#63757 = CARTESIAN_POINT ( 'NONE',  ( -10.72451020669870658, -18.67979575497194134, 44.58442372801901854 ) ) ;
#63758 = CARTESIAN_POINT ( 'NONE',  ( 5.719274019375991003, -21.55341960407610458, 92.70724293864770971 ) ) ;
#63759 = CARTESIAN_POINT ( 'NONE',  ( 18.67979575497194134, -10.72451020669871369, 55.83442372801901854 ) ) ;
#63760 = CARTESIAN_POINT ( 'NONE',  ( 5.049401038298161559, -19.05341960407611168, 22.70724293864769194 ) ) ;
#63761 = ADVANCED_FACE ( 'NONE', ( #180869 ), #80358, .T. ) ;
#63762 = CARTESIAN_POINT ( 'NONE',  ( -19.02544592524342804, 5.153800228976336051, 86.04057627198103830 ) ) ;
#63763 = CARTESIAN_POINT ( 'NONE',  ( 0.05219959533934541429, -16.53943276465976808, 80.00109039468568994 ) ) ;
#63764 = CARTESIAN_POINT ( 'NONE',  ( 8.224510206698953496, -14.34966873604960469, 107.9155762719810241 ) ) ;
#63765 = CARTESIAN_POINT ( 'NONE',  ( 13.89961937509977652, -13.97604488694527269, 108.1239096053143669 ) ) ;
#63766 = CARTESIAN_POINT ( 'NONE',  ( -8.314922557960811034, -14.29746914071050412, 57.08224293864769550 ) ) ;
#63767 = CARTESIAN_POINT ( 'NONE',  ( -8.224510206698948167, 14.34966873604960824, 25.41557627198103120 ) ) ;
#63768 = CARTESIAN_POINT ( 'NONE',  ( 5.153800228976335163, 19.02544592524342804, 69.79057627198103830 ) ) ;
#63769 = CARTESIAN_POINT ( 'NONE',  ( 16.51473224551069308, 9.474510206698969483, 29.16557627198103475 ) ) ;
#63770 = CARTESIAN_POINT ( 'NONE',  ( -21.52544592524343514, 5.823673210054127303, 46.04057627198103830 ) ) ;
#63771 = CARTESIAN_POINT ( 'NONE',  ( -13.89961937509957401, -13.97604488694547875, 34.37609039468566863 ) ) ;
#63774 = CARTESIAN_POINT ( 'NONE',  ( -12.14591786802309592, -12.06949235617757132, 31.87390960531435979 ) ) ;
#63773 = CARTESIAN_POINT ( 'NONE',  ( -17.49999999999999645, -5.499999999999992895, 69.20309617465828467 ) ) ;
#63772 = VECTOR ( 'NONE', #8778, 1000.000000000000000 ) ;
#63775 = CARTESIAN_POINT ( 'NONE',  ( 5.049401038298161559, -19.05341960407611168, 102.7072429386476955 ) ) ;
#63776 = CARTESIAN_POINT ( 'NONE',  ( -5.719274019375665041, -21.55341960407619695, 64.79275706135234714 ) ) ;
#63777 = CARTESIAN_POINT ( 'NONE',  ( 7.284589286804292740, 1.784589286804177277, 1.818019484660534424 ) ) ;
#63778 = CARTESIAN_POINT ( 'NONE',  ( -16.53943276465976808, -0.05219959533934237506, 58.75109039468568994 ) ) ;
#63779 = CARTESIAN_POINT ( 'NONE',  ( -19.02544592524334988, -5.153800228976617603, 63.95942372801899012 ) ) ;
#63780 = CARTESIAN_POINT ( 'NONE',  ( -16.53943276465976808, 0.05219959533911058130, 46.24890960531435979 ) ) ;
#63781 = CARTESIAN_POINT ( 'NONE',  ( 17.50000000000000000, -5.499999999999992895, 51.21769037696435589 ) ) ;
#63782 = CARTESIAN_POINT ( 'NONE',  ( -14.29746914071037622, -8.314922557961029526, 104.1677570613523471 ) ) ;
#63783 = CARTESIAN_POINT ( 'NONE',  ( 5.049401038298161559, -19.05341960407611168, 37.70724293864768839 ) ) ;
#63784 = CARTESIAN_POINT ( 'NONE',  ( -5.049401038298153566, 19.05341960407611168, 55.20724293864769550 ) ) ;
#63785 = CARTESIAN_POINT ( 'NONE',  ( 16.51473224551069308, 9.474510206698969483, 29.16557627198103475 ) ) ;
#63786 = CARTESIAN_POINT ( 'NONE',  ( -10.81492255796105439, 18.62759615963255655, 37.91775706135235424 ) ) ;
#63787 = CARTESIAN_POINT ( 'NONE',  ( -0.05219959533909027116, -19.03943276465977164, 62.49890960531435979 ) ) ;
#63788 = CARTESIAN_POINT ( 'NONE',  ( 5.049401038298161559, -19.05341960407611168, 112.7072429386476813 ) ) ;
#63789 = CARTESIAN_POINT ( 'NONE',  ( -19.05341960407611168, -5.049401038298163336, 46.45724293864768129 ) ) ;
#63790 = CARTESIAN_POINT ( 'NONE',  ( 18.62759615963271287, -10.81492255796078972, 23.33224293864769194 ) ) ;
#63792 = CARTESIAN_POINT ( 'NONE',  ( 19.02544592524343514, -5.153800228976328945, 23.54057627198102054 ) ) ;
#63791 = CARTESIAN_POINT ( 'NONE',  ( 10.81492255796106328, -18.62759615963255655, 65.41775706135234714 ) ) ;
#63793 = CARTESIAN_POINT ( 'NONE',  ( 5.719274019375991003, -21.55341960407610458, 27.70724293864769905 ) ) ;
#63794 = CARTESIAN_POINT ( 'NONE',  ( 12.14591786802327356, -12.06949235617739191, 75.62609039468567573 ) ) ;
#63795 = CARTESIAN_POINT ( 'NONE',  ( -10.81492255796105439, 18.62759615963255655, 107.9177570613523471 ) ) ;
#63796 = PRESENTATION_LAYER_ASSIGNMENT (  '', '', ( #112150 ) ) ;
#63797 = CARTESIAN_POINT ( 'NONE',  ( -4.483927247898782831, 16.52544592524335698, 72.70942372801901854 ) ) ;
#63798 = CARTESIAN_POINT ( 'NONE',  ( 19.05341960407611168, 5.049401038298154454, 98.95724293864766707 ) ) ;
#63799 = CARTESIAN_POINT ( 'NONE',  ( -12.14591786802326823, 12.06949235617739902, 48.12609039468568284 ) ) ;
#63800 = CARTESIAN_POINT ( 'NONE',  ( 12.06949235617739724, 12.14591786802326823, 26.87609039468567218 ) ) ;
#63801 = CARTESIAN_POINT ( 'NONE',  ( -4.483927247898782831, 16.52544592524335698, 97.70942372801904696 ) ) ;
#63802 = CARTESIAN_POINT ( 'NONE',  ( 21.53943276465977519, 0.05219959533937863772, 56.25109039468568284 ) ) ;
#63803 = CARTESIAN_POINT ( 'NONE',  ( -16.46253265017146816, -9.564922557961047289, 104.1677570613523329 ) ) ;
#63804 = CARTESIAN_POINT ( 'NONE',  ( -0.05219959533907301413, -21.53943276465977519, 107.4989096053143669 ) ) ;
#63806 = CARTESIAN_POINT ( 'NONE',  ( -19.02544592524334988, -5.153800228976617603, 103.9594237280190043 ) ) ;
#63805 = CARTESIAN_POINT ( 'NONE',  ( 4.483927247898545687, 16.52544592524342804, 99.79057627198103830 ) ) ;
#63807 = CARTESIAN_POINT ( 'NONE',  ( -14.29746914071037622, -8.314922557961029526, 89.16775706135236135 ) ) ;
#63808 = DIRECTION ( 'NONE',  ( 0.000000000000000000, 0.000000000000000000, 1.000000000000000000 ) ) ;
#63809 = CARTESIAN_POINT ( 'NONE',  ( 5.049401038297881783, 19.05341960407617563, 87.29275706135234714 ) ) ;
#63810 = CARTESIAN_POINT ( 'NONE',  ( -14.29746914071049879, 8.314922557960819915, 40.83224293864769550 ) ) ;
#63811 = CARTESIAN_POINT ( 'NONE',  ( -14.29746914071049879, 8.314922557960819915, 45.83224293864769550 ) ) ;
#63812 = CARTESIAN_POINT ( 'NONE',  ( 14.34966873604960469, 8.224510206698951720, 109.1655762719810383 ) ) ;
#63813 = CARTESIAN_POINT ( 'NONE',  ( 16.51473224551083163, -9.474510206698727899, 50.83442372801899722 ) ) ;
#63814 = CARTESIAN_POINT ( 'NONE',  ( 5.719274019375673035, 21.55341960407619339, 32.29275706135235424 ) ) ;
#63815 = CARTESIAN_POINT ( 'NONE',  ( -13.97604488694547697, 13.89961937509957934, 108.1260903946856331 ) ) ;
#63816 = FACE_OUTER_BOUND ( 'NONE', #142298, .T. ) ;
#63817 = CARTESIAN_POINT ( 'NONE',  ( -16.46253265017160317, 9.564922557960807481, 110.8322429386476955 ) ) ;
#63818 = CARTESIAN_POINT ( 'NONE',  ( 19.05341960407611168, 5.049401038298154454, 83.95724293864766707 ) ) ;
#63819 = CARTESIAN_POINT ( 'NONE',  ( 18.62759615963271287, -10.81492255796078972, 58.33224293864768839 ) ) ;
#63820 = CARTESIAN_POINT ( 'NONE',  ( -14.34966873604960291, -8.224510206698953496, 111.6655762719810525 ) ) ;
#63821 = CARTESIAN_POINT ( 'NONE',  ( 19.05341960407611168, 5.049401038298154454, 68.95724293864769550 ) ) ;
#63822 = CARTESIAN_POINT ( 'NONE',  ( -9.474510206698964154, 16.51473224551069663, 30.41557627198102054 ) ) ;
#63824 = CARTESIAN_POINT ( 'NONE',  ( 10.72451020669871369, 18.67979575497193778, 32.08442372801901854 ) ) ;
#63823 = CIRCLE ( 'NONE', #2474, 8.000000000000001776 ) ;
#63825 = CARTESIAN_POINT ( 'NONE',  ( 10.81492255796106328, -18.62759615963255655, 75.41775706135233293 ) ) ;
#63826 = CARTESIAN_POINT ( 'NONE',  ( 14.29746914071037800, 8.314922557961029526, 96.66775706135234714 ) ) ;
#63827 = CARTESIAN_POINT ( 'NONE',  ( 15.80617190586769283, -15.72974639402175789, 30.62609039468567929 ) ) ;
#63828 = CARTESIAN_POINT ( 'NONE',  ( 15.80617190586769283, -15.72974639402175789, 30.62609039468567929 ) ) ;
#63830 = CARTESIAN_POINT ( 'NONE',  ( -5.153800228976328057, -19.02544592524343514, 77.29057627198099567 ) ) ;
#63829 = CARTESIAN_POINT ( 'NONE',  ( -16.46253265017146816, -9.564922557961047289, 69.16775706135233293 ) ) ;
#63831 = CARTESIAN_POINT ( 'NONE',  ( 5.719274019375673035, 21.55341960407619339, 87.29275706135236135 ) ) ;
#63832 = CARTESIAN_POINT ( 'NONE',  ( 15.80617190586746368, 15.72974639402197994, 84.37390960531438111 ) ) ;
#63833 = CARTESIAN_POINT ( 'NONE',  ( -16.52544592524342804, 4.483927247898546575, 66.04057627198103830 ) ) ;
#63834 = CARTESIAN_POINT ( 'NONE',  ( -21.55341960407619339, 5.719274019375674811, 98.54275706135234714 ) ) ;
#63835 = CARTESIAN_POINT ( 'NONE',  ( 12.14591786802309770, 12.06949235617756955, 89.37390960531435269 ) ) ;
#63836 = CARTESIAN_POINT ( 'NONE',  ( -9.474510206698964154, 16.51473224551069663, 25.41557627198103120 ) ) ;
#63837 = CARTESIAN_POINT ( 'NONE',  ( 13.89961937509957401, 13.97604488694547697, 76.87609039468566152 ) ) ;
#63838 = CARTESIAN_POINT ( 'NONE',  ( -16.52544592524342804, 4.483927247898546575, 31.04057627198102409 ) ) ;
#63840 = EDGE_CURVE ( 'NONE', #186418, #134298, #76530, .T. ) ;
#63839 = CARTESIAN_POINT ( 'NONE',  ( 15.72974639402176855, 15.80617190586768217, 86.87609039468568994 ) ) ;
#63841 = CARTESIAN_POINT ( 'NONE',  ( -5.153800228976328057, -19.02544592524343514, 87.29057627198103830 ) ) ;
#63842 = CARTESIAN_POINT ( 'NONE',  ( -19.05341960407617563, 5.049401038297882671, 58.54275706135234003 ) ) ;
#63843 = CARTESIAN_POINT ( 'NONE',  ( -5.719274019375978568, 21.55341960407610458, 70.20724293864769550 ) ) ;
#63844 = CARTESIAN_POINT ( 'NONE',  ( -10.81492255796078084, -18.62759615963271287, 112.0822429386477097 ) ) ;
#63845 = CARTESIAN_POINT ( 'NONE',  ( 8.224510206698742110, 14.34966873604972548, 22.08442372801901143 ) ) ;
#63846 = CARTESIAN_POINT ( 'NONE',  ( -16.52544592524335698, -4.483927247898792601, 73.95942372801901854 ) ) ;
#63848 = CARTESIAN_POINT ( 'NONE',  ( 15.72974639402176855, 15.80617190586768217, 21.87609039468567573 ) ) ;
#63847 = LINE ( 'NONE', #18351, #103195 ) ;
#63849 =( BOUNDED_CURVE ( )  B_SPLINE_CURVE ( 2, ( #144481, #5965, #114133, #175834, #37307, #98966, #160656, #22148, #191989, #53476, #115153, #176846, #38317 ),
 .UNSPECIFIED., .F., .T. ) 
 B_SPLINE_CURVE_WITH_KNOTS ( ( 3, 2, 2, 2, 2, 2, 3 ),
 ( 0.7129567522165188853, 0.7149122807017543879, 0.7192982456140351033, 0.7236842105263158187, 0.7280701754385965341, 0.7324561403508771384, 0.7343659890140226132 ),
 .UNSPECIFIED. ) 
 CURVE ( )  GEOMETRIC_REPRESENTATION_ITEM ( )  RATIONAL_B_SPLINE_CURVE ( ( 0.9831626618144007068, 0.9848076720550096308, 1.000000000000000000, 0.9659258262890683122, 1.000000000000000000, 0.9659258262890683122, 1.000000000000000000, 0.9659258262890683122, 1.000000000000000000, 0.9659258262890683122, 1.000000000000000000, 0.9851625545550091179, 0.9832469066685282089 ) ) 
 REPRESENTATION_ITEM ( '' )  );
#63850 = CARTESIAN_POINT ( 'NONE',  ( 14.29746914071049879, -8.314922557960816363, 103.3322429386476955 ) ) ;
#63851 = CARTESIAN_POINT ( 'NONE',  ( -36.91746825000001309, -11.99521256947794789, -7.024999997268812635 ) ) ;
#63852 = CARTESIAN_POINT ( 'NONE',  ( 4.379528057220092307, 16.55341960407617563, 32.29275706135235424 ) ) ;
#63853 = CARTESIAN_POINT ( 'NONE',  ( 21.53943276465977519, -0.05219959533907433946, 63.74890960531435979 ) ) ;
#63854 = CARTESIAN_POINT ( 'NONE',  ( -16.55341960407617563, 4.379528057220093196, 103.5427570613523613 ) ) ;
#63855 = CARTESIAN_POINT ( 'NONE',  ( 4.379528057220092307, 16.55341960407617563, 42.29275706135235424 ) ) ;
#63856 = CARTESIAN_POINT ( 'NONE',  ( 0.05219959533909260263, 19.03943276465977164, 34.99890960531435979 ) ) ;
#63857 = CARTESIAN_POINT ( 'NONE',  ( -4.483927247898782831, 16.52544592524335698, 77.70942372801900433 ) ) ;
#63858 = CARTESIAN_POINT ( 'NONE',  ( -19.02544592524334988, -5.153800228976617603, 68.95942372801896170 ) ) ;
#63859 = CARTESIAN_POINT ( 'NONE',  ( -21.53943276465977519, 0.05219959533907696930, 76.24890960531435269 ) ) ;
#63860 = CARTESIAN_POINT ( 'NONE',  ( -16.52544592524335698, -4.483927247898792601, 93.95942372801903275 ) ) ;
#63861 = CARTESIAN_POINT ( 'NONE',  ( 15.80617190586769283, -15.72974639402175789, 80.62609039468567573 ) ) ;
#63862 = CARTESIAN_POINT ( 'NONE',  ( 5.823673210054125526, 21.52544592524343514, 59.79057627198103120 ) ) ;
#63863 = CARTESIAN_POINT ( 'NONE',  ( -15.80617190586745835, -15.72974639402198527, 46.87390960531435979 ) ) ;
#63864 = ORIENTED_EDGE ( 'NONE', *, *, #14853, .T. ) ;
#63865 = ORIENTED_EDGE ( 'NONE', *, *, #146334, .T. ) ;
#63866 = CARTESIAN_POINT ( 'NONE',  ( 14.34966873604972726, -8.224510206698740333, 75.83442372801900433 ) ) ;
#63867 = CARTESIAN_POINT ( 'NONE',  ( -21.52544592524343514, 5.823673210054127303, 46.04057627198103830 ) ) ;
#63868 = EDGE_LOOP ( 'NONE', ( #161094, #81760 ) ) ;
#63869 = CARTESIAN_POINT ( 'NONE',  ( 19.05341960407611168, 5.049401038298154454, 108.9572429386477097 ) ) ;
#63870 = DIRECTION ( 'NONE',  ( 0.8164965809277243691, 0.000000000000000000, -0.5773502691896280625 ) ) ;
#63871 = CARTESIAN_POINT ( 'NONE',  ( -16.51473224551069308, -9.474510206698971260, 31.66557627198102054 ) ) ;
#63872 = CARTESIAN_POINT ( 'NONE',  ( -5.719274019375978568, 21.55341960407610458, 65.20724293864768129 ) ) ;
#63873 = CARTESIAN_POINT ( 'NONE',  ( -16.55341960407617563, 4.379528057220093196, 98.54275706135234714 ) ) ;
#63874 = CARTESIAN_POINT ( 'NONE',  ( 15.72974639402176855, 15.80617190586768217, 46.87609039468568994 ) ) ;
#63875 = CARTESIAN_POINT ( 'NONE',  ( -0.05219959533936034679, 19.03943276465977164, 97.50109039468567573 ) ) ;
#63876 = CARTESIAN_POINT ( 'NONE',  ( 16.52544592524342804, -4.483927247898539470, 103.5405762719810383 ) ) ;
#63877 = CARTESIAN_POINT ( 'NONE',  ( -5.049401038297874678, -19.05341960407617918, 104.7927570613523471 ) ) ;
#63878 = CARTESIAN_POINT ( 'NONE',  ( -9.474510206698964154, 16.51473224551069663, 40.41557627198103120 ) ) ;
#63879 = CARTESIAN_POINT ( 'NONE',  ( 23.31738231874054890, -16.94106989632523508, 140.7999999999999829 ) ) ;
#63880 = CARTESIAN_POINT ( 'NONE',  ( -5.153800228976328057, -19.02544592524343514, 97.29057627198099567 ) ) ;
#63881 = CARTESIAN_POINT ( 'NONE',  ( 16.53943276465976808, 0.05219959533934440121, 71.25109039468568994 ) ) ;
#63882 = CARTESIAN_POINT ( 'NONE',  ( 19.03943276465977164, 0.05219959533936151252, 76.25109039468566152 ) ) ;
#63883 = CARTESIAN_POINT ( 'NONE',  ( 9.564922557961047289, -16.46253265017146816, 20.41775706135233293 ) ) ;
#63884 = CARTESIAN_POINT ( 'NONE',  ( -21.52544592524343514, 5.823673210054127303, 56.04057627198102409 ) ) ;
#63885 = CARTESIAN_POINT ( 'NONE',  ( -12.14591786802326823, 12.06949235617739902, 88.12609039468570415 ) ) ;
#63886 = CARTESIAN_POINT ( 'NONE',  ( 5.049401038297881783, 19.05341960407617563, 77.29275706135231871 ) ) ;
#63887 = CARTESIAN_POINT ( 'NONE',  ( -19.05341960407611168, -5.049401038298163336, 41.45724293864769550 ) ) ;
#63888 = CARTESIAN_POINT ( 'NONE',  ( 13.89961937509977652, -13.97604488694527269, 73.12390960531436690 ) ) ;
#63889 = CARTESIAN_POINT ( 'NONE',  ( -0.05219959533937732626, 21.53943276465977519, 52.50109039468567573 ) ) ;
#63890 = CARTESIAN_POINT ( 'NONE',  ( -9.474510206698964154, 16.51473224551069663, 45.41557627198103120 ) ) ;
#63891 = CARTESIAN_POINT ( 'NONE',  ( -16.46253265017146816, -9.564922557961047289, 79.16775706135234714 ) ) ;
#63892 = LINE ( 'NONE', #191219, #173486 ) ;
#63893 = CARTESIAN_POINT ( 'NONE',  ( 19.05341960407611168, 5.049401038298154454, 113.9572429386477097 ) ) ;
#63894 = CARTESIAN_POINT ( 'NONE',  ( -4.379528057220328563, 16.55341960407611168, 60.20724293864768839 ) ) ;
#63895 = CARTESIAN_POINT ( 'NONE',  ( 15.80617190586746368, 15.72974639402197994, 59.37390960531436690 ) ) ;
#63896 = CARTESIAN_POINT ( 'NONE',  ( 20.28951144177217003, 1.856485852971841544, 102.5000000000000426 ) ) ;
#63897 = CARTESIAN_POINT ( 'NONE',  ( 13.97604488694548053, -13.89961937509957401, 30.62609039468566863 ) ) ;
#63898 =( LENGTH_UNIT ( ) NAMED_UNIT ( * ) SI_UNIT ( .MILLI., .METRE. ) );
#63900 = CARTESIAN_POINT ( 'NONE',  ( 16.51473224551069308, 9.474510206698969483, 79.16557627198103830 ) ) ;
#63899 = CARTESIAN_POINT ( 'NONE',  ( -0.05219959533909027116, -19.03943276465977164, 57.49890960531435979 ) ) ;
#63901 = CARTESIAN_POINT ( 'NONE',  ( 12.06949235617739724, 12.14591786802326823, 56.87609039468568994 ) ) ;
#63902 = CARTESIAN_POINT ( 'NONE',  ( 16.51473224551083163, -9.474510206698727899, 80.83442372801899012 ) ) ;
#63903 = CARTESIAN_POINT ( 'NONE',  ( -17.26172910966780805, 6.454744622555829814, 110.8064690864922568 ) ) ;
#63904 = CARTESIAN_POINT ( 'NONE',  ( -4.483927247898782831, 16.52544592524335698, 87.70942372801901854 ) ) ;
#63905 = CARTESIAN_POINT ( 'NONE',  ( -3.573655867282028392E-15, 2.428612866367529932E-14, -15.00000000000000000 ) ) ;
#63906 = CARTESIAN_POINT ( 'NONE',  ( -12.06949235617739369, -12.14591786802326823, 64.37609039468568994 ) ) ;
#63907 = CARTESIAN_POINT ( 'NONE',  ( -8.314922557961024197, 14.29746914071037800, 37.91775706135235424 ) ) ;
#63909 = DIRECTION ( 'NONE',  ( -0.000000000000000000, -0.000000000000000000, -1.000000000000000000 ) ) ;
#63908 = CARTESIAN_POINT ( 'NONE',  ( 16.46253265017160672, -9.564922557960803928, 58.33224293864769550 ) ) ;
#63910 = CARTESIAN_POINT ( 'NONE',  ( -0.05219959533937732626, 21.53943276465977519, 52.50109039468567573 ) ) ;
#63911 = CARTESIAN_POINT ( 'NONE',  ( -16.51473224551082808, 9.474510206698731452, 68.33442372801900433 ) ) ;
#63912 = CARTESIAN_POINT ( 'NONE',  ( -5.823673210054431948, 21.52544592524334988, 102.7094237280190185 ) ) ;
#63913 = CARTESIAN_POINT ( 'NONE',  ( 5.153800228976335163, 19.02544592524342804, 24.79057627198102765 ) ) ;
#63914 = DIRECTION ( 'NONE',  ( 1.000000000000000000, 0.000000000000000000, 0.000000000000000000 ) ) ;
#63915 = CARTESIAN_POINT ( 'NONE',  ( -21.55341960407610458, -5.719274019375992779, 56.45724293864768839 ) ) ;
#63916 = AXIS2_PLACEMENT_3D ( 'NONE', #177881, #8002, #134370 ) ;
#63917 = CARTESIAN_POINT ( 'NONE',  ( -19.02544592524342804, 5.153800228976336051, 111.0405762719810099 ) ) ;
#63918 = CARTESIAN_POINT ( 'NONE',  ( 16.52544592524342804, -4.483927247898539470, 108.5405762719810241 ) ) ;
#63919 = CARTESIAN_POINT ( 'NONE',  ( -16.53943276465976808, -0.05219959533934237506, 43.75109039468568284 ) ) ;
#63920 = CARTESIAN_POINT ( 'NONE',  ( -12.14591786802309592, -12.06949235617757132, 26.87390960531435979 ) ) ;
#63921 = EDGE_LOOP ( 'NONE', ( #44492, #190801, #79691, #108555 ) ) ;
#63922 = CARTESIAN_POINT ( 'NONE',  ( -10.72451020669870658, -18.67979575497194134, 24.58442372801901499 ) ) ;
#63924 = CARTESIAN_POINT ( 'NONE',  ( -0.05219959533909027116, -19.03943276465977164, 107.4989096053143527 ) ) ;
#63923 = CARTESIAN_POINT ( 'NONE',  ( 14.34966873604960469, 8.224510206698951720, 39.16557627198102409 ) ) ;
#63925 = CARTESIAN_POINT ( 'NONE',  ( 16.51473224551083163, -9.474510206698727899, 100.8344237280190043 ) ) ;
#63926 = CARTESIAN_POINT ( 'NONE',  ( 13.89961937509957401, 13.97604488694547697, 26.87609039468566507 ) ) ;
#63927 = CARTESIAN_POINT ( 'NONE',  ( -14.29746914071049879, 8.314922557960819915, 35.83224293864768839 ) ) ;
#63928 = CARTESIAN_POINT ( 'NONE',  ( -0.05219959533907301413, -21.53943276465977519, 102.4989096053143811 ) ) ;
#63929 = CARTESIAN_POINT ( 'NONE',  ( 0.05219959533907565091, 21.53943276465977519, 69.99890960531435269 ) ) ;
#63930 = CARTESIAN_POINT ( 'NONE',  ( -5.049401038298153566, 19.05341960407611168, 80.20724293864769550 ) ) ;
#63931 = CARTESIAN_POINT ( 'NONE',  ( 0.05219959533910956823, 16.53943276465976808, 44.99890960531435979 ) ) ;
#63932 = CARTESIAN_POINT ( 'NONE',  ( 19.05341960407611168, 5.049401038298154454, 88.95724293864769550 ) ) ;
#63933 = CARTESIAN_POINT ( 'NONE',  ( 13.97604488694527802, 13.89961937509977830, 79.37390960531436690 ) ) ;
#63934 = CARTESIAN_POINT ( 'NONE',  ( 16.46253265017146816, 9.564922557961045513, 36.66775706135233293 ) ) ;
#63935 = CARTESIAN_POINT ( 'NONE',  ( 15.80617190586746368, 15.72974639402197994, 89.37390960531435269 ) ) ;
#63936 = CARTESIAN_POINT ( 'NONE',  ( 0.05219959533910956823, 16.53943276465976808, 99.99890960531436690 ) ) ;
#63937 = CARTESIAN_POINT ( 'NONE',  ( 15.80617190586769283, -15.72974639402175789, 35.62609039468568994 ) ) ;
#63938 = VECTOR ( 'NONE', #65527, 1000.000000000000000 ) ;
#63939 = CARTESIAN_POINT ( 'NONE',  ( -22.44159573604010305, 16.30477369853692338, 140.6750000027311671 ) ) ;
#63940 = CARTESIAN_POINT ( 'NONE',  ( 16.53943276465976808, -0.05219959533910856209, 33.74890960531436690 ) ) ;
#63941 = CARTESIAN_POINT ( 'NONE',  ( 5.153800228976335163, 19.02544592524342804, 29.79057627198102409 ) ) ;
#63942 = CARTESIAN_POINT ( 'NONE',  ( 9.474510206698971260, -16.51473224551069308, 87.91557627198102409 ) ) ;
#63943 = CARTESIAN_POINT ( 'NONE',  ( 18.62759615963271287, -10.81492255796078972, 58.33224293864768839 ) ) ;
#63944 = CARTESIAN_POINT ( 'NONE',  ( -27.73933785331498925, 2.428612866367529932E-14, 138.8750000027311842 ) ) ;
#63945 = CARTESIAN_POINT ( 'NONE',  ( -13.89961937509977652, 13.97604488694528158, 30.62390960531435269 ) ) ;
#63946 = CARTESIAN_POINT ( 'NONE',  ( 4.483927247898545687, 16.52544592524342804, 44.79057627198103120 ) ) ;
#63947 = CARTESIAN_POINT ( 'NONE',  ( -10.81492255796105439, 18.62759615963255655, 67.91775706135234714 ) ) ;
#63949 = CARTESIAN_POINT ( 'NONE',  ( 16.55341960407618274, -4.379528057220086978, 66.04275706135236135 ) ) ;
#63948 = CARTESIAN_POINT ( 'NONE',  ( 21.74014569711068390, -31.09693755439586837, -22.87366378656934174 ) ) ;
#63950 = CARTESIAN_POINT ( 'NONE',  ( 19.05341960407611168, 5.049401038298154454, 53.95724293864770260 ) ) ;
#63951 = CARTESIAN_POINT ( 'NONE',  ( -16.46253265017160317, 9.564922557960807481, 70.83224293864770971 ) ) ;
#63952 = EDGE_LOOP ( 'NONE', ( #147004, #155418, #131303, #166628, #27126, #61404 ) ) ;
#63953 = CARTESIAN_POINT ( 'NONE',  ( -5.719274019375665041, -21.55341960407619695, 104.7927570613523898 ) ) ;
#63954 = CARTESIAN_POINT ( 'NONE',  ( -16.52544592524335698, -4.483927247898792601, 78.95942372801901854 ) ) ;
#63955 = CARTESIAN_POINT ( 'NONE',  ( 21.53943276465977519, 0.05219959533937863772, 101.2510903946856757 ) ) ;
#63956 = CARTESIAN_POINT ( 'NONE',  ( 16.51473224551069308, 9.474510206698969483, 59.16557627198102409 ) ) ;
#63957 = CARTESIAN_POINT ( 'NONE',  ( 21.55341960407610458, 5.719274019375980345, 28.95724293864769905 ) ) ;
#63958 = CARTESIAN_POINT ( 'NONE',  ( -0.05219959533936034679, 19.03943276465977164, 102.5010903946856757 ) ) ;
#63959 = CARTESIAN_POINT ( 'NONE',  ( 21.53943276465977519, 0.05219959533937863772, 86.25109039468568994 ) ) ;
#63960 = CARTESIAN_POINT ( 'NONE',  ( -16.55341960407617563, 4.379528057220093196, 53.54275706135234714 ) ) ;
#63961 = CARTESIAN_POINT ( 'NONE',  ( -10.72451020669898014, 18.67979575497178502, 100.4155762719810241 ) ) ;
#63962 = CARTESIAN_POINT ( 'NONE',  ( -13.89961937509957401, -13.97604488694547875, 99.37609039468567573 ) ) ;
#63963 = CARTESIAN_POINT ( 'NONE',  ( 5.153800228976335163, 19.02544592524342804, 84.79057627198099567 ) ) ;
#63964 = CARTESIAN_POINT ( 'NONE',  ( -9.564922557961040184, 16.46253265017147172, 107.9177570613523471 ) ) ;
#63965 = CARTESIAN_POINT ( 'NONE',  ( 0.05219959533909260263, 19.03943276465977164, 44.99890960531435979 ) ) ;
#63966 = CARTESIAN_POINT ( 'NONE',  ( -4.379528057220086978, -16.55341960407618274, 24.79275706135235779 ) ) ;
#63967 = CARTESIAN_POINT ( 'NONE',  ( 8.314922557960818139, 14.29746914071049879, 64.58224293864769550 ) ) ;
#63968 = CARTESIAN_POINT ( 'NONE',  ( 16.52544592524335698, 4.483927247898782831, 71.45942372801901854 ) ) ;
#63970 = CARTESIAN_POINT ( 'NONE',  ( -16.51473224551069308, -9.474510206698971260, 56.66557627198103120 ) ) ;
#63969 = CARTESIAN_POINT ( 'NONE',  ( -21.52544592524334988, -5.823673210054445271, 28.95942372801902209 ) ) ;
#63971 = CARTESIAN_POINT ( 'NONE',  ( -5.153800228976328057, -19.02544592524343514, 67.29057627198102409 ) ) ;
#63972 = CARTESIAN_POINT ( 'NONE',  ( -12.14591786802326823, 12.06949235617739902, 73.12609039468567573 ) ) ;
#63973 = CARTESIAN_POINT ( 'NONE',  ( 23.31738231874054890, -16.94106989632523508, 147.0500000054623797 ) ) ;
#63974 = ORIENTED_EDGE ( 'NONE', *, *, #168190, .F. ) ;
#63975 = CARTESIAN_POINT ( 'NONE',  ( -15.72974639402176322, -15.80617190586768395, 109.3760903946857042 ) ) ;
#63977 = ADVANCED_FACE ( 'NONE', ( #33872 ), #48058, .T. ) ;
#63976 = CARTESIAN_POINT ( 'NONE',  ( 5.049401038298161559, -19.05341960407611168, 37.70724293864768839 ) ) ;
#63978 = ORIENTED_EDGE ( 'NONE', *, *, #55785, .F. ) ;
#63979 = CARTESIAN_POINT ( 'NONE',  ( -16.53943276465976808, -0.05219959533934237506, 28.75109039468567929 ) ) ;
#63981 = CARTESIAN_POINT ( 'NONE',  ( -4.379528057220086978, -16.55341960407618274, 44.79275706135234714 ) ) ;
#63980 = CARTESIAN_POINT ( 'NONE',  ( -13.89961937509957401, -13.97604488694547875, 49.37609039468567573 ) ) ;
#63982 = CARTESIAN_POINT ( 'NONE',  ( 13.97604488694527802, 13.89961937509977652, 39.37390960531435269 ) ) ;
#63983 = CARTESIAN_POINT ( 'NONE',  ( 5.153800228976335163, 19.02544592524342804, 69.79057627198103830 ) ) ;
#63984 = CARTESIAN_POINT ( 'NONE',  ( -5.719274019375978568, 21.55341960407610458, 80.20724293864769550 ) ) ;
#63986 = CARTESIAN_POINT ( 'NONE',  ( 13.97604488694527802, 13.89961937509977652, 114.3739096053143669 ) ) ;
#63985 = CARTESIAN_POINT ( 'NONE',  ( 16.46253265017160672, -9.564922557960803928, 83.33224293864768129 ) ) ;
#63987 = CARTESIAN_POINT ( 'NONE',  ( -19.05341960407611168, -5.049401038298163336, 61.45724293864769550 ) ) ;
#63988 = DIRECTION ( 'NONE',  ( 0.000000000000000000, 0.000000000000000000, 1.000000000000000000 ) ) ;
#63989 = CARTESIAN_POINT ( 'NONE',  ( 9.474510206698729675, 16.51473224551082808, 102.0844237280190043 ) ) ;
#63990 = CARTESIAN_POINT ( 'NONE',  ( 13.89961937509957401, 13.97604488694547697, 26.87609039468566507 ) ) ;
#63991 = CARTESIAN_POINT ( 'NONE',  ( -16.53943276465976808, 0.05219959533911058130, 56.24890960531436690 ) ) ;
#63992 = CARTESIAN_POINT ( 'NONE',  ( 18.62759615963255655, 10.81492255796105972, 91.66775706135234714 ) ) ;
#63993 = CARTESIAN_POINT ( 'NONE',  ( -16.52544592524342804, 4.483927247898546575, 116.0405762719810383 ) ) ;
#63994 = EDGE_CURVE ( 'NONE', #197337, #169038, #135356, .T. ) ;
#63996 = CARTESIAN_POINT ( 'NONE',  ( -21.55341960407619339, 5.719274019375674811, 88.54275706135236135 ) ) ;
#63995 = CARTESIAN_POINT ( 'NONE',  ( -12.14591786802309592, -12.06949235617757132, 31.87390960531435979 ) ) ;
#63997 = CARTESIAN_POINT ( 'NONE',  ( 16.51473224551069308, 9.474510206698969483, 74.16557627198103830 ) ) ;
#63998 = CARTESIAN_POINT ( 'NONE',  ( -10.72451020669870658, -18.67979575497194134, 49.58442372801901143 ) ) ;
#63999 = CARTESIAN_POINT ( 'NONE',  ( -0.05219959533909027116, -19.03943276465977164, 77.49890960531435269 ) ) ;
#64000 = CARTESIAN_POINT ( 'NONE',  ( -14.29746914071049879, 8.314922557960819915, 100.8322429386477097 ) ) ;
#64001 = CARTESIAN_POINT ( 'NONE',  ( 12.14591786802309770, 12.06949235617756955, 59.37390960531436690 ) ) ;
#64002 = CARTESIAN_POINT ( 'NONE',  ( -0.05219959533907301413, -21.53943276465977519, 72.49890960531435269 ) ) ;
#64003 = CARTESIAN_POINT ( 'NONE',  ( -0.05219959533909027116, -19.03943276465977164, 77.49890960531435269 ) ) ;
#64004 = CARTESIAN_POINT ( 'NONE',  ( 5.823673210054125526, 21.52544592524343514, 89.79057627198103830 ) ) ;
#64005 = CARTESIAN_POINT ( 'NONE',  ( -19.02544592524334988, -5.153800228976617603, 78.95942372801900433 ) ) ;
#64007 = CARTESIAN_POINT ( 'NONE',  ( -4.483927247898539470, -16.52544592524342804, 72.29057627198102409 ) ) ;
#64006 = CARTESIAN_POINT ( 'NONE',  ( 16.46253265017146816, 9.564922557961045513, 36.66775706135233293 ) ) ;
#64008 = CARTESIAN_POINT ( 'NONE',  ( 9.564922557960805705, 16.46253265017160317, 64.58224293864769550 ) ) ;
#64009 = CARTESIAN_POINT ( 'NONE',  ( 18.62759615963271287, -10.81492255796078972, 58.33224293864768839 ) ) ;
#64010 = CARTESIAN_POINT ( 'NONE',  ( 16.38665767535054840, -7.295008042176022833, 27.76400864214547326 ) ) ;
#64012 = CARTESIAN_POINT ( 'NONE',  ( -17.14385361876520264, -23.59649016807271238, 143.6750000027311671 ) ) ;
#64011 = CARTESIAN_POINT ( 'NONE',  ( 12.06949235617739724, 12.14591786802326823, 111.8760903946856615 ) ) ;
#64013 = CARTESIAN_POINT ( 'NONE',  ( 16.46253265017146816, 9.564922557961045513, 101.6677570613523329 ) ) ;
#64014 = CARTESIAN_POINT ( 'NONE',  ( -16.55341960407611168, -4.379528057220339221, 81.45724293864769550 ) ) ;
#64015 = CARTESIAN_POINT ( 'NONE',  ( -17.49999999999998934, 4.013004640162638914, 35.44605720994410092 ) ) ;
#64016 = CARTESIAN_POINT ( 'NONE',  ( 13.97604488694527802, 13.89961937509977652, 79.37390960531435269 ) ) ;
#64017 = CARTESIAN_POINT ( 'NONE',  ( 5.153800228976335163, 19.02544592524342804, 29.79057627198102409 ) ) ;
#64018 = CARTESIAN_POINT ( 'NONE',  ( -8.314922557960811034, -14.29746914071050412, 62.08224293864769550 ) ) ;
#64019 = CARTESIAN_POINT ( 'NONE',  ( -19.02544592524342804, 5.153800228976336051, 96.04057627198103830 ) ) ;
#64021 = CARTESIAN_POINT ( 'NONE',  ( -19.02544592524342804, 5.153800228976336051, 61.04057627198103120 ) ) ;
#64020 = CARTESIAN_POINT ( 'NONE',  ( -9.564922557961040184, 16.46253265017147172, 92.91775706135233293 ) ) ;
#64022 = CARTESIAN_POINT ( 'NONE',  ( 16.46253265017160672, -9.564922557960803928, 83.33224293864768129 ) ) ;
#64023 = CARTESIAN_POINT ( 'NONE',  ( -18.67979575497178146, -10.72451020669898902, 81.66557627198103830 ) ) ;
#64024 = CARTESIAN_POINT ( 'NONE',  ( -12.14591786802326823, 12.06949235617739902, 73.12609039468567573 ) ) ;
#64025 = CARTESIAN_POINT ( 'NONE',  ( -19.03943276465977164, -0.05219959533935946555, 113.7510903946856757 ) ) ;
#64026 = CARTESIAN_POINT ( 'NONE',  ( 19.03943276465977164, -0.05219959533909143690, 58.74890960531435979 ) ) ;
#64027 = CARTESIAN_POINT ( 'NONE',  ( 15.72974639402199770, -15.80617190586745480, 68.12390960531436690 ) ) ;
#64028 = CARTESIAN_POINT ( 'NONE',  ( -5.049401038297874678, -19.05341960407617918, 94.79275706135230450 ) ) ;
#64030 = CARTESIAN_POINT ( 'NONE',  ( 10.81492255796106328, -18.62759615963255655, 45.41775706135234003 ) ) ;
#64029 = CARTESIAN_POINT ( 'NONE',  ( -16.53943276465976808, 0.05219959533911058130, 36.24890960531435979 ) ) ;
#64031 = SPHERICAL_SURFACE ( 'NONE', #131523, 0.5000000000000000000 ) ;
#64033 = CARTESIAN_POINT ( 'NONE',  ( 5.049401038298161559, -19.05341960407611168, 107.7072429386476955 ) ) ;
#64032 = CARTESIAN_POINT ( 'NONE',  ( -16.52544592524335698, -4.483927247898792601, 78.95942372801901854 ) ) ;
#64034 = CARTESIAN_POINT ( 'NONE',  ( 19.03943276465977164, -0.05219959533909143690, 108.7489096053143527 ) ) ;
#64035 = CARTESIAN_POINT ( 'NONE',  ( -16.81555441253554051, -7.025013491695444756, 34.36314554665744225 ) ) ;
#64036 = CARTESIAN_POINT ( 'NONE',  ( 12.14591786802327356, -12.06949235617739191, 95.62609039468568994 ) ) ;
#64037 = CARTESIAN_POINT ( 'NONE',  ( 4.379528057220092307, 16.55341960407617563, 32.29275706135235424 ) ) ;
#64038 = CARTESIAN_POINT ( 'NONE',  ( 13.89961937509977652, -13.97604488694527269, 48.12390960531435979 ) ) ;
#64039 = CARTESIAN_POINT ( 'NONE',  ( -5.049401038298153566, 19.05341960407611168, 50.20724293864770260 ) ) ;
#64040 = CARTESIAN_POINT ( 'NONE',  ( 0.05219959533909260263, 19.03943276465977164, 54.99890960531435979 ) ) ;
#64041 = CARTESIAN_POINT ( 'NONE',  ( -21.53943276465977519, -0.05219959533937600094, 53.75109039468568994 ) ) ;
#64042 = CARTESIAN_POINT ( 'NONE',  ( 16.52544592524335698, 4.483927247898782831, 66.45942372801903275 ) ) ;
#64043 = CARTESIAN_POINT ( 'NONE',  ( 12.06949235617757843, -12.14591786802309237, 38.12390960531436690 ) ) ;
#64044 = CARTESIAN_POINT ( 'NONE',  ( 16.51473224551069308, 9.474510206698969483, 39.16557627198103120 ) ) ;
#64045 = CARTESIAN_POINT ( 'NONE',  ( -19.05341960407611168, -5.049401038298163336, 36.45724293864766707 ) ) ;
#64046 = CARTESIAN_POINT ( 'NONE',  ( -4.379528057220086978, -16.55341960407618274, 34.79275706135235424 ) ) ;
#64047 = CARTESIAN_POINT ( 'NONE',  ( -19.05341960407617563, 5.049401038297882671, 78.54275706135233293 ) ) ;
#64048 = CARTESIAN_POINT ( 'NONE',  ( 16.52544592524342804, -4.483927247898539470, 83.54057627198102409 ) ) ;
#64049 = CARTESIAN_POINT ( 'NONE',  ( 19.02544592524343514, -5.153800228976328945, 53.54057627198102409 ) ) ;
#64051 = CARTESIAN_POINT ( 'NONE',  ( -17.79613651744293890, -24.49428055684527550, 148.2843446568999752 ) ) ;
#64050 = CARTESIAN_POINT ( 'NONE',  ( 13.89961937509957401, 13.97604488694547697, 81.87609039468564731 ) ) ;
#64052 = CARTESIAN_POINT ( 'NONE',  ( 18.67979575497194134, -10.72451020669871369, 75.83442372801900433 ) ) ;
#64053 = CARTESIAN_POINT ( 'NONE',  ( -8.314922557961024197, 14.29746914071037800, 52.91775706135235424 ) ) ;
#64054 = CARTESIAN_POINT ( 'NONE',  ( -17.49999999999999645, 3.805241302050396346, 25.37352472782596280 ) ) ;
#64055 = CARTESIAN_POINT ( 'NONE',  ( -18.67979575497178146, -10.72451020669898902, 51.66557627198102409 ) ) ;
#64056 = CARTESIAN_POINT ( 'NONE',  ( -4.379528057220086978, -16.55341960407618274, 44.79275706135234714 ) ) ;
#64057 = CARTESIAN_POINT ( 'NONE',  ( -23.31738231874055600, 16.94106989632528837, 147.7999999999999829 ) ) ;
#64058 = CARTESIAN_POINT ( 'NONE',  ( -5.153800228976607833, 19.02544592524334988, 22.70942372801899012 ) ) ;
#64059 = CARTESIAN_POINT ( 'NONE',  ( 9.622336364422297450, 11.74387995961029141, -59.83536316257176679 ) ) ;
#64060 = CARTESIAN_POINT ( 'NONE',  ( -19.02544592524342804, 5.153800228976336051, 51.04057627198103120 ) ) ;
#64061 = CARTESIAN_POINT ( 'NONE',  ( 14.67621740152110377, 15.70878279763964258, -56.33456566391306808 ) ) ;
#64062 = CARTESIAN_POINT ( 'NONE',  ( 9.564922557960805705, 16.46253265017160317, 69.58224293864770971 ) ) ;
#64063 = CARTESIAN_POINT ( 'NONE',  ( 17.49999999999999645, -3.237210098469645470, 112.2123698737954243 ) ) ;
#64064 = CARTESIAN_POINT ( 'NONE',  ( -13.97604488694547697, 13.89961937509957934, 23.12609039468565442 ) ) ;
#64065 = CARTESIAN_POINT ( 'NONE',  ( 16.55341960407611168, 4.379528057220329451, 38.95724293864768839 ) ) ;
#64066 = CARTESIAN_POINT ( 'NONE',  ( -13.89961937509977652, 13.97604488694528158, 45.62390960531433848 ) ) ;
#64067 = CARTESIAN_POINT ( 'NONE',  ( -19.02544592524342804, 5.153800228976336051, 101.0405762719810241 ) ) ;
#64068 = CARTESIAN_POINT ( 'NONE',  ( -15.72974639402176322, -15.80617190586768395, 74.37609039468568994 ) ) ;
#64069 = CARTESIAN_POINT ( 'NONE',  ( -13.89961937509977652, 13.97604488694528158, 45.62390960531433848 ) ) ;
#64070 = CARTESIAN_POINT ( 'NONE',  ( 15.72974639402176855, 15.80617190586768217, 66.87609039468568994 ) ) ;
#64071 = CARTESIAN_POINT ( 'NONE',  ( 5.719274019375991003, -21.55341960407610458, 27.70724293864769905 ) ) ;
#64072 = CARTESIAN_POINT ( 'NONE',  ( -5.153800228976328057, -19.02544592524343514, 32.29057627198102409 ) ) ;
#64073 = CARTESIAN_POINT ( 'NONE',  ( -21.53943276465977519, -0.05219959533937600094, 28.75109039468567929 ) ) ;
#64074 = CARTESIAN_POINT ( 'NONE',  ( 16.46253265017146816, 9.564922557961045513, 46.66775706135233293 ) ) ;
#64075 = CARTESIAN_POINT ( 'NONE',  ( -16.51473224551069308, -9.474510206698971260, 26.66557627198103120 ) ) ;
#64076 = CARTESIAN_POINT ( 'NONE',  ( -16.46253265017160317, 9.564922557960807481, 75.83224293864769550 ) ) ;
#64077 = CARTESIAN_POINT ( 'NONE',  ( 5.153800228976615827, -19.02544592524334988, 105.2094237280190185 ) ) ;
#64078 = CARTESIAN_POINT ( 'NONE',  ( -4.379528057220328563, 16.55341960407611168, 75.20724293864769550 ) ) ;
#64079 = CARTESIAN_POINT ( 'NONE',  ( -0.05219959533907301413, -21.53943276465977519, 42.49890960531435979 ) ) ;
#64080 = CARTESIAN_POINT ( 'NONE',  ( -5.049401038297874678, -19.05341960407617918, 99.79275706135234714 ) ) ;
#64081 = CARTESIAN_POINT ( 'NONE',  ( 0.05219959533907565091, 21.53943276465977519, 109.9989096053143527 ) ) ;
#64082 = CARTESIAN_POINT ( 'NONE',  ( 5.719274019375673035, 21.55341960407619339, 62.29275706135236845 ) ) ;
#64084 = CARTESIAN_POINT ( 'NONE',  ( -4.379528057220086978, -16.55341960407618274, 49.79275706135234714 ) ) ;
#64083 = B_SPLINE_CURVE_WITH_KNOTS ( 'NONE', 3,
 ( #154783, #16280, #183149, #77932, #150831, #196355, #57823, #104316, #167971, #120464, #74967, #13302, #182156, #43640, #105303, #166991, #151811, #121457, #106286, #96089, #158750, #20239, #113243, #187141, #32441, #174934, #109270, #21246, #50598, #111260, #4071, #2092 ),
 .UNSPECIFIED., .F., .F.,
 ( 4, 2, 2, 2, 2, 2, 2, 2, 2, 2, 2, 2, 2, 2, 2, 4 ),
 ( 2.281672496420497865E-17, 0.0003712461730036943673, 0.0007424923460073658580, 0.001113738519011037457, 0.001484984692014708948, 0.002227477038022052363, 0.002598723211025727540, 0.002969969384029403584, 0.003341215557033078761, 0.003712461730036753938, 0.004083707903040429549, 0.004454954076044104726, 0.004826200249047780770, 0.005197446422051455947, 0.005568692595055131991, 0.005939938768058807168 ),
 .UNSPECIFIED. ) ;
#64085 = CARTESIAN_POINT ( 'NONE',  ( -12.06949235617739369, -12.14591786802326823, 49.37609039468569705 ) ) ;
#64086 = CARTESIAN_POINT ( 'NONE',  ( 5.719274019375991003, -21.55341960407610458, 67.70724293864769550 ) ) ;
#64087 = CARTESIAN_POINT ( 'NONE',  ( 5.049401038298161559, -19.05341960407611168, 42.70724293864767418 ) ) ;
#64088 = CARTESIAN_POINT ( 'NONE',  ( -8.224510206698735004, -14.34966873604973081, 79.58442372801903275 ) ) ;
#64089 = AXIS2_PLACEMENT_3D ( 'NONE', #198005, #137317, #1781 ) ;
#64090 = CARTESIAN_POINT ( 'NONE',  ( 10.72451020669898902, -18.67979575497178502, 102.9155762719810383 ) ) ;
#64091 = CARTESIAN_POINT ( 'NONE',  ( -12.06949235617756955, 12.14591786802309770, 55.62390960531436690 ) ) ;
#64092 = CARTESIAN_POINT ( 'NONE',  ( 16.46253265017160672, -9.564922557960803928, 68.33224293864770971 ) ) ;
#64093 = CARTESIAN_POINT ( 'NONE',  ( 4.483927247898790824, -16.52544592524335698, 75.20942372801901854 ) ) ;
#64094 = CARTESIAN_POINT ( 'NONE',  ( 14.34966873604972726, -8.224510206698740333, 20.83442372801901143 ) ) ;
#64095 = CARTESIAN_POINT ( 'NONE',  ( -21.53943276465977519, 0.05219959533907696930, 116.2489096053143669 ) ) ;
#64096 = CARTESIAN_POINT ( 'NONE',  ( 8.314922557960818139, 14.29746914071049879, 39.58224293864769550 ) ) ;
#64097 = ORIENTED_EDGE ( 'NONE', *, *, #51432, .T. ) ;
#64098 = CARTESIAN_POINT ( 'NONE',  ( -17.40861289038999971, 6.110651285853370140, 73.62767529172565162 ) ) ;
#64099 =( BOUNDED_CURVE ( )  B_SPLINE_CURVE ( 2, ( #1539, #139062, #185576, #199757, #197773, #170405, #91549, #30906, #60234, #137079, #119931, #123879, #181616 ),
 .UNSPECIFIED., .F., .T. ) 
 B_SPLINE_CURVE_WITH_KNOTS ( ( 3, 2, 2, 2, 2, 2, 3 ),
 ( 0.5551076951965037143, 0.5570175438596490780, 0.5614035087719297934, 0.5657894736842105088, 0.5701754385964912242, 0.5745614035087719396, 0.5765169319940076642 ),
 .UNSPECIFIED. ) 
 CURVE ( )  GEOMETRIC_REPRESENTATION_ITEM ( )  RATIONAL_B_SPLINE_CURVE ( ( 0.9832469066685283199, 0.9851625545550095620, 1.000000000000000000, 0.9659258262890683122, 1.000000000000000000, 0.9659258262890683122, 1.000000000000000000, 0.9659258262890683122, 1.000000000000000000, 0.9659258262890683122, 1.000000000000000000, 0.9848076720550078544, 0.9831626618144001517 ) ) 
 REPRESENTATION_ITEM ( '' )  );
#64100 = CARTESIAN_POINT ( 'NONE',  ( -10.81492255796078084, -18.62759615963271287, 87.08224293864769550 ) ) ;
#64101 = CARTESIAN_POINT ( 'NONE',  ( 14.34966873604960469, 8.224510206698951720, 24.16557627198103120 ) ) ;
#64102 = ORIENTED_EDGE ( 'NONE', *, *, #166008, .T. ) ;
#64103 = CARTESIAN_POINT ( 'NONE',  ( -17.44279575226823908, -5.990770900252486264, 54.16442432485681735 ) ) ;
#64104 = CARTESIAN_POINT ( 'NONE',  ( 0.05219959533907565091, 21.53943276465977519, 99.99890960531436690 ) ) ;
#64105 = CARTESIAN_POINT ( 'NONE',  ( 19.02544592524343514, -5.153800228976328945, 108.5405762719810383 ) ) ;
#64106 = CARTESIAN_POINT ( 'NONE',  ( -15.72974639402197994, 15.80617190586746368, 115.6239096053143669 ) ) ;
#64107 = CARTESIAN_POINT ( 'NONE',  ( 16.55341960407611168, 4.379528057220329451, 48.95724293864770971 ) ) ;
#64108 = CARTESIAN_POINT ( 'NONE',  ( -16.53943276465976808, -0.05219959533934237506, 48.75109039468568284 ) ) ;
#64109 = CARTESIAN_POINT ( 'NONE',  ( -5.049401038298153566, 19.05341960407611168, 55.20724293864769550 ) ) ;
#64110 = B_SPLINE_CURVE_WITH_KNOTS ( 'NONE', 3,
 ( #84064, #148763, #72930, #119424, #116413, #70919, #179114, #23414, #85062, #146744, #164935, #69917, #54741, #181108, #178103, #39571, #42582, #192266, #162918, #104245, #71911, #22414, #117416, #88068, #53748, #163940, #24427, #115422, #55742, #133583, #102252, #118428, #180121, #41589, #26428, #139531, #43571, #153717, #168875, #74900, #93028, #154716, #184067, #44564, #152719, #58725, #197263, #30380 ),
 .UNSPECIFIED., .F., .F.,
 ( 4, 2, 2, 2, 2, 2, 2, 2, 2, 2, 2, 2, 2, 2, 2, 2, 2, 2, 2, 2, 2, 2, 2, 4 ),
 ( 0.04104976116627316596, 0.04252145193039927329, 0.04325729731246233389, 0.04399314269452538756, 0.04472898807658844123, 0.04546483345865150183, 0.04693652422277762998, 0.04840821498690375813, 0.04914406036896680485, 0.04987990575102985852, 0.05135159651515595197, 0.05208744189721900564, 0.05282328727928205236, 0.05429497804340815276, 0.05503082342547122030, 0.05576666880753428784, 0.05723835957166042293, 0.05871005033578655802, 0.05944589571784963944, 0.06018174109991272780, 0.06165343186403891840, 0.06238927724610200676, 0.06312512262816510900, 0.06459681339229128572 ),
 .UNSPECIFIED. ) ;
#64111 = CARTESIAN_POINT ( 'NONE',  ( -13.89961937509957401, -13.97604488694547875, 54.37609039468565442 ) ) ;
#64112 = CARTESIAN_POINT ( 'NONE',  ( 16.46253265017160672, -9.564922557960803928, 83.33224293864768129 ) ) ;
#64113 = VERTEX_POINT ( 'NONE', #157218 ) ;
#64114 = CARTESIAN_POINT ( 'NONE',  ( -15.80617190586745835, -15.72974639402198527, 36.87390960531435979 ) ) ;
#64115 = CARTESIAN_POINT ( 'NONE',  ( -24.94166821950383195, -28.00113106727059176, -18.51304999530125173 ) ) ;
#64116 = CARTESIAN_POINT ( 'NONE',  ( -19.03943276465977164, 0.05219959533909376836, 46.24890960531435979 ) ) ;
#64117 = CARTESIAN_POINT ( 'NONE',  ( -19.05341960407617563, 5.049401038297882671, 113.5427570613523471 ) ) ;
#64118 = CARTESIAN_POINT ( 'NONE',  ( 9.474510206698729675, 16.51473224551082808, 62.08442372801899722 ) ) ;
#64119 = CARTESIAN_POINT ( 'NONE',  ( -15.80617190586745835, -15.72974639402198527, 101.8739096053143811 ) ) ;
#64120 = CARTESIAN_POINT ( 'NONE',  ( -4.379528057220328563, 16.55341960407611168, 35.20724293864768839 ) ) ;
#64121 = CARTESIAN_POINT ( 'NONE',  ( 0.05219959533909260263, 19.03943276465977164, 74.99890960531435269 ) ) ;
#64122 = CARTESIAN_POINT ( 'NONE',  ( -0.05219959533907301413, -21.53943276465977519, 62.49890960531436690 ) ) ;
#64124 = CARTESIAN_POINT ( 'NONE',  ( -16.52544592524335698, -4.483927247898792601, 23.95942372801901143 ) ) ;
#64123 = CARTESIAN_POINT ( 'NONE',  ( 0.05219959533907565091, 21.53943276465977519, 99.99890960531436690 ) ) ;
#64125 = CARTESIAN_POINT ( 'NONE',  ( -5.823673210054116645, -21.52544592524344225, 22.29057627198102765 ) ) ;
#64126 = CARTESIAN_POINT ( 'NONE',  ( -10.72451020669870658, -18.67979575497194134, 94.58442372801901854 ) ) ;
#64127 = CARTESIAN_POINT ( 'NONE',  ( -16.46253265017160317, 9.564922557960807481, 80.83224293864769550 ) ) ;
#64128 = CARTESIAN_POINT ( 'NONE',  ( 19.02544592524343514, -5.153800228976328945, 23.54057627198102054 ) ) ;
#64129 = CARTESIAN_POINT ( 'NONE',  ( -9.474510206698964154, 16.51473224551069663, 85.41557627198102409 ) ) ;
#64130 = CARTESIAN_POINT ( 'NONE',  ( -16.53943276465976808, 0.05219959533911058130, 111.2489096053143669 ) ) ;
#64131 = CARTESIAN_POINT ( 'NONE',  ( -0.05219959533909027116, -19.03943276465977164, 62.49890960531435979 ) ) ;
#64132 = CARTESIAN_POINT ( 'NONE',  ( 16.53943276465976808, 0.05219959533934440121, 26.25109039468567573 ) ) ;
#64133 = LINE ( 'NONE', #156137, #150848 ) ;
#64134 = EDGE_CURVE ( 'NONE', #133361, #12036, #187578, .T. ) ;
#64136 = CARTESIAN_POINT ( 'NONE',  ( -13.97604488694527625, -13.89961937509977652, 111.8739096053143243 ) ) ;
#64135 = CARTESIAN_POINT ( 'NONE',  ( 0.05219959533937995610, -21.53943276465977519, 100.0010903946857042 ) ) ;
#64137 = CARTESIAN_POINT ( 'NONE',  ( 12.14591786802327356, -12.06949235617739191, 85.62609039468568994 ) ) ;
#64138 = FACE_OUTER_BOUND ( 'NONE', #195502, .T. ) ;
#64139 = CARTESIAN_POINT ( 'NONE',  ( 5.153800228976615827, -19.02544592524334988, 70.20942372801899012 ) ) ;
#64140 = CARTESIAN_POINT ( 'NONE',  ( 5.049401038297881783, 19.05341960407617563, 37.29275706135232582 ) ) ;
#64141 = CARTESIAN_POINT ( 'NONE',  ( 11.49674612099286719, -25.26099202438251723, 140.0000000000000000 ) ) ;
#64142 = CARTESIAN_POINT ( 'NONE',  ( 16.51473224551069308, 9.474510206698969483, 34.16557627198102409 ) ) ;
#64143 = CARTESIAN_POINT ( 'NONE',  ( -12.14591786802309592, -12.06949235617757132, 36.87390960531435979 ) ) ;
#64144 = DIRECTION ( 'NONE',  ( -1.000000000000000000, -0.000000000000000000, -0.000000000000000000 ) ) ;
#64145 = CARTESIAN_POINT ( 'NONE',  ( 14.34966873604972726, -8.224510206698740333, 110.8344237280190043 ) ) ;
#64146 = CARTESIAN_POINT ( 'NONE',  ( 16.38665767535055551, 7.295008042176072571, 67.23599135785453029 ) ) ;
#64147 = CARTESIAN_POINT ( 'NONE',  ( -14.34966873604972548, 8.224510206698743886, 83.33442372801903275 ) ) ;
#64148 = CARTESIAN_POINT ( 'NONE',  ( -16.51473224551069308, -9.474510206698971260, 36.66557627198102409 ) ) ;
#64149 = CARTESIAN_POINT ( 'NONE',  ( 10.81492255796106328, -18.62759615963255655, 100.4177570613523471 ) ) ;
#64150 = CARTESIAN_POINT ( 'NONE',  ( 9.474510206698729675, 16.51473224551082808, 97.08442372801900433 ) ) ;
#64151 = CARTESIAN_POINT ( 'NONE',  ( -0.05219959533937732626, 21.53943276465977519, 77.50109039468567573 ) ) ;
#64152 = CARTESIAN_POINT ( 'NONE',  ( -13.89961937509957401, -13.97604488694547875, 59.37609039468566863 ) ) ;
#64153 = CARTESIAN_POINT ( 'NONE',  ( 19.05341960407611168, 5.049401038298154454, 98.95724293864766707 ) ) ;
#64154 = CARTESIAN_POINT ( 'NONE',  ( -13.97604488694527625, -13.89961937509977652, 66.87390960531436690 ) ) ;
#64155 = CARTESIAN_POINT ( 'NONE',  ( 0.000000000000000000, -165.0000000000000000, -23.00000000000000000 ) ) ;
#64156 = CARTESIAN_POINT ( 'NONE',  ( -12.06949235617756955, 12.14591786802309770, 65.62390960531436690 ) ) ;
#64157 = CARTESIAN_POINT ( 'NONE',  ( 18.62759615963271287, -10.81492255796078972, 63.33224293864770260 ) ) ;
#64158 = CARTESIAN_POINT ( 'NONE',  ( -9.474510206698964154, 16.51473224551069663, 50.41557627198102409 ) ) ;
#64160 = CARTESIAN_POINT ( 'NONE',  ( 16.53943276465976808, 0.05219959533934440121, 71.25109039468568994 ) ) ;
#64159 = CARTESIAN_POINT ( 'NONE',  ( 5.719274019375991003, -21.55341960407610458, 87.70724293864769550 ) ) ;
#64161 = ORIENTED_EDGE ( 'NONE', *, *, #24639, .T. ) ;
#64162 = CARTESIAN_POINT ( 'NONE',  ( 19.02544592524343514, -5.153800228976328945, 43.54057627198103120 ) ) ;
#64164 = CARTESIAN_POINT ( 'NONE',  ( -29.86685920354755197, -21.69954338932560134, -6.424999997268812990 ) ) ;
#64163 = CARTESIAN_POINT ( 'NONE',  ( 8.314922557960818139, 14.29746914071049879, 84.58224293864769550 ) ) ;
#64165 = CARTESIAN_POINT ( 'NONE',  ( 16.51473224551069308, 9.474510206698969483, 54.16557627198103120 ) ) ;
#64166 = CARTESIAN_POINT ( 'NONE',  ( -0.05219959533909027116, -19.03943276465977164, 22.49890960531436690 ) ) ;
#64167 = CARTESIAN_POINT ( 'NONE',  ( -5.049401038297874678, -19.05341960407617918, 69.79275706135233293 ) ) ;
#64168 = CARTESIAN_POINT ( 'NONE',  ( -14.29746914071049879, 8.314922557960819915, 70.83224293864770971 ) ) ;
#64169 = CARTESIAN_POINT ( 'NONE',  ( -21.55341960407619339, 5.719274019375674811, 43.54275706135235424 ) ) ;
#64171 = CARTESIAN_POINT ( 'NONE',  ( -18.67979575497178146, -10.72451020669898902, 101.6655762719810383 ) ) ;
#64170 = CARTESIAN_POINT ( 'NONE',  ( 16.51473224551069308, 9.474510206698969483, 39.16557627198103120 ) ) ;
#64172 = CARTESIAN_POINT ( 'NONE',  ( -17.50000000000000000, -5.499999999999992895, 37.50000000000000000 ) ) ;
#64173 = CARTESIAN_POINT ( 'NONE',  ( 4.483927247898545687, 16.52544592524342804, 84.79057627198102409 ) ) ;
#64174 = CARTESIAN_POINT ( 'NONE',  ( 27.53771902582990450, -28.32105632907330062, -18.50180672658675363 ) ) ;
#64175 = CARTESIAN_POINT ( 'NONE',  ( -16.46253265017160317, 9.564922557960807481, 40.83224293864769550 ) ) ;
#64176 = CARTESIAN_POINT ( 'NONE',  ( 17.05116617787822975, 6.768360034955811955, 113.8432444674080557 ) ) ;
#64177 = CARTESIAN_POINT ( 'NONE',  ( -19.03943276465977164, -0.05219959533935918106, 88.75109039468567573 ) ) ;
#64178 = CARTESIAN_POINT ( 'NONE',  ( -5.823673210054431948, 21.52544592524334988, 42.70942372801901854 ) ) ;
#64179 = CARTESIAN_POINT ( 'NONE',  ( -0.05219959533909027116, -19.03943276465977164, 77.49890960531435269 ) ) ;
#64180 = CARTESIAN_POINT ( 'NONE',  ( 13.97604488694548053, -13.89961937509957401, 70.62609039468567573 ) ) ;
#64181 = CARTESIAN_POINT ( 'NONE',  ( 5.153800228976335163, 19.02544592524342804, 39.79057627198100988 ) ) ;
#64182 = CARTESIAN_POINT ( 'NONE',  ( -14.29746914071049879, 8.314922557960819915, 65.83224293864769550 ) ) ;
#64183 = CARTESIAN_POINT ( 'NONE',  ( 0.05219959533910956823, 16.53943276465976808, 64.99890960531435269 ) ) ;
#64184 = CARTESIAN_POINT ( 'NONE',  ( -13.89961937509977652, 13.97604488694528158, 70.62390960531432427 ) ) ;
#64185 = CARTESIAN_POINT ( 'NONE',  ( -0.05219959533907301413, -21.53943276465977519, 97.49890960531436690 ) ) ;
#64186 = CARTESIAN_POINT ( 'NONE',  ( 13.89961937509977652, -13.97604488694527269, 73.12390960531436690 ) ) ;
#64187 = CARTESIAN_POINT ( 'NONE',  ( -15.80617190586768217, 15.72974639402176855, 108.1260903946856757 ) ) ;
#64190 = CARTESIAN_POINT ( 'NONE',  ( 14.34966873604960469, 8.224510206698951720, 109.1655762719810383 ) ) ;
#64189 = CARTESIAN_POINT ( 'NONE',  ( -12.14591786802309592, -12.06949235617757132, 21.87390960531436690 ) ) ;
#64188 = CARTESIAN_POINT ( 'NONE',  ( 19.02544592524343514, -5.153800228976328945, 33.54057627198102409 ) ) ;
#64191 = CARTESIAN_POINT ( 'NONE',  ( -13.89961937509957401, -13.97604488694547875, 99.37609039468567573 ) ) ;
#64192 = ORIENTED_EDGE ( 'NONE', *, *, #37197, .F. ) ;
#64193 = CARTESIAN_POINT ( 'NONE',  ( 21.55341960407619695, -5.719274019375665929, 36.04275706135234714 ) ) ;
#64194 = CARTESIAN_POINT ( 'NONE',  ( -19.02544592524334988, -5.153800228976617603, 53.95942372801898301 ) ) ;
#64195 = CARTESIAN_POINT ( 'NONE',  ( -16.53943276465976808, -0.05219959533934237506, 113.7510903946856757 ) ) ;
#64196 = CARTESIAN_POINT ( 'NONE',  ( 5.823673210054125526, 21.52544592524343514, 74.79057627198105251 ) ) ;
#64197 = CARTESIAN_POINT ( 'NONE',  ( 10.72451020669898902, -18.67979575497178502, 22.91557627198102765 ) ) ;
#64198 = CARTESIAN_POINT ( 'NONE',  ( 4.483927247898545687, 16.52544592524342804, 54.79057627198104541 ) ) ;
#64199 = CARTESIAN_POINT ( 'NONE',  ( -19.02544592524342804, 5.153800228976336051, 36.04057627198100988 ) ) ;
#64200 = CARTESIAN_POINT ( 'NONE',  ( -13.89961937509977652, 13.97604488694528158, 35.62390960531435269 ) ) ;
#64201 = CARTESIAN_POINT ( 'NONE',  ( -19.03943276465977164, -0.05219959533935918106, 33.75109039468566863 ) ) ;
#64202 = CARTESIAN_POINT ( 'NONE',  ( 4.483927247898790824, -16.52544592524335698, 90.20942372801903275 ) ) ;
#64203 = CARTESIAN_POINT ( 'NONE',  ( -12.06949235617739369, -12.14591786802326823, 49.37609039468569705 ) ) ;
#64204 = CARTESIAN_POINT ( 'NONE',  ( 21.55341960407610458, 5.719274019375980345, 23.95724293864769550 ) ) ;
#64206 = CARTESIAN_POINT ( 'NONE',  ( 21.53943276465977519, 0.05219959533937863772, 91.25109039468568994 ) ) ;
#64205 = CARTESIAN_POINT ( 'NONE',  ( 9.474510206698971260, -16.51473224551069308, 57.91557627198103120 ) ) ;
#64207 = CARTESIAN_POINT ( 'NONE',  ( -5.049401038298153566, 19.05341960407611168, 85.20724293864766707 ) ) ;
#64208 = CARTESIAN_POINT ( 'NONE',  ( -8.314922557961024197, 14.29746914071037800, 62.91775706135236135 ) ) ;
#64209 = CARTESIAN_POINT ( 'NONE',  ( 16.55341960407611168, 4.379528057220329451, 108.9572429386476955 ) ) ;
#64210 = ADVANCED_FACE ( 'NONE', ( #186586 ), #42345, .T. ) ;
#64211 = CARTESIAN_POINT ( 'NONE',  ( -4.483927247898539470, -16.52544592524342804, 27.29057627198103120 ) ) ;
#64212 = DIRECTION ( 'NONE',  ( 0.4999999999999945599, -0.5000000000000066613, -0.7071067811865467956 ) ) ;
#64215 = CARTESIAN_POINT ( 'NONE',  ( -19.03943276465977164, 0.05219959533909376836, 76.24890960531435269 ) ) ;
#64214 = CARTESIAN_POINT ( 'NONE',  ( 5.153800228976335163, 19.02544592524342804, 94.79057627198103830 ) ) ;
#64213 = CARTESIAN_POINT ( 'NONE',  ( 15.80617190586769283, -15.72974639402175789, 70.62609039468567573 ) ) ;
#64216 = CARTESIAN_POINT ( 'NONE',  ( -13.97604488694527625, -13.89961937509977652, 111.8739096053143243 ) ) ;
#64217 = CARTESIAN_POINT ( 'NONE',  ( -16.52544592524342804, 4.483927247898546575, 61.04057627198103120 ) ) ;
#64218 = CARTESIAN_POINT ( 'NONE',  ( -14.29746914071037622, -8.314922557961029526, 109.1677570613523613 ) ) ;
#64219 = VERTEX_POINT ( 'NONE', #43331 ) ;
#64220 = CARTESIAN_POINT ( 'NONE',  ( -16.55341960407611168, -4.379528057220339221, 41.45724293864769550 ) ) ;
#64222 = CARTESIAN_POINT ( 'NONE',  ( -2.552343178074577779, 7.052343178074668373, 1.110912703473986074 ) ) ;
#64221 = CARTESIAN_POINT ( 'NONE',  ( -8.224510206698735004, -14.34966873604973081, 39.58442372801901143 ) ) ;
#64223 = CARTESIAN_POINT ( 'NONE',  ( -19.03943276465977164, -0.05219959533935918106, 33.75109039468566863 ) ) ;
#64224 = CARTESIAN_POINT ( 'NONE',  ( 5.049401038298161559, -19.05341960407611168, 82.70724293864770971 ) ) ;
#64225 = CARTESIAN_POINT ( 'NONE',  ( -19.02544592524334988, -5.153800228976617603, 53.95942372801898301 ) ) ;
#64226 = CARTESIAN_POINT ( 'NONE',  ( -5.950531402560715689E-15, 38.81732327939063509, -9.624999997268815832 ) ) ;
#64227 = DIRECTION ( 'NONE',  ( 1.000000000000000000, 0.000000000000000000, 0.000000000000000000 ) ) ;
#64229 = CARTESIAN_POINT ( 'NONE',  ( 8.224510206698742110, 14.34966873604972548, 82.08442372801901854 ) ) ;
#64228 = CARTESIAN_POINT ( 'NONE',  ( 16.51473224551083163, -9.474510206698727899, 85.83442372801900433 ) ) ;
#64230 = CARTESIAN_POINT ( 'NONE',  ( -19.03943276465977164, 0.05219959533909376836, 26.24890960531435624 ) ) ;
#64231 = CARTESIAN_POINT ( 'NONE',  ( 16.51473224551069308, 9.474510206698969483, 99.16557627198102409 ) ) ;
#64232 = CARTESIAN_POINT ( 'NONE',  ( 10.81492255796106328, -18.62759615963255655, 45.41775706135234003 ) ) ;
#64233 = CARTESIAN_POINT ( 'NONE',  ( 19.03943276465977164, 0.05219959533936151252, 96.25109039468567573 ) ) ;
#64235 = CARTESIAN_POINT ( 'NONE',  ( 19.03943276465977164, -0.05219959533909143690, 53.74890960531436690 ) ) ;
#64234 = DIRECTION ( 'NONE',  ( 6.391086490440868450E-16, -1.000000000000000000, 0.000000000000000000 ) ) ;
#64236 = CARTESIAN_POINT ( 'NONE',  ( -19.03943276465977164, 0.05219959533909376836, 106.2489096053143669 ) ) ;
#64238 = CARTESIAN_POINT ( 'NONE',  ( 9.474510206698971260, -16.51473224551069308, 52.91557627198102409 ) ) ;
#64237 = CARTESIAN_POINT ( 'NONE',  ( 4.379528057220339221, -16.55341960407611168, 67.70724293864769550 ) ) ;
#64239 = CARTESIAN_POINT ( 'NONE',  ( -13.97604488694527625, -13.89961937509977652, 61.87390960531435979 ) ) ;
#64240 = CARTESIAN_POINT ( 'NONE',  ( 0.05219959533936267826, -19.03943276465977164, 60.00109039468566863 ) ) ;
#64241 = CARTESIAN_POINT ( 'NONE',  ( 19.03943276465977164, 0.05219959533936151252, 31.25109039468566863 ) ) ;
#64242 = CARTESIAN_POINT ( 'NONE',  ( 9.474510206698971260, -16.51473224551069308, 62.91557627198102409 ) ) ;
#64243 = CARTESIAN_POINT ( 'NONE',  ( 15.72974639402199770, -15.80617190586745480, 73.12390960531436690 ) ) ;
#64245 = CARTESIAN_POINT ( 'NONE',  ( 19.02544592524334988, 5.153800228976608722, 36.45942372801900433 ) ) ;
#64244 = CARTESIAN_POINT ( 'NONE',  ( -4.483927247898539470, -16.52544592524342804, 62.29057627198102409 ) ) ;
#64246 = CARTESIAN_POINT ( 'NONE',  ( -18.67979575497178146, -10.72451020669898902, 51.66557627198102409 ) ) ;
#64247 = CARTESIAN_POINT ( 'NONE',  ( -18.62759615963270932, 10.81492255796079327, 35.83224293864768839 ) ) ;
#64248 = CARTESIAN_POINT ( 'NONE',  ( 5.153800228976335163, 19.02544592524342804, 59.79057627198100988 ) ) ;
#64249 = CARTESIAN_POINT ( 'NONE',  ( 13.89961937509977652, -13.97604488694527269, 43.12390960531434558 ) ) ;
#64250 = CARTESIAN_POINT ( 'NONE',  ( 0.05219959533910956823, 16.53943276465976808, 94.99890960531436690 ) ) ;
#64251 = CARTESIAN_POINT ( 'NONE',  ( 0.05219959533907565091, 21.53943276465977519, 104.9989096053143669 ) ) ;
#64252 = CARTESIAN_POINT ( 'NONE',  ( 9.564922557960805705, 16.46253265017160317, 109.5822429386476955 ) ) ;
#64253 = CARTESIAN_POINT ( 'NONE',  ( 18.67979575497194134, -10.72451020669871369, 25.83442372801901499 ) ) ;
#64254 = CARTESIAN_POINT ( 'NONE',  ( 9.564922557960805705, 16.46253265017160317, 39.58224293864768839 ) ) ;
#64255 = CARTESIAN_POINT ( 'NONE',  ( 5.719274019375991003, -21.55341960407610458, 107.7072429386476955 ) ) ;
#64256 = CARTESIAN_POINT ( 'NONE',  ( -16.46253265017146816, -9.564922557961047289, 49.16775706135233293 ) ) ;
#64257 = CARTESIAN_POINT ( 'NONE',  ( -13.89961937509977652, 13.97604488694528158, 25.62390960531434558 ) ) ;
#64258 = CARTESIAN_POINT ( 'NONE',  ( 18.87075004821566182, -5.500000000000074607, 76.17408112101045958 ) ) ;
#64259 =( NAMED_UNIT ( * ) PLANE_ANGLE_UNIT ( ) SI_UNIT ( $, .RADIAN. ) );
#64260 = CARTESIAN_POINT ( 'NONE',  ( -4.483927247898782831, 16.52544592524335698, 52.70942372801902565 ) ) ;
#64261 = CARTESIAN_POINT ( 'NONE',  ( 19.05341960407611168, 5.049401038298154454, 23.95724293864769194 ) ) ;
#64262 = CARTESIAN_POINT ( 'NONE',  ( 34.40553910806574578, -2.436532241128160692, 90.06585364601157551 ) ) ;
#64263 = CARTESIAN_POINT ( 'NONE',  ( 13.89961937509977652, -13.97604488694527269, 68.12390960531436690 ) ) ;
#64264 = CARTESIAN_POINT ( 'NONE',  ( 4.379528057220339221, -16.55341960407611168, 107.7072429386476955 ) ) ;
#64265 = CARTESIAN_POINT ( 'NONE',  ( -21.52544592524343514, 5.823673210054127303, 41.04057627198103120 ) ) ;
#64266 = CARTESIAN_POINT ( 'NONE',  ( 8.314922557960818139, 14.29746914071049879, 79.58224293864769550 ) ) ;
#64267 = CARTESIAN_POINT ( 'NONE',  ( -8.314922557961024197, 14.29746914071037800, 37.91775706135235424 ) ) ;
#64268 = CARTESIAN_POINT ( 'NONE',  ( -5.823673210054431948, 21.52544592524334988, 87.70942372801901854 ) ) ;
#64269 = CARTESIAN_POINT ( 'NONE',  ( -19.05341960407611168, -5.049401038298163336, 31.45724293864769550 ) ) ;
#64270 = CARTESIAN_POINT ( 'NONE',  ( -14.34966873604972548, 8.224510206698743886, 113.3344237280190328 ) ) ;
#64271 = CARTESIAN_POINT ( 'NONE',  ( -16.52544592524342804, 4.483927247898546575, 61.04057627198103120 ) ) ;
#64272 = CARTESIAN_POINT ( 'NONE',  ( 9.564922557960805705, 16.46253265017160317, 54.58224293864769550 ) ) ;
#64273 = CARTESIAN_POINT ( 'NONE',  ( -21.53943276465977519, -0.05219959533937600094, 93.75109039468567573 ) ) ;
#64274 = CARTESIAN_POINT ( 'NONE',  ( 21.55341960407610458, 5.719274019375980345, 113.9572429386477239 ) ) ;
#64275 = CARTESIAN_POINT ( 'NONE',  ( 18.67979575497194134, -10.72451020669871369, 70.83442372801901854 ) ) ;
#64276 = CARTESIAN_POINT ( 'NONE',  ( -4.379528057220086978, -16.55341960407618274, 44.79275706135234714 ) ) ;
#64278 = CARTESIAN_POINT ( 'NONE',  ( 18.62759615963255655, 10.81492255796105972, 86.66775706135234714 ) ) ;
#64277 = CARTESIAN_POINT ( 'NONE',  ( 0.05219959533910956823, 16.53943276465976808, 84.99890960531436690 ) ) ;
#64279 = CARTESIAN_POINT ( 'NONE',  ( -14.34966873604972548, 8.224510206698743886, 113.3344237280190328 ) ) ;
#64280 = CARTESIAN_POINT ( 'NONE',  ( -17.50000000000000000, 5.624438216177581218, 115.8167034491465017 ) ) ;
#64281 = CARTESIAN_POINT ( 'NONE',  ( 0.05219959533934541429, -16.53943276465976808, 40.00109039468567573 ) ) ;
#64282 = CARTESIAN_POINT ( 'NONE',  ( -12.14591786802309592, -12.06949235617757132, 41.87390960531435979 ) ) ;
#64283 = CARTESIAN_POINT ( 'NONE',  ( 12.14591786802327356, -12.06949235617739191, 85.62609039468568994 ) ) ;
#64284 = CARTESIAN_POINT ( 'NONE',  ( 16.46253265017160672, -9.564922557960803928, 103.3322429386476955 ) ) ;
#64285 = CARTESIAN_POINT ( 'NONE',  ( 16.51473224551069308, 9.474510206698969483, 94.16557627198103830 ) ) ;
#64286 = CARTESIAN_POINT ( 'NONE',  ( -18.67979575497193778, 10.72451020669871902, 98.33442372801901854 ) ) ;
#64287 = CARTESIAN_POINT ( 'NONE',  ( -0.05219959533934338120, 16.53943276465976808, 97.50109039468567573 ) ) ;
#64288 = CARTESIAN_POINT ( 'NONE',  ( 8.314922557960818139, 14.29746914071049879, 69.58224293864769550 ) ) ;
#64289 = CARTESIAN_POINT ( 'NONE',  ( 9.474510206698971260, -16.51473224551069308, 82.91557627198103830 ) ) ;
#64290 = VERTEX_POINT ( 'NONE', #171397 ) ;
#64291 = CARTESIAN_POINT ( 'NONE',  ( 8.224510206698742110, 14.34966873604972548, 27.08442372801901854 ) ) ;
#64292 = CARTESIAN_POINT ( 'NONE',  ( 13.97604488694527802, 13.89961937509977652, 34.37390960531436690 ) ) ;
#64293 = CARTESIAN_POINT ( 'NONE',  ( 13.97604488694527802, 13.89961937509977652, 89.37390960531436690 ) ) ;
#64295 = CARTESIAN_POINT ( 'NONE',  ( 17.72662750342725602, 5.500000000000080824, 68.90179492283743912 ) ) ;
#64294 = CARTESIAN_POINT ( 'NONE',  ( -16.53943276465976808, -0.05219959533934237506, 28.75109039468567929 ) ) ;
#64296 = CARTESIAN_POINT ( 'NONE',  ( 13.89961937509957401, 13.97604488694547697, 41.87609039468566152 ) ) ;
#64297 = CARTESIAN_POINT ( 'NONE',  ( 8.314922557961029526, -14.29746914071037800, 95.41775706135234714 ) ) ;
#64298 = CARTESIAN_POINT ( 'NONE',  ( -5.153800228976607833, 19.02544592524334988, 107.7094237280189759 ) ) ;
#64299 = CARTESIAN_POINT ( 'NONE',  ( 9.564922557960805705, 16.46253265017160317, 29.58224293864769550 ) ) ;
#64300 = CARTESIAN_POINT ( 'NONE',  ( 16.55341960407618274, -4.379528057220086978, 86.04275706135236135 ) ) ;
#64301 = CARTESIAN_POINT ( 'NONE',  ( 12.06949235617739724, 12.14591786802326823, 61.87609039468568284 ) ) ;
#64302 = CARTESIAN_POINT ( 'NONE',  ( 0.05219959533909260263, 19.03943276465977164, 24.99890960531435269 ) ) ;
#64303 = CARTESIAN_POINT ( 'NONE',  ( -19.03943276465977164, -0.05219959533935918106, 63.75109039468566863 ) ) ;
#64304 = CARTESIAN_POINT ( 'NONE',  ( -10.72451020669870658, -18.67979575497194134, 109.5844237280190328 ) ) ;
#64305 = CARTESIAN_POINT ( 'NONE',  ( 9.564922557960805705, 16.46253265017160317, 49.58224293864770260 ) ) ;
#64306 = CARTESIAN_POINT ( 'NONE',  ( 19.05341960407611168, 5.049401038298154454, 88.95724293864769550 ) ) ;
#64307 = CARTESIAN_POINT ( 'NONE',  ( 16.53943276465976808, -0.05219959533910856209, 83.74890960531435269 ) ) ;
#64308 = CARTESIAN_POINT ( 'NONE',  ( 13.97604488694548053, -13.89961937509957401, 60.62609039468564731 ) ) ;
#64309 = CARTESIAN_POINT ( 'NONE',  ( 5.823673210054125526, 21.52544592524343514, 49.79057627198102409 ) ) ;
#64310 = CARTESIAN_POINT ( 'NONE',  ( -21.52544592524334988, -5.823673210054445271, 108.9594237280190185 ) ) ;
#64311 = CARTESIAN_POINT ( 'NONE',  ( -13.89961937509977652, 13.97604488694528158, 90.62390960531432427 ) ) ;
#64312 = CARTESIAN_POINT ( 'NONE',  ( 16.51473224551083163, -9.474510206698727899, 30.83442372801900433 ) ) ;
#64313 = CARTESIAN_POINT ( 'NONE',  ( -15.72974639402197994, 15.80617190586746368, 60.62390960531437401 ) ) ;
#64314 = CARTESIAN_POINT ( 'NONE',  ( -9.564922557960796823, -16.46253265017161027, 112.0822429386476955 ) ) ;
#64315 = CARTESIAN_POINT ( 'NONE',  ( 5.153800228976615827, -19.02544592524334988, 85.20942372801900433 ) ) ;
#64316 = CARTESIAN_POINT ( 'NONE',  ( -2.300691058039471937, -7.143419655154863435, 8.646741581399126630 ) ) ;
#64317 = CARTESIAN_POINT ( 'NONE',  ( 0.05219959533936267826, -19.03943276465977164, 110.0010903946856757 ) ) ;
#64318 = CARTESIAN_POINT ( 'NONE',  ( 4.483927247898545687, 16.52544592524342804, 109.7905762719810383 ) ) ;
#64319 = CARTESIAN_POINT ( 'NONE',  ( 5.153800228976335163, 19.02544592524342804, 99.79057627198102409 ) ) ;
#64320 = CARTESIAN_POINT ( 'NONE',  ( -0.05219959533907301413, -21.53943276465977519, 72.49890960531435269 ) ) ;
#64321 = AXIS2_PLACEMENT_3D ( 'NONE', #113127, #141492, #81773 ) ;
#64322 = CARTESIAN_POINT ( 'NONE',  ( 14.29746914071037800, 8.314922557961029526, 41.66775706135235424 ) ) ;
#64323 = CARTESIAN_POINT ( 'NONE',  ( 18.62759615963255655, 10.81492255796105972, 41.66775706135235424 ) ) ;
#64324 = CARTESIAN_POINT ( 'NONE',  ( -5.823673210054431948, 21.52544592524334988, 97.70942372801904696 ) ) ;
#64325 = CARTESIAN_POINT ( 'NONE',  ( 4.483927247898790824, -16.52544592524335698, 95.20942372801903275 ) ) ;
#64326 = CARTESIAN_POINT ( 'NONE',  ( 0.05219959533909260263, 19.03943276465977164, 89.99890960531436690 ) ) ;
#64327 = CARTESIAN_POINT ( 'NONE',  ( 16.53943276465976808, -0.05219959533910856209, 88.74890960531436690 ) ) ;
#64328 = CARTESIAN_POINT ( 'NONE',  ( 0.05219959533910956823, 16.53943276465976808, 34.99890960531435979 ) ) ;
#64329 = CARTESIAN_POINT ( 'NONE',  ( -5.049401038297874678, -19.05341960407617918, 69.79275706135233293 ) ) ;
#64330 = CARTESIAN_POINT ( 'NONE',  ( 18.62759615963255655, 10.81492255796105972, 41.66775706135235424 ) ) ;
#64331 = CARTESIAN_POINT ( 'NONE',  ( 13.97604488694548053, -13.89961937509957401, 25.62609039468566507 ) ) ;
#64332 = CARTESIAN_POINT ( 'NONE',  ( -0.05219959533910754901, -16.53943276465976808, 92.49890960531436690 ) ) ;
#64333 = CARTESIAN_POINT ( 'NONE',  ( 19.05341960407611168, 5.049401038298154454, 113.9572429386477097 ) ) ;
#64334 = CARTESIAN_POINT ( 'NONE',  ( 8.224510206698742110, 14.34966873604972548, 112.0844237280190185 ) ) ;
#64335 = CARTESIAN_POINT ( 'NONE',  ( 5.719274019375673035, 21.55341960407619339, 87.29275706135236135 ) ) ;
#64336 = CARTESIAN_POINT ( 'NONE',  ( 16.53943276465976808, 0.05219959533934440121, 61.25109039468567573 ) ) ;
#64337 = CARTESIAN_POINT ( 'NONE',  ( -4.483927247898782831, 16.52544592524335698, 102.7094237280190185 ) ) ;
#64338 = CARTESIAN_POINT ( 'NONE',  ( -15.80617190586768217, 15.72974639402176855, 53.12609039468568284 ) ) ;
#64339 = ORIENTED_EDGE ( 'NONE', *, *, #15073, .F. ) ;
#64340 = CARTESIAN_POINT ( 'NONE',  ( 18.62759615963255655, 10.81492255796105972, 31.66775706135234358 ) ) ;
#64341 = CARTESIAN_POINT ( 'NONE',  ( -4.379528057220328563, 16.55341960407611168, 110.2072429386477239 ) ) ;
#64342 = CARTESIAN_POINT ( 'NONE',  ( -9.564922557960796823, -16.46253265017161027, 22.08224293864768839 ) ) ;
#64343 = CARTESIAN_POINT ( 'NONE',  ( 4.483927247898545687, 16.52544592524342804, 59.79057627198103120 ) ) ;
#64344 = CARTESIAN_POINT ( 'NONE',  ( -9.474510206698964154, 16.51473224551069663, 75.41557627198103830 ) ) ;
#64345 = CARTESIAN_POINT ( 'NONE',  ( -8.314922557961024197, 14.29746914071037800, 107.9177570613523471 ) ) ;
#64346 = CARTESIAN_POINT ( 'NONE',  ( -0.05219959533909027116, -19.03943276465977164, 37.49890960531436690 ) ) ;
#64347 = CARTESIAN_POINT ( 'NONE',  ( -21.53943276465977519, 0.05219959533907696930, 51.24890960531436690 ) ) ;
#64348 = CARTESIAN_POINT ( 'NONE',  ( -8.314922557960811034, -14.29746914071050412, 97.08224293864770971 ) ) ;
#64349 = CARTESIAN_POINT ( 'NONE',  ( -10.81492255796078084, -18.62759615963271287, 92.08224293864769550 ) ) ;
#64350 = CARTESIAN_POINT ( 'NONE',  ( 5.153800228976335163, 19.02544592524342804, 94.79057627198103830 ) ) ;
#64352 = CARTESIAN_POINT ( 'NONE',  ( 16.51473224551083163, -9.474510206698727899, 95.83442372801900433 ) ) ;
#64351 = CARTESIAN_POINT ( 'NONE',  ( -13.89961937509977652, 13.97604488694528158, 55.62390960531434558 ) ) ;
#64353 = CARTESIAN_POINT ( 'NONE',  ( 15.80617190586746368, 15.72974639402197994, 49.37390960531436690 ) ) ;
#64354 = CARTESIAN_POINT ( 'NONE',  ( -21.52544592524334988, -5.823673210054445271, 68.95942372801901854 ) ) ;
#64355 = CARTESIAN_POINT ( 'NONE',  ( -19.02544592524342804, 5.153800228976336051, 56.04057627198100988 ) ) ;
#64356 = CARTESIAN_POINT ( 'NONE',  ( -0.05219959533909027116, -19.03943276465977164, 87.49890960531436690 ) ) ;
#64357 = CARTESIAN_POINT ( 'NONE',  ( 0.05219959533934541429, -16.53943276465976808, 65.00109039468568994 ) ) ;
#64358 = CARTESIAN_POINT ( 'NONE',  ( -15.72974639402176322, -15.80617190586768395, 49.37609039468569705 ) ) ;
#64359 = CARTESIAN_POINT ( 'NONE',  ( -15.80617190586768217, 15.72974639402176855, 88.12609039468570415 ) ) ;
#64360 = CARTESIAN_POINT ( 'NONE',  ( -21.55341960407610458, -5.719274019375992779, 101.4572429386476955 ) ) ;
#64362 = CARTESIAN_POINT ( 'NONE',  ( 12.14591786802327356, -12.06949235617739191, 65.62609039468568994 ) ) ;
#64361 = CARTESIAN_POINT ( 'NONE',  ( 21.52544592524334988, 5.823673210054432836, 31.45942372801901854 ) ) ;
#64363 = CARTESIAN_POINT ( 'NONE',  ( 10.72451020669898902, -18.67979575497178502, 62.91557627198102409 ) ) ;
#64364 = CARTESIAN_POINT ( 'NONE',  ( -16.51473224551082808, 9.474510206698731452, 33.33442372801899722 ) ) ;
#64366 = CARTESIAN_POINT ( 'NONE',  ( 14.34966873604960469, 8.224510206698951720, 29.16557627198103120 ) ) ;
#64365 = CARTESIAN_POINT ( 'NONE',  ( -13.97604488694527625, -13.89961937509977652, 61.87390960531435979 ) ) ;
#64367 = CARTESIAN_POINT ( 'NONE',  ( 38.00000000000000000, -12.34694845685040754, -5.099999999999999645 ) ) ;
#64368 = CARTESIAN_POINT ( 'NONE',  ( -9.474510206698964154, 16.51473224551069663, 105.4155762719810383 ) ) ;
#64369 = DIRECTION ( 'NONE',  ( 0.000000000000000000, -0.8164965809277253683, 0.5773502691896268413 ) ) ;
#64370 = ADVANCED_FACE ( 'NONE', ( #32884 ), #58495, .T. ) ;
#64371 = CARTESIAN_POINT ( 'NONE',  ( -19.02544592524334988, -5.153800228976617603, 83.95942372801901854 ) ) ;
#64372 = CARTESIAN_POINT ( 'NONE',  ( 21.55341960407610458, 5.719274019375980345, 53.95724293864770260 ) ) ;
#64373 = CARTESIAN_POINT ( 'NONE',  ( -14.34966873604960291, -8.224510206698953496, 36.66557627198103120 ) ) ;
#64374 = CARTESIAN_POINT ( 'NONE',  ( 16.55341960407618274, -4.379528057220086978, 21.04275706135234714 ) ) ;
#64375 = CARTESIAN_POINT ( 'NONE',  ( -16.51473224551069308, -9.474510206698971260, 31.66557627198102054 ) ) ;
#64376 = CARTESIAN_POINT ( 'NONE',  ( 4.483927247898790824, -16.52544592524335698, 20.20942372801900788 ) ) ;
#64378 = CARTESIAN_POINT ( 'NONE',  ( 13.89961937509957401, 13.97604488694547697, 66.87609039468567573 ) ) ;
#64377 = CARTESIAN_POINT ( 'NONE',  ( 5.823673210054125526, 21.52544592524343514, 94.79057627198105251 ) ) ;
#64379 = CARTESIAN_POINT ( 'NONE',  ( -4.483927247898782831, 16.52544592524335698, 82.70942372801900433 ) ) ;
#64380 = CARTESIAN_POINT ( 'NONE',  ( 19.02544592524343514, -5.153800228976328945, 63.54057627198103830 ) ) ;
#64381 = CARTESIAN_POINT ( 'NONE',  ( -4.379528057220328563, 16.55341960407611168, 70.20724293864769550 ) ) ;
#64382 = CARTESIAN_POINT ( 'NONE',  ( -13.97604488694527625, -13.89961937509977652, 66.87390960531436690 ) ) ;
#64383 = CARTESIAN_POINT ( 'NONE',  ( 4.483927247898545687, 16.52544592524342804, 59.79057627198103120 ) ) ;
#64384 = CARTESIAN_POINT ( 'NONE',  ( -19.03943276465977164, 0.05219959533909376836, 21.24890960531436335 ) ) ;
#64385 = CARTESIAN_POINT ( 'NONE',  ( 1.500000000000020872, 22.80000000000002913, -55.36297086913598520 ) ) ;
#64386 = CARTESIAN_POINT ( 'NONE',  ( 8.314922557960818139, 14.29746914071049879, 44.58224293864769550 ) ) ;
#64387 = CARTESIAN_POINT ( 'NONE',  ( 16.51473224551069308, 9.474510206698969483, 74.16557627198103830 ) ) ;
#64388 = PLANE ( 'NONE',  #167042 ) ;
#64389 = CARTESIAN_POINT ( 'NONE',  ( 0.05219959533936267826, -19.03943276465977164, 40.00109039468566152 ) ) ;
#64390 = CARTESIAN_POINT ( 'NONE',  ( 12.14591786802327356, -12.06949235617739191, 50.62609039468568994 ) ) ;
#64391 = CARTESIAN_POINT ( 'NONE',  ( -18.67979575497178146, -10.72451020669898902, 66.66557627198102409 ) ) ;
#64392 = CARTESIAN_POINT ( 'NONE',  ( 19.03943276465977164, 0.05219959533936151252, 21.25109039468565797 ) ) ;
#64393 = CARTESIAN_POINT ( 'NONE',  ( 9.564922557960805705, 16.46253265017160317, 69.58224293864770971 ) ) ;
#64394 = CYLINDRICAL_SURFACE ( 'NONE', #146876, 6.100000000000006750 ) ;
#64395 = CARTESIAN_POINT ( 'NONE',  ( -13.97604488694527625, -13.89961937509977652, 111.8739096053143243 ) ) ;
#64396 = CARTESIAN_POINT ( 'NONE',  ( -10.72451020669870658, -18.67979575497194134, 44.58442372801901854 ) ) ;
#64397 = CARTESIAN_POINT ( 'NONE',  ( -16.53943276465976808, 0.05219959533911058130, 111.2489096053143669 ) ) ;
#64400 = ORIENTED_EDGE ( 'NONE', *, *, #152637, .T. ) ;
#64399 = CARTESIAN_POINT ( 'NONE',  ( 19.05341960407611168, 5.049401038298154454, 78.95724293864769550 ) ) ;
#64398 = CARTESIAN_POINT ( 'NONE',  ( -15.72974639402197994, 15.80617190586746368, 95.62390960531436690 ) ) ;
#64401 = CARTESIAN_POINT ( 'NONE',  ( 21.55341960407619695, -5.719274019375665929, 26.04275706135235779 ) ) ;
#64402 = VERTEX_POINT ( 'NONE', #49046 ) ;
#64403 = CARTESIAN_POINT ( 'NONE',  ( -5.049401038298153566, 19.05341960407611168, 90.20724293864766707 ) ) ;
#64404 = FACE_OUTER_BOUND ( 'NONE', #125769, .T. ) ;
#64405 = CARTESIAN_POINT ( 'NONE',  ( 9.474510206698971260, -16.51473224551069308, 37.91557627198102409 ) ) ;
#64406 = CARTESIAN_POINT ( 'NONE',  ( -9.564922557961040184, 16.46253265017147172, 102.9177570613523329 ) ) ;
#64407 = DIRECTION ( 'NONE',  ( 0.1039620511844979306, 0.1039620511844979306, -0.9891328443778538704 ) ) ;
#64408 = CARTESIAN_POINT ( 'NONE',  ( -16.52544592524342804, 4.483927247898546575, 111.0405762719810525 ) ) ;
#64409 = CARTESIAN_POINT ( 'NONE',  ( -15.72974639402176322, -15.80617190586768395, 84.37609039468570415 ) ) ;
#64411 = CARTESIAN_POINT ( 'NONE',  ( -18.62759615963255300, -10.81492255796106328, 44.16775706135234714 ) ) ;
#64410 = CARTESIAN_POINT ( 'NONE',  ( 5.153800228976335163, 19.02544592524342804, 79.79057627198102409 ) ) ;
#64412 = CARTESIAN_POINT ( 'NONE',  ( -18.62759615963255300, -10.81492255796106328, 29.16775706135234003 ) ) ;
#64413 = CARTESIAN_POINT ( 'NONE',  ( -5.429308488886486681E-15, 30.30510711980690175, 145.4999999999999432 ) ) ;
#64414 = CARTESIAN_POINT ( 'NONE',  ( -13.97604488694527625, -13.89961937509977652, 86.87390960531436690 ) ) ;
#64415 = CARTESIAN_POINT ( 'NONE',  ( 8.211251140130430670, 27.09903948220703995, 139.9999999999999147 ) ) ;
#64417 = CARTESIAN_POINT ( 'NONE',  ( 15.72974639402199770, -15.80617190586745480, 38.12390960531436690 ) ) ;
#64416 = CARTESIAN_POINT ( 'NONE',  ( -12.14591786802326823, 12.06949235617739902, 43.12609039468568284 ) ) ;
#64418 = CARTESIAN_POINT ( 'NONE',  ( 5.823673210054444382, -21.52544592524334988, 80.20942372801901854 ) ) ;
#64419 = CARTESIAN_POINT ( 'NONE',  ( 6.125853549498594397, 6.687054376293244395, -61.90253133708614541 ) ) ;
#64420 = CARTESIAN_POINT ( 'NONE',  ( -14.29746914071037622, -8.314922557961029526, 19.16775706135234714 ) ) ;
#64421 = CARTESIAN_POINT ( 'NONE',  ( -9.474510206698964154, 16.51473224551069663, 65.41557627198102409 ) ) ;
#64422 = CARTESIAN_POINT ( 'NONE',  ( -19.02544592524342804, 5.153800228976336051, 91.04057627198100988 ) ) ;
#64423 = CARTESIAN_POINT ( 'NONE',  ( -0.05219959533910754901, -16.53943276465976808, 107.4989096053143669 ) ) ;
#64424 = CARTESIAN_POINT ( 'NONE',  ( 8.224510206698953496, -14.34966873604960469, 107.9155762719810241 ) ) ;
#64425 = CARTESIAN_POINT ( 'NONE',  ( -5.049401038298153566, 19.05341960407611168, 105.2072429386476671 ) ) ;
#64426 = CARTESIAN_POINT ( 'NONE',  ( 8.314922557961029526, -14.29746914071037800, 85.41775706135236135 ) ) ;
#64428 = CARTESIAN_POINT ( 'NONE',  ( 13.97604488694527802, 13.89961937509977652, 59.37390960531434558 ) ) ;
#64427 = CARTESIAN_POINT ( 'NONE',  ( 16.52544592524342804, -4.483927247898539470, 53.54057627198103120 ) ) ;
#64429 = CARTESIAN_POINT ( 'NONE',  ( 15.72974639402176855, 15.80617190586768217, 76.87609039468567573 ) ) ;
#64430 = CARTESIAN_POINT ( 'NONE',  ( 18.62759615963255655, 10.81492255796105972, 76.66775706135234714 ) ) ;
#64431 = CARTESIAN_POINT ( 'NONE',  ( -0.05219959533936034679, 19.03943276465977164, 107.5010903946856615 ) ) ;
#64432 = CARTESIAN_POINT ( 'NONE',  ( 16.53943276465976808, -0.05219959533910856209, 68.74890960531435269 ) ) ;
#64433 = CARTESIAN_POINT ( 'NONE',  ( 15.80617190586769283, -15.72974639402175789, 20.62609039468568639 ) ) ;
#64434 = CARTESIAN_POINT ( 'NONE',  ( 15.80617190586746368, 15.72974639402197994, 64.37390960531435269 ) ) ;
#64435 = CARTESIAN_POINT ( 'NONE',  ( -16.88567814943161949, -6.947325034625708717, 106.2900112265259196 ) ) ;
#64436 = CARTESIAN_POINT ( 'NONE',  ( -17.14385361876520619, 23.59649016807275856, 148.5750000027311444 ) ) ;
#64437 = CARTESIAN_POINT ( 'NONE',  ( 16.51473224551069308, 9.474510206698969483, 64.16557627198102409 ) ) ;
#64438 = CARTESIAN_POINT ( 'NONE',  ( -4.483927247898539470, -16.52544592524342804, 37.29057627198102409 ) ) ;
#64439 = CARTESIAN_POINT ( 'NONE',  ( -0.05219959533910754901, -16.53943276465976808, 22.49890960531436335 ) ) ;
#64440 = CARTESIAN_POINT ( 'NONE',  ( -4.379528057220086978, -16.55341960407618274, 99.79275706135234714 ) ) ;
#64441 = CARTESIAN_POINT ( 'NONE',  ( 5.049401038297881783, 19.05341960407617563, 57.29275706135231871 ) ) ;
#64442 = DIRECTION ( 'NONE',  ( -0.000000000000000000, -0.000000000000000000, 1.000000000000000000 ) ) ;
#64443 = CARTESIAN_POINT ( 'NONE',  ( -19.05341960407611168, -5.049401038298163336, 86.45724293864769550 ) ) ;
#64444 = EDGE_CURVE ( 'NONE', #179366, #125647, #32586, .T. ) ;
#64445 = CARTESIAN_POINT ( 'NONE',  ( -4.379528057220328563, 16.55341960407611168, 60.20724293864768839 ) ) ;
#64447 = CARTESIAN_POINT ( 'NONE',  ( -16.51473224551069308, -9.474510206698971260, 111.6655762719810383 ) ) ;
#64446 = CARTESIAN_POINT ( 'NONE',  ( 16.62475595723698873, -7.163666690055304542, 103.0271335181047334 ) ) ;
#64449 = ORIENTED_EDGE ( 'NONE', *, *, #178834, .T. ) ;
#64448 = CARTESIAN_POINT ( 'NONE',  ( 21.53943276465977519, -0.05219959533907433946, 48.74890960531435979 ) ) ;
#64450 = CARTESIAN_POINT ( 'NONE',  ( 16.55341960407611168, 4.379528057220329451, 103.9572429386476813 ) ) ;
#64451 = CARTESIAN_POINT ( 'NONE',  ( 0.05219959533934541429, -16.53943276465976808, 55.00109039468568284 ) ) ;
#64452 = CARTESIAN_POINT ( 'NONE',  ( 4.379528057220339221, -16.55341960407611168, 82.70724293864770971 ) ) ;
#64453 = DIRECTION ( 'NONE',  ( -1.000000000000000000, 4.336808689942018352E-17, 0.000000000000000000 ) ) ;
#64454 = CARTESIAN_POINT ( 'NONE',  ( -16.51473224551082808, 9.474510206698731452, 78.33442372801900433 ) ) ;
#64455 = CARTESIAN_POINT ( 'NONE',  ( 5.153800228976335163, 19.02544592524342804, 114.7905762719810241 ) ) ;
#64457 = EDGE_CURVE ( 'NONE', #179909, #38745, #172381, .T. ) ;
#64456 = CARTESIAN_POINT ( 'NONE',  ( -36.91746825000000598, 2.428612866367529932E-14, -5.124999997268813168 ) ) ;
#64458 = CARTESIAN_POINT ( 'NONE',  ( -22.97168310438084760, 21.16989542479035080, -49.98402367076293018 ) ) ;
#64459 = AXIS2_PLACEMENT_3D ( 'NONE', #107520, #152060, #73253 ) ;
#64461 = CARTESIAN_POINT ( 'NONE',  ( -12.14591786802309592, -12.06949235617757132, 26.87390960531435979 ) ) ;
#64460 = CARTESIAN_POINT ( 'NONE',  ( -0.05219959533934338120, 16.53943276465976808, 42.50109039468567573 ) ) ;
#64462 = B_SPLINE_CURVE_WITH_KNOTS ( 'NONE', 3,
 ( #122734, #30742, #92390, #165295, #64054, #170241, #82170, #31735, #125724, #93383, #81185, #155069, #16564, #78211, #95374, #111544, #142867, #173229, #4346, #50875, #126697, #19540 ),
 .UNSPECIFIED., .F., .F.,
 ( 4, 2, 2, 2, 2, 2, 2, 2, 2, 2, 4 ),
 ( 1.179739509965479003E-17, 0.001309639967555226289, 0.001964459951332832386, 0.002291869943221635109, 0.002455574939166032568, 0.002619279935110430460, 0.002782984931054828352, 0.002946689926999226244, 0.003274099918888021595, 0.003928919902665609261, 0.005238559870220781123 ),
 .UNSPECIFIED. ) ;
#64463 = CARTESIAN_POINT ( 'NONE',  ( 21.52544592524344225, -5.823673210054117533, 53.54057627198103120 ) ) ;
#64464 = CARTESIAN_POINT ( 'NONE',  ( -13.89961937509957401, -13.97604488694547875, 79.37609039468567573 ) ) ;
#64465 = CARTESIAN_POINT ( 'NONE',  ( 10.72451020669898902, -18.67979575497178502, 52.91557627198103830 ) ) ;
#64466 = CARTESIAN_POINT ( 'NONE',  ( -18.67979575497193778, 10.72451020669871902, 78.33442372801901854 ) ) ;
#64467 = CARTESIAN_POINT ( 'NONE',  ( -10.00917710959074824, 9.438666190699219527, -62.55979675456845257 ) ) ;
#64468 = CARTESIAN_POINT ( 'NONE',  ( -14.34966873604972548, 8.224510206698743886, 38.33442372801900433 ) ) ;
#64470 = CARTESIAN_POINT ( 'NONE',  ( 13.89961937509977652, -13.97604488694527269, 88.12390960531438111 ) ) ;
#64469 = CARTESIAN_POINT ( 'NONE',  ( -16.46253265017160317, 9.564922557960807481, 35.83224293864768839 ) ) ;
#64471 = CARTESIAN_POINT ( 'NONE',  ( 9.474510206698971260, -16.51473224551069308, 37.91557627198102409 ) ) ;
#64472 = CARTESIAN_POINT ( 'NONE',  ( -4.483927247898539470, -16.52544592524342804, 107.2905762719810525 ) ) ;
#64473 = CARTESIAN_POINT ( 'NONE',  ( -5.153800228976328057, -19.02544592524343514, 107.2905762719810383 ) ) ;
#64474 = EDGE_LOOP ( 'NONE', ( #24675, #87005, #31166, #72917 ) ) ;
#64475 = CARTESIAN_POINT ( 'NONE',  ( 8.224510206698742110, 14.34966873604972548, 52.08442372801901854 ) ) ;
#64476 = CARTESIAN_POINT ( 'NONE',  ( 0.05219959533907565091, 21.53943276465977519, 89.99890960531438111 ) ) ;
#64477 = CARTESIAN_POINT ( 'NONE',  ( -13.89961937509977652, 13.97604488694528158, 40.62390960531435979 ) ) ;
#64478 = CARTESIAN_POINT ( 'NONE',  ( -18.67979575497193778, 10.72451020669871902, 33.33442372801900433 ) ) ;
#64479 = CARTESIAN_POINT ( 'NONE',  ( 5.049401038298161559, -19.05341960407611168, 77.70724293864765286 ) ) ;
#64480 = CARTESIAN_POINT ( 'NONE',  ( -38.00000000000000711, 2.428612866367529932E-14, -11.74999999453762634 ) ) ;
#64481 = ORIENTED_EDGE ( 'NONE', *, *, #121810, .T. ) ;
#64482 = CARTESIAN_POINT ( 'NONE',  ( -4.483927247898782831, 16.52544592524335698, 32.70942372801900433 ) ) ;
#64483 = CARTESIAN_POINT ( 'NONE',  ( 21.52544592524344225, -5.823673210054117533, 113.5405762719810383 ) ) ;
#64486 = CARTESIAN_POINT ( 'NONE',  ( 19.03943276465977164, 0.05219959533936151252, 81.25109039468567573 ) ) ;
#64485 = CARTESIAN_POINT ( 'NONE',  ( -19.03943276465977164, 0.05219959533909376836, 96.24890960531436690 ) ) ;
#64484 = CARTESIAN_POINT ( 'NONE',  ( 14.29746914071049879, -8.314922557960816363, 113.3322429386476955 ) ) ;
#64487 = CARTESIAN_POINT ( 'NONE',  ( 16.46253265017146816, 9.564922557961045513, 31.66775706135232937 ) ) ;
#64488 = CARTESIAN_POINT ( 'NONE',  ( -21.55341960407610458, -5.719274019375992779, 81.45724293864769550 ) ) ;
#64489 = CARTESIAN_POINT ( 'NONE',  ( -19.02544592524334988, -5.153800228976617603, 28.95942372801900433 ) ) ;
#64490 = CARTESIAN_POINT ( 'NONE',  ( 4.379528057220092307, 16.55341960407617563, 77.29275706135234714 ) ) ;
#64491 = CARTESIAN_POINT ( 'NONE',  ( 0.05219959533909260263, 19.03943276465977164, 99.99890960531436690 ) ) ;
#64492 = CARTESIAN_POINT ( 'NONE',  ( -5.153800228976328057, -19.02544592524343514, 57.29057627198103120 ) ) ;
#64493 = AXIS2_PLACEMENT_3D ( 'NONE', #127492, #16357, #143654 ) ;
#64494 = CARTESIAN_POINT ( 'NONE',  ( 21.53943276465977519, 0.05219959533937863772, 46.25109039468567573 ) ) ;
#64495 = CARTESIAN_POINT ( 'NONE',  ( 5.823673210054444382, -21.52544592524334988, 65.20942372801901854 ) ) ;
#64496 = CARTESIAN_POINT ( 'NONE',  ( 5.153800228976335163, 19.02544592524342804, 79.79057627198102409 ) ) ;
#64497 = CARTESIAN_POINT ( 'NONE',  ( -18.67979575497193778, 10.72451020669871902, 48.33442372801902565 ) ) ;
#64498 = CARTESIAN_POINT ( 'NONE',  ( -19.03943276465977164, -0.05219959533935918106, 93.75109039468566152 ) ) ;
#64499 = CARTESIAN_POINT ( 'NONE',  ( 19.03943276465977164, -0.05219959533909143690, 48.74890960531435979 ) ) ;
#64500 = CARTESIAN_POINT ( 'NONE',  ( 16.46253265017160672, -9.564922557960803928, 98.33224293864769550 ) ) ;
#64501 = CARTESIAN_POINT ( 'NONE',  ( -9.474510206698964154, 16.51473224551069663, 60.41557627198102409 ) ) ;
#64502 = CARTESIAN_POINT ( 'NONE',  ( 13.97604488694527802, 13.89961937509977652, 114.3739096053143669 ) ) ;
#64503 = CARTESIAN_POINT ( 'NONE',  ( -19.05341960407611168, -5.049401038298163336, 51.45724293864770260 ) ) ;
#64504 = CARTESIAN_POINT ( 'NONE',  ( 21.52544592524344225, -5.823673210054117533, 83.54057627198102409 ) ) ;
#64505 = CARTESIAN_POINT ( 'NONE',  ( -16.53943276465976808, -0.05219959533934237506, 73.75109039468567573 ) ) ;
#64506 = CARTESIAN_POINT ( 'NONE',  ( -24.51266705573315718, 8.027923408435372110, 167.0300397585818928 ) ) ;
#64507 = CARTESIAN_POINT ( 'NONE',  ( 13.97604488694548053, -13.89961937509957401, 35.62609039468567573 ) ) ;
#64508 = CARTESIAN_POINT ( 'NONE',  ( -5.153800228976328057, -19.02544592524343514, 62.29057627198100988 ) ) ;
#64509 = CARTESIAN_POINT ( 'NONE',  ( -8.224510206698948167, 14.34966873604960824, 55.41557627198102409 ) ) ;
#64510 = CARTESIAN_POINT ( 'NONE',  ( -14.29746914071049879, 8.314922557960819915, 95.83224293864770971 ) ) ;
#64511 = CARTESIAN_POINT ( 'NONE',  ( 16.46253265017160672, -9.564922557960803928, 103.3322429386476955 ) ) ;
#64512 = CARTESIAN_POINT ( 'NONE',  ( -9.474510206698964154, 16.51473224551069663, 90.41557627198103830 ) ) ;
#64513 = CARTESIAN_POINT ( 'NONE',  ( -5.719274019375665041, -21.55341960407619695, 44.79275706135234714 ) ) ;
#64514 = CARTESIAN_POINT ( 'NONE',  ( -13.97604488694527625, -13.89961937509977652, 101.8739096053143811 ) ) ;
#64515 = CARTESIAN_POINT ( 'NONE',  ( 21.52544592524334988, 5.823673210054432836, 111.4594237280190328 ) ) ;
#64516 = CARTESIAN_POINT ( 'NONE',  ( -12.06949235617739369, -12.14591786802326823, 74.37609039468568994 ) ) ;
#64517 = CARTESIAN_POINT ( 'NONE',  ( 10.81492255796106328, -18.62759615963255655, 40.41775706135234714 ) ) ;
#64518 = CARTESIAN_POINT ( 'NONE',  ( -21.53943276465977519, 0.05219959533907696930, 26.24890960531435624 ) ) ;
#64519 = CARTESIAN_POINT ( 'NONE',  ( 5.719274019375991003, -21.55341960407610458, 102.7072429386476955 ) ) ;
#64520 = CARTESIAN_POINT ( 'NONE',  ( 16.55341960407611168, 4.379528057220329451, 58.95724293864770971 ) ) ;
#64521 = CARTESIAN_POINT ( 'NONE',  ( -5.049401038298153566, 19.05341960407611168, 55.20724293864769550 ) ) ;
#64522 = CARTESIAN_POINT ( 'NONE',  ( -16.53943276465976808, 0.05219959533911058130, 76.24890960531435269 ) ) ;
#64523 = CARTESIAN_POINT ( 'NONE',  ( 0.05219959533907565091, 21.53943276465977519, 44.99890960531435979 ) ) ;
#64524 = CARTESIAN_POINT ( 'NONE',  ( -9.474510206698720793, -16.51473224551083518, 49.58442372801899722 ) ) ;
#64525 = CARTESIAN_POINT ( 'NONE',  ( 12.14591786802309770, 12.06949235617756955, 114.3739096053143527 ) ) ;
#64526 = ORIENTED_EDGE ( 'NONE', *, *, #20577, .F. ) ;
#64527 = CARTESIAN_POINT ( 'NONE',  ( -14.34966873604972548, 8.224510206698743886, 63.33442372801900433 ) ) ;
#64528 = CARTESIAN_POINT ( 'NONE',  ( -0.05219959533909027116, -19.03943276465977164, 72.49890960531435269 ) ) ;
#64529 = CARTESIAN_POINT ( 'NONE',  ( 22.44159573604009594, -16.30477369853687364, 141.6750000027311671 ) ) ;
#64530 = CARTESIAN_POINT ( 'NONE',  ( 16.55341960407611168, 4.379528057220329451, 88.95724293864769550 ) ) ;
#64531 = CARTESIAN_POINT ( 'NONE',  ( -5.823673210054116645, -21.52544592524344225, 42.29057627198103120 ) ) ;
#64532 = ORIENTED_EDGE ( 'NONE', *, *, #89272, .T. ) ;
#64533 = CARTESIAN_POINT ( 'NONE',  ( 0.05219959533934541429, -16.53943276465976808, 110.0010903946856757 ) ) ;
#64534 = CARTESIAN_POINT ( 'NONE',  ( -5.049401038297874678, -19.05341960407617918, 104.7927570613523471 ) ) ;
#64535 = CARTESIAN_POINT ( 'NONE',  ( -21.52544592524334988, -5.823673210054445271, 83.95942372801900433 ) ) ;
#64536 = CARTESIAN_POINT ( 'NONE',  ( 13.89961937509977652, -13.97604488694527269, 88.12390960531438111 ) ) ;
#64537 = CARTESIAN_POINT ( 'NONE',  ( 0.05219959533907565091, 21.53943276465977519, 99.99890960531436690 ) ) ;
#64538 = CARTESIAN_POINT ( 'NONE',  ( 4.483927247898790824, -16.52544592524335698, 60.20942372801902565 ) ) ;
#64539 = CARTESIAN_POINT ( 'NONE',  ( 16.51473224551069308, 9.474510206698969483, 34.16557627198102409 ) ) ;
#64540 = CARTESIAN_POINT ( 'NONE',  ( 16.52544592524335698, 4.483927247898782831, 26.45942372801901854 ) ) ;
#64541 = CARTESIAN_POINT ( 'NONE',  ( 19.05341960407617918, -5.049401038297876454, 96.04275706135231871 ) ) ;
#64542 = EDGE_CURVE ( 'NONE', #105512, #115616, #59090, .T. ) ;
#64543 = CARTESIAN_POINT ( 'NONE',  ( 21.52544592524344225, -5.823673210054117533, 88.54057627198103830 ) ) ;
#64544 = CARTESIAN_POINT ( 'NONE',  ( 19.05341960407617918, -5.049401038297876454, 61.04275706135232582 ) ) ;
#64545 = CARTESIAN_POINT ( 'NONE',  ( -29.15849868437705439, 5.438282248597753110, 174.2683007571264113 ) ) ;
#64546 = CARTESIAN_POINT ( 'NONE',  ( -15.80617190586745835, -15.72974639402198527, 106.8739096053143811 ) ) ;
#64547 = DIRECTION ( 'NONE',  ( -1.000000000000000000, 0.000000000000000000, -0.000000000000000000 ) ) ;
#64548 = CARTESIAN_POINT ( 'NONE',  ( 16.46253265017160672, -9.564922557960803928, 78.33224293864769550 ) ) ;
#64549 = CARTESIAN_POINT ( 'NONE',  ( -14.29746914071037622, -8.314922557961029526, 39.16775706135235424 ) ) ;
#64550 = CARTESIAN_POINT ( 'NONE',  ( -17.97161686094259991, 5.499999999999981348, 100.9963720685924500 ) ) ;
#64551 = B_SPLINE_CURVE_WITH_KNOTS ( 'NONE', 3,
 ( #89267, #104441, #195473, #197455, #180314, #118623, #149950, #55936, #117613, #102444, #150958, #25629, #151933, #13422, #24622, #56949, #164131, #41782, #12452, #103449 ),
 .UNSPECIFIED., .F., .F.,
 ( 4, 2, 2, 2, 2, 2, 2, 2, 2, 4 ),
 ( 3.469446951953614189E-18, 0.0004987090165372656553, 0.0009974180330745278412, 0.001246772541343162729, 0.001496127049611797400, 0.001994836066149071295, 0.002493545082686344973, 0.002742899590954982030, 0.002992254099223618218, 0.003989672132298151264 ),
 .UNSPECIFIED. ) ;
#64552 = CARTESIAN_POINT ( 'NONE',  ( -19.03943276465977164, -0.05219959533935918106, 63.75109039468566863 ) ) ;
#64554 = CARTESIAN_POINT ( 'NONE',  ( -16.52544592524342804, 4.483927247898546575, 71.04057627198103830 ) ) ;
#64553 = CARTESIAN_POINT ( 'NONE',  ( 18.67979575497178502, 10.72451020669898547, 114.1655762719810383 ) ) ;
#64555 = CARTESIAN_POINT ( 'NONE',  ( -13.89961937509977652, 13.97604488694528158, 70.62390960531432427 ) ) ;
#64557 = CARTESIAN_POINT ( 'NONE',  ( -19.03943276465977164, -0.05219959533935918106, 43.75109039468566863 ) ) ;
#64556 = CARTESIAN_POINT ( 'NONE',  ( -4.379528057220086978, -16.55341960407618274, 39.79275706135235424 ) ) ;
#64558 = CARTESIAN_POINT ( 'NONE',  ( 15.80617190586769283, -15.72974639402175789, 55.62609039468568284 ) ) ;
#64559 = CARTESIAN_POINT ( 'NONE',  ( -9.474510206698720793, -16.51473224551083518, 109.5844237280190043 ) ) ;
#64560 = CARTESIAN_POINT ( 'NONE',  ( -16.46253265017160317, 9.564922557960807481, 50.83224293864770260 ) ) ;
#64561 = CARTESIAN_POINT ( 'NONE',  ( 13.97604488694548053, -13.89961937509957401, 75.62609039468564731 ) ) ;
#64562 = CARTESIAN_POINT ( 'NONE',  ( 10.72451020669871369, 18.67979575497193778, 97.08442372801904696 ) ) ;
#64563 = CARTESIAN_POINT ( 'NONE',  ( -5.049401038297874678, -19.05341960407617918, 64.79275706135233293 ) ) ;
#64564 = CARTESIAN_POINT ( 'NONE',  ( 5.153800228976335163, 19.02544592524342804, 34.79057627198102409 ) ) ;
#64565 = CARTESIAN_POINT ( 'NONE',  ( -21.52544592524343514, 5.823673210054127303, 66.04057627198103830 ) ) ;
#64567 = CARTESIAN_POINT ( 'NONE',  ( 16.46253265017146816, 9.564922557961045513, 66.66775706135233293 ) ) ;
#64566 = CARTESIAN_POINT ( 'NONE',  ( 0.05219959533910956823, 16.53943276465976808, 64.99890960531435269 ) ) ;
#64568 = CARTESIAN_POINT ( 'NONE',  ( 19.49401214000076621, 12.39993551617566681, 169.9999999999999716 ) ) ;
#64569 = CARTESIAN_POINT ( 'NONE',  ( -9.474510206698720793, -16.51473224551083518, 24.58442372801900078 ) ) ;
#64570 = CARTESIAN_POINT ( 'NONE',  ( 8.314922557961029526, -14.29746914071037800, 95.41775706135234714 ) ) ;
#64571 = CARTESIAN_POINT ( 'NONE',  ( -12.06949235617756955, 12.14591786802309770, 55.62390960531436690 ) ) ;
#64573 = CARTESIAN_POINT ( 'NONE',  ( -17.14385361876520619, 23.59649016807275856, 140.5750000027311728 ) ) ;
#64572 = CARTESIAN_POINT ( 'NONE',  ( -21.55341960407619339, 5.719274019375674811, 83.54275706135234714 ) ) ;
#64574 = CARTESIAN_POINT ( 'NONE',  ( -15.80617190586745835, -15.72974639402198527, 96.87390960531436690 ) ) ;
#64575 = CARTESIAN_POINT ( 'NONE',  ( 16.46253265017160672, -9.564922557960803928, 53.33224293864768839 ) ) ;
#64576 = CARTESIAN_POINT ( 'NONE',  ( -10.81492255796105439, 18.62759615963255655, 72.91775706135234714 ) ) ;
#64577 = CARTESIAN_POINT ( 'NONE',  ( -19.05341960407611168, -5.049401038298163336, 51.45724293864770260 ) ) ;
#64578 = CARTESIAN_POINT ( 'NONE',  ( -13.89961937509977652, 13.97604488694528158, 65.62390960531436690 ) ) ;
#64579 = CARTESIAN_POINT ( 'NONE',  ( 4.379528057220339221, -16.55341960407611168, 112.7072429386476955 ) ) ;
#64580 = CARTESIAN_POINT ( 'NONE',  ( -19.02544592524342804, 5.153800228976336051, 111.0405762719810099 ) ) ;
#64581 = CARTESIAN_POINT ( 'NONE',  ( 16.53943276465976808, -0.05219959533910856209, 58.74890960531436690 ) ) ;
#64582 = CARTESIAN_POINT ( 'NONE',  ( -0.05219959533909027116, -19.03943276465977164, 32.49890960531435979 ) ) ;
#64583 = CARTESIAN_POINT ( 'NONE',  ( -16.52544592524342804, 4.483927247898546575, 86.04057627198102409 ) ) ;
#64584 = CARTESIAN_POINT ( 'NONE',  ( -15.72974639402197994, 15.80617190586746368, 95.62390960531436690 ) ) ;
#64585 = CARTESIAN_POINT ( 'NONE',  ( -15.80617190586768217, 15.72974639402176855, 38.12609039468567573 ) ) ;
#64586 = CARTESIAN_POINT ( 'NONE',  ( 27.49873734152943427, 21.99873734152882676, 1.818019484660534424 ) ) ;
#64587 = CARTESIAN_POINT ( 'NONE',  ( -14.34966873604972548, 8.224510206698743886, 48.33442372801902565 ) ) ;
#64588 = CARTESIAN_POINT ( 'NONE',  ( -15.80617190586745835, -15.72974639402198527, 86.87390960531438111 ) ) ;
#64590 = CARTESIAN_POINT ( 'NONE',  ( -10.81492255796105439, 18.62759615963255655, 102.9177570613523756 ) ) ;
#64589 = PRODUCT_DEFINITION_CONTEXT ( 'detailed design', #164372, 'design' ) ;
#64591 = CARTESIAN_POINT ( 'NONE',  ( -13.89961937509977652, 13.97604488694528158, 95.62390960531436690 ) ) ;
#64592 = CARTESIAN_POINT ( 'NONE',  ( -15.72974639402176322, -15.80617190586768395, 49.37609039468569705 ) ) ;
#64593 = CARTESIAN_POINT ( 'NONE',  ( 0.05219959533907565091, 21.53943276465977519, 34.99890960531435979 ) ) ;
#64594 = CARTESIAN_POINT ( 'NONE',  ( 12.06949235617739724, 12.14591786802326823, 101.8760903946857042 ) ) ;
#64596 = CARTESIAN_POINT ( 'NONE',  ( 18.67979575497194134, -10.72451020669871369, 80.83442372801901854 ) ) ;
#64595 = CARTESIAN_POINT ( 'NONE',  ( 10.81492255796106328, -18.62759615963255655, 55.41775706135234714 ) ) ;
#64597 = CARTESIAN_POINT ( 'NONE',  ( -13.89961937509957401, -13.97604488694547875, 34.37609039468566863 ) ) ;
#64598 = CARTESIAN_POINT ( 'NONE',  ( -16.55341960407617563, 4.379528057220093196, 93.54275706135234714 ) ) ;
#64599 = CARTESIAN_POINT ( 'NONE',  ( 10.72451020669871369, 18.67979575497193778, 42.08442372801901854 ) ) ;
#64600 = CARTESIAN_POINT ( 'NONE',  ( 9.474510206698971260, -16.51473224551069308, 42.91557627198103120 ) ) ;
#64601 = CARTESIAN_POINT ( 'NONE',  ( 18.62759615963255655, 10.81492255796105972, 106.6677570613523756 ) ) ;
#64602 = CARTESIAN_POINT ( 'NONE',  ( -5.823673210054116645, -21.52544592524344225, 27.29057627198103120 ) ) ;
#64603 = CARTESIAN_POINT ( 'NONE',  ( -21.53943276465977519, -0.05219959533937600094, 18.75109039468568639 ) ) ;
#64604 = VECTOR ( 'NONE', #183526, 1000.000000000000000 ) ;
#64605 = CARTESIAN_POINT ( 'NONE',  ( -21.53943276465977519, 0.05219959533907696930, 76.24890960531435269 ) ) ;
#64607 = CARTESIAN_POINT ( 'NONE',  ( 10.81492255796078972, 18.62759615963270932, 69.58224293864769550 ) ) ;
#64606 = CARTESIAN_POINT ( 'NONE',  ( -17.49999999999999645, -5.500000000000020428, 61.28230962303567964 ) ) ;
#64609 = CARTESIAN_POINT ( 'NONE',  ( 8.224510206698953496, -14.34966873604960469, 57.91557627198103120 ) ) ;
#64608 = CARTESIAN_POINT ( 'NONE',  ( 14.34966873604972726, -8.224510206698740333, 50.83442372801901143 ) ) ;
#64610 = DIRECTION ( 'NONE',  ( -0.000000000000000000, -0.000000000000000000, 1.000000000000000000 ) ) ;
#64611 = CARTESIAN_POINT ( 'NONE',  ( 0.05219959533936267826, -19.03943276465977164, 85.00109039468567573 ) ) ;
#64612 = DIRECTION ( 'NONE',  ( -1.000000000000000000, -0.000000000000000000, -0.000000000000000000 ) ) ;
#64613 = ADVANCED_FACE ( 'NONE', ( #62204 ), #108719, .T. ) ;
#64614 = CARTESIAN_POINT ( 'NONE',  ( -4.483927247898782831, 16.52544592524335698, 22.70942372801901499 ) ) ;
#64615 = CARTESIAN_POINT ( 'NONE',  ( -10.72451020669898014, 18.67979575497178502, 95.41557627198102409 ) ) ;
#64616 = CARTESIAN_POINT ( 'NONE',  ( -15.72974639402197994, 15.80617190586746368, 75.62390960531439532 ) ) ;
#64617 = CARTESIAN_POINT ( 'NONE',  ( 16.51473224551069308, 9.474510206698969483, 109.1655762719810383 ) ) ;
#64618 = CARTESIAN_POINT ( 'NONE',  ( -16.53943276465976808, -0.05219959533934237506, 63.75109039468568284 ) ) ;
#64619 = CARTESIAN_POINT ( 'NONE',  ( -0.05219959533909027116, -19.03943276465977164, 77.49890960531435269 ) ) ;
#64621 = CARTESIAN_POINT ( 'NONE',  ( 16.51473224551083163, -9.474510206698727899, 110.8344237280190043 ) ) ;
#64620 = CARTESIAN_POINT ( 'NONE',  ( -15.80617190586768217, 15.72974639402176855, 38.12609039468567573 ) ) ;
#64622 = CARTESIAN_POINT ( 'NONE',  ( 5.049401038298161559, -19.05341960407611168, 102.7072429386476955 ) ) ;
#64623 = CARTESIAN_POINT ( 'NONE',  ( 9.564922557960805705, 16.46253265017160317, 104.5822429386476955 ) ) ;
#64624 = CARTESIAN_POINT ( 'NONE',  ( -21.55341960407610458, -5.719274019375992779, 101.4572429386476955 ) ) ;
#64625 = CARTESIAN_POINT ( 'NONE',  ( 13.89961937509977652, -13.97604488694527269, 63.12390960531435979 ) ) ;
#64626 = CARTESIAN_POINT ( 'NONE',  ( -17.49999999999999645, 5.499999999999997335, 25.79690382534172244 ) ) ;
#64627 = CARTESIAN_POINT ( 'NONE',  ( -4.483927247898539470, -16.52544592524342804, 87.29057627198103830 ) ) ;
#64628 = CARTESIAN_POINT ( 'NONE',  ( 15.72974639402199770, -15.80617190586745480, 28.12390960531435979 ) ) ;
#64629 = CARTESIAN_POINT ( 'NONE',  ( -5.153800228976328057, -19.02544592524343514, 22.29057627198102765 ) ) ;
#64630 = CARTESIAN_POINT ( 'NONE',  ( 15.72974639402199770, -15.80617190586745480, 103.1239096053143811 ) ) ;
#64631 = CARTESIAN_POINT ( 'NONE',  ( 0.05219959533936267826, -19.03943276465977164, 60.00109039468566863 ) ) ;
#64632 = CARTESIAN_POINT ( 'NONE',  ( 19.03943276465977164, -0.05219959533909143690, 113.7489096053143669 ) ) ;
#64633 = CARTESIAN_POINT ( 'NONE',  ( 5.153800228976335163, 19.02544592524342804, 24.79057627198102765 ) ) ;
#64634 = CARTESIAN_POINT ( 'NONE',  ( -15.80617190586745835, -15.72974639402198527, 61.87390960531436690 ) ) ;
#64635 = CARTESIAN_POINT ( 'NONE',  ( -19.02544592524342804, 5.153800228976336051, 96.04057627198103830 ) ) ;
#64636 = CARTESIAN_POINT ( 'NONE',  ( -15.72974639402176322, -15.80617190586768395, 84.37609039468570415 ) ) ;
#64637 = CARTESIAN_POINT ( 'NONE',  ( -19.05341960407611168, -5.049401038298163336, 46.45724293864768129 ) ) ;
#64638 = ADVANCED_FACE ( 'NONE', ( #93541 ), #140039, .T. ) ;
#64639 = CARTESIAN_POINT ( 'NONE',  ( 16.55341960407611168, 4.379528057220329451, 83.95724293864770971 ) ) ;
#64640 = CARTESIAN_POINT ( 'NONE',  ( -14.29746914071037622, -8.314922557961029526, 39.16775706135235424 ) ) ;
#64641 = CARTESIAN_POINT ( 'NONE',  ( 15.80617190586769283, -15.72974639402175789, 70.62609039468567573 ) ) ;
#64642 = VERTEX_POINT ( 'NONE', #159182 ) ;
#64643 = CARTESIAN_POINT ( 'NONE',  ( -13.97604488694547697, 13.89961937509957934, 23.12609039468565442 ) ) ;
#64644 = CARTESIAN_POINT ( 'NONE',  ( 19.03943276465977164, 0.05219959533936151252, 86.25109039468567573 ) ) ;
#64645 = CARTESIAN_POINT ( 'NONE',  ( 13.89961937509957401, 13.97604488694547697, 36.87609039468565442 ) ) ;
#64646 = CARTESIAN_POINT ( 'NONE',  ( 32.12256032297300834, -23.75458735917137787, -22.83990191704117478 ) ) ;
#64647 = CARTESIAN_POINT ( 'NONE',  ( 5.719274019375673035, 21.55341960407619339, 42.29275706135235424 ) ) ;
#64648 = CARTESIAN_POINT ( 'NONE',  ( -19.39720447994796970, -5.499999999999981348, 44.66317477297180005 ) ) ;
#64649 = CARTESIAN_POINT ( 'NONE',  ( -16.46253265017146816, -9.564922557961047289, 34.16775706135233293 ) ) ;
#64650 = CARTESIAN_POINT ( 'NONE',  ( 19.02544592524343514, -5.153800228976328945, 73.54057627198103830 ) ) ;
#64651 = CARTESIAN_POINT ( 'NONE',  ( -0.05219959533910754901, -16.53943276465976808, 22.49890960531436335 ) ) ;
#64653 = CARTESIAN_POINT ( 'NONE',  ( -21.55341960407619339, 5.719274019375674811, 88.54275706135236135 ) ) ;
#64652 = CARTESIAN_POINT ( 'NONE',  ( 13.89961937509977652, -13.97604488694527269, 113.1239096053143527 ) ) ;
#64654 = CARTESIAN_POINT ( 'NONE',  ( -36.91746825000001309, 11.99521256947798342, -6.724999997268813701 ) ) ;
#64655 = CARTESIAN_POINT ( 'NONE',  ( -33.84581411518095706, 5.355620490906736642, 93.73536670833321693 ) ) ;
#64656 = CARTESIAN_POINT ( 'NONE',  ( 21.55341960407619695, -5.719274019375665929, 91.04275706135236135 ) ) ;
#64657 = CARTESIAN_POINT ( 'NONE',  ( 16.62475595723696742, -7.163666690055224606, 43.02713351810466946 ) ) ;
#64658 = CARTESIAN_POINT ( 'NONE',  ( 0.05219959533909260263, 19.03943276465977164, 104.9989096053143669 ) ) ;
#64659 = CARTESIAN_POINT ( 'NONE',  ( -1.097581692000294984, -31.42649584489976533, -49.72218688481378734 ) ) ;
#64660 = CARTESIAN_POINT ( 'NONE',  ( -19.05341960407611168, -5.049401038298163336, 56.45724293864768129 ) ) ;
#64661 = CARTESIAN_POINT ( 'NONE',  ( -15.72974639402197994, 15.80617190586746368, 50.62390960531435979 ) ) ;
#64662 = CARTESIAN_POINT ( 'NONE',  ( -16.53943276465976808, 0.05219959533911058130, 26.24890960531435624 ) ) ;
#64664 = CARTESIAN_POINT ( 'NONE',  ( 13.89961937509977652, -13.97604488694527269, 88.12390960531438111 ) ) ;
#64663 = CARTESIAN_POINT ( 'NONE',  ( 14.34966873604960469, 8.224510206698951720, 109.1655762719810383 ) ) ;
#64665 = CARTESIAN_POINT ( 'NONE',  ( 5.153800228976615827, -19.02544592524334988, 25.20942372801900433 ) ) ;
#64666 = CARTESIAN_POINT ( 'NONE',  ( -16.52544592524342804, 4.483927247898546575, 96.04057627198102409 ) ) ;
#64667 = CARTESIAN_POINT ( 'NONE',  ( 15.72974639402176855, 15.80617190586768217, 56.87609039468568994 ) ) ;
#64668 = CARTESIAN_POINT ( 'NONE',  ( 0.05219959533909260263, 19.03943276465977164, 114.9989096053143669 ) ) ;
#64669 = CARTESIAN_POINT ( 'NONE',  ( 16.53943276465976808, 0.05219959533934440121, 101.2510903946856757 ) ) ;
#64670 = CARTESIAN_POINT ( 'NONE',  ( -16.51473224551082808, 9.474510206698731452, 68.33442372801900433 ) ) ;
#64671 = CARTESIAN_POINT ( 'NONE',  ( -14.65771419798590181, -37.23161142520606148, -13.64780077568128291 ) ) ;
#64672 = CARTESIAN_POINT ( 'NONE',  ( -19.03943276465977164, 0.05219959533909376836, 116.2489096053143669 ) ) ;
#64673 = CARTESIAN_POINT ( 'NONE',  ( -12.06949235617756955, 12.14591786802309770, 75.62390960531439532 ) ) ;
#64674 = CARTESIAN_POINT ( 'NONE',  ( 9.474510206698729675, 16.51473224551082808, 62.08442372801899722 ) ) ;
#64675 = CARTESIAN_POINT ( 'NONE',  ( 5.049401038298161559, -19.05341960407611168, 57.70724293864769550 ) ) ;
#64676 = CARTESIAN_POINT ( 'NONE',  ( -4.379528057220328563, 16.55341960407611168, 65.20724293864768129 ) ) ;
#64677 = CARTESIAN_POINT ( 'NONE',  ( -5.153800228976607833, 19.02544592524334988, 92.70942372801901854 ) ) ;
#64678 = CARTESIAN_POINT ( 'NONE',  ( 5.719274019375991003, -21.55341960407610458, 47.70724293864770260 ) ) ;
#64679 = ORIENTED_EDGE ( 'NONE', *, *, #115279, .T. ) ;
#64680 = CARTESIAN_POINT ( 'NONE',  ( -14.29746914071049879, 8.314922557960819915, 100.8322429386477097 ) ) ;
#64681 = CARTESIAN_POINT ( 'NONE',  ( -17.26058549869089376, -6.457015423128630971, 31.37745837476069255 ) ) ;
#64683 = CARTESIAN_POINT ( 'NONE',  ( -0.05219959533907301413, -21.53943276465977519, 57.49890960531435979 ) ) ;
#64682 = CARTESIAN_POINT ( 'NONE',  ( -9.474510206698964154, 16.51473224551069663, 55.41557627198103120 ) ) ;
#64684 = CARTESIAN_POINT ( 'NONE',  ( 5.153800228976335163, 19.02544592524342804, 44.79057627198103830 ) ) ;
#64686 = CARTESIAN_POINT ( 'NONE',  ( 13.97604488694527802, 13.89961937509977652, 79.37390960531435269 ) ) ;
#64685 = CARTESIAN_POINT ( 'NONE',  ( -16.55341960407617563, 4.379528057220093196, 93.54275706135234714 ) ) ;
#64687 = CARTESIAN_POINT ( 'NONE',  ( 19.02544592524334988, 5.153800228976608722, 56.45942372801898301 ) ) ;
#64688 = CARTESIAN_POINT ( 'NONE',  ( 5.719274019375673035, 21.55341960407619339, 77.29275706135234714 ) ) ;
#64689 = VERTEX_POINT ( 'NONE', #5503 ) ;
#64690 = CARTESIAN_POINT ( 'NONE',  ( 10.72451020669898902, -18.67979575497178502, 57.91557627198103120 ) ) ;
#64691 = CARTESIAN_POINT ( 'NONE',  ( 5.049401038298161559, -19.05341960407611168, 112.7072429386476813 ) ) ;
#64692 = CARTESIAN_POINT ( 'NONE',  ( 9.474510206698971260, -16.51473224551069308, 37.91557627198102409 ) ) ;
#64693 = CARTESIAN_POINT ( 'NONE',  ( 8.224510206698742110, 14.34966873604972548, 87.08442372801901854 ) ) ;
#64694 = CARTESIAN_POINT ( 'NONE',  ( 16.46253265017146816, 9.564922557961045513, 106.6677570613523471 ) ) ;
#64695 = CARTESIAN_POINT ( 'NONE',  ( -5.153800228976328057, -19.02544592524343514, 27.29057627198103120 ) ) ;
#64696 = CARTESIAN_POINT ( 'NONE',  ( 17.26058549869089376, 6.457015423128627418, 53.87745837476069255 ) ) ;
#64697 = CARTESIAN_POINT ( 'NONE',  ( -21.55341960407619339, 5.719274019375674811, 93.54275706135234714 ) ) ;
#64698 = CARTESIAN_POINT ( 'NONE',  ( -14.29746914071049879, 8.314922557960819915, 60.83224293864769550 ) ) ;
#64699 = CARTESIAN_POINT ( 'NONE',  ( -16.55341960407611168, -4.379528057220339221, 76.45724293864769550 ) ) ;
#64700 = CARTESIAN_POINT ( 'NONE',  ( 15.72974639402199770, -15.80617190586745480, 93.12390960531436690 ) ) ;
#64701 = CARTESIAN_POINT ( 'NONE',  ( 21.53943276465977519, -0.05219959533907433946, 88.74890960531436690 ) ) ;
#64702 = CARTESIAN_POINT ( 'NONE',  ( 23.29544513554940011, 16.92513159979228021, 149.1843446569000093 ) ) ;
#64703 = CARTESIAN_POINT ( 'NONE',  ( -5.719274019375978568, 21.55341960407610458, 45.20724293864769550 ) ) ;
#64704 = CARTESIAN_POINT ( 'NONE',  ( -0.05219959533934338120, 16.53943276465976808, 72.50109039468568994 ) ) ;
#64705 = CARTESIAN_POINT ( 'NONE',  ( 14.34966873604960469, 8.224510206698951720, 89.16557627198102409 ) ) ;
#64706 = CARTESIAN_POINT ( 'NONE',  ( -9.474510206698964154, 16.51473224551069663, 40.41557627198103120 ) ) ;
#64707 = CARTESIAN_POINT ( 'NONE',  ( 34.61318912441599593, -7.252276964307556639, 43.02678305251431823 ) ) ;
#64708 = CARTESIAN_POINT ( 'NONE',  ( 16.53943276465976808, 0.05219959533934440121, 101.2510903946856757 ) ) ;
#64709 = CARTESIAN_POINT ( 'NONE',  ( 0.05219959533937995610, -21.53943276465977519, 30.00109039468568284 ) ) ;
#64710 = CARTESIAN_POINT ( 'NONE',  ( -19.02544592524342804, 5.153800228976336051, 86.04057627198103830 ) ) ;
#64711 = CARTESIAN_POINT ( 'NONE',  ( 18.67979575497194134, -10.72451020669871369, 70.83442372801901854 ) ) ;
#64712 = FACE_OUTER_BOUND ( 'NONE', #117346, .T. ) ;
#64713 = CARTESIAN_POINT ( 'NONE',  ( -0.05219959533909027116, -19.03943276465977164, 22.49890960531436690 ) ) ;
#64714 = ORIENTED_EDGE ( 'NONE', *, *, #482, .T. ) ;
#64715 = CARTESIAN_POINT ( 'NONE',  ( -5.719274019375665041, -21.55341960407619695, 54.79275706135235424 ) ) ;
#64717 = CARTESIAN_POINT ( 'NONE',  ( -0.05219959533909027116, -19.03943276465977164, 22.49890960531436690 ) ) ;
#64716 = CARTESIAN_POINT ( 'NONE',  ( -13.89961937509977652, 13.97604488694528158, 35.62390960531435269 ) ) ;
#64718 = CARTESIAN_POINT ( 'NONE',  ( 0.05219959533909260263, 19.03943276465977164, 94.99890960531436690 ) ) ;
#64719 = CARTESIAN_POINT ( 'NONE',  ( -16.51473224551082808, 9.474510206698731452, 73.33442372801900433 ) ) ;
#64720 = CARTESIAN_POINT ( 'NONE',  ( -15.72974639402176322, -15.80617190586768395, 24.37609039468567573 ) ) ;
#64721 = CARTESIAN_POINT ( 'NONE',  ( -19.02544592524334988, -5.153800228976617603, 53.95942372801898301 ) ) ;
#64722 = CARTESIAN_POINT ( 'NONE',  ( 19.03943276465977164, -0.05219959533909143690, 33.74890960531435979 ) ) ;
#64723 = CARTESIAN_POINT ( 'NONE',  ( -4.379528057220086978, -16.55341960407618274, 99.79275706135234714 ) ) ;
#64724 = CARTESIAN_POINT ( 'NONE',  ( 9.474510206698729675, 16.51473224551082808, 82.08442372801899012 ) ) ;
#64725 = CARTESIAN_POINT ( 'NONE',  ( -16.52544592524342804, 4.483927247898546575, 31.04057627198102409 ) ) ;
#64726 = CARTESIAN_POINT ( 'NONE',  ( 19.05341960407617918, -5.049401038297876454, 56.04275706135234714 ) ) ;
#64727 = CARTESIAN_POINT ( 'NONE',  ( 5.153800228976335163, 19.02544592524342804, 99.79057627198102409 ) ) ;
#64728 = CARTESIAN_POINT ( 'NONE',  ( -5.719274019375665041, -21.55341960407619695, 104.7927570613523898 ) ) ;
#64729 = PRODUCT_DEFINITION_SHAPE ( 'NONE', 'NONE',  #200198 ) ;
#64730 = CARTESIAN_POINT ( 'NONE',  ( -18.67979575497193778, 10.72451020669871902, 103.3344237280190043 ) ) ;
#64731 = CARTESIAN_POINT ( 'NONE',  ( -3.573655867282028392E-15, 2.428612866367529932E-14, 0.000000000000000000 ) ) ;
#64732 = CARTESIAN_POINT ( 'NONE',  ( 18.67979575497194134, -10.72451020669871369, 85.83442372801901854 ) ) ;
#64733 = CARTESIAN_POINT ( 'NONE',  ( -16.52544592524335698, -4.483927247898792601, 28.95942372801902209 ) ) ;
#64734 = CARTESIAN_POINT ( 'NONE',  ( -0.05219959533909027116, -19.03943276465977164, 92.49890960531436690 ) ) ;
#64735 = CARTESIAN_POINT ( 'NONE',  ( 11.74264578624800315, -36.14014761921581709, -9.149999994537626691 ) ) ;
#64736 = CARTESIAN_POINT ( 'NONE',  ( 5.049401038298161559, -19.05341960407611168, 72.70724293864768129 ) ) ;
#64737 = CARTESIAN_POINT ( 'NONE',  ( 17.50000000000000000, 5.499999999999997335, 120.0000000000000142 ) ) ;
#64738 = CARTESIAN_POINT ( 'NONE',  ( -5.049401038297874678, -19.05341960407617918, 64.79275706135233293 ) ) ;
#64739 = CARTESIAN_POINT ( 'NONE',  ( -13.97604488694527625, -13.89961937509977652, 101.8739096053143811 ) ) ;
#64740 = CARTESIAN_POINT ( 'NONE',  ( -18.62759615963255300, -10.81492255796106328, 99.16775706135234714 ) ) ;
#64741 = CARTESIAN_POINT ( 'NONE',  ( -0.05219959533910754901, -16.53943276465976808, 97.49890960531436690 ) ) ;
#64742 = CARTESIAN_POINT ( 'NONE',  ( 0.05219959533907565091, 21.53943276465977519, 44.99890960531435979 ) ) ;
#64743 = CARTESIAN_POINT ( 'NONE',  ( -10.72451020669898014, 18.67979575497178502, 30.41557627198101699 ) ) ;
#64744 = CARTESIAN_POINT ( 'NONE',  ( -16.53943276465976808, 0.05219959533911058130, 106.2489096053143811 ) ) ;
#64745 = FACE_OUTER_BOUND ( 'NONE', #147587, .T. ) ;
#64746 = CARTESIAN_POINT ( 'NONE',  ( -19.03943276465977164, -0.05219959533935918106, 53.75109039468566863 ) ) ;
#64747 = CARTESIAN_POINT ( 'NONE',  ( 8.224510206698953496, -14.34966873604960469, 32.91557627198102409 ) ) ;
#64748 = CARTESIAN_POINT ( 'NONE',  ( -5.049401038298153566, 19.05341960407611168, 100.2072429386476955 ) ) ;
#64749 = CARTESIAN_POINT ( 'NONE',  ( -10.72451020669870658, -18.67979575497194134, 79.58442372801903275 ) ) ;
#64750 = CARTESIAN_POINT ( 'NONE',  ( 21.55341960407610458, 5.719274019375980345, 68.95724293864769550 ) ) ;
#64751 = CARTESIAN_POINT ( 'NONE',  ( 0.05219959533937995610, -21.53943276465977519, 40.00109039468567573 ) ) ;
#64752 = CARTESIAN_POINT ( 'NONE',  ( -21.55341960407610458, -5.719274019375992779, 101.4572429386476955 ) ) ;
#64753 = CARTESIAN_POINT ( 'NONE',  ( -18.62759615963255300, -10.81492255796106328, 49.16775706135234003 ) ) ;
#64754 = CARTESIAN_POINT ( 'NONE',  ( -13.97604488694527625, -13.89961937509977652, 31.87390960531435979 ) ) ;
#64755 = CARTESIAN_POINT ( 'NONE',  ( -13.89961937509977652, 13.97604488694528158, 80.62390960531436690 ) ) ;
#64756 = CARTESIAN_POINT ( 'NONE',  ( 16.53943276465976808, 0.05219959533934440121, 86.25109039468568994 ) ) ;
#64757 = CARTESIAN_POINT ( 'NONE',  ( 12.14591786802309770, 12.06949235617756955, 104.3739096053143669 ) ) ;
#64758 = CARTESIAN_POINT ( 'NONE',  ( 13.97604488694527802, 13.89961937509977652, 104.3739096053143385 ) ) ;
#64759 = CARTESIAN_POINT ( 'NONE',  ( 14.29746914071049879, -8.314922557960816363, 58.33224293864768839 ) ) ;
#64760 = CARTESIAN_POINT ( 'NONE',  ( -12.14591786802309592, -12.06949235617757132, 21.87390960531436690 ) ) ;
#64761 = CARTESIAN_POINT ( 'NONE',  ( 19.03943276465977164, -0.05219959533909143690, 48.74890960531435979 ) ) ;
#64762 = CARTESIAN_POINT ( 'NONE',  ( 16.46253265017160672, -9.564922557960803928, 28.33224293864769550 ) ) ;
#64763 = CARTESIAN_POINT ( 'NONE',  ( -5.823673210054116645, -21.52544592524344225, 42.29057627198103120 ) ) ;
#64764 = CARTESIAN_POINT ( 'NONE',  ( -19.03943276465977164, -0.05219959533935918106, 43.75109039468566863 ) ) ;
#64766 = CARTESIAN_POINT ( 'NONE',  ( 8.314922557960818139, 14.29746914071049879, 39.58224293864769550 ) ) ;
#64765 = FACE_BOUND ( 'NONE', #40802, .T. ) ;
#64767 = VECTOR ( 'NONE', #16546, 1000.000000000000000 ) ;
#64768 = CARTESIAN_POINT ( 'NONE',  ( 5.719274019375673035, 21.55341960407619339, 42.29275706135235424 ) ) ;
#64769 = CARTESIAN_POINT ( 'NONE',  ( -16.49801837613219035, -34.15639402546915449, -27.41207208920364025 ) ) ;
#64770 = CARTESIAN_POINT ( 'NONE',  ( -14.34966873604972548, 8.224510206698743886, 53.33442372801901854 ) ) ;
#64771 = CARTESIAN_POINT ( 'NONE',  ( 13.97604488694548053, -13.89961937509957401, 55.62609039468566863 ) ) ;
#64772 = CARTESIAN_POINT ( 'NONE',  ( 0.05219959533910956823, 16.53943276465976808, 24.99890960531435624 ) ) ;
#64773 = CARTESIAN_POINT ( 'NONE',  ( 16.20579543436676317, -7.371946100355162734, 51.93479165828130562 ) ) ;
#64774 = CARTESIAN_POINT ( 'NONE',  ( 16.55341960407618274, -4.379528057220086978, 101.0427570613523756 ) ) ;
#64775 = CARTESIAN_POINT ( 'NONE',  ( 19.02544592524343514, -5.153800228976328945, 33.54057627198102409 ) ) ;
#64776 = ADVANCED_FACE ( 'NONE', ( #52015 ), #114684, .F. ) ;
#64777 = CARTESIAN_POINT ( 'NONE',  ( -9.564922557960796823, -16.46253265017161027, 67.08224293864769550 ) ) ;
#64778 = CARTESIAN_POINT ( 'NONE',  ( -9.564922557960796823, -16.46253265017161027, 27.08224293864769550 ) ) ;
#64779 = CARTESIAN_POINT ( 'NONE',  ( -5.823673210054431948, 21.52544592524334988, 32.70942372801900433 ) ) ;
#64780 = CARTESIAN_POINT ( 'NONE',  ( 9.564922557960805705, 16.46253265017160317, 49.58224293864770260 ) ) ;
#64781 = CARTESIAN_POINT ( 'NONE',  ( -9.564922557960796823, -16.46253265017161027, 112.0822429386476955 ) ) ;
#64782 = CARTESIAN_POINT ( 'NONE',  ( -9.564922557960796823, -16.46253265017161027, 52.08224293864768839 ) ) ;
#64783 = CARTESIAN_POINT ( 'NONE',  ( 21.55341960407610458, 5.719274019375980345, 23.95724293864769550 ) ) ;
#64785 = CARTESIAN_POINT ( 'NONE',  ( 8.314922557960818139, 14.29746914071049879, 99.58224293864770971 ) ) ;
#64784 = CARTESIAN_POINT ( 'NONE',  ( 10.72451020669871369, 18.67979575497193778, 57.08442372801901854 ) ) ;
#64786 = CARTESIAN_POINT ( 'NONE',  ( -21.52544592524343514, 5.823673210054127303, 26.04057627198103475 ) ) ;
#64787 = CARTESIAN_POINT ( 'NONE',  ( -12.06949235617739369, -12.14591786802326823, 79.37609039468567573 ) ) ;
#64788 = CARTESIAN_POINT ( 'NONE',  ( -18.62759615963255300, -10.81492255796106328, 94.16775706135237556 ) ) ;
#64789 = CARTESIAN_POINT ( 'NONE',  ( 8.314922557961029526, -14.29746914071037800, 50.41775706135235424 ) ) ;
#64790 = CARTESIAN_POINT ( 'NONE',  ( 0.05219959533909260263, 19.03943276465977164, 89.99890960531436690 ) ) ;
#64791 = CARTESIAN_POINT ( 'NONE',  ( -16.55341960407617563, 4.379528057220093196, 43.54275706135235424 ) ) ;
#64792 = CARTESIAN_POINT ( 'NONE',  ( -16.52544592524335698, -4.483927247898792601, 23.95942372801901143 ) ) ;
#64793 = CARTESIAN_POINT ( 'NONE',  ( 14.34966873604972726, -8.224510206698740333, 100.8344237280190185 ) ) ;
#64794 = CARTESIAN_POINT ( 'NONE',  ( 10.72451020669871369, 18.67979575497193778, 52.08442372801901854 ) ) ;
#64795 = CARTESIAN_POINT ( 'NONE',  ( 19.05341960407617918, -5.049401038297876454, 101.0427570613523045 ) ) ;
#64796 = CARTESIAN_POINT ( 'NONE',  ( -5.719274019375665041, -21.55341960407619695, 19.79275706135235069 ) ) ;
#64798 = CARTESIAN_POINT ( 'NONE',  ( -5.049401038297874678, -19.05341960407617918, 109.7927570613523187 ) ) ;
#64797 = CARTESIAN_POINT ( 'NONE',  ( -16.52544592524342804, 4.483927247898546575, 101.0405762719810383 ) ) ;
#64799 = CARTESIAN_POINT ( 'NONE',  ( 14.29746914071037800, 8.314922557961029526, 71.66775706135234714 ) ) ;
#64800 = CARTESIAN_POINT ( 'NONE',  ( 21.98685479826779599, 13.98560643873834231, 165.5209445330007725 ) ) ;
#64801 = CARTESIAN_POINT ( 'NONE',  ( 9.564922557961047289, -16.46253265017146816, 85.41775706135233293 ) ) ;
#64802 = CARTESIAN_POINT ( 'NONE',  ( -16.55341960407611168, -4.379528057220339221, 46.45724293864769550 ) ) ;
#64803 = CARTESIAN_POINT ( 'NONE',  ( 8.224510206698953496, -14.34966873604960469, 47.91557627198102409 ) ) ;
#64804 = CARTESIAN_POINT ( 'NONE',  ( -16.53943276465976808, 0.05219959533911058130, 96.24890960531435269 ) ) ;
#64806 = CARTESIAN_POINT ( 'NONE',  ( -18.87075004821566537, 5.500000000000085265, 88.67408112101047379 ) ) ;
#64805 = CARTESIAN_POINT ( 'NONE',  ( -9.474510206698720793, -16.51473224551083518, 29.58442372801900433 ) ) ;
#64807 = CARTESIAN_POINT ( 'NONE',  ( -21.55341960407619339, 5.719274019375674811, 38.54275706135234714 ) ) ;
#64808 = CARTESIAN_POINT ( 'NONE',  ( 16.51473224551083163, -9.474510206698727899, 100.8344237280190043 ) ) ;
#64809 = CARTESIAN_POINT ( 'NONE',  ( -8.231229499106921921, -38.47007264976929974, -32.24440875978790189 ) ) ;
#64810 = CARTESIAN_POINT ( 'NONE',  ( 19.03943276465977164, -0.05219959533909143690, 88.74890960531436690 ) ) ;
#64811 = CARTESIAN_POINT ( 'NONE',  ( -5.153800228976328057, -19.02544592524343514, 87.29057627198103830 ) ) ;
#64812 = CARTESIAN_POINT ( 'NONE',  ( -10.81492255796078084, -18.62759615963271287, 57.08224293864769550 ) ) ;
#64813 = CARTESIAN_POINT ( 'NONE',  ( 14.29746914071049879, -8.314922557960816363, 98.33224293864769550 ) ) ;
#64814 = CARTESIAN_POINT ( 'NONE',  ( 19.05341960407611168, 5.049401038298154454, 73.95724293864768129 ) ) ;
#64815 = CARTESIAN_POINT ( 'NONE',  ( 16.46253265017160672, -9.564922557960803928, 23.33224293864769194 ) ) ;
#64816 = CARTESIAN_POINT ( 'NONE',  ( -10.72451020669870658, -18.67979575497194134, 39.58442372801901143 ) ) ;
#64817 = CARTESIAN_POINT ( 'NONE',  ( -15.72974639402176322, -15.80617190586768395, 69.37609039468567573 ) ) ;
#64818 = CARTESIAN_POINT ( 'NONE',  ( 16.52544592524335698, 4.483927247898782831, 91.45942372801901854 ) ) ;
#64819 = CARTESIAN_POINT ( 'NONE',  ( 0.05219959533937995610, -21.53943276465977519, 30.00109039468568284 ) ) ;
#64820 = CARTESIAN_POINT ( 'NONE',  ( -21.55341960407619339, 5.719274019375674811, 23.54275706135235424 ) ) ;
#64822 = CARTESIAN_POINT ( 'NONE',  ( 16.46253265017160672, -9.564922557960803928, 83.33224293864768129 ) ) ;
#64821 = CARTESIAN_POINT ( 'NONE',  ( 19.03943276465977164, 0.05219959533936151252, 51.25109039468567573 ) ) ;
#64823 = CARTESIAN_POINT ( 'NONE',  ( -15.80617190586768217, 15.72974639402176855, 83.12609039468568994 ) ) ;
#64824 = CARTESIAN_POINT ( 'NONE',  ( 15.80617190586746368, 15.72974639402197994, 79.37390960531436690 ) ) ;
#64825 = CARTESIAN_POINT ( 'NONE',  ( 16.55341960407611168, 4.379528057220329451, 53.95724293864770260 ) ) ;
#64827 = CARTESIAN_POINT ( 'NONE',  ( 13.89961937509957401, 13.97604488694547697, 31.87609039468566863 ) ) ;
#64826 = CARTESIAN_POINT ( 'NONE',  ( 10.72451020669871369, 18.67979575497193778, 97.08442372801904696 ) ) ;
#64828 = CARTESIAN_POINT ( 'NONE',  ( 16.53943276465976808, -0.05219959533910856209, 73.74890960531433848 ) ) ;
#64829 = CARTESIAN_POINT ( 'NONE',  ( 5.049401038298161559, -19.05341960407611168, 27.70724293864769550 ) ) ;
#64830 = CARTESIAN_POINT ( 'NONE',  ( 5.049401038297881783, 19.05341960407617563, 77.29275706135231871 ) ) ;
#64831 = CARTESIAN_POINT ( 'NONE',  ( -16.52544592524342804, 4.483927247898546575, 41.04057627198103120 ) ) ;
#64832 = CARTESIAN_POINT ( 'NONE',  ( 21.53943276465977519, 0.05219959533937863772, 76.25109039468568994 ) ) ;
#64833 = CARTESIAN_POINT ( 'NONE',  ( -5.049401038298153566, 19.05341960407611168, 80.20724293864769550 ) ) ;
#64834 = CARTESIAN_POINT ( 'NONE',  ( -13.89961937509957401, -13.97604488694547875, 59.37609039468566863 ) ) ;
#64835 = CARTESIAN_POINT ( 'NONE',  ( 5.823673210054125526, 21.52544592524343514, 69.79057627198102409 ) ) ;
#64836 = CARTESIAN_POINT ( 'NONE',  ( -15.80617190586768217, 15.72974639402176855, 23.12609039468567573 ) ) ;
#64837 = CARTESIAN_POINT ( 'NONE',  ( -19.05341960407617563, 5.049401038297882671, 108.5427570613523187 ) ) ;
#64838 = CARTESIAN_POINT ( 'NONE',  ( 8.314922557961029526, -14.29746914071037800, 80.41775706135234714 ) ) ;
#64840 = CARTESIAN_POINT ( 'NONE',  ( -21.55341960407610458, -5.719274019375992779, 111.4572429386476813 ) ) ;
#64839 = CARTESIAN_POINT ( 'NONE',  ( 17.48853670773241831, 5.747243402303172211, 63.83328700250011423 ) ) ;
#64841 = CARTESIAN_POINT ( 'NONE',  ( -16.52544592524342804, 4.483927247898546575, 101.0405762719810383 ) ) ;
#64842 = CARTESIAN_POINT ( 'NONE',  ( -16.31925111598457434, -7.325300261831548809, 99.83575461032749843 ) ) ;
#64843 = CARTESIAN_POINT ( 'NONE',  ( 14.29746914071037800, 8.314922557961029526, 31.66775706135234358 ) ) ;
#64844 = CARTESIAN_POINT ( 'NONE',  ( -15.80617190586745835, -15.72974639402198527, 61.87390960531436690 ) ) ;
#64845 = CARTESIAN_POINT ( 'NONE',  ( -14.29746914071037622, -8.314922557961029526, 99.16775706135234714 ) ) ;
#64846 = CARTESIAN_POINT ( 'NONE',  ( -13.97604488694527625, -13.89961937509977652, 36.87390960531436690 ) ) ;
#64847 = CARTESIAN_POINT ( 'NONE',  ( 16.55341960407618274, -4.379528057220086978, 61.04275706135234714 ) ) ;
#64848 = CARTESIAN_POINT ( 'NONE',  ( 13.89961937509957401, 13.97604488694547697, 76.87609039468566152 ) ) ;
#64849 = CARTESIAN_POINT ( 'NONE',  ( 15.72974639402176855, 15.80617190586768217, 46.87609039468568994 ) ) ;
#64850 = CARTESIAN_POINT ( 'NONE',  ( 10.81492255796078972, 18.62759615963270932, 59.58224293864770260 ) ) ;
#64851 = CARTESIAN_POINT ( 'NONE',  ( -16.55341960407617563, 4.379528057220093196, 98.54275706135234714 ) ) ;
#64852 = CARTESIAN_POINT ( 'NONE',  ( -10.81492255796105439, 18.62759615963255655, 82.91775706135234714 ) ) ;
#64853 = CARTESIAN_POINT ( 'NONE',  ( -18.67979575497178146, -10.72451020669898902, 51.66557627198102409 ) ) ;
#64854 = CARTESIAN_POINT ( 'NONE',  ( -18.67979575497178146, -10.72451020669898902, 46.66557627198102409 ) ) ;
#64855 = CARTESIAN_POINT ( 'NONE',  ( -12.14591786802326823, 12.06949235617739902, 78.12609039468570415 ) ) ;
#64856 = CARTESIAN_POINT ( 'NONE',  ( -5.823673210054116645, -21.52544592524344225, 42.29057627198103120 ) ) ;
#64857 = ORIENTED_EDGE ( 'NONE', *, *, #157461, .F. ) ;
#64858 = CARTESIAN_POINT ( 'NONE',  ( -5.153800228976328057, -19.02544592524343514, 102.2905762719810383 ) ) ;
#64859 = DIRECTION ( 'NONE',  ( -4.336808689942018352E-17, 1.000000000000000000, 0.000000000000000000 ) ) ;
#64860 = CARTESIAN_POINT ( 'NONE',  ( 16.46253265017160672, -9.564922557960803928, 33.33224293864770260 ) ) ;
#64861 = CARTESIAN_POINT ( 'NONE',  ( -21.53943276465977519, 0.05219959533907696930, 66.24890960531436690 ) ) ;
#64862 = CARTESIAN_POINT ( 'NONE',  ( 0.05219959533934541429, -16.53943276465976808, 90.00109039468567573 ) ) ;
#64863 = CARTESIAN_POINT ( 'NONE',  ( -5.719274019375665041, -21.55341960407619695, 44.79275706135234714 ) ) ;
#64864 = CARTESIAN_POINT ( 'NONE',  ( 5.049401038297881783, 19.05341960407617563, 107.2927570613523187 ) ) ;
#64865 = CARTESIAN_POINT ( 'NONE',  ( 0.05219959533910956823, 16.53943276465976808, 99.99890960531436690 ) ) ;
#64866 = CARTESIAN_POINT ( 'NONE',  ( 19.02544592524334988, 5.153800228976608722, 111.4594237280190043 ) ) ;
#64867 = CARTESIAN_POINT ( 'NONE',  ( 19.03943276465977164, -0.05219959533909143690, 38.74890960531436690 ) ) ;
#64868 = CARTESIAN_POINT ( 'NONE',  ( 13.70000000000001528, -0.2066332630087097111, -62.58071313852360618 ) ) ;
#64869 = CARTESIAN_POINT ( 'NONE',  ( 13.97604488694527802, 13.89961937509977652, 94.37390960531436690 ) ) ;
#64870 = EDGE_CURVE ( 'NONE', #11421, #159131, #96514, .T. ) ;
#64871 = CARTESIAN_POINT ( 'NONE',  ( 16.55341960407618274, -4.379528057220086978, 76.04275706135237556 ) ) ;
#64872 = CARTESIAN_POINT ( 'NONE',  ( -0.05219959533937732626, 21.53943276465977519, 112.5010903946857042 ) ) ;
#64873 = CARTESIAN_POINT ( 'NONE',  ( 10.81492255796078972, 18.62759615963270932, 64.58224293864769550 ) ) ;
#64874 = CARTESIAN_POINT ( 'NONE',  ( 16.53943276465976808, 0.05219959533934440121, 86.25109039468568994 ) ) ;
#64875 = CARTESIAN_POINT ( 'NONE',  ( -9.564922557961040184, 16.46253265017147172, 82.91775706135233293 ) ) ;
#64876 = CARTESIAN_POINT ( 'NONE',  ( 5.153800228976335163, 19.02544592524342804, 34.79057627198102409 ) ) ;
#64877 = CARTESIAN_POINT ( 'NONE',  ( -19.03943276465977164, 0.05219959533909376836, 81.24890960531436690 ) ) ;
#64878 = CARTESIAN_POINT ( 'NONE',  ( 13.97604488694527802, 13.89961937509977652, 29.37390960531435979 ) ) ;
#64879 = CARTESIAN_POINT ( 'NONE',  ( -16.46253265017146816, -9.564922557961047289, 69.16775706135233293 ) ) ;
#64880 = CARTESIAN_POINT ( 'NONE',  ( 26.77313074627600287, -4.631999166350020403, 170.7390164845734546 ) ) ;
#64881 = CARTESIAN_POINT ( 'NONE',  ( -19.05341960407611168, -5.049401038298163336, 111.4572429386476671 ) ) ;
#64882 = CARTESIAN_POINT ( 'NONE',  ( -14.29746914071049879, 8.314922557960819915, 65.83224293864769550 ) ) ;
#64883 = CARTESIAN_POINT ( 'NONE',  ( -18.62759615963270932, 10.81492255796079327, 60.83224293864769550 ) ) ;
#64884 = DIRECTION ( 'NONE',  ( -1.000000000000000000, -0.000000000000000000, -0.000000000000000000 ) ) ;
#64885 = CARTESIAN_POINT ( 'NONE',  ( 16.46253265017146816, 9.564922557961045513, 31.66775706135232937 ) ) ;
#64886 = CARTESIAN_POINT ( 'NONE',  ( -18.22780087662122028, 5.500000000000031086, 88.51540105326107266 ) ) ;
#64888 = CARTESIAN_POINT ( 'NONE',  ( -19.03943276465977164, 0.05219959533909376836, 76.24890960531435269 ) ) ;
#64887 = CARTESIAN_POINT ( 'NONE',  ( -13.89961937509977652, 13.97604488694528158, 60.62390960531436690 ) ) ;
#64889 = CARTESIAN_POINT ( 'NONE',  ( 16.53943276465976808, 0.05219959533934440121, 51.25109039468568994 ) ) ;
#64890 = DIRECTION ( 'NONE',  ( -0.000000000000000000, -0.000000000000000000, 1.000000000000000000 ) ) ;
#64891 = CARTESIAN_POINT ( 'NONE',  ( -69.65682714487590488, -71.74905178543390605, 0.000000000000000000 ) ) ;
#64892 = CARTESIAN_POINT ( 'NONE',  ( -14.34966873604972548, 8.224510206698743886, 73.33442372801901854 ) ) ;
#64893 = CARTESIAN_POINT ( 'NONE',  ( -17.97182807773871005, 5.500000000000047073, 78.53038844047287625 ) ) ;
#64894 = CARTESIAN_POINT ( 'NONE',  ( 16.55341960407618274, -4.379528057220086978, 61.04275706135234714 ) ) ;
#64895 = CARTESIAN_POINT ( 'NONE',  ( 12.14591786802327356, -12.06949235617739191, 35.62609039468568994 ) ) ;
#64897 = CARTESIAN_POINT ( 'NONE',  ( -3.573655867282028392E-15, 2.428612866367529932E-14, 155.0000000000000000 ) ) ;
#64896 = CARTESIAN_POINT ( 'NONE',  ( -9.564922557960796823, -16.46253265017161027, 52.08224293864768839 ) ) ;
#64898 = CARTESIAN_POINT ( 'NONE',  ( 18.62759615963255655, 10.81492255796105972, 51.66775706135234714 ) ) ;
#64899 = CARTESIAN_POINT ( 'NONE',  ( 9.474510206698729675, 16.51473224551082808, 62.08442372801899722 ) ) ;
#64900 = CARTESIAN_POINT ( 'NONE',  ( -5.823673210054431948, 21.52544592524334988, 107.7094237280190328 ) ) ;
#64901 = CARTESIAN_POINT ( 'NONE',  ( -9.564922557960796823, -16.46253265017161027, 27.08224293864769550 ) ) ;
#64902 = FACE_OUTER_BOUND ( 'NONE', #184144, .T. ) ;
#64903 = CARTESIAN_POINT ( 'NONE',  ( 5.823673210054125526, 21.52544592524343514, 54.79057627198104541 ) ) ;
#64904 = CARTESIAN_POINT ( 'NONE',  ( 5.049401038298161559, -19.05341960407611168, 107.7072429386476955 ) ) ;
#64905 = CARTESIAN_POINT ( 'NONE',  ( 14.29746914071049879, -8.314922557960816363, 103.3322429386476955 ) ) ;
#64906 = CARTESIAN_POINT ( 'NONE',  ( -16.53943276465976808, -0.05219959533934237506, 38.75109039468567573 ) ) ;
#64907 = CARTESIAN_POINT ( 'NONE',  ( 4.483927247898545687, 16.52544592524342804, 34.79057627198103120 ) ) ;
#64908 = ORIENTED_EDGE ( 'NONE', *, *, #35894, .T. ) ;
#64909 = CARTESIAN_POINT ( 'NONE',  ( -18.67979575497178146, -10.72451020669898902, 96.66557627198102409 ) ) ;
#64911 = CARTESIAN_POINT ( 'NONE',  ( -19.05341960407611168, -5.049401038298163336, 111.4572429386476671 ) ) ;
#64910 = CARTESIAN_POINT ( 'NONE',  ( 4.379528057220339221, -16.55341960407611168, 42.70724293864770260 ) ) ;
#64912 = CARTESIAN_POINT ( 'NONE',  ( 0.05219959533936267826, -19.03943276465977164, 90.00109039468567573 ) ) ;
#64913 = CARTESIAN_POINT ( 'NONE',  ( -19.05341960407617563, 5.049401038297882671, 28.54275706135232937 ) ) ;
#64914 = CARTESIAN_POINT ( 'NONE',  ( 12.06949235617757843, -12.14591786802309237, 28.12390960531435979 ) ) ;
#64915 = CARTESIAN_POINT ( 'NONE',  ( 5.823673210054125526, 21.52544592524343514, 109.7905762719810383 ) ) ;
#64916 = CARTESIAN_POINT ( 'NONE',  ( -15.72974639402197994, 15.80617190586746368, 55.62390960531436690 ) ) ;
#64917 = CARTESIAN_POINT ( 'NONE',  ( -9.564922557960796823, -16.46253265017161027, 82.08224293864768129 ) ) ;
#64918 = CARTESIAN_POINT ( 'NONE',  ( 12.06949235617757843, -12.14591786802309237, 53.12390960531436690 ) ) ;
#64919 = CARTESIAN_POINT ( 'NONE',  ( 19.02544592524343514, -5.153800228976328945, 88.54057627198102409 ) ) ;
#64920 = ORIENTED_EDGE ( 'NONE', *, *, #179710, .T. ) ;
#64921 = CARTESIAN_POINT ( 'NONE',  ( 21.38418241377623019, 7.427326039334300134, 174.4773576836617224 ) ) ;
#64922 = CARTESIAN_POINT ( 'NONE',  ( -13.97604488694547697, 13.89961937509957934, 48.12609039468566863 ) ) ;
#64923 = CARTESIAN_POINT ( 'NONE',  ( -5.719274019375978568, 21.55341960407610458, 85.20724293864770971 ) ) ;
#64924 = CARTESIAN_POINT ( 'NONE',  ( 16.53943276465976808, -0.05219959533910856209, 103.7489096053143669 ) ) ;
#64925 = CARTESIAN_POINT ( 'NONE',  ( 21.55341960407619695, -5.719274019375665929, 31.04275706135234714 ) ) ;
#64926 = CARTESIAN_POINT ( 'NONE',  ( 27.73933785331498214, 9.013057229001095294, 148.4750000027311785 ) ) ;
#64927 = CARTESIAN_POINT ( 'NONE',  ( 14.29746914071037800, 8.314922557961029526, 106.6677570613523756 ) ) ;
#64928 = CARTESIAN_POINT ( 'NONE',  ( 5.049401038298161559, -19.05341960407611168, 42.70724293864767418 ) ) ;
#64929 = B_SPLINE_CURVE_WITH_KNOTS ( 'NONE', 3,
 ( #63132, #171321, #188484, #91467, #137994, #16644, #48971, #153155, #14656, #2456, #79299, #76316, #1454, #106661, #77311, #184505, #17639, #124811, #457, #107640, #95456, #31814 ),
 .UNSPECIFIED., .F., .F.,
 ( 4, 2, 2, 2, 2, 2, 2, 2, 2, 2, 4 ),
 ( 2.775519118949223281E-07, 0.0003140540122564098344, 0.0006278304726009247688, 0.0009416069329454397575, 0.001255383393289954746, 0.001882936313978984724, 0.002510489234668014484, 0.003138042155357044245, 0.003765595076046074439, 0.004393147996735103332, 0.005020700917424133526 ),
 .UNSPECIFIED. ) ;
#64930 = CARTESIAN_POINT ( 'NONE',  ( -19.02544592524342804, 5.153800228976336051, 81.04057627198103830 ) ) ;
#64931 = CARTESIAN_POINT ( 'NONE',  ( 27.73933785331498214, 9.013057229001095294, 139.9750000027311501 ) ) ;
#64932 = CARTESIAN_POINT ( 'NONE',  ( 19.02544592524343514, -5.153800228976328945, 33.54057627198102409 ) ) ;
#64933 = CARTESIAN_POINT ( 'NONE',  ( -12.14591786802309592, -12.06949235617757132, 36.87390960531435979 ) ) ;
#64934 = CARTESIAN_POINT ( 'NONE',  ( 18.67979575497194134, -10.72451020669871369, 75.83442372801900433 ) ) ;
#64936 = CARTESIAN_POINT ( 'NONE',  ( -16.55341960407617563, 4.379528057220093196, 68.54275706135234714 ) ) ;
#64935 = CARTESIAN_POINT ( 'NONE',  ( 19.65168359646968099, -34.19331532915641958, -17.88087567707446013 ) ) ;
#64937 = CARTESIAN_POINT ( 'NONE',  ( -5.153800228976328057, -19.02544592524343514, 57.29057627198103120 ) ) ;
#64938 = CARTESIAN_POINT ( 'NONE',  ( -9.474510206698964154, 16.51473224551069663, 65.41557627198102409 ) ) ;
#64939 = ORIENTED_EDGE ( 'NONE', *, *, #19140, .T. ) ;
#64940 = CARTESIAN_POINT ( 'NONE',  ( 0.05219959533937995610, -21.53943276465977519, 110.0010903946856757 ) ) ;
#64941 = CARTESIAN_POINT ( 'NONE',  ( -14.29746914071037622, -8.314922557961029526, 69.16775706135234714 ) ) ;
#64942 = CARTESIAN_POINT ( 'NONE',  ( 5.719274019375673035, 21.55341960407619339, 102.2927570613523613 ) ) ;
#64943 = CARTESIAN_POINT ( 'NONE',  ( 19.02544592524343514, -5.153800228976328945, 68.54057627198103830 ) ) ;
#64944 = CARTESIAN_POINT ( 'NONE',  ( -15.72974639402197994, 15.80617190586746368, 30.62390960531436335 ) ) ;
#64945 = CARTESIAN_POINT ( 'NONE',  ( 19.05341960407617918, -5.049401038297876454, 111.0427570613523329 ) ) ;
#64946 = CARTESIAN_POINT ( 'NONE',  ( -10.72451020669870658, -18.67979575497194134, 64.58442372801900433 ) ) ;
#64947 = CARTESIAN_POINT ( 'NONE',  ( 4.379528057220092307, 16.55341960407617563, 52.29275706135236135 ) ) ;
#64948 = CARTESIAN_POINT ( 'NONE',  ( -21.52544592524343514, 5.823673210054127303, 106.0405762719810525 ) ) ;
#64949 = CARTESIAN_POINT ( 'NONE',  ( 16.51473224551083163, -9.474510206698727899, 100.8344237280190043 ) ) ;
#64950 = CARTESIAN_POINT ( 'NONE',  ( -16.51473224551069308, -9.474510206698971260, 81.66557627198103830 ) ) ;
#64951 = CARTESIAN_POINT ( 'NONE',  ( 5.049401038297881783, 19.05341960407617563, 112.2927570613523471 ) ) ;
#64952 = CARTESIAN_POINT ( 'NONE',  ( -8.224510206698735004, -14.34966873604973081, 24.58442372801901499 ) ) ;
#64953 = CARTESIAN_POINT ( 'NONE',  ( -14.29746914071049879, 8.314922557960819915, 60.83224293864769550 ) ) ;
#64954 = CARTESIAN_POINT ( 'NONE',  ( 8.314922557961029526, -14.29746914071037800, 70.41775706135236135 ) ) ;
#64956 = CARTESIAN_POINT ( 'NONE',  ( -19.03943276465977164, 0.05219959533909376836, 56.24890960531435979 ) ) ;
#64955 = CARTESIAN_POINT ( 'NONE',  ( -15.72974639402197994, 15.80617190586746368, 115.6239096053143669 ) ) ;
#64957 = CARTESIAN_POINT ( 'NONE',  ( -19.02544592524342804, 5.153800228976336051, 66.04057627198103830 ) ) ;
#64958 = CARTESIAN_POINT ( 'NONE',  ( 8.224510206698742110, 14.34966873604972548, 67.08442372801901854 ) ) ;
#64959 = CARTESIAN_POINT ( 'NONE',  ( 28.79475375365586132, 2.781246896534039337E-14, 148.9843446568999923 ) ) ;
#64960 = EDGE_LOOP ( 'NONE', ( #75055, #126741, #67893, #123820 ) ) ;
#64961 = CARTESIAN_POINT ( 'NONE',  ( 19.05341960407617918, -5.049401038297876454, 21.04275706135232582 ) ) ;
#64962 = EDGE_CURVE ( 'NONE', #193517, #38038, #21682, .T. ) ;
#64963 = CARTESIAN_POINT ( 'NONE',  ( -16.46253265017160317, 9.564922557960807481, 35.83224293864768839 ) ) ;
#64964 = EDGE_LOOP ( 'NONE', ( #18372, #154496, #27885, #105016 ) ) ;
#64965 = CARTESIAN_POINT ( 'NONE',  ( -19.05341960407617563, 5.049401038297882671, 108.5427570613523187 ) ) ;
#64967 = CARTESIAN_POINT ( 'NONE',  ( -16.53943276465976808, -0.05219959533934237506, 23.75109039468567929 ) ) ;
#64966 = CARTESIAN_POINT ( 'NONE',  ( -9.564922557961040184, 16.46253265017147172, 42.91775706135234003 ) ) ;
#64968 = CARTESIAN_POINT ( 'NONE',  ( 19.05341960407611168, 5.049401038298154454, 43.95724293864769550 ) ) ;
#64969 = CARTESIAN_POINT ( 'NONE',  ( -5.153800228976328057, -19.02544592524343514, 62.29057627198100988 ) ) ;
#64970 = CARTESIAN_POINT ( 'NONE',  ( 21.53943276465977519, -0.05219959533907433946, 88.74890960531436690 ) ) ;
#64971 = CARTESIAN_POINT ( 'NONE',  ( 9.474510206698971260, -16.51473224551069308, 107.9155762719810383 ) ) ;
#64972 = CARTESIAN_POINT ( 'NONE',  ( -13.97604488694527625, -13.89961937509977652, 56.87390960531434558 ) ) ;
#64973 = CARTESIAN_POINT ( 'NONE',  ( -27.73933785331498925, -9.013057229001049109, 147.4750000027311785 ) ) ;
#64974 = CARTESIAN_POINT ( 'NONE',  ( -9.564922557961040184, 16.46253265017147172, 92.91775706135233293 ) ) ;
#64975 = CARTESIAN_POINT ( 'NONE',  ( -15.72974639402197994, 15.80617190586746368, 75.62390960531439532 ) ) ;
#64976 = CARTESIAN_POINT ( 'NONE',  ( 9.564922557961047289, -16.46253265017146816, 30.41775706135232937 ) ) ;
#64977 = EDGE_CURVE ( 'NONE', #65515, #147006, #105547, .T. ) ;
#64978 = CARTESIAN_POINT ( 'NONE',  ( -4.379528057220328563, 16.55341960407611168, 65.20724293864768129 ) ) ;
#64979 = CARTESIAN_POINT ( 'NONE',  ( 15.80617190586769283, -15.72974639402175789, 90.62609039468567573 ) ) ;
#64980 = CARTESIAN_POINT ( 'NONE',  ( -13.89961937509977652, 13.97604488694528158, 25.62390960531434558 ) ) ;
#64981 = CARTESIAN_POINT ( 'NONE',  ( -0.05219959533937732626, 21.53943276465977519, 87.50109039468568994 ) ) ;
#64983 = CARTESIAN_POINT ( 'NONE',  ( -5.823673210054431948, 21.52544592524334988, 87.70942372801901854 ) ) ;
#64982 = CARTESIAN_POINT ( 'NONE',  ( 8.314922557960818139, 14.29746914071049879, 29.58224293864769905 ) ) ;
#64984 = CARTESIAN_POINT ( 'NONE',  ( 5.153800228976335163, 19.02544592524342804, 74.79057627198103830 ) ) ;
#64985 = CARTESIAN_POINT ( 'NONE',  ( -21.55341960407619339, 5.719274019375674811, 38.54275706135234714 ) ) ;
#64986 = CARTESIAN_POINT ( 'NONE',  ( -13.89961937509977652, 13.97604488694528158, 75.62390960531438111 ) ) ;
#64987 = CARTESIAN_POINT ( 'NONE',  ( -16.53943276465976808, 0.05219959533911058130, 96.24890960531435269 ) ) ;
#64988 = CARTESIAN_POINT ( 'NONE',  ( -8.314922557960811034, -14.29746914071050412, 67.08224293864770971 ) ) ;
#64989 = CARTESIAN_POINT ( 'NONE',  ( -15.72974639402197994, 15.80617190586746368, 70.62390960531436690 ) ) ;
#64990 = CARTESIAN_POINT ( 'NONE',  ( 16.46253265017160672, -9.564922557960803928, 73.33224293864769550 ) ) ;
#64991 = CARTESIAN_POINT ( 'NONE',  ( -10.81492255796078084, -18.62759615963271287, 87.08224293864769550 ) ) ;
#64992 = CARTESIAN_POINT ( 'NONE',  ( -9.564922557961040184, 16.46253265017147172, 77.91775706135234714 ) ) ;
#64994 = CARTESIAN_POINT ( 'NONE',  ( 4.483927247898545687, 16.52544592524342804, 79.79057627198102409 ) ) ;
#64993 = CARTESIAN_POINT ( 'NONE',  ( -5.153800228976607833, 19.02544592524335343, 37.70942372801899722 ) ) ;
#64995 = CARTESIAN_POINT ( 'NONE',  ( -21.53943276465977519, 0.05219959533907696930, 51.24890960531436690 ) ) ;
#64996 = DIRECTION ( 'NONE',  ( -1.000000000000000000, 0.000000000000000000, 0.000000000000000000 ) ) ;
#64998 = CARTESIAN_POINT ( 'NONE',  ( 17.14385361876520264, 23.59649016807275856, 142.6750000027311103 ) ) ;
#64997 = CARTESIAN_POINT ( 'NONE',  ( -14.29746914071037622, -8.314922557961029526, 99.16775706135234714 ) ) ;
#64999 = CARTESIAN_POINT ( 'NONE',  ( 16.51473224551083163, -9.474510206698727899, 105.8344237280190043 ) ) ;
#65000 = CARTESIAN_POINT ( 'NONE',  ( 4.379528057220339221, -16.55341960407611168, 67.70724293864769550 ) ) ;
#65001 = CARTESIAN_POINT ( 'NONE',  ( -17.50000000000001421, 3.209263204892553567, 34.76196825606270124 ) ) ;
#65002 = CARTESIAN_POINT ( 'NONE',  ( 16.46253265017160672, -9.564922557960803928, 58.33224293864769550 ) ) ;
#65003 = CARTESIAN_POINT ( 'NONE',  ( 8.314922557960818139, 14.29746914071049879, 54.58224293864769550 ) ) ;
#65004 = ADVANCED_FACE ( 'NONE', ( #191528 ), #145016, .T. ) ;
#65005 = CARTESIAN_POINT ( 'NONE',  ( -9.564922557960796823, -16.46253265017161027, 107.0822429386476955 ) ) ;
#65007 = CARTESIAN_POINT ( 'NONE',  ( 5.153800228976335163, 19.02544592524342804, 59.79057627198100988 ) ) ;
#65006 = CARTESIAN_POINT ( 'NONE',  ( -5.049401038297874678, -19.05341960407617918, 89.79275706135230450 ) ) ;
#65008 = CARTESIAN_POINT ( 'NONE',  ( 0.05219959533909260263, 19.03943276465977164, 84.99890960531436690 ) ) ;
#65009 = CARTESIAN_POINT ( 'NONE',  ( 5.049401038298161559, -19.05341960407611168, 92.70724293864769550 ) ) ;
#65010 = CARTESIAN_POINT ( 'NONE',  ( 0.05219959533907565091, 21.53943276465977519, 64.99890960531435269 ) ) ;
#65011 = CARTESIAN_POINT ( 'NONE',  ( -16.55341960407617563, 4.379528057220093196, 53.54275706135234714 ) ) ;
#65012 = CARTESIAN_POINT ( 'NONE',  ( 9.474510206698729675, 16.51473224551082808, 102.0844237280190043 ) ) ;
#65013 = CARTESIAN_POINT ( 'NONE',  ( 5.153800228976335163, 19.02544592524342804, 59.79057627198100988 ) ) ;
#65014 = CARTESIAN_POINT ( 'NONE',  ( 18.62759615963271287, -10.81492255796078972, 63.33224293864770260 ) ) ;
#65015 = SHAPE_REPRESENTATION ( 'Mica Insulated Heating Coil Unit', ( #82054 ), #78902 ) ;
#65016 = CARTESIAN_POINT ( 'NONE',  ( 19.05341960407617918, -5.049401038297876454, 101.0427570613523045 ) ) ;
#65018 = CARTESIAN_POINT ( 'NONE',  ( -10.72451020669870658, -18.67979575497194134, 44.58442372801901854 ) ) ;
#65017 = CARTESIAN_POINT ( 'NONE',  ( 16.53943276465976808, -0.05219959533910856209, 28.74890960531435624 ) ) ;
#65019 = CARTESIAN_POINT ( 'NONE',  ( -4.024989859040965179, -4.710833808339871531, -62.49156203976952639 ) ) ;
#65021 = CARTESIAN_POINT ( 'NONE',  ( 16.53943276465976808, 0.05219959533934440121, 96.25109039468568994 ) ) ;
#65020 = CARTESIAN_POINT ( 'NONE',  ( -16.53943276465976808, -0.05219959533934237506, 78.75109039468568994 ) ) ;
#65022 = CARTESIAN_POINT ( 'NONE',  ( -5.427562675786936573E-15, 30.27659582821221207, 147.7656553485623760 ) ) ;
#65023 = CARTESIAN_POINT ( 'NONE',  ( -16.53943276465976808, -0.05219959533934237506, 78.75109039468568994 ) ) ;
#65024 = CARTESIAN_POINT ( 'NONE',  ( -16.53943276465976808, -0.05219959533934237506, 33.75109039468568284 ) ) ;
#65025 = CARTESIAN_POINT ( 'NONE',  ( -19.05341960407611168, -5.049401038298163336, 46.45724293864768129 ) ) ;
#65026 = CARTESIAN_POINT ( 'NONE',  ( 9.564922557960805705, 16.46253265017160317, 54.58224293864769550 ) ) ;
#65027 = CARTESIAN_POINT ( 'NONE',  ( -0.05219959533909027116, -19.03943276465977164, 62.49890960531435979 ) ) ;
#65028 = CARTESIAN_POINT ( 'NONE',  ( -21.52544592524334988, -5.823673210054445271, 58.95942372801902565 ) ) ;
#65029 = CARTESIAN_POINT ( 'NONE',  ( -12.06949235617739369, -12.14591786802326823, 49.37609039468569705 ) ) ;
#65030 = CARTESIAN_POINT ( 'NONE',  ( -0.05219959533934338120, 16.53943276465976808, 112.5010903946857042 ) ) ;
#65031 = CARTESIAN_POINT ( 'NONE',  ( 5.049401038298161559, -19.05341960407611168, 22.70724293864769194 ) ) ;
#65032 = CARTESIAN_POINT ( 'NONE',  ( 19.05341960407611168, 5.049401038298154454, 38.95724293864767418 ) ) ;
#65033 = CARTESIAN_POINT ( 'NONE',  ( -8.224510206698735004, -14.34966873604973081, 34.58442372801900433 ) ) ;
#65034 = CARTESIAN_POINT ( 'NONE',  ( -13.97604488694547697, 13.89961937509957934, 88.12609039468563310 ) ) ;
#65035 = CARTESIAN_POINT ( 'NONE',  ( 0.05219959533910956823, 16.53943276465976808, 84.99890960531436690 ) ) ;
#65036 = CARTESIAN_POINT ( 'NONE',  ( 5.049401038298161559, -19.05341960407611168, 52.70724293864767418 ) ) ;
#65038 = CARTESIAN_POINT ( 'NONE',  ( 16.38665767535051998, -7.295008042176092999, 92.76400864214544129 ) ) ;
#65037 = CARTESIAN_POINT ( 'NONE',  ( 13.89961937509957401, 13.97604488694547697, 71.87609039468567573 ) ) ;
#65039 = CARTESIAN_POINT ( 'NONE',  ( 5.719274019375673035, 21.55341960407619339, 77.29275706135234714 ) ) ;
#65040 = CARTESIAN_POINT ( 'NONE',  ( -12.14591786802326823, 12.06949235617739902, 53.12609039468568284 ) ) ;
#65041 = CARTESIAN_POINT ( 'NONE',  ( 17.50000000000000000, 5.499999999999997335, 36.70309617465829177 ) ) ;
#65042 = CARTESIAN_POINT ( 'NONE',  ( -15.72974639402197994, 15.80617190586746368, 40.62390960531435269 ) ) ;
#65043 = CARTESIAN_POINT ( 'NONE',  ( -14.29746914071037622, -8.314922557961029526, 29.16775706135234003 ) ) ;
#65044 = CARTESIAN_POINT ( 'NONE',  ( -9.564922557960796823, -16.46253265017161027, 27.08224293864769550 ) ) ;
#65045 = CARTESIAN_POINT ( 'NONE',  ( -9.474510206698720793, -16.51473224551083518, 29.58442372801900433 ) ) ;
#65046 = CARTESIAN_POINT ( 'NONE',  ( 0.000000000000000000, 0.000000000000000000, -64.92279855667830191 ) ) ;
#65047 = CARTESIAN_POINT ( 'NONE',  ( 9.564922557960805705, 16.46253265017160317, 39.58224293864768839 ) ) ;
#65048 = CYLINDRICAL_SURFACE ( 'NONE', #149803, 4.500000000000000000 ) ;
#65049 = CARTESIAN_POINT ( 'NONE',  ( -9.474510206698964154, 16.51473224551069663, 75.41557627198103830 ) ) ;
#65050 = CARTESIAN_POINT ( 'NONE',  ( -18.56101223717333326, -5.499999999999954703, 56.44978406935679516 ) ) ;
#65051 = CARTESIAN_POINT ( 'NONE',  ( -5.049401038297874678, -19.05341960407617918, 19.79275706135233293 ) ) ;
#65052 = CARTESIAN_POINT ( 'NONE',  ( -14.29746914071049879, 8.314922557960819915, 40.83224293864769550 ) ) ;
#65053 = CARTESIAN_POINT ( 'NONE',  ( -13.89961937509977652, 13.97604488694528158, 40.62390960531435979 ) ) ;
#65054 = CARTESIAN_POINT ( 'NONE',  ( -16.51473224551069308, -9.474510206698971260, 106.6655762719810383 ) ) ;
#65055 = CARTESIAN_POINT ( 'NONE',  ( 21.55341960407619695, -5.719274019375665929, 66.04275706135236135 ) ) ;
#65056 = CARTESIAN_POINT ( 'NONE',  ( -19.05341960407611168, -5.049401038298163336, 56.45724293864768129 ) ) ;
#65057 = CARTESIAN_POINT ( 'NONE',  ( 15.80617190586769283, -15.72974639402175789, 70.62609039468567573 ) ) ;
#65058 = CARTESIAN_POINT ( 'NONE',  ( 0.05219959533907565091, 21.53943276465977519, 24.99890960531435624 ) ) ;
#65059 = CARTESIAN_POINT ( 'NONE',  ( 19.02544592524343514, -5.153800228976328945, 38.54057627198103120 ) ) ;
#65060 = CARTESIAN_POINT ( 'NONE',  ( 0.05219959533937995610, -21.53943276465977519, 30.00109039468568284 ) ) ;
#65061 = CARTESIAN_POINT ( 'NONE',  ( -19.02544592524334988, -5.153800228976617603, 53.95942372801898301 ) ) ;
#65062 = CARTESIAN_POINT ( 'NONE',  ( -14.34966873604960291, -8.224510206698953496, 106.6655762719810383 ) ) ;
#65063 = CARTESIAN_POINT ( 'NONE',  ( 13.89961937509977652, -13.97604488694527269, 58.12390960531436690 ) ) ;
#65064 = CARTESIAN_POINT ( 'NONE',  ( -16.53943276465976808, -0.05219959533934237506, 18.75109039468568639 ) ) ;
#65065 = CARTESIAN_POINT ( 'NONE',  ( -12.14591786802309592, -12.06949235617757132, 71.87390960531438111 ) ) ;
#65066 = CARTESIAN_POINT ( 'NONE',  ( 16.51473224551069308, 9.474510206698969483, 114.1655762719810241 ) ) ;
#65067 = CARTESIAN_POINT ( 'NONE',  ( -16.46253265017146816, -9.564922557961047289, 104.1677570613523329 ) ) ;
#65068 = CARTESIAN_POINT ( 'NONE',  ( 5.823673210054125526, 21.52544592524343514, 109.7905762719810383 ) ) ;
#65069 = CARTESIAN_POINT ( 'NONE',  ( -5.823673210054431948, 21.52544592524334988, 52.70942372801902565 ) ) ;
#65070 = CARTESIAN_POINT ( 'NONE',  ( 12.14591786802327356, -12.06949235617739191, 60.62609039468567573 ) ) ;
#65071 = CARTESIAN_POINT ( 'NONE',  ( 12.14591786802327356, -12.06949235617739191, 55.62609039468568284 ) ) ;
#65072 = CARTESIAN_POINT ( 'NONE',  ( -21.52544592524343514, 5.823673210054127303, 51.04057627198103120 ) ) ;
#65073 = CARTESIAN_POINT ( 'NONE',  ( 16.51473224551069308, 9.474510206698969483, 49.16557627198102409 ) ) ;
#65074 = CARTESIAN_POINT ( 'NONE',  ( 12.06949235617739724, 12.14591786802326823, 76.87609039468567573 ) ) ;
#65075 = CARTESIAN_POINT ( 'NONE',  ( -18.62759615963270932, 10.81492255796079327, 95.83224293864770971 ) ) ;
#65076 = CARTESIAN_POINT ( 'NONE',  ( 8.314922557960818139, 14.29746914071049879, 54.58224293864769550 ) ) ;
#65077 = CARTESIAN_POINT ( 'NONE',  ( -0.05219959533909027116, -19.03943276465977164, 67.49890960531436690 ) ) ;
#65078 = CARTESIAN_POINT ( 'NONE',  ( -0.05219959533934338120, 16.53943276465976808, 72.50109039468568994 ) ) ;
#65079 = CARTESIAN_POINT ( 'NONE',  ( -0.05219959533936034679, 19.03943276465977164, 107.5010903946856615 ) ) ;
#65080 = CARTESIAN_POINT ( 'NONE',  ( 5.823673210054125526, 21.52544592524343514, 99.79057627198103830 ) ) ;
#65081 = CARTESIAN_POINT ( 'NONE',  ( 14.34966873604960469, 8.224510206698951720, 44.16557627198103120 ) ) ;
#65082 = ORIENTED_EDGE ( 'NONE', *, *, #87886, .T. ) ;
#65083 = CARTESIAN_POINT ( 'NONE',  ( -16.21995358207302473, 7.366697692864226710, 69.93551001512156517 ) ) ;
#65084 = CARTESIAN_POINT ( 'NONE',  ( 18.67979575497178502, 10.72451020669898547, 84.16557627198103830 ) ) ;
#65085 = CARTESIAN_POINT ( 'NONE',  ( 8.224510206698953496, -14.34966873604960469, 22.91557627198102765 ) ) ;
#65086 = ORIENTED_EDGE ( 'NONE', *, *, #67045, .T. ) ;
#65087 = CARTESIAN_POINT ( 'NONE',  ( 3.181980515339539295, 6.791538853603031889, 1.110912703473986074 ) ) ;
#65088 = CARTESIAN_POINT ( 'NONE',  ( 18.67979575497178502, 10.72451020669898547, 99.16557627198100988 ) ) ;
#65089 = CARTESIAN_POINT ( 'NONE',  ( 5.049401038298161559, -19.05341960407611168, 97.70724293864766707 ) ) ;
#65090 = CARTESIAN_POINT ( 'NONE',  ( -5.719274019375665041, -21.55341960407619695, 19.79275706135235069 ) ) ;
#65091 = CARTESIAN_POINT ( 'NONE',  ( 14.29746914071049879, -8.314922557960816363, 43.33224293864769550 ) ) ;
#65092 = CARTESIAN_POINT ( 'NONE',  ( -16.52544592524335698, -4.483927247898792601, 53.95942372801900433 ) ) ;
#65094 = EDGE_CURVE ( 'NONE', #12036, #149173, #34859, .T. ) ;
#65093 = CARTESIAN_POINT ( 'NONE',  ( 9.564922557960805705, 16.46253265017160317, 44.58224293864769550 ) ) ;
#65095 = CARTESIAN_POINT ( 'NONE',  ( -19.03943276465977164, -0.05219959533935918106, 53.75109039468566863 ) ) ;
#65096 = CARTESIAN_POINT ( 'NONE',  ( 16.46253265017160672, -9.564922557960803928, 78.33224293864769550 ) ) ;
#65097 = CARTESIAN_POINT ( 'NONE',  ( -18.67979575497178146, -10.72451020669898902, 31.66557627198102054 ) ) ;
#65098 = CARTESIAN_POINT ( 'NONE',  ( -29.30938409335406547, -24.40035533028687453, -16.80062434859987874 ) ) ;
#65099 = CARTESIAN_POINT ( 'NONE',  ( -0.05219959533936034679, 19.03943276465977164, 112.5010903946856757 ) ) ;
#65100 = CARTESIAN_POINT ( 'NONE',  ( -5.153800228976607833, 19.02544592524334988, 47.70942372801900433 ) ) ;
#65101 = CARTESIAN_POINT ( 'NONE',  ( 21.53943276465977519, -0.05219959533907433946, 98.74890960531438111 ) ) ;
#65102 = CARTESIAN_POINT ( 'NONE',  ( 8.314922557960818139, 14.29746914071049879, 34.58224293864770260 ) ) ;
#65103 = CARTESIAN_POINT ( 'NONE',  ( -0.05219959533909027116, -19.03943276465977164, 82.49890960531436690 ) ) ;
#65104 = CARTESIAN_POINT ( 'NONE',  ( 5.719274019375991003, -21.55341960407610458, 62.70724293864769550 ) ) ;
#65106 = CARTESIAN_POINT ( 'NONE',  ( 16.52544592524335698, 4.483927247898782831, 31.45942372801901854 ) ) ;
#65105 = CARTESIAN_POINT ( 'NONE',  ( -21.53943276465977519, 0.05219959533907696930, 101.2489096053143669 ) ) ;
#65107 = CARTESIAN_POINT ( 'NONE',  ( 18.67979575497178502, 10.72451020669898547, 24.16557627198103120 ) ) ;
#65108 = CARTESIAN_POINT ( 'NONE',  ( 18.67979575497194134, -10.72451020669871369, 85.83442372801901854 ) ) ;
#65109 = CARTESIAN_POINT ( 'NONE',  ( -19.02544592524342804, 5.153800228976336051, 86.04057627198103830 ) ) ;
#65110 = CARTESIAN_POINT ( 'NONE',  ( -0.05219959533909027116, -19.03943276465977164, 22.49890960531436690 ) ) ;
#65111 = CARTESIAN_POINT ( 'NONE',  ( 13.97604488694527802, 13.89961937509977652, 79.37390960531435269 ) ) ;
#65112 = CARTESIAN_POINT ( 'NONE',  ( 12.06949235617757843, -12.14591786802309237, 108.1239096053143811 ) ) ;
#65113 = CARTESIAN_POINT ( 'NONE',  ( -19.02544592524342804, 5.153800228976336051, 66.04057627198103830 ) ) ;
#65114 = CARTESIAN_POINT ( 'NONE',  ( 9.474510206698729675, 16.51473224551082808, 112.0844237280190043 ) ) ;
#65115 = CARTESIAN_POINT ( 'NONE',  ( 17.50000000000000355, 3.189878218039124302, 32.62948562571244793 ) ) ;
#65116 = CARTESIAN_POINT ( 'NONE',  ( -5.153800228976328057, -19.02544592524343514, 72.29057627198102409 ) ) ;
#65118 = CARTESIAN_POINT ( 'NONE',  ( 21.53943276465977519, -0.05219959533907433946, 23.74890960531435269 ) ) ;
#65117 = CARTESIAN_POINT ( 'NONE',  ( -0.05219959533937732626, 21.53943276465977519, 102.5010903946856899 ) ) ;
#65119 = CARTESIAN_POINT ( 'NONE',  ( 12.06949235617739724, 12.14591786802326823, 91.87609039468568994 ) ) ;
#65120 = CARTESIAN_POINT ( 'NONE',  ( -3.573655867282028392E-15, 2.428612866367529932E-14, 2.000000000000000000 ) ) ;
#65121 = CARTESIAN_POINT ( 'NONE',  ( 19.02544592524334988, 5.153800228976608722, 76.45942372801897591 ) ) ;
#65122 = CARTESIAN_POINT ( 'NONE',  ( -21.53943276465977519, -0.05219959533937600094, 113.7510903946856757 ) ) ;
#65123 = CARTESIAN_POINT ( 'NONE',  ( -16.61371651742604172, -7.165104196376049117, 46.14584930007004715 ) ) ;
#65124 = CARTESIAN_POINT ( 'NONE',  ( 13.97604488694527802, 13.89961937509977652, 34.37390960531436690 ) ) ;
#65125 = CARTESIAN_POINT ( 'NONE',  ( 4.483927247898545687, 16.52544592524342804, 39.79057627198103830 ) ) ;
#65126 = ADVANCED_FACE ( 'NONE', ( #176379 ), #146015, .T. ) ;
#65127 = LINE ( 'NONE', #3450, #146927 ) ;
#65128 = CARTESIAN_POINT ( 'NONE',  ( 16.55341960407618274, -4.379528057220086978, 101.0427570613523756 ) ) ;
#65129 = CARTESIAN_POINT ( 'NONE',  ( -19.01529144963339846, -5.499999999999897859, 86.23431955728437970 ) ) ;
#65130 = CARTESIAN_POINT ( 'NONE',  ( 16.55341960407618274, -4.379528057220086978, 76.04275706135237556 ) ) ;
#65131 = CARTESIAN_POINT ( 'NONE',  ( 19.02544592524343514, -5.153800228976328945, 43.54057627198103120 ) ) ;
#65132 = CARTESIAN_POINT ( 'NONE',  ( -10.81492255796105439, 18.62759615963255655, 92.91775706135236135 ) ) ;
#65133 = CARTESIAN_POINT ( 'NONE',  ( -5.049401038297874678, -19.05341960407617918, 104.7927570613523471 ) ) ;
#65134 = CARTESIAN_POINT ( 'NONE',  ( -18.62759615963255300, -10.81492255796106328, 79.16775706135234714 ) ) ;
#65135 = CARTESIAN_POINT ( 'NONE',  ( -5.049401038297874678, -19.05341960407617918, 59.79275706135231871 ) ) ;
#65136 = CARTESIAN_POINT ( 'NONE',  ( 9.474510206698971260, -16.51473224551069308, 82.91557627198103830 ) ) ;
#65137 = CARTESIAN_POINT ( 'NONE',  ( 9.474510206698971260, -16.51473224551069308, 67.91557627198102409 ) ) ;
#65138 = CARTESIAN_POINT ( 'NONE',  ( 16.31925111598459210, 7.325300261831483084, 72.33575461032744158 ) ) ;
#65139 = CARTESIAN_POINT ( 'NONE',  ( -0.05219959533910754901, -16.53943276465976808, 72.49890960531435269 ) ) ;
#65140 = CARTESIAN_POINT ( 'NONE',  ( 15.80617190586746368, 15.72974639402197994, 54.37390960531435979 ) ) ;
#65141 = CARTESIAN_POINT ( 'NONE',  ( -9.564922557960796823, -16.46253265017161027, 47.08224293864769550 ) ) ;
#65143 = CARTESIAN_POINT ( 'NONE',  ( 16.53943276465976808, 0.05219959533934440121, 76.25109039468568994 ) ) ;
#65142 = CARTESIAN_POINT ( 'NONE',  ( -10.72451020669898014, 18.67979575497178502, 85.41557627198102409 ) ) ;
#65144 = VERTEX_POINT ( 'NONE', #175368 ) ;
#65146 = CARTESIAN_POINT ( 'NONE',  ( -36.91746825000001309, 11.99521256947798342, -0.7249999972688133676 ) ) ;
#65145 = CARTESIAN_POINT ( 'NONE',  ( -8.314922557960811034, -14.29746914071050412, 77.08224293864769550 ) ) ;
#65147 = CARTESIAN_POINT ( 'NONE',  ( -4.379528057220086978, -16.55341960407618274, 39.79275706135235424 ) ) ;
#65148 = CARTESIAN_POINT ( 'NONE',  ( -12.06949235617756955, 12.14591786802309770, 110.6239096053143669 ) ) ;
#65149 = CARTESIAN_POINT ( 'NONE',  ( -5.049401038297874678, -19.05341960407617918, 64.79275706135233293 ) ) ;
#65150 = CARTESIAN_POINT ( 'NONE',  ( 16.53943276465976808, -0.05219959533910856209, 68.74890960531435269 ) ) ;
#65151 = CARTESIAN_POINT ( 'NONE',  ( -10.72451020669870658, -18.67979575497194134, 44.58442372801901854 ) ) ;
#65153 = CARTESIAN_POINT ( 'NONE',  ( 21.55341960407610458, 5.719274019375980345, 93.95724293864770971 ) ) ;
#65152 = DIRECTION ( 'NONE',  ( 0.000000000000000000, 0.000000000000000000, -1.000000000000000000 ) ) ;
#65154 = CARTESIAN_POINT ( 'NONE',  ( 16.46253265017160672, -9.564922557960803928, 113.3322429386476955 ) ) ;
#65155 = CARTESIAN_POINT ( 'NONE',  ( -16.55341960407611168, -4.379528057220339221, 81.45724293864769550 ) ) ;
#65156 = CARTESIAN_POINT ( 'NONE',  ( 24.59647911868938763, -31.70815657101694995, -17.34206816074872037 ) ) ;
#65157 = CARTESIAN_POINT ( 'NONE',  ( -16.46253265017160317, 9.564922557960807481, 45.83224293864769550 ) ) ;
#65158 = CARTESIAN_POINT ( 'NONE',  ( -5.950531402560715689E-15, 38.81732327939063509, -3.124999997268813168 ) ) ;
#65159 = CARTESIAN_POINT ( 'NONE',  ( 19.02544592524334988, 5.153800228976608722, 76.45942372801897591 ) ) ;
#65160 = CARTESIAN_POINT ( 'NONE',  ( 15.72974639402176855, 15.80617190586768217, 36.87609039468568994 ) ) ;
#65161 = CARTESIAN_POINT ( 'NONE',  ( 16.46253265017160672, -9.564922557960803928, 73.33224293864769550 ) ) ;
#65162 = CARTESIAN_POINT ( 'NONE',  ( 9.564922557961047289, -16.46253265017146816, 60.41775706135233293 ) ) ;
#65163 = CARTESIAN_POINT ( 'NONE',  ( -19.05341960407611168, -5.049401038298163336, 41.45724293864769550 ) ) ;
#65164 = CARTESIAN_POINT ( 'NONE',  ( 4.379528057220339221, -16.55341960407611168, 57.70724293864770260 ) ) ;
#65165 = CARTESIAN_POINT ( 'NONE',  ( -4.379528057220328563, 16.55341960407611168, 55.20724293864770260 ) ) ;
#65166 = CARTESIAN_POINT ( 'NONE',  ( 13.89961937509977652, -13.97604488694527269, 78.12390960531433848 ) ) ;
#65167 = CARTESIAN_POINT ( 'NONE',  ( -21.55341960407610458, -5.719274019375992779, 96.45724293864770971 ) ) ;
#65168 = CARTESIAN_POINT ( 'NONE',  ( 13.97604488694527802, 13.89961937509977652, 74.37390960531436690 ) ) ;
#65169 = CARTESIAN_POINT ( 'NONE',  ( 0.05219959533907565091, 21.53943276465977519, 79.99890960531435269 ) ) ;
#65170 = CARTESIAN_POINT ( 'NONE',  ( -15.72974639402176322, -15.80617190586768395, 109.3760903946857042 ) ) ;
#65173 = CARTESIAN_POINT ( 'NONE',  ( -8.314922557960811034, -14.29746914071050412, 97.08224293864770971 ) ) ;
#65172 = CARTESIAN_POINT ( 'NONE',  ( -14.29746914071037622, -8.314922557961029526, 104.1677570613523471 ) ) ;
#65171 = CARTESIAN_POINT ( 'NONE',  ( -16.51473224551069308, -9.474510206698971260, 31.66557627198102054 ) ) ;
#65174 = CARTESIAN_POINT ( 'NONE',  ( -16.51473224551082808, 9.474510206698731452, 108.3344237280190043 ) ) ;
#65175 = ORIENTED_EDGE ( 'NONE', *, *, #155178, .T. ) ;
#65176 = CARTESIAN_POINT ( 'NONE',  ( -15.80617190586768217, 15.72974639402176855, 33.12609039468569705 ) ) ;
#65177 = CARTESIAN_POINT ( 'NONE',  ( -5.049401038297874678, -19.05341960407617918, 54.79275706135234003 ) ) ;
#65178 = CARTESIAN_POINT ( 'NONE',  ( 16.52544592524342804, -4.483927247898539470, 23.54057627198102765 ) ) ;
#65179 = CARTESIAN_POINT ( 'NONE',  ( -10.72451020669898014, 18.67979575497178502, 70.41557627198102409 ) ) ;
#65180 = CARTESIAN_POINT ( 'NONE',  ( -19.03943276465977164, 0.05219959533909376836, 101.2489096053143669 ) ) ;
#65181 = CARTESIAN_POINT ( 'NONE',  ( -14.34966873604960291, -8.224510206698953496, 61.66557627198103120 ) ) ;
#65182 = CARTESIAN_POINT ( 'NONE',  ( -9.564922557960796823, -16.46253265017161027, 27.08224293864769550 ) ) ;
#65183 = CARTESIAN_POINT ( 'NONE',  ( 19.03943276465977164, -0.05219959533909143690, 33.74890960531435979 ) ) ;
#65184 = CARTESIAN_POINT ( 'NONE',  ( 13.97604488694548053, -13.89961937509957401, 25.62609039468566507 ) ) ;
#65185 = CARTESIAN_POINT ( 'NONE',  ( -16.52544592524335698, -4.483927247898792601, 88.95942372801901854 ) ) ;
#65186 = CARTESIAN_POINT ( 'NONE',  ( -5.823673210054431948, 21.52544592524334988, 37.70942372801900433 ) ) ;
#65187 = CARTESIAN_POINT ( 'NONE',  ( -12.14591786802326823, 12.06949235617739902, 43.12609039468568284 ) ) ;
#65188 = CARTESIAN_POINT ( 'NONE',  ( 0.05219959533909260263, 19.03943276465977164, 114.9989096053143669 ) ) ;
#65190 = CARTESIAN_POINT ( 'NONE',  ( 21.52544592524334988, 5.823673210054432836, 91.45942372801901854 ) ) ;
#65189 = CARTESIAN_POINT ( 'NONE',  ( 5.049401038298161559, -19.05341960407611168, 57.70724293864769550 ) ) ;
#65191 = CARTESIAN_POINT ( 'NONE',  ( -9.474510206698964154, 16.51473224551069663, 75.41557627198103830 ) ) ;
#65192 = CARTESIAN_POINT ( 'NONE',  ( 0.05219959533934541429, -16.53943276465976808, 65.00109039468568994 ) ) ;
#65193 = CARTESIAN_POINT ( 'NONE',  ( 12.14591786802309770, 12.06949235617756955, 109.3739096053143811 ) ) ;
#65194 = CARTESIAN_POINT ( 'NONE',  ( -12.06949235617739369, -12.14591786802326823, 109.3760903946857042 ) ) ;
#65195 = CARTESIAN_POINT ( 'NONE',  ( 0.000000000000000000, 0.000000000000000000, -64.92279855667830191 ) ) ;
#65198 = CARTESIAN_POINT ( 'NONE',  ( 9.474510206698971260, -16.51473224551069308, 82.91557627198103830 ) ) ;
#65197 = CARTESIAN_POINT ( 'NONE',  ( -19.05341960407611168, -5.049401038298163336, 96.45724293864769550 ) ) ;
#65196 = CARTESIAN_POINT ( 'NONE',  ( 21.53943276465977519, 0.05219959533937863772, 56.25109039468568284 ) ) ;
#65199 = CARTESIAN_POINT ( 'NONE',  ( 19.03943276465977164, -0.05219959533909143690, 103.7489096053143669 ) ) ;
#65200 = CARTESIAN_POINT ( 'NONE',  ( -16.53943276465976808, 0.05219959533911058130, 46.24890960531435979 ) ) ;
#65201 = CARTESIAN_POINT ( 'NONE',  ( 12.14591786802327356, -12.06949235617739191, 110.6260903946857042 ) ) ;
#65202 = CARTESIAN_POINT ( 'NONE',  ( 12.06949235617757843, -12.14591786802309237, 43.12390960531435269 ) ) ;
#65203 = CARTESIAN_POINT ( 'NONE',  ( -3.573655867282028392E-15, 2.428612866367529932E-14, 2.000000000000000000 ) ) ;
#65204 = CARTESIAN_POINT ( 'NONE',  ( 19.02544592524334988, 5.153800228976608722, 36.45942372801900433 ) ) ;
#65205 = CARTESIAN_POINT ( 'NONE',  ( -19.02544592524342804, 5.153800228976336051, 81.04057627198103830 ) ) ;
#65206 = CARTESIAN_POINT ( 'NONE',  ( 9.474510206698729675, 16.51473224551082808, 57.08442372801900433 ) ) ;
#65207 = CARTESIAN_POINT ( 'NONE',  ( 22.81625015709509441, 31.40387420917330275, -3.324999997268812901 ) ) ;
#65208 = CARTESIAN_POINT ( 'NONE',  ( 18.22780087662119897, -5.500000000000096811, 68.51763182126893525 ) ) ;
#65210 = CARTESIAN_POINT ( 'NONE',  ( -8.224510206698735004, -14.34966873604973081, 74.58442372801901854 ) ) ;
#65209 = CARTESIAN_POINT ( 'NONE',  ( 13.89961937509957401, 13.97604488694547697, 81.87609039468564731 ) ) ;
#65211 = DIRECTION ( 'NONE',  ( 6.718897857320949450E-15, -0.9991276842514722478, 0.04175967627138119087 ) ) ;
#65212 = CARTESIAN_POINT ( 'NONE',  ( -0.05219959533909027116, -19.03943276465977164, 102.4989096053143669 ) ) ;
#65213 = CARTESIAN_POINT ( 'NONE',  ( -18.67979575497193778, 10.72451020669871902, 23.33442372801901499 ) ) ;
#65214 = CARTESIAN_POINT ( 'NONE',  ( -13.89961937509957401, -13.97604488694547875, 94.37609039468566152 ) ) ;
#65216 = CARTESIAN_POINT ( 'NONE',  ( -0.05219959533909027116, -19.03943276465977164, 47.49890960531435979 ) ) ;
#65215 = CARTESIAN_POINT ( 'NONE',  ( -13.89961937509977652, 13.97604488694528158, 115.6239096053143669 ) ) ;
#65217 = CARTESIAN_POINT ( 'NONE',  ( 5.153800228976335163, 19.02544592524342804, 94.79057627198103830 ) ) ;
#65219 = CARTESIAN_POINT ( 'NONE',  ( 13.97604488694527802, 13.89961937509977652, 54.37390960531435979 ) ) ;
#65218 = CARTESIAN_POINT ( 'NONE',  ( -16.53943276465976808, 0.05219959533911058130, 56.24890960531436690 ) ) ;
#65220 = CARTESIAN_POINT ( 'NONE',  ( 13.97604488694527802, 13.89961937509977652, 59.37390960531434558 ) ) ;
#65221 = CARTESIAN_POINT ( 'NONE',  ( 19.02544592524334988, 5.153800228976608722, 61.45942372801900433 ) ) ;
#65222 = CARTESIAN_POINT ( 'NONE',  ( 9.564922557961047289, -16.46253265017146816, 25.41775706135234003 ) ) ;
#65223 = CARTESIAN_POINT ( 'NONE',  ( -5.049401038298153566, 19.05341960407611168, 60.20724293864768129 ) ) ;
#65224 = CARTESIAN_POINT ( 'NONE',  ( 0.05219959533907565091, 21.53943276465977519, 69.99890960531435269 ) ) ;
#65226 = CARTESIAN_POINT ( 'NONE',  ( -5.049401038297874678, -19.05341960407617918, 29.79275706135232227 ) ) ;
#65225 = CARTESIAN_POINT ( 'NONE',  ( 12.06949235617757843, -12.14591786802309237, 73.12390960531436690 ) ) ;
#65227 = FACE_OUTER_BOUND ( 'NONE', #167174, .T. ) ;
#65228 = CARTESIAN_POINT ( 'NONE',  ( -0.05219959533907301413, -21.53943276465977519, 52.49890960531435979 ) ) ;
#65229 = CARTESIAN_POINT ( 'NONE',  ( -18.67979575497178146, -10.72451020669898902, 26.66557627198103475 ) ) ;
#65230 = CARTESIAN_POINT ( 'NONE',  ( -13.97604488694527625, -13.89961937509977652, 46.87390960531435979 ) ) ;
#65231 = CARTESIAN_POINT ( 'NONE',  ( 13.97604488694527802, 13.89961937509977652, 34.37390960531436690 ) ) ;
#65232 = CARTESIAN_POINT ( 'NONE',  ( 12.14591786802309770, 12.06949235617756955, 104.3739096053143669 ) ) ;
#65233 = CARTESIAN_POINT ( 'NONE',  ( 10.72451020669898902, -18.67979575497178502, 107.9155762719810241 ) ) ;
#65234 = DIRECTION ( 'NONE',  ( 0.000000000000000000, 0.000000000000000000, -1.000000000000000000 ) ) ;
#65235 = CARTESIAN_POINT ( 'NONE',  ( 18.62759615963255655, 10.81492255796105972, 31.66775706135234358 ) ) ;
#65236 = CARTESIAN_POINT ( 'NONE',  ( -16.55341960407611168, -4.379528057220339221, 111.4572429386476813 ) ) ;
#65237 = CARTESIAN_POINT ( 'NONE',  ( -18.67979575497193778, 10.72451020669871902, 83.33442372801903275 ) ) ;
#65238 = CARTESIAN_POINT ( 'NONE',  ( 5.719274019375991003, -21.55341960407610458, 87.70724293864769550 ) ) ;
#65239 = CARTESIAN_POINT ( 'NONE',  ( 9.564922557961047289, -16.46253265017146816, 40.41775706135234003 ) ) ;
#65240 = CARTESIAN_POINT ( 'NONE',  ( 5.049401038298161559, -19.05341960407611168, 22.70724293864769194 ) ) ;
#65241 = CARTESIAN_POINT ( 'NONE',  ( 18.22780087662123805, -5.499999999999976019, 78.51763182126894947 ) ) ;
#65242 = CARTESIAN_POINT ( 'NONE',  ( 37.99999999999999289, 2.893978650043524126E-14, -1.000000000000000000 ) ) ;
#65243 = CARTESIAN_POINT ( 'NONE',  ( -4.379528057220086978, -16.55341960407618274, 49.79275706135234714 ) ) ;
#65244 = CARTESIAN_POINT ( 'NONE',  ( 5.153800228976335163, 19.02544592524342804, 29.79057627198102409 ) ) ;
#65245 = CARTESIAN_POINT ( 'NONE',  ( -25.70602947687971351, -7.354137148287275494, 175.2376750527030822 ) ) ;
#65246 = CARTESIAN_POINT ( 'NONE',  ( -19.05341960407611168, -5.049401038298163336, 76.45724293864769550 ) ) ;
#65247 = CARTESIAN_POINT ( 'NONE',  ( -8.314922557960811034, -14.29746914071050412, 97.08224293864770971 ) ) ;
#65248 = CARTESIAN_POINT ( 'NONE',  ( -18.67979575497178146, -10.72451020669898902, 51.66557627198102409 ) ) ;
#65249 = CARTESIAN_POINT ( 'NONE',  ( 12.14591786802309770, 12.06949235617756955, 79.37390960531436690 ) ) ;
#65250 = CARTESIAN_POINT ( 'NONE',  ( -16.52544592524335698, -4.483927247898792601, 38.95942372801901854 ) ) ;
#65251 = CARTESIAN_POINT ( 'NONE',  ( -15.72974639402176322, -15.80617190586768395, 89.37609039468568994 ) ) ;
#65252 = CARTESIAN_POINT ( 'NONE',  ( -0.05219959533909027116, -19.03943276465977164, 27.49890960531435624 ) ) ;
#65253 = CARTESIAN_POINT ( 'NONE',  ( 8.224510206698742110, 14.34966873604972548, 97.08442372801904696 ) ) ;
#65254 = CARTESIAN_POINT ( 'NONE',  ( 16.53943276465976808, -0.05219959533910856209, 43.74890960531435979 ) ) ;
#65255 = CARTESIAN_POINT ( 'NONE',  ( 13.97604488694527802, 13.89961937509977652, 49.37390960531434558 ) ) ;
#65256 = CARTESIAN_POINT ( 'NONE',  ( 21.53943276465977519, 0.05219959533937863772, 91.25109039468568994 ) ) ;
#65257 = CARTESIAN_POINT ( 'NONE',  ( -21.55341960407610458, -5.719274019375992779, 101.4572429386476955 ) ) ;
#65258 = CARTESIAN_POINT ( 'NONE',  ( 5.823673210054444382, -21.52544592524334988, 65.20942372801901854 ) ) ;
#65259 = CARTESIAN_POINT ( 'NONE',  ( 4.483927247898790824, -16.52544592524335698, 45.20942372801901854 ) ) ;
#65261 = CARTESIAN_POINT ( 'NONE',  ( 21.55341960407619695, -5.719274019375665929, 86.04275706135236135 ) ) ;
#65260 = CARTESIAN_POINT ( 'NONE',  ( -14.29746914071049879, 8.314922557960819915, 70.83224293864770971 ) ) ;
#65262 = CARTESIAN_POINT ( 'NONE',  ( 8.224510206698953496, -14.34966873604960469, 22.91557627198102765 ) ) ;
#65263 = CARTESIAN_POINT ( 'NONE',  ( 16.52216118717246118, -7.221426719304361974, 46.42400978952972679 ) ) ;
#65264 = DIRECTION ( 'NONE',  ( 1.000000000000000000, 0.000000000000000000, 0.000000000000000000 ) ) ;
#65265 = CARTESIAN_POINT ( 'NONE',  ( 4.379528057220339221, -16.55341960407611168, 47.70724293864770260 ) ) ;
#65266 = CARTESIAN_POINT ( 'NONE',  ( -16.55341960407617563, 4.379528057220093196, 78.54275706135236135 ) ) ;
#65267 = CARTESIAN_POINT ( 'NONE',  ( -13.89961937509977652, 13.97604488694528158, 90.62390960531432427 ) ) ;
#65268 = CARTESIAN_POINT ( 'NONE',  ( -19.03943276465977164, 0.05219959533909376836, 101.2489096053143669 ) ) ;
#65269 = CARTESIAN_POINT ( 'NONE',  ( -21.55341960407619339, 5.719274019375674811, 83.54275706135234714 ) ) ;
#65270 = CARTESIAN_POINT ( 'NONE',  ( -16.53943276465976808, -0.05219959533934237506, 88.75109039468567573 ) ) ;
#65271 = CARTESIAN_POINT ( 'NONE',  ( -8.314922557960811034, -14.29746914071050412, 67.08224293864770971 ) ) ;
#65272 = CARTESIAN_POINT ( 'NONE',  ( 19.05341960407611168, 5.049401038298154454, 83.95724293864766707 ) ) ;
#65273 = ORIENTED_EDGE ( 'NONE', *, *, #88864, .F. ) ;
#65275 = CARTESIAN_POINT ( 'NONE',  ( -14.34966873604972548, 8.224510206698743886, 28.33442372801902209 ) ) ;
#65274 =( BOUNDED_CURVE ( )  B_SPLINE_CURVE ( 2, ( #59530, #134415, #58551, #56569, #136387, #89885, #120217, #181907, #149570, #26243, #197084 ),
 .UNSPECIFIED., .F., .F. ) 
 B_SPLINE_CURVE_WITH_KNOTS ( ( 3, 2, 2, 2, 2, 3 ),
 ( 0.6000000000000000888, 0.6200000000000001066, 0.6400000000000001243, 0.6600000000000001421, 0.6800000000000001599, 0.7000000000000001776 ),
 .UNSPECIFIED. ) 
 CURVE ( )  GEOMETRIC_REPRESENTATION_ITEM ( )  RATIONAL_B_SPLINE_CURVE ( ( 0.9999999999999997780, 0.9510565162951537532, 1.000000000000000000, 0.9510565162951535312, 1.000000000000000000, 0.9510565162951535312, 1.000000000000000000, 0.9510565162951535312, 1.000000000000000000, 0.9510565162951529761, 1.000000000000000444 ) ) 
 REPRESENTATION_ITEM ( '' )  );
#65276 = CARTESIAN_POINT ( 'NONE',  ( 16.46253265017160672, -9.564922557960803928, 23.33224293864769194 ) ) ;
#65277 = CARTESIAN_POINT ( 'NONE',  ( -5.049401038298153566, 19.05341960407611168, 95.20724293864770971 ) ) ;
#65279 = CARTESIAN_POINT ( 'NONE',  ( 11.40812507854755253, -35.11059874428192273, -10.02499999726881441 ) ) ;
#65278 = CARTESIAN_POINT ( 'NONE',  ( 16.53943276465976808, 0.05219959533934440121, 26.25109039468567573 ) ) ;
#65280 = CARTESIAN_POINT ( 'NONE',  ( 18.67979575497194134, -10.72451020669871369, 110.8344237280190043 ) ) ;
#65281 = CARTESIAN_POINT ( 'NONE',  ( -14.29746914071037622, -8.314922557961029526, 89.16775706135236135 ) ) ;
#65282 = CARTESIAN_POINT ( 'NONE',  ( 16.46253265017146816, 9.564922557961045513, 111.6677570613523329 ) ) ;
#65283 = CARTESIAN_POINT ( 'NONE',  ( 19.05341960407611168, 5.049401038298154454, 38.95724293864767418 ) ) ;
#65284 = CARTESIAN_POINT ( 'NONE',  ( 14.29746914071037800, 8.314922557961029526, 76.66775706135234714 ) ) ;
#65285 = CARTESIAN_POINT ( 'NONE',  ( 8.224510206698742110, 14.34966873604972548, 67.08442372801901854 ) ) ;
#65286 = CARTESIAN_POINT ( 'NONE',  ( 20.76454096204583166, -34.24119976882402483, -10.56784353604181881 ) ) ;
#65287 = CARTESIAN_POINT ( 'NONE',  ( 16.51473224551083163, -9.474510206698727899, 75.83442372801900433 ) ) ;
#65288 = CARTESIAN_POINT ( 'NONE',  ( -10.72451020669870658, -18.67979575497194134, 104.5844237280190185 ) ) ;
#65289 = CARTESIAN_POINT ( 'NONE',  ( -19.02544592524342804, 5.153800228976336051, 51.04057627198103120 ) ) ;
#65290 = CARTESIAN_POINT ( 'NONE',  ( -0.05219959533909027116, -19.03943276465977164, 92.49890960531436690 ) ) ;
#65291 = CARTESIAN_POINT ( 'NONE',  ( -8.314922557960811034, -14.29746914071050412, 82.08224293864768129 ) ) ;
#65292 = CARTESIAN_POINT ( 'NONE',  ( 19.03943276465977164, 0.05219959533936151252, 51.25109039468567573 ) ) ;
#65293 = CARTESIAN_POINT ( 'NONE',  ( -21.55341960407610458, -5.719274019375992779, 46.45724293864769550 ) ) ;
#65294 = CARTESIAN_POINT ( 'NONE',  ( -21.53943276465977519, -0.05219959533937600094, 103.7510903946857042 ) ) ;
#65295 = CARTESIAN_POINT ( 'NONE',  ( 19.05341960407611168, 5.049401038298154454, 93.95724293864769550 ) ) ;
#65296 = CARTESIAN_POINT ( 'NONE',  ( 18.62759615963255655, 10.81492255796105972, 111.6677570613523613 ) ) ;
#65297 = CARTESIAN_POINT ( 'NONE',  ( 21.55341960407610458, 5.719274019375980345, 58.95724293864770971 ) ) ;
#65298 = CARTESIAN_POINT ( 'NONE',  ( -5.153800228976328057, -19.02544592524343514, 92.29057627198099567 ) ) ;
#65299 = CARTESIAN_POINT ( 'NONE',  ( -13.89961937509957401, -13.97604488694547875, 84.37609039468567573 ) ) ;
#65300 = CARTESIAN_POINT ( 'NONE',  ( 13.97604488694527802, 13.89961937509977652, 104.3739096053143385 ) ) ;
#65301 = CARTESIAN_POINT ( 'NONE',  ( -4.379528057220086978, -16.55341960407618274, 19.79275706135235069 ) ) ;
#65302 = CARTESIAN_POINT ( 'NONE',  ( 0.05219959533910956823, 16.53943276465976808, 109.9989096053143527 ) ) ;
#65303 = CARTESIAN_POINT ( 'NONE',  ( 13.89961937509977652, -13.97604488694527269, 83.12390960531436690 ) ) ;
#65304 = CARTESIAN_POINT ( 'NONE',  ( 10.72451020669898902, -18.67979575497178502, 77.91557627198102409 ) ) ;
#65305 = CARTESIAN_POINT ( 'NONE',  ( 16.53943276465976808, 0.05219959533934440121, 41.25109039468568284 ) ) ;
#65306 = CARTESIAN_POINT ( 'NONE',  ( -15.72974639402176322, -15.80617190586768395, 44.37609039468567573 ) ) ;
#65307 = CARTESIAN_POINT ( 'NONE',  ( -15.80617190586768217, 15.72974639402176855, 98.12609039468570415 ) ) ;
#65308 = CARTESIAN_POINT ( 'NONE',  ( 14.34966873604972726, -8.224510206698740333, 90.83442372801901854 ) ) ;
#65309 = CARTESIAN_POINT ( 'NONE',  ( 13.97604488694527802, 13.89961937509977652, 94.37390960531436690 ) ) ;
#65310 = CARTESIAN_POINT ( 'NONE',  ( -12.14591786802309592, -12.06949235617757132, 86.87390960531438111 ) ) ;
#65311 = CARTESIAN_POINT ( 'NONE',  ( 14.34966873604960469, 8.224510206698951720, 29.16557627198103120 ) ) ;
#65312 = CARTESIAN_POINT ( 'NONE',  ( -19.05341960407617563, 5.049401038297882671, 63.54275706135234003 ) ) ;
#65313 = CARTESIAN_POINT ( 'NONE',  ( 18.67979575497194134, -10.72451020669871369, 45.83442372801901854 ) ) ;
#65314 = CARTESIAN_POINT ( 'NONE',  ( -16.51473224551082808, 9.474510206698731452, 28.33442372801900433 ) ) ;
#65315 = CARTESIAN_POINT ( 'NONE',  ( -4.483927247898539470, -16.52544592524342804, 97.29057627198105251 ) ) ;
#65316 = CARTESIAN_POINT ( 'NONE',  ( 16.46253265017160672, -9.564922557960803928, 108.3322429386476955 ) ) ;
#65317 = CARTESIAN_POINT ( 'NONE',  ( 4.379528057220092307, 16.55341960407617563, 112.2927570613523471 ) ) ;
#65318 = CARTESIAN_POINT ( 'NONE',  ( -15.72974639402176322, -15.80617190586768395, 84.37609039468570415 ) ) ;
#65319 = CARTESIAN_POINT ( 'NONE',  ( -0.05219959533934338120, 16.53943276465976808, 52.50109039468567573 ) ) ;
#65320 = CARTESIAN_POINT ( 'NONE',  ( 8.314922557961029526, -14.29746914071037800, 100.4177570613523471 ) ) ;
#65321 = CARTESIAN_POINT ( 'NONE',  ( -10.81492255796105439, 18.62759615963255655, 52.91775706135235424 ) ) ;
#65322 = VERTEX_POINT ( 'NONE', #129829 ) ;
#65323 = CARTESIAN_POINT ( 'NONE',  ( 0.05219959533937995610, -21.53943276465977519, 25.00109039468567218 ) ) ;
#65324 = CARTESIAN_POINT ( 'NONE',  ( -12.14591786802309592, -12.06949235617757132, 106.8739096053143811 ) ) ;
#65325 = CARTESIAN_POINT ( 'NONE',  ( 9.474510206698971260, -16.51473224551069308, 27.91557627198103120 ) ) ;
#65326 = CARTESIAN_POINT ( 'NONE',  ( -16.53943276465976808, 0.05219959533911058130, 66.24890960531436690 ) ) ;
#65327 = CARTESIAN_POINT ( 'NONE',  ( 9.474510206698971260, -16.51473224551069308, 77.91557627198103830 ) ) ;
#65328 = CARTESIAN_POINT ( 'NONE',  ( 12.06949235617739724, 12.14591786802326823, 101.8760903946857042 ) ) ;
#65329 = CARTESIAN_POINT ( 'NONE',  ( 5.153800228976335163, 19.02544592524342804, 39.79057627198100988 ) ) ;
#65330 = CARTESIAN_POINT ( 'NONE',  ( -15.80617190586745835, -15.72974639402198527, 56.87390960531436690 ) ) ;
#65331 = CARTESIAN_POINT ( 'NONE',  ( -0.05219959533910754901, -16.53943276465976808, 87.49890960531436690 ) ) ;
#65332 = CARTESIAN_POINT ( 'NONE',  ( 21.52544592524344225, -5.823673210054117533, 88.54057627198103830 ) ) ;
#65333 = CARTESIAN_POINT ( 'NONE',  ( 9.564922557960805705, 16.46253265017160317, 89.58224293864769550 ) ) ;
#65335 = CARTESIAN_POINT ( 'NONE',  ( 19.03943276465977164, 0.05219959533936151252, 86.25109039468567573 ) ) ;
#65334 = CARTESIAN_POINT ( 'NONE',  ( -0.05219959533909027116, -19.03943276465977164, 57.49890960531435979 ) ) ;
#65336 = CARTESIAN_POINT ( 'NONE',  ( 10.81492255796078972, 18.62759615963270932, 44.58224293864769550 ) ) ;
#65337 = CARTESIAN_POINT ( 'NONE',  ( -21.53943276465977519, -0.05219959533937600094, 73.75109039468567573 ) ) ;
#65338 = CARTESIAN_POINT ( 'NONE',  ( 16.51473224551069308, 9.474510206698969483, 54.16557627198103120 ) ) ;
#65339 = CARTESIAN_POINT ( 'NONE',  ( -16.46253265017160317, 9.564922557960807481, 80.83224293864769550 ) ) ;
#65340 = CARTESIAN_POINT ( 'NONE',  ( 16.55341960407618274, -4.379528057220086978, 61.04275706135234714 ) ) ;
#65341 = CARTESIAN_POINT ( 'NONE',  ( -18.62759615963255300, -10.81492255796106328, 44.16775706135234714 ) ) ;
#65342 = CARTESIAN_POINT ( 'NONE',  ( 0.05219959533937995610, -21.53943276465977519, 70.00109039468568994 ) ) ;
#65343 = CARTESIAN_POINT ( 'NONE',  ( 0.05219959533907565091, 21.53943276465977519, 24.99890960531435624 ) ) ;
#65344 = CARTESIAN_POINT ( 'NONE',  ( 15.72974639402199770, -15.80617190586745480, 98.12390960531436690 ) ) ;
#65346 = CARTESIAN_POINT ( 'NONE',  ( -8.314922557961024197, 14.29746914071037800, 67.91775706135234714 ) ) ;
#65345 = CARTESIAN_POINT ( 'NONE',  ( -15.80617190586768217, 15.72974639402176855, 33.12609039468569705 ) ) ;
#65347 = CARTESIAN_POINT ( 'NONE',  ( 5.823673210054125526, 21.52544592524343514, 59.79057627198103120 ) ) ;
#65348 = CARTESIAN_POINT ( 'NONE',  ( -13.97604488694547697, 13.89961937509957934, 38.12609039468566152 ) ) ;
#65350 = CARTESIAN_POINT ( 'NONE',  ( 14.29746914071049879, -8.314922557960816363, 23.33224293864769194 ) ) ;
#65349 = CARTESIAN_POINT ( 'NONE',  ( -16.46253265017160317, 9.564922557960807481, 70.83224293864770971 ) ) ;
#65351 = CARTESIAN_POINT ( 'NONE',  ( -23.48529157249599919, -32.32473071737749848, -5.700000000000000178 ) ) ;
#65352 = CARTESIAN_POINT ( 'NONE',  ( 19.05341960407611168, 5.049401038298154454, 103.9572429386476671 ) ) ;
#65353 = FACE_OUTER_BOUND ( 'NONE', #149535, .T. ) ;
#65354 = CARTESIAN_POINT ( 'NONE',  ( -9.564922557961040184, 16.46253265017147172, 87.91775706135233293 ) ) ;
#65355 = CARTESIAN_POINT ( 'NONE',  ( 15.80617190586746368, 15.72974639402197994, 54.37390960531435979 ) ) ;
#65356 = CARTESIAN_POINT ( 'NONE',  ( -8.314922557960811034, -14.29746914071050412, 42.08224293864769550 ) ) ;
#65357 = CARTESIAN_POINT ( 'NONE',  ( 19.02544592524334988, 5.153800228976608722, 96.45942372801897591 ) ) ;
#65358 = CARTESIAN_POINT ( 'NONE',  ( -19.02544592524342804, 5.153800228976336051, 36.04057627198100988 ) ) ;
#65359 = CARTESIAN_POINT ( 'NONE',  ( -19.05341960407617563, 5.049401038297882671, 108.5427570613523187 ) ) ;
#65361 = CARTESIAN_POINT ( 'NONE',  ( 9.564922557961047289, -16.46253265017146816, 60.41775706135233293 ) ) ;
#65360 = CARTESIAN_POINT ( 'NONE',  ( 15.72974639402199770, -15.80617190586745480, 93.12390960531436690 ) ) ;
#65362 = CARTESIAN_POINT ( 'NONE',  ( -16.52544592524335698, -4.483927247898792601, 78.95942372801901854 ) ) ;
#65363 = CARTESIAN_POINT ( 'NONE',  ( 0.05219959533909260263, 19.03943276465977164, 64.99890960531436690 ) ) ;
#65364 = CARTESIAN_POINT ( 'NONE',  ( -8.314922557960811034, -14.29746914071050412, 77.08224293864769550 ) ) ;
#65365 = ADVANCED_FACE ( 'NONE', ( #81336 ), #127850, .F. ) ;
#65366 = CARTESIAN_POINT ( 'NONE',  ( 16.51473224551069308, 9.474510206698969483, 54.16557627198103120 ) ) ;
#65367 = CARTESIAN_POINT ( 'NONE',  ( 0.05219959533910956823, 16.53943276465976808, 59.99890960531436690 ) ) ;
#65368 = CARTESIAN_POINT ( 'NONE',  ( 16.51473224551069308, 9.474510206698969483, 24.16557627198102765 ) ) ;
#65369 = CARTESIAN_POINT ( 'NONE',  ( 32.64453336272026718, -1.163414472736631538E-14, 87.50000000000000000 ) ) ;
#65370 = CARTESIAN_POINT ( 'NONE',  ( 8.224510206698953496, -14.34966873604960469, 22.91557627198102765 ) ) ;
#65371 = CARTESIAN_POINT ( 'NONE',  ( -0.05219959533909027116, -19.03943276465977164, 72.49890960531435269 ) ) ;
#65372 = CARTESIAN_POINT ( 'NONE',  ( -18.09805431107246676, 5.500000000000103029, 51.01606229291886763 ) ) ;
#65373 = CARTESIAN_POINT ( 'NONE',  ( -13.97604488694547697, 13.89961937509957934, 33.12609039468566863 ) ) ;
#65374 = CARTESIAN_POINT ( 'NONE',  ( -8.314922557961024197, 14.29746914071037800, 47.91775706135234714 ) ) ;
#65375 = CARTESIAN_POINT ( 'NONE',  ( 15.72974639402199770, -15.80617190586745480, 63.12390960531435979 ) ) ;
#65376 = CARTESIAN_POINT ( 'NONE',  ( -16.46253265017146816, -9.564922557961047289, 19.16775706135233293 ) ) ;
#65377 = CARTESIAN_POINT ( 'NONE',  ( -5.049401038298153566, 19.05341960407611168, 80.20724293864769550 ) ) ;
#65378 = DIRECTION ( 'NONE',  ( -1.000000000000000000, -0.000000000000000000, -0.000000000000000000 ) ) ;
#65379 = CARTESIAN_POINT ( 'NONE',  ( -16.46253265017160317, 9.564922557960807481, 115.8322429386477097 ) ) ;
#65380 = CARTESIAN_POINT ( 'NONE',  ( 10.72451020669871369, 18.67979575497193778, 37.08442372801901143 ) ) ;
#65381 = CARTESIAN_POINT ( 'NONE',  ( -16.55341960407611168, -4.379528057220339221, 101.4572429386476955 ) ) ;
#65384 = CARTESIAN_POINT ( 'NONE',  ( 11.30153831258471797, -180.0000000000000000, -4.999999999999999112 ) ) ;
#65383 = CARTESIAN_POINT ( 'NONE',  ( 19.02544592524343514, -5.153800228976328945, 78.54057627198099567 ) ) ;
#65382 = CARTESIAN_POINT ( 'NONE',  ( -10.81492255796078084, -18.62759615963271287, 107.0822429386476955 ) ) ;
#65385 = CARTESIAN_POINT ( 'NONE',  ( -5.823673210054431948, 21.52544592524334988, 32.70942372801900433 ) ) ;
#65386 = ORIENTED_EDGE ( 'NONE', *, *, #162333, .T. ) ;
#65387 = CARTESIAN_POINT ( 'NONE',  ( 19.05341960407611168, 5.049401038298154454, 88.95724293864769550 ) ) ;
#65388 = CARTESIAN_POINT ( 'NONE',  ( -17.50000000000002842, -5.499999999999952927, 76.28230962303568674 ) ) ;
#65390 = CARTESIAN_POINT ( 'NONE',  ( 19.03943276465977164, -0.05219959533909143690, 38.74890960531436690 ) ) ;
#65389 = CARTESIAN_POINT ( 'NONE',  ( -9.474510206698964154, 16.51473224551069663, 25.41557627198103120 ) ) ;
#65391 = CARTESIAN_POINT ( 'NONE',  ( 9.564922557961047289, -16.46253265017146816, 105.4177570613523471 ) ) ;
#65392 = CARTESIAN_POINT ( 'NONE',  ( 11.40812507854754365, 35.11059874428196537, -7.724999997268813701 ) ) ;
#65393 = CARTESIAN_POINT ( 'NONE',  ( -16.53943276465976808, 0.05219959533911058130, 116.2489096053143669 ) ) ;
#65394 = CARTESIAN_POINT ( 'NONE',  ( 21.55341960407619695, -5.719274019375665929, 86.04275706135236135 ) ) ;
#65396 = CARTESIAN_POINT ( 'NONE',  ( 10.81492255796106328, -18.62759615963255655, 40.41775706135234714 ) ) ;
#65395 = CARTESIAN_POINT ( 'NONE',  ( -0.05219959533909027116, -19.03943276465977164, 57.49890960531435979 ) ) ;
#65397 = CARTESIAN_POINT ( 'NONE',  ( -18.67979575497193778, 10.72451020669871902, 28.33442372801902209 ) ) ;
#65398 = CARTESIAN_POINT ( 'NONE',  ( 17.81289503416610742, 24.51734667627700404, 147.2999999999999545 ) ) ;
#65399 = CARTESIAN_POINT ( 'NONE',  ( 13.89961937509977652, -13.97604488694527269, 83.12390960531436690 ) ) ;
#65400 = LINE ( 'NONE', #69388, #72761 ) ;
#65402 = CARTESIAN_POINT ( 'NONE',  ( 5.823673210054125526, 21.52544592524343514, 44.79057627198103120 ) ) ;
#65401 = CARTESIAN_POINT ( 'NONE',  ( 0.05219959533934541429, -16.53943276465976808, 30.00109039468568284 ) ) ;
#65403 = CARTESIAN_POINT ( 'NONE',  ( 21.53943276465977519, 0.05219959533937863772, 76.25109039468568994 ) ) ;
#65404 = CARTESIAN_POINT ( 'NONE',  ( 5.153800228976335163, 19.02544592524342804, 109.7905762719810099 ) ) ;
#65405 = CARTESIAN_POINT ( 'NONE',  ( 9.564922557961047289, -16.46253265017146816, 100.4177570613523329 ) ) ;
#65406 = CARTESIAN_POINT ( 'NONE',  ( 16.46253265017160672, -9.564922557960803928, 63.33224293864769550 ) ) ;
#65407 = CARTESIAN_POINT ( 'NONE',  ( 5.153800228976335163, 19.02544592524342804, 89.79057627198102409 ) ) ;
#65408 = CARTESIAN_POINT ( 'NONE',  ( -16.52544592524342804, 4.483927247898546575, 101.0405762719810383 ) ) ;
#65409 = CARTESIAN_POINT ( 'NONE',  ( 8.314922557960818139, 14.29746914071049879, 104.5822429386477097 ) ) ;
#65410 = CARTESIAN_POINT ( 'NONE',  ( 5.049401038298161559, -19.05341960407611168, 112.7072429386476813 ) ) ;
#65411 = CARTESIAN_POINT ( 'NONE',  ( 16.53943276465976808, 0.05219959533934440121, 81.25109039468568994 ) ) ;
#65413 = CARTESIAN_POINT ( 'NONE',  ( 13.97604488694527802, 13.89961937509977652, 44.37390960531435269 ) ) ;
#65412 = CARTESIAN_POINT ( 'NONE',  ( -0.05219959533910754901, -16.53943276465976808, 62.49890960531436690 ) ) ;
#65414 = CARTESIAN_POINT ( 'NONE',  ( -15.80617190586768217, 15.72974639402176855, 68.12609039468567573 ) ) ;
#65415 = CARTESIAN_POINT ( 'NONE',  ( -9.564922557961040184, 16.46253265017147172, 92.91775706135233293 ) ) ;
#65416 = CARTESIAN_POINT ( 'NONE',  ( -4.379528057220328563, 16.55341960407611168, 60.20724293864768839 ) ) ;
#65417 = CARTESIAN_POINT ( 'NONE',  ( 21.53943276465977519, 0.05219959533937863772, 21.25109039468567218 ) ) ;
#65418 = CARTESIAN_POINT ( 'NONE',  ( 10.81492255796078972, 18.62759615963270932, 49.58224293864769550 ) ) ;
#65419 = CARTESIAN_POINT ( 'NONE',  ( -17.31747979337945509, -6.344076630961063223, 106.3794486806518194 ) ) ;
#65420 = CARTESIAN_POINT ( 'NONE',  ( 8.906447517083050158, 27.41122689804195645, 139.6500000054623740 ) ) ;
#65421 = CARTESIAN_POINT ( 'NONE',  ( -19.03943276465977164, 0.05219959533909376836, 71.24890960531435269 ) ) ;
#65422 = CARTESIAN_POINT ( 'NONE',  ( -16.52544592524342804, 4.483927247898546575, 41.04057627198103120 ) ) ;
#65423 = CARTESIAN_POINT ( 'NONE',  ( -16.55341960407611168, -4.379528057220339221, 21.45724293864769550 ) ) ;
#65424 = CARTESIAN_POINT ( 'NONE',  ( -12.14591786802326823, 12.06949235617739902, 83.12609039468568994 ) ) ;
#65425 = CARTESIAN_POINT ( 'NONE',  ( 19.03943276465977164, 0.05219959533936151252, 36.25109039468567573 ) ) ;
#65426 = DIRECTION ( 'NONE',  ( 0.000000000000000000, 0.000000000000000000, 1.000000000000000000 ) ) ;
#65427 = CARTESIAN_POINT ( 'NONE',  ( -5.049401038298153566, 19.05341960407611168, 85.20724293864766707 ) ) ;
#65428 = CARTESIAN_POINT ( 'NONE',  ( -12.14591786802309592, -12.06949235617757132, 66.87390960531436690 ) ) ;
#65430 = CARTESIAN_POINT ( 'NONE',  ( 13.97604488694527802, 13.89961937509977652, 114.3739096053143669 ) ) ;
#65429 = CARTESIAN_POINT ( 'NONE',  ( 17.31728774477273802, -6.344390552232379576, 103.3190665168931730 ) ) ;
#65432 = EDGE_LOOP ( 'NONE', ( #157295, #40743, #124777, #27375 ) ) ;
#65431 = CARTESIAN_POINT ( 'NONE',  ( 0.05219959533907565091, 21.53943276465977519, 49.99890960531437401 ) ) ;
#65433 = CARTESIAN_POINT ( 'NONE',  ( 14.34966873604960469, 8.224510206698951720, 104.1655762719810241 ) ) ;
#65434 = CARTESIAN_POINT ( 'NONE',  ( 12.06949235617739724, 12.14591786802326823, 41.87609039468568284 ) ) ;
#65435 = CARTESIAN_POINT ( 'NONE',  ( 0.05219959533910956823, 16.53943276465976808, 84.99890960531436690 ) ) ;
#65436 = LINE ( 'NONE', #127097, #138282 ) ;
#65437 = CARTESIAN_POINT ( 'NONE',  ( 5.049401038297881783, 19.05341960407617563, 77.29275706135231871 ) ) ;
#65438 = CARTESIAN_POINT ( 'NONE',  ( -15.80617190586745835, -15.72974639402198527, 26.87390960531435979 ) ) ;
#65439 = CARTESIAN_POINT ( 'NONE',  ( 36.91746824999999177, 2.880721459617395097E-14, -4.124999997268813168 ) ) ;
#65440 = CARTESIAN_POINT ( 'NONE',  ( -30.00000000000000000, -5.510910596163089556E-15, 47.50000000000000000 ) ) ;
#65442 = CARTESIAN_POINT ( 'NONE',  ( 4.379528057220339221, -16.55341960407611168, 32.70724293864770260 ) ) ;
#65441 = CARTESIAN_POINT ( 'NONE',  ( 12.06949235617739724, 12.14591786802326823, 31.87609039468567929 ) ) ;
#65443 = CARTESIAN_POINT ( 'NONE',  ( 15.72974639402199770, -15.80617190586745480, 53.12390960531436690 ) ) ;
#65444 = CARTESIAN_POINT ( 'NONE',  ( 5.049401038297881783, 19.05341960407617563, 67.29275706135234714 ) ) ;
#65445 = CARTESIAN_POINT ( 'NONE',  ( -5.823673210054116645, -21.52544592524344225, 52.29057627198102409 ) ) ;
#65446 = CARTESIAN_POINT ( 'NONE',  ( -18.62759615963255300, -10.81492255796106328, 69.16775706135234714 ) ) ;
#65447 = CARTESIAN_POINT ( 'NONE',  ( 8.204442743001546745, -36.48291145135366520, -31.77125895174628312 ) ) ;
#65448 = CARTESIAN_POINT ( 'NONE',  ( -4.379528057220086978, -16.55341960407618274, 39.79275706135235424 ) ) ;
#65450 = CARTESIAN_POINT ( 'NONE',  ( -16.51473224551069308, -9.474510206698971260, 86.66557627198102409 ) ) ;
#65449 = CARTESIAN_POINT ( 'NONE',  ( 13.97604488694527802, 13.89961937509977652, 29.37390960531435979 ) ) ;
#65451 = CARTESIAN_POINT ( 'NONE',  ( -19.05341960407611168, -5.049401038298163336, 31.45724293864769550 ) ) ;
#65452 = CARTESIAN_POINT ( 'NONE',  ( -8.314922557960811034, -14.29746914071050412, 107.0822429386476955 ) ) ;
#65453 = CONTEXT_DEPENDENT_SHAPE_REPRESENTATION ( #116512, #53 ) ;
#65454 = CARTESIAN_POINT ( 'NONE',  ( 9.474510206698971260, -16.51473224551069308, 97.91557627198102409 ) ) ;
#65455 = EDGE_LOOP ( 'NONE', ( #127830, #20188, #139134, #116669 ) ) ;
#65456 = CARTESIAN_POINT ( 'NONE',  ( -12.14591786802326823, 12.06949235617739902, 58.12609039468568994 ) ) ;
#65457 = CARTESIAN_POINT ( 'NONE',  ( 10.72451020669898902, -18.67979575497178502, 92.91557627198103830 ) ) ;
#65458 = CARTESIAN_POINT ( 'NONE',  ( 13.89961937509977652, -13.97604488694527269, 48.12390960531435979 ) ) ;
#65460 = CARTESIAN_POINT ( 'NONE',  ( 18.62759615963271287, -10.81492255796078972, 108.3322429386477097 ) ) ;
#65459 = CARTESIAN_POINT ( 'NONE',  ( -19.03943276465977164, -0.05219959533935918106, 73.75109039468566152 ) ) ;
#65461 = CARTESIAN_POINT ( 'NONE',  ( -13.97604488694527625, -13.89961937509977652, 71.87390960531433848 ) ) ;
#65462 = CARTESIAN_POINT ( 'NONE',  ( -5.049401038298153566, 19.05341960407611168, 110.2072429386476671 ) ) ;
#65463 = VERTEX_POINT ( 'NONE', #189555 ) ;
#65464 = CARTESIAN_POINT ( 'NONE',  ( 0.05219959533934541429, -16.53943276465976808, 40.00109039468567573 ) ) ;
#65465 = CARTESIAN_POINT ( 'NONE',  ( 21.55341960407619695, -5.719274019375665929, 21.04275706135234714 ) ) ;
#65468 = CARTESIAN_POINT ( 'NONE',  ( 19.05341960407617918, -5.049401038297876454, 81.04275706135231871 ) ) ;
#65467 = CARTESIAN_POINT ( 'NONE',  ( 16.51473224551069308, 9.474510206698969483, 94.16557627198103830 ) ) ;
#65466 = CARTESIAN_POINT ( 'NONE',  ( 0.05219959533910956823, 16.53943276465976808, 109.9989096053143527 ) ) ;
#65469 = CARTESIAN_POINT ( 'NONE',  ( 10.72451020669898902, -18.67979575497178502, 87.91557627198103830 ) ) ;
#65470 = CARTESIAN_POINT ( 'NONE',  ( 8.314922557960818139, 14.29746914071049879, 49.58224293864769550 ) ) ;
#65471 = CARTESIAN_POINT ( 'NONE',  ( -19.03943276465977164, -0.05219959533935918106, 18.75109039468567218 ) ) ;
#65472 = CARTESIAN_POINT ( 'NONE',  ( -16.52544592524335698, -4.483927247898792601, 73.95942372801901854 ) ) ;
#65474 = ORIENTED_EDGE ( 'NONE', *, *, #53439, .F. ) ;
#65473 = CARTESIAN_POINT ( 'NONE',  ( 19.05341960407611168, 5.049401038298154454, 93.95724293864769550 ) ) ;
#65475 = CARTESIAN_POINT ( 'NONE',  ( 9.564922557960805705, 16.46253265017160317, 44.58224293864769550 ) ) ;
#65476 = CARTESIAN_POINT ( 'NONE',  ( -18.62759615963255300, -10.81492255796106328, 54.16775706135235424 ) ) ;
#65477 = CARTESIAN_POINT ( 'NONE',  ( 21.53943276465977519, 0.05219959533937863772, 61.25109039468567573 ) ) ;
#65478 = CARTESIAN_POINT ( 'NONE',  ( -5.049401038298153566, 19.05341960407611168, 55.20724293864769550 ) ) ;
#65479 = CARTESIAN_POINT ( 'NONE',  ( -18.62759615963255300, -10.81492255796106328, 39.16775706135235424 ) ) ;
#65480 = CARTESIAN_POINT ( 'NONE',  ( -16.51473224551082808, 9.474510206698731452, 83.33442372801899012 ) ) ;
#65481 = CARTESIAN_POINT ( 'NONE',  ( -13.97604488694527625, -13.89961937509977652, 36.87390960531436690 ) ) ;
#65482 = CARTESIAN_POINT ( 'NONE',  ( 16.55341960407618274, -4.379528057220086978, 86.04275706135236135 ) ) ;
#65483 = CARTESIAN_POINT ( 'NONE',  ( -13.97604488694527625, -13.89961937509977652, 61.87390960531435979 ) ) ;
#65484 = CARTESIAN_POINT ( 'NONE',  ( 16.46253265017160672, -9.564922557960803928, 108.3322429386476955 ) ) ;
#65485 = CARTESIAN_POINT ( 'NONE',  ( 5.049401038298161559, -19.05341960407611168, 52.70724293864767418 ) ) ;
#65486 = CARTESIAN_POINT ( 'NONE',  ( -21.55341960407610458, -5.719274019375992779, 91.45724293864769550 ) ) ;
#65487 = CARTESIAN_POINT ( 'NONE',  ( -12.06949235617739369, -12.14591786802326823, 74.37609039468568994 ) ) ;
#65488 = CARTESIAN_POINT ( 'NONE',  ( -24.24393946303101544, 5.863316274098875347, 172.4343578713345266 ) ) ;
#65489 = CARTESIAN_POINT ( 'NONE',  ( 19.03943276465977164, 0.05219959533936151252, 36.25109039468567573 ) ) ;
#65490 = CARTESIAN_POINT ( 'NONE',  ( -19.03943276465977164, 0.05219959533909376836, 61.24890960531436690 ) ) ;
#65491 = CARTESIAN_POINT ( 'NONE',  ( 12.14591786802309770, 12.06949235617756955, 54.37390960531435979 ) ) ;
#65492 = CARTESIAN_POINT ( 'NONE',  ( -8.224510206698948167, 14.34966873604960824, 85.41557627198102409 ) ) ;
#65493 = CARTESIAN_POINT ( 'NONE',  ( -5.049401038298153566, 19.05341960407611168, 100.2072429386476955 ) ) ;
#65494 = CARTESIAN_POINT ( 'NONE',  ( 5.049401038298161559, -19.05341960407611168, 92.70724293864769550 ) ) ;
#65495 = CARTESIAN_POINT ( 'NONE',  ( 15.80617190586769283, -15.72974639402175789, 50.62609039468568994 ) ) ;
#65496 = CARTESIAN_POINT ( 'NONE',  ( -13.89961937509977652, 13.97604488694528158, 105.6239096053143527 ) ) ;
#65497 = CARTESIAN_POINT ( 'NONE',  ( -5.719274019375665041, -21.55341960407619695, 109.7927570613523613 ) ) ;
#65498 = CARTESIAN_POINT ( 'NONE',  ( -4.483927247898782831, 16.52544592524335698, 77.70942372801900433 ) ) ;
#65499 = EDGE_CURVE ( 'NONE', #93191, #158898, #97714, .T. ) ;
#65500 = CARTESIAN_POINT ( 'NONE',  ( 0.05219959533937995610, -21.53943276465977519, 35.00109039468568284 ) ) ;
#65501 = CARTESIAN_POINT ( 'NONE',  ( 16.51473224551069308, 9.474510206698969483, 114.1655762719810241 ) ) ;
#65502 = CARTESIAN_POINT ( 'NONE',  ( 5.823673210054125526, 21.52544592524343514, 104.7905762719810241 ) ) ;
#65503 = CARTESIAN_POINT ( 'NONE',  ( 16.53943276465976808, -0.05219959533910856209, 58.74890960531436690 ) ) ;
#65504 = CARTESIAN_POINT ( 'NONE',  ( -5.153800228976328057, -19.02544592524343514, 52.29057627198100988 ) ) ;
#65505 = CARTESIAN_POINT ( 'NONE',  ( -0.05219959533910754901, -16.53943276465976808, 77.49890960531433848 ) ) ;
#65506 = CARTESIAN_POINT ( 'NONE',  ( 18.67979575497178502, 10.72451020669898547, 34.16557627198102409 ) ) ;
#65507 = CARTESIAN_POINT ( 'NONE',  ( -19.05341960407617563, 5.049401038297882671, 43.54275706135232582 ) ) ;
#65508 = CARTESIAN_POINT ( 'NONE',  ( -9.564922557960796823, -16.46253265017161027, 22.08224293864768839 ) ) ;
#65509 = ORIENTED_EDGE ( 'NONE', *, *, #78263, .F. ) ;
#65510 = CARTESIAN_POINT ( 'NONE',  ( 16.53943276465976808, 0.05219959533934440121, 61.25109039468567573 ) ) ;
#65511 = CARTESIAN_POINT ( 'NONE',  ( 13.97604488694527802, 13.89961937509977652, 74.37390960531436690 ) ) ;
#65512 = CARTESIAN_POINT ( 'NONE',  ( 22.44159573604009239, 16.30477369853692693, 144.0750000027311728 ) ) ;
#65513 = CARTESIAN_POINT ( 'NONE',  ( -14.29746914071049879, 8.314922557960819915, 90.83224293864769550 ) ) ;
#65514 = CARTESIAN_POINT ( 'NONE',  ( -15.80617190586745835, -15.72974639402198527, 41.87390960531435979 ) ) ;
#65515 = VERTEX_POINT ( 'NONE', #7498 ) ;
#65516 = CARTESIAN_POINT ( 'NONE',  ( 14.29746914071037800, 8.314922557961029526, 106.6677570613523756 ) ) ;
#65517 = CARTESIAN_POINT ( 'NONE',  ( 19.03943276465977164, 0.05219959533936151252, 111.2510903946856757 ) ) ;
#65518 = CARTESIAN_POINT ( 'NONE',  ( 0.05219959533937995610, -21.53943276465977519, 75.00109039468568994 ) ) ;
#65519 = CARTESIAN_POINT ( 'NONE',  ( -0.05219959533909027116, -19.03943276465977164, 87.49890960531436690 ) ) ;
#65520 = CARTESIAN_POINT ( 'NONE',  ( -21.55341960407610458, -5.719274019375992779, 101.4572429386476955 ) ) ;
#65521 = CARTESIAN_POINT ( 'NONE',  ( -16.52544592524335698, -4.483927247898792601, 48.95942372801902565 ) ) ;
#65522 = CARTESIAN_POINT ( 'NONE',  ( -0.05219959533909027116, -19.03943276465977164, 32.49890960531435979 ) ) ;
#65523 = CARTESIAN_POINT ( 'NONE',  ( -4.379528057220086978, -16.55341960407618274, 34.79275706135235424 ) ) ;
#65524 = CARTESIAN_POINT ( 'NONE',  ( -5.049401038297874678, -19.05341960407617918, 94.79275706135230450 ) ) ;
#65525 = CARTESIAN_POINT ( 'NONE',  ( 18.62759615963271287, -10.81492255796078972, 93.33224293864769550 ) ) ;
#65526 = CARTESIAN_POINT ( 'NONE',  ( -9.564922557961040184, 16.46253265017147172, 52.91775706135233293 ) ) ;
#65527 = DIRECTION ( 'NONE',  ( -0.000000000000000000, -0.000000000000000000, 1.000000000000000000 ) ) ;
#65528 = CARTESIAN_POINT ( 'NONE',  ( -21.55341960407610458, -5.719274019375992779, 106.4572429386477097 ) ) ;
#65529 = CARTESIAN_POINT ( 'NONE',  ( -17.50000000000000000, -5.499999999999992895, 102.5000000000000142 ) ) ;
#65530 = CARTESIAN_POINT ( 'NONE',  ( -0.05219959533909027116, -19.03943276465977164, 72.49890960531435269 ) ) ;
#65531 = CARTESIAN_POINT ( 'NONE',  ( -0.3535533905933929688, -35.00000000000000000, 5.353553390593268624 ) ) ;
#65532 = CARTESIAN_POINT ( 'NONE',  ( -16.52544592524335698, -4.483927247898792601, 33.95942372801901143 ) ) ;
#65533 = DIRECTION ( 'NONE',  ( -0.000000000000000000, -0.000000000000000000, -1.000000000000000000 ) ) ;
#65535 = CARTESIAN_POINT ( 'NONE',  ( 4.379528057220339221, -16.55341960407611168, 67.70724293864769550 ) ) ;
#65534 = CARTESIAN_POINT ( 'NONE',  ( 10.72451020669871369, 18.67979575497193778, 22.08442372801901143 ) ) ;
#65536 = CARTESIAN_POINT ( 'NONE',  ( 13.89961937509977652, -13.97604488694527269, 73.12390960531436690 ) ) ;
#65538 = CARTESIAN_POINT ( 'NONE',  ( 13.97604488694548053, -13.89961937509957401, 45.62609039468566863 ) ) ;
#65537 = CARTESIAN_POINT ( 'NONE',  ( -16.53943276465976808, -0.05219959533934237506, 43.75109039468568284 ) ) ;
#65539 = AXIS2_PLACEMENT_3D ( 'NONE', #153481, #75642, #181854 ) ;
#65540 = CARTESIAN_POINT ( 'NONE',  ( -21.52544592524334988, -5.823673210054445271, 53.95942372801900433 ) ) ;
#65541 = CARTESIAN_POINT ( 'NONE',  ( -0.05219959533936034679, 19.03943276465977164, 102.5010903946856757 ) ) ;
#65542 = CARTESIAN_POINT ( 'NONE',  ( 19.03943276465977164, -0.05219959533909143690, 58.74890960531435979 ) ) ;
#65543 = CARTESIAN_POINT ( 'NONE',  ( -9.474510206698720793, -16.51473224551083518, 79.58442372801899012 ) ) ;
#65544 = CARTESIAN_POINT ( 'NONE',  ( 0.05219959533937995610, -21.53943276465977519, 85.00109039468568994 ) ) ;
#65545 = CARTESIAN_POINT ( 'NONE',  ( 9.564922557961047289, -16.46253265017146816, 65.41775706135233293 ) ) ;
#65546 = CARTESIAN_POINT ( 'NONE',  ( -5.153800228976328057, -19.02544592524343514, 42.29057627198101699 ) ) ;
#65547 = CARTESIAN_POINT ( 'NONE',  ( 21.52544592524344225, -5.823673210054117533, 53.54057627198103120 ) ) ;
#65549 = CARTESIAN_POINT ( 'NONE',  ( 19.05341960407617918, -5.049401038297876454, 66.04275706135233293 ) ) ;
#65548 = CARTESIAN_POINT ( 'NONE',  ( 14.34966873604960469, 8.224510206698951720, 69.16557627198102409 ) ) ;
#65550 = CARTESIAN_POINT ( 'NONE',  ( -16.20579543436676673, -7.371946100355209808, 25.56520834171879386 ) ) ;
#65551 = CARTESIAN_POINT ( 'NONE',  ( -16.46253265017146816, -9.564922557961047289, 24.16775706135233648 ) ) ;
#65552 = CARTESIAN_POINT ( 'NONE',  ( 4.379528057220092307, 16.55341960407617563, 102.2927570613523613 ) ) ;
#65553 = CARTESIAN_POINT ( 'NONE',  ( -0.05219959533910754901, -16.53943276465976808, 47.49890960531435979 ) ) ;
#65555 = CARTESIAN_POINT ( 'NONE',  ( 27.73933785331498925, -9.013057229001033122, 139.7750000027311899 ) ) ;
#65554 = CARTESIAN_POINT ( 'NONE',  ( 18.67979575497194134, -10.72451020669871369, 85.83442372801901854 ) ) ;
#65556 = CARTESIAN_POINT ( 'NONE',  ( -21.55341960407619339, 5.719274019375674811, 88.54275706135236135 ) ) ;
#65557 = CARTESIAN_POINT ( 'NONE',  ( 15.80617190586746368, 15.72974639402197994, 94.37390960531436690 ) ) ;
#65558 = CARTESIAN_POINT ( 'NONE',  ( 0.05219959533909260263, 19.03943276465977164, 49.99890960531435979 ) ) ;
#65559 = CARTESIAN_POINT ( 'NONE',  ( -18.62759615963255300, -10.81492255796106328, 64.16775706135234714 ) ) ;
#65560 = CARTESIAN_POINT ( 'NONE',  ( 16.51473224551069308, 9.474510206698969483, 49.16557627198102409 ) ) ;
#65561 = CARTESIAN_POINT ( 'NONE',  ( 13.89961937509977652, -13.97604488694527269, 68.12390960531436690 ) ) ;
#65562 = CARTESIAN_POINT ( 'NONE',  ( -8.224510206698948167, 14.34966873604960824, 105.4155762719810383 ) ) ;
#65563 = CARTESIAN_POINT ( 'NONE',  ( -9.564922557960796823, -16.46253265017161027, 112.0822429386476955 ) ) ;
#65564 = CARTESIAN_POINT ( 'NONE',  ( 4.483927247898545687, 16.52544592524342804, 49.79057627198102409 ) ) ;
#65565 = CARTESIAN_POINT ( 'NONE',  ( 16.46253265017160672, -9.564922557960803928, 33.33224293864770260 ) ) ;
#65566 = CARTESIAN_POINT ( 'NONE',  ( -0.05219959533910754901, -16.53943276465976808, 72.49890960531435269 ) ) ;
#65567 = CARTESIAN_POINT ( 'NONE',  ( -21.53943276465977519, 0.05219959533907696930, 96.24890960531435269 ) ) ;
#65568 = CARTESIAN_POINT ( 'NONE',  ( 10.72451020669871369, 18.67979575497193778, 37.08442372801901143 ) ) ;
#65569 = CARTESIAN_POINT ( 'NONE',  ( -28.82186960331499037, 2.428612866367529932E-14, 150.0000000000000000 ) ) ;
#65570 = EDGE_CURVE ( 'NONE', #2854, #117197, #174380, .T. ) ;
#65571 = CARTESIAN_POINT ( 'NONE',  ( -0.05219959533934338120, 16.53943276465976808, 42.50109039468567573 ) ) ;
#65572 = CARTESIAN_POINT ( 'NONE',  ( -15.72974639402197994, 15.80617190586746368, 80.62390960531438111 ) ) ;
#65573 = CARTESIAN_POINT ( 'NONE',  ( -9.474510206698720793, -16.51473224551083518, 19.58442372801899722 ) ) ;
#65574 = CARTESIAN_POINT ( 'NONE',  ( 13.89961937509977652, -13.97604488694527269, 98.12390960531433848 ) ) ;
#65575 = CARTESIAN_POINT ( 'NONE',  ( -15.80617190586768217, 15.72974639402176855, 38.12609039468567573 ) ) ;
#65576 = AXIS2_PLACEMENT_3D ( 'NONE', #10566, #189848, #72230 ) ;
#65577 = CARTESIAN_POINT ( 'NONE',  ( -5.719274019375978568, 21.55341960407610458, 25.20724293864769550 ) ) ;
#65578 = CARTESIAN_POINT ( 'NONE',  ( -8.314922557961024197, 14.29746914071037800, 97.91775706135236135 ) ) ;
#65580 = CARTESIAN_POINT ( 'NONE',  ( -15.72974639402176322, -15.80617190586768395, 89.37609039468568994 ) ) ;
#65579 = CARTESIAN_POINT ( 'NONE',  ( -5.719274019375665041, -21.55341960407619695, 54.79275706135235424 ) ) ;
#65581 = CARTESIAN_POINT ( 'NONE',  ( 9.474510206698729675, 16.51473224551082808, 32.08442372801900433 ) ) ;
#65582 = CARTESIAN_POINT ( 'NONE',  ( 14.29746914071037800, 8.314922557961029526, 86.66775706135234714 ) ) ;
#65583 = CARTESIAN_POINT ( 'NONE',  ( -5.823673210054431948, 21.52544592524334988, 42.70942372801901854 ) ) ;
#65584 = CARTESIAN_POINT ( 'NONE',  ( -0.05219959533909027116, -19.03943276465977164, 27.49890960531435624 ) ) ;
#65585 = CARTESIAN_POINT ( 'NONE',  ( -18.67979575497193778, 10.72451020669871902, 98.33442372801901854 ) ) ;
#65586 = CARTESIAN_POINT ( 'NONE',  ( 19.05341960407611168, 5.049401038298154454, 108.9572429386477097 ) ) ;
#65587 = CARTESIAN_POINT ( 'NONE',  ( -18.67979575497178146, -10.72451020669898902, 106.6655762719810383 ) ) ;
#65588 = CARTESIAN_POINT ( 'NONE',  ( 0.05219959533907565091, 21.53943276465977519, 59.99890960531436690 ) ) ;
#65590 = CARTESIAN_POINT ( 'NONE',  ( -10.81492255796078084, -18.62759615963271287, 72.08224293864769550 ) ) ;
#65589 = DIRECTION ( 'NONE',  ( -0.000000000000000000, -0.000000000000000000, 1.000000000000000000 ) ) ;
#65592 = CARTESIAN_POINT ( 'NONE',  ( 4.379528057220339221, -16.55341960407611168, 67.70724293864769550 ) ) ;
#65591 = CARTESIAN_POINT ( 'NONE',  ( 14.29746914071037800, 8.314922557961029526, 46.66775706135234714 ) ) ;
#65593 = CARTESIAN_POINT ( 'NONE',  ( 18.22780087662122384, -5.500000000000022204, 101.0154010532610869 ) ) ;
#65594 = CARTESIAN_POINT ( 'NONE',  ( -5.153800228976607833, 19.02544592524334988, 92.70942372801901854 ) ) ;
#65595 = CARTESIAN_POINT ( 'NONE',  ( -22.10945809693575370, 1.344113590474837361, -55.87741762761909570 ) ) ;
#65596 = CARTESIAN_POINT ( 'NONE',  ( 0.05219959533934541429, -16.53943276465976808, 20.00109039468568639 ) ) ;
#65597 = CARTESIAN_POINT ( 'NONE',  ( -5.823673210054116645, -21.52544592524344225, 92.29057627198103830 ) ) ;
#65598 = CARTESIAN_POINT ( 'NONE',  ( 0.05219959533907565091, 21.53943276465977519, 79.99890960531435269 ) ) ;
#65599 = CARTESIAN_POINT ( 'NONE',  ( 5.823673210054125526, 21.52544592524343514, 24.79057627198103120 ) ) ;
#65600 = CARTESIAN_POINT ( 'NONE',  ( -4.483927247898782831, 16.52544592524335698, 52.70942372801902565 ) ) ;
#65601 = CARTESIAN_POINT ( 'NONE',  ( 13.89961937509977652, -13.97604488694527269, 78.12390960531433848 ) ) ;
#65603 = CARTESIAN_POINT ( 'NONE',  ( -12.06949235617739369, -12.14591786802326823, 19.37609039468568639 ) ) ;
#65602 = CARTESIAN_POINT ( 'NONE',  ( -21.53943276465977519, -0.05219959533937600094, 28.75109039468567929 ) ) ;
#65604 = CARTESIAN_POINT ( 'NONE',  ( -9.474510206698964154, 16.51473224551069663, 105.4155762719810383 ) ) ;
#65605 = CARTESIAN_POINT ( 'NONE',  ( -5.153800228976328057, -19.02544592524343514, 82.29057627198103830 ) ) ;
#65606 = CARTESIAN_POINT ( 'NONE',  ( 0.05219959533907565091, 21.53943276465977519, 84.99890960531436690 ) ) ;
#65607 = CARTESIAN_POINT ( 'NONE',  ( -13.89961937509977652, 13.97604488694528158, 55.62390960531434558 ) ) ;
#65608 = CARTESIAN_POINT ( 'NONE',  ( 37.99999999999999289, 2.893978650043524126E-14, -1.000000000000000000 ) ) ;
#65609 = CARTESIAN_POINT ( 'NONE',  ( 16.55341960407611168, 4.379528057220329451, 63.95724293864770260 ) ) ;
#65610 = CARTESIAN_POINT ( 'NONE',  ( -21.53943276465977519, 0.05219959533907696930, 26.24890960531435624 ) ) ;
#65611 = CARTESIAN_POINT ( 'NONE',  ( -18.22780087662119541, 5.500000000000102141, 61.01763182126894947 ) ) ;
#65612 = CARTESIAN_POINT ( 'NONE',  ( -21.53943276465977519, 0.05219959533907696930, 106.2489096053143811 ) ) ;
#65613 = CARTESIAN_POINT ( 'NONE',  ( -19.03943276465977164, -0.05219959533935918106, 58.75109039468566863 ) ) ;
#65614 = CARTESIAN_POINT ( 'NONE',  ( 5.049401038298161559, -19.05341960407611168, 112.7072429386476813 ) ) ;
#65615 = CARTESIAN_POINT ( 'NONE',  ( 18.22780087662122739, 5.500000000000000888, 66.48236817873106475 ) ) ;
#65616 = CARTESIAN_POINT ( 'NONE',  ( 15.72974639402199770, -15.80617190586745480, 58.12390960531435979 ) ) ;
#65617 = CARTESIAN_POINT ( 'NONE',  ( -19.02544592524342804, 5.153800228976336051, 86.04057627198103830 ) ) ;
#65618 = CARTESIAN_POINT ( 'NONE',  ( -15.80617190586768217, 15.72974639402176855, 83.12609039468568994 ) ) ;
#65619 = CARTESIAN_POINT ( 'NONE',  ( 16.51473224551069308, 9.474510206698969483, 49.16557627198102409 ) ) ;
#65620 = CARTESIAN_POINT ( 'NONE',  ( -16.53943276465976808, 0.05219959533911058130, 81.24890960531436690 ) ) ;
#65621 = CARTESIAN_POINT ( 'NONE',  ( 16.53943276465976808, 0.05219959533934440121, 41.25109039468568284 ) ) ;
#65622 = CARTESIAN_POINT ( 'NONE',  ( 21.52544592524334988, 5.823673210054432836, 66.45942372801903275 ) ) ;
#65623 = ORIENTED_EDGE ( 'NONE', *, *, #118181, .T. ) ;
#65624 = CARTESIAN_POINT ( 'NONE',  ( -19.05341960407617563, 5.049401038297882671, 23.54275706135233648 ) ) ;
#65625 = CARTESIAN_POINT ( 'NONE',  ( 13.97604488694548053, -13.89961937509957401, 85.62609039468568994 ) ) ;
#65626 = CARTESIAN_POINT ( 'NONE',  ( -5.153800228976607833, 19.02544592524334988, 37.70942372801899722 ) ) ;
#65627 = CARTESIAN_POINT ( 'NONE',  ( 30.74264578624799782, 22.33583958711400541, -6.549999994537627046 ) ) ;
#65628 = CARTESIAN_POINT ( 'NONE',  ( -0.05219959533937732626, 21.53943276465977519, 37.50109039468568284 ) ) ;
#65629 = CARTESIAN_POINT ( 'NONE',  ( -19.49190055781009079, -5.500000000000054179, 45.56116087098781264 ) ) ;
#65630 = CARTESIAN_POINT ( 'NONE',  ( 5.153800228976615827, -19.02544592524334988, 30.20942372801900433 ) ) ;
#65631 = CARTESIAN_POINT ( 'NONE',  ( -19.03943276465977164, 0.05219959533909376836, 61.24890960531436690 ) ) ;
#65632 = CARTESIAN_POINT ( 'NONE',  ( 19.05341960407617918, -5.049401038297876454, 36.04275706135234003 ) ) ;
#65633 = CARTESIAN_POINT ( 'NONE',  ( 12.14591786802327356, -12.06949235617739191, 100.6260903946857184 ) ) ;
#65635 = CARTESIAN_POINT ( 'NONE',  ( 10.72451020669871369, 18.67979575497193778, 87.08442372801901854 ) ) ;
#65634 = CARTESIAN_POINT ( 'NONE',  ( -10.72451020669898014, 18.67979575497178502, 25.41557627198103120 ) ) ;
#65636 = CARTESIAN_POINT ( 'NONE',  ( 3.556970738554033499E-15, -38.81732327939057825, -4.124999997268814056 ) ) ;
#65637 = CARTESIAN_POINT ( 'NONE',  ( -17.49999999999998934, -4.640572885337524767, 34.36211835451161534 ) ) ;
#65638 = CARTESIAN_POINT ( 'NONE',  ( 21.53943276465977519, 0.05219959533937863772, 91.25109039468568994 ) ) ;
#65639 = VECTOR ( 'NONE', #43937, 1000.000000000000000 ) ;
#65640 = CARTESIAN_POINT ( 'NONE',  ( 24.30000000000003268, -0.1103568551765998634, -56.77278709839600168 ) ) ;
#65641 = CARTESIAN_POINT ( 'NONE',  ( -9.564922557960796823, -16.46253265017161027, 97.08224293864769550 ) ) ;
#65642 = CARTESIAN_POINT ( 'NONE',  ( -1.502453648625268645, -30.26186088262145901, -51.11561252063850702 ) ) ;
#65643 = CARTESIAN_POINT ( 'NONE',  ( 19.03943276465977164, -0.05219959533909143690, 53.74890960531436690 ) ) ;
#65644 = CARTESIAN_POINT ( 'NONE',  ( -10.81492255796078084, -18.62759615963271287, 52.08224293864768839 ) ) ;
#65645 = CARTESIAN_POINT ( 'NONE',  ( 4.379528057220339221, -16.55341960407611168, 22.70724293864769194 ) ) ;
#65647 = CARTESIAN_POINT ( 'NONE',  ( 19.02544592524343514, -5.153800228976328945, 98.54057627198100988 ) ) ;
#65646 = CARTESIAN_POINT ( 'NONE',  ( -8.224510206698948167, 14.34966873604960824, 95.41557627198102409 ) ) ;
#65648 = CARTESIAN_POINT ( 'NONE',  ( 16.51473224551083163, -9.474510206698727899, 20.83442372801899722 ) ) ;
#65649 = CARTESIAN_POINT ( 'NONE',  ( -5.153800228976328057, -19.02544592524343514, 42.29057627198101699 ) ) ;
#65650 = CARTESIAN_POINT ( 'NONE',  ( 8.314922557960818139, 14.29746914071049879, 99.58224293864770971 ) ) ;
#65651 = CARTESIAN_POINT ( 'NONE',  ( 15.72974639402176855, 15.80617190586768217, 51.87609039468568284 ) ) ;
#65652 = CARTESIAN_POINT ( 'NONE',  ( 8.224510206698742110, 14.34966873604972548, 107.0844237280190043 ) ) ;
#65653 = CARTESIAN_POINT ( 'NONE',  ( 0.05219959533936267826, -19.03943276465977164, 65.00109039468567573 ) ) ;
#65654 = DIRECTION ( 'NONE',  ( -1.000000000000000000, 0.000000000000000000, -0.000000000000000000 ) ) ;
#65655 = CARTESIAN_POINT ( 'NONE',  ( 9.474510206698971260, -16.51473224551069308, 107.9155762719810383 ) ) ;
#65656 = CARTESIAN_POINT ( 'NONE',  ( 16.53943276465976808, -0.05219959533910856209, 78.74890960531436690 ) ) ;
#65657 = CARTESIAN_POINT ( 'NONE',  ( 9.564922557961047289, -16.46253265017146816, 40.41775706135234003 ) ) ;
#65658 = CARTESIAN_POINT ( 'NONE',  ( -19.03943276465977164, 0.05219959533909376836, 66.24890960531436690 ) ) ;
#65659 = CARTESIAN_POINT ( 'NONE',  ( 14.34966873604960469, 8.224510206698951720, 64.16557627198102409 ) ) ;
#65660 = CARTESIAN_POINT ( 'NONE',  ( -16.51473224551082808, 9.474510206698731452, 83.33442372801899012 ) ) ;
#65661 = CARTESIAN_POINT ( 'NONE',  ( 10.72451020669898902, -18.67979575497178502, 42.91557627198103120 ) ) ;
#65662 = EDGE_LOOP ( 'NONE', ( #106259, #6387, #132538, #133049 ) ) ;
#65663 = CARTESIAN_POINT ( 'NONE',  ( -12.06949235617756955, 12.14591786802309770, 105.6239096053143669 ) ) ;
#65664 = CARTESIAN_POINT ( 'NONE',  ( -17.50000000000003908, -4.658240926743031807, 26.05529582183195103 ) ) ;
#65666 = CARTESIAN_POINT ( 'NONE',  ( -15.80617190586745835, -15.72974639402198527, 56.87390960531436690 ) ) ;
#65665 = CARTESIAN_POINT ( 'NONE',  ( -5.049401038298153566, 19.05341960407611168, 55.20724293864769550 ) ) ;
#65667 = CARTESIAN_POINT ( 'NONE',  ( 16.51473224551069308, 9.474510206698969483, 49.16557627198102409 ) ) ;
#65669 = CARTESIAN_POINT ( 'NONE',  ( -19.03943276465977164, 0.05219959533909376836, 76.24890960531435269 ) ) ;
#65668 = CARTESIAN_POINT ( 'NONE',  ( 16.53943276465976808, 0.05219959533934440121, 96.25109039468568994 ) ) ;
#65670 = CARTESIAN_POINT ( 'NONE',  ( -16.46253265017146816, -9.564922557961047289, 59.16775706135233293 ) ) ;
#65671 = CARTESIAN_POINT ( 'NONE',  ( 15.72974639402176855, 15.80617190586768217, 71.87609039468568994 ) ) ;
#65672 = CARTESIAN_POINT ( 'NONE',  ( 0.05219959533907565091, 21.53943276465977519, 44.99890960531435979 ) ) ;
#65673 = CARTESIAN_POINT ( 'NONE',  ( -5.049401038298153566, 19.05341960407611168, 100.2072429386476955 ) ) ;
#65674 = CARTESIAN_POINT ( 'NONE',  ( 9.564922557960805705, 16.46253265017160317, 24.58224293864769194 ) ) ;
#65675 = CARTESIAN_POINT ( 'NONE',  ( -14.34966873604972548, 8.224510206698743886, 93.33442372801901854 ) ) ;
#65676 = CARTESIAN_POINT ( 'NONE',  ( 16.46253265017146816, 9.564922557961045513, 101.6677570613523329 ) ) ;
#65677 = DIRECTION ( 'NONE',  ( 0.9930308165857338887, 0.1178549842436482642, 0.000000000000000000 ) ) ;
#65678 = DIRECTION ( 'NONE',  ( 0.000000000000000000, 0.000000000000000000, -1.000000000000000000 ) ) ;
#65679 = CARTESIAN_POINT ( 'NONE',  ( -18.67979575497193778, 10.72451020669871902, 93.33442372801901854 ) ) ;
#65680 = CARTESIAN_POINT ( 'NONE',  ( 12.06949235617757843, -12.14591786802309237, 63.12390960531435979 ) ) ;
#65681 = CARTESIAN_POINT ( 'NONE',  ( 16.55341960407611168, 4.379528057220329451, 68.95724293864769550 ) ) ;
#65682 = CARTESIAN_POINT ( 'NONE',  ( 21.53943276465977519, -0.05219959533907433946, 98.74890960531438111 ) ) ;
#65683 = CARTESIAN_POINT ( 'NONE',  ( 5.719274019375991003, -21.55341960407610458, 82.70724293864770971 ) ) ;
#65684 = CARTESIAN_POINT ( 'NONE',  ( 17.50000000000001066, -5.622605283950869115, 96.18792689403893803 ) ) ;
#65685 = CARTESIAN_POINT ( 'NONE',  ( 15.80617190586746368, 15.72974639402197994, 39.37390960531436690 ) ) ;
#65686 = CARTESIAN_POINT ( 'NONE',  ( 16.55341960407618274, -4.379528057220086978, 61.04275706135234714 ) ) ;
#65687 = CARTESIAN_POINT ( 'NONE',  ( 16.52544592524342804, -4.483927247898539470, 88.54057627198103830 ) ) ;
#65688 = CARTESIAN_POINT ( 'NONE',  ( 0.05219959533909260263, 19.03943276465977164, 49.99890960531435979 ) ) ;
#65689 = CARTESIAN_POINT ( 'NONE',  ( 35.31558682697088614, -4.577067960279664227, 39.03840433125808573 ) ) ;
#65690 = CARTESIAN_POINT ( 'NONE',  ( 4.379528057220092307, 16.55341960407617563, 102.2927570613523613 ) ) ;
#65691 = CARTESIAN_POINT ( 'NONE',  ( 21.53943276465977519, 0.05219959533937863772, 31.25109039468568639 ) ) ;
#65692 = CARTESIAN_POINT ( 'NONE',  ( -19.03943276465977164, 0.05219959533909376836, 86.24890960531436690 ) ) ;
#65693 = CARTESIAN_POINT ( 'NONE',  ( 5.823673210054444382, -21.52544592524334988, 65.20942372801901854 ) ) ;
#65694 = CARTESIAN_POINT ( 'NONE',  ( 16.51473224551069308, 9.474510206698969483, 109.1655762719810383 ) ) ;
#65695 = CARTESIAN_POINT ( 'NONE',  ( -15.53529872673524004, -37.10890965030864663, -23.64498726423861186 ) ) ;
#65696 = ORIENTED_EDGE ( 'NONE', *, *, #98431, .F. ) ;
#65697 = CARTESIAN_POINT ( 'NONE',  ( 21.53943276465977519, 0.05219959533937863772, 61.25109039468567573 ) ) ;
#65699 = CARTESIAN_POINT ( 'NONE',  ( 16.51473224551069308, 9.474510206698969483, 114.1655762719810241 ) ) ;
#65698 = CARTESIAN_POINT ( 'NONE',  ( -13.97604488694527625, -13.89961937509977652, 36.87390960531436690 ) ) ;
#65700 = CARTESIAN_POINT ( 'NONE',  ( -16.46253265017146816, -9.564922557961047289, 64.16775706135233293 ) ) ;
#65701 = CARTESIAN_POINT ( 'NONE',  ( -18.67979575497193778, 10.72451020669871902, 28.33442372801902209 ) ) ;
#65702 = CARTESIAN_POINT ( 'NONE',  ( -13.97604488694547697, 13.89961937509957934, 53.12609039468565442 ) ) ;
#65703 = CARTESIAN_POINT ( 'NONE',  ( 19.02544592524343514, -5.153800228976328945, 28.54057627198102409 ) ) ;
#65704 = CARTESIAN_POINT ( 'NONE',  ( -0.05219959533934338120, 16.53943276465976808, 97.50109039468567573 ) ) ;
#65705 = CARTESIAN_POINT ( 'NONE',  ( 19.03943276465977164, 0.05219959533936151252, 61.25109039468566863 ) ) ;
#65706 = CARTESIAN_POINT ( 'NONE',  ( -14.34966873604972548, 8.224510206698743886, 113.3344237280190328 ) ) ;
#65708 = VERTEX_POINT ( 'NONE', #158710 ) ;
#65707 = CARTESIAN_POINT ( 'NONE',  ( 13.97604488694548053, -13.89961937509957401, 50.62609039468566152 ) ) ;
#65709 = CARTESIAN_POINT ( 'NONE',  ( -9.564922557960796823, -16.46253265017161027, 92.08224293864769550 ) ) ;
#65710 = CARTESIAN_POINT ( 'NONE',  ( -18.62759615963255300, -10.81492255796106328, 99.16775706135234714 ) ) ;
#65711 = CARTESIAN_POINT ( 'NONE',  ( 15.80617190586769283, -15.72974639402175789, 110.6260903946857042 ) ) ;
#65712 = DIRECTION ( 'NONE',  ( -1.000000000000000000, 0.000000000000000000, -5.421010862427521184E-16 ) ) ;
#65713 = CARTESIAN_POINT ( 'NONE',  ( -21.53943276465977519, -0.05219959533937600094, 88.75109039468567573 ) ) ;
#65714 = CARTESIAN_POINT ( 'NONE',  ( -14.29746914071037622, -8.314922557961029526, 34.16775706135234714 ) ) ;
#65715 = CARTESIAN_POINT ( 'NONE',  ( 5.049401038298161559, -19.05341960407611168, 87.70724293864769550 ) ) ;
#65716 = CARTESIAN_POINT ( 'NONE',  ( -5.719274019375978568, 21.55341960407610458, 30.20724293864769550 ) ) ;
#65717 = CARTESIAN_POINT ( 'NONE',  ( 22.44159573604009594, -16.30477369853687364, 139.6750000027311955 ) ) ;
#65718 = CARTESIAN_POINT ( 'NONE',  ( 16.46253265017160672, -9.564922557960803928, 83.33224293864768129 ) ) ;
#65719 = CARTESIAN_POINT ( 'NONE',  ( -19.34837522270367671, -5.499999999999745981, 40.86337684832578532 ) ) ;
#65720 = CARTESIAN_POINT ( 'NONE',  ( 5.153800228976615827, -19.02544592524334988, 75.20942372801896170 ) ) ;
#65721 = CARTESIAN_POINT ( 'NONE',  ( -9.474510206698964154, 16.51473224551069663, 100.4155762719810241 ) ) ;
#65722 = CARTESIAN_POINT ( 'NONE',  ( -5.823673210054431948, 21.52544592524334988, 102.7094237280190185 ) ) ;
#65723 = CARTESIAN_POINT ( 'NONE',  ( 16.52544592524342804, -4.483927247898539470, 103.5405762719810383 ) ) ;
#65724 = CARTESIAN_POINT ( 'NONE',  ( 10.81492255796078972, 18.62759615963270932, 44.58224293864769550 ) ) ;
#65725 = CARTESIAN_POINT ( 'NONE',  ( -10.81492255796078084, -18.62759615963271287, 42.08224293864769550 ) ) ;
#65726 = CARTESIAN_POINT ( 'NONE',  ( -12.06949235617756955, 12.14591786802309770, 100.6239096053143811 ) ) ;
#65727 = CARTESIAN_POINT ( 'NONE',  ( -16.09882439466100124, 1.216645939406925780, -61.59766612755959869 ) ) ;
#65728 = CARTESIAN_POINT ( 'NONE',  ( 9.474510206698729675, 16.51473224551082808, 57.08442372801900433 ) ) ;
#65729 = CARTESIAN_POINT ( 'NONE',  ( -8.314922557961024197, 14.29746914071037800, 112.9177570613523329 ) ) ;
#65731 = EDGE_CURVE ( 'NONE', #83417, #131569, #196076, .T. ) ;
#65730 = CARTESIAN_POINT ( 'NONE',  ( -19.02544592524342804, 5.153800228976336051, 96.04057627198103830 ) ) ;
#65732 = CARTESIAN_POINT ( 'NONE',  ( 5.823673210054444382, -21.52544592524334988, 85.20942372801901854 ) ) ;
#65733 = CARTESIAN_POINT ( 'NONE',  ( 15.80617190586746368, 15.72974639402197994, 59.37390960531436690 ) ) ;
#65734 = CARTESIAN_POINT ( 'NONE',  ( 10.81492255796106328, -18.62759615963255655, 50.41775706135235424 ) ) ;
#65735 = CARTESIAN_POINT ( 'NONE',  ( 21.55341960407610458, 5.719274019375980345, 93.95724293864770971 ) ) ;
#65736 = CARTESIAN_POINT ( 'NONE',  ( 21.55341960407619695, -5.719274019375665929, 41.04275706135236135 ) ) ;
#65737 = CARTESIAN_POINT ( 'NONE',  ( -19.05341960407611168, -5.049401038298163336, 21.45724293864768839 ) ) ;
#65738 = CARTESIAN_POINT ( 'NONE',  ( -5.153800228976328057, -19.02544592524343514, 87.29057627198103830 ) ) ;
#65739 = CARTESIAN_POINT ( 'NONE',  ( -8.224510206698735004, -14.34966873604973081, 84.58442372801903275 ) ) ;
#65740 = CARTESIAN_POINT ( 'NONE',  ( -0.05219959533910754901, -16.53943276465976808, 107.4989096053143669 ) ) ;
#65741 = CARTESIAN_POINT ( 'NONE',  ( 9.474510206698971260, -16.51473224551069308, 112.9155762719810383 ) ) ;
#65742 = CARTESIAN_POINT ( 'NONE',  ( -4.379528057220328563, 16.55341960407611168, 55.20724293864770260 ) ) ;
#65743 = CARTESIAN_POINT ( 'NONE',  ( 12.06949235617739724, 12.14591786802326823, 111.8760903946856615 ) ) ;
#65744 = CARTESIAN_POINT ( 'NONE',  ( 0.05219959533909260263, 19.03943276465977164, 54.99890960531435979 ) ) ;
#65745 = CARTESIAN_POINT ( 'NONE',  ( 9.474510206698971260, -16.51473224551069308, 32.91557627198102409 ) ) ;
#65746 = CARTESIAN_POINT ( 'NONE',  ( 21.55341960407610458, 5.719274019375980345, 48.95724293864770971 ) ) ;
#65747 = CARTESIAN_POINT ( 'NONE',  ( 19.03943276465977164, 0.05219959533936151252, 21.25109039468565797 ) ) ;
#65749 = CARTESIAN_POINT ( 'NONE',  ( -16.53943276465976808, 0.05219959533911058130, 36.24890960531435979 ) ) ;
#65748 = LINE ( 'NONE', #124441, #91402 ) ;
#65750 = CARTESIAN_POINT ( 'NONE',  ( 0.05219959533937995610, -21.53943276465977519, 50.00109039468568994 ) ) ;
#65751 = CARTESIAN_POINT ( 'NONE',  ( -19.03943276465977164, 0.05219959533909376836, 116.2489096053143669 ) ) ;
#65752 = CARTESIAN_POINT ( 'NONE',  ( 4.379528057220092307, 16.55341960407617563, 57.29275706135234714 ) ) ;
#65753 = CARTESIAN_POINT ( 'NONE',  ( 9.564922557961047289, -16.46253265017146816, 65.41775706135233293 ) ) ;
#65754 = EDGE_CURVE ( 'NONE', #40357, #98984, #11911, .T. ) ;
#65755 = CARTESIAN_POINT ( 'NONE',  ( -12.14591786802309592, -12.06949235617757132, 31.87390960531435979 ) ) ;
#65756 = CARTESIAN_POINT ( 'NONE',  ( 14.34966873604972726, -8.224510206698740333, 110.8344237280190043 ) ) ;
#65757 = CARTESIAN_POINT ( 'NONE',  ( -5.153800228976328057, -19.02544592524343514, 42.29057627198101699 ) ) ;
#65758 = CARTESIAN_POINT ( 'NONE',  ( 0.05219959533909260263, 19.03943276465977164, 59.99890960531436690 ) ) ;
#65759 = CARTESIAN_POINT ( 'NONE',  ( 16.51473224551069308, 9.474510206698969483, 24.16557627198102765 ) ) ;
#65760 = CARTESIAN_POINT ( 'NONE',  ( 21.53943276465977519, 0.05219959533937863772, 36.25109039468567573 ) ) ;
#65761 = CARTESIAN_POINT ( 'NONE',  ( -5.153800228976328057, -19.02544592524343514, 47.29057627198102409 ) ) ;
#65762 = FACE_OUTER_BOUND ( 'NONE', #87029, .T. ) ;
#65763 = CARTESIAN_POINT ( 'NONE',  ( -5.049401038298153566, 19.05341960407611168, 40.20724293864768839 ) ) ;
#65764 = CARTESIAN_POINT ( 'NONE',  ( 10.81492255796078972, 18.62759615963270932, 29.58224293864769905 ) ) ;
#65766 = CARTESIAN_POINT ( 'NONE',  ( 16.55341960407611168, 4.379528057220329451, 103.9572429386476813 ) ) ;
#65765 = CARTESIAN_POINT ( 'NONE',  ( 18.67979575497194134, -10.72451020669871369, 55.83442372801901854 ) ) ;
#65767 = CARTESIAN_POINT ( 'NONE',  ( 5.049401038298161559, -19.05341960407611168, 107.7072429386476955 ) ) ;
#65768 = VECTOR ( 'NONE', #136928, 1000.000000000000000 ) ;
#65769 = CARTESIAN_POINT ( 'NONE',  ( -8.314922557961024197, 14.29746914071037800, 82.91775706135234714 ) ) ;
#65770 = CARTESIAN_POINT ( 'NONE',  ( 18.62759615963255655, 10.81492255796105972, 86.66775706135234714 ) ) ;
#65771 = CARTESIAN_POINT ( 'NONE',  ( -8.314922557961024197, 14.29746914071037800, 57.91775706135234714 ) ) ;
#65772 = CARTESIAN_POINT ( 'NONE',  ( 13.89961937509977652, -13.97604488694527269, 98.12390960531433848 ) ) ;
#65773 = CARTESIAN_POINT ( 'NONE',  ( 12.06949235617739724, 12.14591786802326823, 46.87609039468568994 ) ) ;
#65774 = CARTESIAN_POINT ( 'NONE',  ( -4.379528057220086978, -16.55341960407618274, 24.79275706135235779 ) ) ;
#65775 = CARTESIAN_POINT ( 'NONE',  ( 4.379528057220092307, 16.55341960407617563, 87.29275706135236135 ) ) ;
#65776 = CARTESIAN_POINT ( 'NONE',  ( -0.05219959533936034679, 19.03943276465977164, 112.5010903946856757 ) ) ;
#65777 = CARTESIAN_POINT ( 'NONE',  ( 21.52544592524344225, -5.823673210054117533, 98.54057627198105251 ) ) ;
#65779 = CARTESIAN_POINT ( 'NONE',  ( -19.02544592524334988, -5.153800228976617603, 98.95942372801900433 ) ) ;
#65778 = CARTESIAN_POINT ( 'NONE',  ( 14.29746914071049879, -8.314922557960816363, 103.3322429386476955 ) ) ;
#65780 = CARTESIAN_POINT ( 'NONE',  ( 8.314922557961029526, -14.29746914071037800, 75.41775706135233293 ) ) ;
#65781 = CARTESIAN_POINT ( 'NONE',  ( -16.29526858892908336, 7.335722546920052878, 44.20329402199734403 ) ) ;
#65782 = CARTESIAN_POINT ( 'NONE',  ( -13.89961937509957401, -13.97604488694547875, 74.37609039468566152 ) ) ;
#65783 = CARTESIAN_POINT ( 'NONE',  ( 16.52544592524342804, -4.483927247898539470, 48.54057627198103120 ) ) ;
#65784 = CARTESIAN_POINT ( 'NONE',  ( 16.55341960407611168, 4.379528057220329451, 28.95724293864769905 ) ) ;
#65785 = CARTESIAN_POINT ( 'NONE',  ( -4.379528057220328563, 16.55341960407611168, 90.20724293864770971 ) ) ;
#65787 = CARTESIAN_POINT ( 'NONE',  ( -17.26058549869092218, 6.457015423128481757, 88.62254162523936429 ) ) ;
#65786 = CARTESIAN_POINT ( 'NONE',  ( -9.474510206698720793, -16.51473224551083518, 39.58442372801899722 ) ) ;
#65788 = CARTESIAN_POINT ( 'NONE',  ( -10.72451020669870658, -18.67979575497194134, 39.58442372801901143 ) ) ;
#65789 = CARTESIAN_POINT ( 'NONE',  ( -5.153800228976607833, 19.02544592524334988, 92.70942372801901854 ) ) ;
#65790 = CARTESIAN_POINT ( 'NONE',  ( -4.521720347981119659, -38.96825017273092584, -33.00000000000000711 ) ) ;
#65791 = CARTESIAN_POINT ( 'NONE',  ( -16.46253265017160317, 9.564922557960807481, 85.83224293864769550 ) ) ;
#65792 = CARTESIAN_POINT ( 'NONE',  ( -19.03943276465977164, 0.05219959533909376836, 96.24890960531436690 ) ) ;
#65793 = CARTESIAN_POINT ( 'NONE',  ( -15.72974639402197994, 15.80617190586746368, 50.62390960531435979 ) ) ;
#65794 = CARTESIAN_POINT ( 'NONE',  ( 12.06949235617757843, -12.14591786802309237, 88.12390960531436690 ) ) ;
#65795 = CARTESIAN_POINT ( 'NONE',  ( -13.97604488694527625, -13.89961937509977652, 76.87390960531433848 ) ) ;
#65796 = CARTESIAN_POINT ( 'NONE',  ( -16.51473224551069308, -9.474510206698971260, 26.66557627198103120 ) ) ;
#65797 = CARTESIAN_POINT ( 'NONE',  ( 5.719274019375673035, 21.55341960407619339, 37.29275706135235424 ) ) ;
#65798 = CARTESIAN_POINT ( 'NONE',  ( 5.823673210054444382, -21.52544592524334988, 80.20942372801901854 ) ) ;
#65799 = CARTESIAN_POINT ( 'NONE',  ( 19.05341960407611168, 5.049401038298154454, 58.95724293864768129 ) ) ;
#65800 = EDGE_CURVE ( 'NONE', #68554, #200018, #130350, .T. ) ;
#65801 = CARTESIAN_POINT ( 'NONE',  ( -0.05219959533934338120, 16.53943276465976808, 82.50109039468568994 ) ) ;
#65802 = CARTESIAN_POINT ( 'NONE',  ( 10.81492255796106328, -18.62759615963255655, 30.41775706135234358 ) ) ;
#65803 = CARTESIAN_POINT ( 'NONE',  ( 18.67979575497194134, -10.72451020669871369, 30.83442372801902209 ) ) ;
#65805 = CARTESIAN_POINT ( 'NONE',  ( 0.05219959533909260263, 19.03943276465977164, 84.99890960531436690 ) ) ;
#65804 = CARTESIAN_POINT ( 'NONE',  ( -5.153800228976607833, 19.02544592524334988, 47.70942372801900433 ) ) ;
#65806 = CARTESIAN_POINT ( 'NONE',  ( -9.474510206698720793, -16.51473224551083518, 34.58442372801899722 ) ) ;
#65807 = CARTESIAN_POINT ( 'NONE',  ( -5.823673210054431948, 21.52544592524334988, 82.70942372801900433 ) ) ;
#65808 = CARTESIAN_POINT ( 'NONE',  ( -10.81492255796078084, -18.62759615963271287, 67.08224293864770971 ) ) ;
#65809 = CARTESIAN_POINT ( 'NONE',  ( -0.05219959533910754901, -16.53943276465976808, 57.49890960531435979 ) ) ;
#65811 = CARTESIAN_POINT ( 'NONE',  ( 5.153800228976615827, -19.02544592524334988, 25.20942372801900433 ) ) ;
#65810 = CARTESIAN_POINT ( 'NONE',  ( -10.72451020669870658, -18.67979575497194134, 84.58442372801903275 ) ) ;
#65812 = CARTESIAN_POINT ( 'NONE',  ( -14.34966873604960291, -8.224510206698953496, 76.66557627198103830 ) ) ;
#65813 = CARTESIAN_POINT ( 'NONE',  ( -14.34966873604960291, -8.224510206698953496, 111.6655762719810525 ) ) ;
#65814 = CARTESIAN_POINT ( 'NONE',  ( -16.46253265017146816, -9.564922557961047289, 74.16775706135234714 ) ) ;
#65815 = CARTESIAN_POINT ( 'NONE',  ( 14.34966873604960469, 8.224510206698951720, 34.16557627198102409 ) ) ;
#65816 = CARTESIAN_POINT ( 'NONE',  ( -21.55341960407619339, 5.719274019375674811, 78.54275706135236135 ) ) ;
#65817 = CARTESIAN_POINT ( 'NONE',  ( 19.02544592524343514, -5.153800228976328945, 73.54057627198103830 ) ) ;
#65818 = CARTESIAN_POINT ( 'NONE',  ( -19.03943276465977164, -0.05219959533935918106, 53.75109039468566863 ) ) ;
#65819 = CARTESIAN_POINT ( 'NONE',  ( 5.719274019375991003, -21.55341960407610458, 47.70724293864770260 ) ) ;
#65820 = CARTESIAN_POINT ( 'NONE',  ( -0.05219959533907301413, -21.53943276465977519, 97.49890960531436690 ) ) ;
#65821 = CARTESIAN_POINT ( 'NONE',  ( 14.34966873604972726, -8.224510206698740333, 20.83442372801901143 ) ) ;
#65822 = CARTESIAN_POINT ( 'NONE',  ( -8.314922557961024197, 14.29746914071037800, 67.91775706135234714 ) ) ;
#65824 = CARTESIAN_POINT ( 'NONE',  ( -5.823673210054116645, -21.52544592524344225, 102.2905762719810383 ) ) ;
#65823 = CARTESIAN_POINT ( 'NONE',  ( 16.20579543436681647, 7.371946100354970000, 63.06520834171877254 ) ) ;
#65825 = CARTESIAN_POINT ( 'NONE',  ( -8.224510206698948167, 14.34966873604960824, 105.4155762719810383 ) ) ;
#65826 = CARTESIAN_POINT ( 'NONE',  ( -17.49999999999998934, -3.305555262949607886, 30.37482847843398659 ) ) ;
#65827 = CARTESIAN_POINT ( 'NONE',  ( -14.29746914071037622, -8.314922557961029526, 39.16775706135235424 ) ) ;
#65828 = CARTESIAN_POINT ( 'NONE',  ( 10.72451020669898902, -18.67979575497178502, 57.91557627198103120 ) ) ;
#65829 = CARTESIAN_POINT ( 'NONE',  ( 4.483927247898790824, -16.52544592524335698, 110.2094237280190185 ) ) ;
#65830 = CARTESIAN_POINT ( 'NONE',  ( -19.03943276465977164, 0.05219959533909376836, 31.24890960531435979 ) ) ;
#65831 = CARTESIAN_POINT ( 'NONE',  ( 16.55341960407618274, -4.379528057220086978, 71.04275706135234714 ) ) ;
#65832 = CARTESIAN_POINT ( 'NONE',  ( -0.05219959533936034679, 19.03943276465977164, 57.50109039468566863 ) ) ;
#65833 = CARTESIAN_POINT ( 'NONE',  ( -15.72974639402176322, -15.80617190586768395, 39.37609039468567573 ) ) ;
#65834 = CARTESIAN_POINT ( 'NONE',  ( 5.823673210054125526, 21.52544592524343514, 59.79057627198103120 ) ) ;
#65835 = CARTESIAN_POINT ( 'NONE',  ( -14.34966873604972548, 8.224510206698743886, 98.33442372801901854 ) ) ;
#65836 = CARTESIAN_POINT ( 'NONE',  ( 10.81492255796106328, -18.62759615963255655, 80.41775706135234714 ) ) ;
#65837 = CARTESIAN_POINT ( 'NONE',  ( -18.67979575497178146, -10.72451020669898902, 46.66557627198102409 ) ) ;
#65838 = CARTESIAN_POINT ( 'NONE',  ( -10.81492255796078084, -18.62759615963271287, 32.08224293864769550 ) ) ;
#65839 = CARTESIAN_POINT ( 'NONE',  ( -16.53943276465976808, -0.05219959533934237506, 78.75109039468568994 ) ) ;
#65840 = CARTESIAN_POINT ( 'NONE',  ( 21.52544592524344225, -5.823673210054117533, 38.54057627198103120 ) ) ;
#65841 = ORIENTED_EDGE ( 'NONE', *, *, #9309, .T. ) ;
#65842 = CARTESIAN_POINT ( 'NONE',  ( 9.474510206698971260, -16.51473224551069308, 97.91557627198102409 ) ) ;
#65843 = CARTESIAN_POINT ( 'NONE',  ( -4.483927247898539470, -16.52544592524342804, 27.29057627198103120 ) ) ;
#65844 = FACE_OUTER_BOUND ( 'NONE', #135665, .T. ) ;
#65845 = CARTESIAN_POINT ( 'NONE',  ( 12.06949235617757843, -12.14591786802309237, 108.1239096053143811 ) ) ;
#65846 = CARTESIAN_POINT ( 'NONE',  ( 10.81492255796078972, 18.62759615963270932, 64.58224293864769550 ) ) ;
#65847 = CARTESIAN_POINT ( 'NONE',  ( 12.14591786802327356, -12.06949235617739191, 85.62609039468568994 ) ) ;
#65848 = CARTESIAN_POINT ( 'NONE',  ( 15.80617190586769283, -15.72974639402175789, 45.62609039468567573 ) ) ;
#65849 = CARTESIAN_POINT ( 'NONE',  ( -16.51473224551082808, 9.474510206698731452, 103.3344237280190043 ) ) ;
#65850 = CARTESIAN_POINT ( 'NONE',  ( -14.34966873604960291, -8.224510206698953496, 106.6655762719810383 ) ) ;
#65851 = CARTESIAN_POINT ( 'NONE',  ( -13.97604488694547697, 13.89961937509957934, 108.1260903946856331 ) ) ;
#65852 = CARTESIAN_POINT ( 'NONE',  ( -13.97604488694527625, -13.89961937509977652, 36.87390960531436690 ) ) ;
#65853 = CARTESIAN_POINT ( 'NONE',  ( 15.38891197842629133, -1.491051326732930171, -61.89130710690760395 ) ) ;
#65854 = CARTESIAN_POINT ( 'NONE',  ( -5.049401038298153566, 19.05341960407611168, 90.20724293864766707 ) ) ;
#65855 = CARTESIAN_POINT ( 'NONE',  ( -16.55341960407617563, 4.379528057220093196, 78.54275706135236135 ) ) ;
#65856 = CARTESIAN_POINT ( 'NONE',  ( 21.52544592524334988, 5.823673210054432836, 101.4594237280190185 ) ) ;
#65857 = CARTESIAN_POINT ( 'NONE',  ( 18.67979575497178502, 10.72451020669898547, 64.16557627198102409 ) ) ;
#65858 = CARTESIAN_POINT ( 'NONE',  ( 4.483927247898790824, -16.52544592524335698, 85.20942372801901854 ) ) ;
#65859 = VECTOR ( 'NONE', #26409, 1000.000000000000000 ) ;
#65860 = CARTESIAN_POINT ( 'NONE',  ( -5.153800228976607833, 19.02544592524334988, 82.70942372801897591 ) ) ;
#65861 = CARTESIAN_POINT ( 'NONE',  ( 19.03943276465977164, -0.05219959533909143690, 38.74890960531436690 ) ) ;
#65862 = CARTESIAN_POINT ( 'NONE',  ( 9.564922557960805705, 16.46253265017160317, 79.58224293864769550 ) ) ;
#65863 = CARTESIAN_POINT ( 'NONE',  ( 9.474510206698971260, -16.51473224551069308, 27.91557627198103120 ) ) ;
#65864 = CARTESIAN_POINT ( 'NONE',  ( 9.474510206698729675, 16.51473224551082808, 67.08442372801900433 ) ) ;
#65865 = CARTESIAN_POINT ( 'NONE',  ( 21.97054992548899222, -8.562709642470922589, 171.7904333278019351 ) ) ;
#65866 = CARTESIAN_POINT ( 'NONE',  ( -9.474510206698964154, 16.51473224551069663, 100.4155762719810241 ) ) ;
#65867 = CARTESIAN_POINT ( 'NONE',  ( -0.05219959533910754901, -16.53943276465976808, 57.49890960531435979 ) ) ;
#65868 = CARTESIAN_POINT ( 'NONE',  ( -0.05219959533907301413, -21.53943276465977519, 62.49890960531436690 ) ) ;
#65869 = CARTESIAN_POINT ( 'NONE',  ( 17.97182807773874202, -5.499999999999957367, 91.03038844047289047 ) ) ;
#65870 = CARTESIAN_POINT ( 'NONE',  ( -16.46253265017146816, -9.564922557961047289, 34.16775706135233293 ) ) ;
#65871 = DIRECTION ( 'NONE',  ( 1.000000000000000000, 0.000000000000000000, 0.000000000000000000 ) ) ;
#65873 = CARTESIAN_POINT ( 'NONE',  ( 13.89961937509977652, -13.97604488694527269, 68.12390960531436690 ) ) ;
#65872 = CARTESIAN_POINT ( 'NONE',  ( -13.97604488694527625, -13.89961937509977652, 56.87390960531434558 ) ) ;
#65874 = CARTESIAN_POINT ( 'NONE',  ( -16.52544592524335698, -4.483927247898792601, 38.95942372801901854 ) ) ;
#65875 = CARTESIAN_POINT ( 'NONE',  ( -33.75684350552029400, -3.359699206722016385, 99.36933870599236229 ) ) ;
#65876 = CARTESIAN_POINT ( 'NONE',  ( 6.154245480356221876, -36.53401430921382342, -8.000000000000003553 ) ) ;
#65877 = CARTESIAN_POINT ( 'NONE',  ( 16.55341960407618274, -4.379528057220086978, 71.04275706135234714 ) ) ;
#65879 = CARTESIAN_POINT ( 'NONE',  ( -0.05219959533907301413, -21.53943276465977519, 97.49890960531436690 ) ) ;
#65878 = CARTESIAN_POINT ( 'NONE',  ( -14.34966873604972548, 8.224510206698743886, 68.33442372801900433 ) ) ;
#65880 = CARTESIAN_POINT ( 'NONE',  ( 12.06949235617739724, 12.14591786802326823, 46.87609039468568994 ) ) ;
#65882 = CARTESIAN_POINT ( 'NONE',  ( 17.57848473335091555, -16.49314274028410310, -56.92152151716637576 ) ) ;
#65881 = CARTESIAN_POINT ( 'NONE',  ( -9.564922557960796823, -16.46253265017161027, 42.08224293864769550 ) ) ;
#65883 = CARTESIAN_POINT ( 'NONE',  ( 10.81492255796106328, -18.62759615963255655, 60.41775706135235424 ) ) ;
#65884 = CARTESIAN_POINT ( 'NONE',  ( -9.564922557961040184, 16.46253265017147172, 62.91775706135233293 ) ) ;
#65885 = CARTESIAN_POINT ( 'NONE',  ( 15.80617190586769283, -15.72974639402175789, 95.62609039468568994 ) ) ;
#65886 = CARTESIAN_POINT ( 'NONE',  ( 19.03943276465977164, -0.05219959533909143690, 33.74890960531435979 ) ) ;
#65887 = CARTESIAN_POINT ( 'NONE',  ( -15.57302527691882688, 1.455916144794820566, -59.63194581529847937 ) ) ;
#65888 = CARTESIAN_POINT ( 'NONE',  ( -18.67979575497178146, -10.72451020669898902, 56.66557627198103830 ) ) ;
#65889 = CARTESIAN_POINT ( 'NONE',  ( 13.97604488694527802, 13.89961937509977652, 99.37390960531436690 ) ) ;
#65890 = CARTESIAN_POINT ( 'NONE',  ( -16.52544592524342804, 4.483927247898546575, 101.0405762719810383 ) ) ;
#65891 = CARTESIAN_POINT ( 'NONE',  ( 0.05219959533934541429, -16.53943276465976808, 40.00109039468567573 ) ) ;
#65892 = CARTESIAN_POINT ( 'NONE',  ( -12.06949235617739369, -12.14591786802326823, 109.3760903946857042 ) ) ;
#65893 = ORIENTED_EDGE ( 'NONE', *, *, #28831, .T. ) ;
#65894 = EDGE_CURVE ( 'NONE', #191214, #82858, #37698, .T. ) ;
#65895 = CARTESIAN_POINT ( 'NONE',  ( 21.55341960407610458, 5.719274019375980345, 98.95724293864770971 ) ) ;
#65897 = CARTESIAN_POINT ( 'NONE',  ( -9.474510206698964154, 16.51473224551069663, 110.4155762719810383 ) ) ;
#65896 = CARTESIAN_POINT ( 'NONE',  ( -12.14591786802309592, -12.06949235617757132, 41.87390960531435979 ) ) ;
#65898 = CARTESIAN_POINT ( 'NONE',  ( -19.05341960407617563, 5.049401038297882671, 88.54275706135230450 ) ) ;
#65899 = CARTESIAN_POINT ( 'NONE',  ( 19.05341960407617918, -5.049401038297876454, 31.04275706135232227 ) ) ;
#65900 = CARTESIAN_POINT ( 'NONE',  ( -0.05219959533910754901, -16.53943276465976808, 32.49890960531435979 ) ) ;
#65901 = CARTESIAN_POINT ( 'NONE',  ( -21.53943276465977519, 0.05219959533907696930, 96.24890960531435269 ) ) ;
#65902 = CARTESIAN_POINT ( 'NONE',  ( -15.80617190586745835, -15.72974639402198527, 56.87390960531436690 ) ) ;
#65903 = VECTOR ( 'NONE', #151948, 1000.000000000000000 ) ;
#65904 = CARTESIAN_POINT ( 'NONE',  ( 9.564922557960805705, 16.46253265017160317, 69.58224293864770971 ) ) ;
#65905 = CARTESIAN_POINT ( 'NONE',  ( 8.314922557960818139, 14.29746914071049879, 34.58224293864770260 ) ) ;
#65906 = CARTESIAN_POINT ( 'NONE',  ( 5.049401038298161559, -19.05341960407611168, 92.70724293864769550 ) ) ;
#65907 = ORIENTED_EDGE ( 'NONE', *, *, #24178, .F. ) ;
#65908 = CARTESIAN_POINT ( 'NONE',  ( 18.39443945427642291, -5.499999999999864997, 61.01745347608654413 ) ) ;
#65909 = CARTESIAN_POINT ( 'NONE',  ( -5.153800228976607833, 19.02544592524334988, 42.70942372801901143 ) ) ;
#65910 = CARTESIAN_POINT ( 'NONE',  ( -5.719274019375978568, 21.55341960407610458, 75.20724293864769550 ) ) ;
#65911 = CARTESIAN_POINT ( 'NONE',  ( -4.483927247898539470, -16.52544592524342804, 102.2905762719810383 ) ) ;
#65912 =( GEOMETRIC_REPRESENTATION_CONTEXT ( 3 ) GLOBAL_UNCERTAINTY_ASSIGNED_CONTEXT ( ( #37796 ) ) GLOBAL_UNIT_ASSIGNED_CONTEXT ( ( #190273, #144751, #100247 ) ) REPRESENTATION_CONTEXT ( 'NONE', 'WORKASPACE' ) );
#65913 = CARTESIAN_POINT ( 'NONE',  ( 15.72974639402176855, 15.80617190586768217, 36.87609039468568994 ) ) ;
#65914 = CARTESIAN_POINT ( 'NONE',  ( -22.44159573604009950, -16.30477369853688430, 143.0750000027311728 ) ) ;
#65915 = CARTESIAN_POINT ( 'NONE',  ( -16.52544592524335698, -4.483927247898792601, 108.9594237280190185 ) ) ;
#65916 = CARTESIAN_POINT ( 'NONE',  ( -9.474510206698964154, 16.51473224551069663, 40.41557627198103120 ) ) ;
#65917 = CARTESIAN_POINT ( 'NONE',  ( 5.153800228976335163, 19.02544592524342804, 84.79057627198099567 ) ) ;
#65918 = CARTESIAN_POINT ( 'NONE',  ( 8.571926809382603096, -26.38167802310801235, 139.4750000027311785 ) ) ;
#65919 = CARTESIAN_POINT ( 'NONE',  ( -5.153800228976328057, -19.02544592524343514, 27.29057627198103120 ) ) ;
#65920 = CARTESIAN_POINT ( 'NONE',  ( -4.379528057220328563, 16.55341960407611168, 40.20724293864769550 ) ) ;
#65921 = CARTESIAN_POINT ( 'NONE',  ( 10.81492255796106328, -18.62759615963255655, 75.41775706135233293 ) ) ;
#65923 = CARTESIAN_POINT ( 'NONE',  ( -4.483927247898782831, 16.52544592524335698, 72.70942372801901854 ) ) ;
#65922 = CARTESIAN_POINT ( 'NONE',  ( 25.08997344983162137, -28.19247641866554233, -20.54396225645222884 ) ) ;
#65924 = CARTESIAN_POINT ( 'NONE',  ( -13.89961937509977652, 13.97604488694528158, 55.62390960531434558 ) ) ;
#65925 = CARTESIAN_POINT ( 'NONE',  ( 0.05219959533909260263, 19.03943276465977164, 64.99890960531436690 ) ) ;
#65926 = VERTEX_POINT ( 'NONE', #38371 ) ;
#65927 = CARTESIAN_POINT ( 'NONE',  ( 21.52544592524334988, 5.823673210054432836, 111.4594237280190328 ) ) ;
#65928 = CARTESIAN_POINT ( 'NONE',  ( -16.55341960407617563, 4.379528057220093196, 68.54275706135234714 ) ) ;
#65929 = CARTESIAN_POINT ( 'NONE',  ( -5.823673210054431948, 21.52544592524334988, 97.70942372801904696 ) ) ;
#65930 = CARTESIAN_POINT ( 'NONE',  ( -19.05341960407611168, -5.049401038298163336, 56.45724293864768129 ) ) ;
#65931 = CARTESIAN_POINT ( 'NONE',  ( 10.81492255796078972, 18.62759615963270932, 34.58224293864770260 ) ) ;
#65932 = CARTESIAN_POINT ( 'NONE',  ( 9.564922557961047289, -16.46253265017146816, 105.4177570613523471 ) ) ;
#65933 = CARTESIAN_POINT ( 'NONE',  ( -5.823673210054431948, 21.52544592524334988, 62.70942372801902565 ) ) ;
#65934 = CARTESIAN_POINT ( 'NONE',  ( -8.224510206698735004, -14.34966873604973081, 54.58442372801901143 ) ) ;
#65935 = CARTESIAN_POINT ( 'NONE',  ( -21.55341960407610458, -5.719274019375992779, 96.45724293864770971 ) ) ;
#65936 = CARTESIAN_POINT ( 'NONE',  ( -13.89961937509957401, -13.97604488694547875, 104.3760903946856757 ) ) ;
#65937 = CARTESIAN_POINT ( 'NONE',  ( 0.05219959533909260263, 19.03943276465977164, 74.99890960531435269 ) ) ;
#65938 = CARTESIAN_POINT ( 'NONE',  ( -14.29746914071037622, -8.314922557961029526, 19.16775706135234714 ) ) ;
#65939 = AXIS2_PLACEMENT_3D ( 'NONE', #94030, #155710, #17206 ) ;
#65940 = CARTESIAN_POINT ( 'NONE',  ( 19.05341960407617918, -5.049401038297876454, 106.0427570613523471 ) ) ;
#65941 = CARTESIAN_POINT ( 'NONE',  ( -8.314922557960811034, -14.29746914071050412, 62.08224293864769550 ) ) ;
#65942 = CARTESIAN_POINT ( 'NONE',  ( 8.224510206698742110, 14.34966873604972548, 77.08442372801901854 ) ) ;
#65944 = CARTESIAN_POINT ( 'NONE',  ( -5.049401038298153566, 19.05341960407611168, 55.20724293864769550 ) ) ;
#65943 = CARTESIAN_POINT ( 'NONE',  ( 15.72974639402176855, 15.80617190586768217, 21.87609039468567573 ) ) ;
#65945 = CARTESIAN_POINT ( 'NONE',  ( -19.03943276465977164, 0.05219959533909376836, 61.24890960531436690 ) ) ;
#65946 = CARTESIAN_POINT ( 'NONE',  ( 12.14591786802327356, -12.06949235617739191, 75.62609039468567573 ) ) ;
#65947 = CARTESIAN_POINT ( 'NONE',  ( -28.82186960331499392, 9.364793116373565596, 144.1500000054623740 ) ) ;
#65948 = ORIENTED_EDGE ( 'NONE', *, *, #136692, .F. ) ;
#65949 = CARTESIAN_POINT ( 'NONE',  ( 0.05219959533937995610, -21.53943276465977519, 110.0010903946856757 ) ) ;
#65950 = FACE_OUTER_BOUND ( 'NONE', #52283, .T. ) ;
#65951 = ORIENTED_EDGE ( 'NONE', *, *, #92301, .F. ) ;
#65952 = CARTESIAN_POINT ( 'NONE',  ( 0.05219959533936267826, -19.03943276465977164, 105.0010903946856615 ) ) ;
#65953 = CARTESIAN_POINT ( 'NONE',  ( 18.62759615963271287, -10.81492255796078972, 48.33224293864770260 ) ) ;
#65955 = CARTESIAN_POINT ( 'NONE',  ( -4.483927247898782831, 16.52544592524335698, 22.70942372801901499 ) ) ;
#65954 = CARTESIAN_POINT ( 'NONE',  ( -19.05341960407617563, 5.049401038297882671, 38.54275706135233293 ) ) ;
#65956 = CARTESIAN_POINT ( 'NONE',  ( 13.89961937509977652, -13.97604488694527269, 43.12390960531434558 ) ) ;
#65957 = CARTESIAN_POINT ( 'NONE',  ( -19.03943276465977164, 0.05219959533909376836, 66.24890960531436690 ) ) ;
#65958 = CARTESIAN_POINT ( 'NONE',  ( 15.80617190586746368, 15.72974639402197994, 84.37390960531438111 ) ) ;
#65959 = CARTESIAN_POINT ( 'NONE',  ( -9.564922557960796823, -16.46253265017161027, 112.0822429386476955 ) ) ;
#65960 = CARTESIAN_POINT ( 'NONE',  ( 5.153800228976335163, 19.02544592524342804, 49.79057627198100988 ) ) ;
#65961 = CARTESIAN_POINT ( 'NONE',  ( -27.73933785331498925, 2.428612866367529932E-14, 149.3750000027311842 ) ) ;
#65962 = CARTESIAN_POINT ( 'NONE',  ( 16.46253265017146816, 9.564922557961045513, 96.66775706135233293 ) ) ;
#65963 = CARTESIAN_POINT ( 'NONE',  ( -16.52544592524342804, 4.483927247898546575, 66.04057627198103830 ) ) ;
#65964 = CARTESIAN_POINT ( 'NONE',  ( 9.564922557961047289, -16.46253265017146816, 25.41775706135234003 ) ) ;
#65965 = AXIS2_PLACEMENT_3D ( 'NONE', #128016, #51191, #131014 ) ;
#65966 = CARTESIAN_POINT ( 'NONE',  ( -0.05219959533910754901, -16.53943276465976808, 57.49890960531435979 ) ) ;
#65967 = CARTESIAN_POINT ( 'NONE',  ( -18.67979575497193778, 10.72451020669871902, 83.33442372801903275 ) ) ;
#65968 = CARTESIAN_POINT ( 'NONE',  ( 5.049401038298161559, -19.05341960407611168, 32.70724293864768129 ) ) ;
#65969 = CARTESIAN_POINT ( 'NONE',  ( -10.81492255796105439, 18.62759615963255655, 92.91775706135236135 ) ) ;
#65971 = CARTESIAN_POINT ( 'NONE',  ( -10.81492255796105439, 18.62759615963255655, 77.91775706135231871 ) ) ;
#65970 = CARTESIAN_POINT ( 'NONE',  ( -14.34966873604960291, -8.224510206698953496, 26.66557627198103475 ) ) ;
#65972 = CARTESIAN_POINT ( 'NONE',  ( -13.89961937509977652, 13.97604488694528158, 65.62390960531436690 ) ) ;
#65973 = EDGE_CURVE ( 'NONE', #182543, #126159, #131372, .T. ) ;
#65974 = CARTESIAN_POINT ( 'NONE',  ( -5.719274019375665041, -21.55341960407619695, 44.79275706135234714 ) ) ;
#65975 = CARTESIAN_POINT ( 'NONE',  ( -13.89961937509977652, 13.97604488694528158, 85.62390960531433848 ) ) ;
#65976 = CARTESIAN_POINT ( 'NONE',  ( 4.379528057220339221, -16.55341960407611168, 97.70724293864772392 ) ) ;
#65977 = CARTESIAN_POINT ( 'NONE',  ( -16.55341960407611168, -4.379528057220339221, 66.45724293864768129 ) ) ;
#65978 = CARTESIAN_POINT ( 'NONE',  ( -21.52544592524343514, 5.823673210054127303, 66.04057627198103830 ) ) ;
#65979 = CARTESIAN_POINT ( 'NONE',  ( 9.474510206698971260, -16.51473224551069308, 72.91557627198102409 ) ) ;
#65980 = CARTESIAN_POINT ( 'NONE',  ( 21.53943276465977519, -0.05219959533907433946, 83.74890960531435269 ) ) ;
#65981 = CARTESIAN_POINT ( 'NONE',  ( 5.049401038297881783, 19.05341960407617563, 67.29275706135234714 ) ) ;
#65983 = CARTESIAN_POINT ( 'NONE',  ( -4.379528057220328563, 16.55341960407611168, 80.20724293864769550 ) ) ;
#65982 = CARTESIAN_POINT ( 'NONE',  ( -16.51473224551082808, 9.474510206698731452, 38.33442372801899722 ) ) ;
#65984 = CARTESIAN_POINT ( 'NONE',  ( 10.72451020669898902, -18.67979575497178502, 47.91557627198102409 ) ) ;
#65985 = DIRECTION ( 'NONE',  ( -1.000000000000000000, 6.391086490440866478E-16, 0.000000000000000000 ) ) ;
#65987 = CARTESIAN_POINT ( 'NONE',  ( 27.73933785331498569, 2.768321779492822058E-14, 142.3750000027311842 ) ) ;
#65986 = CARTESIAN_POINT ( 'NONE',  ( -4.483927247898782831, 16.52544592524335698, 92.70942372801901854 ) ) ;
#65988 = CARTESIAN_POINT ( 'NONE',  ( 9.474510206698729675, 16.51473224551082808, 107.0844237280190043 ) ) ;
#65989 = EDGE_CURVE ( 'NONE', #134824, #103535, #22203, .T. ) ;
#65990 = CARTESIAN_POINT ( 'NONE',  ( -12.14591786802309592, -12.06949235617757132, 61.87390960531436690 ) ) ;
#65991 = CARTESIAN_POINT ( 'NONE',  ( 6.854124442542001816, -1.305043071815303435, -62.35408385982738366 ) ) ;
#65992 = CARTESIAN_POINT ( 'NONE',  ( 5.153800228976335163, 19.02544592524342804, 54.79057627198103120 ) ) ;
#65993 = CARTESIAN_POINT ( 'NONE',  ( -8.224510206698948167, 14.34966873604960824, 55.41557627198102409 ) ) ;
#65994 = CARTESIAN_POINT ( 'NONE',  ( 13.97604488694527802, 13.89961937509977652, 99.37390960531436690 ) ) ;
#65996 = CARTESIAN_POINT ( 'NONE',  ( 0.05219959533909260263, 19.03943276465977164, 64.99890960531436690 ) ) ;
#65995 = CARTESIAN_POINT ( 'NONE',  ( -19.05341960407617563, 5.049401038297882671, 78.54275706135233293 ) ) ;
#65997 = CARTESIAN_POINT ( 'NONE',  ( 13.89961937509977652, -13.97604488694527269, 83.12390960531436690 ) ) ;
#65998 = CARTESIAN_POINT ( 'NONE',  ( -5.049401038298153566, 19.05341960407611168, 90.20724293864766707 ) ) ;
#65999 = CARTESIAN_POINT ( 'NONE',  ( -10.81492255796078084, -18.62759615963271287, 62.08224293864769550 ) ) ;
#66000 = CARTESIAN_POINT ( 'NONE',  ( 14.34966873604972726, -8.224510206698740333, 60.83442372801901854 ) ) ;
#66001 = CARTESIAN_POINT ( 'NONE',  ( 5.049401038297881783, 19.05341960407617918, 102.2927570613523187 ) ) ;
#66002 = CARTESIAN_POINT ( 'NONE',  ( -16.51473224551069308, -9.474510206698971260, 46.66557627198102409 ) ) ;
#66003 = CARTESIAN_POINT ( 'NONE',  ( -10.81492255796078084, -18.62759615963271287, 52.08224293864768839 ) ) ;
#66004 = CARTESIAN_POINT ( 'NONE',  ( -16.46253265017146816, -9.564922557961047289, 99.16775706135233293 ) ) ;
#66005 = APPLICATION_CONTEXT ( 'automotive_design' ) ;
#66007 = CARTESIAN_POINT ( 'NONE',  ( 10.72451020669871369, 18.67979575497193778, 47.08442372801901854 ) ) ;
#66006 = CARTESIAN_POINT ( 'NONE',  ( 4.379528057220339221, -16.55341960407611168, 27.70724293864769905 ) ) ;
#66008 = CARTESIAN_POINT ( 'NONE',  ( 19.02544592524334988, 5.153800228976608722, 36.45942372801900433 ) ) ;
#66010 = CARTESIAN_POINT ( 'NONE',  ( 16.55341960407618274, -4.379528057220086978, 91.04275706135236135 ) ) ;
#66009 = CARTESIAN_POINT ( 'NONE',  ( 8.314922557961029526, -14.29746914071037800, 55.41775706135234714 ) ) ;
#66011 = CARTESIAN_POINT ( 'NONE',  ( -17.49999999999999645, 5.499999999999992895, 53.71769037696436300 ) ) ;
#66012 = CARTESIAN_POINT ( 'NONE',  ( 4.379528057220092307, 16.55341960407617563, 87.29275706135236135 ) ) ;
#66013 = CARTESIAN_POINT ( 'NONE',  ( 4.483927247898790824, -16.52544592524335698, 30.20942372801902565 ) ) ;
#66014 = CARTESIAN_POINT ( 'NONE',  ( 9.474510206698971260, -16.51473224551069308, 42.91557627198103120 ) ) ;
#66015 = CARTESIAN_POINT ( 'NONE',  ( 13.89961937509977652, -13.97604488694527269, 48.12390960531435979 ) ) ;
#66016 = CARTESIAN_POINT ( 'NONE',  ( -19.02544592524342804, 5.153800228976336051, 61.04057627198103120 ) ) ;
#66017 = CARTESIAN_POINT ( 'NONE',  ( -21.55341960407619339, 5.719274019375674811, 53.54275706135234714 ) ) ;
#66018 = CARTESIAN_POINT ( 'NONE',  ( -16.55341960407617563, 4.379528057220093196, 43.54275706135235424 ) ) ;
#66019 = CARTESIAN_POINT ( 'NONE',  ( 0.05219959533934541429, -16.53943276465976808, 110.0010903946856757 ) ) ;
#66020 = CARTESIAN_POINT ( 'NONE',  ( 16.46253265017160672, -9.564922557960803928, 28.33224293864769550 ) ) ;
#66021 = CARTESIAN_POINT ( 'NONE',  ( -5.153800228976607833, 19.02544592524334988, 22.70942372801899012 ) ) ;
#66022 = CARTESIAN_POINT ( 'NONE',  ( 16.53943276465976808, 0.05219959533934440121, 21.25109039468567218 ) ) ;
#66023 = CIRCLE ( 'NONE', #101537, 2.699999999999993960 ) ;
#66024 = CARTESIAN_POINT ( 'NONE',  ( 5.153800228976615827, -19.02544592524334988, 75.20942372801896170 ) ) ;
#66025 = CARTESIAN_POINT ( 'NONE',  ( -4.379528057220328563, 16.55341960407611168, 85.20724293864770971 ) ) ;
#66026 = CARTESIAN_POINT ( 'NONE',  ( 19.05341960407611168, 5.049401038298154454, 38.95724293864767418 ) ) ;
#66028 = CARTESIAN_POINT ( 'NONE',  ( 16.61371651742601685, -7.165104196376144152, 91.35415069992995996 ) ) ;
#66027 = CARTESIAN_POINT ( 'NONE',  ( -16.46253265017146816, -9.564922557961047289, 79.16775706135234714 ) ) ;
#66029 = CARTESIAN_POINT ( 'NONE',  ( -5.823673210054431948, 21.52544592524334988, 82.70942372801900433 ) ) ;
#66030 = CARTESIAN_POINT ( 'NONE',  ( -12.14591786802326823, 12.06949235617739902, 43.12609039468568284 ) ) ;
#66031 = FACE_OUTER_BOUND ( 'NONE', #146743, .T. ) ;
#66032 = CARTESIAN_POINT ( 'NONE',  ( 21.53943276465977519, -0.05219959533907433946, 38.74890960531435979 ) ) ;
#66033 = CARTESIAN_POINT ( 'NONE',  ( -12.14591786802326823, 12.06949235617739902, 28.12609039468568284 ) ) ;
#66034 = CARTESIAN_POINT ( 'NONE',  ( 13.89961937509978007, -13.97604488694527269, 23.12390960531435979 ) ) ;
#66035 = CARTESIAN_POINT ( 'NONE',  ( -9.564922557961040184, 16.46253265017147172, 32.91775706135233293 ) ) ;
#66036 = PLANE ( 'NONE',  #126968 ) ;
#66037 = CARTESIAN_POINT ( 'NONE',  ( 16.46253265017160672, -9.564922557960803928, 43.33224293864769550 ) ) ;
#66038 = PLANE ( 'NONE',  #178825 ) ;
#66039 = CARTESIAN_POINT ( 'NONE',  ( -9.564922557960796823, -16.46253265017161027, 72.08224293864770971 ) ) ;
#66040 = CARTESIAN_POINT ( 'NONE',  ( -19.01533133064923575, 5.499999999999444000, 98.76586590595738357 ) ) ;
#66041 = CARTESIAN_POINT ( 'NONE',  ( -16.51473224551082808, 9.474510206698731452, 23.33442372801900078 ) ) ;
#66042 = CARTESIAN_POINT ( 'NONE',  ( 0.05219959533910956823, 16.53943276465976808, 34.99890960531435979 ) ) ;
#66043 = CARTESIAN_POINT ( 'NONE',  ( -19.02544592524342804, 5.153800228976336051, 46.04057627198101699 ) ) ;
#66044 = CARTESIAN_POINT ( 'NONE',  ( 5.049401038298161559, -19.05341960407611168, 97.70724293864766707 ) ) ;
#66045 = CARTESIAN_POINT ( 'NONE',  ( -0.05219959533937732626, 21.53943276465977519, 72.50109039468568994 ) ) ;
#66046 = CARTESIAN_POINT ( 'NONE',  ( 19.02544592524343514, -5.153800228976328945, 48.54057627198103120 ) ) ;
#66047 = CARTESIAN_POINT ( 'NONE',  ( -10.72451020669870658, -18.67979575497194134, 64.58442372801900433 ) ) ;
#66048 = CARTESIAN_POINT ( 'NONE',  ( 19.05341960407611168, 5.049401038298154454, 113.9572429386477097 ) ) ;
#66049 = CARTESIAN_POINT ( 'NONE',  ( 13.97604488694527802, 13.89961937509977652, 29.37390960531435979 ) ) ;
#66050 = CARTESIAN_POINT ( 'NONE',  ( 5.719274019375991003, -21.55341960407610458, 112.7072429386476955 ) ) ;
#66051 = CARTESIAN_POINT ( 'NONE',  ( -16.46253265017146816, -9.564922557961047289, 29.16775706135232937 ) ) ;
#66052 = CARTESIAN_POINT ( 'NONE',  ( -16.53943276465976808, 0.05219959533911058130, 106.2489096053143811 ) ) ;
#66053 = CARTESIAN_POINT ( 'NONE',  ( -0.05219959533909027116, -19.03943276465977164, 67.49890960531436690 ) ) ;
#66055 = AXIS2_PLACEMENT_3D ( 'NONE', #196597, #27747, #103577 ) ;
#66054 = CARTESIAN_POINT ( 'NONE',  ( -19.05341960407617563, 5.049401038297882671, 113.5427570613523471 ) ) ;
#66056 = CARTESIAN_POINT ( 'NONE',  ( 14.34966873604960469, 8.224510206698951720, 74.16557627198102409 ) ) ;
#66057 = CARTESIAN_POINT ( 'NONE',  ( -16.46253265017160317, 9.564922557960807481, 115.8322429386477097 ) ) ;
#66058 = CARTESIAN_POINT ( 'NONE',  ( 19.02544592524334988, 5.153800228976608722, 86.45942372801900433 ) ) ;
#66059 = CARTESIAN_POINT ( 'NONE',  ( 15.72974639402199770, -15.80617190586745480, 88.12390960531436690 ) ) ;
#66060 = CARTESIAN_POINT ( 'NONE',  ( 21.53943276465977519, 0.05219959533937863772, 61.25109039468567573 ) ) ;
#66061 = CARTESIAN_POINT ( 'NONE',  ( -0.05219959533934338120, 16.53943276465976808, 62.50109039468568284 ) ) ;
#66062 = CARTESIAN_POINT ( 'NONE',  ( 14.34966873604972726, -8.224510206698740333, 55.83442372801901854 ) ) ;
#66063 = CARTESIAN_POINT ( 'NONE',  ( 0.05219959533907565091, 21.53943276465977519, 59.99890960531436690 ) ) ;
#66064 =( GEOMETRIC_REPRESENTATION_CONTEXT ( 3 ) GLOBAL_UNCERTAINTY_ASSIGNED_CONTEXT ( ( #34252 ) ) GLOBAL_UNIT_ASSIGNED_CONTEXT ( ( #151525, #74679, #194053 ) ) REPRESENTATION_CONTEXT ( 'NONE', 'WORKASPACE' ) );
#66065 = CARTESIAN_POINT ( 'NONE',  ( -19.02544592524342804, 5.153800228976336051, 46.04057627198101699 ) ) ;
#66066 = CARTESIAN_POINT ( 'NONE',  ( 3.766062262543149401E-15, -39.95556452105413570, -3.249999994537627224 ) ) ;
#66067 = CARTESIAN_POINT ( 'NONE',  ( 14.29746914071037800, 8.314922557961029526, 81.66775706135236135 ) ) ;
#66068 = CARTESIAN_POINT ( 'NONE',  ( -21.53943276465977519, 0.05219959533907696930, 101.2489096053143669 ) ) ;
#66069 = CARTESIAN_POINT ( 'NONE',  ( 0.05219959533910956823, 16.53943276465976808, 49.99890960531437401 ) ) ;
#66070 = CARTESIAN_POINT ( 'NONE',  ( -16.53943276465976808, -0.05219959533934237506, 58.75109039468568994 ) ) ;
#66071 = CARTESIAN_POINT ( 'NONE',  ( 16.46253265017146816, 9.564922557961045513, 106.6677570613523471 ) ) ;
#66072 = CARTESIAN_POINT ( 'NONE',  ( 21.52544592524344225, -5.823673210054117533, 93.54057627198103830 ) ) ;
#66073 = CARTESIAN_POINT ( 'NONE',  ( -12.06949235617756955, 12.14591786802309770, 50.62390960531435979 ) ) ;
#66074 = ORIENTED_EDGE ( 'NONE', *, *, #64870, .F. ) ;
#66075 = CARTESIAN_POINT ( 'NONE',  ( -17.44270441346519362, 5.991230190322972327, 68.63664920735773478 ) ) ;
#66076 = CARTESIAN_POINT ( 'NONE',  ( 21.55341960407610458, 5.719274019375980345, 78.95724293864769550 ) ) ;
#66077 = CARTESIAN_POINT ( 'NONE',  ( 8.224510206698953496, -14.34966873604960469, 27.91557627198103830 ) ) ;
#66078 = ORIENTED_EDGE ( 'NONE', *, *, #50743, .T. ) ;
#66079 = DIRECTION ( 'NONE',  ( 0.000000000000000000, -0.7071067811865483499, -0.7071067811865466846 ) ) ;
#66080 = CARTESIAN_POINT ( 'NONE',  ( -0.05219959533907301413, -21.53943276465977519, 102.4989096053143811 ) ) ;
#66081 = CARTESIAN_POINT ( 'NONE',  ( -18.67979575497193778, 10.72451020669871902, 23.33442372801901499 ) ) ;
#66082 = CARTESIAN_POINT ( 'NONE',  ( 14.29746914071049879, -8.314922557960816363, 33.33224293864769550 ) ) ;
#66084 = CARTESIAN_POINT ( 'NONE',  ( -14.34966873604972548, 8.224510206698743886, 48.33442372801902565 ) ) ;
#66083 = AXIS2_PLACEMENT_3D ( 'NONE', #9021, #70689, #97986 ) ;
#66085 = CARTESIAN_POINT ( 'NONE',  ( 13.97604488694527802, 13.89961937509977652, 49.37390960531434558 ) ) ;
#66086 = CARTESIAN_POINT ( 'NONE',  ( -19.05341960407611168, -5.049401038298163336, 81.45724293864769550 ) ) ;
#66087 = VERTEX_POINT ( 'NONE', #82857 ) ;
#66088 = CARTESIAN_POINT ( 'NONE',  ( -18.62759615963270932, 10.81492255796079327, 30.83224293864770260 ) ) ;
#66089 = CARTESIAN_POINT ( 'NONE',  ( -13.89961937509977830, 13.97604488694528158, 65.62390960531436690 ) ) ;
#66090 = CARTESIAN_POINT ( 'NONE',  ( 4.379528057220092307, 16.55341960407617563, 22.29275706135235069 ) ) ;
#66091 = CARTESIAN_POINT ( 'NONE',  ( -13.89961937509957401, -13.97604488694547875, 49.37609039468567573 ) ) ;
#66092 = CARTESIAN_POINT ( 'NONE',  ( -10.81492255796078084, -18.62759615963271287, 97.08224293864770971 ) ) ;
#66093 = CARTESIAN_POINT ( 'NONE',  ( 14.34966873604960469, 8.224510206698951720, 39.16557627198102409 ) ) ;
#66094 = CARTESIAN_POINT ( 'NONE',  ( 16.46253265017160672, -9.564922557960803928, 78.33224293864769550 ) ) ;
#66095 = CARTESIAN_POINT ( 'NONE',  ( -5.823673210054116645, -21.52544592524344225, 57.29057627198103120 ) ) ;
#66097 = CARTESIAN_POINT ( 'NONE',  ( -19.05341960407617563, 5.049401038297882671, 113.5427570613523471 ) ) ;
#66096 = CARTESIAN_POINT ( 'NONE',  ( -10.81492255796078084, -18.62759615963271287, 97.08224293864770971 ) ) ;
#66098 = ADVANCED_FACE ( 'NONE', ( #21201 ), #150742, .F. ) ;
#66099 = CARTESIAN_POINT ( 'NONE',  ( 5.719274019375991003, -21.55341960407610458, 27.70724293864769905 ) ) ;
#66100 = CARTESIAN_POINT ( 'NONE',  ( -18.67979575497193778, 10.72451020669871902, 83.33442372801903275 ) ) ;
#66101 = CARTESIAN_POINT ( 'NONE',  ( -5.153800228976328057, -19.02544592524343514, 72.29057627198102409 ) ) ;
#66102 = CARTESIAN_POINT ( 'NONE',  ( -13.89961937509977652, 13.97604488694528158, 30.62390960531435269 ) ) ;
#66103 = CARTESIAN_POINT ( 'NONE',  ( -13.97604488694527625, -13.89961937509977652, 81.87390960531436690 ) ) ;
#66104 = CARTESIAN_POINT ( 'NONE',  ( -8.224510206698948167, 14.34966873604960824, 100.4155762719810241 ) ) ;
#66105 = ORIENTED_EDGE ( 'NONE', *, *, #89035, .T. ) ;
#66106 = CARTESIAN_POINT ( 'NONE',  ( 5.153800228976615827, -19.02544592524334988, 105.2094237280190185 ) ) ;
#66107 = DIRECTION ( 'NONE',  ( -1.000000000000000000, -1.953992523340275511E-14, 0.000000000000000000 ) ) ;
#66108 = CARTESIAN_POINT ( 'NONE',  ( -0.05219959533909027116, -19.03943276465977164, 72.49890960531435269 ) ) ;
#66110 = CARTESIAN_POINT ( 'NONE',  ( -19.05341960407611168, -5.049401038298163336, 111.4572429386476671 ) ) ;
#66109 = CARTESIAN_POINT ( 'NONE',  ( -18.62759615963255300, -10.81492255796106328, 99.16775706135234714 ) ) ;
#66112 = EDGE_CURVE ( 'NONE', #86619, #66459, #35092, .T. ) ;
#66111 = CARTESIAN_POINT ( 'NONE',  ( 14.34966873604972726, -8.224510206698740333, 90.83442372801901854 ) ) ;
#66113 = CARTESIAN_POINT ( 'NONE',  ( -16.31925111598454947, -7.325300261831594106, 74.83575461032751264 ) ) ;
#66114 = CARTESIAN_POINT ( 'NONE',  ( -19.05341960407617563, 5.049401038297882671, 63.54275706135234003 ) ) ;
#66115 = CARTESIAN_POINT ( 'NONE',  ( 5.823673210054444382, -21.52544592524334988, 110.2094237280190185 ) ) ;
#66116 = CARTESIAN_POINT ( 'NONE',  ( 37.47229216401454011, 2.437641287457624095, 40.05669362136319478 ) ) ;
#66117 = CARTESIAN_POINT ( 'NONE',  ( -9.564922557960796823, -16.46253265017161027, 22.08224293864768839 ) ) ;
#66118 = CARTESIAN_POINT ( 'NONE',  ( 12.14591786802309770, 12.06949235617756955, 29.37390960531435269 ) ) ;
#66119 = DIRECTION ( 'NONE',  ( 0.000000000000000000, 0.000000000000000000, 1.000000000000000000 ) ) ;
#66120 = CARTESIAN_POINT ( 'NONE',  ( 14.29746914071037800, 8.314922557961029526, 106.6677570613523756 ) ) ;
#66121 = CARTESIAN_POINT ( 'NONE',  ( -18.22780087662123094, -5.499999999999984901, 86.48459894673892734 ) ) ;
#66122 = CARTESIAN_POINT ( 'NONE',  ( -4.483927247898782831, 16.52544592524335698, 87.70942372801901854 ) ) ;
#66123 = CARTESIAN_POINT ( 'NONE',  ( 19.05341960407611168, 5.049401038298154454, 28.95724293864769550 ) ) ;
#66124 = CARTESIAN_POINT ( 'NONE',  ( 21.53943276465977519, 0.05219959533937863772, 91.25109039468568994 ) ) ;
#66125 = CARTESIAN_POINT ( 'NONE',  ( -19.03943276465977164, -0.05219959533935918106, 103.7510903946856757 ) ) ;
#66126 = CARTESIAN_POINT ( 'NONE',  ( -18.67979575497193778, 10.72451020669871902, 63.33442372801900433 ) ) ;
#66127 = CARTESIAN_POINT ( 'NONE',  ( 5.049401038297881783, 19.05341960407617563, 37.29275706135232582 ) ) ;
#66128 = CARTESIAN_POINT ( 'NONE',  ( 19.05341960407611168, 5.049401038298154454, 83.95724293864766707 ) ) ;
#66129 = CARTESIAN_POINT ( 'NONE',  ( -19.03943276465977164, 0.05219959533909376836, 76.24890960531435269 ) ) ;
#66130 = CARTESIAN_POINT ( 'NONE',  ( -7.143419655154851888, 2.300691058039502135, 8.646741581399137289 ) ) ;
#66131 = CARTESIAN_POINT ( 'NONE',  ( -15.80617190586745835, -15.72974639402198527, 41.87390960531435979 ) ) ;
#66132 = CARTESIAN_POINT ( 'NONE',  ( -13.97604488694527625, -13.89961937509977652, 51.87390960531436690 ) ) ;
#66133 = CARTESIAN_POINT ( 'NONE',  ( -14.34966873604972548, 8.224510206698743886, 78.33442372801901854 ) ) ;
#66134 = ORIENTED_EDGE ( 'NONE', *, *, #135901, .F. ) ;
#66135 = ADVANCED_FACE ( 'NONE', ( #143533 ), #5021, .T. ) ;
#66136 = AXIS2_PLACEMENT_3D ( 'NONE', #96297, #16501, #81120 ) ;
#66138 = CARTESIAN_POINT ( 'NONE',  ( -36.91746825000000598, 2.428612866367529932E-14, -2.624999997268813168 ) ) ;
#66137 = CARTESIAN_POINT ( 'NONE',  ( 8.224510206698953496, -14.34966873604960469, 72.91557627198103830 ) ) ;
#66139 = CARTESIAN_POINT ( 'NONE',  ( 4.483927247898790824, -16.52544592524335698, 40.20942372801901854 ) ) ;
#66140 = CARTESIAN_POINT ( 'NONE',  ( -5.153800228976328057, -19.02544592524343514, 22.29057627198102765 ) ) ;
#66141 = CARTESIAN_POINT ( 'NONE',  ( 5.049401038297881783, 19.05341960407617563, 62.29275706135234003 ) ) ;
#66142 = CARTESIAN_POINT ( 'NONE',  ( -8.314922557960811034, -14.29746914071050412, 67.08224293864770971 ) ) ;
#66143 = CARTESIAN_POINT ( 'NONE',  ( -21.55341960407619339, 5.719274019375674811, 28.54275706135234358 ) ) ;
#66145 = CARTESIAN_POINT ( 'NONE',  ( -18.67979575497178146, -10.72451020669898902, 86.66557627198102409 ) ) ;
#66144 = CARTESIAN_POINT ( 'NONE',  ( -16.46253265017160317, 9.564922557960807481, 25.83224293864769194 ) ) ;
#66146 = CARTESIAN_POINT ( 'NONE',  ( -13.89961937509977652, 13.97604488694528158, 115.6239096053143669 ) ) ;
#66147 = CARTESIAN_POINT ( 'NONE',  ( -8.224510206698948167, 14.34966873604960824, 70.41557627198102409 ) ) ;
#66148 = CARTESIAN_POINT ( 'NONE',  ( 24.90102501248377109, -31.06609936492516866, -21.12314233236756778 ) ) ;
#66149 = CARTESIAN_POINT ( 'NONE',  ( -13.89961937509977652, 13.97604488694528158, 50.62390960531435979 ) ) ;
#66150 = CARTESIAN_POINT ( 'NONE',  ( -11.40812507854755609, 35.11059874428196537, -7.024999997268813523 ) ) ;
#66151 = CARTESIAN_POINT ( 'NONE',  ( 5.049401038297881783, 19.05341960407617563, 87.29275706135234714 ) ) ;
#66152 = CARTESIAN_POINT ( 'NONE',  ( 21.53943276465977519, 0.05219959533937863772, 21.25109039468567218 ) ) ;
#66153 = CARTESIAN_POINT ( 'NONE',  ( -9.564922557960796823, -16.46253265017161027, 67.08224293864769550 ) ) ;
#66154 = CARTESIAN_POINT ( 'NONE',  ( -19.02544592524334988, -5.153800228976617603, 58.95942372801900433 ) ) ;
#66155 = CARTESIAN_POINT ( 'NONE',  ( -5.049401038298153566, 19.05341960407611168, 40.20724293864768839 ) ) ;
#66156 = CARTESIAN_POINT ( 'NONE',  ( -12.06949235617756955, 12.14591786802309770, 65.62390960531436690 ) ) ;
#66157 = CARTESIAN_POINT ( 'NONE',  ( 16.52544592524342804, -4.483927247898539470, 48.54057627198103120 ) ) ;
#66158 = CARTESIAN_POINT ( 'NONE',  ( -9.474510206698964154, 16.51473224551069663, 80.41557627198103830 ) ) ;
#66159 = AXIS2_PLACEMENT_3D ( 'NONE', #187947, #15101, #61585 ) ;
#66160 = CARTESIAN_POINT ( 'NONE',  ( 21.53943276465977519, -0.05219959533907433946, 83.74890960531435269 ) ) ;
#66161 = CARTESIAN_POINT ( 'NONE',  ( -5.153800228976328057, -19.02544592524343514, 77.29057627198099567 ) ) ;
#66162 = CARTESIAN_POINT ( 'NONE',  ( 21.53943276465977519, -0.05219959533907433946, 73.74890960531433848 ) ) ;
#66163 = CARTESIAN_POINT ( 'NONE',  ( 10.72451020669871369, 18.67979575497193778, 112.0844237280190185 ) ) ;
#66166 = CARTESIAN_POINT ( 'NONE',  ( 16.55341960407611168, 4.379528057220329451, 93.95724293864770971 ) ) ;
#66165 = CARTESIAN_POINT ( 'NONE',  ( -4.379528057220086978, -16.55341960407618274, 109.7927570613523613 ) ) ;
#66164 = CARTESIAN_POINT ( 'NONE',  ( -5.153800228976328057, -19.02544592524343514, 22.29057627198102765 ) ) ;
#66167 = CARTESIAN_POINT ( 'NONE',  ( -13.97604488694547697, 13.89961937509957934, 103.1260903946856473 ) ) ;
#66168 = VERTEX_POINT ( 'NONE', #51539 ) ;
#66169 = CARTESIAN_POINT ( 'NONE',  ( -18.62759615963270932, 10.81492255796079327, 115.8322429386477097 ) ) ;
#66170 = CARTESIAN_POINT ( 'NONE',  ( 0.05219959533936267826, -19.03943276465977164, 55.00109039468566863 ) ) ;
#66171 = CARTESIAN_POINT ( 'NONE',  ( -16.53943276465976808, 0.05219959533911058130, 21.24890960531436690 ) ) ;
#66172 = CARTESIAN_POINT ( 'NONE',  ( -5.719274019375978568, 21.55341960407610458, 70.20724293864769550 ) ) ;
#66173 = CARTESIAN_POINT ( 'NONE',  ( -5.153800228976328057, -19.02544592524343514, 102.2905762719810383 ) ) ;
#66174 = CARTESIAN_POINT ( 'NONE',  ( 16.52544592524342804, -4.483927247898539470, 58.54057627198103120 ) ) ;
#66175 = DIRECTION ( 'NONE',  ( 1.000000000000000000, 0.000000000000000000, 0.000000000000000000 ) ) ;
#66176 = CARTESIAN_POINT ( 'NONE',  ( 5.153800228976335163, 19.02544592524342804, 39.79057627198100988 ) ) ;
#66177 = CARTESIAN_POINT ( 'NONE',  ( 15.80617190586769283, -15.72974639402175789, 110.6260903946857042 ) ) ;
#66178 = CARTESIAN_POINT ( 'NONE',  ( 12.14591786802327356, -12.06949235617739191, 85.62609039468568994 ) ) ;
#66179 = CARTESIAN_POINT ( 'NONE',  ( -21.52544592524334988, -5.823673210054445271, 43.95942372801902565 ) ) ;
#66180 = CARTESIAN_POINT ( 'NONE',  ( -16.55341960407617563, 4.379528057220093196, 38.54275706135234714 ) ) ;
#66181 = CARTESIAN_POINT ( 'NONE',  ( 21.53943276465977519, -0.05219959533907433946, 28.74890960531435624 ) ) ;
#66182 = CARTESIAN_POINT ( 'NONE',  ( 19.03943276465977164, -0.05219959533909143690, 53.74890960531436690 ) ) ;
#66183 = CARTESIAN_POINT ( 'NONE',  ( 16.51473224551069308, 9.474510206698969483, 64.16557627198102409 ) ) ;
#66184 =( GEOMETRIC_REPRESENTATION_CONTEXT ( 3 ) GLOBAL_UNCERTAINTY_ASSIGNED_CONTEXT ( ( #98449 ) ) GLOBAL_UNIT_ASSIGNED_CONTEXT ( ( #130067, #114927, #100746 ) ) REPRESENTATION_CONTEXT ( 'NONE', 'WORKASPACE' ) );
#66185 = CARTESIAN_POINT ( 'NONE',  ( 16.53943276465976808, 0.05219959533934440121, 56.25109039468568284 ) ) ;
#66186 = CARTESIAN_POINT ( 'NONE',  ( 8.224510206698953496, -14.34966873604960469, 102.9155762719810383 ) ) ;
#66187 = CARTESIAN_POINT ( 'NONE',  ( -0.05219959533910754901, -16.53943276465976808, 27.49890960531435269 ) ) ;
#66188 = CARTESIAN_POINT ( 'NONE',  ( -30.00000000000000000, -1.163414459189985801E-14, 95.00000000000000000 ) ) ;
#66191 = CARTESIAN_POINT ( 'NONE',  ( 19.05341960407611168, 5.049401038298154454, 83.95724293864766707 ) ) ;
#66190 = CARTESIAN_POINT ( 'NONE',  ( -19.02544592524342804, 5.153800228976336051, 91.04057627198100988 ) ) ;
#66189 = CARTESIAN_POINT ( 'NONE',  ( 15.72974639402176855, 15.80617190586768217, 51.87609039468568284 ) ) ;
#66192 = CARTESIAN_POINT ( 'NONE',  ( 9.564922557960805705, 16.46253265017160317, 99.58224293864770971 ) ) ;
#66193 = CARTESIAN_POINT ( 'NONE',  ( -12.14591786802309592, -12.06949235617757132, 41.87390960531435979 ) ) ;
#66194 = CARTESIAN_POINT ( 'NONE',  ( 4.483927247898790824, -16.52544592524335698, 110.2094237280190185 ) ) ;
#66195 = CARTESIAN_POINT ( 'NONE',  ( 14.29746914071049879, -8.314922557960816363, 43.33224293864769550 ) ) ;
#66196 = AXIS2_PLACEMENT_3D ( 'NONE', #67026, #142864, #144857 ) ;
#66197 = CARTESIAN_POINT ( 'NONE',  ( 19.03943276465977164, 0.05219959533936151252, 41.25109039468566152 ) ) ;
#66198 = CARTESIAN_POINT ( 'NONE',  ( -16.46253265017160317, 9.564922557960807481, 80.83224293864769550 ) ) ;
#66199 = CARTESIAN_POINT ( 'NONE',  ( 16.46253265017146816, 9.564922557961045513, 56.66775706135233293 ) ) ;
#66200 = CARTESIAN_POINT ( 'NONE',  ( -11.40812507854755609, 35.11059874428196537, -9.524999997268816188 ) ) ;
#66201 = DIRECTION ( 'NONE',  ( 0.000000000000000000, -0.8164965809277252573, 0.5773502691896267303 ) ) ;
#66202 = CIRCLE ( 'NONE', #192226, 9.100000000000001421 ) ;
#66204 = CARTESIAN_POINT ( 'NONE',  ( 4.483927247898790824, -16.52544592524335698, 75.20942372801901854 ) ) ;
#66203 = CARTESIAN_POINT ( 'NONE',  ( -9.474510206698720793, -16.51473224551083518, 89.58442372801900433 ) ) ;
#66205 = CARTESIAN_POINT ( 'NONE',  ( 0.05219959533936267826, -19.03943276465977164, 20.00109039468567218 ) ) ;
#66206 = CARTESIAN_POINT ( 'NONE',  ( -17.50000000000000355, -5.500000000000022204, 66.28230962303567253 ) ) ;
#66207 =( BOUNDED_CURVE ( )  B_SPLINE_CURVE ( 2, ( #89005, #41524, #75810, #12194, #152653, #181043, #150696, #27359, #183014, #14143, #73859 ),
 .UNSPECIFIED., .F., .T. ) 
 B_SPLINE_CURVE_WITH_KNOTS ( ( 3, 2, 2, 2, 2, 3 ),
 ( 0.6000000000000033085, 0.6200000000000033262, 0.6400000000000033440, 0.6600000000000034728, 0.6800000000000034905, 0.7000000000000033973 ),
 .UNSPECIFIED. ) 
 CURVE ( )  GEOMETRIC_REPRESENTATION_ITEM ( )  RATIONAL_B_SPLINE_CURVE ( ( 0.9999999999999918954, 0.9510565162951616358, 1.000000000000000000, 0.9510565162951535312, 1.000000000000000000, 0.9510565162951535312, 1.000000000000000000, 0.9510565162951535312, 1.000000000000000000, 0.9510565162951450935, 1.000000000000008438 ) ) 
 REPRESENTATION_ITEM ( '' )  );
#66208 = CARTESIAN_POINT ( 'NONE',  ( -16.51473224551069308, -9.474510206698971260, 101.6655762719810241 ) ) ;
#66209 = CARTESIAN_POINT ( 'NONE',  ( -15.80617190586768217, 15.72974639402176855, 28.12609039468568284 ) ) ;
#66210 = CARTESIAN_POINT ( 'NONE',  ( -19.05341960407617563, 5.049401038297882671, 88.54275706135230450 ) ) ;
#66212 = CARTESIAN_POINT ( 'NONE',  ( -5.049401038298153566, 19.05341960407611168, 45.20724293864769550 ) ) ;
#66211 = CARTESIAN_POINT ( 'NONE',  ( 16.62475595723699939, 7.163666690055252140, 86.97286648189536606 ) ) ;
#66213 = CARTESIAN_POINT ( 'NONE',  ( -19.05341960407611168, -5.049401038298163336, 86.45724293864769550 ) ) ;
#66215 = CARTESIAN_POINT ( 'NONE',  ( 19.03943276465977164, -0.05219959533909143690, 53.74890960531436690 ) ) ;
#66214 = CARTESIAN_POINT ( 'NONE',  ( 16.53943276465976808, -0.05219959533910856209, 43.74890960531435979 ) ) ;
#66216 = CARTESIAN_POINT ( 'NONE',  ( 5.049401038297881783, 19.05341960407617563, 62.29275706135234003 ) ) ;
#66217 = CARTESIAN_POINT ( 'NONE',  ( -16.46253265017146816, -9.564922557961047289, 24.16775706135233648 ) ) ;
#66218 = CARTESIAN_POINT ( 'NONE',  ( -9.474510206698964154, 16.51473224551069663, 60.41557627198102409 ) ) ;
#66219 = CARTESIAN_POINT ( 'NONE',  ( -10.81492255796078084, -18.62759615963271287, 67.08224293864770971 ) ) ;
#66221 = CARTESIAN_POINT ( 'NONE',  ( -16.51473224551082808, 9.474510206698731452, 23.33442372801900078 ) ) ;
#66220 = CARTESIAN_POINT ( 'NONE',  ( -16.55341960407611168, -4.379528057220339221, 66.45724293864768129 ) ) ;
#66222 = CARTESIAN_POINT ( 'NONE',  ( -17.60691670004650788, -5.500000000000066613, 54.13333313366441502 ) ) ;
#66223 = CARTESIAN_POINT ( 'NONE',  ( -13.89961937509977652, 13.97604488694528158, 115.6239096053143669 ) ) ;
#66224 = CARTESIAN_POINT ( 'NONE',  ( -19.05341960407611168, -5.049401038298163336, 51.45724293864770260 ) ) ;
#66225 = CARTESIAN_POINT ( 'NONE',  ( -13.97604488694527625, -13.89961937509977652, 36.87390960531436690 ) ) ;
#66226 = CARTESIAN_POINT ( 'NONE',  ( -12.06949235617756955, 12.14591786802309770, 100.6239096053143811 ) ) ;
#66227 = AXIS2_PLACEMENT_3D ( 'NONE', #105942, #43287, #89784 ) ;
#66228 = CARTESIAN_POINT ( 'NONE',  ( -5.719274019375978568, 21.55341960407610458, 110.2072429386477239 ) ) ;
#66229 = CARTESIAN_POINT ( 'NONE',  ( 25.57682740168941748, -5.495034664247685718, 164.9437814717016408 ) ) ;
#66230 = CARTESIAN_POINT ( 'NONE',  ( -18.67979575497193778, 10.72451020669871902, 28.33442372801902209 ) ) ;
#66231 = CARTESIAN_POINT ( 'NONE',  ( -5.049401038298153566, 19.05341960407611168, 100.2072429386476955 ) ) ;
#66232 = CARTESIAN_POINT ( 'NONE',  ( 16.46253265017160672, -9.564922557960803928, 23.33224293864769194 ) ) ;
#66233 = CARTESIAN_POINT ( 'NONE',  ( -21.55341960407619339, 5.719274019375674811, 73.54275706135234714 ) ) ;
#66234 = CARTESIAN_POINT ( 'NONE',  ( 15.72974639402199770, -15.80617190586745480, 88.12390960531436690 ) ) ;
#66235 = CARTESIAN_POINT ( 'NONE',  ( 5.153800228976615827, -19.02544592524334988, 40.20942372801898301 ) ) ;
#66236 = CARTESIAN_POINT ( 'NONE',  ( -16.46253265017160317, 9.564922557960807481, 25.83224293864769194 ) ) ;
#66237 = FACE_OUTER_BOUND ( 'NONE', #177929, .T. ) ;
#66238 = CARTESIAN_POINT ( 'NONE',  ( 29.02171288343477329, -0.6023940538448767645, -52.52077797743539378 ) ) ;
#66239 = CARTESIAN_POINT ( 'NONE',  ( -8.314922557961024197, 14.29746914071037800, 47.91775706135234714 ) ) ;
#66240 = CARTESIAN_POINT ( 'NONE',  ( -0.05219959533910754901, -16.53943276465976808, 102.4989096053143811 ) ) ;
#66241 = CARTESIAN_POINT ( 'NONE',  ( 34.52594549653174028, -0.3594300054053903293, 89.49999999999896261 ) ) ;
#66242 = CARTESIAN_POINT ( 'NONE',  ( -13.89961937509977652, 13.97604488694528158, 70.62390960531432427 ) ) ;
#66243 = CARTESIAN_POINT ( 'NONE',  ( 4.379528057220339221, -16.55341960407611168, 97.70724293864772392 ) ) ;
#66244 = CARTESIAN_POINT ( 'NONE',  ( -21.53943276465977519, 0.05219959533907696930, 51.24890960531436690 ) ) ;
#66245 = CARTESIAN_POINT ( 'NONE',  ( 0.05219959533910956823, 16.53943276465976808, 64.99890960531435269 ) ) ;
#66246 = CARTESIAN_POINT ( 'NONE',  ( -16.53943276465976808, -0.05219959533934237506, 28.75109039468567929 ) ) ;
#66247 = CARTESIAN_POINT ( 'NONE',  ( -10.81492255796105439, 18.62759615963255655, 82.91775706135234714 ) ) ;
#66248 = CARTESIAN_POINT ( 'NONE',  ( -4.500000000000000888, -120.9970989573719038, 14.58956564881029472 ) ) ;
#66249 = CARTESIAN_POINT ( 'NONE',  ( 8.224510206698742110, 14.34966873604972548, 102.0844237280190185 ) ) ;
#66250 = CARTESIAN_POINT ( 'NONE',  ( -4.379528057220328563, 16.55341960407611168, 40.20724293864769550 ) ) ;
#66251 = CARTESIAN_POINT ( 'NONE',  ( 13.89961937509977652, -13.97604488694527269, 38.12390960531436690 ) ) ;
#66252 = CARTESIAN_POINT ( 'NONE',  ( 5.049401038298161559, -19.05341960407611168, 82.70724293864770971 ) ) ;
#66253 = CARTESIAN_POINT ( 'NONE',  ( 15.72974639402199770, -15.80617190586745480, 113.1239096053143953 ) ) ;
#66254 = CARTESIAN_POINT ( 'NONE',  ( 18.67979575497194134, -10.72451020669871369, 55.83442372801901854 ) ) ;
#66255 = CARTESIAN_POINT ( 'NONE',  ( 16.52544592524335698, 4.483927247898782831, 36.45942372801901143 ) ) ;
#66257 = CARTESIAN_POINT ( 'NONE',  ( 21.55341960407619695, -5.719274019375665929, 91.04275706135236135 ) ) ;
#66256 = CARTESIAN_POINT ( 'NONE',  ( 16.53943276465976808, -0.05219959533910856209, 58.74890960531436690 ) ) ;
#66258 = CARTESIAN_POINT ( 'NONE',  ( 16.53943276465976808, 0.05219959533934440121, 96.25109039468568994 ) ) ;
#66259 = CARTESIAN_POINT ( 'NONE',  ( 17.48847506799968698, 5.747544572773807481, 26.67302562156720924 ) ) ;
#66260 = CARTESIAN_POINT ( 'NONE',  ( -19.49190055781010145, -5.500000000000057732, 65.56116087098779133 ) ) ;
#66261 = CARTESIAN_POINT ( 'NONE',  ( 12.06949235617757843, -12.14591786802309237, 33.12390960531435979 ) ) ;
#66262 = CARTESIAN_POINT ( 'NONE',  ( 8.314922557961029526, -14.29746914071037800, 70.41775706135236135 ) ) ;
#66263 = CARTESIAN_POINT ( 'NONE',  ( 19.02544592524343514, -5.153800228976328945, 83.54057627198100988 ) ) ;
#66264 = CARTESIAN_POINT ( 'NONE',  ( 0.05219959533909260263, 19.03943276465977164, 94.99890960531436690 ) ) ;
#66265 = CARTESIAN_POINT ( 'NONE',  ( -10.72451020669870658, -18.67979575497194134, 79.58442372801903275 ) ) ;
#66266 = EDGE_CURVE ( 'NONE', #81647, #194062, #8617, .T. ) ;
#66267 = CARTESIAN_POINT ( 'NONE',  ( -12.06949235617739369, -12.14591786802326823, 89.37609039468568994 ) ) ;
#66268 = CARTESIAN_POINT ( 'NONE',  ( -16.55341960407611168, -4.379528057220339221, 66.45724293864768129 ) ) ;
#66269 = CARTESIAN_POINT ( 'NONE',  ( 5.049401038298161559, -19.05341960407611168, 67.70724293864769550 ) ) ;
#66270 = ORIENTED_EDGE ( 'NONE', *, *, #90349, .T. ) ;
#66271 = CARTESIAN_POINT ( 'NONE',  ( -0.05219959533934338120, 16.53943276465976808, 22.50109039468567573 ) ) ;
#66272 = CARTESIAN_POINT ( 'NONE',  ( -19.02544592524342804, 5.153800228976336051, 31.04057627198102409 ) ) ;
#66273 = CARTESIAN_POINT ( 'NONE',  ( -5.049401038298153566, 19.05341960407611168, 75.20724293864769550 ) ) ;
#66275 = CARTESIAN_POINT ( 'NONE',  ( -36.91746825000001309, -11.99521256947794789, -8.524999997268812635 ) ) ;
#66274 = CARTESIAN_POINT ( 'NONE',  ( 12.14591786802327356, -12.06949235617739191, 20.62609039468568639 ) ) ;
#66276 = CARTESIAN_POINT ( 'NONE',  ( -5.153800228976607833, 19.02544592524334988, 27.70942372801899722 ) ) ;
#66277 = CARTESIAN_POINT ( 'NONE',  ( -14.29746914071037622, -8.314922557961029526, 79.16775706135234714 ) ) ;
#66278 = CARTESIAN_POINT ( 'NONE',  ( 13.89961937509957401, 13.97604488694547697, 101.8760903946856331 ) ) ;
#66279 = CARTESIAN_POINT ( 'NONE',  ( 0.05219959533909260263, 19.03943276465977164, 24.99890960531435269 ) ) ;
#66280 = CARTESIAN_POINT ( 'NONE',  ( 8.314922557961029526, -14.29746914071037800, 70.41775706135236135 ) ) ;
#66281 = CARTESIAN_POINT ( 'NONE',  ( 16.53943276465976808, 0.05219959533934440121, 56.25109039468568284 ) ) ;
#66282 = CARTESIAN_POINT ( 'NONE',  ( 19.02544592524343514, -5.153800228976328945, 23.54057627198102054 ) ) ;
#66283 = CARTESIAN_POINT ( 'NONE',  ( -5.049401038297874678, -19.05341960407617918, 74.79275706135231871 ) ) ;
#66284 = CARTESIAN_POINT ( 'NONE',  ( 0.05219959533936267826, -19.03943276465977164, 20.00109039468567218 ) ) ;
#66285 = CARTESIAN_POINT ( 'NONE',  ( -9.474510206698964154, 16.51473224551069663, 30.41557627198102054 ) ) ;
#66286 = CARTESIAN_POINT ( 'NONE',  ( 9.474510206698971260, -16.51473224551069308, 82.91557627198103830 ) ) ;
#66287 = CARTESIAN_POINT ( 'NONE',  ( -12.06949235617756955, 12.14591786802309770, 75.62390960531439532 ) ) ;
#66288 = CARTESIAN_POINT ( 'NONE',  ( 9.564922557961047289, -16.46253265017146816, 45.41775706135232582 ) ) ;
#66289 = CARTESIAN_POINT ( 'NONE',  ( -0.05219959533907301413, -21.53943276465977519, 42.49890960531435979 ) ) ;
#66290 = CARTESIAN_POINT ( 'NONE',  ( -18.67979575497193778, 10.72451020669871902, 113.3344237280190328 ) ) ;
#66291 = CARTESIAN_POINT ( 'NONE',  ( -19.05341960407611168, -5.049401038298163336, 96.45724293864769550 ) ) ;
#66292 = CARTESIAN_POINT ( 'NONE',  ( -15.80617190586768217, 15.72974639402176855, 103.1260903946856757 ) ) ;
#66293 = CARTESIAN_POINT ( 'NONE',  ( 10.72451020669898902, -18.67979575497178502, 57.91557627198103120 ) ) ;
#66294 = CARTESIAN_POINT ( 'NONE',  ( 16.46253265017160672, -9.564922557960803928, 98.33224293864769550 ) ) ;
#66295 = CARTESIAN_POINT ( 'NONE',  ( 5.049401038297881783, 19.05341960407617563, 92.29275706135234714 ) ) ;
#66296 = CARTESIAN_POINT ( 'NONE',  ( 9.474510206698971260, -16.51473224551069308, 107.9155762719810383 ) ) ;
#66297 = CARTESIAN_POINT ( 'NONE',  ( 9.474510206698729675, 16.51473224551082808, 97.08442372801900433 ) ) ;
#66298 = CARTESIAN_POINT ( 'NONE',  ( 0.05219959533910956823, 16.53943276465976808, 114.9989096053143669 ) ) ;
#66299 = CARTESIAN_POINT ( 'NONE',  ( 0.05219959533909260263, 19.03943276465977164, 84.99890960531436690 ) ) ;
#66300 = CARTESIAN_POINT ( 'NONE',  ( 5.823673210054125526, 21.52544592524343514, 64.79057627198103830 ) ) ;
#66301 = CARTESIAN_POINT ( 'NONE',  ( -8.224510206698735004, -14.34966873604973081, 39.58442372801901143 ) ) ;
#66302 = CARTESIAN_POINT ( 'NONE',  ( 0.05219959533937995610, -21.53943276465977519, 45.00109039468568284 ) ) ;
#66303 = CARTESIAN_POINT ( 'NONE',  ( -18.62759615963255300, -10.81492255796106328, 99.16775706135234714 ) ) ;
#66304 = CARTESIAN_POINT ( 'NONE',  ( -8.314922557961024197, 14.29746914071037800, 97.91775706135236135 ) ) ;
#66305 = CARTESIAN_POINT ( 'NONE',  ( 19.05341960407611168, 5.049401038298154454, 88.95724293864769550 ) ) ;
#66306 = CARTESIAN_POINT ( 'NONE',  ( -12.06949235617756955, 12.14591786802309770, 95.62390960531436690 ) ) ;
#66307 = CARTESIAN_POINT ( 'NONE',  ( 12.14591786802309770, 12.06949235617756955, 24.37390960531435979 ) ) ;
#66308 = CARTESIAN_POINT ( 'NONE',  ( 5.153800228976615827, -19.02544592524334988, 75.20942372801896170 ) ) ;
#66309 = CARTESIAN_POINT ( 'NONE',  ( -15.80617190586768217, 15.72974639402176855, 48.12609039468568284 ) ) ;
#66310 = CARTESIAN_POINT ( 'NONE',  ( 4.379528057220339221, -16.55341960407611168, 92.70724293864770971 ) ) ;
#66311 = CARTESIAN_POINT ( 'NONE',  ( 16.46253265017160672, -9.564922557960803928, 113.3322429386476955 ) ) ;
#66312 = CARTESIAN_POINT ( 'NONE',  ( -4.379528057220328563, 16.55341960407611168, 25.20724293864769550 ) ) ;
#66313 = CARTESIAN_POINT ( 'NONE',  ( -21.52544592524334988, -5.823673210054445271, 83.95942372801900433 ) ) ;
#66314 = CARTESIAN_POINT ( 'NONE',  ( 16.52544592524335698, 4.483927247898782831, 46.45942372801901854 ) ) ;
#66315 = CARTESIAN_POINT ( 'NONE',  ( 21.53943276465977519, 0.05219959533937863772, 41.25109039468568284 ) ) ;
#66316 = ORIENTED_EDGE ( 'NONE', *, *, #195850, .T. ) ;
#66317 = CARTESIAN_POINT ( 'NONE',  ( -15.80617190586768217, 15.72974639402176855, 28.12609039468568284 ) ) ;
#66318 = CARTESIAN_POINT ( 'NONE',  ( -16.55341960407611168, -4.379528057220339221, 96.45724293864770971 ) ) ;
#66319 = CARTESIAN_POINT ( 'NONE',  ( 20.22402473803820300, 1.857821124618833641, 37.49999999999998579 ) ) ;
#66320 = CARTESIAN_POINT ( 'NONE',  ( -12.14591786802309592, -12.06949235617757132, 66.87390960531436690 ) ) ;
#66321 = CARTESIAN_POINT ( 'NONE',  ( 9.474510206698971260, -16.51473224551069308, 52.91557627198102409 ) ) ;
#66322 = CARTESIAN_POINT ( 'NONE',  ( 4.483927247898790824, -16.52544592524335698, 105.2094237280190328 ) ) ;
#66323 = CARTESIAN_POINT ( 'NONE',  ( -19.03943276465977164, 0.05219959533909376836, 41.24890960531435269 ) ) ;
#66324 = CARTESIAN_POINT ( 'NONE',  ( 21.55341960407610458, 5.719274019375980345, 48.95724293864770971 ) ) ;
#66325 = CARTESIAN_POINT ( 'NONE',  ( -8.224510206698948167, 14.34966873604960824, 75.41557627198102409 ) ) ;
#66326 = VECTOR ( 'NONE', #181084, 1000.000000000000000 ) ;
#66327 = CARTESIAN_POINT ( 'NONE',  ( 21.55341960407610458, 5.719274019375980345, 98.95724293864770971 ) ) ;
#66328 = CARTESIAN_POINT ( 'NONE',  ( 13.97604488694527802, 13.89961937509977652, 94.37390960531436690 ) ) ;
#66330 = CARTESIAN_POINT ( 'NONE',  ( -9.564922557961040184, 16.46253265017147172, 87.91775706135233293 ) ) ;
#66329 = CARTESIAN_POINT ( 'NONE',  ( 19.03943276465977164, -0.05219959533909143690, 43.74890960531435979 ) ) ;
#66331 = CARTESIAN_POINT ( 'NONE',  ( 18.67979575497178502, 10.72451020669898547, 49.16557627198102409 ) ) ;
#66332 = CARTESIAN_POINT ( 'NONE',  ( -18.67979575497193778, 10.72451020669871902, 68.33442372801900433 ) ) ;
#66333 = CARTESIAN_POINT ( 'NONE',  ( 13.97604488694527802, 13.89961937509977652, 54.37390960531435979 ) ) ;
#66334 = CARTESIAN_POINT ( 'NONE',  ( -16.51473224551069308, -9.474510206698971260, 86.66557627198102409 ) ) ;
#66335 = ORIENTED_EDGE ( 'NONE', *, *, #17662, .F. ) ;
#66336 = CARTESIAN_POINT ( 'NONE',  ( -4.379528057220086978, -16.55341960407618274, 59.79275706135234714 ) ) ;
#66337 = CARTESIAN_POINT ( 'NONE',  ( 15.80617190586769283, -15.72974639402175789, 50.62609039468568994 ) ) ;
#66338 = CARTESIAN_POINT ( 'NONE',  ( 10.72451020669871369, 18.67979575497193778, 72.08442372801899012 ) ) ;
#66339 = CARTESIAN_POINT ( 'NONE',  ( -10.81492255796078084, -18.62759615963271287, 22.08224293864769194 ) ) ;
#66340 = CARTESIAN_POINT ( 'NONE',  ( -18.62759615963270932, 10.81492255796079327, 105.8322429386476955 ) ) ;
#66342 = CARTESIAN_POINT ( 'NONE',  ( 12.06949235617739724, 12.14591786802326823, 66.87609039468568994 ) ) ;
#66341 = CARTESIAN_POINT ( 'NONE',  ( -5.823673210054431948, 21.52544592524334988, 32.70942372801900433 ) ) ;
#66343 = CARTESIAN_POINT ( 'NONE',  ( 21.53943276465977519, -0.05219959533907433946, 63.74890960531435979 ) ) ;
#66344 = CARTESIAN_POINT ( 'NONE',  ( -9.564922557961040184, 16.46253265017147172, 37.91775706135233293 ) ) ;
#66346 = CARTESIAN_POINT ( 'NONE',  ( 14.29746914071037800, 8.314922557961029526, 101.6677570613523613 ) ) ;
#66345 = CARTESIAN_POINT ( 'NONE',  ( -19.05341960407611168, -5.049401038298163336, 66.45724293864769550 ) ) ;
#66347 = CARTESIAN_POINT ( 'NONE',  ( -22.00000000000000000, -1.163414459189985801E-14, 97.50000000000000000 ) ) ;
#66348 = CARTESIAN_POINT ( 'NONE',  ( -5.049401038298153566, 19.05341960407611168, 100.2072429386476955 ) ) ;
#66349 = CARTESIAN_POINT ( 'NONE',  ( 20.24680444626657305, 22.34286686445877734, -48.12863666802713425 ) ) ;
#66350 = CARTESIAN_POINT ( 'NONE',  ( 9.474510206698729675, 16.51473224551082808, 87.08442372801900433 ) ) ;
#66351 = CIRCLE ( 'NONE', #4999, 13.70000000000001528 ) ;
#66352 = CARTESIAN_POINT ( 'NONE',  ( 0.05219959533907565091, 21.53943276465977519, 64.99890960531435269 ) ) ;
#66353 = CARTESIAN_POINT ( 'NONE',  ( -0.05219959533910754901, -16.53943276465976808, 32.49890960531435979 ) ) ;
#66354 = CARTESIAN_POINT ( 'NONE',  ( 13.97604488694548053, -13.89961937509957401, 95.62609039468563310 ) ) ;
#66355 = FACE_OUTER_BOUND ( 'NONE', #37582, .T. ) ;
#66356 = CARTESIAN_POINT ( 'NONE',  ( -13.97604488694547697, 13.89961937509957934, 93.12609039468566152 ) ) ;
#66358 = CARTESIAN_POINT ( 'NONE',  ( -19.03943276465977164, -0.05219959533935918106, 63.75109039468566863 ) ) ;
#66357 = CARTESIAN_POINT ( 'NONE',  ( -15.80617190586745835, -15.72974639402198527, 81.87390960531435269 ) ) ;
#66359 = LINE ( 'NONE', #163374, #1533 ) ;
#66360 = CARTESIAN_POINT ( 'NONE',  ( -9.474510206698964154, 16.51473224551069663, 70.41557627198102409 ) ) ;
#66361 = CARTESIAN_POINT ( 'NONE',  ( -16.55341960407611168, -4.379528057220339221, 61.45724293864770260 ) ) ;
#66362 = EDGE_CURVE ( 'NONE', #166806, #45388, #52527, .T. ) ;
#66363 = CARTESIAN_POINT ( 'NONE',  ( -13.89961937509977652, 13.97604488694528158, 50.62390960531435979 ) ) ;
#66364 = CARTESIAN_POINT ( 'NONE',  ( 12.06949235617757843, -12.14591786802309237, 48.12390960531436690 ) ) ;
#66365 = CARTESIAN_POINT ( 'NONE',  ( 19.05341960407611168, 5.049401038298154454, 23.95724293864769194 ) ) ;
#66366 = CARTESIAN_POINT ( 'NONE',  ( 1.469609370623580213, 22.44847579118772529, -55.62606073046919875 ) ) ;
#66367 = CARTESIAN_POINT ( 'NONE',  ( 12.14591786802309770, 12.06949235617756955, 34.37390960531435979 ) ) ;
#66368 = CARTESIAN_POINT ( 'NONE',  ( -19.05341960407611168, -5.049401038298163336, 76.45724293864769550 ) ) ;
#66369 = DIRECTION ( 'NONE',  ( 1.000000000000000000, 0.000000000000000000, 0.000000000000000000 ) ) ;
#66370 = CARTESIAN_POINT ( 'NONE',  ( 0.05219959533936267826, -19.03943276465977164, 35.00109039468566863 ) ) ;
#66371 = CARTESIAN_POINT ( 'NONE',  ( -0.05219959533934338120, 16.53943276465976808, 47.50109039468568994 ) ) ;
#66372 = CARTESIAN_POINT ( 'NONE',  ( 0.05219959533907565091, 21.53943276465977519, 49.99890960531437401 ) ) ;
#66373 = CARTESIAN_POINT ( 'NONE',  ( 0.05219959533937995610, -21.53943276465977519, 110.0010903946856757 ) ) ;
#66374 = CARTESIAN_POINT ( 'NONE',  ( -13.97604488694527625, -13.89961937509977652, 76.87390960531433848 ) ) ;
#66375 = CARTESIAN_POINT ( 'NONE',  ( 16.46253265017160672, -9.564922557960803928, 113.3322429386476955 ) ) ;
#66376 = CARTESIAN_POINT ( 'NONE',  ( -16.51473224551069308, -9.474510206698971260, 106.6655762719810383 ) ) ;
#66377 = CARTESIAN_POINT ( 'NONE',  ( -10.72451020669870658, -18.67979575497194134, 39.58442372801901143 ) ) ;
#66378 = CARTESIAN_POINT ( 'NONE',  ( -4.483927247898539470, -16.52544592524342804, 92.29057627198103830 ) ) ;
#66381 = DIRECTION ( 'NONE',  ( -0.9930308165857338887, 0.1178549842436489581, 0.000000000000000000 ) ) ;
#66380 = CARTESIAN_POINT ( 'NONE',  ( 13.89961937509977652, -13.97604488694527269, 88.12390960531438111 ) ) ;
#66379 = CARTESIAN_POINT ( 'NONE',  ( -5.823673210054116645, -21.52544592524344225, 92.29057627198103830 ) ) ;
#66382 = CARTESIAN_POINT ( 'NONE',  ( 21.55341960407619695, -5.719274019375665929, 21.04275706135234714 ) ) ;
#66383 = EDGE_LOOP ( 'NONE', ( #174642, #97767, #69447, #117609 ) ) ;
#66384 = CARTESIAN_POINT ( 'NONE',  ( -16.46253265017160317, 9.564922557960807481, 80.83224293864769550 ) ) ;
#66385 = CARTESIAN_POINT ( 'NONE',  ( 17.50000000001358558, -5.500000000000039968, 48.29690382535059001 ) ) ;
#66387 = CARTESIAN_POINT ( 'NONE',  ( 19.05341960407611168, 5.049401038298154454, 38.95724293864767418 ) ) ;
#66386 = CARTESIAN_POINT ( 'NONE',  ( -12.06949235617756955, 12.14591786802309770, 115.6239096053143669 ) ) ;
#66388 = CARTESIAN_POINT ( 'NONE',  ( 19.02544592524334988, 5.153800228976608722, 106.4594237280190185 ) ) ;
#66389 = CARTESIAN_POINT ( 'NONE',  ( -36.91746825000001309, -11.99521256947794789, -9.024999997268812635 ) ) ;
#66390 = CARTESIAN_POINT ( 'NONE',  ( 12.06949235617757843, -12.14591786802309237, 113.1239096053143953 ) ) ;
#66391 = CARTESIAN_POINT ( 'NONE',  ( 21.52544592524334988, 5.823673210054432836, 81.45942372801900433 ) ) ;
#66393 = CARTESIAN_POINT ( 'NONE',  ( -10.81492255796105439, 18.62759615963255655, 32.91775706135234714 ) ) ;
#66392 = CARTESIAN_POINT ( 'NONE',  ( -13.97604488694527625, -13.89961937509977652, 61.87390960531435979 ) ) ;
#66394 = CARTESIAN_POINT ( 'NONE',  ( -15.80617190586745835, -15.72974639402198527, 111.8739096053143669 ) ) ;
#66395 = CARTESIAN_POINT ( 'NONE',  ( 17.14385361876520264, 23.59649016807275856, 140.6750000027311387 ) ) ;
#66396 = CARTESIAN_POINT ( 'NONE',  ( -13.89961937509977652, 13.97604488694528158, 90.62390960531432427 ) ) ;
#66397 = CARTESIAN_POINT ( 'NONE',  ( 27.95742675678724609, 7.330130391636824783, 160.9071069586348415 ) ) ;
#66399 = CARTESIAN_POINT ( 'NONE',  ( 18.62759615963271287, -10.81492255796078972, 43.33224293864769550 ) ) ;
#66398 = CARTESIAN_POINT ( 'NONE',  ( -16.53943276465976808, -0.05219959533934237506, 28.75109039468567929 ) ) ;
#66400 = CARTESIAN_POINT ( 'NONE',  ( -10.72451020669870658, -18.67979575497194134, 59.58442372801901854 ) ) ;
#66401 = CARTESIAN_POINT ( 'NONE',  ( 19.03943276465977164, -0.05219959533909143690, 108.7489096053143527 ) ) ;
#66402 = CARTESIAN_POINT ( 'NONE',  ( -16.51473224551082808, 9.474510206698731452, 98.33442372801900433 ) ) ;
#66403 = CARTESIAN_POINT ( 'NONE',  ( -0.05219959533909027116, -19.03943276465977164, 62.49890960531435979 ) ) ;
#66404 = CARTESIAN_POINT ( 'NONE',  ( 5.049401038298161559, -19.05341960407611168, 82.70724293864770971 ) ) ;
#66405 = CARTESIAN_POINT ( 'NONE',  ( 16.52544592524342804, -4.483927247898539470, 93.54057627198103830 ) ) ;
#66406 = CARTESIAN_POINT ( 'NONE',  ( 12.06949235617757843, -12.14591786802309237, 103.1239096053143811 ) ) ;
#66407 = CARTESIAN_POINT ( 'NONE',  ( -21.55341960407610458, -5.719274019375992779, 21.45724293864769550 ) ) ;
#66409 = CARTESIAN_POINT ( 'NONE',  ( -5.049401038298153566, 19.05341960407611168, 35.20724293864768839 ) ) ;
#66408 = CARTESIAN_POINT ( 'NONE',  ( 4.483927247898545687, 16.52544592524342804, 59.79057627198103120 ) ) ;
#66410 = CARTESIAN_POINT ( 'NONE',  ( -10.81492255796105439, 18.62759615963255655, 67.91775706135234714 ) ) ;
#66411 = CARTESIAN_POINT ( 'NONE',  ( -5.049401038297874678, -19.05341960407617918, 89.79275706135230450 ) ) ;
#66412 = CARTESIAN_POINT ( 'NONE',  ( -0.05219959533910754901, -16.53943276465976808, 67.49890960531436690 ) ) ;
#66413 = CARTESIAN_POINT ( 'NONE',  ( -21.55341960407610458, -5.719274019375992779, 106.4572429386477097 ) ) ;
#66414 = CARTESIAN_POINT ( 'NONE',  ( -21.53943276465977519, 0.05219959533907696930, 46.24890960531435979 ) ) ;
#66416 = CARTESIAN_POINT ( 'NONE',  ( -19.05341960407611168, -5.049401038298163336, 111.4572429386476671 ) ) ;
#66415 = TOROIDAL_SURFACE ( 'NONE', #11764, 23.10356920737165254, 3.000000000000000000 ) ;
#66417 = CARTESIAN_POINT ( 'NONE',  ( 22.44159573604009594, -16.30477369853687364, 147.6750000027311671 ) ) ;
#66418 = CARTESIAN_POINT ( 'NONE',  ( -0.05219959533909027116, -19.03943276465977164, 72.49890960531435269 ) ) ;
#66419 = CARTESIAN_POINT ( 'NONE',  ( 16.55341960407611168, 4.379528057220329451, 33.95724293864769550 ) ) ;
#66420 = CARTESIAN_POINT ( 'NONE',  ( -4.483927247898782831, 16.52544592524335698, 107.7094237280190328 ) ) ;
#66421 = CARTESIAN_POINT ( 'NONE',  ( -16.55341960407617563, 4.379528057220093196, 88.54275706135236135 ) ) ;
#66422 = CARTESIAN_POINT ( 'NONE',  ( -0.05219959533936034679, 19.03943276465977164, 42.50109039468566152 ) ) ;
#66423 = CARTESIAN_POINT ( 'NONE',  ( -18.22780087662122028, -5.500000000000014211, 101.4845989467389273 ) ) ;
#66424 = CARTESIAN_POINT ( 'NONE',  ( -5.049401038298153566, 19.05341960407611168, 95.20724293864770971 ) ) ;
#66425 = CARTESIAN_POINT ( 'NONE',  ( 16.51473224551069308, 9.474510206698969483, 44.16557627198103120 ) ) ;
#66426 = CARTESIAN_POINT ( 'NONE',  ( 4.483927247898545687, 16.52544592524342804, 54.79057627198104541 ) ) ;
#66428 = CARTESIAN_POINT ( 'NONE',  ( -16.46253265017160317, 9.564922557960807481, 115.8322429386477097 ) ) ;
#66427 = CARTESIAN_POINT ( 'NONE',  ( -13.89961937509977652, 13.97604488694528158, 25.62390960531434558 ) ) ;
#66429 = CARTESIAN_POINT ( 'NONE',  ( -15.72974639402197994, 15.80617190586746368, 55.62390960531436690 ) ) ;
#66430 = CARTESIAN_POINT ( 'NONE',  ( -4.379528057220328563, 16.55341960407611168, 90.20724293864770971 ) ) ;
#66431 = CARTESIAN_POINT ( 'NONE',  ( -12.14591786802326823, 12.06949235617739902, 33.12609039468569705 ) ) ;
#66432 = CARTESIAN_POINT ( 'NONE',  ( 4.483927247898545687, 16.52544592524342804, 79.79057627198102409 ) ) ;
#66433 = CARTESIAN_POINT ( 'NONE',  ( -19.48894818550241581, 5.500000000000113687, 65.10307310435243267 ) ) ;
#66434 = CARTESIAN_POINT ( 'NONE',  ( -19.02544592524334988, -5.153800228976617603, 73.95942372801900433 ) ) ;
#66435 = CARTESIAN_POINT ( 'NONE',  ( -19.05341960407611168, -5.049401038298163336, 111.4572429386476671 ) ) ;
#66436 = CARTESIAN_POINT ( 'NONE',  ( -22.81625015709510507, 31.40387420917330275, -1.424999997268813212 ) ) ;
#66437 = CARTESIAN_POINT ( 'NONE',  ( -21.26972126690566611, 19.99598863510428970, -52.34638024103106346 ) ) ;
#66439 = CARTESIAN_POINT ( 'NONE',  ( -16.53943276465976808, -0.05219959533934237506, 113.7510903946856757 ) ) ;
#66438 = CARTESIAN_POINT ( 'NONE',  ( -4.379528057220086978, -16.55341960407618274, 24.79275706135235779 ) ) ;
#66440 = CARTESIAN_POINT ( 'NONE',  ( 19.02544592524334988, 5.153800228976608722, 71.45942372801900433 ) ) ;
#66441 = CARTESIAN_POINT ( 'NONE',  ( 15.80617190586746368, 15.72974639402197994, 49.37390960531436690 ) ) ;
#66442 = CARTESIAN_POINT ( 'NONE',  ( 18.67979575497194134, -10.72451020669871369, 70.83442372801901854 ) ) ;
#66443 = CARTESIAN_POINT ( 'NONE',  ( -28.82186960331504721, -9.364793116373462567, 146.3500000054623911 ) ) ;
#66444 = CARTESIAN_POINT ( 'NONE',  ( 16.52544592524335698, 4.483927247898782831, 36.45942372801901143 ) ) ;
#66446 = CARTESIAN_POINT ( 'NONE',  ( 5.153800228976335163, 19.02544592524342804, 84.79057627198099567 ) ) ;
#66445 = CARTESIAN_POINT ( 'NONE',  ( -9.474510206698964154, 16.51473224551069663, 30.41557627198102054 ) ) ;
#66447 = CARTESIAN_POINT ( 'NONE',  ( -13.97604488694527625, -13.89961937509977652, 21.87390960531435979 ) ) ;
#66448 = CARTESIAN_POINT ( 'NONE',  ( -14.34966873604960291, -8.224510206698953496, 96.66557627198102409 ) ) ;
#66449 = ITEM_DEFINED_TRANSFORMATION ( 'NONE', 'NONE', #137228,  #82054 ) ;
#66450 = CARTESIAN_POINT ( 'NONE',  ( 5.049401038298161559, -19.05341960407611168, 97.70724293864766707 ) ) ;
#66451 = ORIENTED_EDGE ( 'NONE', *, *, #11076, .F. ) ;
#66452 = CARTESIAN_POINT ( 'NONE',  ( 9.564922557961047289, -16.46253265017146816, 110.4177570613523471 ) ) ;
#66453 = CARTESIAN_POINT ( 'NONE',  ( 0.05219959533907565091, 21.53943276465977519, 74.99890960531435269 ) ) ;
#66454 = CARTESIAN_POINT ( 'NONE',  ( 16.46253265017160672, -9.564922557960803928, 48.33224293864769550 ) ) ;
#66456 = CARTESIAN_POINT ( 'NONE',  ( -10.81492255796078084, -18.62759615963271287, 112.0822429386477097 ) ) ;
#66455 = CARTESIAN_POINT ( 'NONE',  ( 19.05341960407617918, -5.049401038297876454, 71.04275706135234714 ) ) ;
#66457 = CARTESIAN_POINT ( 'NONE',  ( 13.89961937509977652, -13.97604488694527269, 73.12390960531436690 ) ) ;
#66458 = CARTESIAN_POINT ( 'NONE',  ( -19.05341960407611168, -5.049401038298163336, 106.4572429386476955 ) ) ;
#66459 = VERTEX_POINT ( 'NONE', #195061 ) ;
#66460 = CARTESIAN_POINT ( 'NONE',  ( 16.53943276465976808, 0.05219959533934440121, 36.25109039468567573 ) ) ;
#66461 =( BOUNDED_CURVE ( )  B_SPLINE_CURVE ( 2, ( #11561, #61000, #122672, #134898, #28712, #73227, #184361, #169171, #44856, #61984, #185348, #30675, #90348 ),
 .UNSPECIFIED., .F., .F. ) 
 B_SPLINE_CURVE_WITH_KNOTS ( ( 3, 2, 2, 2, 2, 2, 3 ),
 ( 0.4761146469533609205, 0.4780701754385964786, 0.4824561403508771940, 0.4868421052631579093, 0.4912280701754385692, 0.4956140350877192846, 0.4975238837508647594 ),
 .UNSPECIFIED. ) 
 CURVE ( )  GEOMETRIC_REPRESENTATION_ITEM ( )  RATIONAL_B_SPLINE_CURVE ( ( 0.9831626618144004848, 0.9848076720550091867, 1.000000000000000000, 0.9659258262890683122, 1.000000000000000000, 0.9659258262890683122, 1.000000000000000000, 0.9659258262890683122, 1.000000000000000000, 0.9659258262890683122, 1.000000000000000000, 0.9851625545550091179, 0.9832469066685282089 ) ) 
 REPRESENTATION_ITEM ( '' )  );
#66462 = CARTESIAN_POINT ( 'NONE',  ( 21.55341960407610458, 5.719274019375980345, 98.95724293864770971 ) ) ;
#66465 = CARTESIAN_POINT ( 'NONE',  ( 5.049401038297881783, 19.05341960407617563, 62.29275706135234003 ) ) ;
#66464 = CARTESIAN_POINT ( 'NONE',  ( -5.153800228976328057, -19.02544592524343514, 92.29057627198099567 ) ) ;
#66463 = CARTESIAN_POINT ( 'NONE',  ( 8.224510206698953496, -14.34966873604960469, 102.9155762719810383 ) ) ;
#66466 = CARTESIAN_POINT ( 'NONE',  ( -10.81492255796078084, -18.62759615963271287, 92.08224293864769550 ) ) ;
#66467 = CARTESIAN_POINT ( 'NONE',  ( -16.55341960407611168, -4.379528057220339221, 51.45724293864770260 ) ) ;
#66468 = CARTESIAN_POINT ( 'NONE',  ( 13.89961937509957401, 13.97604488694547697, 26.87609039468566507 ) ) ;
#66469 = CARTESIAN_POINT ( 'NONE',  ( 8.314922557961029526, -14.29746914071037800, 65.41775706135234714 ) ) ;
#66471 = ORIENTED_EDGE ( 'NONE', *, *, #175399, .T. ) ;
#66470 = CARTESIAN_POINT ( 'NONE',  ( 5.049401038298161559, -19.05341960407611168, 87.70724293864769550 ) ) ;
#66472 = CARTESIAN_POINT ( 'NONE',  ( 19.02544592524343514, -5.153800228976328945, 43.54057627198103120 ) ) ;
#66473 = CARTESIAN_POINT ( 'NONE',  ( -5.719274019375665041, -21.55341960407619695, 54.79275706135235424 ) ) ;
#66474 = EDGE_CURVE ( 'NONE', #154069, #71503, #112034, .T. ) ;
#66475 = CARTESIAN_POINT ( 'NONE',  ( 18.67979575497194134, -10.72451020669871369, 65.83442372801900433 ) ) ;
#66476 = CARTESIAN_POINT ( 'NONE',  ( 5.049401038298161559, -19.05341960407611168, 67.70724293864769550 ) ) ;
#66477 = CARTESIAN_POINT ( 'NONE',  ( 0.05219959533937995610, -21.53943276465977519, 30.00109039468568284 ) ) ;
#66478 = CARTESIAN_POINT ( 'NONE',  ( -9.564922557961040184, 16.46253265017147172, 72.91775706135233293 ) ) ;
#66479 = CARTESIAN_POINT ( 'NONE',  ( 13.97604488694527802, 13.89961937509977652, 39.37390960531435269 ) ) ;
#66480 = CARTESIAN_POINT ( 'NONE',  ( 12.06949235617739724, 12.14591786802326823, 86.87609039468568994 ) ) ;
#66481 = CARTESIAN_POINT ( 'NONE',  ( 5.049401038298161559, -19.05341960407611168, 52.70724293864767418 ) ) ;
#66482 = CARTESIAN_POINT ( 'NONE',  ( -19.03943276465977164, 0.05219959533909376836, 106.2489096053143669 ) ) ;
#66483 = CARTESIAN_POINT ( 'NONE',  ( 16.51473224551069308, 9.474510206698969483, 34.16557627198102409 ) ) ;
#66484 = CARTESIAN_POINT ( 'NONE',  ( -10.81492255796078084, -18.62759615963271287, 87.08224293864769550 ) ) ;
#66485 = CARTESIAN_POINT ( 'NONE',  ( -16.53943276465976808, -0.05219959533934237506, 68.75109039468568994 ) ) ;
#66486 = PLANE ( 'NONE',  #39751 ) ;
#66487 = CARTESIAN_POINT ( 'NONE',  ( 9.564922557961047289, -16.46253265017146816, 30.41775706135232937 ) ) ;
#66488 = CARTESIAN_POINT ( 'NONE',  ( 19.03943276465977164, -0.05219959533909143690, 53.74890960531436690 ) ) ;
#66489 = CARTESIAN_POINT ( 'NONE',  ( -12.14591786802309592, -12.06949235617757132, 46.87390960531435979 ) ) ;
#66490 = CARTESIAN_POINT ( 'NONE',  ( -4.483927247898539470, -16.52544592524342804, 77.29057627198102409 ) ) ;
#66491 = CARTESIAN_POINT ( 'NONE',  ( 13.97604488694527802, 13.89961937509977652, 104.3739096053143385 ) ) ;
#66492 = CARTESIAN_POINT ( 'NONE',  ( 19.03943276465977164, -0.05219959533909143690, 78.74890960531436690 ) ) ;
#66493 = CARTESIAN_POINT ( 'NONE',  ( -21.52544592524334988, -5.823673210054445271, 53.95942372801900433 ) ) ;
#66494 = CARTESIAN_POINT ( 'NONE',  ( 9.564922557960805705, 16.46253265017160317, 94.58224293864769550 ) ) ;
#66495 = CARTESIAN_POINT ( 'NONE',  ( 5.823673210054444382, -21.52544592524334988, 95.20942372801903275 ) ) ;
#66496 = CARTESIAN_POINT ( 'NONE',  ( 4.483927247898790824, -16.52544592524335698, 80.20942372801901854 ) ) ;
#66497 = CARTESIAN_POINT ( 'NONE',  ( -10.72451020669870658, -18.67979575497194134, 24.58442372801901499 ) ) ;
#66498 = CARTESIAN_POINT ( 'NONE',  ( -15.72974639402197994, 15.80617190586746368, 105.6239096053143669 ) ) ;
#66499 = CARTESIAN_POINT ( 'NONE',  ( 0.05219959533910956823, 16.53943276465976808, 64.99890960531435269 ) ) ;
#66500 = CARTESIAN_POINT ( 'NONE',  ( 19.03943276465977164, -0.05219959533909143690, 38.74890960531436690 ) ) ;
#66501 = CARTESIAN_POINT ( 'NONE',  ( -12.14591786802309592, -12.06949235617757132, 66.87390960531436690 ) ) ;
#66502 = CARTESIAN_POINT ( 'NONE',  ( 21.55341960407610458, 5.719274019375980345, 23.95724293864769550 ) ) ;
#66503 = CARTESIAN_POINT ( 'NONE',  ( -19.02544592524334988, -5.153800228976617603, 28.95942372801900433 ) ) ;
#66504 = EDGE_CURVE ( 'NONE', #110081, #100463, #177287, .T. ) ;
#66505 = CARTESIAN_POINT ( 'NONE',  ( 4.379528057220339221, -16.55341960407611168, 102.7072429386476955 ) ) ;
#66506 = ORIENTED_EDGE ( 'NONE', *, *, #92660, .T. ) ;
#66507 = CARTESIAN_POINT ( 'NONE',  ( -16.55341960407617563, 4.379528057220093196, 63.54275706135234003 ) ) ;
#66508 = CARTESIAN_POINT ( 'NONE',  ( -19.03943276465977164, 0.05219959533909376836, 66.24890960531436690 ) ) ;
#66509 = CARTESIAN_POINT ( 'NONE',  ( -16.61815367056139436, -6.523988306745442500, 20.69395534479570387 ) ) ;
#66510 = CARTESIAN_POINT ( 'NONE',  ( 14.34966873604960469, 8.224510206698951720, 84.16557627198103830 ) ) ;
#66511 = CARTESIAN_POINT ( 'NONE',  ( -21.53943276465977519, 0.05219959533907696930, 31.24890960531435979 ) ) ;
#66512 = CARTESIAN_POINT ( 'NONE',  ( 4.379528057220092307, 16.55341960407617563, 97.29275706135234714 ) ) ;
#66513 = CARTESIAN_POINT ( 'NONE',  ( -19.03943276465977164, -0.05219959533935918106, 113.7510903946856757 ) ) ;
#66514 = CARTESIAN_POINT ( 'NONE',  ( 10.72451020669871369, 18.67979575497193778, 82.08442372801901854 ) ) ;
#66515 = CARTESIAN_POINT ( 'NONE',  ( 9.564922557960805705, 16.46253265017160317, 89.58224293864769550 ) ) ;
#66516 = CARTESIAN_POINT ( 'NONE',  ( 15.72974639402199770, -15.80617190586745480, 108.1239096053143811 ) ) ;
#66517 = CARTESIAN_POINT ( 'NONE',  ( 12.14591786802327356, -12.06949235617739191, 60.62609039468567573 ) ) ;
#66518 = CARTESIAN_POINT ( 'NONE',  ( 4.483927247898545687, 16.52544592524342804, 114.7905762719810383 ) ) ;
#66519 = CARTESIAN_POINT ( 'NONE',  ( 4.379528057220092307, 16.55341960407617563, 22.29275706135235069 ) ) ;
#66520 = CARTESIAN_POINT ( 'NONE',  ( -16.46253265017146816, -9.564922557961047289, 84.16775706135233293 ) ) ;
#66521 = CARTESIAN_POINT ( 'NONE',  ( -10.81492255796078084, -18.62759615963271287, 72.08224293864769550 ) ) ;
#66522 = CARTESIAN_POINT ( 'NONE',  ( -13.97604488694547697, 13.89961937509957934, 53.12609039468565442 ) ) ;
#66523 = PLANE ( 'NONE',  #99433 ) ;
#66524 = CARTESIAN_POINT ( 'NONE',  ( 21.53943276465977519, -0.05219959533907433946, 108.7489096053143669 ) ) ;
#66525 = CARTESIAN_POINT ( 'NONE',  ( -997.9783121635130101, 0.000000000000000000, 0.000000000000000000 ) ) ;
#66526 = CARTESIAN_POINT ( 'NONE',  ( 0.05219959533909260263, 19.03943276465977164, 74.99890960531435269 ) ) ;
#66527 = DIRECTION ( 'NONE',  ( -0.06104853953485701173, -7.476289853398329258E-18, -0.9981347984218670311 ) ) ;
#66528 = CARTESIAN_POINT ( 'NONE',  ( -14.29746914071037622, -8.314922557961029526, 29.16775706135234003 ) ) ;
#66529 = CARTESIAN_POINT ( 'NONE',  ( 36.79334119018157878, -4.151185298968582238, 48.62628996558957084 ) ) ;
#66531 = CARTESIAN_POINT ( 'NONE',  ( -12.06949235617756955, 12.14591786802309770, 60.62390960531437401 ) ) ;
#66530 = CARTESIAN_POINT ( 'NONE',  ( 15.80617190586746368, 15.72974639402197994, 99.37390960531436690 ) ) ;
#66532 = CARTESIAN_POINT ( 'NONE',  ( 13.97604488694527802, 13.89961937509977652, 64.37390960531436690 ) ) ;
#66533 = CARTESIAN_POINT ( 'NONE',  ( 15.80617190586769283, -15.72974639402175789, 90.62609039468567573 ) ) ;
#66535 = CARTESIAN_POINT ( 'NONE',  ( -13.97604488694547697, 13.89961937509957934, 48.12609039468566863 ) ) ;
#66534 = CARTESIAN_POINT ( 'NONE',  ( -4.483927247898782831, 16.52544592524335698, 37.70942372801900433 ) ) ;
#66536 = CARTESIAN_POINT ( 'NONE',  ( -18.67979575497193778, 10.72451020669871902, 53.33442372801901854 ) ) ;
#66537 = CARTESIAN_POINT ( 'NONE',  ( 21.53943276465977519, -0.05219959533907433946, 58.74890960531436690 ) ) ;
#66538 = CARTESIAN_POINT ( 'NONE',  ( -13.89961937509957401, -13.97604488694547875, 109.3760903946856331 ) ) ;
#66539 = CARTESIAN_POINT ( 'NONE',  ( 5.153800228976335163, 19.02544592524342804, 59.79057627198100988 ) ) ;
#66540 = CARTESIAN_POINT ( 'NONE',  ( 19.05341960407617918, -5.049401038297876454, 86.04275706135233293 ) ) ;
#66541 = CARTESIAN_POINT ( 'NONE',  ( -5.719274019375665041, -21.55341960407619695, 79.79275706135236135 ) ) ;
#66542 = CARTESIAN_POINT ( 'NONE',  ( 13.89961937509957401, 13.97604488694547697, 71.87609039468567573 ) ) ;
#66543 = CARTESIAN_POINT ( 'NONE',  ( -19.02544592524342804, 5.153800228976336051, 41.04057627198103120 ) ) ;
#66544 = CARTESIAN_POINT ( 'NONE',  ( -10.72451020669898014, 18.67979575497178502, 55.41557627198102409 ) ) ;
#66545 = CARTESIAN_POINT ( 'NONE',  ( -8.224510206698948167, 14.34966873604960824, 65.41557627198102409 ) ) ;
#66546 = CARTESIAN_POINT ( 'NONE',  ( 15.50000000000000178, -5.500000000000000888, 20.00000000000000000 ) ) ;
#66547 = CARTESIAN_POINT ( 'NONE',  ( -5.153800228976607833, 19.02544592524334988, 27.70942372801899722 ) ) ;
#66548 = CARTESIAN_POINT ( 'NONE',  ( 16.52544592524335698, 4.483927247898782831, 96.45942372801901854 ) ) ;
#66549 = CARTESIAN_POINT ( 'NONE',  ( -8.314922557960811034, -14.29746914071050412, 52.08224293864768839 ) ) ;
#66550 = CARTESIAN_POINT ( 'NONE',  ( 15.72974639402176855, 15.80617190586768217, 91.87609039468568994 ) ) ;
#66551 = CARTESIAN_POINT ( 'NONE',  ( 10.81492255796106328, -18.62759615963255655, 85.41775706135236135 ) ) ;
#66552 = CARTESIAN_POINT ( 'NONE',  ( 0.05219959533907565091, 21.53943276465977519, 89.99890960531438111 ) ) ;
#66553 = CARTESIAN_POINT ( 'NONE',  ( 5.049401038298161559, -19.05341960407611168, 52.70724293864767418 ) ) ;
#66554 = CARTESIAN_POINT ( 'NONE',  ( -15.72974639402176322, -15.80617190586768395, 64.37609039468568994 ) ) ;
#66555 = CARTESIAN_POINT ( 'NONE',  ( -9.474510206698964154, 16.51473224551069663, 45.41557627198103120 ) ) ;
#66556 = CARTESIAN_POINT ( 'NONE',  ( -19.03943276465977164, 0.05219959533909376836, 61.24890960531436690 ) ) ;
#66557 = CARTESIAN_POINT ( 'NONE',  ( -4.483927247898539470, -16.52544592524342804, 102.2905762719810383 ) ) ;
#66558 = CARTESIAN_POINT ( 'NONE',  ( -19.05341960407611168, -5.049401038298163336, 96.45724293864769550 ) ) ;
#66559 = CARTESIAN_POINT ( 'NONE',  ( 12.14591786802309770, 12.06949235617756955, 54.37390960531435979 ) ) ;
#66560 = CARTESIAN_POINT ( 'NONE',  ( -8.224510206698948167, 14.34966873604960824, 110.4155762719810383 ) ) ;
#66561 = CARTESIAN_POINT ( 'NONE',  ( -21.55341960407610458, -5.719274019375992779, 81.45724293864769550 ) ) ;
#66562 = CARTESIAN_POINT ( 'NONE',  ( -15.80617190586768217, 15.72974639402176855, 33.12609039468569705 ) ) ;
#66563 = LINE ( 'NONE', #23064, #108167 ) ;
#66564 = CARTESIAN_POINT ( 'NONE',  ( 4.379528057220092307, 16.55341960407617563, 42.29275706135235424 ) ) ;
#66565 = CARTESIAN_POINT ( 'NONE',  ( -5.823673210054116645, -21.52544592524344225, 87.29057627198103830 ) ) ;
#66566 = CARTESIAN_POINT ( 'NONE',  ( 15.80617190586769283, -15.72974639402175789, 105.6260903946856899 ) ) ;
#66567 = CARTESIAN_POINT ( 'NONE',  ( 19.03943276465977164, -0.05219959533909143690, 93.74890960531435269 ) ) ;
#66568 = CARTESIAN_POINT ( 'NONE',  ( 5.719274019375673035, 21.55341960407619339, 37.29275706135235424 ) ) ;
#66569 = CARTESIAN_POINT ( 'NONE',  ( -21.55341960407610458, -5.719274019375992779, 31.45724293864769550 ) ) ;
#66570 = CARTESIAN_POINT ( 'NONE',  ( -14.29746914071037622, -8.314922557961029526, 99.16775706135234714 ) ) ;
#66572 = CARTESIAN_POINT ( 'NONE',  ( 15.80617190586769283, -15.72974639402175789, 80.62609039468567573 ) ) ;
#66571 = CARTESIAN_POINT ( 'NONE',  ( -21.53943276465977519, -0.05219959533937600094, 48.75109039468568284 ) ) ;
#66573 = CARTESIAN_POINT ( 'NONE',  ( -18.67979575497193778, 10.72451020669871902, 108.3344237280190185 ) ) ;
#66574 = CARTESIAN_POINT ( 'NONE',  ( -4.483927247898782831, 16.52544592524335698, 77.70942372801900433 ) ) ;
#66575 = CARTESIAN_POINT ( 'NONE',  ( 18.67979575497194134, -10.72451020669871369, 40.83442372801901854 ) ) ;
#66576 = CARTESIAN_POINT ( 'NONE',  ( -16.46253265017160317, 9.564922557960807481, 35.83224293864768839 ) ) ;
#66577 = CARTESIAN_POINT ( 'NONE',  ( -10.81492255796105439, 18.62759615963255655, 107.9177570613523471 ) ) ;
#66578 = CARTESIAN_POINT ( 'NONE',  ( 9.564922557960805705, 16.46253265017160317, 109.5822429386476955 ) ) ;
#66579 = CARTESIAN_POINT ( 'NONE',  ( -21.53943276465977519, 0.05219959533907696930, 101.2489096053143669 ) ) ;
#66581 = CARTESIAN_POINT ( 'NONE',  ( -0.05219959533907301413, -21.53943276465977519, 72.49890960531435269 ) ) ;
#66580 = CARTESIAN_POINT ( 'NONE',  ( 18.87255363501903815, 5.499999999999947597, 83.82513748171827217 ) ) ;
#66584 = CARTESIAN_POINT ( 'NONE',  ( 14.34966873604960469, 8.224510206698951720, 54.16557627198103120 ) ) ;
#66583 = B_SPLINE_CURVE_WITH_KNOTS ( 'NONE', 3,
 ( #14963, #76623, #184804, #154467, #15959, #77619, #139289, #766, #124110, #53245, #144253, #145251, #131083, #67416 ),
 .UNSPECIFIED., .F., .F.,
 ( 4, 2, 2, 2, 2, 2, 4 ),
 ( 3.469446951953614189E-18, 0.002289927113134828090, 0.003434890669702238015, 0.004579854226269648373, 0.006869781339404439600, 0.008014744895971813096, 0.009159708452539187459 ),
 .UNSPECIFIED. ) ;
#66582 = CARTESIAN_POINT ( 'NONE',  ( 16.55341960407618274, -4.379528057220086978, 46.04275706135234714 ) ) ;
#66585 = DIRECTION ( 'NONE',  ( -0.000000000000000000, -0.000000000000000000, 1.000000000000000000 ) ) ;
#66586 = CARTESIAN_POINT ( 'NONE',  ( -13.89961937509957401, -13.97604488694547875, 89.37609039468563310 ) ) ;
#66587 = DIRECTION ( 'NONE',  ( 0.000000000000000000, 0.000000000000000000, 1.000000000000000000 ) ) ;
#66588 = CARTESIAN_POINT ( 'NONE',  ( 14.34966873604972726, -8.224510206698740333, 30.83442372801902209 ) ) ;
#66589 = CARTESIAN_POINT ( 'NONE',  ( 10.72451020669898902, -18.67979575497178502, 102.9155762719810383 ) ) ;
#66590 = CARTESIAN_POINT ( 'NONE',  ( -21.52544592524343514, 5.823673210054127303, 71.04057627198103830 ) ) ;
#66591 = CARTESIAN_POINT ( 'NONE',  ( 0.05219959533909260263, 19.03943276465977164, 109.9989096053143669 ) ) ;
#66592 = CARTESIAN_POINT ( 'NONE',  ( -14.29746914071037622, -8.314922557961029526, 44.16775706135234714 ) ) ;
#66593 = CARTESIAN_POINT ( 'NONE',  ( -9.564922557960796823, -16.46253265017161027, 72.08224293864770971 ) ) ;
#66595 = CARTESIAN_POINT ( 'NONE',  ( -9.474510206698720793, -16.51473224551083518, 94.58442372801900433 ) ) ;
#66594 = CARTESIAN_POINT ( 'NONE',  ( 18.62759615963255655, 10.81492255796105972, 26.66775706135235424 ) ) ;
#66596 = CARTESIAN_POINT ( 'NONE',  ( -5.153800228976328057, -19.02544592524343514, 107.2905762719810383 ) ) ;
#66597 = CARTESIAN_POINT ( 'NONE',  ( 19.05341960407611168, 5.049401038298154454, 93.95724293864769550 ) ) ;
#66598 = CARTESIAN_POINT ( 'NONE',  ( -0.05219959533907301413, -21.53943276465977519, 87.49890960531436690 ) ) ;
#66599 = CARTESIAN_POINT ( 'NONE',  ( 13.97604488694527802, 13.89961937509977652, 54.37390960531435979 ) ) ;
#66600 = CARTESIAN_POINT ( 'NONE',  ( -17.26172910966778318, -6.454744622555873335, 59.19353091350777873 ) ) ;
#66601 = CARTESIAN_POINT ( 'NONE',  ( 12.14591786802309770, 12.06949235617756955, 69.37390960531436690 ) ) ;
#66602 = CARTESIAN_POINT ( 'NONE',  ( -5.823673210054116645, -21.52544592524344225, 27.29057627198103120 ) ) ;
#66603 = CARTESIAN_POINT ( 'NONE',  ( -29.12650189376887511, 0.8004727011106961276, -52.40478149256038876 ) ) ;
#66604 = CARTESIAN_POINT ( 'NONE',  ( 15.80617190586746368, 15.72974639402197994, 89.37390960531435269 ) ) ;
#66605 = CARTESIAN_POINT ( 'NONE',  ( 19.05341960407617918, -5.049401038297876454, 66.04275706135233293 ) ) ;
#66606 = CARTESIAN_POINT ( 'NONE',  ( -18.67979575497178146, -10.72451020669898902, 21.66557627198102409 ) ) ;
#66607 = CARTESIAN_POINT ( 'NONE',  ( 19.39720447994795549, 5.499999999999969802, 67.16317477297174321 ) ) ;
#66608 = CARTESIAN_POINT ( 'NONE',  ( -21.53943276465977519, 0.05219959533907696930, 61.24890960531435979 ) ) ;
#66609 = CARTESIAN_POINT ( 'NONE',  ( -19.03943276465977164, 0.05219959533909376836, 81.24890960531436690 ) ) ;
#66610 = B_SPLINE_CURVE_WITH_KNOTS ( 'NONE', 3,
 ( #55223, #43056, #57238, #116892, #178584, #42070, #163413, #10734, #179595, #24909, #151237, #101724, #9734, #71398, #180596, #166414, #133062, #27908, #12726, #194752, #164419, #141007, #1493, #64176, #90533, #15690, #154200, #137036, #171360, #46022, #31853, #109679 ),
 .UNSPECIFIED., .F., .F.,
 ( 4, 2, 2, 2, 2, 2, 2, 2, 2, 2, 2, 2, 2, 2, 2, 4 ),
 ( 8.673617379884035472E-19, 0.0003712461730036666118, 0.0007424923460073323562, 0.001113738519010998209, 0.001484984692014663845, 0.002227477038021997285, 0.002598723211025675064, 0.002969969384029352410, 0.003341215557033029755, 0.003712461730036707968, 0.004083707903040385313, 0.004454954076044063092, 0.004826200249047740004, 0.005197446422051418650, 0.005568692595055095562, 0.005939938768058774209 ),
 .UNSPECIFIED. ) ;
#66611 = CARTESIAN_POINT ( 'NONE',  ( 21.55341960407619695, -5.719274019375665929, 76.04275706135237556 ) ) ;
#66612 = CARTESIAN_POINT ( 'NONE',  ( 9.474510206698971260, -16.51473224551069308, 57.91557627198103120 ) ) ;
#66613 = CARTESIAN_POINT ( 'NONE',  ( -12.06949235617756955, 12.14591786802309770, 75.62390960531439532 ) ) ;
#66614 = CARTESIAN_POINT ( 'NONE',  ( 4.483927247898790824, -16.52544592524335698, 40.20942372801901854 ) ) ;
#66615 = CARTESIAN_POINT ( 'NONE',  ( 21.52544592524334988, 5.823673210054432836, 71.45942372801901854 ) ) ;
#66616 = ORIENTED_EDGE ( 'NONE', *, *, #97418, .T. ) ;
#66617 = CARTESIAN_POINT ( 'NONE',  ( -16.46253265017146816, -9.564922557961047289, 19.16775706135233293 ) ) ;
#66618 = CARTESIAN_POINT ( 'NONE',  ( 19.03943276465977164, 0.05219959533936151252, 76.25109039468566152 ) ) ;
#66619 = CARTESIAN_POINT ( 'NONE',  ( 28.30127546286013285, -27.84967942650701644, -20.15398247455537373 ) ) ;
#66620 = CARTESIAN_POINT ( 'NONE',  ( -21.55341960407619339, 5.719274019375674811, 38.54275706135234714 ) ) ;
#66621 = CARTESIAN_POINT ( 'NONE',  ( -30.74264578624800492, -22.33583958711396278, -3.549999994537626602 ) ) ;
#66622 = CARTESIAN_POINT ( 'NONE',  ( -9.564922557961040184, 16.46253265017147172, 32.91775706135233293 ) ) ;
#66623 = CARTESIAN_POINT ( 'NONE',  ( -13.97604488694527625, -13.89961937509977652, 56.87390960531434558 ) ) ;
#66624 = CARTESIAN_POINT ( 'NONE',  ( 5.049401038297881783, 19.05341960407617563, 32.29275706135233293 ) ) ;
#66625 = CARTESIAN_POINT ( 'NONE',  ( 0.05219959533934541429, -16.53943276465976808, 105.0010903946856757 ) ) ;
#66627 = CARTESIAN_POINT ( 'NONE',  ( -15.72974639402176322, -15.80617190586768395, 69.37609039468567573 ) ) ;
#66626 = CARTESIAN_POINT ( 'NONE',  ( -5.153800228976328057, -19.02544592524343514, 107.2905762719810383 ) ) ;
#66628 = CARTESIAN_POINT ( 'NONE',  ( -29.86685920354755552, 21.69954338932564397, -2.824999997268813345 ) ) ;
#66629 = CARTESIAN_POINT ( 'NONE',  ( 0.000000000000000000, 0.000000000000000000, 0.000000000000000000 ) ) ;
#66630 = CARTESIAN_POINT ( 'NONE',  ( -21.52544592524334988, -5.823673210054445271, 88.95942372801901854 ) ) ;
#66631 = CARTESIAN_POINT ( 'NONE',  ( 17.48853670773242897, -5.747243402303147342, 41.16671299749989998 ) ) ;
#66632 = CARTESIAN_POINT ( 'NONE',  ( 19.05341960407611168, 5.049401038298154454, 98.95724293864766707 ) ) ;
#66633 = ADVANCED_FACE ( 'NONE', ( #75672 ), #165717, .F. ) ;
#66634 = CARTESIAN_POINT ( 'NONE',  ( 5.049401038297881783, 19.05341960407617563, 27.29275706135232937 ) ) ;
#66635 = CARTESIAN_POINT ( 'NONE',  ( 24.75282386541786650, -28.51018972888594050, -20.68147073028488947 ) ) ;
#66636 = CARTESIAN_POINT ( 'NONE',  ( 0.05219959533909260263, 19.03943276465977164, 44.99890960531435979 ) ) ;
#66637 = CARTESIAN_POINT ( 'NONE',  ( 18.62759615963271287, -10.81492255796078972, 53.33224293864769550 ) ) ;
#66638 = CARTESIAN_POINT ( 'NONE',  ( -12.06949235617756955, 12.14591786802309770, 25.62390960531435624 ) ) ;
#66640 = CARTESIAN_POINT ( 'NONE',  ( 0.05219959533909260263, 19.03943276465977164, 74.99890960531435269 ) ) ;
#66639 = CARTESIAN_POINT ( 'NONE',  ( -8.314922557960811034, -14.29746914071050412, 92.08224293864769550 ) ) ;
#66641 = CARTESIAN_POINT ( 'NONE',  ( 0.05219959533937995610, -21.53943276465977519, 100.0010903946857042 ) ) ;
#66642 = CARTESIAN_POINT ( 'NONE',  ( -19.05341960407611168, -5.049401038298163336, 31.45724293864769550 ) ) ;
#66643 = CARTESIAN_POINT ( 'NONE',  ( -4.379528057220328563, 16.55341960407611168, 105.2072429386477097 ) ) ;
#66644 = CARTESIAN_POINT ( 'NONE',  ( 21.53943276465977519, 0.05219959533937863772, 56.25109039468568284 ) ) ;
#66645 = EDGE_CURVE ( 'NONE', #48040, #177604, #41080, .T. ) ;
#66646 = CARTESIAN_POINT ( 'NONE',  ( -10.81492255796078084, -18.62759615963271287, 82.08224293864768129 ) ) ;
#66647 = CARTESIAN_POINT ( 'NONE',  ( -19.02544592524334988, -5.153800228976617603, 48.95942372801900433 ) ) ;
#66648 = CARTESIAN_POINT ( 'NONE',  ( -20.00287982954261423, -21.32739072855598650, -49.27013238145816842 ) ) ;
#66649 = CARTESIAN_POINT ( 'NONE',  ( 5.153800228976335163, 19.02544592524342804, 104.7905762719809957 ) ) ;
#66650 = CARTESIAN_POINT ( 'NONE',  ( -16.55341960407611168, -4.379528057220339221, 76.45724293864769550 ) ) ;
#66652 = CARTESIAN_POINT ( 'NONE',  ( -19.02544592524334988, -5.153800228976617603, 38.95942372801900433 ) ) ;
#66651 = AXIS2_PLACEMENT_3D ( 'NONE', #136665, #185158, #92134 ) ;
#66653 = CARTESIAN_POINT ( 'NONE',  ( -16.46253265017160317, 9.564922557960807481, 60.83224293864769550 ) ) ;
#66654 = CARTESIAN_POINT ( 'NONE',  ( -16.53943276465976808, 0.05219959533911058130, 61.24890960531435979 ) ) ;
#66655 = CARTESIAN_POINT ( 'NONE',  ( -16.51473224551082808, 9.474510206698731452, 73.33442372801900433 ) ) ;
#66656 = CARTESIAN_POINT ( 'NONE',  ( -5.049401038297874678, -19.05341960407618274, 89.79275706135233293 ) ) ;
#66657 = CARTESIAN_POINT ( 'NONE',  ( -0.05219959533907301413, -21.53943276465977519, 32.49890960531435979 ) ) ;
#66658 = VERTEX_POINT ( 'NONE', #166716 ) ;
#66659 = CARTESIAN_POINT ( 'NONE',  ( -4.379528057220328563, 16.55341960407611168, 95.20724293864769550 ) ) ;
#66660 = DIRECTION ( 'NONE',  ( 2.081668171172168513E-15, -0.8164965809277244801, 0.5773502691896279515 ) ) ;
#66662 = CARTESIAN_POINT ( 'NONE',  ( -15.80617190586745835, -15.72974639402198527, 66.87390960531436690 ) ) ;
#66661 = CARTESIAN_POINT ( 'NONE',  ( 19.02544592524343514, -5.153800228976328945, 58.54057627198102409 ) ) ;
#66663 = CARTESIAN_POINT ( 'NONE',  ( 9.474510206698971260, -16.51473224551069308, 32.91557627198102409 ) ) ;
#66665 = CARTESIAN_POINT ( 'NONE',  ( -9.564922557960796823, -16.46253265017161027, 57.08224293864769550 ) ) ;
#66664 = CARTESIAN_POINT ( 'NONE',  ( 12.06949235617739724, 12.14591786802326823, 76.87609039468567573 ) ) ;
#66666 = CARTESIAN_POINT ( 'NONE',  ( 19.05341960407617918, -5.049401038297876454, 51.04275706135231871 ) ) ;
#66667 = CARTESIAN_POINT ( 'NONE',  ( -5.823673210054431948, 21.52544592524334988, 62.70942372801902565 ) ) ;
#66668 = CARTESIAN_POINT ( 'NONE',  ( -18.62759615963270932, 10.81492255796079327, 50.83224293864770971 ) ) ;
#66669 = CARTESIAN_POINT ( 'NONE',  ( 14.29746914071049879, -8.314922557960816363, 113.3322429386476955 ) ) ;
#66670 = CARTESIAN_POINT ( 'NONE',  ( -14.34966873604972548, 8.224510206698743886, 83.33442372801903275 ) ) ;
#66671 = CARTESIAN_POINT ( 'NONE',  ( -9.564922557961040184, 16.46253265017147172, 102.9177570613523329 ) ) ;
#66672 = CARTESIAN_POINT ( 'NONE',  ( -22.81625015709510507, 31.40387420917330275, -1.424999997268813212 ) ) ;
#66673 = CARTESIAN_POINT ( 'NONE',  ( 17.50000000000001421, 5.622605283950889543, 53.81207310596115434 ) ) ;
#66674 = CARTESIAN_POINT ( 'NONE',  ( 15.80617190586769283, -15.72974639402175789, 100.6260903946857184 ) ) ;
#66675 = VERTEX_POINT ( 'NONE', #164722 ) ;
#66676 = CARTESIAN_POINT ( 'NONE',  ( -12.14591786802309592, -12.06949235617757132, 51.87390960531437401 ) ) ;
#66677 = CARTESIAN_POINT ( 'NONE',  ( -14.29746914071049879, 8.314922557960819915, 55.83224293864770260 ) ) ;
#66678 = CARTESIAN_POINT ( 'NONE',  ( 5.719274019375991003, -21.55341960407610458, 92.70724293864770971 ) ) ;
#66679 = CARTESIAN_POINT ( 'NONE',  ( -10.81492255796078084, -18.62759615963271287, 92.08224293864769550 ) ) ;
#66680 = CARTESIAN_POINT ( 'NONE',  ( -1.495846735942510941, -30.59399807301415208, -47.49088840515941712 ) ) ;
#66681 = CARTESIAN_POINT ( 'NONE',  ( -0.05219959533907301413, -21.53943276465977519, 32.49890960531435979 ) ) ;
#66682 = CARTESIAN_POINT ( 'NONE',  ( 12.06949235617739724, 12.14591786802326823, 71.87609039468568994 ) ) ;
#66683 = CARTESIAN_POINT ( 'NONE',  ( -12.14591786802309592, -12.06949235617757132, 76.87390960531439532 ) ) ;
#66684 = CARTESIAN_POINT ( 'NONE',  ( -13.89961937509977652, 13.97604488694528158, 50.62390960531435979 ) ) ;
#66685 = SHAPE_REPRESENTATION_RELATIONSHIP ( 'NONE' , 'NONE' ,  #85690, #189513 ) ;
#66686 = CARTESIAN_POINT ( 'NONE',  ( -3.503282210674334873, -48.86437366581479580, -35.00000000000000000 ) ) ;
#66687 = CARTESIAN_POINT ( 'NONE',  ( 14.34966873604972726, -8.224510206698740333, 95.83442372801903275 ) ) ;
#66688 = CARTESIAN_POINT ( 'NONE',  ( -15.72974639402197994, 15.80617190586746368, 115.6239096053143669 ) ) ;
#66689 = CARTESIAN_POINT ( 'NONE',  ( 19.05341960407611168, 5.049401038298154454, 88.95724293864769550 ) ) ;
#66690 = CARTESIAN_POINT ( 'NONE',  ( 18.67979575497194134, -10.72451020669871369, 50.83442372801901143 ) ) ;
#66691 = CARTESIAN_POINT ( 'NONE',  ( -18.08554851550293208, -38.44972689945520017, -20.08432885666762502 ) ) ;
#66692 = VERTEX_POINT ( 'NONE', #117207 ) ;
#66693 = CARTESIAN_POINT ( 'NONE',  ( 5.719274019375673035, 21.55341960407619339, 52.29275706135236135 ) ) ;
#66695 = CARTESIAN_POINT ( 'NONE',  ( 0.05219959533909260263, 19.03943276465977164, 114.9989096053143669 ) ) ;
#66694 = CARTESIAN_POINT ( 'NONE',  ( 13.97604488694527802, 13.89961937509977652, 39.37390960531435269 ) ) ;
#66696 = CARTESIAN_POINT ( 'NONE',  ( 9.564922557961047289, -16.46253265017146816, 50.41775706135233293 ) ) ;
#66697 = CARTESIAN_POINT ( 'NONE',  ( 21.53943276465977519, 0.05219959533937863772, 26.25109039468567573 ) ) ;
#66698 = CARTESIAN_POINT ( 'NONE',  ( 5.153800228976615827, -19.02544592524334988, 65.20942372801900433 ) ) ;
#66699 = CARTESIAN_POINT ( 'NONE',  ( -9.474510206698964154, 16.51473224551069663, 25.41557627198103120 ) ) ;
#66700 = CARTESIAN_POINT ( 'NONE',  ( 4.379528057220092307, 16.55341960407617563, 87.29275706135236135 ) ) ;
#66701 = CARTESIAN_POINT ( 'NONE',  ( 5.153800228976615827, -19.02544592524334988, 65.20942372801900433 ) ) ;
#66702 = CARTESIAN_POINT ( 'NONE',  ( 4.379528057220092307, 16.55341960407617563, 107.2927570613523471 ) ) ;
#66704 = ORIENTED_EDGE ( 'NONE', *, *, #192980, .F. ) ;
#66703 = CARTESIAN_POINT ( 'NONE',  ( 9.279464826303303937, 10.38198520235567024, -62.49863477660405664 ) ) ;
#66705 = CARTESIAN_POINT ( 'NONE',  ( -13.97604488694527625, -13.89961937509977652, 91.87390960531432427 ) ) ;
#66706 = CONICAL_SURFACE ( 'NONE', #179762, 2.500000000000000000, 1.029744258676656976 ) ;
#66707 = CARTESIAN_POINT ( 'NONE',  ( -15.72974639402176322, -15.80617190586768395, 99.37609039468568994 ) ) ;
#66709 = EDGE_CURVE ( 'NONE', #155176, #57973, #121697, .T. ) ;
#66708 = CARTESIAN_POINT ( 'NONE',  ( -21.52544592524334988, -5.823673210054445271, 108.9594237280190185 ) ) ;
#66710 = DIRECTION ( 'NONE',  ( 0.7071067811865483499, 2.636779683484746468E-14, -0.7071067811865465735 ) ) ;
#66711 = CARTESIAN_POINT ( 'NONE',  ( 13.89961937509977652, -13.97604488694527269, 98.12390960531433848 ) ) ;
#66712 = CARTESIAN_POINT ( 'NONE',  ( -10.72451020669870658, -18.67979575497194134, 74.58442372801901854 ) ) ;
#66713 = CARTESIAN_POINT ( 'NONE',  ( -12.06949235617739369, -12.14591786802326823, 19.37609039468568639 ) ) ;
#66714 = CARTESIAN_POINT ( 'NONE',  ( 13.89961937509977652, -13.97604488694527269, 78.12390960531433848 ) ) ;
#66715 = CARTESIAN_POINT ( 'NONE',  ( 15.72974639402199770, -15.80617190586745480, 33.12390960531435979 ) ) ;
#66716 = CARTESIAN_POINT ( 'NONE',  ( 0.05219959533909260263, 19.03943276465977164, 94.99890960531436690 ) ) ;
#66717 = DIRECTION ( 'NONE',  ( 1.000000000000000000, 0.000000000000000000, 0.000000000000000000 ) ) ;
#66718 = CARTESIAN_POINT ( 'NONE',  ( 16.51473224551069308, 9.474510206698969483, 59.16557627198102409 ) ) ;
#66719 = CARTESIAN_POINT ( 'NONE',  ( -16.52544592524342804, 4.483927247898546575, 26.04057627198103475 ) ) ;
#66720 = CARTESIAN_POINT ( 'NONE',  ( 37.99999999999999289, 2.893978650043524126E-14, -1.000000000000000000 ) ) ;
#66721 = CARTESIAN_POINT ( 'NONE',  ( -9.474510206698720793, -16.51473224551083518, 69.58442372801901854 ) ) ;
#66722 = CARTESIAN_POINT ( 'NONE',  ( -16.46253265017160317, 9.564922557960807481, 100.8322429386477097 ) ) ;
#66723 = CARTESIAN_POINT ( 'NONE',  ( -21.55341960407619339, 5.719274019375674811, 98.54275706135234714 ) ) ;
#66724 = CARTESIAN_POINT ( 'NONE',  ( 8.314922557960818139, 14.29746914071049879, 79.58224293864769550 ) ) ;
#66725 = CARTESIAN_POINT ( 'NONE',  ( 0.05219959533907565091, 21.53943276465977519, 49.99890960531437401 ) ) ;
#66726 = CARTESIAN_POINT ( 'NONE',  ( -18.67979575497178146, -10.72451020669898902, 41.66557627198103120 ) ) ;
#66727 = CARTESIAN_POINT ( 'NONE',  ( 14.29746914071049879, -8.314922557960816363, 108.3322429386477097 ) ) ;
#66728 = LINE ( 'NONE', #68717, #172681 ) ;
#66729 = CARTESIAN_POINT ( 'NONE',  ( 13.97604488694548053, -13.89961937509957401, 45.62609039468566863 ) ) ;
#66730 = CARTESIAN_POINT ( 'NONE',  ( -14.29746914071049879, 8.314922557960819915, 25.83224293864769194 ) ) ;
#66731 = CARTESIAN_POINT ( 'NONE',  ( -5.153800228976328057, -19.02544592524343514, 97.29057627198099567 ) ) ;
#66732 = CARTESIAN_POINT ( 'NONE',  ( 21.52544592524334988, 5.823673210054432836, 71.45942372801901854 ) ) ;
#66733 = CARTESIAN_POINT ( 'NONE',  ( 21.52544592524344225, -5.823673210054117533, 53.54057627198103120 ) ) ;
#66734 = CARTESIAN_POINT ( 'NONE',  ( -21.53943276465977519, -0.05219959533937600094, 48.75109039468568284 ) ) ;
#66735 = CARTESIAN_POINT ( 'NONE',  ( -18.62759615963270932, 10.81492255796079327, 95.83224293864770971 ) ) ;
#66736 = CARTESIAN_POINT ( 'NONE',  ( 18.67979575497194134, -10.72451020669871369, 35.83442372801901143 ) ) ;
#66737 = CARTESIAN_POINT ( 'NONE',  ( -14.34966873604960291, -8.224510206698953496, 101.6655762719810383 ) ) ;
#66738 = CARTESIAN_POINT ( 'NONE',  ( -5.049401038297874678, -19.05341960407617918, 69.79275706135233293 ) ) ;
#66739 = CARTESIAN_POINT ( 'NONE',  ( 4.483927247898545687, 16.52544592524342804, 109.7905762719810383 ) ) ;
#66740 = CARTESIAN_POINT ( 'NONE',  ( -9.564922557960796823, -16.46253265017161027, 107.0822429386476955 ) ) ;
#66741 = CARTESIAN_POINT ( 'NONE',  ( 16.55341960407611168, 4.379528057220329451, 48.95724293864770971 ) ) ;
#66742 = CARTESIAN_POINT ( 'NONE',  ( 0.05219959533910956823, 16.53943276465976808, 24.99890960531435624 ) ) ;
#66743 = CARTESIAN_POINT ( 'NONE',  ( 16.51473224551069308, 9.474510206698969483, 49.16557627198102409 ) ) ;
#66744 = CARTESIAN_POINT ( 'NONE',  ( -13.97604488694527625, -13.89961937509977652, 26.87390960531434558 ) ) ;
#66745 = CARTESIAN_POINT ( 'NONE',  ( 21.52544592524344225, -5.823673210054117533, 28.54057627198103120 ) ) ;
#66746 = CARTESIAN_POINT ( 'NONE',  ( -19.02544592524334988, -5.153800228976617603, 18.95942372801899722 ) ) ;
#66748 = CARTESIAN_POINT ( 'NONE',  ( 16.52544592524342804, -4.483927247898539470, 33.54057627198102409 ) ) ;
#66747 = DIRECTION ( 'NONE',  ( -1.000000000000000000, 0.000000000000000000, 0.000000000000000000 ) ) ;
#66749 = CARTESIAN_POINT ( 'NONE',  ( 21.55341960407619695, -5.719274019375665929, 51.04275706135234714 ) ) ;
#66750 = CARTESIAN_POINT ( 'NONE',  ( 23.48258780958830982, -5.709364865862134764, 171.6892424014283733 ) ) ;
#66751 = CARTESIAN_POINT ( 'NONE',  ( 4.483927247898790824, -16.52544592524335698, 55.20942372801902565 ) ) ;
#66752 = CARTESIAN_POINT ( 'NONE',  ( 14.34966873604960469, 8.224510206698951720, 29.16557627198103120 ) ) ;
#66753 = CARTESIAN_POINT ( 'NONE',  ( -16.53943276465976808, -0.05219959533934237506, 108.7510903946857042 ) ) ;
#66754 = CARTESIAN_POINT ( 'NONE',  ( 5.049401038298161559, -19.05341960407611168, 32.70724293864768129 ) ) ;
#66755 = CARTESIAN_POINT ( 'NONE',  ( 9.564922557960805705, 16.46253265017160317, 59.58224293864769550 ) ) ;
#66756 = CARTESIAN_POINT ( 'NONE',  ( 16.46253265017160672, -9.564922557960803928, 23.33224293864769194 ) ) ;
#66757 = CARTESIAN_POINT ( 'NONE',  ( 10.81492255796106328, -18.62759615963255655, 30.41775706135234358 ) ) ;
#66758 = CARTESIAN_POINT ( 'NONE',  ( -13.97604488694527625, -13.89961937509977652, 46.87390960531435979 ) ) ;
#66759 = CARTESIAN_POINT ( 'NONE',  ( -11.45643923738959735, 5.000000000000007105, -15.00000000000000000 ) ) ;
#66760 = CARTESIAN_POINT ( 'NONE',  ( 16.46253265017160672, -9.564922557960803928, 33.33224293864770260 ) ) ;
#66761 = CARTESIAN_POINT ( 'NONE',  ( -16.51473224551069308, -9.474510206698971260, 111.6655762719810383 ) ) ;
#66763 = CARTESIAN_POINT ( 'NONE',  ( -4.379528057220328563, 16.55341960407611168, 110.2072429386477239 ) ) ;
#66762 = CARTESIAN_POINT ( 'NONE',  ( -10.81492255796105439, 18.62759615963255655, 62.91775706135236135 ) ) ;
#66764 = CARTESIAN_POINT ( 'NONE',  ( -9.564922557960796823, -16.46253265017161027, 112.0822429386476955 ) ) ;
#66765 = CARTESIAN_POINT ( 'NONE',  ( -14.34966873604972548, 8.224510206698743886, 78.33442372801901854 ) ) ;
#66766 = CARTESIAN_POINT ( 'NONE',  ( -18.62759615963255300, -10.81492255796106328, 89.16775706135236135 ) ) ;
#66767 = CARTESIAN_POINT ( 'NONE',  ( -4.483927247898782831, 16.52544592524335698, 47.70942372801902565 ) ) ;
#66768 = CARTESIAN_POINT ( 'NONE',  ( -0.05219959533909027116, -19.03943276465977164, 97.49890960531436690 ) ) ;
#66769 = CARTESIAN_POINT ( 'NONE',  ( 14.34966873604972726, -8.224510206698740333, 45.83442372801901854 ) ) ;
#66770 = CARTESIAN_POINT ( 'NONE',  ( 8.314922557961029526, -14.29746914071037800, 25.41775706135235779 ) ) ;
#66771 = CARTESIAN_POINT ( 'NONE',  ( 14.34966873604972726, -8.224510206698740333, 80.83442372801901854 ) ) ;
#66772 = CARTESIAN_POINT ( 'NONE',  ( 5.153800228976615827, -19.02544592524334988, 110.2094237280189901 ) ) ;
#66773 = CARTESIAN_POINT ( 'NONE',  ( 5.153800228976335163, 19.02544592524342804, 79.79057627198102409 ) ) ;
#66774 = CARTESIAN_POINT ( 'NONE',  ( -0.05219959533907301413, -21.53943276465977519, 102.4989096053143811 ) ) ;
#66776 = CARTESIAN_POINT ( 'NONE',  ( -19.05341960407617563, 5.049401038297882671, 108.5427570613523187 ) ) ;
#66775 = CARTESIAN_POINT ( 'NONE',  ( 4.379528057220339221, -16.55341960407611168, 107.7072429386476955 ) ) ;
#66777 = CARTESIAN_POINT ( 'NONE',  ( -4.483927247898782831, 16.52544592524335698, 72.70942372801901854 ) ) ;
#66778 = CARTESIAN_POINT ( 'NONE',  ( 28.79475375365586132, 2.781246896534039337E-14, 155.0000000000000000 ) ) ;
#66779 = CARTESIAN_POINT ( 'NONE',  ( 19.05341960407617918, -5.049401038297876454, 76.04275706135230450 ) ) ;
#66780 = CARTESIAN_POINT ( 'NONE',  ( -16.52544592524342804, 4.483927247898546575, 46.04057627198103830 ) ) ;
#66781 = CARTESIAN_POINT ( 'NONE',  ( -14.34966873604960291, -8.224510206698953496, 96.66557627198102409 ) ) ;
#66782 = CARTESIAN_POINT ( 'NONE',  ( 19.03943276465977164, 0.05219959533936151252, 31.25109039468566863 ) ) ;
#66783 = CARTESIAN_POINT ( 'NONE',  ( -5.719274019375665041, -21.55341960407619695, 39.79275706135235424 ) ) ;
#66784 = CARTESIAN_POINT ( 'NONE',  ( -19.02544592524334988, -5.153800228976617603, 93.95942372801900433 ) ) ;
#66785 = CARTESIAN_POINT ( 'NONE',  ( -16.46253265017160317, 9.564922557960807481, 90.83224293864769550 ) ) ;
#66786 = CARTESIAN_POINT ( 'NONE',  ( 5.719274019375673035, 21.55341960407619339, 112.2927570613523471 ) ) ;
#66787 = CARTESIAN_POINT ( 'NONE',  ( 16.51473224551069308, 9.474510206698969483, 94.16557627198103830 ) ) ;
#66788 = CARTESIAN_POINT ( 'NONE',  ( 18.62759615963271287, -10.81492255796078972, 53.33224293864769550 ) ) ;
#66789 = CARTESIAN_POINT ( 'NONE',  ( -0.05219959533910754901, -16.53943276465976808, 87.49890960531436690 ) ) ;
#66790 = CARTESIAN_POINT ( 'NONE',  ( -9.474510206698964154, 16.51473224551069663, 75.41557627198103830 ) ) ;
#66791 = CARTESIAN_POINT ( 'NONE',  ( -4.379528057220328563, 16.55341960407611168, 115.2072429386476955 ) ) ;
#66792 = VECTOR ( 'NONE', #105181, 1000.000000000000000 ) ;
#66793 = CARTESIAN_POINT ( 'NONE',  ( 21.53943276465977519, 0.05219959533937863772, 31.25109039468568639 ) ) ;
#66794 = CARTESIAN_POINT ( 'NONE',  ( 15.80617190586769283, -15.72974639402175789, 75.62609039468567573 ) ) ;
#66795 = CARTESIAN_POINT ( 'NONE',  ( -13.89961937509977652, 13.97604488694528158, 45.62390960531433848 ) ) ;
#66796 = CARTESIAN_POINT ( 'NONE',  ( 8.224510206698742110, 14.34966873604972548, 72.08442372801899012 ) ) ;
#66797 = CARTESIAN_POINT ( 'NONE',  ( 15.72974639402176855, 15.80617190586768217, 26.87609039468567218 ) ) ;
#66798 = CARTESIAN_POINT ( 'NONE',  ( 15.80617190586769283, -15.72974639402175789, 25.62609039468567929 ) ) ;
#66800 = CARTESIAN_POINT ( 'NONE',  ( -19.02544592524342804, 5.153800228976336051, 66.04057627198103830 ) ) ;
#66799 = CARTESIAN_POINT ( 'NONE',  ( -19.03943276465977164, -0.05219959533935918106, 58.75109039468566863 ) ) ;
#66801 = CARTESIAN_POINT ( 'NONE',  ( 19.02544592524334988, 5.153800228976608722, 26.45942372801899722 ) ) ;
#66802 = CARTESIAN_POINT ( 'NONE',  ( 10.72451020669871369, 18.67979575497193778, 87.08442372801901854 ) ) ;
#66803 = CARTESIAN_POINT ( 'NONE',  ( 5.823673210054125526, 21.52544592524343514, 64.79057627198103830 ) ) ;
#66804 = CARTESIAN_POINT ( 'NONE',  ( 0.05219959533910956823, 16.53943276465976808, 54.99890960531435269 ) ) ;
#66806 = CARTESIAN_POINT ( 'NONE',  ( -19.03943276465977164, -0.05219959533935918106, 23.75109039468566152 ) ) ;
#66805 = CARTESIAN_POINT ( 'NONE',  ( -5.719274019375665041, -21.55341960407619695, 84.79275706135234714 ) ) ;
#66807 = CARTESIAN_POINT ( 'NONE',  ( 14.34966873604960469, 8.224510206698951720, 74.16557627198102409 ) ) ;
#66808 = CARTESIAN_POINT ( 'NONE',  ( 9.564922557960805705, 16.46253265017160317, 29.58224293864769550 ) ) ;
#66809 = CARTESIAN_POINT ( 'NONE',  ( -19.02544592524334988, -5.153800228976617603, 53.95942372801898301 ) ) ;
#66810 = CARTESIAN_POINT ( 'NONE',  ( -16.55341960407611168, -4.379528057220339221, 31.45724293864769550 ) ) ;
#66811 = TOROIDAL_SURFACE ( 'NONE', #21641, 1.500000000000001776, 0.5000000000000000000 ) ;
#66812 = CARTESIAN_POINT ( 'NONE',  ( 15.80617190586769283, -15.72974639402175789, 80.62609039468567573 ) ) ;
#66813 = CARTESIAN_POINT ( 'NONE',  ( -9.474510206698964154, 16.51473224551069663, 75.41557627198103830 ) ) ;
#66814 = CARTESIAN_POINT ( 'NONE',  ( 16.51473224551083163, -9.474510206698727899, 50.83442372801899722 ) ) ;
#66815 = CARTESIAN_POINT ( 'NONE',  ( -21.55341960407610458, -5.719274019375992779, 46.45724293864769550 ) ) ;
#66816 = CARTESIAN_POINT ( 'NONE',  ( -21.52544592524334988, -5.823673210054445271, 38.95942372801901854 ) ) ;
#66817 = CARTESIAN_POINT ( 'NONE',  ( -21.53943276465977519, 0.05219959533907696930, 96.24890960531435269 ) ) ;
#66818 = CARTESIAN_POINT ( 'NONE',  ( 16.46253265017146816, 9.564922557961045513, 96.66775706135233293 ) ) ;
#66819 = CARTESIAN_POINT ( 'NONE',  ( 12.06949235617739724, 12.14591786802326823, 61.87609039468568284 ) ) ;
#66821 = CARTESIAN_POINT ( 'NONE',  ( -18.62759615963270932, 10.81492255796079327, 100.8322429386477097 ) ) ;
#66820 = CARTESIAN_POINT ( 'NONE',  ( -15.73785899003303790, -17.57910283142216201, -57.30050143854533218 ) ) ;
#66822 = CARTESIAN_POINT ( 'NONE',  ( 4.483927247898545687, 16.52544592524342804, 109.7905762719810383 ) ) ;
#66823 = CARTESIAN_POINT ( 'NONE',  ( -17.49999999999999645, -5.499999999999992895, 99.20309617465831309 ) ) ;
#66824 = CARTESIAN_POINT ( 'NONE',  ( 14.34966873604972726, -8.224510206698740333, 30.83442372801902209 ) ) ;
#66825 = CARTESIAN_POINT ( 'NONE',  ( -21.55341960407610458, -5.719274019375992779, 66.45724293864768129 ) ) ;
#66826 = CARTESIAN_POINT ( 'NONE',  ( -4.483927247898782831, 16.52544592524335698, 97.70942372801904696 ) ) ;
#66827 = CARTESIAN_POINT ( 'NONE',  ( 5.049401038298161559, -19.05341960407611168, 32.70724293864768129 ) ) ;
#66828 = CARTESIAN_POINT ( 'NONE',  ( -14.34966873604972548, 8.224510206698743886, 63.33442372801900433 ) ) ;
#66829 = CARTESIAN_POINT ( 'NONE',  ( -5.049401038297874678, -19.05341960407617918, 54.79275706135234003 ) ) ;
#66830 = CARTESIAN_POINT ( 'NONE',  ( 21.52544592524334988, 5.823673210054432836, 41.45942372801901143 ) ) ;
#66831 = CARTESIAN_POINT ( 'NONE',  ( -5.823673210054116645, -21.52544592524344225, 62.29057627198102409 ) ) ;
#66832 = CARTESIAN_POINT ( 'NONE',  ( -12.06949235617739369, -12.14591786802326823, 89.37609039468568994 ) ) ;
#66833 = CARTESIAN_POINT ( 'NONE',  ( -21.55341960407619339, 5.719274019375674811, 73.54275706135234714 ) ) ;
#66834 = CARTESIAN_POINT ( 'NONE',  ( -10.81492255796078084, -18.62759615963271287, 57.08224293864769550 ) ) ;
#66835 = CARTESIAN_POINT ( 'NONE',  ( -5.719274019375978568, 21.55341960407610458, 40.20724293864769550 ) ) ;
#66836 = ORIENTED_EDGE ( 'NONE', *, *, #132163, .F. ) ;
#66837 = CARTESIAN_POINT ( 'NONE',  ( 16.55341960407618274, -4.379528057220086978, 71.04275706135234714 ) ) ;
#66838 = CARTESIAN_POINT ( 'NONE',  ( 18.67979575497178502, 10.72451020669898547, 34.16557627198102409 ) ) ;
#66839 = VERTEX_POINT ( 'NONE', #26217 ) ;
#66840 = CARTESIAN_POINT ( 'NONE',  ( -13.89961937509977652, 13.97604488694528158, 100.6239096053143669 ) ) ;
#66841 = CARTESIAN_POINT ( 'NONE',  ( -0.05219959533934338120, 16.53943276465976808, 112.5010903946857042 ) ) ;
#66842 = DIRECTION ( 'NONE',  ( 1.000000000000000000, 0.000000000000000000, 0.000000000000000000 ) ) ;
#66843 = CARTESIAN_POINT ( 'NONE',  ( 4.379528057220339221, -16.55341960407611168, 102.7072429386476955 ) ) ;
#66844 = CARTESIAN_POINT ( 'NONE',  ( -0.05219959533907301413, -21.53943276465977519, 67.49890960531436690 ) ) ;
#66845 = CARTESIAN_POINT ( 'NONE',  ( -4.379528057220086978, -16.55341960407618274, 84.79275706135234714 ) ) ;
#66846 = CARTESIAN_POINT ( 'NONE',  ( -21.53943276465977519, -0.05219959533937600094, 48.75109039468568284 ) ) ;
#66847 = CARTESIAN_POINT ( 'NONE',  ( 9.564922557961047289, -16.46253265017146816, 105.4177570613523471 ) ) ;
#66848 = CARTESIAN_POINT ( 'NONE',  ( -12.06949235617756955, 12.14591786802309770, 105.6239096053143669 ) ) ;
#66849 = CARTESIAN_POINT ( 'NONE',  ( -16.51473224551069308, -9.474510206698971260, 51.66557627198102409 ) ) ;
#66850 = VECTOR ( 'NONE', #35850, 1000.000000000000000 ) ;
#66851 = CARTESIAN_POINT ( 'NONE',  ( -19.03943276465977164, 0.05219959533909376836, 26.24890960531435624 ) ) ;
#66852 = CARTESIAN_POINT ( 'NONE',  ( 0.9809564218223714160, 23.93924616269290340, -54.49512787944463099 ) ) ;
#66853 = CARTESIAN_POINT ( 'NONE',  ( -19.03943276465977164, 0.05219959533909376836, 96.24890960531436690 ) ) ;
#66854 = CARTESIAN_POINT ( 'NONE',  ( -16.53943276465976808, -0.05219959533934237506, 73.75109039468567573 ) ) ;
#66855 = CARTESIAN_POINT ( 'NONE',  ( 21.53943276465977519, 0.05219959533937863772, 111.2510903946856899 ) ) ;
#66856 = CARTESIAN_POINT ( 'NONE',  ( -5.823673210054116645, -21.52544592524344225, 47.29057627198103120 ) ) ;
#66857 = CARTESIAN_POINT ( 'NONE',  ( 4.483927247898790824, -16.52544592524335698, 75.20942372801901854 ) ) ;
#66858 = CARTESIAN_POINT ( 'NONE',  ( -13.97604488694547697, 13.89961937509957934, 78.12609039468567573 ) ) ;
#66859 = CARTESIAN_POINT ( 'NONE',  ( 5.153800228976335163, 19.02544592524342804, 39.79057627198100988 ) ) ;
#66860 = CARTESIAN_POINT ( 'NONE',  ( -9.474510206698964154, 16.51473224551069663, 80.41557627198103830 ) ) ;
#66861 = CARTESIAN_POINT ( 'NONE',  ( 5.049401038298161559, -19.05341960407611168, 37.70724293864768839 ) ) ;
#66862 = CARTESIAN_POINT ( 'NONE',  ( -16.46253265017146816, -9.564922557961047289, 74.16775706135234714 ) ) ;
#66863 = CARTESIAN_POINT ( 'NONE',  ( 24.86475712555791873, -11.37215039201027089, 169.9824823118007657 ) ) ;
#66864 = CARTESIAN_POINT ( 'NONE',  ( -5.049401038298153566, 19.05341960407611168, 100.2072429386476955 ) ) ;
#66865 = CARTESIAN_POINT ( 'NONE',  ( 0.05219959533910956823, 16.53943276465976808, 54.99890960531435269 ) ) ;
#66866 = CARTESIAN_POINT ( 'NONE',  ( 5.719274019375991003, -21.55341960407610458, 47.70724293864770260 ) ) ;
#66867 = CARTESIAN_POINT ( 'NONE',  ( -17.50000000000000000, 3.471454075611697832, 104.4833258114436347 ) ) ;
#66868 = CARTESIAN_POINT ( 'NONE',  ( 5.153800228976615827, -19.02544592524334988, 35.20942372801899722 ) ) ;
#66869 = DIRECTION ( 'NONE',  ( 1.000000000000000000, 0.000000000000000000, 0.000000000000000000 ) ) ;
#66870 = CARTESIAN_POINT ( 'NONE',  ( -19.02544592524342804, 5.153800228976336051, 56.04057627198100988 ) ) ;
#66871 = EDGE_CURVE ( 'NONE', #34377, #37464, #87856, .T. ) ;
#66872 = CARTESIAN_POINT ( 'NONE',  ( -14.29746914071037622, -8.314922557961029526, 34.16775706135234714 ) ) ;
#66873 = DIRECTION ( 'NONE',  ( 1.000000000000000000, 0.000000000000000000, 0.000000000000000000 ) ) ;
#66874 = CARTESIAN_POINT ( 'NONE',  ( 23.58955696227031140, -7.613471476246058245, 172.7063021553927058 ) ) ;
#66875 = CARTESIAN_POINT ( 'NONE',  ( 8.224510206698742110, 14.34966873604972548, 82.08442372801901854 ) ) ;
#66876 = CARTESIAN_POINT ( 'NONE',  ( -15.72974639402197994, 15.80617190586746368, 100.6239096053143811 ) ) ;
#66877 = CARTESIAN_POINT ( 'NONE',  ( 4.483927247898790824, -16.52544592524335698, 40.20942372801901854 ) ) ;
#66879 = CARTESIAN_POINT ( 'NONE',  ( 5.153800228976335163, 19.02544592524342804, 114.7905762719810241 ) ) ;
#66878 = CARTESIAN_POINT ( 'NONE',  ( 16.46253265017160672, -9.564922557960803928, 48.33224293864769550 ) ) ;
#66880 = CARTESIAN_POINT ( 'NONE',  ( -21.52544592524334988, -5.823673210054445271, 43.95942372801902565 ) ) ;
#66881 = CARTESIAN_POINT ( 'NONE',  ( 16.51473224551083163, -9.474510206698727899, 55.83442372801899722 ) ) ;
#66882 = CARTESIAN_POINT ( 'NONE',  ( 0.05219959533937995610, -21.53943276465977519, 100.0010903946857042 ) ) ;
#66883 = CARTESIAN_POINT ( 'NONE',  ( 9.474510206698971260, -16.51473224551069308, 22.91557627198102765 ) ) ;
#66884 = CARTESIAN_POINT ( 'NONE',  ( 16.53943276465976808, -0.05219959533910856209, 43.74890960531435979 ) ) ;
#66885 = CARTESIAN_POINT ( 'NONE',  ( 19.01529144963332030, 5.500000000000156319, 43.73431955728440101 ) ) ;
#66886 = CARTESIAN_POINT ( 'NONE',  ( -5.823673210054116645, -21.52544592524344225, 57.29057627198103120 ) ) ;
#66887 = CARTESIAN_POINT ( 'NONE',  ( -27.73933785331498925, -9.013057229001049109, 142.9750000027312069 ) ) ;
#66888 = CARTESIAN_POINT ( 'NONE',  ( 9.474510206698971260, -16.51473224551069308, 102.9155762719810241 ) ) ;
#66889 = CARTESIAN_POINT ( 'NONE',  ( 4.379528057220339221, -16.55341960407611168, 97.70724293864772392 ) ) ;
#66890 = CARTESIAN_POINT ( 'NONE',  ( -14.29746914071037622, -8.314922557961029526, 19.16775706135234714 ) ) ;
#66891 = CARTESIAN_POINT ( 'NONE',  ( 0.05219959533934541429, -16.53943276465976808, 105.0010903946856757 ) ) ;
#66892 = ORIENTED_EDGE ( 'NONE', *, *, #74956, .T. ) ;
#66894 = CARTESIAN_POINT ( 'NONE',  ( 18.67979575497178502, 10.72451020669898547, 104.1655762719810241 ) ) ;
#66893 = CARTESIAN_POINT ( 'NONE',  ( -13.97604488694527625, -13.89961937509977652, 101.8739096053143811 ) ) ;
#66896 = CARTESIAN_POINT ( 'NONE',  ( 11.74264578624800315, -36.14014761921581709, -9.400000000000000355 ) ) ;
#66895 = CARTESIAN_POINT ( 'NONE',  ( -4.379528057220328563, 16.55341960407611168, 30.20724293864769550 ) ) ;
#66897 = CARTESIAN_POINT ( 'NONE',  ( 5.153800228976615827, -19.02544592524334988, 95.20942372801897591 ) ) ;
#66898 = CARTESIAN_POINT ( 'NONE',  ( -10.81492255796105439, 18.62759615963255655, 107.9177570613523471 ) ) ;
#66899 = CARTESIAN_POINT ( 'NONE',  ( 16.55341960407611168, 4.379528057220329451, 33.95724293864769550 ) ) ;
#66900 = CARTESIAN_POINT ( 'NONE',  ( 18.67979575497178502, 10.72451020669898547, 94.16557627198103830 ) ) ;
#66901 = CARTESIAN_POINT ( 'NONE',  ( 18.62759615963271287, -10.81492255796078972, 53.33224293864769550 ) ) ;
#66902 = CARTESIAN_POINT ( 'NONE',  ( 5.049401038298161559, -19.05341960407611168, 62.70724293864769550 ) ) ;
#66903 = CARTESIAN_POINT ( 'NONE',  ( 16.52544592524342804, -4.483927247898539470, 28.54057627198103120 ) ) ;
#66904 = CARTESIAN_POINT ( 'NONE',  ( -0.05219959533909027116, -19.03943276465977164, 82.49890960531436690 ) ) ;
#66905 = ORIENTED_EDGE ( 'NONE', *, *, #74286, .T. ) ;
#66906 = CARTESIAN_POINT ( 'NONE',  ( -9.474510206698964154, 16.51473224551069663, 80.41557627198103830 ) ) ;
#66907 = CARTESIAN_POINT ( 'NONE',  ( -19.05341960407617563, 5.049401038297882671, 38.54275706135233293 ) ) ;
#66908 = CARTESIAN_POINT ( 'NONE',  ( -10.72451020669898014, 18.67979575497178502, 80.41557627198103830 ) ) ;
#66909 = CARTESIAN_POINT ( 'NONE',  ( 12.14591786802309770, 12.06949235617756955, 84.37390960531438111 ) ) ;
#66910 = CARTESIAN_POINT ( 'NONE',  ( -21.55341960407619339, 5.719274019375674811, 38.54275706135234714 ) ) ;
#66911 = CARTESIAN_POINT ( 'NONE',  ( 17.14385361876520264, -23.59649016807271238, 148.0750000027311728 ) ) ;
#66912 = CARTESIAN_POINT ( 'NONE',  ( -8.224510206698735004, -14.34966873604973081, 109.5844237280190328 ) ) ;
#66913 = CARTESIAN_POINT ( 'NONE',  ( 12.14591786802309770, 12.06949235617756955, 114.3739096053143527 ) ) ;
#66914 = CARTESIAN_POINT ( 'NONE',  ( -9.564922557960796823, -16.46253265017161027, 82.08224293864768129 ) ) ;
#66915 =( LENGTH_UNIT ( ) NAMED_UNIT ( * ) SI_UNIT ( .MILLI., .METRE. ) );
#66916 = CARTESIAN_POINT ( 'NONE',  ( -9.564922557960796823, -16.46253265017161027, 22.08224293864768839 ) ) ;
#66917 = CARTESIAN_POINT ( 'NONE',  ( 14.29746914071049879, -8.314922557960816363, 48.33224293864770260 ) ) ;
#66918 = CARTESIAN_POINT ( 'NONE',  ( 15.72974639402176855, 15.80617190586768217, 56.87609039468568994 ) ) ;
#66919 = CARTESIAN_POINT ( 'NONE',  ( 26.43919995774724185, -26.89423752947832114, -20.34026575423448691 ) ) ;
#66920 = CARTESIAN_POINT ( 'NONE',  ( -5.049401038298153566, 19.05341960407611168, 40.20724293864768839 ) ) ;
#66921 = CARTESIAN_POINT ( 'NONE',  ( 19.03943276465977164, -0.05219959533909143690, 53.74890960531436690 ) ) ;
#66922 = VERTEX_POINT ( 'NONE', #149544 ) ;
#66923 = CARTESIAN_POINT ( 'NONE',  ( 10.72451020669871369, 18.67979575497193778, 107.0844237280190043 ) ) ;
#66924 = CARTESIAN_POINT ( 'NONE',  ( -4.379528057220086978, -16.55341960407618274, 64.79275706135234714 ) ) ;
#66925 = B_SPLINE_CURVE_WITH_KNOTS ( 'NONE', 3,
 ( #20345, #81994, #113350, #175042, #77630, #167668, #59475, #124122, #154477, #32132, #14974, #76634, #125135, #31141, #151509, #15970, #186833, #13001, #121149, #60465, #153478, #109958, #185821, #74664, #182842, #48301, #183828, #138312, #46302, #107958, #92789, #89828 ),
 .UNSPECIFIED., .F., .F.,
 ( 4, 2, 2, 2, 2, 2, 2, 2, 2, 2, 2, 2, 2, 2, 2, 4 ),
 ( 1.599336020787782259E-17, 0.0003712461730036926326, 0.0007424923460073693275, 0.001113738519011045914, 0.001484984692014722609, 0.002227477038022073613, 0.002598723211025752260, 0.002969969384029431340, 0.003341215557033109986, 0.003712461730036789500, 0.004083707903040468580, 0.004454954076044147226, 0.004826200249047826740, 0.005197446422051505387, 0.005568692595055184900, 0.005939938768058864414 ),
 .UNSPECIFIED. ) ;
#66926 = CARTESIAN_POINT ( 'NONE',  ( 21.53943276465977519, 0.05219959533937863772, 96.25109039468568994 ) ) ;
#66927 = CARTESIAN_POINT ( 'NONE',  ( 19.03943276465977164, -0.05219959533909143690, 113.7489096053143669 ) ) ;
#66928 = CARTESIAN_POINT ( 'NONE',  ( -0.05219959533936034679, 19.03943276465977164, 107.5010903946856615 ) ) ;
#66929 = CARTESIAN_POINT ( 'NONE',  ( -15.80617190586768217, 15.72974639402176855, 68.12609039468567573 ) ) ;
#66930 = CARTESIAN_POINT ( 'NONE',  ( -16.52544592524335698, -4.483927247898792601, 33.95942372801901143 ) ) ;
#66931 = CARTESIAN_POINT ( 'NONE',  ( -10.72451020669898014, 18.67979575497178502, 90.41557627198103830 ) ) ;
#66932 = CARTESIAN_POINT ( 'NONE',  ( -19.05341960407617563, 5.049401038297882671, 98.54275706135233293 ) ) ;
#66933 = CARTESIAN_POINT ( 'NONE',  ( -13.89961937509977652, 13.97604488694528158, 65.62390960531436690 ) ) ;
#66934 = CARTESIAN_POINT ( 'NONE',  ( -19.05341960407617563, 5.049401038297882671, 108.5427570613523187 ) ) ;
#66935 = VECTOR ( 'NONE', #162181, 1000.000000000000000 ) ;
#66936 = CARTESIAN_POINT ( 'NONE',  ( 5.153800228976615827, -19.02544592524334988, 100.2094237280190043 ) ) ;
#66937 = CARTESIAN_POINT ( 'NONE',  ( 4.483927247898545687, 16.52544592524342804, 59.79057627198103120 ) ) ;
#66938 = CARTESIAN_POINT ( 'NONE',  ( 0.05219959533936267826, -19.03943276465977164, 75.00109039468566152 ) ) ;
#66939 = CARTESIAN_POINT ( 'NONE',  ( -4.379528057220086978, -16.55341960407618274, 79.79275706135236135 ) ) ;
#66940 = ADVANCED_FACE ( 'NONE', ( #136363 ), #7389, .T. ) ;
#66942 = CARTESIAN_POINT ( 'NONE',  ( 0.05219959533909260263, 19.03943276465977164, 44.99890960531435979 ) ) ;
#66941 = CARTESIAN_POINT ( 'NONE',  ( 21.53943276465977519, -0.05219959533907433946, 113.7489096053143527 ) ) ;
#66943 = CARTESIAN_POINT ( 'NONE',  ( -0.05219959533909027116, -19.03943276465977164, 62.49890960531435979 ) ) ;
#66944 = CARTESIAN_POINT ( 'NONE',  ( -8.314922557961024197, 14.29746914071037800, 77.91775706135231871 ) ) ;
#66945 = CARTESIAN_POINT ( 'NONE',  ( 22.44159573604009594, -16.30477369853687364, 140.1750000027311955 ) ) ;
#66946 = CARTESIAN_POINT ( 'NONE',  ( 17.81289503416610742, 24.51734667627700404, 143.5500000054623513 ) ) ;
#66947 = ORIENTED_EDGE ( 'NONE', *, *, #8998, .T. ) ;
#66948 = CARTESIAN_POINT ( 'NONE',  ( 15.80617190586769283, -15.72974639402175789, 110.6260903946857042 ) ) ;
#66949 = CARTESIAN_POINT ( 'NONE',  ( -16.51473224551069308, -9.474510206698971260, 26.66557627198103120 ) ) ;
#66950 = VERTEX_POINT ( 'NONE', #76808 ) ;
#66951 = CARTESIAN_POINT ( 'NONE',  ( 16.55341960407618274, -4.379528057220086978, 21.04275706135234714 ) ) ;
#66952 = CARTESIAN_POINT ( 'NONE',  ( 15.72974639402199770, -15.80617190586745480, 48.12390960531436690 ) ) ;
#66954 = CARTESIAN_POINT ( 'NONE',  ( -8.314922557961024197, 14.29746914071037800, 32.91775706135234714 ) ) ;
#66953 = CARTESIAN_POINT ( 'NONE',  ( 9.474510206698729675, 16.51473224551082808, 47.08442372801900433 ) ) ;
#66955 = CARTESIAN_POINT ( 'NONE',  ( -9.564922557960796823, -16.46253265017161027, 27.08224293864769550 ) ) ;
#66956 = B_SPLINE_CURVE_WITH_KNOTS ( 'NONE', 3,
 ( #53867, #191372, #161037, #69025, #177229, #178223 ),
 .UNSPECIFIED., .F., .F.,
 ( 4, 2, 4 ),
 ( 0.000000000000000000, 0.0003837532665554159472, 0.0007675065331108318943 ),
 .UNSPECIFIED. ) ;
#66957 = CARTESIAN_POINT ( 'NONE',  ( 19.05341960407611168, 5.049401038298154454, 53.95724293864770260 ) ) ;
#66958 = CARTESIAN_POINT ( 'NONE',  ( 21.52544592524344225, -5.823673210054117533, 88.54057627198103830 ) ) ;
#66959 = DIRECTION ( 'NONE',  ( -1.000000000000000000, 5.392603844284257652E-33, 0.000000000000000000 ) ) ;
#66960 = CARTESIAN_POINT ( 'NONE',  ( 19.03943276465977164, -0.05219959533909143690, 48.74890960531435979 ) ) ;
#66961 = CARTESIAN_POINT ( 'NONE',  ( 27.73933785331498569, 9.013057229001093518, 148.4750000027311785 ) ) ;
#66962 = CARTESIAN_POINT ( 'NONE',  ( 19.03943276465977164, 0.05219959533936151252, 91.25109039468566152 ) ) ;
#66964 = AXIS2_PLACEMENT_3D ( 'NONE', #17397, #127545, #123557 ) ;
#66963 = CARTESIAN_POINT ( 'NONE',  ( -12.06949235617756955, 12.14591786802309770, 60.62390960531437401 ) ) ;
#66965 = CARTESIAN_POINT ( 'NONE',  ( 5.719274019375673035, 21.55341960407619339, 102.2927570613523613 ) ) ;
#66966 = CARTESIAN_POINT ( 'NONE',  ( -18.67979575497178146, -10.72451020669898902, 101.6655762719810383 ) ) ;
#66967 = CARTESIAN_POINT ( 'NONE',  ( 21.53943276465977519, 0.05219959533937863772, 86.25109039468568994 ) ) ;
#66968 = CARTESIAN_POINT ( 'NONE',  ( 9.474510206698971260, -16.51473224551069308, 27.91557627198103120 ) ) ;
#66969 = CARTESIAN_POINT ( 'NONE',  ( 5.823673210054444382, -21.52544592524334988, 80.20942372801901854 ) ) ;
#66971 = CARTESIAN_POINT ( 'NONE',  ( -21.52544592524334988, -5.823673210054445271, 73.95942372801901854 ) ) ;
#66970 = CARTESIAN_POINT ( 'NONE',  ( -12.14591786802326823, 12.06949235617739902, 113.1260903946856899 ) ) ;
#66972 = CARTESIAN_POINT ( 'NONE',  ( -5.049401038298153566, 19.05341960407611168, 70.20724293864769550 ) ) ;
#66973 = CARTESIAN_POINT ( 'NONE',  ( 5.719274019375673035, 21.55341960407619339, 37.29275706135235424 ) ) ;
#66974 = CARTESIAN_POINT ( 'NONE',  ( -19.03943276465977164, 0.05219959533909376836, 86.24890960531436690 ) ) ;
#66975 = CARTESIAN_POINT ( 'NONE',  ( 14.29746914071049879, -8.314922557960816363, 98.33224293864769550 ) ) ;
#66976 = CARTESIAN_POINT ( 'NONE',  ( -4.483927247898539470, -16.52544592524342804, 67.29057627198103830 ) ) ;
#66977 = CARTESIAN_POINT ( 'NONE',  ( -10.81492255796078084, -18.62759615963271287, 67.08224293864770971 ) ) ;
#66978 = CARTESIAN_POINT ( 'NONE',  ( -0.05219959533909027116, -19.03943276465977164, 67.49890960531436690 ) ) ;
#66979 = CARTESIAN_POINT ( 'NONE',  ( 21.55341960407610458, 5.719274019375980345, 88.95724293864769550 ) ) ;
#66980 = CARTESIAN_POINT ( 'NONE',  ( 13.97604488694548053, -13.89961937509957401, 60.62609039468564731 ) ) ;
#66982 = CARTESIAN_POINT ( 'NONE',  ( -16.55341960407611168, -4.379528057220339221, 76.45724293864769550 ) ) ;
#66981 = CARTESIAN_POINT ( 'NONE',  ( -9.564922557961040184, 16.46253265017147172, 37.91775706135233293 ) ) ;
#66983 = VECTOR ( 'NONE', #126675, 1000.000000000000000 ) ;
#66984 = CARTESIAN_POINT ( 'NONE',  ( 10.81492255796078972, 18.62759615963270932, 59.58224293864770260 ) ) ;
#66985 = DIRECTION ( 'NONE',  ( 0.000000000000000000, 0.000000000000000000, 1.000000000000000000 ) ) ;
#66987 = CARTESIAN_POINT ( 'NONE',  ( 1.784210473542230573E-15, -29.16686587814331588, 143.8750000027311842 ) ) ;
#66986 = CARTESIAN_POINT ( 'NONE',  ( -12.06949235617739369, -12.14591786802326823, 94.37609039468568994 ) ) ;
#66988 = CARTESIAN_POINT ( 'NONE',  ( 16.51473224551083163, -9.474510206698727899, 95.83442372801900433 ) ) ;
#66989 = CARTESIAN_POINT ( 'NONE',  ( 16.52544592524342804, -4.483927247898539470, 63.54057627198103830 ) ) ;
#66990 = CARTESIAN_POINT ( 'NONE',  ( 3.889087296526082316, 6.412877669190294228, 1.818019484660534424 ) ) ;
#66991 = CARTESIAN_POINT ( 'NONE',  ( 19.05341960407611168, 5.049401038298154454, 58.95724293864768129 ) ) ;
#66992 = CARTESIAN_POINT ( 'NONE',  ( 4.379528057220339221, -16.55341960407611168, 57.70724293864770260 ) ) ;
#66993 = CARTESIAN_POINT ( 'NONE',  ( -5.049401038298153566, 19.05341960407611168, 105.2072429386476671 ) ) ;
#66995 = CARTESIAN_POINT ( 'NONE',  ( -5.049401038298153566, 19.05341960407611168, 70.20724293864769550 ) ) ;
#66994 = CARTESIAN_POINT ( 'NONE',  ( -5.153800228976607833, 19.02544592524334988, 72.70942372801900433 ) ) ;
#66996 = CARTESIAN_POINT ( 'NONE',  ( -0.05219959533909027116, -19.03943276465977164, 82.49890960531436690 ) ) ;
#66997 = CARTESIAN_POINT ( 'NONE',  ( 5.153800228976335163, 19.02544592524342804, 69.79057627198103830 ) ) ;
#66998 = CARTESIAN_POINT ( 'NONE',  ( -15.72974639402197994, 15.80617190586746368, 65.62390960531436690 ) ) ;
#66999 = CARTESIAN_POINT ( 'NONE',  ( 8.314922557961029526, -14.29746914071037800, 60.41775706135235424 ) ) ;
#67000 = CARTESIAN_POINT ( 'NONE',  ( -16.46253265017146816, -9.564922557961047289, 104.1677570613523329 ) ) ;
#67001 = CARTESIAN_POINT ( 'NONE',  ( 19.02544592524343514, -5.153800228976328945, 43.54057627198103120 ) ) ;
#67002 = CARTESIAN_POINT ( 'NONE',  ( 15.80617190586746368, 15.72974639402197994, 49.37390960531436690 ) ) ;
#67003 = CARTESIAN_POINT ( 'NONE',  ( 16.46253265017146816, 9.564922557961045513, 91.66775706135234714 ) ) ;
#67005 = CARTESIAN_POINT ( 'NONE',  ( 10.72451020669871369, 18.67979575497193778, 32.08442372801901854 ) ) ;
#67004 = CARTESIAN_POINT ( 'NONE',  ( -16.55341960407611168, -4.379528057220339221, 26.45724293864768839 ) ) ;
#67006 = CARTESIAN_POINT ( 'NONE',  ( 19.03943276465977164, 0.05219959533936151252, 31.25109039468566863 ) ) ;
#67008 = CARTESIAN_POINT ( 'NONE',  ( -8.224510206698735004, -14.34966873604973081, 99.58442372801900433 ) ) ;
#67007 = CARTESIAN_POINT ( 'NONE',  ( 16.52544592524335698, 4.483927247898782831, 66.45942372801903275 ) ) ;
#67009 = DIRECTION ( 'NONE',  ( 1.000000000000000000, 0.000000000000000000, -0.000000000000000000 ) ) ;
#67010 = CARTESIAN_POINT ( 'NONE',  ( -8.224510206698735004, -14.34966873604973081, 84.58442372801903275 ) ) ;
#67012 = CARTESIAN_POINT ( 'NONE',  ( -14.34966873604972548, 8.224510206698743886, 33.33442372801900433 ) ) ;
#67011 = CARTESIAN_POINT ( 'NONE',  ( -15.80617190586745835, -15.72974639402198527, 31.87390960531435979 ) ) ;
#67013 = CARTESIAN_POINT ( 'NONE',  ( -13.89961937509977652, 13.97604488694528158, 40.62390960531435979 ) ) ;
#67014 = CARTESIAN_POINT ( 'NONE',  ( 19.03943276465977164, -0.05219959533909143690, 43.74890960531435979 ) ) ;
#67015 = CARTESIAN_POINT ( 'NONE',  ( -9.564922557960796823, -16.46253265017161027, 67.08224293864769550 ) ) ;
#67016 = CARTESIAN_POINT ( 'NONE',  ( -10.72451020669870658, -18.67979575497194134, 44.58442372801901854 ) ) ;
#67017 = CARTESIAN_POINT ( 'NONE',  ( 16.53943276465976808, 0.05219959533934440121, 46.25109039468567573 ) ) ;
#67018 = CARTESIAN_POINT ( 'NONE',  ( -12.14591786802309592, -12.06949235617757132, 21.87390960531436690 ) ) ;
#67019 = CARTESIAN_POINT ( 'NONE',  ( 19.05341960407611168, 5.049401038298154454, 33.95724293864769550 ) ) ;
#67020 = CARTESIAN_POINT ( 'NONE',  ( -18.67979575497193778, 10.72451020669871902, 113.3344237280190328 ) ) ;
#67021 = CARTESIAN_POINT ( 'NONE',  ( -13.89961937509957401, -13.97604488694547875, 104.3760903946856757 ) ) ;
#67022 = CARTESIAN_POINT ( 'NONE',  ( 9.564922557961047289, -16.46253265017146816, 75.41775706135234714 ) ) ;
#67023 = CARTESIAN_POINT ( 'NONE',  ( -8.314922557960811034, -14.29746914071050412, 67.08224293864770971 ) ) ;
#67024 = CARTESIAN_POINT ( 'NONE',  ( 5.049401038298161559, -19.05341960407611168, 32.70724293864768129 ) ) ;
#67026 = CARTESIAN_POINT ( 'NONE',  ( -4.500000000000000888, -139.5000000000000000, 13.35010376910484631 ) ) ;
#67025 = CARTESIAN_POINT ( 'NONE',  ( 5.049401038297881783, 19.05341960407617563, 77.29275706135231871 ) ) ;
#67027 = CARTESIAN_POINT ( 'NONE',  ( -18.67979575497193778, 10.72451020669871902, 78.33442372801901854 ) ) ;
#67028 = CARTESIAN_POINT ( 'NONE',  ( -12.06949235617739369, -12.14591786802326823, 34.37609039468568284 ) ) ;
#67029 = CYLINDRICAL_SURFACE ( 'NONE', #153598, 61.99999999999998579 ) ;
#67030 = CARTESIAN_POINT ( 'NONE',  ( -5.719274019375978568, 21.55341960407610458, 30.20724293864769550 ) ) ;
#67031 = CARTESIAN_POINT ( 'NONE',  ( -16.55341960407617563, 4.379528057220093196, 28.54275706135234358 ) ) ;
#67032 = CARTESIAN_POINT ( 'NONE',  ( 13.97604488694527802, 13.89961937509977830, 29.37390960531435624 ) ) ;
#67033 = CARTESIAN_POINT ( 'NONE',  ( 19.05341960407617918, -5.049401038297876454, 31.04275706135232227 ) ) ;
#67034 = CARTESIAN_POINT ( 'NONE',  ( 32.64453336272026718, -1.163414472736631538E-14, 87.50000000000000000 ) ) ;
#67035 = CARTESIAN_POINT ( 'NONE',  ( 5.153800228976335163, 19.02544592524342804, 39.79057627198100988 ) ) ;
#67036 = CARTESIAN_POINT ( 'NONE',  ( 18.22780087662126647, 5.499999999999818812, 56.48236817873107185 ) ) ;
#67037 = CARTESIAN_POINT ( 'NONE',  ( -5.049401038298153566, 19.05341960407611168, 55.20724293864769550 ) ) ;
#67038 = CARTESIAN_POINT ( 'NONE',  ( 17.50000000000001776, -4.049696124445898882, 111.6803967066594794 ) ) ;
#67039 = CARTESIAN_POINT ( 'NONE',  ( 19.05341960407617918, -5.049401038297876454, 26.04275706135233293 ) ) ;
#67040 = CARTESIAN_POINT ( 'NONE',  ( -14.29746914071049879, 8.314922557960819915, 30.83224293864770260 ) ) ;
#67041 = CARTESIAN_POINT ( 'NONE',  ( 16.51473224551069308, 9.474510206698969483, 34.16557627198102409 ) ) ;
#67042 = CARTESIAN_POINT ( 'NONE',  ( 9.474510206698971260, -16.51473224551069308, 92.91557627198103830 ) ) ;
#67043 = CARTESIAN_POINT ( 'NONE',  ( -15.80617190586768217, 15.72974639402176855, 68.12609039468567573 ) ) ;
#67044 = CARTESIAN_POINT ( 'NONE',  ( 16.46253265017160672, -9.564922557960803928, 33.33224293864770260 ) ) ;
#67045 = EDGE_CURVE ( 'NONE', #92733, #139805, #947, .T. ) ;
#67046 = CARTESIAN_POINT ( 'NONE',  ( 18.62759615963255655, 10.81492255796105972, 71.66775706135234714 ) ) ;
#67048 = CARTESIAN_POINT ( 'NONE',  ( -5.719274019375978568, 21.55341960407610458, 30.20724293864769550 ) ) ;
#67047 = CARTESIAN_POINT ( 'NONE',  ( -16.51473224551082808, 9.474510206698731452, 93.33442372801900433 ) ) ;
#67049 = CARTESIAN_POINT ( 'NONE',  ( 9.564922557960805705, 16.46253265017160317, 39.58224293864768839 ) ) ;
#67050 = CARTESIAN_POINT ( 'NONE',  ( 10.81492255796078972, 18.62759615963270932, 114.5822429386477097 ) ) ;
#67051 = CARTESIAN_POINT ( 'NONE',  ( -9.474510206698720793, -16.51473224551083518, 29.58442372801900433 ) ) ;
#67052 = CARTESIAN_POINT ( 'NONE',  ( 14.34966873604960469, 8.224510206698951720, 114.1655762719810383 ) ) ;
#67053 = CARTESIAN_POINT ( 'NONE',  ( -19.05341960407611168, -5.049401038298163336, 66.45724293864769550 ) ) ;
#67054 = CARTESIAN_POINT ( 'NONE',  ( 19.05341960407617918, -5.049401038297876454, 101.0427570613523045 ) ) ;
#67055 = CARTESIAN_POINT ( 'NONE',  ( -14.29746914071049879, 8.314922557960819915, 75.83224293864769550 ) ) ;
#67056 = CARTESIAN_POINT ( 'NONE',  ( 21.55341960407610458, 5.719274019375980345, 23.95724293864769550 ) ) ;
#67057 = CARTESIAN_POINT ( 'NONE',  ( -9.564922557961040184, 16.46253265017147172, 82.91775706135233293 ) ) ;
#67058 = CARTESIAN_POINT ( 'NONE',  ( -10.81492255796078084, -18.62759615963271287, 87.08224293864769550 ) ) ;
#67059 = CARTESIAN_POINT ( 'NONE',  ( 0.05219959533937995610, -21.53943276465977519, 45.00109039468568284 ) ) ;
#67060 = CARTESIAN_POINT ( 'NONE',  ( -12.06949235617739369, -12.14591786802326823, 49.37609039468569705 ) ) ;
#67062 = CARTESIAN_POINT ( 'NONE',  ( 0.05219959533937995610, -21.53943276465977519, 55.00109039468568284 ) ) ;
#67061 = CARTESIAN_POINT ( 'NONE',  ( -8.224510206698735004, -14.34966873604973081, 49.58442372801901143 ) ) ;
#67063 = CARTESIAN_POINT ( 'NONE',  ( 15.80617190586746368, 15.72974639402197994, 59.37390960531436690 ) ) ;
#67064 = CARTESIAN_POINT ( 'NONE',  ( -5.153800228976328057, -19.02544592524343514, 47.29057627198102409 ) ) ;
#67065 = CARTESIAN_POINT ( 'NONE',  ( 11.74264578624800315, -36.14014761921581709, -7.149999994537626691 ) ) ;
#67066 = CARTESIAN_POINT ( 'NONE',  ( 14.34966873604972726, -8.224510206698740333, 80.83442372801901854 ) ) ;
#67067 = CARTESIAN_POINT ( 'NONE',  ( -21.52544592524343514, 5.823673210054127303, 101.0405762719810383 ) ) ;
#67068 = CARTESIAN_POINT ( 'NONE',  ( 0.05219959533910956823, 16.53943276465976808, 54.99890960531435269 ) ) ;
#67069 = CARTESIAN_POINT ( 'NONE',  ( 4.379528057220092307, 16.55341960407617563, 62.29275706135236845 ) ) ;
#67070 = CARTESIAN_POINT ( 'NONE',  ( -19.02544592524334988, -5.153800228976617603, 103.9594237280190043 ) ) ;
#67071 = CARTESIAN_POINT ( 'NONE',  ( 15.80617190586746368, 15.72974639402197994, 99.37390960531436690 ) ) ;
#67072 = CARTESIAN_POINT ( 'NONE',  ( 8.224510206698953496, -14.34966873604960469, 42.91557627198103120 ) ) ;
#67073 = ORIENTED_EDGE ( 'NONE', *, *, #19257, .F. ) ;
#67074 = CARTESIAN_POINT ( 'NONE',  ( 32.00000000000000000, -1.163414459189985801E-14, 95.00000000000000000 ) ) ;
#67075 = CARTESIAN_POINT ( 'NONE',  ( -5.719274019375978568, 21.55341960407610458, 75.20724293864769550 ) ) ;
#67076 = CARTESIAN_POINT ( 'NONE',  ( -8.314922557960811034, -14.29746914071050412, 22.08224293864769194 ) ) ;
#67077 = ORIENTED_EDGE ( 'NONE', *, *, #69228, .T. ) ;
#67078 = CARTESIAN_POINT ( 'NONE',  ( 35.70266437024449147, 2.428612576286966776E-14, 37.50000000000000000 ) ) ;
#67079 = CARTESIAN_POINT ( 'NONE',  ( 21.52544592524344225, -5.823673210054117533, 103.5405762719810383 ) ) ;
#67080 = CARTESIAN_POINT ( 'NONE',  ( -5.719274019375978568, 21.55341960407610458, 110.2072429386477239 ) ) ;
#67081 = CARTESIAN_POINT ( 'NONE',  ( -12.14591786802309592, -12.06949235617757132, 36.87390960531435979 ) ) ;
#67082 = CARTESIAN_POINT ( 'NONE',  ( 16.53943276465976808, 0.05219959533934440121, 46.25109039468567573 ) ) ;
#67083 = VECTOR ( 'NONE', #50771, 1000.000000000000000 ) ;
#67084 = CARTESIAN_POINT ( 'NONE',  ( -13.97604488694527625, -13.89961937509977652, 51.87390960531436690 ) ) ;
#67085 = CARTESIAN_POINT ( 'NONE',  ( -16.46253265017160317, 9.564922557960807481, 70.83224293864770971 ) ) ;
#67086 = ORIENTED_EDGE ( 'NONE', *, *, #102940, .T. ) ;
#67087 = CARTESIAN_POINT ( 'NONE',  ( -18.67979575497178146, -10.72451020669898902, 36.66557627198103120 ) ) ;
#67088 = CARTESIAN_POINT ( 'NONE',  ( -29.33118895280791349, -23.95254016166466116, -21.73655181065874942 ) ) ;
#67089 = CARTESIAN_POINT ( 'NONE',  ( 9.474510206698729675, 16.51473224551082808, 102.0844237280190043 ) ) ;
#67090 = CARTESIAN_POINT ( 'NONE',  ( -9.564922557961040184, 16.46253265017147172, 52.91775706135233293 ) ) ;
#67091 = CARTESIAN_POINT ( 'NONE',  ( 18.62759615963271287, -10.81492255796078972, 108.3322429386477097 ) ) ;
#67092 = CARTESIAN_POINT ( 'NONE',  ( 12.14591786802309770, 12.06949235617756955, 29.37390960531435269 ) ) ;
#67093 = CARTESIAN_POINT ( 'NONE',  ( 13.89961937509977652, -13.97604488694527269, 78.12390960531433848 ) ) ;
#67094 = CARTESIAN_POINT ( 'NONE',  ( 5.719274019375991003, -21.55341960407610458, 42.70724293864770260 ) ) ;
#67096 = CARTESIAN_POINT ( 'NONE',  ( -8.314922557961024197, 14.29746914071037800, 27.91775706135234358 ) ) ;
#67095 = CARTESIAN_POINT ( 'NONE',  ( 21.53943276465977519, -0.05219959533907433946, 83.74890960531435269 ) ) ;
#67097 = CARTESIAN_POINT ( 'NONE',  ( 15.80617190586746368, 15.72974639402197994, 29.37390960531435269 ) ) ;
#67098 = CARTESIAN_POINT ( 'NONE',  ( -5.823673210054431948, 21.52544592524334988, 77.70942372801900433 ) ) ;
#67099 = CARTESIAN_POINT ( 'NONE',  ( 13.89961937509977652, -13.97604488694527269, 73.12390960531436690 ) ) ;
#67100 = CARTESIAN_POINT ( 'NONE',  ( 13.97604488694527802, 13.89961937509977652, 34.37390960531436690 ) ) ;
#67101 = CARTESIAN_POINT ( 'NONE',  ( 19.05341960407611168, 5.049401038298154454, 83.95724293864766707 ) ) ;
#67102 = CARTESIAN_POINT ( 'NONE',  ( -14.34966873604960291, -8.224510206698953496, 91.66557627198103830 ) ) ;
#67103 = ORIENTED_EDGE ( 'NONE', *, *, #92660, .F. ) ;
#67104 = CARTESIAN_POINT ( 'NONE',  ( -13.97604488694547697, 13.89961937509957934, 108.1260903946856331 ) ) ;
#67105 = DIRECTION ( 'NONE',  ( 1.000000000000000000, 0.000000000000000000, 0.000000000000000000 ) ) ;
#67106 = CARTESIAN_POINT ( 'NONE',  ( 5.049401038298161559, -19.05341960407611168, 67.70724293864769550 ) ) ;
#67107 = VECTOR ( 'NONE', #80692, 1000.000000000000000 ) ;
#67109 = CARTESIAN_POINT ( 'NONE',  ( 16.51473224551069308, 9.474510206698969483, 114.1655762719810241 ) ) ;
#67108 = CARTESIAN_POINT ( 'NONE',  ( 18.67979575497194134, -10.72451020669871369, 90.83442372801901854 ) ) ;
#67110 = CARTESIAN_POINT ( 'NONE',  ( -4.483927247898782831, 16.52544592524335698, 82.70942372801900433 ) ) ;
#67111 = CARTESIAN_POINT ( 'NONE',  ( -29.64248797448946249, 1.297617798568585501, -48.74145669546046378 ) ) ;
#67112 = CARTESIAN_POINT ( 'NONE',  ( -0.05219959533936034679, 19.03943276465977164, 52.50109039468566863 ) ) ;
#67113 = CARTESIAN_POINT ( 'NONE',  ( 0.05219959533936267826, -19.03943276465977164, 20.00109039468567218 ) ) ;
#67114 = CARTESIAN_POINT ( 'NONE',  ( -28.79475375365577250, -9.355982642739318678, 144.0843446569000150 ) ) ;
#67115 = CARTESIAN_POINT ( 'NONE',  ( 3.181980515339834614, 34.99999999999997158, 1.110912703473986074 ) ) ;
#67116 = CARTESIAN_POINT ( 'NONE',  ( 36.91746824999999887, 11.99521256947799053, -6.024999997268811747 ) ) ;
#67117 = CARTESIAN_POINT ( 'NONE',  ( -12.14591786802309592, -12.06949235617757132, 26.87390960531435979 ) ) ;
#67118 = CARTESIAN_POINT ( 'NONE',  ( -19.97888994334923751, -34.65319547504295628, -4.999999999999999112 ) ) ;
#67119 = CARTESIAN_POINT ( 'NONE',  ( -16.52544592524335698, -4.483927247898792601, 103.9594237280190185 ) ) ;
#67120 = CARTESIAN_POINT ( 'NONE',  ( 33.72732726872323639, -21.50529672980692908, -24.82116981130025124 ) ) ;
#67121 = CARTESIAN_POINT ( 'NONE',  ( 16.53943276465976808, 0.05219959533934440121, 86.25109039468568994 ) ) ;
#67122 = CARTESIAN_POINT ( 'NONE',  ( 5.823673210054444382, -21.52544592524334988, 100.2094237280190043 ) ) ;
#67123 = CARTESIAN_POINT ( 'NONE',  ( -13.97604488694547697, 13.89961937509957934, 108.1260903946856331 ) ) ;
#67124 = CARTESIAN_POINT ( 'NONE',  ( 18.67979575497194134, -10.72451020669871369, 60.83442372801901854 ) ) ;
#67125 = CARTESIAN_POINT ( 'NONE',  ( -19.02544592524334988, -5.153800228976617603, 38.95942372801900433 ) ) ;
#67126 = CARTESIAN_POINT ( 'NONE',  ( -16.51473224551069308, -9.474510206698971260, 81.66557627198103830 ) ) ;
#67127 = CARTESIAN_POINT ( 'NONE',  ( -19.03943276465977164, 0.05219959533909376836, 56.24890960531435979 ) ) ;
#67128 = CARTESIAN_POINT ( 'NONE',  ( 26.99873734152913229, -22.49873734152921045, 8.889087296526001936 ) ) ;
#67129 = CARTESIAN_POINT ( 'NONE',  ( -18.67979575497178146, -10.72451020669898902, 96.66557627198102409 ) ) ;
#67130 = CARTESIAN_POINT ( 'NONE',  ( 21.55341960407610458, 5.719274019375980345, 48.95724293864770971 ) ) ;
#67131 = CARTESIAN_POINT ( 'NONE',  ( -0.05219959533909027116, -19.03943276465977164, 42.49890960531435269 ) ) ;
#67132 = CARTESIAN_POINT ( 'NONE',  ( -12.14591786802326823, 12.06949235617739902, 63.12609039468568994 ) ) ;
#67133 = EDGE_CURVE ( 'NONE', #174275, #44164, #61583, .T. ) ;
#67134 = ORIENTED_EDGE ( 'NONE', *, *, #34865, .T. ) ;
#67135 = CARTESIAN_POINT ( 'NONE',  ( -15.72974639402176322, -15.80617190586768395, 49.37609039468569705 ) ) ;
#67137 = CARTESIAN_POINT ( 'NONE',  ( -36.91746825000000598, 2.428612866367529932E-14, -0.6249999972688132788 ) ) ;
#67136 = CARTESIAN_POINT ( 'NONE',  ( -16.52544592524342804, 4.483927247898546575, 66.04057627198103830 ) ) ;
#67138 = CARTESIAN_POINT ( 'NONE',  ( 4.483927247898790824, -16.52544592524335698, 45.20942372801901854 ) ) ;
#67139 = CARTESIAN_POINT ( 'NONE',  ( -8.314922557960811034, -14.29746914071050412, 107.0822429386476955 ) ) ;
#67140 = CARTESIAN_POINT ( 'NONE',  ( -16.51473224551082808, 9.474510206698731452, 58.33442372801900433 ) ) ;
#67141 = CARTESIAN_POINT ( 'NONE',  ( 0.05219959533910956823, 16.53943276465976808, 74.99890960531435269 ) ) ;
#67142 = CARTESIAN_POINT ( 'NONE',  ( 18.62759615963255655, 10.81492255796105972, 26.66775706135235424 ) ) ;
#67144 = CARTESIAN_POINT ( 'NONE',  ( -15.72974639402197994, 15.80617190586746368, 90.62390960531436690 ) ) ;
#67143 = CARTESIAN_POINT ( 'NONE',  ( 21.23184647844211881, -181.1785498424364675, -15.00000000000000000 ) ) ;
#67145 = CARTESIAN_POINT ( 'NONE',  ( -0.05219959533909027116, -19.03943276465977164, 97.49890960531436690 ) ) ;
#67146 = CARTESIAN_POINT ( 'NONE',  ( 14.29746914071049879, -8.314922557960816363, 78.33224293864770971 ) ) ;
#67147 = CARTESIAN_POINT ( 'NONE',  ( 17.67029085834301227, -36.01944455193423522, -22.64778610421477723 ) ) ;
#67148 = CARTESIAN_POINT ( 'NONE',  ( 36.91746824999999177, 11.99521256947799230, -1.524999997268813523 ) ) ;
#67149 = CARTESIAN_POINT ( 'NONE',  ( 19.02544592524334988, 5.153800228976608722, 86.45942372801900433 ) ) ;
#67150 = CARTESIAN_POINT ( 'NONE',  ( 15.72974639402176855, 15.80617190586768217, 26.87609039468567218 ) ) ;
#67151 = CARTESIAN_POINT ( 'NONE',  ( -19.05341960407611168, -5.049401038298163336, 76.45724293864769550 ) ) ;
#67152 = CARTESIAN_POINT ( 'NONE',  ( -9.474510206698720793, -16.51473224551083518, 59.58442372801900433 ) ) ;
#67153 = CARTESIAN_POINT ( 'NONE',  ( 19.02544592524343514, -5.153800228976328945, 43.54057627198103120 ) ) ;
#67154 = PRODUCT_RELATED_PRODUCT_CATEGORY ( 'part', '', ( #29103 ) ) ;
#67155 = CARTESIAN_POINT ( 'NONE',  ( -12.06949235617756955, 12.14591786802309770, 60.62390960531437401 ) ) ;
#67156 = CARTESIAN_POINT ( 'NONE',  ( 4.379528057220339221, -16.55341960407611168, 57.70724293864770260 ) ) ;
#67157 = CARTESIAN_POINT ( 'NONE',  ( -9.564922557960796823, -16.46253265017161027, 77.08224293864769550 ) ) ;
#67158 = CARTESIAN_POINT ( 'NONE',  ( -21.53943276465977519, 0.05219959533907696930, 81.24890960531436690 ) ) ;
#67159 = CARTESIAN_POINT ( 'NONE',  ( -9.564922557960796823, -16.46253265017161027, 67.08224293864769550 ) ) ;
#67160 = CARTESIAN_POINT ( 'NONE',  ( -5.719274019375978568, 21.55341960407610458, 85.20724293864770971 ) ) ;
#67161 = CARTESIAN_POINT ( 'NONE',  ( 0.05219959533936267826, -19.03943276465977164, 20.00109039468567218 ) ) ;
#67164 = CARTESIAN_POINT ( 'NONE',  ( -14.29746914071049879, 8.314922557960819915, 90.83224293864769550 ) ) ;
#67163 = CARTESIAN_POINT ( 'NONE',  ( 8.314922557961029526, -14.29746914071037800, 110.4177570613523756 ) ) ;
#67162 = DIRECTION ( 'NONE',  ( 1.000000000000000000, 0.000000000000000000, 0.000000000000000000 ) ) ;
#67165 = CARTESIAN_POINT ( 'NONE',  ( -19.05341960407617563, 5.049401038297882671, 88.54275706135230450 ) ) ;
#67166 = ORIENTED_EDGE ( 'NONE', *, *, #136461, .T. ) ;
#67167 = CARTESIAN_POINT ( 'NONE',  ( -18.62759615963255300, -10.81492255796106328, 24.16775706135235424 ) ) ;
#67168 = CARTESIAN_POINT ( 'NONE',  ( -16.46253265017146816, -9.564922557961047289, 59.16775706135233293 ) ) ;
#67169 = CARTESIAN_POINT ( 'NONE',  ( -8.224510206698735004, -14.34966873604973081, 99.58442372801900433 ) ) ;
#67170 = CARTESIAN_POINT ( 'NONE',  ( 9.564922557961047289, -16.46253265017146816, 45.41775706135232582 ) ) ;
#67171 = CARTESIAN_POINT ( 'NONE',  ( -19.02544592524342804, 5.153800228976336051, 101.0405762719810241 ) ) ;
#67172 = CARTESIAN_POINT ( 'NONE',  ( 4.483927247898545687, 16.52544592524342804, 59.79057627198103120 ) ) ;
#67173 = DIRECTION ( 'NONE',  ( 0.000000000000000000, 0.000000000000000000, -1.000000000000000000 ) ) ;
#67174 = CARTESIAN_POINT ( 'NONE',  ( 13.89961937509977652, -13.97604488694527269, 38.12390960531436690 ) ) ;
#67175 = CARTESIAN_POINT ( 'NONE',  ( -5.823673210054431948, 21.52544592524334988, 102.7094237280190185 ) ) ;
#67176 = CARTESIAN_POINT ( 'NONE',  ( -16.52544592524335698, -4.483927247898792601, 78.95942372801901854 ) ) ;
#67177 = CARTESIAN_POINT ( 'NONE',  ( -21.55341960407619339, 5.719274019375674811, 38.54275706135234714 ) ) ;
#67178 = CARTESIAN_POINT ( 'NONE',  ( 16.55341960407618274, -4.379528057220086978, 41.04275706135236135 ) ) ;
#67179 = CARTESIAN_POINT ( 'NONE',  ( -19.02544592524342804, 5.153800228976336051, 101.0405762719810241 ) ) ;
#67180 = CARTESIAN_POINT ( 'NONE',  ( 19.05341960407611168, 5.049401038298154454, 53.95724293864770260 ) ) ;
#67181 = CARTESIAN_POINT ( 'NONE',  ( 16.46253265017160672, -9.564922557960803928, 68.33224293864770971 ) ) ;
#67182 = CARTESIAN_POINT ( 'NONE',  ( 16.53943276465976808, 0.05219959533934440121, 51.25109039468568994 ) ) ;
#67183 = CARTESIAN_POINT ( 'NONE',  ( -8.314922557960811034, -14.29746914071050412, 112.0822429386477097 ) ) ;
#67184 = CARTESIAN_POINT ( 'NONE',  ( -0.05219959533910754901, -16.53943276465976808, 22.49890960531436335 ) ) ;
#67185 = DIRECTION ( 'NONE',  ( 0.000000000000000000, 0.000000000000000000, 1.000000000000000000 ) ) ;
#67188 = CARTESIAN_POINT ( 'NONE',  ( 16.46253265017160672, -9.564922557960803928, 58.33224293864769550 ) ) ;
#67187 = CARTESIAN_POINT ( 'NONE',  ( 16.46253265017160672, -9.564922557960803928, 93.33224293864769550 ) ) ;
#67186 = CARTESIAN_POINT ( 'NONE',  ( -18.62759615963255300, -10.81492255796106328, 54.16775706135235424 ) ) ;
#67189 = CARTESIAN_POINT ( 'NONE',  ( 16.51473224551069308, 9.474510206698969483, 94.16557627198103830 ) ) ;
#67190 = CARTESIAN_POINT ( 'NONE',  ( 16.53943276465976808, -0.05219959533910856209, 38.74890960531435979 ) ) ;
#67191 = CARTESIAN_POINT ( 'NONE',  ( 16.53943276465976808, 0.05219959533934440121, 111.2510903946856899 ) ) ;
#67192 = CARTESIAN_POINT ( 'NONE',  ( -12.06949235617756955, 12.14591786802309770, 35.62390960531437401 ) ) ;
#67193 = CARTESIAN_POINT ( 'NONE',  ( 18.09867054820433907, 5.499999999999817923, 56.48393025253586330 ) ) ;
#67194 = CARTESIAN_POINT ( 'NONE',  ( -9.564922557960796823, -16.46253265017161027, 67.08224293864769550 ) ) ;
#67195 = CARTESIAN_POINT ( 'NONE',  ( -0.05219959533936034679, 19.03943276465977164, 42.50109039468566152 ) ) ;
#67196 = CARTESIAN_POINT ( 'NONE',  ( 22.81625015709509441, 31.40387420917330275, -7.824999997268813345 ) ) ;
#67197 = CARTESIAN_POINT ( 'NONE',  ( 9.474510206698971260, -16.51473224551069308, 67.91557627198102409 ) ) ;
#67199 = CARTESIAN_POINT ( 'NONE',  ( -4.483927247898782831, 16.52544592524335698, 62.70942372801902565 ) ) ;
#67198 = CARTESIAN_POINT ( 'NONE',  ( -9.564922557961040184, 16.46253265017147172, 82.91775706135233293 ) ) ;
#67200 = CARTESIAN_POINT ( 'NONE',  ( -24.93942350307309752, 7.769968609432599926, 171.2173313942149946 ) ) ;
#67201 = CARTESIAN_POINT ( 'NONE',  ( 16.51473224551069308, 9.474510206698969483, 94.16557627198103830 ) ) ;
#67202 = CARTESIAN_POINT ( 'NONE',  ( -5.719274019375665041, -21.55341960407619695, 24.79275706135235779 ) ) ;
#67203 = CARTESIAN_POINT ( 'NONE',  ( 16.51473224551083163, -9.474510206698727899, 85.83442372801900433 ) ) ;
#67205 = CARTESIAN_POINT ( 'NONE',  ( 16.46253265017160672, -9.564922557960803928, 53.33224293864768839 ) ) ;
#67204 = CARTESIAN_POINT ( 'NONE',  ( 17.26172910966779028, 6.454744622555872446, 86.69353091350778584 ) ) ;
#67206 = CARTESIAN_POINT ( 'NONE',  ( -13.89961937509977652, 13.97604488694528158, 85.62390960531433848 ) ) ;
#67208 = CARTESIAN_POINT ( 'NONE',  ( -16.46253265017160317, 9.564922557960807481, 45.83224293864769550 ) ) ;
#67207 = CARTESIAN_POINT ( 'NONE',  ( -16.55341960407611168, -4.379528057220339221, 51.45724293864770260 ) ) ;
#67209 = CARTESIAN_POINT ( 'NONE',  ( -5.049401038297874678, -19.05341960407617918, 64.79275706135233293 ) ) ;
#67210 = CARTESIAN_POINT ( 'NONE',  ( -14.29746914071049879, 8.314922557960819915, 90.83224293864769550 ) ) ;
#67211 = CARTESIAN_POINT ( 'NONE',  ( 19.05341960407617918, -5.049401038297876454, 31.04275706135232227 ) ) ;
#67212 = CARTESIAN_POINT ( 'NONE',  ( 13.89961937509977652, -13.97604488694527269, 68.12390960531436690 ) ) ;
#67213 = CARTESIAN_POINT ( 'NONE',  ( 5.823673210054125526, 21.52544592524343514, 64.79057627198103830 ) ) ;
#67215 = CARTESIAN_POINT ( 'NONE',  ( 21.53943276465977519, 0.05219959533937863772, 111.2510903946856899 ) ) ;
#67214 = CARTESIAN_POINT ( 'NONE',  ( -16.53943276465976808, 0.05219959533911058130, 66.24890960531436690 ) ) ;
#67216 = CARTESIAN_POINT ( 'NONE',  ( 9.564922557960805705, 16.46253265017160317, 109.5822429386476955 ) ) ;
#67217 = CARTESIAN_POINT ( 'NONE',  ( -21.52544592524343514, 5.823673210054127303, 31.04057627198102409 ) ) ;
#67218 = CARTESIAN_POINT ( 'NONE',  ( 9.474510206698971260, -16.51473224551069308, 47.91557627198102409 ) ) ;
#67219 = CARTESIAN_POINT ( 'NONE',  ( 13.97604488694527802, 13.89961937509977652, 44.37390960531435269 ) ) ;
#67220 = CARTESIAN_POINT ( 'NONE',  ( -8.224510206698948167, 14.34966873604960824, 95.41557627198102409 ) ) ;
#67221 = CARTESIAN_POINT ( 'NONE',  ( 0.05219959533907565091, 21.53943276465977519, 114.9989096053143669 ) ) ;
#67222 = CARTESIAN_POINT ( 'NONE',  ( 9.474510206698971260, -16.51473224551069308, 97.91557627198102409 ) ) ;
#67223 = CARTESIAN_POINT ( 'NONE',  ( -18.62759615963255300, -10.81492255796106328, 34.16775706135234714 ) ) ;
#67224 = CARTESIAN_POINT ( 'NONE',  ( -19.02544592524342804, 5.153800228976336051, 101.0405762719810241 ) ) ;
#67225 = CARTESIAN_POINT ( 'NONE',  ( 5.049401038298161559, -19.05341960407611168, 22.70724293864769194 ) ) ;
#67226 = CARTESIAN_POINT ( 'NONE',  ( -21.52544592524334988, -5.823673210054445271, 83.95942372801900433 ) ) ;
#67227 = CARTESIAN_POINT ( 'NONE',  ( -5.823673210054116645, -21.52544592524344225, 97.29057627198105251 ) ) ;
#67228 = CARTESIAN_POINT ( 'NONE',  ( -15.06137443927351072, 15.06137443927345210, -56.46919128290398504 ) ) ;
#67229 = CARTESIAN_POINT ( 'NONE',  ( -18.22780087662121673, -5.500000000000062172, 51.48459894673893444 ) ) ;
#67230 = CARTESIAN_POINT ( 'NONE',  ( -23.48529157249599919, -32.32473071737749848, -1.699999999999999956 ) ) ;
#67231 = CARTESIAN_POINT ( 'NONE',  ( -16.52544592524335698, -4.483927247898792601, 48.95942372801902565 ) ) ;
#67232 = CARTESIAN_POINT ( 'NONE',  ( -14.34966873604960291, -8.224510206698953496, 101.6655762719810383 ) ) ;
#67233 = CARTESIAN_POINT ( 'NONE',  ( 33.73406392173259150, -5.500497537618388222, 95.16330145977877919 ) ) ;
#67234 = CARTESIAN_POINT ( 'NONE',  ( 9.564922557960805705, 16.46253265017160317, 54.58224293864769550 ) ) ;
#67235 = CARTESIAN_POINT ( 'NONE',  ( -16.52544592524342804, 4.483927247898546575, 91.04057627198103830 ) ) ;
#67236 = CARTESIAN_POINT ( 'NONE',  ( 10.72451020669898902, -18.67979575497178502, 42.91557627198103120 ) ) ;
#67237 = CARTESIAN_POINT ( 'NONE',  ( -4.483927247898539470, -16.52544592524342804, 62.29057627198102409 ) ) ;
#67238 = CARTESIAN_POINT ( 'NONE',  ( 8.224510206698742110, 14.34966873604972548, 27.08442372801901854 ) ) ;
#67239 = CARTESIAN_POINT ( 'NONE',  ( 21.55341960407619695, -5.719274019375665929, 86.04275706135236135 ) ) ;
#67240 = CARTESIAN_POINT ( 'NONE',  ( 17.44270441346514389, -5.991230190323080684, 76.13664920735770636 ) ) ;
#67241 = CARTESIAN_POINT ( 'NONE',  ( -16.55341960407617563, 4.379528057220093196, 93.54275706135234714 ) ) ;
#67242 = CARTESIAN_POINT ( 'NONE',  ( 16.55341960407611168, 4.379528057220329451, 38.95724293864768839 ) ) ;
#67243 = CARTESIAN_POINT ( 'NONE',  ( 19.02544592524343514, -5.153800228976328945, 38.54057627198103120 ) ) ;
#67244 = CARTESIAN_POINT ( 'NONE',  ( -16.46253265017160317, 9.564922557960807481, 85.83224293864769550 ) ) ;
#67245 = CARTESIAN_POINT ( 'NONE',  ( 5.823673210054125526, 21.52544592524343514, 99.79057627198103830 ) ) ;
#67246 = CARTESIAN_POINT ( 'NONE',  ( -12.06949235617739369, -12.14591786802326823, 44.37609039468567573 ) ) ;
#67248 = CARTESIAN_POINT ( 'NONE',  ( 15.72974639402176855, 15.80617190586768217, 86.87609039468568994 ) ) ;
#67247 = CARTESIAN_POINT ( 'NONE',  ( -4.483927247898539470, -16.52544592524342804, 62.29057627198102409 ) ) ;
#67249 = CIRCLE ( 'NONE', #167451, 61.99999999999998579 ) ;
#67250 = CARTESIAN_POINT ( 'NONE',  ( 8.314922557961029526, -14.29746914071037800, 100.4177570613523471 ) ) ;
#67251 = CARTESIAN_POINT ( 'NONE',  ( 16.21995358207305671, 7.366697692864113911, 27.56448998487843127 ) ) ;
#67252 = DIRECTION ( 'NONE',  ( 0.7071067811865466846, -2.468850131082262977E-15, -0.7071067811865484609 ) ) ;
#67253 = CARTESIAN_POINT ( 'NONE',  ( 16.55341960407611168, 4.379528057220329451, 23.95724293864769550 ) ) ;
#67254 = CARTESIAN_POINT ( 'NONE',  ( 14.34966873604972726, -8.224510206698740333, 75.83442372801900433 ) ) ;
#67255 = CARTESIAN_POINT ( 'NONE',  ( -16.46253265017160317, 9.564922557960807481, 80.83224293864769550 ) ) ;
#67256 = CARTESIAN_POINT ( 'NONE',  ( 5.153800228976335163, 19.02544592524342804, 94.79057627198103830 ) ) ;
#67257 = CARTESIAN_POINT ( 'NONE',  ( -5.719274019375665041, -21.55341960407619695, 89.79275706135236135 ) ) ;
#67258 = CARTESIAN_POINT ( 'NONE',  ( 16.52544592524335698, 4.483927247898782831, 86.45942372801901854 ) ) ;
#67259 = CARTESIAN_POINT ( 'NONE',  ( -14.34966873604960291, -8.224510206698953496, 66.66557627198102409 ) ) ;
#67260 = CARTESIAN_POINT ( 'NONE',  ( 5.049401038298161559, -19.05341960407611168, 72.70724293864768129 ) ) ;
#67261 = ORIENTED_EDGE ( 'NONE', *, *, #79473, .F. ) ;
#67262 = CARTESIAN_POINT ( 'NONE',  ( -19.03943276465977164, -0.05219959533935918106, 103.7510903946856757 ) ) ;
#67263 = CARTESIAN_POINT ( 'NONE',  ( 16.52544592524342804, -4.483927247898539470, 108.5405762719810241 ) ) ;
#67264 = CARTESIAN_POINT ( 'NONE',  ( -9.564922557960796823, -16.46253265017161027, 72.08224293864770971 ) ) ;
#67266 = CARTESIAN_POINT ( 'NONE',  ( 11.40812507854754365, 35.11059874428196537, -9.224999997268813701 ) ) ;
#67265 = CARTESIAN_POINT ( 'NONE',  ( -0.05219959533936034679, 19.03943276465977164, 112.5010903946856757 ) ) ;
#67267 = CARTESIAN_POINT ( 'NONE',  ( -19.03943276465977164, -0.05219959533935918106, 18.75109039468567218 ) ) ;
#67268 = CARTESIAN_POINT ( 'NONE',  ( 4.379528057220092307, 16.55341960407617563, 87.29275706135236135 ) ) ;
#67269 = CARTESIAN_POINT ( 'NONE',  ( 13.89961937509957401, 13.97604488694547697, 106.8760903946856757 ) ) ;
#67270 = CARTESIAN_POINT ( 'NONE',  ( -16.52544592524342804, 4.483927247898546575, 116.0405762719810383 ) ) ;
#67271 = CARTESIAN_POINT ( 'NONE',  ( 4.379528057220092307, 16.55341960407617563, 72.29275706135236135 ) ) ;
#67272 = CARTESIAN_POINT ( 'NONE',  ( -8.314922557961024197, 14.29746914071037800, 47.91775706135234714 ) ) ;
#67273 = FACE_OUTER_BOUND ( 'NONE', #28412, .T. ) ;
#67274 = CARTESIAN_POINT ( 'NONE',  ( -19.02544592524334988, -5.153800228976617603, 73.95942372801900433 ) ) ;
#67275 = CARTESIAN_POINT ( 'NONE',  ( 5.719274019375673035, 21.55341960407619339, 112.2927570613523471 ) ) ;
#67276 = CARTESIAN_POINT ( 'NONE',  ( -9.564922557960796823, -16.46253265017161027, 32.08224293864769550 ) ) ;
#67277 = CARTESIAN_POINT ( 'NONE',  ( 13.89961937509977652, -13.97604488694527269, 73.12390960531436690 ) ) ;
#67278 = CARTESIAN_POINT ( 'NONE',  ( 12.06949235617757843, -12.14591786802309237, 68.12390960531436690 ) ) ;
#67279 = CARTESIAN_POINT ( 'NONE',  ( 9.474510206698729675, 16.51473224551082808, 47.08442372801900433 ) ) ;
#67280 = CARTESIAN_POINT ( 'NONE',  ( 21.53943276465977519, -0.05219959533907433946, 43.74890960531435979 ) ) ;
#67281 = CARTESIAN_POINT ( 'NONE',  ( -0.05219959533937732626, 21.53943276465977519, 112.5010903946857042 ) ) ;
#67282 = CARTESIAN_POINT ( 'NONE',  ( -19.02544592524342804, 5.153800228976336051, 86.04057627198103830 ) ) ;
#67283 = ADVANCED_FACE ( 'NONE', ( #184990 ), #150886, .T. ) ;
#67284 = CARTESIAN_POINT ( 'NONE',  ( -21.53943276465977519, -0.05219959533937600094, 103.7510903946857042 ) ) ;
#67285 = CARTESIAN_POINT ( 'NONE',  ( -21.52544592524343514, 5.823673210054127303, 61.04057627198103120 ) ) ;
#67286 = CARTESIAN_POINT ( 'NONE',  ( -13.89961937509977652, 13.97604488694528158, 90.62390960531432427 ) ) ;
#67287 = CARTESIAN_POINT ( 'NONE',  ( -9.564922557961040184, 16.46253265017147172, 72.91775706135233293 ) ) ;
#67288 = CARTESIAN_POINT ( 'NONE',  ( -5.153800228976328057, -19.02544592524343514, 97.29057627198099567 ) ) ;
#67289 = CARTESIAN_POINT ( 'NONE',  ( -0.05219959533936034679, 19.03943276465977164, 102.5010903946856757 ) ) ;
#67290 = CARTESIAN_POINT ( 'NONE',  ( 8.314922557961029526, -14.29746914071037800, 60.41775706135235424 ) ) ;
#67291 = CARTESIAN_POINT ( 'NONE',  ( -16.51473224551069308, -9.474510206698971260, 21.66557627198102765 ) ) ;
#67292 = CARTESIAN_POINT ( 'NONE',  ( 16.51473224551069308, 9.474510206698969483, 79.16557627198103830 ) ) ;
#67293 = CARTESIAN_POINT ( 'NONE',  ( -10.81492255796078084, -18.62759615963271287, 62.08224293864769550 ) ) ;
#67294 = CARTESIAN_POINT ( 'NONE',  ( -16.52544592524335698, -4.483927247898792601, 38.95942372801901854 ) ) ;
#67295 = CARTESIAN_POINT ( 'NONE',  ( -21.53943276465977519, -0.05219959533937600094, 28.75109039468567929 ) ) ;
#67296 = CARTESIAN_POINT ( 'NONE',  ( -21.52544592524334988, -5.823673210054445271, 83.95942372801900433 ) ) ;
#67297 = CARTESIAN_POINT ( 'NONE',  ( 14.34966873604972726, -8.224510206698740333, 100.8344237280190185 ) ) ;
#67298 = CARTESIAN_POINT ( 'NONE',  ( 16.46253265017160672, -9.564922557960803928, 83.33224293864768129 ) ) ;
#67299 = CARTESIAN_POINT ( 'NONE',  ( -14.29746914071049879, 8.314922557960819915, 75.83224293864769550 ) ) ;
#67300 = CARTESIAN_POINT ( 'NONE',  ( 8.314922557960818139, 14.29746914071049879, 24.58224293864768839 ) ) ;
#67301 = CARTESIAN_POINT ( 'NONE',  ( -13.89961937509957401, -13.97604488694547875, 74.37609039468566152 ) ) ;
#67302 = CARTESIAN_POINT ( 'NONE',  ( 5.823673210054444382, -21.52544592524334988, 50.20942372801901854 ) ) ;
#67303 = CARTESIAN_POINT ( 'NONE',  ( -0.05219959533910754901, -16.53943276465976808, 97.49890960531436690 ) ) ;
#67304 = CARTESIAN_POINT ( 'NONE',  ( -19.03943276465977164, 0.05219959533909376836, 116.2489096053143669 ) ) ;
#67305 = CARTESIAN_POINT ( 'NONE',  ( -8.224510206698735004, -14.34966873604973081, 99.58442372801900433 ) ) ;
#67306 = CARTESIAN_POINT ( 'NONE',  ( 10.72451020669871369, 18.67979575497193778, 92.08442372801901854 ) ) ;
#67307 = CARTESIAN_POINT ( 'NONE',  ( 0.05219959533934541429, -16.53943276465976808, 40.00109039468567573 ) ) ;
#67308 = CARTESIAN_POINT ( 'NONE',  ( 21.52544592524334988, 5.823673210054432836, 36.45942372801901143 ) ) ;
#67309 = ORIENTED_EDGE ( 'NONE', *, *, #30819, .F. ) ;
#67310 = CARTESIAN_POINT ( 'NONE',  ( -21.52544592524343514, 5.823673210054127303, 116.0405762719810383 ) ) ;
#67311 = CARTESIAN_POINT ( 'NONE',  ( 4.379528057220339221, -16.55341960407611168, 87.70724293864769550 ) ) ;
#67312 = CARTESIAN_POINT ( 'NONE',  ( -3.573655867282028392E-15, 2.428612866367529932E-14, 155.0000000000000000 ) ) ;
#67313 = CARTESIAN_POINT ( 'NONE',  ( -4.483927247898539470, -16.52544592524342804, 62.29057627198102409 ) ) ;
#67314 = CARTESIAN_POINT ( 'NONE',  ( -12.06949235617739369, -12.14591786802326823, 104.3760903946856899 ) ) ;
#67315 = CARTESIAN_POINT ( 'NONE',  ( -16.51473224551069308, -9.474510206698971260, 36.66557627198102409 ) ) ;
#67316 = CARTESIAN_POINT ( 'NONE',  ( 5.823673210054125526, 21.52544592524343514, 39.79057627198103830 ) ) ;
#67317 = CARTESIAN_POINT ( 'NONE',  ( -4.483927247898539470, -16.52544592524342804, 72.29057627198102409 ) ) ;
#67318 = CARTESIAN_POINT ( 'NONE',  ( -21.52544592524343514, 5.823673210054127303, 81.04057627198102409 ) ) ;
#67319 = CARTESIAN_POINT ( 'NONE',  ( 13.89961937509977652, -13.97604488694527269, 83.12390960531436690 ) ) ;
#67321 = CARTESIAN_POINT ( 'NONE',  ( 5.153800228976615827, -19.02544592524334988, 95.20942372801897591 ) ) ;
#67320 = CARTESIAN_POINT ( 'NONE',  ( -16.46253265017160317, 9.564922557960807481, 35.83224293864768839 ) ) ;
#67322 = CARTESIAN_POINT ( 'NONE',  ( -21.53943276465977519, 0.05219959533907696930, 36.24890960531435979 ) ) ;
#67323 = CARTESIAN_POINT ( 'NONE',  ( 0.05219959533937995610, -21.53943276465977519, 70.00109039468568994 ) ) ;
#67324 = CARTESIAN_POINT ( 'NONE',  ( 5.049401038298161559, -19.05341960407611168, 47.70724293864770260 ) ) ;
#67325 = CARTESIAN_POINT ( 'NONE',  ( 5.153800228976335163, 19.02544592524342804, 89.79057627198102409 ) ) ;
#67326 = VERTEX_POINT ( 'NONE', #124300 ) ;
#67327 = CARTESIAN_POINT ( 'NONE',  ( 4.483927247898790824, -16.52544592524335698, 65.20942372801901854 ) ) ;
#67328 = CARTESIAN_POINT ( 'NONE',  ( -5.823673210054431948, 21.52544592524334988, 42.70942372801901854 ) ) ;
#67329 = CARTESIAN_POINT ( 'NONE',  ( -21.53943276465977519, -0.05219959533937600094, 78.75109039468568994 ) ) ;
#67330 = CARTESIAN_POINT ( 'NONE',  ( -15.72974639402197994, 15.80617190586746368, 25.62390960531435624 ) ) ;
#67331 = CARTESIAN_POINT ( 'NONE',  ( -18.67979575497178146, -10.72451020669898902, 91.66557627198103830 ) ) ;
#67333 = CARTESIAN_POINT ( 'NONE',  ( 16.52544592524335698, 4.483927247898782831, 66.45942372801903275 ) ) ;
#67332 = CARTESIAN_POINT ( 'NONE',  ( -15.72974639402176322, -15.80617190586768395, 19.37609039468568639 ) ) ;
#67334 = CARTESIAN_POINT ( 'NONE',  ( 5.719274019375991003, -21.55341960407610458, 57.70724293864770260 ) ) ;
#67335 = CARTESIAN_POINT ( 'NONE',  ( -19.05341960407617563, 5.049401038297882671, 23.54275706135233648 ) ) ;
#67337 = CARTESIAN_POINT ( 'NONE',  ( 8.224510206698742110, 14.34966873604972548, 107.0844237280190043 ) ) ;
#67336 = CARTESIAN_POINT ( 'NONE',  ( 19.03943276465977164, -0.05219959533909143690, 63.74890960531435979 ) ) ;
#67338 = CARTESIAN_POINT ( 'NONE',  ( 37.99999999999999289, 2.893978650043524126E-14, -5.000000000000000000 ) ) ;
#67339 = B_SPLINE_CURVE_WITH_KNOTS ( 'NONE', 3,
 ( #15908, #172572, #125071, #77566, #93727, #713, #108901, #60404, #91720, #45254, #187759, #155409 ),
 .UNSPECIFIED., .F., .F.,
 ( 4, 2, 2, 2, 2, 4 ),
 ( 0.002611479512216078464, 0.003262097472420399501, 0.003912715432624720539, 0.004563333392829041144, 0.004888642372931204481, 0.005213951353033367819 ),
 .UNSPECIFIED. ) ;
#67340 = CARTESIAN_POINT ( 'NONE',  ( 5.049401038298161559, -19.05341960407611168, 92.70724293864769550 ) ) ;
#67341 = CARTESIAN_POINT ( 'NONE',  ( 20.70663425419854420, 22.78165926218171222, -47.27781451939568313 ) ) ;
#67342 = CARTESIAN_POINT ( 'NONE',  ( 19.02544592524334988, 5.153800228976608722, 76.45942372801897591 ) ) ;
#67343 = CARTESIAN_POINT ( 'NONE',  ( 21.53943276465977519, -0.05219959533907433946, 58.74890960531436690 ) ) ;
#67344 = CARTESIAN_POINT ( 'NONE',  ( 0.05219959533910956823, 16.53943276465976808, 24.99890960531435624 ) ) ;
#67345 = CARTESIAN_POINT ( 'NONE',  ( -13.97604488694547697, 13.89961937509957934, 93.12609039468566152 ) ) ;
#67346 = CARTESIAN_POINT ( 'NONE',  ( -16.46253265017160317, 9.564922557960807481, 40.83224293864769550 ) ) ;
#67347 = CARTESIAN_POINT ( 'NONE',  ( 19.03943276465977164, 0.05219959533936151252, 91.25109039468566152 ) ) ;
#67349 = CARTESIAN_POINT ( 'NONE',  ( -16.46253265017146816, -9.564922557961047289, 64.16775706135233293 ) ) ;
#67348 = CARTESIAN_POINT ( 'NONE',  ( 21.52544592524344225, -5.823673210054117533, 93.54057627198103830 ) ) ;
#67350 = CARTESIAN_POINT ( 'NONE',  ( 17.31728774477274513, 6.344390552232368918, 106.6809334831068128 ) ) ;
#67351 = CARTESIAN_POINT ( 'NONE',  ( -19.03943276465977164, 0.05219959533909376836, 51.24890960531436690 ) ) ;
#67352 = CARTESIAN_POINT ( 'NONE',  ( -0.05219959533910754901, -16.53943276465976808, 62.49890960531436690 ) ) ;
#67353 = CARTESIAN_POINT ( 'NONE',  ( 19.05341960407611168, 5.049401038298154454, 48.95724293864768129 ) ) ;
#67354 = CARTESIAN_POINT ( 'NONE',  ( 14.34966873604960469, 8.224510206698951720, 49.16557627198102409 ) ) ;
#67355 = DIRECTION ( 'NONE',  ( 1.000000000000000000, 0.000000000000000000, 0.000000000000000000 ) ) ;
#67356 = CARTESIAN_POINT ( 'NONE',  ( 31.91599925174810792, -5.957486376704251185, 90.41819350476903594 ) ) ;
#67357 = CARTESIAN_POINT ( 'NONE',  ( 12.06949235617757843, -12.14591786802309237, 33.12390960531435979 ) ) ;
#67358 = CARTESIAN_POINT ( 'NONE',  ( 19.02544592524343514, -5.153800228976328945, 58.54057627198102409 ) ) ;
#67359 = CARTESIAN_POINT ( 'NONE',  ( -9.564922557961040184, 16.46253265017147172, 72.91775706135233293 ) ) ;
#67360 = CARTESIAN_POINT ( 'NONE',  ( -19.05341960407617563, 5.049401038297882671, 43.54275706135232582 ) ) ;
#67361 = CARTESIAN_POINT ( 'NONE',  ( 8.224510206698742110, 14.34966873604972548, 47.08442372801901854 ) ) ;
#67362 = CARTESIAN_POINT ( 'NONE',  ( -5.823673210054116645, -21.52544592524344225, 47.29057627198103120 ) ) ;
#67363 = CARTESIAN_POINT ( 'NONE',  ( -10.72451020669870658, -18.67979575497194134, 109.5844237280190328 ) ) ;
#67364 = CARTESIAN_POINT ( 'NONE',  ( -5.049401038298153566, 19.05341960407611168, 70.20724293864769550 ) ) ;
#67365 = CARTESIAN_POINT ( 'NONE',  ( 22.55670631985092456, -22.55670631985084995, -49.13275782002545355 ) ) ;
#67366 = CARTESIAN_POINT ( 'NONE',  ( 19.03943276465977164, -0.05219959533909143690, 113.7489096053143669 ) ) ;
#67367 = CARTESIAN_POINT ( 'NONE',  ( 29.86685920354754842, -21.69954338932559068, -1.824999997268813345 ) ) ;
#67368 = CARTESIAN_POINT ( 'NONE',  ( 0.05219959533937995610, -21.53943276465977519, 45.00109039468568284 ) ) ;
#67369 = CARTESIAN_POINT ( 'NONE',  ( -4.483927247898539470, -16.52544592524342804, 87.29057627198103830 ) ) ;
#67371 = CARTESIAN_POINT ( 'NONE',  ( -0.05219959533909027116, -19.03943276465977164, 87.49890960531436690 ) ) ;
#67370 = CARTESIAN_POINT ( 'NONE',  ( -15.72974639402197994, 15.80617190586746368, 90.62390960531436690 ) ) ;
#67372 = CARTESIAN_POINT ( 'NONE',  ( 13.89961937509977652, -13.97604488694527269, 83.12390960531436690 ) ) ;
#67373 = CARTESIAN_POINT ( 'NONE',  ( -21.55341960407619339, 5.719274019375674811, 23.54275706135235424 ) ) ;
#67374 = EDGE_CURVE ( 'NONE', #27352, #133752, #185997, .T. ) ;
#67375 = ORIENTED_EDGE ( 'NONE', *, *, #166248, .F. ) ;
#67376 = CARTESIAN_POINT ( 'NONE',  ( -5.153800228976328057, -19.02544592524343514, 77.29057627198099567 ) ) ;
#67377 = CARTESIAN_POINT ( 'NONE',  ( -28.79475375365586842, 2.428612866367529932E-14, 147.9843446568999923 ) ) ;
#67379 = CARTESIAN_POINT ( 'NONE',  ( -16.51473224551069308, -9.474510206698971260, 36.66557627198102409 ) ) ;
#67378 = CARTESIAN_POINT ( 'NONE',  ( -9.564922557960796823, -16.46253265017161027, 22.08224293864768839 ) ) ;
#67380 = CARTESIAN_POINT ( 'NONE',  ( 19.03943276465977164, 0.05219959533936151252, 106.2510903946856615 ) ) ;
#67381 = CARTESIAN_POINT ( 'NONE',  ( 11.40812507854755253, -35.11059874428192273, -10.52499999726881263 ) ) ;
#67382 = CARTESIAN_POINT ( 'NONE',  ( -14.34966873604960291, -8.224510206698953496, 111.6655762719810525 ) ) ;
#67383 = CARTESIAN_POINT ( 'NONE',  ( 21.52544592524334988, 5.823673210054432836, 76.45942372801901854 ) ) ;
#67385 = CARTESIAN_POINT ( 'NONE',  ( -5.719274019375665041, -21.55341960407619695, 29.79275706135234358 ) ) ;
#67384 = CARTESIAN_POINT ( 'NONE',  ( 16.46253265017160672, -9.564922557960803928, 68.33224293864770971 ) ) ;
#67386 = CARTESIAN_POINT ( 'NONE',  ( 18.67979575497178502, 10.72451020669898547, 114.1655762719810383 ) ) ;
#67387 = CARTESIAN_POINT ( 'NONE',  ( 17.81289503416611453, -24.51734667627695785, 148.6999999999999602 ) ) ;
#67388 = CARTESIAN_POINT ( 'NONE',  ( 0.05219959533909260263, 19.03943276465977164, 79.99890960531436690 ) ) ;
#67389 = CARTESIAN_POINT ( 'NONE',  ( -5.000000000000000888, -130.0000000000000000, -13.99999999999999822 ) ) ;
#67391 = CARTESIAN_POINT ( 'NONE',  ( 10.81492255796078972, 18.62759615963270932, 39.58224293864769550 ) ) ;
#67390 = CARTESIAN_POINT ( 'NONE',  ( -14.34966873604972548, 8.224510206698743886, 28.33442372801902209 ) ) ;
#67392 = CARTESIAN_POINT ( 'NONE',  ( -0.05219959533937732626, 21.53943276465977519, 62.50109039468568284 ) ) ;
#67393 = CARTESIAN_POINT ( 'NONE',  ( 19.02544592524343514, -5.153800228976328945, 108.5405762719810383 ) ) ;
#67394 =( BOUNDED_CURVE ( )  B_SPLINE_CURVE ( 2, ( #132814, #194500, #27662, #197489, #135819, #102480, #40810, #116646, #58956, #117650, #178336, #100471, #179347 ),
 .UNSPECIFIED., .F., .T. ) 
 B_SPLINE_CURVE_WITH_KNOTS ( ( 3, 2, 2, 2, 2, 2, 3 ),
 ( 0.1603251732691504117, 0.1622807017543859698, 0.1666666666666666574, 0.1710526315789473728, 0.1754385964912280604, 0.1798245614035087758, 0.1817344100666542506 ),
 .UNSPECIFIED. ) 
 CURVE ( )  GEOMETRIC_REPRESENTATION_ITEM ( )  RATIONAL_B_SPLINE_CURVE ( ( 0.9831626618144004848, 0.9848076720550091867, 1.000000000000000000, 0.9659258262890683122, 1.000000000000000000, 0.9659258262890683122, 1.000000000000000000, 0.9659258262890683122, 1.000000000000000000, 0.9659258262890683122, 1.000000000000000000, 0.9851625545550090068, 0.9832469066685280978 ) ) 
 REPRESENTATION_ITEM ( '' )  );
#67395 = CARTESIAN_POINT ( 'NONE',  ( -9.564922557961040184, 16.46253265017147172, 97.91775706135233293 ) ) ;
#67396 = CARTESIAN_POINT ( 'NONE',  ( 19.05341960407611168, 5.049401038298154454, 43.95724293864769550 ) ) ;
#67397 = CARTESIAN_POINT ( 'NONE',  ( 5.049401038298161559, -19.05341960407611168, 87.70724293864769550 ) ) ;
#67398 = CARTESIAN_POINT ( 'NONE',  ( -12.14591786802309592, -12.06949235617757132, 91.87390960531436690 ) ) ;
#67399 = CARTESIAN_POINT ( 'NONE',  ( 0.05219959533910956823, 16.53943276465976808, 94.99890960531436690 ) ) ;
#67401 = EDGE_CURVE ( 'NONE', #28211, #173655, #191943, .T. ) ;
#67400 = CARTESIAN_POINT ( 'NONE',  ( 13.89961937509977652, -13.97604488694527269, 108.1239096053143669 ) ) ;
#67403 = CARTESIAN_POINT ( 'NONE',  ( 19.02544592524343514, -5.153800228976328945, 38.54057627198103120 ) ) ;
#67402 = CARTESIAN_POINT ( 'NONE',  ( -16.52544592524342804, 4.483927247898546575, 51.04057627198103120 ) ) ;
#67404 = CARTESIAN_POINT ( 'NONE',  ( 0.05219959533937995610, -21.53943276465977519, 60.00109039468568284 ) ) ;
#67405 = CARTESIAN_POINT ( 'NONE',  ( 19.05341960407617918, -5.049401038297876454, 96.04275706135231871 ) ) ;
#67406 = CARTESIAN_POINT ( 'NONE',  ( -4.483927247898539470, -16.52544592524342804, 57.29057627198103120 ) ) ;
#67407 = CARTESIAN_POINT ( 'NONE',  ( -10.72451020669898014, 18.67979575497178502, 115.4155762719810241 ) ) ;
#67408 = CARTESIAN_POINT ( 'NONE',  ( 21.55341960407610458, 5.719274019375980345, 48.95724293864770971 ) ) ;
#67409 = CARTESIAN_POINT ( 'NONE',  ( -19.05341960407611168, -5.049401038298163336, 106.4572429386476955 ) ) ;
#67410 = CARTESIAN_POINT ( 'NONE',  ( 28.82186960331498327, 2.781578969918950771E-14, 139.2500000054623683 ) ) ;
#67411 = CARTESIAN_POINT ( 'NONE',  ( -13.97604488694527625, -13.89961937509977652, 61.87390960531435979 ) ) ;
#67412 = CARTESIAN_POINT ( 'NONE',  ( 16.53943276465976808, -0.05219959533910856209, 38.74890960531435979 ) ) ;
#67413 = CARTESIAN_POINT ( 'NONE',  ( 4.379528057220092307, 16.55341960407617563, 97.29275706135234714 ) ) ;
#67414 = CARTESIAN_POINT ( 'NONE',  ( -12.06949235617739369, -12.14591786802326823, 79.37609039468567573 ) ) ;
#67415 = CARTESIAN_POINT ( 'NONE',  ( -16.51473224551082808, 9.474510206698731452, 33.33442372801899722 ) ) ;
#67416 = CARTESIAN_POINT ( 'NONE',  ( -24.81835718235489097, -6.052279806424480491, 168.4265042179603427 ) ) ;
#67417 = CARTESIAN_POINT ( 'NONE',  ( -13.89961937509977652, 13.97604488694528158, 95.62390960531436690 ) ) ;
#67418 = CARTESIAN_POINT ( 'NONE',  ( 16.46253265017160672, -9.564922557960803928, 48.33224293864769550 ) ) ;
#67419 = CARTESIAN_POINT ( 'NONE',  ( -16.53943276465976808, 0.05219959533911058130, 56.24890960531436690 ) ) ;
#67421 = CARTESIAN_POINT ( 'NONE',  ( 21.55341960407610458, 5.719274019375980345, 23.95724293864769550 ) ) ;
#67420 = CARTESIAN_POINT ( 'NONE',  ( -13.97604488694527625, -13.89961937509977652, 21.87390960531435979 ) ) ;
#67422 = CARTESIAN_POINT ( 'NONE',  ( -18.62759615963270932, 10.81492255796079327, 40.83224293864769550 ) ) ;
#67423 = CARTESIAN_POINT ( 'NONE',  ( 16.55341960407611168, 4.379528057220329451, 83.95724293864770971 ) ) ;
#67424 = CARTESIAN_POINT ( 'NONE',  ( 4.379528057220092307, 16.55341960407617563, 32.29275706135235424 ) ) ;
#67425 = CARTESIAN_POINT ( 'NONE',  ( 8.224510206698953496, -14.34966873604960469, 72.91557627198103830 ) ) ;
#67426 = CARTESIAN_POINT ( 'NONE',  ( 26.53315420742544717, 7.611574518544833801, 168.2743882774363726 ) ) ;
#67427 = CARTESIAN_POINT ( 'NONE',  ( -16.51473224551082808, 9.474510206698731452, 73.33442372801900433 ) ) ;
#67428 = CARTESIAN_POINT ( 'NONE',  ( 13.97604488694527802, 13.89961937509977652, 104.3739096053143385 ) ) ;
#67429 = CARTESIAN_POINT ( 'NONE',  ( -29.86685920354755197, -21.69954338932560134, -4.924999997268813878 ) ) ;
#67430 = CARTESIAN_POINT ( 'NONE',  ( 18.82182630884605601, 5.499999999999964473, 101.5751632728302383 ) ) ;
#67432 = CARTESIAN_POINT ( 'NONE',  ( -16.53943276465976808, 0.05219959533911058130, 21.24890960531436690 ) ) ;
#67431 = CARTESIAN_POINT ( 'NONE',  ( -14.34966873604972548, 8.224510206698743886, 33.33442372801900433 ) ) ;
#67433 = CARTESIAN_POINT ( 'NONE',  ( 9.474510206698729675, 16.51473224551082808, 77.08442372801900433 ) ) ;
#67434 = CARTESIAN_POINT ( 'NONE',  ( -10.72451020669898014, 18.67979575497178502, 55.41557627198102409 ) ) ;
#67435 = CARTESIAN_POINT ( 'NONE',  ( -21.55341960407619339, 5.719274019375674811, 68.54275706135234714 ) ) ;
#67436 = DIRECTION ( 'NONE',  ( 1.000000000000000000, 0.000000000000000000, 0.000000000000000000 ) ) ;
#67437 = CARTESIAN_POINT ( 'NONE',  ( 12.14591786802327356, -12.06949235617739191, 40.62609039468567573 ) ) ;
#67439 = CARTESIAN_POINT ( 'NONE',  ( -19.05341960407611168, -5.049401038298163336, 81.45724293864769550 ) ) ;
#67438 = CARTESIAN_POINT ( 'NONE',  ( 19.03943276465977164, -0.05219959533909143690, 28.74890960531435624 ) ) ;
#67440 = CARTESIAN_POINT ( 'NONE',  ( 19.03943276465977164, -0.05219959533909143690, 23.74890960531435269 ) ) ;
#67441 = CARTESIAN_POINT ( 'NONE',  ( 8.314922557960818139, 14.29746914071049879, 84.58224293864769550 ) ) ;
#67442 = APPLICATION_PROTOCOL_DEFINITION ( 'draft international standard', 'automotive_design', 1998, #124181 ) ;
#67443 = CARTESIAN_POINT ( 'NONE',  ( 16.51473224551069308, 9.474510206698969483, 89.16557627198103830 ) ) ;
#67444 = VERTEX_POINT ( 'NONE', #158613 ) ;
#67445 = CARTESIAN_POINT ( 'NONE',  ( 5.153800228976615827, -19.02544592524334988, 100.2094237280190043 ) ) ;
#67446 = CARTESIAN_POINT ( 'NONE',  ( -21.55341960407610458, -5.719274019375992779, 76.45724293864769550 ) ) ;
#67447 = CARTESIAN_POINT ( 'NONE',  ( -5.153800228976328057, -19.02544592524343514, 47.29057627198102409 ) ) ;
#67449 = CARTESIAN_POINT ( 'NONE',  ( 10.81492255796106328, -18.62759615963255655, 20.41775706135234714 ) ) ;
#67448 = CARTESIAN_POINT ( 'NONE',  ( -13.97604488694547697, 13.89961937509957934, 68.12609039468563310 ) ) ;
#67450 = CARTESIAN_POINT ( 'NONE',  ( 19.03943276465977164, -0.05219959533909143690, 63.74890960531435979 ) ) ;
#67451 = CARTESIAN_POINT ( 'NONE',  ( 13.97604488694527802, 13.89961937509977652, 109.3739096053143669 ) ) ;
#67452 = ORIENTED_EDGE ( 'NONE', *, *, #128971, .T. ) ;
#67453 = CARTESIAN_POINT ( 'NONE',  ( 16.52544592524335698, 4.483927247898782831, 31.45942372801901854 ) ) ;
#67454 = CARTESIAN_POINT ( 'NONE',  ( 15.72974639402199770, -15.80617190586745480, 103.1239096053143811 ) ) ;
#67457 = CARTESIAN_POINT ( 'NONE',  ( 19.03943276465977164, 0.05219959533936151252, 66.25109039468567573 ) ) ;
#67456 = CARTESIAN_POINT ( 'NONE',  ( -16.51473224551069308, -9.474510206698971260, 91.66557627198103830 ) ) ;
#67455 = CARTESIAN_POINT ( 'NONE',  ( 16.52544592524342804, -4.483927247898539470, 103.5405762719810383 ) ) ;
#67458 = CARTESIAN_POINT ( 'NONE',  ( -21.55341960407610458, -5.719274019375992779, 86.45724293864770971 ) ) ;
#67459 = CARTESIAN_POINT ( 'NONE',  ( -0.05219959533910754901, -16.53943276465976808, 52.49890960531435979 ) ) ;
#67460 = CARTESIAN_POINT ( 'NONE',  ( 9.474510206698729675, 16.51473224551082808, 22.08442372801899722 ) ) ;
#67461 = CARTESIAN_POINT ( 'NONE',  ( -16.53943276465976808, -0.05219959533934237506, 58.75109039468568994 ) ) ;
#67462 = CARTESIAN_POINT ( 'NONE',  ( 9.564922557960805705, 16.46253265017160317, 94.58224293864769550 ) ) ;
#67463 = CARTESIAN_POINT ( 'NONE',  ( -19.03943276465977164, 0.05219959533909376836, 41.24890960531435269 ) ) ;
#67464 = CARTESIAN_POINT ( 'NONE',  ( -0.05219959533937732626, 21.53943276465977519, 52.50109039468567573 ) ) ;
#67465 = CARTESIAN_POINT ( 'NONE',  ( 5.719274019375673035, 21.55341960407619339, 67.29275706135234714 ) ) ;
#67466 = CARTESIAN_POINT ( 'NONE',  ( 5.153800228976335163, 19.02544592524342804, 54.79057627198103120 ) ) ;
#67467 = CARTESIAN_POINT ( 'NONE',  ( -15.80617190586768217, 15.72974639402176855, 33.12609039468569705 ) ) ;
#67468 = CARTESIAN_POINT ( 'NONE',  ( -13.89961937509957401, -13.97604488694547875, 69.37609039468564731 ) ) ;
#67469 = CARTESIAN_POINT ( 'NONE',  ( -5.153800228976607833, 19.02544592524334988, 72.70942372801900433 ) ) ;
#67470 = CARTESIAN_POINT ( 'NONE',  ( 19.03943276465977164, -0.05219959533909143690, 33.74890960531435979 ) ) ;
#67471 = CARTESIAN_POINT ( 'NONE',  ( 12.14591786802327356, -12.06949235617739191, 85.62609039468568994 ) ) ;
#67472 = CARTESIAN_POINT ( 'NONE',  ( -5.049401038298153566, 19.05341960407611168, 50.20724293864770260 ) ) ;
#67473 = CARTESIAN_POINT ( 'NONE',  ( 19.05341960407611168, 5.049401038298154454, 23.95724293864769194 ) ) ;
#67474 = CARTESIAN_POINT ( 'NONE',  ( 19.02544592524343514, -5.153800228976328945, 98.54057627198100988 ) ) ;
#67475 = CARTESIAN_POINT ( 'NONE',  ( 19.03943276465977164, -0.05219959533909143690, 38.74890960531436690 ) ) ;
#67476 = CARTESIAN_POINT ( 'NONE',  ( -0.05219959533907301413, -21.53943276465977519, 87.49890960531436690 ) ) ;
#67477 = CARTESIAN_POINT ( 'NONE',  ( -0.05219959533934338120, 16.53943276465976808, 57.50109039468568994 ) ) ;
#67478 = CARTESIAN_POINT ( 'NONE',  ( -0.05219959533936034679, 19.03943276465977164, 32.50109039468566863 ) ) ;
#67479 = EDGE_CURVE ( 'NONE', #38003, #60305, #53428, .T. ) ;
#67480 = CARTESIAN_POINT ( 'NONE',  ( 19.05341960407611168, 5.049401038298154454, 53.95724293864770260 ) ) ;
#67481 = CARTESIAN_POINT ( 'NONE',  ( -8.224510206698948167, 14.34966873604960824, 50.41557627198103120 ) ) ;
#67482 = CARTESIAN_POINT ( 'NONE',  ( -0.05219959533910754901, -16.53943276465976808, 82.49890960531436690 ) ) ;
#67483 = VECTOR ( 'NONE', #148723, 1000.000000000000000 ) ;
#67484 = CARTESIAN_POINT ( 'NONE',  ( -19.02544592524342804, 5.153800228976336051, 91.04057627198100988 ) ) ;
#67485 = CARTESIAN_POINT ( 'NONE',  ( -19.02544592524342804, 5.153800228976336051, 76.04057627198102409 ) ) ;
#67486 = CARTESIAN_POINT ( 'NONE',  ( 18.62759615963255655, 10.81492255796105972, 31.66775706135234358 ) ) ;
#67487 = CARTESIAN_POINT ( 'NONE',  ( -13.97604488694527625, -13.89961937509977652, 96.87390960531433848 ) ) ;
#67488 = CARTESIAN_POINT ( 'NONE',  ( -15.72974639402176322, -15.80617190586768395, 94.37609039468568994 ) ) ;
#67489 = CARTESIAN_POINT ( 'NONE',  ( -16.53943276465976808, -0.05219959533934237506, 73.75109039468567573 ) ) ;
#67490 = CARTESIAN_POINT ( 'NONE',  ( -15.72974639402176322, -15.80617190586768395, 29.37609039468568284 ) ) ;
#67491 = ADVANCED_FACE ( 'NONE', ( #98920 ), #115105, .T. ) ;
#67492 = CARTESIAN_POINT ( 'NONE',  ( -21.53943276465977519, 0.05219959533907696930, 96.24890960531435269 ) ) ;
#67493 = CARTESIAN_POINT ( 'NONE',  ( -4.379528057220328563, 16.55341960407611168, 45.20724293864769550 ) ) ;
#67494 = CARTESIAN_POINT ( 'NONE',  ( -19.05341960407611168, -5.049401038298163336, 36.45724293864766707 ) ) ;
#67495 = CARTESIAN_POINT ( 'NONE',  ( -4.483927247898539470, -16.52544592524342804, 72.29057627198102409 ) ) ;
#67496 = CARTESIAN_POINT ( 'NONE',  ( -0.05219959533907301413, -21.53943276465977519, 32.49890960531435979 ) ) ;
#67497 = CARTESIAN_POINT ( 'NONE',  ( -19.05341960407617563, 5.049401038297882671, 28.54275706135232937 ) ) ;
#67498 = CARTESIAN_POINT ( 'NONE',  ( -14.34966873604960291, -8.224510206698953496, 101.6655762719810383 ) ) ;
#67499 = CARTESIAN_POINT ( 'NONE',  ( 0.05219959533909260263, 19.03943276465977164, 104.9989096053143669 ) ) ;
#67500 = ORIENTED_EDGE ( 'NONE', *, *, #198323, .F. ) ;
#67501 = CARTESIAN_POINT ( 'NONE',  ( 12.14591786802327356, -12.06949235617739191, 55.62609039468568284 ) ) ;
#67502 = CARTESIAN_POINT ( 'NONE',  ( 13.97604488694527802, 13.89961937509977652, 69.37390960531436690 ) ) ;
#67503 = CARTESIAN_POINT ( 'NONE',  ( -5.359611314223446995E-15, 29.16686587814335851, 140.3750000027311842 ) ) ;
#67504 = CARTESIAN_POINT ( 'NONE',  ( 5.823673210054125526, 21.52544592524343514, 29.79057627198102409 ) ) ;
#67505 = CARTESIAN_POINT ( 'NONE',  ( 14.29746914071037800, 8.314922557961029526, 91.66775706135234714 ) ) ;
#67506 = CARTESIAN_POINT ( 'NONE',  ( -0.05219959533936034679, 19.03943276465977164, 112.5010903946856757 ) ) ;
#67507 = CARTESIAN_POINT ( 'NONE',  ( -10.72451020669870658, -18.67979575497194134, 79.58442372801903275 ) ) ;
#67508 = CARTESIAN_POINT ( 'NONE',  ( 0.05219959533909260263, 19.03943276465977164, 69.99890960531435269 ) ) ;
#67509 = CARTESIAN_POINT ( 'NONE',  ( -5.719274019375978568, 21.55341960407610458, 110.2072429386477239 ) ) ;
#67510 = CARTESIAN_POINT ( 'NONE',  ( 14.29746914071037800, 8.314922557961029526, 56.66775706135235424 ) ) ;
#67511 = CARTESIAN_POINT ( 'NONE',  ( 16.55341960407611168, 4.379528057220329451, 113.9572429386477239 ) ) ;
#67512 = CARTESIAN_POINT ( 'NONE',  ( -12.06949235617739369, -12.14591786802326823, 24.37609039468567573 ) ) ;
#67513 = CARTESIAN_POINT ( 'NONE',  ( -13.97604488694547697, 13.89961937509957934, 88.12609039468563310 ) ) ;
#67514 = CARTESIAN_POINT ( 'NONE',  ( 18.67979575497178502, 10.72451020669898547, 74.16557627198102409 ) ) ;
#67515 = CARTESIAN_POINT ( 'NONE',  ( 5.049401038297881783, 19.05341960407617563, 57.29275706135231871 ) ) ;
#67516 = CARTESIAN_POINT ( 'NONE',  ( -5.000000000000000888, 4.999999999999999112, -15.00000000000000000 ) ) ;
#67517 = CARTESIAN_POINT ( 'NONE',  ( -5.823673210054116645, -21.52544592524344225, 97.29057627198105251 ) ) ;
#67518 = CARTESIAN_POINT ( 'NONE',  ( -28.82186960331499037, 2.428612866367529932E-14, 148.0000000000000000 ) ) ;
#67519 = CARTESIAN_POINT ( 'NONE',  ( -9.564922557960796823, -16.46253265017161027, 72.08224293864770971 ) ) ;
#67520 = PLANE ( 'NONE',  #169145 ) ;
#67521 = CARTESIAN_POINT ( 'NONE',  ( 16.53943276465976808, 0.05219959533934440121, 26.25109039468567573 ) ) ;
#67522 = CARTESIAN_POINT ( 'NONE',  ( 36.77116682341763010, -5.223593267096956261, 46.75914592492880217 ) ) ;
#67524 = CARTESIAN_POINT ( 'NONE',  ( -8.314922557960811034, -14.29746914071050412, 62.08224293864769550 ) ) ;
#67523 = CARTESIAN_POINT ( 'NONE',  ( -15.80617190586745835, -15.72974639402198527, 96.87390960531436690 ) ) ;
#67525 = CARTESIAN_POINT ( 'NONE',  ( 19.03943276465977164, -0.05219959533909143690, 73.74890960531435269 ) ) ;
#67526 = CARTESIAN_POINT ( 'NONE',  ( -15.72974639402176322, -15.80617190586768395, 74.37609039468568994 ) ) ;
#67528 = CARTESIAN_POINT ( 'NONE',  ( -13.89961937509957401, -13.97604488694547875, 44.37609039468566863 ) ) ;
#67527 = CARTESIAN_POINT ( 'NONE',  ( 12.14591786802327356, -12.06949235617739191, 35.62609039468568994 ) ) ;
#67529 = CARTESIAN_POINT ( 'NONE',  ( 21.55341960407619695, -5.719274019375665929, 46.04275706135234714 ) ) ;
#67530 = CARTESIAN_POINT ( 'NONE',  ( 0.05219959533907565091, 21.53943276465977519, 64.99890960531435269 ) ) ;
#67531 = CARTESIAN_POINT ( 'NONE',  ( -16.53943276465976808, -0.05219959533934237506, 18.75109039468568639 ) ) ;
#67532 = CARTESIAN_POINT ( 'NONE',  ( 16.51473224551069308, 9.474510206698969483, 54.16557627198103120 ) ) ;
#67533 = CARTESIAN_POINT ( 'NONE',  ( -9.564922557961040184, 16.46253265017147172, 72.91775706135233293 ) ) ;
#67534 = CARTESIAN_POINT ( 'NONE',  ( 18.62759615963255655, 10.81492255796105972, 86.66775706135234714 ) ) ;
#67535 = CARTESIAN_POINT ( 'NONE',  ( -9.474510206698720793, -16.51473224551083518, 54.58442372801899722 ) ) ;
#67536 = CARTESIAN_POINT ( 'NONE',  ( -13.89961937509977652, 13.97604488694528158, 35.62390960531435269 ) ) ;
#67537 = CARTESIAN_POINT ( 'NONE',  ( -5.823673210054116645, -21.52544592524344225, 62.29057627198102409 ) ) ;
#67538 = CARTESIAN_POINT ( 'NONE',  ( -8.314922557960811034, -14.29746914071050412, 47.08224293864770260 ) ) ;
#67539 = CARTESIAN_POINT ( 'NONE',  ( 21.59136165864583390, 7.527668378163610896, 173.8290135686407893 ) ) ;
#67540 = CARTESIAN_POINT ( 'NONE',  ( -19.02544592524334988, -5.153800228976617603, 33.95942372801897591 ) ) ;
#67541 = CARTESIAN_POINT ( 'NONE',  ( -14.34966873604972548, 8.224510206698743886, 83.33442372801903275 ) ) ;
#67542 = CARTESIAN_POINT ( 'NONE',  ( 16.52544592524342804, -4.483927247898539470, 58.54057627198103120 ) ) ;
#67543 = CARTESIAN_POINT ( 'NONE',  ( -21.53943276465977519, -0.05219959533937600094, 93.75109039468567573 ) ) ;
#67544 = CARTESIAN_POINT ( 'NONE',  ( 15.80617190586769283, -15.72974639402175789, 85.62609039468568994 ) ) ;
#67545 = CARTESIAN_POINT ( 'NONE',  ( -0.05219959533907301413, -21.53943276465977519, 87.49890960531436690 ) ) ;
#67546 = CARTESIAN_POINT ( 'NONE',  ( -19.02544592524342804, 5.153800228976336051, 51.04057627198103120 ) ) ;
#67547 = CARTESIAN_POINT ( 'NONE',  ( 0.05219959533937995610, -21.53943276465977519, 60.00109039468568284 ) ) ;
#67548 = CARTESIAN_POINT ( 'NONE',  ( -19.03943276465977164, 0.05219959533909376836, 36.24890960531436690 ) ) ;
#67549 = EDGE_LOOP ( 'NONE', ( #84079, #163146, #154002 ) ) ;
#67550 = CARTESIAN_POINT ( 'NONE',  ( -19.03943276465977164, 0.05219959533909376836, 56.24890960531435979 ) ) ;
#67551 = CARTESIAN_POINT ( 'NONE',  ( 12.14591786802309770, 12.06949235617756955, 109.3739096053143811 ) ) ;
#67552 = CARTESIAN_POINT ( 'NONE',  ( -13.89961937509977652, 13.97604488694528158, 95.62390960531436690 ) ) ;
#67553 = CARTESIAN_POINT ( 'NONE',  ( -0.05219959533910754901, -16.53943276465976808, 57.49890960531435979 ) ) ;
#67554 = CARTESIAN_POINT ( 'NONE',  ( -14.34966873604960291, -8.224510206698953496, 106.6655762719810383 ) ) ;
#67555 = CARTESIAN_POINT ( 'NONE',  ( 15.80617190586746368, 15.72974639402197994, 79.37390960531436690 ) ) ;
#67556 = CARTESIAN_POINT ( 'NONE',  ( -21.52544592524334988, -5.823673210054445271, 23.95942372801901143 ) ) ;
#67557 = CARTESIAN_POINT ( 'NONE',  ( 27.60788766665615768, -7.718175339870845697, 162.2452582881560943 ) ) ;
#67558 = CARTESIAN_POINT ( 'NONE',  ( -8.314922557961024197, 14.29746914071037800, 42.91775706135235424 ) ) ;
#67559 = ORIENTED_EDGE ( 'NONE', *, *, #193913, .F. ) ;
#67560 = CARTESIAN_POINT ( 'NONE',  ( -5.823673210054116645, -21.52544592524344225, 67.29057627198103830 ) ) ;
#67561 = CARTESIAN_POINT ( 'NONE',  ( 10.72451020669871369, 18.67979575497193778, 112.0844237280190185 ) ) ;
#67562 = CARTESIAN_POINT ( 'NONE',  ( -0.05219959533909027116, -19.03943276465977164, 92.49890960531436690 ) ) ;
#67563 = CARTESIAN_POINT ( 'NONE',  ( 10.72451020669871369, 18.67979575497193778, 27.08442372801901854 ) ) ;
#67564 = CARTESIAN_POINT ( 'NONE',  ( -10.72451020669898014, 18.67979575497178502, 30.41557627198101699 ) ) ;
#67565 = CARTESIAN_POINT ( 'NONE',  ( 14.34966873604972726, -8.224510206698740333, 105.8344237280190328 ) ) ;
#67567 = CARTESIAN_POINT ( 'NONE',  ( 18.67979575497194134, -10.72451020669871369, 85.83442372801901854 ) ) ;
#67566 = CARTESIAN_POINT ( 'NONE',  ( 18.62759615963255655, 10.81492255796105972, 46.66775706135234714 ) ) ;
#67568 = CARTESIAN_POINT ( 'NONE',  ( -16.46253265017146816, -9.564922557961047289, 19.16775706135233293 ) ) ;
#67569 = CARTESIAN_POINT ( 'NONE',  ( 8.314922557961029526, -14.29746914071037800, 70.41775706135236135 ) ) ;
#67570 = CARTESIAN_POINT ( 'NONE',  ( -15.72974639402176322, -15.80617190586768395, 44.37609039468567573 ) ) ;
#67571 = CARTESIAN_POINT ( 'NONE',  ( -19.05341960407611168, -5.049401038298163336, 36.45724293864766707 ) ) ;
#67572 = CARTESIAN_POINT ( 'NONE',  ( -21.53943276465977519, -0.05219959533937600094, 103.7510903946857042 ) ) ;
#67573 = CARTESIAN_POINT ( 'NONE',  ( 13.89961937509977652, -13.97604488694527269, 113.1239096053143527 ) ) ;
#67574 = B_SPLINE_CURVE_WITH_KNOTS ( 'NONE', 3,
 ( #115457, #116454, #98253, #190300, #117451, #144780 ),
 .UNSPECIFIED., .F., .F.,
 ( 4, 2, 4 ),
 ( 0.000000000000000000, 0.0003837532665554014731, 0.0007675065331108029461 ),
 .UNSPECIFIED. ) ;
#67575 = CARTESIAN_POINT ( 'NONE',  ( -0.05219959533907301413, -21.53943276465977519, 107.4989096053143669 ) ) ;
#67577 = CARTESIAN_POINT ( 'NONE',  ( 5.823673210054125526, 21.52544592524343514, 64.79057627198103830 ) ) ;
#67576 = CARTESIAN_POINT ( 'NONE',  ( 19.01529144963338069, 5.499999999999978684, 83.73431955728436549 ) ) ;
#67579 = CARTESIAN_POINT ( 'NONE',  ( 14.29746914071049879, -8.314922557960816363, 43.33224293864769550 ) ) ;
#67578 = CARTESIAN_POINT ( 'NONE',  ( -14.34966873604972548, 8.224510206698743886, 48.33442372801902565 ) ) ;
#67580 = CARTESIAN_POINT ( 'NONE',  ( 22.67087683854552083, 7.530304285672279718, 173.4975851171454622 ) ) ;
#67581 = CARTESIAN_POINT ( 'NONE',  ( -16.46253265017146816, -9.564922557961047289, 79.16775706135234714 ) ) ;
#67582 = CARTESIAN_POINT ( 'NONE',  ( -16.88567814943161949, 6.947325034625681184, 103.7099887734741372 ) ) ;
#67583 = CARTESIAN_POINT ( 'NONE',  ( 8.314922557961029526, -14.29746914071037800, 30.41775706135234358 ) ) ;
#67584 = CARTESIAN_POINT ( 'NONE',  ( 21.55341960407610458, 5.719274019375980345, 98.95724293864770971 ) ) ;
#67585 = CARTESIAN_POINT ( 'NONE',  ( 0.05219959533910956823, 16.53943276465976808, 64.99890960531435269 ) ) ;
#67586 = CARTESIAN_POINT ( 'NONE',  ( 16.46253265017160672, -9.564922557960803928, 108.3322429386476955 ) ) ;
#67587 = CARTESIAN_POINT ( 'NONE',  ( -0.05219959533934338120, 16.53943276465976808, 42.50109039468567573 ) ) ;
#67588 = CARTESIAN_POINT ( 'NONE',  ( 5.049401038298161559, -19.05341960407611168, 62.70724293864769550 ) ) ;
#67590 = CARTESIAN_POINT ( 'NONE',  ( 5.049401038297881783, 19.05341960407617563, 92.29275706135234714 ) ) ;
#67589 = CARTESIAN_POINT ( 'NONE',  ( -15.72974639402176322, -15.80617190586768395, 34.37609039468568284 ) ) ;
#67591 = CARTESIAN_POINT ( 'NONE',  ( -0.05219959533909027116, -19.03943276465977164, 112.4989096053143669 ) ) ;
#67592 = CARTESIAN_POINT ( 'NONE',  ( -16.46253265017160317, 9.564922557960807481, 90.83224293864769550 ) ) ;
#67593 = CARTESIAN_POINT ( 'NONE',  ( -18.62759615963270932, 10.81492255796079327, 95.83224293864770971 ) ) ;
#67594 = CARTESIAN_POINT ( 'NONE',  ( 16.51473224551069308, 9.474510206698969483, 59.16557627198102409 ) ) ;
#67595 = CARTESIAN_POINT ( 'NONE',  ( 2.500000000000000000, 2.357898499370431722, -2.818925648462311528E-15 ) ) ;
#67596 = CARTESIAN_POINT ( 'NONE',  ( 16.55341960407611168, 4.379528057220329451, 68.95724293864769550 ) ) ;
#67597 = CARTESIAN_POINT ( 'NONE',  ( -13.89961937509977652, 13.97604488694528158, 105.6239096053143527 ) ) ;
#67598 = CARTESIAN_POINT ( 'NONE',  ( 17.59990181671015819, -15.82965471272139091, -54.72698953881466366 ) ) ;
#67599 = CARTESIAN_POINT ( 'NONE',  ( -13.89961937509957401, -13.97604488694547875, 84.37609039468567573 ) ) ;
#67600 = CARTESIAN_POINT ( 'NONE',  ( -21.53943276465977519, 0.05219959533907696930, 86.24890960531436690 ) ) ;
#67601 = CARTESIAN_POINT ( 'NONE',  ( 19.05341960407617918, -5.049401038297876454, 46.04275706135233293 ) ) ;
#67602 = CARTESIAN_POINT ( 'NONE',  ( -19.02544592524342804, 5.153800228976336051, 111.0405762719810099 ) ) ;
#67603 = CARTESIAN_POINT ( 'NONE',  ( 10.81492255796078972, 18.62759615963270932, 59.58224293864770260 ) ) ;
#67604 = CARTESIAN_POINT ( 'NONE',  ( 13.89961937509977652, -13.97604488694527269, 83.12390960531436690 ) ) ;
#67605 = CARTESIAN_POINT ( 'NONE',  ( 21.55341960407619695, -5.719274019375665929, 81.04275706135236135 ) ) ;
#67606 = CARTESIAN_POINT ( 'NONE',  ( 19.02544592524343514, -5.153800228976328945, 43.54057627198103120 ) ) ;
#67607 = CARTESIAN_POINT ( 'NONE',  ( 0.05219959533910956823, 16.53943276465976808, 69.99890960531435269 ) ) ;
#67608 = CARTESIAN_POINT ( 'NONE',  ( 14.34966873604972726, -8.224510206698740333, 25.83442372801901499 ) ) ;
#67609 = CARTESIAN_POINT ( 'NONE',  ( 10.72451020669871369, 18.67979575497193778, 72.08442372801899012 ) ) ;
#67610 = ORIENTED_EDGE ( 'NONE', *, *, #52643, .T. ) ;
#67611 = CARTESIAN_POINT ( 'NONE',  ( 5.049401038297881783, 19.05341960407617563, 32.29275706135233293 ) ) ;
#67612 = CARTESIAN_POINT ( 'NONE',  ( 19.03943276465977164, 0.05219959533936151252, 81.25109039468567573 ) ) ;
#67613 = DIRECTION ( 'NONE',  ( 0.000000000000000000, -0.000000000000000000, 1.000000000000000000 ) ) ;
#67614 = CARTESIAN_POINT ( 'NONE',  ( -21.52544592524343514, 5.823673210054127303, 116.0405762719810383 ) ) ;
#67615 = CARTESIAN_POINT ( 'NONE',  ( 19.24578484527059175, -180.9428398739492820, -4.999999999999999112 ) ) ;
#67616 = CARTESIAN_POINT ( 'NONE',  ( -9.474510206698720793, -16.51473224551083518, 24.58442372801900078 ) ) ;
#67617 = CARTESIAN_POINT ( 'NONE',  ( -0.05219959533909027116, -19.03943276465977164, 57.49890960531435979 ) ) ;
#67618 = CARTESIAN_POINT ( 'NONE',  ( -0.05219959533936034679, 19.03943276465977164, 22.50109039468566152 ) ) ;
#67619 = CARTESIAN_POINT ( 'NONE',  ( -12.06949235617739369, -12.14591786802326823, 104.3760903946856899 ) ) ;
#67621 = CARTESIAN_POINT ( 'NONE',  ( 18.62759615963255655, 10.81492255796105972, 66.66775706135234714 ) ) ;
#67620 = CARTESIAN_POINT ( 'NONE',  ( 19.02544592524343514, -5.153800228976328945, 98.54057627198100988 ) ) ;
#67622 = CIRCLE ( 'NONE', #32137, 214.0437394197456911 ) ;
#67623 = CARTESIAN_POINT ( 'NONE',  ( 36.91746824999999887, 11.99521256947799053, -7.524999997268814411 ) ) ;
#67624 = CARTESIAN_POINT ( 'NONE',  ( -33.74157273865942130, 3.640299887980672722, 99.13851753912355491 ) ) ;
#67625 = CARTESIAN_POINT ( 'NONE',  ( -0.05219959533937732626, 21.53943276465977519, 87.50109039468568994 ) ) ;
#67626 = CARTESIAN_POINT ( 'NONE',  ( 18.67979575497194134, -10.72451020669871369, 100.8344237280190185 ) ) ;
#67627 = DIRECTION ( 'NONE',  ( 0.000000000000000000, 0.000000000000000000, 1.000000000000000000 ) ) ;
#67628 = CARTESIAN_POINT ( 'NONE',  ( 13.97604488694527802, 13.89961937509977652, 104.3739096053143385 ) ) ;
#67629 = CARTESIAN_POINT ( 'NONE',  ( 13.97604488694548053, -13.89961937509957401, 25.62609039468566507 ) ) ;
#67630 = DIRECTION ( 'NONE',  ( 0.7071067811865483499, 0.000000000000000000, -0.7071067811865466846 ) ) ;
#67631 = CARTESIAN_POINT ( 'NONE',  ( -5.049401038298153566, 19.05341960407611168, 35.20724293864768839 ) ) ;
#67633 = EDGE_CURVE ( 'NONE', #166185, #30659, #148266, .T. ) ;
#67632 = CARTESIAN_POINT ( 'NONE',  ( -21.55341960407610458, -5.719274019375992779, 61.45724293864770260 ) ) ;
#67634 = CARTESIAN_POINT ( 'NONE',  ( -4.483927247898782831, 16.52544592524335698, 102.7094237280190185 ) ) ;
#67636 = CARTESIAN_POINT ( 'NONE',  ( -19.05341960407611168, -5.049401038298163336, 81.45724293864769550 ) ) ;
#67635 = CARTESIAN_POINT ( 'NONE',  ( -4.483927247898539470, -16.52544592524342804, 102.2905762719810383 ) ) ;
#67637 = CARTESIAN_POINT ( 'NONE',  ( 18.67979575497194134, -10.72451020669871369, 100.8344237280190185 ) ) ;
#67638 = CARTESIAN_POINT ( 'NONE',  ( 9.564922557960805705, 16.46253265017160317, 34.58224293864770260 ) ) ;
#67639 = CARTESIAN_POINT ( 'NONE',  ( -0.05219959533910754901, -16.53943276465976808, 97.49890960531436690 ) ) ;
#67640 = CARTESIAN_POINT ( 'NONE',  ( -5.823673210054431948, 21.52544592524334988, 52.70942372801902565 ) ) ;
#67641 = CARTESIAN_POINT ( 'NONE',  ( -10.81492255796078084, -18.62759615963271287, 92.08224293864769550 ) ) ;
#67642 = CARTESIAN_POINT ( 'NONE',  ( -16.46253265017146816, -9.564922557961047289, 49.16775706135233293 ) ) ;
#67643 = CARTESIAN_POINT ( 'NONE',  ( -15.58352941493655131, -36.85276851793626207, -13.27801782995927660 ) ) ;
#67644 = CARTESIAN_POINT ( 'NONE',  ( 16.46253265017160672, -9.564922557960803928, 93.33224293864769550 ) ) ;
#67645 = CARTESIAN_POINT ( 'NONE',  ( -8.224510206698948167, 14.34966873604960824, 75.41557627198102409 ) ) ;
#67646 = EDGE_CURVE ( 'NONE', #17032, #120193, #116105, .T. ) ;
#67647 = CARTESIAN_POINT ( 'NONE',  ( 5.153800228976615827, -19.02544592524334988, 50.20942372801897591 ) ) ;
#67649 = VECTOR ( 'NONE', #170791, 1000.000000000000000 ) ;
#67648 = CARTESIAN_POINT ( 'NONE',  ( 16.51473224551069308, 9.474510206698969483, 69.16557627198102409 ) ) ;
#67650 = CARTESIAN_POINT ( 'NONE',  ( -4.379528057220328563, 16.55341960407611168, 50.20724293864769550 ) ) ;
#67651 = CARTESIAN_POINT ( 'NONE',  ( -13.89961937509957401, -13.97604488694547875, 84.37609039468567573 ) ) ;
#67652 = DIRECTION ( 'NONE',  ( 3.469446951953612217E-15, 0.000000000000000000, -1.000000000000000000 ) ) ;
#67653 = CARTESIAN_POINT ( 'NONE',  ( 5.823673210054125526, 21.52544592524343514, 34.79057627198103120 ) ) ;
#67654 = CARTESIAN_POINT ( 'NONE',  ( 16.52544592524342804, -4.483927247898539470, 103.5405762719810383 ) ) ;
#67655 = CARTESIAN_POINT ( 'NONE',  ( -17.50000000000001776, -3.850315288878612741, 25.73370869396545046 ) ) ;
#67657 = CARTESIAN_POINT ( 'NONE',  ( 18.62759615963271287, -10.81492255796078972, 58.33224293864768839 ) ) ;
#67656 = CARTESIAN_POINT ( 'NONE',  ( -19.05341960407611168, -5.049401038298163336, 61.45724293864769550 ) ) ;
#67658 = CARTESIAN_POINT ( 'NONE',  ( 9.474510206698971260, -16.51473224551069308, 27.91557627198103120 ) ) ;
#67660 = CARTESIAN_POINT ( 'NONE',  ( 5.153800228976335163, 19.02544592524342804, 59.79057627198100988 ) ) ;
#67659 = CARTESIAN_POINT ( 'NONE',  ( -14.34966873604972548, 8.224510206698743886, 83.33442372801903275 ) ) ;
#67661 = CARTESIAN_POINT ( 'NONE',  ( -16.46253265017146816, -9.564922557961047289, 54.16775706135234003 ) ) ;
#67662 = CARTESIAN_POINT ( 'NONE',  ( -21.53943276465977519, -0.05219959533937600094, 68.75109039468568994 ) ) ;
#67663 = ORIENTED_EDGE ( 'NONE', *, *, #186227, .T. ) ;
#67664 = CARTESIAN_POINT ( 'NONE',  ( -15.80617190586745835, -15.72974639402198527, 46.87390960531435979 ) ) ;
#67665 = CARTESIAN_POINT ( 'NONE',  ( -16.51473224551069308, -9.474510206698971260, 26.66557627198103120 ) ) ;
#67666 = CARTESIAN_POINT ( 'NONE',  ( 0.05219959533934541429, -16.53943276465976808, 90.00109039468567573 ) ) ;
#67667 = CARTESIAN_POINT ( 'NONE',  ( -5.153800228976607833, 19.02544592524334988, 107.7094237280189759 ) ) ;
#67668 = CARTESIAN_POINT ( 'NONE',  ( -9.474510206698964154, 16.51473224551069663, 25.41557627198103120 ) ) ;
#67670 = CARTESIAN_POINT ( 'NONE',  ( -21.53943276465977519, 0.05219959533907696930, 56.24890960531436690 ) ) ;
#67669 = CARTESIAN_POINT ( 'NONE',  ( 17.48853670773243962, 5.747243402303178428, 53.83328700250012133 ) ) ;
#67671 = CARTESIAN_POINT ( 'NONE',  ( -21.52544592524334988, -5.823673210054445271, 93.95942372801903275 ) ) ;
#67672 = CARTESIAN_POINT ( 'NONE',  ( -14.29746914071049879, 8.314922557960819915, 50.83224293864770971 ) ) ;
#67673 = CARTESIAN_POINT ( 'NONE',  ( -16.53943276465976808, 0.05219959533911058130, 51.24890960531436690 ) ) ;
#67674 = CARTESIAN_POINT ( 'NONE',  ( -0.05219959533907301413, -21.53943276465977519, 82.49890960531436690 ) ) ;
#67675 = CARTESIAN_POINT ( 'NONE',  ( -18.67979575497178146, -10.72451020669898902, 91.66557627198103830 ) ) ;
#67676 = CARTESIAN_POINT ( 'NONE',  ( -1.376802789500885194, -29.79829367730026846, -48.54110828511537079 ) ) ;
#67677 = CARTESIAN_POINT ( 'NONE',  ( 21.53943276465977519, -0.05219959533907433946, 38.74890960531435979 ) ) ;
#67678 = CARTESIAN_POINT ( 'NONE',  ( 4.483927247898790824, -16.52544592524335698, 70.20942372801904696 ) ) ;
#67679 = CARTESIAN_POINT ( 'NONE',  ( -14.29746914071049879, 8.314922557960819915, 75.83224293864769550 ) ) ;
#67680 = CARTESIAN_POINT ( 'NONE',  ( 19.03943276465977164, -0.05219959533909143690, 38.74890960531436690 ) ) ;
#67681 = SURFACE_STYLE_FILL_AREA ( #160692 ) ;
#67682 = CARTESIAN_POINT ( 'NONE',  ( 35.41276914313061752, -3.966036006072659603, 38.62970943314351757 ) ) ;
#67683 = EDGE_LOOP ( 'NONE', ( #162996, #169034, #56829, #75921 ) ) ;
#67684 = CARTESIAN_POINT ( 'NONE',  ( 4.483927247898790824, -16.52544592524335698, 90.20942372801903275 ) ) ;
#67685 = CARTESIAN_POINT ( 'NONE',  ( 15.72974639402199770, -15.80617190586745480, 113.1239096053143953 ) ) ;
#67686 = CARTESIAN_POINT ( 'NONE',  ( -5.049401038298153566, 19.05341960407611168, 80.20724293864769550 ) ) ;
#67687 = CARTESIAN_POINT ( 'NONE',  ( -0.05219959533937732626, 21.53943276465977519, 52.50109039468567573 ) ) ;
#67688 = CARTESIAN_POINT ( 'NONE',  ( -19.03943276465977164, 0.05219959533909376836, 106.2489096053143669 ) ) ;
#67689 = CARTESIAN_POINT ( 'NONE',  ( -8.106210103297929237, -39.71824525391685512, -25.55638568641365893 ) ) ;
#67690 = ORIENTED_EDGE ( 'NONE', *, *, #174924, .F. ) ;
#67691 = CARTESIAN_POINT ( 'NONE',  ( -15.80617190586768217, 15.72974639402176855, 43.12609039468568284 ) ) ;
#67693 = CARTESIAN_POINT ( 'NONE',  ( 5.049401038298161559, -19.05341960407611168, 97.70724293864766707 ) ) ;
#67692 = CARTESIAN_POINT ( 'NONE',  ( 5.049401038298161559, -19.05341960407611168, 37.70724293864768839 ) ) ;
#67694 = CARTESIAN_POINT ( 'NONE',  ( -9.474510206698720793, -16.51473224551083518, 54.58442372801899722 ) ) ;
#67695 = CARTESIAN_POINT ( 'NONE',  ( -5.823673210054431948, 21.52544592524334988, 32.70942372801900433 ) ) ;
#67696 = CARTESIAN_POINT ( 'NONE',  ( 19.03943276465977164, 0.05219959533936151252, 51.25109039468567573 ) ) ;
#67697 = CARTESIAN_POINT ( 'NONE',  ( -16.46253265017160317, 9.564922557960807481, 25.83224293864769194 ) ) ;
#67698 = CARTESIAN_POINT ( 'NONE',  ( -12.14591786802326823, 12.06949235617739902, 93.12609039468568994 ) ) ;
#67699 = CARTESIAN_POINT ( 'NONE',  ( 16.46253265017146816, 9.564922557961045513, 61.66775706135234003 ) ) ;
#67700 = CARTESIAN_POINT ( 'NONE',  ( -12.14591786802326823, 12.06949235617739902, 108.1260903946856757 ) ) ;
#67701 = CARTESIAN_POINT ( 'NONE',  ( -3.573655867282028392E-15, 2.428612866367529932E-14, -0.1220970790697140096 ) ) ;
#67702 = CARTESIAN_POINT ( 'NONE',  ( -5.049401038298153566, 19.05341960407611168, 80.20724293864769550 ) ) ;
#67703 = CARTESIAN_POINT ( 'NONE',  ( -10.81492255796105439, 18.62759615963255655, 97.91775706135236135 ) ) ;
#67704 = CARTESIAN_POINT ( 'NONE',  ( 10.81492255796106328, -18.62759615963255655, 105.4177570613523613 ) ) ;
#67705 = DIRECTION ( 'NONE',  ( -1.000000000000000000, 0.000000000000000000, 0.000000000000000000 ) ) ;
#67706 = CARTESIAN_POINT ( 'NONE',  ( -13.89961937509977652, 13.97604488694528158, 100.6239096053143669 ) ) ;
#67707 = CARTESIAN_POINT ( 'NONE',  ( -15.72974639402176322, -15.80617190586768395, 69.37609039468567573 ) ) ;
#67708 = CARTESIAN_POINT ( 'NONE',  ( 4.483927247898790824, -16.52544592524335698, 20.20942372801900788 ) ) ;
#67709 = CARTESIAN_POINT ( 'NONE',  ( 0.05219959533909260263, 19.03943276465977164, 79.99890960531436690 ) ) ;
#67710 = CARTESIAN_POINT ( 'NONE',  ( 18.62759615963271287, -10.81492255796078972, 28.33224293864769550 ) ) ;
#67711 = CARTESIAN_POINT ( 'NONE',  ( -19.03943276465977164, 0.05219959533909376836, 91.24890960531436690 ) ) ;
#67712 = CARTESIAN_POINT ( 'NONE',  ( 27.83212366386711523, -25.89052209088936607, -16.12745387078193815 ) ) ;
#67713 = CARTESIAN_POINT ( 'NONE',  ( 13.97604488694527802, 13.89961937509977652, 74.37390960531436690 ) ) ;
#67714 = CARTESIAN_POINT ( 'NONE',  ( -9.564922557960796823, -16.46253265017161027, 67.08224293864769550 ) ) ;
#67715 = CARTESIAN_POINT ( 'NONE',  ( -14.29746914071037622, -8.314922557961029526, 109.1677570613523613 ) ) ;
#67716 = CARTESIAN_POINT ( 'NONE',  ( -19.01529144963332030, -5.500000000000166978, 41.23431955728439391 ) ) ;
#67717 = CARTESIAN_POINT ( 'NONE',  ( 9.564922557961047289, -16.46253265017146816, 70.41775706135233293 ) ) ;
#67718 = CARTESIAN_POINT ( 'NONE',  ( 16.46253265017160672, -9.564922557960803928, 88.33224293864769550 ) ) ;
#67719 = CARTESIAN_POINT ( 'NONE',  ( -12.14591786802309592, -12.06949235617757132, 86.87390960531438111 ) ) ;
#67720 = CARTESIAN_POINT ( 'NONE',  ( -18.62759615963270932, 10.81492255796079327, 40.83224293864769550 ) ) ;
#67721 = CARTESIAN_POINT ( 'NONE',  ( 21.53943276465977519, -0.05219959533907433946, 23.74890960531435269 ) ) ;
#67722 = CARTESIAN_POINT ( 'NONE',  ( -14.34966873604960291, -8.224510206698953496, 106.6655762719810383 ) ) ;
#67723 = CARTESIAN_POINT ( 'NONE',  ( -17.48853670773242541, 5.747243402303156223, 53.66671299749993551 ) ) ;
#67724 = CARTESIAN_POINT ( 'NONE',  ( -16.46253265017146816, -9.564922557961047289, 39.16775706135234003 ) ) ;
#67725 = CARTESIAN_POINT ( 'NONE',  ( 12.06949235617757843, -12.14591786802309237, 28.12390960531435979 ) ) ;
#67726 = CARTESIAN_POINT ( 'NONE',  ( -5.049401038298153566, 19.05341960407611168, 105.2072429386476671 ) ) ;
#67727 = CARTESIAN_POINT ( 'NONE',  ( -10.72451020669870658, -18.67979575497194134, 64.58442372801900433 ) ) ;
#67728 = CARTESIAN_POINT ( 'NONE',  ( 0.05219959533907565091, 21.53943276465977519, 59.99890960531436690 ) ) ;
#67729 = CARTESIAN_POINT ( 'NONE',  ( 10.81492255796106328, -18.62759615963255655, 25.41775706135235779 ) ) ;
#67730 = CARTESIAN_POINT ( 'NONE',  ( -15.72974639402197994, 15.80617190586746368, 80.62390960531438111 ) ) ;
#67731 = CARTESIAN_POINT ( 'NONE',  ( -21.53943276465977519, -0.05219959533937600094, 43.75109039468568284 ) ) ;
#67732 = CARTESIAN_POINT ( 'NONE',  ( 14.29746914071049879, -8.314922557960816363, 108.3322429386477097 ) ) ;
#67733 = CARTESIAN_POINT ( 'NONE',  ( -16.46253265017146816, -9.564922557961047289, 64.16775706135233293 ) ) ;
#67734 = CARTESIAN_POINT ( 'NONE',  ( 13.97604488694527802, 13.89961937509977652, 49.37390960531434558 ) ) ;
#67735 = CARTESIAN_POINT ( 'NONE',  ( -16.52544592524342804, 4.483927247898546575, 86.04057627198102409 ) ) ;
#67736 = CARTESIAN_POINT ( 'NONE',  ( 19.05341960407611168, 5.049401038298154454, 103.9572429386476671 ) ) ;
#67737 = CARTESIAN_POINT ( 'NONE',  ( -19.03943276465977164, 0.05219959533909376836, 26.24890960531435624 ) ) ;
#67738 = CARTESIAN_POINT ( 'NONE',  ( -8.314922557960811034, -14.29746914071050412, 42.08224293864769550 ) ) ;
#67739 = CARTESIAN_POINT ( 'NONE',  ( -8.224510206698735004, -14.34966873604973081, 94.58442372801901854 ) ) ;
#67740 = CARTESIAN_POINT ( 'NONE',  ( -19.03943276465977164, 0.05219959533909376836, 56.24890960531435979 ) ) ;
#67741 = CARTESIAN_POINT ( 'NONE',  ( 19.02544592524343514, -5.153800228976328945, 23.54057627198102054 ) ) ;
#67742 = CARTESIAN_POINT ( 'NONE',  ( 16.46253265017146816, 9.564922557961045513, 26.66775706135234003 ) ) ;
#67744 = CARTESIAN_POINT ( 'NONE',  ( -8.224510206698948167, 14.34966873604960824, 35.41557627198102409 ) ) ;
#67743 = CARTESIAN_POINT ( 'NONE',  ( 5.153800228976335163, 19.02544592524342804, 109.7905762719810099 ) ) ;
#67745 = CARTESIAN_POINT ( 'NONE',  ( 18.67979575497194134, -10.72451020669871369, 45.83442372801901854 ) ) ;
#67746 = CARTESIAN_POINT ( 'NONE',  ( 19.05341960407611168, 5.049401038298154454, 113.9572429386477097 ) ) ;
#67747 = CARTESIAN_POINT ( 'NONE',  ( 4.379528057220092307, 16.55341960407617563, 62.29275706135236845 ) ) ;
#67748 = CARTESIAN_POINT ( 'NONE',  ( 16.53943276465976808, -0.05219959533910856209, 23.74890960531435269 ) ) ;
#67749 = CARTESIAN_POINT ( 'NONE',  ( 16.55341960407618274, -4.379528057220086978, 106.0427570613523471 ) ) ;
#67750 = CARTESIAN_POINT ( 'NONE',  ( -8.314922557961024197, 14.29746914071037800, 22.91775706135235069 ) ) ;
#67751 = CARTESIAN_POINT ( 'NONE',  ( 9.474510206698971260, -16.51473224551069308, 47.91557627198102409 ) ) ;
#67752 = CARTESIAN_POINT ( 'NONE',  ( 12.06949235617757843, -12.14591786802309237, 108.1239096053143811 ) ) ;
#67753 = CARTESIAN_POINT ( 'NONE',  ( -18.62759615963255300, -10.81492255796106328, 24.16775706135235424 ) ) ;
#67754 = CARTESIAN_POINT ( 'NONE',  ( 13.89961937509977652, -13.97604488694527269, 43.12390960531434558 ) ) ;
#67755 = CARTESIAN_POINT ( 'NONE',  ( -5.361383004202544100, -6.881117414448073788, -61.98550895074578193 ) ) ;
#67756 = CARTESIAN_POINT ( 'NONE',  ( -16.46253265017160317, 9.564922557960807481, 35.83224293864768839 ) ) ;
#67757 = CARTESIAN_POINT ( 'NONE',  ( 10.72451020669898902, -18.67979575497178502, 22.91557627198102765 ) ) ;
#67758 = CARTESIAN_POINT ( 'NONE',  ( -17.26172910966780805, -6.454744622555800504, 34.19353091350776452 ) ) ;
#67759 = VECTOR ( 'NONE', #157393, 1000.000000000000000 ) ;
#67760 = CARTESIAN_POINT ( 'NONE',  ( -19.05341960407611168, -5.049401038298163336, 96.45724293864769550 ) ) ;
#67762 = CARTESIAN_POINT ( 'NONE',  ( -12.06949235617756955, 12.14591786802309770, 100.6239096053143811 ) ) ;
#67761 = CARTESIAN_POINT ( 'NONE',  ( 15.72974639402176855, 15.80617190586768217, 46.87609039468568994 ) ) ;
#67763 = CARTESIAN_POINT ( 'NONE',  ( 19.02544592524343514, -5.153800228976328945, 108.5405762719810383 ) ) ;
#67764 = CARTESIAN_POINT ( 'NONE',  ( 193.3062444957835453, -155.7167183371837496, -4.999999999999999112 ) ) ;
#67765 = CARTESIAN_POINT ( 'NONE',  ( -14.29746914071037622, -8.314922557961029526, 74.16775706135231871 ) ) ;
#67766 = CARTESIAN_POINT ( 'NONE',  ( -5.823673210054431948, 21.52544592524334988, 97.70942372801904696 ) ) ;
#67767 = CARTESIAN_POINT ( 'NONE',  ( -4.483927247898782831, 16.52544592524335698, 52.70942372801902565 ) ) ;
#67768 = CARTESIAN_POINT ( 'NONE',  ( 9.474510206698971260, -16.51473224551069308, 97.91557627198102409 ) ) ;
#67769 = CARTESIAN_POINT ( 'NONE',  ( -4.379528057220086978, -16.55341960407618274, 44.79275706135234714 ) ) ;
#67770 = CARTESIAN_POINT ( 'NONE',  ( 13.89961937509957401, 13.97604488694547697, 111.8760903946856757 ) ) ;
#67771 = CARTESIAN_POINT ( 'NONE',  ( -16.55341960407617563, 4.379528057220093196, 88.54275706135236135 ) ) ;
#67772 = CARTESIAN_POINT ( 'NONE',  ( 5.049401038297881783, 19.05341960407617563, 112.2927570613523471 ) ) ;
#67773 = CARTESIAN_POINT ( 'NONE',  ( -19.05341960407611168, -5.049401038298163336, 76.45724293864769550 ) ) ;
#67774 = CARTESIAN_POINT ( 'NONE',  ( -21.55341960407610458, -5.719274019375992779, 91.45724293864769550 ) ) ;
#67776 = CARTESIAN_POINT ( 'NONE',  ( 9.564922557961047289, -16.46253265017146816, 105.4177570613523471 ) ) ;
#67775 = CARTESIAN_POINT ( 'NONE',  ( 4.483927247898545687, 16.52544592524342804, 104.7905762719810241 ) ) ;
#67777 = CARTESIAN_POINT ( 'NONE',  ( 16.55341960407618274, -4.379528057220086978, 71.04275706135234714 ) ) ;
#67778 = CARTESIAN_POINT ( 'NONE',  ( 21.51693143705272959, 9.260949364272169859, 168.7281092719942990 ) ) ;
#67779 = CARTESIAN_POINT ( 'NONE',  ( 19.05341960407617918, -5.049401038297876454, 71.04275706135234714 ) ) ;
#67780 = CARTESIAN_POINT ( 'NONE',  ( -16.53943276465976808, 0.05219959533911058130, 26.24890960531435624 ) ) ;
#67781 = CARTESIAN_POINT ( 'NONE',  ( 16.53943276465976808, -0.05219959533910856209, 93.74890960531436690 ) ) ;
#67783 = CARTESIAN_POINT ( 'NONE',  ( -17.12812012977028431, 6.668231424565927767, 88.64051240676862164 ) ) ;
#67782 = CARTESIAN_POINT ( 'NONE',  ( 9.474510206698729675, 16.51473224551082808, 37.08442372801899722 ) ) ;
#67784 = CARTESIAN_POINT ( 'NONE',  ( -15.80617190586768217, 15.72974639402176855, 33.12609039468569705 ) ) ;
#67785 = CARTESIAN_POINT ( 'NONE',  ( 5.049401038297881783, 19.05341960407617563, 92.29275706135234714 ) ) ;
#67786 = CARTESIAN_POINT ( 'NONE',  ( -16.46253265017160317, 9.564922557960807481, 115.8322429386477097 ) ) ;
#67787 = CARTESIAN_POINT ( 'NONE',  ( 0.05219959533909260263, 19.03943276465977164, 94.99890960531436690 ) ) ;
#67788 = CARTESIAN_POINT ( 'NONE',  ( 5.823673210054444382, -21.52544592524334988, 90.20942372801903275 ) ) ;
#67789 = CARTESIAN_POINT ( 'NONE',  ( 19.02544592524343514, -5.153800228976328945, 73.54057627198103830 ) ) ;
#67790 = EDGE_LOOP ( 'NONE', ( #190263, #173129, #62856, #73565, #21569 ) ) ;
#67791 = CARTESIAN_POINT ( 'NONE',  ( -21.53943276465977519, 0.05219959533907696930, 41.24890960531435269 ) ) ;
#67792 = CARTESIAN_POINT ( 'NONE',  ( 12.14591786802309770, 12.06949235617756955, 99.37390960531436690 ) ) ;
#67793 = CARTESIAN_POINT ( 'NONE',  ( 13.89961937509977652, -13.97604488694527269, 53.12390960531434558 ) ) ;
#67794 = CARTESIAN_POINT ( 'NONE',  ( 14.29746914071049879, -8.314922557960816363, 108.3322429386477097 ) ) ;
#67795 = CARTESIAN_POINT ( 'NONE',  ( 15.72974639402176855, 15.80617190586768217, 26.87609039468567218 ) ) ;
#67796 = AXIS2_PLACEMENT_3D ( 'NONE', #128420, #191111, #52585 ) ;
#67797 = CARTESIAN_POINT ( 'NONE',  ( 10.72451020669871369, 18.67979575497193778, 77.08442372801901854 ) ) ;
#67798 = CARTESIAN_POINT ( 'NONE',  ( 0.05219959533909260263, 19.03943276465977164, 44.99890960531435979 ) ) ;
#67799 = CARTESIAN_POINT ( 'NONE',  ( -16.53943276465976808, -0.05219959533934237506, 78.75109039468568994 ) ) ;
#67800 = CARTESIAN_POINT ( 'NONE',  ( 21.53943276465977519, 0.05219959533937863772, 21.25109039468567218 ) ) ;
#67801 = ORIENTED_EDGE ( 'NONE', *, *, #171282, .T. ) ;
#67802 = CARTESIAN_POINT ( 'NONE',  ( 15.72974639402176855, 15.80617190586768217, 31.87609039468567929 ) ) ;
#67804 = CARTESIAN_POINT ( 'NONE',  ( -16.51473224551069308, -9.474510206698971260, 61.66557627198103120 ) ) ;
#67803 = CARTESIAN_POINT ( 'NONE',  ( 0.05219959533936267826, -19.03943276465977164, 55.00109039468566863 ) ) ;
#67805 = CARTESIAN_POINT ( 'NONE',  ( -19.05341960407617563, 5.049401038297882671, 38.54275706135233293 ) ) ;
#67806 = CARTESIAN_POINT ( 'NONE',  ( 5.719274019375673035, 21.55341960407619339, 72.29275706135236135 ) ) ;
#67807 = CARTESIAN_POINT ( 'NONE',  ( 18.67979575497178502, 10.72451020669898547, 74.16557627198102409 ) ) ;
#67808 = CARTESIAN_POINT ( 'NONE',  ( -14.29746914071049879, 8.314922557960819915, 45.83224293864769550 ) ) ;
#67810 = CARTESIAN_POINT ( 'NONE',  ( -9.474510206698720793, -16.51473224551083518, 34.58442372801899722 ) ) ;
#67809 = CARTESIAN_POINT ( 'NONE',  ( -18.67979575497193778, 10.72451020669871902, 93.33442372801901854 ) ) ;
#67811 = CARTESIAN_POINT ( 'NONE',  ( 4.379528057220339221, -16.55341960407611168, 67.70724293864769550 ) ) ;
#67812 = CARTESIAN_POINT ( 'NONE',  ( -4.379528057220328563, 16.55341960407611168, 115.2072429386476955 ) ) ;
#67813 = CARTESIAN_POINT ( 'NONE',  ( -0.05219959533936034679, 19.03943276465977164, 52.50109039468566863 ) ) ;
#67814 = CARTESIAN_POINT ( 'NONE',  ( -12.14591786802326823, 12.06949235617739902, 113.1260903946856899 ) ) ;
#67815 = CARTESIAN_POINT ( 'NONE',  ( 15.80617190586769283, -15.72974639402175789, 85.62609039468568994 ) ) ;
#67816 = CARTESIAN_POINT ( 'NONE',  ( -16.46253265017146816, -9.564922557961047289, 44.16775706135232582 ) ) ;
#67817 = CARTESIAN_POINT ( 'NONE',  ( -21.55341960407610458, -5.719274019375992779, 56.45724293864768839 ) ) ;
#67818 = CARTESIAN_POINT ( 'NONE',  ( -18.62759615963255300, -10.81492255796106328, 49.16775706135234003 ) ) ;
#67819 = CARTESIAN_POINT ( 'NONE',  ( 15.72974639402199770, -15.80617190586745480, 98.12390960531436690 ) ) ;
#67820 = CARTESIAN_POINT ( 'NONE',  ( -16.46253265017146816, -9.564922557961047289, 99.16775706135233293 ) ) ;
#67821 = CARTESIAN_POINT ( 'NONE',  ( 14.34966873604972726, -8.224510206698740333, 70.83442372801901854 ) ) ;
#67823 = CARTESIAN_POINT ( 'NONE',  ( 21.55341960407610458, 5.719274019375980345, 103.9572429386476813 ) ) ;
#67822 = CARTESIAN_POINT ( 'NONE',  ( -3.573655867282028392E-15, 2.428612866367529932E-14, -25.00000000000000000 ) ) ;
#67824 = CARTESIAN_POINT ( 'NONE',  ( -14.34966873604960291, -8.224510206698953496, 91.66557627198103830 ) ) ;
#67825 = CARTESIAN_POINT ( 'NONE',  ( -17.50000000000011369, -3.417042746627175109, 29.82619603767520644 ) ) ;
#67826 = CARTESIAN_POINT ( 'NONE',  ( 14.34966873604972726, -8.224510206698740333, 35.83442372801901143 ) ) ;
#67827 = CARTESIAN_POINT ( 'NONE',  ( 15.80617190586746368, 15.72974639402197994, 54.37390960531435979 ) ) ;
#67828 = CARTESIAN_POINT ( 'NONE',  ( 14.34966873604972726, -8.224510206698740333, 95.83442372801903275 ) ) ;
#67829 = DIRECTION ( 'NONE',  ( 0.000000000000000000, 0.000000000000000000, -1.000000000000000000 ) ) ;
#67830 = CARTESIAN_POINT ( 'NONE',  ( -8.314922557961024197, 14.29746914071037800, 72.91775706135234714 ) ) ;
#67831 = CARTESIAN_POINT ( 'NONE',  ( 0.05219959533937995610, -21.53943276465977519, 45.00109039468568284 ) ) ;
#67832 = CARTESIAN_POINT ( 'NONE',  ( 21.52544592524344225, -5.823673210054117533, 63.54057627198103830 ) ) ;
#67833 = CARTESIAN_POINT ( 'NONE',  ( -16.53943276465976808, -0.05219959533934237506, 83.75109039468568994 ) ) ;
#67834 = CARTESIAN_POINT ( 'NONE',  ( 21.53943276465977519, 0.05219959533937863772, 76.25109039468568994 ) ) ;
#67835 = CARTESIAN_POINT ( 'NONE',  ( 21.55341960407610458, 5.719274019375980345, 58.95724293864770971 ) ) ;
#67836 = CARTESIAN_POINT ( 'NONE',  ( -18.67979575497178146, -10.72451020669898902, 36.66557627198103120 ) ) ;
#67837 = CARTESIAN_POINT ( 'NONE',  ( -12.06949235617739369, -12.14591786802326823, 59.37609039468568284 ) ) ;
#67838 = CARTESIAN_POINT ( 'NONE',  ( -10.81492255796078084, -18.62759615963271287, 32.08224293864769550 ) ) ;
#67839 = ORIENTED_EDGE ( 'NONE', *, *, #89447, .F. ) ;
#67840 = CARTESIAN_POINT ( 'NONE',  ( 9.474510206698971260, -16.51473224551069308, 92.91557627198103830 ) ) ;
#67841 = CARTESIAN_POINT ( 'NONE',  ( 12.06949235617739724, 12.14591786802326823, 106.8760903946856899 ) ) ;
#67842 = CARTESIAN_POINT ( 'NONE',  ( 18.00321789565200703, -35.67122027912853355, -27.04300662093937291 ) ) ;
#67843 = CARTESIAN_POINT ( 'NONE',  ( 16.55341960407611168, 4.379528057220329451, 113.9572429386477239 ) ) ;
#67844 = CARTESIAN_POINT ( 'NONE',  ( -0.05219959533907301413, -21.53943276465977519, 52.49890960531435979 ) ) ;
#67845 = CARTESIAN_POINT ( 'NONE',  ( 16.51473224551069308, 9.474510206698969483, 49.16557627198102409 ) ) ;
#67846 = CARTESIAN_POINT ( 'NONE',  ( 4.483927247898790824, -16.52544592524335698, 95.20942372801903275 ) ) ;
#67847 = CARTESIAN_POINT ( 'NONE',  ( -5.719274019375665041, -21.55341960407619695, 39.79275706135235424 ) ) ;
#67848 = CARTESIAN_POINT ( 'NONE',  ( 5.153800228976615827, -19.02544592524334988, 85.20942372801900433 ) ) ;
#67849 = CARTESIAN_POINT ( 'NONE',  ( -16.52544592524342804, 4.483927247898546575, 106.0405762719810525 ) ) ;
#67850 = CARTESIAN_POINT ( 'NONE',  ( 9.564922557960805705, 16.46253265017160317, 54.58224293864769550 ) ) ;
#67851 = CARTESIAN_POINT ( 'NONE',  ( 5.000000000000000888, -129.0000000000000000, -13.99999999999999822 ) ) ;
#67852 = CARTESIAN_POINT ( 'NONE',  ( 17.97161686093727795, -5.499999999999996447, 63.49637206859166838 ) ) ;
#67853 = CARTESIAN_POINT ( 'NONE',  ( 13.97604488694527802, 13.89961937509977652, 79.37390960531435269 ) ) ;
#67854 = CARTESIAN_POINT ( 'NONE',  ( -16.52544592524335698, -4.483927247898792601, 68.95942372801901854 ) ) ;
#67855 = CARTESIAN_POINT ( 'NONE',  ( 21.53943276465977519, 0.05219959533937863772, 106.2510903946856757 ) ) ;
#67856 = CARTESIAN_POINT ( 'NONE',  ( -10.81492255796078084, -18.62759615963271287, 47.08224293864770260 ) ) ;
#67857 = CARTESIAN_POINT ( 'NONE',  ( 4.483927247898790824, -16.52544592524335698, 70.20942372801904696 ) ) ;
#67858 = CARTESIAN_POINT ( 'NONE',  ( -9.564922557961040184, 16.46253265017147172, 67.91775706135233293 ) ) ;
#67859 = VERTEX_POINT ( 'NONE', #96931 ) ;
#67860 = CARTESIAN_POINT ( 'NONE',  ( -21.55341960407619339, 5.719274019375674811, 68.54275706135234714 ) ) ;
#67861 = CARTESIAN_POINT ( 'NONE',  ( 0.05219959533909260263, 19.03943276465977164, 64.99890960531436690 ) ) ;
#67862 = CARTESIAN_POINT ( 'NONE',  ( 13.97604488694527802, 13.89961937509977652, 34.37390960531436690 ) ) ;
#67863 = CARTESIAN_POINT ( 'NONE',  ( -13.97604488694547697, 13.89961937509957934, 53.12609039468565442 ) ) ;
#67864 = CARTESIAN_POINT ( 'NONE',  ( -16.46253265017160317, 9.564922557960807481, 115.8322429386477097 ) ) ;
#67865 = CARTESIAN_POINT ( 'NONE',  ( -16.51473224551069308, -9.474510206698971260, 91.66557627198103830 ) ) ;
#67866 = CARTESIAN_POINT ( 'NONE',  ( 4.379528057220339221, -16.55341960407611168, 57.70724293864770260 ) ) ;
#67867 = CARTESIAN_POINT ( 'NONE',  ( 10.81492255796078972, 18.62759615963270932, 44.58224293864769550 ) ) ;
#67868 = CARTESIAN_POINT ( 'NONE',  ( 37.99626262588765258, 2.893932880411085066E-14, 2.000000000000000000 ) ) ;
#67869 = CARTESIAN_POINT ( 'NONE',  ( 13.89961937509957401, 13.97604488694547697, 26.87609039468566507 ) ) ;
#67870 = FACE_OUTER_BOUND ( 'NONE', #164723, .T. ) ;
#67871 = CARTESIAN_POINT ( 'NONE',  ( 19.02544592524343514, -5.153800228976328945, 48.54057627198103120 ) ) ;
#67872 = CARTESIAN_POINT ( 'NONE',  ( 16.52544592524335698, 4.483927247898782831, 31.45942372801901854 ) ) ;
#67873 = CARTESIAN_POINT ( 'NONE',  ( -18.39639308325437739, -5.500000000000015099, 101.4825224618219863 ) ) ;
#67874 = FACE_OUTER_BOUND ( 'NONE', #159501, .T. ) ;
#67875 = CARTESIAN_POINT ( 'NONE',  ( -16.53943276465976808, -0.05219959533934237506, 78.75109039468568994 ) ) ;
#67877 = EDGE_CURVE ( 'NONE', #48812, #96464, #102423, .T. ) ;
#67876 = CARTESIAN_POINT ( 'NONE',  ( -0.05219959533907301413, -21.53943276465977519, 102.4989096053143811 ) ) ;
#67879 = CARTESIAN_POINT ( 'NONE',  ( 7.500000000000000888, -1.380023386739103852, 4.327083394447440057 ) ) ;
#67878 = CARTESIAN_POINT ( 'NONE',  ( 13.97604488694527802, 13.89961937509977652, 39.37390960531435269 ) ) ;
#67880 = CARTESIAN_POINT ( 'NONE',  ( 10.72451020669871369, 18.67979575497193778, 37.08442372801901143 ) ) ;
#67881 = CARTESIAN_POINT ( 'NONE',  ( 9.564922557961047289, -16.46253265017146816, 50.41775706135233293 ) ) ;
#67882 = CARTESIAN_POINT ( 'NONE',  ( 5.153800228976335163, 19.02544592524342804, 44.79057627198103830 ) ) ;
#67883 = CARTESIAN_POINT ( 'NONE',  ( 21.55341960407619695, -5.719274019375665929, 101.0427570613523756 ) ) ;
#67884 = CARTESIAN_POINT ( 'NONE',  ( -13.97604488694527625, -13.89961937509977652, 21.87390960531435979 ) ) ;
#67885 = CARTESIAN_POINT ( 'NONE',  ( -4.483927247898539470, -16.52544592524342804, 42.29057627198103120 ) ) ;
#67886 = CARTESIAN_POINT ( 'NONE',  ( 19.35543954521082100, 5.499999999999578115, 42.08901960356453031 ) ) ;
#67887 = CARTESIAN_POINT ( 'NONE',  ( -10.72451020669898014, 18.67979575497178502, 60.41557627198102409 ) ) ;
#67888 = CARTESIAN_POINT ( 'NONE',  ( -17.14385361876520975, 23.59649016807275856, 140.5750000027311444 ) ) ;
#67889 = CARTESIAN_POINT ( 'NONE',  ( 13.97604488694527802, 13.89961937509977652, 109.3739096053143669 ) ) ;
#67890 = CARTESIAN_POINT ( 'NONE',  ( 16.55341960407611168, 4.379528057220329451, 88.95724293864769550 ) ) ;
#67891 = CARTESIAN_POINT ( 'NONE',  ( -14.34966873604972548, 8.224510206698743886, 28.33442372801902209 ) ) ;
#67892 = CARTESIAN_POINT ( 'NONE',  ( -16.55341960407617563, 4.379528057220093196, 103.5427570613523613 ) ) ;
#67893 = ORIENTED_EDGE ( 'NONE', *, *, #67633, .F. ) ;
#67895 = CARTESIAN_POINT ( 'NONE',  ( 18.67979575497178502, 10.72451020669898547, 99.16557627198100988 ) ) ;
#67894 = CARTESIAN_POINT ( 'NONE',  ( -5.049401038298153566, 19.05341960407611168, 100.2072429386476955 ) ) ;
#67897 = CARTESIAN_POINT ( 'NONE',  ( -5.153800228976328057, -19.02544592524343514, 97.29057627198099567 ) ) ;
#67896 = CARTESIAN_POINT ( 'NONE',  ( 12.06949235617757843, -12.14591786802309237, 28.12390960531435979 ) ) ;
#67898 = CARTESIAN_POINT ( 'NONE',  ( -16.51473224551082808, 9.474510206698731452, 93.33442372801900433 ) ) ;
#67899 = CARTESIAN_POINT ( 'NONE',  ( 21.52544592524334988, 5.823673210054432836, 106.4594237280190328 ) ) ;
#67900 = CARTESIAN_POINT ( 'NONE',  ( -10.72451020669898014, 18.67979575497178502, 85.41557627198102409 ) ) ;
#67901 = CARTESIAN_POINT ( 'NONE',  ( 15.80617190586746368, 15.72974639402197994, 54.37390960531435979 ) ) ;
#67902 = CARTESIAN_POINT ( 'NONE',  ( 5.049401038298161559, -19.05341960407611168, 57.70724293864769550 ) ) ;
#67903 = CARTESIAN_POINT ( 'NONE',  ( -16.55341960407611168, -4.379528057220339221, 36.45724293864768839 ) ) ;
#67904 = CARTESIAN_POINT ( 'NONE',  ( 0.05219959533909260263, 19.03943276465977164, 79.99890960531436690 ) ) ;
#67905 = ORIENTED_EDGE ( 'NONE', *, *, #71198, .T. ) ;
#67906 = CARTESIAN_POINT ( 'NONE',  ( 1.300000000000000044, 0.000000000000000000, 0.000000000000000000 ) ) ;
#67907 = CARTESIAN_POINT ( 'NONE',  ( -16.51473224551082808, 9.474510206698731452, 43.33442372801900433 ) ) ;
#67908 = CARTESIAN_POINT ( 'NONE',  ( -0.05219959533907301413, -21.53943276465977519, 77.49890960531433848 ) ) ;
#67909 = CARTESIAN_POINT ( 'NONE',  ( 14.29746914071049879, -8.314922557960816363, 83.33224293864769550 ) ) ;
#67910 = CARTESIAN_POINT ( 'NONE',  ( -18.67979575497193778, 10.72451020669871902, 23.33442372801901499 ) ) ;
#67911 = CARTESIAN_POINT ( 'NONE',  ( 27.73933785331498925, -9.013057229001033122, 146.2750000027311899 ) ) ;
#67912 = CARTESIAN_POINT ( 'NONE',  ( 4.483927247898790824, -16.52544592524335698, 110.2094237280190185 ) ) ;
#67913 = CARTESIAN_POINT ( 'NONE',  ( -5.049401038298153566, 19.05341960407611168, 25.20724293864768484 ) ) ;
#67914 = CARTESIAN_POINT ( 'NONE',  ( -19.03943276465977164, 0.05219959533909376836, 71.24890960531435269 ) ) ;
#67915 = SURFACE_STYLE_USAGE ( .BOTH. , #6236 ) ;
#67916 = CARTESIAN_POINT ( 'NONE',  ( -38.00000000000000711, 2.428612866367529932E-14, -9.749999994537626336 ) ) ;
#67917 = CARTESIAN_POINT ( 'NONE',  ( 16.53943276465976808, -0.05219959533910856209, 48.74890960531435979 ) ) ;
#67918 = CARTESIAN_POINT ( 'NONE',  ( 10.81492255796106328, -18.62759615963255655, 55.41775706135234714 ) ) ;
#67919 = CARTESIAN_POINT ( 'NONE',  ( 25.38628342471155364, -27.91043139587388566, -20.44818103819207167 ) ) ;
#67920 = CARTESIAN_POINT ( 'NONE',  ( -5.153800228976328057, -19.02544592524343514, 37.29057627198102409 ) ) ;
#67921 = CARTESIAN_POINT ( 'NONE',  ( 0.05219959533909260263, 19.03943276465977164, 54.99890960531435979 ) ) ;
#67922 = ORIENTED_EDGE ( 'NONE', *, *, #114385, .F. ) ;
#67923 = CARTESIAN_POINT ( 'NONE',  ( -15.72974639402176322, -15.80617190586768395, 109.3760903946857042 ) ) ;
#67924 = CARTESIAN_POINT ( 'NONE',  ( -16.53943276465976808, -0.05219959533934237506, 63.75109039468568284 ) ) ;
#67925 = CARTESIAN_POINT ( 'NONE',  ( 21.52544592524334988, 5.823673210054432836, 86.45942372801901854 ) ) ;
#67926 = CARTESIAN_POINT ( 'NONE',  ( -19.02544592524342804, 5.153800228976336051, 116.0405762719810383 ) ) ;
#67927 = CARTESIAN_POINT ( 'NONE',  ( 0.05219959533936267826, -19.03943276465977164, 95.00109039468567573 ) ) ;
#67928 = CARTESIAN_POINT ( 'NONE',  ( -21.53943276465977519, -0.05219959533937600094, 68.75109039468568994 ) ) ;
#67929 = CARTESIAN_POINT ( 'NONE',  ( 16.52544592524335698, 4.483927247898782831, 41.45942372801901143 ) ) ;
#67930 = CARTESIAN_POINT ( 'NONE',  ( 21.53943276465977519, -0.05219959533907433946, 88.74890960531436690 ) ) ;
#67931 = CARTESIAN_POINT ( 'NONE',  ( 9.564922557961047289, -16.46253265017146816, 105.4177570613523471 ) ) ;
#67932 = CARTESIAN_POINT ( 'NONE',  ( 16.51473224551069308, 9.474510206698969483, 59.16557627198102409 ) ) ;
#67933 = CARTESIAN_POINT ( 'NONE',  ( 13.97604488694548053, -13.89961937509957401, 95.62609039468563310 ) ) ;
#67934 = AXIS2_PLACEMENT_3D ( 'NONE', #360, #91364, #152079 ) ;
#67935 = CARTESIAN_POINT ( 'NONE',  ( -9.564922557961040184, 16.46253265017147172, 97.91775706135233293 ) ) ;
#67936 = CARTESIAN_POINT ( 'NONE',  ( -0.05219959533910754901, -16.53943276465976808, 52.49890960531435979 ) ) ;
#67937 = CARTESIAN_POINT ( 'NONE',  ( -5.153800228976607833, 19.02544592524334988, 82.70942372801897591 ) ) ;
#67938 = CARTESIAN_POINT ( 'NONE',  ( 16.53943276465976808, 0.05219959533934440121, 61.25109039468567573 ) ) ;
#67940 = CARTESIAN_POINT ( 'NONE',  ( 13.89961937509977652, -13.97604488694527269, 38.12390960531436690 ) ) ;
#67939 = CARTESIAN_POINT ( 'NONE',  ( -21.52544592524334988, -5.823673210054445271, 18.95942372801901143 ) ) ;
#67941 = CARTESIAN_POINT ( 'NONE',  ( 9.564922557960805705, 16.46253265017160317, 49.58224293864770260 ) ) ;
#67942 = CARTESIAN_POINT ( 'NONE',  ( -14.29746914071037622, -8.314922557961029526, 54.16775706135235424 ) ) ;
#67943 = CARTESIAN_POINT ( 'NONE',  ( 30.00000000000000711, -1.163414459189985801E-14, 95.00000000000000000 ) ) ;
#67944 = CARTESIAN_POINT ( 'NONE',  ( -28.82186960331499392, 9.364793116373565596, 146.1500000054623456 ) ) ;
#67945 = CARTESIAN_POINT ( 'NONE',  ( -5.049401038298153566, 19.05341960407611168, 100.2072429386476955 ) ) ;
#67946 = LINE ( 'NONE', #178145, #136566 ) ;
#67947 = CARTESIAN_POINT ( 'NONE',  ( -5.153800228976607833, 19.02544592524334988, 112.7094237280190043 ) ) ;
#67948 = CARTESIAN_POINT ( 'NONE',  ( 5.823673210054125526, 21.52544592524343514, 34.79057627198103120 ) ) ;
#67950 = CARTESIAN_POINT ( 'NONE',  ( -8.224510206698735004, -14.34966873604973081, 34.58442372801900433 ) ) ;
#67949 = CARTESIAN_POINT ( 'NONE',  ( 9.474510206698729675, 16.51473224551082808, 42.08442372801900433 ) ) ;
#67951 = CARTESIAN_POINT ( 'NONE',  ( 19.05341960407611168, 5.049401038298154454, 33.95724293864769550 ) ) ;
#67952 = CARTESIAN_POINT ( 'NONE',  ( -13.97604488694527625, -13.89961937509977652, 51.87390960531436690 ) ) ;
#67953 = CARTESIAN_POINT ( 'NONE',  ( 15.72974639402199770, -15.80617190586745480, 88.12390960531436690 ) ) ;
#67954 = CARTESIAN_POINT ( 'NONE',  ( -5.153800228976328057, -19.02544592524343514, 97.29057627198099567 ) ) ;
#67955 = CARTESIAN_POINT ( 'NONE',  ( -5.153800228976328057, -19.02544592524343514, 47.29057627198102409 ) ) ;
#67956 = CARTESIAN_POINT ( 'NONE',  ( -27.73933785331498925, 2.428612866367529932E-14, 141.3750000027311842 ) ) ;
#67957 = CARTESIAN_POINT ( 'NONE',  ( -16.46253265017146816, -9.564922557961047289, 84.16775706135233293 ) ) ;
#67958 = CARTESIAN_POINT ( 'NONE',  ( -4.483927247898539470, -16.52544592524342804, 72.29057627198102409 ) ) ;
#67959 = CARTESIAN_POINT ( 'NONE',  ( 18.67979575497194134, -10.72451020669871369, 100.8344237280190185 ) ) ;
#67960 = CARTESIAN_POINT ( 'NONE',  ( 21.55341960407610458, 5.719274019375980345, 93.95724293864770971 ) ) ;
#67961 = CARTESIAN_POINT ( 'NONE',  ( -5.823673210054431948, 21.52544592524334988, 82.70942372801900433 ) ) ;
#67962 = B_SPLINE_CURVE_WITH_KNOTS ( 'NONE', 3,
 ( #49138, #157307, #113764, #36931, #98593, #126945, #80449, #142122, #160287, #3607, #65286, #111792, #173480, #34953, #158294, #19783, #73296, #9619, #57122, #25798, #87444, #162283 ),
 .UNSPECIFIED., .F., .F.,
 ( 4, 2, 2, 2, 2, 2, 2, 2, 2, 2, 4 ),
 ( -3.098386792753634396E-05, 0.0007621651712067583836, 0.001555314210341053084, 0.003141612288609643786, 0.006314208445146832563, 0.01265940075822121792, 0.01583199691475840887, 0.01900459307129559808, 0.02059089114956419789, 0.02217718922783280117, 0.02534978538437000078 ),
 .UNSPECIFIED. ) ;
#67963 = CARTESIAN_POINT ( 'NONE',  ( 15.80617190586769283, -15.72974639402175789, 80.62609039468567573 ) ) ;
#67964 = CARTESIAN_POINT ( 'NONE',  ( 13.89961937509977652, -13.97604488694527269, 103.1239096053143527 ) ) ;
#67966 = CARTESIAN_POINT ( 'NONE',  ( 18.67979575497194134, -10.72451020669871369, 80.83442372801901854 ) ) ;
#67965 = CARTESIAN_POINT ( 'NONE',  ( 0.05219959533934541429, -16.53943276465976808, 110.0010903946856757 ) ) ;
#67967 = CARTESIAN_POINT ( 'NONE',  ( -19.03943276465977164, 0.05219959533909376836, 61.24890960531436690 ) ) ;
#67968 = CARTESIAN_POINT ( 'NONE',  ( -21.55341960407619339, 5.719274019375674811, 43.54275706135235424 ) ) ;
#67969 = CARTESIAN_POINT ( 'NONE',  ( -13.97604488694527625, -13.89961937509977652, 81.87390960531436690 ) ) ;
#67970 = CARTESIAN_POINT ( 'NONE',  ( 4.379528057220339221, -16.55341960407611168, 82.70724293864770971 ) ) ;
#67971 = CARTESIAN_POINT ( 'NONE',  ( 8.314922557960818139, 14.29746914071049879, 54.58224293864769550 ) ) ;
#67972 = CARTESIAN_POINT ( 'NONE',  ( 10.81492255796078972, 18.62759615963270932, 54.58224293864769550 ) ) ;
#67973 = CARTESIAN_POINT ( 'NONE',  ( 5.049401038298161559, -19.05341960407611168, 62.70724293864769550 ) ) ;
#67974 = CARTESIAN_POINT ( 'NONE',  ( -0.05219959533907301413, -21.53943276465977519, 77.49890960531433848 ) ) ;
#67975 = CARTESIAN_POINT ( 'NONE',  ( 19.05341960407617918, -5.049401038297876454, 71.04275706135234714 ) ) ;
#67977 = CARTESIAN_POINT ( 'NONE',  ( -0.05219959533910754901, -16.53943276465976808, 72.49890960531435269 ) ) ;
#67976 = CARTESIAN_POINT ( 'NONE',  ( 13.97604488694548053, -13.89961937509957401, 35.62609039468567573 ) ) ;
#67978 = CARTESIAN_POINT ( 'NONE',  ( 21.53943276465977519, -0.05219959533907433946, 58.74890960531436690 ) ) ;
#67979 = CARTESIAN_POINT ( 'NONE',  ( -17.49999999999999289, 5.500000000000032863, 70.79690382534172954 ) ) ;
#67981 = CARTESIAN_POINT ( 'NONE',  ( -22.44159573604009950, -16.30477369853688430, 143.5750000027311728 ) ) ;
#67980 = CARTESIAN_POINT ( 'NONE',  ( 14.34966873604972726, -8.224510206698740333, 95.83442372801903275 ) ) ;
#67982 = CARTESIAN_POINT ( 'NONE',  ( 0.05219959533936267826, -19.03943276465977164, 105.0010903946856615 ) ) ;
#67983 = CARTESIAN_POINT ( 'NONE',  ( -16.55341960407611168, -4.379528057220339221, 71.45724293864769550 ) ) ;
#67984 = CARTESIAN_POINT ( 'NONE',  ( -17.50000000000002132, 3.850315288878720654, 34.26629130603451046 ) ) ;
#67985 = CARTESIAN_POINT ( 'NONE',  ( -0.05219959533909027116, -19.03943276465977164, 62.49890960531435979 ) ) ;
#67986 = CARTESIAN_POINT ( 'NONE',  ( 8.224510206698953496, -14.34966873604960469, 47.91557627198102409 ) ) ;
#67987 = CARTESIAN_POINT ( 'NONE',  ( -13.97604488694527625, -13.89961937509977652, 91.87390960531432427 ) ) ;
#67989 = CARTESIAN_POINT ( 'NONE',  ( -19.03943276465977164, 0.05219959533909376836, 61.24890960531436690 ) ) ;
#67988 = CARTESIAN_POINT ( 'NONE',  ( 13.89961937509957401, 13.97604488694547697, 76.87609039468566152 ) ) ;
#67990 = CARTESIAN_POINT ( 'NONE',  ( 19.02544592524343514, -5.153800228976328945, 83.54057627198100988 ) ) ;
#67991 = CIRCLE ( 'NONE', #164886, 206.0437394197456911 ) ;
#67992 = CARTESIAN_POINT ( 'NONE',  ( -0.05219959533909027116, -19.03943276465977164, 67.49890960531436690 ) ) ;
#67993 = CARTESIAN_POINT ( 'NONE',  ( -21.53943276465977519, 0.05219959533907696930, 66.24890960531436690 ) ) ;
#67994 = CARTESIAN_POINT ( 'NONE',  ( -14.29746914071037622, -8.314922557961029526, 54.16775706135235424 ) ) ;
#67995 = CARTESIAN_POINT ( 'NONE',  ( -16.51473224551082808, 9.474510206698731452, 103.3344237280190043 ) ) ;
#67996 = CARTESIAN_POINT ( 'NONE',  ( 5.153800228976335163, 19.02544592524342804, 44.79057627198103830 ) ) ;
#67997 = CARTESIAN_POINT ( 'NONE',  ( -18.67979575497178146, -10.72451020669898902, 56.66557627198103830 ) ) ;
#67998 = CARTESIAN_POINT ( 'NONE',  ( 19.03943276465977164, 0.05219959533936151252, 81.25109039468567573 ) ) ;
#67999 = CARTESIAN_POINT ( 'NONE',  ( 8.224510206698953496, -14.34966873604960469, 22.91557627198102765 ) ) ;
#68000 = EDGE_CURVE ( 'NONE', #53519, #101425, #83047, .T. ) ;
#68001 = CARTESIAN_POINT ( 'NONE',  ( 19.03943276465977164, 0.05219959533936151252, 41.25109039468566152 ) ) ;
#68003 = CARTESIAN_POINT ( 'NONE',  ( -12.06949235617739369, -12.14591786802326823, 99.37609039468568994 ) ) ;
#68002 = CARTESIAN_POINT ( 'NONE',  ( 14.34966873604972726, -8.224510206698740333, 60.83442372801901854 ) ) ;
#68004 = CARTESIAN_POINT ( 'NONE',  ( -17.97182807773874558, 5.499999999999870326, 53.53038844047288336 ) ) ;
#68005 = CARTESIAN_POINT ( 'NONE',  ( -12.06949235617739369, -12.14591786802326823, 79.37609039468567573 ) ) ;
#68006 = CARTESIAN_POINT ( 'NONE',  ( 21.53943276465977519, -0.05219959533907433946, 23.74890960531435269 ) ) ;
#68007 = CARTESIAN_POINT ( 'NONE',  ( -19.02544592524342804, 5.153800228976336051, 46.04057627198101699 ) ) ;
#68008 = CARTESIAN_POINT ( 'NONE',  ( -16.51473224551069308, -9.474510206698971260, 46.66557627198102409 ) ) ;
#68009 = CARTESIAN_POINT ( 'NONE',  ( -16.51473224551069308, -9.474510206698971260, 46.66557627198102409 ) ) ;
#68010 = CARTESIAN_POINT ( 'NONE',  ( 10.81492255796106328, -18.62759615963255655, 40.41775706135234714 ) ) ;
#68011 = CARTESIAN_POINT ( 'NONE',  ( -8.314922557961024197, 14.29746914071037800, 47.91775706135234714 ) ) ;
#68012 = CARTESIAN_POINT ( 'NONE',  ( 14.29746914071037800, 8.314922557961029526, 111.6677570613523613 ) ) ;
#68013 = CARTESIAN_POINT ( 'NONE',  ( -19.02544592524342804, 5.153800228976336051, 26.04057627198103120 ) ) ;
#68014 = CARTESIAN_POINT ( 'NONE',  ( -13.89961937509957401, -13.97604488694547875, 19.37609039468566507 ) ) ;
#68015 = CARTESIAN_POINT ( 'NONE',  ( 0.05219959533936267826, -19.03943276465977164, 110.0010903946856757 ) ) ;
#68016 = CARTESIAN_POINT ( 'NONE',  ( 5.049401038297881783, 19.05341960407617563, 62.29275706135234003 ) ) ;
#68017 = CARTESIAN_POINT ( 'NONE',  ( 16.53943276465976808, -0.05219959533910856209, 63.74890960531435979 ) ) ;
#68018 = CARTESIAN_POINT ( 'NONE',  ( 16.46253265017160672, -9.564922557960803928, 38.33224293864768839 ) ) ;
#68020 = CARTESIAN_POINT ( 'NONE',  ( 17.31728774477273092, -6.344390552232384017, 93.31906651689317300 ) ) ;
#68019 = CARTESIAN_POINT ( 'NONE',  ( -19.02544592524334988, -5.153800228976617603, 73.95942372801900433 ) ) ;
#68021 = CARTESIAN_POINT ( 'NONE',  ( -15.72974639402176322, -15.80617190586768395, 74.37609039468568994 ) ) ;
#68022 = CARTESIAN_POINT ( 'NONE',  ( 8.224510206698742110, 14.34966873604972548, 37.08442372801901143 ) ) ;
#68023 = CARTESIAN_POINT ( 'NONE',  ( -29.44685852473304166, -27.07773368778541112, -16.45956342659044580 ) ) ;
#68024 = CARTESIAN_POINT ( 'NONE',  ( 15.72974639402199770, -15.80617190586745480, 33.12390960531435979 ) ) ;
#68025 = CARTESIAN_POINT ( 'NONE',  ( 14.34966873604972726, -8.224510206698740333, 25.83442372801901499 ) ) ;
#68026 = CARTESIAN_POINT ( 'NONE',  ( -16.46253265017160317, 9.564922557960807481, 30.83224293864769550 ) ) ;
#68027 = CARTESIAN_POINT ( 'NONE',  ( -19.02544592524334988, -5.153800228976617603, 18.95942372801899722 ) ) ;
#68028 = DIRECTION ( 'NONE',  ( 1.000000000000000000, 0.000000000000000000, 0.000000000000000000 ) ) ;
#68029 = CARTESIAN_POINT ( 'NONE',  ( 9.474510206698971260, -16.51473224551069308, 37.91557627198102409 ) ) ;
#68030 = CARTESIAN_POINT ( 'NONE',  ( -13.97604488694547520, 13.89961937509957934, 58.12609039468566863 ) ) ;
#68031 = CARTESIAN_POINT ( 'NONE',  ( -9.564922557960796823, -16.46253265017161027, 62.08224293864769550 ) ) ;
#68032 = CARTESIAN_POINT ( 'NONE',  ( -15.72974639402176322, -15.80617190586768395, 64.37609039468568994 ) ) ;
#68033 = CARTESIAN_POINT ( 'NONE',  ( 21.55341960407619695, -5.719274019375665929, 111.0427570613523613 ) ) ;
#68034 = CARTESIAN_POINT ( 'NONE',  ( 8.224510206698953496, -14.34966873604960469, 27.91557627198103830 ) ) ;
#68035 = CARTESIAN_POINT ( 'NONE',  ( 19.05341960407611168, 5.049401038298154454, 28.95724293864769550 ) ) ;
#68036 = CARTESIAN_POINT ( 'NONE',  ( -16.51473224551069308, -9.474510206698971260, 96.66557627198102409 ) ) ;
#68037 = CARTESIAN_POINT ( 'NONE',  ( -5.719274019375665041, -21.55341960407619695, 59.79275706135234714 ) ) ;
#68038 = CARTESIAN_POINT ( 'NONE',  ( -19.02544592524342804, 5.153800228976336051, 36.04057627198100988 ) ) ;
#68039 = CARTESIAN_POINT ( 'NONE',  ( 5.719274019375673035, 21.55341960407619339, 62.29275706135236845 ) ) ;
#68041 = CARTESIAN_POINT ( 'NONE',  ( -9.564922557960796823, -16.46253265017161027, 107.0822429386476955 ) ) ;
#68040 = CARTESIAN_POINT ( 'NONE',  ( 0.05219959533936267826, -19.03943276465977164, 90.00109039468567573 ) ) ;
#68042 = CARTESIAN_POINT ( 'NONE',  ( -16.51473224551069308, -9.474510206698971260, 26.66557627198103120 ) ) ;
#68043 = CARTESIAN_POINT ( 'NONE',  ( 10.72451020669898902, -18.67979575497178502, 112.9155762719810383 ) ) ;
#68044 = CARTESIAN_POINT ( 'NONE',  ( 13.97604488694548053, -13.89961937509957401, 30.62609039468566863 ) ) ;
#68045 = CARTESIAN_POINT ( 'NONE',  ( 14.29746914071049879, -8.314922557960816363, 113.3322429386476955 ) ) ;
#68046 = CARTESIAN_POINT ( 'NONE',  ( 9.564922557960805705, 16.46253265017160317, 59.58224293864769550 ) ) ;
#68047 = CARTESIAN_POINT ( 'NONE',  ( -19.05341960407617563, 5.049401038297882671, 98.54275706135233293 ) ) ;
#68048 = CARTESIAN_POINT ( 'NONE',  ( 8.224510206698953496, -14.34966873604960469, 62.91557627198102409 ) ) ;
#68049 = CARTESIAN_POINT ( 'NONE',  ( 5.823673210054125526, 21.52544592524343514, 24.79057627198103120 ) ) ;
#68050 = CARTESIAN_POINT ( 'NONE',  ( -19.05341960407617563, 5.049401038297882671, 88.54275706135230450 ) ) ;
#68051 = CARTESIAN_POINT ( 'NONE',  ( -15.72974639402197994, 15.80617190586746368, 85.62390960531436690 ) ) ;
#68052 = CARTESIAN_POINT ( 'NONE',  ( -0.05219959533937732626, 21.53943276465977519, 47.50109039468568994 ) ) ;
#68053 = CARTESIAN_POINT ( 'NONE',  ( -14.34966873604972548, 8.224510206698743886, 38.33442372801900433 ) ) ;
#68055 = CARTESIAN_POINT ( 'NONE',  ( -21.52544592524334988, -5.823673210054445271, 53.95942372801900433 ) ) ;
#68054 = CARTESIAN_POINT ( 'NONE',  ( -16.55341960407617563, 4.379528057220093196, 38.54275706135234714 ) ) ;
#68056 = CARTESIAN_POINT ( 'NONE',  ( -21.52544592524343514, 5.823673210054127303, 61.04057627198103120 ) ) ;
#68057 = CARTESIAN_POINT ( 'NONE',  ( 19.05341960407611168, 5.049401038298154454, 33.95724293864769550 ) ) ;
#68058 = CARTESIAN_POINT ( 'NONE',  ( -23.48529157249599919, -32.32473071737750558, -5.449999994537626513 ) ) ;
#68059 = CARTESIAN_POINT ( 'NONE',  ( -4.379528057220086978, -16.55341960407618274, 69.79275706135234714 ) ) ;
#68060 = CARTESIAN_POINT ( 'NONE',  ( 21.53943276465977519, -0.05219959533907433946, 103.7489096053143669 ) ) ;
#68061 = CARTESIAN_POINT ( 'NONE',  ( -12.14591786802309592, -12.06949235617757132, 41.87390960531435979 ) ) ;
#68062 = CARTESIAN_POINT ( 'NONE',  ( -4.483927247898782831, 16.52544592524335698, 62.70942372801902565 ) ) ;
#68063 = CARTESIAN_POINT ( 'NONE',  ( 9.564922557961047289, -16.46253265017146816, 100.4177570613523329 ) ) ;
#68064 = CARTESIAN_POINT ( 'NONE',  ( 15.72974639402199770, -15.80617190586745480, 98.12390960531436690 ) ) ;
#68065 = CARTESIAN_POINT ( 'NONE',  ( -8.314922557960811034, -14.29746914071050412, 27.08224293864769550 ) ) ;
#68066 = EDGE_LOOP ( 'NONE', ( #113417, #80674, #58377, #183854 ) ) ;
#68067 = CARTESIAN_POINT ( 'NONE',  ( -16.52544592524335698, -4.483927247898792601, 78.95942372801901854 ) ) ;
#68068 = DIRECTION ( 'NONE',  ( 0.000000000000000000, 0.000000000000000000, -1.000000000000000000 ) ) ;
#68069 = CARTESIAN_POINT ( 'NONE',  ( 10.81492255796078972, 18.62759615963270932, 74.58224293864768129 ) ) ;
#68070 = CARTESIAN_POINT ( 'NONE',  ( 4.483927247898790824, -16.52544592524335698, 110.2094237280190185 ) ) ;
#68071 = VERTEX_POINT ( 'NONE', #193964 ) ;
#68072 = CARTESIAN_POINT ( 'NONE',  ( -23.48529157249599919, -32.32473071737749848, -3.699999999999999734 ) ) ;
#68073 = CARTESIAN_POINT ( 'NONE',  ( -5.823673210054116645, -21.52544592524344225, 102.2905762719810383 ) ) ;
#68074 = CARTESIAN_POINT ( 'NONE',  ( -21.53943276465977519, 0.05219959533907696930, 106.2489096053143811 ) ) ;
#68075 = CARTESIAN_POINT ( 'NONE',  ( -16.55341960407611168, -4.379528057220339221, 36.45724293864768839 ) ) ;
#68076 = CARTESIAN_POINT ( 'NONE',  ( 12.06949235617739724, 12.14591786802326823, 41.87609039468568284 ) ) ;
#68077 = CARTESIAN_POINT ( 'NONE',  ( 19.02544592524343514, -5.153800228976328945, 43.54057627198103120 ) ) ;
#68078 = CARTESIAN_POINT ( 'NONE',  ( -9.564922557960796823, -16.46253265017161027, 62.08224293864769550 ) ) ;
#68079 = ORIENTED_EDGE ( 'NONE', *, *, #142437, .F. ) ;
#68080 = EDGE_CURVE ( 'NONE', #136632, #113568, #101935, .T. ) ;
#68081 = CARTESIAN_POINT ( 'NONE',  ( -13.89961937509977652, 13.97604488694528158, 110.6239096053143243 ) ) ;
#68082 = CARTESIAN_POINT ( 'NONE',  ( -26.28653040952168141, -27.04268878403664900, -20.33571853020666609 ) ) ;
#68083 = CARTESIAN_POINT ( 'NONE',  ( 0.05219959533936267826, -19.03943276465977164, 105.0010903946856615 ) ) ;
#68084 = CARTESIAN_POINT ( 'NONE',  ( 13.89961937509957401, 13.97604488694547697, 46.87609039468565442 ) ) ;
#68085 = CARTESIAN_POINT ( 'NONE',  ( 15.72974639402199770, -15.80617190586745480, 83.12390960531436690 ) ) ;
#68086 = CARTESIAN_POINT ( 'NONE',  ( -0.05219959533934338120, 16.53943276465976808, 112.5010903946857042 ) ) ;
#68087 = CARTESIAN_POINT ( 'NONE',  ( -10.81492255796078084, -18.62759615963271287, 47.08224293864770260 ) ) ;
#68089 = CARTESIAN_POINT ( 'NONE',  ( 9.564922557961047289, -16.46253265017146816, 110.4177570613523471 ) ) ;
#68088 = CARTESIAN_POINT ( 'NONE',  ( 5.719274019375991003, -21.55341960407610458, 82.70724293864770971 ) ) ;
#68090 = CARTESIAN_POINT ( 'NONE',  ( 15.80617190586746368, 15.72974639402197994, 24.37390960531435979 ) ) ;
#68091 = CARTESIAN_POINT ( 'NONE',  ( 18.62759615963255655, 10.81492255796105972, 76.66775706135234714 ) ) ;
#68093 = EDGE_CURVE ( 'NONE', #113568, #60986, #118697, .T. ) ;
#68092 = CARTESIAN_POINT ( 'NONE',  ( 19.03943276465977164, -0.05219959533909143690, 73.74890960531435269 ) ) ;
#68094 = CARTESIAN_POINT ( 'NONE',  ( 32.64453336272026718, -1.163414472736631538E-14, 87.50000000000000000 ) ) ;
#68095 = CARTESIAN_POINT ( 'NONE',  ( -13.97604488694527625, -13.89961937509977652, 76.87390960531433848 ) ) ;
#68096 = CARTESIAN_POINT ( 'NONE',  ( -8.314922557960811034, -14.29746914071050412, 87.08224293864769550 ) ) ;
#68097 = ORIENTED_EDGE ( 'NONE', *, *, #73850, .F. ) ;
#68098 = CARTESIAN_POINT ( 'NONE',  ( 19.05341960407617918, -5.049401038297876454, 111.0427570613523329 ) ) ;
#68099 = CARTESIAN_POINT ( 'NONE',  ( 17.50000000000000355, -5.624438216177593652, 83.31670344914645909 ) ) ;
#68100 = CARTESIAN_POINT ( 'NONE',  ( -13.97604488694527625, -13.89961937509977652, 76.87390960531433848 ) ) ;
#68102 = CARTESIAN_POINT ( 'NONE',  ( -19.02544592524342804, 5.153800228976336051, 96.04057627198103830 ) ) ;
#68101 = CARTESIAN_POINT ( 'NONE',  ( -15.72974639402176322, -15.80617190586768395, 79.37609039468567573 ) ) ;
#68103 = CARTESIAN_POINT ( 'NONE',  ( -8.224510206698735004, -14.34966873604973081, 74.58442372801901854 ) ) ;
#68104 = CARTESIAN_POINT ( 'NONE',  ( -17.26058549869093284, -6.457015423128470211, 76.37745837476069255 ) ) ;
#68105 = CARTESIAN_POINT ( 'NONE',  ( 19.02544592524334988, 5.153800228976608722, 61.45942372801900433 ) ) ;
#68106 = CARTESIAN_POINT ( 'NONE',  ( 13.89961937509957401, 13.97604488694547697, 21.87609039468566152 ) ) ;
#68107 = CARTESIAN_POINT ( 'NONE',  ( 22.73749492396215288, -155.7167183371838064, -15.00000000000000178 ) ) ;
#68108 = CARTESIAN_POINT ( 'NONE',  ( -12.49999999999997691, -89.99999999999997158, -4.999999999999999112 ) ) ;
#68109 = CARTESIAN_POINT ( 'NONE',  ( 11.40812507854755253, -35.11059874428192273, -2.524999997268813523 ) ) ;
#68110 = CARTESIAN_POINT ( 'NONE',  ( -14.34966873604960291, -8.224510206698953496, 26.66557627198103475 ) ) ;
#68111 = DIRECTION ( 'NONE',  ( 0.000000000000000000, 0.7660444431189784575, -0.6427876096865388078 ) ) ;
#68112 = CARTESIAN_POINT ( 'NONE',  ( 14.29746914071037800, 8.314922557961029526, 101.6677570613523613 ) ) ;
#68113 = CARTESIAN_POINT ( 'NONE',  ( 16.19135201231365784, 7.376712067591955524, 67.68680854052030327 ) ) ;
#68114 = CARTESIAN_POINT ( 'NONE',  ( 4.483927247898790824, -16.52544592524335698, 80.20942372801901854 ) ) ;
#68115 = CARTESIAN_POINT ( 'NONE',  ( 10.81492255796106328, -18.62759615963255655, 85.41775706135236135 ) ) ;
#68116 = CARTESIAN_POINT ( 'NONE',  ( -5.049401038297874678, -19.05341960407617918, 94.79275706135230450 ) ) ;
#68117 = CARTESIAN_POINT ( 'NONE',  ( -5.153800228976607833, 19.02544592524334988, 42.70942372801901143 ) ) ;
#68118 = CARTESIAN_POINT ( 'NONE',  ( 16.51473224551069308, 9.474510206698969483, 74.16557627198103830 ) ) ;
#68119 = CARTESIAN_POINT ( 'NONE',  ( -19.05341960407611168, -5.049401038298163336, 51.45724293864770260 ) ) ;
#68120 = CARTESIAN_POINT ( 'NONE',  ( 18.22780087662123805, -5.499999999999976019, 88.51763182126893525 ) ) ;
#68121 = CARTESIAN_POINT ( 'NONE',  ( -15.72974639402197994, 15.80617190586746368, 95.62390960531436690 ) ) ;
#68122 = CARTESIAN_POINT ( 'NONE',  ( 10.81492255796078972, 18.62759615963270932, 44.58224293864769550 ) ) ;
#68123 = CARTESIAN_POINT ( 'NONE',  ( 5.049401038298161559, -19.05341960407611168, 42.70724293864767418 ) ) ;
#68124 = CARTESIAN_POINT ( 'NONE',  ( -8.314922557961024197, 14.29746914071037800, 57.91775706135234714 ) ) ;
#68125 = UNCERTAINTY_MEASURE_WITH_UNIT (LENGTH_MEASURE( 1.000000000000000082E-05 ), #63898, 'distance_accuracy_value', 'NONE');
#68126 = VERTEX_POINT ( 'NONE', #8937 ) ;
#68127 = CARTESIAN_POINT ( 'NONE',  ( -21.53943276465977519, -0.05219959533937600094, 48.75109039468568284 ) ) ;
#68129 = CARTESIAN_POINT ( 'NONE',  ( 30.74264578624799782, 22.33583958711400541, -0.7999999999999999334 ) ) ;
#68128 = CARTESIAN_POINT ( 'NONE',  ( 0.05219959533910956823, 16.53943276465976808, 64.99890960531435269 ) ) ;
#68130 = CARTESIAN_POINT ( 'NONE',  ( -14.34966873604972548, 8.224510206698743886, 43.33442372801901143 ) ) ;
#68131 = CARTESIAN_POINT ( 'NONE',  ( -12.06949235617756955, 12.14591786802309770, 105.6239096053143669 ) ) ;
#68132 = CARTESIAN_POINT ( 'NONE',  ( -9.564922557961040184, 16.46253265017147172, 57.91775706135233293 ) ) ;
#68133 = CARTESIAN_POINT ( 'NONE',  ( 14.34966873604960469, 8.224510206698951720, 69.16557627198102409 ) ) ;
#68134 = CARTESIAN_POINT ( 'NONE',  ( -0.05219959533937732626, 21.53943276465977519, 32.50109039468568284 ) ) ;
#68136 = CARTESIAN_POINT ( 'NONE',  ( 15.80617190586746368, 15.72974639402197994, 94.37390960531436690 ) ) ;
#68135 = LINE ( 'NONE', #19652, #37547 ) ;
#68137 = CARTESIAN_POINT ( 'NONE',  ( -5.153800228976328057, -19.02544592524343514, 107.2905762719810383 ) ) ;
#68138 = CARTESIAN_POINT ( 'NONE',  ( 12.06949235617757843, -12.14591786802309237, 68.12390960531436690 ) ) ;
#68139 = CARTESIAN_POINT ( 'NONE',  ( 13.97604488694527802, 13.89961937509977652, 114.3739096053143669 ) ) ;
#68140 = CARTESIAN_POINT ( 'NONE',  ( 36.91746824999999177, 11.99521256947799230, -5.524999997268812635 ) ) ;
#68141 = CARTESIAN_POINT ( 'NONE',  ( 9.474510206698729675, 16.51473224551082808, 77.08442372801900433 ) ) ;
#68142 = CARTESIAN_POINT ( 'NONE',  ( -15.72974639402176322, -15.80617190586768395, 29.37609039468568284 ) ) ;
#68143 = CARTESIAN_POINT ( 'NONE',  ( 9.474510206698971260, -16.51473224551069308, 72.91557627198102409 ) ) ;
#68144 = CARTESIAN_POINT ( 'NONE',  ( -5.153800228976607833, 19.02544592524334988, 57.70942372801899012 ) ) ;
#68145 = CARTESIAN_POINT ( 'NONE',  ( 16.51473224551069308, 9.474510206698969483, 29.16557627198103475 ) ) ;
#68146 = CARTESIAN_POINT ( 'NONE',  ( 21.55341960407619695, -5.719274019375665929, 76.04275706135237556 ) ) ;
#68147 = CARTESIAN_POINT ( 'NONE',  ( 16.53943276465976808, -0.05219959533910856209, 63.74890960531435979 ) ) ;
#68148 = CARTESIAN_POINT ( 'NONE',  ( -4.379528057220328563, 16.55341960407611168, 60.20724293864768839 ) ) ;
#68149 = CARTESIAN_POINT ( 'NONE',  ( -16.46253265017160317, 9.564922557960807481, 65.83224293864769550 ) ) ;
#68150 = CARTESIAN_POINT ( 'NONE',  ( -21.55341960407610458, -5.719274019375992779, 91.45724293864769550 ) ) ;
#68151 = CARTESIAN_POINT ( 'NONE',  ( 9.474510206698971260, -16.51473224551069308, 62.91557627198102409 ) ) ;
#68152 = CARTESIAN_POINT ( 'NONE',  ( -18.67979575497178146, -10.72451020669898902, 76.66557627198103830 ) ) ;
#68153 = CARTESIAN_POINT ( 'NONE',  ( 0.05219959533937995610, -21.53943276465977519, 100.0010903946857042 ) ) ;
#68156 = CARTESIAN_POINT ( 'NONE',  ( -16.53943276465976808, 0.05219959533911058130, 101.2489096053143669 ) ) ;
#68155 = CARTESIAN_POINT ( 'NONE',  ( -16.52544592524335698, -4.483927247898792601, 108.9594237280190185 ) ) ;
#68154 = DIRECTION ( 'NONE',  ( 0.000000000000000000, 0.000000000000000000, -1.000000000000000000 ) ) ;
#68157 = CARTESIAN_POINT ( 'NONE',  ( -19.05341960407617563, 5.049401038297882671, 98.54275706135233293 ) ) ;
#68158 = VERTEX_POINT ( 'NONE', #163617 ) ;
#68159 = CARTESIAN_POINT ( 'NONE',  ( 0.05219959533907565091, 21.53943276465977519, 114.9989096053143669 ) ) ;
#68160 = CARTESIAN_POINT ( 'NONE',  ( -9.564922557961040184, 16.46253265017147172, 57.91775706135233293 ) ) ;
#68161 = CARTESIAN_POINT ( 'NONE',  ( -8.314922557961024197, 14.29746914071037800, 97.91775706135236135 ) ) ;
#68162 = CARTESIAN_POINT ( 'NONE',  ( 19.03943276465977164, 0.05219959533936151252, 36.25109039468567573 ) ) ;
#68163 = CARTESIAN_POINT ( 'NONE',  ( -5.049401038298153566, 19.05341960407611168, 105.2072429386476671 ) ) ;
#68164 = CARTESIAN_POINT ( 'NONE',  ( -18.62759615963270932, 10.81492255796079327, 65.83224293864769550 ) ) ;
#68165 = CARTESIAN_POINT ( 'NONE',  ( -25.78958964901898554, 10.70071173758531557, 166.5174151181484490 ) ) ;
#68166 = CARTESIAN_POINT ( 'NONE',  ( -5.049401038298153566, 19.05341960407611168, 30.20724293864768839 ) ) ;
#68167 = CARTESIAN_POINT ( 'NONE',  ( -19.03943276465977164, -0.05219959533935918106, 18.75109039468567218 ) ) ;
#68168 = CARTESIAN_POINT ( 'NONE',  ( 8.314922557961029526, -14.29746914071037800, 70.41775706135236135 ) ) ;
#68169 = CARTESIAN_POINT ( 'NONE',  ( 0.05219959533937995610, -21.53943276465977519, 25.00109039468567218 ) ) ;
#68170 = CARTESIAN_POINT ( 'NONE',  ( -0.05219959533934338120, 16.53943276465976808, 42.50109039468567573 ) ) ;
#68171 = CARTESIAN_POINT ( 'NONE',  ( -19.05341960407611168, -5.049401038298163336, 106.4572429386476955 ) ) ;
#68172 = CARTESIAN_POINT ( 'NONE',  ( -19.02544592524342804, 5.153800228976336051, 51.04057627198103120 ) ) ;
#68173 = CARTESIAN_POINT ( 'NONE',  ( 9.474510206698971260, -16.51473224551069308, 62.91557627198102409 ) ) ;
#68174 = CARTESIAN_POINT ( 'NONE',  ( 4.379528057220092307, 16.55341960407617563, 52.29275706135236135 ) ) ;
#68175 = CARTESIAN_POINT ( 'NONE',  ( 16.52544592524342804, -4.483927247898539470, 93.54057627198103830 ) ) ;
#68176 = CARTESIAN_POINT ( 'NONE',  ( 16.55341960407618274, -4.379528057220086978, 106.0427570613523471 ) ) ;
#68177 = CARTESIAN_POINT ( 'NONE',  ( 1.300000000000000044, 0.7216878364870328300, -1.250000000000000000 ) ) ;
#68180 = CARTESIAN_POINT ( 'NONE',  ( -0.05219959533909027116, -19.03943276465977164, 62.49890960531435979 ) ) ;
#68179 = CARTESIAN_POINT ( 'NONE',  ( -9.564922557960796823, -16.46253265017161027, 77.08224293864769550 ) ) ;
#68178 = CARTESIAN_POINT ( 'NONE',  ( -21.53943276465977519, -0.05219959533937600094, 53.75109039468568994 ) ) ;
#68181 = CARTESIAN_POINT ( 'NONE',  ( -16.46253265017160317, 9.564922557960807481, 90.83224293864769550 ) ) ;
#68182 = CARTESIAN_POINT ( 'NONE',  ( 12.06949235617757843, -12.14591786802309237, 48.12390960531436690 ) ) ;
#68183 = CARTESIAN_POINT ( 'NONE',  ( 16.52544592524335698, 4.483927247898782831, 96.45942372801901854 ) ) ;
#68184 = CARTESIAN_POINT ( 'NONE',  ( 8.314922557960818139, 14.29746914071049879, 39.58224293864769550 ) ) ;
#68185 = ORIENTED_EDGE ( 'NONE', *, *, #141668, .F. ) ;
#68186 = CARTESIAN_POINT ( 'NONE',  ( -5.153800228976607833, 19.02544592524334988, 37.70942372801899722 ) ) ;
#68187 = CARTESIAN_POINT ( 'NONE',  ( 16.51473224551069308, 9.474510206698969483, 114.1655762719810241 ) ) ;
#68188 = CARTESIAN_POINT ( 'NONE',  ( -0.05219959533909027116, -19.03943276465977164, 62.49890960531435979 ) ) ;
#68189 = CARTESIAN_POINT ( 'NONE',  ( -9.564922557961040184, 16.46253265017147172, 37.91775706135233293 ) ) ;
#68190 = CARTESIAN_POINT ( 'NONE',  ( 29.86685920354754842, -21.69954338932559068, -8.324999997268813345 ) ) ;
#68191 = CARTESIAN_POINT ( 'NONE',  ( 17.97214573761830536, 5.500000000000079048, 58.96970049038655759 ) ) ;
#68193 = CARTESIAN_POINT ( 'NONE',  ( -8.314922557961024197, 14.29746914071037800, 67.91775706135234714 ) ) ;
#68192 = CARTESIAN_POINT ( 'NONE',  ( 19.05341960407617918, -5.049401038297876454, 81.04275706135231871 ) ) ;
#68194 = DIRECTION ( 'NONE',  ( 0.000000000000000000, -0.04175967627138118393, -0.9991276842514721368 ) ) ;
#68195 = CARTESIAN_POINT ( 'NONE',  ( -19.03943276465977164, 0.05219959533909376836, 86.24890960531436690 ) ) ;
#68196 = CARTESIAN_POINT ( 'NONE',  ( 5.719274019375673035, 21.55341960407619339, 32.29275706135235424 ) ) ;
#68197 = CARTESIAN_POINT ( 'NONE',  ( -19.02544592524334988, -5.153800228976617603, 73.95942372801900433 ) ) ;
#68199 = CARTESIAN_POINT ( 'NONE',  ( -19.03943276465977164, 0.05219959533909376836, 46.24890960531435979 ) ) ;
#68198 = DIRECTION ( 'NONE',  ( 1.000000000000000000, 0.000000000000000000, 0.000000000000000000 ) ) ;
#68200 = CARTESIAN_POINT ( 'NONE',  ( -5.153800228976328057, -19.02544592524343514, 92.29057627198099567 ) ) ;
#68202 = CARTESIAN_POINT ( 'NONE',  ( 19.05341960407611168, 5.049401038298154454, 33.95724293864769550 ) ) ;
#68201 = CARTESIAN_POINT ( 'NONE',  ( 16.53943276465976808, -0.05219959533910856209, 48.74890960531435979 ) ) ;
#68203 = CARTESIAN_POINT ( 'NONE',  ( 16.46253265017146816, 9.564922557961045513, 46.66775706135233293 ) ) ;
#68204 = CARTESIAN_POINT ( 'NONE',  ( 14.34966873604960469, 8.224510206698951720, 89.16557627198102409 ) ) ;
#68205 = CARTESIAN_POINT ( 'NONE',  ( -16.46253265017146816, -9.564922557961047289, 29.16775706135232937 ) ) ;
#68206 = CARTESIAN_POINT ( 'NONE',  ( -19.03943276465977164, 0.05219959533909376836, 71.24890960531435269 ) ) ;
#68207 =( BOUNDED_CURVE ( )  B_SPLINE_CURVE ( 3, ( #22083, #19107, #3913, #83734 ),
 .UNSPECIFIED., .F., .F. ) 
 B_SPLINE_CURVE_WITH_KNOTS ( ( 4, 4 ),
 ( 1.025647941782810824, 1.570796326794896558 ),
 .UNSPECIFIED. ) 
 CURVE ( )  GEOMETRIC_REPRESENTATION_ITEM ( )  RATIONAL_B_SPLINE_CURVE ( ( 1.000000000000000000, 0.9753873905749756990, 0.9753873905749756990, 1.000000000000000000 ) ) 
 REPRESENTATION_ITEM ( '' )  );
#68208 = CARTESIAN_POINT ( 'NONE',  ( 21.55341960407610458, 5.719274019375980345, 63.95724293864770260 ) ) ;
#68210 = CARTESIAN_POINT ( 'NONE',  ( -5.153800228976607833, 19.02544592524334988, 27.70942372801899722 ) ) ;
#68209 = CARTESIAN_POINT ( 'NONE',  ( -0.05219959533910754901, -16.53943276465976808, 57.49890960531435979 ) ) ;
#68211 = CARTESIAN_POINT ( 'NONE',  ( 9.474510206698971260, -16.51473224551069308, 112.9155762719810383 ) ) ;
#68212 = CARTESIAN_POINT ( 'NONE',  ( 5.823673210054125526, 21.52544592524343514, 24.79057627198103120 ) ) ;
#68213 = CARTESIAN_POINT ( 'NONE',  ( -16.51473224551069308, -9.474510206698971260, 46.66557627198102409 ) ) ;
#68214 = CARTESIAN_POINT ( 'NONE',  ( 19.03943276465977164, -0.05219959533909143690, 43.74890960531435979 ) ) ;
#68215 = CARTESIAN_POINT ( 'NONE',  ( 16.55341960407611168, 4.379528057220329451, 103.9572429386476813 ) ) ;
#68216 = CARTESIAN_POINT ( 'NONE',  ( 18.67979575497178502, 10.72451020669898547, 109.1655762719810383 ) ) ;
#68217 = CARTESIAN_POINT ( 'NONE',  ( 0.05219959533909260263, 19.03943276465977164, 94.99890960531436690 ) ) ;
#68218 = CARTESIAN_POINT ( 'NONE',  ( 5.823673210054444382, -21.52544592524334988, 20.20942372801900788 ) ) ;
#68219 = CARTESIAN_POINT ( 'NONE',  ( -13.97604488694527625, -13.89961937509977652, 101.8739096053143811 ) ) ;
#68220 = CARTESIAN_POINT ( 'NONE',  ( 8.224510206698953496, -14.34966873604960469, 112.9155762719810383 ) ) ;
#68221 = CARTESIAN_POINT ( 'NONE',  ( -5.823673210054431948, 21.52544592524334988, 82.70942372801900433 ) ) ;
#68222 = CARTESIAN_POINT ( 'NONE',  ( 21.53943276465977519, -0.05219959533907433946, 93.74890960531436690 ) ) ;
#68223 = CARTESIAN_POINT ( 'NONE',  ( 16.52216118717207749, -7.221426719304518294, 106.4240097895300892 ) ) ;
#68224 = CARTESIAN_POINT ( 'NONE',  ( 9.564922557960805705, 16.46253265017160317, 59.58224293864769550 ) ) ;
#68225 = CARTESIAN_POINT ( 'NONE',  ( -12.06949235617739369, -12.14591786802326823, 44.37609039468567573 ) ) ;
#68226 = CARTESIAN_POINT ( 'NONE',  ( 8.224510206698953496, -14.34966873604960469, 107.9155762719810241 ) ) ;
#68227 = CARTESIAN_POINT ( 'NONE',  ( -17.50000000000001066, -3.237210098469584185, 110.2876301262045615 ) ) ;
#68228 = CARTESIAN_POINT ( 'NONE',  ( 9.474510206698971260, -16.51473224551069308, 52.91557627198102409 ) ) ;
#68229 = CARTESIAN_POINT ( 'NONE',  ( 4.483927247898545687, 16.52544592524342804, 99.79057627198103830 ) ) ;
#68230 = CARTESIAN_POINT ( 'NONE',  ( -0.05219959533907301413, -21.53943276465977519, 47.49890960531435979 ) ) ;
#68231 = CARTESIAN_POINT ( 'NONE',  ( 12.14591786802309770, 12.06949235617756955, 64.37390960531435269 ) ) ;
#68232 = CARTESIAN_POINT ( 'NONE',  ( -12.06949235617739369, -12.14591786802326823, 24.37609039468567573 ) ) ;
#68233 = CARTESIAN_POINT ( 'NONE',  ( -15.80617190586768217, 15.72974639402176855, 68.12609039468567573 ) ) ;
#68234 = CARTESIAN_POINT ( 'NONE',  ( 16.46253265017146816, 9.564922557961045513, 61.66775706135234003 ) ) ;
#68235 = CARTESIAN_POINT ( 'NONE',  ( 16.55341960407618274, -4.379528057220086978, 101.0427570613523756 ) ) ;
#68236 = CARTESIAN_POINT ( 'NONE',  ( 0.05219959533910956823, 16.53943276465976808, 44.99890960531435979 ) ) ;
#68237 = CARTESIAN_POINT ( 'NONE',  ( 5.049401038298161559, -19.05341960407611168, 37.70724293864768839 ) ) ;
#68238 = CARTESIAN_POINT ( 'NONE',  ( -19.05341960407611168, -5.049401038298163336, 91.45724293864766707 ) ) ;
#68239 = CARTESIAN_POINT ( 'NONE',  ( 21.52544592524344225, -5.823673210054117533, 98.54057627198105251 ) ) ;
#68240 = CARTESIAN_POINT ( 'NONE',  ( 4.483927247898790824, -16.52544592524335698, 30.20942372801902565 ) ) ;
#68242 = CARTESIAN_POINT ( 'NONE',  ( 18.67979575497194134, -10.72451020669871369, 75.83442372801900433 ) ) ;
#68241 = CARTESIAN_POINT ( 'NONE',  ( -12.14591786802309592, -12.06949235617757132, 61.87390960531436690 ) ) ;
#68243 = B_SPLINE_CURVE_WITH_KNOTS ( 'NONE', 3,
 ( #54432, #165611, #87752, #100916, #86759, #41268, #57440, #12924, #194953, #39260, #147446, #58420, #193961, #162601, #88756, #70603, #59400, #27110, #120087, #164615, #89751, #134280, #74588, #136256, #117095, #150449, #102930, #26109, #197932, #119113, #24105, #103931, #177790, #85759, #195968, #42273, #8934, #132270, #179799, #178790, #55424, #40259 ),
 .UNSPECIFIED., .F., .F.,
 ( 4, 2, 2, 2, 2, 2, 2, 2, 2, 2, 2, 2, 2, 2, 2, 2, 2, 2, 2, 2, 4 ),
 ( 0.0002562179899358165238, 0.004844394232870628293, 0.009432570475805439683, 0.01172665859727284841, 0.01402074671874025888, 0.01860892296167508675, 0.02319709920460991115, 0.02778527544754473902, 0.03237345169047955995, 0.03466753981194697909, 0.03696162793341439129, 0.04154980417634921569, 0.04384389229781662095, 0.04613798041928402621, 0.05072615666221883673, 0.05302024478368623506, 0.05531433290515364032, 0.05990250914808845084, 0.06449068539102326136, 0.06907886163395808576, 0.07366703787689289629 ),
 .UNSPECIFIED. ) ;
#68244 = EDGE_CURVE ( 'NONE', #190550, #116695, #63682, .T. ) ;
#68245 = CARTESIAN_POINT ( 'NONE',  ( -16.55341960407617563, 4.379528057220093196, 93.54275706135234714 ) ) ;
#68246 = FACE_OUTER_BOUND ( 'NONE', #153423, .T. ) ;
#68247 = CARTESIAN_POINT ( 'NONE',  ( 1.820000000000000062, 4.653657836759941744E-16, -3.799999999999999378 ) ) ;
#68248 = CARTESIAN_POINT ( 'NONE',  ( -4.483927247898539470, -16.52544592524342804, 22.29057627198102765 ) ) ;
#68249 = CARTESIAN_POINT ( 'NONE',  ( 14.29746914071037800, 8.314922557961029526, 71.66775706135234714 ) ) ;
#68250 = CARTESIAN_POINT ( 'NONE',  ( -16.46253265017160317, 9.564922557960807481, 85.83224293864769550 ) ) ;
#68251 = CARTESIAN_POINT ( 'NONE',  ( -5.049401038298153566, 19.05341960407611168, 105.2072429386476671 ) ) ;
#68252 = CARTESIAN_POINT ( 'NONE',  ( -18.67979575497193778, 10.72451020669871902, 83.33442372801903275 ) ) ;
#68253 = CARTESIAN_POINT ( 'NONE',  ( -16.55341960407617563, 4.379528057220093196, 93.54275706135234714 ) ) ;
#68254 = CARTESIAN_POINT ( 'NONE',  ( -14.34966873604960291, -8.224510206698953496, 56.66557627198103830 ) ) ;
#68255 = CARTESIAN_POINT ( 'NONE',  ( -13.97604488694527625, -13.89961937509977652, 71.87390960531433848 ) ) ;
#68256 = ORIENTED_EDGE ( 'NONE', *, *, #42127, .F. ) ;
#68257 = CARTESIAN_POINT ( 'NONE',  ( -16.51473224551082808, 9.474510206698731452, 113.3344237280190043 ) ) ;
#68258 = CARTESIAN_POINT ( 'NONE',  ( -12.14591786802309592, -12.06949235617757132, 106.8739096053143811 ) ) ;
#68259 = CARTESIAN_POINT ( 'NONE',  ( 13.89961937509977652, -13.97604488694527269, 73.12390960531436690 ) ) ;
#68261 = CARTESIAN_POINT ( 'NONE',  ( -11.40812507854755609, 35.11059874428196537, -9.024999997268814411 ) ) ;
#68260 = CARTESIAN_POINT ( 'NONE',  ( 8.314922557961029526, -14.29746914071037800, 25.41775706135235779 ) ) ;
#68262 = CARTESIAN_POINT ( 'NONE',  ( -13.89961937509957401, -13.97604488694547875, 19.37609039468566507 ) ) ;
#68263 = CARTESIAN_POINT ( 'NONE',  ( 12.06949235617739724, 12.14591786802326823, 76.87609039468567573 ) ) ;
#68264 = CARTESIAN_POINT ( 'NONE',  ( 0.05219959533936267826, -19.03943276465977164, 95.00109039468567573 ) ) ;
#68265 = CARTESIAN_POINT ( 'NONE',  ( 9.564922557960805705, 16.46253265017160317, 24.58224293864769194 ) ) ;
#68266 = CARTESIAN_POINT ( 'NONE',  ( 8.224510206698742110, 14.34966873604972548, 67.08442372801901854 ) ) ;
#68267 = CARTESIAN_POINT ( 'NONE',  ( -16.55341960407617563, 4.379528057220093196, 58.54275706135235424 ) ) ;
#68268 = CARTESIAN_POINT ( 'NONE',  ( -13.97604488694527625, -13.89961937509977652, 26.87390960531434558 ) ) ;
#68269 = CARTESIAN_POINT ( 'NONE',  ( 19.03943276465977164, 0.05219959533936151252, 51.25109039468567573 ) ) ;
#68270 = CARTESIAN_POINT ( 'NONE',  ( 5.719274019375673035, 21.55341960407619339, 92.29275706135236135 ) ) ;
#68271 = CARTESIAN_POINT ( 'NONE',  ( 9.564922557960805705, 16.46253265017160317, 29.58224293864769550 ) ) ;
#68272 = CARTESIAN_POINT ( 'NONE',  ( 19.02544592524343514, -5.153800228976328945, 73.54057627198103830 ) ) ;
#68273 = CARTESIAN_POINT ( 'NONE',  ( 12.06949235617757843, -12.14591786802309237, 73.12390960531436690 ) ) ;
#68274 = CARTESIAN_POINT ( 'NONE',  ( -18.62759615963255300, -10.81492255796106328, 89.16775706135236135 ) ) ;
#68275 = EDGE_CURVE ( 'NONE', #67859, #15498, #134872, .T. ) ;
#68276 = CARTESIAN_POINT ( 'NONE',  ( -13.89961937509957401, -13.97604488694547875, 64.37609039468567573 ) ) ;
#68277 = CARTESIAN_POINT ( 'NONE',  ( -5.153800228976607833, 19.02544592524334988, 42.70942372801901143 ) ) ;
#68278 = CARTESIAN_POINT ( 'NONE',  ( 21.52544592524344225, -5.823673210054117533, 38.54057627198103120 ) ) ;
#68279 = CARTESIAN_POINT ( 'NONE',  ( 18.67979575497194134, -10.72451020669871369, 105.8344237280190328 ) ) ;
#68280 = CARTESIAN_POINT ( 'NONE',  ( -0.05219959533909027116, -19.03943276465977164, 77.49890960531435269 ) ) ;
#68281 = CARTESIAN_POINT ( 'NONE',  ( -18.67979575497193778, 10.72451020669871902, 103.3344237280190043 ) ) ;
#68282 = CARTESIAN_POINT ( 'NONE',  ( 0.05219959533907565091, 21.53943276465977519, 44.99890960531435979 ) ) ;
#68283 = CARTESIAN_POINT ( 'NONE',  ( 5.153800228976335163, 19.02544592524342804, 99.79057627198102409 ) ) ;
#68284 = CARTESIAN_POINT ( 'NONE',  ( 5.049401038297881783, 19.05341960407617563, 77.29275706135231871 ) ) ;
#68285 = CARTESIAN_POINT ( 'NONE',  ( -9.564922557960796823, -16.46253265017161027, 107.0822429386476955 ) ) ;
#68286 = CARTESIAN_POINT ( 'NONE',  ( -5.153800228976607833, 19.02544592524334988, 92.70942372801901854 ) ) ;
#68287 = CARTESIAN_POINT ( 'NONE',  ( 16.52544592524335698, 4.483927247898782831, 41.45942372801901143 ) ) ;
#68288 = CARTESIAN_POINT ( 'NONE',  ( -12.14591786802309592, -12.06949235617757132, 96.87390960531436690 ) ) ;
#68289 = CARTESIAN_POINT ( 'NONE',  ( 16.51473224551069308, 9.474510206698969483, 89.16557627198103830 ) ) ;
#68290 = CARTESIAN_POINT ( 'NONE',  ( -21.53943276465977519, 0.05219959533907696930, 66.24890960531436690 ) ) ;
#68291 = CARTESIAN_POINT ( 'NONE',  ( -0.05219959533934338120, 16.53943276465976808, 32.50109039468568284 ) ) ;
#68292 = CARTESIAN_POINT ( 'NONE',  ( -5.823673210054431948, 21.52544592524334988, 27.70942372801901854 ) ) ;
#68293 = CARTESIAN_POINT ( 'NONE',  ( -15.80617190586768217, 15.72974639402176855, 83.12609039468568994 ) ) ;
#68294 = CARTESIAN_POINT ( 'NONE',  ( -4.483927247898782831, 16.52544592524335698, 87.70942372801901854 ) ) ;
#68295 = CARTESIAN_POINT ( 'NONE',  ( 19.03943276465977164, -0.05219959533909143690, 78.74890960531436690 ) ) ;
#68296 = CARTESIAN_POINT ( 'NONE',  ( -14.29746914071049879, 8.314922557960819915, 80.83224293864769550 ) ) ;
#68297 = CARTESIAN_POINT ( 'NONE',  ( -16.53943276465976808, -0.05219959533934237506, 113.7510903946856757 ) ) ;
#68298 = CARTESIAN_POINT ( 'NONE',  ( -19.05341960407617563, 5.049401038297882671, 58.54275706135234003 ) ) ;
#68299 = CARTESIAN_POINT ( 'NONE',  ( -18.62759615963255300, -10.81492255796106328, 39.16775706135235424 ) ) ;
#68300 = CARTESIAN_POINT ( 'NONE',  ( 12.06949235617757843, -12.14591786802309237, 78.12390960531436690 ) ) ;
#68301 = CARTESIAN_POINT ( 'NONE',  ( 19.05341960407611168, 5.049401038298154454, 108.9572429386477097 ) ) ;
#68302 = CARTESIAN_POINT ( 'NONE',  ( 16.53943276465976808, 0.05219959533934440121, 96.25109039468568994 ) ) ;
#68303 = CARTESIAN_POINT ( 'NONE',  ( 15.80617190586769283, -15.72974639402175789, 80.62609039468567573 ) ) ;
#68304 = CARTESIAN_POINT ( 'NONE',  ( 16.53943276465976808, 0.05219959533934440121, 41.25109039468568284 ) ) ;
#68305 = CARTESIAN_POINT ( 'NONE',  ( -15.80617190586768217, 15.72974639402176855, 43.12609039468568284 ) ) ;
#68306 = VERTEX_POINT ( 'NONE', #136259 ) ;
#68307 = CARTESIAN_POINT ( 'NONE',  ( -10.72451020669870658, -18.67979575497194134, 19.58442372801901143 ) ) ;
#68308 = CARTESIAN_POINT ( 'NONE',  ( -8.224510206698948167, 14.34966873604960824, 95.41557627198102409 ) ) ;
#68309 = CARTESIAN_POINT ( 'NONE',  ( -18.22780087662121673, -5.500000000000063061, 51.48459894673893444 ) ) ;
#68310 = CARTESIAN_POINT ( 'NONE',  ( 14.29746914071049879, -8.314922557960816363, 53.33224293864769550 ) ) ;
#68311 = CARTESIAN_POINT ( 'NONE',  ( -8.314922557961024197, 14.29746914071037800, 97.91775706135236135 ) ) ;
#68312 = CARTESIAN_POINT ( 'NONE',  ( -13.89961937509977652, 13.97604488694528158, 35.62390960531435269 ) ) ;
#68313 = CARTESIAN_POINT ( 'NONE',  ( -15.72974639402197994, 15.80617190586746368, 40.62390960531435269 ) ) ;
#68314 = CARTESIAN_POINT ( 'NONE',  ( 4.379528057220339221, -16.55341960407611168, 82.70724293864770971 ) ) ;
#68315 = CARTESIAN_POINT ( 'NONE',  ( -10.81492255796078084, -18.62759615963271287, 77.08224293864769550 ) ) ;
#68316 = CARTESIAN_POINT ( 'NONE',  ( -16.51473224551069308, -9.474510206698971260, 91.66557627198103830 ) ) ;
#68318 = CARTESIAN_POINT ( 'NONE',  ( 9.474510206698729675, 16.51473224551082808, 92.08442372801900433 ) ) ;
#68317 = CARTESIAN_POINT ( 'NONE',  ( 16.51473224551069308, 9.474510206698969483, 44.16557627198103120 ) ) ;
#68319 = EDGE_CURVE ( 'NONE', #194525, #115704, #59403, .T. ) ;
#68320 = CARTESIAN_POINT ( 'NONE',  ( -18.67979575497178146, -10.72451020669898902, 26.66557627198103475 ) ) ;
#68321 = CARTESIAN_POINT ( 'NONE',  ( -0.05219959533937732626, 21.53943276465977519, 52.50109039468567573 ) ) ;
#68322 = CARTESIAN_POINT ( 'NONE',  ( 16.51473224551069308, 9.474510206698969483, 49.16557627198102409 ) ) ;
#68323 = CARTESIAN_POINT ( 'NONE',  ( -19.03943276465977164, 0.05219959533909376836, 86.24890960531436690 ) ) ;
#68324 = EDGE_LOOP ( 'NONE', ( #18598, #198466, #173582, #130520 ) ) ;
#68325 = CARTESIAN_POINT ( 'NONE',  ( -12.06949235617739369, -12.14591786802326823, 54.37609039468568994 ) ) ;
#68326 = CARTESIAN_POINT ( 'NONE',  ( 15.80617190586769283, -15.72974639402175789, 25.62609039468567929 ) ) ;
#68327 = CARTESIAN_POINT ( 'NONE',  ( -18.62759615963255300, -10.81492255796106328, 79.16775706135234714 ) ) ;
#68328 = CARTESIAN_POINT ( 'NONE',  ( 18.62759615963271287, -10.81492255796078972, 23.33224293864769194 ) ) ;
#68329 = CARTESIAN_POINT ( 'NONE',  ( -0.05219959533907301413, -21.53943276465977519, 87.49890960531436690 ) ) ;
#68331 = CARTESIAN_POINT ( 'NONE',  ( 4.483927247898790824, -16.52544592524335698, 60.20942372801902565 ) ) ;
#68330 = CARTESIAN_POINT ( 'NONE',  ( -21.53943276465977519, 0.05219959533907696930, 116.2489096053143669 ) ) ;
#68332 = CARTESIAN_POINT ( 'NONE',  ( -18.62759615963270932, 10.81492255796079327, 60.83224293864769550 ) ) ;
#68333 = CARTESIAN_POINT ( 'NONE',  ( 16.46253265017146816, 9.564922557961045513, 21.66775706135233648 ) ) ;
#68334 = CARTESIAN_POINT ( 'NONE',  ( 0.05219959533909260263, 19.03943276465977164, 64.99890960531436690 ) ) ;
#68335 = CARTESIAN_POINT ( 'NONE',  ( -19.05341960407611168, -5.049401038298163336, 106.4572429386476955 ) ) ;
#68336 = CARTESIAN_POINT ( 'NONE',  ( -19.03943276465977164, 0.05219959533909376836, 86.24890960531436690 ) ) ;
#68337 = FACE_OUTER_BOUND ( 'NONE', #63921, .T. ) ;
#68338 = CARTESIAN_POINT ( 'NONE',  ( -16.51473224551082808, 9.474510206698731452, 63.33442372801900433 ) ) ;
#68339 = CARTESIAN_POINT ( 'NONE',  ( -18.67979575497178146, -10.72451020669898902, 51.66557627198102409 ) ) ;
#68340 = CARTESIAN_POINT ( 'NONE',  ( -14.34966873604960291, -8.224510206698953496, 26.66557627198103475 ) ) ;
#68341 = CARTESIAN_POINT ( 'NONE',  ( -16.51473224551082808, 9.474510206698731452, 103.3344237280190043 ) ) ;
#68342 = DIRECTION ( 'NONE',  ( 0.000000000000000000, 0.000000000000000000, 1.000000000000000000 ) ) ;
#68343 = CARTESIAN_POINT ( 'NONE',  ( 5.049401038297881783, 19.05341960407617563, 97.29275706135233293 ) ) ;
#68345 = CARTESIAN_POINT ( 'NONE',  ( 9.474510206698729675, 16.51473224551082808, 52.08442372801900433 ) ) ;
#68344 = CARTESIAN_POINT ( 'NONE',  ( -18.62759615963270932, 10.81492255796079327, 90.83224293864769550 ) ) ;
#68346 = CARTESIAN_POINT ( 'NONE',  ( 17.05587630539787369, 6.762274262135677283, 106.7581969096268750 ) ) ;
#68347 = CARTESIAN_POINT ( 'NONE',  ( -19.02544592524342804, 5.153800228976336051, 61.04057627198103120 ) ) ;
#68348 = CARTESIAN_POINT ( 'NONE',  ( -12.14591786802309592, -12.06949235617757132, 61.87390960531436690 ) ) ;
#68349 = CARTESIAN_POINT ( 'NONE',  ( 5.049401038298161559, -19.05341960407611168, 42.70724293864767418 ) ) ;
#68350 = CARTESIAN_POINT ( 'NONE',  ( 14.34966873604960469, 8.224510206698951720, 59.16557627198103120 ) ) ;
#68351 = CARTESIAN_POINT ( 'NONE',  ( -32.99455490591380169, -22.60464286593628458, -23.90693389968298277 ) ) ;
#68352 = CARTESIAN_POINT ( 'NONE',  ( -16.52544592524342804, 4.483927247898546575, 26.04057627198103475 ) ) ;
#68353 = CARTESIAN_POINT ( 'NONE',  ( -19.03943276465977164, 0.05219959533909376836, 61.24890960531436690 ) ) ;
#68354 = CARTESIAN_POINT ( 'NONE',  ( -17.60728821186567217, 5.500000000000037303, 50.86690927743004664 ) ) ;
#68355 = CARTESIAN_POINT ( 'NONE',  ( -16.51473224551082808, 9.474510206698731452, 23.33442372801900078 ) ) ;
#68356 = CARTESIAN_POINT ( 'NONE',  ( -14.29746914071037622, -8.314922557961029526, 44.16775706135234714 ) ) ;
#68357 = CARTESIAN_POINT ( 'NONE',  ( -21.55341960407610458, -5.719274019375992779, 51.45724293864770260 ) ) ;
#68359 = ORIENTED_EDGE ( 'NONE', *, *, #190638, .F. ) ;
#68358 = CARTESIAN_POINT ( 'NONE',  ( -15.80617190586768217, 15.72974639402176855, 103.1260903946856757 ) ) ;
#68360 = CARTESIAN_POINT ( 'NONE',  ( -5.153800228976328057, -19.02544592524343514, 57.29057627198103120 ) ) ;
#68361 = CARTESIAN_POINT ( 'NONE',  ( 17.18269478283316332, -17.18269478283309226, -64.92279855667830191 ) ) ;
#68362 = CARTESIAN_POINT ( 'NONE',  ( -16.46253265017160317, 9.564922557960807481, 95.83224293864769550 ) ) ;
#68363 = CARTESIAN_POINT ( 'NONE',  ( -36.91746825000000598, 2.428612866367529932E-14, -0.6249999972688132788 ) ) ;
#68364 = CARTESIAN_POINT ( 'NONE',  ( -18.62759615963255300, -10.81492255796106328, 24.16775706135235424 ) ) ;
#68365 = CARTESIAN_POINT ( 'NONE',  ( 8.314922557960818139, 14.29746914071049879, 99.58224293864770971 ) ) ;
#68367 = CARTESIAN_POINT ( 'NONE',  ( 9.474510206698971260, -16.51473224551069308, 67.91557627198102409 ) ) ;
#68366 = CARTESIAN_POINT ( 'NONE',  ( -21.55341960407610458, -5.719274019375992779, 86.45724293864770971 ) ) ;
#68368 = CARTESIAN_POINT ( 'NONE',  ( 9.474510206698971260, -16.51473224551069308, 82.91557627198103830 ) ) ;
#68369 = CARTESIAN_POINT ( 'NONE',  ( -18.62759615963270932, 10.81492255796079327, 110.8322429386476955 ) ) ;
#68370 = ORIENTED_EDGE ( 'NONE', *, *, #142150, .F. ) ;
#68371 = CARTESIAN_POINT ( 'NONE',  ( 19.05341960407611168, 5.049401038298154454, 68.95724293864769550 ) ) ;
#68372 = CARTESIAN_POINT ( 'NONE',  ( 19.46398650005388120, -5.500000000000036415, 97.68269651486373562 ) ) ;
#68374 = CARTESIAN_POINT ( 'NONE',  ( -13.89961937509977652, 13.97604488694528158, 35.62390960531435269 ) ) ;
#68373 = CARTESIAN_POINT ( 'NONE',  ( 0.05219959533910956823, 16.53943276465976808, 109.9989096053143527 ) ) ;
#68375 = CARTESIAN_POINT ( 'NONE',  ( 5.049401038297881783, 19.05341960407617563, 97.29275706135233293 ) ) ;
#68376 = CARTESIAN_POINT ( 'NONE',  ( 4.483927247898545687, 16.52544592524342804, 104.7905762719810241 ) ) ;
#68377 = CARTESIAN_POINT ( 'NONE',  ( 5.719274019375673035, 21.55341960407619339, 72.29275706135236135 ) ) ;
#68379 = CARTESIAN_POINT ( 'NONE',  ( 15.72974639402176855, 15.80617190586768217, 36.87609039468568994 ) ) ;
#68378 = CARTESIAN_POINT ( 'NONE',  ( -5.153800228976328057, -19.02544592524343514, 57.29057627198103120 ) ) ;
#68380 = CARTESIAN_POINT ( 'NONE',  ( -10.72451020669870658, -18.67979575497194134, 19.58442372801901143 ) ) ;
#68381 = CARTESIAN_POINT ( 'NONE',  ( -28.82186960331499037, 2.428612866367529932E-14, 144.0000000000000000 ) ) ;
#68382 = CARTESIAN_POINT ( 'NONE',  ( 9.564922557960805705, 16.46253265017160317, 69.58224293864770971 ) ) ;
#68383 = CARTESIAN_POINT ( 'NONE',  ( 27.83962847748220781, 7.578403945688395815, 161.1890875223823514 ) ) ;
#68385 = CARTESIAN_POINT ( 'NONE',  ( -15.80617190586745835, -15.72974639402198527, 26.87390960531435979 ) ) ;
#68384 = CARTESIAN_POINT ( 'NONE',  ( -16.55341960407617563, 4.379528057220093196, 23.54275706135235424 ) ) ;
#68386 = CARTESIAN_POINT ( 'NONE',  ( -21.52544592524334988, -5.823673210054445271, 63.95942372801901854 ) ) ;
#68387 = CARTESIAN_POINT ( 'NONE',  ( -19.05341960407611168, -5.049401038298163336, 106.4572429386476955 ) ) ;
#68388 = CARTESIAN_POINT ( 'NONE',  ( 19.02544592524334988, 5.153800228976608722, 101.4594237280189759 ) ) ;
#68389 = CARTESIAN_POINT ( 'NONE',  ( 0.05219959533909260263, 19.03943276465977164, 49.99890960531435979 ) ) ;
#68390 = CARTESIAN_POINT ( 'NONE',  ( 9.564922557960805705, 16.46253265017160317, 74.58224293864769550 ) ) ;
#68391 = CARTESIAN_POINT ( 'NONE',  ( 4.379528057220339221, -16.55341960407611168, 92.70724293864770971 ) ) ;
#68392 = CARTESIAN_POINT ( 'NONE',  ( 19.02544592524343514, -5.153800228976328945, 108.5405762719810383 ) ) ;
#68393 = CARTESIAN_POINT ( 'NONE',  ( -16.53943276465976808, 0.05219959533911058130, 86.24890960531436690 ) ) ;
#68394 = CARTESIAN_POINT ( 'NONE',  ( -19.05341960407611168, -5.049401038298163336, 101.4572429386476955 ) ) ;
#68396 = CARTESIAN_POINT ( 'NONE',  ( -13.89961937509977652, 13.97604488694528158, 35.62390960531435269 ) ) ;
#68395 = CARTESIAN_POINT ( 'NONE',  ( 12.06949235617757843, -12.14591786802309237, 63.12390960531435979 ) ) ;
#68397 = CARTESIAN_POINT ( 'NONE',  ( 5.823673210054444382, -21.52544592524334988, 55.20942372801902565 ) ) ;
#68398 = CARTESIAN_POINT ( 'NONE',  ( 5.153800228976615827, -19.02544592524334988, 95.20942372801897591 ) ) ;
#68399 = CARTESIAN_POINT ( 'NONE',  ( 8.314922557960818139, 14.29746914071049879, 49.58224293864769550 ) ) ;
#68400 = CARTESIAN_POINT ( 'NONE',  ( 18.67979575497194134, -10.72451020669871369, 20.83442372801901143 ) ) ;
#68401 = CARTESIAN_POINT ( 'NONE',  ( -5.823673210054116645, -21.52544592524344225, 42.29057627198103120 ) ) ;
#68403 = CARTESIAN_POINT ( 'NONE',  ( 4.483927247898545687, 16.52544592524342804, 89.79057627198103830 ) ) ;
#68402 = CARTESIAN_POINT ( 'NONE',  ( 0.05219959533909260263, 19.03943276465977164, 114.9989096053143669 ) ) ;
#68404 = CARTESIAN_POINT ( 'NONE',  ( 17.81289503416610742, 24.51734667627700404, 139.5500000054623229 ) ) ;
#68405 = CARTESIAN_POINT ( 'NONE',  ( 9.474510206698971260, -16.51473224551069308, 62.91557627198102409 ) ) ;
#68406 = CARTESIAN_POINT ( 'NONE',  ( -8.314922557961024197, 14.29746914071037800, 112.9177570613523329 ) ) ;
#68407 = CARTESIAN_POINT ( 'NONE',  ( 14.29746914071037800, 8.314922557961029526, 101.6677570613523613 ) ) ;
#68408 = CARTESIAN_POINT ( 'NONE',  ( 0.05219959533934541429, -16.53943276465976808, 80.00109039468568994 ) ) ;
#68409 = CARTESIAN_POINT ( 'NONE',  ( -19.02544592524334988, -5.153800228976617603, 38.95942372801900433 ) ) ;
#68410 = CARTESIAN_POINT ( 'NONE',  ( -22.40075113267185714, 13.33491755757043506, 165.5209445330008009 ) ) ;
#68411 = CARTESIAN_POINT ( 'NONE',  ( 9.474510206698971260, -16.51473224551069308, 97.91557627198102409 ) ) ;
#68412 = CARTESIAN_POINT ( 'NONE',  ( 5.049401038298161559, -19.05341960407611168, 47.70724293864770260 ) ) ;
#68413 = CARTESIAN_POINT ( 'NONE',  ( 14.29746914071049879, -8.314922557960816363, 58.33224293864768839 ) ) ;
#68415 = CARTESIAN_POINT ( 'NONE',  ( -13.97604488694527625, -13.89961937509977652, 106.8739096053143669 ) ) ;
#68414 = CARTESIAN_POINT ( 'NONE',  ( 9.474510206698971260, -16.51473224551069308, 112.9155762719810383 ) ) ;
#68416 = CARTESIAN_POINT ( 'NONE',  ( -10.72451020669898014, 18.67979575497178502, 45.41557627198103830 ) ) ;
#68417 = CARTESIAN_POINT ( 'NONE',  ( 0.05219959533910956823, 16.53943276465976808, 84.99890960531436690 ) ) ;
#68418 = CARTESIAN_POINT ( 'NONE',  ( -14.29746914071037622, -8.314922557961029526, 39.16775706135235424 ) ) ;
#68419 = EDGE_CURVE ( 'NONE', #116580, #111465, #28109, .T. ) ;
#68420 = AXIS2_PLACEMENT_3D ( 'NONE', #166962, #120434, #106258 ) ;
#68421 = CARTESIAN_POINT ( 'NONE',  ( 14.29746914071049879, -8.314922557960816363, 78.33224293864770971 ) ) ;
#68422 = CYLINDRICAL_SURFACE ( 'NONE', #83405, 10.00000000000000178 ) ;
#68423 = CARTESIAN_POINT ( 'NONE',  ( 16.46253265017146816, 9.564922557961045513, 71.66775706135233293 ) ) ;
#68424 = CARTESIAN_POINT ( 'NONE',  ( 19.05341960407611168, 5.049401038298154454, 108.9572429386477097 ) ) ;
#68425 = CARTESIAN_POINT ( 'NONE',  ( -19.03943276465977164, -0.05219959533935918106, 73.75109039468566152 ) ) ;
#68426 = DIRECTION ( 'NONE',  ( -0.000000000000000000, -0.000000000000000000, 1.000000000000000000 ) ) ;
#68428 = CARTESIAN_POINT ( 'NONE',  ( -4.379528057220086978, -16.55341960407618274, 109.7927570613523613 ) ) ;
#68427 = CARTESIAN_POINT ( 'NONE',  ( -14.29746914071037622, -8.314922557961029526, 24.16775706135235424 ) ) ;
#68429 = CARTESIAN_POINT ( 'NONE',  ( 19.03943276465977164, 0.05219959533936151252, 71.25109039468566152 ) ) ;
#68430 = CARTESIAN_POINT ( 'NONE',  ( 15.72974639402199770, -15.80617190586745480, 33.12390960531435979 ) ) ;
#68431 = CARTESIAN_POINT ( 'NONE',  ( 21.53943276465977519, 0.05219959533937863772, 71.25109039468568994 ) ) ;
#68432 = CARTESIAN_POINT ( 'NONE',  ( -22.37486833544133091, -13.37560805684351450, 165.5209445320977864 ) ) ;
#68433 = CARTESIAN_POINT ( 'NONE',  ( -4.379528057220086978, -16.55341960407618274, 24.79275706135235779 ) ) ;
#68435 = CARTESIAN_POINT ( 'NONE',  ( 13.89961937509977652, -13.97604488694527269, 93.12390960531436690 ) ) ;
#68434 = DIRECTION ( 'NONE',  ( 0.000000000000000000, 0.6427876096865404731, 0.7660444431189771253 ) ) ;
#68436 = CARTESIAN_POINT ( 'NONE',  ( 5.049401038298161559, -19.05341960407611168, 27.70724293864769550 ) ) ;
#68438 = CARTESIAN_POINT ( 'NONE',  ( -19.02544592524342804, 5.153800228976336051, 86.04057627198103830 ) ) ;
#68437 = CARTESIAN_POINT ( 'NONE',  ( 14.34966873604960469, 8.224510206698951720, 94.16557627198103830 ) ) ;
#68439 = ITEM_DEFINED_TRANSFORMATION ( 'NONE', 'NONE', #162921,  #82054 ) ;
#68440 = CARTESIAN_POINT ( 'NONE',  ( -16.51473224551069308, -9.474510206698971260, 81.66557627198103830 ) ) ;
#68441 = ORIENTED_EDGE ( 'NONE', *, *, #117511, .F. ) ;
#68442 = CARTESIAN_POINT ( 'NONE',  ( 5.153800228976615827, -19.02544592524334988, 85.20942372801900433 ) ) ;
#68443 = CARTESIAN_POINT ( 'NONE',  ( -0.05219959533907301413, -21.53943276465977519, 77.49890960531433848 ) ) ;
#68444 = CARTESIAN_POINT ( 'NONE',  ( -9.564922557960796823, -16.46253265017161027, 42.08224293864769550 ) ) ;
#68446 = CARTESIAN_POINT ( 'NONE',  ( -0.05219959533907301413, -21.53943276465977519, 112.4989096053143669 ) ) ;
#68445 = CARTESIAN_POINT ( 'NONE',  ( -5.049401038297874678, -19.05341960407617918, 74.79275706135231871 ) ) ;
#68447 = CARTESIAN_POINT ( 'NONE',  ( -19.02544592524342804, 5.153800228976336051, 71.04057627198099567 ) ) ;
#68448 = CARTESIAN_POINT ( 'NONE',  ( 0.05219959533909260263, 19.03943276465977164, 104.9989096053143669 ) ) ;
#68449 = ORIENTED_EDGE ( 'NONE', *, *, #41619, .T. ) ;
#68450 = CARTESIAN_POINT ( 'NONE',  ( -8.314922557961024197, 14.29746914071037800, 32.91775706135234714 ) ) ;
#68451 = CARTESIAN_POINT ( 'NONE',  ( 18.67979575497178502, 10.72451020669898547, 104.1655762719810241 ) ) ;
#68454 = CARTESIAN_POINT ( 'NONE',  ( -13.89961937509957401, -13.97604488694547875, 59.37609039468566863 ) ) ;
#68453 = CARTESIAN_POINT ( 'NONE',  ( 9.474510206698971260, -16.51473224551069308, 82.91557627198103830 ) ) ;
#68452 = CARTESIAN_POINT ( 'NONE',  ( -14.34966873604960291, -8.224510206698953496, 101.6655762719810383 ) ) ;
#68455 = CARTESIAN_POINT ( 'NONE',  ( 10.72451020669898902, -18.67979575497178502, 92.91557627198103830 ) ) ;
#68456 = CARTESIAN_POINT ( 'NONE',  ( 10.81492255796078972, 18.62759615963270932, 69.58224293864769550 ) ) ;
#68457 = CARTESIAN_POINT ( 'NONE',  ( 4.379528057220339221, -16.55341960407611168, 42.70724293864770260 ) ) ;
#68458 = CARTESIAN_POINT ( 'NONE',  ( 13.89961937509957401, 13.97604488694547697, 21.87609039468566152 ) ) ;
#68459 = CARTESIAN_POINT ( 'NONE',  ( -4.483927247898782831, 16.52544592524335698, 67.70942372801901854 ) ) ;
#68460 = CARTESIAN_POINT ( 'NONE',  ( -19.05341960407611168, -5.049401038298163336, 96.45724293864769550 ) ) ;
#68461 = CARTESIAN_POINT ( 'NONE',  ( 16.51473224551069308, 9.474510206698969483, 49.16557627198102409 ) ) ;
#68462 = CARTESIAN_POINT ( 'NONE',  ( 10.72451020669871369, 18.67979575497193778, 47.08442372801901854 ) ) ;
#68463 = CARTESIAN_POINT ( 'NONE',  ( -21.53943276465977519, -0.05219959533937600094, 48.75109039468568284 ) ) ;
#68464 = CARTESIAN_POINT ( 'NONE',  ( 19.05341960407611168, 5.049401038298154454, 63.95724293864769550 ) ) ;
#68465 = CARTESIAN_POINT ( 'NONE',  ( 21.52544592524334988, 5.823673210054432836, 36.45942372801901143 ) ) ;
#68466 = CARTESIAN_POINT ( 'NONE',  ( -5.153800228976607833, 19.02544592524334988, 72.70942372801900433 ) ) ;
#68467 = CARTESIAN_POINT ( 'NONE',  ( 5.153800228976615827, -19.02544592524334988, 75.20942372801896170 ) ) ;
#68468 = CARTESIAN_POINT ( 'NONE',  ( 0.05219959533909260263, 19.03943276465977164, 39.99890960531436690 ) ) ;
#68469 = CARTESIAN_POINT ( 'NONE',  ( 16.55341960407618274, -4.379528057220086978, 91.04275706135236135 ) ) ;
#68470 = CARTESIAN_POINT ( 'NONE',  ( 16.51473224551069308, 9.474510206698969483, 59.16557627198102409 ) ) ;
#68471 = CARTESIAN_POINT ( 'NONE',  ( 21.47377332592399668, -5.474134792251643233, 173.8918256800999984 ) ) ;
#68472 = CARTESIAN_POINT ( 'NONE',  ( 13.89961937509977652, -13.97604488694527269, 98.12390960531433848 ) ) ;
#68473 = CARTESIAN_POINT ( 'NONE',  ( -13.89961937509977652, 13.97604488694528158, 35.62390960531435269 ) ) ;
#68474 = CARTESIAN_POINT ( 'NONE',  ( 5.823673210054125526, 21.52544592524343514, 89.79057627198103830 ) ) ;
#68475 = CARTESIAN_POINT ( 'NONE',  ( 0.05219959533934541429, -16.53943276465976808, 65.00109039468568994 ) ) ;
#68476 = CARTESIAN_POINT ( 'NONE',  ( -15.80617190586768217, 15.72974639402176855, 108.1260903946856757 ) ) ;
#68477 = CARTESIAN_POINT ( 'NONE',  ( -16.51473224551069308, -9.474510206698971260, 46.66557627198102409 ) ) ;
#68478 = CARTESIAN_POINT ( 'NONE',  ( 12.06949235617757843, -12.14591786802309237, 48.12390960531436690 ) ) ;
#68479 = CARTESIAN_POINT ( 'NONE',  ( -8.314922557960811034, -14.29746914071050412, 82.08224293864768129 ) ) ;
#68480 = CARTESIAN_POINT ( 'NONE',  ( -0.05219959533909027116, -19.03943276465977164, 72.49890960531435269 ) ) ;
#68481 = CARTESIAN_POINT ( 'NONE',  ( 10.72451020669871369, 18.67979575497193778, 37.08442372801901143 ) ) ;
#68482 = CARTESIAN_POINT ( 'NONE',  ( 13.89961937509977652, -13.97604488694527269, 98.12390960531433848 ) ) ;
#68483 = CARTESIAN_POINT ( 'NONE',  ( 15.80617190586769283, -15.72974639402175789, 95.62609039468568994 ) ) ;
#68484 = CARTESIAN_POINT ( 'NONE',  ( 8.224510206698742110, 14.34966873604972548, 82.08442372801901854 ) ) ;
#68485 = CARTESIAN_POINT ( 'NONE',  ( -15.72974639402176322, -15.80617190586768395, 24.37609039468567573 ) ) ;
#68486 = CARTESIAN_POINT ( 'NONE',  ( 16.51473224551069308, 9.474510206698969483, 114.1655762719810241 ) ) ;
#68487 = CARTESIAN_POINT ( 'NONE',  ( 5.823673210054125526, 21.52544592524343514, 84.79057627198102409 ) ) ;
#68488 = CARTESIAN_POINT ( 'NONE',  ( 14.29746914071049879, -8.314922557960816363, 53.33224293864769550 ) ) ;
#68489 = CARTESIAN_POINT ( 'NONE',  ( 9.474510206698971260, -16.51473224551069308, 42.91557627198103120 ) ) ;
#68490 = CARTESIAN_POINT ( 'NONE',  ( 16.52544592524342804, -4.483927247898539470, 63.54057627198103830 ) ) ;
#68491 = CARTESIAN_POINT ( 'NONE',  ( 10.81492255796078972, 18.62759615963270932, 34.58224293864770260 ) ) ;
#68492 = CARTESIAN_POINT ( 'NONE',  ( -16.51473224551082808, 9.474510206698731452, 28.33442372801900433 ) ) ;
#68493 = CARTESIAN_POINT ( 'NONE',  ( 16.53943276465976808, -0.05219959533910856209, 93.74890960531436690 ) ) ;
#68494 = CARTESIAN_POINT ( 'NONE',  ( -5.049401038298153566, 19.05341960407611168, 105.2072429386476671 ) ) ;
#68495 = ORIENTED_EDGE ( 'NONE', *, *, #178481, .T. ) ;
#68496 = CARTESIAN_POINT ( 'NONE',  ( 8.224510206698742110, 14.34966873604972548, 47.08442372801901854 ) ) ;
#68497 = CARTESIAN_POINT ( 'NONE',  ( -5.153800228976328057, -19.02544592524343514, 52.29057627198100988 ) ) ;
#68498 = CARTESIAN_POINT ( 'NONE',  ( 27.73933785331498569, 2.768321779492822058E-14, 139.8750000027311842 ) ) ;
#68499 = CARTESIAN_POINT ( 'NONE',  ( 8.314922557961029526, -14.29746914071037800, 95.41775706135234714 ) ) ;
#68500 = CARTESIAN_POINT ( 'NONE',  ( -16.51473224551082808, 9.474510206698731452, 103.3344237280190043 ) ) ;
#68501 = CARTESIAN_POINT ( 'NONE',  ( 21.53943276465977519, 0.05219959533937863772, 76.25109039468568994 ) ) ;
#68502 = CARTESIAN_POINT ( 'NONE',  ( 9.564922557960805705, 16.46253265017160317, 69.58224293864770971 ) ) ;
#68503 = CARTESIAN_POINT ( 'NONE',  ( -15.72974639402197994, 15.80617190586746368, 110.6239096053143669 ) ) ;
#68504 = CARTESIAN_POINT ( 'NONE',  ( 16.52544592524335698, 4.483927247898782831, 51.45942372801901854 ) ) ;
#68505 = CARTESIAN_POINT ( 'NONE',  ( -8.224510206698948167, 14.34966873604960824, 115.4155762719810241 ) ) ;
#68506 = CARTESIAN_POINT ( 'NONE',  ( -14.34966873604972548, 8.224510206698743886, 23.33442372801901499 ) ) ;
#68507 = EDGE_CURVE ( 'NONE', #4269, #24637, #89754, .T. ) ;
#68508 = CARTESIAN_POINT ( 'NONE',  ( 9.564922557961047289, -16.46253265017146816, 80.41775706135234714 ) ) ;
#68509 = CARTESIAN_POINT ( 'NONE',  ( -5.823673210054116645, -21.52544592524344225, 82.29057627198103830 ) ) ;
#68510 = CARTESIAN_POINT ( 'NONE',  ( 0.05219959533936267826, -19.03943276465977164, 60.00109039468566863 ) ) ;
#68511 = CARTESIAN_POINT ( 'NONE',  ( 5.153800228976335163, 19.02544592524342804, 114.7905762719810241 ) ) ;
#68512 = CARTESIAN_POINT ( 'NONE',  ( -5.823673210054116645, -21.52544592524344225, 102.2905762719810383 ) ) ;
#68513 = CARTESIAN_POINT ( 'NONE',  ( 17.81289503416611453, -24.51734667627695785, 148.6999999999999602 ) ) ;
#68514 = CARTESIAN_POINT ( 'NONE',  ( -16.46253265017160317, 9.564922557960807481, 65.83224293864769550 ) ) ;
#68515 = CARTESIAN_POINT ( 'NONE',  ( -17.49999999999999645, 7.499999999999998224, 22.00000000000000711 ) ) ;
#68516 = CARTESIAN_POINT ( 'NONE',  ( 19.02544592524334988, 5.153800228976608722, 111.4594237280190043 ) ) ;
#68517 = CARTESIAN_POINT ( 'NONE',  ( 24.39440776506090103, 8.562465606919662520, 166.7298475161184683 ) ) ;
#68518 = CARTESIAN_POINT ( 'NONE',  ( -21.52544592524334988, -5.823673210054445271, 53.95942372801900433 ) ) ;
#68520 = CARTESIAN_POINT ( 'NONE',  ( -12.14591786802309592, -12.06949235617757132, 66.87390960531436690 ) ) ;
#68519 = CARTESIAN_POINT ( 'NONE',  ( -15.80617190586745835, -15.72974639402198527, 106.8739096053143811 ) ) ;
#68521 = CARTESIAN_POINT ( 'NONE',  ( -13.97604488694527625, -13.89961937509977652, 71.87390960531433848 ) ) ;
#68522 = CARTESIAN_POINT ( 'NONE',  ( 15.72974639402176855, 15.80617190586768217, 76.87609039468567573 ) ) ;
#68524 = CARTESIAN_POINT ( 'NONE',  ( 19.05341960407617918, -5.049401038297876454, 31.04275706135232227 ) ) ;
#68523 = CARTESIAN_POINT ( 'NONE',  ( 4.379528057220092307, 16.55341960407617563, 27.29275706135234358 ) ) ;
#68525 = CARTESIAN_POINT ( 'NONE',  ( 18.67979575497194134, -10.72451020669871369, 45.83442372801901854 ) ) ;
#68526 = CARTESIAN_POINT ( 'NONE',  ( 0.05219959533907565091, 21.53943276465977519, 109.9989096053143527 ) ) ;
#68527 = CARTESIAN_POINT ( 'NONE',  ( -10.81492255796078084, -18.62759615963271287, 62.08224293864769550 ) ) ;
#68528 = CARTESIAN_POINT ( 'NONE',  ( -19.05341960407617563, 5.049401038297882671, 93.54275706135234714 ) ) ;
#68529 = CARTESIAN_POINT ( 'NONE',  ( 19.02544592524334988, 5.153800228976608722, 66.45942372801899012 ) ) ;
#68530 = CARTESIAN_POINT ( 'NONE',  ( 18.67979575497194134, -10.72451020669871369, 85.83442372801901854 ) ) ;
#68531 = CARTESIAN_POINT ( 'NONE',  ( 13.89961937509957401, 13.97604488694547697, 51.87609039468566863 ) ) ;
#68532 = CARTESIAN_POINT ( 'NONE',  ( -16.46253265017160317, 9.564922557960807481, 35.83224293864768839 ) ) ;
#68533 = CARTESIAN_POINT ( 'NONE',  ( 21.52544592524344225, -5.823673210054117533, 58.54057627198103120 ) ) ;
#68534 = CARTESIAN_POINT ( 'NONE',  ( -12.06949235617756955, 12.14591786802309770, 55.62390960531436690 ) ) ;
#68535 = CARTESIAN_POINT ( 'NONE',  ( -18.56453257813365809, 5.499999999999960920, 95.99000423690688422 ) ) ;
#68536 = CARTESIAN_POINT ( 'NONE',  ( -16.46253265017146816, -9.564922557961047289, 29.16775706135232937 ) ) ;
#68537 = CARTESIAN_POINT ( 'NONE',  ( 14.29746914071037800, 8.314922557961029526, 86.66775706135234714 ) ) ;
#68538 = CARTESIAN_POINT ( 'NONE',  ( 4.483927247898545687, 16.52544592524342804, 54.79057627198104541 ) ) ;
#68539 = CARTESIAN_POINT ( 'NONE',  ( 10.81492255796106328, -18.62759615963255655, 80.41775706135234714 ) ) ;
#68540 = CARTESIAN_POINT ( 'NONE',  ( 10.72451020669871369, 18.67979575497193778, 77.08442372801901854 ) ) ;
#68541 = CARTESIAN_POINT ( 'NONE',  ( -10.72451020669898014, 18.67979575497178502, 75.41557627198102409 ) ) ;
#68542 = CARTESIAN_POINT ( 'NONE',  ( 13.97604488694527802, 13.89961937509977652, 39.37390960531435269 ) ) ;
#68543 = CARTESIAN_POINT ( 'NONE',  ( -10.72451020669870658, -18.67979575497194134, 54.58442372801901143 ) ) ;
#68544 = CARTESIAN_POINT ( 'NONE',  ( 19.05341960407611168, 5.049401038298154454, 33.95724293864769550 ) ) ;
#68545 = CARTESIAN_POINT ( 'NONE',  ( -19.05341960407611168, -5.049401038298163336, 46.45724293864768129 ) ) ;
#68546 = CARTESIAN_POINT ( 'NONE',  ( -16.53943276465976808, 0.05219959533911058130, 106.2489096053143811 ) ) ;
#68547 = CARTESIAN_POINT ( 'NONE',  ( 16.51473224551069308, 9.474510206698969483, 104.1655762719810241 ) ) ;
#68548 = CARTESIAN_POINT ( 'NONE',  ( 16.52544592524342804, -4.483927247898539470, 38.54057627198103120 ) ) ;
#68549 = CARTESIAN_POINT ( 'NONE',  ( 16.55341960407611168, 4.379528057220329451, 113.9572429386477239 ) ) ;
#68550 = CARTESIAN_POINT ( 'NONE',  ( 15.72974639402199770, -15.80617190586745480, 88.12390960531436690 ) ) ;
#68551 = CARTESIAN_POINT ( 'NONE',  ( 0.05219959533937995610, -21.53943276465977519, 20.00109039468568639 ) ) ;
#68552 = DIRECTION ( 'NONE',  ( -0.000000000000000000, -0.000000000000000000, -1.000000000000000000 ) ) ;
#68553 = CARTESIAN_POINT ( 'NONE',  ( -0.05219959533934338120, 16.53943276465976808, 32.50109039468568284 ) ) ;
#68554 = VERTEX_POINT ( 'NONE', #133265 ) ;
#68555 = CARTESIAN_POINT ( 'NONE',  ( -15.80617190586745835, -15.72974639402198527, 66.87390960531436690 ) ) ;
#68556 = CARTESIAN_POINT ( 'NONE',  ( -18.67979575497193778, 10.72451020669871902, 88.33442372801901854 ) ) ;
#68557 = CARTESIAN_POINT ( 'NONE',  ( 13.97604488694527802, 13.89961937509977652, 89.37390960531436690 ) ) ;
#68558 = CARTESIAN_POINT ( 'NONE',  ( 21.53943276465977519, 0.05219959533937863772, 36.25109039468567573 ) ) ;
#68559 = CARTESIAN_POINT ( 'NONE',  ( -18.67979575497178146, -10.72451020669898902, 26.66557627198103475 ) ) ;
#68560 = CARTESIAN_POINT ( 'NONE',  ( 16.55341960407618274, -4.379528057220086978, 86.04275706135236135 ) ) ;
#68561 = CARTESIAN_POINT ( 'NONE',  ( -21.52544592524334988, -5.823673210054445271, 88.95942372801901854 ) ) ;
#68562 = CARTESIAN_POINT ( 'NONE',  ( -5.153800228976607833, 19.02544592524334988, 22.70942372801899012 ) ) ;
#68563 = CARTESIAN_POINT ( 'NONE',  ( 16.52544592524335698, 4.483927247898782831, 71.45942372801901854 ) ) ;
#68564 = CARTESIAN_POINT ( 'NONE',  ( -18.67979575497193778, 10.72451020669871902, 23.33442372801901499 ) ) ;
#68565 = CARTESIAN_POINT ( 'NONE',  ( 9.564922557960805705, 16.46253265017160317, 34.58224293864770260 ) ) ;
#68566 = CARTESIAN_POINT ( 'NONE',  ( -18.62759615963255300, -10.81492255796106328, 109.1677570613523613 ) ) ;
#68567 = CARTESIAN_POINT ( 'NONE',  ( 13.89961937509977652, -13.97604488694527269, 108.1239096053143669 ) ) ;
#68568 = CARTESIAN_POINT ( 'NONE',  ( 10.72451020669898902, -18.67979575497178502, 107.9155762719810241 ) ) ;
#68570 = CARTESIAN_POINT ( 'NONE',  ( -18.62759615963270932, 10.81492255796079327, 60.83224293864769550 ) ) ;
#68569 = CARTESIAN_POINT ( 'NONE',  ( 2.552343178074615970, -7.052343178074640839, 1.110912703473986074 ) ) ;
#68572 = CARTESIAN_POINT ( 'NONE',  ( 4.483927247898545687, 16.52544592524342804, 54.79057627198104541 ) ) ;
#68571 = CARTESIAN_POINT ( 'NONE',  ( 14.29746914071037800, 8.314922557961029526, 51.66775706135234714 ) ) ;
#68573 = CARTESIAN_POINT ( 'NONE',  ( 19.33860699428957020, -5.500000000000004441, 101.6010922787093733 ) ) ;
#68574 = CARTESIAN_POINT ( 'NONE',  ( 5.049401038297881783, 19.05341960407617563, 72.29275706135234714 ) ) ;
#68575 =( BOUNDED_SURFACE ( )  B_SPLINE_SURFACE ( 3, 2, ( 
 ( #37739, #130739, #6389 ),
 ( #40744, #36725, #191419 ),
 ( #116581, #54908, #100405 ),
 ( #176267, #192431, #132747 ),
 ( #190430, #8408, #129722 ),
 ( #69072, #193432, #178270 ),
 ( #83231, #23580, #144906 ),
 ( #179279, #70082, #39733 ),
 ( #101394, #162086, #131750 ),
 ( #194435, #128734, #52895 ),
 ( #99400, #163087, #161083 ),
 ( #53913, #85228, #22578 ),
 ( #146919, #24591, #86239 ),
 ( #55906, #117579, #84225 ),
 ( #145904, #7388, #115588 ),
 ( #180282, #152880, #27594 ),
 ( #183242, #195442, #73092 ),
 ( #58889, #75056, #44723 ),
 ( #106379, #14375, #120555 ),
 ( #60864, #76041, #137716 ),
 ( #119587, #165094, #197423 ),
 ( #12419, #182248, #148927 ),
 ( #56917, #199400, #43733 ),
 ( #72074, #28583, #89232 ) ),
 .UNSPECIFIED., .F., .F., .T. ) 
 B_SPLINE_SURFACE_WITH_KNOTS ( ( 4, 2, 2, 2, 2, 2, 2, 2, 2, 2, 2, 4 ),
 ( 3, 3 ),
 ( -8.673617379884035472E-19, 0.001899702839891689908, 0.002849554259837535405, 0.003799405679783380684, 0.005699108519675071677, 0.006648959939620916956, 0.007598811359566762236, 0.008548662779512607515, 0.009498514199458452795, 0.01139821703935014335, 0.01329791987924183391, 0.01519762271913352447 ),
 ( 0.000000000000000000, 1.000000000000000000 ),
 .UNSPECIFIED. ) 
 GEOMETRIC_REPRESENTATION_ITEM ( )  RATIONAL_B_SPLINE_SURFACE ( (
 ( 1.000000000000000000, 0.7660444431189777914, 1.000000000000000000),
 ( 1.000000000000000000, 0.7753720600381861505, 1.000000000000000000),
 ( 1.000000000000000000, 0.7832595754286625356, 1.000000000000000000),
 ( 1.000000000000000000, 0.7928595458705119947, 1.000000000000000000),
 ( 1.000000000000000000, 0.7956872332516092827, 1.000000000000000000),
 ( 1.000000000000000000, 0.8005750596157589216, 1.000000000000000000),
 ( 1.000000000000000000, 0.8026302056541690932, 1.000000000000000000),
 ( 1.000000000000000000, 0.8075080643848435713, 1.000000000000000000),
 ( 1.000000000000000000, 0.8091143015809740824, 1.000000000000000000),
 ( 1.000000000000000000, 0.8093067629633081683, 1.000000000000000000),
 ( 1.000000000000000000, 0.8089952915731970506, 1.000000000000000000),
 ( 1.000000000000000000, 0.8076919994861997409, 1.000000000000000000),
 ( 1.000000000000000000, 0.8067078407648531346, 1.000000000000000000),
 ( 1.000000000000000000, 0.8041786842467797403, 1.000000000000000000),
 ( 1.000000000000000000, 0.8026334674877259046, 1.000000000000000000),
 ( 1.000000000000000000, 0.7990747329469148896, 1.000000000000000000),
 ( 1.000000000000000000, 0.7970509760942132704, 1.000000000000000000),
 ( 1.000000000000000000, 0.7904793850862674720, 1.000000000000000000),
 ( 1.000000000000000000, 0.7855040224314492336, 1.000000000000000000),
 ( 1.000000000000000000, 0.7751942650506803423, 1.000000000000000000),
 ( 1.000000000000000000, 0.7698260778211011290, 1.000000000000000000),
 ( 1.000000000000000000, 0.7598259884961470201, 1.000000000000000000),
 ( 1.000000000000000000, 0.7551428682219897270, 1.000000000000000000),
 ( 1.000000000000000000, 0.7510191126010854479, 1.000000000000000000) ) ) 
 REPRESENTATION_ITEM ( '' )  SURFACE ( )  );
#68576 = CARTESIAN_POINT ( 'NONE',  ( -17.49999999999999645, 5.624438216177585659, 105.8167034491464449 ) ) ;
#68577 = CARTESIAN_POINT ( 'NONE',  ( 4.379528057220092307, 16.55341960407617563, 22.29275706135235069 ) ) ;
#68578 = CARTESIAN_POINT ( 'NONE',  ( -5.719274019375978568, 21.55341960407610458, 100.2072429386476955 ) ) ;
#68579 = CARTESIAN_POINT ( 'NONE',  ( 16.53943276465976808, -0.05219959533910856209, 58.74890960531436690 ) ) ;
#68580 = CARTESIAN_POINT ( 'NONE',  ( -9.564922557960796823, -16.46253265017161027, 107.0822429386476955 ) ) ;
#68581 = CARTESIAN_POINT ( 'NONE',  ( 16.53943276465976808, 0.05219959533934440121, 46.25109039468567573 ) ) ;
#68582 = CARTESIAN_POINT ( 'NONE',  ( -0.05219959533909027116, -19.03943276465977164, 52.49890960531436690 ) ) ;
#68584 = CARTESIAN_POINT ( 'NONE',  ( -13.97604488694547697, 13.89961937509957934, 103.1260903946856473 ) ) ;
#68583 = CARTESIAN_POINT ( 'NONE',  ( -21.55341960407619339, 5.719274019375674811, 28.54275706135234358 ) ) ;
#68585 = CARTESIAN_POINT ( 'NONE',  ( -16.51473224551069308, -9.474510206698971260, 101.6655762719810241 ) ) ;
#68586 = CARTESIAN_POINT ( 'NONE',  ( -16.46253265017160317, 9.564922557960807481, 85.83224293864769550 ) ) ;
#68587 = CARTESIAN_POINT ( 'NONE',  ( -5.823673210054116645, -21.52544592524344225, 92.29057627198103830 ) ) ;
#68588 = CARTESIAN_POINT ( 'NONE',  ( -9.564922557960796823, -16.46253265017161027, 52.08224293864768839 ) ) ;
#68589 = CARTESIAN_POINT ( 'NONE',  ( -11.74264578624800670, 36.14014761921585972, -0.3999999999999999112 ) ) ;
#68590 = CARTESIAN_POINT ( 'NONE',  ( -16.53943276465976808, 0.05219959533911058130, 66.24890960531436690 ) ) ;
#68591 = CARTESIAN_POINT ( 'NONE',  ( 5.153800228976335163, 19.02544592524342804, 109.7905762719810099 ) ) ;
#68592 = CARTESIAN_POINT ( 'NONE',  ( -31.67901979315909600, 0.7913989229881625009, -49.40962234820035093 ) ) ;
#68593 = CARTESIAN_POINT ( 'NONE',  ( 16.51473224551083163, -9.474510206698727899, 80.83442372801899012 ) ) ;
#68594 = CARTESIAN_POINT ( 'NONE',  ( -10.72451020669898014, 18.67979575497178502, 85.41557627198102409 ) ) ;
#68595 = CARTESIAN_POINT ( 'NONE',  ( 5.153800228976615827, -19.02544592524334988, 45.20942372801901143 ) ) ;
#68596 = CARTESIAN_POINT ( 'NONE',  ( 16.51473224551069308, 9.474510206698969483, 104.1655762719810241 ) ) ;
#68597 = CARTESIAN_POINT ( 'NONE',  ( 17.72560187377284890, 5.500000000000043521, 76.57814504131320632 ) ) ;
#68598 = CARTESIAN_POINT ( 'NONE',  ( 15.80617190586746368, 15.72974639402197994, 39.37390960531436690 ) ) ;
#68599 = CARTESIAN_POINT ( 'NONE',  ( -9.564922557960796823, -16.46253265017161027, 82.08224293864768129 ) ) ;
#68600 = CARTESIAN_POINT ( 'NONE',  ( -10.81492255796105439, 18.62759615963255655, 67.91775706135234714 ) ) ;
#68601 = CARTESIAN_POINT ( 'NONE',  ( 19.05341960407611168, 5.049401038298154454, 33.95724293864769550 ) ) ;
#68602 = CARTESIAN_POINT ( 'NONE',  ( -16.53943276465976808, 0.05219959533911058130, 71.24890960531435269 ) ) ;
#68603 = CARTESIAN_POINT ( 'NONE',  ( 16.55341960407618274, -4.379528057220086978, 21.04275706135234714 ) ) ;
#68604 = CARTESIAN_POINT ( 'NONE',  ( 5.719274019375673035, 21.55341960407619339, 52.29275706135236135 ) ) ;
#68605 = ORIENTED_EDGE ( 'NONE', *, *, #42638, .T. ) ;
#68606 = CARTESIAN_POINT ( 'NONE',  ( 0.000000000000000000, 0.000000000000000000, -61.34707691135562868 ) ) ;
#68607 = CARTESIAN_POINT ( 'NONE',  ( 5.153800228976615827, -19.02544592524334988, 75.20942372801896170 ) ) ;
#68608 = CARTESIAN_POINT ( 'NONE',  ( 0.000000000000000000, 0.000000000000000000, -65.00100000000003320 ) ) ;
#68609 = CARTESIAN_POINT ( 'NONE',  ( 15.72974639402176855, 15.80617190586768217, 26.87609039468567218 ) ) ;
#68610 = EDGE_CURVE ( 'NONE', #150223, #30088, #92827, .T. ) ;
#68611 = CARTESIAN_POINT ( 'NONE',  ( -19.25176906914649422, -5.499999999999741540, 45.99927264242278113 ) ) ;
#68612 = CARTESIAN_POINT ( 'NONE',  ( -21.53943276465977519, -0.05219959533937600094, 108.7510903946857042 ) ) ;
#68613 = CARTESIAN_POINT ( 'NONE',  ( 9.564922557960805705, 16.46253265017160317, 49.58224293864770260 ) ) ;
#68614 = CARTESIAN_POINT ( 'NONE',  ( 18.67979575497194134, -10.72451020669871369, 110.8344237280190043 ) ) ;
#68615 = CARTESIAN_POINT ( 'NONE',  ( 16.55341960407618274, -4.379528057220086978, 101.0427570613523756 ) ) ;
#68617 = CARTESIAN_POINT ( 'NONE',  ( -10.72451020669870658, -18.67979575497194134, 79.58442372801903275 ) ) ;
#68616 = CARTESIAN_POINT ( 'NONE',  ( -13.97604488694527625, -13.89961937509977652, 96.87390960531433848 ) ) ;
#68618 = CARTESIAN_POINT ( 'NONE',  ( 17.14385361876520264, -23.59649016807271238, 148.0750000027311728 ) ) ;
#68619 = CARTESIAN_POINT ( 'NONE',  ( -18.10062525802553424, 5.500000000000031974, 98.51383468041922242 ) ) ;
#68620 = CARTESIAN_POINT ( 'NONE',  ( 22.99604614807110892, -21.65681935926113866, -46.12383121077565562 ) ) ;
#68621 = CARTESIAN_POINT ( 'NONE',  ( 18.62759615963255655, 10.81492255796105972, 71.66775706135234714 ) ) ;
#68622 = CARTESIAN_POINT ( 'NONE',  ( 5.719274019375673035, 21.55341960407619339, 107.2927570613523471 ) ) ;
#68623 = CARTESIAN_POINT ( 'NONE',  ( -9.687362902255733488, 9.687362902255692632, -62.58071313852362039 ) ) ;
#68624 = CARTESIAN_POINT ( 'NONE',  ( -9.564922557960796823, -16.46253265017161027, 87.08224293864769550 ) ) ;
#68625 = CARTESIAN_POINT ( 'NONE',  ( -0.05219959533936034679, 19.03943276465977164, 27.50109039468566507 ) ) ;
#68626 = EDGE_CURVE ( 'NONE', #91848, #141307, #100919, .T. ) ;
#68627 = CARTESIAN_POINT ( 'NONE',  ( 26.58214507596527199, -26.75488679838896289, -20.35119661315284390 ) ) ;
#68628 = CARTESIAN_POINT ( 'NONE',  ( 13.97604488694527802, 13.89961937509977652, 34.37390960531436690 ) ) ;
#68629 = CARTESIAN_POINT ( 'NONE',  ( -18.62759615963270932, 10.81492255796079327, 55.83224293864770260 ) ) ;
#68630 = CARTESIAN_POINT ( 'NONE',  ( -14.34966873604972548, 8.224510206698743886, 103.3344237280190043 ) ) ;
#68632 = CARTESIAN_POINT ( 'NONE',  ( -5.153800228976328057, -19.02544592524343514, 87.29057627198103830 ) ) ;
#68631 = CARTESIAN_POINT ( 'NONE',  ( 14.29746914071049879, -8.314922557960816363, 98.33224293864769550 ) ) ;
#68633 = CARTESIAN_POINT ( 'NONE',  ( -10.72451020669870658, -18.67979575497194134, 104.5844237280190185 ) ) ;
#68634 = CARTESIAN_POINT ( 'NONE',  ( -13.97604488694527625, -13.89961937509977652, 41.87390960531435979 ) ) ;
#68635 = CARTESIAN_POINT ( 'NONE',  ( 14.34966873604960469, 8.224510206698951720, 89.16557627198102409 ) ) ;
#68636 = CARTESIAN_POINT ( 'NONE',  ( -18.62759615963255300, -10.81492255796106328, 49.16775706135234003 ) ) ;
#68637 = CARTESIAN_POINT ( 'NONE',  ( -0.05219959533907301413, -21.53943276465977519, 87.49890960531436690 ) ) ;
#68638 = CARTESIAN_POINT ( 'NONE',  ( 5.049401038297881783, 19.05341960407617563, 52.29275706135234003 ) ) ;
#68639 = CARTESIAN_POINT ( 'NONE',  ( -27.04846034099724505, -29.46915111869712334, -5.722710424963890929 ) ) ;
#68640 = CARTESIAN_POINT ( 'NONE',  ( -13.97604488694527625, -13.89961937509977652, 91.87390960531432427 ) ) ;
#68641 = CARTESIAN_POINT ( 'NONE',  ( 8.224510206698953496, -14.34966873604960469, 57.91557627198103120 ) ) ;
#68642 = CARTESIAN_POINT ( 'NONE',  ( 19.02544592524334988, 5.153800228976608722, 46.45942372801899012 ) ) ;
#68643 = CARTESIAN_POINT ( 'NONE',  ( 0.05219959533909260263, 19.03943276465977164, 49.99890960531435979 ) ) ;
#68644 = CARTESIAN_POINT ( 'NONE',  ( -8.224510206698948167, 14.34966873604960824, 45.41557627198103830 ) ) ;
#68645 = CARTESIAN_POINT ( 'NONE',  ( 9.564922557961047289, -16.46253265017146816, 80.41775706135234714 ) ) ;
#68646 = CARTESIAN_POINT ( 'NONE',  ( -19.01533133064924996, 5.499999999999451106, 83.76586590595742621 ) ) ;
#68647 = CARTESIAN_POINT ( 'NONE',  ( -10.81492255796078084, -18.62759615963271287, 42.08224293864769550 ) ) ;
#68648 = CARTESIAN_POINT ( 'NONE',  ( 0.05219959533910956823, 16.53943276465976808, 104.9989096053143669 ) ) ;
#68649 = CARTESIAN_POINT ( 'NONE',  ( 2.995967610389833449E-15, -78.64189009824762877, -14.99999966871768642 ) ) ;
#68651 = CARTESIAN_POINT ( 'NONE',  ( -21.52544592524343514, 5.823673210054127303, 51.04057627198103120 ) ) ;
#68650 = CARTESIAN_POINT ( 'NONE',  ( 13.97604488694527802, 13.89961937509977652, 54.37390960531435979 ) ) ;
#68652 = CARTESIAN_POINT ( 'NONE',  ( -9.474510206698964154, 16.51473224551069663, 30.41557627198102054 ) ) ;
#68654 = CARTESIAN_POINT ( 'NONE',  ( -13.97604488694527625, -13.89961937509977652, 61.87390960531435979 ) ) ;
#68653 = CARTESIAN_POINT ( 'NONE',  ( -8.314922557961024197, 14.29746914071037800, 77.91775706135231871 ) ) ;
#68656 = EDGE_CURVE ( 'NONE', #64642, #80486, #28222, .T. ) ;
#68655 = CARTESIAN_POINT ( 'NONE',  ( 13.89961937509957401, 13.97604488694547697, 46.87609039468565442 ) ) ;
#68657 = CARTESIAN_POINT ( 'NONE',  ( -10.81492255796105439, 18.62759615963255655, 67.91775706135234714 ) ) ;
#68658 = CARTESIAN_POINT ( 'NONE',  ( 15.72974639402199770, -15.80617190586745480, 48.12390960531436690 ) ) ;
#68659 = CARTESIAN_POINT ( 'NONE',  ( 19.03943276465977164, -0.05219959533909143690, 28.74890960531435624 ) ) ;
#68660 = CARTESIAN_POINT ( 'NONE',  ( 19.03943276465977164, 0.05219959533936151252, 106.2510903946856615 ) ) ;
#68661 = CARTESIAN_POINT ( 'NONE',  ( -0.05219959533909027116, -19.03943276465977164, 22.49890960531436690 ) ) ;
#68663 = CARTESIAN_POINT ( 'NONE',  ( 21.53943276465977519, -0.05219959533907433946, 53.74890960531437401 ) ) ;
#68662 = CARTESIAN_POINT ( 'NONE',  ( -1.245073757422965999, -21.94104750614015487, -58.42286556281734988 ) ) ;
#68664 = CARTESIAN_POINT ( 'NONE',  ( 5.049401038298161559, -19.05341960407611168, 22.70724293864769194 ) ) ;
#68665 = CARTESIAN_POINT ( 'NONE',  ( -21.55341960407619339, 5.719274019375674811, 78.54275706135236135 ) ) ;
#68666 = CARTESIAN_POINT ( 'NONE',  ( 16.55341960407611168, 4.379528057220329451, 48.95724293864770971 ) ) ;
#68667 = CARTESIAN_POINT ( 'NONE',  ( 12.06949235617757843, -12.14591786802309237, 58.12390960531435979 ) ) ;
#68668 = CARTESIAN_POINT ( 'NONE',  ( -5.823673210054116645, -21.52544592524344225, 77.29057627198102409 ) ) ;
#68669 = APPLICATION_CONTEXT ( 'automotive_design' ) ;
#68670 = CARTESIAN_POINT ( 'NONE',  ( 5.719274019375991003, -21.55341960407610458, 72.70724293864769550 ) ) ;
#68671 = CARTESIAN_POINT ( 'NONE',  ( -0.1353689087803485180, -28.90000000000005187, -49.67367017693150899 ) ) ;
#68672 = CARTESIAN_POINT ( 'NONE',  ( 18.67979575497178502, 10.72451020669898547, 29.16557627198103120 ) ) ;
#68673 = CARTESIAN_POINT ( 'NONE',  ( -12.14591786802326823, 12.06949235617739902, 48.12609039468568284 ) ) ;
#68674 = CARTESIAN_POINT ( 'NONE',  ( 16.55341960407611168, 4.379528057220329451, 83.95724293864770971 ) ) ;
#68675 = CARTESIAN_POINT ( 'NONE',  ( -13.97604488694527625, -13.89961937509977652, 26.87390960531434558 ) ) ;
#68676 = CARTESIAN_POINT ( 'NONE',  ( 18.09918380851992481, 5.500000000000035527, 48.98618307335610922 ) ) ;
#68677 = ORIENTED_EDGE ( 'NONE', *, *, #28409, .T. ) ;
#68678 = CARTESIAN_POINT ( 'NONE',  ( -8.224510206698735004, -14.34966873604973081, 84.58442372801903275 ) ) ;
#68679 = CARTESIAN_POINT ( 'NONE',  ( 5.823673210054444382, -21.52544592524334988, 25.20942372801901854 ) ) ;
#68680 = CARTESIAN_POINT ( 'NONE',  ( -5.049401038298153566, 19.05341960407611168, 85.20724293864766707 ) ) ;
#68681 = CARTESIAN_POINT ( 'NONE',  ( 18.62759615963255655, 10.81492255796105972, 51.66775706135234714 ) ) ;
#68682 = CARTESIAN_POINT ( 'NONE',  ( -16.51473224551069308, -9.474510206698971260, 111.6655762719810383 ) ) ;
#68683 = CARTESIAN_POINT ( 'NONE',  ( -14.09403216839727158, -37.74807521950489075, -24.22002746647715554 ) ) ;
#68684 = ORIENTED_EDGE ( 'NONE', *, *, #43478, .F. ) ;
#68685 = CARTESIAN_POINT ( 'NONE',  ( -5.719274019375665041, -21.55341960407619695, 39.79275706135235424 ) ) ;
#68687 = CARTESIAN_POINT ( 'NONE',  ( 0.05219959533909260263, 19.03943276465977164, 104.9989096053143669 ) ) ;
#68686 = CARTESIAN_POINT ( 'NONE',  ( 13.97604488694527802, 13.89961937509977652, 34.37390960531436690 ) ) ;
#68688 = CARTESIAN_POINT ( 'NONE',  ( -0.05219959533936034679, 19.03943276465977164, 52.50109039468566863 ) ) ;
#68689 = CARTESIAN_POINT ( 'NONE',  ( -10.72451020669870658, -18.67979575497194134, 29.58442372801901854 ) ) ;
#68690 = CARTESIAN_POINT ( 'NONE',  ( -16.46253265017146816, -9.564922557961047289, 44.16775706135232582 ) ) ;
#68691 = CARTESIAN_POINT ( 'NONE',  ( -5.049401038298153566, 19.05341960407611168, 25.20724293864768484 ) ) ;
#68692 = CARTESIAN_POINT ( 'NONE',  ( -8.224510206698735004, -14.34966873604973081, 89.58442372801901854 ) ) ;
#68693 = CARTESIAN_POINT ( 'NONE',  ( -0.05219959533936034679, 19.03943276465977164, 67.50109039468566152 ) ) ;
#68694 = CARTESIAN_POINT ( 'NONE',  ( -16.55341960407617563, 4.379528057220093196, 108.5427570613523756 ) ) ;
#68695 = CARTESIAN_POINT ( 'NONE',  ( 9.244353370540800086, 10.58303160951403221, -62.45107349144919340 ) ) ;
#68696 = CARTESIAN_POINT ( 'NONE',  ( -0.05219959533909027116, -19.03943276465977164, 87.49890960531436690 ) ) ;
#68697 = CARTESIAN_POINT ( 'NONE',  ( -0.05219959533937732626, 21.53943276465977519, 97.50109039468567573 ) ) ;
#68698 = CARTESIAN_POINT ( 'NONE',  ( -10.81492255796105439, 18.62759615963255655, 107.9177570613523471 ) ) ;
#68699 = CARTESIAN_POINT ( 'NONE',  ( -12.73749492396214578, -155.7167183371837496, -15.00000000000000000 ) ) ;
#68700 = CARTESIAN_POINT ( 'NONE',  ( -19.05341960407611168, -5.049401038298163336, 106.4572429386476955 ) ) ;
#68701 = CARTESIAN_POINT ( 'NONE',  ( -21.52544592524334988, -5.823673210054445271, 68.95942372801901854 ) ) ;
#68702 = CARTESIAN_POINT ( 'NONE',  ( 16.53943276465976808, 0.05219959533934440121, 21.25109039468567218 ) ) ;
#68703 = CARTESIAN_POINT ( 'NONE',  ( 19.05341960407611168, 5.049401038298154454, 83.95724293864766707 ) ) ;
#68704 = CARTESIAN_POINT ( 'NONE',  ( 10.81492255796078972, 18.62759615963270932, 29.58224293864769905 ) ) ;
#68705 = CARTESIAN_POINT ( 'NONE',  ( 13.97604488694527802, 13.89961937509977652, 94.37390960531436690 ) ) ;
#68706 = CARTESIAN_POINT ( 'NONE',  ( -16.52216118717209170, -7.221426719304498754, 91.07599021046998189 ) ) ;
#68707 = CARTESIAN_POINT ( 'NONE',  ( -9.564922557960796823, -16.46253265017161027, 72.08224293864770971 ) ) ;
#68708 = CARTESIAN_POINT ( 'NONE',  ( -13.89961937509977652, 13.97604488694528158, 70.62390960531432427 ) ) ;
#68709 = CARTESIAN_POINT ( 'NONE',  ( 16.55341960407618274, -4.379528057220086978, 106.0427570613523471 ) ) ;
#68710 = CARTESIAN_POINT ( 'NONE',  ( 69.65682714487590488, -71.74905178543389184, -15.00000000000000178 ) ) ;
#68711 = CARTESIAN_POINT ( 'NONE',  ( -5.049401038297874678, -19.05341960407617918, 69.79275706135233293 ) ) ;
#68712 = CARTESIAN_POINT ( 'NONE',  ( 19.05341960407611168, 5.049401038298154454, 98.95724293864766707 ) ) ;
#68713 = CARTESIAN_POINT ( 'NONE',  ( -4.379528057220328563, 16.55341960407611168, 85.20724293864770971 ) ) ;
#68714 = CARTESIAN_POINT ( 'NONE',  ( -10.72451020669898014, 18.67979575497178502, 30.41557627198101699 ) ) ;
#68715 = CARTESIAN_POINT ( 'NONE',  ( 9.564922557960805705, 16.46253265017160317, 114.5822429386476955 ) ) ;
#68716 = CARTESIAN_POINT ( 'NONE',  ( -4.379528057220328563, 16.55341960407611168, 90.20724293864770971 ) ) ;
#68717 = CARTESIAN_POINT ( 'NONE',  ( -35.00000000000000000, -3.181980515339470905, 8.889087296526001936 ) ) ;
#68718 = CARTESIAN_POINT ( 'NONE',  ( 16.46253265017146816, 9.564922557961045513, 41.66775706135234003 ) ) ;
#68719 = CARTESIAN_POINT ( 'NONE',  ( -4.483927247898539470, -16.52544592524342804, 27.29057627198103120 ) ) ;
#68720 = CARTESIAN_POINT ( 'NONE',  ( -0.05219959533909027116, -19.03943276465977164, 102.4989096053143669 ) ) ;
#68721 = CARTESIAN_POINT ( 'NONE',  ( 0.05219959533937995610, -21.53943276465977519, 60.00109039468568284 ) ) ;
#68722 = CARTESIAN_POINT ( 'NONE',  ( 21.53943276465977519, -0.05219959533907433946, 53.74890960531437401 ) ) ;
#68723 = CARTESIAN_POINT ( 'NONE',  ( 5.719274019375673035, 21.55341960407619339, 32.29275706135235424 ) ) ;
#68724 = CARTESIAN_POINT ( 'NONE',  ( -15.80617190586745835, -15.72974639402198527, 76.87390960531439532 ) ) ;
#68725 = CARTESIAN_POINT ( 'NONE',  ( 10.81492255796106328, -18.62759615963255655, 35.41775706135234003 ) ) ;
#68726 = CARTESIAN_POINT ( 'NONE',  ( 12.14591786802309770, 12.06949235617756955, 104.3739096053143669 ) ) ;
#68727 = CARTESIAN_POINT ( 'NONE',  ( -16.46253265017146816, -9.564922557961047289, 69.16775706135233293 ) ) ;
#68728 = CARTESIAN_POINT ( 'NONE',  ( 9.474510206698971260, -16.51473224551069308, 47.91557627198102409 ) ) ;
#68730 = CARTESIAN_POINT ( 'NONE',  ( -9.564922557960796823, -16.46253265017161027, 92.08224293864769550 ) ) ;
#68729 = CARTESIAN_POINT ( 'NONE',  ( 16.52544592524342804, -4.483927247898539470, 93.54057627198103830 ) ) ;
#68731 = CARTESIAN_POINT ( 'NONE',  ( -13.89961937509977652, 13.97604488694528158, 95.62390960531436690 ) ) ;
#68732 = CARTESIAN_POINT ( 'NONE',  ( 12.06949235617757843, -12.14591786802309237, 113.1239096053143953 ) ) ;
#68733 = CARTESIAN_POINT ( 'NONE',  ( 16.55341960407611168, 4.379528057220329451, 43.95724293864769550 ) ) ;
#68734 = CARTESIAN_POINT ( 'NONE',  ( -0.05219959533934338120, 16.53943276465976808, 97.50109039468567573 ) ) ;
#68735 = CARTESIAN_POINT ( 'NONE',  ( 16.51473224551069308, 9.474510206698969483, 54.16557627198103120 ) ) ;
#68736 = CARTESIAN_POINT ( 'NONE',  ( -16.51473224551069308, -9.474510206698971260, 21.66557627198102765 ) ) ;
#68737 = CARTESIAN_POINT ( 'NONE',  ( 16.46253265017146816, 9.564922557961045513, 21.66775706135233648 ) ) ;
#68739 = CARTESIAN_POINT ( 'NONE',  ( 14.34966873604960469, 8.224510206698951720, 24.16557627198103120 ) ) ;
#68738 = CARTESIAN_POINT ( 'NONE',  ( -3.573655867282028392E-15, 2.428612866367529932E-14, -8.000000000000000000 ) ) ;
#68740 = CARTESIAN_POINT ( 'NONE',  ( -5.823673210054431948, 21.52544592524334988, 47.70942372801902565 ) ) ;
#68741 = CARTESIAN_POINT ( 'NONE',  ( 19.02544592524343514, -5.153800228976328945, 108.5405762719810383 ) ) ;
#68742 = CARTESIAN_POINT ( 'NONE',  ( 8.314922557961029526, -14.29746914071037800, 45.41775706135234003 ) ) ;
#68743 = CARTESIAN_POINT ( 'NONE',  ( -0.05219959533910754901, -16.53943276465976808, 32.49890960531435979 ) ) ;
#68744 = CARTESIAN_POINT ( 'NONE',  ( 0.05219959533909260263, 19.03943276465977164, 49.99890960531435979 ) ) ;
#68745 = CARTESIAN_POINT ( 'NONE',  ( 8.314922557961029526, -14.29746914071037800, 90.41775706135236135 ) ) ;
#68746 = CARTESIAN_POINT ( 'NONE',  ( 16.52544592524335698, 4.483927247898782831, 26.45942372801901854 ) ) ;
#68747 = CARTESIAN_POINT ( 'NONE',  ( -16.51473224551069308, -9.474510206698971260, 41.66557627198103120 ) ) ;
#68748 = AXIS2_PLACEMENT_3D ( 'NONE', #156783, #126428, #18276 ) ;
#68749 = CARTESIAN_POINT ( 'NONE',  ( -4.483927247898539470, -16.52544592524342804, 102.2905762719810383 ) ) ;
#68750 = CARTESIAN_POINT ( 'NONE',  ( -18.62759615963255300, -10.81492255796106328, 19.16775706135234714 ) ) ;
#68751 = CARTESIAN_POINT ( 'NONE',  ( 5.153800228976335163, 19.02544592524342804, 44.79057627198103830 ) ) ;
#68752 = CARTESIAN_POINT ( 'NONE',  ( 13.89961937509977652, -13.97604488694527269, 103.1239096053143527 ) ) ;
#68753 = CARTESIAN_POINT ( 'NONE',  ( 5.153800228976335163, 19.02544592524342804, 29.79057627198102409 ) ) ;
#68754 = CARTESIAN_POINT ( 'NONE',  ( -9.564922557960796823, -16.46253265017161027, 107.0822429386476955 ) ) ;
#68755 = CARTESIAN_POINT ( 'NONE',  ( -17.49999999999999645, -5.500000000000000888, 104.2030961746582847 ) ) ;
#68756 = CARTESIAN_POINT ( 'NONE',  ( -13.97604488694527625, -13.89961937509977652, 101.8739096053143811 ) ) ;
#68758 = CARTESIAN_POINT ( 'NONE',  ( 12.06949235617757843, -12.14591786802309237, 103.1239096053143811 ) ) ;
#68757 = CARTESIAN_POINT ( 'NONE',  ( -15.72974639402176322, -15.80617190586768395, 39.37609039468567573 ) ) ;
#68759 = CARTESIAN_POINT ( 'NONE',  ( 5.153800228976335163, 19.02544592524342804, 104.7905762719809957 ) ) ;
#68760 = CARTESIAN_POINT ( 'NONE',  ( -27.88129983271673851, -6.733757357603135318, 162.1517353552107750 ) ) ;
#68761 = CARTESIAN_POINT ( 'NONE',  ( 8.224510206698742110, 14.34966873604972548, 67.08442372801901854 ) ) ;
#68762 = CARTESIAN_POINT ( 'NONE',  ( -10.81492255796105439, 18.62759615963255655, 87.91775706135234714 ) ) ;
#68763 = CARTESIAN_POINT ( 'NONE',  ( -12.14591786802326823, 12.06949235617739902, 38.12609039468567573 ) ) ;
#68764 = CARTESIAN_POINT ( 'NONE',  ( -19.05341960407611168, -5.049401038298163336, 76.45724293864769550 ) ) ;
#68765 = CARTESIAN_POINT ( 'NONE',  ( -0.05219959533934338120, 16.53943276465976808, 37.50109039468568284 ) ) ;
#68766 = CARTESIAN_POINT ( 'NONE',  ( 5.049401038297881783, 19.05341960407617563, 102.2927570613523045 ) ) ;
#68767 = CARTESIAN_POINT ( 'NONE',  ( -0.05219959533934338120, 16.53943276465976808, 82.50109039468568994 ) ) ;
#68768 = CARTESIAN_POINT ( 'NONE',  ( -19.02544592524334988, -5.153800228976617603, 93.95942372801900433 ) ) ;
#68769 = CARTESIAN_POINT ( 'NONE',  ( -13.89961937509977652, 13.97604488694528158, 75.62390960531438111 ) ) ;
#68770 = CARTESIAN_POINT ( 'NONE',  ( -10.72451020669898014, 18.67979575497178502, 100.4155762719810241 ) ) ;
#68772 = CARTESIAN_POINT ( 'NONE',  ( 19.03943276465977164, 0.05219959533936151252, 91.25109039468566152 ) ) ;
#68771 = CARTESIAN_POINT ( 'NONE',  ( -4.379528057220328563, 16.55341960407611168, 95.20724293864769550 ) ) ;
#68773 = CARTESIAN_POINT ( 'NONE',  ( -14.29746914071037622, -8.314922557961029526, 74.16775706135231871 ) ) ;
#68774 = CARTESIAN_POINT ( 'NONE',  ( -16.20579543436696568, 7.371946100355094345, 44.43479165828048849 ) ) ;
#68776 = EDGE_CURVE ( 'NONE', #114881, #24708, #8850, .T. ) ;
#68775 = CARTESIAN_POINT ( 'NONE',  ( -16.46253265017146816, -9.564922557961047289, 74.16775706135234714 ) ) ;
#68777 = CARTESIAN_POINT ( 'NONE',  ( 14.29746914071049879, -8.314922557960816363, 33.33224293864769550 ) ) ;
#68778 = CARTESIAN_POINT ( 'NONE',  ( 4.483927247898545687, 16.52544592524342804, 99.79057627198103830 ) ) ;
#68780 = CARTESIAN_POINT ( 'NONE',  ( 5.153800228976617603, -19.02544592524335343, 45.20942372801900433 ) ) ;
#68779 = CARTESIAN_POINT ( 'NONE',  ( -16.51473224551082808, 9.474510206698731452, 33.33442372801899722 ) ) ;
#68781 = CARTESIAN_POINT ( 'NONE',  ( -15.72974639402197994, 15.80617190586746368, 115.6239096053143669 ) ) ;
#68782 = CARTESIAN_POINT ( 'NONE',  ( 15.50000000000000178, -5.500000000000000888, 22.00000000000000000 ) ) ;
#68783 = CARTESIAN_POINT ( 'NONE',  ( 13.89961937509977652, -13.97604488694527269, 93.12390960531436690 ) ) ;
#68784 = CARTESIAN_POINT ( 'NONE',  ( -10.81492255796105439, 18.62759615963255655, 102.9177570613523756 ) ) ;
#68785 = CARTESIAN_POINT ( 'NONE',  ( -19.03943276465977164, 0.05219959533909376836, 71.24890960531435269 ) ) ;
#68786 = CARTESIAN_POINT ( 'NONE',  ( -5.823673210054116645, -21.52544592524344225, 47.29057627198103120 ) ) ;
#68787 = CARTESIAN_POINT ( 'NONE',  ( 4.483927247898545687, 16.52544592524342804, 94.79057627198105251 ) ) ;
#68788 = CARTESIAN_POINT ( 'NONE',  ( -9.474510206698964154, 16.51473224551069663, 60.41557627198102409 ) ) ;
#68789 = EDGE_CURVE ( 'NONE', #1415, #84042, #150452, .T. ) ;
#68790 = CARTESIAN_POINT ( 'NONE',  ( 16.55341960407611168, 4.379528057220329451, 108.9572429386476955 ) ) ;
#68791 = CARTESIAN_POINT ( 'NONE',  ( -18.62759615963255300, -10.81492255796106328, 29.16775706135234003 ) ) ;
#68792 = CARTESIAN_POINT ( 'NONE',  ( -15.80617190586768217, 15.72974639402176855, 68.12609039468567573 ) ) ;
#68793 = CARTESIAN_POINT ( 'NONE',  ( 19.03943276465977164, -0.05219959533909143690, 48.74890960531435979 ) ) ;
#68794 = CARTESIAN_POINT ( 'NONE',  ( -14.34966873604972548, 8.224510206698743886, 83.33442372801903275 ) ) ;
#68795 = CARTESIAN_POINT ( 'NONE',  ( 21.55341960407610458, 5.719274019375980345, 113.9572429386477239 ) ) ;
#68796 = VERTEX_POINT ( 'NONE', #149440 ) ;
#68797 = CARTESIAN_POINT ( 'NONE',  ( -5.823673210054116645, -21.52544592524344225, 107.2905762719810525 ) ) ;
#68799 = CARTESIAN_POINT ( 'NONE',  ( -9.474510206698964154, 16.51473224551069663, 60.41557627198102409 ) ) ;
#68798 = CARTESIAN_POINT ( 'NONE',  ( -19.05341960407617563, 5.049401038297882671, 53.54275706135231871 ) ) ;
#68800 = CARTESIAN_POINT ( 'NONE',  ( 5.153800228976615827, -19.02544592524334988, 35.20942372801899722 ) ) ;
#68801 = CARTESIAN_POINT ( 'NONE',  ( 10.81492255796106328, -18.62759615963255655, 70.41775706135236135 ) ) ;
#68802 = CARTESIAN_POINT ( 'NONE',  ( 21.52544592524344225, -5.823673210054117533, 68.54057627198103830 ) ) ;
#68803 = CARTESIAN_POINT ( 'NONE',  ( 14.34966873604960469, 8.224510206698951720, 54.16557627198103120 ) ) ;
#68805 = CARTESIAN_POINT ( 'NONE',  ( 13.97604488694548053, -13.89961937509957401, 30.62609039468566863 ) ) ;
#68804 = CARTESIAN_POINT ( 'NONE',  ( -5.719274019375665041, -21.55341960407619695, 89.79275706135236135 ) ) ;
#68806 = CARTESIAN_POINT ( 'NONE',  ( -4.379528057220328563, 16.55341960407611168, 65.20724293864768129 ) ) ;
#68807 = CARTESIAN_POINT ( 'NONE',  ( 12.06949235617757843, -12.14591786802309237, 108.1239096053143811 ) ) ;
#68808 = CARTESIAN_POINT ( 'NONE',  ( 19.02544592524334988, 5.153800228976608722, 51.45942372801900433 ) ) ;
#68809 = CARTESIAN_POINT ( 'NONE',  ( 8.314922557960818139, 14.29746914071049879, 24.58224293864768839 ) ) ;
#68810 = CARTESIAN_POINT ( 'NONE',  ( -21.53943276465977519, -0.05219959533937600094, 73.75109039468567573 ) ) ;
#68811 = B_SPLINE_CURVE_WITH_KNOTS ( 'NONE', 3,
 ( #125612, #139770, #17443, #170126, #109442, #184314, #93271, #92279, #107447, #49769, #3257, #157941, #95266, #153963, #4238, #45795, #62935, #124615, #173121, #77117 ),
 .UNSPECIFIED., .F., .F.,
 ( 4, 2, 2, 2, 2, 2, 2, 2, 2, 4 ),
 ( 0.004000878361811927020, 0.004499404418915936912, 0.004997930476019946805, 0.005496456533123957565, 0.005994982590227967457, 0.006244245618779961995, 0.006493508647331957401, 0.006992034704435969895, 0.007490560761539982390, 0.007989086818643994017 ),
 .UNSPECIFIED. ) ;
#68812 = CARTESIAN_POINT ( 'NONE',  ( -16.51473224551069308, -9.474510206698971260, 71.66557627198102409 ) ) ;
#68813 = CARTESIAN_POINT ( 'NONE',  ( 13.97604488694548053, -13.89961937509957401, 45.62609039468566863 ) ) ;
#68814 = CARTESIAN_POINT ( 'NONE',  ( -0.05219959533907301413, -21.53943276465977519, 52.49890960531435979 ) ) ;
#68815 = CARTESIAN_POINT ( 'NONE',  ( -15.72974639402176322, -15.80617190586768395, 44.37609039468567573 ) ) ;
#68816 = CARTESIAN_POINT ( 'NONE',  ( -0.05219959533907301413, -21.53943276465977519, 107.4989096053143669 ) ) ;
#68817 = CARTESIAN_POINT ( 'NONE',  ( -9.474510206698720793, -16.51473224551083518, 104.5844237280190043 ) ) ;
#68818 = CARTESIAN_POINT ( 'NONE',  ( 12.06949235617739724, 12.14591786802326823, 71.87609039468568994 ) ) ;
#68820 = CARTESIAN_POINT ( 'NONE',  ( -5.719274019375978568, 21.55341960407610458, 105.2072429386477097 ) ) ;
#68819 = CARTESIAN_POINT ( 'NONE',  ( -23.48298174826589602, -32.32155151706772500, -5.702157773949823039 ) ) ;
#68821 = CARTESIAN_POINT ( 'NONE',  ( -16.52544592524342804, 4.483927247898546575, 96.04057627198102409 ) ) ;
#68822 = CARTESIAN_POINT ( 'NONE',  ( -17.49999999999998579, -3.805241302050414998, 29.62647527217406562 ) ) ;
#68823 = CARTESIAN_POINT ( 'NONE',  ( 16.53943276465976808, 0.05219959533934440121, 26.25109039468567573 ) ) ;
#68824 = CARTESIAN_POINT ( 'NONE',  ( -21.53943276465977519, 0.05219959533907696930, 46.24890960531435979 ) ) ;
#68825 = CARTESIAN_POINT ( 'NONE',  ( 0.05219959533934541429, -16.53943276465976808, 85.00109039468568994 ) ) ;
#68826 = CARTESIAN_POINT ( 'NONE',  ( 36.85948423281453046, 2.394443620734153289, -8.000000000000001776 ) ) ;
#68827 = B_SPLINE_CURVE_WITH_KNOTS ( 'NONE', 3,
 ( #82712, #147409, #8896, #70564, #193924, #37222, #40216, #148405, #56391, #10897, #89720, #117057, #71560, #57406, #25077, #58388, #28080, #88722, #178752, #120055 ),
 .UNSPECIFIED., .F., .F.,
 ( 4, 2, 2, 2, 2, 2, 2, 2, 2, 4 ),
 ( 2.784207231363245562E-07, 0.0003311547508960723256, 0.0006620310810690082683, 0.0009929074112419442651, 0.001323783741414880262, 0.002647289062106632923, 0.003309041722452508820, 0.003970794382798385584, 0.004632547043144262348, 0.005294299703490139113 ),
 .UNSPECIFIED. ) ;
#68828 = CARTESIAN_POINT ( 'NONE',  ( 4.379528057220092307, 16.55341960407617563, 62.29275706135236845 ) ) ;
#68829 = CARTESIAN_POINT ( 'NONE',  ( 0.05219959533937995610, -21.53943276465977519, 35.00109039468568284 ) ) ;
#68830 = CARTESIAN_POINT ( 'NONE',  ( -21.52544592524343514, 5.823673210054127303, 61.04057627198103120 ) ) ;
#68831 = CARTESIAN_POINT ( 'NONE',  ( -14.29746914071037622, -8.314922557961029526, 84.16775706135234714 ) ) ;
#68832 = CARTESIAN_POINT ( 'NONE',  ( -0.05219959533909027116, -19.03943276465977164, 102.4989096053143669 ) ) ;
#68833 = CARTESIAN_POINT ( 'NONE',  ( 10.81492255796106328, -18.62759615963255655, 70.41775706135236135 ) ) ;
#68834 = CARTESIAN_POINT ( 'NONE',  ( -15.72974639402197994, 15.80617190586746368, 45.62390960531436690 ) ) ;
#68835 = CARTESIAN_POINT ( 'NONE',  ( -21.52544592524343514, 5.823673210054127303, 31.04057627198102409 ) ) ;
#68836 = ORIENTED_EDGE ( 'NONE', *, *, #104283, .T. ) ;
#68837 = CARTESIAN_POINT ( 'NONE',  ( -16.51473224551082808, 9.474510206698731452, 58.33442372801900433 ) ) ;
#68838 = CARTESIAN_POINT ( 'NONE',  ( -14.34966873604972548, 8.224510206698743886, 68.33442372801900433 ) ) ;
#68839 = CARTESIAN_POINT ( 'NONE',  ( -0.05219959533907301413, -21.53943276465977519, 37.49890960531436690 ) ) ;
#68840 = ORIENTED_EDGE ( 'NONE', *, *, #110986, .T. ) ;
#68841 = CARTESIAN_POINT ( 'NONE',  ( -16.46253265017160317, 9.564922557960807481, 85.83224293864769550 ) ) ;
#68842 = CARTESIAN_POINT ( 'NONE',  ( -16.52544592524342804, 4.483927247898546575, 26.04057627198103475 ) ) ;
#68843 = CARTESIAN_POINT ( 'NONE',  ( 193.3062444957835453, -155.7167183371837496, -15.00000000000000178 ) ) ;
#68844 = CARTESIAN_POINT ( 'NONE',  ( -12.06949235617756955, 12.14591786802309770, 110.6239096053143669 ) ) ;
#68845 = CARTESIAN_POINT ( 'NONE',  ( -5.719274019375978568, 21.55341960407610458, 50.20724293864769550 ) ) ;
#68846 = CARTESIAN_POINT ( 'NONE',  ( -9.474510206698964154, 16.51473224551069663, 50.41557627198102409 ) ) ;
#68847 = CARTESIAN_POINT ( 'NONE',  ( -14.29746914071037622, -8.314922557961029526, 89.16775706135236135 ) ) ;
#68848 = CARTESIAN_POINT ( 'NONE',  ( 21.52544592524334988, 5.823673210054432836, 36.45942372801901143 ) ) ;
#68849 = CARTESIAN_POINT ( 'NONE',  ( 16.51473224551083163, -9.474510206698727899, 85.83442372801900433 ) ) ;
#68850 = CARTESIAN_POINT ( 'NONE',  ( 4.379528057220339221, -16.55341960407611168, 92.70724293864770971 ) ) ;
#68851 = CARTESIAN_POINT ( 'NONE',  ( 13.89961937509977652, -13.97604488694527269, 58.12390960531436690 ) ) ;
#68852 = CARTESIAN_POINT ( 'NONE',  ( -19.05341960407611168, -5.049401038298163336, 31.45724293864769550 ) ) ;
#68853 = DIRECTION ( 'NONE',  ( 0.000000000000000000, 0.000000000000000000, -1.000000000000000000 ) ) ;
#68854 = CARTESIAN_POINT ( 'NONE',  ( -0.05219959533909027116, -19.03943276465977164, 72.49890960531435269 ) ) ;
#68855 = CARTESIAN_POINT ( 'NONE',  ( -8.314922557961024197, 14.29746914071037800, 57.91775706135234714 ) ) ;
#68856 = CARTESIAN_POINT ( 'NONE',  ( -18.67979575497193778, 10.72451020669871902, 108.3344237280190185 ) ) ;
#68857 = CARTESIAN_POINT ( 'NONE',  ( -5.719274019375978568, 21.55341960407610458, 55.20724293864770260 ) ) ;
#68858 = CARTESIAN_POINT ( 'NONE',  ( -8.224510206698735004, -14.34966873604973081, 69.58442372801900433 ) ) ;
#68859 = CARTESIAN_POINT ( 'NONE',  ( -5.049401038297874678, -19.05341960407617918, 54.79275706135234003 ) ) ;
#68860 = CARTESIAN_POINT ( 'NONE',  ( 16.46253265017146816, 9.564922557961045513, 61.66775706135234003 ) ) ;
#68861 = ORIENTED_EDGE ( 'NONE', *, *, #163318, .F. ) ;
#68862 = CARTESIAN_POINT ( 'NONE',  ( 5.719274019375673035, 21.55341960407619339, 62.29275706135236845 ) ) ;
#68863 = CARTESIAN_POINT ( 'NONE',  ( 9.564922557960805705, 16.46253265017160317, 64.58224293864769550 ) ) ;
#68864 = CARTESIAN_POINT ( 'NONE',  ( -19.02544592524342804, 5.153800228976336051, 31.04057627198102409 ) ) ;
#68865 = CARTESIAN_POINT ( 'NONE',  ( -19.02544592524334988, -5.153800228976617603, 58.95942372801900433 ) ) ;
#68866 = CARTESIAN_POINT ( 'NONE',  ( 19.05341960407611168, 5.049401038298154454, 113.9572429386477097 ) ) ;
#68867 = CARTESIAN_POINT ( 'NONE',  ( 16.46253265017160672, -9.564922557960803928, 93.33224293864769550 ) ) ;
#68868 = CARTESIAN_POINT ( 'NONE',  ( -16.53943276465976808, 0.05219959533911058130, 56.24890960531436690 ) ) ;
#68869 = CARTESIAN_POINT ( 'NONE',  ( 5.719274019375991003, -21.55341960407610458, 52.70724293864769550 ) ) ;
#68870 = CARTESIAN_POINT ( 'NONE',  ( -17.50000000000000355, 5.076555817581253294, 103.8204850795022907 ) ) ;
#68871 = CARTESIAN_POINT ( 'NONE',  ( 15.72974639402176855, 15.80617190586768217, 111.8760903946856615 ) ) ;
#68872 = CARTESIAN_POINT ( 'NONE',  ( -17.05587630539788435, -6.762274262135696823, 79.25819690962690345 ) ) ;
#68873 = CARTESIAN_POINT ( 'NONE',  ( 0.05219959533909260263, 19.03943276465977164, 49.99890960531435979 ) ) ;
#68874 = CARTESIAN_POINT ( 'NONE',  ( -33.80700117934221538, -2.275881256356159010, 100.0103016164005112 ) ) ;
#68875 = CARTESIAN_POINT ( 'NONE',  ( -4.500000000000001776, -116.8122400552013431, 54.87277500418469600 ) ) ;
#68876 = CARTESIAN_POINT ( 'NONE',  ( 4.483927247898790824, -16.52544592524335698, 70.20942372801904696 ) ) ;
#68877 = CARTESIAN_POINT ( 'NONE',  ( 18.67979575497178502, 10.72451020669898547, 94.16557627198103830 ) ) ;
#68878 = CARTESIAN_POINT ( 'NONE',  ( 4.379528057220339221, -16.55341960407611168, 47.70724293864770260 ) ) ;
#68880 = CARTESIAN_POINT ( 'NONE',  ( 23.48529157249600630, -32.32473071737748427, -5.049999994537627046 ) ) ;
#68879 = CARTESIAN_POINT ( 'NONE',  ( 13.89961937509977652, -13.97604488694527269, 48.12390960531435979 ) ) ;
#68881 = CARTESIAN_POINT ( 'NONE',  ( 0.05219959533937995610, -21.53943276465977519, 35.00109039468568284 ) ) ;
#68882 = CARTESIAN_POINT ( 'NONE',  ( 5.153800228976615827, -19.02544592524334988, 45.20942372801901143 ) ) ;
#68883 = CARTESIAN_POINT ( 'NONE',  ( -16.46253265017160317, 9.564922557960807481, 45.83224293864769550 ) ) ;
#68884 = CARTESIAN_POINT ( 'NONE',  ( -15.80617190586768217, 15.72974639402176855, 98.12609039468570415 ) ) ;
#68885 = CARTESIAN_POINT ( 'NONE',  ( 17.44270441346517941, 5.991230190323027394, 98.86335079264229364 ) ) ;
#68886 = VERTEX_POINT ( 'NONE', #10936 ) ;
#68887 = CARTESIAN_POINT ( 'NONE',  ( 4.483927247898545687, 16.52544592524342804, 44.79057627198103120 ) ) ;
#68888 = CARTESIAN_POINT ( 'NONE',  ( 19.49190055781009079, 5.500000000000045297, 43.06116087098784817 ) ) ;
#68889 = CARTESIAN_POINT ( 'NONE',  ( -5.823673210054116645, -21.52544592524344225, 47.29057627198103120 ) ) ;
#68890 = CARTESIAN_POINT ( 'NONE',  ( 27.73933785331498569, 9.013057229001093518, 143.9750000027312069 ) ) ;
#68891 = CARTESIAN_POINT ( 'NONE',  ( -16.51473224551069308, -9.474510206698971260, 101.6655762719810241 ) ) ;
#68892 = CARTESIAN_POINT ( 'NONE',  ( 0.05219959533910956823, 16.53943276465976808, 84.99890960531436690 ) ) ;
#68893 = CARTESIAN_POINT ( 'NONE',  ( 0.05219959533934541429, -16.53943276465976808, 20.00109039468568639 ) ) ;
#68894 = CARTESIAN_POINT ( 'NONE',  ( 0.05219959533934541429, -16.53943276465976808, 110.0010903946856757 ) ) ;
#68895 = ORIENTED_EDGE ( 'NONE', *, *, #174899, .F. ) ;
#68897 = CARTESIAN_POINT ( 'NONE',  ( -15.72974639402197994, 15.80617190586746368, 105.6239096053143669 ) ) ;
#68896 = CARTESIAN_POINT ( 'NONE',  ( 19.03943276465977164, -0.05219959533909143690, 93.74890960531435269 ) ) ;
#68898 = AXIS2_PLACEMENT_3D ( 'NONE', #31934, #15772, #76440 ) ;
#68900 = CARTESIAN_POINT ( 'NONE',  ( 0.05219959533909260263, 19.03943276465977164, 104.9989096053143669 ) ) ;
#68899 = CARTESIAN_POINT ( 'NONE',  ( -12.06949235617756955, 12.14591786802309770, 30.62390960531436335 ) ) ;
#68901 = CARTESIAN_POINT ( 'NONE',  ( -5.153800228976607833, 19.02544592524334988, 77.70942372801900433 ) ) ;
#68902 = CARTESIAN_POINT ( 'NONE',  ( -19.03943276465977164, -0.05219959533935918106, 18.75109039468567218 ) ) ;
#68903 = CARTESIAN_POINT ( 'NONE',  ( 21.55341960407610458, 5.719274019375980345, 88.95724293864769550 ) ) ;
#68904 = CARTESIAN_POINT ( 'NONE',  ( -18.67979575497178146, -10.72451020669898902, 56.66557627198103830 ) ) ;
#68905 = CARTESIAN_POINT ( 'NONE',  ( -13.97604488694527625, -13.89961937509977652, 66.87390960531436690 ) ) ;
#68906 = CARTESIAN_POINT ( 'NONE',  ( -12.14591786802309592, -12.06949235617757132, 31.87390960531435979 ) ) ;
#68907 = CARTESIAN_POINT ( 'NONE',  ( 5.049401038298161559, -19.05341960407611168, 72.70724293864768129 ) ) ;
#68908 = ORIENTED_EDGE ( 'NONE', *, *, #163998, .T. ) ;
#68909 = DIRECTION ( 'NONE',  ( 0.000000000000000000, 0.000000000000000000, 1.000000000000000000 ) ) ;
#68910 = CARTESIAN_POINT ( 'NONE',  ( -13.89961937509957401, -13.97604488694547875, 29.37609039468565797 ) ) ;
#68911 = CARTESIAN_POINT ( 'NONE',  ( 8.314922557960818139, 14.29746914071049879, 84.58224293864769550 ) ) ;
#68912 = CARTESIAN_POINT ( 'NONE',  ( 5.719274019375673035, 21.55341960407619339, 27.29275706135234358 ) ) ;
#68913 = CARTESIAN_POINT ( 'NONE',  ( 8.571926809382603096, -26.38167802310801235, 141.9750000027312069 ) ) ;
#68914 = CARTESIAN_POINT ( 'NONE',  ( 8.314922557961029526, -14.29746914071037800, 100.4177570613523471 ) ) ;
#68915 = CARTESIAN_POINT ( 'NONE',  ( -19.05341960407611168, -5.049401038298163336, 21.45724293864768839 ) ) ;
#68916 = CARTESIAN_POINT ( 'NONE',  ( -5.153800228976328057, -19.02544592524343514, 72.29057627198102409 ) ) ;
#68917 = SHAPE_REPRESENTATION_RELATIONSHIP ( 'NONE' , 'NONE' ,  #92179, #100331 ) ;
#68918 = CARTESIAN_POINT ( 'NONE',  ( 37.99626262588765258, 2.893932880411085066E-14, -4.747842220587804363 ) ) ;
#68919 = CARTESIAN_POINT ( 'NONE',  ( 12.14591786802309770, 12.06949235617756955, 29.37390960531435269 ) ) ;
#68920 = CARTESIAN_POINT ( 'NONE',  ( -18.62759615963255300, -10.81492255796106328, 59.16775706135234714 ) ) ;
#68921 = CARTESIAN_POINT ( 'NONE',  ( 24.48191864109216098, -29.02791343561681003, -16.65471697699033982 ) ) ;
#68922 = CARTESIAN_POINT ( 'NONE',  ( -15.80617190586768217, 15.72974639402176855, 88.12609039468570415 ) ) ;
#68923 = CARTESIAN_POINT ( 'NONE',  ( 16.46253265017160672, -9.564922557960803928, 43.33224293864769550 ) ) ;
#68924 = CARTESIAN_POINT ( 'NONE',  ( 9.564922557960805705, 16.46253265017160317, 54.58224293864769550 ) ) ;
#68925 = ORIENTED_EDGE ( 'NONE', *, *, #132407, .T. ) ;
#68926 = CARTESIAN_POINT ( 'NONE',  ( 18.67979575497194134, -10.72451020669871369, 100.8344237280190185 ) ) ;
#68927 = CARTESIAN_POINT ( 'NONE',  ( -4.483927247898782831, 16.52544592524335698, 62.70942372801902565 ) ) ;
#68928 = CARTESIAN_POINT ( 'NONE',  ( -5.823673210054431948, 21.52544592524334988, 82.70942372801900433 ) ) ;
#68929 = CARTESIAN_POINT ( 'NONE',  ( 15.72974639402199770, -15.80617190586745480, 28.12390960531435979 ) ) ;
#68930 = CARTESIAN_POINT ( 'NONE',  ( 16.51473224551083163, -9.474510206698727899, 90.83442372801900433 ) ) ;
#68931 = CARTESIAN_POINT ( 'NONE',  ( -15.72974639402176322, -15.80617190586768395, 64.37609039468568994 ) ) ;
#68932 = CARTESIAN_POINT ( 'NONE',  ( 4.483927247898790824, -16.52544592524335698, 40.20942372801901854 ) ) ;
#68933 = CARTESIAN_POINT ( 'NONE',  ( 15.72974639402199770, -15.80617190586745480, 83.12390960531436690 ) ) ;
#68934 = CARTESIAN_POINT ( 'NONE',  ( 9.474510206698729675, 16.51473224551082808, 82.08442372801899012 ) ) ;
#68935 = CARTESIAN_POINT ( 'NONE',  ( -16.46253265017160317, 9.564922557960807481, 65.83224293864769550 ) ) ;
#68936 = CARTESIAN_POINT ( 'NONE',  ( -9.474510206698720793, -16.51473224551083518, 94.58442372801900433 ) ) ;
#68937 = CARTESIAN_POINT ( 'NONE',  ( 16.51473224551083163, -9.474510206698727899, 105.8344237280190043 ) ) ;
#68938 = CARTESIAN_POINT ( 'NONE',  ( -16.52544592524342804, 4.483927247898546575, 51.04057627198103120 ) ) ;
#68939 = CARTESIAN_POINT ( 'NONE',  ( 13.97604488694548053, -13.89961937509957401, 80.62609039468567573 ) ) ;
#68940 = CARTESIAN_POINT ( 'NONE',  ( 0.05219959533934541429, -16.53943276465976808, 65.00109039468568994 ) ) ;
#68941 = CARTESIAN_POINT ( 'NONE',  ( 19.03943276465977164, -0.05219959533909143690, 38.74890960531436690 ) ) ;
#68942 = CARTESIAN_POINT ( 'NONE',  ( -19.05341960407611168, -5.049401038298163336, 56.45724293864768129 ) ) ;
#68943 = CARTESIAN_POINT ( 'NONE',  ( 16.53943276465976808, 0.05219959533934440121, 56.25109039468568284 ) ) ;
#68944 = DIRECTION ( 'NONE',  ( 0.000000000000000000, -0.7071067811865483499, -0.7071067811865465735 ) ) ;
#68945 = CARTESIAN_POINT ( 'NONE',  ( -27.73933785331498925, 9.013057229001089965, 148.7750000027311899 ) ) ;
#68946 = CARTESIAN_POINT ( 'NONE',  ( -9.564922557960796823, -16.46253265017161027, 112.0822429386476955 ) ) ;
#68947 = CARTESIAN_POINT ( 'NONE',  ( -9.564922557960796823, -16.46253265017161027, 27.08224293864769550 ) ) ;
#68948 = EDGE_LOOP ( 'NONE', ( #43973, #42107, #58434, #7114 ) ) ;
#68949 = CARTESIAN_POINT ( 'NONE',  ( -16.51473224551082808, 9.474510206698731452, 108.3344237280190043 ) ) ;
#68950 = CARTESIAN_POINT ( 'NONE',  ( -0.05219959533907301413, -21.53943276465977519, 42.49890960531435979 ) ) ;
#68952 = CARTESIAN_POINT ( 'NONE',  ( 4.483927247898790824, -16.52544592524335698, 30.20942372801902565 ) ) ;
#68951 = CARTESIAN_POINT ( 'NONE',  ( -9.564922557961040184, 16.46253265017147172, 32.91775706135233293 ) ) ;
#68953 = CARTESIAN_POINT ( 'NONE',  ( -5.049401038298153566, 19.05341960407611168, 25.20724293864768484 ) ) ;
#68954 = CARTESIAN_POINT ( 'NONE',  ( 19.03943276465977164, -0.05219959533909143690, 48.74890960531435979 ) ) ;
#68955 = CARTESIAN_POINT ( 'NONE',  ( -0.05219959533907301413, -21.53943276465977519, 77.49890960531433848 ) ) ;
#68956 = CARTESIAN_POINT ( 'NONE',  ( -16.51473224551069308, -9.474510206698971260, 96.66557627198102409 ) ) ;
#68957 = VECTOR ( 'NONE', #99707, 1000.000000000000000 ) ;
#68958 = CARTESIAN_POINT ( 'NONE',  ( 13.97604488694527802, 13.89961937509977652, 44.37390960531435269 ) ) ;
#68959 = CARTESIAN_POINT ( 'NONE',  ( 27.73933785331498569, 2.768321779492822058E-14, 144.3750000027311842 ) ) ;
#68960 = CARTESIAN_POINT ( 'NONE',  ( -9.474510206698720793, -16.51473224551083518, 79.58442372801899012 ) ) ;
#68961 = CARTESIAN_POINT ( 'NONE',  ( 14.29746914071049879, -8.314922557960816363, 68.33224293864769550 ) ) ;
#68962 = CARTESIAN_POINT ( 'NONE',  ( 10.72451020669898902, -18.67979575497178502, 52.91557627198103830 ) ) ;
#68963 = CARTESIAN_POINT ( 'NONE',  ( 21.52544592524334988, 5.823673210054432836, 111.4594237280190328 ) ) ;
#68964 = CARTESIAN_POINT ( 'NONE',  ( 21.55341960407610458, 5.719274019375980345, 98.95724293864770971 ) ) ;
#68965 = CARTESIAN_POINT ( 'NONE',  ( 10.81492255796106328, -18.62759615963255655, 70.41775706135236135 ) ) ;
#68966 = CARTESIAN_POINT ( 'NONE',  ( 0.05219959533937995610, -21.53943276465977519, 80.00109039468568994 ) ) ;
#68967 = CARTESIAN_POINT ( 'NONE',  ( 19.05341960407611168, 5.049401038298154454, 113.9572429386477097 ) ) ;
#68969 = CARTESIAN_POINT ( 'NONE',  ( 10.72451020669871369, 18.67979575497193778, 72.08442372801899012 ) ) ;
#68968 = CARTESIAN_POINT ( 'NONE',  ( 16.53943276465976808, 0.05219959533934440121, 106.2510903946856757 ) ) ;
#68970 = CARTESIAN_POINT ( 'NONE',  ( -13.97604488694527625, -13.89961937509977652, 66.87390960531436690 ) ) ;
#68971 = CARTESIAN_POINT ( 'NONE',  ( 0.05219959533937995610, -21.53943276465977519, 30.00109039468568284 ) ) ;
#68972 = CARTESIAN_POINT ( 'NONE',  ( -16.46253265017160317, 9.564922557960807481, 65.83224293864769550 ) ) ;
#68973 = CARTESIAN_POINT ( 'NONE',  ( 8.314922557960818139, 14.29746914071049879, 74.58224293864768129 ) ) ;
#68974 = CARTESIAN_POINT ( 'NONE',  ( 14.34966873604960469, 8.224510206698951720, 54.16557627198103120 ) ) ;
#68975 = CARTESIAN_POINT ( 'NONE',  ( 21.53943276465977519, -0.05219959533907433946, 53.74890960531437401 ) ) ;
#68976 = CARTESIAN_POINT ( 'NONE',  ( 5.049401038298161559, -19.05341960407611168, 67.70724293864769550 ) ) ;
#68977 = CARTESIAN_POINT ( 'NONE',  ( -10.72451020669898014, 18.67979575497178502, 75.41557627198102409 ) ) ;
#68978 = CARTESIAN_POINT ( 'NONE',  ( 19.03943276465977164, 0.05219959533936151252, 61.25109039468566863 ) ) ;
#68980 = CARTESIAN_POINT ( 'NONE',  ( -12.14591786802309592, -12.06949235617757132, 66.87390960531436690 ) ) ;
#68979 = CARTESIAN_POINT ( 'NONE',  ( -5.153800228976607833, 19.02544592524335343, 22.70942372801899367 ) ) ;
#68981 = CARTESIAN_POINT ( 'NONE',  ( -0.05219959533907301413, -21.53943276465977519, 37.49890960531436690 ) ) ;
#68982 = ORIENTED_EDGE ( 'NONE', *, *, #9460, .F. ) ;
#68983 = EDGE_CURVE ( 'NONE', #149173, #122541, #104927, .T. ) ;
#68984 = CARTESIAN_POINT ( 'NONE',  ( -17.72662750342724891, -5.500000000000089706, 41.40179492283743912 ) ) ;
#68986 = CARTESIAN_POINT ( 'NONE',  ( 27.73933785331498569, 9.013057229001093518, 140.4750000027312069 ) ) ;
#68985 = CARTESIAN_POINT ( 'NONE',  ( 8.224510206698742110, 14.34966873604972548, 97.08442372801904696 ) ) ;
#68987 = CARTESIAN_POINT ( 'NONE',  ( -16.46253265017146816, -9.564922557961047289, 94.16775706135233293 ) ) ;
#68988 = CARTESIAN_POINT ( 'NONE',  ( 4.379528057220339221, -16.55341960407611168, 72.70724293864769550 ) ) ;
#68989 = DIRECTION ( 'NONE',  ( -1.000000000000000000, 1.065814103640150121E-14, 0.000000000000000000 ) ) ;
#68990 = CARTESIAN_POINT ( 'NONE',  ( -9.564922557960796823, -16.46253265017161027, 57.08224293864769550 ) ) ;
#68991 = CARTESIAN_POINT ( 'NONE',  ( 12.06949235617757843, -12.14591786802309237, 58.12390960531435979 ) ) ;
#68992 = CARTESIAN_POINT ( 'NONE',  ( 19.02544592524343514, -5.153800228976328945, 83.54057627198100988 ) ) ;
#68994 = CARTESIAN_POINT ( 'NONE',  ( -19.02544592524342804, 5.153800228976336051, 51.04057627198103120 ) ) ;
#68993 = CARTESIAN_POINT ( 'NONE',  ( -19.03943276465977164, -0.05219959533935918106, 78.75109039468567573 ) ) ;
#68995 = CARTESIAN_POINT ( 'NONE',  ( -13.89961937509977652, 13.97604488694528158, 80.62390960531436690 ) ) ;
#68996 = CARTESIAN_POINT ( 'NONE',  ( 9.564922557960805705, 16.46253265017160317, 69.58224293864770971 ) ) ;
#68997 = CARTESIAN_POINT ( 'NONE',  ( -21.55341960407610458, -5.719274019375992779, 61.45724293864770260 ) ) ;
#68998 = CARTESIAN_POINT ( 'NONE',  ( 13.97604488694527802, 13.89961937509977652, 49.37390960531434558 ) ) ;
#68999 = CARTESIAN_POINT ( 'NONE',  ( -18.67979575497178146, -10.72451020669898902, 51.66557627198102409 ) ) ;
#69000 = CARTESIAN_POINT ( 'NONE',  ( 5.049401038297881783, 19.05341960407617563, 77.29275706135231871 ) ) ;
#69001 = CARTESIAN_POINT ( 'NONE',  ( -8.314922557961024197, 14.29746914071037800, 97.91775706135236135 ) ) ;
#69002 = CARTESIAN_POINT ( 'NONE',  ( 5.049401038297881783, 19.05341960407617563, 32.29275706135233293 ) ) ;
#69004 = CARTESIAN_POINT ( 'NONE',  ( -14.29746914071037622, -8.314922557961029526, 94.16775706135237556 ) ) ;
#69003 = CARTESIAN_POINT ( 'NONE',  ( 14.34966873604972726, -8.224510206698740333, 65.83442372801900433 ) ) ;
#69005 = CARTESIAN_POINT ( 'NONE',  ( -28.79475375365586842, 9.355982642739222754, 148.1656553485623533 ) ) ;
#69006 = CARTESIAN_POINT ( 'NONE',  ( 4.379528057220092307, 16.55341960407617563, 77.29275706135234714 ) ) ;
#69007 = CARTESIAN_POINT ( 'NONE',  ( 15.80617190586746368, 15.72974639402197994, 29.37390960531435269 ) ) ;
#69008 = CARTESIAN_POINT ( 'NONE',  ( -19.03943276465977164, 0.05219959533909376836, 36.24890960531436690 ) ) ;
#69009 = CARTESIAN_POINT ( 'NONE',  ( 14.34966873604972726, -8.224510206698740333, 35.83442372801901143 ) ) ;
#69010 = CARTESIAN_POINT ( 'NONE',  ( 5.153800228976335163, 19.02544592524342804, 44.79057627198103830 ) ) ;
#69011 = CARTESIAN_POINT ( 'NONE',  ( 21.55341960407619695, -5.719274019375665929, 46.04275706135234714 ) ) ;
#69012 = CARTESIAN_POINT ( 'NONE',  ( -4.379528057220086978, -16.55341960407618274, 44.79275706135234714 ) ) ;
#69013 = CARTESIAN_POINT ( 'NONE',  ( -16.53943276465976808, 0.05219959533911058130, 21.24890960531436690 ) ) ;
#69014 = CARTESIAN_POINT ( 'NONE',  ( -13.89961937509977652, 13.97604488694528158, 30.62390960531435269 ) ) ;
#69015 = CARTESIAN_POINT ( 'NONE',  ( 0.05219959533936267826, -19.03943276465977164, 25.00109039468566152 ) ) ;
#69017 = EDGE_CURVE ( 'NONE', #59237, #57160, #69403, .T. ) ;
#69016 = CARTESIAN_POINT ( 'NONE',  ( -5.153800228976607833, 19.02544592524334988, 107.7094237280189759 ) ) ;
#69018 = CARTESIAN_POINT ( 'NONE',  ( -13.97604488694547697, 13.89961937509957934, 68.12609039468563310 ) ) ;
#69019 = CARTESIAN_POINT ( 'NONE',  ( 8.224510206698953496, -14.34966873604960469, 72.91557627198103830 ) ) ;
#69020 = CARTESIAN_POINT ( 'NONE',  ( 9.564922557960805705, 16.46253265017160317, 34.58224293864770260 ) ) ;
#69022 = CARTESIAN_POINT ( 'NONE',  ( 69.65682714487590488, -71.74905178543389184, -15.00000000000000178 ) ) ;
#69021 = CARTESIAN_POINT ( 'NONE',  ( -13.97604488694547697, 13.89961937509957934, 68.12609039468563310 ) ) ;
#69023 = CARTESIAN_POINT ( 'NONE',  ( -21.55341960407619339, 5.719274019375674811, 68.54275706135234714 ) ) ;
#69024 = CARTESIAN_POINT ( 'NONE',  ( 8.314922557961029526, -14.29746914071037800, 45.41775706135234003 ) ) ;
#69025 = CARTESIAN_POINT ( 'NONE',  ( 17.72517630441461023, -5.499999999999981348, 73.42175719257603816 ) ) ;
#69026 = CARTESIAN_POINT ( 'NONE',  ( 5.719274019375991003, -21.55341960407610458, 32.70724293864770260 ) ) ;
#69027 = CARTESIAN_POINT ( 'NONE',  ( -4.483927247898782831, 16.52544592524335698, 22.70942372801901499 ) ) ;
#69028 = CARTESIAN_POINT ( 'NONE',  ( 17.97161686093727795, -5.499999999999970690, 98.49637206859168259 ) ) ;
#69029 = CARTESIAN_POINT ( 'NONE',  ( -21.94905633995364269, 8.886455535323596777, 171.4390084046502523 ) ) ;
#69030 = CARTESIAN_POINT ( 'NONE',  ( -9.564922557960796823, -16.46253265017161027, 42.08224293864769550 ) ) ;
#69031 = CARTESIAN_POINT ( 'NONE',  ( -15.72974639402176322, -15.80617190586768395, 109.3760903946857042 ) ) ;
#69032 = CARTESIAN_POINT ( 'NONE',  ( -16.51473224551069308, -9.474510206698971260, 51.66557627198102409 ) ) ;
#69033 = CARTESIAN_POINT ( 'NONE',  ( 18.62759615963255655, 10.81492255796105972, 66.66775706135234714 ) ) ;
#69034 = CARTESIAN_POINT ( 'NONE',  ( -10.81492255796105439, 18.62759615963255655, 107.9177570613523471 ) ) ;
#69035 = CARTESIAN_POINT ( 'NONE',  ( -16.53943276465976808, -0.05219959533934237506, 113.7510903946856757 ) ) ;
#69036 = CARTESIAN_POINT ( 'NONE',  ( -16.46253265017160317, 9.564922557960807481, 35.83224293864768839 ) ) ;
#69037 = CARTESIAN_POINT ( 'NONE',  ( -13.89961937509977652, 13.97604488694528158, 90.62390960531432427 ) ) ;
#69038 = CARTESIAN_POINT ( 'NONE',  ( -10.81492255796105439, 18.62759615963255655, 52.91775706135235424 ) ) ;
#69039 = CARTESIAN_POINT ( 'NONE',  ( -19.05341960407611168, -5.049401038298163336, 36.45724293864766707 ) ) ;
#69040 = CIRCLE ( 'NONE', #114198, 2.649999999999999911 ) ;
#69041 = CARTESIAN_POINT ( 'NONE',  ( -21.53943276465977519, -0.05219959533937600094, 48.75109039468568284 ) ) ;
#69043 = CARTESIAN_POINT ( 'NONE',  ( 19.02544592524343514, -5.153800228976328945, 103.5405762719809957 ) ) ;
#69042 = CARTESIAN_POINT ( 'NONE',  ( 13.89961937509957401, 13.97604488694547697, 96.87609039468566152 ) ) ;
#69044 = CARTESIAN_POINT ( 'NONE',  ( -8.314922557960811034, -14.29746914071050412, 112.0822429386477097 ) ) ;
#69045 = CARTESIAN_POINT ( 'NONE',  ( -18.62759615963270932, 10.81492255796079327, 110.8322429386476955 ) ) ;
#69046 = CARTESIAN_POINT ( 'NONE',  ( -9.474510206698720793, -16.51473224551083518, 34.58442372801899722 ) ) ;
#69047 = CARTESIAN_POINT ( 'NONE',  ( 16.55341960407611168, 4.379528057220329451, 113.9572429386477239 ) ) ;
#69048 = CARTESIAN_POINT ( 'NONE',  ( 13.89961937509977652, -13.97604488694527269, 63.12390960531435979 ) ) ;
#69049 = CARTESIAN_POINT ( 'NONE',  ( 16.46253265017146816, 9.564922557961045513, 96.66775706135233293 ) ) ;
#69050 = CARTESIAN_POINT ( 'NONE',  ( 14.29746914071049879, -8.314922557960816363, 68.33224293864769550 ) ) ;
#69051 = CARTESIAN_POINT ( 'NONE',  ( -16.46253265017146816, -9.564922557961047289, 24.16775706135233648 ) ) ;
#69052 = CARTESIAN_POINT ( 'NONE',  ( 19.02544592524343514, -5.153800228976328945, 113.5405762719810241 ) ) ;
#69053 = CARTESIAN_POINT ( 'NONE',  ( -5.153800228976607833, 19.02544592524334988, 92.70942372801901854 ) ) ;
#69054 = CARTESIAN_POINT ( 'NONE',  ( 0.05219959533907565091, 21.53943276465977519, 89.99890960531438111 ) ) ;
#69055 = CARTESIAN_POINT ( 'NONE',  ( -21.52544592524334988, -5.823673210054445271, 38.95942372801901854 ) ) ;
#69056 = CARTESIAN_POINT ( 'NONE',  ( 12.06949235617739724, 12.14591786802326823, 46.87609039468568994 ) ) ;
#69057 = CARTESIAN_POINT ( 'NONE',  ( -14.34966873604972548, 8.224510206698743886, 103.3344237280190043 ) ) ;
#69059 = CARTESIAN_POINT ( 'NONE',  ( -15.72974639402176322, -15.80617190586768395, 44.37609039468567573 ) ) ;
#69058 = CARTESIAN_POINT ( 'NONE',  ( -16.53943276465976808, -0.05219959533934237506, 43.75109039468568284 ) ) ;
#69060 = CARTESIAN_POINT ( 'NONE',  ( 0.05219959533907565091, 21.53943276465977519, 49.99890960531437401 ) ) ;
#69061 = CARTESIAN_POINT ( 'NONE',  ( 13.97604488694527802, 13.89961937509977652, 29.37390960531435979 ) ) ;
#69062 = CARTESIAN_POINT ( 'NONE',  ( -30.74264578624800492, -22.33583958711396278, -5.549999994537627046 ) ) ;
#69063 = CARTESIAN_POINT ( 'NONE',  ( 16.55341960407618274, -4.379528057220086978, 61.04275706135234714 ) ) ;
#69064 = CARTESIAN_POINT ( 'NONE',  ( 18.67979575497178502, 10.72451020669898547, 89.16557627198102409 ) ) ;
#69065 = CARTESIAN_POINT ( 'NONE',  ( 4.483927247898545687, 16.52544592524342804, 44.79057627198103120 ) ) ;
#69066 = CARTESIAN_POINT ( 'NONE',  ( 12.06949235617739724, 12.14591786802326823, 66.87609039468568994 ) ) ;
#69067 = CARTESIAN_POINT ( 'NONE',  ( 9.564922557961047289, -16.46253265017146816, 105.4177570613523471 ) ) ;
#69068 = CARTESIAN_POINT ( 'NONE',  ( 10.72451020669898902, -18.67979575497178502, 97.91557627198103830 ) ) ;
#69069 = CARTESIAN_POINT ( 'NONE',  ( -12.14591786802309592, -12.06949235617757132, 36.87390960531435979 ) ) ;
#69070 = ORIENTED_EDGE ( 'NONE', *, *, #120968, .T. ) ;
#69071 = CARTESIAN_POINT ( 'NONE',  ( -8.224510206698735004, -14.34966873604973081, 79.58442372801903275 ) ) ;
#69072 = CARTESIAN_POINT ( 'NONE',  ( 20.93662873023604121, 11.00447265502299388, 170.1964094900432372 ) ) ;
#69073 = CARTESIAN_POINT ( 'NONE',  ( -18.62759615963270932, 10.81492255796079327, 80.83224293864769550 ) ) ;
#69074 = ORIENTED_EDGE ( 'NONE', *, *, #53677, .T. ) ;
#69075 = CARTESIAN_POINT ( 'NONE',  ( -16.55341960407617563, 4.379528057220093196, 103.5427570613523613 ) ) ;
#69076 = ORIENTED_EDGE ( 'NONE', *, *, #107363, .F. ) ;
#69077 = CARTESIAN_POINT ( 'NONE',  ( 19.52851543214743657, 5.500000000000030198, 87.89357721762581832 ) ) ;
#69078 = CARTESIAN_POINT ( 'NONE',  ( -5.719274019375978568, 21.55341960407610458, 90.20724293864770971 ) ) ;
#69079 = CARTESIAN_POINT ( 'NONE',  ( 0.05219959533907565091, 21.53943276465977519, 104.9989096053143669 ) ) ;
#69080 = CARTESIAN_POINT ( 'NONE',  ( 12.06949235617757843, -12.14591786802309237, 38.12390960531436690 ) ) ;
#69081 = CARTESIAN_POINT ( 'NONE',  ( -12.06949235617739369, -12.14591786802326823, 29.37609039468568284 ) ) ;
#69082 = CARTESIAN_POINT ( 'NONE',  ( -19.05341960407611168, -5.049401038298163336, 41.45724293864769550 ) ) ;
#69083 = CARTESIAN_POINT ( 'NONE',  ( -13.89961937509977652, 13.97604488694528158, 65.62390960531436690 ) ) ;
#69084 = CARTESIAN_POINT ( 'NONE',  ( 5.719274019375991003, -21.55341960407610458, 27.70724293864769905 ) ) ;
#69085 = CARTESIAN_POINT ( 'NONE',  ( -13.89961937509977652, 13.97604488694528158, 115.6239096053143669 ) ) ;
#69086 = CARTESIAN_POINT ( 'NONE',  ( 9.474510206698729675, 16.51473224551082808, 107.0844237280190043 ) ) ;
#69087 = CARTESIAN_POINT ( 'NONE',  ( 13.97604488694548053, -13.89961937509957401, 50.62609039468566152 ) ) ;
#69088 = CARTESIAN_POINT ( 'NONE',  ( -10.72451020669898014, 18.67979575497178502, 90.41557627198103830 ) ) ;
#69089 = CARTESIAN_POINT ( 'NONE',  ( 8.224510206698742110, 14.34966873604972548, 107.0844237280190043 ) ) ;
#69090 = CARTESIAN_POINT ( 'NONE',  ( -15.80617190586745835, -15.72974639402198527, 46.87390960531435979 ) ) ;
#69092 = CARTESIAN_POINT ( 'NONE',  ( 19.05341960407617918, -5.049401038297876454, 111.0427570613523329 ) ) ;
#69091 = CARTESIAN_POINT ( 'NONE',  ( -21.55341960407610458, -5.719274019375992779, 86.45724293864770971 ) ) ;
#69093 = CARTESIAN_POINT ( 'NONE',  ( -13.89961937509977652, 13.97604488694528158, 100.6239096053143669 ) ) ;
#69094 = CARTESIAN_POINT ( 'NONE',  ( -15.80617190586768217, 15.72974639402176855, 78.12609039468570415 ) ) ;
#69095 = CARTESIAN_POINT ( 'NONE',  ( -16.51473224551069308, -9.474510206698971260, 71.66557627198102409 ) ) ;
#69096 = CARTESIAN_POINT ( 'NONE',  ( 32.15509708611484996, 4.949069787320328651, 89.34338315600291480 ) ) ;
#69097 = CARTESIAN_POINT ( 'NONE',  ( -13.89961937509977652, 13.97604488694528158, 70.62390960531432427 ) ) ;
#69098 = CARTESIAN_POINT ( 'NONE',  ( 16.55341960407611168, 4.379528057220329451, 88.95724293864769550 ) ) ;
#69099 = VERTEX_POINT ( 'NONE', #138243 ) ;
#69100 = CARTESIAN_POINT ( 'NONE',  ( 16.51473224551083163, -9.474510206698727899, 110.8344237280190043 ) ) ;
#69101 = CIRCLE ( 'NONE', #94941, 59.99999999999998579 ) ;
#69102 = CARTESIAN_POINT ( 'NONE',  ( 16.19135201231366494, -7.376712067591922661, 82.31319145947968252 ) ) ;
#69103 = CARTESIAN_POINT ( 'NONE',  ( 16.51473224551069308, 9.474510206698969483, 69.16557627198102409 ) ) ;
#69105 = CARTESIAN_POINT ( 'NONE',  ( -16.51473224551069308, -9.474510206698971260, 106.6655762719810383 ) ) ;
#69104 = CARTESIAN_POINT ( 'NONE',  ( -18.67979575497193778, 10.72451020669871902, 88.33442372801901854 ) ) ;
#69106 = CARTESIAN_POINT ( 'NONE',  ( 16.55341960407618274, -4.379528057220086978, 76.04275706135237556 ) ) ;
#69107 = CARTESIAN_POINT ( 'NONE',  ( -30.27664185797782537, 1.503321482105818507, -47.91583118997741053 ) ) ;
#69108 = CARTESIAN_POINT ( 'NONE',  ( 9.564922557961047289, -16.46253265017146816, 50.41775706135233293 ) ) ;
#69109 = CARTESIAN_POINT ( 'NONE',  ( -10.81492255796105439, 18.62759615963255655, 107.9177570613523471 ) ) ;
#69110 = DIRECTION ( 'NONE',  ( 1.000000000000000000, 0.000000000000000000, 3.709348145883536076E-20 ) ) ;
#69111 = CARTESIAN_POINT ( 'NONE',  ( 6.412877669190332419, 3.889087296526017479, 8.181980515339454030 ) ) ;
#69112 = LINE ( 'NONE', #88026, #46384 ) ;
#69113 = CARTESIAN_POINT ( 'NONE',  ( 0.05219959533934541429, -16.53943276465976808, 110.0010903946856757 ) ) ;
#69114 = CARTESIAN_POINT ( 'NONE',  ( -34.67225235875025646, -7.109416101192573834, 42.56171885070867944 ) ) ;
#69115 = CARTESIAN_POINT ( 'NONE',  ( 14.29746914071037800, 8.314922557961029526, 91.66775706135234714 ) ) ;
#69116 = CARTESIAN_POINT ( 'NONE',  ( 28.79475375365586132, 2.781246896534039337E-14, 140.9843446568999923 ) ) ;
#69117 = CARTESIAN_POINT ( 'NONE',  ( 14.29746914071037800, 8.314922557961029526, 66.66775706135234714 ) ) ;
#69118 = CARTESIAN_POINT ( 'NONE',  ( -5.823673210054431948, 21.52544592524334988, 77.70942372801900433 ) ) ;
#69119 = CARTESIAN_POINT ( 'NONE',  ( 19.02544592524334988, 5.153800228976608722, 86.45942372801900433 ) ) ;
#69120 = CARTESIAN_POINT ( 'NONE',  ( 16.51473224551083163, -9.474510206698727899, 35.83442372801899722 ) ) ;
#69121 = CARTESIAN_POINT ( 'NONE',  ( -5.049401038298153566, 19.05341960407611168, 65.20724293864765286 ) ) ;
#69122 = CARTESIAN_POINT ( 'NONE',  ( -19.02544592524342804, 5.153800228976336051, 56.04057627198100988 ) ) ;
#69123 = CARTESIAN_POINT ( 'NONE',  ( -9.564922557960796823, -16.46253265017161027, 87.08224293864769550 ) ) ;
#69124 = CARTESIAN_POINT ( 'NONE',  ( -10.72451020669898014, 18.67979575497178502, 85.41557627198102409 ) ) ;
#69125 = AXIS2_PLACEMENT_3D ( 'NONE', #173731, #69523, #5844 ) ;
#69126 = CARTESIAN_POINT ( 'NONE',  ( -10.81492255796078084, -18.62759615963271287, 52.08224293864768839 ) ) ;
#69127 = CARTESIAN_POINT ( 'NONE',  ( -19.05341960407611168, -5.049401038298163336, 31.45724293864769550 ) ) ;
#69128 = CARTESIAN_POINT ( 'NONE',  ( 16.53943276465976808, 0.05219959533934440121, 66.25109039468567573 ) ) ;
#69129 = ORIENTED_EDGE ( 'NONE', *, *, #167140, .T. ) ;
#69130 = CARTESIAN_POINT ( 'NONE',  ( -10.81492255796105439, 18.62759615963255655, 47.91775706135234714 ) ) ;
#69132 = CARTESIAN_POINT ( 'NONE',  ( 23.48529157249599919, 32.32473071737754111, -0.6999999999999998446 ) ) ;
#69131 = CARTESIAN_POINT ( 'NONE',  ( -4.483927247898539470, -16.52544592524342804, 62.29057627198102409 ) ) ;
#69133 = CARTESIAN_POINT ( 'NONE',  ( -0.05219959533934338120, 16.53943276465976808, 37.50109039468568284 ) ) ;
#69134 = CARTESIAN_POINT ( 'NONE',  ( 0.05219959533910956823, 16.53943276465976808, 104.9989096053143669 ) ) ;
#69135 = CARTESIAN_POINT ( 'NONE',  ( -19.05341960407617563, 5.049401038297882671, 58.54275706135234003 ) ) ;
#69136 = CARTESIAN_POINT ( 'NONE',  ( 12.14591786802309770, 12.06949235617756955, 54.37390960531435979 ) ) ;
#69137 = CARTESIAN_POINT ( 'NONE',  ( -15.80617190586768217, 15.72974639402176855, 38.12609039468567573 ) ) ;
#69139 = CARTESIAN_POINT ( 'NONE',  ( 10.72451020669898902, -18.67979575497178502, 92.91557627198103830 ) ) ;
#69138 = CARTESIAN_POINT ( 'NONE',  ( 13.97604488694527802, 13.89961937509977652, 24.37390960531435624 ) ) ;
#69140 = CARTESIAN_POINT ( 'NONE',  ( 9.474510206698971260, -16.51473224551069308, 97.91557627198102409 ) ) ;
#69141 = CARTESIAN_POINT ( 'NONE',  ( 4.483927247898545687, 16.52544592524342804, 79.79057627198102409 ) ) ;
#69142 = CARTESIAN_POINT ( 'NONE',  ( -5.153800228976328057, -19.02544592524343514, 112.2905762719810099 ) ) ;
#69143 = CARTESIAN_POINT ( 'NONE',  ( -36.91746825000000598, 11.99521256947798520, -2.724999997268813701 ) ) ;
#69144 = CARTESIAN_POINT ( 'NONE',  ( -13.89961937509957401, -13.97604488694547875, 79.37609039468567573 ) ) ;
#69145 = CARTESIAN_POINT ( 'NONE',  ( -15.72974639402176322, -15.80617190586768395, 24.37609039468567573 ) ) ;
#69146 = CARTESIAN_POINT ( 'NONE',  ( 5.153800228976335163, 19.02544592524342804, 64.79057627198100988 ) ) ;
#69147 = CARTESIAN_POINT ( 'NONE',  ( -13.97604488694547697, 13.89961937509957934, 63.12609039468566152 ) ) ;
#69148 = CARTESIAN_POINT ( 'NONE',  ( 19.05341960407611168, 5.049401038298154454, 28.95724293864769550 ) ) ;
#69149 = EDGE_CURVE ( 'NONE', #14377, #70166, #36716, .T. ) ;
#69150 = CARTESIAN_POINT ( 'NONE',  ( 21.55341960407619695, -5.719274019375665929, 66.04275706135236135 ) ) ;
#69151 = CARTESIAN_POINT ( 'NONE',  ( -16.31925111598454947, -7.325300261831595883, 69.83575461032751264 ) ) ;
#69152 = CARTESIAN_POINT ( 'NONE',  ( -4.483927247898539470, -16.52544592524342804, 52.29057627198102409 ) ) ;
#69153 = CARTESIAN_POINT ( 'NONE',  ( 0.05219959533909260263, 19.03943276465977164, 59.99890960531436690 ) ) ;
#69154 = CARTESIAN_POINT ( 'NONE',  ( -21.55341960407610458, -5.719274019375992779, 86.45724293864770971 ) ) ;
#69155 = CARTESIAN_POINT ( 'NONE',  ( 16.46253265017160672, -9.564922557960803928, 63.33224293864769550 ) ) ;
#69156 = ORIENTED_EDGE ( 'NONE', *, *, #22880, .F. ) ;
#69157 = CARTESIAN_POINT ( 'NONE',  ( 21.53943276465977519, -0.05219959533907433946, 78.74890960531436690 ) ) ;
#69158 = CARTESIAN_POINT ( 'NONE',  ( 18.67979575497194134, -10.72451020669871369, 95.83442372801903275 ) ) ;
#69161 = CARTESIAN_POINT ( 'NONE',  ( 4.379528057220339221, -16.55341960407611168, 97.70724293864772392 ) ) ;
#69160 = CARTESIAN_POINT ( 'NONE',  ( 4.379528057220092307, 16.55341960407617563, 97.29275706135234714 ) ) ;
#69159 = CARTESIAN_POINT ( 'NONE',  ( -16.51473224551069308, -9.474510206698971260, 21.66557627198102765 ) ) ;
#69162 = CARTESIAN_POINT ( 'NONE',  ( 9.474510206698729675, 16.51473224551082808, 87.08442372801900433 ) ) ;
#69163 = ORIENTED_EDGE ( 'NONE', *, *, #140897, .T. ) ;
#69164 = CARTESIAN_POINT ( 'NONE',  ( -15.72974639402176322, -15.80617190586768395, 24.37609039468567573 ) ) ;
#69165 = CARTESIAN_POINT ( 'NONE',  ( 19.03943276465977164, 0.05219959533936151252, 46.25109039468566863 ) ) ;
#69166 = CARTESIAN_POINT ( 'NONE',  ( -12.14591786802326823, 12.06949235617739902, 103.1260903946856757 ) ) ;
#69167 = CARTESIAN_POINT ( 'NONE',  ( 16.51473224551083163, -9.474510206698727899, 35.83442372801899722 ) ) ;
#69168 = CARTESIAN_POINT ( 'NONE',  ( 19.03943276465977164, -0.05219959533909143690, 98.74890960531436690 ) ) ;
#69169 = CARTESIAN_POINT ( 'NONE',  ( 10.72451020669898902, -18.67979575497178502, 62.91557627198102409 ) ) ;
#69170 = DIRECTION ( 'NONE',  ( -0.000000000000000000, 0.000000000000000000, 1.000000000000000000 ) ) ;
#69171 = CARTESIAN_POINT ( 'NONE',  ( 13.97604488694527802, 13.89961937509977652, 24.37390960531435624 ) ) ;
#69172 = EDGE_CURVE ( 'NONE', #63497, #71844, #108895, .T. ) ;
#69173 = CARTESIAN_POINT ( 'NONE',  ( -19.02544592524334988, -5.153800228976617603, 18.95942372801899722 ) ) ;
#69174 = CARTESIAN_POINT ( 'NONE',  ( 16.55341960407618274, -4.379528057220086978, 71.04275706135234714 ) ) ;
#69175 = CARTESIAN_POINT ( 'NONE',  ( 15.72974639402176855, 15.80617190586768217, 31.87609039468567929 ) ) ;
#69176 = CARTESIAN_POINT ( 'NONE',  ( 4.483927247898790824, -16.52544592524335698, 35.20942372801901854 ) ) ;
#69177 = CARTESIAN_POINT ( 'NONE',  ( 19.03943276465977164, -0.05219959533909143690, 103.7489096053143669 ) ) ;
#69178 = CARTESIAN_POINT ( 'NONE',  ( -5.153800228976328057, -19.02544592524343514, 42.29057627198101699 ) ) ;
#69179 = CARTESIAN_POINT ( 'NONE',  ( -5.153800228976328057, -19.02544592524343514, 72.29057627198102409 ) ) ;
#69180 = CARTESIAN_POINT ( 'NONE',  ( -12.14591786802326823, 12.06949235617739902, 48.12609039468568284 ) ) ;
#69181 = CARTESIAN_POINT ( 'NONE',  ( -4.483927247898539470, -16.52544592524342804, 87.29057627198103830 ) ) ;
#69182 = CARTESIAN_POINT ( 'NONE',  ( 16.53943276465976808, 0.05219959533934440121, 96.25109039468568994 ) ) ;
#69185 = CARTESIAN_POINT ( 'NONE',  ( 19.03943276465977164, -0.05219959533909143690, 58.74890960531435979 ) ) ;
#69184 = CARTESIAN_POINT ( 'NONE',  ( -19.02544592524342804, 5.153800228976336051, 76.04057627198102409 ) ) ;
#69183 = CARTESIAN_POINT ( 'NONE',  ( 21.55341960407619695, -5.719274019375665929, 56.04275706135235424 ) ) ;
#69186 = CARTESIAN_POINT ( 'NONE',  ( -19.02544592524342804, 5.153800228976336051, 91.04057627198100988 ) ) ;
#69187 = CARTESIAN_POINT ( 'NONE',  ( 16.52544592524342804, -4.483927247898539470, 43.54057627198103830 ) ) ;
#69188 = CARTESIAN_POINT ( 'NONE',  ( -16.55341960407617563, 4.379528057220093196, 93.54275706135234714 ) ) ;
#69189 = VERTEX_POINT ( 'NONE', #91714 ) ;
#69190 = CARTESIAN_POINT ( 'NONE',  ( 13.97604488694548053, -13.89961937509957401, 50.62609039468566152 ) ) ;
#69191 = CARTESIAN_POINT ( 'NONE',  ( 5.153800228976335163, 19.02544592524342804, 114.7905762719810241 ) ) ;
#69192 = CARTESIAN_POINT ( 'NONE',  ( 13.89961937509977652, -13.97604488694527269, 63.12390960531435979 ) ) ;
#69193 = CARTESIAN_POINT ( 'NONE',  ( -19.05341960407617563, 5.049401038297882671, 33.54275706135231871 ) ) ;
#69194 = CARTESIAN_POINT ( 'NONE',  ( -11.40812507854755609, 35.11059874428196537, -5.024999997268813523 ) ) ;
#69195 = CARTESIAN_POINT ( 'NONE',  ( 19.25663599770061651, -5.499999999999440448, 71.49419308057203182 ) ) ;
#69196 = CARTESIAN_POINT ( 'NONE',  ( 14.29746914071037800, 8.314922557961029526, 51.66775706135234714 ) ) ;
#69198 = CARTESIAN_POINT ( 'NONE',  ( -16.52544592524335698, -4.483927247898792601, 73.95942372801901854 ) ) ;
#69197 = CARTESIAN_POINT ( 'NONE',  ( -0.05219959533936034679, 19.03943276465977164, 77.50109039468566152 ) ) ;
#69199 = CARTESIAN_POINT ( 'NONE',  ( 17.44270441346517231, 5.991230190323027394, 93.86335079264232206 ) ) ;
#69200 = CARTESIAN_POINT ( 'NONE',  ( 13.97604488694527802, 13.89961937509977652, 84.37390960531433848 ) ) ;
#69201 = CARTESIAN_POINT ( 'NONE',  ( 21.55341960407619695, -5.719274019375665929, 31.04275706135234714 ) ) ;
#69202 = CARTESIAN_POINT ( 'NONE',  ( 9.474510206698729675, 16.51473224551082808, 82.08442372801899012 ) ) ;
#69204 = CARTESIAN_POINT ( 'NONE',  ( 9.564922557960805705, 16.46253265017160317, 39.58224293864768839 ) ) ;
#69203 = CARTESIAN_POINT ( 'NONE',  ( 16.31925111598457434, 7.325300261831476867, 87.33575461032751264 ) ) ;
#69205 = CARTESIAN_POINT ( 'NONE',  ( -19.05341960407611168, -5.049401038298163336, 96.45724293864769550 ) ) ;
#69207 = CARTESIAN_POINT ( 'NONE',  ( -9.564922557960796823, -16.46253265017161027, 42.08224293864769550 ) ) ;
#69206 = CARTESIAN_POINT ( 'NONE',  ( 8.224510206698953496, -14.34966873604960469, 42.91557627198103120 ) ) ;
#69208 = CARTESIAN_POINT ( 'NONE',  ( -16.46253265017146816, -9.564922557961047289, 49.16775706135233293 ) ) ;
#69209 = CARTESIAN_POINT ( 'NONE',  ( 8.224510206698953496, -14.34966873604960469, 82.91557627198103830 ) ) ;
#69210 = CARTESIAN_POINT ( 'NONE',  ( 16.51473224551083163, -9.474510206698727899, 20.83442372801899722 ) ) ;
#69211 = CARTESIAN_POINT ( 'NONE',  ( 5.049401038298161559, -19.05341960407611168, 52.70724293864767418 ) ) ;
#69212 = VECTOR ( 'NONE', #141444, 1000.000000000000000 ) ;
#69213 = CARTESIAN_POINT ( 'NONE',  ( 18.67979575497178502, 10.72451020669898547, 59.16557627198103120 ) ) ;
#69215 = CARTESIAN_POINT ( 'NONE',  ( 19.05341960407617918, -5.049401038297876454, 21.04275706135232582 ) ) ;
#69214 = CARTESIAN_POINT ( 'NONE',  ( 0.05219959533910956823, 16.53943276465976808, 54.99890960531435269 ) ) ;
#69216 = CARTESIAN_POINT ( 'NONE',  ( 16.51473224551069308, 9.474510206698969483, 104.1655762719810241 ) ) ;
#69217 = CARTESIAN_POINT ( 'NONE',  ( 13.89961937509977652, -13.97604488694527269, 113.1239096053143527 ) ) ;
#69218 = CARTESIAN_POINT ( 'NONE',  ( 13.97604488694527802, 13.89961937509977652, 49.37390960531434558 ) ) ;
#69219 = CARTESIAN_POINT ( 'NONE',  ( 19.05341960407611168, 5.049401038298154454, 23.95724293864769194 ) ) ;
#69220 = CARTESIAN_POINT ( 'NONE',  ( 14.34966873604960469, 8.224510206698951720, 94.16557627198103830 ) ) ;
#69221 = CARTESIAN_POINT ( 'NONE',  ( -0.05219959533907301413, -21.53943276465977519, 102.4989096053143811 ) ) ;
#69222 = CARTESIAN_POINT ( 'NONE',  ( -19.05341960407611168, -5.049401038298163336, 106.4572429386476955 ) ) ;
#69223 = CARTESIAN_POINT ( 'NONE',  ( 10.81492255796078972, 18.62759615963270932, 114.5822429386477097 ) ) ;
#69224 = CARTESIAN_POINT ( 'NONE',  ( -0.05219959533909027116, -19.03943276465977164, 102.4989096053143669 ) ) ;
#69225 = CARTESIAN_POINT ( 'NONE',  ( -5.153800228976328057, -19.02544592524343514, 22.29057627198102765 ) ) ;
#69226 = CARTESIAN_POINT ( 'NONE',  ( -18.62759615963255300, -10.81492255796106328, 79.16775706135234714 ) ) ;
#69227 = CARTESIAN_POINT ( 'NONE',  ( -18.67979575497178146, -10.72451020669898902, 91.66557627198103830 ) ) ;
#69228 = EDGE_CURVE ( 'NONE', #33312, #61533, #2711, .T. ) ;
#69229 = PLANE ( 'NONE',  #69794 ) ;
#69230 = CARTESIAN_POINT ( 'NONE',  ( -16.51473224551069308, -9.474510206698971260, 51.66557627198102409 ) ) ;
#69231 = CARTESIAN_POINT ( 'NONE',  ( 31.88380457335793849, -0.2515199893712269930, -49.15318026754363245 ) ) ;
#69232 = CARTESIAN_POINT ( 'NONE',  ( 8.314922557961029526, -14.29746914071037800, 35.41775706135234003 ) ) ;
#69234 = VECTOR ( 'NONE', #90097, 1000.000000000000000 ) ;
#69233 = CARTESIAN_POINT ( 'NONE',  ( 8.314922557960818139, 14.29746914071049879, 104.5822429386477097 ) ) ;
#69235 = CARTESIAN_POINT ( 'NONE',  ( -17.50000000000013500, -3.292511757969763586, 109.9347972978946331 ) ) ;
#69236 = CARTESIAN_POINT ( 'NONE',  ( 13.97604488694527802, 13.89961937509977652, 59.37390960531434558 ) ) ;
#69237 = CARTESIAN_POINT ( 'NONE',  ( 12.06949235617757843, -12.14591786802309237, 93.12390960531436690 ) ) ;
#69238 = CARTESIAN_POINT ( 'NONE',  ( 18.67979575497178502, 10.72451020669898547, 39.16557627198102409 ) ) ;
#69239 = CARTESIAN_POINT ( 'NONE',  ( -14.29746914071049879, 8.314922557960819915, 65.83224293864769550 ) ) ;
#69240 = CARTESIAN_POINT ( 'NONE',  ( 0.05219959533934541429, -16.53943276465976808, 20.00109039468568639 ) ) ;
#69241 = CARTESIAN_POINT ( 'NONE',  ( 10.72451020669871369, 18.67979575497193778, 67.08442372801901854 ) ) ;
#69242 = DIRECTION ( 'NONE',  ( -1.000000000000000000, 0.000000000000000000, 0.000000000000000000 ) ) ;
#69243 = CARTESIAN_POINT ( 'NONE',  ( 9.474510206698971260, -16.51473224551069308, 107.9155762719810383 ) ) ;
#69244 = CARTESIAN_POINT ( 'NONE',  ( 4.483927247898790824, -16.52544592524335698, 100.2094237280190043 ) ) ;
#69245 = CARTESIAN_POINT ( 'NONE',  ( -0.05219959533909027116, -19.03943276465977164, 42.49890960531435269 ) ) ;
#69246 = CARTESIAN_POINT ( 'NONE',  ( -13.89961937509977652, 13.97604488694528158, 85.62390960531433848 ) ) ;
#69247 = CARTESIAN_POINT ( 'NONE',  ( -5.823673210054116645, -21.52544592524344225, 92.29057627198103830 ) ) ;
#69248 = CARTESIAN_POINT ( 'NONE',  ( -4.379528057220086978, -16.55341960407618274, 19.79275706135235069 ) ) ;
#69250 = CARTESIAN_POINT ( 'NONE',  ( -5.823673210054431948, 21.52544592524334988, 67.70942372801901854 ) ) ;
#69249 = CARTESIAN_POINT ( 'NONE',  ( -8.224510206698948167, 14.34966873604960824, 60.41557627198102409 ) ) ;
#69251 = CARTESIAN_POINT ( 'NONE',  ( 12.06949235617739724, 12.14591786802326823, 101.8760903946857042 ) ) ;
#69252 = CARTESIAN_POINT ( 'NONE',  ( 16.38665767535053774, 7.295008042176051255, 27.23599135785455871 ) ) ;
#69253 = DIRECTION ( 'NONE',  ( 0.7071067811865483499, -7.406550393246807469E-15, -0.7071067811865467956 ) ) ;
#69254 = CARTESIAN_POINT ( 'NONE',  ( -4.379528057220328563, 16.55341960407611168, 25.20724293864769550 ) ) ;
#69255 = CARTESIAN_POINT ( 'NONE',  ( -16.53943276465976808, -0.05219959533934237506, 68.75109039468568994 ) ) ;
#69256 = CARTESIAN_POINT ( 'NONE',  ( -9.564922557960796823, -16.46253265017161027, 92.08224293864769550 ) ) ;
#69257 = CARTESIAN_POINT ( 'NONE',  ( -19.02544592524342804, 5.153800228976336051, 81.04057627198103830 ) ) ;
#69258 = CARTESIAN_POINT ( 'NONE',  ( -15.72974639402176322, -15.80617190586768395, 84.37609039468570415 ) ) ;
#69259 = CARTESIAN_POINT ( 'NONE',  ( -4.483927247898782831, 16.52544592524335698, 87.70942372801901854 ) ) ;
#69260 = CARTESIAN_POINT ( 'NONE',  ( -8.314922557960811034, -14.29746914071050412, 57.08224293864769550 ) ) ;
#69261 = CARTESIAN_POINT ( 'NONE',  ( -0.05219959533909027116, -19.03943276465977164, 67.49890960531436690 ) ) ;
#69262 = EDGE_LOOP ( 'NONE', ( #14670, #27198, #71458 ) ) ;
#69263 = CARTESIAN_POINT ( 'NONE',  ( -9.564922557961040184, 16.46253265017147172, 112.9177570613523329 ) ) ;
#69264 = CARTESIAN_POINT ( 'NONE',  ( 0.05219959533910956823, 16.53943276465976808, 114.9989096053143669 ) ) ;
#69265 = CARTESIAN_POINT ( 'NONE',  ( 13.89961937509977652, -13.97604488694527269, 78.12390960531433848 ) ) ;
#69267 = CARTESIAN_POINT ( 'NONE',  ( -22.81625015709509441, -31.40387420917324590, -6.324999997268815122 ) ) ;
#69266 = CARTESIAN_POINT ( 'NONE',  ( -13.97604488694547697, 13.89961937509957934, 108.1260903946856331 ) ) ;
#69268 = CARTESIAN_POINT ( 'NONE',  ( -19.05341960407617563, 5.049401038297882671, 28.54275706135232937 ) ) ;
#69269 = CARTESIAN_POINT ( 'NONE',  ( 8.314922557961029526, -14.29746914071037800, 80.41775706135234714 ) ) ;
#69270 = CARTESIAN_POINT ( 'NONE',  ( -19.03943276465977164, -0.05219959533935918106, 88.75109039468567573 ) ) ;
#69271 = CARTESIAN_POINT ( 'NONE',  ( 0.05219959533910956823, 16.53943276465976808, 109.9989096053143527 ) ) ;
#69272 = CARTESIAN_POINT ( 'NONE',  ( 16.52544592524335698, 4.483927247898782831, 71.45942372801901854 ) ) ;
#69273 = CARTESIAN_POINT ( 'NONE',  ( -17.49999999999999645, -5.500000000000000888, 34.20309617465829177 ) ) ;
#69274 = CARTESIAN_POINT ( 'NONE',  ( -9.474510206698720793, -16.51473224551083518, 54.58442372801899722 ) ) ;
#69275 = CARTESIAN_POINT ( 'NONE',  ( 21.55341960407619695, -5.719274019375665929, 96.04275706135236135 ) ) ;
#69276 = CARTESIAN_POINT ( 'NONE',  ( -5.049401038298153566, 19.05341960407611168, 40.20724293864768839 ) ) ;
#69277 = CARTESIAN_POINT ( 'NONE',  ( -5.153800228976328057, -19.02544592524343514, 77.29057627198099567 ) ) ;
#69278 = CARTESIAN_POINT ( 'NONE',  ( -0.05219959533910754901, -16.53943276465976808, 72.49890960531435269 ) ) ;
#69279 = AXIS2_PLACEMENT_3D ( 'NONE', #151519, #12030, #119193 ) ;
#69280 = CARTESIAN_POINT ( 'NONE',  ( 5.823673210054444382, -21.52544592524334988, 85.20942372801901854 ) ) ;
#69281 = CARTESIAN_POINT ( 'NONE',  ( 5.049401038297881783, 19.05341960407617563, 57.29275706135231871 ) ) ;
#69282 = CARTESIAN_POINT ( 'NONE',  ( 13.89961937509957401, 13.97604488694547697, 46.87609039468565442 ) ) ;
#69283 = CARTESIAN_POINT ( 'NONE',  ( -10.81492255796078084, -18.62759615963271287, 42.08224293864769550 ) ) ;
#69284 = CARTESIAN_POINT ( 'NONE',  ( 21.55341960407619695, -5.719274019375665929, 96.04275706135236135 ) ) ;
#69285 = CARTESIAN_POINT ( 'NONE',  ( 9.474510206698971260, -16.51473224551069308, 72.91557627198102409 ) ) ;
#69286 = CARTESIAN_POINT ( 'NONE',  ( 10.72451020669871369, 18.67979575497193778, 107.0844237280190043 ) ) ;
#69287 = CARTESIAN_POINT ( 'NONE',  ( -21.53943276465977519, 0.05219959533907696930, 56.24890960531436690 ) ) ;
#69288 = CARTESIAN_POINT ( 'NONE',  ( 16.46253265017160672, -9.564922557960803928, 103.3322429386476955 ) ) ;
#69289 = CARTESIAN_POINT ( 'NONE',  ( -13.89961937509957401, -13.97604488694547875, 69.37609039468564731 ) ) ;
#69290 = CARTESIAN_POINT ( 'NONE',  ( 16.46253265017160672, -9.564922557960803928, 103.3322429386476955 ) ) ;
#69291 = CARTESIAN_POINT ( 'NONE',  ( 19.03943276465977164, 0.05219959533936151252, 101.2510903946856757 ) ) ;
#69292 = CARTESIAN_POINT ( 'NONE',  ( 8.224510206698742110, 14.34966873604972548, 42.08442372801901854 ) ) ;
#69293 = CARTESIAN_POINT ( 'NONE',  ( 12.14591786802309770, 12.06949235617756955, 99.37390960531436690 ) ) ;
#69294 = CARTESIAN_POINT ( 'NONE',  ( 13.97604488694527802, 13.89961937509977652, 89.37390960531436690 ) ) ;
#69295 = CARTESIAN_POINT ( 'NONE',  ( 21.55341960407610458, 5.719274019375980345, 58.95724293864770971 ) ) ;
#69296 = CARTESIAN_POINT ( 'NONE',  ( -12.14591786802326823, 12.06949235617739902, 33.12609039468569705 ) ) ;
#69297 = CARTESIAN_POINT ( 'NONE',  ( -18.62759615963255300, -10.81492255796106328, 34.16775706135234714 ) ) ;
#69298 = CARTESIAN_POINT ( 'NONE',  ( -10.81492255796105439, 18.62759615963255655, 77.91775706135231871 ) ) ;
#69299 = CARTESIAN_POINT ( 'NONE',  ( 14.29746914071037800, 8.314922557961029526, 81.66775706135236135 ) ) ;
#69300 = CARTESIAN_POINT ( 'NONE',  ( -19.03943276465977164, 0.05219959533909376836, 76.24890960531435269 ) ) ;
#69301 = CARTESIAN_POINT ( 'NONE',  ( 12.06949235617757843, -12.14591786802309237, 73.12390960531436690 ) ) ;
#69302 = CARTESIAN_POINT ( 'NONE',  ( -8.224510206698735004, -14.34966873604973081, 109.5844237280190328 ) ) ;
#69303 = CARTESIAN_POINT ( 'NONE',  ( 16.46253265017146816, 9.564922557961045513, 56.66775706135233293 ) ) ;
#69304 = CARTESIAN_POINT ( 'NONE',  ( 0.05219959533937995610, -21.53943276465977519, 30.00109039468568284 ) ) ;
#69305 = CARTESIAN_POINT ( 'NONE',  ( -16.52544592524342804, 4.483927247898546575, 81.04057627198102409 ) ) ;
#69306 = CARTESIAN_POINT ( 'NONE',  ( -19.02544592524342804, 5.153800228976336051, 106.0405762719810241 ) ) ;
#69307 = CARTESIAN_POINT ( 'NONE',  ( 16.55341960407618274, -4.379528057220086978, 106.0427570613523471 ) ) ;
#69308 = CARTESIAN_POINT ( 'NONE',  ( -10.72451020669870658, -18.67979575497194134, 69.58442372801900433 ) ) ;
#69309 = CARTESIAN_POINT ( 'NONE',  ( -8.224510206698735004, -14.34966873604973081, 49.58442372801901143 ) ) ;
#69310 = CARTESIAN_POINT ( 'NONE',  ( -18.62759615963255300, -10.81492255796106328, 44.16775706135234714 ) ) ;
#69311 = CARTESIAN_POINT ( 'NONE',  ( -12.14591786802309592, -12.06949235617757132, 66.87390960531436690 ) ) ;
#69312 = ORIENTED_EDGE ( 'NONE', *, *, #93066, .T. ) ;
#69313 = CARTESIAN_POINT ( 'NONE',  ( -15.72974639402176322, -15.80617190586768395, 19.37609039468568639 ) ) ;
#69314 = CARTESIAN_POINT ( 'NONE',  ( -16.55341960407611168, -4.379528057220339221, 91.45724293864769550 ) ) ;
#69315 = CARTESIAN_POINT ( 'NONE',  ( -19.49671883438229258, -5.499999999999982236, 49.89279849105685116 ) ) ;
#69316 = CARTESIAN_POINT ( 'NONE',  ( -16.55341960407611168, -4.379528057220339221, 46.45724293864769550 ) ) ;
#69317 = CARTESIAN_POINT ( 'NONE',  ( -19.05341960407611168, -5.049401038298163336, 26.45724293864769550 ) ) ;
#69318 = CARTESIAN_POINT ( 'NONE',  ( -21.55341960407610458, -5.719274019375992779, 41.45724293864769550 ) ) ;
#69319 = CARTESIAN_POINT ( 'NONE',  ( 8.224510206698953496, -14.34966873604960469, 82.91557627198103830 ) ) ;
#69320 = CARTESIAN_POINT ( 'NONE',  ( 15.72974639402199770, -15.80617190586745480, 83.12390960531436690 ) ) ;
#69321 = CARTESIAN_POINT ( 'NONE',  ( 9.564922557960805705, 16.46253265017160317, 84.58224293864769550 ) ) ;
#69323 = CARTESIAN_POINT ( 'NONE',  ( -9.474510206698720793, -16.51473224551083518, 74.58442372801900433 ) ) ;
#69322 = CARTESIAN_POINT ( 'NONE',  ( 16.46253265017160672, -9.564922557960803928, 43.33224293864769550 ) ) ;
#69325 = CARTESIAN_POINT ( 'NONE',  ( -5.823673210054116645, -21.52544592524344225, 62.29057627198102409 ) ) ;
#69324 = CARTESIAN_POINT ( 'NONE',  ( -18.67979575497193778, 10.72451020669871902, 58.33442372801901143 ) ) ;
#69326 = CARTESIAN_POINT ( 'NONE',  ( -16.46253265017160317, 9.564922557960807481, 40.83224293864769550 ) ) ;
#69327 = CARTESIAN_POINT ( 'NONE',  ( -5.049401038298153566, 19.05341960407611168, 70.20724293864769550 ) ) ;
#69328 = ORIENTED_EDGE ( 'NONE', *, *, #4868, .F. ) ;
#69329 = CARTESIAN_POINT ( 'NONE',  ( 14.29746914071037800, 8.314922557961029526, 51.66775706135234714 ) ) ;
#69330 = CARTESIAN_POINT ( 'NONE',  ( -0.05219959533937732626, 21.53943276465977519, 32.50109039468568284 ) ) ;
#69331 = CARTESIAN_POINT ( 'NONE',  ( -15.72974639402176322, -15.80617190586768395, 74.37609039468568994 ) ) ;
#69332 = CARTESIAN_POINT ( 'NONE',  ( 21.52544592524344225, -5.823673210054117533, 28.54057627198103120 ) ) ;
#69333 = CARTESIAN_POINT ( 'NONE',  ( -10.72451020669898014, 18.67979575497178502, 80.41557627198103830 ) ) ;
#69335 = CARTESIAN_POINT ( 'NONE',  ( 12.14591786802327356, -12.06949235617739191, 50.62609039468568994 ) ) ;
#69334 = CARTESIAN_POINT ( 'NONE',  ( -10.72451020669870658, -18.67979575497194134, 19.58442372801901143 ) ) ;
#69336 = CARTESIAN_POINT ( 'NONE',  ( -18.62759615963270932, 10.81492255796079327, 45.83224293864769550 ) ) ;
#69337 = CARTESIAN_POINT ( 'NONE',  ( 0.05219959533937995610, -21.53943276465977519, 110.0010903946856757 ) ) ;
#69338 = CARTESIAN_POINT ( 'NONE',  ( -5.153800228976328057, -19.02544592524343514, 52.29057627198100988 ) ) ;
#69339 = CARTESIAN_POINT ( 'NONE',  ( -13.89961937509977652, 13.97604488694528158, 115.6239096053143669 ) ) ;
#69340 = CARTESIAN_POINT ( 'NONE',  ( 9.564922557960805705, 16.46253265017160317, 94.58224293864769550 ) ) ;
#69341 = CARTESIAN_POINT ( 'NONE',  ( 22.55670631985092811, 22.55670631985084640, -45.64921306006598201 ) ) ;
#69342 = CARTESIAN_POINT ( 'NONE',  ( -13.89961937509957401, -13.97604488694547875, 74.37609039468566152 ) ) ;
#69343 = CARTESIAN_POINT ( 'NONE',  ( -18.67979575497178146, -10.72451020669898902, 46.66557627198102409 ) ) ;
#69344 = CARTESIAN_POINT ( 'NONE',  ( -4.483927247898539470, -16.52544592524342804, 27.29057627198103120 ) ) ;
#69345 = CARTESIAN_POINT ( 'NONE',  ( -9.564922557961040184, 16.46253265017147172, 102.9177570613523329 ) ) ;
#69346 = CARTESIAN_POINT ( 'NONE',  ( 17.60769864724392875, -5.499999999999830358, 51.15024842019163742 ) ) ;
#69347 = CARTESIAN_POINT ( 'NONE',  ( -19.03943276465977164, -0.05219959533935918106, 18.75109039468567218 ) ) ;
#69348 = CARTESIAN_POINT ( 'NONE',  ( -9.564922557961040184, 16.46253265017147172, 92.91775706135233293 ) ) ;
#69350 = CARTESIAN_POINT ( 'NONE',  ( 13.89961937509957401, 13.97604488694547697, 56.87609039468564731 ) ) ;
#69349 = CARTESIAN_POINT ( 'NONE',  ( -21.55341960407610458, -5.719274019375992779, 81.45724293864769550 ) ) ;
#69351 = CARTESIAN_POINT ( 'NONE',  ( 18.22780087662126647, 5.499999999999818812, 51.48236817873107896 ) ) ;
#69352 = CARTESIAN_POINT ( 'NONE',  ( -13.97604488694527625, -13.89961937509977652, 56.87390960531434558 ) ) ;
#69353 = CARTESIAN_POINT ( 'NONE',  ( 16.55341960407611168, 4.379528057220329451, 68.95724293864769550 ) ) ;
#69354 = CARTESIAN_POINT ( 'NONE',  ( -0.05219959533909027116, -19.03943276465977164, 37.49890960531436690 ) ) ;
#69355 = CARTESIAN_POINT ( 'NONE',  ( -8.314922557960811034, -14.29746914071050412, 37.08224293864768129 ) ) ;
#69356 = CARTESIAN_POINT ( 'NONE',  ( 23.48298174826589246, 32.32155151706776053, -6.447842220587803652 ) ) ;
#69357 = CARTESIAN_POINT ( 'NONE',  ( -16.52544592524335698, -4.483927247898792601, 108.9594237280190185 ) ) ;
#69358 = CARTESIAN_POINT ( 'NONE',  ( 13.89961937509977652, -13.97604488694527269, 58.12390960531436690 ) ) ;
#69359 = CARTESIAN_POINT ( 'NONE',  ( -5.049401038297874678, -19.05341960407617918, 24.79275706135233648 ) ) ;
#69360 = CARTESIAN_POINT ( 'NONE',  ( -12.14591786802326823, 12.06949235617739902, 38.12609039468567573 ) ) ;
#69361 = CARTESIAN_POINT ( 'NONE',  ( -10.72451020669898014, 18.67979575497178502, 55.41557627198102409 ) ) ;
#69363 = ORIENTED_EDGE ( 'NONE', *, *, #25526, .T. ) ;
#69362 = CARTESIAN_POINT ( 'NONE',  ( -5.823673210054431948, 21.52544592524334988, 102.7094237280190185 ) ) ;
#69364 = CARTESIAN_POINT ( 'NONE',  ( -13.97604488694527625, -13.89961937509977652, 56.87390960531434558 ) ) ;
#69365 = CARTESIAN_POINT ( 'NONE',  ( 13.97604488694527802, 13.89961937509977652, 114.3739096053143669 ) ) ;
#69366 = CARTESIAN_POINT ( 'NONE',  ( -19.03943276465977164, 0.05219959533909376836, 96.24890960531436690 ) ) ;
#69367 = CARTESIAN_POINT ( 'NONE',  ( -29.86685920354755197, -21.69954338932560134, -2.424999997268813434 ) ) ;
#69368 = CARTESIAN_POINT ( 'NONE',  ( 21.53943276465977519, 0.05219959533937863772, 21.25109039468567218 ) ) ;
#69369 = CARTESIAN_POINT ( 'NONE',  ( -4.379528057220328563, 16.55341960407611168, 95.20724293864769550 ) ) ;
#69371 = CARTESIAN_POINT ( 'NONE',  ( 5.153800228976335163, 19.02544592524342804, 64.79057627198100988 ) ) ;
#69370 = CARTESIAN_POINT ( 'NONE',  ( -10.81492255796078084, -18.62759615963271287, 87.08224293864769550 ) ) ;
#69372 = CARTESIAN_POINT ( 'NONE',  ( 19.02544592524343514, -5.153800228976328945, 68.54057627198103830 ) ) ;
#69373 = CARTESIAN_POINT ( 'NONE',  ( 18.67979575497178502, 10.72451020669898547, 114.1655762719810383 ) ) ;
#69374 = ORIENTED_EDGE ( 'NONE', *, *, #148621, .T. ) ;
#69375 = CARTESIAN_POINT ( 'NONE',  ( 13.89961937509977652, -13.97604488694527269, 73.12390960531436690 ) ) ;
#69376 = DIRECTION ( 'NONE',  ( 1.000000000000000000, 0.000000000000000000, 0.000000000000000000 ) ) ;
#69378 = CARTESIAN_POINT ( 'NONE',  ( 9.474510206698971260, -16.51473224551069308, 22.91557627198102765 ) ) ;
#69377 = CARTESIAN_POINT ( 'NONE',  ( 0.05219959533910956823, 16.53943276465976808, 104.9989096053143669 ) ) ;
#69379 = CARTESIAN_POINT ( 'NONE',  ( -13.89961937509957401, -13.97604488694547875, 99.37609039468567573 ) ) ;
#69380 = CIRCLE ( 'NONE', #153380, 5.000000000000000888 ) ;
#69381 = CARTESIAN_POINT ( 'NONE',  ( 12.14591786802309770, 12.06949235617756955, 94.37390960531436690 ) ) ;
#69382 = CARTESIAN_POINT ( 'NONE',  ( 21.55341960407619695, -5.719274019375665929, 76.04275706135237556 ) ) ;
#69384 = CARTESIAN_POINT ( 'NONE',  ( 5.719274019375673035, 21.55341960407619339, 32.29275706135235424 ) ) ;
#69383 = CARTESIAN_POINT ( 'NONE',  ( 16.51473224551069308, 9.474510206698969483, 59.16557627198102409 ) ) ;
#69385 = CARTESIAN_POINT ( 'NONE',  ( -10.81492255796078084, -18.62759615963271287, 112.0822429386477097 ) ) ;
#69386 = CARTESIAN_POINT ( 'NONE',  ( 17.81289503416611453, -24.51734667627695785, 142.6999999999999886 ) ) ;
#69387 = CARTESIAN_POINT ( 'NONE',  ( 13.97604488694527802, 13.89961937509977652, 74.37390960531436690 ) ) ;
#69388 = CARTESIAN_POINT ( 'NONE',  ( -3.889087296525703508, 30.00000000000004263, 8.181980515339454030 ) ) ;
#69390 = CARTESIAN_POINT ( 'NONE',  ( 18.67979575497178502, 10.72451020669898547, 24.16557627198103120 ) ) ;
#69389 = CARTESIAN_POINT ( 'NONE',  ( -14.29746914071037622, -8.314922557961029526, 24.16775706135235424 ) ) ;
#69391 = CARTESIAN_POINT ( 'NONE',  ( 15.72974639402176855, 15.80617190586768217, 66.87609039468568994 ) ) ;
#69392 = PRESENTATION_LAYER_ASSIGNMENT (  '', '', ( #88743 ) ) ;
#69393 = CARTESIAN_POINT ( 'NONE',  ( -5.049401038298153566, 19.05341960407611168, 105.2072429386476671 ) ) ;
#69394 = CARTESIAN_POINT ( 'NONE',  ( -19.02544592524334988, -5.153800228976617603, 98.95942372801900433 ) ) ;
#69395 = CARTESIAN_POINT ( 'NONE',  ( -9.474510206698964154, 16.51473224551069663, 45.41557627198103120 ) ) ;
#69396 = CARTESIAN_POINT ( 'NONE',  ( 5.049401038298161559, -19.05341960407611168, 72.70724293864768129 ) ) ;
#69397 = EDGE_CURVE ( 'NONE', #157920, #136724, #186529, .T. ) ;
#69398 = CARTESIAN_POINT ( 'NONE',  ( -14.29746914071049879, 8.314922557960819915, 95.83224293864770971 ) ) ;
#69399 = CARTESIAN_POINT ( 'NONE',  ( 16.51473224551069308, 9.474510206698969483, 99.16557627198102409 ) ) ;
#69400 = CARTESIAN_POINT ( 'NONE',  ( -14.29746914071049879, 8.314922557960819915, 90.83224293864769550 ) ) ;
#69401 = CARTESIAN_POINT ( 'NONE',  ( 13.89961937509977652, -13.97604488694527269, 103.1239096053143527 ) ) ;
#69404 = CARTESIAN_POINT ( 'NONE',  ( -13.89961937509977652, 13.97604488694528158, 45.62390960531433848 ) ) ;
#69403 =( BOUNDED_CURVE ( )  B_SPLINE_CURVE ( 2, ( #177793, #85762, #117098, #178793, #9940, #194956, #56433, #118113, #156393, #62379, #182771 ),
 .UNSPECIFIED., .F., .T. ) 
 B_SPLINE_CURVE_WITH_KNOTS ( ( 3, 2, 2, 2, 2, 3 ),
 ( 0.5000000000000004441, 0.5200000000000004619, 0.5400000000000004796, 0.5600000000000006084, 0.5800000000000005151, 0.6000000000000005329 ),
 .UNSPECIFIED. ) 
 CURVE ( )  GEOMETRIC_REPRESENTATION_ITEM ( )  RATIONAL_B_SPLINE_CURVE ( ( 0.9999999999999988898, 0.9510565162951546414, 1.000000000000000000, 0.9510565162951535312, 1.000000000000000000, 0.9510565162951535312, 1.000000000000000000, 0.9510565162951535312, 1.000000000000000000, 0.9510565162951521989, 1.000000000000001332 ) ) 
 REPRESENTATION_ITEM ( '' )  );
#69402 = CARTESIAN_POINT ( 'NONE',  ( 14.29746914071049879, -8.314922557960816363, 48.33224293864770260 ) ) ;
#69405 = CARTESIAN_POINT ( 'NONE',  ( -5.823673210054431948, 21.52544592524334988, 62.70942372801902565 ) ) ;
#69406 = CARTESIAN_POINT ( 'NONE',  ( 19.02544592524334988, 5.153800228976608722, 96.45942372801897591 ) ) ;
#69407 = CARTESIAN_POINT ( 'NONE',  ( 0.05219959533910956823, 16.53943276465976808, 44.99890960531435979 ) ) ;
#69408 = CARTESIAN_POINT ( 'NONE',  ( -5.823673210054116645, -21.52544592524344225, 102.2905762719810383 ) ) ;
#69409 = CARTESIAN_POINT ( 'NONE',  ( 15.72974639402199770, -15.80617190586745480, 48.12390960531436690 ) ) ;
#69411 = CARTESIAN_POINT ( 'NONE',  ( 16.52544592524342804, -4.483927247898539470, 83.54057627198102409 ) ) ;
#69410 = CARTESIAN_POINT ( 'NONE',  ( -13.89961937509977652, 13.97604488694528158, 110.6239096053143243 ) ) ;
#69412 = CARTESIAN_POINT ( 'NONE',  ( -16.51473224551069308, -9.474510206698971260, 56.66557627198103120 ) ) ;
#69413 = CARTESIAN_POINT ( 'NONE',  ( 4.379528057220339221, -16.55341960407611168, 27.70724293864769905 ) ) ;
#69414 = CARTESIAN_POINT ( 'NONE',  ( 0.05219959533934541429, -16.53943276465976808, 105.0010903946856757 ) ) ;
#69415 = CARTESIAN_POINT ( 'NONE',  ( -14.29746914071037622, -8.314922557961029526, 84.16775706135234714 ) ) ;
#69416 = CARTESIAN_POINT ( 'NONE',  ( -13.97604488694547697, 13.89961937509957934, 38.12609039468566152 ) ) ;
#69418 = CARTESIAN_POINT ( 'NONE',  ( 9.564922557960805705, 16.46253265017160317, 104.5822429386476955 ) ) ;
#69417 = DIRECTION ( 'NONE',  ( -0.000000000000000000, -0.000000000000000000, 1.000000000000000000 ) ) ;
#69419 = CARTESIAN_POINT ( 'NONE',  ( 19.02544592524343514, -5.153800228976328945, 73.54057627198103830 ) ) ;
#69420 = CARTESIAN_POINT ( 'NONE',  ( 13.97604488694527802, 13.89961937509977652, 34.37390960531436690 ) ) ;
#69421 = CARTESIAN_POINT ( 'NONE',  ( -8.314922557960811034, -14.29746914071050412, 42.08224293864769550 ) ) ;
#69423 = CARTESIAN_POINT ( 'NONE',  ( -9.564922557960796823, -16.46253265017161027, 102.0822429386477097 ) ) ;
#69422 = CARTESIAN_POINT ( 'NONE',  ( 19.05341960407611168, 5.049401038298154454, 113.9572429386477097 ) ) ;
#69424 = CARTESIAN_POINT ( 'NONE',  ( -21.52544592524343514, 5.823673210054127303, 46.04057627198103830 ) ) ;
#69425 = CARTESIAN_POINT ( 'NONE',  ( -12.14591786802309592, -12.06949235617757132, 86.87390960531438111 ) ) ;
#69426 = CARTESIAN_POINT ( 'NONE',  ( -12.14591786802326823, 12.06949235617739902, 38.12609039468567573 ) ) ;
#69427 = CARTESIAN_POINT ( 'NONE',  ( 4.483927247898545687, 16.52544592524342804, 59.79057627198103120 ) ) ;
#69428 = CARTESIAN_POINT ( 'NONE',  ( 29.14368513529645099, -0.8274645171313743663, -49.37167794572895474 ) ) ;
#69429 = CARTESIAN_POINT ( 'NONE',  ( 13.97604488694548053, -13.89961937509957401, 60.62609039468564731 ) ) ;
#69430 = CARTESIAN_POINT ( 'NONE',  ( 19.02544592524343514, -5.153800228976328945, 98.54057627198100988 ) ) ;
#69431 = CARTESIAN_POINT ( 'NONE',  ( -0.05219959533936034679, 19.03943276465977164, 72.50109039468566152 ) ) ;
#69432 = CARTESIAN_POINT ( 'NONE',  ( 16.51473224551083163, -9.474510206698727899, 95.83442372801900433 ) ) ;
#69434 = CARTESIAN_POINT ( 'NONE',  ( -8.314922557961024197, 14.29746914071037800, 102.9177570613523756 ) ) ;
#69433 = CARTESIAN_POINT ( 'NONE',  ( 16.55341960407618274, -4.379528057220086978, 31.04275706135234714 ) ) ;
#69435 = CARTESIAN_POINT ( 'NONE',  ( 16.51473224551083163, -9.474510206698727899, 70.83442372801900433 ) ) ;
#69436 = CARTESIAN_POINT ( 'NONE',  ( 18.67979575497178502, 10.72451020669898547, 39.16557627198102409 ) ) ;
#69437 = CARTESIAN_POINT ( 'NONE',  ( -5.719274019375665041, -21.55341960407619695, 69.79275706135234714 ) ) ;
#69438 = CARTESIAN_POINT ( 'NONE',  ( -21.35462415990328822, -9.648971641163925028, 168.5494316893072835 ) ) ;
#69439 = CARTESIAN_POINT ( 'NONE',  ( 19.05341960407617918, -5.049401038297876454, 111.0427570613523329 ) ) ;
#69441 = CARTESIAN_POINT ( 'NONE',  ( -13.89961937509977652, 13.97604488694528158, 75.62390960531438111 ) ) ;
#69440 = DIRECTION ( 'NONE',  ( 0.000000000000000000, -0.7660444431189766812, 0.6427876096865408062 ) ) ;
#69442 = CARTESIAN_POINT ( 'NONE',  ( 14.61899031675406846, 16.10093921903347081, -58.57166825620328154 ) ) ;
#69444 = CARTESIAN_POINT ( 'NONE',  ( -0.05219959533909027116, -19.03943276465977164, 72.49890960531435269 ) ) ;
#69443 = CARTESIAN_POINT ( 'NONE',  ( 16.53943276465976808, -0.05219959533910856209, 83.74890960531435269 ) ) ;
#69445 = ITEM_DEFINED_TRANSFORMATION ( 'NONE', 'NONE', #49912,  #82054 ) ;
#69446 = CARTESIAN_POINT ( 'NONE',  ( 19.03943276465977164, -0.05219959533909143690, 93.74890960531435269 ) ) ;
#69447 = ORIENTED_EDGE ( 'NONE', *, *, #55785, .T. ) ;
#69448 = CARTESIAN_POINT ( 'NONE',  ( 9.474510206698729675, 16.51473224551082808, 87.08442372801900433 ) ) ;
#69449 = CARTESIAN_POINT ( 'NONE',  ( -21.52544592524343514, 5.823673210054127303, 76.04057627198102409 ) ) ;
#69450 = CARTESIAN_POINT ( 'NONE',  ( -13.97604488694527625, -13.89961937509977652, 26.87390960531434558 ) ) ;
#69452 = CARTESIAN_POINT ( 'NONE',  ( -21.53943276465977519, 0.05219959533907696930, 111.2489096053143669 ) ) ;
#69451 = CARTESIAN_POINT ( 'NONE',  ( -9.564922557961040184, 16.46253265017147172, 72.91775706135233293 ) ) ;
#69453 = CARTESIAN_POINT ( 'NONE',  ( -5.153800228976328057, -19.02544592524343514, 72.29057627198102409 ) ) ;
#69454 = CARTESIAN_POINT ( 'NONE',  ( -9.564922557960796823, -16.46253265017161027, 102.0822429386477097 ) ) ;
#69455 = ORIENTED_EDGE ( 'NONE', *, *, #149391, .T. ) ;
#69456 = CARTESIAN_POINT ( 'NONE',  ( 15.80617190586746368, 15.72974639402197994, 99.37390960531436690 ) ) ;
#69459 = CARTESIAN_POINT ( 'NONE',  ( -0.05219959533936034679, 19.03943276465977164, 57.50109039468566863 ) ) ;
#69458 = CARTESIAN_POINT ( 'NONE',  ( 0.05219959533909260263, 19.03943276465977164, 84.99890960531436690 ) ) ;
#69457 = CARTESIAN_POINT ( 'NONE',  ( -4.483927247898539470, -16.52544592524342804, 97.29057627198105251 ) ) ;
#69460 = CARTESIAN_POINT ( 'NONE',  ( 21.52544592524344225, -5.823673210054117533, 83.54057627198102409 ) ) ;
#69461 = CARTESIAN_POINT ( 'NONE',  ( -5.823673210054116645, -21.52544592524344225, 67.29057627198103830 ) ) ;
#69462 = VECTOR ( 'NONE', #84230, 1000.000000000000114 ) ;
#69463 = CARTESIAN_POINT ( 'NONE',  ( -4.379528057220328563, 16.55341960407611168, 40.20724293864769550 ) ) ;
#69464 = CARTESIAN_POINT ( 'NONE',  ( 15.80617190586769283, -15.72974639402175789, 110.6260903946857042 ) ) ;
#69465 = CARTESIAN_POINT ( 'NONE',  ( 8.224510206698742110, 14.34966873604972548, 62.08442372801901143 ) ) ;
#69466 = CARTESIAN_POINT ( 'NONE',  ( -16.46253265017160317, 9.564922557960807481, 90.83224293864769550 ) ) ;
#69467 = CARTESIAN_POINT ( 'NONE',  ( -19.05341960407611168, -5.049401038298163336, 31.45724293864769550 ) ) ;
#69468 = CARTESIAN_POINT ( 'NONE',  ( 18.67979575497194134, -10.72451020669871369, 40.83442372801901854 ) ) ;
#69469 = CARTESIAN_POINT ( 'NONE',  ( 5.719274019375673035, 21.55341960407619339, 57.29275706135234714 ) ) ;
#69470 = CARTESIAN_POINT ( 'NONE',  ( 13.97604488694527802, 13.89961937509977652, 64.37390960531436690 ) ) ;
#69471 = CARTESIAN_POINT ( 'NONE',  ( -21.53943276465977519, -0.05219959533937600094, 33.75109039468568284 ) ) ;
#69472 = EDGE_CURVE ( 'NONE', #161389, #94667, #34219, .T. ) ;
#69473 = CARTESIAN_POINT ( 'NONE',  ( 19.05341960407617918, -5.049401038297876454, 76.04275706135230450 ) ) ;
#69474 = CARTESIAN_POINT ( 'NONE',  ( 13.97604488694548053, -13.89961937509957401, 75.62609039468564731 ) ) ;
#69475 = CARTESIAN_POINT ( 'NONE',  ( 19.05341960407611168, 5.049401038298154454, 43.95724293864769550 ) ) ;
#69476 = CARTESIAN_POINT ( 'NONE',  ( -16.53943276465976808, -0.05219959533934237506, 83.75109039468568994 ) ) ;
#69477 = CARTESIAN_POINT ( 'NONE',  ( 9.474510206698971260, -16.51473224551069308, 57.91557627198103120 ) ) ;
#69478 = CARTESIAN_POINT ( 'NONE',  ( 23.75112013235311892, -10.51683317207933399, 166.0021274478077942 ) ) ;
#69479 = CARTESIAN_POINT ( 'NONE',  ( 13.97604488694527802, 13.89961937509977652, 99.37390960531436690 ) ) ;
#69480 = CARTESIAN_POINT ( 'NONE',  ( 13.89961937509977652, -13.97604488694527269, 43.12390960531434558 ) ) ;
#69481 = VECTOR ( 'NONE', #153273, 1000.000000000000000 ) ;
#69482 = CARTESIAN_POINT ( 'NONE',  ( 0.05219959533907565091, 21.53943276465977519, 74.99890960531435269 ) ) ;
#69483 = CARTESIAN_POINT ( 'NONE',  ( -8.314922557961024197, 14.29746914071037800, 62.91775706135236135 ) ) ;
#69484 = CARTESIAN_POINT ( 'NONE',  ( -19.02544592524334988, -5.153800228976617603, 18.95942372801899722 ) ) ;
#69485 = CARTESIAN_POINT ( 'NONE',  ( 16.46253265017160672, -9.564922557960803928, 48.33224293864769550 ) ) ;
#69486 = CARTESIAN_POINT ( 'NONE',  ( 8.224510206698953496, -14.34966873604960469, 47.91557627198102409 ) ) ;
#69487 = CARTESIAN_POINT ( 'NONE',  ( -12.14591786802309592, -12.06949235617757132, 76.87390960531439532 ) ) ;
#69488 = CARTESIAN_POINT ( 'NONE',  ( -5.153800228976328057, -19.02544592524343514, 82.29057627198103830 ) ) ;
#69489 = CARTESIAN_POINT ( 'NONE',  ( 21.55341960407619695, -5.719274019375665929, 41.04275706135236135 ) ) ;
#69490 = CARTESIAN_POINT ( 'NONE',  ( 19.05341960407611168, 5.049401038298154454, 93.95724293864769550 ) ) ;
#69491 = CARTESIAN_POINT ( 'NONE',  ( 18.67979575497194134, -10.72451020669871369, 105.8344237280190328 ) ) ;
#69492 = CARTESIAN_POINT ( 'NONE',  ( -12.14591786802326823, 12.06949235617739902, 63.12609039468568994 ) ) ;
#69493 = CARTESIAN_POINT ( 'NONE',  ( -15.80617190586768217, 15.72974639402176855, 28.12609039468568284 ) ) ;
#69494 = CARTESIAN_POINT ( 'NONE',  ( -16.46253265017160317, 9.564922557960807481, 105.8322429386476955 ) ) ;
#69495 = CARTESIAN_POINT ( 'NONE',  ( 21.55341960407610458, 5.719274019375980345, 88.95724293864769550 ) ) ;
#69496 = CARTESIAN_POINT ( 'NONE',  ( 16.53943276465976808, -0.05219959533910856209, 48.74890960531435979 ) ) ;
#69497 = CARTESIAN_POINT ( 'NONE',  ( -9.474510206698964154, 16.51473224551069663, 35.41557627198102409 ) ) ;
#69498 = CARTESIAN_POINT ( 'NONE',  ( -12.06949235617756955, 12.14591786802309770, 65.62390960531436690 ) ) ;
#69499 = CARTESIAN_POINT ( 'NONE',  ( -5.823673210054116645, -21.52544592524344225, 32.29057627198102409 ) ) ;
#69500 = CARTESIAN_POINT ( 'NONE',  ( 16.46253265017146816, 9.564922557961045513, 26.66775706135234003 ) ) ;
#69501 = CARTESIAN_POINT ( 'NONE',  ( -14.29746914071049879, 8.314922557960819915, 95.83224293864770971 ) ) ;
#69502 = CARTESIAN_POINT ( 'NONE',  ( -16.46253265017160317, 9.564922557960807481, 105.8322429386476955 ) ) ;
#69503 = VERTEX_POINT ( 'NONE', #75569 ) ;
#69504 = CARTESIAN_POINT ( 'NONE',  ( -16.52544592524335698, -4.483927247898792601, 53.95942372801900433 ) ) ;
#69505 = CARTESIAN_POINT ( 'NONE',  ( 13.89961937509977652, -13.97604488694527269, 53.12390960531434558 ) ) ;
#69506 = CARTESIAN_POINT ( 'NONE',  ( -16.60608727067442558, -6.680868421854470718, 20.82238414752631073 ) ) ;
#69507 = CARTESIAN_POINT ( 'NONE',  ( 13.97604488694548053, -13.89961937509957401, 65.62609039468567573 ) ) ;
#69508 = CARTESIAN_POINT ( 'NONE',  ( -8.314922557961024197, 14.29746914071037800, 92.91775706135236135 ) ) ;
#69509 = CARTESIAN_POINT ( 'NONE',  ( 9.564922557961047289, -16.46253265017146816, 100.4177570613523329 ) ) ;
#69510 = CARTESIAN_POINT ( 'NONE',  ( 21.53943276465977519, 0.05219959533937863772, 71.25109039468568994 ) ) ;
#69511 = CARTESIAN_POINT ( 'NONE',  ( -9.564922557960796823, -16.46253265017161027, 72.08224293864770971 ) ) ;
#69512 = CARTESIAN_POINT ( 'NONE',  ( -21.55341960407610458, -5.719274019375992779, 86.45724293864770971 ) ) ;
#69513 = CARTESIAN_POINT ( 'NONE',  ( -4.379528057220086978, -16.55341960407618274, 44.79275706135234714 ) ) ;
#69515 = CARTESIAN_POINT ( 'NONE',  ( 16.55341960407611168, 4.379528057220329451, 108.9572429386476955 ) ) ;
#69514 = VECTOR ( 'NONE', #113856, 1000.000000000000000 ) ;
#69516 = CARTESIAN_POINT ( 'NONE',  ( -5.153800228976607833, 19.02544592524334988, 82.70942372801897591 ) ) ;
#69517 = CARTESIAN_POINT ( 'NONE',  ( -15.80617190586745835, -15.72974639402198527, 71.87390960531438111 ) ) ;
#69518 = CARTESIAN_POINT ( 'NONE',  ( -5.049401038297874678, -19.05341960407617918, 44.79275706135232582 ) ) ;
#69519 = DIRECTION ( 'NONE',  ( 1.000000000000000000, 0.000000000000000000, 0.000000000000000000 ) ) ;
#69520 = CARTESIAN_POINT ( 'NONE',  ( 0.05219959533907565091, 21.53943276465977519, 89.99890960531438111 ) ) ;
#69521 = CARTESIAN_POINT ( 'NONE',  ( 17.50000000000147082, 3.202012800152233662, 27.57177583972747215 ) ) ;
#69522 = CARTESIAN_POINT ( 'NONE',  ( -5.049401038298153566, 19.05341960407611168, 65.20724293864765286 ) ) ;
#69523 = DIRECTION ( 'NONE',  ( -0.000000000000000000, 0.3420201433256656043, 0.9396926207859095381 ) ) ;
#69524 = CARTESIAN_POINT ( 'NONE',  ( -14.29746914071037622, -8.314922557961029526, 24.16775706135235424 ) ) ;
#69525 = DIRECTION ( 'NONE',  ( 1.000000000000000000, -0.000000000000000000, -0.000000000000000000 ) ) ;
#69526 = CARTESIAN_POINT ( 'NONE',  ( -9.564922557960796823, -16.46253265017161027, 52.08224293864768839 ) ) ;
#69528 = CARTESIAN_POINT ( 'NONE',  ( -0.05219959533910754901, -16.53943276465976808, 57.49890960531435979 ) ) ;
#69527 = CARTESIAN_POINT ( 'NONE',  ( 5.719274019375991003, -21.55341960407610458, 107.7072429386476955 ) ) ;
#69529 = CARTESIAN_POINT ( 'NONE',  ( 19.02544592524343514, -5.153800228976328945, 53.54057627198102409 ) ) ;
#69530 = CIRCLE ( 'NONE', #108348, 1.000000000000000888 ) ;
#69531 = CARTESIAN_POINT ( 'NONE',  ( -21.52544592524334988, -5.823673210054445271, 73.95942372801901854 ) ) ;
#69533 = CARTESIAN_POINT ( 'NONE',  ( 19.05341960407617918, -5.049401038297876454, 26.04275706135233293 ) ) ;
#69532 = CARTESIAN_POINT ( 'NONE',  ( 4.483927247898790824, -16.52544592524335698, 20.20942372801900788 ) ) ;
#69534 = CARTESIAN_POINT ( 'NONE',  ( 16.52544592524342804, -4.483927247898539470, 33.54057627198102409 ) ) ;
#69535 = CARTESIAN_POINT ( 'NONE',  ( -5.719274019375665041, -21.55341960407619695, 44.79275706135234714 ) ) ;
#69536 = CARTESIAN_POINT ( 'NONE',  ( 10.81492255796106328, -18.62759615963255655, 20.41775706135234714 ) ) ;
#69537 = CARTESIAN_POINT ( 'NONE',  ( -15.72974639402197994, 15.80617190586746368, 65.62390960531436690 ) ) ;
#69538 = CARTESIAN_POINT ( 'NONE',  ( 5.153800228976615827, -19.02544592524334988, 95.20942372801897591 ) ) ;
#69539 = CARTESIAN_POINT ( 'NONE',  ( -0.05219959533936034679, 19.03943276465977164, 62.50109039468566863 ) ) ;
#69540 = CARTESIAN_POINT ( 'NONE',  ( 18.67979575497194134, -10.72451020669871369, 65.83442372801900433 ) ) ;
#69541 = CARTESIAN_POINT ( 'NONE',  ( -13.89961937509957401, -13.97604488694547875, 54.37609039468565442 ) ) ;
#69542 = CARTESIAN_POINT ( 'NONE',  ( -19.03943276465977164, 0.05219959533909376836, 21.24890960531436335 ) ) ;
#69543 = CARTESIAN_POINT ( 'NONE',  ( 15.80617190586746368, 15.72974639402197994, 59.37390960531436690 ) ) ;
#69544 = CARTESIAN_POINT ( 'NONE',  ( -0.05219959533910754901, -16.53943276465976808, 47.49890960531435979 ) ) ;
#69545 = CARTESIAN_POINT ( 'NONE',  ( -19.35633801406907750, 5.499999999999677591, 94.13373818172762242 ) ) ;
#69546 = CARTESIAN_POINT ( 'NONE',  ( 21.52544592524334988, 5.823673210054432836, 111.4594237280190328 ) ) ;
#69547 = CARTESIAN_POINT ( 'NONE',  ( 8.224510206698742110, 14.34966873604972548, 87.08442372801901854 ) ) ;
#69548 = CARTESIAN_POINT ( 'NONE',  ( 16.55341960407611168, 4.379528057220329451, 38.95724293864768839 ) ) ;
#69549 = CARTESIAN_POINT ( 'NONE',  ( -5.719274019375665041, -21.55341960407619695, 79.79275706135236135 ) ) ;
#69550 = CARTESIAN_POINT ( 'NONE',  ( 10.81492255796106328, -18.62759615963255655, 75.41775706135233293 ) ) ;
#69551 = CARTESIAN_POINT ( 'NONE',  ( -21.55341960407610458, -5.719274019375992779, 81.45724293864769550 ) ) ;
#69552 = CARTESIAN_POINT ( 'NONE',  ( 19.02544592524343514, -5.153800228976328945, 43.54057627198103120 ) ) ;
#69553 = CARTESIAN_POINT ( 'NONE',  ( 21.55341960407619695, -5.719274019375665929, 61.04275706135234714 ) ) ;
#69554 = CARTESIAN_POINT ( 'NONE',  ( -9.474510206698964154, 16.51473224551069663, 35.41557627198102409 ) ) ;
#69555 = CARTESIAN_POINT ( 'NONE',  ( 19.02544592524343514, -5.153800228976328945, 53.54057627198102409 ) ) ;
#69556 = CARTESIAN_POINT ( 'NONE',  ( 12.06949235617757843, -12.14591786802309237, 88.12390960531436690 ) ) ;
#69557 = CARTESIAN_POINT ( 'NONE',  ( -16.46253265017160317, 9.564922557960807481, 100.8322429386477097 ) ) ;
#69558 = CARTESIAN_POINT ( 'NONE',  ( -14.29746914071049879, 8.314922557960819915, 40.83224293864769550 ) ) ;
#69559 = CARTESIAN_POINT ( 'NONE',  ( -4.379528057220328563, 16.55341960407611168, 110.2072429386477239 ) ) ;
#69560 = CARTESIAN_POINT ( 'NONE',  ( -15.72974639402197994, 15.80617190586746368, 80.62390960531438111 ) ) ;
#69561 = CARTESIAN_POINT ( 'NONE',  ( -0.05219959533937732626, 21.53943276465977519, 22.50109039468567573 ) ) ;
#69562 = DIRECTION ( 'NONE',  ( -1.000000000000000000, -0.000000000000000000, -0.000000000000000000 ) ) ;
#69563 = CARTESIAN_POINT ( 'NONE',  ( -16.52544592524335698, -4.483927247898792601, 38.95942372801901854 ) ) ;
#69564 = CARTESIAN_POINT ( 'NONE',  ( 0.05219959533907565091, 21.53943276465977519, 74.99890960531435269 ) ) ;
#69565 = CARTESIAN_POINT ( 'NONE',  ( -5.719274019375665041, -21.55341960407619695, 94.79275706135234714 ) ) ;
#69566 = CARTESIAN_POINT ( 'NONE',  ( -19.02544592524342804, 5.153800228976336051, 76.04057627198102409 ) ) ;
#69567 = CARTESIAN_POINT ( 'NONE',  ( -15.72974639402176322, -15.80617190586768395, 24.37609039468567573 ) ) ;
#69568 = EDGE_CURVE ( 'NONE', #27470, #116009, #192870, .T. ) ;
#69569 = CARTESIAN_POINT ( 'NONE',  ( 0.05219959533909260263, 19.03943276465977164, 114.9989096053143669 ) ) ;
#69570 = CARTESIAN_POINT ( 'NONE',  ( 14.34966873604972726, -8.224510206698740333, 95.83442372801903275 ) ) ;
#69571 = CARTESIAN_POINT ( 'NONE',  ( -15.80617190586768217, 15.72974639402176855, 73.12609039468567573 ) ) ;
#69572 = CARTESIAN_POINT ( 'NONE',  ( 13.97604488694548053, -13.89961937509957401, 20.62609039468567573 ) ) ;
#69573 = CARTESIAN_POINT ( 'NONE',  ( 16.53943276465976808, 0.05219959533934440121, 71.25109039468568994 ) ) ;
#69574 = CARTESIAN_POINT ( 'NONE',  ( 0.05219959533937995610, -21.53943276465977519, 30.00109039468568284 ) ) ;
#69575 = CARTESIAN_POINT ( 'NONE',  ( -16.46253265017160317, 9.564922557960807481, 30.83224293864769550 ) ) ;
#69576 = CARTESIAN_POINT ( 'NONE',  ( -15.72974639402176322, -15.80617190586768395, 89.37609039468568994 ) ) ;
#69577 = CARTESIAN_POINT ( 'NONE',  ( 5.153800228976335163, 19.02544592524342804, 94.79057627198103830 ) ) ;
#69578 = CARTESIAN_POINT ( 'NONE',  ( -18.67979575497178146, -10.72451020669898902, 96.66557627198102409 ) ) ;
#69580 = CARTESIAN_POINT ( 'NONE',  ( 5.823673210054125526, 21.52544592524343514, 54.79057627198104541 ) ) ;
#69579 = CARTESIAN_POINT ( 'NONE',  ( 69.65682714487590488, -71.74905178543389184, 0.000000000000000000 ) ) ;
#69582 = CARTESIAN_POINT ( 'NONE',  ( 12.06949235617757843, -12.14591786802309237, 48.12390960531436690 ) ) ;
#69581 = CARTESIAN_POINT ( 'NONE',  ( -16.51473224551069308, -9.474510206698971260, 96.66557627198102409 ) ) ;
#69583 = CARTESIAN_POINT ( 'NONE',  ( 11.82759615478249593, -9.696917953820088698, -61.96080966668566248 ) ) ;
#69584 = CARTESIAN_POINT ( 'NONE',  ( 16.51473224551083163, -9.474510206698727899, 75.83442372801900433 ) ) ;
#69585 = CARTESIAN_POINT ( 'NONE',  ( 5.199999999999996625, 3.306546357697854226E-16, 2.700000000000000622 ) ) ;
#69586 = CARTESIAN_POINT ( 'NONE',  ( 5.049401038297881783, 19.05341960407617563, 107.2927570613523187 ) ) ;
#69587 = CARTESIAN_POINT ( 'NONE',  ( 15.80617190586746368, 15.72974639402197994, 89.37390960531435269 ) ) ;
#69588 = CARTESIAN_POINT ( 'NONE',  ( -16.55341960407611168, -4.379528057220339221, 66.45724293864768129 ) ) ;
#69589 = CARTESIAN_POINT ( 'NONE',  ( -16.51473224551069308, -9.474510206698971260, 96.66557627198102409 ) ) ;
#69590 = CARTESIAN_POINT ( 'NONE',  ( -16.52544592524335698, -4.483927247898792601, 38.95942372801901854 ) ) ;
#69591 = CARTESIAN_POINT ( 'NONE',  ( -13.89961937509977652, 13.97604488694528158, 55.62390960531434558 ) ) ;
#69593 = CARTESIAN_POINT ( 'NONE',  ( -16.51473224551082808, 9.474510206698731452, 98.33442372801900433 ) ) ;
#69592 = CARTESIAN_POINT ( 'NONE',  ( 15.72974639402176855, 15.80617190586768217, 26.87609039468567218 ) ) ;
#69594 = CARTESIAN_POINT ( 'NONE',  ( -5.049401038298153566, 19.05341960407611168, 100.2072429386476955 ) ) ;
#69595 = CARTESIAN_POINT ( 'NONE',  ( 5.049401038298161559, -19.05341960407611168, 87.70724293864769550 ) ) ;
#69596 = CARTESIAN_POINT ( 'NONE',  ( -10.72451020669898014, 18.67979575497178502, 90.41557627198103830 ) ) ;
#69597 = CARTESIAN_POINT ( 'NONE',  ( 16.46253265017160672, -9.564922557960803928, 48.33224293864769550 ) ) ;
#69598 = CARTESIAN_POINT ( 'NONE',  ( -17.05116617787826883, -6.768360034955705373, 61.34324446740804859 ) ) ;
#69599 = CARTESIAN_POINT ( 'NONE',  ( 14.34966873604960469, 8.224510206698951720, 74.16557627198102409 ) ) ;
#69600 = CARTESIAN_POINT ( 'NONE',  ( -16.51473224551069308, -9.474510206698971260, 106.6655762719810383 ) ) ;
#69601 = CARTESIAN_POINT ( 'NONE',  ( -29.18776880969891607, 0.8894290736110457285, -52.33677266386640525 ) ) ;
#69602 = CARTESIAN_POINT ( 'NONE',  ( -5.049401038297874678, -19.05341960407617918, 59.79275706135231871 ) ) ;
#69603 = CIRCLE ( 'NONE', #198797, 2.649999999999992806 ) ;
#69604 = CARTESIAN_POINT ( 'NONE',  ( -21.55341960407610458, -5.719274019375992779, 86.45724293864770971 ) ) ;
#69605 = CARTESIAN_POINT ( 'NONE',  ( 13.97604488694548053, -13.89961937509957401, 55.62609039468566863 ) ) ;
#69606 = CARTESIAN_POINT ( 'NONE',  ( -19.03943276465977164, 0.05219959533909376836, 106.2489096053143669 ) ) ;
#69607 = CYLINDRICAL_SURFACE ( 'NONE', #37171, 37.99626262588765968 ) ;
#69608 = CARTESIAN_POINT ( 'NONE',  ( -18.62759615963270932, 10.81492255796079327, 40.83224293864769550 ) ) ;
#69609 = CARTESIAN_POINT ( 'NONE',  ( 16.46253265017160672, -9.564922557960803928, 88.33224293864769550 ) ) ;
#69610 = CARTESIAN_POINT ( 'NONE',  ( 21.55341960407619695, -5.719274019375665929, 66.04275706135236135 ) ) ;
#69611 = CARTESIAN_POINT ( 'NONE',  ( -9.564922557960796823, -16.46253265017161027, 32.08224293864769550 ) ) ;
#69612 = CARTESIAN_POINT ( 'NONE',  ( -16.52544592524342804, 4.483927247898546575, 76.04057627198102409 ) ) ;
#69613 = CARTESIAN_POINT ( 'NONE',  ( -8.314922557961024197, 14.29746914071037800, 22.91775706135235069 ) ) ;
#69614 = CARTESIAN_POINT ( 'NONE',  ( 18.62759615963255655, 10.81492255796105972, 56.66775706135235424 ) ) ;
#69615 = ORIENTED_EDGE ( 'NONE', *, *, #157116, .T. ) ;
#69616 = CARTESIAN_POINT ( 'NONE',  ( -9.474510206698964154, 16.51473224551069663, 115.4155762719810241 ) ) ;
#69617 = CARTESIAN_POINT ( 'NONE',  ( 5.049401038297881783, 19.05341960407617563, 62.29275706135234003 ) ) ;
#69618 = CARTESIAN_POINT ( 'NONE',  ( -19.80295450558176640, 12.05995242899444797, 167.9999999999999716 ) ) ;
#69619 = CARTESIAN_POINT ( 'NONE',  ( 15.80617190586769283, -15.72974639402175789, 20.62609039468568639 ) ) ;
#69620 = CARTESIAN_POINT ( 'NONE',  ( 19.03943276465977164, -0.05219959533909143690, 63.74890960531435979 ) ) ;
#69621 = CARTESIAN_POINT ( 'NONE',  ( 38.00000000000000711, -12.34694845685040754, -4.849999994537625092 ) ) ;
#69622 = CARTESIAN_POINT ( 'NONE',  ( -16.46253265017146816, -9.564922557961047289, 24.16775706135233648 ) ) ;
#69623 = CARTESIAN_POINT ( 'NONE',  ( -19.05341960407611168, -5.049401038298163336, 56.45724293864768129 ) ) ;
#69624 = CARTESIAN_POINT ( 'NONE',  ( -21.55341960407619339, 5.719274019375674811, 108.5427570613523756 ) ) ;
#69625 = CARTESIAN_POINT ( 'NONE',  ( 14.34966873604972726, -8.224510206698740333, 105.8344237280190328 ) ) ;
#69627 = CARTESIAN_POINT ( 'NONE',  ( -15.80617190586768217, 15.72974639402176855, 73.12609039468567573 ) ) ;
#69626 = CARTESIAN_POINT ( 'NONE',  ( 9.474510206698971260, -16.51473224551069308, 107.9155762719810383 ) ) ;
#69628 = CARTESIAN_POINT ( 'NONE',  ( 8.571926809382603096, -26.38167802310801235, 147.9750000027311785 ) ) ;
#69629 = CARTESIAN_POINT ( 'NONE',  ( 5.153800228976335163, 19.02544592524342804, 109.7905762719810099 ) ) ;
#69630 = CARTESIAN_POINT ( 'NONE',  ( 17.50000000000000000, 5.499999999999992895, 96.70309617465829888 ) ) ;
#69632 = CARTESIAN_POINT ( 'NONE',  ( -21.52544592524334988, -5.823673210054445271, 73.95942372801901854 ) ) ;
#69631 = CARTESIAN_POINT ( 'NONE',  ( 8.314922557961029526, -14.29746914071037800, 60.41775706135235424 ) ) ;
#69633 = CARTESIAN_POINT ( 'NONE',  ( -21.53943276465977519, -0.05219959533937600094, 108.7510903946857042 ) ) ;
#69634 = DIRECTION ( 'NONE',  ( -1.000000000000000000, 0.000000000000000000, 0.000000000000000000 ) ) ;
#69635 = CARTESIAN_POINT ( 'NONE',  ( 16.46253265017160672, -9.564922557960803928, 88.33224293864769550 ) ) ;
#69636 = CARTESIAN_POINT ( 'NONE',  ( -19.03943276465977164, 0.05219959533909376836, 106.2489096053143669 ) ) ;
#69637 = ORIENTED_EDGE ( 'NONE', *, *, #133011, .F. ) ;
#69638 = CARTESIAN_POINT ( 'NONE',  ( 17.48847506799967277, 5.747544572773803928, 41.67302562156719858 ) ) ;
#69639 = CARTESIAN_POINT ( 'NONE',  ( 9.564922557960805705, 16.46253265017160317, 39.58224293864768839 ) ) ;
#69640 = CARTESIAN_POINT ( 'NONE',  ( 10.81492255796078972, 18.62759615963270932, 39.58224293864769550 ) ) ;
#69641 = CARTESIAN_POINT ( 'NONE',  ( 8.314922557961029526, -14.29746914071037800, 110.4177570613523756 ) ) ;
#69643 = CARTESIAN_POINT ( 'NONE',  ( 9.474510206698971260, -16.51473224551069308, 82.91557627198103830 ) ) ;
#69642 = CARTESIAN_POINT ( 'NONE',  ( 16.55341960407611168, 4.379528057220329451, 98.95724293864770971 ) ) ;
#69644 = CARTESIAN_POINT ( 'NONE',  ( -21.55341960407619339, 5.719274019375674811, 103.5427570613523613 ) ) ;
#69645 = CARTESIAN_POINT ( 'NONE',  ( 16.51473224551069308, 9.474510206698969483, 34.16557627198102409 ) ) ;
#69646 = CARTESIAN_POINT ( 'NONE',  ( 16.52544592524342804, -4.483927247898539470, 93.54057627198103830 ) ) ;
#69647 = CARTESIAN_POINT ( 'NONE',  ( 10.81492255796106328, -18.62759615963255655, 40.41775706135234714 ) ) ;
#69648 = CARTESIAN_POINT ( 'NONE',  ( 15.80617190586746368, 15.72974639402197994, 84.37390960531438111 ) ) ;
#69649 = CARTESIAN_POINT ( 'NONE',  ( -9.474510206698720793, -16.51473224551083518, 49.58442372801899722 ) ) ;
#69650 = CARTESIAN_POINT ( 'NONE',  ( 18.22780087662121673, 5.500000000000056843, 63.98459894673894155 ) ) ;
#69651 = CARTESIAN_POINT ( 'NONE',  ( 9.564922557960805705, 16.46253265017160317, 99.58224293864770971 ) ) ;
#69652 = CARTESIAN_POINT ( 'NONE',  ( 12.14591786802309770, 12.06949235617756955, 69.37390960531436690 ) ) ;
#69653 = CARTESIAN_POINT ( 'NONE',  ( 16.53943276465976808, -0.05219959533910856209, 53.74890960531437401 ) ) ;
#69654 = CARTESIAN_POINT ( 'NONE',  ( -9.474510206698720793, -16.51473224551083518, 84.58442372801900433 ) ) ;
#69655 = CARTESIAN_POINT ( 'NONE',  ( 0.000000000000000000, 0.000000000000000000, -25.00000000000000000 ) ) ;
#69656 = CARTESIAN_POINT ( 'NONE',  ( 21.53943276465977519, -0.05219959533907433946, 23.74890960531435269 ) ) ;
#69657 = ADVANCED_FACE ( 'NONE', ( #47236, #153408, #33060, #94715, #137245, #93721, #141220, #170574, #32065, #45248, #168575, #76568, #199927, #61390, #46233, #173568, #37021, #126056 ), #175546, .T. ) ;
#69658 = CARTESIAN_POINT ( 'NONE',  ( -14.29746914071049879, 8.314922557960819915, 90.83224293864769550 ) ) ;
#69659 = DIRECTION ( 'NONE',  ( -1.000000000000000000, 0.000000000000000000, 0.000000000000000000 ) ) ;
#69661 = CARTESIAN_POINT ( 'NONE',  ( 21.53943276465977519, -0.05219959533907433946, 53.74890960531437401 ) ) ;
#69660 = CARTESIAN_POINT ( 'NONE',  ( -19.02544592524342804, 5.153800228976336051, 51.04057627198103120 ) ) ;
#69662 = CARTESIAN_POINT ( 'NONE',  ( -19.05341960407611168, -5.049401038298163336, 31.45724293864769550 ) ) ;
#69664 = CARTESIAN_POINT ( 'NONE',  ( 19.05341960407611168, 5.049401038298154454, 63.95724293864769550 ) ) ;
#69663 = CARTESIAN_POINT ( 'NONE',  ( -16.55341960407617563, 4.379528057220093196, 73.54275706135234714 ) ) ;
#69665 = CARTESIAN_POINT ( 'NONE',  ( -5.049401038297874678, -19.05341960407617918, 34.79275706135233293 ) ) ;
#69666 = CARTESIAN_POINT ( 'NONE',  ( -21.52544592524334988, -5.823673210054445271, 73.95942372801901854 ) ) ;
#69667 = CARTESIAN_POINT ( 'NONE',  ( -21.53943276465977519, 0.05219959533907696930, 31.24890960531435979 ) ) ;
#69668 = CARTESIAN_POINT ( 'NONE',  ( -0.05219959533910754901, -16.53943276465976808, 112.4989096053143669 ) ) ;
#69669 = CARTESIAN_POINT ( 'NONE',  ( -19.02544592524334988, -5.153800228976617603, 88.95942372801897591 ) ) ;
#69670 = CARTESIAN_POINT ( 'NONE',  ( 22.81625015709510151, -31.40387420917324590, -6.424999997268811214 ) ) ;
#69672 = CARTESIAN_POINT ( 'NONE',  ( 5.719274019375991003, -21.55341960407610458, 42.70724293864770260 ) ) ;
#69671 = CARTESIAN_POINT ( 'NONE',  ( 17.50000000000000711, 3.556738311678228737, 37.24728836128200982 ) ) ;
#69673 = CARTESIAN_POINT ( 'NONE',  ( 16.52216118717209525, -7.221426719304495201, 66.42400978953006074 ) ) ;
#69674 = CARTESIAN_POINT ( 'NONE',  ( 10.72451020669871369, 18.67979575497193778, 77.08442372801901854 ) ) ;
#69675 = CARTESIAN_POINT ( 'NONE',  ( -12.14591786802309592, -12.06949235617757132, 46.87390960531435979 ) ) ;
#69677 = CARTESIAN_POINT ( 'NONE',  ( 4.483927247898545687, 16.52544592524342804, 54.79057627198104541 ) ) ;
#69676 = CARTESIAN_POINT ( 'NONE',  ( 0.05219959533934541429, -16.53943276465976808, 75.00109039468568994 ) ) ;
#69678 = CARTESIAN_POINT ( 'NONE',  ( -15.72974639402197994, 15.80617190586746368, 80.62390960531438111 ) ) ;
#69679 = CARTESIAN_POINT ( 'NONE',  ( -21.53943276465977519, 0.05219959533907696930, 81.24890960531436690 ) ) ;
#69680 = DIRECTION ( 'NONE',  ( -0.000000000000000000, -0.000000000000000000, -1.000000000000000000 ) ) ;
#69681 = CARTESIAN_POINT ( 'NONE',  ( -15.80617190586745835, -15.72974639402198527, 26.87390960531435979 ) ) ;
#69682 = CARTESIAN_POINT ( 'NONE',  ( -4.483927247898782831, 16.52544592524335698, 47.70942372801902565 ) ) ;
#69683 = CARTESIAN_POINT ( 'NONE',  ( -16.55341960407611168, -4.379528057220339221, 76.45724293864769550 ) ) ;
#69684 = CARTESIAN_POINT ( 'NONE',  ( 5.153800228976335163, 19.02544592524342804, 64.79057627198100988 ) ) ;
#69685 = CARTESIAN_POINT ( 'NONE',  ( 9.474510206698971260, -16.51473224551069308, 37.91557627198102409 ) ) ;
#69686 = LINE ( 'NONE', #162692, #176945 ) ;
#69687 = CARTESIAN_POINT ( 'NONE',  ( -16.53943276465976808, -0.05219959533934237506, 83.75109039468568994 ) ) ;
#69688 = CARTESIAN_POINT ( 'NONE',  ( 10.81492255796106328, -18.62759615963255655, 20.41775706135234714 ) ) ;
#69689 = CARTESIAN_POINT ( 'NONE',  ( -19.05341960407611168, -5.049401038298163336, 66.45724293864769550 ) ) ;
#69690 = CARTESIAN_POINT ( 'NONE',  ( -10.72451020669870658, -18.67979575497194134, 54.58442372801901143 ) ) ;
#69691 = CARTESIAN_POINT ( 'NONE',  ( -16.46253265017160317, 9.564922557960807481, 115.8322429386477097 ) ) ;
#69692 = CARTESIAN_POINT ( 'NONE',  ( -6.767138868727710310, -40.03474714072286389, -25.59093536067524610 ) ) ;
#69693 = ORIENTED_EDGE ( 'NONE', *, *, #12667, .T. ) ;
#69694 = CARTESIAN_POINT ( 'NONE',  ( 18.67979575497194134, -10.72451020669871369, 45.83442372801901854 ) ) ;
#69696 = CARTESIAN_POINT ( 'NONE',  ( 19.05341960407611168, 5.049401038298154454, 103.9572429386476671 ) ) ;
#69695 = CARTESIAN_POINT ( 'NONE',  ( -16.46253265017160317, 9.564922557960807481, 115.8322429386477097 ) ) ;
#69697 = CARTESIAN_POINT ( 'NONE',  ( -16.51473224551082808, 9.474510206698731452, 58.33442372801900433 ) ) ;
#69698 = CARTESIAN_POINT ( 'NONE',  ( 21.53943276465977519, 0.05219959533937863772, 21.25109039468567218 ) ) ;
#69699 = CARTESIAN_POINT ( 'NONE',  ( 5.153800228976615827, -19.02544592524334988, 45.20942372801901143 ) ) ;
#69700 = CARTESIAN_POINT ( 'NONE',  ( -19.05341960407617563, 5.049401038297882671, 63.54275706135234003 ) ) ;
#69701 = CARTESIAN_POINT ( 'NONE',  ( -14.34966873604972548, 8.224510206698743886, 103.3344237280190043 ) ) ;
#69703 = EDGE_LOOP ( 'NONE', ( #56921, #199659, #181360, #98385 ) ) ;
#69702 = DIRECTION ( 'NONE',  ( 1.000000000000000000, 0.000000000000000000, 0.000000000000000000 ) ) ;
#69704 = CARTESIAN_POINT ( 'NONE',  ( -9.474510206698964154, 16.51473224551069663, 80.41557627198103830 ) ) ;
#69705 = VECTOR ( 'NONE', #137265, 1000.000000000000000 ) ;
#69706 = CARTESIAN_POINT ( 'NONE',  ( -0.05219959533937732626, 21.53943276465977519, 87.50109039468568994 ) ) ;
#69707 = CARTESIAN_POINT ( 'NONE',  ( 18.62759615963255655, 10.81492255796105972, 91.66775706135234714 ) ) ;
#69708 = CARTESIAN_POINT ( 'NONE',  ( 4.500000000000000888, -139.5000000000000000, 13.35010376910484098 ) ) ;
#69709 = CARTESIAN_POINT ( 'NONE',  ( -9.564922557960796823, -16.46253265017161027, 102.0822429386477097 ) ) ;
#69710 = CARTESIAN_POINT ( 'NONE',  ( -18.62759615963255300, -10.81492255796106328, 79.16775706135234714 ) ) ;
#69711 = CARTESIAN_POINT ( 'NONE',  ( -16.52544592524335698, -4.483927247898792601, 18.95942372801901143 ) ) ;
#69712 = CARTESIAN_POINT ( 'NONE',  ( -13.89961937509977652, 13.97604488694528158, 75.62390960531438111 ) ) ;
#69713 = CARTESIAN_POINT ( 'NONE',  ( 5.719274019375991003, -21.55341960407610458, 27.70724293864769905 ) ) ;
#69714 = CARTESIAN_POINT ( 'NONE',  ( -16.46253265017160317, 9.564922557960807481, 90.83224293864769550 ) ) ;
#69715 = CARTESIAN_POINT ( 'NONE',  ( -16.88567814943164436, -6.947325034625694506, 91.29001122652587696 ) ) ;
#69716 = CARTESIAN_POINT ( 'NONE',  ( 9.564922557960805705, 16.46253265017160317, 79.58224293864769550 ) ) ;
#69717 = CARTESIAN_POINT ( 'NONE',  ( 19.05341960407611168, 5.049401038298154454, 63.95724293864769550 ) ) ;
#69718 = CARTESIAN_POINT ( 'NONE',  ( -15.72974639402197994, 15.80617190586746368, 110.6239096053143669 ) ) ;
#69719 = CARTESIAN_POINT ( 'NONE',  ( -4.483927247898782831, 16.52544592524335698, 102.7094237280190185 ) ) ;
#69720 = DIRECTION ( 'NONE',  ( -1.000000000000000000, 0.000000000000000000, 0.000000000000000000 ) ) ;
#69721 = CARTESIAN_POINT ( 'NONE',  ( 0.05219959533936267826, -19.03943276465977164, 60.00109039468566863 ) ) ;
#69722 = CARTESIAN_POINT ( 'NONE',  ( 9.474510206698971260, -16.51473224551069308, 97.91557627198102409 ) ) ;
#69723 = CARTESIAN_POINT ( 'NONE',  ( -0.05219959533910754901, -16.53943276465976808, 87.49890960531436690 ) ) ;
#69724 = CARTESIAN_POINT ( 'NONE',  ( 21.55341960407610458, 5.719274019375980345, 33.95724293864769550 ) ) ;
#69725 = CARTESIAN_POINT ( 'NONE',  ( -5.153800228976328057, -19.02544592524343514, 112.2905762719810099 ) ) ;
#69726 = CARTESIAN_POINT ( 'NONE',  ( 12.06949235617757843, -12.14591786802309237, 93.12390960531436690 ) ) ;
#69727 = CARTESIAN_POINT ( 'NONE',  ( -17.31728774477274158, 6.344390552232391123, 55.81906651689321563 ) ) ;
#69728 = CARTESIAN_POINT ( 'NONE',  ( 19.02544592524334988, 5.153800228976608722, 41.45942372801900433 ) ) ;
#69729 = CARTESIAN_POINT ( 'NONE',  ( -14.29746914071037622, -8.314922557961029526, 104.1677570613523471 ) ) ;
#69730 = CARTESIAN_POINT ( 'NONE',  ( 5.049401038298161559, -19.05341960407611168, 87.70724293864769550 ) ) ;
#69731 = CARTESIAN_POINT ( 'NONE',  ( 15.72974639402176855, 15.80617190586768217, 66.87609039468568994 ) ) ;
#69732 = CARTESIAN_POINT ( 'NONE',  ( -21.55341960407610458, -5.719274019375992779, 51.45724293864770260 ) ) ;
#69733 = CARTESIAN_POINT ( 'NONE',  ( 15.80617190586769283, -15.72974639402175789, 35.62609039468568994 ) ) ;
#69734 = CARTESIAN_POINT ( 'NONE',  ( 18.62759615963271287, -10.81492255796078972, 88.33224293864769550 ) ) ;
#69735 = CARTESIAN_POINT ( 'NONE',  ( 16.52544592524342804, -4.483927247898539470, 103.5405762719810383 ) ) ;
#69736 = CARTESIAN_POINT ( 'NONE',  ( -13.89961937509957401, -13.97604488694547875, 74.37609039468566152 ) ) ;
#69737 = CARTESIAN_POINT ( 'NONE',  ( 9.564922557960805705, 16.46253265017160317, 44.58224293864769550 ) ) ;
#69738 = CARTESIAN_POINT ( 'NONE',  ( 16.51473224551069308, 9.474510206698969483, 99.16557627198102409 ) ) ;
#69739 = CARTESIAN_POINT ( 'NONE',  ( 19.05341960407611168, 5.049401038298154454, 88.95724293864769550 ) ) ;
#69740 = CARTESIAN_POINT ( 'NONE',  ( 12.14591786802309770, 12.06949235617756955, 114.3739096053143527 ) ) ;
#69741 = CARTESIAN_POINT ( 'NONE',  ( -4.379528057220328563, 16.55341960407611168, 45.20724293864769550 ) ) ;
#69742 = CARTESIAN_POINT ( 'NONE',  ( -16.55341960407617563, 4.379528057220093196, 38.54275706135234714 ) ) ;
#69743 = CARTESIAN_POINT ( 'NONE',  ( 5.153800228976335163, 19.02544592524342804, 24.79057627198102765 ) ) ;
#69744 = CARTESIAN_POINT ( 'NONE',  ( 10.81492255796106328, -18.62759615963255655, 100.4177570613523471 ) ) ;
#69746 = CARTESIAN_POINT ( 'NONE',  ( 4.379528057220339221, -16.55341960407611168, 22.70724293864769194 ) ) ;
#69745 = CARTESIAN_POINT ( 'NONE',  ( 19.03943276465977164, -0.05219959533909143690, 108.7489096053143527 ) ) ;
#69747 = CARTESIAN_POINT ( 'NONE',  ( -10.72451020669870658, -18.67979575497194134, 29.58442372801901854 ) ) ;
#69748 = CARTESIAN_POINT ( 'NONE',  ( 0.05219959533909260263, 19.03943276465977164, 104.9989096053143669 ) ) ;
#69749 = CARTESIAN_POINT ( 'NONE',  ( 12.06949235617739724, 12.14591786802326823, 51.87609039468568284 ) ) ;
#69750 = CARTESIAN_POINT ( 'NONE',  ( 12.14591786802327356, -12.06949235617739191, 110.6260903946857042 ) ) ;
#69751 = CARTESIAN_POINT ( 'NONE',  ( 8.224510206698742110, 14.34966873604972548, 87.08442372801901854 ) ) ;
#69752 = CARTESIAN_POINT ( 'NONE',  ( 14.29746914071037800, 8.314922557961029526, 31.66775706135234358 ) ) ;
#69753 = CARTESIAN_POINT ( 'NONE',  ( -13.97604488694527625, -13.89961937509977652, 51.87390960531436690 ) ) ;
#69754 = CARTESIAN_POINT ( 'NONE',  ( 14.29746914071049879, -8.314922557960816363, 103.3322429386476955 ) ) ;
#69755 = CARTESIAN_POINT ( 'NONE',  ( 18.67979575497194134, -10.72451020669871369, 20.83442372801901143 ) ) ;
#69756 = CARTESIAN_POINT ( 'NONE',  ( -5.049401038298153566, 19.05341960407611168, 30.20724293864768839 ) ) ;
#69757 = CARTESIAN_POINT ( 'NONE',  ( 16.51473224551069308, 9.474510206698969483, 99.16557627198102409 ) ) ;
#69758 = CARTESIAN_POINT ( 'NONE',  ( -9.564922557960796823, -16.46253265017161027, 32.08224293864769550 ) ) ;
#69759 = EDGE_CURVE ( 'NONE', #122026, #45563, #70190, .T. ) ;
#69760 = CARTESIAN_POINT ( 'NONE',  ( 16.46253265017160672, -9.564922557960803928, 98.33224293864769550 ) ) ;
#69761 = DIRECTION ( 'NONE',  ( 0.7071067811865414665, -0.7071067811865536790, -0.000000000000000000 ) ) ;
#69762 = CARTESIAN_POINT ( 'NONE',  ( -5.153800228976328057, -19.02544592524343514, 102.2905762719810383 ) ) ;
#69764 = CARTESIAN_POINT ( 'NONE',  ( 0.05219959533910956823, 16.53943276465976808, 94.99890960531436690 ) ) ;
#69763 = CARTESIAN_POINT ( 'NONE',  ( -21.52544592524334988, -5.823673210054445271, 43.95942372801902565 ) ) ;
#69765 = CARTESIAN_POINT ( 'NONE',  ( 5.153800228976335163, 19.02544592524342804, 114.7905762719810241 ) ) ;
#69766 = CARTESIAN_POINT ( 'NONE',  ( -3.573655867282028392E-15, 2.428612866367529932E-14, 167.9999999999999716 ) ) ;
#69768 =( BOUNDED_SURFACE ( )  B_SPLINE_SURFACE ( 3, 2, ( 
 ( #65751, #82903, #110269, #34432, #7060, #112260, #96092, #125449, #173952, #187145, #4074, #67746, #35419, #158753, #127420, #171950, #156787, #114235, #48618, #20242, #79935, #141605, #152330, #86914, #45159, #121984, #84898, #162755, #29987, #195107, #198844, #29009, #102087, #163771, #105826, #147601, #24264, #68741, #161760, #71747, #115256, #85913, #120984, #59315, #131417, #133418, #9088, #137155, #25272, #146577, #106815, #101070, #13816, #8072, #69748, #75482, #148597, #182682, #70756, #193105, #44167, #10089, #168489, #167513, #60308, #132424, #194115, #192097, #90648, #53579, #55579, #176949, #183674, #54579, #117253, #91626, #153314, #178945, #130399, #38418, #40416, #100075, #23255, #116251, #177943, #39410, #199834, #50123, #109794, #3598, #138153, #110787, #107794, #48137, #80440, #96596, #142113, #169478, #184658, #32966, #126936, #65277, #188644, #171477, #111783, #78449, #49129, #94620, #33955, #172468, #170479, #61301, #46140, #95613, #156299, #173471, #140123, #34944, #122971, #2616, #14815, #17800, #30979, #79457, #125960, #76476, #92626, #141126, #155310, #64293, #154317, #15806, #77467, #1614, #139137, #614, #63290, #62284, #47142, #187658, #124970, #186667, #16799, #123952, #185650, #157298, #108800, #31969, #18795, #93625, #38936, #176461, #131944, #8603, #174461, #52098, #116770, #84418, #85425, #115778, #191610, #53089, #192622, #36922, #51109, #161275, #4580, #113755, #7579, #146095, #20760, #22770, #175451, #23775, #114767, #35930, #193628, #190623, #100593, #97576, #159264, #162275, #37934, #69265, #98584, #82415, #130931, #99595, #55100, #54104, #147116, #160278, #21769, #81415, #177467, #143101, #83420, #66273, #70276, #144104, #145097, #178461, #39928, #6580, #158285, #19774, #129910, #68259, #127932, #189634, #5584, #112768, #67264, #128922, #196636, #90408, #24786, #197612, #194629, #134958, #167271, #183430, #28770, #56099, #71276, #119775, #13577, #152093, #75244, #58105, #198602, #165290, #135942, #181459, #120744, #59077, #57114, #148120, #132941, #182443, #42937, #136915, #26783, #60070, #9611, #89427, #121738, #104601, #117780, #166289, #12608, #101597, #163285, #27785, #41948, #151116, #86434, #102611, #179474, #88425, #164297, #40939, #150119, #25790, #133950, #74272, #11620, #73288, #103614, #87436, #149121, #43923, #10612, #72273, #105585, #195641, #118788, #180477, #18551, #95369, #61057, #138893, #3361, #171232, #172222, #2369, #78206, #139876, #79210, #123710, #373, #44915, #33707, #157054, #124723, #80199, #32721, #137908, #108558, #186421, #106571, #64049, #168248, #29744, #141870, #65036, #1365, #63044, #170236, #47897, #93378, #91379, #153068, #45900, #126692, #187418, #14570, #125719, #48886, #76228, #199590, #122729, #184420, #109551, #94373, #107553, #156053, #169231, #31730, #30738, #92385, #17550, #154072, #15566, #140879, #110541, #77224, #155064, #62045, #185407, #46898, #16559, #35691, #85174, #100353, #162032, #70030, #99349, #160033, #52844, #50870, #161032, #173224, #130685, #144855, #112528, #81180, #98334, #159024, #21520, #19535, #114514, #142862, #83181, #192379, #6338, #4341, #49874, #97338, #190380, #20517, #66026, #145853, #188396, #68018, #22526, #115536, #174222, #129670, #177224, #176215, #38697, #84173, #191367, #158045, #37684, #23528, #146863, #8355, #7335, #82165, #127693, #69020, #189393, #143861, #53862, #111539, #34700, #5340, #96357, #175209, #67024, #128683, #36674, #51855, #113515, #167028, #10366, #25550, #101344, #135700, #89180, #133696, #103365, #147880, #118541, #116530, #72023, #41700, #104355, #180231, #194387, #90166, #195388, #151849, #164051, #88180, #56866, #165043, #26536, #178218, #39682, #42694, #120503, #9366, #166039, #11369, #12366, #149864, #105341, #182194, #71031, #87194, #13340, #57863, #58836, #150872, #73039, #134711, #27539, #196394, #148875, #131699, #24540, #119535, #163033, #181218 ),
 ( #197371, #74029, #43679, #28530, #132698, #193380, #54856, #86190, #55854, #117528, #179226, #40692, #102362, #139636, #59825, #138651, #183189, #47658, #14323, #15321, #140641, #1124, #123471, #93136, #78966, #46654, #107311, #77969, #121495, #91140, #44671, #106324, #110304, #169993, #63812, #198351, #170988, #168010, #108313, #2131, #156822, #125485, #29506, #152829, #154821, #187181, #48652, #171986, #31484, #33474, #132, #109309, #16319, #94134, #32481, #30488, #75988, #137661, #155813, #62798, #95132, #61801, #75004, #199348, #124480, #136669, #186176, #60813, #17311, #122487, #184178, #45660, #168984, #76980, #92139, #153826, #185163, #53615, #98089, #68778, #6101, #111299, #81922, #159787, #79971, #175976, #141639, #18314, #130435, #7096, #174970, #113279, #143614, #36434, #66781, #3129, #64804, #19304, #38454, #160797, #188163, #37445, #99105, #126465, #172988, #34466, #115291, #21282, #67781, #49636, #82939, #96125, #5098, #100109, #145617, #191137, #176984, #157814, #144617, #80952, #142627, #4106, #22285, #114272, #173984, #65785, #127454, #83936, #129438, #189160, #128442, #192134, #50633, #52610, #112294, #35453, #97104, #158788, #20276, #190139, #51614, #195144, #102122, #26299, #146613, #162789, #197136, #148634, #24298, #120269, #25308, #181961, #194149, #118299, #86950, #10124, #163806, #8105, #69783, #72800, #150635, #39443, #134470, #41458, #42454, #179991, #135468, #12131, #177975, #55613, #43443, #87940, #88944, #119295, #56625, #103123, #196155, #40448, #117287, #161793, #54611, #164804, #131451, #178981, #11125, #149627, #85946, #57628, #71784, #27297, #180978, #101103, #58603, #133454, #104118, #147635, #9124, #165800, #73795, #23288, #84932, #70790, #193138, #116285, #132458, #92901, #105112, #198120, #108072, #151620, #199107, #154587, #16083, #167778, #169756, #122250, #170756, #61569, #182955, #140406, #137427, #185936, #44438, #106092, #109077, #123238, #31251, #60574, #29276, #77741, #46414, #1895, #139407, #32245, #107078, #168750, #28299, #889, #89939, #30253, #13113, #62564, #90908, #45425, #93903, #124241, #153587, #184929, #155581, #76746, #183940, #47421, #74777, #121261, #136439, #59587, #63575, #200101, #17076, #152593, #78730, #14084, #138421, #125249, #186947, #166798, #75750, #91896, #15085, #160558, #175728, #114031, #4864, #82695, #49400, #83699, #156585, #67542, #144379, #3874, #94901, #18080, #5866, #143372, #145377, #112064, #98863, #79735, #36201, #6859, #189910, #64571, #51385, #159544, #22048, #68538, #81690, #188926, #113046, #33243, #111063, #130193, #35220, #172751, #48418, #173752, #110074, #80717, #66549, #96873, #158557, #50404, #141404, #2892, #21042, #37207, #126236, #129200, #128213, #190898, #174738, #171754, #187931, #34232, #142395, #95894, #97855, #157577, #52374, #19070, #65553, #127212, #20047, #85708, #99872, #56376, #161556, #117043, #11898, #119064, #164565, #150402, #23049, #133211, #53373, #192903, #57391, #7861, #177741, #10883, #165563, #39210, #88706, #103883, #27060, #73561, #102880, #163563, #118059, #54380, #26059, #176743, #134231, #148391, #116052, #84694, #101881, #162548, #25063, #146374, #179749, #69548, #86706, #195916, #9885, #131212, #115051, #100866, #193909, #24052, #147394, #149387, #191889, #71545, #87702, #180746, #8882, #194902, #42222, #41219, #38216, #72553, #70550, #132217, #55373, #178738, #40201, #32012, #92668, #105864, #151390, #138193, #74545, #182720, #14856, #106853, #108842, #197885, #58373, #122022, #59354, #44205, #183713, #123995, #120040, #170523, #13853, #29046, #104875, #139179, #154356, #137195, #168528, #12880, #45199, #181727, #75520, #30026, #107834, #62325, #185693, #76517, #47183, #123011, #28063, #198881, #199876, #196906, #15849, #43208, #135234, #93669, #155354, #91664, #153354, #60348, #61340, #184697, #166564, #89704, #136210, #16844, #77508, #121023, #655, #167551, #90686 ),
 ( #152368, #46181, #169518, #31018, #17844, #18839, #146902, #145889, #126979, #99385, #85212, #50168, #110831, #84209, #63338, #94665, #48182, #125015, #116566, #176252, #70067, #1660, #177260, #171521, #114554, #8392, #163070, #131735, #33010, #109838, #161068, #193417, #54892, #178255, #37723, #115573, #79502, #39716, #186711, #100390, #38732, #34000, #156344, #141171, #162068, #22563, #101379, #142158, #78494, #2660, #69057, #140167, #7372, #64337, #130724, #192416, #126006, #187702, #53898, #80484, #23564, #49172, #172515, #95656, #65320, #157344, #3642, #188688, #44707, #56901, #181253, #149898, #88214, #26571, #9400, #71066, #135736, #13376, #102398, #197407, #104392, #105378, #42730, #198387, #75040, #40728, #118575, #183226, #150909, #151886, #182232, #57898, #119570, #58873, #103399, #180265, #24575, #117563, #27578, #132732, #41735, #74065, #12403, #87228, #89216, #165077, #90203, #166075, #164085, #59864, #11405, #167065, #25584, #148910, #28566, #120539, #43717, #73074, #10400, #136706, #196428, #121531, #72057, #106361, #194420, #86224, #147914, #133731, #179263, #134746, #195424, #55890, #199384, #32517, #60848, #1159, #172019, #62834, #184213, #29542, #77015, #170030, #138687, #45695, #125518, #168045, #124518, #79001, #95167, #92176, #186213, #156855, #155848, #18350, #2167, #109344, #137699, #171026, #80005, #141674, #64838, #187215, #168, #107346, #94169, #169019, #15359, #47694, #139671, #3165, #30524, #91175, #154858, #153861, #61836, #16356, #126500, #152864, #188198, #46690, #123506, #122523, #33508, #48686, #31520, #17345, #185199, #78004, #14359, #108351, #140675, #63846, #49670, #76024, #110338, #93173, #99146, #4143, #175009, #52649, #173024, #68818, #34503, #111334, #161830, #100149, #67821, #6139, #36473, #129476, #159827, #96161, #157850, #112331, #131489, #53655, #80989, #130477, #192174, #19342, #65822, #127491, #146651, #191175, #160835, #142664, #176015, #189196, #98130, #193176, #38493, #83974, #69822, #50671, #114313, #174021, #35492, #177023, #97142, #158825, #115332, #84969, #20313, #8145, #23325, #81961, #143653, #22324, #5137, #66819, #128482, #37484, #190178, #51653, #113317, #145654, #7135, #21322, #82980, #144656, #73834, #150671, #10162, #101140, #24335, #12169, #149666, #89975, #118336, #105149, #162826, #42493, #151656, #196194, #70829, #57666, #165838, #28336, #13150, #87978, #195182, #119333, #39479, #55651, #74813, #41498, #117323, #136475, #180029, #54649, #86987, #11164, #103162, #164842, #56663, #85985, #147674, #27335, #43482, #132497, #88981, #134508, #135505, #72838, #116323, #166835, #194186, #148674, #178012, #181019, #181999, #197175, #104157, #58640, #120306, #133490, #71822, #9162, #179019, #40487, #102159, #26338, #163845, #25346, #137464, #31284, #168785, #170790, #184963, #152629, #78763, #45460, #185971, #14119, #75786, #109111, #46447, #92935, #107114, #199144, #169791, #154623, #140440, #16117, #32282, #153624, #15120, #121299, #77774, #182991, #76782, #44474, #139441, #60610, #91932, #93937, #923, #138453, #108107, #155616, #61603, #183974, #62597, #106129, #122285, #167813, #29312, #17112, #123272, #1930, #59625, #124275, #90942, #47455, #63609, #198155, #30287, #200134, #163494, #57316, #88632, #151317, #105791, #28972, #58302, #90614, #166492, #71475, #42151, #119969, #40128, #136138, #101806, #178665, #152296, #167477, #135161, #73488, #103811, #196834, #26987, #24992, #86636, #179676, #198808, #120949, #148319, #197814, #59279, #9814, #133140, #194831, #13780, #181655, #27990, #56304, #43134, #117986, #165491, #60273, #75447, #12806, #137122, #41148, #104803, #102811, #164496, #44132, #25989, #87632, #182648, #149318, #10812, #72482, #134155, #195843, #118992, #89629, #150328, #74473, #180675, #11823, #170562, #18878, #110869, #173556, #35025, #33048, #140206, #64376, #184736, #695, #96680, #186750, #62367, #158368, #63376 ),
 ( #80524, #17885, #19857, #50212, #15890, #93709, #81497, #126044, #127020, #157385, #94703, #156380, #34040, #78532, #155391, #199915, #92707, #2699, #46221, #16881, #49211, #187740, #124036, #172554, #1700, #65359, #79539, #77548, #61379, #32052, #142198, #139220, #185735, #3681, #95697, #154395, #141209, #188727, #123050, #111866, #47224, #169562, #107874, #31059, #108883, #125053, #48220, #109874, #171558, #178544, #51192, #162358, #39021, #98669, #189719, #112853, #100676, #38023, #40010, #6665, #193715, #174544, #131016, #176547, #36011, #113838, #23859, #54189, #116853, #101683, #99679, #83504, #7664, #128017, #144185, #163372, #129994, #5671, #24869, #68343, #143184, #175534, #161363, #191694, #53177, #145181, #97660, #159349, #115862, #132026, #20845, #177552, #22854, #85510, #84501, #4664, #55184, #82503, #37008, #66356, #69348, #70359, #147198, #146179, #192706, #8689, #21853, #160363, #67347, #129007, #190707, #52180, #114853, #136022, #74356, #149206, #151202, #103697, #152179, #43020, #164381, #121825, #118875, #167359, #25874, #87518, #90497, #104687, #12690, #180559, #10697, #89512, #27871, #183519, #197696, #13663, #88513, #150209, #9695, #59162, #71360, #11706, #194714, #120830, #72360, #26870, #75330, #182530, #135045, #166375, #137001, #58189, #42033, #44012, #133024, #102693, #56183, #117867, #45002, #181541, #198689, #179557, #106662, #73373, #60156, #41027, #105673, #119857, #134034, #57200, #28857, #168335, #86518, #148202, #195727, #196721, #165376, #14657, #30825, #65121, #16645, #92473, #188485, #93466, #49964, #62133, #186512, #155153, #78292, #31815, #76317, #137995, #140969, #18638, #107641, #2457, #109639, #110627, #47986, #3445, #80284, #45986, #123797, #111628, #156142, #157142, #187505, #63133, #124812, #64139, #108645, #185495, #29831, #122816, #32810, #199679, #46986, #79300, #17640, #154161, #94461, #170323, #141956, #139966, #1455, #61144, #33797, #48972, #171322, #125803, #169318, #172308, #184506, #95457, #126779, #91468, #153156, #15653, #77312, #138980, #458, #66114, #36762, #114606, #34788, #130774, #96443, #173313, #23619, #162122, #129757, #68105, #98425, #191454, #21610, #158130, #19622, #174308, #193469, #115625, #142945, #192466, #53949, #81264, #127779, #189479, #8445, #52931, #22616, #4427, #37775, #50957, #160122, #54946, #100442, #145943, #131789, #112616, #176303, #35777, #97424, #38785, #159110, #20604, #177314, #146957, #82256, #70118, #85266, #83268, #99439, #144942, #143948, #5428, #67112, #128770, #190469, #51942, #113602, #175296, #6424, #161119, #84262, #7424, #69108, #166132, #24628, #181308, #86276, #41789, #136760, #43771, #89275, #75093, #147967, #57954, #178307, #117620, #182291, #132785, #102451, #135791, #90257, #164139, #13429, #28620, #151940, #198445, #27634, #88269, #42786, #179318, #133788, #103456, #9455, #197462, #40782, #71119, #26626, #87280, #149957, #194472, #104449, #55944, #11463, #120596, #73134, #25636, #39770, #148965, #118630, #10454, #72115, #74120, #116618, #134804, #150965, #105435, #195480, #196484, #167120, #12460, #101434, #58928, #119625, #56956, #163125, #180321, #165134, #159625, #20124, #30582, #76077, #65632, #199437, #107403, #142475, #34311, #36277, #122581, #183280, #49479, #184269, #169076, #21120, #111142, #81768, #113122, #138742, #153919, #29595, #66624, #143455, #61892, #95974, #137753, #172832, #44762, #224, #157658, #35297, #189986, #174812, #3953, #97932, #50480, #152917, #123562, #127292, #121585, #4940, #106416, #59917, #82776, #51460, #19147, #80797, #144457, #173832, #189005, #112140, #45751, #77072, #188009, #91226, #128288, #92234, #14413, #96953, #15414, #158633, #60905, #168097, #37284, #39286, #9963, #100943, #22123, #67618, #115126, #7941, #176819, #83773, #163641, #5942, #162627, #117122, #133289, #130270, #24134, #194979, #193989, #56458, #40286, #147472, #175811, #8962 ),
 ( #52451, #99945, #55451, #178816, #25143, #38291, #161631, #118137, #85786, #145453, #41296, #23125, #86785, #6935, #68614, #71623, #70630, #132297, #84770, #191965, #101960, #148470, #102957, #179826, #164641, #69624, #131290, #129279, #26136, #190974, #192978, #114108, #87779, #53451, #146448, #98941, #160632, #54457, #116127, #177816, #121102, #181803, #152440, #134308, #165637, #119139, #195994, #184771, #44279, #138267, #72633, #45271, #42298, #182796, #14931, #31095, #76591, #103958, #180819, #167622, #61414, #199950, #123085, #105937, #183785, #150475, #46257, #57467, #168598, #106925, #104951, #27135, #88782, #30098, #29118, #107912, #11970, #73635, #60421, #169597, #135306, #122094, #90757, #91738, #13926, #149464, #10959, #196978, #43282, #58445, #75593, #120113, #153433, #137272, #198954, #166637, #28139, #89779, #151464, #12952, #74617, #136283, #197959, #59428, #80557, #111902, #125088, #1735, #4701, #49244, #170598, #128053, #186786, #173590, #32088, #93745, #96714, #110902, #18912, #48256, #155426, #95732, #34074, #189755, #142232, #158402, #94738, #156418, #15925, #157418, #77583, #17919, #731, #65394, #16916, #33082, #19891, #3717, #141243, #172588, #81532, #64409, #109910, #127055, #139255, #108918, #62403, #124073, #51227, #187774, #143219, #185774, #188762, #47261, #126078, #66391, #174582, #112888, #78569, #140243, #50246, #92743, #154431, #63413, #35059, #171594, #79574, #2732, #144222, #55217, #132060, #191728, #82540, #5706, #193749, #131051, #71392, #99712, #86550, #67383, #23892, #69382, #129040, #6699, #116886, #147231, #9728, #133056, #192741, #176582, #100709, #20882, #37046, #194746, #22888, #98705, #56218, #161396, #117900, #68377, #54223, #84534, #146211, #38056, #115894, #36047, #7699, #148234, #190741, #85545, #177584, #52215, #130029, #178578, #8723, #97696, #159387, #39051, #162389, #70392, #113872, #160399, #175569, #40043, #21888, #83538, #101717, #145217, #53210, #163407, #24903, #114888, #181572, #164413, #25905, #90527, #168366, #57232, #152209, #59192, #60187, #197726, #153186, #29862, #195758, #73404, #138028, #105704, #106693, #137030, #12720, #74386, #13693, #58218, #135075, #179589, #72392, #182561, #87550, #196751, #28887, #167391, #198720, #11737, #88544, #91499, #136051, #118906, #14689, #119887, #121857, #180590, #42064, #183549, #120861, #75360, #43050, #103728, #44044, #45035, #76351, #199711, #61176, #104716, #166407, #102724, #41061, #149237, #27902, #10728, #134068, #165408, #89545, #26901, #150242, #151231, #141000, #126808, #94491, #155185, #125834, #107672, #139011, #92505, #169349, #158159, #17672, #111658, #46016, #18667, #15684, #156173, #188516, #4453, #49993, #77345, #154194, #2488, #34816, #173345, #96471, #79330, #157173, #123828, #19651, #30858, #141986, #80313, #78324, #491, #62164, #3474, #65151, #47018, #185526, #32841, #93498, #64169, #108677, #187537, #170355, #49002, #81292, #110658, #31847, #184536, #16675, #124843, #139997, #1486, #142976, #122848, #172338, #33827, #63164, #186543, #95487, #48016, #109672, #171352, #100470, #7453, #35806, #69137, #54975, #193496, #163153, #23645, #36792, #82287, #130804, #5460, #113631, #145971, #37806, #39798, #128800, #189510, #52960, #190499, #175326, #24656, #114636, #85293, #116645, #144972, #160151, #97452, #70147, #146985, #68134, #99468, #143979, #176335, #50984, #6453, #161148, #38812, #178335, #101462, #192495, #86305, #53979, #159138, #129785, #115651, #127806, #8472, #112644, #66143, #147994, #174336, #22645, #84292, #191482, #177341, #162149, #20635, #67142, #51972, #98458, #131817, #21643, #83296, #167148, #194499, #164166, #102479, #44789, #27661, #58955, #117649, #74146, #179346, #134831, #29619, #136787, #182319, #168123, #40809, #150993, #71147, #10482, #75119, #25664, #195509, #28647, #183307, #56982, #106442, #121612, #91251, #9483, #120623, #181334, #135818, #72142 ),
 ( #55972, #43799, #198473, #87309, #105462, #89301, #90283, #12485, #132813, #59944, #148992, #103483, #133818, #197488, #118656, #151967, #42813, #104475, #13455, #88296, #165161, #180347, #41815, #26653, #149984, #11490, #73161, #196510, #57980, #119652, #166160, #64915, #109427, #30609, #188277, #185283, #33587, #92262, #153946, #156935, #171106, #79084, #46775, #15441, #155932, #94252, #49750, #140757, #18432, #154939, #16436, #76104, #17427, #137779, #78085, #60932, #125597, #77100, #93253, #80082, #2245, #1240, #32599, #141751, #124599, #108434, #63928, #199465, #169102, #122606, #184296, #111419, #47774, #3241, #45778, #48765, #107430, #186294, #126576, #34582, #173105, #138769, #250, #187294, #152942, #14441, #61919, #110420, #172101, #123589, #170110, #31604, #95250, #139753, #62919, #142743, #65901, #53742, #191253, #131577, #159913, #146737, #4223, #84059, #129553, #127575, #66900, #115416, #7218, #69911, #193261, #52728, #36555, #160915, #81065, #97219, #54735, #83060, #177105, #189276, #50752, #112410, #116407, #114393, #145737, #174102, #22408, #35571, #21402, #178096, #23408, #68903, #96239, #158905, #37565, #157927, #20396, #161914, #82043, #143740, #38576, #19417, #5219, #128563, #8233, #190258, #51735, #130562, #67900, #192260, #113397, #175087, #144734, #98209, #100232, #6221, #176095, #99228, #85056, #72925, #70913, #104240, #132581, #134594, #43566, #196280, #55736, #101224, #148757, #41583, #10246, #117410, #197258, #39566, #57749, #150756, #166919, #163934, #119419, #28420, #27419, #90057, #73916, #181103, #9246, #42577, #151739, #13232, #136558, #58720, #71905, #179107, #165923, #40576, #87072, #89065, #11251, #74895, #102246, #162913, #26422, #25431, #133577, #198239, #88062, #120389, #59710, #118422, #195267, #194269, #105231, #182083, #103247, #12254, #56751, #149749, #24421, #180115, #135586, #121383, #86070, #147760, #164929, #33358, #170875, #75872, #46538, #124363, #44558, #140527, #106213, #183075, #95017, #171869, #139525, #77858, #108197, #1008, #31372, #167897, #29397, #184061, #3013, #125371, #152713, #2017, #186059, #47542, #79857, #32366, #187067, #185050, #169879, #91027, #109196, #14204, #93022, #137548, #155700, #122372, #123357, #48537, #94019, #154710, #62682, #110191, #16203, #15207, #17195, #199231, #60696, #45544, #107199, #18199, #78849, #156705, #168869, #63696, #30374, #141525, #64690, #92018, #153711, #76866, #138536, #14, #61688, #53494, #192009, #82819, #160674, #127334, #161674, #34352, #145497, #22166, #81810, #172871, #96013, #83817, #21163, #23170, #190030, #176864, #157698, #114152, #159667, #19188, #96993, #6977, #37326, #99989, #84813, #144500, #66668, #191017, #111181, #189046, #146493, #113165, #50521, #7984, #51504, #126351, #158676, #112184, #142514, #68658, #188048, #5984, #98985, #115171, #173872, #67664, #38333, #175854, #49518, #130313, #129320, #80837, #52492, #3992, #65672, #35342, #20165, #143498, #4982, #128331, #174854, #36320, #97974, #44078, #46050, #132342, #193022, #59225, #194034, #178863, #30892, #120894, #91533, #122881, #151263, #166439, #39330, #76385, #29895, #74418, #105737, #85830, #182594, #54499, #12753, #13727, #131334, #70676, #138062, #147519, #55498, #153220, #107705, #117167, #169384, #184569, #92539, #154228, #183583, #167424, #137065, #43081, #89577, #197758, #100989, #14725, #104748, #162673, #28920, #27934, #90560, #24180, #198755, #9008, #152242, #199743, #75393, #136084, #60220, #121890, #69667, #45068, #106726, #61209, #116171, #168400, #177861, #143013, #140033, #33864, #4491, #3512, #66181, #50031, #157210, #185560, #18704, #127843, #189549, #112682, #173383, #186579, #31881, #80351, #155220, #63200, #95524, #187571, #51021, #78359, #139046, #2524, #1522, #124880, #174374, #64204, #34853, #35844, #94527, #109708, #47054, #19688, #96508, #17709, #49039, #93535, #125871, #526, #156209 ),
 ( #188553, #16709, #79366, #81330, #142023, #110694, #65188, #97490, #172374, #48052, #126847, #62198, #171390, #108711, #123862, #15718, #111696, #77378, #170390, #158198, #32877, #141037, #24695, #40846, #86344, #113668, #128836, #177379, #71186, #148031, #9520, #115691, #132850, #56009, #116682, #129823, #175362, #162187, #98496, #6491, #38851, #130843, #194538, #21679, #82325, #146009, #83333, #68171, #117687, #7492, #178372, #179384, #37846, #52999, #190535, #163191, #39836, #161187, #192534, #36830, #69177, #144015, #99506, #54017, #131855, #159176, #20671, #100508, #5496, #147025, #52009, #22683, #23685, #67179, #101502, #160189, #145010, #191522, #114677, #85333, #8509, #84330, #70187, #193538, #176373, #55012, #103522, #122643, #44826, #72183, #121649, #59982, #87346, #57021, #195547, #137819, #120659, #152005, #10520, #167185, #133857, #27696, #184333, #29657, #75156, #60969, #118694, #43835, #164203, #165198, #168160, #180386, #88333, #183344, #76141, #150024, #199503, #14479, #102520, #25701, #13491, #74184, #28684, #26693, #119687, #89337, #41856, #106481, #11529, #73199, #12520, #134869, #135854, #196547, #90319, #58017, #197524, #91289, #58992, #181370, #104514, #42849, #149032, #166195, #151029, #152980, #182357, #105499, #136827, #198511, #170146, #63963, #173140, #33622, #96274, #80116, #187330, #15481, #48801, #34615, #138807, #110455, #92300, #139789, #95285, #156969, #64950, #78120, #154975, #157960, #2280, #123624, #81099, #1277, #126609, #185319, #46810, #49788, #125632, #172136, #62954, #108469, #18465, #141784, #142777, #3278, #111454, #47811, #109461, #169142, #188311, #30647, #171144, #153984, #19451, #31641, #186329, #4258, #65937, #94287, #127609, #45815, #17462, #124635, #107466, #77138, #61957, #288, #93290, #16471, #140792, #32633, #155965, #79119, #82078, #22440, #54768, #70944, #116442, #143771, #158939, #7250, #101257, #178131, #39598, #145768, #23441, #190290, #24453, #97251, #8266, #85088, #144768, #35605, #20428, #146772, #84089, #86102, #52757, #162946, #5252, #177138, #68935, #66933, #159945, #69945, #100265, #147793, #9279, #130597, #129586, #53773, #174134, #51766, #189308, #176128, #113427, #50785, #112445, #6253, #128596, #175119, #114426, #37598, #191282, #36587, #98242, #161946, #21432, #83092, #131609, #192294, #193294, #115447, #67932, #99260, #160947, #38609, #91057, #58750, #59743, #90086, #165954, #27454, #166947, #11282, #26452, #132612, #104272, #106244, #195300, #55767, #119449, #56782, #41614, #152744, #181134, #151768, #183106, #72956, #88094, #102278, #136587, #13261, #134625, #89096, #148789, #42608, #117441, #196309, #150787, #105261, #121413, #44587, #12282, #167926, #120419, #25464, #57779, #73947, #194301, #74924, #179139, #40608, #29426, #14234, #135616, #197287, #182110, #43595, #28450, #163966, #87104, #133607, #10278, #198267, #71937, #118454, #180145, #103279, #164959, #149780, #111215, #94052, #125402, #184094, #140559, #45577, #1042, #96045, #3046, #48569, #34385, #107230, #17228, #137580, #76897, #141557, #92053, #61721, #95050, #49552, #123389, #172907, #188081, #157732, #75905, #187099, #47574, #2048, #138568, #93055, #62715, #168901, #156739, #46, #30407, #186092, #46570, #109226, #153743, #63727, #15238, #170905, #79887, #32397, #185081, #77890, #108231, #199263, #169912, #31404, #33391, #60730, #155730, #110222, #64722, #154742, #78880, #126384, #171903, #122404, #18233, #16238, #139558, #124397, #53526, #192045, #161709, #83848, #5017, #112214, #191050, #35373, #81841, #129355, #130346, #6018, #160708, #97025, #100022, #65703, #145530, #22199, #190059, #4025, #127369, #7009, #144532, #23205, #174887, #115204, #189081, #175888, #67697, #50554, #66699, #68691, #99017, #38367, #84848, #52523, #113198, #114184, #173904, #158706, #19221, #21197, #20195, #80871, #142547, #37359, #143529, #128363, #176896, #51535, #36353 ) ),
 .UNSPECIFIED., .T., .F., .F. ) 
 B_SPLINE_SURFACE_WITH_KNOTS ( ( 4, 3, 4 ),
 ( 3, 2, 2, 2, 2, 2, 2, 2, 2, 2, 2, 2, 2, 2, 2, 2, 2, 2, 2, 2, 2, 2, 2, 2, 2, 2, 2, 2, 2, 2, 2, 2, 2, 2, 2, 2, 2, 2, 2, 2, 2, 2, 2, 2, 2, 2, 2, 2, 2, 2, 2, 2, 2, 2, 2, 2, 2, 2, 2, 2, 2, 2, 2, 2, 2, 2, 2, 2, 2, 2, 2, 2, 2, 2, 2, 2, 2, 2, 2, 2, 2, 2, 2, 2, 2, 2, 2, 2, 2, 2, 2, 2, 2, 2, 2, 2, 2, 2, 2, 2, 2, 2, 2, 2, 2, 2, 2, 2, 2, 2, 2, 2, 2, 2, 2, 2, 2, 2, 2, 2, 2, 2, 2, 2, 2, 2, 2, 2, 2, 2, 2, 2, 2, 2, 2, 2, 2, 2, 2, 2, 2, 2, 2, 2, 2, 2, 2, 2, 2, 2, 2, 2, 2, 2, 2, 2, 2, 2, 2, 2, 2, 2, 2, 2, 2, 2, 2, 2, 2, 2, 2, 2, 2, 2, 2, 2, 2, 2, 2, 2, 2, 2, 2, 2, 2, 2, 2, 2, 2, 2, 2, 2, 2, 2, 2, 2, 2, 2, 2, 2, 2, 2, 2, 2, 2, 2, 2, 2, 2, 2, 2, 2, 2, 2, 2, 2, 2, 2, 2, 2, 2, 2, 2, 2, 2, 2, 2, 2, 3 ),
 ( 0.000000000000000000, 0.5000000000000000000, 1.000000000000000000 ),
 ( 0.000000000000000000, 0.004385964912280701511, 0.008771929824561403022, 0.01315789473684210453, 0.01754385964912280604, 0.02192982456140350755, 0.02631578947368420907, 0.03070175438596491058, 0.03508771929824561209, 0.03947368421052631360, 0.04385964912280701511, 0.04824561403508771662, 0.05263157894736841813, 0.05701754385964911964, 0.06140350877192982115, 0.06578947368421052266, 0.07017543859649122417, 0.07456140350877192569, 0.07894736842105262720, 0.08333333333333332871, 0.08771929824561403022, 0.09210526315789473173, 0.09649122807017543324, 0.1008771929824561348, 0.1052631578947368363, 0.1096491228070175378, 0.1140350877192982393, 0.1184210526315789408, 0.1228070175438596423, 0.1271929824561403577, 0.1315789473684210453, 0.1359649122807017607, 0.1403508771929824483, 0.1447368421052631637, 0.1491228070175438514, 0.1535087719298245668, 0.1578947368421052544, 0.1622807017543859698, 0.1666666666666666574, 0.1710526315789473728, 0.1754385964912280604, 0.1798245614035087758, 0.1842105263157894635, 0.1885964912280701788, 0.1929824561403508665, 0.1973684210526315819, 0.2017543859649122695, 0.2061403508771929849, 0.2105263157894736725, 0.2149122807017543879, 0.2192982456140350755, 0.2236842105263157909, 0.2280701754385964786, 0.2324561403508771940, 0.2368421052631578816, 0.2412280701754385970, 0.2456140350877192846, 0.2500000000000000000, 0.2543859649122807154, 0.2587719298245614308, 0.2631578947368420907, 0.2675438596491228060, 0.2719298245614035214, 0.2763157894736842368, 0.2807017543859648967, 0.2850877192982456121, 0.2894736842105263275, 0.2938596491228070429, 0.2982456140350877027, 0.3026315789473684181, 0.3070175438596491335, 0.3114035087719298489, 0.3157894736842105088, 0.3201754385964912242, 0.3245614035087719396, 0.3289473684210526550, 0.3333333333333333148, 0.3377192982456140302, 0.3421052631578947456, 0.3464912280701754610, 0.3508771929824561209, 0.3552631578947368363, 0.3596491228070175517, 0.3640350877192982670, 0.3684210526315789269, 0.3728070175438596423, 0.3771929824561403577, 0.3815789473684210731, 0.3859649122807017330, 0.3903508771929824483, 0.3947368421052631637, 0.3991228070175438791, 0.4035087719298245390, 0.4078947368421052544, 0.4122807017543859698, 0.4166666666666666852, 0.4210526315789473450, 0.4254385964912280604, 0.4298245614035087758, 0.4342105263157894912, 0.4385964912280701511, 0.4429824561403508665, 0.4473684210526315819, 0.4517543859649122973, 0.4561403508771929571, 0.4605263157894736725, 0.4649122807017543879, 0.4692982456140351033, 0.4736842105263157632, 0.4780701754385964786, 0.4824561403508771940, 0.4868421052631579093, 0.4912280701754385692, 0.4956140350877192846, 0.5000000000000000000, 0.5043859649122807154, 0.5087719298245614308, 0.5131578947368421462, 0.5175438596491228616, 0.5219298245614034659, 0.5263157894736841813, 0.5307017543859648967, 0.5350877192982456121, 0.5394736842105263275, 0.5438596491228070429, 0.5482456140350877583, 0.5526315789473684736, 0.5570175438596490780, 0.5614035087719297934, 0.5657894736842105088, 0.5701754385964912242, 0.5745614035087719396, 0.5789473684210526550, 0.5833333333333333703, 0.5877192982456140857, 0.5921052631578946901, 0.5964912280701754055, 0.6008771929824561209, 0.6052631578947368363, 0.6096491228070175517, 0.6140350877192982670, 0.6184210526315789824, 0.6228070175438596978, 0.6271929824561403022, 0.6315789473684210176, 0.6359649122807017330, 0.6403508771929824483, 0.6447368421052631637, 0.6491228070175438791, 0.6535087719298245945, 0.6578947368421053099, 0.6622807017543859143, 0.6666666666666666297, 0.6710526315789473450, 0.6754385964912280604, 0.6798245614035087758, 0.6842105263157894912, 0.6885964912280702066, 0.6929824561403509220, 0.6973684210526315264, 0.7017543859649122417, 0.7061403508771929571, 0.7105263157894736725, 0.7149122807017543879, 0.7192982456140351033, 0.7236842105263158187, 0.7280701754385965341, 0.7324561403508771384, 0.7368421052631578538, 0.7412280701754385692, 0.7456140350877192846, 0.7500000000000000000, 0.7543859649122807154, 0.7587719298245614308, 0.7631578947368421462, 0.7675438596491228616, 0.7719298245614034659, 0.7763157894736841813, 0.7807017543859648967, 0.7850877192982456121, 0.7894736842105263275, 0.7938596491228070429, 0.7982456140350877583, 0.8026315789473684736, 0.8070175438596490780, 0.8114035087719297934, 0.8157894736842105088, 0.8201754385964912242, 0.8245614035087719396, 0.8289473684210526550, 0.8333333333333333703, 0.8377192982456140857, 0.8421052631578946901, 0.8464912280701754055, 0.8508771929824561209, 0.8552631578947368363, 0.8596491228070175517, 0.8640350877192982670, 0.8684210526315789824, 0.8728070175438596978, 0.8771929824561403022, 0.8815789473684210176, 0.8859649122807017330, 0.8903508771929824483, 0.8947368421052631637, 0.8991228070175438791, 0.9035087719298245945, 0.9078947368421053099, 0.9122807017543859143, 0.9166666666666666297, 0.9210526315789473450, 0.9254385964912280604, 0.9298245614035087758, 0.9342105263157894912, 0.9385964912280702066, 0.9429824561403509220, 0.9473684210526315264, 0.9517543859649122417, 0.9561403508771929571, 0.9605263157894736725, 0.9649122807017543879, 0.9692982456140351033, 0.9736842105263158187, 0.9780701754385965341, 0.9824561403508771384, 0.9868421052631578538, 0.9912280701754385692, 0.9956140350877192846, 1.000000000000000000 ),
 .UNSPECIFIED. ) 
 GEOMETRIC_REPRESENTATION_ITEM ( )  RATIONAL_B_SPLINE_SURFACE ( (
 ( 1.000000000000000000, 0.9659258262890683122, 1.000000000000000000, 0.9659258262890683122, 1.000000000000000000, 0.9659258262890683122, 1.000000000000000000, 0.9659258262890683122, 1.000000000000000000, 0.9659258262890683122, 1.000000000000000000, 0.9659258262890683122, 1.000000000000000000, 0.9659258262890683122, 1.000000000000000000, 0.9659258262890683122, 1.000000000000000000, 0.9659258262890683122, 1.000000000000000000, 0.9659258262890683122, 1.000000000000000000, 0.9659258262890683122, 1.000000000000000000, 0.9659258262890683122, 1.000000000000000000, 0.9659258262890683122, 1.000000000000000000, 0.9659258262890683122, 1.000000000000000000, 0.9659258262890683122, 1.000000000000000000, 0.9659258262890683122, 1.000000000000000000, 0.9659258262890683122, 1.000000000000000000, 0.9659258262890683122, 1.000000000000000000, 0.9659258262890683122, 1.000000000000000000, 0.9659258262890683122, 1.000000000000000000, 0.9659258262890683122, 1.000000000000000000, 0.9659258262890683122, 1.000000000000000000, 0.9659258262890683122, 1.000000000000000000, 0.9659258262890683122, 1.000000000000000000, 0.9659258262890683122, 1.000000000000000000, 0.9659258262890683122, 1.000000000000000000, 0.9659258262890683122, 1.000000000000000000, 0.9659258262890683122, 1.000000000000000000, 0.9659258262890683122, 1.000000000000000000, 0.9659258262890683122, 1.000000000000000000, 0.9659258262890683122, 1.000000000000000000, 0.9659258262890683122, 1.000000000000000000, 0.9659258262890683122, 1.000000000000000000, 0.9659258262890683122, 1.000000000000000000, 0.9659258262890683122, 1.000000000000000000, 0.9659258262890683122, 1.000000000000000000, 0.9659258262890683122, 1.000000000000000000, 0.9659258262890683122, 1.000000000000000000, 0.9659258262890683122, 1.000000000000000000, 0.9659258262890683122, 1.000000000000000000, 0.9659258262890683122, 1.000000000000000000, 0.9659258262890683122, 1.000000000000000000, 0.9659258262890683122, 1.000000000000000000, 0.9659258262890683122, 1.000000000000000000, 0.9659258262890683122, 1.000000000000000000, 0.9659258262890683122, 1.000000000000000000, 0.9659258262890683122, 1.000000000000000000, 0.9659258262890683122, 1.000000000000000000, 0.9659258262890683122, 1.000000000000000000, 0.9659258262890683122, 1.000000000000000000, 0.9659258262890683122, 1.000000000000000000, 0.9659258262890683122, 1.000000000000000000, 0.9659258262890683122, 1.000000000000000000, 0.9659258262890683122, 1.000000000000000000, 0.9659258262890683122, 1.000000000000000000, 0.9659258262890683122, 1.000000000000000000, 0.9659258262890683122, 1.000000000000000000, 0.9659258262890683122, 1.000000000000000000, 0.9659258262890683122, 1.000000000000000000, 0.9659258262890683122, 1.000000000000000000, 0.9659258262890683122, 1.000000000000000000, 0.9659258262890683122, 1.000000000000000000, 0.9659258262890683122, 1.000000000000000000, 0.9659258262890683122, 1.000000000000000000, 0.9659258262890683122, 1.000000000000000000, 0.9659258262890683122, 1.000000000000000000, 0.9659258262890683122, 1.000000000000000000, 0.9659258262890683122, 1.000000000000000000, 0.9659258262890683122, 1.000000000000000000, 0.9659258262890683122, 1.000000000000000000, 0.9659258262890683122, 1.000000000000000000, 0.9659258262890683122, 1.000000000000000000, 0.9659258262890683122, 1.000000000000000000, 0.9659258262890683122, 1.000000000000000000, 0.9659258262890683122, 1.000000000000000000, 0.9659258262890683122, 1.000000000000000000, 0.9659258262890683122, 1.000000000000000000, 0.9659258262890683122, 1.000000000000000000, 0.9659258262890683122, 1.000000000000000000, 0.9659258262890683122, 1.000000000000000000, 0.9659258262890683122, 1.000000000000000000, 0.9659258262890683122, 1.000000000000000000, 0.9659258262890683122, 1.000000000000000000, 0.9659258262890683122, 1.000000000000000000, 0.9659258262890683122, 1.000000000000000000, 0.9659258262890683122, 1.000000000000000000, 0.9659258262890683122, 1.000000000000000000, 0.9659258262890683122, 1.000000000000000000, 0.9659258262890683122, 1.000000000000000000, 0.9659258262890683122, 1.000000000000000000, 0.9659258262890683122, 1.000000000000000000, 0.9659258262890683122, 1.000000000000000000, 0.9659258262890683122, 1.000000000000000000, 0.9659258262890683122, 1.000000000000000000, 0.9659258262890683122, 1.000000000000000000, 0.9659258262890683122, 1.000000000000000000, 0.9659258262890683122, 1.000000000000000000, 0.9659258262890683122, 1.000000000000000000, 0.9659258262890683122, 1.000000000000000000, 0.9659258262890683122, 1.000000000000000000, 0.9659258262890683122, 1.000000000000000000, 0.9659258262890683122, 1.000000000000000000, 0.9659258262890683122, 1.000000000000000000, 0.9659258262890683122, 1.000000000000000000, 0.9659258262890683122, 1.000000000000000000, 0.9659258262890683122, 1.000000000000000000, 0.9659258262890683122, 1.000000000000000000, 0.9659258262890683122, 1.000000000000000000, 0.9659258262890683122, 1.000000000000000000, 0.9659258262890683122, 1.000000000000000000, 0.9659258262890683122, 1.000000000000000000, 0.9659258262890683122, 1.000000000000000000, 0.9659258262890683122, 1.000000000000000000, 0.9659258262890683122, 1.000000000000000000, 0.9659258262890683122, 1.000000000000000000, 0.9659258262890683122, 1.000000000000000000, 0.9659258262890683122, 1.000000000000000000, 0.9659258262890683122, 1.000000000000000000, 0.9659258262890683122, 1.000000000000000000, 0.9659258262890683122, 1.000000000000000000, 0.9659258262890683122, 1.000000000000000000, 0.9659258262890683122, 1.000000000000000000, 0.9659258262890683122, 1.000000000000000000, 0.9659258262890683122, 1.000000000000000000, 0.9659258262890683122, 1.000000000000000000, 0.9659258262890683122, 1.000000000000000000, 0.9659258262890683122, 1.000000000000000000, 0.9659258262890683122, 1.000000000000000000, 0.9659258262890683122, 1.000000000000000000, 0.9659258262890683122, 1.000000000000000000, 0.9659258262890683122, 1.000000000000000000, 0.9659258262890683122, 1.000000000000000000, 0.9659258262890683122, 1.000000000000000000, 0.9659258262890683122, 1.000000000000000000, 0.9659258262890683122, 1.000000000000000000, 0.9659258262890683122, 1.000000000000000000, 0.9659258262890683122, 1.000000000000000000, 0.9659258262890683122, 1.000000000000000000, 0.9659258262890683122, 1.000000000000000000, 0.9659258262890683122, 1.000000000000000000, 0.9659258262890683122, 1.000000000000000000, 0.9659258262890683122, 1.000000000000000000, 0.9659258262890683122, 1.000000000000000000, 0.9659258262890683122, 1.000000000000000000, 0.9659258262890683122, 1.000000000000000000, 0.9659258262890683122, 1.000000000000000000, 0.9659258262890683122, 1.000000000000000000, 0.9659258262890683122, 1.000000000000000000, 0.9659258262890683122, 1.000000000000000000, 0.9659258262890683122, 1.000000000000000000, 0.9659258262890683122, 1.000000000000000000, 0.9659258262890683122, 1.000000000000000000, 0.9659258262890683122, 1.000000000000000000, 0.9659258262890683122, 1.000000000000000000, 0.9659258262890683122, 1.000000000000000000, 0.9659258262890683122, 1.000000000000000000, 0.9659258262890683122, 1.000000000000000000, 0.9659258262890683122, 1.000000000000000000, 0.9659258262890683122, 1.000000000000000000, 0.9659258262890683122, 1.000000000000000000, 0.9659258262890683122, 1.000000000000000000, 0.9659258262890683122, 1.000000000000000000, 0.9659258262890683122, 1.000000000000000000, 0.9659258262890683122, 1.000000000000000000, 0.9659258262890683122, 1.000000000000000000, 0.9659258262890683122, 1.000000000000000000, 0.9659258262890683122, 1.000000000000000000, 0.9659258262890683122, 1.000000000000000000, 0.9659258262890683122, 1.000000000000000000, 0.9659258262890683122, 1.000000000000000000, 0.9659258262890683122, 1.000000000000000000, 0.9659258262890683122, 1.000000000000000000, 0.9659258262890683122, 1.000000000000000000, 0.9659258262890683122, 1.000000000000000000, 0.9659258262890683122, 1.000000000000000000, 0.9659258262890683122, 1.000000000000000000, 0.9659258262890683122, 1.000000000000000000, 0.9659258262890683122, 1.000000000000000000, 0.9659258262890683122, 1.000000000000000000, 0.9659258262890683122, 1.000000000000000000, 0.9659258262890683122, 1.000000000000000000, 0.9659258262890683122, 1.000000000000000000, 0.9659258262890683122, 1.000000000000000000, 0.9659258262890683122, 1.000000000000000000, 0.9659258262890683122, 1.000000000000000000, 0.9659258262890683122, 1.000000000000000000, 0.9659258262890683122, 1.000000000000000000, 0.9659258262890683122, 1.000000000000000000, 0.9659258262890683122, 1.000000000000000000, 0.9659258262890683122, 1.000000000000000000, 0.9659258262890683122, 1.000000000000000000, 0.9659258262890683122, 1.000000000000000000, 0.9659258262890683122, 1.000000000000000000, 0.9659258262890683122, 1.000000000000000000, 0.9659258262890683122, 1.000000000000000000, 0.9659258262890683122, 1.000000000000000000, 0.9659258262890683122, 1.000000000000000000, 0.9659258262890683122, 1.000000000000000000, 0.9659258262890683122, 1.000000000000000000, 0.9659258262890683122, 1.000000000000000000, 0.9659258262890683122, 1.000000000000000000, 0.9659258262890683122, 1.000000000000000000, 0.9659258262890683122, 1.000000000000000000, 0.9659258262890683122, 1.000000000000000000, 0.9659258262890683122, 1.000000000000000000, 0.9659258262890683122, 1.000000000000000000, 0.9659258262890683122, 1.000000000000000000, 0.9659258262890683122, 1.000000000000000000, 0.9659258262890683122, 1.000000000000000000, 0.9659258262890683122, 1.000000000000000000, 0.9659258262890683122, 1.000000000000000000, 0.9659258262890683122, 1.000000000000000000, 0.9659258262890683122, 1.000000000000000000, 0.9659258262890683122, 1.000000000000000000, 0.9659258262890683122, 1.000000000000000000, 0.9659258262890683122, 1.000000000000000000, 0.9659258262890683122, 1.000000000000000000, 0.9659258262890683122, 1.000000000000000000, 0.9659258262890683122, 1.000000000000000000, 0.9659258262890683122, 1.000000000000000000, 0.9659258262890683122, 1.000000000000000000, 0.9659258262890683122, 1.000000000000000000, 0.9659258262890683122, 1.000000000000000000, 0.9659258262890683122, 1.000000000000000000, 0.9659258262890683122, 1.000000000000000000, 0.9659258262890683122, 1.000000000000000000, 0.9659258262890683122, 1.000000000000000000, 0.9659258262890683122, 1.000000000000000000),
 ( 0.3333333333333333703, 0.3219752754296894559, 0.3333333333333333703, 0.3219752754296894559, 0.3333333333333333703, 0.3219752754296894559, 0.3333333333333333703, 0.3219752754296894559, 0.3333333333333333703, 0.3219752754296894559, 0.3333333333333333703, 0.3219752754296894559, 0.3333333333333333703, 0.3219752754296894559, 0.3333333333333333703, 0.3219752754296894559, 0.3333333333333333703, 0.3219752754296894559, 0.3333333333333333703, 0.3219752754296894559, 0.3333333333333333703, 0.3219752754296894559, 0.3333333333333333703, 0.3219752754296894559, 0.3333333333333333703, 0.3219752754296894559, 0.3333333333333333703, 0.3219752754296894559, 0.3333333333333333703, 0.3219752754296894559, 0.3333333333333333703, 0.3219752754296894559, 0.3333333333333333703, 0.3219752754296894559, 0.3333333333333333703, 0.3219752754296894559, 0.3333333333333333703, 0.3219752754296894559, 0.3333333333333333703, 0.3219752754296894559, 0.3333333333333333703, 0.3219752754296894559, 0.3333333333333333703, 0.3219752754296894559, 0.3333333333333333703, 0.3219752754296894559, 0.3333333333333333703, 0.3219752754296894559, 0.3333333333333333703, 0.3219752754296894559, 0.3333333333333333703, 0.3219752754296894559, 0.3333333333333333703, 0.3219752754296894559, 0.3333333333333333703, 0.3219752754296894559, 0.3333333333333333703, 0.3219752754296894559, 0.3333333333333333703, 0.3219752754296894559, 0.3333333333333333703, 0.3219752754296894559, 0.3333333333333333703, 0.3219752754296894559, 0.3333333333333333703, 0.3219752754296894559, 0.3333333333333333703, 0.3219752754296894559, 0.3333333333333333703, 0.3219752754296894559, 0.3333333333333333703, 0.3219752754296894559, 0.3333333333333333703, 0.3219752754296894559, 0.3333333333333333703, 0.3219752754296894559, 0.3333333333333333703, 0.3219752754296894559, 0.3333333333333333703, 0.3219752754296894559, 0.3333333333333333703, 0.3219752754296894559, 0.3333333333333333703, 0.3219752754296894559, 0.3333333333333333703, 0.3219752754296894559, 0.3333333333333333703, 0.3219752754296894559, 0.3333333333333333703, 0.3219752754296894559, 0.3333333333333333703, 0.3219752754296894559, 0.3333333333333333703, 0.3219752754296894559, 0.3333333333333333703, 0.3219752754296894559, 0.3333333333333333703, 0.3219752754296894559, 0.3333333333333333703, 0.3219752754296894559, 0.3333333333333333703, 0.3219752754296894559, 0.3333333333333333703, 0.3219752754296894559, 0.3333333333333333703, 0.3219752754296894559, 0.3333333333333333703, 0.3219752754296894559, 0.3333333333333333703, 0.3219752754296894559, 0.3333333333333333703, 0.3219752754296894559, 0.3333333333333333703, 0.3219752754296894559, 0.3333333333333333703, 0.3219752754296894559, 0.3333333333333333703, 0.3219752754296894559, 0.3333333333333333703, 0.3219752754296894559, 0.3333333333333333703, 0.3219752754296894559, 0.3333333333333333703, 0.3219752754296894559, 0.3333333333333333703, 0.3219752754296894559, 0.3333333333333333703, 0.3219752754296894559, 0.3333333333333333703, 0.3219752754296894559, 0.3333333333333333703, 0.3219752754296894559, 0.3333333333333333703, 0.3219752754296894559, 0.3333333333333333703, 0.3219752754296894559, 0.3333333333333333703, 0.3219752754296894559, 0.3333333333333333703, 0.3219752754296894559, 0.3333333333333333703, 0.3219752754296894559, 0.3333333333333333703, 0.3219752754296894559, 0.3333333333333333703, 0.3219752754296894559, 0.3333333333333333703, 0.3219752754296894559, 0.3333333333333333703, 0.3219752754296894559, 0.3333333333333333703, 0.3219752754296894559, 0.3333333333333333703, 0.3219752754296894559, 0.3333333333333333703, 0.3219752754296894559, 0.3333333333333333703, 0.3219752754296894559, 0.3333333333333333703, 0.3219752754296894559, 0.3333333333333333703, 0.3219752754296894559, 0.3333333333333333703, 0.3219752754296894559, 0.3333333333333333703, 0.3219752754296894559, 0.3333333333333333703, 0.3219752754296894559, 0.3333333333333333703, 0.3219752754296894559, 0.3333333333333333703, 0.3219752754296894559, 0.3333333333333333703, 0.3219752754296894559, 0.3333333333333333703, 0.3219752754296894559, 0.3333333333333333703, 0.3219752754296894559, 0.3333333333333333703, 0.3219752754296894559, 0.3333333333333333703, 0.3219752754296894559, 0.3333333333333333703, 0.3219752754296894559, 0.3333333333333333703, 0.3219752754296894559, 0.3333333333333333703, 0.3219752754296894559, 0.3333333333333333703, 0.3219752754296894559, 0.3333333333333333703, 0.3219752754296894559, 0.3333333333333333703, 0.3219752754296894559, 0.3333333333333333703, 0.3219752754296894559, 0.3333333333333333703, 0.3219752754296894559, 0.3333333333333333703, 0.3219752754296894559, 0.3333333333333333703, 0.3219752754296894559, 0.3333333333333333703, 0.3219752754296894559, 0.3333333333333333703, 0.3219752754296894559, 0.3333333333333333703, 0.3219752754296894559, 0.3333333333333333703, 0.3219752754296894559, 0.3333333333333333703, 0.3219752754296894559, 0.3333333333333333703, 0.3219752754296894559, 0.3333333333333333703, 0.3219752754296894559, 0.3333333333333333703, 0.3219752754296894559, 0.3333333333333333703, 0.3219752754296894559, 0.3333333333333333703, 0.3219752754296894559, 0.3333333333333333703, 0.3219752754296894559, 0.3333333333333333703, 0.3219752754296894559, 0.3333333333333333703, 0.3219752754296894559, 0.3333333333333333703, 0.3219752754296894559, 0.3333333333333333703, 0.3219752754296894559, 0.3333333333333333703, 0.3219752754296894559, 0.3333333333333333703, 0.3219752754296894559, 0.3333333333333333703, 0.3219752754296894559, 0.3333333333333333703, 0.3219752754296894559, 0.3333333333333333703, 0.3219752754296894559, 0.3333333333333333703, 0.3219752754296894559, 0.3333333333333333703, 0.3219752754296894559, 0.3333333333333333703, 0.3219752754296894559, 0.3333333333333333703, 0.3219752754296894559, 0.3333333333333333703, 0.3219752754296894559, 0.3333333333333333703, 0.3219752754296894559, 0.3333333333333333703, 0.3219752754296894559, 0.3333333333333333703, 0.3219752754296894559, 0.3333333333333333703, 0.3219752754296894559, 0.3333333333333333703, 0.3219752754296894559, 0.3333333333333333703, 0.3219752754296894559, 0.3333333333333333703, 0.3219752754296894559, 0.3333333333333333703, 0.3219752754296894559, 0.3333333333333333703, 0.3219752754296894559, 0.3333333333333333703, 0.3219752754296894559, 0.3333333333333333703, 0.3219752754296894559, 0.3333333333333333703, 0.3219752754296894559, 0.3333333333333333703, 0.3219752754296894559, 0.3333333333333333703, 0.3219752754296894559, 0.3333333333333333703, 0.3219752754296894559, 0.3333333333333333703, 0.3219752754296894559, 0.3333333333333333703, 0.3219752754296894559, 0.3333333333333333703, 0.3219752754296894559, 0.3333333333333333703, 0.3219752754296894559, 0.3333333333333333703, 0.3219752754296894559, 0.3333333333333333703, 0.3219752754296894559, 0.3333333333333333703, 0.3219752754296894559, 0.3333333333333333703, 0.3219752754296894559, 0.3333333333333333703, 0.3219752754296894559, 0.3333333333333333703, 0.3219752754296894559, 0.3333333333333333703, 0.3219752754296894559, 0.3333333333333333703, 0.3219752754296894559, 0.3333333333333333703, 0.3219752754296894559, 0.3333333333333333703, 0.3219752754296894559, 0.3333333333333333703, 0.3219752754296894559, 0.3333333333333333703, 0.3219752754296894559, 0.3333333333333333703, 0.3219752754296894559, 0.3333333333333333703, 0.3219752754296894559, 0.3333333333333333703, 0.3219752754296894559, 0.3333333333333333703, 0.3219752754296894559, 0.3333333333333333703, 0.3219752754296894559, 0.3333333333333333703, 0.3219752754296894559, 0.3333333333333333703, 0.3219752754296894559, 0.3333333333333333703, 0.3219752754296894559, 0.3333333333333333703, 0.3219752754296894559, 0.3333333333333333703, 0.3219752754296894559, 0.3333333333333333703, 0.3219752754296894559, 0.3333333333333333703, 0.3219752754296894559, 0.3333333333333333703, 0.3219752754296894559, 0.3333333333333333703, 0.3219752754296894559, 0.3333333333333333703, 0.3219752754296894559, 0.3333333333333333703, 0.3219752754296894559, 0.3333333333333333703, 0.3219752754296894559, 0.3333333333333333703, 0.3219752754296894559, 0.3333333333333333703, 0.3219752754296894559, 0.3333333333333333703, 0.3219752754296894559, 0.3333333333333333703, 0.3219752754296894559, 0.3333333333333333703, 0.3219752754296894559, 0.3333333333333333703, 0.3219752754296894559, 0.3333333333333333703, 0.3219752754296894559, 0.3333333333333333703, 0.3219752754296894559, 0.3333333333333333703, 0.3219752754296894559, 0.3333333333333333703, 0.3219752754296894559, 0.3333333333333333703, 0.3219752754296894559, 0.3333333333333333703, 0.3219752754296894559, 0.3333333333333333703, 0.3219752754296894559, 0.3333333333333333703, 0.3219752754296894559, 0.3333333333333333703, 0.3219752754296894559, 0.3333333333333333703, 0.3219752754296894559, 0.3333333333333333703, 0.3219752754296894559, 0.3333333333333333703, 0.3219752754296894559, 0.3333333333333333703, 0.3219752754296894559, 0.3333333333333333703, 0.3219752754296894559, 0.3333333333333333703, 0.3219752754296894559, 0.3333333333333333703, 0.3219752754296894559, 0.3333333333333333703, 0.3219752754296894559, 0.3333333333333333703, 0.3219752754296894559, 0.3333333333333333703, 0.3219752754296894559, 0.3333333333333333703, 0.3219752754296894559, 0.3333333333333333703, 0.3219752754296894559, 0.3333333333333333703, 0.3219752754296894559, 0.3333333333333333703, 0.3219752754296894559, 0.3333333333333333703, 0.3219752754296894559, 0.3333333333333333703, 0.3219752754296894559, 0.3333333333333333703, 0.3219752754296894559, 0.3333333333333333703, 0.3219752754296894559, 0.3333333333333333703, 0.3219752754296894559, 0.3333333333333333703, 0.3219752754296894559, 0.3333333333333333703, 0.3219752754296894559, 0.3333333333333333703, 0.3219752754296894559, 0.3333333333333333703, 0.3219752754296894559, 0.3333333333333333703, 0.3219752754296894559, 0.3333333333333333703, 0.3219752754296894559, 0.3333333333333333703, 0.3219752754296894559, 0.3333333333333333703, 0.3219752754296894559, 0.3333333333333333703, 0.3219752754296894559, 0.3333333333333333703, 0.3219752754296894559, 0.3333333333333333703, 0.3219752754296894559, 0.3333333333333333703, 0.3219752754296894559, 0.3333333333333333703, 0.3219752754296894559, 0.3333333333333333703, 0.3219752754296894559, 0.3333333333333333703, 0.3219752754296894559, 0.3333333333333333703, 0.3219752754296894559, 0.3333333333333333703, 0.3219752754296894559, 0.3333333333333333703, 0.3219752754296894559, 0.3333333333333333703, 0.3219752754296894559, 0.3333333333333333703, 0.3219752754296894559, 0.3333333333333333703),
 ( 0.3333333333333333703, 0.3219752754296894559, 0.3333333333333333703, 0.3219752754296894559, 0.3333333333333333703, 0.3219752754296894559, 0.3333333333333333703, 0.3219752754296894559, 0.3333333333333333703, 0.3219752754296894559, 0.3333333333333333703, 0.3219752754296894559, 0.3333333333333333703, 0.3219752754296894559, 0.3333333333333333703, 0.3219752754296894559, 0.3333333333333333703, 0.3219752754296894559, 0.3333333333333333703, 0.3219752754296894559, 0.3333333333333333703, 0.3219752754296894559, 0.3333333333333333703, 0.3219752754296894559, 0.3333333333333333703, 0.3219752754296894559, 0.3333333333333333703, 0.3219752754296894559, 0.3333333333333333703, 0.3219752754296894559, 0.3333333333333333703, 0.3219752754296894559, 0.3333333333333333703, 0.3219752754296894559, 0.3333333333333333703, 0.3219752754296894559, 0.3333333333333333703, 0.3219752754296894559, 0.3333333333333333703, 0.3219752754296894559, 0.3333333333333333703, 0.3219752754296894559, 0.3333333333333333703, 0.3219752754296894559, 0.3333333333333333703, 0.3219752754296894559, 0.3333333333333333703, 0.3219752754296894559, 0.3333333333333333703, 0.3219752754296894559, 0.3333333333333333703, 0.3219752754296894559, 0.3333333333333333703, 0.3219752754296894559, 0.3333333333333333703, 0.3219752754296894559, 0.3333333333333333703, 0.3219752754296894559, 0.3333333333333333703, 0.3219752754296894559, 0.3333333333333333703, 0.3219752754296894559, 0.3333333333333333703, 0.3219752754296894559, 0.3333333333333333703, 0.3219752754296894559, 0.3333333333333333703, 0.3219752754296894559, 0.3333333333333333703, 0.3219752754296894559, 0.3333333333333333703, 0.3219752754296894559, 0.3333333333333333703, 0.3219752754296894559, 0.3333333333333333703, 0.3219752754296894559, 0.3333333333333333703, 0.3219752754296894559, 0.3333333333333333703, 0.3219752754296894559, 0.3333333333333333703, 0.3219752754296894559, 0.3333333333333333703, 0.3219752754296894559, 0.3333333333333333703, 0.3219752754296894559, 0.3333333333333333703, 0.3219752754296894559, 0.3333333333333333703, 0.3219752754296894559, 0.3333333333333333703, 0.3219752754296894559, 0.3333333333333333703, 0.3219752754296894559, 0.3333333333333333703, 0.3219752754296894559, 0.3333333333333333703, 0.3219752754296894559, 0.3333333333333333703, 0.3219752754296894559, 0.3333333333333333703, 0.3219752754296894559, 0.3333333333333333703, 0.3219752754296894559, 0.3333333333333333703, 0.3219752754296894559, 0.3333333333333333703, 0.3219752754296894559, 0.3333333333333333703, 0.3219752754296894559, 0.3333333333333333703, 0.3219752754296894559, 0.3333333333333333703, 0.3219752754296894559, 0.3333333333333333703, 0.3219752754296894559, 0.3333333333333333703, 0.3219752754296894559, 0.3333333333333333703, 0.3219752754296894559, 0.3333333333333333703, 0.3219752754296894559, 0.3333333333333333703, 0.3219752754296894559, 0.3333333333333333703, 0.3219752754296894559, 0.3333333333333333703, 0.3219752754296894559, 0.3333333333333333703, 0.3219752754296894559, 0.3333333333333333703, 0.3219752754296894559, 0.3333333333333333703, 0.3219752754296894559, 0.3333333333333333703, 0.3219752754296894559, 0.3333333333333333703, 0.3219752754296894559, 0.3333333333333333703, 0.3219752754296894559, 0.3333333333333333703, 0.3219752754296894559, 0.3333333333333333703, 0.3219752754296894559, 0.3333333333333333703, 0.3219752754296894559, 0.3333333333333333703, 0.3219752754296894559, 0.3333333333333333703, 0.3219752754296894559, 0.3333333333333333703, 0.3219752754296894559, 0.3333333333333333703, 0.3219752754296894559, 0.3333333333333333703, 0.3219752754296894559, 0.3333333333333333703, 0.3219752754296894559, 0.3333333333333333703, 0.3219752754296894559, 0.3333333333333333703, 0.3219752754296894559, 0.3333333333333333703, 0.3219752754296894559, 0.3333333333333333703, 0.3219752754296894559, 0.3333333333333333703, 0.3219752754296894559, 0.3333333333333333703, 0.3219752754296894559, 0.3333333333333333703, 0.3219752754296894559, 0.3333333333333333703, 0.3219752754296894559, 0.3333333333333333703, 0.3219752754296894559, 0.3333333333333333703, 0.3219752754296894559, 0.3333333333333333703, 0.3219752754296894559, 0.3333333333333333703, 0.3219752754296894559, 0.3333333333333333703, 0.3219752754296894559, 0.3333333333333333703, 0.3219752754296894559, 0.3333333333333333703, 0.3219752754296894559, 0.3333333333333333703, 0.3219752754296894559, 0.3333333333333333703, 0.3219752754296894559, 0.3333333333333333703, 0.3219752754296894559, 0.3333333333333333703, 0.3219752754296894559, 0.3333333333333333703, 0.3219752754296894559, 0.3333333333333333703, 0.3219752754296894559, 0.3333333333333333703, 0.3219752754296894559, 0.3333333333333333703, 0.3219752754296894559, 0.3333333333333333703, 0.3219752754296894559, 0.3333333333333333703, 0.3219752754296894559, 0.3333333333333333703, 0.3219752754296894559, 0.3333333333333333703, 0.3219752754296894559, 0.3333333333333333703, 0.3219752754296894559, 0.3333333333333333703, 0.3219752754296894559, 0.3333333333333333703, 0.3219752754296894559, 0.3333333333333333703, 0.3219752754296894559, 0.3333333333333333703, 0.3219752754296894559, 0.3333333333333333703, 0.3219752754296894559, 0.3333333333333333703, 0.3219752754296894559, 0.3333333333333333703, 0.3219752754296894559, 0.3333333333333333703, 0.3219752754296894559, 0.3333333333333333703, 0.3219752754296894559, 0.3333333333333333703, 0.3219752754296894559, 0.3333333333333333703, 0.3219752754296894559, 0.3333333333333333703, 0.3219752754296894559, 0.3333333333333333703, 0.3219752754296894559, 0.3333333333333333703, 0.3219752754296894559, 0.3333333333333333703, 0.3219752754296894559, 0.3333333333333333703, 0.3219752754296894559, 0.3333333333333333703, 0.3219752754296894559, 0.3333333333333333703, 0.3219752754296894559, 0.3333333333333333703, 0.3219752754296894559, 0.3333333333333333703, 0.3219752754296894559, 0.3333333333333333703, 0.3219752754296894559, 0.3333333333333333703, 0.3219752754296894559, 0.3333333333333333703, 0.3219752754296894559, 0.3333333333333333703, 0.3219752754296894559, 0.3333333333333333703, 0.3219752754296894559, 0.3333333333333333703, 0.3219752754296894559, 0.3333333333333333703, 0.3219752754296894559, 0.3333333333333333703, 0.3219752754296894559, 0.3333333333333333703, 0.3219752754296894559, 0.3333333333333333703, 0.3219752754296894559, 0.3333333333333333703, 0.3219752754296894559, 0.3333333333333333703, 0.3219752754296894559, 0.3333333333333333703, 0.3219752754296894559, 0.3333333333333333703, 0.3219752754296894559, 0.3333333333333333703, 0.3219752754296894559, 0.3333333333333333703, 0.3219752754296894559, 0.3333333333333333703, 0.3219752754296894559, 0.3333333333333333703, 0.3219752754296894559, 0.3333333333333333703, 0.3219752754296894559, 0.3333333333333333703, 0.3219752754296894559, 0.3333333333333333703, 0.3219752754296894559, 0.3333333333333333703, 0.3219752754296894559, 0.3333333333333333703, 0.3219752754296894559, 0.3333333333333333703, 0.3219752754296894559, 0.3333333333333333703, 0.3219752754296894559, 0.3333333333333333703, 0.3219752754296894559, 0.3333333333333333703, 0.3219752754296894559, 0.3333333333333333703, 0.3219752754296894559, 0.3333333333333333703, 0.3219752754296894559, 0.3333333333333333703, 0.3219752754296894559, 0.3333333333333333703, 0.3219752754296894559, 0.3333333333333333703, 0.3219752754296894559, 0.3333333333333333703, 0.3219752754296894559, 0.3333333333333333703, 0.3219752754296894559, 0.3333333333333333703, 0.3219752754296894559, 0.3333333333333333703, 0.3219752754296894559, 0.3333333333333333703, 0.3219752754296894559, 0.3333333333333333703, 0.3219752754296894559, 0.3333333333333333703, 0.3219752754296894559, 0.3333333333333333703, 0.3219752754296894559, 0.3333333333333333703, 0.3219752754296894559, 0.3333333333333333703, 0.3219752754296894559, 0.3333333333333333703, 0.3219752754296894559, 0.3333333333333333703, 0.3219752754296894559, 0.3333333333333333703, 0.3219752754296894559, 0.3333333333333333703, 0.3219752754296894559, 0.3333333333333333703, 0.3219752754296894559, 0.3333333333333333703, 0.3219752754296894559, 0.3333333333333333703, 0.3219752754296894559, 0.3333333333333333703, 0.3219752754296894559, 0.3333333333333333703, 0.3219752754296894559, 0.3333333333333333703, 0.3219752754296894559, 0.3333333333333333703, 0.3219752754296894559, 0.3333333333333333703, 0.3219752754296894559, 0.3333333333333333703, 0.3219752754296894559, 0.3333333333333333703, 0.3219752754296894559, 0.3333333333333333703, 0.3219752754296894559, 0.3333333333333333703, 0.3219752754296894559, 0.3333333333333333703, 0.3219752754296894559, 0.3333333333333333703, 0.3219752754296894559, 0.3333333333333333703, 0.3219752754296894559, 0.3333333333333333703, 0.3219752754296894559, 0.3333333333333333703, 0.3219752754296894559, 0.3333333333333333703, 0.3219752754296894559, 0.3333333333333333703, 0.3219752754296894559, 0.3333333333333333703, 0.3219752754296894559, 0.3333333333333333703, 0.3219752754296894559, 0.3333333333333333703, 0.3219752754296894559, 0.3333333333333333703, 0.3219752754296894559, 0.3333333333333333703, 0.3219752754296894559, 0.3333333333333333703, 0.3219752754296894559, 0.3333333333333333703, 0.3219752754296894559, 0.3333333333333333703, 0.3219752754296894559, 0.3333333333333333703, 0.3219752754296894559, 0.3333333333333333703, 0.3219752754296894559, 0.3333333333333333703, 0.3219752754296894559, 0.3333333333333333703, 0.3219752754296894559, 0.3333333333333333703, 0.3219752754296894559, 0.3333333333333333703, 0.3219752754296894559, 0.3333333333333333703, 0.3219752754296894559, 0.3333333333333333703, 0.3219752754296894559, 0.3333333333333333703, 0.3219752754296894559, 0.3333333333333333703, 0.3219752754296894559, 0.3333333333333333703, 0.3219752754296894559, 0.3333333333333333703, 0.3219752754296894559, 0.3333333333333333703, 0.3219752754296894559, 0.3333333333333333703, 0.3219752754296894559, 0.3333333333333333703, 0.3219752754296894559, 0.3333333333333333703, 0.3219752754296894559, 0.3333333333333333703, 0.3219752754296894559, 0.3333333333333333703, 0.3219752754296894559, 0.3333333333333333703, 0.3219752754296894559, 0.3333333333333333703, 0.3219752754296894559, 0.3333333333333333703, 0.3219752754296894559, 0.3333333333333333703, 0.3219752754296894559, 0.3333333333333333703, 0.3219752754296894559, 0.3333333333333333703, 0.3219752754296894559, 0.3333333333333333703, 0.3219752754296894559, 0.3333333333333333703, 0.3219752754296894559, 0.3333333333333333703, 0.3219752754296894559, 0.3333333333333333703, 0.3219752754296894559, 0.3333333333333333703),
 ( 1.000000000000000000, 0.9659258262890683122, 1.000000000000000000, 0.9659258262890683122, 1.000000000000000000, 0.9659258262890683122, 1.000000000000000000, 0.9659258262890683122, 1.000000000000000000, 0.9659258262890683122, 1.000000000000000000, 0.9659258262890683122, 1.000000000000000000, 0.9659258262890683122, 1.000000000000000000, 0.9659258262890683122, 1.000000000000000000, 0.9659258262890683122, 1.000000000000000000, 0.9659258262890683122, 1.000000000000000000, 0.9659258262890683122, 1.000000000000000000, 0.9659258262890683122, 1.000000000000000000, 0.9659258262890683122, 1.000000000000000000, 0.9659258262890683122, 1.000000000000000000, 0.9659258262890683122, 1.000000000000000000, 0.9659258262890683122, 1.000000000000000000, 0.9659258262890683122, 1.000000000000000000, 0.9659258262890683122, 1.000000000000000000, 0.9659258262890683122, 1.000000000000000000, 0.9659258262890683122, 1.000000000000000000, 0.9659258262890683122, 1.000000000000000000, 0.9659258262890683122, 1.000000000000000000, 0.9659258262890683122, 1.000000000000000000, 0.9659258262890683122, 1.000000000000000000, 0.9659258262890683122, 1.000000000000000000, 0.9659258262890683122, 1.000000000000000000, 0.9659258262890683122, 1.000000000000000000, 0.9659258262890683122, 1.000000000000000000, 0.9659258262890683122, 1.000000000000000000, 0.9659258262890683122, 1.000000000000000000, 0.9659258262890683122, 1.000000000000000000, 0.9659258262890683122, 1.000000000000000000, 0.9659258262890683122, 1.000000000000000000, 0.9659258262890683122, 1.000000000000000000, 0.9659258262890683122, 1.000000000000000000, 0.9659258262890683122, 1.000000000000000000, 0.9659258262890683122, 1.000000000000000000, 0.9659258262890683122, 1.000000000000000000, 0.9659258262890683122, 1.000000000000000000, 0.9659258262890683122, 1.000000000000000000, 0.9659258262890683122, 1.000000000000000000, 0.9659258262890683122, 1.000000000000000000, 0.9659258262890683122, 1.000000000000000000, 0.9659258262890683122, 1.000000000000000000, 0.9659258262890683122, 1.000000000000000000, 0.9659258262890683122, 1.000000000000000000, 0.9659258262890683122, 1.000000000000000000, 0.9659258262890683122, 1.000000000000000000, 0.9659258262890683122, 1.000000000000000000, 0.9659258262890683122, 1.000000000000000000, 0.9659258262890683122, 1.000000000000000000, 0.9659258262890683122, 1.000000000000000000, 0.9659258262890683122, 1.000000000000000000, 0.9659258262890683122, 1.000000000000000000, 0.9659258262890683122, 1.000000000000000000, 0.9659258262890683122, 1.000000000000000000, 0.9659258262890683122, 1.000000000000000000, 0.9659258262890683122, 1.000000000000000000, 0.9659258262890683122, 1.000000000000000000, 0.9659258262890683122, 1.000000000000000000, 0.9659258262890683122, 1.000000000000000000, 0.9659258262890683122, 1.000000000000000000, 0.9659258262890683122, 1.000000000000000000, 0.9659258262890683122, 1.000000000000000000, 0.9659258262890683122, 1.000000000000000000, 0.9659258262890683122, 1.000000000000000000, 0.9659258262890683122, 1.000000000000000000, 0.9659258262890683122, 1.000000000000000000, 0.9659258262890683122, 1.000000000000000000, 0.9659258262890683122, 1.000000000000000000, 0.9659258262890683122, 1.000000000000000000, 0.9659258262890683122, 1.000000000000000000, 0.9659258262890683122, 1.000000000000000000, 0.9659258262890683122, 1.000000000000000000, 0.9659258262890683122, 1.000000000000000000, 0.9659258262890683122, 1.000000000000000000, 0.9659258262890683122, 1.000000000000000000, 0.9659258262890683122, 1.000000000000000000, 0.9659258262890683122, 1.000000000000000000, 0.9659258262890683122, 1.000000000000000000, 0.9659258262890683122, 1.000000000000000000, 0.9659258262890683122, 1.000000000000000000, 0.9659258262890683122, 1.000000000000000000, 0.9659258262890683122, 1.000000000000000000, 0.9659258262890683122, 1.000000000000000000, 0.9659258262890683122, 1.000000000000000000, 0.9659258262890683122, 1.000000000000000000, 0.9659258262890683122, 1.000000000000000000, 0.9659258262890683122, 1.000000000000000000, 0.9659258262890683122, 1.000000000000000000, 0.9659258262890683122, 1.000000000000000000, 0.9659258262890683122, 1.000000000000000000, 0.9659258262890683122, 1.000000000000000000, 0.9659258262890683122, 1.000000000000000000, 0.9659258262890683122, 1.000000000000000000, 0.9659258262890683122, 1.000000000000000000, 0.9659258262890683122, 1.000000000000000000, 0.9659258262890683122, 1.000000000000000000, 0.9659258262890683122, 1.000000000000000000, 0.9659258262890683122, 1.000000000000000000, 0.9659258262890683122, 1.000000000000000000, 0.9659258262890683122, 1.000000000000000000, 0.9659258262890683122, 1.000000000000000000, 0.9659258262890683122, 1.000000000000000000, 0.9659258262890683122, 1.000000000000000000, 0.9659258262890683122, 1.000000000000000000, 0.9659258262890683122, 1.000000000000000000, 0.9659258262890683122, 1.000000000000000000, 0.9659258262890683122, 1.000000000000000000, 0.9659258262890683122, 1.000000000000000000, 0.9659258262890683122, 1.000000000000000000, 0.9659258262890683122, 1.000000000000000000, 0.9659258262890683122, 1.000000000000000000, 0.9659258262890683122, 1.000000000000000000, 0.9659258262890683122, 1.000000000000000000, 0.9659258262890683122, 1.000000000000000000, 0.9659258262890683122, 1.000000000000000000, 0.9659258262890683122, 1.000000000000000000, 0.9659258262890683122, 1.000000000000000000, 0.9659258262890683122, 1.000000000000000000, 0.9659258262890683122, 1.000000000000000000, 0.9659258262890683122, 1.000000000000000000, 0.9659258262890683122, 1.000000000000000000, 0.9659258262890683122, 1.000000000000000000, 0.9659258262890683122, 1.000000000000000000, 0.9659258262890683122, 1.000000000000000000, 0.9659258262890683122, 1.000000000000000000, 0.9659258262890683122, 1.000000000000000000, 0.9659258262890683122, 1.000000000000000000, 0.9659258262890683122, 1.000000000000000000, 0.9659258262890683122, 1.000000000000000000, 0.9659258262890683122, 1.000000000000000000, 0.9659258262890683122, 1.000000000000000000, 0.9659258262890683122, 1.000000000000000000, 0.9659258262890683122, 1.000000000000000000, 0.9659258262890683122, 1.000000000000000000, 0.9659258262890683122, 1.000000000000000000, 0.9659258262890683122, 1.000000000000000000, 0.9659258262890683122, 1.000000000000000000, 0.9659258262890683122, 1.000000000000000000, 0.9659258262890683122, 1.000000000000000000, 0.9659258262890683122, 1.000000000000000000, 0.9659258262890683122, 1.000000000000000000, 0.9659258262890683122, 1.000000000000000000, 0.9659258262890683122, 1.000000000000000000, 0.9659258262890683122, 1.000000000000000000, 0.9659258262890683122, 1.000000000000000000, 0.9659258262890683122, 1.000000000000000000, 0.9659258262890683122, 1.000000000000000000, 0.9659258262890683122, 1.000000000000000000, 0.9659258262890683122, 1.000000000000000000, 0.9659258262890683122, 1.000000000000000000, 0.9659258262890683122, 1.000000000000000000, 0.9659258262890683122, 1.000000000000000000, 0.9659258262890683122, 1.000000000000000000, 0.9659258262890683122, 1.000000000000000000, 0.9659258262890683122, 1.000000000000000000, 0.9659258262890683122, 1.000000000000000000, 0.9659258262890683122, 1.000000000000000000, 0.9659258262890683122, 1.000000000000000000, 0.9659258262890683122, 1.000000000000000000, 0.9659258262890683122, 1.000000000000000000, 0.9659258262890683122, 1.000000000000000000, 0.9659258262890683122, 1.000000000000000000, 0.9659258262890683122, 1.000000000000000000, 0.9659258262890683122, 1.000000000000000000, 0.9659258262890683122, 1.000000000000000000, 0.9659258262890683122, 1.000000000000000000, 0.9659258262890683122, 1.000000000000000000, 0.9659258262890683122, 1.000000000000000000, 0.9659258262890683122, 1.000000000000000000, 0.9659258262890683122, 1.000000000000000000, 0.9659258262890683122, 1.000000000000000000, 0.9659258262890683122, 1.000000000000000000, 0.9659258262890683122, 1.000000000000000000, 0.9659258262890683122, 1.000000000000000000, 0.9659258262890683122, 1.000000000000000000, 0.9659258262890683122, 1.000000000000000000, 0.9659258262890683122, 1.000000000000000000, 0.9659258262890683122, 1.000000000000000000, 0.9659258262890683122, 1.000000000000000000, 0.9659258262890683122, 1.000000000000000000, 0.9659258262890683122, 1.000000000000000000, 0.9659258262890683122, 1.000000000000000000, 0.9659258262890683122, 1.000000000000000000, 0.9659258262890683122, 1.000000000000000000, 0.9659258262890683122, 1.000000000000000000, 0.9659258262890683122, 1.000000000000000000, 0.9659258262890683122, 1.000000000000000000, 0.9659258262890683122, 1.000000000000000000, 0.9659258262890683122, 1.000000000000000000, 0.9659258262890683122, 1.000000000000000000, 0.9659258262890683122, 1.000000000000000000, 0.9659258262890683122, 1.000000000000000000, 0.9659258262890683122, 1.000000000000000000, 0.9659258262890683122, 1.000000000000000000, 0.9659258262890683122, 1.000000000000000000, 0.9659258262890683122, 1.000000000000000000, 0.9659258262890683122, 1.000000000000000000, 0.9659258262890683122, 1.000000000000000000, 0.9659258262890683122, 1.000000000000000000, 0.9659258262890683122, 1.000000000000000000, 0.9659258262890683122, 1.000000000000000000, 0.9659258262890683122, 1.000000000000000000, 0.9659258262890683122, 1.000000000000000000, 0.9659258262890683122, 1.000000000000000000, 0.9659258262890683122, 1.000000000000000000, 0.9659258262890683122, 1.000000000000000000, 0.9659258262890683122, 1.000000000000000000, 0.9659258262890683122, 1.000000000000000000, 0.9659258262890683122, 1.000000000000000000, 0.9659258262890683122, 1.000000000000000000, 0.9659258262890683122, 1.000000000000000000, 0.9659258262890683122, 1.000000000000000000, 0.9659258262890683122, 1.000000000000000000, 0.9659258262890683122, 1.000000000000000000, 0.9659258262890683122, 1.000000000000000000, 0.9659258262890683122, 1.000000000000000000, 0.9659258262890683122, 1.000000000000000000, 0.9659258262890683122, 1.000000000000000000, 0.9659258262890683122, 1.000000000000000000, 0.9659258262890683122, 1.000000000000000000, 0.9659258262890683122, 1.000000000000000000, 0.9659258262890683122, 1.000000000000000000, 0.9659258262890683122, 1.000000000000000000, 0.9659258262890683122, 1.000000000000000000, 0.9659258262890683122, 1.000000000000000000, 0.9659258262890683122, 1.000000000000000000),
 ( 0.3333333333333333703, 0.3219752754296894559, 0.3333333333333333703, 0.3219752754296894559, 0.3333333333333333703, 0.3219752754296894559, 0.3333333333333333703, 0.3219752754296894559, 0.3333333333333333703, 0.3219752754296894559, 0.3333333333333333703, 0.3219752754296894559, 0.3333333333333333703, 0.3219752754296894559, 0.3333333333333333703, 0.3219752754296894559, 0.3333333333333333703, 0.3219752754296894559, 0.3333333333333333703, 0.3219752754296894559, 0.3333333333333333703, 0.3219752754296894559, 0.3333333333333333703, 0.3219752754296894559, 0.3333333333333333703, 0.3219752754296894559, 0.3333333333333333703, 0.3219752754296894559, 0.3333333333333333703, 0.3219752754296894559, 0.3333333333333333703, 0.3219752754296894559, 0.3333333333333333703, 0.3219752754296894559, 0.3333333333333333703, 0.3219752754296894559, 0.3333333333333333703, 0.3219752754296894559, 0.3333333333333333703, 0.3219752754296894559, 0.3333333333333333703, 0.3219752754296894559, 0.3333333333333333703, 0.3219752754296894559, 0.3333333333333333703, 0.3219752754296894559, 0.3333333333333333703, 0.3219752754296894559, 0.3333333333333333703, 0.3219752754296894559, 0.3333333333333333703, 0.3219752754296894559, 0.3333333333333333703, 0.3219752754296894559, 0.3333333333333333703, 0.3219752754296894559, 0.3333333333333333703, 0.3219752754296894559, 0.3333333333333333703, 0.3219752754296894559, 0.3333333333333333703, 0.3219752754296894559, 0.3333333333333333703, 0.3219752754296894559, 0.3333333333333333703, 0.3219752754296894559, 0.3333333333333333703, 0.3219752754296894559, 0.3333333333333333703, 0.3219752754296894559, 0.3333333333333333703, 0.3219752754296894559, 0.3333333333333333703, 0.3219752754296894559, 0.3333333333333333703, 0.3219752754296894559, 0.3333333333333333703, 0.3219752754296894559, 0.3333333333333333703, 0.3219752754296894559, 0.3333333333333333703, 0.3219752754296894559, 0.3333333333333333703, 0.3219752754296894559, 0.3333333333333333703, 0.3219752754296894559, 0.3333333333333333703, 0.3219752754296894559, 0.3333333333333333703, 0.3219752754296894559, 0.3333333333333333703, 0.3219752754296894559, 0.3333333333333333703, 0.3219752754296894559, 0.3333333333333333703, 0.3219752754296894559, 0.3333333333333333703, 0.3219752754296894559, 0.3333333333333333703, 0.3219752754296894559, 0.3333333333333333703, 0.3219752754296894559, 0.3333333333333333703, 0.3219752754296894559, 0.3333333333333333703, 0.3219752754296894559, 0.3333333333333333703, 0.3219752754296894559, 0.3333333333333333703, 0.3219752754296894559, 0.3333333333333333703, 0.3219752754296894559, 0.3333333333333333703, 0.3219752754296894559, 0.3333333333333333703, 0.3219752754296894559, 0.3333333333333333703, 0.3219752754296894559, 0.3333333333333333703, 0.3219752754296894559, 0.3333333333333333703, 0.3219752754296894559, 0.3333333333333333703, 0.3219752754296894559, 0.3333333333333333703, 0.3219752754296894559, 0.3333333333333333703, 0.3219752754296894559, 0.3333333333333333703, 0.3219752754296894559, 0.3333333333333333703, 0.3219752754296894559, 0.3333333333333333703, 0.3219752754296894559, 0.3333333333333333703, 0.3219752754296894559, 0.3333333333333333703, 0.3219752754296894559, 0.3333333333333333703, 0.3219752754296894559, 0.3333333333333333703, 0.3219752754296894559, 0.3333333333333333703, 0.3219752754296894559, 0.3333333333333333703, 0.3219752754296894559, 0.3333333333333333703, 0.3219752754296894559, 0.3333333333333333703, 0.3219752754296894559, 0.3333333333333333703, 0.3219752754296894559, 0.3333333333333333703, 0.3219752754296894559, 0.3333333333333333703, 0.3219752754296894559, 0.3333333333333333703, 0.3219752754296894559, 0.3333333333333333703, 0.3219752754296894559, 0.3333333333333333703, 0.3219752754296894559, 0.3333333333333333703, 0.3219752754296894559, 0.3333333333333333703, 0.3219752754296894559, 0.3333333333333333703, 0.3219752754296894559, 0.3333333333333333703, 0.3219752754296894559, 0.3333333333333333703, 0.3219752754296894559, 0.3333333333333333703, 0.3219752754296894559, 0.3333333333333333703, 0.3219752754296894559, 0.3333333333333333703, 0.3219752754296894559, 0.3333333333333333703, 0.3219752754296894559, 0.3333333333333333703, 0.3219752754296894559, 0.3333333333333333703, 0.3219752754296894559, 0.3333333333333333703, 0.3219752754296894559, 0.3333333333333333703, 0.3219752754296894559, 0.3333333333333333703, 0.3219752754296894559, 0.3333333333333333703, 0.3219752754296894559, 0.3333333333333333703, 0.3219752754296894559, 0.3333333333333333703, 0.3219752754296894559, 0.3333333333333333703, 0.3219752754296894559, 0.3333333333333333703, 0.3219752754296894559, 0.3333333333333333703, 0.3219752754296894559, 0.3333333333333333703, 0.3219752754296894559, 0.3333333333333333703, 0.3219752754296894559, 0.3333333333333333703, 0.3219752754296894559, 0.3333333333333333703, 0.3219752754296894559, 0.3333333333333333703, 0.3219752754296894559, 0.3333333333333333703, 0.3219752754296894559, 0.3333333333333333703, 0.3219752754296894559, 0.3333333333333333703, 0.3219752754296894559, 0.3333333333333333703, 0.3219752754296894559, 0.3333333333333333703, 0.3219752754296894559, 0.3333333333333333703, 0.3219752754296894559, 0.3333333333333333703, 0.3219752754296894559, 0.3333333333333333703, 0.3219752754296894559, 0.3333333333333333703, 0.3219752754296894559, 0.3333333333333333703, 0.3219752754296894559, 0.3333333333333333703, 0.3219752754296894559, 0.3333333333333333703, 0.3219752754296894559, 0.3333333333333333703, 0.3219752754296894559, 0.3333333333333333703, 0.3219752754296894559, 0.3333333333333333703, 0.3219752754296894559, 0.3333333333333333703, 0.3219752754296894559, 0.3333333333333333703, 0.3219752754296894559, 0.3333333333333333703, 0.3219752754296894559, 0.3333333333333333703, 0.3219752754296894559, 0.3333333333333333703, 0.3219752754296894559, 0.3333333333333333703, 0.3219752754296894559, 0.3333333333333333703, 0.3219752754296894559, 0.3333333333333333703, 0.3219752754296894559, 0.3333333333333333703, 0.3219752754296894559, 0.3333333333333333703, 0.3219752754296894559, 0.3333333333333333703, 0.3219752754296894559, 0.3333333333333333703, 0.3219752754296894559, 0.3333333333333333703, 0.3219752754296894559, 0.3333333333333333703, 0.3219752754296894559, 0.3333333333333333703, 0.3219752754296894559, 0.3333333333333333703, 0.3219752754296894559, 0.3333333333333333703, 0.3219752754296894559, 0.3333333333333333703, 0.3219752754296894559, 0.3333333333333333703, 0.3219752754296894559, 0.3333333333333333703, 0.3219752754296894559, 0.3333333333333333703, 0.3219752754296894559, 0.3333333333333333703, 0.3219752754296894559, 0.3333333333333333703, 0.3219752754296894559, 0.3333333333333333703, 0.3219752754296894559, 0.3333333333333333703, 0.3219752754296894559, 0.3333333333333333703, 0.3219752754296894559, 0.3333333333333333703, 0.3219752754296894559, 0.3333333333333333703, 0.3219752754296894559, 0.3333333333333333703, 0.3219752754296894559, 0.3333333333333333703, 0.3219752754296894559, 0.3333333333333333703, 0.3219752754296894559, 0.3333333333333333703, 0.3219752754296894559, 0.3333333333333333703, 0.3219752754296894559, 0.3333333333333333703, 0.3219752754296894559, 0.3333333333333333703, 0.3219752754296894559, 0.3333333333333333703, 0.3219752754296894559, 0.3333333333333333703, 0.3219752754296894559, 0.3333333333333333703, 0.3219752754296894559, 0.3333333333333333703, 0.3219752754296894559, 0.3333333333333333703, 0.3219752754296894559, 0.3333333333333333703, 0.3219752754296894559, 0.3333333333333333703, 0.3219752754296894559, 0.3333333333333333703, 0.3219752754296894559, 0.3333333333333333703, 0.3219752754296894559, 0.3333333333333333703, 0.3219752754296894559, 0.3333333333333333703, 0.3219752754296894559, 0.3333333333333333703, 0.3219752754296894559, 0.3333333333333333703, 0.3219752754296894559, 0.3333333333333333703, 0.3219752754296894559, 0.3333333333333333703, 0.3219752754296894559, 0.3333333333333333703, 0.3219752754296894559, 0.3333333333333333703, 0.3219752754296894559, 0.3333333333333333703, 0.3219752754296894559, 0.3333333333333333703, 0.3219752754296894559, 0.3333333333333333703, 0.3219752754296894559, 0.3333333333333333703, 0.3219752754296894559, 0.3333333333333333703, 0.3219752754296894559, 0.3333333333333333703, 0.3219752754296894559, 0.3333333333333333703, 0.3219752754296894559, 0.3333333333333333703, 0.3219752754296894559, 0.3333333333333333703, 0.3219752754296894559, 0.3333333333333333703, 0.3219752754296894559, 0.3333333333333333703, 0.3219752754296894559, 0.3333333333333333703, 0.3219752754296894559, 0.3333333333333333703, 0.3219752754296894559, 0.3333333333333333703, 0.3219752754296894559, 0.3333333333333333703, 0.3219752754296894559, 0.3333333333333333703, 0.3219752754296894559, 0.3333333333333333703, 0.3219752754296894559, 0.3333333333333333703, 0.3219752754296894559, 0.3333333333333333703, 0.3219752754296894559, 0.3333333333333333703, 0.3219752754296894559, 0.3333333333333333703, 0.3219752754296894559, 0.3333333333333333703, 0.3219752754296894559, 0.3333333333333333703, 0.3219752754296894559, 0.3333333333333333703, 0.3219752754296894559, 0.3333333333333333703, 0.3219752754296894559, 0.3333333333333333703, 0.3219752754296894559, 0.3333333333333333703, 0.3219752754296894559, 0.3333333333333333703, 0.3219752754296894559, 0.3333333333333333703, 0.3219752754296894559, 0.3333333333333333703, 0.3219752754296894559, 0.3333333333333333703, 0.3219752754296894559, 0.3333333333333333703, 0.3219752754296894559, 0.3333333333333333703, 0.3219752754296894559, 0.3333333333333333703, 0.3219752754296894559, 0.3333333333333333703, 0.3219752754296894559, 0.3333333333333333703, 0.3219752754296894559, 0.3333333333333333703, 0.3219752754296894559, 0.3333333333333333703, 0.3219752754296894559, 0.3333333333333333703, 0.3219752754296894559, 0.3333333333333333703, 0.3219752754296894559, 0.3333333333333333703, 0.3219752754296894559, 0.3333333333333333703, 0.3219752754296894559, 0.3333333333333333703, 0.3219752754296894559, 0.3333333333333333703, 0.3219752754296894559, 0.3333333333333333703, 0.3219752754296894559, 0.3333333333333333703, 0.3219752754296894559, 0.3333333333333333703, 0.3219752754296894559, 0.3333333333333333703, 0.3219752754296894559, 0.3333333333333333703, 0.3219752754296894559, 0.3333333333333333703, 0.3219752754296894559, 0.3333333333333333703, 0.3219752754296894559, 0.3333333333333333703, 0.3219752754296894559, 0.3333333333333333703, 0.3219752754296894559, 0.3333333333333333703, 0.3219752754296894559, 0.3333333333333333703, 0.3219752754296894559, 0.3333333333333333703),
 ( 0.3333333333333333703, 0.3219752754296894559, 0.3333333333333333703, 0.3219752754296894559, 0.3333333333333333703, 0.3219752754296894559, 0.3333333333333333703, 0.3219752754296894559, 0.3333333333333333703, 0.3219752754296894559, 0.3333333333333333703, 0.3219752754296894559, 0.3333333333333333703, 0.3219752754296894559, 0.3333333333333333703, 0.3219752754296894559, 0.3333333333333333703, 0.3219752754296894559, 0.3333333333333333703, 0.3219752754296894559, 0.3333333333333333703, 0.3219752754296894559, 0.3333333333333333703, 0.3219752754296894559, 0.3333333333333333703, 0.3219752754296894559, 0.3333333333333333703, 0.3219752754296894559, 0.3333333333333333703, 0.3219752754296894559, 0.3333333333333333703, 0.3219752754296894559, 0.3333333333333333703, 0.3219752754296894559, 0.3333333333333333703, 0.3219752754296894559, 0.3333333333333333703, 0.3219752754296894559, 0.3333333333333333703, 0.3219752754296894559, 0.3333333333333333703, 0.3219752754296894559, 0.3333333333333333703, 0.3219752754296894559, 0.3333333333333333703, 0.3219752754296894559, 0.3333333333333333703, 0.3219752754296894559, 0.3333333333333333703, 0.3219752754296894559, 0.3333333333333333703, 0.3219752754296894559, 0.3333333333333333703, 0.3219752754296894559, 0.3333333333333333703, 0.3219752754296894559, 0.3333333333333333703, 0.3219752754296894559, 0.3333333333333333703, 0.3219752754296894559, 0.3333333333333333703, 0.3219752754296894559, 0.3333333333333333703, 0.3219752754296894559, 0.3333333333333333703, 0.3219752754296894559, 0.3333333333333333703, 0.3219752754296894559, 0.3333333333333333703, 0.3219752754296894559, 0.3333333333333333703, 0.3219752754296894559, 0.3333333333333333703, 0.3219752754296894559, 0.3333333333333333703, 0.3219752754296894559, 0.3333333333333333703, 0.3219752754296894559, 0.3333333333333333703, 0.3219752754296894559, 0.3333333333333333703, 0.3219752754296894559, 0.3333333333333333703, 0.3219752754296894559, 0.3333333333333333703, 0.3219752754296894559, 0.3333333333333333703, 0.3219752754296894559, 0.3333333333333333703, 0.3219752754296894559, 0.3333333333333333703, 0.3219752754296894559, 0.3333333333333333703, 0.3219752754296894559, 0.3333333333333333703, 0.3219752754296894559, 0.3333333333333333703, 0.3219752754296894559, 0.3333333333333333703, 0.3219752754296894559, 0.3333333333333333703, 0.3219752754296894559, 0.3333333333333333703, 0.3219752754296894559, 0.3333333333333333703, 0.3219752754296894559, 0.3333333333333333703, 0.3219752754296894559, 0.3333333333333333703, 0.3219752754296894559, 0.3333333333333333703, 0.3219752754296894559, 0.3333333333333333703, 0.3219752754296894559, 0.3333333333333333703, 0.3219752754296894559, 0.3333333333333333703, 0.3219752754296894559, 0.3333333333333333703, 0.3219752754296894559, 0.3333333333333333703, 0.3219752754296894559, 0.3333333333333333703, 0.3219752754296894559, 0.3333333333333333703, 0.3219752754296894559, 0.3333333333333333703, 0.3219752754296894559, 0.3333333333333333703, 0.3219752754296894559, 0.3333333333333333703, 0.3219752754296894559, 0.3333333333333333703, 0.3219752754296894559, 0.3333333333333333703, 0.3219752754296894559, 0.3333333333333333703, 0.3219752754296894559, 0.3333333333333333703, 0.3219752754296894559, 0.3333333333333333703, 0.3219752754296894559, 0.3333333333333333703, 0.3219752754296894559, 0.3333333333333333703, 0.3219752754296894559, 0.3333333333333333703, 0.3219752754296894559, 0.3333333333333333703, 0.3219752754296894559, 0.3333333333333333703, 0.3219752754296894559, 0.3333333333333333703, 0.3219752754296894559, 0.3333333333333333703, 0.3219752754296894559, 0.3333333333333333703, 0.3219752754296894559, 0.3333333333333333703, 0.3219752754296894559, 0.3333333333333333703, 0.3219752754296894559, 0.3333333333333333703, 0.3219752754296894559, 0.3333333333333333703, 0.3219752754296894559, 0.3333333333333333703, 0.3219752754296894559, 0.3333333333333333703, 0.3219752754296894559, 0.3333333333333333703, 0.3219752754296894559, 0.3333333333333333703, 0.3219752754296894559, 0.3333333333333333703, 0.3219752754296894559, 0.3333333333333333703, 0.3219752754296894559, 0.3333333333333333703, 0.3219752754296894559, 0.3333333333333333703, 0.3219752754296894559, 0.3333333333333333703, 0.3219752754296894559, 0.3333333333333333703, 0.3219752754296894559, 0.3333333333333333703, 0.3219752754296894559, 0.3333333333333333703, 0.3219752754296894559, 0.3333333333333333703, 0.3219752754296894559, 0.3333333333333333703, 0.3219752754296894559, 0.3333333333333333703, 0.3219752754296894559, 0.3333333333333333703, 0.3219752754296894559, 0.3333333333333333703, 0.3219752754296894559, 0.3333333333333333703, 0.3219752754296894559, 0.3333333333333333703, 0.3219752754296894559, 0.3333333333333333703, 0.3219752754296894559, 0.3333333333333333703, 0.3219752754296894559, 0.3333333333333333703, 0.3219752754296894559, 0.3333333333333333703, 0.3219752754296894559, 0.3333333333333333703, 0.3219752754296894559, 0.3333333333333333703, 0.3219752754296894559, 0.3333333333333333703, 0.3219752754296894559, 0.3333333333333333703, 0.3219752754296894559, 0.3333333333333333703, 0.3219752754296894559, 0.3333333333333333703, 0.3219752754296894559, 0.3333333333333333703, 0.3219752754296894559, 0.3333333333333333703, 0.3219752754296894559, 0.3333333333333333703, 0.3219752754296894559, 0.3333333333333333703, 0.3219752754296894559, 0.3333333333333333703, 0.3219752754296894559, 0.3333333333333333703, 0.3219752754296894559, 0.3333333333333333703, 0.3219752754296894559, 0.3333333333333333703, 0.3219752754296894559, 0.3333333333333333703, 0.3219752754296894559, 0.3333333333333333703, 0.3219752754296894559, 0.3333333333333333703, 0.3219752754296894559, 0.3333333333333333703, 0.3219752754296894559, 0.3333333333333333703, 0.3219752754296894559, 0.3333333333333333703, 0.3219752754296894559, 0.3333333333333333703, 0.3219752754296894559, 0.3333333333333333703, 0.3219752754296894559, 0.3333333333333333703, 0.3219752754296894559, 0.3333333333333333703, 0.3219752754296894559, 0.3333333333333333703, 0.3219752754296894559, 0.3333333333333333703, 0.3219752754296894559, 0.3333333333333333703, 0.3219752754296894559, 0.3333333333333333703, 0.3219752754296894559, 0.3333333333333333703, 0.3219752754296894559, 0.3333333333333333703, 0.3219752754296894559, 0.3333333333333333703, 0.3219752754296894559, 0.3333333333333333703, 0.3219752754296894559, 0.3333333333333333703, 0.3219752754296894559, 0.3333333333333333703, 0.3219752754296894559, 0.3333333333333333703, 0.3219752754296894559, 0.3333333333333333703, 0.3219752754296894559, 0.3333333333333333703, 0.3219752754296894559, 0.3333333333333333703, 0.3219752754296894559, 0.3333333333333333703, 0.3219752754296894559, 0.3333333333333333703, 0.3219752754296894559, 0.3333333333333333703, 0.3219752754296894559, 0.3333333333333333703, 0.3219752754296894559, 0.3333333333333333703, 0.3219752754296894559, 0.3333333333333333703, 0.3219752754296894559, 0.3333333333333333703, 0.3219752754296894559, 0.3333333333333333703, 0.3219752754296894559, 0.3333333333333333703, 0.3219752754296894559, 0.3333333333333333703, 0.3219752754296894559, 0.3333333333333333703, 0.3219752754296894559, 0.3333333333333333703, 0.3219752754296894559, 0.3333333333333333703, 0.3219752754296894559, 0.3333333333333333703, 0.3219752754296894559, 0.3333333333333333703, 0.3219752754296894559, 0.3333333333333333703, 0.3219752754296894559, 0.3333333333333333703, 0.3219752754296894559, 0.3333333333333333703, 0.3219752754296894559, 0.3333333333333333703, 0.3219752754296894559, 0.3333333333333333703, 0.3219752754296894559, 0.3333333333333333703, 0.3219752754296894559, 0.3333333333333333703, 0.3219752754296894559, 0.3333333333333333703, 0.3219752754296894559, 0.3333333333333333703, 0.3219752754296894559, 0.3333333333333333703, 0.3219752754296894559, 0.3333333333333333703, 0.3219752754296894559, 0.3333333333333333703, 0.3219752754296894559, 0.3333333333333333703, 0.3219752754296894559, 0.3333333333333333703, 0.3219752754296894559, 0.3333333333333333703, 0.3219752754296894559, 0.3333333333333333703, 0.3219752754296894559, 0.3333333333333333703, 0.3219752754296894559, 0.3333333333333333703, 0.3219752754296894559, 0.3333333333333333703, 0.3219752754296894559, 0.3333333333333333703, 0.3219752754296894559, 0.3333333333333333703, 0.3219752754296894559, 0.3333333333333333703, 0.3219752754296894559, 0.3333333333333333703, 0.3219752754296894559, 0.3333333333333333703, 0.3219752754296894559, 0.3333333333333333703, 0.3219752754296894559, 0.3333333333333333703, 0.3219752754296894559, 0.3333333333333333703, 0.3219752754296894559, 0.3333333333333333703, 0.3219752754296894559, 0.3333333333333333703, 0.3219752754296894559, 0.3333333333333333703, 0.3219752754296894559, 0.3333333333333333703, 0.3219752754296894559, 0.3333333333333333703, 0.3219752754296894559, 0.3333333333333333703, 0.3219752754296894559, 0.3333333333333333703, 0.3219752754296894559, 0.3333333333333333703, 0.3219752754296894559, 0.3333333333333333703, 0.3219752754296894559, 0.3333333333333333703, 0.3219752754296894559, 0.3333333333333333703, 0.3219752754296894559, 0.3333333333333333703, 0.3219752754296894559, 0.3333333333333333703, 0.3219752754296894559, 0.3333333333333333703, 0.3219752754296894559, 0.3333333333333333703, 0.3219752754296894559, 0.3333333333333333703, 0.3219752754296894559, 0.3333333333333333703, 0.3219752754296894559, 0.3333333333333333703, 0.3219752754296894559, 0.3333333333333333703, 0.3219752754296894559, 0.3333333333333333703, 0.3219752754296894559, 0.3333333333333333703, 0.3219752754296894559, 0.3333333333333333703, 0.3219752754296894559, 0.3333333333333333703, 0.3219752754296894559, 0.3333333333333333703, 0.3219752754296894559, 0.3333333333333333703, 0.3219752754296894559, 0.3333333333333333703, 0.3219752754296894559, 0.3333333333333333703, 0.3219752754296894559, 0.3333333333333333703, 0.3219752754296894559, 0.3333333333333333703, 0.3219752754296894559, 0.3333333333333333703, 0.3219752754296894559, 0.3333333333333333703, 0.3219752754296894559, 0.3333333333333333703, 0.3219752754296894559, 0.3333333333333333703, 0.3219752754296894559, 0.3333333333333333703, 0.3219752754296894559, 0.3333333333333333703, 0.3219752754296894559, 0.3333333333333333703, 0.3219752754296894559, 0.3333333333333333703, 0.3219752754296894559, 0.3333333333333333703, 0.3219752754296894559, 0.3333333333333333703, 0.3219752754296894559, 0.3333333333333333703, 0.3219752754296894559, 0.3333333333333333703, 0.3219752754296894559, 0.3333333333333333703, 0.3219752754296894559, 0.3333333333333333703),
 ( 1.000000000000000000, 0.9659258262890683122, 1.000000000000000000, 0.9659258262890683122, 1.000000000000000000, 0.9659258262890683122, 1.000000000000000000, 0.9659258262890683122, 1.000000000000000000, 0.9659258262890683122, 1.000000000000000000, 0.9659258262890683122, 1.000000000000000000, 0.9659258262890683122, 1.000000000000000000, 0.9659258262890683122, 1.000000000000000000, 0.9659258262890683122, 1.000000000000000000, 0.9659258262890683122, 1.000000000000000000, 0.9659258262890683122, 1.000000000000000000, 0.9659258262890683122, 1.000000000000000000, 0.9659258262890683122, 1.000000000000000000, 0.9659258262890683122, 1.000000000000000000, 0.9659258262890683122, 1.000000000000000000, 0.9659258262890683122, 1.000000000000000000, 0.9659258262890683122, 1.000000000000000000, 0.9659258262890683122, 1.000000000000000000, 0.9659258262890683122, 1.000000000000000000, 0.9659258262890683122, 1.000000000000000000, 0.9659258262890683122, 1.000000000000000000, 0.9659258262890683122, 1.000000000000000000, 0.9659258262890683122, 1.000000000000000000, 0.9659258262890683122, 1.000000000000000000, 0.9659258262890683122, 1.000000000000000000, 0.9659258262890683122, 1.000000000000000000, 0.9659258262890683122, 1.000000000000000000, 0.9659258262890683122, 1.000000000000000000, 0.9659258262890683122, 1.000000000000000000, 0.9659258262890683122, 1.000000000000000000, 0.9659258262890683122, 1.000000000000000000, 0.9659258262890683122, 1.000000000000000000, 0.9659258262890683122, 1.000000000000000000, 0.9659258262890683122, 1.000000000000000000, 0.9659258262890683122, 1.000000000000000000, 0.9659258262890683122, 1.000000000000000000, 0.9659258262890683122, 1.000000000000000000, 0.9659258262890683122, 1.000000000000000000, 0.9659258262890683122, 1.000000000000000000, 0.9659258262890683122, 1.000000000000000000, 0.9659258262890683122, 1.000000000000000000, 0.9659258262890683122, 1.000000000000000000, 0.9659258262890683122, 1.000000000000000000, 0.9659258262890683122, 1.000000000000000000, 0.9659258262890683122, 1.000000000000000000, 0.9659258262890683122, 1.000000000000000000, 0.9659258262890683122, 1.000000000000000000, 0.9659258262890683122, 1.000000000000000000, 0.9659258262890683122, 1.000000000000000000, 0.9659258262890683122, 1.000000000000000000, 0.9659258262890683122, 1.000000000000000000, 0.9659258262890683122, 1.000000000000000000, 0.9659258262890683122, 1.000000000000000000, 0.9659258262890683122, 1.000000000000000000, 0.9659258262890683122, 1.000000000000000000, 0.9659258262890683122, 1.000000000000000000, 0.9659258262890683122, 1.000000000000000000, 0.9659258262890683122, 1.000000000000000000, 0.9659258262890683122, 1.000000000000000000, 0.9659258262890683122, 1.000000000000000000, 0.9659258262890683122, 1.000000000000000000, 0.9659258262890683122, 1.000000000000000000, 0.9659258262890683122, 1.000000000000000000, 0.9659258262890683122, 1.000000000000000000, 0.9659258262890683122, 1.000000000000000000, 0.9659258262890683122, 1.000000000000000000, 0.9659258262890683122, 1.000000000000000000, 0.9659258262890683122, 1.000000000000000000, 0.9659258262890683122, 1.000000000000000000, 0.9659258262890683122, 1.000000000000000000, 0.9659258262890683122, 1.000000000000000000, 0.9659258262890683122, 1.000000000000000000, 0.9659258262890683122, 1.000000000000000000, 0.9659258262890683122, 1.000000000000000000, 0.9659258262890683122, 1.000000000000000000, 0.9659258262890683122, 1.000000000000000000, 0.9659258262890683122, 1.000000000000000000, 0.9659258262890683122, 1.000000000000000000, 0.9659258262890683122, 1.000000000000000000, 0.9659258262890683122, 1.000000000000000000, 0.9659258262890683122, 1.000000000000000000, 0.9659258262890683122, 1.000000000000000000, 0.9659258262890683122, 1.000000000000000000, 0.9659258262890683122, 1.000000000000000000, 0.9659258262890683122, 1.000000000000000000, 0.9659258262890683122, 1.000000000000000000, 0.9659258262890683122, 1.000000000000000000, 0.9659258262890683122, 1.000000000000000000, 0.9659258262890683122, 1.000000000000000000, 0.9659258262890683122, 1.000000000000000000, 0.9659258262890683122, 1.000000000000000000, 0.9659258262890683122, 1.000000000000000000, 0.9659258262890683122, 1.000000000000000000, 0.9659258262890683122, 1.000000000000000000, 0.9659258262890683122, 1.000000000000000000, 0.9659258262890683122, 1.000000000000000000, 0.9659258262890683122, 1.000000000000000000, 0.9659258262890683122, 1.000000000000000000, 0.9659258262890683122, 1.000000000000000000, 0.9659258262890683122, 1.000000000000000000, 0.9659258262890683122, 1.000000000000000000, 0.9659258262890683122, 1.000000000000000000, 0.9659258262890683122, 1.000000000000000000, 0.9659258262890683122, 1.000000000000000000, 0.9659258262890683122, 1.000000000000000000, 0.9659258262890683122, 1.000000000000000000, 0.9659258262890683122, 1.000000000000000000, 0.9659258262890683122, 1.000000000000000000, 0.9659258262890683122, 1.000000000000000000, 0.9659258262890683122, 1.000000000000000000, 0.9659258262890683122, 1.000000000000000000, 0.9659258262890683122, 1.000000000000000000, 0.9659258262890683122, 1.000000000000000000, 0.9659258262890683122, 1.000000000000000000, 0.9659258262890683122, 1.000000000000000000, 0.9659258262890683122, 1.000000000000000000, 0.9659258262890683122, 1.000000000000000000, 0.9659258262890683122, 1.000000000000000000, 0.9659258262890683122, 1.000000000000000000, 0.9659258262890683122, 1.000000000000000000, 0.9659258262890683122, 1.000000000000000000, 0.9659258262890683122, 1.000000000000000000, 0.9659258262890683122, 1.000000000000000000, 0.9659258262890683122, 1.000000000000000000, 0.9659258262890683122, 1.000000000000000000, 0.9659258262890683122, 1.000000000000000000, 0.9659258262890683122, 1.000000000000000000, 0.9659258262890683122, 1.000000000000000000, 0.9659258262890683122, 1.000000000000000000, 0.9659258262890683122, 1.000000000000000000, 0.9659258262890683122, 1.000000000000000000, 0.9659258262890683122, 1.000000000000000000, 0.9659258262890683122, 1.000000000000000000, 0.9659258262890683122, 1.000000000000000000, 0.9659258262890683122, 1.000000000000000000, 0.9659258262890683122, 1.000000000000000000, 0.9659258262890683122, 1.000000000000000000, 0.9659258262890683122, 1.000000000000000000, 0.9659258262890683122, 1.000000000000000000, 0.9659258262890683122, 1.000000000000000000, 0.9659258262890683122, 1.000000000000000000, 0.9659258262890683122, 1.000000000000000000, 0.9659258262890683122, 1.000000000000000000, 0.9659258262890683122, 1.000000000000000000, 0.9659258262890683122, 1.000000000000000000, 0.9659258262890683122, 1.000000000000000000, 0.9659258262890683122, 1.000000000000000000, 0.9659258262890683122, 1.000000000000000000, 0.9659258262890683122, 1.000000000000000000, 0.9659258262890683122, 1.000000000000000000, 0.9659258262890683122, 1.000000000000000000, 0.9659258262890683122, 1.000000000000000000, 0.9659258262890683122, 1.000000000000000000, 0.9659258262890683122, 1.000000000000000000, 0.9659258262890683122, 1.000000000000000000, 0.9659258262890683122, 1.000000000000000000, 0.9659258262890683122, 1.000000000000000000, 0.9659258262890683122, 1.000000000000000000, 0.9659258262890683122, 1.000000000000000000, 0.9659258262890683122, 1.000000000000000000, 0.9659258262890683122, 1.000000000000000000, 0.9659258262890683122, 1.000000000000000000, 0.9659258262890683122, 1.000000000000000000, 0.9659258262890683122, 1.000000000000000000, 0.9659258262890683122, 1.000000000000000000, 0.9659258262890683122, 1.000000000000000000, 0.9659258262890683122, 1.000000000000000000, 0.9659258262890683122, 1.000000000000000000, 0.9659258262890683122, 1.000000000000000000, 0.9659258262890683122, 1.000000000000000000, 0.9659258262890683122, 1.000000000000000000, 0.9659258262890683122, 1.000000000000000000, 0.9659258262890683122, 1.000000000000000000, 0.9659258262890683122, 1.000000000000000000, 0.9659258262890683122, 1.000000000000000000, 0.9659258262890683122, 1.000000000000000000, 0.9659258262890683122, 1.000000000000000000, 0.9659258262890683122, 1.000000000000000000, 0.9659258262890683122, 1.000000000000000000, 0.9659258262890683122, 1.000000000000000000, 0.9659258262890683122, 1.000000000000000000, 0.9659258262890683122, 1.000000000000000000, 0.9659258262890683122, 1.000000000000000000, 0.9659258262890683122, 1.000000000000000000, 0.9659258262890683122, 1.000000000000000000, 0.9659258262890683122, 1.000000000000000000, 0.9659258262890683122, 1.000000000000000000, 0.9659258262890683122, 1.000000000000000000, 0.9659258262890683122, 1.000000000000000000, 0.9659258262890683122, 1.000000000000000000, 0.9659258262890683122, 1.000000000000000000, 0.9659258262890683122, 1.000000000000000000, 0.9659258262890683122, 1.000000000000000000, 0.9659258262890683122, 1.000000000000000000, 0.9659258262890683122, 1.000000000000000000, 0.9659258262890683122, 1.000000000000000000, 0.9659258262890683122, 1.000000000000000000, 0.9659258262890683122, 1.000000000000000000, 0.9659258262890683122, 1.000000000000000000, 0.9659258262890683122, 1.000000000000000000, 0.9659258262890683122, 1.000000000000000000, 0.9659258262890683122, 1.000000000000000000, 0.9659258262890683122, 1.000000000000000000, 0.9659258262890683122, 1.000000000000000000, 0.9659258262890683122, 1.000000000000000000, 0.9659258262890683122, 1.000000000000000000, 0.9659258262890683122, 1.000000000000000000, 0.9659258262890683122, 1.000000000000000000, 0.9659258262890683122, 1.000000000000000000, 0.9659258262890683122, 1.000000000000000000, 0.9659258262890683122, 1.000000000000000000, 0.9659258262890683122, 1.000000000000000000, 0.9659258262890683122, 1.000000000000000000, 0.9659258262890683122, 1.000000000000000000, 0.9659258262890683122, 1.000000000000000000, 0.9659258262890683122, 1.000000000000000000, 0.9659258262890683122, 1.000000000000000000, 0.9659258262890683122, 1.000000000000000000, 0.9659258262890683122, 1.000000000000000000, 0.9659258262890683122, 1.000000000000000000, 0.9659258262890683122, 1.000000000000000000, 0.9659258262890683122, 1.000000000000000000, 0.9659258262890683122, 1.000000000000000000, 0.9659258262890683122, 1.000000000000000000, 0.9659258262890683122, 1.000000000000000000, 0.9659258262890683122, 1.000000000000000000, 0.9659258262890683122, 1.000000000000000000, 0.9659258262890683122, 1.000000000000000000) ) ) 
 REPRESENTATION_ITEM ( '' )  SURFACE ( )  );
#69767 = CARTESIAN_POINT ( 'NONE',  ( -8.314922557961024197, 14.29746914071037800, 62.91775706135236135 ) ) ;
#69769 = CARTESIAN_POINT ( 'NONE',  ( -5.823673210054431948, 21.52544592524334988, 72.70942372801901854 ) ) ;
#69770 = CARTESIAN_POINT ( 'NONE',  ( 16.53943276465976808, 0.05219959533934440121, 46.25109039468567573 ) ) ;
#69771 = CARTESIAN_POINT ( 'NONE',  ( -5.153800228976328057, -19.02544592524343514, 77.29057627198099567 ) ) ;
#69772 = CARTESIAN_POINT ( 'NONE',  ( 19.05341960407617918, -5.049401038297876454, 106.0427570613523471 ) ) ;
#69773 = CARTESIAN_POINT ( 'NONE',  ( 16.53943276465976808, 0.05219959533934440121, 86.25109039468568994 ) ) ;
#69774 = CARTESIAN_POINT ( 'NONE',  ( -9.474510206698720793, -16.51473224551083518, 89.58442372801900433 ) ) ;
#69775 = CARTESIAN_POINT ( 'NONE',  ( 19.02544592524343514, -5.153800228976328945, 58.54057627198102409 ) ) ;
#69776 = CARTESIAN_POINT ( 'NONE',  ( 5.719274019375991003, -21.55341960407610458, 92.70724293864770971 ) ) ;
#69778 = CARTESIAN_POINT ( 'NONE',  ( 13.89961937509957401, 13.97604488694547697, 91.87609039468567573 ) ) ;
#69777 = CARTESIAN_POINT ( 'NONE',  ( -12.06949235617756955, 12.14591786802309770, 95.62390960531436690 ) ) ;
#69779 = CARTESIAN_POINT ( 'NONE',  ( -4.483927247898782831, 16.52544592524335698, 62.70942372801902565 ) ) ;
#69780 = CARTESIAN_POINT ( 'NONE',  ( 17.48847506799971185, -5.747544572773693794, 63.32697437843280852 ) ) ;
#69781 = CARTESIAN_POINT ( 'NONE',  ( -13.97604488694547697, 13.89961937509957934, 68.12609039468563310 ) ) ;
#69782 = CARTESIAN_POINT ( 'NONE',  ( -16.52544592524342804, 4.483927247898546575, 26.04057627198103475 ) ) ;
#69783 = CARTESIAN_POINT ( 'NONE',  ( 14.29746914071049879, -8.314922557960816363, 83.33224293864769550 ) ) ;
#69785 = CARTESIAN_POINT ( 'NONE',  ( -17.26058549869106429, 6.457015423128171783, 38.62254162523935008 ) ) ;
#69784 = CARTESIAN_POINT ( 'NONE',  ( 13.97604488694548053, -13.89961937509957401, 25.62609039468566507 ) ) ;
#69786 = CARTESIAN_POINT ( 'NONE',  ( 10.81492255796106328, -18.62759615963255655, 20.41775706135234714 ) ) ;
#69787 = CARTESIAN_POINT ( 'NONE',  ( -19.02544592524342804, 5.153800228976336051, 116.0405762719810383 ) ) ;
#69788 = CARTESIAN_POINT ( 'NONE',  ( 19.03943276465977164, -0.05219959533909143690, 83.74890960531436690 ) ) ;
#69789 = CARTESIAN_POINT ( 'NONE',  ( -18.62759615963255300, -10.81492255796106328, 99.16775706135234714 ) ) ;
#69790 = CARTESIAN_POINT ( 'NONE',  ( -13.89961937509977652, 13.97604488694528158, 75.62390960531438111 ) ) ;
#69791 = CARTESIAN_POINT ( 'NONE',  ( 10.81492255796078972, 18.62759615963270932, 49.58224293864769550 ) ) ;
#69792 = CARTESIAN_POINT ( 'NONE',  ( 4.483927247898545687, 16.52544592524342804, 79.79057627198102409 ) ) ;
#69793 = CARTESIAN_POINT ( 'NONE',  ( -19.05341960407611168, -5.049401038298163336, 56.45724293864768129 ) ) ;
#69794 = AXIS2_PLACEMENT_3D ( 'NONE', #127896, #147080, #39887 ) ;
#69795 = CARTESIAN_POINT ( 'NONE',  ( -12.14591786802309592, -12.06949235617757132, 106.8739096053143811 ) ) ;
#69796 = CARTESIAN_POINT ( 'NONE',  ( 15.80617190586769283, -15.72974639402175789, 25.62609039468567929 ) ) ;
#69797 = CARTESIAN_POINT ( 'NONE',  ( 21.55341960407619695, -5.719274019375665929, 56.04275706135235424 ) ) ;
#69798 = CARTESIAN_POINT ( 'NONE',  ( 9.474510206698971260, -16.51473224551069308, 42.91557627198103120 ) ) ;
#69799 = CARTESIAN_POINT ( 'NONE',  ( -12.14591786802326823, 12.06949235617739902, 83.12609039468568994 ) ) ;
#69800 = CARTESIAN_POINT ( 'NONE',  ( -10.81492255796078084, -18.62759615963271287, 112.0822429386477097 ) ) ;
#69801 = CARTESIAN_POINT ( 'NONE',  ( -0.05219959533907301413, -21.53943276465977519, 112.4989096053143669 ) ) ;
#69803 = CARTESIAN_POINT ( 'NONE',  ( -13.89961937509977652, 13.97604488694528158, 60.62390960531436690 ) ) ;
#69802 = CARTESIAN_POINT ( 'NONE',  ( 19.03943276465977164, 0.05219959533936151252, 46.25109039468566863 ) ) ;
#69804 = CARTESIAN_POINT ( 'NONE',  ( -13.97604488694547697, 13.89961937509957934, 38.12609039468566152 ) ) ;
#69805 = CARTESIAN_POINT ( 'NONE',  ( 21.53943276465977519, 0.05219959533937863772, 71.25109039468568994 ) ) ;
#69806 = ADVANCED_FACE ( 'NONE', ( #112865 ), #34052, .F. ) ;
#69807 = CARTESIAN_POINT ( 'NONE',  ( 18.62759615963271287, -10.81492255796078972, 68.33224293864769550 ) ) ;
#69808 = CARTESIAN_POINT ( 'NONE',  ( 14.29746914071049879, -8.314922557960816363, 33.33224293864769550 ) ) ;
#69810 = CARTESIAN_POINT ( 'NONE',  ( -15.80617190586768217, 15.72974639402176855, 108.1260903946856757 ) ) ;
#69809 = CARTESIAN_POINT ( 'NONE',  ( 15.80617190586769283, -15.72974639402175789, 95.62609039468568994 ) ) ;
#69811 = CARTESIAN_POINT ( 'NONE',  ( -14.29746914071049879, 8.314922557960819915, 55.83224293864770260 ) ) ;
#69812 = CARTESIAN_POINT ( 'NONE',  ( -12.06949235617756955, 12.14591786802309770, 105.6239096053143669 ) ) ;
#69813 = CARTESIAN_POINT ( 'NONE',  ( 19.03943276465977164, 0.05219959533936151252, 61.25109039468566863 ) ) ;
#69814 = CARTESIAN_POINT ( 'NONE',  ( 4.379528057220339221, -16.55341960407611168, 22.70724293864769194 ) ) ;
#69815 = CARTESIAN_POINT ( 'NONE',  ( -15.80617190586768217, 15.72974639402176855, 63.12609039468568994 ) ) ;
#69816 = CARTESIAN_POINT ( 'NONE',  ( 16.51473224551069308, 9.474510206698969483, 74.16557627198103830 ) ) ;
#69817 = CARTESIAN_POINT ( 'NONE',  ( -0.05219959533936034679, 19.03943276465977164, 42.50109039468566152 ) ) ;
#69818 = CARTESIAN_POINT ( 'NONE',  ( 21.55341960407610458, 5.719274019375980345, 48.95724293864770971 ) ) ;
#69819 = CARTESIAN_POINT ( 'NONE',  ( 21.55341960407619695, -5.719274019375665929, 41.04275706135236135 ) ) ;
#69820 = CARTESIAN_POINT ( 'NONE',  ( 0.05219959533907565091, 21.53943276465977519, 104.9989096053143669 ) ) ;
#69821 = CARTESIAN_POINT ( 'NONE',  ( -9.564922557961040184, 16.46253265017147172, 97.91775706135233293 ) ) ;
#69822 = CARTESIAN_POINT ( 'NONE',  ( 8.314922557961029526, -14.29746914071037800, 65.41775706135234714 ) ) ;
#69824 = CARTESIAN_POINT ( 'NONE',  ( 15.72974639402199770, -15.80617190586745480, 98.12390960531436690 ) ) ;
#69823 = CARTESIAN_POINT ( 'NONE',  ( 30.73962218707677962, -22.33364281372841376, -5.202157773949823927 ) ) ;
#69825 = CARTESIAN_POINT ( 'NONE',  ( -12.06949235617756955, 12.14591786802309770, 90.62390960531436690 ) ) ;
#69826 = CARTESIAN_POINT ( 'NONE',  ( -21.64789649210654687, -31.17538106138195175, -22.95353217465975249 ) ) ;
#69827 = CARTESIAN_POINT ( 'NONE',  ( 8.314922557961029526, -14.29746914071037800, 20.41775706135234714 ) ) ;
#69828 = CARTESIAN_POINT ( 'NONE',  ( 21.52544592524344225, -5.823673210054117533, 43.54057627198103830 ) ) ;
#69829 = CARTESIAN_POINT ( 'NONE',  ( 16.55341960407618274, -4.379528057220086978, 91.04275706135236135 ) ) ;
#69830 = CARTESIAN_POINT ( 'NONE',  ( -5.153800228976328057, -19.02544592524343514, 22.29057627198102765 ) ) ;
#69831 = CARTESIAN_POINT ( 'NONE',  ( -12.06949235617739369, -12.14591786802326823, 59.37609039468568284 ) ) ;
#69832 = CARTESIAN_POINT ( 'NONE',  ( 21.53943276465977519, 0.05219959533937863772, 26.25109039468567573 ) ) ;
#69833 = CARTESIAN_POINT ( 'NONE',  ( 5.823673210054125526, 21.52544592524343514, 49.79057627198102409 ) ) ;
#69834 = CARTESIAN_POINT ( 'NONE',  ( 14.34966873604972726, -8.224510206698740333, 90.83442372801901854 ) ) ;
#69835 = CARTESIAN_POINT ( 'NONE',  ( 9.474510206698971260, -16.51473224551069308, 102.9155762719810241 ) ) ;
#69836 = CARTESIAN_POINT ( 'NONE',  ( -18.62759615963255300, -10.81492255796106328, 74.16775706135231871 ) ) ;
#69837 = CARTESIAN_POINT ( 'NONE',  ( 0.05219959533907565091, 21.53943276465977519, 44.99890960531435979 ) ) ;
#69838 = CARTESIAN_POINT ( 'NONE',  ( 10.81492255796078972, 18.62759615963270932, 34.58224293864770260 ) ) ;
#69839 = VERTEX_POINT ( 'NONE', #157397 ) ;
#69840 = CARTESIAN_POINT ( 'NONE',  ( -13.89961937509957401, -13.97604488694547875, 49.37609039468567573 ) ) ;
#69841 = CARTESIAN_POINT ( 'NONE',  ( 8.314922557961029526, -14.29746914071037800, 65.41775706135234714 ) ) ;
#69842 = CARTESIAN_POINT ( 'NONE',  ( 21.53943276465977519, -0.05219959533907433946, 33.74890960531436690 ) ) ;
#69843 = ORIENTED_EDGE ( 'NONE', *, *, #107568, .T. ) ;
#69844 = CARTESIAN_POINT ( 'NONE',  ( -19.05341960407611168, -5.049401038298163336, 91.45724293864766707 ) ) ;
#69845 = CARTESIAN_POINT ( 'NONE',  ( -4.379528057220086978, -16.55341960407618274, 109.7927570613523613 ) ) ;
#69846 = CARTESIAN_POINT ( 'NONE',  ( 6.674792076160520615, -4.273745901508142708, 5.990689250852172520 ) ) ;
#69847 = CARTESIAN_POINT ( 'NONE',  ( -4.379528057220328563, 16.55341960407611168, 105.2072429386477097 ) ) ;
#69848 = CARTESIAN_POINT ( 'NONE',  ( -5.823673210054116645, -21.52544592524344225, 42.29057627198103120 ) ) ;
#69849 = CARTESIAN_POINT ( 'NONE',  ( 9.564922557960805705, 16.46253265017160317, 44.58224293864769550 ) ) ;
#69850 = CARTESIAN_POINT ( 'NONE',  ( 14.29746914071037800, 8.314922557961029526, 81.66775706135236135 ) ) ;
#69851 = CARTESIAN_POINT ( 'NONE',  ( 15.72974639402176855, 15.80617190586768217, 31.87609039468567929 ) ) ;
#69852 = CARTESIAN_POINT ( 'NONE',  ( -13.97604488694547697, 13.89961937509957934, 88.12609039468563310 ) ) ;
#69853 = CARTESIAN_POINT ( 'NONE',  ( -8.224510206698948167, 14.34966873604960824, 85.41557627198102409 ) ) ;
#69854 = CARTESIAN_POINT ( 'NONE',  ( 5.153800228976335163, 19.02544592524342804, 59.79057627198100988 ) ) ;
#69855 = CIRCLE ( 'NONE', #102193, 2.000000000000001776 ) ;
#69856 = CARTESIAN_POINT ( 'NONE',  ( -5.049401038298153566, 19.05341960407611168, 25.20724293864768484 ) ) ;
#69857 = CARTESIAN_POINT ( 'NONE',  ( -5.719274019375665041, -21.55341960407619695, 104.7927570613523898 ) ) ;
#69858 = CARTESIAN_POINT ( 'NONE',  ( 0.05219959533909260263, 19.03943276465977164, 79.99890960531436690 ) ) ;
#69859 = CARTESIAN_POINT ( 'NONE',  ( -8.224510206698735004, -14.34966873604973081, 59.58442372801901854 ) ) ;
#69860 = CARTESIAN_POINT ( 'NONE',  ( -15.80617190586768217, 15.72974639402176855, 98.12609039468570415 ) ) ;
#69861 = CARTESIAN_POINT ( 'NONE',  ( -0.05219959533907301413, -21.53943276465977519, 47.49890960531435979 ) ) ;
#69862 = CARTESIAN_POINT ( 'NONE',  ( -12.14591786802326823, 12.06949235617739902, 78.12609039468570415 ) ) ;
#69863 = CARTESIAN_POINT ( 'NONE',  ( 16.51473224551083163, -9.474510206698727899, 45.83442372801900433 ) ) ;
#69864 = CARTESIAN_POINT ( 'NONE',  ( -19.02544592524334988, -5.153800228976617603, 63.95942372801899012 ) ) ;
#69865 = EDGE_LOOP ( 'NONE', ( #143208, #75584, #99403, #99520 ) ) ;
#69866 = CARTESIAN_POINT ( 'NONE',  ( -18.67979575497193778, 10.72451020669871902, 68.33442372801900433 ) ) ;
#69867 = CARTESIAN_POINT ( 'NONE',  ( -16.51473224551069308, -9.474510206698971260, 66.66557627198102409 ) ) ;
#69868 = CARTESIAN_POINT ( 'NONE',  ( 13.89961937509978007, -13.97604488694527269, 58.12390960531435979 ) ) ;
#69869 = CARTESIAN_POINT ( 'NONE',  ( -16.51473224551082808, 9.474510206698731452, 58.33442372801900433 ) ) ;
#69870 = CARTESIAN_POINT ( 'NONE',  ( -25.25560589046783733, 4.310829775027161581, 167.9999999999999716 ) ) ;
#69871 = CARTESIAN_POINT ( 'NONE',  ( -13.97604488694527625, -13.89961937509977652, 91.87390960531432427 ) ) ;
#69872 = CARTESIAN_POINT ( 'NONE',  ( -8.224510206698948167, 14.34966873604960824, 50.41557627198103120 ) ) ;
#69873 = CARTESIAN_POINT ( 'NONE',  ( 21.53943276465977519, -0.05219959533907433946, 48.74890960531435979 ) ) ;
#69874 = DIRECTION ( 'NONE',  ( -0.000000000000000000, 1.000000000000000000, 0.000000000000000000 ) ) ;
#69875 = CARTESIAN_POINT ( 'NONE',  ( 19.05341960407617918, -5.049401038297876454, 21.04275706135232582 ) ) ;
#69876 = CARTESIAN_POINT ( 'NONE',  ( 0.000000000000000000, 0.000000000000000000, -64.92279855667830191 ) ) ;
#69877 = CARTESIAN_POINT ( 'NONE',  ( 0.05219959533909260263, 19.03943276465977164, 44.99890960531435979 ) ) ;
#69878 = CARTESIAN_POINT ( 'NONE',  ( 18.22780087662121673, 5.500000000000056843, 83.98459894673892734 ) ) ;
#69879 = CARTESIAN_POINT ( 'NONE',  ( -6.020228577223754586E-15, 39.95556452105416412, -4.500000000000000888 ) ) ;
#69880 = CARTESIAN_POINT ( 'NONE',  ( -30.73962218707678318, -22.33364281372842441, -1.802157773949823127 ) ) ;
#69881 = CARTESIAN_POINT ( 'NONE',  ( 14.34966873604972726, -8.224510206698740333, 60.83442372801901854 ) ) ;
#69882 = CARTESIAN_POINT ( 'NONE',  ( -21.55341960407610458, -5.719274019375992779, 86.45724293864770971 ) ) ;
#69883 = CARTESIAN_POINT ( 'NONE',  ( 8.314922557960818139, 14.29746914071049879, 59.58224293864770260 ) ) ;
#69885 = CARTESIAN_POINT ( 'NONE',  ( -4.500000000000001776, -130.0000000000000000, 13.99999999999999822 ) ) ;
#69884 = CARTESIAN_POINT ( 'NONE',  ( -13.97604488694527625, -13.89961937509977652, 46.87390960531435979 ) ) ;
#69886 = CARTESIAN_POINT ( 'NONE',  ( 15.72974639402176855, 15.80617190586768217, 36.87609039468568994 ) ) ;
#69887 = CARTESIAN_POINT ( 'NONE',  ( -5.153800228976607833, 19.02544592524334988, 47.70942372801900433 ) ) ;
#69888 = CARTESIAN_POINT ( 'NONE',  ( 19.05341960407611168, 5.049401038298154454, 38.95724293864767418 ) ) ;
#69889 = CARTESIAN_POINT ( 'NONE',  ( -10.72451020669870658, -18.67979575497194134, 89.58442372801901854 ) ) ;
#69890 = CIRCLE ( 'NONE', #182914, 8.000000000000000000 ) ;
#69891 = CARTESIAN_POINT ( 'NONE',  ( -17.72696623605160582, 5.499999999999857003, 48.59811031808417425 ) ) ;
#69892 = ORIENTED_EDGE ( 'NONE', *, *, #138165, .F. ) ;
#69893 = CARTESIAN_POINT ( 'NONE',  ( -16.53943276465976808, 0.05219959533911058130, 36.24890960531435979 ) ) ;
#69894 = CARTESIAN_POINT ( 'NONE',  ( -16.64782025964801093, 0.4052355915355428384, -59.15693706287431297 ) ) ;
#69895 = CARTESIAN_POINT ( 'NONE',  ( 10.81492255796078972, 18.62759615963270932, 34.58224293864770260 ) ) ;
#69896 = CARTESIAN_POINT ( 'NONE',  ( -27.73933785331498925, 2.428612866367529932E-14, 140.8750000027311842 ) ) ;
#69897 = VECTOR ( 'NONE', #48771, 1000.000000000000114 ) ;
#69898 = CARTESIAN_POINT ( 'NONE',  ( -19.03943276465977164, 0.05219959533909376836, 91.24890960531436690 ) ) ;
#69899 = CARTESIAN_POINT ( 'NONE',  ( 8.224510206698953496, -14.34966873604960469, 82.91557627198103830 ) ) ;
#69900 = CARTESIAN_POINT ( 'NONE',  ( 8.314922557961029526, -14.29746914071037800, 30.41775706135234358 ) ) ;
#69901 = CARTESIAN_POINT ( 'NONE',  ( -4.483927247898782831, 16.52544592524335698, 112.7094237280190328 ) ) ;
#69902 = EDGE_LOOP ( 'NONE', ( #32299, #24832, #114292, #142539 ) ) ;
#69903 = EDGE_CURVE ( 'NONE', #146141, #18152, #35037, .T. ) ;
#69904 = CARTESIAN_POINT ( 'NONE',  ( -5.153800228976328057, -19.02544592524343514, 52.29057627198100988 ) ) ;
#69906 = CARTESIAN_POINT ( 'NONE',  ( 21.55341960407610458, 5.719274019375980345, 93.95724293864770971 ) ) ;
#69905 = CARTESIAN_POINT ( 'NONE',  ( -9.474510206698964154, 16.51473224551069663, 80.41557627198103830 ) ) ;
#69908 = CARTESIAN_POINT ( 'NONE',  ( -5.153800228976328057, -19.02544592524343514, 107.2905762719810383 ) ) ;
#69907 = CARTESIAN_POINT ( 'NONE',  ( 14.29746914071049879, -8.314922557960816363, 23.33224293864769194 ) ) ;
#69909 = CARTESIAN_POINT ( 'NONE',  ( 19.03943276465977164, 0.05219959533936151252, 76.25109039468566152 ) ) ;
#69910 = CARTESIAN_POINT ( 'NONE',  ( -21.52544592524334988, -5.823673210054445271, 103.9594237280190185 ) ) ;
#69911 = CARTESIAN_POINT ( 'NONE',  ( 21.52544592524344225, -5.823673210054117533, 93.54057627198103830 ) ) ;
#69912 = CARTESIAN_POINT ( 'NONE',  ( 15.80617190586746368, 15.72974639402197994, 34.37390960531435979 ) ) ;
#69913 = CARTESIAN_POINT ( 'NONE',  ( 9.474510206698971260, -16.51473224551069308, 67.91557627198102409 ) ) ;
#69914 = CARTESIAN_POINT ( 'NONE',  ( 0.05219959533934541429, -16.53943276465976808, 110.0010903946856757 ) ) ;
#69915 = CARTESIAN_POINT ( 'NONE',  ( -5.153800228976328057, -19.02544592524343514, 72.29057627198102409 ) ) ;
#69916 = VERTEX_POINT ( 'NONE', #111878 ) ;
#69917 = CARTESIAN_POINT ( 'NONE',  ( -32.22964258392465098, -4.577260022299249442, 89.03854312871814614 ) ) ;
#69918 = CARTESIAN_POINT ( 'NONE',  ( 5.153800228976615827, -19.02544592524334988, 30.20942372801900433 ) ) ;
#69919 = CARTESIAN_POINT ( 'NONE',  ( -14.34966873604960291, -8.224510206698953496, 91.66557627198103830 ) ) ;
#69920 = CARTESIAN_POINT ( 'NONE',  ( -18.67979575497193778, 10.72451020669871902, 28.33442372801902209 ) ) ;
#69921 = CARTESIAN_POINT ( 'NONE',  ( -8.571926809382608425, 26.38167802310805854, 146.9750000027311785 ) ) ;
#69922 = CARTESIAN_POINT ( 'NONE',  ( 10.81492255796078972, 18.62759615963270932, 69.58224293864769550 ) ) ;
#69923 = CARTESIAN_POINT ( 'NONE',  ( 4.483927247898790824, -16.52544592524335698, 95.20942372801903275 ) ) ;
#69924 = CARTESIAN_POINT ( 'NONE',  ( -16.51473224551069308, -9.474510206698971260, 26.66557627198103120 ) ) ;
#69925 = CARTESIAN_POINT ( 'NONE',  ( 19.03943276465977164, -0.05219959533909143690, 78.74890960531436690 ) ) ;
#69926 = FILL_AREA_STYLE_COLOUR ( '', #182283 ) ;
#69927 = CARTESIAN_POINT ( 'NONE',  ( 11.74264578624799427, 36.14014761921585972, -10.34999999453762598 ) ) ;
#69928 = CARTESIAN_POINT ( 'NONE',  ( -14.34966873604960291, -8.224510206698953496, 36.66557627198103120 ) ) ;
#69929 = EDGE_CURVE ( 'NONE', #157949, #89709, #55236, .T. ) ;
#69930 = CARTESIAN_POINT ( 'NONE',  ( -5.719274019375665041, -21.55341960407619695, 64.79275706135234714 ) ) ;
#69931 = CARTESIAN_POINT ( 'NONE',  ( -0.05219959533909027116, -19.03943276465977164, 107.4989096053143527 ) ) ;
#69932 = CARTESIAN_POINT ( 'NONE',  ( 21.55341960407619695, -5.719274019375665929, 91.04275706135236135 ) ) ;
#69933 = CARTESIAN_POINT ( 'NONE',  ( -5.049401038298153566, 19.05341960407611168, 45.20724293864769550 ) ) ;
#69934 = CARTESIAN_POINT ( 'NONE',  ( -5.153800228976328057, -19.02544592524343514, 57.29057627198103120 ) ) ;
#69935 = VERTEX_POINT ( 'NONE', #127032 ) ;
#69936 = CARTESIAN_POINT ( 'NONE',  ( -5.823673210054431948, 21.52544592524334988, 97.70942372801904696 ) ) ;
#69937 = CARTESIAN_POINT ( 'NONE',  ( -0.05219959533934338120, 16.53943276465976808, 67.50109039468568994 ) ) ;
#69938 = CARTESIAN_POINT ( 'NONE',  ( -21.55341960407619339, 5.719274019375674811, 88.54275706135236135 ) ) ;
#69939 = CARTESIAN_POINT ( 'NONE',  ( 18.67979575497178502, 10.72451020669898547, 24.16557627198103120 ) ) ;
#69940 = CARTESIAN_POINT ( 'NONE',  ( -19.03943276465977164, -0.05219959533935918106, 93.75109039468566152 ) ) ;
#69941 = CARTESIAN_POINT ( 'NONE',  ( 10.81492255796106328, -18.62759615963255655, 60.41775706135235424 ) ) ;
#69942 = CARTESIAN_POINT ( 'NONE',  ( -8.224510206698735004, -14.34966873604973081, 34.58442372801900433 ) ) ;
#69943 = CARTESIAN_POINT ( 'NONE',  ( 5.719274019375991003, -21.55341960407610458, 87.70724293864769550 ) ) ;
#69944 = CARTESIAN_POINT ( 'NONE',  ( -19.05341960407617563, 5.049401038297882671, 83.54275706135233293 ) ) ;
#69945 = CARTESIAN_POINT ( 'NONE',  ( -5.049401038298153566, 19.05341960407611168, 65.20724293864765286 ) ) ;
#69946 = CARTESIAN_POINT ( 'NONE',  ( 13.89961937509957401, 13.97604488694547697, 96.87609039468566152 ) ) ;
#69947 = CARTESIAN_POINT ( 'NONE',  ( -5.049401038297874678, -19.05341960407617918, 104.7927570613523471 ) ) ;
#69948 = CARTESIAN_POINT ( 'NONE',  ( 16.55341960407611168, 4.379528057220329451, 48.95724293864770971 ) ) ;
#69949 = CARTESIAN_POINT ( 'NONE',  ( -19.05341960407617563, 5.049401038297882671, 83.54275706135233293 ) ) ;
#69950 = CARTESIAN_POINT ( 'NONE',  ( -16.53943276465976808, -0.05219959533934237506, 58.75109039468568994 ) ) ;
#69951 = CARTESIAN_POINT ( 'NONE',  ( -5.153800228976607833, 19.02544592524334988, 42.70942372801901143 ) ) ;
#69952 = CARTESIAN_POINT ( 'NONE',  ( 19.05341960407611168, 5.049401038298154454, 38.95724293864767418 ) ) ;
#69953 = CARTESIAN_POINT ( 'NONE',  ( 5.049401038298161559, -19.05341960407611168, 52.70724293864767418 ) ) ;
#69954 = CARTESIAN_POINT ( 'NONE',  ( -16.52544592524335698, -4.483927247898792601, 53.95942372801900433 ) ) ;
#69955 = CARTESIAN_POINT ( 'NONE',  ( 27.73933785331498569, 2.768321779492822058E-14, 140.3750000027311842 ) ) ;
#69956 = CARTESIAN_POINT ( 'NONE',  ( -5.359611314223446995E-15, 29.16686587814335496, 148.3750000027311842 ) ) ;
#69957 = CARTESIAN_POINT ( 'NONE',  ( 5.153800228976335163, 19.02544592524342804, 109.7905762719810099 ) ) ;
#69958 = CARTESIAN_POINT ( 'NONE',  ( -19.02544592524342804, 5.153800228976336051, 26.04057627198103120 ) ) ;
#69959 = ORIENTED_EDGE ( 'NONE', *, *, #7934, .T. ) ;
#69960 = CARTESIAN_POINT ( 'NONE',  ( -19.03943276465977164, -0.05219959533935918106, 98.75109039468567573 ) ) ;
#69961 = CARTESIAN_POINT ( 'NONE',  ( -15.72974639402197994, 15.80617190586746368, 40.62390960531435269 ) ) ;
#69963 = CARTESIAN_POINT ( 'NONE',  ( -16.51473224551082808, 9.474510206698731452, 113.3344237280190043 ) ) ;
#69962 = CARTESIAN_POINT ( 'NONE',  ( -19.05341960407617563, 5.049401038297882671, 33.54275706135231871 ) ) ;
#69964 = CARTESIAN_POINT ( 'NONE',  ( -13.89961937509977652, 13.97604488694528158, 35.62390960531435269 ) ) ;
#69965 = CARTESIAN_POINT ( 'NONE',  ( 0.05219959533909260263, 19.03943276465977164, 44.99890960531435979 ) ) ;
#69966 = CARTESIAN_POINT ( 'NONE',  ( -0.05219959533907301413, -21.53943276465977519, 67.49890960531436690 ) ) ;
#69967 = CARTESIAN_POINT ( 'NONE',  ( 9.474510206698971260, -16.51473224551069308, 102.9155762719810241 ) ) ;
#69968 = CARTESIAN_POINT ( 'NONE',  ( 19.03943276465977164, -0.05219959533909143690, 38.74890960531436690 ) ) ;
#69969 = CARTESIAN_POINT ( 'NONE',  ( -27.73933785331498925, -9.013057229001049109, 141.4750000027312069 ) ) ;
#69970 = CARTESIAN_POINT ( 'NONE',  ( -16.46253265017146816, -9.564922557961047289, 89.16775706135234714 ) ) ;
#69971 = CARTESIAN_POINT ( 'NONE',  ( -16.53943276465976808, 0.05219959533911058130, 51.24890960531436690 ) ) ;
#69972 = CARTESIAN_POINT ( 'NONE',  ( 10.72451020669898902, -18.67979575497178502, 47.91557627198102409 ) ) ;
#69973 = CARTESIAN_POINT ( 'NONE',  ( -21.52544592524334988, -5.823673210054445271, 108.9594237280190185 ) ) ;
#69974 = CARTESIAN_POINT ( 'NONE',  ( -18.67979575497178146, -10.72451020669898902, 96.66557627198102409 ) ) ;
#69975 = CARTESIAN_POINT ( 'NONE',  ( 21.52544592524334988, 5.823673210054432836, 66.45942372801903275 ) ) ;
#69976 = CARTESIAN_POINT ( 'NONE',  ( -15.72974639402176322, -15.80617190586768395, 79.37609039468567573 ) ) ;
#69977 = CARTESIAN_POINT ( 'NONE',  ( -16.46253265017160317, 9.564922557960807481, 110.8322429386476955 ) ) ;
#69979 = CARTESIAN_POINT ( 'NONE',  ( -5.719274019375665041, -21.55341960407619695, 59.79275706135234714 ) ) ;
#69978 = CARTESIAN_POINT ( 'NONE',  ( -4.483927247898782831, 16.52544592524335698, 102.7094237280190185 ) ) ;
#69980 = CARTESIAN_POINT ( 'NONE',  ( -13.89961937509977652, 13.97604488694528158, 70.62390960531432427 ) ) ;
#69981 = CARTESIAN_POINT ( 'NONE',  ( 9.474510206698729675, 16.51473224551082808, 32.08442372801900433 ) ) ;
#69982 = CARTESIAN_POINT ( 'NONE',  ( -15.72974639402176322, -15.80617190586768395, 34.37609039468568284 ) ) ;
#69983 = CARTESIAN_POINT ( 'NONE',  ( 16.46253265017160672, -9.564922557960803928, 73.33224293864769550 ) ) ;
#69984 = CARTESIAN_POINT ( 'NONE',  ( 14.34966873604960469, 8.224510206698951720, 79.16557627198103830 ) ) ;
#69985 = CARTESIAN_POINT ( 'NONE',  ( 16.55341960407611168, 4.379528057220329451, 43.95724293864769550 ) ) ;
#69986 = CARTESIAN_POINT ( 'NONE',  ( -10.81492255796078084, -18.62759615963271287, 52.08224293864768839 ) ) ;
#69987 = CARTESIAN_POINT ( 'NONE',  ( 9.474510206698971260, -16.51473224551069308, 67.91557627198102409 ) ) ;
#69988 = CARTESIAN_POINT ( 'NONE',  ( 18.62759615963271287, -10.81492255796078972, 68.33224293864769550 ) ) ;
#69989 = CARTESIAN_POINT ( 'NONE',  ( 9.564922557961047289, -16.46253265017146816, 60.41775706135233293 ) ) ;
#69991 = CARTESIAN_POINT ( 'NONE',  ( 4.379528057220339221, -16.55341960407611168, 57.70724293864770260 ) ) ;
#69990 = CARTESIAN_POINT ( 'NONE',  ( 5.153800228976617603, -19.02544592524335343, 20.20942372801899722 ) ) ;
#69992 = CARTESIAN_POINT ( 'NONE',  ( 0.05219959533907565091, 21.53943276465977519, 39.99890960531436690 ) ) ;
#69993 = ORIENTED_EDGE ( 'NONE', *, *, #52209, .F. ) ;
#69994 = DIRECTION ( 'NONE',  ( 0.000000000000000000, 0.000000000000000000, 1.000000000000000000 ) ) ;
#69996 = CARTESIAN_POINT ( 'NONE',  ( 8.571926809382597767, 26.38167802310806209, 148.2750000027311899 ) ) ;
#69995 = CARTESIAN_POINT ( 'NONE',  ( -16.52544592524335698, -4.483927247898792601, 83.95942372801900433 ) ) ;
#69997 = CARTESIAN_POINT ( 'NONE',  ( 5.049401038297881783, 19.05341960407617563, 82.29275706135229029 ) ) ;
#69998 = CARTESIAN_POINT ( 'NONE',  ( 12.14591786802309770, 12.06949235617756955, 54.37390960531435979 ) ) ;
#69999 = CARTESIAN_POINT ( 'NONE',  ( -9.564922557960796823, -16.46253265017161027, 47.08224293864769550 ) ) ;
#70000 = CARTESIAN_POINT ( 'NONE',  ( -12.06949235617756955, 12.14591786802309770, 45.62390960531436690 ) ) ;
#70001 = CARTESIAN_POINT ( 'NONE',  ( 16.51473224551069308, 9.474510206698969483, 89.16557627198103830 ) ) ;
#70002 = CARTESIAN_POINT ( 'NONE',  ( -9.564922557960796823, -16.46253265017161027, 47.08224293864769550 ) ) ;
#70003 = CARTESIAN_POINT ( 'NONE',  ( 21.52544592524334988, 5.823673210054432836, 61.45942372801901854 ) ) ;
#70004 = CARTESIAN_POINT ( 'NONE',  ( 16.46253265017160672, -9.564922557960803928, 68.33224293864770971 ) ) ;
#70005 = CARTESIAN_POINT ( 'NONE',  ( 19.02544592524343514, -5.153800228976328945, 23.54057627198102054 ) ) ;
#70006 = CARTESIAN_POINT ( 'NONE',  ( 5.049401038298161559, -19.05341960407611168, 77.70724293864765286 ) ) ;
#70007 = ADVANCED_FACE ( 'NONE', ( #110881 ), #64388, .T. ) ;
#70008 = CARTESIAN_POINT ( 'NONE',  ( -21.52544592524343514, 5.823673210054127303, 46.04057627198103830 ) ) ;
#70009 = CARTESIAN_POINT ( 'NONE',  ( -9.474510206698964154, 16.51473224551069663, 55.41557627198103120 ) ) ;
#70010 = CARTESIAN_POINT ( 'NONE',  ( -18.62759615963270932, 10.81492255796079327, 50.83224293864770971 ) ) ;
#70011 = CARTESIAN_POINT ( 'NONE',  ( -5.049401038297874678, -19.05341960407617918, 79.79275706135233293 ) ) ;
#70012 = CARTESIAN_POINT ( 'NONE',  ( 0.05219959533934541429, -16.53943276465976808, 100.0010903946857042 ) ) ;
#70013 = CARTESIAN_POINT ( 'NONE',  ( -13.97604488694547697, 13.89961937509957934, 38.12609039468566152 ) ) ;
#70015 = CARTESIAN_POINT ( 'NONE',  ( 8.224510206698742110, 14.34966873604972548, 82.08442372801901854 ) ) ;
#70014 = CARTESIAN_POINT ( 'NONE',  ( 16.53943276465976808, 0.05219959533934440121, 66.25109039468567573 ) ) ;
#70016 = FACE_OUTER_BOUND ( 'NONE', #16194, .T. ) ;
#70017 = CARTESIAN_POINT ( 'NONE',  ( 4.483927247898790824, -16.52544592524335698, 65.20942372801901854 ) ) ;
#70018 = CARTESIAN_POINT ( 'NONE',  ( 0.05219959533909260263, 19.03943276465977164, 114.9989096053143669 ) ) ;
#70019 = CARTESIAN_POINT ( 'NONE',  ( 19.02544592524343514, -5.153800228976328945, 28.54057627198102409 ) ) ;
#70020 = CARTESIAN_POINT ( 'NONE',  ( -8.224510206698735004, -14.34966873604973081, 44.58442372801901854 ) ) ;
#70021 = CARTESIAN_POINT ( 'NONE',  ( 19.03943276465977164, -0.05219959533909143690, 43.74890960531435979 ) ) ;
#70022 = CARTESIAN_POINT ( 'NONE',  ( -15.80617190586768217, 15.72974639402176855, 43.12609039468568284 ) ) ;
#70023 = CARTESIAN_POINT ( 'NONE',  ( 4.483927247898790824, -16.52544592524335698, 40.20942372801901854 ) ) ;
#70024 = CARTESIAN_POINT ( 'NONE',  ( -0.05219959533934338120, 16.53943276465976808, 102.5010903946856899 ) ) ;
#70025 = CARTESIAN_POINT ( 'NONE',  ( -28.28060372831499336, 2.428612866367529932E-14, 148.5625000040967620 ) ) ;
#70026 = CARTESIAN_POINT ( 'NONE',  ( 15.80617190586769283, -15.72974639402175789, 110.6260903946857042 ) ) ;
#70027 = CARTESIAN_POINT ( 'NONE',  ( 0.05219959533936267826, -19.03943276465977164, 105.0010903946856615 ) ) ;
#70028 = CARTESIAN_POINT ( 'NONE',  ( -5.049401038297874678, -19.05341960407617918, 64.79275706135233293 ) ) ;
#70029 = CARTESIAN_POINT ( 'NONE',  ( 4.379528057220339221, -16.55341960407611168, 67.70724293864769550 ) ) ;
#70030 = CARTESIAN_POINT ( 'NONE',  ( 16.51473224551069308, 9.474510206698969483, 44.16557627198103120 ) ) ;
#70032 = CARTESIAN_POINT ( 'NONE',  ( 17.31728774477212696, -6.344390552233678982, 58.31906651689306642 ) ) ;
#70031 = CARTESIAN_POINT ( 'NONE',  ( -9.564922557961040184, 16.46253265017147172, 62.91775706135233293 ) ) ;
#70033 = CARTESIAN_POINT ( 'NONE',  ( 18.62759615963255655, 10.81492255796105972, 66.66775706135234714 ) ) ;
#70034 = CARTESIAN_POINT ( 'NONE',  ( 14.34966873604972726, -8.224510206698740333, 40.83442372801901854 ) ) ;
#70035 = CARTESIAN_POINT ( 'NONE',  ( 17.49999999999999289, 5.622605283950886879, 38.81207310596112592 ) ) ;
#70036 = CARTESIAN_POINT ( 'NONE',  ( -15.80617190586745835, -15.72974639402198527, 21.87390960531436690 ) ) ;
#70037 = CARTESIAN_POINT ( 'NONE',  ( -13.97604488694547697, 13.89961937509957934, 103.1260903946856473 ) ) ;
#70038 = CARTESIAN_POINT ( 'NONE',  ( -13.97604488694527625, -13.89961937509977652, 111.8739096053143243 ) ) ;
#70039 = FACE_OUTER_BOUND ( 'NONE', #140806, .T. ) ;
#70040 = CARTESIAN_POINT ( 'NONE',  ( -0.05219959533909027116, -19.03943276465977164, 27.49890960531435624 ) ) ;
#70041 = CARTESIAN_POINT ( 'NONE',  ( 21.55341960407619695, -5.719274019375665929, 111.0427570613523613 ) ) ;
#70042 = CARTESIAN_POINT ( 'NONE',  ( 9.474510206698971260, -16.51473224551069308, 52.91557627198102409 ) ) ;
#70044 = CARTESIAN_POINT ( 'NONE',  ( -10.72451020669870658, -18.67979575497194134, 59.58442372801901854 ) ) ;
#70043 = AXIS2_PLACEMENT_3D ( 'NONE', #113202, #146529, #99021 ) ;
#70045 = CARTESIAN_POINT ( 'NONE',  ( 21.52544592524334988, 5.823673210054432836, 96.45942372801901854 ) ) ;
#70046 = CARTESIAN_POINT ( 'NONE',  ( 16.52544592524342804, -4.483927247898539470, 23.54057627198102765 ) ) ;
#70047 = CARTESIAN_POINT ( 'NONE',  ( -16.51473224551069308, -9.474510206698971260, 31.66557627198102054 ) ) ;
#70048 = CARTESIAN_POINT ( 'NONE',  ( -5.049401038298153566, 19.05341960407611168, 75.20724293864769550 ) ) ;
#70049 = CARTESIAN_POINT ( 'NONE',  ( 10.72451020669871369, 18.67979575497193778, 57.08442372801901854 ) ) ;
#70050 = CARTESIAN_POINT ( 'NONE',  ( -5.049401038298153566, 19.05341960407611168, 40.20724293864768839 ) ) ;
#70051 = CARTESIAN_POINT ( 'NONE',  ( -5.823673210054431948, 21.52544592524334988, 52.70942372801902565 ) ) ;
#70053 = CARTESIAN_POINT ( 'NONE',  ( 16.51473224551069308, 9.474510206698969483, 99.16557627198102409 ) ) ;
#70052 = CARTESIAN_POINT ( 'NONE',  ( 9.564922557961047289, -16.46253265017146816, 80.41775706135234714 ) ) ;
#70054 = CARTESIAN_POINT ( 'NONE',  ( -16.55341960407611168, -4.379528057220339221, 111.4572429386476813 ) ) ;
#70055 = CARTESIAN_POINT ( 'NONE',  ( -21.52544592524343514, 5.823673210054127303, 106.0405762719810525 ) ) ;
#70056 = CARTESIAN_POINT ( 'NONE',  ( 19.02544592524334988, 5.153800228976608722, 31.45942372801900433 ) ) ;
#70057 = CARTESIAN_POINT ( 'NONE',  ( 4.379528057220339221, -16.55341960407611168, 92.70724293864770971 ) ) ;
#70058 = CARTESIAN_POINT ( 'NONE',  ( 19.02544592524343514, -5.153800228976328945, 48.54057627198103120 ) ) ;
#70059 = CARTESIAN_POINT ( 'NONE',  ( -5.049401038297874678, -19.05341960407617918, 94.79275706135230450 ) ) ;
#70060 = CARTESIAN_POINT ( 'NONE',  ( 16.55341960407611168, 4.379528057220329451, 58.95724293864770971 ) ) ;
#70061 = CARTESIAN_POINT ( 'NONE',  ( 5.719274019375673035, 21.55341960407619339, 107.2927570613523471 ) ) ;
#70062 = CARTESIAN_POINT ( 'NONE',  ( -13.89961937509977652, 13.97604488694528158, 100.6239096053143669 ) ) ;
#70063 = CARTESIAN_POINT ( 'NONE',  ( -19.03943276465977164, -0.05219959533935918106, 93.75109039468566152 ) ) ;
#70064 = CARTESIAN_POINT ( 'NONE',  ( 18.67979575497178502, 10.72451020669898547, 94.16557627198103830 ) ) ;
#70065 = CARTESIAN_POINT ( 'NONE',  ( 15.80617190586769283, -15.72974639402175789, 50.62609039468568994 ) ) ;
#70066 = CARTESIAN_POINT ( 'NONE',  ( 12.14591786802327356, -12.06949235617739191, 45.62609039468567573 ) ) ;
#70067 = CARTESIAN_POINT ( 'NONE',  ( -8.224510206698735004, -14.34966873604973081, 109.5844237280190328 ) ) ;
#70069 = CARTESIAN_POINT ( 'NONE',  ( -5.719274019375665041, -21.55341960407619695, 49.79275706135234714 ) ) ;
#70068 = CARTESIAN_POINT ( 'NONE',  ( 12.14591786802327356, -12.06949235617739191, 45.62609039468567573 ) ) ;
#70070 = CARTESIAN_POINT ( 'NONE',  ( 21.55341960407610458, 5.719274019375980345, 38.95724293864768839 ) ) ;
#70071 = CARTESIAN_POINT ( 'NONE',  ( 19.03943276465977164, -0.05219959533909143690, 33.74890960531435979 ) ) ;
#70072 = CARTESIAN_POINT ( 'NONE',  ( 23.48529157249599919, 32.32473071737754111, -6.449999994537626513 ) ) ;
#70073 = CARTESIAN_POINT ( 'NONE',  ( 14.29746914071037800, 8.314922557961029526, 66.66775706135234714 ) ) ;
#70074 = CARTESIAN_POINT ( 'NONE',  ( 15.72974639402199770, -15.80617190586745480, 83.12390960531436690 ) ) ;
#70075 = CARTESIAN_POINT ( 'NONE',  ( 14.34966873604960469, 8.224510206698951720, 34.16557627198102409 ) ) ;
#70076 = CARTESIAN_POINT ( 'NONE',  ( -12.14591786802326823, 12.06949235617739902, 63.12609039468568994 ) ) ;
#70077 = CARTESIAN_POINT ( 'NONE',  ( 13.89961937509977652, -13.97604488694527269, 63.12390960531435979 ) ) ;
#70078 = CARTESIAN_POINT ( 'NONE',  ( 13.97604488694548053, -13.89961937509957401, 95.62609039468563310 ) ) ;
#70079 = CARTESIAN_POINT ( 'NONE',  ( 5.823673210054125526, 21.52544592524343514, 79.79057627198102409 ) ) ;
#70080 = CARTESIAN_POINT ( 'NONE',  ( -16.55341960407611168, -4.379528057220339221, 31.45724293864769550 ) ) ;
#70081 = VERTEX_POINT ( 'NONE', #95709 ) ;
#70082 = CARTESIAN_POINT ( 'NONE',  ( 24.86475712555687423, 11.37215039201022293, 169.9824823118007657 ) ) ;
#70083 = CARTESIAN_POINT ( 'NONE',  ( -15.72974639402197994, 15.80617190586746368, 70.62390960531436690 ) ) ;
#70084 = CARTESIAN_POINT ( 'NONE',  ( -16.52544592524335698, -4.483927247898792601, 108.9594237280190185 ) ) ;
#70085 = ORIENTED_EDGE ( 'NONE', *, *, #122826, .F. ) ;
#70086 = CARTESIAN_POINT ( 'NONE',  ( 17.49999999999999645, -5.099703775203614065, 103.2332118591204448 ) ) ;
#70087 = CARTESIAN_POINT ( 'NONE',  ( -0.05219959533907301413, -21.53943276465977519, 92.49890960531436690 ) ) ;
#70088 = CARTESIAN_POINT ( 'NONE',  ( 18.62759615963271287, -10.81492255796078972, 108.3322429386477097 ) ) ;
#70089 = CARTESIAN_POINT ( 'NONE',  ( -16.52544592524342804, 4.483927247898546575, 31.04057627198102409 ) ) ;
#70090 = CARTESIAN_POINT ( 'NONE',  ( -16.55341960407617563, 4.379528057220093196, 28.54275706135234358 ) ) ;
#70091 = CARTESIAN_POINT ( 'NONE',  ( 16.51473224551069308, 9.474510206698969483, 39.16557627198103120 ) ) ;
#70092 = CARTESIAN_POINT ( 'NONE',  ( -9.474510206698964154, 16.51473224551069663, 65.41557627198102409 ) ) ;
#70093 = CARTESIAN_POINT ( 'NONE',  ( 8.571926809382597767, 26.38167802310806209, 140.7750000027311899 ) ) ;
#70094 = CARTESIAN_POINT ( 'NONE',  ( -5.823673210054116645, -21.52544592524344225, 27.29057627198103120 ) ) ;
#70095 = CARTESIAN_POINT ( 'NONE',  ( 1.499999999999961586, 30.23919084766313858, -51.14197153238884397 ) ) ;
#70096 = CARTESIAN_POINT ( 'NONE',  ( 9.564922557961047289, -16.46253265017146816, 110.4177570613523471 ) ) ;
#70097 = CARTESIAN_POINT ( 'NONE',  ( 16.46253265017146816, 9.564922557961045513, 41.66775706135234003 ) ) ;
#70098 = CARTESIAN_POINT ( 'NONE',  ( -15.72974639402197994, 15.80617190586746368, 85.62390960531436690 ) ) ;
#70099 = CARTESIAN_POINT ( 'NONE',  ( -4.379528057220086978, -16.55341960407618274, 109.7927570613523613 ) ) ;
#70100 = CARTESIAN_POINT ( 'NONE',  ( 10.81492255796078972, 18.62759615963270932, 39.58224293864769550 ) ) ;
#70102 = CARTESIAN_POINT ( 'NONE',  ( 16.46253265017146816, 9.564922557961045513, 101.6677570613523329 ) ) ;
#70101 = CARTESIAN_POINT ( 'NONE',  ( 5.823673210054125526, 21.52544592524343514, 84.79057627198102409 ) ) ;
#70103 = CARTESIAN_POINT ( 'NONE',  ( 13.89961937509977652, -13.97604488694527269, 103.1239096053143527 ) ) ;
#70104 = CARTESIAN_POINT ( 'NONE',  ( -21.53943276465977519, -0.05219959533937600094, 78.75109039468568994 ) ) ;
#70105 = CARTESIAN_POINT ( 'NONE',  ( 9.474510206698971260, -16.51473224551069308, 77.91557627198103830 ) ) ;
#70106 = CARTESIAN_POINT ( 'NONE',  ( 16.53943276465976808, -0.05219959533910856209, 98.74890960531438111 ) ) ;
#70107 = DIRECTION ( 'NONE',  ( 0.000000000000000000, 0.000000000000000000, 1.000000000000000000 ) ) ;
#70108 = CARTESIAN_POINT ( 'NONE',  ( 9.564922557960805705, 16.46253265017160317, 69.58224293864770971 ) ) ;
#70109 = CARTESIAN_POINT ( 'NONE',  ( 4.483927247898545687, 16.52544592524342804, 84.79057627198102409 ) ) ;
#70110 = ORIENTED_EDGE ( 'NONE', *, *, #162970, .T. ) ;
#70111 = CARTESIAN_POINT ( 'NONE',  ( 5.049401038297881783, 19.05341960407617563, 107.2927570613523187 ) ) ;
#70112 = CARTESIAN_POINT ( 'NONE',  ( -4.500000000000001776, -130.0000000000000000, 12.99999999999999822 ) ) ;
#70113 = CARTESIAN_POINT ( 'NONE',  ( 19.03943276465977164, -0.05219959533909143690, 53.74890960531436690 ) ) ;
#70115 = CARTESIAN_POINT ( 'NONE',  ( -19.05341960407611168, -5.049401038298163336, 96.45724293864769550 ) ) ;
#70114 = CARTESIAN_POINT ( 'NONE',  ( -5.823673210054431948, 21.52544592524334988, 87.70942372801901854 ) ) ;
#70116 = CARTESIAN_POINT ( 'NONE',  ( -14.34966873604972548, 8.224510206698743886, 83.33442372801903275 ) ) ;
#70117 = CARTESIAN_POINT ( 'NONE',  ( -38.00000000000000711, 2.893978650043524126E-14, -15.00000000000000000 ) ) ;
#70118 = CARTESIAN_POINT ( 'NONE',  ( -19.02544592524334988, -5.153800228976617603, 53.95942372801898301 ) ) ;
#70119 = CARTESIAN_POINT ( 'NONE',  ( 10.81492255796106328, -18.62759615963255655, 100.4177570613523471 ) ) ;
#70120 = CARTESIAN_POINT ( 'NONE',  ( 37.43947335741457039, 2.756686112915584630, 40.22705064412460985 ) ) ;
#70121 = CARTESIAN_POINT ( 'NONE',  ( 4.313351365237948265, 4.313351365237946489, -62.50719930893269805 ) ) ;
#70122 = CARTESIAN_POINT ( 'NONE',  ( -16.55341960407617563, 4.379528057220093196, 108.5427570613523756 ) ) ;
#70123 = CARTESIAN_POINT ( 'NONE',  ( 16.70000000000002416, -0.1037895044722859789, -59.13370768023892055 ) ) ;
#70124 = CARTESIAN_POINT ( 'NONE',  ( 8.314922557961029526, -14.29746914071037800, 90.41775706135236135 ) ) ;
#70125 = CARTESIAN_POINT ( 'NONE',  ( -17.79613651744294600, 24.49428055684532524, 145.9656553485623647 ) ) ;
#70126 = CARTESIAN_POINT ( 'NONE',  ( 4.483927247898790824, -16.52544592524335698, 65.20942372801901854 ) ) ;
#70127 = CARTESIAN_POINT ( 'NONE',  ( 11.30153831258471797, -180.0000000000000000, -14.99999999999999822 ) ) ;
#70128 = CARTESIAN_POINT ( 'NONE',  ( -10.81492255796105439, 18.62759615963255655, 77.91775706135231871 ) ) ;
#70129 = CARTESIAN_POINT ( 'NONE',  ( -9.474510206698720793, -16.51473224551083518, 89.58442372801900433 ) ) ;
#70130 = CARTESIAN_POINT ( 'NONE',  ( -13.89961937509957401, -13.97604488694547875, 44.37609039468566863 ) ) ;
#70131 = CARTESIAN_POINT ( 'NONE',  ( -16.51473224551069308, -9.474510206698971260, 61.66557627198103120 ) ) ;
#70132 = CARTESIAN_POINT ( 'NONE',  ( -16.51473224551069308, -9.474510206698971260, 61.66557627198103120 ) ) ;
#70133 = CARTESIAN_POINT ( 'NONE',  ( 6.938893903907228378E-15, 22.80000000000002913, -65.00100000000003320 ) ) ;
#70134 = CARTESIAN_POINT ( 'NONE',  ( -21.53943276465977519, 0.05219959533907696930, 76.24890960531435269 ) ) ;
#70135 = AXIS2_PLACEMENT_3D ( 'NONE', #118619, #114595, #176292 ) ;
#70136 = CARTESIAN_POINT ( 'NONE',  ( -18.62759615963270932, 10.81492255796079327, 40.83224293864769550 ) ) ;
#70137 = CARTESIAN_POINT ( 'NONE',  ( -13.89961937509977652, 13.97604488694528158, 35.62390960531435269 ) ) ;
#70138 = CARTESIAN_POINT ( 'NONE',  ( -4.483927247898782831, 16.52544592524335698, 67.70942372801901854 ) ) ;
#70139 = ORIENTED_EDGE ( 'NONE', *, *, #68610, .F. ) ;
#70140 = CARTESIAN_POINT ( 'NONE',  ( -21.53943276465977519, -0.05219959533937600094, 33.75109039468568284 ) ) ;
#70142 = CARTESIAN_POINT ( 'NONE',  ( 22.81625015709509441, 31.40387420917330275, -9.324999997268813345 ) ) ;
#70141 = CARTESIAN_POINT ( 'NONE',  ( 14.34966873604960469, 8.224510206698951720, 64.16557627198102409 ) ) ;
#70143 = CARTESIAN_POINT ( 'NONE',  ( -8.314922557961024197, 14.29746914071037800, 27.91775706135234358 ) ) ;
#70144 = CARTESIAN_POINT ( 'NONE',  ( 13.97604488694548053, -13.89961937509957401, 55.62609039468566863 ) ) ;
#70145 = VECTOR ( 'NONE', #137229, 1000.000000000000000 ) ;
#70146 = CARTESIAN_POINT ( 'NONE',  ( 12.06949235617757843, -12.14591786802309237, 58.12390960531435979 ) ) ;
#70147 = CARTESIAN_POINT ( 'NONE',  ( -10.81492255796105439, 18.62759615963255655, 32.91775706135234714 ) ) ;
#70149 = CARTESIAN_POINT ( 'NONE',  ( -21.55341960407610458, -5.719274019375992779, 71.45724293864769550 ) ) ;
#70148 = LINE ( 'NONE', #195510, #21384 ) ;
#70150 = CARTESIAN_POINT ( 'NONE',  ( 19.03943276465977164, -0.05219959533909143690, 98.74890960531436690 ) ) ;
#70151 = CARTESIAN_POINT ( 'NONE',  ( -8.314922557960811034, -14.29746914071050412, 72.08224293864769550 ) ) ;
#70152 = CARTESIAN_POINT ( 'NONE',  ( 30.57338251523173156, -25.88377959333006118, -17.25078043576312936 ) ) ;
#70153 = LINE ( 'NONE', #10488, #76388 ) ;
#70154 = CARTESIAN_POINT ( 'NONE',  ( -5.049401038297874678, -19.05341960407617918, 74.79275706135231871 ) ) ;
#70155 = CARTESIAN_POINT ( 'NONE',  ( -21.52544592524334988, -5.823673210054445271, 23.95942372801901143 ) ) ;
#70156 = CARTESIAN_POINT ( 'NONE',  ( -19.02544592524342804, 5.153800228976336051, 56.04057627198100988 ) ) ;
#70157 = CARTESIAN_POINT ( 'NONE',  ( 13.89961937509957401, 13.97604488694547697, 41.87609039468566152 ) ) ;
#70158 = CARTESIAN_POINT ( 'NONE',  ( 13.89961937509977652, -13.97604488694527269, 33.12390960531434558 ) ) ;
#70159 = CARTESIAN_POINT ( 'NONE',  ( 5.823673210054444382, -21.52544592524334988, 60.20942372801902565 ) ) ;
#70160 = AXIS2_PLACEMENT_3D ( 'NONE', #6944, #82784, #67627 ) ;
#70161 = CARTESIAN_POINT ( 'NONE',  ( -6.434671708797631950, -6.434671708797536027, -61.89430850415821794 ) ) ;
#70162 = CARTESIAN_POINT ( 'NONE',  ( -4.483927247898539470, -16.52544592524342804, 47.29057627198103120 ) ) ;
#70163 = CARTESIAN_POINT ( 'NONE',  ( 16.46253265017160672, -9.564922557960803928, 68.33224293864770971 ) ) ;
#70164 = CARTESIAN_POINT ( 'NONE',  ( -5.719274019375978568, 21.55341960407610458, 85.20724293864770971 ) ) ;
#70165 = CARTESIAN_POINT ( 'NONE',  ( -5.153800228976328057, -19.02544592524343514, 62.29057627198100988 ) ) ;
#70166 = VERTEX_POINT ( 'NONE', #18890 ) ;
#70167 = CARTESIAN_POINT ( 'NONE',  ( -10.81492255796078084, -18.62759615963271287, 72.08224293864769550 ) ) ;
#70168 = EDGE_CURVE ( 'NONE', #137721, #74853, #80536, .T. ) ;
#70169 = CARTESIAN_POINT ( 'NONE',  ( 5.823673210054444382, -21.52544592524334988, 105.2094237280190328 ) ) ;
#70172 = CARTESIAN_POINT ( 'NONE',  ( -12.14591786802309592, -12.06949235617757132, 76.87390960531439532 ) ) ;
#70171 = CARTESIAN_POINT ( 'NONE',  ( 16.53943276465976808, 0.05219959533934440121, 91.25109039468568994 ) ) ;
#70170 = FACE_OUTER_BOUND ( 'NONE', #191446, .T. ) ;
#70173 = CARTESIAN_POINT ( 'NONE',  ( -13.97604488694547697, 13.89961937509957934, 98.12609039468566152 ) ) ;
#70174 = VERTEX_POINT ( 'NONE', #97672 ) ;
#70175 = CARTESIAN_POINT ( 'NONE',  ( -21.55341960407619339, 5.719274019375674811, 23.54275706135235424 ) ) ;
#70176 = CARTESIAN_POINT ( 'NONE',  ( 19.02544592524334988, 5.153800228976608722, 46.45942372801899012 ) ) ;
#70177 = CARTESIAN_POINT ( 'NONE',  ( 4.379528057220092307, 16.55341960407617563, 97.29275706135234714 ) ) ;
#70178 = CARTESIAN_POINT ( 'NONE',  ( 13.89961937509957401, 13.97604488694547697, 36.87609039468565442 ) ) ;
#70179 = CARTESIAN_POINT ( 'NONE',  ( 9.564922557960805705, 16.46253265017160317, 89.58224293864769550 ) ) ;
#70180 = CARTESIAN_POINT ( 'NONE',  ( 15.72974639402199770, -15.80617190586745480, 58.12390960531435979 ) ) ;
#70181 = CARTESIAN_POINT ( 'NONE',  ( -28.79475375365484524, 9.355982642740638511, 140.1656553485623533 ) ) ;
#70182 = CARTESIAN_POINT ( 'NONE',  ( -0.05219959533909027116, -19.03943276465977164, 22.49890960531436690 ) ) ;
#70183 = CARTESIAN_POINT ( 'NONE',  ( 21.55341960407619695, -5.719274019375665929, 111.0427570613523613 ) ) ;
#70184 = CARTESIAN_POINT ( 'NONE',  ( 16.53943276465976808, 0.05219959533934440121, 76.25109039468568994 ) ) ;
#70185 = CARTESIAN_POINT ( 'NONE',  ( 10.72451020669871369, 18.67979575497193778, 32.08442372801901854 ) ) ;
#70186 = CARTESIAN_POINT ( 'NONE',  ( -16.52544592524335698, -4.483927247898792601, 33.95942372801901143 ) ) ;
#70187 = CARTESIAN_POINT ( 'NONE',  ( 16.51473224551069308, 9.474510206698969483, 99.16557627198102409 ) ) ;
#70188 = CARTESIAN_POINT ( 'NONE',  ( -16.46253265017160317, 9.564922557960807481, 35.83224293864768839 ) ) ;
#70189 = CARTESIAN_POINT ( 'NONE',  ( -19.03943276465977164, 0.05219959533909376836, 61.24890960531436690 ) ) ;
#70190 = CIRCLE ( 'NONE', #31498, 0.2000000000000057288 ) ;
#70191 = CARTESIAN_POINT ( 'NONE',  ( 16.55341960407618274, -4.379528057220086978, 51.04275706135234714 ) ) ;
#70192 = CARTESIAN_POINT ( 'NONE',  ( 14.34966873604960469, 8.224510206698951720, 99.16557627198100988 ) ) ;
#70193 = CARTESIAN_POINT ( 'NONE',  ( 0.05219959533934541429, -16.53943276465976808, 95.00109039468568994 ) ) ;
#70196 = CARTESIAN_POINT ( 'NONE',  ( -0.05219959533909027116, -19.03943276465977164, 67.49890960531436690 ) ) ;
#70195 = CARTESIAN_POINT ( 'NONE',  ( 5.049401038298161559, -19.05341960407611168, 72.70724293864768129 ) ) ;
#70194 = CARTESIAN_POINT ( 'NONE',  ( -10.72451020669870658, -18.67979575497194134, 49.58442372801901143 ) ) ;
#70197 = CARTESIAN_POINT ( 'NONE',  ( -16.51473224551069308, -9.474510206698971260, 101.6655762719810241 ) ) ;
#70198 = CARTESIAN_POINT ( 'NONE',  ( -0.05219959533910754901, -16.53943276465976808, 32.49890960531435979 ) ) ;
#70199 = CARTESIAN_POINT ( 'NONE',  ( 4.483927247898790824, -16.52544592524335698, 105.2094237280190328 ) ) ;
#70200 = ORIENTED_EDGE ( 'NONE', *, *, #51432, .F. ) ;
#70201 = CARTESIAN_POINT ( 'NONE',  ( 19.02544592524334988, 5.153800228976608722, 41.45942372801900433 ) ) ;
#70202 = CARTESIAN_POINT ( 'NONE',  ( -9.474510206698964154, 16.51473224551069663, 110.4155762719810383 ) ) ;
#70203 = CARTESIAN_POINT ( 'NONE',  ( 13.97604488694527802, 13.89961937509977652, 69.37390960531436690 ) ) ;
#70204 = CARTESIAN_POINT ( 'NONE',  ( -19.05341960407617563, 5.049401038297882671, 38.54275706135233293 ) ) ;
#70205 = CARTESIAN_POINT ( 'NONE',  ( 36.91746824999999177, 2.880721459617395097E-14, -3.624999997268813168 ) ) ;
#70206 = CARTESIAN_POINT ( 'NONE',  ( -16.18388926212241330, -7.379444403734410685, 65.43953151366150678 ) ) ;
#70207 = CARTESIAN_POINT ( 'NONE',  ( 16.52544592524335698, 4.483927247898782831, 36.45942372801901143 ) ) ;
#70209 = CARTESIAN_POINT ( 'NONE',  ( -12.14591786802326823, 12.06949235617739902, 53.12609039468568284 ) ) ;
#70208 = CARTESIAN_POINT ( 'NONE',  ( 13.97604488694548053, -13.89961937509957401, 75.62609039468564731 ) ) ;
#70210 = CARTESIAN_POINT ( 'NONE',  ( 6.542287240554228056, -4.421942842314275701, -64.21309694765785991 ) ) ;
#70211 = CARTESIAN_POINT ( 'NONE',  ( -16.51473224551069308, -9.474510206698971260, 96.66557627198102409 ) ) ;
#70212 = CARTESIAN_POINT ( 'NONE',  ( -5.719274019375978568, 21.55341960407610458, 110.2072429386477239 ) ) ;
#70213 = CARTESIAN_POINT ( 'NONE',  ( -16.51473224551082808, 9.474510206698731452, 83.33442372801899012 ) ) ;
#70215 = CARTESIAN_POINT ( 'NONE',  ( -9.474510206698964154, 16.51473224551069663, 35.41557627198102409 ) ) ;
#70214 = CARTESIAN_POINT ( 'NONE',  ( -0.05219959533909027116, -19.03943276465977164, 102.4989096053143669 ) ) ;
#70216 = CARTESIAN_POINT ( 'NONE',  ( 16.51473224551069308, 9.474510206698969483, 74.16557627198103830 ) ) ;
#70218 = CARTESIAN_POINT ( 'NONE',  ( -0.05219959533909027116, -19.03943276465977164, 32.49890960531435979 ) ) ;
#70217 = CARTESIAN_POINT ( 'NONE',  ( -0.05219959533910754901, -16.53943276465976808, 47.49890960531435979 ) ) ;
#70219 = CARTESIAN_POINT ( 'NONE',  ( -19.02544592524334988, -5.153800228976617603, 53.95942372801898301 ) ) ;
#70220 = CARTESIAN_POINT ( 'NONE',  ( -8.314922557960811034, -14.29746914071050412, 87.08224293864769550 ) ) ;
#70221 = CARTESIAN_POINT ( 'NONE',  ( 5.049401038297881783, 19.05341960407617563, 22.29275706135233648 ) ) ;
#70222 = CARTESIAN_POINT ( 'NONE',  ( 19.05341960407611168, 5.049401038298154454, 48.95724293864768129 ) ) ;
#70223 = CARTESIAN_POINT ( 'NONE',  ( -0.05219959533907301413, -21.53943276465977519, 52.49890960531435979 ) ) ;
#70225 = CARTESIAN_POINT ( 'NONE',  ( -16.51473224551082808, 9.474510206698731452, 28.33442372801900433 ) ) ;
#70224 = CARTESIAN_POINT ( 'NONE',  ( -12.14591786802309592, -12.06949235617757132, 56.87390960531436690 ) ) ;
#70226 = CARTESIAN_POINT ( 'NONE',  ( -19.03943276465977164, 0.05219959533909376836, 101.2489096053143669 ) ) ;
#70227 = CARTESIAN_POINT ( 'NONE',  ( 19.03943276465977164, -0.05219959533909143690, 108.7489096053143527 ) ) ;
#70228 = CARTESIAN_POINT ( 'NONE',  ( -5.153800228976328057, -19.02544592524343514, 42.29057627198101699 ) ) ;
#70229 = CARTESIAN_POINT ( 'NONE',  ( -16.46253265017160317, 9.564922557960807481, 30.83224293864769550 ) ) ;
#70230 = CARTESIAN_POINT ( 'NONE',  ( -16.55341960407611168, -4.379528057220339221, 91.45724293864769550 ) ) ;
#70231 = CARTESIAN_POINT ( 'NONE',  ( 21.53943276465977519, -0.05219959533907433946, 98.74890960531438111 ) ) ;
#70232 = CARTESIAN_POINT ( 'NONE',  ( 19.02544592524343514, -5.153800228976328945, 98.54057627198100988 ) ) ;
#70233 = CARTESIAN_POINT ( 'NONE',  ( -10.81492255796078084, -18.62759615963271287, 107.0822429386476955 ) ) ;
#70234 = CARTESIAN_POINT ( 'NONE',  ( -16.51473224551069308, -9.474510206698971260, 106.6655762719810383 ) ) ;
#70236 = CARTESIAN_POINT ( 'NONE',  ( -0.05219959533910754901, -16.53943276465976808, 107.4989096053143669 ) ) ;
#70235 = FACE_OUTER_BOUND ( 'NONE', #35973, .T. ) ;
#70237 = CARTESIAN_POINT ( 'NONE',  ( 16.51473224551069308, 9.474510206698969483, 74.16557627198103830 ) ) ;
#70238 = CARTESIAN_POINT ( 'NONE',  ( -21.52544592524343514, 5.823673210054127303, 86.04057627198102409 ) ) ;
#70239 = CARTESIAN_POINT ( 'NONE',  ( 17.12812012977027365, -6.668231424565973064, 106.1405124067685506 ) ) ;
#70240 = CARTESIAN_POINT ( 'NONE',  ( -21.96449396329681392, -6.689387493872139601, 170.9254202302468855 ) ) ;
#70242 = CARTESIAN_POINT ( 'NONE',  ( 18.22780087662122384, -5.500000000000022204, 66.01540105326107266 ) ) ;
#70241 = CARTESIAN_POINT ( 'NONE',  ( 18.67979575497178502, 10.72451020669898547, 34.16557627198102409 ) ) ;
#70243 = CARTESIAN_POINT ( 'NONE',  ( 14.29746914071037800, 8.314922557961029526, 36.66775706135234714 ) ) ;
#70244 = CARTESIAN_POINT ( 'NONE',  ( 8.314922557960818139, 14.29746914071049879, 89.58224293864768129 ) ) ;
#70245 = CYLINDRICAL_SURFACE ( 'NONE', #28986, 2.500000000000000000 ) ;
#70246 = CARTESIAN_POINT ( 'NONE',  ( -19.02544592524342804, 5.153800228976336051, 56.04057627198100988 ) ) ;
#70247 = CARTESIAN_POINT ( 'NONE',  ( -8.224510206698948167, 14.34966873604960824, 75.41557627198102409 ) ) ;
#70248 = CARTESIAN_POINT ( 'NONE',  ( -15.80617190586745835, -15.72974639402198527, 26.87390960531435979 ) ) ;
#70249 = CARTESIAN_POINT ( 'NONE',  ( -16.53943276465976808, 0.05219959533911058130, 61.24890960531435979 ) ) ;
#70250 = CARTESIAN_POINT ( 'NONE',  ( 14.29746914071037800, 8.314922557961029526, 26.66775706135235424 ) ) ;
#70251 = CARTESIAN_POINT ( 'NONE',  ( -15.72974639402176322, -15.80617190586768395, 74.37609039468568994 ) ) ;
#70252 = CARTESIAN_POINT ( 'NONE',  ( 16.20579543436678449, -7.371946100355083686, 76.93479165828125588 ) ) ;
#70253 = CARTESIAN_POINT ( 'NONE',  ( 0.05219959533909260263, 19.03943276465977164, 114.9989096053143669 ) ) ;
#70254 = CARTESIAN_POINT ( 'NONE',  ( 16.53943276465976808, 0.05219959533934440121, 86.25109039468568994 ) ) ;
#70255 = CARTESIAN_POINT ( 'NONE',  ( 16.46253265017160672, -9.564922557960803928, 33.33224293864770260 ) ) ;
#70256 = CARTESIAN_POINT ( 'NONE',  ( 13.97604488694527802, 13.89961937509977652, 84.37390960531433848 ) ) ;
#70257 = CARTESIAN_POINT ( 'NONE',  ( 21.55341960407610458, 5.719274019375980345, 88.95724293864769550 ) ) ;
#70258 = CARTESIAN_POINT ( 'NONE',  ( -12.14591786802326823, 12.06949235617739902, 23.12609039468567573 ) ) ;
#70260 = CARTESIAN_POINT ( 'NONE',  ( 5.719274019375673035, 21.55341960407619339, 72.29275706135236135 ) ) ;
#70259 = CARTESIAN_POINT ( 'NONE',  ( -4.379528057220328563, 16.55341960407611168, 45.20724293864769550 ) ) ;
#70261 = CARTESIAN_POINT ( 'NONE',  ( 16.55341960407618274, -4.379528057220086978, 106.0427570613523471 ) ) ;
#70262 = CARTESIAN_POINT ( 'NONE',  ( 19.02544592524343514, -5.153800228976328945, 113.5405762719810241 ) ) ;
#70263 = LINE ( 'NONE', #181445, #193831 ) ;
#70264 = CARTESIAN_POINT ( 'NONE',  ( -12.14591786802326823, 12.06949235617739902, 108.1260903946856757 ) ) ;
#70265 = CARTESIAN_POINT ( 'NONE',  ( 14.34966873604972726, -8.224510206698740333, 65.83442372801900433 ) ) ;
#70267 = ORIENTED_EDGE ( 'NONE', *, *, #151508, .F. ) ;
#70266 = CARTESIAN_POINT ( 'NONE',  ( -5.153800228976328057, -19.02544592524343514, 77.29057627198099567 ) ) ;
#70268 = CARTESIAN_POINT ( 'NONE',  ( -0.05219959533909027116, -19.03943276465977164, 82.49890960531436690 ) ) ;
#70269 = CARTESIAN_POINT ( 'NONE',  ( -21.52544592524334988, -5.823673210054445271, 73.95942372801901854 ) ) ;
#70270 = CARTESIAN_POINT ( 'NONE',  ( -12.06949235617739369, -12.14591786802326823, 69.37609039468567573 ) ) ;
#70271 = CARTESIAN_POINT ( 'NONE',  ( 16.55341960407611168, 4.379528057220329451, 63.95724293864770260 ) ) ;
#70272 = CARTESIAN_POINT ( 'NONE',  ( -5.049401038298153566, 19.05341960407611168, 50.20724293864770260 ) ) ;
#70273 = VERTEX_POINT ( 'NONE', #81509 ) ;
#70274 = CARTESIAN_POINT ( 'NONE',  ( 0.05219959533936267826, -19.03943276465977164, 105.0010903946856615 ) ) ;
#70275 = CARTESIAN_POINT ( 'NONE',  ( 14.34966873604960469, 8.224510206698951720, 109.1655762719810383 ) ) ;
#70276 = CARTESIAN_POINT ( 'NONE',  ( 0.05219959533909260263, 19.03943276465977164, 74.99890960531435269 ) ) ;
#70278 = CARTESIAN_POINT ( 'NONE',  ( 38.00000000000000711, -12.34694845685040754, -3.100000000000000533 ) ) ;
#70277 = CARTESIAN_POINT ( 'NONE',  ( 16.55341960407618274, -4.379528057220086978, 21.04275706135234714 ) ) ;
#70279 = CARTESIAN_POINT ( 'NONE',  ( -15.72974639402176322, -15.80617190586768395, 99.37609039468568994 ) ) ;
#70280 = CARTESIAN_POINT ( 'NONE',  ( 16.52544592524335698, 4.483927247898782831, 76.45942372801901854 ) ) ;
#70281 = CARTESIAN_POINT ( 'NONE',  ( 9.474510206698729675, 16.51473224551082808, 87.08442372801900433 ) ) ;
#70282 = CARTESIAN_POINT ( 'NONE',  ( 19.02544592524343514, -5.153800228976328945, 23.54057627198102054 ) ) ;
#70283 = CARTESIAN_POINT ( 'NONE',  ( 4.483927247898790824, -16.52544592524335698, 70.20942372801904696 ) ) ;
#70284 = DIRECTION ( 'NONE',  ( 0.000000000000000000, 0.000000000000000000, 1.000000000000000000 ) ) ;
#70285 = CARTESIAN_POINT ( 'NONE',  ( 5.153800228976615827, -19.02544592524334988, 60.20942372801899012 ) ) ;
#70286 = CARTESIAN_POINT ( 'NONE',  ( -21.52544592524334988, -5.823673210054445271, 93.95942372801903275 ) ) ;
#70287 = CARTESIAN_POINT ( 'NONE',  ( -5.153800228976328057, -19.02544592524343514, 32.29057627198102409 ) ) ;
#70288 = CARTESIAN_POINT ( 'NONE',  ( 19.02544592524343514, -5.153800228976328945, 78.54057627198099567 ) ) ;
#70289 = CARTESIAN_POINT ( 'NONE',  ( 16.52544592524342804, -4.483927247898539470, 78.54057627198103830 ) ) ;
#70290 = CARTESIAN_POINT ( 'NONE',  ( -21.52544592524334988, -5.823673210054445271, 83.95942372801900433 ) ) ;
#70291 = CARTESIAN_POINT ( 'NONE',  ( -0.05219959533936034679, 19.03943276465977164, 52.50109039468566863 ) ) ;
#70292 = CARTESIAN_POINT ( 'NONE',  ( 19.03943276465977164, 0.05219959533936151252, 36.25109039468567573 ) ) ;
#70293 = CARTESIAN_POINT ( 'NONE',  ( -0.05219959533907301413, -21.53943276465977519, 32.49890960531435979 ) ) ;
#70294 = CARTESIAN_POINT ( 'NONE',  ( -0.05219959533937732626, 21.53943276465977519, 102.5010903946856899 ) ) ;
#70295 = CARTESIAN_POINT ( 'NONE',  ( -19.05341960407611168, -5.049401038298163336, 81.45724293864769550 ) ) ;
#70296 = CARTESIAN_POINT ( 'NONE',  ( 18.62759615963255655, 10.81492255796105972, 86.66775706135234714 ) ) ;
#70297 = CARTESIAN_POINT ( 'NONE',  ( -10.81492255796078084, -18.62759615963271287, 57.08224293864769550 ) ) ;
#70298 = CARTESIAN_POINT ( 'NONE',  ( 0.05219959533909260263, 19.03943276465977164, 89.99890960531436690 ) ) ;
#70299 = CARTESIAN_POINT ( 'NONE',  ( -9.474510206698720793, -16.51473224551083518, 69.58442372801901854 ) ) ;
#70300 = CARTESIAN_POINT ( 'NONE',  ( 16.51473224551069308, 9.474510206698969483, 89.16557627198103830 ) ) ;
#70301 = CARTESIAN_POINT ( 'NONE',  ( 19.03943276465977164, 0.05219959533936151252, 91.25109039468566152 ) ) ;
#70302 = CARTESIAN_POINT ( 'NONE',  ( 16.52544592524335698, 4.483927247898782831, 36.45942372801901143 ) ) ;
#70303 = CARTESIAN_POINT ( 'NONE',  ( 4.379528057220339221, -16.55341960407611168, 97.70724293864772392 ) ) ;
#70304 = CARTESIAN_POINT ( 'NONE',  ( 5.153800228976335163, 19.02544592524342804, 74.79057627198103830 ) ) ;
#70305 = CARTESIAN_POINT ( 'NONE',  ( -0.05219959533907301413, -21.53943276465977519, 62.49890960531436690 ) ) ;
#70306 = CARTESIAN_POINT ( 'NONE',  ( 4.483927247898790824, -16.52544592524335698, 30.20942372801902565 ) ) ;
#70307 = CARTESIAN_POINT ( 'NONE',  ( -5.823673210054431948, 21.52544592524334988, 32.70942372801900433 ) ) ;
#70308 = CARTESIAN_POINT ( 'NONE',  ( 15.80617190586769283, -15.72974639402175789, 85.62609039468568994 ) ) ;
#70309 = CARTESIAN_POINT ( 'NONE',  ( 4.483927247898790824, -16.52544592524335698, 80.20942372801901854 ) ) ;
#70310 = CARTESIAN_POINT ( 'NONE',  ( 13.89961937509977652, -13.97604488694527269, 78.12390960531433848 ) ) ;
#70311 = CARTESIAN_POINT ( 'NONE',  ( 8.314922557960818139, 14.29746914071049879, 79.58224293864769550 ) ) ;
#70312 = CARTESIAN_POINT ( 'NONE',  ( 8.314922557961029526, -14.29746914071037800, 100.4177570613523471 ) ) ;
#70313 = CARTESIAN_POINT ( 'NONE',  ( -16.46253265017146816, -9.564922557961047289, 49.16775706135233293 ) ) ;
#70314 = EDGE_CURVE ( 'NONE', #93191, #45948, #167116, .T. ) ;
#70315 = AXIS2_PLACEMENT_3D ( 'NONE', #176829, #4947, #189994 ) ;
#70316 = CARTESIAN_POINT ( 'NONE',  ( -0.05219959533937732626, 21.53943276465977519, 27.50109039468567929 ) ) ;
#70317 = CARTESIAN_POINT ( 'NONE',  ( 12.06949235617757843, -12.14591786802309237, 83.12390960531436690 ) ) ;
#70318 = CARTESIAN_POINT ( 'NONE',  ( -19.03943276465977164, 0.05219959533909376836, 96.24890960531436690 ) ) ;
#70319 = CARTESIAN_POINT ( 'NONE',  ( 16.53943276465976808, 0.05219959533934440121, 101.2510903946856757 ) ) ;
#70320 = CARTESIAN_POINT ( 'NONE',  ( 21.53943276465977519, 0.05219959533937863772, 71.25109039468568994 ) ) ;
#70321 = CARTESIAN_POINT ( 'NONE',  ( 14.34966873604972726, -8.224510206698740333, 45.83442372801901854 ) ) ;
#70322 = CARTESIAN_POINT ( 'NONE',  ( 10.81492255796106328, -18.62759615963255655, 40.41775706135234714 ) ) ;
#70323 = CARTESIAN_POINT ( 'NONE',  ( 4.483927247898545687, 16.52544592524342804, 69.79057627198102409 ) ) ;
#70324 = ORIENTED_EDGE ( 'NONE', *, *, #150999, .T. ) ;
#70325 = CARTESIAN_POINT ( 'NONE',  ( 10.72451020669898902, -18.67979575497178502, 112.9155762719810383 ) ) ;
#70326 = CARTESIAN_POINT ( 'NONE',  ( 17.50000000000000355, -5.499999999999992006, 26.21769037696436300 ) ) ;
#70327 = CARTESIAN_POINT ( 'NONE',  ( -16.53943276465976808, 0.05219959533911058130, 46.24890960531435979 ) ) ;
#70328 = CARTESIAN_POINT ( 'NONE',  ( 9.564922557960805705, 16.46253265017160317, 24.58224293864769194 ) ) ;
#70329 = CARTESIAN_POINT ( 'NONE',  ( -18.67979575497178146, -10.72451020669898902, 31.66557627198102054 ) ) ;
#70330 = CARTESIAN_POINT ( 'NONE',  ( 8.314922557960818139, 14.29746914071049879, 74.58224293864768129 ) ) ;
#70331 = CARTESIAN_POINT ( 'NONE',  ( -0.05219959533907301413, -21.53943276465977519, 82.49890960531436690 ) ) ;
#70332 = CARTESIAN_POINT ( 'NONE',  ( 16.51473224551069308, 9.474510206698969483, 79.16557627198103830 ) ) ;
#70334 = CARTESIAN_POINT ( 'NONE',  ( 9.474510206698729675, 16.51473224551082808, 77.08442372801900433 ) ) ;
#70333 = CARTESIAN_POINT ( 'NONE',  ( 9.564922557960805705, 16.46253265017160317, 39.58224293864768839 ) ) ;
#70336 = CARTESIAN_POINT ( 'NONE',  ( -15.72974639402197994, 15.80617190586746368, 60.62390960531437401 ) ) ;
#70335 = CARTESIAN_POINT ( 'NONE',  ( 18.67979575497194134, -10.72451020669871369, 50.83442372801901143 ) ) ;
#70337 = CARTESIAN_POINT ( 'NONE',  ( 19.02544592524343514, -5.153800228976328945, 33.54057627198102409 ) ) ;
#70338 = CARTESIAN_POINT ( 'NONE',  ( 0.05219959533909260263, 19.03943276465977164, 74.99890960531435269 ) ) ;
#70339 = ORIENTED_EDGE ( 'NONE', *, *, #46382, .T. ) ;
#70340 = CARTESIAN_POINT ( 'NONE',  ( 8.314922557961029526, -14.29746914071037800, 55.41775706135234714 ) ) ;
#70341 = CARTESIAN_POINT ( 'NONE',  ( 21.52544592524334988, 5.823673210054432836, 36.45942372801901143 ) ) ;
#70342 = CARTESIAN_POINT ( 'NONE',  ( -21.55341960407619339, 5.719274019375674811, 58.54275706135235424 ) ) ;
#70343 = CARTESIAN_POINT ( 'NONE',  ( 19.03943276465977164, -0.05219959533909143690, 108.7489096053143527 ) ) ;
#70344 = CARTESIAN_POINT ( 'NONE',  ( -21.53943276465977519, 0.05219959533907696930, 91.24890960531436690 ) ) ;
#70346 = CARTESIAN_POINT ( 'NONE',  ( 4.483927247898790824, -16.52544592524335698, 45.20942372801901854 ) ) ;
#70345 = CARTESIAN_POINT ( 'NONE',  ( 5.823673210054444382, -21.52544592524334988, 25.20942372801901854 ) ) ;
#70347 = CARTESIAN_POINT ( 'NONE',  ( -5.719274019375978568, 21.55341960407610458, 45.20724293864769550 ) ) ;
#70348 = CARTESIAN_POINT ( 'NONE',  ( -9.474510206698720793, -16.51473224551083518, 19.58442372801899722 ) ) ;
#70349 = CARTESIAN_POINT ( 'NONE',  ( 19.02544592524343514, -5.153800228976328945, 53.54057627198102409 ) ) ;
#70350 = CARTESIAN_POINT ( 'NONE',  ( -19.03943276465977164, 0.05219959533909376836, 116.2489096053143669 ) ) ;
#70351 = CARTESIAN_POINT ( 'NONE',  ( -19.05341960407611168, -5.049401038298163336, 91.45724293864766707 ) ) ;
#70352 = CARTESIAN_POINT ( 'NONE',  ( -13.97604488694547520, 13.89961937509957934, 53.12609039468566152 ) ) ;
#70353 = CARTESIAN_POINT ( 'NONE',  ( 0.05219959533936267826, -19.03943276465977164, 70.00109039468566152 ) ) ;
#70354 = CARTESIAN_POINT ( 'NONE',  ( -21.52544592524343514, 5.823673210054127303, 46.04057627198103830 ) ) ;
#70355 = CARTESIAN_POINT ( 'NONE',  ( 4.379528057220339221, -16.55341960407611168, 22.70724293864769194 ) ) ;
#70356 = CARTESIAN_POINT ( 'NONE',  ( 5.049401038297881783, 19.05341960407617563, 87.29275706135234714 ) ) ;
#70357 = CARTESIAN_POINT ( 'NONE',  ( 16.46253265017160672, -9.564922557960803928, 23.33224293864769194 ) ) ;
#70358 = CARTESIAN_POINT ( 'NONE',  ( 18.62759615963255655, 10.81492255796105972, 111.6677570613523613 ) ) ;
#70359 = CARTESIAN_POINT ( 'NONE',  ( -5.153800228976607833, 19.02544592524334988, 92.70942372801901854 ) ) ;
#70360 = CARTESIAN_POINT ( 'NONE',  ( -19.03943276465977164, -0.05219959533935918106, 38.75109039468566152 ) ) ;
#70361 = CARTESIAN_POINT ( 'NONE',  ( 24.02706313830236695, -14.44797190822832889, 165.8682408883346397 ) ) ;
#70362 = CARTESIAN_POINT ( 'NONE',  ( -5.153800228976328057, -19.02544592524343514, 52.29057627198100988 ) ) ;
#70363 = CARTESIAN_POINT ( 'NONE',  ( 4.483927247898545687, 16.52544592524342804, 64.79057627198103830 ) ) ;
#70364 = CARTESIAN_POINT ( 'NONE',  ( 19.03943276465977164, -0.05219959533909143690, 33.74890960531435979 ) ) ;
#70365 = CARTESIAN_POINT ( 'NONE',  ( 8.314922557960818139, 14.29746914071049879, 34.58224293864770260 ) ) ;
#70366 = CARTESIAN_POINT ( 'NONE',  ( 18.22780087662122384, -5.500000000000022204, 56.01540105326107977 ) ) ;
#70367 = CARTESIAN_POINT ( 'NONE',  ( -4.483927247898782831, 16.52544592524335698, 102.7094237280190185 ) ) ;
#70368 = CARTESIAN_POINT ( 'NONE',  ( 16.46253265017160672, -9.564922557960803928, 63.33224293864769550 ) ) ;
#70369 = CARTESIAN_POINT ( 'NONE',  ( 9.564922557961047289, -16.46253265017146816, 20.41775706135233293 ) ) ;
#70370 = CARTESIAN_POINT ( 'NONE',  ( -4.483927247898782831, 16.52544592524335698, 27.70942372801901854 ) ) ;
#70371 = CARTESIAN_POINT ( 'NONE',  ( 21.55341960407610458, 5.719274019375980345, 48.95724293864770971 ) ) ;
#70373 = ORIENTED_EDGE ( 'NONE', *, *, #11302, .F. ) ;
#70372 = CARTESIAN_POINT ( 'NONE',  ( 21.55341960407619695, -5.719274019375665929, 106.0427570613523471 ) ) ;
#70374 = CARTESIAN_POINT ( 'NONE',  ( -19.05341960407611168, -5.049401038298163336, 61.45724293864769550 ) ) ;
#70375 = CARTESIAN_POINT ( 'NONE',  ( -19.02544592524342804, 5.153800228976336051, 111.0405762719810099 ) ) ;
#70376 = CARTESIAN_POINT ( 'NONE',  ( -9.564922557960796823, -16.46253265017161027, 102.0822429386477097 ) ) ;
#70377 = CARTESIAN_POINT ( 'NONE',  ( 36.91746824999999177, 2.880721459617395097E-14, -3.624999997268813168 ) ) ;
#70378 = CARTESIAN_POINT ( 'NONE',  ( -15.80617190586768217, 15.72974639402176855, 28.12609039468568284 ) ) ;
#70379 = CARTESIAN_POINT ( 'NONE',  ( -16.52544592524342804, 4.483927247898546575, 91.04057627198103830 ) ) ;
#70381 = CARTESIAN_POINT ( 'NONE',  ( -5.153800228976328057, -19.02544592524343514, 62.29057627198100988 ) ) ;
#70380 = CARTESIAN_POINT ( 'NONE',  ( 15.72974639402199770, -15.80617190586745480, 83.12390960531436690 ) ) ;
#70382 = CARTESIAN_POINT ( 'NONE',  ( 9.564922557960805705, 16.46253265017160317, 69.58224293864770971 ) ) ;
#70383 = CARTESIAN_POINT ( 'NONE',  ( 15.72974639402199770, -15.80617190586745480, 113.1239096053143953 ) ) ;
#70384 = ORIENTED_EDGE ( 'NONE', *, *, #22791, .T. ) ;
#70385 = CARTESIAN_POINT ( 'NONE',  ( 19.02544592524343514, -5.153800228976328945, 68.54057627198103830 ) ) ;
#70386 = CYLINDRICAL_SURFACE ( 'NONE', #143133, 2.500000000000000000 ) ;
#70388 = CARTESIAN_POINT ( 'NONE',  ( -3.573655867282028392E-15, 2.428612866367529932E-14, 150.0000000000000000 ) ) ;
#70387 = CARTESIAN_POINT ( 'NONE',  ( 8.224510206698953496, -14.34966873604960469, 107.9155762719810241 ) ) ;
#70389 = CARTESIAN_POINT ( 'NONE',  ( 9.474510206698971260, -16.51473224551069308, 67.91557627198102409 ) ) ;
#70390 = CARTESIAN_POINT ( 'NONE',  ( 19.05341960407617918, -5.049401038297876454, 91.04275706135234714 ) ) ;
#70391 = CARTESIAN_POINT ( 'NONE',  ( 14.34966873604960469, 8.224510206698951720, 99.16557627198100988 ) ) ;
#70392 = CARTESIAN_POINT ( 'NONE',  ( -15.80617190586768217, 15.72974639402176855, 68.12609039468567573 ) ) ;
#70394 = CARTESIAN_POINT ( 'NONE',  ( -21.55341960407619339, 5.719274019375674811, 33.54275706135234714 ) ) ;
#70393 = CARTESIAN_POINT ( 'NONE',  ( 13.89961937509977652, -13.97604488694527269, 43.12390960531434558 ) ) ;
#70395 = CARTESIAN_POINT ( 'NONE',  ( -0.05219959533907301413, -21.53943276465977519, 107.4989096053143669 ) ) ;
#70396 = CARTESIAN_POINT ( 'NONE',  ( -5.429308488886486681E-15, 30.30510711980690175, 141.5000000000000000 ) ) ;
#70397 = CARTESIAN_POINT ( 'NONE',  ( -5.153800228976328057, -19.02544592524343514, 72.29057627198102409 ) ) ;
#70398 = CARTESIAN_POINT ( 'NONE',  ( 1.508955259217861487E-14, -71.74905152827281540, -24.99410988490251029 ) ) ;
#70400 = CARTESIAN_POINT ( 'NONE',  ( 0.05219959533907565091, 21.53943276465977519, 34.99890960531435979 ) ) ;
#70399 = CARTESIAN_POINT ( 'NONE',  ( -16.46253265017146816, -9.564922557961047289, 104.1677570613523329 ) ) ;
#70401 = CARTESIAN_POINT ( 'NONE',  ( 18.62759615963255655, 10.81492255796105972, 66.66775706135234714 ) ) ;
#70402 = CARTESIAN_POINT ( 'NONE',  ( -16.46253265017160317, 9.564922557960807481, 90.83224293864769550 ) ) ;
#70403 = CARTESIAN_POINT ( 'NONE',  ( -13.97604488694547697, 13.89961937509957934, 78.12609039468567573 ) ) ;
#70404 = CARTESIAN_POINT ( 'NONE',  ( -9.474510206698964154, 16.51473224551069663, 50.41557627198102409 ) ) ;
#70405 = CARTESIAN_POINT ( 'NONE',  ( 13.89961937509977652, -13.97604488694527269, 68.12390960531436690 ) ) ;
#70406 = CARTESIAN_POINT ( 'NONE',  ( -4.379528057220328563, 16.55341960407611168, 90.20724293864770971 ) ) ;
#70407 = CARTESIAN_POINT ( 'NONE',  ( 9.474510206698971260, -16.51473224551069308, 97.91557627198102409 ) ) ;
#70408 = CARTESIAN_POINT ( 'NONE',  ( -14.34966873604960291, -8.224510206698953496, 86.66557627198102409 ) ) ;
#70409 = CARTESIAN_POINT ( 'NONE',  ( 19.05341960407611168, 5.049401038298154454, 93.95724293864769550 ) ) ;
#70410 = EDGE_CURVE ( 'NONE', #183245, #67326, #56426, .T. ) ;
#70412 = CARTESIAN_POINT ( 'NONE',  ( -9.564922557960796823, -16.46253265017161027, 32.08224293864769550 ) ) ;
#70411 = CARTESIAN_POINT ( 'NONE',  ( 0.05219959533910956823, 16.53943276465976808, 39.99890960531436690 ) ) ;
#70413 = VERTEX_POINT ( 'NONE', #154054 ) ;
#70414 = CARTESIAN_POINT ( 'NONE',  ( -0.05219959533937732626, 21.53943276465977519, 57.50109039468568994 ) ) ;
#70415 = CARTESIAN_POINT ( 'NONE',  ( 19.05341960407617918, -5.049401038297876454, 86.04275706135233293 ) ) ;
#70416 = CARTESIAN_POINT ( 'NONE',  ( 12.14591786802309770, 12.06949235617756955, 44.37390960531435979 ) ) ;
#70417 = CARTESIAN_POINT ( 'NONE',  ( -10.72451020669898014, 18.67979575497178502, 95.41557627198102409 ) ) ;
#70418 = CARTESIAN_POINT ( 'NONE',  ( 10.72451020669898902, -18.67979575497178502, 27.91557627198103830 ) ) ;
#70419 = CARTESIAN_POINT ( 'NONE',  ( 14.29746914071049879, -8.314922557960816363, 88.33224293864769550 ) ) ;
#70420 = CARTESIAN_POINT ( 'NONE',  ( 9.474510206698971260, -16.51473224551069308, 57.91557627198103120 ) ) ;
#70421 = CARTESIAN_POINT ( 'NONE',  ( 14.29746914071049879, -8.314922557960816363, 23.33224293864769194 ) ) ;
#70422 = AXIS2_PLACEMENT_3D ( 'NONE', #43490, #183983, #13158 ) ;
#70423 = CARTESIAN_POINT ( 'NONE',  ( -12.06949235617739369, -12.14591786802326823, 99.37609039468568994 ) ) ;
#70424 = CARTESIAN_POINT ( 'NONE',  ( 12.06949235617739724, 12.14591786802326823, 76.87609039468567573 ) ) ;
#70425 = CARTESIAN_POINT ( 'NONE',  ( 9.564922557961047289, -16.46253265017146816, 25.41775706135234003 ) ) ;
#70426 = CARTESIAN_POINT ( 'NONE',  ( -19.03943276465977164, 0.05219959533909376836, 101.2489096053143669 ) ) ;
#70427 = CARTESIAN_POINT ( 'NONE',  ( 0.05219959533909260263, 19.03943276465977164, 74.99890960531435269 ) ) ;
#70428 = CARTESIAN_POINT ( 'NONE',  ( -19.03943276465977164, 0.05219959533909376836, 31.24890960531435979 ) ) ;
#70429 = CARTESIAN_POINT ( 'NONE',  ( 16.52544592524342804, -4.483927247898539470, 48.54057627198103120 ) ) ;
#70430 = CARTESIAN_POINT ( 'NONE',  ( -13.97604488694527625, -13.89961937509977652, 101.8739096053143811 ) ) ;
#70431 = CARTESIAN_POINT ( 'NONE',  ( 10.72451020669898902, -18.67979575497178502, 42.91557627198103120 ) ) ;
#70432 = CARTESIAN_POINT ( 'NONE',  ( 16.55341960407611168, 4.379528057220329451, 78.95724293864769550 ) ) ;
#70433 = CARTESIAN_POINT ( 'NONE',  ( -0.05219959533934338120, 16.53943276465976808, 27.50109039468567929 ) ) ;
#70434 = CARTESIAN_POINT ( 'NONE',  ( -0.05219959533910754901, -16.53943276465976808, 67.49890960531436690 ) ) ;
#70435 = CARTESIAN_POINT ( 'NONE',  ( 29.20736712825158321, -0.9155518048963849909, -49.29216761470111408 ) ) ;
#70436 = CARTESIAN_POINT ( 'NONE',  ( 19.03943276465977164, 0.05219959533936151252, 66.25109039468567573 ) ) ;
#70437 = CARTESIAN_POINT ( 'NONE',  ( 19.05341960407611168, 5.049401038298154454, 103.9572429386476671 ) ) ;
#70438 = CARTESIAN_POINT ( 'NONE',  ( -5.153800228976607833, 19.02544592524334988, 77.70942372801900433 ) ) ;
#70439 = CARTESIAN_POINT ( 'NONE',  ( -17.58332526062528345, -7.635886036038592728, 39.07665040441535353 ) ) ;
#70441 = CARTESIAN_POINT ( 'NONE',  ( 14.34966873604972726, -8.224510206698740333, 105.8344237280190328 ) ) ;
#70440 = CARTESIAN_POINT ( 'NONE',  ( -16.51473224551082808, 9.474510206698731452, 113.3344237280190043 ) ) ;
#70442 = CARTESIAN_POINT ( 'NONE',  ( -5.153800228976328057, -19.02544592524343514, 37.29057627198102409 ) ) ;
#70443 = CARTESIAN_POINT ( 'NONE',  ( -5.719274019375978568, 21.55341960407610458, 35.20724293864768839 ) ) ;
#70444 = CARTESIAN_POINT ( 'NONE',  ( 10.81492255796106328, -18.62759615963255655, 60.41775706135235424 ) ) ;
#70445 = CARTESIAN_POINT ( 'NONE',  ( -24.51266705573320692, -8.027923408435210462, 167.0300397585817791 ) ) ;
#70446 = CARTESIAN_POINT ( 'NONE',  ( -8.224510206698735004, -14.34966873604973081, 24.58442372801901499 ) ) ;
#70448 = CARTESIAN_POINT ( 'NONE',  ( -5.049401038298153566, 19.05341960407611168, 70.20724293864769550 ) ) ;
#70447 = CARTESIAN_POINT ( 'NONE',  ( 17.49999999999985079, 3.193340300986046820, 22.66536441064387475 ) ) ;
#70449 = CIRCLE ( 'NONE', #8977, 5.500000000001017852 ) ;
#70450 = CARTESIAN_POINT ( 'NONE',  ( -16.51473224551069308, -9.474510206698971260, 21.66557627198102765 ) ) ;
#70452 = CARTESIAN_POINT ( 'NONE',  ( -9.474510206698964154, 16.51473224551069663, 70.41557627198102409 ) ) ;
#70451 = CARTESIAN_POINT ( 'NONE',  ( 12.14591786802309770, 12.06949235617756955, 84.37390960531438111 ) ) ;
#70453 = CARTESIAN_POINT ( 'NONE',  ( -16.46253265017160317, 9.564922557960807481, 90.83224293864769550 ) ) ;
#70454 = ORIENTED_EDGE ( 'NONE', *, *, #55, .T. ) ;
#70455 = CARTESIAN_POINT ( 'NONE',  ( -9.564922557961040184, 16.46253265017147172, 87.91775706135233293 ) ) ;
#70456 = CARTESIAN_POINT ( 'NONE',  ( 5.719274019375991003, -21.55341960407610458, 62.70724293864769550 ) ) ;
#70457 = CARTESIAN_POINT ( 'NONE',  ( 16.51473224551069308, 9.474510206698969483, 24.16557627198102765 ) ) ;
#70458 = CARTESIAN_POINT ( 'NONE',  ( -16.51473224551082808, 9.474510206698731452, 53.33442372801900433 ) ) ;
#70459 = CARTESIAN_POINT ( 'NONE',  ( -19.03943276465977164, 0.05219959533909376836, 61.24890960531436690 ) ) ;
#70460 = CARTESIAN_POINT ( 'NONE',  ( 16.46253265017160672, -9.564922557960803928, 88.33224293864769550 ) ) ;
#70461 = ORIENTED_EDGE ( 'NONE', *, *, #192965, .F. ) ;
#70462 = CARTESIAN_POINT ( 'NONE',  ( -15.72974639402197994, 15.80617190586746368, 100.6239096053143811 ) ) ;
#70465 = CARTESIAN_POINT ( 'NONE',  ( -19.05341960407617563, 5.049401038297882671, 58.54275706135234003 ) ) ;
#70464 = CARTESIAN_POINT ( 'NONE',  ( -16.46253265017160317, 9.564922557960807481, 85.83224293864769550 ) ) ;
#70463 = CARTESIAN_POINT ( 'NONE',  ( -12.14591786802309592, -12.06949235617757132, 91.87390960531436690 ) ) ;
#70466 = CARTESIAN_POINT ( 'NONE',  ( 5.823673210054125526, 21.52544592524343514, 94.79057627198105251 ) ) ;
#70467 = CARTESIAN_POINT ( 'NONE',  ( 21.55341960407610458, 5.719274019375980345, 68.95724293864769550 ) ) ;
#70468 = CARTESIAN_POINT ( 'NONE',  ( 4.483927247898545687, 16.52544592524342804, 34.79057627198103120 ) ) ;
#70469 = CARTESIAN_POINT ( 'NONE',  ( -15.80617190586768217, 15.72974639402176855, 98.12609039468570415 ) ) ;
#70470 = CARTESIAN_POINT ( 'NONE',  ( 12.14591786802327356, -12.06949235617739191, 60.62609039468567573 ) ) ;
#70471 = CARTESIAN_POINT ( 'NONE',  ( -19.05341960407611168, -5.049401038298163336, 81.45724293864769550 ) ) ;
#70472 = CARTESIAN_POINT ( 'NONE',  ( 13.89961937509977652, -13.97604488694527269, 28.12390960531435624 ) ) ;
#70473 = CARTESIAN_POINT ( 'NONE',  ( -21.53943276465977519, -0.05219959533937600094, 33.75109039468568284 ) ) ;
#70474 = CARTESIAN_POINT ( 'NONE',  ( -21.52544592524334988, -5.823673210054445271, 48.95942372801902565 ) ) ;
#70475 = CARTESIAN_POINT ( 'NONE',  ( -9.564922557960796823, -16.46253265017161027, 47.08224293864769550 ) ) ;
#70476 = CARTESIAN_POINT ( 'NONE',  ( -5.719274019375978568, 21.55341960407610458, 115.2072429386476955 ) ) ;
#70477 = CARTESIAN_POINT ( 'NONE',  ( 13.97604488694548053, -13.89961937509957401, 70.62609039468567573 ) ) ;
#70478 = CARTESIAN_POINT ( 'NONE',  ( -16.46253265017146816, -9.564922557961047289, 74.16775706135234714 ) ) ;
#70479 = CARTESIAN_POINT ( 'NONE',  ( 9.564922557960805705, 16.46253265017160317, 29.58224293864769550 ) ) ;
#70480 = CARTESIAN_POINT ( 'NONE',  ( -16.53943276465976808, -0.05219959533934237506, 78.75109039468568994 ) ) ;
#70481 = CARTESIAN_POINT ( 'NONE',  ( 9.474510206698971260, -16.51473224551069308, 47.91557627198102409 ) ) ;
#70482 = FACE_OUTER_BOUND ( 'NONE', #19410, .T. ) ;
#70483 = CARTESIAN_POINT ( 'NONE',  ( -13.97604488694527625, -13.89961937509977652, 96.87390960531433848 ) ) ;
#70484 = CARTESIAN_POINT ( 'NONE',  ( 19.05341960407611168, 5.049401038298154454, 38.95724293864767418 ) ) ;
#70485 = CARTESIAN_POINT ( 'NONE',  ( 21.53943276465977519, -0.05219959533907433946, 68.74890960531435269 ) ) ;
#70486 = CARTESIAN_POINT ( 'NONE',  ( 14.34966873604972726, -8.224510206698740333, 55.83442372801901854 ) ) ;
#70487 = CARTESIAN_POINT ( 'NONE',  ( -18.62759615963255300, -10.81492255796106328, 109.1677570613523613 ) ) ;
#70488 = CARTESIAN_POINT ( 'NONE',  ( 0.05219959533909260263, 19.03943276465977164, 54.99890960531435979 ) ) ;
#70489 = CARTESIAN_POINT ( 'NONE',  ( 12.06949235617757843, -12.14591786802309237, 33.12390960531435979 ) ) ;
#70490 = CARTESIAN_POINT ( 'NONE',  ( 14.29746914071049879, -8.314922557960816363, 68.33224293864769550 ) ) ;
#70491 = CARTESIAN_POINT ( 'NONE',  ( -19.03943276465977164, 0.05219959533909376836, 76.24890960531435269 ) ) ;
#70492 = CARTESIAN_POINT ( 'NONE',  ( -0.05219959533937732626, 21.53943276465977519, 42.50109039468567573 ) ) ;
#70493 = CARTESIAN_POINT ( 'NONE',  ( 5.049401038298161559, -19.05341960407611168, 87.70724293864769550 ) ) ;
#70494 = CARTESIAN_POINT ( 'NONE',  ( 0.05219959533937995610, -21.53943276465977519, 100.0010903946857042 ) ) ;
#70495 = CARTESIAN_POINT ( 'NONE',  ( 4.379528057220092307, 16.55341960407617563, 67.29275706135234714 ) ) ;
#70496 = CARTESIAN_POINT ( 'NONE',  ( -19.05341960407611168, -5.049401038298163336, 111.4572429386476671 ) ) ;
#70497 = CARTESIAN_POINT ( 'NONE',  ( 5.823673210054125526, 21.52544592524343514, 94.79057627198105251 ) ) ;
#70498 = CARTESIAN_POINT ( 'NONE',  ( 0.05219959533910956823, 16.53943276465976808, 49.99890960531437401 ) ) ;
#70499 = CARTESIAN_POINT ( 'NONE',  ( 19.03943276465977164, -0.05219959533909143690, 43.74890960531435979 ) ) ;
#70500 = CARTESIAN_POINT ( 'NONE',  ( -8.224510206698735004, -14.34966873604973081, 54.58442372801901143 ) ) ;
#70501 = CARTESIAN_POINT ( 'NONE',  ( 12.06949235617757843, -12.14591786802309237, 63.12390960531435979 ) ) ;
#70502 = CARTESIAN_POINT ( 'NONE',  ( 19.05341960407611168, 5.049401038298154454, 113.9572429386477097 ) ) ;
#70503 = CARTESIAN_POINT ( 'NONE',  ( 18.62759615963271287, -10.81492255796078972, 38.33224293864768839 ) ) ;
#70504 = CARTESIAN_POINT ( 'NONE',  ( 13.89961937509957401, 13.97604488694547697, 26.87609039468566507 ) ) ;
#70505 = CARTESIAN_POINT ( 'NONE',  ( -4.379528057220328563, 16.55341960407611168, 95.20724293864769550 ) ) ;
#70506 = CARTESIAN_POINT ( 'NONE',  ( 0.05219959533909260263, 19.03943276465977164, 109.9989096053143669 ) ) ;
#70507 = VERTEX_POINT ( 'NONE', #78189 ) ;
#70508 = CARTESIAN_POINT ( 'NONE',  ( 4.379528057220092307, 16.55341960407617563, 52.29275706135236135 ) ) ;
#70509 = CARTESIAN_POINT ( 'NONE',  ( 16.51473224551069308, 9.474510206698969483, 59.16557627198102409 ) ) ;
#70510 = CARTESIAN_POINT ( 'NONE',  ( 22.44159573604009239, 16.30477369853692693, 140.0750000027311728 ) ) ;
#70511 = CARTESIAN_POINT ( 'NONE',  ( 9.474510206698729675, 16.51473224551082808, 52.08442372801900433 ) ) ;
#70512 = CARTESIAN_POINT ( 'NONE',  ( -14.29746914071037622, -8.314922557961029526, 99.16775706135234714 ) ) ;
#70513 = CARTESIAN_POINT ( 'NONE',  ( -16.51473224551082808, 9.474510206698731452, 98.33442372801900433 ) ) ;
#70514 = CARTESIAN_POINT ( 'NONE',  ( 5.823673210054444382, -21.52544592524334988, 65.20942372801901854 ) ) ;
#70515 = CARTESIAN_POINT ( 'NONE',  ( 0.05219959533909260263, 19.03943276465977164, 74.99890960531435269 ) ) ;
#70516 = CARTESIAN_POINT ( 'NONE',  ( -5.719274019375978568, 21.55341960407610458, 95.20724293864769550 ) ) ;
#70517 = CARTESIAN_POINT ( 'NONE',  ( -8.224510206698948167, 14.34966873604960824, 110.4155762719810383 ) ) ;
#70518 = CARTESIAN_POINT ( 'NONE',  ( -13.89961937509957401, -13.97604488694547875, 79.37609039468567573 ) ) ;
#70519 = CARTESIAN_POINT ( 'NONE',  ( 15.72974639402199770, -15.80617190586745480, 73.12390960531436690 ) ) ;
#70520 = CARTESIAN_POINT ( 'NONE',  ( -13.97604488694547697, 13.89961937509957934, 38.12609039468566152 ) ) ;
#70521 = CARTESIAN_POINT ( 'NONE',  ( 19.01529144963337004, 5.500000000000029310, 98.73431955728440812 ) ) ;
#70522 = CARTESIAN_POINT ( 'NONE',  ( -15.72974639402197994, 15.80617190586746368, 90.62390960531436690 ) ) ;
#70523 = CARTESIAN_POINT ( 'NONE',  ( -19.25663599770061651, 5.499999999999450218, 53.99419308057203182 ) ) ;
#70524 = CARTESIAN_POINT ( 'NONE',  ( -19.05341960407611168, -5.049401038298163336, 66.45724293864769550 ) ) ;
#70525 = CYLINDRICAL_SURFACE ( 'NONE', #75622, 38.00000000000000000 ) ;
#70526 = CARTESIAN_POINT ( 'NONE',  ( 12.14591786802327356, -12.06949235617739191, 25.62609039468567929 ) ) ;
#70527 = CARTESIAN_POINT ( 'NONE',  ( 24.60782464877076947, 7.576768089025934572, 167.2921030401324742 ) ) ;
#70528 = CARTESIAN_POINT ( 'NONE',  ( 16.46253265017160672, -9.564922557960803928, 48.33224293864769550 ) ) ;
#70529 = CARTESIAN_POINT ( 'NONE',  ( -19.05341960407611168, -5.049401038298163336, 111.4572429386476671 ) ) ;
#70531 = CARTESIAN_POINT ( 'NONE',  ( -0.05219959533910754901, -16.53943276465976808, 52.49890960531435979 ) ) ;
#70530 = CARTESIAN_POINT ( 'NONE',  ( -10.81492255796078084, -18.62759615963271287, 102.0822429386476955 ) ) ;
#70532 = CARTESIAN_POINT ( 'NONE',  ( -5.719274019375665041, -21.55341960407619695, 74.79275706135234714 ) ) ;
#70534 = CARTESIAN_POINT ( 'NONE',  ( -16.46253265017146816, -9.564922557961047289, 34.16775706135233293 ) ) ;
#70533 = CARTESIAN_POINT ( 'NONE',  ( 14.34966873604972726, -8.224510206698740333, 30.83442372801902209 ) ) ;
#70535 = CARTESIAN_POINT ( 'NONE',  ( 12.06949235617757843, -12.14591786802309237, 33.12390960531435979 ) ) ;
#70536 = CARTESIAN_POINT ( 'NONE',  ( 21.55341960407619695, -5.719274019375665929, 41.04275706135236135 ) ) ;
#70537 = CARTESIAN_POINT ( 'NONE',  ( -0.05219959533907301413, -21.53943276465977519, 112.4989096053143669 ) ) ;
#70538 = CARTESIAN_POINT ( 'NONE',  ( 12.06949235617757843, -12.14591786802309237, 43.12390960531435269 ) ) ;
#70539 = CARTESIAN_POINT ( 'NONE',  ( 16.51473224551083163, -9.474510206698727899, 100.8344237280190043 ) ) ;
#70540 = EDGE_CURVE ( 'NONE', #34840, #42860, #80181, .T. ) ;
#70541 = CARTESIAN_POINT ( 'NONE',  ( 0.05219959533936267826, -19.03943276465977164, 70.00109039468566152 ) ) ;
#70542 = CARTESIAN_POINT ( 'NONE',  ( 5.719274019375673035, 21.55341960407619339, 67.29275706135234714 ) ) ;
#70543 = CARTESIAN_POINT ( 'NONE',  ( -5.049401038297874678, -19.05341960407617918, 49.79275706135231871 ) ) ;
#70544 = CARTESIAN_POINT ( 'NONE',  ( 0.05219959533909260263, 19.03943276465977164, 24.99890960531435269 ) ) ;
#70545 = CARTESIAN_POINT ( 'NONE',  ( 21.53943276465977519, -0.05219959533907433946, 43.74890960531435979 ) ) ;
#70546 = CARTESIAN_POINT ( 'NONE',  ( 8.314922557960818139, 14.29746914071049879, 54.58224293864769550 ) ) ;
#70547 = CARTESIAN_POINT ( 'NONE',  ( -30.74264578624800492, 22.33583958711400186, -1.949999994537626735 ) ) ;
#70548 = CARTESIAN_POINT ( 'NONE',  ( 5.823673210054444382, -21.52544592524334988, 110.2094237280190185 ) ) ;
#70549 = CARTESIAN_POINT ( 'NONE',  ( 4.379528057220092307, 16.55341960407617563, 87.29275706135236135 ) ) ;
#70550 = CARTESIAN_POINT ( 'NONE',  ( 8.314922557960818139, 14.29746914071049879, 34.58224293864770260 ) ) ;
#70551 = CARTESIAN_POINT ( 'NONE',  ( -15.72974639402176322, -15.80617190586768395, 69.37609039468567573 ) ) ;
#70552 = CARTESIAN_POINT ( 'NONE',  ( -10.72451020669870658, -18.67979575497194134, 84.58442372801903275 ) ) ;
#70553 = CARTESIAN_POINT ( 'NONE',  ( -10.81492255796078084, -18.62759615963271287, 82.08224293864768129 ) ) ;
#70554 = CARTESIAN_POINT ( 'NONE',  ( 16.46253265017160672, -9.564922557960803928, 38.33224293864768839 ) ) ;
#70555 = CARTESIAN_POINT ( 'NONE',  ( 21.53943276465977519, 0.05219959533937863772, 61.25109039468567573 ) ) ;
#70556 = CARTESIAN_POINT ( 'NONE',  ( 13.89961937509977652, -13.97604488694527269, 38.12390960531436690 ) ) ;
#70557 = CARTESIAN_POINT ( 'NONE',  ( 13.97604488694527802, 13.89961937509977652, 49.37390960531434558 ) ) ;
#70558 = CARTESIAN_POINT ( 'NONE',  ( -16.55341960407611168, -4.379528057220339221, 86.45724293864770971 ) ) ;
#70559 = CARTESIAN_POINT ( 'NONE',  ( 9.564922557960805705, 16.46253265017160317, 94.58224293864769550 ) ) ;
#70560 = CARTESIAN_POINT ( 'NONE',  ( -16.52544592524342804, 4.483927247898546575, 41.04057627198103120 ) ) ;
#70561 = CARTESIAN_POINT ( 'NONE',  ( 12.14591786802309770, 12.06949235617756955, 114.3739096053143527 ) ) ;
#70562 = CARTESIAN_POINT ( 'NONE',  ( -18.67979575497178146, -10.72451020669898902, 76.66557627198103830 ) ) ;
#70563 = CARTESIAN_POINT ( 'NONE',  ( 5.823673210054125526, 21.52544592524343514, 114.7905762719810383 ) ) ;
#70564 = CARTESIAN_POINT ( 'NONE',  ( -15.41147372653650116, 14.79648886421073506, -56.42550976940268015 ) ) ;
#70566 = CARTESIAN_POINT ( 'NONE',  ( 14.34966873604972726, -8.224510206698740333, 20.83442372801901143 ) ) ;
#70565 = CARTESIAN_POINT ( 'NONE',  ( -13.97604488694527625, -13.89961937509977652, 81.87390960531436690 ) ) ;
#70567 = CARTESIAN_POINT ( 'NONE',  ( 10.81492255796078972, 18.62759615963270932, 74.58224293864768129 ) ) ;
#70568 = CARTESIAN_POINT ( 'NONE',  ( 21.55341960407619695, -5.719274019375665929, 96.04275706135236135 ) ) ;
#70569 = CARTESIAN_POINT ( 'NONE',  ( -16.46253265017160317, 9.564922557960807481, 75.83224293864769550 ) ) ;
#70570 = CARTESIAN_POINT ( 'NONE',  ( 10.81492255796106328, -18.62759615963255655, 35.41775706135234003 ) ) ;
#70571 = CARTESIAN_POINT ( 'NONE',  ( -15.80617190586745835, -15.72974639402198527, 21.87390960531436690 ) ) ;
#70572 = CARTESIAN_POINT ( 'NONE',  ( -8.224510206698735004, -14.34966873604973081, 84.58442372801903275 ) ) ;
#70573 = CARTESIAN_POINT ( 'NONE',  ( 15.72974639402176855, 15.80617190586768217, 66.87609039468568994 ) ) ;
#70574 = CARTESIAN_POINT ( 'NONE',  ( -21.55341960407619339, 5.719274019375674811, 103.5427570613523613 ) ) ;
#70575 = CARTESIAN_POINT ( 'NONE',  ( 14.34966873604972726, -8.224510206698740333, 80.83442372801901854 ) ) ;
#70576 = CARTESIAN_POINT ( 'NONE',  ( -21.53943276465977519, -0.05219959533937600094, 23.75109039468567929 ) ) ;
#70577 = CARTESIAN_POINT ( 'NONE',  ( 9.474510206698971260, -16.51473224551069308, 22.91557627198102765 ) ) ;
#70578 = CARTESIAN_POINT ( 'NONE',  ( 0.05219959533937995610, -21.53943276465977519, 95.00109039468568994 ) ) ;
#70579 = CARTESIAN_POINT ( 'NONE',  ( 5.049401038298161559, -19.05341960407611168, 87.70724293864769550 ) ) ;
#70580 = CARTESIAN_POINT ( 'NONE',  ( -15.72974639402197994, 15.80617190586746368, 85.62390960531436690 ) ) ;
#70581 = CARTESIAN_POINT ( 'NONE',  ( 19.05341960407617918, -5.049401038297876454, 56.04275706135234714 ) ) ;
#70583 = CARTESIAN_POINT ( 'NONE',  ( 21.53943276465977519, -0.05219959533907433946, 53.74890960531437401 ) ) ;
#70582 = CARTESIAN_POINT ( 'NONE',  ( -2.662494480112494788, -37.13692398601925504, -32.59999999999999432 ) ) ;
#70585 = CARTESIAN_POINT ( 'NONE',  ( -0.05219959533910754901, -16.53943276465976808, 52.49890960531435979 ) ) ;
#70584 = CARTESIAN_POINT ( 'NONE',  ( 9.564922557960805705, 16.46253265017160317, 89.58224293864769550 ) ) ;
#70586 = DIRECTION ( 'NONE',  ( -0.7071067811865492381, 8.659560562354911904E-17, -0.7071067811865457964 ) ) ;
#70587 = CARTESIAN_POINT ( 'NONE',  ( -19.02544592524334988, -5.153800228976617603, 83.95942372801901854 ) ) ;
#70588 = AXIS2_PLACEMENT_3D ( 'NONE', #93550, #13740, #183598 ) ;
#70589 = CARTESIAN_POINT ( 'NONE',  ( -0.7792920370541464026, -16.49741402511618915, -61.43171317168469869 ) ) ;
#70590 = CARTESIAN_POINT ( 'NONE',  ( -19.05341960407617563, 5.049401038297882671, 113.5427570613523471 ) ) ;
#70591 = CARTESIAN_POINT ( 'NONE',  ( 21.55341960407610458, 5.719274019375980345, 78.95724293864769550 ) ) ;
#70592 = CARTESIAN_POINT ( 'NONE',  ( -12.14591786802309592, -12.06949235617757132, 66.87390960531436690 ) ) ;
#70593 = CARTESIAN_POINT ( 'NONE',  ( -19.03943276465977164, 0.05219959533909376836, 96.24890960531436690 ) ) ;
#70594 = CARTESIAN_POINT ( 'NONE',  ( 12.06949235617739724, 12.14591786802326823, 41.87609039468568284 ) ) ;
#70595 = CARTESIAN_POINT ( 'NONE',  ( 16.46253265017160672, -9.564922557960803928, 58.33224293864769550 ) ) ;
#70597 = CARTESIAN_POINT ( 'NONE',  ( 13.89961937509957401, 13.97604488694547697, 86.87609039468567573 ) ) ;
#70596 = CARTESIAN_POINT ( 'NONE',  ( -18.67979575497178146, -10.72451020669898902, 111.6655762719810525 ) ) ;
#70598 = CARTESIAN_POINT ( 'NONE',  ( -13.97604488694527625, -13.89961937509977652, 96.87390960531433848 ) ) ;
#70599 =( BOUNDED_CURVE ( )  B_SPLINE_CURVE ( 2, ( #162723, #24228, #85879, #39378, #146541, #102053, #118229, #54546, #177910, #103052, #9052, #52539, #194083 ),
 .UNSPECIFIED., .F., .F. ) 
 B_SPLINE_CURVE_WITH_KNOTS ( ( 3, 2, 2, 2, 2, 2, 3 ),
 ( 0.2656340109859774423, 0.2675438596491228060, 0.2719298245614035214, 0.2763157894736842368, 0.2807017543859648967, 0.2850877192982456121, 0.2870432477834812812 ),
 .UNSPECIFIED. ) 
 CURVE ( )  GEOMETRIC_REPRESENTATION_ITEM ( )  RATIONAL_B_SPLINE_CURVE ( ( 0.9832469066685285419, 0.9851625545550100060, 1.000000000000000000, 0.9659258262890683122, 1.000000000000000000, 0.9659258262890683122, 1.000000000000000000, 0.9659258262890683122, 1.000000000000000000, 0.9659258262890683122, 1.000000000000000000, 0.9848076720550082985, 0.9831626618144002627 ) ) 
 REPRESENTATION_ITEM ( '' )  );
#70600 = CARTESIAN_POINT ( 'NONE',  ( 13.89961937509977652, -13.97604488694527269, 78.12390960531433848 ) ) ;
#70601 = CARTESIAN_POINT ( 'NONE',  ( -10.72451020669898014, 18.67979575497178502, 80.41557627198103830 ) ) ;
#70602 = CARTESIAN_POINT ( 'NONE',  ( -9.564922557960796823, -16.46253265017161027, 47.08224293864769550 ) ) ;
#70603 = CARTESIAN_POINT ( 'NONE',  ( -0.3641133308643078048, 37.60169961596129440, -7.999999999999994671 ) ) ;
#70604 = CARTESIAN_POINT ( 'NONE',  ( 4.379528057220339221, -16.55341960407611168, 52.70724293864769550 ) ) ;
#70605 = CARTESIAN_POINT ( 'NONE',  ( -9.564922557960796823, -16.46253265017161027, 97.08224293864769550 ) ) ;
#70606 = DIRECTION ( 'NONE',  ( 1.000000000000000000, 0.000000000000000000, 0.000000000000000000 ) ) ;
#70607 = CARTESIAN_POINT ( 'NONE',  ( 9.474510206698729675, 16.51473224551082808, 67.08442372801900433 ) ) ;
#70608 = CARTESIAN_POINT ( 'NONE',  ( 10.72451020669898902, -18.67979575497178502, 92.91557627198103830 ) ) ;
#70609 = CARTESIAN_POINT ( 'NONE',  ( -5.049401038297874678, -19.05341960407617918, 44.79275706135232582 ) ) ;
#70610 = CARTESIAN_POINT ( 'NONE',  ( -9.564922557960796823, -16.46253265017161027, 97.08224293864769550 ) ) ;
#70611 = CARTESIAN_POINT ( 'NONE',  ( 11.62258226397313798, -9.495678640448794283, -59.91195431507608049 ) ) ;
#70612 = CARTESIAN_POINT ( 'NONE',  ( 5.719274019375991003, -21.55341960407610458, 42.70724293864770260 ) ) ;
#70613 = CARTESIAN_POINT ( 'NONE',  ( 13.97604488694527802, 13.89961937509977652, 69.37390960531436690 ) ) ;
#70614 = CARTESIAN_POINT ( 'NONE',  ( 18.67979575497194134, -10.72451020669871369, 65.83442372801900433 ) ) ;
#70615 = CARTESIAN_POINT ( 'NONE',  ( -16.46253265017160317, 9.564922557960807481, 35.83224293864768839 ) ) ;
#70616 = EDGE_CURVE ( 'NONE', #184655, #171099, #1348, .T. ) ;
#70618 = ORIENTED_EDGE ( 'NONE', *, *, #137192, .T. ) ;
#70617 = CARTESIAN_POINT ( 'NONE',  ( 4.483927247898545687, 16.52544592524342804, 74.79057627198105251 ) ) ;
#70619 = CARTESIAN_POINT ( 'NONE',  ( 16.52544592524335698, 4.483927247898782831, 26.45942372801901854 ) ) ;
#70620 = CARTESIAN_POINT ( 'NONE',  ( 15.72974639402176855, 15.80617190586768217, 56.87609039468568994 ) ) ;
#70621 = ORIENTED_EDGE ( 'NONE', *, *, #59834, .F. ) ;
#70622 = CARTESIAN_POINT ( 'NONE',  ( -27.81654016797119766, -7.031644252044944920, 140.0000000000000284 ) ) ;
#70623 = CARTESIAN_POINT ( 'NONE',  ( -0.05219959533936034679, 19.03943276465977164, 67.50109039468566152 ) ) ;
#70624 = CARTESIAN_POINT ( 'NONE',  ( 27.00987238947314850, -29.10436634937579115, -20.14159902729967300 ) ) ;
#70625 = CARTESIAN_POINT ( 'NONE',  ( -21.53943276465977519, 0.05219959533907696930, 116.2489096053143669 ) ) ;
#70626 = CARTESIAN_POINT ( 'NONE',  ( 13.97604488694527802, 13.89961937509977652, 54.37390960531435979 ) ) ;
#70627 = CARTESIAN_POINT ( 'NONE',  ( 23.48529157249599919, 32.32473071737754111, -4.449999994537627401 ) ) ;
#70628 = CARTESIAN_POINT ( 'NONE',  ( 19.05341960407617918, -5.049401038297876454, 26.04275706135233293 ) ) ;
#70629 = CARTESIAN_POINT ( 'NONE',  ( 19.05341960407611168, 5.049401038298154454, 43.95724293864769550 ) ) ;
#70630 = CARTESIAN_POINT ( 'NONE',  ( 10.81492255796106328, -18.62759615963255655, 110.4177570613523756 ) ) ;
#70631 = CARTESIAN_POINT ( 'NONE',  ( 12.06949235617739724, 12.14591786802326823, 86.87609039468568994 ) ) ;
#70632 = EDGE_CURVE ( 'NONE', #159210, #150536, #196229, .T. ) ;
#70634 = CARTESIAN_POINT ( 'NONE',  ( -21.53943276465977519, -0.05219959533937600094, 68.75109039468568994 ) ) ;
#70633 = CARTESIAN_POINT ( 'NONE',  ( 16.51473224551069308, 9.474510206698969483, 99.16557627198102409 ) ) ;
#70635 = CARTESIAN_POINT ( 'NONE',  ( 36.91746824999999177, 2.880721459617395097E-14, -9.624999997268814056 ) ) ;
#70636 = CARTESIAN_POINT ( 'NONE',  ( -19.03943276465977164, 0.05219959533909376836, 116.2489096053143669 ) ) ;
#70637 = CARTESIAN_POINT ( 'NONE',  ( 22.15208335914313409, 5.528296758471276107, 173.4118699040215006 ) ) ;
#70639 = CARTESIAN_POINT ( 'NONE',  ( -18.62759615963255300, -10.81492255796106328, 69.16775706135234714 ) ) ;
#70638 = CARTESIAN_POINT ( 'NONE',  ( -12.14591786802326823, 12.06949235617739902, 53.12609039468568284 ) ) ;
#70640 = CARTESIAN_POINT ( 'NONE',  ( 5.823673210054444382, -21.52544592524334988, 100.2094237280190043 ) ) ;
#70641 = CARTESIAN_POINT ( 'NONE',  ( 6.434671708797586653, 6.434671708797580436, -63.95112321872120731 ) ) ;
#70642 = CARTESIAN_POINT ( 'NONE',  ( -16.53943276465976808, -0.05219959533934237506, 38.75109039468567573 ) ) ;
#70643 = CARTESIAN_POINT ( 'NONE',  ( 13.89961937509977652, -13.97604488694527269, 83.12390960531436690 ) ) ;
#70644 = CARTESIAN_POINT ( 'NONE',  ( -19.02544592524342804, 5.153800228976336051, 111.0405762719810099 ) ) ;
#70645 = ORIENTED_EDGE ( 'NONE', *, *, #137830, .T. ) ;
#70646 = CARTESIAN_POINT ( 'NONE',  ( 16.88567814943166212, 6.947325034625596807, 43.79001122652586986 ) ) ;
#70647 = CARTESIAN_POINT ( 'NONE',  ( 13.97604488694527802, 13.89961937509977652, 39.37390960531435269 ) ) ;
#70648 = CARTESIAN_POINT ( 'NONE',  ( 10.81492255796078972, 18.62759615963270932, 49.58224293864769550 ) ) ;
#70649 = CARTESIAN_POINT ( 'NONE',  ( -16.52544592524335698, -4.483927247898792601, 108.9594237280190185 ) ) ;
#70651 = CARTESIAN_POINT ( 'NONE',  ( -16.51473224551069308, -9.474510206698971260, 76.66557627198103830 ) ) ;
#70650 = CARTESIAN_POINT ( 'NONE',  ( -4.379528057220328563, 16.55341960407611168, 85.20724293864770971 ) ) ;
#70652 = CARTESIAN_POINT ( 'NONE',  ( -10.81492255796105439, 18.62759615963255655, 107.9177570613523471 ) ) ;
#70653 = CARTESIAN_POINT ( 'NONE',  ( 8.314922557961029526, -14.29746914071037800, 20.41775706135234714 ) ) ;
#70654 = CARTESIAN_POINT ( 'NONE',  ( -14.29746914071049879, 8.314922557960819915, 85.83224293864768129 ) ) ;
#70655 = CARTESIAN_POINT ( 'NONE',  ( 10.81492255796106328, -18.62759615963255655, 35.41775706135234003 ) ) ;
#70656 = CARTESIAN_POINT ( 'NONE',  ( 5.823673210054125526, 21.52544592524343514, 69.79057627198102409 ) ) ;
#70657 = CARTESIAN_POINT ( 'NONE',  ( 13.89961937509957401, 13.97604488694547697, 56.87609039468564731 ) ) ;
#70658 = CARTESIAN_POINT ( 'NONE',  ( -34.54575687042841281, 4.960469055748716549, 50.63070180855214630 ) ) ;
#70659 = CARTESIAN_POINT ( 'NONE',  ( -0.05219959533909027116, -19.03943276465977164, 92.49890960531436690 ) ) ;
#70660 = CARTESIAN_POINT ( 'NONE',  ( -0.05219959533910754901, -16.53943276465976808, 62.49890960531436690 ) ) ;
#70661 = CARTESIAN_POINT ( 'NONE',  ( -12.06949235617756955, 12.14591786802309770, 50.62390960531435979 ) ) ;
#70662 = CARTESIAN_POINT ( 'NONE',  ( 14.29746914071037800, 8.314922557961029526, 111.6677570613523613 ) ) ;
#70663 = CARTESIAN_POINT ( 'NONE',  ( 5.153800228976615827, -19.02544592524334988, 70.20942372801899012 ) ) ;
#70664 = FACE_OUTER_BOUND ( 'NONE', #77511, .T. ) ;
#70665 = CARTESIAN_POINT ( 'NONE',  ( -5.823673210054116645, -21.52544592524344225, 27.29057627198103120 ) ) ;
#70666 = CARTESIAN_POINT ( 'NONE',  ( 4.379528057220339221, -16.55341960407611168, 87.70724293864769550 ) ) ;
#70667 = FACE_OUTER_BOUND ( 'NONE', #176575, .T. ) ;
#70669 = CARTESIAN_POINT ( 'NONE',  ( 5.719274019375991003, -21.55341960407610458, 42.70724293864770260 ) ) ;
#70668 = CARTESIAN_POINT ( 'NONE',  ( -9.564922557960796823, -16.46253265017161027, 42.08224293864769550 ) ) ;
#70670 = CARTESIAN_POINT ( 'NONE',  ( -9.474510206698964154, 16.51473224551069663, 25.41557627198103120 ) ) ;
#70672 = CARTESIAN_POINT ( 'NONE',  ( 9.564922557960805705, 16.46253265017160317, 64.58224293864769550 ) ) ;
#70671 = CARTESIAN_POINT ( 'NONE',  ( -12.06949235617739369, -12.14591786802326823, 64.37609039468568994 ) ) ;
#70673 = CARTESIAN_POINT ( 'NONE',  ( 5.153800228976615827, -19.02544592524334988, 40.20942372801898301 ) ) ;
#70674 = CARTESIAN_POINT ( 'NONE',  ( -18.67979575497193778, 10.72451020669871902, 53.33442372801901854 ) ) ;
#70675 = ORIENTED_EDGE ( 'NONE', *, *, #65094, .T. ) ;
#70676 = CARTESIAN_POINT ( 'NONE',  ( 15.72974639402199770, -15.80617190586745480, 38.12390960531436690 ) ) ;
#70677 = CARTESIAN_POINT ( 'NONE',  ( 8.314922557960818139, 14.29746914071049879, 99.58224293864770971 ) ) ;
#70678 = CARTESIAN_POINT ( 'NONE',  ( -9.564922557961040184, 16.46253265017147172, 92.91775706135233293 ) ) ;
#70679 = CARTESIAN_POINT ( 'NONE',  ( -11.40812507854754720, -35.11059874428192273, -6.724999997268813701 ) ) ;
#70681 = CARTESIAN_POINT ( 'NONE',  ( 21.53943276465977519, -0.05219959533907433946, 48.74890960531435979 ) ) ;
#70680 = DIRECTION ( 'NONE',  ( -1.000000000000000000, 0.000000000000000000, 0.000000000000000000 ) ) ;
#70682 = CARTESIAN_POINT ( 'NONE',  ( -5.153800228976328057, -19.02544592524343514, 27.29057627198103120 ) ) ;
#70683 = CARTESIAN_POINT ( 'NONE',  ( -15.72974639402176322, -15.80617190586768395, 89.37609039468568994 ) ) ;
#70684 = CARTESIAN_POINT ( 'NONE',  ( -14.29746914071049879, 8.314922557960819915, 45.83224293864769550 ) ) ;
#70686 = CARTESIAN_POINT ( 'NONE',  ( -16.55341960407611168, -4.379528057220339221, 56.45724293864768839 ) ) ;
#70685 = CARTESIAN_POINT ( 'NONE',  ( -14.34966873604972548, 8.224510206698743886, 58.33442372801901143 ) ) ;
#70687 = CARTESIAN_POINT ( 'NONE',  ( 15.72974639402199770, -15.80617190586745480, 88.12390960531436690 ) ) ;
#70688 = CARTESIAN_POINT ( 'NONE',  ( -18.62759615963270932, 10.81492255796079327, 70.83224293864770971 ) ) ;
#70689 = DIRECTION ( 'NONE',  ( -1.000000000000000000, -0.000000000000000000, -0.000000000000000000 ) ) ;
#70691 = CARTESIAN_POINT ( 'NONE',  ( 15.80617190586746368, 15.72974639402197994, 24.37390960531435979 ) ) ;
#70690 = CARTESIAN_POINT ( 'NONE',  ( -0.05219959533936034679, 19.03943276465977164, 87.50109039468567573 ) ) ;
#70692 = CARTESIAN_POINT ( 'NONE',  ( -5.049401038298153566, 19.05341960407611168, 65.20724293864765286 ) ) ;
#70693 = CARTESIAN_POINT ( 'NONE',  ( -16.51473224551069308, -9.474510206698971260, 36.66557627198102409 ) ) ;
#70694 = DIRECTION ( 'NONE',  ( 1.000000000000000000, -0.000000000000000000, -0.000000000000000000 ) ) ;
#70695 = CARTESIAN_POINT ( 'NONE',  ( -8.314922557961024197, 14.29746914071037800, 87.91775706135234714 ) ) ;
#70696 = CARTESIAN_POINT ( 'NONE',  ( 0.05219959533937995610, -21.53943276465977519, 25.00109039468567218 ) ) ;
#70697 = CARTESIAN_POINT ( 'NONE',  ( -9.564922557960796823, -16.46253265017161027, 67.08224293864769550 ) ) ;
#70698 = CARTESIAN_POINT ( 'NONE',  ( -18.67979575497193778, 10.72451020669871902, 53.33442372801901854 ) ) ;
#70699 = CARTESIAN_POINT ( 'NONE',  ( -5.049401038298153566, 19.05341960407611168, 90.20724293864766707 ) ) ;
#70700 = CARTESIAN_POINT ( 'NONE',  ( -24.59647911869062042, -31.70815657101477925, -17.34206816075075253 ) ) ;
#70701 = VERTEX_POINT ( 'NONE', #2350 ) ;
#70702 = CARTESIAN_POINT ( 'NONE',  ( -21.52544592524334988, -5.823673210054445271, 43.95942372801902565 ) ) ;
#70704 = CARTESIAN_POINT ( 'NONE',  ( -9.564922557960796823, -16.46253265017161027, 107.0822429386476955 ) ) ;
#70703 = CARTESIAN_POINT ( 'NONE',  ( -19.05341960407611168, -5.049401038298163336, 26.45724293864769550 ) ) ;
#70705 = CARTESIAN_POINT ( 'NONE',  ( -0.05219959533936034679, 19.03943276465977164, 47.50109039468566863 ) ) ;
#70706 = CARTESIAN_POINT ( 'NONE',  ( -15.80617190586745835, -15.72974639402198527, 106.8739096053143811 ) ) ;
#70707 = CARTESIAN_POINT ( 'NONE',  ( -19.05341960407617563, 5.049401038297882671, 48.54275706135233293 ) ) ;
#70708 = CARTESIAN_POINT ( 'NONE',  ( 16.51473224551083163, -9.474510206698727899, 45.83442372801900433 ) ) ;
#70709 = CARTESIAN_POINT ( 'NONE',  ( 16.53943276465976808, 0.05219959533934440121, 111.2510903946856899 ) ) ;
#70711 = ORIENTED_EDGE ( 'NONE', *, *, #44529, .T. ) ;
#70710 = CARTESIAN_POINT ( 'NONE',  ( 9.408549014593489801, 11.42987701755554752, -62.15975709196300869 ) ) ;
#70712 = CARTESIAN_POINT ( 'NONE',  ( -19.02544592524342804, 5.153800228976336051, 76.04057627198102409 ) ) ;
#70713 = CARTESIAN_POINT ( 'NONE',  ( 5.719274019375673035, 21.55341960407619339, 82.29275706135234714 ) ) ;
#70714 = CARTESIAN_POINT ( 'NONE',  ( -5.719274019375665041, -21.55341960407619695, 94.79275706135234714 ) ) ;
#70715 = CARTESIAN_POINT ( 'NONE',  ( 0.000000000000000000, 0.000000000000000000, -62.58071313852362039 ) ) ;
#70716 = CARTESIAN_POINT ( 'NONE',  ( -16.51473224551069308, -9.474510206698971260, 96.66557627198102409 ) ) ;
#70717 = CARTESIAN_POINT ( 'NONE',  ( -21.53943276465977519, -0.05219959533937600094, 73.75109039468567573 ) ) ;
#70718 = CARTESIAN_POINT ( 'NONE',  ( -8.224510206698735004, -14.34966873604973081, 19.58442372801901143 ) ) ;
#70719 = CARTESIAN_POINT ( 'NONE',  ( 9.474510206698971260, -16.51473224551069308, 77.91557627198103830 ) ) ;
#70721 = EDGE_CURVE ( 'NONE', #12139, #114764, #180063, .T. ) ;
#70720 = CARTESIAN_POINT ( 'NONE',  ( 0.05219959533909260263, 19.03943276465977164, 114.9989096053143669 ) ) ;
#70722 = CARTESIAN_POINT ( 'NONE',  ( 19.03943276465977164, -0.05219959533909143690, 88.74890960531436690 ) ) ;
#70723 = DIRECTION ( 'NONE',  ( 0.000000000000000000, 0.000000000000000000, 1.000000000000000000 ) ) ;
#70724 = CARTESIAN_POINT ( 'NONE',  ( 9.564922557960805705, 16.46253265017160317, 84.58224293864769550 ) ) ;
#70725 = CARTESIAN_POINT ( 'NONE',  ( 16.46253265017160672, -9.564922557960803928, 63.33224293864769550 ) ) ;
#70726 = CARTESIAN_POINT ( 'NONE',  ( -10.81492255796078084, -18.62759615963271287, 107.0822429386476955 ) ) ;
#70727 = CARTESIAN_POINT ( 'NONE',  ( 12.14591786802327356, -12.06949235617739191, 105.6260903946856899 ) ) ;
#70728 = DIRECTION ( 'NONE',  ( -0.5000000000000002220, -0.4999999999999985567, 0.7071067811865484609 ) ) ;
#70729 = CARTESIAN_POINT ( 'NONE',  ( 19.03943276465977164, 0.05219959533936151252, 56.25109039468566863 ) ) ;
#70730 = CARTESIAN_POINT ( 'NONE',  ( 16.51473224551069308, 9.474510206698969483, 94.16557627198103830 ) ) ;
#70731 = CARTESIAN_POINT ( 'NONE',  ( 4.379528057220339221, -16.55341960407611168, 87.70724293864769550 ) ) ;
#70732 = CARTESIAN_POINT ( 'NONE',  ( 9.564922557960805705, 16.46253265017160317, 24.58224293864769194 ) ) ;
#70733 = CARTESIAN_POINT ( 'NONE',  ( -15.80617190586745835, -15.72974639402198527, 31.87390960531435979 ) ) ;
#70734 = CARTESIAN_POINT ( 'NONE',  ( 21.52544592524344225, -5.823673210054117533, 23.54057627198102765 ) ) ;
#70735 = CARTESIAN_POINT ( 'NONE',  ( 16.53943276465976808, -0.05219959533910856209, 98.74890960531438111 ) ) ;
#70736 = CARTESIAN_POINT ( 'NONE',  ( -1.197744245042869471, -6.691772886347793659, -62.38710104649958055 ) ) ;
#70737 = CARTESIAN_POINT ( 'NONE',  ( -19.02544592524334988, -5.153800228976617603, 38.95942372801900433 ) ) ;
#70738 = CARTESIAN_POINT ( 'NONE',  ( -4.483927247898782831, 16.52544592524335698, 107.7094237280190328 ) ) ;
#70739 = CARTESIAN_POINT ( 'NONE',  ( 5.049401038298161559, -19.05341960407611168, 82.70724293864770971 ) ) ;
#70740 = CARTESIAN_POINT ( 'NONE',  ( -18.62759615963255300, -10.81492255796106328, 69.16775706135234714 ) ) ;
#70741 = CARTESIAN_POINT ( 'NONE',  ( 21.52544592524344225, -5.823673210054117533, 43.54057627198103830 ) ) ;
#70742 = CARTESIAN_POINT ( 'NONE',  ( -5.719274019375665041, -21.55341960407619695, 34.79275706135235424 ) ) ;
#70743 = CARTESIAN_POINT ( 'NONE',  ( -18.67979575497178146, -10.72451020669898902, 86.66557627198102409 ) ) ;
#70744 = CARTESIAN_POINT ( 'NONE',  ( -4.379528057220328563, 16.55341960407611168, 105.2072429386477097 ) ) ;
#70745 = CARTESIAN_POINT ( 'NONE',  ( -0.05219959533936034679, 19.03943276465977164, 67.50109039468566152 ) ) ;
#70746 = CARTESIAN_POINT ( 'NONE',  ( -16.46253265017160317, 9.564922557960807481, 50.83224293864770260 ) ) ;
#70747 = CARTESIAN_POINT ( 'NONE',  ( 19.02544592524343514, -5.153800228976328945, 98.54057627198100988 ) ) ;
#70748 = CARTESIAN_POINT ( 'NONE',  ( -5.153800228976328057, -19.02544592524343514, 97.29057627198099567 ) ) ;
#70749 = CARTESIAN_POINT ( 'NONE',  ( 16.52544592524342804, -4.483927247898539470, 113.5405762719810383 ) ) ;
#70750 = CARTESIAN_POINT ( 'NONE',  ( -14.29746914071049879, 8.314922557960819915, 45.83224293864769550 ) ) ;
#70751 = CARTESIAN_POINT ( 'NONE',  ( -0.05219959533934338120, 16.53943276465976808, 37.50109039468568284 ) ) ;
#70752 = CARTESIAN_POINT ( 'NONE',  ( 10.81492255796106328, -18.62759615963255655, 105.4177570613523613 ) ) ;
#70754 = CARTESIAN_POINT ( 'NONE',  ( 14.29746914071049879, -8.314922557960816363, 23.33224293864769194 ) ) ;
#70753 = SPHERICAL_SURFACE ( 'NONE', #175277, 2.000000000000000000 ) ;
#70755 = CARTESIAN_POINT ( 'NONE',  ( 18.62759615963255655, 10.81492255796105972, 26.66775706135235424 ) ) ;
#70756 = CARTESIAN_POINT ( 'NONE',  ( 16.51473224551069308, 9.474510206698969483, 104.1655762719810241 ) ) ;
#70757 = CARTESIAN_POINT ( 'NONE',  ( 16.55341960407618274, -4.379528057220086978, 111.0427570613523613 ) ) ;
#70758 = CARTESIAN_POINT ( 'NONE',  ( -16.55341960407617563, 4.379528057220093196, 93.54275706135234714 ) ) ;
#70759 = CARTESIAN_POINT ( 'NONE',  ( 12.14591786802327356, -12.06949235617739191, 30.62609039468567929 ) ) ;
#70760 = CARTESIAN_POINT ( 'NONE',  ( -13.89961937509977652, 13.97604488694528158, 45.62390960531433848 ) ) ;
#70761 = CARTESIAN_POINT ( 'NONE',  ( -12.06949235617756955, 12.14591786802309770, 105.6239096053143669 ) ) ;
#70762 = CARTESIAN_POINT ( 'NONE',  ( -18.62759615963270932, 10.81492255796079327, 115.8322429386477097 ) ) ;
#70763 = CARTESIAN_POINT ( 'NONE',  ( -5.049401038298153566, 19.05341960407611168, 35.20724293864768839 ) ) ;
#70764 = CARTESIAN_POINT ( 'NONE',  ( -19.05341960407611168, -5.049401038298163336, 111.4572429386476671 ) ) ;
#70765 = CARTESIAN_POINT ( 'NONE',  ( 21.53943276465977519, 0.05219959533937863772, 26.25109039468567573 ) ) ;
#70766 = CARTESIAN_POINT ( 'NONE',  ( 13.97604488694527802, 13.89961937509977652, 34.37390960531436690 ) ) ;
#70767 = CARTESIAN_POINT ( 'NONE',  ( -19.02544592524342804, 5.153800228976336051, 106.0405762719810241 ) ) ;
#70768 = DIRECTION ( 'NONE',  ( 0.000000000000000000, 0.000000000000000000, 1.000000000000000000 ) ) ;
#70769 = CARTESIAN_POINT ( 'NONE',  ( -5.049401038298153566, 19.05341960407611168, 100.2072429386476955 ) ) ;
#70771 = CARTESIAN_POINT ( 'NONE',  ( 12.14591786802309770, 12.06949235617756955, 89.37390960531435269 ) ) ;
#70770 = CARTESIAN_POINT ( 'NONE',  ( 10.81492255796106328, -18.62759615963255655, 45.41775706135234003 ) ) ;
#70772 = CARTESIAN_POINT ( 'NONE',  ( 16.51473224551069308, 9.474510206698969483, 94.16557627198103830 ) ) ;
#70773 = CARTESIAN_POINT ( 'NONE',  ( -27.79720911487485324, -7.618197028333625553, 161.3616953378478343 ) ) ;
#70774 = CARTESIAN_POINT ( 'NONE',  ( -14.34966873604972548, 8.224510206698743886, 68.33442372801900433 ) ) ;
#70775 = CARTESIAN_POINT ( 'NONE',  ( -21.55341960407619339, 5.719274019375674811, 83.54275706135234714 ) ) ;
#70776 = CARTESIAN_POINT ( 'NONE',  ( 16.53943276465976808, 0.05219959533934440121, 36.25109039468567573 ) ) ;
#70778 = ADVANCED_FACE ( 'NONE', ( #155047 ), #105691, .T. ) ;
#70777 = CARTESIAN_POINT ( 'NONE',  ( 5.049401038298161559, -19.05341960407611168, 77.70724293864765286 ) ) ;
#70779 = CARTESIAN_POINT ( 'NONE',  ( 19.02544592524334988, 5.153800228976608722, 106.4594237280190185 ) ) ;
#70780 = CARTESIAN_POINT ( 'NONE',  ( 14.34966873604972726, -8.224510206698740333, 75.83442372801900433 ) ) ;
#70781 = CARTESIAN_POINT ( 'NONE',  ( 19.03943276465977164, 0.05219959533936151252, 91.25109039468566152 ) ) ;
#70782 = CARTESIAN_POINT ( 'NONE',  ( -9.474510206698964154, 16.51473224551069663, 65.41557627198102409 ) ) ;
#70783 = CARTESIAN_POINT ( 'NONE',  ( 10.81492255796078972, 18.62759615963270932, 89.58224293864768129 ) ) ;
#70785 = CARTESIAN_POINT ( 'NONE',  ( -16.51473224551082808, 9.474510206698731452, 88.33442372801900433 ) ) ;
#70784 = CARTESIAN_POINT ( 'NONE',  ( -16.53943276465976808, 0.05219959533911058130, 96.24890960531435269 ) ) ;
#70786 = CARTESIAN_POINT ( 'NONE',  ( -16.53943276465976808, -0.05219959533934237506, 53.75109039468568994 ) ) ;
#70787 = CARTESIAN_POINT ( 'NONE',  ( 24.40828949532285819, 2.848420800298366196, 173.9378174459544937 ) ) ;
#70788 = CARTESIAN_POINT ( 'NONE',  ( -13.97604488694547697, 13.89961937509957934, 63.12609039468566152 ) ) ;
#70789 = CARTESIAN_POINT ( 'NONE',  ( -12.14591786802309592, -12.06949235617757132, 36.87390960531435979 ) ) ;
#70790 = CARTESIAN_POINT ( 'NONE',  ( 12.14591786802309770, 12.06949235617756955, 74.37390960531436690 ) ) ;
#70792 = CARTESIAN_POINT ( 'NONE',  ( -16.61371651742640410, 7.165104196375922108, 38.85415069992971127 ) ) ;
#70791 = CARTESIAN_POINT ( 'NONE',  ( 19.03943276465977164, 0.05219959533936151252, 26.25109039468566507 ) ) ;
#70793 = CARTESIAN_POINT ( 'NONE',  ( 21.52544592524334988, 5.823673210054432836, 21.45942372801901499 ) ) ;
#70794 = CARTESIAN_POINT ( 'NONE',  ( 0.8613000766924048257, -7.878827036337491485, 6.568406857878970939 ) ) ;
#70795 = CARTESIAN_POINT ( 'NONE',  ( -9.564922557960796823, -16.46253265017161027, 77.08224293864769550 ) ) ;
#70796 = CARTESIAN_POINT ( 'NONE',  ( 21.52544592524334988, 5.823673210054432836, 96.45942372801901854 ) ) ;
#70797 = CARTESIAN_POINT ( 'NONE',  ( -9.564922557960796823, -16.46253265017161027, 77.08224293864769550 ) ) ;
#70798 = CARTESIAN_POINT ( 'NONE',  ( 10.81492255796078972, 18.62759615963270932, 44.58224293864769550 ) ) ;
#70799 = CARTESIAN_POINT ( 'NONE',  ( -14.34966873604960291, -8.224510206698953496, 81.66557627198103830 ) ) ;
#70800 = CARTESIAN_POINT ( 'NONE',  ( -19.02544592524342804, 5.153800228976336051, 61.04057627198103120 ) ) ;
#70801 = CARTESIAN_POINT ( 'NONE',  ( -8.314922557960811034, -14.29746914071050412, 112.0822429386477097 ) ) ;
#70802 = CARTESIAN_POINT ( 'NONE',  ( 5.823673210054444382, -21.52544592524334988, 20.20942372801900788 ) ) ;
#70803 = CARTESIAN_POINT ( 'NONE',  ( -5.719274019375665041, -21.55341960407619695, 64.79275706135234714 ) ) ;
#70804 = CARTESIAN_POINT ( 'NONE',  ( -13.97604488694527625, -13.89961937509977652, 46.87390960531435979 ) ) ;
#70805 = CARTESIAN_POINT ( 'NONE',  ( -8.224510206698735004, -14.34966873604973081, 69.58442372801900433 ) ) ;
#70806 = ADVANCED_FACE ( 'NONE', ( #44897 ), #172204, .T. ) ;
#70807 = CARTESIAN_POINT ( 'NONE',  ( -18.62759615963270932, 10.81492255796079327, 115.8322429386477097 ) ) ;
#70808 = CARTESIAN_POINT ( 'NONE',  ( 21.52544592524344225, -5.823673210054117533, 108.5405762719810241 ) ) ;
#70810 = CARTESIAN_POINT ( 'NONE',  ( 16.51473224551069308, 9.474510206698969483, 59.16557627198102409 ) ) ;
#70809 = CARTESIAN_POINT ( 'NONE',  ( -13.97604488694547697, 13.89961937509957934, 33.12609039468566863 ) ) ;
#70811 = CARTESIAN_POINT ( 'NONE',  ( -7.652493125987827050, -39.26116846142902261, -15.00000000000000000 ) ) ;
#70812 = CARTESIAN_POINT ( 'NONE',  ( 15.80617190586769283, -15.72974639402175789, 65.62609039468568994 ) ) ;
#70813 = CARTESIAN_POINT ( 'NONE',  ( 18.62759615963271287, -10.81492255796078972, 53.33224293864769550 ) ) ;
#70814 = CARTESIAN_POINT ( 'NONE',  ( 8.314922557960818139, 14.29746914071049879, 39.58224293864769550 ) ) ;
#70816 = CARTESIAN_POINT ( 'NONE',  ( 10.81492255796106328, -18.62759615963255655, 110.4177570613523756 ) ) ;
#70815 = CARTESIAN_POINT ( 'NONE',  ( -5.719274019375665041, -21.55341960407619695, 74.79275706135234714 ) ) ;
#70817 = CARTESIAN_POINT ( 'NONE',  ( 16.55341960407611168, 4.379528057220329451, 58.95724293864770971 ) ) ;
#70818 = CARTESIAN_POINT ( 'NONE',  ( 12.14591786802309770, 12.06949235617756955, 99.37390960531436690 ) ) ;
#70819 = CARTESIAN_POINT ( 'NONE',  ( -16.51473224551082808, 9.474510206698731452, 58.33442372801900433 ) ) ;
#70820 = CARTESIAN_POINT ( 'NONE',  ( 12.06949235617757843, -12.14591786802309237, 28.12390960531435979 ) ) ;
#70821 = CARTESIAN_POINT ( 'NONE',  ( -18.62759615963255300, -10.81492255796106328, 69.16775706135234714 ) ) ;
#70822 = CARTESIAN_POINT ( 'NONE',  ( 13.89961937509977652, -13.97604488694527269, 78.12390960531433848 ) ) ;
#70823 = CARTESIAN_POINT ( 'NONE',  ( 5.153800228976615827, -19.02544592524334988, 35.20942372801899722 ) ) ;
#70824 = CARTESIAN_POINT ( 'NONE',  ( -18.62759615963270932, 10.81492255796079327, 40.83224293864769550 ) ) ;
#70825 = CARTESIAN_POINT ( 'NONE',  ( 21.52544592524334988, 5.823673210054432836, 36.45942372801901143 ) ) ;
#70826 = VECTOR ( 'NONE', #141720, 1000.000000000000114 ) ;
#70827 = CARTESIAN_POINT ( 'NONE',  ( -5.823673210054116645, -21.52544592524344225, 87.29057627198103830 ) ) ;
#70828 = CARTESIAN_POINT ( 'NONE',  ( -13.89961937509957401, -13.97604488694547875, 104.3760903946856757 ) ) ;
#70829 = CARTESIAN_POINT ( 'NONE',  ( 14.29746914071037800, 8.314922557961029526, 56.66775706135235424 ) ) ;
#70831 = CARTESIAN_POINT ( 'NONE',  ( -15.72974639402197994, 15.80617190586746368, 90.62390960531436690 ) ) ;
#70830 = CARTESIAN_POINT ( 'NONE',  ( -11.74264578624800670, 36.14014761921585972, -6.400000000000000355 ) ) ;
#70832 = CARTESIAN_POINT ( 'NONE',  ( 8.314922557960818139, 14.29746914071049879, 84.58224293864769550 ) ) ;
#70833 = CARTESIAN_POINT ( 'NONE',  ( -17.26058549869091507, -6.457015423128549259, 101.3774583747607210 ) ) ;
#70834 = CARTESIAN_POINT ( 'NONE',  ( 9.474510206698729675, 16.51473224551082808, 112.0844237280190043 ) ) ;
#70835 = CARTESIAN_POINT ( 'NONE',  ( -18.67979575497178146, -10.72451020669898902, 51.66557627198102409 ) ) ;
#70836 = CARTESIAN_POINT ( 'NONE',  ( 12.14591786802327356, -12.06949235617739191, 90.62609039468567573 ) ) ;
#70837 = DIRECTION ( 'NONE',  ( -1.000000000000000000, 0.000000000000000000, 0.000000000000000000 ) ) ;
#70838 = CARTESIAN_POINT ( 'NONE',  ( -0.05219959533934338120, 16.53943276465976808, 47.50109039468568994 ) ) ;
#70839 = CARTESIAN_POINT ( 'NONE',  ( -18.62759615963255300, -10.81492255796106328, 29.16775706135234003 ) ) ;
#70840 = CARTESIAN_POINT ( 'NONE',  ( -15.80617190586745835, -15.72974639402198527, 41.87390960531435979 ) ) ;
#70841 = CARTESIAN_POINT ( 'NONE',  ( 8.224510206698742110, 14.34966873604972548, 87.08442372801901854 ) ) ;
#70842 = CARTESIAN_POINT ( 'NONE',  ( -9.474510206698964154, 16.51473224551069663, 95.41557627198102409 ) ) ;
#70843 = CARTESIAN_POINT ( 'NONE',  ( 0.05219959533937995610, -21.53943276465977519, 75.00109039468568994 ) ) ;
#70844 = CARTESIAN_POINT ( 'NONE',  ( -21.55341960407610458, -5.719274019375992779, 36.45724293864768839 ) ) ;
#70845 = CARTESIAN_POINT ( 'NONE',  ( 16.46253265017160672, -9.564922557960803928, 113.3322429386476955 ) ) ;
#70846 = CARTESIAN_POINT ( 'NONE',  ( -19.02544592524334988, -5.153800228976617603, 53.95942372801898301 ) ) ;
#70847 = CARTESIAN_POINT ( 'NONE',  ( 14.34966873604972726, -8.224510206698740333, 70.83442372801901854 ) ) ;
#70848 = CARTESIAN_POINT ( 'NONE',  ( 15.72974639402199770, -15.80617190586745480, 23.12390960531436335 ) ) ;
#70849 = ORIENTED_EDGE ( 'NONE', *, *, #200059, .T. ) ;
#70850 = CARTESIAN_POINT ( 'NONE',  ( -16.51473224551069308, -9.474510206698971260, 86.66557627198102409 ) ) ;
#70851 = CARTESIAN_POINT ( 'NONE',  ( -12.14591786802326823, 12.06949235617739902, 103.1260903946856757 ) ) ;
#70852 = CARTESIAN_POINT ( 'NONE',  ( -17.97058386085788229, -5.499999999999976019, 79.00390968646219392 ) ) ;
#70853 = CARTESIAN_POINT ( 'NONE',  ( -16.53943276465976808, 0.05219959533911058130, 91.24890960531436690 ) ) ;
#70854 = CARTESIAN_POINT ( 'NONE',  ( 21.53943276465977519, -0.05219959533907433946, 43.74890960531435979 ) ) ;
#70855 = CARTESIAN_POINT ( 'NONE',  ( -19.05341960407611168, -5.049401038298163336, 36.45724293864766707 ) ) ;
#70856 = CARTESIAN_POINT ( 'NONE',  ( -14.34966873604972548, 8.224510206698743886, 83.33442372801903275 ) ) ;
#70857 = CARTESIAN_POINT ( 'NONE',  ( 15.80617190586769283, -15.72974639402175789, 35.62609039468568994 ) ) ;
#70858 = CARTESIAN_POINT ( 'NONE',  ( 9.564922557961047289, -16.46253265017146816, 95.41775706135233293 ) ) ;
#70859 = CARTESIAN_POINT ( 'NONE',  ( 4.379528057220339221, -16.55341960407611168, 87.70724293864769550 ) ) ;
#70860 = CARTESIAN_POINT ( 'NONE',  ( 5.153800228976335163, 19.02544592524342804, 54.79057627198103120 ) ) ;
#70861 = AXIS2_PLACEMENT_3D ( 'NONE', #159828, #86988, #21323 ) ;
#70862 = CARTESIAN_POINT ( 'NONE',  ( 19.02544592524343514, -5.153800228976328945, 23.54057627198102054 ) ) ;
#70863 = CARTESIAN_POINT ( 'NONE',  ( 10.81492255796106328, -18.62759615963255655, 105.4177570613523613 ) ) ;
#70864 = CARTESIAN_POINT ( 'NONE',  ( 13.89961937509977652, -13.97604488694527269, 83.12390960531436690 ) ) ;
#70865 = CARTESIAN_POINT ( 'NONE',  ( -14.29746914071037622, -8.314922557961029526, 59.16775706135234714 ) ) ;
#70866 = CARTESIAN_POINT ( 'NONE',  ( -10.72451020669870658, -18.67979575497194134, 94.58442372801901854 ) ) ;
#70867 = CARTESIAN_POINT ( 'NONE',  ( 8.224510206698742110, 14.34966873604972548, 77.08442372801901854 ) ) ;
#70868 = CARTESIAN_POINT ( 'NONE',  ( 5.153800228976615827, -19.02544592524334988, 55.20942372801899722 ) ) ;
#70869 = CARTESIAN_POINT ( 'NONE',  ( 0.05219959533936267826, -19.03943276465977164, 65.00109039468567573 ) ) ;
#70870 = VERTEX_POINT ( 'NONE', #63028 ) ;
#70871 = CARTESIAN_POINT ( 'NONE',  ( 0.05219959533937995610, -21.53943276465977519, 65.00109039468568994 ) ) ;
#70872 = CARTESIAN_POINT ( 'NONE',  ( 19.02544592524343514, -5.153800228976328945, 63.54057627198103830 ) ) ;
#70873 = CARTESIAN_POINT ( 'NONE',  ( -13.97604488694527625, -13.89961937509977652, 26.87390960531434558 ) ) ;
#70874 = CARTESIAN_POINT ( 'NONE',  ( -16.46253265017146816, -9.564922557961047289, 59.16775706135233293 ) ) ;
#70875 = CARTESIAN_POINT ( 'NONE',  ( -25.31894786019269361, 4.571304203950368183, 167.3973414147895085 ) ) ;
#70876 = CARTESIAN_POINT ( 'NONE',  ( -9.564922557960796823, -16.46253265017161027, 87.08224293864769550 ) ) ;
#70877 = CARTESIAN_POINT ( 'NONE',  ( -16.53943276465976808, 0.05219959533911058130, 36.24890960531435979 ) ) ;
#70878 = CARTESIAN_POINT ( 'NONE',  ( -0.05219959533907301413, -21.53943276465977519, 47.49890960531435979 ) ) ;
#70879 = LINE ( 'NONE', #73883, #67483 ) ;
#70880 = CARTESIAN_POINT ( 'NONE',  ( -15.80617190586768217, 15.72974639402176855, 108.1260903946856757 ) ) ;
#70881 = CARTESIAN_POINT ( 'NONE',  ( -16.29526858892875296, -7.335722546920122156, 80.79670597800208043 ) ) ;
#70882 = CARTESIAN_POINT ( 'NONE',  ( -16.51473224551069308, -9.474510206698971260, 31.66557627198102054 ) ) ;
#70883 = CARTESIAN_POINT ( 'NONE',  ( 16.51473224551069308, 9.474510206698969483, 24.16557627198102765 ) ) ;
#70884 = CARTESIAN_POINT ( 'NONE',  ( -34.51794252349512249, -0.7246179257117795203, 89.53606970770105988 ) ) ;
#70885 = CARTESIAN_POINT ( 'NONE',  ( -5.719274019375665041, -21.55341960407619695, 69.79275706135234714 ) ) ;
#70886 = CARTESIAN_POINT ( 'NONE',  ( -34.94848686537405769, -14.38147731881034375, -7.999999999999994671 ) ) ;
#70887 = CARTESIAN_POINT ( 'NONE',  ( -8.314922557961024197, 14.29746914071037800, 62.91775706135236135 ) ) ;
#70888 = CARTESIAN_POINT ( 'NONE',  ( -15.72974639402197994, 15.80617190586746368, 85.62390960531436690 ) ) ;
#70889 = CARTESIAN_POINT ( 'NONE',  ( 4.379528057220339221, -16.55341960407611168, 57.70724293864770260 ) ) ;
#70891 = CARTESIAN_POINT ( 'NONE',  ( 0.05219959533909260263, 19.03943276465977164, 114.9989096053143669 ) ) ;
#70890 = CARTESIAN_POINT ( 'NONE',  ( 16.51473224551069308, 9.474510206698969483, 34.16557627198102409 ) ) ;
#70892 = CARTESIAN_POINT ( 'NONE',  ( -15.72974639402176322, -15.80617190586768395, 39.37609039468567573 ) ) ;
#70893 = CARTESIAN_POINT ( 'NONE',  ( -13.89961937509957401, -13.97604488694547875, 44.37609039468566863 ) ) ;
#70894 = CARTESIAN_POINT ( 'NONE',  ( 13.89961937509977652, -13.97604488694527269, 28.12390960531435624 ) ) ;
#70895 = CARTESIAN_POINT ( 'NONE',  ( 18.67979575497194134, -10.72451020669871369, 85.83442372801901854 ) ) ;
#70896 = CARTESIAN_POINT ( 'NONE',  ( -5.153800228976328057, -19.02544592524343514, 22.29057627198102765 ) ) ;
#70897 = CARTESIAN_POINT ( 'NONE',  ( 12.06949235617757843, -12.14591786802309237, 38.12390960531436690 ) ) ;
#70898 = DIRECTION ( 'NONE',  ( -1.000000000000000000, -6.938893903907222461E-16, -0.000000000000000000 ) ) ;
#70899 = CARTESIAN_POINT ( 'NONE',  ( -10.72451020669898014, 18.67979575497178502, 45.41557627198103830 ) ) ;
#70900 = CARTESIAN_POINT ( 'NONE',  ( 8.571926809382597767, 26.38167802310806209, 142.2750000027311899 ) ) ;
#70901 = CARTESIAN_POINT ( 'NONE',  ( 0.05219959533909260263, 19.03943276465977164, 94.99890960531436690 ) ) ;
#70902 = CARTESIAN_POINT ( 'NONE',  ( 4.483927247898545687, 16.52544592524342804, 89.79057627198103830 ) ) ;
#70903 = CARTESIAN_POINT ( 'NONE',  ( 12.14591786802327356, -12.06949235617739191, 30.62609039468567929 ) ) ;
#70904 = CARTESIAN_POINT ( 'NONE',  ( -10.81492255796078084, -18.62759615963271287, 62.08224293864769550 ) ) ;
#70905 = ORIENTED_EDGE ( 'NONE', *, *, #58993, .F. ) ;
#70906 = CARTESIAN_POINT ( 'NONE',  ( -13.97604488694527625, -13.89961937509977652, 36.87390960531436690 ) ) ;
#70908 = CARTESIAN_POINT ( 'NONE',  ( 18.67979575497178502, 10.72451020669898547, 94.16557627198103830 ) ) ;
#70907 = CARTESIAN_POINT ( 'NONE',  ( 9.564922557960805705, 16.46253265017160317, 79.58224293864769550 ) ) ;
#70910 = CARTESIAN_POINT ( 'NONE',  ( 16.46253265017160672, -9.564922557960803928, 98.33224293864769550 ) ) ;
#70909 = CARTESIAN_POINT ( 'NONE',  ( -0.05219959533910754901, -16.53943276465976808, 27.49890960531435269 ) ) ;
#70911 = CARTESIAN_POINT ( 'NONE',  ( -13.89961937509957401, -13.97604488694547875, 84.37609039468567573 ) ) ;
#70912 = CARTESIAN_POINT ( 'NONE',  ( -21.53943276465977519, -0.05219959533937600094, 108.7510903946857042 ) ) ;
#70913 = CARTESIAN_POINT ( 'NONE',  ( 10.72451020669898902, -18.67979575497178502, 82.91557627198103830 ) ) ;
#70914 = CARTESIAN_POINT ( 'NONE',  ( 21.52544592524344225, -5.823673210054117533, 33.54057627198102409 ) ) ;
#70915 = CARTESIAN_POINT ( 'NONE',  ( -5.049401038298153566, 19.05341960407611168, 55.20724293864769550 ) ) ;
#70916 = CARTESIAN_POINT ( 'NONE',  ( -8.314922557960811034, -14.29746914071050412, 27.08224293864769550 ) ) ;
#70917 = CARTESIAN_POINT ( 'NONE',  ( 13.89961937509977652, -13.97604488694527269, 73.12390960531436690 ) ) ;
#70918 = ORIENTED_EDGE ( 'NONE', *, *, #141068, .T. ) ;
#70919 = CARTESIAN_POINT ( 'NONE',  ( -32.53128430053963172, -2.419343514923748550, 87.89668391837240335 ) ) ;
#70920 = CARTESIAN_POINT ( 'NONE',  ( -9.474510206698720793, -16.51473224551083518, 29.58442372801900433 ) ) ;
#70921 = CARTESIAN_POINT ( 'NONE',  ( 16.55341960407611168, 4.379528057220329451, 83.95724293864770971 ) ) ;
#70922 = CARTESIAN_POINT ( 'NONE',  ( -10.72451020669870658, -18.67979575497194134, 19.58442372801901143 ) ) ;
#70923 = CARTESIAN_POINT ( 'NONE',  ( 27.73933785331498214, 9.013057229001095294, 146.4750000027311501 ) ) ;
#70924 = CARTESIAN_POINT ( 'NONE',  ( 21.53943276465977519, -0.05219959533907433946, 53.74890960531437401 ) ) ;
#70925 = CARTESIAN_POINT ( 'NONE',  ( -0.05219959533934338120, 16.53943276465976808, 87.50109039468568994 ) ) ;
#70926 = CARTESIAN_POINT ( 'NONE',  ( -8.224510206698948167, 14.34966873604960824, 115.4155762719810241 ) ) ;
#70927 = CARTESIAN_POINT ( 'NONE',  ( -5.049401038298153566, 19.05341960407611168, 70.20724293864769550 ) ) ;
#70928 = CARTESIAN_POINT ( 'NONE',  ( -23.48529157249600985, 32.32473071737754111, -10.04999999453762705 ) ) ;
#70929 = CARTESIAN_POINT ( 'NONE',  ( 16.52544592524342804, -4.483927247898539470, 23.54057627198102765 ) ) ;
#70930 = CARTESIAN_POINT ( 'NONE',  ( -21.52544592524334988, -5.823673210054445271, 63.95942372801901854 ) ) ;
#70931 = CARTESIAN_POINT ( 'NONE',  ( 19.02544592524343514, -5.153800228976328945, 113.5405762719810241 ) ) ;
#70932 = CARTESIAN_POINT ( 'NONE',  ( 10.81492255796106328, -18.62759615963255655, 95.41775706135234714 ) ) ;
#70933 = CARTESIAN_POINT ( 'NONE',  ( -16.51473224551069308, -9.474510206698971260, 41.66557627198103120 ) ) ;
#70934 = CARTESIAN_POINT ( 'NONE',  ( 13.89961937509977652, -13.97604488694527269, 48.12390960531435979 ) ) ;
#70935 = ORIENTED_EDGE ( 'NONE', *, *, #145468, .T. ) ;
#70936 = CARTESIAN_POINT ( 'NONE',  ( 21.52544592524334988, 5.823673210054432836, 101.4594237280190185 ) ) ;
#70937 = CARTESIAN_POINT ( 'NONE',  ( 12.14591786802327356, -12.06949235617739191, 65.62609039468568994 ) ) ;
#70938 = CARTESIAN_POINT ( 'NONE',  ( -0.05219959533937732626, 21.53943276465977519, 82.50109039468568994 ) ) ;
#70939 = CARTESIAN_POINT ( 'NONE',  ( -0.05219959533907301413, -21.53943276465977519, 27.49890960531435269 ) ) ;
#70940 = CARTESIAN_POINT ( 'NONE',  ( -16.46253265017146816, -9.564922557961047289, 99.16775706135233293 ) ) ;
#70941 = CARTESIAN_POINT ( 'NONE',  ( -18.62759615963255300, -10.81492255796106328, 49.16775706135234003 ) ) ;
#70942 = CARTESIAN_POINT ( 'NONE',  ( 16.52544592524335698, 4.483927247898782831, 36.45942372801901143 ) ) ;
#70943 = CARTESIAN_POINT ( 'NONE',  ( 19.02544592524334988, 5.153800228976608722, 81.45942372801897591 ) ) ;
#70944 = CARTESIAN_POINT ( 'NONE',  ( -19.02544592524342804, 5.153800228976336051, 71.04057627198099567 ) ) ;
#70945 = CARTESIAN_POINT ( 'NONE',  ( -16.46253265017146816, -9.564922557961047289, 99.16775706135233293 ) ) ;
#70946 = CARTESIAN_POINT ( 'NONE',  ( 9.564922557961047289, -16.46253265017146816, 95.41775706135233293 ) ) ;
#70947 = CARTESIAN_POINT ( 'NONE',  ( 8.314922557960818139, 14.29746914071049879, 54.58224293864769550 ) ) ;
#70948 = CARTESIAN_POINT ( 'NONE',  ( -19.03943276465977164, -0.05219959533935918106, 73.75109039468566152 ) ) ;
#70949 = CARTESIAN_POINT ( 'NONE',  ( -12.14591786802326823, 12.06949235617739902, 58.12609039468568994 ) ) ;
#70950 = CARTESIAN_POINT ( 'NONE',  ( -19.03943276465977164, -0.05219959533935918106, 23.75109039468566152 ) ) ;
#70951 = CARTESIAN_POINT ( 'NONE',  ( 5.153800228976335163, 19.02544592524342804, 34.79057627198102409 ) ) ;
#70952 = CARTESIAN_POINT ( 'NONE',  ( -16.51473224551069308, -9.474510206698971260, 36.66557627198102409 ) ) ;
#70953 = CARTESIAN_POINT ( 'NONE',  ( 14.34966873604972726, -8.224510206698740333, 60.83442372801901854 ) ) ;
#70954 = CARTESIAN_POINT ( 'NONE',  ( 17.14385361876520264, -23.59649016807271238, 140.0750000027311728 ) ) ;
#70955 = EDGE_CURVE ( 'NONE', #40791, #53699, #125901, .T. ) ;
#70956 = CARTESIAN_POINT ( 'NONE',  ( 8.906447517083050158, 27.41122689804195645, 139.6500000054623740 ) ) ;
#70957 = CARTESIAN_POINT ( 'NONE',  ( 5.049401038298161559, -19.05341960407611168, 102.7072429386476955 ) ) ;
#70958 = CARTESIAN_POINT ( 'NONE',  ( -17.49999999999999645, 5.499999999999997335, 120.0000000000000142 ) ) ;
#70959 = ORIENTED_EDGE ( 'NONE', *, *, #72533, .F. ) ;
#70960 = CARTESIAN_POINT ( 'NONE',  ( -16.46253265017146816, -9.564922557961047289, 104.1677570613523329 ) ) ;
#70962 = CARTESIAN_POINT ( 'NONE',  ( 15.80617190586746368, 15.72974639402197994, 34.37390960531435979 ) ) ;
#70961 = AXIS2_PLACEMENT_3D ( 'NONE', #98554, #160248, #117745 ) ;
#70964 = CARTESIAN_POINT ( 'NONE',  ( -12.06949235617739369, -12.14591786802326823, 19.37609039468568639 ) ) ;
#70963 = CARTESIAN_POINT ( 'NONE',  ( -9.474510206698720793, -16.51473224551083518, 29.58442372801900433 ) ) ;
#70965 = CARTESIAN_POINT ( 'NONE',  ( 13.97604488694527802, 13.89961937509977652, 29.37390960531435979 ) ) ;
#70966 = CARTESIAN_POINT ( 'NONE',  ( -13.97604488694527625, -13.89961937509977652, 56.87390960531434558 ) ) ;
#70967 = CARTESIAN_POINT ( 'NONE',  ( -21.53943276465977519, 0.05219959533907696930, 76.24890960531435269 ) ) ;
#70968 = CARTESIAN_POINT ( 'NONE',  ( 5.049401038298161559, -19.05341960407611168, 102.7072429386476955 ) ) ;
#70969 = CARTESIAN_POINT ( 'NONE',  ( -9.474510206698964154, 16.51473224551069663, 35.41557627198102409 ) ) ;
#70970 = CARTESIAN_POINT ( 'NONE',  ( -8.571926809382608425, 26.38167802310805854, 142.9750000027312069 ) ) ;
#70971 = CARTESIAN_POINT ( 'NONE',  ( 16.51473224551083163, -9.474510206698727899, 85.83442372801900433 ) ) ;
#70972 = CARTESIAN_POINT ( 'NONE',  ( 16.52544592524342804, -4.483927247898539470, 48.54057627198103120 ) ) ;
#70973 = CARTESIAN_POINT ( 'NONE',  ( 5.719274019375991003, -21.55341960407610458, 27.70724293864769905 ) ) ;
#70974 = CARTESIAN_POINT ( 'NONE',  ( -15.72974639402176322, -15.80617190586768395, 104.3760903946856899 ) ) ;
#70975 = CARTESIAN_POINT ( 'NONE',  ( -18.62759615963270932, 10.81492255796079327, 100.8322429386477097 ) ) ;
#70976 = CARTESIAN_POINT ( 'NONE',  ( -21.55341960407619339, 5.719274019375674811, 68.54275706135234714 ) ) ;
#70977 = CARTESIAN_POINT ( 'NONE',  ( -0.05219959533937732626, 21.53943276465977519, 77.50109039468567573 ) ) ;
#70978 = CARTESIAN_POINT ( 'NONE',  ( -19.05341960407611168, -5.049401038298163336, 106.4572429386476955 ) ) ;
#70980 = CARTESIAN_POINT ( 'NONE',  ( -0.05219959533937732626, 21.53943276465977519, 62.50109039468568284 ) ) ;
#70979 = CARTESIAN_POINT ( 'NONE',  ( 16.52544592524335698, 4.483927247898782831, 111.4594237280190328 ) ) ;
#70981 = CARTESIAN_POINT ( 'NONE',  ( -13.97604488694527625, -13.89961937509977652, 56.87390960531434558 ) ) ;
#70982 = CARTESIAN_POINT ( 'NONE',  ( 0.05219959533936267826, -19.03943276465977164, 40.00109039468566152 ) ) ;
#70983 = CARTESIAN_POINT ( 'NONE',  ( 5.823673210054444382, -21.52544592524334988, 30.20942372801902565 ) ) ;
#70984 = CARTESIAN_POINT ( 'NONE',  ( -0.05219959533909027116, -19.03943276465977164, 72.49890960531435269 ) ) ;
#70985 = CARTESIAN_POINT ( 'NONE',  ( 4.379528057220339221, -16.55341960407611168, 77.70724293864770971 ) ) ;
#70986 = CARTESIAN_POINT ( 'NONE',  ( 0.05219959533910956823, 16.53943276465976808, 49.99890960531437401 ) ) ;
#70987 = CARTESIAN_POINT ( 'NONE',  ( -5.719274019375978568, 21.55341960407610458, 60.20724293864768839 ) ) ;
#70988 = CARTESIAN_POINT ( 'NONE',  ( 9.474510206698971260, -16.51473224551069308, 57.91557627198103120 ) ) ;
#70989 = CARTESIAN_POINT ( 'NONE',  ( 15.72974639402199770, -15.80617190586745480, 78.12390960531436690 ) ) ;
#70990 = CARTESIAN_POINT ( 'NONE',  ( 9.474510206698729675, 16.51473224551082808, 57.08442372801900433 ) ) ;
#70992 = CARTESIAN_POINT ( 'NONE',  ( 0.05219959533910956823, 16.53943276465976808, 59.99890960531436690 ) ) ;
#70991 = CARTESIAN_POINT ( 'NONE',  ( -19.02544592524335343, -5.153800228976618492, 18.95942372801899367 ) ) ;
#70994 = AXIS2_PLACEMENT_3D ( 'NONE', #130305, #85822, #147510 ) ;
#70993 = CARTESIAN_POINT ( 'NONE',  ( -10.81492255796078084, -18.62759615963271287, 37.08224293864768129 ) ) ;
#70995 = ORIENTED_EDGE ( 'NONE', *, *, #140816, .T. ) ;
#70996 = CARTESIAN_POINT ( 'NONE',  ( 21.30000000000002913, 0.000000000000000000, -56.46919128290398504 ) ) ;
#70998 = CARTESIAN_POINT ( 'NONE',  ( 17.14385361876520264, -23.59649016807270883, 147.5750000027311728 ) ) ;
#70997 = CARTESIAN_POINT ( 'NONE',  ( 16.55341960407618274, -4.379528057220086978, 81.04275706135236135 ) ) ;
#70999 = CARTESIAN_POINT ( 'NONE',  ( -19.03943276465977164, -0.05219959533935918106, 88.75109039468567573 ) ) ;
#71000 = CARTESIAN_POINT ( 'NONE',  ( 14.29746914071049879, -8.314922557960816363, 48.33224293864770260 ) ) ;
#71001 = DIRECTION ( 'NONE',  ( 0.000000000000000000, 0.000000000000000000, 1.000000000000000000 ) ) ;
#71002 = CARTESIAN_POINT ( 'NONE',  ( -16.51473224551069308, -9.474510206698971260, 46.66557627198102409 ) ) ;
#71003 = CARTESIAN_POINT ( 'NONE',  ( -4.379528057220328563, 16.55341960407611168, 40.20724293864769550 ) ) ;
#71004 = CARTESIAN_POINT ( 'NONE',  ( 16.51473224551069308, 9.474510206698969483, 94.16557627198103830 ) ) ;
#71005 = CARTESIAN_POINT ( 'NONE',  ( 13.97604488694527802, 13.89961937509977652, 54.37390960531435979 ) ) ;
#71006 = CARTESIAN_POINT ( 'NONE',  ( -15.80617190586768217, 15.72974639402176855, 58.12609039468568994 ) ) ;
#71007 = CARTESIAN_POINT ( 'NONE',  ( -9.564922557960796823, -16.46253265017161027, 77.08224293864769550 ) ) ;
#71008 = CARTESIAN_POINT ( 'NONE',  ( -19.02544592524342804, 5.153800228976336051, 31.04057627198102409 ) ) ;
#71009 = CARTESIAN_POINT ( 'NONE',  ( 9.474510206698971260, -16.51473224551069308, 77.91557627198103830 ) ) ;
#71010 = CARTESIAN_POINT ( 'NONE',  ( 5.823673210054125526, 21.52544592524343514, 49.79057627198102409 ) ) ;
#71011 = CARTESIAN_POINT ( 'NONE',  ( -9.474510206698964154, 16.51473224551069663, 40.41557627198103120 ) ) ;
#71012 = CARTESIAN_POINT ( 'NONE',  ( -18.67979575497178146, -10.72451020669898902, 36.66557627198103120 ) ) ;
#71013 = CARTESIAN_POINT ( 'NONE',  ( 14.34966873604972726, -8.224510206698740333, 110.8344237280190043 ) ) ;
#71014 = CARTESIAN_POINT ( 'NONE',  ( -0.05219959533936034679, 19.03943276465977164, 22.50109039468566152 ) ) ;
#71016 = CARTESIAN_POINT ( 'NONE',  ( 16.53943276465976808, 0.05219959533934440121, 81.25109039468568994 ) ) ;
#71015 = CARTESIAN_POINT ( 'NONE',  ( -4.379528057220086978, -16.55341960407618274, 44.79275706135234714 ) ) ;
#71017 = DIRECTION ( 'NONE',  ( 0.000000000000000000, 0.7071067811865467956, -0.7071067811865483499 ) ) ;
#71018 = CARTESIAN_POINT ( 'NONE',  ( 14.34966873604972726, -8.224510206698740333, 70.83442372801901854 ) ) ;
#71019 = CARTESIAN_POINT ( 'NONE',  ( -18.67979575497178146, -10.72451020669898902, 31.66557627198102054 ) ) ;
#71020 = CARTESIAN_POINT ( 'NONE',  ( -19.02544592524342804, 5.153800228976336051, 31.04057627198102409 ) ) ;
#71021 = CARTESIAN_POINT ( 'NONE',  ( -14.29746914071037622, -8.314922557961029526, 44.16775706135234714 ) ) ;
#71022 = CARTESIAN_POINT ( 'NONE',  ( -19.05341960407611168, -5.049401038298163336, 46.45724293864768129 ) ) ;
#71023 = CARTESIAN_POINT ( 'NONE',  ( 15.80617190586769283, -15.72974639402175789, 45.62609039468567573 ) ) ;
#71024 = CARTESIAN_POINT ( 'NONE',  ( 16.55341960407618274, -4.379528057220086978, 41.04275706135236135 ) ) ;
#71025 = CARTESIAN_POINT ( 'NONE',  ( -0.05219959533934338120, 16.53943276465976808, 97.50109039468567573 ) ) ;
#71026 = DIRECTION ( 'NONE',  ( -1.000000000000000000, -4.336808689942018352E-17, 3.574525976782710181E-31 ) ) ;
#71027 = CARTESIAN_POINT ( 'NONE',  ( 21.55341960407619695, -5.719274019375665929, 96.04275706135236135 ) ) ;
#71028 = CARTESIAN_POINT ( 'NONE',  ( -19.05341960407617563, 5.049401038297882671, 93.54275706135234714 ) ) ;
#71029 = CARTESIAN_POINT ( 'NONE',  ( -13.89961937509957401, -13.97604488694547875, 49.37609039468567573 ) ) ;
#71030 = CARTESIAN_POINT ( 'NONE',  ( -14.29746914071049879, 8.314922557960819915, 75.83224293864769550 ) ) ;
#71031 = CARTESIAN_POINT ( 'NONE',  ( 13.97604488694527802, 13.89961937509977652, 24.37390960531435624 ) ) ;
#71033 = CARTESIAN_POINT ( 'NONE',  ( 16.18388926212238133, 7.379444403734545688, 77.93953151366154941 ) ) ;
#71032 = CARTESIAN_POINT ( 'NONE',  ( -0.05219959533936034679, 19.03943276465977164, 62.50109039468566863 ) ) ;
#71034 = CARTESIAN_POINT ( 'NONE',  ( -0.05219959533937732626, 21.53943276465977519, 57.50109039468568994 ) ) ;
#71035 = CARTESIAN_POINT ( 'NONE',  ( -8.224510206698735004, -14.34966873604973081, 29.58442372801901854 ) ) ;
#71036 = DIRECTION ( 'NONE',  ( 1.000000000000000000, 0.000000000000000000, 0.000000000000000000 ) ) ;
#71037 = CARTESIAN_POINT ( 'NONE',  ( 5.823673210054125526, 21.52544592524343514, 24.79057627198103120 ) ) ;
#71038 = CARTESIAN_POINT ( 'NONE',  ( 5.049401038297881783, 19.05341960407617563, 102.2927570613523045 ) ) ;
#71039 = CARTESIAN_POINT ( 'NONE',  ( -13.89961937509977652, 13.97604488694528158, 110.6239096053143243 ) ) ;
#71040 = CARTESIAN_POINT ( 'NONE',  ( -26.38458505201399618, 8.641005086744664609, 167.3773361139123494 ) ) ;
#71041 = CARTESIAN_POINT ( 'NONE',  ( -4.379528057220328563, 16.55341960407611168, 115.2072429386476955 ) ) ;
#71042 = CARTESIAN_POINT ( 'NONE',  ( 10.81492255796106328, -18.62759615963255655, 110.4177570613523756 ) ) ;
#71043 = CARTESIAN_POINT ( 'NONE',  ( 19.05341960407611168, 5.049401038298154454, 58.95724293864768129 ) ) ;
#71044 = CARTESIAN_POINT ( 'NONE',  ( -5.719274019375665041, -21.55341960407619695, 59.79275706135234714 ) ) ;
#71045 = CARTESIAN_POINT ( 'NONE',  ( 5.719274019375673035, 21.55341960407619339, 107.2927570613523471 ) ) ;
#71046 = CARTESIAN_POINT ( 'NONE',  ( -16.53943276465976808, -0.05219959533934237506, 98.75109039468568994 ) ) ;
#71047 = EDGE_CURVE ( 'NONE', #126834, #155489, #35741, .T. ) ;
#71048 = CARTESIAN_POINT ( 'NONE',  ( -16.46253265017160317, 9.564922557960807481, 80.83224293864769550 ) ) ;
#71049 = CARTESIAN_POINT ( 'NONE',  ( -21.52544592524334988, -5.823673210054445271, 53.95942372801900433 ) ) ;
#71050 = CARTESIAN_POINT ( 'NONE',  ( -18.67979575497193778, 10.72451020669871902, 58.33442372801901143 ) ) ;
#71052 = CARTESIAN_POINT ( 'NONE',  ( 19.03943276465977164, -0.05219959533909143690, 108.7489096053143527 ) ) ;
#71051 = CARTESIAN_POINT ( 'NONE',  ( 0.05219959533936267826, -19.03943276465977164, 75.00109039468566152 ) ) ;
#71053 = CARTESIAN_POINT ( 'NONE',  ( 16.51473224551069308, 9.474510206698969483, 24.16557627198102765 ) ) ;
#71054 = CARTESIAN_POINT ( 'NONE',  ( 21.55341960407610458, 5.719274019375980345, 93.95724293864770971 ) ) ;
#71055 = CARTESIAN_POINT ( 'NONE',  ( 5.049401038297881783, 19.05341960407617563, 27.29275706135232937 ) ) ;
#71056 = CARTESIAN_POINT ( 'NONE',  ( 8.314922557960818139, 14.29746914071049879, 99.58224293864770971 ) ) ;
#71057 = CARTESIAN_POINT ( 'NONE',  ( 0.05219959533909260263, 19.03943276465977164, 49.99890960531435979 ) ) ;
#71058 = CARTESIAN_POINT ( 'NONE',  ( -13.97604488694547697, 13.89961937509957934, 103.1260903946856473 ) ) ;
#71059 = CARTESIAN_POINT ( 'NONE',  ( -14.29746914071049879, 8.314922557960819915, 65.83224293864769550 ) ) ;
#71060 = CARTESIAN_POINT ( 'NONE',  ( -18.62759615963255300, -10.81492255796106328, 109.1677570613523613 ) ) ;
#71061 = CARTESIAN_POINT ( 'NONE',  ( 19.03943276465977164, -0.05219959533909143690, 98.74890960531436690 ) ) ;
#71062 = CARTESIAN_POINT ( 'NONE',  ( -13.89961937509957401, -13.97604488694547875, 74.37609039468566152 ) ) ;
#71063 = CARTESIAN_POINT ( 'NONE',  ( -0.05219959533907301413, -21.53943276465977519, 82.49890960531436690 ) ) ;
#71064 = CARTESIAN_POINT ( 'NONE',  ( 15.80617190586769283, -15.72974639402175789, 40.62609039468567573 ) ) ;
#71065 = CARTESIAN_POINT ( 'NONE',  ( -0.05219959533934338120, 16.53943276465976808, 42.50109039468567573 ) ) ;
#71066 = CARTESIAN_POINT ( 'NONE',  ( -12.14591786802326823, 12.06949235617739902, 98.12609039468570415 ) ) ;
#71068 = CARTESIAN_POINT ( 'NONE',  ( 15.72974639402176855, 15.80617190586768217, 31.87609039468567929 ) ) ;
#71067 = CARTESIAN_POINT ( 'NONE',  ( -4.483927247898782831, 16.52544592524335698, 37.70942372801900433 ) ) ;
#71069 = CARTESIAN_POINT ( 'NONE',  ( 21.55341960407610458, 5.719274019375980345, 43.95724293864769550 ) ) ;
#71070 = CARTESIAN_POINT ( 'NONE',  ( -13.97604488694527625, -13.89961937509977652, 31.87390960531435979 ) ) ;
#71071 = CARTESIAN_POINT ( 'NONE',  ( 11.74264578624800315, -36.14014761921581709, -9.149999994537626691 ) ) ;
#71072 = CARTESIAN_POINT ( 'NONE',  ( 16.55341960407618274, -4.379528057220086978, 56.04275706135235424 ) ) ;
#71073 = CARTESIAN_POINT ( 'NONE',  ( 15.80617190586746368, 15.72974639402197994, 89.37390960531435269 ) ) ;
#71074 = CARTESIAN_POINT ( 'NONE',  ( -16.55341960407611168, -4.379528057220339221, 36.45724293864768839 ) ) ;
#71075 = CARTESIAN_POINT ( 'NONE',  ( -8.224510206698735004, -14.34966873604973081, 44.58442372801901854 ) ) ;
#71076 = CARTESIAN_POINT ( 'NONE',  ( -19.05341960407611168, -5.049401038298163336, 56.45724293864768129 ) ) ;
#71077 = CARTESIAN_POINT ( 'NONE',  ( -9.474510206698720793, -16.51473224551083518, 89.58442372801900433 ) ) ;
#71078 = CARTESIAN_POINT ( 'NONE',  ( -5.719274019375978568, 21.55341960407610458, 85.20724293864770971 ) ) ;
#71079 = CARTESIAN_POINT ( 'NONE',  ( -16.52544592524342804, 4.483927247898546575, 36.04057627198102409 ) ) ;
#71080 = ORIENTED_EDGE ( 'NONE', *, *, #122412, .F. ) ;
#71081 = DIRECTION ( 'NONE',  ( 0.000000000000000000, 0.000000000000000000, -1.000000000000000000 ) ) ;
#71082 = CARTESIAN_POINT ( 'NONE',  ( 21.55341960407610458, 5.719274019375980345, 58.95724293864770971 ) ) ;
#71083 = CARTESIAN_POINT ( 'NONE',  ( -16.55341960407617563, 4.379528057220093196, 108.5427570613523756 ) ) ;
#71084 = VERTEX_POINT ( 'NONE', #156035 ) ;
#71085 = CARTESIAN_POINT ( 'NONE',  ( 19.39056639909673763, 5.500000000000049738, 88.28948781074345220 ) ) ;
#71086 = CARTESIAN_POINT ( 'NONE',  ( -0.05219959533907301413, -21.53943276465977519, 87.49890960531436690 ) ) ;
#71087 = CARTESIAN_POINT ( 'NONE',  ( -12.06949235617756955, 12.14591786802309770, 25.62390960531435624 ) ) ;
#71088 = CARTESIAN_POINT ( 'NONE',  ( -16.53943276465976808, -0.05219959533934237506, 38.75109039468567573 ) ) ;
#71089 = CARTESIAN_POINT ( 'NONE',  ( -19.03943276465977164, 0.05219959533909376836, 41.24890960531435269 ) ) ;
#71090 = CARTESIAN_POINT ( 'NONE',  ( 5.049401038298161559, -19.05341960407611168, 67.70724293864769550 ) ) ;
#71091 = CARTESIAN_POINT ( 'NONE',  ( -27.73933785331498925, -9.013057229001049109, 139.4750000027311785 ) ) ;
#71092 = CARTESIAN_POINT ( 'NONE',  ( 18.62759615963271287, -10.81492255796078972, 28.33224293864769550 ) ) ;
#71093 = CARTESIAN_POINT ( 'NONE',  ( 1.358751706670194404, 29.75846941761153985, -51.69462059227841877 ) ) ;
#71094 = CARTESIAN_POINT ( 'NONE',  ( 14.34966873604972726, -8.224510206698740333, 105.8344237280190328 ) ) ;
#71095 = CARTESIAN_POINT ( 'NONE',  ( -16.46253265017146816, -9.564922557961047289, 109.1677570613523471 ) ) ;
#71096 = CARTESIAN_POINT ( 'NONE',  ( 0.05219959533936267826, -19.03943276465977164, 40.00109039468566152 ) ) ;
#71097 = CARTESIAN_POINT ( 'NONE',  ( -15.80617190586745835, -15.72974639402198527, 86.87390960531438111 ) ) ;
#71098 = CARTESIAN_POINT ( 'NONE',  ( -0.05219959533910754901, -16.53943276465976808, 27.49890960531435269 ) ) ;
#71099 = CARTESIAN_POINT ( 'NONE',  ( -15.80617190586745835, -15.72974639402198527, 51.87390960531437401 ) ) ;
#71101 = CARTESIAN_POINT ( 'NONE',  ( -19.02544592524334988, -5.153800228976617603, 103.9594237280190043 ) ) ;
#71100 = CARTESIAN_POINT ( 'NONE',  ( -21.55341960407610458, -5.719274019375992779, 76.45724293864769550 ) ) ;
#71102 = CARTESIAN_POINT ( 'NONE',  ( 9.474510206698971260, -16.51473224551069308, 107.9155762719810383 ) ) ;
#71103 = CARTESIAN_POINT ( 'NONE',  ( -18.62759615963255300, -10.81492255796106328, 69.16775706135234714 ) ) ;
#71104 = CARTESIAN_POINT ( 'NONE',  ( 16.51473224551069308, 9.474510206698969483, 59.16557627198102409 ) ) ;
#71105 = AXIS2_PLACEMENT_3D ( 'NONE', #173564, #5679, #67355 ) ;
#71106 = CARTESIAN_POINT ( 'NONE',  ( -16.55341960407611168, -4.379528057220339221, 96.45724293864770971 ) ) ;
#71107 = CARTESIAN_POINT ( 'NONE',  ( 31.37700036491431632, 7.446261808816053041, 93.97872476790939800 ) ) ;
#71108 = CARTESIAN_POINT ( 'NONE',  ( -5.049401038298153566, 19.05341960407611168, 75.20724293864769550 ) ) ;
#71109 = CARTESIAN_POINT ( 'NONE',  ( -16.52544592524342804, 4.483927247898546575, 96.04057627198102409 ) ) ;
#71110 = ORIENTED_EDGE ( 'NONE', *, *, #80930, .T. ) ;
#71111 = CARTESIAN_POINT ( 'NONE',  ( -19.02544592524334988, -5.153800228976617603, 88.95942372801897591 ) ) ;
#71112 = CARTESIAN_POINT ( 'NONE',  ( 17.12812012977029852, -6.668231424565925991, 81.14051240676860743 ) ) ;
#71113 = CARTESIAN_POINT ( 'NONE',  ( 13.97604488694527802, 13.89961937509977652, 54.37390960531435979 ) ) ;
#71114 = CARTESIAN_POINT ( 'NONE',  ( 31.76083434626055535, -6.487688756757409969, 91.22915654580297939 ) ) ;
#71116 = CARTESIAN_POINT ( 'NONE',  ( 5.153800228976335163, 19.02544592524342804, 94.79057627198103830 ) ) ;
#71115 = CARTESIAN_POINT ( 'NONE',  ( 5.823673210054444382, -21.52544592524334988, 85.20942372801901854 ) ) ;
#71117 = CARTESIAN_POINT ( 'NONE',  ( -16.55341960407617563, 4.379528057220093196, 63.54275706135234003 ) ) ;
#71118 = DIRECTION ( 'NONE',  ( 1.000000000000000000, 0.000000000000000000, 0.000000000000000000 ) ) ;
#71119 = CARTESIAN_POINT ( 'NONE',  ( -19.05341960407617563, 5.049401038297882671, 43.54275706135232582 ) ) ;
#71120 = CARTESIAN_POINT ( 'NONE',  ( 21.55341960407619695, -5.719274019375665929, 101.0427570613523756 ) ) ;
#71121 = CARTESIAN_POINT ( 'NONE',  ( 36.95577132204471837, 5.312067825339672922, 43.56319566887929540 ) ) ;
#71122 = CARTESIAN_POINT ( 'NONE',  ( 23.48529157249600630, -32.32473071737748427, -7.049999994537626158 ) ) ;
#71123 = CARTESIAN_POINT ( 'NONE',  ( -8.314922557961024197, 14.29746914071037800, 97.91775706135236135 ) ) ;
#71124 = CARTESIAN_POINT ( 'NONE',  ( -34.36934878537049798, -7.254149193659903183, 46.92043707032850364 ) ) ;
#71125 = CARTESIAN_POINT ( 'NONE',  ( -16.52544592524335698, -4.483927247898792601, 98.95942372801903275 ) ) ;
#71126 = CARTESIAN_POINT ( 'NONE',  ( 32.61313261257514284, -23.16473864289021378, -21.41836715626212495 ) ) ;
#71127 = CARTESIAN_POINT ( 'NONE',  ( 8.224510206698742110, 14.34966873604972548, 62.08442372801901143 ) ) ;
#71128 = ORIENTED_EDGE ( 'NONE', *, *, #829, .F. ) ;
#71129 = CARTESIAN_POINT ( 'NONE',  ( -5.719274019375665041, -21.55341960407619695, 79.79275706135236135 ) ) ;
#71130 = CARTESIAN_POINT ( 'NONE',  ( -19.03943276465977164, -0.05219959533935918106, 93.75109039468566152 ) ) ;
#71131 = CARTESIAN_POINT ( 'NONE',  ( -5.153800228976607833, 19.02544592524334988, 32.70942372801899722 ) ) ;
#71132 = CARTESIAN_POINT ( 'NONE',  ( -5.153800228976328057, -19.02544592524343514, 72.29057627198102409 ) ) ;
#71133 = CARTESIAN_POINT ( 'NONE',  ( 0.05219959533909260263, 19.03943276465977164, 54.99890960531435979 ) ) ;
#71134 = CARTESIAN_POINT ( 'NONE',  ( 16.30887417027163622, -7.330987202194335417, 22.64566514850552181 ) ) ;
#71135 = CARTESIAN_POINT ( 'NONE',  ( 10.81492255796078972, 18.62759615963270932, 74.58224293864768129 ) ) ;
#71136 = CIRCLE ( 'NONE', #109943, 12.00000000000000000 ) ;
#71137 = CARTESIAN_POINT ( 'NONE',  ( 0.05219959533907565091, 21.53943276465977519, 39.99890960531436690 ) ) ;
#71138 = CARTESIAN_POINT ( 'NONE',  ( 9.564922557960805705, 16.46253265017160317, 29.58224293864769550 ) ) ;
#71139 = CARTESIAN_POINT ( 'NONE',  ( 16.52544592524335698, 4.483927247898782831, 66.45942372801903275 ) ) ;
#71140 = ORIENTED_EDGE ( 'NONE', *, *, #2746, .F. ) ;
#71141 = CARTESIAN_POINT ( 'NONE',  ( 18.67979575497194134, -10.72451020669871369, 25.83442372801901499 ) ) ;
#71143 = CARTESIAN_POINT ( 'NONE',  ( -11.74264578624800670, 36.14014761921585972, -2.400000000000000355 ) ) ;
#71142 = CARTESIAN_POINT ( 'NONE',  ( -4.379528057220328563, 16.55341960407611168, 65.20724293864768129 ) ) ;
#71144 = CARTESIAN_POINT ( 'NONE',  ( 12.06949235617739724, 12.14591786802326823, 26.87609039468567218 ) ) ;
#71145 = CARTESIAN_POINT ( 'NONE',  ( -19.02544592524334988, -5.153800228976617603, 53.95942372801898301 ) ) ;
#71146 = CARTESIAN_POINT ( 'NONE',  ( -12.14591786802309592, -12.06949235617757132, 51.87390960531437401 ) ) ;
#71148 = ADVANCED_FACE ( 'NONE', ( #170219 ), #64031, .T. ) ;
#71147 = CARTESIAN_POINT ( 'NONE',  ( 15.72974639402176855, 15.80617190586768217, 21.87609039468567573 ) ) ;
#71149 = CARTESIAN_POINT ( 'NONE',  ( 10.72451020669898902, -18.67979575497178502, 72.91557627198103830 ) ) ;
#71150 = CARTESIAN_POINT ( 'NONE',  ( -13.97604488694527625, -13.89961937509977652, 101.8739096053143811 ) ) ;
#71151 = CARTESIAN_POINT ( 'NONE',  ( -14.29746914071049879, 8.314922557960819915, 65.83224293864769550 ) ) ;
#71152 = CARTESIAN_POINT ( 'NONE',  ( -16.46253265017160317, 9.564922557960807481, 115.8322429386477097 ) ) ;
#71153 = LINE ( 'NONE', #27667, #47391 ) ;
#71154 = CARTESIAN_POINT ( 'NONE',  ( 19.02544592524334988, 5.153800228976608722, 66.45942372801899012 ) ) ;
#71155 = CARTESIAN_POINT ( 'NONE',  ( 21.55341960407610458, 5.719274019375980345, 113.9572429386477239 ) ) ;
#71156 = CARTESIAN_POINT ( 'NONE',  ( 19.03943276465977164, -0.05219959533909143690, 53.74890960531436690 ) ) ;
#71157 = CARTESIAN_POINT ( 'NONE',  ( -16.51473224551082808, 9.474510206698731452, 48.33442372801900433 ) ) ;
#71158 = CARTESIAN_POINT ( 'NONE',  ( 0.05219959533909260263, 19.03943276465977164, 34.99890960531435979 ) ) ;
#71159 = CARTESIAN_POINT ( 'NONE',  ( 18.67979575497194134, -10.72451020669871369, 65.83442372801900433 ) ) ;
#71160 = DIRECTION ( 'NONE',  ( -1.000000000000000000, 0.000000000000000000, 0.000000000000000000 ) ) ;
#71161 = EDGE_CURVE ( 'NONE', #33072, #97924, #44359, .T. ) ;
#71162 = CARTESIAN_POINT ( 'NONE',  ( -12.14591786802309592, -12.06949235617757132, 36.87390960531435979 ) ) ;
#71163 = CARTESIAN_POINT ( 'NONE',  ( 5.153800228976335163, 19.02544592524342804, 59.79057627198100988 ) ) ;
#71164 = CARTESIAN_POINT ( 'NONE',  ( -10.81492255796078084, -18.62759615963271287, 72.08224293864769550 ) ) ;
#71165 = CARTESIAN_POINT ( 'NONE',  ( -19.03943276465977164, 0.05219959533909376836, 61.24890960531436690 ) ) ;
#71166 = ORIENTED_EDGE ( 'NONE', *, *, #18906, .T. ) ;
#71167 = CARTESIAN_POINT ( 'NONE',  ( -21.52544592524343514, 5.823673210054127303, 66.04057627198103830 ) ) ;
#71168 = EDGE_LOOP ( 'NONE', ( #75864, #52922, #178029, #6159, #24356 ) ) ;
#71169 = CARTESIAN_POINT ( 'NONE',  ( -0.05219959533937732626, 21.53943276465977519, 102.5010903946856899 ) ) ;
#71172 = CARTESIAN_POINT ( 'NONE',  ( 4.483927247898545687, 16.52544592524342804, 79.79057627198102409 ) ) ;
#71171 = CARTESIAN_POINT ( 'NONE',  ( 14.29746914071037800, 8.314922557961029526, 101.6677570613523613 ) ) ;
#71170 = CARTESIAN_POINT ( 'NONE',  ( -9.248023074035629065, -10.74802307403544077, -60.25555373585994090 ) ) ;
#71173 = CARTESIAN_POINT ( 'NONE',  ( -5.049401038297874678, -19.05341960407617918, 89.79275706135230450 ) ) ;
#71174 = ORIENTED_EDGE ( 'NONE', *, *, #113718, .T. ) ;
#71175 = CARTESIAN_POINT ( 'NONE',  ( 0.05219959533936267826, -19.03943276465977164, 45.00109039468566863 ) ) ;
#71176 = CARTESIAN_POINT ( 'NONE',  ( 16.53943276465976808, 0.05219959533934440121, 106.2510903946856757 ) ) ;
#71177 = CARTESIAN_POINT ( 'NONE',  ( 16.46253265017146816, 9.564922557961045513, 31.66775706135232937 ) ) ;
#71178 = CARTESIAN_POINT ( 'NONE',  ( 5.153800228976335163, 19.02544592524342804, 94.79057627198103830 ) ) ;
#71179 = CARTESIAN_POINT ( 'NONE',  ( 21.52544592524344225, -5.823673210054117533, 63.54057627198103830 ) ) ;
#71180 = DIRECTION ( 'NONE',  ( -0.5000000000000051070, 0.000000000000000000, 0.8660254037844355990 ) ) ;
#71181 = CARTESIAN_POINT ( 'NONE',  ( -13.97604488694527625, -13.89961937509977652, 21.87390960531435979 ) ) ;
#71182 = CARTESIAN_POINT ( 'NONE',  ( 18.62759615963255655, 10.81492255796105972, 91.66775706135234714 ) ) ;
#71183 = CARTESIAN_POINT ( 'NONE',  ( 14.34966873604972726, -8.224510206698740333, 70.83442372801901854 ) ) ;
#71184 = CARTESIAN_POINT ( 'NONE',  ( -5.719274019375665041, -21.55341960407619695, 29.79275706135234358 ) ) ;
#71185 = CARTESIAN_POINT ( 'NONE',  ( 14.29746914071037800, 8.314922557961029526, 36.66775706135234714 ) ) ;
#71186 = CARTESIAN_POINT ( 'NONE',  ( -9.474510206698964154, 16.51473224551069663, 110.4155762719810383 ) ) ;
#71187 = CARTESIAN_POINT ( 'NONE',  ( 13.97604488694527802, 13.89961937509977652, 34.37390960531436690 ) ) ;
#71188 = CARTESIAN_POINT ( 'NONE',  ( 9.474510206698971260, -16.51473224551069308, 47.91557627198102409 ) ) ;
#71189 = CARTESIAN_POINT ( 'NONE',  ( 12.06949235617739724, 12.14591786802326823, 51.87609039468568284 ) ) ;
#71190 = CARTESIAN_POINT ( 'NONE',  ( -12.14591786802309592, -12.06949235617757132, 91.87390960531436690 ) ) ;
#71191 = CARTESIAN_POINT ( 'NONE',  ( 4.379528057220092307, 16.55341960407617563, 97.29275706135234714 ) ) ;
#71194 = CARTESIAN_POINT ( 'NONE',  ( -5.153800228976328057, -19.02544592524343514, 62.29057627198100988 ) ) ;
#71193 = CARTESIAN_POINT ( 'NONE',  ( 9.564922557960805705, 16.46253265017160317, 84.58224293864769550 ) ) ;
#71192 = CARTESIAN_POINT ( 'NONE',  ( 21.53943276465977519, 0.05219959533937863772, 41.25109039468568284 ) ) ;
#71195 = CARTESIAN_POINT ( 'NONE',  ( -16.51473224551069308, -9.474510206698971260, 81.66557627198103830 ) ) ;
#71196 = CARTESIAN_POINT ( 'NONE',  ( 8.314922557960818139, 14.29746914071049879, 34.58224293864770260 ) ) ;
#71197 = CARTESIAN_POINT ( 'NONE',  ( -16.55341960407617563, 4.379528057220093196, 103.5427570613523613 ) ) ;
#71198 = EDGE_CURVE ( 'NONE', #193343, #40990, #43907, .T. ) ;
#71199 = ORIENTED_EDGE ( 'NONE', *, *, #186126, .T. ) ;
#71200 = CARTESIAN_POINT ( 'NONE',  ( -13.89961937509957401, -13.97604488694547875, 39.37609039468566152 ) ) ;
#71201 = CARTESIAN_POINT ( 'NONE',  ( 5.049401038298161559, -19.05341960407611168, 112.7072429386476813 ) ) ;
#71202 = CARTESIAN_POINT ( 'NONE',  ( -9.564922557960796823, -16.46253265017161027, 57.08224293864769550 ) ) ;
#71203 = CARTESIAN_POINT ( 'NONE',  ( 5.049401038297881783, 19.05341960407617563, 37.29275706135232582 ) ) ;
#71204 = CARTESIAN_POINT ( 'NONE',  ( -22.81625015709509441, -31.40387420917324590, -4.324999997268812457 ) ) ;
#71205 = CARTESIAN_POINT ( 'NONE',  ( 8.314922557961029526, -14.29746914071037800, 40.41775706135234714 ) ) ;
#71207 = CARTESIAN_POINT ( 'NONE',  ( 8.314922557961029526, -14.29746914071037800, 55.41775706135234714 ) ) ;
#71206 = CARTESIAN_POINT ( 'NONE',  ( -5.153800228976607833, 19.02544592524334988, 77.70942372801900433 ) ) ;
#71208 = CARTESIAN_POINT ( 'NONE',  ( -16.46253265017160317, 9.564922557960807481, 115.8322429386477097 ) ) ;
#71209 = CARTESIAN_POINT ( 'NONE',  ( -9.474510206698964154, 16.51473224551069663, 90.41557627198103830 ) ) ;
#71210 = CARTESIAN_POINT ( 'NONE',  ( -15.80617190586745835, -15.72974639402198527, 106.8739096053143811 ) ) ;
#71211 = CARTESIAN_POINT ( 'NONE',  ( -19.05341960407617563, 5.049401038297882671, 83.54275706135233293 ) ) ;
#71213 = CARTESIAN_POINT ( 'NONE',  ( 19.02544592524343514, -5.153800228976328945, 38.54057627198103120 ) ) ;
#71212 = CARTESIAN_POINT ( 'NONE',  ( 19.05341960407611168, 5.049401038298154454, 103.9572429386476671 ) ) ;
#71214 = CARTESIAN_POINT ( 'NONE',  ( -9.474510206698964154, 16.51473224551069663, 70.41557627198102409 ) ) ;
#71216 = CARTESIAN_POINT ( 'NONE',  ( -0.05219959533909027116, -19.03943276465977164, 42.49890960531435269 ) ) ;
#71215 = CARTESIAN_POINT ( 'NONE',  ( 14.29746914071049879, -8.314922557960816363, 38.33224293864768839 ) ) ;
#71217 = CARTESIAN_POINT ( 'NONE',  ( 5.153800228976615827, -19.02544592524334988, 50.20942372801897591 ) ) ;
#71218 = CARTESIAN_POINT ( 'NONE',  ( 4.483927247898545687, 16.52544592524342804, 89.79057627198103830 ) ) ;
#71219 = CARTESIAN_POINT ( 'NONE',  ( -18.67979575497193778, 10.72451020669871902, 108.3344237280190185 ) ) ;
#71220 = CARTESIAN_POINT ( 'NONE',  ( -5.153800228976328057, -19.02544592524343514, 47.29057627198102409 ) ) ;
#71221 = CARTESIAN_POINT ( 'NONE',  ( 21.52544592524344225, -5.823673210054117533, 53.54057627198103120 ) ) ;
#71223 = CARTESIAN_POINT ( 'NONE',  ( -5.719274019375665041, -21.55341960407619695, 99.79275706135234714 ) ) ;
#71222 = CARTESIAN_POINT ( 'NONE',  ( -8.314922557960811034, -14.29746914071050412, 52.08224293864768839 ) ) ;
#71224 = CARTESIAN_POINT ( 'NONE',  ( 13.89961937509977652, -13.97604488694527269, 113.1239096053143527 ) ) ;
#71225 = CARTESIAN_POINT ( 'NONE',  ( -16.51473224551069308, -9.474510206698971260, 101.6655762719810241 ) ) ;
#71226 = CARTESIAN_POINT ( 'NONE',  ( 13.97604488694527802, 13.89961937509977652, 34.37390960531436690 ) ) ;
#71227 = CARTESIAN_POINT ( 'NONE',  ( -19.03943276465977164, 0.05219959533909376836, 26.24890960531435624 ) ) ;
#71228 = CARTESIAN_POINT ( 'NONE',  ( 16.55341960407611168, 4.379528057220329451, 88.95724293864769550 ) ) ;
#71229 = CARTESIAN_POINT ( 'NONE',  ( 15.72974639402199770, -15.80617190586745480, 98.12390960531436690 ) ) ;
#71230 = CARTESIAN_POINT ( 'NONE',  ( 5.153800228976335163, 19.02544592524342804, 104.7905762719809957 ) ) ;
#71231 = CARTESIAN_POINT ( 'NONE',  ( -18.67979575497178146, -10.72451020669898902, 111.6655762719810525 ) ) ;
#71232 = CARTESIAN_POINT ( 'NONE',  ( -13.89961937509977652, 13.97604488694528158, 85.62390960531433848 ) ) ;
#71234 = CARTESIAN_POINT ( 'NONE',  ( 14.29746914071049879, -8.314922557960816363, 98.33224293864769550 ) ) ;
#71233 = DIRECTION ( 'NONE',  ( 0.000000000000000000, 0.000000000000000000, 1.000000000000000000 ) ) ;
#71235 = CARTESIAN_POINT ( 'NONE',  ( -19.05341960407611168, -5.049401038298163336, 71.45724293864766707 ) ) ;
#71236 = CARTESIAN_POINT ( 'NONE',  ( -15.72974639402197994, 15.80617190586746368, 75.62390960531439532 ) ) ;
#71237 = CARTESIAN_POINT ( 'NONE',  ( -31.72709406046302760, 0.4964181571218586053, 102.5000000000000284 ) ) ;
#71238 = CARTESIAN_POINT ( 'NONE',  ( 0.000000000000000000, -105.0000000000000000, 12.00000000000000355 ) ) ;
#71240 = CARTESIAN_POINT ( 'NONE',  ( 18.56453257813360835, -5.500000000000033751, 68.49000423690685579 ) ) ;
#71239 = CARTESIAN_POINT ( 'NONE',  ( 10.72451020669898902, -18.67979575497178502, 27.91557627198103830 ) ) ;
#71241 = CARTESIAN_POINT ( 'NONE',  ( -8.314922557961024197, 14.29746914071037800, 37.91775706135235424 ) ) ;
#71242 = CARTESIAN_POINT ( 'NONE',  ( 12.14591786802309770, 12.06949235617756955, 89.37390960531435269 ) ) ;
#71243 = DIRECTION ( 'NONE',  ( 1.000000000000000000, 0.000000000000000000, 0.000000000000000000 ) ) ;
#71244 = CARTESIAN_POINT ( 'NONE',  ( 9.564922557960805705, 16.46253265017160317, 94.58224293864769550 ) ) ;
#71245 = CARTESIAN_POINT ( 'NONE',  ( -5.049401038298153566, 19.05341960407611168, 45.20724293864769550 ) ) ;
#71246 = CARTESIAN_POINT ( 'NONE',  ( -8.314922557960811034, -14.29746914071050412, 82.08224293864768129 ) ) ;
#71247 = CARTESIAN_POINT ( 'NONE',  ( 21.53943276465977519, -0.05219959533907433946, 38.74890960531435979 ) ) ;
#71248 = CARTESIAN_POINT ( 'NONE',  ( 12.14591786802309770, 12.06949235617756955, 54.37390960531435979 ) ) ;
#71249 = CARTESIAN_POINT ( 'NONE',  ( 19.05341960407617918, -5.049401038297876454, 111.0427570613523329 ) ) ;
#71250 = CARTESIAN_POINT ( 'NONE',  ( -10.72451020669870658, -18.67979575497194134, 79.58442372801903275 ) ) ;
#71251 = CARTESIAN_POINT ( 'NONE',  ( 17.14385361876520264, -23.59649016807270883, 145.5750000027311728 ) ) ;
#71252 = CARTESIAN_POINT ( 'NONE',  ( -15.80617190586745835, -15.72974639402198527, 21.87390960531436690 ) ) ;
#71253 = CARTESIAN_POINT ( 'NONE',  ( -14.29746914071037622, -8.314922557961029526, 89.16775706135236135 ) ) ;
#71254 = CARTESIAN_POINT ( 'NONE',  ( -19.05341960407611168, -5.049401038298163336, 26.45724293864769550 ) ) ;
#71255 = CARTESIAN_POINT ( 'NONE',  ( -5.049401038298153566, 19.05341960407611168, 80.20724293864769550 ) ) ;
#71256 = CARTESIAN_POINT ( 'NONE',  ( -21.55341960407610458, -5.719274019375992779, 96.45724293864770971 ) ) ;
#71257 = CARTESIAN_POINT ( 'NONE',  ( 8.314922557961029526, -14.29746914071037800, 25.41775706135235779 ) ) ;
#71259 = CARTESIAN_POINT ( 'NONE',  ( -18.62759615963255300, -10.81492255796106328, 74.16775706135231871 ) ) ;
#71258 = CARTESIAN_POINT ( 'NONE',  ( -16.55341960407611168, -4.379528057220339221, 46.45724293864769550 ) ) ;
#71261 = CARTESIAN_POINT ( 'NONE',  ( 10.72451020669898902, -18.67979575497178502, 22.91557627198102765 ) ) ;
#71260 = CARTESIAN_POINT ( 'NONE',  ( 8.224510206698742110, 14.34966873604972548, 92.08442372801901854 ) ) ;
#71262 = CARTESIAN_POINT ( 'NONE',  ( 26.26106931734003425, 9.140213825779245127, 167.1341548181404164 ) ) ;
#71263 = DIRECTION ( 'NONE',  ( -6.982962677686266711E-15, 0.000000000000000000, 1.000000000000000000 ) ) ;
#71264 = CARTESIAN_POINT ( 'NONE',  ( -4.379528057220086978, -16.55341960407618274, 109.7927570613523613 ) ) ;
#71265 = CARTESIAN_POINT ( 'NONE',  ( -16.52544592524335698, -4.483927247898792601, 63.95942372801901854 ) ) ;
#71266 = CARTESIAN_POINT ( 'NONE',  ( -5.049401038298153566, 19.05341960407611168, 70.20724293864769550 ) ) ;
#71267 = CARTESIAN_POINT ( 'NONE',  ( -19.03943276465977164, 0.05219959533909376836, 91.24890960531436690 ) ) ;
#71268 = CARTESIAN_POINT ( 'NONE',  ( 18.67979575497194134, -10.72451020669871369, 65.83442372801900433 ) ) ;
#71269 = CARTESIAN_POINT ( 'NONE',  ( -16.55341960407617563, 4.379528057220093196, 78.54275706135236135 ) ) ;
#71270 = CARTESIAN_POINT ( 'NONE',  ( -8.314922557960811034, -14.29746914071050412, 42.08224293864769550 ) ) ;
#71271 = CARTESIAN_POINT ( 'NONE',  ( 19.03943276465977164, -0.05219959533909143690, 58.74890960531435979 ) ) ;
#71272 = CARTESIAN_POINT ( 'NONE',  ( 16.51473224551069308, 9.474510206698969483, 44.16557627198103120 ) ) ;
#71273 = ORIENTED_EDGE ( 'NONE', *, *, #55067, .T. ) ;
#71274 = CARTESIAN_POINT ( 'NONE',  ( -16.51473224551082808, 9.474510206698731452, 108.3344237280190043 ) ) ;
#71275 = CARTESIAN_POINT ( 'NONE',  ( -16.52544592524342804, 4.483927247898546575, 116.0405762719810383 ) ) ;
#71276 = CARTESIAN_POINT ( 'NONE',  ( 9.564922557960805705, 16.46253265017160317, 69.58224293864770971 ) ) ;
#71278 = CARTESIAN_POINT ( 'NONE',  ( 3.766062262543149401E-15, -39.95556452105413570, -3.499999999999999556 ) ) ;
#71277 = CARTESIAN_POINT ( 'NONE',  ( 16.46253265017146816, 9.564922557961045513, 101.6677570613523329 ) ) ;
#71279 = CARTESIAN_POINT ( 'NONE',  ( -0.05219959533937732626, 21.53943276465977519, 97.50109039468567573 ) ) ;
#71280 = CARTESIAN_POINT ( 'NONE',  ( 8.314922557961029526, -14.29746914071037800, 70.41775706135236135 ) ) ;
#71281 = CARTESIAN_POINT ( 'NONE',  ( 13.97604488694548053, -13.89961937509957401, 95.62609039468563310 ) ) ;
#71282 = CARTESIAN_POINT ( 'NONE',  ( 21.52544592524344225, -5.823673210054117533, 63.54057627198103830 ) ) ;
#71283 = CARTESIAN_POINT ( 'NONE',  ( 12.06949235617739724, 12.14591786802326823, 51.87609039468568284 ) ) ;
#71284 = DIRECTION ( 'NONE',  ( 0.000000000000000000, -0.6427876096865287048, -0.7660444431189871173 ) ) ;
#71285 = CARTESIAN_POINT ( 'NONE',  ( 19.05341960407617918, -5.049401038297876454, 56.04275706135234714 ) ) ;
#71286 = CARTESIAN_POINT ( 'NONE',  ( 18.67979575497194134, -10.72451020669871369, 90.83442372801901854 ) ) ;
#71287 = CARTESIAN_POINT ( 'NONE',  ( -5.049401038298153566, 19.05341960407611168, 25.20724293864768484 ) ) ;
#71288 = CARTESIAN_POINT ( 'NONE',  ( 9.564922557960805705, 16.46253265017160317, 64.58224293864769550 ) ) ;
#71289 = CARTESIAN_POINT ( 'NONE',  ( 12.14591786802309770, 12.06949235617756955, 64.37390960531435269 ) ) ;
#71290 = VECTOR ( 'NONE', #104096, 1000.000000000000000 ) ;
#71291 = ADVANCED_FACE ( 'NONE', ( #183999 ), #15143, .F. ) ;
#71292 = CARTESIAN_POINT ( 'NONE',  ( -15.80617190586768217, 15.72974639402176855, 93.12609039468568994 ) ) ;
#71293 = CARTESIAN_POINT ( 'NONE',  ( -16.51473224551082808, 9.474510206698731452, 43.33442372801900433 ) ) ;
#71294 = CARTESIAN_POINT ( 'NONE',  ( -9.474510206698720793, -16.51473224551083518, 24.58442372801900078 ) ) ;
#71295 = CARTESIAN_POINT ( 'NONE',  ( 5.823673210054125526, 21.52544592524343514, 24.79057627198103120 ) ) ;
#71296 = CARTESIAN_POINT ( 'NONE',  ( -15.80617190586768217, 15.72974639402176855, 103.1260903946856757 ) ) ;
#71297 = CARTESIAN_POINT ( 'NONE',  ( -19.03943276465977164, 0.05219959533909376836, 76.24890960531435269 ) ) ;
#71298 = CARTESIAN_POINT ( 'NONE',  ( 21.55341960407619695, -5.719274019375665929, 91.04275706135236135 ) ) ;
#71299 = CARTESIAN_POINT ( 'NONE',  ( 15.72974639402199770, -15.80617190586745480, 53.12390960531436690 ) ) ;
#71300 = CARTESIAN_POINT ( 'NONE',  ( 5.049401038298161559, -19.05341960407611168, 77.70724293864765286 ) ) ;
#71301 = CARTESIAN_POINT ( 'NONE',  ( 16.46253265017146816, 9.564922557961045513, 81.66775706135233293 ) ) ;
#71302 = CARTESIAN_POINT ( 'NONE',  ( -19.05341960407611168, -5.049401038298163336, 41.45724293864769550 ) ) ;
#71303 = CARTESIAN_POINT ( 'NONE',  ( 19.03943276465977164, -0.05219959533909143690, 83.74890960531436690 ) ) ;
#71304 = CARTESIAN_POINT ( 'NONE',  ( -5.153800228976607833, 19.02544592524334988, 87.70942372801897591 ) ) ;
#71305 = CARTESIAN_POINT ( 'NONE',  ( -16.55341960407617563, 4.379528057220093196, 48.54275706135234714 ) ) ;
#71306 = CARTESIAN_POINT ( 'NONE',  ( 16.53943276465976808, -0.05219959533910856209, 103.7489096053143669 ) ) ;
#71307 = CARTESIAN_POINT ( 'NONE',  ( 19.03943276465977164, -0.05219959533909143690, 68.74890960531436690 ) ) ;
#71308 = CARTESIAN_POINT ( 'NONE',  ( 5.823673210054125526, 21.52544592524343514, 44.79057627198103120 ) ) ;
#71309 = CARTESIAN_POINT ( 'NONE',  ( -5.153800228976607833, 19.02544592524334988, 112.7094237280190043 ) ) ;
#71310 = CARTESIAN_POINT ( 'NONE',  ( -21.53943276465977519, -0.05219959533937600094, 33.75109039468568284 ) ) ;
#71311 = CARTESIAN_POINT ( 'NONE',  ( 15.80617190586769283, -15.72974639402175789, 90.62609039468567573 ) ) ;
#71312 = CARTESIAN_POINT ( 'NONE',  ( -14.29746914071037622, -8.314922557961029526, 89.16775706135236135 ) ) ;
#71313 = CARTESIAN_POINT ( 'NONE',  ( 16.46253265017160672, -9.564922557960803928, 73.33224293864769550 ) ) ;
#71314 = CARTESIAN_POINT ( 'NONE',  ( 12.06949235617739724, 12.14591786802326823, 101.8760903946857042 ) ) ;
#71315 = CARTESIAN_POINT ( 'NONE',  ( 5.049401038297881783, 19.05341960407617563, 52.29275706135234003 ) ) ;
#71316 = CARTESIAN_POINT ( 'NONE',  ( -5.823673210054431948, 21.52544592524334988, 32.70942372801900433 ) ) ;
#71317 = CARTESIAN_POINT ( 'NONE',  ( 14.29746914071049879, -8.314922557960816363, 78.33224293864770971 ) ) ;
#71318 = CARTESIAN_POINT ( 'NONE',  ( -16.51473224551069308, -9.474510206698971260, 96.66557627198102409 ) ) ;
#71319 = CARTESIAN_POINT ( 'NONE',  ( 4.483927247898790824, -16.52544592524335698, 105.2094237280190328 ) ) ;
#71320 = CARTESIAN_POINT ( 'NONE',  ( -21.55341960407619339, 5.719274019375674811, 78.54275706135236135 ) ) ;
#71321 = CARTESIAN_POINT ( 'NONE',  ( 16.52544592524335698, 4.483927247898782831, 36.45942372801901143 ) ) ;
#71322 = CARTESIAN_POINT ( 'NONE',  ( 21.53943276465977519, 0.05219959533937863772, 31.25109039468568639 ) ) ;
#71323 = CARTESIAN_POINT ( 'NONE',  ( 8.224510206698953496, -14.34966873604960469, 72.91557627198103830 ) ) ;
#71324 = EDGE_CURVE ( 'NONE', #88586, #4577, #27098, .T. ) ;
#71325 = ORIENTED_EDGE ( 'NONE', *, *, #104490, .T. ) ;
#71326 = CARTESIAN_POINT ( 'NONE',  ( 18.62759615963271287, -10.81492255796078972, 103.3322429386476955 ) ) ;
#71327 = CARTESIAN_POINT ( 'NONE',  ( -12.14591786802309592, -12.06949235617757132, 56.87390960531436690 ) ) ;
#71328 = CARTESIAN_POINT ( 'NONE',  ( 13.97604488694527802, 13.89961937509977652, 24.37390960531435624 ) ) ;
#71329 = CARTESIAN_POINT ( 'NONE',  ( 0.05219959533907565091, 21.53943276465977519, 24.99890960531435624 ) ) ;
#71330 = CARTESIAN_POINT ( 'NONE',  ( 5.719274019375673035, 21.55341960407619339, 52.29275706135236135 ) ) ;
#71331 = CARTESIAN_POINT ( 'NONE',  ( 8.314922557960818139, 14.29746914071049879, 59.58224293864770260 ) ) ;
#71332 = CARTESIAN_POINT ( 'NONE',  ( 21.55341960407610458, 5.719274019375980345, 83.95724293864770971 ) ) ;
#71333 = CARTESIAN_POINT ( 'NONE',  ( -13.89961937509977652, 13.97604488694528158, 70.62390960531432427 ) ) ;
#71335 = CARTESIAN_POINT ( 'NONE',  ( -13.89961937509957401, -13.97604488694547875, 79.37609039468567573 ) ) ;
#71334 = CARTESIAN_POINT ( 'NONE',  ( -19.05341960407611168, -5.049401038298163336, 31.45724293864769550 ) ) ;
#71337 = CARTESIAN_POINT ( 'NONE',  ( 10.72451020669898902, -18.67979575497178502, 62.91557627198102409 ) ) ;
#71336 = CARTESIAN_POINT ( 'NONE',  ( -21.53943276465977519, -0.05219959533937600094, 53.75109039468568994 ) ) ;
#71338 = CARTESIAN_POINT ( 'NONE',  ( 19.03943276465977164, -0.05219959533909143690, 38.74890960531436690 ) ) ;
#71339 = CARTESIAN_POINT ( 'NONE',  ( -0.05219959533909027116, -19.03943276465977164, 72.49890960531435269 ) ) ;
#71340 = EDGE_LOOP ( 'NONE', ( #74505, #92312, #182159, #176265 ) ) ;
#71341 = CARTESIAN_POINT ( 'NONE',  ( 8.314922557961029526, -14.29746914071037800, 45.41775706135234003 ) ) ;
#71342 = CARTESIAN_POINT ( 'NONE',  ( 0.05219959533937995610, -21.53943276465977519, 35.00109039468568284 ) ) ;
#71343 = CARTESIAN_POINT ( 'NONE',  ( 15.80617190586769283, -15.72974639402175789, 65.62609039468568994 ) ) ;
#71344 = CARTESIAN_POINT ( 'NONE',  ( 9.564922557960805705, 16.46253265017160317, 99.58224293864770971 ) ) ;
#71345 = CARTESIAN_POINT ( 'NONE',  ( 21.55341960407610458, 5.719274019375980345, 83.95724293864770971 ) ) ;
#71347 = CARTESIAN_POINT ( 'NONE',  ( 8.224510206698742110, 14.34966873604972548, 47.08442372801901854 ) ) ;
#71346 = CARTESIAN_POINT ( 'NONE',  ( 21.53943276465977519, 0.05219959533937863772, 26.25109039468567573 ) ) ;
#71348 = CARTESIAN_POINT ( 'NONE',  ( -5.719274019375978568, 21.55341960407610458, 50.20724293864769550 ) ) ;
#71349 = CARTESIAN_POINT ( 'NONE',  ( -9.474510206698720793, -16.51473224551083518, 24.58442372801900078 ) ) ;
#71350 = CARTESIAN_POINT ( 'NONE',  ( 16.46253265017160672, -9.564922557960803928, 53.33224293864768839 ) ) ;
#71351 = CARTESIAN_POINT ( 'NONE',  ( -5.153800228976328057, -19.02544592524343514, 112.2905762719810099 ) ) ;
#71352 = CARTESIAN_POINT ( 'NONE',  ( -5.153800228976328057, -19.02544592524343514, 92.29057627198099567 ) ) ;
#71353 = CARTESIAN_POINT ( 'NONE',  ( 7.500000000000000000, 9.184850993605147944E-16, 10.00000000000000000 ) ) ;
#71354 = CARTESIAN_POINT ( 'NONE',  ( -16.46253265017146816, -9.564922557961047289, 74.16775706135234714 ) ) ;
#71355 = CARTESIAN_POINT ( 'NONE',  ( 18.67979575497178502, 10.72451020669898547, 49.16557627198102409 ) ) ;
#71356 = CARTESIAN_POINT ( 'NONE',  ( 16.52544592524342804, -4.483927247898539470, 28.54057627198103120 ) ) ;
#71357 = CARTESIAN_POINT ( 'NONE',  ( -9.474510206698720793, -16.51473224551083518, 79.58442372801899012 ) ) ;
#71358 = CARTESIAN_POINT ( 'NONE',  ( -14.98843538525856722, -15.13431349328839914, -58.85720012050613548 ) ) ;
#71359 = CARTESIAN_POINT ( 'NONE',  ( -9.564922557961040184, 16.46253265017147172, 22.91775706135233648 ) ) ;
#71360 = CARTESIAN_POINT ( 'NONE',  ( -9.474510206698720793, -16.51473224551083518, 84.58442372801900433 ) ) ;
#71361 = CARTESIAN_POINT ( 'NONE',  ( 16.51473224551083163, -9.474510206698727899, 45.83442372801900433 ) ) ;
#71362 = CARTESIAN_POINT ( 'NONE',  ( 16.88567814943159817, 6.947325034625697171, 108.7900112265258912 ) ) ;
#71363 = CARTESIAN_POINT ( 'NONE',  ( 16.46253265017160672, -9.564922557960803928, 58.33224293864769550 ) ) ;
#71364 = CARTESIAN_POINT ( 'NONE',  ( -4.379528057220328563, 16.55341960407611168, 50.20724293864769550 ) ) ;
#71365 = CARTESIAN_POINT ( 'NONE',  ( 19.03943276465977164, -0.05219959533909143690, 28.74890960531435624 ) ) ;
#71366 = CARTESIAN_POINT ( 'NONE',  ( -4.483927247898539470, -16.52544592524342804, 42.29057627198103120 ) ) ;
#71367 = CARTESIAN_POINT ( 'NONE',  ( -27.81822689058051878, -28.32190533958856449, -20.09416750255129713 ) ) ;
#71368 = CARTESIAN_POINT ( 'NONE',  ( 14.29746914071037800, 8.314922557961029526, 111.6677570613523613 ) ) ;
#71369 = CARTESIAN_POINT ( 'NONE',  ( -5.049401038298153566, 19.05341960407611168, 45.20724293864769550 ) ) ;
#71370 = CARTESIAN_POINT ( 'NONE',  ( -16.46253265017146816, -9.564922557961047289, 19.16775706135233293 ) ) ;
#71371 = CARTESIAN_POINT ( 'NONE',  ( -16.55341960407617563, 4.379528057220093196, 38.54275706135234714 ) ) ;
#71372 = CARTESIAN_POINT ( 'NONE',  ( 18.62759615963271287, -10.81492255796078972, 33.33224293864769550 ) ) ;
#71374 = ORIENTED_EDGE ( 'NONE', *, *, #121851, .F. ) ;
#71373 = CARTESIAN_POINT ( 'NONE',  ( 5.823673210054444382, -21.52544592524334988, 90.20942372801903275 ) ) ;
#71375 = CARTESIAN_POINT ( 'NONE',  ( 16.46253265017160672, -9.564922557960803928, 63.33224293864769550 ) ) ;
#71376 = CARTESIAN_POINT ( 'NONE',  ( -5.049401038298153566, 19.05341960407611168, 105.2072429386476671 ) ) ;
#71377 = CARTESIAN_POINT ( 'NONE',  ( 16.46253265017160672, -9.564922557960803928, 93.33224293864769550 ) ) ;
#71378 = CARTESIAN_POINT ( 'NONE',  ( 29.86685920354754487, 21.69954338932564752, -3.424999997268813434 ) ) ;
#71379 = CARTESIAN_POINT ( 'NONE',  ( 0.05219959533937995610, -21.53943276465977519, 30.00109039468568284 ) ) ;
#71380 = CARTESIAN_POINT ( 'NONE',  ( 16.52544592524342804, -4.483927247898539470, 83.54057627198102409 ) ) ;
#71382 = CARTESIAN_POINT ( 'NONE',  ( -19.05341960407611168, -5.049401038298163336, 71.45724293864766707 ) ) ;
#71381 = CARTESIAN_POINT ( 'NONE',  ( -0.05219959533907301413, -21.53943276465977519, 77.49890960531433848 ) ) ;
#71383 = CARTESIAN_POINT ( 'NONE',  ( -16.46253265017160317, 9.564922557960807481, 70.83224293864770971 ) ) ;
#71384 = CARTESIAN_POINT ( 'NONE',  ( -18.62759615963270932, 10.81492255796079327, 115.8322429386477097 ) ) ;
#71385 = ORIENTED_EDGE ( 'NONE', *, *, #193069, .F. ) ;
#71386 = CARTESIAN_POINT ( 'NONE',  ( -19.03943276465977164, 0.05219959533909376836, 71.24890960531435269 ) ) ;
#71388 = DIRECTION ( 'NONE',  ( 0.000000000000000000, 0.000000000000000000, 1.000000000000000000 ) ) ;
#71387 = CARTESIAN_POINT ( 'NONE',  ( 16.55341960407611168, 4.379528057220329451, 103.9572429386476813 ) ) ;
#71389 = CARTESIAN_POINT ( 'NONE',  ( 0.05219959533909260263, 19.03943276465977164, 59.99890960531436690 ) ) ;
#71390 = CARTESIAN_POINT ( 'NONE',  ( -5.049401038297874678, -19.05341960407617918, 89.79275706135230450 ) ) ;
#71391 = CARTESIAN_POINT ( 'NONE',  ( -8.224510206698948167, 14.34966873604960824, 95.41557627198102409 ) ) ;
#71392 = CARTESIAN_POINT ( 'NONE',  ( 10.72451020669871369, 18.67979575497193778, 77.08442372801901854 ) ) ;
#71394 = CARTESIAN_POINT ( 'NONE',  ( -10.72451020669870658, -18.67979575497194134, 24.58442372801901499 ) ) ;
#71393 = CARTESIAN_POINT ( 'NONE',  ( -16.46253265017160317, 9.564922557960807481, 55.83224293864769550 ) ) ;
#71395 = CARTESIAN_POINT ( 'NONE',  ( -16.53943276465976808, 0.05219959533911058130, 96.24890960531435269 ) ) ;
#71396 = CARTESIAN_POINT ( 'NONE',  ( 28.82186960331498327, 2.781578969918950771E-14, 145.0000000000000000 ) ) ;
#71397 = CARTESIAN_POINT ( 'NONE',  ( 19.02544592524343514, -5.153800228976328945, 68.54057627198103830 ) ) ;
#71398 = CARTESIAN_POINT ( 'NONE',  ( 16.21995358207305316, 7.366697692864170754, 112.5644899848783496 ) ) ;
#71400 = CARTESIAN_POINT ( 'NONE',  ( -5.823673210054116645, -21.52544592524344225, 32.29057627198102409 ) ) ;
#71399 = CARTESIAN_POINT ( 'NONE',  ( -9.564922557961040184, 16.46253265017147172, 107.9177570613523471 ) ) ;
#71401 = CARTESIAN_POINT ( 'NONE',  ( 18.62759615963255655, 10.81492255796105972, 51.66775706135234714 ) ) ;
#71402 = CARTESIAN_POINT ( 'NONE',  ( -9.474510206698964154, 16.51473224551069663, 90.41557627198103830 ) ) ;
#71403 = CARTESIAN_POINT ( 'NONE',  ( 16.51473224551083163, -9.474510206698727899, 85.83442372801900433 ) ) ;
#71404 = CARTESIAN_POINT ( 'NONE',  ( 19.03943276465977164, -0.05219959533909143690, 68.74890960531436690 ) ) ;
#71405 = CARTESIAN_POINT ( 'NONE',  ( 4.379528057220339221, -16.55341960407611168, 82.70724293864770971 ) ) ;
#71406 = CARTESIAN_POINT ( 'NONE',  ( -5.153800228976328057, -19.02544592524343514, 102.2905762719810383 ) ) ;
#71407 = CARTESIAN_POINT ( 'NONE',  ( 12.14591786802309770, 12.06949235617756955, 94.37390960531436690 ) ) ;
#71408 = CARTESIAN_POINT ( 'NONE',  ( 19.02544592524343514, -5.153800228976328945, 93.54057627198102409 ) ) ;
#71410 = CARTESIAN_POINT ( 'NONE',  ( -19.05341960407611168, -5.049401038298163336, 21.45724293864768839 ) ) ;
#71409 = CARTESIAN_POINT ( 'NONE',  ( -12.06949235617756955, 12.14591786802309770, 45.62390960531436690 ) ) ;
#71411 = ORIENTED_EDGE ( 'NONE', *, *, #95173, .T. ) ;
#71412 = CARTESIAN_POINT ( 'NONE',  ( 18.62759615963255655, 10.81492255796105972, 61.66775706135235424 ) ) ;
#71413 = CARTESIAN_POINT ( 'NONE',  ( -9.564922557961040184, 16.46253265017147172, 77.91775706135234714 ) ) ;
#71414 = CARTESIAN_POINT ( 'NONE',  ( 4.379528057220339221, -16.55341960407611168, 52.70724293864769550 ) ) ;
#71415 = CARTESIAN_POINT ( 'NONE',  ( -15.80617190586745835, -15.72974639402198527, 96.87390960531436690 ) ) ;
#71416 = CARTESIAN_POINT ( 'NONE',  ( 15.80617190586746368, 15.72974639402197994, 34.37390960531435979 ) ) ;
#71417 = CARTESIAN_POINT ( 'NONE',  ( 4.379528057220339221, -16.55341960407611168, 82.70724293864770971 ) ) ;
#71418 = CARTESIAN_POINT ( 'NONE',  ( 5.049401038298161559, -19.05341960407611168, 52.70724293864767418 ) ) ;
#71419 = CARTESIAN_POINT ( 'NONE',  ( 0.05219959533910956823, 16.53943276465976808, 29.99890960531435979 ) ) ;
#71420 = CARTESIAN_POINT ( 'NONE',  ( -14.29746914071037622, -8.314922557961029526, 89.16775706135236135 ) ) ;
#71421 = CARTESIAN_POINT ( 'NONE',  ( 14.34966873604972726, -8.224510206698740333, 75.83442372801900433 ) ) ;
#71422 = CARTESIAN_POINT ( 'NONE',  ( 19.03943276465977164, 0.05219959533936151252, 26.25109039468566507 ) ) ;
#71423 = CARTESIAN_POINT ( 'NONE',  ( 0.05219959533909260263, 19.03943276465977164, 89.99890960531436690 ) ) ;
#71424 = CARTESIAN_POINT ( 'NONE',  ( -9.474510206698964154, 16.51473224551069663, 75.41557627198103830 ) ) ;
#71425 = CARTESIAN_POINT ( 'NONE',  ( 14.29746914071037800, 8.314922557961029526, 81.66775706135236135 ) ) ;
#71426 = CARTESIAN_POINT ( 'NONE',  ( 0.05219959533909260263, 19.03943276465977164, 34.99890960531435979 ) ) ;
#71427 = CARTESIAN_POINT ( 'NONE',  ( -16.53943276465976808, 0.05219959533911058130, 51.24890960531436690 ) ) ;
#71429 = CARTESIAN_POINT ( 'NONE',  ( 5.049401038298161559, -19.05341960407611168, 102.7072429386476955 ) ) ;
#71428 = CARTESIAN_POINT ( 'NONE',  ( 19.03943276465977164, -0.05219959533909143690, 113.7489096053143669 ) ) ;
#71430 = CARTESIAN_POINT ( 'NONE',  ( 0.05219959533907565091, 21.53943276465977519, 39.99890960531436690 ) ) ;
#71431 = CARTESIAN_POINT ( 'NONE',  ( -16.55341960407611168, -4.379528057220339221, 76.45724293864769550 ) ) ;
#71432 = CARTESIAN_POINT ( 'NONE',  ( 16.53943276465976808, 0.05219959533934440121, 21.25109039468567218 ) ) ;
#71433 = B_SPLINE_CURVE_WITH_KNOTS ( 'NONE', 3,
 ( #196049, #30152, #149520, #91794, #136341, #181860, #43339, #27191, #57524, #121159, #14984, #135365, #166693, #44335, #197036, #118193, #89838, #58503, #105007, #137326, #105992, #88838 ),
 .UNSPECIFIED., .F., .F.,
 ( 4, 2, 2, 2, 2, 2, 2, 2, 2, 2, 4 ),
 ( 0.000000000000000000, 0.001027542925581684209, 0.002055085851163368418, 0.002568857313954213666, 0.003082628776745058915, 0.004110171702326815765, 0.004623943165117716525, 0.005137714627908618152, 0.006165257553490454366, 0.007192800479072292315, 0.008220343404654129396 ),
 .UNSPECIFIED. ) ;
#71434 = CARTESIAN_POINT ( 'NONE',  ( -8.314922557960811034, -14.29746914071050412, 72.08224293864769550 ) ) ;
#71435 = CARTESIAN_POINT ( 'NONE',  ( 0.000000000000000000, 0.000000000000000000, -62.50719930893269805 ) ) ;
#71436 = CARTESIAN_POINT ( 'NONE',  ( -13.97604488694547697, 13.89961937509957934, 58.12609039468566863 ) ) ;
#71437 = CARTESIAN_POINT ( 'NONE',  ( 16.51473224551069308, 9.474510206698969483, 109.1655762719810383 ) ) ;
#71438 = CARTESIAN_POINT ( 'NONE',  ( -9.474510206698720793, -16.51473224551083518, 79.58442372801899012 ) ) ;
#71440 = CARTESIAN_POINT ( 'NONE',  ( -8.314922557961024197, 14.29746914071037800, 92.91775706135236135 ) ) ;
#71439 = CARTESIAN_POINT ( 'NONE',  ( 16.46253265017146816, 9.564922557961045513, 106.6677570613523471 ) ) ;
#71441 = CARTESIAN_POINT ( 'NONE',  ( 0.05219959533909260263, 19.03943276465977164, 34.99890960531435979 ) ) ;
#71442 = CARTESIAN_POINT ( 'NONE',  ( 15.80617190586746368, 15.72974639402197994, 29.37390960531435269 ) ) ;
#71443 = CARTESIAN_POINT ( 'NONE',  ( -10.72451020669870658, -18.67979575497194134, 54.58442372801901143 ) ) ;
#71444 = CARTESIAN_POINT ( 'NONE',  ( -19.03943276465977164, -0.05219959533935918106, 113.7510903946856757 ) ) ;
#71446 = CARTESIAN_POINT ( 'NONE',  ( 13.89961937509977652, -13.97604488694527269, 68.12390960531436690 ) ) ;
#71445 = CARTESIAN_POINT ( 'NONE',  ( 9.564922557961047289, -16.46253265017146816, 55.41775706135234003 ) ) ;
#71447 = CARTESIAN_POINT ( 'NONE',  ( -5.049401038298153566, 19.05341960407611168, 115.2072429386477097 ) ) ;
#71449 = CARTESIAN_POINT ( 'NONE',  ( 13.89961937509977652, -13.97604488694527269, 73.12390960531436690 ) ) ;
#71448 = CARTESIAN_POINT ( 'NONE',  ( -14.29746914071049879, 8.314922557960819915, 80.83224293864769550 ) ) ;
#71450 = CARTESIAN_POINT ( 'NONE',  ( -5.049401038298153566, 19.05341960407611168, 85.20724293864766707 ) ) ;
#71451 = VERTEX_POINT ( 'NONE', #76805 ) ;
#71452 = CARTESIAN_POINT ( 'NONE',  ( 16.51473224551083163, -9.474510206698727899, 90.83442372801900433 ) ) ;
#71453 = CARTESIAN_POINT ( 'NONE',  ( 15.80617190586746368, 15.72974639402197994, 59.37390960531436690 ) ) ;
#71454 = CARTESIAN_POINT ( 'NONE',  ( 0.05219959533909260263, 19.03943276465977164, 34.99890960531435979 ) ) ;
#71455 = CARTESIAN_POINT ( 'NONE',  ( -16.51473224551082808, 9.474510206698731452, 63.33442372801900433 ) ) ;
#71456 = CARTESIAN_POINT ( 'NONE',  ( -16.51473224551069308, -9.474510206698971260, 51.66557627198102409 ) ) ;
#71457 = CARTESIAN_POINT ( 'NONE',  ( -19.05341960407611168, -5.049401038298163336, 86.45724293864769550 ) ) ;
#71458 = ORIENTED_EDGE ( 'NONE', *, *, #88386, .F. ) ;
#71459 = CARTESIAN_POINT ( 'NONE',  ( -15.80617190586745835, -15.72974639402198527, 91.87390960531436690 ) ) ;
#71461 = CARTESIAN_POINT ( 'NONE',  ( -19.02544592524334988, -5.153800228976617603, 53.95942372801898301 ) ) ;
#71460 = CARTESIAN_POINT ( 'NONE',  ( 8.314922557960818139, 14.29746914071049879, 99.58224293864770971 ) ) ;
#71462 = CARTESIAN_POINT ( 'NONE',  ( -5.823673210054116645, -21.52544592524344225, 87.29057627198103830 ) ) ;
#71463 = CARTESIAN_POINT ( 'NONE',  ( 18.67979575497178502, 10.72451020669898547, 74.16557627198102409 ) ) ;
#71464 = CARTESIAN_POINT ( 'NONE',  ( 16.53943276465976808, -0.05219959533910856209, 33.74890960531436690 ) ) ;
#71465 = CARTESIAN_POINT ( 'NONE',  ( -10.81492255796105439, 18.62759615963255655, 102.9177570613523756 ) ) ;
#71466 = CARTESIAN_POINT ( 'NONE',  ( 0.05219959533934541429, -16.53943276465976808, 50.00109039468568994 ) ) ;
#71467 = CARTESIAN_POINT ( 'NONE',  ( 13.89961937509977652, -13.97604488694527269, 83.12390960531436690 ) ) ;
#71468 = CARTESIAN_POINT ( 'NONE',  ( -19.03943276465977164, 0.05219959533909376836, 26.24890960531435624 ) ) ;
#71469 = CARTESIAN_POINT ( 'NONE',  ( -15.80617190586768217, 15.72974639402176855, 38.12609039468567573 ) ) ;
#71470 = CARTESIAN_POINT ( 'NONE',  ( 15.80617190586769283, -15.72974639402175789, 60.62609039468567573 ) ) ;
#71471 = CARTESIAN_POINT ( 'NONE',  ( 16.51473224551069308, 9.474510206698969483, 54.16557627198103120 ) ) ;
#71472 = CARTESIAN_POINT ( 'NONE',  ( 0.05219959533907565091, 21.53943276465977519, 114.9989096053143669 ) ) ;
#71473 = CARTESIAN_POINT ( 'NONE',  ( -5.153800228976607833, 19.02544592524334988, 57.70942372801899012 ) ) ;
#71474 = CARTESIAN_POINT ( 'NONE',  ( -16.51473224551082808, 9.474510206698731452, 68.33442372801900433 ) ) ;
#71475 = CARTESIAN_POINT ( 'NONE',  ( -12.14591786802326823, 12.06949235617739902, 33.12609039468569705 ) ) ;
#71476 = PLANE ( 'NONE',  #146739 ) ;
#71477 = CARTESIAN_POINT ( 'NONE',  ( -14.29746914071037622, -8.314922557961029526, 74.16775706135231871 ) ) ;
#71478 = CARTESIAN_POINT ( 'NONE',  ( 19.02544592524343514, -5.153800228976328945, 43.54057627198103120 ) ) ;
#71479 = CARTESIAN_POINT ( 'NONE',  ( 23.63516320021125594, -9.722623904421409335, 168.4908852323012809 ) ) ;
#71480 = CARTESIAN_POINT ( 'NONE',  ( 9.474510206698971260, -16.51473224551069308, 92.91557627198103830 ) ) ;
#71481 = CARTESIAN_POINT ( 'NONE',  ( 16.55341960407611168, 4.379528057220329451, 113.9572429386477239 ) ) ;
#71482 = CARTESIAN_POINT ( 'NONE',  ( -21.53943276465977519, 0.05219959533907696930, 76.24890960531435269 ) ) ;
#71483 = CARTESIAN_POINT ( 'NONE',  ( -0.05219959533934338120, 16.53943276465976808, 62.50109039468568284 ) ) ;
#71484 = CARTESIAN_POINT ( 'NONE',  ( -21.52544592524334988, -5.823673210054445271, 108.9594237280190185 ) ) ;
#71485 = CARTESIAN_POINT ( 'NONE',  ( -9.474510206698964154, 16.51473224551069663, 45.41557627198103120 ) ) ;
#71486 = CARTESIAN_POINT ( 'NONE',  ( -16.53943276465976808, 0.05219959533911058130, 26.24890960531435624 ) ) ;
#71487 = CARTESIAN_POINT ( 'NONE',  ( -0.05219959533910754901, -16.53943276465976808, 62.49890960531436690 ) ) ;
#71488 = CARTESIAN_POINT ( 'NONE',  ( -16.46253265017160317, 9.564922557960807481, 70.83224293864770971 ) ) ;
#71489 = CARTESIAN_POINT ( 'NONE',  ( -0.05219959533937732626, 21.53943276465977519, 32.50109039468568284 ) ) ;
#71490 = CARTESIAN_POINT ( 'NONE',  ( 5.049401038298161559, -19.05341960407611168, 77.70724293864765286 ) ) ;
#71491 = CARTESIAN_POINT ( 'NONE',  ( 5.719274019375673035, 21.55341960407619339, 82.29275706135234714 ) ) ;
#71492 = CARTESIAN_POINT ( 'NONE',  ( -16.55341960407617563, 4.379528057220093196, 63.54275706135234003 ) ) ;
#71493 = CARTESIAN_POINT ( 'NONE',  ( 9.564922557960805705, 16.46253265017160317, 104.5822429386476955 ) ) ;
#71494 = CARTESIAN_POINT ( 'NONE',  ( 4.483927247898545687, 16.52544592524342804, 44.79057627198103120 ) ) ;
#71495 = CARTESIAN_POINT ( 'NONE',  ( -13.97604488694527625, -13.89961937509977652, 21.87390960531435979 ) ) ;
#71496 = CARTESIAN_POINT ( 'NONE',  ( 16.55341960407618274, -4.379528057220086978, 51.04275706135234714 ) ) ;
#71497 = CARTESIAN_POINT ( 'NONE',  ( 8.314922557960818139, 14.29746914071049879, 54.58224293864769550 ) ) ;
#71498 = CARTESIAN_POINT ( 'NONE',  ( 16.46253265017160672, -9.564922557960803928, 113.3322429386476955 ) ) ;
#71499 = CARTESIAN_POINT ( 'NONE',  ( -10.72451020669898014, 18.67979575497178502, 30.41557627198101699 ) ) ;
#71500 = CARTESIAN_POINT ( 'NONE',  ( 0.05219959533936267826, -19.03943276465977164, 20.00109039468567218 ) ) ;
#71501 = CARTESIAN_POINT ( 'NONE',  ( -14.34966873604960291, -8.224510206698953496, 91.66557627198103830 ) ) ;
#71502 = CARTESIAN_POINT ( 'NONE',  ( -13.89961937509977652, 13.97604488694528158, 90.62390960531432427 ) ) ;
#71503 = VERTEX_POINT ( 'NONE', #16140 ) ;
#71504 = CARTESIAN_POINT ( 'NONE',  ( -4.483927247898782831, 16.52544592524335698, 57.70942372801901143 ) ) ;
#71505 = CARTESIAN_POINT ( 'NONE',  ( 19.03943276465977164, -0.05219959533909143690, 58.74890960531435979 ) ) ;
#71506 = DIRECTION ( 'NONE',  ( 0.000000000000000000, 0.000000000000000000, 1.000000000000000000 ) ) ;
#71507 = CARTESIAN_POINT ( 'NONE',  ( -0.05219959533936034679, 19.03943276465977164, 42.50109039468566152 ) ) ;
#71508 = CARTESIAN_POINT ( 'NONE',  ( 0.05219959533934541429, -16.53943276465976808, 80.00109039468568994 ) ) ;
#71509 = CARTESIAN_POINT ( 'NONE',  ( -19.03943276465977164, -0.05219959533935918106, 98.75109039468567573 ) ) ;
#71510 = CARTESIAN_POINT ( 'NONE',  ( 10.81492255796106328, -18.62759615963255655, 70.41775706135236135 ) ) ;
#71511 = CARTESIAN_POINT ( 'NONE',  ( 9.474510206698971260, -16.51473224551069308, 72.91557627198102409 ) ) ;
#71512 = CARTESIAN_POINT ( 'NONE',  ( 5.823673210054125526, 21.52544592524343514, 89.79057627198103830 ) ) ;
#71513 = CARTESIAN_POINT ( 'NONE',  ( 16.52544592524342804, -4.483927247898539470, 98.54057627198105251 ) ) ;
#71514 = CARTESIAN_POINT ( 'NONE',  ( 5.049401038297881783, 19.05341960407617563, 67.29275706135234714 ) ) ;
#71515 = CARTESIAN_POINT ( 'NONE',  ( -18.67979575497178146, -10.72451020669898902, 61.66557627198103120 ) ) ;
#71516 = CARTESIAN_POINT ( 'NONE',  ( 19.05341960407617918, -5.049401038297876454, 36.04275706135234003 ) ) ;
#71517 = FACE_BOUND ( 'NONE', #186012, .T. ) ;
#71518 = CARTESIAN_POINT ( 'NONE',  ( -18.67979575497178146, -10.72451020669898902, 96.66557627198102409 ) ) ;
#71519 = CARTESIAN_POINT ( 'NONE',  ( -19.46398650005389541, 5.499999999999947597, 55.18269651486371430 ) ) ;
#71520 = CARTESIAN_POINT ( 'NONE',  ( 0.05219959533909260263, 19.03943276465977164, 69.99890960531435269 ) ) ;
#71521 = CARTESIAN_POINT ( 'NONE',  ( -5.153800228976328057, -19.02544592524343514, 92.29057627198102409 ) ) ;
#71522 = CARTESIAN_POINT ( 'NONE',  ( 9.564922557961047289, -16.46253265017146816, 110.4177570613523471 ) ) ;
#71523 = CARTESIAN_POINT ( 'NONE',  ( 37.43820758241026425, -2.754439498815792753, 40.23603015349058154 ) ) ;
#71524 = CARTESIAN_POINT ( 'NONE',  ( -9.564922557960796823, -16.46253265017161027, 42.08224293864769550 ) ) ;
#71525 = CARTESIAN_POINT ( 'NONE',  ( -19.02544592524342804, 5.153800228976336051, 116.0405762719810383 ) ) ;
#71527 = CARTESIAN_POINT ( 'NONE',  ( -16.52544592524342804, 4.483927247898546575, 46.04057627198103830 ) ) ;
#71526 = CARTESIAN_POINT ( 'NONE',  ( -15.80617190586745835, -15.72974639402198527, 86.87390960531438111 ) ) ;
#71528 = CARTESIAN_POINT ( 'NONE',  ( 5.823673210054444382, -21.52544592524334988, 70.20942372801904696 ) ) ;
#71531 = CARTESIAN_POINT ( 'NONE',  ( -5.049401038297874678, -19.05341960407617918, 29.79275706135232227 ) ) ;
#71530 = CARTESIAN_POINT ( 'NONE',  ( -14.29746914071037622, -8.314922557961029526, 29.16775706135234003 ) ) ;
#71529 = SHAPE_REPRESENTATION ( 'socket button head screw_iso_ISO 7380 - M4 x 8 - 8N', ( #82054 ), #17734 ) ;
#71532 = CARTESIAN_POINT ( 'NONE',  ( 16.53943276465976808, -0.05219959533910856209, 28.74890960531435624 ) ) ;
#71533 = CARTESIAN_POINT ( 'NONE',  ( -15.72974639402197994, 15.80617190586746368, 115.6239096053143669 ) ) ;
#71534 = CARTESIAN_POINT ( 'NONE',  ( -4.483927247898539470, -16.52544592524342804, 52.29057627198102409 ) ) ;
#71535 = CARTESIAN_POINT ( 'NONE',  ( 13.97604488694548053, -13.89961937509957401, 100.6260903946856615 ) ) ;
#71536 = CARTESIAN_POINT ( 'NONE',  ( 9.564922557961047289, -16.46253265017146816, 65.41775706135233293 ) ) ;
#71537 = CARTESIAN_POINT ( 'NONE',  ( -21.55341960407619339, 5.719274019375674811, 73.54275706135234714 ) ) ;
#71538 = CARTESIAN_POINT ( 'NONE',  ( -9.564922557961040184, 16.46253265017147172, 52.91775706135233293 ) ) ;
#71539 = CARTESIAN_POINT ( 'NONE',  ( -0.05219959533910754901, -16.53943276465976808, 112.4989096053143669 ) ) ;
#71540 = CARTESIAN_POINT ( 'NONE',  ( -5.719274019375978568, 21.55341960407610458, 50.20724293864769550 ) ) ;
#71541 = CARTESIAN_POINT ( 'NONE',  ( 16.52544592524342804, -4.483927247898539470, 43.54057627198103830 ) ) ;
#71542 = CARTESIAN_POINT ( 'NONE',  ( -18.09918380851992481, -5.500000000000039968, 51.48618307335613054 ) ) ;
#71543 = CARTESIAN_POINT ( 'NONE',  ( 10.72451020669871369, 18.67979575497193778, 112.0844237280190185 ) ) ;
#71544 = CARTESIAN_POINT ( 'NONE',  ( 12.14591786802327356, -12.06949235617739191, 90.62609039468567573 ) ) ;
#71545 = CARTESIAN_POINT ( 'NONE',  ( -16.55341960407611168, -4.379528057220339221, 36.45724293864768839 ) ) ;
#71546 = CARTESIAN_POINT ( 'NONE',  ( 0.05219959533937995610, -21.53943276465977519, 75.00109039468568994 ) ) ;
#71547 = CARTESIAN_POINT ( 'NONE',  ( 18.62759615963255655, 10.81492255796105972, 71.66775706135234714 ) ) ;
#71548 = CARTESIAN_POINT ( 'NONE',  ( 10.72451020669898902, -18.67979575497178502, 77.91557627198102409 ) ) ;
#71549 = ADVANCED_FACE ( 'NONE', ( #32305 ), #157356, .F. ) ;
#71550 = CARTESIAN_POINT ( 'NONE',  ( -13.97604488694527625, -13.89961937509977652, 36.87390960531436690 ) ) ;
#71551 = CARTESIAN_POINT ( 'NONE',  ( -15.80617190586768217, 15.72974639402176855, 53.12609039468568284 ) ) ;
#71552 = CARTESIAN_POINT ( 'NONE',  ( 13.97604488694527802, 13.89961937509977652, 39.37390960531435269 ) ) ;
#71553 = CARTESIAN_POINT ( 'NONE',  ( -0.05219959533909027116, -19.03943276465977164, 47.49890960531435979 ) ) ;
#71554 = CARTESIAN_POINT ( 'NONE',  ( 16.52544592524342804, -4.483927247898539470, 93.54057627198103830 ) ) ;
#71555 = CARTESIAN_POINT ( 'NONE',  ( -16.51473224551069308, -9.474510206698971260, 81.66557627198103830 ) ) ;
#71556 = CARTESIAN_POINT ( 'NONE',  ( -16.55341960407611168, -4.379528057220339221, 46.45724293864769550 ) ) ;
#71557 = CARTESIAN_POINT ( 'NONE',  ( -0.05219959533910754901, -16.53943276465976808, 102.4989096053143811 ) ) ;
#71558 = CARTESIAN_POINT ( 'NONE',  ( -18.67979575497178146, -10.72451020669898902, 66.66557627198102409 ) ) ;
#71559 = CARTESIAN_POINT ( 'NONE',  ( -0.05219959533937732626, 21.53943276465977519, 27.50109039468567929 ) ) ;
#71560 = CARTESIAN_POINT ( 'NONE',  ( -17.41439684931615517, 15.33930553228139004, -55.09142748592167038 ) ) ;
#71562 = CARTESIAN_POINT ( 'NONE',  ( 16.52544592524335698, 4.483927247898782831, 21.45942372801901499 ) ) ;
#71561 = CARTESIAN_POINT ( 'NONE',  ( 13.97604488694527802, 13.89961937509977652, 84.37390960531433848 ) ) ;
#71563 = CARTESIAN_POINT ( 'NONE',  ( -10.81492255796078084, -18.62759615963271287, 77.08224293864769550 ) ) ;
#71564 = CARTESIAN_POINT ( 'NONE',  ( 10.81492255796106328, -18.62759615963255655, 100.4177570613523471 ) ) ;
#71565 = CARTESIAN_POINT ( 'NONE',  ( 19.03943276465977164, -0.05219959533909143690, 83.74890960531436690 ) ) ;
#71566 = CARTESIAN_POINT ( 'NONE',  ( -21.53943276465977519, -0.05219959533937600094, 18.75109039468568639 ) ) ;
#71567 = CARTESIAN_POINT ( 'NONE',  ( -16.46253265017160317, 9.564922557960807481, 110.8322429386476955 ) ) ;
#71568 = CARTESIAN_POINT ( 'NONE',  ( 14.34966873604972726, -8.224510206698740333, 90.83442372801901854 ) ) ;
#71569 = CARTESIAN_POINT ( 'NONE',  ( -18.62759615963255300, -10.81492255796106328, 69.16775706135234714 ) ) ;
#71570 = CARTESIAN_POINT ( 'NONE',  ( -10.72451020669870658, -18.67979575497194134, 99.58442372801900433 ) ) ;
#71571 = CARTESIAN_POINT ( 'NONE',  ( 12.06949235617739724, 12.14591786802326823, 66.87609039468568994 ) ) ;
#71572 = CARTESIAN_POINT ( 'NONE',  ( -10.72451020669870658, -18.67979575497194134, 29.58442372801901854 ) ) ;
#71573 = CARTESIAN_POINT ( 'NONE',  ( -18.67979575497193778, 10.72451020669871902, 93.33442372801901854 ) ) ;
#71574 = CARTESIAN_POINT ( 'NONE',  ( 16.46253265017160672, -9.564922557960803928, 98.33224293864769550 ) ) ;
#71575 = CARTESIAN_POINT ( 'NONE',  ( -21.52544592524343514, 5.823673210054127303, 91.04057627198103830 ) ) ;
#71576 = CARTESIAN_POINT ( 'NONE',  ( 9.564922557961047289, -16.46253265017146816, 65.41775706135233293 ) ) ;
#71578 = CARTESIAN_POINT ( 'NONE',  ( 15.72974639402199770, -15.80617190586745480, 58.12390960531435979 ) ) ;
#71577 = CARTESIAN_POINT ( 'NONE',  ( -8.779096689238560458, -37.67883572780603174, -23.98624440746952757 ) ) ;
#71580 = CARTESIAN_POINT ( 'NONE',  ( -16.53943276465976808, 0.05219959533911058130, 36.24890960531435979 ) ) ;
#71579 = CARTESIAN_POINT ( 'NONE',  ( 19.02544592524343514, -5.153800228976328945, 88.54057627198102409 ) ) ;
#71581 = CARTESIAN_POINT ( 'NONE',  ( 19.80313217313587870, 12.05975691044382181, 167.9999999999999147 ) ) ;
#71582 = CARTESIAN_POINT ( 'NONE',  ( 16.46253265017146816, 9.564922557961045513, 71.66775706135233293 ) ) ;
#71583 = CARTESIAN_POINT ( 'NONE',  ( -1.322671946311490432, -15.93273212980864173, -61.66661032175889545 ) ) ;
#71584 = CARTESIAN_POINT ( 'NONE',  ( -0.05219959533936034679, 19.03943276465977164, 107.5010903946856615 ) ) ;
#71585 = CARTESIAN_POINT ( 'NONE',  ( -21.53943276465977519, 0.05219959533907696930, 81.24890960531436690 ) ) ;
#71586 = CARTESIAN_POINT ( 'NONE',  ( 8.224510206698953496, -14.34966873604960469, 67.91557627198102409 ) ) ;
#71587 = CARTESIAN_POINT ( 'NONE',  ( -9.474510206698964154, 16.51473224551069663, 95.41557627198102409 ) ) ;
#71588 = CARTESIAN_POINT ( 'NONE',  ( -4.379528057220086978, -16.55341960407618274, 24.79275706135235779 ) ) ;
#71589 = CARTESIAN_POINT ( 'NONE',  ( 16.51473224551069308, 9.474510206698969483, 64.16557627198102409 ) ) ;
#71591 = CARTESIAN_POINT ( 'NONE',  ( -19.03943276465977164, -0.05219959533935918106, 78.75109039468567573 ) ) ;
#71590 = CARTESIAN_POINT ( 'NONE',  ( -15.80617190586745835, -15.72974639402198527, 111.8739096053143669 ) ) ;
#71592 = CARTESIAN_POINT ( 'NONE',  ( -9.474510206698964154, 16.51473224551069663, 95.41557627198102409 ) ) ;
#71593 = CARTESIAN_POINT ( 'NONE',  ( 5.153800228976335163, 19.02544592524342804, 69.79057627198103830 ) ) ;
#71594 = CARTESIAN_POINT ( 'NONE',  ( -5.823673210054116645, -21.52544592524344225, 72.29057627198102409 ) ) ;
#71595 = CARTESIAN_POINT ( 'NONE',  ( -5.153800228976328057, -19.02544592524343514, 42.29057627198101699 ) ) ;
#71596 = DIRECTION ( 'NONE',  ( -0.000000000000000000, -0.000000000000000000, 1.000000000000000000 ) ) ;
#71597 = CARTESIAN_POINT ( 'NONE',  ( 0.05219959533910956823, 16.53943276465976808, 49.99890960531437401 ) ) ;
#71598 = CARTESIAN_POINT ( 'NONE',  ( -13.89961937509977652, 13.97604488694528158, 100.6239096053143669 ) ) ;
#71599 = DIRECTION ( 'NONE',  ( -0.000000000000000000, -0.000000000000000000, 1.000000000000000000 ) ) ;
#71600 = CARTESIAN_POINT ( 'NONE',  ( 9.474510206698729675, 16.51473224551082808, 62.08442372801899722 ) ) ;
#71601 = CARTESIAN_POINT ( 'NONE',  ( 18.67979575497178502, 10.72451020669898547, 84.16557627198103830 ) ) ;
#71602 = CARTESIAN_POINT ( 'NONE',  ( -16.46253265017146816, -9.564922557961047289, 49.16775706135233293 ) ) ;
#71603 = CARTESIAN_POINT ( 'NONE',  ( 5.049401038298161559, -19.05341960407611168, 102.7072429386476955 ) ) ;
#71604 = CARTESIAN_POINT ( 'NONE',  ( 9.687362902255731711, -9.687362902255694408, -60.44446360152740993 ) ) ;
#71605 = CARTESIAN_POINT ( 'NONE',  ( 15.80617190586746368, 15.72974639402197994, 44.37390960531435979 ) ) ;
#71606 = CARTESIAN_POINT ( 'NONE',  ( 19.05341960407611168, 5.049401038298154454, 78.95724293864769550 ) ) ;
#71607 = CARTESIAN_POINT ( 'NONE',  ( 0.05219959533937995610, -21.53943276465977519, 65.00109039468568994 ) ) ;
#71608 = CARTESIAN_POINT ( 'NONE',  ( -16.51473224551069308, -9.474510206698971260, 41.66557627198103120 ) ) ;
#71610 = VERTEX_POINT ( 'NONE', #155639 ) ;
#71609 = CARTESIAN_POINT ( 'NONE',  ( -10.72451020669898014, 18.67979575497178502, 115.4155762719810241 ) ) ;
#71611 = CARTESIAN_POINT ( 'NONE',  ( -15.80617190586768217, 15.72974639402176855, 58.12609039468568994 ) ) ;
#71612 = ORIENTED_EDGE ( 'NONE', *, *, #183693, .T. ) ;
#71613 = CARTESIAN_POINT ( 'NONE',  ( 19.05341960407611168, 5.049401038298154454, 113.9572429386477097 ) ) ;
#71614 = CARTESIAN_POINT ( 'NONE',  ( -13.97604488694547697, 13.89961937509957934, 68.12609039468563310 ) ) ;
#71615 = CIRCLE ( 'NONE', #103950, 1.250000000000006439 ) ;
#71616 = CARTESIAN_POINT ( 'NONE',  ( 22.78725946537545965, -32.81619059092827939, -22.84582334174698559 ) ) ;
#71617 = CARTESIAN_POINT ( 'NONE',  ( -18.67979575497178146, -10.72451020669898902, 111.6655762719810525 ) ) ;
#71618 = CARTESIAN_POINT ( 'NONE',  ( 19.05341960407611168, 5.049401038298154454, 63.95724293864769550 ) ) ;
#71619 = CARTESIAN_POINT ( 'NONE',  ( -4.483927247898782831, 16.52544592524335698, 37.70942372801900433 ) ) ;
#71620 = CARTESIAN_POINT ( 'NONE',  ( 11.74264578624799427, 36.14014761921585972, -8.349999994537625980 ) ) ;
#71621 = CARTESIAN_POINT ( 'NONE',  ( -18.67979575497193778, 10.72451020669871902, 98.33442372801901854 ) ) ;
#71622 = CARTESIAN_POINT ( 'NONE',  ( -5.153800228976328057, -19.02544592524343514, 37.29057627198102409 ) ) ;
#71623 = CARTESIAN_POINT ( 'NONE',  ( 15.80617190586769283, -15.72974639402175789, 110.6260903946857042 ) ) ;
#71624 = CARTESIAN_POINT ( 'NONE',  ( -8.314922557961024197, 14.29746914071037800, 87.91775706135234714 ) ) ;
#71626 = CARTESIAN_POINT ( 'NONE',  ( 10.81492255796106328, -18.62759615963255655, 55.41775706135234714 ) ) ;
#71625 = CARTESIAN_POINT ( 'NONE',  ( -0.05219959533909027116, -19.03943276465977164, 92.49890960531436690 ) ) ;
#71627 = CARTESIAN_POINT ( 'NONE',  ( 3.556970738554033499E-15, -38.81732327939057825, -10.12499999726881228 ) ) ;
#71628 = CARTESIAN_POINT ( 'NONE',  ( -19.02544592524342804, 5.153800228976336051, 116.0405762719810383 ) ) ;
#71629 = CARTESIAN_POINT ( 'NONE',  ( -1.784589286804201480, 7.284589286804282970, 1.818019484660534424 ) ) ;
#71631 = CARTESIAN_POINT ( 'NONE',  ( 15.80617190586769283, -15.72974639402175789, 70.62609039468567573 ) ) ;
#71630 = CARTESIAN_POINT ( 'NONE',  ( -14.34966873604972548, 8.224510206698743886, 53.33442372801901854 ) ) ;
#71632 = CARTESIAN_POINT ( 'NONE',  ( 15.72974639402176855, 15.80617190586768217, 106.8760903946856899 ) ) ;
#71633 = FACE_OUTER_BOUND ( 'NONE', #44445, .T. ) ;
#71634 = CARTESIAN_POINT ( 'NONE',  ( 16.55341960407618274, -4.379528057220086978, 26.04275706135235779 ) ) ;
#71635 = CARTESIAN_POINT ( 'NONE',  ( 13.97604488694527802, 13.89961937509977652, 89.37390960531436690 ) ) ;
#71636 = CARTESIAN_POINT ( 'NONE',  ( 13.97604488694527802, 13.89961937509977652, 109.3739096053143669 ) ) ;
#71637 = ORIENTED_EDGE ( 'NONE', *, *, #85633, .T. ) ;
#71638 = CARTESIAN_POINT ( 'NONE',  ( 16.18388926212241685, 7.379444403734403579, 42.93953151366154231 ) ) ;
#71639 = CARTESIAN_POINT ( 'NONE',  ( -12.06949235617756955, 12.14591786802309770, 115.6239096053143669 ) ) ;
#71640 = CARTESIAN_POINT ( 'NONE',  ( -18.62759615963270932, 10.81492255796079327, 40.83224293864769550 ) ) ;
#71641 = CARTESIAN_POINT ( 'NONE',  ( -16.53943276465976808, -0.05219959533934237506, 108.7510903946857042 ) ) ;
#71643 = CARTESIAN_POINT ( 'NONE',  ( 5.153800228976335163, 19.02544592524342804, 64.79057627198100988 ) ) ;
#71642 = CARTESIAN_POINT ( 'NONE',  ( 4.379528057220339221, -16.55341960407611168, 87.70724293864769550 ) ) ;
#71644 = CARTESIAN_POINT ( 'NONE',  ( -5.823673210054431948, 21.52544592524334988, 87.70942372801901854 ) ) ;
#71645 = CARTESIAN_POINT ( 'NONE',  ( 4.483927247898790824, -16.52544592524335698, 30.20942372801902565 ) ) ;
#71646 = CARTESIAN_POINT ( 'NONE',  ( 16.52544592524342804, -4.483927247898539470, 88.54057627198103830 ) ) ;
#71647 = CARTESIAN_POINT ( 'NONE',  ( -21.53943276465977519, -0.05219959533937600094, 38.75109039468567573 ) ) ;
#71648 = CARTESIAN_POINT ( 'NONE',  ( -18.67979575497178146, -10.72451020669898902, 76.66557627198103830 ) ) ;
#71649 = CARTESIAN_POINT ( 'NONE',  ( -9.474510206698720793, -16.51473224551083518, 34.58442372801899722 ) ) ;
#71650 = CARTESIAN_POINT ( 'NONE',  ( -34.38590767368159362, 6.751198732549906545, 48.30327006964593295 ) ) ;
#71651 = CARTESIAN_POINT ( 'NONE',  ( -0.05219959533909027116, -19.03943276465977164, 97.49890960531436690 ) ) ;
#71652 = CARTESIAN_POINT ( 'NONE',  ( 16.53943276465976808, -0.05219959533910856209, 68.74890960531435269 ) ) ;
#71653 = CARTESIAN_POINT ( 'NONE',  ( 14.34966873604960469, 8.224510206698951720, 54.16557627198103120 ) ) ;
#71654 = CARTESIAN_POINT ( 'NONE',  ( -14.34966873604960291, -8.224510206698953496, 21.66557627198102409 ) ) ;
#71655 = CARTESIAN_POINT ( 'NONE',  ( 9.564922557961047289, -16.46253265017146816, 70.41775706135233293 ) ) ;
#71656 = CARTESIAN_POINT ( 'NONE',  ( 19.39056639909672342, 5.500000000000042633, 53.28948781074348773 ) ) ;
#71657 = CARTESIAN_POINT ( 'NONE',  ( -16.46253265017160317, 9.564922557960807481, 115.8322429386477097 ) ) ;
#71658 = CARTESIAN_POINT ( 'NONE',  ( 16.52544592524342804, -4.483927247898539470, 83.54057627198102409 ) ) ;
#71659 = CARTESIAN_POINT ( 'NONE',  ( 0.000000000000000000, 0.000000000000000000, -64.53213882399991519 ) ) ;
#71661 = CARTESIAN_POINT ( 'NONE',  ( 21.53943276465977519, -0.05219959533907433946, 48.74890960531435979 ) ) ;
#71660 = CARTESIAN_POINT ( 'NONE',  ( 13.97604488694527802, 13.89961937509977652, 44.37390960531435269 ) ) ;
#71662 = CARTESIAN_POINT ( 'NONE',  ( -15.80617190586745835, -15.72974639402198527, 86.87390960531438111 ) ) ;
#71663 = CARTESIAN_POINT ( 'NONE',  ( 12.14591786802309770, 12.06949235617756955, 114.3739096053143527 ) ) ;
#71665 = CARTESIAN_POINT ( 'NONE',  ( -19.02544592524342804, 5.153800228976336051, 51.04057627198103120 ) ) ;
#71664 = CARTESIAN_POINT ( 'NONE',  ( -14.34966873604972548, 8.224510206698743886, 63.33442372801900433 ) ) ;
#71666 = CARTESIAN_POINT ( 'NONE',  ( 0.05219959533936267826, -19.03943276465977164, 40.00109039468566152 ) ) ;
#71667 = CARTESIAN_POINT ( 'NONE',  ( 21.55341960407619695, -5.719274019375665929, 56.04275706135235424 ) ) ;
#71668 = CARTESIAN_POINT ( 'NONE',  ( 12.14591786802309770, 12.06949235617756955, 109.3739096053143811 ) ) ;
#71669 = CARTESIAN_POINT ( 'NONE',  ( 9.564922557961047289, -16.46253265017146816, 85.41775706135233293 ) ) ;
#71670 = CARTESIAN_POINT ( 'NONE',  ( -11.40812507854755609, 35.11059874428196537, -5.524999997268813523 ) ) ;
#71672 = CARTESIAN_POINT ( 'NONE',  ( -0.05219959533907301413, -21.53943276465977519, 52.49890960531435979 ) ) ;
#71671 = CARTESIAN_POINT ( 'NONE',  ( 17.50000000000000000, 5.499999999999997335, 36.70309617465829177 ) ) ;
#71673 = CARTESIAN_POINT ( 'NONE',  ( 16.51473224551069308, 9.474510206698969483, 29.16557627198103475 ) ) ;
#71674 = CARTESIAN_POINT ( 'NONE',  ( -10.72451020669870658, -18.67979575497194134, 79.58442372801903275 ) ) ;
#71675 = CARTESIAN_POINT ( 'NONE',  ( 16.55341960407611168, 4.379528057220329451, 28.95724293864769905 ) ) ;
#71677 = CARTESIAN_POINT ( 'NONE',  ( 8.314922557960818139, 14.29746914071049879, 44.58224293864769550 ) ) ;
#71676 = CARTESIAN_POINT ( 'NONE',  ( 16.53943276465976808, 0.05219959533934440121, 56.25109039468568284 ) ) ;
#71678 = CARTESIAN_POINT ( 'NONE',  ( -10.72451020669898014, 18.67979575497178502, 75.41557627198102409 ) ) ;
#71679 = CARTESIAN_POINT ( 'NONE',  ( -21.55341960407610458, -5.719274019375992779, 81.45724293864769550 ) ) ;
#71680 = CARTESIAN_POINT ( 'NONE',  ( -18.22780087662122028, 5.500000000000031086, 68.51540105326107266 ) ) ;
#71683 = ADVANCED_FACE ( 'NONE', ( #17134 ), #61627, .T. ) ;
#71682 = CARTESIAN_POINT ( 'NONE',  ( -0.05219959533909027116, -19.03943276465977164, 112.4989096053143669 ) ) ;
#71681 = CARTESIAN_POINT ( 'NONE',  ( 0.05219959533936267826, -19.03943276465977164, 85.00109039468567573 ) ) ;
#71684 = CARTESIAN_POINT ( 'NONE',  ( 16.46253265017160672, -9.564922557960803928, 43.33224293864769550 ) ) ;
#71685 = CARTESIAN_POINT ( 'NONE',  ( -16.46253265017160317, 9.564922557960807481, 35.83224293864768839 ) ) ;
#71686 = CARTESIAN_POINT ( 'NONE',  ( -17.97161686093728150, 5.499999999999980460, 75.99637206859166838 ) ) ;
#71687 = EDGE_LOOP ( 'NONE', ( #161897, #10237, #194813, #98215 ) ) ;
#71688 = CARTESIAN_POINT ( 'NONE',  ( -14.29746914071037622, -8.314922557961029526, 89.16775706135236135 ) ) ;
#71689 = CARTESIAN_POINT ( 'NONE',  ( -21.55341960407610458, -5.719274019375992779, 106.4572429386477097 ) ) ;
#71690 = CARTESIAN_POINT ( 'NONE',  ( 16.46253265017160672, -9.564922557960803928, 68.33224293864770971 ) ) ;
#71691 = CARTESIAN_POINT ( 'NONE',  ( 10.72451020669871369, 18.67979575497193778, 47.08442372801901854 ) ) ;
#71692 = CARTESIAN_POINT ( 'NONE',  ( -5.049401038298153566, 19.05341960407611168, 100.2072429386476955 ) ) ;
#71693 = CARTESIAN_POINT ( 'NONE',  ( -24.90102501248286160, -31.06609936492528945, -21.12314233236282845 ) ) ;
#71694 = ORIENTED_EDGE ( 'NONE', *, *, #188107, .T. ) ;
#71695 = CARTESIAN_POINT ( 'NONE',  ( 21.52544592524334988, 5.823673210054432836, 36.45942372801901143 ) ) ;
#71697 = CARTESIAN_POINT ( 'NONE',  ( 9.564922557960805705, 16.46253265017160317, 104.5822429386476955 ) ) ;
#71696 = CARTESIAN_POINT ( 'NONE',  ( 16.51473224551069308, 9.474510206698969483, 114.1655762719810241 ) ) ;
#71698 = CARTESIAN_POINT ( 'NONE',  ( 16.51473224551083163, -9.474510206698727899, 35.83442372801899722 ) ) ;
#71699 = CARTESIAN_POINT ( 'NONE',  ( 15.72974639402176855, 15.80617190586768217, 21.87609039468567573 ) ) ;
#71700 = CARTESIAN_POINT ( 'NONE',  ( -13.89961937509957401, -13.97604488694547875, 44.37609039468566863 ) ) ;
#71701 = CARTESIAN_POINT ( 'NONE',  ( 19.03943276465977164, 0.05219959533936151252, 51.25109039468567573 ) ) ;
#71702 = CARTESIAN_POINT ( 'NONE',  ( -12.06949235617739369, -12.14591786802326823, 89.37609039468568994 ) ) ;
#71703 = CARTESIAN_POINT ( 'NONE',  ( 13.97604488694527802, 13.89961937509977652, 114.3739096053143669 ) ) ;
#71704 = CARTESIAN_POINT ( 'NONE',  ( 13.89961937509977652, -13.97604488694527269, 73.12390960531436690 ) ) ;
#71705 = CARTESIAN_POINT ( 'NONE',  ( 21.52544592524334988, 5.823673210054432836, 76.45942372801901854 ) ) ;
#71706 = CARTESIAN_POINT ( 'NONE',  ( -15.72974639402176322, -15.80617190586768395, 89.37609039468568994 ) ) ;
#71707 = CARTESIAN_POINT ( 'NONE',  ( 5.000000000000001776, -120.0000000000000142, -15.00000000000000000 ) ) ;
#71708 = CARTESIAN_POINT ( 'NONE',  ( -9.564922557960796823, -16.46253265017161027, 87.08224293864769550 ) ) ;
#71709 = CARTESIAN_POINT ( 'NONE',  ( -15.80617190586768217, 15.72974639402176855, 68.12609039468567573 ) ) ;
#71710 = CARTESIAN_POINT ( 'NONE',  ( 19.05341960407617918, -5.049401038297876454, 106.0427570613523471 ) ) ;
#71711 = CARTESIAN_POINT ( 'NONE',  ( 13.89961937509977652, -13.97604488694527269, 63.12390960531435979 ) ) ;
#71712 = CARTESIAN_POINT ( 'NONE',  ( -16.46253265017160317, 9.564922557960807481, 115.8322429386477097 ) ) ;
#71713 = CARTESIAN_POINT ( 'NONE',  ( -19.02544592524342804, 5.153800228976336051, 76.04057627198102409 ) ) ;
#71714 = DIRECTION ( 'NONE',  ( 0.000000000000000000, -0.000000000000000000, -1.000000000000000000 ) ) ;
#71715 = CARTESIAN_POINT ( 'NONE',  ( 19.05341960407611168, 5.049401038298154454, 68.95724293864769550 ) ) ;
#71716 = CARTESIAN_POINT ( 'NONE',  ( -13.89961937509977652, 13.97604488694528158, 55.62390960531434558 ) ) ;
#71717 = CARTESIAN_POINT ( 'NONE',  ( 15.72974639402199770, -15.80617190586745480, 108.1239096053143811 ) ) ;
#71718 = CARTESIAN_POINT ( 'NONE',  ( 8.314922557961029526, -14.29746914071037800, 105.4177570613523613 ) ) ;
#71719 = CARTESIAN_POINT ( 'NONE',  ( 0.5019701148545779867, 16.61710099588754019, -61.38173178550033526 ) ) ;
#71720 = CARTESIAN_POINT ( 'NONE',  ( -16.51473224551082808, 9.474510206698731452, 63.33442372801900433 ) ) ;
#71721 = CARTESIAN_POINT ( 'NONE',  ( -5.049401038298153566, 19.05341960407611168, 90.20724293864766707 ) ) ;
#71722 = CARTESIAN_POINT ( 'NONE',  ( 8.224510206698953496, -14.34966873604960469, 67.91557627198102409 ) ) ;
#71723 = CARTESIAN_POINT ( 'NONE',  ( 16.55341960407611168, 4.379528057220329451, 103.9572429386476813 ) ) ;
#71724 = CARTESIAN_POINT ( 'NONE',  ( -5.823673210054116645, -21.52544592524344225, 27.29057627198103120 ) ) ;
#71725 = CARTESIAN_POINT ( 'NONE',  ( 10.81492255796078972, 18.62759615963270932, 29.58224293864769905 ) ) ;
#71726 = CARTESIAN_POINT ( 'NONE',  ( -8.224510206698948167, 14.34966873604960824, 90.41557627198103830 ) ) ;
#71727 = CARTESIAN_POINT ( 'NONE',  ( -16.51473224551069308, -9.474510206698971260, 81.66557627198103830 ) ) ;
#71728 = CARTESIAN_POINT ( 'NONE',  ( 5.049401038297881783, 19.05341960407617563, 27.29275706135232937 ) ) ;
#71729 = CARTESIAN_POINT ( 'NONE',  ( 8.224510206698742110, 14.34966873604972548, 102.0844237280190185 ) ) ;
#71730 = CARTESIAN_POINT ( 'NONE',  ( 19.05341960407611168, 5.049401038298154454, 93.95724293864769550 ) ) ;
#71731 = CARTESIAN_POINT ( 'NONE',  ( -18.67979575497193778, 10.72451020669871902, 48.33442372801902565 ) ) ;
#71732 = CARTESIAN_POINT ( 'NONE',  ( 0.05219959533907565091, 21.53943276465977519, 49.99890960531437401 ) ) ;
#71733 = CARTESIAN_POINT ( 'NONE',  ( 18.62759615963255655, 10.81492255796105972, 26.66775706135235424 ) ) ;
#71734 = CARTESIAN_POINT ( 'NONE',  ( 21.55341960407610458, 5.719274019375980345, 78.95724293864769550 ) ) ;
#71735 = CARTESIAN_POINT ( 'NONE',  ( 16.55341960407611168, 4.379528057220329451, 98.95724293864770971 ) ) ;
#71736 = CARTESIAN_POINT ( 'NONE',  ( -13.97604488694547697, 13.89961937509957934, 53.12609039468565442 ) ) ;
#71737 = CARTESIAN_POINT ( 'NONE',  ( -19.03943276465977164, 0.05219959533909376836, 41.24890960531435269 ) ) ;
#71738 = CARTESIAN_POINT ( 'NONE',  ( 19.02544592524343514, -5.153800228976328945, 93.54057627198102409 ) ) ;
#71739 = CARTESIAN_POINT ( 'NONE',  ( 9.474510206698971260, -16.51473224551069308, 92.91557627198103830 ) ) ;
#71740 = CARTESIAN_POINT ( 'NONE',  ( -8.224510206698948167, 14.34966873604960824, 110.4155762719810383 ) ) ;
#71741 = CARTESIAN_POINT ( 'NONE',  ( 12.14591786802309770, 12.06949235617756955, 44.37390960531435979 ) ) ;
#71742 = CARTESIAN_POINT ( 'NONE',  ( 16.52544592524335698, 4.483927247898782831, 36.45942372801901143 ) ) ;
#71743 = CARTESIAN_POINT ( 'NONE',  ( -10.72451020669870658, -18.67979575497194134, 104.5844237280190185 ) ) ;
#71745 = CARTESIAN_POINT ( 'NONE',  ( 14.34966873604972726, -8.224510206698740333, 110.8344237280190043 ) ) ;
#71744 = LINE ( 'NONE', #7056, #181795 ) ;
#71746 = CARTESIAN_POINT ( 'NONE',  ( 15.80617190586769283, -15.72974639402175789, 30.62609039468567929 ) ) ;
#71747 = CARTESIAN_POINT ( 'NONE',  ( 13.89961937509977652, -13.97604488694527269, 108.1239096053143669 ) ) ;
#71748 = EDGE_CURVE ( 'NONE', #13448, #120001, #48474, .T. ) ;
#71749 = CARTESIAN_POINT ( 'NONE',  ( 8.224510206698742110, 14.34966873604972548, 57.08442372801901854 ) ) ;
#71750 = CARTESIAN_POINT ( 'NONE',  ( -16.53943276465976808, 0.05219959533911058130, 21.24890960531436690 ) ) ;
#71751 = B_SPLINE_CURVE_WITH_KNOTS ( 'NONE', 3,
 ( #154478, #136332, #47309, #170645, #198006, #93791, #199994, #92790, #139300, #155471, #122141, #106969, #16963, #1782, #61461, #63460, #90803, #91785, #125136, #153479, #107959, #14975, #186834, #76635, #48302, #109959, #28187, #138313, #152486, #184818, #169646, #4568 ),
 .UNSPECIFIED., .F., .F.,
 ( 4, 2, 2, 2, 2, 2, 2, 2, 2, 2, 2, 2, 2, 2, 2, 4 ),
 ( 2.711112516444420852E-17, 0.0003712461730036998968, 0.0007424923460073726885, 0.001113738519011045480, 0.001484984692014718272, 0.002227477038022064072, 0.002598723211025740984, 0.002969969384029417896, 0.003341215557033094374, 0.003712461730036770852, 0.004083707903040447763, 0.004454954076044124675, 0.004826200249047800719, 0.005197446422051477631, 0.005568692595055154543, 0.005939938768058831454 ),
 .UNSPECIFIED. ) ;
#71752 = CARTESIAN_POINT ( 'NONE',  ( 0.05219959533934541429, -16.53943276465976808, 90.00109039468567573 ) ) ;
#71753 = CARTESIAN_POINT ( 'NONE',  ( 12.14591786802327356, -12.06949235617739191, 25.62609039468567929 ) ) ;
#71754 = CARTESIAN_POINT ( 'NONE',  ( 5.049401038298161559, -19.05341960407611168, 42.70724293864767418 ) ) ;
#71755 = CARTESIAN_POINT ( 'NONE',  ( -0.05219959533910754901, -16.53943276465976808, 112.4989096053143669 ) ) ;
#71756 = CARTESIAN_POINT ( 'NONE',  ( -21.53943276465977519, 0.05219959533907696930, 116.2489096053143669 ) ) ;
#71757 = CARTESIAN_POINT ( 'NONE',  ( -19.05341960407611168, -5.049401038298163336, 36.45724293864766707 ) ) ;
#71758 = CARTESIAN_POINT ( 'NONE',  ( 0.05219959533909260263, 19.03943276465977164, 104.9989096053143669 ) ) ;
#71759 = CARTESIAN_POINT ( 'NONE',  ( -10.81492255796105439, 18.62759615963255655, 27.91775706135234358 ) ) ;
#71760 = CARTESIAN_POINT ( 'NONE',  ( 9.474510206698971260, -16.51473224551069308, 22.91557627198102765 ) ) ;
#71761 = CARTESIAN_POINT ( 'NONE',  ( -5.049401038298153566, 19.05341960407611168, 105.2072429386476671 ) ) ;
#71762 = CARTESIAN_POINT ( 'NONE',  ( 16.18388926212238843, -7.379444403734509272, 112.0604684863385074 ) ) ;
#71763 = CARTESIAN_POINT ( 'NONE',  ( -16.46253265017160317, 9.564922557960807481, 100.8322429386477097 ) ) ;
#71765 = CARTESIAN_POINT ( 'NONE',  ( 16.53943276465976808, -0.05219959533910856209, 93.74890960531436690 ) ) ;
#71764 = CARTESIAN_POINT ( 'NONE',  ( 5.719274019375673035, 21.55341960407619339, 52.29275706135236135 ) ) ;
#71766 = CARTESIAN_POINT ( 'NONE',  ( -9.564922557960796823, -16.46253265017161027, 97.08224293864769550 ) ) ;
#71767 = CARTESIAN_POINT ( 'NONE',  ( 18.10062525802553424, -5.500000000000022204, 96.01383468041922242 ) ) ;
#71768 = CARTESIAN_POINT ( 'NONE',  ( 14.29746914071037800, 8.314922557961029526, 66.66775706135234714 ) ) ;
#71769 = CARTESIAN_POINT ( 'NONE',  ( 5.823673210054444382, -21.52544592524334988, 85.20942372801901854 ) ) ;
#71770 = CARTESIAN_POINT ( 'NONE',  ( -16.52544592524335698, -4.483927247898792601, 38.95942372801901854 ) ) ;
#71771 = CARTESIAN_POINT ( 'NONE',  ( 16.51473224551069308, 9.474510206698969483, 84.16557627198102409 ) ) ;
#71772 = CARTESIAN_POINT ( 'NONE',  ( -4.379528057220086978, -16.55341960407618274, 19.79275706135235069 ) ) ;
#71773 = CARTESIAN_POINT ( 'NONE',  ( 12.14591786802327356, -12.06949235617739191, 65.62609039468568994 ) ) ;
#71774 = CARTESIAN_POINT ( 'NONE',  ( 16.51473224551083163, -9.474510206698727899, 20.83442372801899722 ) ) ;
#71775 = CARTESIAN_POINT ( 'NONE',  ( -19.03943276465977164, -0.05219959533935918106, 88.75109039468567573 ) ) ;
#71776 = CARTESIAN_POINT ( 'NONE',  ( 13.97604488694527802, 13.89961937509977652, 69.37390960531436690 ) ) ;
#71777 = CARTESIAN_POINT ( 'NONE',  ( -21.52544592524343514, 5.823673210054127303, 81.04057627198102409 ) ) ;
#71779 = CARTESIAN_POINT ( 'NONE',  ( 19.05341960407617918, -5.049401038297876454, 96.04275706135231871 ) ) ;
#71778 = CARTESIAN_POINT ( 'NONE',  ( -8.314922557960811034, -14.29746914071050412, 87.08224293864769550 ) ) ;
#71780 = CARTESIAN_POINT ( 'NONE',  ( -8.314922557961024197, 14.29746914071037800, 57.91775706135234714 ) ) ;
#71781 = CARTESIAN_POINT ( 'NONE',  ( 24.04614410382215084, 5.408324479805897589, 174.2944578187874072 ) ) ;
#71782 = CARTESIAN_POINT ( 'NONE',  ( 19.05341960407617918, -5.049401038297876454, 61.04275706135232582 ) ) ;
#71783 = CARTESIAN_POINT ( 'NONE',  ( -4.483927247898539470, -16.52544592524342804, 32.29057627198102409 ) ) ;
#71784 = CARTESIAN_POINT ( 'NONE',  ( -8.314922557960811034, -14.29746914071050412, 77.08224293864769550 ) ) ;
#71786 = CARTESIAN_POINT ( 'NONE',  ( -16.20579543436696568, 7.371946100355090792, 39.43479165828050270 ) ) ;
#71785 = CARTESIAN_POINT ( 'NONE',  ( -5.719274019375665041, -21.55341960407619695, 109.7927570613523613 ) ) ;
#71787 = CARTESIAN_POINT ( 'NONE',  ( 21.55341960407619695, -5.719274019375665929, 21.04275706135234714 ) ) ;
#71788 =( BOUNDED_SURFACE ( )  B_SPLINE_SURFACE ( 1, 2, ( 
 ( #184660, #153316, #170481, #107796, #169480, #17802, #187660, #31971, #32968, #14817, #183676, #95615, #45161, #106817, #168491, #29989, #94622, #93627, #15808, #76478, #16801, #172470, #79459, #141128, #2618, #125962, #124972, #199836, #47144, #171479, #92628, #616, #49131, #78451, #77469, #110789, #60310, #62286, #1616, #123954, #138155, #63292, #61303, #185652, #48139, #108802, #33957, #18797, #53091, #85427, #96598, #7581, #54106, #115780, #129912, #158287, #143103, #69267, #35932, #20762, #174463, #4582, #126938, #6582, #130933, #159266, #146097, #175453, #99597, #51111, #23777, #84420, #177469, #128924, #173473, #3600, #19776, #36924, #81417, #66275, #38938, #144106, #5586, #98586, #68261, #100595, #67266, #97578, #145099, #82417, #192624, #190625, #162277, #114769, #65279, #188646, #50125, #52100, #37936, #111785, #191612 ),
 ( #160280, #112770, #34946, #21771, #127934, #189636, #176463, #113757, #83422, #161277, #22772, #28772, #39930, #151118, #197614, #59079, #73290, #132943, #42939, #167273, #194631, #88427, #164299, #56101, #26785, #181461, #118790, #195643, #147118, #9613, #134960, #70278, #8605, #165292, #196638, #71278, #89429, #120746, #58107, #102613, #180479, #119777, #87438, #41950, #133952, #27787, #117782, #86436, #131946, #179476, #150121, #103616, #25792, #43925, #40941, #149123, #104603, #12610, #178463, #10614, #101599, #163287, #193630, #11622, #24788, #166291, #182445, #74274, #135944, #105587, #55102, #116772, #148122, #72275, #57116, #154074, #187420, #78208, #153070, #62047, #140881, #124725, #156055, #152095, #185409, #172224, #44917, #29746, #94375, #122731, #107555, #61059, #91381, #13579, #93380, #17552, #45902, #32723, #123712, #186423, #137910 ) ),
 .UNSPECIFIED., .F., .F., .T. ) 
 B_SPLINE_SURFACE_WITH_KNOTS ( ( 2, 2 ),
 ( 3, 2, 2, 2, 2, 2, 2, 2, 2, 2, 2, 2, 2, 2, 2, 2, 2, 2, 2, 2, 2, 2, 2, 2, 2, 2, 2, 2, 2, 2, 2, 2, 2, 2, 2, 2, 2, 2, 2, 2, 2, 2, 2, 2, 2, 2, 2, 2, 2, 2, 3 ),
 ( 0.000000000000000000, 1.000000000000000000 ),
 ( 0.000000000000000000, 0.02000000000000000042, 0.04000000000000000083, 0.05999999999999999778, 0.08000000000000000167, 0.1000000000000000056, 0.1199999999999999956, 0.1400000000000000133, 0.1600000000000000033, 0.1799999999999999933, 0.2000000000000000111, 0.2200000000000000011, 0.2399999999999999911, 0.2600000000000000089, 0.2800000000000000266, 0.2999999999999999889, 0.3200000000000000067, 0.3400000000000000244, 0.3599999999999999867, 0.3800000000000000044, 0.4000000000000000222, 0.4199999999999999845, 0.4400000000000000022, 0.4600000000000000200, 0.4799999999999999822, 0.5000000000000000000, 0.5200000000000000178, 0.5400000000000000355, 0.5600000000000000533, 0.5799999999999999600, 0.5999999999999999778, 0.6199999999999999956, 0.6400000000000000133, 0.6600000000000000311, 0.6800000000000000488, 0.6999999999999999556, 0.7199999999999999734, 0.7399999999999999911, 0.7600000000000000089, 0.7800000000000000266, 0.8000000000000000444, 0.8199999999999999512, 0.8399999999999999689, 0.8599999999999999867, 0.8800000000000000044, 0.9000000000000000222, 0.9200000000000000400, 0.9399999999999999467, 0.9599999999999999645, 0.9799999999999999822, 1.000000000000000000 ),
 .UNSPECIFIED. ) 
 GEOMETRIC_REPRESENTATION_ITEM ( )  RATIONAL_B_SPLINE_SURFACE ( (
 ( 1.000000000000000000, 0.9510565162951535312, 1.000000000000000000, 0.9510565162951535312, 1.000000000000000000, 0.9510565162951535312, 1.000000000000000000, 0.9510565162951535312, 1.000000000000000000, 0.9510565162951535312, 1.000000000000000000, 0.9510565162951535312, 1.000000000000000000, 0.9510565162951535312, 1.000000000000000000, 0.9510565162951535312, 1.000000000000000000, 0.9510565162951535312, 1.000000000000000000, 0.9510565162951535312, 1.000000000000000000, 0.9510565162951535312, 1.000000000000000000, 0.9510565162951535312, 1.000000000000000000, 0.9510565162951535312, 1.000000000000000000, 0.9510565162951535312, 1.000000000000000000, 0.9510565162951535312, 1.000000000000000000, 0.9510565162951535312, 1.000000000000000000, 0.9510565162951535312, 1.000000000000000000, 0.9510565162951535312, 1.000000000000000000, 0.9510565162951535312, 1.000000000000000000, 0.9510565162951535312, 1.000000000000000000, 0.9510565162951535312, 1.000000000000000000, 0.9510565162951535312, 1.000000000000000000, 0.9510565162951535312, 1.000000000000000000, 0.9510565162951535312, 1.000000000000000000, 0.9510565162951535312, 1.000000000000000000, 0.9510565162951535312, 1.000000000000000000, 0.9510565162951535312, 1.000000000000000000, 0.9510565162951535312, 1.000000000000000000, 0.9510565162951535312, 1.000000000000000000, 0.9510565162951535312, 1.000000000000000000, 0.9510565162951535312, 1.000000000000000000, 0.9510565162951535312, 1.000000000000000000, 0.9510565162951535312, 1.000000000000000000, 0.9510565162951535312, 1.000000000000000000, 0.9510565162951535312, 1.000000000000000000, 0.9510565162951535312, 1.000000000000000000, 0.9510565162951535312, 1.000000000000000000, 0.9510565162951535312, 1.000000000000000000, 0.9510565162951535312, 1.000000000000000000, 0.9510565162951535312, 1.000000000000000000, 0.9510565162951535312, 1.000000000000000000, 0.9510565162951535312, 1.000000000000000000, 0.9510565162951535312, 1.000000000000000000, 0.9510565162951535312, 1.000000000000000000, 0.9510565162951535312, 1.000000000000000000, 0.9510565162951535312, 1.000000000000000000, 0.9510565162951535312, 1.000000000000000000, 0.9510565162951535312, 1.000000000000000000, 0.9510565162951535312, 1.000000000000000000, 0.9510565162951535312, 1.000000000000000000),
 ( 1.000000000000000000, 0.9510565162951535312, 1.000000000000000000, 0.9510565162951535312, 1.000000000000000000, 0.9510565162951535312, 1.000000000000000000, 0.9510565162951535312, 1.000000000000000000, 0.9510565162951535312, 1.000000000000000000, 0.9510565162951535312, 1.000000000000000000, 0.9510565162951535312, 1.000000000000000000, 0.9510565162951535312, 1.000000000000000000, 0.9510565162951535312, 1.000000000000000000, 0.9510565162951535312, 1.000000000000000000, 0.9510565162951535312, 1.000000000000000000, 0.9510565162951535312, 1.000000000000000000, 0.9510565162951535312, 1.000000000000000000, 0.9510565162951535312, 1.000000000000000000, 0.9510565162951535312, 1.000000000000000000, 0.9510565162951535312, 1.000000000000000000, 0.9510565162951535312, 1.000000000000000000, 0.9510565162951535312, 1.000000000000000000, 0.9510565162951535312, 1.000000000000000000, 0.9510565162951535312, 1.000000000000000000, 0.9510565162951535312, 1.000000000000000000, 0.9510565162951535312, 1.000000000000000000, 0.9510565162951535312, 1.000000000000000000, 0.9510565162951535312, 1.000000000000000000, 0.9510565162951535312, 1.000000000000000000, 0.9510565162951535312, 1.000000000000000000, 0.9510565162951535312, 1.000000000000000000, 0.9510565162951535312, 1.000000000000000000, 0.9510565162951535312, 1.000000000000000000, 0.9510565162951535312, 1.000000000000000000, 0.9510565162951535312, 1.000000000000000000, 0.9510565162951535312, 1.000000000000000000, 0.9510565162951535312, 1.000000000000000000, 0.9510565162951535312, 1.000000000000000000, 0.9510565162951535312, 1.000000000000000000, 0.9510565162951535312, 1.000000000000000000, 0.9510565162951535312, 1.000000000000000000, 0.9510565162951535312, 1.000000000000000000, 0.9510565162951535312, 1.000000000000000000, 0.9510565162951535312, 1.000000000000000000, 0.9510565162951535312, 1.000000000000000000, 0.9510565162951535312, 1.000000000000000000, 0.9510565162951535312, 1.000000000000000000, 0.9510565162951535312, 1.000000000000000000, 0.9510565162951535312, 1.000000000000000000, 0.9510565162951535312, 1.000000000000000000, 0.9510565162951535312, 1.000000000000000000, 0.9510565162951535312, 1.000000000000000000, 0.9510565162951535312, 1.000000000000000000, 0.9510565162951535312, 1.000000000000000000) ) ) 
 REPRESENTATION_ITEM ( '' )  SURFACE ( )  );
#71789 = CARTESIAN_POINT ( 'NONE',  ( 5.153800228976335163, 19.02544592524342804, 104.7905762719809957 ) ) ;
#71790 = CARTESIAN_POINT ( 'NONE',  ( 16.51473224551069308, 9.474510206698969483, 84.16557627198102409 ) ) ;
#71791 = CARTESIAN_POINT ( 'NONE',  ( -18.67979575497193778, 10.72451020669871902, 93.33442372801901854 ) ) ;
#71792 = CARTESIAN_POINT ( 'NONE',  ( 9.564922557960805705, 16.46253265017160317, 74.58224293864769550 ) ) ;
#71793 = CARTESIAN_POINT ( 'NONE',  ( 18.62759615963271287, -10.81492255796078972, 43.33224293864769550 ) ) ;
#71794 = CARTESIAN_POINT ( 'NONE',  ( 4.483927247898545687, 16.52544592524342804, 74.79057627198105251 ) ) ;
#71795 = CARTESIAN_POINT ( 'NONE',  ( 16.51473224551069308, 9.474510206698969483, 39.16557627198103120 ) ) ;
#71796 = CARTESIAN_POINT ( 'NONE',  ( -12.14591786802309592, -12.06949235617757132, 91.87390960531436690 ) ) ;
#71797 = CARTESIAN_POINT ( 'NONE',  ( 21.52544592524344225, -5.823673210054117533, 113.5405762719810383 ) ) ;
#71798 = CARTESIAN_POINT ( 'NONE',  ( -10.72451020669870658, -18.67979575497194134, 59.58442372801901854 ) ) ;
#71799 = CARTESIAN_POINT ( 'NONE',  ( 9.474510206698971260, -16.51473224551069308, 27.91557627198103120 ) ) ;
#71800 = CARTESIAN_POINT ( 'NONE',  ( -16.52544592524335698, -4.483927247898792601, 58.95942372801902565 ) ) ;
#71801 = CARTESIAN_POINT ( 'NONE',  ( 18.67979575497194134, -10.72451020669871369, 20.83442372801901143 ) ) ;
#71802 = CARTESIAN_POINT ( 'NONE',  ( -0.05219959533907301413, -21.53943276465977519, 107.4989096053143669 ) ) ;
#71804 = CARTESIAN_POINT ( 'NONE',  ( 19.05341960407611168, 5.049401038298154454, 48.95724293864768129 ) ) ;
#71803 = CARTESIAN_POINT ( 'NONE',  ( 13.97604488694548053, -13.89961937509957401, 40.62609039468564731 ) ) ;
#71805 = FACE_OUTER_BOUND ( 'NONE', #197279, .T. ) ;
#71806 = CARTESIAN_POINT ( 'NONE',  ( -21.55341960407619339, 5.719274019375674811, 68.54275706135234714 ) ) ;
#71807 = CARTESIAN_POINT ( 'NONE',  ( 18.62759615963271287, -10.81492255796078972, 58.33224293864768839 ) ) ;
#71808 = CARTESIAN_POINT ( 'NONE',  ( 16.53943276465976808, -0.05219959533910856209, 33.74890960531436690 ) ) ;
#71810 = CARTESIAN_POINT ( 'NONE',  ( 15.80617190586769283, -15.72974639402175789, 110.6260903946857042 ) ) ;
#71809 = CARTESIAN_POINT ( 'NONE',  ( -15.80617190586768217, 15.72974639402176855, 78.12609039468570415 ) ) ;
#71811 = CARTESIAN_POINT ( 'NONE',  ( 16.52544592524342804, -4.483927247898539470, 53.54057627198103120 ) ) ;
#71812 = CARTESIAN_POINT ( 'NONE',  ( 4.379528057220339221, -16.55341960407611168, 107.7072429386476955 ) ) ;
#71813 = CARTESIAN_POINT ( 'NONE',  ( 13.89961937509957401, 13.97604488694547697, 46.87609039468565442 ) ) ;
#71814 = CARTESIAN_POINT ( 'NONE',  ( -8.314922557961024197, 14.29746914071037800, 102.9177570613523756 ) ) ;
#71815 = CARTESIAN_POINT ( 'NONE',  ( -5.823673210054431948, 21.52544592524334988, 67.70942372801901854 ) ) ;
#71816 = CARTESIAN_POINT ( 'NONE',  ( -13.89961937509977652, 13.97604488694528158, 55.62390960531434558 ) ) ;
#71817 = CARTESIAN_POINT ( 'NONE',  ( -5.153800228976607833, 19.02544592524334988, 32.70942372801899722 ) ) ;
#71818 = CARTESIAN_POINT ( 'NONE',  ( 21.55341960407610458, 5.719274019375980345, 38.95724293864768839 ) ) ;
#71819 = CARTESIAN_POINT ( 'NONE',  ( 15.80617190586769283, -15.72974639402175789, 30.62609039468567929 ) ) ;
#71820 = CARTESIAN_POINT ( 'NONE',  ( 5.719274019375991003, -21.55341960407610458, 82.70724293864770971 ) ) ;
#71821 = CARTESIAN_POINT ( 'NONE',  ( 9.564922557961047289, -16.46253265017146816, 80.41775706135234714 ) ) ;
#71822 = CARTESIAN_POINT ( 'NONE',  ( -8.314922557961024197, 14.29746914071037800, 47.91775706135234714 ) ) ;
#71824 = CARTESIAN_POINT ( 'NONE',  ( -5.823673210054116645, -21.52544592524344225, 87.29057627198103830 ) ) ;
#71823 = CARTESIAN_POINT ( 'NONE',  ( 17.50000000000050449, -4.380085919831727459, 36.54968126928942240 ) ) ;
#71825 = CARTESIAN_POINT ( 'NONE',  ( 16.53943276465976808, -0.05219959533910856209, 73.74890960531433848 ) ) ;
#71826 = CARTESIAN_POINT ( 'NONE',  ( -26.58214507596518672, -26.75488679838906947, -20.35119661315286521 ) ) ;
#71827 = CARTESIAN_POINT ( 'NONE',  ( -16.52544592524335698, -4.483927247898792601, 18.95942372801901143 ) ) ;
#71828 = CARTESIAN_POINT ( 'NONE',  ( -5.719274019375978568, 21.55341960407610458, 45.20724293864769550 ) ) ;
#71829 = CARTESIAN_POINT ( 'NONE',  ( -16.53943276465976808, -0.05219959533934237506, 78.75109039468568994 ) ) ;
#71830 = CARTESIAN_POINT ( 'NONE',  ( 22.00000000000000000, -5.510910596163089556E-15, 42.49999999999999289 ) ) ;
#71831 = CARTESIAN_POINT ( 'NONE',  ( 12.06949235617739724, 12.14591786802326823, 51.87609039468568284 ) ) ;
#71832 = CARTESIAN_POINT ( 'NONE',  ( -10.81492255796105439, 18.62759615963255655, 27.91775706135234358 ) ) ;
#71833 = CARTESIAN_POINT ( 'NONE',  ( -21.52544592524343514, 5.823673210054127303, 46.04057627198103830 ) ) ;
#71834 = CARTESIAN_POINT ( 'NONE',  ( -14.34966873604972548, 8.224510206698743886, 68.33442372801900433 ) ) ;
#71835 = CARTESIAN_POINT ( 'NONE',  ( -19.05341960407611168, -5.049401038298163336, 101.4572429386476955 ) ) ;
#71837 = CARTESIAN_POINT ( 'NONE',  ( -16.46253265017160317, 9.564922557960807481, 30.83224293864769550 ) ) ;
#71836 = CARTESIAN_POINT ( 'NONE',  ( -5.823673210054431948, 21.52544592524334988, 62.70942372801902565 ) ) ;
#71838 = CARTESIAN_POINT ( 'NONE',  ( -5.823673210054116645, -21.52544592524344225, 37.29057627198102409 ) ) ;
#71839 = CARTESIAN_POINT ( 'NONE',  ( -21.52544592524343514, 5.823673210054127303, 26.04057627198103475 ) ) ;
#71840 = ORIENTED_EDGE ( 'NONE', *, *, #100439, .F. ) ;
#71841 = CARTESIAN_POINT ( 'NONE',  ( 9.474510206698729675, 16.51473224551082808, 37.08442372801899722 ) ) ;
#71842 = CARTESIAN_POINT ( 'NONE',  ( 16.55341960407618274, -4.379528057220086978, 56.04275706135235424 ) ) ;
#71843 = CARTESIAN_POINT ( 'NONE',  ( 5.049401038298161559, -19.05341960407611168, 112.7072429386476813 ) ) ;
#71844 = VERTEX_POINT ( 'NONE', #92959 ) ;
#71845 = CARTESIAN_POINT ( 'NONE',  ( -5.153800228976328057, -19.02544592524343514, 82.29057627198103830 ) ) ;
#71846 = CARTESIAN_POINT ( 'NONE',  ( 4.483927247898790824, -16.52544592524335698, 95.20942372801903275 ) ) ;
#71847 = DIRECTION ( 'NONE',  ( -0.000000000000000000, -0.000000000000000000, -1.000000000000000000 ) ) ;
#71848 = CARTESIAN_POINT ( 'NONE',  ( -8.224510206698948167, 14.34966873604960824, 90.41557627198103830 ) ) ;
#71849 = CARTESIAN_POINT ( 'NONE',  ( 5.823673210054125526, 21.52544592524343514, 54.79057627198104541 ) ) ;
#71850 = CARTESIAN_POINT ( 'NONE',  ( -5.153800228976328057, -19.02544592524343514, 32.29057627198102409 ) ) ;
#71851 = CARTESIAN_POINT ( 'NONE',  ( -12.06949235617739369, -12.14591786802326823, 79.37609039468567573 ) ) ;
#71852 = CARTESIAN_POINT ( 'NONE',  ( 10.81492255796106328, -18.62759615963255655, 35.41775706135234003 ) ) ;
#71853 = CARTESIAN_POINT ( 'NONE',  ( 19.05341960407617918, -5.049401038297876454, 91.04275706135234714 ) ) ;
#71854 = CARTESIAN_POINT ( 'NONE',  ( -13.89961937509977652, 13.97604488694528158, 45.62390960531433848 ) ) ;
#71855 = CARTESIAN_POINT ( 'NONE',  ( -5.153800228976328057, -19.02544592524343514, 107.2905762719810383 ) ) ;
#71856 = CARTESIAN_POINT ( 'NONE',  ( 18.62759615963255655, 10.81492255796105972, 101.6677570613523613 ) ) ;
#71857 = CARTESIAN_POINT ( 'NONE',  ( 19.05341960407611168, 5.049401038298154454, 78.95724293864769550 ) ) ;
#71858 = CARTESIAN_POINT ( 'NONE',  ( 12.06949235617739724, 12.14591786802326823, 66.87609039468568994 ) ) ;
#71859 = CARTESIAN_POINT ( 'NONE',  ( -10.81492255796105439, 18.62759615963255655, 92.91775706135236135 ) ) ;
#71860 = CARTESIAN_POINT ( 'NONE',  ( -5.049401038297874678, -19.05341960407617918, 49.79275706135231871 ) ) ;
#71861 = CARTESIAN_POINT ( 'NONE',  ( -19.03943276465977164, -0.05219959533935918106, 63.75109039468566863 ) ) ;
#71862 = ORIENTED_EDGE ( 'NONE', *, *, #196878, .F. ) ;
#71863 = CARTESIAN_POINT ( 'NONE',  ( -18.67979575497193778, 10.72451020669871902, 63.33442372801900433 ) ) ;
#71864 = CARTESIAN_POINT ( 'NONE',  ( -19.05341960407611168, -5.049401038298163336, 66.45724293864769550 ) ) ;
#71865 = CARTESIAN_POINT ( 'NONE',  ( 15.50000000000000178, -5.500000000000000888, 22.00000000000000711 ) ) ;
#71866 = CARTESIAN_POINT ( 'NONE',  ( -5.049401038297874678, -19.05341960407617918, 54.79275706135234003 ) ) ;
#71867 = FACE_OUTER_BOUND ( 'NONE', #5882, .T. ) ;
#71868 = CARTESIAN_POINT ( 'NONE',  ( -0.05219959533909027116, -19.03943276465977164, 82.49890960531436690 ) ) ;
#71869 = CARTESIAN_POINT ( 'NONE',  ( -14.29746914071049879, 8.314922557960819915, 40.83224293864769550 ) ) ;
#71870 = CARTESIAN_POINT ( 'NONE',  ( 10.72451020669898902, -18.67979575497178502, 37.91557627198102409 ) ) ;
#71871 = CARTESIAN_POINT ( 'NONE',  ( -18.09918380851993192, -5.500000000000014211, 96.48618307335613054 ) ) ;
#71872 = CARTESIAN_POINT ( 'NONE',  ( 5.049401038297881783, 19.05341960407617563, 22.29275706135233648 ) ) ;
#71873 = FACE_OUTER_BOUND ( 'NONE', #155655, .T. ) ;
#71874 = CARTESIAN_POINT ( 'NONE',  ( 5.049401038298161559, -19.05341960407611168, 42.70724293864767418 ) ) ;
#71875 = CARTESIAN_POINT ( 'NONE',  ( 9.564922557960805705, 16.46253265017160317, 29.58224293864769550 ) ) ;
#71876 = DIRECTION ( 'NONE',  ( 0.000000000000000000, 0.000000000000000000, 1.000000000000000000 ) ) ;
#71877 = CARTESIAN_POINT ( 'NONE',  ( 15.80617190586769283, -15.72974639402175789, 70.62609039468567573 ) ) ;
#71878 = DIRECTION ( 'NONE',  ( 0.000000000000000000, 0.000000000000000000, 1.000000000000000000 ) ) ;
#71879 = CARTESIAN_POINT ( 'NONE',  ( 16.55341960407618274, -4.379528057220086978, 66.04275706135236135 ) ) ;
#71880 = CARTESIAN_POINT ( 'NONE',  ( 10.81492255796078972, 18.62759615963270932, 79.58224293864769550 ) ) ;
#71881 = CARTESIAN_POINT ( 'NONE',  ( 16.55341960407611168, 4.379528057220329451, 48.95724293864770971 ) ) ;
#71883 = CARTESIAN_POINT ( 'NONE',  ( -9.564922557960796823, -16.46253265017161027, 107.0822429386476955 ) ) ;
#71882 = CARTESIAN_POINT ( 'NONE',  ( -5.153800228976328057, -19.02544592524343514, 27.29057627198103120 ) ) ;
#71884 = CARTESIAN_POINT ( 'NONE',  ( 21.52544592524334988, 5.823673210054432836, 31.45942372801901854 ) ) ;
#71885 = CARTESIAN_POINT ( 'NONE',  ( -9.474510206698720793, -16.51473224551083518, 49.58442372801899722 ) ) ;
#71886 = CARTESIAN_POINT ( 'NONE',  ( 0.05219959533909260263, 19.03943276465977164, 29.99890960531435979 ) ) ;
#71887 = CARTESIAN_POINT ( 'NONE',  ( 15.72974639402176855, 15.80617190586768217, 86.87609039468568994 ) ) ;
#71888 = CARTESIAN_POINT ( 'NONE',  ( 17.26058549869090086, -6.457015423128600773, 31.12254162523932166 ) ) ;
#71889 = CARTESIAN_POINT ( 'NONE',  ( 12.06949235617757843, -12.14591786802309237, 33.12390960531435979 ) ) ;
#71890 = CARTESIAN_POINT ( 'NONE',  ( 17.50000000000000000, 3.345213924137398820, 112.9123137690565528 ) ) ;
#71891 = CARTESIAN_POINT ( 'NONE',  ( -15.72974639402197994, 15.80617190586746368, 45.62390960531436690 ) ) ;
#71892 = CARTESIAN_POINT ( 'NONE',  ( 8.945614359730875265, -0.6701480022146872884, -63.98123544873406132 ) ) ;
#71893 = CARTESIAN_POINT ( 'NONE',  ( 19.03943276465977164, -0.05219959533909143690, 93.74890960531435269 ) ) ;
#71894 = CARTESIAN_POINT ( 'NONE',  ( 4.379528057220339221, -16.55341960407611168, 87.70724293864769550 ) ) ;
#71895 = CARTESIAN_POINT ( 'NONE',  ( -19.03943276465977164, -0.05219959533935918106, 108.7510903946856615 ) ) ;
#71896 = CARTESIAN_POINT ( 'NONE',  ( 5.719274019375991003, -21.55341960407610458, 57.70724293864770260 ) ) ;
#71897 = ORIENTED_EDGE ( 'NONE', *, *, #37374, .F. ) ;
#71898 = CARTESIAN_POINT ( 'NONE',  ( 16.51473224551069308, 9.474510206698969483, 34.16557627198102409 ) ) ;
#71900 = CARTESIAN_POINT ( 'NONE',  ( 10.81492255796078972, 18.62759615963270932, 94.58224293864769550 ) ) ;
#71899 = CARTESIAN_POINT ( 'NONE',  ( -16.51473224551069308, -9.474510206698971260, 81.66557627198103830 ) ) ;
#71902 = CARTESIAN_POINT ( 'NONE',  ( -13.97604488694527625, -13.89961937509977652, 106.8739096053143669 ) ) ;
#71901 = CARTESIAN_POINT ( 'NONE',  ( 4.483927247898790824, -16.52544592524335698, 105.2094237280190328 ) ) ;
#71903 = CARTESIAN_POINT ( 'NONE',  ( -19.02544592524334988, -5.153800228976617603, 73.95942372801900433 ) ) ;
#71904 = CARTESIAN_POINT ( 'NONE',  ( -10.72451020669870658, -18.67979575497194134, 94.58442372801901854 ) ) ;
#71905 = CARTESIAN_POINT ( 'NONE',  ( -18.67979575497178146, -10.72451020669898902, 76.66557627198103830 ) ) ;
#71906 = CARTESIAN_POINT ( 'NONE',  ( 15.72974639402199770, -15.80617190586745480, 38.12390960531436690 ) ) ;
#71907 = CARTESIAN_POINT ( 'NONE',  ( 13.89961937509977652, -13.97604488694527269, 48.12390960531435979 ) ) ;
#71908 = CARTESIAN_POINT ( 'NONE',  ( -16.55341960407617563, 4.379528057220093196, 108.5427570613523756 ) ) ;
#71909 = CARTESIAN_POINT ( 'NONE',  ( -0.05219959533909027116, -19.03943276465977164, 67.49890960531436690 ) ) ;
#71910 = ORIENTED_EDGE ( 'NONE', *, *, #194452, .F. ) ;
#71911 = CARTESIAN_POINT ( 'NONE',  ( -31.48242569098778176, -7.251655820954945320, 93.02470426148724414 ) ) ;
#71912 = CARTESIAN_POINT ( 'NONE',  ( -13.97604488694547697, 13.89961937509957934, 33.12609039468566863 ) ) ;
#71913 = CARTESIAN_POINT ( 'NONE',  ( -12.06949235617756955, 12.14591786802309770, 75.62390960531439532 ) ) ;
#71914 = CARTESIAN_POINT ( 'NONE',  ( 10.81492255796106328, -18.62759615963255655, 25.41775706135235779 ) ) ;
#71915 = CARTESIAN_POINT ( 'NONE',  ( -22.44159573604009950, -16.30477369853688430, 141.5750000027311728 ) ) ;
#71917 = ADVANCED_FACE ( 'NONE', ( #49455 ), #111117, .T. ) ;
#71916 = CARTESIAN_POINT ( 'NONE',  ( -15.80617190586745835, -15.72974639402198527, 56.87390960531436690 ) ) ;
#71918 = CARTESIAN_POINT ( 'NONE',  ( 16.55341960407618274, -4.379528057220086978, 96.04275706135236135 ) ) ;
#71919 = CARTESIAN_POINT ( 'NONE',  ( -12.06949235617756955, 12.14591786802309770, 105.6239096053143669 ) ) ;
#71920 = CARTESIAN_POINT ( 'NONE',  ( 16.51473224551069308, 9.474510206698969483, 79.16557627198103830 ) ) ;
#71921 = CARTESIAN_POINT ( 'NONE',  ( 8.224510206698953496, -14.34966873604960469, 32.91557627198102409 ) ) ;
#71922 = ORIENTED_EDGE ( 'NONE', *, *, #62447, .F. ) ;
#71923 = CARTESIAN_POINT ( 'NONE',  ( -18.62759615963255300, -10.81492255796106328, 44.16775706135234714 ) ) ;
#71924 = CARTESIAN_POINT ( 'NONE',  ( -5.153800228976328057, -19.02544592524343514, 107.2905762719810383 ) ) ;
#71925 = CARTESIAN_POINT ( 'NONE',  ( -15.72974639402176322, -15.80617190586768395, 79.37609039468567573 ) ) ;
#71926 = CARTESIAN_POINT ( 'NONE',  ( -9.474510206698964154, 16.51473224551069663, 30.41557627198102054 ) ) ;
#71927 = CARTESIAN_POINT ( 'NONE',  ( 5.049401038298161559, -19.05341960407611168, 32.70724293864768129 ) ) ;
#71928 = VERTEX_POINT ( 'NONE', #154645 ) ;
#71929 = CARTESIAN_POINT ( 'NONE',  ( 10.72451020669871369, 18.67979575497193778, 92.08442372801901854 ) ) ;
#71930 = CARTESIAN_POINT ( 'NONE',  ( 16.55341960407618274, -4.379528057220086978, 46.04275706135234714 ) ) ;
#71931 = CARTESIAN_POINT ( 'NONE',  ( -10.81492255796105439, 18.62759615963255655, 72.91775706135234714 ) ) ;
#71932 = CARTESIAN_POINT ( 'NONE',  ( 9.474510206698971260, -16.51473224551069308, 107.9155762719810383 ) ) ;
#71933 = CARTESIAN_POINT ( 'NONE',  ( -13.97604488694547697, 13.89961937509957934, 98.12609039468566152 ) ) ;
#71934 = CARTESIAN_POINT ( 'NONE',  ( 0.05219959533937995610, -21.53943276465977519, 60.00109039468568284 ) ) ;
#71935 = CARTESIAN_POINT ( 'NONE',  ( -12.14591786802326823, 12.06949235617739902, 23.12609039468567573 ) ) ;
#71936 = CARTESIAN_POINT ( 'NONE',  ( 9.564922557961047289, -16.46253265017146816, 80.41775706135234714 ) ) ;
#71937 = CARTESIAN_POINT ( 'NONE',  ( -19.03943276465977164, 0.05219959533909376836, 46.24890960531435979 ) ) ;
#71938 = CARTESIAN_POINT ( 'NONE',  ( 16.46253265017146816, 9.564922557961045513, 101.6677570613523329 ) ) ;
#71939 = CARTESIAN_POINT ( 'NONE',  ( 16.53943276465976808, -0.05219959533910856209, 23.74890960531435269 ) ) ;
#71940 = CARTESIAN_POINT ( 'NONE',  ( -19.03943276465977164, -0.05219959533935918106, 83.75109039468567573 ) ) ;
#71941 = CARTESIAN_POINT ( 'NONE',  ( 4.379528057220339221, -16.55341960407611168, 47.70724293864770260 ) ) ;
#71942 = CARTESIAN_POINT ( 'NONE',  ( 16.46253265017146816, 9.564922557961045513, 61.66775706135234003 ) ) ;
#71943 = CARTESIAN_POINT ( 'NONE',  ( -4.379528057220086978, -16.55341960407618274, 64.79275706135234714 ) ) ;
#71944 = CARTESIAN_POINT ( 'NONE',  ( 16.46253265017146816, 9.564922557961045513, 21.66775706135233648 ) ) ;
#71945 = CARTESIAN_POINT ( 'NONE',  ( 5.049401038298161559, -19.05341960407611168, 22.70724293864769194 ) ) ;
#71946 = CARTESIAN_POINT ( 'NONE',  ( 16.46253265017160672, -9.564922557960803928, 38.33224293864768839 ) ) ;
#71947 = CARTESIAN_POINT ( 'NONE',  ( 4.483927247898790824, -16.52544592524335698, 55.20942372801902565 ) ) ;
#71948 = LINE ( 'NONE', #137591, #69234 ) ;
#71949 = CARTESIAN_POINT ( 'NONE',  ( 27.73933785331498925, -9.013057229001033122, 147.7750000027311899 ) ) ;
#71950 = CARTESIAN_POINT ( 'NONE',  ( 19.05341960407611168, 5.049401038298154454, 88.95724293864769550 ) ) ;
#71951 = CARTESIAN_POINT ( 'NONE',  ( -13.89961937509957401, -13.97604488694547697, 84.37609039468567573 ) ) ;
#71952 = ORIENTED_EDGE ( 'NONE', *, *, #51668, .T. ) ;
#71953 = CARTESIAN_POINT ( 'NONE',  ( -19.03943276465977164, -0.05219959533935918106, 103.7510903946856757 ) ) ;
#71954 = CARTESIAN_POINT ( 'NONE',  ( -18.62759615963270932, 10.81492255796079327, 35.83224293864768839 ) ) ;
#71956 = CARTESIAN_POINT ( 'NONE',  ( 19.02544592524334988, 5.153800228976608722, 111.4594237280190043 ) ) ;
#71955 = CARTESIAN_POINT ( 'NONE',  ( 0.05219959533936267826, -19.03943276465977164, 25.00109039468566152 ) ) ;
#71957 = CARTESIAN_POINT ( 'NONE',  ( 16.55341960407611168, 4.379528057220329451, 108.9572429386476955 ) ) ;
#71958 = CARTESIAN_POINT ( 'NONE',  ( 9.564922557960805705, 16.46253265017160317, 34.58224293864770260 ) ) ;
#71959 = CARTESIAN_POINT ( 'NONE',  ( -18.62759615963270932, 10.81492255796079327, 70.83224293864770971 ) ) ;
#71960 = CARTESIAN_POINT ( 'NONE',  ( -13.89961937509977652, 13.97604488694528158, 30.62390960531435269 ) ) ;
#71961 = CARTESIAN_POINT ( 'NONE',  ( 17.14385361876520264, -23.59649016807270883, 142.0750000027311444 ) ) ;
#71962 = CARTESIAN_POINT ( 'NONE',  ( 19.03943276465977164, 0.05219959533936151252, 81.25109039468567573 ) ) ;
#71963 = CARTESIAN_POINT ( 'NONE',  ( 16.52544592524342804, -4.483927247898539470, 53.54057627198103120 ) ) ;
#71964 = CARTESIAN_POINT ( 'NONE',  ( -5.823673210054116645, -21.52544592524344225, 27.29057627198103120 ) ) ;
#71965 = CARTESIAN_POINT ( 'NONE',  ( 18.67979575497194134, -10.72451020669871369, 90.83442372801901854 ) ) ;
#71966 = CARTESIAN_POINT ( 'NONE',  ( 21.55341960407610458, 5.719274019375980345, 83.95724293864770971 ) ) ;
#71967 = CARTESIAN_POINT ( 'NONE',  ( -15.80617190586768217, 15.72974639402176855, 78.12609039468570415 ) ) ;
#71968 = CARTESIAN_POINT ( 'NONE',  ( 21.52544592524334988, 5.823673210054432836, 66.45942372801903275 ) ) ;
#71969 = CARTESIAN_POINT ( 'NONE',  ( -19.03943276465977164, 0.05219959533909376836, 116.2489096053143669 ) ) ;
#71971 = CARTESIAN_POINT ( 'NONE',  ( 21.55341960407619695, -5.719274019375665929, 61.04275706135234714 ) ) ;
#71970 = CARTESIAN_POINT ( 'NONE',  ( 16.53943276465976808, 0.05219959533934440121, 111.2510903946856899 ) ) ;
#71972 = CARTESIAN_POINT ( 'NONE',  ( -9.564922557960796823, -16.46253265017161027, 57.08224293864769550 ) ) ;
#71973 = CARTESIAN_POINT ( 'NONE',  ( 18.62759615963255655, 10.81492255796105972, 36.66775706135234714 ) ) ;
#71974 = CARTESIAN_POINT ( 'NONE',  ( 5.049401038298161559, -19.05341960407611168, 72.70724293864768129 ) ) ;
#71975 = CARTESIAN_POINT ( 'NONE',  ( 4.483927247898545687, 16.52544592524342804, 79.79057627198102409 ) ) ;
#71976 = CARTESIAN_POINT ( 'NONE',  ( -14.29746914071049879, 8.314922557960819915, 50.83224293864770971 ) ) ;
#71977 = CARTESIAN_POINT ( 'NONE',  ( 15.72974639402199770, -15.80617190586745480, 58.12390960531435979 ) ) ;
#71978 = CARTESIAN_POINT ( 'NONE',  ( 13.89961937509977652, -13.97604488694527269, 48.12390960531435979 ) ) ;
#71979 = CARTESIAN_POINT ( 'NONE',  ( -10.81492255796078084, -18.62759615963271287, 62.08224293864769550 ) ) ;
#71980 = CARTESIAN_POINT ( 'NONE',  ( 9.474510206698729675, 16.51473224551082808, 52.08442372801900433 ) ) ;
#71982 = CARTESIAN_POINT ( 'NONE',  ( -4.483927247898539470, -16.52544592524342804, 67.29057627198103830 ) ) ;
#71981 = CARTESIAN_POINT ( 'NONE',  ( 13.97604488694548053, -13.89961937509957401, 20.62609039468567218 ) ) ;
#71983 = CARTESIAN_POINT ( 'NONE',  ( -18.62759615963270932, 10.81492255796079327, 45.83224293864769550 ) ) ;
#71984 = ORIENTED_EDGE ( 'NONE', *, *, #69472, .T. ) ;
#71985 = CARTESIAN_POINT ( 'NONE',  ( 19.24578484527059175, -180.9428398739492820, -1.787262988391354872E-28 ) ) ;
#71987 = CARTESIAN_POINT ( 'NONE',  ( 0.7618971401916020403, 6.292798783326192691, -64.49505886858686665 ) ) ;
#71986 = CARTESIAN_POINT ( 'NONE',  ( 4.379528057220092307, 16.55341960407617563, 87.29275706135236135 ) ) ;
#71988 = ADVANCED_FACE ( 'NONE', ( #157633 ), #95947, .T. ) ;
#71989 = CARTESIAN_POINT ( 'NONE',  ( 9.474510206698729675, 16.51473224551082808, 87.08442372801900433 ) ) ;
#71990 = CARTESIAN_POINT ( 'NONE',  ( 14.34966873604960469, 8.224510206698951720, 59.16557627198103120 ) ) ;
#71991 = DIRECTION ( 'NONE',  ( 0.000000000000000000, 0.000000000000000000, 1.000000000000000000 ) ) ;
#71992 = CARTESIAN_POINT ( 'NONE',  ( 0.05219959533909260263, 19.03943276465977164, 49.99890960531435979 ) ) ;
#71993 = CARTESIAN_POINT ( 'NONE',  ( 4.483927247898545687, 16.52544592524342804, 44.79057627198103120 ) ) ;
#71994 = CARTESIAN_POINT ( 'NONE',  ( -16.46253265017160317, 9.564922557960807481, 90.83224293864769550 ) ) ;
#71995 = CARTESIAN_POINT ( 'NONE',  ( 19.03943276465977164, -0.05219959533909143690, 48.74890960531435979 ) ) ;
#71996 = CARTESIAN_POINT ( 'NONE',  ( -15.72974639402176322, -15.80617190586768395, 54.37609039468568994 ) ) ;
#71997 = CARTESIAN_POINT ( 'NONE',  ( 19.03943276465977164, -0.05219959533909143690, 78.74890960531436690 ) ) ;
#71998 = CARTESIAN_POINT ( 'NONE',  ( -13.89961937509977652, 13.97604488694528158, 25.62390960531434558 ) ) ;
#71999 = CARTESIAN_POINT ( 'NONE',  ( 16.51473224551069308, 9.474510206698969483, 64.16557627198102409 ) ) ;
#72000 = CARTESIAN_POINT ( 'NONE',  ( 18.62759615963271287, -10.81492255796078972, 43.33224293864769550 ) ) ;
#72001 = CARTESIAN_POINT ( 'NONE',  ( 0.05219959533909260263, 19.03943276465977164, 34.99890960531435979 ) ) ;
#72002 = CARTESIAN_POINT ( 'NONE',  ( 5.719274019375991003, -21.55341960407610458, 47.70724293864770260 ) ) ;
#72003 = B_SPLINE_CURVE_WITH_KNOTS ( 'NONE', 3,
 ( #151446, #105918, #163622, #150458, #165619, #148450, #44261, #41276, #196960, #102938, #27118, #136265, #26117, #195976, #180802, #182778, #10941, #117103, #29099, #178798, #72614, #197940 ),
 .UNSPECIFIED., .F., .F.,
 ( 4, 2, 2, 2, 2, 2, 2, 2, 2, 2, 4 ),
 ( 0.000000000000000000, 0.001309639967555287438, 0.001964459951332926061, 0.002291869943221736157, 0.002455574939166141855, 0.002619279935110547120, 0.002782984931054952819, 0.002946689926999358517, 0.003274099918888195501, 0.003928919902665849520, 0.005238559870221154088 ),
 .UNSPECIFIED. ) ;
#72004 = CARTESIAN_POINT ( 'NONE',  ( -16.55341960407617563, 4.379528057220093196, 103.5427570613523613 ) ) ;
#72005 = CARTESIAN_POINT ( 'NONE',  ( 5.153800228976615827, -19.02544592524334988, 20.20942372801899722 ) ) ;
#72007 = CARTESIAN_POINT ( 'NONE',  ( -12.06949235617739369, -12.14591786802326823, 79.37609039468567573 ) ) ;
#72006 = CARTESIAN_POINT ( 'NONE',  ( 12.06949235617739724, 12.14591786802326823, 41.87609039468568284 ) ) ;
#72008 = DIRECTION ( 'NONE',  ( 1.000000000000000000, 0.000000000000000000, 0.000000000000000000 ) ) ;
#72009 = CARTESIAN_POINT ( 'NONE',  ( -14.29746914071037622, -8.314922557961029526, 64.16775706135234714 ) ) ;
#72010 = CARTESIAN_POINT ( 'NONE',  ( -8.224510206698735004, -14.34966873604973081, 59.58442372801901854 ) ) ;
#72011 = CARTESIAN_POINT ( 'NONE',  ( -0.05219959533909027116, -19.03943276465977164, 112.4989096053143669 ) ) ;
#72012 = CARTESIAN_POINT ( 'NONE',  ( 5.049401038298161559, -19.05341960407611168, 32.70724293864768129 ) ) ;
#72013 = CARTESIAN_POINT ( 'NONE',  ( -8.314922557961024197, 14.29746914071037800, 32.91775706135234714 ) ) ;
#72014 = CARTESIAN_POINT ( 'NONE',  ( 13.89961937509977652, -13.97604488694527269, 53.12390960531434558 ) ) ;
#72015 = CARTESIAN_POINT ( 'NONE',  ( -0.05219959533937732626, 21.53943276465977519, 32.50109039468568284 ) ) ;
#72016 = CARTESIAN_POINT ( 'NONE',  ( 16.53943276465976808, 0.05219959533934440121, 41.25109039468568284 ) ) ;
#72017 = CARTESIAN_POINT ( 'NONE',  ( -8.314922557961024197, 14.29746914071037800, 92.91775706135236135 ) ) ;
#72018 = CARTESIAN_POINT ( 'NONE',  ( 18.22780087662121673, 5.500000000000056843, 58.98459894673892023 ) ) ;
#72019 = CARTESIAN_POINT ( 'NONE',  ( -5.719274019375665041, -21.55341960407619695, 99.79275706135234714 ) ) ;
#72020 = CARTESIAN_POINT ( 'NONE',  ( 5.049401038297881783, 19.05341960407617563, 92.29275706135234714 ) ) ;
#72021 = CARTESIAN_POINT ( 'NONE',  ( -13.89961937509957401, -13.97604488694547875, 59.37609039468566863 ) ) ;
#72022 = CARTESIAN_POINT ( 'NONE',  ( -0.05219959533910754901, -16.53943276465976808, 62.49890960531436690 ) ) ;
#72023 = CARTESIAN_POINT ( 'NONE',  ( 13.97604488694527802, 13.89961937509977652, 29.37390960531435979 ) ) ;
#72025 = CARTESIAN_POINT ( 'NONE',  ( -11.74264578624799782, -36.14014761921581709, -3.349999994537626868 ) ) ;
#72024 = CARTESIAN_POINT ( 'NONE',  ( -9.474510206698720793, -16.51473224551083518, 64.58442372801900433 ) ) ;
#72026 = CARTESIAN_POINT ( 'NONE',  ( -0.05219959533937732626, 21.53943276465977519, 67.50109039468568994 ) ) ;
#72027 = CARTESIAN_POINT ( 'NONE',  ( 12.14591786802327356, -12.06949235617739191, 25.62609039468567929 ) ) ;
#72028 = CARTESIAN_POINT ( 'NONE',  ( 16.20579543436677383, 7.371946100355107667, 83.06520834171875833 ) ) ;
#72029 = CARTESIAN_POINT ( 'NONE',  ( -0.05219959533907301413, -21.53943276465977519, 27.49890960531435269 ) ) ;
#72030 = CARTESIAN_POINT ( 'NONE',  ( 16.46253265017146816, 9.564922557961045513, 111.6677570613523329 ) ) ;
#72031 = CARTESIAN_POINT ( 'NONE',  ( 8.906447517083050158, 27.41122689804195645, 147.4000000000000057 ) ) ;
#72032 = CARTESIAN_POINT ( 'NONE',  ( -20.14845677604832375, 11.85354687992394496, 170.0217845860066745 ) ) ;
#72033 = CARTESIAN_POINT ( 'NONE',  ( -19.02544592524342804, 5.153800228976336051, 26.04057627198103120 ) ) ;
#72034 = CARTESIAN_POINT ( 'NONE',  ( -10.81492255796105439, 18.62759615963255655, 107.9177570613523471 ) ) ;
#72035 = CARTESIAN_POINT ( 'NONE',  ( 16.46253265017160672, -9.564922557960803928, 43.33224293864769550 ) ) ;
#72036 = CARTESIAN_POINT ( 'NONE',  ( -18.62759615963255300, -10.81492255796106328, 64.16775706135234714 ) ) ;
#72037 = CARTESIAN_POINT ( 'NONE',  ( 5.823673210054444382, -21.52544592524334988, 105.2094237280190328 ) ) ;
#72038 = CARTESIAN_POINT ( 'NONE',  ( -12.06949235617739369, -12.14591786802326823, 104.3760903946856899 ) ) ;
#72039 = CARTESIAN_POINT ( 'NONE',  ( -19.05341960407611168, -5.049401038298163336, 81.45724293864769550 ) ) ;
#72040 = CARTESIAN_POINT ( 'NONE',  ( -15.80617190586768217, 15.72974639402176855, 58.12609039468568994 ) ) ;
#72041 = CARTESIAN_POINT ( 'NONE',  ( -0.05219959533937732626, 21.53943276465977519, 57.50109039468568994 ) ) ;
#72043 = CARTESIAN_POINT ( 'NONE',  ( 9.564922557960805705, 16.46253265017160317, 109.5822429386476955 ) ) ;
#72042 = CARTESIAN_POINT ( 'NONE',  ( -13.97604488694547697, 13.89961937509957934, 73.12609039468568994 ) ) ;
#72044 = CARTESIAN_POINT ( 'NONE',  ( -16.46253265017160317, 9.564922557960807481, 25.83224293864769194 ) ) ;
#72045 = CARTESIAN_POINT ( 'NONE',  ( -15.80617190586745835, -15.72974639402198527, 96.87390960531436690 ) ) ;
#72046 = CARTESIAN_POINT ( 'NONE',  ( 19.02544592524334988, 5.153800228976608722, 26.45942372801899722 ) ) ;
#72047 = CARTESIAN_POINT ( 'NONE',  ( -12.06949235617756955, 12.14591786802309770, 100.6239096053143811 ) ) ;
#72048 = CARTESIAN_POINT ( 'NONE',  ( 13.89961937509977652, -13.97604488694527269, 48.12390960531435979 ) ) ;
#72049 = CARTESIAN_POINT ( 'NONE',  ( 13.97604488694548053, -13.89961937509957401, 80.62609039468567573 ) ) ;
#72050 = CARTESIAN_POINT ( 'NONE',  ( 4.483927247898545687, 16.52544592524342804, 59.79057627198103120 ) ) ;
#72051 = CARTESIAN_POINT ( 'NONE',  ( -10.81492255796105439, 18.62759615963255655, 102.9177570613523756 ) ) ;
#72052 = CARTESIAN_POINT ( 'NONE',  ( -5.049401038298153566, 19.05341960407611168, 110.2072429386476671 ) ) ;
#72053 = CARTESIAN_POINT ( 'NONE',  ( 13.89961937509957401, 13.97604488694547697, 76.87609039468566152 ) ) ;
#72054 = CARTESIAN_POINT ( 'NONE',  ( 0.05219959533907565091, 21.53943276465977519, 74.99890960531435269 ) ) ;
#72055 = CARTESIAN_POINT ( 'NONE',  ( 15.72974639402176855, 15.80617190586768217, 36.87609039468568994 ) ) ;
#72056 = CARTESIAN_POINT ( 'NONE',  ( 14.34966873604972726, -8.224510206698740333, 30.83442372801902209 ) ) ;
#72057 = CARTESIAN_POINT ( 'NONE',  ( -14.34966873604972548, 8.224510206698743886, 88.33442372801901854 ) ) ;
#72059 = CARTESIAN_POINT ( 'NONE',  ( 5.719274019375673035, 21.55341960407619339, 42.29275706135235424 ) ) ;
#72058 = CARTESIAN_POINT ( 'NONE',  ( -8.314922557961024197, 14.29746914071037800, 42.91775706135235424 ) ) ;
#72060 = CARTESIAN_POINT ( 'NONE',  ( 18.62759615963271287, -10.81492255796078972, 43.33224293864769550 ) ) ;
#72061 = CARTESIAN_POINT ( 'NONE',  ( 5.153800228976335163, 19.02544592524342804, 34.79057627198102409 ) ) ;
#72062 = CARTESIAN_POINT ( 'NONE',  ( -38.00000000000000711, 2.428612866367529932E-14, -7.749999994537626336 ) ) ;
#72064 = VECTOR ( 'NONE', #13689, 1000.000000000000114 ) ;
#72063 = CARTESIAN_POINT ( 'NONE',  ( 16.53943276465976808, 0.05219959533934440121, 66.25109039468567573 ) ) ;
#72065 = CARTESIAN_POINT ( 'NONE',  ( 21.52544592524344225, -5.823673210054117533, 88.54057627198103830 ) ) ;
#72066 = CARTESIAN_POINT ( 'NONE',  ( 16.55341960407611168, 4.379528057220329451, 43.95724293864769550 ) ) ;
#72067 = CARTESIAN_POINT ( 'NONE',  ( -8.224510206698735004, -14.34966873604973081, 49.58442372801901143 ) ) ;
#72068 = CARTESIAN_POINT ( 'NONE',  ( 13.97604488694527802, 13.89961937509977652, 54.37390960531435979 ) ) ;
#72069 = CARTESIAN_POINT ( 'NONE',  ( -16.53943276465976808, -0.05219959533934237506, 88.75109039468567573 ) ) ;
#72070 = CARTESIAN_POINT ( 'NONE',  ( -19.03943276465977164, -0.05219959533935918106, 83.75109039468567573 ) ) ;
#72071 = CARTESIAN_POINT ( 'NONE',  ( 21.53943276465977519, -0.05219959533907433946, 88.74890960531436690 ) ) ;
#72072 = CARTESIAN_POINT ( 'NONE',  ( 8.314922557960818139, 14.29746914071049879, 29.58224293864769905 ) ) ;
#72073 = ORIENTED_EDGE ( 'NONE', *, *, #94442, .T. ) ;
#72074 = CARTESIAN_POINT ( 'NONE',  ( 21.36928693577338834, 7.422813773936193016, 174.5222352431090087 ) ) ;
#72075 = CARTESIAN_POINT ( 'NONE',  ( 5.823673210054125526, 21.52544592524343514, 54.79057627198104541 ) ) ;
#72076 = VERTEX_POINT ( 'NONE', #173808 ) ;
#72077 = CARTESIAN_POINT ( 'NONE',  ( -4.483927247898782831, 16.52544592524335698, 102.7094237280190185 ) ) ;
#72078 = ORIENTED_EDGE ( 'NONE', *, *, #81519, .F. ) ;
#72079 = CARTESIAN_POINT ( 'NONE',  ( 21.55341960407610458, 5.719274019375980345, 28.95724293864769905 ) ) ;
#72080 = CARTESIAN_POINT ( 'NONE',  ( 30.74264578624800137, -22.33583958711395212, -3.200000000000000178 ) ) ;
#72081 = CARTESIAN_POINT ( 'NONE',  ( -21.52544592524343514, 5.823673210054127303, 91.04057627198103830 ) ) ;
#72082 = CARTESIAN_POINT ( 'NONE',  ( -14.34966873604960291, -8.224510206698953496, 26.66557627198103475 ) ) ;
#72083 = CARTESIAN_POINT ( 'NONE',  ( 4.379528057220092307, 16.55341960407617563, 37.29275706135235424 ) ) ;
#72084 = CARTESIAN_POINT ( 'NONE',  ( 9.564922557960805705, 16.46253265017160317, 29.58224293864769550 ) ) ;
#72085 = CARTESIAN_POINT ( 'NONE',  ( 8.314922557961029526, -14.29746914071037800, 30.41775706135234358 ) ) ;
#72086 = CARTESIAN_POINT ( 'NONE',  ( -9.564922557960796823, -16.46253265017161027, 57.08224293864769550 ) ) ;
#72087 = CARTESIAN_POINT ( 'NONE',  ( 23.31738231874054890, -16.94106989632523508, 148.7999999999999829 ) ) ;
#72088 = CARTESIAN_POINT ( 'NONE',  ( 5.153800228976335163, 19.02544592524342804, 109.7905762719810099 ) ) ;
#72089 = CARTESIAN_POINT ( 'NONE',  ( 19.05341960407611168, 5.049401038298154454, 113.9572429386477097 ) ) ;
#72090 = CARTESIAN_POINT ( 'NONE',  ( 12.06949235617739724, 12.14591786802326823, 101.8760903946857042 ) ) ;
#72091 = CARTESIAN_POINT ( 'NONE',  ( -0.05219959533936034679, 19.03943276465977164, 87.50109039468567573 ) ) ;
#72092 = CARTESIAN_POINT ( 'NONE',  ( 5.153800228976615827, -19.02544592524334988, 40.20942372801898301 ) ) ;
#72093 = CARTESIAN_POINT ( 'NONE',  ( 0.05219959533907565091, 21.53943276465977519, 89.99890960531438111 ) ) ;
#72094 = EDGE_CURVE ( 'NONE', #46039, #4246, #111922, .T. ) ;
#72095 = CARTESIAN_POINT ( 'NONE',  ( -14.34966873604960291, -8.224510206698953496, 21.66557627198102409 ) ) ;
#72096 = AXIS2_PLACEMENT_3D ( 'NONE', #6544, #115744, #177431 ) ;
#72097 = CARTESIAN_POINT ( 'NONE',  ( -15.72974639402197994, 15.80617190586746368, 35.62390960531437401 ) ) ;
#72098 = CARTESIAN_POINT ( 'NONE',  ( 5.153800228976615827, -19.02544592524334988, 105.2094237280190185 ) ) ;
#72099 = CARTESIAN_POINT ( 'NONE',  ( 13.97604488694527802, 13.89961937509977652, 109.3739096053143669 ) ) ;
#72100 = CARTESIAN_POINT ( 'NONE',  ( 18.67979575497194134, -10.72451020669871369, 65.83442372801900433 ) ) ;
#72101 = CARTESIAN_POINT ( 'NONE',  ( 0.05219959533909260263, 19.03943276465977164, 59.99890960531436690 ) ) ;
#72102 = CARTESIAN_POINT ( 'NONE',  ( -8.224510206698948167, 14.34966873604960824, 95.41557627198102409 ) ) ;
#72103 = CARTESIAN_POINT ( 'NONE',  ( 31.68361083058364613, 1.948458647159017509, 102.2466786067742959 ) ) ;
#72104 = CARTESIAN_POINT ( 'NONE',  ( 14.34966873604960469, 8.224510206698951720, 84.16557627198103830 ) ) ;
#72105 = ORIENTED_EDGE ( 'NONE', *, *, #141591, .T. ) ;
#72106 = CARTESIAN_POINT ( 'NONE',  ( -13.89961937509957401, -13.97604488694547875, 94.37609039468566152 ) ) ;
#72107 = CARTESIAN_POINT ( 'NONE',  ( -4.500000000000001776, -139.5000000000000000, 21.32407087589996308 ) ) ;
#72108 = CARTESIAN_POINT ( 'NONE',  ( -13.89961937509977652, 13.97604488694528158, 65.62390960531436690 ) ) ;
#72109 = CARTESIAN_POINT ( 'NONE',  ( 16.36317988757097552, -7.306389748694710917, 71.59789608363172420 ) ) ;
#72111 = CARTESIAN_POINT ( 'NONE',  ( -16.46253265017160317, 9.564922557960807481, 100.8322429386477097 ) ) ;
#72110 = CARTESIAN_POINT ( 'NONE',  ( 9.564922557960805705, 16.46253265017160317, 79.58224293864769550 ) ) ;
#72112 = CARTESIAN_POINT ( 'NONE',  ( 12.06949235617739724, 12.14591786802326823, 66.87609039468568994 ) ) ;
#72113 = CARTESIAN_POINT ( 'NONE',  ( -17.13100169013299734, -6.664070546373170423, 49.23210164300151348 ) ) ;
#72114 = B_SPLINE_CURVE_WITH_KNOTS ( 'NONE', 3,
 ( #129290, #175822, #160644, #18169, #83786, #189015, #145465, #2980, #64659, #49490, #172841, #34320, #95983, #65642, #50489, #178831, #134321, #181818, #102971, #164656, #84784, #40300, #146463, #7955, #72647, #24150, #23139, #54471 ),
 .UNSPECIFIED., .F., .F.,
 ( 4, 2, 2, 2, 2, 2, 2, 2, 2, 2, 2, 2, 2, 4 ),
 ( 1.961533960389205320E-07, 0.0003775868847195711629, 0.0007549776160431033488, 0.001132368347366635806, 0.001509759078690167938, 0.002264540541337212252, 0.003019322003984256566, 0.003774103466631300880, 0.004151494197954830843, 0.004528884929278359506, 0.004906275660601889903, 0.005283666391925419432, 0.005661057123248948962, 0.006038447854572478492 ),
 .UNSPECIFIED. ) ;
#72115 = CARTESIAN_POINT ( 'NONE',  ( 9.564922557961047289, -16.46253265017146816, 40.41775706135234003 ) ) ;
#72116 = CARTESIAN_POINT ( 'NONE',  ( 15.80617190586769283, -15.72974639402175789, 95.62609039468568994 ) ) ;
#72117 = FACE_OUTER_BOUND ( 'NONE', #131810, .T. ) ;
#72118 = CARTESIAN_POINT ( 'NONE',  ( -5.153800228976328057, -19.02544592524343514, 107.2905762719810383 ) ) ;
#72119 = CARTESIAN_POINT ( 'NONE',  ( 16.53943276465976808, 0.05219959533934440121, 96.25109039468568994 ) ) ;
#72120 = CARTESIAN_POINT ( 'NONE',  ( -34.77074502975527537, -6.826893893699448768, 41.88499232265944983 ) ) ;
#72121 = CARTESIAN_POINT ( 'NONE',  ( 12.06949235617739724, 12.14591786802326823, 96.87609039468568994 ) ) ;
#72122 = CARTESIAN_POINT ( 'NONE',  ( 0.000000000000000000, 0.000000000000000000, -65.00100000000003320 ) ) ;
#72123 = CARTESIAN_POINT ( 'NONE',  ( -16.52544592524335698, -4.483927247898792601, 68.95942372801901854 ) ) ;
#72124 = DIRECTION ( 'NONE',  ( 0.4999999999999933387, -0.5000000000000055511, 0.7071067811865484609 ) ) ;
#72125 = CARTESIAN_POINT ( 'NONE',  ( -18.62759615963255300, -10.81492255796106328, 84.16775706135234714 ) ) ;
#72126 = CARTESIAN_POINT ( 'NONE',  ( -16.51473224551082808, 9.474510206698731452, 83.33442372801899012 ) ) ;
#72127 = CARTESIAN_POINT ( 'NONE',  ( 16.46253265017146816, 9.564922557961045513, 21.66775706135233648 ) ) ;
#72128 = CARTESIAN_POINT ( 'NONE',  ( -19.05341960407611168, -5.049401038298163336, 61.45724293864769550 ) ) ;
#72129 = CARTESIAN_POINT ( 'NONE',  ( 19.05341960407611168, 5.049401038298154454, 43.95724293864769550 ) ) ;
#72130 = FACE_OUTER_BOUND ( 'NONE', #169521, .T. ) ;
#72131 = CARTESIAN_POINT ( 'NONE',  ( 10.81492255796078972, 18.62759615963270932, 84.58224293864769550 ) ) ;
#72132 = CARTESIAN_POINT ( 'NONE',  ( 18.62759615963271287, -10.81492255796078972, 38.33224293864768839 ) ) ;
#72133 = CARTESIAN_POINT ( 'NONE',  ( 0.05219959533909260263, 19.03943276465977164, 29.99890960531435979 ) ) ;
#72134 = CARTESIAN_POINT ( 'NONE',  ( 16.53943276465976808, 0.05219959533934440121, 56.25109039468568284 ) ) ;
#72135 = ORIENTED_EDGE ( 'NONE', *, *, #113474, .T. ) ;
#72136 = CARTESIAN_POINT ( 'NONE',  ( -15.80617190586768217, 15.72974639402176855, 38.12609039468567573 ) ) ;
#72138 = CARTESIAN_POINT ( 'NONE',  ( 22.81625015709510151, -31.40387420917324590, -7.924999997268812990 ) ) ;
#72137 = CARTESIAN_POINT ( 'NONE',  ( -16.53943276465976808, 0.05219959533911058130, 56.24890960531436690 ) ) ;
#72139 = CARTESIAN_POINT ( 'NONE',  ( -12.14591786802326823, 12.06949235617739902, 23.12609039468567573 ) ) ;
#72140 = CARTESIAN_POINT ( 'NONE',  ( -19.02544592524334988, -5.153800228976617603, 43.95942372801899012 ) ) ;
#72141 = CARTESIAN_POINT ( 'NONE',  ( 12.14591786802309770, 12.06949235617756955, 64.37390960531435269 ) ) ;
#72142 = CARTESIAN_POINT ( 'NONE',  ( -21.53943276465977519, -0.05219959533937600094, 18.75109039468568639 ) ) ;
#72144 = CARTESIAN_POINT ( 'NONE',  ( 15.72974639402199770, -15.80617190586745480, 73.12390960531436690 ) ) ;
#72143 = CARTESIAN_POINT ( 'NONE',  ( 32.00000000000000000, -1.163414459189985801E-14, 95.00000000000000000 ) ) ;
#72145 = CARTESIAN_POINT ( 'NONE',  ( -19.05341960407611168, -5.049401038298163336, 86.45724293864769550 ) ) ;
#72146 = CARTESIAN_POINT ( 'NONE',  ( -0.05219959533910754901, -16.53943276465976808, 67.49890960531436690 ) ) ;
#72147 = CARTESIAN_POINT ( 'NONE',  ( 16.46253265017160672, -9.564922557960803928, 98.33224293864769550 ) ) ;
#72148 = CARTESIAN_POINT ( 'NONE',  ( -18.22780087662119541, 5.500000000000102141, 46.01763182126894947 ) ) ;
#72149 = CARTESIAN_POINT ( 'NONE',  ( -13.89961937509957401, -13.97604488694547875, 74.37609039468566152 ) ) ;
#72150 = CARTESIAN_POINT ( 'NONE',  ( -0.05219959533907301413, -21.53943276465977519, 112.4989096053143669 ) ) ;
#72151 = CARTESIAN_POINT ( 'NONE',  ( 9.474510206698971260, -16.51473224551069308, 62.91557627198102409 ) ) ;
#72152 = CARTESIAN_POINT ( 'NONE',  ( -9.474510206698720793, -16.51473224551083518, 44.58442372801900433 ) ) ;
#72153 = CARTESIAN_POINT ( 'NONE',  ( 0.05219959533909260263, 19.03943276465977164, 24.99890960531435269 ) ) ;
#72154 = AXIS2_PLACEMENT_3D ( 'NONE', #68606, #23118, #176812 ) ;
#72155 = CARTESIAN_POINT ( 'NONE',  ( 18.62759615963255655, 10.81492255796105972, 66.66775706135234714 ) ) ;
#72156 = CARTESIAN_POINT ( 'NONE',  ( -16.61371651742604172, -7.165104196376156587, 71.14584930007008268 ) ) ;
#72157 = CARTESIAN_POINT ( 'NONE',  ( 8.314922557960818139, 14.29746914071049879, 39.58224293864769550 ) ) ;
#72158 = CARTESIAN_POINT ( 'NONE',  ( -13.97604488694527625, -13.89961937509977652, 56.87390960531434558 ) ) ;
#72159 = CARTESIAN_POINT ( 'NONE',  ( 21.55341960407610458, 5.719274019375980345, 68.95724293864769550 ) ) ;
#72160 = CARTESIAN_POINT ( 'NONE',  ( 8.571926809382603096, -26.38167802310801235, 145.4750000027311785 ) ) ;
#72161 = CARTESIAN_POINT ( 'NONE',  ( -16.46253265017160317, 9.564922557960807481, 60.83224293864769550 ) ) ;
#72162 = EDGE_LOOP ( 'NONE', ( #132311, #82652, #43273, #183903 ) ) ;
#72163 = CARTESIAN_POINT ( 'NONE',  ( -0.05219959533907301413, -21.53943276465977519, 72.49890960531435269 ) ) ;
#72164 = ORIENTED_EDGE ( 'NONE', *, *, #169778, .T. ) ;
#72165 = CARTESIAN_POINT ( 'NONE',  ( 21.52544592524334988, 5.823673210054432836, 106.4594237280190328 ) ) ;
#72168 = CARTESIAN_POINT ( 'NONE',  ( 16.52544592524342804, -4.483927247898539470, 78.54057627198103830 ) ) ;
#72167 = CARTESIAN_POINT ( 'NONE',  ( -16.52544592524335698, -4.483927247898792601, 98.95942372801903275 ) ) ;
#72166 = CARTESIAN_POINT ( 'NONE',  ( 6.020883695542538661, -38.43099163646597560, -23.90977630326271353 ) ) ;
#72169 = CARTESIAN_POINT ( 'NONE',  ( -5.049401038298153566, 19.05341960407611168, 65.20724293864765286 ) ) ;
#72170 = ORIENTED_EDGE ( 'NONE', *, *, #112694, .T. ) ;
#72171 = CARTESIAN_POINT ( 'NONE',  ( -19.02544592524334988, -5.153800228976617603, 33.95942372801897591 ) ) ;
#72172 = CARTESIAN_POINT ( 'NONE',  ( 14.29746914071037800, 8.314922557961029526, 86.66775706135234714 ) ) ;
#72173 = EDGE_CURVE ( 'NONE', #94189, #27850, #132602, .T. ) ;
#72174 = CARTESIAN_POINT ( 'NONE',  ( 13.97604488694548053, -13.89961937509957401, 35.62609039468567573 ) ) ;
#72175 = CARTESIAN_POINT ( 'NONE',  ( 16.46253265017160672, -9.564922557960803928, 93.33224293864769550 ) ) ;
#72176 = CARTESIAN_POINT ( 'NONE',  ( -5.719274019375978568, 21.55341960407610458, 55.20724293864770260 ) ) ;
#72177 = CARTESIAN_POINT ( 'NONE',  ( 2.500000000000000000, 0.000000000000000000, 2.041999999999999815 ) ) ;
#72178 = CARTESIAN_POINT ( 'NONE',  ( -5.153800228976328057, -19.02544592524343514, 27.29057627198103120 ) ) ;
#72179 = CARTESIAN_POINT ( 'NONE',  ( -15.80617190586768217, 15.72974639402176855, 98.12609039468570415 ) ) ;
#72180 = CARTESIAN_POINT ( 'NONE',  ( 14.29746914071037800, 8.314922557961029526, 61.66775706135235424 ) ) ;
#72181 = CARTESIAN_POINT ( 'NONE',  ( -21.53943276465977519, -0.05219959533937600094, 28.75109039468567929 ) ) ;
#72182 = CARTESIAN_POINT ( 'NONE',  ( -16.52544592524335698, -4.483927247898792601, 23.95942372801901143 ) ) ;
#72183 = CARTESIAN_POINT ( 'NONE',  ( 5.049401038298161559, -19.05341960407611168, 97.70724293864766707 ) ) ;
#72184 = CARTESIAN_POINT ( 'NONE',  ( -19.05341960407611168, -5.049401038298163336, 41.45724293864769550 ) ) ;
#72185 = CARTESIAN_POINT ( 'NONE',  ( -19.05341960407611168, -5.049401038298163336, 51.45724293864770260 ) ) ;
#72186 = CARTESIAN_POINT ( 'NONE',  ( 4.379528057220092307, 16.55341960407617563, 37.29275706135235424 ) ) ;
#72187 = CARTESIAN_POINT ( 'NONE',  ( -8.224510206698948167, 14.34966873604960824, 95.41557627198102409 ) ) ;
#72188 = CARTESIAN_POINT ( 'NONE',  ( 16.55341960407618274, -4.379528057220086978, 101.0427570613523756 ) ) ;
#72191 = CARTESIAN_POINT ( 'NONE',  ( -19.02544592524342804, 5.153800228976336051, 46.04057627198101699 ) ) ;
#72190 = CARTESIAN_POINT ( 'NONE',  ( 0.05219959533909260263, 19.03943276465977164, 74.99890960531435269 ) ) ;
#72189 = CARTESIAN_POINT ( 'NONE',  ( -10.72451020669870658, -18.67979575497194134, 44.58442372801901854 ) ) ;
#72193 = ADVANCED_FACE ( 'NONE', ( #159598 ), #20100, .T. ) ;
#72192 = CARTESIAN_POINT ( 'NONE',  ( -19.05341960407611168, -5.049401038298163336, 86.45724293864769550 ) ) ;
#72194 = CARTESIAN_POINT ( 'NONE',  ( 14.29746914071049879, -8.314922557960816363, 33.33224293864769550 ) ) ;
#72195 = CARTESIAN_POINT ( 'NONE',  ( 8.224510206698742110, 14.34966873604972548, 97.08442372801904696 ) ) ;
#72196 = VERTEX_POINT ( 'NONE', #114084 ) ;
#72197 = CARTESIAN_POINT ( 'NONE',  ( -19.05341960407617563, 5.049401038297882671, 43.54275706135232582 ) ) ;
#72198 = CARTESIAN_POINT ( 'NONE',  ( 13.97604488694527802, 13.89961937509977652, 114.3739096053143669 ) ) ;
#72199 = CARTESIAN_POINT ( 'NONE',  ( 19.02544592524343514, -5.153800228976328945, 53.54057627198102409 ) ) ;
#72200 = CARTESIAN_POINT ( 'NONE',  ( 16.46253265017146816, 9.564922557961045513, 21.66775706135233648 ) ) ;
#72201 = CARTESIAN_POINT ( 'NONE',  ( 36.91746825000000598, -11.99521256947793546, -7.724999997268812812 ) ) ;
#72202 = CARTESIAN_POINT ( 'NONE',  ( 4.379528057220092307, 16.55341960407617563, 37.29275706135235424 ) ) ;
#72204 = CARTESIAN_POINT ( 'NONE',  ( 8.314922557961029526, -14.29746914071037800, 50.41775706135235424 ) ) ;
#72203 = CARTESIAN_POINT ( 'NONE',  ( 0.05219959533936267826, -19.03943276465977164, 75.00109039468566152 ) ) ;
#72205 = CARTESIAN_POINT ( 'NONE',  ( -9.474510206698964154, 16.51473224551069663, 115.4155762719810241 ) ) ;
#72206 = CARTESIAN_POINT ( 'NONE',  ( 5.153800228976335163, 19.02544592524342804, 79.79057627198102409 ) ) ;
#72207 = CARTESIAN_POINT ( 'NONE',  ( 21.52544592524334988, 5.823673210054432836, 21.45942372801901499 ) ) ;
#72208 = CARTESIAN_POINT ( 'NONE',  ( -13.97604488694547697, 13.89961937509957934, 83.12609039468564731 ) ) ;
#72210 = CARTESIAN_POINT ( 'NONE',  ( -9.474510206698964154, 16.51473224551069663, 30.41557627198102054 ) ) ;
#72209 = CARTESIAN_POINT ( 'NONE',  ( -5.049401038298153566, 19.05341960407611168, 105.2072429386476671 ) ) ;
#72211 = CARTESIAN_POINT ( 'NONE',  ( 0.05219959533909260263, 19.03943276465977164, 74.99890960531435269 ) ) ;
#72213 = CARTESIAN_POINT ( 'NONE',  ( 5.153800228976335163, 19.02544592524342804, 34.79057627198102409 ) ) ;
#72212 = CARTESIAN_POINT ( 'NONE',  ( 16.53943276465976808, -0.05219959533910856209, 28.74890960531435624 ) ) ;
#72214 = CARTESIAN_POINT ( 'NONE',  ( -19.05341960407617563, 5.049401038297882671, 53.54275706135231871 ) ) ;
#72215 = CARTESIAN_POINT ( 'NONE',  ( -12.14591786802309592, -12.06949235617757132, 76.87390960531439532 ) ) ;
#72216 = CARTESIAN_POINT ( 'NONE',  ( 9.474510206698729675, 16.51473224551082808, 22.08442372801899722 ) ) ;
#72217 = CARTESIAN_POINT ( 'NONE',  ( -5.049401038298153566, 19.05341960407611168, 50.20724293864770260 ) ) ;
#72218 = CARTESIAN_POINT ( 'NONE',  ( 10.72451020669898902, -18.67979575497178502, 52.91557627198103830 ) ) ;
#72220 = CARTESIAN_POINT ( 'NONE',  ( 15.80617190586769283, -15.72974639402175789, 100.6260903946857184 ) ) ;
#72219 = CARTESIAN_POINT ( 'NONE',  ( -16.53943276465976808, 0.05219959533911058130, 51.24890960531436690 ) ) ;
#72221 = CARTESIAN_POINT ( 'NONE',  ( 9.564922557960805705, 16.46253265017160317, 94.58224293864769550 ) ) ;
#72222 = CARTESIAN_POINT ( 'NONE',  ( 13.97604488694527802, 13.89961937509977652, 114.3739096053143669 ) ) ;
#72223 = CARTESIAN_POINT ( 'NONE',  ( -19.05341960407611168, -5.049401038298163336, 41.45724293864769550 ) ) ;
#72224 = CARTESIAN_POINT ( 'NONE',  ( -8.224510206698948167, 14.34966873604960824, 115.4155762719810241 ) ) ;
#72225 = CARTESIAN_POINT ( 'NONE',  ( 8.314922557960818139, 14.29746914071049879, 89.58224293864768129 ) ) ;
#72226 = CARTESIAN_POINT ( 'NONE',  ( -21.53943276465977519, 0.05219959533907696930, 101.2489096053143669 ) ) ;
#72227 = CARTESIAN_POINT ( 'NONE',  ( -13.89961937509977652, 13.97604488694528158, 85.62390960531433848 ) ) ;
#72228 = CARTESIAN_POINT ( 'NONE',  ( 0.05219959533907565091, 21.53943276465977519, 114.9989096053143669 ) ) ;
#72229 = CARTESIAN_POINT ( 'NONE',  ( -5.049401038298153566, 19.05341960407611168, 95.20724293864770971 ) ) ;
#72231 = CARTESIAN_POINT ( 'NONE',  ( 12.14591786802309770, 12.06949235617756955, 104.3739096053143669 ) ) ;
#72230 = DIRECTION ( 'NONE',  ( 1.000000000000000000, 0.000000000000000000, 0.000000000000000000 ) ) ;
#72232 = CARTESIAN_POINT ( 'NONE',  ( 5.049401038298161559, -19.05341960407611168, 72.70724293864768129 ) ) ;
#72233 = CARTESIAN_POINT ( 'NONE',  ( 0.05219959533907565091, 21.53943276465977519, 79.99890960531435269 ) ) ;
#72234 = CARTESIAN_POINT ( 'NONE',  ( 5.000000000000000000, -120.6140767358124180, 14.26817184396703020 ) ) ;
#72236 = CARTESIAN_POINT ( 'NONE',  ( 1.300000000000000044, 1.443375672974065216, 7.017607234860990640E-28 ) ) ;
#72235 = CARTESIAN_POINT ( 'NONE',  ( -18.62759615963270932, 10.81492255796079327, 25.83224293864769194 ) ) ;
#72237 = CARTESIAN_POINT ( 'NONE',  ( -16.53943276465976808, -0.05219959533934237506, 33.75109039468568284 ) ) ;
#72238 = CARTESIAN_POINT ( 'NONE',  ( -14.29746914071049879, 8.314922557960819915, 100.8322429386477097 ) ) ;
#72239 = CARTESIAN_POINT ( 'NONE',  ( -17.49999999999999645, -5.500000000000000000, 111.2823096230356725 ) ) ;
#72240 = CARTESIAN_POINT ( 'NONE',  ( 5.049401038298161559, -19.05341960407611168, 82.70724293864770971 ) ) ;
#72241 = CARTESIAN_POINT ( 'NONE',  ( 19.03943276465977164, -0.05219959533909143690, 43.74890960531435979 ) ) ;
#72242 = CARTESIAN_POINT ( 'NONE',  ( 16.55341960407611168, 4.379528057220329451, 73.95724293864769550 ) ) ;
#72243 = CARTESIAN_POINT ( 'NONE',  ( -21.52544592524343514, 5.823673210054127303, 36.04057627198102409 ) ) ;
#72244 = CARTESIAN_POINT ( 'NONE',  ( 16.52544592524342804, -4.483927247898539470, 53.54057627198103120 ) ) ;
#72245 = CARTESIAN_POINT ( 'NONE',  ( -19.05341960407617563, 5.049401038297882671, 108.5427570613523187 ) ) ;
#72246 = CARTESIAN_POINT ( 'NONE',  ( 15.72974639402176855, 15.80617190586768217, 71.87609039468568994 ) ) ;
#72247 = CARTESIAN_POINT ( 'NONE',  ( -27.73933785331498925, -9.013057229001049109, 144.9750000027312069 ) ) ;
#72248 = CARTESIAN_POINT ( 'NONE',  ( 5.153800228976335163, 19.02544592524342804, 109.7905762719810099 ) ) ;
#72249 = CARTESIAN_POINT ( 'NONE',  ( -4.483927247898782831, 16.52544592524335698, 87.70942372801901854 ) ) ;
#72250 = CARTESIAN_POINT ( 'NONE',  ( -17.40805194821983548, 6.112264579160783917, 95.83371272510609629 ) ) ;
#72251 = CARTESIAN_POINT ( 'NONE',  ( 5.049401038298161559, -19.05341960407611168, 72.70724293864768129 ) ) ;
#72252 = CARTESIAN_POINT ( 'NONE',  ( 15.80617190586746368, 15.72974639402197994, 79.37390960531436690 ) ) ;
#72253 = CARTESIAN_POINT ( 'NONE',  ( -8.224510206698735004, -14.34966873604973081, 24.58442372801901499 ) ) ;
#72255 = CARTESIAN_POINT ( 'NONE',  ( -5.719274019375665041, -21.55341960407619695, 74.79275706135234714 ) ) ;
#72254 = CARTESIAN_POINT ( 'NONE',  ( -8.314922557960811034, -14.29746914071050412, 52.08224293864768839 ) ) ;
#72257 = CARTESIAN_POINT ( 'NONE',  ( -21.52544592524343514, 5.823673210054127303, 26.04057627198103475 ) ) ;
#72256 = CARTESIAN_POINT ( 'NONE',  ( -12.06949235617739369, -12.14591786802326823, 84.37609039468570415 ) ) ;
#72258 = CARTESIAN_POINT ( 'NONE',  ( -19.03943276465977164, 0.05219959533909376836, 116.2489096053143669 ) ) ;
#72259 = DIRECTION ( 'NONE',  ( 0.000000000000000000, 0.000000000000000000, 1.000000000000000000 ) ) ;
#72260 = CARTESIAN_POINT ( 'NONE',  ( 0.05219959533934541429, -16.53943276465976808, 110.0010903946856757 ) ) ;
#72261 = CARTESIAN_POINT ( 'NONE',  ( -4.379528057220086978, -16.55341960407618274, 54.79275706135235424 ) ) ;
#72263 = EDGE_LOOP ( 'NONE', ( #118839, #79880, #155116, #150361 ) ) ;
#72262 = CARTESIAN_POINT ( 'NONE',  ( 13.89961937509977652, -13.97604488694527269, 78.12390960531433848 ) ) ;
#72264 = CARTESIAN_POINT ( 'NONE',  ( 13.97604488694527802, 13.89961937509977652, 84.37390960531433848 ) ) ;
#72265 = CARTESIAN_POINT ( 'NONE',  ( -18.67979575497193778, 10.72451020669871902, 73.33442372801901854 ) ) ;
#72266 = CARTESIAN_POINT ( 'NONE',  ( -14.34966873604972548, 8.224510206698743886, 73.33442372801901854 ) ) ;
#72267 = CARTESIAN_POINT ( 'NONE',  ( -0.05219959533910754901, -16.53943276465976808, 52.49890960531435979 ) ) ;
#72268 = CARTESIAN_POINT ( 'NONE',  ( 19.03943276465977164, -0.05219959533909143690, 48.74890960531435979 ) ) ;
#72269 = CARTESIAN_POINT ( 'NONE',  ( 13.97604488694527802, 13.89961937509977652, 49.37390960531434558 ) ) ;
#72270 = ORIENTED_EDGE ( 'NONE', *, *, #115041, .F. ) ;
#72271 = CARTESIAN_POINT ( 'NONE',  ( 13.97604488694548053, -13.89961937509957401, 90.62609039468567573 ) ) ;
#72272 = CARTESIAN_POINT ( 'NONE',  ( 16.52544592524342804, -4.483927247898539470, 93.54057627198103830 ) ) ;
#72273 = CARTESIAN_POINT ( 'NONE',  ( 13.97604488694527802, 13.89961937509977652, 59.37390960531434558 ) ) ;
#72275 = CARTESIAN_POINT ( 'NONE',  ( 23.48529157249600630, -32.32473071737749137, -7.299999999999998934 ) ) ;
#72274 = CARTESIAN_POINT ( 'NONE',  ( -16.46253265017146816, -9.564922557961047289, 94.16775706135233293 ) ) ;
#72276 = CARTESIAN_POINT ( 'NONE',  ( -18.62759615963255300, -10.81492255796106328, 109.1677570613523613 ) ) ;
#72277 = CARTESIAN_POINT ( 'NONE',  ( 12.06949235617739724, 12.14591786802326823, 66.87609039468568994 ) ) ;
#72278 = CARTESIAN_POINT ( 'NONE',  ( -5.153800228976607833, 19.02544592524334988, 87.70942372801897591 ) ) ;
#72279 = CARTESIAN_POINT ( 'NONE',  ( 21.52544592524344225, -5.823673210054117533, 68.54057627198103830 ) ) ;
#72280 = CARTESIAN_POINT ( 'NONE',  ( -0.05219959533934338120, 16.53943276465976808, 52.50109039468567573 ) ) ;
#72281 = CARTESIAN_POINT ( 'NONE',  ( -3.573655867282028392E-15, 2.428612866367529932E-14, 169.9999999999999716 ) ) ;
#72282 = CARTESIAN_POINT ( 'NONE',  ( -19.02544592524334988, -5.153800228976617603, 53.95942372801898301 ) ) ;
#72283 = CARTESIAN_POINT ( 'NONE',  ( -21.55341960407619339, 5.719274019375674811, 98.54275706135234714 ) ) ;
#72284 = CARTESIAN_POINT ( 'NONE',  ( -16.53943276465976808, 0.05219959533911058130, 111.2489096053143669 ) ) ;
#72285 = CARTESIAN_POINT ( 'NONE',  ( -19.02544592524342804, 5.153800228976336051, 66.04057627198103830 ) ) ;
#72286 = CARTESIAN_POINT ( 'NONE',  ( -16.52544592524342804, 4.483927247898546575, 61.04057627198103120 ) ) ;
#72287 = CARTESIAN_POINT ( 'NONE',  ( -5.823673210054431948, 21.52544592524334988, 87.70942372801901854 ) ) ;
#72288 = CARTESIAN_POINT ( 'NONE',  ( 5.049401038297881783, 19.05341960407617563, 52.29275706135234003 ) ) ;
#72289 = CARTESIAN_POINT ( 'NONE',  ( -13.97604488694547697, 13.89961937509957934, 28.12609039468565797 ) ) ;
#72290 = CARTESIAN_POINT ( 'NONE',  ( -10.81492255796078084, -18.62759615963271287, 27.08224293864769550 ) ) ;
#72291 = CARTESIAN_POINT ( 'NONE',  ( 10.81492255796106328, -18.62759615963255655, 100.4177570613523471 ) ) ;
#72292 = CARTESIAN_POINT ( 'NONE',  ( 16.51473224551069308, 9.474510206698969483, 79.16557627198103830 ) ) ;
#72293 = CARTESIAN_POINT ( 'NONE',  ( -18.67979575497193778, 10.72451020669871902, 98.33442372801901854 ) ) ;
#72294 = CARTESIAN_POINT ( 'NONE',  ( 21.53943276465977519, -0.05219959533907433946, 53.74890960531437401 ) ) ;
#72295 = CARTESIAN_POINT ( 'NONE',  ( 13.97604488694527802, 13.89961937509977652, 89.37390960531436690 ) ) ;
#72296 = CARTESIAN_POINT ( 'NONE',  ( 9.564922557961047289, -16.46253265017146816, 60.41775706135233293 ) ) ;
#72297 = CARTESIAN_POINT ( 'NONE',  ( -9.564922557960796823, -16.46253265017161027, 42.08224293864769550 ) ) ;
#72298 = CARTESIAN_POINT ( 'NONE',  ( 19.03943276465977164, -0.05219959533909143690, 88.74890960531436690 ) ) ;
#72299 = EDGE_CURVE ( 'NONE', #29646, #44580, #3071, .T. ) ;
#72300 = CARTESIAN_POINT ( 'NONE',  ( 19.05341960407617918, -5.049401038297876454, 86.04275706135233293 ) ) ;
#72301 = CARTESIAN_POINT ( 'NONE',  ( 12.14591786802327356, -12.06949235617739191, 45.62609039468567573 ) ) ;
#72302 = CARTESIAN_POINT ( 'NONE',  ( -8.224510206698948167, 14.34966873604960824, 100.4155762719810241 ) ) ;
#72303 = CARTESIAN_POINT ( 'NONE',  ( -19.03943276465977164, 0.05219959533909376836, 71.24890960531435269 ) ) ;
#72304 = CARTESIAN_POINT ( 'NONE',  ( -18.62759615963270932, 10.81492255796079327, 50.83224293864770971 ) ) ;
#72305 = CARTESIAN_POINT ( 'NONE',  ( -19.02544592524334988, -5.153800228976617603, 108.9594237280189759 ) ) ;
#72306 = CARTESIAN_POINT ( 'NONE',  ( -18.67979575497193778, 10.72451020669871902, 23.33442372801901499 ) ) ;
#72307 = CARTESIAN_POINT ( 'NONE',  ( 21.52544592524334988, 5.823673210054432836, 76.45942372801901854 ) ) ;
#72308 = CARTESIAN_POINT ( 'NONE',  ( -4.483927247898782831, 16.52544592524335698, 77.70942372801900433 ) ) ;
#72309 = AXIS2_PLACEMENT_3D ( 'NONE', #129302, #173854, #95994 ) ;
#72310 = CARTESIAN_POINT ( 'NONE',  ( -5.153800228976328057, -19.02544592524343514, 72.29057627198102409 ) ) ;
#72311 = CARTESIAN_POINT ( 'NONE',  ( 4.483927247898790824, -16.52544592524335698, 100.2094237280190043 ) ) ;
#72312 = CARTESIAN_POINT ( 'NONE',  ( -13.89961937509957401, -13.97604488694547875, 44.37609039468566863 ) ) ;
#72313 = CARTESIAN_POINT ( 'NONE',  ( 5.823673210054444382, -21.52544592524334988, 35.20942372801901854 ) ) ;
#72314 = EDGE_CURVE ( 'NONE', #103711, #21447, #68243, .T. ) ;
#72315 = CARTESIAN_POINT ( 'NONE',  ( -4.379528057220328563, 16.55341960407611168, 85.20724293864770971 ) ) ;
#72316 = CARTESIAN_POINT ( 'NONE',  ( -13.89961937509977652, 13.97604488694528158, 105.6239096053143527 ) ) ;
#72317 = CARTESIAN_POINT ( 'NONE',  ( -16.53943276465976808, -0.05219959533934237506, 88.75109039468567573 ) ) ;
#72318 = CARTESIAN_POINT ( 'NONE',  ( -15.72974639402176322, -15.80617190586768395, 69.37609039468567573 ) ) ;
#72319 = CARTESIAN_POINT ( 'NONE',  ( -16.53943276465976808, -0.05219959533934237506, 33.75109039468568284 ) ) ;
#72320 = CARTESIAN_POINT ( 'NONE',  ( 15.72974639402176855, 15.80617190586768217, 31.87609039468567929 ) ) ;
#72321 = CARTESIAN_POINT ( 'NONE',  ( 14.34966873604960469, 8.224510206698951720, 74.16557627198102409 ) ) ;
#72322 = ORIENTED_EDGE ( 'NONE', *, *, #178834, .F. ) ;
#72323 = CARTESIAN_POINT ( 'NONE',  ( -18.67979575497178146, -10.72451020669898902, 96.66557627198102409 ) ) ;
#72324 = CARTESIAN_POINT ( 'NONE',  ( 8.314922557960818139, 14.29746914071049879, 54.58224293864769550 ) ) ;
#72325 = ORIENTED_EDGE ( 'NONE', *, *, #172057, .T. ) ;
#72326 = CARTESIAN_POINT ( 'NONE',  ( 0.05219959533909260263, 19.03943276465977164, 29.99890960531435979 ) ) ;
#72327 = CARTESIAN_POINT ( 'NONE',  ( 5.823673210054125526, 21.52544592524343514, 34.79057627198103120 ) ) ;
#72328 = CARTESIAN_POINT ( 'NONE',  ( -0.05219959533937732626, 21.53943276465977519, 32.50109039468568284 ) ) ;
#72329 = CARTESIAN_POINT ( 'NONE',  ( -16.53943276465976808, 0.05219959533911058130, 66.24890960531436690 ) ) ;
#72330 = AXIS2_PLACEMENT_3D ( 'NONE', #39811, #194512, #114650 ) ;
#72331 = CARTESIAN_POINT ( 'NONE',  ( 21.55341960407610458, 5.719274019375980345, 68.95724293864769550 ) ) ;
#72332 = CARTESIAN_POINT ( 'NONE',  ( 9.564922557960805705, 16.46253265017160317, 74.58224293864769550 ) ) ;
#72334 = CARTESIAN_POINT ( 'NONE',  ( -13.89961937509957401, -13.97604488694547875, 84.37609039468567573 ) ) ;
#72333 = CARTESIAN_POINT ( 'NONE',  ( -19.02544592524342804, 5.153800228976336051, 26.04057627198103120 ) ) ;
#72335 = CARTESIAN_POINT ( 'NONE',  ( 10.81492255796078972, 18.62759615963270932, 59.58224293864770260 ) ) ;
#72336 = CARTESIAN_POINT ( 'NONE',  ( -19.05341960407611168, -5.049401038298163336, 41.45724293864769550 ) ) ;
#72337 = CARTESIAN_POINT ( 'NONE',  ( 19.05341960407611168, 5.049401038298154454, 73.95724293864768129 ) ) ;
#72338 = ORIENTED_EDGE ( 'NONE', *, *, #114385, .T. ) ;
#72339 = CARTESIAN_POINT ( 'NONE',  ( -8.224510206698735004, -14.34966873604973081, 54.58442372801901143 ) ) ;
#72340 = CARTESIAN_POINT ( 'NONE',  ( 5.719274019375673035, 21.55341960407619339, 27.29275706135234358 ) ) ;
#72341 = EDGE_CURVE ( 'NONE', #153137, #111465, #181775, .T. ) ;
#72342 = CARTESIAN_POINT ( 'NONE',  ( -21.55341960407619339, 5.719274019375674811, 53.54275706135234714 ) ) ;
#72343 = CARTESIAN_POINT ( 'NONE',  ( 13.89961937509977652, -13.97604488694527269, 98.12390960531433848 ) ) ;
#72344 = CARTESIAN_POINT ( 'NONE',  ( 10.81492255796078972, 18.62759615963270932, 69.58224293864769550 ) ) ;
#72346 = CARTESIAN_POINT ( 'NONE',  ( 0.05219959533934541429, -16.53943276465976808, 50.00109039468568994 ) ) ;
#72345 = CARTESIAN_POINT ( 'NONE',  ( 15.80617190586746368, 15.72974639402197994, 114.3739096053143527 ) ) ;
#72347 = CARTESIAN_POINT ( 'NONE',  ( 18.67979575497178502, 10.72451020669898547, 49.16557627198102409 ) ) ;
#72348 = CARTESIAN_POINT ( 'NONE',  ( -21.55341960407619339, 5.719274019375674811, 108.5427570613523756 ) ) ;
#72349 = CARTESIAN_POINT ( 'NONE',  ( -16.46253265017160317, 9.564922557960807481, 55.83224293864769550 ) ) ;
#72350 = CARTESIAN_POINT ( 'NONE',  ( -13.89961937509977652, 13.97604488694528158, 110.6239096053143243 ) ) ;
#72351 = CARTESIAN_POINT ( 'NONE',  ( -16.46253265017160317, 9.564922557960807481, 75.83224293864769550 ) ) ;
#72352 = CARTESIAN_POINT ( 'NONE',  ( -28.47622644277399928, -25.16156846422451920, -16.68312038616162951 ) ) ;
#72353 = CARTESIAN_POINT ( 'NONE',  ( -19.03943276465977164, -0.05219959533935918106, 73.75109039468566152 ) ) ;
#72355 = CARTESIAN_POINT ( 'NONE',  ( -15.72974639402197994, 15.80617190586746368, 40.62390960531435269 ) ) ;
#72354 = CARTESIAN_POINT ( 'NONE',  ( -13.89961937509957401, -13.97604488694547875, 19.37609039468566507 ) ) ;
#72356 = CARTESIAN_POINT ( 'NONE',  ( -0.05219959533934338120, 16.53943276465976808, 102.5010903946856899 ) ) ;
#72357 = CARTESIAN_POINT ( 'NONE',  ( -9.564922557961040184, 16.46253265017147172, 82.91775706135233293 ) ) ;
#72358 = CARTESIAN_POINT ( 'NONE',  ( -17.49999999999999645, 5.624438216177593652, 60.81670344914646620 ) ) ;
#72359 = CARTESIAN_POINT ( 'NONE',  ( 16.51473224551083163, -9.474510206698727899, 25.83442372801900078 ) ) ;
#72360 = CARTESIAN_POINT ( 'NONE',  ( -19.03943276465977164, -0.05219959533935918106, 83.75109039468567573 ) ) ;
#72361 = CARTESIAN_POINT ( 'NONE',  ( 5.153800228976615827, -19.02544592524334988, 45.20942372801901143 ) ) ;
#72362 = CARTESIAN_POINT ( 'NONE',  ( -17.48847506799968698, -5.747544572773811034, 44.17302562156721280 ) ) ;
#72363 = CARTESIAN_POINT ( 'NONE',  ( -19.02544592524342804, 5.153800228976336051, 41.04057627198103120 ) ) ;
#72364 = CARTESIAN_POINT ( 'NONE',  ( -0.05219959533910754901, -16.53943276465976808, 52.49890960531435979 ) ) ;
#72365 = CARTESIAN_POINT ( 'NONE',  ( -19.03943276465977164, 0.05219959533909376836, 36.24890960531436690 ) ) ;
#72366 = CARTESIAN_POINT ( 'NONE',  ( 0.05219959533910956823, 16.53943276465976808, 44.99890960531435979 ) ) ;
#72367 = CARTESIAN_POINT ( 'NONE',  ( 17.97182807773875979, -5.499999999999868550, 46.03038844047287625 ) ) ;
#72368 = CARTESIAN_POINT ( 'NONE',  ( -12.14591786802309592, -12.06949235617757132, 21.87390960531436690 ) ) ;
#72369 = CARTESIAN_POINT ( 'NONE',  ( -9.474510206698964154, 16.51473224551069663, 55.41557627198103120 ) ) ;
#72370 = CARTESIAN_POINT ( 'NONE',  ( 5.049401038297881783, 19.05341960407617563, 27.29275706135232937 ) ) ;
#72371 = CARTESIAN_POINT ( 'NONE',  ( -0.05219959533934338120, 16.53943276465976808, 37.50109039468568284 ) ) ;
#72372 = CARTESIAN_POINT ( 'NONE',  ( 18.67979575497178502, 10.72451020669898547, 39.16557627198102409 ) ) ;
#72374 = ORIENTED_EDGE ( 'NONE', *, *, #155151, .F. ) ;
#72373 = CARTESIAN_POINT ( 'NONE',  ( 5.719274019375673035, 21.55341960407619339, 97.29275706135234714 ) ) ;
#72375 = CARTESIAN_POINT ( 'NONE',  ( -16.51473224551069308, -9.474510206698971260, 111.6655762719810383 ) ) ;
#72376 = CARTESIAN_POINT ( 'NONE',  ( -16.46253265017160317, 9.564922557960807481, 100.8322429386477097 ) ) ;
#72377 = CARTESIAN_POINT ( 'NONE',  ( 11.40812507854754365, 35.11059874428196537, -9.224999997268813701 ) ) ;
#72378 = CARTESIAN_POINT ( 'NONE',  ( -21.52544592524334988, -5.823673210054445271, 18.95942372801901143 ) ) ;
#72379 = CARTESIAN_POINT ( 'NONE',  ( -14.34966873604960291, -8.224510206698953496, 76.66557627198103830 ) ) ;
#72381 = CARTESIAN_POINT ( 'NONE',  ( -19.03943276465977164, 0.05219959533909376836, 66.24890960531436690 ) ) ;
#72380 = CARTESIAN_POINT ( 'NONE',  ( -10.81492255796078084, -18.62759615963271287, 77.08224293864769550 ) ) ;
#72382 = CARTESIAN_POINT ( 'NONE',  ( 16.51473224551069308, 9.474510206698969483, 79.16557627198103830 ) ) ;
#72383 = CARTESIAN_POINT ( 'NONE',  ( -18.67979575497178146, -10.72451020669898902, 106.6655762719810383 ) ) ;
#72384 = ORIENTED_EDGE ( 'NONE', *, *, #38861, .F. ) ;
#72385 = CARTESIAN_POINT ( 'NONE',  ( -16.46253265017160317, 9.564922557960807481, 55.83224293864769550 ) ) ;
#72386 = CIRCLE ( 'NONE', #185376, 4.250000000000000000 ) ;
#72388 = CARTESIAN_POINT ( 'NONE',  ( -3.573655867282028392E-15, 2.428612866367529932E-14, -25.00000000000000000 ) ) ;
#72387 = CARTESIAN_POINT ( 'NONE',  ( 4.379528057220339221, -16.55341960407611168, 102.7072429386476955 ) ) ;
#72389 = CARTESIAN_POINT ( 'NONE',  ( 13.89961937509977652, -13.97604488694527269, 58.12390960531436690 ) ) ;
#72390 = CARTESIAN_POINT ( 'NONE',  ( 16.46253265017146816, 9.564922557961045513, 86.66775706135233293 ) ) ;
#72391 = CARTESIAN_POINT ( 'NONE',  ( 14.29746914071049879, -8.314922557960816363, 98.33224293864769550 ) ) ;
#72392 = CARTESIAN_POINT ( 'NONE',  ( 10.81492255796106328, -18.62759615963255655, 60.41775706135235424 ) ) ;
#72394 = CARTESIAN_POINT ( 'NONE',  ( 18.67979575497194134, -10.72451020669871369, 20.83442372801901143 ) ) ;
#72393 = CARTESIAN_POINT ( 'NONE',  ( 9.564922557960805705, 16.46253265017160317, 54.58224293864769550 ) ) ;
#72395 = CARTESIAN_POINT ( 'NONE',  ( -14.34966873604960291, -8.224510206698953496, 101.6655762719810383 ) ) ;
#72396 = CARTESIAN_POINT ( 'NONE',  ( 28.82186960331498327, 9.364793116373570925, 141.0999999999999943 ) ) ;
#72397 = CARTESIAN_POINT ( 'NONE',  ( -0.05219959533909027116, -19.03943276465977164, 77.49890960531435269 ) ) ;
#72398 = CARTESIAN_POINT ( 'NONE',  ( -28.82186960331499392, -9.364793116373526516, 138.3500000054623911 ) ) ;
#72400 = CARTESIAN_POINT ( 'NONE',  ( -21.55341960407610458, -5.719274019375992779, 31.45724293864769550 ) ) ;
#72399 = CARTESIAN_POINT ( 'NONE',  ( -5.153800228976607833, 19.02544592524334988, 107.7094237280189759 ) ) ;
#72401 = CARTESIAN_POINT ( 'NONE',  ( -15.80617190586768217, 15.72974639402176855, 48.12609039468568284 ) ) ;
#72402 = CARTESIAN_POINT ( 'NONE',  ( -19.03943276465977164, 0.05219959533909376836, 91.24890960531436690 ) ) ;
#72403 = CARTESIAN_POINT ( 'NONE',  ( -13.89961937509957401, -13.97604488694547875, 89.37609039468563310 ) ) ;
#72404 = CARTESIAN_POINT ( 'NONE',  ( -19.03943276465977164, 0.05219959533909376836, 66.24890960531436690 ) ) ;
#72405 = CARTESIAN_POINT ( 'NONE',  ( -12.06949235617756955, 12.14591786802309770, 85.62390960531436690 ) ) ;
#72406 = CARTESIAN_POINT ( 'NONE',  ( -5.153800228976328057, -19.02544592524343514, 107.2905762719810383 ) ) ;
#72407 = CARTESIAN_POINT ( 'NONE',  ( -12.06949235617756955, 12.14591786802309770, 75.62390960531439532 ) ) ;
#72408 = CARTESIAN_POINT ( 'NONE',  ( 13.89961937509977652, -13.97604488694527269, 98.12390960531433848 ) ) ;
#72409 = CARTESIAN_POINT ( 'NONE',  ( 13.97604488694548053, -13.89961937509957401, 50.62609039468566152 ) ) ;
#72412 = CARTESIAN_POINT ( 'NONE',  ( -5.153800228976328057, -19.02544592524343514, 27.29057627198103120 ) ) ;
#72411 = CARTESIAN_POINT ( 'NONE',  ( 8.314922557960818139, 14.29746914071049879, 39.58224293864769550 ) ) ;
#72410 = CARTESIAN_POINT ( 'NONE',  ( -19.05341960407611168, -5.049401038298163336, 46.45724293864768129 ) ) ;
#72413 = ORIENTED_EDGE ( 'NONE', *, *, #173531, .F. ) ;
#72414 = CARTESIAN_POINT ( 'NONE',  ( 18.67979575497194134, -10.72451020669871369, 50.83442372801901143 ) ) ;
#72415 = CARTESIAN_POINT ( 'NONE',  ( 19.02544592524334988, 5.153800228976608722, 76.45942372801897591 ) ) ;
#72416 = CARTESIAN_POINT ( 'NONE',  ( 16.55341960407611168, 4.379528057220329451, 48.95724293864770971 ) ) ;
#72417 = CARTESIAN_POINT ( 'NONE',  ( -5.719274019375978568, 21.55341960407610458, 100.2072429386476955 ) ) ;
#72418 = CARTESIAN_POINT ( 'NONE',  ( 18.67979575497178502, 10.72451020669898547, 39.16557627198102409 ) ) ;
#72419 = CARTESIAN_POINT ( 'NONE',  ( -4.379528057220328563, 16.55341960407611168, 80.20724293864769550 ) ) ;
#72420 = CARTESIAN_POINT ( 'NONE',  ( 19.03943276465977164, -0.05219959533909143690, 48.74890960531435979 ) ) ;
#72421 = CARTESIAN_POINT ( 'NONE',  ( -14.34966873604972548, 8.224510206698743886, 113.3344237280190328 ) ) ;
#72422 = CARTESIAN_POINT ( 'NONE',  ( 8.224510206698742110, 14.34966873604972548, 87.08442372801901854 ) ) ;
#72423 = CARTESIAN_POINT ( 'NONE',  ( 4.483927247898790824, -16.52544592524335698, 65.20942372801901854 ) ) ;
#72424 = CARTESIAN_POINT ( 'NONE',  ( 19.02544592524334988, 5.153800228976608722, 26.45942372801899722 ) ) ;
#72425 = CARTESIAN_POINT ( 'NONE',  ( -13.89961937509977652, 13.97604488694528158, 95.62390960531436690 ) ) ;
#72426 = CARTESIAN_POINT ( 'NONE',  ( 9.564922557960805705, 16.46253265017160317, 79.58224293864769550 ) ) ;
#72427 = CARTESIAN_POINT ( 'NONE',  ( -8.314922557961024197, 14.29746914071037800, 72.91775706135234714 ) ) ;
#72428 = CARTESIAN_POINT ( 'NONE',  ( -13.89961937509977652, 13.97604488694528158, 35.62390960531435269 ) ) ;
#72429 = CARTESIAN_POINT ( 'NONE',  ( 4.379528057220339221, -16.55341960407611168, 52.70724293864769550 ) ) ;
#72431 = CARTESIAN_POINT ( 'NONE',  ( 19.03943276465977164, -0.05219959533909143690, 108.7489096053143527 ) ) ;
#72430 = CARTESIAN_POINT ( 'NONE',  ( 16.51473224551069308, 9.474510206698969483, 114.1655762719810241 ) ) ;
#72433 = ADVANCED_FACE ( 'NONE', ( #149437, #180794 ), #72606, .F. ) ;
#72432 = CARTESIAN_POINT ( 'NONE',  ( -15.72974639402197994, 15.80617190586746368, 30.62390960531436335 ) ) ;
#72434 = AXIS2_PLACEMENT_3D ( 'NONE', #91069, #44600, #149791 ) ;
#72435 = CARTESIAN_POINT ( 'NONE',  ( 4.379528057220339221, -16.55341960407611168, 72.70724293864769550 ) ) ;
#72436 = CARTESIAN_POINT ( 'NONE',  ( -12.06949235617756955, 12.14591786802309770, 70.62390960531436690 ) ) ;
#72438 = AXIS2_PLACEMENT_3D ( 'NONE', #64897, #50733, #186276 ) ;
#72437 = CARTESIAN_POINT ( 'NONE',  ( 30.74964850363291546, -1.467638476639183009, -47.27948696604331502 ) ) ;
#72439 = CARTESIAN_POINT ( 'NONE',  ( -19.05341960407617563, 5.049401038297882671, 68.54275706135230450 ) ) ;
#72440 = CARTESIAN_POINT ( 'NONE',  ( 13.97604488694527802, 13.89961937509977652, 84.37390960531433848 ) ) ;
#72441 = CARTESIAN_POINT ( 'NONE',  ( 0.05219959533936267826, -19.03943276465977164, 75.00109039468566152 ) ) ;
#72442 = CARTESIAN_POINT ( 'NONE',  ( -5.049401038297874678, -19.05341960407618274, 94.79275706135233293 ) ) ;
#72444 = CARTESIAN_POINT ( 'NONE',  ( 16.53943276465976808, 0.05219959533934440121, 96.25109039468568994 ) ) ;
#72443 = CARTESIAN_POINT ( 'NONE',  ( -12.06949235617739369, -12.14591786802326823, 19.37609039468568639 ) ) ;
#72446 = CARTESIAN_POINT ( 'NONE',  ( 16.51473224551069308, 9.474510206698969483, 39.16557627198103120 ) ) ;
#72445 = PRESENTATION_LAYER_ASSIGNMENT (  '', '', ( #117611 ) ) ;
#72447 = CARTESIAN_POINT ( 'NONE',  ( -0.05219959533909027116, -19.03943276465977164, 112.4989096053143669 ) ) ;
#72448 = CARTESIAN_POINT ( 'NONE',  ( -5.719274019375665041, -21.55341960407619695, 54.79275706135235424 ) ) ;
#72449 = CARTESIAN_POINT ( 'NONE',  ( -16.52544592524335698, -4.483927247898792601, 23.95942372801901143 ) ) ;
#72451 = CARTESIAN_POINT ( 'NONE',  ( -13.97604488694527625, -13.89961937509977652, 76.87390960531433848 ) ) ;
#72450 = FACE_OUTER_BOUND ( 'NONE', #39824, .T. ) ;
#72452 = CARTESIAN_POINT ( 'NONE',  ( -19.02544592524342804, 5.153800228976336051, 116.0405762719810383 ) ) ;
#72454 = CARTESIAN_POINT ( 'NONE',  ( 9.564922557960805705, 16.46253265017160317, 74.58224293864769550 ) ) ;
#72453 = CARTESIAN_POINT ( 'NONE',  ( -4.483927247898539470, -16.52544592524342804, 77.29057627198102409 ) ) ;
#72455 = CONTEXT_DEPENDENT_SHAPE_REPRESENTATION ( #185017, #198619 ) ;
#72456 = CARTESIAN_POINT ( 'NONE',  ( 13.89961937509977652, -13.97604488694527269, 73.12390960531436690 ) ) ;
#72457 = ORIENTED_EDGE ( 'NONE', *, *, #151524, .F. ) ;
#72458 = CARTESIAN_POINT ( 'NONE',  ( -16.51473224551082808, 9.474510206698731452, 93.33442372801900433 ) ) ;
#72459 = CARTESIAN_POINT ( 'NONE',  ( 18.62759615963271287, -10.81492255796078972, 68.33224293864769550 ) ) ;
#72460 = CARTESIAN_POINT ( 'NONE',  ( -5.049401038298153566, 19.05341960407611168, 35.20724293864768839 ) ) ;
#72461 = CARTESIAN_POINT ( 'NONE',  ( 9.474510206698729675, 16.51473224551082808, 62.08442372801899722 ) ) ;
#72462 = CARTESIAN_POINT ( 'NONE',  ( 19.02544592524343514, -5.153800228976328945, 53.54057627198102409 ) ) ;
#72464 = EDGE_CURVE ( 'NONE', #84310, #85102, #125174, .T. ) ;
#72463 = CARTESIAN_POINT ( 'NONE',  ( -13.97604488694527625, -13.89961937509977652, 91.87390960531432427 ) ) ;
#72465 = ORIENTED_EDGE ( 'NONE', *, *, #79617, .F. ) ;
#72466 = CARTESIAN_POINT ( 'NONE',  ( 5.823673210054125526, 21.52544592524343514, 89.79057627198103830 ) ) ;
#72468 = CARTESIAN_POINT ( 'NONE',  ( 9.474510206698729675, 16.51473224551082808, 52.08442372801900433 ) ) ;
#72467 = CARTESIAN_POINT ( 'NONE',  ( -12.06949235617756955, 12.14591786802309770, 95.62390960531436690 ) ) ;
#72469 = CARTESIAN_POINT ( 'NONE',  ( -15.72974639402197994, 15.80617190586746368, 85.62390960531436690 ) ) ;
#72470 = CARTESIAN_POINT ( 'NONE',  ( -15.80617190586745835, -15.72974639402198527, 71.87390960531438111 ) ) ;
#72471 = CARTESIAN_POINT ( 'NONE',  ( 12.06949235617757843, -12.14591786802309237, 38.12390960531436690 ) ) ;
#72472 = CARTESIAN_POINT ( 'NONE',  ( 5.823673210054444382, -21.52544592524334988, 110.2094237280190185 ) ) ;
#72473 = CARTESIAN_POINT ( 'NONE',  ( -16.46253265017160317, 9.564922557960807481, 75.83224293864769550 ) ) ;
#72474 = CARTESIAN_POINT ( 'NONE',  ( -9.474510206698964154, 16.51473224551069663, 35.41557627198102409 ) ) ;
#72475 = AXIS2_PLACEMENT_3D ( 'NONE', #152494, #199007, #60474 ) ;
#72476 = CARTESIAN_POINT ( 'NONE',  ( 15.80617190586769283, -15.72974639402175789, 35.62609039468568994 ) ) ;
#72477 = CARTESIAN_POINT ( 'NONE',  ( -15.80617190586768217, 15.72974639402176855, 58.12609039468568994 ) ) ;
#72478 = CARTESIAN_POINT ( 'NONE',  ( -19.05341960407611168, -5.049401038298163336, 41.45724293864769550 ) ) ;
#72479 = CARTESIAN_POINT ( 'NONE',  ( -0.05219959533937732626, 21.53943276465977519, 22.50109039468567573 ) ) ;
#72480 = CARTESIAN_POINT ( 'NONE',  ( -5.049401038297874678, -19.05341960407617918, 54.79275706135234003 ) ) ;
#72481 = CARTESIAN_POINT ( 'NONE',  ( 9.474510206698971260, -16.51473224551069308, 37.91557627198102409 ) ) ;
#72482 = CARTESIAN_POINT ( 'NONE',  ( -16.55341960407617563, 4.379528057220093196, 23.54275706135235424 ) ) ;
#72483 = CARTESIAN_POINT ( 'NONE',  ( -13.89961937509977652, 13.97604488694528158, 25.62390960531434558 ) ) ;
#72484 = CARTESIAN_POINT ( 'NONE',  ( -16.55341960407617563, 4.379528057220093196, 73.54275706135234714 ) ) ;
#72485 = CARTESIAN_POINT ( 'NONE',  ( -19.05341960407611168, -5.049401038298163336, 41.45724293864769550 ) ) ;
#72486 = CARTESIAN_POINT ( 'NONE',  ( 21.92083080610821355, -6.374575339255582840, 171.4095429173268599 ) ) ;
#72487 = CARTESIAN_POINT ( 'NONE',  ( -16.46253265017160317, 9.564922557960807481, 80.83224293864769550 ) ) ;
#72488 = CARTESIAN_POINT ( 'NONE',  ( -16.51473224551069308, -9.474510206698971260, 31.66557627198102054 ) ) ;
#72489 = CARTESIAN_POINT ( 'NONE',  ( -21.52544592524343514, 5.823673210054127303, 76.04057627198102409 ) ) ;
#72490 = CARTESIAN_POINT ( 'NONE',  ( 16.55341960407618274, -4.379528057220086978, 41.04275706135236135 ) ) ;
#72491 = CARTESIAN_POINT ( 'NONE',  ( 5.049401038297881783, 19.05341960407617563, 22.29275706135233648 ) ) ;
#72492 = CARTESIAN_POINT ( 'NONE',  ( 0.05219959533909260263, 19.03943276465977164, 44.99890960531435979 ) ) ;
#72493 = CARTESIAN_POINT ( 'NONE',  ( -16.55341960407611168, -4.379528057220339221, 26.45724293864768839 ) ) ;
#72494 = CARTESIAN_POINT ( 'NONE',  ( 12.14591786802309770, 12.06949235617756955, 74.37390960531436690 ) ) ;
#72495 = CARTESIAN_POINT ( 'NONE',  ( -9.474510206698964154, 16.51473224551069663, 65.41557627198102409 ) ) ;
#72496 = CARTESIAN_POINT ( 'NONE',  ( 21.55341960407619695, -5.719274019375665929, 111.0427570613523613 ) ) ;
#72497 = CARTESIAN_POINT ( 'NONE',  ( 5.719274019375673035, 21.55341960407619339, 27.29275706135234358 ) ) ;
#72498 = CARTESIAN_POINT ( 'NONE',  ( -13.97604488694527625, -13.89961937509977652, 76.87390960531433848 ) ) ;
#72499 = CARTESIAN_POINT ( 'NONE',  ( -15.72974639402176322, -15.80617190586768395, 84.37609039468570415 ) ) ;
#72500 = CARTESIAN_POINT ( 'NONE',  ( -4.379528057220086978, -16.55341960407618274, 59.79275706135234714 ) ) ;
#72501 = CARTESIAN_POINT ( 'NONE',  ( -8.314922557961024197, 14.29746914071037800, 22.91775706135235069 ) ) ;
#72503 = CARTESIAN_POINT ( 'NONE',  ( 13.89961937509977652, -13.97604488694527269, 108.1239096053143669 ) ) ;
#72502 = CARTESIAN_POINT ( 'NONE',  ( -16.53943276465976808, 0.05219959533911058130, 91.24890960531436690 ) ) ;
#72504 = CARTESIAN_POINT ( 'NONE',  ( -16.53943276465976808, 0.05219959533911058130, 36.24890960531435979 ) ) ;
#72505 = CARTESIAN_POINT ( 'NONE',  ( 0.05219959533909260263, 19.03943276465977164, 24.99890960531435269 ) ) ;
#72506 = CARTESIAN_POINT ( 'NONE',  ( -16.52544592524335698, -4.483927247898792601, 48.95942372801902565 ) ) ;
#72507 = CARTESIAN_POINT ( 'NONE',  ( 14.29746914071049879, -8.314922557960816363, 53.33224293864769550 ) ) ;
#72508 = CARTESIAN_POINT ( 'NONE',  ( -8.224510206698735004, -14.34966873604973081, 99.58442372801900433 ) ) ;
#72509 = CARTESIAN_POINT ( 'NONE',  ( 9.564922557960805705, 16.46253265017160317, 114.5822429386476955 ) ) ;
#72510 = CARTESIAN_POINT ( 'NONE',  ( -21.52544592524343514, 5.823673210054127303, 31.04057627198102409 ) ) ;
#72511 = CARTESIAN_POINT ( 'NONE',  ( -13.89961937509957401, -13.97604488694547875, 19.37609039468566507 ) ) ;
#72512 = CARTESIAN_POINT ( 'NONE',  ( 8.224510206698953496, -14.34966873604960469, 82.91557627198103830 ) ) ;
#72513 = CARTESIAN_POINT ( 'NONE',  ( 0.05219959533909260263, 19.03943276465977164, 99.99890960531436690 ) ) ;
#72514 = EDGE_LOOP ( 'NONE', ( #22064, #148295, #113623, #178558, #92196, #113988, #197660, #162618, #97000 ) ) ;
#72515 = CARTESIAN_POINT ( 'NONE',  ( 12.14591786802327356, -12.06949235617739191, 40.62609039468567573 ) ) ;
#72516 = CARTESIAN_POINT ( 'NONE',  ( -19.02544592524342804, 5.153800228976336051, 56.04057627198100988 ) ) ;
#72517 = CYLINDRICAL_SURFACE ( 'NONE', #134066, 5.000000000000000000 ) ;
#72518 = CARTESIAN_POINT ( 'NONE',  ( 16.51473224551083163, -9.474510206698727899, 50.83442372801899722 ) ) ;
#72519 = CARTESIAN_POINT ( 'NONE',  ( 16.46253265017160672, -9.564922557960803928, 43.33224293864769550 ) ) ;
#72520 = CARTESIAN_POINT ( 'NONE',  ( -12.06949235617739369, -12.14591786802326823, 74.37609039468568994 ) ) ;
#72521 = CARTESIAN_POINT ( 'NONE',  ( -5.153800228976607833, 19.02544592524334988, 92.70942372801901854 ) ) ;
#72522 = CARTESIAN_POINT ( 'NONE',  ( 5.049401038298161559, -19.05341960407611168, 62.70724293864769550 ) ) ;
#72523 = CARTESIAN_POINT ( 'NONE',  ( 15.72974639402199770, -15.80617190586745480, 88.12390960531436690 ) ) ;
#72524 = CARTESIAN_POINT ( 'NONE',  ( -14.34966873604960291, -8.224510206698953496, 96.66557627198102409 ) ) ;
#72525 = CARTESIAN_POINT ( 'NONE',  ( -13.89961937509957401, -13.97604488694547875, 74.37609039468566152 ) ) ;
#72526 = CARTESIAN_POINT ( 'NONE',  ( 10.72451020669898902, -18.67979575497178502, 57.91557627198103120 ) ) ;
#72527 = CARTESIAN_POINT ( 'NONE',  ( 5.049401038297881783, 19.05341960407617563, 42.29275706135234003 ) ) ;
#72528 = CARTESIAN_POINT ( 'NONE',  ( 9.564922557960805705, 16.46253265017160317, 114.5822429386476955 ) ) ;
#72529 = CARTESIAN_POINT ( 'NONE',  ( -0.05219959533907301413, -21.53943276465977519, 92.49890960531436690 ) ) ;
#72530 = CARTESIAN_POINT ( 'NONE',  ( -19.52837319214027900, 5.499999999999901412, 54.60471352585540217 ) ) ;
#72531 = CARTESIAN_POINT ( 'NONE',  ( 19.03943276465977164, 0.05219959533936151252, 106.2510903946856615 ) ) ;
#72532 = CARTESIAN_POINT ( 'NONE',  ( -17.97058386085786452, -5.500000000000008882, 99.00390968646219392 ) ) ;
#72533 = EDGE_CURVE ( 'NONE', #197947, #144280, #176850, .T. ) ;
#72534 = CARTESIAN_POINT ( 'NONE',  ( -12.14591786802326823, 12.06949235617739902, 23.12609039468567573 ) ) ;
#72535 = CARTESIAN_POINT ( 'NONE',  ( -19.03943276465977164, 0.05219959533909376836, 46.24890960531435979 ) ) ;
#72536 = CARTESIAN_POINT ( 'NONE',  ( 5.049401038298161559, -19.05341960407611168, 112.7072429386476813 ) ) ;
#72537 = CARTESIAN_POINT ( 'NONE',  ( 21.55341960407610458, 5.719274019375980345, 83.95724293864770971 ) ) ;
#72538 = CARTESIAN_POINT ( 'NONE',  ( 10.81492255796106328, -18.62759615963255655, 65.41775706135234714 ) ) ;
#72540 = CARTESIAN_POINT ( 'NONE',  ( 13.89961937509957401, 13.97604488694547697, 26.87609039468566507 ) ) ;
#72539 = CARTESIAN_POINT ( 'NONE',  ( 19.05341960407617918, -5.049401038297876454, 111.0427570613523329 ) ) ;
#72541 = CARTESIAN_POINT ( 'NONE',  ( -16.53943276465976808, 0.05219959533911058130, 26.24890960531435624 ) ) ;
#72542 = CARTESIAN_POINT ( 'NONE',  ( 21.55341960407610458, 5.719274019375980345, 103.9572429386476813 ) ) ;
#72543 = CARTESIAN_POINT ( 'NONE',  ( -14.29746914071049879, 8.314922557960819915, 55.83224293864770260 ) ) ;
#72544 = CARTESIAN_POINT ( 'NONE',  ( 5.049401038297881783, 19.05341960407617563, 92.29275706135234714 ) ) ;
#72545 = CARTESIAN_POINT ( 'NONE',  ( 0.05219959533936267826, -19.03943276465977164, 60.00109039468566863 ) ) ;
#72546 = CARTESIAN_POINT ( 'NONE',  ( 15.80617190586769283, -15.72974639402175789, 75.62609039468567573 ) ) ;
#72547 = CARTESIAN_POINT ( 'NONE',  ( 0.05219959533936267826, -19.03943276465977164, 40.00109039468566152 ) ) ;
#72548 = CARTESIAN_POINT ( 'NONE',  ( -13.97604488694527625, -13.89961937509977652, 21.87390960531435979 ) ) ;
#72549 = CARTESIAN_POINT ( 'NONE',  ( -10.81492255796078084, -18.62759615963271287, 47.08224293864770260 ) ) ;
#72550 = CARTESIAN_POINT ( 'NONE',  ( -4.483927247898539470, -16.52544592524342804, 37.29057627198102409 ) ) ;
#72551 = CARTESIAN_POINT ( 'NONE',  ( -21.52544592524334988, -5.823673210054445271, 108.9594237280190185 ) ) ;
#72552 = CARTESIAN_POINT ( 'NONE',  ( 14.34966873604972726, -8.224510206698740333, 75.83442372801900433 ) ) ;
#72553 = CARTESIAN_POINT ( 'NONE',  ( 4.483927247898545687, 16.52544592524342804, 34.79057627198103120 ) ) ;
#72554 = CARTESIAN_POINT ( 'NONE',  ( 5.719274019375673035, 21.55341960407619339, 72.29275706135236135 ) ) ;
#72556 = EDGE_CURVE ( 'NONE', #27838, #59417, #151032, .T. ) ;
#72555 = CARTESIAN_POINT ( 'NONE',  ( 21.52544592524334988, 5.823673210054432836, 61.45942372801901854 ) ) ;
#72557 = CARTESIAN_POINT ( 'NONE',  ( -10.72451020669898014, 18.67979575497178502, 65.41557627198102409 ) ) ;
#72558 = VECTOR ( 'NONE', #134446, 1000.000000000000000 ) ;
#72559 = EDGE_LOOP ( 'NONE', ( #117642, #196272 ) ) ;
#72560 = CARTESIAN_POINT ( 'NONE',  ( 0.05219959533909260263, 19.03943276465977164, 34.99890960531435979 ) ) ;
#72561 = CARTESIAN_POINT ( 'NONE',  ( 5.823673210054444382, -21.52544592524334988, 40.20942372801901854 ) ) ;
#72562 = CARTESIAN_POINT ( 'NONE',  ( -13.97604488694527625, -13.89961937509977652, 26.87390960531434558 ) ) ;
#72563 = CARTESIAN_POINT ( 'NONE',  ( -9.564922557960796823, -16.46253265017161027, 42.08224293864769550 ) ) ;
#72564 = CARTESIAN_POINT ( 'NONE',  ( -4.483927247898539470, -16.52544592524342804, 92.29057627198103830 ) ) ;
#72565 = CARTESIAN_POINT ( 'NONE',  ( 19.05341960407611168, 5.049401038298154454, 78.95724293864769550 ) ) ;
#72566 = CARTESIAN_POINT ( 'NONE',  ( 8.314922557960818139, 14.29746914071049879, 34.58224293864770260 ) ) ;
#72567 = CARTESIAN_POINT ( 'NONE',  ( -12.06949235617756955, 12.14591786802309770, 100.6239096053143811 ) ) ;
#72568 = CARTESIAN_POINT ( 'NONE',  ( 21.55341960407610458, 5.719274019375980345, 63.95724293864770260 ) ) ;
#72569 = CARTESIAN_POINT ( 'NONE',  ( -10.72451020669898014, 18.67979575497178502, 110.4155762719810383 ) ) ;
#72570 = CARTESIAN_POINT ( 'NONE',  ( 19.05341960407611168, 5.049401038298154454, 113.9572429386477097 ) ) ;
#72572 = CARTESIAN_POINT ( 'NONE',  ( 12.14591786802327356, -12.06949235617739191, 25.62609039468567929 ) ) ;
#72571 = CARTESIAN_POINT ( 'NONE',  ( 0.05219959533909260263, 19.03943276465977164, 59.99890960531436690 ) ) ;
#72573 = CARTESIAN_POINT ( 'NONE',  ( -15.80617190586745835, -15.72974639402198527, 51.87390960531437401 ) ) ;
#72574 = AXIS2_PLACEMENT_3D ( 'NONE', #13272, #89108, #12294 ) ;
#72575 = CARTESIAN_POINT ( 'NONE',  ( 18.67979575497194134, -10.72451020669871369, 90.83442372801901854 ) ) ;
#72576 = CARTESIAN_POINT ( 'NONE',  ( -9.564922557960796823, -16.46253265017161027, 77.08224293864769550 ) ) ;
#72577 = CARTESIAN_POINT ( 'NONE',  ( -21.52544592524343514, 5.823673210054127303, 116.0405762719810383 ) ) ;
#72578 = CARTESIAN_POINT ( 'NONE',  ( -9.564922557960796823, -16.46253265017161027, 112.0822429386476955 ) ) ;
#72579 = CARTESIAN_POINT ( 'NONE',  ( 16.53943276465976808, 0.05219959533934440121, 91.25109039468568994 ) ) ;
#72580 = CARTESIAN_POINT ( 'NONE',  ( 10.72451020669871369, 18.67979575497193778, 77.08442372801901854 ) ) ;
#72581 = CARTESIAN_POINT ( 'NONE',  ( -21.55341960407619339, 5.719274019375674811, 98.54275706135234714 ) ) ;
#72582 = CARTESIAN_POINT ( 'NONE',  ( 4.379528057220092307, 16.55341960407617563, 62.29275706135236845 ) ) ;
#72583 = CARTESIAN_POINT ( 'NONE',  ( 5.823673210054444382, -21.52544592524334988, 30.20942372801902565 ) ) ;
#72584 = CARTESIAN_POINT ( 'NONE',  ( -19.05341960407611168, -5.049401038298163336, 111.4572429386476671 ) ) ;
#72585 = CARTESIAN_POINT ( 'NONE',  ( 21.52544592524334988, 5.823673210054432836, 86.45942372801901854 ) ) ;
#72586 = CARTESIAN_POINT ( 'NONE',  ( 16.51473224551069308, 9.474510206698969483, 94.16557627198103830 ) ) ;
#72587 = CARTESIAN_POINT ( 'NONE',  ( 18.67979575497178502, 10.72451020669898547, 89.16557627198102409 ) ) ;
#72588 = CARTESIAN_POINT ( 'NONE',  ( 5.049401038297881783, 19.05341960407617563, 47.29275706135231161 ) ) ;
#72589 = CARTESIAN_POINT ( 'NONE',  ( 15.80617190586746368, 15.72974639402197994, 59.37390960531436690 ) ) ;
#72591 = CARTESIAN_POINT ( 'NONE',  ( 8.224510206698953496, -14.34966873604960469, 32.91557627198102409 ) ) ;
#72590 = CARTESIAN_POINT ( 'NONE',  ( 9.564922557960805705, 16.46253265017160317, 99.58224293864770971 ) ) ;
#72592 = CARTESIAN_POINT ( 'NONE',  ( 21.97143472835163891, 7.273127645264538366, 170.2116391040482313 ) ) ;
#72593 = CARTESIAN_POINT ( 'NONE',  ( 13.97604488694548053, -13.89961937509957401, 65.62609039468567573 ) ) ;
#72594 = CARTESIAN_POINT ( 'NONE',  ( 0.4098915413868572943, 13.74273402794541177, -60.42614997978301972 ) ) ;
#72595 = CARTESIAN_POINT ( 'NONE',  ( 5.153800228976615827, -19.02544592524334988, 105.2094237280190185 ) ) ;
#72596 = CARTESIAN_POINT ( 'NONE',  ( -21.55341960407610458, -5.719274019375992779, 91.45724293864769550 ) ) ;
#72597 = CARTESIAN_POINT ( 'NONE',  ( 8.314922557960818139, 14.29746914071049879, 54.58224293864769550 ) ) ;
#72598 = CARTESIAN_POINT ( 'NONE',  ( -4.379528057220086978, -16.55341960407618274, 34.79275706135235424 ) ) ;
#72599 = CARTESIAN_POINT ( 'NONE',  ( 9.564922557960805705, 16.46253265017160317, 49.58224293864770260 ) ) ;
#72601 = CARTESIAN_POINT ( 'NONE',  ( 9.564922557961047289, -16.46253265017146816, 90.41775706135234714 ) ) ;
#72600 = CARTESIAN_POINT ( 'NONE',  ( 21.53943276465977519, -0.05219959533907433946, 113.7489096053143527 ) ) ;
#72602 = CARTESIAN_POINT ( 'NONE',  ( 19.03943276465977164, -0.05219959533909143690, 88.74890960531436690 ) ) ;
#72603 = CARTESIAN_POINT ( 'NONE',  ( -9.564922557960796823, -16.46253265017161027, 72.08224293864770971 ) ) ;
#72604 = CARTESIAN_POINT ( 'NONE',  ( -21.55341960407610458, -5.719274019375992779, 76.45724293864769550 ) ) ;
#72605 = CARTESIAN_POINT ( 'NONE',  ( 19.05341960407611168, 5.049401038298154454, 48.95724293864768129 ) ) ;
#72606 = PLANE ( 'NONE',  #167188 ) ;
#72607 = CARTESIAN_POINT ( 'NONE',  ( 8.314922557960818139, 14.29746914071049879, 54.58224293864769550 ) ) ;
#72608 = CARTESIAN_POINT ( 'NONE',  ( -0.05219959533909027116, -19.03943276465977164, 87.49890960531436690 ) ) ;
#72609 = CARTESIAN_POINT ( 'NONE',  ( 28.82186960331480208, -9.364793116373776982, 141.1500000054623740 ) ) ;
#72610 = CARTESIAN_POINT ( 'NONE',  ( -9.564922557961040184, 16.46253265017147172, 62.91775706135233293 ) ) ;
#72611 = CARTESIAN_POINT ( 'NONE',  ( -18.62759615963270932, 10.81492255796079327, 75.83224293864769550 ) ) ;
#72612 = CARTESIAN_POINT ( 'NONE',  ( -5.153800228976607833, 19.02544592524334988, 32.70942372801899722 ) ) ;
#72613 = CARTESIAN_POINT ( 'NONE',  ( -13.97604488694527625, -13.89961937509977652, 101.8739096053143811 ) ) ;
#72614 = CARTESIAN_POINT ( 'NONE',  ( -17.49999999999999645, 5.076555817581247965, 113.8204850795022907 ) ) ;
#72615 = CARTESIAN_POINT ( 'NONE',  ( -5.823673210054116645, -21.52544592524344225, 42.29057627198103120 ) ) ;
#72616 = CIRCLE ( 'NONE', #117929, 214.0437394197456911 ) ;
#72617 = CARTESIAN_POINT ( 'NONE',  ( 19.05341960407611168, 5.049401038298154454, 73.95724293864768129 ) ) ;
#72618 = CARTESIAN_POINT ( 'NONE',  ( 0.05219959533937995610, -21.53943276465977519, 60.00109039468568284 ) ) ;
#72619 = CARTESIAN_POINT ( 'NONE',  ( 19.05341960407611168, 5.049401038298154454, 23.95724293864769194 ) ) ;
#72621 = ORIENTED_EDGE ( 'NONE', *, *, #75628, .T. ) ;
#72620 = CARTESIAN_POINT ( 'NONE',  ( -21.52544592524343514, 5.823673210054127303, 116.0405762719810383 ) ) ;
#72622 = CARTESIAN_POINT ( 'NONE',  ( -10.81492255796105439, 18.62759615963255655, 47.91775706135234714 ) ) ;
#72623 = ORIENTED_EDGE ( 'NONE', *, *, #43155, .T. ) ;
#72624 = CARTESIAN_POINT ( 'NONE',  ( -5.153800228976328057, -19.02544592524343514, 97.29057627198099567 ) ) ;
#72625 = CARTESIAN_POINT ( 'NONE',  ( -0.05219959533936034679, 19.03943276465977164, 72.50109039468566152 ) ) ;
#72626 = CARTESIAN_POINT ( 'NONE',  ( -21.38418241377624085, 5.438282248597754887, 174.2683007571264113 ) ) ;
#72627 = CARTESIAN_POINT ( 'NONE',  ( -5.823673210054116645, -21.52544592524344225, 107.2905762719810525 ) ) ;
#72628 = CARTESIAN_POINT ( 'NONE',  ( 9.474510206698971260, -16.51473224551069308, 57.91557627198103120 ) ) ;
#72629 = CARTESIAN_POINT ( 'NONE',  ( -14.34966873604972548, 8.224510206698743886, 33.33442372801900433 ) ) ;
#72630 = CARTESIAN_POINT ( 'NONE',  ( -11.74264578624799782, -36.14014761921581709, -9.349999994537627757 ) ) ;
#72631 = CARTESIAN_POINT ( 'NONE',  ( 5.719274019375673035, 21.55341960407619339, 97.29275706135234714 ) ) ;
#72632 = CARTESIAN_POINT ( 'NONE',  ( 19.02544592524343514, -5.153800228976328945, 43.54057627198103120 ) ) ;
#72633 = CARTESIAN_POINT ( 'NONE',  ( -18.67979575497193778, 10.72451020669871902, 103.3344237280190043 ) ) ;
#72635 = CARTESIAN_POINT ( 'NONE',  ( -21.53943276465977519, -0.05219959533937600094, 53.75109039468568994 ) ) ;
#72634 = CARTESIAN_POINT ( 'NONE',  ( 9.474510206698971260, -16.51473224551069308, 82.91557627198103830 ) ) ;
#72636 = CARTESIAN_POINT ( 'NONE',  ( -36.91746825000001309, -11.99521256947794789, -10.52499999726881441 ) ) ;
#72637 = CARTESIAN_POINT ( 'NONE',  ( -16.51473224551069308, -9.474510206698971260, 111.6655762719810383 ) ) ;
#72638 = CARTESIAN_POINT ( 'NONE',  ( 0.000000000000000000, 4.653657836759941744E-16, -3.799999999999999378 ) ) ;
#72640 = CARTESIAN_POINT ( 'NONE',  ( -0.05219959533937732626, 21.53943276465977519, 67.50109039468568994 ) ) ;
#72639 = CARTESIAN_POINT ( 'NONE',  ( 8.224510206698742110, 14.34966873604972548, 47.08442372801901854 ) ) ;
#72641 = CARTESIAN_POINT ( 'NONE',  ( -10.72451020669870658, -18.67979575497194134, 94.58442372801901854 ) ) ;
#72642 = CARTESIAN_POINT ( 'NONE',  ( -9.840250911107732534, 9.549542882988092174, -60.43989527633940639 ) ) ;
#72643 = CARTESIAN_POINT ( 'NONE',  ( 14.29746914071037800, 8.314922557961029526, 21.66775706135235069 ) ) ;
#72644 = CARTESIAN_POINT ( 'NONE',  ( 16.51473224551069308, 9.474510206698969483, 84.16557627198102409 ) ) ;
#72645 = CARTESIAN_POINT ( 'NONE',  ( 0.05219959533909260263, 19.03943276465977164, 114.9989096053143669 ) ) ;
#72646 = VERTEX_POINT ( 'NONE', #166611 ) ;
#72647 = CARTESIAN_POINT ( 'NONE',  ( -0.4911207797134861108, -28.97745891950397024, -52.56957762865166472 ) ) ;
#72648 = CARTESIAN_POINT ( 'NONE',  ( 8.314922557960818139, 14.29746914071049879, 114.5822429386477097 ) ) ;
#72649 = CARTESIAN_POINT ( 'NONE',  ( 18.62759615963271287, -10.81492255796078972, 43.33224293864769550 ) ) ;
#72650 = CARTESIAN_POINT ( 'NONE',  ( 14.29746914071037800, 8.314922557961029526, 91.66775706135234714 ) ) ;
#72652 = CARTESIAN_POINT ( 'NONE',  ( 19.03943276465977164, -0.05219959533909143690, 63.74890960531435979 ) ) ;
#72651 = CARTESIAN_POINT ( 'NONE',  ( -14.34966873604960291, -8.224510206698953496, 81.66557627198103830 ) ) ;
#72653 = CARTESIAN_POINT ( 'NONE',  ( 5.823673210054444382, -21.52544592524334988, 85.20942372801901854 ) ) ;
#72654 = CARTESIAN_POINT ( 'NONE',  ( 11.30153831258470021, -180.0000000000000000, -15.00000000000000178 ) ) ;
#72655 = CARTESIAN_POINT ( 'NONE',  ( -19.05341960407617563, 5.049401038297882671, 113.5427570613523471 ) ) ;
#72656 = CARTESIAN_POINT ( 'NONE',  ( 14.34966873604960469, 8.224510206698951720, 84.16557627198103830 ) ) ;
#72657 = CARTESIAN_POINT ( 'NONE',  ( 5.823673210054444382, -21.52544592524334988, 40.20942372801901854 ) ) ;
#72658 = CARTESIAN_POINT ( 'NONE',  ( -5.719274019375978568, 21.55341960407610458, 75.20724293864769550 ) ) ;
#72659 = CARTESIAN_POINT ( 'NONE',  ( -19.03943276465977164, -0.05219959533935918106, 43.75109039468566863 ) ) ;
#72660 = CARTESIAN_POINT ( 'NONE',  ( 17.59860650958989936, 7.585241751807028088, 44.07662985737508166 ) ) ;
#72661 = CARTESIAN_POINT ( 'NONE',  ( 9.474510206698971260, -16.51473224551069308, 77.91557627198103830 ) ) ;
#72662 = CARTESIAN_POINT ( 'NONE',  ( 16.52544592524342804, -4.483927247898539470, 68.54057627198103830 ) ) ;
#72663 = CARTESIAN_POINT ( 'NONE',  ( -16.53943276465976808, 0.05219959533911058130, 36.24890960531435979 ) ) ;
#72664 = CARTESIAN_POINT ( 'NONE',  ( 16.52544592524335698, 4.483927247898782831, 106.4594237280190328 ) ) ;
#72665 = CARTESIAN_POINT ( 'NONE',  ( -19.03943276465977164, -0.05219959533935918106, 68.75109039468566152 ) ) ;
#72666 = CARTESIAN_POINT ( 'NONE',  ( 17.31728774477273447, 6.344390552232407998, 46.68093348310681279 ) ) ;
#72667 = CARTESIAN_POINT ( 'NONE',  ( -9.474510206698964154, 16.51473224551069663, 115.4155762719810241 ) ) ;
#72668 = CARTESIAN_POINT ( 'NONE',  ( -16.55341960407611168, -4.379528057220339221, 91.45724293864769550 ) ) ;
#72669 = DIRECTION ( 'NONE',  ( -0.000000000000000000, -0.000000000000000000, 1.000000000000000000 ) ) ;
#72671 = CARTESIAN_POINT ( 'NONE',  ( -18.62759615963270932, 10.81492255796079327, 45.83224293864769550 ) ) ;
#72670 = CARTESIAN_POINT ( 'NONE',  ( -19.05341960407611168, -5.049401038298163336, 46.45724293864768129 ) ) ;
#72672 = CARTESIAN_POINT ( 'NONE',  ( 21.52544592524344225, -5.823673210054117533, 68.54057627198103830 ) ) ;
#72673 = CARTESIAN_POINT ( 'NONE',  ( -13.97604488694527625, -13.89961937509977652, 21.87390960531435979 ) ) ;
#72675 = CARTESIAN_POINT ( 'NONE',  ( -13.89961937509977652, 13.97604488694528158, 50.62390960531435979 ) ) ;
#72674 = CARTESIAN_POINT ( 'NONE',  ( -4.379528057220086978, -16.55341960407618274, 59.79275706135234714 ) ) ;
#72676 = AXIS2_PLACEMENT_3D ( 'NONE', #26234, #24233, #179925 ) ;
#72677 = CARTESIAN_POINT ( 'NONE',  ( -21.55341960407619339, 5.719274019375674811, 53.54275706135234714 ) ) ;
#72678 = CARTESIAN_POINT ( 'NONE',  ( 0.05219959533910956823, 16.53943276465976808, 99.99890960531436690 ) ) ;
#72679 = EDGE_CURVE ( 'NONE', #93860, #112813, #63823, .T. ) ;
#72680 = CARTESIAN_POINT ( 'NONE',  ( 13.89961937509957401, 13.97604488694547697, 91.87609039468567573 ) ) ;
#72681 = CARTESIAN_POINT ( 'NONE',  ( -5.950531402560715689E-15, 38.81732327939063509, -1.624999997268813390 ) ) ;
#72683 = CARTESIAN_POINT ( 'NONE',  ( -21.52544592524343514, 5.823673210054127303, 51.04057627198103120 ) ) ;
#72682 = DIRECTION ( 'NONE',  ( 1.000000000000000000, 0.000000000000000000, 0.000000000000000000 ) ) ;
#72684 = CARTESIAN_POINT ( 'NONE',  ( 17.49999999999999645, -5.624438216177594541, 68.31670344914645909 ) ) ;
#72685 = CARTESIAN_POINT ( 'NONE',  ( -18.62759615963255300, -10.81492255796106328, 79.16775706135234714 ) ) ;
#72687 = CARTESIAN_POINT ( 'NONE',  ( -12.14591786802309592, -12.06949235617757132, 36.87390960531435979 ) ) ;
#72686 = CARTESIAN_POINT ( 'NONE',  ( 14.34966873604972726, -8.224510206698740333, 55.83442372801901854 ) ) ;
#72688 = CARTESIAN_POINT ( 'NONE',  ( 18.67979575497178502, 10.72451020669898547, 74.16557627198102409 ) ) ;
#72689 = CARTESIAN_POINT ( 'NONE',  ( -15.72974639402197994, 15.80617190586746368, 75.62390960531439532 ) ) ;
#72690 = CARTESIAN_POINT ( 'NONE',  ( -20.02432819973542877, 11.96332215053014636, 170.0134113894037000 ) ) ;
#72692 = CARTESIAN_POINT ( 'NONE',  ( 13.97604488694527802, 13.89961937509977652, 109.3739096053143669 ) ) ;
#72691 = CARTESIAN_POINT ( 'NONE',  ( -19.05341960407617563, 5.049401038297882671, 88.54275706135230450 ) ) ;
#72693 = CARTESIAN_POINT ( 'NONE',  ( 0.05219959533909260263, 19.03943276465977164, 54.99890960531435979 ) ) ;
#72694 = CARTESIAN_POINT ( 'NONE',  ( 16.53943276465976808, -0.05219959533910856209, 113.7489096053143527 ) ) ;
#72695 = SURFACE_STYLE_USAGE ( .BOTH. , #165699 ) ;
#72696 = CARTESIAN_POINT ( 'NONE',  ( -9.100000000000001421, 9.789526074884739315E-14, -63.95112321872120731 ) ) ;
#72697 = ORIENTED_EDGE ( 'NONE', *, *, #143807, .T. ) ;
#72699 = CARTESIAN_POINT ( 'NONE',  ( -16.52544592524335698, -4.483927247898792601, 88.95942372801901854 ) ) ;
#72698 = CIRCLE ( 'NONE', #150207, 4.999999999999998224 ) ;
#72700 = CARTESIAN_POINT ( 'NONE',  ( 5.823673210054125526, 21.52544592524343514, 104.7905762719810241 ) ) ;
#72701 = CARTESIAN_POINT ( 'NONE',  ( -5.049401038298153566, 19.05341960407611168, 65.20724293864765286 ) ) ;
#72702 = CARTESIAN_POINT ( 'NONE',  ( -15.80617190586768217, 15.72974639402176855, 38.12609039468567573 ) ) ;
#72703 = CARTESIAN_POINT ( 'NONE',  ( -19.05341960407611168, -5.049401038298163336, 96.45724293864769550 ) ) ;
#72705 = EDGE_CURVE ( 'NONE', #106856, #142504, #151437, .T. ) ;
#72704 = CARTESIAN_POINT ( 'NONE',  ( -30.36026264928165119, -25.76863830326744775, -21.12575414590727618 ) ) ;
#72706 = ORIENTED_EDGE ( 'NONE', *, *, #86027, .T. ) ;
#72707 = CARTESIAN_POINT ( 'NONE',  ( 21.53943276465977519, 0.05219959533937863772, 31.25109039468568639 ) ) ;
#72709 = CARTESIAN_POINT ( 'NONE',  ( -19.02544592524334988, -5.153800228976617603, 88.95942372801897591 ) ) ;
#72708 = CARTESIAN_POINT ( 'NONE',  ( -0.05219959533909027116, -19.03943276465977164, 22.49890960531436690 ) ) ;
#72710 = CARTESIAN_POINT ( 'NONE',  ( 19.03943276465977164, 0.05219959533936151252, 41.25109039468566152 ) ) ;
#72711 = CARTESIAN_POINT ( 'NONE',  ( -18.62759615963255300, -10.81492255796106328, 19.16775706135234714 ) ) ;
#72712 = CARTESIAN_POINT ( 'NONE',  ( -19.02544592524334988, -5.153800228976617603, 38.95942372801900433 ) ) ;
#72713 = CARTESIAN_POINT ( 'NONE',  ( -16.46253265017146816, -9.564922557961047289, 44.16775706135232582 ) ) ;
#72714 = CARTESIAN_POINT ( 'NONE',  ( 14.29746914071037800, 8.314922557961029526, 91.66775706135234714 ) ) ;
#72715 = DIRECTION ( 'NONE',  ( 0.000000000000000000, 0.9396926207859095381, -0.3420201433256656043 ) ) ;
#72716 = CARTESIAN_POINT ( 'NONE',  ( 16.46253265017160672, -9.564922557960803928, 68.33224293864770971 ) ) ;
#72717 = MECHANICAL_DESIGN_GEOMETRIC_PRESENTATION_REPRESENTATION (  '', ( #179239 ), #108182 ) ;
#72718 = CARTESIAN_POINT ( 'NONE',  ( 18.67979575497194134, -10.72451020669871369, 75.83442372801900433 ) ) ;
#72719 = CARTESIAN_POINT ( 'NONE',  ( -0.05219959533937732626, 21.53943276465977519, 92.50109039468567573 ) ) ;
#72720 = CARTESIAN_POINT ( 'NONE',  ( -0.9199430937698453992, -8.788868155854853370, -64.01178436185549003 ) ) ;
#72721 = CARTESIAN_POINT ( 'NONE',  ( 0.05219959533909260263, 19.03943276465977164, 84.99890960531436690 ) ) ;
#72722 = CARTESIAN_POINT ( 'NONE',  ( -5.823673210054431948, 21.52544592524334988, 62.70942372801902565 ) ) ;
#72723 = CARTESIAN_POINT ( 'NONE',  ( -13.97604488694547697, 13.89961937509957934, 103.1260903946856473 ) ) ;
#72724 = CARTESIAN_POINT ( 'NONE',  ( -13.89961937509977652, 13.97604488694528158, 65.62390960531436690 ) ) ;
#72725 = CARTESIAN_POINT ( 'NONE',  ( -10.81492255796078084, -18.62759615963271287, 22.08224293864769194 ) ) ;
#72726 = CARTESIAN_POINT ( 'NONE',  ( 9.564922557960805705, 16.46253265017160317, 74.58224293864769550 ) ) ;
#72727 = CARTESIAN_POINT ( 'NONE',  ( 2.552343178074723884, 7.052343178074616858, 8.889087296526001936 ) ) ;
#72728 = CARTESIAN_POINT ( 'NONE',  ( -16.51473224551069308, -9.474510206698971260, 61.66557627198103120 ) ) ;
#72729 = CARTESIAN_POINT ( 'NONE',  ( -9.564922557960796823, -16.46253265017161027, 47.08224293864769550 ) ) ;
#72730 = CARTESIAN_POINT ( 'NONE',  ( 21.52544592524344225, -5.823673210054117533, 113.5405762719810383 ) ) ;
#72731 = CARTESIAN_POINT ( 'NONE',  ( 14.34966873604972726, -8.224510206698740333, 95.83442372801903275 ) ) ;
#72732 = CARTESIAN_POINT ( 'NONE',  ( -18.56399227203345603, -5.499999999999827693, 38.97830131249903474 ) ) ;
#72733 = AXIS2_PLACEMENT_3D ( 'NONE', #59317, #75484, #120986 ) ;
#72734 = CARTESIAN_POINT ( 'NONE',  ( 8.725106586199796510, -0.9968436689772890436, -64.02420483255117745 ) ) ;
#72735 = CARTESIAN_POINT ( 'NONE',  ( 5.049401038297881783, 19.05341960407617563, 62.29275706135234003 ) ) ;
#72736 = CARTESIAN_POINT ( 'NONE',  ( -13.97604488694527625, -13.89961937509977652, 76.87390960531433848 ) ) ;
#72737 = CARTESIAN_POINT ( 'NONE',  ( -16.52544592524342804, 4.483927247898546575, 71.04057627198103830 ) ) ;
#72738 = CARTESIAN_POINT ( 'NONE',  ( 16.52544592524342804, -4.483927247898539470, 103.5405762719810383 ) ) ;
#72739 = VECTOR ( 'NONE', #92475, 999.9999999999998863 ) ;
#72740 = CARTESIAN_POINT ( 'NONE',  ( 15.72974639402199770, -15.80617190586745480, 38.12390960531436690 ) ) ;
#72741 =( BOUNDED_CURVE ( )  B_SPLINE_CURVE ( 2, ( #152839, #107321, #185173, #61811, #137672, #76990, #88189, #45670, #184188, #149873, #14333, #123481, #75998 ),
 .UNSPECIFIED., .F., .F. ) 
 B_SPLINE_CURVE_WITH_KNOTS ( ( 3, 2, 2, 2, 2, 2, 3 ),
 ( 0.6603708530912405505, 0.6622807017543859143, 0.6666666666666666297, 0.6710526315789473450, 0.6754385964912280604, 0.6798245614035087758, 0.6817800898887445005 ),
 .UNSPECIFIED. ) 
 CURVE ( )  GEOMETRIC_REPRESENTATION_ITEM ( )  RATIONAL_B_SPLINE_CURVE ( ( 0.9832469066685283199, 0.9851625545550095620, 1.000000000000000000, 0.9659258262890683122, 1.000000000000000000, 0.9659258262890683122, 1.000000000000000000, 0.9659258262890683122, 1.000000000000000000, 0.9659258262890683122, 1.000000000000000000, 0.9848076720550078544, 0.9831626618144001517 ) ) 
 REPRESENTATION_ITEM ( '' )  );
#72742 = CARTESIAN_POINT ( 'NONE',  ( 5.153800228976335163, 19.02544592524342804, 109.7905762719810099 ) ) ;
#72743 = CARTESIAN_POINT ( 'NONE',  ( -4.483927247898539470, -16.52544592524342804, 97.29057627198105251 ) ) ;
#72744 = CARTESIAN_POINT ( 'NONE',  ( -13.97604488694527625, -13.89961937509977830, 81.87390960531436690 ) ) ;
#72745 = CARTESIAN_POINT ( 'NONE',  ( 19.02544592524334988, 5.153800228976608722, 26.45942372801899722 ) ) ;
#72746 = CARTESIAN_POINT ( 'NONE',  ( -16.52544592524335698, -4.483927247898792601, 103.9594237280190185 ) ) ;
#72747 = CARTESIAN_POINT ( 'NONE',  ( -0.05219959533909027116, -19.03943276465977164, 87.49890960531436690 ) ) ;
#72748 = CARTESIAN_POINT ( 'NONE',  ( 18.62759615963255655, 10.81492255796105972, 46.66775706135234714 ) ) ;
#72749 = CARTESIAN_POINT ( 'NONE',  ( 5.719274019375991003, -21.55341960407610458, 37.70724293864769550 ) ) ;
#72750 = CARTESIAN_POINT ( 'NONE',  ( -15.80617190586745835, -15.72974639402198527, 111.8739096053143669 ) ) ;
#72751 = CARTESIAN_POINT ( 'NONE',  ( -10.72451020669898014, 18.67979575497178502, 75.41557627198102409 ) ) ;
#72752 = CARTESIAN_POINT ( 'NONE',  ( -12.06949235617756955, 12.14591786802309770, 90.62390960531436690 ) ) ;
#72753 = CARTESIAN_POINT ( 'NONE',  ( -19.02544592524334988, -5.153800228976617603, 58.95942372801900433 ) ) ;
#72754 = CARTESIAN_POINT ( 'NONE',  ( -13.89961937509977652, 13.97604488694528158, 30.62390960531435269 ) ) ;
#72755 = CARTESIAN_POINT ( 'NONE',  ( 13.89961937509977652, -13.97604488694527269, 98.12390960531433848 ) ) ;
#72756 = CARTESIAN_POINT ( 'NONE',  ( -19.05341960407611168, -5.049401038298163336, 91.45724293864766707 ) ) ;
#72757 = CARTESIAN_POINT ( 'NONE',  ( 16.52544592524342804, -4.483927247898539470, 108.5405762719810241 ) ) ;
#72758 = CARTESIAN_POINT ( 'NONE',  ( -14.29746914071049879, 8.314922557960819915, 25.83224293864769194 ) ) ;
#72759 = CARTESIAN_POINT ( 'NONE',  ( 16.55341960407618274, -4.379528057220086978, 41.04275706135236135 ) ) ;
#72761 = VECTOR ( 'NONE', #127061, 1000.000000000000000 ) ;
#72760 = CARTESIAN_POINT ( 'NONE',  ( -18.62759615963255300, -10.81492255796106328, 104.1677570613523471 ) ) ;
#72763 = CARTESIAN_POINT ( 'NONE',  ( 16.53943276465976808, -0.05219959533910856209, 23.74890960531435269 ) ) ;
#72762 = CARTESIAN_POINT ( 'NONE',  ( -13.97604488694527625, -13.89961937509977652, 101.8739096053143811 ) ) ;
#72764 = CARTESIAN_POINT ( 'NONE',  ( 18.62759615963255655, 10.81492255796105972, 36.66775706135234714 ) ) ;
#72765 = CARTESIAN_POINT ( 'NONE',  ( -13.89961937509977652, 13.97604488694528158, 45.62390960531433848 ) ) ;
#72766 = CARTESIAN_POINT ( 'NONE',  ( 16.55341960407618274, -4.379528057220086978, 51.04275706135234714 ) ) ;
#72767 = CARTESIAN_POINT ( 'NONE',  ( 16.52544592524335698, 4.483927247898782831, 111.4594237280190328 ) ) ;
#72768 = CARTESIAN_POINT ( 'NONE',  ( -16.53943276465976808, -0.05219959533934237506, 98.75109039468568994 ) ) ;
#72769 = CARTESIAN_POINT ( 'NONE',  ( -16.46253265017146816, -9.564922557961047289, 104.1677570613523329 ) ) ;
#72770 = CARTESIAN_POINT ( 'NONE',  ( 9.564922557960805705, 16.46253265017160317, 39.58224293864768839 ) ) ;
#72771 = CARTESIAN_POINT ( 'NONE',  ( 16.52544592524342804, -4.483927247898539470, 93.54057627198103830 ) ) ;
#72772 = CARTESIAN_POINT ( 'NONE',  ( -10.72451020669898014, 18.67979575497178502, 105.4155762719810383 ) ) ;
#72773 = CARTESIAN_POINT ( 'NONE',  ( -0.05219959533909027116, -19.03943276465977164, 37.49890960531436690 ) ) ;
#72774 = CARTESIAN_POINT ( 'NONE',  ( -16.51473224551069308, -9.474510206698971260, 101.6655762719810241 ) ) ;
#72775 = CARTESIAN_POINT ( 'NONE',  ( 5.719274019375673035, 21.55341960407619339, 27.29275706135234358 ) ) ;
#72776 = CARTESIAN_POINT ( 'NONE',  ( 2.500000000000000000, -165.0000000000000000, 12.00000000000000355 ) ) ;
#72777 = CARTESIAN_POINT ( 'NONE',  ( 9.474510206698971260, -16.51473224551069308, 102.9155762719810241 ) ) ;
#72778 = LINE ( 'NONE', #57604, #80916 ) ;
#72779 = CARTESIAN_POINT ( 'NONE',  ( -19.02544592524342804, 5.153800228976336051, 91.04057627198100988 ) ) ;
#72781 = CARTESIAN_POINT ( 'NONE',  ( -12.14591786802309592, -12.06949235617757132, 96.87390960531436690 ) ) ;
#72780 = CARTESIAN_POINT ( 'NONE',  ( -5.719274019375665041, -21.55341960407619695, 34.79275706135235424 ) ) ;
#72782 = CARTESIAN_POINT ( 'NONE',  ( 19.03943276465977164, -0.05219959533909143690, 93.74890960531435269 ) ) ;
#72783 = CARTESIAN_POINT ( 'NONE',  ( 16.51473224551083163, -9.474510206698727899, 25.83442372801900078 ) ) ;
#72784 = CARTESIAN_POINT ( 'NONE',  ( -12.06949235617739369, -12.14591786802326823, 59.37609039468568284 ) ) ;
#72785 = CARTESIAN_POINT ( 'NONE',  ( -21.53943276465977519, -0.05219959533937600094, 73.75109039468567573 ) ) ;
#72786 = CARTESIAN_POINT ( 'NONE',  ( 8.314922557961029526, -14.29746914071037800, 45.41775706135234003 ) ) ;
#72787 = CARTESIAN_POINT ( 'NONE',  ( -19.02544592524342804, 5.153800228976336051, 86.04057627198103830 ) ) ;
#72788 = CARTESIAN_POINT ( 'NONE',  ( -16.46253265017146816, -9.564922557961047289, 89.16775706135234714 ) ) ;
#72789 = CARTESIAN_POINT ( 'NONE',  ( -8.314922557961024197, 14.29746914071037800, 72.91775706135234714 ) ) ;
#72790 = CARTESIAN_POINT ( 'NONE',  ( 10.72451020669871369, 18.67979575497193778, 107.0844237280190043 ) ) ;
#72791 = CARTESIAN_POINT ( 'NONE',  ( 13.89961937509957401, 13.97604488694547697, 96.87609039468566152 ) ) ;
#72792 = CARTESIAN_POINT ( 'NONE',  ( 9.474510206698971260, -16.51473224551069308, 67.91557627198102409 ) ) ;
#72793 = CARTESIAN_POINT ( 'NONE',  ( 5.719274019375991003, -21.55341960407610458, 77.70724293864770971 ) ) ;
#72795 = CARTESIAN_POINT ( 'NONE',  ( 5.153800228976615827, -19.02544592524334988, 90.20942372801900433 ) ) ;
#72794 = CARTESIAN_POINT ( 'NONE',  ( -14.29746914071049879, 8.314922557960819915, 85.83224293864768129 ) ) ;
#72796 = CARTESIAN_POINT ( 'NONE',  ( 12.14591786802327356, -12.06949235617739191, 65.62609039468568994 ) ) ;
#72797 = CARTESIAN_POINT ( 'NONE',  ( 24.66578506923905323, 3.377805382905409104, 172.1149105766468494 ) ) ;
#72798 = CARTESIAN_POINT ( 'NONE',  ( 16.51473224551083163, -9.474510206698727899, 60.83442372801900433 ) ) ;
#72799 = CARTESIAN_POINT ( 'NONE',  ( 12.06949235617757843, -12.14591786802309237, 23.12390960531436335 ) ) ;
#72800 = CARTESIAN_POINT ( 'NONE',  ( 12.06949235617757843, -12.14591786802309237, 83.12390960531436690 ) ) ;
#72802 = CARTESIAN_POINT ( 'NONE',  ( -17.44279575226786250, 5.990770900253883369, 40.83557567514318265 ) ) ;
#72801 = CARTESIAN_POINT ( 'NONE',  ( -16.46253265017146816, -9.564922557961047289, 19.16775706135233293 ) ) ;
#72803 = CARTESIAN_POINT ( 'NONE',  ( -21.52544592524334988, -5.823673210054445271, 18.95942372801901143 ) ) ;
#72804 = CARTESIAN_POINT ( 'NONE',  ( 9.474510206698971260, -16.51473224551069308, 97.91557627198102409 ) ) ;
#72805 = CARTESIAN_POINT ( 'NONE',  ( -5.049401038298153566, 19.05341960407611168, 80.20724293864769550 ) ) ;
#72806 = CARTESIAN_POINT ( 'NONE',  ( -21.52544592524334988, -5.823673210054445271, 88.95942372801901854 ) ) ;
#72807 = CARTESIAN_POINT ( 'NONE',  ( -16.51473224551069308, -9.474510206698971260, 66.66557627198102409 ) ) ;
#72808 = CARTESIAN_POINT ( 'NONE',  ( 21.53943276465977519, -0.05219959533907433946, 28.74890960531435624 ) ) ;
#72809 = AXIS2_PLACEMENT_3D ( 'NONE', #164101, #167081, #150925 ) ;
#72810 = CARTESIAN_POINT ( 'NONE',  ( 14.29746914071049879, -8.314922557960816363, 78.33224293864770971 ) ) ;
#72811 = CARTESIAN_POINT ( 'NONE',  ( -16.46253265017160317, 9.564922557960807481, 40.83224293864769550 ) ) ;
#72812 = CARTESIAN_POINT ( 'NONE',  ( -0.05219959533910754901, -16.53943276465976808, 102.4989096053143811 ) ) ;
#72813 = CARTESIAN_POINT ( 'NONE',  ( 5.823673210054125526, 21.52544592524343514, 104.7905762719810241 ) ) ;
#72814 = CARTESIAN_POINT ( 'NONE',  ( 18.67979575497194134, -10.72451020669871369, 60.83442372801901854 ) ) ;
#72815 = CARTESIAN_POINT ( 'NONE',  ( -9.474510206698964154, 16.51473224551069663, 30.41557627198102054 ) ) ;
#72816 = CARTESIAN_POINT ( 'NONE',  ( -8.224510206698735004, -14.34966873604973081, 64.58442372801900433 ) ) ;
#72817 = CARTESIAN_POINT ( 'NONE',  ( -15.80617190586745835, -15.72974639402198527, 106.8739096053143811 ) ) ;
#72818 = CARTESIAN_POINT ( 'NONE',  ( -5.823673210054116645, -21.52544592524344225, 112.2905762719810241 ) ) ;
#72820 = CARTESIAN_POINT ( 'NONE',  ( 5.049401038298161559, -19.05341960407611168, 47.70724293864770260 ) ) ;
#72819 = CARTESIAN_POINT ( 'NONE',  ( 13.97604488694548053, -13.89961937509957401, 45.62609039468566863 ) ) ;
#72821 = CARTESIAN_POINT ( 'NONE',  ( -17.72696623605158806, 5.500000000000047962, 83.59811031808415294 ) ) ;
#72822 = CARTESIAN_POINT ( 'NONE',  ( -0.05219959533937732626, 21.53943276465977519, 62.50109039468568284 ) ) ;
#72823 = CARTESIAN_POINT ( 'NONE',  ( 15.80617190586746368, 15.72974639402197994, 54.37390960531435979 ) ) ;
#72824 = CARTESIAN_POINT ( 'NONE',  ( -14.34966873604960291, -8.224510206698953496, 31.66557627198102054 ) ) ;
#72826 = CARTESIAN_POINT ( 'NONE',  ( 18.62759615963255655, 10.81492255796105972, 111.6677570613523613 ) ) ;
#72825 = CARTESIAN_POINT ( 'NONE',  ( -0.05219959533937732626, 21.53943276465977519, 72.50109039468568994 ) ) ;
#72827 = CARTESIAN_POINT ( 'NONE',  ( 0.05219959533910956823, 16.53943276465976808, 54.99890960531435269 ) ) ;
#72828 = CARTESIAN_POINT ( 'NONE',  ( 0.05219959533910956823, 16.53943276465976808, 104.9989096053143669 ) ) ;
#72829 = CARTESIAN_POINT ( 'NONE',  ( -9.474510206698720793, -16.51473224551083518, 39.58442372801899722 ) ) ;
#72830 = CARTESIAN_POINT ( 'NONE',  ( -14.34966873604972548, 8.224510206698743886, 98.33442372801901854 ) ) ;
#72831 = CARTESIAN_POINT ( 'NONE',  ( 0.05219959533937995610, -21.53943276465977519, 65.00109039468568994 ) ) ;
#72832 = CARTESIAN_POINT ( 'NONE',  ( 19.05341960407611168, 5.049401038298154454, 58.95724293864768129 ) ) ;
#72833 = CARTESIAN_POINT ( 'NONE',  ( -16.46253265017146816, -9.564922557961047289, 34.16775706135233293 ) ) ;
#72834 = CARTESIAN_POINT ( 'NONE',  ( 18.67979575497178502, 10.72451020669898547, 39.16557627198102409 ) ) ;
#72835 = CARTESIAN_POINT ( 'NONE',  ( -21.52544592524334988, -5.823673210054445271, 28.95942372801902209 ) ) ;
#72836 = CARTESIAN_POINT ( 'NONE',  ( -10.81492255796078084, -18.62759615963271287, 82.08224293864768129 ) ) ;
#72837 = CARTESIAN_POINT ( 'NONE',  ( 0.05219959533936267826, -19.03943276465977164, 90.00109039468567573 ) ) ;
#72838 = CARTESIAN_POINT ( 'NONE',  ( 12.14591786802327356, -12.06949235617739191, 50.62609039468568994 ) ) ;
#72840 = CARTESIAN_POINT ( 'NONE',  ( -0.05219959533907301413, -21.53943276465977519, 97.49890960531436690 ) ) ;
#72839 = CARTESIAN_POINT ( 'NONE',  ( 17.50000000000050093, -3.947464652946276242, 36.72413553410236631 ) ) ;
#72842 = CARTESIAN_POINT ( 'NONE',  ( -16.53943276465976808, 0.05219959533911058130, 76.24890960531435269 ) ) ;
#72841 = CARTESIAN_POINT ( 'NONE',  ( -16.52544592524335698, -4.483927247898792601, 83.95942372801900433 ) ) ;
#72843 = CARTESIAN_POINT ( 'NONE',  ( -17.44270441346515454, -5.991230190323027394, 101.3633507926422794 ) ) ;
#72844 = CARTESIAN_POINT ( 'NONE',  ( -0.05219959533934338120, 16.53943276465976808, 27.50109039468567929 ) ) ;
#72845 = EDGE_CURVE ( 'NONE', #30659, #104408, #104446, .T. ) ;
#72846 = CARTESIAN_POINT ( 'NONE',  ( 15.80617190586746368, 15.72974639402197994, 39.37390960531436690 ) ) ;
#72847 = CARTESIAN_POINT ( 'NONE',  ( 4.379528057220092307, 16.55341960407617563, 72.29275706135236135 ) ) ;
#72848 = CARTESIAN_POINT ( 'NONE',  ( -16.55341960407617563, 4.379528057220093196, 53.54275706135234714 ) ) ;
#72849 = CARTESIAN_POINT ( 'NONE',  ( 10.72451020669871369, 18.67979575497193778, 32.08442372801901854 ) ) ;
#72850 = CARTESIAN_POINT ( 'NONE',  ( 18.67979575497178502, 10.72451020669898547, 49.16557627198102409 ) ) ;
#72851 = CARTESIAN_POINT ( 'NONE',  ( 12.14591786802327356, -12.06949235617739191, 75.62609039468567573 ) ) ;
#72852 = CARTESIAN_POINT ( 'NONE',  ( -5.153800228976328057, -19.02544592524343514, 82.29057627198103830 ) ) ;
#72854 = CARTESIAN_POINT ( 'NONE',  ( 9.474510206698971260, -16.51473224551069308, 32.91557627198102409 ) ) ;
#72853 = CARTESIAN_POINT ( 'NONE',  ( -5.823673210054431948, 21.52544592524334988, 57.70942372801901143 ) ) ;
#72855 = CARTESIAN_POINT ( 'NONE',  ( -10.81492255796078084, -18.62759615963271287, 42.08224293864769550 ) ) ;
#72856 = CARTESIAN_POINT ( 'NONE',  ( -18.62759615963270932, 10.81492255796079327, 25.83224293864769194 ) ) ;
#72857 = ORIENTED_EDGE ( 'NONE', *, *, #67133, .T. ) ;
#72858 = CARTESIAN_POINT ( 'NONE',  ( 0.05219959533936267826, -19.03943276465977164, 45.00109039468566863 ) ) ;
#72859 = CARTESIAN_POINT ( 'NONE',  ( -12.14591786802326823, 12.06949235617739902, 48.12609039468568284 ) ) ;
#72860 = CARTESIAN_POINT ( 'NONE',  ( 13.89961937509977652, -13.97604488694527269, 108.1239096053143669 ) ) ;
#72861 = ORIENTED_EDGE ( 'NONE', *, *, #62108, .F. ) ;
#72862 = CARTESIAN_POINT ( 'NONE',  ( -0.05219959533909027116, -19.03943276465977164, 82.49890960531436690 ) ) ;
#72863 = CARTESIAN_POINT ( 'NONE',  ( -16.53943276465976808, -0.05219959533934237506, 103.7510903946857042 ) ) ;
#72864 = DIRECTION ( 'NONE',  ( 1.000000000000000000, 0.000000000000000000, 0.000000000000000000 ) ) ;
#72865 = CARTESIAN_POINT ( 'NONE',  ( 16.53943276465976808, -0.05219959533910856209, 98.74890960531438111 ) ) ;
#72866 = CARTESIAN_POINT ( 'NONE',  ( -10.81492255796078084, -18.62759615963271287, 32.08224293864769550 ) ) ;
#72867 = CARTESIAN_POINT ( 'NONE',  ( -16.51473224551069308, -9.474510206698971260, 26.66557627198103120 ) ) ;
#72868 = CARTESIAN_POINT ( 'NONE',  ( -14.29746914071037622, -8.314922557961029526, 84.16775706135234714 ) ) ;
#72869 = CARTESIAN_POINT ( 'NONE',  ( 18.62759615963255655, 10.81492255796105972, 21.66775706135235069 ) ) ;
#72870 = CARTESIAN_POINT ( 'NONE',  ( -9.474510206698720793, -16.51473224551083518, 74.58442372801900433 ) ) ;
#72871 = CARTESIAN_POINT ( 'NONE',  ( -5.049401038298153566, 19.05341960407611168, 35.20724293864768839 ) ) ;
#72872 = AXIS2_PLACEMENT_3D ( 'NONE', #97033, #3054, #7017 ) ;
#72873 = CARTESIAN_POINT ( 'NONE',  ( -0.05219959533909027116, -19.03943276465977164, 112.4989096053143669 ) ) ;
#72874 = CARTESIAN_POINT ( 'NONE',  ( 21.55341960407619695, -5.719274019375665929, 106.0427570613523471 ) ) ;
#72875 = CARTESIAN_POINT ( 'NONE',  ( 19.03943276465977164, -0.05219959533909143690, 63.74890960531435979 ) ) ;
#72876 = CARTESIAN_POINT ( 'NONE',  ( 16.55341960407618274, -4.379528057220086978, 46.04275706135234714 ) ) ;
#72877 = CARTESIAN_POINT ( 'NONE',  ( 21.52544592524334988, 5.823673210054432836, 86.45942372801901854 ) ) ;
#72878 = CARTESIAN_POINT ( 'NONE',  ( -0.05219959533936034679, 19.03943276465977164, 47.50109039468566863 ) ) ;
#72879 = CARTESIAN_POINT ( 'NONE',  ( 9.564922557961047289, -16.46253265017146816, 55.41775706135234003 ) ) ;
#72880 = ORIENTED_EDGE ( 'NONE', *, *, #166372, .F. ) ;
#72881 = CARTESIAN_POINT ( 'NONE',  ( -21.55341960407619339, 5.719274019375674811, 48.54275706135234714 ) ) ;
#72882 = DIRECTION ( 'NONE',  ( -1.000000000000000000, 0.000000000000000000, 0.000000000000000000 ) ) ;
#72883 = CARTESIAN_POINT ( 'NONE',  ( 13.89961937509957401, 13.97604488694547697, 46.87609039468565442 ) ) ;
#72884 = CARTESIAN_POINT ( 'NONE',  ( -19.05341960407611168, -5.049401038298163336, 96.45724293864769550 ) ) ;
#72885 = CARTESIAN_POINT ( 'NONE',  ( 5.049401038298161559, -19.05341960407611168, 77.70724293864765286 ) ) ;
#72886 = CARTESIAN_POINT ( 'NONE',  ( 4.379528057220339221, -16.55341960407611168, 32.70724293864770260 ) ) ;
#72887 = CARTESIAN_POINT ( 'NONE',  ( 5.823673210054125526, 21.52544592524343514, 29.79057627198102409 ) ) ;
#72888 = AXIS2_PLACEMENT_3D ( 'NONE', #20134, #143466, #67630 ) ;
#72889 = CARTESIAN_POINT ( 'NONE',  ( 29.86685920354754487, 21.69954338932564752, -1.924999997268813212 ) ) ;
#72890 = CARTESIAN_POINT ( 'NONE',  ( 20.23564678862950927, 22.32700255269481104, -51.30755147637196956 ) ) ;
#72891 = CARTESIAN_POINT ( 'NONE',  ( -5.153800228976607833, 19.02544592524334988, 22.70942372801899012 ) ) ;
#72892 = LINE ( 'NONE', #196248, #108979 ) ;
#72893 = CARTESIAN_POINT ( 'NONE',  ( 16.46253265017160672, -9.564922557960803928, 43.33224293864769550 ) ) ;
#72894 = CARTESIAN_POINT ( 'NONE',  ( 16.46253265017160672, -9.564922557960803928, 23.33224293864769194 ) ) ;
#72895 = CARTESIAN_POINT ( 'NONE',  ( -9.574135874901902099, -11.69267847920397685, -59.86604769085835187 ) ) ;
#72896 = CARTESIAN_POINT ( 'NONE',  ( -18.30394412277474103, -32.66729986584498135, -8.000000000000000000 ) ) ;
#72897 = CARTESIAN_POINT ( 'NONE',  ( -0.05219959533934338120, 16.53943276465976808, 67.50109039468568994 ) ) ;
#72898 = CARTESIAN_POINT ( 'NONE',  ( 18.67979575497178502, 10.72451020669898547, 89.16557627198102409 ) ) ;
#72899 = CARTESIAN_POINT ( 'NONE',  ( 16.55341960407611168, 4.379528057220329451, 53.95724293864770260 ) ) ;
#72901 = CARTESIAN_POINT ( 'NONE',  ( 9.474510206698971260, -16.51473224551069308, 112.9155762719810383 ) ) ;
#72900 = CARTESIAN_POINT ( 'NONE',  ( 19.05341960407611168, 5.049401038298154454, 28.95724293864769550 ) ) ;
#72902 = CARTESIAN_POINT ( 'NONE',  ( 10.72451020669871369, 18.67979575497193778, 32.08442372801901854 ) ) ;
#72903 = CARTESIAN_POINT ( 'NONE',  ( 19.02544592524334988, 5.153800228976608722, 36.45942372801900433 ) ) ;
#72904 = CARTESIAN_POINT ( 'NONE',  ( -13.97604488694527625, -13.89961937509977652, 36.87390960531436690 ) ) ;
#72905 = CARTESIAN_POINT ( 'NONE',  ( -18.62759615963255300, -10.81492255796106328, 79.16775706135234714 ) ) ;
#72906 = DIRECTION ( 'NONE',  ( -1.000000000000000000, 0.000000000000000000, 0.000000000000000000 ) ) ;
#72907 = CARTESIAN_POINT ( 'NONE',  ( -4.379528057220328563, 16.55341960407611168, 25.20724293864769550 ) ) ;
#72908 = CARTESIAN_POINT ( 'NONE',  ( 11.40812507854755253, -35.11059874428192273, -2.524999997268813523 ) ) ;
#72909 = CARTESIAN_POINT ( 'NONE',  ( 5.719274019375991003, -21.55341960407610458, 47.70724293864770260 ) ) ;
#72910 = CARTESIAN_POINT ( 'NONE',  ( 0.05219959533910956823, 16.53943276465976808, 109.9989096053143527 ) ) ;
#72911 = CARTESIAN_POINT ( 'NONE',  ( 4.158454644149660595, -48.51789971941278168, -23.00000000000000000 ) ) ;
#72912 = CARTESIAN_POINT ( 'NONE',  ( -19.02544592524342804, 5.153800228976336051, 86.04057627198103830 ) ) ;
#72913 = CARTESIAN_POINT ( 'NONE',  ( 14.34966873604960469, 8.224510206698951720, 79.16557627198103830 ) ) ;
#72914 = CARTESIAN_POINT ( 'NONE',  ( -19.02544592524334988, -5.153800228976617603, 103.9594237280190043 ) ) ;
#72915 = EDGE_CURVE ( 'NONE', #150593, #136632, #92231, .T. ) ;
#72916 = CARTESIAN_POINT ( 'NONE',  ( 15.80617190586746368, 15.72974639402197994, 69.37390960531436690 ) ) ;
#72917 = ORIENTED_EDGE ( 'NONE', *, *, #74806, .F. ) ;
#72918 = CARTESIAN_POINT ( 'NONE',  ( 19.02544592524343514, -5.153800228976328945, 28.54057627198102409 ) ) ;
#72920 = CARTESIAN_POINT ( 'NONE',  ( 18.62759615963271287, -10.81492255796078972, 93.33224293864769550 ) ) ;
#72919 = CARTESIAN_POINT ( 'NONE',  ( -13.89961937509977652, 13.97604488694528158, 90.62390960531432427 ) ) ;
#72922 = CARTESIAN_POINT ( 'NONE',  ( 5.049401038298161559, -19.05341960407611168, 92.70724293864769550 ) ) ;
#72921 = CARTESIAN_POINT ( 'NONE',  ( 14.29746914071037800, 8.314922557961029526, 101.6677570613523613 ) ) ;
#72923 = CARTESIAN_POINT ( 'NONE',  ( 19.05341960407617918, -5.049401038297876454, 86.04275706135233293 ) ) ;
#72924 = CARTESIAN_POINT ( 'NONE',  ( 18.62759615963255655, 10.81492255796105972, 96.66775706135234714 ) ) ;
#72925 = CARTESIAN_POINT ( 'NONE',  ( 15.72974639402199770, -15.80617190586745480, 83.12390960531436690 ) ) ;
#72926 = CARTESIAN_POINT ( 'NONE',  ( 15.80617190586746368, 15.72974639402197994, 39.37390960531436690 ) ) ;
#72927 = CARTESIAN_POINT ( 'NONE',  ( 5.153800228976335163, 19.02544592524342804, 49.79057627198100988 ) ) ;
#72928 = CARTESIAN_POINT ( 'NONE',  ( -4.483927247898539470, -16.52544592524342804, 27.29057627198103120 ) ) ;
#72929 = CARTESIAN_POINT ( 'NONE',  ( 19.05341960407611168, 5.049401038298154454, 63.95724293864769550 ) ) ;
#72930 = CARTESIAN_POINT ( 'NONE',  ( -32.63052366545711180, -0.9798963808688879729, 87.54781425814060469 ) ) ;
#72931 = CARTESIAN_POINT ( 'NONE',  ( 13.97604488694548053, -13.89961937509957401, 25.62609039468566507 ) ) ;
#72932 = CARTESIAN_POINT ( 'NONE',  ( -8.314922557960811034, -14.29746914071050412, 77.08224293864769550 ) ) ;
#72933 = CARTESIAN_POINT ( 'NONE',  ( -18.67979575497178146, -10.72451020669898902, 111.6655762719810525 ) ) ;
#72934 = CARTESIAN_POINT ( 'NONE',  ( -27.73933785331498925, 2.428612866367529932E-14, 139.3750000027311842 ) ) ;
#72935 = CARTESIAN_POINT ( 'NONE',  ( -10.72451020669898014, 18.67979575497178502, 55.41557627198102409 ) ) ;
#72936 = CARTESIAN_POINT ( 'NONE',  ( 16.52544592524335698, 4.483927247898782831, 91.45942372801901854 ) ) ;
#72937 = CARTESIAN_POINT ( 'NONE',  ( -16.52544592524342804, 4.483927247898546575, 101.0405762719810383 ) ) ;
#72938 = CARTESIAN_POINT ( 'NONE',  ( 5.153800228976335163, 19.02544592524342804, 59.79057627198100988 ) ) ;
#72939 =( NAMED_UNIT ( * ) SI_UNIT ( $, .STERADIAN. ) SOLID_ANGLE_UNIT ( ) );
#72940 = CARTESIAN_POINT ( 'NONE',  ( -14.29746914071049879, 8.314922557960819915, 35.83224293864768839 ) ) ;
#72941 = CARTESIAN_POINT ( 'NONE',  ( 21.55341960407619695, -5.719274019375665929, 41.04275706135236135 ) ) ;
#72942 = CARTESIAN_POINT ( 'NONE',  ( -13.89961937509977652, 13.97604488694528158, 110.6239096053143243 ) ) ;
#72943 = CARTESIAN_POINT ( 'NONE',  ( -18.62759615963255300, -10.81492255796106328, 79.16775706135234714 ) ) ;
#72944 = CARTESIAN_POINT ( 'NONE',  ( -13.97604488694527625, -13.89961937509977652, 26.87390960531434558 ) ) ;
#72945 = CARTESIAN_POINT ( 'NONE',  ( -5.049401038298153566, 19.05341960407611168, 40.20724293864768839 ) ) ;
#72946 = VERTEX_POINT ( 'NONE', #90729 ) ;
#72947 = CARTESIAN_POINT ( 'NONE',  ( 15.80617190586769283, -15.72974639402175789, 90.62609039468567573 ) ) ;
#72948 = CARTESIAN_POINT ( 'NONE',  ( -16.52544592524335698, -4.483927247898792601, 43.95942372801902565 ) ) ;
#72949 = CARTESIAN_POINT ( 'NONE',  ( 18.62759615963255655, 10.81492255796105972, 71.66775706135234714 ) ) ;
#72950 = CARTESIAN_POINT ( 'NONE',  ( -0.05219959533909027116, -19.03943276465977164, 107.4989096053143527 ) ) ;
#72951 = CARTESIAN_POINT ( 'NONE',  ( 9.474510206698729675, 16.51473224551082808, 87.08442372801900433 ) ) ;
#72952 = CARTESIAN_POINT ( 'NONE',  ( -10.72451020669870658, -18.67979575497194134, 54.58442372801901143 ) ) ;
#72953 = CARTESIAN_POINT ( 'NONE',  ( 19.02544592524334988, 5.153800228976608722, 111.4594237280190043 ) ) ;
#72954 = VECTOR ( 'NONE', #169236, 1000.000000000000000 ) ;
#72955 = CARTESIAN_POINT ( 'NONE',  ( -13.97604488694547697, 13.89961937509957934, 83.12609039468564731 ) ) ;
#72956 = CARTESIAN_POINT ( 'NONE',  ( 19.05341960407611168, 5.049401038298154454, 53.95724293864770260 ) ) ;
#72957 = CARTESIAN_POINT ( 'NONE',  ( -19.02544592524334988, -5.153800228976617603, 83.95942372801901854 ) ) ;
#72958 = CARTESIAN_POINT ( 'NONE',  ( -14.34966873604972548, 8.224510206698743886, 113.3344237280190328 ) ) ;
#72959 = CARTESIAN_POINT ( 'NONE',  ( 19.03943276465977164, 0.05219959533936151252, 91.25109039468566152 ) ) ;
#72960 = CARTESIAN_POINT ( 'NONE',  ( -14.34966873604960291, -8.224510206698953496, 36.66557627198103120 ) ) ;
#72961 = CARTESIAN_POINT ( 'NONE',  ( -9.564922557961040184, 16.46253265017147172, 67.91775706135233293 ) ) ;
#72962 = CARTESIAN_POINT ( 'NONE',  ( 16.52544592524335698, 4.483927247898782831, 46.45942372801901854 ) ) ;
#72963 = CARTESIAN_POINT ( 'NONE',  ( -9.564922557961040184, 16.46253265017147172, 27.91775706135232582 ) ) ;
#72964 = CARTESIAN_POINT ( 'NONE',  ( 0.05219959533910956823, 16.53943276465976808, 114.9989096053143669 ) ) ;
#72965 = CARTESIAN_POINT ( 'NONE',  ( 9.564922557960805705, 16.46253265017160317, 39.58224293864768839 ) ) ;
#72966 = CARTESIAN_POINT ( 'NONE',  ( -16.52544592524335698, -4.483927247898792601, 43.95942372801902565 ) ) ;
#72967 = LINE ( 'NONE', #183117, #104758 ) ;
#72968 = CARTESIAN_POINT ( 'NONE',  ( -23.31738231874055245, -16.94106989632524574, 142.4500000054623854 ) ) ;
#72969 = CARTESIAN_POINT ( 'NONE',  ( -16.51473224551069308, -9.474510206698971260, 86.66557627198102409 ) ) ;
#72970 = CARTESIAN_POINT ( 'NONE',  ( 17.66907692000856400, -2.165031582821545175, 102.5000000000000000 ) ) ;
#72971 = ORIENTED_EDGE ( 'NONE', *, *, #80196, .T. ) ;
#72972 = CARTESIAN_POINT ( 'NONE',  ( -16.51473224551082808, 9.474510206698731452, 93.33442372801900433 ) ) ;
#72973 = CARTESIAN_POINT ( 'NONE',  ( -18.67979575497178146, -10.72451020669898902, 26.66557627198103475 ) ) ;
#72975 = CARTESIAN_POINT ( 'NONE',  ( -5.049401038297874678, -19.05341960407617918, 104.7927570613523471 ) ) ;
#72974 = CARTESIAN_POINT ( 'NONE',  ( 16.51473224551083163, -9.474510206698727899, 25.83442372801900078 ) ) ;
#72976 = CARTESIAN_POINT ( 'NONE',  ( 16.53943276465976808, -0.05219959533910856209, 108.7489096053143669 ) ) ;
#72977 = CARTESIAN_POINT ( 'NONE',  ( 5.153800228976335163, 19.02544592524342804, 34.79057627198102409 ) ) ;
#72978 = CARTESIAN_POINT ( 'NONE',  ( 15.72974639402199770, -15.80617190586745480, 68.12390960531436690 ) ) ;
#72979 = CARTESIAN_POINT ( 'NONE',  ( -0.05219959533909027116, -19.03943276465977164, 37.49890960531436690 ) ) ;
#72980 = CARTESIAN_POINT ( 'NONE',  ( 10.65970682939788716, -25.60940286011448919, 139.9999999999999716 ) ) ;
#72981 = CARTESIAN_POINT ( 'NONE',  ( -16.46253265017146816, -9.564922557961047289, 74.16775706135234714 ) ) ;
#72982 = CARTESIAN_POINT ( 'NONE',  ( 16.53943276465976808, -0.05219959533910856209, 58.74890960531436690 ) ) ;
#72983 = CARTESIAN_POINT ( 'NONE',  ( 10.81492255796078972, 18.62759615963270932, 34.58224293864770260 ) ) ;
#72984 = CARTESIAN_POINT ( 'NONE',  ( 15.80617190586769283, -15.72974639402175789, 90.62609039468567573 ) ) ;
#72985 = CARTESIAN_POINT ( 'NONE',  ( 15.80617190586746368, 15.72974639402197994, 84.37390960531438111 ) ) ;
#72986 = CARTESIAN_POINT ( 'NONE',  ( 5.719274019375673035, 21.55341960407619339, 77.29275706135234714 ) ) ;
#72987 = CARTESIAN_POINT ( 'NONE',  ( -18.67979575497193778, 10.72451020669871902, 58.33442372801901143 ) ) ;
#72988 = CARTESIAN_POINT ( 'NONE',  ( 19.05341960407611168, 5.049401038298154454, 98.95724293864766707 ) ) ;
#72990 = CARTESIAN_POINT ( 'NONE',  ( -10.81492255796105439, 18.62759615963255655, 62.91775706135236135 ) ) ;
#72989 = CARTESIAN_POINT ( 'NONE',  ( -14.34966873604972548, 8.224510206698743886, 88.33442372801901854 ) ) ;
#72991 = CARTESIAN_POINT ( 'NONE',  ( 13.97604488694527802, 13.89961937509977652, 59.37390960531434558 ) ) ;
#72992 = CARTESIAN_POINT ( 'NONE',  ( 21.52544592524334988, 5.823673210054432836, 36.45942372801901143 ) ) ;
#72993 = CARTESIAN_POINT ( 'NONE',  ( 9.564922557960805705, 16.46253265017160317, 69.58224293864770971 ) ) ;
#72994 = CARTESIAN_POINT ( 'NONE',  ( 4.483927247898545687, 16.52544592524342804, 64.79057627198103830 ) ) ;
#72995 = CARTESIAN_POINT ( 'NONE',  ( 8.224510206698953496, -14.34966873604960469, 27.91557627198103830 ) ) ;
#72996 = CARTESIAN_POINT ( 'NONE',  ( 18.62759615963271287, -10.81492255796078972, 48.33224293864770260 ) ) ;
#72997 = CONICAL_SURFACE ( 'NONE', #131132, 30.82560697742735556, 0.1745329251994333364 ) ;
#72998 = CARTESIAN_POINT ( 'NONE',  ( -5.153800228976328057, -19.02544592524343514, 47.29057627198102409 ) ) ;
#72999 = CARTESIAN_POINT ( 'NONE',  ( -0.05219959533907301413, -21.53943276465977519, 52.49890960531435979 ) ) ;
#73000 = CARTESIAN_POINT ( 'NONE',  ( 16.51473224551083163, -9.474510206698727899, 55.83442372801899722 ) ) ;
#73002 = CARTESIAN_POINT ( 'NONE',  ( 8.224510206698953496, -14.34966873604960469, 62.91557627198102409 ) ) ;
#73001 = CARTESIAN_POINT ( 'NONE',  ( -20.96320343559654020, -25.54568634023494411, 7.533197955354854258 ) ) ;
#73003 = CARTESIAN_POINT ( 'NONE',  ( 21.52544592524344225, -5.823673210054117533, 38.54057627198103120 ) ) ;
#73004 = ORIENTED_EDGE ( 'NONE', *, *, #146462, .T. ) ;
#73005 = DIRECTION ( 'NONE',  ( 0.000000000000000000, 0.000000000000000000, -1.000000000000000000 ) ) ;
#73006 = CARTESIAN_POINT ( 'NONE',  ( 0.05219959533934541429, -16.53943276465976808, 80.00109039468568994 ) ) ;
#73007 = CARTESIAN_POINT ( 'NONE',  ( -9.564922557961040184, 16.46253265017147172, 87.91775706135233293 ) ) ;
#73008 = CARTESIAN_POINT ( 'NONE',  ( -14.29746914071049879, 8.314922557960819915, 60.83224293864769550 ) ) ;
#73009 = PLANE ( 'NONE',  #145128 ) ;
#73010 = CARTESIAN_POINT ( 'NONE',  ( 9.564922557960805705, 16.46253265017160317, 54.58224293864769550 ) ) ;
#73011 = CARTESIAN_POINT ( 'NONE',  ( -0.05219959533910754901, -16.53943276465976808, 37.49890960531436690 ) ) ;
#73012 = CARTESIAN_POINT ( 'NONE',  ( -13.97604488694527625, -13.89961937509977652, 51.87390960531436690 ) ) ;
#73013 = CARTESIAN_POINT ( 'NONE',  ( 19.02544592524343514, -5.153800228976328945, 78.54057627198099567 ) ) ;
#73014 = CARTESIAN_POINT ( 'NONE',  ( -5.049401038298153566, 19.05341960407611168, 40.20724293864768839 ) ) ;
#73015 = CARTESIAN_POINT ( 'NONE',  ( -21.52544592524334988, -5.823673210054445271, 48.95942372801902565 ) ) ;
#73016 = CARTESIAN_POINT ( 'NONE',  ( 9.474510206698971260, -16.51473224551069308, 67.91557627198102409 ) ) ;
#73017 = CARTESIAN_POINT ( 'NONE',  ( -9.474510206698964154, 16.51473224551069663, 25.41557627198103120 ) ) ;
#73018 = CARTESIAN_POINT ( 'NONE',  ( 16.51473224551069308, 9.474510206698969483, 54.16557627198103120 ) ) ;
#73019 = CARTESIAN_POINT ( 'NONE',  ( 10.81492255796078972, 18.62759615963270932, 49.58224293864769550 ) ) ;
#73020 = CARTESIAN_POINT ( 'NONE',  ( 13.97604488694527802, 13.89961937509977652, 29.37390960531435979 ) ) ;
#73021 = CARTESIAN_POINT ( 'NONE',  ( 18.67979575497178502, 10.72451020669898547, 44.16557627198103120 ) ) ;
#73022 = CARTESIAN_POINT ( 'NONE',  ( 4.379528057220092307, 16.55341960407617563, 107.2927570613523471 ) ) ;
#73023 = CARTESIAN_POINT ( 'NONE',  ( 13.97604488694548053, -13.89961937509957401, 25.62609039468566507 ) ) ;
#73025 = CARTESIAN_POINT ( 'NONE',  ( -8.314922557961024197, 14.29746914071037800, 82.91775706135234714 ) ) ;
#73024 = CARTESIAN_POINT ( 'NONE',  ( 0.05219959533934541429, -16.53943276465976808, 50.00109039468568994 ) ) ;
#73026 = CARTESIAN_POINT ( 'NONE',  ( -3.573655867282028392E-15, 2.428612866367529932E-14, 139.9999999999999716 ) ) ;
#73027 = CARTESIAN_POINT ( 'NONE',  ( 0.05219959533934541429, -16.53943276465976808, 70.00109039468568994 ) ) ;
#73028 = CARTESIAN_POINT ( 'NONE',  ( -4.483927247898782831, 16.52544592524335698, 57.70942372801901143 ) ) ;
#73029 = CARTESIAN_POINT ( 'NONE',  ( -13.89961937509977652, 13.97604488694528158, 105.6239096053143527 ) ) ;
#73030 = CARTESIAN_POINT ( 'NONE',  ( 16.53943276465976808, 0.05219959533934440121, 36.25109039468567573 ) ) ;
#73031 = CARTESIAN_POINT ( 'NONE',  ( 13.89961937509977652, -13.97604488694527269, 33.12390960531434558 ) ) ;
#73032 = CARTESIAN_POINT ( 'NONE',  ( 5.719274019375673035, 21.55341960407619339, 32.29275706135235424 ) ) ;
#73033 = CARTESIAN_POINT ( 'NONE',  ( -16.52544592524335698, -4.483927247898792601, 38.95942372801901854 ) ) ;
#73034 = CARTESIAN_POINT ( 'NONE',  ( -12.06949235617739369, -12.14591786802326823, 104.3760903946856899 ) ) ;
#73035 = DIRECTION ( 'NONE',  ( -1.000000000000000000, -0.000000000000000000, 0.000000000000000000 ) ) ;
#73036 = CARTESIAN_POINT ( 'NONE',  ( 15.72974639402176855, 15.80617190586768217, 106.8760903946856899 ) ) ;
#73037 = CARTESIAN_POINT ( 'NONE',  ( -9.564922557961040184, 16.46253265017147172, 97.91775706135233293 ) ) ;
#73038 = CARTESIAN_POINT ( 'NONE',  ( -12.14591786802309592, -12.06949235617757132, 61.87390960531436690 ) ) ;
#73039 = CARTESIAN_POINT ( 'NONE',  ( 13.89961937509977652, -13.97604488694527269, 23.12390960531436335 ) ) ;
#73041 = CARTESIAN_POINT ( 'NONE',  ( 9.656827144875922642, -71.74905178543389184, -15.00000000000000178 ) ) ;
#73040 = CARTESIAN_POINT ( 'NONE',  ( -0.05219959533936034679, 19.03943276465977164, 57.50109039468566863 ) ) ;
#73042 = CARTESIAN_POINT ( 'NONE',  ( -18.67979575497193778, 10.72451020669871902, 63.33442372801900433 ) ) ;
#73043 = CARTESIAN_POINT ( 'NONE',  ( -12.14591786802326823, 12.06949235617739902, 33.12609039468569705 ) ) ;
#73044 = CARTESIAN_POINT ( 'NONE',  ( 16.21995358207306737, 7.366697692864124569, 82.56448998487843483 ) ) ;
#73045 = CARTESIAN_POINT ( 'NONE',  ( -16.46253265017160317, 9.564922557960807481, 115.8322429386477097 ) ) ;
#73046 = CARTESIAN_POINT ( 'NONE',  ( 13.89961937509957401, 13.97604488694547697, 111.8760903946856757 ) ) ;
#73047 = CARTESIAN_POINT ( 'NONE',  ( -5.000000000000000000, 6.123233995736766282E-16, -18.00000000000000000 ) ) ;
#73048 = CARTESIAN_POINT ( 'NONE',  ( -21.36928693577339544, 7.422813773936193016, 174.5222352431090087 ) ) ;
#73049 = CARTESIAN_POINT ( 'NONE',  ( -12.06949235617756955, 12.14591786802309770, 115.6239096053143669 ) ) ;
#73050 = CARTESIAN_POINT ( 'NONE',  ( 5.823673210054444382, -21.52544592524334988, 105.2094237280190328 ) ) ;
#73051 = CARTESIAN_POINT ( 'NONE',  ( 13.89961937509977652, -13.97604488694527269, 43.12390960531434558 ) ) ;
#73052 = CIRCLE ( 'NONE', #89051, 69.99999999999997158 ) ;
#73053 = CARTESIAN_POINT ( 'NONE',  ( 18.67979575497194134, -10.72451020669871369, 55.83442372801901854 ) ) ;
#73054 = CARTESIAN_POINT ( 'NONE',  ( 18.67979575497194134, -10.72451020669871369, 100.8344237280190185 ) ) ;
#73055 = CARTESIAN_POINT ( 'NONE',  ( 0.05219959533934541429, -16.53943276465976808, 105.0010903946856757 ) ) ;
#73056 = CARTESIAN_POINT ( 'NONE',  ( -13.97604488694527625, -13.89961937509977652, 76.87390960531433848 ) ) ;
#73057 = CARTESIAN_POINT ( 'NONE',  ( -21.55341960407619339, 5.719274019375674811, 43.54275706135235424 ) ) ;
#73058 = CARTESIAN_POINT ( 'NONE',  ( -10.81492255796105439, 18.62759615963255655, 57.91775706135234714 ) ) ;
#73060 = CARTESIAN_POINT ( 'NONE',  ( 16.46253265017160672, -9.564922557960803928, 98.33224293864769550 ) ) ;
#73059 = CARTESIAN_POINT ( 'NONE',  ( 19.02544592524334988, 5.153800228976608722, 81.45942372801897591 ) ) ;
#73061 = CARTESIAN_POINT ( 'NONE',  ( 14.34966873604960469, 8.224510206698951720, 104.1655762719810241 ) ) ;
#73062 = CARTESIAN_POINT ( 'NONE',  ( -5.823673210054116645, -21.52544592524344225, 97.29057627198105251 ) ) ;
#73063 = CARTESIAN_POINT ( 'NONE',  ( -5.049401038297874678, -19.05341960407617918, 24.79275706135233648 ) ) ;
#73064 = CARTESIAN_POINT ( 'NONE',  ( -16.52544592524342804, 4.483927247898546575, 96.04057627198102409 ) ) ;
#73065 = CARTESIAN_POINT ( 'NONE',  ( -5.153800228976328057, -19.02544592524343514, 47.29057627198102409 ) ) ;
#73066 = CARTESIAN_POINT ( 'NONE',  ( 16.46253265017146816, 9.564922557961045513, 81.66775706135233293 ) ) ;
#73067 = CARTESIAN_POINT ( 'NONE',  ( 16.53943276465976808, -0.05219959533910856209, 43.74890960531435979 ) ) ;
#73068 = CARTESIAN_POINT ( 'NONE',  ( -18.67979575497193778, 10.72451020669871902, 113.3344237280190328 ) ) ;
#73069 = CARTESIAN_POINT ( 'NONE',  ( -19.02544592524342804, 5.153800228976336051, 111.0405762719810099 ) ) ;
#73070 = CARTESIAN_POINT ( 'NONE',  ( 0.05219959533936267826, -19.03943276465977164, 80.00109039468567573 ) ) ;
#73071 = CARTESIAN_POINT ( 'NONE',  ( 21.53943276465977519, -0.05219959533907433946, 83.74890960531435269 ) ) ;
#73072 = CARTESIAN_POINT ( 'NONE',  ( -0.05219959533937732626, 21.53943276465977519, 27.50109039468567929 ) ) ;
#73073 = CARTESIAN_POINT ( 'NONE',  ( -12.06949235617739369, -12.14591786802326823, 34.37609039468568284 ) ) ;
#73074 = CARTESIAN_POINT ( 'NONE',  ( -12.06949235617739369, -12.14591786802326823, 89.37609039468568994 ) ) ;
#73076 = CARTESIAN_POINT ( 'NONE',  ( 10.81492255796106328, -18.62759615963255655, 30.41775706135234358 ) ) ;
#73075 = CARTESIAN_POINT ( 'NONE',  ( -19.02544592524342804, 5.153800228976336051, 26.04057627198103120 ) ) ;
#73077 = CARTESIAN_POINT ( 'NONE',  ( -15.72974639402197994, 15.80617190586746368, 45.62390960531436690 ) ) ;
#73078 = CARTESIAN_POINT ( 'NONE',  ( -12.06949235617756955, 12.14591786802309770, 110.6239096053143669 ) ) ;
#73079 = CARTESIAN_POINT ( 'NONE',  ( 30.74264578624800137, -22.33583958711395212, -8.949999994537627401 ) ) ;
#73080 = CARTESIAN_POINT ( 'NONE',  ( -12.14591786802326823, 12.06949235617739902, 63.12609039468568994 ) ) ;
#73081 = EDGE_CURVE ( 'NONE', #17083, #132603, #186462, .T. ) ;
#73082 = CARTESIAN_POINT ( 'NONE',  ( 12.06949235617757843, -12.14591786802309237, 88.12390960531436690 ) ) ;
#73083 = CARTESIAN_POINT ( 'NONE',  ( 18.62759615963271287, -10.81492255796078972, 73.33224293864769550 ) ) ;
#73084 = CARTESIAN_POINT ( 'NONE',  ( 8.224510206698742110, 14.34966873604972548, 112.0844237280190185 ) ) ;
#73085 = CARTESIAN_POINT ( 'NONE',  ( -14.34966873604972548, 8.224510206698743886, 53.33442372801901854 ) ) ;
#73086 = CARTESIAN_POINT ( 'NONE',  ( -19.03943276465977164, 0.05219959533909376836, 56.24890960531435979 ) ) ;
#73087 = CARTESIAN_POINT ( 'NONE',  ( 8.224510206698742110, 14.34966873604972548, 87.08442372801901854 ) ) ;
#73088 = CARTESIAN_POINT ( 'NONE',  ( 16.46253265017146816, 9.564922557961045513, 86.66775706135233293 ) ) ;
#73089 = CARTESIAN_POINT ( 'NONE',  ( 18.67979575497178502, 10.72451020669898547, 84.16557627198103830 ) ) ;
#73090 = CARTESIAN_POINT ( 'NONE',  ( 16.55341960407618274, -4.379528057220086978, 106.0427570613523471 ) ) ;
#73091 = VERTEX_POINT ( 'NONE', #14903 ) ;
#73092 = CARTESIAN_POINT ( 'NONE',  ( 26.78465914369782297, 5.761000505272440897, 169.4491075441771670 ) ) ;
#73093 = CARTESIAN_POINT ( 'NONE',  ( 0.05219959533907565091, 21.53943276465977519, 59.99890960531436690 ) ) ;
#73094 = CARTESIAN_POINT ( 'NONE',  ( -12.06949235617739369, -12.14591786802326823, 89.37609039468568994 ) ) ;
#73095 = ORIENTED_EDGE ( 'NONE', *, *, #137670, .F. ) ;
#73096 = CARTESIAN_POINT ( 'NONE',  ( -5.823673210054116645, -21.52544592524344225, 32.29057627198102409 ) ) ;
#73097 = CARTESIAN_POINT ( 'NONE',  ( -18.56453257813363678, 5.500000000000057732, 75.99000423690684158 ) ) ;
#73098 = CARTESIAN_POINT ( 'NONE',  ( 5.823673210054125526, 21.52544592524343514, 84.79057627198102409 ) ) ;
#73099 = AXIS2_PLACEMENT_3D ( 'NONE', #77101, #152943, #1241 ) ;
#73100 = CARTESIAN_POINT ( 'NONE',  ( -12.06949235617756955, 12.14591786802309770, 30.62390960531436335 ) ) ;
#73101 = CARTESIAN_POINT ( 'NONE',  ( -4.483927247898782831, 16.52544592524335698, 32.70942372801900433 ) ) ;
#73102 = CARTESIAN_POINT ( 'NONE',  ( 0.05219959533909260263, 19.03943276465977164, 39.99890960531436690 ) ) ;
#73103 = CARTESIAN_POINT ( 'NONE',  ( -8.224510206698735004, -14.34966873604973081, 24.58442372801901499 ) ) ;
#73104 = AXIS2_PLACEMENT_3D ( 'NONE', #94498, #155192, #29868 ) ;
#73105 = CARTESIAN_POINT ( 'NONE',  ( -0.05219959533909027116, -19.03943276465977164, 52.49890960531436690 ) ) ;
#73106 = CARTESIAN_POINT ( 'NONE',  ( 8.906447517083057264, -27.41122689804191026, 146.5999999999999943 ) ) ;
#73107 = CARTESIAN_POINT ( 'NONE',  ( -9.564922557960796823, -16.46253265017161027, 107.0822429386476955 ) ) ;
#73108 = CARTESIAN_POINT ( 'NONE',  ( 16.46253265017160672, -9.564922557960803928, 103.3322429386476955 ) ) ;
#73109 = CARTESIAN_POINT ( 'NONE',  ( -8.224510206698735004, -14.34966873604973081, 99.58442372801900433 ) ) ;
#73110 = CARTESIAN_POINT ( 'NONE',  ( -16.51473224551082808, 9.474510206698731452, 98.33442372801900433 ) ) ;
#73111 = CARTESIAN_POINT ( 'NONE',  ( 13.89961937509957401, 13.97604488694547697, 41.87609039468566152 ) ) ;
#73112 = CARTESIAN_POINT ( 'NONE',  ( -15.80617190586745835, -15.72974639402198527, 71.87390960531438111 ) ) ;
#73114 = B_SPLINE_CURVE_WITH_KNOTS ( 'NONE', 3,
 ( #105974, #42334, #89818, #165673, #27172, #58483 ),
 .UNSPECIFIED., .F., .F.,
 ( 4, 2, 4 ),
 ( 0.003239945802372203986, 0.003620412082092052709, 0.004000878361811900999 ),
 .UNSPECIFIED. ) ;
#73113 = CARTESIAN_POINT ( 'NONE',  ( -4.483927247898782831, 16.52544592524335698, 102.7094237280190185 ) ) ;
#73115 = CARTESIAN_POINT ( 'NONE',  ( 18.67979575497178502, 10.72451020669898547, 34.16557627198102409 ) ) ;
#73116 = CARTESIAN_POINT ( 'NONE',  ( 16.46253265017146816, 9.564922557961045513, 96.66775706135233293 ) ) ;
#73117 = CARTESIAN_POINT ( 'NONE',  ( 0.05219959533909260263, 19.03943276465977164, 49.99890960531435979 ) ) ;
#73118 = CARTESIAN_POINT ( 'NONE',  ( -5.153800228976328057, -19.02544592524343514, 102.2905762719810383 ) ) ;
#73119 = CARTESIAN_POINT ( 'NONE',  ( 15.72974639402176855, 15.80617190586768217, 66.87609039468568994 ) ) ;
#73120 = CARTESIAN_POINT ( 'NONE',  ( -9.564922557960796823, -16.46253265017161027, 67.08224293864769550 ) ) ;
#73121 = CARTESIAN_POINT ( 'NONE',  ( 0.05219959533910956823, 16.53943276465976808, 104.9989096053143669 ) ) ;
#73122 = CARTESIAN_POINT ( 'NONE',  ( -17.44270441346519007, -5.991230190322947458, 86.36335079264233627 ) ) ;
#73123 = CARTESIAN_POINT ( 'NONE',  ( 16.55341960407611168, 4.379528057220329451, 83.95724293864770971 ) ) ;
#73124 = CARTESIAN_POINT ( 'NONE',  ( -15.80617190586745835, -15.72974639402198527, 76.87390960531439532 ) ) ;
#73125 = ORIENTED_EDGE ( 'NONE', *, *, #168721, .F. ) ;
#73126 = CARTESIAN_POINT ( 'NONE',  ( -5.153800228976607833, 19.02544592524334988, 87.70942372801897591 ) ) ;
#73127 = CARTESIAN_POINT ( 'NONE',  ( 17.50000000000001066, -5.622605283950866450, 81.18792689403893803 ) ) ;
#73128 = CARTESIAN_POINT ( 'NONE',  ( 13.97604488694527802, 13.89961937509977652, 64.37390960531436690 ) ) ;
#73129 = CARTESIAN_POINT ( 'NONE',  ( 31.65994483839895679, -2.419126180341553578, 102.1034561864645980 ) ) ;
#73131 = CARTESIAN_POINT ( 'NONE',  ( 19.02544592524343514, -5.153800228976328945, 88.54057627198102409 ) ) ;
#73130 = CARTESIAN_POINT ( 'NONE',  ( -0.05219959533909027116, -19.03943276465977164, 72.49890960531435269 ) ) ;
#73132 = CARTESIAN_POINT ( 'NONE',  ( -14.34966873604972548, 8.224510206698743886, 58.33442372801901143 ) ) ;
#73133 = CARTESIAN_POINT ( 'NONE',  ( -16.62475595723696742, -7.163666690055265462, 49.47286648189535185 ) ) ;
#73134 = CARTESIAN_POINT ( 'NONE',  ( 16.46253265017146816, 9.564922557961045513, 41.66775706135234003 ) ) ;
#73135 = CARTESIAN_POINT ( 'NONE',  ( 36.77035430826401097, 5.154579508995670523, 46.92692430510571455 ) ) ;
#73136 = CARTESIAN_POINT ( 'NONE',  ( -9.474510206698964154, 16.51473224551069663, 110.4155762719810383 ) ) ;
#73137 = CARTESIAN_POINT ( 'NONE',  ( -14.34966873604972548, 8.224510206698743886, 98.33442372801901854 ) ) ;
#73138 = CARTESIAN_POINT ( 'NONE',  ( -34.67490716095264958, -3.335491994402104865, 51.73554620185603170 ) ) ;
#73139 = CARTESIAN_POINT ( 'NONE',  ( 0.05219959533934541429, -16.53943276465976808, 95.00109039468568994 ) ) ;
#73140 = CARTESIAN_POINT ( 'NONE',  ( -17.49999999999999645, 5.622605283950868227, 28.68792689403889895 ) ) ;
#73141 = CARTESIAN_POINT ( 'NONE',  ( -4.483927247898782831, 16.52544592524335698, 67.70942372801901854 ) ) ;
#73142 = CARTESIAN_POINT ( 'NONE',  ( 2.500000000000000000, 0.000000000000000000, 0.000000000000000000 ) ) ;
#73143 = CARTESIAN_POINT ( 'NONE',  ( -21.53943276465977519, -0.05219959533937600094, 73.75109039468567573 ) ) ;
#73144 = CARTESIAN_POINT ( 'NONE',  ( -9.474510206698720793, -16.51473224551083518, 74.58442372801900433 ) ) ;
#73145 = CARTESIAN_POINT ( 'NONE',  ( 13.89961937509957401, 13.97604488694547697, 26.87609039468566507 ) ) ;
#73146 = CARTESIAN_POINT ( 'NONE',  ( 19.02544592524343514, -5.153800228976328945, 63.54057627198103830 ) ) ;
#73147 = CARTESIAN_POINT ( 'NONE',  ( -9.564922557960796823, -16.46253265017161027, 42.08224293864769550 ) ) ;
#73148 = CARTESIAN_POINT ( 'NONE',  ( -19.97888994334928014, -34.65319547504296338, -5.175670227483850638 ) ) ;
#73149 = CARTESIAN_POINT ( 'NONE',  ( 21.55341960407610458, 5.719274019375980345, 83.95724293864770971 ) ) ;
#73150 = CARTESIAN_POINT ( 'NONE',  ( -10.72451020669898014, 18.67979575497178502, 35.41557627198102409 ) ) ;
#73151 = CARTESIAN_POINT ( 'NONE',  ( -16.51473224551069308, -9.474510206698971260, 36.66557627198102409 ) ) ;
#73152 = CARTESIAN_POINT ( 'NONE',  ( -16.52544592524335698, -4.483927247898792601, 48.95942372801902565 ) ) ;
#73153 = EDGE_CURVE ( 'NONE', #116695, #41844, #53556, .T. ) ;
#73154 = ORIENTED_EDGE ( 'NONE', *, *, #156319, .T. ) ;
#73155 = CARTESIAN_POINT ( 'NONE',  ( 10.72451020669871369, 18.67979575497193778, 32.08442372801901854 ) ) ;
#73157 = CARTESIAN_POINT ( 'NONE',  ( 38.00000000000000000, 12.34694845685046616, -2.900000000000000355 ) ) ;
#73156 = CARTESIAN_POINT ( 'NONE',  ( -14.34966873604960291, -8.224510206698953496, 56.66557627198103830 ) ) ;
#73158 = CARTESIAN_POINT ( 'NONE',  ( -8.224510206698735004, -14.34966873604973081, 29.58442372801901854 ) ) ;
#73159 = CARTESIAN_POINT ( 'NONE',  ( 16.51473224551083163, -9.474510206698727899, 35.83442372801899722 ) ) ;
#73160 = CARTESIAN_POINT ( 'NONE',  ( -12.14591786802309592, -12.06949235617757132, 61.87390960531436690 ) ) ;
#73161 = CARTESIAN_POINT ( 'NONE',  ( -18.62759615963270932, 10.81492255796079327, 110.8322429386476955 ) ) ;
#73163 = CARTESIAN_POINT ( 'NONE',  ( -5.823673210054116645, -21.52544592524344225, 82.29057627198103830 ) ) ;
#73162 = CARTESIAN_POINT ( 'NONE',  ( 30.00000000000000711, -1.163414459189985801E-14, 95.00000000000000000 ) ) ;
#73164 = CARTESIAN_POINT ( 'NONE',  ( -19.02544592524342804, 5.153800228976336051, 96.04057627198103830 ) ) ;
#73165 = CARTESIAN_POINT ( 'NONE',  ( -16.55341960407611168, -4.379528057220339221, 66.45724293864768129 ) ) ;
#73166 = CARTESIAN_POINT ( 'NONE',  ( 9.564922557960805705, 16.46253265017160317, 99.58224293864770971 ) ) ;
#73167 = CARTESIAN_POINT ( 'NONE',  ( -37.01127658466555914, 5.144934411046666156, 43.04759647146321555 ) ) ;
#73168 = CARTESIAN_POINT ( 'NONE',  ( 16.46253265017146816, 9.564922557961045513, 71.66775706135233293 ) ) ;
#73169 = CARTESIAN_POINT ( 'NONE',  ( -21.55341960407610458, -5.719274019375992779, 101.4572429386476955 ) ) ;
#73170 = CARTESIAN_POINT ( 'NONE',  ( 19.05341960407611168, 5.049401038298154454, 58.95724293864768129 ) ) ;
#73171 = CARTESIAN_POINT ( 'NONE',  ( 19.03943276465977164, 0.05219959533936151252, 46.25109039468566863 ) ) ;
#73172 = CARTESIAN_POINT ( 'NONE',  ( 14.34966873604960469, 8.224510206698951720, 114.1655762719810383 ) ) ;
#73173 = CARTESIAN_POINT ( 'NONE',  ( -21.55341960407619339, 5.719274019375674811, 58.54275706135235424 ) ) ;
#73174 = CARTESIAN_POINT ( 'NONE',  ( -17.12812012977030562, -6.668231424565919774, 71.35948759323142099 ) ) ;
#73175 = CARTESIAN_POINT ( 'NONE',  ( 4.483927247898545687, 16.52544592524342804, 44.79057627198103120 ) ) ;
#73176 = CARTESIAN_POINT ( 'NONE',  ( -19.02544592524342804, 5.153800228976336051, 51.04057627198103120 ) ) ;
#73177 = CARTESIAN_POINT ( 'NONE',  ( -5.049401038298153566, 19.05341960407611168, 115.2072429386477097 ) ) ;
#73178 = CARTESIAN_POINT ( 'NONE',  ( -18.62759615963270932, 10.81492255796079327, 70.83224293864770971 ) ) ;
#73179 = CARTESIAN_POINT ( 'NONE',  ( 17.14385361876520264, 23.59649016807275856, 144.1750000027311671 ) ) ;
#73180 = CARTESIAN_POINT ( 'NONE',  ( 9.564922557960805705, 16.46253265017160317, 49.58224293864770260 ) ) ;
#73181 = CARTESIAN_POINT ( 'NONE',  ( -15.72974639402197994, 15.80617190586746368, 65.62390960531436690 ) ) ;
#73182 = ORIENTED_EDGE ( 'NONE', *, *, #114876, .F. ) ;
#73183 = CARTESIAN_POINT ( 'NONE',  ( 0.05219959533937995610, -21.53943276465977519, 90.00109039468567573 ) ) ;
#73186 = CARTESIAN_POINT ( 'NONE',  ( 16.53943276465976808, -0.05219959533910856209, 88.74890960531436690 ) ) ;
#73185 = CARTESIAN_POINT ( 'NONE',  ( 16.53943276465976808, 0.05219959533934440121, 96.25109039468568994 ) ) ;
#73184 = CARTESIAN_POINT ( 'NONE',  ( 7.980598154334715311, -36.52039581308737581, -31.83703727319202414 ) ) ;
#73187 = CARTESIAN_POINT ( 'NONE',  ( 19.02544592524343514, -5.153800228976328945, 73.54057627198103830 ) ) ;
#73188 = ORIENTED_EDGE ( 'NONE', *, *, #106983, .F. ) ;
#73189 = CARTESIAN_POINT ( 'NONE',  ( 5.153800228976615827, -19.02544592524334988, 40.20942372801898301 ) ) ;
#73190 = CARTESIAN_POINT ( 'NONE',  ( 8.224510206698742110, 14.34966873604972548, 82.08442372801901854 ) ) ;
#73191 = CARTESIAN_POINT ( 'NONE',  ( -19.05341960407617563, 5.049401038297882671, 23.54275706135233648 ) ) ;
#73192 = CARTESIAN_POINT ( 'NONE',  ( 16.46253265017160672, -9.564922557960803928, 83.33224293864768129 ) ) ;
#73193 = CARTESIAN_POINT ( 'NONE',  ( 0.05219959533907565091, 21.53943276465977519, 44.99890960531435979 ) ) ;
#73194 = CARTESIAN_POINT ( 'NONE',  ( -6.918342302711550929, -47.27039221922506584, -24.65254351866712668 ) ) ;
#73195 = CARTESIAN_POINT ( 'NONE',  ( -21.52544592524334988, -5.823673210054445271, 98.95942372801903275 ) ) ;
#73196 = CARTESIAN_POINT ( 'NONE',  ( -14.34966873604972548, 8.224510206698743886, 58.33442372801901143 ) ) ;
#73197 = CARTESIAN_POINT ( 'NONE',  ( 21.52544592524344225, -5.823673210054117533, 108.5405762719810241 ) ) ;
#73198 = CARTESIAN_POINT ( 'NONE',  ( 8.224510206698742110, 14.34966873604972548, 37.08442372801901143 ) ) ;
#73199 = CARTESIAN_POINT ( 'NONE',  ( 13.97604488694527802, 13.89961937509977652, 89.37390960531436690 ) ) ;
#73200 = CARTESIAN_POINT ( 'NONE',  ( 9.564922557960805705, 16.46253265017160317, 34.58224293864770260 ) ) ;
#73201 = CARTESIAN_POINT ( 'NONE',  ( -0.05219959533909027116, -19.03943276465977164, 47.49890960531435979 ) ) ;
#73202 = CARTESIAN_POINT ( 'NONE',  ( -16.55341960407617563, 4.379528057220093196, 28.54275706135234358 ) ) ;
#73203 = CARTESIAN_POINT ( 'NONE',  ( 8.314922557960818139, 14.29746914071049879, 79.58224293864769550 ) ) ;
#73204 = CARTESIAN_POINT ( 'NONE',  ( -8.314922557961024197, 14.29746914071037800, 92.91775706135236135 ) ) ;
#73207 = CARTESIAN_POINT ( 'NONE',  ( 5.049401038298161559, -19.05341960407611168, 57.70724293864769550 ) ) ;
#73206 = CARTESIAN_POINT ( 'NONE',  ( -16.51473224551069308, -9.474510206698971260, 71.66557627198102409 ) ) ;
#73205 = CARTESIAN_POINT ( 'NONE',  ( 15.72974639402176855, 15.80617190586768217, 41.87609039468568284 ) ) ;
#73208 = CARTESIAN_POINT ( 'NONE',  ( -13.89961937509977652, 13.97604488694528158, 85.62390960531433848 ) ) ;
#73209 = CARTESIAN_POINT ( 'NONE',  ( -12.06949235617756955, 12.14591786802309770, 30.62390960531436335 ) ) ;
#73210 = CARTESIAN_POINT ( 'NONE',  ( 4.483927247898790824, -16.52544592524335698, 90.20942372801903275 ) ) ;
#73211 = ORIENTED_EDGE ( 'NONE', *, *, #187522, .F. ) ;
#73212 = CARTESIAN_POINT ( 'NONE',  ( 9.564922557961047289, -16.46253265017146816, 25.41775706135234003 ) ) ;
#73213 = CARTESIAN_POINT ( 'NONE',  ( -19.05341960407611168, -5.049401038298163336, 96.45724293864769550 ) ) ;
#73214 = CARTESIAN_POINT ( 'NONE',  ( 9.474510206698971260, -16.51473224551069308, 47.91557627198102409 ) ) ;
#73215 = CARTESIAN_POINT ( 'NONE',  ( 3.556970738554033499E-15, -38.81732327939057825, -6.124999997268812280 ) ) ;
#73216 = CARTESIAN_POINT ( 'NONE',  ( 16.53943276465976808, 0.05219959533934440121, 41.25109039468568284 ) ) ;
#73218 = CARTESIAN_POINT ( 'NONE',  ( 16.55341960407618274, -4.379528057220086978, 56.04275706135235424 ) ) ;
#73217 = CARTESIAN_POINT ( 'NONE',  ( -5.049401038297874678, -19.05341960407617918, 74.79275706135231871 ) ) ;
#73219 = DIRECTION ( 'NONE',  ( -0.8660254037844410391, 0.000000000000000000, 0.4999999999999958367 ) ) ;
#73220 = CARTESIAN_POINT ( 'NONE',  ( 5.153800228976335163, 19.02544592524342804, 74.79057627198103830 ) ) ;
#73221 = CARTESIAN_POINT ( 'NONE',  ( -21.52544592524334988, -5.823673210054445271, 18.95942372801901143 ) ) ;
#73222 = CARTESIAN_POINT ( 'NONE',  ( -19.03943276465977164, -0.05219959533935918106, 63.75109039468566863 ) ) ;
#73224 = CARTESIAN_POINT ( 'NONE',  ( 9.564922557960805705, 16.46253265017160317, 34.58224293864770260 ) ) ;
#73223 = CARTESIAN_POINT ( 'NONE',  ( 19.05341960407611168, 5.049401038298154454, 108.9572429386477097 ) ) ;
#73225 = CARTESIAN_POINT ( 'NONE',  ( -5.153800228976328057, -19.02544592524343514, 82.29057627198103830 ) ) ;
#73227 = CARTESIAN_POINT ( 'NONE',  ( -5.049401038298153566, 19.05341960407611168, 70.20724293864769550 ) ) ;
#73226 = CARTESIAN_POINT ( 'NONE',  ( -16.52544592524342804, 4.483927247898546575, 41.04057627198103120 ) ) ;
#73228 = CARTESIAN_POINT ( 'NONE',  ( 9.474510206698729675, 16.51473224551082808, 37.08442372801899722 ) ) ;
#73229 = CARTESIAN_POINT ( 'NONE',  ( 12.14591786802309770, 12.06949235617756955, 79.37390960531436690 ) ) ;
#73230 = CARTESIAN_POINT ( 'NONE',  ( 16.46253265017146816, 9.564922557961045513, 21.66775706135233648 ) ) ;
#73231 = CARTESIAN_POINT ( 'NONE',  ( 19.02544592524343514, -5.153800228976328945, 48.54057627198103120 ) ) ;
#73233 = CARTESIAN_POINT ( 'NONE',  ( 5.719274019375673035, 21.55341960407619339, 107.2927570613523471 ) ) ;
#73232 = CARTESIAN_POINT ( 'NONE',  ( -8.224510206698948167, 14.34966873604960824, 35.41557627198102409 ) ) ;
#73234 = CARTESIAN_POINT ( 'NONE',  ( 0.05219959533909260263, 19.03943276465977164, 89.99890960531436690 ) ) ;
#73235 = CARTESIAN_POINT ( 'NONE',  ( -16.46253265017160317, 9.564922557960807481, 105.8322429386476955 ) ) ;
#73236 = CARTESIAN_POINT ( 'NONE',  ( -5.049401038298153566, 19.05341960407611168, 45.20724293864769550 ) ) ;
#73237 = CARTESIAN_POINT ( 'NONE',  ( 13.89961937509977652, -13.97604488694527269, 28.12390960531435624 ) ) ;
#73238 = CARTESIAN_POINT ( 'NONE',  ( -0.05219959533910754901, -16.53943276465976808, 82.49890960531436690 ) ) ;
#73239 = CARTESIAN_POINT ( 'NONE',  ( 10.72451020669898902, -18.67979575497178502, 102.9155762719810383 ) ) ;
#73240 = CARTESIAN_POINT ( 'NONE',  ( 9.564922557960805705, 16.46253265017160317, 94.58224293864769550 ) ) ;
#73241 = CARTESIAN_POINT ( 'NONE',  ( 5.719274019375991003, -21.55341960407610458, 92.70724293864770971 ) ) ;
#73242 = CARTESIAN_POINT ( 'NONE',  ( 13.89961937509977652, -13.97604488694527269, 93.12390960531436690 ) ) ;
#73244 = CARTESIAN_POINT ( 'NONE',  ( -16.52544592524342804, 4.483927247898546575, 101.0405762719810383 ) ) ;
#73243 = DIRECTION ( 'NONE',  ( -0.000000000000000000, 0.000000000000000000, 1.000000000000000000 ) ) ;
#73246 = CARTESIAN_POINT ( 'NONE',  ( -9.564922557960796823, -16.46253265017161027, 67.08224293864769550 ) ) ;
#73245 = AXIS2_PLACEMENT_3D ( 'NONE', #1528, #64212, #82332 ) ;
#73247 = CARTESIAN_POINT ( 'NONE',  ( 18.62759615963271287, -10.81492255796078972, 73.33224293864769550 ) ) ;
#73248 = DIRECTION ( 'NONE',  ( -0.000000000000000000, -0.000000000000000000, -1.000000000000000000 ) ) ;
#73250 = CARTESIAN_POINT ( 'NONE',  ( 6.412877669190335972, -3.889087296526014814, 1.818019484660534424 ) ) ;
#73249 = CARTESIAN_POINT ( 'NONE',  ( 5.719274019375991003, -21.55341960407610458, 22.70724293864769194 ) ) ;
#73251 = CARTESIAN_POINT ( 'NONE',  ( -16.53943276465976808, -0.05219959533934237506, 38.75109039468567573 ) ) ;
#73252 = CARTESIAN_POINT ( 'NONE',  ( -0.05219959533910754901, -16.53943276465976808, 97.49890960531436690 ) ) ;
#73253 = DIRECTION ( 'NONE',  ( -1.000000000000000000, 0.000000000000000000, 0.000000000000000000 ) ) ;
#73254 = CARTESIAN_POINT ( 'NONE',  ( -5.153800228976328057, -19.02544592524343514, 92.29057627198099567 ) ) ;
#73255 = CARTESIAN_POINT ( 'NONE',  ( 5.153800228976335163, 19.02544592524342804, 49.79057627198100988 ) ) ;
#73257 = EDGE_CURVE ( 'NONE', #149684, #185073, #181441, .T. ) ;
#73256 = CARTESIAN_POINT ( 'NONE',  ( 4.379528057220339221, -16.55341960407611168, 77.70724293864770971 ) ) ;
#73258 = CARTESIAN_POINT ( 'NONE',  ( -5.823673210054116645, -21.52544592524344225, 22.29057627198102765 ) ) ;
#73259 = CARTESIAN_POINT ( 'NONE',  ( 12.06949235617757843, -12.14591786802309237, 58.12390960531435979 ) ) ;
#73260 = CARTESIAN_POINT ( 'NONE',  ( 19.03943276465977164, 0.05219959533936151252, 96.25109039468567573 ) ) ;
#73261 = CARTESIAN_POINT ( 'NONE',  ( -5.719274019375665041, -21.55341960407619695, 59.79275706135234714 ) ) ;
#73262 = CARTESIAN_POINT ( 'NONE',  ( 17.14385361876520264, 23.59649016807275856, 146.1750000027311387 ) ) ;
#73263 = CARTESIAN_POINT ( 'NONE',  ( -9.564922557960796823, -16.46253265017161027, 102.0822429386477097 ) ) ;
#73264 = CARTESIAN_POINT ( 'NONE',  ( -8.224510206698735004, -14.34966873604973081, 89.58442372801901854 ) ) ;
#73265 = LINE ( 'NONE', #167250, #129122 ) ;
#73266 = CARTESIAN_POINT ( 'NONE',  ( 16.46253265017160672, -9.564922557960803928, 78.33224293864769550 ) ) ;
#73267 = CARTESIAN_POINT ( 'NONE',  ( 18.62759615963271287, -10.81492255796078972, 83.33224293864769550 ) ) ;
#73268 = CARTESIAN_POINT ( 'NONE',  ( 9.474510206698729675, 16.51473224551082808, 112.0844237280190043 ) ) ;
#73270 = CARTESIAN_POINT ( 'NONE',  ( -5.719274019375665041, -21.55341960407619695, 64.79275706135234714 ) ) ;
#73269 = CARTESIAN_POINT ( 'NONE',  ( 8.224510206698953496, -14.34966873604960469, 57.91557627198103120 ) ) ;
#73272 = CARTESIAN_POINT ( 'NONE',  ( -15.80617190586745835, -15.72974639402198527, 26.87390960531435979 ) ) ;
#73271 = CARTESIAN_POINT ( 'NONE',  ( 12.14591786802327356, -12.06949235617739191, 80.62609039468567573 ) ) ;
#73273 = CARTESIAN_POINT ( 'NONE',  ( 13.89961937509978007, -13.97604488694527269, 113.1239096053143669 ) ) ;
#73274 = PLANE ( 'NONE',  #151956 ) ;
#73275 = CARTESIAN_POINT ( 'NONE',  ( -8.314922557961024197, 14.29746914071037800, 107.9177570613523471 ) ) ;
#73276 = CARTESIAN_POINT ( 'NONE',  ( 16.52544592524335698, 4.483927247898782831, 66.45942372801903275 ) ) ;
#73277 = CARTESIAN_POINT ( 'NONE',  ( 13.97604488694527802, 13.89961937509977652, 69.37390960531436690 ) ) ;
#73278 = CARTESIAN_POINT ( 'NONE',  ( 19.03943276465977164, -0.05219959533909143690, 83.74890960531436690 ) ) ;
#73279 = CARTESIAN_POINT ( 'NONE',  ( -21.55341960407619339, 5.719274019375674811, 78.54275706135236135 ) ) ;
#73280 = CARTESIAN_POINT ( 'NONE',  ( -4.379528057220086978, -16.55341960407618274, 79.79275706135236135 ) ) ;
#73281 = CARTESIAN_POINT ( 'NONE',  ( 12.06949235617757843, -12.14591786802309237, 53.12390960531436690 ) ) ;
#73282 = CARTESIAN_POINT ( 'NONE',  ( 5.049401038298161559, -19.05341960407611168, 52.70724293864767418 ) ) ;
#73283 = CARTESIAN_POINT ( 'NONE',  ( -19.05341960407611168, -5.049401038298163336, 51.45724293864770260 ) ) ;
#73285 = ORIENTED_EDGE ( 'NONE', *, *, #20112, .T. ) ;
#73284 = CARTESIAN_POINT ( 'NONE',  ( 8.314922557961029526, -14.29746914071037800, 45.41775706135234003 ) ) ;
#73286 = CARTESIAN_POINT ( 'NONE',  ( 16.51473224551083163, -9.474510206698727899, 100.8344237280190043 ) ) ;
#73287 = CARTESIAN_POINT ( 'NONE',  ( -4.379528057220328563, 16.55341960407611168, 100.2072429386476955 ) ) ;
#73288 = CARTESIAN_POINT ( 'NONE',  ( -13.89961937509977652, 13.97604488694528158, 60.62390960531436690 ) ) ;
#73290 = CARTESIAN_POINT ( 'NONE',  ( -11.74264578624799782, -36.14014761921581709, -1.599999999999999867 ) ) ;
#73289 = CARTESIAN_POINT ( 'NONE',  ( 13.97604488694548053, -13.89961937509957401, 105.6260903946856757 ) ) ;
#73291 = CARTESIAN_POINT ( 'NONE',  ( -21.53943276465977519, -0.05219959533937600094, 103.7510903946857042 ) ) ;
#73292 = CARTESIAN_POINT ( 'NONE',  ( -16.53943276465976808, -0.05219959533934237506, 63.75109039468568284 ) ) ;
#73293 = CYLINDRICAL_SURFACE ( 'NONE', #143915, 61.99999999999998579 ) ;
#73294 = CARTESIAN_POINT ( 'NONE',  ( -21.52544592524343514, 5.823673210054127303, 66.04057627198103830 ) ) ;
#73295 = CARTESIAN_POINT ( 'NONE',  ( 4.379528057220092307, 16.55341960407617563, 47.29275706135234003 ) ) ;
#73296 = CARTESIAN_POINT ( 'NONE',  ( 12.73189700295822213, -37.92323000020837753, -14.26360274717254129 ) ) ;
#73297 = CARTESIAN_POINT ( 'NONE',  ( -5.153800228976607833, 19.02544592524334988, 47.70942372801900433 ) ) ;
#73298 = CARTESIAN_POINT ( 'NONE',  ( -9.564922557960796823, -16.46253265017161027, 87.08224293864769550 ) ) ;
#73299 = CARTESIAN_POINT ( 'NONE',  ( 13.97604488694527802, 13.89961937509977652, 24.37390960531435624 ) ) ;
#73300 = CARTESIAN_POINT ( 'NONE',  ( 19.03943276465977164, -0.05219959533909143690, 58.74890960531435979 ) ) ;
#73301 = CARTESIAN_POINT ( 'NONE',  ( -14.34966873604960291, -8.224510206698953496, 61.66557627198103120 ) ) ;
#73302 = CARTESIAN_POINT ( 'NONE',  ( -5.823673210054431948, 21.52544592524334988, 72.70942372801901854 ) ) ;
#73303 = CARTESIAN_POINT ( 'NONE',  ( -16.46253265017146816, -9.564922557961047289, 49.16775706135233293 ) ) ;
#73304 = CARTESIAN_POINT ( 'NONE',  ( -19.05341960407617563, 5.049401038297882671, 28.54275706135232937 ) ) ;
#73305 = CARTESIAN_POINT ( 'NONE',  ( -19.02544592524342804, 5.153800228976336051, 51.04057627198103120 ) ) ;
#73306 = CARTESIAN_POINT ( 'NONE',  ( 10.81492255796078972, 18.62759615963270932, 29.58224293864769905 ) ) ;
#73307 = CARTESIAN_POINT ( 'NONE',  ( 10.72451020669871369, 18.67979575497193778, 102.0844237280190185 ) ) ;
#73308 = CARTESIAN_POINT ( 'NONE',  ( 19.03943276465977164, -0.05219959533909143690, 63.74890960531435979 ) ) ;
#73309 = CARTESIAN_POINT ( 'NONE',  ( -0.05219959533937732626, 21.53943276465977519, 97.50109039468567573 ) ) ;
#73310 = CARTESIAN_POINT ( 'NONE',  ( 10.81492255796078972, 18.62759615963270932, 34.58224293864770260 ) ) ;
#73311 = CARTESIAN_POINT ( 'NONE',  ( -5.153800228976328057, -19.02544592524343514, 82.29057627198103830 ) ) ;
#73312 = CARTESIAN_POINT ( 'NONE',  ( -16.46253265017146816, -9.564922557961047289, 64.16775706135233293 ) ) ;
#73313 = CARTESIAN_POINT ( 'NONE',  ( 19.03943276465977164, -0.05219959533909143690, 38.74890960531436690 ) ) ;
#73314 = CARTESIAN_POINT ( 'NONE',  ( -19.05341960407611168, -5.049401038298163336, 86.45724293864769550 ) ) ;
#73315 = CARTESIAN_POINT ( 'NONE',  ( 14.34966873604972726, -8.224510206698740333, 30.83442372801902209 ) ) ;
#73316 = CARTESIAN_POINT ( 'NONE',  ( -16.53943276465976808, 0.05219959533911058130, 86.24890960531436690 ) ) ;
#73317 = CARTESIAN_POINT ( 'NONE',  ( -13.97604488694527625, -13.89961937509977652, 66.87390960531436690 ) ) ;
#73318 = CARTESIAN_POINT ( 'NONE',  ( -15.72974639402197994, 15.80617190586746368, 45.62390960531436690 ) ) ;
#73319 = CARTESIAN_POINT ( 'NONE',  ( -12.06949235617739369, -12.14591786802326823, 19.37609039468568639 ) ) ;
#73320 = CARTESIAN_POINT ( 'NONE',  ( 21.52544592524334988, 5.823673210054432836, 26.45942372801901854 ) ) ;
#73321 = CARTESIAN_POINT ( 'NONE',  ( 18.67979575497194134, -10.72451020669871369, 65.83442372801900433 ) ) ;
#73322 = CARTESIAN_POINT ( 'NONE',  ( -16.55341960407617563, 4.379528057220093196, 73.54275706135234714 ) ) ;
#73323 = CARTESIAN_POINT ( 'NONE',  ( 14.34966873604972726, -8.224510206698740333, 65.83442372801900433 ) ) ;
#73324 = CARTESIAN_POINT ( 'NONE',  ( 9.474510206698971260, -16.51473224551069308, 57.91557627198103120 ) ) ;
#73325 = CARTESIAN_POINT ( 'NONE',  ( -16.52544592524335698, -4.483927247898792601, 98.95942372801903275 ) ) ;
#73326 = CARTESIAN_POINT ( 'NONE',  ( 19.03943276465977164, 0.05219959533936151252, 41.25109039468566152 ) ) ;
#73327 = CARTESIAN_POINT ( 'NONE',  ( -21.53943276465977519, -0.05219959533937600094, 28.75109039468567929 ) ) ;
#73328 = CARTESIAN_POINT ( 'NONE',  ( -4.483927247898539470, -16.52544592524342804, 62.29057627198102409 ) ) ;
#73329 = CARTESIAN_POINT ( 'NONE',  ( -13.97604488694527625, -13.89961937509977652, 96.87390960531433848 ) ) ;
#73330 = CARTESIAN_POINT ( 'NONE',  ( 16.55341960407618274, -4.379528057220086978, 91.04275706135236135 ) ) ;
#73331 = CARTESIAN_POINT ( 'NONE',  ( -10.81492255796105439, 18.62759615963255655, 77.91775706135231871 ) ) ;
#73332 = CARTESIAN_POINT ( 'NONE',  ( -14.34966873604972548, 8.224510206698743886, 33.33442372801900433 ) ) ;
#73333 = CARTESIAN_POINT ( 'NONE',  ( -15.80617190586768217, 15.72974639402176855, 23.12609039468567573 ) ) ;
#73334 = CARTESIAN_POINT ( 'NONE',  ( -12.14591786802309592, -12.06949235617757132, 56.87390960531436690 ) ) ;
#73335 = ORIENTED_EDGE ( 'NONE', *, *, #84390, .F. ) ;
#73336 = CARTESIAN_POINT ( 'NONE',  ( 15.72974639402199770, -15.80617190586745480, 98.12390960531436690 ) ) ;
#73337 = CARTESIAN_POINT ( 'NONE',  ( 8.224510206698953496, -14.34966873604960469, 42.91557627198103120 ) ) ;
#73338 = ORIENTED_EDGE ( 'NONE', *, *, #166372, .T. ) ;
#73339 = CARTESIAN_POINT ( 'NONE',  ( 16.46253265017160672, -9.564922557960803928, 23.33224293864769194 ) ) ;
#73340 = CARTESIAN_POINT ( 'NONE',  ( 21.53943276465977519, -0.05219959533907433946, 33.74890960531436690 ) ) ;
#73341 = CARTESIAN_POINT ( 'NONE',  ( 21.53943276465977519, 0.05219959533937863772, 41.25109039468568284 ) ) ;
#73342 = CARTESIAN_POINT ( 'NONE',  ( -4.379528057220328563, 16.55341960407611168, 70.20724293864769550 ) ) ;
#73343 = CARTESIAN_POINT ( 'NONE',  ( -18.62759615963270932, 10.81492255796079327, 60.83224293864769550 ) ) ;
#73344 = CARTESIAN_POINT ( 'NONE',  ( 19.02544592524343514, -5.153800228976328945, 73.54057627198103830 ) ) ;
#73346 = CARTESIAN_POINT ( 'NONE',  ( -9.564922557961040184, 16.46253265017147172, 82.91775706135233293 ) ) ;
#73345 = CARTESIAN_POINT ( 'NONE',  ( 16.46253265017160672, -9.564922557960803928, 23.33224293864769194 ) ) ;
#73347 = EDGE_CURVE ( 'NONE', #191417, #89861, #162075, .T. ) ;
#73348 = CARTESIAN_POINT ( 'NONE',  ( -21.53943276465977519, 0.05219959533907696930, 46.24890960531435979 ) ) ;
#73349 = CARTESIAN_POINT ( 'NONE',  ( 9.564922557960805705, 16.46253265017160317, 39.58224293864768839 ) ) ;
#73350 = CARTESIAN_POINT ( 'NONE',  ( 16.51473224551069308, 9.474510206698969483, 74.16557627198103830 ) ) ;
#73351 = ORIENTED_EDGE ( 'NONE', *, *, #142462, .F. ) ;
#73352 = CARTESIAN_POINT ( 'NONE',  ( 4.379528057220092307, 16.55341960407617563, 37.29275706135235424 ) ) ;
#73353 = CARTESIAN_POINT ( 'NONE',  ( -0.05219959533907301413, -21.53943276465977519, 112.4989096053143669 ) ) ;
#73354 = CARTESIAN_POINT ( 'NONE',  ( -8.314922557960811034, -14.29746914071050412, 42.08224293864769550 ) ) ;
#73355 = CARTESIAN_POINT ( 'NONE',  ( 13.89961937509977652, -13.97604488694527269, 103.1239096053143527 ) ) ;
#73356 = CARTESIAN_POINT ( 'NONE',  ( -18.62759615963270932, 10.81492255796079327, 75.83224293864769550 ) ) ;
#73358 = CARTESIAN_POINT ( 'NONE',  ( 12.06949235617739724, 12.14591786802326823, 56.87609039468568994 ) ) ;
#73357 = CARTESIAN_POINT ( 'NONE',  ( 10.72451020669898902, -18.67979575497178502, 107.9155762719810241 ) ) ;
#73359 = VECTOR ( 'NONE', #112103, 1000.000000000000000 ) ;
#73360 = CARTESIAN_POINT ( 'NONE',  ( 21.52544592524344225, -5.823673210054117533, 53.54057627198103120 ) ) ;
#73361 = CARTESIAN_POINT ( 'NONE',  ( -5.719274019375665041, -21.55341960407619695, 99.79275706135234714 ) ) ;
#73362 = CARTESIAN_POINT ( 'NONE',  ( 5.049401038298161559, -19.05341960407611168, 57.70724293864769550 ) ) ;
#73363 = CARTESIAN_POINT ( 'NONE',  ( 19.05341960407611168, 5.049401038298154454, 103.9572429386476671 ) ) ;
#73364 = CARTESIAN_POINT ( 'NONE',  ( -16.46253265017160317, 9.564922557960807481, 80.83224293864769550 ) ) ;
#73365 = FACE_OUTER_BOUND ( 'NONE', #104942, .T. ) ;
#73366 = CARTESIAN_POINT ( 'NONE',  ( 19.03943276465977164, 0.05219959533936151252, 51.25109039468567573 ) ) ;
#73368 = CARTESIAN_POINT ( 'NONE',  ( 15.80617190586746368, 15.72974639402197994, 34.37390960531435979 ) ) ;
#73367 = CARTESIAN_POINT ( 'NONE',  ( 21.52544592524334988, 5.823673210054432836, 111.4594237280190328 ) ) ;
#73369 = CARTESIAN_POINT ( 'NONE',  ( -12.14591786802326823, 12.06949235617739902, 103.1260903946856757 ) ) ;
#73370 = CARTESIAN_POINT ( 'NONE',  ( -5.049401038297874678, -19.05341960407617918, 84.79275706135233293 ) ) ;
#73371 = CARTESIAN_POINT ( 'NONE',  ( -17.12812012977025944, 6.668231424566050336, 58.64051240676859322 ) ) ;
#73372 = CARTESIAN_POINT ( 'NONE',  ( 0.05219959533909260263, 19.03943276465977164, 104.9989096053143669 ) ) ;
#73373 = CARTESIAN_POINT ( 'NONE',  ( -5.049401038297874678, -19.05341960407617918, 79.79275706135233293 ) ) ;
#73374 = CARTESIAN_POINT ( 'NONE',  ( 13.89961937509957401, 13.97604488694547697, 46.87609039468565442 ) ) ;
#73375 = CARTESIAN_POINT ( 'NONE',  ( 17.50000000000000000, 5.499999999999992895, 71.70309617465829888 ) ) ;
#73376 = CARTESIAN_POINT ( 'NONE',  ( -0.05219959533909027116, -19.03943276465977164, 47.49890960531435979 ) ) ;
#73377 = CARTESIAN_POINT ( 'NONE',  ( 12.06949235617757843, -12.14591786802309237, 53.12390960531436690 ) ) ;
#73378 = CARTESIAN_POINT ( 'NONE',  ( 19.03943276465977164, -0.05219959533909143690, 38.74890960531436690 ) ) ;
#73379 = CARTESIAN_POINT ( 'NONE',  ( -14.29746914071049879, 8.314922557960819915, 35.83224293864768839 ) ) ;
#73380 = CARTESIAN_POINT ( 'NONE',  ( -37.45873412500000654, 2.428612866367529932E-14, -0.3124999986344065839 ) ) ;
#73381 = CARTESIAN_POINT ( 'NONE',  ( 4.483927247898790824, -16.52544592524335698, 105.2094237280190328 ) ) ;
#73382 = CARTESIAN_POINT ( 'NONE',  ( 19.05341960407611168, 5.049401038298154454, 53.95724293864770260 ) ) ;
#73383 = CARTESIAN_POINT ( 'NONE',  ( -21.53943276465977519, -0.05219959533937600094, 113.7510903946856757 ) ) ;
#73384 = CARTESIAN_POINT ( 'NONE',  ( -14.29746914071037622, -8.314922557961029526, 29.16775706135234003 ) ) ;
#73385 = CARTESIAN_POINT ( 'NONE',  ( -21.55341960407610458, -5.719274019375992779, 36.45724293864768839 ) ) ;
#73387 = EDGE_LOOP ( 'NONE', ( #48815, #71128, #182253 ) ) ;
#73386 = CARTESIAN_POINT ( 'NONE',  ( 18.62759615963255655, 10.81492255796105972, 86.66775706135234714 ) ) ;
#73388 = CARTESIAN_POINT ( 'NONE',  ( 5.153800228976335163, 19.02544592524342804, 99.79057627198102409 ) ) ;
#73389 = CARTESIAN_POINT ( 'NONE',  ( -19.02544592524342804, 5.153800228976336051, 86.04057627198103830 ) ) ;
#73390 = CARTESIAN_POINT ( 'NONE',  ( -36.91746825000000598, -11.99521256947794789, -8.524999997268812635 ) ) ;
#73391 = CARTESIAN_POINT ( 'NONE',  ( -15.72974639402197994, 15.80617190586746368, 105.6239096053143669 ) ) ;
#73392 = AXIS2_PLACEMENT_3D ( 'NONE', #132346, #84818, #39334 ) ;
#73393 = CARTESIAN_POINT ( 'NONE',  ( -4.483927247898539470, -16.52544592524342804, 77.29057627198102409 ) ) ;
#73394 = CARTESIAN_POINT ( 'NONE',  ( 21.55341960407610458, 5.719274019375980345, 68.95724293864769550 ) ) ;
#73395 = CARTESIAN_POINT ( 'NONE',  ( 19.03943276465977164, -0.05219959533909143690, 73.74890960531435269 ) ) ;
#73396 = CARTESIAN_POINT ( 'NONE',  ( -0.05219959533907301413, -21.53943276465977519, 97.49890960531436690 ) ) ;
#73397 = ORIENTED_EDGE ( 'NONE', *, *, #136828, .F. ) ;
#73398 = CARTESIAN_POINT ( 'NONE',  ( 9.564922557960805705, 16.46253265017160317, 64.58224293864769550 ) ) ;
#73400 = CARTESIAN_POINT ( 'NONE',  ( 28.26755983467668898, -28.30239183792592428, -15.36609880857821153 ) ) ;
#73399 = CARTESIAN_POINT ( 'NONE',  ( 16.52544592524342804, -4.483927247898539470, 93.54057627198103830 ) ) ;
#73401 = CARTESIAN_POINT ( 'NONE',  ( -19.03943276465977164, 0.05219959533909376836, 66.24890960531436690 ) ) ;
#73402 = CARTESIAN_POINT ( 'NONE',  ( -9.474510206698720793, -16.51473224551083518, 74.58442372801900433 ) ) ;
#73403 = CARTESIAN_POINT ( 'NONE',  ( 12.06949235617757843, -12.14591786802309237, 98.12390960531436690 ) ) ;
#73404 = CARTESIAN_POINT ( 'NONE',  ( -5.823673210054431948, 21.52544592524334988, 62.70942372801902565 ) ) ;
#73406 = CARTESIAN_POINT ( 'NONE',  ( -5.719274019375665041, -21.55341960407619695, 19.79275706135235069 ) ) ;
#73405 = CARTESIAN_POINT ( 'NONE',  ( 19.05341960407611168, 5.049401038298154454, 53.95724293864770260 ) ) ;
#73407 = CARTESIAN_POINT ( 'NONE',  ( -8.224510206698948167, 14.34966873604960824, 100.4155762719810241 ) ) ;
#73408 = DIRECTION ( 'NONE',  ( 1.000000000000000000, 0.000000000000000000, 0.000000000000000000 ) ) ;
#73409 = CARTESIAN_POINT ( 'NONE',  ( 9.564922557960805705, 16.46253265017160317, 59.58224293864769550 ) ) ;
#73410 = CARTESIAN_POINT ( 'NONE',  ( -21.49604614807126524, -21.49604614807088154, -64.92279855667830191 ) ) ;
#73412 = CARTESIAN_POINT ( 'NONE',  ( -9.564922557960796823, -16.46253265017161027, 112.0822429386476955 ) ) ;
#73411 = CARTESIAN_POINT ( 'NONE',  ( 13.97604488694548053, -13.89961937509957401, 105.6260903946856757 ) ) ;
#73413 = CARTESIAN_POINT ( 'NONE',  ( 21.55341960407619695, -5.719274019375665929, 51.04275706135234714 ) ) ;
#73414 = CARTESIAN_POINT ( 'NONE',  ( -5.049401038298153566, 19.05341960407611168, 95.20724293864770971 ) ) ;
#73415 = CARTESIAN_POINT ( 'NONE',  ( -19.05341960407617563, 5.049401038297882671, 83.54275706135233293 ) ) ;
#73416 = CARTESIAN_POINT ( 'NONE',  ( -16.51473224551069308, -9.474510206698971260, 61.66557627198103120 ) ) ;
#73417 = CARTESIAN_POINT ( 'NONE',  ( 4.379528057220339221, -16.55341960407611168, 77.70724293864770971 ) ) ;
#73418 = CARTESIAN_POINT ( 'NONE',  ( -9.474510206698964154, 16.51473224551069663, 95.41557627198102409 ) ) ;
#73419 = CARTESIAN_POINT ( 'NONE',  ( 4.379528057220339221, -16.55341960407611168, 77.70724293864770971 ) ) ;
#73420 = CARTESIAN_POINT ( 'NONE',  ( 13.97604488694527802, 13.89961937509977652, 79.37390960531435269 ) ) ;
#73421 = CARTESIAN_POINT ( 'NONE',  ( 9.474510206698729675, 16.51473224551082808, 32.08442372801900433 ) ) ;
#73424 = CARTESIAN_POINT ( 'NONE',  ( 5.049401038298161559, -19.05341960407611168, 32.70724293864768129 ) ) ;
#73423 = CARTESIAN_POINT ( 'NONE',  ( -4.483927247898539470, -16.52544592524342804, 47.29057627198103120 ) ) ;
#73422 = CARTESIAN_POINT ( 'NONE',  ( -16.51473224551069308, -9.474510206698971260, 51.66557627198102409 ) ) ;
#73425 = EDGE_LOOP ( 'NONE', ( #86497, #144164 ) ) ;
#73426 = CARTESIAN_POINT ( 'NONE',  ( -10.81492255796105439, 18.62759615963255655, 42.91775706135235424 ) ) ;
#73427 = CARTESIAN_POINT ( 'NONE',  ( 16.51473224551083163, -9.474510206698727899, 75.83442372801900433 ) ) ;
#73428 = CARTESIAN_POINT ( 'NONE',  ( -8.314922557960811034, -14.29746914071050412, 42.08224293864769550 ) ) ;
#73429 = CARTESIAN_POINT ( 'NONE',  ( 15.80617190586746368, 15.72974639402197994, 94.37390960531436690 ) ) ;
#73430 = CARTESIAN_POINT ( 'NONE',  ( 10.72451020669898902, -18.67979575497178502, 32.91557627198102409 ) ) ;
#73431 = CARTESIAN_POINT ( 'NONE',  ( 14.34966873604960469, 8.224510206698951720, 74.16557627198102409 ) ) ;
#73432 = CARTESIAN_POINT ( 'NONE',  ( -19.05341960407611168, -5.049401038298163336, 36.45724293864766707 ) ) ;
#73433 = CARTESIAN_POINT ( 'NONE',  ( 0.05219959533934541429, -16.53943276465976808, 105.0010903946856757 ) ) ;
#73434 = CARTESIAN_POINT ( 'NONE',  ( -8.224510206698735004, -14.34966873604973081, 64.58442372801900433 ) ) ;
#73435 = CARTESIAN_POINT ( 'NONE',  ( 13.89961937509957401, 13.97604488694547697, 31.87609039468566863 ) ) ;
#73436 = CARTESIAN_POINT ( 'NONE',  ( 19.05341960407611168, 5.049401038298154454, 98.95724293864766707 ) ) ;
#73437 = CARTESIAN_POINT ( 'NONE',  ( -16.51473224551069308, -9.474510206698971260, 76.66557627198103830 ) ) ;
#73438 = CARTESIAN_POINT ( 'NONE',  ( 4.379528057220092307, 16.55341960407617563, 72.29275706135236135 ) ) ;
#73439 = CARTESIAN_POINT ( 'NONE',  ( -16.51473224551069308, -9.474510206698971260, 41.66557627198103120 ) ) ;
#73440 = CARTESIAN_POINT ( 'NONE',  ( 14.29746914071049879, -8.314922557960816363, 53.33224293864769550 ) ) ;
#73442 = CARTESIAN_POINT ( 'NONE',  ( -19.03943276465977164, 0.05219959533909376836, 96.24890960531436690 ) ) ;
#73441 = CARTESIAN_POINT ( 'NONE',  ( -0.05219959533909027116, -19.03943276465977164, 107.4989096053143527 ) ) ;
#73443 = CARTESIAN_POINT ( 'NONE',  ( 18.67979575497178502, 10.72451020669898547, 24.16557627198103120 ) ) ;
#73444 = CARTESIAN_POINT ( 'NONE',  ( -14.34966873604960291, -8.224510206698953496, 71.66557627198100988 ) ) ;
#73445 = CARTESIAN_POINT ( 'NONE',  ( -12.14591786802309592, -12.06949235617757132, 71.87390960531438111 ) ) ;
#73447 = DIRECTION ( 'NONE',  ( -0.000000000000000000, -0.000000000000000000, 1.000000000000000000 ) ) ;
#73446 = CARTESIAN_POINT ( 'NONE',  ( 8.224510206698742110, 14.34966873604972548, 57.08442372801901854 ) ) ;
#73448 = CARTESIAN_POINT ( 'NONE',  ( 5.049401038297881783, 19.05341960407617563, 67.29275706135234714 ) ) ;
#73449 = CARTESIAN_POINT ( 'NONE',  ( 9.564922557960805705, 16.46253265017160317, 84.58224293864769550 ) ) ;
#73450 = CARTESIAN_POINT ( 'NONE',  ( 9.564922557961047289, -16.46253265017146816, 60.41775706135233293 ) ) ;
#73451 = CARTESIAN_POINT ( 'NONE',  ( 0.05219959533936267826, -19.03943276465977164, 40.00109039468566152 ) ) ;
#73453 = CARTESIAN_POINT ( 'NONE',  ( 16.52544592524335698, 4.483927247898782831, 101.4594237280190185 ) ) ;
#73452 = CARTESIAN_POINT ( 'NONE',  ( 0.05219959533934541429, -16.53943276465976808, 20.00109039468568639 ) ) ;
#73454 = CARTESIAN_POINT ( 'NONE',  ( -16.51473224551069308, -9.474510206698971260, 36.66557627198102409 ) ) ;
#73455 = CARTESIAN_POINT ( 'NONE',  ( 18.67979575497178502, 10.72451020669898547, 24.16557627198103120 ) ) ;
#73456 = CARTESIAN_POINT ( 'NONE',  ( -21.52544592524334988, -5.823673210054445271, 58.95942372801902565 ) ) ;
#73457 = CARTESIAN_POINT ( 'NONE',  ( 13.89961937509957401, 13.97604488694547697, 106.8760903946856757 ) ) ;
#73459 = CARTESIAN_POINT ( 'NONE',  ( 19.03943276465977164, -0.05219959533909143690, 73.74890960531435269 ) ) ;
#73458 = DIRECTION ( 'NONE',  ( 0.1045284632676537068, 0.000000000000000000, 0.9945218953682734009 ) ) ;
#73460 = CARTESIAN_POINT ( 'NONE',  ( -16.51473224551069308, -9.474510206698971260, 111.6655762719810383 ) ) ;
#73462 = CARTESIAN_POINT ( 'NONE',  ( 9.474510206698971260, -16.51473224551069308, 82.91557627198103830 ) ) ;
#73461 = CARTESIAN_POINT ( 'NONE',  ( 0.05219959533910956823, 16.53943276465976808, 74.99890960531435269 ) ) ;
#73463 = ITEM_DEFINED_TRANSFORMATION ( 'NONE', 'NONE', #188772,  #82054 ) ;
#73464 = CARTESIAN_POINT ( 'NONE',  ( 19.03943276465977164, -0.05219959533909143690, 73.74890960531435269 ) ) ;
#73465 = CARTESIAN_POINT ( 'NONE',  ( 13.89961937509957401, 13.97604488694547697, 76.87609039468566152 ) ) ;
#73466 = CARTESIAN_POINT ( 'NONE',  ( 15.72974639402199770, -15.80617190586745480, 63.12390960531435979 ) ) ;
#73467 = CARTESIAN_POINT ( 'NONE',  ( -16.53943276465976808, 0.05219959533911058130, 116.2489096053143669 ) ) ;
#73468 = CARTESIAN_POINT ( 'NONE',  ( 19.05341960407617918, -5.049401038297876454, 61.04275706135232582 ) ) ;
#73469 = CARTESIAN_POINT ( 'NONE',  ( 9.564922557960805705, 16.46253265017160317, 54.58224293864769550 ) ) ;
#73470 = CARTESIAN_POINT ( 'NONE',  ( 19.02544592524343514, -5.153800228976328945, 93.54057627198102409 ) ) ;
#73471 = VERTEX_POINT ( 'NONE', #151935 ) ;
#73472 = CARTESIAN_POINT ( 'NONE',  ( 21.53943276465977519, -0.05219959533907433946, 83.74890960531435269 ) ) ;
#73474 = CARTESIAN_POINT ( 'NONE',  ( 9.474510206698729675, 16.51473224551082808, 42.08442372801900433 ) ) ;
#73473 = CARTESIAN_POINT ( 'NONE',  ( 12.06949235617757843, -12.14591786802309237, 98.12390960531436690 ) ) ;
#73475 = CARTESIAN_POINT ( 'NONE',  ( 5.719274019375991003, -21.55341960407610458, 77.70724293864770971 ) ) ;
#73476 = CARTESIAN_POINT ( 'NONE',  ( -18.62759615963270932, 10.81492255796079327, 65.83224293864769550 ) ) ;
#73477 = CARTESIAN_POINT ( 'NONE',  ( 12.14591786802309770, 12.06949235617756955, 39.37390960531436690 ) ) ;
#73478 = CARTESIAN_POINT ( 'NONE',  ( 21.55341960407619695, -5.719274019375665929, 111.0427570613523613 ) ) ;
#73479 = CARTESIAN_POINT ( 'NONE',  ( 5.153800228976335163, 19.02544592524342804, 84.79057627198099567 ) ) ;
#73480 = CARTESIAN_POINT ( 'NONE',  ( -5.049401038298153566, 19.05341960407611168, 30.20724293864768839 ) ) ;
#73481 = AXIS2_PLACEMENT_3D ( 'NONE', #185246, #60892, #134791 ) ;
#73482 = CARTESIAN_POINT ( 'NONE',  ( -10.81492255796105439, 18.62759615963255655, 42.91775706135235424 ) ) ;
#73483 = CARTESIAN_POINT ( 'NONE',  ( 21.55341960407619695, -5.719274019375665929, 36.04275706135234714 ) ) ;
#73484 = CARTESIAN_POINT ( 'NONE',  ( 9.564922557960805705, 16.46253265017160317, 49.58224293864770260 ) ) ;
#73485 = CARTESIAN_POINT ( 'NONE',  ( -18.67979575497193778, 10.72451020669871902, 23.33442372801901499 ) ) ;
#73486 = CARTESIAN_POINT ( 'NONE',  ( 5.049401038297881783, 19.05341960407617563, 57.29275706135231871 ) ) ;
#73487 = CARTESIAN_POINT ( 'NONE',  ( -19.02544592524342804, 5.153800228976336051, 31.04057627198102409 ) ) ;
#73488 = CARTESIAN_POINT ( 'NONE',  ( 16.55341960407618274, -4.379528057220086978, 31.04275706135234714 ) ) ;
#73489 = CARTESIAN_POINT ( 'NONE',  ( -9.564922557960796823, -16.46253265017161027, 32.08224293864769550 ) ) ;
#73490 = CARTESIAN_POINT ( 'NONE',  ( 16.52544592524335698, 4.483927247898782831, 76.45942372801901854 ) ) ;
#73491 = CARTESIAN_POINT ( 'NONE',  ( 19.03943276465977164, -0.05219959533909143690, 43.74890960531435979 ) ) ;
#73492 = CARTESIAN_POINT ( 'NONE',  ( -24.95262708931866058, -12.69764001896745143, 166.0532406165023360 ) ) ;
#73493 = CARTESIAN_POINT ( 'NONE',  ( -9.474510206698964154, 16.51473224551069663, 80.41557627198103830 ) ) ;
#73495 = EDGE_CURVE ( 'NONE', #127301, #42534, #141326, .T. ) ;
#73494 = CARTESIAN_POINT ( 'NONE',  ( 19.02544592524343514, -5.153800228976328945, 28.54057627198102409 ) ) ;
#73496 = CARTESIAN_POINT ( 'NONE',  ( -18.67979575497178146, -10.72451020669898902, 71.66557627198100988 ) ) ;
#73497 = CARTESIAN_POINT ( 'NONE',  ( 8.314922557961029526, -14.29746914071037800, 45.41775706135234003 ) ) ;
#73498 = CARTESIAN_POINT ( 'NONE',  ( 15.72974639402176855, 15.80617190586768217, 96.87609039468568994 ) ) ;
#73499 = CARTESIAN_POINT ( 'NONE',  ( 5.153800228976335163, 19.02544592524342804, 34.79057627198102409 ) ) ;
#73500 = CARTESIAN_POINT ( 'NONE',  ( -8.314922557960811034, -14.29746914071050412, 27.08224293864769550 ) ) ;
#73501 = CARTESIAN_POINT ( 'NONE',  ( -8.224510206698948167, 14.34966873604960824, 65.41557627198102409 ) ) ;
#73502 = CARTESIAN_POINT ( 'NONE',  ( 19.03943276465977164, -0.05219959533909143690, 63.74890960531435979 ) ) ;
#73503 = CARTESIAN_POINT ( 'NONE',  ( -18.62759615963255300, -10.81492255796106328, 104.1677570613523471 ) ) ;
#73504 = CARTESIAN_POINT ( 'NONE',  ( -15.80617190586768217, 15.72974639402176855, 23.12609039468567573 ) ) ;
#73505 = CARTESIAN_POINT ( 'NONE',  ( -19.02544592524342804, 5.153800228976336051, 81.04057627198103830 ) ) ;
#73506 = CARTESIAN_POINT ( 'NONE',  ( -18.67979575497193778, 10.72451020669871902, 88.33442372801901854 ) ) ;
#73507 = CARTESIAN_POINT ( 'NONE',  ( 8.314922557961029526, -14.29746914071037800, 55.41775706135234714 ) ) ;
#73508 = CARTESIAN_POINT ( 'NONE',  ( 8.314922557961029526, -14.29746914071037800, 25.41775706135235779 ) ) ;
#73510 = CARTESIAN_POINT ( 'NONE',  ( 21.55341960407619695, -5.719274019375665929, 96.04275706135236135 ) ) ;
#73509 = CARTESIAN_POINT ( 'NONE',  ( -8.314922557960811034, -14.29746914071050412, 92.08224293864769550 ) ) ;
#73511 = AXIS2_PLACEMENT_3D ( 'NONE', #196479, #14408, #119620 ) ;
#73512 = CARTESIAN_POINT ( 'NONE',  ( 16.55341960407611168, 4.379528057220329451, 28.95724293864769905 ) ) ;
#73513 = CARTESIAN_POINT ( 'NONE',  ( 13.97604488694527802, 13.89961937509977652, 29.37390960531435979 ) ) ;
#73514 = CARTESIAN_POINT ( 'NONE',  ( -12.14591786802326823, 12.06949235617739902, 53.12609039468568284 ) ) ;
#73515 = CARTESIAN_POINT ( 'NONE',  ( 14.34966873604960469, 8.224510206698951720, 54.16557627198103120 ) ) ;
#73516 = CARTESIAN_POINT ( 'NONE',  ( 8.224510206698742110, 14.34966873604972548, 97.08442372801904696 ) ) ;
#73517 = CARTESIAN_POINT ( 'NONE',  ( 9.474510206698971260, -16.51473224551069308, 112.9155762719810383 ) ) ;
#73518 = CARTESIAN_POINT ( 'NONE',  ( -15.72974639402197994, 15.80617190586746368, 35.62390960531437401 ) ) ;
#73519 = CARTESIAN_POINT ( 'NONE',  ( -19.02544592524334988, -5.153800228976617603, 18.95942372801899722 ) ) ;
#73520 = CARTESIAN_POINT ( 'NONE',  ( 12.06949235617757843, -12.14591786802309237, 93.12390960531436690 ) ) ;
#73521 = CARTESIAN_POINT ( 'NONE',  ( 19.05341960407611168, 5.049401038298154454, 98.95724293864766707 ) ) ;
#73522 = ORIENTED_EDGE ( 'NONE', *, *, #157036, .T. ) ;
#73523 = CARTESIAN_POINT ( 'NONE',  ( 14.34966873604972726, -8.224510206698740333, 40.83442372801901854 ) ) ;
#73524 = CARTESIAN_POINT ( 'NONE',  ( -19.02544592524342804, 5.153800228976336051, 36.04057627198100988 ) ) ;
#73526 = SURFACE_STYLE_USAGE ( .BOTH. , #180711 ) ;
#73525 = CARTESIAN_POINT ( 'NONE',  ( -16.53943276465976808, -0.05219959533934237506, 48.75109039468568284 ) ) ;
#73527 = CARTESIAN_POINT ( 'NONE',  ( -9.474510206698720793, -16.51473224551083518, 54.58442372801899722 ) ) ;
#73528 = CARTESIAN_POINT ( 'NONE',  ( 5.153800228976335163, 19.02544592524342804, 39.79057627198100988 ) ) ;
#73529 = CARTESIAN_POINT ( 'NONE',  ( -0.05219959533934338120, 16.53943276465976808, 82.50109039468568994 ) ) ;
#73530 = CARTESIAN_POINT ( 'NONE',  ( -9.564922557961040184, 16.46253265017147172, 97.91775706135233293 ) ) ;
#73531 = CARTESIAN_POINT ( 'NONE',  ( 19.03943276465977164, 0.05219959533936151252, 26.25109039468566507 ) ) ;
#73532 = CARTESIAN_POINT ( 'NONE',  ( 16.51473224551069308, 9.474510206698969483, 59.16557627198102409 ) ) ;
#73533 = CARTESIAN_POINT ( 'NONE',  ( 16.52544592524342804, -4.483927247898539470, 93.54057627198103830 ) ) ;
#73534 = CARTESIAN_POINT ( 'NONE',  ( 13.89961937509957401, 13.97604488694547697, 66.87609039468567573 ) ) ;
#73535 = CARTESIAN_POINT ( 'NONE',  ( -10.72451020669898014, 18.67979575497178502, 65.41557627198102409 ) ) ;
#73536 = CARTESIAN_POINT ( 'NONE',  ( 0.05219959533936267826, -19.03943276465977164, 35.00109039468566863 ) ) ;
#73537 = CARTESIAN_POINT ( 'NONE',  ( 13.97604488694527802, 13.89961937509977652, 104.3739096053143385 ) ) ;
#73538 = CARTESIAN_POINT ( 'NONE',  ( -21.52544592524343514, 5.823673210054127303, 91.04057627198103830 ) ) ;
#73539 = CARTESIAN_POINT ( 'NONE',  ( -16.88567814943162659, 6.947325034625692730, 83.70998877347415146 ) ) ;
#73540 = CARTESIAN_POINT ( 'NONE',  ( -16.51473224551082808, 9.474510206698731452, 98.33442372801900433 ) ) ;
#73541 = CARTESIAN_POINT ( 'NONE',  ( -17.49999999999999645, -5.499999999999992895, 99.20309617465831309 ) ) ;
#73542 = CARTESIAN_POINT ( 'NONE',  ( -8.314922557961024197, 14.29746914071037800, 22.91775706135235069 ) ) ;
#73543 = CARTESIAN_POINT ( 'NONE',  ( -0.05219959533909027116, -19.03943276465977164, 52.49890960531436690 ) ) ;
#73544 = CARTESIAN_POINT ( 'NONE',  ( 19.05341960407611168, 5.049401038298154454, 108.9572429386477097 ) ) ;
#73545 = CARTESIAN_POINT ( 'NONE',  ( 15.72974639402199770, -15.80617190586745480, 93.12390960531436690 ) ) ;
#73546 = CARTESIAN_POINT ( 'NONE',  ( 21.53943276465977519, 0.05219959533937863772, 56.25109039468568284 ) ) ;
#73548 = CARTESIAN_POINT ( 'NONE',  ( 19.02544592524334988, 5.153800228976608722, 21.45942372801899012 ) ) ;
#73547 = CARTESIAN_POINT ( 'NONE',  ( -16.51473224551082808, 9.474510206698731452, 108.3344237280190043 ) ) ;
#73549 = CARTESIAN_POINT ( 'NONE',  ( 16.52544592524335698, 4.483927247898782831, 106.4594237280190328 ) ) ;
#73550 = CARTESIAN_POINT ( 'NONE',  ( -5.719274019375978568, 21.55341960407610458, 105.2072429386477097 ) ) ;
#73551 = CARTESIAN_POINT ( 'NONE',  ( -16.52544592524342804, 4.483927247898546575, 51.04057627198103120 ) ) ;
#73552 = CARTESIAN_POINT ( 'NONE',  ( -19.02544592524334988, -5.153800228976617603, 78.95942372801900433 ) ) ;
#73553 = CARTESIAN_POINT ( 'NONE',  ( 13.89961937509957401, 13.97604488694547697, 56.87609039468564731 ) ) ;
#73554 = CARTESIAN_POINT ( 'NONE',  ( -5.719274019375665041, -21.55341960407619695, 74.79275706135234714 ) ) ;
#73555 = CARTESIAN_POINT ( 'NONE',  ( -9.474510206698720793, -16.51473224551083518, 34.58442372801899722 ) ) ;
#73556 = CARTESIAN_POINT ( 'NONE',  ( 5.049401038298161559, -19.05341960407611168, 27.70724293864769550 ) ) ;
#73557 = CARTESIAN_POINT ( 'NONE',  ( -21.52544592524343514, 5.823673210054127303, 41.04057627198103120 ) ) ;
#73558 = CARTESIAN_POINT ( 'NONE',  ( -16.52544592524342804, 4.483927247898546575, 31.04057627198102409 ) ) ;
#73559 = CARTESIAN_POINT ( 'NONE',  ( 21.52544592524334988, 5.823673210054432836, 106.4594237280190328 ) ) ;
#73560 = CARTESIAN_POINT ( 'NONE',  ( 12.06949235617739724, 12.14591786802326823, 76.87609039468567573 ) ) ;
#73561 = CARTESIAN_POINT ( 'NONE',  ( -4.483927247898539470, -16.52544592524342804, 42.29057627198103120 ) ) ;
#73562 = CARTESIAN_POINT ( 'NONE',  ( 5.823673210054444382, -21.52544592524334988, 65.20942372801901854 ) ) ;
#73563 = CARTESIAN_POINT ( 'NONE',  ( -21.55341960407619339, 5.719274019375674811, 63.54275706135234003 ) ) ;
#73564 = CARTESIAN_POINT ( 'NONE',  ( -5.823673210054116645, -21.52544592524344225, 67.29057627198103830 ) ) ;
#73565 = ORIENTED_EDGE ( 'NONE', *, *, #153660, .T. ) ;
#73566 = CARTESIAN_POINT ( 'NONE',  ( 5.049401038298161559, -19.05341960407611168, 27.70724293864769550 ) ) ;
#73567 = CARTESIAN_POINT ( 'NONE',  ( -15.80617190586768217, 15.72974639402176855, 48.12609039468568284 ) ) ;
#73568 = CARTESIAN_POINT ( 'NONE',  ( -9.474510206698964154, 16.51473224551069663, 25.41557627198103120 ) ) ;
#73569 = CARTESIAN_POINT ( 'NONE',  ( 16.46253265017160672, -9.564922557960803928, 43.33224293864769550 ) ) ;
#73570 = CARTESIAN_POINT ( 'NONE',  ( 4.379528057220339221, -16.55341960407611168, 92.70724293864770971 ) ) ;
#73571 = CARTESIAN_POINT ( 'NONE',  ( 19.05341960407611168, 5.049401038298154454, 88.95724293864769550 ) ) ;
#73572 = CARTESIAN_POINT ( 'NONE',  ( -0.05219959533910754901, -16.53943276465976808, 27.49890960531435269 ) ) ;
#73573 = CARTESIAN_POINT ( 'NONE',  ( -4.483927247898539470, -16.52544592524342804, 102.2905762719810383 ) ) ;
#73574 = CARTESIAN_POINT ( 'NONE',  ( 0.05219959533907565091, 21.53943276465977519, 69.99890960531435269 ) ) ;
#73575 = CARTESIAN_POINT ( 'NONE',  ( -0.05219959533907301413, -21.53943276465977519, 102.4989096053143811 ) ) ;
#73576 = CARTESIAN_POINT ( 'NONE',  ( 19.03943276465977164, -0.05219959533909143690, 108.7489096053143527 ) ) ;
#73578 = CARTESIAN_POINT ( 'NONE',  ( 14.29746914071037800, 8.314922557961029526, 26.66775706135235424 ) ) ;
#73577 = CARTESIAN_POINT ( 'NONE',  ( 13.89961937509977652, -13.97604488694527269, 68.12390960531436690 ) ) ;
#73579 = EDGE_CURVE ( 'NONE', #197846, #24501, #118770, .T. ) ;
#73580 = CARTESIAN_POINT ( 'NONE',  ( 21.55341960407610458, 5.719274019375980345, 58.95724293864770971 ) ) ;
#73581 = CARTESIAN_POINT ( 'NONE',  ( -0.05219959533937732626, 21.53943276465977519, 87.50109039468568994 ) ) ;
#73582 = CARTESIAN_POINT ( 'NONE',  ( 9.564922557960805705, 16.46253265017160317, 79.58224293864769550 ) ) ;
#73583 = CARTESIAN_POINT ( 'NONE',  ( -21.53943276465977519, 0.05219959533907696930, 21.24890960531436690 ) ) ;
#73584 = CARTESIAN_POINT ( 'NONE',  ( -12.14591786802326823, 12.06949235617739902, 73.12609039468567573 ) ) ;
#73585 = CARTESIAN_POINT ( 'NONE',  ( 15.80617190586769283, -15.72974639402175789, 70.62609039468567573 ) ) ;
#73586 = CARTESIAN_POINT ( 'NONE',  ( 18.67979575497194134, -10.72451020669871369, 95.83442372801903275 ) ) ;
#73587 = CARTESIAN_POINT ( 'NONE',  ( -4.483927247898782831, 16.52544592524335698, 62.70942372801902565 ) ) ;
#73588 = CARTESIAN_POINT ( 'NONE',  ( 10.81492255796106328, -18.62759615963255655, 20.41775706135234714 ) ) ;
#73589 = CARTESIAN_POINT ( 'NONE',  ( 16.51473224551069308, 9.474510206698969483, 24.16557627198102765 ) ) ;
#73590 = CARTESIAN_POINT ( 'NONE',  ( 0.05219959533907565091, 21.53943276465977519, 94.99890960531436690 ) ) ;
#73591 = CARTESIAN_POINT ( 'NONE',  ( -16.51473224551082808, 9.474510206698731452, 53.33442372801900433 ) ) ;
#73592 = CARTESIAN_POINT ( 'NONE',  ( 18.67979575497178502, 10.72451020669898547, 59.16557627198103120 ) ) ;
#73594 = CARTESIAN_POINT ( 'NONE',  ( 12.06949235617757843, -12.14591786802309237, 38.12390960531436690 ) ) ;
#73593 = CARTESIAN_POINT ( 'NONE',  ( -19.05341960407611168, -5.049401038298163336, 96.45724293864769550 ) ) ;
#73595 = CARTESIAN_POINT ( 'NONE',  ( 17.50000000000000000, 5.499999999999992895, 91.70309617465828467 ) ) ;
#73596 = CARTESIAN_POINT ( 'NONE',  ( -19.20446147854526231, -5.500000000000010658, 79.38999695167677828 ) ) ;
#73597 = CARTESIAN_POINT ( 'NONE',  ( -19.03943276465977164, -0.05219959533935918106, 113.7510903946856757 ) ) ;
#73598 = CARTESIAN_POINT ( 'NONE',  ( 15.72974639402199770, -15.80617190586745480, 73.12390960531436690 ) ) ;
#73599 = CARTESIAN_POINT ( 'NONE',  ( -8.224510206698948167, 14.34966873604960824, 45.41557627198103830 ) ) ;
#73600 = CARTESIAN_POINT ( 'NONE',  ( -0.05219959533934338120, 16.53943276465976808, 27.50109039468567929 ) ) ;
#73601 = CARTESIAN_POINT ( 'NONE',  ( -19.03943276465977164, 0.05219959533909376836, 51.24890960531436690 ) ) ;
#73603 = CARTESIAN_POINT ( 'NONE',  ( 13.89961937509957401, 13.97604488694547697, 81.87609039468564731 ) ) ;
#73602 = CARTESIAN_POINT ( 'NONE',  ( -21.52544592524343514, 5.823673210054127303, 111.0405762719810525 ) ) ;
#73604 = ADVANCED_FACE ( 'NONE', ( #91221 ), #152912, .T. ) ;
#73605 = CARTESIAN_POINT ( 'NONE',  ( -16.46253265017160317, 9.564922557960807481, 80.83224293864769550 ) ) ;
#73606 = CARTESIAN_POINT ( 'NONE',  ( -5.049401038298153566, 19.05341960407611168, 70.20724293864769550 ) ) ;
#73607 = CARTESIAN_POINT ( 'NONE',  ( 21.53943276465977519, -0.05219959533907433946, 73.74890960531433848 ) ) ;
#73608 = CARTESIAN_POINT ( 'NONE',  ( 19.05341960407611168, 5.049401038298154454, 33.95724293864769550 ) ) ;
#73609 = CARTESIAN_POINT ( 'NONE',  ( 0.000000000000000000, 0.000000000000000000, -25.00000000000000000 ) ) ;
#73610 = CARTESIAN_POINT ( 'NONE',  ( -8.314922557960811034, -14.29746914071050412, 57.08224293864769550 ) ) ;
#73611 = CARTESIAN_POINT ( 'NONE',  ( -19.02544592524342804, 5.153800228976336051, 91.04057627198100988 ) ) ;
#73612 = CARTESIAN_POINT ( 'NONE',  ( -28.82186960331499037, 2.428612866367529932E-14, 140.2500000054623683 ) ) ;
#73613 = CARTESIAN_POINT ( 'NONE',  ( 16.51473224551083163, -9.474510206698727899, 60.83442372801900433 ) ) ;
#73614 = CARTESIAN_POINT ( 'NONE',  ( 15.80617190586746368, 15.72974639402197994, 79.37390960531436690 ) ) ;
#73615 = CARTESIAN_POINT ( 'NONE',  ( 9.564922557961047289, -16.46253265017146816, 30.41775706135232937 ) ) ;
#73616 = CARTESIAN_POINT ( 'NONE',  ( -0.05219959533909027116, -19.03943276465977164, 92.49890960531436690 ) ) ;
#73617 = DIRECTION ( 'NONE',  ( 6.716189716306310304E-15, -0.9991276842514723588, 0.04175967627138119781 ) ) ;
#73618 = CARTESIAN_POINT ( 'NONE',  ( 10.72451020669898902, -18.67979575497178502, 32.91557627198102409 ) ) ;
#73619 = AXIS2_PLACEMENT_3D ( 'NONE', #198496, #75141, #151015 ) ;
#73620 = CARTESIAN_POINT ( 'NONE',  ( -13.89961937509977652, 13.97604488694528158, 75.62390960531438111 ) ) ;
#73621 = CARTESIAN_POINT ( 'NONE',  ( -21.52544592524334988, -5.823673210054445271, 53.95942372801900433 ) ) ;
#73622 = CARTESIAN_POINT ( 'NONE',  ( 9.564922557960805705, 16.46253265017160317, 24.58224293864769194 ) ) ;
#73624 = ORIENTED_EDGE ( 'NONE', *, *, #155268, .T. ) ;
#73623 = CARTESIAN_POINT ( 'NONE',  ( 15.80617190586746368, 15.72974639402197994, 109.3739096053143811 ) ) ;
#73625 = CARTESIAN_POINT ( 'NONE',  ( -0.05219959533937732626, 21.53943276465977519, 37.50109039468568284 ) ) ;
#73626 = ORIENTED_EDGE ( 'NONE', *, *, #104106, .T. ) ;
#73627 = CARTESIAN_POINT ( 'NONE',  ( -16.51473224551069308, -9.474510206698971260, 96.66557627198102409 ) ) ;
#73628 = CARTESIAN_POINT ( 'NONE',  ( -21.81399809961444802, 8.291606000631404072, 169.3279294801716617 ) ) ;
#73629 = CARTESIAN_POINT ( 'NONE',  ( -21.55341960407610458, -5.719274019375992779, 101.4572429386476955 ) ) ;
#73630 = CARTESIAN_POINT ( 'NONE',  ( -16.51473224551069308, -9.474510206698971260, 66.66557627198102409 ) ) ;
#73631 = CARTESIAN_POINT ( 'NONE',  ( -14.29746914071037622, -8.314922557961029526, 19.16775706135234714 ) ) ;
#73632 = CARTESIAN_POINT ( 'NONE',  ( 23.48529157249599919, 32.32473071737754111, -6.449999994537626513 ) ) ;
#73633 = CARTESIAN_POINT ( 'NONE',  ( -15.72974639402176322, -15.80617190586768395, 104.3760903946856899 ) ) ;
#73634 = CARTESIAN_POINT ( 'NONE',  ( 13.97604488694527802, 13.89961937509977652, 39.37390960531435269 ) ) ;
#73635 = CARTESIAN_POINT ( 'NONE',  ( -5.823673210054431948, 21.52544592524334988, 97.70942372801904696 ) ) ;
#73637 = CARTESIAN_POINT ( 'NONE',  ( 5.719274019375673035, 21.55341960407619339, 62.29275706135236845 ) ) ;
#73636 = CARTESIAN_POINT ( 'NONE',  ( 19.03943276465977164, -0.05219959533909143690, 93.74890960531435269 ) ) ;
#73638 = CARTESIAN_POINT ( 'NONE',  ( 1.784210473542230573E-15, -29.16686587814331588, 141.8750000027311842 ) ) ;
#73639 = CYLINDRICAL_SURFACE ( 'NONE', #144978, 8.000000000000000000 ) ;
#73640 = CARTESIAN_POINT ( 'NONE',  ( -14.62203461105304036, -16.12203461105356794, -56.14925526931841659 ) ) ;
#73643 = CARTESIAN_POINT ( 'NONE',  ( 5.823673210054444382, -21.52544592524334988, 60.20942372801902565 ) ) ;
#73642 = CARTESIAN_POINT ( 'NONE',  ( -14.34966873604972548, 8.224510206698743886, 68.33442372801900433 ) ) ;
#73641 = CARTESIAN_POINT ( 'NONE',  ( -4.379528057220086978, -16.55341960407618274, 54.79275706135235424 ) ) ;
#73644 = CARTESIAN_POINT ( 'NONE',  ( -21.55341960407619339, 5.719274019375674811, 88.54275706135236135 ) ) ;
#73645 = DIRECTION ( 'NONE',  ( 1.000000000000000000, -0.000000000000000000, -0.000000000000000000 ) ) ;
#73646 = CARTESIAN_POINT ( 'NONE',  ( -12.06949235617739369, -12.14591786802326823, 29.37609039468568284 ) ) ;
#73647 = CARTESIAN_POINT ( 'NONE',  ( 16.46253265017160672, -9.564922557960803928, 78.33224293864769550 ) ) ;
#73648 = CARTESIAN_POINT ( 'NONE',  ( -9.564922557960796823, -16.46253265017161027, 92.08224293864769550 ) ) ;
#73649 = CARTESIAN_POINT ( 'NONE',  ( 16.81555441253550498, 7.025013491695491830, 41.86314554665747778 ) ) ;
#73650 = CARTESIAN_POINT ( 'NONE',  ( -19.03943276465977164, 0.05219959533909376836, 31.24890960531435979 ) ) ;
#73651 = CARTESIAN_POINT ( 'NONE',  ( 21.53943276465977519, -0.05219959533907433946, 48.74890960531435979 ) ) ;
#73652 = CARTESIAN_POINT ( 'NONE',  ( -16.52544592524335698, -4.483927247898792601, 88.95942372801901854 ) ) ;
#73654 = CARTESIAN_POINT ( 'NONE',  ( -0.05219959533909027116, -19.03943276465977164, 72.49890960531435269 ) ) ;
#73653 = CARTESIAN_POINT ( 'NONE',  ( 12.14591786802309770, 12.06949235617756955, 84.37390960531438111 ) ) ;
#73655 = CARTESIAN_POINT ( 'NONE',  ( 18.67979575497194134, -10.72451020669871369, 85.83442372801901854 ) ) ;
#73656 = CARTESIAN_POINT ( 'NONE',  ( -8.898068258721469448, -27.38543819252872069, 144.6656553485624102 ) ) ;
#73657 = CARTESIAN_POINT ( 'NONE',  ( -16.53943276465976808, -0.05219959533934237506, 28.75109039468567929 ) ) ;
#73658 = CARTESIAN_POINT ( 'NONE',  ( -12.06949235617756955, 12.14591786802309770, 70.62390960531436690 ) ) ;
#73659 = CARTESIAN_POINT ( 'NONE',  ( -5.823673210054431948, 21.52544592524334988, 47.70942372801902565 ) ) ;
#73660 = CARTESIAN_POINT ( 'NONE',  ( -21.53943276465977519, 0.05219959533907696930, 76.24890960531435269 ) ) ;
#73661 = CARTESIAN_POINT ( 'NONE',  ( -13.89961937509957401, -13.97604488694547875, 44.37609039468566863 ) ) ;
#73662 = CARTESIAN_POINT ( 'NONE',  ( 5.153800228976335163, 19.02544592524342804, 44.79057627198103120 ) ) ;
#73663 = CARTESIAN_POINT ( 'NONE',  ( -19.05341960407611168, -5.049401038298163336, 81.45724293864769550 ) ) ;
#73664 = CARTESIAN_POINT ( 'NONE',  ( -12.06949235617756955, 12.14591786802309770, 45.62390960531436690 ) ) ;
#73665 = CARTESIAN_POINT ( 'NONE',  ( 16.55341960407611168, 4.379528057220329451, 28.95724293864769905 ) ) ;
#73666 = CARTESIAN_POINT ( 'NONE',  ( -12.14591786802309592, -12.06949235617757132, 21.87390960531436690 ) ) ;
#73667 = CARTESIAN_POINT ( 'NONE',  ( -9.564922557961040184, 16.46253265017147172, 62.91775706135233293 ) ) ;
#73668 = CARTESIAN_POINT ( 'NONE',  ( -997.9783121635130101, 0.000000000000000000, 0.000000000000000000 ) ) ;
#73669 = CARTESIAN_POINT ( 'NONE',  ( 10.81492255796078972, 18.62759615963270932, 29.58224293864769905 ) ) ;
#73670 = CARTESIAN_POINT ( 'NONE',  ( 16.53943276465976808, -0.05219959533910856209, 93.74890960531436690 ) ) ;
#73671 = CARTESIAN_POINT ( 'NONE',  ( 11.80868324581538253, -11.80868324581533457, -64.92279855667830191 ) ) ;
#73673 = CARTESIAN_POINT ( 'NONE',  ( -21.55341960407610458, -5.719274019375992779, 31.45724293864769550 ) ) ;
#73672 = CARTESIAN_POINT ( 'NONE',  ( -9.474510206698964154, 16.51473224551069663, 45.41557627198103120 ) ) ;
#73674 = CARTESIAN_POINT ( 'NONE',  ( -18.67979575497178146, -10.72451020669898902, 66.66557627198102409 ) ) ;
#73675 = CARTESIAN_POINT ( 'NONE',  ( 13.89961937509977652, -13.97604488694527269, 23.12390960531436335 ) ) ;
#73677 = CARTESIAN_POINT ( 'NONE',  ( 9.474510206698971260, -16.51473224551069308, 52.91557627198102409 ) ) ;
#73676 = CARTESIAN_POINT ( 'NONE',  ( -0.05219959533934338120, 16.53943276465976808, 62.50109039468568284 ) ) ;
#73678 = CARTESIAN_POINT ( 'NONE',  ( -0.05219959533937732626, 21.53943276465977519, 52.50109039468567573 ) ) ;
#73679 = ORIENTED_EDGE ( 'NONE', *, *, #91683, .F. ) ;
#73680 = CARTESIAN_POINT ( 'NONE',  ( 4.483927247898545687, 16.52544592524342804, 99.79057627198103830 ) ) ;
#73681 = EDGE_CURVE ( 'NONE', #99125, #49756, #199432, .T. ) ;
#73682 = CARTESIAN_POINT ( 'NONE',  ( 19.05341960407617918, -5.049401038297876454, 96.04275706135231871 ) ) ;
#73683 = CARTESIAN_POINT ( 'NONE',  ( -11.40812507854755609, 35.11059874428196537, -7.524999997268813523 ) ) ;
#73685 = CARTESIAN_POINT ( 'NONE',  ( 18.67979575497178502, 10.72451020669898547, 29.16557627198103120 ) ) ;
#73684 = CARTESIAN_POINT ( 'NONE',  ( -18.22780087662123805, 5.499999999999981348, 71.01763182126894947 ) ) ;
#73686 = DIRECTION ( 'NONE',  ( 0.000000000000000000, 0.5000000000000011102, 0.8660254037844380415 ) ) ;
#73687 = CARTESIAN_POINT ( 'NONE',  ( 18.67979575497194134, -10.72451020669871369, 75.83442372801900433 ) ) ;
#73688 = VERTEX_POINT ( 'NONE', #184264 ) ;
#73690 = CARTESIAN_POINT ( 'NONE',  ( 16.52544592524342804, -4.483927247898539470, 43.54057627198103830 ) ) ;
#73689 = CARTESIAN_POINT ( 'NONE',  ( -12.06949235617739369, -12.14591786802326823, 59.37609039468568284 ) ) ;
#73691 = CARTESIAN_POINT ( 'NONE',  ( 18.62759615963271287, -10.81492255796078972, 68.33224293864769550 ) ) ;
#73692 = CARTESIAN_POINT ( 'NONE',  ( -10.81492255796078084, -18.62759615963271287, 62.08224293864769550 ) ) ;
#73693 = DIRECTION ( 'NONE',  ( 0.000000000000000000, 0.000000000000000000, -1.000000000000000000 ) ) ;
#73695 = CARTESIAN_POINT ( 'NONE',  ( 5.719274019375991003, -21.55341960407610458, 22.70724293864769194 ) ) ;
#73694 = CARTESIAN_POINT ( 'NONE',  ( -5.153800228976607833, 19.02544592524334988, 82.70942372801897591 ) ) ;
#73696 = CARTESIAN_POINT ( 'NONE',  ( -19.02544592524342804, 5.153800228976336051, 51.04057627198103120 ) ) ;
#73698 = EDGE_CURVE ( 'NONE', #54292, #11758, #76072, .T. ) ;
#73697 = CARTESIAN_POINT ( 'NONE',  ( 19.02544592524343514, -5.153800228976328945, 23.54057627198102054 ) ) ;
#73699 = CARTESIAN_POINT ( 'NONE',  ( -19.03943276465977164, 0.05219959533909376836, 111.2489096053143669 ) ) ;
#73700 = ORIENTED_EDGE ( 'NONE', *, *, #11846, .F. ) ;
#73701 = CARTESIAN_POINT ( 'NONE',  ( -16.55341960407617563, 4.379528057220093196, 73.54275706135234714 ) ) ;
#73702 = CARTESIAN_POINT ( 'NONE',  ( -18.67979575497178146, -10.72451020669898902, 106.6655762719810383 ) ) ;
#73703 = CARTESIAN_POINT ( 'NONE',  ( -5.153800228976328057, -19.02544592524343514, 67.29057627198102409 ) ) ;
#73704 = CARTESIAN_POINT ( 'NONE',  ( -21.55341960407619339, 5.719274019375674811, 43.54275706135235424 ) ) ;
#73705 = CARTESIAN_POINT ( 'NONE',  ( -0.05219959533909027116, -19.03943276465977164, 102.4989096053143669 ) ) ;
#73706 = CARTESIAN_POINT ( 'NONE',  ( -24.05628303387027600, -31.51879896407069737, -19.31700871830652844 ) ) ;
#73707 = ORIENTED_EDGE ( 'NONE', *, *, #4758, .F. ) ;
#73708 = CARTESIAN_POINT ( 'NONE',  ( -5.823673210054431948, 21.52544592524334988, 32.70942372801900433 ) ) ;
#73710 = CARTESIAN_POINT ( 'NONE',  ( -5.153800228976607833, 19.02544592524334988, 82.70942372801897591 ) ) ;
#73709 = CARTESIAN_POINT ( 'NONE',  ( -9.474510206698964154, 16.51473224551069663, 25.41557627198103120 ) ) ;
#73711 = CARTESIAN_POINT ( 'NONE',  ( -13.97604488694547697, 13.89961937509957934, 38.12609039468566152 ) ) ;
#73712 = CARTESIAN_POINT ( 'NONE',  ( -10.81492255796078084, -18.62759615963271287, 112.0822429386477097 ) ) ;
#73713 = CARTESIAN_POINT ( 'NONE',  ( -19.05341960407617563, 5.049401038297882671, 33.54275706135231871 ) ) ;
#73714 = CARTESIAN_POINT ( 'NONE',  ( -5.153800228976607833, 19.02544592524334988, 52.70942372801900433 ) ) ;
#73715 = CARTESIAN_POINT ( 'NONE',  ( -14.34966873604972548, 8.224510206698743886, 98.33442372801901854 ) ) ;
#73716 = CARTESIAN_POINT ( 'NONE',  ( 23.71437922609630178, -10.61260870832703773, 165.9744018657352456 ) ) ;
#73717 = CARTESIAN_POINT ( 'NONE',  ( 19.02544592524343514, -5.153800228976328945, 73.54057627198103830 ) ) ;
#73718 = CARTESIAN_POINT ( 'NONE',  ( -5.823673210054431948, 21.52544592524334988, 82.70942372801900433 ) ) ;
#73719 = CARTESIAN_POINT ( 'NONE',  ( -15.80617190586768217, 15.72974639402176855, 93.12609039468568994 ) ) ;
#73720 = CARTESIAN_POINT ( 'NONE',  ( 17.50000000000000000, 5.499999999999997335, 26.70309617465829888 ) ) ;
#73721 = CARTESIAN_POINT ( 'NONE',  ( 9.564922557960805705, 16.46253265017160317, 94.58224293864769550 ) ) ;
#73722 = CARTESIAN_POINT ( 'NONE',  ( -21.53943276465977519, -0.05219959533937600094, 58.75109039468568994 ) ) ;
#73723 = CARTESIAN_POINT ( 'NONE',  ( 19.03943276465977164, 0.05219959533936151252, 106.2510903946856615 ) ) ;
#73724 = CARTESIAN_POINT ( 'NONE',  ( -0.05219959533909027116, -19.03943276465977164, 62.49890960531435979 ) ) ;
#73725 = CARTESIAN_POINT ( 'NONE',  ( -16.46253265017160317, 9.564922557960807481, 110.8322429386476955 ) ) ;
#73726 = CARTESIAN_POINT ( 'NONE',  ( -5.049401038298153566, 19.05341960407611168, 85.20724293864766707 ) ) ;
#73727 = CARTESIAN_POINT ( 'NONE',  ( -17.50000000000002132, -5.499999999999948486, 91.28230962303565832 ) ) ;
#73728 = CARTESIAN_POINT ( 'NONE',  ( 19.02544592524343514, -5.153800228976328945, 68.54057627198103830 ) ) ;
#73729 = CARTESIAN_POINT ( 'NONE',  ( -19.03943276465977164, 0.05219959533909376836, 46.24890960531435979 ) ) ;
#73730 = CARTESIAN_POINT ( 'NONE',  ( -5.823673210054116645, -21.52544592524344225, 112.2905762719810241 ) ) ;
#73731 = CARTESIAN_POINT ( 'NONE',  ( -0.05219959533934338120, 16.53943276465976808, 82.50109039468568994 ) ) ;
#73732 = CARTESIAN_POINT ( 'NONE',  ( 8.516692751257743055, -1.203296689329369729, -64.06477955746662190 ) ) ;
#73733 = CARTESIAN_POINT ( 'NONE',  ( -9.474510206698720793, -16.51473224551083518, 49.58442372801899722 ) ) ;
#73734 = CARTESIAN_POINT ( 'NONE',  ( 19.05341960407611168, 5.049401038298154454, 73.95724293864768129 ) ) ;
#73735 = CARTESIAN_POINT ( 'NONE',  ( 12.06949235617757843, -12.14591786802309237, 73.12390960531436690 ) ) ;
#73736 = CARTESIAN_POINT ( 'NONE',  ( 0.05219959533910956823, 16.53943276465976808, 109.9989096053143527 ) ) ;
#73737 = CARTESIAN_POINT ( 'NONE',  ( -9.564922557960796823, -16.46253265017161027, 112.0822429386476955 ) ) ;
#73738 = ORIENTED_EDGE ( 'NONE', *, *, #139548, .T. ) ;
#73739 = CARTESIAN_POINT ( 'NONE',  ( -16.51473224551069308, -9.474510206698971260, 106.6655762719810383 ) ) ;
#73740 = CARTESIAN_POINT ( 'NONE',  ( 12.14591786802309770, 12.06949235617756955, 74.37390960531436690 ) ) ;
#73741 = CARTESIAN_POINT ( 'NONE',  ( 16.51473224551069308, 9.474510206698969483, 114.1655762719810241 ) ) ;
#73742 = CARTESIAN_POINT ( 'NONE',  ( 0.05219959533936267826, -19.03943276465977164, 35.00109039468566863 ) ) ;
#73743 = CARTESIAN_POINT ( 'NONE',  ( -8.314922557961024197, 14.29746914071037800, 102.9177570613523756 ) ) ;
#73744 = CARTESIAN_POINT ( 'NONE',  ( 19.02544592524343514, -5.153800228976328945, 88.54057627198102409 ) ) ;
#73745 = CARTESIAN_POINT ( 'NONE',  ( 5.719274019375673035, 21.55341960407619339, 57.29275706135234714 ) ) ;
#73746 = CARTESIAN_POINT ( 'NONE',  ( 21.52544592524344225, -5.823673210054117533, 48.54057627198103120 ) ) ;
#73747 = CARTESIAN_POINT ( 'NONE',  ( -10.81492255796078084, -18.62759615963271287, 112.0822429386477097 ) ) ;
#73748 = CARTESIAN_POINT ( 'NONE',  ( -5.823673210054116645, -21.52544592524344225, 67.29057627198103830 ) ) ;
#73749 = CARTESIAN_POINT ( 'NONE',  ( 14.29746914071049879, -8.314922557960816363, 88.33224293864769550 ) ) ;
#73750 = CARTESIAN_POINT ( 'NONE',  ( -9.474510206698720793, -16.51473224551083518, 54.58442372801899722 ) ) ;
#73751 = CARTESIAN_POINT ( 'NONE',  ( -13.89961937509977652, 13.97604488694528158, 25.62390960531434558 ) ) ;
#73752 = CARTESIAN_POINT ( 'NONE',  ( -9.474510206698964154, 16.51473224551069663, 80.41557627198103830 ) ) ;
#73753 = CARTESIAN_POINT ( 'NONE',  ( -19.02544592524342804, 5.153800228976336051, 86.04057627198103830 ) ) ;
#73754 = CARTESIAN_POINT ( 'NONE',  ( -8.224510206698948167, 14.34966873604960824, 100.4155762719810241 ) ) ;
#73755 = ORIENTED_EDGE ( 'NONE', *, *, #123102, .T. ) ;
#73756 = CARTESIAN_POINT ( 'NONE',  ( -4.483927247898539470, -16.52544592524342804, 27.29057627198103120 ) ) ;
#73757 = CARTESIAN_POINT ( 'NONE',  ( 8.314922557961029526, -14.29746914071037800, 40.41775706135234714 ) ) ;
#73758 = CARTESIAN_POINT ( 'NONE',  ( 5.823673210054444382, -21.52544592524334988, 105.2094237280190328 ) ) ;
#73759 = CARTESIAN_POINT ( 'NONE',  ( -19.02544592524342804, 5.153800228976336051, 96.04057627198103830 ) ) ;
#73760 = CARTESIAN_POINT ( 'NONE',  ( -21.55341960407619339, 5.719274019375674811, 38.54275706135234714 ) ) ;
#73761 = CARTESIAN_POINT ( 'NONE',  ( 19.03943276465977164, -0.05219959533909143690, 48.74890960531435979 ) ) ;
#73762 = CARTESIAN_POINT ( 'NONE',  ( 0.05219959533934541429, -16.53943276465976808, 40.00109039468567573 ) ) ;
#73763 = CARTESIAN_POINT ( 'NONE',  ( -5.049401038297874678, -19.05341960407617918, 104.7927570613523471 ) ) ;
#73764 = CARTESIAN_POINT ( 'NONE',  ( -9.474510206698964154, 16.51473224551069663, 40.41557627198103120 ) ) ;
#73765 = CARTESIAN_POINT ( 'NONE',  ( -8.314922557960811034, -14.29746914071050412, 97.08224293864770971 ) ) ;
#73766 = CARTESIAN_POINT ( 'NONE',  ( -15.72974639402197994, 15.80617190586746368, 105.6239096053143669 ) ) ;
#73767 = CARTESIAN_POINT ( 'NONE',  ( 16.51473224551083163, -9.474510206698727899, 75.83442372801900433 ) ) ;
#73768 = CARTESIAN_POINT ( 'NONE',  ( -16.51473224551069308, -9.474510206698971260, 31.66557627198102054 ) ) ;
#73769 = CARTESIAN_POINT ( 'NONE',  ( 9.474510206698971260, -16.51473224551069308, 92.91557627198103830 ) ) ;
#73770 = CARTESIAN_POINT ( 'NONE',  ( 21.55341960407619695, -5.719274019375665929, 36.04275706135234714 ) ) ;
#73771 = CARTESIAN_POINT ( 'NONE',  ( -6.019987952026119621E-15, 39.95163481335720235, -4.247842220587803475 ) ) ;
#73772 = CARTESIAN_POINT ( 'NONE',  ( -5.153800228976328057, -19.02544592524343514, 97.29057627198099567 ) ) ;
#73773 = CARTESIAN_POINT ( 'NONE',  ( 17.79613651744294245, -24.49428055684527195, 142.6843446568999809 ) ) ;
#73774 = CARTESIAN_POINT ( 'NONE',  ( 19.05341960407611168, 5.049401038298154454, 88.95724293864769550 ) ) ;
#73776 = CARTESIAN_POINT ( 'NONE',  ( -8.314922557960811034, -14.29746914071050412, 87.08224293864769550 ) ) ;
#73775 = CARTESIAN_POINT ( 'NONE',  ( -0.05219959533937732626, 21.53943276465977519, 37.50109039468568284 ) ) ;
#73777 = CARTESIAN_POINT ( 'NONE',  ( 13.89961937509977652, -13.97604488694527269, 93.12390960531436690 ) ) ;
#73778 = CARTESIAN_POINT ( 'NONE',  ( 0.05219959533936267826, -19.03943276465977164, 25.00109039468566152 ) ) ;
#73779 = CARTESIAN_POINT ( 'NONE',  ( -16.52544592524335698, -4.483927247898792601, 53.95942372801900433 ) ) ;
#73780 = CARTESIAN_POINT ( 'NONE',  ( -15.72974639402176322, -15.80617190586768395, 74.37609039468568994 ) ) ;
#73781 = AXIS2_PLACEMENT_3D ( 'NONE', #110945, #64453, #129083 ) ;
#73782 = CARTESIAN_POINT ( 'NONE',  ( 12.06949235617739724, 12.14591786802326823, 26.87609039468567218 ) ) ;
#73783 = CARTESIAN_POINT ( 'NONE',  ( -19.05341960407611168, -5.049401038298163336, 66.45724293864769550 ) ) ;
#73784 = CARTESIAN_POINT ( 'NONE',  ( -19.05341960407617563, 5.049401038297882671, 98.54275706135233293 ) ) ;
#73785 = CARTESIAN_POINT ( 'NONE',  ( -0.05219959533934338120, 16.53943276465976808, 72.50109039468568994 ) ) ;
#73786 = CARTESIAN_POINT ( 'NONE',  ( 9.564922557961047289, -16.46253265017146816, 20.41775706135233293 ) ) ;
#73787 = CARTESIAN_POINT ( 'NONE',  ( -13.89961937509957401, -13.97604488694547875, 74.37609039468566152 ) ) ;
#73788 = CARTESIAN_POINT ( 'NONE',  ( -5.049401038298153566, 19.05341960407611168, 60.20724293864768129 ) ) ;
#73789 = CARTESIAN_POINT ( 'NONE',  ( 21.52544592524344225, -5.823673210054117533, 78.54057627198103830 ) ) ;
#73791 = CARTESIAN_POINT ( 'NONE',  ( 5.049401038297881783, 19.05341960407617563, 82.29275706135229029 ) ) ;
#73790 = CARTESIAN_POINT ( 'NONE',  ( -14.29746914071049879, 8.314922557960819915, 75.83224293864769550 ) ) ;
#73792 = CARTESIAN_POINT ( 'NONE',  ( 16.29526858892873165, -7.335722546920202092, 61.70329402199800484 ) ) ;
#73793 = CARTESIAN_POINT ( 'NONE',  ( 16.46253265017146816, 9.564922557961045513, 51.66775706135233293 ) ) ;
#73794 = CARTESIAN_POINT ( 'NONE',  ( -0.05219959533934338120, 16.53943276465976808, 112.5010903946857042 ) ) ;
#73795 = CARTESIAN_POINT ( 'NONE',  ( 0.05219959533910956823, 16.53943276465976808, 74.99890960531435269 ) ) ;
#73797 = CARTESIAN_POINT ( 'NONE',  ( -27.73933785331498925, -9.013057229001049109, 144.9750000027312069 ) ) ;
#73796 = CARTESIAN_POINT ( 'NONE',  ( -13.89961937509957401, -13.97604488694547875, 24.37609039468565442 ) ) ;
#73798 = CARTESIAN_POINT ( 'NONE',  ( -21.53943276465977519, 0.05219959533907696930, 111.2489096053143669 ) ) ;
#73799 = CARTESIAN_POINT ( 'NONE',  ( -19.03943276465977164, 0.05219959533909376836, 101.2489096053143669 ) ) ;
#73800 = CARTESIAN_POINT ( 'NONE',  ( 16.51473224551069308, 9.474510206698969483, 74.16557627198103830 ) ) ;
#73801 = CARTESIAN_POINT ( 'NONE',  ( 0.05219959533937995610, -21.53943276465977519, 80.00109039468568994 ) ) ;
#73802 = CARTESIAN_POINT ( 'NONE',  ( -5.153800228976328057, -19.02544592524343514, 57.29057627198103120 ) ) ;
#73803 = ORIENTED_EDGE ( 'NONE', *, *, #164773, .T. ) ;
#73804 = CARTESIAN_POINT ( 'NONE',  ( 16.46253265017160672, -9.564922557960803928, 43.33224293864769550 ) ) ;
#73805 = CARTESIAN_POINT ( 'NONE',  ( -10.72451020669898014, 18.67979575497178502, 25.41557627198103120 ) ) ;
#73806 = CARTESIAN_POINT ( 'NONE',  ( -14.29746914071049879, 8.314922557960819915, 80.83224293864769550 ) ) ;
#73807 = CARTESIAN_POINT ( 'NONE',  ( -16.51473224551069308, -9.474510206698971260, 41.66557627198103120 ) ) ;
#73808 = CARTESIAN_POINT ( 'NONE',  ( -4.483927247898539470, -16.52544592524342804, 102.2905762719810383 ) ) ;
#73809 = CARTESIAN_POINT ( 'NONE',  ( 15.72974639402199770, -15.80617190586745480, 103.1239096053143811 ) ) ;
#73810 = EDGE_CURVE ( 'NONE', #94299, #66950, #118669, .T. ) ;
#73811 = B_SPLINE_CURVE_WITH_KNOTS ( 'NONE', 3,
 ( #141531, #112189, #35347, #140533, #172877, #63701 ),
 .UNSPECIFIED., .F., .F.,
 ( 4, 2, 4 ),
 ( 0.000000000000000000, 0.0003837532665634976444, 0.0007675065331269952888 ),
 .UNSPECIFIED. ) ;
#73812 = CARTESIAN_POINT ( 'NONE',  ( -21.55341960407619339, 5.719274019375674811, 48.54275706135234714 ) ) ;
#73813 = CARTESIAN_POINT ( 'NONE',  ( -13.89961937509977652, 13.97604488694528158, 35.62390960531435269 ) ) ;
#73814 = CARTESIAN_POINT ( 'NONE',  ( 12.06949235617739724, 12.14591786802326823, 61.87609039468568284 ) ) ;
#73815 = CARTESIAN_POINT ( 'NONE',  ( -18.67979575497178146, -10.72451020669898902, 106.6655762719810383 ) ) ;
#73816 = CARTESIAN_POINT ( 'NONE',  ( 15.80617190586746368, 15.72974639402197994, 99.37390960531436690 ) ) ;
#73818 = CARTESIAN_POINT ( 'NONE',  ( -19.05341960407611168, -5.049401038298163336, 46.45724293864768129 ) ) ;
#73817 = CARTESIAN_POINT ( 'NONE',  ( 19.02544592524334988, 5.153800228976608722, 36.45942372801900433 ) ) ;
#73819 = CARTESIAN_POINT ( 'NONE',  ( 19.02544592524343514, -5.153800228976328945, 113.5405762719810241 ) ) ;
#73820 = CARTESIAN_POINT ( 'NONE',  ( -21.52544592524334988, -5.823673210054445271, 58.95942372801902565 ) ) ;
#73821 = CARTESIAN_POINT ( 'NONE',  ( -10.81492255796078084, -18.62759615963271287, 52.08224293864768839 ) ) ;
#73822 = CARTESIAN_POINT ( 'NONE',  ( -8.314922557960811034, -14.29746914071050412, 37.08224293864768129 ) ) ;
#73824 = CARTESIAN_POINT ( 'NONE',  ( 15.72974639402176855, 15.80617190586768217, 111.8760903946856615 ) ) ;
#73823 = CARTESIAN_POINT ( 'NONE',  ( -21.53943276465977519, -0.05219959533937600094, 73.75109039468567573 ) ) ;
#73825 = CARTESIAN_POINT ( 'NONE',  ( -16.51473224551082808, 9.474510206698731452, 48.33442372801900433 ) ) ;
#73826 = CARTESIAN_POINT ( 'NONE',  ( -12.14591786802326823, 12.06949235617739902, 98.12609039468570415 ) ) ;
#73827 = CARTESIAN_POINT ( 'NONE',  ( -18.67979575497193778, 10.72451020669871902, 53.33442372801901854 ) ) ;
#73828 = CARTESIAN_POINT ( 'NONE',  ( -5.049401038298153566, 19.05341960407611168, 55.20724293864769550 ) ) ;
#73829 = CARTESIAN_POINT ( 'NONE',  ( -13.97604488694547697, 13.89961937509957934, 28.12609039468565797 ) ) ;
#73830 = CARTESIAN_POINT ( 'NONE',  ( -15.72974639402197994, 15.80617190586746368, 35.62390960531437401 ) ) ;
#73831 = CARTESIAN_POINT ( 'NONE',  ( 18.67979575497194134, -10.72451020669871369, 35.83442372801901143 ) ) ;
#73832 = CARTESIAN_POINT ( 'NONE',  ( 5.719274019375991003, -21.55341960407610458, 92.70724293864770971 ) ) ;
#73833 = CARTESIAN_POINT ( 'NONE',  ( -9.474510206698720793, -16.51473224551083518, 84.58442372801900433 ) ) ;
#73834 = CARTESIAN_POINT ( 'NONE',  ( -8.224510206698735004, -14.34966873604973081, 59.58442372801901854 ) ) ;
#73836 = CARTESIAN_POINT ( 'NONE',  ( -10.81492255796078084, -18.62759615963271287, 87.08224293864769550 ) ) ;
#73835 = CARTESIAN_POINT ( 'NONE',  ( -6.824288631998610022, 4.978841623633250890, -62.04929096494494445 ) ) ;
#73838 = CARTESIAN_POINT ( 'NONE',  ( -16.53943276465976808, 0.05219959533911058130, 81.24890960531436690 ) ) ;
#73837 = CARTESIAN_POINT ( 'NONE',  ( -12.14591786802326823, 12.06949235617739902, 78.12609039468570415 ) ) ;
#73839 = CARTESIAN_POINT ( 'NONE',  ( -16.79531203550646978, -7.028104445595615424, 101.2524498822044450 ) ) ;
#73840 = CARTESIAN_POINT ( 'NONE',  ( -13.97604488694547697, 13.89961937509957934, 103.1260903946856473 ) ) ;
#73841 = CARTESIAN_POINT ( 'NONE',  ( 5.823673210054125526, 21.52544592524343514, 29.79057627198102409 ) ) ;
#73842 = DIRECTION ( 'NONE',  ( 0.000000000000000000, 0.000000000000000000, -1.000000000000000000 ) ) ;
#73843 = CARTESIAN_POINT ( 'NONE',  ( 4.483927247898790824, -16.52544592524335698, 50.20942372801901854 ) ) ;
#73844 = CARTESIAN_POINT ( 'NONE',  ( -10.72451020669870658, -18.67979575497194134, 24.58442372801901499 ) ) ;
#73845 = CARTESIAN_POINT ( 'NONE',  ( -10.81492255796078084, -18.62759615963271287, 47.08224293864770260 ) ) ;
#73846 = CARTESIAN_POINT ( 'NONE',  ( 16.52544592524335698, 4.483927247898782831, 66.45942372801903275 ) ) ;
#73847 = CARTESIAN_POINT ( 'NONE',  ( 16.51473224551069308, 9.474510206698969483, 79.16557627198103830 ) ) ;
#73849 = CARTESIAN_POINT ( 'NONE',  ( -9.474510206698964154, 16.51473224551069663, 30.41557627198102054 ) ) ;
#73848 = CARTESIAN_POINT ( 'NONE',  ( -21.53943276465977519, -0.05219959533937600094, 58.75109039468568994 ) ) ;
#73850 = EDGE_CURVE ( 'NONE', #33153, #42657, #12454, .T. ) ;
#73851 = CARTESIAN_POINT ( 'NONE',  ( 21.52544592524344225, -5.823673210054117533, 28.54057627198103120 ) ) ;
#73852 = ORIENTED_EDGE ( 'NONE', *, *, #119482, .T. ) ;
#73853 = CARTESIAN_POINT ( 'NONE',  ( -13.97604488694547697, 13.89961937509957934, 38.12609039468566152 ) ) ;
#73854 = CARTESIAN_POINT ( 'NONE',  ( -8.314922557961024197, 14.29746914071037800, 57.91775706135234714 ) ) ;
#73855 = CARTESIAN_POINT ( 'NONE',  ( -15.80617190586745835, -15.72974639402198527, 21.87390960531436690 ) ) ;
#73856 = ORIENTED_EDGE ( 'NONE', *, *, #160998, .T. ) ;
#73857 = CARTESIAN_POINT ( 'NONE',  ( -9.564922557960796823, -16.46253265017161027, 77.08224293864769550 ) ) ;
#73858 = CARTESIAN_POINT ( 'NONE',  ( -16.55341960407617563, 4.379528057220093196, 103.5427570613523613 ) ) ;
#73859 = CARTESIAN_POINT ( 'NONE',  ( 28.79475375365586132, 2.781246896534039337E-14, 141.2656553485623760 ) ) ;
#73860 = CARTESIAN_POINT ( 'NONE',  ( 8.224510206698953496, -14.34966873604960469, 97.91557627198103830 ) ) ;
#73861 = CARTESIAN_POINT ( 'NONE',  ( -18.62759615963270932, 10.81492255796079327, 40.83224293864769550 ) ) ;
#73862 = CARTESIAN_POINT ( 'NONE',  ( 13.89961937509977652, -13.97604488694527269, 38.12390960531436690 ) ) ;
#73863 = CARTESIAN_POINT ( 'NONE',  ( -14.29746914071037622, -8.314922557961029526, 74.16775706135231871 ) ) ;
#73864 = CARTESIAN_POINT ( 'NONE',  ( 15.80617190586769283, -15.72974639402175789, 20.62609039468568639 ) ) ;
#73865 = CARTESIAN_POINT ( 'NONE',  ( -19.03943276465977164, -0.05219959533935918106, 78.75109039468567573 ) ) ;
#73866 = CARTESIAN_POINT ( 'NONE',  ( 5.049401038298161559, -19.05341960407611168, 37.70724293864768839 ) ) ;
#73867 = CARTESIAN_POINT ( 'NONE',  ( -19.03943276465977164, 0.05219959533909376836, 111.2489096053143669 ) ) ;
#73868 = CARTESIAN_POINT ( 'NONE',  ( 21.53943276465977519, 0.05219959533937863772, 86.25109039468568994 ) ) ;
#73869 = CARTESIAN_POINT ( 'NONE',  ( 19.03943276465977164, -0.05219959533909143690, 58.74890960531435979 ) ) ;
#73870 = CARTESIAN_POINT ( 'NONE',  ( 12.14591786802327356, -12.06949235617739191, 50.62609039468568994 ) ) ;
#73871 = CARTESIAN_POINT ( 'NONE',  ( 15.72974639402176855, 15.80617190586768217, 76.87609039468567573 ) ) ;
#73872 = CARTESIAN_POINT ( 'NONE',  ( -16.46253265017146816, -9.564922557961047289, 44.16775706135232582 ) ) ;
#73873 = CARTESIAN_POINT ( 'NONE',  ( -19.02544592524334988, -5.153800228976617603, 53.95942372801898301 ) ) ;
#73874 = ORIENTED_EDGE ( 'NONE', *, *, #57511, .T. ) ;
#73875 = CARTESIAN_POINT ( 'NONE',  ( 21.53943276465977519, 0.05219959533937863772, 56.25109039468568284 ) ) ;
#73876 = CARTESIAN_POINT ( 'NONE',  ( 19.03943276465977164, -0.05219959533909143690, 23.74890960531435269 ) ) ;
#73877 = CARTESIAN_POINT ( 'NONE',  ( 16.46253265017146816, 9.564922557961045513, 41.66775706135234003 ) ) ;
#73878 = CARTESIAN_POINT ( 'NONE',  ( 13.97604488694527802, 13.89961937509977652, 104.3739096053143385 ) ) ;
#73879 = CARTESIAN_POINT ( 'NONE',  ( 19.02544592524343514, -5.153800228976328945, 83.54057627198100988 ) ) ;
#73880 = CARTESIAN_POINT ( 'NONE',  ( 0.05219959533910956823, 16.53943276465976808, 39.99890960531436690 ) ) ;
#73881 = CARTESIAN_POINT ( 'NONE',  ( 5.719274019375991003, -21.55341960407610458, 37.70724293864769550 ) ) ;
#73882 = CARTESIAN_POINT ( 'NONE',  ( -29.86685920354755552, 21.69954338932564397, -5.324999997268814234 ) ) ;
#73883 = CARTESIAN_POINT ( 'NONE',  ( -38.00000000000000711, 2.893978650043524126E-14, -25.00000000000000000 ) ) ;
#73884 = CARTESIAN_POINT ( 'NONE',  ( 21.55341960407619695, -5.719274019375665929, 96.04275706135236135 ) ) ;
#73885 = CARTESIAN_POINT ( 'NONE',  ( -27.88129983271662837, 6.733757357602863536, 162.1517353552117982 ) ) ;
#73886 = CARTESIAN_POINT ( 'NONE',  ( 9.564922557960805705, 16.46253265017160317, 39.58224293864768839 ) ) ;
#73887 = CARTESIAN_POINT ( 'NONE',  ( 9.474510206698971260, -16.51473224551069308, 107.9155762719810383 ) ) ;
#73888 = CARTESIAN_POINT ( 'NONE',  ( -32.52061478538139028, -19.14287791848993336, -8.000000000000003553 ) ) ;
#73889 = CARTESIAN_POINT ( 'NONE',  ( 4.379528057220092307, 16.55341960407617563, 57.29275706135234714 ) ) ;
#73890 = CARTESIAN_POINT ( 'NONE',  ( 5.719274019375991003, -21.55341960407610458, 77.70724293864770971 ) ) ;
#73891 = CARTESIAN_POINT ( 'NONE',  ( -16.53943276465976808, 0.05219959533911058130, 41.24890960531435269 ) ) ;
#73893 = CARTESIAN_POINT ( 'NONE',  ( 5.049401038298161559, -19.05341960407611168, 112.7072429386476813 ) ) ;
#73892 = CARTESIAN_POINT ( 'NONE',  ( 13.89961937509977652, -13.97604488694527269, 33.12390960531434558 ) ) ;
#73894 = CARTESIAN_POINT ( 'NONE',  ( 0.05219959533937995610, -21.53943276465977519, 30.00109039468568284 ) ) ;
#73895 = CARTESIAN_POINT ( 'NONE',  ( -13.97604488694547697, 13.89961937509957934, 33.12609039468566863 ) ) ;
#73896 = CARTESIAN_POINT ( 'NONE',  ( 13.97604488694527802, 13.89961937509977652, 39.37390960531435269 ) ) ;
#73897 = CARTESIAN_POINT ( 'NONE',  ( -18.62759615963255300, -10.81492255796106328, 84.16775706135234714 ) ) ;
#73898 = DIRECTION ( 'NONE',  ( -0.000000000000000000, -0.000000000000000000, 1.000000000000000000 ) ) ;
#73899 = CARTESIAN_POINT ( 'NONE',  ( 12.14591786802309770, 12.06949235617756955, 24.37390960531435979 ) ) ;
#73900 = CARTESIAN_POINT ( 'NONE',  ( 11.40812507854754365, 35.11059874428196537, -3.724999997268813701 ) ) ;
#73901 = CARTESIAN_POINT ( 'NONE',  ( 15.72974639402199770, -15.80617190586745480, 23.12390960531436335 ) ) ;
#73902 = CARTESIAN_POINT ( 'NONE',  ( -14.29746914071049879, 8.314922557960819915, 105.8322429386476955 ) ) ;
#73903 = CARTESIAN_POINT ( 'NONE',  ( 9.979912183652610125, -44.24332767168409930, -21.75883150241362429 ) ) ;
#73904 = CARTESIAN_POINT ( 'NONE',  ( -16.46253265017160317, 9.564922557960807481, 85.83224293864769550 ) ) ;
#73905 = CARTESIAN_POINT ( 'NONE',  ( -4.483927247898539470, -16.52544592524342804, 72.29057627198102409 ) ) ;
#73906 = CARTESIAN_POINT ( 'NONE',  ( 13.97604488694548053, -13.89961937509957401, 100.6260903946856615 ) ) ;
#73907 = CARTESIAN_POINT ( 'NONE',  ( -5.823673210054116645, -21.52544592524344225, 67.29057627198103830 ) ) ;
#73908 = ORIENTED_EDGE ( 'NONE', *, *, #588, .T. ) ;
#73909 = CARTESIAN_POINT ( 'NONE',  ( -19.05341960407611168, -5.049401038298163336, 36.45724293864766707 ) ) ;
#73911 = CARTESIAN_POINT ( 'NONE',  ( -5.823673210054116645, -21.52544592524344225, 87.29057627198103830 ) ) ;
#73910 = CARTESIAN_POINT ( 'NONE',  ( 16.46253265017160672, -9.564922557960803928, 88.33224293864769550 ) ) ;
#73913 = CARTESIAN_POINT ( 'NONE',  ( 19.05341960407611168, 5.049401038298154454, 83.95724293864766707 ) ) ;
#73912 = CARTESIAN_POINT ( 'NONE',  ( -14.29746914071037622, -8.314922557961029526, 99.16775706135234714 ) ) ;
#73914 = CARTESIAN_POINT ( 'NONE',  ( -16.51473224551082808, 9.474510206698731452, 68.33442372801900433 ) ) ;
#73915 = CARTESIAN_POINT ( 'NONE',  ( 18.62759615963255655, 10.81492255796105972, 101.6677570613523613 ) ) ;
#73916 = CARTESIAN_POINT ( 'NONE',  ( 18.62759615963271287, -10.81492255796078972, 78.33224293864770971 ) ) ;
#73917 = CARTESIAN_POINT ( 'NONE',  ( -10.72451020669898014, 18.67979575497178502, 35.41557627198102409 ) ) ;
#73918 = CARTESIAN_POINT ( 'NONE',  ( 16.46253265017160672, -9.564922557960803928, 48.33224293864769550 ) ) ;
#73919 = CARTESIAN_POINT ( 'NONE',  ( -16.53943276465976808, 0.05219959533911058130, 26.24890960531435624 ) ) ;
#73920 = CARTESIAN_POINT ( 'NONE',  ( -9.564922557960796823, -16.46253265017161027, 62.08224293864769550 ) ) ;
#73921 = DIRECTION ( 'NONE',  ( -0.000000000000000000, -0.000000000000000000, 1.000000000000000000 ) ) ;
#73922 = CARTESIAN_POINT ( 'NONE',  ( 0.05219959533936267826, -19.03943276465977164, 20.00109039468567218 ) ) ;
#73923 = CARTESIAN_POINT ( 'NONE',  ( -16.52544592524342804, 4.483927247898546575, 76.04057627198102409 ) ) ;
#73924 =( BOUNDED_CURVE ( )  B_SPLINE_CURVE ( 3, ( #22425, #84075, #5238, #7236 ),
 .UNSPECIFIED., .F., .F. ) 
 B_SPLINE_CURVE_WITH_KNOTS ( ( 4, 4 ),
 ( 5.150538010968860547, 5.257537365396776075 ),
 .UNSPECIFIED. ) 
 CURVE ( )  GEOMETRIC_REPRESENTATION_ITEM ( )  RATIONAL_B_SPLINE_CURVE ( ( 1.000000000000000000, 0.9990461557208837329, 0.9990461557208837329, 1.000000000000000000 ) ) 
 REPRESENTATION_ITEM ( '' )  );
#73925 = CARTESIAN_POINT ( 'NONE',  ( -18.62759615963270932, 10.81492255796079327, 110.8322429386476955 ) ) ;
#73926 = CARTESIAN_POINT ( 'NONE',  ( 18.62759615963271287, -10.81492255796078972, 108.3322429386477097 ) ) ;
#73927 = CARTESIAN_POINT ( 'NONE',  ( -5.183909576824695442, 3.882848763669461967, -64.47227361656568689 ) ) ;
#73928 = CARTESIAN_POINT ( 'NONE',  ( -5.719274019375978568, 21.55341960407610458, 65.20724293864768129 ) ) ;
#73929 = CARTESIAN_POINT ( 'NONE',  ( -4.379528057220086978, -16.55341960407618274, 99.79275706135234714 ) ) ;
#73930 = CARTESIAN_POINT ( 'NONE',  ( 16.52544592524342804, -4.483927247898539470, 103.5405762719810383 ) ) ;
#73931 = CARTESIAN_POINT ( 'NONE',  ( -19.02544592524342804, 5.153800228976336051, 66.04057627198103830 ) ) ;
#73932 = SHAPE_REPRESENTATION_RELATIONSHIP ( 'NONE' , 'NONE' ,  #8335, #117169 ) ;
#73933 = CARTESIAN_POINT ( 'NONE',  ( -14.29746914071037622, -8.314922557961029526, 109.1677570613523613 ) ) ;
#73934 = CARTESIAN_POINT ( 'NONE',  ( -5.823673210054431948, 21.52544592524334988, 52.70942372801902565 ) ) ;
#73935 = CARTESIAN_POINT ( 'NONE',  ( 13.97604488694527802, 13.89961937509977652, 104.3739096053143385 ) ) ;
#73936 = CARTESIAN_POINT ( 'NONE',  ( 10.72451020669871369, 18.67979575497193778, 82.08442372801901854 ) ) ;
#73937 = CARTESIAN_POINT ( 'NONE',  ( -13.89961937509977652, 13.97604488694528158, 25.62390960531434558 ) ) ;
#73938 = CARTESIAN_POINT ( 'NONE',  ( -19.02544592524342804, 5.153800228976336051, 41.04057627198103120 ) ) ;
#73939 = VERTEX_POINT ( 'NONE', #166127 ) ;
#73940 = CARTESIAN_POINT ( 'NONE',  ( -15.72974639402176322, -15.80617190586768395, 84.37609039468570415 ) ) ;
#73941 = CARTESIAN_POINT ( 'NONE',  ( 10.72451020669871369, 18.67979575497193778, 67.08442372801901854 ) ) ;
#73942 = CARTESIAN_POINT ( 'NONE',  ( 9.564922557960805705, 16.46253265017160317, 109.5822429386476955 ) ) ;
#73943 = CARTESIAN_POINT ( 'NONE',  ( 13.89961937509957401, 13.97604488694547697, 81.87609039468564731 ) ) ;
#73944 = CARTESIAN_POINT ( 'NONE',  ( 21.53943276465977519, 0.05219959533937863772, 51.25109039468568994 ) ) ;
#73945 = CARTESIAN_POINT ( 'NONE',  ( -4.379528057220086978, -16.55341960407618274, 24.79275706135235779 ) ) ;
#73946 = CARTESIAN_POINT ( 'NONE',  ( 13.89961937509957401, 13.97604488694547697, 76.87609039468566152 ) ) ;
#73947 = CARTESIAN_POINT ( 'NONE',  ( 5.153800228976335163, 19.02544592524342804, 49.79057627198100988 ) ) ;
#73948 = CARTESIAN_POINT ( 'NONE',  ( -5.153800228976607833, 19.02544592524334988, 77.70942372801900433 ) ) ;
#73950 = MANIFOLD_SOLID_BREP ( 'Cavity1', #117602 ) ;
#73949 = CARTESIAN_POINT ( 'NONE',  ( 12.06949235617739724, 12.14591786802326823, 111.8760903946856615 ) ) ;
#73951 = CARTESIAN_POINT ( 'NONE',  ( -13.97604488694547697, 13.89961937509957934, 88.12609039468563310 ) ) ;
#73952 = CARTESIAN_POINT ( 'NONE',  ( -4.379528057220328563, 16.55341960407611168, 40.20724293864769550 ) ) ;
#73953 = CARTESIAN_POINT ( 'NONE',  ( -9.474510206698720793, -16.51473224551083518, 69.58442372801901854 ) ) ;
#73954 = CARTESIAN_POINT ( 'NONE',  ( -16.55341960407617563, 4.379528057220093196, 43.54275706135235424 ) ) ;
#73955 = CARTESIAN_POINT ( 'NONE',  ( -0.05219959533936034679, 19.03943276465977164, 22.50109039468566152 ) ) ;
#73956 = CARTESIAN_POINT ( 'NONE',  ( -13.97604488694527625, -13.89961937509977652, 36.87390960531436690 ) ) ;
#73957 = CARTESIAN_POINT ( 'NONE',  ( -17.49999999999999645, -5.499999999999992895, 64.20309617465829888 ) ) ;
#73958 = CARTESIAN_POINT ( 'NONE',  ( 0.05219959533934541429, -16.53943276465976808, 40.00109039468567573 ) ) ;
#73959 = CYLINDRICAL_SURFACE ( 'NONE', #30560, 28.79475375365586487 ) ;
#73960 = CARTESIAN_POINT ( 'NONE',  ( 17.14385361876520264, -23.59649016807271238, 145.5750000027312012 ) ) ;
#73961 = CARTESIAN_POINT ( 'NONE',  ( -19.02544592524342804, 5.153800228976336051, 96.04057627198103830 ) ) ;
#73962 = CARTESIAN_POINT ( 'NONE',  ( 16.51473224551083163, -9.474510206698727899, 85.83442372801900433 ) ) ;
#73963 = ORIENTED_EDGE ( 'NONE', *, *, #44832, .F. ) ;
#73964 = CARTESIAN_POINT ( 'NONE',  ( 19.02544592524334988, 5.153800228976608722, 101.4594237280189759 ) ) ;
#73965 = CARTESIAN_POINT ( 'NONE',  ( 18.67979575497178502, 10.72451020669898547, 24.16557627198103120 ) ) ;
#73967 = CARTESIAN_POINT ( 'NONE',  ( -19.03943276465977164, -0.05219959533935918106, 108.7510903946856615 ) ) ;
#73966 = CARTESIAN_POINT ( 'NONE',  ( -15.80617190586768217, 15.72974639402176855, 113.1260903946856899 ) ) ;
#73968 = CARTESIAN_POINT ( 'NONE',  ( -12.14591786802309592, -12.06949235617757132, 111.8739096053143669 ) ) ;
#73969 = CARTESIAN_POINT ( 'NONE',  ( -16.46253265017160317, 9.564922557960807481, 30.83224293864769550 ) ) ;
#73970 = CARTESIAN_POINT ( 'NONE',  ( 5.719274019375991003, -21.55341960407610458, 62.70724293864769550 ) ) ;
#73971 = CARTESIAN_POINT ( 'NONE',  ( -13.97604488694527625, -13.89961937509977652, 36.87390960531436690 ) ) ;
#73972 = DIRECTION ( 'NONE',  ( 1.000000000000000000, -4.336808689942018352E-17, 0.000000000000000000 ) ) ;
#73973 = CARTESIAN_POINT ( 'NONE',  ( 13.89961937509957401, 13.97604488694547697, 76.87609039468566152 ) ) ;
#73974 = CARTESIAN_POINT ( 'NONE',  ( -8.314922557960811034, -14.29746914071050412, 47.08224293864770260 ) ) ;
#73975 = CARTESIAN_POINT ( 'NONE',  ( 21.55341960407610458, 5.719274019375980345, 28.95724293864769905 ) ) ;
#73976 = CARTESIAN_POINT ( 'NONE',  ( -21.52544592524334988, -5.823673210054445271, 93.95942372801903275 ) ) ;
#73977 = CARTESIAN_POINT ( 'NONE',  ( -18.62759615963270932, 10.81492255796079327, 90.83224293864769550 ) ) ;
#73978 = CARTESIAN_POINT ( 'NONE',  ( -21.53943276465977519, -0.05219959533937600094, 63.75109039468568284 ) ) ;
#73979 = CARTESIAN_POINT ( 'NONE',  ( 15.72974639402176855, 15.80617190586768217, 66.87609039468568994 ) ) ;
#73980 = CARTESIAN_POINT ( 'NONE',  ( 9.564922557960805705, 16.46253265017160317, 99.58224293864770971 ) ) ;
#73982 = CARTESIAN_POINT ( 'NONE',  ( -5.823673210054431948, 21.52544592524334988, 62.70942372801902565 ) ) ;
#73981 = CARTESIAN_POINT ( 'NONE',  ( -0.05219959533934338120, 16.53943276465976808, 97.50109039468567573 ) ) ;
#73983 = CARTESIAN_POINT ( 'NONE',  ( 16.51473224551069308, 9.474510206698969483, 54.16557627198103120 ) ) ;
#73984 = CARTESIAN_POINT ( 'NONE',  ( -0.05219959533909027116, -19.03943276465977164, 22.49890960531436690 ) ) ;
#73985 = CARTESIAN_POINT ( 'NONE',  ( -9.474510206698964154, 16.51473224551069663, 55.41557627198103120 ) ) ;
#73986 = CARTESIAN_POINT ( 'NONE',  ( 16.55341960407611168, 4.379528057220329451, 63.95724293864770260 ) ) ;
#73987 = CARTESIAN_POINT ( 'NONE',  ( -8.314922557960811034, -14.29746914071050412, 37.08224293864768129 ) ) ;
#73988 = CARTESIAN_POINT ( 'NONE',  ( -15.72974639402197994, 15.80617190586746368, 40.62390960531435269 ) ) ;
#73989 = CARTESIAN_POINT ( 'NONE',  ( -19.05341960407611168, -5.049401038298163336, 46.45724293864768129 ) ) ;
#73990 = CARTESIAN_POINT ( 'NONE',  ( 5.823673210054125526, 21.52544592524343514, 59.79057627198103120 ) ) ;
#73991 = CARTESIAN_POINT ( 'NONE',  ( 19.05341960407617918, -5.049401038297876454, 51.04275706135231871 ) ) ;
#73993 = CARTESIAN_POINT ( 'NONE',  ( 12.06949235617757843, -12.14591786802309237, 48.12390960531436690 ) ) ;
#73992 = DIRECTION ( 'NONE',  ( 0.000000000000000000, 0.000000000000000000, -1.000000000000000000 ) ) ;
#73994 = CARTESIAN_POINT ( 'NONE',  ( 21.53943276465977519, -0.05219959533907433946, 23.74890960531435269 ) ) ;
#73995 = EDGE_LOOP ( 'NONE', ( #46826, #144997, #194438, #189 ) ) ;
#73996 = CARTESIAN_POINT ( 'NONE',  ( 16.38665767535054130, 7.295008042176128527, 102.2359913578545303 ) ) ;
#73997 = CARTESIAN_POINT ( 'NONE',  ( -12.14591786802326823, 12.06949235617739902, 83.12609039468568994 ) ) ;
#73998 = CARTESIAN_POINT ( 'NONE',  ( 5.153800228976615827, -19.02544592524334988, 70.20942372801899012 ) ) ;
#73999 = CARTESIAN_POINT ( 'NONE',  ( 0.05219959533910956823, 16.53943276465976808, 59.99890960531436690 ) ) ;
#74000 = DIRECTION ( 'NONE',  ( -8.551662891793917213E-31, 1.000000000000000000, 1.224646799147353207E-16 ) ) ;
#74001 = CARTESIAN_POINT ( 'NONE',  ( 12.14591786802309770, 12.06949235617756955, 34.37390960531435979 ) ) ;
#74002 = CARTESIAN_POINT ( 'NONE',  ( -9.474510206698964154, 16.51473224551069663, 55.41557627198103120 ) ) ;
#74003 = CARTESIAN_POINT ( 'NONE',  ( -9.564922557960796823, -16.46253265017161027, 77.08224293864769550 ) ) ;
#74004 = CARTESIAN_POINT ( 'NONE',  ( -9.474510206698964154, 16.51473224551069663, 35.41557627198102409 ) ) ;
#74005 = CARTESIAN_POINT ( 'NONE',  ( -5.719274019375665041, -21.55341960407619695, 39.79275706135235424 ) ) ;
#74006 = CARTESIAN_POINT ( 'NONE',  ( -5.153800228976328057, -19.02544592524343514, 72.29057627198102409 ) ) ;
#74007 = CARTESIAN_POINT ( 'NONE',  ( 19.02544592524343514, -5.153800228976328945, 58.54057627198102409 ) ) ;
#74008 = CARTESIAN_POINT ( 'NONE',  ( -10.72451020669898014, 18.67979575497178502, 30.41557627198101699 ) ) ;
#74009 = VECTOR ( 'NONE', #2215, 1000.000000000000000 ) ;
#74010 = CARTESIAN_POINT ( 'NONE',  ( -0.05219959533909027116, -19.03943276465977164, 37.49890960531436690 ) ) ;
#74011 = CARTESIAN_POINT ( 'NONE',  ( 5.823673210054125526, 21.52544592524343514, 44.79057627198103120 ) ) ;
#74012 = CARTESIAN_POINT ( 'NONE',  ( -0.05219959533934338120, 16.53943276465976808, 92.50109039468567573 ) ) ;
#74013 = CARTESIAN_POINT ( 'NONE',  ( 13.89961937509957401, 13.97604488694547697, 21.87609039468566152 ) ) ;
#74015 = CARTESIAN_POINT ( 'NONE',  ( 14.29746914071037800, 8.314922557961029526, 76.66775706135234714 ) ) ;
#74014 = CARTESIAN_POINT ( 'NONE',  ( 16.53943276465976808, 0.05219959533934440121, 51.25109039468568994 ) ) ;
#74016 = DIRECTION ( 'NONE',  ( -0.000000000000000000, -0.000000000000000000, 1.000000000000000000 ) ) ;
#74017 = CARTESIAN_POINT ( 'NONE',  ( 8.224510206698742110, 14.34966873604972548, 62.08442372801901143 ) ) ;
#74018 = CARTESIAN_POINT ( 'NONE',  ( -16.53943276465976808, -0.05219959533934237506, 43.75109039468568284 ) ) ;
#74019 = CARTESIAN_POINT ( 'NONE',  ( 16.51473224551069308, 9.474510206698969483, 114.1655762719810241 ) ) ;
#74020 = CARTESIAN_POINT ( 'NONE',  ( -12.06949235617739369, -12.14591786802326823, 24.37609039468567573 ) ) ;
#74021 = CARTESIAN_POINT ( 'NONE',  ( 9.474510206698971260, -16.51473224551069308, 37.91557627198102409 ) ) ;
#74022 = CARTESIAN_POINT ( 'NONE',  ( 15.80617190586769283, -15.72974639402175789, 25.62609039468567929 ) ) ;
#74023 = CARTESIAN_POINT ( 'NONE',  ( -0.05219959533934338120, 16.53943276465976808, 37.50109039468568284 ) ) ;
#74024 = CARTESIAN_POINT ( 'NONE',  ( -8.224510206698735004, -14.34966873604973081, 94.58442372801901854 ) ) ;
#74025 = CARTESIAN_POINT ( 'NONE',  ( -3.573655867282028392E-15, 2.428612866367529932E-14, 149.6527036446661327 ) ) ;
#74026 = CARTESIAN_POINT ( 'NONE',  ( 10.72451020669871369, 18.67979575497193778, 102.0844237280190185 ) ) ;
#74027 = CARTESIAN_POINT ( 'NONE',  ( -9.564922557961040184, 16.46253265017147172, 92.91775706135233293 ) ) ;
#74028 = CARTESIAN_POINT ( 'NONE',  ( 0.05219959533910956823, 16.53943276465976808, 59.99890960531436690 ) ) ;
#74029 = CARTESIAN_POINT ( 'NONE',  ( -16.52544592524342804, 4.483927247898546575, 116.0405762719810383 ) ) ;
#74031 = CARTESIAN_POINT ( 'NONE',  ( 16.21995358207306026, 7.366697692864119240, 77.56448998487844904 ) ) ;
#74030 = CARTESIAN_POINT ( 'NONE',  ( -9.474510206698720793, -16.51473224551083518, 59.58442372801900433 ) ) ;
#74032 = CARTESIAN_POINT ( 'NONE',  ( -5.719274019375665041, -21.55341960407619695, 54.79275706135235424 ) ) ;
#74033 = CARTESIAN_POINT ( 'NONE',  ( 16.55341960407618274, -4.379528057220086978, 31.04275706135234714 ) ) ;
#74034 = DIRECTION ( 'NONE',  ( 0.000000000000000000, 0.000000000000000000, -1.000000000000000000 ) ) ;
#74035 = CARTESIAN_POINT ( 'NONE',  ( -19.02544592524342804, 5.153800228976336051, 116.0405762719810383 ) ) ;
#74036 = CARTESIAN_POINT ( 'NONE',  ( -0.05219959533907301413, -21.53943276465977519, 72.49890960531435269 ) ) ;
#74037 = CARTESIAN_POINT ( 'NONE',  ( 19.03943276465977164, 0.05219959533936151252, 106.2510903946856615 ) ) ;
#74038 = CARTESIAN_POINT ( 'NONE',  ( -16.46253265017160317, 9.564922557960807481, 100.8322429386477097 ) ) ;
#74039 = CARTESIAN_POINT ( 'NONE',  ( -9.708182408413708941, -26.42831169063299157, 139.9999999999999716 ) ) ;
#74040 = CARTESIAN_POINT ( 'NONE',  ( 19.02544592524343514, -5.153800228976328945, 23.54057627198102054 ) ) ;
#74041 = CARTESIAN_POINT ( 'NONE',  ( -18.62759615963255300, -10.81492255796106328, 89.16775706135236135 ) ) ;
#74042 = CARTESIAN_POINT ( 'NONE',  ( -9.564922557960796823, -16.46253265017161027, 42.08224293864769550 ) ) ;
#74043 = CARTESIAN_POINT ( 'NONE',  ( -21.55341960407619339, 5.719274019375674811, 53.54275706135234714 ) ) ;
#74044 = CARTESIAN_POINT ( 'NONE',  ( -18.62759615963255300, -10.81492255796106328, 94.16775706135237556 ) ) ;
#74045 = CARTESIAN_POINT ( 'NONE',  ( 14.29746914071037800, 8.314922557961029526, 101.6677570613523613 ) ) ;
#74046 = CARTESIAN_POINT ( 'NONE',  ( -5.153800228976328057, -19.02544592524343514, 82.29057627198103830 ) ) ;
#74047 = CARTESIAN_POINT ( 'NONE',  ( -0.05219959533937732626, 21.53943276465977519, 42.50109039468567573 ) ) ;
#74048 = CARTESIAN_POINT ( 'NONE',  ( -21.55341960407619339, 5.719274019375674811, 38.54275706135234714 ) ) ;
#74050 = CARTESIAN_POINT ( 'NONE',  ( -9.474510206698964154, 16.51473224551069663, 90.41557627198103830 ) ) ;
#74049 = CARTESIAN_POINT ( 'NONE',  ( 9.474510206698729675, 16.51473224551082808, 77.08442372801900433 ) ) ;
#74051 = CARTESIAN_POINT ( 'NONE',  ( -8.314922557960811034, -14.29746914071050412, 107.0822429386476955 ) ) ;
#74052 = CARTESIAN_POINT ( 'NONE',  ( -18.62759615963270932, 10.81492255796079327, 95.83224293864770971 ) ) ;
#74053 = CARTESIAN_POINT ( 'NONE',  ( -16.53943276465976808, 0.05219959533911058130, 81.24890960531436690 ) ) ;
#74054 = CARTESIAN_POINT ( 'NONE',  ( 13.89961937509957401, 13.97604488694547697, 21.87609039468566152 ) ) ;
#74055 = CARTESIAN_POINT ( 'NONE',  ( -4.483927247898539470, -16.52544592524342804, 97.29057627198105251 ) ) ;
#74056 = CARTESIAN_POINT ( 'NONE',  ( 16.51473224551069308, 9.474510206698969483, 54.16557627198103120 ) ) ;
#74057 = CARTESIAN_POINT ( 'NONE',  ( -9.564922557961040184, 16.46253265017147172, 87.91775706135233293 ) ) ;
#74058 = CARTESIAN_POINT ( 'NONE',  ( -16.53943276465976808, 0.05219959533911058130, 46.24890960531435979 ) ) ;
#74059 = CARTESIAN_POINT ( 'NONE',  ( -21.55341960407619339, 5.719274019375674811, 113.5427570613523756 ) ) ;
#74060 = CARTESIAN_POINT ( 'NONE',  ( -0.05219959533909027116, -19.03943276465977164, 102.4989096053143669 ) ) ;
#74061 = CARTESIAN_POINT ( 'NONE',  ( 16.51473224551083163, -9.474510206698727899, 75.83442372801900433 ) ) ;
#74062 = CARTESIAN_POINT ( 'NONE',  ( 5.823673210054125526, 21.52544592524343514, 84.79057627198102409 ) ) ;
#74063 = CARTESIAN_POINT ( 'NONE',  ( -18.67979575497193778, 10.72451020669871902, 33.33442372801900433 ) ) ;
#74064 = CARTESIAN_POINT ( 'NONE',  ( 4.379528057220092307, 16.55341960407617563, 32.29275706135235424 ) ) ;
#74065 = CARTESIAN_POINT ( 'NONE',  ( -4.483927247898782831, 16.52544592524335698, 92.70942372801901854 ) ) ;
#74067 = CARTESIAN_POINT ( 'NONE',  ( 15.72974639402176855, 15.80617190586768217, 41.87609039468568284 ) ) ;
#74066 = CARTESIAN_POINT ( 'NONE',  ( 5.049401038298161559, -19.05341960407611168, 22.70724293864769194 ) ) ;
#74068 = CARTESIAN_POINT ( 'NONE',  ( -19.03943276465977164, 0.05219959533909376836, 26.24890960531435624 ) ) ;
#74069 = CARTESIAN_POINT ( 'NONE',  ( -23.48529157249599919, -32.32473071737750558, -9.449999994537623849 ) ) ;
#74070 = CARTESIAN_POINT ( 'NONE',  ( 12.14591786802327356, -12.06949235617739191, 50.62609039468568994 ) ) ;
#74071 = CARTESIAN_POINT ( 'NONE',  ( -16.52544592524342804, 4.483927247898546575, 81.04057627198102409 ) ) ;
#74072 = CARTESIAN_POINT ( 'NONE',  ( 15.80617190586746368, 15.72974639402197994, 74.37390960531436690 ) ) ;
#74073 = CARTESIAN_POINT ( 'NONE',  ( 16.52544592524342804, -4.483927247898539470, 28.54057627198103120 ) ) ;
#74074 = CARTESIAN_POINT ( 'NONE',  ( -16.52544592524335698, -4.483927247898792601, 53.95942372801900433 ) ) ;
#74075 = CARTESIAN_POINT ( 'NONE',  ( -19.02544592524342804, 5.153800228976336051, 46.04057627198101699 ) ) ;
#74076 = CARTESIAN_POINT ( 'NONE',  ( -8.224510206698735004, -14.34966873604973081, 99.58442372801900433 ) ) ;
#74077 = CARTESIAN_POINT ( 'NONE',  ( 5.153800228976615827, -19.02544592524334988, 90.20942372801900433 ) ) ;
#74078 = CARTESIAN_POINT ( 'NONE',  ( -18.67979575497178146, -10.72451020669898902, 81.66557627198103830 ) ) ;
#74079 = CARTESIAN_POINT ( 'NONE',  ( 4.379528057220092307, 16.55341960407617563, 107.2927570613523471 ) ) ;
#74080 = ORIENTED_EDGE ( 'NONE', *, *, #182203, .F. ) ;
#74081 = CARTESIAN_POINT ( 'NONE',  ( 13.89961937509977652, -13.97604488694527269, 113.1239096053143527 ) ) ;
#74082 = ADVANCED_FACE ( 'NONE', ( #187266 ), #183319, .T. ) ;
#74083 = CARTESIAN_POINT ( 'NONE',  ( -18.62759615963270932, 10.81492255796079327, 65.83224293864769550 ) ) ;
#74084 = ORIENTED_EDGE ( 'NONE', *, *, #26286, .T. ) ;
#74085 = CARTESIAN_POINT ( 'NONE',  ( -4.483927247898782831, 16.52544592524335698, 97.70942372801904696 ) ) ;
#74086 = ORIENTED_EDGE ( 'NONE', *, *, #156994, .F. ) ;
#74087 = CARTESIAN_POINT ( 'NONE',  ( -0.05219959533907301413, -21.53943276465977519, 32.49890960531435979 ) ) ;
#74088 = CARTESIAN_POINT ( 'NONE',  ( 17.50000000000003553, 4.049696124445888223, 108.3196032933406201 ) ) ;
#74089 = CARTESIAN_POINT ( 'NONE',  ( -21.52544592524343514, 5.823673210054127303, 81.04057627198102409 ) ) ;
#74090 = CARTESIAN_POINT ( 'NONE',  ( 0.05219959533910956823, 16.53943276465976808, 24.99890960531435624 ) ) ;
#74091 = CARTESIAN_POINT ( 'NONE',  ( 4.379528057220092307, 16.55341960407617563, 22.29275706135235069 ) ) ;
#74092 = CARTESIAN_POINT ( 'NONE',  ( 9.474510206698971260, -16.51473224551069308, 32.91557627198102409 ) ) ;
#74093 = CARTESIAN_POINT ( 'NONE',  ( 16.55341960407618274, -4.379528057220086978, 31.04275706135234714 ) ) ;
#74094 = CARTESIAN_POINT ( 'NONE',  ( -9.564922557960796823, -16.46253265017161027, 47.08224293864769550 ) ) ;
#74095 = CARTESIAN_POINT ( 'NONE',  ( 28.82186960331498327, 2.781578969918950771E-14, 147.0000000000000000 ) ) ;
#74096 = CARTESIAN_POINT ( 'NONE',  ( 0.05219959533909260263, 19.03943276465977164, 109.9989096053143669 ) ) ;
#74097 = CARTESIAN_POINT ( 'NONE',  ( -5.153800228976328057, -19.02544592524343514, 102.2905762719810383 ) ) ;
#74098 = CARTESIAN_POINT ( 'NONE',  ( -16.52544592524335698, -4.483927247898792601, 93.95942372801903275 ) ) ;
#74099 = CARTESIAN_POINT ( 'NONE',  ( 19.02544592524334988, 5.153800228976608722, 86.45942372801900433 ) ) ;
#74100 = CARTESIAN_POINT ( 'NONE',  ( 13.89961937509957401, 13.97604488694547697, 31.87609039468566863 ) ) ;
#74101 = CARTESIAN_POINT ( 'NONE',  ( -0.05219959533907301413, -21.53943276465977519, 77.49890960531433848 ) ) ;
#74102 = CARTESIAN_POINT ( 'NONE',  ( -16.52544592524335698, -4.483927247898792601, 103.9594237280190185 ) ) ;
#74103 = CARTESIAN_POINT ( 'NONE',  ( 5.823673210054125526, 21.52544592524343514, 34.79057627198103120 ) ) ;
#74104 = CARTESIAN_POINT ( 'NONE',  ( 0.05219959533936267826, -19.03943276465977164, 100.0010903946856757 ) ) ;
#74105 = CARTESIAN_POINT ( 'NONE',  ( -13.89961937509977652, 13.97604488694528158, 45.62390960531433848 ) ) ;
#74106 = CARTESIAN_POINT ( 'NONE',  ( -16.51473224551069308, -9.474510206698971260, 86.66557627198102409 ) ) ;
#74107 = CARTESIAN_POINT ( 'NONE',  ( 5.823673210054444382, -21.52544592524334988, 65.20942372801901854 ) ) ;
#74108 = CARTESIAN_POINT ( 'NONE',  ( 0.05219959533909260263, 19.03943276465977164, 54.99890960531435979 ) ) ;
#74109 = CARTESIAN_POINT ( 'NONE',  ( 12.14591786802309770, 12.06949235617756955, 99.37390960531436690 ) ) ;
#74110 = CARTESIAN_POINT ( 'NONE',  ( 23.64729612845458817, -13.72274676820368633, 169.8070494178799663 ) ) ;
#74111 = CARTESIAN_POINT ( 'NONE',  ( 8.314922557960818139, 14.29746914071049879, 84.58224293864769550 ) ) ;
#74112 = CARTESIAN_POINT ( 'NONE',  ( -10.72451020669898014, 18.67979575497178502, 70.41557627198102409 ) ) ;
#74113 = CARTESIAN_POINT ( 'NONE',  ( 19.02544592524334988, 5.153800228976608722, 91.45942372801900433 ) ) ;
#74114 = CARTESIAN_POINT ( 'NONE',  ( 17.26058549869093284, -6.457015423128480869, 81.12254162523936429 ) ) ;
#74115 = CARTESIAN_POINT ( 'NONE',  ( -19.05341960407611168, -5.049401038298163336, 56.45724293864768129 ) ) ;
#74117 = CARTESIAN_POINT ( 'NONE',  ( -16.46253265017160317, 9.564922557960807481, 80.83224293864769550 ) ) ;
#74116 = CARTESIAN_POINT ( 'NONE',  ( 19.02544592524343514, -5.153800228976328945, 78.54057627198099567 ) ) ;
#74118 = CARTESIAN_POINT ( 'NONE',  ( -16.53943276465976808, -0.05219959533934237506, 68.75109039468568994 ) ) ;
#74119 = CARTESIAN_POINT ( 'NONE',  ( -17.05587630539785238, -6.762274262135719027, 49.25819690962688213 ) ) ;
#74120 = CARTESIAN_POINT ( 'NONE',  ( 5.153800228976615827, -19.02544592524334988, 40.20942372801898301 ) ) ;
#74121 = CARTESIAN_POINT ( 'NONE',  ( 36.77100073307799022, 4.779104515855422619, 47.74589100149061949 ) ) ;
#74122 = CARTESIAN_POINT ( 'NONE',  ( -19.03943276465977164, 0.05219959533909376836, 111.2489096053143669 ) ) ;
#74123 = CARTESIAN_POINT ( 'NONE',  ( 4.379528057220092307, 16.55341960407617563, 102.2927570613523613 ) ) ;
#74124 = CARTESIAN_POINT ( 'NONE',  ( -0.5379555815578647149, -24.20415418211123892, -54.28961862586980658 ) ) ;
#74125 = CARTESIAN_POINT ( 'NONE',  ( -16.52544592524335698, -4.483927247898792601, 78.95942372801901854 ) ) ;
#74126 = CARTESIAN_POINT ( 'NONE',  ( 25.25560589046783022, -4.310829775027113620, 167.9999999999999716 ) ) ;
#74127 = CARTESIAN_POINT ( 'NONE',  ( 12.14591786802327356, -12.06949235617739191, 60.62609039468567573 ) ) ;
#74128 = CARTESIAN_POINT ( 'NONE',  ( -18.22780087662123805, 5.499999999999981348, 76.01763182126894947 ) ) ;
#74129 = CARTESIAN_POINT ( 'NONE',  ( 18.62759615963255655, 10.81492255796105972, 71.66775706135234714 ) ) ;
#74130 = CARTESIAN_POINT ( 'NONE',  ( 13.97604488694548053, -13.89961937509957401, 70.62609039468567573 ) ) ;
#74131 = CARTESIAN_POINT ( 'NONE',  ( -9.564922557961040184, 16.46253265017147172, 22.91775706135233648 ) ) ;
#74132 = CARTESIAN_POINT ( 'NONE',  ( 16.51473224551069308, 9.474510206698969483, 49.16557627198102409 ) ) ;
#74133 = CARTESIAN_POINT ( 'NONE',  ( -13.89961937509977652, 13.97604488694528158, 40.62390960531435979 ) ) ;
#74134 = CARTESIAN_POINT ( 'NONE',  ( 16.20063489777861676, -7.373262058553140541, 22.00000000000000711 ) ) ;
#74135 = CARTESIAN_POINT ( 'NONE',  ( -18.67979575497178146, -10.72451020669898902, 71.66557627198100988 ) ) ;
#74136 = CARTESIAN_POINT ( 'NONE',  ( 5.823673210054125526, 21.52544592524343514, 29.79057627198102409 ) ) ;
#74137 = CARTESIAN_POINT ( 'NONE',  ( -5.153800228976328057, -19.02544592524343514, 22.29057627198102765 ) ) ;
#74138 = CARTESIAN_POINT ( 'NONE',  ( -0.05219959533934338120, 16.53943276465976808, 52.50109039468567573 ) ) ;
#74139 = ORIENTED_EDGE ( 'NONE', *, *, #172113, .F. ) ;
#74140 = CARTESIAN_POINT ( 'NONE',  ( 18.67979575497194134, -10.72451020669871369, 35.83442372801901143 ) ) ;
#74142 = CARTESIAN_POINT ( 'NONE',  ( -38.00000000000001421, 12.34694845685046438, -4.100000000000000533 ) ) ;
#74141 = CARTESIAN_POINT ( 'NONE',  ( 14.29746914071049879, -8.314922557960816363, 48.33224293864770260 ) ) ;
#74143 = CARTESIAN_POINT ( 'NONE',  ( 8.224510206698742110, 14.34966873604972548, 22.08442372801901143 ) ) ;
#74144 = CARTESIAN_POINT ( 'NONE',  ( 9.564922557961047289, -16.46253265017146816, 35.41775706135233293 ) ) ;
#74145 = CARTESIAN_POINT ( 'NONE',  ( -16.52544592524342804, 4.483927247898546575, 46.04057627198103830 ) ) ;
#74146 = CARTESIAN_POINT ( 'NONE',  ( -21.53943276465977519, -0.05219959533937600094, 23.75109039468567929 ) ) ;
#74148 = CARTESIAN_POINT ( 'NONE',  ( -5.719274019375978568, 21.55341960407610458, 75.20724293864769550 ) ) ;
#74147 = DIRECTION ( 'NONE',  ( 0.000000000000000000, 0.000000000000000000, -1.000000000000000000 ) ) ;
#74149 = CARTESIAN_POINT ( 'NONE',  ( -13.97604488694527625, -13.89961937509977652, 91.87390960531432427 ) ) ;
#74150 = CARTESIAN_POINT ( 'NONE',  ( 4.379528057220339221, -16.55341960407611168, 57.70724293864770260 ) ) ;
#74151 = CARTESIAN_POINT ( 'NONE',  ( -13.89961937509977652, 13.97604488694528158, 105.6239096053143527 ) ) ;
#74152 = AXIS2_PLACEMENT_3D ( 'NONE', #55824, #82132, #7304 ) ;
#74153 = CARTESIAN_POINT ( 'NONE',  ( -37.36578165719733846, 3.357000025855910064, 40.62839678089418527 ) ) ;
#74154 = CARTESIAN_POINT ( 'NONE',  ( -9.474510206698720793, -16.51473224551083518, 59.58442372801900433 ) ) ;
#74155 = CARTESIAN_POINT ( 'NONE',  ( 21.52544592524344225, -5.823673210054117533, 103.5405762719810383 ) ) ;
#74156 = CARTESIAN_POINT ( 'NONE',  ( 19.02544592524343514, -5.153800228976328945, 38.54057627198103120 ) ) ;
#74157 = CARTESIAN_POINT ( 'NONE',  ( 8.314922557960818139, 14.29746914071049879, 109.5822429386476955 ) ) ;
#74158 = CARTESIAN_POINT ( 'NONE',  ( -18.62759615963255300, -10.81492255796106328, 54.16775706135235424 ) ) ;
#74159 = CARTESIAN_POINT ( 'NONE',  ( 8.571926809382603096, -26.38167802310801235, 145.4750000027311785 ) ) ;
#74160 = CARTESIAN_POINT ( 'NONE',  ( 8.314922557960818139, 14.29746914071049879, 44.58224293864769550 ) ) ;
#74161 = CARTESIAN_POINT ( 'NONE',  ( 19.02544592524343514, -5.153800228976328945, 43.54057627198103120 ) ) ;
#74162 = CARTESIAN_POINT ( 'NONE',  ( 5.049401038298161559, -19.05341960407611168, 102.7072429386476955 ) ) ;
#74163 = CARTESIAN_POINT ( 'NONE',  ( 21.55341960407610458, 5.719274019375980345, 78.95724293864769550 ) ) ;
#74164 = CARTESIAN_POINT ( 'NONE',  ( 17.14385361876520264, -23.59649016807271238, 147.5750000027311444 ) ) ;
#74165 = CARTESIAN_POINT ( 'NONE',  ( -19.02544592524342804, 5.153800228976336051, 51.04057627198103120 ) ) ;
#74166 = VERTEX_POINT ( 'NONE', #48735 ) ;
#74167 = CARTESIAN_POINT ( 'NONE',  ( -21.53943276465977519, 0.05219959533907696930, 66.24890960531436690 ) ) ;
#74168 = ORIENTED_EDGE ( 'NONE', *, *, #90391, .F. ) ;
#74169 = CARTESIAN_POINT ( 'NONE',  ( 5.719274019375673035, 21.55341960407619339, 92.29275706135236135 ) ) ;
#74172 = CARTESIAN_POINT ( 'NONE',  ( -4.379528057220328563, 16.55341960407611168, 80.20724293864769550 ) ) ;
#74171 = CARTESIAN_POINT ( 'NONE',  ( 0.05219959533934541429, -16.53943276465976808, 80.00109039468568994 ) ) ;
#74170 = CARTESIAN_POINT ( 'NONE',  ( -17.49999999999999645, 5.499999999999985789, 38.71769037696434879 ) ) ;
#74173 = CARTESIAN_POINT ( 'NONE',  ( 16.51473224551069308, 9.474510206698969483, 69.16557627198102409 ) ) ;
#74174 = ORIENTED_EDGE ( 'NONE', *, *, #27973, .T. ) ;
#74175 = CARTESIAN_POINT ( 'NONE',  ( 0.05219959533936267826, -19.03943276465977164, 30.00109039468566863 ) ) ;
#74176 = CARTESIAN_POINT ( 'NONE',  ( -16.55341960407617563, 4.379528057220093196, 88.54275706135236135 ) ) ;
#74177 = CARTESIAN_POINT ( 'NONE',  ( 21.53943276465977519, 0.05219959533937863772, 106.2510903946856757 ) ) ;
#74178 = CARTESIAN_POINT ( 'NONE',  ( -9.474510206698964154, 16.51473224551069663, 75.41557627198103830 ) ) ;
#74179 = CARTESIAN_POINT ( 'NONE',  ( -18.62759615963270932, 10.81492255796079327, 45.83224293864769550 ) ) ;
#74180 = CARTESIAN_POINT ( 'NONE',  ( 10.81492255796106328, -18.62759615963255655, 90.41775706135236135 ) ) ;
#74181 = CARTESIAN_POINT ( 'NONE',  ( 14.29746914071037800, 8.314922557961029526, 56.66775706135235424 ) ) ;
#74182 = CARTESIAN_POINT ( 'NONE',  ( 10.72451020669898902, -18.67979575497178502, 112.9155762719810383 ) ) ;
#74183 = CARTESIAN_POINT ( 'NONE',  ( 9.474510206698729675, 16.51473224551082808, 112.0844237280190043 ) ) ;
#74184 = CARTESIAN_POINT ( 'NONE',  ( -19.02544592524342804, 5.153800228976336051, 91.04057627198100988 ) ) ;
#74185 = CARTESIAN_POINT ( 'NONE',  ( -12.14591786802326823, 12.06949235617739902, 33.12609039468569705 ) ) ;
#74186 = CARTESIAN_POINT ( 'NONE',  ( -16.46253265017160317, 9.564922557960807481, 55.83224293864769550 ) ) ;
#74187 = VECTOR ( 'NONE', #20314, 1000.000000000000000 ) ;
#74188 = CARTESIAN_POINT ( 'NONE',  ( 12.06949235617739724, 12.14591786802326823, 36.87609039468568994 ) ) ;
#74189 = CARTESIAN_POINT ( 'NONE',  ( -8.224510206698948167, 14.34966873604960824, 75.41557627198102409 ) ) ;
#74190 = CARTESIAN_POINT ( 'NONE',  ( -14.29746914071037622, -8.314922557961029526, 84.16775706135234714 ) ) ;
#74192 = CARTESIAN_POINT ( 'NONE',  ( 13.97604488694527802, 13.89961937509977652, 59.37390960531434558 ) ) ;
#74191 = CARTESIAN_POINT ( 'NONE',  ( -5.823673210054431948, 21.52544592524334988, 42.70942372801901854 ) ) ;
#74193 = CARTESIAN_POINT ( 'NONE',  ( 16.51473224551069308, 9.474510206698969483, 79.16557627198103830 ) ) ;
#74194 = CARTESIAN_POINT ( 'NONE',  ( 14.34966873604972726, -8.224510206698740333, 90.83442372801901854 ) ) ;
#74195 = CARTESIAN_POINT ( 'NONE',  ( -4.313351365237961588, 4.313351365237934054, -62.50719930893269805 ) ) ;
#74196 = ORIENTED_EDGE ( 'NONE', *, *, #115703, .T. ) ;
#74197 = CARTESIAN_POINT ( 'NONE',  ( -9.564922557961040184, 16.46253265017147172, 27.91775706135232582 ) ) ;
#74198 = CARTESIAN_POINT ( 'NONE',  ( -9.474510206698964154, 16.51473224551069663, 100.4155762719810241 ) ) ;
#74199 = CARTESIAN_POINT ( 'NONE',  ( 16.51473224551069308, 9.474510206698969483, 49.16557627198102409 ) ) ;
#74200 = CARTESIAN_POINT ( 'NONE',  ( -19.05341960407611168, -5.049401038298163336, 111.4572429386476671 ) ) ;
#74201 = CARTESIAN_POINT ( 'NONE',  ( 0.05219959533934541429, -16.53943276465976808, 45.00109039468568284 ) ) ;
#74203 = CARTESIAN_POINT ( 'NONE',  ( 0.05219959533934541429, -16.53943276465976808, 60.00109039468568284 ) ) ;
#74202 = CARTESIAN_POINT ( 'NONE',  ( -16.46253265017146816, -9.564922557961047289, 59.16775706135233293 ) ) ;
#74204 = CARTESIAN_POINT ( 'NONE',  ( -6.412877669190332419, -3.889087296526017479, 8.181980515339454030 ) ) ;
#74205 = CARTESIAN_POINT ( 'NONE',  ( 19.02544592524343514, -5.153800228976328945, 83.54057627198100988 ) ) ;
#74206 = CARTESIAN_POINT ( 'NONE',  ( 18.62759615963271287, -10.81492255796078972, 108.3322429386477097 ) ) ;
#74207 = CARTESIAN_POINT ( 'NONE',  ( 13.89961937509957401, 13.97604488694547697, 61.87609039468566863 ) ) ;
#74209 = CARTESIAN_POINT ( 'NONE',  ( 5.049401038298161559, -19.05341960407611168, 22.70724293864769194 ) ) ;
#74208 = CARTESIAN_POINT ( 'NONE',  ( -5.153800228976328057, -19.02544592524343514, 97.29057627198099567 ) ) ;
#74210 = EDGE_CURVE ( 'NONE', #104760, #18152, #173885, .T. ) ;
#74211 = CARTESIAN_POINT ( 'NONE',  ( -16.51473224551069308, -9.474510206698971260, 76.66557627198103830 ) ) ;
#74213 = CARTESIAN_POINT ( 'NONE',  ( 9.564922557960805705, 16.46253265017160317, 24.58224293864769194 ) ) ;
#74212 = CARTESIAN_POINT ( 'NONE',  ( -16.53943276465976808, 0.05219959533911058130, 36.24890960531435979 ) ) ;
#74214 = CARTESIAN_POINT ( 'NONE',  ( -9.474510206698720793, -16.51473224551083518, 44.58442372801900433 ) ) ;
#74215 = CARTESIAN_POINT ( 'NONE',  ( 4.483927247898545687, 16.52544592524342804, 69.79057627198102409 ) ) ;
#74216 = CARTESIAN_POINT ( 'NONE',  ( 15.80617190586769283, -15.72974639402175789, 100.6260903946857184 ) ) ;
#74217 = CARTESIAN_POINT ( 'NONE',  ( -0.05219959533909027116, -19.03943276465977164, 37.49890960531436690 ) ) ;
#74219 = CARTESIAN_POINT ( 'NONE',  ( -21.53943276465977519, -0.05219959533937600094, 98.75109039468568994 ) ) ;
#74218 = CARTESIAN_POINT ( 'NONE',  ( -8.314922557960811034, -14.29746914071050412, 37.08224293864768129 ) ) ;
#74220 = CARTESIAN_POINT ( 'NONE',  ( 5.153800228976335163, 19.02544592524342804, 99.79057627198102409 ) ) ;
#74221 = CARTESIAN_POINT ( 'NONE',  ( 5.153800228976335163, 19.02544592524342804, 89.79057627198102409 ) ) ;
#74222 = CARTESIAN_POINT ( 'NONE',  ( -19.02544592524342804, 5.153800228976336051, 41.04057627198103120 ) ) ;
#74223 = CARTESIAN_POINT ( 'NONE',  ( 14.34966873604960469, 8.224510206698951720, 104.1655762719810241 ) ) ;
#74224 = CARTESIAN_POINT ( 'NONE',  ( 8.314922557960818139, 14.29746914071049879, 74.58224293864768129 ) ) ;
#74225 = CARTESIAN_POINT ( 'NONE',  ( -21.53943276465977519, 0.05219959533907696930, 86.24890960531436690 ) ) ;
#74226 = CARTESIAN_POINT ( 'NONE',  ( -9.474510206698964154, 16.51473224551069663, 85.41557627198102409 ) ) ;
#74227 = CARTESIAN_POINT ( 'NONE',  ( -18.67979575497178146, -10.72451020669898902, 101.6655762719810383 ) ) ;
#74228 = CARTESIAN_POINT ( 'NONE',  ( -5.153800228976328057, -19.02544592524343514, 92.29057627198099567 ) ) ;
#74230 = CARTESIAN_POINT ( 'NONE',  ( 14.34966873604960469, 8.224510206698951720, 99.16557627198100988 ) ) ;
#74229 = CARTESIAN_POINT ( 'NONE',  ( -19.34837522270365540, -5.499999999999852562, 90.86337684832578532 ) ) ;
#74231 = CARTESIAN_POINT ( 'NONE',  ( 9.564922557960805705, 16.46253265017160317, 74.58224293864769550 ) ) ;
#74232 = CARTESIAN_POINT ( 'NONE',  ( 15.72974639402199770, -15.80617190586745480, 83.12390960531436690 ) ) ;
#74233 = CARTESIAN_POINT ( 'NONE',  ( 23.31738231874054890, -16.94106989632523508, 146.7999999999999829 ) ) ;
#74235 = LINE ( 'NONE', #147083, #27273 ) ;
#74234 = CARTESIAN_POINT ( 'NONE',  ( -21.55341960407610458, -5.719274019375992779, 31.45724293864769550 ) ) ;
#74236 = CARTESIAN_POINT ( 'NONE',  ( -19.03943276465977164, -0.05219959533935918106, 113.7510903946856757 ) ) ;
#74237 = CARTESIAN_POINT ( 'NONE',  ( -14.34966873604960291, -8.224510206698953496, 96.66557627198102409 ) ) ;
#74238 = CARTESIAN_POINT ( 'NONE',  ( -16.52216118717208815, -7.221426719304519182, 96.07599021046995347 ) ) ;
#74239 = CARTESIAN_POINT ( 'NONE',  ( -9.564922557960796823, -16.46253265017161027, 82.08224293864768129 ) ) ;
#74240 = CARTESIAN_POINT ( 'NONE',  ( 16.46253265017160672, -9.564922557960803928, 43.33224293864769550 ) ) ;
#74241 = CARTESIAN_POINT ( 'NONE',  ( -14.29746914071049879, 8.314922557960819915, 85.83224293864768129 ) ) ;
#74242 = CARTESIAN_POINT ( 'NONE',  ( -16.51473224551069308, -9.474510206698971260, 111.6655762719810383 ) ) ;
#74243 = CARTESIAN_POINT ( 'NONE',  ( 4.379528057220339221, -16.55341960407611168, 57.70724293864770260 ) ) ;
#74244 = CARTESIAN_POINT ( 'NONE',  ( 16.51473224551083163, -9.474510206698727899, 100.8344237280190043 ) ) ;
#74245 = CARTESIAN_POINT ( 'NONE',  ( 5.823673210054444382, -21.52544592524334988, 65.20942372801901854 ) ) ;
#74246 = CARTESIAN_POINT ( 'NONE',  ( 22.44159573604009239, 16.30477369853692693, 146.0750000027311728 ) ) ;
#74247 = CARTESIAN_POINT ( 'NONE',  ( 16.51473224551069308, 9.474510206698969483, 94.16557627198103830 ) ) ;
#74248 = CARTESIAN_POINT ( 'NONE',  ( 10.81492255796078972, 18.62759615963270932, 84.58224293864769550 ) ) ;
#74249 = CARTESIAN_POINT ( 'NONE',  ( 8.314922557961029526, -14.29746914071037800, 90.41775706135236135 ) ) ;
#74250 = CARTESIAN_POINT ( 'NONE',  ( -5.153800228976328057, -19.02544592524343514, 22.29057627198102765 ) ) ;
#74251 = CARTESIAN_POINT ( 'NONE',  ( 5.153800228976335163, 19.02544592524342804, 74.79057627198103830 ) ) ;
#74252 = CARTESIAN_POINT ( 'NONE',  ( 15.72974639402199770, -15.80617190586745480, 83.12390960531436690 ) ) ;
#74253 = CARTESIAN_POINT ( 'NONE',  ( 9.474510206698729675, 16.51473224551082808, 107.0844237280190043 ) ) ;
#74255 = CARTESIAN_POINT ( 'NONE',  ( 21.52544592524334988, 5.823673210054432836, 56.45942372801902565 ) ) ;
#74254 = CARTESIAN_POINT ( 'NONE',  ( -14.29746914071049879, 8.314922557960819915, 50.83224293864770971 ) ) ;
#74257 = CARTESIAN_POINT ( 'NONE',  ( -10.81492255796078084, -18.62759615963271287, 22.08224293864769194 ) ) ;
#74256 = CARTESIAN_POINT ( 'NONE',  ( -14.34966873604972548, 8.224510206698743886, 83.33442372801903275 ) ) ;
#74258 = CARTESIAN_POINT ( 'NONE',  ( -9.474510206698964154, 16.51473224551069663, 110.4155762719810383 ) ) ;
#74259 = CARTESIAN_POINT ( 'NONE',  ( 18.22780087662119897, -5.500000000000096811, 58.51763182126894947 ) ) ;
#74260 = CARTESIAN_POINT ( 'NONE',  ( -12.14591786802326823, 12.06949235617739902, 103.1260903946856757 ) ) ;
#74261 = CARTESIAN_POINT ( 'NONE',  ( -12.06949235617739369, -12.14591786802326823, 64.37609039468568994 ) ) ;
#74262 = CARTESIAN_POINT ( 'NONE',  ( 5.049401038298161559, -19.05341960407611168, 52.70724293864767418 ) ) ;
#74263 = CARTESIAN_POINT ( 'NONE',  ( 5.153800228976335163, 19.02544592524342804, 69.79057627198103830 ) ) ;
#74264 = CARTESIAN_POINT ( 'NONE',  ( 16.53943276465976808, 0.05219959533934440121, 76.25109039468568994 ) ) ;
#74265 = CARTESIAN_POINT ( 'NONE',  ( -16.53943276465976808, 0.05219959533911058130, 51.24890960531436690 ) ) ;
#74266 = CARTESIAN_POINT ( 'NONE',  ( 16.51473224551069308, 9.474510206698969483, 59.16557627198102409 ) ) ;
#74267 = CARTESIAN_POINT ( 'NONE',  ( -13.97604488694527625, -13.89961937509977652, 46.87390960531435979 ) ) ;
#74269 = ORIENTED_EDGE ( 'NONE', *, *, #119223, .T. ) ;
#74268 = CARTESIAN_POINT ( 'NONE',  ( 14.34966873604972726, -8.224510206698740333, 35.83442372801901143 ) ) ;
#74270 = CARTESIAN_POINT ( 'NONE',  ( 9.474510206698729675, 16.51473224551082808, 92.08442372801900433 ) ) ;
#74271 = CARTESIAN_POINT ( 'NONE',  ( -4.379528057220328563, 16.55341960407611168, 95.20724293864769550 ) ) ;
#74272 = CARTESIAN_POINT ( 'NONE',  ( -19.02544592524342804, 5.153800228976336051, 61.04057627198103120 ) ) ;
#74274 = CARTESIAN_POINT ( 'NONE',  ( 23.48529157249599919, 32.32473071737754111, -6.700000000000001066 ) ) ;
#74273 = CARTESIAN_POINT ( 'NONE',  ( -16.46253265017146816, -9.564922557961047289, 99.16775706135233293 ) ) ;
#74275 = CARTESIAN_POINT ( 'NONE',  ( -5.719274019375665041, -21.55341960407619695, 109.7927570613523613 ) ) ;
#74276 = CARTESIAN_POINT ( 'NONE',  ( -14.34966873604972548, 8.224510206698743886, 73.33442372801901854 ) ) ;
#74277 = DIRECTION ( 'NONE',  ( 0.000000000000000000, 0.000000000000000000, 1.000000000000000000 ) ) ;
#74278 = CARTESIAN_POINT ( 'NONE',  ( -10.81492255796078084, -18.62759615963271287, 62.08224293864769550 ) ) ;
#74279 = CARTESIAN_POINT ( 'NONE',  ( -16.53943276465976808, -0.05219959533934237506, 53.75109039468568994 ) ) ;
#74280 = CARTESIAN_POINT ( 'NONE',  ( -16.51473224551069308, -9.474510206698971260, 31.66557627198102054 ) ) ;
#74281 = CARTESIAN_POINT ( 'NONE',  ( -16.51473224551082808, 9.474510206698731452, 38.33442372801899722 ) ) ;
#74282 = CARTESIAN_POINT ( 'NONE',  ( -16.46253265017160317, 9.564922557960807481, 90.83224293864769550 ) ) ;
#74283 = CARTESIAN_POINT ( 'NONE',  ( 16.55341960407611168, 4.379528057220329451, 113.9572429386477239 ) ) ;
#74284 = CARTESIAN_POINT ( 'NONE',  ( 0.05219959533909260263, 19.03943276465977164, 69.99890960531435269 ) ) ;
#74285 = CARTESIAN_POINT ( 'NONE',  ( -15.72974639402176322, -15.80617190586768395, 79.37609039468567573 ) ) ;
#74286 = EDGE_CURVE ( 'NONE', #142306, #189322, #193231, .T. ) ;
#74287 = CARTESIAN_POINT ( 'NONE',  ( -9.564922557961040184, 16.46253265017147172, 52.91775706135233293 ) ) ;
#74288 = CARTESIAN_POINT ( 'NONE',  ( 13.97604488694548053, -13.89961937509957401, 25.62609039468566507 ) ) ;
#74289 = CARTESIAN_POINT ( 'NONE',  ( 19.03943276465977164, -0.05219959533909143690, 58.74890960531435979 ) ) ;
#74290 = CARTESIAN_POINT ( 'NONE',  ( 16.46253265017160672, -9.564922557960803928, 113.3322429386476955 ) ) ;
#74291 = CARTESIAN_POINT ( 'NONE',  ( -18.62759615963255300, -10.81492255796106328, 84.16775706135234714 ) ) ;
#74292 = CARTESIAN_POINT ( 'NONE',  ( -19.02544592524342804, 5.153800228976336051, 61.04057627198103120 ) ) ;
#74293 = CARTESIAN_POINT ( 'NONE',  ( -10.72451020669870658, -18.67979575497194134, 94.58442372801901854 ) ) ;
#74294 = CARTESIAN_POINT ( 'NONE',  ( -15.80617190586745835, -15.72974639402198527, 31.87390960531435979 ) ) ;
#74295 = CARTESIAN_POINT ( 'NONE',  ( -16.51473224551069308, -9.474510206698971260, 86.66557627198102409 ) ) ;
#74296 = CARTESIAN_POINT ( 'NONE',  ( -21.53943276465977519, -0.05219959533937600094, 43.75109039468568284 ) ) ;
#74297 = CARTESIAN_POINT ( 'NONE',  ( 16.46253265017146816, 9.564922557961045513, 56.66775706135233293 ) ) ;
#74298 = CARTESIAN_POINT ( 'NONE',  ( -19.02544592524342804, 5.153800228976336051, 36.04057627198100988 ) ) ;
#74299 = CARTESIAN_POINT ( 'NONE',  ( -19.03943276465977164, 0.05219959533909376836, 91.24890960531436690 ) ) ;
#74300 = CARTESIAN_POINT ( 'NONE',  ( 12.14591786802327356, -12.06949235617739191, 25.62609039468567929 ) ) ;
#74301 = CARTESIAN_POINT ( 'NONE',  ( 0.05219959533910956823, 16.53943276465976808, 94.99890960531436690 ) ) ;
#74302 = CARTESIAN_POINT ( 'NONE',  ( 16.51473224551069308, 9.474510206698969483, 74.16557627198103830 ) ) ;
#74303 = ADVANCED_FACE ( 'NONE', ( #171076 ), #112381, .F. ) ;
#74304 = CARTESIAN_POINT ( 'NONE',  ( 5.823673210054125526, 21.52544592524343514, 54.79057627198104541 ) ) ;
#74305 = CIRCLE ( 'NONE', #45274, 8.000000000000000000 ) ;
#74306 = CARTESIAN_POINT ( 'NONE',  ( -16.51473224551082808, 9.474510206698731452, 113.3344237280190043 ) ) ;
#74307 = CARTESIAN_POINT ( 'NONE',  ( 0.05219959533937995610, -21.53943276465977519, 20.00109039468568639 ) ) ;
#74308 = CARTESIAN_POINT ( 'NONE',  ( -21.52544592524334988, -5.823673210054445271, 73.95942372801901854 ) ) ;
#74309 = CARTESIAN_POINT ( 'NONE',  ( -16.53943276465976808, -0.05219959533934237506, 63.75109039468568284 ) ) ;
#74310 = CARTESIAN_POINT ( 'NONE',  ( -12.06949235617739369, -12.14591786802326823, 64.37609039468568994 ) ) ;
#74311 = CARTESIAN_POINT ( 'NONE',  ( -19.03943276465977164, 0.05219959533909376836, 61.24890960531436690 ) ) ;
#74312 = CARTESIAN_POINT ( 'NONE',  ( -14.34966873604972548, 8.224510206698743886, 98.33442372801901854 ) ) ;
#74313 = CARTESIAN_POINT ( 'NONE',  ( -5.153800228976607833, 19.02544592524334988, 47.70942372801900433 ) ) ;
#74314 = CARTESIAN_POINT ( 'NONE',  ( 10.81492255796078972, 18.62759615963270932, 114.5822429386477097 ) ) ;
#74315 = CARTESIAN_POINT ( 'NONE',  ( -8.224510206698948167, 14.34966873604960824, 60.41557627198102409 ) ) ;
#74316 = CARTESIAN_POINT ( 'NONE',  ( -19.05341960407611168, -5.049401038298163336, 91.45724293864766707 ) ) ;
#74317 = CARTESIAN_POINT ( 'NONE',  ( 8.314922557961029526, -14.29746914071037800, 90.41775706135236135 ) ) ;
#74318 = CARTESIAN_POINT ( 'NONE',  ( -10.72451020669870658, -18.67979575497194134, 64.58442372801900433 ) ) ;
#74319 = CARTESIAN_POINT ( 'NONE',  ( 16.55341960407618274, -4.379528057220086978, 31.04275706135234714 ) ) ;
#74320 = CARTESIAN_POINT ( 'NONE',  ( 10.81492255796106328, -18.62759615963255655, 30.41775706135234358 ) ) ;
#74321 = CARTESIAN_POINT ( 'NONE',  ( 8.224510206698953496, -14.34966873604960469, 57.91557627198103120 ) ) ;
#74322 = ORIENTED_EDGE ( 'NONE', *, *, #93154, .F. ) ;
#74323 = CARTESIAN_POINT ( 'NONE',  ( -0.05219959533907301413, -21.53943276465977519, 102.4989096053143811 ) ) ;
#74324 = CARTESIAN_POINT ( 'NONE',  ( 0.05219959533910956823, 16.53943276465976808, 39.99890960531436690 ) ) ;
#74325 = EDGE_LOOP ( 'NONE', ( #10609, #38471, #139930, #115678 ) ) ;
#74326 = CARTESIAN_POINT ( 'NONE',  ( 34.48171762721879929, 5.660481407866305936, 49.94458042978408940 ) ) ;
#74327 = CARTESIAN_POINT ( 'NONE',  ( 18.67979575497178502, 10.72451020669898547, 34.16557627198102409 ) ) ;
#74328 = CARTESIAN_POINT ( 'NONE',  ( -15.80617190586768217, 15.72974639402176855, 38.12609039468567573 ) ) ;
#74329 = CARTESIAN_POINT ( 'NONE',  ( -12.06949235617756955, 12.14591786802309770, 70.62390960531436690 ) ) ;
#74330 = CIRCLE ( 'NONE', #77479, 69.99999999999997158 ) ;
#74331 = CARTESIAN_POINT ( 'NONE',  ( -21.52544592524343514, 5.823673210054127303, 71.04057627198103830 ) ) ;
#74332 = CARTESIAN_POINT ( 'NONE',  ( -13.89961937509977652, 13.97604488694528158, 80.62390960531436690 ) ) ;
#74334 = CARTESIAN_POINT ( 'NONE',  ( 16.51473224551083163, -9.474510206698727899, 65.83442372801900433 ) ) ;
#74333 = CARTESIAN_POINT ( 'NONE',  ( 9.474510206698971260, -16.51473224551069308, 27.91557627198103120 ) ) ;
#74335 = CARTESIAN_POINT ( 'NONE',  ( 21.53943276465977519, -0.05219959533907433946, 48.74890960531435979 ) ) ;
#74336 = CARTESIAN_POINT ( 'NONE',  ( 19.05341960407611168, 5.049401038298154454, 63.95724293864769550 ) ) ;
#74337 = CARTESIAN_POINT ( 'NONE',  ( -14.34966873604972548, 8.224510206698743886, 38.33442372801900433 ) ) ;
#74338 = CARTESIAN_POINT ( 'NONE',  ( 10.81492255796078972, 18.62759615963270932, 109.5822429386476955 ) ) ;
#74339 = CARTESIAN_POINT ( 'NONE',  ( -16.52544592524342804, 4.483927247898546575, 51.04057627198103120 ) ) ;
#74340 = CARTESIAN_POINT ( 'NONE',  ( 5.153800228976335163, 19.02544592524342804, 104.7905762719809957 ) ) ;
#74341 = CARTESIAN_POINT ( 'NONE',  ( 18.67979575497178502, 10.72451020669898547, 69.16557627198102409 ) ) ;
#74343 = CARTESIAN_POINT ( 'NONE',  ( 16.53943276465976808, 0.05219959533934440121, 41.25109039468568284 ) ) ;
#74342 = CARTESIAN_POINT ( 'NONE',  ( 15.72974639402199770, -15.80617190586745480, 108.1239096053143811 ) ) ;
#74344 = CARTESIAN_POINT ( 'NONE',  ( 10.72451020669898902, -18.67979575497178502, 42.91557627198103120 ) ) ;
#74345 = CARTESIAN_POINT ( 'NONE',  ( 21.55341960407619695, -5.719274019375665929, 96.04275706135236135 ) ) ;
#74346 = CARTESIAN_POINT ( 'NONE',  ( -19.02544592524342804, 5.153800228976336051, 41.04057627198103120 ) ) ;
#74347 = CARTESIAN_POINT ( 'NONE',  ( 19.03943276465977164, -0.05219959533909143690, 93.74890960531435269 ) ) ;
#74348 = CARTESIAN_POINT ( 'NONE',  ( -19.03943276465977164, 0.05219959533909376836, 76.24890960531435269 ) ) ;
#74349 = CARTESIAN_POINT ( 'NONE',  ( 17.31728774477213406, -6.344390552233679870, 88.31906651689307353 ) ) ;
#74350 = CARTESIAN_POINT ( 'NONE',  ( -0.05219959533936034679, 19.03943276465977164, 52.50109039468566863 ) ) ;
#74352 = CARTESIAN_POINT ( 'NONE',  ( -10.72451020669898014, 18.67979575497178502, 35.41557627198102409 ) ) ;
#74351 = CARTESIAN_POINT ( 'NONE',  ( -18.62759615963255300, -10.81492255796106328, 109.1677570613523613 ) ) ;
#74353 = CARTESIAN_POINT ( 'NONE',  ( -8.224510206698735004, -14.34966873604973081, 109.5844237280190328 ) ) ;
#74354 = CARTESIAN_POINT ( 'NONE',  ( 13.97604488694548053, -13.89961937509957401, 90.62609039468567573 ) ) ;
#74355 = CARTESIAN_POINT ( 'NONE',  ( -14.81363604427072644, -15.38158542220645408, -58.82267548686223080 ) ) ;
#74356 = CARTESIAN_POINT ( 'NONE',  ( 0.05219959533936267826, -19.03943276465977164, 90.00109039468567573 ) ) ;
#74357 = CARTESIAN_POINT ( 'NONE',  ( 13.97604488694548053, -13.89961937509957401, 50.62609039468566152 ) ) ;
#74358 = CARTESIAN_POINT ( 'NONE',  ( -16.38665767535053064, -7.295008042176048590, 44.73599135785455871 ) ) ;
#74359 = CARTESIAN_POINT ( 'NONE',  ( -16.46253265017160317, 9.564922557960807481, 40.83224293864769550 ) ) ;
#74360 = CARTESIAN_POINT ( 'NONE',  ( 4.483927247898545687, 16.52544592524342804, 49.79057627198102409 ) ) ;
#74361 = CARTESIAN_POINT ( 'NONE',  ( -17.31728774477273802, -6.344390552232371583, 109.1809334831068412 ) ) ;
#74362 = CARTESIAN_POINT ( 'NONE',  ( 4.483927247898545687, 16.52544592524342804, 24.79057627198103120 ) ) ;
#74363 = CARTESIAN_POINT ( 'NONE',  ( 1.500000000004810818, 7.599999999999482725, -64.24270632869257724 ) ) ;
#74364 = CARTESIAN_POINT ( 'NONE',  ( -8.224510206698735004, -14.34966873604973081, 94.58442372801901854 ) ) ;
#74365 = CARTESIAN_POINT ( 'NONE',  ( 0.05219959533909260263, 19.03943276465977164, 54.99890960531435979 ) ) ;
#74366 = CARTESIAN_POINT ( 'NONE',  ( -18.67979575497193778, 10.72451020669871902, 103.3344237280190043 ) ) ;
#74367 = CARTESIAN_POINT ( 'NONE',  ( -4.483927247898782831, 16.52544592524335698, 22.70942372801901499 ) ) ;
#74368 = CARTESIAN_POINT ( 'NONE',  ( 5.719274019375991003, -21.55341960407610458, 37.70724293864769550 ) ) ;
#74370 = ORIENTED_EDGE ( 'NONE', *, *, #169635, .T. ) ;
#74369 = CARTESIAN_POINT ( 'NONE',  ( -21.55341960407619339, 5.719274019375674811, 98.54275706135234714 ) ) ;
#74371 = CARTESIAN_POINT ( 'NONE',  ( 16.51473224551069308, 9.474510206698969483, 99.16557627198102409 ) ) ;
#74372 = CARTESIAN_POINT ( 'NONE',  ( 0.05219959533909260263, 19.03943276465977164, 84.99890960531436690 ) ) ;
#74373 = CARTESIAN_POINT ( 'NONE',  ( 29.86685920354754487, 21.69954338932564752, -9.424999997268814766 ) ) ;
#74374 = CARTESIAN_POINT ( 'NONE',  ( 21.55341960407610458, 5.719274019375980345, 103.9572429386476813 ) ) ;
#74375 = CARTESIAN_POINT ( 'NONE',  ( -14.34966873604960291, -8.224510206698953496, 81.66557627198103830 ) ) ;
#74376 = CARTESIAN_POINT ( 'NONE',  ( -5.823673210054116645, -21.52544592524344225, 77.29057627198102409 ) ) ;
#74377 = CARTESIAN_POINT ( 'NONE',  ( 5.153800228976335163, 19.02544592524342804, 54.79057627198103120 ) ) ;
#74378 = CARTESIAN_POINT ( 'NONE',  ( -18.62759615963270932, 10.81492255796079327, 95.83224293864770971 ) ) ;
#74379 = ORIENTED_EDGE ( 'NONE', *, *, #153559, .F. ) ;
#74380 = CARTESIAN_POINT ( 'NONE',  ( -9.474510206698964154, 16.51473224551069663, 65.41557627198102409 ) ) ;
#74382 = CARTESIAN_POINT ( 'NONE',  ( 21.94595931813856637, -7.591279830614304558, 169.8931963588656231 ) ) ;
#74381 = CARTESIAN_POINT ( 'NONE',  ( 16.52544592524342804, -4.483927247898539470, 98.54057627198105251 ) ) ;
#74383 = CARTESIAN_POINT ( 'NONE',  ( 16.51473224551069308, 9.474510206698969483, 69.16557627198102409 ) ) ;
#74384 = CARTESIAN_POINT ( 'NONE',  ( -0.05219959533936034679, 19.03943276465977164, 82.50109039468567573 ) ) ;
#74385 = CARTESIAN_POINT ( 'NONE',  ( -14.29746914071049879, 8.314922557960819915, 90.83224293864769550 ) ) ;
#74386 = CARTESIAN_POINT ( 'NONE',  ( 21.52544592524334988, 5.823673210054432836, 61.45942372801901854 ) ) ;
#74388 = CARTESIAN_POINT ( 'NONE',  ( 18.62759615963271287, -10.81492255796078972, 113.3322429386476955 ) ) ;
#74387 = CARTESIAN_POINT ( 'NONE',  ( 19.05341960407611168, 5.049401038298154454, 48.95724293864768129 ) ) ;
#74389 = CARTESIAN_POINT ( 'NONE',  ( -12.14591786802309592, -12.06949235617757132, 106.8739096053143811 ) ) ;
#74390 = DIRECTION ( 'NONE',  ( 1.000000000000000000, 0.000000000000000000, 0.000000000000000000 ) ) ;
#74391 = CARTESIAN_POINT ( 'NONE',  ( 16.51473224551069308, 9.474510206698969483, 59.16557627198102409 ) ) ;
#74392 = CARTESIAN_POINT ( 'NONE',  ( -24.99873734152929217, -24.49873734152903282, 5.353553390593269512 ) ) ;
#74394 = CARTESIAN_POINT ( 'NONE',  ( -19.03943276465977164, 0.05219959533909376836, 106.2489096053143669 ) ) ;
#74393 = CARTESIAN_POINT ( 'NONE',  ( -5.153800228976607833, 19.02544592524334988, 112.7094237280190043 ) ) ;
#74395 = CARTESIAN_POINT ( 'NONE',  ( -18.62759615963255300, -10.81492255796106328, 54.16775706135235424 ) ) ;
#74396 = CARTESIAN_POINT ( 'NONE',  ( 19.05341960407611168, 5.049401038298154454, 98.95724293864766707 ) ) ;
#74397 = CARTESIAN_POINT ( 'NONE',  ( -13.97604488694547697, 13.89961937509957934, 88.12609039468563310 ) ) ;
#74398 = CARTESIAN_POINT ( 'NONE',  ( 9.564922557960805705, 16.46253265017160317, 64.58224293864769550 ) ) ;
#74399 = CARTESIAN_POINT ( 'NONE',  ( -12.14591786802309592, -12.06949235617757132, 76.87390960531439532 ) ) ;
#74400 = CARTESIAN_POINT ( 'NONE',  ( -4.379528057220328563, 16.55341960407611168, 85.20724293864770971 ) ) ;
#74401 = CARTESIAN_POINT ( 'NONE',  ( -5.153800228976328057, -19.02544592524343514, 87.29057627198103830 ) ) ;
#74402 = CARTESIAN_POINT ( 'NONE',  ( 4.379528057220339221, -16.55341960407611168, 72.70724293864769550 ) ) ;
#74403 = CARTESIAN_POINT ( 'NONE',  ( 19.05341960407611168, 5.049401038298154454, 83.95724293864766707 ) ) ;
#74404 = CARTESIAN_POINT ( 'NONE',  ( 19.03943276465977164, 0.05219959533936151252, 26.25109039468566507 ) ) ;
#74407 = CARTESIAN_POINT ( 'NONE',  ( -19.05341960407611168, -5.049401038298163336, 26.45724293864769550 ) ) ;
#74406 = CARTESIAN_POINT ( 'NONE',  ( 0.05219959533910956823, 16.53943276465976808, 34.99890960531435979 ) ) ;
#74405 = CARTESIAN_POINT ( 'NONE',  ( 0.05219959533909260263, 19.03943276465977164, 54.99890960531435979 ) ) ;
#74408 = EDGE_LOOP ( 'NONE', ( #114038, #196910, #108990 ) ) ;
#74409 = CARTESIAN_POINT ( 'NONE',  ( -21.52544592524334988, -5.823673210054445271, 48.95942372801902565 ) ) ;
#74410 = CARTESIAN_POINT ( 'NONE',  ( -19.05341960407617563, 5.049401038297882671, 78.54275706135233293 ) ) ;
#74411 = CARTESIAN_POINT ( 'NONE',  ( 8.314922557960818139, 14.29746914071049879, 34.58224293864770260 ) ) ;
#74412 = CARTESIAN_POINT ( 'NONE',  ( 5.719274019375991003, -21.55341960407610458, 92.70724293864770971 ) ) ;
#74413 = CARTESIAN_POINT ( 'NONE',  ( -15.80617190586745835, -15.72974639402198527, 36.87390960531435979 ) ) ;
#74414 = CARTESIAN_POINT ( 'NONE',  ( -14.29746914071049879, 8.314922557960819915, 65.83224293864769550 ) ) ;
#74415 = CARTESIAN_POINT ( 'NONE',  ( 16.46253265017160672, -9.564922557960803928, 48.33224293864769550 ) ) ;
#74416 = CARTESIAN_POINT ( 'NONE',  ( 16.52544592524335698, 4.483927247898782831, 96.45942372801901854 ) ) ;
#74417 = CARTESIAN_POINT ( 'NONE',  ( 16.53943276465976808, 0.05219959533934440121, 76.25109039468568994 ) ) ;
#74418 = CARTESIAN_POINT ( 'NONE',  ( 5.823673210054125526, 21.52544592524343514, 39.79057627198103830 ) ) ;
#74419 = CARTESIAN_POINT ( 'NONE',  ( -5.049401038297874678, -19.05341960407617918, 24.79275706135233648 ) ) ;
#74420 = CARTESIAN_POINT ( 'NONE',  ( 16.51473224551069308, 9.474510206698969483, 89.16557627198103830 ) ) ;
#74421 = CARTESIAN_POINT ( 'NONE',  ( -0.05219959533934338120, 16.53943276465976808, 67.50109039468568994 ) ) ;
#74422 = CARTESIAN_POINT ( 'NONE',  ( -16.53943276465976808, 0.05219959533911058130, 116.2489096053143669 ) ) ;
#74423 = CARTESIAN_POINT ( 'NONE',  ( 8.314922557960818139, 14.29746914071049879, 34.58224293864770260 ) ) ;
#74425 = CARTESIAN_POINT ( 'NONE',  ( -9.564922557960796823, -16.46253265017161027, 97.08224293864769550 ) ) ;
#74424 = CARTESIAN_POINT ( 'NONE',  ( -13.89961937509977652, 13.97604488694528158, 100.6239096053143669 ) ) ;
#74426 = CARTESIAN_POINT ( 'NONE',  ( 0.05219959533907565091, 21.53943276465977519, 29.99890960531435979 ) ) ;
#74427 = CARTESIAN_POINT ( 'NONE',  ( -16.52544592524342804, 4.483927247898546575, 71.04057627198103830 ) ) ;
#74428 = CARTESIAN_POINT ( 'NONE',  ( 16.55341960407611168, 4.379528057220329451, 53.95724293864770260 ) ) ;
#74430 = DIRECTION ( 'NONE',  ( 0.000000000000000000, 0.000000000000000000, 1.000000000000000000 ) ) ;
#74429 = CARTESIAN_POINT ( 'NONE',  ( -16.53943276465976808, -0.05219959533934237506, 58.75109039468568994 ) ) ;
#74431 = CARTESIAN_POINT ( 'NONE',  ( 16.51473224551083163, -9.474510206698727899, 50.83442372801899722 ) ) ;
#74432 = CARTESIAN_POINT ( 'NONE',  ( 5.153800228976335163, 19.02544592524342804, 89.79057627198102409 ) ) ;
#74433 = CARTESIAN_POINT ( 'NONE',  ( 5.049401038297881783, 19.05341960407617563, 72.29275706135234714 ) ) ;
#74434 = CARTESIAN_POINT ( 'NONE',  ( 17.14385361876520264, -23.59649016807271238, 146.0750000027311728 ) ) ;
#74435 = CARTESIAN_POINT ( 'NONE',  ( 16.46253265017146816, 9.564922557961045513, 56.66775706135233293 ) ) ;
#74437 = CARTESIAN_POINT ( 'NONE',  ( 4.483927247898790824, -16.52544592524335698, 90.20942372801903275 ) ) ;
#74436 = CARTESIAN_POINT ( 'NONE',  ( 19.02544592524334988, 5.153800228976608722, 111.4594237280190043 ) ) ;
#74438 = CARTESIAN_POINT ( 'NONE',  ( 22.44159573604009594, -16.30477369853687364, 148.1750000027311671 ) ) ;
#74439 = CARTESIAN_POINT ( 'NONE',  ( -13.97604488694527625, -13.89961937509977652, 41.87390960531435979 ) ) ;
#74440 = CARTESIAN_POINT ( 'NONE',  ( -9.564922557960796823, -16.46253265017161027, 112.0822429386476955 ) ) ;
#74441 = CARTESIAN_POINT ( 'NONE',  ( -18.62759615963255300, -10.81492255796106328, 59.16775706135234714 ) ) ;
#74442 = CARTESIAN_POINT ( 'NONE',  ( -9.564922557961040184, 16.46253265017147172, 97.91775706135233293 ) ) ;
#74444 = CARTESIAN_POINT ( 'NONE',  ( -19.02544592524342804, 5.153800228976336051, 61.04057627198103120 ) ) ;
#74443 = DIRECTION ( 'NONE',  ( 1.000000000000000000, -0.000000000000000000, -0.000000000000000000 ) ) ;
#74445 = EDGE_CURVE ( 'NONE', #117961, #182543, #154157, .T. ) ;
#74446 = CARTESIAN_POINT ( 'NONE',  ( -16.46253265017160317, 9.564922557960807481, 110.8322429386476955 ) ) ;
#74448 = CARTESIAN_POINT ( 'NONE',  ( 13.97604488694527802, 13.89961937509977652, 64.37390960531436690 ) ) ;
#74447 = CARTESIAN_POINT ( 'NONE',  ( -8.224510206698948167, 14.34966873604960824, 80.41557627198103830 ) ) ;
#74449 = CARTESIAN_POINT ( 'NONE',  ( -9.564922557960796823, -16.46253265017161027, 72.08224293864770971 ) ) ;
#74450 = CARTESIAN_POINT ( 'NONE',  ( 9.474510206698729675, 16.51473224551082808, 72.08442372801900433 ) ) ;
#74451 = CARTESIAN_POINT ( 'NONE',  ( -15.80617190586745835, -15.72974639402198527, 61.87390960531436690 ) ) ;
#74452 = CARTESIAN_POINT ( 'NONE',  ( 0.05219959533910956823, 16.53943276465976808, 109.9989096053143527 ) ) ;
#74453 = CARTESIAN_POINT ( 'NONE',  ( 19.05341960407617918, -5.049401038297876454, 56.04275706135234714 ) ) ;
#74454 = CARTESIAN_POINT ( 'NONE',  ( 5.049401038298161559, -19.05341960407611168, 62.70724293864769550 ) ) ;
#74455 = CARTESIAN_POINT ( 'NONE',  ( 9.564922557960805705, 16.46253265017160317, 89.58224293864769550 ) ) ;
#74456 = CARTESIAN_POINT ( 'NONE',  ( 5.719274019375991003, -21.55341960407610458, 92.70724293864770971 ) ) ;
#74458 = CARTESIAN_POINT ( 'NONE',  ( 13.89961937509957401, 13.97604488694547697, 51.87609039468566863 ) ) ;
#74457 = CARTESIAN_POINT ( 'NONE',  ( 16.52544592524342804, -4.483927247898539470, 83.54057627198102409 ) ) ;
#74459 = CARTESIAN_POINT ( 'NONE',  ( -10.81492255796078084, -18.62759615963271287, 82.08224293864768129 ) ) ;
#74460 = CARTESIAN_POINT ( 'NONE',  ( -21.55341960407610458, -5.719274019375992779, 56.45724293864768839 ) ) ;
#74461 = CARTESIAN_POINT ( 'NONE',  ( 14.34966873604960469, 8.224510206698951720, 39.16557627198102409 ) ) ;
#74462 = CARTESIAN_POINT ( 'NONE',  ( 21.55341960407619695, -5.719274019375665929, 91.04275706135236135 ) ) ;
#74463 = CARTESIAN_POINT ( 'NONE',  ( -16.46253265017160317, 9.564922557960807481, 85.83224293864769550 ) ) ;
#74464 = CARTESIAN_POINT ( 'NONE',  ( -19.05341960407611168, -5.049401038298163336, 21.45724293864768839 ) ) ;
#74465 = CIRCLE ( 'NONE', #96937, 5.000000000000000000 ) ;
#74466 = CARTESIAN_POINT ( 'NONE',  ( -15.72974639402176322, -15.80617190586768395, 29.37609039468568284 ) ) ;
#74467 = CARTESIAN_POINT ( 'NONE',  ( -15.72974639402176322, -15.80617190586768395, 34.37609039468568284 ) ) ;
#74468 = CARTESIAN_POINT ( 'NONE',  ( -19.03943276465977164, 0.05219959533909376836, 51.24890960531436690 ) ) ;
#74469 = CARTESIAN_POINT ( 'NONE',  ( 21.52544592524334988, 5.823673210054432836, 26.45942372801901854 ) ) ;
#74470 = CARTESIAN_POINT ( 'NONE',  ( -13.89961937509957401, -13.97604488694547875, 64.37609039468567573 ) ) ;
#74471 = EDGE_CURVE ( 'NONE', #49235, #77030, #92804, .T. ) ;
#74472 = CARTESIAN_POINT ( 'NONE',  ( -19.03943276465977164, 0.05219959533909376836, 41.24890960531435269 ) ) ;
#74473 = CARTESIAN_POINT ( 'NONE',  ( 4.379528057220092307, 16.55341960407617563, 22.29275706135235069 ) ) ;
#74474 = CARTESIAN_POINT ( 'NONE',  ( -19.05341960407611168, -5.049401038298163336, 31.45724293864769550 ) ) ;
#74475 = CARTESIAN_POINT ( 'NONE',  ( 12.14591786802327356, -12.06949235617739191, 70.62609039468567573 ) ) ;
#74476 = CARTESIAN_POINT ( 'NONE',  ( -19.02544592524342804, 5.153800228976336051, 41.04057627198103120 ) ) ;
#74477 = CARTESIAN_POINT ( 'NONE',  ( -25.85231681326418851, -7.957828899753048191, 172.6576833274880869 ) ) ;
#74478 = CARTESIAN_POINT ( 'NONE',  ( 19.03943276465977164, -0.05219959533909143690, 88.74890960531436690 ) ) ;
#74479 = CARTESIAN_POINT ( 'NONE',  ( -12.06949235617756955, 12.14591786802309770, 115.6239096053143669 ) ) ;
#74480 = CARTESIAN_POINT ( 'NONE',  ( -15.80617190586745835, -15.72974639402198527, 61.87390960531436690 ) ) ;
#74481 = CARTESIAN_POINT ( 'NONE',  ( -16.52544592524335698, -4.483927247898792601, 53.95942372801900433 ) ) ;
#74482 = CARTESIAN_POINT ( 'NONE',  ( 5.823673210054444382, -21.52544592524334988, 100.2094237280190043 ) ) ;
#74483 = CARTESIAN_POINT ( 'NONE',  ( 0.05219959533909260263, 19.03943276465977164, 39.99890960531436690 ) ) ;
#74484 = CARTESIAN_POINT ( 'NONE',  ( -8.224510206698948167, 14.34966873604960824, 35.41557627198102409 ) ) ;
#74485 = CARTESIAN_POINT ( 'NONE',  ( 16.55341960407611168, 4.379528057220329451, 63.95724293864770260 ) ) ;
#74486 = CARTESIAN_POINT ( 'NONE',  ( -19.02544592524342804, 5.153800228976336051, 71.04057627198099567 ) ) ;
#74487 = CARTESIAN_POINT ( 'NONE',  ( -18.67979575497193778, 10.72451020669871902, 113.3344237280190328 ) ) ;
#74488 = CARTESIAN_POINT ( 'NONE',  ( 18.62759615963255655, 10.81492255796105972, 26.66775706135235424 ) ) ;
#74489 = CARTESIAN_POINT ( 'NONE',  ( -5.153800228976328057, -19.02544592524343514, 82.29057627198103830 ) ) ;
#74490 = CARTESIAN_POINT ( 'NONE',  ( 5.823673210054444382, -21.52544592524334988, 90.20942372801903275 ) ) ;
#74491 = CARTESIAN_POINT ( 'NONE',  ( 4.483927247898790824, -16.52544592524335698, 50.20942372801901854 ) ) ;
#74492 = CARTESIAN_POINT ( 'NONE',  ( 14.34966873604972726, -8.224510206698740333, 35.83442372801901143 ) ) ;
#74494 = CARTESIAN_POINT ( 'NONE',  ( -21.55341960407619339, 5.719274019375674811, 98.54275706135234714 ) ) ;
#74493 = CARTESIAN_POINT ( 'NONE',  ( -16.55341960407611168, -4.379528057220339221, 86.45724293864770971 ) ) ;
#74495 = CARTESIAN_POINT ( 'NONE',  ( -8.224510206698948167, 14.34966873604960824, 40.41557627198103120 ) ) ;
#74496 = CARTESIAN_POINT ( 'NONE',  ( 13.89961937509977652, -13.97604488694527269, 28.12390960531435624 ) ) ;
#74497 = CARTESIAN_POINT ( 'NONE',  ( -12.14591786802326823, 12.06949235617739902, 48.12609039468568284 ) ) ;
#74498 = CARTESIAN_POINT ( 'NONE',  ( 4.379528057220339221, -16.55341960407611168, 57.70724293864770260 ) ) ;
#74499 = CARTESIAN_POINT ( 'NONE',  ( 0.05219959533934541429, -16.53943276465976808, 95.00109039468568994 ) ) ;
#74500 = CARTESIAN_POINT ( 'NONE',  ( 21.52544592524344225, -5.823673210054117533, 23.54057627198102765 ) ) ;
#74501 = CARTESIAN_POINT ( 'NONE',  ( 19.02544592524343514, -5.153800228976328945, 108.5405762719810383 ) ) ;
#74502 = CARTESIAN_POINT ( 'NONE',  ( 0.05219959533937995610, -21.53943276465977519, 110.0010903946856757 ) ) ;
#74503 = CARTESIAN_POINT ( 'NONE',  ( -8.314922557960811034, -14.29746914071050412, 92.08224293864769550 ) ) ;
#74504 = CARTESIAN_POINT ( 'NONE',  ( 9.564922557960805705, 16.46253265017160317, 94.58224293864769550 ) ) ;
#74505 = ORIENTED_EDGE ( 'NONE', *, *, #21468, .F. ) ;
#74506 = CARTESIAN_POINT ( 'NONE',  ( 12.14591786802327356, -12.06949235617739191, 35.62609039468568994 ) ) ;
#74507 = CARTESIAN_POINT ( 'NONE',  ( -9.564922557960796823, -16.46253265017161027, 47.08224293864769550 ) ) ;
#74509 = PLANE ( 'NONE',  #127534 ) ;
#74508 = CARTESIAN_POINT ( 'NONE',  ( 8.314922557961029526, -14.29746914071037800, 50.41775706135235424 ) ) ;
#74510 = CARTESIAN_POINT ( 'NONE',  ( -19.03943276465977164, -0.05219959533935918106, 43.75109039468566863 ) ) ;
#74511 = CARTESIAN_POINT ( 'NONE',  ( 9.474510206698971260, -16.51473224551069308, 42.91557627198103120 ) ) ;
#74512 = CARTESIAN_POINT ( 'NONE',  ( 0.05219959533934541429, -16.53943276465976808, 85.00109039468568994 ) ) ;
#74513 = CARTESIAN_POINT ( 'NONE',  ( -16.46253265017146816, -9.564922557961047289, 79.16775706135234714 ) ) ;
#74514 = CARTESIAN_POINT ( 'NONE',  ( -19.05341960407617563, 5.049401038297882671, 28.54275706135232937 ) ) ;
#74515 = CARTESIAN_POINT ( 'NONE',  ( -9.474510206698964154, 16.51473224551069663, 65.41557627198102409 ) ) ;
#74516 = CARTESIAN_POINT ( 'NONE',  ( 14.34966873604960469, 8.224510206698951720, 104.1655762719810241 ) ) ;
#74517 = EDGE_CURVE ( 'NONE', #185763, #30659, #157899, .T. ) ;
#74518 = CARTESIAN_POINT ( 'NONE',  ( -9.564922557961040184, 16.46253265017147172, 62.91775706135233293 ) ) ;
#74519 = CARTESIAN_POINT ( 'NONE',  ( 21.55341960407610458, 5.719274019375980345, 63.95724293864770260 ) ) ;
#74520 = CARTESIAN_POINT ( 'NONE',  ( 9.474510206698729675, 16.51473224551082808, 32.08442372801900433 ) ) ;
#74521 = CARTESIAN_POINT ( 'NONE',  ( -5.049401038298153566, 19.05341960407611168, 105.2072429386476671 ) ) ;
#74522 = CARTESIAN_POINT ( 'NONE',  ( -15.80617190586745835, -15.72974639402198527, 76.87390960531439532 ) ) ;
#74523 = CARTESIAN_POINT ( 'NONE',  ( -16.79531203550646623, 7.028104445595604766, 83.74755011779558345 ) ) ;
#74524 = CARTESIAN_POINT ( 'NONE',  ( -0.05219959533936034679, 19.03943276465977164, 107.5010903946856615 ) ) ;
#74525 = CARTESIAN_POINT ( 'NONE',  ( -17.72560187377284180, -5.500000000000007105, 99.07814504131322053 ) ) ;
#74526 = CARTESIAN_POINT ( 'NONE',  ( -16.53943276465976808, -0.05219959533934237506, 33.75109039468568284 ) ) ;
#74527 = CARTESIAN_POINT ( 'NONE',  ( 13.89961937509977652, -13.97604488694527269, 28.12390960531435624 ) ) ;
#74528 = CARTESIAN_POINT ( 'NONE',  ( -5.153800228976328057, -19.02544592524343514, 112.2905762719810099 ) ) ;
#74529 = CARTESIAN_POINT ( 'NONE',  ( -18.67979575497178146, -10.72451020669898902, 86.66557627198102409 ) ) ;
#74530 = CARTESIAN_POINT ( 'NONE',  ( -5.823673210054431948, 21.52544592524334988, 62.70942372801902565 ) ) ;
#74532 = CARTESIAN_POINT ( 'NONE',  ( -13.89961937509957401, -13.97604488694547875, 19.37609039468566507 ) ) ;
#74531 = CARTESIAN_POINT ( 'NONE',  ( 9.474510206698729675, 16.51473224551082808, 112.0844237280190043 ) ) ;
#74533 = CARTESIAN_POINT ( 'NONE',  ( -16.55341960407617563, 4.379528057220093196, 103.5427570613523613 ) ) ;
#74534 = CARTESIAN_POINT ( 'NONE',  ( -21.53943276465977519, 0.05219959533907696930, 101.2489096053143669 ) ) ;
#74535 = CARTESIAN_POINT ( 'NONE',  ( 16.55341960407611168, 4.379528057220329451, 53.95724293864770260 ) ) ;
#74536 = CARTESIAN_POINT ( 'NONE',  ( -13.97604488694547697, 13.89961937509957934, 83.12609039468564731 ) ) ;
#74537 = CARTESIAN_POINT ( 'NONE',  ( 13.97604488694548053, -13.89961937509957401, 55.62609039468566863 ) ) ;
#74538 = CARTESIAN_POINT ( 'NONE',  ( 10.72451020669871369, 18.67979575497193778, 57.08442372801901854 ) ) ;
#74539 = CARTESIAN_POINT ( 'NONE',  ( -13.89961937509957401, -13.97604488694547875, 34.37609039468566863 ) ) ;
#74540 = CARTESIAN_POINT ( 'NONE',  ( -8.224510206698948167, 14.34966873604960824, 100.4155762719810241 ) ) ;
#74541 = CARTESIAN_POINT ( 'NONE',  ( 5.719274019375991003, -21.55341960407610458, 47.70724293864770260 ) ) ;
#74542 = CARTESIAN_POINT ( 'NONE',  ( 12.14591786802309770, 12.06949235617756955, 39.37390960531436690 ) ) ;
#74543 = CARTESIAN_POINT ( 'NONE',  ( -5.823673210054431948, 21.52544592524334988, 102.7094237280190185 ) ) ;
#74544 = CARTESIAN_POINT ( 'NONE',  ( 16.53943276465976808, 0.05219959533934440121, 66.25109039468567573 ) ) ;
#74545 = CARTESIAN_POINT ( 'NONE',  ( -0.05219959533910754901, -16.53943276465976808, 32.49890960531435979 ) ) ;
#74546 = CARTESIAN_POINT ( 'NONE',  ( -5.719274019375665041, -21.55341960407619695, 64.79275706135234714 ) ) ;
#74547 = CARTESIAN_POINT ( 'NONE',  ( -10.81492255796105439, 18.62759615963255655, 62.91775706135236135 ) ) ;
#74548 = CARTESIAN_POINT ( 'NONE',  ( 18.67979575497178502, 10.72451020669898547, 69.16557627198102409 ) ) ;
#74549 = CARTESIAN_POINT ( 'NONE',  ( 21.52544592524334988, 5.823673210054432836, 46.45942372801901854 ) ) ;
#74550 = CARTESIAN_POINT ( 'NONE',  ( 5.153800228976335163, 19.02544592524342804, 24.79057627198102765 ) ) ;
#74551 = CARTESIAN_POINT ( 'NONE',  ( 13.89961937509977652, -13.97604488694527269, 38.12390960531436690 ) ) ;
#74552 = CARTESIAN_POINT ( 'NONE',  ( -8.224510206698948167, 14.34966873604960824, 80.41557627198103830 ) ) ;
#74553 = CARTESIAN_POINT ( 'NONE',  ( -19.05341960407611168, -5.049401038298163336, 91.45724293864766707 ) ) ;
#74554 = CARTESIAN_POINT ( 'NONE',  ( -16.55341960407617563, 4.379528057220093196, 113.5427570613523756 ) ) ;
#74555 = CARTESIAN_POINT ( 'NONE',  ( -0.05219959533910754901, -16.53943276465976808, 97.49890960531436690 ) ) ;
#74556 = CARTESIAN_POINT ( 'NONE',  ( -21.55341960407610458, -5.719274019375992779, 71.45724293864769550 ) ) ;
#74557 = CARTESIAN_POINT ( 'NONE',  ( -18.67979575497178146, -10.72451020669898902, 111.6655762719810525 ) ) ;
#74558 = CARTESIAN_POINT ( 'NONE',  ( -16.51473224551069308, -9.474510206698971260, 111.6655762719810383 ) ) ;
#74560 = CARTESIAN_POINT ( 'NONE',  ( 13.97604488694548053, -13.89961937509957401, 100.6260903946856615 ) ) ;
#74559 = CARTESIAN_POINT ( 'NONE',  ( 0.05219959533909260263, 19.03943276465977164, 69.99890960531435269 ) ) ;
#74561 = CARTESIAN_POINT ( 'NONE',  ( 21.52544592524344225, -5.823673210054117533, 58.54057627198103120 ) ) ;
#74562 = CARTESIAN_POINT ( 'NONE',  ( -5.823673210054431948, 21.52544592524334988, 87.70942372801901854 ) ) ;
#74563 = CARTESIAN_POINT ( 'NONE',  ( 5.153800228976335163, 19.02544592524342804, 64.79057627198100988 ) ) ;
#74564 = CARTESIAN_POINT ( 'NONE',  ( 13.97604488694527802, 13.89961937509977652, 99.37390960531436690 ) ) ;
#74565 = CARTESIAN_POINT ( 'NONE',  ( 8.224510206698742110, 14.34966873604972548, 72.08442372801899012 ) ) ;
#74566 = CARTESIAN_POINT ( 'NONE',  ( 10.72451020669871369, 18.67979575497193778, 62.08442372801901143 ) ) ;
#74567 = CARTESIAN_POINT ( 'NONE',  ( -21.52544592524334988, -5.823673210054445271, 93.95942372801903275 ) ) ;
#74568 = CARTESIAN_POINT ( 'NONE',  ( 21.55341960407610458, 5.719274019375980345, 113.9572429386477239 ) ) ;
#74569 = CARTESIAN_POINT ( 'NONE',  ( 15.80617190586746368, 15.72974639402197994, 84.37390960531438111 ) ) ;
#74570 = CARTESIAN_POINT ( 'NONE',  ( 19.05341960407617918, -5.049401038297876454, 41.04275706135233293 ) ) ;
#74571 = CARTESIAN_POINT ( 'NONE',  ( -21.52544592524343514, 5.823673210054127303, 36.04057627198102409 ) ) ;
#74573 = CARTESIAN_POINT ( 'NONE',  ( -14.29746914071049879, 8.314922557960819915, 35.83224293864768839 ) ) ;
#74572 = CARTESIAN_POINT ( 'NONE',  ( 19.02544592524343514, -5.153800228976328945, 83.54057627198100988 ) ) ;
#74574 = CARTESIAN_POINT ( 'NONE',  ( -17.49999999999999645, 5.499999999999992895, 63.71769037696435589 ) ) ;
#74575 = LINE ( 'NONE', #90716, #44323 ) ;
#74576 = CARTESIAN_POINT ( 'NONE',  ( 13.89961937509957401, 13.97604488694547697, 96.87609039468566152 ) ) ;
#74577 = CARTESIAN_POINT ( 'NONE',  ( -21.55341960407610458, -5.719274019375992779, 66.45724293864768129 ) ) ;
#74578 = CARTESIAN_POINT ( 'NONE',  ( -12.06949235617756955, 12.14591786802309770, 50.62390960531435979 ) ) ;
#74579 = CARTESIAN_POINT ( 'NONE',  ( 16.52544592524335698, 4.483927247898782831, 36.45942372801901143 ) ) ;
#74580 = CARTESIAN_POINT ( 'NONE',  ( -19.02544592524342804, 5.153800228976336051, 51.04057627198103120 ) ) ;
#74582 = CARTESIAN_POINT ( 'NONE',  ( 5.153800228976615827, -19.02544592524334988, 85.20942372801900433 ) ) ;
#74581 = CARTESIAN_POINT ( 'NONE',  ( 15.72974639402199770, -15.80617190586745480, 108.1239096053143811 ) ) ;
#74583 = CARTESIAN_POINT ( 'NONE',  ( -13.89961937509977652, 13.97604488694528158, 75.62390960531438111 ) ) ;
#74584 = CARTESIAN_POINT ( 'NONE',  ( -4.483927247898539470, -16.52544592524342804, 92.29057627198103830 ) ) ;
#74585 = CARTESIAN_POINT ( 'NONE',  ( 13.97604488694527802, 13.89961937509977652, 79.37390960531435269 ) ) ;
#74586 = CARTESIAN_POINT ( 'NONE',  ( -5.719274019375978568, 21.55341960407610458, 80.20724293864769550 ) ) ;
#74587 = CARTESIAN_POINT ( 'NONE',  ( 16.46253265017160672, -9.564922557960803928, 28.33224293864769550 ) ) ;
#74588 = CARTESIAN_POINT ( 'NONE',  ( 10.18315950979500251, 36.03432976468644000, -8.000000000000003553 ) ) ;
#74589 = CARTESIAN_POINT ( 'NONE',  ( 12.14591786802309770, 12.06949235617756955, 59.37390960531436690 ) ) ;
#74590 = CARTESIAN_POINT ( 'NONE',  ( 13.89961937509977652, -13.97604488694527269, 93.12390960531436690 ) ) ;
#74591 = CARTESIAN_POINT ( 'NONE',  ( 17.81289503416611453, -24.51734667627695785, 140.9500000054623570 ) ) ;
#74592 = CARTESIAN_POINT ( 'NONE',  ( -13.89961937509957401, -13.97604488694547875, 49.37609039468567573 ) ) ;
#74593 = CARTESIAN_POINT ( 'NONE',  ( 14.29746914071037800, 8.314922557961029526, 56.66775706135235424 ) ) ;
#74594 = CARTESIAN_POINT ( 'NONE',  ( 5.823673210054125526, 21.52544592524343514, 74.79057627198105251 ) ) ;
#74595 = CARTESIAN_POINT ( 'NONE',  ( 5.153800228976615827, -19.02544592524334988, 40.20942372801898301 ) ) ;
#74596 = CARTESIAN_POINT ( 'NONE',  ( 5.153800228976335163, 19.02544592524342804, 84.79057627198099567 ) ) ;
#74597 = CARTESIAN_POINT ( 'NONE',  ( 11.09567578556706025, -9.260623346590088900, -60.14574966503957398 ) ) ;
#74598 = CARTESIAN_POINT ( 'NONE',  ( -21.52544592524343514, 5.823673210054127303, 31.04057627198102409 ) ) ;
#74599 = MANIFOLD_SOLID_BREP ( 'Hex', #30422 ) ;
#74600 = CARTESIAN_POINT ( 'NONE',  ( -5.153800228976328057, -19.02544592524343514, 72.29057627198102409 ) ) ;
#74601 = CARTESIAN_POINT ( 'NONE',  ( 21.55341960407619695, -5.719274019375665929, 46.04275706135234714 ) ) ;
#74602 = CARTESIAN_POINT ( 'NONE',  ( -14.29746914071049879, 8.314922557960819915, 115.8322429386477097 ) ) ;
#74605 = ORIENTED_EDGE ( 'NONE', *, *, #38962, .T. ) ;
#74604 = CARTESIAN_POINT ( 'NONE',  ( 19.02544592524343514, -5.153800228976328945, 98.54057627198100988 ) ) ;
#74603 = CARTESIAN_POINT ( 'NONE',  ( -21.53943276465977519, -0.05219959533937600094, 18.75109039468568639 ) ) ;
#74606 = CARTESIAN_POINT ( 'NONE',  ( -18.62759615963255300, -10.81492255796106328, 34.16775706135234714 ) ) ;
#74607 = ORIENTED_EDGE ( 'NONE', *, *, #142789, .F. ) ;
#74608 = CARTESIAN_POINT ( 'NONE',  ( -19.03943276465977164, 0.05219959533909376836, 106.2489096053143669 ) ) ;
#74609 = ADVANCED_FACE ( 'NONE', ( #191225, #84028 ), #174073, .F. ) ;
#74610 = DIRECTION ( 'NONE',  ( -0.000000000000000000, -0.000000000000000000, 1.000000000000000000 ) ) ;
#74611 = CARTESIAN_POINT ( 'NONE',  ( 18.67979575497178502, 10.72451020669898547, 114.1655762719810383 ) ) ;
#74612 = CARTESIAN_POINT ( 'NONE',  ( 13.97604488694527802, 13.89961937509977652, 49.37390960531434558 ) ) ;
#74613 = CARTESIAN_POINT ( 'NONE',  ( -8.224510206698735004, -14.34966873604973081, 29.58442372801901854 ) ) ;
#74614 = CARTESIAN_POINT ( 'NONE',  ( 29.86685920354754487, 21.69954338932564752, -1.924999997268813212 ) ) ;
#74615 = CARTESIAN_POINT ( 'NONE',  ( 15.72974639402176855, 15.80617190586768217, 101.8760903946857042 ) ) ;
#74616 = CARTESIAN_POINT ( 'NONE',  ( 19.03943276465977164, -0.05219959533909143690, 48.74890960531435979 ) ) ;
#74617 = CARTESIAN_POINT ( 'NONE',  ( -10.81492255796105439, 18.62759615963255655, 92.91775706135236135 ) ) ;
#74619 = CARTESIAN_POINT ( 'NONE',  ( -15.72974639402176322, -15.80617190586768395, 59.37609039468568284 ) ) ;
#74618 = CARTESIAN_POINT ( 'NONE',  ( -13.89961937509977652, 13.97604488694528158, 95.62390960531436690 ) ) ;
#74620 = CARTESIAN_POINT ( 'NONE',  ( 8.571926809382603096, -26.38167802310801235, 145.9750000027311785 ) ) ;
#74621 = CARTESIAN_POINT ( 'NONE',  ( -16.46253265017160317, 9.564922557960807481, 95.83224293864769550 ) ) ;
#74622 = CARTESIAN_POINT ( 'NONE',  ( -17.49999999999999289, 3.345213924137299788, 29.58768623094355732 ) ) ;
#74625 = CARTESIAN_POINT ( 'NONE',  ( 10.72451020669871369, 18.67979575497193778, 52.08442372801901854 ) ) ;
#74624 = CARTESIAN_POINT ( 'NONE',  ( -4.483927247898782831, 16.52544592524335698, 62.70942372801902565 ) ) ;
#74623 = CARTESIAN_POINT ( 'NONE',  ( -0.05219959533934338120, 16.53943276465976808, 52.50109039468567573 ) ) ;
#74626 = CARTESIAN_POINT ( 'NONE',  ( 10.72451020669871369, 18.67979575497193778, 92.08442372801901854 ) ) ;
#74627 = DIRECTION ( 'NONE',  ( 1.908195823574487804E-15, 0.000000000000000000, -1.000000000000000000 ) ) ;
#74628 = CARTESIAN_POINT ( 'NONE',  ( -14.29746914071037622, -8.314922557961029526, 29.16775706135234003 ) ) ;
#74629 = CARTESIAN_POINT ( 'NONE',  ( 13.97604488694527802, 13.89961937509977652, 79.37390960531435269 ) ) ;
#74630 = CARTESIAN_POINT ( 'NONE',  ( 9.474510206698971260, -16.51473224551069308, 102.9155762719810241 ) ) ;
#74631 = FACE_OUTER_BOUND ( 'NONE', #12884, .T. ) ;
#74632 = B_SPLINE_CURVE_WITH_KNOTS ( 'NONE', 3,
 ( #45750, #33562, #17401, #153918, #79058, #95224, #168096, #60904, #29594, #156910, #2220, #223, #18407, #136759, #59916, #183279, #169075, #122579, #184268, #107402, #144708, #142717, #96214, #174077, #84030, #100205 ),
 .UNSPECIFIED., .F., .F.,
 ( 4, 2, 2, 2, 2, 2, 2, 2, 2, 2, 2, 2, 4 ),
 ( 8.673617379884035472E-19, 0.002268141957793348533, 0.004536283915586696198, 0.006804425873380042997, 0.009072567831173390662, 0.01360885174676007212, 0.01814513566234675704, 0.02268141957793343502, 0.02721770349352011995, 0.02948584545131345894, 0.03175398740910680140, 0.03402212936690014039, 0.03629027132469347938 ),
 .UNSPECIFIED. ) ;
#74633 = CARTESIAN_POINT ( 'NONE',  ( 13.89961937509977652, -13.97604488694527269, 23.12390960531436335 ) ) ;
#74634 = CARTESIAN_POINT ( 'NONE',  ( -10.72451020669898014, 18.67979575497178502, 35.41557627198102409 ) ) ;
#74635 = CARTESIAN_POINT ( 'NONE',  ( 8.224510206698742110, 14.34966873604972548, 97.08442372801904696 ) ) ;
#74637 = CARTESIAN_POINT ( 'NONE',  ( 19.02544592524343514, -5.153800228976328945, 68.54057627198103830 ) ) ;
#74636 = CARTESIAN_POINT ( 'NONE',  ( 8.224510206698953496, -14.34966873604960469, 67.91557627198102409 ) ) ;
#74638 = CARTESIAN_POINT ( 'NONE',  ( 10.72451020669871369, 18.67979575497193778, 97.08442372801904696 ) ) ;
#74639 = FACE_OUTER_BOUND ( 'NONE', #63649, .T. ) ;
#74640 = CARTESIAN_POINT ( 'NONE',  ( 16.52544592524335698, 4.483927247898782831, 26.45942372801901854 ) ) ;
#74641 = CARTESIAN_POINT ( 'NONE',  ( 8.314922557960818139, 14.29746914071049879, 79.58224293864769550 ) ) ;
#74642 = CARTESIAN_POINT ( 'NONE',  ( 15.72974639402176855, 15.80617190586768217, 21.87609039468567573 ) ) ;
#74643 = CARTESIAN_POINT ( 'NONE',  ( -0.05219959533907301413, -21.53943276465977519, 77.49890960531433848 ) ) ;
#74644 = CARTESIAN_POINT ( 'NONE',  ( 5.049401038297881783, 19.05341960407617563, 37.29275706135232582 ) ) ;
#74645 = CARTESIAN_POINT ( 'NONE',  ( -28.82186960331499392, 9.364793116373565596, 148.1500000054624024 ) ) ;
#74646 = CARTESIAN_POINT ( 'NONE',  ( 0.05219959533909260263, 19.03943276465977164, 84.99890960531436690 ) ) ;
#74647 = CARTESIAN_POINT ( 'NONE',  ( 16.55341960407611168, 4.379528057220329451, 43.95724293864769550 ) ) ;
#74648 = CARTESIAN_POINT ( 'NONE',  ( 4.379528057220339221, -16.55341960407611168, 37.70724293864769550 ) ) ;
#74649 = CARTESIAN_POINT ( 'NONE',  ( 16.55341960407611168, 4.379528057220329451, 23.95724293864769550 ) ) ;
#74650 = CARTESIAN_POINT ( 'NONE',  ( 19.05341960407617918, -5.049401038297876454, 61.04275706135232582 ) ) ;
#74651 = CARTESIAN_POINT ( 'NONE',  ( 18.56101223717332616, 5.499999999999941380, 53.94978406935679516 ) ) ;
#74652 = CARTESIAN_POINT ( 'NONE',  ( -19.02544592524342804, 5.153800228976336051, 101.0405762719810241 ) ) ;
#74653 = CARTESIAN_POINT ( 'NONE',  ( 16.55341960407611168, 4.379528057220329451, 68.95724293864769550 ) ) ;
#74654 = CARTESIAN_POINT ( 'NONE',  ( 19.17291183240699581, -5.500000000000061284, 38.15094504727040459 ) ) ;
#74656 = CARTESIAN_POINT ( 'NONE',  ( -18.67979575497178146, -10.72451020669898902, 41.66557627198103120 ) ) ;
#74655 = CARTESIAN_POINT ( 'NONE',  ( -5.153800228976328057, -19.02544592524343514, 27.29057627198103120 ) ) ;
#74657 = CARTESIAN_POINT ( 'NONE',  ( -5.823673210054116645, -21.52544592524344225, 72.29057627198102409 ) ) ;
#74658 = CARTESIAN_POINT ( 'NONE',  ( 4.483927247898545687, 16.52544592524342804, 109.7905762719810383 ) ) ;
#74660 = CARTESIAN_POINT ( 'NONE',  ( -16.46253265017160317, 9.564922557960807481, 40.83224293864769550 ) ) ;
#74659 = CARTESIAN_POINT ( 'NONE',  ( -16.55341960407617563, 4.379528057220093196, 63.54275706135234003 ) ) ;
#74661 = CARTESIAN_POINT ( 'NONE',  ( 0.05219959533937995610, -21.53943276465977519, 60.00109039468568284 ) ) ;
#74662 = ORIENTED_EDGE ( 'NONE', *, *, #53692, .F. ) ;
#74663 = CARTESIAN_POINT ( 'NONE',  ( 16.55341960407611168, 4.379528057220329451, 103.9572429386476813 ) ) ;
#74664 = CARTESIAN_POINT ( 'NONE',  ( 17.05116617787826527, -6.768360034955669846, 36.15675553259198693 ) ) ;
#74665 = CARTESIAN_POINT ( 'NONE',  ( -36.91746825000000598, -11.99521256947794789, -11.02499999726881263 ) ) ;
#74666 = CARTESIAN_POINT ( 'NONE',  ( -0.05219959533907301413, -21.53943276465977519, 37.49890960531436690 ) ) ;
#74667 = CYLINDRICAL_SURFACE ( 'NONE', #17203, 7.500000000000000000 ) ;
#74669 = CARTESIAN_POINT ( 'NONE',  ( 1.500000000000345945, 22.97976134357531564, -57.70670369762110141 ) ) ;
#74668 = CARTESIAN_POINT ( 'NONE',  ( -15.72974639402176322, -15.80617190586768395, 74.37609039468568994 ) ) ;
#74671 = CARTESIAN_POINT ( 'NONE',  ( 16.53943276465976808, -0.05219959533910856209, 38.74890960531435979 ) ) ;
#74670 = CARTESIAN_POINT ( 'NONE',  ( 16.52544592524335698, 4.483927247898782831, 61.45942372801901854 ) ) ;
#74672 = CARTESIAN_POINT ( 'NONE',  ( -5.823673210054116645, -21.52544592524344225, 62.29057627198102409 ) ) ;
#74673 = CARTESIAN_POINT ( 'NONE',  ( 21.55341960407610458, 5.719274019375980345, 58.95724293864770971 ) ) ;
#74674 = CARTESIAN_POINT ( 'NONE',  ( 31.88558403383513706, -20.67508902814666882, -24.22575984094845936 ) ) ;
#74676 = CARTESIAN_POINT ( 'NONE',  ( 0.05219959533907565091, 21.53943276465977519, 24.99890960531435624 ) ) ;
#74675 = CARTESIAN_POINT ( 'NONE',  ( -9.564922557961040184, 16.46253265017147172, 87.91775706135233293 ) ) ;
#74677 = CARTESIAN_POINT ( 'NONE',  ( -19.03943276465977164, 0.05219959533909376836, 46.24890960531435979 ) ) ;
#74678 = CARTESIAN_POINT ( 'NONE',  ( 19.03943276465977164, -0.05219959533909143690, 23.74890960531435269 ) ) ;
#74679 =( NAMED_UNIT ( * ) PLANE_ANGLE_UNIT ( ) SI_UNIT ( $, .RADIAN. ) );
#74680 = DIRECTION ( 'NONE',  ( -0.000000000000000000, -0.000000000000000000, -1.000000000000000000 ) ) ;
#74681 = ORIENTED_EDGE ( 'NONE', *, *, #182367, .F. ) ;
#74682 = CARTESIAN_POINT ( 'NONE',  ( -16.52544592524335698, -4.483927247898792601, 68.95942372801901854 ) ) ;
#74683 = CARTESIAN_POINT ( 'NONE',  ( 21.55341960407610458, 5.719274019375980345, 103.9572429386476813 ) ) ;
#74684 = CARTESIAN_POINT ( 'NONE',  ( -13.97604488694527625, -13.89961937509977652, 61.87390960531435979 ) ) ;
#74685 = CARTESIAN_POINT ( 'NONE',  ( -0.05219959533937732626, 21.53943276465977519, 37.50109039468568284 ) ) ;
#74686 = CARTESIAN_POINT ( 'NONE',  ( -0.05219959533909027116, -19.03943276465977164, 97.49890960531436690 ) ) ;
#74687 = CARTESIAN_POINT ( 'NONE',  ( -25.95926362436877710, -29.82107321766972774, -18.67624575278512822 ) ) ;
#74688 = ORIENTED_EDGE ( 'NONE', *, *, #67133, .F. ) ;
#74689 = CARTESIAN_POINT ( 'NONE',  ( 15.80617190586769283, -15.72974639402175789, 30.62609039468567929 ) ) ;
#74691 = CARTESIAN_POINT ( 'NONE',  ( 16.51473224551083163, -9.474510206698727899, 85.83442372801900433 ) ) ;
#74690 = CARTESIAN_POINT ( 'NONE',  ( -19.05341960407611168, -5.049401038298163336, 106.4572429386476955 ) ) ;
#74692 = EDGE_CURVE ( 'NONE', #8743, #92102, #137705, .T. ) ;
#74693 = CARTESIAN_POINT ( 'NONE',  ( -13.97604488694547697, 13.89961937509957934, 43.12609039468566152 ) ) ;
#74694 = CARTESIAN_POINT ( 'NONE',  ( 15.80617190586746368, 15.72974639402197994, 94.37390960531436690 ) ) ;
#74695 = CARTESIAN_POINT ( 'NONE',  ( 19.03943276465977164, 0.05219959533936151252, 36.25109039468567573 ) ) ;
#74696 = CARTESIAN_POINT ( 'NONE',  ( 5.153800228976615827, -19.02544592524334988, 50.20942372801897591 ) ) ;
#74697 = CARTESIAN_POINT ( 'NONE',  ( -0.05219959533934338120, 16.53943276465976808, 97.50109039468567573 ) ) ;
#74699 = VERTEX_POINT ( 'NONE', #8201 ) ;
#74698 = CARTESIAN_POINT ( 'NONE',  ( 5.000000000000000000, -132.8113331068338425, 10.91562811307057679 ) ) ;
#74700 = CARTESIAN_POINT ( 'NONE',  ( -19.05341960407611168, -5.049401038298163336, 66.45724293864769550 ) ) ;
#74701 = CARTESIAN_POINT ( 'NONE',  ( -21.55341960407619339, 5.719274019375674811, 83.54275706135234714 ) ) ;
#74702 = CARTESIAN_POINT ( 'NONE',  ( 10.81492255796106328, -18.62759615963255655, 75.41775706135233293 ) ) ;
#74703 = DIRECTION ( 'NONE',  ( 0.4999999999999966693, -0.5000000000000019984, -0.7071067811865483499 ) ) ;
#74704 = CARTESIAN_POINT ( 'NONE',  ( 9.474510206698971260, -16.51473224551069308, 87.91557627198102409 ) ) ;
#74705 = CARTESIAN_POINT ( 'NONE',  ( 15.80617190586769283, -15.72974639402175789, 55.62609039468568284 ) ) ;
#74706 = CARTESIAN_POINT ( 'NONE',  ( 0.05219959533936267826, -19.03943276465977164, 100.0010903946856757 ) ) ;
#74707 = ADVANCED_FACE ( 'NONE', ( #193229 ), #97189, .F. ) ;
#74708 = CARTESIAN_POINT ( 'NONE',  ( -5.153800228976328057, -19.02544592524343514, 67.29057627198102409 ) ) ;
#74709 = CARTESIAN_POINT ( 'NONE',  ( -13.97604488694527625, -13.89961937509977652, 106.8739096053143669 ) ) ;
#74710 = CARTESIAN_POINT ( 'NONE',  ( 5.153800228976335163, 19.02544592524342804, 84.79057627198099567 ) ) ;
#74711 = CARTESIAN_POINT ( 'NONE',  ( 17.50000000000000000, -3.456093896842488800, 22.00000000000000711 ) ) ;
#74712 = CARTESIAN_POINT ( 'NONE',  ( -16.46253265017160317, 9.564922557960807481, 60.83224293864769550 ) ) ;
#74713 = CARTESIAN_POINT ( 'NONE',  ( -16.46253265017160317, 9.564922557960807481, 55.83224293864769550 ) ) ;
#74714 = CARTESIAN_POINT ( 'NONE',  ( -5.719274019375978568, 21.55341960407610458, 95.20724293864769550 ) ) ;
#74715 = CARTESIAN_POINT ( 'NONE',  ( -16.52544592524335698, -4.483927247898792601, 88.95942372801901854 ) ) ;
#74716 = FACE_OUTER_BOUND ( 'NONE', #182787, .T. ) ;
#74717 = CARTESIAN_POINT ( 'NONE',  ( -9.474510206698720793, -16.51473224551083518, 44.58442372801900433 ) ) ;
#74718 = CARTESIAN_POINT ( 'NONE',  ( -19.05341960407611168, -5.049401038298163336, 76.45724293864769550 ) ) ;
#74719 = CARTESIAN_POINT ( 'NONE',  ( 16.53943276465976808, -0.05219959533910856209, 68.74890960531435269 ) ) ;
#74720 = CARTESIAN_POINT ( 'NONE',  ( 8.314922557960818139, 14.29746914071049879, 114.5822429386477097 ) ) ;
#74721 = CARTESIAN_POINT ( 'NONE',  ( -5.823673210054116645, -21.52544592524344225, 22.29057627198102765 ) ) ;
#74722 = CARTESIAN_POINT ( 'NONE',  ( -19.03943276465977164, 0.05219959533909376836, 101.2489096053143669 ) ) ;
#74723 = CARTESIAN_POINT ( 'NONE',  ( -4.379528057220328563, 16.55341960407611168, 85.20724293864770971 ) ) ;
#74724 = CARTESIAN_POINT ( 'NONE',  ( 13.89961937509957401, 13.97604488694547697, 26.87609039468566507 ) ) ;
#74725 = CARTESIAN_POINT ( 'NONE',  ( 16.53943276465976808, 0.05219959533934440121, 91.25109039468568994 ) ) ;
#74726 = CARTESIAN_POINT ( 'NONE',  ( 5.153800228976335163, 19.02544592524342804, 79.79057627198102409 ) ) ;
#74727 = CARTESIAN_POINT ( 'NONE',  ( -21.53943276465977519, -0.05219959533937600094, 53.75109039468568994 ) ) ;
#74728 = CARTESIAN_POINT ( 'NONE',  ( 18.62759615963271287, -10.81492255796078972, 48.33224293864770260 ) ) ;
#74729 = CARTESIAN_POINT ( 'NONE',  ( -0.05219959533937732626, 21.53943276465977519, 22.50109039468567573 ) ) ;
#74730 = CARTESIAN_POINT ( 'NONE',  ( -18.62759615963270932, 10.81492255796079327, 70.83224293864770971 ) ) ;
#74731 = CARTESIAN_POINT ( 'NONE',  ( 8.224510206698953496, -14.34966873604960469, 92.91557627198103830 ) ) ;
#74732 = CARTESIAN_POINT ( 'NONE',  ( 0.05219959533936267826, -19.03943276465977164, 55.00109039468566863 ) ) ;
#74733 = CARTESIAN_POINT ( 'NONE',  ( 13.89961937509977652, -13.97604488694527269, 38.12390960531436690 ) ) ;
#74734 =( BOUNDED_CURVE ( )  B_SPLINE_CURVE ( 2, ( #157118, #21585, #83243, #66089, #125780, #187482, #189456, #48949, #50934, #172284, #18614, #80261, #8423 ),
 .UNSPECIFIED., .F., .T. ) 
 B_SPLINE_CURVE_WITH_KNOTS ( ( 3, 2, 2, 2, 2, 2, 3 ),
 ( 0.5287462259007293941, 0.5307017543859648967, 0.5350877192982456121, 0.5394736842105263275, 0.5438596491228070429, 0.5482456140350877583, 0.5501554626982332330 ),
 .UNSPECIFIED. ) 
 CURVE ( )  GEOMETRIC_REPRESENTATION_ITEM ( )  RATIONAL_B_SPLINE_CURVE ( ( 0.9831626618144007068, 0.9848076720550096308, 1.000000000000000000, 0.9659258262890683122, 1.000000000000000000, 0.9659258262890683122, 1.000000000000000000, 0.9659258262890683122, 1.000000000000000000, 0.9659258262890683122, 1.000000000000000000, 0.9851625545550091179, 0.9832469066685282089 ) ) 
 REPRESENTATION_ITEM ( '' )  );
#74735 = CARTESIAN_POINT ( 'NONE',  ( -9.564922557960796823, -16.46253265017161027, 87.08224293864769550 ) ) ;
#74736 = CARTESIAN_POINT ( 'NONE',  ( 16.46253265017160672, -9.564922557960803928, 88.33224293864769550 ) ) ;
#74737 = CARTESIAN_POINT ( 'NONE',  ( -16.52544592524342804, 4.483927247898546575, 96.04057627198102409 ) ) ;
#74738 = CARTESIAN_POINT ( 'NONE',  ( 16.55341960407611168, 4.379528057220329451, 28.95724293864769905 ) ) ;
#74739 = CARTESIAN_POINT ( 'NONE',  ( -4.483927247898782831, 16.52544592524335698, 32.70942372801900433 ) ) ;
#74740 = CARTESIAN_POINT ( 'NONE',  ( -18.62759615963255300, -10.81492255796106328, 89.16775706135236135 ) ) ;
#74741 = CARTESIAN_POINT ( 'NONE',  ( 19.03943276465977164, -0.05219959533909143690, 103.7489096053143669 ) ) ;
#74742 = CARTESIAN_POINT ( 'NONE',  ( 10.72451020669871369, 18.67979575497193778, 22.08442372801901143 ) ) ;
#74743 = CARTESIAN_POINT ( 'NONE',  ( -13.97604488694527625, -13.89961937509977652, 41.87390960531435979 ) ) ;
#74744 = CARTESIAN_POINT ( 'NONE',  ( 8.314922557961029526, -14.29746914071037800, 50.41775706135235424 ) ) ;
#74745 = CARTESIAN_POINT ( 'NONE',  ( 16.46253265017146816, 9.564922557961045513, 101.6677570613523329 ) ) ;
#74746 = CARTESIAN_POINT ( 'NONE',  ( 9.474510206698971260, -16.51473224551069308, 37.91557627198102409 ) ) ;
#74747 = CARTESIAN_POINT ( 'NONE',  ( 14.29746914071049879, -8.314922557960816363, 98.33224293864769550 ) ) ;
#74748 = CARTESIAN_POINT ( 'NONE',  ( -10.72451020669898014, 18.67979575497178502, 110.4155762719810383 ) ) ;
#74749 = CARTESIAN_POINT ( 'NONE',  ( 16.46253265017146816, 9.564922557961045513, 81.66775706135233293 ) ) ;
#74750 = CARTESIAN_POINT ( 'NONE',  ( -16.51473224551069308, -9.474510206698971260, 21.66557627198102765 ) ) ;
#74751 = CARTESIAN_POINT ( 'NONE',  ( -9.474510206698964154, 16.51473224551069663, 85.41557627198102409 ) ) ;
#74752 = CARTESIAN_POINT ( 'NONE',  ( 5.719274019375991003, -21.55341960407610458, 112.7072429386476955 ) ) ;
#74753 = CARTESIAN_POINT ( 'NONE',  ( -13.89961937509977652, 13.97604488694528158, 25.62390960531434558 ) ) ;
#74754 = CARTESIAN_POINT ( 'NONE',  ( -16.51473224551069308, -9.474510206698971260, 86.66557627198102409 ) ) ;
#74755 = CARTESIAN_POINT ( 'NONE',  ( 16.21995358207305671, -7.366697692864175195, 112.4355100151216504 ) ) ;
#74756 = B_SPLINE_CURVE_WITH_KNOTS ( 'NONE', 3,
 ( #190471, #192468, #21612, #23621, #191456, #85268, #177316, #66116, #70120, #127781, #100444, #131791, #112618, #54948, #174310, #35779, #195482, #71121, #39772, #179320, #27635, #163127, #194474, #104450, #26627, #132787, #73135, #118631, #74121, #121586, #42787, #166133, #24630, #56957, #55946, #101436, #40784, #89276, #59918, #151941, #103457, #88270 ),
 .UNSPECIFIED., .F., .F.,
 ( 4, 2, 2, 2, 2, 2, 2, 2, 2, 2, 2, 2, 2, 2, 2, 2, 2, 2, 2, 2, 4 ),
 ( 0.004226304204691699526, 0.005303825792898752590, 0.005842586587002279556, 0.006381347381105806522, 0.007458868969312861322, 0.008536390557519916988, 0.009613912145726972655, 0.01069143373393402832, 0.01123019452803756396, 0.01176895532214110307, 0.01284647691034817608, 0.01392399849855525083, 0.01446275929265878647, 0.01500152008676232558, 0.01607904167496940206, 0.01715656326317647334, 0.01823408485138354809, 0.01877284564548709067, 0.01931160643959063325, 0.02038912802779771494, 0.02146664961600480703 ),
 .UNSPECIFIED. ) ;
#74757 = CARTESIAN_POINT ( 'NONE',  ( 19.03943276465977164, -0.05219959533909143690, 83.74890960531436690 ) ) ;
#74759 = CARTESIAN_POINT ( 'NONE',  ( -4.379528057220328563, 16.55341960407611168, 75.20724293864769550 ) ) ;
#74758 = CARTESIAN_POINT ( 'NONE',  ( -5.823673210054431948, 21.52544592524334988, 37.70942372801900433 ) ) ;
#74760 = CARTESIAN_POINT ( 'NONE',  ( -19.02544592524342804, 5.153800228976336051, 101.0405762719810241 ) ) ;
#74761 = CARTESIAN_POINT ( 'NONE',  ( 9.474510206698729675, 16.51473224551082808, 27.08442372801900433 ) ) ;
#74762 = CARTESIAN_POINT ( 'NONE',  ( 0.05219959533934541429, -16.53943276465976808, 45.00109039468568284 ) ) ;
#74763 = CARTESIAN_POINT ( 'NONE',  ( 18.62759615963255655, 10.81492255796105972, 61.66775706135235424 ) ) ;
#74764 = CARTESIAN_POINT ( 'NONE',  ( 14.29746914071037800, 8.314922557961029526, 31.66775706135234358 ) ) ;
#74765 = CARTESIAN_POINT ( 'NONE',  ( 16.51473224551069308, 9.474510206698969483, 69.16557627198102409 ) ) ;
#74766 = CARTESIAN_POINT ( 'NONE',  ( -13.89961937509957401, -13.97604488694547875, 99.37609039468567573 ) ) ;
#74767 = CARTESIAN_POINT ( 'NONE',  ( 16.52544592524335698, 4.483927247898782831, 66.45942372801903275 ) ) ;
#74768 = CARTESIAN_POINT ( 'NONE',  ( 10.81492255796106328, -18.62759615963255655, 105.4177570613523613 ) ) ;
#74769 = CARTESIAN_POINT ( 'NONE',  ( 19.03943276465977164, 0.05219959533936151252, 81.25109039468567573 ) ) ;
#74770 = CARTESIAN_POINT ( 'NONE',  ( 16.46253265017160672, -9.564922557960803928, 53.33224293864768839 ) ) ;
#74771 = CARTESIAN_POINT ( 'NONE',  ( 15.80617190586746368, 15.72974639402197994, 84.37390960531438111 ) ) ;
#74773 = CARTESIAN_POINT ( 'NONE',  ( -9.564922557961040184, 16.46253265017147172, 72.91775706135233293 ) ) ;
#74772 = CARTESIAN_POINT ( 'NONE',  ( 14.34966873604960469, 8.224510206698951720, 74.16557627198102409 ) ) ;
#74774 = LINE ( 'NONE', #136436, #186190 ) ;
#74775 = CARTESIAN_POINT ( 'NONE',  ( -13.89961937509957401, -13.97604488694547875, 59.37609039468566863 ) ) ;
#74776 = CARTESIAN_POINT ( 'NONE',  ( -16.53943276465976808, 0.05219959533911058130, 21.24890960531436690 ) ) ;
#74777 = CARTESIAN_POINT ( 'NONE',  ( 16.53943276465976808, -0.05219959533910856209, 63.74890960531435979 ) ) ;
#74779 = CARTESIAN_POINT ( 'NONE',  ( -17.14385361876520264, -23.59649016807271593, 143.1750000027311671 ) ) ;
#74778 = CARTESIAN_POINT ( 'NONE',  ( -5.719274019375665041, -21.55341960407619695, 104.7927570613523898 ) ) ;
#74780 = CARTESIAN_POINT ( 'NONE',  ( -10.81492255796078084, -18.62759615963271287, 102.0822429386476955 ) ) ;
#74781 = CARTESIAN_POINT ( 'NONE',  ( -16.46253265017160317, 9.564922557960807481, 60.83224293864769550 ) ) ;
#74782 = CARTESIAN_POINT ( 'NONE',  ( -10.81492255796105439, 18.62759615963255655, 82.91775706135234714 ) ) ;
#74783 = CARTESIAN_POINT ( 'NONE',  ( -19.02544592524342804, 5.153800228976336051, 66.04057627198103830 ) ) ;
#74784 = CARTESIAN_POINT ( 'NONE',  ( -19.05341960407611168, -5.049401038298163336, 21.45724293864768839 ) ) ;
#74785 = CARTESIAN_POINT ( 'NONE',  ( 21.55341960407610458, 5.719274019375980345, 33.95724293864769550 ) ) ;
#74786 = CARTESIAN_POINT ( 'NONE',  ( -4.483927247898539470, -16.52544592524342804, 67.29057627198103830 ) ) ;
#74787 = CARTESIAN_POINT ( 'NONE',  ( 5.153800228976335163, 19.02544592524342804, 39.79057627198100988 ) ) ;
#74788 = CARTESIAN_POINT ( 'NONE',  ( -16.55341960407611168, -4.379528057220339221, 96.45724293864770971 ) ) ;
#74789 = CARTESIAN_POINT ( 'NONE',  ( 21.52544592524344225, -5.823673210054117533, 108.5405762719810241 ) ) ;
#74790 = CARTESIAN_POINT ( 'NONE',  ( -10.81492255796105439, 18.62759615963255655, 47.91775706135234714 ) ) ;
#74791 = CARTESIAN_POINT ( 'NONE',  ( 0.05219959533909260263, 19.03943276465977164, 34.99890960531435979 ) ) ;
#74792 = CARTESIAN_POINT ( 'NONE',  ( -4.379528057220086978, -16.55341960407618274, 69.79275706135234714 ) ) ;
#74793 = CARTESIAN_POINT ( 'NONE',  ( -5.823673210054116645, -21.52544592524344225, 107.2905762719810525 ) ) ;
#74794 = CARTESIAN_POINT ( 'NONE',  ( 18.62759615963271287, -10.81492255796078972, 103.3322429386476955 ) ) ;
#74796 = CARTESIAN_POINT ( 'NONE',  ( -16.51473224551069308, -9.474510206698971260, 56.66557627198103120 ) ) ;
#74795 = CARTESIAN_POINT ( 'NONE',  ( 16.46253265017146816, 9.564922557961045513, 26.66775706135234003 ) ) ;
#74797 = CARTESIAN_POINT ( 'NONE',  ( -17.97182807773870650, 5.500000000000046185, 83.53038844047284783 ) ) ;
#74798 = CARTESIAN_POINT ( 'NONE',  ( -5.823673210054431948, 21.52544592524334988, 57.70942372801901143 ) ) ;
#74799 = CARTESIAN_POINT ( 'NONE',  ( -18.62759615963270932, 10.81492255796079327, 50.83224293864770971 ) ) ;
#74800 = CARTESIAN_POINT ( 'NONE',  ( -16.52544592524342804, 4.483927247898546575, 26.04057627198103475 ) ) ;
#74802 = CARTESIAN_POINT ( 'NONE',  ( -0.05219959533937732626, 21.53943276465977519, 97.50109039468567573 ) ) ;
#74801 = CARTESIAN_POINT ( 'NONE',  ( -18.62759615963255300, -10.81492255796106328, 79.16775706135234714 ) ) ;
#74803 = CARTESIAN_POINT ( 'NONE',  ( -16.46253265017146816, -9.564922557961047289, 39.16775706135234003 ) ) ;
#74804 = CARTESIAN_POINT ( 'NONE',  ( 4.379528057220092307, 16.55341960407617563, 107.2927570613523471 ) ) ;
#74806 = EDGE_CURVE ( 'NONE', #138761, #8238, #54143, .T. ) ;
#74805 = CARTESIAN_POINT ( 'NONE',  ( 15.72974639402176855, 15.80617190586768217, 51.87609039468568284 ) ) ;
#74807 = CARTESIAN_POINT ( 'NONE',  ( -9.564922557960796823, -16.46253265017161027, 62.08224293864769550 ) ) ;
#74808 = CARTESIAN_POINT ( 'NONE',  ( -19.02544592524334988, -5.153800228976617603, 18.95942372801899722 ) ) ;
#74809 = CARTESIAN_POINT ( 'NONE',  ( 21.55341960407610458, 5.719274019375980345, 33.95724293864769550 ) ) ;
#74810 = CARTESIAN_POINT ( 'NONE',  ( 15.80617190586769283, -15.72974639402175789, 35.62609039468568994 ) ) ;
#74811 = CARTESIAN_POINT ( 'NONE',  ( 10.81492255796078972, 18.62759615963270932, 84.58224293864769550 ) ) ;
#74812 = CARTESIAN_POINT ( 'NONE',  ( 19.03943276465977164, 0.05219959533936151252, 91.25109039468566152 ) ) ;
#74813 = CARTESIAN_POINT ( 'NONE',  ( -8.224510206698735004, -14.34966873604973081, 54.58442372801901143 ) ) ;
#74815 = CARTESIAN_POINT ( 'NONE',  ( -15.72974639402197994, 15.80617190586746368, 85.62390960531436690 ) ) ;
#74814 = CARTESIAN_POINT ( 'NONE',  ( 17.50000000000000000, 5.500000000000013323, 63.78230962303565832 ) ) ;
#74817 = CARTESIAN_POINT ( 'NONE',  ( -0.05219959533910754901, -16.53943276465976808, 72.49890960531435269 ) ) ;
#74816 = CARTESIAN_POINT ( 'NONE',  ( 16.55341960407618274, -4.379528057220086978, 71.04275706135234714 ) ) ;
#74818 = CARTESIAN_POINT ( 'NONE',  ( 1.499999999999986677, 30.24381343224601437, -47.95930528970760776 ) ) ;
#74819 = CARTESIAN_POINT ( 'NONE',  ( 16.51473224551083163, -9.474510206698727899, 100.8344237280190043 ) ) ;
#74820 = CARTESIAN_POINT ( 'NONE',  ( -10.81492255796078084, -18.62759615963271287, 37.08224293864768129 ) ) ;
#74821 = SPHERICAL_SURFACE ( 'NONE', #60732, 0.5000000000000000000 ) ;
#74822 = ADVANCED_FACE ( 'NONE', ( #67870 ), #52699, .F. ) ;
#74823 = CARTESIAN_POINT ( 'NONE',  ( 14.29746914071037800, 8.314922557961029526, 36.66775706135234714 ) ) ;
#74824 = CARTESIAN_POINT ( 'NONE',  ( 18.62759615963271287, -10.81492255796078972, 108.3322429386477097 ) ) ;
#74825 = CARTESIAN_POINT ( 'NONE',  ( -10.72451020669898014, 18.67979575497178502, 30.41557627198101699 ) ) ;
#74826 = CARTESIAN_POINT ( 'NONE',  ( 16.53943276465976808, 0.05219959533934440121, 71.25109039468568994 ) ) ;
#74827 = CARTESIAN_POINT ( 'NONE',  ( 9.474510206698971260, -16.51473224551069308, 87.91557627198102409 ) ) ;
#74829 = CARTESIAN_POINT ( 'NONE',  ( -5.153800228976328057, -19.02544592524343514, 32.29057627198102409 ) ) ;
#74828 = CARTESIAN_POINT ( 'NONE',  ( -0.05219959533937732626, 21.53943276465977519, 62.50109039468568284 ) ) ;
#74830 = CARTESIAN_POINT ( 'NONE',  ( -15.80617190586745835, -15.72974639402198527, 21.87390960531436690 ) ) ;
#74831 = CARTESIAN_POINT ( 'NONE',  ( 13.97604488694548053, -13.89961937509957401, 40.62609039468564731 ) ) ;
#74832 = CARTESIAN_POINT ( 'NONE',  ( -12.14591786802326823, 12.06949235617739902, 53.12609039468568284 ) ) ;
#74833 = CARTESIAN_POINT ( 'NONE',  ( -5.719274019375978568, 21.55341960407610458, 25.20724293864769550 ) ) ;
#74834 = CARTESIAN_POINT ( 'NONE',  ( 19.05341960407611168, 5.049401038298154454, 73.95724293864768129 ) ) ;
#74835 = CARTESIAN_POINT ( 'NONE',  ( 14.34966873604972726, -8.224510206698740333, 100.8344237280190185 ) ) ;
#74836 = CARTESIAN_POINT ( 'NONE',  ( -4.483927247898539470, -16.52544592524342804, 92.29057627198103830 ) ) ;
#74837 = CARTESIAN_POINT ( 'NONE',  ( -21.55341960407610458, -5.719274019375992779, 36.45724293864768839 ) ) ;
#74838 = CARTESIAN_POINT ( 'NONE',  ( -5.049401038298153566, 19.05341960407611168, 30.20724293864768839 ) ) ;
#74839 = CARTESIAN_POINT ( 'NONE',  ( -12.06949235617739369, -12.14591786802326823, 64.37609039468568994 ) ) ;
#74840 = CARTESIAN_POINT ( 'NONE',  ( -15.72974639402176322, -15.80617190586768395, 19.37609039468568639 ) ) ;
#74841 = CARTESIAN_POINT ( 'NONE',  ( -16.51473224551082808, 9.474510206698731452, 83.33442372801899012 ) ) ;
#74842 = CARTESIAN_POINT ( 'NONE',  ( -19.03943276465977164, 0.05219959533909376836, 46.24890960531435979 ) ) ;
#74843 = CARTESIAN_POINT ( 'NONE',  ( -5.823673210054116645, -21.52544592524344225, 67.29057627198103830 ) ) ;
#74844 = CARTESIAN_POINT ( 'NONE',  ( 13.97604488694527802, 13.89961937509977652, 109.3739096053143669 ) ) ;
#74845 = CARTESIAN_POINT ( 'NONE',  ( -5.719274019375665041, -21.55341960407619695, 94.79275706135234714 ) ) ;
#74846 = CARTESIAN_POINT ( 'NONE',  ( -5.049401038298153566, 19.05341960407611168, 65.20724293864765286 ) ) ;
#74847 = CARTESIAN_POINT ( 'NONE',  ( 14.29746914071037800, 8.314922557961029526, 51.66775706135234714 ) ) ;
#74848 = CARTESIAN_POINT ( 'NONE',  ( -5.049401038298153566, 19.05341960407611168, 65.20724293864765286 ) ) ;
#74849 = CARTESIAN_POINT ( 'NONE',  ( -21.55341960407619339, 5.719274019375674811, 83.54275706135234714 ) ) ;
#74850 = CARTESIAN_POINT ( 'NONE',  ( -13.97604488694547697, 13.89961937509957934, 38.12609039468566152 ) ) ;
#74851 = EDGE_CURVE ( 'NONE', #169095, #22637, #40543, .T. ) ;
#74852 = CARTESIAN_POINT ( 'NONE',  ( -16.46253265017146816, -9.564922557961047289, 59.16775706135233293 ) ) ;
#74853 = VERTEX_POINT ( 'NONE', #42545 ) ;
#74854 = CARTESIAN_POINT ( 'NONE',  ( 21.52544592524334988, 5.823673210054432836, 56.45942372801902565 ) ) ;
#74855 = CARTESIAN_POINT ( 'NONE',  ( -7.989781499195968806, 1.461410587780254788, -62.12232043736380405 ) ) ;
#74856 = CARTESIAN_POINT ( 'NONE',  ( 16.46253265017146816, 9.564922557961045513, 51.66775706135233293 ) ) ;
#74857 = CARTESIAN_POINT ( 'NONE',  ( 16.46253265017160672, -9.564922557960803928, 103.3322429386476955 ) ) ;
#74858 = CARTESIAN_POINT ( 'NONE',  ( -19.02544592524342804, 5.153800228976336051, 76.04057627198102409 ) ) ;
#74859 = CARTESIAN_POINT ( 'NONE',  ( -16.52544592524342804, 4.483927247898546575, 36.04057627198102409 ) ) ;
#74860 = CARTESIAN_POINT ( 'NONE',  ( 18.62759615963271287, -10.81492255796078972, 33.33224293864769550 ) ) ;
#74861 = CARTESIAN_POINT ( 'NONE',  ( 11.40812507854754365, 35.11059874428196537, -7.724999997268813701 ) ) ;
#74862 = LINE ( 'NONE', #125336, #157975 ) ;
#74863 = CARTESIAN_POINT ( 'NONE',  ( 10.81492255796106328, -18.62759615963255655, 100.4177570613523471 ) ) ;
#74864 = CARTESIAN_POINT ( 'NONE',  ( -27.89965394715913760, 6.788920637341050224, 161.9771076211713137 ) ) ;
#74865 = CARTESIAN_POINT ( 'NONE',  ( 13.89961937509977652, -13.97604488694527269, 33.12390960531434558 ) ) ;
#74866 = CARTESIAN_POINT ( 'NONE',  ( -0.05219959533909027116, -19.03943276465977164, 112.4989096053143669 ) ) ;
#74867 = CARTESIAN_POINT ( 'NONE',  ( 34.40575365382723305, 2.434396366613707396, 90.06480789948632548 ) ) ;
#74868 = CARTESIAN_POINT ( 'NONE',  ( 4.483927247898790824, -16.52544592524335698, 50.20942372801901854 ) ) ;
#74869 = CARTESIAN_POINT ( 'NONE',  ( -10.81492255796078084, -18.62759615963271287, 72.08224293864769550 ) ) ;
#74870 = CARTESIAN_POINT ( 'NONE',  ( -16.53943276465976808, 0.05219959533911058130, 46.24890960531435979 ) ) ;
#74872 = CARTESIAN_POINT ( 'NONE',  ( 16.46253265017160672, -9.564922557960803928, 103.3322429386476955 ) ) ;
#74871 = CARTESIAN_POINT ( 'NONE',  ( -5.049401038298153566, 19.05341960407611168, 30.20724293864768839 ) ) ;
#74873 = CARTESIAN_POINT ( 'NONE',  ( 5.719274019375673035, 21.55341960407619339, 27.29275706135234358 ) ) ;
#74874 = CARTESIAN_POINT ( 'NONE',  ( -9.474510206698720793, -16.51473224551083518, 39.58442372801899722 ) ) ;
#74875 = CARTESIAN_POINT ( 'NONE',  ( -12.14591786802309592, -12.06949235617757132, 111.8739096053143669 ) ) ;
#74876 = CARTESIAN_POINT ( 'NONE',  ( 10.81492255796106328, -18.62759615963255655, 75.41775706135233293 ) ) ;
#74877 = CARTESIAN_POINT ( 'NONE',  ( 16.62475595723696031, -7.163666690055223718, 33.02713351810466236 ) ) ;
#74878 = CARTESIAN_POINT ( 'NONE',  ( 12.14591786802309770, 12.06949235617756955, 34.37390960531435979 ) ) ;
#74879 = CARTESIAN_POINT ( 'NONE',  ( 17.49999999999999645, 4.013004640162542991, 112.0539427900559417 ) ) ;
#74880 = CARTESIAN_POINT ( 'NONE',  ( 21.52544592524344225, -5.823673210054117533, 28.54057627198103120 ) ) ;
#74881 = CARTESIAN_POINT ( 'NONE',  ( 4.483927247898545687, 16.52544592524342804, 94.79057627198105251 ) ) ;
#74882 = CARTESIAN_POINT ( 'NONE',  ( -17.49999999999999645, -5.500000000000000888, 39.20309617465829177 ) ) ;
#74883 = CARTESIAN_POINT ( 'NONE',  ( -19.02544592524342804, 5.153800228976336051, 81.04057627198103830 ) ) ;
#74884 = CARTESIAN_POINT ( 'NONE',  ( -12.14591786802309592, -12.06949235617757132, 76.87390960531439532 ) ) ;
#74885 = CARTESIAN_POINT ( 'NONE',  ( 19.03943276465977164, 0.05219959533936151252, 101.2510903946856757 ) ) ;
#74886 = CARTESIAN_POINT ( 'NONE',  ( 15.80617190586746368, 15.72974639402197994, 64.37390960531435269 ) ) ;
#74887 = VERTEX_POINT ( 'NONE', #137517 ) ;
#74888 = CARTESIAN_POINT ( 'NONE',  ( 19.03943276465977164, -0.05219959533909143690, 38.74890960531436690 ) ) ;
#74890 = CARTESIAN_POINT ( 'NONE',  ( 5.823673210054125526, 21.52544592524343514, 69.79057627198102409 ) ) ;
#74889 = CARTESIAN_POINT ( 'NONE',  ( -5.153800228976328057, -19.02544592524343514, 77.29057627198099567 ) ) ;
#74892 = CARTESIAN_POINT ( 'NONE',  ( 19.03943276465977164, -0.05219959533909143690, 83.74890960531436690 ) ) ;
#74891 = CARTESIAN_POINT ( 'NONE',  ( 16.52544592524335698, 4.483927247898782831, 106.4594237280190328 ) ) ;
#74893 = CARTESIAN_POINT ( 'NONE',  ( -19.02544592524334988, -5.153800228976617603, 68.95942372801896170 ) ) ;
#74894 = CARTESIAN_POINT ( 'NONE',  ( -15.72974639402176322, -15.80617190586768395, 94.37609039468568994 ) ) ;
#74895 = CARTESIAN_POINT ( 'NONE',  ( -5.719274019375978568, 21.55341960407610458, 75.20724293864769550 ) ) ;
#74896 = CARTESIAN_POINT ( 'NONE',  ( 15.80617190586746368, 15.72974639402197994, 24.37390960531435979 ) ) ;
#74897 = CARTESIAN_POINT ( 'NONE',  ( -5.153800228976328057, -19.02544592524343514, 52.29057627198100988 ) ) ;
#74898 = CARTESIAN_POINT ( 'NONE',  ( 0.05219959533934541429, -16.53943276465976808, 95.00109039468568994 ) ) ;
#74899 = CARTESIAN_POINT ( 'NONE',  ( -5.049401038298153566, 19.05341960407611168, 65.20724293864765286 ) ) ;
#74900 = CARTESIAN_POINT ( 'NONE',  ( -31.56677620984798338, -3.765895691706333093, 101.5045925518948593 ) ) ;
#74901 = CARTESIAN_POINT ( 'NONE',  ( 5.823673210054444382, -21.52544592524334988, 110.2094237280190185 ) ) ;
#74902 = CARTESIAN_POINT ( 'NONE',  ( 14.29746914071049879, -8.314922557960816363, 73.33224293864769550 ) ) ;
#74903 = CARTESIAN_POINT ( 'NONE',  ( 21.53943276465977519, -0.05219959533907433946, 103.7489096053143669 ) ) ;
#74904 = CARTESIAN_POINT ( 'NONE',  ( -0.05219959533907301413, -21.53943276465977519, 102.4989096053143811 ) ) ;
#74905 = DIRECTION ( 'NONE',  ( 0.8660254037844410391, 0.000000000000000000, 0.4999999999999958367 ) ) ;
#74906 = CARTESIAN_POINT ( 'NONE',  ( 5.823673210054125526, 21.52544592524343514, 64.79057627198103830 ) ) ;
#74907 = CARTESIAN_POINT ( 'NONE',  ( 16.55341960407618274, -4.379528057220086978, 81.04275706135236135 ) ) ;
#74908 = CARTESIAN_POINT ( 'NONE',  ( -4.483927247898539470, -16.52544592524342804, 102.2905762719810383 ) ) ;
#74909 = CARTESIAN_POINT ( 'NONE',  ( -5.049401038298153566, 19.05341960407611168, 60.20724293864768129 ) ) ;
#74910 = FILL_AREA_STYLE ('',( #41598 ) ) ;
#74911 = CARTESIAN_POINT ( 'NONE',  ( -16.53943276465976808, -0.05219959533934237506, 113.7510903946856757 ) ) ;
#74912 = CARTESIAN_POINT ( 'NONE',  ( 0.05219959533937995610, -21.53943276465977519, 50.00109039468568994 ) ) ;
#74913 = CARTESIAN_POINT ( 'NONE',  ( -9.474510206698964154, 16.51473224551069663, 100.4155762719810241 ) ) ;
#74914 = CARTESIAN_POINT ( 'NONE',  ( -5.823673210054431948, 21.52544592524334988, 77.70942372801900433 ) ) ;
#74915 = CARTESIAN_POINT ( 'NONE',  ( 5.153800228976335163, 19.02544592524342804, 24.79057627198102765 ) ) ;
#74916 = CARTESIAN_POINT ( 'NONE',  ( 9.564922557960805705, 16.46253265017160317, 34.58224293864770260 ) ) ;
#74917 = ORIENTED_EDGE ( 'NONE', *, *, #79855, .T. ) ;
#74918 = CARTESIAN_POINT ( 'NONE',  ( 18.62759615963255655, 10.81492255796105972, 76.66775706135234714 ) ) ;
#74919 = CARTESIAN_POINT ( 'NONE',  ( -13.89961937509977652, 13.97604488694528158, 100.6239096053143669 ) ) ;
#74920 = CARTESIAN_POINT ( 'NONE',  ( 9.564922557961047289, -16.46253265017146816, 85.41775706135233293 ) ) ;
#74921 = CARTESIAN_POINT ( 'NONE',  ( 0.05219959533937995610, -21.53943276465977519, 45.00109039468568284 ) ) ;
#74922 = CARTESIAN_POINT ( 'NONE',  ( 16.55341960407618274, -4.379528057220086978, 26.04275706135235779 ) ) ;
#74923 = CARTESIAN_POINT ( 'NONE',  ( -19.02544592524334988, -5.153800228976617603, 68.95942372801896170 ) ) ;
#74924 = CARTESIAN_POINT ( 'NONE',  ( 13.97604488694527802, 13.89961937509977652, 49.37390960531434558 ) ) ;
#74925 = CARTESIAN_POINT ( 'NONE',  ( 0.05219959533936267826, -19.03943276465977164, 85.00109039468567573 ) ) ;
#74926 = CARTESIAN_POINT ( 'NONE',  ( 14.34966873604960469, 8.224510206698951720, 29.16557627198103120 ) ) ;
#74927 = CARTESIAN_POINT ( 'NONE',  ( -9.564922557961040184, 16.46253265017147172, 87.91775706135233293 ) ) ;
#74928 = CARTESIAN_POINT ( 'NONE',  ( 14.29746914071049879, -8.314922557960816363, 38.33224293864768839 ) ) ;
#74929 = CARTESIAN_POINT ( 'NONE',  ( 0.05219959533936267826, -19.03943276465977164, 70.00109039468566152 ) ) ;
#74930 = CARTESIAN_POINT ( 'NONE',  ( 12.14591786802327356, -12.06949235617739191, 50.62609039468568994 ) ) ;
#74931 = CARTESIAN_POINT ( 'NONE',  ( -19.03943276465977164, -0.05219959533935918106, 18.75109039468567218 ) ) ;
#74932 = CARTESIAN_POINT ( 'NONE',  ( 19.02544592524343514, -5.153800228976328945, 38.54057627198103120 ) ) ;
#74933 = CARTESIAN_POINT ( 'NONE',  ( -17.26058549869088310, -6.457015423128632747, 66.37745837476067834 ) ) ;
#74934 = CARTESIAN_POINT ( 'NONE',  ( 16.55341960407618274, -4.379528057220086978, 51.04275706135234714 ) ) ;
#74935 = CARTESIAN_POINT ( 'NONE',  ( -193.3062444957834884, -155.7167183371838064, -15.00000000000000000 ) ) ;
#74936 = CARTESIAN_POINT ( 'NONE',  ( -27.73933785331498925, -9.013057229001049109, 146.9750000027311785 ) ) ;
#74937 = CARTESIAN_POINT ( 'NONE',  ( -5.049401038298153566, 19.05341960407611168, 90.20724293864766707 ) ) ;
#74938 = CARTESIAN_POINT ( 'NONE',  ( -15.49999999999999822, -5.500000000000000888, 118.0000000000000142 ) ) ;
#74939 = VERTEX_POINT ( 'NONE', #182051 ) ;
#74940 = CARTESIAN_POINT ( 'NONE',  ( 13.97604488694548053, -13.89961937509957401, 80.62609039468567573 ) ) ;
#74941 = CARTESIAN_POINT ( 'NONE',  ( -18.62759615963270932, 10.81492255796079327, 25.83224293864769194 ) ) ;
#74943 = CARTESIAN_POINT ( 'NONE',  ( 19.05341960407617918, -5.049401038297876454, 101.0427570613523045 ) ) ;
#74942 = CARTESIAN_POINT ( 'NONE',  ( -19.02544592524334988, -5.153800228976617603, 23.95942372801900078 ) ) ;
#74944 = CARTESIAN_POINT ( 'NONE',  ( -9.564922557960796823, -16.46253265017161027, 22.08224293864768839 ) ) ;
#74945 = CARTESIAN_POINT ( 'NONE',  ( 5.049401038298161559, -19.05341960407611168, 32.70724293864768129 ) ) ;
#74946 = CARTESIAN_POINT ( 'NONE',  ( -15.80617190586745835, -15.72974639402198527, 56.87390960531436690 ) ) ;
#74947 = CARTESIAN_POINT ( 'NONE',  ( -12.06949235617756955, 12.14591786802309770, 115.6239096053143669 ) ) ;
#74948 = CYLINDRICAL_SURFACE ( 'NONE', #30657, 2.500000000000002220 ) ;
#74949 = CARTESIAN_POINT ( 'NONE',  ( 5.049401038297881783, 19.05341960407617563, 77.29275706135231871 ) ) ;
#74950 = CARTESIAN_POINT ( 'NONE',  ( 14.34966873604960469, 8.224510206698951720, 44.16557627198103120 ) ) ;
#74951 = CARTESIAN_POINT ( 'NONE',  ( 21.53943276465977519, -0.05219959533907433946, 28.74890960531435624 ) ) ;
#74952 = CARTESIAN_POINT ( 'NONE',  ( 15.72974639402176855, 15.80617190586768217, 96.87609039468568994 ) ) ;
#74953 = CARTESIAN_POINT ( 'NONE',  ( 18.62759615963271287, -10.81492255796078972, 88.33224293864769550 ) ) ;
#74954 = CARTESIAN_POINT ( 'NONE',  ( -0.05219959533937732626, 21.53943276465977519, 52.50109039468567573 ) ) ;
#74955 = CARTESIAN_POINT ( 'NONE',  ( 10.81492255796106328, -18.62759615963255655, 65.41775706135234714 ) ) ;
#74956 = EDGE_CURVE ( 'NONE', #80629, #183542, #165889, .T. ) ;
#74957 = CARTESIAN_POINT ( 'NONE',  ( 19.02544592524343514, -5.153800228976328945, 93.54057627198102409 ) ) ;
#74959 = CARTESIAN_POINT ( 'NONE',  ( 15.80617190586769283, -15.72974639402175789, 55.62609039468568284 ) ) ;
#74958 = CARTESIAN_POINT ( 'NONE',  ( -14.29746914071037622, -8.314922557961029526, 99.16775706135234714 ) ) ;
#74960 = CARTESIAN_POINT ( 'NONE',  ( 14.34966873604960469, 8.224510206698951720, 114.1655762719810383 ) ) ;
#74961 = CARTESIAN_POINT ( 'NONE',  ( -16.55341960407611168, -4.379528057220339221, 61.45724293864770260 ) ) ;
#74962 = CARTESIAN_POINT ( 'NONE',  ( 4.379528057220339221, -16.55341960407611168, 37.70724293864769550 ) ) ;
#74963 = CARTESIAN_POINT ( 'NONE',  ( 10.81492255796078972, 18.62759615963270932, 44.58224293864769550 ) ) ;
#74964 = CARTESIAN_POINT ( 'NONE',  ( 5.049401038298161559, -19.05341960407611168, 52.70724293864767418 ) ) ;
#74965 = CARTESIAN_POINT ( 'NONE',  ( 18.62759615963271287, -10.81492255796078972, 58.33224293864768839 ) ) ;
#74966 = CARTESIAN_POINT ( 'NONE',  ( 19.05341960407617918, -5.049401038297876454, 46.04275706135233293 ) ) ;
#74968 = CARTESIAN_POINT ( 'NONE',  ( -4.483927247898539470, -16.52544592524342804, 52.29057627198102409 ) ) ;
#74967 = CARTESIAN_POINT ( 'NONE',  ( -16.62475595723695676, -7.163666690055263686, 39.47286648189535896 ) ) ;
#74969 = CARTESIAN_POINT ( 'NONE',  ( -15.80617190586745835, -15.72974639402198527, 21.87390960531436690 ) ) ;
#74970 = VERTEX_POINT ( 'NONE', #43534 ) ;
#74971 = EDGE_LOOP ( 'NONE', ( #1033, #56198 ) ) ;
#74972 = CARTESIAN_POINT ( 'NONE',  ( 1.820000000000000062, 0.000000000000000000, 3.799999999999999378 ) ) ;
#74973 = CARTESIAN_POINT ( 'NONE',  ( -14.34966873604972548, 8.224510206698743886, 73.33442372801901854 ) ) ;
#74974 = CARTESIAN_POINT ( 'NONE',  ( 13.97604488694548053, -13.89961937509957401, 80.62609039468567573 ) ) ;
#74975 = CARTESIAN_POINT ( 'NONE',  ( -16.53943276465976808, 0.05219959533911058130, 36.24890960531435979 ) ) ;
#74976 = FACE_OUTER_BOUND ( 'NONE', #128348, .T. ) ;
#74977 = CARTESIAN_POINT ( 'NONE',  ( -8.314922557960811034, -14.29746914071050412, 22.08224293864769194 ) ) ;
#74978 = CARTESIAN_POINT ( 'NONE',  ( -19.03943276465977164, 0.05219959533909376836, 46.24890960531435979 ) ) ;
#74979 = CARTESIAN_POINT ( 'NONE',  ( 0.05219959533909260263, 19.03943276465977164, 69.99890960531435269 ) ) ;
#74980 = CARTESIAN_POINT ( 'NONE',  ( 19.03943276465977164, -0.05219959533909143690, 33.74890960531435979 ) ) ;
#74981 = CARTESIAN_POINT ( 'NONE',  ( -18.67979575497193778, 10.72451020669871902, 48.33442372801902565 ) ) ;
#74982 = CARTESIAN_POINT ( 'NONE',  ( 9.474510206698971260, -16.51473224551069308, 57.91557627198103120 ) ) ;
#74983 = FACE_BOUND ( 'NONE', #27439, .T. ) ;
#74984 = CARTESIAN_POINT ( 'NONE',  ( 9.564922557960805705, 16.46253265017160317, 59.58224293864769550 ) ) ;
#74985 = CARTESIAN_POINT ( 'NONE',  ( 10.81492255796078972, 18.62759615963270932, 39.58224293864769550 ) ) ;
#74986 = CARTESIAN_POINT ( 'NONE',  ( 19.02544592524343514, -5.153800228976328945, 33.54057627198102409 ) ) ;
#74987 = CARTESIAN_POINT ( 'NONE',  ( -18.62759615963270932, 10.81492255796079327, 35.83224293864768839 ) ) ;
#74988 = CARTESIAN_POINT ( 'NONE',  ( 4.379528057220092307, 16.55341960407617563, 87.29275706135236135 ) ) ;
#74989 = CARTESIAN_POINT ( 'NONE',  ( 0.05219959533937995610, -21.53943276465977519, 100.0010903946857042 ) ) ;
#74990 = CARTESIAN_POINT ( 'NONE',  ( -4.379528057220086978, -16.55341960407618274, 64.79275706135234714 ) ) ;
#74991 = CARTESIAN_POINT ( 'NONE',  ( -16.46253265017160317, 9.564922557960807481, 105.8322429386476955 ) ) ;
#74992 = CARTESIAN_POINT ( 'NONE',  ( 12.14591786802327356, -12.06949235617739191, 55.62609039468568284 ) ) ;
#74993 = CARTESIAN_POINT ( 'NONE',  ( 16.52544592524335698, 4.483927247898782831, 36.45942372801901143 ) ) ;
#74994 = CARTESIAN_POINT ( 'NONE',  ( 13.97604488694527802, 13.89961937509977652, 104.3739096053143385 ) ) ;
#74995 = CARTESIAN_POINT ( 'NONE',  ( -16.52544592524335698, -4.483927247898792601, 28.95942372801902209 ) ) ;
#74996 = CARTESIAN_POINT ( 'NONE',  ( 5.049401038298161559, -19.05341960407611168, 32.70724293864768129 ) ) ;
#74997 = CARTESIAN_POINT ( 'NONE',  ( -10.72451020669870658, -18.67979575497194134, 24.58442372801901499 ) ) ;
#74998 = CARTESIAN_POINT ( 'NONE',  ( 16.53943276465976808, 0.05219959533934440121, 21.25109039468567218 ) ) ;
#74999 = CARTESIAN_POINT ( 'NONE',  ( 8.314922557961029526, -14.29746914071037800, 90.41775706135236135 ) ) ;
#75000 = CARTESIAN_POINT ( 'NONE',  ( -6.020228577223754586E-15, 39.95556452105416412, -4.249999994537626336 ) ) ;
#75001 = CARTESIAN_POINT ( 'NONE',  ( -21.55341960407619339, 5.719274019375674811, 98.54275706135234714 ) ) ;
#75002 = CARTESIAN_POINT ( 'NONE',  ( 19.05341960407617918, -5.049401038297876454, 91.04275706135234714 ) ) ;
#75003 = CARTESIAN_POINT ( 'NONE',  ( 0.05219959533910956823, 16.53943276465976808, 54.99890960531435269 ) ) ;
#75004 = CARTESIAN_POINT ( 'NONE',  ( 14.29746914071049879, -8.314922557960816363, 103.3322429386476955 ) ) ;
#75006 = CARTESIAN_POINT ( 'NONE',  ( -7.990187535671161356, 1.461319442807373692, -64.16708268805474802 ) ) ;
#75005 = CARTESIAN_POINT ( 'NONE',  ( 9.564922557961047289, -16.46253265017146816, 45.41775706135232582 ) ) ;
#75007 = CARTESIAN_POINT ( 'NONE',  ( 15.72974639402176855, 15.80617190586768217, 51.87609039468568284 ) ) ;
#75008 = CARTESIAN_POINT ( 'NONE',  ( 16.52544592524335698, 4.483927247898782831, 31.45942372801901854 ) ) ;
#75009 = CARTESIAN_POINT ( 'NONE',  ( 17.12812012977029141, 6.668231424565952636, 83.85948759323147783 ) ) ;
#75010 = CARTESIAN_POINT ( 'NONE',  ( -19.03943276465977164, 0.05219959533909376836, 111.2489096053143669 ) ) ;
#75011 = CARTESIAN_POINT ( 'NONE',  ( 18.62759615963271287, -10.81492255796078972, 68.33224293864769550 ) ) ;
#75012 = CARTESIAN_POINT ( 'NONE',  ( -9.474510206698720793, -16.51473224551083518, 94.58442372801900433 ) ) ;
#75013 = CARTESIAN_POINT ( 'NONE',  ( -9.564922557960796823, -16.46253265017161027, 102.0822429386477097 ) ) ;
#75014 = CARTESIAN_POINT ( 'NONE',  ( -21.95653654802720922, 8.266568072468359674, 172.1684357517875412 ) ) ;
#75015 = CARTESIAN_POINT ( 'NONE',  ( -16.55341960407611168, -4.379528057220339221, 111.4572429386476813 ) ) ;
#75016 = CARTESIAN_POINT ( 'NONE',  ( -21.53943276465977519, -0.05219959533937600094, 98.75109039468568994 ) ) ;
#75017 = CARTESIAN_POINT ( 'NONE',  ( -0.05219959533909027116, -19.03943276465977164, 47.49890960531435979 ) ) ;
#75018 = CARTESIAN_POINT ( 'NONE',  ( -5.719274019375665041, -21.55341960407619695, 54.79275706135235424 ) ) ;
#75019 = CARTESIAN_POINT ( 'NONE',  ( 0.05219959533937995610, -21.53943276465977519, 85.00109039468568994 ) ) ;
#75020 = CARTESIAN_POINT ( 'NONE',  ( 8.314922557961029526, -14.29746914071037800, 110.4177570613523756 ) ) ;
#75021 = CARTESIAN_POINT ( 'NONE',  ( -5.153800228976328057, -19.02544592524343514, 67.29057627198102409 ) ) ;
#75022 = CARTESIAN_POINT ( 'NONE',  ( -15.80617190586768217, 15.72974639402176855, 38.12609039468567573 ) ) ;
#75023 = CARTESIAN_POINT ( 'NONE',  ( -21.52544592524334988, -5.823673210054445271, 33.95942372801901143 ) ) ;
#75025 = CARTESIAN_POINT ( 'NONE',  ( 16.46253265017160672, -9.564922557960803928, 93.33224293864769550 ) ) ;
#75024 = CARTESIAN_POINT ( 'NONE',  ( 13.89961937509957401, 13.97604488694547697, 71.87609039468567573 ) ) ;
#75026 = CARTESIAN_POINT ( 'NONE',  ( 14.34966873604960469, 8.224510206698951720, 109.1655762719810383 ) ) ;
#75027 = CARTESIAN_POINT ( 'NONE',  ( -21.55341960407610458, -5.719274019375992779, 96.45724293864770971 ) ) ;
#75028 = CARTESIAN_POINT ( 'NONE',  ( 12.14591786802309770, 12.06949235617756955, 69.37390960531436690 ) ) ;
#75029 = CARTESIAN_POINT ( 'NONE',  ( 5.719274019375673035, 21.55341960407619339, 112.2927570613523471 ) ) ;
#75030 = CARTESIAN_POINT ( 'NONE',  ( 12.06949235617757843, -12.14591786802309237, 88.12390960531436690 ) ) ;
#75031 = CARTESIAN_POINT ( 'NONE',  ( 5.049401038298161559, -19.05341960407611168, 42.70724293864767418 ) ) ;
#75032 = CARTESIAN_POINT ( 'NONE',  ( 19.02544592524334988, 5.153800228976608722, 81.45942372801897591 ) ) ;
#75033 = CARTESIAN_POINT ( 'NONE',  ( 14.29746914071049879, -8.314922557960816363, 48.33224293864770260 ) ) ;
#75034 = CARTESIAN_POINT ( 'NONE',  ( -21.52544592524334988, -5.823673210054445271, 98.95942372801903275 ) ) ;
#75035 = CARTESIAN_POINT ( 'NONE',  ( 19.02544592524343514, -5.153800228976328945, 93.54057627198102409 ) ) ;
#75036 = CARTESIAN_POINT ( 'NONE',  ( -19.03943276465977164, -0.05219959533935918106, 68.75109039468566152 ) ) ;
#75037 = CARTESIAN_POINT ( 'NONE',  ( -10.81492255796078084, -18.62759615963271287, 77.08224293864769550 ) ) ;
#75038 = CARTESIAN_POINT ( 'NONE',  ( 5.719274019375673035, 21.55341960407619339, 27.29275706135234358 ) ) ;
#75039 = CARTESIAN_POINT ( 'NONE',  ( -16.53943276465976808, -0.05219959533934237506, 23.75109039468567929 ) ) ;
#75040 = CARTESIAN_POINT ( 'NONE',  ( 16.53943276465976808, 0.05219959533934440121, 96.25109039468568994 ) ) ;
#75042 = CARTESIAN_POINT ( 'NONE',  ( -0.05219959533937732626, 21.53943276465977519, 42.50109039468567573 ) ) ;
#75041 = CARTESIAN_POINT ( 'NONE',  ( 19.05341960407611168, 5.049401038298154454, 23.95724293864769194 ) ) ;
#75043 = CARTESIAN_POINT ( 'NONE',  ( 5.049401038298161559, -19.05341960407611168, 27.70724293864769550 ) ) ;
#75044 = CARTESIAN_POINT ( 'NONE',  ( 38.00000000000000000, 12.34694845685046616, -10.64999999453762491 ) ) ;
#75045 = CARTESIAN_POINT ( 'NONE',  ( 0.05219959533934541429, -16.53943276465976808, 45.00109039468568284 ) ) ;
#75046 = CARTESIAN_POINT ( 'NONE',  ( 4.483927247898545687, 16.52544592524342804, 74.79057627198105251 ) ) ;
#75047 = CARTESIAN_POINT ( 'NONE',  ( 18.67979575497178502, 10.72451020669898547, 69.16557627198102409 ) ) ;
#75048 = CARTESIAN_POINT ( 'NONE',  ( -16.53943276465976808, 0.05219959533911058130, 26.24890960531435624 ) ) ;
#75049 = CARTESIAN_POINT ( 'NONE',  ( 8.314922557961029526, -14.29746914071037800, 55.41775706135234714 ) ) ;
#75050 = CARTESIAN_POINT ( 'NONE',  ( -9.564922557960796823, -16.46253265017161027, 47.08224293864769550 ) ) ;
#75051 = CARTESIAN_POINT ( 'NONE',  ( -14.29746914071037622, -8.314922557961029526, 99.16775706135234714 ) ) ;
#75052 = CARTESIAN_POINT ( 'NONE',  ( 16.51473224551083163, -9.474510206698727899, 80.83442372801899012 ) ) ;
#75053 = CARTESIAN_POINT ( 'NONE',  ( 15.72974639402199770, -15.80617190586745480, 68.12390960531436690 ) ) ;
#75054 = CARTESIAN_POINT ( 'NONE',  ( 4.379528057220092307, 16.55341960407617563, 112.2927570613523471 ) ) ;
#75055 = ORIENTED_EDGE ( 'NONE', *, *, #16747, .T. ) ;
#75056 = CARTESIAN_POINT ( 'NONE',  ( 25.82893184620815319, 8.167111171437667849, 172.3011985515803701 ) ) ;
#75057 = CARTESIAN_POINT ( 'NONE',  ( 0.05219959533907565091, 21.53943276465977519, 64.99890960531435269 ) ) ;
#75058 = EDGE_LOOP ( 'NONE', ( #177831, #121549, #75297, #198654 ) ) ;
#75059 = CARTESIAN_POINT ( 'NONE',  ( 14.29746914071037800, 8.314922557961029526, 91.66775706135234714 ) ) ;
#75060 = ORIENTED_EDGE ( 'NONE', *, *, #37703, .F. ) ;
#75061 = CARTESIAN_POINT ( 'NONE',  ( 5.049401038298161559, -19.05341960407611168, 107.7072429386476955 ) ) ;
#75062 = DIRECTION ( 'NONE',  ( 0.000000000000000000, 0.000000000000000000, 1.000000000000000000 ) ) ;
#75063 = CARTESIAN_POINT ( 'NONE',  ( 5.823673210054125526, 21.52544592524343514, 69.79057627198102409 ) ) ;
#75064 = CARTESIAN_POINT ( 'NONE',  ( 14.34966873604972726, -8.224510206698740333, 105.8344237280190328 ) ) ;
#75065 = CARTESIAN_POINT ( 'NONE',  ( -16.53943276465976808, -0.05219959533934237506, 18.75109039468568639 ) ) ;
#75066 = CARTESIAN_POINT ( 'NONE',  ( -5.153800228976328057, -19.02544592524343514, 22.29057627198102765 ) ) ;
#75067 = CARTESIAN_POINT ( 'NONE',  ( -12.06949235617739369, -12.14591786802326823, 29.37609039468568284 ) ) ;
#75068 = CARTESIAN_POINT ( 'NONE',  ( 13.97604488694527802, 13.89961937509977652, 59.37390960531434558 ) ) ;
#75069 = CARTESIAN_POINT ( 'NONE',  ( 28.82186960331499392, -9.364793116373510529, 144.9000000000000057 ) ) ;
#75070 = CARTESIAN_POINT ( 'NONE',  ( 13.97604488694527802, 13.89961937509977652, 99.37390960531436690 ) ) ;
#75071 = CARTESIAN_POINT ( 'NONE',  ( -16.53943276465976808, -0.05219959533934237506, 93.75109039468567573 ) ) ;
#75072 = CARTESIAN_POINT ( 'NONE',  ( -9.564922557961040184, 16.46253265017147172, 87.91775706135233293 ) ) ;
#75073 = CARTESIAN_POINT ( 'NONE',  ( -13.89961937509957401, -13.97604488694547875, 19.37609039468566507 ) ) ;
#75074 = CARTESIAN_POINT ( 'NONE',  ( 10.81492255796078972, 18.62759615963270932, 69.58224293864769550 ) ) ;
#75075 = CARTESIAN_POINT ( 'NONE',  ( -16.52544592524335698, -4.483927247898792601, 93.95942372801903275 ) ) ;
#75076 = CARTESIAN_POINT ( 'NONE',  ( 16.51473224551083163, -9.474510206698727899, 90.83442372801900433 ) ) ;
#75077 = CARTESIAN_POINT ( 'NONE',  ( -16.51473224551069308, -9.474510206698971260, 51.66557627198102409 ) ) ;
#75078 = CARTESIAN_POINT ( 'NONE',  ( -16.51473224551069308, -9.474510206698971260, 96.66557627198102409 ) ) ;
#75079 = CARTESIAN_POINT ( 'NONE',  ( -18.62759615963255300, -10.81492255796106328, 64.16775706135234714 ) ) ;
#75080 = CARTESIAN_POINT ( 'NONE',  ( -13.89961937509977652, 13.97604488694528158, 65.62390960531436690 ) ) ;
#75081 = CARTESIAN_POINT ( 'NONE',  ( -8.224510206698948167, 14.34966873604960824, 90.41557627198103830 ) ) ;
#75082 = CARTESIAN_POINT ( 'NONE',  ( -17.13100169013300444, -6.664070546373138448, 84.23210164300149927 ) ) ;
#75083 = CARTESIAN_POINT ( 'NONE',  ( -14.34966873604960291, -8.224510206698953496, 81.66557627198103830 ) ) ;
#75084 = CARTESIAN_POINT ( 'NONE',  ( 5.823673210054125526, 21.52544592524343514, 79.79057627198102409 ) ) ;
#75085 =( BOUNDED_CURVE ( )  B_SPLINE_CURVE ( 2, ( #170633, #110935, #173623, #156455, #78604, #16950, #123119, #79607, #93779, #92778, #95766 ),
 .UNSPECIFIED., .F., .T. ) 
 B_SPLINE_CURVE_WITH_KNOTS ( ( 3, 2, 2, 2, 2, 3 ),
 ( 0.8000000000000000444, 0.8199999999999999512, 0.8399999999999999689, 0.8599999999999999867, 0.8800000000000000044, 0.9000000000000000222 ),
 .UNSPECIFIED. ) 
 CURVE ( )  GEOMETRIC_REPRESENTATION_ITEM ( )  RATIONAL_B_SPLINE_CURVE ( ( 1.000000000000000000, 0.9510565162951535312, 1.000000000000000000, 0.9510565162951535312, 1.000000000000000000, 0.9510565162951535312, 1.000000000000000000, 0.9510565162951535312, 1.000000000000000000, 0.9510565162951535312, 1.000000000000000000 ) ) 
 REPRESENTATION_ITEM ( '' )  );
#75086 = CARTESIAN_POINT ( 'NONE',  ( 0.000000000000000000, 0.000000000000000000, -60.44446360152740283 ) ) ;
#75087 = CARTESIAN_POINT ( 'NONE',  ( 5.153800228976615827, -19.02544592524334988, 40.20942372801898301 ) ) ;
#75088 = CARTESIAN_POINT ( 'NONE',  ( 17.44279575226788026, -5.990770900253884257, 73.33557567514321818 ) ) ;
#75090 = CARTESIAN_POINT ( 'NONE',  ( -5.049401038298153566, 19.05341960407611168, 85.20724293864766707 ) ) ;
#75089 = CARTESIAN_POINT ( 'NONE',  ( 13.97604488694527802, 13.89961937509977652, 74.37390960531436690 ) ) ;
#75091 = CARTESIAN_POINT ( 'NONE',  ( 16.52544592524335698, 4.483927247898782831, 61.45942372801901854 ) ) ;
#75092 = CARTESIAN_POINT ( 'NONE',  ( -26.79475375365586842, 2.428612866367529932E-14, 139.9999999999999716 ) ) ;
#75093 = CARTESIAN_POINT ( 'NONE',  ( -19.05341960407617563, 5.049401038297882671, 48.54275706135233293 ) ) ;
#75094 = CARTESIAN_POINT ( 'NONE',  ( 16.85867132384987244, 6.968984503517829054, 21.84742265313312259 ) ) ;
#75095 = CARTESIAN_POINT ( 'NONE',  ( 19.02544592524343514, -5.153800228976328945, 113.5405762719810241 ) ) ;
#75096 = CARTESIAN_POINT ( 'NONE',  ( 8.224510206698742110, 14.34966873604972548, 87.08442372801901854 ) ) ;
#75097 = CARTESIAN_POINT ( 'NONE',  ( -3.874011537017815421, -5.374011537017721274, -64.44758591613756948 ) ) ;
#75098 = CARTESIAN_POINT ( 'NONE',  ( 12.14591786802327356, -12.06949235617739191, 75.62609039468567573 ) ) ;
#75099 = FACE_OUTER_BOUND ( 'NONE', #16606, .T. ) ;
#75100 = CARTESIAN_POINT ( 'NONE',  ( -12.14591786802326823, 12.06949235617739902, 48.12609039468568284 ) ) ;
#75101 = LINE ( 'NONE', #41797, #172887 ) ;
#75102 = CARTESIAN_POINT ( 'NONE',  ( 18.62759615963255655, 10.81492255796105972, 61.66775706135235424 ) ) ;
#75103 = CARTESIAN_POINT ( 'NONE',  ( 13.97604488694548053, -13.89961937509957401, 80.62609039468567573 ) ) ;
#75104 = CARTESIAN_POINT ( 'NONE',  ( 13.97604488694548053, -13.89961937509957401, 20.62609039468567573 ) ) ;
#75105 = CARTESIAN_POINT ( 'NONE',  ( -16.51473224551069308, -9.474510206698971260, 51.66557627198102409 ) ) ;
#75106 = CARTESIAN_POINT ( 'NONE',  ( 9.564922557960805705, 16.46253265017160317, 39.58224293864768839 ) ) ;
#75107 = CARTESIAN_POINT ( 'NONE',  ( 28.79475375365586132, 2.781246896534039337E-14, 155.0000000000000000 ) ) ;
#75108 = CARTESIAN_POINT ( 'NONE',  ( 15.72974639402199770, -15.80617190586745480, 63.12390960531435979 ) ) ;
#75109 = CARTESIAN_POINT ( 'NONE',  ( -13.89961937509977652, 13.97604488694528158, 115.6239096053143669 ) ) ;
#75110 = CARTESIAN_POINT ( 'NONE',  ( 14.29746914071049879, -8.314922557960816363, 113.3322429386476955 ) ) ;
#75111 = CARTESIAN_POINT ( 'NONE',  ( -14.29746914071037622, -8.314922557961029526, 49.16775706135234003 ) ) ;
#75112 = ORIENTED_EDGE ( 'NONE', *, *, #38764, .F. ) ;
#75113 = CARTESIAN_POINT ( 'NONE',  ( -5.719274019375978568, 21.55341960407610458, 115.2072429386476955 ) ) ;
#75115 = CARTESIAN_POINT ( 'NONE',  ( 30.74264578624799782, 22.33583958711400541, -2.799999999999999822 ) ) ;
#75114 = CARTESIAN_POINT ( 'NONE',  ( -14.29746914071049879, 8.314922557960819915, 55.83224293864770260 ) ) ;
#75116 = CARTESIAN_POINT ( 'NONE',  ( -19.02544592524334988, -5.153800228976617603, 108.9594237280189759 ) ) ;
#75117 = CARTESIAN_POINT ( 'NONE',  ( -13.97604488694547697, 13.89961937509957934, 38.12609039468566152 ) ) ;
#75118 = CARTESIAN_POINT ( 'NONE',  ( 4.483927247898545687, 16.52544592524342804, 39.79057627198103830 ) ) ;
#75119 = CARTESIAN_POINT ( 'NONE',  ( 21.52544592524334988, 5.823673210054432836, 21.45942372801901499 ) ) ;
#75121 = CARTESIAN_POINT ( 'NONE',  ( 15.72974639402199770, -15.80617190586745480, 58.12390960531435979 ) ) ;
#75120 = CARTESIAN_POINT ( 'NONE',  ( 17.48853670773242186, 5.747243402303175763, 33.83328700250010002 ) ) ;
#75122 = CARTESIAN_POINT ( 'NONE',  ( -13.97604488694527625, -13.89961937509977652, 86.87390960531436690 ) ) ;
#75123 = CARTESIAN_POINT ( 'NONE',  ( -4.483927247898539470, -16.52544592524342804, 57.29057627198103120 ) ) ;
#75124 = CARTESIAN_POINT ( 'NONE',  ( 13.97604488694527802, 13.89961937509977652, 109.3739096053143669 ) ) ;
#75125 = CARTESIAN_POINT ( 'NONE',  ( -36.77234560139673647, 5.215770478161305235, 46.75454185840153798 ) ) ;
#75126 = CARTESIAN_POINT ( 'NONE',  ( -19.02544592524334988, -5.153800228976617603, 48.95942372801900433 ) ) ;
#75127 = CARTESIAN_POINT ( 'NONE',  ( 21.55341960407610458, 5.719274019375980345, 103.9572429386476813 ) ) ;
#75128 = CARTESIAN_POINT ( 'NONE',  ( 0.05219959533909260263, 19.03943276465977164, 49.99890960531435979 ) ) ;
#75129 = CARTESIAN_POINT ( 'NONE',  ( -14.29746914071049879, 8.314922557960819915, 110.8322429386476955 ) ) ;
#75130 = CARTESIAN_POINT ( 'NONE',  ( 21.53943276465977519, 0.05219959533937863772, 46.25109039468567573 ) ) ;
#75131 = CARTESIAN_POINT ( 'NONE',  ( 17.14385361876520264, 23.59649016807275856, 144.1750000027311671 ) ) ;
#75132 = CARTESIAN_POINT ( 'NONE',  ( 0.05219959533910956823, 16.53943276465976808, 29.99890960531435979 ) ) ;
#75133 = CARTESIAN_POINT ( 'NONE',  ( -9.564922557960796823, -16.46253265017161027, 47.08224293864769550 ) ) ;
#75134 = CARTESIAN_POINT ( 'NONE',  ( 16.51473224551069308, 9.474510206698969483, 104.1655762719810241 ) ) ;
#75135 = CARTESIAN_POINT ( 'NONE',  ( 18.62759615963271287, -10.81492255796078972, 73.33224293864769550 ) ) ;
#75136 = CARTESIAN_POINT ( 'NONE',  ( -17.14385361876520264, -23.59649016807271593, 145.1750000027311387 ) ) ;
#75138 = CARTESIAN_POINT ( 'NONE',  ( -9.474510206698964154, 16.51473224551069663, 40.41557627198103120 ) ) ;
#75137 = B_SPLINE_CURVE_WITH_KNOTS ( 'NONE', 3,
 ( #168006, #14319, #46648, #76975, #75984, #137657, #199344, #45655, #30483, #138646, #15316, #169988, #93131, #79966, #20272, #52607, #68774, #65781, #97100, #82936, #141635, #36431, #95128, #51611, #112290, #173980, #33470, #129435, #144614, #48648, #188159, #3125 ),
 .UNSPECIFIED., .F., .F.,
 ( 4, 2, 2, 2, 2, 2, 2, 2, 2, 2, 2, 2, 2, 2, 2, 4 ),
 ( 1.638340482224582059E-15, 0.0003712461730052129009, 0.0007424923460087874639, 0.001113738519012362135, 0.001484984692015936698, 0.002227477038023092330, 0.002598723211026670362, 0.002969969384030248395, 0.003341215557033825993, 0.003712461730037403592, 0.004083707903040982058, 0.004454954076044560091, 0.004826200249048137256, 0.005197446422051715288, 0.005568692595055293321, 0.005939938768058871353 ),
 .UNSPECIFIED. ) ;
#75139 = CARTESIAN_POINT ( 'NONE',  ( -21.53943276465977519, 0.05219959533907696930, 56.24890960531436690 ) ) ;
#75140 = CARTESIAN_POINT ( 'NONE',  ( 21.55341960407619695, -5.719274019375665929, 91.04275706135236135 ) ) ;
#75143 = CARTESIAN_POINT ( 'NONE',  ( -8.224510206698948167, 14.34966873604960824, 65.41557627198102409 ) ) ;
#75142 = CARTESIAN_POINT ( 'NONE',  ( -14.29746914071037622, -8.314922557961029526, 79.16775706135234714 ) ) ;
#75141 = DIRECTION ( 'NONE',  ( 0.000000000000000000, -1.000000000000000000, 0.000000000000000000 ) ) ;
#75144 = CARTESIAN_POINT ( 'NONE',  ( 5.153800228976335163, 19.02544592524342804, 74.79057627198103830 ) ) ;
#75145 = EDGE_LOOP ( 'NONE', ( #181565, #105697, #36494 ) ) ;
#75146 = CARTESIAN_POINT ( 'NONE',  ( -5.153800228976607833, 19.02544592524334988, 27.70942372801899722 ) ) ;
#75147 = CARTESIAN_POINT ( 'NONE',  ( -8.224510206698735004, -14.34966873604973081, 89.58442372801901854 ) ) ;
#75148 = CARTESIAN_POINT ( 'NONE',  ( -19.03943276465977164, -0.05219959533935918106, 23.75109039468566152 ) ) ;
#75149 = CARTESIAN_POINT ( 'NONE',  ( -5.153800228976328057, -19.02544592524343514, 72.29057627198102409 ) ) ;
#75150 = CARTESIAN_POINT ( 'NONE',  ( 18.62759615963271287, -10.81492255796078972, 48.33224293864770260 ) ) ;
#75151 = CARTESIAN_POINT ( 'NONE',  ( 16.53943276465976808, 0.05219959533934440121, 31.25109039468568639 ) ) ;
#75152 = CARTESIAN_POINT ( 'NONE',  ( 21.52544592524334988, 5.823673210054432836, 81.45942372801900433 ) ) ;
#75153 = CARTESIAN_POINT ( 'NONE',  ( -14.34966873604972548, 8.224510206698743886, 63.33442372801900433 ) ) ;
#75154 = CARTESIAN_POINT ( 'NONE',  ( -5.823673210054116645, -21.52544592524344225, 112.2905762719810241 ) ) ;
#75155 = CARTESIAN_POINT ( 'NONE',  ( 8.224510206698742110, 14.34966873604972548, 22.08442372801901143 ) ) ;
#75156 = CARTESIAN_POINT ( 'NONE',  ( 9.564922557960805705, 16.46253265017160317, 94.58224293864769550 ) ) ;
#75157 = CARTESIAN_POINT ( 'NONE',  ( -16.55341960407617563, 4.379528057220093196, 28.54275706135234358 ) ) ;
#75158 = CARTESIAN_POINT ( 'NONE',  ( 19.03943276465977164, -0.05219959533909143690, 53.74890960531436690 ) ) ;
#75159 = CARTESIAN_POINT ( 'NONE',  ( 0.05219959533934541429, -16.53943276465976808, 35.00109039468568284 ) ) ;
#75160 = CARTESIAN_POINT ( 'NONE',  ( -8.314922557960811034, -14.29746914071050412, 82.08224293864768129 ) ) ;
#75161 = CARTESIAN_POINT ( 'NONE',  ( 16.53943276465976808, 0.05219959533934440121, 86.25109039468568994 ) ) ;
#75163 = CARTESIAN_POINT ( 'NONE',  ( 0.05219959533909260263, 19.03943276465977164, 64.99890960531436690 ) ) ;
#75162 = CARTESIAN_POINT ( 'NONE',  ( 0.05219959533937995610, -21.53943276465977519, 25.00109039468567218 ) ) ;
#75164 = CARTESIAN_POINT ( 'NONE',  ( -13.97604488694527625, -13.89961937509977652, 76.87390960531433848 ) ) ;
#75165 = CARTESIAN_POINT ( 'NONE',  ( -16.52544592524335698, -4.483927247898792601, 88.95942372801901854 ) ) ;
#75167 = ORIENTED_EDGE ( 'NONE', *, *, #132905, .T. ) ;
#75166 = CARTESIAN_POINT ( 'NONE',  ( -24.83221077041872960, -4.296110748029300375, 170.3917201292314303 ) ) ;
#75168 = VERTEX_POINT ( 'NONE', #105199 ) ;
#75169 = CARTESIAN_POINT ( 'NONE',  ( 16.51473224551083163, -9.474510206698727899, 30.83442372801900433 ) ) ;
#75170 = CARTESIAN_POINT ( 'NONE',  ( 9.474510206698971260, -16.51473224551069308, 97.91557627198102409 ) ) ;
#75171 = CARTESIAN_POINT ( 'NONE',  ( -5.049401038298153566, 19.05341960407611168, 55.20724293864769550 ) ) ;
#75172 = CARTESIAN_POINT ( 'NONE',  ( -16.46253265017160317, 9.564922557960807481, 115.8322429386477097 ) ) ;
#75173 = CARTESIAN_POINT ( 'NONE',  ( -0.05219959533934338120, 16.53943276465976808, 32.50109039468568284 ) ) ;
#75175 = CARTESIAN_POINT ( 'NONE',  ( 8.314922557961029526, -14.29746914071037800, 40.41775706135234714 ) ) ;
#75174 = CARTESIAN_POINT ( 'NONE',  ( -13.89961937509957401, -13.97604488694547875, 54.37609039468565442 ) ) ;
#75176 = CARTESIAN_POINT ( 'NONE',  ( -5.153800228976328057, -19.02544592524343514, 107.2905762719810383 ) ) ;
#75177 = CARTESIAN_POINT ( 'NONE',  ( -19.05341960407611168, -5.049401038298163336, 71.45724293864766707 ) ) ;
#75178 = CARTESIAN_POINT ( 'NONE',  ( -21.53943276465977519, 0.05219959533907696930, 101.2489096053143669 ) ) ;
#75179 = CARTESIAN_POINT ( 'NONE',  ( 5.153800228976615827, -19.02544592524334988, 70.20942372801899012 ) ) ;
#75181 = FACE_OUTER_BOUND ( 'NONE', #169155, .T. ) ;
#75180 = CARTESIAN_POINT ( 'NONE',  ( -16.51473224551069308, -9.474510206698971260, 86.66557627198102409 ) ) ;
#75182 = CARTESIAN_POINT ( 'NONE',  ( 19.02544592524343514, -5.153800228976328945, 58.54057627198102409 ) ) ;
#75184 = CARTESIAN_POINT ( 'NONE',  ( -16.46253265017160317, 9.564922557960807481, 25.83224293864769194 ) ) ;
#75183 = CARTESIAN_POINT ( 'NONE',  ( -14.29746914071049879, 8.314922557960819915, 40.83224293864769550 ) ) ;
#75185 = CARTESIAN_POINT ( 'NONE',  ( -16.51473224551082808, 9.474510206698731452, 43.33442372801900433 ) ) ;
#75186 = CARTESIAN_POINT ( 'NONE',  ( -14.34966873604960291, -8.224510206698953496, 76.66557627198103830 ) ) ;
#75187 = CARTESIAN_POINT ( 'NONE',  ( 21.52544592524334988, 5.823673210054432836, 96.45942372801901854 ) ) ;
#75188 = CARTESIAN_POINT ( 'NONE',  ( 9.564922557960805705, 16.46253265017160317, 39.58224293864768839 ) ) ;
#75189 = CARTESIAN_POINT ( 'NONE',  ( -12.06949235617739369, -12.14591786802326823, 54.37609039468568994 ) ) ;
#75190 = EDGE_CURVE ( 'NONE', #139805, #184086, #2452, .T. ) ;
#75192 = CARTESIAN_POINT ( 'NONE',  ( -18.62759615963255300, -10.81492255796106328, 104.1677570613523471 ) ) ;
#75191 = CARTESIAN_POINT ( 'NONE',  ( 12.14591786802309770, 12.06949235617756955, 39.37390960531436690 ) ) ;
#75193 = CARTESIAN_POINT ( 'NONE',  ( 5.049401038298161559, -19.05341960407611168, 92.70724293864769550 ) ) ;
#75194 = CARTESIAN_POINT ( 'NONE',  ( 5.049401038298161559, -19.05341960407611168, 97.70724293864766707 ) ) ;
#75195 = CARTESIAN_POINT ( 'NONE',  ( -13.97604488694527625, -13.89961937509977652, 21.87390960531435979 ) ) ;
#75196 = CARTESIAN_POINT ( 'NONE',  ( -16.55341960407611168, -4.379528057220339221, 106.4572429386477097 ) ) ;
#75197 = CARTESIAN_POINT ( 'NONE',  ( -12.14591786802309592, -12.06949235617757132, 71.87390960531438111 ) ) ;
#75198 = CARTESIAN_POINT ( 'NONE',  ( 10.81492255796078972, 18.62759615963270932, 79.58224293864769550 ) ) ;
#75199 = CARTESIAN_POINT ( 'NONE',  ( 5.153800228976335163, 19.02544592524342804, 89.79057627198102409 ) ) ;
#75200 = CARTESIAN_POINT ( 'NONE',  ( 15.72974639402199770, -15.80617190586745480, 93.12390960531436690 ) ) ;
#75201 = CARTESIAN_POINT ( 'NONE',  ( 5.153800228976335163, 19.02544592524342804, 94.79057627198103830 ) ) ;
#75203 = CARTESIAN_POINT ( 'NONE',  ( -14.34966873604960291, -8.224510206698953496, 91.66557627198103830 ) ) ;
#75202 = CARTESIAN_POINT ( 'NONE',  ( -19.39056639909674473, -5.499999999999968026, 90.78948781074345220 ) ) ;
#75204 = CARTESIAN_POINT ( 'NONE',  ( 13.89961937509977652, -13.97604488694527269, 58.12390960531436690 ) ) ;
#75205 = CARTESIAN_POINT ( 'NONE',  ( -15.72974639402197994, 15.80617190586746368, 70.62390960531436690 ) ) ;
#75206 = CARTESIAN_POINT ( 'NONE',  ( 17.05116617787827948, -6.768360034955676952, 26.15675553259199759 ) ) ;
#75208 = CARTESIAN_POINT ( 'NONE',  ( -27.73933785331498925, 2.428612866367529932E-14, 149.3750000027311842 ) ) ;
#75207 = CARTESIAN_POINT ( 'NONE',  ( -16.55341960407611168, -4.379528057220339221, 21.45724293864769550 ) ) ;
#75209 = CARTESIAN_POINT ( 'NONE',  ( 8.314922557961029526, -14.29746914071037800, 25.41775706135235779 ) ) ;
#75210 = CARTESIAN_POINT ( 'NONE',  ( -14.34966873604960291, -8.224510206698953496, 76.66557627198103830 ) ) ;
#75211 = CARTESIAN_POINT ( 'NONE',  ( -18.09918380851992481, -5.500000000000039968, 46.48618307335612343 ) ) ;
#75212 = CARTESIAN_POINT ( 'NONE',  ( 9.474510206698971260, -16.51473224551069308, 77.91557627198103830 ) ) ;
#75213 = CARTESIAN_POINT ( 'NONE',  ( -19.03943276465977164, 0.05219959533909376836, 41.24890960531435269 ) ) ;
#75214 = CARTESIAN_POINT ( 'NONE',  ( -4.483927247898539470, -16.52544592524342804, 67.29057627198103830 ) ) ;
#75215 = CARTESIAN_POINT ( 'NONE',  ( 13.89961937509977652, -13.97604488694527269, 113.1239096053143527 ) ) ;
#75216 = CARTESIAN_POINT ( 'NONE',  ( -19.02544592524334988, -5.153800228976617603, 98.95942372801900433 ) ) ;
#75217 = CARTESIAN_POINT ( 'NONE',  ( 18.67979575497194134, -10.72451020669871369, 60.83442372801901854 ) ) ;
#75218 = CARTESIAN_POINT ( 'NONE',  ( -9.474510206698964154, 16.51473224551069663, 95.41557627198102409 ) ) ;
#75219 = CARTESIAN_POINT ( 'NONE',  ( 0.05219959533907565091, 21.53943276465977519, 79.99890960531435269 ) ) ;
#75220 = CARTESIAN_POINT ( 'NONE',  ( -16.52544592524335698, -4.483927247898792601, 73.95942372801901854 ) ) ;
#75221 = CARTESIAN_POINT ( 'NONE',  ( 5.153800228976335163, 19.02544592524342804, 24.79057627198102765 ) ) ;
#75222 = CARTESIAN_POINT ( 'NONE',  ( 0.05219959533909260263, 19.03943276465977164, 69.99890960531435269 ) ) ;
#75223 = CARTESIAN_POINT ( 'NONE',  ( 5.719274019375991003, -21.55341960407610458, 87.70724293864769550 ) ) ;
#75224 = CARTESIAN_POINT ( 'NONE',  ( -0.05219959533936034679, 19.03943276465977164, 102.5010903946856757 ) ) ;
#75225 = AXIS2_PLACEMENT_3D ( 'NONE', #133052, #162386, #42060 ) ;
#75227 = CARTESIAN_POINT ( 'NONE',  ( -15.72974639402176322, -15.80617190586768395, 64.37609039468568994 ) ) ;
#75226 = CARTESIAN_POINT ( 'NONE',  ( 4.379528057220339221, -16.55341960407611168, 42.70724293864770260 ) ) ;
#75229 = CARTESIAN_POINT ( 'NONE',  ( 5.153800228976335163, 19.02544592524342804, 109.7905762719810099 ) ) ;
#75228 = CARTESIAN_POINT ( 'NONE',  ( 12.14591786802327356, -12.06949235617739191, 90.62609039468567573 ) ) ;
#75230 = CARTESIAN_POINT ( 'NONE',  ( 16.51473224551069308, 9.474510206698969483, 104.1655762719810241 ) ) ;
#75231 = CARTESIAN_POINT ( 'NONE',  ( 7.500000000000000000, 9.184850993605147944E-16, 0.000000000000000000 ) ) ;
#75232 = CARTESIAN_POINT ( 'NONE',  ( -4.379528057220086978, -16.55341960407618274, 94.79275706135234714 ) ) ;
#75233 = CARTESIAN_POINT ( 'NONE',  ( 16.55341960407618274, -4.379528057220086978, 51.04275706135234714 ) ) ;
#75234 = CARTESIAN_POINT ( 'NONE',  ( 9.564922557960805705, 16.46253265017160317, 54.58224293864769550 ) ) ;
#75235 = CARTESIAN_POINT ( 'NONE',  ( 5.153800228976335163, 19.02544592524342804, 74.79057627198103830 ) ) ;
#75236 = CARTESIAN_POINT ( 'NONE',  ( -18.62759615963255300, -10.81492255796106328, 69.16775706135234714 ) ) ;
#75237 = CARTESIAN_POINT ( 'NONE',  ( -4.483927247898782831, 16.52544592524335698, 67.70942372801901854 ) ) ;
#75238 = CARTESIAN_POINT ( 'NONE',  ( -16.55341960407611168, -4.379528057220339221, 46.45724293864769550 ) ) ;
#75239 = CARTESIAN_POINT ( 'NONE',  ( -19.02544592524342804, 5.153800228976336051, 46.04057627198101699 ) ) ;
#75240 = CARTESIAN_POINT ( 'NONE',  ( 19.02544592524343514, -5.153800228976328945, 53.54057627198102409 ) ) ;
#75241 = CARTESIAN_POINT ( 'NONE',  ( 8.224510206698742110, 14.34966873604972548, 37.08442372801901143 ) ) ;
#75242 = CARTESIAN_POINT ( 'NONE',  ( -9.474510206698720793, -16.51473224551083518, 89.58442372801900433 ) ) ;
#75243 = CARTESIAN_POINT ( 'NONE',  ( -16.53943276465976808, 0.05219959533911058130, 91.24890960531436690 ) ) ;
#75244 = CARTESIAN_POINT ( 'NONE',  ( 19.03943276465977164, -0.05219959533909143690, 68.74890960531436690 ) ) ;
#75246 = CARTESIAN_POINT ( 'NONE',  ( 28.79475375365609935, -9.355982642738862154, 148.8843446569000264 ) ) ;
#75245 = CARTESIAN_POINT ( 'NONE',  ( 19.03943276465977164, 0.05219959533936151252, 101.2510903946856757 ) ) ;
#75247 = CARTESIAN_POINT ( 'NONE',  ( 21.53943276465977519, 0.05219959533937863772, 91.25109039468568994 ) ) ;
#75248 = CARTESIAN_POINT ( 'NONE',  ( 16.55341960407618274, -4.379528057220086978, 61.04275706135234714 ) ) ;
#75249 = CARTESIAN_POINT ( 'NONE',  ( 0.000000000000000000, 0.000000000000000000, -56.77278709839600879 ) ) ;
#75250 = CARTESIAN_POINT ( 'NONE',  ( -0.05219959533907301413, -21.53943276465977519, 47.49890960531435979 ) ) ;
#75251 = CARTESIAN_POINT ( 'NONE',  ( 0.05219959533934541429, -16.53943276465976808, 55.00109039468568284 ) ) ;
#75252 = CARTESIAN_POINT ( 'NONE',  ( 17.58332526062526568, -7.635886036038552760, 38.42334959558466778 ) ) ;
#75253 = CARTESIAN_POINT ( 'NONE',  ( 13.89961937509957401, 13.97604488694547697, 41.87609039468566152 ) ) ;
#75254 = CARTESIAN_POINT ( 'NONE',  ( -19.03943276465977164, 0.05219959533909376836, 86.24890960531436690 ) ) ;
#75255 = CARTESIAN_POINT ( 'NONE',  ( -9.564922557960796823, -16.46253265017161027, 22.08224293864768839 ) ) ;
#75256 = CARTESIAN_POINT ( 'NONE',  ( -5.153800228976328057, -19.02544592524343514, 62.29057627198100988 ) ) ;
#75257 = CARTESIAN_POINT ( 'NONE',  ( 15.06137443927350361, 15.06137443927346098, -56.46919128290398504 ) ) ;
#75258 = CARTESIAN_POINT ( 'NONE',  ( -18.67979575497193778, 10.72451020669871902, 78.33442372801901854 ) ) ;
#75259 = CARTESIAN_POINT ( 'NONE',  ( -18.39639308325436673, -5.500000000000040856, 56.48252246182197212 ) ) ;
#75260 = CARTESIAN_POINT ( 'NONE',  ( -19.03943276465977164, -0.05219959533935918106, 38.75109039468566152 ) ) ;
#75261 = CARTESIAN_POINT ( 'NONE',  ( -5.153800228976607833, 19.02544592524334988, 27.70942372801899722 ) ) ;
#75262 = CARTESIAN_POINT ( 'NONE',  ( -4.379528057220328563, 16.55341960407611168, 50.20724293864769550 ) ) ;
#75263 = CARTESIAN_POINT ( 'NONE',  ( 19.03943276465977164, -0.05219959533909143690, 53.74890960531436690 ) ) ;
#75264 = CARTESIAN_POINT ( 'NONE',  ( 21.55341960407610458, 5.719274019375980345, 23.95724293864769550 ) ) ;
#75265 = CARTESIAN_POINT ( 'NONE',  ( -21.55341960407619339, 5.719274019375674811, 78.54275706135236135 ) ) ;
#75266 = CARTESIAN_POINT ( 'NONE',  ( 5.049401038298161559, -19.05341960407611168, 67.70724293864769550 ) ) ;
#75267 = AXIS2_PLACEMENT_3D ( 'NONE', #33435, #188125, #98051 ) ;
#75268 = CARTESIAN_POINT ( 'NONE',  ( 21.53943276465977519, 0.05219959533937863772, 76.25109039468568994 ) ) ;
#75269 = CARTESIAN_POINT ( 'NONE',  ( 21.52544592524344225, -5.823673210054117533, 33.54057627198102409 ) ) ;
#75270 = CARTESIAN_POINT ( 'NONE',  ( -5.823673210054431948, 21.52544592524334988, 42.70942372801901854 ) ) ;
#75271 = CARTESIAN_POINT ( 'NONE',  ( -19.05341960407617563, 5.049401038297882671, 63.54275706135234003 ) ) ;
#75272 = CARTESIAN_POINT ( 'NONE',  ( -5.049401038298153566, 19.05341960407611168, 45.20724293864769550 ) ) ;
#75273 = CARTESIAN_POINT ( 'NONE',  ( 9.474510206698971260, -16.51473224551069308, 82.91557627198103830 ) ) ;
#75274 = CARTESIAN_POINT ( 'NONE',  ( 12.06949235617739724, 12.14591786802326823, 31.87609039468567929 ) ) ;
#75275 = CARTESIAN_POINT ( 'NONE',  ( -4.483927247898539470, -16.52544592524342804, 82.29057627198103830 ) ) ;
#75276 = CARTESIAN_POINT ( 'NONE',  ( -19.05341960407611168, -5.049401038298163336, 51.45724293864770260 ) ) ;
#75277 = CARTESIAN_POINT ( 'NONE',  ( 21.53943276465977519, -0.05219959533907433946, 48.74890960531435979 ) ) ;
#75278 = CARTESIAN_POINT ( 'NONE',  ( 14.34966873604972726, -8.224510206698740333, 20.83442372801901143 ) ) ;
#75279 = CARTESIAN_POINT ( 'NONE',  ( 15.80617190586769283, -15.72974639402175789, 25.62609039468567929 ) ) ;
#75280 = CARTESIAN_POINT ( 'NONE',  ( 10.72451020669871369, 18.67979575497193778, 77.08442372801901854 ) ) ;
#75281 = CARTESIAN_POINT ( 'NONE',  ( 12.14591786802327356, -12.06949235617739191, 75.62609039468567573 ) ) ;
#75282 = CARTESIAN_POINT ( 'NONE',  ( -8.224510206698735004, -14.34966873604973081, 64.58442372801900433 ) ) ;
#75283 = CARTESIAN_POINT ( 'NONE',  ( -5.153800228976328057, -19.02544592524343514, 57.29057627198103120 ) ) ;
#75284 = CARTESIAN_POINT ( 'NONE',  ( -16.53943276465976808, -0.05219959533934237506, 88.75109039468567573 ) ) ;
#75285 = CARTESIAN_POINT ( 'NONE',  ( -13.97604488694547697, 13.89961937509957934, 48.12609039468566863 ) ) ;
#75286 = CARTESIAN_POINT ( 'NONE',  ( -21.55341960407619339, 5.719274019375674811, 23.54275706135235424 ) ) ;
#75287 = CARTESIAN_POINT ( 'NONE',  ( -8.314922557960811034, -14.29746914071050412, 62.08224293864769550 ) ) ;
#75288 = CARTESIAN_POINT ( 'NONE',  ( 9.474510206698971260, -16.51473224551069308, 82.91557627198103830 ) ) ;
#75289 = CARTESIAN_POINT ( 'NONE',  ( 8.314922557961029526, -14.29746914071037800, 95.41775706135234714 ) ) ;
#75290 = CARTESIAN_POINT ( 'NONE',  ( -21.55341960407619339, 5.719274019375674811, 58.54275706135235424 ) ) ;
#75291 = CARTESIAN_POINT ( 'NONE',  ( -14.29746914071037622, -8.314922557961029526, 29.16775706135234003 ) ) ;
#75292 = CARTESIAN_POINT ( 'NONE',  ( -15.72974639402197994, 15.80617190586746368, 105.6239096053143669 ) ) ;
#75293 = CARTESIAN_POINT ( 'NONE',  ( -8.224510206698948167, 14.34966873604960824, 55.41557627198102409 ) ) ;
#75294 = ORIENTED_EDGE ( 'NONE', *, *, #139940, .T. ) ;
#75295 = CARTESIAN_POINT ( 'NONE',  ( -15.72974639402197994, 15.80617190586746368, 95.62390960531436690 ) ) ;
#75296 = CARTESIAN_POINT ( 'NONE',  ( 0.05219959533910956823, 16.53943276465976808, 44.99890960531435979 ) ) ;
#75297 = ORIENTED_EDGE ( 'NONE', *, *, #45175, .F. ) ;
#75298 = CARTESIAN_POINT ( 'NONE',  ( 34.36935609104189382, 7.254501760396902199, 46.91913033384989262 ) ) ;
#75299 = CARTESIAN_POINT ( 'NONE',  ( -9.474510206698964154, 16.51473224551069663, 115.4155762719810241 ) ) ;
#75300 = CARTESIAN_POINT ( 'NONE',  ( -18.67979575497193778, 10.72451020669871902, 43.33442372801901143 ) ) ;
#75301 = CARTESIAN_POINT ( 'NONE',  ( -12.14591786802309592, -12.06949235617757132, 61.87390960531436690 ) ) ;
#75302 = CARTESIAN_POINT ( 'NONE',  ( -9.474510206698964154, 16.51473224551069663, 60.41557627198102409 ) ) ;
#75304 = CARTESIAN_POINT ( 'NONE',  ( 5.049401038297881783, 19.05341960407617563, 67.29275706135234714 ) ) ;
#75303 = CARTESIAN_POINT ( 'NONE',  ( -13.89961937509977652, 13.97604488694528158, 30.62390960531435269 ) ) ;
#75305 = CARTESIAN_POINT ( 'NONE',  ( -5.823673210054116645, -21.52544592524344225, 42.29057627198103120 ) ) ;
#75306 = CARTESIAN_POINT ( 'NONE',  ( -24.21728366753307071, -29.00647930567809851, -20.95994360448459659 ) ) ;
#75307 = CARTESIAN_POINT ( 'NONE',  ( 5.153800228976335163, 19.02544592524342804, 64.79057627198100988 ) ) ;
#75308 = CARTESIAN_POINT ( 'NONE',  ( 14.29746914071037800, 8.314922557961029526, 36.66775706135234714 ) ) ;
#75309 = CARTESIAN_POINT ( 'NONE',  ( 5.823673210054125526, 21.52544592524343514, 109.7905762719810383 ) ) ;
#75310 = CARTESIAN_POINT ( 'NONE',  ( -16.52544592524342804, 4.483927247898546575, 41.04057627198103120 ) ) ;
#75311 = ORIENTED_EDGE ( 'NONE', *, *, #114623, .F. ) ;
#75312 = CARTESIAN_POINT ( 'NONE',  ( -5.153800228976328057, -19.02544592524343514, 92.29057627198099567 ) ) ;
#75313 = CARTESIAN_POINT ( 'NONE',  ( 0.05219959533907565091, 21.53943276465977519, 69.99890960531435269 ) ) ;
#75315 = CARTESIAN_POINT ( 'NONE',  ( 8.314922557961029526, -14.29746914071037800, 40.41775706135234714 ) ) ;
#75314 = CARTESIAN_POINT ( 'NONE',  ( 15.72974639402199770, -15.80617190586745480, 113.1239096053143953 ) ) ;
#75316 = CARTESIAN_POINT ( 'NONE',  ( 15.80617190586746368, 15.72974639402197994, 34.37390960531435979 ) ) ;
#75317 = CARTESIAN_POINT ( 'NONE',  ( 5.719274019375673035, 21.55341960407619339, 107.2927570613523471 ) ) ;
#75318 = CARTESIAN_POINT ( 'NONE',  ( 19.02544592524343514, -5.153800228976328945, 103.5405762719809957 ) ) ;
#75319 = CARTESIAN_POINT ( 'NONE',  ( -5.153800228976328057, -19.02544592524343514, 47.29057627198102409 ) ) ;
#75320 = CARTESIAN_POINT ( 'NONE',  ( 13.97604488694527802, 13.89961937509977652, 94.37390960531436690 ) ) ;
#75321 = CARTESIAN_POINT ( 'NONE',  ( -5.153800228976328057, -19.02544592524343514, 77.29057627198099567 ) ) ;
#75322 = CARTESIAN_POINT ( 'NONE',  ( 16.18388926212248791, -7.379444403734420455, 87.06046848633769741 ) ) ;
#75323 = EDGE_CURVE ( 'NONE', #193525, #120616, #166886, .T. ) ;
#75324 = CARTESIAN_POINT ( 'NONE',  ( 9.474510206698729675, 16.51473224551082808, 57.08442372801900433 ) ) ;
#75326 = CARTESIAN_POINT ( 'NONE',  ( 10.81492255796078972, 18.62759615963270932, 34.58224293864770260 ) ) ;
#75325 = CARTESIAN_POINT ( 'NONE',  ( 0.05219959533936267826, -19.03943276465977164, 20.00109039468567218 ) ) ;
#75327 = CARTESIAN_POINT ( 'NONE',  ( 12.14591786802327356, -12.06949235617739191, 110.6260903946857042 ) ) ;
#75328 = CARTESIAN_POINT ( 'NONE',  ( -19.03943276465977164, -0.05219959533935918106, 78.75109039468567573 ) ) ;
#75329 = CARTESIAN_POINT ( 'NONE',  ( 13.97604488694527802, 13.89961937509977830, 39.37390960531435979 ) ) ;
#75330 = CARTESIAN_POINT ( 'NONE',  ( -16.51473224551082808, 9.474510206698731452, 83.33442372801899012 ) ) ;
#75331 = CARTESIAN_POINT ( 'NONE',  ( -19.05341960407617563, 5.049401038297882671, 33.54275706135231871 ) ) ;
#75332 = CARTESIAN_POINT ( 'NONE',  ( 16.79531203550646623, 7.028104445595620753, 108.7524498822044023 ) ) ;
#75333 = CARTESIAN_POINT ( 'NONE',  ( -5.049401038298153566, 19.05341960407611168, 40.20724293864768839 ) ) ;
#75334 = CARTESIAN_POINT ( 'NONE',  ( 4.483927247898545687, 16.52544592524342804, 54.79057627198104541 ) ) ;
#75335 = CARTESIAN_POINT ( 'NONE',  ( -19.05341960407611168, -5.049401038298163336, 21.45724293864768839 ) ) ;
#75336 = CARTESIAN_POINT ( 'NONE',  ( -16.55341960407611168, -4.379528057220339221, 21.45724293864769550 ) ) ;
#75337 = CARTESIAN_POINT ( 'NONE',  ( 18.22780087662122384, -5.500000000000022204, 46.01540105326107266 ) ) ;
#75338 = CARTESIAN_POINT ( 'NONE',  ( 8.224510206698742110, 14.34966873604972548, 97.08442372801904696 ) ) ;
#75339 = CARTESIAN_POINT ( 'NONE',  ( -19.03943276465977164, 0.05219959533909376836, 56.24890960531435979 ) ) ;
#75340 = CARTESIAN_POINT ( 'NONE',  ( -18.62759615963255300, -10.81492255796106328, 109.1677570613523613 ) ) ;
#75341 = CARTESIAN_POINT ( 'NONE',  ( 12.14591786802327356, -12.06949235617739191, 20.62609039468568639 ) ) ;
#75343 = VERTEX_POINT ( 'NONE', #104208 ) ;
#75342 = CARTESIAN_POINT ( 'NONE',  ( 21.52544592524334988, 5.823673210054432836, 91.45942372801901854 ) ) ;
#75344 = CARTESIAN_POINT ( 'NONE',  ( -9.474510206698964154, 16.51473224551069663, 95.41557627198102409 ) ) ;
#75345 = CARTESIAN_POINT ( 'NONE',  ( 19.03943276465977164, -0.05219959533909143690, 88.74890960531436690 ) ) ;
#75346 = CARTESIAN_POINT ( 'NONE',  ( 36.91746824999999177, 11.99521256947799230, -9.524999997268812635 ) ) ;
#75347 = CARTESIAN_POINT ( 'NONE',  ( 21.55341960407610458, 5.719274019375980345, 113.9572429386477239 ) ) ;
#75348 = CARTESIAN_POINT ( 'NONE',  ( 14.34966873604960469, 8.224510206698951720, 79.16557627198103830 ) ) ;
#75349 = CARTESIAN_POINT ( 'NONE',  ( 15.80617190586746368, 15.72974639402197994, 74.37390960531436690 ) ) ;
#75350 = CARTESIAN_POINT ( 'NONE',  ( -16.46253265017160317, 9.564922557960807481, 65.83224293864769550 ) ) ;
#75352 = CARTESIAN_POINT ( 'NONE',  ( -4.379528057220086978, -16.55341960407618274, 89.79275706135236135 ) ) ;
#75351 = CARTESIAN_POINT ( 'NONE',  ( 10.81492255796078972, 18.62759615963270932, 99.58224293864770971 ) ) ;
#75353 = ORIENTED_EDGE ( 'NONE', *, *, #8545, .T. ) ;
#75354 = CARTESIAN_POINT ( 'NONE',  ( -13.97604488694527625, -13.89961937509977652, 66.87390960531436690 ) ) ;
#75356 = CARTESIAN_POINT ( 'NONE',  ( 17.50000000000000000, 5.500000000000001776, 33.78230962303567253 ) ) ;
#75355 = CARTESIAN_POINT ( 'NONE',  ( -16.53943276465976808, 0.05219959533911058130, 86.24890960531436690 ) ) ;
#75357 = CARTESIAN_POINT ( 'NONE',  ( 16.46253265017160672, -9.564922557960803928, 48.33224293864769550 ) ) ;
#75358 = CARTESIAN_POINT ( 'NONE',  ( 16.51473224551083163, -9.474510206698727899, 75.83442372801900433 ) ) ;
#75359 = CARTESIAN_POINT ( 'NONE',  ( 14.34966873604960469, 8.224510206698951720, 79.16557627198103830 ) ) ;
#75360 = CARTESIAN_POINT ( 'NONE',  ( 21.52544592524334988, 5.823673210054432836, 56.45942372801902565 ) ) ;
#75362 = CARTESIAN_POINT ( 'NONE',  ( -21.52544592524343514, 5.823673210054127303, 116.0405762719810383 ) ) ;
#75361 = CARTESIAN_POINT ( 'NONE',  ( -13.97604488694527625, -13.89961937509977652, 36.87390960531436690 ) ) ;
#75363 = CARTESIAN_POINT ( 'NONE',  ( -12.14591786802309592, -12.06949235617757132, 101.8739096053143811 ) ) ;
#75364 = CARTESIAN_POINT ( 'NONE',  ( 14.29384609392659833, -37.08231061483255075, -29.62140346006600922 ) ) ;
#75365 = CARTESIAN_POINT ( 'NONE',  ( -13.97604488694527625, -13.89961937509977652, 61.87390960531435979 ) ) ;
#75366 = CARTESIAN_POINT ( 'NONE',  ( 19.19724070472090105, 5.500000000000154543, 48.56193348274384647 ) ) ;
#75368 = CARTESIAN_POINT ( 'NONE',  ( 0.05219959533909260263, 19.03943276465977164, 109.9989096053143669 ) ) ;
#75367 = CARTESIAN_POINT ( 'NONE',  ( 13.97604488694548053, -13.89961937509957401, 100.6260903946856615 ) ) ;
#75369 = CARTESIAN_POINT ( 'NONE',  ( 21.55341960407619695, -5.719274019375665929, 46.04275706135234714 ) ) ;
#75370 = CARTESIAN_POINT ( 'NONE',  ( 19.03943276465977164, -0.05219959533909143690, 83.74890960531436690 ) ) ;
#75371 = CARTESIAN_POINT ( 'NONE',  ( -13.89961937509957401, -13.97604488694547875, 74.37609039468566152 ) ) ;
#75372 = CARTESIAN_POINT ( 'NONE',  ( 5.049401038298161559, -19.05341960407611168, 57.70724293864769550 ) ) ;
#75373 = CARTESIAN_POINT ( 'NONE',  ( -0.05219959533910754901, -16.53943276465976808, 82.49890960531436690 ) ) ;
#75374 = CARTESIAN_POINT ( 'NONE',  ( -4.483927247898539470, -16.52544592524342804, 67.29057627198103830 ) ) ;
#75375 = CARTESIAN_POINT ( 'NONE',  ( -0.05219959533909027116, -19.03943276465977164, 87.49890960531436690 ) ) ;
#75376 = CARTESIAN_POINT ( 'NONE',  ( 16.52544592524342804, -4.483927247898539470, 73.54057627198102409 ) ) ;
#75377 = CARTESIAN_POINT ( 'NONE',  ( -9.474510206698964154, 16.51473224551069663, 80.41557627198103830 ) ) ;
#75378 = CARTESIAN_POINT ( 'NONE',  ( 19.02544592524334988, 5.153800228976608722, 31.45942372801900433 ) ) ;
#75381 = CARTESIAN_POINT ( 'NONE',  ( -19.03943276465977164, 0.05219959533909376836, 21.24890960531436335 ) ) ;
#75380 = CARTESIAN_POINT ( 'NONE',  ( -14.34966873604960291, -8.224510206698953496, 31.66557627198102054 ) ) ;
#75379 = CARTESIAN_POINT ( 'NONE',  ( -13.97604488694527625, -13.89961937509977652, 46.87390960531435979 ) ) ;
#75382 = ORIENTED_EDGE ( 'NONE', *, *, #137500, .F. ) ;
#75383 = CARTESIAN_POINT ( 'NONE',  ( 15.80617190586769283, -15.72974639402175789, 40.62609039468567573 ) ) ;
#75384 = CARTESIAN_POINT ( 'NONE',  ( 9.474510206698729675, 16.51473224551082808, 62.08442372801899722 ) ) ;
#75385 = CARTESIAN_POINT ( 'NONE',  ( 16.52544592524342804, -4.483927247898539470, 33.54057627198102409 ) ) ;
#75386 = CARTESIAN_POINT ( 'NONE',  ( -5.719274019375978568, 21.55341960407610458, 80.20724293864769550 ) ) ;
#75387 = CARTESIAN_POINT ( 'NONE',  ( -15.72974639402197994, 15.80617190586746368, 25.62390960531435624 ) ) ;
#75388 = CARTESIAN_POINT ( 'NONE',  ( 8.314922557960818139, 14.29746914071049879, 64.58224293864769550 ) ) ;
#75389 = CARTESIAN_POINT ( 'NONE',  ( 19.02544592524343514, -5.153800228976328945, 43.54057627198103120 ) ) ;
#75390 = CARTESIAN_POINT ( 'NONE',  ( -5.049401038297874678, -19.05341960407617918, 44.79275706135232582 ) ) ;
#75391 = CARTESIAN_POINT ( 'NONE',  ( 16.53943276465976808, 0.05219959533934440121, 106.2510903946856757 ) ) ;
#75392 = CARTESIAN_POINT ( 'NONE',  ( 4.379528057220092307, 16.55341960407617563, 62.29275706135236845 ) ) ;
#75393 = CARTESIAN_POINT ( 'NONE',  ( -10.81492255796078084, -18.62759615963271287, 32.08224293864769550 ) ) ;
#75394 = CARTESIAN_POINT ( 'NONE',  ( -21.53943276465977519, -0.05219959533937600094, 103.7510903946857042 ) ) ;
#75395 = CARTESIAN_POINT ( 'NONE',  ( 0.05219959533909260263, 19.03943276465977164, 94.99890960531436690 ) ) ;
#75396 = CARTESIAN_POINT ( 'NONE',  ( -12.14591786802326823, 12.06949235617739902, 73.12609039468567573 ) ) ;
#75397 = CARTESIAN_POINT ( 'NONE',  ( -19.02544592524342804, 5.153800228976336051, 26.04057627198103120 ) ) ;
#75398 = ADVANCED_FACE ( 'NONE', ( #71873 ), #151708, .F. ) ;
#75399 = CARTESIAN_POINT ( 'NONE',  ( -16.53943276465976808, 0.05219959533911058130, 36.24890960531435979 ) ) ;
#75401 = CARTESIAN_POINT ( 'NONE',  ( -5.153800228976328057, -19.02544592524343514, 97.29057627198099567 ) ) ;
#75400 = CARTESIAN_POINT ( 'NONE',  ( 19.02544592524343514, -5.153800228976328945, 98.54057627198100988 ) ) ;
#75402 = CARTESIAN_POINT ( 'NONE',  ( -18.67979575497178146, -10.72451020669898902, 21.66557627198102409 ) ) ;
#75403 = CARTESIAN_POINT ( 'NONE',  ( 0.05219959533910956823, 16.53943276465976808, 69.99890960531435269 ) ) ;
#75404 = CARTESIAN_POINT ( 'NONE',  ( -0.05219959533910754901, -16.53943276465976808, 37.49890960531436690 ) ) ;
#75405 = AXIS2_PLACEMENT_3D ( 'NONE', #99311, #66985, #127655 ) ;
#75406 = CARTESIAN_POINT ( 'NONE',  ( -12.06949235617756955, 12.14591786802309770, 55.62390960531436690 ) ) ;
#75407 = EDGE_LOOP ( 'NONE', ( #17697, #124592, #195444, #186083 ) ) ;
#75408 = CARTESIAN_POINT ( 'NONE',  ( 16.52544592524335698, 4.483927247898782831, 56.45942372801902565 ) ) ;
#75409 = CARTESIAN_POINT ( 'NONE',  ( 19.05341960407617918, -5.049401038297876454, 56.04275706135234714 ) ) ;
#75410 = CARTESIAN_POINT ( 'NONE',  ( 9.474510206698971260, -16.51473224551069308, 82.91557627198103830 ) ) ;
#75411 = CARTESIAN_POINT ( 'NONE',  ( 13.89961937509957401, 13.97604488694547697, 71.87609039468567573 ) ) ;
#75412 = CARTESIAN_POINT ( 'NONE',  ( -27.73933785331498925, -9.013057229001049109, 141.4750000027311785 ) ) ;
#75413 = CARTESIAN_POINT ( 'NONE',  ( 16.51473224551083163, -9.474510206698727899, 50.83442372801899722 ) ) ;
#75415 = CARTESIAN_POINT ( 'NONE',  ( -16.55341960407617563, 4.379528057220093196, 98.54275706135234714 ) ) ;
#75414 = CARTESIAN_POINT ( 'NONE',  ( 13.97604488694548053, -13.89961937509957401, 95.62609039468563310 ) ) ;
#75416 = CARTESIAN_POINT ( 'NONE',  ( 8.571926809382603096, -26.38167802310801235, 145.9750000027311785 ) ) ;
#75417 = CARTESIAN_POINT ( 'NONE',  ( 9.564922557960805705, 16.46253265017160317, 24.58224293864769194 ) ) ;
#75418 = CARTESIAN_POINT ( 'NONE',  ( 5.719274019375991003, -21.55341960407610458, 22.70724293864769194 ) ) ;
#75419 = CARTESIAN_POINT ( 'NONE',  ( 15.80617190586769283, -15.72974639402175789, 45.62609039468567573 ) ) ;
#75420 = CARTESIAN_POINT ( 'NONE',  ( 16.46253265017146816, 9.564922557961045513, 106.6677570613523471 ) ) ;
#75422 = CARTESIAN_POINT ( 'NONE',  ( 5.049401038298161559, -19.05341960407611168, 57.70724293864769550 ) ) ;
#75421 = CARTESIAN_POINT ( 'NONE',  ( 17.49999999999999645, -4.013004640162614933, 107.9460572099440725 ) ) ;
#75423 = FACE_OUTER_BOUND ( 'NONE', #142552, .T. ) ;
#75425 = CARTESIAN_POINT ( 'NONE',  ( -9.474510206698964154, 16.51473224551069663, 65.41557627198102409 ) ) ;
#75424 = CARTESIAN_POINT ( 'NONE',  ( -8.314922557960811034, -14.29746914071050412, 77.08224293864769550 ) ) ;
#75426 = CARTESIAN_POINT ( 'NONE',  ( -19.05341960407611168, -5.049401038298163336, 76.45724293864769550 ) ) ;
#75427 = CARTESIAN_POINT ( 'NONE',  ( -9.474510206698720793, -16.51473224551083518, 79.58442372801899012 ) ) ;
#75428 = CARTESIAN_POINT ( 'NONE',  ( -18.67979575497178146, -10.72451020669898902, 51.66557627198102409 ) ) ;
#75429 = CARTESIAN_POINT ( 'NONE',  ( 16.53943276465976808, -0.05219959533910856209, 108.7489096053143669 ) ) ;
#75430 = CARTESIAN_POINT ( 'NONE',  ( -9.474510206698720793, -16.51473224551083518, 39.58442372801899722 ) ) ;
#75431 = CARTESIAN_POINT ( 'NONE',  ( 5.153800228976335163, 19.02544592524342804, 79.79057627198102409 ) ) ;
#75432 = CARTESIAN_POINT ( 'NONE',  ( -5.823673210054116645, -21.52544592524344225, 72.29057627198102409 ) ) ;
#75434 = CARTESIAN_POINT ( 'NONE',  ( -9.564922557961040184, 16.46253265017147172, 42.91775706135234003 ) ) ;
#75433 = CARTESIAN_POINT ( 'NONE',  ( -16.55341960407611168, -4.379528057220339221, 86.45724293864770971 ) ) ;
#75435 = CARTESIAN_POINT ( 'NONE',  ( 5.823673210054125526, 21.52544592524343514, 74.79057627198105251 ) ) ;
#75436 = CARTESIAN_POINT ( 'NONE',  ( -10.72451020669898014, 18.67979575497178502, 65.41557627198102409 ) ) ;
#75437 = CARTESIAN_POINT ( 'NONE',  ( 10.72451020669898902, -18.67979575497178502, 37.91557627198102409 ) ) ;
#75438 = CARTESIAN_POINT ( 'NONE',  ( 21.52544592524334988, 5.823673210054432836, 96.45942372801901854 ) ) ;
#75439 = CARTESIAN_POINT ( 'NONE',  ( -16.46253265017160317, 9.564922557960807481, 70.83224293864770971 ) ) ;
#75440 = CARTESIAN_POINT ( 'NONE',  ( 13.97604488694527802, 13.89961937509977652, 24.37390960531435624 ) ) ;
#75441 = CARTESIAN_POINT ( 'NONE',  ( 18.62759615963255655, 10.81492255796105972, 31.66775706135234358 ) ) ;
#75442 = CARTESIAN_POINT ( 'NONE',  ( -18.62759615963255300, -10.81492255796106328, 44.16775706135234714 ) ) ;
#75443 = CARTESIAN_POINT ( 'NONE',  ( -13.97604488694527625, -13.89961937509977652, 31.87390960531435979 ) ) ;
#75444 = CARTESIAN_POINT ( 'NONE',  ( 18.67979575497178502, 10.72451020669898547, 109.1655762719810383 ) ) ;
#75445 = CARTESIAN_POINT ( 'NONE',  ( -19.03943276465977164, -0.05219959533935918106, 58.75109039468566863 ) ) ;
#75446 = CARTESIAN_POINT ( 'NONE',  ( -0.05219959533909027116, -19.03943276465977164, 42.49890960531435269 ) ) ;
#75447 = CARTESIAN_POINT ( 'NONE',  ( 16.53943276465976808, 0.05219959533934440121, 26.25109039468567573 ) ) ;
#75448 = SURFACE_STYLE_FILL_AREA ( #156264 ) ;
#75449 = CARTESIAN_POINT ( 'NONE',  ( 12.14591786802327356, -12.06949235617739191, 55.62609039468568284 ) ) ;
#75450 = CARTESIAN_POINT ( 'NONE',  ( 9.564922557960805705, 16.46253265017160317, 34.58224293864770260 ) ) ;
#75451 = CARTESIAN_POINT ( 'NONE',  ( -21.73861122199297924, -7.688394669363364464, 173.2969830217473941 ) ) ;
#75452 = CARTESIAN_POINT ( 'NONE',  ( 16.46253265017160672, -9.564922557960803928, 83.33224293864768129 ) ) ;
#75453 = CARTESIAN_POINT ( 'NONE',  ( 0.05219959533910956823, 16.53943276465976808, 114.9989096053143669 ) ) ;
#75454 = CARTESIAN_POINT ( 'NONE',  ( -0.05219959533907301413, -21.53943276465977519, 62.49890960531436690 ) ) ;
#75455 = CARTESIAN_POINT ( 'NONE',  ( 4.483927247898790824, -16.52544592524335698, 50.20942372801901854 ) ) ;
#75456 = CARTESIAN_POINT ( 'NONE',  ( 10.81492255796106328, -18.62759615963255655, 105.4177570613523613 ) ) ;
#75457 = CARTESIAN_POINT ( 'NONE',  ( -19.03943276465977164, 0.05219959533909376836, 41.24890960531435269 ) ) ;
#75458 = CARTESIAN_POINT ( 'NONE',  ( 4.379528057220339221, -16.55341960407611168, 22.70724293864769194 ) ) ;
#75459 = CARTESIAN_POINT ( 'NONE',  ( 4.483927247898545687, 16.52544592524342804, 54.79057627198104541 ) ) ;
#75460 = CARTESIAN_POINT ( 'NONE',  ( -9.564922557960796823, -16.46253265017161027, 67.08224293864769550 ) ) ;
#75461 = CARTESIAN_POINT ( 'NONE',  ( 18.67979575497194134, -10.72451020669871369, 105.8344237280190328 ) ) ;
#75462 = CARTESIAN_POINT ( 'NONE',  ( 0.05219959533937995610, -21.53943276465977519, 25.00109039468567218 ) ) ;
#75463 = CIRCLE ( 'NONE', #10968, 0.5000000000000004441 ) ;
#75464 = CARTESIAN_POINT ( 'NONE',  ( 10.81492255796106328, -18.62759615963255655, 80.41775706135234714 ) ) ;
#75465 = CARTESIAN_POINT ( 'NONE',  ( 16.52544592524335698, 4.483927247898782831, 46.45942372801901854 ) ) ;
#75466 = CARTESIAN_POINT ( 'NONE',  ( -16.52544592524335698, -4.483927247898792601, 23.95942372801901143 ) ) ;
#75468 = CARTESIAN_POINT ( 'NONE',  ( -21.53943276465977519, -0.05219959533937600094, 93.75109039468567573 ) ) ;
#75467 = CARTESIAN_POINT ( 'NONE',  ( 12.14591786802309770, 12.06949235617756955, 79.37390960531436690 ) ) ;
#75469 = CARTESIAN_POINT ( 'NONE',  ( -12.06949235617756955, 12.14591786802309770, 35.62390960531437401 ) ) ;
#75470 = CARTESIAN_POINT ( 'NONE',  ( -17.26058549869090086, 6.457015423128545706, 113.6225416252393501 ) ) ;
#75471 = CARTESIAN_POINT ( 'NONE',  ( 12.06949235617739724, 12.14591786802326823, 41.87609039468568284 ) ) ;
#75472 = CARTESIAN_POINT ( 'NONE',  ( 16.52544592524342804, -4.483927247898539470, 53.54057627198103120 ) ) ;
#75473 = CARTESIAN_POINT ( 'NONE',  ( -12.14591786802326823, 12.06949235617739902, 93.12609039468568994 ) ) ;
#75474 = CARTESIAN_POINT ( 'NONE',  ( 19.05341960407611168, 5.049401038298154454, 98.95724293864766707 ) ) ;
#75475 = CARTESIAN_POINT ( 'NONE',  ( 9.564922557960805705, 16.46253265017160317, 114.5822429386476955 ) ) ;
#75476 = CARTESIAN_POINT ( 'NONE',  ( -18.62759615963255300, -10.81492255796106328, 109.1677570613523613 ) ) ;
#75477 = CARTESIAN_POINT ( 'NONE',  ( 4.379528057220339221, -16.55341960407611168, 82.70724293864770971 ) ) ;
#75478 = CARTESIAN_POINT ( 'NONE',  ( 5.153800228976335163, 19.02544592524342804, 99.79057627198102409 ) ) ;
#75479 = ORIENTED_EDGE ( 'NONE', *, *, #35102, .T. ) ;
#75480 = CARTESIAN_POINT ( 'NONE',  ( 16.55341960407618274, -4.379528057220086978, 36.04275706135234714 ) ) ;
#75481 = CARTESIAN_POINT ( 'NONE',  ( -5.049401038298153566, 19.05341960407611168, 40.20724293864768839 ) ) ;
#75482 = CARTESIAN_POINT ( 'NONE',  ( 5.153800228976335163, 19.02544592524342804, 104.7905762719809957 ) ) ;
#75484 = DIRECTION ( 'NONE',  ( 0.000000000000000000, 0.000000000000000000, -1.000000000000000000 ) ) ;
#75483 = CARTESIAN_POINT ( 'NONE',  ( 14.34966873604972726, -8.224510206698740333, 40.83442372801901854 ) ) ;
#75485 = CARTESIAN_POINT ( 'NONE',  ( -5.153800228976607833, 19.02544592524334988, 37.70942372801899722 ) ) ;
#75486 = CARTESIAN_POINT ( 'NONE',  ( -19.03943276465977164, 0.05219959533909376836, 41.24890960531435269 ) ) ;
#75487 = CARTESIAN_POINT ( 'NONE',  ( -16.53943276465976808, -0.05219959533934237506, 83.75109039468568994 ) ) ;
#75488 = CARTESIAN_POINT ( 'NONE',  ( -19.02544592524334988, -5.153800228976617603, 78.95942372801900433 ) ) ;
#75489 = CARTESIAN_POINT ( 'NONE',  ( 13.89961937509957401, 13.97604488694547697, 31.87609039468566863 ) ) ;
#75490 = CARTESIAN_POINT ( 'NONE',  ( -5.049401038298153566, 19.05341960407611168, 55.20724293864769550 ) ) ;
#75491 = CARTESIAN_POINT ( 'NONE',  ( -14.34966873604960291, -8.224510206698953496, 101.6655762719810383 ) ) ;
#75492 = CARTESIAN_POINT ( 'NONE',  ( 16.46253265017146816, 9.564922557961045513, 71.66775706135233293 ) ) ;
#75493 = CARTESIAN_POINT ( 'NONE',  ( 21.52544592524344225, -5.823673210054117533, 68.54057627198103830 ) ) ;
#75494 = CARTESIAN_POINT ( 'NONE',  ( 19.02544592524334988, 5.153800228976608722, 21.45942372801899012 ) ) ;
#75495 = CARTESIAN_POINT ( 'NONE',  ( 13.97604488694527802, 13.89961937509977652, 109.3739096053143669 ) ) ;
#75496 = CARTESIAN_POINT ( 'NONE',  ( -5.823673210054116645, -21.52544592524344225, 72.29057627198102409 ) ) ;
#75497 = CARTESIAN_POINT ( 'NONE',  ( -13.97604488694527625, -13.89961937509977652, 111.8739096053143243 ) ) ;
#75498 = CARTESIAN_POINT ( 'NONE',  ( 19.05341960407617918, -5.049401038297876454, 101.0427570613523045 ) ) ;
#75499 = CARTESIAN_POINT ( 'NONE',  ( -13.97604488694547520, 13.89961937509957934, 98.12609039468566152 ) ) ;
#75500 = CARTESIAN_POINT ( 'NONE',  ( 14.29746914071037800, 8.314922557961029526, 21.66775706135235069 ) ) ;
#75501 = CARTESIAN_POINT ( 'NONE',  ( 5.153800228976335163, 19.02544592524342804, 29.79057627198102409 ) ) ;
#75502 = CARTESIAN_POINT ( 'NONE',  ( 9.474510206698971260, -16.51473224551069308, 102.9155762719810241 ) ) ;
#75504 = B_SPLINE_CURVE_WITH_KNOTS ( 'NONE', 3,
 ( #161242, #127898, #69231, #82382, #22736, #142078, #19740, #130898, #36885, #95578, #173437, #98551, #160245, #84384, #143066, #146061, #175417, #3564, #21734, #81381, #113721, #192588, #83387, #66238, #144070, #145064, #189600, #51073 ),
 .UNSPECIFIED., .F., .F.,
 ( 4, 2, 2, 2, 2, 2, 2, 2, 2, 2, 2, 2, 2, 4 ),
 ( 1.961533959443023196E-07, 0.0003775868847194836678, 0.0007549776160430232263, 0.001132368347366562514, 0.001509759078690102235, 0.002264540541337181027, 0.003019322003984260035, 0.003774103466631338610, 0.004151494197954877681, 0.004528884929278417619, 0.004906275660601956690, 0.005283666391925495760, 0.005661057123249034831, 0.006038447854572573902 ),
 .UNSPECIFIED. ) ;
#75503 = CARTESIAN_POINT ( 'NONE',  ( 5.719274019375991003, -21.55341960407610458, 87.70724293864769550 ) ) ;
#75505 = CARTESIAN_POINT ( 'NONE',  ( 15.72974639402176855, 15.80617190586768217, 61.87609039468568284 ) ) ;
#75507 = CARTESIAN_POINT ( 'NONE',  ( -21.55341960407619339, 5.719274019375674811, 113.5427570613523756 ) ) ;
#75506 = CARTESIAN_POINT ( 'NONE',  ( -16.46253265017146816, -9.564922557961047289, 104.1677570613523329 ) ) ;
#75508 = CARTESIAN_POINT ( 'NONE',  ( 12.06949235617757843, -12.14591786802309237, 23.12390960531436335 ) ) ;
#75509 = CARTESIAN_POINT ( 'NONE',  ( -18.62759615963270932, 10.81492255796079327, 105.8322429386476955 ) ) ;
#75510 = CARTESIAN_POINT ( 'NONE',  ( 12.06949235617757843, -12.14591786802309237, 38.12390960531436690 ) ) ;
#75511 = CARTESIAN_POINT ( 'NONE',  ( -9.474510206698720793, -16.51473224551083518, 84.58442372801900433 ) ) ;
#75512 = CARTESIAN_POINT ( 'NONE',  ( -13.89961937509957401, -13.97604488694547875, 54.37609039468565442 ) ) ;
#75513 = CARTESIAN_POINT ( 'NONE',  ( -21.53943276465977519, -0.05219959533937600094, 58.75109039468568994 ) ) ;
#75514 = CARTESIAN_POINT ( 'NONE',  ( 13.97604488694548053, -13.89961937509957401, 45.62609039468566863 ) ) ;
#75515 = CARTESIAN_POINT ( 'NONE',  ( 14.34966873604960469, 8.224510206698951720, 104.1655762719810241 ) ) ;
#75516 = CARTESIAN_POINT ( 'NONE',  ( 18.67979575497178502, 10.72451020669898547, 29.16557627198103120 ) ) ;
#75517 = CARTESIAN_POINT ( 'NONE',  ( -8.314922557960811034, -14.29746914071050412, 37.08224293864768129 ) ) ;
#75518 = CARTESIAN_POINT ( 'NONE',  ( -10.81492255796105439, 18.62759615963255655, 92.91775706135236135 ) ) ;
#75519 = CARTESIAN_POINT ( 'NONE',  ( -8.314922557961024197, 14.29746914071037800, 67.91775706135234714 ) ) ;
#75520 = CARTESIAN_POINT ( 'NONE',  ( -0.05219959533910754901, -16.53943276465976808, 27.49890960531435269 ) ) ;
#75521 = CARTESIAN_POINT ( 'NONE',  ( 15.72974639402176855, 15.80617190586768217, 66.87609039468568994 ) ) ;
#75522 = CARTESIAN_POINT ( 'NONE',  ( -21.52544592524334988, -5.823673210054445271, 68.95942372801901854 ) ) ;
#75523 = CARTESIAN_POINT ( 'NONE',  ( -10.81492255796078084, -18.62759615963271287, 72.08224293864769550 ) ) ;
#75524 = ORIENTED_EDGE ( 'NONE', *, *, #122751, .F. ) ;
#75525 = CARTESIAN_POINT ( 'NONE',  ( 0.05219959533909260263, 19.03943276465977164, 29.99890960531435979 ) ) ;
#75526 = CARTESIAN_POINT ( 'NONE',  ( -21.52544592524334988, -5.823673210054445271, 43.95942372801902565 ) ) ;
#75527 = CARTESIAN_POINT ( 'NONE',  ( -12.06949235617756955, 12.14591786802309770, 115.6239096053143669 ) ) ;
#75528 = CARTESIAN_POINT ( 'NONE',  ( -16.51473224551069308, -9.474510206698971260, 41.66557627198103120 ) ) ;
#75529 = CARTESIAN_POINT ( 'NONE',  ( 8.224510206698953496, -14.34966873604960469, 82.91557627198103830 ) ) ;
#75530 = CARTESIAN_POINT ( 'NONE',  ( 16.46253265017160672, -9.564922557960803928, 83.33224293864768129 ) ) ;
#75531 = CARTESIAN_POINT ( 'NONE',  ( 0.05219959533910956823, 16.53943276465976808, 29.99890960531435979 ) ) ;
#75532 = CARTESIAN_POINT ( 'NONE',  ( 18.62759615963271287, -10.81492255796078972, 73.33224293864769550 ) ) ;
#75533 = CARTESIAN_POINT ( 'NONE',  ( -21.52544592524343514, 5.823673210054127303, 111.0405762719810525 ) ) ;
#75534 = DIRECTION ( 'NONE',  ( -0.06104853953485701173, -7.476289853398329258E-18, -0.9981347984218670311 ) ) ;
#75536 = CARTESIAN_POINT ( 'NONE',  ( 16.51473224551083163, -9.474510206698727899, 105.8344237280190043 ) ) ;
#75535 = CARTESIAN_POINT ( 'NONE',  ( -5.153800228976328057, -19.02544592524343514, 67.29057627198102409 ) ) ;
#75537 = CARTESIAN_POINT ( 'NONE',  ( 18.67979575497178502, 10.72451020669898547, 59.16557627198103120 ) ) ;
#75538 = CARTESIAN_POINT ( 'NONE',  ( 21.53943276465977519, 0.05219959533937863772, 76.25109039468568994 ) ) ;
#75539 = CARTESIAN_POINT ( 'NONE',  ( -16.46253265017160317, 9.564922557960807481, 60.83224293864769550 ) ) ;
#75540 = VECTOR ( 'NONE', #73408, 1000.000000000000000 ) ;
#75541 = CARTESIAN_POINT ( 'NONE',  ( 9.474510206698971260, -16.51473224551069308, 92.91557627198103830 ) ) ;
#75542 = CARTESIAN_POINT ( 'NONE',  ( 8.314922557961029526, -14.29746914071037800, 80.41775706135234714 ) ) ;
#75543 = CARTESIAN_POINT ( 'NONE',  ( 0.05219959533937995610, -21.53943276465977519, 60.00109039468568284 ) ) ;
#75544 = CARTESIAN_POINT ( 'NONE',  ( -5.823673210054431948, 21.52544592524334988, 82.70942372801900433 ) ) ;
#75545 = CARTESIAN_POINT ( 'NONE',  ( 5.823673210054125526, 21.52544592524343514, 109.7905762719810383 ) ) ;
#75546 = CARTESIAN_POINT ( 'NONE',  ( 15.80617190586746368, 15.72974639402197994, 79.37390960531436690 ) ) ;
#75547 = CARTESIAN_POINT ( 'NONE',  ( 5.049401038297881783, 19.05341960407617563, 42.29275706135234003 ) ) ;
#75548 = CARTESIAN_POINT ( 'NONE',  ( 15.80617190586746368, 15.72974639402197994, 39.37390960531436690 ) ) ;
#75550 = CARTESIAN_POINT ( 'NONE',  ( -8.314922557960811034, -14.29746914071050412, 32.08224293864769550 ) ) ;
#75549 = CARTESIAN_POINT ( 'NONE',  ( 19.05341960407611168, 5.049401038298154454, 83.95724293864766707 ) ) ;
#75551 = CARTESIAN_POINT ( 'NONE',  ( -6.412877669190335972, 3.889087296526014814, 1.818019484660534424 ) ) ;
#75552 = CARTESIAN_POINT ( 'NONE',  ( -8.388830574159379737E-16, -13.70000000000001528, -62.58071313852362039 ) ) ;
#75553 = EDGE_CURVE ( 'NONE', #16229, #2773, #24582, .T. ) ;
#75554 = CARTESIAN_POINT ( 'NONE',  ( 9.564922557961047289, -16.46253265017146816, 90.41775706135234714 ) ) ;
#75555 = CARTESIAN_POINT ( 'NONE',  ( 15.72974639402199770, -15.80617190586745480, 68.12390960531436690 ) ) ;
#75556 = CARTESIAN_POINT ( 'NONE',  ( 12.06949235617757843, -12.14591786802309237, 58.12390960531435979 ) ) ;
#75557 = CARTESIAN_POINT ( 'NONE',  ( 14.29746914071037800, 8.314922557961029526, 26.66775706135235424 ) ) ;
#75558 = CARTESIAN_POINT ( 'NONE',  ( -19.03943276465977164, 0.05219959533909376836, 41.24890960531435269 ) ) ;
#75560 = CARTESIAN_POINT ( 'NONE',  ( -16.51473224551082808, 9.474510206698731452, 73.33442372801900433 ) ) ;
#75559 = CARTESIAN_POINT ( 'NONE',  ( 5.823673210054125526, 21.52544592524343514, 104.7905762719810241 ) ) ;
#75561 = CARTESIAN_POINT ( 'NONE',  ( -5.153800228976328057, -19.02544592524343514, 87.29057627198103830 ) ) ;
#75562 = CARTESIAN_POINT ( 'NONE',  ( 16.52544592524342804, -4.483927247898539470, 83.54057627198102409 ) ) ;
#75563 = CARTESIAN_POINT ( 'NONE',  ( -0.05219959533909027116, -19.03943276465977164, 62.49890960531435979 ) ) ;
#75564 = CARTESIAN_POINT ( 'NONE',  ( 0.05219959533910956823, 16.53943276465976808, 64.99890960531435269 ) ) ;
#75565 = CARTESIAN_POINT ( 'NONE',  ( -13.97604488694527625, -13.89961937509977652, 36.87390960531436690 ) ) ;
#75566 = CARTESIAN_POINT ( 'NONE',  ( -17.13361728884595081, -5.330296506332817152, 20.84482979903667754 ) ) ;
#75567 = CARTESIAN_POINT ( 'NONE',  ( -16.52544592524342804, 4.483927247898546575, 46.04057627198103830 ) ) ;
#75568 = CARTESIAN_POINT ( 'NONE',  ( 9.564922557960805705, 16.46253265017160317, 94.58224293864769550 ) ) ;
#75569 = CARTESIAN_POINT ( 'NONE',  ( -20.43538597629128262, 20.43538597629122222, -49.67367017693150189 ) ) ;
#75570 = CARTESIAN_POINT ( 'NONE',  ( -16.51473224551082808, 9.474510206698731452, 58.33442372801900433 ) ) ;
#75571 = CARTESIAN_POINT ( 'NONE',  ( -12.14591786802326823, 12.06949235617739902, 63.12609039468568994 ) ) ;
#75572 = CARTESIAN_POINT ( 'NONE',  ( 15.72974639402199770, -15.80617190586745480, 78.12390960531436690 ) ) ;
#75573 = CARTESIAN_POINT ( 'NONE',  ( 19.03943276465977164, 0.05219959533936151252, 36.25109039468567573 ) ) ;
#75574 = CARTESIAN_POINT ( 'NONE',  ( 0.05219959533909260263, 19.03943276465977164, 84.99890960531436690 ) ) ;
#75575 = CARTESIAN_POINT ( 'NONE',  ( -20.29787683430801692, -22.40769709776935059, -48.02032541638636332 ) ) ;
#75576 = CARTESIAN_POINT ( 'NONE',  ( -0.05219959533907301413, -21.53943276465977519, 22.49890960531436335 ) ) ;
#75577 = CARTESIAN_POINT ( 'NONE',  ( -16.51473224551069308, -9.474510206698971260, 61.66557627198103120 ) ) ;
#75578 = CARTESIAN_POINT ( 'NONE',  ( -18.62759615963255300, -10.81492255796106328, 54.16775706135235424 ) ) ;
#75579 = CARTESIAN_POINT ( 'NONE',  ( -8.224510206698948167, 14.34966873604960824, 115.4155762719810241 ) ) ;
#75582 = ORIENTED_EDGE ( 'NONE', *, *, #26705, .T. ) ;
#75581 = CARTESIAN_POINT ( 'NONE',  ( 13.89961937509977652, -13.97604488694527269, 98.12390960531433848 ) ) ;
#75580 = CARTESIAN_POINT ( 'NONE',  ( -5.719274019375665041, -21.55341960407619695, 19.79275706135235069 ) ) ;
#75583 = CARTESIAN_POINT ( 'NONE',  ( -18.62759615963255300, -10.81492255796106328, 39.16775706135235424 ) ) ;
#75584 = ORIENTED_EDGE ( 'NONE', *, *, #165816, .T. ) ;
#75585 = CARTESIAN_POINT ( 'NONE',  ( 19.02544592524343514, -5.153800228976328945, 103.5405762719809957 ) ) ;
#75586 = CARTESIAN_POINT ( 'NONE',  ( 31.99364916730973363, -1.163414459185697237E-14, 92.35000000000020748 ) ) ;
#75587 = CARTESIAN_POINT ( 'NONE',  ( -21.55341960407610458, -5.719274019375992779, 106.4572429386477097 ) ) ;
#75588 = CARTESIAN_POINT ( 'NONE',  ( 19.02544592524343514, -5.153800228976328945, 53.54057627198102409 ) ) ;
#75589 = CARTESIAN_POINT ( 'NONE',  ( -16.53943276465976808, -0.05219959533934237506, 23.75109039468567929 ) ) ;
#75590 = CARTESIAN_POINT ( 'NONE',  ( -5.950531402560715689E-15, 38.81732327939063509, -1.624999997268813612 ) ) ;
#75591 = CARTESIAN_POINT ( 'NONE',  ( -18.62759615963255300, -10.81492255796106328, 99.16775706135234714 ) ) ;
#75592 = CARTESIAN_POINT ( 'NONE',  ( 5.049401038298161559, -19.05341960407611168, 32.70724293864768129 ) ) ;
#75593 = CARTESIAN_POINT ( 'NONE',  ( 0.05219959533937995610, -21.53943276465977519, 95.00109039468568994 ) ) ;
#75595 = CARTESIAN_POINT ( 'NONE',  ( 0.05219959533937995610, -21.53943276465977519, 55.00109039468568284 ) ) ;
#75594 = CARTESIAN_POINT ( 'NONE',  ( -13.97604488694527625, -13.89961937509977652, 86.87390960531436690 ) ) ;
#75596 = CARTESIAN_POINT ( 'NONE',  ( 1.784210473542230573E-15, -29.16686587814331588, 143.8750000027311557 ) ) ;
#75597 = CARTESIAN_POINT ( 'NONE',  ( 13.97604488694527802, 13.89961937509977652, 94.37390960531436690 ) ) ;
#75598 = CARTESIAN_POINT ( 'NONE',  ( -19.30190589895974185, 21.36759865781276346, 139.9999999999999716 ) ) ;
#75601 = CARTESIAN_POINT ( 'NONE',  ( -10.72451020669870658, -18.67979575497194134, 54.58442372801901143 ) ) ;
#75600 = CARTESIAN_POINT ( 'NONE',  ( 12.06949235617739724, 12.14591786802326823, 71.87609039468568994 ) ) ;
#75599 = CARTESIAN_POINT ( 'NONE',  ( 14.29746914071037800, 8.314922557961029526, 41.66775706135235424 ) ) ;
#75602 = CARTESIAN_POINT ( 'NONE',  ( -15.80617190586768217, 15.72974639402176855, 83.12609039468568994 ) ) ;
#75603 = PLANE ( 'NONE',  #173649 ) ;
#75604 = CARTESIAN_POINT ( 'NONE',  ( -13.97604488694547697, 13.89961937509957934, 113.1260903946856757 ) ) ;
#75605 = CARTESIAN_POINT ( 'NONE',  ( 5.049401038298161559, -19.05341960407611168, 77.70724293864765286 ) ) ;
#75606 = CARTESIAN_POINT ( 'NONE',  ( 5.049401038298161559, -19.05341960407611168, 92.70724293864769550 ) ) ;
#75607 = CARTESIAN_POINT ( 'NONE',  ( -8.224510206698948167, 14.34966873604960824, 115.4155762719810241 ) ) ;
#75608 = CARTESIAN_POINT ( 'NONE',  ( -21.52544592524343514, 5.823673210054127303, 26.04057627198103475 ) ) ;
#75609 = CARTESIAN_POINT ( 'NONE',  ( -4.483927247898782831, 16.52544592524335698, 92.70942372801901854 ) ) ;
#75611 = CARTESIAN_POINT ( 'NONE',  ( -13.89961937509977652, 13.97604488694528158, 60.62390960531436690 ) ) ;
#75610 = CARTESIAN_POINT ( 'NONE',  ( 8.314922557960818139, 14.29746914071049879, 64.58224293864769550 ) ) ;
#75612 = CARTESIAN_POINT ( 'NONE',  ( -0.05219959533937732626, 21.53943276465977519, 92.50109039468567573 ) ) ;
#75613 = CARTESIAN_POINT ( 'NONE',  ( 4.000000000000000888, -105.0000000000000000, 12.00000000000000355 ) ) ;
#75614 = CARTESIAN_POINT ( 'NONE',  ( 19.05341960407617918, -5.049401038297876454, 111.0427570613523329 ) ) ;
#75615 = CARTESIAN_POINT ( 'NONE',  ( -12.06949235617756955, 12.14591786802309770, 80.62390960531438111 ) ) ;
#75616 = CARTESIAN_POINT ( 'NONE',  ( 21.55341960407619695, -5.719274019375665929, 31.04275706135234714 ) ) ;
#75617 = CARTESIAN_POINT ( 'NONE',  ( 5.823673210054125526, 21.52544592524343514, 59.79057627198103120 ) ) ;
#75618 = CARTESIAN_POINT ( 'NONE',  ( -13.89961937509957401, -13.97604488694547875, 39.37609039468566152 ) ) ;
#75619 = CARTESIAN_POINT ( 'NONE',  ( -35.69940131823277341, 0.4911691522781976293, 37.51200899188186355 ) ) ;
#75620 = CARTESIAN_POINT ( 'NONE',  ( -9.474510206698964154, 16.51473224551069663, 80.41557627198103830 ) ) ;
#75621 = CARTESIAN_POINT ( 'NONE',  ( 16.52544592524342804, -4.483927247898539470, 53.54057627198103120 ) ) ;
#75622 = AXIS2_PLACEMENT_3D ( 'NONE', #179725, #167287, #28784 ) ;
#75623 = CARTESIAN_POINT ( 'NONE',  ( 4.483927247898545687, 16.52544592524342804, 34.79057627198103120 ) ) ;
#75624 = CARTESIAN_POINT ( 'NONE',  ( 8.224510206698742110, 14.34966873604972548, 97.08442372801904696 ) ) ;
#75625 = CARTESIAN_POINT ( 'NONE',  ( 16.46253265017146816, 9.564922557961045513, 56.66775706135233293 ) ) ;
#75626 = FACE_OUTER_BOUND ( 'NONE', #45341, .T. ) ;
#75627 = CARTESIAN_POINT ( 'NONE',  ( 0.05219959533909260263, 19.03943276465977164, 99.99890960531436690 ) ) ;
#75628 = EDGE_CURVE ( 'NONE', #39588, #92192, #167865, .T. ) ;
#75629 = CARTESIAN_POINT ( 'NONE',  ( -12.06949235617756955, 12.14591786802309770, 80.62390960531438111 ) ) ;
#75630 = CARTESIAN_POINT ( 'NONE',  ( -0.05219959533936034679, 19.03943276465977164, 47.50109039468566863 ) ) ;
#75632 = CARTESIAN_POINT ( 'NONE',  ( -21.55341960407610458, -5.719274019375992779, 36.45724293864768839 ) ) ;
#75631 = CARTESIAN_POINT ( 'NONE',  ( -16.46253265017160317, 9.564922557960807481, 30.83224293864769550 ) ) ;
#75633 = CARTESIAN_POINT ( 'NONE',  ( 21.52544592524344225, -5.823673210054117533, 73.54057627198102409 ) ) ;
#75634 = CARTESIAN_POINT ( 'NONE',  ( -16.53943276465976808, 0.05219959533911058130, 106.2489096053143811 ) ) ;
#75636 = CARTESIAN_POINT ( 'NONE',  ( -9.564922557960796823, -16.46253265017161027, 47.08224293864769550 ) ) ;
#75635 = CARTESIAN_POINT ( 'NONE',  ( 4.379528057220092307, 16.55341960407617563, 47.29275706135234003 ) ) ;
#75637 = CARTESIAN_POINT ( 'NONE',  ( -0.05219959533937732626, 21.53943276465977519, 42.50109039468567573 ) ) ;
#75638 = CARTESIAN_POINT ( 'NONE',  ( -16.52544592524342804, 4.483927247898546575, 86.04057627198102409 ) ) ;
#75639 = FACE_OUTER_BOUND ( 'NONE', #127342, .T. ) ;
#75640 = CARTESIAN_POINT ( 'NONE',  ( -11.40812507854755609, 35.11059874428196537, -9.524999997268816188 ) ) ;
#75641 = CARTESIAN_POINT ( 'NONE',  ( 18.62759615963271287, -10.81492255796078972, 33.33224293864769550 ) ) ;
#75642 = DIRECTION ( 'NONE',  ( -0.000000000000000000, -0.000000000000000000, -1.000000000000000000 ) ) ;
#75643 = DIRECTION ( 'NONE',  ( 4.336808689942018352E-17, -1.000000000000000000, 0.000000000000000000 ) ) ;
#75645 = CARTESIAN_POINT ( 'NONE',  ( 8.314922557960818139, 14.29746914071049879, 49.58224293864769550 ) ) ;
#75644 = CARTESIAN_POINT ( 'NONE',  ( -14.34966873604972548, 8.224510206698743886, 38.33442372801900433 ) ) ;
#75646 = CARTESIAN_POINT ( 'NONE',  ( 10.72451020669898902, -18.67979575497178502, 67.91557627198102409 ) ) ;
#75647 = CARTESIAN_POINT ( 'NONE',  ( 18.67979575497178502, 10.72451020669898547, 64.16557627198102409 ) ) ;
#75648 = CARTESIAN_POINT ( 'NONE',  ( 29.94898851760540026, -23.39111959325554935, -18.65171477573349179 ) ) ;
#75650 = CARTESIAN_POINT ( 'NONE',  ( -16.46253265017160317, 9.564922557960807481, 105.8322429386476955 ) ) ;
#75649 = CARTESIAN_POINT ( 'NONE',  ( -16.51473224551069308, -9.474510206698971260, 41.66557627198103120 ) ) ;
#75651 = CARTESIAN_POINT ( 'NONE',  ( -9.474510206698964154, 16.51473224551069663, 50.41557627198102409 ) ) ;
#75652 = CARTESIAN_POINT ( 'NONE',  ( 16.53943276465976808, -0.05219959533910856209, 108.7489096053143669 ) ) ;
#75653 = CARTESIAN_POINT ( 'NONE',  ( 0.000000000000000000, 0.000000000000000000, 0.000000000000000000 ) ) ;
#75654 = CARTESIAN_POINT ( 'NONE',  ( -5.049401038298153566, 19.05341960407611168, 115.2072429386477097 ) ) ;
#75655 = AXIS2_PLACEMENT_3D ( 'NONE', #189718, #177550, #39019 ) ;
#75656 = ORIENTED_EDGE ( 'NONE', *, *, #183623, .T. ) ;
#75657 = CARTESIAN_POINT ( 'NONE',  ( -8.224510206698735004, -14.34966873604973081, 69.58442372801900433 ) ) ;
#75658 = CARTESIAN_POINT ( 'NONE',  ( 5.823673210054125526, 21.52544592524343514, 109.7905762719810383 ) ) ;
#75659 = CARTESIAN_POINT ( 'NONE',  ( -16.51473224551069308, -9.474510206698971260, 51.66557627198102409 ) ) ;
#75660 = CARTESIAN_POINT ( 'NONE',  ( 21.52544592524334988, 5.823673210054432836, 41.45942372801901143 ) ) ;
#75661 = CARTESIAN_POINT ( 'NONE',  ( -0.05219959533909027116, -19.03943276465977164, 87.49890960531436690 ) ) ;
#75662 = CARTESIAN_POINT ( 'NONE',  ( 23.29544513554940011, 16.92513159979228021, 145.1843446569000093 ) ) ;
#75663 = VERTEX_POINT ( 'NONE', #75839 ) ;
#75664 = CARTESIAN_POINT ( 'NONE',  ( 21.55341960407619695, -5.719274019375665929, 31.04275706135234714 ) ) ;
#75666 = CARTESIAN_POINT ( 'NONE',  ( -0.05219959533936034679, 19.03943276465977164, 87.50109039468567573 ) ) ;
#75665 = CARTESIAN_POINT ( 'NONE',  ( -0.05219959533909027116, -19.03943276465977164, 107.4989096053143527 ) ) ;
#75667 = CARTESIAN_POINT ( 'NONE',  ( 0.05219959533936267826, -19.03943276465977164, 45.00109039468566863 ) ) ;
#75668 = CARTESIAN_POINT ( 'NONE',  ( -21.55341960407610458, -5.719274019375992779, 106.4572429386477097 ) ) ;
#75669 = CARTESIAN_POINT ( 'NONE',  ( -19.05341960407617563, 5.049401038297882671, 28.54275706135232937 ) ) ;
#75670 = CARTESIAN_POINT ( 'NONE',  ( 5.049401038297881783, 19.05341960407617563, 32.29275706135233293 ) ) ;
#75671 = CARTESIAN_POINT ( 'NONE',  ( 8.314922557961029526, -14.29746914071037800, 90.41775706135236135 ) ) ;
#75672 = FACE_OUTER_BOUND ( 'NONE', #136094, .T. ) ;
#75673 = CARTESIAN_POINT ( 'NONE',  ( -19.02544592524342804, 5.153800228976336051, 56.04057627198100988 ) ) ;
#75674 = CARTESIAN_POINT ( 'NONE',  ( -21.53943276465977519, -0.05219959533937600094, 63.75109039468568284 ) ) ;
#75675 = CARTESIAN_POINT ( 'NONE',  ( 5.719274019375673035, 21.55341960407619339, 87.29275706135236135 ) ) ;
#75676 = CARTESIAN_POINT ( 'NONE',  ( 9.564922557960805705, 16.46253265017160317, 79.58224293864769550 ) ) ;
#75677 = CARTESIAN_POINT ( 'NONE',  ( -5.719274019375665041, -21.55341960407619695, 59.79275706135234714 ) ) ;
#75678 = CARTESIAN_POINT ( 'NONE',  ( 13.89961937509957401, 13.97604488694547697, 96.87609039468566152 ) ) ;
#75679 = CARTESIAN_POINT ( 'NONE',  ( -19.02544592524342804, 5.153800228976336051, 61.04057627198103120 ) ) ;
#75680 = CARTESIAN_POINT ( 'NONE',  ( 19.03943276465977164, -0.05219959533909143690, 93.74890960531435269 ) ) ;
#75681 = CARTESIAN_POINT ( 'NONE',  ( 13.97604488694527802, 13.89961937509977652, 79.37390960531435269 ) ) ;
#75682 = CARTESIAN_POINT ( 'NONE',  ( -16.70000000000002061, 1.759457951533292443E-13, -61.34707691135562868 ) ) ;
#75683 = CARTESIAN_POINT ( 'NONE',  ( 19.05341960407611168, 5.049401038298154454, 63.95724293864769550 ) ) ;
#75684 = CARTESIAN_POINT ( 'NONE',  ( 21.55341960407610458, 5.719274019375980345, 93.95724293864770971 ) ) ;
#75685 = CARTESIAN_POINT ( 'NONE',  ( 0.05219959533934541429, -16.53943276465976808, 85.00109039468568994 ) ) ;
#75686 = CARTESIAN_POINT ( 'NONE',  ( -31.74999999999995737, 0.000000000000000000, 0.000000000000000000 ) ) ;
#75687 = CARTESIAN_POINT ( 'NONE',  ( -9.564922557961040184, 16.46253265017147172, 42.91775706135234003 ) ) ;
#75688 = CARTESIAN_POINT ( 'NONE',  ( 5.153800228976335163, 19.02544592524342804, 74.79057627198103830 ) ) ;
#75689 = CARTESIAN_POINT ( 'NONE',  ( -16.55341960407611168, -4.379528057220339221, 71.45724293864769550 ) ) ;
#75690 = CARTESIAN_POINT ( 'NONE',  ( -12.14591786802309592, -12.06949235617757132, 106.8739096053143811 ) ) ;
#75691 = CARTESIAN_POINT ( 'NONE',  ( 15.80617190586746368, 15.72974639402197994, 24.37390960531435979 ) ) ;
#75692 = CARTESIAN_POINT ( 'NONE',  ( 9.564922557960805705, 16.46253265017160317, 104.5822429386476955 ) ) ;
#75693 = DIRECTION ( 'NONE',  ( -0.8660254037844391517, 0.000000000000000000, 0.4999999999999989453 ) ) ;
#75694 = CARTESIAN_POINT ( 'NONE',  ( 5.153800228976615827, -19.02544592524334988, 25.20942372801900433 ) ) ;
#75695 = CARTESIAN_POINT ( 'NONE',  ( -14.29746914071037622, -8.314922557961029526, 89.16775706135236135 ) ) ;
#75696 = CARTESIAN_POINT ( 'NONE',  ( -13.97604488694527625, -13.89961937509977652, 76.87390960531433848 ) ) ;
#75697 = CARTESIAN_POINT ( 'NONE',  ( -5.719274019375665041, -21.55341960407619695, 54.79275706135235424 ) ) ;
#75698 = CARTESIAN_POINT ( 'NONE',  ( -15.80617190586745835, -15.72974639402198527, 31.87390960531435979 ) ) ;
#75699 = CARTESIAN_POINT ( 'NONE',  ( -10.81492255796105439, 18.62759615963255655, 22.91775706135235069 ) ) ;
#75700 = CARTESIAN_POINT ( 'NONE',  ( 5.823673210054125526, 21.52544592524343514, 74.79057627198105251 ) ) ;
#75701 = CARTESIAN_POINT ( 'NONE',  ( 0.05219959533910956823, 16.53943276465976808, 89.99890960531438111 ) ) ;
#75702 = CARTESIAN_POINT ( 'NONE',  ( 5.049401038297881783, 19.05341960407617563, 57.29275706135231871 ) ) ;
#75703 = CIRCLE ( 'NONE', #46706, 206.0437394197456342 ) ;
#75704 = CARTESIAN_POINT ( 'NONE',  ( -16.46253265017160317, 9.564922557960807481, 30.83224293864769550 ) ) ;
#75705 = CARTESIAN_POINT ( 'NONE',  ( 13.89961937509977652, -13.97604488694527269, 78.12390960531433848 ) ) ;
#75706 = CARTESIAN_POINT ( 'NONE',  ( 13.89961937509977652, -13.97604488694527269, 83.12390960531436690 ) ) ;
#75707 = DIRECTION ( 'NONE',  ( 0.8164965809277243691, 0.000000000000000000, -0.5773502691896280625 ) ) ;
#75708 = CARTESIAN_POINT ( 'NONE',  ( -14.29746914071049879, 8.314922557960819915, 100.8322429386477097 ) ) ;
#75709 = ORIENTED_EDGE ( 'NONE', *, *, #49944, .T. ) ;
#75710 = CARTESIAN_POINT ( 'NONE',  ( -4.483927247898539470, -16.52544592524342804, 32.29057627198102409 ) ) ;
#75711 = CARTESIAN_POINT ( 'NONE',  ( -8.224510206698735004, -14.34966873604973081, 24.58442372801901499 ) ) ;
#75712 = CARTESIAN_POINT ( 'NONE',  ( -15.72974639402176322, -15.80617190586768395, 89.37609039468568994 ) ) ;
#75713 = CARTESIAN_POINT ( 'NONE',  ( 19.05341960407611168, 5.049401038298154454, 103.9572429386476671 ) ) ;
#75714 = CARTESIAN_POINT ( 'NONE',  ( 5.719274019375991003, -21.55341960407610458, 112.7072429386476955 ) ) ;
#75715 = CARTESIAN_POINT ( 'NONE',  ( 16.51473224551069308, 9.474510206698969483, 39.16557627198103120 ) ) ;
#75716 = CARTESIAN_POINT ( 'NONE',  ( -14.29746914071037622, -8.314922557961029526, 44.16775706135234714 ) ) ;
#75717 = AXIS2_PLACEMENT_3D ( 'NONE', #162957, #86113, #147804 ) ;
#75718 = CARTESIAN_POINT ( 'NONE',  ( 5.049401038297881783, 19.05341960407617563, 112.2927570613523471 ) ) ;
#75719 = EDGE_CURVE ( 'NONE', #35005, #159084, #88029, .T. ) ;
#75720 = CARTESIAN_POINT ( 'NONE',  ( -19.03943276465977164, 0.05219959533909376836, 31.24890960531435979 ) ) ;
#75721 = CARTESIAN_POINT ( 'NONE',  ( -8.224510206698948167, 14.34966873604960824, 100.4155762719810241 ) ) ;
#75722 = CARTESIAN_POINT ( 'NONE',  ( 15.80617190586746368, 15.72974639402197994, 109.3739096053143811 ) ) ;
#75723 = CARTESIAN_POINT ( 'NONE',  ( 5.049401038297881783, 19.05341960407617563, 62.29275706135234003 ) ) ;
#75724 = PRESENTATION_STYLE_ASSIGNMENT (( #124212 ) ) ;
#75725 = CARTESIAN_POINT ( 'NONE',  ( 15.80617190586769283, -15.72974639402175789, 25.62609039468567929 ) ) ;
#75726 = CARTESIAN_POINT ( 'NONE',  ( -5.000000000000000888, -129.0000000000000000, -13.99999999999999822 ) ) ;
#75727 = CARTESIAN_POINT ( 'NONE',  ( -19.02544592524342804, 5.153800228976336051, 86.04057627198103830 ) ) ;
#75728 = AXIS2_PLACEMENT_3D ( 'NONE', #30345, #153681, #77827 ) ;
#75729 = CARTESIAN_POINT ( 'NONE',  ( 1.988064558232696151E-15, -30.27659582821216588, 142.4843446568999923 ) ) ;
#75730 = CARTESIAN_POINT ( 'NONE',  ( 0.05219959533909260263, 19.03943276465977164, 79.99890960531436690 ) ) ;
#75732 = CARTESIAN_POINT ( 'NONE',  ( 14.29746914071049879, -8.314922557960816363, 83.33224293864769550 ) ) ;
#75731 = CARTESIAN_POINT ( 'NONE',  ( -18.67979575497193778, 10.72451020669871902, 38.33442372801900433 ) ) ;
#75733 = CARTESIAN_POINT ( 'NONE',  ( -9.564922557960796823, -16.46253265017161027, 82.08224293864768129 ) ) ;
#75735 = CARTESIAN_POINT ( 'NONE',  ( -16.46253265017146816, -9.564922557961047289, 54.16775706135234003 ) ) ;
#75734 = CARTESIAN_POINT ( 'NONE',  ( -0.05219959533934338120, 16.53943276465976808, 47.50109039468568994 ) ) ;
#75736 = CARTESIAN_POINT ( 'NONE',  ( -5.719274019375665041, -21.55341960407619695, 59.79275706135234714 ) ) ;
#75737 = CARTESIAN_POINT ( 'NONE',  ( -8.224510206698735004, -14.34966873604973081, 24.58442372801901499 ) ) ;
#75738 = CARTESIAN_POINT ( 'NONE',  ( -5.049401038298153566, 19.05341960407611168, 70.20724293864769550 ) ) ;
#75739 = CARTESIAN_POINT ( 'NONE',  ( 9.564922557961047289, -16.46253265017146816, 95.41775706135233293 ) ) ;
#75740 = CARTESIAN_POINT ( 'NONE',  ( 12.06949235617739724, 12.14591786802326823, 56.87609039468568994 ) ) ;
#75741 = CARTESIAN_POINT ( 'NONE',  ( -0.05219959533937732626, 21.53943276465977519, 102.5010903946856899 ) ) ;
#75742 = CARTESIAN_POINT ( 'NONE',  ( 19.02544592524334988, 5.153800228976608722, 81.45942372801897591 ) ) ;
#75743 = CARTESIAN_POINT ( 'NONE',  ( -16.46253265017160317, 9.564922557960807481, 45.83224293864769550 ) ) ;
#75744 = CARTESIAN_POINT ( 'NONE',  ( 15.80617190586746368, 15.72974639402197994, 64.37390960531435269 ) ) ;
#75746 = CARTESIAN_POINT ( 'NONE',  ( -0.05219959533936034679, 19.03943276465977164, 72.50109039468566152 ) ) ;
#75745 = CARTESIAN_POINT ( 'NONE',  ( -8.314922557960811034, -14.29746914071050412, 77.08224293864769550 ) ) ;
#75747 = CARTESIAN_POINT ( 'NONE',  ( 17.44270441346518652, -5.991230190322998972, 61.13664920735772768 ) ) ;
#75748 = CARTESIAN_POINT ( 'NONE',  ( -9.474510206698720793, -16.51473224551083518, 49.58442372801899722 ) ) ;
#75749 = CARTESIAN_POINT ( 'NONE',  ( 0.05219959533910956823, 16.53943276465976808, 24.99890960531435624 ) ) ;
#75750 = CARTESIAN_POINT ( 'NONE',  ( -14.29746914071049879, 8.314922557960819915, 60.83224293864769550 ) ) ;
#75752 = CARTESIAN_POINT ( 'NONE',  ( 17.14385361876520264, -23.59649016807271238, 143.5750000027312012 ) ) ;
#75751 = CARTESIAN_POINT ( 'NONE',  ( 18.62759615963255655, 10.81492255796105972, 96.66775706135234714 ) ) ;
#75753 = CARTESIAN_POINT ( 'NONE',  ( -15.72974639402197994, 15.80617190586746368, 110.6239096053143669 ) ) ;
#75754 = CARTESIAN_POINT ( 'NONE',  ( 19.05341960407611168, 5.049401038298154454, 68.95724293864769550 ) ) ;
#75755 = CARTESIAN_POINT ( 'NONE',  ( -5.823673210054431948, 21.52544592524334988, 87.70942372801901854 ) ) ;
#75756 = CARTESIAN_POINT ( 'NONE',  ( -9.474510206698964154, 16.51473224551069663, 65.41557627198102409 ) ) ;
#75757 = EDGE_LOOP ( 'NONE', ( #191246, #14812, #101514, #22192 ) ) ;
#75758 = CARTESIAN_POINT ( 'NONE',  ( 12.06949235617757843, -12.14591786802309237, 113.1239096053143953 ) ) ;
#75759 = CARTESIAN_POINT ( 'NONE',  ( -5.719274019375978568, 21.55341960407610458, 35.20724293864768839 ) ) ;
#75760 = CARTESIAN_POINT ( 'NONE',  ( 16.53943276465976808, -0.05219959533910856209, 73.74890960531433848 ) ) ;
#75761 = CARTESIAN_POINT ( 'NONE',  ( 9.474510206698971260, -16.51473224551069308, 42.91557627198103120 ) ) ;
#75762 = CARTESIAN_POINT ( 'NONE',  ( 8.314922557960818139, 14.29746914071049879, 94.58224293864769550 ) ) ;
#75763 = CIRCLE ( 'NONE', #82080, 12.50000000000000000 ) ;
#75764 = CARTESIAN_POINT ( 'NONE',  ( -21.52544592524343514, 5.823673210054127303, 106.0405762719810525 ) ) ;
#75765 = CARTESIAN_POINT ( 'NONE',  ( 10.81492255796106328, -18.62759615963255655, 45.41775706135234003 ) ) ;
#75766 = CARTESIAN_POINT ( 'NONE',  ( -9.474510206698964154, 16.51473224551069663, 35.41557627198102409 ) ) ;
#75767 = CARTESIAN_POINT ( 'NONE',  ( 14.34966873604972726, -8.224510206698740333, 45.83442372801901854 ) ) ;
#75768 = CARTESIAN_POINT ( 'NONE',  ( 21.52544592524344225, -5.823673210054117533, 98.54057627198105251 ) ) ;
#75769 = CARTESIAN_POINT ( 'NONE',  ( 15.72974639402199770, -15.80617190586745480, 98.12390960531436690 ) ) ;
#75771 = CARTESIAN_POINT ( 'NONE',  ( -13.97604488694527625, -13.89961937509977652, 51.87390960531436690 ) ) ;
#75770 = CARTESIAN_POINT ( 'NONE',  ( 5.153800228976615827, -19.02544592524334988, 25.20942372801900433 ) ) ;
#75772 = CARTESIAN_POINT ( 'NONE',  ( 19.02544592524343514, -5.153800228976328945, 108.5405762719810383 ) ) ;
#75773 = CARTESIAN_POINT ( 'NONE',  ( 5.719274019375673035, 21.55341960407619339, 52.29275706135236135 ) ) ;
#75774 = CARTESIAN_POINT ( 'NONE',  ( 5.719274019375991003, -21.55341960407610458, 47.70724293864770260 ) ) ;
#75775 = CARTESIAN_POINT ( 'NONE',  ( 16.52544592524335698, 4.483927247898782831, 111.4594237280190328 ) ) ;
#75777 = CARTESIAN_POINT ( 'NONE',  ( -15.72974639402176322, -15.80617190586768395, 94.37609039468568994 ) ) ;
#75776 = CARTESIAN_POINT ( 'NONE',  ( -15.80617190586768217, 15.72974639402176855, 63.12609039468568994 ) ) ;
#75778 = CARTESIAN_POINT ( 'NONE',  ( -13.89961937509957401, -13.97604488694547875, 44.37609039468566863 ) ) ;
#75779 = CARTESIAN_POINT ( 'NONE',  ( 4.483927247898790824, -16.52544592524335698, 105.2094237280190328 ) ) ;
#75780 = CARTESIAN_POINT ( 'NONE',  ( 5.719274019375673035, 21.55341960407619339, 57.29275706135234714 ) ) ;
#75781 = CARTESIAN_POINT ( 'NONE',  ( -16.46253265017160317, 9.564922557960807481, 55.83224293864769550 ) ) ;
#75782 = CARTESIAN_POINT ( 'NONE',  ( 0.05219959533937995610, -21.53943276465977519, 110.0010903946856757 ) ) ;
#75783 = CARTESIAN_POINT ( 'NONE',  ( -15.72974639402197994, 15.80617190586746368, 25.62390960531435624 ) ) ;
#75784 = CARTESIAN_POINT ( 'NONE',  ( -21.52544592524343514, 5.823673210054127303, 111.0405762719810525 ) ) ;
#75785 = CARTESIAN_POINT ( 'NONE',  ( 5.823673210054125526, 21.52544592524343514, 74.79057627198105251 ) ) ;
#75786 = CARTESIAN_POINT ( 'NONE',  ( -14.29746914071037622, -8.314922557961029526, 44.16775706135234714 ) ) ;
#75788 = CARTESIAN_POINT ( 'NONE',  ( 21.55341960407610458, 5.719274019375980345, 78.95724293864769550 ) ) ;
#75787 = CYLINDRICAL_SURFACE ( 'NONE', #167704, 8.000000000000000000 ) ;
#75790 = CARTESIAN_POINT ( 'NONE',  ( -16.53943276465976808, 0.05219959533911058130, 71.24890960531435269 ) ) ;
#75789 = CARTESIAN_POINT ( 'NONE',  ( -14.34966873604972548, 8.224510206698743886, 68.33442372801900433 ) ) ;
#75791 = CARTESIAN_POINT ( 'NONE',  ( 1.475613392205543661, 30.08492190595072557, -48.16867494856833787 ) ) ;
#75792 = CARTESIAN_POINT ( 'NONE',  ( -9.474510206698720793, -16.51473224551083518, 109.5844237280190043 ) ) ;
#75793 = CARTESIAN_POINT ( 'NONE',  ( -10.72451020669898014, 18.67979575497178502, 40.41557627198103120 ) ) ;
#75794 = CARTESIAN_POINT ( 'NONE',  ( 0.05219959533909260263, 19.03943276465977164, 94.99890960531436690 ) ) ;
#75795 = CARTESIAN_POINT ( 'NONE',  ( 8.314922557961029526, -14.29746914071037800, 35.41775706135234003 ) ) ;
#75796 = CARTESIAN_POINT ( 'NONE',  ( -10.72451020669898014, 18.67979575497178502, 105.4155762719810383 ) ) ;
#75797 = CARTESIAN_POINT ( 'NONE',  ( -21.52544592524343514, 5.823673210054127303, 31.04057627198102409 ) ) ;
#75798 = CARTESIAN_POINT ( 'NONE',  ( -4.379528057220086978, -16.55341960407618274, 64.79275706135234714 ) ) ;
#75799 = CARTESIAN_POINT ( 'NONE',  ( 13.89961937509977652, -13.97604488694527269, 88.12390960531438111 ) ) ;
#75801 = CARTESIAN_POINT ( 'NONE',  ( 13.89961937509977652, -13.97604488694527269, 33.12390960531434558 ) ) ;
#75800 = CARTESIAN_POINT ( 'NONE',  ( -18.67979575497193778, 10.72451020669871902, 58.33442372801901143 ) ) ;
#75802 = CARTESIAN_POINT ( 'NONE',  ( -15.72974639402197994, 15.80617190586746368, 30.62390960531436335 ) ) ;
#75803 = ORIENTED_EDGE ( 'NONE', *, *, #83344, .F. ) ;
#75804 = CARTESIAN_POINT ( 'NONE',  ( -19.02544592524334988, -5.153800228976617603, 33.95942372801897591 ) ) ;
#75805 = CARTESIAN_POINT ( 'NONE',  ( 16.53943276465976808, 0.05219959533934440121, 56.25109039468568284 ) ) ;
#75806 = CARTESIAN_POINT ( 'NONE',  ( -16.51473224551069308, -9.474510206698971260, 101.6655762719810241 ) ) ;
#75807 = CARTESIAN_POINT ( 'NONE',  ( -18.62759615963270932, 10.81492255796079327, 100.8322429386477097 ) ) ;
#75808 = CARTESIAN_POINT ( 'NONE',  ( 16.46253265017160672, -9.564922557960803928, 68.33224293864770971 ) ) ;
#75809 = CARTESIAN_POINT ( 'NONE',  ( -17.13100169013300444, 6.664070546373152659, 25.76789835699850073 ) ) ;
#75810 = CARTESIAN_POINT ( 'NONE',  ( -23.29544513554941076, 16.92513159979227666, 142.0656553485623590 ) ) ;
#75811 = CARTESIAN_POINT ( 'NONE',  ( -14.34966873604960291, -8.224510206698953496, 86.66557627198102409 ) ) ;
#75812 = CARTESIAN_POINT ( 'NONE',  ( -5.823673210054116645, -21.52544592524344225, 32.29057627198102409 ) ) ;
#75813 = CARTESIAN_POINT ( 'NONE',  ( -16.31925111598457789, 7.325300261831451998, 35.16424538967250868 ) ) ;
#75814 = CARTESIAN_POINT ( 'NONE',  ( -14.29746914071037622, -8.314922557961029526, 69.16775706135234714 ) ) ;
#75815 = CARTESIAN_POINT ( 'NONE',  ( -5.719274019375978568, 21.55341960407610458, 115.2072429386476955 ) ) ;
#75816 = CARTESIAN_POINT ( 'NONE',  ( 9.564922557961047289, -16.46253265017146816, 75.41775706135234714 ) ) ;
#75817 = CARTESIAN_POINT ( 'NONE',  ( -9.564922557960796823, -16.46253265017161027, 37.08224293864768839 ) ) ;
#75818 = CARTESIAN_POINT ( 'NONE',  ( 21.55341960407610458, 5.719274019375980345, 63.95724293864770260 ) ) ;
#75819 = CARTESIAN_POINT ( 'NONE',  ( -0.05219959533909027116, -19.03943276465977164, 97.49890960531436690 ) ) ;
#75820 = CARTESIAN_POINT ( 'NONE',  ( 15.72974639402176855, 15.80617190586768217, 96.87609039468568994 ) ) ;
#75821 = CARTESIAN_POINT ( 'NONE',  ( -19.02544592524342804, 5.153800228976336051, 66.04057627198103830 ) ) ;
#75822 = EDGE_CURVE ( 'NONE', #9294, #34941, #72892, .T. ) ;
#75823 = CARTESIAN_POINT ( 'NONE',  ( -14.29746914071037622, -8.314922557961029526, 44.16775706135234714 ) ) ;
#75824 = CARTESIAN_POINT ( 'NONE',  ( 19.03943276465977164, -0.05219959533909143690, 53.74890960531436690 ) ) ;
#75825 = CARTESIAN_POINT ( 'NONE',  ( 0.05219959533937995610, -21.53943276465977519, 75.00109039468568994 ) ) ;
#75826 = CARTESIAN_POINT ( 'NONE',  ( -9.564922557961040184, 16.46253265017147172, 42.91775706135234003 ) ) ;
#75827 = CARTESIAN_POINT ( 'NONE',  ( -16.46253265017146816, -9.564922557961047289, 54.16775706135234003 ) ) ;
#75828 = CARTESIAN_POINT ( 'NONE',  ( 5.823673210054444382, -21.52544592524334988, 50.20942372801901854 ) ) ;
#75829 = CARTESIAN_POINT ( 'NONE',  ( -8.898623008803063783, 0.7571601631682653988, -61.93576936796790022 ) ) ;
#75830 = CARTESIAN_POINT ( 'NONE',  ( -13.97604488694547697, 13.89961937509957934, 48.12609039468566863 ) ) ;
#75831 = CARTESIAN_POINT ( 'NONE',  ( -5.153800228976328057, -19.02544592524343514, 102.2905762719810383 ) ) ;
#75832 = CARTESIAN_POINT ( 'NONE',  ( -13.89961937509977652, 13.97604488694528158, 75.62390960531438111 ) ) ;
#75833 = CARTESIAN_POINT ( 'NONE',  ( 0.05219959533910956823, 16.53943276465976808, 29.99890960531435979 ) ) ;
#75835 = CARTESIAN_POINT ( 'NONE',  ( 18.62759615963255655, 10.81492255796105972, 101.6677570613523613 ) ) ;
#75834 = CARTESIAN_POINT ( 'NONE',  ( -18.62759615963270932, 10.81492255796079327, 30.83224293864770260 ) ) ;
#75836 = CARTESIAN_POINT ( 'NONE',  ( -11.40812507854754720, -35.11059874428192273, -8.724999997268813701 ) ) ;
#75837 = CARTESIAN_POINT ( 'NONE',  ( -34.35276339089875108, 2.907959671212060559, 90.32815265678038941 ) ) ;
#75838 = CARTESIAN_POINT ( 'NONE',  ( -5.719274019375665041, -21.55341960407619695, 99.79275706135234714 ) ) ;
#75839 = CARTESIAN_POINT ( 'NONE',  ( -22.94331271462294808, 3.784814030245898575, 190.0000000000000000 ) ) ;
#75841 = CARTESIAN_POINT ( 'NONE',  ( 5.049401038298161559, -19.05341960407611168, 27.70724293864769550 ) ) ;
#75840 = PRODUCT_DEFINITION ( 'UNKNOWN', '', #179267, #20065 ) ;
#75842 = CARTESIAN_POINT ( 'NONE',  ( -13.97604488694527625, -13.89961937509977652, 111.8739096053143243 ) ) ;
#75843 = CARTESIAN_POINT ( 'NONE',  ( 34.52594549653174028, 0.3596637467104462083, 89.49999999999900524 ) ) ;
#75844 = AXIS2_PLACEMENT_3D ( 'NONE', #10351, #134698, #57850 ) ;
#75845 = CARTESIAN_POINT ( 'NONE',  ( -8.314922557961024197, 14.29746914071037800, 52.91775706135235424 ) ) ;
#75846 = CARTESIAN_POINT ( 'NONE',  ( -5.719274019375978568, 21.55341960407610458, 70.20724293864769550 ) ) ;
#75847 = CARTESIAN_POINT ( 'NONE',  ( -12.14591786802309592, -12.06949235617757132, 41.87390960531435979 ) ) ;
#75849 = CARTESIAN_POINT ( 'NONE',  ( 13.89961937509977652, -13.97604488694527269, 113.1239096053143527 ) ) ;
#75848 = CARTESIAN_POINT ( 'NONE',  ( 4.379528057220339221, -16.55341960407611168, 112.7072429386476955 ) ) ;
#75850 = CARTESIAN_POINT ( 'NONE',  ( 16.46253265017146816, 9.564922557961045513, 41.66775706135234003 ) ) ;
#75851 = CARTESIAN_POINT ( 'NONE',  ( 14.29746914071049879, -8.314922557960816363, 113.3322429386476955 ) ) ;
#75852 = CARTESIAN_POINT ( 'NONE',  ( -10.81492255796105439, 18.62759615963255655, 67.91775706135234714 ) ) ;
#75853 = FACE_OUTER_BOUND ( 'NONE', #63188, .T. ) ;
#75854 = CARTESIAN_POINT ( 'NONE',  ( 0.05219959533910956823, 16.53943276465976808, 24.99890960531435624 ) ) ;
#75855 = CARTESIAN_POINT ( 'NONE',  ( -5.950531402560715689E-15, 38.81732327939063509, -7.624999997268814056 ) ) ;
#75856 = CARTESIAN_POINT ( 'NONE',  ( 21.53943276465977519, -0.05219959533907433946, 28.74890960531435624 ) ) ;
#75857 = CARTESIAN_POINT ( 'NONE',  ( 16.55341960407611168, 4.379528057220329451, 83.95724293864770971 ) ) ;
#75858 = AXIS2_PLACEMENT_3D ( 'NONE', #19875, #161380, #128035 ) ;
#75859 = CARTESIAN_POINT ( 'NONE',  ( 9.100000000000004974, -0.1000365528946606797, -63.95112321872119310 ) ) ;
#75860 = CARTESIAN_POINT ( 'NONE',  ( -13.97604488694527625, -13.89961937509977652, 81.87390960531436690 ) ) ;
#75861 = CARTESIAN_POINT ( 'NONE',  ( 14.34966873604960469, 8.224510206698951720, 69.16557627198102409 ) ) ;
#75862 = CARTESIAN_POINT ( 'NONE',  ( 9.564922557961047289, -16.46253265017146816, 105.4177570613523471 ) ) ;
#75863 = CARTESIAN_POINT ( 'NONE',  ( -15.72974639402197994, 15.80617190586746368, 50.62390960531435979 ) ) ;
#75864 = ORIENTED_EDGE ( 'NONE', *, *, #69149, .T. ) ;
#75865 = CARTESIAN_POINT ( 'NONE',  ( 16.53943276465976808, -0.05219959533910856209, 108.7489096053143669 ) ) ;
#75867 = CARTESIAN_POINT ( 'NONE',  ( -21.55341960407610458, -5.719274019375992779, 76.45724293864769550 ) ) ;
#75866 = CARTESIAN_POINT ( 'NONE',  ( -19.05341960407611168, -5.049401038298163336, 76.45724293864769550 ) ) ;
#75869 = CARTESIAN_POINT ( 'NONE',  ( -19.05341960407611168, -5.049401038298163336, 81.45724293864769550 ) ) ;
#75868 = CARTESIAN_POINT ( 'NONE',  ( -16.55341960407617563, 4.379528057220093196, 103.5427570613523613 ) ) ;
#75870 = CARTESIAN_POINT ( 'NONE',  ( 19.03943276465977164, 0.05219959533936151252, 66.25109039468567573 ) ) ;
#75871 = CARTESIAN_POINT ( 'NONE',  ( 0.05219959533937995610, -21.53943276465977519, 90.00109039468567573 ) ) ;
#75872 = CARTESIAN_POINT ( 'NONE',  ( 15.80617190586746368, 15.72974639402197994, 69.37390960531436690 ) ) ;
#75873 = CARTESIAN_POINT ( 'NONE',  ( 15.80617190586746368, 15.72974639402197994, 29.37390960531435269 ) ) ;
#75874 = CARTESIAN_POINT ( 'NONE',  ( -5.049401038298153566, 19.05341960407611168, 35.20724293864768839 ) ) ;
#75875 = CARTESIAN_POINT ( 'NONE',  ( -16.53943276465976808, -0.05219959533934237506, 103.7510903946857042 ) ) ;
#75876 = CARTESIAN_POINT ( 'NONE',  ( 13.97604488694527802, 13.89961937509977652, 59.37390960531434558 ) ) ;
#75877 = CARTESIAN_POINT ( 'NONE',  ( 8.224510206698742110, 14.34966873604972548, 22.08442372801901143 ) ) ;
#75878 = CARTESIAN_POINT ( 'NONE',  ( -3.573655867282028392E-15, 2.428612866367529932E-14, 169.9999999999999716 ) ) ;
#75879 = CARTESIAN_POINT ( 'NONE',  ( -15.80617190586768217, 15.72974639402176855, 108.1260903946856757 ) ) ;
#75880 = CARTESIAN_POINT ( 'NONE',  ( -16.55341960407611168, -4.379528057220339221, 76.45724293864769550 ) ) ;
#75881 = PRODUCT_DEFINITION_FORMATION_WITH_SPECIFIED_SOURCE ( 'ANY', '', #95384, .NOT_KNOWN. ) ;
#75882 = CARTESIAN_POINT ( 'NONE',  ( 15.80617190586746368, 15.72974639402197994, 114.3739096053143527 ) ) ;
#75883 = CARTESIAN_POINT ( 'NONE',  ( -0.05219959533907301413, -21.53943276465977519, 107.4989096053143669 ) ) ;
#75884 = DIRECTION ( 'NONE',  ( 1.000000000000000000, 0.000000000000000000, 0.000000000000000000 ) ) ;
#75885 = CARTESIAN_POINT ( 'NONE',  ( 5.823673210054125526, 21.52544592524343514, 39.79057627198103830 ) ) ;
#75886 = CARTESIAN_POINT ( 'NONE',  ( -4.483927247898782831, 16.52544592524335698, 82.70942372801900433 ) ) ;
#75887 = CARTESIAN_POINT ( 'NONE',  ( 8.314922557960818139, 14.29746914071049879, 99.58224293864770971 ) ) ;
#75888 = CARTESIAN_POINT ( 'NONE',  ( -16.51473224551069308, -9.474510206698971260, 56.66557627198103120 ) ) ;
#75889 =( NAMED_UNIT ( * ) PLANE_ANGLE_UNIT ( ) SI_UNIT ( $, .RADIAN. ) );
#75890 = CARTESIAN_POINT ( 'NONE',  ( -0.05219959533910754901, -16.53943276465976808, 22.49890960531436335 ) ) ;
#75891 = VERTEX_POINT ( 'NONE', #19155 ) ;
#75892 = CARTESIAN_POINT ( 'NONE',  ( 18.62759615963255655, 10.81492255796105972, 41.66775706135235424 ) ) ;
#75893 = CARTESIAN_POINT ( 'NONE',  ( 5.153800228976335163, 19.02544592524342804, 94.79057627198103830 ) ) ;
#75894 = CARTESIAN_POINT ( 'NONE',  ( 15.72974639402176855, 15.80617190586768217, 76.87609039468567573 ) ) ;
#75895 = CARTESIAN_POINT ( 'NONE',  ( 0.05219959533909260263, 19.03943276465977164, 34.99890960531435979 ) ) ;
#75896 = CARTESIAN_POINT ( 'NONE',  ( -19.05341960407611168, -5.049401038298163336, 21.45724293864768839 ) ) ;
#75897 =( BOUNDED_CURVE ( )  B_SPLINE_CURVE ( 2, ( #62448, #47308, #170644, #155470, #93790 ),
 .UNSPECIFIED., .F., .F. ) 
 B_SPLINE_CURVE_WITH_KNOTS ( ( 3, 2, 3 ),
 ( 0.9744993486534860860, 0.9799999999999999822, 1.000000000000000000 ),
 .UNSPECIFIED. ) 
 CURVE ( )  GEOMETRIC_REPRESENTATION_ITEM ( )  RATIONAL_B_SPLINE_CURVE ( ( 0.9804823514139775487, 0.9865389480227928498, 1.000000000000000000, 0.9510565162951535312, 1.000000000000000000 ) ) 
 REPRESENTATION_ITEM ( '' )  );
#75898 = ORIENTED_EDGE ( 'NONE', *, *, #44361, .F. ) ;
#75899 = CARTESIAN_POINT ( 'NONE',  ( 15.80617190586769283, -15.72974639402175789, 70.62609039468567573 ) ) ;
#75900 = CARTESIAN_POINT ( 'NONE',  ( -16.51473224551069308, -9.474510206698971260, 101.6655762719810241 ) ) ;
#75901 = CARTESIAN_POINT ( 'NONE',  ( -19.02544592524334988, -5.153800228976617603, 73.95942372801900433 ) ) ;
#75902 = CARTESIAN_POINT ( 'NONE',  ( -0.05219959533937732626, 21.53943276465977519, 47.50109039468568994 ) ) ;
#75903 = CARTESIAN_POINT ( 'NONE',  ( -8.224510206698735004, -14.34966873604973081, 19.58442372801901143 ) ) ;
#75904 = CARTESIAN_POINT ( 'NONE',  ( 19.02544592524334988, 5.153800228976608722, 66.45942372801899012 ) ) ;
#75905 = CARTESIAN_POINT ( 'NONE',  ( 0.05219959533909260263, 19.03943276465977164, 39.99890960531436690 ) ) ;
#75906 = CARTESIAN_POINT ( 'NONE',  ( -9.564922557961040184, 16.46253265017147172, 87.91775706135233293 ) ) ;
#75907 = AXIS2_PLACEMENT_3D ( 'NONE', #22129, #145459, #188254 ) ;
#75908 = CARTESIAN_POINT ( 'NONE',  ( 12.06949235617757843, -12.14591786802309237, 23.12390960531436335 ) ) ;
#75909 = CARTESIAN_POINT ( 'NONE',  ( 5.049401038297881783, 19.05341960407617563, 82.29275706135229029 ) ) ;
#75910 = CARTESIAN_POINT ( 'NONE',  ( 14.34966873604960469, 8.224510206698951720, 34.16557627198102409 ) ) ;
#75911 = CARTESIAN_POINT ( 'NONE',  ( 19.03943276465977164, 0.05219959533936151252, 66.25109039468567573 ) ) ;
#75912 = CARTESIAN_POINT ( 'NONE',  ( -21.52544592524334988, -5.823673210054445271, 108.9594237280190185 ) ) ;
#75913 = CARTESIAN_POINT ( 'NONE',  ( 9.564922557961047289, -16.46253265017146816, 30.41775706135232937 ) ) ;
#75914 = CARTESIAN_POINT ( 'NONE',  ( 19.05341960407611168, 5.049401038298154454, 28.95724293864769550 ) ) ;
#75915 = CARTESIAN_POINT ( 'NONE',  ( -16.88567814943164436, -6.947325034625593254, 66.29001122652586275 ) ) ;
#75916 = CARTESIAN_POINT ( 'NONE',  ( -4.483927247898782831, 16.52544592524335698, 47.70942372801902565 ) ) ;
#75917 = CARTESIAN_POINT ( 'NONE',  ( 23.31738231874054534, 16.94106989632529192, 139.4500000054623570 ) ) ;
#75918 = CARTESIAN_POINT ( 'NONE',  ( 27.73933785331498925, -9.013057229001033122, 145.7750000027311899 ) ) ;
#75919 = CARTESIAN_POINT ( 'NONE',  ( 9.474510206698971260, -16.51473224551069308, 87.91557627198102409 ) ) ;
#75920 = CARTESIAN_POINT ( 'NONE',  ( -28.82186960331480208, 9.364793116373830273, 141.9000000000000057 ) ) ;
#75921 = ORIENTED_EDGE ( 'NONE', *, *, #68080, .F. ) ;
#75922 = CARTESIAN_POINT ( 'NONE',  ( -13.89961937509957401, -13.97604488694547875, 89.37609039468563310 ) ) ;
#75923 = CARTESIAN_POINT ( 'NONE',  ( -10.72451020669898014, 18.67979575497178502, 25.41557627198103120 ) ) ;
#75925 = CARTESIAN_POINT ( 'NONE',  ( -0.05219959533936034679, 19.03943276465977164, 102.5010903946856757 ) ) ;
#75924 = CARTESIAN_POINT ( 'NONE',  ( 13.97604488694548053, -13.89961937509957401, 20.62609039468567573 ) ) ;
#75926 = CARTESIAN_POINT ( 'NONE',  ( 8.224510206698953496, -14.34966873604960469, 107.9155762719810241 ) ) ;
#75927 = CARTESIAN_POINT ( 'NONE',  ( 5.153800228976335163, 19.02544592524342804, 29.79057627198102409 ) ) ;
#75928 = CARTESIAN_POINT ( 'NONE',  ( -10.81492255796078084, -18.62759615963271287, 57.08224293864769550 ) ) ;
#75929 = CARTESIAN_POINT ( 'NONE',  ( -18.67979575497178146, -10.72451020669898902, 46.66557627198102409 ) ) ;
#75930 = CARTESIAN_POINT ( 'NONE',  ( -5.049401038298153566, 19.05341960407611168, 25.20724293864768484 ) ) ;
#75931 = LINE ( 'NONE', #151793, #101664 ) ;
#75932 = CARTESIAN_POINT ( 'NONE',  ( -5.049401038297874678, -19.05341960407617918, 74.79275706135231871 ) ) ;
#75933 = CARTESIAN_POINT ( 'NONE',  ( -8.314922557960811034, -14.29746914071050412, 37.08224293864768129 ) ) ;
#75934 = CARTESIAN_POINT ( 'NONE',  ( -15.80617190586745835, -15.72974639402198527, 21.87390960531436690 ) ) ;
#75935 = CARTESIAN_POINT ( 'NONE',  ( -10.72451020669870658, -18.67979575497194134, 89.58442372801901854 ) ) ;
#75936 = CARTESIAN_POINT ( 'NONE',  ( -15.72974639402197994, 15.80617190586746368, 80.62390960531438111 ) ) ;
#75937 = CARTESIAN_POINT ( 'NONE',  ( 18.62759615963255655, 10.81492255796105972, 56.66775706135235424 ) ) ;
#75938 = CARTESIAN_POINT ( 'NONE',  ( -10.81492255796105439, 18.62759615963255655, 67.91775706135234714 ) ) ;
#75939 = CARTESIAN_POINT ( 'NONE',  ( 13.89961937509977652, -13.97604488694527269, 98.12390960531433848 ) ) ;
#75941 = CARTESIAN_POINT ( 'NONE',  ( -21.53943276465977519, -0.05219959533937600094, 53.75109039468568994 ) ) ;
#75940 = CARTESIAN_POINT ( 'NONE',  ( -16.53943276465976808, -0.05219959533934237506, 93.75109039468567573 ) ) ;
#75942 = CARTESIAN_POINT ( 'NONE',  ( -19.02544592524342804, 5.153800228976336051, 26.04057627198103120 ) ) ;
#75943 = CARTESIAN_POINT ( 'NONE',  ( -31.37858599332832910, 5.662547894918618319, 99.94225302722342974 ) ) ;
#75944 = AXIS2_PLACEMENT_3D ( 'NONE', #126521, #62858, #173047 ) ;
#75945 = CARTESIAN_POINT ( 'NONE',  ( -12.06949235617756955, 12.14591786802309770, 65.62390960531436690 ) ) ;
#75946 = CARTESIAN_POINT ( 'NONE',  ( -8.224510206698948167, 14.34966873604960824, 35.41557627198102409 ) ) ;
#75947 = CARTESIAN_POINT ( 'NONE',  ( 13.97604488694527802, 13.89961937509977652, 69.37390960531436690 ) ) ;
#75948 = CARTESIAN_POINT ( 'NONE',  ( 16.51473224551069308, 9.474510206698969483, 54.16557627198103120 ) ) ;
#75949 = CARTESIAN_POINT ( 'NONE',  ( 5.823673210054125526, 21.52544592524343514, 54.79057627198104541 ) ) ;
#75950 = CARTESIAN_POINT ( 'NONE',  ( 9.474510206698729675, 16.51473224551082808, 37.08442372801899722 ) ) ;
#75952 = CARTESIAN_POINT ( 'NONE',  ( 14.29746914071049879, -8.314922557960816363, 53.33224293864769550 ) ) ;
#75951 = CARTESIAN_POINT ( 'NONE',  ( 22.83054850305942907, -22.20849125555281489, -49.19912570997622936 ) ) ;
#75953 = CARTESIAN_POINT ( 'NONE',  ( -9.474510206698964154, 16.51473224551069663, 115.4155762719810241 ) ) ;
#75954 = ORIENTED_EDGE ( 'NONE', *, *, #74210, .T. ) ;
#75955 = CARTESIAN_POINT ( 'NONE',  ( -28.75808110634262604, -1.452795517301058048, 139.9999999999999716 ) ) ;
#75956 = CARTESIAN_POINT ( 'NONE',  ( 16.55341960407618274, -4.379528057220086978, 66.04275706135236135 ) ) ;
#75957 = CARTESIAN_POINT ( 'NONE',  ( 0.05219959533936267826, -19.03943276465977164, 80.00109039468567573 ) ) ;
#75958 = CARTESIAN_POINT ( 'NONE',  ( 16.55341960407611168, 4.379528057220329451, 43.95724293864769550 ) ) ;
#75959 = CARTESIAN_POINT ( 'NONE',  ( 31.99999999999936051, 1.011767027235951731E-12, 92.30000000000021032 ) ) ;
#75960 = CARTESIAN_POINT ( 'NONE',  ( -16.55341960407617563, 4.379528057220093196, 113.5427570613523756 ) ) ;
#75961 = CARTESIAN_POINT ( 'NONE',  ( 9.564922557960805705, 16.46253265017160317, 54.58224293864769550 ) ) ;
#75962 = EDGE_CURVE ( 'NONE', #99310, #57684, #2693, .T. ) ;
#75963 = CARTESIAN_POINT ( 'NONE',  ( -5.049401038298153566, 19.05341960407611168, 75.20724293864769550 ) ) ;
#75964 = CARTESIAN_POINT ( 'NONE',  ( -16.46253265017160317, 9.564922557960807481, 45.83224293864769550 ) ) ;
#75965 = CARTESIAN_POINT ( 'NONE',  ( -10.81492255796105439, 18.62759615963255655, 47.91775706135234714 ) ) ;
#75966 = CARTESIAN_POINT ( 'NONE',  ( 19.02544592524343514, -5.153800228976328945, 53.54057627198102409 ) ) ;
#75967 = CARTESIAN_POINT ( 'NONE',  ( 24.30000000000003268, 0.000000000000000000, -56.77278709839600879 ) ) ;
#75968 = CARTESIAN_POINT ( 'NONE',  ( 9.474510206698971260, -16.51473224551069308, 62.91557627198102409 ) ) ;
#75969 = CARTESIAN_POINT ( 'NONE',  ( -21.52544592524343514, 5.823673210054127303, 36.04057627198102409 ) ) ;
#75970 = CARTESIAN_POINT ( 'NONE',  ( 13.97604488694527802, 13.89961937509977652, 24.37390960531435624 ) ) ;
#75971 = CARTESIAN_POINT ( 'NONE',  ( 21.53943276465977519, -0.05219959533907433946, 28.74890960531435624 ) ) ;
#75972 = CARTESIAN_POINT ( 'NONE',  ( -14.29746914071037622, -8.314922557961029526, 94.16775706135237556 ) ) ;
#75973 = CARTESIAN_POINT ( 'NONE',  ( -18.62759615963255300, -10.81492255796106328, 104.1677570613523471 ) ) ;
#75974 = CARTESIAN_POINT ( 'NONE',  ( 16.52544592524335698, 4.483927247898782831, 61.45942372801901854 ) ) ;
#75975 = CARTESIAN_POINT ( 'NONE',  ( -19.02544592524342804, 5.153800228976336051, 106.0405762719810241 ) ) ;
#75976 = CARTESIAN_POINT ( 'NONE',  ( 4.379528057220092307, 16.55341960407617563, 52.29275706135236135 ) ) ;
#75977 = CARTESIAN_POINT ( 'NONE',  ( -8.314922557961024197, 14.29746914071037800, 42.91775706135235424 ) ) ;
#75978 = CARTESIAN_POINT ( 'NONE',  ( 9.564922557960805705, 16.46253265017160317, 109.5822429386476955 ) ) ;
#75979 = CARTESIAN_POINT ( 'NONE',  ( 16.55341960407618274, -4.379528057220086978, 26.04275706135235779 ) ) ;
#75980 = CARTESIAN_POINT ( 'NONE',  ( -9.564922557960796823, -16.46253265017161027, 32.08224293864769550 ) ) ;
#75981 = CARTESIAN_POINT ( 'NONE',  ( -15.72974639402197994, 15.80617190586746368, 105.6239096053143669 ) ) ;
#75982 = CARTESIAN_POINT ( 'NONE',  ( -16.52544592524335698, -4.483927247898792601, 18.95942372801901143 ) ) ;
#75983 = CARTESIAN_POINT ( 'NONE',  ( 12.14591786802327356, -12.06949235617739191, 85.62609039468568994 ) ) ;
#75984 = CARTESIAN_POINT ( 'NONE',  ( -17.40805194821984259, 6.112264579160790134, 45.83371272510608918 ) ) ;
#75985 = CARTESIAN_POINT ( 'NONE',  ( -10.72451020669870658, -18.67979575497194134, 89.58442372801901854 ) ) ;
#75986 = CARTESIAN_POINT ( 'NONE',  ( -9.474510206698720793, -16.51473224551083518, 79.58442372801899012 ) ) ;
#75987 = CARTESIAN_POINT ( 'NONE',  ( -12.06949235617756955, 12.14591786802309770, 60.62390960531437401 ) ) ;
#75988 = CARTESIAN_POINT ( 'NONE',  ( 8.314922557960818139, 14.29746914071049879, 104.5822429386477097 ) ) ;
#75990 = CARTESIAN_POINT ( 'NONE',  ( 17.50000000000001421, -5.622605283950835364, 56.18792689403892382 ) ) ;
#75989 = CARTESIAN_POINT ( 'NONE',  ( 5.049401038297881783, 19.05341960407617563, 52.29275706135234003 ) ) ;
#75991 = CARTESIAN_POINT ( 'NONE',  ( -21.55341960407619339, 5.719274019375674811, 53.54275706135234714 ) ) ;
#75992 = CARTESIAN_POINT ( 'NONE',  ( -16.46253265017146816, -9.564922557961047289, 104.1677570613523329 ) ) ;
#75993 = CARTESIAN_POINT ( 'NONE',  ( -17.49999999999999645, 5.499999999999997335, 120.0000000000000142 ) ) ;
#75994 = CARTESIAN_POINT ( 'NONE',  ( -19.03943276465977164, 0.05219959533909376836, 106.2489096053143669 ) ) ;
#75995 = CARTESIAN_POINT ( 'NONE',  ( -5.823673210054116645, -21.52544592524344225, 72.29057627198102409 ) ) ;
#75996 = CARTESIAN_POINT ( 'NONE',  ( -16.51473224551082808, 9.474510206698731452, 93.33442372801900433 ) ) ;
#75997 = CARTESIAN_POINT ( 'NONE',  ( -9.474510206698964154, 16.51473224551069663, 105.4155762719810383 ) ) ;
#75998 = CARTESIAN_POINT ( 'NONE',  ( -18.22780087662126647, -5.499999999999827693, 48.98236817873107185 ) ) ;
#75999 = CARTESIAN_POINT ( 'NONE',  ( 16.55341960407611168, 4.379528057220329451, 108.9572429386476955 ) ) ;
#76000 = CARTESIAN_POINT ( 'NONE',  ( 15.80617190586769283, -15.72974639402175789, 90.62609039468567573 ) ) ;
#76001 = CARTESIAN_POINT ( 'NONE',  ( -19.02544592524342804, 5.153800228976336051, 41.04057627198103120 ) ) ;
#76002 = AXIS2_PLACEMENT_3D ( 'NONE', #13037, #188593, #182880 ) ;
#76003 = CARTESIAN_POINT ( 'NONE',  ( 5.719274019375673035, 21.55341960407619339, 57.29275706135234714 ) ) ;
#76004 = CARTESIAN_POINT ( 'NONE',  ( -15.72974639402176322, -15.80617190586768395, 89.37609039468568994 ) ) ;
#76005 = CARTESIAN_POINT ( 'NONE',  ( 0.05219959533934541429, -16.53943276465976808, 95.00109039468568994 ) ) ;
#76006 = CARTESIAN_POINT ( 'NONE',  ( 15.72974639402176855, 15.80617190586768217, 41.87609039468568284 ) ) ;
#76007 = CARTESIAN_POINT ( 'NONE',  ( -18.67979575497193778, 10.72451020669871902, 43.33442372801901143 ) ) ;
#76009 = CARTESIAN_POINT ( 'NONE',  ( -9.474510206698964154, 16.51473224551069663, 95.41557627198102409 ) ) ;
#76008 = CARTESIAN_POINT ( 'NONE',  ( 13.97604488694548053, -13.89961937509957401, 65.62609039468567573 ) ) ;
#76010 = CARTESIAN_POINT ( 'NONE',  ( 12.14591786802309770, 12.06949235617756955, 104.3739096053143669 ) ) ;
#76011 = CARTESIAN_POINT ( 'NONE',  ( -10.81492255796078084, -18.62759615963271287, 82.08224293864768129 ) ) ;
#76012 = CARTESIAN_POINT ( 'NONE',  ( 8.224510206698953496, -14.34966873604960469, 67.91557627198102409 ) ) ;
#76013 = CARTESIAN_POINT ( 'NONE',  ( -18.62759615963255300, -10.81492255796106328, 99.16775706135234714 ) ) ;
#76014 = CARTESIAN_POINT ( 'NONE',  ( 16.52544592524342804, -4.483927247898539470, 78.54057627198103830 ) ) ;
#76015 = CARTESIAN_POINT ( 'NONE',  ( -16.46253265017160317, 9.564922557960807481, 40.83224293864769550 ) ) ;
#76016 = CARTESIAN_POINT ( 'NONE',  ( -19.02544592524334988, -5.153800228976617603, 83.95942372801901854 ) ) ;
#76017 = CARTESIAN_POINT ( 'NONE',  ( -12.06949235617756955, 12.14591786802309770, 50.62390960531435979 ) ) ;
#76018 = CARTESIAN_POINT ( 'NONE',  ( -21.53943276465977519, -0.05219959533937600094, 93.75109039468567573 ) ) ;
#76019 = CARTESIAN_POINT ( 'NONE',  ( -16.46253265017160317, 9.564922557960807481, 85.83224293864769550 ) ) ;
#76020 = CARTESIAN_POINT ( 'NONE',  ( 16.46253265017146816, 9.564922557961045513, 61.66775706135234003 ) ) ;
#76021 = CARTESIAN_POINT ( 'NONE',  ( 18.67979575497178502, 10.72451020669898547, 69.16557627198102409 ) ) ;
#76022 = CARTESIAN_POINT ( 'NONE',  ( -18.62759615963255300, -10.81492255796106328, 24.16775706135235424 ) ) ;
#76023 = CARTESIAN_POINT ( 'NONE',  ( 4.379528057220092307, 16.55341960407617563, 27.29275706135234358 ) ) ;
#76024 = CARTESIAN_POINT ( 'NONE',  ( -16.55341960407617563, 4.379528057220093196, 73.54275706135234714 ) ) ;
#76026 = CARTESIAN_POINT ( 'NONE',  ( 18.67979575497178502, 10.72451020669898547, 114.1655762719810383 ) ) ;
#76025 = CARTESIAN_POINT ( 'NONE',  ( -0.05219959533909027116, -19.03943276465977164, 27.49890960531435624 ) ) ;
#76027 = CARTESIAN_POINT ( 'NONE',  ( -8.314922557960811034, -14.29746914071050412, 112.0822429386477097 ) ) ;
#76028 = CARTESIAN_POINT ( 'NONE',  ( -22.81625015709509441, -31.40387420917324590, -6.824999997268814234 ) ) ;
#76029 = CARTESIAN_POINT ( 'NONE',  ( 16.52544592524335698, 4.483927247898782831, 51.45942372801901854 ) ) ;
#76030 = CARTESIAN_POINT ( 'NONE',  ( 16.53943276465976808, -0.05219959533910856209, 73.74890960531433848 ) ) ;
#76031 = CARTESIAN_POINT ( 'NONE',  ( -0.05219959533907301413, -21.53943276465977519, 77.49890960531433848 ) ) ;
#76032 = CIRCLE ( 'NONE', #189064, 5.000000000000001776 ) ;
#76033 = CARTESIAN_POINT ( 'NONE',  ( -16.55341960407611168, -4.379528057220339221, 21.45724293864769550 ) ) ;
#76034 = CARTESIAN_POINT ( 'NONE',  ( 14.34966873604972726, -8.224510206698740333, 40.83442372801901854 ) ) ;
#76035 = CARTESIAN_POINT ( 'NONE',  ( -0.05219959533909027116, -19.03943276465977164, 42.49890960531435269 ) ) ;
#76036 = CARTESIAN_POINT ( 'NONE',  ( -8.224510206698735004, -14.34966873604973081, 79.58442372801903275 ) ) ;
#76037 = CARTESIAN_POINT ( 'NONE',  ( -5.153800228976607833, 19.02544592524334988, 72.70942372801900433 ) ) ;
#76038 = CARTESIAN_POINT ( 'NONE',  ( -21.52544592524343514, 5.823673210054127303, 76.04057627198102409 ) ) ;
#76039 = CARTESIAN_POINT ( 'NONE',  ( -16.53943276465976808, -0.05219959533934237506, 113.7510903946856757 ) ) ;
#76040 = ORIENTED_EDGE ( 'NONE', *, *, #115218, .T. ) ;
#76041 = CARTESIAN_POINT ( 'NONE',  ( 25.86526910843881311, 7.630673861714906359, 173.3900163844835731 ) ) ;
#76042 = CARTESIAN_POINT ( 'NONE',  ( 0.05219959533907565091, 21.53943276465977519, 44.99890960531435979 ) ) ;
#76043 = VERTEX_POINT ( 'NONE', #95981 ) ;
#76044 = CARTESIAN_POINT ( 'NONE',  ( 14.29746914071037800, 8.314922557961029526, 96.66775706135234714 ) ) ;
#76045 = ORIENTED_EDGE ( 'NONE', *, *, #63738, .F. ) ;
#76046 = CARTESIAN_POINT ( 'NONE',  ( 9.564922557960805705, 16.46253265017160317, 114.5822429386476955 ) ) ;
#76047 = CARTESIAN_POINT ( 'NONE',  ( -23.48529157249600985, 32.32473071737754111, -8.049999994537627046 ) ) ;
#76048 = CARTESIAN_POINT ( 'NONE',  ( 0.05219959533907565091, 21.53943276465977519, 74.99890960531435269 ) ) ;
#76049 = CARTESIAN_POINT ( 'NONE',  ( 8.224510206698742110, 14.34966873604972548, 107.0844237280190043 ) ) ;
#76050 = CARTESIAN_POINT ( 'NONE',  ( 5.719274019375673035, 21.55341960407619339, 57.29275706135234714 ) ) ;
#76051 = CARTESIAN_POINT ( 'NONE',  ( -9.564922557961040184, 16.46253265017147172, 112.9177570613523329 ) ) ;
#76052 = CARTESIAN_POINT ( 'NONE',  ( 9.474510206698971260, -16.51473224551069308, 22.91557627198102765 ) ) ;
#76053 = CARTESIAN_POINT ( 'NONE',  ( -14.34966873604972548, 8.224510206698743886, 23.33442372801901499 ) ) ;
#76054 = CARTESIAN_POINT ( 'NONE',  ( -19.03943276465977164, 0.05219959533909376836, 56.24890960531435979 ) ) ;
#76055 = CARTESIAN_POINT ( 'NONE',  ( 28.82186960331498327, 2.781578969918950771E-14, 145.0000000000000000 ) ) ;
#76056 = CARTESIAN_POINT ( 'NONE',  ( -0.05219959533909027116, -19.03943276465977164, 107.4989096053143527 ) ) ;
#76057 = EDGE_CURVE ( 'NONE', #105306, #18425, #163852, .T. ) ;
#76058 = CARTESIAN_POINT ( 'NONE',  ( 12.06949235617739724, 12.14591786802326823, 91.87609039468568994 ) ) ;
#76059 = CARTESIAN_POINT ( 'NONE',  ( -19.03943276465977164, -0.05219959533935918106, 93.75109039468566152 ) ) ;
#76060 = CARTESIAN_POINT ( 'NONE',  ( -5.049401038297874678, -19.05341960407617918, 24.79275706135233648 ) ) ;
#76061 = CARTESIAN_POINT ( 'NONE',  ( 15.80617190586746368, 15.72974639402197994, 69.37390960531436690 ) ) ;
#76062 = CARTESIAN_POINT ( 'NONE',  ( 12.06949235617739724, 12.14591786802326823, 96.87609039468568994 ) ) ;
#76063 = CARTESIAN_POINT ( 'NONE',  ( 13.89961937509957401, 13.97604488694547697, 96.87609039468566152 ) ) ;
#76064 = CARTESIAN_POINT ( 'NONE',  ( 0.05219959533909260263, 19.03943276465977164, 54.99890960531435979 ) ) ;
#76065 = CARTESIAN_POINT ( 'NONE',  ( 13.97604488694527802, 13.89961937509977652, 94.37390960531436690 ) ) ;
#76066 = CARTESIAN_POINT ( 'NONE',  ( -5.823673210054431948, 21.52544592524334988, 52.70942372801902565 ) ) ;
#76067 = CARTESIAN_POINT ( 'NONE',  ( -19.05341960407611168, -5.049401038298163336, 46.45724293864768129 ) ) ;
#76068 = CARTESIAN_POINT ( 'NONE',  ( -12.06949235617756955, 12.14591786802309770, 65.62390960531436690 ) ) ;
#76069 = CARTESIAN_POINT ( 'NONE',  ( -18.62759615963270932, 10.81492255796079327, 75.83224293864769550 ) ) ;
#76070 = DIRECTION ( 'NONE',  ( -1.000000000000000000, 0.000000000000000000, 0.000000000000000000 ) ) ;
#76071 = CARTESIAN_POINT ( 'NONE',  ( 13.89961937509957401, 13.97604488694547697, 46.87609039468565442 ) ) ;
#76072 = LINE ( 'NONE', #133782, #180036 ) ;
#76074 = CARTESIAN_POINT ( 'NONE',  ( -13.89961937509977652, 13.97604488694528158, 90.62390960531432427 ) ) ;
#76073 = CARTESIAN_POINT ( 'NONE',  ( 16.46253265017160672, -9.564922557960803928, 73.33224293864769550 ) ) ;
#76075 = CARTESIAN_POINT ( 'NONE',  ( -4.483927247898782831, 16.52544592524335698, 57.70942372801901143 ) ) ;
#76076 = CARTESIAN_POINT ( 'NONE',  ( -28.82186960331483760, 9.364793116373787640, 143.9000000000000057 ) ) ;
#76077 = CARTESIAN_POINT ( 'NONE',  ( 19.03943276465977164, 0.05219959533936151252, 36.25109039468567573 ) ) ;
#76078 = CARTESIAN_POINT ( 'NONE',  ( 18.22780087662123805, -5.499999999999976019, 93.51763182126896368 ) ) ;
#76079 = CARTESIAN_POINT ( 'NONE',  ( -8.314922557961024197, 14.29746914071037800, 92.91775706135236135 ) ) ;
#76080 = EDGE_CURVE ( 'NONE', #193619, #120101, #90078, .T. ) ;
#76081 = CARTESIAN_POINT ( 'NONE',  ( -16.53943276465976808, -0.05219959533934237506, 78.75109039468568994 ) ) ;
#76082 = CARTESIAN_POINT ( 'NONE',  ( 16.53943276465976808, 0.05219959533934440121, 56.25109039468568284 ) ) ;
#76084 = CARTESIAN_POINT ( 'NONE',  ( -13.89961937509977830, 13.97604488694528158, 75.62390960531436690 ) ) ;
#76083 = CARTESIAN_POINT ( 'NONE',  ( 19.02544592524343514, -5.153800228976328945, 53.54057627198102409 ) ) ;
#76085 = CARTESIAN_POINT ( 'NONE',  ( -10.81492255796105439, 18.62759615963255655, 62.91775706135236135 ) ) ;
#76086 = CARTESIAN_POINT ( 'NONE',  ( -13.89961937509957401, -13.97604488694547875, 74.37609039468566152 ) ) ;
#76087 = CARTESIAN_POINT ( 'NONE',  ( 18.62759615963255655, 10.81492255796105972, 111.6677570613523613 ) ) ;
#76088 = AXIS2_PLACEMENT_3D ( 'NONE', #43928, #105590, #153073 ) ;
#76089 = CARTESIAN_POINT ( 'NONE',  ( 9.474510206698971260, -16.51473224551069308, 57.91557627198103120 ) ) ;
#76090 = CARTESIAN_POINT ( 'NONE',  ( -0.05219959533909027116, -19.03943276465977164, 37.49890960531436690 ) ) ;
#76091 = CARTESIAN_POINT ( 'NONE',  ( -15.13939621930183854, 14.98335265924511717, -58.85720012050611416 ) ) ;
#76092 = CARTESIAN_POINT ( 'NONE',  ( -10.81492255796078084, -18.62759615963271287, 72.08224293864769550 ) ) ;
#76093 = CARTESIAN_POINT ( 'NONE',  ( -13.89961937509977652, 13.97604488694528158, 110.6239096053143243 ) ) ;
#76094 = CARTESIAN_POINT ( 'NONE',  ( 16.52544592524342804, -4.483927247898539470, 113.5405762719810383 ) ) ;
#76095 = CARTESIAN_POINT ( 'NONE',  ( 0.05219959533934541429, -16.53943276465976808, 45.00109039468568284 ) ) ;
#76096 = CARTESIAN_POINT ( 'NONE',  ( 8.314922557960818139, 14.29746914071049879, 34.58224293864770260 ) ) ;
#76097 = ORIENTED_EDGE ( 'NONE', *, *, #125462, .T. ) ;
#76098 = CARTESIAN_POINT ( 'NONE',  ( -5.719274019375978568, 21.55341960407610458, 110.2072429386477239 ) ) ;
#76100 = CARTESIAN_POINT ( 'NONE',  ( 11.74264578624799427, 36.14014761921585972, -2.600000000000000533 ) ) ;
#76099 = CARTESIAN_POINT ( 'NONE',  ( 0.05219959533910956823, 16.53943276465976808, 49.99890960531437401 ) ) ;
#76101 = CARTESIAN_POINT ( 'NONE',  ( -19.03943276465977164, -0.05219959533935918106, 113.7510903946856757 ) ) ;
#76102 = CARTESIAN_POINT ( 'NONE',  ( -16.51473224551082808, 9.474510206698731452, 38.33442372801899722 ) ) ;
#76103 = CARTESIAN_POINT ( 'NONE',  ( -12.06949235617756955, 12.14591786802309770, 45.62390960531436690 ) ) ;
#76104 = CARTESIAN_POINT ( 'NONE',  ( -15.72974639402197994, 15.80617190586746368, 105.6239096053143669 ) ) ;
#76106 = CARTESIAN_POINT ( 'NONE',  ( 5.719274019375991003, -21.55341960407610458, 57.70724293864770260 ) ) ;
#76105 = DIRECTION ( 'NONE',  ( -0.000000000000000000, -0.000000000000000000, 1.000000000000000000 ) ) ;
#76107 = CARTESIAN_POINT ( 'NONE',  ( 13.89961937509977652, -13.97604488694527269, 73.12390960531436690 ) ) ;
#76108 = CARTESIAN_POINT ( 'NONE',  ( 12.06949235617757843, -12.14591786802309237, 48.12390960531436690 ) ) ;
#76109 = CARTESIAN_POINT ( 'NONE',  ( 19.03943276465977164, -0.05219959533909143690, 103.7489096053143669 ) ) ;
#76110 = CARTESIAN_POINT ( 'NONE',  ( -32.00000000000000711, -5.180255960393304182E-15, 47.70000000000000284 ) ) ;
#76111 = CARTESIAN_POINT ( 'NONE',  ( 9.564922557961047289, -16.46253265017146816, 55.41775706135234003 ) ) ;
#76112 = CARTESIAN_POINT ( 'NONE',  ( 15.72974639402199770, -15.80617190586745480, 93.12390960531436690 ) ) ;
#76113 = CARTESIAN_POINT ( 'NONE',  ( -9.474510206698964154, 16.51473224551069663, 45.41557627198103120 ) ) ;
#76114 = CARTESIAN_POINT ( 'NONE',  ( 16.53943276465976808, -0.05219959533910856209, 113.7489096053143527 ) ) ;
#76115 = CARTESIAN_POINT ( 'NONE',  ( 18.67979575497194134, -10.72451020669871369, 55.83442372801901854 ) ) ;
#76116 = CARTESIAN_POINT ( 'NONE',  ( 1.784210473542230573E-15, -29.16686587814331588, 145.3750000027311842 ) ) ;
#76117 = CARTESIAN_POINT ( 'NONE',  ( -8.224510206698948167, 14.34966873604960824, 25.41557627198103120 ) ) ;
#76118 = CARTESIAN_POINT ( 'NONE',  ( 0.05219959533909260263, 19.03943276465977164, 54.99890960531435979 ) ) ;
#76119 = CARTESIAN_POINT ( 'NONE',  ( -13.89961937509977652, 13.97604488694528158, 100.6239096053143669 ) ) ;
#76120 = CARTESIAN_POINT ( 'NONE',  ( -21.53943276465977519, 0.05219959533907696930, 66.24890960531436690 ) ) ;
#76121 = CARTESIAN_POINT ( 'NONE',  ( -5.359611314223446995E-15, 29.16686587814335496, 146.3750000027311842 ) ) ;
#76122 = CARTESIAN_POINT ( 'NONE',  ( 13.89961937509977652, -13.97604488694527269, 43.12390960531434558 ) ) ;
#76123 = CARTESIAN_POINT ( 'NONE',  ( 10.81492255796078972, 18.62759615963270932, 54.58224293864769550 ) ) ;
#76124 = CARTESIAN_POINT ( 'NONE',  ( 10.72451020669871369, 18.67979575497193778, 82.08442372801901854 ) ) ;
#76127 = CARTESIAN_POINT ( 'NONE',  ( 8.314922557960818139, 14.29746914071049879, 69.58224293864769550 ) ) ;
#76126 = CARTESIAN_POINT ( 'NONE',  ( -16.53943276465976808, -0.05219959533934237506, 88.75109039468567573 ) ) ;
#76125 = CARTESIAN_POINT ( 'NONE',  ( 22.55660001725822994, -30.45235066353972542, -22.16622550485903886 ) ) ;
#76128 = CARTESIAN_POINT ( 'NONE',  ( 14.34966873604972726, -8.224510206698740333, 85.83442372801901854 ) ) ;
#76129 = CARTESIAN_POINT ( 'NONE',  ( -19.03943276465977164, 0.05219959533909376836, 71.24890960531435269 ) ) ;
#76130 = VERTEX_POINT ( 'NONE', #47509 ) ;
#76131 = CARTESIAN_POINT ( 'NONE',  ( 19.05341960407617918, -5.049401038297876454, 31.04275706135232227 ) ) ;
#76132 = CARTESIAN_POINT ( 'NONE',  ( -0.05219959533934338120, 16.53943276465976808, 87.50109039468568994 ) ) ;
#76133 = CARTESIAN_POINT ( 'NONE',  ( 19.05341960407617918, -5.049401038297876454, 21.04275706135232582 ) ) ;
#76134 = CARTESIAN_POINT ( 'NONE',  ( 19.03943276465977164, -0.05219959533909143690, 78.74890960531436690 ) ) ;
#76135 = CARTESIAN_POINT ( 'NONE',  ( -18.67979575497178146, -10.72451020669898902, 41.66557627198103120 ) ) ;
#76136 = CARTESIAN_POINT ( 'NONE',  ( -14.34966873604972548, 8.224510206698743886, 23.33442372801901499 ) ) ;
#76137 = CARTESIAN_POINT ( 'NONE',  ( -0.05219959533937732626, 21.53943276465977519, 77.50109039468567573 ) ) ;
#76138 = CARTESIAN_POINT ( 'NONE',  ( 4.379528057220092307, 16.55341960407617563, 62.29275706135236845 ) ) ;
#76139 = CARTESIAN_POINT ( 'NONE',  ( -15.72974639402197994, 15.80617190586746368, 110.6239096053143669 ) ) ;
#76140 = CARTESIAN_POINT ( 'NONE',  ( 9.474510206698729675, 16.51473224551082808, 107.0844237280190043 ) ) ;
#76141 = CARTESIAN_POINT ( 'NONE',  ( -0.05219959533909027116, -19.03943276465977164, 92.49890960531436690 ) ) ;
#76142 = CARTESIAN_POINT ( 'NONE',  ( 8.314922557961029526, -14.29746914071037800, 30.41775706135234358 ) ) ;
#76143 = CARTESIAN_POINT ( 'NONE',  ( 13.89961937509977652, -13.97604488694527269, 38.12390960531436690 ) ) ;
#76144 = CARTESIAN_POINT ( 'NONE',  ( 12.06949235617739724, 12.14591786802326823, 21.87609039468567573 ) ) ;
#76145 = CARTESIAN_POINT ( 'NONE',  ( 14.34966873604960469, 8.224510206698951720, 84.16557627198103830 ) ) ;
#76146 = CARTESIAN_POINT ( 'NONE',  ( -0.05219959533934338120, 16.53943276465976808, 82.50109039468568994 ) ) ;
#76148 = CARTESIAN_POINT ( 'NONE',  ( -9.564922557960796823, -16.46253265017161027, 67.08224293864769550 ) ) ;
#76147 = CARTESIAN_POINT ( 'NONE',  ( -21.55341960407619339, 5.719274019375674811, 23.54275706135235424 ) ) ;
#76149 = CARTESIAN_POINT ( 'NONE',  ( 13.97604488694527802, 13.89961937509977652, 69.37390960531436690 ) ) ;
#76150 = CARTESIAN_POINT ( 'NONE',  ( 14.29746914071037800, 8.314922557961029526, 91.66775706135234714 ) ) ;
#76152 = EDGE_LOOP ( 'NONE', ( #87533, #156483, #87543 ) ) ;
#76151 = CARTESIAN_POINT ( 'NONE',  ( -24.85901545656360767, -5.346793810781480083, 169.1018111888377291 ) ) ;
#76153 = ORIENTED_EDGE ( 'NONE', *, *, #193676, .T. ) ;
#76154 = CARTESIAN_POINT ( 'NONE',  ( 13.97604488694548053, -13.89961937509957401, 35.62609039468567573 ) ) ;
#76155 = EDGE_CURVE ( 'NONE', #89992, #106494, #46029, .T. ) ;
#76156 = CARTESIAN_POINT ( 'NONE',  ( -19.05341960407611168, -5.049401038298163336, 51.45724293864770260 ) ) ;
#76158 = VERTEX_POINT ( 'NONE', #128295 ) ;
#76157 = CARTESIAN_POINT ( 'NONE',  ( -19.02544592524342804, 5.153800228976336051, 111.0405762719810099 ) ) ;
#76159 = CARTESIAN_POINT ( 'NONE',  ( 16.53943276465976808, 0.05219959533934440121, 26.25109039468567573 ) ) ;
#76161 = CARTESIAN_POINT ( 'NONE',  ( 4.379528057220092307, 16.55341960407617563, 47.29275706135234003 ) ) ;
#76160 = CARTESIAN_POINT ( 'NONE',  ( -19.02544592524334988, -5.153800228976617603, 53.95942372801898301 ) ) ;
#76162 = CARTESIAN_POINT ( 'NONE',  ( 0.05219959533909260263, 19.03943276465977164, 99.99890960531436690 ) ) ;
#76163 = CARTESIAN_POINT ( 'NONE',  ( 16.51473224551069308, 9.474510206698969483, 74.16557627198103830 ) ) ;
#76164 = CARTESIAN_POINT ( 'NONE',  ( 21.55341960407610458, 5.719274019375980345, 103.9572429386476813 ) ) ;
#76165 = CARTESIAN_POINT ( 'NONE',  ( -9.564922557961040184, 16.46253265017147172, 67.91775706135233293 ) ) ;
#76167 = CYLINDRICAL_SURFACE ( 'NONE', #5201, 28.82186960331498682 ) ;
#76166 = CARTESIAN_POINT ( 'NONE',  ( -9.474510206698964154, 16.51473224551069663, 85.41557627198102409 ) ) ;
#76168 = CARTESIAN_POINT ( 'NONE',  ( 9.564922557960805705, 16.46253265017160317, 59.58224293864769550 ) ) ;
#76170 = CARTESIAN_POINT ( 'NONE',  ( 5.049401038298161559, -19.05341960407611168, 27.70724293864769550 ) ) ;
#76169 = CARTESIAN_POINT ( 'NONE',  ( 14.29746914071049879, -8.314922557960816363, 23.33224293864769194 ) ) ;
#76171 = CARTESIAN_POINT ( 'NONE',  ( -5.153800228976607833, 19.02544592524334988, 37.70942372801899722 ) ) ;
#76172 = CARTESIAN_POINT ( 'NONE',  ( -12.06949235617756955, 12.14591786802309770, 75.62390960531439532 ) ) ;
#76173 = CARTESIAN_POINT ( 'NONE',  ( 0.05219959533937995610, -21.53943276465977519, 95.00109039468568994 ) ) ;
#76174 = CARTESIAN_POINT ( 'NONE',  ( 13.89961937509977652, -13.97604488694527269, 43.12390960531434558 ) ) ;
#76175 = CARTESIAN_POINT ( 'NONE',  ( -16.53943276465976808, -0.05219959533934237506, 48.75109039468568284 ) ) ;
#76177 = CARTESIAN_POINT ( 'NONE',  ( 21.53943276465977519, 0.05219959533937863772, 91.25109039468568994 ) ) ;
#76176 = CARTESIAN_POINT ( 'NONE',  ( -12.06949235617756955, 12.14591786802309770, 45.62390960531436690 ) ) ;
#76178 = CARTESIAN_POINT ( 'NONE',  ( -0.05219959533909027116, -19.03943276465977164, 97.49890960531436690 ) ) ;
#76179 = CARTESIAN_POINT ( 'NONE',  ( 13.89961937509977652, -13.97604488694527269, 98.12390960531433848 ) ) ;
#76180 = CARTESIAN_POINT ( 'NONE',  ( -0.05219959533910754901, -16.53943276465976808, 107.4989096053143669 ) ) ;
#76181 = CARTESIAN_POINT ( 'NONE',  ( 14.29746914071049879, -8.314922557960816363, 68.33224293864769550 ) ) ;
#76182 = CARTESIAN_POINT ( 'NONE',  ( 5.719274019375991003, -21.55341960407610458, 77.70724293864770971 ) ) ;
#76183 = CARTESIAN_POINT ( 'NONE',  ( 19.03943276465977164, -0.05219959533909143690, 93.74890960531435269 ) ) ;
#76184 = CARTESIAN_POINT ( 'NONE',  ( 5.823673210054125526, 21.52544592524343514, 104.7905762719810241 ) ) ;
#76185 = CARTESIAN_POINT ( 'NONE',  ( 5.049401038297881783, 19.05341960407617563, 72.29275706135234714 ) ) ;
#76188 = CARTESIAN_POINT ( 'NONE',  ( 8.314922557960818139, 14.29746914071049879, 89.58224293864768129 ) ) ;
#76187 = CARTESIAN_POINT ( 'NONE',  ( -19.53091890409953990, -5.499999999999944933, 90.06097431831425126 ) ) ;
#76186 = CIRCLE ( 'NONE', #14869, 38.00000000000000000 ) ;
#76189 = CARTESIAN_POINT ( 'NONE',  ( 19.02544592524343514, -5.153800228976328945, 53.54057627198102409 ) ) ;
#76190 = CARTESIAN_POINT ( 'NONE',  ( -0.05219959533907301413, -21.53943276465977519, 67.49890960531436690 ) ) ;
#76191 = CARTESIAN_POINT ( 'NONE',  ( 19.50973618000807619, 5.499999999999992895, 102.5000000000000142 ) ) ;
#76193 = CARTESIAN_POINT ( 'NONE',  ( 0.000000000000000000, 0.000000000000000000, -63.95112321872120731 ) ) ;
#76192 = CARTESIAN_POINT ( 'NONE',  ( 16.52544592524335698, 4.483927247898782831, 106.4594237280190328 ) ) ;
#76194 = CARTESIAN_POINT ( 'NONE',  ( -14.34966873604972548, 8.224510206698743886, 23.33442372801901499 ) ) ;
#76195 = CARTESIAN_POINT ( 'NONE',  ( -0.05219959533910754901, -16.53943276465976808, 87.49890960531436690 ) ) ;
#76196 = LINE ( 'NONE', #153035, #170967 ) ;
#76197 = CARTESIAN_POINT ( 'NONE',  ( -5.049401038298153566, 19.05341960407611168, 70.20724293864769550 ) ) ;
#76198 = CARTESIAN_POINT ( 'NONE',  ( -9.564922557960796823, -16.46253265017161027, 37.08224293864768839 ) ) ;
#76199 = CARTESIAN_POINT ( 'NONE',  ( -14.34966873604960291, -8.224510206698953496, 66.66557627198102409 ) ) ;
#76200 = CARTESIAN_POINT ( 'NONE',  ( -21.52544592524343514, 5.823673210054127303, 26.04057627198103475 ) ) ;
#76201 = CARTESIAN_POINT ( 'NONE',  ( 9.474510206698729675, 16.51473224551082808, 97.08442372801900433 ) ) ;
#76202 = CARTESIAN_POINT ( 'NONE',  ( -13.89961937509977652, 13.97604488694528158, 100.6239096053143669 ) ) ;
#76203 = CARTESIAN_POINT ( 'NONE',  ( -18.62759615963270932, 10.81492255796079327, 80.83224293864769550 ) ) ;
#76204 = CARTESIAN_POINT ( 'NONE',  ( -4.483927247898782831, 16.52544592524335698, 77.70942372801900433 ) ) ;
#76205 = CARTESIAN_POINT ( 'NONE',  ( -16.46253265017146816, -9.564922557961047289, 109.1677570613523471 ) ) ;
#76206 = CARTESIAN_POINT ( 'NONE',  ( -16.51473224551069308, -9.474510206698971260, 56.66557627198103120 ) ) ;
#76207 = CARTESIAN_POINT ( 'NONE',  ( 15.80617190586746368, 15.72974639402197994, 64.37390960531435269 ) ) ;
#76208 = CARTESIAN_POINT ( 'NONE',  ( -5.153800228976607833, 19.02544592524334988, 102.7094237280189759 ) ) ;
#76210 = CARTESIAN_POINT ( 'NONE',  ( 18.62759615963255655, 10.81492255796105972, 61.66775706135235424 ) ) ;
#76209 = CARTESIAN_POINT ( 'NONE',  ( 14.29746914071049879, -8.314922557960816363, 43.33224293864769550 ) ) ;
#76211 = CARTESIAN_POINT ( 'NONE',  ( 28.82186960331498327, 2.781578969918950771E-14, 145.2500000054623683 ) ) ;
#76213 = CARTESIAN_POINT ( 'NONE',  ( -16.46253265017160317, 9.564922557960807481, 100.8322429386477097 ) ) ;
#76212 = CARTESIAN_POINT ( 'NONE',  ( 0.05219959533934541429, -16.53943276465976808, 75.00109039468568994 ) ) ;
#76214 = CARTESIAN_POINT ( 'NONE',  ( -9.564922557960796823, -16.46253265017161027, 107.0822429386476955 ) ) ;
#76215 = FACE_OUTER_BOUND ( 'NONE', #166207, .T. ) ;
#76216 = CARTESIAN_POINT ( 'NONE',  ( -16.52544592524335698, -4.483927247898792601, 98.95942372801903275 ) ) ;
#76217 = CARTESIAN_POINT ( 'NONE',  ( -16.52544592524335698, -4.483927247898792601, 43.95942372801902565 ) ) ;
#76218 = CARTESIAN_POINT ( 'NONE',  ( 19.03943276465977164, -0.05219959533909143690, 53.74890960531436690 ) ) ;
#76219 = CARTESIAN_POINT ( 'NONE',  ( 9.474510206698971260, -16.51473224551069308, 72.91557627198102409 ) ) ;
#76220 = CARTESIAN_POINT ( 'NONE',  ( 21.52544592524334988, 5.823673210054432836, 66.45942372801903275 ) ) ;
#76221 = CARTESIAN_POINT ( 'NONE',  ( 16.55341960407618274, -4.379528057220086978, 61.04275706135234714 ) ) ;
#76222 = CARTESIAN_POINT ( 'NONE',  ( -12.06949235617756955, 12.14591786802309770, 30.62390960531436335 ) ) ;
#76223 = CARTESIAN_POINT ( 'NONE',  ( 9.564922557960805705, 16.46253265017160317, 39.58224293864768839 ) ) ;
#76224 = CARTESIAN_POINT ( 'NONE',  ( 16.51473224551069308, 9.474510206698969483, 34.16557627198102409 ) ) ;
#76225 = CARTESIAN_POINT ( 'NONE',  ( -14.29746914071037622, -8.314922557961029526, 34.16775706135234714 ) ) ;
#76226 = CARTESIAN_POINT ( 'NONE',  ( 9.564922557961047289, -16.46253265017146816, 100.4177570613523329 ) ) ;
#76227 = CARTESIAN_POINT ( 'NONE',  ( -14.34966873604960291, -8.224510206698953496, 101.6655762719810383 ) ) ;
#76228 = CARTESIAN_POINT ( 'NONE',  ( 5.153800228976335163, 19.02544592524342804, 49.79057627198100988 ) ) ;
#76230 = CARTESIAN_POINT ( 'NONE',  ( 8.898068258721473001, -27.38543819252872069, 148.5843446568999866 ) ) ;
#76229 = CARTESIAN_POINT ( 'NONE',  ( 13.97604488694548053, -13.89961937509957401, 85.62609039468568994 ) ) ;
#76231 = CARTESIAN_POINT ( 'NONE',  ( 10.72451020669871369, 18.67979575497193778, 92.08442372801901854 ) ) ;
#76232 = CARTESIAN_POINT ( 'NONE',  ( -12.14591786802326823, 12.06949235617739902, 58.12609039468568994 ) ) ;
#76233 = CARTESIAN_POINT ( 'NONE',  ( -18.22780087662126647, -5.499999999999827693, 48.98236817873107185 ) ) ;
#76234 = CARTESIAN_POINT ( 'NONE',  ( -10.81492255796078084, -18.62759615963271287, 52.08224293864768839 ) ) ;
#76235 = CARTESIAN_POINT ( 'NONE',  ( 12.14591786802327356, -12.06949235617739191, 35.62609039468568994 ) ) ;
#76236 = CARTESIAN_POINT ( 'NONE',  ( -18.39635199886970796, 5.499999999999980460, 71.01967076360004683 ) ) ;
#76237 = CARTESIAN_POINT ( 'NONE',  ( -19.05341960407617563, 5.049401038297882671, 38.54275706135233293 ) ) ;
#76238 = AXIS2_PLACEMENT_3D ( 'NONE', #8473, #162150, #131818 ) ;
#76239 = CARTESIAN_POINT ( 'NONE',  ( 19.05341960407611168, 5.049401038298154454, 93.95724293864769550 ) ) ;
#76240 = CARTESIAN_POINT ( 'NONE',  ( -5.153800228976328057, -19.02544592524343514, 57.29057627198103120 ) ) ;
#76241 = CARTESIAN_POINT ( 'NONE',  ( -21.02754888379051934, -22.92766777125494215, -50.14365614045077990 ) ) ;
#76242 = CARTESIAN_POINT ( 'NONE',  ( 5.719274019375673035, 21.55341960407619339, 77.29275706135234714 ) ) ;
#76243 = CARTESIAN_POINT ( 'NONE',  ( -15.49999999999999822, 0.000000000000000000, 120.0000000000000142 ) ) ;
#76244 = CARTESIAN_POINT ( 'NONE',  ( 0.05219959533936267826, -19.03943276465977164, 35.00109039468566863 ) ) ;
#76245 = CARTESIAN_POINT ( 'NONE',  ( 19.05341960407617918, -5.049401038297876454, 21.04275706135232582 ) ) ;
#76246 = CARTESIAN_POINT ( 'NONE',  ( -16.52544592524342804, 4.483927247898546575, 51.04057627198103120 ) ) ;
#76247 = CARTESIAN_POINT ( 'NONE',  ( -19.03943276465977164, 0.05219959533909376836, 56.24890960531435979 ) ) ;
#76248 = CARTESIAN_POINT ( 'NONE',  ( -9.474510206698964154, 16.51473224551069663, 110.4155762719810383 ) ) ;
#76249 = CARTESIAN_POINT ( 'NONE',  ( 18.62759615963255655, 10.81492255796105972, 86.66775706135234714 ) ) ;
#76250 = CARTESIAN_POINT ( 'NONE',  ( 9.564922557960805705, 16.46253265017160317, 69.58224293864770971 ) ) ;
#76251 = CARTESIAN_POINT ( 'NONE',  ( 15.80617190586769283, -15.72974639402175789, 75.62609039468567573 ) ) ;
#76252 = CARTESIAN_POINT ( 'NONE',  ( 21.53943276465977519, -0.05219959533907433946, 33.74890960531436690 ) ) ;
#76253 = CARTESIAN_POINT ( 'NONE',  ( -21.53943276465977519, -0.05219959533937600094, 33.75109039468568284 ) ) ;
#76254 = CARTESIAN_POINT ( 'NONE',  ( -19.02544592524334988, -5.153800228976617603, 63.95942372801899012 ) ) ;
#76255 = CARTESIAN_POINT ( 'NONE',  ( 13.97604488694527802, 13.89961937509977652, 24.37390960531435624 ) ) ;
#76256 = CARTESIAN_POINT ( 'NONE',  ( -16.46253265017160317, 9.564922557960807481, 70.83224293864770971 ) ) ;
#76257 = CARTESIAN_POINT ( 'NONE',  ( 16.53943276465976808, 0.05219959533934440121, 31.25109039468568639 ) ) ;
#76258 = CARTESIAN_POINT ( 'NONE',  ( -16.52544592524342804, 4.483927247898546575, 86.04057627198102409 ) ) ;
#76259 = CARTESIAN_POINT ( 'NONE',  ( -16.51473224551069308, -9.474510206698971260, 61.66557627198103120 ) ) ;
#76260 = CARTESIAN_POINT ( 'NONE',  ( 5.823673210054125526, 21.52544592524343514, 39.79057627198103830 ) ) ;
#76261 = CARTESIAN_POINT ( 'NONE',  ( -9.474510206698720793, -16.51473224551083518, 104.5844237280190043 ) ) ;
#76262 = CARTESIAN_POINT ( 'NONE',  ( -10.72451020669898014, 18.67979575497178502, 115.4155762719810241 ) ) ;
#76263 = CARTESIAN_POINT ( 'NONE',  ( 21.53943276465977519, 0.05219959533937863772, 76.25109039468568994 ) ) ;
#76264 = CARTESIAN_POINT ( 'NONE',  ( -4.379528057220086978, -16.55341960407618274, 74.79275706135234714 ) ) ;
#76265 = CARTESIAN_POINT ( 'NONE',  ( -16.53943276465976808, -0.05219959533934237506, 68.75109039468568994 ) ) ;
#76266 =( BOUNDED_CURVE ( )  B_SPLINE_CURVE ( 3, ( #88409, #132927, #149108, #178449 ),
 .UNSPECIFIED., .F., .F. ) 
 B_SPLINE_CURVE_WITH_KNOTS ( ( 4, 4 ),
 ( 5.503250352303675541, 7.063120262055496923 ),
 .UNSPECIFIED. ) 
 CURVE ( )  GEOMETRIC_REPRESENTATION_ITEM ( )  RATIONAL_B_SPLINE_CURVE ( ( 1.000000000000000000, 0.8073061876036304874, 0.8073061876036304874, 1.000000000000000000 ) ) 
 REPRESENTATION_ITEM ( '' )  );
#76267 = CARTESIAN_POINT ( 'NONE',  ( -13.97604488694527625, -13.89961937509977652, 66.87390960531436690 ) ) ;
#76268 = CARTESIAN_POINT ( 'NONE',  ( -4.379528057220086978, -16.55341960407618274, 84.79275706135234714 ) ) ;
#76269 = CARTESIAN_POINT ( 'NONE',  ( 9.474510206698729675, 16.51473224551082808, 42.08442372801900433 ) ) ;
#76270 = CARTESIAN_POINT ( 'NONE',  ( 10.72451020669898902, -18.67979575497178502, 112.9155762719810383 ) ) ;
#76271 = CARTESIAN_POINT ( 'NONE',  ( 12.14591786802309770, 12.06949235617756955, 69.37390960531436690 ) ) ;
#76272 = CARTESIAN_POINT ( 'NONE',  ( 9.564922557960805705, 16.46253265017160317, 79.58224293864769550 ) ) ;
#76273 = CARTESIAN_POINT ( 'NONE',  ( 4.483927247898790824, -16.52544592524335698, 85.20942372801901854 ) ) ;
#76274 = CARTESIAN_POINT ( 'NONE',  ( 0.05219959533937995610, -21.53943276465977519, 65.00109039468568994 ) ) ;
#76275 = CARTESIAN_POINT ( 'NONE',  ( -5.153800228976607833, 19.02544592524334988, 112.7094237280190043 ) ) ;
#76276 = CARTESIAN_POINT ( 'NONE',  ( 15.80617190586769283, -15.72974639402175789, 20.62609039468568639 ) ) ;
#76277 = CARTESIAN_POINT ( 'NONE',  ( -8.314922557960811034, -14.29746914071050412, 57.08224293864769550 ) ) ;
#76278 = ORIENTED_EDGE ( 'NONE', *, *, #125471, .T. ) ;
#76279 = CARTESIAN_POINT ( 'NONE',  ( 21.53943276465977519, -0.05219959533907433946, 93.74890960531436690 ) ) ;
#76280 = CARTESIAN_POINT ( 'NONE',  ( -12.06949235617756955, 12.14591786802309770, 40.62390960531435269 ) ) ;
#76281 = EDGE_LOOP ( 'NONE', ( #155101, #39000, #195471, #107189, #70085, #185308, #187235, #45625, #158910, #95189, #191607, #150012, #43000, #93816, #79614, #164129, #40581, #104497, #8715, #133354, #161342, #97212, #46799, #199114, #146668, #175736, #104197, #27593, #92497, #66947, #112957, #57741, #26848, #89146, #26150, #29668, #106611, #42599, #156165, #160852, #7819, #36577, #153120, #155544, #101396, #69615, #124388, #98881, #47428, #42183, #151350, #56446, #68359, #36753, #1663, #75382 ) ) ;
#76282 = DIRECTION ( 'NONE',  ( 0.000000000000000000, 0.000000000000000000, 1.000000000000000000 ) ) ;
#76283 = CARTESIAN_POINT ( 'NONE',  ( 10.81492255796078972, 18.62759615963270932, 109.5822429386476955 ) ) ;
#76284 = CARTESIAN_POINT ( 'NONE',  ( 5.153800228976335163, 19.02544592524342804, 109.7905762719810099 ) ) ;
#76285 = CARTESIAN_POINT ( 'NONE',  ( 21.55341960407619695, -5.719274019375665929, 31.04275706135234714 ) ) ;
#76286 = CARTESIAN_POINT ( 'NONE',  ( -16.55341960407611168, -4.379528057220339221, 51.45724293864770260 ) ) ;
#76288 = EDGE_CURVE ( 'NONE', #112813, #139989, #115137, .T. ) ;
#76287 = CARTESIAN_POINT ( 'NONE',  ( -19.05341960407611168, -5.049401038298163336, 56.45724293864768129 ) ) ;
#76289 = B_SPLINE_CURVE_WITH_KNOTS ( 'NONE', 3,
 ( #119144, #151469, #152445, #133295, #121107, #103964 ),
 .UNSPECIFIED., .F., .F.,
 ( 4, 2, 4 ),
 ( 0.003989672132298028098, 0.004372778065220453078, 0.004755883998142877191 ),
 .UNSPECIFIED. ) ;
#76290 = CARTESIAN_POINT ( 'NONE',  ( 9.474510206698729675, 16.51473224551082808, 62.08442372801899722 ) ) ;
#76291 = CARTESIAN_POINT ( 'NONE',  ( 5.153800228976335163, 19.02544592524342804, 89.79057627198102409 ) ) ;
#76292 = CARTESIAN_POINT ( 'NONE',  ( 18.67979575497178502, 10.72451020669898547, 54.16557627198103120 ) ) ;
#76293 = CARTESIAN_POINT ( 'NONE',  ( -22.27567441218681665, -30.36413145305472483, -19.29304740691864950 ) ) ;
#76294 = CARTESIAN_POINT ( 'NONE',  ( -9.564922557960796823, -16.46253265017161027, 57.08224293864769550 ) ) ;
#76295 = CARTESIAN_POINT ( 'NONE',  ( 16.53943276465976808, 0.05219959533934440121, 41.25109039468568284 ) ) ;
#76296 = CARTESIAN_POINT ( 'NONE',  ( -19.03943276465977164, -0.05219959533935918106, 68.75109039468566152 ) ) ;
#76297 = CARTESIAN_POINT ( 'NONE',  ( -21.55341960407610458, -5.719274019375992779, 111.4572429386476813 ) ) ;
#76298 = CARTESIAN_POINT ( 'NONE',  ( -12.14591786802309592, -12.06949235617757132, 51.87390960531437401 ) ) ;
#76299 = ORIENTED_EDGE ( 'NONE', *, *, #9338, .F. ) ;
#76300 = CARTESIAN_POINT ( 'NONE',  ( 0.05219959533909260263, 19.03943276465977164, 84.99890960531436690 ) ) ;
#76301 = CARTESIAN_POINT ( 'NONE',  ( 18.67979575497178502, 10.72451020669898547, 74.16557627198102409 ) ) ;
#76303 = CARTESIAN_POINT ( 'NONE',  ( 16.52544592524335698, 4.483927247898782831, 36.45942372801901143 ) ) ;
#76302 = CARTESIAN_POINT ( 'NONE',  ( 21.55341960407610458, 5.719274019375980345, 103.9572429386476813 ) ) ;
#76304 = CARTESIAN_POINT ( 'NONE',  ( 10.81492255796078972, 18.62759615963270932, 34.58224293864770260 ) ) ;
#76305 = CARTESIAN_POINT ( 'NONE',  ( 18.67979575497194134, -10.72451020669871369, 100.8344237280190185 ) ) ;
#76306 = CARTESIAN_POINT ( 'NONE',  ( -19.02544592524342804, 5.153800228976336051, 91.04057627198100988 ) ) ;
#76307 = CARTESIAN_POINT ( 'NONE',  ( -19.02544592524342804, 5.153800228976336051, 46.04057627198101699 ) ) ;
#76308 = CARTESIAN_POINT ( 'NONE',  ( -19.05341960407611168, -5.049401038298163336, 101.4572429386476955 ) ) ;
#76309 = CARTESIAN_POINT ( 'NONE',  ( -13.97604488694527625, -13.89961937509977652, 71.87390960531433848 ) ) ;
#76310 = CARTESIAN_POINT ( 'NONE',  ( 16.52544592524335698, 4.483927247898782831, 21.45942372801901499 ) ) ;
#76311 = CARTESIAN_POINT ( 'NONE',  ( 4.500000000000000888, -140.0000000000000000, 21.32407087589996308 ) ) ;
#76312 = CARTESIAN_POINT ( 'NONE',  ( -19.03943276465977164, -0.05219959533935918106, 53.75109039468566863 ) ) ;
#76314 = CARTESIAN_POINT ( 'NONE',  ( 5.823673210054125526, 21.52544592524343514, 34.79057627198103120 ) ) ;
#76313 = CARTESIAN_POINT ( 'NONE',  ( -5.719274019375665041, -21.55341960407619695, 104.7927570613523898 ) ) ;
#76315 = CARTESIAN_POINT ( 'NONE',  ( 4.379528057220092307, 16.55341960407617563, 102.2927570613523613 ) ) ;
#76316 = CARTESIAN_POINT ( 'NONE',  ( 22.02260766363856348, -20.08456848261498351, -48.57241000235018191 ) ) ;
#76317 = CARTESIAN_POINT ( 'NONE',  ( -16.46253265017146816, -9.564922557961047289, 74.16775706135234714 ) ) ;
#76318 = CARTESIAN_POINT ( 'NONE',  ( 5.049401038297881783, 19.05341960407617563, 27.29275706135232937 ) ) ;
#76319 = LINE ( 'NONE', #184508, #14545 ) ;
#76320 = CARTESIAN_POINT ( 'NONE',  ( -16.46253265017160317, 9.564922557960807481, 45.83224293864769550 ) ) ;
#76321 = CARTESIAN_POINT ( 'NONE',  ( -14.34966873604960291, -8.224510206698953496, 41.66557627198103120 ) ) ;
#76322 = EDGE_CURVE ( 'NONE', #189816, #36546, #54467, .T. ) ;
#76323 = CARTESIAN_POINT ( 'NONE',  ( -16.79531203550645202, -7.028104445595626082, 111.2524498822044023 ) ) ;
#76324 = CARTESIAN_POINT ( 'NONE',  ( 12.06949235617757843, -12.14591786802309237, 33.12390960531435979 ) ) ;
#76325 = CARTESIAN_POINT ( 'NONE',  ( 2.500000000000000000, 2.357898499370431722, -2.818925648462311528E-15 ) ) ;
#76326 = CARTESIAN_POINT ( 'NONE',  ( -4.483927247898782831, 16.52544592524335698, 92.70942372801901854 ) ) ;
#76327 = CARTESIAN_POINT ( 'NONE',  ( 5.153800228976335163, 19.02544592524342804, 34.79057627198102409 ) ) ;
#76328 = CARTESIAN_POINT ( 'NONE',  ( -5.823673210054431948, 21.52544592524334988, 112.7094237280190328 ) ) ;
#76329 = CARTESIAN_POINT ( 'NONE',  ( -16.53943276465976808, -0.05219959533934237506, 18.75109039468568639 ) ) ;
#76331 = ORIENTED_EDGE ( 'NONE', *, *, #135199, .T. ) ;
#76330 = CARTESIAN_POINT ( 'NONE',  ( -15.72974639402176322, -15.80617190586768395, 84.37609039468570415 ) ) ;
#76332 = CARTESIAN_POINT ( 'NONE',  ( 19.02544592524334988, 5.153800228976608722, 71.45942372801900433 ) ) ;
#76333 = CARTESIAN_POINT ( 'NONE',  ( -19.02544592524342804, 5.153800228976336051, 96.04057627198103830 ) ) ;
#76334 = CARTESIAN_POINT ( 'NONE',  ( -9.564922557960796823, -16.46253265017161027, 87.08224293864769550 ) ) ;
#76335 = ADVANCED_FACE ( 'NONE', ( #83783 ), #116137, .F. ) ;
#76336 = CARTESIAN_POINT ( 'NONE',  ( 11.40812507854755253, -35.11059874428192273, -6.024999997268814411 ) ) ;
#76337 = CARTESIAN_POINT ( 'NONE',  ( 5.823673210054125526, 21.52544592524343514, 114.7905762719810383 ) ) ;
#76338 = AXIS2_PLACEMENT_3D ( 'NONE', #161208, #111716, #66201 ) ;
#76339 = CARTESIAN_POINT ( 'NONE',  ( 0.05219959533910956823, 16.53943276465976808, 69.99890960531435269 ) ) ;
#76340 = CARTESIAN_POINT ( 'NONE',  ( -0.05219959533907301413, -21.53943276465977519, 57.49890960531435979 ) ) ;
#76341 = CARTESIAN_POINT ( 'NONE',  ( -19.02544592524342804, 5.153800228976336051, 66.04057627198103830 ) ) ;
#76343 = CARTESIAN_POINT ( 'NONE',  ( -14.29746914071037622, -8.314922557961029526, 84.16775706135234714 ) ) ;
#76342 = CARTESIAN_POINT ( 'NONE',  ( 18.67979575497178502, 10.72451020669898547, 94.16557627198103830 ) ) ;
#76344 = ORIENTED_EDGE ( 'NONE', *, *, #104192, .T. ) ;
#76345 = CARTESIAN_POINT ( 'NONE',  ( -13.97604488694527625, -13.89961937509977652, 56.87390960531434558 ) ) ;
#76347 = LINE ( 'NONE', #89541, #159202 ) ;
#76346 = CARTESIAN_POINT ( 'NONE',  ( -0.05219959533910754901, -16.53943276465976808, 92.49890960531436690 ) ) ;
#76348 = CARTESIAN_POINT ( 'NONE',  ( -13.89961937509977652, 13.97604488694528158, 45.62390960531433848 ) ) ;
#76349 = CARTESIAN_POINT ( 'NONE',  ( -13.97604488694547697, 13.89961937509957934, 83.12609039468564731 ) ) ;
#76350 = CARTESIAN_POINT ( 'NONE',  ( 16.52544592524342804, -4.483927247898539470, 78.54057627198103830 ) ) ;
#76351 = CARTESIAN_POINT ( 'NONE',  ( 10.81492255796106328, -18.62759615963255655, 55.41775706135234714 ) ) ;
#76353 = CARTESIAN_POINT ( 'NONE',  ( -10.72451020669898014, 18.67979575497178502, 105.4155762719810383 ) ) ;
#76352 = CARTESIAN_POINT ( 'NONE',  ( -19.02544592524342804, 5.153800228976336051, 41.04057627198103120 ) ) ;
#76354 = B_SPLINE_CURVE_WITH_KNOTS ( 'NONE', 3,
 ( #194487, #196498, #57968, #10469, #151954, #42801, #147982, #27649, #103470, #165149, #59932, #44776, #40797, #71134, #104463, #105450, #26640, #74134 ),
 .UNSPECIFIED., .F., .F.,
 ( 4, 2, 2, 2, 2, 2, 2, 2, 4 ),
 ( 9.540979117872439019E-18, 0.0003942454150793282125, 0.0007884908301586468840, 0.001182736245237965556, 0.001576981660317284227, 0.001971227075396602899, 0.002365472490475921570, 0.002759717905555240242, 0.003153963320634558913 ),
 .UNSPECIFIED. ) ;
#76355 = CARTESIAN_POINT ( 'NONE',  ( -8.314922557960811034, -14.29746914071050412, 87.08224293864769550 ) ) ;
#76356 = CARTESIAN_POINT ( 'NONE',  ( 18.09918380851993192, 5.500000000000009770, 93.98618307335613054 ) ) ;
#76357 = CARTESIAN_POINT ( 'NONE',  ( 19.05341960407611168, 5.049401038298154454, 63.95724293864769550 ) ) ;
#76358 = CARTESIAN_POINT ( 'NONE',  ( 18.87255363501902394, 5.499999999999941380, 48.82513748171827217 ) ) ;
#76360 = CARTESIAN_POINT ( 'NONE',  ( -0.05219959533909027116, -19.03943276465977164, 112.4989096053143669 ) ) ;
#76359 = CARTESIAN_POINT ( 'NONE',  ( -19.03943276465977164, -0.05219959533935918106, 98.75109039468567573 ) ) ;
#76361 = CARTESIAN_POINT ( 'NONE',  ( 5.719274019375673035, 21.55341960407619339, 37.29275706135235424 ) ) ;
#76362 = CARTESIAN_POINT ( 'NONE',  ( 19.02544592524343514, -5.153800228976328945, 78.54057627198099567 ) ) ;
#76363 = CARTESIAN_POINT ( 'NONE',  ( 9.564922557961047289, -16.46253265017146816, 65.41775706135233293 ) ) ;
#76364 = CARTESIAN_POINT ( 'NONE',  ( -9.564922557960796823, -16.46253265017161027, 57.08224293864769550 ) ) ;
#76365 = CARTESIAN_POINT ( 'NONE',  ( -16.55341960407611168, -4.379528057220339221, 81.45724293864769550 ) ) ;
#76366 = CARTESIAN_POINT ( 'NONE',  ( 8.224510206698953496, -14.34966873604960469, 72.91557627198103830 ) ) ;
#76367 = CARTESIAN_POINT ( 'NONE',  ( -16.51473224551069308, -9.474510206698971260, 91.66557627198103830 ) ) ;
#76368 = CARTESIAN_POINT ( 'NONE',  ( 8.314922557960818139, 14.29746914071049879, 84.58224293864769550 ) ) ;
#76369 = CARTESIAN_POINT ( 'NONE',  ( 13.97604488694527802, 13.89961937509977652, 89.37390960531436690 ) ) ;
#76370 = CARTESIAN_POINT ( 'NONE',  ( -16.46253265017146816, -9.564922557961047289, 34.16775706135233293 ) ) ;
#76373 = CARTESIAN_POINT ( 'NONE',  ( 4.483927247898545687, 16.52544592524342804, 104.7905762719810241 ) ) ;
#76372 = CARTESIAN_POINT ( 'NONE',  ( 16.52544592524342804, -4.483927247898539470, 28.54057627198103120 ) ) ;
#76371 = CARTESIAN_POINT ( 'NONE',  ( -5.153800228976328057, -19.02544592524343514, 32.29057627198102409 ) ) ;
#76374 = VERTEX_POINT ( 'NONE', #68623 ) ;
#76375 = CARTESIAN_POINT ( 'NONE',  ( -15.80617190586768217, 15.72974639402176855, 38.12609039468567573 ) ) ;
#76376 = CARTESIAN_POINT ( 'NONE',  ( 16.46253265017146816, 9.564922557961045513, 71.66775706135233293 ) ) ;
#76377 = CARTESIAN_POINT ( 'NONE',  ( -0.05219959533910754901, -16.53943276465976808, 32.49890960531435979 ) ) ;
#76378 = CARTESIAN_POINT ( 'NONE',  ( -21.52544592524343514, 5.823673210054127303, 91.04057627198103830 ) ) ;
#76379 = CARTESIAN_POINT ( 'NONE',  ( -15.80617190586745835, -15.72974639402198527, 26.87390960531435979 ) ) ;
#76380 = CARTESIAN_POINT ( 'NONE',  ( 14.29746914071049879, -8.314922557960816363, 73.33224293864769550 ) ) ;
#76381 = CARTESIAN_POINT ( 'NONE',  ( 9.564922557960805705, 16.46253265017160317, 44.58224293864769550 ) ) ;
#76382 = CARTESIAN_POINT ( 'NONE',  ( -16.46253265017146816, -9.564922557961047289, 24.16775706135233648 ) ) ;
#76383 = CARTESIAN_POINT ( 'NONE',  ( -4.483927247898782831, 16.52544592524335698, 102.7094237280190185 ) ) ;
#76384 = CARTESIAN_POINT ( 'NONE',  ( -8.314922557961024197, 14.29746914071037800, 57.91775706135234714 ) ) ;
#76385 = CARTESIAN_POINT ( 'NONE',  ( -5.719274019375978568, 21.55341960407610458, 40.20724293864769550 ) ) ;
#76386 = CARTESIAN_POINT ( 'NONE',  ( -15.80617190586768217, 15.72974639402176855, 108.1260903946856757 ) ) ;
#76387 = CARTESIAN_POINT ( 'NONE',  ( -5.049401038298153566, 19.05341960407611168, 80.20724293864769550 ) ) ;
#76388 = VECTOR ( 'NONE', #38818, 1000.000000000000000 ) ;
#76389 = CARTESIAN_POINT ( 'NONE',  ( 16.52544592524335698, 4.483927247898782831, 76.45942372801901854 ) ) ;
#76390 = CARTESIAN_POINT ( 'NONE',  ( -13.89961937509977652, 13.97604488694528158, 25.62390960531434558 ) ) ;
#76391 = CARTESIAN_POINT ( 'NONE',  ( 16.52544592524342804, -4.483927247898539470, 38.54057627198103120 ) ) ;
#76393 = CARTESIAN_POINT ( 'NONE',  ( 0.05219959533909260263, 19.03943276465977164, 94.99890960531436690 ) ) ;
#76392 = CARTESIAN_POINT ( 'NONE',  ( -13.89961937509977652, 13.97604488694528158, 105.6239096053143527 ) ) ;
#76394 = CARTESIAN_POINT ( 'NONE',  ( -15.80617190586745835, -15.72974639402198527, 31.87390960531435979 ) ) ;
#76395 = CARTESIAN_POINT ( 'NONE',  ( -8.224510206698948167, 14.34966873604960824, 55.41557627198102409 ) ) ;
#76396 = CARTESIAN_POINT ( 'NONE',  ( 16.53943276465976808, -0.05219959533910856209, 38.74890960531435979 ) ) ;
#76397 = ORIENTED_EDGE ( 'NONE', *, *, #178712, .T. ) ;
#76398 = CARTESIAN_POINT ( 'NONE',  ( 14.29746914071049879, -8.314922557960816363, 58.33224293864768839 ) ) ;
#76400 = CARTESIAN_POINT ( 'NONE',  ( -7.284589286804265207, -1.784589286804211916, 1.818019484660534424 ) ) ;
#76399 = CARTESIAN_POINT ( 'NONE',  ( -12.14591786802326823, 12.06949235617739902, 38.12609039468567573 ) ) ;
#76401 = CARTESIAN_POINT ( 'NONE',  ( -0.05219959533936034679, 19.03943276465977164, 47.50109039468566863 ) ) ;
#76402 = CARTESIAN_POINT ( 'NONE',  ( -9.474510206698964154, 16.51473224551069663, 90.41557627198103830 ) ) ;
#76403 = CARTESIAN_POINT ( 'NONE',  ( 19.02544592524334988, 5.153800228976608722, 61.45942372801900433 ) ) ;
#76404 = CARTESIAN_POINT ( 'NONE',  ( 8.571926809382597767, 26.38167802310806209, 144.7750000027311899 ) ) ;
#76405 = CARTESIAN_POINT ( 'NONE',  ( -19.03943276465977164, -0.05219959533935918106, 53.75109039468566863 ) ) ;
#76407 = CARTESIAN_POINT ( 'NONE',  ( 16.55341960407618274, -4.379528057220086978, 76.04275706135237556 ) ) ;
#76406 = CARTESIAN_POINT ( 'NONE',  ( -9.474510206698720793, -16.51473224551083518, 99.58442372801900433 ) ) ;
#76408 = CARTESIAN_POINT ( 'NONE',  ( 8.571926809382603096, -26.38167802310801235, 147.9750000027311785 ) ) ;
#76409 = CARTESIAN_POINT ( 'NONE',  ( 19.05341960407611168, 5.049401038298154454, 23.95724293864769194 ) ) ;
#76410 = CARTESIAN_POINT ( 'NONE',  ( 21.53943276465977519, -0.05219959533907433946, 23.74890960531435269 ) ) ;
#76411 = CARTESIAN_POINT ( 'NONE',  ( -0.05219959533937732626, 21.53943276465977519, 37.50109039468568284 ) ) ;
#76412 = CARTESIAN_POINT ( 'NONE',  ( -16.46253265017146816, -9.564922557961047289, 99.16775706135233293 ) ) ;
#76414 = CARTESIAN_POINT ( 'NONE',  ( -0.05219959533909027116, -19.03943276465977164, 57.49890960531435979 ) ) ;
#76413 = CARTESIAN_POINT ( 'NONE',  ( 17.49999999999999289, -3.237210098469628150, 107.2123698737954243 ) ) ;
#76415 = CARTESIAN_POINT ( 'NONE',  ( 9.474510206698971260, -16.51473224551069308, 107.9155762719810383 ) ) ;
#76417 = CARTESIAN_POINT ( 'NONE',  ( -16.46253265017160317, 9.564922557960807481, 60.83224293864769550 ) ) ;
#76416 = CARTESIAN_POINT ( 'NONE',  ( -8.224510206698948167, 14.34966873604960824, 65.41557627198102409 ) ) ;
#76418 = CARTESIAN_POINT ( 'NONE',  ( 9.474510206698971260, -16.51473224551069308, 77.91557627198103830 ) ) ;
#76419 = CARTESIAN_POINT ( 'NONE',  ( 0.05219959533936267826, -19.03943276465977164, 80.00109039468567573 ) ) ;
#76420 = CARTESIAN_POINT ( 'NONE',  ( -10.81492255796078084, -18.62759615963271287, 57.08224293864769550 ) ) ;
#76421 = CARTESIAN_POINT ( 'NONE',  ( -0.05219959533910754901, -16.53943276465976808, 107.4989096053143669 ) ) ;
#76422 = CARTESIAN_POINT ( 'NONE',  ( 9.474510206698729675, 16.51473224551082808, 47.08442372801900433 ) ) ;
#76423 = CARTESIAN_POINT ( 'NONE',  ( -19.02544592524342804, 5.153800228976336051, 86.04057627198103830 ) ) ;
#76424 = CARTESIAN_POINT ( 'NONE',  ( -21.53943276465977519, 0.05219959533907696930, 71.24890960531435269 ) ) ;
#76426 = CARTESIAN_POINT ( 'NONE',  ( 16.46253265017146816, 9.564922557961045513, 41.66775706135234003 ) ) ;
#76425 = CARTESIAN_POINT ( 'NONE',  ( 0.05219959533910956823, 16.53943276465976808, 79.99890960531435269 ) ) ;
#76427 = CARTESIAN_POINT ( 'NONE',  ( 21.55341960407610458, 5.719274019375980345, 78.95724293864769550 ) ) ;
#76428 = CARTESIAN_POINT ( 'NONE',  ( 15.80617190586746368, 15.72974639402197994, 59.37390960531436690 ) ) ;
#76429 = CARTESIAN_POINT ( 'NONE',  ( 10.72451020669898902, -18.67979575497178502, 42.91557627198103120 ) ) ;
#76430 = CARTESIAN_POINT ( 'NONE',  ( 18.67979575497194134, -10.72451020669871369, 85.83442372801901854 ) ) ;
#76431 = CARTESIAN_POINT ( 'NONE',  ( 9.474510206698971260, -16.51473224551069308, 62.91557627198102409 ) ) ;
#76432 = CARTESIAN_POINT ( 'NONE',  ( 8.224510206698953496, -14.34966873604960469, 112.9155762719810383 ) ) ;
#76433 = CARTESIAN_POINT ( 'NONE',  ( -10.72451020669870658, -18.67979575497194134, 19.58442372801901143 ) ) ;
#76434 = CARTESIAN_POINT ( 'NONE',  ( -17.60691670004650788, -5.500000000000068390, 49.13333313366439370 ) ) ;
#76435 = CARTESIAN_POINT ( 'NONE',  ( -10.81492255796105439, 18.62759615963255655, 37.91775706135235424 ) ) ;
#76436 = CARTESIAN_POINT ( 'NONE',  ( -9.474510206698964154, 16.51473224551069663, 40.41557627198103120 ) ) ;
#76437 = CARTESIAN_POINT ( 'NONE',  ( 18.62759615963271287, -10.81492255796078972, 103.3322429386476955 ) ) ;
#76438 = CARTESIAN_POINT ( 'NONE',  ( -13.97604488694547697, 13.89961937509957934, 53.12609039468565442 ) ) ;
#76439 = CARTESIAN_POINT ( 'NONE',  ( -5.153800228976328057, -19.02544592524343514, 42.29057627198101699 ) ) ;
#76440 = DIRECTION ( 'NONE',  ( 1.000000000000000000, 0.000000000000000000, 0.000000000000000000 ) ) ;
#76441 = CARTESIAN_POINT ( 'NONE',  ( 16.21926038945174398, -7.366295777783752996, 21.89088085486532620 ) ) ;
#76442 = CARTESIAN_POINT ( 'NONE',  ( -14.29746914071037622, -8.314922557961029526, 54.16775706135235424 ) ) ;
#76443 = CARTESIAN_POINT ( 'NONE',  ( 5.049401038298161559, -19.05341960407611168, 27.70724293864769550 ) ) ;
#76444 = CARTESIAN_POINT ( 'NONE',  ( -23.64874990377911601, -15.04272038711346582, 165.8682408883346397 ) ) ;
#76445 = CARTESIAN_POINT ( 'NONE',  ( -13.89961937509977652, 13.97604488694528158, 80.62390960531436690 ) ) ;
#76446 = CARTESIAN_POINT ( 'NONE',  ( -16.52544592524342804, 4.483927247898546575, 106.0405762719810525 ) ) ;
#76447 = CARTESIAN_POINT ( 'NONE',  ( 10.81492255796078972, 18.62759615963270932, 54.58224293864769550 ) ) ;
#76448 = CARTESIAN_POINT ( 'NONE',  ( -4.483927247898782831, 16.52544592524335698, 47.70942372801902565 ) ) ;
#76449 = CARTESIAN_POINT ( 'NONE',  ( -10.72451020669870658, -18.67979575497194134, 99.58442372801900433 ) ) ;
#76450 = CARTESIAN_POINT ( 'NONE',  ( -13.89961937509977652, 13.97604488694528158, 30.62390960531435269 ) ) ;
#76451 = CARTESIAN_POINT ( 'NONE',  ( -16.55341960407611168, -4.379528057220339221, 21.45724293864769550 ) ) ;
#76452 = CARTESIAN_POINT ( 'NONE',  ( -8.224510206698948167, 14.34966873604960824, 50.41557627198103120 ) ) ;
#76453 = CARTESIAN_POINT ( 'NONE',  ( -19.03943276465977164, 0.05219959533909376836, 56.24890960531435979 ) ) ;
#76454 = CARTESIAN_POINT ( 'NONE',  ( -0.05219959533937732626, 21.53943276465977519, 112.5010903946857042 ) ) ;
#76455 = CARTESIAN_POINT ( 'NONE',  ( -18.62759615963255300, -10.81492255796106328, 19.16775706135234714 ) ) ;
#76456 = CARTESIAN_POINT ( 'NONE',  ( 5.823673210054444382, -21.52544592524334988, 75.20942372801901854 ) ) ;
#76457 = CARTESIAN_POINT ( 'NONE',  ( 8.314922557961029526, -14.29746914071037800, 50.41775706135235424 ) ) ;
#76458 = CARTESIAN_POINT ( 'NONE',  ( 16.52544592524335698, 4.483927247898782831, 31.45942372801901854 ) ) ;
#76459 = EDGE_CURVE ( 'NONE', #25627, #77120, #162638, .T. ) ;
#76461 = CARTESIAN_POINT ( 'NONE',  ( -21.55341960407619339, 5.719274019375674811, 93.54275706135234714 ) ) ;
#76460 = CARTESIAN_POINT ( 'NONE',  ( -0.05219959533910754901, -16.53943276465976808, 72.49890960531435269 ) ) ;
#76462 = CARTESIAN_POINT ( 'NONE',  ( 4.483927247898545687, 16.52544592524342804, 39.79057627198103830 ) ) ;
#76463 = CARTESIAN_POINT ( 'NONE',  ( -17.49999999999999645, 5.499999999999997335, 115.7969038253417438 ) ) ;
#76464 = CARTESIAN_POINT ( 'NONE',  ( -14.29746914071037622, -8.314922557961029526, 39.16775706135235424 ) ) ;
#76465 = CARTESIAN_POINT ( 'NONE',  ( -0.05219959533910754901, -16.53943276465976808, 42.49890960531435979 ) ) ;
#76466 = CARTESIAN_POINT ( 'NONE',  ( 14.29746914071037800, 8.314922557961029526, 91.66775706135234714 ) ) ;
#76467 = CARTESIAN_POINT ( 'NONE',  ( -13.89961937509977652, 13.97604488694528158, 100.6239096053143669 ) ) ;
#76468 = CARTESIAN_POINT ( 'NONE',  ( -16.46253265017160317, 9.564922557960807481, 115.8322429386477097 ) ) ;
#76469 = CARTESIAN_POINT ( 'NONE',  ( 15.72974639402176855, 15.80617190586768217, 96.87609039468568994 ) ) ;
#76470 = CARTESIAN_POINT ( 'NONE',  ( -8.314922557961024197, 14.29746914071037800, 97.91775706135236135 ) ) ;
#76471 = CARTESIAN_POINT ( 'NONE',  ( -0.05219959533910754901, -16.53943276465976808, 72.49890960531435269 ) ) ;
#76472 = CARTESIAN_POINT ( 'NONE',  ( 19.02544592524343514, -5.153800228976328945, 83.54057627198100988 ) ) ;
#76473 = EDGE_LOOP ( 'NONE', ( #165939, #102501, #1727, #123156 ) ) ;
#76474 = CARTESIAN_POINT ( 'NONE',  ( 0.05219959533934541429, -16.53943276465976808, 45.00109039468568284 ) ) ;
#76475 = CARTESIAN_POINT ( 'NONE',  ( -0.05219959533909027116, -19.03943276465977164, 37.49890960531436690 ) ) ;
#76476 = CARTESIAN_POINT ( 'NONE',  ( -5.049401038298153566, 19.05341960407611168, 90.20724293864766707 ) ) ;
#76478 = CARTESIAN_POINT ( 'NONE',  ( -36.91746825000001309, -11.99521256947794789, -2.524999997268813523 ) ) ;
#76477 = CARTESIAN_POINT ( 'NONE',  ( 14.29746914071037800, 8.314922557961029526, 36.66775706135234714 ) ) ;
#76479 = CARTESIAN_POINT ( 'NONE',  ( -5.153800228976607833, 19.02544592524334988, 32.70942372801899722 ) ) ;
#76480 = CARTESIAN_POINT ( 'NONE',  ( -16.52544592524335698, -4.483927247898792601, 93.95942372801903275 ) ) ;
#76481 = CARTESIAN_POINT ( 'NONE',  ( -5.049401038298153566, 19.05341960407611168, 30.20724293864768839 ) ) ;
#76482 = CARTESIAN_POINT ( 'NONE',  ( 12.06949235617739724, 12.14591786802326823, 81.87609039468568994 ) ) ;
#76483 = CARTESIAN_POINT ( 'NONE',  ( 14.29746914071037800, 8.314922557961029526, 66.66775706135234714 ) ) ;
#76484 = CARTESIAN_POINT ( 'NONE',  ( 0.05219959533936267826, -19.03943276465977164, 85.00109039468567573 ) ) ;
#76485 = CARTESIAN_POINT ( 'NONE',  ( 0.05219959533936267826, -19.03943276465977164, 30.00109039468566863 ) ) ;
#76486 = CARTESIAN_POINT ( 'NONE',  ( -16.51473224551069308, -9.474510206698971260, 56.66557627198103120 ) ) ;
#76487 = CARTESIAN_POINT ( 'NONE',  ( 8.224510206698953496, -14.34966873604960469, 87.91557627198103830 ) ) ;
#76488 = VECTOR ( 'NONE', #198276, 1000.000000000000000 ) ;
#76489 = CARTESIAN_POINT ( 'NONE',  ( 0.05219959533936267826, -19.03943276465977164, 60.00109039468566863 ) ) ;
#76490 = CARTESIAN_POINT ( 'NONE',  ( -5.823673210054116645, -21.52544592524344225, 47.29057627198103120 ) ) ;
#76491 = CARTESIAN_POINT ( 'NONE',  ( 0.05219959533936267826, -19.03943276465977164, 25.00109039468566152 ) ) ;
#76492 = CARTESIAN_POINT ( 'NONE',  ( -16.51473224551069308, -9.474510206698971260, 106.6655762719810383 ) ) ;
#76493 = CARTESIAN_POINT ( 'NONE',  ( -5.719274019375978568, 21.55341960407610458, 80.20724293864769550 ) ) ;
#76494 = CARTESIAN_POINT ( 'NONE',  ( 16.51473224551069308, 9.474510206698969483, 104.1655762719810241 ) ) ;
#76495 = VECTOR ( 'NONE', #133249, 1000.000000000000000 ) ;
#76496 = CARTESIAN_POINT ( 'NONE',  ( 9.474510206698729675, 16.51473224551082808, 102.0844237280190043 ) ) ;
#76497 = CARTESIAN_POINT ( 'NONE',  ( 0.05219959533909260263, 19.03943276465977164, 109.9989096053143669 ) ) ;
#76498 = CARTESIAN_POINT ( 'NONE',  ( -9.564922557961040184, 16.46253265017147172, 102.9177570613523329 ) ) ;
#76499 = CARTESIAN_POINT ( 'NONE',  ( 16.46253265017160672, -9.564922557960803928, 38.33224293864768839 ) ) ;
#76500 = CARTESIAN_POINT ( 'NONE',  ( -16.51473224551069308, -9.474510206698971260, 96.66557627198102409 ) ) ;
#76501 = CARTESIAN_POINT ( 'NONE',  ( -21.55341960407610458, -5.719274019375992779, 81.45724293864769550 ) ) ;
#76502 = CARTESIAN_POINT ( 'NONE',  ( -4.379528057220086978, -16.55341960407618274, 64.79275706135234714 ) ) ;
#76503 = CARTESIAN_POINT ( 'NONE',  ( 18.62759615963255655, 10.81492255796105972, 66.66775706135234714 ) ) ;
#76505 = CARTESIAN_POINT ( 'NONE',  ( 5.719274019375673035, 21.55341960407619339, 112.2927570613523471 ) ) ;
#76504 = CARTESIAN_POINT ( 'NONE',  ( 19.02544592524334988, 5.153800228976608722, 111.4594237280190043 ) ) ;
#76506 = CARTESIAN_POINT ( 'NONE',  ( 0.05219959533934541429, -16.53943276465976808, 105.0010903946856757 ) ) ;
#76507 = CARTESIAN_POINT ( 'NONE',  ( -18.67979575497178146, -10.72451020669898902, 101.6655762719810383 ) ) ;
#76508 = CARTESIAN_POINT ( 'NONE',  ( 0.05219959533910956823, 16.53943276465976808, 39.99890960531436690 ) ) ;
#76509 = CARTESIAN_POINT ( 'NONE',  ( -9.474510206698720793, -16.51473224551083518, 79.58442372801899012 ) ) ;
#76510 = CARTESIAN_POINT ( 'NONE',  ( 15.80617190586769283, -15.72974639402175789, 60.62609039468567573 ) ) ;
#76511 = CARTESIAN_POINT ( 'NONE',  ( -5.153800228976607833, 19.02544592524334988, 37.70942372801899722 ) ) ;
#76512 = CARTESIAN_POINT ( 'NONE',  ( -8.314922557960811034, -14.29746914071050412, 102.0822429386476955 ) ) ;
#76513 = CARTESIAN_POINT ( 'NONE',  ( -21.53943276465977519, 0.05219959533907696930, 26.24890960531435624 ) ) ;
#76514 = CARTESIAN_POINT ( 'NONE',  ( -12.06949235617756955, 12.14591786802309770, 35.62390960531437401 ) ) ;
#76515 = CARTESIAN_POINT ( 'NONE',  ( -18.67979575497193778, 10.72451020669871902, 98.33442372801901854 ) ) ;
#76516 = CARTESIAN_POINT ( 'NONE',  ( 16.55341960407618274, -4.379528057220086978, 76.04275706135237556 ) ) ;
#76517 = CARTESIAN_POINT ( 'NONE',  ( -16.55341960407611168, -4.379528057220339221, 26.45724293864768839 ) ) ;
#76518 = CARTESIAN_POINT ( 'NONE',  ( -21.53943276465977519, -0.05219959533937600094, 58.75109039468568994 ) ) ;
#76519 = CARTESIAN_POINT ( 'NONE',  ( -0.05219959533937732626, 21.53943276465977519, 52.50109039468567573 ) ) ;
#76520 = ORIENTED_EDGE ( 'NONE', *, *, #60120, .F. ) ;
#76521 = CARTESIAN_POINT ( 'NONE',  ( -0.05219959533909027116, -19.03943276465977164, 27.49890960531435624 ) ) ;
#76522 = CARTESIAN_POINT ( 'NONE',  ( -21.55341960407619339, 5.719274019375674811, 38.54275706135234714 ) ) ;
#76523 = CARTESIAN_POINT ( 'NONE',  ( -13.89961937509977652, 13.97604488694528158, 25.62390960531434558 ) ) ;
#76524 = CARTESIAN_POINT ( 'NONE',  ( 19.02544592524343514, -5.153800228976328945, 38.54057627198103120 ) ) ;
#76525 = CARTESIAN_POINT ( 'NONE',  ( -12.14591786802309592, -12.06949235617757132, 81.87390960531435269 ) ) ;
#76526 = CARTESIAN_POINT ( 'NONE',  ( 19.05341960407611168, 5.049401038298154454, 73.95724293864768129 ) ) ;
#76527 = CARTESIAN_POINT ( 'NONE',  ( 12.14591786802309770, 12.06949235617756955, 29.37390960531435269 ) ) ;
#76528 = CARTESIAN_POINT ( 'NONE',  ( 15.72974639402199770, -15.80617190586745480, 58.12390960531435979 ) ) ;
#76529 = CARTESIAN_POINT ( 'NONE',  ( 16.53943276465976808, -0.05219959533910856209, 93.74890960531436690 ) ) ;
#76530 = CIRCLE ( 'NONE', #31358, 2.700000000000001066 ) ;
#76531 = CARTESIAN_POINT ( 'NONE',  ( 10.72451020669898902, -18.67979575497178502, 112.9155762719810383 ) ) ;
#76532 = CARTESIAN_POINT ( 'NONE',  ( 9.474510206698971260, -16.51473224551069308, 107.9155762719810383 ) ) ;
#76534 = CARTESIAN_POINT ( 'NONE',  ( 19.02544592524334988, 5.153800228976608722, 106.4594237280190185 ) ) ;
#76533 = CARTESIAN_POINT ( 'NONE',  ( -5.049401038298153566, 19.05341960407611168, 70.20724293864769550 ) ) ;
#76535 = CARTESIAN_POINT ( 'NONE',  ( 21.52544592524344225, -5.823673210054117533, 53.54057627198103120 ) ) ;
#76536 = CARTESIAN_POINT ( 'NONE',  ( 21.55341960407619695, -5.719274019375665929, 81.04275706135236135 ) ) ;
#76537 = CARTESIAN_POINT ( 'NONE',  ( -19.05341960407611168, -5.049401038298163336, 66.45724293864769550 ) ) ;
#76538 = CARTESIAN_POINT ( 'NONE',  ( 5.153800228976335163, 19.02544592524342804, 104.7905762719809957 ) ) ;
#76539 = CARTESIAN_POINT ( 'NONE',  ( 12.06949235617739724, 12.14591786802326823, 81.87609039468568994 ) ) ;
#76540 = CARTESIAN_POINT ( 'NONE',  ( 10.81492255796106328, -18.62759615963255655, 55.41775706135234714 ) ) ;
#76541 = CARTESIAN_POINT ( 'NONE',  ( 15.72974639402176855, 15.80617190586768217, 81.87609039468568994 ) ) ;
#76542 = CARTESIAN_POINT ( 'NONE',  ( 10.81492255796078972, 18.62759615963270932, 109.5822429386476955 ) ) ;
#76543 = CARTESIAN_POINT ( 'NONE',  ( -12.14591786802326823, 12.06949235617739902, 83.12609039468568994 ) ) ;
#76544 = CARTESIAN_POINT ( 'NONE',  ( -5.719274019375978568, 21.55341960407610458, 70.20724293864769550 ) ) ;
#76545 = CARTESIAN_POINT ( 'NONE',  ( 16.51473224551083163, -9.474510206698727899, 45.83442372801900433 ) ) ;
#76546 = CARTESIAN_POINT ( 'NONE',  ( 0.05219959533907565091, 21.53943276465977519, 39.99890960531436690 ) ) ;
#76548 = CARTESIAN_POINT ( 'NONE',  ( -4.483927247898782831, 16.52544592524335698, 112.7094237280190328 ) ) ;
#76547 = CARTESIAN_POINT ( 'NONE',  ( 0.05219959533909260263, 19.03943276465977164, 74.99890960531435269 ) ) ;
#76549 = CARTESIAN_POINT ( 'NONE',  ( -17.48853670773241831, 5.747243402303156223, 63.66671299749991420 ) ) ;
#76550 = CARTESIAN_POINT ( 'NONE',  ( 0.05219959533909260263, 19.03943276465977164, 114.9989096053143669 ) ) ;
#76551 = CARTESIAN_POINT ( 'NONE',  ( 18.22780087662122739, 5.500000000000000888, 81.48236817873103632 ) ) ;
#76552 = CARTESIAN_POINT ( 'NONE',  ( -19.05341960407617563, 5.049401038297882671, 93.54275706135234714 ) ) ;
#76553 = CARTESIAN_POINT ( 'NONE',  ( 15.80617190586746368, 15.72974639402197994, 74.37390960531436690 ) ) ;
#76554 = CARTESIAN_POINT ( 'NONE',  ( 16.53943276465976808, -0.05219959533910856209, 53.74890960531437401 ) ) ;
#76555 = CARTESIAN_POINT ( 'NONE',  ( 12.14591786802327356, -12.06949235617739191, 20.62609039468568639 ) ) ;
#76556 = CARTESIAN_POINT ( 'NONE',  ( -13.97604488694527625, -13.89961937509977652, 26.87390960531434558 ) ) ;
#76558 = CARTESIAN_POINT ( 'NONE',  ( -13.97604488694547697, 13.89961937509957934, 68.12609039468563310 ) ) ;
#76557 = CARTESIAN_POINT ( 'NONE',  ( -10.81492255796078084, -18.62759615963271287, 97.08224293864770971 ) ) ;
#76559 = CARTESIAN_POINT ( 'NONE',  ( 19.03943276465977164, -0.05219959533909143690, 78.74890960531436690 ) ) ;
#76560 = CARTESIAN_POINT ( 'NONE',  ( -0.05219959533910754901, -16.53943276465976808, 77.49890960531433848 ) ) ;
#76561 = ADVANCED_FACE ( 'NONE', ( #114117 ), #52459, .T. ) ;
#76562 = CARTESIAN_POINT ( 'NONE',  ( 9.474510206698971260, -16.51473224551069308, 57.91557627198103120 ) ) ;
#76563 = CARTESIAN_POINT ( 'NONE',  ( -14.29746914071049879, 8.314922557960819915, 60.83224293864769550 ) ) ;
#76564 = CARTESIAN_POINT ( 'NONE',  ( -5.049401038298153566, 19.05341960407611168, 30.20724293864768839 ) ) ;
#76565 = CARTESIAN_POINT ( 'NONE',  ( 2.577820198429831642E-15, 9.100000000000001421, -61.89430850415821794 ) ) ;
#76566 = CARTESIAN_POINT ( 'NONE',  ( 14.34966873604960469, 8.224510206698951720, 39.16557627198102409 ) ) ;
#76567 = CARTESIAN_POINT ( 'NONE',  ( -19.05341960407611168, -5.049401038298163336, 86.45724293864769550 ) ) ;
#76568 = FACE_BOUND ( 'NONE', #127324, .T. ) ;
#76569 = CARTESIAN_POINT ( 'NONE',  ( -13.97604488694547697, 13.89961937509957934, 48.12609039468566863 ) ) ;
#76570 = CARTESIAN_POINT ( 'NONE',  ( 12.06949235617739724, 12.14591786802326823, 66.87609039468568994 ) ) ;
#76571 = CARTESIAN_POINT ( 'NONE',  ( -18.62759615963270932, 10.81492255796079327, 70.83224293864770971 ) ) ;
#76572 = CARTESIAN_POINT ( 'NONE',  ( -0.05219959533936034679, 19.03943276465977164, 37.50109039468567573 ) ) ;
#76573 = CARTESIAN_POINT ( 'NONE',  ( -19.03943276465977164, 0.05219959533909376836, 86.24890960531436690 ) ) ;
#76574 = FACE_OUTER_BOUND ( 'NONE', #96794, .T. ) ;
#76575 = CARTESIAN_POINT ( 'NONE',  ( 0.05219959533907565091, 21.53943276465977519, 24.99890960531435624 ) ) ;
#76576 = CARTESIAN_POINT ( 'NONE',  ( -13.89961937509977652, 13.97604488694528158, 55.62390960531434558 ) ) ;
#76577 = CARTESIAN_POINT ( 'NONE',  ( 18.62759615963255655, 10.81492255796105972, 46.66775706135234714 ) ) ;
#76578 = CARTESIAN_POINT ( 'NONE',  ( 14.34966873604960469, 8.224510206698951720, 104.1655762719810241 ) ) ;
#76581 = EDGE_LOOP ( 'NONE', ( #72465, #172106, #192282, #96783 ) ) ;
#76580 = CARTESIAN_POINT ( 'NONE',  ( 19.02544592524343514, -5.153800228976328945, 88.54057627198102409 ) ) ;
#76579 = CARTESIAN_POINT ( 'NONE',  ( 0.05219959533907565091, 21.53943276465977519, 99.99890960531436690 ) ) ;
#76582 = CARTESIAN_POINT ( 'NONE',  ( -15.80617190586768217, 15.72974639402176855, 43.12609039468568284 ) ) ;
#76583 = ORIENTED_EDGE ( 'NONE', *, *, #168500, .T. ) ;
#76584 = CARTESIAN_POINT ( 'NONE',  ( 16.46253265017160672, -9.564922557960803928, 103.3322429386476955 ) ) ;
#76585 = CARTESIAN_POINT ( 'NONE',  ( 9.564922557960805705, 16.46253265017160317, 89.58224293864769550 ) ) ;
#76586 = CARTESIAN_POINT ( 'NONE',  ( -15.80617190586745835, -15.72974639402198527, 91.87390960531436690 ) ) ;
#76587 = CARTESIAN_POINT ( 'NONE',  ( 19.05341960407611168, 5.049401038298154454, 43.95724293864769550 ) ) ;
#76588 = CARTESIAN_POINT ( 'NONE',  ( 16.53943276465976808, 0.05219959533934440121, 21.25109039468567218 ) ) ;
#76589 = CARTESIAN_POINT ( 'NONE',  ( -30.74264578624800492, -22.33583958711396278, -11.54999999453762527 ) ) ;
#76590 = CARTESIAN_POINT ( 'NONE',  ( -16.51473224551069308, -9.474510206698971260, 26.66557627198103120 ) ) ;
#76591 = CARTESIAN_POINT ( 'NONE',  ( 10.72451020669871369, 18.67979575497193778, 102.0844237280190185 ) ) ;
#76593 = CARTESIAN_POINT ( 'NONE',  ( 5.719274019375673035, 21.55341960407619339, 42.29275706135235424 ) ) ;
#76592 = CARTESIAN_POINT ( 'NONE',  ( -0.05219959533909027116, -19.03943276465977164, 82.49890960531436690 ) ) ;
#76594 = CARTESIAN_POINT ( 'NONE',  ( 1.784210473542230573E-15, -29.16686587814331588, 145.8750000027311273 ) ) ;
#76595 = CARTESIAN_POINT ( 'NONE',  ( 16.51473224551069308, 9.474510206698969483, 94.16557627198103830 ) ) ;
#76596 = CARTESIAN_POINT ( 'NONE',  ( 18.76835711872175594, 20.78600286866540969, 140.0000000000000000 ) ) ;
#76599 = CARTESIAN_POINT ( 'NONE',  ( -21.53943276465977519, -0.05219959533937600094, 63.75109039468568284 ) ) ;
#76598 = CARTESIAN_POINT ( 'NONE',  ( -12.14591786802326823, 12.06949235617739902, 68.12609039468567573 ) ) ;
#76597 = CARTESIAN_POINT ( 'NONE',  ( 14.29746914071037800, 8.314922557961029526, 36.66775706135234714 ) ) ;
#76600 = CARTESIAN_POINT ( 'NONE',  ( -21.52544592524334988, -5.823673210054445271, 73.95942372801901854 ) ) ;
#76601 = CARTESIAN_POINT ( 'NONE',  ( 4.176031345420748941, 6.297279900606364222, -62.24169944404282973 ) ) ;
#76602 = CARTESIAN_POINT ( 'NONE',  ( 16.53943276465976808, 0.05219959533934440121, 21.25109039468567218 ) ) ;
#76603 = CARTESIAN_POINT ( 'NONE',  ( 13.97604488694527802, 13.89961937509977652, 74.37390960531436690 ) ) ;
#76604 = CARTESIAN_POINT ( 'NONE',  ( 9.564922557960805705, 16.46253265017160317, 104.5822429386476955 ) ) ;
#76605 = CARTESIAN_POINT ( 'NONE',  ( 4.483927247898545687, 16.52544592524342804, 109.7905762719810383 ) ) ;
#76606 = CARTESIAN_POINT ( 'NONE',  ( 10.81492255796078972, 18.62759615963270932, 29.58224293864769905 ) ) ;
#76607 = CARTESIAN_POINT ( 'NONE',  ( -16.55341960407617563, 4.379528057220093196, 88.54275706135236135 ) ) ;
#76609 = CARTESIAN_POINT ( 'NONE',  ( -0.05219959533909027116, -19.03943276465977164, 52.49890960531436690 ) ) ;
#76608 = CARTESIAN_POINT ( 'NONE',  ( 8.314922557960818139, 14.29746914071049879, 74.58224293864768129 ) ) ;
#76610 = CARTESIAN_POINT ( 'NONE',  ( 5.823673210054444382, -21.52544592524334988, 75.20942372801901854 ) ) ;
#76611 = CARTESIAN_POINT ( 'NONE',  ( -24.11964846217544078, 0.7207009035789223583, -56.90195918390940477 ) ) ;
#76612 = CARTESIAN_POINT ( 'NONE',  ( 13.97604488694548053, -13.89961937509957401, 100.6260903946856615 ) ) ;
#76613 = CARTESIAN_POINT ( 'NONE',  ( 0.05219959533910956823, 16.53943276465976808, 74.99890960531435269 ) ) ;
#76614 = CARTESIAN_POINT ( 'NONE',  ( 18.62759615963255655, 10.81492255796105972, 26.66775706135235424 ) ) ;
#76615 = CARTESIAN_POINT ( 'NONE',  ( -5.823673210054116645, -21.52544592524344225, 62.29057627198102409 ) ) ;
#76616 = CARTESIAN_POINT ( 'NONE',  ( -17.44279575226825330, -5.990770900252416098, 104.1644243248568387 ) ) ;
#76617 = CARTESIAN_POINT ( 'NONE',  ( -28.82186960331499392, 9.364793116373565596, 144.1500000054623740 ) ) ;
#76618 = CARTESIAN_POINT ( 'NONE',  ( 19.02544592524343514, -5.153800228976328945, 78.54057627198099567 ) ) ;
#76619 = CARTESIAN_POINT ( 'NONE',  ( -8.224510206698948167, 14.34966873604960824, 50.41557627198103120 ) ) ;
#76620 = CARTESIAN_POINT ( 'NONE',  ( -14.34966873604960291, -8.224510206698953496, 41.66557627198103120 ) ) ;
#76621 = CARTESIAN_POINT ( 'NONE',  ( -8.314922557961024197, 14.29746914071037800, 102.9177570613523756 ) ) ;
#76622 = CARTESIAN_POINT ( 'NONE',  ( 9.474510206698729675, 16.51473224551082808, 47.08442372801900433 ) ) ;
#76623 = CARTESIAN_POINT ( 'NONE',  ( -22.40074995931641055, -13.33491940220945793, 165.5209445330007725 ) ) ;
#76624 = CARTESIAN_POINT ( 'NONE',  ( -16.46253265017160317, 9.564922557960807481, 110.8322429386476955 ) ) ;
#76625 = CARTESIAN_POINT ( 'NONE',  ( 12.06949235617757843, -12.14591786802309237, 68.12390960531436690 ) ) ;
#76626 = CARTESIAN_POINT ( 'NONE',  ( -13.97604488694547697, 13.89961937509957934, 48.12609039468566863 ) ) ;
#76628 = CARTESIAN_POINT ( 'NONE',  ( 10.81492255796078972, 18.62759615963270932, 34.58224293864770260 ) ) ;
#76627 = CARTESIAN_POINT ( 'NONE',  ( 13.97604488694527802, 13.89961937509977652, 34.37390960531436690 ) ) ;
#76629 = CARTESIAN_POINT ( 'NONE',  ( -21.52544592524343514, 5.823673210054127303, 61.04057627198103120 ) ) ;
#76630 = CARTESIAN_POINT ( 'NONE',  ( 8.224510206698953496, -14.34966873604960469, 102.9155762719810383 ) ) ;
#76631 = CARTESIAN_POINT ( 'NONE',  ( -8.314922557961024197, 14.29746914071037800, 47.91775706135234714 ) ) ;
#76632 = CARTESIAN_POINT ( 'NONE',  ( 10.72451020669871369, 18.67979575497193778, 47.08442372801901854 ) ) ;
#76633 = CARTESIAN_POINT ( 'NONE',  ( 12.06949235617757843, -12.14591786802309237, 98.12390960531436690 ) ) ;
#76634 = CARTESIAN_POINT ( 'NONE',  ( 16.38665767535054840, -7.295008042176023721, 37.76400864214549102 ) ) ;
#76635 = CARTESIAN_POINT ( 'NONE',  ( -17.05116617787826527, 6.768360034955678728, 48.65675553259197983 ) ) ;
#76636 = CARTESIAN_POINT ( 'NONE',  ( -21.52544592524343514, 5.823673210054127303, 31.04057627198102409 ) ) ;
#76637 = DIRECTION ( 'NONE',  ( 0.000000000000000000, 0.000000000000000000, -1.000000000000000000 ) ) ;
#76638 = CARTESIAN_POINT ( 'NONE',  ( 1.468080482507219120, 23.15813577935543677, -57.58210375345692711 ) ) ;
#76640 = CARTESIAN_POINT ( 'NONE',  ( 14.29746914071049879, -8.314922557960816363, 28.33224293864769550 ) ) ;
#76639 = CARTESIAN_POINT ( 'NONE',  ( 16.53943276465976808, 0.05219959533934440121, 46.25109039468567573 ) ) ;
#76641 = CARTESIAN_POINT ( 'NONE',  ( -0.05219959533907301413, -21.53943276465977519, 67.49890960531436690 ) ) ;
#76642 = CARTESIAN_POINT ( 'NONE',  ( -5.049401038297874678, -19.05341960407617918, 89.79275706135230450 ) ) ;
#76643 = CARTESIAN_POINT ( 'NONE',  ( -21.55341960407610458, -5.719274019375992779, 66.45724293864768129 ) ) ;
#76644 = CARTESIAN_POINT ( 'NONE',  ( 29.40087336786514527, -24.08182305020411462, -17.68713395559149859 ) ) ;
#76645 = CARTESIAN_POINT ( 'NONE',  ( 4.379528057220092307, 16.55341960407617563, 47.29275706135234003 ) ) ;
#76647 = CARTESIAN_POINT ( 'NONE',  ( 9.474510206698971260, -16.51473224551069308, 107.9155762719810383 ) ) ;
#76646 = CARTESIAN_POINT ( 'NONE',  ( 16.46253265017160672, -9.564922557960803928, 33.33224293864770260 ) ) ;
#76648 = PRESENTATION_LAYER_ASSIGNMENT (  '', '', ( #5623 ) ) ;
#76649 = CARTESIAN_POINT ( 'NONE',  ( 13.97604488694527802, 13.89961937509977652, 39.37390960531435269 ) ) ;
#76650 = CARTESIAN_POINT ( 'NONE',  ( -16.53943276465976808, 0.05219959533911058130, 116.2489096053143669 ) ) ;
#76651 = CARTESIAN_POINT ( 'NONE',  ( 1.179611963664228824E-13, -165.0000000000000000, 17.19999999999998508 ) ) ;
#76652 = CARTESIAN_POINT ( 'NONE',  ( 16.46253265017160672, -9.564922557960803928, 113.3322429386476955 ) ) ;
#76653 = CARTESIAN_POINT ( 'NONE',  ( -0.05219959533934338120, 16.53943276465976808, 67.50109039468568994 ) ) ;
#76654 = CARTESIAN_POINT ( 'NONE',  ( 21.52544592524344225, -5.823673210054117533, 93.54057627198103830 ) ) ;
#76655 = CARTESIAN_POINT ( 'NONE',  ( -16.51473224551069308, -9.474510206698971260, 56.66557627198103120 ) ) ;
#76656 = CARTESIAN_POINT ( 'NONE',  ( -21.55341960407619339, 5.719274019375674811, 33.54275706135234714 ) ) ;
#76657 = CARTESIAN_POINT ( 'NONE',  ( -16.51473224551069308, -9.474510206698971260, 86.66557627198102409 ) ) ;
#76658 = CARTESIAN_POINT ( 'NONE',  ( 16.46253265017160672, -9.564922557960803928, 113.3322429386476955 ) ) ;
#76659 = ORIENTED_EDGE ( 'NONE', *, *, #193305, .T. ) ;
#76660 = CARTESIAN_POINT ( 'NONE',  ( -21.52544592524334988, -5.823673210054445271, 18.95942372801901143 ) ) ;
#76663 = CARTESIAN_POINT ( 'NONE',  ( 0.05219959533936267826, -19.03943276465977164, 95.00109039468567573 ) ) ;
#76662 = CARTESIAN_POINT ( 'NONE',  ( -9.474510206698964154, 16.51473224551069663, 100.4155762719810241 ) ) ;
#76661 = CARTESIAN_POINT ( 'NONE',  ( 9.564922557960805705, 16.46253265017160317, 24.58224293864769194 ) ) ;
#76664 = CARTESIAN_POINT ( 'NONE',  ( 19.05341960407617918, -5.049401038297876454, 26.04275706135233293 ) ) ;
#76665 = CARTESIAN_POINT ( 'NONE',  ( -0.05219959533907301413, -21.53943276465977519, 102.4989096053143811 ) ) ;
#76666 = CARTESIAN_POINT ( 'NONE',  ( -5.153800228976607833, 19.02544592524334988, 32.70942372801899722 ) ) ;
#76667 = CARTESIAN_POINT ( 'NONE',  ( 4.379528057220092307, 16.55341960407617563, 82.29275706135234714 ) ) ;
#76669 = ORIENTED_EDGE ( 'NONE', *, *, #78822, .T. ) ;
#76668 = CARTESIAN_POINT ( 'NONE',  ( -5.049401038298153566, 19.05341960407611168, 105.2072429386476671 ) ) ;
#76670 = CARTESIAN_POINT ( 'NONE',  ( 9.564922557960805705, 16.46253265017160317, 54.58224293864769550 ) ) ;
#76671 = VECTOR ( 'NONE', #147449, 1000.000000000000000 ) ;
#76672 = CARTESIAN_POINT ( 'NONE',  ( 5.719274019375673035, 21.55341960407619339, 62.29275706135236845 ) ) ;
#76673 = CARTESIAN_POINT ( 'NONE',  ( -18.62759615963255300, -10.81492255796106328, 79.16775706135234714 ) ) ;
#76674 = DIRECTION ( 'NONE',  ( 0.000000000000000000, -0.7071067811865466846, 0.7071067811865484609 ) ) ;
#76675 = CARTESIAN_POINT ( 'NONE',  ( 0.05219959533909260263, 19.03943276465977164, 74.99890960531435269 ) ) ;
#76676 = CARTESIAN_POINT ( 'NONE',  ( 5.823673210054444382, -21.52544592524334988, 50.20942372801901854 ) ) ;
#76677 = CARTESIAN_POINT ( 'NONE',  ( 9.564922557961047289, -16.46253265017146816, 90.41775706135234714 ) ) ;
#76678 = CARTESIAN_POINT ( 'NONE',  ( 16.46253265017160672, -9.564922557960803928, 48.33224293864769550 ) ) ;
#76679 = CARTESIAN_POINT ( 'NONE',  ( -16.46253265017160317, 9.564922557960807481, 100.8322429386477097 ) ) ;
#76680 = CARTESIAN_POINT ( 'NONE',  ( 13.97604488694527802, 13.89961937509977652, 64.37390960531436690 ) ) ;
#76681 = CARTESIAN_POINT ( 'NONE',  ( 17.50000000000009237, -3.443395144217226367, 22.69309096419004845 ) ) ;
#76682 = CARTESIAN_POINT ( 'NONE',  ( -16.51473224551069308, -9.474510206698971260, 56.66557627198103120 ) ) ;
#76683 = CARTESIAN_POINT ( 'NONE',  ( -21.53943276465977519, 0.05219959533907696930, 101.2489096053143669 ) ) ;
#76684 = CARTESIAN_POINT ( 'NONE',  ( -12.06949235617739369, -12.14591786802326823, 84.37609039468570415 ) ) ;
#76685 = CARTESIAN_POINT ( 'NONE',  ( -21.94381615377086447, 13.26253372808103848, 167.9278110240108788 ) ) ;
#76686 = CARTESIAN_POINT ( 'NONE',  ( 13.97604488694548053, -13.89961937509957401, 45.62609039468566863 ) ) ;
#76687 = CARTESIAN_POINT ( 'NONE',  ( 9.474510206698971260, -16.51473224551069308, 67.91557627198102409 ) ) ;
#76688 = CARTESIAN_POINT ( 'NONE',  ( 4.379528057220339221, -16.55341960407611168, 62.70724293864769550 ) ) ;
#76689 = CARTESIAN_POINT ( 'NONE',  ( 12.06949235617757843, -12.14591786802309237, 93.12390960531436690 ) ) ;
#76690 = CARTESIAN_POINT ( 'NONE',  ( 19.05341960407611168, 5.049401038298154454, 113.9572429386477097 ) ) ;
#76691 = CARTESIAN_POINT ( 'NONE',  ( -9.564922557960796823, -16.46253265017161027, 102.0822429386477097 ) ) ;
#76692 = CARTESIAN_POINT ( 'NONE',  ( -19.03943276465977164, 0.05219959533909376836, 111.2489096053143669 ) ) ;
#76693 = CARTESIAN_POINT ( 'NONE',  ( -15.80617190586768217, 15.72974639402176855, 113.1260903946856899 ) ) ;
#76694 = CARTESIAN_POINT ( 'NONE',  ( 14.29746914071037800, 8.314922557961029526, 86.66775706135234714 ) ) ;
#76696 = EDGE_CURVE ( 'NONE', #150038, #123761, #24144, .T. ) ;
#76695 = CARTESIAN_POINT ( 'NONE',  ( -5.049401038298153566, 19.05341960407611168, 80.20724293864769550 ) ) ;
#76697 = CARTESIAN_POINT ( 'NONE',  ( 21.55341960407619695, -5.719274019375665929, 46.04275706135234714 ) ) ;
#76698 = CARTESIAN_POINT ( 'NONE',  ( 15.72974639402199770, -15.80617190586745480, 28.12390960531435979 ) ) ;
#76699 = CARTESIAN_POINT ( 'NONE',  ( -21.52544592524343514, 5.823673210054127303, 116.0405762719810383 ) ) ;
#76700 = CARTESIAN_POINT ( 'NONE',  ( 21.55341960407610458, 5.719274019375980345, 73.95724293864769550 ) ) ;
#76701 = CARTESIAN_POINT ( 'NONE',  ( 12.06949235617757843, -12.14591786802309237, 88.12390960531436690 ) ) ;
#76702 = CARTESIAN_POINT ( 'NONE',  ( -0.05219959533936034679, 19.03943276465977164, 42.50109039468566152 ) ) ;
#76703 = CARTESIAN_POINT ( 'NONE',  ( -5.153800228976328057, -19.02544592524343514, 32.29057627198102409 ) ) ;
#76704 = CARTESIAN_POINT ( 'NONE',  ( -0.05219959533909027116, -19.03943276465977164, 77.49890960531435269 ) ) ;
#76705 = CARTESIAN_POINT ( 'NONE',  ( -19.05341960407611168, -5.049401038298163336, 76.45724293864769550 ) ) ;
#76706 = CARTESIAN_POINT ( 'NONE',  ( -27.73933785331498925, -9.013057229001049109, 140.9750000027311785 ) ) ;
#76707 = CARTESIAN_POINT ( 'NONE',  ( 16.55341960407611168, 4.379528057220329451, 98.95724293864770971 ) ) ;
#76708 = ORIENTED_EDGE ( 'NONE', *, *, #90570, .F. ) ;
#76709 = CARTESIAN_POINT ( 'NONE',  ( 14.34966873604960469, 8.224510206698951720, 34.16557627198102409 ) ) ;
#76710 = CARTESIAN_POINT ( 'NONE',  ( -8.314922557961024197, 14.29746914071037800, 32.91775706135234714 ) ) ;
#76711 = CARTESIAN_POINT ( 'NONE',  ( -0.05219959533937732626, 21.53943276465977519, 92.50109039468567573 ) ) ;
#76712 = CARTESIAN_POINT ( 'NONE',  ( -19.05341960407611168, -5.049401038298163336, 101.4572429386476955 ) ) ;
#76713 = CARTESIAN_POINT ( 'NONE',  ( -21.55341960407619339, 5.719274019375674811, 23.54275706135235424 ) ) ;
#76714 = CARTESIAN_POINT ( 'NONE',  ( -16.46253265017160317, 9.564922557960807481, 40.83224293864769550 ) ) ;
#76715 = CARTESIAN_POINT ( 'NONE',  ( -8.224510206698735004, -14.34966873604973081, 34.58442372801900433 ) ) ;
#76716 = CARTESIAN_POINT ( 'NONE',  ( 0.05219959533936267826, -19.03943276465977164, 110.0010903946856757 ) ) ;
#76717 = CARTESIAN_POINT ( 'NONE',  ( -18.67979575497178146, -10.72451020669898902, 101.6655762719810383 ) ) ;
#76718 = CARTESIAN_POINT ( 'NONE',  ( 19.02544592524334988, 5.153800228976608722, 71.45942372801900433 ) ) ;
#76719 = CARTESIAN_POINT ( 'NONE',  ( 28.82186960331498327, 2.428612866367529932E-14, 139.9999999999999716 ) ) ;
#76720 = CARTESIAN_POINT ( 'NONE',  ( 5.823673210054125526, 21.52544592524343514, 114.7905762719810383 ) ) ;
#76721 = CARTESIAN_POINT ( 'NONE',  ( 13.89961937509978007, -13.97604488694527269, 73.12390960531436690 ) ) ;
#76722 = CARTESIAN_POINT ( 'NONE',  ( 19.05341960407611168, 5.049401038298154454, 93.95724293864769550 ) ) ;
#76723 = CARTESIAN_POINT ( 'NONE',  ( 19.60416288135285967, -34.86663519103794329, -6.666020143318704072 ) ) ;
#76724 = B_SPLINE_CURVE_WITH_KNOTS ( 'NONE', 3,
 ( #82250, #68099, #143941, #7418, #175290, #129751, #37769, #193463, #99431, #22609, #84255, #54940, #145937, #177307, #69102, #130768, #192460, #53943, #135784, #134796, #136753, #28612, #10447, #167111, #71112, #74114, #196477, #86270, #121578, #179311, #73127, #181301 ),
 .UNSPECIFIED., .F., .F.,
 ( 4, 2, 2, 2, 2, 2, 2, 2, 2, 2, 2, 2, 2, 2, 2, 4 ),
 ( 2.281672496420497865E-17, 0.0003712461730036837964, 0.0007424923460073447161, 0.001113738519011005582, 0.001484984692014666664, 0.002227477038022000321, 0.002598723211025685039, 0.002969969384029369323, 0.003341215557033053608, 0.003712461730036737458, 0.004083707903040420875, 0.004454954076044104726, 0.004826200249047788576, 0.005197446422051473294, 0.005568692595055157145, 0.005939938768058841863 ),
 .UNSPECIFIED. ) ;
#76725 = CARTESIAN_POINT ( 'NONE',  ( -16.51473224551069308, -9.474510206698971260, 81.66557627198103830 ) ) ;
#76727 = CARTESIAN_POINT ( 'NONE',  ( 16.53943276465976808, -0.05219959533910856209, 73.74890960531433848 ) ) ;
#76726 = CARTESIAN_POINT ( 'NONE',  ( 15.72974639402176855, 15.80617190586768217, 31.87609039468567929 ) ) ;
#76728 = CARTESIAN_POINT ( 'NONE',  ( 13.89961937509977652, -13.97604488694527269, 83.12390960531436690 ) ) ;
#76730 = CARTESIAN_POINT ( 'NONE',  ( 13.97604488694548053, -13.89961937509957401, 60.62609039468564731 ) ) ;
#76729 = CARTESIAN_POINT ( 'NONE',  ( 12.14591786802327356, -12.06949235617739191, 55.62609039468568284 ) ) ;
#76731 = CARTESIAN_POINT ( 'NONE',  ( 21.52544592524334988, 5.823673210054432836, 66.45942372801903275 ) ) ;
#76732 = CARTESIAN_POINT ( 'NONE',  ( -16.52544592524335698, -4.483927247898792601, 23.95942372801901143 ) ) ;
#76733 = CARTESIAN_POINT ( 'NONE',  ( -16.46253265017160317, 9.564922557960807481, 65.83224293864769550 ) ) ;
#76734 = CARTESIAN_POINT ( 'NONE',  ( 19.05341960407617918, -5.049401038297876454, 96.04275706135231871 ) ) ;
#76735 = CARTESIAN_POINT ( 'NONE',  ( 0.05219959533934541429, -16.53943276465976808, 60.00109039468568284 ) ) ;
#76737 = B_SPLINE_CURVE_WITH_KNOTS ( 'NONE', 3,
 ( #145709, #34556, #96215, #7191, #130534, #53713, #65876, #157904, #127550, #189251, #50728, #112386, #12225, #134564, #9219, #56722, #119391, #179078, #148730, #42549, #26394, #72896, #54707, #25403, #117381, #88033, #149721, #197230, #90028, #182054, #133548, #58691, #73888, #102218, #118393, #10218, #70886, #181074, #196252, #116379, #40549, #43537, #163907, #57721, #55709, #11221 ),
 .UNSPECIFIED., .F., .F.,
 ( 4, 2, 2, 2, 2, 2, 2, 2, 2, 2, 2, 2, 2, 2, 2, 2, 2, 2, 2, 2, 2, 2, 4 ),
 ( 0.000000000000000000, 0.004592541348721043692, 0.006888812023081562069, 0.009185082697442082181, 0.01148135337180260229, 0.01377762404616312067, 0.01837016539488416089, 0.02296270674360520112, 0.02755524809232623787, 0.02985151876668676665, 0.03214778944104729197, 0.03674033078976832872, 0.04133287213848937242, 0.04592541348721041611, 0.04822168416157093795, 0.05051795483593145980, 0.05511049618465248268, 0.05740676685901301146, 0.05970303753337353331, 0.06429557888209455618, 0.06659184955645508497, 0.06888812023081561375, 0.07348066157953664357 ),
 .UNSPECIFIED. ) ;
#76736 = CARTESIAN_POINT ( 'NONE',  ( -21.55341960407619339, 5.719274019375674811, 93.54275706135234714 ) ) ;
#76738 = CARTESIAN_POINT ( 'NONE',  ( -9.564922557961040184, 16.46253265017147172, 82.91775706135233293 ) ) ;
#76739 = CARTESIAN_POINT ( 'NONE',  ( 5.049401038298161559, -19.05341960407611168, 52.70724293864767418 ) ) ;
#76740 = CARTESIAN_POINT ( 'NONE',  ( -5.823673210054116645, -21.52544592524344225, 72.29057627198102409 ) ) ;
#76742 = CARTESIAN_POINT ( 'NONE',  ( -16.51473224551082808, 9.474510206698731452, 78.33442372801900433 ) ) ;
#76741 = CARTESIAN_POINT ( 'NONE',  ( 4.379528057220339221, -16.55341960407611168, 72.70724293864769550 ) ) ;
#76743 = CARTESIAN_POINT ( 'NONE',  ( -3.573655867282028392E-15, 2.428612866367529932E-14, 139.9999999999999716 ) ) ;
#76744 = CARTESIAN_POINT ( 'NONE',  ( 0.05219959533936267826, -19.03943276465977164, 45.00109039468566863 ) ) ;
#76745 = CARTESIAN_POINT ( 'NONE',  ( -8.224510206698948167, 14.34966873604960824, 25.41557627198103120 ) ) ;
#76746 = CARTESIAN_POINT ( 'NONE',  ( 12.14591786802309770, 12.06949235617756955, 64.37390960531435269 ) ) ;
#76748 = CARTESIAN_POINT ( 'NONE',  ( -17.14385361876520619, 23.59649016807275856, 146.5750000027311444 ) ) ;
#76747 = CARTESIAN_POINT ( 'NONE',  ( 15.80617190586769283, -15.72974639402175789, 105.6260903946856899 ) ) ;
#76749 = CARTESIAN_POINT ( 'NONE',  ( -15.80617190586745835, -15.72974639402198527, 111.8739096053143669 ) ) ;
#76750 = CARTESIAN_POINT ( 'NONE',  ( -13.97604488694527625, -13.89961937509977652, 61.87390960531435979 ) ) ;
#76751 = CARTESIAN_POINT ( 'NONE',  ( 0.05219959533937995610, -21.53943276465977519, 85.00109039468568994 ) ) ;
#76752 = CARTESIAN_POINT ( 'NONE',  ( -13.97604488694527625, -13.89961937509977652, 61.87390960531435979 ) ) ;
#76753 = CARTESIAN_POINT ( 'NONE',  ( -9.474510206698964154, 16.51473224551069663, 30.41557627198102054 ) ) ;
#76754 = CARTESIAN_POINT ( 'NONE',  ( 0.05219959533907565091, 21.53943276465977519, 29.99890960531435979 ) ) ;
#76755 = CARTESIAN_POINT ( 'NONE',  ( -16.55341960407611168, -4.379528057220339221, 71.45724293864769550 ) ) ;
#76756 = CARTESIAN_POINT ( 'NONE',  ( 0.05219959533909260263, 19.03943276465977164, 34.99890960531435979 ) ) ;
#76757 = CARTESIAN_POINT ( 'NONE',  ( -14.29746914071049879, 8.314922557960819915, 85.83224293864768129 ) ) ;
#76758 = VECTOR ( 'NONE', #105484, 1000.000000000000000 ) ;
#76759 = CARTESIAN_POINT ( 'NONE',  ( -0.05219959533907301413, -21.53943276465977519, 97.49890960531436690 ) ) ;
#76760 = CARTESIAN_POINT ( 'NONE',  ( 5.823673210054444382, -21.52544592524334988, 45.20942372801901854 ) ) ;
#76761 = CARTESIAN_POINT ( 'NONE',  ( -28.82186960331499392, 9.364793116373565596, 149.9000000000000057 ) ) ;
#76762 = EDGE_CURVE ( 'NONE', #140047, #118127, #191974, .T. ) ;
#76763 = CARTESIAN_POINT ( 'NONE',  ( 14.34966873604972726, -8.224510206698740333, 55.83442372801901854 ) ) ;
#76764 = CARTESIAN_POINT ( 'NONE',  ( -21.52544592524343514, 5.823673210054127303, 101.0405762719810383 ) ) ;
#76766 = CARTESIAN_POINT ( 'NONE',  ( -5.049401038298153566, 19.05341960407611168, 40.20724293864768839 ) ) ;
#76765 = CARTESIAN_POINT ( 'NONE',  ( 16.51473224551083163, -9.474510206698727899, 30.83442372801900433 ) ) ;
#76767 = CARTESIAN_POINT ( 'NONE',  ( -16.51473224551069308, -9.474510206698971260, 101.6655762719810241 ) ) ;
#76768 = CARTESIAN_POINT ( 'NONE',  ( 18.67979575497194134, -10.72451020669871369, 60.83442372801901854 ) ) ;
#76769 = CARTESIAN_POINT ( 'NONE',  ( -15.72974639402197994, 15.80617190586746368, 40.62390960531435269 ) ) ;
#76770 = CARTESIAN_POINT ( 'NONE',  ( 14.29746914071037800, 8.314922557961029526, 111.6677570613523613 ) ) ;
#76772 = CARTESIAN_POINT ( 'NONE',  ( -5.823673210054431948, 21.52544592524334988, 97.70942372801904696 ) ) ;
#76771 = CARTESIAN_POINT ( 'NONE',  ( -5.823673210054431948, 21.52544592524334988, 62.70942372801902565 ) ) ;
#76773 = CARTESIAN_POINT ( 'NONE',  ( 0.05219959533936267826, -19.03943276465977164, 30.00109039468566863 ) ) ;
#76774 = CARTESIAN_POINT ( 'NONE',  ( -0.05219959533934338120, 16.53943276465976808, 92.50109039468567573 ) ) ;
#76775 = CARTESIAN_POINT ( 'NONE',  ( -21.52544592524334988, -5.823673210054445271, 53.95942372801900433 ) ) ;
#76776 = CARTESIAN_POINT ( 'NONE',  ( -19.02544592524342804, 5.153800228976336051, 46.04057627198101699 ) ) ;
#76777 = CARTESIAN_POINT ( 'NONE',  ( -10.81492255796105439, 18.62759615963255655, 112.9177570613523329 ) ) ;
#76778 = CARTESIAN_POINT ( 'NONE',  ( 19.03943276465977164, -0.05219959533909143690, 113.7489096053143669 ) ) ;
#76779 = EDGE_CURVE ( 'NONE', #120616, #88998, #39296, .T. ) ;
#76780 = CARTESIAN_POINT ( 'NONE',  ( -5.719274019375978568, 21.55341960407610458, 110.2072429386477239 ) ) ;
#76781 = CARTESIAN_POINT ( 'NONE',  ( 21.55341960407610458, 5.719274019375980345, 68.95724293864769550 ) ) ;
#76782 = CARTESIAN_POINT ( 'NONE',  ( 14.34966873604972726, -8.224510206698740333, 40.83442372801901854 ) ) ;
#76784 = CARTESIAN_POINT ( 'NONE',  ( 5.823673210054125526, 21.52544592524343514, 74.79057627198105251 ) ) ;
#76783 = LINE ( 'NONE', #125285, #67649 ) ;
#76786 = CARTESIAN_POINT ( 'NONE',  ( -12.14591786802309592, -12.06949235617757132, 61.87390960531436690 ) ) ;
#76785 = CARTESIAN_POINT ( 'NONE',  ( 4.379528057220092307, 16.55341960407617563, 67.29275706135234714 ) ) ;
#76787 = CARTESIAN_POINT ( 'NONE',  ( -22.55670631985092456, 22.55670631985084995, -45.64921306006598201 ) ) ;
#76788 = CARTESIAN_POINT ( 'NONE',  ( 13.97604488694548053, -13.89961937509957401, 110.6260903946856615 ) ) ;
#76789 = CARTESIAN_POINT ( 'NONE',  ( 21.52544592524344225, -5.823673210054117533, 38.54057627198103120 ) ) ;
#76790 = AXIS2_PLACEMENT_3D ( 'NONE', #121112, #44289, #105947 ) ;
#76791 = CARTESIAN_POINT ( 'NONE',  ( 8.224510206698742110, 14.34966873604972548, 42.08442372801901854 ) ) ;
#76792 = CARTESIAN_POINT ( 'NONE',  ( -10.72451020669898014, 18.67979575497178502, 110.4155762719810383 ) ) ;
#76793 = CARTESIAN_POINT ( 'NONE',  ( -10.72451020669898014, 18.67979575497178502, 35.41557627198102409 ) ) ;
#76794 = CARTESIAN_POINT ( 'NONE',  ( -16.52544592524335698, -4.483927247898792601, 58.95942372801902565 ) ) ;
#76795 = CARTESIAN_POINT ( 'NONE',  ( 16.46253265017160672, -9.564922557960803928, 78.33224293864769550 ) ) ;
#76797 = CARTESIAN_POINT ( 'NONE',  ( -19.03943276465977164, -0.05219959533935918106, 108.7510903946856615 ) ) ;
#76796 = CARTESIAN_POINT ( 'NONE',  ( -15.80617190586768217, 15.72974639402176855, 43.12609039468568284 ) ) ;
#76798 = CARTESIAN_POINT ( 'NONE',  ( -10.72451020669898014, 18.67979575497178502, 25.41557627198103120 ) ) ;
#76799 = ORIENTED_EDGE ( 'NONE', *, *, #99588, .T. ) ;
#76800 = CARTESIAN_POINT ( 'NONE',  ( -19.05341960407617563, 5.049401038297882671, 28.54275706135232937 ) ) ;
#76801 = CARTESIAN_POINT ( 'NONE',  ( -0.05219959533934338120, 16.53943276465976808, 37.50109039468568284 ) ) ;
#76802 = CARTESIAN_POINT ( 'NONE',  ( -13.89961937509977652, 13.97604488694528158, 95.62390960531436690 ) ) ;
#76803 = CARTESIAN_POINT ( 'NONE',  ( 15.80617190586746368, 15.72974639402197994, 109.3739096053143811 ) ) ;
#76804 = CARTESIAN_POINT ( 'NONE',  ( 16.51473224551069308, 9.474510206698969483, 74.16557627198103830 ) ) ;
#76805 = CARTESIAN_POINT ( 'NONE',  ( -5.000000000000000888, 11.45643923738960090, -15.00000000000000000 ) ) ;
#76806 = CARTESIAN_POINT ( 'NONE',  ( -16.53943276465976808, 0.05219959533911058130, 81.24890960531436690 ) ) ;
#76807 = CARTESIAN_POINT ( 'NONE',  ( -5.719274019375978568, 21.55341960407610458, 40.20724293864769550 ) ) ;
#76808 = CARTESIAN_POINT ( 'NONE',  ( -5.000000000000000000, -139.5000000000000000, 21.32407087589995953 ) ) ;
#76809 = CARTESIAN_POINT ( 'NONE',  ( 0.05219959533934541429, -16.53943276465976808, 65.00109039468568994 ) ) ;
#76810 = CARTESIAN_POINT ( 'NONE',  ( -18.67979575497178146, -10.72451020669898902, 106.6655762719810383 ) ) ;
#76811 = CARTESIAN_POINT ( 'NONE',  ( 16.51473224551083163, -9.474510206698727899, 80.83442372801899012 ) ) ;
#76812 = CARTESIAN_POINT ( 'NONE',  ( 19.03943276465977164, -0.05219959533909143690, 33.74890960531435979 ) ) ;
#76813 = CARTESIAN_POINT ( 'NONE',  ( 18.67979575497178502, 10.72451020669898547, 69.16557627198102409 ) ) ;
#76814 = CARTESIAN_POINT ( 'NONE',  ( -19.05341960407611168, -5.049401038298163336, 96.45724293864769550 ) ) ;
#76815 = CARTESIAN_POINT ( 'NONE',  ( 15.80617190586769283, -15.72974639402175789, 95.62609039468568994 ) ) ;
#76816 = CARTESIAN_POINT ( 'NONE',  ( -16.46253265017160317, 9.564922557960807481, 60.83224293864769550 ) ) ;
#76817 = CARTESIAN_POINT ( 'NONE',  ( -14.34966873604972548, 8.224510206698743886, 43.33442372801901143 ) ) ;
#76818 = CARTESIAN_POINT ( 'NONE',  ( 13.97604488694527802, 13.89961937509977652, 54.37390960531435979 ) ) ;
#76819 = CARTESIAN_POINT ( 'NONE',  ( -10.72451020669870658, -18.67979575497194134, 79.58442372801903275 ) ) ;
#76820 = EDGE_LOOP ( 'NONE', ( #26201, #133839 ) ) ;
#76821 = CARTESIAN_POINT ( 'NONE',  ( -19.02544592524334988, -5.153800228976617603, 43.95942372801899012 ) ) ;
#76822 = CARTESIAN_POINT ( 'NONE',  ( -9.474510206698720793, -16.51473224551083518, 59.58442372801900433 ) ) ;
#76823 = CARTESIAN_POINT ( 'NONE',  ( -5.823673210054431948, 21.52544592524334988, 52.70942372801902565 ) ) ;
#76824 = CARTESIAN_POINT ( 'NONE',  ( -9.090072183657234461, 0.1985533113406500183, -61.89635373339110913 ) ) ;
#76825 = CARTESIAN_POINT ( 'NONE',  ( 13.89961937509957401, 13.97604488694547697, 41.87609039468566152 ) ) ;
#76826 = CARTESIAN_POINT ( 'NONE',  ( -9.564922557960796823, -16.46253265017161027, 97.08224293864769550 ) ) ;
#76827 = CARTESIAN_POINT ( 'NONE',  ( -16.51473224551069308, -9.474510206698971260, 66.66557627198102409 ) ) ;
#76828 = CARTESIAN_POINT ( 'NONE',  ( 12.06949235617739724, 12.14591786802326823, 111.8760903946856615 ) ) ;
#76830 = CARTESIAN_POINT ( 'NONE',  ( 10.81492255796106328, -18.62759615963255655, 90.41775706135236135 ) ) ;
#76829 = CARTESIAN_POINT ( 'NONE',  ( 21.55341960407610458, 5.719274019375980345, 23.95724293864769550 ) ) ;
#76831 = CARTESIAN_POINT ( 'NONE',  ( 11.40812507854755253, -35.11059874428192273, -8.524999997268814411 ) ) ;
#76832 = CARTESIAN_POINT ( 'NONE',  ( 16.88567814943164791, 6.947325034625594142, 58.79001122652586275 ) ) ;
#76833 = CARTESIAN_POINT ( 'NONE',  ( -10.81492255796105439, 18.62759615963255655, 102.9177570613523756 ) ) ;
#76834 = DIRECTION ( 'NONE',  ( -1.000000000000000000, 0.000000000000000000, 0.000000000000000000 ) ) ;
#76835 = CARTESIAN_POINT ( 'NONE',  ( 16.55341960407611168, 4.379528057220329451, 113.9572429386477239 ) ) ;
#76836 = CARTESIAN_POINT ( 'NONE',  ( -7.500000000000000000, 0.000000000000000000, 4.292893218813445877 ) ) ;
#76837 = CARTESIAN_POINT ( 'NONE',  ( -26.26106931734002004, -9.140213825779254009, 167.1341548181403596 ) ) ;
#76838 = CARTESIAN_POINT ( 'NONE',  ( 8.314922557961029526, -14.29746914071037800, 55.41775706135234714 ) ) ;
#76839 = CARTESIAN_POINT ( 'NONE',  ( 0.05219959533907565091, 21.53943276465977519, 69.99890960531435269 ) ) ;
#76840 = CARTESIAN_POINT ( 'NONE',  ( -0.05219959533910754901, -16.53943276465976808, 42.49890960531435979 ) ) ;
#76842 = CARTESIAN_POINT ( 'NONE',  ( -19.05341960407611168, -5.049401038298163336, 96.45724293864769550 ) ) ;
#76841 = CARTESIAN_POINT ( 'NONE',  ( -4.379528057220328563, 16.55341960407611168, 105.2072429386477097 ) ) ;
#76843 = CARTESIAN_POINT ( 'NONE',  ( 16.46253265017146816, 9.564922557961045513, 31.66775706135232937 ) ) ;
#76844 = CARTESIAN_POINT ( 'NONE',  ( 8.224510206698953496, -14.34966873604960469, 112.9155762719810383 ) ) ;
#76845 = CARTESIAN_POINT ( 'NONE',  ( -18.67979575497193778, 10.72451020669871902, 73.33442372801901854 ) ) ;
#76846 = CARTESIAN_POINT ( 'NONE',  ( -13.97604488694527625, -13.89961937509977830, 96.87390960531435269 ) ) ;
#76847 = CARTESIAN_POINT ( 'NONE',  ( -8.314922557961024197, 14.29746914071037800, 112.9177570613523329 ) ) ;
#76848 = CARTESIAN_POINT ( 'NONE',  ( 17.58332526062524437, 7.635886036038643354, 66.57665040441534643 ) ) ;
#76849 = CARTESIAN_POINT ( 'NONE',  ( 21.55341960407610458, 5.719274019375980345, 28.95724293864769905 ) ) ;
#76850 = CARTESIAN_POINT ( 'NONE',  ( 8.224510206698953496, -14.34966873604960469, 92.91557627198103830 ) ) ;
#76851 = CARTESIAN_POINT ( 'NONE',  ( -9.474510206698720793, -16.51473224551083518, 54.58442372801899722 ) ) ;
#76852 = CARTESIAN_POINT ( 'NONE',  ( -13.89961937509977652, 13.97604488694528158, 75.62390960531438111 ) ) ;
#76853 = CARTESIAN_POINT ( 'NONE',  ( 8.224510206698953496, -14.34966873604960469, 72.91557627198103830 ) ) ;
#76854 = CARTESIAN_POINT ( 'NONE',  ( 19.03943276465977164, 0.05219959533936151252, 86.25109039468567573 ) ) ;
#76855 = CARTESIAN_POINT ( 'NONE',  ( 21.55341960407610458, 5.719274019375980345, 43.95724293864769550 ) ) ;
#76856 = VERTEX_POINT ( 'NONE', #51469 ) ;
#76857 = CARTESIAN_POINT ( 'NONE',  ( -0.05219959533909027116, -19.03943276465977164, 22.49890960531436690 ) ) ;
#76858 = CARTESIAN_POINT ( 'NONE',  ( -17.49999999999999645, -5.500000000000005329, 31.28230962303567253 ) ) ;
#76859 = EDGE_CURVE ( 'NONE', #171824, #124248, #192993, .T. ) ;
#76861 = CARTESIAN_POINT ( 'NONE',  ( -10.81492255796078084, -18.62759615963271287, 77.08224293864769550 ) ) ;
#76860 = CARTESIAN_POINT ( 'NONE',  ( -5.153800228976328057, -19.02544592524343514, 67.29057627198102409 ) ) ;
#76863 = CARTESIAN_POINT ( 'NONE',  ( -9.564922557960796823, -16.46253265017161027, 92.08224293864769550 ) ) ;
#76862 = CARTESIAN_POINT ( 'NONE',  ( 8.314922557961029526, -14.29746914071037800, 90.41775706135236135 ) ) ;
#76864 = CARTESIAN_POINT ( 'NONE',  ( -19.05341960407617563, 5.049401038297882671, 73.54275706135233293 ) ) ;
#76865 = CARTESIAN_POINT ( 'NONE',  ( 18.62759615963255655, 10.81492255796105972, 86.66775706135234714 ) ) ;
#76866 = CARTESIAN_POINT ( 'NONE',  ( -5.823673210054116645, -21.52544592524344225, 57.29057627198103120 ) ) ;
#76867 = CARTESIAN_POINT ( 'NONE',  ( -10.72451020669898014, 18.67979575497178502, 30.41557627198101699 ) ) ;
#76868 = CARTESIAN_POINT ( 'NONE',  ( 9.474510206698971260, -16.51473224551069308, 32.91557627198102409 ) ) ;
#76869 = CARTESIAN_POINT ( 'NONE',  ( -0.05219959533934338120, 16.53943276465976808, 102.5010903946856899 ) ) ;
#76870 = CARTESIAN_POINT ( 'NONE',  ( -5.049401038298153566, 19.05341960407611168, 45.20724293864769550 ) ) ;
#76871 = CARTESIAN_POINT ( 'NONE',  ( -13.97604488694547697, 13.89961937509957934, 113.1260903946856757 ) ) ;
#76872 = CARTESIAN_POINT ( 'NONE',  ( 17.31728774477272736, 6.344390552232407110, 51.68093348310683410 ) ) ;
#76873 = CARTESIAN_POINT ( 'NONE',  ( -10.81492255796105439, 18.62759615963255655, 107.9177570613523471 ) ) ;
#76874 = CARTESIAN_POINT ( 'NONE',  ( -14.34966873604960291, -8.224510206698953496, 56.66557627198103830 ) ) ;
#76875 = CARTESIAN_POINT ( 'NONE',  ( 18.62759615963271287, -10.81492255796078972, 103.3322429386476955 ) ) ;
#76876 = CARTESIAN_POINT ( 'NONE',  ( -21.55341960407610458, -5.719274019375992779, 106.4572429386477097 ) ) ;
#76877 = CARTESIAN_POINT ( 'NONE',  ( -5.773271879485258218, 3.915140329348332671, -64.38756054665735462 ) ) ;
#76878 = CARTESIAN_POINT ( 'NONE',  ( 21.53943276465977519, -0.05219959533907433946, 43.74890960531435979 ) ) ;
#76879 = CARTESIAN_POINT ( 'NONE',  ( 4.483927247898790824, -16.52544592524335698, 75.20942372801901854 ) ) ;
#76880 = CARTESIAN_POINT ( 'NONE',  ( 4.379528057220339221, -16.55341960407611168, 92.70724293864770971 ) ) ;
#76881 = CARTESIAN_POINT ( 'NONE',  ( 19.05341960407611168, 5.049401038298154454, 53.95724293864770260 ) ) ;
#76882 = CARTESIAN_POINT ( 'NONE',  ( 27.05641397906351386, -3.631740835637518927, 169.9999999999999716 ) ) ;
#76883 = CARTESIAN_POINT ( 'NONE',  ( -4.483927247898782831, 16.52544592524335698, 107.7094237280190328 ) ) ;
#76884 = CARTESIAN_POINT ( 'NONE',  ( 21.53943276465977519, 0.05219959533937863772, 36.25109039468567573 ) ) ;
#76885 = CARTESIAN_POINT ( 'NONE',  ( -5.049401038298153566, 19.05341960407611168, 95.20724293864770971 ) ) ;
#76886 = CARTESIAN_POINT ( 'NONE',  ( -15.80617190586768217, 15.72974639402176855, 63.12609039468568994 ) ) ;
#76887 = DIRECTION ( 'NONE',  ( 0.000000000000000000, -1.000000000000000000, 0.000000000000000000 ) ) ;
#76888 = CARTESIAN_POINT ( 'NONE',  ( -19.03943276465977164, 0.05219959533909376836, 21.24890960531436335 ) ) ;
#76889 = ORIENTED_EDGE ( 'NONE', *, *, #184713, .T. ) ;
#76890 = CARTESIAN_POINT ( 'NONE',  ( 5.823673210054444382, -21.52544592524334988, 60.20942372801902565 ) ) ;
#76891 = CARTESIAN_POINT ( 'NONE',  ( -9.474510206698964154, 16.51473224551069663, 45.41557627198103120 ) ) ;
#76892 = CARTESIAN_POINT ( 'NONE',  ( -9.474510206698964154, 16.51473224551069663, 95.41557627198102409 ) ) ;
#76893 = CARTESIAN_POINT ( 'NONE',  ( -19.05341960407617563, 5.049401038297882671, 68.54275706135230450 ) ) ;
#76894 = CARTESIAN_POINT ( 'NONE',  ( 21.55341960407619695, -5.719274019375665929, 36.04275706135234714 ) ) ;
#76895 = CARTESIAN_POINT ( 'NONE',  ( 13.89961937509957401, 13.97604488694547697, 106.8760903946856757 ) ) ;
#76896 = CARTESIAN_POINT ( 'NONE',  ( -16.51473224551082808, 9.474510206698731452, 78.33442372801900433 ) ) ;
#76897 = CARTESIAN_POINT ( 'NONE',  ( -9.564922557960796823, -16.46253265017161027, 42.08224293864769550 ) ) ;
#76898 = CARTESIAN_POINT ( 'NONE',  ( -19.02544592524334988, -5.153800228976617603, 78.95942372801900433 ) ) ;
#76899 = CARTESIAN_POINT ( 'NONE',  ( -8.224510206698735004, -14.34966873604973081, 99.58442372801900433 ) ) ;
#76900 = CARTESIAN_POINT ( 'NONE',  ( 5.049401038297881783, 19.05341960407617563, 72.29275706135234714 ) ) ;
#76901 = CARTESIAN_POINT ( 'NONE',  ( -14.29746914071049879, 8.314922557960819915, 40.83224293864769550 ) ) ;
#76902 = CARTESIAN_POINT ( 'NONE',  ( -16.51473224551082808, 9.474510206698731452, 48.33442372801900433 ) ) ;
#76903 = CARTESIAN_POINT ( 'NONE',  ( 18.67979575497194134, -10.72451020669871369, 100.8344237280190185 ) ) ;
#76904 = CARTESIAN_POINT ( 'NONE',  ( -13.97604488694547697, 13.89961937509957934, 28.12609039468565797 ) ) ;
#76905 = CARTESIAN_POINT ( 'NONE',  ( 5.153800228976335163, 19.02544592524342804, 34.79057627198102409 ) ) ;
#76906 = CARTESIAN_POINT ( 'NONE',  ( 15.72974639402176855, 15.80617190586768217, 86.87609039468568994 ) ) ;
#76907 = CARTESIAN_POINT ( 'NONE',  ( 14.34966873604972726, -8.224510206698740333, 40.83442372801901854 ) ) ;
#76908 = CARTESIAN_POINT ( 'NONE',  ( -0.05219959533909027116, -19.03943276465977164, 87.49890960531436690 ) ) ;
#76909 = CARTESIAN_POINT ( 'NONE',  ( -22.44159573604009950, -16.30477369853688430, 145.0750000027311728 ) ) ;
#76910 = CARTESIAN_POINT ( 'NONE',  ( -16.46253265017160317, 9.564922557960807481, 80.83224293864769550 ) ) ;
#76911 = LINE ( 'NONE', #141572, #32936 ) ;
#76912 = ORIENTED_EDGE ( 'NONE', *, *, #59414, .T. ) ;
#76913 = CARTESIAN_POINT ( 'NONE',  ( -5.049401038297874678, -19.05341960407617918, 84.79275706135233293 ) ) ;
#76914 = CARTESIAN_POINT ( 'NONE',  ( -21.55341960407610458, -5.719274019375992779, 21.45724293864769550 ) ) ;
#76916 = CARTESIAN_POINT ( 'NONE',  ( 5.153800228976615827, -19.02544592524334988, 95.20942372801897591 ) ) ;
#76915 = CARTESIAN_POINT ( 'NONE',  ( 5.823673210054444382, -21.52544592524334988, 110.2094237280190185 ) ) ;
#76917 = CARTESIAN_POINT ( 'NONE',  ( -8.314922557960811034, -14.29746914071050412, 102.0822429386476955 ) ) ;
#76918 = CARTESIAN_POINT ( 'NONE',  ( 5.049401038298161559, -19.05341960407611168, 22.70724293864769194 ) ) ;
#76919 = CARTESIAN_POINT ( 'NONE',  ( -21.53943276465977519, 0.05219959533907696930, 61.24890960531435979 ) ) ;
#76920 = CARTESIAN_POINT ( 'NONE',  ( 21.55341960407610458, 5.719274019375980345, 48.95724293864770971 ) ) ;
#76921 = CARTESIAN_POINT ( 'NONE',  ( -14.29746914071049879, 8.314922557960819915, 115.8322429386477097 ) ) ;
#76922 = FACE_OUTER_BOUND ( 'NONE', #13996, .T. ) ;
#76923 = CARTESIAN_POINT ( 'NONE',  ( 13.97604488694548053, -13.89961937509957401, 75.62609039468564731 ) ) ;
#76925 = VECTOR ( 'NONE', #142283, 1000.000000000000114 ) ;
#76924 = CARTESIAN_POINT ( 'NONE',  ( -16.55341960407611168, -4.379528057220339221, 46.45724293864769550 ) ) ;
#76927 = ADVANCED_FACE ( 'NONE', ( #190982 ), #20131, .F. ) ;
#76926 = CARTESIAN_POINT ( 'NONE',  ( -21.53943276465977519, 0.05219959533907696930, 21.24890960531436690 ) ) ;
#76928 = CARTESIAN_POINT ( 'NONE',  ( 0.05219959533937995610, -21.53943276465977519, 85.00109039468568994 ) ) ;
#76929 = CARTESIAN_POINT ( 'NONE',  ( 18.67979575497178502, 10.72451020669898547, 74.16557627198102409 ) ) ;
#76930 = CARTESIAN_POINT ( 'NONE',  ( 5.823673210054444382, -21.52544592524334988, 65.20942372801901854 ) ) ;
#76931 = CARTESIAN_POINT ( 'NONE',  ( -15.80617190586768217, 15.72974639402176855, 48.12609039468568284 ) ) ;
#76932 = CARTESIAN_POINT ( 'NONE',  ( -0.05219959533909027116, -19.03943276465977164, 82.49890960531436690 ) ) ;
#76933 = CARTESIAN_POINT ( 'NONE',  ( 16.55341960407618274, -4.379528057220086978, 96.04275706135236135 ) ) ;
#76934 = CARTESIAN_POINT ( 'NONE',  ( -12.14591786802309592, -12.06949235617757132, 111.8739096053143669 ) ) ;
#76935 = CARTESIAN_POINT ( 'NONE',  ( -31.60134953801818014, 3.338644055332177896, 101.7340227041930234 ) ) ;
#76936 = CARTESIAN_POINT ( 'NONE',  ( -8.224510206698948167, 14.34966873604960824, 65.41557627198102409 ) ) ;
#76937 = CARTESIAN_POINT ( 'NONE',  ( -14.34966873604960291, -8.224510206698953496, 31.66557627198102054 ) ) ;
#76938 = CARTESIAN_POINT ( 'NONE',  ( 5.153800228976335163, 19.02544592524342804, 64.79057627198100988 ) ) ;
#76939 = CARTESIAN_POINT ( 'NONE',  ( 19.03943276465977164, -0.05219959533909143690, 38.74890960531436690 ) ) ;
#76940 = CARTESIAN_POINT ( 'NONE',  ( -18.62759615963270932, 10.81492255796079327, 40.83224293864769550 ) ) ;
#76941 = CARTESIAN_POINT ( 'NONE',  ( -5.153800228976607833, 19.02544592524334988, 32.70942372801899722 ) ) ;
#76943 = CARTESIAN_POINT ( 'NONE',  ( 16.52544592524342804, -4.483927247898539470, 48.54057627198103120 ) ) ;
#76942 = CARTESIAN_POINT ( 'NONE',  ( 11.45643923738959735, 5.000000000000007105, -18.00000000000000000 ) ) ;
#76944 = CARTESIAN_POINT ( 'NONE',  ( -18.67979575497178146, -10.72451020669898902, 26.66557627198103475 ) ) ;
#76945 = DIRECTION ( 'NONE',  ( 0.000000000000000000, 0.000000000000000000, 1.000000000000000000 ) ) ;
#76946 = CARTESIAN_POINT ( 'NONE',  ( -4.483927247898782831, 16.52544592524335698, 77.70942372801900433 ) ) ;
#76947 = CARTESIAN_POINT ( 'NONE',  ( 9.564922557961047289, -16.46253265017146816, 80.41775706135234714 ) ) ;
#76948 = ADVANCED_FACE ( 'NONE', ( #36285 ), #97941, .T. ) ;
#76949 = CARTESIAN_POINT ( 'NONE',  ( -12.06949235617756955, 12.14591786802309770, 45.62390960531436690 ) ) ;
#76950 = CARTESIAN_POINT ( 'NONE',  ( 16.21995358207308158, -7.366697692864041969, 52.43551001512160781 ) ) ;
#76951 = CARTESIAN_POINT ( 'NONE',  ( 4.379528057220339221, -16.55341960407611168, 27.70724293864769905 ) ) ;
#76952 = CARTESIAN_POINT ( 'NONE',  ( 19.03943276465977164, -0.05219959533909143690, 48.74890960531435979 ) ) ;
#76953 = CARTESIAN_POINT ( 'NONE',  ( 0.05219959533909260263, 19.03943276465977164, 79.99890960531436690 ) ) ;
#76954 = CARTESIAN_POINT ( 'NONE',  ( 16.51473224551069308, 9.474510206698969483, 44.16557627198103120 ) ) ;
#76955 = CARTESIAN_POINT ( 'NONE',  ( 18.62759615963255655, 10.81492255796105972, 41.66775706135235424 ) ) ;
#76956 = CARTESIAN_POINT ( 'NONE',  ( 19.03943276465977164, -0.05219959533909143690, 58.74890960531435979 ) ) ;
#76957 = CARTESIAN_POINT ( 'NONE',  ( 193.3062444957835453, -155.7167183371837496, -25.00000000000000000 ) ) ;
#76958 = CARTESIAN_POINT ( 'NONE',  ( -13.97604488694527625, -13.89961937509977652, 46.87390960531435979 ) ) ;
#76959 = CARTESIAN_POINT ( 'NONE',  ( -21.53943276465977519, 0.05219959533907696930, 41.24890960531435269 ) ) ;
#76961 = CARTESIAN_POINT ( 'NONE',  ( 12.14591786802309770, 12.06949235617756955, 114.3739096053143527 ) ) ;
#76960 = CARTESIAN_POINT ( 'NONE',  ( 18.62759615963255655, 10.81492255796105972, 71.66775706135234714 ) ) ;
#76962 = CARTESIAN_POINT ( 'NONE',  ( -5.719274019375978568, 21.55341960407610458, 25.20724293864769550 ) ) ;
#76963 = CARTESIAN_POINT ( 'NONE',  ( -0.05219959533934338120, 16.53943276465976808, 97.50109039468567573 ) ) ;
#76964 = CARTESIAN_POINT ( 'NONE',  ( -15.72974639402176322, -15.80617190586768395, 99.37609039468568994 ) ) ;
#76965 = CARTESIAN_POINT ( 'NONE',  ( 14.34966873604972726, -8.224510206698740333, 65.83442372801900433 ) ) ;
#76966 = CARTESIAN_POINT ( 'NONE',  ( -0.05219959533909027116, -19.03943276465977164, 112.4989096053143669 ) ) ;
#76967 = CARTESIAN_POINT ( 'NONE',  ( 4.483927247898790824, -16.52544592524335698, 55.20942372801902565 ) ) ;
#76968 = CARTESIAN_POINT ( 'NONE',  ( -14.29746914071037622, -8.314922557961029526, 39.16775706135235424 ) ) ;
#76969 = CARTESIAN_POINT ( 'NONE',  ( -8.314922557961024197, 14.29746914071037800, 97.91775706135236135 ) ) ;
#76970 = CARTESIAN_POINT ( 'NONE',  ( -21.53943276465977519, -0.05219959533937600094, 58.75109039468568994 ) ) ;
#76971 = CARTESIAN_POINT ( 'NONE',  ( 14.29746914071037800, 8.314922557961029526, 26.66775706135235424 ) ) ;
#76972 = CARTESIAN_POINT ( 'NONE',  ( -10.72451020669898014, 18.67979575497178502, 110.4155762719810383 ) ) ;
#76973 = CARTESIAN_POINT ( 'NONE',  ( 16.55341960407618274, -4.379528057220086978, 21.04275706135234714 ) ) ;
#76974 = CARTESIAN_POINT ( 'NONE',  ( -14.34966873604972548, 8.224510206698743886, 83.33442372801903275 ) ) ;
#76975 = CARTESIAN_POINT ( 'NONE',  ( -17.44279575226787316, 5.990770900253887810, 45.83557567514318976 ) ) ;
#76976 = CARTESIAN_POINT ( 'NONE',  ( 21.52544592524334988, 5.823673210054432836, 81.45942372801900433 ) ) ;
#76977 = CARTESIAN_POINT ( 'NONE',  ( -19.05341960407617563, 5.049401038297882671, 88.54275706135230450 ) ) ;
#76978 = CARTESIAN_POINT ( 'NONE',  ( 16.52544592524342804, -4.483927247898539470, 58.54057627198103120 ) ) ;
#76979 = CARTESIAN_POINT ( 'NONE',  ( -8.224510206698948167, 14.34966873604960824, 40.41557627198103120 ) ) ;
#76980 = CARTESIAN_POINT ( 'NONE',  ( -16.52544592524342804, 4.483927247898546575, 101.0405762719810383 ) ) ;
#76982 = CARTESIAN_POINT ( 'NONE',  ( -9.100000000000001421, 9.789526074884739315E-14, -63.95112321872120731 ) ) ;
#76981 = CARTESIAN_POINT ( 'NONE',  ( -5.049401038297874678, -19.05341960407617918, 49.79275706135231871 ) ) ;
#76983 = CARTESIAN_POINT ( 'NONE',  ( 5.719274019375673035, 21.55341960407619339, 47.29275706135234003 ) ) ;
#76984 = CARTESIAN_POINT ( 'NONE',  ( -5.153800228976607833, 19.02544592524334988, 107.7094237280189759 ) ) ;
#76985 = DIRECTION ( 'NONE',  ( 0.000000000000000000, 0.000000000000000000, 1.000000000000000000 ) ) ;
#76986 = CARTESIAN_POINT ( 'NONE',  ( 13.97604488694527802, 13.89961937509977652, 99.37390960531436690 ) ) ;
#76987 = CARTESIAN_POINT ( 'NONE',  ( 21.53943276465977519, -0.05219959533907433946, 73.74890960531433848 ) ) ;
#76988 = CARTESIAN_POINT ( 'NONE',  ( 13.89961937509957401, 13.97604488694547697, 96.87609039468566152 ) ) ;
#76989 = CARTESIAN_POINT ( 'NONE',  ( -13.89961937509977652, 13.97604488694528158, 105.6239096053143527 ) ) ;
#76990 = CARTESIAN_POINT ( 'NONE',  ( 5.153800228976617603, -19.02544592524335343, 50.20942372801899012 ) ) ;
#76991 = CARTESIAN_POINT ( 'NONE',  ( 12.14591786802309770, 12.06949235617756955, 104.3739096053143669 ) ) ;
#76992 = CARTESIAN_POINT ( 'NONE',  ( 10.81492255796106328, -18.62759615963255655, 95.41775706135234714 ) ) ;
#76993 = CARTESIAN_POINT ( 'NONE',  ( -19.05341960407611168, -5.049401038298163336, 31.45724293864769550 ) ) ;
#76994 = CARTESIAN_POINT ( 'NONE',  ( 15.72974639402176855, 15.80617190586768217, 46.87609039468568994 ) ) ;
#76995 = CARTESIAN_POINT ( 'NONE',  ( 18.67979575497194134, -10.72451020669871369, 85.83442372801901854 ) ) ;
#76996 = CARTESIAN_POINT ( 'NONE',  ( -4.483927247898782831, 16.52544592524335698, 87.70942372801901854 ) ) ;
#76997 = CARTESIAN_POINT ( 'NONE',  ( -18.62759615963255300, -10.81492255796106328, 49.16775706135234003 ) ) ;
#76998 = CARTESIAN_POINT ( 'NONE',  ( -10.81492255796105439, 18.62759615963255655, 37.91775706135235424 ) ) ;
#77000 = CARTESIAN_POINT ( 'NONE',  ( 16.51473224551069308, 9.474510206698969483, 89.16557627198103830 ) ) ;
#76999 = CARTESIAN_POINT ( 'NONE',  ( 16.51473224551083163, -9.474510206698727899, 60.83442372801900433 ) ) ;
#77001 = CARTESIAN_POINT ( 'NONE',  ( 16.52544592524342804, -4.483927247898539470, 108.5405762719810241 ) ) ;
#77002 = CARTESIAN_POINT ( 'NONE',  ( 10.72451020669898902, -18.67979575497178502, 77.91557627198102409 ) ) ;
#77003 = CARTESIAN_POINT ( 'NONE',  ( -8.224510206698948167, 14.34966873604960824, 70.41557627198102409 ) ) ;
#77004 = CARTESIAN_POINT ( 'NONE',  ( -10.72451020669870658, -18.67979575497194134, 104.5844237280190185 ) ) ;
#77005 = CARTESIAN_POINT ( 'NONE',  ( 8.314922557960818139, 14.29746914071049879, 84.58224293864769550 ) ) ;
#77006 = CARTESIAN_POINT ( 'NONE',  ( 5.049401038298161559, -19.05341960407611168, 32.70724293864768129 ) ) ;
#77007 = CARTESIAN_POINT ( 'NONE',  ( -13.97604488694547697, 13.89961937509957934, 73.12609039468568994 ) ) ;
#77008 = CARTESIAN_POINT ( 'NONE',  ( -0.05219959533910754901, -16.53943276465976808, 52.49890960531435979 ) ) ;
#77009 = CARTESIAN_POINT ( 'NONE',  ( 21.53943276465977519, 0.05219959533937863772, 91.25109039468568994 ) ) ;
#77010 = CARTESIAN_POINT ( 'NONE',  ( -16.46253265017160317, 9.564922557960807481, 95.83224293864769550 ) ) ;
#77011 = CARTESIAN_POINT ( 'NONE',  ( 13.97604488694548053, -13.89961937509957401, 55.62609039468566863 ) ) ;
#77012 = CARTESIAN_POINT ( 'NONE',  ( -18.62759615963270932, 10.81492255796079327, 70.83224293864770971 ) ) ;
#77013 = CARTESIAN_POINT ( 'NONE',  ( -21.55341960407619339, 5.719274019375674811, 23.54275706135235424 ) ) ;
#77014 = CARTESIAN_POINT ( 'NONE',  ( -9.564922557961040184, 16.46253265017147172, 112.9177570613523329 ) ) ;
#77015 = CARTESIAN_POINT ( 'NONE',  ( -8.224510206698735004, -14.34966873604973081, 84.58442372801903275 ) ) ;
#77017 = CARTESIAN_POINT ( 'NONE',  ( 0.05219959533937995610, -21.53943276465977519, 25.00109039468567218 ) ) ;
#77016 = CARTESIAN_POINT ( 'NONE',  ( -0.05219959533909027116, -19.03943276465977164, 22.49890960531436690 ) ) ;
#77018 = CARTESIAN_POINT ( 'NONE',  ( 12.14591786802309770, 12.06949235617756955, 114.3739096053143527 ) ) ;
#77019 = CARTESIAN_POINT ( 'NONE',  ( -36.91746825000000598, 2.428612866367529932E-14, -9.124999997268814056 ) ) ;
#77020 = CARTESIAN_POINT ( 'NONE',  ( 8.314922557961029526, -14.29746914071037800, 50.41775706135235424 ) ) ;
#77021 = CARTESIAN_POINT ( 'NONE',  ( -4.379528057220328563, 16.55341960407611168, 80.20724293864769550 ) ) ;
#77022 = CARTESIAN_POINT ( 'NONE',  ( 21.52544592524344225, -5.823673210054117533, 73.54057627198102409 ) ) ;
#77023 = CARTESIAN_POINT ( 'NONE',  ( 14.34966873604960469, 8.224510206698951720, 29.16557627198103120 ) ) ;
#77024 = CARTESIAN_POINT ( 'NONE',  ( -12.14591786802326823, 12.06949235617739902, 33.12609039468569705 ) ) ;
#77025 = CARTESIAN_POINT ( 'NONE',  ( -9.474510206698964154, 16.51473224551069663, 40.41557627198103120 ) ) ;
#77026 = CARTESIAN_POINT ( 'NONE',  ( -8.224510206698735004, -14.34966873604973081, 84.58442372801903275 ) ) ;
#77027 = CARTESIAN_POINT ( 'NONE',  ( -19.02544592524334988, -5.153800228976617603, 73.95942372801900433 ) ) ;
#77028 = CARTESIAN_POINT ( 'NONE',  ( -15.72974639402197994, 15.80617190586746368, 65.62390960531436690 ) ) ;
#77029 = CARTESIAN_POINT ( 'NONE',  ( -0.05219959533934338120, 16.53943276465976808, 112.5010903946857042 ) ) ;
#77030 = VERTEX_POINT ( 'NONE', #8972 ) ;
#77031 = CARTESIAN_POINT ( 'NONE',  ( 21.52544592524334988, 5.823673210054432836, 86.45942372801901854 ) ) ;
#77032 = CARTESIAN_POINT ( 'NONE',  ( -15.80617190586745835, -15.72974639402198527, 41.87390960531435979 ) ) ;
#77033 = ORIENTED_EDGE ( 'NONE', *, *, #155268, .F. ) ;
#77034 = ORIENTED_EDGE ( 'NONE', *, *, #181949, .T. ) ;
#77035 = CARTESIAN_POINT ( 'NONE',  ( 12.06949235617739724, 12.14591786802326823, 96.87609039468568994 ) ) ;
#77036 = CARTESIAN_POINT ( 'NONE',  ( 15.80617190586746368, 15.72974639402197994, 39.37390960531436690 ) ) ;
#77037 = ORIENTED_EDGE ( 'NONE', *, *, #82699, .T. ) ;
#77038 = CARTESIAN_POINT ( 'NONE',  ( -13.97604488694527625, -13.89961937509977652, 106.8739096053143669 ) ) ;
#77039 = CARTESIAN_POINT ( 'NONE',  ( 11.74264578624799427, 36.14014761921585972, -8.349999994537625980 ) ) ;
#77040 = CARTESIAN_POINT ( 'NONE',  ( -13.97604488694527625, -13.89961937509977652, 31.87390960531435979 ) ) ;
#77041 = CARTESIAN_POINT ( 'NONE',  ( -21.53943276465977519, 0.05219959533907696930, 71.24890960531435269 ) ) ;
#77042 = CARTESIAN_POINT ( 'NONE',  ( 4.379528057220092307, 16.55341960407617563, 102.2927570613523613 ) ) ;
#77043 = CARTESIAN_POINT ( 'NONE',  ( -21.52544592524334988, -5.823673210054445271, 63.95942372801901854 ) ) ;
#77044 = CARTESIAN_POINT ( 'NONE',  ( -8.314922557961024197, 14.29746914071037800, 22.91775706135235069 ) ) ;
#77045 = CARTESIAN_POINT ( 'NONE',  ( -16.53943276465976808, 0.05219959533911058130, 116.2489096053143669 ) ) ;
#77046 = CARTESIAN_POINT ( 'NONE',  ( 13.89961937509957401, 13.97604488694547697, 106.8760903946856757 ) ) ;
#77047 = CARTESIAN_POINT ( 'NONE',  ( -16.46253265017160317, 9.564922557960807481, 35.83224293864768839 ) ) ;
#77048 = CARTESIAN_POINT ( 'NONE',  ( 8.906447517083050158, 27.41122689804195645, 145.4000000000000057 ) ) ;
#77049 = CARTESIAN_POINT ( 'NONE',  ( 9.564922557960805705, 16.46253265017160317, 104.5822429386476955 ) ) ;
#77050 = CARTESIAN_POINT ( 'NONE',  ( 4.379528057220092307, 16.55341960407617563, 92.29275706135236135 ) ) ;
#77051 = CARTESIAN_POINT ( 'NONE',  ( 5.153800228976615827, -19.02544592524334988, 80.20942372801901854 ) ) ;
#77052 = CARTESIAN_POINT ( 'NONE',  ( -13.89961937509957401, -13.97604488694547875, 24.37609039468565442 ) ) ;
#77053 = CARTESIAN_POINT ( 'NONE',  ( -10.81492255796078084, -18.62759615963271287, 77.08224293864769550 ) ) ;
#77054 = CARTESIAN_POINT ( 'NONE',  ( 16.52544592524335698, 4.483927247898782831, 86.45942372801901854 ) ) ;
#77055 = CARTESIAN_POINT ( 'NONE',  ( -13.89961937509957401, -13.97604488694547875, 89.37609039468563310 ) ) ;
#77056 = CARTESIAN_POINT ( 'NONE',  ( -16.46253265017160317, 9.564922557960807481, 50.83224293864770260 ) ) ;
#77057 = CARTESIAN_POINT ( 'NONE',  ( 5.153800228976335163, 19.02544592524342804, 94.79057627198103830 ) ) ;
#77058 = CARTESIAN_POINT ( 'NONE',  ( -21.55341960407619339, 5.719274019375674811, 48.54275706135234714 ) ) ;
#77059 = CARTESIAN_POINT ( 'NONE',  ( 19.03943276465977164, -0.05219959533909143690, 48.74890960531435979 ) ) ;
#77060 = CARTESIAN_POINT ( 'NONE',  ( -16.29526858892877783, -7.335722546920120379, 85.79670597800210885 ) ) ;
#77061 = CARTESIAN_POINT ( 'NONE',  ( -13.97604488694527625, -13.89961937509977652, 111.8739096053143243 ) ) ;
#77062 = CARTESIAN_POINT ( 'NONE',  ( -14.34966873604960291, -8.224510206698953496, 61.66557627198103120 ) ) ;
#77063 = CARTESIAN_POINT ( 'NONE',  ( 5.823673210054125526, 21.52544592524343514, 69.79057627198102409 ) ) ;
#77064 = LINE ( 'NONE', #50721, #54646 ) ;
#77065 = CARTESIAN_POINT ( 'NONE',  ( -13.89961937509957401, -13.97604488694547875, 44.37609039468566863 ) ) ;
#77066 = CARTESIAN_POINT ( 'NONE',  ( 21.76480897080536181, -7.725232727579773417, 173.1951875983967852 ) ) ;
#77067 = VECTOR ( 'NONE', #94545, 1000.000000000000000 ) ;
#77069 = CARTESIAN_POINT ( 'NONE',  ( 19.05341960407611168, 5.049401038298154454, 73.95724293864768129 ) ) ;
#77068 = CARTESIAN_POINT ( 'NONE',  ( 5.049401038298161559, -19.05341960407611168, 67.70724293864769550 ) ) ;
#77070 = CARTESIAN_POINT ( 'NONE',  ( 14.34966873604972726, -8.224510206698740333, 45.83442372801901854 ) ) ;
#77071 = CARTESIAN_POINT ( 'NONE',  ( -17.60779699588840330, -5.500000000000021316, 66.34981316670106821 ) ) ;
#77072 = CARTESIAN_POINT ( 'NONE',  ( 16.51473224551083163, -9.474510206698727899, 25.83442372801900078 ) ) ;
#77073 = DIRECTION ( 'NONE',  ( 1.000000000000000000, 0.000000000000000000, 0.000000000000000000 ) ) ;
#77074 = CARTESIAN_POINT ( 'NONE',  ( -16.55341960407617563, 4.379528057220093196, 88.54275706135236135 ) ) ;
#77075 = CARTESIAN_POINT ( 'NONE',  ( -3.950025424479786551, -4.892422815249006796, -64.50280008989093972 ) ) ;
#77076 = CARTESIAN_POINT ( 'NONE',  ( -12.06949235617739369, -12.14591786802326823, 84.37609039468570415 ) ) ;
#77077 =( BOUNDED_CURVE ( )  B_SPLINE_CURVE ( 2, ( #25641, #196488, #7430, #117625, #87286, #181312, #130780, #192472, #9461, #149961, #53955, #115630, #180325 ),
 .UNSPECIFIED., .F., .T. ) 
 B_SPLINE_CURVE_WITH_KNOTS ( ( 3, 2, 2, 2, 2, 2, 3 ),
 ( 0.3972129583543985154, 0.3991228070175438791, 0.4035087719298245390, 0.4078947368421052544, 0.4122807017543859698, 0.4166666666666666852, 0.4186221951519023543 ),
 .UNSPECIFIED. ) 
 CURVE ( )  GEOMETRIC_REPRESENTATION_ITEM ( )  RATIONAL_B_SPLINE_CURVE ( ( 0.9832469066685285419, 0.9851625545550100060, 1.000000000000000000, 0.9659258262890683122, 1.000000000000000000, 0.9659258262890683122, 1.000000000000000000, 0.9659258262890683122, 1.000000000000000000, 0.9659258262890683122, 1.000000000000000000, 0.9848076720550081875, 0.9831626618144004848 ) ) 
 REPRESENTATION_ITEM ( '' )  );
#77078 = CARTESIAN_POINT ( 'NONE',  ( -4.483927247898782831, 16.52544592524335698, 52.70942372801902565 ) ) ;
#77079 = CARTESIAN_POINT ( 'NONE',  ( 9.474510206698729675, 16.51473224551082808, 27.08442372801900433 ) ) ;
#77081 = DIRECTION ( 'NONE',  ( 3.469446951953612217E-15, 0.000000000000000000, -1.000000000000000000 ) ) ;
#77080 = CARTESIAN_POINT ( 'NONE',  ( -9.474510206698964154, 16.51473224551069663, 50.41557627198102409 ) ) ;
#77082 = CARTESIAN_POINT ( 'NONE',  ( -5.719274019375665041, -21.55341960407619695, 64.79275706135234714 ) ) ;
#77083 = CARTESIAN_POINT ( 'NONE',  ( 0.05219959533936267826, -19.03943276465977164, 80.00109039468567573 ) ) ;
#77084 = CARTESIAN_POINT ( 'NONE',  ( -21.55341960407619339, 5.719274019375674811, 103.5427570613523613 ) ) ;
#77085 = CARTESIAN_POINT ( 'NONE',  ( -9.564922557960796823, -16.46253265017161027, 37.08224293864768839 ) ) ;
#77086 = CARTESIAN_POINT ( 'NONE',  ( -16.91340028822897068, 14.83455351965406877, -58.07447375877293894 ) ) ;
#77087 = CARTESIAN_POINT ( 'NONE',  ( -15.80617190586745835, -15.72974639402198527, 61.87390960531436690 ) ) ;
#77088 = CARTESIAN_POINT ( 'NONE',  ( -5.823673210054116645, -21.52544592524344225, 22.29057627198102765 ) ) ;
#77089 = CARTESIAN_POINT ( 'NONE',  ( -4.379528057220328563, 16.55341960407611168, 110.2072429386477239 ) ) ;
#77090 = CARTESIAN_POINT ( 'NONE',  ( -14.34966873604972548, 8.224510206698743886, 33.33442372801900433 ) ) ;
#77091 = CARTESIAN_POINT ( 'NONE',  ( -8.224510206698948167, 14.34966873604960824, 25.41557627198103120 ) ) ;
#77092 = EDGE_LOOP ( 'NONE', ( #58102, #8490, #8225 ) ) ;
#77093 = EDGE_CURVE ( 'NONE', #100463, #79565, #47785, .T. ) ;
#77094 = CARTESIAN_POINT ( 'NONE',  ( -21.52544592524334988, -5.823673210054445271, 18.95942372801901143 ) ) ;
#77096 = CARTESIAN_POINT ( 'NONE',  ( -6.020228577223754586E-15, 39.95556452105416412, -6.500000000000000000 ) ) ;
#77095 = CARTESIAN_POINT ( 'NONE',  ( -16.52544592524342804, 4.483927247898546575, 36.04057627198102409 ) ) ;
#77097 = CARTESIAN_POINT ( 'NONE',  ( -13.89961937509957401, -13.97604488694547875, 104.3760903946856757 ) ) ;
#77098 = CARTESIAN_POINT ( 'NONE',  ( -9.474510206698720793, -16.51473224551083518, 24.58442372801900078 ) ) ;
#77099 = CARTESIAN_POINT ( 'NONE',  ( -14.34966873604960291, -8.224510206698953496, 41.66557627198103120 ) ) ;
#77100 = CARTESIAN_POINT ( 'NONE',  ( 15.80617190586746368, 15.72974639402197994, 104.3739096053143669 ) ) ;
#77102 = CARTESIAN_POINT ( 'NONE',  ( -10.72451020669898014, 18.67979575497178502, 60.41557627198102409 ) ) ;
#77101 = CARTESIAN_POINT ( 'NONE',  ( 22.00000000000000000, -5.510910596163089556E-15, 45.00000000000000000 ) ) ;
#77103 = CARTESIAN_POINT ( 'NONE',  ( -5.153800228976328057, -19.02544592524343514, 72.29057627198102409 ) ) ;
#77104 = CARTESIAN_POINT ( 'NONE',  ( -4.379528057220328563, 16.55341960407611168, 50.20724293864769550 ) ) ;
#77105 = CARTESIAN_POINT ( 'NONE',  ( 16.51473224551069308, 9.474510206698969483, 89.16557627198103830 ) ) ;
#77106 = DIRECTION ( 'NONE',  ( 0.000000000000000000, 0.000000000000000000, -1.000000000000000000 ) ) ;
#77107 = CARTESIAN_POINT ( 'NONE',  ( -19.05341960407617563, 5.049401038297882671, 53.54275706135231871 ) ) ;
#77108 = CARTESIAN_POINT ( 'NONE',  ( 21.55341960407610458, 5.719274019375980345, 88.95724293864769550 ) ) ;
#77109 = CARTESIAN_POINT ( 'NONE',  ( 5.049401038298161559, -19.05341960407611168, 47.70724293864770260 ) ) ;
#77110 = CARTESIAN_POINT ( 'NONE',  ( -12.06949235617756955, 12.14591786802309770, 105.6239096053143669 ) ) ;
#77111 = CARTESIAN_POINT ( 'NONE',  ( -5.823673210054431948, 21.52544592524334988, 47.70942372801902565 ) ) ;
#77112 = CARTESIAN_POINT ( 'NONE',  ( -17.14385361876520619, 23.59649016807275856, 146.5750000027311444 ) ) ;
#77113 = CARTESIAN_POINT ( 'NONE',  ( -14.29746914071049879, 8.314922557960819915, 25.83224293864769194 ) ) ;
#77114 = CARTESIAN_POINT ( 'NONE',  ( -16.46253265017160317, 9.564922557960807481, 45.83224293864769550 ) ) ;
#77115 = CARTESIAN_POINT ( 'NONE',  ( -9.474510206698964154, 16.51473224551069663, 95.41557627198102409 ) ) ;
#77116 = CARTESIAN_POINT ( 'NONE',  ( -18.62759615963270932, 10.81492255796079327, 55.83224293864770260 ) ) ;
#77117 = CARTESIAN_POINT ( 'NONE',  ( -18.22780087662119541, 5.500000000000102141, 46.01763182126894947 ) ) ;
#77118 = CARTESIAN_POINT ( 'NONE',  ( 16.46253265017160672, -9.564922557960803928, 48.33224293864769550 ) ) ;
#77119 = CARTESIAN_POINT ( 'NONE',  ( -5.823673210054116645, -21.52544592524344225, 47.29057627198103120 ) ) ;
#77120 = VERTEX_POINT ( 'NONE', #131300 ) ;
#77121 = CARTESIAN_POINT ( 'NONE',  ( 0.05219959533937995610, -21.53943276465977519, 85.00109039468568994 ) ) ;
#77123 = CARTESIAN_POINT ( 'NONE',  ( -12.14591786802326823, 12.06949235617739902, 88.12609039468570415 ) ) ;
#77122 = CARTESIAN_POINT ( 'NONE',  ( 8.963443992379767522, -45.12205215321816354, -22.08927284594079765 ) ) ;
#77124 = CARTESIAN_POINT ( 'NONE',  ( -12.06949235617739369, -12.14591786802326823, 89.37609039468568994 ) ) ;
#77125 = CARTESIAN_POINT ( 'NONE',  ( 16.51473224551069308, 9.474510206698969483, 59.16557627198102409 ) ) ;
#77126 = CARTESIAN_POINT ( 'NONE',  ( 0.05219959533909260263, 19.03943276465977164, 59.99890960531436690 ) ) ;
#77127 = ORIENTED_EDGE ( 'NONE', *, *, #195610, .T. ) ;
#77128 = CARTESIAN_POINT ( 'NONE',  ( 9.564922557961047289, -16.46253265017146816, 25.41775706135234003 ) ) ;
#77129 = CARTESIAN_POINT ( 'NONE',  ( 0.05219959533934541429, -16.53943276465976808, 80.00109039468568994 ) ) ;
#77130 = CARTESIAN_POINT ( 'NONE',  ( 10.72451020669871369, 18.67979575497193778, 107.0844237280190043 ) ) ;
#77131 = CARTESIAN_POINT ( 'NONE',  ( 16.51473224551069308, 9.474510206698969483, 79.16557627198103830 ) ) ;
#77132 = CARTESIAN_POINT ( 'NONE',  ( -18.67979575497178146, -10.72451020669898902, 51.66557627198102409 ) ) ;
#77133 = CARTESIAN_POINT ( 'NONE',  ( 4.483927247898790824, -16.52544592524335698, 20.20942372801900788 ) ) ;
#77134 = CARTESIAN_POINT ( 'NONE',  ( -21.55341960407619339, 5.719274019375674811, 83.54275706135234714 ) ) ;
#77135 = CARTESIAN_POINT ( 'NONE',  ( -14.29746914071037622, -8.314922557961029526, 44.16775706135234714 ) ) ;
#77136 = CARTESIAN_POINT ( 'NONE',  ( 10.72451020669898902, -18.67979575497178502, 107.9155762719810241 ) ) ;
#77137 = CARTESIAN_POINT ( 'NONE',  ( 5.049401038297881783, 19.05341960407617563, 112.2927570613523471 ) ) ;
#77138 = CARTESIAN_POINT ( 'NONE',  ( 19.02544592524343514, -5.153800228976328945, 73.54057627198103830 ) ) ;
#77139 = CARTESIAN_POINT ( 'NONE',  ( 4.379528057220092307, 16.55341960407617563, 27.29275706135234358 ) ) ;
#77140 = CARTESIAN_POINT ( 'NONE',  ( -19.03943276465977164, 0.05219959533909376836, 41.24890960531435269 ) ) ;
#77141 = CARTESIAN_POINT ( 'NONE',  ( 16.55341960407618274, -4.379528057220086978, 21.04275706135234714 ) ) ;
#77142 = CARTESIAN_POINT ( 'NONE',  ( 14.34966873604960469, 8.224510206698951720, 74.16557627198102409 ) ) ;
#77143 = CARTESIAN_POINT ( 'NONE',  ( -4.379528057220086978, -16.55341960407618274, 89.79275706135236135 ) ) ;
#77145 = CARTESIAN_POINT ( 'NONE',  ( -19.02544592524342804, 5.153800228976336051, 66.04057627198103830 ) ) ;
#77144 = CARTESIAN_POINT ( 'NONE',  ( -15.72974639402176322, -15.80617190586768395, 34.37609039468568284 ) ) ;
#77146 = CARTESIAN_POINT ( 'NONE',  ( 19.02544592524343514, -5.153800228976328945, 68.54057627198103830 ) ) ;
#77147 = CARTESIAN_POINT ( 'NONE',  ( -16.55341960407617563, 4.379528057220093196, 83.54275706135234714 ) ) ;
#77149 = ORIENTED_EDGE ( 'NONE', *, *, #176999, .F. ) ;
#77148 = CARTESIAN_POINT ( 'NONE',  ( -21.88033147701211689, -7.974798826780787664, 169.5716465351736986 ) ) ;
#77150 = ORIENTED_EDGE ( 'NONE', *, *, #172493, .F. ) ;
#77151 = CARTESIAN_POINT ( 'NONE',  ( 13.89961937509957401, 13.97604488694547697, 31.87609039468566863 ) ) ;
#77152 = CARTESIAN_POINT ( 'NONE',  ( -19.05341960407611168, -5.049401038298163336, 31.45724293864769550 ) ) ;
#77154 = ORIENTED_EDGE ( 'NONE', *, *, #96372, .T. ) ;
#77153 = CARTESIAN_POINT ( 'NONE',  ( 5.049401038298161559, -19.05341960407611168, 112.7072429386476813 ) ) ;
#77155 = CARTESIAN_POINT ( 'NONE',  ( -8.314922557961024197, 14.29746914071037800, 27.91775706135234358 ) ) ;
#77156 = AXIS2_PLACEMENT_3D ( 'NONE', #72122, #27640, #59923 ) ;
#77158 = CARTESIAN_POINT ( 'NONE',  ( -4.379528057220086978, -16.55341960407618274, 39.79275706135235424 ) ) ;
#77157 = CARTESIAN_POINT ( 'NONE',  ( 5.049401038297881783, 19.05341960407617563, 52.29275706135234003 ) ) ;
#77159 = CARTESIAN_POINT ( 'NONE',  ( -19.02544592524342804, 5.153800228976336051, 101.0405762719810241 ) ) ;
#77160 = CARTESIAN_POINT ( 'NONE',  ( 19.02544592524343514, -5.153800228976328945, 63.54057627198103830 ) ) ;
#77161 = CARTESIAN_POINT ( 'NONE',  ( -5.823673210054116645, -21.52544592524344225, 102.2905762719810383 ) ) ;
#77163 = CARTESIAN_POINT ( 'NONE',  ( 16.46253265017160672, -9.564922557960803928, 23.33224293864769194 ) ) ;
#77162 = CARTESIAN_POINT ( 'NONE',  ( -13.97604488694527625, -13.89961937509977652, 91.87390960531432427 ) ) ;
#77164 = CARTESIAN_POINT ( 'NONE',  ( -5.153800228976328057, -19.02544592524343514, 62.29057627198100988 ) ) ;
#77166 = CARTESIAN_POINT ( 'NONE',  ( -9.564922557960796823, -16.46253265017161027, 22.08224293864768839 ) ) ;
#77165 = CARTESIAN_POINT ( 'NONE',  ( 4.379528057220092307, 16.55341960407617563, 112.2927570613523471 ) ) ;
#77167 = CARTESIAN_POINT ( 'NONE',  ( 16.46253265017146816, 9.564922557961045513, 36.66775706135233293 ) ) ;
#77168 = CARTESIAN_POINT ( 'NONE',  ( 16.53943276465976808, -0.05219959533910856209, 63.74890960531435979 ) ) ;
#77169 = CARTESIAN_POINT ( 'NONE',  ( -0.05219959533937732626, 21.53943276465977519, 102.5010903946856899 ) ) ;
#77170 = CARTESIAN_POINT ( 'NONE',  ( 19.02544592524343514, -5.153800228976328945, 38.54057627198103120 ) ) ;
#77171 = CARTESIAN_POINT ( 'NONE',  ( -12.14591786802326823, 12.06949235617739902, 58.12609039468568994 ) ) ;
#77173 = CARTESIAN_POINT ( 'NONE',  ( 5.719274019375673035, 21.55341960407619339, 92.29275706135236135 ) ) ;
#77172 = CARTESIAN_POINT ( 'NONE',  ( -16.53943276465976808, 0.05219959533911058130, 41.24890960531435269 ) ) ;
#77174 = CARTESIAN_POINT ( 'NONE',  ( -5.049401038298153566, 19.05341960407611168, 75.20724293864769550 ) ) ;
#77175 = CARTESIAN_POINT ( 'NONE',  ( 16.51473224551069308, 9.474510206698969483, 99.16557627198102409 ) ) ;
#77176 = CARTESIAN_POINT ( 'NONE',  ( 14.29746914071049879, -8.314922557960816363, 108.3322429386477097 ) ) ;
#77177 = CARTESIAN_POINT ( 'NONE',  ( 4.379528057220339221, -16.55341960407611168, 77.70724293864770971 ) ) ;
#77178 = CARTESIAN_POINT ( 'NONE',  ( 0.05219959533907565091, 21.53943276465977519, 84.99890960531436690 ) ) ;
#77179 = CARTESIAN_POINT ( 'NONE',  ( -5.049401038298153566, 19.05341960407611168, 75.20724293864769550 ) ) ;
#77180 = CARTESIAN_POINT ( 'NONE',  ( 5.823673210054125526, 21.52544592524343514, 94.79057627198105251 ) ) ;
#77181 = CARTESIAN_POINT ( 'NONE',  ( -0.05219959533936034679, 19.03943276465977164, 72.50109039468566152 ) ) ;
#77183 = CARTESIAN_POINT ( 'NONE',  ( -8.224510206698948167, 14.34966873604960824, 90.41557627198103830 ) ) ;
#77182 = CARTESIAN_POINT ( 'NONE',  ( 35.00000000000000000, 3.181980515339470905, 8.889087296526001936 ) ) ;
#77184 = CARTESIAN_POINT ( 'NONE',  ( 9.474510206698971260, -16.51473224551069308, 62.91557627198102409 ) ) ;
#77185 = CARTESIAN_POINT ( 'NONE',  ( -18.62759615963270932, 10.81492255796079327, 65.83224293864769550 ) ) ;
#77186 = CARTESIAN_POINT ( 'NONE',  ( 1.500000000000000888, 15.20000000000002061, -59.79525829764741474 ) ) ;
#77188 = DIRECTION ( 'NONE',  ( 0.000000000000000000, 0.000000000000000000, 1.000000000000000000 ) ) ;
#77187 = CARTESIAN_POINT ( 'NONE',  ( -4.379528057220328563, 16.55341960407611168, 25.20724293864769550 ) ) ;
#77189 = CARTESIAN_POINT ( 'NONE',  ( -5.049401038297874678, -19.05341960407617918, 109.7927570613523187 ) ) ;
#77190 = ADVANCED_FACE ( 'NONE', ( #192989 ), #100953, .F. ) ;
#77191 = CARTESIAN_POINT ( 'NONE',  ( -0.05219959533910754901, -16.53943276465976808, 82.49890960531436690 ) ) ;
#77192 = CARTESIAN_POINT ( 'NONE',  ( 22.00000000000000000, -1.163414459189985801E-14, 95.00000000000000000 ) ) ;
#77193 = CARTESIAN_POINT ( 'NONE',  ( -16.51473224551069308, -9.474510206698971260, 76.66557627198103830 ) ) ;
#77194 = CARTESIAN_POINT ( 'NONE',  ( 9.564922557960805705, 16.46253265017160317, 34.58224293864770260 ) ) ;
#77195 = CARTESIAN_POINT ( 'NONE',  ( 14.29746914071049879, -8.314922557960816363, 68.33224293864769550 ) ) ;
#77196 = CARTESIAN_POINT ( 'NONE',  ( 13.97604488694527802, 13.89961937509977652, 109.3739096053143669 ) ) ;
#77197 = CARTESIAN_POINT ( 'NONE',  ( 19.02544592524334988, 5.153800228976608722, 91.45942372801900433 ) ) ;
#77198 = CARTESIAN_POINT ( 'NONE',  ( -16.51473224551069308, -9.474510206698971260, 96.66557627198102409 ) ) ;
#77199 = CARTESIAN_POINT ( 'NONE',  ( -0.05219959533907301413, -21.53943276465977519, 77.49890960531433848 ) ) ;
#77200 = CARTESIAN_POINT ( 'NONE',  ( 14.34966873604972726, -8.224510206698740333, 65.83442372801900433 ) ) ;
#77201 = CARTESIAN_POINT ( 'NONE',  ( -17.48853670773245739, 5.747243402303007009, 93.66671299749994262 ) ) ;
#77202 = CARTESIAN_POINT ( 'NONE',  ( -0.05219959533909027116, -19.03943276465977164, 57.49890960531435979 ) ) ;
#77203 = CARTESIAN_POINT ( 'NONE',  ( -5.823673210054116645, -21.52544592524344225, 62.29057627198102409 ) ) ;
#77204 = CARTESIAN_POINT ( 'NONE',  ( -13.97604488694547697, 13.89961937509957934, 108.1260903946856331 ) ) ;
#77206 = CARTESIAN_POINT ( 'NONE',  ( -10.81492255796105439, 18.62759615963255655, 47.91775706135234714 ) ) ;
#77205 = CARTESIAN_POINT ( 'NONE',  ( 14.34966873604960469, 8.224510206698951720, 44.16557627198103120 ) ) ;
#77207 = CARTESIAN_POINT ( 'NONE',  ( -26.79475375365586842, 2.428612866367529932E-14, 155.0000000000000000 ) ) ;
#77209 = CARTESIAN_POINT ( 'NONE',  ( -0.05219959533909027116, -19.03943276465977164, 107.4989096053143527 ) ) ;
#77208 = CARTESIAN_POINT ( 'NONE',  ( -16.55341960407617563, 4.379528057220093196, 78.54275706135236135 ) ) ;
#77210 = CARTESIAN_POINT ( 'NONE',  ( -5.153800228976328057, -19.02544592524343514, 102.2905762719810241 ) ) ;
#77211 = CARTESIAN_POINT ( 'NONE',  ( -19.03943276465977164, -1.327063459122257427E-13, 115.0000000000000142 ) ) ;
#77212 = CARTESIAN_POINT ( 'NONE',  ( 14.29746914071037800, 8.314922557961029526, 91.66775706135234714 ) ) ;
#77213 = CARTESIAN_POINT ( 'NONE',  ( -16.55341960407617563, 4.379528057220093196, 53.54275706135234714 ) ) ;
#77214 = CARTESIAN_POINT ( 'NONE',  ( -0.05219959533909027116, -19.03943276465977164, 52.49890960531436690 ) ) ;
#77215 = CARTESIAN_POINT ( 'NONE',  ( -0.05219959533909027116, -19.03943276465977164, 72.49890960531435269 ) ) ;
#77216 = CARTESIAN_POINT ( 'NONE',  ( 21.53943276465977519, 0.05219959533937863772, 51.25109039468568994 ) ) ;
#77217 = CARTESIAN_POINT ( 'NONE',  ( -0.05219959533934338120, 16.53943276465976808, 67.50109039468568994 ) ) ;
#77218 = CARTESIAN_POINT ( 'NONE',  ( 16.55341960407611168, 4.379528057220329451, 33.95724293864769550 ) ) ;
#77219 = CARTESIAN_POINT ( 'NONE',  ( 19.05341960407611168, 5.049401038298154454, 43.95724293864769550 ) ) ;
#77220 = CARTESIAN_POINT ( 'NONE',  ( -16.46253265017160317, 9.564922557960807481, 30.83224293864769550 ) ) ;
#77221 = CARTESIAN_POINT ( 'NONE',  ( -12.06949235617739369, -12.14591786802326823, 29.37609039468568284 ) ) ;
#77222 = CARTESIAN_POINT ( 'NONE',  ( 19.02544592524334988, 5.153800228976608722, 76.45942372801897591 ) ) ;
#77223 = CARTESIAN_POINT ( 'NONE',  ( 14.29746914071049879, -8.314922557960816363, 88.33224293864769550 ) ) ;
#77224 = CARTESIAN_POINT ( 'NONE',  ( -19.03943276465977164, 0.05219959533909376836, 46.24890960531435979 ) ) ;
#77226 = CARTESIAN_POINT ( 'NONE',  ( 0.000000000000000000, 0.000000000000000000, -15.00000000000000000 ) ) ;
#77225 = CARTESIAN_POINT ( 'NONE',  ( 5.049401038297881783, 19.05341960407617563, 87.29275706135234714 ) ) ;
#77227 = CARTESIAN_POINT ( 'NONE',  ( -15.72974639402176322, -15.80617190586768395, 84.37609039468570415 ) ) ;
#77228 = CARTESIAN_POINT ( 'NONE',  ( -16.53943276465976808, -0.05219959533934237506, 48.75109039468568284 ) ) ;
#77229 = PLANE ( 'NONE',  #192291 ) ;
#77230 = CARTESIAN_POINT ( 'NONE',  ( 21.52544592524344225, -5.823673210054117533, 53.54057627198103120 ) ) ;
#77231 = CARTESIAN_POINT ( 'NONE',  ( -16.53943276465976808, -0.05219959533934237506, 33.75109039468568284 ) ) ;
#77232 = CARTESIAN_POINT ( 'NONE',  ( 9.564922557960805705, 16.46253265017160317, 34.58224293864770260 ) ) ;
#77233 = CARTESIAN_POINT ( 'NONE',  ( 5.049401038297881783, 19.05341960407617563, 42.29275706135234003 ) ) ;
#77234 = CARTESIAN_POINT ( 'NONE',  ( 16.51473224551069308, 9.474510206698969483, 79.16557627198103830 ) ) ;
#77235 = CARTESIAN_POINT ( 'NONE',  ( -5.153800228976328057, -19.02544592524343514, 47.29057627198102409 ) ) ;
#77236 = CARTESIAN_POINT ( 'NONE',  ( 16.83259678516731839, 17.45991095687928762, -54.25516819912628108 ) ) ;
#77237 = CARTESIAN_POINT ( 'NONE',  ( 10.72451020669871369, 18.67979575497193778, 72.08442372801899012 ) ) ;
#77238 = LINE ( 'NONE', #62059, #14282 ) ;
#77239 = CARTESIAN_POINT ( 'NONE',  ( 9.564922557961047289, -16.46253265017146816, 30.41775706135232937 ) ) ;
#77240 = CARTESIAN_POINT ( 'NONE',  ( -15.72974639402176322, -15.80617190586768395, 104.3760903946856899 ) ) ;
#77241 = CARTESIAN_POINT ( 'NONE',  ( 16.53943276465976808, -0.05219959533910856209, 43.74890960531435979 ) ) ;
#77242 = CARTESIAN_POINT ( 'NONE',  ( 5.153800228976335163, 19.02544592524342804, 44.79057627198103830 ) ) ;
#77243 = CARTESIAN_POINT ( 'NONE',  ( -13.97604488694527625, -13.89961937509977652, 101.8739096053143811 ) ) ;
#77244 = CARTESIAN_POINT ( 'NONE',  ( 15.80617190586769283, -15.72974639402175789, 85.62609039468568994 ) ) ;
#77245 = CARTESIAN_POINT ( 'NONE',  ( 9.474510206698971260, -16.51473224551069308, 57.91557627198103120 ) ) ;
#77246 = CARTESIAN_POINT ( 'NONE',  ( 5.719274019375673035, 21.55341960407619339, 82.29275706135234714 ) ) ;
#77247 = CARTESIAN_POINT ( 'NONE',  ( -21.55341960407610458, -5.719274019375992779, 36.45724293864768839 ) ) ;
#77248 = CARTESIAN_POINT ( 'NONE',  ( 10.72451020669871369, 18.67979575497193778, 32.08442372801901854 ) ) ;
#77249 = CARTESIAN_POINT ( 'NONE',  ( 0.05219959533936267826, -19.03943276465977164, 55.00109039468566863 ) ) ;
#77250 = CARTESIAN_POINT ( 'NONE',  ( 9.474510206698971260, -16.51473224551069308, 22.91557627198102765 ) ) ;
#77251 = CARTESIAN_POINT ( 'NONE',  ( 0.05219959533909260263, 19.03943276465977164, 79.99890960531436690 ) ) ;
#77252 = CARTESIAN_POINT ( 'NONE',  ( -4.379528057220086978, -16.55341960407618274, 34.79275706135235424 ) ) ;
#77253 = CARTESIAN_POINT ( 'NONE',  ( 14.29746914071049879, -8.314922557960816363, 93.33224293864769550 ) ) ;
#77254 = CARTESIAN_POINT ( 'NONE',  ( 13.89961937509977652, -13.97604488694527269, 58.12390960531436690 ) ) ;
#77255 = CARTESIAN_POINT ( 'NONE',  ( 21.55341960407610458, 5.719274019375980345, 33.95724293864769550 ) ) ;
#77256 = CARTESIAN_POINT ( 'NONE',  ( 9.474510206698729675, 16.51473224551082808, 102.0844237280190043 ) ) ;
#77257 = CARTESIAN_POINT ( 'NONE',  ( -15.72974639402197994, 15.80617190586746368, 105.6239096053143669 ) ) ;
#77258 = CARTESIAN_POINT ( 'NONE',  ( -18.62759615963255300, -10.81492255796106328, 59.16775706135234714 ) ) ;
#77259 = CARTESIAN_POINT ( 'NONE',  ( 16.53943276465976808, 0.05219959533934440121, 66.25109039468567573 ) ) ;
#77260 = CARTESIAN_POINT ( 'NONE',  ( 4.379528057220092307, 16.55341960407617563, 72.29275706135236135 ) ) ;
#77261 = CARTESIAN_POINT ( 'NONE',  ( -0.05219959533909027116, -19.03943276465977164, 62.49890960531435979 ) ) ;
#77262 = CARTESIAN_POINT ( 'NONE',  ( 12.14591786802327356, -12.06949235617739191, 90.62609039468567573 ) ) ;
#77263 = CARTESIAN_POINT ( 'NONE',  ( 0.05219959533907565091, 21.53943276465977519, 114.9989096053143669 ) ) ;
#77264 = CARTESIAN_POINT ( 'NONE',  ( 4.483927247898545687, 16.52544592524342804, 69.79057627198102409 ) ) ;
#77265 = CARTESIAN_POINT ( 'NONE',  ( -9.474510206698964154, 16.51473224551069663, 80.41557627198103830 ) ) ;
#77266 = CARTESIAN_POINT ( 'NONE',  ( 14.34966873604972726, -8.224510206698740333, 70.83442372801901854 ) ) ;
#77267 = CARTESIAN_POINT ( 'NONE',  ( -21.55341960407619339, 5.719274019375674811, 63.54275706135234003 ) ) ;
#77268 = CARTESIAN_POINT ( 'NONE',  ( 0.05219959533936267826, -19.03943276465977164, 110.0010903946856757 ) ) ;
#77269 = CARTESIAN_POINT ( 'NONE',  ( -10.72451020669898014, 18.67979575497178502, 115.4155762719810241 ) ) ;
#77270 = CARTESIAN_POINT ( 'NONE',  ( -16.53943276465976808, 0.05219959533911058130, 61.24890960531435979 ) ) ;
#77271 = VERTEX_POINT ( 'NONE', #11980 ) ;
#77272 = CARTESIAN_POINT ( 'NONE',  ( -16.20579543436679160, 7.371946100355093456, 69.43479165828128430 ) ) ;
#77273 = CARTESIAN_POINT ( 'NONE',  ( -5.719274019375978568, 21.55341960407610458, 85.20724293864770971 ) ) ;
#77274 = CARTESIAN_POINT ( 'NONE',  ( 4.483927247898545687, 16.52544592524342804, 34.79057627198103120 ) ) ;
#77275 = ORIENTED_EDGE ( 'NONE', *, *, #167369, .T. ) ;
#77276 = CARTESIAN_POINT ( 'NONE',  ( 34.98624150382327969, 6.090157606732328865, 40.61607269374898266 ) ) ;
#77277 = CARTESIAN_POINT ( 'NONE',  ( 15.72974639402176855, 15.80617190586768217, 21.87609039468567573 ) ) ;
#77278 = CARTESIAN_POINT ( 'NONE',  ( -19.05341960407611168, -5.049401038298163336, 106.4572429386476955 ) ) ;
#77279 = CARTESIAN_POINT ( 'NONE',  ( 10.81492255796106328, -18.62759615963255655, 25.41775706135235779 ) ) ;
#77280 = CARTESIAN_POINT ( 'NONE',  ( -14.29746914071049879, 8.314922557960819915, 45.83224293864769550 ) ) ;
#77281 = CARTESIAN_POINT ( 'NONE',  ( 16.52544592524335698, 4.483927247898782831, 61.45942372801901854 ) ) ;
#77282 = CARTESIAN_POINT ( 'NONE',  ( 19.05341960407611168, 5.049401038298154454, 58.95724293864768129 ) ) ;
#77283 = CARTESIAN_POINT ( 'NONE',  ( -5.049401038297874678, -19.05341960407617918, 59.79275706135231871 ) ) ;
#77284 = CARTESIAN_POINT ( 'NONE',  ( -9.564922557960796823, -16.46253265017161027, 82.08224293864768129 ) ) ;
#77285 = CARTESIAN_POINT ( 'NONE',  ( 15.80617190586746368, 15.72974639402197994, 44.37390960531435979 ) ) ;
#77286 = CARTESIAN_POINT ( 'NONE',  ( -7.213464565008907314, -38.12638803158534984, -24.00445952849389641 ) ) ;
#77287 = CARTESIAN_POINT ( 'NONE',  ( 16.46253265017160672, -9.564922557960803928, 53.33224293864768839 ) ) ;
#77288 = CARTESIAN_POINT ( 'NONE',  ( -4.379528057220086978, -16.55341960407618274, 34.79275706135235424 ) ) ;
#77289 = CARTESIAN_POINT ( 'NONE',  ( 19.03943276465977164, 0.05219959533936151252, 66.25109039468567573 ) ) ;
#77290 = CARTESIAN_POINT ( 'NONE',  ( 10.81492255796078972, 18.62759615963270932, 114.5822429386477097 ) ) ;
#77291 = CARTESIAN_POINT ( 'NONE',  ( 12.06949235617757843, -12.14591786802309237, 53.12390960531436690 ) ) ;
#77292 = CARTESIAN_POINT ( 'NONE',  ( 13.97604488694527802, 13.89961937509977652, 94.37390960531436690 ) ) ;
#77293 = CARTESIAN_POINT ( 'NONE',  ( -15.72974639402197994, 15.80617190586746368, 60.62390960531437401 ) ) ;
#77295 = CARTESIAN_POINT ( 'NONE',  ( -12.14591786802326823, 12.06949235617739902, 33.12609039468569705 ) ) ;
#77294 = CARTESIAN_POINT ( 'NONE',  ( -10.72451020669898014, 18.67979575497178502, 95.41557627198102409 ) ) ;
#77296 = ADVANCED_FACE ( 'NONE', ( #102966 ), #86473, .T. ) ;
#77297 = CARTESIAN_POINT ( 'NONE',  ( -0.05219959533907301413, -21.53943276465977519, 32.49890960531435979 ) ) ;
#77298 = CARTESIAN_POINT ( 'NONE',  ( 18.67979575497194134, -10.72451020669871369, 90.83442372801901854 ) ) ;
#77299 = CARTESIAN_POINT ( 'NONE',  ( 13.97604488694527802, 13.89961937509977652, 84.37390960531433848 ) ) ;
#77300 = AXIS2_PLACEMENT_3D ( 'NONE', #130653, #102331, #71001 ) ;
#77301 = CARTESIAN_POINT ( 'NONE',  ( -0.05219959533909027116, -19.03943276465977164, 37.49890960531436690 ) ) ;
#77302 = CARTESIAN_POINT ( 'NONE',  ( -19.03943276465977164, 0.05219959533909376836, 101.2489096053143669 ) ) ;
#77303 = CARTESIAN_POINT ( 'NONE',  ( 14.34966873604960469, 8.224510206698951720, 104.1655762719810241 ) ) ;
#77304 = CARTESIAN_POINT ( 'NONE',  ( -19.02544592524342804, 5.153800228976336051, 61.04057627198103120 ) ) ;
#77305 = CARTESIAN_POINT ( 'NONE',  ( 16.55341960407618274, -4.379528057220086978, 21.04275706135234714 ) ) ;
#77306 = CARTESIAN_POINT ( 'NONE',  ( 17.50000000000001776, 3.850315288878741526, 33.23370869396553928 ) ) ;
#77308 = CARTESIAN_POINT ( 'NONE',  ( -10.81492255796078084, -18.62759615963271287, 27.08224293864769550 ) ) ;
#77307 = CARTESIAN_POINT ( 'NONE',  ( -18.67979575497193778, 10.72451020669871902, 98.33442372801901854 ) ) ;
#77310 = EDGE_CURVE ( 'NONE', #42462, #1415, #9109, .T. ) ;
#77309 = CARTESIAN_POINT ( 'NONE',  ( -16.53943276465976808, -0.05219959533934237506, 88.75109039468567573 ) ) ;
#77311 = CARTESIAN_POINT ( 'NONE',  ( 22.46875132164074884, -20.34737474481815056, -47.91687182510066378 ) ) ;
#77312 = CARTESIAN_POINT ( 'NONE',  ( -16.46253265017146816, -9.564922557961047289, 64.16775706135233293 ) ) ;
#77313 = CARTESIAN_POINT ( 'NONE',  ( -16.51473224551082808, 9.474510206698731452, 28.33442372801900433 ) ) ;
#77314 = CARTESIAN_POINT ( 'NONE',  ( 16.94467121224478134, -22.03697309902838697, 139.9999999999999432 ) ) ;
#77315 = CARTESIAN_POINT ( 'NONE',  ( -9.474510206698964154, 16.51473224551069663, 30.41557627198102054 ) ) ;
#77316 = CARTESIAN_POINT ( 'NONE',  ( -4.379528057220328563, 16.55341960407611168, 35.20724293864768839 ) ) ;
#77317 = CARTESIAN_POINT ( 'NONE',  ( -17.05587630539786304, -6.762274262135681724, 109.2581969096268466 ) ) ;
#77318 = CARTESIAN_POINT ( 'NONE',  ( -16.52544592524342804, 4.483927247898546575, 31.04057627198102409 ) ) ;
#77319 = CARTESIAN_POINT ( 'NONE',  ( 21.71562642307798185, -20.00551537737228713, -51.98609762351841113 ) ) ;
#77320 = CARTESIAN_POINT ( 'NONE',  ( 0.05219959533934541429, -16.53943276465976808, 95.00109039468568994 ) ) ;
#77321 = CARTESIAN_POINT ( 'NONE',  ( 13.89961937509977652, -13.97604488694527269, 33.12390960531434558 ) ) ;
#77322 = CARTESIAN_POINT ( 'NONE',  ( 15.72974639402176855, 15.80617190586768217, 111.8760903946856615 ) ) ;
#77323 = CARTESIAN_POINT ( 'NONE',  ( -5.153800228976607833, 19.02544592524334988, 112.7094237280190043 ) ) ;
#77324 = CARTESIAN_POINT ( 'NONE',  ( -21.53943276465977519, -0.05219959533937600094, 78.75109039468568994 ) ) ;
#77325 = CARTESIAN_POINT ( 'NONE',  ( 19.03943276465977164, 0.05219959533936151252, 56.25109039468566863 ) ) ;
#77326 = CARTESIAN_POINT ( 'NONE',  ( -9.474510206698964154, 16.51473224551069663, 90.41557627198103830 ) ) ;
#77327 = CARTESIAN_POINT ( 'NONE',  ( 16.46253265017160672, -9.564922557960803928, 78.33224293864769550 ) ) ;
#77328 = CARTESIAN_POINT ( 'NONE',  ( -18.87075004821571866, 5.499999999999899636, 38.67408112101045958 ) ) ;
#77329 = CARTESIAN_POINT ( 'NONE',  ( -21.53943276465977519, 0.05219959533907696930, 91.24890960531436690 ) ) ;
#77330 = CIRCLE ( 'NONE', #90181, 26.05799246640827960 ) ;
#77331 = CARTESIAN_POINT ( 'NONE',  ( 4.483927247898545687, 16.52544592524342804, 64.79057627198103830 ) ) ;
#77332 = CARTESIAN_POINT ( 'NONE',  ( -15.80617190586745835, -15.72974639402198527, 56.87390960531436690 ) ) ;
#77333 = CARTESIAN_POINT ( 'NONE',  ( -5.049401038298153566, 19.05341960407611168, 55.20724293864769550 ) ) ;
#77335 = CARTESIAN_POINT ( 'NONE',  ( 12.06949235617739724, 12.14591786802326823, 96.87609039468568994 ) ) ;
#77334 = CARTESIAN_POINT ( 'NONE',  ( 18.62759615963271287, -10.81492255796078972, 83.33224293864769550 ) ) ;
#77336 = ORIENTED_EDGE ( 'NONE', *, *, #97058, .F. ) ;
#77337 = CARTESIAN_POINT ( 'NONE',  ( 9.474510206698971260, -16.51473224551069308, 47.91557627198102409 ) ) ;
#77338 = EDGE_CURVE ( 'NONE', #34628, #54169, #141446, .T. ) ;
#77340 = CARTESIAN_POINT ( 'NONE',  ( 21.81399809961443381, -8.291606000631404072, 169.3279294801716048 ) ) ;
#77339 = CARTESIAN_POINT ( 'NONE',  ( 16.52544592524342804, -4.483927247898539470, 88.54057627198103830 ) ) ;
#77341 = CARTESIAN_POINT ( 'NONE',  ( 5.153800228976335163, 19.02544592524342804, 44.79057627198103830 ) ) ;
#77342 = CARTESIAN_POINT ( 'NONE',  ( 19.02544592524343514, -5.153800228976328945, 23.54057627198102054 ) ) ;
#77343 = CARTESIAN_POINT ( 'NONE',  ( 5.049401038297881783, 19.05341960407617563, 67.29275706135234714 ) ) ;
#77344 = CARTESIAN_POINT ( 'NONE',  ( 4.379528057220339221, -16.55341960407611168, 87.70724293864769550 ) ) ;
#77345 = CARTESIAN_POINT ( 'NONE',  ( -15.80617190586768217, 15.72974639402176855, 48.12609039468568284 ) ) ;
#77347 = CARTESIAN_POINT ( 'NONE',  ( -21.55341960407610458, -5.719274019375992779, 101.4572429386476955 ) ) ;
#77346 = CARTESIAN_POINT ( 'NONE',  ( -16.51473224551069308, -9.474510206698971260, 36.66557627198102409 ) ) ;
#77348 = CARTESIAN_POINT ( 'NONE',  ( 12.14591786802309770, 12.06949235617756955, 84.37390960531438111 ) ) ;
#77349 = CARTESIAN_POINT ( 'NONE',  ( 8.863853373469035901, -46.11448583660357770, -24.15755306339434227 ) ) ;
#77350 = CARTESIAN_POINT ( 'NONE',  ( 9.564922557960805705, 16.46253265017160317, 64.58224293864769550 ) ) ;
#77351 = CARTESIAN_POINT ( 'NONE',  ( -11.30013253874036216, -12.15106144227211438, -61.39618700965100828 ) ) ;
#77353 = CARTESIAN_POINT ( 'NONE',  ( 18.62759615963271287, -10.81492255796078972, 23.33224293864769194 ) ) ;
#77352 = CARTESIAN_POINT ( 'NONE',  ( -19.02544592524334988, -5.153800228976617603, 98.95942372801900433 ) ) ;
#77354 = CARTESIAN_POINT ( 'NONE',  ( 5.719274019375673035, 21.55341960407619339, 32.29275706135235424 ) ) ;
#77355 = CARTESIAN_POINT ( 'NONE',  ( -9.564922557960796823, -16.46253265017161027, 77.08224293864769550 ) ) ;
#77356 = CARTESIAN_POINT ( 'NONE',  ( -16.51473224551082808, 9.474510206698731452, 63.33442372801900433 ) ) ;
#77357 = CARTESIAN_POINT ( 'NONE',  ( -16.51473224551069308, -9.474510206698971260, 51.66557627198102409 ) ) ;
#77358 = CARTESIAN_POINT ( 'NONE',  ( 14.29746914071049879, -8.314922557960816363, 78.33224293864770971 ) ) ;
#77359 = CARTESIAN_POINT ( 'NONE',  ( -16.52544592524342804, 4.483927247898546575, 71.04057627198103830 ) ) ;
#77360 = CARTESIAN_POINT ( 'NONE',  ( 13.97604488694527802, 13.89961937509977652, 94.37390960531436690 ) ) ;
#77361 = CARTESIAN_POINT ( 'NONE',  ( -21.53943276465977519, 0.05219959533907696930, 106.2489096053143811 ) ) ;
#77362 = CARTESIAN_POINT ( 'NONE',  ( 19.02544592524343514, -5.153800228976328945, 83.54057627198100988 ) ) ;
#77363 = CARTESIAN_POINT ( 'NONE',  ( -9.474510206698720793, -16.51473224551083518, 29.58442372801900433 ) ) ;
#77366 = CARTESIAN_POINT ( 'NONE',  ( 16.55341960407611168, 4.379528057220329451, 108.9572429386476955 ) ) ;
#77365 = CARTESIAN_POINT ( 'NONE',  ( 14.34966873604960469, 8.224510206698951720, 29.16557627198103120 ) ) ;
#77364 = CARTESIAN_POINT ( 'NONE',  ( -19.02544592524342804, 5.153800228976336051, 31.04057627198102409 ) ) ;
#77367 = ORIENTED_EDGE ( 'NONE', *, *, #4454, .F. ) ;
#77368 = CARTESIAN_POINT ( 'NONE',  ( -18.62759615963255300, -10.81492255796106328, 34.16775706135234714 ) ) ;
#77369 = CARTESIAN_POINT ( 'NONE',  ( -13.97604488694547697, 13.89961937509957934, 73.12609039468568994 ) ) ;
#77370 = CARTESIAN_POINT ( 'NONE',  ( -16.52544592524342804, 4.483927247898546575, 31.04057627198102409 ) ) ;
#77371 = CARTESIAN_POINT ( 'NONE',  ( 0.05219959533907565091, 21.53943276465977519, 89.99890960531438111 ) ) ;
#77372 = CARTESIAN_POINT ( 'NONE',  ( -0.05219959533907301413, -21.53943276465977519, 22.49890960531436335 ) ) ;
#77373 = CARTESIAN_POINT ( 'NONE',  ( -8.314922557960811034, -14.29746914071050412, 67.08224293864770971 ) ) ;
#77374 = CARTESIAN_POINT ( 'NONE',  ( 16.51473224551069308, 9.474510206698969483, 24.16557627198102765 ) ) ;
#77375 = CARTESIAN_POINT ( 'NONE',  ( 9.474510206698729675, 16.51473224551082808, 22.08442372801899722 ) ) ;
#77376 = CARTESIAN_POINT ( 'NONE',  ( 16.55341960407618274, -4.379528057220086978, 101.0427570613523756 ) ) ;
#77377 = CARTESIAN_POINT ( 'NONE',  ( -16.55341960407617563, 4.379528057220093196, 58.54275706135235424 ) ) ;
#77378 = CARTESIAN_POINT ( 'NONE',  ( 5.049401038298161559, -19.05341960407611168, 112.7072429386476813 ) ) ;
#77379 = CARTESIAN_POINT ( 'NONE',  ( -0.05219959533937732626, 21.53943276465977519, 107.5010903946856899 ) ) ;
#77380 = CARTESIAN_POINT ( 'NONE',  ( 9.564922557960805705, 16.46253265017160317, 84.58224293864769550 ) ) ;
#77381 = CARTESIAN_POINT ( 'NONE',  ( 4.483927247898790824, -16.52544592524335698, 60.20942372801902565 ) ) ;
#77382 = CARTESIAN_POINT ( 'NONE',  ( 8.224510206698953496, -14.34966873604960469, 112.9155762719810383 ) ) ;
#77383 = CARTESIAN_POINT ( 'NONE',  ( -14.34966873604960291, -8.224510206698953496, 36.66557627198103120 ) ) ;
#77384 = DIRECTION ( 'NONE',  ( -1.000000000000000000, 5.392603844284257652E-33, 0.000000000000000000 ) ) ;
#77386 = CARTESIAN_POINT ( 'NONE',  ( 19.05341960407611168, 5.049401038298154454, 93.95724293864769550 ) ) ;
#77385 = CARTESIAN_POINT ( 'NONE',  ( -19.02544592524342804, 5.153800228976336051, 111.0405762719810099 ) ) ;
#77387 = CARTESIAN_POINT ( 'NONE',  ( -19.05341960407611168, -5.049401038298163336, 111.4572429386476671 ) ) ;
#77388 = CARTESIAN_POINT ( 'NONE',  ( -4.483927247898539470, -16.52544592524342804, 57.29057627198103120 ) ) ;
#77389 = CARTESIAN_POINT ( 'NONE',  ( 4.483927247898545687, 16.52544592524342804, 39.79057627198103830 ) ) ;
#77390 = CARTESIAN_POINT ( 'NONE',  ( -12.14591786802309592, -12.06949235617757132, 51.87390960531437401 ) ) ;
#77392 = FACE_OUTER_BOUND ( 'NONE', #169763, .T. ) ;
#77391 = CARTESIAN_POINT ( 'NONE',  ( -4.379528057220086978, -16.55341960407618274, 44.79275706135234714 ) ) ;
#77393 = CARTESIAN_POINT ( 'NONE',  ( 9.474510206698729675, 16.51473224551082808, 52.08442372801900433 ) ) ;
#77394 = CARTESIAN_POINT ( 'NONE',  ( 9.474510206698971260, -16.51473224551069308, 77.91557627198103830 ) ) ;
#77395 = CARTESIAN_POINT ( 'NONE',  ( -9.474510206698720793, -16.51473224551083518, 64.58442372801900433 ) ) ;
#77396 = CARTESIAN_POINT ( 'NONE',  ( -8.571926809382608425, 26.38167802310805854, 144.9750000027312069 ) ) ;
#77397 = CARTESIAN_POINT ( 'NONE',  ( -16.51473224551082808, 9.474510206698731452, 58.33442372801900433 ) ) ;
#77399 = CARTESIAN_POINT ( 'NONE',  ( 14.29746914071037800, 8.314922557961029526, 81.66775706135236135 ) ) ;
#77398 = CARTESIAN_POINT ( 'NONE',  ( -5.153800228976607833, 19.02544592524334988, 102.7094237280189759 ) ) ;
#77400 = CARTESIAN_POINT ( 'NONE',  ( -8.571926809382601320, -26.38167802310801591, 145.7750000027311899 ) ) ;
#77401 = CARTESIAN_POINT ( 'NONE',  ( -0.05219959533909027116, -19.03943276465977164, 32.49890960531435979 ) ) ;
#77402 = CARTESIAN_POINT ( 'NONE',  ( 19.03943276465977164, -0.05219959533909143690, 98.74890960531436690 ) ) ;
#77403 = CARTESIAN_POINT ( 'NONE',  ( 15.72974639402176855, 15.80617190586768217, 46.87609039468568994 ) ) ;
#77404 = CARTESIAN_POINT ( 'NONE',  ( -19.02544592524334988, -5.153800228976617603, 103.9594237280190043 ) ) ;
#77406 = CARTESIAN_POINT ( 'NONE',  ( 13.97604488694527802, 13.89961937509977652, 64.37390960531436690 ) ) ;
#77405 = CARTESIAN_POINT ( 'NONE',  ( 17.50000000000000355, -3.209263204892577548, 107.2619682560627581 ) ) ;
#77407 = CARTESIAN_POINT ( 'NONE',  ( 5.049401038298161559, -19.05341960407611168, 102.7072429386476955 ) ) ;
#77409 = CARTESIAN_POINT ( 'NONE',  ( 13.97604488694527802, 13.89961937509977652, 59.37390960531434558 ) ) ;
#77408 = CARTESIAN_POINT ( 'NONE',  ( -4.483927247898539470, -16.52544592524342804, 62.29057627198102409 ) ) ;
#77410 = CARTESIAN_POINT ( 'NONE',  ( 0.05219959533909260263, 19.03943276465977164, 59.99890960531436690 ) ) ;
#77411 = CARTESIAN_POINT ( 'NONE',  ( -16.46253265017146816, -9.564922557961047289, 84.16775706135233293 ) ) ;
#77412 = CARTESIAN_POINT ( 'NONE',  ( -5.823673210054116645, -21.52544592524344225, 57.29057627198103120 ) ) ;
#77413 = CARTESIAN_POINT ( 'NONE',  ( 14.34966873604960469, 8.224510206698951720, 114.1655762719810383 ) ) ;
#77414 = CARTESIAN_POINT ( 'NONE',  ( 16.46253265017146816, 9.564922557961045513, 46.66775706135233293 ) ) ;
#77415 = CARTESIAN_POINT ( 'NONE',  ( 5.153800228976335163, 19.02544592524342804, 84.79057627198099567 ) ) ;
#77416 = CARTESIAN_POINT ( 'NONE',  ( 15.72974639402199770, -15.80617190586745480, 83.12390960531436690 ) ) ;
#77418 = CARTESIAN_POINT ( 'NONE',  ( -19.05341960407617563, 5.049401038297882671, 38.54275706135233293 ) ) ;
#77417 = CARTESIAN_POINT ( 'NONE',  ( 8.314922557960818139, 14.29746914071049879, 79.58224293864769550 ) ) ;
#77419 = CARTESIAN_POINT ( 'NONE',  ( 5.823673210054125526, 21.52544592524343514, 59.79057627198103120 ) ) ;
#77420 = CARTESIAN_POINT ( 'NONE',  ( -5.719274019375978568, 21.55341960407610458, 45.20724293864769550 ) ) ;
#77421 = CARTESIAN_POINT ( 'NONE',  ( -15.80617190586768217, 15.72974639402176855, 93.12609039468568994 ) ) ;
#77422 = CARTESIAN_POINT ( 'NONE',  ( 19.03943276465977164, -0.05219959533909143690, 68.74890960531436690 ) ) ;
#77423 = CARTESIAN_POINT ( 'NONE',  ( 4.379528057220339221, -16.55341960407611168, 112.7072429386476955 ) ) ;
#77424 = CARTESIAN_POINT ( 'NONE',  ( -0.05219959533937732626, 21.53943276465977519, 32.50109039468568284 ) ) ;
#77426 = ADVANCED_FACE ( 'NONE', ( #71633 ), #149473, .T. ) ;
#77425 = CARTESIAN_POINT ( 'NONE',  ( 1.500000000000163203, 15.29469527405681184, -61.93010668218706627 ) ) ;
#77427 = CARTESIAN_POINT ( 'NONE',  ( 5.823673210054444382, -21.52544592524334988, 45.20942372801901854 ) ) ;
#77428 = CARTESIAN_POINT ( 'NONE',  ( -5.153800228976328057, -19.02544592524343514, 37.29057627198102409 ) ) ;
#77429 = CARTESIAN_POINT ( 'NONE',  ( -15.80617190586745835, -15.72974639402198527, 101.8739096053143811 ) ) ;
#77430 = CARTESIAN_POINT ( 'NONE',  ( 13.89961937509957401, 13.97604488694547697, 46.87609039468565442 ) ) ;
#77431 = CARTESIAN_POINT ( 'NONE',  ( 19.03943276465977164, -0.05219959533909143690, 23.74890960531435269 ) ) ;
#77432 = CARTESIAN_POINT ( 'NONE',  ( 31.99999999999934275, 1.011436372600181938E-12, 95.00000000000021316 ) ) ;
#77433 = CARTESIAN_POINT ( 'NONE',  ( 8.224510206698742110, 14.34966873604972548, 62.08442372801901143 ) ) ;
#77434 = CARTESIAN_POINT ( 'NONE',  ( 9.564922557960805705, 16.46253265017160317, 24.58224293864769194 ) ) ;
#77435 = CARTESIAN_POINT ( 'NONE',  ( -21.51693143705271893, -10.15780255052857406, 170.5200780514254859 ) ) ;
#77436 = CARTESIAN_POINT ( 'NONE',  ( -19.02544592524342804, 5.153800228976336051, 76.04057627198102409 ) ) ;
#77437 = CARTESIAN_POINT ( 'NONE',  ( -8.224510206698948167, 14.34966873604960824, 105.4155762719810383 ) ) ;
#77438 = CARTESIAN_POINT ( 'NONE',  ( 21.52544592524344225, -5.823673210054117533, 63.54057627198103830 ) ) ;
#77439 = CARTESIAN_POINT ( 'NONE',  ( -16.52544592524335698, -4.483927247898792601, 33.95942372801901143 ) ) ;
#77440 = CARTESIAN_POINT ( 'NONE',  ( -21.55341960407619339, 5.719274019375674811, 98.54275706135234714 ) ) ;
#77441 = DIRECTION ( 'NONE',  ( -9.445700745138859830E-17, 1.000000000000000000, 0.000000000000000000 ) ) ;
#77442 = CARTESIAN_POINT ( 'NONE',  ( -0.05219959533934338120, 16.53943276465976808, 112.5010903946857042 ) ) ;
#77443 = CARTESIAN_POINT ( 'NONE',  ( 14.34966873604960469, 8.224510206698951720, 49.16557627198102409 ) ) ;
#77444 = VECTOR ( 'NONE', #51200, 1000.000000000000000 ) ;
#77445 = CARTESIAN_POINT ( 'NONE',  ( -9.474510206698964154, 16.51473224551069663, 45.41557627198103120 ) ) ;
#77446 = CARTESIAN_POINT ( 'NONE',  ( -21.53943276465977519, -0.05219959533937600094, 98.75109039468568994 ) ) ;
#77447 = CARTESIAN_POINT ( 'NONE',  ( -10.81492255796078084, -18.62759615963271287, 107.0822429386476955 ) ) ;
#77448 = CARTESIAN_POINT ( 'NONE',  ( 10.81492255796106328, -18.62759615963255655, 70.41775706135236135 ) ) ;
#77449 = CARTESIAN_POINT ( 'NONE',  ( 14.29746914071037800, 8.314922557961029526, 51.66775706135234714 ) ) ;
#77451 = CARTESIAN_POINT ( 'NONE',  ( -5.823673210054431948, 21.52544592524334988, 97.70942372801904696 ) ) ;
#77450 = CARTESIAN_POINT ( 'NONE',  ( 16.55341960407611168, 4.379528057220329451, 83.95724293864770971 ) ) ;
#77452 = CARTESIAN_POINT ( 'NONE',  ( -12.14591786802326823, 12.06949235617739902, 113.1260903946856899 ) ) ;
#77453 = CARTESIAN_POINT ( 'NONE',  ( 8.898068258721473001, -27.38543819252872069, 140.8656553485623704 ) ) ;
#77454 = CARTESIAN_POINT ( 'NONE',  ( 16.53943276465976808, 0.05219959533934440121, 36.25109039468567573 ) ) ;
#77455 = CARTESIAN_POINT ( 'NONE',  ( -16.55341960407611168, -4.379528057220339221, 46.45724293864769550 ) ) ;
#77456 = CARTESIAN_POINT ( 'NONE',  ( -14.29746914071037622, -8.314922557961029526, 89.16775706135236135 ) ) ;
#77457 = CARTESIAN_POINT ( 'NONE',  ( -19.03943276465977164, 0.05219959533909376836, 96.24890960531436690 ) ) ;
#77458 = CARTESIAN_POINT ( 'NONE',  ( -5.153800228976328057, -19.02544592524343514, 112.2905762719810099 ) ) ;
#77459 = CARTESIAN_POINT ( 'NONE',  ( -5.719274019375665041, -21.55341960407619695, 99.79275706135234714 ) ) ;
#77460 = EDGE_CURVE ( 'NONE', #111025, #12839, #60708, .T. ) ;
#77461 = CARTESIAN_POINT ( 'NONE',  ( -0.05219959533934338120, 16.53943276465976808, 107.5010903946856899 ) ) ;
#77462 = CARTESIAN_POINT ( 'NONE',  ( 16.52544592524342804, -4.483927247898539470, 68.54057627198103830 ) ) ;
#77463 = CARTESIAN_POINT ( 'NONE',  ( -5.153800228976328057, -19.02544592524343514, 77.29057627198099567 ) ) ;
#77464 = ORIENTED_EDGE ( 'NONE', *, *, #18367, .F. ) ;
#77465 = CARTESIAN_POINT ( 'NONE',  ( -14.34966873604972548, 8.224510206698743886, 33.33442372801900433 ) ) ;
#77466 = CARTESIAN_POINT ( 'NONE',  ( 19.02544592524343514, -5.153800228976328945, 28.54057627198102409 ) ) ;
#77467 = CARTESIAN_POINT ( 'NONE',  ( 19.03943276465977164, -0.05219959533909143690, 88.74890960531436690 ) ) ;
#77469 = CARTESIAN_POINT ( 'NONE',  ( 11.40812507854755253, -35.11059874428192273, -4.024999997268814411 ) ) ;
#77468 = CARTESIAN_POINT ( 'NONE',  ( -14.29746914071037622, -8.314922557961029526, 29.16775706135234003 ) ) ;
#77470 = CARTESIAN_POINT ( 'NONE',  ( 5.153800228976615827, -19.02544592524334988, 35.20942372801899722 ) ) ;
#77471 = CARTESIAN_POINT ( 'NONE',  ( -8.314922557961024197, 14.29746914071037800, 92.91775706135236135 ) ) ;
#77472 = CARTESIAN_POINT ( 'NONE',  ( 5.049401038298161559, -19.05341960407611168, 37.70724293864768839 ) ) ;
#77473 = CARTESIAN_POINT ( 'NONE',  ( 0.05219959533934541429, -16.53943276465976808, 75.00109039468568994 ) ) ;
#77474 = CARTESIAN_POINT ( 'NONE',  ( 8.314922557961029526, -14.29746914071037800, 60.41775706135235424 ) ) ;
#77475 = CARTESIAN_POINT ( 'NONE',  ( -16.46253265017146816, -9.564922557961047289, 84.16775706135233293 ) ) ;
#77476 = CARTESIAN_POINT ( 'NONE',  ( 16.46253265017146816, 9.564922557961045513, 31.66775706135232937 ) ) ;
#77477 = CARTESIAN_POINT ( 'NONE',  ( 13.97604488694527802, 13.89961937509977652, 44.37390960531435269 ) ) ;
#77478 = CARTESIAN_POINT ( 'NONE',  ( -16.53943276465976808, 0.05219959533911058130, 86.24890960531436690 ) ) ;
#77479 = AXIS2_PLACEMENT_3D ( 'NONE', #131326, #143489, #193014 ) ;
#77480 = CARTESIAN_POINT ( 'NONE',  ( -5.049401038297874678, -19.05341960407617918, 59.79275706135231871 ) ) ;
#77481 = CARTESIAN_POINT ( 'NONE',  ( -10.72451020669898014, 18.67979575497178502, 50.41557627198103120 ) ) ;
#77482 = CARTESIAN_POINT ( 'NONE',  ( 5.049401038297881783, 19.05341960407617563, 27.29275706135232937 ) ) ;
#77483 = CARTESIAN_POINT ( 'NONE',  ( -9.564922557960796823, -16.46253265017161027, 107.0822429386476955 ) ) ;
#77484 = CARTESIAN_POINT ( 'NONE',  ( -0.05219959533907301413, -21.53943276465977519, 77.49890960531433848 ) ) ;
#77485 = CARTESIAN_POINT ( 'NONE',  ( 5.153800228976335163, 19.02544592524342804, 114.7905762719810241 ) ) ;
#77486 = CARTESIAN_POINT ( 'NONE',  ( 9.564922557961047289, -16.46253265017146816, 90.41775706135234714 ) ) ;
#77487 = CARTESIAN_POINT ( 'NONE',  ( -17.49999999999999645, 3.471454075611712042, 109.4833258114436347 ) ) ;
#77488 = CARTESIAN_POINT ( 'NONE',  ( 5.049401038297881783, 19.05341960407617563, 112.2927570613523471 ) ) ;
#77489 = CARTESIAN_POINT ( 'NONE',  ( -16.51473224551069308, -9.474510206698971260, 31.66557627198102054 ) ) ;
#77490 = CARTESIAN_POINT ( 'NONE',  ( 9.564922557960805705, 16.46253265017160317, 94.58224293864769550 ) ) ;
#77491 = CARTESIAN_POINT ( 'NONE',  ( -10.81492255796078084, -18.62759615963271287, 72.08224293864769550 ) ) ;
#77492 = CARTESIAN_POINT ( 'NONE',  ( -0.05219959533934338120, 16.53943276465976808, 47.50109039468568994 ) ) ;
#77493 = CARTESIAN_POINT ( 'NONE',  ( 15.80617190586769283, -15.72974639402175789, 50.62609039468568994 ) ) ;
#77495 = CARTESIAN_POINT ( 'NONE',  ( 10.81492255796106328, -18.62759615963255655, 105.4177570613523613 ) ) ;
#77494 = CARTESIAN_POINT ( 'NONE',  ( -13.97604488694547697, 13.89961937509957934, 88.12609039468563310 ) ) ;
#77496 = CARTESIAN_POINT ( 'NONE',  ( 16.55341960407618274, -4.379528057220086978, 111.0427570613523613 ) ) ;
#77497 = CARTESIAN_POINT ( 'NONE',  ( -16.46253265017160317, 9.564922557960807481, 100.8322429386477097 ) ) ;
#77498 = CARTESIAN_POINT ( 'NONE',  ( -4.379528057220328563, 16.55341960407611168, 85.20724293864770971 ) ) ;
#77499 = CARTESIAN_POINT ( 'NONE',  ( 4.379528057220339221, -16.55341960407611168, 42.70724293864770260 ) ) ;
#77500 = CARTESIAN_POINT ( 'NONE',  ( 19.03943276465977164, 0.05219959533936151252, 76.25109039468566152 ) ) ;
#77501 = CARTESIAN_POINT ( 'NONE',  ( 21.53943276465977519, 0.05219959533937863772, 61.25109039468567573 ) ) ;
#77502 = CARTESIAN_POINT ( 'NONE',  ( -19.02544592524334988, -5.153800228976617603, 23.95942372801900078 ) ) ;
#77503 = CARTESIAN_POINT ( 'NONE',  ( 16.55341960407611168, 4.379528057220329451, 98.95724293864770971 ) ) ;
#77504 = CARTESIAN_POINT ( 'NONE',  ( -15.72974639402197994, 15.80617190586746368, 25.62390960531435624 ) ) ;
#77505 = CARTESIAN_POINT ( 'NONE',  ( -4.483927247898539470, -16.52544592524342804, 27.29057627198103120 ) ) ;
#77506 = CARTESIAN_POINT ( 'NONE',  ( 0.05219959533937995610, -21.53943276465977519, 100.0010903946857042 ) ) ;
#77507 = CARTESIAN_POINT ( 'NONE',  ( -16.53943276465976808, -0.05219959533934237506, 63.75109039468568284 ) ) ;
#77508 = CARTESIAN_POINT ( 'NONE',  ( -8.314922557960811034, -14.29746914071050412, 22.08224293864769194 ) ) ;
#77509 = CARTESIAN_POINT ( 'NONE',  ( -5.823673210054431948, 21.52544592524334988, 57.70942372801901143 ) ) ;
#77510 = CARTESIAN_POINT ( 'NONE',  ( 0.05219959533937995610, -21.53943276465977519, 55.00109039468568284 ) ) ;
#77511 = EDGE_LOOP ( 'NONE', ( #37931, #59760, #132052, #84834 ) ) ;
#77512 = CARTESIAN_POINT ( 'NONE',  ( -16.51473224551069308, -9.474510206698971260, 61.66557627198103120 ) ) ;
#77513 = CARTESIAN_POINT ( 'NONE',  ( 10.72451020669871369, 18.67979575497193778, 27.08442372801901854 ) ) ;
#77514 = CARTESIAN_POINT ( 'NONE',  ( 4.379528057220339221, -16.55341960407611168, 102.7072429386476955 ) ) ;
#77515 = CARTESIAN_POINT ( 'NONE',  ( 9.564922557960805705, 16.46253265017160317, 29.58224293864769550 ) ) ;
#77516 = CARTESIAN_POINT ( 'NONE',  ( 4.483927247898545687, 16.52544592524342804, 74.79057627198105251 ) ) ;
#77517 = CARTESIAN_POINT ( 'NONE',  ( 16.46253265017160672, -9.564922557960803928, 68.33224293864770971 ) ) ;
#77518 = CARTESIAN_POINT ( 'NONE',  ( -16.53943276465976808, 0.05219959533911058130, 26.24890960531435624 ) ) ;
#77519 = CARTESIAN_POINT ( 'NONE',  ( -18.62759615963270932, 10.81492255796079327, 55.83224293864770260 ) ) ;
#77520 = CARTESIAN_POINT ( 'NONE',  ( 8.224510206698953496, -14.34966873604960469, 92.91557627198103830 ) ) ;
#77521 = CARTESIAN_POINT ( 'NONE',  ( -0.05219959533907301413, -21.53943276465977519, 92.49890960531436690 ) ) ;
#77522 = CARTESIAN_POINT ( 'NONE',  ( -9.474510206698964154, 16.51473224551069663, 95.41557627198102409 ) ) ;
#77524 = CARTESIAN_POINT ( 'NONE',  ( -13.97604488694547697, 13.89961937509957934, 103.1260903946856473 ) ) ;
#77523 = CARTESIAN_POINT ( 'NONE',  ( -19.05341960407611168, -5.049401038298163336, 51.45724293864770260 ) ) ;
#77525 = CARTESIAN_POINT ( 'NONE',  ( 5.719274019375991003, -21.55341960407610458, 42.70724293864770260 ) ) ;
#77526 = CARTESIAN_POINT ( 'NONE',  ( 18.67979575497194134, -10.72451020669871369, 80.83442372801901854 ) ) ;
#77527 = CARTESIAN_POINT ( 'NONE',  ( -19.03943276465977164, 0.05219959533909376836, 66.24890960531436690 ) ) ;
#77528 = CARTESIAN_POINT ( 'NONE',  ( -9.564922557960796823, -16.46253265017161027, 102.0822429386477097 ) ) ;
#77529 = CARTESIAN_POINT ( 'NONE',  ( -8.314922557961024197, 14.29746914071037800, 82.91775706135234714 ) ) ;
#77530 = CARTESIAN_POINT ( 'NONE',  ( -5.823673210054431948, 21.52544592524334988, 62.70942372801902565 ) ) ;
#77531 = CARTESIAN_POINT ( 'NONE',  ( 5.823673210054444382, -21.52544592524334988, 90.20942372801903275 ) ) ;
#77532 = CARTESIAN_POINT ( 'NONE',  ( 21.55341960407619695, -5.719274019375665929, 21.04275706135234714 ) ) ;
#77534 = CARTESIAN_POINT ( 'NONE',  ( 12.06949235617739724, 12.14591786802326823, 76.87609039468567573 ) ) ;
#77533 = CARTESIAN_POINT ( 'NONE',  ( -18.62759615963255300, -10.81492255796106328, 44.16775706135234714 ) ) ;
#77535 = CARTESIAN_POINT ( 'NONE',  ( 21.55341960407610458, 5.719274019375980345, 78.95724293864769550 ) ) ;
#77536 = CARTESIAN_POINT ( 'NONE',  ( 9.474510206698729675, 16.51473224551082808, 27.08442372801900433 ) ) ;
#77537 = CARTESIAN_POINT ( 'NONE',  ( 18.67979575497178502, 10.72451020669898547, 44.16557627198103120 ) ) ;
#77539 = CARTESIAN_POINT ( 'NONE',  ( -16.52544592524342804, 4.483927247898546575, 26.04057627198103475 ) ) ;
#77538 = CARTESIAN_POINT ( 'NONE',  ( -9.564922557960796823, -16.46253265017161027, 87.08224293864769550 ) ) ;
#77540 = FACE_BOUND ( 'NONE', #91970, .T. ) ;
#77541 = CARTESIAN_POINT ( 'NONE',  ( 16.46253265017160672, -9.564922557960803928, 98.33224293864769550 ) ) ;
#77542 = DIRECTION ( 'NONE',  ( 0.000000000000000000, 0.000000000000000000, -1.000000000000000000 ) ) ;
#77543 = CARTESIAN_POINT ( 'NONE',  ( 5.049401038297881783, 19.05341960407617563, 97.29275706135233293 ) ) ;
#77544 = CARTESIAN_POINT ( 'NONE',  ( -5.719274019375978568, 21.55341960407610458, 70.20724293864769550 ) ) ;
#77545 = CARTESIAN_POINT ( 'NONE',  ( 14.34966873604960469, 8.224510206698951720, 34.16557627198102409 ) ) ;
#77546 = CARTESIAN_POINT ( 'NONE',  ( -16.51473224551082808, 9.474510206698731452, 108.3344237280190043 ) ) ;
#77547 = CARTESIAN_POINT ( 'NONE',  ( -19.03943276465977164, 0.05219959533909376836, 36.24890960531436690 ) ) ;
#77548 = CARTESIAN_POINT ( 'NONE',  ( -13.97604488694547697, 13.89961937509957934, 108.1260903946856331 ) ) ;
#77550 = CARTESIAN_POINT ( 'NONE',  ( -19.02544592524334988, -5.153800228976617603, 73.95942372801900433 ) ) ;
#77549 = CARTESIAN_POINT ( 'NONE',  ( -21.53943276465977519, 0.05219959533907696930, 101.2489096053143669 ) ) ;
#77551 = CARTESIAN_POINT ( 'NONE',  ( -12.06949235617739369, -12.14591786802326823, 79.37609039468567573 ) ) ;
#77552 = CARTESIAN_POINT ( 'NONE',  ( 5.153800228976335163, 19.02544592524342804, 84.79057627198099567 ) ) ;
#77553 = CARTESIAN_POINT ( 'NONE',  ( 16.53943276465976808, -0.05219959533910856209, 73.74890960531433848 ) ) ;
#77554 = CARTESIAN_POINT ( 'NONE',  ( 13.97604488694527802, 13.89961937509977652, 64.37390960531436690 ) ) ;
#77555 = CARTESIAN_POINT ( 'NONE',  ( 0.05219959533910956823, 16.53943276465976808, 69.99890960531435269 ) ) ;
#77556 = CARTESIAN_POINT ( 'NONE',  ( -16.46253265017160317, 9.564922557960807481, 35.83224293864768839 ) ) ;
#77557 = CARTESIAN_POINT ( 'NONE',  ( -36.81601778013477855, -3.637449627666676122, 49.14141020753753963 ) ) ;
#77558 = CARTESIAN_POINT ( 'NONE',  ( -0.05219959533910754901, -16.53943276465976808, 47.49890960531435979 ) ) ;
#77559 = CARTESIAN_POINT ( 'NONE',  ( -13.89961937509977652, 13.97604488694528158, 80.62390960531436690 ) ) ;
#77560 = DIRECTION ( 'NONE',  ( -1.000000000000000000, 0.000000000000000000, 0.000000000000000000 ) ) ;
#77561 = CARTESIAN_POINT ( 'NONE',  ( 19.02544592524334988, 5.153800228976608722, 46.45942372801899012 ) ) ;
#77562 = CARTESIAN_POINT ( 'NONE',  ( -16.52544592524335698, -4.483927247898792601, 63.95942372801901854 ) ) ;
#77563 = CARTESIAN_POINT ( 'NONE',  ( 10.81492255796078972, 18.62759615963270932, 64.58224293864769550 ) ) ;
#77564 = CARTESIAN_POINT ( 'NONE',  ( 13.97604488694548053, -13.89961937509957401, 25.62609039468566507 ) ) ;
#77565 = CARTESIAN_POINT ( 'NONE',  ( -19.03943276465977164, 0.05219959533909376836, 91.24890960531436690 ) ) ;
#77566 = CARTESIAN_POINT ( 'NONE',  ( 1.338944653035268662, 22.09907077859329405, -58.31495840562853061 ) ) ;
#77567 = CARTESIAN_POINT ( 'NONE',  ( -10.81492255796078084, -18.62759615963271287, 27.08224293864769550 ) ) ;
#77568 = CARTESIAN_POINT ( 'NONE',  ( 13.97604488694527802, 13.89961937509977652, 59.37390960531434558 ) ) ;
#77569 = CARTESIAN_POINT ( 'NONE',  ( 10.72451020669871369, 18.67979575497193778, 47.08442372801901854 ) ) ;
#77570 = CARTESIAN_POINT ( 'NONE',  ( 14.29746914071049879, -8.314922557960816363, 108.3322429386477097 ) ) ;
#77573 = ORIENTED_EDGE ( 'NONE', *, *, #30682, .F. ) ;
#77572 = CARTESIAN_POINT ( 'NONE',  ( -19.02544592524342804, 5.153800228976336051, 96.04057627198103830 ) ) ;
#77571 = CARTESIAN_POINT ( 'NONE',  ( -0.05219959533907301413, -21.53943276465977519, 102.4989096053143811 ) ) ;
#77574 = CARTESIAN_POINT ( 'NONE',  ( -10.81492255796105439, 18.62759615963255655, 32.91775706135234714 ) ) ;
#77575 = ORIENTED_EDGE ( 'NONE', *, *, #173518, .F. ) ;
#77576 = CARTESIAN_POINT ( 'NONE',  ( -9.564922557960796823, -16.46253265017161027, 92.08224293864769550 ) ) ;
#77577 = CARTESIAN_POINT ( 'NONE',  ( 18.22780087662123805, -5.499999999999976019, 83.51763182126894947 ) ) ;
#77578 = CARTESIAN_POINT ( 'NONE',  ( 10.72451020669898902, -18.67979575497178502, 92.91557627198103830 ) ) ;
#77579 = CARTESIAN_POINT ( 'NONE',  ( 13.89961937509977652, -13.97604488694527269, 53.12390960531434558 ) ) ;
#77580 = CARTESIAN_POINT ( 'NONE',  ( 12.14591786802327356, -12.06949235617739191, 20.62609039468568639 ) ) ;
#77581 = CARTESIAN_POINT ( 'NONE',  ( 22.81625015709509441, 31.40387420917330275, -1.824999997268813567 ) ) ;
#77582 = CARTESIAN_POINT ( 'NONE',  ( -5.049401038298153566, 19.05341960407611168, 30.20724293864768839 ) ) ;
#77583 = CARTESIAN_POINT ( 'NONE',  ( 18.62759615963255655, 10.81492255796105972, 86.66775706135234714 ) ) ;
#77585 = CARTESIAN_POINT ( 'NONE',  ( 21.55341960407619695, -5.719274019375665929, 51.04275706135234714 ) ) ;
#77584 = CARTESIAN_POINT ( 'NONE',  ( 5.153800228976335163, 19.02544592524342804, 69.79057627198103830 ) ) ;
#77586 = AXIS2_PLACEMENT_3D ( 'NONE', #10461, #136766, #13435 ) ;
#77587 = CARTESIAN_POINT ( 'NONE',  ( 15.72974639402176855, 15.80617190586768217, 31.87609039468567929 ) ) ;
#77588 = CARTESIAN_POINT ( 'NONE',  ( -17.14385361876520264, -23.59649016807271593, 145.6750000027311671 ) ) ;
#77589 = CARTESIAN_POINT ( 'NONE',  ( 13.89961937509977652, -13.97604488694527269, 103.1239096053143527 ) ) ;
#77590 = CARTESIAN_POINT ( 'NONE',  ( -18.43223033536927957, 22.10073931973474970, 139.9999999999999716 ) ) ;
#77593 = CARTESIAN_POINT ( 'NONE',  ( 18.62759615963255655, 10.81492255796105972, 61.66775706135235424 ) ) ;
#77592 = CARTESIAN_POINT ( 'NONE',  ( -16.55341960407617563, 4.379528057220093196, 68.54275706135234714 ) ) ;
#77591 = CARTESIAN_POINT ( 'NONE',  ( -16.55341960407617563, 4.379528057220093196, 33.54275706135234714 ) ) ;
#77594 = CARTESIAN_POINT ( 'NONE',  ( 10.72451020669871369, 18.67979575497193778, 82.08442372801901854 ) ) ;
#77595 = PLANE ( 'NONE',  #21946 ) ;
#77596 = CARTESIAN_POINT ( 'NONE',  ( 13.97604488694548053, -13.89961937509957401, 110.6260903946856615 ) ) ;
#77597 = CARTESIAN_POINT ( 'NONE',  ( 19.03943276465977164, -0.05219959533909143690, 63.74890960531435979 ) ) ;
#77598 = CARTESIAN_POINT ( 'NONE',  ( 16.51473224551069308, 9.474510206698969483, 104.1655762719810241 ) ) ;
#77599 = CARTESIAN_POINT ( 'NONE',  ( 4.483927247898545687, 16.52544592524342804, 104.7905762719810241 ) ) ;
#77600 = CARTESIAN_POINT ( 'NONE',  ( -14.29746914071049879, 8.314922557960819915, 100.8322429386477097 ) ) ;
#77601 = CARTESIAN_POINT ( 'NONE',  ( 21.52544592524344225, -5.823673210054117533, 33.54057627198102409 ) ) ;
#77602 = CARTESIAN_POINT ( 'NONE',  ( 12.14591786802327356, -12.06949235617739191, 85.62609039468568994 ) ) ;
#77604 = CARTESIAN_POINT ( 'NONE',  ( -5.049401038298153566, 19.05341960407611168, 50.20724293864770260 ) ) ;
#77603 = CARTESIAN_POINT ( 'NONE',  ( -8.224510206698948167, 14.34966873604960824, 70.41557627198102409 ) ) ;
#77605 = CARTESIAN_POINT ( 'NONE',  ( 21.53943276465977519, 0.05219959533937863772, 71.25109039468568994 ) ) ;
#77606 = CARTESIAN_POINT ( 'NONE',  ( 18.67979575497194134, -10.72451020669871369, 70.83442372801901854 ) ) ;
#77607 = CARTESIAN_POINT ( 'NONE',  ( 19.02544592524334988, 5.153800228976608722, 111.4594237280190043 ) ) ;
#77608 = CARTESIAN_POINT ( 'NONE',  ( -4.483927247898539470, -16.52544592524342804, 72.29057627198102409 ) ) ;
#77609 = CARTESIAN_POINT ( 'NONE',  ( -21.55341960407619339, 5.719274019375674811, 23.54275706135235424 ) ) ;
#77610 = CARTESIAN_POINT ( 'NONE',  ( -21.55341960407610458, -5.719274019375992779, 66.45724293864768129 ) ) ;
#77611 = CARTESIAN_POINT ( 'NONE',  ( -17.05116617787824396, -6.768360034955828830, 106.3432444674080273 ) ) ;
#77612 = CARTESIAN_POINT ( 'NONE',  ( -35.52763170759350686, 3.100152895725881930, 38.16632899394345912 ) ) ;
#77613 = CARTESIAN_POINT ( 'NONE',  ( 16.51473224551069308, 9.474510206698969483, 69.16557627198102409 ) ) ;
#77614 = CARTESIAN_POINT ( 'NONE',  ( -4.483927247898539470, -16.52544592524342804, 52.29057627198102409 ) ) ;
#77615 = AXIS2_PLACEMENT_3D ( 'NONE', #41934, #102598, #195627 ) ;
#77616 = CARTESIAN_POINT ( 'NONE',  ( 14.34966873604960469, 8.224510206698951720, 24.16557627198103120 ) ) ;
#77617 = CARTESIAN_POINT ( 'NONE',  ( -14.34966873604972548, 8.224510206698743886, 103.3344237280190043 ) ) ;
#77618 = CARTESIAN_POINT ( 'NONE',  ( 19.02544592524334988, 5.153800228976608722, 56.45942372801898301 ) ) ;
#77619 = CARTESIAN_POINT ( 'NONE',  ( -23.71437531004594135, -10.61261859643794558, 165.9743991446059113 ) ) ;
#77620 = CARTESIAN_POINT ( 'NONE',  ( -13.97604488694527625, -13.89961937509977652, 106.8739096053143669 ) ) ;
#77621 = CARTESIAN_POINT ( 'NONE',  ( -16.55341960407611168, -4.379528057220339221, 71.45724293864769550 ) ) ;
#77622 = CARTESIAN_POINT ( 'NONE',  ( 9.564922557961047289, -16.46253265017146816, 50.41775706135233293 ) ) ;
#77624 = CARTESIAN_POINT ( 'NONE',  ( 15.80617190586746368, 15.72974639402197994, 39.37390960531436690 ) ) ;
#77623 = CARTESIAN_POINT ( 'NONE',  ( 13.89961937509977652, -13.97604488694527269, 38.12390960531436690 ) ) ;
#77626 = ORIENTED_EDGE ( 'NONE', *, *, #175018, .F. ) ;
#77625 = CARTESIAN_POINT ( 'NONE',  ( 18.67979575497178502, 10.72451020669898547, 54.16557627198103120 ) ) ;
#77627 = CARTESIAN_POINT ( 'NONE',  ( 16.52544592524342804, -4.483927247898539470, 93.54057627198103830 ) ) ;
#77628 = CARTESIAN_POINT ( 'NONE',  ( -8.314922557961024197, 14.29746914071037800, 57.91775706135234714 ) ) ;
#77629 = CARTESIAN_POINT ( 'NONE',  ( -8.224510206698948167, 14.34966873604960824, 90.41557627198103830 ) ) ;
#77630 = CARTESIAN_POINT ( 'NONE',  ( 17.40805194822032931, -6.112264579159339739, 38.33371272510613181 ) ) ;
#77631 = CARTESIAN_POINT ( 'NONE',  ( -11.40812507854754720, -35.11059874428192273, -10.72499999726881548 ) ) ;
#77632 = CARTESIAN_POINT ( 'NONE',  ( -5.719274019375978568, 21.55341960407610458, 30.20724293864769550 ) ) ;
#77633 = DIRECTION ( 'NONE',  ( 0.000000000000000000, 0.000000000000000000, -1.000000000000000000 ) ) ;
#77634 = CARTESIAN_POINT ( 'NONE',  ( 23.31738231874054890, -16.94106989632523508, 142.7999999999999829 ) ) ;
#77636 = CARTESIAN_POINT ( 'NONE',  ( 4.483927247898545687, 16.52544592524342804, 29.79057627198102409 ) ) ;
#77635 = CARTESIAN_POINT ( 'NONE',  ( 4.379528057220092307, 16.55341960407617563, 47.29275706135234003 ) ) ;
#77637 = CARTESIAN_POINT ( 'NONE',  ( -18.62759615963270932, 10.81492255796079327, 50.83224293864770971 ) ) ;
#77638 = CARTESIAN_POINT ( 'NONE',  ( 16.46253265017146816, 9.564922557961045513, 86.66775706135233293 ) ) ;
#77639 = CARTESIAN_POINT ( 'NONE',  ( 15.72974639402199770, -15.80617190586745480, 63.12390960531435979 ) ) ;
#77640 = CARTESIAN_POINT ( 'NONE',  ( 18.67979575497194134, -10.72451020669871369, 75.83442372801900433 ) ) ;
#77641 = DIRECTION ( 'NONE',  ( -1.000000000000000000, -0.000000000000000000, -0.000000000000000000 ) ) ;
#77642 = CARTESIAN_POINT ( 'NONE',  ( -4.483927247898782831, 16.52544592524335698, 47.70942372801902565 ) ) ;
#77644 = CARTESIAN_POINT ( 'NONE',  ( -19.02544592524342804, 5.153800228976336051, 101.0405762719810241 ) ) ;
#77643 = CARTESIAN_POINT ( 'NONE',  ( -13.97604488694527625, -13.89961937509977652, 31.87390960531435979 ) ) ;
#77645 = CARTESIAN_POINT ( 'NONE',  ( -9.474510206698964154, 16.51473224551069663, 35.41557627198102409 ) ) ;
#77646 = CARTESIAN_POINT ( 'NONE',  ( 16.53943276465976808, -0.05219959533910856209, 103.7489096053143669 ) ) ;
#77647 = DIRECTION ( 'NONE',  ( 0.000000000000000000, 0.000000000000000000, 1.000000000000000000 ) ) ;
#77648 = FACE_BOUND ( 'NONE', #53633, .T. ) ;
#77649 = ORIENTED_EDGE ( 'NONE', *, *, #48243, .F. ) ;
#77650 = CARTESIAN_POINT ( 'NONE',  ( -14.29746914071037622, -8.314922557961029526, 64.16775706135234714 ) ) ;
#77651 = CARTESIAN_POINT ( 'NONE',  ( 0.05219959533907565091, 21.53943276465977519, 84.99890960531436690 ) ) ;
#77652 = CARTESIAN_POINT ( 'NONE',  ( 16.46253265017160672, -9.564922557960803928, 53.33224293864768839 ) ) ;
#77653 = CARTESIAN_POINT ( 'NONE',  ( -10.81492255796105439, 18.62759615963255655, 27.91775706135234358 ) ) ;
#77654 = CARTESIAN_POINT ( 'NONE',  ( 13.97604488694527802, 13.89961937509977652, 89.37390960531436690 ) ) ;
#77655 = CARTESIAN_POINT ( 'NONE',  ( 2.300691058039529224, 7.143419655154843007, 8.646741581399139065 ) ) ;
#77656 = ORIENTED_EDGE ( 'NONE', *, *, #37032, .T. ) ;
#77657 = CARTESIAN_POINT ( 'NONE',  ( -10.72451020669870658, -18.67979575497194134, 24.58442372801901499 ) ) ;
#77660 = CARTESIAN_POINT ( 'NONE',  ( 5.049401038297881783, 19.05341960407617563, 72.29275706135234714 ) ) ;
#77659 = CARTESIAN_POINT ( 'NONE',  ( 9.564922557960805705, 16.46253265017160317, 109.5822429386476955 ) ) ;
#77658 = CARTESIAN_POINT ( 'NONE',  ( -9.564922557960796823, -16.46253265017161027, 22.08224293864768839 ) ) ;
#77661 = CARTESIAN_POINT ( 'NONE',  ( 13.89961937509957401, 13.97604488694547697, 31.87609039468566863 ) ) ;
#77662 = CARTESIAN_POINT ( 'NONE',  ( -15.72974639402197994, 15.80617190586746368, 100.6239096053143811 ) ) ;
#77663 = CARTESIAN_POINT ( 'NONE',  ( 0.05219959533936267826, -19.03943276465977164, 30.00109039468566863 ) ) ;
#77664 = CARTESIAN_POINT ( 'NONE',  ( 12.14591786802327356, -12.06949235617739191, 75.62609039468567573 ) ) ;
#77665 = CARTESIAN_POINT ( 'NONE',  ( -13.97604488694527625, -13.89961937509977652, 106.8739096053143669 ) ) ;
#77666 = CARTESIAN_POINT ( 'NONE',  ( -13.89961937509977652, 13.97604488694528158, 55.62390960531434558 ) ) ;
#77667 = CARTESIAN_POINT ( 'NONE',  ( -10.72451020669870658, -18.67979575497194134, 69.58442372801900433 ) ) ;
#77668 = CARTESIAN_POINT ( 'NONE',  ( 21.55341960407619695, -5.719274019375665929, 81.04275706135236135 ) ) ;
#77669 = CARTESIAN_POINT ( 'NONE',  ( 16.51473224551069308, 9.474510206698969483, 69.16557627198102409 ) ) ;
#77670 = CARTESIAN_POINT ( 'NONE',  ( -21.53943276465977519, -0.05219959533937600094, 48.75109039468568284 ) ) ;
#77671 = CARTESIAN_POINT ( 'NONE',  ( -9.474510206698720793, -16.51473224551083518, 89.58442372801900433 ) ) ;
#77672 = CARTESIAN_POINT ( 'NONE',  ( 13.97604488694527802, 13.89961937509977652, 49.37390960531434558 ) ) ;
#77673 = CARTESIAN_POINT ( 'NONE',  ( -5.049401038298153566, 19.05341960407611168, 100.2072429386476955 ) ) ;
#77674 = CARTESIAN_POINT ( 'NONE',  ( 19.02544592524343514, -5.153800228976328945, 68.54057627198103830 ) ) ;
#77675 = CARTESIAN_POINT ( 'NONE',  ( -19.05341960407611168, -5.049401038298163336, 111.4572429386476671 ) ) ;
#77676 = CARTESIAN_POINT ( 'NONE',  ( -5.153800228976328057, -19.02544592524343514, 57.29057627198103120 ) ) ;
#77677 = CARTESIAN_POINT ( 'NONE',  ( -21.55341960407610458, -5.719274019375992779, 101.4572429386476955 ) ) ;
#77678 = CARTESIAN_POINT ( 'NONE',  ( 4.483927247898790824, -16.52544592524335698, 70.20942372801904696 ) ) ;
#77679 = VECTOR ( 'NONE', #30824, 1000.000000000000000 ) ;
#77680 = CARTESIAN_POINT ( 'NONE',  ( -20.93662873023660254, 10.44628751056252725, 168.2749732860604013 ) ) ;
#77681 = CARTESIAN_POINT ( 'NONE',  ( -13.89961937509957401, -13.97604488694547875, 44.37609039468566863 ) ) ;
#77682 = CARTESIAN_POINT ( 'NONE',  ( 5.153800228976335163, 19.02544592524342804, 59.79057627198100988 ) ) ;
#77683 = CARTESIAN_POINT ( 'NONE',  ( -0.05219959533910754901, -16.53943276465976808, 57.49890960531435979 ) ) ;
#77684 = CARTESIAN_POINT ( 'NONE',  ( 4.483927247898545687, 16.52544592524342804, 89.79057627198103830 ) ) ;
#77685 = CARTESIAN_POINT ( 'NONE',  ( -19.02544592524342804, 5.153800228976336051, 111.0405762719810099 ) ) ;
#77686 = CARTESIAN_POINT ( 'NONE',  ( -9.564922557960796823, -16.46253265017161027, 97.08224293864769550 ) ) ;
#77687 = CARTESIAN_POINT ( 'NONE',  ( 9.564922557960805705, 16.46253265017160317, 104.5822429386476955 ) ) ;
#77688 = CARTESIAN_POINT ( 'NONE',  ( -5.823673210054431948, 21.52544592524334988, 107.7094237280190328 ) ) ;
#77689 = CARTESIAN_POINT ( 'NONE',  ( 12.06949235617739724, 12.14591786802326823, 96.87609039468568994 ) ) ;
#77690 = CARTESIAN_POINT ( 'NONE',  ( 9.474510206698971260, -16.51473224551069308, 77.91557627198103830 ) ) ;
#77691 = CARTESIAN_POINT ( 'NONE',  ( -0.05219959533937732626, 21.53943276465977519, 37.50109039468568284 ) ) ;
#77692 = CARTESIAN_POINT ( 'NONE',  ( -15.80617190586745835, -15.72974639402198527, 36.87390960531435979 ) ) ;
#77693 = CARTESIAN_POINT ( 'NONE',  ( -18.67979575497178146, -10.72451020669898902, 101.6655762719810383 ) ) ;
#77694 = CARTESIAN_POINT ( 'NONE',  ( -0.05219959533910754901, -16.53943276465976808, 62.49890960531436690 ) ) ;
#77695 = CARTESIAN_POINT ( 'NONE',  ( -19.03943276465977164, 0.05219959533909376836, 56.24890960531435979 ) ) ;
#77696 = CARTESIAN_POINT ( 'NONE',  ( 12.06949235617757843, -12.14591786802309237, 83.12390960531436690 ) ) ;
#77697 = CARTESIAN_POINT ( 'NONE',  ( 16.46253265017146816, 9.564922557961045513, 41.66775706135234003 ) ) ;
#77698 = EDGE_CURVE ( 'NONE', #114568, #173841, #147383, .T. ) ;
#77699 = CARTESIAN_POINT ( 'NONE',  ( 16.53943276465976808, -0.05219959533910856209, 108.7489096053143669 ) ) ;
#77700 = CARTESIAN_POINT ( 'NONE',  ( -5.049401038298153566, 19.05341960407611168, 80.20724293864769550 ) ) ;
#77701 = CARTESIAN_POINT ( 'NONE',  ( -9.474510206698964154, 16.51473224551069663, 75.41557627198103830 ) ) ;
#77702 = CARTESIAN_POINT ( 'NONE',  ( 22.44159573604009594, -16.30477369853687364, 143.6750000027311671 ) ) ;
#77703 = CARTESIAN_POINT ( 'NONE',  ( 12.14591786802309770, 12.06949235617756955, 94.37390960531436690 ) ) ;
#77704 = VERTEX_POINT ( 'NONE', #70641 ) ;
#77705 = CARTESIAN_POINT ( 'NONE',  ( 16.53943276465976808, 0.05219959533934440121, 101.2510903946856757 ) ) ;
#77706 = CARTESIAN_POINT ( 'NONE',  ( 16.55341960407618274, -4.379528057220086978, 31.04275706135234714 ) ) ;
#77707 = CARTESIAN_POINT ( 'NONE',  ( -21.53943276465977519, -0.05219959533937600094, 98.75109039468568994 ) ) ;
#77708 = CARTESIAN_POINT ( 'NONE',  ( -19.03943276465977164, 0.05219959533909376836, 91.24890960531436690 ) ) ;
#77709 = CARTESIAN_POINT ( 'NONE',  ( -5.823673210054431948, 21.52544592524334988, 22.70942372801901499 ) ) ;
#77710 = CARTESIAN_POINT ( 'NONE',  ( 0.05219959533909260263, 19.03943276465977164, 24.99890960531435269 ) ) ;
#77711 = CARTESIAN_POINT ( 'NONE',  ( 14.29746914071037800, 8.314922557961029526, 26.66775706135235424 ) ) ;
#77712 = CARTESIAN_POINT ( 'NONE',  ( -13.97604488694547697, 13.89961937509957934, 93.12609039468566152 ) ) ;
#77713 = CARTESIAN_POINT ( 'NONE',  ( 10.81492255796078972, 18.62759615963270932, 94.58224293864769550 ) ) ;
#77714 = CARTESIAN_POINT ( 'NONE',  ( 9.564922557961047289, -16.46253265017146816, 70.41775706135233293 ) ) ;
#77715 = SURFACE_SIDE_STYLE ('',( #43416 ) ) ;
#77716 = CARTESIAN_POINT ( 'NONE',  ( 15.72974639402199770, -15.80617190586745480, 113.1239096053143953 ) ) ;
#77717 = CYLINDRICAL_SURFACE ( 'NONE', #130537, 28.79475375365586487 ) ;
#77718 = CARTESIAN_POINT ( 'NONE',  ( 13.89961937509977652, -13.97604488694527269, 93.12390960531436690 ) ) ;
#77719 = CARTESIAN_POINT ( 'NONE',  ( 16.55341960407618274, -4.379528057220086978, 46.04275706135234714 ) ) ;
#77720 = CARTESIAN_POINT ( 'NONE',  ( 17.83380816373549038, -35.80792897213662940, -9.022620566401460707 ) ) ;
#77721 = CARTESIAN_POINT ( 'NONE',  ( -19.02544592524334988, -5.153800228976617603, 58.95942372801900433 ) ) ;
#77723 = CARTESIAN_POINT ( 'NONE',  ( 8.314922557960818139, 14.29746914071049879, 79.58224293864769550 ) ) ;
#77722 = CARTESIAN_POINT ( 'NONE',  ( 21.52544592524334988, 5.823673210054432836, 21.45942372801901499 ) ) ;
#77724 = CARTESIAN_POINT ( 'NONE',  ( -0.05219959533909027116, -19.03943276465977164, 87.49890960531436690 ) ) ;
#77726 = CARTESIAN_POINT ( 'NONE',  ( 9.474510206698729675, 16.51473224551082808, 57.08442372801900433 ) ) ;
#77725 = CARTESIAN_POINT ( 'NONE',  ( 14.34966873604972726, -8.224510206698740333, 45.83442372801901854 ) ) ;
#77727 = CARTESIAN_POINT ( 'NONE',  ( 10.81492255796106328, -18.62759615963255655, 70.41775706135236135 ) ) ;
#77728 = CARTESIAN_POINT ( 'NONE',  ( 14.34966873604972726, -8.224510206698740333, 30.83442372801902209 ) ) ;
#77729 = CARTESIAN_POINT ( 'NONE',  ( -19.05341960407611168, -5.049401038298163336, 71.45724293864766707 ) ) ;
#77730 = CARTESIAN_POINT ( 'NONE',  ( 19.03943276465977164, 0.05219959533936151252, 81.25109039468567573 ) ) ;
#77731 = CARTESIAN_POINT ( 'NONE',  ( -16.52544592524335698, -4.483927247898792601, 58.95942372801902565 ) ) ;
#77732 = CARTESIAN_POINT ( 'NONE',  ( 10.72451020669871369, 18.67979575497193778, 92.08442372801901854 ) ) ;
#77733 = CARTESIAN_POINT ( 'NONE',  ( -19.03943276465977164, -0.05219959533935918106, 78.75109039468567573 ) ) ;
#77734 = CARTESIAN_POINT ( 'NONE',  ( -16.46253265017160317, 9.564922557960807481, 50.83224293864770260 ) ) ;
#77735 = CARTESIAN_POINT ( 'NONE',  ( 15.80617190586746368, 15.72974639402197994, 74.37390960531436690 ) ) ;
#77737 = CARTESIAN_POINT ( 'NONE',  ( -13.89961937509957401, -13.97604488694547875, 84.37609039468567573 ) ) ;
#77736 = CARTESIAN_POINT ( 'NONE',  ( -14.34966873604960291, -8.224510206698953496, 81.66557627198103830 ) ) ;
#77738 = CARTESIAN_POINT ( 'NONE',  ( -18.22780087662123094, -5.499999999999984901, 71.48459894673891313 ) ) ;
#77739 = CARTESIAN_POINT ( 'NONE',  ( 16.46253265017146816, 9.564922557961045513, 41.66775706135234003 ) ) ;
#77740 = CARTESIAN_POINT ( 'NONE',  ( -12.14591786802326823, 12.06949235617739902, 98.12609039468570415 ) ) ;
#77741 = CARTESIAN_POINT ( 'NONE',  ( 16.52544592524342804, -4.483927247898539470, 68.54057627198103830 ) ) ;
#77743 = CARTESIAN_POINT ( 'NONE',  ( -17.14385361876520619, 23.59649016807275856, 142.5750000027312012 ) ) ;
#77742 = CARTESIAN_POINT ( 'NONE',  ( 18.67979575497194134, -10.72451020669871369, 100.8344237280190185 ) ) ;
#77744 = CARTESIAN_POINT ( 'NONE',  ( 18.67979575497178502, 10.72451020669898547, 109.1655762719810383 ) ) ;
#77745 = CARTESIAN_POINT ( 'NONE',  ( 19.05341960407611168, 5.049401038298154454, 58.95724293864768129 ) ) ;
#77746 = CARTESIAN_POINT ( 'NONE',  ( 21.55341960407619695, -5.719274019375665929, 76.04275706135237556 ) ) ;
#77747 = CARTESIAN_POINT ( 'NONE',  ( 16.51473224551069308, 9.474510206698969483, 54.16557627198103120 ) ) ;
#77748 = ORIENTED_EDGE ( 'NONE', *, *, #157667, .T. ) ;
#77749 = CARTESIAN_POINT ( 'NONE',  ( 5.049401038298161559, -19.05341960407611168, 27.70724293864769550 ) ) ;
#77750 = CARTESIAN_POINT ( 'NONE',  ( -21.55341960407610458, -5.719274019375992779, 21.45724293864769550 ) ) ;
#77751 = CARTESIAN_POINT ( 'NONE',  ( -12.06949235617756955, 12.14591786802309770, 65.62390960531436690 ) ) ;
#77752 = CARTESIAN_POINT ( 'NONE',  ( 13.97604488694527802, 13.89961937509977652, 24.37390960531435624 ) ) ;
#77753 = CARTESIAN_POINT ( 'NONE',  ( 4.483927247898545687, 16.52544592524342804, 84.79057627198102409 ) ) ;
#77754 = CARTESIAN_POINT ( 'NONE',  ( 5.719274019375991003, -21.55341960407610458, 92.70724293864770971 ) ) ;
#77755 = CARTESIAN_POINT ( 'NONE',  ( 5.719274019375673035, 21.55341960407619339, 42.29275706135235424 ) ) ;
#77756 = CARTESIAN_POINT ( 'NONE',  ( 1.304798881014889833, 6.853701371036049039, -62.35416993336013292 ) ) ;
#77757 = CARTESIAN_POINT ( 'NONE',  ( 4.379528057220092307, 16.55341960407617563, 47.29275706135234003 ) ) ;
#77758 = CARTESIAN_POINT ( 'NONE',  ( 21.53943276465977519, -0.05219959533907433946, 103.7489096053143669 ) ) ;
#77759 = CARTESIAN_POINT ( 'NONE',  ( 19.05341960407617918, -5.049401038297876454, 26.04275706135233293 ) ) ;
#77760 = CARTESIAN_POINT ( 'NONE',  ( -19.05341960407611168, -5.049401038298163336, 111.4572429386476671 ) ) ;
#77761 = CARTESIAN_POINT ( 'NONE',  ( 18.67979575497194134, -10.72451020669871369, 40.83442372801901854 ) ) ;
#77762 = CARTESIAN_POINT ( 'NONE',  ( 5.823673210054125526, 21.52544592524343514, 49.79057627198102409 ) ) ;
#77763 = CARTESIAN_POINT ( 'NONE',  ( -0.05219959533910754901, -16.53943276465976808, 27.49890960531435269 ) ) ;
#77765 = CARTESIAN_POINT ( 'NONE',  ( -21.53943276465977519, -0.05219959533937600094, 98.75109039468568994 ) ) ;
#77764 = CARTESIAN_POINT ( 'NONE',  ( 5.823673210054444382, -21.52544592524334988, 65.20942372801901854 ) ) ;
#77766 = CARTESIAN_POINT ( 'NONE',  ( 9.564922557961047289, -16.46253265017146816, 25.41775706135234003 ) ) ;
#77767 = CARTESIAN_POINT ( 'NONE',  ( 16.53943276465976808, 0.05219959533934440121, 91.25109039468568994 ) ) ;
#77768 = CARTESIAN_POINT ( 'NONE',  ( 21.53943276465977519, 0.05219959533937863772, 51.25109039468568994 ) ) ;
#77769 = CARTESIAN_POINT ( 'NONE',  ( -5.049401038298153566, 19.05341960407611168, 40.20724293864768839 ) ) ;
#77770 = CARTESIAN_POINT ( 'NONE',  ( -0.05219959533937732626, 21.53943276465977519, 112.5010903946857042 ) ) ;
#77771 = CARTESIAN_POINT ( 'NONE',  ( 18.67979575497178502, 10.72451020669898547, 24.16557627198103120 ) ) ;
#77772 = CARTESIAN_POINT ( 'NONE',  ( 5.823673210054444382, -21.52544592524334988, 25.20942372801901854 ) ) ;
#77773 = CARTESIAN_POINT ( 'NONE',  ( -21.52544592524343514, 5.823673210054127303, 76.04057627198102409 ) ) ;
#77774 = CARTESIAN_POINT ( 'NONE',  ( 16.53943276465976808, 0.05219959533934440121, 41.25109039468568284 ) ) ;
#77775 = CARTESIAN_POINT ( 'NONE',  ( 5.719274019375991003, -21.55341960407610458, 77.70724293864770971 ) ) ;
#77777 = CARTESIAN_POINT ( 'NONE',  ( 16.52544592524342804, -4.483927247898539470, 63.54057627198103830 ) ) ;
#77776 = CARTESIAN_POINT ( 'NONE',  ( 16.53943276465976808, 0.05219959533934440121, 66.25109039468567573 ) ) ;
#77778 = CARTESIAN_POINT ( 'NONE',  ( -22.65278057777883092, 22.46063206192296136, -45.64921306006598911 ) ) ;
#77779 = CARTESIAN_POINT ( 'NONE',  ( 16.46253265017146816, 9.564922557961045513, 101.6677570613523329 ) ) ;
#77780 = CARTESIAN_POINT ( 'NONE',  ( 20.43538597629129328, 20.43538597629121156, -49.67367017693150189 ) ) ;
#77781 = CARTESIAN_POINT ( 'NONE',  ( 12.14591786802327356, -12.06949235617739191, 40.62609039468567573 ) ) ;
#77782 = CARTESIAN_POINT ( 'NONE',  ( -21.52544592524343514, 5.823673210054127303, 116.0405762719810383 ) ) ;
#77783 = CARTESIAN_POINT ( 'NONE',  ( -5.823673210054116645, -21.52544592524344225, 37.29057627198102409 ) ) ;
#77784 = CARTESIAN_POINT ( 'NONE',  ( 16.52544592524335698, 4.483927247898782831, 51.45942372801901854 ) ) ;
#77785 = CARTESIAN_POINT ( 'NONE',  ( 5.049401038298161559, -19.05341960407611168, 72.70724293864768129 ) ) ;
#77787 = CARTESIAN_POINT ( 'NONE',  ( -19.02544592524334988, -5.153800228976617603, 108.9594237280189759 ) ) ;
#77786 = CARTESIAN_POINT ( 'NONE',  ( -18.67979575497193778, 10.72451020669871902, 48.33442372801902565 ) ) ;
#77788 = CARTESIAN_POINT ( 'NONE',  ( 21.55341960407610458, 5.719274019375980345, 23.95724293864769550 ) ) ;
#77789 = ORIENTED_EDGE ( 'NONE', *, *, #47276, .T. ) ;
#77790 = CARTESIAN_POINT ( 'NONE',  ( 5.049401038297881783, 19.05341960407617563, 32.29275706135233293 ) ) ;
#77791 = CARTESIAN_POINT ( 'NONE',  ( 16.53943276465976808, 0.05219959533934440121, 36.25109039468567573 ) ) ;
#77792 = CARTESIAN_POINT ( 'NONE',  ( 9.564922557960805705, 16.46253265017160317, 99.58224293864770971 ) ) ;
#77793 = CARTESIAN_POINT ( 'NONE',  ( 18.67979575497178502, 10.72451020669898547, 109.1655762719810383 ) ) ;
#77794 = CARTESIAN_POINT ( 'NONE',  ( -16.51473224551069308, -9.474510206698971260, 76.66557627198103830 ) ) ;
#77795 = CARTESIAN_POINT ( 'NONE',  ( -17.26172910966779028, 6.454744622555852018, 25.80646908649224613 ) ) ;
#77796 = CARTESIAN_POINT ( 'NONE',  ( -4.483927247898539470, -16.52544592524342804, 82.29057627198103830 ) ) ;
#77797 = CARTESIAN_POINT ( 'NONE',  ( 10.72451020669898902, -18.67979575497178502, 22.91557627198102765 ) ) ;
#77798 = CARTESIAN_POINT ( 'NONE',  ( 12.99999999999999822, 0.000000000000000000, 0.000000000000000000 ) ) ;
#77799 = CARTESIAN_POINT ( 'NONE',  ( -4.379528057220086978, -16.55341960407618274, 64.79275706135234714 ) ) ;
#77800 = CARTESIAN_POINT ( 'NONE',  ( 18.67979575497178502, 10.72451020669898547, 104.1655762719810241 ) ) ;
#77801 = CARTESIAN_POINT ( 'NONE',  ( -19.02544592524334988, -5.153800228976617603, 58.95942372801900433 ) ) ;
#77802 = CARTESIAN_POINT ( 'NONE',  ( 10.72451020669898902, -18.67979575497178502, 32.91557627198102409 ) ) ;
#77803 = CARTESIAN_POINT ( 'NONE',  ( -5.049401038298153566, 19.05341960407611168, 25.20724293864768484 ) ) ;
#77804 = CARTESIAN_POINT ( 'NONE',  ( -10.81492255796078084, -18.62759615963271287, 72.08224293864769550 ) ) ;
#77805 = CARTESIAN_POINT ( 'NONE',  ( 13.89961937509977652, -13.97604488694527269, 93.12390960531436690 ) ) ;
#77806 = CARTESIAN_POINT ( 'NONE',  ( 18.62759615963255655, 10.81492255796105972, 91.66775706135234714 ) ) ;
#77807 = CARTESIAN_POINT ( 'NONE',  ( 5.153800228976335163, 19.02544592524342804, 54.79057627198103120 ) ) ;
#77808 = CARTESIAN_POINT ( 'NONE',  ( 8.224510206698742110, 14.34966873604972548, 32.08442372801901854 ) ) ;
#77809 = CARTESIAN_POINT ( 'NONE',  ( 13.89961937509977652, -13.97604488694527269, 53.12390960531434558 ) ) ;
#77810 = CARTESIAN_POINT ( 'NONE',  ( 21.55341960407619695, -5.719274019375665929, 86.04275706135236135 ) ) ;
#77811 = ORIENTED_EDGE ( 'NONE', *, *, #66266, .T. ) ;
#77812 = CARTESIAN_POINT ( 'NONE',  ( -0.05219959533936034679, 19.03943276465977164, 42.50109039468566152 ) ) ;
#77813 = CARTESIAN_POINT ( 'NONE',  ( 16.46253265017146816, 9.564922557961045513, 41.66775706135234003 ) ) ;
#77814 = CARTESIAN_POINT ( 'NONE',  ( 18.62759615963255655, 10.81492255796105972, 41.66775706135235424 ) ) ;
#77815 = CARTESIAN_POINT ( 'NONE',  ( 5.153800228976335163, 19.02544592524342804, 54.79057627198103120 ) ) ;
#77816 = CARTESIAN_POINT ( 'NONE',  ( 19.02544592524334988, 5.153800228976608722, 26.45942372801899722 ) ) ;
#77817 = CARTESIAN_POINT ( 'NONE',  ( -19.03943276465977164, 0.05219959533909376836, 86.24890960531436690 ) ) ;
#77818 = CARTESIAN_POINT ( 'NONE',  ( 16.51473224551069308, 9.474510206698969483, 64.16557627198102409 ) ) ;
#77819 = CARTESIAN_POINT ( 'NONE',  ( -16.52544592524342804, 4.483927247898546575, 31.04057627198102409 ) ) ;
#77821 = CARTESIAN_POINT ( 'NONE',  ( -21.53943276465977519, -0.05219959533937600094, 83.75109039468568994 ) ) ;
#77820 = CARTESIAN_POINT ( 'NONE',  ( -9.564922557960796823, -16.46253265017161027, 112.0822429386476955 ) ) ;
#77822 = CARTESIAN_POINT ( 'NONE',  ( 11.40812507854754365, 35.11059874428196537, -1.224999997268813479 ) ) ;
#77823 = CARTESIAN_POINT ( 'NONE',  ( 17.44270441346513323, 5.991230190323100224, 58.86335079264229364 ) ) ;
#77824 = CARTESIAN_POINT ( 'NONE',  ( -21.52544592524334988, -5.823673210054445271, 93.95942372801903275 ) ) ;
#77825 = CARTESIAN_POINT ( 'NONE',  ( 21.39352396646988552, -0.5319302666794151202, -58.79417398750191381 ) ) ;
#77826 = CARTESIAN_POINT ( 'NONE',  ( -16.51473224551069308, -9.474510206698971260, 26.66557627198103120 ) ) ;
#77827 = DIRECTION ( 'NONE',  ( 1.000000000000000000, 0.000000000000000000, 0.000000000000000000 ) ) ;
#77828 = EDGE_CURVE ( 'NONE', #59417, #165210, #199477, .T. ) ;
#77829 = CARTESIAN_POINT ( 'NONE',  ( 33.86350577294170705, 5.311679113341320146, 93.56182321589975004 ) ) ;
#77830 = CARTESIAN_POINT ( 'NONE',  ( -12.06949235617739369, -12.14591786802326823, 54.37609039468568994 ) ) ;
#77831 = CARTESIAN_POINT ( 'NONE',  ( 18.67979575497178502, 10.72451020669898547, 69.16557627198102409 ) ) ;
#77832 = CARTESIAN_POINT ( 'NONE',  ( -16.52544592524342804, 4.483927247898546575, 36.04057627198102409 ) ) ;
#77834 = CARTESIAN_POINT ( 'NONE',  ( -5.049401038298153566, 19.05341960407611168, 90.20724293864766707 ) ) ;
#77833 = CARTESIAN_POINT ( 'NONE',  ( 4.379528057220339221, -16.55341960407611168, 107.7072429386476955 ) ) ;
#77835 = CARTESIAN_POINT ( 'NONE',  ( -19.03943276465977164, -0.05219959533935918106, 23.75109039468566152 ) ) ;
#77836 = CARTESIAN_POINT ( 'NONE',  ( -16.53943276465976808, 0.05219959533911058130, 116.2489096053143669 ) ) ;
#77837 = CARTESIAN_POINT ( 'NONE',  ( 10.72451020669871369, 18.67979575497193778, 72.08442372801899012 ) ) ;
#77838 = CARTESIAN_POINT ( 'NONE',  ( -19.02544592524342804, 5.153800228976336051, 111.0405762719810099 ) ) ;
#77839 = CARTESIAN_POINT ( 'NONE',  ( 8.224510206698742110, 14.34966873604972548, 112.0844237280190185 ) ) ;
#77840 = CARTESIAN_POINT ( 'NONE',  ( 19.03943276465977164, 0.05219959533936151252, 71.25109039468566152 ) ) ;
#77841 = CARTESIAN_POINT ( 'NONE',  ( -36.91746825000000598, -11.99521256947794789, -5.024999997268813523 ) ) ;
#77842 = CARTESIAN_POINT ( 'NONE',  ( 13.89961937509977652, -13.97604488694527269, 108.1239096053143669 ) ) ;
#77843 = CARTESIAN_POINT ( 'NONE',  ( 12.14591786802309770, 12.06949235617756955, 94.37390960531436690 ) ) ;
#77844 = CARTESIAN_POINT ( 'NONE',  ( -0.05219959533936034679, 19.03943276465977164, 62.50109039468566863 ) ) ;
#77845 = CARTESIAN_POINT ( 'NONE',  ( 0.05219959533909260263, 19.03943276465977164, 69.99890960531435269 ) ) ;
#77846 = CARTESIAN_POINT ( 'NONE',  ( 14.29746914071049879, -8.314922557960816363, 68.33224293864769550 ) ) ;
#77847 = CARTESIAN_POINT ( 'NONE',  ( 19.02544592524334988, 5.153800228976608722, 91.45942372801900433 ) ) ;
#77848 = CARTESIAN_POINT ( 'NONE',  ( -18.67979575497178146, -10.72451020669898902, 46.66557627198102409 ) ) ;
#77849 = EDGE_LOOP ( 'NONE', ( #63687, #5649, #158842, #168060 ) ) ;
#77850 = CARTESIAN_POINT ( 'NONE',  ( -14.29746914071049879, 8.314922557960819915, 110.8322429386476955 ) ) ;
#77851 = CARTESIAN_POINT ( 'NONE',  ( 9.564922557961047289, -16.46253265017146816, 100.4177570613523329 ) ) ;
#77853 = CARTESIAN_POINT ( 'NONE',  ( -21.52544592524343514, 5.823673210054127303, 71.04057627198103830 ) ) ;
#77852 = CARTESIAN_POINT ( 'NONE',  ( -16.51473224551069308, -9.474510206698971260, 71.66557627198102409 ) ) ;
#77855 = CARTESIAN_POINT ( 'NONE',  ( 13.89961937509977652, -13.97604488694527269, 68.12390960531436690 ) ) ;
#77854 = CARTESIAN_POINT ( 'NONE',  ( 14.34966873604972726, -8.224510206698740333, 95.83442372801903275 ) ) ;
#77856 = CARTESIAN_POINT ( 'NONE',  ( -19.03943276465977164, -0.05219959533935918106, 63.75109039468566863 ) ) ;
#77857 = CARTESIAN_POINT ( 'NONE',  ( -5.823673210054431948, 21.52544592524334988, 87.70942372801901854 ) ) ;
#77858 = CARTESIAN_POINT ( 'NONE',  ( -5.823673210054116645, -21.52544592524344225, 67.29057627198103830 ) ) ;
#77859 = CARTESIAN_POINT ( 'NONE',  ( 0.05219959533907565091, 21.53943276465977519, 24.99890960531435624 ) ) ;
#77860 = CARTESIAN_POINT ( 'NONE',  ( 16.46253265017160672, -9.564922557960803928, 38.33224293864768839 ) ) ;
#77861 = CARTESIAN_POINT ( 'NONE',  ( -14.34966873604972548, 8.224510206698743886, 98.33442372801901854 ) ) ;
#77862 = CARTESIAN_POINT ( 'NONE',  ( -13.97604488694527625, -13.89961937509977652, 46.87390960531435979 ) ) ;
#77863 = CARTESIAN_POINT ( 'NONE',  ( 16.52544592524335698, 4.483927247898782831, 21.45942372801901499 ) ) ;
#77864 = CARTESIAN_POINT ( 'NONE',  ( -30.00000000000000000, -5.510910596163089556E-15, 45.00000000000000000 ) ) ;
#77865 = CARTESIAN_POINT ( 'NONE',  ( 19.02544592524334988, 5.153800228976608722, 21.45942372801899012 ) ) ;
#77866 = CARTESIAN_POINT ( 'NONE',  ( 0.05219959533910956823, 16.53943276465976808, 54.99890960531435269 ) ) ;
#77867 = CARTESIAN_POINT ( 'NONE',  ( -18.67979575497178146, -10.72451020669898902, 101.6655762719810383 ) ) ;
#77868 = CARTESIAN_POINT ( 'NONE',  ( 5.823673210054125526, 21.52544592524343514, 104.7905762719810241 ) ) ;
#77869 = CARTESIAN_POINT ( 'NONE',  ( 16.79531203550648044, -7.028104445595601213, 96.24755011779556924 ) ) ;
#77870 = CARTESIAN_POINT ( 'NONE',  ( 5.719274019375991003, -21.55341960407610458, 47.70724293864770260 ) ) ;
#77871 = CARTESIAN_POINT ( 'NONE',  ( 4.379528057220092307, 16.55341960407617563, 82.29275706135234714 ) ) ;
#77872 = CARTESIAN_POINT ( 'NONE',  ( -16.53943276465976808, 0.05219959533911058130, 86.24890960531436690 ) ) ;
#77873 = CARTESIAN_POINT ( 'NONE',  ( -13.97604488694527625, -13.89961937509977652, 46.87390960531435979 ) ) ;
#77874 = CARTESIAN_POINT ( 'NONE',  ( -25.83521962401025007, -30.44105770729785121, -17.07601944841967523 ) ) ;
#77875 = CARTESIAN_POINT ( 'NONE',  ( -8.314922557961024197, 14.29746914071037800, 107.9177570613523471 ) ) ;
#77876 = CARTESIAN_POINT ( 'NONE',  ( -10.81492255796105439, 18.62759615963255655, 27.91775706135234358 ) ) ;
#77877 = CARTESIAN_POINT ( 'NONE',  ( -13.97604488694527625, -13.89961937509977652, 101.8739096053143811 ) ) ;
#77878 = CARTESIAN_POINT ( 'NONE',  ( 5.719274019375673035, 21.55341960407619339, 62.29275706135236845 ) ) ;
#77879 = FACE_OUTER_BOUND ( 'NONE', #27253, .T. ) ;
#77880 = CYLINDRICAL_SURFACE ( 'NONE', #115449, 12.50000000000000000 ) ;
#77881 = ORIENTED_EDGE ( 'NONE', *, *, #22446, .T. ) ;
#77882 = CARTESIAN_POINT ( 'NONE',  ( 10.81492255796106328, -18.62759615963255655, 60.41775706135235424 ) ) ;
#77884 = CARTESIAN_POINT ( 'NONE',  ( 17.60728821187776916, -5.500000000000036415, 58.36690927743609336 ) ) ;
#77883 = CARTESIAN_POINT ( 'NONE',  ( -16.46253265017160317, 9.564922557960807481, 45.83224293864769550 ) ) ;
#77885 = CARTESIAN_POINT ( 'NONE',  ( 9.474510206698971260, -16.51473224551069308, 92.91557627198103830 ) ) ;
#77886 = CARTESIAN_POINT ( 'NONE',  ( 16.51473224551083163, -9.474510206698727899, 65.83442372801900433 ) ) ;
#77887 = CARTESIAN_POINT ( 'NONE',  ( 15.80617190586769283, -15.72974639402175789, 40.62609039468567573 ) ) ;
#77888 = CARTESIAN_POINT ( 'NONE',  ( 9.564922557961047289, -16.46253265017146816, 105.4177570613523471 ) ) ;
#77889 = CARTESIAN_POINT ( 'NONE',  ( -13.97604488694547697, 13.89961937509957934, 68.12609039468563310 ) ) ;
#77890 = CARTESIAN_POINT ( 'NONE',  ( -13.89961937509977652, 13.97604488694528158, 35.62390960531435269 ) ) ;
#77891 = CARTESIAN_POINT ( 'NONE',  ( -12.06949235617739369, -12.14591786802326823, 109.3760903946857042 ) ) ;
#77892 = CARTESIAN_POINT ( 'NONE',  ( -9.564922557961040184, 16.46253265017147172, 77.91775706135234714 ) ) ;
#77893 = CARTESIAN_POINT ( 'NONE',  ( -8.314922557960811034, -14.29746914071050412, 22.08224293864769194 ) ) ;
#77894 = CARTESIAN_POINT ( 'NONE',  ( 9.564922557961047289, -16.46253265017146816, 45.41775706135232582 ) ) ;
#77895 = CARTESIAN_POINT ( 'NONE',  ( 18.67979575497194134, -10.72451020669871369, 105.8344237280190328 ) ) ;
#77897 = EDGE_CURVE ( 'NONE', #119352, #182346, #115620, .T. ) ;
#77896 = CARTESIAN_POINT ( 'NONE',  ( -19.05341960407617563, 5.049401038297882671, 23.54275706135233648 ) ) ;
#77898 = CARTESIAN_POINT ( 'NONE',  ( -19.03943276465977164, 0.05219959533909376836, 31.24890960531435979 ) ) ;
#77899 = CARTESIAN_POINT ( 'NONE',  ( 5.719274019375673035, 21.55341960407619339, 82.29275706135234714 ) ) ;
#77900 = CARTESIAN_POINT ( 'NONE',  ( -8.314922557961024197, 14.29746914071037800, 27.91775706135234358 ) ) ;
#77901 = CARTESIAN_POINT ( 'NONE',  ( -19.05341960407611168, -5.049401038298163336, 91.45724293864766707 ) ) ;
#77902 = CARTESIAN_POINT ( 'NONE',  ( 27.73933785331498569, 2.768321779492822058E-14, 141.8750000027311842 ) ) ;
#77903 = CARTESIAN_POINT ( 'NONE',  ( -13.89961937509977652, 13.97604488694528158, 75.62390960531438111 ) ) ;
#77904 = CARTESIAN_POINT ( 'NONE',  ( -17.44279575226783763, 5.990770900254001496, 100.8355756751431898 ) ) ;
#77905 = CARTESIAN_POINT ( 'NONE',  ( -16.51473224551082808, 9.474510206698731452, 78.33442372801900433 ) ) ;
#77906 = CARTESIAN_POINT ( 'NONE',  ( -16.46253265017160317, 9.564922557960807481, 110.8322429386476955 ) ) ;
#77907 = CARTESIAN_POINT ( 'NONE',  ( 0.05219959533937995610, -21.53943276465977519, 110.0010903946856757 ) ) ;
#77908 = CARTESIAN_POINT ( 'NONE',  ( -8.314922557960811034, -14.29746914071050412, 92.08224293864769550 ) ) ;
#77909 = CARTESIAN_POINT ( 'NONE',  ( -19.05341960407611168, -5.049401038298163336, 26.45724293864769550 ) ) ;
#77910 = CARTESIAN_POINT ( 'NONE',  ( -21.55341960407610458, -5.719274019375992779, 61.45724293864770260 ) ) ;
#77911 = CARTESIAN_POINT ( 'NONE',  ( 15.80617190586746368, 15.72974639402197994, 39.37390960531436690 ) ) ;
#77912 = CARTESIAN_POINT ( 'NONE',  ( 14.29746914071049879, -8.314922557960816363, 113.3322429386476955 ) ) ;
#77913 = CARTESIAN_POINT ( 'NONE',  ( -0.3920586954752057207, -9.051216217265922737, -61.90435651123959104 ) ) ;
#77914 = CARTESIAN_POINT ( 'NONE',  ( -16.51473224551082808, 9.474510206698731452, 63.33442372801900433 ) ) ;
#77915 = CARTESIAN_POINT ( 'NONE',  ( -14.34966873604960291, -8.224510206698953496, 46.66557627198102409 ) ) ;
#77916 = CARTESIAN_POINT ( 'NONE',  ( -19.03943276465977164, 0.05219959533909376836, 116.2489096053143669 ) ) ;
#77917 = CARTESIAN_POINT ( 'NONE',  ( 0.05219959533937995610, -21.53943276465977519, 75.00109039468568994 ) ) ;
#77918 = CARTESIAN_POINT ( 'NONE',  ( 15.72974639402199770, -15.80617190586745480, 68.12390960531436690 ) ) ;
#77919 = CARTESIAN_POINT ( 'NONE',  ( 10.72451020669871369, 18.67979575497193778, 57.08442372801901854 ) ) ;
#77920 = CARTESIAN_POINT ( 'NONE',  ( 21.55341960407610458, 5.719274019375980345, 98.95724293864770971 ) ) ;
#77921 = CARTESIAN_POINT ( 'NONE',  ( 21.53943276465977519, 0.05219959533937863772, 46.25109039468567573 ) ) ;
#77922 = CARTESIAN_POINT ( 'NONE',  ( 9.474510206698971260, -16.51473224551069308, 77.91557627198103830 ) ) ;
#77923 = CARTESIAN_POINT ( 'NONE',  ( 4.483927247898790824, -16.52544592524335698, 85.20942372801901854 ) ) ;
#77924 = CARTESIAN_POINT ( 'NONE',  ( -0.05219959533909027116, -19.03943276465977164, 27.49890960531435624 ) ) ;
#77925 = DIRECTION ( 'NONE',  ( -0.9526137857479314297, -0.3041824702427711746, 0.000000000000000000 ) ) ;
#77926 = CARTESIAN_POINT ( 'NONE',  ( -12.06949235617756955, 12.14591786802309770, 60.62390960531437401 ) ) ;
#77927 = CARTESIAN_POINT ( 'NONE',  ( 16.55341960407611168, 4.379528057220329451, 23.95724293864769550 ) ) ;
#77928 = CARTESIAN_POINT ( 'NONE',  ( 13.89961937509977652, -13.97604488694527269, 63.12390960531435979 ) ) ;
#77929 = CARTESIAN_POINT ( 'NONE',  ( 9.564922557960805705, 16.46253265017160317, 34.58224293864770260 ) ) ;
#77930 = CARTESIAN_POINT ( 'NONE',  ( -15.72974639402197994, 15.80617190586746368, 45.62390960531436690 ) ) ;
#77931 = CARTESIAN_POINT ( 'NONE',  ( -19.05341960407617563, 5.049401038297882671, 38.54275706135233293 ) ) ;
#77933 = CARTESIAN_POINT ( 'NONE',  ( 12.14591786802309770, 12.06949235617756955, 54.37390960531435979 ) ) ;
#77932 = CARTESIAN_POINT ( 'NONE',  ( -17.44279575226822843, -5.990770900252486264, 39.16442432485683156 ) ) ;
#77934 = CARTESIAN_POINT ( 'NONE',  ( 10.72451020669898902, -18.67979575497178502, 32.91557627198102409 ) ) ;
#77935 = LINE ( 'NONE', #186141, #187299 ) ;
#77936 = CARTESIAN_POINT ( 'NONE',  ( 0.05219959533934541429, -16.53943276465976808, 70.00109039468568994 ) ) ;
#77937 = CARTESIAN_POINT ( 'NONE',  ( 19.03943276465977164, 0.05219959533936151252, 76.25109039468566152 ) ) ;
#77938 = CARTESIAN_POINT ( 'NONE',  ( -4.379528057220328563, 16.55341960407611168, 45.20724293864769550 ) ) ;
#77939 = CARTESIAN_POINT ( 'NONE',  ( -19.25176906914648711, -5.499999999999851674, 75.99927264242275271 ) ) ;
#77940 = CARTESIAN_POINT ( 'NONE',  ( 16.52544592524342804, -4.483927247898539470, 23.54057627198102765 ) ) ;
#77941 = CARTESIAN_POINT ( 'NONE',  ( -19.03943276465977164, 0.05219959533909376836, 36.24890960531436690 ) ) ;
#77942 = CARTESIAN_POINT ( 'NONE',  ( -16.51473224551069308, -9.474510206698971260, 56.66557627198103120 ) ) ;
#77943 = CARTESIAN_POINT ( 'NONE',  ( -16.51473224551069308, -9.474510206698971260, 21.66557627198102765 ) ) ;
#77944 = CARTESIAN_POINT ( 'NONE',  ( 5.823673210054444382, -21.52544592524334988, 30.20942372801902565 ) ) ;
#77945 = CARTESIAN_POINT ( 'NONE',  ( -9.564922557960796823, -16.46253265017161027, 62.08224293864769550 ) ) ;
#77946 = FACE_OUTER_BOUND ( 'NONE', #127929, .T. ) ;
#77947 = CARTESIAN_POINT ( 'NONE',  ( -19.05341960407611168, -5.049401038298163336, 41.45724293864769550 ) ) ;
#77948 = CARTESIAN_POINT ( 'NONE',  ( -0.05219959533907301413, -21.53943276465977519, 37.49890960531436690 ) ) ;
#77950 = CARTESIAN_POINT ( 'NONE',  ( -13.97604488694527625, -13.89961937509977652, 21.87390960531435979 ) ) ;
#77949 = CARTESIAN_POINT ( 'NONE',  ( 21.52544592524334988, 5.823673210054432836, 61.45942372801901854 ) ) ;
#77951 = CARTESIAN_POINT ( 'NONE',  ( -18.62759615963270932, 10.81492255796079327, 30.83224293864770260 ) ) ;
#77952 = CARTESIAN_POINT ( 'NONE',  ( -16.55341960407617563, 4.379528057220093196, 88.54275706135236135 ) ) ;
#77953 = CARTESIAN_POINT ( 'NONE',  ( 21.55341960407619695, -5.719274019375665929, 101.0427570613523756 ) ) ;
#77954 = CARTESIAN_POINT ( 'NONE',  ( -8.224510206698735004, -14.34966873604973081, 69.58442372801900433 ) ) ;
#77955 = CARTESIAN_POINT ( 'NONE',  ( 5.153800228976335163, 19.02544592524342804, 114.7905762719810241 ) ) ;
#77956 = CARTESIAN_POINT ( 'NONE',  ( 16.53943276465976808, 0.05219959533934440121, 56.25109039468568284 ) ) ;
#77957 = CARTESIAN_POINT ( 'NONE',  ( -16.52544592524335698, -4.483927247898792601, 38.95942372801901854 ) ) ;
#77958 = CARTESIAN_POINT ( 'NONE',  ( 14.34966873604972726, -8.224510206698740333, 90.83442372801901854 ) ) ;
#77959 = CARTESIAN_POINT ( 'NONE',  ( -18.67979575497193778, 10.72451020669871902, 53.33442372801901854 ) ) ;
#77960 = CARTESIAN_POINT ( 'NONE',  ( 4.483927247898790824, -16.52544592524335698, 20.20942372801900788 ) ) ;
#77961 = CARTESIAN_POINT ( 'NONE',  ( -21.52544592524343514, 5.823673210054127303, 106.0405762719810525 ) ) ;
#77962 = CARTESIAN_POINT ( 'NONE',  ( 14.29746914071037800, 8.314922557961029526, 26.66775706135235424 ) ) ;
#77963 = CARTESIAN_POINT ( 'NONE',  ( 8.224510206698742110, 14.34966873604972548, 92.08442372801901854 ) ) ;
#77964 = CARTESIAN_POINT ( 'NONE',  ( -2.552343178074661267, -7.052343178074616858, 8.889087296526001936 ) ) ;
#77965 = CARTESIAN_POINT ( 'NONE',  ( -0.05219959533937732626, 21.53943276465977519, 92.50109039468567573 ) ) ;
#77966 = CARTESIAN_POINT ( 'NONE',  ( 19.02544592524334988, 5.153800228976608722, 81.45942372801897591 ) ) ;
#77967 = CARTESIAN_POINT ( 'NONE',  ( 16.55341960407611168, 4.379528057220329451, 63.95724293864770260 ) ) ;
#77968 = CARTESIAN_POINT ( 'NONE',  ( 12.06949235617757843, -12.14591786802309237, 38.12390960531436690 ) ) ;
#77969 = CARTESIAN_POINT ( 'NONE',  ( -12.06949235617756955, 12.14591786802309770, 110.6239096053143669 ) ) ;
#77971 = SURFACE_SIDE_STYLE ('',( #16321 ) ) ;
#77970 = CARTESIAN_POINT ( 'NONE',  ( 13.97604488694548053, -13.89961937509957401, 45.62609039468566863 ) ) ;
#77972 = CARTESIAN_POINT ( 'NONE',  ( 5.823673210054444382, -21.52544592524334988, 50.20942372801901854 ) ) ;
#77973 = CARTESIAN_POINT ( 'NONE',  ( 9.564922557961047289, -16.46253265017146816, 110.4177570613523471 ) ) ;
#77974 = FACE_OUTER_BOUND ( 'NONE', #128601, .T. ) ;
#77975 = CARTESIAN_POINT ( 'NONE',  ( -16.46253265017160317, 9.564922557960807481, 100.8322429386477097 ) ) ;
#77976 = CARTESIAN_POINT ( 'NONE',  ( -15.80617190586745835, -15.72974639402198527, 76.87390960531439532 ) ) ;
#77977 = CARTESIAN_POINT ( 'NONE',  ( -9.564922557961040184, 16.46253265017147172, 92.91775706135233293 ) ) ;
#77978 = CARTESIAN_POINT ( 'NONE',  ( -19.02544592524342804, 5.153800228976336051, 106.0405762719810241 ) ) ;
#77979 = CARTESIAN_POINT ( 'NONE',  ( 0.05219959533907565091, 21.53943276465977519, 59.99890960531436690 ) ) ;
#77980 = CARTESIAN_POINT ( 'NONE',  ( -8.224510206698948167, 14.34966873604960824, 105.4155762719810383 ) ) ;
#77981 = CARTESIAN_POINT ( 'NONE',  ( -13.97604488694527625, -13.89961937509977652, 71.87390960531433848 ) ) ;
#77982 = CARTESIAN_POINT ( 'NONE',  ( -13.89961937509977652, 13.97604488694528158, 35.62390960531435269 ) ) ;
#77983 = CARTESIAN_POINT ( 'NONE',  ( 21.53943276465977519, 0.05219959533937863772, 36.25109039468567573 ) ) ;
#77984 = CARTESIAN_POINT ( 'NONE',  ( 5.823673210054444382, -21.52544592524334988, 85.20942372801901854 ) ) ;
#77985 = CARTESIAN_POINT ( 'NONE',  ( -16.52544592524335698, -4.483927247898792601, 83.95942372801900433 ) ) ;
#77986 = CARTESIAN_POINT ( 'NONE',  ( 15.80617190586769283, -15.72974639402175789, 35.62609039468568994 ) ) ;
#77987 = CARTESIAN_POINT ( 'NONE',  ( -18.67979575497193778, 10.72451020669871902, 38.33442372801900433 ) ) ;
#77989 = CARTESIAN_POINT ( 'NONE',  ( 9.564922557960805705, 16.46253265017160317, 79.58224293864769550 ) ) ;
#77988 = CARTESIAN_POINT ( 'NONE',  ( 13.97604488694548053, -13.89961937509957401, 60.62609039468564731 ) ) ;
#77990 = CARTESIAN_POINT ( 'NONE',  ( 21.52544592524334988, 5.823673210054432836, 81.45942372801900433 ) ) ;
#77991 = CARTESIAN_POINT ( 'NONE',  ( -18.62759615963270932, 10.81492255796079327, 85.83224293864768129 ) ) ;
#77992 = CARTESIAN_POINT ( 'NONE',  ( 4.379528057220339221, -16.55341960407611168, 57.70724293864770260 ) ) ;
#77993 = CARTESIAN_POINT ( 'NONE',  ( -18.67979575497193778, 10.72451020669871902, 108.3344237280190185 ) ) ;
#77994 = CARTESIAN_POINT ( 'NONE',  ( 4.483927247898545687, 16.52544592524342804, 89.79057627198103830 ) ) ;
#77995 = CARTESIAN_POINT ( 'NONE',  ( -19.05341960407611168, -5.049401038298163336, 41.45724293864769550 ) ) ;
#77996 = CARTESIAN_POINT ( 'NONE',  ( 19.03943276465977164, 0.05219959533936151252, 66.25109039468567573 ) ) ;
#77997 = CARTESIAN_POINT ( 'NONE',  ( -12.14591786802309592, -12.06949235617757132, 36.87390960531435979 ) ) ;
#77998 = CARTESIAN_POINT ( 'NONE',  ( -5.719274019375665041, -21.55341960407619695, 89.79275706135236135 ) ) ;
#77999 = CARTESIAN_POINT ( 'NONE',  ( 16.46253265017160672, -9.564922557960803928, 93.33224293864769550 ) ) ;
#78000 = CARTESIAN_POINT ( 'NONE',  ( 19.02544592524334988, 5.153800228976608722, 61.45942372801900433 ) ) ;
#78001 = CARTESIAN_POINT ( 'NONE',  ( -18.67979575497178146, -10.72451020669898902, 71.66557627198100988 ) ) ;
#78002 = CARTESIAN_POINT ( 'NONE',  ( 0.05219959533937995610, -21.53943276465977519, 20.00109039468568639 ) ) ;
#78003 = CARTESIAN_POINT ( 'NONE',  ( 13.89961937509957401, 13.97604488694547697, 106.8760903946856757 ) ) ;
#78004 = CARTESIAN_POINT ( 'NONE',  ( -4.379528057220086978, -16.55341960407618274, 74.79275706135234714 ) ) ;
#78006 = CARTESIAN_POINT ( 'NONE',  ( -10.81492255796105439, 18.62759615963255655, 27.91775706135234358 ) ) ;
#78005 = DIRECTION ( 'NONE',  ( 0.7071067811865485719, 0.000000000000000000, 0.7071067811865465735 ) ) ;
#78007 = CARTESIAN_POINT ( 'NONE',  ( -16.53943276465976808, 0.05219959533911058130, 106.2489096053143811 ) ) ;
#78008 = CARTESIAN_POINT ( 'NONE',  ( -22.81625015709509441, -31.40387420917324590, -4.824999997268813345 ) ) ;
#78009 = CARTESIAN_POINT ( 'NONE',  ( -16.53943276465976808, -0.05219959533934237506, 43.75109039468568284 ) ) ;
#78010 = CARTESIAN_POINT ( 'NONE',  ( -0.05219959533907301413, -21.53943276465977519, 57.49890960531435979 ) ) ;
#78011 = CARTESIAN_POINT ( 'NONE',  ( -4.379528057220086978, -16.55341960407618274, 99.79275706135234714 ) ) ;
#78012 = CARTESIAN_POINT ( 'NONE',  ( -12.06949235617739369, -12.14591786802326823, 39.37609039468567573 ) ) ;
#78013 = CARTESIAN_POINT ( 'NONE',  ( -19.03943276465977164, 0.05219959533909376836, 51.24890960531436690 ) ) ;
#78014 = CARTESIAN_POINT ( 'NONE',  ( -14.34966873604972548, 8.224510206698743886, 73.33442372801901854 ) ) ;
#78015 = CARTESIAN_POINT ( 'NONE',  ( 9.474510206698729675, 16.51473224551082808, 67.08442372801900433 ) ) ;
#78016 = CARTESIAN_POINT ( 'NONE',  ( -0.05219959533907301413, -21.53943276465977519, 67.49890960531436690 ) ) ;
#78017 = CARTESIAN_POINT ( 'NONE',  ( -12.14591786802326823, 12.06949235617739902, 103.1260903946856757 ) ) ;
#78018 = CARTESIAN_POINT ( 'NONE',  ( -5.823673210054431948, 21.52544592524334988, 87.70942372801901854 ) ) ;
#78019 = CARTESIAN_POINT ( 'NONE',  ( -5.719274019375978568, 21.55341960407610458, 70.20724293864769550 ) ) ;
#78020 = CARTESIAN_POINT ( 'NONE',  ( 21.55341960407610458, 5.719274019375980345, 53.95724293864770260 ) ) ;
#78021 = VERTEX_POINT ( 'NONE', #136293 ) ;
#78022 = CARTESIAN_POINT ( 'NONE',  ( -14.34966873604972548, 8.224510206698743886, 78.33442372801901854 ) ) ;
#78023 = CARTESIAN_POINT ( 'NONE',  ( 21.52544592524344225, -5.823673210054117533, 48.54057627198103120 ) ) ;
#78024 = ORIENTED_EDGE ( 'NONE', *, *, #62342, .T. ) ;
#78025 = CARTESIAN_POINT ( 'NONE',  ( -15.80617190586745835, -15.72974639402198527, 21.87390960531436690 ) ) ;
#78026 = CARTESIAN_POINT ( 'NONE',  ( -21.38418241377623374, -7.427326039334300134, 174.4773576836617224 ) ) ;
#78027 = CARTESIAN_POINT ( 'NONE',  ( -19.05341960407611168, -5.049401038298163336, 26.45724293864769550 ) ) ;
#78028 = CARTESIAN_POINT ( 'NONE',  ( 10.72451020669898902, -18.67979575497178502, 72.91557627198103830 ) ) ;
#78029 = CARTESIAN_POINT ( 'NONE',  ( -12.06949235617739369, -12.14591786802326823, 99.37609039468568994 ) ) ;
#78030 = CARTESIAN_POINT ( 'NONE',  ( -18.67979575497193778, 10.72451020669871902, 43.33442372801901143 ) ) ;
#78031 = CARTESIAN_POINT ( 'NONE',  ( -9.474510206698720793, -16.51473224551083518, 104.5844237280190043 ) ) ;
#78032 = CARTESIAN_POINT ( 'NONE',  ( 16.55341960407611168, 4.379528057220329451, 113.9572429386477239 ) ) ;
#78033 = CARTESIAN_POINT ( 'NONE',  ( 9.564922557961047289, -16.46253265017146816, 105.4177570613523471 ) ) ;
#78034 = CARTESIAN_POINT ( 'NONE',  ( -16.51473224551069308, -9.474510206698971260, 36.66557627198102409 ) ) ;
#78035 = CARTESIAN_POINT ( 'NONE',  ( 23.31738231874054890, -16.94106989632523508, 144.7999999999999829 ) ) ;
#78036 = CARTESIAN_POINT ( 'NONE',  ( 16.51473224551069308, 9.474510206698969483, 94.16557627198103830 ) ) ;
#78037 = CARTESIAN_POINT ( 'NONE',  ( -4.379528057220086978, -16.55341960407618274, 69.79275706135234714 ) ) ;
#78038 = CARTESIAN_POINT ( 'NONE',  ( -16.46253265017146816, -9.564922557961047289, 74.16775706135234714 ) ) ;
#78039 = CARTESIAN_POINT ( 'NONE',  ( 13.89961937509957401, 13.97604488694547697, 21.87609039468566152 ) ) ;
#78040 = CARTESIAN_POINT ( 'NONE',  ( 15.72974639402199770, -15.80617190586745480, 68.12390960531436690 ) ) ;
#78041 = CARTESIAN_POINT ( 'NONE',  ( -0.05219959533934338120, 16.53943276465976808, 82.50109039468568994 ) ) ;
#78042 = CARTESIAN_POINT ( 'NONE',  ( 13.89961937509957401, 13.97604488694547697, 81.87609039468564731 ) ) ;
#78043 = CARTESIAN_POINT ( 'NONE',  ( 19.05341960407611168, 5.049401038298154454, 33.95724293864769550 ) ) ;
#78044 = CARTESIAN_POINT ( 'NONE',  ( 9.474510206698971260, -16.51473224551069308, 92.91557627198103830 ) ) ;
#78045 = CARTESIAN_POINT ( 'NONE',  ( 21.53943276465977519, 0.05219959533937863772, 46.25109039468567573 ) ) ;
#78046 = CARTESIAN_POINT ( 'NONE',  ( -19.02544592524342804, 5.153800228976336051, 41.04057627198103120 ) ) ;
#78047 = CARTESIAN_POINT ( 'NONE',  ( 21.47376810972761163, -7.452933495370365868, 174.2084625793492307 ) ) ;
#78048 = CARTESIAN_POINT ( 'NONE',  ( -19.02544592524342804, 5.153800228976336051, 106.0405762719810241 ) ) ;
#78049 = CARTESIAN_POINT ( 'NONE',  ( 16.55341960407611168, 4.379528057220329451, 58.95724293864770971 ) ) ;
#78050 = CARTESIAN_POINT ( 'NONE',  ( -15.80617190586745835, -15.72974639402198527, 56.87390960531436690 ) ) ;
#78051 = LINE ( 'NONE', #110387, #135360 ) ;
#78052 = CARTESIAN_POINT ( 'NONE',  ( -0.05219959533936034679, 19.03943276465977164, 47.50109039468566863 ) ) ;
#78054 = CARTESIAN_POINT ( 'NONE',  ( 9.564922557960805705, 16.46253265017160317, 69.58224293864770971 ) ) ;
#78053 = CARTESIAN_POINT ( 'NONE',  ( -19.03943276465977164, 0.05219959533909376836, 61.24890960531436690 ) ) ;
#78055 = EDGE_CURVE ( 'NONE', #49927, #80629, #89793, .T. ) ;
#78056 = CARTESIAN_POINT ( 'NONE',  ( 16.52544592524335698, 4.483927247898782831, 56.45942372801902565 ) ) ;
#78057 = CARTESIAN_POINT ( 'NONE',  ( -17.97214573761831247, -5.500000000000092371, 66.46970049038654338 ) ) ;
#78058 = CARTESIAN_POINT ( 'NONE',  ( 0.000000000000000000, -5.795830589372932273, 190.0000000000000000 ) ) ;
#78059 = CARTESIAN_POINT ( 'NONE',  ( -12.06949235617739369, -12.14591786802326823, 94.37609039468568994 ) ) ;
#78060 = CARTESIAN_POINT ( 'NONE',  ( -4.243048740927896745, -4.383653989548000673, -64.53213882399991519 ) ) ;
#78061 = CARTESIAN_POINT ( 'NONE',  ( 16.55341960407618274, -4.379528057220086978, 86.04275706135236135 ) ) ;
#78062 = CARTESIAN_POINT ( 'NONE',  ( -16.53943276465976808, -0.05219959533934237506, 53.75109039468568994 ) ) ;
#78063 = CARTESIAN_POINT ( 'NONE',  ( -19.05341960407617563, 5.049401038297882671, 28.54275706135232937 ) ) ;
#78065 = CARTESIAN_POINT ( 'NONE',  ( 17.18269478283316332, -17.18269478283309226, -56.77278709839600879 ) ) ;
#78064 = CARTESIAN_POINT ( 'NONE',  ( 19.05341960407611168, 5.049401038298154454, 48.95724293864768129 ) ) ;
#78066 = CARTESIAN_POINT ( 'NONE',  ( 5.719274019375673035, 21.55341960407619339, 52.29275706135236135 ) ) ;
#78067 = CARTESIAN_POINT ( 'NONE',  ( 9.474510206698729675, 16.51473224551082808, 57.08442372801900433 ) ) ;
#78068 = CARTESIAN_POINT ( 'NONE',  ( -13.89961937509957401, -13.97604488694547875, 19.37609039468566507 ) ) ;
#78069 = CARTESIAN_POINT ( 'NONE',  ( 0.05219959533909260263, 19.03943276465977164, 24.99890960531435269 ) ) ;
#78070 = CARTESIAN_POINT ( 'NONE',  ( -17.49235657833709467, 16.74109322108048659, -56.83968056806632774 ) ) ;
#78071 = CARTESIAN_POINT ( 'NONE',  ( 10.81492255796078972, 18.62759615963270932, 69.58224293864769550 ) ) ;
#78072 = CARTESIAN_POINT ( 'NONE',  ( -15.80617190586745835, -15.72974639402198527, 21.87390960531436690 ) ) ;
#78073 = CARTESIAN_POINT ( 'NONE',  ( -4.483927247898539470, -16.52544592524342804, 112.2905762719810241 ) ) ;
#78074 = CARTESIAN_POINT ( 'NONE',  ( -16.52544592524335698, -4.483927247898792601, 33.95942372801901143 ) ) ;
#78075 = CARTESIAN_POINT ( 'NONE',  ( -14.34966873604960291, -8.224510206698953496, 31.66557627198102054 ) ) ;
#78076 = ORIENTED_EDGE ( 'NONE', *, *, #49797, .T. ) ;
#78078 = CARTESIAN_POINT ( 'NONE',  ( -21.52544592524343514, 5.823673210054127303, 111.0405762719810525 ) ) ;
#78077 = B_SPLINE_CURVE_WITH_KNOTS ( 'NONE', 3,
 ( #173405, #98520, #83357, #188577, #130867, #53022, #82350, #176396, #111719, #114703, #191545, #99529, #128858, #34876, #129846, #113689, #37870, #142047, #160213, #189571, #51043, #112705, #21703, #161211, #174397, #22706, #192557, #7514, #69199, #115714, #95547, #35867 ),
 .UNSPECIFIED., .F., .F.,
 ( 4, 2, 2, 2, 2, 2, 2, 2, 2, 2, 2, 2, 2, 2, 2, 4 ),
 ( 1.346507514538369135E-17, 0.0003712461730036979452, 0.0007424923460073824463, 0.001113738519011066947, 0.001484984692014751449, 0.002227477038022120451, 0.002598723211025787388, 0.002969969384029454759, 0.003341215557033121696, 0.003712461730036789500, 0.004083707903040457304, 0.004454954076044123808, 0.004826200249047792046, 0.005197446422051459416, 0.005568692595055126787, 0.005939938768058793291 ),
 .UNSPECIFIED. ) ;
#78080 = LINE ( 'NONE', #126572, #1017 ) ;
#78079 = CARTESIAN_POINT ( 'NONE',  ( 8.314922557960818139, 14.29746914071049879, 39.58224293864769550 ) ) ;
#78081 = AXIS2_PLACEMENT_3D ( 'NONE', #84102, #161958, #23454 ) ;
#78082 = CARTESIAN_POINT ( 'NONE',  ( -9.564922557961040184, 16.46253265017147172, 112.9177570613523329 ) ) ;
#78083 = CARTESIAN_POINT ( 'NONE',  ( 13.97604488694548053, -13.89961937509957401, 25.62609039468566507 ) ) ;
#78084 = CARTESIAN_POINT ( 'NONE',  ( -14.29746914071049879, 8.314922557960819915, 50.83224293864770971 ) ) ;
#78085 = CARTESIAN_POINT ( 'NONE',  ( 0.05219959533907565091, 21.53943276465977519, 104.9989096053143669 ) ) ;
#78087 = CARTESIAN_POINT ( 'NONE',  ( -10.81492255796078084, -18.62759615963271287, 62.08224293864769550 ) ) ;
#78086 = CARTESIAN_POINT ( 'NONE',  ( 16.88567814943164436, 6.947325034625594142, 33.79001122652586986 ) ) ;
#78088 = CARTESIAN_POINT ( 'NONE',  ( -16.46253265017160317, 9.564922557960807481, 80.83224293864769550 ) ) ;
#78089 = CARTESIAN_POINT ( 'NONE',  ( -4.483927247898539470, -16.52544592524342804, 42.29057627198103120 ) ) ;
#78090 = CARTESIAN_POINT ( 'NONE',  ( -9.474510206698964154, 16.51473224551069663, 85.41557627198102409 ) ) ;
#78091 = CARTESIAN_POINT ( 'NONE',  ( -36.85386064174076637, 2.754345082724620752, 49.76404540304364588 ) ) ;
#78092 = CARTESIAN_POINT ( 'NONE',  ( 19.05341960407617918, -5.049401038297876454, 51.04275706135231871 ) ) ;
#78093 = CARTESIAN_POINT ( 'NONE',  ( -15.72974639402197994, 15.80617190586746368, 95.62390960531436690 ) ) ;
#78094 = CARTESIAN_POINT ( 'NONE',  ( -4.483927247898539470, -16.52544592524342804, 97.29057627198105251 ) ) ;
#78095 = CARTESIAN_POINT ( 'NONE',  ( 15.80617190586769283, -15.72974639402175789, 45.62609039468567573 ) ) ;
#78096 = CARTESIAN_POINT ( 'NONE',  ( 17.14385361876520264, -23.59649016807271238, 147.5750000027311444 ) ) ;
#78097 = CARTESIAN_POINT ( 'NONE',  ( 16.52544592524342804, -4.483927247898539470, 33.54057627198102409 ) ) ;
#78098 = CARTESIAN_POINT ( 'NONE',  ( -9.564922557960796823, -16.46253265017161027, 37.08224293864768839 ) ) ;
#78099 = CARTESIAN_POINT ( 'NONE',  ( -19.03943276465977164, 0.05219959533909376836, 101.2489096053143669 ) ) ;
#78100 = CARTESIAN_POINT ( 'NONE',  ( -18.67979575497178146, -10.72451020669898902, 61.66557627198103120 ) ) ;
#78101 = CARTESIAN_POINT ( 'NONE',  ( -27.73933785331498925, -9.013057229001049109, 138.9750000027311785 ) ) ;
#78102 = CARTESIAN_POINT ( 'NONE',  ( 19.05341960407611168, 5.049401038298154454, 33.95724293864769550 ) ) ;
#78103 = CARTESIAN_POINT ( 'NONE',  ( 18.67979575497178502, 10.72451020669898547, 49.16557627198102409 ) ) ;
#78104 = CARTESIAN_POINT ( 'NONE',  ( -21.55341960407619339, 5.719274019375674811, 73.54275706135234714 ) ) ;
#78106 = CARTESIAN_POINT ( 'NONE',  ( 16.55341960407618274, -4.379528057220086978, 71.04275706135234714 ) ) ;
#78105 = CARTESIAN_POINT ( 'NONE',  ( 8.122171662651544111, -45.80197342711153397, -22.32604245071861371 ) ) ;
#78107 = CARTESIAN_POINT ( 'NONE',  ( 19.03943276465977164, -0.05219959533909143690, 53.74890960531436690 ) ) ;
#78108 = CARTESIAN_POINT ( 'NONE',  ( 16.51473224551069308, 9.474510206698969483, 64.16557627198102409 ) ) ;
#78109 = ORIENTED_EDGE ( 'NONE', *, *, #77828, .T. ) ;
#78110 = CARTESIAN_POINT ( 'NONE',  ( 9.474510206698729675, 16.51473224551082808, 22.08442372801899722 ) ) ;
#78111 = CARTESIAN_POINT ( 'NONE',  ( 4.483927247898790824, -16.52544592524335698, 80.20942372801901854 ) ) ;
#78112 = CARTESIAN_POINT ( 'NONE',  ( 15.72974639402176855, 15.80617190586768217, 96.87609039468568994 ) ) ;
#78113 = CARTESIAN_POINT ( 'NONE',  ( -13.97604488694527625, -13.89961937509977652, 81.87390960531436690 ) ) ;
#78114 = CARTESIAN_POINT ( 'NONE',  ( -5.719274019375978568, 21.55341960407610458, 30.20724293864769550 ) ) ;
#78115 = CARTESIAN_POINT ( 'NONE',  ( 19.02544592524334988, 5.153800228976608722, 106.4594237280190185 ) ) ;
#78116 = CARTESIAN_POINT ( 'NONE',  ( -15.80617190586768217, 15.72974639402176855, 78.12609039468570415 ) ) ;
#78117 = CARTESIAN_POINT ( 'NONE',  ( -8.314922557961024197, 14.29746914071037800, 52.91775706135235424 ) ) ;
#78118 = CARTESIAN_POINT ( 'NONE',  ( 5.823673210054125526, 21.52544592524343514, 94.79057627198105251 ) ) ;
#78119 = CARTESIAN_POINT ( 'NONE',  ( -8.224510206698735004, -14.34966873604973081, 19.58442372801901143 ) ) ;
#78120 = CARTESIAN_POINT ( 'NONE',  ( -19.05341960407611168, -5.049401038298163336, 81.45724293864769550 ) ) ;
#78121 = CARTESIAN_POINT ( 'NONE',  ( -16.52544592524335698, -4.483927247898792601, 23.95942372801901143 ) ) ;
#78122 = CARTESIAN_POINT ( 'NONE',  ( -19.03943276465977164, 0.05219959533909376836, 36.24890960531436690 ) ) ;
#78123 = CARTESIAN_POINT ( 'NONE',  ( -5.049401038297874678, -19.05341960407617918, 109.7927570613523187 ) ) ;
#78124 = CARTESIAN_POINT ( 'NONE',  ( -16.53943276465976808, 0.05219959533911058130, 71.24890960531435269 ) ) ;
#78125 = CARTESIAN_POINT ( 'NONE',  ( 14.29746914071037800, 8.314922557961029526, 71.66775706135234714 ) ) ;
#78126 = EDGE_CURVE ( 'NONE', #8650, #45202, #167632, .T. ) ;
#78128 = CARTESIAN_POINT ( 'NONE',  ( 16.46253265017160672, -9.564922557960803928, 53.33224293864768839 ) ) ;
#78127 = CARTESIAN_POINT ( 'NONE',  ( -5.719274019375665041, -21.55341960407619695, 34.79275706135235424 ) ) ;
#78129 = CARTESIAN_POINT ( 'NONE',  ( -19.03943276465977164, 0.05219959533909376836, 71.24890960531435269 ) ) ;
#78130 = CARTESIAN_POINT ( 'NONE',  ( 16.52544592524335698, 4.483927247898782831, 71.45942372801901854 ) ) ;
#78132 = ORIENTED_EDGE ( 'NONE', *, *, #77093, .F. ) ;
#78131 = CARTESIAN_POINT ( 'NONE',  ( -21.92083080610932200, -6.374575339255695638, 171.4095429173266325 ) ) ;
#78133 = VERTEX_POINT ( 'NONE', #49254 ) ;
#78134 = CARTESIAN_POINT ( 'NONE',  ( -15.80617190586768217, 15.72974639402176855, 113.1260903946856899 ) ) ;
#78135 = CARTESIAN_POINT ( 'NONE',  ( -16.51473224551069308, -9.474510206698971260, 36.66557627198102409 ) ) ;
#78137 = ORIENTED_EDGE ( 'NONE', *, *, #185806, .T. ) ;
#78136 = CARTESIAN_POINT ( 'NONE',  ( -19.02544592524342804, 5.153800228976336051, 116.0405762719810383 ) ) ;
#78138 = CARTESIAN_POINT ( 'NONE',  ( -4.483927247898782831, 16.52544592524335698, 27.70942372801901854 ) ) ;
#78140 = CARTESIAN_POINT ( 'NONE',  ( 0.05219959533934541429, -16.53943276465976808, 40.00109039468567573 ) ) ;
#78139 = CARTESIAN_POINT ( 'NONE',  ( 13.97604488694548053, -13.89961937509957401, 60.62609039468564731 ) ) ;
#78141 = CARTESIAN_POINT ( 'NONE',  ( -5.153800228976328057, -19.02544592524343514, 42.29057627198101699 ) ) ;
#78142 = CARTESIAN_POINT ( 'NONE',  ( 5.049401038298161559, -19.05341960407611168, 112.7072429386476813 ) ) ;
#78143 = CARTESIAN_POINT ( 'NONE',  ( -9.474510206698964154, 16.51473224551069663, 60.41557627198102409 ) ) ;
#78144 = CARTESIAN_POINT ( 'NONE',  ( -10.81492255796078084, -18.62759615963271287, 102.0822429386476955 ) ) ;
#78146 = CARTESIAN_POINT ( 'NONE',  ( 9.474510206698971260, -16.51473224551069308, 27.91557627198103120 ) ) ;
#78145 = CARTESIAN_POINT ( 'NONE',  ( 19.02544592524343514, -5.153800228976328945, 93.54057627198102409 ) ) ;
#78147 = CARTESIAN_POINT ( 'NONE',  ( 5.153800228976335163, 19.02544592524342804, 59.79057627198100988 ) ) ;
#78149 = CYLINDRICAL_SURFACE ( 'NONE', #85491, 1.499999999999997780 ) ;
#78148 = CARTESIAN_POINT ( 'NONE',  ( -8.314922557960811034, -14.29746914071050412, 22.08224293864769194 ) ) ;
#78150 = CARTESIAN_POINT ( 'NONE',  ( -5.153800228976607833, 19.02544592524334988, 97.70942372801900433 ) ) ;
#78151 = CARTESIAN_POINT ( 'NONE',  ( 13.97604488694548053, -13.89961937509957401, 30.62609039468566863 ) ) ;
#78152 = CARTESIAN_POINT ( 'NONE',  ( -14.29746914071049879, 8.314922557960819915, 55.83224293864770260 ) ) ;
#78153 = CARTESIAN_POINT ( 'NONE',  ( 5.719274019375673035, 21.55341960407619339, 97.29275706135234714 ) ) ;
#78154 = CARTESIAN_POINT ( 'NONE',  ( -13.97604488694527625, -13.89961937509977652, 41.87390960531435979 ) ) ;
#78156 = CARTESIAN_POINT ( 'NONE',  ( 5.823673210054444382, -21.52544592524334988, 85.20942372801901854 ) ) ;
#78155 = CARTESIAN_POINT ( 'NONE',  ( 12.14591786802309770, 12.06949235617756955, 29.37390960531435269 ) ) ;
#78157 = CARTESIAN_POINT ( 'NONE',  ( -16.51473224551069308, -9.474510206698971260, 76.66557627198103830 ) ) ;
#78158 = CARTESIAN_POINT ( 'NONE',  ( 0.05219959533909260263, 19.03943276465977164, 94.99890960531436690 ) ) ;
#78159 = CARTESIAN_POINT ( 'NONE',  ( 12.06949235617757843, -12.14591786802309237, 93.12390960531436690 ) ) ;
#78160 = CARTESIAN_POINT ( 'NONE',  ( 14.29746914071049879, -8.314922557960816363, 73.33224293864769550 ) ) ;
#78161 = CARTESIAN_POINT ( 'NONE',  ( -5.719274019375978568, 21.55341960407610458, 85.20724293864770971 ) ) ;
#78162 = CARTESIAN_POINT ( 'NONE',  ( -13.89961937509977652, 13.97604488694528158, 80.62390960531436690 ) ) ;
#78163 = CARTESIAN_POINT ( 'NONE',  ( -21.53943276465977519, 0.05219959533907696930, 81.24890960531436690 ) ) ;
#78164 = CARTESIAN_POINT ( 'NONE',  ( 13.97604488694548053, -13.89961937509957401, 75.62609039468564731 ) ) ;
#78166 = CARTESIAN_POINT ( 'NONE',  ( -4.483927247898539470, -16.52544592524342804, 92.29057627198103830 ) ) ;
#78165 = DIRECTION ( 'NONE',  ( 0.000000000000000000, 0.000000000000000000, 1.000000000000000000 ) ) ;
#78167 = CARTESIAN_POINT ( 'NONE',  ( 0.05219959533909260263, 19.03943276465977164, 54.99890960531435979 ) ) ;
#78168 = CARTESIAN_POINT ( 'NONE',  ( 18.62759615963271287, -10.81492255796078972, 63.33224293864770260 ) ) ;
#78169 = LINE ( 'NONE', #60033, #165770 ) ;
#78170 = CARTESIAN_POINT ( 'NONE',  ( -8.224510206698948167, 14.34966873604960824, 25.41557627198103120 ) ) ;
#78171 = CARTESIAN_POINT ( 'NONE',  ( -16.53943276465976808, -0.05219959533934237506, 18.75109039468568639 ) ) ;
#78172 = CARTESIAN_POINT ( 'NONE',  ( -14.34966873604960291, -8.224510206698953496, 86.66557627198102409 ) ) ;
#78173 = CARTESIAN_POINT ( 'NONE',  ( 7.503800738396989800, -1.500046863536464992, -62.22166870076608092 ) ) ;
#78174 = CARTESIAN_POINT ( 'NONE',  ( 5.049401038298161559, -19.05341960407611168, 72.70724293864768129 ) ) ;
#78175 = CARTESIAN_POINT ( 'NONE',  ( -19.02544592524342804, 5.153800228976336051, 31.04057627198102409 ) ) ;
#78176 = CARTESIAN_POINT ( 'NONE',  ( 8.314922557960818139, 14.29746914071049879, 64.58224293864769550 ) ) ;
#78177 = CARTESIAN_POINT ( 'NONE',  ( -16.46253265017160317, 9.564922557960807481, 105.8322429386476955 ) ) ;
#78179 = CARTESIAN_POINT ( 'NONE',  ( 19.03943276465977164, -0.05219959533909143690, 83.74890960531436690 ) ) ;
#78178 = CARTESIAN_POINT ( 'NONE',  ( -9.474510206698720793, -16.51473224551083518, 84.58442372801900433 ) ) ;
#78180 = CARTESIAN_POINT ( 'NONE',  ( -16.51473224551069308, -9.474510206698971260, 86.66557627198102409 ) ) ;
#78181 = CARTESIAN_POINT ( 'NONE',  ( -5.719274019375978568, 21.55341960407610458, 80.20724293864769550 ) ) ;
#78182 = CARTESIAN_POINT ( 'NONE',  ( 14.34966873604972726, -8.224510206698740333, 70.83442372801901854 ) ) ;
#78183 = CARTESIAN_POINT ( 'NONE',  ( -19.05341960407617918, 5.049401038297883559, 113.5427570613523329 ) ) ;
#78184 = CARTESIAN_POINT ( 'NONE',  ( -13.89961937509977652, 13.97604488694528158, 65.62390960531436690 ) ) ;
#78185 = CARTESIAN_POINT ( 'NONE',  ( 5.719274019375991003, -21.55341960407610458, 67.70724293864769550 ) ) ;
#78186 = CARTESIAN_POINT ( 'NONE',  ( 5.153800228976615827, -19.02544592524334988, 90.20942372801900433 ) ) ;
#78188 = CARTESIAN_POINT ( 'NONE',  ( 0.05219959533937995610, -21.53943276465977519, 40.00109039468567573 ) ) ;
#78187 = CARTESIAN_POINT ( 'NONE',  ( -4.483927247898539470, -16.52544592524342804, 32.29057627198102409 ) ) ;
#78189 = CARTESIAN_POINT ( 'NONE',  ( -19.24578484527059175, -180.9428398739491684, 1.787262988391354872E-28 ) ) ;
#78191 = CARTESIAN_POINT ( 'NONE',  ( -13.97604488694527625, -13.89961937509977652, 101.8739096053143811 ) ) ;
#78190 = CARTESIAN_POINT ( 'NONE',  ( -8.224510206698735004, -14.34966873604973081, 79.58442372801903275 ) ) ;
#78192 = DIRECTION ( 'NONE',  ( -0.000000000000000000, -0.000000000000000000, 1.000000000000000000 ) ) ;
#78193 = DIRECTION ( 'NONE',  ( 0.000000000000000000, 0.04175967627138096189, 0.9991276842514722478 ) ) ;
#78194 = CARTESIAN_POINT ( 'NONE',  ( 12.14591786802327356, -12.06949235617739191, 100.6260903946857184 ) ) ;
#78195 = CARTESIAN_POINT ( 'NONE',  ( -0.05219959533934338120, 16.53943276465976808, 42.50109039468567573 ) ) ;
#78196 = CARTESIAN_POINT ( 'NONE',  ( -9.564922557960796823, -16.46253265017161027, 57.08224293864769550 ) ) ;
#78197 = CARTESIAN_POINT ( 'NONE',  ( -16.51473224551069308, -9.474510206698971260, 66.66557627198102409 ) ) ;
#78198 = CARTESIAN_POINT ( 'NONE',  ( -18.62759615963255300, -10.81492255796106328, 49.16775706135234003 ) ) ;
#78199 = CARTESIAN_POINT ( 'NONE',  ( -14.29746914071037622, -8.314922557961029526, 64.16775706135234714 ) ) ;
#78200 = CARTESIAN_POINT ( 'NONE',  ( 12.14591786802309770, 12.06949235617756955, 39.37390960531436690 ) ) ;
#78201 = CARTESIAN_POINT ( 'NONE',  ( -5.153800228976328057, -19.02544592524343514, 47.29057627198102409 ) ) ;
#78202 = CARTESIAN_POINT ( 'NONE',  ( -19.03943276465977164, 0.05219959533909376836, 41.24890960531435269 ) ) ;
#78203 = CARTESIAN_POINT ( 'NONE',  ( 16.53943276465976808, 0.05219959533934440121, 31.25109039468568639 ) ) ;
#78204 = CARTESIAN_POINT ( 'NONE',  ( -0.05219959533936034679, 19.03943276465977164, 77.50109039468566152 ) ) ;
#78205 = CARTESIAN_POINT ( 'NONE',  ( -16.53943276465976808, 0.05219959533911058130, 86.24890960531436690 ) ) ;
#78206 = CARTESIAN_POINT ( 'NONE',  ( -16.51473224551069308, -9.474510206698971260, 56.66557627198103120 ) ) ;
#78208 = CARTESIAN_POINT ( 'NONE',  ( -23.48529157249599919, -32.32473071737750558, -7.699999999999999289 ) ) ;
#78207 = CARTESIAN_POINT ( 'NONE',  ( 19.03943276465977164, 0.05219959533936151252, 86.25109039468567573 ) ) ;
#78209 = CARTESIAN_POINT ( 'NONE',  ( -18.62759615963255300, -10.81492255796106328, 84.16775706135234714 ) ) ;
#78210 = CARTESIAN_POINT ( 'NONE',  ( 12.14591786802327356, -12.06949235617739191, 55.62609039468568284 ) ) ;
#78211 = CARTESIAN_POINT ( 'NONE',  ( -17.49999999999997158, 3.305555262949582129, 24.62517152156607736 ) ) ;
#78212 = CARTESIAN_POINT ( 'NONE',  ( 21.55341960407610458, 5.719274019375980345, 53.95724293864770260 ) ) ;
#78213 = CARTESIAN_POINT ( 'NONE',  ( 8.224510206698742110, 14.34966873604972548, 37.08442372801901143 ) ) ;
#78214 = CARTESIAN_POINT ( 'NONE',  ( -17.49999999999999645, -5.500000000000000888, 22.00000000000000711 ) ) ;
#78215 = CARTESIAN_POINT ( 'NONE',  ( -16.46253265017146816, -9.564922557961047289, 34.16775706135233293 ) ) ;
#78216 = CARTESIAN_POINT ( 'NONE',  ( 16.51473224551069308, 9.474510206698969483, 74.16557627198103830 ) ) ;
#78217 = CARTESIAN_POINT ( 'NONE',  ( -0.05219959533909027116, -19.03943276465977164, 57.49890960531435979 ) ) ;
#78218 = DIRECTION ( 'NONE',  ( 0.000000000000000000, 1.000000000000000000, 0.000000000000000000 ) ) ;
#78219 = CARTESIAN_POINT ( 'NONE',  ( -16.46253265017160317, 9.564922557960807481, 70.83224293864770971 ) ) ;
#78220 = CARTESIAN_POINT ( 'NONE',  ( 17.50000000000000000, -5.076555817581248853, 111.3204850795022480 ) ) ;
#78221 = CARTESIAN_POINT ( 'NONE',  ( -19.05341960407617563, 5.049401038297882671, 28.54275706135232937 ) ) ;
#78222 = CARTESIAN_POINT ( 'NONE',  ( -21.53943276465977519, -0.05219959533937600094, 103.7510903946857042 ) ) ;
#78223 = CARTESIAN_POINT ( 'NONE',  ( 16.53943276465976808, -0.05219959533910856209, 33.74890960531436690 ) ) ;
#78224 = CARTESIAN_POINT ( 'NONE',  ( 5.153800228976335163, 19.02544592524342804, 49.79057627198100988 ) ) ;
#78225 = CARTESIAN_POINT ( 'NONE',  ( 19.05341960407611168, 5.049401038298154454, 108.9572429386477097 ) ) ;
#78226 = CARTESIAN_POINT ( 'NONE',  ( -21.55341960407619339, 5.719274019375674811, 83.54275706135234714 ) ) ;
#78227 = CARTESIAN_POINT ( 'NONE',  ( 19.03943276465977164, -0.05219959533909143690, 48.74890960531435979 ) ) ;
#78228 = EDGE_CURVE ( 'NONE', #39558, #121632, #195771, .T. ) ;
#78229 = CARTESIAN_POINT ( 'NONE',  ( 21.55341960407619695, -5.719274019375665929, 76.04275706135237556 ) ) ;
#78230 = CARTESIAN_POINT ( 'NONE',  ( -10.81492255796078084, -18.62759615963271287, 22.08224293864769194 ) ) ;
#78231 = CARTESIAN_POINT ( 'NONE',  ( 21.53943276465977519, 0.05219959533937863772, 26.25109039468567573 ) ) ;
#78232 = CARTESIAN_POINT ( 'NONE',  ( 19.02544592524334988, 5.153800228976608722, 51.45942372801900433 ) ) ;
#78233 = CARTESIAN_POINT ( 'NONE',  ( 19.05341960407611168, 5.049401038298154454, 33.95724293864769550 ) ) ;
#78234 = CARTESIAN_POINT ( 'NONE',  ( -19.02544592524342804, 5.153800228976336051, 81.04057627198103830 ) ) ;
#78235 = CARTESIAN_POINT ( 'NONE',  ( 5.153800228976615827, -19.02544592524334988, 110.2094237280189901 ) ) ;
#78236 = CARTESIAN_POINT ( 'NONE',  ( 8.314922557960818139, 14.29746914071049879, 69.58224293864769550 ) ) ;
#78237 = CARTESIAN_POINT ( 'NONE',  ( 21.52544592524344225, -5.823673210054117533, 38.54057627198103120 ) ) ;
#78238 = CARTESIAN_POINT ( 'NONE',  ( 0.05219959533936267826, -19.03943276465977164, 95.00109039468567573 ) ) ;
#78239 = CARTESIAN_POINT ( 'NONE',  ( 21.55341960407610458, 5.719274019375980345, 98.95724293864770971 ) ) ;
#78240 = CARTESIAN_POINT ( 'NONE',  ( -21.53943276465977519, -0.05219959533937600094, 63.75109039468568284 ) ) ;
#78241 = CARTESIAN_POINT ( 'NONE',  ( 12.14591786802327356, -12.06949235617739191, 55.62609039468568284 ) ) ;
#78242 = CARTESIAN_POINT ( 'NONE',  ( -12.06949235617739369, -12.14591786802326823, 59.37609039468568284 ) ) ;
#78243 = CARTESIAN_POINT ( 'NONE',  ( 19.05341960407611168, 5.049401038298154454, 43.95724293864769550 ) ) ;
#78244 = CARTESIAN_POINT ( 'NONE',  ( 14.34966873604972726, -8.224510206698740333, 85.83442372801901854 ) ) ;
#78245 = CARTESIAN_POINT ( 'NONE',  ( 18.67979575497178502, 10.72451020669898547, 114.1655762719810383 ) ) ;
#78246 = CARTESIAN_POINT ( 'NONE',  ( 16.53943276465976808, -0.05219959533910856209, 53.74890960531437401 ) ) ;
#78247 = CARTESIAN_POINT ( 'NONE',  ( -19.03943276465977164, 0.05219959533909376836, 86.24890960531436690 ) ) ;
#78248 = CARTESIAN_POINT ( 'NONE',  ( -0.05219959533934338120, 16.53943276465976808, 77.50109039468567573 ) ) ;
#78249 = CARTESIAN_POINT ( 'NONE',  ( -0.05219959533937732626, 21.53943276465977519, 62.50109039468568284 ) ) ;
#78250 = CARTESIAN_POINT ( 'NONE',  ( -16.46253265017146816, -9.564922557961047289, 109.1677570613523471 ) ) ;
#78251 = CARTESIAN_POINT ( 'NONE',  ( 5.719274019375991003, -21.55341960407610458, 112.7072429386476955 ) ) ;
#78252 = CARTESIAN_POINT ( 'NONE',  ( -16.55341960407611168, -4.379528057220339221, 46.45724293864769550 ) ) ;
#78253 = VERTEX_POINT ( 'NONE', #13936 ) ;
#78254 = CARTESIAN_POINT ( 'NONE',  ( -16.38665767535054130, 7.295008042176037044, 75.26400864214548392 ) ) ;
#78255 = CARTESIAN_POINT ( 'NONE',  ( 10.81492255796078972, 18.62759615963270932, 84.58224293864769550 ) ) ;
#78256 = CARTESIAN_POINT ( 'NONE',  ( -16.53943276465976808, 0.05219959533911058130, 31.24890960531435979 ) ) ;
#78257 = EDGE_LOOP ( 'NONE', ( #21422, #82768, #175288, #139458 ) ) ;
#78258 = CARTESIAN_POINT ( 'NONE',  ( 34.46971384048857345, 7.497988128173094680, 44.47943501004273514 ) ) ;
#78259 = CARTESIAN_POINT ( 'NONE',  ( -21.55341960407619339, 5.719274019375674811, 23.54275706135235424 ) ) ;
#78260 = CARTESIAN_POINT ( 'NONE',  ( 19.05341960407611168, 5.049401038298154454, 113.9572429386477097 ) ) ;
#78261 = CARTESIAN_POINT ( 'NONE',  ( 15.72974639402176855, 15.80617190586768217, 21.87609039468567573 ) ) ;
#78262 = CARTESIAN_POINT ( 'NONE',  ( -8.224510206698948167, 14.34966873604960824, 55.41557627198102409 ) ) ;
#78263 = EDGE_CURVE ( 'NONE', #194207, #28673, #164231, .T. ) ;
#78264 = CARTESIAN_POINT ( 'NONE',  ( -16.53943276465976808, -0.05219959533934237506, 63.75109039468568284 ) ) ;
#78265 = CARTESIAN_POINT ( 'NONE',  ( -13.97604488694527625, -13.89961937509977652, 56.87390960531434558 ) ) ;
#78266 = CARTESIAN_POINT ( 'NONE',  ( 19.05341960407617918, -5.049401038297876454, 66.04275706135233293 ) ) ;
#78267 = CARTESIAN_POINT ( 'NONE',  ( 9.564922557960805705, 16.46253265017160317, 84.58224293864769550 ) ) ;
#78268 = CARTESIAN_POINT ( 'NONE',  ( 15.72974639402199770, -15.80617190586745480, 38.12390960531436690 ) ) ;
#78269 = CARTESIAN_POINT ( 'NONE',  ( -23.37981185087361524, -29.75599608462389156, -21.51565039292586690 ) ) ;
#78270 = CARTESIAN_POINT ( 'NONE',  ( 0.05219959533909260263, 19.03943276465977164, 54.99890960531435979 ) ) ;
#78271 = CARTESIAN_POINT ( 'NONE',  ( 8.314922557961029526, -14.29746914071037800, 25.41775706135235779 ) ) ;
#78272 = CARTESIAN_POINT ( 'NONE',  ( -0.05219959533936034679, 19.03943276465977164, 67.50109039468566152 ) ) ;
#78273 = CARTESIAN_POINT ( 'NONE',  ( 21.55341960407610458, 5.719274019375980345, 98.95724293864770971 ) ) ;
#78274 = CARTESIAN_POINT ( 'NONE',  ( 16.55341960407611168, 4.379528057220329451, 38.95724293864768839 ) ) ;
#78275 = CARTESIAN_POINT ( 'NONE',  ( 19.02544592524343514, -5.153800228976328945, 93.54057627198102409 ) ) ;
#78276 = CARTESIAN_POINT ( 'NONE',  ( -18.62759615963270932, 10.81492255796079327, 55.83224293864770260 ) ) ;
#78278 = CARTESIAN_POINT ( 'NONE',  ( 12.14591786802327356, -12.06949235617739191, 40.62609039468567573 ) ) ;
#78277 = CARTESIAN_POINT ( 'NONE',  ( -21.52544592524343514, 5.823673210054127303, 91.04057627198103830 ) ) ;
#78279 = CARTESIAN_POINT ( 'NONE',  ( -15.80617190586745835, -15.72974639402198527, 41.87390960531435979 ) ) ;
#78280 = CARTESIAN_POINT ( 'NONE',  ( -5.719274019375665041, -21.55341960407619695, 89.79275706135236135 ) ) ;
#78281 = CARTESIAN_POINT ( 'NONE',  ( -13.89961937509977652, 13.97604488694528158, 90.62390960531432427 ) ) ;
#78282 = CARTESIAN_POINT ( 'NONE',  ( 5.049401038298161559, -19.05341960407611168, 27.70724293864769550 ) ) ;
#78283 = CARTESIAN_POINT ( 'NONE',  ( -19.02544592524342804, 5.153800228976336051, 86.04057627198103830 ) ) ;
#78284 = CARTESIAN_POINT ( 'NONE',  ( 16.55341960407611168, 4.379528057220329451, 108.9572429386476955 ) ) ;
#78285 = CARTESIAN_POINT ( 'NONE',  ( -13.97604488694527625, -13.89961937509977652, 66.87390960531436690 ) ) ;
#78286 = CARTESIAN_POINT ( 'NONE',  ( -4.379528057220086978, -16.55341960407618274, 19.79275706135235069 ) ) ;
#78287 = CARTESIAN_POINT ( 'NONE',  ( 16.46253265017146816, 9.564922557961045513, 41.66775706135234003 ) ) ;
#78289 = CARTESIAN_POINT ( 'NONE',  ( 16.46253265017160672, -9.564922557960803928, 108.3322429386476955 ) ) ;
#78288 = CARTESIAN_POINT ( 'NONE',  ( -10.72451020669870658, -18.67979575497194134, 94.58442372801901854 ) ) ;
#78290 = CARTESIAN_POINT ( 'NONE',  ( -8.314922557961024197, 14.29746914071037800, 87.91775706135234714 ) ) ;
#78291 = DIRECTION ( 'NONE',  ( 0.000000000000000000, 0.000000000000000000, 1.000000000000000000 ) ) ;
#78292 = CARTESIAN_POINT ( 'NONE',  ( -9.474510206698720793, -16.51473224551083518, 74.58442372801900433 ) ) ;
#78293 = CARTESIAN_POINT ( 'NONE',  ( -16.51473224551082808, 9.474510206698731452, 33.33442372801899722 ) ) ;
#78294 = CARTESIAN_POINT ( 'NONE',  ( 3.920520744267807167, 4.990514878257738651, -64.49346902751020139 ) ) ;
#78295 = CARTESIAN_POINT ( 'NONE',  ( -19.05341960407611168, -5.049401038298163336, 31.45724293864769550 ) ) ;
#78296 = CARTESIAN_POINT ( 'NONE',  ( -12.06949235617756955, 12.14591786802309770, 30.62390960531436335 ) ) ;
#78297 = CARTESIAN_POINT ( 'NONE',  ( 16.46253265017160672, -9.564922557960803928, 23.33224293864769194 ) ) ;
#78298 = CARTESIAN_POINT ( 'NONE',  ( 14.29746914071049879, -8.314922557960816363, 28.33224293864769550 ) ) ;
#78299 = CARTESIAN_POINT ( 'NONE',  ( -19.49671883438224995, -5.500000000000074607, 84.89279849105676590 ) ) ;
#78300 = CARTESIAN_POINT ( 'NONE',  ( -16.53943276465976808, -0.05219959533934237506, 98.75109039468568994 ) ) ;
#78301 = CARTESIAN_POINT ( 'NONE',  ( -5.153800228976328057, -19.02544592524343514, 42.29057627198101699 ) ) ;
#78302 = EDGE_CURVE ( 'NONE', #45716, #59419, #140254, .T. ) ;
#78303 = CARTESIAN_POINT ( 'NONE',  ( 5.823673210054444382, -21.52544592524334988, 90.20942372801903275 ) ) ;
#78304 = CARTESIAN_POINT ( 'NONE',  ( 12.14591786802327356, -12.06949235617739191, 25.62609039468567929 ) ) ;
#78305 = CARTESIAN_POINT ( 'NONE',  ( -5.823673210054431948, 21.52544592524334988, 82.70942372801900433 ) ) ;
#78306 = CARTESIAN_POINT ( 'NONE',  ( 16.46253265017146816, 9.564922557961045513, 46.66775706135233293 ) ) ;
#78307 = CARTESIAN_POINT ( 'NONE',  ( -0.05219959533909027116, -19.03943276465977164, 87.49890960531436690 ) ) ;
#78308 = CARTESIAN_POINT ( 'NONE',  ( 16.51473224551069308, 9.474510206698969483, 74.16557627198103830 ) ) ;
#78309 = DIRECTION ( 'NONE',  ( 0.000000000000000000, 0.000000000000000000, 1.000000000000000000 ) ) ;
#78310 = CARTESIAN_POINT ( 'NONE',  ( -16.52544592524342804, 4.483927247898546575, 71.04057627198103830 ) ) ;
#78311 = CARTESIAN_POINT ( 'NONE',  ( 5.823673210054125526, 21.52544592524343514, 59.79057627198103120 ) ) ;
#78312 = CARTESIAN_POINT ( 'NONE',  ( -19.03943276465977164, 0.05219959533909376836, 61.24890960531436690 ) ) ;
#78314 = CARTESIAN_POINT ( 'NONE',  ( -4.379528057220086978, -16.55341960407618274, 79.79275706135236135 ) ) ;
#78313 = CARTESIAN_POINT ( 'NONE',  ( 15.80617190586746368, 15.72974639402197994, 79.37390960531436690 ) ) ;
#78315 = EDGE_CURVE ( 'NONE', #144387, #176032, #186652, .T. ) ;
#78316 = VERTEX_POINT ( 'NONE', #137282 ) ;
#78317 = CARTESIAN_POINT ( 'NONE',  ( -0.05219959533909027116, -19.03943276465977164, 52.49890960531436690 ) ) ;
#78319 = DIRECTION ( 'NONE',  ( 1.000000000000000000, 0.000000000000000000, 0.000000000000000000 ) ) ;
#78318 = CARTESIAN_POINT ( 'NONE',  ( -14.34966873604960291, -8.224510206698953496, 81.66557627198103830 ) ) ;
#78320 = CARTESIAN_POINT ( 'NONE',  ( 19.02544592524343514, -5.153800228976328945, 53.54057627198102409 ) ) ;
#78321 = CARTESIAN_POINT ( 'NONE',  ( -8.314922557960811034, -14.29746914071050412, 112.0822429386477097 ) ) ;
#78322 = CARTESIAN_POINT ( 'NONE',  ( -13.89961937509957401, -13.97604488694547875, 64.37609039468567573 ) ) ;
#78323 = CARTESIAN_POINT ( 'NONE',  ( 16.53943276465976808, -0.05219959533910856209, 83.74890960531435269 ) ) ;
#78324 = CARTESIAN_POINT ( 'NONE',  ( 10.81492255796106328, -18.62759615963255655, 45.41775706135234003 ) ) ;
#78326 = CARTESIAN_POINT ( 'NONE',  ( 15.80617190586746368, 15.72974639402197994, 104.3739096053143669 ) ) ;
#78325 = CARTESIAN_POINT ( 'NONE',  ( -5.153800228976328057, -19.02544592524343514, 42.29057627198101699 ) ) ;
#78327 = CARTESIAN_POINT ( 'NONE',  ( 6.434671708797603529, -6.434671708797564449, -64.92279855667830191 ) ) ;
#78328 = CARTESIAN_POINT ( 'NONE',  ( 8.314922557960818139, 14.29746914071049879, 89.58224293864768129 ) ) ;
#78329 = CARTESIAN_POINT ( 'NONE',  ( 22.88436389169569196, -32.73361847831127847, -22.76175135428369956 ) ) ;
#78330 = CARTESIAN_POINT ( 'NONE',  ( -19.02544592524342804, 5.153800228976336051, 51.04057627198103120 ) ) ;
#78331 = DIRECTION ( 'NONE',  ( 0.000000000000000000, 0.000000000000000000, -1.000000000000000000 ) ) ;
#78333 = CARTESIAN_POINT ( 'NONE',  ( 16.51473224551069308, 9.474510206698969483, 104.1655762719810241 ) ) ;
#78332 = CARTESIAN_POINT ( 'NONE',  ( 0.05219959533936267826, -19.03943276465977164, 90.00109039468567573 ) ) ;
#78334 = CARTESIAN_POINT ( 'NONE',  ( 21.55341960407619695, -5.719274019375665929, 41.04275706135236135 ) ) ;
#78335 = CARTESIAN_POINT ( 'NONE',  ( -13.89961937509977652, 13.97604488694528158, 80.62390960531436690 ) ) ;
#78336 = CARTESIAN_POINT ( 'NONE',  ( -9.474510206698720793, -16.51473224551083518, 74.58442372801900433 ) ) ;
#78337 = CARTESIAN_POINT ( 'NONE',  ( 16.51473224551069308, 9.474510206698969483, 49.16557627198102409 ) ) ;
#78338 = CARTESIAN_POINT ( 'NONE',  ( -8.314922557960811034, -14.29746914071050412, 77.08224293864769550 ) ) ;
#78339 = CARTESIAN_POINT ( 'NONE',  ( -16.55341960407611168, -4.379528057220339221, 61.45724293864770260 ) ) ;
#78340 = CARTESIAN_POINT ( 'NONE',  ( 16.51473224551069308, 9.474510206698969483, 79.16557627198103830 ) ) ;
#78341 = CARTESIAN_POINT ( 'NONE',  ( -5.823673210054116645, -21.52544592524344225, 107.2905762719810525 ) ) ;
#78342 = CARTESIAN_POINT ( 'NONE',  ( -5.049401038298153566, 19.05341960407611168, 75.20724293864769550 ) ) ;
#78343 = CARTESIAN_POINT ( 'NONE',  ( -19.02544592524334988, -5.153800228976617603, 18.95942372801899722 ) ) ;
#78346 = CARTESIAN_POINT ( 'NONE',  ( -4.483927247898539470, -16.52544592524342804, 107.2905762719810525 ) ) ;
#78345 = CARTESIAN_POINT ( 'NONE',  ( -16.55341960407611168, -4.379528057220339221, 36.45724293864768839 ) ) ;
#78344 = CARTESIAN_POINT ( 'NONE',  ( -16.51473224551069308, -9.474510206698971260, 36.66557627198102409 ) ) ;
#78347 = CARTESIAN_POINT ( 'NONE',  ( -16.51473224551082808, 9.474510206698731452, 103.3344237280190043 ) ) ;
#78348 = ORIENTED_EDGE ( 'NONE', *, *, #73681, .T. ) ;
#78349 = CARTESIAN_POINT ( 'NONE',  ( 21.52544592524334988, 5.823673210054432836, 26.45942372801901854 ) ) ;
#78350 = CARTESIAN_POINT ( 'NONE',  ( 5.153800228976615827, -19.02544592524334988, 65.20942372801900433 ) ) ;
#78351 = CARTESIAN_POINT ( 'NONE',  ( 16.55341960407611168, 4.379528057220329451, 23.95724293864769550 ) ) ;
#78352 = CARTESIAN_POINT ( 'NONE',  ( -15.80617190586745835, -15.72974639402198527, 81.87390960531435269 ) ) ;
#78353 = CARTESIAN_POINT ( 'NONE',  ( 21.55341960407610458, 5.719274019375980345, 23.95724293864769550 ) ) ;
#78354 = CARTESIAN_POINT ( 'NONE',  ( 4.379528057220339221, -16.55341960407611168, 52.70724293864769550 ) ) ;
#78355 = CARTESIAN_POINT ( 'NONE',  ( -13.89961937509977652, 13.97604488694528158, 35.62390960531435269 ) ) ;
#78356 = CARTESIAN_POINT ( 'NONE',  ( 19.05341960407617918, -5.049401038297876454, 21.04275706135232582 ) ) ;
#78357 = CARTESIAN_POINT ( 'NONE',  ( -14.29746914071037622, -8.314922557961029526, 84.16775706135234714 ) ) ;
#78358 = CARTESIAN_POINT ( 'NONE',  ( 14.34966873604972726, -8.224510206698740333, 55.83442372801901854 ) ) ;
#78359 = CARTESIAN_POINT ( 'NONE',  ( -5.719274019375978568, 21.55341960407610458, 25.20724293864769550 ) ) ;
#78360 = CARTESIAN_POINT ( 'NONE',  ( -15.72974639402176322, -15.80617190586768395, 104.3760903946856899 ) ) ;
#78361 = CARTESIAN_POINT ( 'NONE',  ( 16.46253265017160672, -9.564922557960803928, 83.33224293864768129 ) ) ;
#78362 = CARTESIAN_POINT ( 'NONE',  ( -16.55341960407617563, 4.379528057220093196, 63.54275706135234003 ) ) ;
#78363 = CARTESIAN_POINT ( 'NONE',  ( -12.14591786802309592, -12.06949235617757132, 106.8739096053143811 ) ) ;
#78364 = CARTESIAN_POINT ( 'NONE',  ( -4.379528057220328563, 16.55341960407611168, 35.20724293864768839 ) ) ;
#78365 = CARTESIAN_POINT ( 'NONE',  ( -18.22780087662122028, 5.500000000000031086, 38.51540105326107266 ) ) ;
#78368 = CARTESIAN_POINT ( 'NONE',  ( 13.89961937509977652, -13.97604488694527269, 73.12390960531436690 ) ) ;
#78367 = CARTESIAN_POINT ( 'NONE',  ( -13.97604488694527625, -13.89961937509977652, 91.87390960531432427 ) ) ;
#78366 = CARTESIAN_POINT ( 'NONE',  ( 15.72974639402176855, 15.80617190586768217, 71.87609039468568994 ) ) ;
#78369 = CARTESIAN_POINT ( 'NONE',  ( 13.97604488694527802, 13.89961937509977652, 109.3739096053143669 ) ) ;
#78370 = CARTESIAN_POINT ( 'NONE',  ( -16.55341960407611168, -4.379528057220339221, 61.45724293864770260 ) ) ;
#78371 = CARTESIAN_POINT ( 'NONE',  ( -16.53943276465976808, 0.05219959533911058130, 31.24890960531435979 ) ) ;
#78372 = CARTESIAN_POINT ( 'NONE',  ( -0.05219959533910754901, -16.53943276465976808, 57.49890960531435979 ) ) ;
#78374 = CARTESIAN_POINT ( 'NONE',  ( 17.49999999999999289, -3.565345528327872771, 31.92494486806480580 ) ) ;
#78373 = CARTESIAN_POINT ( 'NONE',  ( -14.29746914071037622, -8.314922557961029526, 39.16775706135235424 ) ) ;
#78375 = CARTESIAN_POINT ( 'NONE',  ( -5.049401038297874678, -19.05341960407617918, 44.79275706135232582 ) ) ;
#78376 = CARTESIAN_POINT ( 'NONE',  ( 9.564922557960805705, 16.46253265017160317, 69.58224293864770971 ) ) ;
#78377 = CARTESIAN_POINT ( 'NONE',  ( 19.03943276465977164, 0.05219959533936151252, 46.25109039468566863 ) ) ;
#78378 = CARTESIAN_POINT ( 'NONE',  ( 5.049401038297881783, 19.05341960407617563, 52.29275706135234003 ) ) ;
#78380 = CARTESIAN_POINT ( 'NONE',  ( -16.52544592524335698, -4.483927247898792601, 88.95942372801901854 ) ) ;
#78379 = CARTESIAN_POINT ( 'NONE',  ( -9.474510206698720793, -16.51473224551083518, 104.5844237280190043 ) ) ;
#78381 = CARTESIAN_POINT ( 'NONE',  ( 27.73933785331498569, 2.768321779492822058E-14, 146.3750000027311842 ) ) ;
#78382 = CARTESIAN_POINT ( 'NONE',  ( -5.049401038298153566, 19.05341960407611168, 25.20724293864768484 ) ) ;
#78383 = CARTESIAN_POINT ( 'NONE',  ( 13.89961937509977652, -13.97604488694527269, 108.1239096053143669 ) ) ;
#78384 = CARTESIAN_POINT ( 'NONE',  ( 18.62759615963255655, 10.81492255796105972, 36.66775706135234714 ) ) ;
#78385 = CARTESIAN_POINT ( 'NONE',  ( -0.05219959533936034679, 19.03943276465977164, 92.50109039468566152 ) ) ;
#78387 = CARTESIAN_POINT ( 'NONE',  ( -19.02544592524342804, 5.153800228976336051, 56.04057627198100988 ) ) ;
#78386 = CARTESIAN_POINT ( 'NONE',  ( 37.99999999999999289, 2.893978650043524126E-14, -3.000000000000000000 ) ) ;
#78388 = CARTESIAN_POINT ( 'NONE',  ( -19.03943276465977164, 0.05219959533909376836, 101.2489096053143669 ) ) ;
#78390 = CARTESIAN_POINT ( 'NONE',  ( -13.89961937509977652, 13.97604488694528158, 65.62390960531436690 ) ) ;
#78389 = CARTESIAN_POINT ( 'NONE',  ( -8.224510206698948167, 14.34966873604960824, 55.41557627198102409 ) ) ;
#78391 = CARTESIAN_POINT ( 'NONE',  ( 16.51473224551069308, 9.474510206698969483, 59.16557627198102409 ) ) ;
#78392 = CARTESIAN_POINT ( 'NONE',  ( -9.474510206698720793, -16.51473224551083518, 59.58442372801900433 ) ) ;
#78393 = CARTESIAN_POINT ( 'NONE',  ( 5.823673210054125526, 21.52544592524343514, 54.79057627198104541 ) ) ;
#78394 = CARTESIAN_POINT ( 'NONE',  ( -9.564922557961040184, 16.46253265017147172, 37.91775706135233293 ) ) ;
#78395 = CARTESIAN_POINT ( 'NONE',  ( 9.564922557960805705, 16.46253265017160317, 74.58224293864769550 ) ) ;
#78396 = CARTESIAN_POINT ( 'NONE',  ( -10.81492255796078084, -18.62759615963271287, 82.08224293864768129 ) ) ;
#78398 = CARTESIAN_POINT ( 'NONE',  ( 0.05219959533936267826, -19.03943276465977164, 30.00109039468566863 ) ) ;
#78397 = CARTESIAN_POINT ( 'NONE',  ( 8.314922557960818139, 14.29746914071049879, 74.58224293864768129 ) ) ;
#78399 = CARTESIAN_POINT ( 'NONE',  ( 18.67979575497178502, 10.72451020669898547, 49.16557627198102409 ) ) ;
#78400 = CARTESIAN_POINT ( 'NONE',  ( -5.719274019375978568, 21.55341960407610458, 40.20724293864769550 ) ) ;
#78401 = CARTESIAN_POINT ( 'NONE',  ( 9.564922557960805705, 16.46253265017160317, 69.58224293864770971 ) ) ;
#78402 = CARTESIAN_POINT ( 'NONE',  ( 16.46253265017160672, -9.564922557960803928, 53.33224293864768839 ) ) ;
#78403 = CARTESIAN_POINT ( 'NONE',  ( 19.02544592524343514, -5.153800228976328945, 23.54057627198102054 ) ) ;
#78404 = CARTESIAN_POINT ( 'NONE',  ( 5.719274019375673035, 21.55341960407619339, 22.29275706135235069 ) ) ;
#78405 = CARTESIAN_POINT ( 'NONE',  ( 25.77168321198462664, -6.124454116751252286, 163.0898522765300811 ) ) ;
#78406 = CARTESIAN_POINT ( 'NONE',  ( 5.719274019375673035, 21.55341960407619339, 27.29275706135234358 ) ) ;
#78407 = CARTESIAN_POINT ( 'NONE',  ( -5.049401038298153566, 19.05341960407611168, 35.20724293864768839 ) ) ;
#78408 = CARTESIAN_POINT ( 'NONE',  ( 18.62759615963271287, -10.81492255796078972, 108.3322429386477097 ) ) ;
#78409 = CARTESIAN_POINT ( 'NONE',  ( -19.03943276465977164, -0.05219959533935918106, 43.75109039468566863 ) ) ;
#78410 = CARTESIAN_POINT ( 'NONE',  ( 9.474510206698971260, -16.51473224551069308, 27.91557627198103120 ) ) ;
#78411 = CARTESIAN_POINT ( 'NONE',  ( -13.97604488694527625, -13.89961937509977652, 21.87390960531435979 ) ) ;
#78412 = DIRECTION ( 'NONE',  ( -0.000000000000000000, 0.000000000000000000, 1.000000000000000000 ) ) ;
#78413 = CARTESIAN_POINT ( 'NONE',  ( -4.379528057220086978, -16.55341960407618274, 64.79275706135234714 ) ) ;
#78414 = CARTESIAN_POINT ( 'NONE',  ( 13.97604488694527802, 13.89961937509977652, 24.37390960531435624 ) ) ;
#78415 = CARTESIAN_POINT ( 'NONE',  ( 33.74160284725414982, -3.639722220971261635, 99.13931652913686321 ) ) ;
#78416 = CARTESIAN_POINT ( 'NONE',  ( 9.564922557960805705, 16.46253265017160317, 74.58224293864769550 ) ) ;
#78417 = CARTESIAN_POINT ( 'NONE',  ( -14.29746914071049879, 8.314922557960819915, 105.8322429386476955 ) ) ;
#78418 = AXIS2_PLACEMENT_3D ( 'NONE', #23733, #85382, #8559 ) ;
#78419 = CARTESIAN_POINT ( 'NONE',  ( -21.52544592524343514, 5.823673210054127303, 66.04057627198103830 ) ) ;
#78420 = CARTESIAN_POINT ( 'NONE',  ( 16.53943276465976808, -0.05219959533910856209, 73.74890960531433848 ) ) ;
#78421 = CARTESIAN_POINT ( 'NONE',  ( -4.379528057220086978, -16.55341960407618274, 29.79275706135234358 ) ) ;
#78422 = CARTESIAN_POINT ( 'NONE',  ( -15.80617190586768217, 15.72974639402176855, 88.12609039468570415 ) ) ;
#78423 = EDGE_CURVE ( 'NONE', #16157, #41521, #57480, .T. ) ;
#78424 = CARTESIAN_POINT ( 'NONE',  ( -19.02544592524342804, 5.153800228976336051, 31.04057627198102409 ) ) ;
#78425 = CARTESIAN_POINT ( 'NONE',  ( 16.53943276465976808, 0.05219959533934440121, 111.2510903946856899 ) ) ;
#78426 = CARTESIAN_POINT ( 'NONE',  ( 14.34966873604960469, 8.224510206698951720, 54.16557627198103120 ) ) ;
#78427 = CARTESIAN_POINT ( 'NONE',  ( 16.46253265017160672, -9.564922557960803928, 53.33224293864768839 ) ) ;
#78428 = CARTESIAN_POINT ( 'NONE',  ( 21.52544592524334988, 5.823673210054432836, 101.4594237280190185 ) ) ;
#78429 = CARTESIAN_POINT ( 'NONE',  ( -15.80617190586745835, -15.72974639402198527, 101.8739096053143811 ) ) ;
#78430 = CARTESIAN_POINT ( 'NONE',  ( -10.72451020669870658, -18.67979575497194134, 74.58442372801901854 ) ) ;
#78431 = CARTESIAN_POINT ( 'NONE',  ( -4.379528057220086978, -16.55341960407618274, 39.79275706135235424 ) ) ;
#78433 = CARTESIAN_POINT ( 'NONE',  ( 15.80617190586769283, -15.72974639402175789, 85.62609039468568994 ) ) ;
#78432 = CARTESIAN_POINT ( 'NONE',  ( 4.483927247898545687, 16.52544592524342804, 84.79057627198102409 ) ) ;
#78434 = ADVANCED_FACE ( 'NONE', ( #15936 ), #77595, .F. ) ;
#78435 = CARTESIAN_POINT ( 'NONE',  ( 14.29746914071049879, -8.314922557960816363, 23.33224293864769194 ) ) ;
#78436 = CARTESIAN_POINT ( 'NONE',  ( -16.61371651742599198, 7.165104196376160139, 113.8541506999300026 ) ) ;
#78437 = CARTESIAN_POINT ( 'NONE',  ( -8.314922557961024197, 14.29746914071037800, 42.91775706135235424 ) ) ;
#78438 = CARTESIAN_POINT ( 'NONE',  ( -14.29746914071049879, 8.314922557960819915, 35.83224293864768839 ) ) ;
#78439 = CARTESIAN_POINT ( 'NONE',  ( -8.314922557961024197, 14.29746914071037800, 92.91775706135236135 ) ) ;
#78440 = CARTESIAN_POINT ( 'NONE',  ( -9.474510206698964154, 16.51473224551069663, 100.4155762719810241 ) ) ;
#78441 = CARTESIAN_POINT ( 'NONE',  ( 5.153800228976335163, 19.02544592524342804, 114.7905762719810241 ) ) ;
#78442 = CARTESIAN_POINT ( 'NONE',  ( 0.05219959533937995610, -21.53943276465977519, 105.0010903946856757 ) ) ;
#78443 = CARTESIAN_POINT ( 'NONE',  ( -14.29746914071037622, -8.314922557961029526, 104.1677570613523471 ) ) ;
#78444 = CARTESIAN_POINT ( 'NONE',  ( -14.34966873604960291, -8.224510206698953496, 71.66557627198100988 ) ) ;
#78445 = CARTESIAN_POINT ( 'NONE',  ( -19.03943276465977164, 0.05219959533909376836, 81.24890960531436690 ) ) ;
#78446 = ORIENTED_EDGE ( 'NONE', *, *, #100204, .F. ) ;
#78447 = CARTESIAN_POINT ( 'NONE',  ( 16.53943276465976808, 0.05219959533934440121, 26.25109039468567573 ) ) ;
#78448 = CARTESIAN_POINT ( 'NONE',  ( 5.049401038298161559, -19.05341960407611168, 22.70724293864769194 ) ) ;
#78449 = CARTESIAN_POINT ( 'NONE',  ( 13.97604488694527802, 13.89961937509977652, 94.37390960531436690 ) ) ;
#78451 = CARTESIAN_POINT ( 'NONE',  ( 22.81625015709510151, -31.40387420917324590, -3.924999997268811658 ) ) ;
#78450 = CARTESIAN_POINT ( 'NONE',  ( -4.483927247898782831, 16.52544592524335698, 32.70942372801900433 ) ) ;
#78452 = CARTESIAN_POINT ( 'NONE',  ( 19.03943276465977164, 0.05219959533936151252, 36.25109039468567573 ) ) ;
#78453 = CARTESIAN_POINT ( 'NONE',  ( -0.05219959533934338120, 16.53943276465976808, 87.50109039468568994 ) ) ;
#78454 = CARTESIAN_POINT ( 'NONE',  ( 9.474510206698729675, 16.51473224551082808, 102.0844237280190043 ) ) ;
#78455 = CARTESIAN_POINT ( 'NONE',  ( 19.02544592524343514, -5.153800228976328945, 38.54057627198103120 ) ) ;
#78456 = CARTESIAN_POINT ( 'NONE',  ( 4.483927247898790824, -16.52544592524335698, 85.20942372801901854 ) ) ;
#78457 = CARTESIAN_POINT ( 'NONE',  ( -14.29746914071037622, -8.314922557961029526, 69.16775706135234714 ) ) ;
#78458 = CARTESIAN_POINT ( 'NONE',  ( -0.05219959533936034679, 19.03943276465977164, 77.50109039468566152 ) ) ;
#78459 = CARTESIAN_POINT ( 'NONE',  ( -9.474510206698720793, -16.51473224551083518, 19.58442372801899722 ) ) ;
#78460 = CARTESIAN_POINT ( 'NONE',  ( -16.51473224551069308, -9.474510206698971260, 41.66557627198103120 ) ) ;
#78461 = CARTESIAN_POINT ( 'NONE',  ( -0.05219959533909027116, -19.03943276465977164, 97.49890960531436690 ) ) ;
#78462 = CARTESIAN_POINT ( 'NONE',  ( -14.29746914071049879, 8.314922557960819915, 80.83224293864769550 ) ) ;
#78463 = CARTESIAN_POINT ( 'NONE',  ( 13.89961937509957401, 13.97604488694547697, 51.87609039468566863 ) ) ;
#78464 = CARTESIAN_POINT ( 'NONE',  ( 18.67979575497178502, 10.72451020669898547, 49.16557627198102409 ) ) ;
#78465 = CARTESIAN_POINT ( 'NONE',  ( 19.02544592524334988, 5.153800228976608722, 26.45942372801899722 ) ) ;
#78466 = CARTESIAN_POINT ( 'NONE',  ( -19.03943276465977164, 0.05219959533909376836, 96.24890960531436690 ) ) ;
#78467 = EDGE_CURVE ( 'NONE', #196449, #160325, #190701, .T. ) ;
#78468 = CARTESIAN_POINT ( 'NONE',  ( 19.05341960407617918, -5.049401038297876454, 26.04275706135233293 ) ) ;
#78469 = CARTESIAN_POINT ( 'NONE',  ( 5.823673210054125526, 21.52544592524343514, 74.79057627198105251 ) ) ;
#78470 = CARTESIAN_POINT ( 'NONE',  ( 16.46253265017160672, -9.564922557960803928, 108.3322429386476955 ) ) ;
#78471 = CARTESIAN_POINT ( 'NONE',  ( 13.89961937509957401, 13.97604488694547697, 81.87609039468564731 ) ) ;
#78472 = FACE_OUTER_BOUND ( 'NONE', #9269, .T. ) ;
#78473 = CARTESIAN_POINT ( 'NONE',  ( -16.52544592524335698, -4.483927247898792601, 18.95942372801901143 ) ) ;
#78474 = B_SPLINE_CURVE_WITH_KNOTS ( 'NONE', 3,
 ( #152929, #76091, #46762, #93240, #3228, #45764, #15427, #79070, #61904, #169089, #156922, #77086, #170096, #154925, #138755, #123575, #94237, #124586, #139738, #78070, #108421, #16423, #1227, #62905 ),
 .UNSPECIFIED., .F., .F.,
 ( 4, 2, 2, 2, 2, 2, 2, 2, 2, 2, 2, 4 ),
 ( 2.784816138783909714E-07, 0.0003261688173017302525, 0.0006520591529895821293, 0.0009779494886774341145, 0.001303839824365285883, 0.001955620495740971205, 0.002607401167116656527, 0.003259181838492341415, 0.003910962509868023268, 0.004562743181243703386, 0.004888633516931540843, 0.005214523852619376565 ),
 .UNSPECIFIED. ) ;
#78475 = CARTESIAN_POINT ( 'NONE',  ( 16.46253265017160672, -9.564922557960803928, 33.33224293864770260 ) ) ;
#78476 = CARTESIAN_POINT ( 'NONE',  ( -19.03943276465977164, 0.05219959533909376836, 91.24890960531436690 ) ) ;
#78477 = CARTESIAN_POINT ( 'NONE',  ( -5.719274019375978568, 21.55341960407610458, 70.20724293864769550 ) ) ;
#78478 = CARTESIAN_POINT ( 'NONE',  ( 12.06949235617739724, 12.14591786802326823, 51.87609039468568284 ) ) ;
#78479 = CARTESIAN_POINT ( 'NONE',  ( 10.81492255796106328, -18.62759615963255655, 45.41775706135234003 ) ) ;
#78481 = CARTESIAN_POINT ( 'NONE',  ( 21.52544592524334988, 5.823673210054432836, 96.45942372801901854 ) ) ;
#78480 = CARTESIAN_POINT ( 'NONE',  ( 13.89961937509957401, 13.97604488694547697, 86.87609039468567573 ) ) ;
#78482 = CARTESIAN_POINT ( 'NONE',  ( 14.29746914071037800, 8.314922557961029526, 91.66775706135234714 ) ) ;
#78483 = CARTESIAN_POINT ( 'NONE',  ( -9.474510206698964154, 16.51473224551069663, 95.41557627198102409 ) ) ;
#78484 = CARTESIAN_POINT ( 'NONE',  ( -16.52544592524342804, 4.483927247898546575, 96.04057627198102409 ) ) ;
#78485 = CARTESIAN_POINT ( 'NONE',  ( -16.53943276465976808, 0.05219959533911058130, 36.24890960531435979 ) ) ;
#78486 = CARTESIAN_POINT ( 'NONE',  ( -19.03943276465977164, -0.05219959533935918106, 73.75109039468566152 ) ) ;
#78487 = CARTESIAN_POINT ( 'NONE',  ( -5.823673210054431948, 21.52544592524334988, 62.70942372801902565 ) ) ;
#78488 = CARTESIAN_POINT ( 'NONE',  ( -0.05219959533936034679, 19.03943276465977164, 22.50109039468566152 ) ) ;
#78489 = CARTESIAN_POINT ( 'NONE',  ( -14.34966873604960291, -8.224510206698953496, 106.6655762719810383 ) ) ;
#78490 = CARTESIAN_POINT ( 'NONE',  ( -10.81492255796078084, -18.62759615963271287, 37.08224293864768129 ) ) ;
#78491 = CARTESIAN_POINT ( 'NONE',  ( 14.29746914071037800, 8.314922557961029526, 111.6677570613523613 ) ) ;
#78492 = CARTESIAN_POINT ( 'NONE',  ( 21.52544592524334988, 5.823673210054432836, 96.45942372801901854 ) ) ;
#78493 = CARTESIAN_POINT ( 'NONE',  ( -4.483927247898782831, 16.52544592524335698, 62.70942372801902565 ) ) ;
#78494 = CARTESIAN_POINT ( 'NONE',  ( -16.53943276465976808, -0.05219959533934237506, 103.7510903946857042 ) ) ;
#78495 = CARTESIAN_POINT ( 'NONE',  ( -15.80617190586768217, 15.72974639402176855, 53.12609039468568284 ) ) ;
#78496 = CARTESIAN_POINT ( 'NONE',  ( -5.719274019375665041, -21.55341960407619695, 59.79275706135234714 ) ) ;
#78497 = ORIENTED_EDGE ( 'NONE', *, *, #36811, .T. ) ;
#78498 = CARTESIAN_POINT ( 'NONE',  ( -5.719274019375665041, -21.55341960407619695, 29.79275706135234358 ) ) ;
#78499 = CARTESIAN_POINT ( 'NONE',  ( -4.379528057220328563, 16.55341960407611168, 100.2072429386476955 ) ) ;
#78500 = CARTESIAN_POINT ( 'NONE',  ( 19.03943276465977164, -0.05219959533909143690, 28.74890960531435624 ) ) ;
#78501 = CARTESIAN_POINT ( 'NONE',  ( -14.29746914071049879, 8.314922557960819915, 85.83224293864768129 ) ) ;
#78502 = CARTESIAN_POINT ( 'NONE',  ( -19.03943276465977164, 0.05219959533909376836, 66.24890960531436690 ) ) ;
#78503 = CARTESIAN_POINT ( 'NONE',  ( 0.05219959533934541429, -16.53943276465976808, 110.0010903946856757 ) ) ;
#78504 = CARTESIAN_POINT ( 'NONE',  ( -10.81492255796078084, -18.62759615963271287, 57.08224293864769550 ) ) ;
#78505 = CARTESIAN_POINT ( 'NONE',  ( -16.55341960407611168, -4.379528057220339221, 86.45724293864770971 ) ) ;
#78506 = CARTESIAN_POINT ( 'NONE',  ( -5.823673210054116645, -21.52544592524344225, 97.29057627198105251 ) ) ;
#78507 = CARTESIAN_POINT ( 'NONE',  ( -16.51473224551069308, -9.474510206698971260, 96.66557627198102409 ) ) ;
#78509 = CARTESIAN_POINT ( 'NONE',  ( 13.89961937509957401, 13.97604488694547697, 111.8760903946856757 ) ) ;
#78508 = CARTESIAN_POINT ( 'NONE',  ( -5.153800228976328057, -19.02544592524343514, 52.29057627198100988 ) ) ;
#78510 = CARTESIAN_POINT ( 'NONE',  ( 21.53943276465977519, -0.05219959533907433946, 38.74890960531435979 ) ) ;
#78511 = CARTESIAN_POINT ( 'NONE',  ( 21.52544592524334988, 5.823673210054432836, 71.45942372801901854 ) ) ;
#78512 = CARTESIAN_POINT ( 'NONE',  ( 19.02544592524343514, -5.153800228976328945, 68.54057627198103830 ) ) ;
#78513 = CARTESIAN_POINT ( 'NONE',  ( 5.049401038298161559, -19.05341960407611168, 102.7072429386476955 ) ) ;
#78514 = CARTESIAN_POINT ( 'NONE',  ( -14.29746914071037622, -8.314922557961029526, 59.16775706135234714 ) ) ;
#78515 = CARTESIAN_POINT ( 'NONE',  ( -0.05219959533937732626, 21.53943276465977519, 42.50109039468567573 ) ) ;
#78516 = CARTESIAN_POINT ( 'NONE',  ( -10.72451020669870658, -18.67979575497194134, 84.58442372801903275 ) ) ;
#78517 = CARTESIAN_POINT ( 'NONE',  ( 10.72451020669898902, -18.67979575497178502, 97.91557627198103830 ) ) ;
#78519 = CARTESIAN_POINT ( 'NONE',  ( 8.314922557961029526, -14.29746914071037800, 80.41775706135234714 ) ) ;
#78518 = CARTESIAN_POINT ( 'NONE',  ( -15.72974639402176322, -15.80617190586768395, 39.37609039468567573 ) ) ;
#78520 = CARTESIAN_POINT ( 'NONE',  ( -18.62759615963270932, 10.81492255796079327, 75.83224293864769550 ) ) ;
#78521 = CARTESIAN_POINT ( 'NONE',  ( -16.46253265017146816, -9.564922557961047289, 39.16775706135234003 ) ) ;
#78523 = CARTESIAN_POINT ( 'NONE',  ( -8.314922557961024197, 14.29746914071037800, 112.9177570613523329 ) ) ;
#78522 = CARTESIAN_POINT ( 'NONE',  ( 9.474510206698971260, -16.51473224551069308, 87.91557627198102409 ) ) ;
#78524 = CARTESIAN_POINT ( 'NONE',  ( -17.12812012977024168, 6.668231424566043231, 63.64051240676855770 ) ) ;
#78525 = CARTESIAN_POINT ( 'NONE',  ( -19.03943276465977164, 0.05219959533909376836, 101.2489096053143669 ) ) ;
#78526 = PLANE ( 'NONE',  #179871 ) ;
#78527 = CARTESIAN_POINT ( 'NONE',  ( 19.03943276465977164, 0.05219959533936151252, 91.25109039468566152 ) ) ;
#78528 = CARTESIAN_POINT ( 'NONE',  ( 18.62759615963271287, -10.81492255796078972, 53.33224293864769550 ) ) ;
#78529 = CARTESIAN_POINT ( 'NONE',  ( 16.52544592524342804, -4.483927247898539470, 43.54057627198103830 ) ) ;
#78530 = CARTESIAN_POINT ( 'NONE',  ( -8.314922557961024197, 14.29746914071037800, 22.91775706135235069 ) ) ;
#78531 = CARTESIAN_POINT ( 'NONE',  ( -9.474510206698964154, 16.51473224551069663, 25.41557627198103120 ) ) ;
#78532 = CARTESIAN_POINT ( 'NONE',  ( 19.05341960407617918, -5.049401038297876454, 111.0427570613523329 ) ) ;
#78534 = CARTESIAN_POINT ( 'NONE',  ( -19.03943276465977164, -0.05219959533935918106, 68.75109039468566152 ) ) ;
#78533 = CARTESIAN_POINT ( 'NONE',  ( 18.62759615963271287, -10.81492255796078972, 98.33224293864769550 ) ) ;
#78535 = CARTESIAN_POINT ( 'NONE',  ( -16.55341960407617563, 4.379528057220093196, 78.54275706135236135 ) ) ;
#78536 = CARTESIAN_POINT ( 'NONE',  ( -16.46253265017160317, 9.564922557960807481, 70.83224293864770971 ) ) ;
#78537 = CARTESIAN_POINT ( 'NONE',  ( -16.52544592524342804, 4.483927247898546575, 71.04057627198103830 ) ) ;
#78538 = CARTESIAN_POINT ( 'NONE',  ( -9.474510206698964154, 16.51473224551069663, 65.41557627198102409 ) ) ;
#78539 = CARTESIAN_POINT ( 'NONE',  ( -16.53943276465976808, 0.05219959533911058130, 71.24890960531435269 ) ) ;
#78540 = DIRECTION ( 'NONE',  ( 0.000000000000000000, -0.4999999999999993894, 0.8660254037844389297 ) ) ;
#78541 = CARTESIAN_POINT ( 'NONE',  ( -36.79334119018159299, -4.151185298968584014, 48.62628996558957084 ) ) ;
#78542 = CARTESIAN_POINT ( 'NONE',  ( -14.29746914071049879, 8.314922557960819915, 35.83224293864768839 ) ) ;
#78543 = CARTESIAN_POINT ( 'NONE',  ( 5.153800228976335163, 19.02544592524342804, 79.79057627198102409 ) ) ;
#78544 = DIRECTION ( 'NONE',  ( 0.000000000000000000, 0.000000000000000000, -1.000000000000000000 ) ) ;
#78545 = CARTESIAN_POINT ( 'NONE',  ( 9.474510206698729675, 16.51473224551082808, 57.08442372801900433 ) ) ;
#78546 = CARTESIAN_POINT ( 'NONE',  ( 12.14591786802327356, -12.06949235617739191, 65.62609039468568994 ) ) ;
#78547 = CARTESIAN_POINT ( 'NONE',  ( -21.55341960407610458, -5.719274019375992779, 61.45724293864770260 ) ) ;
#78548 = CARTESIAN_POINT ( 'NONE',  ( -19.05341960407617563, 5.049401038297882671, 23.54275706135233648 ) ) ;
#78549 = CARTESIAN_POINT ( 'NONE',  ( 19.03943276465977164, -0.05219959533909143690, 78.74890960531436690 ) ) ;
#78550 = CARTESIAN_POINT ( 'NONE',  ( 12.24802307403557577, -10.74802307403608737, -59.32879157176802920 ) ) ;
#78551 = CARTESIAN_POINT ( 'NONE',  ( 19.05341960407611168, 5.049401038298154454, 113.9572429386477097 ) ) ;
#78552 = CARTESIAN_POINT ( 'NONE',  ( 9.564922557960805705, 16.46253265017160317, 64.58224293864769550 ) ) ;
#78553 = CARTESIAN_POINT ( 'NONE',  ( 21.53943276465977519, 0.05219959533937863772, 41.25109039468568284 ) ) ;
#78554 = CARTESIAN_POINT ( 'NONE',  ( 16.53943276465976808, -0.05219959533910856209, 103.7489096053143669 ) ) ;
#78557 = ORIENTED_EDGE ( 'NONE', *, *, #40630, .F. ) ;
#78556 = CARTESIAN_POINT ( 'NONE',  ( 16.51473224551069308, 9.474510206698969483, 94.16557627198103830 ) ) ;
#78555 = CARTESIAN_POINT ( 'NONE',  ( -21.55341960407610458, -5.719274019375992779, 96.45724293864770971 ) ) ;
#78558 = CARTESIAN_POINT ( 'NONE',  ( -10.81492255796105439, 18.62759615963255655, 27.91775706135234358 ) ) ;
#78559 = ADVANCED_FACE ( 'NONE', ( #33093 ), #75603, .T. ) ;
#78560 = ORIENTED_EDGE ( 'NONE', *, *, #150015, .F. ) ;
#78561 = CARTESIAN_POINT ( 'NONE',  ( 16.46253265017160672, -9.564922557960803928, 83.33224293864768129 ) ) ;
#78562 = CIRCLE ( 'NONE', #46250, 28.82186960331498682 ) ;
#78563 = CARTESIAN_POINT ( 'NONE',  ( -6.434671708797603529, 6.434671708797564449, -61.89430850415821794 ) ) ;
#78564 = CARTESIAN_POINT ( 'NONE',  ( -5.719274019375978568, 21.55341960407610458, 100.2072429386476955 ) ) ;
#78565 = CARTESIAN_POINT ( 'NONE',  ( 0.05219959533909260263, 19.03943276465977164, 44.99890960531435979 ) ) ;
#78566 = CARTESIAN_POINT ( 'NONE',  ( -0.05219959533936034679, 19.03943276465977164, 107.5010903946856615 ) ) ;
#78567 = CARTESIAN_POINT ( 'NONE',  ( -36.91746825000001309, 11.99521256947798342, -3.224999997268813257 ) ) ;
#78568 = CARTESIAN_POINT ( 'NONE',  ( 5.049401038298161559, -19.05341960407611168, 22.70724293864769194 ) ) ;
#78569 = CARTESIAN_POINT ( 'NONE',  ( 18.67979575497194134, -10.72451020669871369, 80.83442372801901854 ) ) ;
#78571 = CARTESIAN_POINT ( 'NONE',  ( -15.80617190586768217, 15.72974639402176855, 43.12609039468568284 ) ) ;
#78570 = CARTESIAN_POINT ( 'NONE',  ( -5.153800228976328057, -19.02544592524343514, 82.29057627198103830 ) ) ;
#78572 = CARTESIAN_POINT ( 'NONE',  ( 18.67979575497194134, -10.72451020669871369, 30.83442372801902209 ) ) ;
#78573 = CARTESIAN_POINT ( 'NONE',  ( -23.31738231874055600, 16.94106989632528837, 147.7999999999999829 ) ) ;
#78574 = CARTESIAN_POINT ( 'NONE',  ( 13.97604488694527802, 13.89961937509977652, 84.37390960531433848 ) ) ;
#78575 = CARTESIAN_POINT ( 'NONE',  ( 0.4100696261202915749, 28.38346208463798348, 140.0000000000000853 ) ) ;
#78578 = CARTESIAN_POINT ( 'NONE',  ( 0.05219959533937995610, -21.53943276465977519, 40.00109039468567573 ) ) ;
#78577 = CARTESIAN_POINT ( 'NONE',  ( 21.55341960407610458, 5.719274019375980345, 43.95724293864769550 ) ) ;
#78576 = CARTESIAN_POINT ( 'NONE',  ( 4.379528057220092307, 16.55341960407617563, 42.29275706135235424 ) ) ;
#78579 = CARTESIAN_POINT ( 'NONE',  ( 18.67979575497194134, -10.72451020669871369, 70.83442372801901854 ) ) ;
#78580 = CARTESIAN_POINT ( 'NONE',  ( 4.023452810412280201, 4.713873842512024126, -62.49134662286012087 ) ) ;
#78581 = CARTESIAN_POINT ( 'NONE',  ( -19.02544592524334988, -5.153800228976617603, 108.9594237280189759 ) ) ;
#78582 = CARTESIAN_POINT ( 'NONE',  ( -19.05341960407611168, -5.049401038298163336, 61.45724293864769550 ) ) ;
#78583 = CARTESIAN_POINT ( 'NONE',  ( -19.05341960407611168, -5.049401038298163336, 81.45724293864769550 ) ) ;
#78584 = CARTESIAN_POINT ( 'NONE',  ( -16.55341960407611168, -4.379528057220339221, 106.4572429386477097 ) ) ;
#78585 = CARTESIAN_POINT ( 'NONE',  ( -12.06949235617756955, 12.14591786802309770, 105.6239096053143669 ) ) ;
#78587 = EDGE_CURVE ( 'NONE', #142920, #164159, #141253, .T. ) ;
#78586 = CARTESIAN_POINT ( 'NONE',  ( 10.81492255796078972, 18.62759615963270932, 34.58224293864770260 ) ) ;
#78588 = CARTESIAN_POINT ( 'NONE',  ( -12.06949235617739369, -12.14591786802326823, 79.37609039468567573 ) ) ;
#78590 = CARTESIAN_POINT ( 'NONE',  ( 19.05341960407611168, 5.049401038298154454, 58.95724293864768129 ) ) ;
#78589 = CARTESIAN_POINT ( 'NONE',  ( 4.483927247898545687, 16.52544592524342804, 64.79057627198103830 ) ) ;
#78591 = CARTESIAN_POINT ( 'NONE',  ( 10.72451020669871369, 18.67979575497193778, 82.08442372801901854 ) ) ;
#78592 = CARTESIAN_POINT ( 'NONE',  ( -18.62759615963255300, -10.81492255796106328, 69.16775706135234714 ) ) ;
#78593 = CARTESIAN_POINT ( 'NONE',  ( 16.46253265017146816, 9.564922557961045513, 111.6677570613523329 ) ) ;
#78594 = CARTESIAN_POINT ( 'NONE',  ( -16.55341960407611168, -4.379528057220339221, 56.45724293864768839 ) ) ;
#78595 = CARTESIAN_POINT ( 'NONE',  ( 5.719274019375673035, 21.55341960407619339, 27.29275706135234358 ) ) ;
#78596 = CARTESIAN_POINT ( 'NONE',  ( 5.823673210054125526, 21.52544592524343514, 64.79057627198103830 ) ) ;
#78597 = CARTESIAN_POINT ( 'NONE',  ( 19.01529144963336648, 5.499999999999971578, 73.73431955728440812 ) ) ;
#78598 = CARTESIAN_POINT ( 'NONE',  ( 1.993301997531345292E-15, -30.30510711980685912, 144.7500000054623399 ) ) ;
#78599 = CARTESIAN_POINT ( 'NONE',  ( 0.05219959533909260263, 19.03943276465977164, 74.99890960531435269 ) ) ;
#78600 = CARTESIAN_POINT ( 'NONE',  ( -8.224510206698948167, 14.34966873604960824, 30.41557627198101699 ) ) ;
#78601 = CARTESIAN_POINT ( 'NONE',  ( -4.483927247898539470, -16.52544592524342804, 22.29057627198102765 ) ) ;
#78602 = CARTESIAN_POINT ( 'NONE',  ( -4.483927247898782831, 16.52544592524335698, 92.70942372801901854 ) ) ;
#78603 = CARTESIAN_POINT ( 'NONE',  ( -16.51473224551082808, 9.474510206698731452, 58.33442372801900433 ) ) ;
#78604 = CARTESIAN_POINT ( 'NONE',  ( -11.74264578624800670, 36.14014761921585972, -8.400000000000000355 ) ) ;
#78605 = CARTESIAN_POINT ( 'NONE',  ( 9.474510206698971260, -16.51473224551069308, 102.9155762719810241 ) ) ;
#78606 = CARTESIAN_POINT ( 'NONE',  ( 12.14591786802309770, 12.06949235617756955, 74.37390960531436690 ) ) ;
#78607 = CARTESIAN_POINT ( 'NONE',  ( -19.02544592524334988, -5.153800228976617603, 48.95942372801900433 ) ) ;
#78609 = CARTESIAN_POINT ( 'NONE',  ( -19.03943276465977164, 0.05219959533909376836, 116.2489096053143669 ) ) ;
#78608 = CARTESIAN_POINT ( 'NONE',  ( -5.153800228976328057, -19.02544592524343514, 37.29057627198102409 ) ) ;
#78611 = ORIENTED_EDGE ( 'NONE', *, *, #154603, .T. ) ;
#78610 = CARTESIAN_POINT ( 'NONE',  ( -10.72451020669898014, 18.67979575497178502, 50.41557627198103120 ) ) ;
#78612 = CARTESIAN_POINT ( 'NONE',  ( -16.52544592524342804, 4.483927247898546575, 96.04057627198102409 ) ) ;
#78613 = CARTESIAN_POINT ( 'NONE',  ( -14.34966873604972548, 8.224510206698743886, 58.33442372801901143 ) ) ;
#78614 = CARTESIAN_POINT ( 'NONE',  ( 8.224510206698953496, -14.34966873604960469, 92.91557627198103830 ) ) ;
#78615 = DIRECTION ( 'NONE',  ( -5.392603844284257652E-33, -1.000000000000000000, -0.000000000000000000 ) ) ;
#78616 = CARTESIAN_POINT ( 'NONE',  ( -36.91746825000000598, 2.428612866367529932E-14, -9.124999997268814056 ) ) ;
#78617 = CARTESIAN_POINT ( 'NONE',  ( -5.049401038298153566, 19.05341960407611168, 110.2072429386476671 ) ) ;
#78618 = CARTESIAN_POINT ( 'NONE',  ( 29.86685920354754842, -21.69954338932559068, -4.324999997268814234 ) ) ;
#78619 = DIRECTION ( 'NONE',  ( 0.000000000000000000, -1.000000000000000000, 0.000000000000000000 ) ) ;
#78621 = CARTESIAN_POINT ( 'NONE',  ( 16.52544592524342804, -4.483927247898539470, 23.54057627198102765 ) ) ;
#78620 = CARTESIAN_POINT ( 'NONE',  ( -16.52544592524335698, -4.483927247898792601, 43.95942372801902565 ) ) ;
#78622 = CARTESIAN_POINT ( 'NONE',  ( -15.80617190586745835, -15.72974639402198527, 56.87390960531436690 ) ) ;
#78624 = CARTESIAN_POINT ( 'NONE',  ( 16.51473224551083163, -9.474510206698727899, 80.83442372801899012 ) ) ;
#78623 = CIRCLE ( 'NONE', #46310, 2.000000000000000000 ) ;
#78625 = CARTESIAN_POINT ( 'NONE',  ( -18.62759615963270932, 10.81492255796079327, 45.83224293864769550 ) ) ;
#78626 = CARTESIAN_POINT ( 'NONE',  ( 18.67979575497194134, -10.72451020669871369, 80.83442372801901854 ) ) ;
#78627 = CARTESIAN_POINT ( 'NONE',  ( -12.20200080651912344, 10.33258783678502546, -61.66593582935060880 ) ) ;
#78628 = CARTESIAN_POINT ( 'NONE',  ( -0.05219959533934338120, 16.53943276465976808, 47.50109039468568994 ) ) ;
#78630 = CARTESIAN_POINT ( 'NONE',  ( 0.05219959533909260263, 19.03943276465977164, 99.99890960531436690 ) ) ;
#78629 = CARTESIAN_POINT ( 'NONE',  ( 16.51473224551069308, 9.474510206698969483, 39.16557627198103120 ) ) ;
#78631 = CARTESIAN_POINT ( 'NONE',  ( -19.02544592524342804, 5.153800228976336051, 41.04057627198103120 ) ) ;
#78632 = CARTESIAN_POINT ( 'NONE',  ( 14.34966873604960469, 8.224510206698951720, 104.1655762719810241 ) ) ;
#78633 = CARTESIAN_POINT ( 'NONE',  ( 36.99999999999968736, 4.791014396527177230E-13, 45.00000000000025580 ) ) ;
#78634 = CARTESIAN_POINT ( 'NONE',  ( 16.51473224551069308, 9.474510206698969483, 99.16557627198102409 ) ) ;
#78635 = ORIENTED_EDGE ( 'NONE', *, *, #77310, .F. ) ;
#78636 = CARTESIAN_POINT ( 'NONE',  ( -0.05219959533934338120, 16.53943276465976808, 52.50109039468567573 ) ) ;
#78637 = CARTESIAN_POINT ( 'NONE',  ( 5.719274019375991003, -21.55341960407610458, 92.70724293864770971 ) ) ;
#78638 = CARTESIAN_POINT ( 'NONE',  ( -13.97604488694527625, -13.89961937509977652, 51.87390960531436690 ) ) ;
#78639 = CARTESIAN_POINT ( 'NONE',  ( 10.81492255796106328, -18.62759615963255655, 25.41775706135235779 ) ) ;
#78640 = CARTESIAN_POINT ( 'NONE',  ( -5.153800228976328057, -19.02544592524343514, 82.29057627198103830 ) ) ;
#78641 = CARTESIAN_POINT ( 'NONE',  ( 0.000000000000000000, 0.000000000000000000, 0.000000000000000000 ) ) ;
#78642 = ORIENTED_EDGE ( 'NONE', *, *, #110020, .F. ) ;
#78643 = CARTESIAN_POINT ( 'NONE',  ( -16.55341960407617563, 4.379528057220093196, 53.54275706135234714 ) ) ;
#78644 = CARTESIAN_POINT ( 'NONE',  ( 18.67979575497194134, -10.72451020669871369, 20.83442372801901143 ) ) ;
#78647 = CARTESIAN_POINT ( 'NONE',  ( -9.564922557961040184, 16.46253265017147172, 72.91775706135233293 ) ) ;
#78646 = CARTESIAN_POINT ( 'NONE',  ( 16.46253265017160672, -9.564922557960803928, 103.3322429386476955 ) ) ;
#78645 = CARTESIAN_POINT ( 'NONE',  ( 0.05219959533909260263, 19.03943276465977164, 29.99890960531435979 ) ) ;
#78648 = CARTESIAN_POINT ( 'NONE',  ( 16.51473224551083163, -9.474510206698727899, 30.83442372801900433 ) ) ;
#78649 = CARTESIAN_POINT ( 'NONE',  ( 21.53943276465977519, -0.05219959533907433946, 88.74890960531436690 ) ) ;
#78650 = CARTESIAN_POINT ( 'NONE',  ( -9.564922557961040184, 16.46253265017147172, 32.91775706135233293 ) ) ;
#78651 = CARTESIAN_POINT ( 'NONE',  ( 8.314922557961029526, -14.29746914071037800, 80.41775706135234714 ) ) ;
#78652 = CARTESIAN_POINT ( 'NONE',  ( -0.05219959533909027116, -19.03943276465977164, 102.4989096053143669 ) ) ;
#78653 = CARTESIAN_POINT ( 'NONE',  ( -5.153800228976328057, -19.02544592524343514, 62.29057627198100988 ) ) ;
#78654 = CARTESIAN_POINT ( 'NONE',  ( 5.719274019375673035, 21.55341960407619339, 72.29275706135236135 ) ) ;
#78655 = CARTESIAN_POINT ( 'NONE',  ( -0.05219959533937732626, 21.53943276465977519, 87.50109039468568994 ) ) ;
#78656 = CARTESIAN_POINT ( 'NONE',  ( -16.51473224551069308, -9.474510206698971260, 71.66557627198102409 ) ) ;
#78657 = CARTESIAN_POINT ( 'NONE',  ( -0.05219959533937732626, 21.53943276465977519, 52.50109039468567573 ) ) ;
#78658 = CARTESIAN_POINT ( 'NONE',  ( -13.97604488694547697, 13.89961937509957934, 83.12609039468564731 ) ) ;
#78659 = CARTESIAN_POINT ( 'NONE',  ( 19.03943276465977164, -0.05219959533909143690, 53.74890960531436690 ) ) ;
#78660 = CARTESIAN_POINT ( 'NONE',  ( -13.97604488694527625, -13.89961937509977652, 101.8739096053143811 ) ) ;
#78661 = CARTESIAN_POINT ( 'NONE',  ( -16.46253265017160317, 9.564922557960807481, 70.83224293864770971 ) ) ;
#78662 = CARTESIAN_POINT ( 'NONE',  ( 16.51473224551069308, 9.474510206698969483, 114.1655762719810241 ) ) ;
#78663 = CARTESIAN_POINT ( 'NONE',  ( 16.51473224551069308, 9.474510206698969483, 49.16557627198102409 ) ) ;
#78664 = CARTESIAN_POINT ( 'NONE',  ( -15.80617190586745835, -15.72974639402198527, 96.87390960531436690 ) ) ;
#78665 = CARTESIAN_POINT ( 'NONE',  ( 8.224510206698742110, 14.34966873604972548, 77.08442372801901854 ) ) ;
#78666 = CARTESIAN_POINT ( 'NONE',  ( -23.63516320021239636, 9.722623904421405783, 168.4908852323012809 ) ) ;
#78667 = CARTESIAN_POINT ( 'NONE',  ( 19.05341960407617918, -5.049401038297876454, 31.04275706135232227 ) ) ;
#78668 = ADVANCED_FACE ( 'NONE', ( #159397 ), #131406, .T. ) ;
#78669 = CARTESIAN_POINT ( 'NONE',  ( -16.46253265017160317, 9.564922557960807481, 60.83224293864769550 ) ) ;
#78670 = CARTESIAN_POINT ( 'NONE',  ( 16.53943276465976808, -0.05219959533910856209, 63.74890960531435979 ) ) ;
#78671 = CARTESIAN_POINT ( 'NONE',  ( 12.06949235617757843, -12.14591786802309237, 88.12390960531436690 ) ) ;
#78672 = CARTESIAN_POINT ( 'NONE',  ( 19.05341960407611168, 5.049401038298154454, 103.9572429386476671 ) ) ;
#78673 = CARTESIAN_POINT ( 'NONE',  ( -13.97604488694527625, -13.89961937509977652, 91.87390960531432427 ) ) ;
#78674 = CARTESIAN_POINT ( 'NONE',  ( -16.51473224551069308, -9.474510206698971260, 106.6655762719810383 ) ) ;
#78675 = CARTESIAN_POINT ( 'NONE',  ( -10.72451020669870658, -18.67979575497194134, 109.5844237280190328 ) ) ;
#78676 = CARTESIAN_POINT ( 'NONE',  ( -12.14591786802326823, 12.06949235617739902, 88.12609039468570415 ) ) ;
#78677 = CARTESIAN_POINT ( 'NONE',  ( 0.05219959533937995610, -21.53943276465977519, 40.00109039468567573 ) ) ;
#78678 = CARTESIAN_POINT ( 'NONE',  ( -18.67979575497178146, -10.72451020669898902, 31.66557627198102054 ) ) ;
#78679 = CARTESIAN_POINT ( 'NONE',  ( -10.81492255796078084, -18.62759615963271287, 107.0822429386476955 ) ) ;
#78680 = CARTESIAN_POINT ( 'NONE',  ( 0.05219959533910956823, 16.53943276465976808, 54.99890960531435269 ) ) ;
#78681 = CARTESIAN_POINT ( 'NONE',  ( 9.474510206698971260, -16.51473224551069308, 52.91557627198102409 ) ) ;
#78682 = CARTESIAN_POINT ( 'NONE',  ( -0.05219959533910754901, -16.53943276465976808, 87.49890960531436690 ) ) ;
#78683 = CARTESIAN_POINT ( 'NONE',  ( 15.80617190586746368, 15.72974639402197994, 49.37390960531436690 ) ) ;
#78684 = CARTESIAN_POINT ( 'NONE',  ( 5.049401038297881783, 19.05341960407617563, 42.29275706135234003 ) ) ;
#78685 = CARTESIAN_POINT ( 'NONE',  ( 5.153800228976335163, 19.02544592524342804, 24.79057627198102765 ) ) ;
#78686 = EDGE_LOOP ( 'NONE', ( #153966, #8599, #125621, #156957, #108188, #160994, #110425, #136810 ) ) ;
#78687 = CARTESIAN_POINT ( 'NONE',  ( -16.55341960407617563, 4.379528057220093196, 73.54275706135234714 ) ) ;
#78688 = CARTESIAN_POINT ( 'NONE',  ( 5.049401038298161559, -19.05341960407611168, 62.70724293864769550 ) ) ;
#78689 = CARTESIAN_POINT ( 'NONE',  ( 27.73933785331498569, 2.768321779492822058E-14, 143.8750000027311842 ) ) ;
#78690 = CARTESIAN_POINT ( 'NONE',  ( 12.14591786802309770, 12.06949235617756955, 89.37390960531435269 ) ) ;
#78691 = CARTESIAN_POINT ( 'NONE',  ( 21.52544592524344225, -5.823673210054117533, 43.54057627198103830 ) ) ;
#78692 = ORIENTED_EDGE ( 'NONE', *, *, #151524, .T. ) ;
#78693 = CARTESIAN_POINT ( 'NONE',  ( 12.06949235617739724, 12.14591786802326823, 106.8760903946856899 ) ) ;
#78694 = CARTESIAN_POINT ( 'NONE',  ( -12.06949235617739369, -12.14591786802326823, 29.37609039468568284 ) ) ;
#78695 = CARTESIAN_POINT ( 'NONE',  ( 10.72451020669871369, 18.67979575497193778, 97.08442372801904696 ) ) ;
#78696 = CARTESIAN_POINT ( 'NONE',  ( 13.97604488694527802, 13.89961937509977652, 89.37390960531436690 ) ) ;
#78697 = CARTESIAN_POINT ( 'NONE',  ( 18.67979575497178502, 10.72451020669898547, 114.1655762719810383 ) ) ;
#78698 = CARTESIAN_POINT ( 'NONE',  ( 9.474510206698971260, -16.51473224551069308, 27.91557627198103120 ) ) ;
#78699 = CARTESIAN_POINT ( 'NONE',  ( -8.314922557961024197, 14.29746914071037800, 27.91775706135234358 ) ) ;
#78700 = CARTESIAN_POINT ( 'NONE',  ( -5.153800228976607833, 19.02544592524334988, 97.70942372801900433 ) ) ;
#78701 = AXIS2_PLACEMENT_3D ( 'NONE', #136379, #30192, #91834 ) ;
#78702 = CARTESIAN_POINT ( 'NONE',  ( 21.55341960407610458, 5.719274019375980345, 83.95724293864770971 ) ) ;
#78703 = CARTESIAN_POINT ( 'NONE',  ( 9.474510206698729675, 16.51473224551082808, 67.08442372801900433 ) ) ;
#78704 = LINE ( 'NONE', #79710, #92943 ) ;
#78705 = CARTESIAN_POINT ( 'NONE',  ( -10.81492255796105439, 18.62759615963255655, 22.91775706135235069 ) ) ;
#78706 = CARTESIAN_POINT ( 'NONE',  ( -5.153800228976328057, -19.02544592524343514, 72.29057627198102409 ) ) ;
#78707 = CARTESIAN_POINT ( 'NONE',  ( 5.049401038298161559, -19.05341960407611168, 82.70724293864770971 ) ) ;
#78708 = CARTESIAN_POINT ( 'NONE',  ( -8.224510206698735004, -14.34966873604973081, 39.58442372801901143 ) ) ;
#78709 = DIRECTION ( 'NONE',  ( 0.000000000000000000, 0.000000000000000000, -1.000000000000000000 ) ) ;
#78710 = CARTESIAN_POINT ( 'NONE',  ( -19.02544592524334988, -5.153800228976617603, 63.95942372801899012 ) ) ;
#78712 = CARTESIAN_POINT ( 'NONE',  ( 16.55341960407611168, 4.379528057220329451, 73.95724293864769550 ) ) ;
#78711 = CARTESIAN_POINT ( 'NONE',  ( 18.67979575497194134, -10.72451020669871369, 20.83442372801901143 ) ) ;
#78713 = CARTESIAN_POINT ( 'NONE',  ( 13.97604488694527802, 13.89961937509977652, 84.37390960531433848 ) ) ;
#78715 = CARTESIAN_POINT ( 'NONE',  ( -19.05341960407617563, 5.049401038297882671, 48.54275706135233293 ) ) ;
#78714 = CARTESIAN_POINT ( 'NONE',  ( -14.29746914071037622, -8.314922557961029526, 34.16775706135234714 ) ) ;
#78716 = CARTESIAN_POINT ( 'NONE',  ( 5.823673210054444382, -21.52544592524334988, 60.20942372801902565 ) ) ;
#78717 = CARTESIAN_POINT ( 'NONE',  ( 5.153800228976615827, -19.02544592524334988, 105.2094237280190185 ) ) ;
#78718 = CARTESIAN_POINT ( 'NONE',  ( 19.05341960407611168, 5.049401038298154454, 58.95724293864768129 ) ) ;
#78719 = CARTESIAN_POINT ( 'NONE',  ( 16.46253265017146816, 9.564922557961045513, 76.66775706135234714 ) ) ;
#78720 = CARTESIAN_POINT ( 'NONE',  ( 12.14591786802327356, -12.06949235617739191, 50.62609039468568994 ) ) ;
#78721 = CARTESIAN_POINT ( 'NONE',  ( 18.62759615963255655, 10.81492255796105972, 96.66775706135234714 ) ) ;
#78722 = CARTESIAN_POINT ( 'NONE',  ( 9.564922557961047289, -16.46253265017146816, 70.41775706135233293 ) ) ;
#78723 = CARTESIAN_POINT ( 'NONE',  ( -19.03943276465977164, 0.05219959533909376836, 46.24890960531435979 ) ) ;
#78724 = CARTESIAN_POINT ( 'NONE',  ( 0.05219959533907565091, 21.53943276465977519, 69.99890960531435269 ) ) ;
#78726 = CARTESIAN_POINT ( 'NONE',  ( -19.05341960407617563, 5.049401038297882671, 63.54275706135234003 ) ) ;
#78725 = CARTESIAN_POINT ( 'NONE',  ( 12.14591786802309770, 12.06949235617756955, 69.37390960531436690 ) ) ;
#78727 = CARTESIAN_POINT ( 'NONE',  ( 20.02446474427094003, 11.96320450740734032, 170.0134183209139849 ) ) ;
#78728 = CARTESIAN_POINT ( 'NONE',  ( 13.97604488694548053, -13.89961937509957401, 40.62609039468564731 ) ) ;
#78729 = CARTESIAN_POINT ( 'NONE',  ( 16.53943276465976808, 0.05219959533934440121, 96.25109039468568994 ) ) ;
#78730 = CARTESIAN_POINT ( 'NONE',  ( -8.314922557960811034, -14.29746914071050412, 62.08224293864769550 ) ) ;
#78732 = CARTESIAN_POINT ( 'NONE',  ( 17.14385361876520264, -23.59649016807271238, 139.5750000027311444 ) ) ;
#78731 = CARTESIAN_POINT ( 'NONE',  ( -10.81492255796105439, 18.62759615963255655, 97.91775706135236135 ) ) ;
#78733 = CARTESIAN_POINT ( 'NONE',  ( 10.72451020669898902, -18.67979575497178502, 97.91557627198103830 ) ) ;
#78734 = CARTESIAN_POINT ( 'NONE',  ( 9.474510206698971260, -16.51473224551069308, 52.91557627198102409 ) ) ;
#78735 = CARTESIAN_POINT ( 'NONE',  ( 0.05219959533937995610, -21.53943276465977519, 75.00109039468568994 ) ) ;
#78736 = CARTESIAN_POINT ( 'NONE',  ( -9.474510206698964154, 16.51473224551069663, 55.41557627198103120 ) ) ;
#78737 = CARTESIAN_POINT ( 'NONE',  ( -9.564922557960796823, -16.46253265017161027, 67.08224293864769550 ) ) ;
#78738 = CARTESIAN_POINT ( 'NONE',  ( 16.46253265017160672, -9.564922557960803928, 28.33224293864769550 ) ) ;
#78739 = CARTESIAN_POINT ( 'NONE',  ( -9.564922557960796823, -16.46253265017161027, 107.0822429386476955 ) ) ;
#78740 = CARTESIAN_POINT ( 'NONE',  ( 16.52544592524342804, -4.483927247898539470, 68.54057627198103830 ) ) ;
#78741 = CARTESIAN_POINT ( 'NONE',  ( 19.05341960407611168, 5.049401038298154454, 33.95724293864769550 ) ) ;
#78742 = CARTESIAN_POINT ( 'NONE',  ( -0.05219959533910754901, -16.53943276465976808, 82.49890960531436690 ) ) ;
#78743 = CARTESIAN_POINT ( 'NONE',  ( -10.72451020669898014, 18.67979575497178502, 90.41557627198103830 ) ) ;
#78744 = CARTESIAN_POINT ( 'NONE',  ( 18.62759615963255655, 10.81492255796105972, 31.66775706135234358 ) ) ;
#78745 = CARTESIAN_POINT ( 'NONE',  ( 3.735172737399431091E-16, 6.100000000000006750, -62.50719930893269805 ) ) ;
#78746 = CARTESIAN_POINT ( 'NONE',  ( 16.52544592524335698, 4.483927247898782831, 46.45942372801901854 ) ) ;
#78747 = CARTESIAN_POINT ( 'NONE',  ( 21.52544592524344225, -5.823673210054117533, 83.54057627198102409 ) ) ;
#78748 = CARTESIAN_POINT ( 'NONE',  ( 15.72974639402176855, 15.80617190586768217, 111.8760903946856615 ) ) ;
#78749 = CARTESIAN_POINT ( 'NONE',  ( -19.03943276465977164, 0.05219959533909376836, 106.2489096053143669 ) ) ;
#78750 = CARTESIAN_POINT ( 'NONE',  ( 10.81492255796106328, -18.62759615963255655, 45.41775706135234003 ) ) ;
#78751 = CARTESIAN_POINT ( 'NONE',  ( 21.53943276465977519, -0.05219959533907433946, 48.74890960531435979 ) ) ;
#78752 = CARTESIAN_POINT ( 'NONE',  ( 8.224510206698742110, 14.34966873604972548, 102.0844237280190185 ) ) ;
#78754 = CARTESIAN_POINT ( 'NONE',  ( 15.80617190586769283, -15.72974639402175789, 100.6260903946857184 ) ) ;
#78753 = CARTESIAN_POINT ( 'NONE',  ( -10.81492255796105439, 18.62759615963255655, 62.91775706135236135 ) ) ;
#78755 = CARTESIAN_POINT ( 'NONE',  ( -9.474510206698720793, -16.51473224551083518, 34.58442372801899722 ) ) ;
#78756 = CARTESIAN_POINT ( 'NONE',  ( 14.29746914071037800, 8.314922557961029526, 81.66775706135236135 ) ) ;
#78757 = CARTESIAN_POINT ( 'NONE',  ( -15.80617190586768217, 15.72974639402176855, 43.12609039468568284 ) ) ;
#78758 = CARTESIAN_POINT ( 'NONE',  ( -0.05219959533909027116, -19.03943276465977164, 47.49890960531435979 ) ) ;
#78759 = CARTESIAN_POINT ( 'NONE',  ( -5.153800228976607833, 19.02544592524334988, 22.70942372801899012 ) ) ;
#78760 = CARTESIAN_POINT ( 'NONE',  ( -21.53943276465977519, 0.05219959533907696930, 26.24890960531435624 ) ) ;
#78761 = CARTESIAN_POINT ( 'NONE',  ( -10.81492255796078084, -18.62759615963271287, 112.0822429386477097 ) ) ;
#78762 = CARTESIAN_POINT ( 'NONE',  ( -10.72451020669898014, 18.67979575497178502, 75.41557627198102409 ) ) ;
#78763 = CARTESIAN_POINT ( 'NONE',  ( 0.05219959533934541429, -16.53943276465976808, 45.00109039468568284 ) ) ;
#78765 = CARTESIAN_POINT ( 'NONE',  ( 10.72451020669898902, -18.67979575497178502, 77.91557627198102409 ) ) ;
#78764 = CARTESIAN_POINT ( 'NONE',  ( 193.3062444957835453, -155.7167183371837496, -25.00000000000000000 ) ) ;
#78767 = CARTESIAN_POINT ( 'NONE',  ( -16.52544592524342804, 4.483927247898546575, 61.04057627198103120 ) ) ;
#78766 = CARTESIAN_POINT ( 'NONE',  ( 16.52544592524335698, 4.483927247898782831, 71.45942372801901854 ) ) ;
#78768 = CARTESIAN_POINT ( 'NONE',  ( -22.73357338108569081, 22.35296335725854533, -45.67722784712131556 ) ) ;
#78769 = CARTESIAN_POINT ( 'NONE',  ( 5.153800228976615827, -19.02544592524334988, 85.20942372801900433 ) ) ;
#78770 = VECTOR ( 'NONE', #57495, 1000.000000000000000 ) ;
#78771 = CARTESIAN_POINT ( 'NONE',  ( -11.30153831258470731, -188.0000000000000000, 0.000000000000000000 ) ) ;
#78772 = CARTESIAN_POINT ( 'NONE',  ( -16.52544592524335698, -4.483927247898792601, 43.95942372801902565 ) ) ;
#78773 = CARTESIAN_POINT ( 'NONE',  ( -18.62759615963255300, -10.81492255796106328, 19.16775706135234714 ) ) ;
#78774 = CARTESIAN_POINT ( 'NONE',  ( -21.55341960407610458, -5.719274019375992779, 81.45724293864769550 ) ) ;
#78775 = CARTESIAN_POINT ( 'NONE',  ( -0.05219959533907301413, -21.53943276465977519, 22.49890960531436335 ) ) ;
#78776 = CARTESIAN_POINT ( 'NONE',  ( 4.483927247898790824, -16.52544592524335698, 60.20942372801902565 ) ) ;
#78777 = CARTESIAN_POINT ( 'NONE',  ( 5.049401038298161559, -19.05341960407611168, 77.70724293864765286 ) ) ;
#78779 = CARTESIAN_POINT ( 'NONE',  ( -9.474510206698720793, -16.51473224551083518, 109.5844237280190043 ) ) ;
#78778 = CARTESIAN_POINT ( 'NONE',  ( -21.55341960407619339, 5.719274019375674811, 43.54275706135235424 ) ) ;
#78780 = CARTESIAN_POINT ( 'NONE',  ( -5.049401038298153566, 19.05341960407611168, 110.2072429386476671 ) ) ;
#78781 = CARTESIAN_POINT ( 'NONE',  ( 9.474510206698729675, 16.51473224551082808, 32.08442372801900433 ) ) ;
#78782 = CARTESIAN_POINT ( 'NONE',  ( -8.314922557961024197, 14.29746914071037800, 42.91775706135235424 ) ) ;
#78783 = CARTESIAN_POINT ( 'NONE',  ( 19.02544592524343514, -5.153800228976328945, 98.54057627198100988 ) ) ;
#78784 = CARTESIAN_POINT ( 'NONE',  ( 5.823673210054125526, 21.52544592524343514, 104.7905762719810241 ) ) ;
#78785 = CARTESIAN_POINT ( 'NONE',  ( 19.03943276465977164, -0.05219959533909143690, 63.74890960531435979 ) ) ;
#78786 = CARTESIAN_POINT ( 'NONE',  ( -16.20579543436682357, 7.371946100354950460, 24.43479165828125232 ) ) ;
#78787 = CARTESIAN_POINT ( 'NONE',  ( 16.52544592524342804, -4.483927247898539470, 83.54057627198102409 ) ) ;
#78788 = CARTESIAN_POINT ( 'NONE',  ( 5.153800228976335163, 19.02544592524342804, 114.7905762719810241 ) ) ;
#78789 = CARTESIAN_POINT ( 'NONE',  ( -13.97604488694527625, -13.89961937509977652, 21.87390960531435979 ) ) ;
#78790 = CARTESIAN_POINT ( 'NONE',  ( -5.823673210054116645, -21.52544592524344225, 102.2905762719810383 ) ) ;
#78791 = CARTESIAN_POINT ( 'NONE',  ( 13.89961937509957401, 13.97604488694547697, 66.87609039468567573 ) ) ;
#78792 = CARTESIAN_POINT ( 'NONE',  ( 5.719274019375991003, -21.55341960407610458, 37.70724293864769550 ) ) ;
#78793 = CARTESIAN_POINT ( 'NONE',  ( 16.51473224551069308, 9.474510206698969483, 29.16557627198103475 ) ) ;
#78794 = CARTESIAN_POINT ( 'NONE',  ( -21.55341960407610458, -5.719274019375992779, 61.45724293864770260 ) ) ;
#78795 = AXIS2_PLACEMENT_3D ( 'NONE', #99481, #161162, #163166 ) ;
#78796 = CARTESIAN_POINT ( 'NONE',  ( 0.05219959533909260263, 19.03943276465977164, 99.99890960531436690 ) ) ;
#78797 = CARTESIAN_POINT ( 'NONE',  ( 5.823673210054444382, -21.52544592524334988, 85.20942372801901854 ) ) ;
#78798 = CARTESIAN_POINT ( 'NONE',  ( -9.564922557960796823, -16.46253265017161027, 57.08224293864769550 ) ) ;
#78799 = CARTESIAN_POINT ( 'NONE',  ( -16.53943276465976808, 0.05219959533911058130, 91.24890960531436690 ) ) ;
#78800 = CARTESIAN_POINT ( 'NONE',  ( 12.06949235617739724, 12.14591786802326823, 31.87609039468567929 ) ) ;
#78801 = CARTESIAN_POINT ( 'NONE',  ( 5.049401038298161559, -19.05341960407611168, 62.70724293864769550 ) ) ;
#78802 = CARTESIAN_POINT ( 'NONE',  ( 21.55341960407619695, -5.719274019375665929, 71.04275706135234714 ) ) ;
#78803 = EDGE_LOOP ( 'NONE', ( #97445, #135756, #72697, #141795, #49687, #16460, #136839, #106521, #130568, #141693, #32373, #94044, #73338, #29884 ) ) ;
#78804 = CARTESIAN_POINT ( 'NONE',  ( 0.05219959533936267826, -19.03943276465977164, 30.00109039468566863 ) ) ;
#78805 = CARTESIAN_POINT ( 'NONE',  ( 16.51473224551083163, -9.474510206698727899, 45.83442372801900433 ) ) ;
#78806 = LINE ( 'NONE', #189980, #166578 ) ;
#78807 = CARTESIAN_POINT ( 'NONE',  ( 21.52544592524334988, 5.823673210054432836, 36.45942372801901143 ) ) ;
#78808 = CARTESIAN_POINT ( 'NONE',  ( -6.293264767923588465, 0.7627558185761745824, -62.46802126132831035 ) ) ;
#78809 = CARTESIAN_POINT ( 'NONE',  ( -19.02544592524334988, -5.153800228976617603, 33.95942372801897591 ) ) ;
#78810 = CARTESIAN_POINT ( 'NONE',  ( -5.049401038298153566, 19.05341960407611168, 90.20724293864766707 ) ) ;
#78811 = CARTESIAN_POINT ( 'NONE',  ( 9.564922557960805705, 16.46253265017160317, 69.58224293864770971 ) ) ;
#78812 = CARTESIAN_POINT ( 'NONE',  ( 16.53943276465976808, -0.05219959533910856209, 23.74890960531435269 ) ) ;
#78814 = CARTESIAN_POINT ( 'NONE',  ( 21.55341960407619695, -5.719274019375665929, 81.04275706135236135 ) ) ;
#78813 = CARTESIAN_POINT ( 'NONE',  ( -21.55341960407610458, -5.719274019375992779, 26.45724293864768839 ) ) ;
#78815 = CARTESIAN_POINT ( 'NONE',  ( -29.86685920354755197, -21.69954338932560134, -8.924999997268812990 ) ) ;
#78816 = CARTESIAN_POINT ( 'NONE',  ( -34.48736576873178450, 1.429538131128952561, 89.67663809442002787 ) ) ;
#78817 = CARTESIAN_POINT ( 'NONE',  ( -5.719274019375665041, -21.55341960407619695, 84.79275706135234714 ) ) ;
#78818 = CARTESIAN_POINT ( 'NONE',  ( 16.29526858892873520, -7.335722546920258935, 41.70329402199793378 ) ) ;
#78819 = CARTESIAN_POINT ( 'NONE',  ( -5.049401038298153566, 19.05341960407611168, 105.2072429386476671 ) ) ;
#78820 = CARTESIAN_POINT ( 'NONE',  ( 34.42157296979474523, 2.272259278789490189, 89.98812102125175727 ) ) ;
#78822 = EDGE_CURVE ( 'NONE', #128850, #196699, #22037, .T. ) ;
#78821 = CARTESIAN_POINT ( 'NONE',  ( -5.719274019375978568, 21.55341960407610458, 65.20724293864768129 ) ) ;
#78823 = CARTESIAN_POINT ( 'NONE',  ( -16.53943276465976808, 0.05219959533911058130, 31.24890960531435979 ) ) ;
#78825 = CARTESIAN_POINT ( 'NONE',  ( 5.153800228976335163, 19.02544592524342804, 89.79057627198102409 ) ) ;
#78824 = CARTESIAN_POINT ( 'NONE',  ( -12.06949235617756955, 12.14591786802309770, 110.6239096053143669 ) ) ;
#78826 = CARTESIAN_POINT ( 'NONE',  ( 16.46253265017146816, 9.564922557961045513, 21.66775706135233648 ) ) ;
#78827 = CARTESIAN_POINT ( 'NONE',  ( -4.483927247898539470, -16.52544592524342804, 102.2905762719810383 ) ) ;
#78828 = CARTESIAN_POINT ( 'NONE',  ( -15.80617190586768217, 15.72974639402176855, 68.12609039468567573 ) ) ;
#78829 = CARTESIAN_POINT ( 'NONE',  ( -5.153800228976328057, -19.02544592524343514, 97.29057627198102409 ) ) ;
#78830 = CARTESIAN_POINT ( 'NONE',  ( 16.55341960407618274, -4.379528057220086978, 111.0427570613523613 ) ) ;
#78831 = CARTESIAN_POINT ( 'NONE',  ( 16.51473224551083163, -9.474510206698727899, 65.83442372801900433 ) ) ;
#78832 = CARTESIAN_POINT ( 'NONE',  ( -17.50000000000000711, -5.500000000000025757, 51.28230962303570095 ) ) ;
#78833 = CARTESIAN_POINT ( 'NONE',  ( 19.03943276465977164, -0.05219959533909143690, 103.7489096053143669 ) ) ;
#78834 = CARTESIAN_POINT ( 'NONE',  ( 14.34966873604960469, 8.224510206698951720, 94.16557627198103830 ) ) ;
#78835 = CARTESIAN_POINT ( 'NONE',  ( 9.564922557961047289, -16.46253265017146816, 60.41775706135233293 ) ) ;
#78836 = CARTESIAN_POINT ( 'NONE',  ( 5.049401038298161559, -19.05341960407611168, 77.70724293864765286 ) ) ;
#78837 = CARTESIAN_POINT ( 'NONE',  ( -12.14591786802309592, -12.06949235617757132, 56.87390960531436690 ) ) ;
#78838 = CARTESIAN_POINT ( 'NONE',  ( -16.46253265017146816, -9.564922557961047289, 89.16775706135234714 ) ) ;
#78839 = CARTESIAN_POINT ( 'NONE',  ( 18.67979575497178502, 10.72451020669898547, 49.16557627198102409 ) ) ;
#78840 = ORIENTED_EDGE ( 'NONE', *, *, #5261, .F. ) ;
#78841 = CARTESIAN_POINT ( 'NONE',  ( -4.483927247898539470, -16.52544592524342804, 112.2905762719810241 ) ) ;
#78842 = CARTESIAN_POINT ( 'NONE',  ( 18.22780087662122384, -5.500000000000022204, 101.0154010532610869 ) ) ;
#78844 = CARTESIAN_POINT ( 'NONE',  ( -0.05219959533907301413, -21.53943276465977519, 77.49890960531433848 ) ) ;
#78843 = CARTESIAN_POINT ( 'NONE',  ( 5.049401038298161559, -19.05341960407611168, 72.70724293864768129 ) ) ;
#78846 = CARTESIAN_POINT ( 'NONE',  ( 0.05219959533909260263, 19.03943276465977164, 74.99890960531435269 ) ) ;
#78845 = CARTESIAN_POINT ( 'NONE',  ( -0.05219959533934338120, 16.53943276465976808, 97.50109039468567573 ) ) ;
#78847 = CARTESIAN_POINT ( 'NONE',  ( 13.97604488694548053, -13.89961937509957401, 50.62609039468566152 ) ) ;
#78848 = CARTESIAN_POINT ( 'NONE',  ( -15.80617190586768217, 15.72974639402176855, 88.12609039468570415 ) ) ;
#78849 = CARTESIAN_POINT ( 'NONE',  ( 18.67979575497178502, 10.72451020669898547, 59.16557627198103120 ) ) ;
#78850 = CARTESIAN_POINT ( 'NONE',  ( -15.80617190586745835, -15.72974639402198527, 26.87390960531435979 ) ) ;
#78851 = CARTESIAN_POINT ( 'NONE',  ( -5.153800228976328057, -19.02544592524343514, 37.29057627198102409 ) ) ;
#78852 = CARTESIAN_POINT ( 'NONE',  ( -16.52544592524335698, -4.483927247898792601, 103.9594237280190185 ) ) ;
#78853 = CARTESIAN_POINT ( 'NONE',  ( -12.06949235617739369, -12.14591786802326823, 24.37609039468567573 ) ) ;
#78854 = DIRECTION ( 'NONE',  ( -0.000000000000000000, -0.000000000000000000, 1.000000000000000000 ) ) ;
#78855 = CARTESIAN_POINT ( 'NONE',  ( -5.719274019375665041, -21.55341960407619695, 94.79275706135234714 ) ) ;
#78856 = CARTESIAN_POINT ( 'NONE',  ( -14.34966873604960291, -8.224510206698953496, 61.66557627198103120 ) ) ;
#78857 = CARTESIAN_POINT ( 'NONE',  ( 21.52544592524344225, -5.823673210054117533, 98.54057627198105251 ) ) ;
#78858 = CARTESIAN_POINT ( 'NONE',  ( 15.80617190586746368, 15.72974639402197994, 89.37390960531435269 ) ) ;
#78859 = DIRECTION ( 'NONE',  ( -1.000000000000000000, 5.392603844284257652E-33, -0.000000000000000000 ) ) ;
#78860 = CARTESIAN_POINT ( 'NONE',  ( -0.05219959533907301413, -21.53943276465977519, 42.49890960531435979 ) ) ;
#78861 = CARTESIAN_POINT ( 'NONE',  ( 8.224510206698742110, 14.34966873604972548, 72.08442372801899012 ) ) ;
#78862 = CARTESIAN_POINT ( 'NONE',  ( -14.34966873604960291, -8.224510206698953496, 91.66557627198103830 ) ) ;
#78863 = CARTESIAN_POINT ( 'NONE',  ( 9.474510206698971260, -16.51473224551069308, 47.91557627198102409 ) ) ;
#78864 = CARTESIAN_POINT ( 'NONE',  ( -5.000000000000000000, 11.45643923738959913, -18.00000000000000000 ) ) ;
#78865 = CARTESIAN_POINT ( 'NONE',  ( -8.224510206698735004, -14.34966873604973081, 99.58442372801900433 ) ) ;
#78866 = CARTESIAN_POINT ( 'NONE',  ( 15.80617190586769283, -15.72974639402175789, 35.62609039468568994 ) ) ;
#78867 = CARTESIAN_POINT ( 'NONE',  ( 13.89961937509977652, -13.97604488694527269, 98.12390960531433848 ) ) ;
#78868 = CARTESIAN_POINT ( 'NONE',  ( -18.67979575497193778, 10.72451020669871902, 73.33442372801901854 ) ) ;
#78869 = CARTESIAN_POINT ( 'NONE',  ( 16.46253265017160672, -9.564922557960803928, 23.33224293864769194 ) ) ;
#78870 = CARTESIAN_POINT ( 'NONE',  ( -16.51473224551069308, -9.474510206698971260, 26.66557627198103120 ) ) ;
#78871 = CIRCLE ( 'NONE', #98331, 5.000000000000000000 ) ;
#78872 = ORIENTED_EDGE ( 'NONE', *, *, #23760, .F. ) ;
#78873 = CARTESIAN_POINT ( 'NONE',  ( -15.80617190586768217, 15.72974639402176855, 63.12609039468568994 ) ) ;
#78875 = CARTESIAN_POINT ( 'NONE',  ( -19.03943276465977164, 0.05219959533909376836, 116.2489096053143669 ) ) ;
#78874 = CARTESIAN_POINT ( 'NONE',  ( -0.05219959533909027116, -19.03943276465977164, 47.49890960531435979 ) ) ;
#78876 = CARTESIAN_POINT ( 'NONE',  ( -5.049401038298153566, 19.05341960407611168, 95.20724293864770971 ) ) ;
#78877 = CARTESIAN_POINT ( 'NONE',  ( 16.46253265017146816, 9.564922557961045513, 66.66775706135233293 ) ) ;
#78878 = CARTESIAN_POINT ( 'NONE',  ( 21.53943276465977519, 0.05219959533937863772, 41.25109039468568284 ) ) ;
#78879 = CARTESIAN_POINT ( 'NONE',  ( 9.564922557961047289, -16.46253265017146816, 60.41775706135233293 ) ) ;
#78880 = CARTESIAN_POINT ( 'NONE',  ( 16.46253265017160672, -9.564922557960803928, 33.33224293864770260 ) ) ;
#78881 = CARTESIAN_POINT ( 'NONE',  ( 8.314922557961029526, -14.29746914071037800, 100.4177570613523471 ) ) ;
#78882 = CARTESIAN_POINT ( 'NONE',  ( -19.05341960407617563, 5.049401038297882671, 73.54275706135233293 ) ) ;
#78883 = CARTESIAN_POINT ( 'NONE',  ( 14.34966873604960469, 8.224510206698951720, 29.16557627198103120 ) ) ;
#78884 = CARTESIAN_POINT ( 'NONE',  ( -9.474510206698720793, -16.51473224551083518, 49.58442372801899722 ) ) ;
#78885 = CARTESIAN_POINT ( 'NONE',  ( 13.97604488694527802, 13.89961937509977652, 99.37390960531436690 ) ) ;
#78886 = CARTESIAN_POINT ( 'NONE',  ( 5.823673210054444382, -21.52544592524334988, 110.2094237280190185 ) ) ;
#78887 = CARTESIAN_POINT ( 'NONE',  ( -16.46253265017146816, -9.564922557961047289, 29.16775706135232937 ) ) ;
#78888 = CARTESIAN_POINT ( 'NONE',  ( 19.03943276465977164, -0.05219959533909143690, 28.74890960531435624 ) ) ;
#78889 = CARTESIAN_POINT ( 'NONE',  ( -10.81492255796105439, 18.62759615963255655, 92.91775706135236135 ) ) ;
#78890 = CARTESIAN_POINT ( 'NONE',  ( -8.314922557961024197, 14.29746914071037800, 32.91775706135234714 ) ) ;
#78891 = CARTESIAN_POINT ( 'NONE',  ( -13.89961937509977652, 13.97604488694528158, 95.62390960531436690 ) ) ;
#78892 = CARTESIAN_POINT ( 'NONE',  ( -27.05641397906351742, 3.631740835637567333, 169.9999999999999716 ) ) ;
#78893 = CARTESIAN_POINT ( 'NONE',  ( 16.51473224551069308, 9.474510206698969483, 74.16557627198103830 ) ) ;
#78894 = LINE ( 'NONE', #126399, #113583 ) ;
#78895 = VECTOR ( 'NONE', #54281, 1000.000000000000000 ) ;
#78896 = CARTESIAN_POINT ( 'NONE',  ( -5.049401038297874678, -19.05341960407617918, 89.79275706135230450 ) ) ;
#78897 = CARTESIAN_POINT ( 'NONE',  ( 19.03943276465977164, -0.05219959533909143690, 108.7489096053143527 ) ) ;
#78898 = CARTESIAN_POINT ( 'NONE',  ( -21.52544592524334988, -5.823673210054445271, 98.95942372801903275 ) ) ;
#78899 = CARTESIAN_POINT ( 'NONE',  ( 14.29746914071049879, -8.314922557960816363, 103.3322429386476955 ) ) ;
#78900 = CARTESIAN_POINT ( 'NONE',  ( -13.89961937509977652, 13.97604488694528158, 30.62390960531435269 ) ) ;
#78901 = CARTESIAN_POINT ( 'NONE',  ( -21.53943276465977519, 0.05219959533907696930, 41.24890960531435269 ) ) ;
#78902 =( GEOMETRIC_REPRESENTATION_CONTEXT ( 3 ) GLOBAL_UNCERTAINTY_ASSIGNED_CONTEXT ( ( #144963 ) ) GLOBAL_UNIT_ASSIGNED_CONTEXT ( ( #183092, #195283, #49536 ) ) REPRESENTATION_CONTEXT ( 'NONE', 'WORKASPACE' ) );
#78903 = CARTESIAN_POINT ( 'NONE',  ( -21.52544592524343514, 5.823673210054127303, 31.04057627198102409 ) ) ;
#78904 = CARTESIAN_POINT ( 'NONE',  ( 0.05219959533909260263, 19.03943276465977164, 24.99890960531435269 ) ) ;
#78905 = CARTESIAN_POINT ( 'NONE',  ( -15.66706267174403067, 1.428615351859272575, -61.77652290643390387 ) ) ;
#78906 = CARTESIAN_POINT ( 'NONE',  ( -5.153800228976607833, 19.02544592524334988, 62.70942372801899722 ) ) ;
#78907 = CARTESIAN_POINT ( 'NONE',  ( 14.29746914071049879, -8.314922557960816363, 38.33224293864768839 ) ) ;
#78908 = CARTESIAN_POINT ( 'NONE',  ( 21.52544592524344225, -5.823673210054117533, 23.54057627198102765 ) ) ;
#78909 = CARTESIAN_POINT ( 'NONE',  ( 10.72451020669871369, 18.67979575497193778, 82.08442372801901854 ) ) ;
#78910 = CARTESIAN_POINT ( 'NONE',  ( -15.80617190586745835, -15.72974639402198527, 76.87390960531439532 ) ) ;
#78911 = CARTESIAN_POINT ( 'NONE',  ( 15.80617190586769283, -15.72974639402175789, 50.62609039468568994 ) ) ;
#78912 = CARTESIAN_POINT ( 'NONE',  ( -10.81492255796078084, -18.62759615963271287, 97.08224293864770971 ) ) ;
#78913 = CARTESIAN_POINT ( 'NONE',  ( 18.62759615963255655, 10.81492255796105972, 56.66775706135235424 ) ) ;
#78914 = CARTESIAN_POINT ( 'NONE',  ( -9.564922557960796823, -16.46253265017161027, 27.08224293864769550 ) ) ;
#78915 = CARTESIAN_POINT ( 'NONE',  ( 9.564922557960805705, 16.46253265017160317, 84.58224293864769550 ) ) ;
#78916 = CARTESIAN_POINT ( 'NONE',  ( 12.14591786802327356, -12.06949235617739191, 85.62609039468568994 ) ) ;
#78917 = CARTESIAN_POINT ( 'NONE',  ( -8.314922557960811034, -14.29746914071050412, 107.0822429386476955 ) ) ;
#78918 = CARTESIAN_POINT ( 'NONE',  ( 9.564922557960805705, 16.46253265017160317, 109.5822429386476955 ) ) ;
#78919 = CARTESIAN_POINT ( 'NONE',  ( -16.55341960407611168, -4.379528057220339221, 56.45724293864768839 ) ) ;
#78920 = CARTESIAN_POINT ( 'NONE',  ( -16.55341960407611168, -4.379528057220339221, 21.45724293864769550 ) ) ;
#78921 = CARTESIAN_POINT ( 'NONE',  ( -9.474510206698964154, 16.51473224551069663, 60.41557627198102409 ) ) ;
#78922 = CARTESIAN_POINT ( 'NONE',  ( -13.89961937509977652, 13.97604488694528158, 35.62390960531435269 ) ) ;
#78923 = CARTESIAN_POINT ( 'NONE',  ( 21.53943276465977519, -0.05219959533907433946, 48.74890960531435979 ) ) ;
#78925 = AXIS2_PLACEMENT_3D ( 'NONE', #86879, #148564, #71714 ) ;
#78924 = CARTESIAN_POINT ( 'NONE',  ( 0.05219959533936267826, -19.03943276465977164, 35.00109039468566863 ) ) ;
#78927 = CARTESIAN_POINT ( 'NONE',  ( 4.379528057220339221, -16.55341960407611168, 42.70724293864770260 ) ) ;
#78926 = DIRECTION ( 'NONE',  ( 0.000000000000000000, 0.000000000000000000, 1.000000000000000000 ) ) ;
#78928 = CARTESIAN_POINT ( 'NONE',  ( 9.564922557960805705, 16.46253265017160317, 109.5822429386476955 ) ) ;
#78929 = CARTESIAN_POINT ( 'NONE',  ( -5.719274019375665041, -21.55341960407619695, 54.79275706135235424 ) ) ;
#78930 = CARTESIAN_POINT ( 'NONE',  ( -20.34036572606774484, 20.41983568886641365, 139.9999999999999716 ) ) ;
#78931 = CARTESIAN_POINT ( 'NONE',  ( 8.314922557961029526, -14.29746914071037800, 65.41775706135234714 ) ) ;
#78932 = CARTESIAN_POINT ( 'NONE',  ( 0.05219959533936267826, -19.03943276465977164, 65.00109039468567573 ) ) ;
#78933 = CARTESIAN_POINT ( 'NONE',  ( -14.29746914071049879, 8.314922557960819915, 35.83224293864768839 ) ) ;
#78934 = CARTESIAN_POINT ( 'NONE',  ( 16.29526858892872454, -7.335722546920200315, 51.70329402199800484 ) ) ;
#78935 = CARTESIAN_POINT ( 'NONE',  ( -12.06949235617756955, 12.14591786802309770, 25.62390960531435624 ) ) ;
#78936 = CARTESIAN_POINT ( 'NONE',  ( 0.05219959533909260263, 19.03943276465977164, 44.99890960531435979 ) ) ;
#78937 = CARTESIAN_POINT ( 'NONE',  ( 19.03943276465977164, -0.05219959533909143690, 58.74890960531435979 ) ) ;
#78938 = CARTESIAN_POINT ( 'NONE',  ( -19.02544592524342804, 5.153800228976336051, 31.04057627198102409 ) ) ;
#78939 = CARTESIAN_POINT ( 'NONE',  ( -0.05219959533937732626, 21.53943276465977519, 27.50109039468567929 ) ) ;
#78940 = CARTESIAN_POINT ( 'NONE',  ( 19.03943276465977164, -0.05219959533909143690, 53.74890960531436690 ) ) ;
#78941 = CARTESIAN_POINT ( 'NONE',  ( -19.99999999999998224, -180.0000000000000000, -4.999999999999999112 ) ) ;
#78942 = CARTESIAN_POINT ( 'NONE',  ( 5.153800228976335163, 19.02544592524342804, 44.79057627198103830 ) ) ;
#78943 = CARTESIAN_POINT ( 'NONE',  ( 21.55341960407610458, 5.719274019375980345, 28.95724293864769905 ) ) ;
#78945 = CARTESIAN_POINT ( 'NONE',  ( -5.153800228976328057, -19.02544592524343514, 22.29057627198102765 ) ) ;
#78944 = CARTESIAN_POINT ( 'NONE',  ( -21.52544592524334988, -5.823673210054445271, 53.95942372801900433 ) ) ;
#78946 = CARTESIAN_POINT ( 'NONE',  ( -15.72974639402197994, 15.80617190586746368, 30.62390960531436335 ) ) ;
#78947 = CARTESIAN_POINT ( 'NONE',  ( -16.55341960407617563, 4.379528057220093196, 73.54275706135234714 ) ) ;
#78948 = EDGE_CURVE ( 'NONE', #77271, #108481, #45400, .T. ) ;
#78949 = CARTESIAN_POINT ( 'NONE',  ( 15.80617190586769283, -15.72974639402175789, 105.6260903946856899 ) ) ;
#78950 = CARTESIAN_POINT ( 'NONE',  ( 0.05219959533934541429, -16.53943276465976808, 70.00109039468568994 ) ) ;
#78951 = CARTESIAN_POINT ( 'NONE',  ( 9.564922557960805705, 16.46253265017160317, 99.58224293864770971 ) ) ;
#78952 = CARTESIAN_POINT ( 'NONE',  ( -16.55341960407617563, 4.379528057220093196, 48.54275706135234714 ) ) ;
#78953 = CARTESIAN_POINT ( 'NONE',  ( -12.06949235617739369, -12.14591786802326823, 29.37609039468568284 ) ) ;
#78954 = CARTESIAN_POINT ( 'NONE',  ( 4.379528057220092307, 16.55341960407617563, 97.29275706135234714 ) ) ;
#78955 = CARTESIAN_POINT ( 'NONE',  ( -5.719274019375665041, -21.55341960407619695, 54.79275706135235424 ) ) ;
#78956 = CARTESIAN_POINT ( 'NONE',  ( 9.564922557961047289, -16.46253265017146816, 105.4177570613523471 ) ) ;
#78957 = CARTESIAN_POINT ( 'NONE',  ( 10.72451020669898902, -18.67979575497178502, 107.9155762719810241 ) ) ;
#78959 = CARTESIAN_POINT ( 'NONE',  ( -19.03943276465977164, -0.05219959533935918106, 113.7510903946856757 ) ) ;
#78958 = CARTESIAN_POINT ( 'NONE',  ( -14.34966873604960291, -8.224510206698953496, 106.6655762719810383 ) ) ;
#78960 = CARTESIAN_POINT ( 'NONE',  ( 16.53943276465976808, 0.05219959533934440121, 86.25109039468568994 ) ) ;
#78961 = DIRECTION ( 'NONE',  ( -1.000000000000000000, -0.000000000000000000, -0.000000000000000000 ) ) ;
#78962 = CARTESIAN_POINT ( 'NONE',  ( 5.719274019375673035, 21.55341960407619339, 87.29275706135236135 ) ) ;
#78963 = CARTESIAN_POINT ( 'NONE',  ( 0.05219959533936267826, -19.03943276465977164, 80.00109039468567573 ) ) ;
#78964 = CARTESIAN_POINT ( 'NONE',  ( 12.14591786802309770, 12.06949235617756955, 44.37390960531435979 ) ) ;
#78965 = CARTESIAN_POINT ( 'NONE',  ( 16.55341960407611168, 4.379528057220329451, 48.95724293864770971 ) ) ;
#78966 = CARTESIAN_POINT ( 'NONE',  ( -16.53943276465976808, 0.05219959533911058130, 111.2489096053143669 ) ) ;
#78968 = CARTESIAN_POINT ( 'NONE',  ( 17.44270441346523626, -5.991230190322815119, 56.13664920735774899 ) ) ;
#78967 = CARTESIAN_POINT ( 'NONE',  ( 9.474510206698729675, 16.51473224551082808, 42.08442372801900433 ) ) ;
#78969 = CARTESIAN_POINT ( 'NONE',  ( -5.823673210054431948, 21.52544592524334988, 32.70942372801900433 ) ) ;
#78970 = CARTESIAN_POINT ( 'NONE',  ( 13.89961937509957401, 13.97604488694547697, 111.8760903946856757 ) ) ;
#78971 = DIRECTION ( 'NONE',  ( -1.000000000000000000, -0.000000000000000000, -0.000000000000000000 ) ) ;
#78972 = CARTESIAN_POINT ( 'NONE',  ( -5.153800228976328057, -19.02544592524343514, 107.2905762719810383 ) ) ;
#78973 = CARTESIAN_POINT ( 'NONE',  ( -18.67979575497178146, -10.72451020669898902, 61.66557627198103120 ) ) ;
#78974 = CARTESIAN_POINT ( 'NONE',  ( 9.564922557960805705, 16.46253265017160317, 84.58224293864769550 ) ) ;
#78975 = CARTESIAN_POINT ( 'NONE',  ( 5.719274019375991003, -21.55341960407610458, 52.70724293864769550 ) ) ;
#78976 = CARTESIAN_POINT ( 'NONE',  ( -14.34966873604960291, -8.224510206698953496, 106.6655762719810383 ) ) ;
#78977 = CARTESIAN_POINT ( 'NONE',  ( 9.474510206698971260, -16.51473224551069308, 72.91557627198102409 ) ) ;
#78978 = CARTESIAN_POINT ( 'NONE',  ( 13.97604488694527802, 13.89961937509977652, 34.37390960531436690 ) ) ;
#78979 = CARTESIAN_POINT ( 'NONE',  ( -0.05219959533937732626, 21.53943276465977519, 32.50109039468568284 ) ) ;
#78980 = CARTESIAN_POINT ( 'NONE',  ( -10.81492255796105439, 18.62759615963255655, 77.91775706135231871 ) ) ;
#78981 = CARTESIAN_POINT ( 'NONE',  ( 16.53943276465976808, 0.05219959533934440121, 96.25109039468568994 ) ) ;
#78982 = CARTESIAN_POINT ( 'NONE',  ( 18.67979575497194134, -10.72451020669871369, 25.83442372801901499 ) ) ;
#78983 = CARTESIAN_POINT ( 'NONE',  ( -5.823673210054431948, 21.52544592524334988, 32.70942372801900433 ) ) ;
#78985 = CARTESIAN_POINT ( 'NONE',  ( 9.564922557960805705, 16.46253265017160317, 84.58224293864769550 ) ) ;
#78984 = CARTESIAN_POINT ( 'NONE',  ( -5.049401038297874678, -19.05341960407617918, 59.79275706135231871 ) ) ;
#78986 = CARTESIAN_POINT ( 'NONE',  ( -0.05219959533937732626, 21.53943276465977519, 77.50109039468567573 ) ) ;
#78987 = CIRCLE ( 'NONE', #36990, 2.500000000000000000 ) ;
#78988 = CARTESIAN_POINT ( 'NONE',  ( 15.72974639402199770, -15.80617190586745480, 83.12390960531436690 ) ) ;
#78989 = CARTESIAN_POINT ( 'NONE',  ( 16.53943276465976808, -0.05219959533910856209, 63.74890960531435979 ) ) ;
#78990 = CARTESIAN_POINT ( 'NONE',  ( -21.52544592524334988, -5.823673210054445271, 98.95942372801903275 ) ) ;
#78991 = CARTESIAN_POINT ( 'NONE',  ( -8.224510206698948167, 14.34966873604960824, 85.41557627198102409 ) ) ;
#78992 = CARTESIAN_POINT ( 'NONE',  ( -19.03943276465977164, 0.05219959533909376836, 41.24890960531435269 ) ) ;
#78993 = CARTESIAN_POINT ( 'NONE',  ( -13.89961937509957401, -13.97604488694547875, 69.37609039468564731 ) ) ;
#78994 = CARTESIAN_POINT ( 'NONE',  ( 4.483927247898545687, 16.52544592524342804, 34.79057627198103120 ) ) ;
#78995 = CARTESIAN_POINT ( 'NONE',  ( -18.67979575497193778, 10.72451020669871902, 98.33442372801901854 ) ) ;
#78996 = CARTESIAN_POINT ( 'NONE',  ( 13.97604488694527802, 13.89961937509977652, 94.37390960531436690 ) ) ;
#78997 = CARTESIAN_POINT ( 'NONE',  ( 19.03943276465977164, 0.05219959533936151252, 66.25109039468567573 ) ) ;
#78998 = CARTESIAN_POINT ( 'NONE',  ( -21.53943276465977519, 0.05219959533907696930, 71.24890960531435269 ) ) ;
#78999 = CARTESIAN_POINT ( 'NONE',  ( -21.53943276465977519, -0.05219959533937600094, 18.75109039468568639 ) ) ;
#79000 = CARTESIAN_POINT ( 'NONE',  ( 5.049401038297881783, 19.05341960407617563, 112.2927570613523471 ) ) ;
#79001 = CARTESIAN_POINT ( 'NONE',  ( -12.14591786802326823, 12.06949235617739902, 83.12609039468568994 ) ) ;
#79003 = CARTESIAN_POINT ( 'NONE',  ( -10.72451020669870658, -18.67979575497194134, 19.58442372801901143 ) ) ;
#79002 = CARTESIAN_POINT ( 'NONE',  ( 2.285367203649815956E-16, -78.65850330665435308, -13.00000000000000000 ) ) ;
#79004 = CARTESIAN_POINT ( 'NONE',  ( 16.52544592524342804, -4.483927247898539470, 108.5405762719810241 ) ) ;
#79005 = CARTESIAN_POINT ( 'NONE',  ( 36.91746825000000598, -11.99521256947793546, -6.224999997268814589 ) ) ;
#79006 = CARTESIAN_POINT ( 'NONE',  ( -14.34966873604972548, 8.224510206698743886, 33.33442372801900433 ) ) ;
#79007 = CARTESIAN_POINT ( 'NONE',  ( 10.72451020669898902, -18.67979575497178502, 62.91557627198102409 ) ) ;
#79008 = CARTESIAN_POINT ( 'NONE',  ( 14.29746914071037800, 8.314922557961029526, 106.6677570613523756 ) ) ;
#79009 = CARTESIAN_POINT ( 'NONE',  ( 14.29746914071037800, 8.314922557961029526, 36.66775706135234714 ) ) ;
#79010 = CARTESIAN_POINT ( 'NONE',  ( -5.049401038298153566, 19.05341960407611168, 30.20724293864768839 ) ) ;
#79011 = CARTESIAN_POINT ( 'NONE',  ( 16.53943276465976808, 0.05219959533934440121, 81.25109039468568994 ) ) ;
#79012 = CARTESIAN_POINT ( 'NONE',  ( -19.03943276465977164, -0.05219959533935918106, 73.75109039468566152 ) ) ;
#79013 = CARTESIAN_POINT ( 'NONE',  ( -5.823673210054116645, -21.52544592524344225, 72.29057627198102409 ) ) ;
#79014 = CARTESIAN_POINT ( 'NONE',  ( -14.29746914071037622, -8.314922557961029526, 104.1677570613523471 ) ) ;
#79015 = CARTESIAN_POINT ( 'NONE',  ( -0.05219959533937732626, 21.53943276465977519, 82.50109039468568994 ) ) ;
#79016 = CARTESIAN_POINT ( 'NONE',  ( 5.719274019375991003, -21.55341960407610458, 62.70724293864769550 ) ) ;
#79017 = CARTESIAN_POINT ( 'NONE',  ( 21.52544592524344225, -5.823673210054117533, 53.54057627198103120 ) ) ;
#79018 = ORIENTED_EDGE ( 'NONE', *, *, #43792, .T. ) ;
#79019 = CARTESIAN_POINT ( 'NONE',  ( -14.29746914071037622, -8.314922557961029526, 84.16775706135234714 ) ) ;
#79020 = CARTESIAN_POINT ( 'NONE',  ( 10.81492255796078972, 18.62759615963270932, 49.58224293864769550 ) ) ;
#79021 = ORIENTED_EDGE ( 'NONE', *, *, #58712, .F. ) ;
#79022 = CARTESIAN_POINT ( 'NONE',  ( 9.474510206698971260, -16.51473224551069308, 112.9155762719810383 ) ) ;
#79023 = FACE_OUTER_BOUND ( 'NONE', #65432, .T. ) ;
#79024 = CARTESIAN_POINT ( 'NONE',  ( 16.51473224551069308, 9.474510206698969483, 29.16557627198103475 ) ) ;
#79025 = CARTESIAN_POINT ( 'NONE',  ( -0.05219959533907301413, -21.53943276465977519, 62.49890960531436690 ) ) ;
#79026 = CARTESIAN_POINT ( 'NONE',  ( -12.06949235617739369, -12.14591786802326823, 104.3760903946856899 ) ) ;
#79027 = CARTESIAN_POINT ( 'NONE',  ( 10.81492255796106328, -18.62759615963255655, 40.41775706135234714 ) ) ;
#79028 = CARTESIAN_POINT ( 'NONE',  ( -9.564922557961040184, 16.46253265017147172, 97.91775706135233293 ) ) ;
#79029 = CARTESIAN_POINT ( 'NONE',  ( -16.52544592524342804, 4.483927247898546575, 116.0405762719810383 ) ) ;
#79030 = CARTESIAN_POINT ( 'NONE',  ( -16.51473224551082808, 9.474510206698731452, 113.3344237280190043 ) ) ;
#79031 = CARTESIAN_POINT ( 'NONE',  ( -16.51473224551069308, -9.474510206698971260, 46.66557627198102409 ) ) ;
#79032 = EDGE_CURVE ( 'NONE', #1947, #50775, #70449, .T. ) ;
#79033 = CARTESIAN_POINT ( 'NONE',  ( -23.31738231874055245, -16.94106989632524574, 140.1999999999999886 ) ) ;
#79034 = CARTESIAN_POINT ( 'NONE',  ( 9.474510206698971260, -16.51473224551069308, 87.91557627198102409 ) ) ;
#79035 = CARTESIAN_POINT ( 'NONE',  ( 4.483927247898790824, -16.52544592524335698, 75.20942372801901854 ) ) ;
#79036 = CARTESIAN_POINT ( 'NONE',  ( -9.474510206698720793, -16.51473224551083518, 79.58442372801899012 ) ) ;
#79037 = CARTESIAN_POINT ( 'NONE',  ( -0.05219959533936034679, 19.03943276465977164, 22.50109039468566152 ) ) ;
#79038 = CARTESIAN_POINT ( 'NONE',  ( -21.52544592524343514, 5.823673210054127303, 66.04057627198103830 ) ) ;
#79039 = CARTESIAN_POINT ( 'NONE',  ( 16.52544592524335698, 4.483927247898782831, 91.45942372801901854 ) ) ;
#79040 = CARTESIAN_POINT ( 'NONE',  ( -13.89961937509957401, -13.97604488694547875, 84.37609039468567573 ) ) ;
#79041 = CARTESIAN_POINT ( 'NONE',  ( 9.564922557960805705, 16.46253265017160317, 34.58224293864770260 ) ) ;
#79043 = AXIS2_PLACEMENT_3D ( 'NONE', #77226, #121740, #170238 ) ;
#79042 = CARTESIAN_POINT ( 'NONE',  ( -13.97604488694527625, -13.89961937509977652, 81.87390960531436690 ) ) ;
#79044 = CARTESIAN_POINT ( 'NONE',  ( 18.67979575497194134, -10.72451020669871369, 50.83442372801901143 ) ) ;
#79045 = CARTESIAN_POINT ( 'NONE',  ( 19.02544592524343514, -5.153800228976328945, 53.54057627198102409 ) ) ;
#79046 = CARTESIAN_POINT ( 'NONE',  ( -19.03943276465977164, -0.05219959533935918106, 68.75109039468566152 ) ) ;
#79047 = CARTESIAN_POINT ( 'NONE',  ( 37.99999999999999289, 2.893978650043524126E-14, -5.000000000000000000 ) ) ;
#79048 = CARTESIAN_POINT ( 'NONE',  ( 9.564922557960805705, 16.46253265017160317, 114.5822429386476955 ) ) ;
#79049 = CARTESIAN_POINT ( 'NONE',  ( 0.05219959533910956823, 16.53943276465976808, 69.99890960531435269 ) ) ;
#79050 = CARTESIAN_POINT ( 'NONE',  ( -10.81492255796078084, -18.62759615963271287, 62.08224293864769550 ) ) ;
#79051 = CARTESIAN_POINT ( 'NONE',  ( 19.96322699617726570, -3.697860406115397680, 102.5000000000000568 ) ) ;
#79052 = STYLED_ITEM ( 'NONE', ( #117187 ), #22986 ) ;
#79053 = CARTESIAN_POINT ( 'NONE',  ( -19.02544592524334988, -5.153800228976617603, 28.95942372801900433 ) ) ;
#79054 = CARTESIAN_POINT ( 'NONE',  ( -17.49999999999999645, 5.499999999999992895, 88.71769037696435589 ) ) ;
#79056 = CARTESIAN_POINT ( 'NONE',  ( 19.05341960407611168, 5.049401038298154454, 78.95724293864769550 ) ) ;
#79055 = CARTESIAN_POINT ( 'NONE',  ( -9.564922557960796823, -16.46253265017161027, 67.08224293864769550 ) ) ;
#79057 = CARTESIAN_POINT ( 'NONE',  ( -0.05219959533934338120, 16.53943276465976808, 52.50109039468567573 ) ) ;
#79058 = CARTESIAN_POINT ( 'NONE',  ( 6.918342302711550040, -47.27039221922507295, -24.65254351866712668 ) ) ;
#79059 = DIRECTION ( 'NONE',  ( 1.000000000000000000, 0.000000000000000000, 0.000000000000000000 ) ) ;
#79060 = CARTESIAN_POINT ( 'NONE',  ( 4.483927247898790824, -16.52544592524335698, 90.20942372801903275 ) ) ;
#79061 = CARTESIAN_POINT ( 'NONE',  ( 23.22614267028769675, 5.670187745555516301, 172.0618673401326646 ) ) ;
#79062 = CARTESIAN_POINT ( 'NONE',  ( 12.06949235617739724, 12.14591786802326823, 71.87609039468568994 ) ) ;
#79063 = CARTESIAN_POINT ( 'NONE',  ( -12.14591786802326823, 12.06949235617739902, 43.12609039468568284 ) ) ;
#79065 = CARTESIAN_POINT ( 'NONE',  ( -11.30153831258470731, -190.0000000000000000, -25.00000000000000000 ) ) ;
#79064 = CARTESIAN_POINT ( 'NONE',  ( 5.153800228976335163, 19.02544592524342804, 54.79057627198103120 ) ) ;
#79066 = CARTESIAN_POINT ( 'NONE',  ( -21.52544592524334988, -5.823673210054445271, 53.95942372801900433 ) ) ;
#79067 = CARTESIAN_POINT ( 'NONE',  ( 5.153800228976615827, -19.02544592524334988, 65.20942372801900433 ) ) ;
#79068 = CARTESIAN_POINT ( 'NONE',  ( -18.62759615963255300, -10.81492255796106328, 109.1677570613523613 ) ) ;
#79069 = CARTESIAN_POINT ( 'NONE',  ( -9.474510206698964154, 16.51473224551069663, 25.41557627198103120 ) ) ;
#79070 = CARTESIAN_POINT ( 'NONE',  ( -16.00195535827013771, 14.62341493535840264, -58.61703605924742533 ) ) ;
#79071 = CARTESIAN_POINT ( 'NONE',  ( 10.72451020669898902, -18.67979575497178502, 52.91557627198103830 ) ) ;
#79072 = AXIS2_PLACEMENT_3D ( 'NONE', #158135, #127784, #128776 ) ;
#79073 = CARTESIAN_POINT ( 'NONE',  ( -5.153800228976328057, -19.02544592524343514, 112.2905762719810099 ) ) ;
#79074 = CARTESIAN_POINT ( 'NONE',  ( -16.52544592524342804, 4.483927247898546575, 96.04057627198102409 ) ) ;
#79075 = CARTESIAN_POINT ( 'NONE',  ( 4.483927247898790824, -16.52544592524335698, 40.20942372801901854 ) ) ;
#79076 = CARTESIAN_POINT ( 'NONE',  ( -16.53943276465976808, 0.05219959533911058130, 31.24890960531435979 ) ) ;
#79077 = ORIENTED_EDGE ( 'NONE', *, *, #100282, .F. ) ;
#79078 = CARTESIAN_POINT ( 'NONE',  ( 15.72974639402176855, 15.80617190586768217, 21.87609039468567573 ) ) ;
#79080 = CARTESIAN_POINT ( 'NONE',  ( -5.153800228976328057, -19.02544592524343514, 112.2905762719810099 ) ) ;
#79079 = CARTESIAN_POINT ( 'NONE',  ( -4.379528057220328563, 16.55341960407611168, 45.20724293864769550 ) ) ;
#79081 = CARTESIAN_POINT ( 'NONE',  ( 19.02544592524334988, 5.153800228976608722, 101.4594237280189759 ) ) ;
#79082 = CARTESIAN_POINT ( 'NONE',  ( 16.51473224551083163, -9.474510206698727899, 30.83442372801900433 ) ) ;
#79083 = CARTESIAN_POINT ( 'NONE',  ( 0.05219959533910956823, 16.53943276465976808, 34.99890960531435979 ) ) ;
#79084 = CARTESIAN_POINT ( 'NONE',  ( 5.719274019375991003, -21.55341960407610458, 107.7072429386476955 ) ) ;
#79085 = CARTESIAN_POINT ( 'NONE',  ( 15.80617190586746368, 15.72974639402197994, 59.37390960531436690 ) ) ;
#79086 = CARTESIAN_POINT ( 'NONE',  ( 16.46253265017160672, -9.564922557960803928, 73.33224293864769550 ) ) ;
#79087 = CARTESIAN_POINT ( 'NONE',  ( 4.483927247898545687, 16.52544592524342804, 44.79057627198103120 ) ) ;
#79088 = CARTESIAN_POINT ( 'NONE',  ( -5.049401038298153566, 19.05341960407611168, 95.20724293864770971 ) ) ;
#79089 = CARTESIAN_POINT ( 'NONE',  ( 18.56399227203345603, 5.499999999999817923, 56.47830131249901342 ) ) ;
#79090 = CARTESIAN_POINT ( 'NONE',  ( 9.474510206698729675, 16.51473224551082808, 42.08442372801900433 ) ) ;
#79091 = CARTESIAN_POINT ( 'NONE',  ( 5.823673210054125526, 21.52544592524343514, 89.79057627198103830 ) ) ;
#79092 = CARTESIAN_POINT ( 'NONE',  ( 0.05219959533910956823, 16.53943276465976808, 94.99890960531436690 ) ) ;
#79093 = CARTESIAN_POINT ( 'NONE',  ( -10.81492255796105439, 18.62759615963255655, 32.91775706135234714 ) ) ;
#79094 = CARTESIAN_POINT ( 'NONE',  ( -22.44159573604010305, 16.30477369853692338, 142.6750000027311671 ) ) ;
#79095 = CARTESIAN_POINT ( 'NONE',  ( 0.05219959533910956823, 16.53943276465976808, 24.99890960531435624 ) ) ;
#79096 = CARTESIAN_POINT ( 'NONE',  ( -16.46253265017160317, 9.564922557960807481, 30.83224293864769550 ) ) ;
#79097 = CARTESIAN_POINT ( 'NONE',  ( 9.564922557960805705, 16.46253265017160317, 89.58224293864769550 ) ) ;
#79098 = CARTESIAN_POINT ( 'NONE',  ( 18.62759615963271287, -10.81492255796078972, 63.33224293864770260 ) ) ;
#79099 = CARTESIAN_POINT ( 'NONE',  ( -17.14385361876520264, -23.59649016807271593, 141.1750000027311671 ) ) ;
#79100 = CARTESIAN_POINT ( 'NONE',  ( -16.46253265017160317, 9.564922557960807481, 25.83224293864769194 ) ) ;
#79101 = CARTESIAN_POINT ( 'NONE',  ( -0.05219959533907301413, -21.53943276465977519, 57.49890960531435979 ) ) ;
#79102 = CARTESIAN_POINT ( 'NONE',  ( -18.67979575497193778, 10.72451020669871902, 68.33442372801900433 ) ) ;
#79104 = CARTESIAN_POINT ( 'NONE',  ( -16.53943276465976808, -0.05219959533934237506, 63.75109039468568284 ) ) ;
#79103 = CARTESIAN_POINT ( 'NONE',  ( 23.38845648566366364, -29.41134498177906309, -18.89001425235115406 ) ) ;
#79105 = CARTESIAN_POINT ( 'NONE',  ( -5.049401038298153566, 19.05341960407611168, 55.20724293864769550 ) ) ;
#79106 = CARTESIAN_POINT ( 'NONE',  ( 19.05341960407611168, 5.049401038298154454, 68.95724293864769550 ) ) ;
#79107 = ORIENTED_EDGE ( 'NONE', *, *, #55941, .T. ) ;
#79108 = CARTESIAN_POINT ( 'NONE',  ( 18.67979575497194134, -10.72451020669871369, 105.8344237280190328 ) ) ;
#79109 = CARTESIAN_POINT ( 'NONE',  ( 14.29746914071037800, 8.314922557961029526, 71.66775706135234714 ) ) ;
#79110 = CARTESIAN_POINT ( 'NONE',  ( 10.81492255796106328, -18.62759615963255655, 100.4177570613523471 ) ) ;
#79111 = CARTESIAN_POINT ( 'NONE',  ( -19.05341960407611168, -5.049401038298163336, 61.45724293864769550 ) ) ;
#79112 = CARTESIAN_POINT ( 'NONE',  ( 21.52544592524344225, -5.823673210054117533, 28.54057627198103120 ) ) ;
#79113 = CARTESIAN_POINT ( 'NONE',  ( -16.51473224551082808, 9.474510206698731452, 103.3344237280190043 ) ) ;
#79114 = CARTESIAN_POINT ( 'NONE',  ( -18.67979575497193778, 10.72451020669871902, 88.33442372801901854 ) ) ;
#79115 = CARTESIAN_POINT ( 'NONE',  ( -12.14591786802326823, 12.06949235617739902, 43.12609039468568284 ) ) ;
#79117 = CARTESIAN_POINT ( 'NONE',  ( 15.72974639402199770, -15.80617190586745480, 93.12390960531436690 ) ) ;
#79116 = VECTOR ( 'NONE', #75062, 1000.000000000000000 ) ;
#79118 = CARTESIAN_POINT ( 'NONE',  ( -5.153800228976607833, 19.02544592524334988, 102.7094237280189759 ) ) ;
#79119 = CARTESIAN_POINT ( 'NONE',  ( -13.97604488694527625, -13.89961937509977652, 71.87390960531433848 ) ) ;
#79120 = CARTESIAN_POINT ( 'NONE',  ( -19.02544592524334988, -5.153800228976617603, 108.9594237280189759 ) ) ;
#79121 = CARTESIAN_POINT ( 'NONE',  ( -9.474510206698964154, 16.51473224551069663, 35.41557627198102409 ) ) ;
#79122 = CARTESIAN_POINT ( 'NONE',  ( 4.379528057220092307, 16.55341960407617563, 22.29275706135235069 ) ) ;
#79123 = CARTESIAN_POINT ( 'NONE',  ( 16.53943276465976808, -0.05219959533910856209, 63.74890960531435979 ) ) ;
#79124 = CARTESIAN_POINT ( 'NONE',  ( -16.53943276465976808, -0.05219959533934237506, 78.75109039468568994 ) ) ;
#79126 = CARTESIAN_POINT ( 'NONE',  ( -5.049401038298153566, 19.05341960407611168, 45.20724293864769550 ) ) ;
#79125 = CARTESIAN_POINT ( 'NONE',  ( 18.62759615963255655, 10.81492255796105972, 31.66775706135234358 ) ) ;
#79127 = CARTESIAN_POINT ( 'NONE',  ( -13.89961937509977652, 13.97604488694528158, 70.62390960531432427 ) ) ;
#79128 = CARTESIAN_POINT ( 'NONE',  ( -8.224510206698735004, -14.34966873604973081, 69.58442372801900433 ) ) ;
#79129 = VECTOR ( 'NONE', #60012, 1000.000000000000000 ) ;
#79130 = FACE_OUTER_BOUND ( 'NONE', #86431, .T. ) ;
#79131 = ORIENTED_EDGE ( 'NONE', *, *, #749, .F. ) ;
#79132 = CARTESIAN_POINT ( 'NONE',  ( 15.72974639402176855, 15.80617190586768217, 111.8760903946856615 ) ) ;
#79133 = CARTESIAN_POINT ( 'NONE',  ( 16.51473224551069308, 9.474510206698969483, 39.16557627198103120 ) ) ;
#79135 = ORIENTED_EDGE ( 'NONE', *, *, #80827, .T. ) ;
#79134 = CARTESIAN_POINT ( 'NONE',  ( -19.03943276465977164, 0.05219959533909376836, 96.24890960531436690 ) ) ;
#79136 = CARTESIAN_POINT ( 'NONE',  ( -8.224510206698735004, -14.34966873604973081, 29.58442372801901854 ) ) ;
#79138 = CARTESIAN_POINT ( 'NONE',  ( 14.34966873604972726, -8.224510206698740333, 45.83442372801901854 ) ) ;
#79137 = CARTESIAN_POINT ( 'NONE',  ( 19.02544592524334988, 5.153800228976608722, 41.45942372801900433 ) ) ;
#79139 = CARTESIAN_POINT ( 'NONE',  ( -5.153800228976328057, -19.02544592524343514, 47.29057627198102409 ) ) ;
#79140 = CARTESIAN_POINT ( 'NONE',  ( -9.474510206698964154, 16.51473224551069663, 100.4155762719810241 ) ) ;
#79141 = CARTESIAN_POINT ( 'NONE',  ( -13.89961937509977652, 13.97604488694528158, 65.62390960531436690 ) ) ;
#79142 = CARTESIAN_POINT ( 'NONE',  ( 10.81492255796078972, 18.62759615963270932, 99.58224293864770971 ) ) ;
#79144 = CARTESIAN_POINT ( 'NONE',  ( 19.05341960407611168, 5.049401038298154454, 108.9572429386477097 ) ) ;
#79143 = CARTESIAN_POINT ( 'NONE',  ( -9.474510206698964154, 16.51473224551069663, 80.41557627198103830 ) ) ;
#79145 = CARTESIAN_POINT ( 'NONE',  ( 13.89961937509977652, -13.97604488694527269, 68.12390960531436690 ) ) ;
#79146 = DIRECTION ( 'NONE',  ( -1.000000000000000000, 0.000000000000000000, 0.000000000000000000 ) ) ;
#79147 = CARTESIAN_POINT ( 'NONE',  ( -16.51473224551082808, 9.474510206698731452, 93.33442372801900433 ) ) ;
#79148 = EDGE_CURVE ( 'NONE', #184761, #137566, #2600, .T. ) ;
#79149 = CARTESIAN_POINT ( 'NONE',  ( -5.049401038297874678, -19.05341960407617918, 19.79275706135233293 ) ) ;
#79150 = CARTESIAN_POINT ( 'NONE',  ( 0.05219959533910956823, 16.53943276465976808, 64.99890960531435269 ) ) ;
#79151 = CARTESIAN_POINT ( 'NONE',  ( 18.67979575497194134, -10.72451020669871369, 90.83442372801901854 ) ) ;
#79152 = CARTESIAN_POINT ( 'NONE',  ( -13.97604488694527625, -13.89961937509977652, 21.87390960531435979 ) ) ;
#79154 = CARTESIAN_POINT ( 'NONE',  ( 15.80617190586769283, -15.72974639402175789, 95.62609039468568994 ) ) ;
#79153 = CARTESIAN_POINT ( 'NONE',  ( -16.55341960407617563, 4.379528057220093196, 113.5427570613523756 ) ) ;
#79155 = CARTESIAN_POINT ( 'NONE',  ( -13.89961937509977652, 13.97604488694528158, 80.62390960531436690 ) ) ;
#79156 = CARTESIAN_POINT ( 'NONE',  ( -5.719274019375665041, -21.55341960407619695, 49.79275706135234714 ) ) ;
#79157 = CARTESIAN_POINT ( 'NONE',  ( -9.564922557960796823, -16.46253265017161027, 82.08224293864768129 ) ) ;
#79158 = CARTESIAN_POINT ( 'NONE',  ( -4.379528057220328563, 16.55341960407611168, 95.20724293864769550 ) ) ;
#79159 = CARTESIAN_POINT ( 'NONE',  ( -16.55341960407611168, -4.379528057220339221, 61.45724293864770260 ) ) ;
#79160 = CARTESIAN_POINT ( 'NONE',  ( -18.67979575497178146, -10.72451020669898902, 71.66557627198100988 ) ) ;
#79161 = CARTESIAN_POINT ( 'NONE',  ( 5.049401038298161559, -19.05341960407611168, 72.70724293864768129 ) ) ;
#79162 = CARTESIAN_POINT ( 'NONE',  ( -15.72974639402197994, 15.80617190586746368, 90.62390960531436690 ) ) ;
#79163 = CIRCLE ( 'NONE', #172718, 10.00000000000000355 ) ;
#79164 = CARTESIAN_POINT ( 'NONE',  ( 13.89961937509957401, 13.97604488694547697, 81.87609039468564731 ) ) ;
#79166 = CARTESIAN_POINT ( 'NONE',  ( -14.29746914071049879, 8.314922557960819915, 70.83224293864770971 ) ) ;
#79165 = CARTESIAN_POINT ( 'NONE',  ( -18.22780087662124160, -5.499999999999927169, 88.98236817873107896 ) ) ;
#79167 = CARTESIAN_POINT ( 'NONE',  ( 13.97604488694527802, 13.89961937509977652, 54.37390960531435979 ) ) ;
#79168 = CARTESIAN_POINT ( 'NONE',  ( 18.67979575497178502, 10.72451020669898547, 64.16557627198102409 ) ) ;
#79169 = DIRECTION ( 'NONE',  ( 0.000000000000000000, 0.000000000000000000, 1.000000000000000000 ) ) ;
#79171 = CARTESIAN_POINT ( 'NONE',  ( -3.874011537017815865, -5.374011537017721274, -64.92279855667830191 ) ) ;
#79170 = CARTESIAN_POINT ( 'NONE',  ( 8.224510206698742110, 14.34966873604972548, 107.0844237280190043 ) ) ;
#79172 = CARTESIAN_POINT ( 'NONE',  ( 9.564922557961047289, -16.46253265017146816, 95.41775706135233293 ) ) ;
#79173 = CARTESIAN_POINT ( 'NONE',  ( 8.314922557960818139, 14.29746914071049879, 84.58224293864769550 ) ) ;
#79174 = CARTESIAN_POINT ( 'NONE',  ( 7.989781499195996339, -1.461410587780195947, -62.12232043736379694 ) ) ;
#79175 = CARTESIAN_POINT ( 'NONE',  ( 0.05219959533909260263, 19.03943276465977164, 79.99890960531436690 ) ) ;
#79176 = CARTESIAN_POINT ( 'NONE',  ( -5.153800228976328057, -19.02544592524343514, 32.29057627198102409 ) ) ;
#79177 = CARTESIAN_POINT ( 'NONE',  ( 0.05219959533910956823, 16.53943276465976808, 69.99890960531435269 ) ) ;
#79178 = CARTESIAN_POINT ( 'NONE',  ( -16.51473224551069308, -9.474510206698971260, 96.66557627198102409 ) ) ;
#79180 = CARTESIAN_POINT ( 'NONE',  ( -19.03943276465977164, 0.05219959533909376836, 71.24890960531435269 ) ) ;
#79179 = CARTESIAN_POINT ( 'NONE',  ( -9.564922557961040184, 16.46253265017147172, 87.91775706135233293 ) ) ;
#79181 = COLOUR_RGB ( '', 0.40784314, 0.44705882, 0.49803922) ;
#79182 = CARTESIAN_POINT ( 'NONE',  ( -13.89961937509977652, 13.97604488694528158, 90.62390960531432427 ) ) ;
#79183 = CARTESIAN_POINT ( 'NONE',  ( 5.719274019375991003, -21.55341960407610458, 82.70724293864770971 ) ) ;
#79184 = CARTESIAN_POINT ( 'NONE',  ( -0.05219959533934338120, 16.53943276465976808, 67.50109039468568994 ) ) ;
#79185 = CARTESIAN_POINT ( 'NONE',  ( -9.474510206698720793, -16.51473224551083518, 109.5844237280190043 ) ) ;
#79186 = CARTESIAN_POINT ( 'NONE',  ( 19.03943276465977164, -0.05219959533909143690, 63.74890960531435979 ) ) ;
#79187 = CARTESIAN_POINT ( 'NONE',  ( -5.823673210054116645, -21.52544592524344225, 72.29057627198102409 ) ) ;
#79188 = CARTESIAN_POINT ( 'NONE',  ( 5.153800228976615827, -19.02544592524334988, 95.20942372801897591 ) ) ;
#79190 = CARTESIAN_POINT ( 'NONE',  ( 15.72974639402176855, 15.80617190586768217, 46.87609039468568994 ) ) ;
#79189 = CARTESIAN_POINT ( 'NONE',  ( -0.05219959533910754901, -16.53943276465976808, 37.49890960531436690 ) ) ;
#79191 = EDGE_CURVE ( 'NONE', #90959, #72946, #154561, .T. ) ;
#79192 = CARTESIAN_POINT ( 'NONE',  ( 18.22780087662122739, 5.500000000000000888, 71.48236817873106475 ) ) ;
#79194 = CARTESIAN_POINT ( 'NONE',  ( 13.97604488694527802, 13.89961937509977652, 109.3739096053143669 ) ) ;
#79193 = CARTESIAN_POINT ( 'NONE',  ( 0.05219959533934541429, -16.53943276465976808, 70.00109039468568994 ) ) ;
#79195 = DIRECTION ( 'NONE',  ( 0.000000000000000000, 0.000000000000000000, 1.000000000000000000 ) ) ;
#79196 = CARTESIAN_POINT ( 'NONE',  ( -17.31728774477275579, -6.344390552232334279, 34.18093348310681989 ) ) ;
#79197 = CARTESIAN_POINT ( 'NONE',  ( 14.29746914071037800, 8.314922557961029526, 96.66775706135234714 ) ) ;
#79198 = CARTESIAN_POINT ( 'NONE',  ( -0.05219959533934338120, 16.53943276465976808, 32.50109039468568284 ) ) ;
#79199 = CARTESIAN_POINT ( 'NONE',  ( -16.51473224551069308, -9.474510206698971260, 51.66557627198102409 ) ) ;
#79200 = CARTESIAN_POINT ( 'NONE',  ( -0.05219959533909027116, -19.03943276465977164, 47.49890960531435979 ) ) ;
#79201 = CARTESIAN_POINT ( 'NONE',  ( -9.564922557960796823, -16.46253265017161027, 62.08224293864769550 ) ) ;
#79202 = CARTESIAN_POINT ( 'NONE',  ( 0.05219959533937995610, -21.53943276465977519, 55.00109039468568284 ) ) ;
#79203 = CARTESIAN_POINT ( 'NONE',  ( -14.34966873604972548, 8.224510206698743886, 68.33442372801900433 ) ) ;
#79204 = CARTESIAN_POINT ( 'NONE',  ( -8.314922557960811034, -14.29746914071050412, 32.08224293864769550 ) ) ;
#79205 = CARTESIAN_POINT ( 'NONE',  ( -9.474510206698964154, 16.51473224551069663, 40.41557627198103120 ) ) ;
#79206 = CARTESIAN_POINT ( 'NONE',  ( -5.049401038298153566, 19.05341960407611168, 30.20724293864768839 ) ) ;
#79207 = CARTESIAN_POINT ( 'NONE',  ( 8.314922557961029526, -14.29746914071037800, 25.41775706135235779 ) ) ;
#79208 = CARTESIAN_POINT ( 'NONE',  ( 19.03943276465977164, 0.05219959533936151252, 81.25109039468567573 ) ) ;
#79209 = CARTESIAN_POINT ( 'NONE',  ( -16.52544592524342804, 4.483927247898546575, 81.04057627198102409 ) ) ;
#79210 = CARTESIAN_POINT ( 'NONE',  ( -19.03943276465977164, 0.05219959533909376836, 56.24890960531435979 ) ) ;
#79212 = CARTESIAN_POINT ( 'NONE',  ( -23.29544513554940721, -16.92513159979223403, 148.1843446569000093 ) ) ;
#79211 = CARTESIAN_POINT ( 'NONE',  ( -9.474510206698720793, -16.51473224551083518, 89.58442372801900433 ) ) ;
#79213 = CARTESIAN_POINT ( 'NONE',  ( -10.81492255796105439, 18.62759615963255655, 87.91775706135234714 ) ) ;
#79214 = CARTESIAN_POINT ( 'NONE',  ( 14.34966873604972726, -8.224510206698740333, 50.83442372801901143 ) ) ;
#79215 = CARTESIAN_POINT ( 'NONE',  ( 17.26058549869090086, 6.457015423128631859, 38.87745837476068544 ) ) ;
#79216 = CARTESIAN_POINT ( 'NONE',  ( 21.55341960407610458, 5.719274019375980345, 43.95724293864769550 ) ) ;
#79217 = CARTESIAN_POINT ( 'NONE',  ( 8.314922557961029526, -14.29746914071037800, 45.41775706135234003 ) ) ;
#79218 = CARTESIAN_POINT ( 'NONE',  ( -28.82186960331499037, 2.428612866367529617E-14, 148.0000000000000000 ) ) ;
#79219 = CARTESIAN_POINT ( 'NONE',  ( -19.05341960407617563, 5.049401038297882671, 23.54275706135233648 ) ) ;
#79220 = CARTESIAN_POINT ( 'NONE',  ( -16.51473224551069308, -9.474510206698971260, 81.66557627198103830 ) ) ;
#79221 = CARTESIAN_POINT ( 'NONE',  ( 9.262594875851847931, 10.97788116290291249, -60.18097545586278585 ) ) ;
#79222 = CARTESIAN_POINT ( 'NONE',  ( 5.049401038298161559, -19.05341960407611168, 52.70724293864767418 ) ) ;
#79223 = MANIFOLD_SOLID_BREP ( 'Boss-Extrude2', #195120 ) ;
#79224 = DIRECTION ( 'NONE',  ( -3.469446951953611033E-15, 0.000000000000000000, -1.000000000000000000 ) ) ;
#79225 = CARTESIAN_POINT ( 'NONE',  ( -5.153800228976328057, -19.02544592524343514, 72.29057627198102409 ) ) ;
#79226 = CARTESIAN_POINT ( 'NONE',  ( -19.39056639909671986, -5.500000000000052403, 55.78948781074346641 ) ) ;
#79227 = CARTESIAN_POINT ( 'NONE',  ( -5.049401038297874678, -19.05341960407617918, 24.79275706135233648 ) ) ;
#79228 = CARTESIAN_POINT ( 'NONE',  ( -19.03943276465977164, -0.05219959533935918106, 18.75109039468567218 ) ) ;
#79229 = CARTESIAN_POINT ( 'NONE',  ( -8.224510206698948167, 14.34966873604960824, 35.41557627198102409 ) ) ;
#79230 = CARTESIAN_POINT ( 'NONE',  ( -9.474510206698964154, 16.51473224551069663, 40.41557627198103120 ) ) ;
#79231 = CARTESIAN_POINT ( 'NONE',  ( 19.02544592524343514, -5.153800228976328945, 108.5405762719810383 ) ) ;
#79232 = CARTESIAN_POINT ( 'NONE',  ( -15.72974639402176322, -15.80617190586768395, 69.37609039468567573 ) ) ;
#79233 = CARTESIAN_POINT ( 'NONE',  ( -19.05341960407611168, -5.049401038298163336, 46.45724293864768129 ) ) ;
#79234 = CARTESIAN_POINT ( 'NONE',  ( 10.72451020669871369, 18.67979575497193778, 77.08442372801901854 ) ) ;
#79235 = CARTESIAN_POINT ( 'NONE',  ( 15.80617190586746368, 15.72974639402197994, 29.37390960531435269 ) ) ;
#79236 = CARTESIAN_POINT ( 'NONE',  ( 0.05219959533909260263, 19.03943276465977164, 34.99890960531435979 ) ) ;
#79237 = CARTESIAN_POINT ( 'NONE',  ( 5.823673210054444382, -21.52544592524334988, 30.20942372801902565 ) ) ;
#79238 = CARTESIAN_POINT ( 'NONE',  ( 9.474510206698729675, 16.51473224551082808, 47.08442372801900433 ) ) ;
#79239 = CARTESIAN_POINT ( 'NONE',  ( 5.049401038298161559, -19.05341960407611168, 32.70724293864768129 ) ) ;
#79240 = CARTESIAN_POINT ( 'NONE',  ( -9.564922557960796823, -16.46253265017161027, 72.08224293864770971 ) ) ;
#79241 = CARTESIAN_POINT ( 'NONE',  ( 16.51473224551083163, -9.474510206698727899, 105.8344237280190043 ) ) ;
#79242 = CARTESIAN_POINT ( 'NONE',  ( -12.14591786802309592, -12.06949235617757132, 76.87390960531439532 ) ) ;
#79243 = CARTESIAN_POINT ( 'NONE',  ( 5.719274019375991003, -21.55341960407610458, 32.70724293864770260 ) ) ;
#79244 = CARTESIAN_POINT ( 'NONE',  ( -0.05219959533936034679, 19.03943276465977164, 97.50109039468567573 ) ) ;
#79245 = CARTESIAN_POINT ( 'NONE',  ( 21.53943276465977519, -0.05219959533907433946, 108.7489096053143669 ) ) ;
#79246 = CARTESIAN_POINT ( 'NONE',  ( 10.72451020669871369, 18.67979575497193778, 62.08442372801901143 ) ) ;
#79247 = CARTESIAN_POINT ( 'NONE',  ( -16.52544592524335698, -4.483927247898792601, 58.95942372801902565 ) ) ;
#79248 = CARTESIAN_POINT ( 'NONE',  ( -4.379528057220086978, -16.55341960407618274, 49.79275706135234714 ) ) ;
#79249 = CARTESIAN_POINT ( 'NONE',  ( 18.62759615963271287, -10.81492255796078972, 73.33224293864769550 ) ) ;
#79250 = CARTESIAN_POINT ( 'NONE',  ( -13.89961937509977652, 13.97604488694528158, 45.62390960531433848 ) ) ;
#79251 = CARTESIAN_POINT ( 'NONE',  ( -16.52544592524335698, -4.483927247898792601, 93.95942372801903275 ) ) ;
#79252 = CARTESIAN_POINT ( 'NONE',  ( 5.719274019375991003, -21.55341960407610458, 97.70724293864772392 ) ) ;
#79253 = CARTESIAN_POINT ( 'NONE',  ( 16.53943276465976808, -0.05219959533910856209, 58.74890960531436690 ) ) ;
#79254 = CARTESIAN_POINT ( 'NONE',  ( -19.03943276465977164, 0.05219959533909376836, 71.24890960531435269 ) ) ;
#79255 = CARTESIAN_POINT ( 'NONE',  ( -16.52544592524335698, -4.483927247898792601, 78.95942372801901854 ) ) ;
#79256 = CARTESIAN_POINT ( 'NONE',  ( -9.564922557961040184, 16.46253265017147172, 112.9177570613523329 ) ) ;
#79257 = CARTESIAN_POINT ( 'NONE',  ( -0.05219959533907301413, -21.53943276465977519, 112.4989096053143669 ) ) ;
#79258 = CARTESIAN_POINT ( 'NONE',  ( -12.06949235617756955, 12.14591786802309770, 40.62390960531435269 ) ) ;
#79259 = ORIENTED_EDGE ( 'NONE', *, *, #60885, .F. ) ;
#79260 = CARTESIAN_POINT ( 'NONE',  ( -16.31925111598456013, 7.325300261831604764, 75.16424538967253000 ) ) ;
#79261 = CARTESIAN_POINT ( 'NONE',  ( 15.80617190586746368, 15.72974639402197994, 89.37390960531435269 ) ) ;
#79262 = CARTESIAN_POINT ( 'NONE',  ( 8.314922557960818139, 14.29746914071049879, 29.58224293864769905 ) ) ;
#79263 = EDGE_LOOP ( 'NONE', ( #22434, #80024, #37767, #105307, #173042, #26443, #11273, #75311, #124064, #153209, #151455, #130339, #43168, #81239, #62392, #40274, #2422, #30790, #148486, #100280, #149295, #121776, #41285, #175376, #147038, #79354, #35177, #3038, #183671, #115724, #41102, #172150, #46246, #45057, #59126, #123202, #22817, #28931, #107365, #75112, #91545 ) ) ;
#79264 = DIRECTION ( 'NONE',  ( -1.000000000000000000, -0.000000000000000000, -0.000000000000000000 ) ) ;
#79265 = CARTESIAN_POINT ( 'NONE',  ( -15.80617190586745835, -15.72974639402198527, 106.8739096053143811 ) ) ;
#79266 = AXIS2_PLACEMENT_3D ( 'NONE', #118793, #197617, #90413 ) ;
#79267 = CARTESIAN_POINT ( 'NONE',  ( -19.03943276465977164, 0.05219959533909376836, 106.2489096053143669 ) ) ;
#79268 = CARTESIAN_POINT ( 'NONE',  ( -21.52544592524343514, 5.823673210054127303, 116.0405762719810383 ) ) ;
#79269 = CARTESIAN_POINT ( 'NONE',  ( 8.224510206698953496, -14.34966873604960469, 52.91557627198103830 ) ) ;
#79270 = CARTESIAN_POINT ( 'NONE',  ( -12.06949235617739369, -12.14591786802326823, 54.37609039468568994 ) ) ;
#79271 = CARTESIAN_POINT ( 'NONE',  ( 19.05341960407611168, 5.049401038298154454, 63.95724293864769550 ) ) ;
#79272 = CARTESIAN_POINT ( 'NONE',  ( 13.89961937509957401, 13.97604488694547697, 51.87609039468566863 ) ) ;
#79273 = CARTESIAN_POINT ( 'NONE',  ( -5.049401038298153566, 19.05341960407611168, 80.20724293864769550 ) ) ;
#79274 = EDGE_CURVE ( 'NONE', #41082, #151987, #107053, .T. ) ;
#79275 = CARTESIAN_POINT ( 'NONE',  ( 15.72974639402199770, -15.80617190586745480, 33.12390960531435979 ) ) ;
#79276 = CARTESIAN_POINT ( 'NONE',  ( -36.30973463498060738, -18.33876584755894612, -18.81039752656815622 ) ) ;
#79277 = CARTESIAN_POINT ( 'NONE',  ( -19.05341960407611168, -5.049401038298163336, 51.45724293864770260 ) ) ;
#79278 = CARTESIAN_POINT ( 'NONE',  ( -8.224510206698735004, -14.34966873604973081, 19.58442372801901143 ) ) ;
#79279 = CARTESIAN_POINT ( 'NONE',  ( 9.564922557961047289, -16.46253265017146816, 70.41775706135233293 ) ) ;
#79280 = CARTESIAN_POINT ( 'NONE',  ( 5.823673210054125526, 21.52544592524343514, 104.7905762719810241 ) ) ;
#79281 = CARTESIAN_POINT ( 'NONE',  ( -14.34966873604960291, -8.224510206698953496, 36.66557627198103120 ) ) ;
#79282 = CARTESIAN_POINT ( 'NONE',  ( -16.51473224551069308, -9.474510206698971260, 81.66557627198103830 ) ) ;
#79283 = CARTESIAN_POINT ( 'NONE',  ( 0.05219959533907565091, 21.53943276465977519, 64.99890960531435269 ) ) ;
#79285 = CARTESIAN_POINT ( 'NONE',  ( -4.379528057220086978, -16.55341960407618274, 29.79275706135234358 ) ) ;
#79284 = CARTESIAN_POINT ( 'NONE',  ( -18.62759615963270932, 10.81492255796079327, 100.8322429386477097 ) ) ;
#79286 = CARTESIAN_POINT ( 'NONE',  ( 13.97604488694527802, 13.89961937509977652, 114.3739096053143669 ) ) ;
#79287 = CARTESIAN_POINT ( 'NONE',  ( -5.823673210054431948, 21.52544592524334988, 92.70942372801901854 ) ) ;
#79289 = ADVANCED_FACE ( 'NONE', ( #199081 ), #60549, .T. ) ;
#79288 = CARTESIAN_POINT ( 'NONE',  ( -19.05341960407611168, -5.049401038298163336, 81.45724293864769550 ) ) ;
#79290 = CARTESIAN_POINT ( 'NONE',  ( -5.153800228976328057, -19.02544592524343514, 32.29057627198102409 ) ) ;
#79291 = CARTESIAN_POINT ( 'NONE',  ( -5.049401038298153566, 19.05341960407611168, 90.20724293864766707 ) ) ;
#79292 = CARTESIAN_POINT ( 'NONE',  ( 4.379528057220339221, -16.55341960407611168, 102.7072429386476955 ) ) ;
#79293 = CARTESIAN_POINT ( 'NONE',  ( 19.05341960407611168, 5.049401038298154454, 63.95724293864769550 ) ) ;
#79294 = CARTESIAN_POINT ( 'NONE',  ( 0.05219959533934541429, -16.53943276465976808, 20.00109039468568639 ) ) ;
#79295 = CARTESIAN_POINT ( 'NONE',  ( -13.97604488694547520, 13.89961937509957934, 43.12609039468566152 ) ) ;
#79297 = CARTESIAN_POINT ( 'NONE',  ( -5.153800228976328057, -19.02544592524343514, 107.2905762719810383 ) ) ;
#79296 = CARTESIAN_POINT ( 'NONE',  ( 18.62759615963255655, 10.81492255796105972, 91.66775706135234714 ) ) ;
#79298 = CARTESIAN_POINT ( 'NONE',  ( -8.224510206698735004, -14.34966873604973081, 94.58442372801901854 ) ) ;
#79299 = CARTESIAN_POINT ( 'NONE',  ( 21.75275980508837392, -20.01158182446510736, -48.88299994772790313 ) ) ;
#79300 = CARTESIAN_POINT ( 'NONE',  ( -19.05341960407617563, 5.049401038297882671, 68.54275706135230450 ) ) ;
#79301 = CARTESIAN_POINT ( 'NONE',  ( 5.049401038297881783, 19.05341960407617563, 32.29275706135233293 ) ) ;
#79302 = CARTESIAN_POINT ( 'NONE',  ( 22.00000000000000000, -1.163414459189985801E-14, 92.50000000000000000 ) ) ;
#79303 = CARTESIAN_POINT ( 'NONE',  ( 16.46253265017160672, -9.564922557960803928, 28.33224293864769550 ) ) ;
#79304 = CARTESIAN_POINT ( 'NONE',  ( -0.05219959533910754901, -16.53943276465976808, 42.49890960531435979 ) ) ;
#79305 = LINE ( 'NONE', #175302, #195302 ) ;
#79306 = CARTESIAN_POINT ( 'NONE',  ( 4.483927247898790824, -16.52544592524335698, 110.2094237280190185 ) ) ;
#79307 = DIRECTION ( 'NONE',  ( -1.000000000000000000, 0.000000000000000000, 0.000000000000000000 ) ) ;
#79308 = CARTESIAN_POINT ( 'NONE',  ( 12.14591786802327356, -12.06949235617739191, 85.62609039468568994 ) ) ;
#79309 = CARTESIAN_POINT ( 'NONE',  ( 13.97604488694527802, 13.89961937509977652, 39.37390960531435269 ) ) ;
#79310 = CARTESIAN_POINT ( 'NONE',  ( -5.823673210054431948, 21.52544592524334988, 87.70942372801901854 ) ) ;
#79311 = CARTESIAN_POINT ( 'NONE',  ( -16.51473224551082808, 9.474510206698731452, 108.3344237280190043 ) ) ;
#79312 = CARTESIAN_POINT ( 'NONE',  ( 21.53943276465977519, 0.05219959533937863772, 81.25109039468568994 ) ) ;
#79313 = CARTESIAN_POINT ( 'NONE',  ( 19.03943276465977164, 0.05219959533936151252, 51.25109039468567573 ) ) ;
#79314 = CARTESIAN_POINT ( 'NONE',  ( -13.89961937509977652, 13.97604488694528158, 95.62390960531436690 ) ) ;
#79315 = CARTESIAN_POINT ( 'NONE',  ( -5.049401038298153566, 19.05341960407611168, 75.20724293864769550 ) ) ;
#79316 = CARTESIAN_POINT ( 'NONE',  ( -19.35633801406906329, 5.499999999999779732, 39.13373818172762242 ) ) ;
#79317 = CARTESIAN_POINT ( 'NONE',  ( -16.53943276465976808, 0.05219959533911058130, 71.24890960531435269 ) ) ;
#79318 = CARTESIAN_POINT ( 'NONE',  ( 15.72974639402199770, -15.80617190586745480, 58.12390960531435979 ) ) ;
#79319 = CARTESIAN_POINT ( 'NONE',  ( -19.05341960407611168, -5.049401038298163336, 41.45724293864769550 ) ) ;
#79321 = CARTESIAN_POINT ( 'NONE',  ( 16.52544592524335698, 4.483927247898782831, 71.45942372801901854 ) ) ;
#79320 = CARTESIAN_POINT ( 'NONE',  ( 10.81492255796078972, 18.62759615963270932, 89.58224293864768129 ) ) ;
#79322 = EDGE_LOOP ( 'NONE', ( #60124, #114868, #134001, #36784, #185899, #22115, #151761, #91433 ) ) ;
#79323 = CARTESIAN_POINT ( 'NONE',  ( 9.564922557960805705, 16.46253265017160317, 49.58224293864770260 ) ) ;
#79325 = CARTESIAN_POINT ( 'NONE',  ( 11.40812507854754365, 35.11059874428196537, -5.224999997268813701 ) ) ;
#79324 = CARTESIAN_POINT ( 'NONE',  ( 8.314922557960818139, 14.29746914071049879, 79.58224293864769550 ) ) ;
#79326 = CARTESIAN_POINT ( 'NONE',  ( 19.03943276465977164, -0.05219959533909143690, 48.74890960531435979 ) ) ;
#79327 = CARTESIAN_POINT ( 'NONE',  ( 12.14591786802309770, 12.06949235617756955, 114.3739096053143527 ) ) ;
#79328 = CARTESIAN_POINT ( 'NONE',  ( -9.564922557961040184, 16.46253265017147172, 72.91775706135233293 ) ) ;
#79329 = CARTESIAN_POINT ( 'NONE',  ( -16.55341960407611168, -4.379528057220339221, 76.45724293864769550 ) ) ;
#79330 = CARTESIAN_POINT ( 'NONE',  ( 15.72974639402176855, 15.80617190586768217, 46.87609039468568994 ) ) ;
#79332 = CARTESIAN_POINT ( 'NONE',  ( -18.67979575497178146, -10.72451020669898902, 106.6655762719810383 ) ) ;
#79331 = CARTESIAN_POINT ( 'NONE',  ( -16.51473224551069308, -9.474510206698971260, 31.66557627198102054 ) ) ;
#79333 = DIRECTION ( 'NONE',  ( -1.000000000000000000, 3.552713678800500929E-15, 0.000000000000000000 ) ) ;
#79334 = CARTESIAN_POINT ( 'NONE',  ( 16.53943276465976808, -0.05219959533910856209, 88.74890960531436690 ) ) ;
#79335 = CARTESIAN_POINT ( 'NONE',  ( 24.03200911576290366, -31.81637637394766571, -21.77892875004970819 ) ) ;
#79336 = CARTESIAN_POINT ( 'NONE',  ( 0.05219959533909260263, 19.03943276465977164, 44.99890960531435979 ) ) ;
#79337 = CARTESIAN_POINT ( 'NONE',  ( 19.39720447994796260, 5.499999999999971578, 47.16317477297181426 ) ) ;
#79339 = CARTESIAN_POINT ( 'NONE',  ( -5.049401038298153566, 19.05341960407611168, 105.2072429386476671 ) ) ;
#79338 = CARTESIAN_POINT ( 'NONE',  ( -19.03943276465977164, -0.05219959533935918106, 93.75109039468566152 ) ) ;
#79340 = CARTESIAN_POINT ( 'NONE',  ( 15.72974639402176855, 15.80617190586768217, 31.87609039468567929 ) ) ;
#79341 = CARTESIAN_POINT ( 'NONE',  ( -13.89961937509977652, 13.97604488694528158, 85.62390960531433848 ) ) ;
#79342 = CARTESIAN_POINT ( 'NONE',  ( 9.474510206698729675, 16.51473224551082808, 72.08442372801900433 ) ) ;
#79343 = CARTESIAN_POINT ( 'NONE',  ( 19.05341960407611168, 5.049401038298154454, 43.95724293864769550 ) ) ;
#79344 = CARTESIAN_POINT ( 'NONE',  ( -12.14591786802309592, -12.06949235617757132, 61.87390960531436690 ) ) ;
#79345 = CARTESIAN_POINT ( 'NONE',  ( 4.483927247898545687, 16.52544592524342804, 69.79057627198102409 ) ) ;
#79346 = CARTESIAN_POINT ( 'NONE',  ( -5.153800228976328057, -19.02544592524343514, 72.29057627198102409 ) ) ;
#79347 = CARTESIAN_POINT ( 'NONE',  ( -15.72974639402197994, 15.80617190586746368, 105.6239096053143669 ) ) ;
#79348 = CARTESIAN_POINT ( 'NONE',  ( 0.05219959533909260263, 19.03943276465977164, 64.99890960531436690 ) ) ;
#79349 = CARTESIAN_POINT ( 'NONE',  ( -21.52544592524334988, -5.823673210054445271, 108.9594237280190185 ) ) ;
#79352 = CARTESIAN_POINT ( 'NONE',  ( 16.53943276465976808, -0.05219959533910856209, 108.7489096053143669 ) ) ;
#79351 = CARTESIAN_POINT ( 'NONE',  ( -4.483927247898782831, 16.52544592524335698, 112.7094237280190328 ) ) ;
#79350 = CARTESIAN_POINT ( 'NONE',  ( -19.05341960407611168, -5.049401038298163336, 41.45724293864769550 ) ) ;
#79353 = CARTESIAN_POINT ( 'NONE',  ( 5.049401038297881783, 19.05341960407617563, 107.2927570613523187 ) ) ;
#79354 = ORIENTED_EDGE ( 'NONE', *, *, #73579, .F. ) ;
#79355 = CARTESIAN_POINT ( 'NONE',  ( -10.72451020669870658, -18.67979575497194134, 24.58442372801901499 ) ) ;
#79356 = CARTESIAN_POINT ( 'NONE',  ( 5.153800228976615827, -19.02544592524334988, 50.20942372801897591 ) ) ;
#79357 = CARTESIAN_POINT ( 'NONE',  ( -12.06949235617739369, -12.14591786802326823, 109.3760903946857042 ) ) ;
#79358 = CARTESIAN_POINT ( 'NONE',  ( 0.05219959533907565091, 21.53943276465977519, 74.99890960531435269 ) ) ;
#79359 = CARTESIAN_POINT ( 'NONE',  ( -21.52544592524343514, 5.823673210054127303, 26.04057627198103475 ) ) ;
#79360 = CARTESIAN_POINT ( 'NONE',  ( 16.53943276465976808, -0.05219959533910856209, 53.74890960531437401 ) ) ;
#79361 = CARTESIAN_POINT ( 'NONE',  ( 9.564922557960805705, 16.46253265017160317, 29.58224293864769550 ) ) ;
#79362 = CARTESIAN_POINT ( 'NONE',  ( -13.89961937509977652, 13.97604488694528158, 40.62390960531435979 ) ) ;
#79363 = CARTESIAN_POINT ( 'NONE',  ( -9.564922557961040184, 16.46253265017147172, 32.91775706135233293 ) ) ;
#79364 = CARTESIAN_POINT ( 'NONE',  ( 8.314922557961029526, -14.29746914071037800, 95.41775706135234714 ) ) ;
#79365 = CARTESIAN_POINT ( 'NONE',  ( -0.05219959533934338120, 16.53943276465976808, 57.50109039468568994 ) ) ;
#79366 = CARTESIAN_POINT ( 'NONE',  ( -16.46253265017160317, 9.564922557960807481, 115.8322429386477097 ) ) ;
#79368 = CARTESIAN_POINT ( 'NONE',  ( -21.52544592524334988, -5.823673210054445271, 108.9594237280190185 ) ) ;
#79367 = CARTESIAN_POINT ( 'NONE',  ( 5.153800228976335163, 19.02544592524342804, 59.79057627198100988 ) ) ;
#79369 = CARTESIAN_POINT ( 'NONE',  ( -13.89961937509977652, 13.97604488694528158, 80.62390960531436690 ) ) ;
#79370 = VECTOR ( 'NONE', #85780, 1000.000000000000000 ) ;
#79371 = CARTESIAN_POINT ( 'NONE',  ( 8.224510206698742110, 14.34966873604972548, 67.08442372801901854 ) ) ;
#79372 = CARTESIAN_POINT ( 'NONE',  ( 14.34966873604960469, 8.224510206698951720, 104.1655762719810241 ) ) ;
#79373 = CARTESIAN_POINT ( 'NONE',  ( 16.55341960407611168, 4.379528057220329451, 23.95724293864769550 ) ) ;
#79374 = CARTESIAN_POINT ( 'NONE',  ( -17.72517630440433933, 5.499999999999974243, 70.92175719257211597 ) ) ;
#79377 = CARTESIAN_POINT ( 'NONE',  ( -13.97604488694527625, -13.89961937509977652, 71.87390960531433848 ) ) ;
#79376 = CARTESIAN_POINT ( 'NONE',  ( -16.51473224551069308, -9.474510206698971260, 86.66557627198102409 ) ) ;
#79375 = CARTESIAN_POINT ( 'NONE',  ( 18.62759615963255655, 10.81492255796105972, 76.66775706135234714 ) ) ;
#79378 = CARTESIAN_POINT ( 'NONE',  ( 0.05219959533909260263, 19.03943276465977164, 104.9989096053143669 ) ) ;
#79379 = CARTESIAN_POINT ( 'NONE',  ( 14.34966873604960469, 8.224510206698951720, 54.16557627198103120 ) ) ;
#79380 = ADVANCED_FACE ( 'NONE', ( #1868 ), #66523, .F. ) ;
#79381 = CARTESIAN_POINT ( 'NONE',  ( 0.05219959533934541429, -16.53943276465976808, 110.0010903946856757 ) ) ;
#79382 = ORIENTED_EDGE ( 'NONE', *, *, #103239, .T. ) ;
#79383 = CARTESIAN_POINT ( 'NONE',  ( -12.14591786802309592, -12.06949235617757132, 36.87390960531435979 ) ) ;
#79385 = DIRECTION ( 'NONE',  ( -0.000000000000000000, -0.000000000000000000, 1.000000000000000000 ) ) ;
#79384 = CARTESIAN_POINT ( 'NONE',  ( -4.483927247898782831, 16.52544592524335698, 42.70942372801901854 ) ) ;
#79386 = CARTESIAN_POINT ( 'NONE',  ( -9.474510206698720793, -16.51473224551083518, 39.58442372801899722 ) ) ;
#79387 = CARTESIAN_POINT ( 'NONE',  ( 5.049401038298161559, -19.05341960407611168, 77.70724293864765286 ) ) ;
#79388 = CARTESIAN_POINT ( 'NONE',  ( -9.564922557961040184, 16.46253265017147172, 52.91775706135233293 ) ) ;
#79389 = CARTESIAN_POINT ( 'NONE',  ( -36.91746825000001309, 11.99521256947798342, -2.724999997268813701 ) ) ;
#79391 = CARTESIAN_POINT ( 'NONE',  ( -8.224510206698735004, -14.34966873604973081, 84.58442372801903275 ) ) ;
#79390 = CARTESIAN_POINT ( 'NONE',  ( -5.049401038297874678, -19.05341960407617918, 99.79275706135234714 ) ) ;
#79392 = CARTESIAN_POINT ( 'NONE',  ( 13.97604488694527802, 13.89961937509977652, 24.37390960531435624 ) ) ;
#79393 = CARTESIAN_POINT ( 'NONE',  ( 9.564922557960805705, 16.46253265017160317, 99.58224293864770971 ) ) ;
#79394 = CARTESIAN_POINT ( 'NONE',  ( -15.80617190586768217, 15.72974639402176855, 48.12609039468568284 ) ) ;
#79395 = CARTESIAN_POINT ( 'NONE',  ( 13.89961937509957401, 13.97604488694547697, 86.87609039468567573 ) ) ;
#79397 = CARTESIAN_POINT ( 'NONE',  ( 19.03943276465977164, -0.05219959533909143690, 43.74890960531435979 ) ) ;
#79396 = CYLINDRICAL_SURFACE ( 'NONE', #86294, 2.000000000000001776 ) ;
#79398 = CARTESIAN_POINT ( 'NONE',  ( -16.46253265017160317, 9.564922557960807481, 105.8322429386476955 ) ) ;
#79400 = CARTESIAN_POINT ( 'NONE',  ( -13.89961937509977652, 13.97604488694528158, 55.62390960531434558 ) ) ;
#79399 = CARTESIAN_POINT ( 'NONE',  ( -4.483927247898539470, -16.52544592524342804, 67.29057627198103830 ) ) ;
#79401 = CARTESIAN_POINT ( 'NONE',  ( -5.049401038298153566, 19.05341960407611168, 65.20724293864765286 ) ) ;
#79402 = CARTESIAN_POINT ( 'NONE',  ( -19.02544592524334988, -5.153800228976617603, 58.95942372801900433 ) ) ;
#79403 = CARTESIAN_POINT ( 'NONE',  ( -16.51473224551082808, 9.474510206698731452, 43.33442372801900433 ) ) ;
#79404 = CARTESIAN_POINT ( 'NONE',  ( -16.51473224551069308, -9.474510206698971260, 71.66557627198102409 ) ) ;
#79405 = CARTESIAN_POINT ( 'NONE',  ( -21.53943276465977519, 0.05219959533907696930, 81.24890960531436690 ) ) ;
#79407 = CARTESIAN_POINT ( 'NONE',  ( -9.474510206698720793, -16.51473224551083518, 39.58442372801899722 ) ) ;
#79406 = CARTESIAN_POINT ( 'NONE',  ( -8.224510206698948167, 14.34966873604960824, 70.41557627198102409 ) ) ;
#79408 = CARTESIAN_POINT ( 'NONE',  ( 10.81492255796078972, 18.62759615963270932, 49.58224293864769550 ) ) ;
#79409 = AXIS2_PLACEMENT_3D ( 'NONE', #41816, #150994, #146986 ) ;
#79410 = CARTESIAN_POINT ( 'NONE',  ( 0.05219959533907565091, 21.53943276465977519, 39.99890960531436690 ) ) ;
#79411 = CARTESIAN_POINT ( 'NONE',  ( 13.97604488694527802, 13.89961937509977652, 64.37390960531436690 ) ) ;
#79412 = CARTESIAN_POINT ( 'NONE',  ( -9.564922557960796823, -16.46253265017161027, 42.08224293864769550 ) ) ;
#79413 = CARTESIAN_POINT ( 'NONE',  ( -16.53943276465976808, 0.05219959533911058130, 101.2489096053143669 ) ) ;
#79414 = CARTESIAN_POINT ( 'NONE',  ( -15.72974639402197994, 15.80617190586746368, 110.6239096053143669 ) ) ;
#79415 = CARTESIAN_POINT ( 'NONE',  ( -28.47622644277399928, -25.16156846422451920, -16.68312038616162951 ) ) ;
#79416 = CARTESIAN_POINT ( 'NONE',  ( 0.05219959533937995610, -21.53943276465977519, 30.00109039468568284 ) ) ;
#79417 = CARTESIAN_POINT ( 'NONE',  ( -19.02544592524342804, 5.153800228976336051, 36.04057627198100988 ) ) ;
#79418 = CARTESIAN_POINT ( 'NONE',  ( -0.05219959533907301413, -21.53943276465977519, 112.4989096053143669 ) ) ;
#79419 = CARTESIAN_POINT ( 'NONE',  ( 0.05219959533936267826, -19.03943276465977164, 45.00109039468566863 ) ) ;
#79420 = CARTESIAN_POINT ( 'NONE',  ( 19.02544592524343514, -5.153800228976328945, 23.54057627198102054 ) ) ;
#79421 = CARTESIAN_POINT ( 'NONE',  ( -5.153800228976328057, -19.02544592524343514, 27.29057627198103120 ) ) ;
#79422 = CARTESIAN_POINT ( 'NONE',  ( 4.483927247898790824, -16.52544592524335698, 40.20942372801901854 ) ) ;
#79423 = CARTESIAN_POINT ( 'NONE',  ( 19.02544592524343514, -5.153800228976328945, 28.54057627198102409 ) ) ;
#79424 = CARTESIAN_POINT ( 'NONE',  ( -25.85392304583074008, -7.514126903510844002, 173.7688241862487644 ) ) ;
#79425 = CARTESIAN_POINT ( 'NONE',  ( -5.049401038298153566, 19.05341960407611168, 75.20724293864769550 ) ) ;
#79426 = CARTESIAN_POINT ( 'NONE',  ( 16.53943276465976808, -0.05219959533910856209, 113.7489096053143527 ) ) ;
#79427 = CARTESIAN_POINT ( 'NONE',  ( 5.719274019375991003, -21.55341960407610458, 52.70724293864769550 ) ) ;
#79428 = CARTESIAN_POINT ( 'NONE',  ( -16.55341960407611168, -4.379528057220339221, 81.45724293864769550 ) ) ;
#79429 = CARTESIAN_POINT ( 'NONE',  ( -14.29746914071037622, -8.314922557961029526, 29.16775706135234003 ) ) ;
#79430 = CARTESIAN_POINT ( 'NONE',  ( 21.52544592524334988, 5.823673210054432836, 86.45942372801901854 ) ) ;
#79431 = CARTESIAN_POINT ( 'NONE',  ( -19.03943276465977164, 0.05219959533909376836, 31.24890960531435979 ) ) ;
#79432 = CARTESIAN_POINT ( 'NONE',  ( -16.55341960407617563, 4.379528057220093196, 113.5427570613523756 ) ) ;
#79433 = CARTESIAN_POINT ( 'NONE',  ( -12.06949235617756955, 12.14591786802309770, 50.62390960531435979 ) ) ;
#79434 = CARTESIAN_POINT ( 'NONE',  ( 13.97604488694527802, 13.89961937509977652, 54.37390960531435979 ) ) ;
#79435 = CARTESIAN_POINT ( 'NONE',  ( 15.72974639402176855, 15.80617190586768217, 101.8760903946857042 ) ) ;
#79436 = CARTESIAN_POINT ( 'NONE',  ( 5.719274019375991003, -21.55341960407610458, 112.7072429386476955 ) ) ;
#79437 = CARTESIAN_POINT ( 'NONE',  ( -21.52544592524334988, -5.823673210054445271, 78.95942372801901854 ) ) ;
#79438 = CARTESIAN_POINT ( 'NONE',  ( 8.314922557961029526, -14.29746914071037800, 35.41775706135234003 ) ) ;
#79440 = CARTESIAN_POINT ( 'NONE',  ( -10.81492255796105439, 18.62759615963255655, 87.91775706135234714 ) ) ;
#79439 = CARTESIAN_POINT ( 'NONE',  ( -8.224510206698948167, 14.34966873604960824, 75.41557627198102409 ) ) ;
#79441 = EDGE_CURVE ( 'NONE', #6927, #115616, #141379, .T. ) ;
#79442 = CARTESIAN_POINT ( 'NONE',  ( 14.34966873604972726, -8.224510206698740333, 110.8344237280190043 ) ) ;
#79443 = CARTESIAN_POINT ( 'NONE',  ( -17.13100169013301510, 6.664070546373117132, 115.7678983569985292 ) ) ;
#79444 = CARTESIAN_POINT ( 'NONE',  ( 16.55341960407618274, -4.379528057220086978, 41.04275706135236135 ) ) ;
#79445 = CARTESIAN_POINT ( 'NONE',  ( -4.483927247898539470, -16.52544592524342804, 37.29057627198102409 ) ) ;
#79446 = CARTESIAN_POINT ( 'NONE',  ( -0.05219959533934338120, 16.53943276465976808, 82.50109039468568994 ) ) ;
#79447 = CARTESIAN_POINT ( 'NONE',  ( -5.049401038298153566, 19.05341960407611168, 95.20724293864770971 ) ) ;
#79448 = CARTESIAN_POINT ( 'NONE',  ( -16.46253265017160317, 9.564922557960807481, 95.83224293864769550 ) ) ;
#79449 = CARTESIAN_POINT ( 'NONE',  ( -18.67979575497193778, 10.72451020669871902, 103.3344237280190043 ) ) ;
#79450 = CARTESIAN_POINT ( 'NONE',  ( 4.483927247898790824, -16.52544592524335698, 100.2094237280190043 ) ) ;
#79451 = CARTESIAN_POINT ( 'NONE',  ( -12.14591786802309592, -12.06949235617757132, 71.87390960531438111 ) ) ;
#79452 = CARTESIAN_POINT ( 'NONE',  ( -19.03943276465977164, 0.05219959533909376836, 86.24890960531436690 ) ) ;
#79453 = ORIENTED_EDGE ( 'NONE', *, *, #192121, .F. ) ;
#79455 = CARTESIAN_POINT ( 'NONE',  ( -8.314922557961024197, 14.29746914071037800, 27.91775706135234358 ) ) ;
#79454 =( BOUNDED_SURFACE ( )  B_SPLINE_SURFACE ( 1, 2, ( 
 ( #67137, #65146, #128795, #189504, #139992, #51967, #1481, #97447, #50979, #98453, #142971, #4448, #124838, #95482, #187532, #96466, #158154, #113626, #143974, #82282, #66138, #110653, #80308, #19646, #112639, #173339, #109667, #126803, #141981, #171347, #188511, #127801, #34811, #2483, #81287, #36787, #175321, #160146, #21637, #5454, #63159, #174331, #35801, #3469, #49988, #48997, #79325, #48011, #159133, #20630, #186538, #32836, #94486, #156168, #17667, #172333, #125829, #140995, #64164, #33822, #157168, #18662, #117645, #164162, #132809, #10478, #54971, #55968, #176330, #52955, #8468, #53974, #163149, #72138, #86301, #39794, #192491, #148988, #115647, #177337, #194495, #40805, #102475, #25660, #87305, #147990, #22640, #70142, #179342, #9479, #133814, #195505, #118652, #38808, #56978, #83291, #162145, #129780, #191477, #180343, #7448 ),
 ( #100466, #161143, #41811, #116641, #103479, #165157, #37800, #69132, #68129, #114631, #131813, #144967, #84287, #23641, #6448, #99463, #24652, #145966, #178331, #193492, #130800, #101458, #85289, #146981, #71143, #44785, #76100, #150989, #75115, #73157, #29615, #106438, #58951, #168119, #169098, #137775, #13451, #107426, #12481, #166156, #88292, #74142, #91247, #183303, #182315, #123585, #89297, #135814, #181330, #61914, #136783, #152938, #121608, #198469, #184292, #26649, #59940, #199461, #60928, #197484, #14437, #120619, #122602, #185279, #28643, #77096, #43795, #45773, #30605, #119648, #92258, #46771, #105458, #153942, #15437, #90279, #138765, #167144, #246, #108430, #149980, #151963, #11486, #134827, #196506, #57976, #42809, #104471, #27657, #188273, #128559, #48761, #172097, #186290, #66896, #35567, #18428, #16432, #97215, #125593, #112406 ) ),
 .UNSPECIFIED., .F., .F., .F. ) 
 B_SPLINE_SURFACE_WITH_KNOTS ( ( 2, 2 ),
 ( 3, 2, 2, 2, 2, 2, 2, 2, 2, 2, 2, 2, 2, 2, 2, 2, 2, 2, 2, 2, 2, 2, 2, 2, 2, 2, 2, 2, 2, 2, 2, 2, 2, 2, 2, 2, 2, 2, 2, 2, 2, 2, 2, 2, 2, 2, 2, 2, 2, 2, 3 ),
 ( 0.000000000000000000, 1.000000000000000000 ),
 ( 0.000000000000000000, 0.02000000000000000042, 0.04000000000000000083, 0.05999999999999999778, 0.08000000000000000167, 0.1000000000000000056, 0.1199999999999999956, 0.1400000000000000133, 0.1600000000000000033, 0.1799999999999999933, 0.2000000000000000111, 0.2200000000000000011, 0.2399999999999999911, 0.2600000000000000089, 0.2800000000000000266, 0.2999999999999999889, 0.3200000000000000067, 0.3400000000000000244, 0.3599999999999999867, 0.3800000000000000044, 0.4000000000000000222, 0.4199999999999999845, 0.4400000000000000022, 0.4600000000000000200, 0.4799999999999999822, 0.5000000000000000000, 0.5200000000000000178, 0.5400000000000000355, 0.5600000000000000533, 0.5799999999999999600, 0.5999999999999999778, 0.6199999999999999956, 0.6400000000000000133, 0.6600000000000000311, 0.6800000000000000488, 0.6999999999999999556, 0.7199999999999999734, 0.7399999999999999911, 0.7600000000000000089, 0.7800000000000000266, 0.8000000000000000444, 0.8199999999999999512, 0.8399999999999999689, 0.8599999999999999867, 0.8800000000000000044, 0.9000000000000000222, 0.9200000000000000400, 0.9399999999999999467, 0.9599999999999999645, 0.9799999999999999822, 1.000000000000000000 ),
 .UNSPECIFIED. ) 
 GEOMETRIC_REPRESENTATION_ITEM ( )  RATIONAL_B_SPLINE_SURFACE ( (
 ( 1.000000000000000000, 0.9510565162951535312, 1.000000000000000000, 0.9510565162951535312, 1.000000000000000000, 0.9510565162951535312, 1.000000000000000000, 0.9510565162951535312, 1.000000000000000000, 0.9510565162951535312, 1.000000000000000000, 0.9510565162951535312, 1.000000000000000000, 0.9510565162951535312, 1.000000000000000000, 0.9510565162951535312, 1.000000000000000000, 0.9510565162951535312, 1.000000000000000000, 0.9510565162951535312, 1.000000000000000000, 0.9510565162951535312, 1.000000000000000000, 0.9510565162951535312, 1.000000000000000000, 0.9510565162951535312, 1.000000000000000000, 0.9510565162951535312, 1.000000000000000000, 0.9510565162951535312, 1.000000000000000000, 0.9510565162951535312, 1.000000000000000000, 0.9510565162951535312, 1.000000000000000000, 0.9510565162951535312, 1.000000000000000000, 0.9510565162951535312, 1.000000000000000000, 0.9510565162951535312, 1.000000000000000000, 0.9510565162951535312, 1.000000000000000000, 0.9510565162951535312, 1.000000000000000000, 0.9510565162951535312, 1.000000000000000000, 0.9510565162951535312, 1.000000000000000000, 0.9510565162951535312, 1.000000000000000000, 0.9510565162951535312, 1.000000000000000000, 0.9510565162951535312, 1.000000000000000000, 0.9510565162951535312, 1.000000000000000000, 0.9510565162951535312, 1.000000000000000000, 0.9510565162951535312, 1.000000000000000000, 0.9510565162951535312, 1.000000000000000000, 0.9510565162951535312, 1.000000000000000000, 0.9510565162951535312, 1.000000000000000000, 0.9510565162951535312, 1.000000000000000000, 0.9510565162951535312, 1.000000000000000000, 0.9510565162951535312, 1.000000000000000000, 0.9510565162951535312, 1.000000000000000000, 0.9510565162951535312, 1.000000000000000000, 0.9510565162951535312, 1.000000000000000000, 0.9510565162951535312, 1.000000000000000000, 0.9510565162951535312, 1.000000000000000000, 0.9510565162951535312, 1.000000000000000000, 0.9510565162951535312, 1.000000000000000000, 0.9510565162951535312, 1.000000000000000000, 0.9510565162951535312, 1.000000000000000000, 0.9510565162951535312, 1.000000000000000000, 0.9510565162951535312, 1.000000000000000000, 0.9510565162951535312, 1.000000000000000000, 0.9510565162951535312, 1.000000000000000000, 0.9510565162951535312, 1.000000000000000000),
 ( 1.000000000000000000, 0.9510565162951535312, 1.000000000000000000, 0.9510565162951535312, 1.000000000000000000, 0.9510565162951535312, 1.000000000000000000, 0.9510565162951535312, 1.000000000000000000, 0.9510565162951535312, 1.000000000000000000, 0.9510565162951535312, 1.000000000000000000, 0.9510565162951535312, 1.000000000000000000, 0.9510565162951535312, 1.000000000000000000, 0.9510565162951535312, 1.000000000000000000, 0.9510565162951535312, 1.000000000000000000, 0.9510565162951535312, 1.000000000000000000, 0.9510565162951535312, 1.000000000000000000, 0.9510565162951535312, 1.000000000000000000, 0.9510565162951535312, 1.000000000000000000, 0.9510565162951535312, 1.000000000000000000, 0.9510565162951535312, 1.000000000000000000, 0.9510565162951535312, 1.000000000000000000, 0.9510565162951535312, 1.000000000000000000, 0.9510565162951535312, 1.000000000000000000, 0.9510565162951535312, 1.000000000000000000, 0.9510565162951535312, 1.000000000000000000, 0.9510565162951535312, 1.000000000000000000, 0.9510565162951535312, 1.000000000000000000, 0.9510565162951535312, 1.000000000000000000, 0.9510565162951535312, 1.000000000000000000, 0.9510565162951535312, 1.000000000000000000, 0.9510565162951535312, 1.000000000000000000, 0.9510565162951535312, 1.000000000000000000, 0.9510565162951535312, 1.000000000000000000, 0.9510565162951535312, 1.000000000000000000, 0.9510565162951535312, 1.000000000000000000, 0.9510565162951535312, 1.000000000000000000, 0.9510565162951535312, 1.000000000000000000, 0.9510565162951535312, 1.000000000000000000, 0.9510565162951535312, 1.000000000000000000, 0.9510565162951535312, 1.000000000000000000, 0.9510565162951535312, 1.000000000000000000, 0.9510565162951535312, 1.000000000000000000, 0.9510565162951535312, 1.000000000000000000, 0.9510565162951535312, 1.000000000000000000, 0.9510565162951535312, 1.000000000000000000, 0.9510565162951535312, 1.000000000000000000, 0.9510565162951535312, 1.000000000000000000, 0.9510565162951535312, 1.000000000000000000, 0.9510565162951535312, 1.000000000000000000, 0.9510565162951535312, 1.000000000000000000, 0.9510565162951535312, 1.000000000000000000, 0.9510565162951535312, 1.000000000000000000, 0.9510565162951535312, 1.000000000000000000, 0.9510565162951535312, 1.000000000000000000) ) ) 
 REPRESENTATION_ITEM ( '' )  SURFACE ( )  );
#79456 = CARTESIAN_POINT ( 'NONE',  ( -13.89961937509977652, 13.97604488694528158, 30.62390960531435269 ) ) ;
#79457 = CARTESIAN_POINT ( 'NONE',  ( -13.89961937509977652, 13.97604488694528158, 90.62390960531432427 ) ) ;
#79459 = CARTESIAN_POINT ( 'NONE',  ( -29.86685920354755552, 21.69954338932564397, -2.824999997268813345 ) ) ;
#79458 = CARTESIAN_POINT ( 'NONE',  ( -12.14591786802326823, 12.06949235617739902, 38.12609039468567573 ) ) ;
#79460 = CARTESIAN_POINT ( 'NONE',  ( 9.564922557961047289, -16.46253265017146816, 30.41775706135232937 ) ) ;
#79461 = CARTESIAN_POINT ( 'NONE',  ( 0.05219959533934541429, -16.53943276465976808, 95.00109039468568994 ) ) ;
#79462 = CARTESIAN_POINT ( 'NONE',  ( 19.02544592524334988, 5.153800228976608722, 101.4594237280189759 ) ) ;
#79463 = CARTESIAN_POINT ( 'NONE',  ( 5.049401038298161559, -19.05341960407611168, 32.70724293864768129 ) ) ;
#79464 = CARTESIAN_POINT ( 'NONE',  ( -12.14591786802326823, 12.06949235617739902, 78.12609039468570415 ) ) ;
#79465 = CARTESIAN_POINT ( 'NONE',  ( -8.224510206698735004, -14.34966873604973081, 69.58442372801900433 ) ) ;
#79466 = CARTESIAN_POINT ( 'NONE',  ( 9.474510206698971260, -16.51473224551069308, 22.91557627198102765 ) ) ;
#79467 = CARTESIAN_POINT ( 'NONE',  ( -5.049401038297874678, -19.05341960407617918, 69.79275706135233293 ) ) ;
#79468 = CARTESIAN_POINT ( 'NONE',  ( 15.72974639402176855, 15.80617190586768217, 106.8760903946856899 ) ) ;
#79469 = CARTESIAN_POINT ( 'NONE',  ( -5.049401038298153566, 19.05341960407611168, 50.20724293864770260 ) ) ;
#79470 = AXIS2_PLACEMENT_3D ( 'NONE', #92592, #126900, #15771 ) ;
#79471 = CARTESIAN_POINT ( 'NONE',  ( -16.51473224551069308, -9.474510206698971260, 91.66557627198103830 ) ) ;
#79472 = CARTESIAN_POINT ( 'NONE',  ( -8.314922557960811034, -14.29746914071050412, 92.08224293864769550 ) ) ;
#79473 = EDGE_CURVE ( 'NONE', #71451, #194525, #125223, .T. ) ;
#79474 = CARTESIAN_POINT ( 'NONE',  ( -19.02544592524334988, -5.153800228976617603, 58.95942372801900433 ) ) ;
#79475 = CARTESIAN_POINT ( 'NONE',  ( -15.80617190586745835, -15.72974639402198527, 56.87390960531436690 ) ) ;
#79476 = CARTESIAN_POINT ( 'NONE',  ( 21.52544592524334988, 5.823673210054432836, 106.4594237280190328 ) ) ;
#79477 = CARTESIAN_POINT ( 'NONE',  ( -19.02544592524342804, 5.153800228976336051, 96.04057627198103830 ) ) ;
#79478 = CARTESIAN_POINT ( 'NONE',  ( -9.474510206698720793, -16.51473224551083518, 24.58442372801900078 ) ) ;
#79479 = CARTESIAN_POINT ( 'NONE',  ( -18.62759615963270932, 10.81492255796079327, 60.83224293864769550 ) ) ;
#79480 = CARTESIAN_POINT ( 'NONE',  ( 0.05219959533909260263, 19.03943276465977164, 104.9989096053143669 ) ) ;
#79481 = CARTESIAN_POINT ( 'NONE',  ( 19.03943276465977164, 0.05219959533936151252, 86.25109039468567573 ) ) ;
#79482 = CARTESIAN_POINT ( 'NONE',  ( -38.00000000000000711, 2.428612866367529932E-14, 0.000000000000000000 ) ) ;
#79483 = CARTESIAN_POINT ( 'NONE',  ( -5.049401038297874678, -19.05341960407617918, 104.7927570613523471 ) ) ;
#79484 = CARTESIAN_POINT ( 'NONE',  ( -14.29746914071049879, 8.314922557960819915, 110.8322429386476955 ) ) ;
#79485 = CARTESIAN_POINT ( 'NONE',  ( -5.049401038298153566, 19.05341960407611168, 100.2072429386476955 ) ) ;
#79486 = CARTESIAN_POINT ( 'NONE',  ( -0.05219959533907301413, -21.53943276465977519, 77.49890960531433848 ) ) ;
#79487 = CARTESIAN_POINT ( 'NONE',  ( 4.379528057220092307, 16.55341960407617563, 47.29275706135234003 ) ) ;
#79488 = CARTESIAN_POINT ( 'NONE',  ( 10.72451020669871369, 18.67979575497193778, 42.08442372801901854 ) ) ;
#79489 = CARTESIAN_POINT ( 'NONE',  ( 18.62759615963255655, 10.81492255796105972, 96.66775706135234714 ) ) ;
#79490 = CARTESIAN_POINT ( 'NONE',  ( 8.314922557961029526, -14.29746914071037800, 95.41775706135234714 ) ) ;
#79491 = CARTESIAN_POINT ( 'NONE',  ( 19.02544592524343514, -5.153800228976328945, 83.54057627198100988 ) ) ;
#79492 = CARTESIAN_POINT ( 'NONE',  ( 16.55341960407611168, 4.379528057220329451, 88.95724293864769550 ) ) ;
#79493 = CARTESIAN_POINT ( 'NONE',  ( -12.06949235617756955, 12.14591786802309770, 30.62390960531436335 ) ) ;
#79494 = CARTESIAN_POINT ( 'NONE',  ( -19.02544592524334988, -5.153800228976617603, 63.95942372801899012 ) ) ;
#79495 = CARTESIAN_POINT ( 'NONE',  ( 21.55341960407619695, -5.719274019375665929, 46.04275706135234714 ) ) ;
#79496 = CARTESIAN_POINT ( 'NONE',  ( -9.474510206698720793, -16.51473224551083518, 29.58442372801900433 ) ) ;
#79497 = CARTESIAN_POINT ( 'NONE',  ( 14.34966873604960469, 8.224510206698951720, 94.16557627198103830 ) ) ;
#79498 = CARTESIAN_POINT ( 'NONE',  ( 9.474510206698971260, -16.51473224551069308, 112.9155762719810383 ) ) ;
#79499 = CARTESIAN_POINT ( 'NONE',  ( 12.06949235617757843, -12.14591786802309237, 23.12390960531436335 ) ) ;
#79500 = CARTESIAN_POINT ( 'NONE',  ( -18.67979575497193778, 10.72451020669871902, 88.33442372801901854 ) ) ;
#79501 = CARTESIAN_POINT ( 'NONE',  ( -0.05219959533934338120, 16.53943276465976808, 57.50109039468568994 ) ) ;
#79502 = CARTESIAN_POINT ( 'NONE',  ( 16.53943276465976808, 0.05219959533934440121, 106.2510903946856757 ) ) ;
#79503 = CARTESIAN_POINT ( 'NONE',  ( 18.67979575497194134, -10.72451020669871369, 60.83442372801901854 ) ) ;
#79504 = CARTESIAN_POINT ( 'NONE',  ( 5.823673210054444382, -21.52544592524334988, 30.20942372801902565 ) ) ;
#79505 = CARTESIAN_POINT ( 'NONE',  ( -12.14591786802309592, -12.06949235617757132, 101.8739096053143811 ) ) ;
#79506 = CARTESIAN_POINT ( 'NONE',  ( -16.51473224551069308, -9.474510206698971260, 21.66557627198102765 ) ) ;
#79507 = CARTESIAN_POINT ( 'NONE',  ( 0.05219959533910956823, 16.53943276465976808, 59.99890960531436690 ) ) ;
#79508 = CARTESIAN_POINT ( 'NONE',  ( 13.97604488694527802, 13.89961937509977652, 69.37390960531436690 ) ) ;
#79509 = CARTESIAN_POINT ( 'NONE',  ( 16.55341960407618274, -4.379528057220086978, 111.0427570613523613 ) ) ;
#79510 = CARTESIAN_POINT ( 'NONE',  ( 10.81492255796078972, 18.62759615963270932, 59.58224293864770260 ) ) ;
#79511 = CARTESIAN_POINT ( 'NONE',  ( -16.55341960407611168, -4.379528057220339221, 96.45724293864770971 ) ) ;
#79512 = AXIS2_PLACEMENT_3D ( 'NONE', #155808, #61796, #125481 ) ;
#79513 = CARTESIAN_POINT ( 'NONE',  ( -10.72451020669898014, 18.67979575497178502, 95.41557627198102409 ) ) ;
#79514 = CARTESIAN_POINT ( 'NONE',  ( -9.474510206698964154, 16.51473224551069663, 105.4155762719810383 ) ) ;
#79516 = CARTESIAN_POINT ( 'NONE',  ( 16.51473224551083163, -9.474510206698727899, 90.83442372801900433 ) ) ;
#79515 = CARTESIAN_POINT ( 'NONE',  ( 13.89961937509977652, -13.97604488694527269, 53.12390960531434558 ) ) ;
#79517 = CARTESIAN_POINT ( 'NONE',  ( 21.52544592524344225, -5.823673210054117533, 48.54057627198103120 ) ) ;
#79518 = CARTESIAN_POINT ( 'NONE',  ( 10.72451020669871369, 18.67979575497193778, 62.08442372801901143 ) ) ;
#79519 = CARTESIAN_POINT ( 'NONE',  ( -5.153800228976328057, -19.02544592524343514, 47.29057627198102409 ) ) ;
#79520 = CARTESIAN_POINT ( 'NONE',  ( -0.05219959533909027116, -19.03943276465977164, 82.49890960531436690 ) ) ;
#79521 = CARTESIAN_POINT ( 'NONE',  ( -8.314922557961024197, 14.29746914071037800, 67.91775706135234714 ) ) ;
#79522 = CARTESIAN_POINT ( 'NONE',  ( 5.823673210054444382, -21.52544592524334988, 40.20942372801901854 ) ) ;
#79523 = CARTESIAN_POINT ( 'NONE',  ( -21.55341960407619339, 5.719274019375674811, 88.54275706135236135 ) ) ;
#79524 = CARTESIAN_POINT ( 'NONE',  ( 18.67979575497178502, 10.72451020669898547, 99.16557627198100988 ) ) ;
#79526 = CARTESIAN_POINT ( 'NONE',  ( 8.314922557961029526, -14.29746914071037800, 65.41775706135234714 ) ) ;
#79525 = CARTESIAN_POINT ( 'NONE',  ( -10.81492255796105439, 18.62759615963255655, 37.91775706135235424 ) ) ;
#79527 = CARTESIAN_POINT ( 'NONE',  ( 18.62759615963271287, -10.81492255796078972, 73.33224293864769550 ) ) ;
#79528 = CARTESIAN_POINT ( 'NONE',  ( 5.049401038297881783, 19.05341960407617563, 32.29275706135233293 ) ) ;
#79530 = CARTESIAN_POINT ( 'NONE',  ( 16.52544592524335698, 4.483927247898782831, 111.4594237280190328 ) ) ;
#79529 = CARTESIAN_POINT ( 'NONE',  ( -0.05219959533909027116, -19.03943276465977164, 62.49890960531435979 ) ) ;
#79531 = CARTESIAN_POINT ( 'NONE',  ( -17.49999999999999645, -3.345213924137415251, 105.4123137690565670 ) ) ;
#79532 = CARTESIAN_POINT ( 'NONE',  ( -5.049401038298153566, 19.05341960407611168, 105.2072429386476671 ) ) ;
#79533 = CARTESIAN_POINT ( 'NONE',  ( -3.573655867282028392E-15, 2.428612866367529932E-14, 139.9999999999999716 ) ) ;
#79534 = CARTESIAN_POINT ( 'NONE',  ( 16.51473224551083163, -9.474510206698727899, 85.83442372801900433 ) ) ;
#79535 = CARTESIAN_POINT ( 'NONE',  ( 10.81492255796078972, 18.62759615963270932, 54.58224293864769550 ) ) ;
#79536 = CARTESIAN_POINT ( 'NONE',  ( 14.29746914071049879, -8.314922557960816363, 33.33224293864769550 ) ) ;
#79537 = CARTESIAN_POINT ( 'NONE',  ( -0.05219959533936034679, 19.03943276465977164, 112.5010903946856757 ) ) ;
#79538 = CARTESIAN_POINT ( 'NONE',  ( 16.51473224551069308, 9.474510206698969483, 29.16557627198103475 ) ) ;
#79539 = CARTESIAN_POINT ( 'NONE',  ( -16.51473224551082808, 9.474510206698731452, 108.3344237280190043 ) ) ;
#79541 = CARTESIAN_POINT ( 'NONE',  ( 9.564922557961047289, -16.46253265017146816, 70.41775706135233293 ) ) ;
#79540 = CARTESIAN_POINT ( 'NONE',  ( -5.719274019375978568, 21.55341960407610458, 95.20724293864769550 ) ) ;
#79542 = CARTESIAN_POINT ( 'NONE',  ( 14.34966873604972726, -8.224510206698740333, 75.83442372801900433 ) ) ;
#79543 = CARTESIAN_POINT ( 'NONE',  ( -9.474510206698964154, 16.51473224551069663, 65.41557627198102409 ) ) ;
#79544 = CARTESIAN_POINT ( 'NONE',  ( -12.14591786802309592, -12.06949235617757132, 76.87390960531439532 ) ) ;
#79545 = CARTESIAN_POINT ( 'NONE',  ( 9.564922557960805705, 16.46253265017160317, 54.58224293864769550 ) ) ;
#79546 = CARTESIAN_POINT ( 'NONE',  ( -12.14591786802309592, -12.06949235617757132, 61.87390960531436690 ) ) ;
#79547 = CARTESIAN_POINT ( 'NONE',  ( 30.00000000000000000, 0.000000000000000000, 0.000000000000000000 ) ) ;
#79548 = CARTESIAN_POINT ( 'NONE',  ( -36.77116682341763010, -5.223593267096957149, 46.75914592492878796 ) ) ;
#79549 = CARTESIAN_POINT ( 'NONE',  ( -8.314922557960811034, -14.29746914071050412, 37.08224293864768129 ) ) ;
#79550 = CARTESIAN_POINT ( 'NONE',  ( 19.03943276465977164, -0.05219959533909143690, 78.74890960531436690 ) ) ;
#79551 = CARTESIAN_POINT ( 'NONE',  ( 11.30153831258470731, -180.0000000000000000, 0.000000000000000000 ) ) ;
#79552 = CARTESIAN_POINT ( 'NONE',  ( -13.89961937509957401, -13.97604488694547875, 39.37609039468566152 ) ) ;
#79553 = CARTESIAN_POINT ( 'NONE',  ( 16.52544592524335698, 4.483927247898782831, 51.45942372801901854 ) ) ;
#79554 = AXIS2_PLACEMENT_3D ( 'NONE', #50279, #157452, #140278 ) ;
#79555 = CARTESIAN_POINT ( 'NONE',  ( -5.823673210054116645, -21.52544592524344225, 62.29057627198102409 ) ) ;
#79556 = CARTESIAN_POINT ( 'NONE',  ( 16.46253265017146816, 9.564922557961045513, 21.66775706135233648 ) ) ;
#79557 = CARTESIAN_POINT ( 'NONE',  ( 0.05219959533909260263, 19.03943276465977164, 69.99890960531435269 ) ) ;
#79558 = DIRECTION ( 'NONE',  ( -0.000000000000000000, -0.000000000000000000, 1.000000000000000000 ) ) ;
#79559 = CARTESIAN_POINT ( 'NONE',  ( -9.474510206698964154, 16.51473224551069663, 105.4155762719810383 ) ) ;
#79560 = CARTESIAN_POINT ( 'NONE',  ( 0.05219959533937995610, -21.53943276465977519, 40.00109039468567573 ) ) ;
#79561 = AXIS2_PLACEMENT_3D ( 'NONE', #19423, #81070, #20402 ) ;
#79562 = CARTESIAN_POINT ( 'NONE',  ( -16.53943276465976808, 0.05219959533911058130, 101.2489096053143669 ) ) ;
#79565 = VERTEX_POINT ( 'NONE', #5840 ) ;
#79564 = CARTESIAN_POINT ( 'NONE',  ( -19.05341960407611168, -5.049401038298163336, 81.45724293864769550 ) ) ;
#79563 = CARTESIAN_POINT ( 'NONE',  ( 21.52544592524344225, -5.823673210054117533, 98.54057627198105251 ) ) ;
#79566 = CARTESIAN_POINT ( 'NONE',  ( 15.80617190586769283, -15.72974639402175789, 20.62609039468568639 ) ) ;
#79567 = ORIENTED_EDGE ( 'NONE', *, *, #34959, .T. ) ;
#79568 = CARTESIAN_POINT ( 'NONE',  ( -16.51473224551069308, -9.474510206698971260, 91.66557627198103830 ) ) ;
#79569 = CARTESIAN_POINT ( 'NONE',  ( 19.53037848336980531, -5.499999999999891642, 82.35532783611442653 ) ) ;
#79570 = CARTESIAN_POINT ( 'NONE',  ( 5.153800228976335163, 19.02544592524342804, 29.79057627198102409 ) ) ;
#79571 = CARTESIAN_POINT ( 'NONE',  ( 16.46253265017146816, 9.564922557961045513, 106.6677570613523471 ) ) ;
#79572 = CARTESIAN_POINT ( 'NONE',  ( 26.56065628307858262, 9.391201389438098346, 155.7923318601102380 ) ) ;
#79573 = CARTESIAN_POINT ( 'NONE',  ( 4.379528057220339221, -16.55341960407611168, 112.7072429386476955 ) ) ;
#79574 = CARTESIAN_POINT ( 'NONE',  ( -18.62759615963255300, -10.81492255796106328, 79.16775706135234714 ) ) ;
#79576 = CARTESIAN_POINT ( 'NONE',  ( -21.55341960407619339, 5.719274019375674811, 43.54275706135235424 ) ) ;
#79575 = CARTESIAN_POINT ( 'NONE',  ( 9.564922557960805705, 16.46253265017160317, 79.58224293864769550 ) ) ;
#79577 = CARTESIAN_POINT ( 'NONE',  ( 15.80617190586769283, -15.72974639402175789, 25.62609039468567929 ) ) ;
#79578 = CARTESIAN_POINT ( 'NONE',  ( -23.31738231874055245, -16.94106989632524574, 148.1999999999999886 ) ) ;
#79579 = CARTESIAN_POINT ( 'NONE',  ( -0.05219959533909027116, -19.03943276465977164, 92.49890960531436690 ) ) ;
#79580 = CARTESIAN_POINT ( 'NONE',  ( -2.996983800768426409, 28.38061290966174255, 139.9999999999999716 ) ) ;
#79582 = CARTESIAN_POINT ( 'NONE',  ( -5.719274019375978568, 21.55341960407610458, 40.20724293864769550 ) ) ;
#79581 = CARTESIAN_POINT ( 'NONE',  ( 16.53943276465976808, 0.05219959533934440121, 46.25109039468567573 ) ) ;
#79583 = CARTESIAN_POINT ( 'NONE',  ( 21.55341960407619695, -5.719274019375665929, 71.04275706135234714 ) ) ;
#79584 = DIRECTION ( 'NONE',  ( 0.000000000000000000, -1.000000000000000000, 0.000000000000000000 ) ) ;
#79585 = CARTESIAN_POINT ( 'NONE',  ( 19.05341960407617918, -5.049401038297876454, 106.0427570613523471 ) ) ;
#79586 = CARTESIAN_POINT ( 'NONE',  ( 9.564922557960805705, 16.46253265017160317, 54.58224293864769550 ) ) ;
#79587 = CARTESIAN_POINT ( 'NONE',  ( 19.03943276465977164, -0.05219959533909143690, 78.74890960531436690 ) ) ;
#79588 = CARTESIAN_POINT ( 'NONE',  ( -0.05219959533910754901, -16.53943276465976808, 112.4989096053143669 ) ) ;
#79589 = CARTESIAN_POINT ( 'NONE',  ( 4.483927247898545687, 16.52544592524342804, 104.7905762719810241 ) ) ;
#79590 = CARTESIAN_POINT ( 'NONE',  ( -19.05341960407611168, -5.049401038298163336, 106.4572429386476955 ) ) ;
#79591 = CARTESIAN_POINT ( 'NONE',  ( -8.224510206698735004, -14.34966873604973081, 79.58442372801903275 ) ) ;
#79593 = CARTESIAN_POINT ( 'NONE',  ( 13.89961937509977652, -13.97604488694527269, 58.12390960531436690 ) ) ;
#79592 = CARTESIAN_POINT ( 'NONE',  ( -14.29746914071049879, 8.314922557960819915, 60.83224293864769550 ) ) ;
#79594 = CARTESIAN_POINT ( 'NONE',  ( -10.81492255796105439, 18.62759615963255655, 77.91775706135231871 ) ) ;
#79595 = CARTESIAN_POINT ( 'NONE',  ( 10.72451020669871369, 18.67979575497193778, 72.08442372801899012 ) ) ;
#79596 = CARTESIAN_POINT ( 'NONE',  ( 5.153800228976615827, -19.02544592524334988, 110.2094237280189901 ) ) ;
#79597 = CARTESIAN_POINT ( 'NONE',  ( -16.52544592524342804, 4.483927247898546575, 61.04057627198103120 ) ) ;
#79598 = CARTESIAN_POINT ( 'NONE',  ( -18.62759615963270932, 10.81492255796079327, 110.8322429386476955 ) ) ;
#79599 = CARTESIAN_POINT ( 'NONE',  ( 15.80617190586746368, 15.72974639402197994, 54.37390960531435979 ) ) ;
#79600 = DIRECTION ( 'NONE',  ( -1.000000000000000000, 0.000000000000000000, 0.000000000000000000 ) ) ;
#79601 = CARTESIAN_POINT ( 'NONE',  ( -27.73933785331498925, 2.428612866367529932E-14, 148.8750000027311842 ) ) ;
#79602 = CARTESIAN_POINT ( 'NONE',  ( -9.564922557960796823, -16.46253265017161027, 67.08224293864769550 ) ) ;
#79603 = CARTESIAN_POINT ( 'NONE',  ( 12.14591786802309770, 12.06949235617756955, 39.37390960531436690 ) ) ;
#79604 = CARTESIAN_POINT ( 'NONE',  ( -8.314922557960811034, -14.29746914071050412, 27.08224293864769550 ) ) ;
#79605 = CARTESIAN_POINT ( 'NONE',  ( -0.05219959533934338120, 16.53943276465976808, 102.5010903946856899 ) ) ;
#79606 = CARTESIAN_POINT ( 'NONE',  ( -19.03943276465977164, -0.05219959533935918106, 58.75109039468566863 ) ) ;
#79607 = CARTESIAN_POINT ( 'NONE',  ( 23.48529157249599564, 32.32473071737754111, -8.700000000000002842 ) ) ;
#79608 = CARTESIAN_POINT ( 'NONE',  ( -19.05341960407611168, -5.049401038298163336, 91.45724293864766707 ) ) ;
#79609 = CARTESIAN_POINT ( 'NONE',  ( -8.314922557960811034, -14.29746914071050412, 62.08224293864769550 ) ) ;
#79610 = B_SPLINE_CURVE_WITH_KNOTS ( 'NONE', 3,
 ( #89046, #57731, #197240, #58701, #106195, #11232, #163917, #149731, #151721, #13214, #74877, #152695, #10228, #182064, #12236, #133558, #91009, #88043, #55719, #119401, #134575, #41565, #25413, #87055, #121363, #71888, #136539, #44540, #167879, #198220, #29378, #14184 ),
 .UNSPECIFIED., .F., .F.,
 ( 4, 2, 2, 2, 2, 2, 2, 2, 2, 2, 2, 2, 2, 2, 2, 4 ),
 ( 8.673617379884035472E-18, 0.0003712461730036821701, 0.0007424923460073556665, 0.001113738519011029217, 0.001484984692014702659, 0.002227477038022057567, 0.002598723211025738382, 0.002969969384029419197, 0.003341215557033099578, 0.003712461730036780826, 0.004083707903040461641, 0.004454954076044142022, 0.004826200249047823271, 0.005197446422051503652, 0.005568692595055184900, 0.005939938768058865282 ),
 .UNSPECIFIED. ) ;
#79612 = CARTESIAN_POINT ( 'NONE',  ( -10.81492255796078084, -18.62759615963271287, 22.08224293864769194 ) ) ;
#79611 = CARTESIAN_POINT ( 'NONE',  ( 18.09805431107520590, -5.500000000000095923, 48.51606229291890315 ) ) ;
#79614 = ORIENTED_EDGE ( 'NONE', *, *, #138961, .F. ) ;
#79613 = CARTESIAN_POINT ( 'NONE',  ( -18.62759615963270932, 10.81492255796079327, 50.83224293864770971 ) ) ;
#79615 = CARTESIAN_POINT ( 'NONE',  ( 12.14591786802309770, 12.06949235617756955, 94.37390960531436690 ) ) ;
#79616 = CARTESIAN_POINT ( 'NONE',  ( -8.314922557961024197, 14.29746914071037800, 52.91775706135235424 ) ) ;
#79617 = EDGE_CURVE ( 'NONE', #40993, #179372, #49375, .T. ) ;
#79618 = CARTESIAN_POINT ( 'NONE',  ( 12.06949235617757843, -12.14591786802309237, 78.12390960531436690 ) ) ;
#79619 = LINE ( 'NONE', #81575, #25293 ) ;
#79620 = CARTESIAN_POINT ( 'NONE',  ( -9.564922557961040184, 16.46253265017147172, 82.91775706135233293 ) ) ;
#79621 = CARTESIAN_POINT ( 'NONE',  ( 9.564922557960805705, 16.46253265017160317, 109.5822429386476955 ) ) ;
#79622 = CARTESIAN_POINT ( 'NONE',  ( -29.86685920354755552, 21.69954338932564397, -3.324999997268813345 ) ) ;
#79623 = CARTESIAN_POINT ( 'NONE',  ( -22.64734518408119612, 22.46606745562059970, -49.13275782002548198 ) ) ;
#79625 = CARTESIAN_POINT ( 'NONE',  ( 12.14591786802309770, 12.06949235617756955, 29.37390960531435269 ) ) ;
#79624 = CARTESIAN_POINT ( 'NONE',  ( -16.55341960407617563, 4.379528057220093196, 48.54275706135234714 ) ) ;
#79626 = CARTESIAN_POINT ( 'NONE',  ( -5.719274019375978568, 21.55341960407610458, 55.20724293864770260 ) ) ;
#79627 = CARTESIAN_POINT ( 'NONE',  ( -5.049401038297874678, -19.05341960407617918, 84.79275706135233293 ) ) ;
#79628 = CARTESIAN_POINT ( 'NONE',  ( -18.67979575497178146, -10.72451020669898902, 51.66557627198102409 ) ) ;
#79629 = CARTESIAN_POINT ( 'NONE',  ( 0.05219959533937995610, -21.53943276465977519, 80.00109039468568994 ) ) ;
#79630 = CARTESIAN_POINT ( 'NONE',  ( -11.42987701755558128, 9.408549014593454274, -62.15975709196302290 ) ) ;
#79631 = CARTESIAN_POINT ( 'NONE',  ( 14.29746914071037800, 8.314922557961029526, 31.66775706135234358 ) ) ;
#79633 = CARTESIAN_POINT ( 'NONE',  ( -5.049401038298153566, 19.05341960407611168, 100.2072429386476955 ) ) ;
#79632 = CARTESIAN_POINT ( 'NONE',  ( 9.474510206698971260, -16.51473224551069308, 42.91557627198103120 ) ) ;
#79634 = CARTESIAN_POINT ( 'NONE',  ( -16.46253265017160317, 9.564922557960807481, 40.83224293864769550 ) ) ;
#79635 = CARTESIAN_POINT ( 'NONE',  ( 4.483927247898545687, 16.52544592524342804, 104.7905762719810241 ) ) ;
#79636 = DIRECTION ( 'NONE',  ( 5.551115123125774690E-17, 9.714451465470120961E-17, -1.000000000000000000 ) ) ;
#79637 = CARTESIAN_POINT ( 'NONE',  ( 19.02544592524343514, -5.153800228976328945, 98.54057627198100988 ) ) ;
#79638 = VERTEX_POINT ( 'NONE', #144353 ) ;
#79639 = CARTESIAN_POINT ( 'NONE',  ( -8.314922557961024197, 14.29746914071037800, 52.91775706135235424 ) ) ;
#79640 = CARTESIAN_POINT ( 'NONE',  ( -15.72974639402197994, 15.80617190586746368, 90.62390960531436690 ) ) ;
#79641 = CARTESIAN_POINT ( 'NONE',  ( 5.049401038298161559, -19.05341960407611168, 42.70724293864767418 ) ) ;
#79642 = CARTESIAN_POINT ( 'NONE',  ( 21.53943276465977519, 0.05219959533937863772, 26.25109039468567573 ) ) ;
#79643 = CARTESIAN_POINT ( 'NONE',  ( 19.05341960407611168, 5.049401038298154454, 78.95724293864769550 ) ) ;
#79644 = CARTESIAN_POINT ( 'NONE',  ( 24.95432927374997334, 0.000000000000000000, 190.0000000000000000 ) ) ;
#79645 = EDGE_LOOP ( 'NONE', ( #14379, #119836, #126598, #131941, #24352, #87609, #56334, #26924 ) ) ;
#79646 = CARTESIAN_POINT ( 'NONE',  ( -8.224510206698735004, -14.34966873604973081, 49.58442372801901143 ) ) ;
#79647 = CARTESIAN_POINT ( 'NONE',  ( -18.67979575497178146, -10.72451020669898902, 111.6655762719810525 ) ) ;
#79650 = CARTESIAN_POINT ( 'NONE',  ( -16.46253265017146816, -9.564922557961047289, 69.16775706135233293 ) ) ;
#79649 = CARTESIAN_POINT ( 'NONE',  ( 9.474510206698971260, -16.51473224551069308, 97.91557627198102409 ) ) ;
#79648 = CARTESIAN_POINT ( 'NONE',  ( 16.53943276465976808, -0.05219959533910856209, 103.7489096053143669 ) ) ;
#79651 = CARTESIAN_POINT ( 'NONE',  ( -19.05341960407617563, 5.049401038297882671, 33.54275706135231871 ) ) ;
#79652 = CARTESIAN_POINT ( 'NONE',  ( 21.55341960407610458, 5.719274019375980345, 88.95724293864769550 ) ) ;
#79653 = CARTESIAN_POINT ( 'NONE',  ( 19.02544592524334988, 5.153800228976608722, 21.45942372801899012 ) ) ;
#79654 = CARTESIAN_POINT ( 'NONE',  ( -8.224510206698735004, -14.34966873604973081, 79.58442372801903275 ) ) ;
#79655 = CARTESIAN_POINT ( 'NONE',  ( -5.049401038298153566, 19.05341960407611168, 100.2072429386476955 ) ) ;
#79656 = CARTESIAN_POINT ( 'NONE',  ( 19.03943276465977164, -0.05219959533909143690, 58.74890960531435979 ) ) ;
#79657 = VECTOR ( 'NONE', #115786, 1000.000000000000000 ) ;
#79658 = CARTESIAN_POINT ( 'NONE',  ( 21.55341960407619695, -5.719274019375665929, 71.04275706135234714 ) ) ;
#79659 = CARTESIAN_POINT ( 'NONE',  ( -0.05219959533937732626, 21.53943276465977519, 67.50109039468568994 ) ) ;
#79660 = CARTESIAN_POINT ( 'NONE',  ( -19.05341960407611168, -5.049401038298163336, 76.45724293864769550 ) ) ;
#79661 = CARTESIAN_POINT ( 'NONE',  ( -15.80617190586768217, 15.72974639402176855, 53.12609039468568284 ) ) ;
#79662 = CARTESIAN_POINT ( 'NONE',  ( -13.97604488694547697, 13.89961937509957934, 93.12609039468566152 ) ) ;
#79663 = CARTESIAN_POINT ( 'NONE',  ( -13.89961937509977652, 13.97604488694528158, 50.62390960531435979 ) ) ;
#79664 = CARTESIAN_POINT ( 'NONE',  ( 0.05219959533909260263, 19.03943276465977164, 94.99890960531436690 ) ) ;
#79665 = CARTESIAN_POINT ( 'NONE',  ( 13.97604488694527802, 13.89961937509977652, 69.37390960531436690 ) ) ;
#79666 = CARTESIAN_POINT ( 'NONE',  ( -23.48298174826590667, 32.32155151706776053, -2.047842220587803297 ) ) ;
#79667 = CARTESIAN_POINT ( 'NONE',  ( 19.02544592524343514, -5.153800228976328945, 48.54057627198103120 ) ) ;
#79668 = CARTESIAN_POINT ( 'NONE',  ( 18.67979575497178502, 10.72451020669898547, 89.16557627198102409 ) ) ;
#79669 = CARTESIAN_POINT ( 'NONE',  ( 12.14591786802327356, -12.06949235617739191, 70.62609039468567573 ) ) ;
#79670 = CARTESIAN_POINT ( 'NONE',  ( -24.10180676228322483, 9.559744493757339256, 166.3058469464611164 ) ) ;
#79671 = CARTESIAN_POINT ( 'NONE',  ( -9.474510206698720793, -16.51473224551083518, 29.58442372801900433 ) ) ;
#79672 = CARTESIAN_POINT ( 'NONE',  ( -16.46253265017160317, 9.564922557960807481, 65.83224293864769550 ) ) ;
#79673 = CARTESIAN_POINT ( 'NONE',  ( -16.53943276465976808, 0.05219959533911058130, 56.24890960531436690 ) ) ;
#79674 = CARTESIAN_POINT ( 'NONE',  ( -16.53943276465976808, 0.05219959533911058130, 101.2489096053143669 ) ) ;
#79675 = CARTESIAN_POINT ( 'NONE',  ( -9.564922557960796823, -16.46253265017161027, 97.08224293864769550 ) ) ;
#79676 = CARTESIAN_POINT ( 'NONE',  ( -5.153800228976328057, -19.02544592524343514, 97.29057627198099567 ) ) ;
#79677 = CARTESIAN_POINT ( 'NONE',  ( 21.55341960407619695, -5.719274019375665929, 51.04275706135234714 ) ) ;
#79678 = CARTESIAN_POINT ( 'NONE',  ( 19.02544592524343514, -5.153800228976328945, 108.5405762719810383 ) ) ;
#79679 = CARTESIAN_POINT ( 'NONE',  ( 5.153800228976615827, -19.02544592524334988, 20.20942372801899722 ) ) ;
#79680 = CARTESIAN_POINT ( 'NONE',  ( -4.483927247898782831, 16.52544592524335698, 82.70942372801900433 ) ) ;
#79681 = B_SPLINE_CURVE_WITH_KNOTS ( 'NONE', 3,
 ( #48391, #34206, #171728, #143348, #50379, #33216, #96849, #4836, #95869, #18056, #81665, #20023, #175701, #128186, #112039, #94876, #157552, #173727, #19045, #98836 ),
 .UNSPECIFIED., .F., .F.,
 ( 4, 2, 2, 2, 2, 2, 2, 2, 2, 4 ),
 ( 0.004000878361811959112, 0.004499404418915953392, 0.004997930476019946805, 0.005496456533123941085, 0.005994982590227935365, 0.006244245618779932505, 0.006493508647331928778, 0.006992034704435923058, 0.007490560761539916471, 0.007989086818643910751 ),
 .UNSPECIFIED. ) ;
#79682 = CARTESIAN_POINT ( 'NONE',  ( 18.62759615963255655, 10.81492255796105972, 36.66775706135234714 ) ) ;
#79683 = CARTESIAN_POINT ( 'NONE',  ( -5.823673210054116645, -21.52544592524344225, 37.29057627198102409 ) ) ;
#79684 = CARTESIAN_POINT ( 'NONE',  ( 21.52544592524344225, -5.823673210054117533, 103.5405762719810383 ) ) ;
#79685 = CARTESIAN_POINT ( 'NONE',  ( -14.34966873604960291, -8.224510206698953496, 56.66557627198103830 ) ) ;
#79686 = CARTESIAN_POINT ( 'NONE',  ( 19.02544592524343514, -5.153800228976328945, 48.54057627198103120 ) ) ;
#79687 = CARTESIAN_POINT ( 'NONE',  ( -14.29746914071049879, 8.314922557960819915, 80.83224293864769550 ) ) ;
#79688 = CARTESIAN_POINT ( 'NONE',  ( 21.52544592524344225, -5.823673210054117533, 38.54057627198103120 ) ) ;
#79689 = CARTESIAN_POINT ( 'NONE',  ( 9.564922557961047289, -16.46253265017146816, 40.41775706135234003 ) ) ;
#79690 = CARTESIAN_POINT ( 'NONE',  ( 14.34966873604960469, 8.224510206698951720, 114.1655762719810383 ) ) ;
#79691 = ORIENTED_EDGE ( 'NONE', *, *, #156319, .F. ) ;
#79692 = CARTESIAN_POINT ( 'NONE',  ( -14.34966873604972548, 8.224510206698743886, 68.33442372801900433 ) ) ;
#79693 = CARTESIAN_POINT ( 'NONE',  ( 5.049401038298161559, -19.05341960407611168, 72.70724293864768129 ) ) ;
#79694 = CARTESIAN_POINT ( 'NONE',  ( -27.73933785331498925, 2.428612866367529932E-14, 144.8750000027311842 ) ) ;
#79695 = CARTESIAN_POINT ( 'NONE',  ( 4.483927247898545687, 16.52544592524342804, 89.79057627198103830 ) ) ;
#79696 = CARTESIAN_POINT ( 'NONE',  ( 10.72451020669898902, -18.67979575497178502, 37.91557627198102409 ) ) ;
#79697 = CARTESIAN_POINT ( 'NONE',  ( -4.483927247898782831, 16.52544592524335698, 107.7094237280190328 ) ) ;
#79698 = CARTESIAN_POINT ( 'NONE',  ( -13.97604488694547697, 13.89961937509957934, 113.1260903946856757 ) ) ;
#79699 = CARTESIAN_POINT ( 'NONE',  ( -21.52544592524334988, -5.823673210054445271, 78.95942372801901854 ) ) ;
#79700 = CARTESIAN_POINT ( 'NONE',  ( -19.03943276465977164, 0.05219959533909376836, 86.24890960531436690 ) ) ;
#79701 = CARTESIAN_POINT ( 'NONE',  ( -15.72974639402197994, 15.80617190586746368, 100.6239096053143811 ) ) ;
#79702 = CARTESIAN_POINT ( 'NONE',  ( 14.34966873604972726, -8.224510206698740333, 60.83442372801901854 ) ) ;
#79703 = CARTESIAN_POINT ( 'NONE',  ( -9.474510206698964154, 16.51473224551069663, 30.41557627198102054 ) ) ;
#79704 = AXIS2_PLACEMENT_3D ( 'NONE', #160679, #37331, #100993 ) ;
#79705 = CARTESIAN_POINT ( 'NONE',  ( 4.379528057220092307, 16.55341960407617563, 27.29275706135234358 ) ) ;
#79706 = EDGE_CURVE ( 'NONE', #101739, #103252, #111038, .T. ) ;
#79707 = CARTESIAN_POINT ( 'NONE',  ( -16.51473224551082808, 9.474510206698731452, 88.33442372801900433 ) ) ;
#79708 = CARTESIAN_POINT ( 'NONE',  ( 18.67979575497178502, 10.72451020669898547, 89.16557627198102409 ) ) ;
#79709 = CARTESIAN_POINT ( 'NONE',  ( -16.51473224551082808, 9.474510206698731452, 48.33442372801900433 ) ) ;
#79710 = CARTESIAN_POINT ( 'NONE',  ( 17.50000000000000000, -7.500000000000000888, 102.5000000000000142 ) ) ;
#79711 = CARTESIAN_POINT ( 'NONE',  ( -5.719274019375978568, 21.55341960407610458, 110.2072429386477239 ) ) ;
#79712 = CARTESIAN_POINT ( 'NONE',  ( -17.59860650958991002, -7.585241751807008548, 71.57662985737509587 ) ) ;
#79713 = CARTESIAN_POINT ( 'NONE',  ( -16.51473224551069308, -9.474510206698971260, 76.66557627198103830 ) ) ;
#79714 = CARTESIAN_POINT ( 'NONE',  ( 0.05219959533934541429, -16.53943276465976808, 30.00109039468568284 ) ) ;
#79715 = FACE_BOUND ( 'NONE', #82846, .T. ) ;
#79716 = CARTESIAN_POINT ( 'NONE',  ( 16.51473224551083163, -9.474510206698727899, 55.83442372801899722 ) ) ;
#79718 = CARTESIAN_POINT ( 'NONE',  ( -14.34966873604960291, -8.224510206698953496, 61.66557627198103120 ) ) ;
#79717 = CARTESIAN_POINT ( 'NONE',  ( 10.81492255796106328, -18.62759615963255655, 20.41775706135234714 ) ) ;
#79719 = CARTESIAN_POINT ( 'NONE',  ( -19.05341960407611168, -5.049401038298163336, 66.45724293864769550 ) ) ;
#79721 = CARTESIAN_POINT ( 'NONE',  ( 5.049401038297881783, 19.05341960407617563, 47.29275706135231161 ) ) ;
#79720 = CARTESIAN_POINT ( 'NONE',  ( -12.14591786802326823, 12.06949235617739902, 38.12609039468567573 ) ) ;
#79722 = CARTESIAN_POINT ( 'NONE',  ( -5.719274019375665041, -21.55341960407619695, 49.79275706135234714 ) ) ;
#79723 = CARTESIAN_POINT ( 'NONE',  ( -19.03943276465977164, -0.05219959533935918106, 113.7510903946856757 ) ) ;
#79724 = CARTESIAN_POINT ( 'NONE',  ( 13.97604488694527802, 13.89961937509977652, 59.37390960531434558 ) ) ;
#79725 = CARTESIAN_POINT ( 'NONE',  ( -16.51473224551082808, 9.474510206698731452, 88.33442372801900433 ) ) ;
#79726 = CARTESIAN_POINT ( 'NONE',  ( -18.67979575497193778, 10.72451020669871902, 93.33442372801901854 ) ) ;
#79727 = CARTESIAN_POINT ( 'NONE',  ( -9.564922557961040184, 16.46253265017147172, 67.91775706135233293 ) ) ;
#79728 = CARTESIAN_POINT ( 'NONE',  ( 16.51473224551069308, 9.474510206698969483, 39.16557627198103120 ) ) ;
#79729 = CARTESIAN_POINT ( 'NONE',  ( -18.62759615963270932, 10.81492255796079327, 75.83224293864769550 ) ) ;
#79731 = CARTESIAN_POINT ( 'NONE',  ( -5.049401038297874678, -19.05341960407617918, 64.79275706135233293 ) ) ;
#79730 = CARTESIAN_POINT ( 'NONE',  ( 8.314922557960818139, 14.29746914071049879, 59.58224293864770260 ) ) ;
#79732 = CARTESIAN_POINT ( 'NONE',  ( -16.81555441253554051, -7.025013491695444756, 24.36314554665744225 ) ) ;
#79733 = CARTESIAN_POINT ( 'NONE',  ( 0.05219959533936267826, -19.03943276465977164, 25.00109039468566152 ) ) ;
#79734 = CARTESIAN_POINT ( 'NONE',  ( -0.05219959533934338120, 16.53943276465976808, 92.50109039468567573 ) ) ;
#79735 = CARTESIAN_POINT ( 'NONE',  ( -16.55341960407611168, -4.379528057220339221, 56.45724293864768839 ) ) ;
#79737 = CARTESIAN_POINT ( 'NONE',  ( -27.73933785331498925, 9.013057229001089965, 140.7750000027311899 ) ) ;
#79736 = CARTESIAN_POINT ( 'NONE',  ( 5.823673210054444382, -21.52544592524334988, 85.20942372801901854 ) ) ;
#79738 = CARTESIAN_POINT ( 'NONE',  ( 10.81492255796078972, 18.62759615963270932, 99.58224293864770971 ) ) ;
#79739 = CARTESIAN_POINT ( 'NONE',  ( 5.049401038298161559, -19.05341960407611168, 57.70724293864769550 ) ) ;
#79740 = CARTESIAN_POINT ( 'NONE',  ( 0.05219959533937995610, -21.53943276465977519, 70.00109039468568994 ) ) ;
#79741 = CARTESIAN_POINT ( 'NONE',  ( 13.97604488694527802, 13.89961937509977652, 49.37390960531434558 ) ) ;
#79742 = ORIENTED_EDGE ( 'NONE', *, *, #104490, .F. ) ;
#79743 = CARTESIAN_POINT ( 'NONE',  ( -16.51473224551069308, -9.474510206698971260, 66.66557627198102409 ) ) ;
#79744 = CARTESIAN_POINT ( 'NONE',  ( -4.379528057220328563, 16.55341960407611168, 100.2072429386476955 ) ) ;
#79745 = CARTESIAN_POINT ( 'NONE',  ( 16.51473224551069308, 9.474510206698969483, 109.1655762719810383 ) ) ;
#79746 = CARTESIAN_POINT ( 'NONE',  ( -12.14591786802309592, -12.06949235617757132, 51.87390960531437401 ) ) ;
#79747 = CARTESIAN_POINT ( 'NONE',  ( 13.97604488694527802, 13.89961937509977652, 34.37390960531436690 ) ) ;
#79748 = CARTESIAN_POINT ( 'NONE',  ( 14.29746914071049879, -8.314922557960816363, 78.33224293864770971 ) ) ;
#79749 = CARTESIAN_POINT ( 'NONE',  ( 18.67979575497178502, 10.72451020669898547, 99.16557627198100988 ) ) ;
#79750 = CARTESIAN_POINT ( 'NONE',  ( 5.823673210054444382, -21.52544592524334988, 30.20942372801902565 ) ) ;
#79751 = CARTESIAN_POINT ( 'NONE',  ( 27.96122637818066181, -7.045120623242188351, 161.2893955982186185 ) ) ;
#79752 = CARTESIAN_POINT ( 'NONE',  ( -12.14591786802326823, 12.06949235617739902, 53.12609039468568284 ) ) ;
#79753 = CARTESIAN_POINT ( 'NONE',  ( -5.719274019375978568, 21.55341960407610458, 80.20724293864769550 ) ) ;
#79754 = CARTESIAN_POINT ( 'NONE',  ( -15.80617190586768217, 15.72974639402176855, 108.1260903946856757 ) ) ;
#79755 = CARTESIAN_POINT ( 'NONE',  ( -19.02544592524342804, 5.153800228976336051, 106.0405762719810241 ) ) ;
#79756 = CARTESIAN_POINT ( 'NONE',  ( -0.05219959533937732626, 21.53943276465977519, 37.50109039468568284 ) ) ;
#79757 = CARTESIAN_POINT ( 'NONE',  ( -10.81492255796078084, -18.62759615963271287, 37.08224293864768129 ) ) ;
#79758 = CARTESIAN_POINT ( 'NONE',  ( 8.224510206698742110, 14.34966873604972548, 97.08442372801904696 ) ) ;
#79760 = CARTESIAN_POINT ( 'NONE',  ( 10.81492255796106328, -18.62759615963255655, 85.41775706135236135 ) ) ;
#79759 = CARTESIAN_POINT ( 'NONE',  ( 10.72451020669871369, 18.67979575497193778, 67.08442372801901854 ) ) ;
#79761 = CARTESIAN_POINT ( 'NONE',  ( -9.564922557961040184, 16.46253265017147172, 27.91775706135232582 ) ) ;
#79762 = CARTESIAN_POINT ( 'NONE',  ( 12.14591786802327356, -12.06949235617739191, 90.62609039468567573 ) ) ;
#79763 = CARTESIAN_POINT ( 'NONE',  ( 10.81492255796106328, -18.62759615963255655, 35.41775706135234003 ) ) ;
#79764 = CARTESIAN_POINT ( 'NONE',  ( 0.05219959533909260263, 19.03943276465977164, 44.99890960531435979 ) ) ;
#79765 = CARTESIAN_POINT ( 'NONE',  ( 10.81492255796106328, -18.62759615963255655, 105.4177570613523613 ) ) ;
#79766 = CARTESIAN_POINT ( 'NONE',  ( 15.72974639402199770, -15.80617190586745480, 23.12390960531436335 ) ) ;
#79767 = B_SPLINE_CURVE_WITH_KNOTS ( 'NONE', 3,
 ( #153158, #138982, #94463, #170325, #460, #32812, #187507, #109641, #1457, #14659, #15655, #140971, #137997, #199681, #171324, #2459, #77314, #61146, #188487, #17642, #64141, #108647 ),
 .UNSPECIFIED., .F., .F.,
 ( 4, 2, 2, 2, 2, 2, 2, 2, 2, 2, 4 ),
 ( 0.000000000000000000, 0.005439051211804343464, 0.01087810242360868693, 0.01359762802951085953, 0.01631715363541303213, 0.02175620484721737039, 0.02719525605902171211, 0.03263430727082605037, 0.03807335848263039557, 0.04079288408853257164, 0.04351240969443474077 ),
 .UNSPECIFIED. ) ;
#79768 = CARTESIAN_POINT ( 'NONE',  ( -10.72451020669870658, -18.67979575497194134, 24.58442372801901499 ) ) ;
#79769 = CARTESIAN_POINT ( 'NONE',  ( 10.72451020669898902, -18.67979575497178502, 77.91557627198102409 ) ) ;
#79771 = CARTESIAN_POINT ( 'NONE',  ( 5.823673210054125526, 21.52544592524343514, 69.79057627198102409 ) ) ;
#79770 = CARTESIAN_POINT ( 'NONE',  ( 5.000000000000000000, -116.8122400552013431, 54.87277500418469600 ) ) ;
#79773 = CARTESIAN_POINT ( 'NONE',  ( 16.55341960407611168, 4.379528057220329451, 58.95724293864770971 ) ) ;
#79772 = CARTESIAN_POINT ( 'NONE',  ( -16.55341960407617563, 4.379528057220093196, 58.54275706135235424 ) ) ;
#79774 = CARTESIAN_POINT ( 'NONE',  ( 21.54612633733962568, 7.439814990119595350, 174.3585332542395463 ) ) ;
#79775 = CARTESIAN_POINT ( 'NONE',  ( 5.153800228976615827, -19.02544592524334988, 95.20942372801897591 ) ) ;
#79776 = CARTESIAN_POINT ( 'NONE',  ( -21.53159096656795768, 0.8285391498305729741, -56.30101842015761804 ) ) ;
#79777 = CARTESIAN_POINT ( 'NONE',  ( -16.55341960407617563, 4.379528057220093196, 23.54275706135235424 ) ) ;
#79778 = CARTESIAN_POINT ( 'NONE',  ( 10.72451020669898902, -18.67979575497178502, 97.91557627198103830 ) ) ;
#79779 = CARTESIAN_POINT ( 'NONE',  ( 21.52544592524344225, -5.823673210054117533, 78.54057627198103830 ) ) ;
#79780 = CARTESIAN_POINT ( 'NONE',  ( 5.153800228976335163, 19.02544592524342804, 114.7905762719810241 ) ) ;
#79781 = CARTESIAN_POINT ( 'NONE',  ( -16.53943276465976808, -0.05219959533934237506, 53.75109039468568994 ) ) ;
#79782 = CARTESIAN_POINT ( 'NONE',  ( -13.89961937509977652, 13.97604488694528158, 65.62390960531436690 ) ) ;
#79784 = CARTESIAN_POINT ( 'NONE',  ( 19.05341960407617918, -5.049401038297876454, 111.0427570613523329 ) ) ;
#79783 = CARTESIAN_POINT ( 'NONE',  ( -21.53943276465977519, -0.05219959533937600094, 38.75109039468567573 ) ) ;
#79785 = CARTESIAN_POINT ( 'NONE',  ( 13.89961937509977652, -13.97604488694527269, 103.1239096053143527 ) ) ;
#79786 = CARTESIAN_POINT ( 'NONE',  ( 5.153800228976615827, -19.02544592524334988, 30.20942372801900433 ) ) ;
#79787 = CARTESIAN_POINT ( 'NONE',  ( -5.049401038298153566, 19.05341960407611168, 105.2072429386476671 ) ) ;
#79788 = CARTESIAN_POINT ( 'NONE',  ( 21.55341960407610458, 5.719274019375980345, 103.9572429386476813 ) ) ;
#79789 = CARTESIAN_POINT ( 'NONE',  ( 16.46253265017160672, -9.564922557960803928, 63.33224293864769550 ) ) ;
#79790 = CARTESIAN_POINT ( 'NONE',  ( 2.400000000000000799, 0.000000000000000000, 0.000000000000000000 ) ) ;
#79791 = CARTESIAN_POINT ( 'NONE',  ( -16.55341960407611168, -4.379528057220339221, 76.45724293864769550 ) ) ;
#79792 = CARTESIAN_POINT ( 'NONE',  ( -9.474510206698964154, 16.51473224551069663, 110.4155762719810383 ) ) ;
#79793 = CARTESIAN_POINT ( 'NONE',  ( 0.05219959533909260263, 19.03943276465977164, 24.99890960531435269 ) ) ;
#79794 = CARTESIAN_POINT ( 'NONE',  ( -10.72451020669898014, 18.67979575497178502, 100.4155762719810241 ) ) ;
#79795 = CARTESIAN_POINT ( 'NONE',  ( 19.02544592524334988, 5.153800228976608722, 66.45942372801899012 ) ) ;
#79796 = CARTESIAN_POINT ( 'NONE',  ( 9.474510206698971260, -16.51473224551069308, 112.9155762719810383 ) ) ;
#79797 = CARTESIAN_POINT ( 'NONE',  ( -19.02544592524342804, 5.153800228976336051, 31.04057627198102409 ) ) ;
#79798 = CARTESIAN_POINT ( 'NONE',  ( -21.53943276465977519, 0.05219959533907696930, 56.24890960531436690 ) ) ;
#79799 = CIRCLE ( 'NONE', #186482, 38.00000000000000000 ) ;
#79800 = CARTESIAN_POINT ( 'NONE',  ( 5.049401038298161559, -19.05341960407611168, 97.70724293864766707 ) ) ;
#79801 = CARTESIAN_POINT ( 'NONE',  ( -5.823673210054431948, 21.52544592524334988, 72.70942372801901854 ) ) ;
#79802 = CARTESIAN_POINT ( 'NONE',  ( 16.51473224551069308, 9.474510206698969483, 54.16557627198103120 ) ) ;
#79803 = CARTESIAN_POINT ( 'NONE',  ( 12.06949235617757843, -12.14591786802309237, 88.12390960531436690 ) ) ;
#79804 = CARTESIAN_POINT ( 'NONE',  ( -12.06949235617739369, -12.14591786802326823, 39.37609039468567573 ) ) ;
#79805 = CARTESIAN_POINT ( 'NONE',  ( 18.62759615963255655, 10.81492255796105972, 61.66775706135235424 ) ) ;
#79806 = ORIENTED_EDGE ( 'NONE', *, *, #186365, .F. ) ;
#79807 = CARTESIAN_POINT ( 'NONE',  ( 19.05341960407617918, -5.049401038297876454, 31.04275706135232227 ) ) ;
#79808 = CARTESIAN_POINT ( 'NONE',  ( -19.03943276465977164, -0.05219959533935918106, 83.75109039468567573 ) ) ;
#79809 = CARTESIAN_POINT ( 'NONE',  ( -19.05341960407617563, 5.049401038297882671, 38.54275706135233293 ) ) ;
#79810 = CARTESIAN_POINT ( 'NONE',  ( 28.82186960331498327, 2.781578969918950771E-14, 147.2500000054623683 ) ) ;
#79811 = CARTESIAN_POINT ( 'NONE',  ( -18.67979575497193778, 10.72451020669871902, 38.33442372801900433 ) ) ;
#79812 = AXIS2_PLACEMENT_3D ( 'NONE', #184500, #157136, #199672 ) ;
#79813 = ADVANCED_FACE ( 'NONE', ( #126210 ), #156556, .T. ) ;
#79814 = CARTESIAN_POINT ( 'NONE',  ( 23.48529157249599919, 32.32473071737754111, -2.449999994537626069 ) ) ;
#79815 = CARTESIAN_POINT ( 'NONE',  ( -5.153800228976607833, 19.02544592524334988, 32.70942372801899722 ) ) ;
#79816 = CARTESIAN_POINT ( 'NONE',  ( -13.89961937509977652, 13.97604488694528158, 65.62390960531436690 ) ) ;
#79817 = CARTESIAN_POINT ( 'NONE',  ( -16.55341960407617563, 4.379528057220093196, 113.5427570613523756 ) ) ;
#79819 = CARTESIAN_POINT ( 'NONE',  ( -18.62759615963255300, -10.81492255796106328, 89.16775706135236135 ) ) ;
#79818 = CARTESIAN_POINT ( 'NONE',  ( 0.05219959533907565091, 21.53943276465977519, 24.99890960531435624 ) ) ;
#79820 = CARTESIAN_POINT ( 'NONE',  ( -5.950531402560715689E-15, 38.81732327939063509, -7.124999997268814944 ) ) ;
#79821 = CARTESIAN_POINT ( 'NONE',  ( -17.50000000000002487, -3.805241302050037522, 34.62647527217417576 ) ) ;
#79822 = CARTESIAN_POINT ( 'NONE',  ( 5.719274019375673035, 21.55341960407619339, 82.29275706135234714 ) ) ;
#79823 = CARTESIAN_POINT ( 'NONE',  ( -30.73962218707677962, -22.33364281372842441, -3.547842220587803297 ) ) ;
#79824 = CARTESIAN_POINT ( 'NONE',  ( 9.564922557960805705, 16.46253265017160317, 99.58224293864770971 ) ) ;
#79825 = ADVANCED_FACE ( 'NONE', ( #127187 ), #129173, .F. ) ;
#79826 = CARTESIAN_POINT ( 'NONE',  ( 31.73029476377072555, -20.92000799991017246, -24.48145274275710292 ) ) ;
#79827 = CARTESIAN_POINT ( 'NONE',  ( -9.474510206698964154, 16.51473224551069663, 55.41557627198103120 ) ) ;
#79828 = CARTESIAN_POINT ( 'NONE',  ( -18.62759615963270932, 10.81492255796079327, 50.83224293864770971 ) ) ;
#79829 = CARTESIAN_POINT ( 'NONE',  ( -0.05219959533910754901, -16.53943276465976808, 27.49890960531435269 ) ) ;
#79831 = CARTESIAN_POINT ( 'NONE',  ( -13.89961937509977652, 13.97604488694528158, 90.62390960531432427 ) ) ;
#79830 = CARTESIAN_POINT ( 'NONE',  ( 12.14591786802309770, 12.06949235617756955, 109.3739096053143811 ) ) ;
#79832 = CARTESIAN_POINT ( 'NONE',  ( 19.03943276465977164, 0.05219959533936151252, 21.25109039468565797 ) ) ;
#79833 = CARTESIAN_POINT ( 'NONE',  ( -16.55341960407611168, -4.379528057220339221, 96.45724293864770971 ) ) ;
#79834 = CARTESIAN_POINT ( 'NONE',  ( 5.823673210054444382, -21.52544592524334988, 65.20942372801901854 ) ) ;
#79835 = CARTESIAN_POINT ( 'NONE',  ( 19.03943276465977164, -0.05219959533909143690, 113.7489096053143669 ) ) ;
#79836 = CARTESIAN_POINT ( 'NONE',  ( 4.379528057220092307, 16.55341960407617563, 102.2927570613523613 ) ) ;
#79837 = CARTESIAN_POINT ( 'NONE',  ( -5.049401038297874678, -19.05341960407617918, 64.79275706135233293 ) ) ;
#79838 = CARTESIAN_POINT ( 'NONE',  ( 29.86685920354754487, 21.69954338932564752, -5.924999997268813878 ) ) ;
#79839 = CARTESIAN_POINT ( 'NONE',  ( 5.153800228976335163, 19.02544592524342804, 114.7905762719810241 ) ) ;
#79840 = CARTESIAN_POINT ( 'NONE',  ( -4.483927247898539470, -16.52544592524342804, 82.29057627198103830 ) ) ;
#79841 = CARTESIAN_POINT ( 'NONE',  ( -5.153800228976607833, 19.02544592524334988, 62.70942372801899722 ) ) ;
#79842 = VECTOR ( 'NONE', #41271, 1000.000000000000000 ) ;
#79843 = CARTESIAN_POINT ( 'NONE',  ( -5.049401038298153566, 19.05341960407611168, 60.20724293864768129 ) ) ;
#79844 = CARTESIAN_POINT ( 'NONE',  ( -4.483927247898539470, -16.52544592524342804, 62.29057627198102409 ) ) ;
#79845 = CARTESIAN_POINT ( 'NONE',  ( 5.049401038297881783, 19.05341960407617563, 87.29275706135234714 ) ) ;
#79846 = CARTESIAN_POINT ( 'NONE',  ( -10.72451020669898014, 18.67979575497178502, 50.41557627198103120 ) ) ;
#79847 = ORIENTED_EDGE ( 'NONE', *, *, #192729, .T. ) ;
#79848 = CARTESIAN_POINT ( 'NONE',  ( 0.05219959533909260263, 19.03943276465977164, 24.99890960531435269 ) ) ;
#79849 = CARTESIAN_POINT ( 'NONE',  ( -16.38665767535053064, -7.295008042176051255, 29.73599135785456227 ) ) ;
#79851 = CARTESIAN_POINT ( 'NONE',  ( 18.67979575497178502, 10.72451020669898547, 59.16557627198103120 ) ) ;
#79850 = CARTESIAN_POINT ( 'NONE',  ( -13.89961937509977652, 13.97604488694528158, 60.62390960531436690 ) ) ;
#79853 = CARTESIAN_POINT ( 'NONE',  ( 0.05219959533909260263, 19.03943276465977164, 69.99890960531435269 ) ) ;
#79852 = CARTESIAN_POINT ( 'NONE',  ( -14.34966873604972548, 8.224510206698743886, 88.33442372801901854 ) ) ;
#79855 = EDGE_CURVE ( 'NONE', #133811, #120648, #79681, .T. ) ;
#79854 = CARTESIAN_POINT ( 'NONE',  ( -9.564922557961040184, 16.46253265017147172, 47.91775706135233293 ) ) ;
#79856 = CARTESIAN_POINT ( 'NONE',  ( 21.53943276465977519, 0.05219959533937863772, 81.25109039468568994 ) ) ;
#79857 = CARTESIAN_POINT ( 'NONE',  ( 10.81492255796078972, 18.62759615963270932, 64.58224293864769550 ) ) ;
#79858 = CARTESIAN_POINT ( 'NONE',  ( -16.51473224551069308, -9.474510206698971260, 101.6655762719810241 ) ) ;
#79859 = CARTESIAN_POINT ( 'NONE',  ( 19.02544592524343514, -5.153800228976328945, 38.54057627198103120 ) ) ;
#79860 = CARTESIAN_POINT ( 'NONE',  ( 14.34966873604972726, -8.224510206698740333, 90.83442372801901854 ) ) ;
#79861 = CARTESIAN_POINT ( 'NONE',  ( 9.474510206698729675, 16.51473224551082808, 112.0844237280190043 ) ) ;
#79862 = CARTESIAN_POINT ( 'NONE',  ( 1.300000000000000044, -0.7216878364870319418, 1.249999999999999778 ) ) ;
#79863 = CARTESIAN_POINT ( 'NONE',  ( -15.72974639402176322, -15.80617190586768395, 99.37609039468568994 ) ) ;
#79864 = CARTESIAN_POINT ( 'NONE',  ( -12.14591786802309592, -12.06949235617757132, 61.87390960531436690 ) ) ;
#79865 = CARTESIAN_POINT ( 'NONE',  ( -8.314922557960811034, -14.29746914071050412, 67.08224293864770971 ) ) ;
#79866 = CARTESIAN_POINT ( 'NONE',  ( 5.823673210054125526, 21.52544592524343514, 99.79057627198103830 ) ) ;
#79867 = CARTESIAN_POINT ( 'NONE',  ( 21.55341960407610458, 5.719274019375980345, 83.95724293864770971 ) ) ;
#79868 = CARTESIAN_POINT ( 'NONE',  ( 17.40861289039002457, -6.110651285853308856, 96.12767529172566583 ) ) ;
#79869 = CARTESIAN_POINT ( 'NONE',  ( -18.67979575497178146, -10.72451020669898902, 51.66557627198102409 ) ) ;
#79870 = CARTESIAN_POINT ( 'NONE',  ( -8.224510206698735004, -14.34966873604973081, 64.58442372801900433 ) ) ;
#79871 = CARTESIAN_POINT ( 'NONE',  ( -16.53943276465976808, 0.05219959533911058130, 96.24890960531435269 ) ) ;
#79872 = CARTESIAN_POINT ( 'NONE',  ( -16.51473224551069308, -9.474510206698971260, 46.66557627198102409 ) ) ;
#79873 = CARTESIAN_POINT ( 'NONE',  ( 34.41611627805853857, -6.381310488372548662, 48.94841969467694298 ) ) ;
#79874 = CARTESIAN_POINT ( 'NONE',  ( -14.34966873604972548, 8.224510206698743886, 93.33442372801901854 ) ) ;
#79875 = CARTESIAN_POINT ( 'NONE',  ( -18.67979575497193778, 10.72451020669871902, 38.33442372801900433 ) ) ;
#79876 = CARTESIAN_POINT ( 'NONE',  ( -16.46253265017160317, 9.564922557960807481, 85.83224293864769550 ) ) ;
#79877 = CARTESIAN_POINT ( 'NONE',  ( 21.53943276465977519, 0.05219959533937863772, 61.25109039468567573 ) ) ;
#79878 = FACE_OUTER_BOUND ( 'NONE', #29669, .T. ) ;
#79879 = CARTESIAN_POINT ( 'NONE',  ( 5.153800228976335163, 19.02544592524342804, 29.79057627198102409 ) ) ;
#79880 = ORIENTED_EDGE ( 'NONE', *, *, #75962, .F. ) ;
#79881 = CARTESIAN_POINT ( 'NONE',  ( 10.81492255796106328, -18.62759615963255655, 65.41775706135234714 ) ) ;
#79882 = CARTESIAN_POINT ( 'NONE',  ( 5.049401038298161559, -19.05341960407611168, 32.70724293864768129 ) ) ;
#79883 = CARTESIAN_POINT ( 'NONE',  ( -13.97604488694527625, -13.89961937509977652, 91.87390960531432427 ) ) ;
#79884 = CARTESIAN_POINT ( 'NONE',  ( -13.97604488694547697, 13.89961937509957934, 68.12609039468563310 ) ) ;
#79885 = CARTESIAN_POINT ( 'NONE',  ( -5.719274019375665041, -21.55341960407619695, 24.79275706135235779 ) ) ;
#79886 = CARTESIAN_POINT ( 'NONE',  ( -5.049401038297874678, -19.05341960407617918, 54.79275706135234003 ) ) ;
#79887 = CARTESIAN_POINT ( 'NONE',  ( -19.03943276465977164, 0.05219959533909376836, 36.24890960531436690 ) ) ;
#79888 = CARTESIAN_POINT ( 'NONE',  ( -16.53943276465976808, -0.05219959533934237506, 98.75109039468568994 ) ) ;
#79889 = CARTESIAN_POINT ( 'NONE',  ( -5.049401038297874678, -19.05341960407617918, 69.79275706135233293 ) ) ;
#79890 = CARTESIAN_POINT ( 'NONE',  ( -16.55341960407611168, -4.379528057220339221, 26.45724293864768839 ) ) ;
#79891 = CARTESIAN_POINT ( 'NONE',  ( -0.05219959533936034679, 19.03943276465977164, 52.50109039468566863 ) ) ;
#79892 = CARTESIAN_POINT ( 'NONE',  ( 19.02544592524343514, -5.153800228976328945, 103.5405762719809957 ) ) ;
#79893 = CARTESIAN_POINT ( 'NONE',  ( -21.53943276465977519, -0.05219959533937600094, 108.7510903946857042 ) ) ;
#79894 = CARTESIAN_POINT ( 'NONE',  ( -5.823673210054431948, 21.52544592524334988, 112.7094237280190328 ) ) ;
#79895 = CARTESIAN_POINT ( 'NONE',  ( 5.049401038298161559, -19.05341960407611168, 27.70724293864769550 ) ) ;
#79896 = CARTESIAN_POINT ( 'NONE',  ( -5.719274019375665041, -21.55341960407619695, 89.79275706135236135 ) ) ;
#79897 = CARTESIAN_POINT ( 'NONE',  ( -16.52544592524335698, -4.483927247898792601, 33.95942372801901143 ) ) ;
#79898 = CARTESIAN_POINT ( 'NONE',  ( 13.89961937509977652, -13.97604488694527269, 93.12390960531436690 ) ) ;
#79899 = CARTESIAN_POINT ( 'NONE',  ( 37.99999999999999289, 2.893978650043524126E-14, -8.749999994537628112 ) ) ;
#79900 = CARTESIAN_POINT ( 'NONE',  ( 9.564922557960805705, 16.46253265017160317, 74.58224293864769550 ) ) ;
#79901 = LINE ( 'NONE', #64737, #120105 ) ;
#79902 = CARTESIAN_POINT ( 'NONE',  ( 5.153800228976615827, -19.02544592524334988, 65.20942372801900433 ) ) ;
#79903 = CARTESIAN_POINT ( 'NONE',  ( -19.02544592524342804, 5.153800228976336051, 111.0405762719810099 ) ) ;
#79904 = CARTESIAN_POINT ( 'NONE',  ( 18.67979575497194134, -10.72451020669871369, 95.83442372801903275 ) ) ;
#79905 = CARTESIAN_POINT ( 'NONE',  ( 4.379528057220339221, -16.55341960407611168, 102.7072429386476955 ) ) ;
#79906 = CARTESIAN_POINT ( 'NONE',  ( 21.55341960407610458, 5.719274019375980345, 48.95724293864770971 ) ) ;
#79907 = CARTESIAN_POINT ( 'NONE',  ( 5.823673210054125526, 21.52544592524343514, 34.79057627198103120 ) ) ;
#79908 = CARTESIAN_POINT ( 'NONE',  ( 4.483927247898545687, 16.52544592524342804, 109.7905762719810383 ) ) ;
#79909 = CARTESIAN_POINT ( 'NONE',  ( -1.314123079931730054, -8.348819774032584462, -62.04874212273343659 ) ) ;
#79910 = CARTESIAN_POINT ( 'NONE',  ( -13.89961937509957401, -13.97604488694547875, 59.37609039468566863 ) ) ;
#79911 = CARTESIAN_POINT ( 'NONE',  ( -12.14591786802326823, 12.06949235617739902, 113.1260903946856899 ) ) ;
#79912 = CARTESIAN_POINT ( 'NONE',  ( 0.05219959533909260263, 19.03943276465977164, 114.9989096053143669 ) ) ;
#79913 = CARTESIAN_POINT ( 'NONE',  ( 18.62759615963255655, 10.81492255796105972, 81.66775706135236135 ) ) ;
#79914 = CARTESIAN_POINT ( 'NONE',  ( -15.72974639402197994, 15.80617190586746368, 70.62390960531436690 ) ) ;
#79915 = CARTESIAN_POINT ( 'NONE',  ( 5.823673210054444382, -21.52544592524334988, 40.20942372801901854 ) ) ;
#79916 = CARTESIAN_POINT ( 'NONE',  ( 0.05219959533907565091, 21.53943276465977519, 99.99890960531436690 ) ) ;
#79917 = CARTESIAN_POINT ( 'NONE',  ( -21.53943276465977519, -0.05219959533937600094, 53.75109039468568994 ) ) ;
#79918 = CARTESIAN_POINT ( 'NONE',  ( 9.474510206698971260, -16.51473224551069308, 32.91557627198102409 ) ) ;
#79919 = CARTESIAN_POINT ( 'NONE',  ( -5.049401038298153566, 19.05341960407611168, 80.20724293864769550 ) ) ;
#79920 = CARTESIAN_POINT ( 'NONE',  ( -4.483927247898782831, 16.52544592524335698, 82.70942372801900433 ) ) ;
#79921 = CARTESIAN_POINT ( 'NONE',  ( -16.53943276465976808, 0.05219959533911058130, 101.2489096053143669 ) ) ;
#79922 = CARTESIAN_POINT ( 'NONE',  ( -5.049401038298153566, 19.05341960407611168, 105.2072429386476671 ) ) ;
#79923 = CARTESIAN_POINT ( 'NONE',  ( -12.14591786802309592, -12.06949235617757132, 51.87390960531437401 ) ) ;
#79924 = CARTESIAN_POINT ( 'NONE',  ( 8.224510206698742110, 14.34966873604972548, 112.0844237280190185 ) ) ;
#79925 = CARTESIAN_POINT ( 'NONE',  ( 5.153800228976335163, 19.02544592524342804, 59.79057627198100988 ) ) ;
#79926 = CARTESIAN_POINT ( 'NONE',  ( -19.02544592524342804, 5.153800228976336051, 41.04057627198103120 ) ) ;
#79927 = CARTESIAN_POINT ( 'NONE',  ( 10.72451020669898902, -18.67979575497178502, 47.91557627198102409 ) ) ;
#79928 = CARTESIAN_POINT ( 'NONE',  ( 13.97604488694548053, -13.89961937509957401, 35.62609039468567573 ) ) ;
#79931 = CARTESIAN_POINT ( 'NONE',  ( 0.05219959533910956823, 16.53943276465976808, 39.99890960531436690 ) ) ;
#79930 = DIRECTION ( 'NONE',  ( 0.9526137857479317628, 0.3041824702427701199, 0.000000000000000000 ) ) ;
#79929 = VECTOR ( 'NONE', #67173, 1000.000000000000000 ) ;
#79932 = CARTESIAN_POINT ( 'NONE',  ( 19.05341960407611168, 5.049401038298154454, 103.9572429386476671 ) ) ;
#79933 = CARTESIAN_POINT ( 'NONE',  ( 5.823673210054444382, -21.52544592524334988, 45.20942372801901854 ) ) ;
#79934 = EDGE_CURVE ( 'NONE', #148543, #147212, #131784, .T. ) ;
#79935 = CARTESIAN_POINT ( 'NONE',  ( -9.564922557960796823, -16.46253265017161027, 112.0822429386476955 ) ) ;
#79936 = CARTESIAN_POINT ( 'NONE',  ( -12.06949235617739369, -12.14591786802326823, 59.37609039468568284 ) ) ;
#79937 = CARTESIAN_POINT ( 'NONE',  ( 0.05219959533936267826, -19.03943276465977164, 60.00109039468566863 ) ) ;
#79938 = CARTESIAN_POINT ( 'NONE',  ( 12.06949235617757843, -12.14591786802309237, 33.12390960531435979 ) ) ;
#79939 = CARTESIAN_POINT ( 'NONE',  ( -17.49999999999999645, 5.499999999999997335, 120.0000000000000142 ) ) ;
#79940 = CARTESIAN_POINT ( 'NONE',  ( -0.05219959533934338120, 16.53943276465976808, 107.5010903946856899 ) ) ;
#79941 = CARTESIAN_POINT ( 'NONE',  ( 16.51473224551069308, 9.474510206698969483, 34.16557627198102409 ) ) ;
#79942 = CARTESIAN_POINT ( 'NONE',  ( 19.02544592524343514, -5.153800228976328945, 63.54057627198103830 ) ) ;
#79943 = CARTESIAN_POINT ( 'NONE',  ( -19.05341960407611168, -5.049401038298163336, 31.45724293864769550 ) ) ;
#79944 = CARTESIAN_POINT ( 'NONE',  ( -21.53943276465977519, -0.05219959533937600094, 28.75109039468567929 ) ) ;
#79945 = CARTESIAN_POINT ( 'NONE',  ( -9.474510206698964154, 16.51473224551069663, 40.41557627198103120 ) ) ;
#79946 = CARTESIAN_POINT ( 'NONE',  ( -0.05219959533909027116, -19.03943276465977164, 112.4989096053143669 ) ) ;
#79947 = CARTESIAN_POINT ( 'NONE',  ( -5.153800228976328057, -19.02544592524343514, 47.29057627198102409 ) ) ;
#79948 = CARTESIAN_POINT ( 'NONE',  ( 19.02544592524343514, -5.153800228976328945, 113.5405762719810241 ) ) ;
#79950 = CARTESIAN_POINT ( 'NONE',  ( -16.53943276465976808, 0.05219959533911058130, 111.2489096053143669 ) ) ;
#79949 = CARTESIAN_POINT ( 'NONE',  ( -0.05219959533937732626, 21.53943276465977519, 52.50109039468567573 ) ) ;
#79951 = CARTESIAN_POINT ( 'NONE',  ( 21.52544592524344225, -5.823673210054117533, 28.54057627198103120 ) ) ;
#79952 = CARTESIAN_POINT ( 'NONE',  ( 8.224510206698742110, 14.34966873604972548, 72.08442372801899012 ) ) ;
#79953 = CARTESIAN_POINT ( 'NONE',  ( -21.55341960407619339, 5.719274019375674811, 98.54275706135234714 ) ) ;
#79954 = VECTOR ( 'NONE', #5950, 1000.000000000000114 ) ;
#79955 = CARTESIAN_POINT ( 'NONE',  ( 8.224510206698742110, 14.34966873604972548, 52.08442372801901854 ) ) ;
#79956 = CARTESIAN_POINT ( 'NONE',  ( -5.049401038298153566, 19.05341960407611168, 90.20724293864766707 ) ) ;
#79957 = CARTESIAN_POINT ( 'NONE',  ( 0.05219959533934541429, -16.53943276465976808, 45.00109039468568284 ) ) ;
#79958 = CARTESIAN_POINT ( 'NONE',  ( -4.483927247898782831, 16.52544592524335698, 27.70942372801901854 ) ) ;
#79959 = CARTESIAN_POINT ( 'NONE',  ( -14.29746914071037622, -8.314922557961029526, 99.16775706135234714 ) ) ;
#79960 = CARTESIAN_POINT ( 'NONE',  ( -18.67979575497193778, 10.72451020669871902, 58.33442372801901143 ) ) ;
#79961 = CARTESIAN_POINT ( 'NONE',  ( 5.153800228976615827, -19.02544592524334988, 105.2094237280190185 ) ) ;
#79962 = CARTESIAN_POINT ( 'NONE',  ( -18.62759615963270932, 10.81492255796079327, 110.8322429386476955 ) ) ;
#79964 = CARTESIAN_POINT ( 'NONE',  ( 16.51473224551083163, -9.474510206698727899, 105.8344237280190043 ) ) ;
#79963 = CARTESIAN_POINT ( 'NONE',  ( -4.483927247898539470, -16.52544592524342804, 102.2905762719810383 ) ) ;
#79965 = CARTESIAN_POINT ( 'NONE',  ( -4.483927247898782831, 16.52544592524335698, 77.70942372801900433 ) ) ;
#79966 = CARTESIAN_POINT ( 'NONE',  ( -16.21995358207275473, 7.366697692864369706, 44.93551001512068410 ) ) ;
#79968 = EDGE_CURVE ( 'NONE', #136632, #2296, #51359, .T. ) ;
#79967 = CARTESIAN_POINT ( 'NONE',  ( -19.02544592524334988, -5.153800228976617603, 78.95942372801900433 ) ) ;
#79969 = CARTESIAN_POINT ( 'NONE',  ( -14.29746914071049879, 8.314922557960819915, 50.83224293864770971 ) ) ;
#79970 = CARTESIAN_POINT ( 'NONE',  ( 4.483927247898545687, 16.52544592524342804, 39.79057627198103830 ) ) ;
#79971 = CARTESIAN_POINT ( 'NONE',  ( 16.53943276465976808, -0.05219959533910856209, 98.74890960531438111 ) ) ;
#79973 = CARTESIAN_POINT ( 'NONE',  ( -18.39443945427639093, 5.500000000000031974, 88.51745347608650150 ) ) ;
#79972 = CARTESIAN_POINT ( 'NONE',  ( -19.05341960407617563, 5.049401038297882671, 38.54275706135233293 ) ) ;
#79974 = CARTESIAN_POINT ( 'NONE',  ( 15.80617190586769283, -15.72974639402175789, 35.62609039468568994 ) ) ;
#79975 = CARTESIAN_POINT ( 'NONE',  ( 5.153800228976615827, -19.02544592524334988, 100.2094237280190043 ) ) ;
#79976 = CARTESIAN_POINT ( 'NONE',  ( 22.73749492396215288, -155.7167183371838064, 0.000000000000000000 ) ) ;
#79977 = CARTESIAN_POINT ( 'NONE',  ( 19.05341960407611168, 5.049401038298154454, 88.95724293864769550 ) ) ;
#79978 = CARTESIAN_POINT ( 'NONE',  ( -16.46253265017160317, 9.564922557960807481, 95.83224293864769550 ) ) ;
#79979 = CARTESIAN_POINT ( 'NONE',  ( 10.81492255796078972, 18.62759615963270932, 59.58224293864770260 ) ) ;
#79980 = CARTESIAN_POINT ( 'NONE',  ( -4.483927247898539470, -16.52544592524342804, 92.29057627198103830 ) ) ;
#79981 = CARTESIAN_POINT ( 'NONE',  ( 19.03943276465977164, -0.05219959533909143690, 68.74890960531436690 ) ) ;
#79982 = CARTESIAN_POINT ( 'NONE',  ( 19.02544592524343514, -5.153800228976328945, 23.54057627198102054 ) ) ;
#79983 = CARTESIAN_POINT ( 'NONE',  ( 21.52544592524334988, 5.823673210054432836, 41.45942372801901143 ) ) ;
#79984 = CARTESIAN_POINT ( 'NONE',  ( 5.823673210054444382, -21.52544592524334988, 70.20942372801904696 ) ) ;
#79985 = CARTESIAN_POINT ( 'NONE',  ( -12.14591786802326823, 12.06949235617739902, 93.12609039468568994 ) ) ;
#79986 = CARTESIAN_POINT ( 'NONE',  ( -18.67979575497193778, 10.72451020669871902, 23.33442372801901499 ) ) ;
#79987 = CARTESIAN_POINT ( 'NONE',  ( 21.55341960407619695, -5.719274019375665929, 21.04275706135234714 ) ) ;
#79989 = CARTESIAN_POINT ( 'NONE',  ( 0.05219959533909260263, 19.03943276465977164, 74.99890960531435269 ) ) ;
#79988 = CARTESIAN_POINT ( 'NONE',  ( 16.46253265017146816, 9.564922557961045513, 56.66775706135233293 ) ) ;
#79990 = CARTESIAN_POINT ( 'NONE',  ( 21.53943276465977519, 0.05219959533937863772, 81.25109039468568994 ) ) ;
#79991 = CARTESIAN_POINT ( 'NONE',  ( 10.81492255796078972, 18.62759615963270932, 89.58224293864768129 ) ) ;
#79992 = CARTESIAN_POINT ( 'NONE',  ( 12.06949235617757843, -12.14591786802309237, 48.12390960531436690 ) ) ;
#79994 = CARTESIAN_POINT ( 'NONE',  ( -16.46253265017146816, -9.564922557961047289, 34.16775706135233293 ) ) ;
#79993 = CARTESIAN_POINT ( 'NONE',  ( 21.52544592524334988, 5.823673210054432836, 101.4594237280190185 ) ) ;
#79995 = CARTESIAN_POINT ( 'NONE',  ( -12.06949235617756955, 12.14591786802309770, 75.62390960531439532 ) ) ;
#79996 = CARTESIAN_POINT ( 'NONE',  ( 12.06949235617757843, -12.14591786802309237, 113.1239096053143953 ) ) ;
#79997 = CARTESIAN_POINT ( 'NONE',  ( 16.51473224551083163, -9.474510206698727899, 75.83442372801900433 ) ) ;
#79998 = CARTESIAN_POINT ( 'NONE',  ( 0.05219959533910956823, 16.53943276465976808, 39.99890960531436690 ) ) ;
#79999 = CARTESIAN_POINT ( 'NONE',  ( -15.80617190586768217, 15.72974639402176855, 83.12609039468568994 ) ) ;
#80000 = CARTESIAN_POINT ( 'NONE',  ( 5.049401038298161559, -19.05341960407611168, 77.70724293864765286 ) ) ;
#80001 = CARTESIAN_POINT ( 'NONE',  ( 19.05341960407617918, -5.049401038297876454, 66.04275706135233293 ) ) ;
#80002 = CARTESIAN_POINT ( 'NONE',  ( 0.05219959533907565091, 21.53943276465977519, 64.99890960531435269 ) ) ;
#80003 = CARTESIAN_POINT ( 'NONE',  ( 0.05219959533907565091, 21.53943276465977519, 109.9989096053143527 ) ) ;
#80004 = CARTESIAN_POINT ( 'NONE',  ( 19.03943276465977164, 0.05219959533936151252, 111.2510903946856757 ) ) ;
#80005 = CARTESIAN_POINT ( 'NONE',  ( 14.34966873604972726, -8.224510206698740333, 80.83442372801901854 ) ) ;
#80007 = CARTESIAN_POINT ( 'NONE',  ( -18.67979575497193778, 10.72451020669871902, 23.33442372801901499 ) ) ;
#80006 = CARTESIAN_POINT ( 'NONE',  ( -6.677994727576218814, 3.424326230466335996, 1.353258418600855606 ) ) ;
#80008 = CARTESIAN_POINT ( 'NONE',  ( 8.224510206698953496, -14.34966873604960469, 102.9155762719810383 ) ) ;
#80009 = CARTESIAN_POINT ( 'NONE',  ( -36.91746825000001309, -11.99521256947794789, -5.024999997268813523 ) ) ;
#80010 = CARTESIAN_POINT ( 'NONE',  ( 16.52544592524335698, 4.483927247898782831, 41.45942372801901143 ) ) ;
#80011 = CARTESIAN_POINT ( 'NONE',  ( -10.81492255796078084, -18.62759615963271287, 57.08224293864769550 ) ) ;
#80012 = CARTESIAN_POINT ( 'NONE',  ( -16.53943276465976808, -0.05219959533934237506, 98.75109039468568994 ) ) ;
#80013 = CARTESIAN_POINT ( 'NONE',  ( 16.51473224551069308, 9.474510206698969483, 29.16557627198103475 ) ) ;
#80014 = CARTESIAN_POINT ( 'NONE',  ( 0.05219959533934541429, -16.53943276465976808, 80.00109039468568994 ) ) ;
#80015 = CARTESIAN_POINT ( 'NONE',  ( 0.05219959533936267826, -19.03943276465977164, 70.00109039468566152 ) ) ;
#80016 = CARTESIAN_POINT ( 'NONE',  ( 10.72451020669871369, 18.67979575497193778, 37.08442372801901143 ) ) ;
#80017 = CARTESIAN_POINT ( 'NONE',  ( -15.80617190586745835, -15.72974639402198527, 61.87390960531436690 ) ) ;
#80018 = CARTESIAN_POINT ( 'NONE',  ( -4.483927247898782831, 16.52544592524335698, 92.70942372801901854 ) ) ;
#80019 = CARTESIAN_POINT ( 'NONE',  ( 21.55341960407619695, -5.719274019375665929, 86.04275706135236135 ) ) ;
#80020 = CARTESIAN_POINT ( 'NONE',  ( -10.72451020669898014, 18.67979575497178502, 50.41557627198103120 ) ) ;
#80021 = CARTESIAN_POINT ( 'NONE',  ( 21.53943276465977519, -0.05219959533907433946, 43.74890960531435979 ) ) ;
#80022 = CARTESIAN_POINT ( 'NONE',  ( -12.14591786802326823, 12.06949235617739902, 83.12609039468568994 ) ) ;
#80023 = CARTESIAN_POINT ( 'NONE',  ( -21.55341960407610458, -5.719274019375992779, 51.45724293864770260 ) ) ;
#80024 = ORIENTED_EDGE ( 'NONE', *, *, #117330, .F. ) ;
#80025 = CARTESIAN_POINT ( 'NONE',  ( 0.05219959533909260263, 19.03943276465977164, 104.9989096053143669 ) ) ;
#80026 = CARTESIAN_POINT ( 'NONE',  ( -25.12473289294612755, 7.795855283352524090, 170.9710361440363613 ) ) ;
#80027 = CARTESIAN_POINT ( 'NONE',  ( 19.03943276465977164, -0.05219959533909143690, 23.74890960531435269 ) ) ;
#80028 = CARTESIAN_POINT ( 'NONE',  ( -15.80617190586745835, -15.72974639402198527, 66.87390960531436690 ) ) ;
#80029 = CARTESIAN_POINT ( 'NONE',  ( -4.483927247898782831, 16.52544592524335698, 92.70942372801901854 ) ) ;
#80030 = CARTESIAN_POINT ( 'NONE',  ( 18.62759615963255655, 10.81492255796105972, 46.66775706135234714 ) ) ;
#80031 = CARTESIAN_POINT ( 'NONE',  ( -9.474510206698720793, -16.51473224551083518, 99.58442372801900433 ) ) ;
#80032 = CARTESIAN_POINT ( 'NONE',  ( 14.29746914071049879, -8.314922557960816363, 103.3322429386476955 ) ) ;
#80033 = CARTESIAN_POINT ( 'NONE',  ( 16.53943276465976808, 0.05219959533934440121, 21.25109039468567218 ) ) ;
#80034 = CARTESIAN_POINT ( 'NONE',  ( 13.89961937509977652, -13.97604488694527269, 43.12390960531434558 ) ) ;
#80035 = CARTESIAN_POINT ( 'NONE',  ( 13.90353822939981931, -0.7813480796679665996, -62.49831333862085359 ) ) ;
#80036 = CARTESIAN_POINT ( 'NONE',  ( 19.03943276465977164, -0.05219959533909143690, 88.74890960531436690 ) ) ;
#80037 = CARTESIAN_POINT ( 'NONE',  ( 16.52544592524335698, 4.483927247898782831, 81.45942372801900433 ) ) ;
#80038 = CARTESIAN_POINT ( 'NONE',  ( 18.67979575497194134, -10.72451020669871369, 105.8344237280190328 ) ) ;
#80039 = CARTESIAN_POINT ( 'NONE',  ( -21.55341960407610458, -5.719274019375992779, 61.45724293864770260 ) ) ;
#80040 = CARTESIAN_POINT ( 'NONE',  ( 14.34966873604972726, -8.224510206698740333, 85.83442372801901854 ) ) ;
#80041 = CARTESIAN_POINT ( 'NONE',  ( 0.05219959533936267826, -19.03943276465977164, 75.00109039468566152 ) ) ;
#80042 = CARTESIAN_POINT ( 'NONE',  ( 0.05219959533909260263, 19.03943276465977164, 34.99890960531435979 ) ) ;
#80043 = CARTESIAN_POINT ( 'NONE',  ( 19.02544592524343514, -5.153800228976328945, 83.54057627198100988 ) ) ;
#80044 = CARTESIAN_POINT ( 'NONE',  ( -15.72974639402176322, -15.80617190586768395, 44.37609039468567573 ) ) ;
#80045 = CARTESIAN_POINT ( 'NONE',  ( -9.564922557960796823, -16.46253265017161027, 47.08224293864769550 ) ) ;
#80046 = CARTESIAN_POINT ( 'NONE',  ( -13.89961937509957401, -13.97604488694547875, 69.37609039468564731 ) ) ;
#80047 = CARTESIAN_POINT ( 'NONE',  ( 26.45594755429551626, -8.318738267476710746, 167.5492909577866101 ) ) ;
#80048 = CARTESIAN_POINT ( 'NONE',  ( -13.89961937509977652, 13.97604488694528158, 115.6239096053143669 ) ) ;
#80049 = CARTESIAN_POINT ( 'NONE',  ( 8.224510206698953496, -14.34966873604960469, 67.91557627198102409 ) ) ;
#80050 = CARTESIAN_POINT ( 'NONE',  ( 5.719274019375991003, -21.55341960407610458, 62.70724293864769550 ) ) ;
#80051 = LINE ( 'NONE', #35540, #70826 ) ;
#80052 = CARTESIAN_POINT ( 'NONE',  ( 16.51473224551083163, -9.474510206698727899, 30.83442372801900433 ) ) ;
#80054 = CARTESIAN_POINT ( 'NONE',  ( -19.02544592524342804, 5.153800228976336051, 71.04057627198099567 ) ) ;
#80053 = CARTESIAN_POINT ( 'NONE',  ( -9.564922557960796823, -16.46253265017161027, 62.08224293864769550 ) ) ;
#80055 = CARTESIAN_POINT ( 'NONE',  ( -14.29746914071037622, -8.314922557961029526, 54.16775706135235424 ) ) ;
#80056 = CARTESIAN_POINT ( 'NONE',  ( -9.656827144875922642, -71.74905178543390605, -4.999999999999999112 ) ) ;
#80057 = DIRECTION ( 'NONE',  ( 0.4999999999999933387, -0.5000000000000055511, 0.7071067811865484609 ) ) ;
#80058 = CARTESIAN_POINT ( 'NONE',  ( -12.06949235617739369, -12.14591786802326823, 79.37609039468567573 ) ) ;
#80059 = PLANE ( 'NONE',  #75907 ) ;
#80060 = CARTESIAN_POINT ( 'NONE',  ( 4.379528057220092307, 16.55341960407617563, 62.29275706135236845 ) ) ;
#80061 = CARTESIAN_POINT ( 'NONE',  ( 14.29746914071037800, 8.314922557961029526, 36.66775706135234714 ) ) ;
#80063 = CARTESIAN_POINT ( 'NONE',  ( -40.00000000000002842, 1.938754146708588393E-14, 0.000000000000000000 ) ) ;
#80062 = CARTESIAN_POINT ( 'NONE',  ( 13.89961937509977652, -13.97604488694527269, 53.12390960531434558 ) ) ;
#80064 = CARTESIAN_POINT ( 'NONE',  ( -10.81492255796105439, 18.62759615963255655, 57.91775706135234714 ) ) ;
#80065 = CARTESIAN_POINT ( 'NONE',  ( -5.153800228976607833, 19.02544592524334988, 62.70942372801899722 ) ) ;
#80066 = CARTESIAN_POINT ( 'NONE',  ( -10.81492255796105439, 18.62759615963255655, 107.9177570613523471 ) ) ;
#80067 = CARTESIAN_POINT ( 'NONE',  ( -9.474510206698964154, 16.51473224551069663, 30.41557627198102054 ) ) ;
#80068 = CARTESIAN_POINT ( 'NONE',  ( 17.18050156595283795, 6.597016869166541397, 23.86958650019716544 ) ) ;
#80069 = CARTESIAN_POINT ( 'NONE',  ( 18.62759615963271287, -10.81492255796078972, 53.33224293864769550 ) ) ;
#80070 = AXIS2_PLACEMENT_3D ( 'NONE', #171888, #129340, #173890 ) ;
#80071 = CARTESIAN_POINT ( 'NONE',  ( 9.474510206698971260, -16.51473224551069308, 107.9155762719810383 ) ) ;
#80072 = CARTESIAN_POINT ( 'NONE',  ( -12.14591786802309592, -12.06949235617757132, 106.8739096053143811 ) ) ;
#80073 = CARTESIAN_POINT ( 'NONE',  ( -4.483927247898782831, 16.52544592524335698, 42.70942372801901854 ) ) ;
#80074 = CARTESIAN_POINT ( 'NONE',  ( -16.53943276465976808, 0.05219959533911058130, 26.24890960531435624 ) ) ;
#80075 = ORIENTED_EDGE ( 'NONE', *, *, #95661, .T. ) ;
#80076 = CARTESIAN_POINT ( 'NONE',  ( -10.72451020669898014, 18.67979575497178502, 100.4155762719810241 ) ) ;
#80078 = CARTESIAN_POINT ( 'NONE',  ( -5.049401038298153566, 19.05341960407611168, 115.2072429386477097 ) ) ;
#80077 = CARTESIAN_POINT ( 'NONE',  ( 12.14591786802309770, 12.06949235617756955, 44.37390960531435979 ) ) ;
#80079 = CARTESIAN_POINT ( 'NONE',  ( 19.03943276465977164, 0.05219959533936151252, 96.25109039468567573 ) ) ;
#80080 = CARTESIAN_POINT ( 'NONE',  ( 16.51473224551083163, -9.474510206698727899, 25.83442372801900078 ) ) ;
#80081 = CARTESIAN_POINT ( 'NONE',  ( -8.224510206698948167, 14.34966873604960824, 35.41557627198102409 ) ) ;
#80082 = CARTESIAN_POINT ( 'NONE',  ( 21.55341960407610458, 5.719274019375980345, 103.9572429386476813 ) ) ;
#80083 = CARTESIAN_POINT ( 'NONE',  ( -5.719274019375978568, 21.55341960407610458, 50.20724293864769550 ) ) ;
#80084 = CARTESIAN_POINT ( 'NONE',  ( -16.46253265017160317, 9.564922557960807481, 75.83224293864769550 ) ) ;
#80085 = CARTESIAN_POINT ( 'NONE',  ( -16.55341960407611168, -4.379528057220339221, 41.45724293864769550 ) ) ;
#80086 = CARTESIAN_POINT ( 'NONE',  ( -19.05341960407611168, -5.049401038298163336, 91.45724293864766707 ) ) ;
#80087 = VERTEX_POINT ( 'NONE', #97829 ) ;
#80088 = CARTESIAN_POINT ( 'NONE',  ( 19.01533133064922154, -5.499999999999651834, 61.26586590595741200 ) ) ;
#80089 = CARTESIAN_POINT ( 'NONE',  ( 9.564922557961047289, -16.46253265017146816, 35.41775706135233293 ) ) ;
#80090 = CARTESIAN_POINT ( 'NONE',  ( -15.72974639402197994, 15.80617190586746368, 80.62390960531438111 ) ) ;
#80091 = CARTESIAN_POINT ( 'NONE',  ( 12.14591786802309770, 12.06949235617756955, 104.3739096053143669 ) ) ;
#80092 = CARTESIAN_POINT ( 'NONE',  ( 21.52544592524334988, 5.823673210054432836, 31.45942372801901854 ) ) ;
#80093 = CARTESIAN_POINT ( 'NONE',  ( -27.73933785331498925, -9.013057229001049109, 138.9750000027311785 ) ) ;
#80094 = CARTESIAN_POINT ( 'NONE',  ( 12.14591786802327356, -12.06949235617739191, 110.6260903946857042 ) ) ;
#80095 = CARTESIAN_POINT ( 'NONE',  ( -9.564922557960796823, -16.46253265017161027, 42.08224293864769550 ) ) ;
#80096 = CARTESIAN_POINT ( 'NONE',  ( -0.05219959533909027116, -19.03943276465977164, 82.49890960531436690 ) ) ;
#80097 = CARTESIAN_POINT ( 'NONE',  ( -9.564922557961040184, 16.46253265017147172, 92.91775706135233293 ) ) ;
#80098 = CARTESIAN_POINT ( 'NONE',  ( 19.02544592524343514, -5.153800228976328945, 28.54057627198102409 ) ) ;
#80099 = CARTESIAN_POINT ( 'NONE',  ( -8.224510206698948167, 14.34966873604960824, 45.41557627198103830 ) ) ;
#80100 = CARTESIAN_POINT ( 'NONE',  ( 21.55341960407619695, -5.719274019375665929, 76.04275706135237556 ) ) ;
#80102 = CARTESIAN_POINT ( 'NONE',  ( 0.05219959533934541429, -16.53943276465976808, 70.00109039468568994 ) ) ;
#80101 = CARTESIAN_POINT ( 'NONE',  ( 22.64239272338469178, -30.05593529206061021, -19.14955533182169845 ) ) ;
#80103 = CARTESIAN_POINT ( 'NONE',  ( -16.51473224551069308, -9.474510206698971260, 61.66557627198103120 ) ) ;
#80104 = CARTESIAN_POINT ( 'NONE',  ( 5.049401038298161559, -19.05341960407611168, 62.70724293864769550 ) ) ;
#80105 = ORIENTED_EDGE ( 'NONE', *, *, #163400, .T. ) ;
#80106 = CARTESIAN_POINT ( 'NONE',  ( -0.05219959533937732626, 21.53943276465977519, 102.5010903946856899 ) ) ;
#80107 = CARTESIAN_POINT ( 'NONE',  ( 0.05219959533934541429, -16.53943276465976808, 70.00109039468568994 ) ) ;
#80108 = CARTESIAN_POINT ( 'NONE',  ( -10.72451020669870658, -18.67979575497194134, 99.58442372801900433 ) ) ;
#80109 = CARTESIAN_POINT ( 'NONE',  ( 19.03943276465977164, -0.05219959533909143690, 68.74890960531436690 ) ) ;
#80110 = CARTESIAN_POINT ( 'NONE',  ( 15.72974639402199770, -15.80617190586745480, 33.12390960531435979 ) ) ;
#80111 = CARTESIAN_POINT ( 'NONE',  ( 13.89961937509957401, 13.97604488694547697, 106.8760903946856757 ) ) ;
#80112 = CARTESIAN_POINT ( 'NONE',  ( 0.05219959533937995610, -21.53943276465977519, 75.00109039468568994 ) ) ;
#80113 = CARTESIAN_POINT ( 'NONE',  ( -12.14591786802326823, 12.06949235617739902, 48.12609039468568284 ) ) ;
#80114 = CARTESIAN_POINT ( 'NONE',  ( 10.81492255796078972, 18.62759615963270932, 99.58224293864770971 ) ) ;
#80115 = CARTESIAN_POINT ( 'NONE',  ( -5.049401038297874678, -19.05341960407617918, 104.7927570613523471 ) ) ;
#80116 = CARTESIAN_POINT ( 'NONE',  ( 19.05341960407611168, 5.049401038298154454, 83.95724293864766707 ) ) ;
#80117 = CARTESIAN_POINT ( 'NONE',  ( -5.153800228976607833, 19.02544592524334988, 107.7094237280189759 ) ) ;
#80118 = CARTESIAN_POINT ( 'NONE',  ( -12.14591786802326823, 12.06949235617739902, 23.12609039468567573 ) ) ;
#80119 = CARTESIAN_POINT ( 'NONE',  ( 14.29746914071049879, -8.314922557960816363, 63.33224293864770260 ) ) ;
#80120 = CARTESIAN_POINT ( 'NONE',  ( -8.314922557961024197, 14.29746914071037800, 67.91775706135234714 ) ) ;
#80122 = CARTESIAN_POINT ( 'NONE',  ( -19.03943276465977164, 0.05219959533909376836, 51.24890960531436690 ) ) ;
#80121 = CARTESIAN_POINT ( 'NONE',  ( -21.52544592524343514, 5.823673210054127303, 111.0405762719810525 ) ) ;
#80123 = CARTESIAN_POINT ( 'NONE',  ( 0.05219959533909260263, 19.03943276465977164, 74.99890960531435269 ) ) ;
#80124 = CARTESIAN_POINT ( 'NONE',  ( -12.06949235617739369, -12.14591786802326823, 69.37609039468567573 ) ) ;
#80125 = CARTESIAN_POINT ( 'NONE',  ( 8.906447517083050158, 27.41122689804195645, 143.6500000054623740 ) ) ;
#80126 = ORIENTED_EDGE ( 'NONE', *, *, #106448, .T. ) ;
#80127 = CARTESIAN_POINT ( 'NONE',  ( -18.62759615963255300, -10.81492255796106328, 109.1677570613523613 ) ) ;
#80128 = CARTESIAN_POINT ( 'NONE',  ( -19.02544592524342804, 5.153800228976336051, 36.04057627198100988 ) ) ;
#80129 = ORIENTED_EDGE ( 'NONE', *, *, #23510, .F. ) ;
#80130 = CARTESIAN_POINT ( 'NONE',  ( -16.53943276465976808, -0.05219959533934237506, 18.75109039468568639 ) ) ;
#80132 = CARTESIAN_POINT ( 'NONE',  ( -16.52544592524335698, -4.483927247898792601, 23.95942372801901143 ) ) ;
#80131 = CARTESIAN_POINT ( 'NONE',  ( 19.03943276465977164, 0.05219959533936151252, 51.25109039468567573 ) ) ;
#80133 = CARTESIAN_POINT ( 'NONE',  ( -13.97604488694527625, -13.89961937509977652, 46.87390960531435979 ) ) ;
#80134 = CARTESIAN_POINT ( 'NONE',  ( 9.474510206698971260, -16.51473224551069308, 67.91557627198102409 ) ) ;
#80135 = CARTESIAN_POINT ( 'NONE',  ( 5.719274019375991003, -21.55341960407610458, 87.70724293864769550 ) ) ;
#80136 = CARTESIAN_POINT ( 'NONE',  ( 5.153800228976335163, 19.02544592524342804, 109.7905762719810099 ) ) ;
#80137 = CARTESIAN_POINT ( 'NONE',  ( 19.03943276465977164, -0.05219959533909143690, 43.74890960531435979 ) ) ;
#80138 = CARTESIAN_POINT ( 'NONE',  ( -17.72696623605160582, 5.499999999999962697, 93.59811031808420978 ) ) ;
#80139 = CARTESIAN_POINT ( 'NONE',  ( 19.02544592524334988, 5.153800228976608722, 96.45942372801897591 ) ) ;
#80140 = CARTESIAN_POINT ( 'NONE',  ( -18.62759615963270932, 10.81492255796079327, 70.83224293864770971 ) ) ;
#80141 = CARTESIAN_POINT ( 'NONE',  ( 5.049401038297881783, 19.05341960407617563, 27.29275706135232937 ) ) ;
#80142 = CARTESIAN_POINT ( 'NONE',  ( -14.29746914071049879, 8.314922557960819915, 60.83224293864769550 ) ) ;
#80143 = CARTESIAN_POINT ( 'NONE',  ( 15.80617190586769283, -15.72974639402175789, 85.62609039468568994 ) ) ;
#80144 = CARTESIAN_POINT ( 'NONE',  ( -16.46253265017160317, 9.564922557960807481, 25.83224293864769194 ) ) ;
#80146 = CARTESIAN_POINT ( 'NONE',  ( 21.55341960407619695, -5.719274019375665929, 96.04275706135236135 ) ) ;
#80145 = CARTESIAN_POINT ( 'NONE',  ( 0.05219959533910956823, 16.53943276465976808, 29.99890960531435979 ) ) ;
#80147 = CARTESIAN_POINT ( 'NONE',  ( 0.05219959533909260263, 19.03943276465977164, 74.99890960531435269 ) ) ;
#80148 = CARTESIAN_POINT ( 'NONE',  ( 5.823673210054444382, -21.52544592524334988, 40.20942372801901854 ) ) ;
#80149 = CARTESIAN_POINT ( 'NONE',  ( 0.05219959533909260263, 19.03943276465977164, 79.99890960531436690 ) ) ;
#80150 = CARTESIAN_POINT ( 'NONE',  ( -12.06949235617756955, 12.14591786802309770, 90.62390960531436690 ) ) ;
#80151 = CARTESIAN_POINT ( 'NONE',  ( -8.224510206698948167, 14.34966873604960824, 60.41557627198102409 ) ) ;
#80152 = CARTESIAN_POINT ( 'NONE',  ( 18.62759615963271287, -10.81492255796078972, 73.33224293864769550 ) ) ;
#80153 = CARTESIAN_POINT ( 'NONE',  ( -16.46253265017160317, 9.564922557960807481, 75.83224293864769550 ) ) ;
#80154 = CARTESIAN_POINT ( 'NONE',  ( -0.05219959533907301413, -21.53943276465977519, 82.49890960531436690 ) ) ;
#80155 = CARTESIAN_POINT ( 'NONE',  ( -16.51473224551082808, 9.474510206698731452, 83.33442372801899012 ) ) ;
#80157 = CARTESIAN_POINT ( 'NONE',  ( -12.14591786802309592, -12.06949235617757132, 71.87390960531438111 ) ) ;
#80156 = CARTESIAN_POINT ( 'NONE',  ( -16.46253265017146816, -9.564922557961047289, 34.16775706135233293 ) ) ;
#80158 = CARTESIAN_POINT ( 'NONE',  ( 18.67979575497178502, 10.72451020669898547, 59.16557627198103120 ) ) ;
#80159 = DIRECTION ( 'NONE',  ( 1.000000000000000000, 0.000000000000000000, 0.000000000000000000 ) ) ;
#80161 = CARTESIAN_POINT ( 'NONE',  ( 22.44159573604009594, -16.30477369853687364, 144.1750000027311671 ) ) ;
#80160 = CARTESIAN_POINT ( 'NONE',  ( -12.06949235617739369, -12.14591786802326823, 104.3760903946856899 ) ) ;
#80162 = CARTESIAN_POINT ( 'NONE',  ( -9.474510206698720793, -16.51473224551083518, 99.58442372801900433 ) ) ;
#80163 = CARTESIAN_POINT ( 'NONE',  ( -12.06949235617756955, 12.14591786802309770, 65.62390960531436690 ) ) ;
#80164 = CARTESIAN_POINT ( 'NONE',  ( -17.50000000000001421, 3.189878218039099878, 34.87051437428754497 ) ) ;
#80165 = CARTESIAN_POINT ( 'NONE',  ( -19.03943276465977164, 0.05219959533909376836, 61.24890960531436690 ) ) ;
#80166 = CARTESIAN_POINT ( 'NONE',  ( -13.97604488694527625, -13.89961937509977652, 26.87390960531434558 ) ) ;
#80167 = CARTESIAN_POINT ( 'NONE',  ( 12.14591786802309770, 12.06949235617756955, 59.37390960531436690 ) ) ;
#80168 = CARTESIAN_POINT ( 'NONE',  ( 19.03943276465977164, -0.05219959533909143690, 103.7489096053143669 ) ) ;
#80170 = CARTESIAN_POINT ( 'NONE',  ( 16.51473224551069308, 9.474510206698969483, 64.16557627198102409 ) ) ;
#80169 = CARTESIAN_POINT ( 'NONE',  ( -19.03943276465977164, -0.05219959533935918106, 83.75109039468567573 ) ) ;
#80171 = CARTESIAN_POINT ( 'NONE',  ( -0.05219959533909027116, -19.03943276465977164, 87.49890960531436690 ) ) ;
#80172 = CARTESIAN_POINT ( 'NONE',  ( -9.564922557960796823, -16.46253265017161027, 87.08224293864769550 ) ) ;
#80173 = CARTESIAN_POINT ( 'NONE',  ( 21.52544592524344225, -5.823673210054117533, 63.54057627198103830 ) ) ;
#80174 = CARTESIAN_POINT ( 'NONE',  ( 12.06949235617739724, 12.14591786802326823, 56.87609039468568994 ) ) ;
#80175 = CARTESIAN_POINT ( 'NONE',  ( 0.05219959533936267826, -19.03943276465977164, 110.0010903946856757 ) ) ;
#80176 = CARTESIAN_POINT ( 'NONE',  ( -16.51473224551069308, -9.474510206698971260, 61.66557627198103120 ) ) ;
#80177 = CARTESIAN_POINT ( 'NONE',  ( -18.62759615963270932, 10.81492255796079327, 70.83224293864770971 ) ) ;
#80178 = CARTESIAN_POINT ( 'NONE',  ( -19.03943276465977164, -0.05219959533935918106, 98.75109039468567573 ) ) ;
#80180 = CARTESIAN_POINT ( 'NONE',  ( -5.823673210054431948, 21.52544592524334988, 47.70942372801902565 ) ) ;
#80179 = CARTESIAN_POINT ( 'NONE',  ( -12.14591786802309592, -12.06949235617757132, 26.87390960531435979 ) ) ;
#80181 = LINE ( 'NONE', #77207, #41189 ) ;
#80183 = CARTESIAN_POINT ( 'NONE',  ( -14.34966873604972548, 8.224510206698743886, 98.33442372801901854 ) ) ;
#80182 = CARTESIAN_POINT ( 'NONE',  ( 4.379528057220092307, 16.55341960407617563, 67.29275706135234714 ) ) ;
#80184 = CARTESIAN_POINT ( 'NONE',  ( -17.79613651744294600, 24.49428055684532524, 147.9656553485623647 ) ) ;
#80185 = CARTESIAN_POINT ( 'NONE',  ( -4.483927247898782831, 16.52544592524335698, 77.70942372801900433 ) ) ;
#80186 = CARTESIAN_POINT ( 'NONE',  ( 8.314922557961029526, -14.29746914071037800, 30.41775706135234358 ) ) ;
#80187 = CARTESIAN_POINT ( 'NONE',  ( -5.049401038298153566, 19.05341960407611168, 45.20724293864769550 ) ) ;
#80188 = CARTESIAN_POINT ( 'NONE',  ( 13.97604488694527802, 13.89961937509977652, 44.37390960531435269 ) ) ;
#80189 = CARTESIAN_POINT ( 'NONE',  ( 19.05341960407611168, 5.049401038298154454, 53.95724293864770260 ) ) ;
#80190 = CARTESIAN_POINT ( 'NONE',  ( -5.823673210054431948, 21.52544592524334988, 52.70942372801902565 ) ) ;
#80191 = CARTESIAN_POINT ( 'NONE',  ( 14.29746914071037800, 8.314922557961029526, 51.66775706135234714 ) ) ;
#80192 = CARTESIAN_POINT ( 'NONE',  ( -16.53943276465976808, 0.05219959533911058130, 36.24890960531435979 ) ) ;
#80193 = CARTESIAN_POINT ( 'NONE',  ( -9.474510206698964154, 16.51473224551069663, 30.41557627198102054 ) ) ;
#80194 = CARTESIAN_POINT ( 'NONE',  ( -16.46253265017160317, 9.564922557960807481, 40.83224293864769550 ) ) ;
#80196 = EDGE_CURVE ( 'NONE', #26208, #112608, #78704, .T. ) ;
#80195 = CARTESIAN_POINT ( 'NONE',  ( 16.52544592524335698, 4.483927247898782831, 26.45942372801901854 ) ) ;
#80197 = CARTESIAN_POINT ( 'NONE',  ( 19.03943276465977164, 0.05219959533936151252, 86.25109039468567573 ) ) ;
#80198 = CARTESIAN_POINT ( 'NONE',  ( 4.379528057220339221, -16.55341960407611168, 77.70724293864770971 ) ) ;
#80199 = CARTESIAN_POINT ( 'NONE',  ( 5.153800228976335163, 19.02544592524342804, 54.79057627198103120 ) ) ;
#80201 = CARTESIAN_POINT ( 'NONE',  ( 17.26058549869091507, -6.457015423128539489, 91.12254162523935008 ) ) ;
#80200 = CARTESIAN_POINT ( 'NONE',  ( 19.03943276465977164, 0.05219959533936151252, 91.25109039468566152 ) ) ;
#80202 = CARTESIAN_POINT ( 'NONE',  ( -0.05219959533937732626, 21.53943276465977519, 82.50109039468568994 ) ) ;
#80203 = CARTESIAN_POINT ( 'NONE',  ( 8.314922557961029526, -14.29746914071037800, 55.41775706135234714 ) ) ;
#80204 = DIRECTION ( 'NONE',  ( -0.9945218953682734009, 0.000000000000000000, -0.1045284632676528741 ) ) ;
#80205 = CARTESIAN_POINT ( 'NONE',  ( 21.52544592524344225, -5.823673210054117533, 38.54057627198103120 ) ) ;
#80206 = CARTESIAN_POINT ( 'NONE',  ( 14.29746914071037800, 8.314922557961029526, 36.66775706135234714 ) ) ;
#80207 = CARTESIAN_POINT ( 'NONE',  ( -5.153800228976328057, -19.02544592524343514, 27.29057627198103120 ) ) ;
#80208 = CARTESIAN_POINT ( 'NONE',  ( 16.51473224551083163, -9.474510206698727899, 30.83442372801900433 ) ) ;
#80209 = DIRECTION ( 'NONE',  ( 1.000000000000000000, 0.000000000000000000, 0.000000000000000000 ) ) ;
#80210 = CARTESIAN_POINT ( 'NONE',  ( 19.02544592524343514, -5.153800228976328945, 33.54057627198102409 ) ) ;
#80211 = CARTESIAN_POINT ( 'NONE',  ( -23.29544513554940721, -16.92513159979223758, 142.4656553485623647 ) ) ;
#80212 = CARTESIAN_POINT ( 'NONE',  ( 19.02544592524343514, -5.153800228976328945, 68.54057627198103830 ) ) ;
#80213 = CARTESIAN_POINT ( 'NONE',  ( 17.50000000000147438, -3.254303733634560825, 112.5239589307140449 ) ) ;
#80214 = CARTESIAN_POINT ( 'NONE',  ( 19.02544592524334988, 5.153800228976608722, 21.45942372801899012 ) ) ;
#80215 = CARTESIAN_POINT ( 'NONE',  ( 12.06949235617757843, -12.14591786802309237, 43.12390960531435269 ) ) ;
#80216 = CARTESIAN_POINT ( 'NONE',  ( -9.474510206698964154, 16.51473224551069663, 45.41557627198103120 ) ) ;
#80217 = CARTESIAN_POINT ( 'NONE',  ( 9.564922557960805705, 16.46253265017160317, 99.58224293864770971 ) ) ;
#80218 = CARTESIAN_POINT ( 'NONE',  ( 5.719274019375673035, 21.55341960407619339, 72.29275706135236135 ) ) ;
#80219 = CARTESIAN_POINT ( 'NONE',  ( -5.153800228976328057, -19.02544592524343514, 57.29057627198103120 ) ) ;
#80220 = CARTESIAN_POINT ( 'NONE',  ( -10.81492255796105439, 18.62759615963255655, 67.91775706135234714 ) ) ;
#80221 = CARTESIAN_POINT ( 'NONE',  ( -5.049401038298153566, 19.05341960407611168, 115.2072429386477097 ) ) ;
#80222 = CARTESIAN_POINT ( 'NONE',  ( -9.474510206698964154, 16.51473224551069663, 30.41557627198102054 ) ) ;
#80223 = CARTESIAN_POINT ( 'NONE',  ( -10.81492255796105439, 18.62759615963255655, 27.91775706135234358 ) ) ;
#80224 = CARTESIAN_POINT ( 'NONE',  ( -5.153800228976607833, 19.02544592524334988, 42.70942372801901143 ) ) ;
#80225 = CARTESIAN_POINT ( 'NONE',  ( 0.05219959533909260263, 19.03943276465977164, 24.99890960531435269 ) ) ;
#80226 = CARTESIAN_POINT ( 'NONE',  ( -5.153800228976328057, -19.02544592524343514, 57.29057627198103120 ) ) ;
#80227 = CARTESIAN_POINT ( 'NONE',  ( -19.02544592524334988, -5.153800228976617603, 108.9594237280189759 ) ) ;
#80228 = CARTESIAN_POINT ( 'NONE',  ( 16.55341960407611168, 4.379528057220329451, 78.95724293864769550 ) ) ;
#80229 = CARTESIAN_POINT ( 'NONE',  ( -18.62759615963270932, 10.81492255796079327, 30.83224293864770260 ) ) ;
#80230 = CARTESIAN_POINT ( 'NONE',  ( 9.474510206698729675, 16.51473224551082808, 97.08442372801900433 ) ) ;
#80231 = CARTESIAN_POINT ( 'NONE',  ( 0.05219959533907565091, 21.53943276465977519, 99.99890960531436690 ) ) ;
#80232 = CARTESIAN_POINT ( 'NONE',  ( -15.80617190586768217, 15.72974639402176855, 63.12609039468568994 ) ) ;
#80233 = CARTESIAN_POINT ( 'NONE',  ( -14.29746914071037622, -8.314922557961029526, 59.16775706135234714 ) ) ;
#80234 = CARTESIAN_POINT ( 'NONE',  ( -8.314922557961024197, 14.29746914071037800, 57.91775706135234714 ) ) ;
#80235 = CARTESIAN_POINT ( 'NONE',  ( -5.823673210054116645, -21.52544592524344225, 57.29057627198103120 ) ) ;
#80236 = CARTESIAN_POINT ( 'NONE',  ( 16.51473224551069308, 9.474510206698969483, 54.16557627198103120 ) ) ;
#80237 = CARTESIAN_POINT ( 'NONE',  ( -12.06949235617739369, -12.14591786802326823, 69.37609039468567573 ) ) ;
#80238 = AXIS2_PLACEMENT_3D ( 'NONE', #71435, #23935, #118949 ) ;
#80239 = CARTESIAN_POINT ( 'NONE',  ( 0.05219959533907565091, 21.53943276465977519, 99.99890960531436690 ) ) ;
#80240 = CARTESIAN_POINT ( 'NONE',  ( 12.14591786802309770, 12.06949235617756955, 49.37390960531436690 ) ) ;
#80241 = CARTESIAN_POINT ( 'NONE',  ( 19.05341960407611168, 5.049401038298154454, 73.95724293864768129 ) ) ;
#80242 = CARTESIAN_POINT ( 'NONE',  ( -4.379528057220086978, -16.55341960407618274, 79.79275706135236135 ) ) ;
#80243 = CARTESIAN_POINT ( 'NONE',  ( -19.05341960407617563, 5.049401038297882671, 108.5427570613523187 ) ) ;
#80244 = CARTESIAN_POINT ( 'NONE',  ( 10.72451020669898902, -18.67979575497178502, 102.9155762719810383 ) ) ;
#80245 = CARTESIAN_POINT ( 'NONE',  ( 4.483927247898545687, 16.52544592524342804, 49.79057627198102409 ) ) ;
#80246 = ORIENTED_EDGE ( 'NONE', *, *, #7150, .T. ) ;
#80247 = CARTESIAN_POINT ( 'NONE',  ( -16.19135201231366494, 7.376712067591930655, 69.81319145947971094 ) ) ;
#80248 = CARTESIAN_POINT ( 'NONE',  ( -18.67979575497178146, -10.72451020669898902, 86.66557627198102409 ) ) ;
#80249 = CARTESIAN_POINT ( 'NONE',  ( 4.483927247898545687, 16.52544592524342804, 24.79057627198103120 ) ) ;
#80250 = ORIENTED_EDGE ( 'NONE', *, *, #105310, .T. ) ;
#80251 = CARTESIAN_POINT ( 'NONE',  ( -17.12812012977024168, -6.668231424566069876, 56.35948759323144941 ) ) ;
#80252 = CARTESIAN_POINT ( 'NONE',  ( -15.80617190586745835, -15.72974639402198527, 96.87390960531436690 ) ) ;
#80253 = CARTESIAN_POINT ( 'NONE',  ( 5.049401038298161559, -19.05341960407611168, 102.7072429386476955 ) ) ;
#80254 = CARTESIAN_POINT ( 'NONE',  ( 21.53943276465977519, 0.05219959533937863772, 26.25109039468567573 ) ) ;
#80255 = CARTESIAN_POINT ( 'NONE',  ( -12.14591786802309592, -12.06949235617757132, 46.87390960531435979 ) ) ;
#80256 = CARTESIAN_POINT ( 'NONE',  ( 12.06949235617739724, 12.14591786802326823, 46.87609039468568994 ) ) ;
#80257 = CARTESIAN_POINT ( 'NONE',  ( -16.51473224551069308, -9.474510206698971260, 46.66557627198102409 ) ) ;
#80258 = CARTESIAN_POINT ( 'NONE',  ( -0.05219959533936034679, 19.03943276465977164, 47.50109039468566863 ) ) ;
#80259 = CARTESIAN_POINT ( 'NONE',  ( 19.05341960407611168, 5.049401038298154454, 78.95724293864769550 ) ) ;
#80260 = CARTESIAN_POINT ( 'NONE',  ( -15.72974639402197994, 15.80617190586746368, 35.62390960531437401 ) ) ;
#80261 = CARTESIAN_POINT ( 'NONE',  ( 17.59860650958989936, 7.585241751807028088, 64.07662985737508166 ) ) ;
#80262 = CARTESIAN_POINT ( 'NONE',  ( -5.153800228976607833, 19.02544592524334988, 112.7094237280190043 ) ) ;
#80263 = CARTESIAN_POINT ( 'NONE',  ( -16.46253265017146816, -9.564922557961047289, 54.16775706135234003 ) ) ;
#80264 = CARTESIAN_POINT ( 'NONE',  ( 15.72974639402199770, -15.80617190586745480, 108.1239096053143811 ) ) ;
#80265 = CARTESIAN_POINT ( 'NONE',  ( 14.29746914071049879, -8.314922557960816363, 38.33224293864768839 ) ) ;
#80266 = CARTESIAN_POINT ( 'NONE',  ( 9.474510206698971260, -16.51473224551069308, 77.91557627198103830 ) ) ;
#80267 = CARTESIAN_POINT ( 'NONE',  ( 15.80617190586746368, 15.72974639402197994, 64.37390960531435269 ) ) ;
#80269 = CARTESIAN_POINT ( 'NONE',  ( -8.224510206698735004, -14.34966873604973081, 19.58442372801901143 ) ) ;
#80268 = CARTESIAN_POINT ( 'NONE',  ( -18.62759615963270932, 10.81492255796079327, 95.83224293864770971 ) ) ;
#80270 = CARTESIAN_POINT ( 'NONE',  ( -9.564922557960796823, -16.46253265017161027, 112.0822429386476955 ) ) ;
#80271 = CARTESIAN_POINT ( 'NONE',  ( -15.80617190586768217, 15.72974639402176855, 93.12609039468568994 ) ) ;
#80272 = CARTESIAN_POINT ( 'NONE',  ( 19.03943276465977164, -0.05219959533909143690, 88.74890960531436690 ) ) ;
#80273 = CARTESIAN_POINT ( 'NONE',  ( -9.474510206698964154, 16.51473224551069663, 30.41557627198102054 ) ) ;
#80274 = CARTESIAN_POINT ( 'NONE',  ( 0.05219959533909260263, 19.03943276465977164, 84.99890960531436690 ) ) ;
#80275 = CARTESIAN_POINT ( 'NONE',  ( 8.314922557960818139, 14.29746914071049879, 104.5822429386477097 ) ) ;
#80276 = CARTESIAN_POINT ( 'NONE',  ( -5.049401038298153566, 19.05341960407611168, 65.20724293864765286 ) ) ;
#80277 = CARTESIAN_POINT ( 'NONE',  ( 8.314922557961029526, -14.29746914071037800, 20.41775706135234714 ) ) ;
#80278 = DIRECTION ( 'NONE',  ( -0.000000000000000000, -0.000000000000000000, 1.000000000000000000 ) ) ;
#80279 = CARTESIAN_POINT ( 'NONE',  ( 9.474510206698971260, -16.51473224551069308, 72.91557627198102409 ) ) ;
#80281 = CARTESIAN_POINT ( 'NONE',  ( -16.46253265017160317, 9.564922557960807481, 115.8322429386477097 ) ) ;
#80280 = CARTESIAN_POINT ( 'NONE',  ( -5.823673210054431948, 21.52544592524334988, 102.7094237280190185 ) ) ;
#80282 = CARTESIAN_POINT ( 'NONE',  ( -14.34966873604972548, 8.224510206698743886, 93.33442372801901854 ) ) ;
#80283 = CARTESIAN_POINT ( 'NONE',  ( -3.573655867282028392E-15, 2.428612866367529932E-14, -25.00000000000000000 ) ) ;
#80284 = CARTESIAN_POINT ( 'NONE',  ( 9.474510206698729675, 16.51473224551082808, 72.08442372801900433 ) ) ;
#80285 = CARTESIAN_POINT ( 'NONE',  ( 9.564922557961047289, -16.46253265017146816, 20.41775706135233293 ) ) ;
#80286 = CARTESIAN_POINT ( 'NONE',  ( 3.874965782148156457, 5.576804854476206330, -64.41982836185009376 ) ) ;
#80287 = CARTESIAN_POINT ( 'NONE',  ( -19.02544592524342804, 5.153800228976336051, 26.04057627198103120 ) ) ;
#80288 = CARTESIAN_POINT ( 'NONE',  ( -8.224510206698948167, 14.34966873604960824, 35.41557627198102409 ) ) ;
#80289 = DIRECTION ( 'NONE',  ( 1.000000000000000000, -0.000000000000000000, -0.000000000000000000 ) ) ;
#80290 = CARTESIAN_POINT ( 'NONE',  ( 16.52544592524335698, 4.483927247898782831, 101.4594237280190185 ) ) ;
#80291 = CARTESIAN_POINT ( 'NONE',  ( -3.573655867282028392E-15, 2.428612866367529932E-14, -8.000000000000000000 ) ) ;
#80292 = CARTESIAN_POINT ( 'NONE',  ( 16.52544592524335698, 4.483927247898782831, 76.45942372801901854 ) ) ;
#80293 = CARTESIAN_POINT ( 'NONE',  ( -19.02544592524342804, 5.153800228976336051, 31.04057627198102409 ) ) ;
#80294 = CARTESIAN_POINT ( 'NONE',  ( -21.55341960407619339, 5.719274019375674811, 93.54275706135234714 ) ) ;
#80295 = CARTESIAN_POINT ( 'NONE',  ( 16.51473224551083163, -9.474510206698727899, 95.83442372801900433 ) ) ;
#80296 = CARTESIAN_POINT ( 'NONE',  ( 5.823673210054444382, -21.52544592524334988, 75.20942372801901854 ) ) ;
#80297 = CARTESIAN_POINT ( 'NONE',  ( -19.03943276465977164, -0.05219959533935918106, 58.75109039468566863 ) ) ;
#80298 = CARTESIAN_POINT ( 'NONE',  ( 19.05341960407611168, 5.049401038298154454, 73.95724293864768129 ) ) ;
#80299 = CARTESIAN_POINT ( 'NONE',  ( 16.46253265017160672, -9.564922557960803928, 73.33224293864769550 ) ) ;
#80300 = CARTESIAN_POINT ( 'NONE',  ( 16.21995358207305671, 7.366697692864125457, 72.56448998487839219 ) ) ;
#80301 = CARTESIAN_POINT ( 'NONE',  ( 8.314922557960818139, 14.29746914071049879, 64.58224293864769550 ) ) ;
#80302 = CARTESIAN_POINT ( 'NONE',  ( -15.72974639402197994, 15.80617190586746368, 60.62390960531437401 ) ) ;
#80303 = CARTESIAN_POINT ( 'NONE',  ( 5.153800228976335163, 19.02544592524342804, 49.79057627198100988 ) ) ;
#80305 = CARTESIAN_POINT ( 'NONE',  ( -16.55341960407617563, 4.379528057220093196, 83.54275706135234714 ) ) ;
#80304 = CARTESIAN_POINT ( 'NONE',  ( 21.53943276465977519, -0.05219959533907433946, 88.74890960531436690 ) ) ;
#80306 = EDGE_LOOP ( 'NONE', ( #141979, #48425, #97620, #80680, #122632 ) ) ;
#80308 = CARTESIAN_POINT ( 'NONE',  ( -29.86685920354755552, 21.69954338932564397, -2.824999997268813345 ) ) ;
#80307 = CARTESIAN_POINT ( 'NONE',  ( 14.29746914071049879, -8.314922557960816363, 78.33224293864770971 ) ) ;
#80309 = CARTESIAN_POINT ( 'NONE',  ( -16.52544592524335698, -4.483927247898792601, 33.95942372801901143 ) ) ;
#80310 = CARTESIAN_POINT ( 'NONE',  ( -16.46253265017160317, 9.564922557960807481, 25.83224293864769194 ) ) ;
#80311 = CARTESIAN_POINT ( 'NONE',  ( 5.153800228976615827, -19.02544592524334988, 65.20942372801900433 ) ) ;
#80312 = CARTESIAN_POINT ( 'NONE',  ( -14.29746914071049879, 8.314922557960819915, 65.83224293864769550 ) ) ;
#80313 = CARTESIAN_POINT ( 'NONE',  ( 15.80617190586769283, -15.72974639402175789, 45.62609039468567573 ) ) ;
#80315 = CARTESIAN_POINT ( 'NONE',  ( -21.53943276465977519, 0.05219959533907696930, 96.24890960531435269 ) ) ;
#80314 = CARTESIAN_POINT ( 'NONE',  ( 9.474510206698971260, -16.51473224551069308, 22.91557627198102765 ) ) ;
#80316 = DIRECTION ( 'NONE',  ( 0.000000000000000000, 0.000000000000000000, 1.000000000000000000 ) ) ;
#80317 = CARTESIAN_POINT ( 'NONE',  ( 16.53943276465976808, -0.05219959533910856209, 93.74890960531436690 ) ) ;
#80318 = CARTESIAN_POINT ( 'NONE',  ( 25.90378602754583071, -30.37248848106526822, -17.06839622125441736 ) ) ;
#80319 = CARTESIAN_POINT ( 'NONE',  ( -5.049401038298153566, 19.05341960407611168, 50.20724293864770260 ) ) ;
#80320 = CARTESIAN_POINT ( 'NONE',  ( -29.86685920354755552, 21.69954338932564397, -6.824999997268814234 ) ) ;
#80321 = CARTESIAN_POINT ( 'NONE',  ( 5.049401038297881783, 19.05341960407617563, 82.29275706135229029 ) ) ;
#80322 = CARTESIAN_POINT ( 'NONE',  ( -18.67979575497193778, 10.72451020669871902, 33.33442372801900433 ) ) ;
#80323 = CARTESIAN_POINT ( 'NONE',  ( -19.05341960407611168, -5.049401038298163336, 71.45724293864766707 ) ) ;
#80324 = CARTESIAN_POINT ( 'NONE',  ( 13.97604488694548053, -13.89961937509957401, 55.62609039468566863 ) ) ;
#80325 = CARTESIAN_POINT ( 'NONE',  ( -13.89961937509977652, 13.97604488694528158, 45.62390960531433848 ) ) ;
#80326 = EDGE_CURVE ( 'NONE', #139245, #123348, #21013, .T. ) ;
#80327 = CARTESIAN_POINT ( 'NONE',  ( 8.224510206698953496, -14.34966873604960469, 67.91557627198102409 ) ) ;
#80328 = CARTESIAN_POINT ( 'NONE',  ( -14.29746914071049879, 8.314922557960819915, 50.83224293864770971 ) ) ;
#80329 = CARTESIAN_POINT ( 'NONE',  ( -9.564922557960796823, -16.46253265017161027, 72.08224293864770971 ) ) ;
#80330 = CARTESIAN_POINT ( 'NONE',  ( -5.823673210054116645, -21.52544592524344225, 97.29057627198105251 ) ) ;
#80331 = CARTESIAN_POINT ( 'NONE',  ( 19.02544592524343514, -5.153800228976328945, 68.54057627198103830 ) ) ;
#80332 = CARTESIAN_POINT ( 'NONE',  ( -5.823673210054116645, -21.52544592524344225, 82.29057627198103830 ) ) ;
#80333 = CARTESIAN_POINT ( 'NONE',  ( -5.153800228976607833, 19.02544592524334988, 22.70942372801899012 ) ) ;
#80336 = CARTESIAN_POINT ( 'NONE',  ( -16.55341960407611168, -4.379528057220339221, 91.45724293864769550 ) ) ;
#80335 = CARTESIAN_POINT ( 'NONE',  ( -4.379528057220086978, -16.55341960407618274, 104.7927570613523898 ) ) ;
#80334 = CARTESIAN_POINT ( 'NONE',  ( 19.05341960407611168, 5.049401038298154454, 38.95724293864767418 ) ) ;
#80337 = CARTESIAN_POINT ( 'NONE',  ( 19.05341960407617918, -5.049401038297876454, 111.0427570613523329 ) ) ;
#80338 = ORIENTED_EDGE ( 'NONE', *, *, #13111, .T. ) ;
#80339 = CARTESIAN_POINT ( 'NONE',  ( 15.80617190586769283, -15.72974639402175789, 35.62609039468568994 ) ) ;
#80340 = CARTESIAN_POINT ( 'NONE',  ( -16.51473224551082808, 9.474510206698731452, 48.33442372801900433 ) ) ;
#80341 = CARTESIAN_POINT ( 'NONE',  ( 12.06949235617757843, -12.14591786802309237, 28.12390960531435979 ) ) ;
#80342 = CARTESIAN_POINT ( 'NONE',  ( 15.72974639402199770, -15.80617190586745480, 73.12390960531436690 ) ) ;
#80343 = CARTESIAN_POINT ( 'NONE',  ( -19.03943276465977164, 0.05219959533909376836, 96.24890960531436690 ) ) ;
#80344 = CARTESIAN_POINT ( 'NONE',  ( 0.05219959533910956823, 16.53943276465976808, 59.99890960531436690 ) ) ;
#80345 = CARTESIAN_POINT ( 'NONE',  ( 5.153800228976335163, 19.02544592524342804, 29.79057627198102409 ) ) ;
#80346 = CARTESIAN_POINT ( 'NONE',  ( -0.05219959533909027116, -19.03943276465977164, 32.49890960531435979 ) ) ;
#80347 = CARTESIAN_POINT ( 'NONE',  ( 0.05219959533936267826, -19.03943276465977164, 30.00109039468566863 ) ) ;
#80348 = CARTESIAN_POINT ( 'NONE',  ( 0.05219959533934541429, -16.53943276465976808, 95.00109039468568994 ) ) ;
#80349 = CARTESIAN_POINT ( 'NONE',  ( -10.81492255796105439, 18.62759615963255655, 37.91775706135235424 ) ) ;
#80350 = CARTESIAN_POINT ( 'NONE',  ( -14.29746914071037622, -8.314922557961029526, 44.16775706135234714 ) ) ;
#80351 = CARTESIAN_POINT ( 'NONE',  ( -21.55341960407610458, -5.719274019375992779, 26.45724293864768839 ) ) ;
#80353 = CARTESIAN_POINT ( 'NONE',  ( 21.55341960407619695, -5.719274019375665929, 96.04275706135236135 ) ) ;
#80352 = CARTESIAN_POINT ( 'NONE',  ( 9.564922557960805705, 16.46253265017160317, 49.58224293864770260 ) ) ;
#80354 = CARTESIAN_POINT ( 'NONE',  ( -19.03943276465977164, 0.05219959533909376836, 81.24890960531436690 ) ) ;
#80355 = CARTESIAN_POINT ( 'NONE',  ( -12.06949235617739369, -12.14591786802326823, 59.37609039468568284 ) ) ;
#80356 = CARTESIAN_POINT ( 'NONE',  ( -4.379528057220328563, 16.55341960407611168, 110.2072429386477239 ) ) ;
#80357 = CARTESIAN_POINT ( 'NONE',  ( 14.34966873604972726, -8.224510206698740333, 110.8344237280190043 ) ) ;
#80358 = CYLINDRICAL_SURFACE ( 'NONE', #24889, 0.5000000000000004441 ) ;
#80361 = CARTESIAN_POINT ( 'NONE',  ( -19.05341960407611168, -5.049401038298163336, 71.45724293864766707 ) ) ;
#80360 = CARTESIAN_POINT ( 'NONE',  ( 13.97604488694527802, 13.89961937509977652, 94.37390960531436690 ) ) ;
#80359 = CARTESIAN_POINT ( 'NONE',  ( -21.55341960407619339, 5.719274019375674811, 58.54275706135235424 ) ) ;
#80362 = CARTESIAN_POINT ( 'NONE',  ( -9.474510206698964154, 16.51473224551069663, 115.4155762719810241 ) ) ;
#80363 = CARTESIAN_POINT ( 'NONE',  ( 16.55341960407611168, 4.379528057220329451, 38.95724293864768839 ) ) ;
#80364 = CARTESIAN_POINT ( 'NONE',  ( 8.224510206698742110, 14.34966873604972548, 112.0844237280190185 ) ) ;
#80365 = CARTESIAN_POINT ( 'NONE',  ( 8.314922557960818139, 14.29746914071049879, 34.58224293864770260 ) ) ;
#80366 = DIRECTION ( 'NONE',  ( 0.000000000000000000, -0.000000000000000000, 1.000000000000000000 ) ) ;
#80367 = CARTESIAN_POINT ( 'NONE',  ( -13.97604488694547697, 13.89961937509957934, 33.12609039468566863 ) ) ;
#80368 = CARTESIAN_POINT ( 'NONE',  ( 9.564922557960805705, 16.46253265017160317, 79.58224293864769550 ) ) ;
#80369 = CARTESIAN_POINT ( 'NONE',  ( 9.474510206698729675, 16.51473224551082808, 52.08442372801900433 ) ) ;
#80370 = CARTESIAN_POINT ( 'NONE',  ( 29.86685920354754842, -21.69954338932559068, -10.32499999726881335 ) ) ;
#80371 = CARTESIAN_POINT ( 'NONE',  ( 5.199999999999996625, 0.000000000000000000, 2.500000000000000444 ) ) ;
#80373 = CARTESIAN_POINT ( 'NONE',  ( -12.14591786802326823, 12.06949235617739902, 78.12609039468570415 ) ) ;
#80372 = CARTESIAN_POINT ( 'NONE',  ( -19.05341960407617563, 5.049401038297882671, 88.54275706135230450 ) ) ;
#80374 = FACE_OUTER_BOUND ( 'NONE', #192669, .T. ) ;
#80375 =( BOUNDED_SURFACE ( )  B_SPLINE_SURFACE ( 3, 2, ( 
 ( #25379, #59657, #106163, #181051, #44507, #165871, #132530, #12203, #26371, #194219, #121331, #11197, #183024, #14152, #150705, #90007, #149699, #167846, #72873, #196230, #119368, #120337, #166868, #104189, #73867, #103196, #88011, #135537, #151691, #13181, #118370, #29346, #90975, #74844, #55684, #136507, #117358, #198187, #179054, #102194, #163882, #87021, #10195, #71855, #133524, #195216, #56697, #180064, #164876, #187013, #32315, #139474, #199178, #15153, #109143, #17143, #111127, #60644, #30322, #168817, #172816, #93968, #125317, #184010, #140474, #954, #62631, #122318, #49464, #187994, #95958, #170822, #1962, #126297, #63642, #45492, #155648, #94966, #78796, #137497, #91964, #110139, #46481, #48484, #124307, #153657, #34296, #156650, #157642, #79800, #75819, #169825, #171818, #18146, #107147, #76814, #33306, #64635, #138485, #141472, #2956, #200167, #61636, #123304, #184997, #108141, #31317, #92969, #186005, #154655, #16151, #77805, #47487, #175796, #80782, #50466, #19131, #131274, #100926, #82762, #188990, #38277, #112126, #99931, #177801, #142459, #160618, #161617, #130255, #23110, #7924, #114094, #37269, #116112, #69609, #5928, #53436, #22109, #83759, #127277, #84756, #3937, #173817, #98927, #192962, #65617, #115111, #35282, #52436, #146434, #96938, #97917, #129265, #158619, #20109, #4927, #145439, #128274, #6921, #67604, #39270, #36263, #190959, #81753, #68599, #143441, #21107, #54441, #66609, #189971, #51446, #191951, #159609, #113107, #176805, #174797, #144443, #58430, #8945, #71606, #132280, #10943, #135290, #87762, #11955, #88767, #166621, #101943, #104935, #182780, #181785, #43266, #42283, #120097, #180804, #73620, #150460, #151448, #103941, #44263, #165621, #118121, #27120, #72617, #28123, #134291, #196962, #55434, #89763, #12935, #119123, #74600, #136267, #197942, #26119, #85769, #163624, #195978, #59411, #121086, #147456, #117105, #178800, #162611, #24116, #70613, #193972, #40270, #149447, #57451, #25127, #86769, #148452, #9947, #133272, #194963, #56441, #179809, #41279, #102941, #164625, #31080, #168583, #184756, #106910, #16901, #13911, #47245, #78552, #32073, #1720, #92727, #48240, #715, #154416, #105921, #61398, #63396, #198939, #183770, #62387, #91722, #75577, #140227, #109895, #123070, #139240, #185757, #30081, #125073, #15910, #14915, #90740, #77568, #46241, #137254, #107895, #93729, #45256, #60406, #108903, #122079, #169582, #124057, #199935, #170582, #155411, #186770, #153417, #171579, #138252, #76576, #167606, #29101, #152423, #198598, #119770, #86430, #166283, #180471, #148116, #75240, #165285, #13573, #168244, #181454, #43919, #103609, #136911, #26778, #88420, #73283, #12603, #120740, #150114, #11615, #57109, #41943, #134953, #196631, #27780, #72269, #60066, #121734, #106567, #182439, #132937, #195636, #56095, #58100, #59073, #42932, #135937, #74267, #90403, #25786, #28766, #9607, #105581, #167267, #89422, #152088, #104596, #197607, #183426, #44910, #71272, #151111, #194624, #117776, #179470, #40935, #102607, #164293, #87432, #149117, #10608, #133946, #118783, #32717, #78202, #45896, #80194, #48882, #111535, #33702, #3357, #123704, #94369, #110537, #188392, #65032, #140875, #18547, #29740, #172218, #187414, #153064, #17545, #156048, #138889, #2364, #199585, #64045, #93373, #184415, #137903, #141866, #62040, #186416, #91373, #61053, #14566, #126688, #76224, #155060, #122725, #95365, #107549, #157050, #49869, #169225, #171228, #30734, #125715, #92381, #154067, #124718, #47893, #15562, #77220, #16555, #369, #79206, #185402, #46893, #108553, #170232, #31725, #109546, #139872, #1361, #63040, #111655, #32838, #16672, #171349, #94488, #156170, #154191, #49990, #125831, #173341, #2485, #80310, #142973, #158156, #62161, #48999, #139994, #140997, #93495, #17669, #155182, #34813, #77342, #141983, #96468, #126805, #19648, #64166, #66140, #107669, #187534, #1483, #169346, #81289 ),
 ( #15681, #4450, #63161, #110655, #30855, #139008, #92502, #127803, #189506, #79327, #488, #188513, #123825, #185523, #47015, #108674, #172335, #170352, #18664, #31844, #78321, #33824, #95484, #124840, #186540, #157170, #3471, #65148, #48013, #109669, #72910, #112641, #20632, #145968, #42563, #174333, #149735, #119405, #143976, #150740, #5456, #129782, #161145, #97449, #67139, #36789, #7450, #160148, #84289, #37802, #73902, #68131, #22642, #12240, #69134, #128797, #52957, #134579, #165907, #35803, #190496, #133562, #191479, #144969, #195252, #26408, #135572, #11236, #159135, #21639, #82284, #99465, #88047, #176332, #103232, #180101, #57735, #51969, #196266, #50981, #181088, #104226, #56737, #27405, #118407, #164914, #89050, #113628, #175323, #41569, #98455, #83293, #6450, #114633, #30359, #16188, #15191, #58705, #13218, #31356, #167883, #4849, #45529, #74881, #47525, #77843, #78834, #993, #170860, #91013, #46522, #90043, #76850, #124347, #153695, #186042, #108181, #138521, #60682, #120375, #136543, #92001, #61673, #32351, #182068, #151725, #198224, #94004, #62667, #122357, #106199, #184046, #107183, #168854, #43551, #139510, #123342, #109181, #185035, #169862, #155685, #17180, #59696, #93007, #29382, #154693, #183060, #197244, #44544, #105217, #166904, #28404, #121367, #152699, #14188, #75857, #137533, #199215, #35322, #140512, #80820, #129304, #33343, #79840, #4964, #49502, #171855, #82801, #37309, #142498, #81793, #190012, #188032, #52476, #173856, #172854, #63680, #20148, #3976, #95002, #65656, #97958, #141510, #156689, #51486, #18183, #50503, #96976, #19171, #158657, #143480, #66650, #2995, #128312, #157681, #64673, #67645, #114135, #189029, #175836, #113148, #2001, #174838, #34335, #125355, #191000, #127318, #98968, #22150, #36303, #159650, #112167, #160658, #21146, #144483, #5967, #187052, #48522, #110176, #126335, #111165, #95996, #85815, #132326, #25173, #69652, #10989, #196021, #71652, #72662, #101990, #165666, #163671, #39314, #86815, #194018, #179854, #55481, #24164, #134337, #176848, #23154, #148501, #193008, #115155, #26166, #180849, #147501, #9992, #133319, #131318, #57497, #117151, #116155, #6961, #195008, #8992, #38319, #70660, #41325, #84798, #99974, #56486, #161658, #178846, #40313, #162658, #118164, #102985, #164670, #146477, #87807, #100973, #7969, #119166, #42326, #149493, #103987, #83800, #145480, #68641, #177846, #130297, #191991, #53478, #54485, #108948, #122124, #184800, #44308, #154463, #167652, #105967, #13955, #153462, #61443, #29148, #90785, #197988, #182826, #152469, #75621, #168626, #12983, #15955, #139285, #14959, #77614, #45301, #27164, #106953, #137301, #30126, #198982, #123115, #60449, #76619, #120142, #91767, #762, #183812, #62433, #138297, #199978, #46286, #150504, #166667, #107942, #169629, #124105, #12001, #181833, #43312, #185805, #31125, #92773, #136313, #47292, #88812, #73664, #135336, #197009, #58475, #104980, #28168, #89810, #151492, #74647, #59458, #121132, #2762, #3745, #156450, #95762, #17950, #174609, #140273, #143246, #36075, #189783, #20909, #65422, #129067, #96741, #127083, #170629, #63443, #109942, #35088, #79603, #1766, #112915, #67412, #172617, #111932, #19918, #141272, #82568, #188791, #64438, #93775, #50274, #110931, #125119, #34105, #128080, #171624, #186817, #81560, #48287, #80587, #173618, #49273, #158430, #4729, #66419, #33112, #51255, #187804, #94768, #97724, #144249, #18942, #5733, #159414, #32118, #190768, #126108, #155456, #52243, #157447, #16946, #78600, #142261, #71419, #131079, #41090, #54251, #192768, #100737, #40070, #148262, #115923, #177613, #84563, #69413, #39081, #162418, #55246, #99741, #102753, #25935, #101747, #164441, #132088, #195789, #193777, #23920, #116914, #85574, #9755, #147261, #163436, #6728, #178607, #87578, #70421, #149265, #24933, #86578, #8751, #37074, #53241, #133083, #194773, #10757, #98734 ),
 ( #56247, #117928, #72421, #134098, #68406, #179618, #146241, #113900, #161425, #175598, #22917, #160427, #83568, #21916, #145247, #130058, #191758, #114918, #176611, #38085, #7727, #57261, #197756, #46048, #42093, #11767, #150272, #92537, #61207, #182592, #166437, #120892, #44076, #105735, #103758, #199741, #75391, #122879, #152240, #29893, #154226, #107703, #73433, #198753, #89575, #90558, #43079, #167422, #104746, #184567, #26932, #91531, #169382, #76383, #30890, #13725, #15716, #183581, #137063, #118935, #59223, #77376, #135104, #196780, #121888, #27932, #88574, #139044, #180620, #28918, #60218, #106724, #151261, #165437, #45066, #12751, #58248, #168398, #153218, #119916, #14723, #138060, #181602, #74416, #136082, #16707, #110691, #157207, #79364, #18701, #80348, #126844, #63198, #142020, #17707, #93533, #127840, #174371, #49036, #112679, #33861, #524, #3509, #94525, #62196, #189546, #141035, #51018, #82322, #95521, #158195, #2522, #35841, #64202, #125869, #187569, #188550, #34850, #172371, #65185, #171388, #156207, #50028, #111693, #173380, #186577, #97487, #159173, #96505, #20668, #19685, #123860, #81327, #143010, #4488, #66178, #185558, #47052, #108709, #155218, #170388, #31879, #78357, #140031, #1520, #124878, #48050, #109706, #32875, #177376, #85330, #179381, #132847, #38848, #100505, #40843, #194535, #130840, #178369, #147022, #8506, #52006, #163188, #5493, #113665, #162184, #56006, #67176, #39833, #9517, #36827, #102517, #98493, #22680, #54014, #190532, #160186, #129820, #23682, #52996, #70184, #192531, #164200, #161184, #115688, #25698, #131852, #21676, #146006, #24692, #117684, #128833, #83330, #193535, #84327, #37843, #55009, #116679, #144012, #101499, #175359, #114674, #145007, #86341, #148028, #69174, #71183, #6488, #68168, #191519, #176370, #99503, #7489, #106478, #167182, #44823, #105496, #136824, #60966, #199500, #107463, #120656, #152002, #137816, #13488, #57018, #182354, #168157, #28681, #149029, #103519, #121646, #58014, #90316, #135851, #165195, #122640, #29654, #169139, #91286, #184330, #181367, #75153, #152977, #45812, #87343, #198508, #76138, #10517, #14476, #72180, #133854, #59979, #183341, #196544, #195544, #118691, #180383, #151026, #41853, #26690, #88330, #119684, #43832, #150021, #11526, #73196, #134866, #42846, #12517, #104511, #166192, #27693, #89334, #74181, #197521, #58989, #111450, #141781, #173137, #48798, #34612, #125629, #3275, #65934, #81096, #185316, #172133, #62951, #63960, #16468, #155962, #78117, #96271, #285, #64947, #157957, #49785, #142774, #187327, #189305, #156965, #110452, #30644, #171141, #19448, #123621, #170143, #95282, #139786, #61954, #4255, #127606, #32630, #33619, #80113, #1274, #50782, #18462, #124631, #153981, #126606, #94284, #46807, #17459, #188308, #31638, #108466, #112442, #93287, #140788, #92297, #109458, #15478, #77135, #138804, #154972, #186326, #47808, #79115, #2277, #147790, #22437, #86099, #7247, #174131, #53770, #67929, #35602, #162943, #52754, #101254, #55765, #68932, #131606, #191279, #24450, #114423, #176124, #160944, #100262, #8262, #37595, #99257, #144765, #129583, #84086, #145765, #115444, #159942, #9276, #70942, #161943, #132610, #192290, #97248, #177135, #130594, #38606, #23438, #69942, #85085, #146769, #66930, #193291, #194299, #54765, #158936, #116439, #178128, #39595, #20425, #113424, #82075, #143768, #5249, #128593, #190287, #51763, #175116, #36584, #98239, #83089, #21429, #6250, #104270, #163964, #59741, #14232, #119447, #58748, #166945, #164957, #29424, #150785, #149778, #40605, #197285, #57777, #148787, #181132, #74922, #56779, #10276, #28448, #133605, #27452, #73945, #196307, #135614, #120417, #43593, #180143, #182108, #134623, #71935, #44585, #91055, #165952, #152742, #12280, #117439, #105259, #11280, #179137, #106242, #42606, #167924, #199261, #90084, #136585, #89093, #75903, #151766, #13259, #198265, #121410 ),
 ( #183104, #195298, #137577, #102276, #25462, #87102, #118452, #41612, #103277, #26450, #88092, #72953, #160460, #113934, #50309, #97760, #66452, #128113, #168899, #82600, #122402, #30405, #158465, #52276, #184092, #159447, #129103, #153740, #21951, #15236, #139556, #173657, #107228, #76895, #46568, #19953, #169909, #96776, #111965, #83601, #77888, #35124, #145280, #81595, #138566, #62713, #144281, #175633, #45575, #44, #143279, #1040, #154740, #4765, #36108, #60728, #20943, #92051, #31402, #61719, #189817, #5770, #186090, #112950, #51289, #67445, #123387, #190802, #185079, #108229, #174643, #37107, #93053, #98766, #16236, #124395, #103789, #99776, #85609, #116949, #53274, #22951, #192803, #101782, #25967, #133117, #42128, #57292, #161461, #148296, #39114, #40104, #54286, #132120, #115958, #10790, #176646, #179653, #72458, #87610, #118969, #163470, #165469, #194806, #24967, #6763, #147296, #195821, #84599, #146278, #71452, #177646, #38122, #149296, #26965, #8785, #9790, #56280, #100770, #180652, #86613, #162453, #130096, #117962, #70455, #7765, #193813, #164473, #69448, #131115, #41123, #23954, #178641, #102787, #55278, #134132, #88608, #68442, #191793, #114953, #167456, #43113, #77411, #123898, #198787, #62230, #183618, #150304, #29929, #44111, #11801, #139081, #28952, #559, #31915, #45101, #107739, #90593, #185597, #152275, #13759, #137101, #76419, #184603, #75427, #60253, #120927, #105769, #121924, #106758, #91568, #136116, #47086, #108747, #138095, #170423, #168433, #73465, #153256, #14758, #199776, #61243, #46084, #122915, #169420, #104781, #30925, #135138, #92573, #196812, #154261, #15752, #58279, #119948, #181633, #166469, #27967, #89607, #151296, #12785, #74450, #197792, #59258, #182626, #124914, #35876, #190567, #95557, #34886, #143045, #141073, #5529, #126881, #125906, #16743, #173415, #33900, #186612, #157244, #51052, #32910, #48084, #4523, #109740, #3543, #50068, #172411, #111729, #96541, #19719, #156243, #158229, #110730, #171424, #20703, #67209, #142057, #128867, #188587, #93568, #81361, #187605, #155254, #82359, #18738, #144047, #175394, #66216, #112714, #80385, #52042, #65221, #127876, #189580, #174407, #97522, #159209, #113698, #64240, #49074, #78392, #140068, #1559, #79402, #63235, #94564, #17745, #2558, #55043, #118727, #116713, #192566, #178403, #147058, #132880, #8541, #86375, #129856, #39867, #164235, #193571, #25731, #148060, #101533, #100539, #160222, #176405, #70219, #163226, #72214, #21712, #191554, #53031, #133888, #40878, #162218, #146040, #23717, #85365, #131886, #83366, #179413, #24726, #9551, #56039, #71217, #195580, #87377, #114712, #194569, #69208, #117717, #22715, #102551, #84362, #149062, #6524, #10550, #57052, #36862, #98529, #145042, #68203, #54049, #37880, #99538, #161220, #7524, #130876, #115723, #177411, #38882, #74214, #41887, #169172, #59021, #107495, #61985, #75185, #137851, #197553, #30676, #120688, #182387, #167216, #106513, #14509, #43865, #105530, #151057, #135882, #28713, #90350, #121680, #166224, #92329, #154015, #168191, #15510, #198542, #180415, #60013, #152035, #183376, #13520, #76171, #136857, #29687, #73228, #44857, #77167, #91319, #138837, #153010, #199531, #61001, #103554, #119716, #122673, #184362, #317, #165229, #134899, #196576, #26724, #45843, #88363, #89368, #150056, #11562, #58046, #181400, #42878, #104543, #27725, #12548, #49815, #158966, #174163, #78151, #64976, #155995, #156995, #109493, #48828, #171176, #127635, #93322, #96300, #189335, #142803, #35633, #18493, #82107, #111480, #80141, #123651, #63990, #112470, #16503, #62986, #188337, #32663, #155006, #65964, #20457, #125661, #126635, #173165, #94317, #97278, #141811, #17491, #46839, #3304, #187358, #139819, #110481, #81123, #124665, #1308, #34641, #186361, #33649, #157986, #2309, #19477, #4284, #50813, #47841, #143799, #79149, #5282, #140820, #172164, #185349, #108499 ),
 ( #95310, #170179, #31672, #84117, #53801, #193323, #101286, #7279, #145796, #37626, #22469, #68963, #115477, #8295, #52785, #194330, #179168, #54797, #55798, #85118, #148818, #146802, #130625, #69973, #177165, #162976, #38638, #116472, #159973, #131640, #117470, #23469, #40636, #178161, #39626, #192321, #190318, #6281, #100295, #24481, #102305, #51795, #21460, #83122, #163994, #70974, #161973, #176155, #86131, #147823, #9308, #113454, #132642, #25491, #87133, #66965, #128625, #175147, #36615, #144798, #98271, #99289, #67959, #114454, #129614, #160975, #191309, #180175, #183134, #14266, #29455, #60761, #105288, #168931, #136615, #166976, #10308, #150814, #199294, #103308, #149808, #74952, #119478, #41643, #152774, #107260, #12311, #151797, #59773, #57807, #122433, #43625, #42637, #133639, #90113, #73976, #164987, #135645, #167956, #11314, #26482, #121442, #88124, #120447, #28479, #89126, #13288, #198296, #118484, #91087, #71965, #72984, #44618, #184125, #195330, #106271, #75935, #134653, #30437, #196339, #197315, #182141, #56810, #181161, #104300, #137610, #45607, #92084, #58779, #165983, #27483, #63755, #50582, #48597, #31431, #155758, #172934, #65732, #76928, #93085, #171930, #94079, #47600, #125429, #126411, #173933, #49580, #79, #62744, #123417, #2076, #188108, #78909, #3073, #79913, #157761, #154769, #96071, #35401, #34413, #19251, #33419, #111243, #95078, #64749, #127400, #189109, #153773, #187125, #18260, #4054, #141585, #185110, #110249, #80898, #156766, #15268, #169940, #142575, #124424, #112242, #138597, #16266, #61749, #46600, #108260, #77917, #139584, #109254, #1069, #186120, #170933, #32425, #17256, #140586, #97052, #116235, #54563, #20224, #84879, #161740, #6049, #8052, #66732, #131399, #160738, #51564, #5046, #9070, #129385, #53558, #158734, #128392, #81872, #70740, #178929, #22230, #190089, #177926, #113228, #39394, #55562, #143564, #38398, #101054, #69731, #162739, #85896, #192076, #115236, #194100, #147584, #83879, #193087, #100054, #23235, #67727, #174918, #24247, #117236, #99049, #146556, #132408, #144563, #36382, #130378, #191081, #98036, #176928, #37391, #159733, #145561, #21230, #82885, #52554, #114215, #175920, #7039, #68721, #119245, #58555, #197088, #166746, #103070, #181911, #57575, #133401, #167728, #14032, #88891, #152544, #73745, #40399, #120221, #134419, #102070, #29226, #180929, #90859, #122200, #135417, #198068, #42404, #75697, #104067, #165749, #27242, #28249, #74727, #150583, #12082, #11070, #196105, #43391, #105062, #89889, #26247, #137377, #199056, #151572, #60525, #13061, #163755, #136391, #59534, #121213, #182903, #44387, #106042, #25255, #195090, #86897, #148581, #10072, #71731, #56573, #118247, #179938, #41405, #164752, #87887, #149574, #72748, #168702, #138373, #76697, #19019, #187880, #109026, #92851, #47371, #170705, #32195, #30204, #126184, #93852, #48365, #2839, #110021, #80665, #34180, #200053, #125198, #16033, #17024, #169706, #155529, #31200, #49347, #153539, #156529, #111009, #64517, #95841, #78677, #142341, #171700, #140353, #183892, #124185, #172695, #61522, #123191, #33189, #1841, #185886, #77691, #63523, #18028, #3821, #79682, #91845, #154537, #15036, #186894, #141352, #94848, #157525, #65500, #45377, #184880, #107030, #46362, #108020, #139359, #840, #62513, #175677, #145324, #146320, #84643, #131158, #52322, #160504, #22995, #21994, #35168, #113979, #53318, #37151, #188869, #19995, #130140, #112994, #83647, #67490, #81639, #7809, #114996, #192847, #176691, #69493, #36152, #6807, #38165, #127161, #50352, #191837, #112011, #173700, #96823, #158508, #4809, #99820, #161505, #129148, #143322, #174688, #66497, #68485, #159493, #97804, #128160, #98811, #189860, #20988, #82643, #51334, #144326, #5815, #190845, #180914, #148567, #42389, #87871, #25241, #149559, #179923, #165732, #41390, #119230, #162726, #11055, #197074, #26232, #58541, #104052 ),
 ( #178915, #133385, #195076, #56555, #116222, #12068, #118232, #134403, #88876, #196090, #105047, #120207, #24231, #72730, #102056, #103055, #55548, #164737, #117221, #73730, #39381, #27228, #181897, #43375, #57560, #166731, #150569, #69718, #135403, #163741, #131385, #28235, #10057, #89875, #151558, #193074, #54549, #86882, #177913, #71717, #101040, #85882, #147570, #9055, #70726, #132393, #40382, #194086, #15022, #61509, #154523, #199042, #140341, #125186, #171687, #124171, #91832, #185872, #31186, #168689, #92838, #123178, #109013, #184867, #62500, #106029, #16020, #1829, #169692, #63511, #47358, #77677, #76683, #136377, #152531, #46349, #139346, #48352, #198054, #167715, #29213, #110006, #17012, #138359, #122187, #200040, #108007, #825, #59520, #155517, #170692, #32181, #93837, #78664, #33176, #186882, #90846, #94835, #45364, #13047, #60512, #74714, #183879, #121197, #182890, #44373, #14018, #75684, #137363, #107017, #30190, #153525, #51320, #156514, #96809, #145312, #49334, #95828, #20974, #65486, #187866, #98799, #53307, #158495, #97791, #5803, #3808, #68474, #189846, #188856, #79668, #36139, #19982, #110996, #81625, #113966, #157512, #172682, #67476, #34166, #66484, #112981, #35153, #174674, #159480, #82631, #19006, #144313, #173687, #80652, #129136, #114985, #6796, #143308, #190833, #52309, #175665, #64504, #37140, #18015, #126171, #160493, #130129, #141339, #21983, #83635, #142328, #176678, #127148, #4795, #128146, #2826, #50339, #111996, #191826, #38154, #164503, #86643, #119976, #116980, #9821, #196841, #194838, #177677, #101813, #118999, #11830, #22982, #39145, #117994, #40136, #193844, #71482, #72489, #181662, #195851, #146309, #8815, #69482, #148326, #134162, #24999, #149325, #25996, #103818, #100800, #42158, #99808, #180682, #165498, #179683, #57323, #41155, #10819, #73496, #135168, #161494, #133147, #87639, #150335, #26994, #131147, #56311, #88639, #102818, #84632, #115988, #58308, #70485, #7798, #192835, #162484, #54316, #23985, #85642, #147328, #132151, #55308, #178672, #163501, #1586, #78419, #154289, #31941, #43141, #62257, #585, #166499, #30952, #107765, #152303, #15779, #12813, #77438, #106787, #197821, #151325, #155281, #75454, #199805, #104810, #74480, #27997, #16771, #124941, #108772, #137128, #59287, #139110, #123925, #63261, #89636, #184631, #185623, #47113, #170450, #93595, #138124, #136145, #169450, #61272, #120956, #183646, #140095, #182655, #44139, #92599, #13787, #105798, #167484, #28980, #45128, #46112, #90621, #198815, #60280, #76447, #121953, #168461, #122942, #29959, #91596, #153286, #14787, #125931, #79427, #97549, #2585, #96568, #143073, #65248, #4551, #66244, #112740, #49100, #127904, #3570, #141098, #113727, #160251, #34912, #98557, #19746, #186638, #189606, #80412, #48109, #175424, #126908, #36892, #68230, #81387, #144076, #188614, #21741, #50095, #111755, #173444, #174433, #20731, #158256, #51080, #157269, #142084, #35903, #159237, #82388, #172439, #83393, #145070, #6552, #5557, #67236, #128895, #190594, #52070, #109765, #171449, #32937, #94592, #156270, #64265, #17772, #187630, #110758, #33927, #95585, #18765, #193600, #53061, #69238, #163256, #71247, #165259, #114740, #84391, #22742, #26753, #133920, #55072, #38909, #116742, #178432, #39899, #176434, #72243, #101565, #194598, #149092, #56070, #88393, #180446, #146067, #132911, #162248, #24758, #115751, #86405, #177439, #195611, #99567, #102582, #57083, #10582, #41918, #148090, #37908, #103584, #23747, #9581, #191583, #161248, #129883, #150086, #11590, #118757, #85396, #7552, #40909, #130904, #192594, #54077, #117750, #100566, #164266, #147089, #8573, #179443, #25761, #70248, #131916, #87407, #107524, #76200, #137879, #181428, #92357, #134927, #42906, #168219, #62014, #196604, #169201, #138865, #166254, #170207, #27754, #152064, #183403, #119745, #89397, #73258, #345, #199560, #61029, #60042, #93349 ),
 ( #123678, #29716, #31700, #122701, #91348, #58075, #13549, #185377, #151086, #12577, #184391, #182415, #104572, #15538, #155035, #75215, #14539, #45871, #120716, #46867, #106543, #105558, #74242, #153040, #136887, #135911, #198572, #30707, #197582, #59049, #154043, #43895, #44886, #77196, #121710, #108528, #167244, #28743, #90379, #158014, #33676, #109521, #143829, #190347, #65005, #128652, #49843, #16530, #96327, #110510, #78177, #5309, #95338, #66993, #98301, #111507, #174191, #157023, #51823, #18521, #80168, #3331, #142832, #50840, #113483, #35659, #139846, #20486, #175177, #172191, #81150, #97307, #36643, #1335, #127663, #63015, #124694, #158993, #82135, #186391, #4311, #65994, #125688, #189363, #47868, #112497, #141840, #171203, #32693, #94344, #48855, #173193, #156023, #17520, #79178, #140849, #2338, #64019, #126662, #187387, #188366, #34669, #19505, #41672, #101316, #40665, #71004, #102334, #148847, #54828, #116502, #56838, #10338, #146832, #194360, #163005, #24512, #67987, #179197, #21490, #129641, #178190, #71994, #83151, #55827, #25520, #52815, #118513, #114482, #38668, #70001, #6309, #176186, #160002, #87166, #86162, #147852, #8326, #180203, #177195, #131671, #144825, #39655, #37655, #162002, #164024, #133668, #191337, #99320, #9339, #100323, #53833, #193352, #132672, #161004, #117500, #22498, #68992, #84145, #195358, #145824, #85146, #7307, #130656, #192350, #115507, #23498, #123442, #122459, #184152, #183162, #60788, #121470, #152803, #76953, #15293, #185135, #136641, #167984, #153799, #29482, #73013, #198324, #45633, #44646, #165016, #119509, #137636, #74003, #106298, #151824, #181190, #182168, #91113, #59800, #14295, #166013, #75963, #120477, #196368, #30462, #138623, #13313, #104, #199323, #103336, #107285, #197345, #26509, #92110, #43653, #61774, #88153, #168956, #149838, #105316, #11342, #167003, #28505, #90139, #134682, #57836, #74979, #42668, #135673, #58808, #104329, #27513, #89154, #150843, #12339, #158759, #5072, #157787, #125456, #19277, #64777, #2103, #126438, #156794, #142601, #18287, #96098, #139609, #188136, #173958, #3099, #35425, #80924, #49607, #110277, #169964, #186148, #79942, #111270, #81896, #31457, #1095, #62771, #143589, #50607, #171958, #155786, #33446, #95105, #141612, #93109, #189135, #172961, #34439, #65758, #4080, #66755, #97078, #124452, #127427, #78937, #112266, #32454, #20249, #94107, #128416, #16292, #46626, #108286, #154794, #77942, #47627, #109282, #170960, #17283, #140613, #187153, #63784, #48625, #129409, #54583, #99076, #21254, #132428, #86920, #192103, #131423, #39414, #37416, #102091, #23260, #22256, #113252, #69753, #130405, #82909, #53586, #147605, #191106, #144587, #101074, #6073, #100080, #146583, #36405, #194120, #176955, #116256, #9093, #177947, #25277, #40420, #67751, #193109, #83905, #84903, #175947, #115262, #160766, #55583, #159759, #162759, #117257, #70760, #163776, #8077, #148602, #24268, #85917, #190112, #38424, #178950, #52580, #114240, #10094, #145588, #7066, #71754, #51587, #161765, #174943, #98060, #68747, #48146, #166768, #165769, #56595, #13081, #73764, #164774, #135437, #90880, #72770, #26268, #44408, #149596, #43412, #89907, #12101, #151590, #74746, #59554, #196125, #136409, #150605, #87910, #63299, #109803, #181930, #171486, #28269, #133423, #198088, #27264, #195112, #124979, #197107, #186676, #17809, #121232, #152563, #58574, #32975, #120240, #105082, #182925, #106062, #167748, #29246, #14052, #104087, #88913, #75720, #137396, #199077, #119265, #94629, #156308, #118269, #179959, #41426, #103092, #11094, #134440, #57596, #180948, #42425, #189643, #128931, #172477, #97585, #6589, #35939, #68268, #190632, #159273, #143110, #2625, #18804, #112777, #20769, #114776, #64302, #33964, #95622, #176470, #83429, #4589, #188653, #66282, #127941, #51118, #79466, #129919, #144113, #5593, #174470, #99604, #96605, #82424, #37944 ) ),
 .UNSPECIFIED., .T., .F., .F. ) 
 B_SPLINE_SURFACE_WITH_KNOTS ( ( 4, 3, 4 ),
 ( 3, 2, 2, 2, 2, 2, 2, 2, 2, 2, 2, 2, 2, 2, 2, 2, 2, 2, 2, 2, 2, 2, 2, 2, 2, 2, 2, 2, 2, 2, 2, 2, 2, 2, 2, 2, 2, 2, 2, 2, 2, 2, 2, 2, 2, 2, 2, 2, 2, 2, 2, 2, 2, 2, 2, 2, 2, 2, 2, 2, 2, 2, 2, 2, 2, 2, 2, 2, 2, 2, 2, 2, 2, 2, 2, 2, 2, 2, 2, 2, 2, 2, 2, 2, 2, 2, 2, 2, 2, 2, 2, 2, 2, 2, 2, 2, 2, 2, 2, 2, 2, 2, 2, 2, 2, 2, 2, 2, 2, 2, 2, 2, 2, 2, 2, 2, 2, 2, 2, 2, 2, 2, 2, 2, 2, 2, 2, 2, 2, 2, 2, 2, 2, 2, 2, 2, 2, 2, 2, 2, 2, 2, 2, 2, 2, 2, 2, 2, 2, 2, 2, 2, 2, 2, 2, 2, 2, 2, 2, 2, 2, 2, 2, 2, 2, 2, 2, 2, 2, 2, 2, 2, 2, 2, 2, 2, 2, 2, 2, 2, 2, 2, 2, 2, 2, 2, 2, 2, 2, 2, 2, 2, 2, 2, 2, 2, 2, 2, 2, 2, 2, 2, 2, 2, 2, 2, 2, 2, 2, 2, 2, 2, 2, 2, 2, 2, 2, 2, 2, 2, 2, 2, 2, 2, 2, 2, 2, 2, 3 ),
 ( 0.000000000000000000, 0.5000000000000000000, 1.000000000000000000 ),
 ( 0.000000000000000000, 0.004385964912280701511, 0.008771929824561403022, 0.01315789473684210453, 0.01754385964912280604, 0.02192982456140350755, 0.02631578947368420907, 0.03070175438596491058, 0.03508771929824561209, 0.03947368421052631360, 0.04385964912280701511, 0.04824561403508771662, 0.05263157894736841813, 0.05701754385964911964, 0.06140350877192982115, 0.06578947368421052266, 0.07017543859649122417, 0.07456140350877192569, 0.07894736842105262720, 0.08333333333333332871, 0.08771929824561403022, 0.09210526315789473173, 0.09649122807017543324, 0.1008771929824561348, 0.1052631578947368363, 0.1096491228070175378, 0.1140350877192982393, 0.1184210526315789408, 0.1228070175438596423, 0.1271929824561403577, 0.1315789473684210453, 0.1359649122807017607, 0.1403508771929824483, 0.1447368421052631637, 0.1491228070175438514, 0.1535087719298245668, 0.1578947368421052544, 0.1622807017543859698, 0.1666666666666666574, 0.1710526315789473728, 0.1754385964912280604, 0.1798245614035087758, 0.1842105263157894635, 0.1885964912280701788, 0.1929824561403508665, 0.1973684210526315819, 0.2017543859649122695, 0.2061403508771929849, 0.2105263157894736725, 0.2149122807017543879, 0.2192982456140350755, 0.2236842105263157909, 0.2280701754385964786, 0.2324561403508771940, 0.2368421052631578816, 0.2412280701754385970, 0.2456140350877192846, 0.2500000000000000000, 0.2543859649122807154, 0.2587719298245614308, 0.2631578947368420907, 0.2675438596491228060, 0.2719298245614035214, 0.2763157894736842368, 0.2807017543859648967, 0.2850877192982456121, 0.2894736842105263275, 0.2938596491228070429, 0.2982456140350877027, 0.3026315789473684181, 0.3070175438596491335, 0.3114035087719298489, 0.3157894736842105088, 0.3201754385964912242, 0.3245614035087719396, 0.3289473684210526550, 0.3333333333333333148, 0.3377192982456140302, 0.3421052631578947456, 0.3464912280701754610, 0.3508771929824561209, 0.3552631578947368363, 0.3596491228070175517, 0.3640350877192982670, 0.3684210526315789269, 0.3728070175438596423, 0.3771929824561403577, 0.3815789473684210731, 0.3859649122807017330, 0.3903508771929824483, 0.3947368421052631637, 0.3991228070175438791, 0.4035087719298245390, 0.4078947368421052544, 0.4122807017543859698, 0.4166666666666666852, 0.4210526315789473450, 0.4254385964912280604, 0.4298245614035087758, 0.4342105263157894912, 0.4385964912280701511, 0.4429824561403508665, 0.4473684210526315819, 0.4517543859649122973, 0.4561403508771929571, 0.4605263157894736725, 0.4649122807017543879, 0.4692982456140351033, 0.4736842105263157632, 0.4780701754385964786, 0.4824561403508771940, 0.4868421052631579093, 0.4912280701754385692, 0.4956140350877192846, 0.5000000000000000000, 0.5043859649122807154, 0.5087719298245614308, 0.5131578947368421462, 0.5175438596491228616, 0.5219298245614034659, 0.5263157894736841813, 0.5307017543859648967, 0.5350877192982456121, 0.5394736842105263275, 0.5438596491228070429, 0.5482456140350877583, 0.5526315789473684736, 0.5570175438596490780, 0.5614035087719297934, 0.5657894736842105088, 0.5701754385964912242, 0.5745614035087719396, 0.5789473684210526550, 0.5833333333333333703, 0.5877192982456140857, 0.5921052631578946901, 0.5964912280701754055, 0.6008771929824561209, 0.6052631578947368363, 0.6096491228070175517, 0.6140350877192982670, 0.6184210526315789824, 0.6228070175438596978, 0.6271929824561403022, 0.6315789473684210176, 0.6359649122807017330, 0.6403508771929824483, 0.6447368421052631637, 0.6491228070175438791, 0.6535087719298245945, 0.6578947368421053099, 0.6622807017543859143, 0.6666666666666666297, 0.6710526315789473450, 0.6754385964912280604, 0.6798245614035087758, 0.6842105263157894912, 0.6885964912280702066, 0.6929824561403509220, 0.6973684210526315264, 0.7017543859649122417, 0.7061403508771929571, 0.7105263157894736725, 0.7149122807017543879, 0.7192982456140351033, 0.7236842105263158187, 0.7280701754385965341, 0.7324561403508771384, 0.7368421052631578538, 0.7412280701754385692, 0.7456140350877192846, 0.7500000000000000000, 0.7543859649122807154, 0.7587719298245614308, 0.7631578947368421462, 0.7675438596491228616, 0.7719298245614034659, 0.7763157894736841813, 0.7807017543859648967, 0.7850877192982456121, 0.7894736842105263275, 0.7938596491228070429, 0.7982456140350877583, 0.8026315789473684736, 0.8070175438596490780, 0.8114035087719297934, 0.8157894736842105088, 0.8201754385964912242, 0.8245614035087719396, 0.8289473684210526550, 0.8333333333333333703, 0.8377192982456140857, 0.8421052631578946901, 0.8464912280701754055, 0.8508771929824561209, 0.8552631578947368363, 0.8596491228070175517, 0.8640350877192982670, 0.8684210526315789824, 0.8728070175438596978, 0.8771929824561403022, 0.8815789473684210176, 0.8859649122807017330, 0.8903508771929824483, 0.8947368421052631637, 0.8991228070175438791, 0.9035087719298245945, 0.9078947368421053099, 0.9122807017543859143, 0.9166666666666666297, 0.9210526315789473450, 0.9254385964912280604, 0.9298245614035087758, 0.9342105263157894912, 0.9385964912280702066, 0.9429824561403509220, 0.9473684210526315264, 0.9517543859649122417, 0.9561403508771929571, 0.9605263157894736725, 0.9649122807017543879, 0.9692982456140351033, 0.9736842105263158187, 0.9780701754385965341, 0.9824561403508771384, 0.9868421052631578538, 0.9912280701754385692, 0.9956140350877192846, 1.000000000000000000 ),
 .UNSPECIFIED. ) 
 GEOMETRIC_REPRESENTATION_ITEM ( )  RATIONAL_B_SPLINE_SURFACE ( (
 ( 1.000000000000000000, 0.9659258262890683122, 1.000000000000000000, 0.9659258262890683122, 1.000000000000000000, 0.9659258262890683122, 1.000000000000000000, 0.9659258262890683122, 1.000000000000000000, 0.9659258262890683122, 1.000000000000000000, 0.9659258262890683122, 1.000000000000000000, 0.9659258262890683122, 1.000000000000000000, 0.9659258262890683122, 1.000000000000000000, 0.9659258262890683122, 1.000000000000000000, 0.9659258262890683122, 1.000000000000000000, 0.9659258262890683122, 1.000000000000000000, 0.9659258262890683122, 1.000000000000000000, 0.9659258262890683122, 1.000000000000000000, 0.9659258262890683122, 1.000000000000000000, 0.9659258262890683122, 1.000000000000000000, 0.9659258262890683122, 1.000000000000000000, 0.9659258262890683122, 1.000000000000000000, 0.9659258262890683122, 1.000000000000000000, 0.9659258262890683122, 1.000000000000000000, 0.9659258262890683122, 1.000000000000000000, 0.9659258262890683122, 1.000000000000000000, 0.9659258262890683122, 1.000000000000000000, 0.9659258262890683122, 1.000000000000000000, 0.9659258262890683122, 1.000000000000000000, 0.9659258262890683122, 1.000000000000000000, 0.9659258262890683122, 1.000000000000000000, 0.9659258262890683122, 1.000000000000000000, 0.9659258262890683122, 1.000000000000000000, 0.9659258262890683122, 1.000000000000000000, 0.9659258262890683122, 1.000000000000000000, 0.9659258262890683122, 1.000000000000000000, 0.9659258262890683122, 1.000000000000000000, 0.9659258262890683122, 1.000000000000000000, 0.9659258262890683122, 1.000000000000000000, 0.9659258262890683122, 1.000000000000000000, 0.9659258262890683122, 1.000000000000000000, 0.9659258262890683122, 1.000000000000000000, 0.9659258262890683122, 1.000000000000000000, 0.9659258262890683122, 1.000000000000000000, 0.9659258262890683122, 1.000000000000000000, 0.9659258262890683122, 1.000000000000000000, 0.9659258262890683122, 1.000000000000000000, 0.9659258262890683122, 1.000000000000000000, 0.9659258262890683122, 1.000000000000000000, 0.9659258262890683122, 1.000000000000000000, 0.9659258262890683122, 1.000000000000000000, 0.9659258262890683122, 1.000000000000000000, 0.9659258262890683122, 1.000000000000000000, 0.9659258262890683122, 1.000000000000000000, 0.9659258262890683122, 1.000000000000000000, 0.9659258262890683122, 1.000000000000000000, 0.9659258262890683122, 1.000000000000000000, 0.9659258262890683122, 1.000000000000000000, 0.9659258262890683122, 1.000000000000000000, 0.9659258262890683122, 1.000000000000000000, 0.9659258262890683122, 1.000000000000000000, 0.9659258262890683122, 1.000000000000000000, 0.9659258262890683122, 1.000000000000000000, 0.9659258262890683122, 1.000000000000000000, 0.9659258262890683122, 1.000000000000000000, 0.9659258262890683122, 1.000000000000000000, 0.9659258262890683122, 1.000000000000000000, 0.9659258262890683122, 1.000000000000000000, 0.9659258262890683122, 1.000000000000000000, 0.9659258262890683122, 1.000000000000000000, 0.9659258262890683122, 1.000000000000000000, 0.9659258262890683122, 1.000000000000000000, 0.9659258262890683122, 1.000000000000000000, 0.9659258262890683122, 1.000000000000000000, 0.9659258262890683122, 1.000000000000000000, 0.9659258262890683122, 1.000000000000000000, 0.9659258262890683122, 1.000000000000000000, 0.9659258262890683122, 1.000000000000000000, 0.9659258262890683122, 1.000000000000000000, 0.9659258262890683122, 1.000000000000000000, 0.9659258262890683122, 1.000000000000000000, 0.9659258262890683122, 1.000000000000000000, 0.9659258262890683122, 1.000000000000000000, 0.9659258262890683122, 1.000000000000000000, 0.9659258262890683122, 1.000000000000000000, 0.9659258262890683122, 1.000000000000000000, 0.9659258262890683122, 1.000000000000000000, 0.9659258262890683122, 1.000000000000000000, 0.9659258262890683122, 1.000000000000000000, 0.9659258262890683122, 1.000000000000000000, 0.9659258262890683122, 1.000000000000000000, 0.9659258262890683122, 1.000000000000000000, 0.9659258262890683122, 1.000000000000000000, 0.9659258262890683122, 1.000000000000000000, 0.9659258262890683122, 1.000000000000000000, 0.9659258262890683122, 1.000000000000000000, 0.9659258262890683122, 1.000000000000000000, 0.9659258262890683122, 1.000000000000000000, 0.9659258262890683122, 1.000000000000000000, 0.9659258262890683122, 1.000000000000000000, 0.9659258262890683122, 1.000000000000000000, 0.9659258262890683122, 1.000000000000000000, 0.9659258262890683122, 1.000000000000000000, 0.9659258262890683122, 1.000000000000000000, 0.9659258262890683122, 1.000000000000000000, 0.9659258262890683122, 1.000000000000000000, 0.9659258262890683122, 1.000000000000000000, 0.9659258262890683122, 1.000000000000000000, 0.9659258262890683122, 1.000000000000000000, 0.9659258262890683122, 1.000000000000000000, 0.9659258262890683122, 1.000000000000000000, 0.9659258262890683122, 1.000000000000000000, 0.9659258262890683122, 1.000000000000000000, 0.9659258262890683122, 1.000000000000000000, 0.9659258262890683122, 1.000000000000000000, 0.9659258262890683122, 1.000000000000000000, 0.9659258262890683122, 1.000000000000000000, 0.9659258262890683122, 1.000000000000000000, 0.9659258262890683122, 1.000000000000000000, 0.9659258262890683122, 1.000000000000000000, 0.9659258262890683122, 1.000000000000000000, 0.9659258262890683122, 1.000000000000000000, 0.9659258262890683122, 1.000000000000000000, 0.9659258262890683122, 1.000000000000000000, 0.9659258262890683122, 1.000000000000000000, 0.9659258262890683122, 1.000000000000000000, 0.9659258262890683122, 1.000000000000000000, 0.9659258262890683122, 1.000000000000000000, 0.9659258262890683122, 1.000000000000000000, 0.9659258262890683122, 1.000000000000000000, 0.9659258262890683122, 1.000000000000000000, 0.9659258262890683122, 1.000000000000000000, 0.9659258262890683122, 1.000000000000000000, 0.9659258262890683122, 1.000000000000000000, 0.9659258262890683122, 1.000000000000000000, 0.9659258262890683122, 1.000000000000000000, 0.9659258262890683122, 1.000000000000000000, 0.9659258262890683122, 1.000000000000000000, 0.9659258262890683122, 1.000000000000000000, 0.9659258262890683122, 1.000000000000000000, 0.9659258262890683122, 1.000000000000000000, 0.9659258262890683122, 1.000000000000000000, 0.9659258262890683122, 1.000000000000000000, 0.9659258262890683122, 1.000000000000000000, 0.9659258262890683122, 1.000000000000000000, 0.9659258262890683122, 1.000000000000000000, 0.9659258262890683122, 1.000000000000000000, 0.9659258262890683122, 1.000000000000000000, 0.9659258262890683122, 1.000000000000000000, 0.9659258262890683122, 1.000000000000000000, 0.9659258262890683122, 1.000000000000000000, 0.9659258262890683122, 1.000000000000000000, 0.9659258262890683122, 1.000000000000000000, 0.9659258262890683122, 1.000000000000000000, 0.9659258262890683122, 1.000000000000000000, 0.9659258262890683122, 1.000000000000000000, 0.9659258262890683122, 1.000000000000000000, 0.9659258262890683122, 1.000000000000000000, 0.9659258262890683122, 1.000000000000000000, 0.9659258262890683122, 1.000000000000000000, 0.9659258262890683122, 1.000000000000000000, 0.9659258262890683122, 1.000000000000000000, 0.9659258262890683122, 1.000000000000000000, 0.9659258262890683122, 1.000000000000000000, 0.9659258262890683122, 1.000000000000000000, 0.9659258262890683122, 1.000000000000000000, 0.9659258262890683122, 1.000000000000000000, 0.9659258262890683122, 1.000000000000000000, 0.9659258262890683122, 1.000000000000000000, 0.9659258262890683122, 1.000000000000000000, 0.9659258262890683122, 1.000000000000000000, 0.9659258262890683122, 1.000000000000000000, 0.9659258262890683122, 1.000000000000000000, 0.9659258262890683122, 1.000000000000000000, 0.9659258262890683122, 1.000000000000000000, 0.9659258262890683122, 1.000000000000000000, 0.9659258262890683122, 1.000000000000000000, 0.9659258262890683122, 1.000000000000000000, 0.9659258262890683122, 1.000000000000000000, 0.9659258262890683122, 1.000000000000000000, 0.9659258262890683122, 1.000000000000000000, 0.9659258262890683122, 1.000000000000000000, 0.9659258262890683122, 1.000000000000000000, 0.9659258262890683122, 1.000000000000000000, 0.9659258262890683122, 1.000000000000000000, 0.9659258262890683122, 1.000000000000000000, 0.9659258262890683122, 1.000000000000000000, 0.9659258262890683122, 1.000000000000000000, 0.9659258262890683122, 1.000000000000000000, 0.9659258262890683122, 1.000000000000000000, 0.9659258262890683122, 1.000000000000000000, 0.9659258262890683122, 1.000000000000000000, 0.9659258262890683122, 1.000000000000000000, 0.9659258262890683122, 1.000000000000000000, 0.9659258262890683122, 1.000000000000000000, 0.9659258262890683122, 1.000000000000000000, 0.9659258262890683122, 1.000000000000000000, 0.9659258262890683122, 1.000000000000000000, 0.9659258262890683122, 1.000000000000000000, 0.9659258262890683122, 1.000000000000000000, 0.9659258262890683122, 1.000000000000000000, 0.9659258262890683122, 1.000000000000000000, 0.9659258262890683122, 1.000000000000000000, 0.9659258262890683122, 1.000000000000000000, 0.9659258262890683122, 1.000000000000000000, 0.9659258262890683122, 1.000000000000000000, 0.9659258262890683122, 1.000000000000000000, 0.9659258262890683122, 1.000000000000000000, 0.9659258262890683122, 1.000000000000000000, 0.9659258262890683122, 1.000000000000000000, 0.9659258262890683122, 1.000000000000000000, 0.9659258262890683122, 1.000000000000000000, 0.9659258262890683122, 1.000000000000000000, 0.9659258262890683122, 1.000000000000000000, 0.9659258262890683122, 1.000000000000000000, 0.9659258262890683122, 1.000000000000000000, 0.9659258262890683122, 1.000000000000000000, 0.9659258262890683122, 1.000000000000000000, 0.9659258262890683122, 1.000000000000000000, 0.9659258262890683122, 1.000000000000000000, 0.9659258262890683122, 1.000000000000000000, 0.9659258262890683122, 1.000000000000000000, 0.9659258262890683122, 1.000000000000000000, 0.9659258262890683122, 1.000000000000000000, 0.9659258262890683122, 1.000000000000000000, 0.9659258262890683122, 1.000000000000000000, 0.9659258262890683122, 1.000000000000000000, 0.9659258262890683122, 1.000000000000000000, 0.9659258262890683122, 1.000000000000000000, 0.9659258262890683122, 1.000000000000000000, 0.9659258262890683122, 1.000000000000000000, 0.9659258262890683122, 1.000000000000000000, 0.9659258262890683122, 1.000000000000000000),
 ( 0.3333333333333333703, 0.3219752754296894559, 0.3333333333333333703, 0.3219752754296894559, 0.3333333333333333703, 0.3219752754296894559, 0.3333333333333333703, 0.3219752754296894559, 0.3333333333333333703, 0.3219752754296894559, 0.3333333333333333703, 0.3219752754296894559, 0.3333333333333333703, 0.3219752754296894559, 0.3333333333333333703, 0.3219752754296894559, 0.3333333333333333703, 0.3219752754296894559, 0.3333333333333333703, 0.3219752754296894559, 0.3333333333333333703, 0.3219752754296894559, 0.3333333333333333703, 0.3219752754296894559, 0.3333333333333333703, 0.3219752754296894559, 0.3333333333333333703, 0.3219752754296894559, 0.3333333333333333703, 0.3219752754296894559, 0.3333333333333333703, 0.3219752754296894559, 0.3333333333333333703, 0.3219752754296894559, 0.3333333333333333703, 0.3219752754296894559, 0.3333333333333333703, 0.3219752754296894559, 0.3333333333333333703, 0.3219752754296894559, 0.3333333333333333703, 0.3219752754296894559, 0.3333333333333333703, 0.3219752754296894559, 0.3333333333333333703, 0.3219752754296894559, 0.3333333333333333703, 0.3219752754296894559, 0.3333333333333333703, 0.3219752754296894559, 0.3333333333333333703, 0.3219752754296894559, 0.3333333333333333703, 0.3219752754296894559, 0.3333333333333333703, 0.3219752754296894559, 0.3333333333333333703, 0.3219752754296894559, 0.3333333333333333703, 0.3219752754296894559, 0.3333333333333333703, 0.3219752754296894559, 0.3333333333333333703, 0.3219752754296894559, 0.3333333333333333703, 0.3219752754296894559, 0.3333333333333333703, 0.3219752754296894559, 0.3333333333333333703, 0.3219752754296894559, 0.3333333333333333703, 0.3219752754296894559, 0.3333333333333333703, 0.3219752754296894559, 0.3333333333333333703, 0.3219752754296894559, 0.3333333333333333703, 0.3219752754296894559, 0.3333333333333333703, 0.3219752754296894559, 0.3333333333333333703, 0.3219752754296894559, 0.3333333333333333703, 0.3219752754296894559, 0.3333333333333333703, 0.3219752754296894559, 0.3333333333333333703, 0.3219752754296894559, 0.3333333333333333703, 0.3219752754296894559, 0.3333333333333333703, 0.3219752754296894559, 0.3333333333333333703, 0.3219752754296894559, 0.3333333333333333703, 0.3219752754296894559, 0.3333333333333333703, 0.3219752754296894559, 0.3333333333333333703, 0.3219752754296894559, 0.3333333333333333703, 0.3219752754296894559, 0.3333333333333333703, 0.3219752754296894559, 0.3333333333333333703, 0.3219752754296894559, 0.3333333333333333703, 0.3219752754296894559, 0.3333333333333333703, 0.3219752754296894559, 0.3333333333333333703, 0.3219752754296894559, 0.3333333333333333703, 0.3219752754296894559, 0.3333333333333333703, 0.3219752754296894559, 0.3333333333333333703, 0.3219752754296894559, 0.3333333333333333703, 0.3219752754296894559, 0.3333333333333333703, 0.3219752754296894559, 0.3333333333333333703, 0.3219752754296894559, 0.3333333333333333703, 0.3219752754296894559, 0.3333333333333333703, 0.3219752754296894559, 0.3333333333333333703, 0.3219752754296894559, 0.3333333333333333703, 0.3219752754296894559, 0.3333333333333333703, 0.3219752754296894559, 0.3333333333333333703, 0.3219752754296894559, 0.3333333333333333703, 0.3219752754296894559, 0.3333333333333333703, 0.3219752754296894559, 0.3333333333333333703, 0.3219752754296894559, 0.3333333333333333703, 0.3219752754296894559, 0.3333333333333333703, 0.3219752754296894559, 0.3333333333333333703, 0.3219752754296894559, 0.3333333333333333703, 0.3219752754296894559, 0.3333333333333333703, 0.3219752754296894559, 0.3333333333333333703, 0.3219752754296894559, 0.3333333333333333703, 0.3219752754296894559, 0.3333333333333333703, 0.3219752754296894559, 0.3333333333333333703, 0.3219752754296894559, 0.3333333333333333703, 0.3219752754296894559, 0.3333333333333333703, 0.3219752754296894559, 0.3333333333333333703, 0.3219752754296894559, 0.3333333333333333703, 0.3219752754296894559, 0.3333333333333333703, 0.3219752754296894559, 0.3333333333333333703, 0.3219752754296894559, 0.3333333333333333703, 0.3219752754296894559, 0.3333333333333333703, 0.3219752754296894559, 0.3333333333333333703, 0.3219752754296894559, 0.3333333333333333703, 0.3219752754296894559, 0.3333333333333333703, 0.3219752754296894559, 0.3333333333333333703, 0.3219752754296894559, 0.3333333333333333703, 0.3219752754296894559, 0.3333333333333333703, 0.3219752754296894559, 0.3333333333333333703, 0.3219752754296894559, 0.3333333333333333703, 0.3219752754296894559, 0.3333333333333333703, 0.3219752754296894559, 0.3333333333333333703, 0.3219752754296894559, 0.3333333333333333703, 0.3219752754296894559, 0.3333333333333333703, 0.3219752754296894559, 0.3333333333333333703, 0.3219752754296894559, 0.3333333333333333703, 0.3219752754296894559, 0.3333333333333333703, 0.3219752754296894559, 0.3333333333333333703, 0.3219752754296894559, 0.3333333333333333703, 0.3219752754296894559, 0.3333333333333333703, 0.3219752754296894559, 0.3333333333333333703, 0.3219752754296894559, 0.3333333333333333703, 0.3219752754296894559, 0.3333333333333333703, 0.3219752754296894559, 0.3333333333333333703, 0.3219752754296894559, 0.3333333333333333703, 0.3219752754296894559, 0.3333333333333333703, 0.3219752754296894559, 0.3333333333333333703, 0.3219752754296894559, 0.3333333333333333703, 0.3219752754296894559, 0.3333333333333333703, 0.3219752754296894559, 0.3333333333333333703, 0.3219752754296894559, 0.3333333333333333703, 0.3219752754296894559, 0.3333333333333333703, 0.3219752754296894559, 0.3333333333333333703, 0.3219752754296894559, 0.3333333333333333703, 0.3219752754296894559, 0.3333333333333333703, 0.3219752754296894559, 0.3333333333333333703, 0.3219752754296894559, 0.3333333333333333703, 0.3219752754296894559, 0.3333333333333333703, 0.3219752754296894559, 0.3333333333333333703, 0.3219752754296894559, 0.3333333333333333703, 0.3219752754296894559, 0.3333333333333333703, 0.3219752754296894559, 0.3333333333333333703, 0.3219752754296894559, 0.3333333333333333703, 0.3219752754296894559, 0.3333333333333333703, 0.3219752754296894559, 0.3333333333333333703, 0.3219752754296894559, 0.3333333333333333703, 0.3219752754296894559, 0.3333333333333333703, 0.3219752754296894559, 0.3333333333333333703, 0.3219752754296894559, 0.3333333333333333703, 0.3219752754296894559, 0.3333333333333333703, 0.3219752754296894559, 0.3333333333333333703, 0.3219752754296894559, 0.3333333333333333703, 0.3219752754296894559, 0.3333333333333333703, 0.3219752754296894559, 0.3333333333333333703, 0.3219752754296894559, 0.3333333333333333703, 0.3219752754296894559, 0.3333333333333333703, 0.3219752754296894559, 0.3333333333333333703, 0.3219752754296894559, 0.3333333333333333703, 0.3219752754296894559, 0.3333333333333333703, 0.3219752754296894559, 0.3333333333333333703, 0.3219752754296894559, 0.3333333333333333703, 0.3219752754296894559, 0.3333333333333333703, 0.3219752754296894559, 0.3333333333333333703, 0.3219752754296894559, 0.3333333333333333703, 0.3219752754296894559, 0.3333333333333333703, 0.3219752754296894559, 0.3333333333333333703, 0.3219752754296894559, 0.3333333333333333703, 0.3219752754296894559, 0.3333333333333333703, 0.3219752754296894559, 0.3333333333333333703, 0.3219752754296894559, 0.3333333333333333703, 0.3219752754296894559, 0.3333333333333333703, 0.3219752754296894559, 0.3333333333333333703, 0.3219752754296894559, 0.3333333333333333703, 0.3219752754296894559, 0.3333333333333333703, 0.3219752754296894559, 0.3333333333333333703, 0.3219752754296894559, 0.3333333333333333703, 0.3219752754296894559, 0.3333333333333333703, 0.3219752754296894559, 0.3333333333333333703, 0.3219752754296894559, 0.3333333333333333703, 0.3219752754296894559, 0.3333333333333333703, 0.3219752754296894559, 0.3333333333333333703, 0.3219752754296894559, 0.3333333333333333703, 0.3219752754296894559, 0.3333333333333333703, 0.3219752754296894559, 0.3333333333333333703, 0.3219752754296894559, 0.3333333333333333703, 0.3219752754296894559, 0.3333333333333333703, 0.3219752754296894559, 0.3333333333333333703, 0.3219752754296894559, 0.3333333333333333703, 0.3219752754296894559, 0.3333333333333333703, 0.3219752754296894559, 0.3333333333333333703, 0.3219752754296894559, 0.3333333333333333703, 0.3219752754296894559, 0.3333333333333333703, 0.3219752754296894559, 0.3333333333333333703, 0.3219752754296894559, 0.3333333333333333703, 0.3219752754296894559, 0.3333333333333333703, 0.3219752754296894559, 0.3333333333333333703, 0.3219752754296894559, 0.3333333333333333703, 0.3219752754296894559, 0.3333333333333333703, 0.3219752754296894559, 0.3333333333333333703, 0.3219752754296894559, 0.3333333333333333703, 0.3219752754296894559, 0.3333333333333333703, 0.3219752754296894559, 0.3333333333333333703, 0.3219752754296894559, 0.3333333333333333703, 0.3219752754296894559, 0.3333333333333333703, 0.3219752754296894559, 0.3333333333333333703, 0.3219752754296894559, 0.3333333333333333703, 0.3219752754296894559, 0.3333333333333333703, 0.3219752754296894559, 0.3333333333333333703, 0.3219752754296894559, 0.3333333333333333703, 0.3219752754296894559, 0.3333333333333333703, 0.3219752754296894559, 0.3333333333333333703, 0.3219752754296894559, 0.3333333333333333703, 0.3219752754296894559, 0.3333333333333333703, 0.3219752754296894559, 0.3333333333333333703, 0.3219752754296894559, 0.3333333333333333703, 0.3219752754296894559, 0.3333333333333333703, 0.3219752754296894559, 0.3333333333333333703, 0.3219752754296894559, 0.3333333333333333703, 0.3219752754296894559, 0.3333333333333333703, 0.3219752754296894559, 0.3333333333333333703, 0.3219752754296894559, 0.3333333333333333703, 0.3219752754296894559, 0.3333333333333333703, 0.3219752754296894559, 0.3333333333333333703, 0.3219752754296894559, 0.3333333333333333703, 0.3219752754296894559, 0.3333333333333333703, 0.3219752754296894559, 0.3333333333333333703, 0.3219752754296894559, 0.3333333333333333703, 0.3219752754296894559, 0.3333333333333333703, 0.3219752754296894559, 0.3333333333333333703, 0.3219752754296894559, 0.3333333333333333703, 0.3219752754296894559, 0.3333333333333333703, 0.3219752754296894559, 0.3333333333333333703, 0.3219752754296894559, 0.3333333333333333703, 0.3219752754296894559, 0.3333333333333333703, 0.3219752754296894559, 0.3333333333333333703, 0.3219752754296894559, 0.3333333333333333703, 0.3219752754296894559, 0.3333333333333333703, 0.3219752754296894559, 0.3333333333333333703, 0.3219752754296894559, 0.3333333333333333703, 0.3219752754296894559, 0.3333333333333333703, 0.3219752754296894559, 0.3333333333333333703, 0.3219752754296894559, 0.3333333333333333703, 0.3219752754296894559, 0.3333333333333333703),
 ( 0.3333333333333333703, 0.3219752754296894559, 0.3333333333333333703, 0.3219752754296894559, 0.3333333333333333703, 0.3219752754296894559, 0.3333333333333333703, 0.3219752754296894559, 0.3333333333333333703, 0.3219752754296894559, 0.3333333333333333703, 0.3219752754296894559, 0.3333333333333333703, 0.3219752754296894559, 0.3333333333333333703, 0.3219752754296894559, 0.3333333333333333703, 0.3219752754296894559, 0.3333333333333333703, 0.3219752754296894559, 0.3333333333333333703, 0.3219752754296894559, 0.3333333333333333703, 0.3219752754296894559, 0.3333333333333333703, 0.3219752754296894559, 0.3333333333333333703, 0.3219752754296894559, 0.3333333333333333703, 0.3219752754296894559, 0.3333333333333333703, 0.3219752754296894559, 0.3333333333333333703, 0.3219752754296894559, 0.3333333333333333703, 0.3219752754296894559, 0.3333333333333333703, 0.3219752754296894559, 0.3333333333333333703, 0.3219752754296894559, 0.3333333333333333703, 0.3219752754296894559, 0.3333333333333333703, 0.3219752754296894559, 0.3333333333333333703, 0.3219752754296894559, 0.3333333333333333703, 0.3219752754296894559, 0.3333333333333333703, 0.3219752754296894559, 0.3333333333333333703, 0.3219752754296894559, 0.3333333333333333703, 0.3219752754296894559, 0.3333333333333333703, 0.3219752754296894559, 0.3333333333333333703, 0.3219752754296894559, 0.3333333333333333703, 0.3219752754296894559, 0.3333333333333333703, 0.3219752754296894559, 0.3333333333333333703, 0.3219752754296894559, 0.3333333333333333703, 0.3219752754296894559, 0.3333333333333333703, 0.3219752754296894559, 0.3333333333333333703, 0.3219752754296894559, 0.3333333333333333703, 0.3219752754296894559, 0.3333333333333333703, 0.3219752754296894559, 0.3333333333333333703, 0.3219752754296894559, 0.3333333333333333703, 0.3219752754296894559, 0.3333333333333333703, 0.3219752754296894559, 0.3333333333333333703, 0.3219752754296894559, 0.3333333333333333703, 0.3219752754296894559, 0.3333333333333333703, 0.3219752754296894559, 0.3333333333333333703, 0.3219752754296894559, 0.3333333333333333703, 0.3219752754296894559, 0.3333333333333333703, 0.3219752754296894559, 0.3333333333333333703, 0.3219752754296894559, 0.3333333333333333703, 0.3219752754296894559, 0.3333333333333333703, 0.3219752754296894559, 0.3333333333333333703, 0.3219752754296894559, 0.3333333333333333703, 0.3219752754296894559, 0.3333333333333333703, 0.3219752754296894559, 0.3333333333333333703, 0.3219752754296894559, 0.3333333333333333703, 0.3219752754296894559, 0.3333333333333333703, 0.3219752754296894559, 0.3333333333333333703, 0.3219752754296894559, 0.3333333333333333703, 0.3219752754296894559, 0.3333333333333333703, 0.3219752754296894559, 0.3333333333333333703, 0.3219752754296894559, 0.3333333333333333703, 0.3219752754296894559, 0.3333333333333333703, 0.3219752754296894559, 0.3333333333333333703, 0.3219752754296894559, 0.3333333333333333703, 0.3219752754296894559, 0.3333333333333333703, 0.3219752754296894559, 0.3333333333333333703, 0.3219752754296894559, 0.3333333333333333703, 0.3219752754296894559, 0.3333333333333333703, 0.3219752754296894559, 0.3333333333333333703, 0.3219752754296894559, 0.3333333333333333703, 0.3219752754296894559, 0.3333333333333333703, 0.3219752754296894559, 0.3333333333333333703, 0.3219752754296894559, 0.3333333333333333703, 0.3219752754296894559, 0.3333333333333333703, 0.3219752754296894559, 0.3333333333333333703, 0.3219752754296894559, 0.3333333333333333703, 0.3219752754296894559, 0.3333333333333333703, 0.3219752754296894559, 0.3333333333333333703, 0.3219752754296894559, 0.3333333333333333703, 0.3219752754296894559, 0.3333333333333333703, 0.3219752754296894559, 0.3333333333333333703, 0.3219752754296894559, 0.3333333333333333703, 0.3219752754296894559, 0.3333333333333333703, 0.3219752754296894559, 0.3333333333333333703, 0.3219752754296894559, 0.3333333333333333703, 0.3219752754296894559, 0.3333333333333333703, 0.3219752754296894559, 0.3333333333333333703, 0.3219752754296894559, 0.3333333333333333703, 0.3219752754296894559, 0.3333333333333333703, 0.3219752754296894559, 0.3333333333333333703, 0.3219752754296894559, 0.3333333333333333703, 0.3219752754296894559, 0.3333333333333333703, 0.3219752754296894559, 0.3333333333333333703, 0.3219752754296894559, 0.3333333333333333703, 0.3219752754296894559, 0.3333333333333333703, 0.3219752754296894559, 0.3333333333333333703, 0.3219752754296894559, 0.3333333333333333703, 0.3219752754296894559, 0.3333333333333333703, 0.3219752754296894559, 0.3333333333333333703, 0.3219752754296894559, 0.3333333333333333703, 0.3219752754296894559, 0.3333333333333333703, 0.3219752754296894559, 0.3333333333333333703, 0.3219752754296894559, 0.3333333333333333703, 0.3219752754296894559, 0.3333333333333333703, 0.3219752754296894559, 0.3333333333333333703, 0.3219752754296894559, 0.3333333333333333703, 0.3219752754296894559, 0.3333333333333333703, 0.3219752754296894559, 0.3333333333333333703, 0.3219752754296894559, 0.3333333333333333703, 0.3219752754296894559, 0.3333333333333333703, 0.3219752754296894559, 0.3333333333333333703, 0.3219752754296894559, 0.3333333333333333703, 0.3219752754296894559, 0.3333333333333333703, 0.3219752754296894559, 0.3333333333333333703, 0.3219752754296894559, 0.3333333333333333703, 0.3219752754296894559, 0.3333333333333333703, 0.3219752754296894559, 0.3333333333333333703, 0.3219752754296894559, 0.3333333333333333703, 0.3219752754296894559, 0.3333333333333333703, 0.3219752754296894559, 0.3333333333333333703, 0.3219752754296894559, 0.3333333333333333703, 0.3219752754296894559, 0.3333333333333333703, 0.3219752754296894559, 0.3333333333333333703, 0.3219752754296894559, 0.3333333333333333703, 0.3219752754296894559, 0.3333333333333333703, 0.3219752754296894559, 0.3333333333333333703, 0.3219752754296894559, 0.3333333333333333703, 0.3219752754296894559, 0.3333333333333333703, 0.3219752754296894559, 0.3333333333333333703, 0.3219752754296894559, 0.3333333333333333703, 0.3219752754296894559, 0.3333333333333333703, 0.3219752754296894559, 0.3333333333333333703, 0.3219752754296894559, 0.3333333333333333703, 0.3219752754296894559, 0.3333333333333333703, 0.3219752754296894559, 0.3333333333333333703, 0.3219752754296894559, 0.3333333333333333703, 0.3219752754296894559, 0.3333333333333333703, 0.3219752754296894559, 0.3333333333333333703, 0.3219752754296894559, 0.3333333333333333703, 0.3219752754296894559, 0.3333333333333333703, 0.3219752754296894559, 0.3333333333333333703, 0.3219752754296894559, 0.3333333333333333703, 0.3219752754296894559, 0.3333333333333333703, 0.3219752754296894559, 0.3333333333333333703, 0.3219752754296894559, 0.3333333333333333703, 0.3219752754296894559, 0.3333333333333333703, 0.3219752754296894559, 0.3333333333333333703, 0.3219752754296894559, 0.3333333333333333703, 0.3219752754296894559, 0.3333333333333333703, 0.3219752754296894559, 0.3333333333333333703, 0.3219752754296894559, 0.3333333333333333703, 0.3219752754296894559, 0.3333333333333333703, 0.3219752754296894559, 0.3333333333333333703, 0.3219752754296894559, 0.3333333333333333703, 0.3219752754296894559, 0.3333333333333333703, 0.3219752754296894559, 0.3333333333333333703, 0.3219752754296894559, 0.3333333333333333703, 0.3219752754296894559, 0.3333333333333333703, 0.3219752754296894559, 0.3333333333333333703, 0.3219752754296894559, 0.3333333333333333703, 0.3219752754296894559, 0.3333333333333333703, 0.3219752754296894559, 0.3333333333333333703, 0.3219752754296894559, 0.3333333333333333703, 0.3219752754296894559, 0.3333333333333333703, 0.3219752754296894559, 0.3333333333333333703, 0.3219752754296894559, 0.3333333333333333703, 0.3219752754296894559, 0.3333333333333333703, 0.3219752754296894559, 0.3333333333333333703, 0.3219752754296894559, 0.3333333333333333703, 0.3219752754296894559, 0.3333333333333333703, 0.3219752754296894559, 0.3333333333333333703, 0.3219752754296894559, 0.3333333333333333703, 0.3219752754296894559, 0.3333333333333333703, 0.3219752754296894559, 0.3333333333333333703, 0.3219752754296894559, 0.3333333333333333703, 0.3219752754296894559, 0.3333333333333333703, 0.3219752754296894559, 0.3333333333333333703, 0.3219752754296894559, 0.3333333333333333703, 0.3219752754296894559, 0.3333333333333333703, 0.3219752754296894559, 0.3333333333333333703, 0.3219752754296894559, 0.3333333333333333703, 0.3219752754296894559, 0.3333333333333333703, 0.3219752754296894559, 0.3333333333333333703, 0.3219752754296894559, 0.3333333333333333703, 0.3219752754296894559, 0.3333333333333333703, 0.3219752754296894559, 0.3333333333333333703, 0.3219752754296894559, 0.3333333333333333703, 0.3219752754296894559, 0.3333333333333333703, 0.3219752754296894559, 0.3333333333333333703, 0.3219752754296894559, 0.3333333333333333703, 0.3219752754296894559, 0.3333333333333333703, 0.3219752754296894559, 0.3333333333333333703, 0.3219752754296894559, 0.3333333333333333703, 0.3219752754296894559, 0.3333333333333333703, 0.3219752754296894559, 0.3333333333333333703, 0.3219752754296894559, 0.3333333333333333703, 0.3219752754296894559, 0.3333333333333333703, 0.3219752754296894559, 0.3333333333333333703, 0.3219752754296894559, 0.3333333333333333703, 0.3219752754296894559, 0.3333333333333333703, 0.3219752754296894559, 0.3333333333333333703, 0.3219752754296894559, 0.3333333333333333703, 0.3219752754296894559, 0.3333333333333333703, 0.3219752754296894559, 0.3333333333333333703, 0.3219752754296894559, 0.3333333333333333703, 0.3219752754296894559, 0.3333333333333333703, 0.3219752754296894559, 0.3333333333333333703, 0.3219752754296894559, 0.3333333333333333703, 0.3219752754296894559, 0.3333333333333333703, 0.3219752754296894559, 0.3333333333333333703, 0.3219752754296894559, 0.3333333333333333703, 0.3219752754296894559, 0.3333333333333333703, 0.3219752754296894559, 0.3333333333333333703, 0.3219752754296894559, 0.3333333333333333703, 0.3219752754296894559, 0.3333333333333333703, 0.3219752754296894559, 0.3333333333333333703, 0.3219752754296894559, 0.3333333333333333703, 0.3219752754296894559, 0.3333333333333333703, 0.3219752754296894559, 0.3333333333333333703, 0.3219752754296894559, 0.3333333333333333703, 0.3219752754296894559, 0.3333333333333333703, 0.3219752754296894559, 0.3333333333333333703, 0.3219752754296894559, 0.3333333333333333703, 0.3219752754296894559, 0.3333333333333333703, 0.3219752754296894559, 0.3333333333333333703, 0.3219752754296894559, 0.3333333333333333703, 0.3219752754296894559, 0.3333333333333333703, 0.3219752754296894559, 0.3333333333333333703, 0.3219752754296894559, 0.3333333333333333703, 0.3219752754296894559, 0.3333333333333333703),
 ( 1.000000000000000000, 0.9659258262890683122, 1.000000000000000000, 0.9659258262890683122, 1.000000000000000000, 0.9659258262890683122, 1.000000000000000000, 0.9659258262890683122, 1.000000000000000000, 0.9659258262890683122, 1.000000000000000000, 0.9659258262890683122, 1.000000000000000000, 0.9659258262890683122, 1.000000000000000000, 0.9659258262890683122, 1.000000000000000000, 0.9659258262890683122, 1.000000000000000000, 0.9659258262890683122, 1.000000000000000000, 0.9659258262890683122, 1.000000000000000000, 0.9659258262890683122, 1.000000000000000000, 0.9659258262890683122, 1.000000000000000000, 0.9659258262890683122, 1.000000000000000000, 0.9659258262890683122, 1.000000000000000000, 0.9659258262890683122, 1.000000000000000000, 0.9659258262890683122, 1.000000000000000000, 0.9659258262890683122, 1.000000000000000000, 0.9659258262890683122, 1.000000000000000000, 0.9659258262890683122, 1.000000000000000000, 0.9659258262890683122, 1.000000000000000000, 0.9659258262890683122, 1.000000000000000000, 0.9659258262890683122, 1.000000000000000000, 0.9659258262890683122, 1.000000000000000000, 0.9659258262890683122, 1.000000000000000000, 0.9659258262890683122, 1.000000000000000000, 0.9659258262890683122, 1.000000000000000000, 0.9659258262890683122, 1.000000000000000000, 0.9659258262890683122, 1.000000000000000000, 0.9659258262890683122, 1.000000000000000000, 0.9659258262890683122, 1.000000000000000000, 0.9659258262890683122, 1.000000000000000000, 0.9659258262890683122, 1.000000000000000000, 0.9659258262890683122, 1.000000000000000000, 0.9659258262890683122, 1.000000000000000000, 0.9659258262890683122, 1.000000000000000000, 0.9659258262890683122, 1.000000000000000000, 0.9659258262890683122, 1.000000000000000000, 0.9659258262890683122, 1.000000000000000000, 0.9659258262890683122, 1.000000000000000000, 0.9659258262890683122, 1.000000000000000000, 0.9659258262890683122, 1.000000000000000000, 0.9659258262890683122, 1.000000000000000000, 0.9659258262890683122, 1.000000000000000000, 0.9659258262890683122, 1.000000000000000000, 0.9659258262890683122, 1.000000000000000000, 0.9659258262890683122, 1.000000000000000000, 0.9659258262890683122, 1.000000000000000000, 0.9659258262890683122, 1.000000000000000000, 0.9659258262890683122, 1.000000000000000000, 0.9659258262890683122, 1.000000000000000000, 0.9659258262890683122, 1.000000000000000000, 0.9659258262890683122, 1.000000000000000000, 0.9659258262890683122, 1.000000000000000000, 0.9659258262890683122, 1.000000000000000000, 0.9659258262890683122, 1.000000000000000000, 0.9659258262890683122, 1.000000000000000000, 0.9659258262890683122, 1.000000000000000000, 0.9659258262890683122, 1.000000000000000000, 0.9659258262890683122, 1.000000000000000000, 0.9659258262890683122, 1.000000000000000000, 0.9659258262890683122, 1.000000000000000000, 0.9659258262890683122, 1.000000000000000000, 0.9659258262890683122, 1.000000000000000000, 0.9659258262890683122, 1.000000000000000000, 0.9659258262890683122, 1.000000000000000000, 0.9659258262890683122, 1.000000000000000000, 0.9659258262890683122, 1.000000000000000000, 0.9659258262890683122, 1.000000000000000000, 0.9659258262890683122, 1.000000000000000000, 0.9659258262890683122, 1.000000000000000000, 0.9659258262890683122, 1.000000000000000000, 0.9659258262890683122, 1.000000000000000000, 0.9659258262890683122, 1.000000000000000000, 0.9659258262890683122, 1.000000000000000000, 0.9659258262890683122, 1.000000000000000000, 0.9659258262890683122, 1.000000000000000000, 0.9659258262890683122, 1.000000000000000000, 0.9659258262890683122, 1.000000000000000000, 0.9659258262890683122, 1.000000000000000000, 0.9659258262890683122, 1.000000000000000000, 0.9659258262890683122, 1.000000000000000000, 0.9659258262890683122, 1.000000000000000000, 0.9659258262890683122, 1.000000000000000000, 0.9659258262890683122, 1.000000000000000000, 0.9659258262890683122, 1.000000000000000000, 0.9659258262890683122, 1.000000000000000000, 0.9659258262890683122, 1.000000000000000000, 0.9659258262890683122, 1.000000000000000000, 0.9659258262890683122, 1.000000000000000000, 0.9659258262890683122, 1.000000000000000000, 0.9659258262890683122, 1.000000000000000000, 0.9659258262890683122, 1.000000000000000000, 0.9659258262890683122, 1.000000000000000000, 0.9659258262890683122, 1.000000000000000000, 0.9659258262890683122, 1.000000000000000000, 0.9659258262890683122, 1.000000000000000000, 0.9659258262890683122, 1.000000000000000000, 0.9659258262890683122, 1.000000000000000000, 0.9659258262890683122, 1.000000000000000000, 0.9659258262890683122, 1.000000000000000000, 0.9659258262890683122, 1.000000000000000000, 0.9659258262890683122, 1.000000000000000000, 0.9659258262890683122, 1.000000000000000000, 0.9659258262890683122, 1.000000000000000000, 0.9659258262890683122, 1.000000000000000000, 0.9659258262890683122, 1.000000000000000000, 0.9659258262890683122, 1.000000000000000000, 0.9659258262890683122, 1.000000000000000000, 0.9659258262890683122, 1.000000000000000000, 0.9659258262890683122, 1.000000000000000000, 0.9659258262890683122, 1.000000000000000000, 0.9659258262890683122, 1.000000000000000000, 0.9659258262890683122, 1.000000000000000000, 0.9659258262890683122, 1.000000000000000000, 0.9659258262890683122, 1.000000000000000000, 0.9659258262890683122, 1.000000000000000000, 0.9659258262890683122, 1.000000000000000000, 0.9659258262890683122, 1.000000000000000000, 0.9659258262890683122, 1.000000000000000000, 0.9659258262890683122, 1.000000000000000000, 0.9659258262890683122, 1.000000000000000000, 0.9659258262890683122, 1.000000000000000000, 0.9659258262890683122, 1.000000000000000000, 0.9659258262890683122, 1.000000000000000000, 0.9659258262890683122, 1.000000000000000000, 0.9659258262890683122, 1.000000000000000000, 0.9659258262890683122, 1.000000000000000000, 0.9659258262890683122, 1.000000000000000000, 0.9659258262890683122, 1.000000000000000000, 0.9659258262890683122, 1.000000000000000000, 0.9659258262890683122, 1.000000000000000000, 0.9659258262890683122, 1.000000000000000000, 0.9659258262890683122, 1.000000000000000000, 0.9659258262890683122, 1.000000000000000000, 0.9659258262890683122, 1.000000000000000000, 0.9659258262890683122, 1.000000000000000000, 0.9659258262890683122, 1.000000000000000000, 0.9659258262890683122, 1.000000000000000000, 0.9659258262890683122, 1.000000000000000000, 0.9659258262890683122, 1.000000000000000000, 0.9659258262890683122, 1.000000000000000000, 0.9659258262890683122, 1.000000000000000000, 0.9659258262890683122, 1.000000000000000000, 0.9659258262890683122, 1.000000000000000000, 0.9659258262890683122, 1.000000000000000000, 0.9659258262890683122, 1.000000000000000000, 0.9659258262890683122, 1.000000000000000000, 0.9659258262890683122, 1.000000000000000000, 0.9659258262890683122, 1.000000000000000000, 0.9659258262890683122, 1.000000000000000000, 0.9659258262890683122, 1.000000000000000000, 0.9659258262890683122, 1.000000000000000000, 0.9659258262890683122, 1.000000000000000000, 0.9659258262890683122, 1.000000000000000000, 0.9659258262890683122, 1.000000000000000000, 0.9659258262890683122, 1.000000000000000000, 0.9659258262890683122, 1.000000000000000000, 0.9659258262890683122, 1.000000000000000000, 0.9659258262890683122, 1.000000000000000000, 0.9659258262890683122, 1.000000000000000000, 0.9659258262890683122, 1.000000000000000000, 0.9659258262890683122, 1.000000000000000000, 0.9659258262890683122, 1.000000000000000000, 0.9659258262890683122, 1.000000000000000000, 0.9659258262890683122, 1.000000000000000000, 0.9659258262890683122, 1.000000000000000000, 0.9659258262890683122, 1.000000000000000000, 0.9659258262890683122, 1.000000000000000000, 0.9659258262890683122, 1.000000000000000000, 0.9659258262890683122, 1.000000000000000000, 0.9659258262890683122, 1.000000000000000000, 0.9659258262890683122, 1.000000000000000000, 0.9659258262890683122, 1.000000000000000000, 0.9659258262890683122, 1.000000000000000000, 0.9659258262890683122, 1.000000000000000000, 0.9659258262890683122, 1.000000000000000000, 0.9659258262890683122, 1.000000000000000000, 0.9659258262890683122, 1.000000000000000000, 0.9659258262890683122, 1.000000000000000000, 0.9659258262890683122, 1.000000000000000000, 0.9659258262890683122, 1.000000000000000000, 0.9659258262890683122, 1.000000000000000000, 0.9659258262890683122, 1.000000000000000000, 0.9659258262890683122, 1.000000000000000000, 0.9659258262890683122, 1.000000000000000000, 0.9659258262890683122, 1.000000000000000000, 0.9659258262890683122, 1.000000000000000000, 0.9659258262890683122, 1.000000000000000000, 0.9659258262890683122, 1.000000000000000000, 0.9659258262890683122, 1.000000000000000000, 0.9659258262890683122, 1.000000000000000000, 0.9659258262890683122, 1.000000000000000000, 0.9659258262890683122, 1.000000000000000000, 0.9659258262890683122, 1.000000000000000000, 0.9659258262890683122, 1.000000000000000000, 0.9659258262890683122, 1.000000000000000000, 0.9659258262890683122, 1.000000000000000000, 0.9659258262890683122, 1.000000000000000000, 0.9659258262890683122, 1.000000000000000000, 0.9659258262890683122, 1.000000000000000000, 0.9659258262890683122, 1.000000000000000000, 0.9659258262890683122, 1.000000000000000000, 0.9659258262890683122, 1.000000000000000000, 0.9659258262890683122, 1.000000000000000000, 0.9659258262890683122, 1.000000000000000000, 0.9659258262890683122, 1.000000000000000000, 0.9659258262890683122, 1.000000000000000000, 0.9659258262890683122, 1.000000000000000000, 0.9659258262890683122, 1.000000000000000000, 0.9659258262890683122, 1.000000000000000000, 0.9659258262890683122, 1.000000000000000000, 0.9659258262890683122, 1.000000000000000000, 0.9659258262890683122, 1.000000000000000000, 0.9659258262890683122, 1.000000000000000000, 0.9659258262890683122, 1.000000000000000000, 0.9659258262890683122, 1.000000000000000000, 0.9659258262890683122, 1.000000000000000000, 0.9659258262890683122, 1.000000000000000000, 0.9659258262890683122, 1.000000000000000000, 0.9659258262890683122, 1.000000000000000000, 0.9659258262890683122, 1.000000000000000000, 0.9659258262890683122, 1.000000000000000000, 0.9659258262890683122, 1.000000000000000000, 0.9659258262890683122, 1.000000000000000000, 0.9659258262890683122, 1.000000000000000000, 0.9659258262890683122, 1.000000000000000000, 0.9659258262890683122, 1.000000000000000000),
 ( 0.3333333333333333703, 0.3219752754296894559, 0.3333333333333333703, 0.3219752754296894559, 0.3333333333333333703, 0.3219752754296894559, 0.3333333333333333703, 0.3219752754296894559, 0.3333333333333333703, 0.3219752754296894559, 0.3333333333333333703, 0.3219752754296894559, 0.3333333333333333703, 0.3219752754296894559, 0.3333333333333333703, 0.3219752754296894559, 0.3333333333333333703, 0.3219752754296894559, 0.3333333333333333703, 0.3219752754296894559, 0.3333333333333333703, 0.3219752754296894559, 0.3333333333333333703, 0.3219752754296894559, 0.3333333333333333703, 0.3219752754296894559, 0.3333333333333333703, 0.3219752754296894559, 0.3333333333333333703, 0.3219752754296894559, 0.3333333333333333703, 0.3219752754296894559, 0.3333333333333333703, 0.3219752754296894559, 0.3333333333333333703, 0.3219752754296894559, 0.3333333333333333703, 0.3219752754296894559, 0.3333333333333333703, 0.3219752754296894559, 0.3333333333333333703, 0.3219752754296894559, 0.3333333333333333703, 0.3219752754296894559, 0.3333333333333333703, 0.3219752754296894559, 0.3333333333333333703, 0.3219752754296894559, 0.3333333333333333703, 0.3219752754296894559, 0.3333333333333333703, 0.3219752754296894559, 0.3333333333333333703, 0.3219752754296894559, 0.3333333333333333703, 0.3219752754296894559, 0.3333333333333333703, 0.3219752754296894559, 0.3333333333333333703, 0.3219752754296894559, 0.3333333333333333703, 0.3219752754296894559, 0.3333333333333333703, 0.3219752754296894559, 0.3333333333333333703, 0.3219752754296894559, 0.3333333333333333703, 0.3219752754296894559, 0.3333333333333333703, 0.3219752754296894559, 0.3333333333333333703, 0.3219752754296894559, 0.3333333333333333703, 0.3219752754296894559, 0.3333333333333333703, 0.3219752754296894559, 0.3333333333333333703, 0.3219752754296894559, 0.3333333333333333703, 0.3219752754296894559, 0.3333333333333333703, 0.3219752754296894559, 0.3333333333333333703, 0.3219752754296894559, 0.3333333333333333703, 0.3219752754296894559, 0.3333333333333333703, 0.3219752754296894559, 0.3333333333333333703, 0.3219752754296894559, 0.3333333333333333703, 0.3219752754296894559, 0.3333333333333333703, 0.3219752754296894559, 0.3333333333333333703, 0.3219752754296894559, 0.3333333333333333703, 0.3219752754296894559, 0.3333333333333333703, 0.3219752754296894559, 0.3333333333333333703, 0.3219752754296894559, 0.3333333333333333703, 0.3219752754296894559, 0.3333333333333333703, 0.3219752754296894559, 0.3333333333333333703, 0.3219752754296894559, 0.3333333333333333703, 0.3219752754296894559, 0.3333333333333333703, 0.3219752754296894559, 0.3333333333333333703, 0.3219752754296894559, 0.3333333333333333703, 0.3219752754296894559, 0.3333333333333333703, 0.3219752754296894559, 0.3333333333333333703, 0.3219752754296894559, 0.3333333333333333703, 0.3219752754296894559, 0.3333333333333333703, 0.3219752754296894559, 0.3333333333333333703, 0.3219752754296894559, 0.3333333333333333703, 0.3219752754296894559, 0.3333333333333333703, 0.3219752754296894559, 0.3333333333333333703, 0.3219752754296894559, 0.3333333333333333703, 0.3219752754296894559, 0.3333333333333333703, 0.3219752754296894559, 0.3333333333333333703, 0.3219752754296894559, 0.3333333333333333703, 0.3219752754296894559, 0.3333333333333333703, 0.3219752754296894559, 0.3333333333333333703, 0.3219752754296894559, 0.3333333333333333703, 0.3219752754296894559, 0.3333333333333333703, 0.3219752754296894559, 0.3333333333333333703, 0.3219752754296894559, 0.3333333333333333703, 0.3219752754296894559, 0.3333333333333333703, 0.3219752754296894559, 0.3333333333333333703, 0.3219752754296894559, 0.3333333333333333703, 0.3219752754296894559, 0.3333333333333333703, 0.3219752754296894559, 0.3333333333333333703, 0.3219752754296894559, 0.3333333333333333703, 0.3219752754296894559, 0.3333333333333333703, 0.3219752754296894559, 0.3333333333333333703, 0.3219752754296894559, 0.3333333333333333703, 0.3219752754296894559, 0.3333333333333333703, 0.3219752754296894559, 0.3333333333333333703, 0.3219752754296894559, 0.3333333333333333703, 0.3219752754296894559, 0.3333333333333333703, 0.3219752754296894559, 0.3333333333333333703, 0.3219752754296894559, 0.3333333333333333703, 0.3219752754296894559, 0.3333333333333333703, 0.3219752754296894559, 0.3333333333333333703, 0.3219752754296894559, 0.3333333333333333703, 0.3219752754296894559, 0.3333333333333333703, 0.3219752754296894559, 0.3333333333333333703, 0.3219752754296894559, 0.3333333333333333703, 0.3219752754296894559, 0.3333333333333333703, 0.3219752754296894559, 0.3333333333333333703, 0.3219752754296894559, 0.3333333333333333703, 0.3219752754296894559, 0.3333333333333333703, 0.3219752754296894559, 0.3333333333333333703, 0.3219752754296894559, 0.3333333333333333703, 0.3219752754296894559, 0.3333333333333333703, 0.3219752754296894559, 0.3333333333333333703, 0.3219752754296894559, 0.3333333333333333703, 0.3219752754296894559, 0.3333333333333333703, 0.3219752754296894559, 0.3333333333333333703, 0.3219752754296894559, 0.3333333333333333703, 0.3219752754296894559, 0.3333333333333333703, 0.3219752754296894559, 0.3333333333333333703, 0.3219752754296894559, 0.3333333333333333703, 0.3219752754296894559, 0.3333333333333333703, 0.3219752754296894559, 0.3333333333333333703, 0.3219752754296894559, 0.3333333333333333703, 0.3219752754296894559, 0.3333333333333333703, 0.3219752754296894559, 0.3333333333333333703, 0.3219752754296894559, 0.3333333333333333703, 0.3219752754296894559, 0.3333333333333333703, 0.3219752754296894559, 0.3333333333333333703, 0.3219752754296894559, 0.3333333333333333703, 0.3219752754296894559, 0.3333333333333333703, 0.3219752754296894559, 0.3333333333333333703, 0.3219752754296894559, 0.3333333333333333703, 0.3219752754296894559, 0.3333333333333333703, 0.3219752754296894559, 0.3333333333333333703, 0.3219752754296894559, 0.3333333333333333703, 0.3219752754296894559, 0.3333333333333333703, 0.3219752754296894559, 0.3333333333333333703, 0.3219752754296894559, 0.3333333333333333703, 0.3219752754296894559, 0.3333333333333333703, 0.3219752754296894559, 0.3333333333333333703, 0.3219752754296894559, 0.3333333333333333703, 0.3219752754296894559, 0.3333333333333333703, 0.3219752754296894559, 0.3333333333333333703, 0.3219752754296894559, 0.3333333333333333703, 0.3219752754296894559, 0.3333333333333333703, 0.3219752754296894559, 0.3333333333333333703, 0.3219752754296894559, 0.3333333333333333703, 0.3219752754296894559, 0.3333333333333333703, 0.3219752754296894559, 0.3333333333333333703, 0.3219752754296894559, 0.3333333333333333703, 0.3219752754296894559, 0.3333333333333333703, 0.3219752754296894559, 0.3333333333333333703, 0.3219752754296894559, 0.3333333333333333703, 0.3219752754296894559, 0.3333333333333333703, 0.3219752754296894559, 0.3333333333333333703, 0.3219752754296894559, 0.3333333333333333703, 0.3219752754296894559, 0.3333333333333333703, 0.3219752754296894559, 0.3333333333333333703, 0.3219752754296894559, 0.3333333333333333703, 0.3219752754296894559, 0.3333333333333333703, 0.3219752754296894559, 0.3333333333333333703, 0.3219752754296894559, 0.3333333333333333703, 0.3219752754296894559, 0.3333333333333333703, 0.3219752754296894559, 0.3333333333333333703, 0.3219752754296894559, 0.3333333333333333703, 0.3219752754296894559, 0.3333333333333333703, 0.3219752754296894559, 0.3333333333333333703, 0.3219752754296894559, 0.3333333333333333703, 0.3219752754296894559, 0.3333333333333333703, 0.3219752754296894559, 0.3333333333333333703, 0.3219752754296894559, 0.3333333333333333703, 0.3219752754296894559, 0.3333333333333333703, 0.3219752754296894559, 0.3333333333333333703, 0.3219752754296894559, 0.3333333333333333703, 0.3219752754296894559, 0.3333333333333333703, 0.3219752754296894559, 0.3333333333333333703, 0.3219752754296894559, 0.3333333333333333703, 0.3219752754296894559, 0.3333333333333333703, 0.3219752754296894559, 0.3333333333333333703, 0.3219752754296894559, 0.3333333333333333703, 0.3219752754296894559, 0.3333333333333333703, 0.3219752754296894559, 0.3333333333333333703, 0.3219752754296894559, 0.3333333333333333703, 0.3219752754296894559, 0.3333333333333333703, 0.3219752754296894559, 0.3333333333333333703, 0.3219752754296894559, 0.3333333333333333703, 0.3219752754296894559, 0.3333333333333333703, 0.3219752754296894559, 0.3333333333333333703, 0.3219752754296894559, 0.3333333333333333703, 0.3219752754296894559, 0.3333333333333333703, 0.3219752754296894559, 0.3333333333333333703, 0.3219752754296894559, 0.3333333333333333703, 0.3219752754296894559, 0.3333333333333333703, 0.3219752754296894559, 0.3333333333333333703, 0.3219752754296894559, 0.3333333333333333703, 0.3219752754296894559, 0.3333333333333333703, 0.3219752754296894559, 0.3333333333333333703, 0.3219752754296894559, 0.3333333333333333703, 0.3219752754296894559, 0.3333333333333333703, 0.3219752754296894559, 0.3333333333333333703, 0.3219752754296894559, 0.3333333333333333703, 0.3219752754296894559, 0.3333333333333333703, 0.3219752754296894559, 0.3333333333333333703, 0.3219752754296894559, 0.3333333333333333703, 0.3219752754296894559, 0.3333333333333333703, 0.3219752754296894559, 0.3333333333333333703, 0.3219752754296894559, 0.3333333333333333703, 0.3219752754296894559, 0.3333333333333333703, 0.3219752754296894559, 0.3333333333333333703, 0.3219752754296894559, 0.3333333333333333703, 0.3219752754296894559, 0.3333333333333333703, 0.3219752754296894559, 0.3333333333333333703, 0.3219752754296894559, 0.3333333333333333703, 0.3219752754296894559, 0.3333333333333333703, 0.3219752754296894559, 0.3333333333333333703, 0.3219752754296894559, 0.3333333333333333703, 0.3219752754296894559, 0.3333333333333333703, 0.3219752754296894559, 0.3333333333333333703, 0.3219752754296894559, 0.3333333333333333703, 0.3219752754296894559, 0.3333333333333333703, 0.3219752754296894559, 0.3333333333333333703, 0.3219752754296894559, 0.3333333333333333703, 0.3219752754296894559, 0.3333333333333333703, 0.3219752754296894559, 0.3333333333333333703, 0.3219752754296894559, 0.3333333333333333703, 0.3219752754296894559, 0.3333333333333333703, 0.3219752754296894559, 0.3333333333333333703, 0.3219752754296894559, 0.3333333333333333703, 0.3219752754296894559, 0.3333333333333333703, 0.3219752754296894559, 0.3333333333333333703, 0.3219752754296894559, 0.3333333333333333703, 0.3219752754296894559, 0.3333333333333333703, 0.3219752754296894559, 0.3333333333333333703, 0.3219752754296894559, 0.3333333333333333703, 0.3219752754296894559, 0.3333333333333333703, 0.3219752754296894559, 0.3333333333333333703, 0.3219752754296894559, 0.3333333333333333703),
 ( 0.3333333333333333703, 0.3219752754296894559, 0.3333333333333333703, 0.3219752754296894559, 0.3333333333333333703, 0.3219752754296894559, 0.3333333333333333703, 0.3219752754296894559, 0.3333333333333333703, 0.3219752754296894559, 0.3333333333333333703, 0.3219752754296894559, 0.3333333333333333703, 0.3219752754296894559, 0.3333333333333333703, 0.3219752754296894559, 0.3333333333333333703, 0.3219752754296894559, 0.3333333333333333703, 0.3219752754296894559, 0.3333333333333333703, 0.3219752754296894559, 0.3333333333333333703, 0.3219752754296894559, 0.3333333333333333703, 0.3219752754296894559, 0.3333333333333333703, 0.3219752754296894559, 0.3333333333333333703, 0.3219752754296894559, 0.3333333333333333703, 0.3219752754296894559, 0.3333333333333333703, 0.3219752754296894559, 0.3333333333333333703, 0.3219752754296894559, 0.3333333333333333703, 0.3219752754296894559, 0.3333333333333333703, 0.3219752754296894559, 0.3333333333333333703, 0.3219752754296894559, 0.3333333333333333703, 0.3219752754296894559, 0.3333333333333333703, 0.3219752754296894559, 0.3333333333333333703, 0.3219752754296894559, 0.3333333333333333703, 0.3219752754296894559, 0.3333333333333333703, 0.3219752754296894559, 0.3333333333333333703, 0.3219752754296894559, 0.3333333333333333703, 0.3219752754296894559, 0.3333333333333333703, 0.3219752754296894559, 0.3333333333333333703, 0.3219752754296894559, 0.3333333333333333703, 0.3219752754296894559, 0.3333333333333333703, 0.3219752754296894559, 0.3333333333333333703, 0.3219752754296894559, 0.3333333333333333703, 0.3219752754296894559, 0.3333333333333333703, 0.3219752754296894559, 0.3333333333333333703, 0.3219752754296894559, 0.3333333333333333703, 0.3219752754296894559, 0.3333333333333333703, 0.3219752754296894559, 0.3333333333333333703, 0.3219752754296894559, 0.3333333333333333703, 0.3219752754296894559, 0.3333333333333333703, 0.3219752754296894559, 0.3333333333333333703, 0.3219752754296894559, 0.3333333333333333703, 0.3219752754296894559, 0.3333333333333333703, 0.3219752754296894559, 0.3333333333333333703, 0.3219752754296894559, 0.3333333333333333703, 0.3219752754296894559, 0.3333333333333333703, 0.3219752754296894559, 0.3333333333333333703, 0.3219752754296894559, 0.3333333333333333703, 0.3219752754296894559, 0.3333333333333333703, 0.3219752754296894559, 0.3333333333333333703, 0.3219752754296894559, 0.3333333333333333703, 0.3219752754296894559, 0.3333333333333333703, 0.3219752754296894559, 0.3333333333333333703, 0.3219752754296894559, 0.3333333333333333703, 0.3219752754296894559, 0.3333333333333333703, 0.3219752754296894559, 0.3333333333333333703, 0.3219752754296894559, 0.3333333333333333703, 0.3219752754296894559, 0.3333333333333333703, 0.3219752754296894559, 0.3333333333333333703, 0.3219752754296894559, 0.3333333333333333703, 0.3219752754296894559, 0.3333333333333333703, 0.3219752754296894559, 0.3333333333333333703, 0.3219752754296894559, 0.3333333333333333703, 0.3219752754296894559, 0.3333333333333333703, 0.3219752754296894559, 0.3333333333333333703, 0.3219752754296894559, 0.3333333333333333703, 0.3219752754296894559, 0.3333333333333333703, 0.3219752754296894559, 0.3333333333333333703, 0.3219752754296894559, 0.3333333333333333703, 0.3219752754296894559, 0.3333333333333333703, 0.3219752754296894559, 0.3333333333333333703, 0.3219752754296894559, 0.3333333333333333703, 0.3219752754296894559, 0.3333333333333333703, 0.3219752754296894559, 0.3333333333333333703, 0.3219752754296894559, 0.3333333333333333703, 0.3219752754296894559, 0.3333333333333333703, 0.3219752754296894559, 0.3333333333333333703, 0.3219752754296894559, 0.3333333333333333703, 0.3219752754296894559, 0.3333333333333333703, 0.3219752754296894559, 0.3333333333333333703, 0.3219752754296894559, 0.3333333333333333703, 0.3219752754296894559, 0.3333333333333333703, 0.3219752754296894559, 0.3333333333333333703, 0.3219752754296894559, 0.3333333333333333703, 0.3219752754296894559, 0.3333333333333333703, 0.3219752754296894559, 0.3333333333333333703, 0.3219752754296894559, 0.3333333333333333703, 0.3219752754296894559, 0.3333333333333333703, 0.3219752754296894559, 0.3333333333333333703, 0.3219752754296894559, 0.3333333333333333703, 0.3219752754296894559, 0.3333333333333333703, 0.3219752754296894559, 0.3333333333333333703, 0.3219752754296894559, 0.3333333333333333703, 0.3219752754296894559, 0.3333333333333333703, 0.3219752754296894559, 0.3333333333333333703, 0.3219752754296894559, 0.3333333333333333703, 0.3219752754296894559, 0.3333333333333333703, 0.3219752754296894559, 0.3333333333333333703, 0.3219752754296894559, 0.3333333333333333703, 0.3219752754296894559, 0.3333333333333333703, 0.3219752754296894559, 0.3333333333333333703, 0.3219752754296894559, 0.3333333333333333703, 0.3219752754296894559, 0.3333333333333333703, 0.3219752754296894559, 0.3333333333333333703, 0.3219752754296894559, 0.3333333333333333703, 0.3219752754296894559, 0.3333333333333333703, 0.3219752754296894559, 0.3333333333333333703, 0.3219752754296894559, 0.3333333333333333703, 0.3219752754296894559, 0.3333333333333333703, 0.3219752754296894559, 0.3333333333333333703, 0.3219752754296894559, 0.3333333333333333703, 0.3219752754296894559, 0.3333333333333333703, 0.3219752754296894559, 0.3333333333333333703, 0.3219752754296894559, 0.3333333333333333703, 0.3219752754296894559, 0.3333333333333333703, 0.3219752754296894559, 0.3333333333333333703, 0.3219752754296894559, 0.3333333333333333703, 0.3219752754296894559, 0.3333333333333333703, 0.3219752754296894559, 0.3333333333333333703, 0.3219752754296894559, 0.3333333333333333703, 0.3219752754296894559, 0.3333333333333333703, 0.3219752754296894559, 0.3333333333333333703, 0.3219752754296894559, 0.3333333333333333703, 0.3219752754296894559, 0.3333333333333333703, 0.3219752754296894559, 0.3333333333333333703, 0.3219752754296894559, 0.3333333333333333703, 0.3219752754296894559, 0.3333333333333333703, 0.3219752754296894559, 0.3333333333333333703, 0.3219752754296894559, 0.3333333333333333703, 0.3219752754296894559, 0.3333333333333333703, 0.3219752754296894559, 0.3333333333333333703, 0.3219752754296894559, 0.3333333333333333703, 0.3219752754296894559, 0.3333333333333333703, 0.3219752754296894559, 0.3333333333333333703, 0.3219752754296894559, 0.3333333333333333703, 0.3219752754296894559, 0.3333333333333333703, 0.3219752754296894559, 0.3333333333333333703, 0.3219752754296894559, 0.3333333333333333703, 0.3219752754296894559, 0.3333333333333333703, 0.3219752754296894559, 0.3333333333333333703, 0.3219752754296894559, 0.3333333333333333703, 0.3219752754296894559, 0.3333333333333333703, 0.3219752754296894559, 0.3333333333333333703, 0.3219752754296894559, 0.3333333333333333703, 0.3219752754296894559, 0.3333333333333333703, 0.3219752754296894559, 0.3333333333333333703, 0.3219752754296894559, 0.3333333333333333703, 0.3219752754296894559, 0.3333333333333333703, 0.3219752754296894559, 0.3333333333333333703, 0.3219752754296894559, 0.3333333333333333703, 0.3219752754296894559, 0.3333333333333333703, 0.3219752754296894559, 0.3333333333333333703, 0.3219752754296894559, 0.3333333333333333703, 0.3219752754296894559, 0.3333333333333333703, 0.3219752754296894559, 0.3333333333333333703, 0.3219752754296894559, 0.3333333333333333703, 0.3219752754296894559, 0.3333333333333333703, 0.3219752754296894559, 0.3333333333333333703, 0.3219752754296894559, 0.3333333333333333703, 0.3219752754296894559, 0.3333333333333333703, 0.3219752754296894559, 0.3333333333333333703, 0.3219752754296894559, 0.3333333333333333703, 0.3219752754296894559, 0.3333333333333333703, 0.3219752754296894559, 0.3333333333333333703, 0.3219752754296894559, 0.3333333333333333703, 0.3219752754296894559, 0.3333333333333333703, 0.3219752754296894559, 0.3333333333333333703, 0.3219752754296894559, 0.3333333333333333703, 0.3219752754296894559, 0.3333333333333333703, 0.3219752754296894559, 0.3333333333333333703, 0.3219752754296894559, 0.3333333333333333703, 0.3219752754296894559, 0.3333333333333333703, 0.3219752754296894559, 0.3333333333333333703, 0.3219752754296894559, 0.3333333333333333703, 0.3219752754296894559, 0.3333333333333333703, 0.3219752754296894559, 0.3333333333333333703, 0.3219752754296894559, 0.3333333333333333703, 0.3219752754296894559, 0.3333333333333333703, 0.3219752754296894559, 0.3333333333333333703, 0.3219752754296894559, 0.3333333333333333703, 0.3219752754296894559, 0.3333333333333333703, 0.3219752754296894559, 0.3333333333333333703, 0.3219752754296894559, 0.3333333333333333703, 0.3219752754296894559, 0.3333333333333333703, 0.3219752754296894559, 0.3333333333333333703, 0.3219752754296894559, 0.3333333333333333703, 0.3219752754296894559, 0.3333333333333333703, 0.3219752754296894559, 0.3333333333333333703, 0.3219752754296894559, 0.3333333333333333703, 0.3219752754296894559, 0.3333333333333333703, 0.3219752754296894559, 0.3333333333333333703, 0.3219752754296894559, 0.3333333333333333703, 0.3219752754296894559, 0.3333333333333333703, 0.3219752754296894559, 0.3333333333333333703, 0.3219752754296894559, 0.3333333333333333703, 0.3219752754296894559, 0.3333333333333333703, 0.3219752754296894559, 0.3333333333333333703, 0.3219752754296894559, 0.3333333333333333703, 0.3219752754296894559, 0.3333333333333333703, 0.3219752754296894559, 0.3333333333333333703, 0.3219752754296894559, 0.3333333333333333703, 0.3219752754296894559, 0.3333333333333333703, 0.3219752754296894559, 0.3333333333333333703, 0.3219752754296894559, 0.3333333333333333703, 0.3219752754296894559, 0.3333333333333333703, 0.3219752754296894559, 0.3333333333333333703, 0.3219752754296894559, 0.3333333333333333703, 0.3219752754296894559, 0.3333333333333333703, 0.3219752754296894559, 0.3333333333333333703, 0.3219752754296894559, 0.3333333333333333703, 0.3219752754296894559, 0.3333333333333333703, 0.3219752754296894559, 0.3333333333333333703, 0.3219752754296894559, 0.3333333333333333703, 0.3219752754296894559, 0.3333333333333333703, 0.3219752754296894559, 0.3333333333333333703, 0.3219752754296894559, 0.3333333333333333703, 0.3219752754296894559, 0.3333333333333333703, 0.3219752754296894559, 0.3333333333333333703, 0.3219752754296894559, 0.3333333333333333703, 0.3219752754296894559, 0.3333333333333333703, 0.3219752754296894559, 0.3333333333333333703, 0.3219752754296894559, 0.3333333333333333703, 0.3219752754296894559, 0.3333333333333333703, 0.3219752754296894559, 0.3333333333333333703, 0.3219752754296894559, 0.3333333333333333703, 0.3219752754296894559, 0.3333333333333333703, 0.3219752754296894559, 0.3333333333333333703, 0.3219752754296894559, 0.3333333333333333703),
 ( 1.000000000000000000, 0.9659258262890683122, 1.000000000000000000, 0.9659258262890683122, 1.000000000000000000, 0.9659258262890683122, 1.000000000000000000, 0.9659258262890683122, 1.000000000000000000, 0.9659258262890683122, 1.000000000000000000, 0.9659258262890683122, 1.000000000000000000, 0.9659258262890683122, 1.000000000000000000, 0.9659258262890683122, 1.000000000000000000, 0.9659258262890683122, 1.000000000000000000, 0.9659258262890683122, 1.000000000000000000, 0.9659258262890683122, 1.000000000000000000, 0.9659258262890683122, 1.000000000000000000, 0.9659258262890683122, 1.000000000000000000, 0.9659258262890683122, 1.000000000000000000, 0.9659258262890683122, 1.000000000000000000, 0.9659258262890683122, 1.000000000000000000, 0.9659258262890683122, 1.000000000000000000, 0.9659258262890683122, 1.000000000000000000, 0.9659258262890683122, 1.000000000000000000, 0.9659258262890683122, 1.000000000000000000, 0.9659258262890683122, 1.000000000000000000, 0.9659258262890683122, 1.000000000000000000, 0.9659258262890683122, 1.000000000000000000, 0.9659258262890683122, 1.000000000000000000, 0.9659258262890683122, 1.000000000000000000, 0.9659258262890683122, 1.000000000000000000, 0.9659258262890683122, 1.000000000000000000, 0.9659258262890683122, 1.000000000000000000, 0.9659258262890683122, 1.000000000000000000, 0.9659258262890683122, 1.000000000000000000, 0.9659258262890683122, 1.000000000000000000, 0.9659258262890683122, 1.000000000000000000, 0.9659258262890683122, 1.000000000000000000, 0.9659258262890683122, 1.000000000000000000, 0.9659258262890683122, 1.000000000000000000, 0.9659258262890683122, 1.000000000000000000, 0.9659258262890683122, 1.000000000000000000, 0.9659258262890683122, 1.000000000000000000, 0.9659258262890683122, 1.000000000000000000, 0.9659258262890683122, 1.000000000000000000, 0.9659258262890683122, 1.000000000000000000, 0.9659258262890683122, 1.000000000000000000, 0.9659258262890683122, 1.000000000000000000, 0.9659258262890683122, 1.000000000000000000, 0.9659258262890683122, 1.000000000000000000, 0.9659258262890683122, 1.000000000000000000, 0.9659258262890683122, 1.000000000000000000, 0.9659258262890683122, 1.000000000000000000, 0.9659258262890683122, 1.000000000000000000, 0.9659258262890683122, 1.000000000000000000, 0.9659258262890683122, 1.000000000000000000, 0.9659258262890683122, 1.000000000000000000, 0.9659258262890683122, 1.000000000000000000, 0.9659258262890683122, 1.000000000000000000, 0.9659258262890683122, 1.000000000000000000, 0.9659258262890683122, 1.000000000000000000, 0.9659258262890683122, 1.000000000000000000, 0.9659258262890683122, 1.000000000000000000, 0.9659258262890683122, 1.000000000000000000, 0.9659258262890683122, 1.000000000000000000, 0.9659258262890683122, 1.000000000000000000, 0.9659258262890683122, 1.000000000000000000, 0.9659258262890683122, 1.000000000000000000, 0.9659258262890683122, 1.000000000000000000, 0.9659258262890683122, 1.000000000000000000, 0.9659258262890683122, 1.000000000000000000, 0.9659258262890683122, 1.000000000000000000, 0.9659258262890683122, 1.000000000000000000, 0.9659258262890683122, 1.000000000000000000, 0.9659258262890683122, 1.000000000000000000, 0.9659258262890683122, 1.000000000000000000, 0.9659258262890683122, 1.000000000000000000, 0.9659258262890683122, 1.000000000000000000, 0.9659258262890683122, 1.000000000000000000, 0.9659258262890683122, 1.000000000000000000, 0.9659258262890683122, 1.000000000000000000, 0.9659258262890683122, 1.000000000000000000, 0.9659258262890683122, 1.000000000000000000, 0.9659258262890683122, 1.000000000000000000, 0.9659258262890683122, 1.000000000000000000, 0.9659258262890683122, 1.000000000000000000, 0.9659258262890683122, 1.000000000000000000, 0.9659258262890683122, 1.000000000000000000, 0.9659258262890683122, 1.000000000000000000, 0.9659258262890683122, 1.000000000000000000, 0.9659258262890683122, 1.000000000000000000, 0.9659258262890683122, 1.000000000000000000, 0.9659258262890683122, 1.000000000000000000, 0.9659258262890683122, 1.000000000000000000, 0.9659258262890683122, 1.000000000000000000, 0.9659258262890683122, 1.000000000000000000, 0.9659258262890683122, 1.000000000000000000, 0.9659258262890683122, 1.000000000000000000, 0.9659258262890683122, 1.000000000000000000, 0.9659258262890683122, 1.000000000000000000, 0.9659258262890683122, 1.000000000000000000, 0.9659258262890683122, 1.000000000000000000, 0.9659258262890683122, 1.000000000000000000, 0.9659258262890683122, 1.000000000000000000, 0.9659258262890683122, 1.000000000000000000, 0.9659258262890683122, 1.000000000000000000, 0.9659258262890683122, 1.000000000000000000, 0.9659258262890683122, 1.000000000000000000, 0.9659258262890683122, 1.000000000000000000, 0.9659258262890683122, 1.000000000000000000, 0.9659258262890683122, 1.000000000000000000, 0.9659258262890683122, 1.000000000000000000, 0.9659258262890683122, 1.000000000000000000, 0.9659258262890683122, 1.000000000000000000, 0.9659258262890683122, 1.000000000000000000, 0.9659258262890683122, 1.000000000000000000, 0.9659258262890683122, 1.000000000000000000, 0.9659258262890683122, 1.000000000000000000, 0.9659258262890683122, 1.000000000000000000, 0.9659258262890683122, 1.000000000000000000, 0.9659258262890683122, 1.000000000000000000, 0.9659258262890683122, 1.000000000000000000, 0.9659258262890683122, 1.000000000000000000, 0.9659258262890683122, 1.000000000000000000, 0.9659258262890683122, 1.000000000000000000, 0.9659258262890683122, 1.000000000000000000, 0.9659258262890683122, 1.000000000000000000, 0.9659258262890683122, 1.000000000000000000, 0.9659258262890683122, 1.000000000000000000, 0.9659258262890683122, 1.000000000000000000, 0.9659258262890683122, 1.000000000000000000, 0.9659258262890683122, 1.000000000000000000, 0.9659258262890683122, 1.000000000000000000, 0.9659258262890683122, 1.000000000000000000, 0.9659258262890683122, 1.000000000000000000, 0.9659258262890683122, 1.000000000000000000, 0.9659258262890683122, 1.000000000000000000, 0.9659258262890683122, 1.000000000000000000, 0.9659258262890683122, 1.000000000000000000, 0.9659258262890683122, 1.000000000000000000, 0.9659258262890683122, 1.000000000000000000, 0.9659258262890683122, 1.000000000000000000, 0.9659258262890683122, 1.000000000000000000, 0.9659258262890683122, 1.000000000000000000, 0.9659258262890683122, 1.000000000000000000, 0.9659258262890683122, 1.000000000000000000, 0.9659258262890683122, 1.000000000000000000, 0.9659258262890683122, 1.000000000000000000, 0.9659258262890683122, 1.000000000000000000, 0.9659258262890683122, 1.000000000000000000, 0.9659258262890683122, 1.000000000000000000, 0.9659258262890683122, 1.000000000000000000, 0.9659258262890683122, 1.000000000000000000, 0.9659258262890683122, 1.000000000000000000, 0.9659258262890683122, 1.000000000000000000, 0.9659258262890683122, 1.000000000000000000, 0.9659258262890683122, 1.000000000000000000, 0.9659258262890683122, 1.000000000000000000, 0.9659258262890683122, 1.000000000000000000, 0.9659258262890683122, 1.000000000000000000, 0.9659258262890683122, 1.000000000000000000, 0.9659258262890683122, 1.000000000000000000, 0.9659258262890683122, 1.000000000000000000, 0.9659258262890683122, 1.000000000000000000, 0.9659258262890683122, 1.000000000000000000, 0.9659258262890683122, 1.000000000000000000, 0.9659258262890683122, 1.000000000000000000, 0.9659258262890683122, 1.000000000000000000, 0.9659258262890683122, 1.000000000000000000, 0.9659258262890683122, 1.000000000000000000, 0.9659258262890683122, 1.000000000000000000, 0.9659258262890683122, 1.000000000000000000, 0.9659258262890683122, 1.000000000000000000, 0.9659258262890683122, 1.000000000000000000, 0.9659258262890683122, 1.000000000000000000, 0.9659258262890683122, 1.000000000000000000, 0.9659258262890683122, 1.000000000000000000, 0.9659258262890683122, 1.000000000000000000, 0.9659258262890683122, 1.000000000000000000, 0.9659258262890683122, 1.000000000000000000, 0.9659258262890683122, 1.000000000000000000, 0.9659258262890683122, 1.000000000000000000, 0.9659258262890683122, 1.000000000000000000, 0.9659258262890683122, 1.000000000000000000, 0.9659258262890683122, 1.000000000000000000, 0.9659258262890683122, 1.000000000000000000, 0.9659258262890683122, 1.000000000000000000, 0.9659258262890683122, 1.000000000000000000, 0.9659258262890683122, 1.000000000000000000, 0.9659258262890683122, 1.000000000000000000, 0.9659258262890683122, 1.000000000000000000, 0.9659258262890683122, 1.000000000000000000, 0.9659258262890683122, 1.000000000000000000, 0.9659258262890683122, 1.000000000000000000, 0.9659258262890683122, 1.000000000000000000, 0.9659258262890683122, 1.000000000000000000, 0.9659258262890683122, 1.000000000000000000, 0.9659258262890683122, 1.000000000000000000, 0.9659258262890683122, 1.000000000000000000, 0.9659258262890683122, 1.000000000000000000, 0.9659258262890683122, 1.000000000000000000, 0.9659258262890683122, 1.000000000000000000, 0.9659258262890683122, 1.000000000000000000, 0.9659258262890683122, 1.000000000000000000, 0.9659258262890683122, 1.000000000000000000, 0.9659258262890683122, 1.000000000000000000, 0.9659258262890683122, 1.000000000000000000, 0.9659258262890683122, 1.000000000000000000, 0.9659258262890683122, 1.000000000000000000, 0.9659258262890683122, 1.000000000000000000, 0.9659258262890683122, 1.000000000000000000, 0.9659258262890683122, 1.000000000000000000, 0.9659258262890683122, 1.000000000000000000, 0.9659258262890683122, 1.000000000000000000, 0.9659258262890683122, 1.000000000000000000, 0.9659258262890683122, 1.000000000000000000, 0.9659258262890683122, 1.000000000000000000, 0.9659258262890683122, 1.000000000000000000, 0.9659258262890683122, 1.000000000000000000, 0.9659258262890683122, 1.000000000000000000, 0.9659258262890683122, 1.000000000000000000, 0.9659258262890683122, 1.000000000000000000, 0.9659258262890683122, 1.000000000000000000, 0.9659258262890683122, 1.000000000000000000, 0.9659258262890683122, 1.000000000000000000, 0.9659258262890683122, 1.000000000000000000, 0.9659258262890683122, 1.000000000000000000, 0.9659258262890683122, 1.000000000000000000, 0.9659258262890683122, 1.000000000000000000, 0.9659258262890683122, 1.000000000000000000, 0.9659258262890683122, 1.000000000000000000, 0.9659258262890683122, 1.000000000000000000, 0.9659258262890683122, 1.000000000000000000) ) ) 
 REPRESENTATION_ITEM ( '' )  SURFACE ( )  );
#80376 = CARTESIAN_POINT ( 'NONE',  ( 16.46253265017160672, -9.564922557960803928, 108.3322429386476955 ) ) ;
#80377 = CARTESIAN_POINT ( 'NONE',  ( 5.823673210054444382, -21.52544592524334988, 25.20942372801901854 ) ) ;
#80378 = CARTESIAN_POINT ( 'NONE',  ( -13.97604488694547697, 13.89961937509957934, 88.12609039468563310 ) ) ;
#80380 = CARTESIAN_POINT ( 'NONE',  ( -19.02544592524342804, 5.153800228976336051, 46.04057627198101699 ) ) ;
#80379 = DIRECTION ( 'NONE',  ( 0.000000000000000000, 0.000000000000000000, 1.000000000000000000 ) ) ;
#80381 = CARTESIAN_POINT ( 'NONE',  ( 16.51473224551069308, 9.474510206698969483, 89.16557627198103830 ) ) ;
#80383 = CARTESIAN_POINT ( 'NONE',  ( -19.03943276465977164, 0.05219959533909376836, 46.24890960531435979 ) ) ;
#80382 = CARTESIAN_POINT ( 'NONE',  ( 0.05219959533910956823, 16.53943276465976808, 64.99890960531435269 ) ) ;
#80384 = CARTESIAN_POINT ( 'NONE',  ( -13.89961937509977652, 13.97604488694528158, 60.62390960531436690 ) ) ;
#80385 = CARTESIAN_POINT ( 'NONE',  ( 13.89961937509957401, 13.97604488694547697, 61.87609039468566863 ) ) ;
#80386 = CARTESIAN_POINT ( 'NONE',  ( 19.05341960407617918, -5.049401038297876454, 26.04275706135233293 ) ) ;
#80387 = CARTESIAN_POINT ( 'NONE',  ( 16.51473224551069308, 9.474510206698969483, 69.16557627198102409 ) ) ;
#80388 = CARTESIAN_POINT ( 'NONE',  ( 18.67979575497178502, 10.72451020669898547, 64.16557627198102409 ) ) ;
#80390 = CARTESIAN_POINT ( 'NONE',  ( -19.05341960407617563, 5.049401038297882671, 33.54275706135231871 ) ) ;
#80389 = CARTESIAN_POINT ( 'NONE',  ( 12.14591786802309770, 12.06949235617756955, 64.37390960531435269 ) ) ;
#80391 = CARTESIAN_POINT ( 'NONE',  ( -0.2000799437544613923, -6.100000000000011191, -64.53213882399992940 ) ) ;
#80392 = CARTESIAN_POINT ( 'NONE',  ( -10.72451020669898014, 18.67979575497178502, 45.41557627198103830 ) ) ;
#80393 = CARTESIAN_POINT ( 'NONE',  ( 21.52544592524344225, -5.823673210054117533, 23.54057627198102765 ) ) ;
#80394 = CARTESIAN_POINT ( 'NONE',  ( 19.03943276465977164, -0.05219959533909143690, 48.74890960531435979 ) ) ;
#80395 = CARTESIAN_POINT ( 'NONE',  ( 5.153800228976335163, 19.02544592524342804, 39.79057627198100988 ) ) ;
#80396 = CARTESIAN_POINT ( 'NONE',  ( 12.06949235617757843, -12.14591786802309237, 103.1239096053143811 ) ) ;
#80397 = CARTESIAN_POINT ( 'NONE',  ( 15.80617190586746368, 15.72974639402197994, 114.3739096053143527 ) ) ;
#80398 = CARTESIAN_POINT ( 'NONE',  ( 16.51473224551069308, 9.474510206698969483, 109.1655762719810383 ) ) ;
#80399 = CARTESIAN_POINT ( 'NONE',  ( 21.53943276465977519, 0.05219959533937863772, 21.25109039468567218 ) ) ;
#80400 = CARTESIAN_POINT ( 'NONE',  ( 12.14591786802309770, 12.06949235617756955, 114.3739096053143527 ) ) ;
#80401 = CARTESIAN_POINT ( 'NONE',  ( -10.72451020669898014, 18.67979575497178502, 95.41557627198102409 ) ) ;
#80402 = EDGE_CURVE ( 'NONE', #173153, #25217, #157618, .T. ) ;
#80403 = CARTESIAN_POINT ( 'NONE',  ( -19.03943276465977164, -0.05219959533935918106, 53.75109039468566863 ) ) ;
#80404 = CARTESIAN_POINT ( 'NONE',  ( 13.97604488694527802, 13.89961937509977652, 24.37390960531435624 ) ) ;
#80405 = CARTESIAN_POINT ( 'NONE',  ( 9.564922557960805705, 16.46253265017160317, 29.58224293864769550 ) ) ;
#80406 = CARTESIAN_POINT ( 'NONE',  ( -11.74264578624799782, -36.14014761921581709, -1.599999999999999867 ) ) ;
#80407 = CARTESIAN_POINT ( 'NONE',  ( 8.224510206698742110, 14.34966873604972548, 42.08442372801901854 ) ) ;
#80408 = CARTESIAN_POINT ( 'NONE',  ( 0.05219959533910956823, 16.53943276465976808, 114.9989096053143669 ) ) ;
#80409 = CARTESIAN_POINT ( 'NONE',  ( -7.652493125962417153, -39.26116846143397510, -13.00000000000000000 ) ) ;
#80410 = CARTESIAN_POINT ( 'NONE',  ( -16.46253265017160317, 9.564922557960807481, 75.83224293864769550 ) ) ;
#80411 = CARTESIAN_POINT ( 'NONE',  ( 0.05219959533910956823, 16.53943276465976808, 94.99890960531436690 ) ) ;
#80412 = CARTESIAN_POINT ( 'NONE',  ( 21.52544592524344225, -5.823673210054117533, 48.54057627198103120 ) ) ;
#80413 = CARTESIAN_POINT ( 'NONE',  ( -12.14591786802309592, -12.06949235617757132, 81.87390960531435269 ) ) ;
#80414 = CARTESIAN_POINT ( 'NONE',  ( 4.379528057220092307, 16.55341960407617563, 32.29275706135235424 ) ) ;
#80415 = CARTESIAN_POINT ( 'NONE',  ( -18.67979575497193778, 10.72451020669871902, 88.33442372801901854 ) ) ;
#80416 = CARTESIAN_POINT ( 'NONE',  ( 5.153800228976335163, 19.02544592524342804, 29.79057627198102409 ) ) ;
#80417 = CARTESIAN_POINT ( 'NONE',  ( -8.224510206698735004, -14.34966873604973081, 94.58442372801901854 ) ) ;
#80418 = CARTESIAN_POINT ( 'NONE',  ( 4.379528057220339221, -16.55341960407611168, 47.70724293864770260 ) ) ;
#80419 = CARTESIAN_POINT ( 'NONE',  ( -9.564922557960796823, -16.46253265017161027, 52.08224293864768839 ) ) ;
#80420 = CARTESIAN_POINT ( 'NONE',  ( -15.72974639402176322, -15.80617190586768395, 99.37609039468568994 ) ) ;
#80421 = CARTESIAN_POINT ( 'NONE',  ( 18.67979575497178502, 10.72451020669898547, 114.1655762719810383 ) ) ;
#80422 = CARTESIAN_POINT ( 'NONE',  ( 21.52544592524334988, 5.823673210054432836, 66.45942372801903275 ) ) ;
#80423 = CARTESIAN_POINT ( 'NONE',  ( 4.483927247898790824, -16.52544592524335698, 40.20942372801901854 ) ) ;
#80425 = CARTESIAN_POINT ( 'NONE',  ( -15.72974639402176322, -15.80617190586768395, 89.37609039468568994 ) ) ;
#80424 = CARTESIAN_POINT ( 'NONE',  ( 14.29746914071049879, -8.314922557960816363, 63.33224293864770260 ) ) ;
#80426 = CARTESIAN_POINT ( 'NONE',  ( 14.34966873604960469, 8.224510206698951720, 24.16557627198103120 ) ) ;
#80427 = CARTESIAN_POINT ( 'NONE',  ( 17.05587630539707433, -6.762274262136759084, 48.24180309037284076 ) ) ;
#80428 = DIRECTION ( 'NONE',  ( 1.000000000000000000, 0.000000000000000000, 0.000000000000000000 ) ) ;
#80429 = CARTESIAN_POINT ( 'NONE',  ( -12.06949235617756955, 12.14591786802309770, 45.62390960531436690 ) ) ;
#80430 = CARTESIAN_POINT ( 'NONE',  ( 4.379528057220092307, 16.55341960407617563, 67.29275706135234714 ) ) ;
#80431 = CARTESIAN_POINT ( 'NONE',  ( -9.474510206698964154, 16.51473224551069663, 85.41557627198102409 ) ) ;
#80432 = CARTESIAN_POINT ( 'NONE',  ( -0.05219959533909027116, -19.03943276465977164, 97.49890960531436690 ) ) ;
#80433 = CARTESIAN_POINT ( 'NONE',  ( 18.62759615963255655, 10.81492255796105972, 86.66775706135234714 ) ) ;
#80434 = CARTESIAN_POINT ( 'NONE',  ( 8.224510206698742110, 14.34966873604972548, 107.0844237280190043 ) ) ;
#80435 = CARTESIAN_POINT ( 'NONE',  ( 14.29746914071049879, -8.314922557960816363, 78.33224293864770971 ) ) ;
#80436 = CARTESIAN_POINT ( 'NONE',  ( -16.46253265017160317, 9.564922557960807481, 80.83224293864769550 ) ) ;
#80437 = ORIENTED_EDGE ( 'NONE', *, *, #160998, .F. ) ;
#80438 = CARTESIAN_POINT ( 'NONE',  ( 16.52544592524335698, 4.483927247898782831, 26.45942372801901854 ) ) ;
#80439 = CARTESIAN_POINT ( 'NONE',  ( 5.153800228976335163, 19.02544592524342804, 29.79057627198102409 ) ) ;
#80440 = CARTESIAN_POINT ( 'NONE',  ( -16.51473224551069308, -9.474510206698971260, 96.66557627198102409 ) ) ;
#80442 = FACE_OUTER_BOUND ( 'NONE', #106675, .T. ) ;
#80441 = CARTESIAN_POINT ( 'NONE',  ( 14.29746914071037800, 8.314922557961029526, 26.66775706135235424 ) ) ;
#80443 = CARTESIAN_POINT ( 'NONE',  ( -5.153800228976607833, 19.02544592524334988, 22.70942372801899012 ) ) ;
#80444 = CARTESIAN_POINT ( 'NONE',  ( 0.05219959533934541429, -16.53943276465976808, 90.00109039468567573 ) ) ;
#80445 = CARTESIAN_POINT ( 'NONE',  ( 5.049401038297881783, 19.05341960407617563, 112.2927570613523471 ) ) ;
#80446 = CARTESIAN_POINT ( 'NONE',  ( -19.05341960407611168, -5.049401038298163336, 26.45724293864769550 ) ) ;
#80447 = CARTESIAN_POINT ( 'NONE',  ( -12.14591786802326823, 12.06949235617739902, 83.12609039468568994 ) ) ;
#80448 = CARTESIAN_POINT ( 'NONE',  ( 12.06949235617739724, 12.14591786802326823, 71.87609039468568994 ) ) ;
#80449 = CARTESIAN_POINT ( 'NONE',  ( 26.21537839388344793, -30.21513421080428685, -6.441064297728048338 ) ) ;
#80450 = CARTESIAN_POINT ( 'NONE',  ( 19.05341960407617918, -5.049401038297876454, 71.04275706135234714 ) ) ;
#80451 = CARTESIAN_POINT ( 'NONE',  ( -18.62759615963255300, -10.81492255796106328, 109.1677570613523613 ) ) ;
#80452 = CARTESIAN_POINT ( 'NONE',  ( -0.05219959533909027116, -19.03943276465977164, 52.49890960531436690 ) ) ;
#80453 = CARTESIAN_POINT ( 'NONE',  ( -19.05341960407611168, -5.049401038298163336, 91.45724293864766707 ) ) ;
#80454 = CARTESIAN_POINT ( 'NONE',  ( 16.55341960407611168, 4.379528057220329451, 83.95724293864770971 ) ) ;
#80455 = CARTESIAN_POINT ( 'NONE',  ( -13.97604488694547697, 13.89961937509957934, 53.12609039468565442 ) ) ;
#80456 = CARTESIAN_POINT ( 'NONE',  ( -0.05219959533907301413, -21.53943276465977519, 52.49890960531435979 ) ) ;
#80457 = CARTESIAN_POINT ( 'NONE',  ( -21.55341960407619339, 5.719274019375674811, 108.5427570613523756 ) ) ;
#80458 = CARTESIAN_POINT ( 'NONE',  ( 0.05219959533909260263, 19.03943276465977164, 89.99890960531436690 ) ) ;
#80459 = CARTESIAN_POINT ( 'NONE',  ( 18.67979575497194134, -10.72451020669871369, 110.8344237280190043 ) ) ;
#80460 = CARTESIAN_POINT ( 'NONE',  ( -5.719274019375978568, 21.55341960407610458, 65.20724293864768129 ) ) ;
#80461 = CARTESIAN_POINT ( 'NONE',  ( 5.049401038298161559, -19.05341960407611168, 92.70724293864769550 ) ) ;
#80462 = CARTESIAN_POINT ( 'NONE',  ( -5.049401038297874678, -19.05341960407617918, 89.79275706135230450 ) ) ;
#80463 = CARTESIAN_POINT ( 'NONE',  ( -9.564922557960796823, -16.46253265017161027, 97.08224293864769550 ) ) ;
#80464 = CARTESIAN_POINT ( 'NONE',  ( -13.89961937509957401, -13.97604488694547875, 104.3760903946856757 ) ) ;
#80465 = CARTESIAN_POINT ( 'NONE',  ( -13.97604488694527625, -13.89961937509977652, 21.87390960531435979 ) ) ;
#80466 = CARTESIAN_POINT ( 'NONE',  ( -13.89961937509977652, 13.97604488694528158, 80.62390960531436690 ) ) ;
#80467 = CARTESIAN_POINT ( 'NONE',  ( 5.719274019375991003, -21.55341960407610458, 82.70724293864770971 ) ) ;
#80468 = AXIS2_PLACEMENT_3D ( 'NONE', #27384, #69874, #89030 ) ;
#80469 = CARTESIAN_POINT ( 'NONE',  ( -16.52544592524335698, -4.483927247898792601, 48.95942372801902565 ) ) ;
#80470 = CARTESIAN_POINT ( 'NONE',  ( 21.53943276465977519, 0.05219959533937863772, 46.25109039468567573 ) ) ;
#80471 = CARTESIAN_POINT ( 'NONE',  ( -10.81492255796105439, 18.62759615963255655, 92.91775706135236135 ) ) ;
#80472 = CARTESIAN_POINT ( 'NONE',  ( 16.55341960407618274, -4.379528057220086978, 91.04275706135236135 ) ) ;
#80473 = CARTESIAN_POINT ( 'NONE',  ( -13.89961937509977652, 13.97604488694528158, 85.62390960531433848 ) ) ;
#80474 = CARTESIAN_POINT ( 'NONE',  ( 14.29746914071049879, -8.314922557960816363, 88.33224293864769550 ) ) ;
#80475 = CARTESIAN_POINT ( 'NONE',  ( -16.55341960407611168, -4.379528057220339221, 26.45724293864768839 ) ) ;
#80476 = CARTESIAN_POINT ( 'NONE',  ( -5.049401038297874678, -19.05341960407617918, 64.79275706135233293 ) ) ;
#80477 = CARTESIAN_POINT ( 'NONE',  ( -21.55341960407619339, 5.719274019375674811, 48.54275706135234714 ) ) ;
#80478 = CARTESIAN_POINT ( 'NONE',  ( 19.03943276465977164, 0.05219959533936151252, 26.25109039468566507 ) ) ;
#80479 = CARTESIAN_POINT ( 'NONE',  ( 12.06949235617757843, -12.14591786802309237, 98.12390960531436690 ) ) ;
#80480 = CARTESIAN_POINT ( 'NONE',  ( -21.53943276465977519, 0.05219959533907696930, 21.24890960531436690 ) ) ;
#80481 = CARTESIAN_POINT ( 'NONE',  ( -16.55341960407611168, -4.379528057220339221, 26.45724293864768839 ) ) ;
#80482 = CARTESIAN_POINT ( 'NONE',  ( -21.53943276465977519, -0.05219959533937600094, 83.75109039468568994 ) ) ;
#80483 = CARTESIAN_POINT ( 'NONE',  ( -12.14591786802326823, 12.06949235617739902, 53.12609039468568284 ) ) ;
#80484 = CARTESIAN_POINT ( 'NONE',  ( 16.52544592524335698, 4.483927247898782831, 101.4594237280190185 ) ) ;
#80485 = CARTESIAN_POINT ( 'NONE',  ( -15.72974639402176322, -15.80617190586768395, 59.37609039468568284 ) ) ;
#80486 = VERTEX_POINT ( 'NONE', #119040 ) ;
#80487 = CARTESIAN_POINT ( 'NONE',  ( 21.53943276465977519, 0.05219959533937863772, 26.25109039468567573 ) ) ;
#80488 = CARTESIAN_POINT ( 'NONE',  ( -16.52544592524342804, 4.483927247898546575, 106.0405762719810525 ) ) ;
#80489 = CARTESIAN_POINT ( 'NONE',  ( -5.153800228976328057, -19.02544592524343514, 32.29057627198102409 ) ) ;
#80490 = CARTESIAN_POINT ( 'NONE',  ( -12.06949235617756955, 12.14591786802309770, 70.62390960531436690 ) ) ;
#80491 = CARTESIAN_POINT ( 'NONE',  ( -0.05219959533909027116, -19.03943276465977164, 72.49890960531435269 ) ) ;
#80492 = CARTESIAN_POINT ( 'NONE',  ( 8.314922557961029526, -14.29746914071037800, 110.4177570613523756 ) ) ;
#80493 = CARTESIAN_POINT ( 'NONE',  ( 9.474510206698971260, -16.51473224551069308, 32.91557627198102409 ) ) ;
#80494 = CARTESIAN_POINT ( 'NONE',  ( -15.72974639402197994, 15.80617190586746368, 50.62390960531435979 ) ) ;
#80495 = CARTESIAN_POINT ( 'NONE',  ( -12.14591786802309592, -12.06949235617757132, 91.87390960531436690 ) ) ;
#80496 = AXIS2_PLACEMENT_3D ( 'NONE', #141675, #81962, #108352 ) ;
#80497 = CARTESIAN_POINT ( 'NONE',  ( 5.719274019375991003, -21.55341960407610458, 92.70724293864770971 ) ) ;
#80498 = CARTESIAN_POINT ( 'NONE',  ( -5.049401038298153566, 19.05341960407611168, 100.2072429386476955 ) ) ;
#80500 = CARTESIAN_POINT ( 'NONE',  ( 0.05219959533936267826, -19.03943276465977164, 90.00109039468567573 ) ) ;
#80499 = CARTESIAN_POINT ( 'NONE',  ( 19.02544592524343514, -5.153800228976328945, 53.54057627198102409 ) ) ;
#80501 = CARTESIAN_POINT ( 'NONE',  ( 21.52544592524344225, -5.823673210054117533, 43.54057627198103830 ) ) ;
#80502 = CARTESIAN_POINT ( 'NONE',  ( -5.719274019375665041, -21.55341960407619695, 64.79275706135234714 ) ) ;
#80503 = CARTESIAN_POINT ( 'NONE',  ( 5.153800228976335163, 19.02544592524342804, 54.79057627198103120 ) ) ;
#80504 = CARTESIAN_POINT ( 'NONE',  ( -19.02544592524342804, 5.153800228976336051, 91.04057627198100988 ) ) ;
#80505 = CARTESIAN_POINT ( 'NONE',  ( -4.379528057220086978, -16.55341960407618274, 64.79275706135234714 ) ) ;
#80506 = CARTESIAN_POINT ( 'NONE',  ( -18.67979575497193778, 10.72451020669871902, 38.33442372801900433 ) ) ;
#80507 = CARTESIAN_POINT ( 'NONE',  ( -18.62759615963255300, -10.81492255796106328, 74.16775706135231871 ) ) ;
#80508 = CARTESIAN_POINT ( 'NONE',  ( -21.55341960407610458, -5.719274019375992779, 26.45724293864768839 ) ) ;
#80509 = CARTESIAN_POINT ( 'NONE',  ( -15.80617190586745835, -15.72974639402198527, 101.8739096053143811 ) ) ;
#80511 = CARTESIAN_POINT ( 'NONE',  ( -16.55341960407617563, 4.379528057220093196, 58.54275706135235424 ) ) ;
#80510 = CARTESIAN_POINT ( 'NONE',  ( -15.80617190586768217, 15.72974639402176855, 38.12609039468567573 ) ) ;
#80512 = CARTESIAN_POINT ( 'NONE',  ( 15.72974639402199770, -15.80617190586745480, 68.12390960531436690 ) ) ;
#80513 = CARTESIAN_POINT ( 'NONE',  ( 9.564922557961047289, -16.46253265017146816, 30.41775706135232937 ) ) ;
#80515 = CARTESIAN_POINT ( 'NONE',  ( -8.224510206698735004, -14.34966873604973081, 109.5844237280190328 ) ) ;
#80514 = CARTESIAN_POINT ( 'NONE',  ( 5.153800228976335163, 19.02544592524342804, 74.79057627198103830 ) ) ;
#80516 = FACE_OUTER_BOUND ( 'NONE', #15853, .T. ) ;
#80517 = CARTESIAN_POINT ( 'NONE',  ( 0.05219959533909260263, 19.03943276465977164, 104.9989096053143669 ) ) ;
#80518 = CARTESIAN_POINT ( 'NONE',  ( -17.49999999999999645, 5.499999999999997335, 120.0000000000000142 ) ) ;
#80519 = CARTESIAN_POINT ( 'NONE',  ( 19.03943276465977164, 0.05219959533936151252, 81.25109039468567573 ) ) ;
#80520 = CARTESIAN_POINT ( 'NONE',  ( -5.823673210054116645, -21.52544592524344225, 52.29057627198102409 ) ) ;
#80521 = CARTESIAN_POINT ( 'NONE',  ( -14.29746914071049879, 8.314922557960819915, 35.83224293864768839 ) ) ;
#80522 = CARTESIAN_POINT ( 'NONE',  ( -14.34966873604972548, 8.224510206698743886, 23.33442372801901499 ) ) ;
#80523 = CARTESIAN_POINT ( 'NONE',  ( 5.153800228976335163, 19.02544592524342804, 34.79057627198102409 ) ) ;
#80524 = CARTESIAN_POINT ( 'NONE',  ( -19.03943276465977164, -0.05219959533935918106, 113.7510903946856757 ) ) ;
#80526 = CARTESIAN_POINT ( 'NONE',  ( -19.02544592524334988, -5.153800228976617603, 63.95942372801899012 ) ) ;
#80525 = CARTESIAN_POINT ( 'NONE',  ( 0.05219959533907565091, 21.53943276465977519, 84.99890960531436690 ) ) ;
#80527 = CARTESIAN_POINT ( 'NONE',  ( 0.05219959533934541429, -16.53943276465976808, 80.00109039468568994 ) ) ;
#80528 = CARTESIAN_POINT ( 'NONE',  ( 19.02544592524343514, -5.153800228976328945, 68.54057627198103830 ) ) ;
#80529 = CARTESIAN_POINT ( 'NONE',  ( -4.379528057220328563, 16.55341960407611168, 75.20724293864769550 ) ) ;
#80530 = CARTESIAN_POINT ( 'NONE',  ( -19.03943276465977164, 0.05219959533909376836, 41.24890960531435269 ) ) ;
#80531 = CARTESIAN_POINT ( 'NONE',  ( -0.05219959533910754901, -16.53943276465976808, 52.49890960531435979 ) ) ;
#80532 = CARTESIAN_POINT ( 'NONE',  ( -16.51473224551069308, -9.474510206698971260, 21.66557627198102765 ) ) ;
#80533 = CARTESIAN_POINT ( 'NONE',  ( 1.314372631020014115, 8.348397508521239629, -62.04882876100633382 ) ) ;
#80534 = CARTESIAN_POINT ( 'NONE',  ( -14.34966873604960291, -8.224510206698953496, 26.66557627198103475 ) ) ;
#80535 = CARTESIAN_POINT ( 'NONE',  ( 13.97604488694527802, 13.89961937509977652, 74.37390960531436690 ) ) ;
#80536 = LINE ( 'NONE', #21866, #144485 ) ;
#80537 = CARTESIAN_POINT ( 'NONE',  ( 5.049401038297881783, 19.05341960407617563, 37.29275706135232582 ) ) ;
#80538 = CARTESIAN_POINT ( 'NONE',  ( -0.05219959533934338120, 16.53943276465976808, 52.50109039468567573 ) ) ;
#80539 = CARTESIAN_POINT ( 'NONE',  ( 15.80617190586746368, 15.72974639402197994, 69.37390960531436690 ) ) ;
#80540 = CARTESIAN_POINT ( 'NONE',  ( 9.474510206698729675, 16.51473224551082808, 27.08442372801900433 ) ) ;
#80541 = CARTESIAN_POINT ( 'NONE',  ( 9.474510206698971260, -16.51473224551069308, 72.91557627198102409 ) ) ;
#80542 = CARTESIAN_POINT ( 'NONE',  ( 35.00000000000000000, 3.181980515339470905, 8.889087296526001936 ) ) ;
#80543 = CARTESIAN_POINT ( 'NONE',  ( 13.97604488694527802, 13.89961937509977652, 114.3739096053143669 ) ) ;
#80544 = CARTESIAN_POINT ( 'NONE',  ( 18.67979575497194134, -10.72451020669871369, 40.83442372801901854 ) ) ;
#80545 = CARTESIAN_POINT ( 'NONE',  ( -4.483927247898539470, -16.52544592524342804, 102.2905762719810383 ) ) ;
#80548 = EDGE_LOOP ( 'NONE', ( #73125, #110031, #139516, #43644, #105823 ) ) ;
#80547 = CARTESIAN_POINT ( 'NONE',  ( 16.46253265017160672, -9.564922557960803928, 78.33224293864769550 ) ) ;
#80546 = CARTESIAN_POINT ( 'NONE',  ( -15.80617190586745835, -15.72974639402198527, 106.8739096053143811 ) ) ;
#80549 = CARTESIAN_POINT ( 'NONE',  ( -21.52544592524334988, -5.823673210054445271, 23.95942372801901143 ) ) ;
#80550 = ORIENTED_EDGE ( 'NONE', *, *, #99297, .T. ) ;
#80551 = CARTESIAN_POINT ( 'NONE',  ( 13.89961937509977652, -13.97604488694527269, 93.12390960531436690 ) ) ;
#80552 = DIRECTION ( 'NONE',  ( -0.000000000000000000, -0.000000000000000000, 1.000000000000000000 ) ) ;
#80553 = CARTESIAN_POINT ( 'NONE',  ( 19.03943276465977164, -0.05219959533909143690, 33.74890960531435979 ) ) ;
#80554 = CARTESIAN_POINT ( 'NONE',  ( 16.51473224551083163, -9.474510206698727899, 110.8344237280190043 ) ) ;
#80555 = CARTESIAN_POINT ( 'NONE',  ( -36.91746825000001309, 11.99521256947798342, -9.224999997268813701 ) ) ;
#80556 = CARTESIAN_POINT ( 'NONE',  ( 16.55341960407611168, 4.379528057220329451, 108.9572429386476955 ) ) ;
#80557 = CARTESIAN_POINT ( 'NONE',  ( 10.72451020669871369, 18.67979575497193778, 92.08442372801901854 ) ) ;
#80559 = CARTESIAN_POINT ( 'NONE',  ( 18.67979575497194134, -10.72451020669871369, 40.83442372801901854 ) ) ;
#80558 = CARTESIAN_POINT ( 'NONE',  ( 19.03943276465977164, -0.05219959533909143690, 78.74890960531436690 ) ) ;
#80560 = CARTESIAN_POINT ( 'NONE',  ( 21.52544592524334988, 5.823673210054432836, 21.45942372801901499 ) ) ;
#80561 = CARTESIAN_POINT ( 'NONE',  ( -28.82186960331499392, 9.364793116373565596, 149.9000000000000057 ) ) ;
#80562 = CARTESIAN_POINT ( 'NONE',  ( -19.02544592524342804, 5.153800228976336051, 81.04057627198103830 ) ) ;
#80563 = DIRECTION ( 'NONE',  ( 1.000000000000000000, 0.000000000000000000, 0.000000000000000000 ) ) ;
#80565 = CARTESIAN_POINT ( 'NONE',  ( 15.80617190586746368, 15.72974639402197994, 44.37390960531435979 ) ) ;
#80564 = CARTESIAN_POINT ( 'NONE',  ( 16.55341960407618274, -4.379528057220086978, 31.04275706135234714 ) ) ;
#80566 = CARTESIAN_POINT ( 'NONE',  ( -0.05219959533937732626, 21.53943276465977519, 82.50109039468568994 ) ) ;
#80567 = CARTESIAN_POINT ( 'NONE',  ( -13.97604488694527625, -13.89961937509977652, 111.8739096053143243 ) ) ;
#80568 = CARTESIAN_POINT ( 'NONE',  ( 5.049401038297881783, 19.05341960407617563, 92.29275706135234714 ) ) ;
#80569 = CARTESIAN_POINT ( 'NONE',  ( 5.153800228976335163, 19.02544592524342804, 64.79057627198100988 ) ) ;
#80570 = CARTESIAN_POINT ( 'NONE',  ( -5.049401038298153566, 19.05341960407611168, 80.20724293864769550 ) ) ;
#80571 = EDGE_CURVE ( 'NONE', #35831, #11669, #161688, .T. ) ;
#80572 = CARTESIAN_POINT ( 'NONE',  ( 14.29746914071049879, -8.314922557960816363, 103.3322429386476955 ) ) ;
#80573 = CARTESIAN_POINT ( 'NONE',  ( -16.53943276465976808, 0.05219959533911058130, 106.2489096053143811 ) ) ;
#80574 = CARTESIAN_POINT ( 'NONE',  ( -19.02544592524342804, 5.153800228976336051, 106.0405762719810241 ) ) ;
#80575 = CARTESIAN_POINT ( 'NONE',  ( -8.314922557961024197, 14.29746914071037800, 77.91775706135231871 ) ) ;
#80577 = CARTESIAN_POINT ( 'NONE',  ( 19.03943276465977164, -0.05219959533909143690, 38.74890960531436690 ) ) ;
#80576 = CARTESIAN_POINT ( 'NONE',  ( 8.224510206698953496, -14.34966873604960469, 52.91557627198103830 ) ) ;
#80578 = CARTESIAN_POINT ( 'NONE',  ( 21.52544592524334988, 5.823673210054432836, 81.45942372801900433 ) ) ;
#80579 = CARTESIAN_POINT ( 'NONE',  ( 21.53943276465977519, 0.05219959533937863772, 76.25109039468568994 ) ) ;
#80580 = CARTESIAN_POINT ( 'NONE',  ( -19.05341960407617563, 5.049401038297882671, 88.54275706135230450 ) ) ;
#80581 = CARTESIAN_POINT ( 'NONE',  ( 12.06949235617757843, -12.14591786802309237, 58.12390960531435979 ) ) ;
#80582 = CARTESIAN_POINT ( 'NONE',  ( -10.81492255796078084, -18.62759615963271287, 107.0822429386476955 ) ) ;
#80583 = CARTESIAN_POINT ( 'NONE',  ( -15.80617190586745835, -15.72974639402198527, 51.87390960531437401 ) ) ;
#80584 = CARTESIAN_POINT ( 'NONE',  ( -16.81555441253553340, -7.025013491695471401, 104.3631455466574494 ) ) ;
#80585 = CARTESIAN_POINT ( 'NONE',  ( 22.44159573604009239, 16.30477369853692693, 148.0750000027312012 ) ) ;
#80586 = CARTESIAN_POINT ( 'NONE',  ( 16.46253265017160672, -9.564922557960803928, 68.33224293864770971 ) ) ;
#80587 = CARTESIAN_POINT ( 'NONE',  ( 0.05219959533910956823, 16.53943276465976808, 34.99890960531435979 ) ) ;
#80588 = CARTESIAN_POINT ( 'NONE',  ( 4.379528057220339221, -16.55341960407611168, 27.70724293864769905 ) ) ;
#80589 = CARTESIAN_POINT ( 'NONE',  ( -4.483927247898782831, 16.52544592524335698, 82.70942372801900433 ) ) ;
#80590 = CARTESIAN_POINT ( 'NONE',  ( 13.89961937509957401, 13.97604488694547697, 36.87609039468565442 ) ) ;
#80591 = CARTESIAN_POINT ( 'NONE',  ( -32.00000000000000000, -1.130961319012580892E-14, 92.35000000000000853 ) ) ;
#80592 = CARTESIAN_POINT ( 'NONE',  ( -9.474510206698964154, 16.51473224551069663, 85.41557627198102409 ) ) ;
#80593 = EDGE_CURVE ( 'NONE', #183244, #88998, #83672, .T. ) ;
#80594 = CARTESIAN_POINT ( 'NONE',  ( -8.314922557960811034, -14.29746914071050412, 57.08224293864769550 ) ) ;
#80596 = CARTESIAN_POINT ( 'NONE',  ( 5.823673210054125526, 21.52544592524343514, 24.79057627198103120 ) ) ;
#80595 = CARTESIAN_POINT ( 'NONE',  ( -19.05341960407611168, -5.049401038298163336, 21.45724293864768839 ) ) ;
#80597 = CARTESIAN_POINT ( 'NONE',  ( -10.72451020669898014, 18.67979575497178502, 55.41557627198102409 ) ) ;
#80598 = CARTESIAN_POINT ( 'NONE',  ( -8.314922557960811034, -14.29746914071050412, 92.08224293864769550 ) ) ;
#80599 = CARTESIAN_POINT ( 'NONE',  ( -14.29746914071037622, -8.314922557961029526, 34.16775706135234714 ) ) ;
#80600 = CARTESIAN_POINT ( 'NONE',  ( -16.52544592524342804, 4.483927247898546575, 76.04057627198102409 ) ) ;
#80601 = DIRECTION ( 'NONE',  ( 1.000000000000000000, 0.000000000000000000, -0.000000000000000000 ) ) ;
#80602 = CARTESIAN_POINT ( 'NONE',  ( 13.97604488694548053, -13.89961937509957401, 80.62609039468567573 ) ) ;
#80603 = CARTESIAN_POINT ( 'NONE',  ( 19.05341960407611168, 5.049401038298154454, 113.9572429386477097 ) ) ;
#80604 = CARTESIAN_POINT ( 'NONE',  ( -11.40812507854755609, 35.11059874428196537, -5.524999997268813523 ) ) ;
#80605 = CARTESIAN_POINT ( 'NONE',  ( 5.049401038298163336, -19.05341960407611168, 42.70724293864768839 ) ) ;
#80606 = CIRCLE ( 'NONE', #3107, 24.30000000000003268 ) ;
#80608 = CARTESIAN_POINT ( 'NONE',  ( 14.29746914071049879, -8.314922557960816363, 33.33224293864769550 ) ) ;
#80607 = CARTESIAN_POINT ( 'NONE',  ( -4.379528057220086978, -16.55341960407618274, 34.79275706135235424 ) ) ;
#80609 = CARTESIAN_POINT ( 'NONE',  ( 18.62759615963271287, -10.81492255796078972, 58.33224293864768839 ) ) ;
#80610 = CARTESIAN_POINT ( 'NONE',  ( 13.97604488694548053, -13.89961937509957401, 85.62609039468568994 ) ) ;
#80611 = CARTESIAN_POINT ( 'NONE',  ( 18.67979575497178502, 10.72451020669898547, 54.16557627198103120 ) ) ;
#80612 = CARTESIAN_POINT ( 'NONE',  ( 21.55341960407619695, -5.719274019375665929, 86.04275706135236135 ) ) ;
#80613 = CARTESIAN_POINT ( 'NONE',  ( 2.662494480112515660, -37.13692398601924793, -32.59999999999999432 ) ) ;
#80614 = CARTESIAN_POINT ( 'NONE',  ( -14.29746914071037622, -8.314922557961029526, 29.16775706135234003 ) ) ;
#80616 = CARTESIAN_POINT ( 'NONE',  ( 19.02544592524343514, -5.153800228976328945, 88.54057627198102409 ) ) ;
#80615 = CARTESIAN_POINT ( 'NONE',  ( 17.59860650958994555, -7.585241751806880650, 55.92337014262493966 ) ) ;
#80617 = CARTESIAN_POINT ( 'NONE',  ( -0.05219959533909027116, -19.03943276465977164, 32.49890960531435979 ) ) ;
#80618 = CARTESIAN_POINT ( 'NONE',  ( 8.314922557960818139, 14.29746914071049879, 104.5822429386477097 ) ) ;
#80619 = SHAPE_DEFINITION_REPRESENTATION ( #156746, #85690 ) ;
#80620 = CARTESIAN_POINT ( 'NONE',  ( -0.05219959533909027116, -19.03943276465977164, 102.4989096053143669 ) ) ;
#80621 = ORIENTED_EDGE ( 'NONE', *, *, #125103, .F. ) ;
#80622 = CARTESIAN_POINT ( 'NONE',  ( 4.483927247898790824, -16.52544592524335698, 60.20942372801902565 ) ) ;
#80623 = CARTESIAN_POINT ( 'NONE',  ( -10.81492255796078084, -18.62759615963271287, 97.08224293864770971 ) ) ;
#80624 = CARTESIAN_POINT ( 'NONE',  ( 5.049401038298161559, -19.05341960407611168, 47.70724293864770260 ) ) ;
#80626 = CARTESIAN_POINT ( 'NONE',  ( 21.52544592524334988, 5.823673210054432836, 31.45942372801901854 ) ) ;
#80625 = CARTESIAN_POINT ( 'NONE',  ( 19.03943276465977164, 0.05219959533936151252, 71.25109039468566152 ) ) ;
#80627 = CARTESIAN_POINT ( 'NONE',  ( 19.02544592524343514, -5.153800228976328945, 68.54057627198103830 ) ) ;
#80628 = CARTESIAN_POINT ( 'NONE',  ( -16.46253265017160317, 9.564922557960807481, 100.8322429386477097 ) ) ;
#80629 = VERTEX_POINT ( 'NONE', #117016 ) ;
#80630 = CARTESIAN_POINT ( 'NONE',  ( -12.06949235617739369, -12.14591786802326823, 34.37609039468568284 ) ) ;
#80631 = CARTESIAN_POINT ( 'NONE',  ( -21.53943276465977519, -0.05219959533937600094, 23.75109039468567929 ) ) ;
#80634 = CARTESIAN_POINT ( 'NONE',  ( 5.049401038297881783, 19.05341960407617563, 77.29275706135231871 ) ) ;
#80633 = CARTESIAN_POINT ( 'NONE',  ( 9.564922557960805705, 16.46253265017160317, 89.58224293864769550 ) ) ;
#80632 = CARTESIAN_POINT ( 'NONE',  ( -14.29746914071049879, 8.314922557960819915, 100.8322429386477097 ) ) ;
#80635 = CARTESIAN_POINT ( 'NONE',  ( -21.55341960407610458, -5.719274019375992779, 91.45724293864769550 ) ) ;
#80636 = CARTESIAN_POINT ( 'NONE',  ( 4.483927247898545687, 16.52544592524342804, 49.79057627198102409 ) ) ;
#80637 = CARTESIAN_POINT ( 'NONE',  ( -19.02544592524334988, -5.153800228976617603, 18.95942372801899722 ) ) ;
#80638 = CARTESIAN_POINT ( 'NONE',  ( -4.379528057220086978, -16.55341960407618274, 74.79275706135234714 ) ) ;
#80639 = CARTESIAN_POINT ( 'NONE',  ( -19.02544592524342804, 5.153800228976336051, 106.0405762719810241 ) ) ;
#80640 = CARTESIAN_POINT ( 'NONE',  ( -19.02544592524342804, 5.153800228976336051, 46.04057627198101699 ) ) ;
#80641 = CARTESIAN_POINT ( 'NONE',  ( -5.823673210054431948, 21.52544592524334988, 52.70942372801902565 ) ) ;
#80642 = CARTESIAN_POINT ( 'NONE',  ( -21.53943276465977519, -0.05219959533937600094, 73.75109039468567573 ) ) ;
#80643 = CARTESIAN_POINT ( 'NONE',  ( -16.46253265017160317, 9.564922557960807481, 55.83224293864769550 ) ) ;
#80644 = CARTESIAN_POINT ( 'NONE',  ( -21.52544592524334988, -5.823673210054445271, 48.95942372801902565 ) ) ;
#80645 = ADVANCED_FACE ( 'NONE', ( #163536, #162521, #8854, #25036, #86679, #84667, #193881, #9858, #71517, #147365 ), #43447, .T. ) ;
#80646 = CARTESIAN_POINT ( 'NONE',  ( 9.474510206698729675, 16.51473224551082808, 87.08442372801900433 ) ) ;
#80647 = CARTESIAN_POINT ( 'NONE',  ( 13.89961937509977652, -13.97604488694527269, 38.12390960531436690 ) ) ;
#80648 = CARTESIAN_POINT ( 'NONE',  ( 16.52544592524335698, 4.483927247898782831, 86.45942372801901854 ) ) ;
#80649 = CARTESIAN_POINT ( 'NONE',  ( 0.05219959533909260263, 19.03943276465977164, 59.99890960531436690 ) ) ;
#80650 = CARTESIAN_POINT ( 'NONE',  ( 5.049401038298161559, -19.05341960407611168, 112.7072429386476813 ) ) ;
#80651 = CARTESIAN_POINT ( 'NONE',  ( -13.89961937509977652, 13.97604488694528158, 45.62390960531433848 ) ) ;
#80652 = CARTESIAN_POINT ( 'NONE',  ( -5.719274019375978568, 21.55341960407610458, 85.20724293864770971 ) ) ;
#80653 = CARTESIAN_POINT ( 'NONE',  ( -0.05219959533934338120, 16.53943276465976808, 67.50109039468568994 ) ) ;
#80654 = CARTESIAN_POINT ( 'NONE',  ( -24.29042230868038388, 8.936166115090465212, 166.5611006352799848 ) ) ;
#80655 = CARTESIAN_POINT ( 'NONE',  ( 0.05219959533936267826, -19.03943276465977164, 25.00109039468566152 ) ) ;
#80656 = CARTESIAN_POINT ( 'NONE',  ( -5.049401038298153566, 19.05341960407611168, 65.20724293864765286 ) ) ;
#80657 = CARTESIAN_POINT ( 'NONE',  ( 16.52544592524342804, -4.483927247898539470, 53.54057627198103120 ) ) ;
#80658 = CARTESIAN_POINT ( 'NONE',  ( -16.52544592524342804, 4.483927247898546575, 96.04057627198102409 ) ) ;
#80659 = CARTESIAN_POINT ( 'NONE',  ( 16.51473224551069308, 9.474510206698969483, 104.1655762719810241 ) ) ;
#80660 = CARTESIAN_POINT ( 'NONE',  ( -5.153800228976328057, -19.02544592524343514, 87.29057627198103830 ) ) ;
#80661 = CARTESIAN_POINT ( 'NONE',  ( -21.55341960407619339, 5.719274019375674811, 53.54275706135234714 ) ) ;
#80662 = CARTESIAN_POINT ( 'NONE',  ( 9.474510206698971260, -16.51473224551069308, 102.9155762719810241 ) ) ;
#80663 = CARTESIAN_POINT ( 'NONE',  ( 15.80617190586769283, -15.72974639402175789, 110.6260903946857042 ) ) ;
#80664 = CARTESIAN_POINT ( 'NONE',  ( 0.05219959533934541429, -16.53943276465976808, 85.00109039468568994 ) ) ;
#80665 = CARTESIAN_POINT ( 'NONE',  ( -15.80617190586768217, 15.72974639402176855, 43.12609039468568284 ) ) ;
#80666 = CARTESIAN_POINT ( 'NONE',  ( 19.05341960407611168, 5.049401038298154454, 108.9572429386477097 ) ) ;
#80667 = CARTESIAN_POINT ( 'NONE',  ( 10.72451020669898902, -18.67979575497178502, 107.9155762719810241 ) ) ;
#80668 = CARTESIAN_POINT ( 'NONE',  ( -0.05219959533910754901, -16.53943276465976808, 57.49890960531435979 ) ) ;
#80669 = CARTESIAN_POINT ( 'NONE',  ( 13.89961937509977652, -13.97604488694527269, 53.12390960531434558 ) ) ;
#80670 = CARTESIAN_POINT ( 'NONE',  ( -14.29746914071049879, 8.314922557960819915, 85.83224293864768129 ) ) ;
#80671 = CARTESIAN_POINT ( 'NONE',  ( 18.62759615963271287, -10.81492255796078972, 28.33224293864769550 ) ) ;
#80672 = CARTESIAN_POINT ( 'NONE',  ( 16.51473224551083163, -9.474510206698727899, 40.83442372801900433 ) ) ;
#80673 = CARTESIAN_POINT ( 'NONE',  ( -16.53943276465976808, 0.05219959533911058130, 116.2489096053143669 ) ) ;
#80674 = ORIENTED_EDGE ( 'NONE', *, *, #120835, .T. ) ;
#80675 = CARTESIAN_POINT ( 'NONE',  ( 14.29746914071037800, 8.314922557961029526, 61.66775706135235424 ) ) ;
#80676 = CARTESIAN_POINT ( 'NONE',  ( -16.51473224551069308, -9.474510206698971260, 71.66557627198102409 ) ) ;
#80677 = CARTESIAN_POINT ( 'NONE',  ( 17.14385361876520264, 23.59649016807275856, 146.1750000027311387 ) ) ;
#80678 = CARTESIAN_POINT ( 'NONE',  ( -12.14591786802309592, -12.06949235617757132, 91.87390960531436690 ) ) ;
#80679 = CARTESIAN_POINT ( 'NONE',  ( -5.823673210054116645, -21.52544592524344225, 32.29057627198102409 ) ) ;
#80680 = ORIENTED_EDGE ( 'NONE', *, *, #13338, .T. ) ;
#80681 = CARTESIAN_POINT ( 'NONE',  ( 12.06949235617739724, 12.14591786802326823, 101.8760903946857042 ) ) ;
#80682 = CARTESIAN_POINT ( 'NONE',  ( -16.51473224551082808, 9.474510206698731452, 113.3344237280190043 ) ) ;
#80683 = CARTESIAN_POINT ( 'NONE',  ( -0.05219959533937732626, 21.53943276465977519, 82.50109039468568994 ) ) ;
#80684 = CARTESIAN_POINT ( 'NONE',  ( -5.153800228976328057, -19.02544592524343514, 92.29057627198099567 ) ) ;
#80685 = CARTESIAN_POINT ( 'NONE',  ( -5.823673210054116645, -21.52544592524344225, 107.2905762719810525 ) ) ;
#80686 = CARTESIAN_POINT ( 'NONE',  ( 16.52544592524335698, 4.483927247898782831, 61.45942372801901854 ) ) ;
#80687 = CARTESIAN_POINT ( 'NONE',  ( 13.97604488694527802, 13.89961937509977652, 24.37390960531435624 ) ) ;
#80688 = CARTESIAN_POINT ( 'NONE',  ( 12.06949235617739724, 12.14591786802326823, 36.87609039468568994 ) ) ;
#80689 = CARTESIAN_POINT ( 'NONE',  ( -16.51473224551082808, 9.474510206698731452, 98.33442372801900433 ) ) ;
#80690 = CARTESIAN_POINT ( 'NONE',  ( -15.72974639402197994, 15.80617190586746368, 85.62390960531436690 ) ) ;
#80691 = CARTESIAN_POINT ( 'NONE',  ( 19.03943276465977164, 0.05219959533936151252, 61.25109039468566863 ) ) ;
#80692 = DIRECTION ( 'NONE',  ( -1.000000000000000000, -0.000000000000000000, 0.000000000000000000 ) ) ;
#80693 = CARTESIAN_POINT ( 'NONE',  ( 5.719274019375991003, -21.55341960407610458, 97.70724293864772392 ) ) ;
#80694 = CARTESIAN_POINT ( 'NONE',  ( -1.227931366032057224E-14, -24.30000000000003268, -54.21489346206828230 ) ) ;
#80695 = CARTESIAN_POINT ( 'NONE',  ( -9.564922557960796823, -16.46253265017161027, 82.08224293864768129 ) ) ;
#80696 = CARTESIAN_POINT ( 'NONE',  ( -8.314922557961024197, 14.29746914071037800, 32.91775706135234714 ) ) ;
#80697 = CARTESIAN_POINT ( 'NONE',  ( 23.48298174826589246, 32.32155151706776053, -6.702157773949822150 ) ) ;
#80698 = CARTESIAN_POINT ( 'NONE',  ( 16.46253265017146816, 9.564922557961045513, 56.66775706135233293 ) ) ;
#80700 = CARTESIAN_POINT ( 'NONE',  ( 12.06949235617757843, -12.14591786802309237, 58.12390960531435979 ) ) ;
#80699 = CARTESIAN_POINT ( 'NONE',  ( -15.80617190586745835, -15.72974639402198527, 111.8739096053143669 ) ) ;
#80701 = CARTESIAN_POINT ( 'NONE',  ( -16.46253265017160317, 9.564922557960807481, 65.83224293864769550 ) ) ;
#80703 = CARTESIAN_POINT ( 'NONE',  ( -16.51473224551082808, 9.474510206698731452, 48.33442372801900433 ) ) ;
#80702 = CARTESIAN_POINT ( 'NONE',  ( 16.53943276465976808, 0.05219959533934440121, 31.25109039468568639 ) ) ;
#80704 = CARTESIAN_POINT ( 'NONE',  ( 0.05219959533937995610, -21.53943276465977519, 50.00109039468568994 ) ) ;
#80705 = CARTESIAN_POINT ( 'NONE',  ( 9.564922557961047289, -16.46253265017146816, 105.4177570613523471 ) ) ;
#80706 = CARTESIAN_POINT ( 'NONE',  ( -16.51473224551069308, -9.474510206698971260, 56.66557627198103120 ) ) ;
#80707 = CARTESIAN_POINT ( 'NONE',  ( -16.51473224551082808, 9.474510206698731452, 78.33442372801900433 ) ) ;
#80708 = CARTESIAN_POINT ( 'NONE',  ( -5.823673210054431948, 21.52544592524334988, 87.70942372801901854 ) ) ;
#80709 = CARTESIAN_POINT ( 'NONE',  ( -5.153800228976607833, 19.02544592524334988, 67.70942372801900433 ) ) ;
#80710 = CARTESIAN_POINT ( 'NONE',  ( 16.46253265017160672, -9.564922557960803928, 43.33224293864769550 ) ) ;
#80711 = CARTESIAN_POINT ( 'NONE',  ( 18.62759615963271287, -10.81492255796078972, 58.33224293864768839 ) ) ;
#80713 = CARTESIAN_POINT ( 'NONE',  ( 13.97604488694548053, -13.89961937509957401, 65.62609039468567573 ) ) ;
#80712 = CARTESIAN_POINT ( 'NONE',  ( -12.14591786802309592, -12.06949235617757132, 61.87390960531436690 ) ) ;
#80714 = CARTESIAN_POINT ( 'NONE',  ( 21.64434376887848899, 9.890319055725232289, 170.6724019390510421 ) ) ;
#80715 = CARTESIAN_POINT ( 'NONE',  ( -0.05219959533936034679, 19.03943276465977164, 27.50109039468566507 ) ) ;
#80716 = CARTESIAN_POINT ( 'NONE',  ( -16.53943276465976808, -0.05219959533934237506, 103.7510903946857042 ) ) ;
#80717 = CARTESIAN_POINT ( 'NONE',  ( -4.483927247898539470, -16.52544592524342804, 52.29057627198102409 ) ) ;
#80719 = CARTESIAN_POINT ( 'NONE',  ( 17.14385361876520264, -23.59649016807271238, 141.5750000027312012 ) ) ;
#80718 = CARTESIAN_POINT ( 'NONE',  ( 21.55341960407619695, -5.719274019375665929, 86.04275706135236135 ) ) ;
#80720 = CARTESIAN_POINT ( 'NONE',  ( -18.67979575497193778, 10.72451020669871902, 88.33442372801901854 ) ) ;
#80721 = CARTESIAN_POINT ( 'NONE',  ( -5.719274019375978568, 21.55341960407610458, 95.20724293864769550 ) ) ;
#80722 = CARTESIAN_POINT ( 'NONE',  ( 0.05219959533909260263, 19.03943276465977164, 44.99890960531435979 ) ) ;
#80723 = CARTESIAN_POINT ( 'NONE',  ( -21.52544592524334988, -5.823673210054445271, 68.95942372801901854 ) ) ;
#80724 = CARTESIAN_POINT ( 'NONE',  ( -5.049401038298153566, 19.05341960407611168, 55.20724293864769550 ) ) ;
#80725 = CARTESIAN_POINT ( 'NONE',  ( 19.03943276465977164, -0.05219959533909143690, 63.74890960531435979 ) ) ;
#80726 = CARTESIAN_POINT ( 'NONE',  ( -4.483927247898539470, -16.52544592524342804, 107.2905762719810525 ) ) ;
#80727 = CARTESIAN_POINT ( 'NONE',  ( -16.46253265017160317, 9.564922557960807481, 110.8322429386476955 ) ) ;
#80728 = CARTESIAN_POINT ( 'NONE',  ( 0.05219959533910956823, 16.53943276465976808, 49.99890960531437401 ) ) ;
#80729 = CARTESIAN_POINT ( 'NONE',  ( -0.05219959533909027116, -19.03943276465977164, 27.49890960531435624 ) ) ;
#80730 = CARTESIAN_POINT ( 'NONE',  ( -12.14591786802309592, -12.06949235617757132, 81.87390960531435269 ) ) ;
#80731 = CARTESIAN_POINT ( 'NONE',  ( 18.62759615963271287, -10.81492255796078972, 93.33224293864769550 ) ) ;
#80732 = CARTESIAN_POINT ( 'NONE',  ( -0.05219959533937732626, 21.53943276465977519, 37.50109039468568284 ) ) ;
#80733 = CARTESIAN_POINT ( 'NONE',  ( -23.31738231874055600, 16.94106989632528837, 149.7999999999999829 ) ) ;
#80734 = CARTESIAN_POINT ( 'NONE',  ( -14.34966873604972548, 8.224510206698743886, 33.33442372801900433 ) ) ;
#80735 = CARTESIAN_POINT ( 'NONE',  ( 21.55341960407610458, 5.719274019375980345, 83.95724293864770971 ) ) ;
#80736 = CARTESIAN_POINT ( 'NONE',  ( -16.46253265017146816, -9.564922557961047289, 19.16775706135233293 ) ) ;
#80737 = CARTESIAN_POINT ( 'NONE',  ( 13.89961937509977652, -13.97604488694527269, 88.12390960531438111 ) ) ;
#80738 = CARTESIAN_POINT ( 'NONE',  ( -15.72974639402176322, -15.80617190586768395, 39.37609039468567573 ) ) ;
#80739 = EDGE_CURVE ( 'NONE', #34342, #56776, #164654, .T. ) ;
#80740 = CARTESIAN_POINT ( 'NONE',  ( -15.80617190586745835, -15.72974639402198527, 31.87390960531435979 ) ) ;
#80741 = CARTESIAN_POINT ( 'NONE',  ( -8.224510206698735004, -14.34966873604973081, 104.5844237280190185 ) ) ;
#80743 = CARTESIAN_POINT ( 'NONE',  ( -10.72451020669870658, -18.67979575497194134, 84.58442372801903275 ) ) ;
#80742 = CARTESIAN_POINT ( 'NONE',  ( 21.52544592524334988, 5.823673210054432836, 51.45942372801901854 ) ) ;
#80744 = CARTESIAN_POINT ( 'NONE',  ( 19.05341960407617918, -5.049401038297876454, 26.04275706135233293 ) ) ;
#80745 = CARTESIAN_POINT ( 'NONE',  ( 16.53943276465976808, 0.05219959533934440121, 86.25109039468568994 ) ) ;
#80746 = CARTESIAN_POINT ( 'NONE',  ( 18.62759615963255655, 10.81492255796105972, 41.66775706135235424 ) ) ;
#80747 = CARTESIAN_POINT ( 'NONE',  ( -9.564922557960796823, -16.46253265017161027, 47.08224293864769550 ) ) ;
#80748 = CARTESIAN_POINT ( 'NONE',  ( 10.81492255796106328, -18.62759615963255655, 100.4177570613523471 ) ) ;
#80749 = CARTESIAN_POINT ( 'NONE',  ( 16.46253265017160672, -9.564922557960803928, 113.3322429386476955 ) ) ;
#80750 = CARTESIAN_POINT ( 'NONE',  ( -18.62759615963270932, 10.81492255796079327, 100.8322429386477097 ) ) ;
#80751 = AXIS2_PLACEMENT_3D ( 'NONE', #34102, #125116, #48284 ) ;
#80752 = CARTESIAN_POINT ( 'NONE',  ( -21.55341960407610458, -5.719274019375992779, 66.45724293864768129 ) ) ;
#80754 = CARTESIAN_POINT ( 'NONE',  ( 21.52544592524344225, -5.823673210054117533, 63.54057627198103830 ) ) ;
#80753 = DIRECTION ( 'NONE',  ( 1.000000000000000000, 5.372046893347532792E-15, 0.000000000000000000 ) ) ;
#80756 = CARTESIAN_POINT ( 'NONE',  ( -0.05219959533910754901, -16.53943276465976808, 62.49890960531436690 ) ) ;
#80755 = CARTESIAN_POINT ( 'NONE',  ( -12.14591786802326823, 12.06949235617739902, 48.12609039468568284 ) ) ;
#80757 = DIRECTION ( 'NONE',  ( 1.000000000000000000, 0.000000000000000000, 0.000000000000000000 ) ) ;
#80758 = CARTESIAN_POINT ( 'NONE',  ( 19.03943276465977164, 0.05219959533936151252, 96.25109039468567573 ) ) ;
#80759 = PLANE ( 'NONE',  #144315 ) ;
#80760 = CARTESIAN_POINT ( 'NONE',  ( 8.314922557961029526, -14.29746914071037800, 20.41775706135234714 ) ) ;
#80761 = CARTESIAN_POINT ( 'NONE',  ( 10.81492255796078972, 18.62759615963270932, 94.58224293864769550 ) ) ;
#80762 = CARTESIAN_POINT ( 'NONE',  ( 21.53943276465977519, -0.05219959533907433946, 73.74890960531433848 ) ) ;
#80763 = CARTESIAN_POINT ( 'NONE',  ( 21.52544592524344225, -5.823673210054117533, 23.54057627198102765 ) ) ;
#80764 = CARTESIAN_POINT ( 'NONE',  ( -4.379528057220086978, -16.55341960407618274, 54.79275706135235424 ) ) ;
#80765 = CARTESIAN_POINT ( 'NONE',  ( 13.97604488694527802, 13.89961937509977652, 69.37390960531436690 ) ) ;
#80767 = CARTESIAN_POINT ( 'NONE',  ( 5.153800228976615827, -19.02544592524334988, 105.2094237280190185 ) ) ;
#80766 = CARTESIAN_POINT ( 'NONE',  ( -0.05219959533937732626, 21.53943276465977519, 32.50109039468568284 ) ) ;
#80768 = CARTESIAN_POINT ( 'NONE',  ( -19.05341960407611168, -5.049401038298163336, 111.4572429386476671 ) ) ;
#80769 = CARTESIAN_POINT ( 'NONE',  ( 13.89961937509977652, -13.97604488694527269, 83.12390960531436690 ) ) ;
#80770 = CARTESIAN_POINT ( 'NONE',  ( 18.62759615963271287, -10.81492255796078972, 88.33224293864769550 ) ) ;
#80771 = CARTESIAN_POINT ( 'NONE',  ( -19.02544592524342804, 5.153800228976336051, 56.04057627198100988 ) ) ;
#80772 = CARTESIAN_POINT ( 'NONE',  ( -16.62475595723695676, -7.163666690055258357, 59.47286648189533054 ) ) ;
#80773 = CARTESIAN_POINT ( 'NONE',  ( 0.05219959533910956823, 16.53943276465976808, 64.99890960531435269 ) ) ;
#80774 = CARTESIAN_POINT ( 'NONE',  ( -19.02544592524342804, 5.153800228976336051, 116.0405762719810383 ) ) ;
#80775 = CARTESIAN_POINT ( 'NONE',  ( -31.90000000000002700, 0.1282610754047256441, -49.13275782002543934 ) ) ;
#80776 = CARTESIAN_POINT ( 'NONE',  ( 21.53943276465977519, -0.05219959533907433946, 108.7489096053143669 ) ) ;
#80777 = CARTESIAN_POINT ( 'NONE',  ( 16.46253265017146816, 9.564922557961045513, 61.66775706135234003 ) ) ;
#80778 = CARTESIAN_POINT ( 'NONE',  ( 19.02544592524343514, -5.153800228976328945, 113.5405762719810241 ) ) ;
#80779 = CARTESIAN_POINT ( 'NONE',  ( -9.564922557960796823, -16.46253265017161027, 27.08224293864769550 ) ) ;
#80780 = CARTESIAN_POINT ( 'NONE',  ( -18.67979575497178146, -10.72451020669898902, 51.66557627198102409 ) ) ;
#80781 = AXIS2_PLACEMENT_3D ( 'NONE', #143089, #50111, #36909 ) ;
#80782 = CARTESIAN_POINT ( 'NONE',  ( -0.05219959533909027116, -19.03943276465977164, 92.49890960531436690 ) ) ;
#80783 = CARTESIAN_POINT ( 'NONE',  ( -21.52544592524334988, -5.823673210054445271, 78.95942372801901854 ) ) ;
#80784 = CARTESIAN_POINT ( 'NONE',  ( -19.05341960407611168, -5.049401038298163336, 56.45724293864768129 ) ) ;
#80785 = CARTESIAN_POINT ( 'NONE',  ( 4.379528057220339221, -16.55341960407611168, 82.70724293864770971 ) ) ;
#80786 = CARTESIAN_POINT ( 'NONE',  ( 0.05219959533934541429, -16.53943276465976808, 40.00109039468567573 ) ) ;
#80787 = CARTESIAN_POINT ( 'NONE',  ( -10.72451020669870658, -18.67979575497194134, 59.58442372801901854 ) ) ;
#80788 = VERTEX_POINT ( 'NONE', #191976 ) ;
#80789 = CARTESIAN_POINT ( 'NONE',  ( -19.03943276465977164, -0.05219959533935918106, 28.75109039468566507 ) ) ;
#80790 = CARTESIAN_POINT ( 'NONE',  ( -0.05219959533936034679, 19.03943276465977164, 77.50109039468566152 ) ) ;
#80791 = CARTESIAN_POINT ( 'NONE',  ( -0.05219959533936034679, 19.03943276465977164, 42.50109039468566152 ) ) ;
#80792 = CARTESIAN_POINT ( 'NONE',  ( 15.50000000000000178, -5.500000000000000888, 118.0000000000000142 ) ) ;
#80793 = CARTESIAN_POINT ( 'NONE',  ( 15.80617190586769283, -15.72974639402175789, 35.62609039468568994 ) ) ;
#80794 = CARTESIAN_POINT ( 'NONE',  ( -23.48529157249599919, -32.32473071737750558, -3.449999994537626957 ) ) ;
#80795 = CARTESIAN_POINT ( 'NONE',  ( 19.05341960407617918, -5.049401038297876454, 31.04275706135232227 ) ) ;
#80796 = CARTESIAN_POINT ( 'NONE',  ( -16.46253265017160317, 9.564922557960807481, 50.83224293864770260 ) ) ;
#80797 = CARTESIAN_POINT ( 'NONE',  ( 9.474510206698729675, 16.51473224551082808, 27.08442372801900433 ) ) ;
#80798 = CARTESIAN_POINT ( 'NONE',  ( 14.29746914071037800, 8.314922557961029526, 101.6677570613523613 ) ) ;
#80800 = CARTESIAN_POINT ( 'NONE',  ( 0.05219959533937995610, -21.53943276465977519, 85.00109039468568994 ) ) ;
#80799 = CARTESIAN_POINT ( 'NONE',  ( 5.153800228976335163, 19.02544592524342804, 109.7905762719810099 ) ) ;
#80801 = CARTESIAN_POINT ( 'NONE',  ( -29.86685920354755552, 21.69954338932564397, -6.824999997268814234 ) ) ;
#80802 = CARTESIAN_POINT ( 'NONE',  ( -33.75669036400348944, 3.362847000060358305, 99.36731340788949751 ) ) ;
#80803 = CARTESIAN_POINT ( 'NONE',  ( -10.81492255796105439, 18.62759615963255655, 87.91775706135234714 ) ) ;
#80804 = CARTESIAN_POINT ( 'NONE',  ( 21.52594032250407352, -0.8193109935767731722, -58.70475745007095014 ) ) ;
#80805 = CARTESIAN_POINT ( 'NONE',  ( 0.05219959533909260263, 19.03943276465977164, 99.99890960531436690 ) ) ;
#80806 = CARTESIAN_POINT ( 'NONE',  ( 5.049401038298161559, -19.05341960407611168, 52.70724293864767418 ) ) ;
#80807 = CARTESIAN_POINT ( 'NONE',  ( -15.80617190586745835, -15.72974639402198527, 56.87390960531436690 ) ) ;
#80808 = CARTESIAN_POINT ( 'NONE',  ( -4.379528057220328563, 16.55341960407611168, 25.20724293864769550 ) ) ;
#80810 = CARTESIAN_POINT ( 'NONE',  ( 19.02544592524343514, -5.153800228976328945, 93.54057627198102409 ) ) ;
#80809 = CARTESIAN_POINT ( 'NONE',  ( -0.05219959533910754901, -16.53943276465976808, 102.4989096053143811 ) ) ;
#80811 = CARTESIAN_POINT ( 'NONE',  ( -21.55341960407619339, 5.719274019375674811, 113.5427570613523756 ) ) ;
#80812 = ADVANCED_FACE ( 'NONE', ( #99958 ), #13896, .T. ) ;
#80813 = CARTESIAN_POINT ( 'NONE',  ( -16.46253265017160317, 9.564922557960807481, 30.83224293864769550 ) ) ;
#80814 = CARTESIAN_POINT ( 'NONE',  ( -14.34966873604960291, -8.224510206698953496, 101.6655762719810383 ) ) ;
#80815 = CARTESIAN_POINT ( 'NONE',  ( -5.719274019375665041, -21.55341960407619695, 59.79275706135234714 ) ) ;
#80816 = CARTESIAN_POINT ( 'NONE',  ( 16.52544592524335698, 4.483927247898782831, 111.4594237280190328 ) ) ;
#80817 = CARTESIAN_POINT ( 'NONE',  ( 5.049401038297881783, 19.05341960407617563, 67.29275706135234714 ) ) ;
#80818 = CARTESIAN_POINT ( 'NONE',  ( -11.23589665953924666, -38.39309219976287579, -14.62820445599025199 ) ) ;
#80819 = CARTESIAN_POINT ( 'NONE',  ( 19.05341960407611168, 5.049401038298154454, 108.9572429386477097 ) ) ;
#80820 = CARTESIAN_POINT ( 'NONE',  ( 8.224510206698953496, -14.34966873604960469, 82.91557627198103830 ) ) ;
#80821 = CARTESIAN_POINT ( 'NONE',  ( -19.03943276465977164, -0.05219959533935918106, 53.75109039468566863 ) ) ;
#80822 = CARTESIAN_POINT ( 'NONE',  ( -5.153800228976328057, -19.02544592524343514, 67.29057627198102409 ) ) ;
#80823 = CARTESIAN_POINT ( 'NONE',  ( 14.34966873604960469, 8.224510206698951720, 59.16557627198103120 ) ) ;
#80824 = CARTESIAN_POINT ( 'NONE',  ( -19.03943276465977164, -0.05219959533935918106, 93.75109039468566152 ) ) ;
#80825 = CARTESIAN_POINT ( 'NONE',  ( 21.53943276465977519, -0.05219959533907433946, 38.74890960531435979 ) ) ;
#80826 = ORIENTED_EDGE ( 'NONE', *, *, #199141, .T. ) ;
#80827 = EDGE_CURVE ( 'NONE', #162507, #188321, #146761, .T. ) ;
#80828 = CARTESIAN_POINT ( 'NONE',  ( -8.314922557960811034, -14.29746914071050412, 102.0822429386476955 ) ) ;
#80829 = CARTESIAN_POINT ( 'NONE',  ( -18.22780087662123805, -5.499999999999968026, 98.98236817873106475 ) ) ;
#80831 = CARTESIAN_POINT ( 'NONE',  ( -21.53943276465977519, 0.05219959533907696930, 61.24890960531435979 ) ) ;
#80830 = CARTESIAN_POINT ( 'NONE',  ( 9.564922557960805705, 16.46253265017160317, 59.58224293864769550 ) ) ;
#80832 = CARTESIAN_POINT ( 'NONE',  ( 19.05341960407611168, 5.049401038298154454, 38.95724293864767418 ) ) ;
#80834 = CARTESIAN_POINT ( 'NONE',  ( -9.474510206698964154, 16.51473224551069663, 75.41557627198103830 ) ) ;
#80833 = CARTESIAN_POINT ( 'NONE',  ( -16.52544592524335698, -4.483927247898792601, 93.95942372801903275 ) ) ;
#80835 = CARTESIAN_POINT ( 'NONE',  ( 5.049401038297881783, 19.05341960407617563, 57.29275706135231871 ) ) ;
#80836 = CARTESIAN_POINT ( 'NONE',  ( -21.55341960407619339, 5.719274019375674811, 73.54275706135234714 ) ) ;
#80837 = CARTESIAN_POINT ( 'NONE',  ( -15.72974639402197994, 15.80617190586746368, 45.62390960531436690 ) ) ;
#80838 = CARTESIAN_POINT ( 'NONE',  ( 19.03943276465977164, -0.05219959533909143690, 108.7489096053143527 ) ) ;
#80839 = CARTESIAN_POINT ( 'NONE',  ( 19.05341960407611168, 5.049401038298154454, 23.95724293864769194 ) ) ;
#80840 = CARTESIAN_POINT ( 'NONE',  ( 16.52544592524335698, 4.483927247898782831, 81.45942372801900433 ) ) ;
#80841 = CARTESIAN_POINT ( 'NONE',  ( -5.153800228976607833, 19.02544592524334988, 102.7094237280189759 ) ) ;
#80842 = CARTESIAN_POINT ( 'NONE',  ( 23.64874990377914799, 15.04272038711346049, 165.8682408883346397 ) ) ;
#80843 = CARTESIAN_POINT ( 'NONE',  ( 19.53091890409951858, 5.500000000000028422, 77.56097431831419442 ) ) ;
#80844 = CARTESIAN_POINT ( 'NONE',  ( -18.62759615963255300, -10.81492255796106328, 99.16775706135234714 ) ) ;
#80845 = ORIENTED_EDGE ( 'NONE', *, *, #179869, .T. ) ;
#80846 = CARTESIAN_POINT ( 'NONE',  ( -14.29746914071049879, 8.314922557960819915, 65.83224293864769550 ) ) ;
#80847 = CARTESIAN_POINT ( 'NONE',  ( -4.483927247898539470, -16.52544592524342804, 72.29057627198102409 ) ) ;
#80848 = CARTESIAN_POINT ( 'NONE',  ( 10.72451020669898902, -18.67979575497178502, 97.91557627198103830 ) ) ;
#80849 = CARTESIAN_POINT ( 'NONE',  ( 15.72974639402199770, -15.80617190586745480, 83.12390960531436690 ) ) ;
#80850 = DIRECTION ( 'NONE',  ( 0.000000000000000000, 0.000000000000000000, -1.000000000000000000 ) ) ;
#80851 = CARTESIAN_POINT ( 'NONE',  ( 10.72451020669898902, -18.67979575497178502, 32.91557627198102409 ) ) ;
#80852 = CARTESIAN_POINT ( 'NONE',  ( -0.05219959533934338120, 16.53943276465976808, 67.50109039468568994 ) ) ;
#80853 = CARTESIAN_POINT ( 'NONE',  ( -16.55341960407611168, -4.379528057220339221, 91.45724293864769550 ) ) ;
#80854 = CARTESIAN_POINT ( 'NONE',  ( 19.02544592524343514, -5.153800228976328945, 43.54057627198103120 ) ) ;
#80855 =( NAMED_UNIT ( * ) PLANE_ANGLE_UNIT ( ) SI_UNIT ( $, .RADIAN. ) );
#80856 = CARTESIAN_POINT ( 'NONE',  ( 35.44379935611745225, -3.753814927773954757, 38.50236686201311187 ) ) ;
#80857 = CARTESIAN_POINT ( 'NONE',  ( -12.14591786802326823, 12.06949235617739902, 98.12609039468570415 ) ) ;
#80858 = CARTESIAN_POINT ( 'NONE',  ( -21.53943276465977519, -0.05219959533937600094, 33.75109039468568284 ) ) ;
#80859 = CARTESIAN_POINT ( 'NONE',  ( 16.51473224551069308, 9.474510206698969483, 79.16557627198103830 ) ) ;
#80860 = CARTESIAN_POINT ( 'NONE',  ( 15.72974639402176855, 15.80617190586768217, 71.87609039468568994 ) ) ;
#80861 = FACE_OUTER_BOUND ( 'NONE', #85615, .T. ) ;
#80862 = CARTESIAN_POINT ( 'NONE',  ( -17.75813068129445327, -35.78296932995274204, -27.23805928211587002 ) ) ;
#80863 = ORIENTED_EDGE ( 'NONE', *, *, #127587, .F. ) ;
#80864 = CARTESIAN_POINT ( 'NONE',  ( -18.67979575497193778, 10.72451020669871902, 53.33442372801901854 ) ) ;
#80866 = CARTESIAN_POINT ( 'NONE',  ( 2.649999999999999911, -105.0000000000000000, -15.00000000000000000 ) ) ;
#80865 = CARTESIAN_POINT ( 'NONE',  ( 19.05341960407611168, 5.049401038298154454, 33.95724293864769550 ) ) ;
#80867 = CARTESIAN_POINT ( 'NONE',  ( 19.05341960407611168, 5.049401038298154454, 88.95724293864769550 ) ) ;
#80868 = CARTESIAN_POINT ( 'NONE',  ( 9.474510206698729675, 16.51473224551082808, 67.08442372801900433 ) ) ;
#80869 = CARTESIAN_POINT ( 'NONE',  ( -10.81492255796105439, 18.62759615963255655, 22.91775706135235069 ) ) ;
#80870 = CARTESIAN_POINT ( 'NONE',  ( -19.05341960407617563, 5.049401038297882671, 63.54275706135234003 ) ) ;
#80871 = CARTESIAN_POINT ( 'NONE',  ( 5.049401038298161559, -19.05341960407611168, 22.70724293864769194 ) ) ;
#80872 = CARTESIAN_POINT ( 'NONE',  ( -0.05219959533934338120, 16.53943276465976808, 102.5010903946856899 ) ) ;
#80873 = CARTESIAN_POINT ( 'NONE',  ( 0.05219959533936267826, -19.03943276465977164, 65.00109039468567573 ) ) ;
#80874 = CARTESIAN_POINT ( 'NONE',  ( 16.52544592524342804, -4.483927247898539470, 23.54057627198102765 ) ) ;
#80875 = CARTESIAN_POINT ( 'NONE',  ( 16.51473224551083163, -9.474510206698727899, 50.83442372801899722 ) ) ;
#80876 = CARTESIAN_POINT ( 'NONE',  ( 13.89961937509977652, -13.97604488694527269, 83.12390960531436690 ) ) ;
#80877 = CARTESIAN_POINT ( 'NONE',  ( -21.52544592524334988, -5.823673210054445271, 93.95942372801903275 ) ) ;
#80878 = CARTESIAN_POINT ( 'NONE',  ( 5.719274019375673035, 21.55341960407619339, 107.2927570613523471 ) ) ;
#80879 = DIRECTION ( 'NONE',  ( -1.000000000000000000, 0.000000000000000000, 0.000000000000000000 ) ) ;
#80880 = CARTESIAN_POINT ( 'NONE',  ( 18.62759615963255655, 10.81492255796105972, 91.66775706135234714 ) ) ;
#80881 = CARTESIAN_POINT ( 'NONE',  ( -8.314922557961024197, 14.29746914071037800, 37.91775706135235424 ) ) ;
#80882 = CARTESIAN_POINT ( 'NONE',  ( 16.46253265017160672, -9.564922557960803928, 93.33224293864769550 ) ) ;
#80883 = CARTESIAN_POINT ( 'NONE',  ( 15.80617190586746368, 15.72974639402197994, 24.37390960531435979 ) ) ;
#80884 = DIRECTION ( 'NONE',  ( 0.000000000000000000, 0.7071067811865466846, 0.7071067811865484609 ) ) ;
#80885 = CARTESIAN_POINT ( 'NONE',  ( 5.153800228976335163, 19.02544592524342804, 84.79057627198099567 ) ) ;
#80886 = CARTESIAN_POINT ( 'NONE',  ( -18.87255363501902394, -5.499999999999949374, 41.32513748171826506 ) ) ;
#80887 = CARTESIAN_POINT ( 'NONE',  ( 16.46253265017146816, 9.564922557961045513, 71.66775706135233293 ) ) ;
#80888 = CARTESIAN_POINT ( 'NONE',  ( 16.46253265017160672, -9.564922557960803928, 108.3322429386476955 ) ) ;
#80889 = CARTESIAN_POINT ( 'NONE',  ( -5.719274019375665041, -21.55341960407619695, 104.7927570613523898 ) ) ;
#80890 = CARTESIAN_POINT ( 'NONE',  ( -12.14591786802309592, -12.06949235617757132, 101.8739096053143811 ) ) ;
#80891 = CARTESIAN_POINT ( 'NONE',  ( -5.823673210054116645, -21.52544592524344225, 52.29057627198102409 ) ) ;
#80892 = CARTESIAN_POINT ( 'NONE',  ( -21.53943276465977519, 0.05219959533907696930, 41.24890960531435269 ) ) ;
#80893 = CARTESIAN_POINT ( 'NONE',  ( 8.224510206698953496, -14.34966873604960469, 107.9155762719810241 ) ) ;
#80894 = DIRECTION ( 'NONE',  ( 0.000000000000000000, 0.000000000000000000, -1.000000000000000000 ) ) ;
#80895 = CARTESIAN_POINT ( 'NONE',  ( -13.97604488694547697, 13.89961937509957934, 63.12609039468566152 ) ) ;
#80896 = CARTESIAN_POINT ( 'NONE',  ( 16.53943276465976808, -0.05219959533910856209, 23.74890960531435269 ) ) ;
#80897 = CARTESIAN_POINT ( 'NONE',  ( 0.05219959533909260263, 19.03943276465977164, 99.99890960531436690 ) ) ;
#80898 = CARTESIAN_POINT ( 'NONE',  ( -0.05219959533937732626, 21.53943276465977519, 77.50109039468567573 ) ) ;
#80899 = CARTESIAN_POINT ( 'NONE',  ( -18.67979575497178146, -10.72451020669898902, 66.66557627198102409 ) ) ;
#80900 = CARTESIAN_POINT ( 'NONE',  ( -21.52544592524334988, -5.823673210054445271, 38.95942372801901854 ) ) ;
#80901 = CARTESIAN_POINT ( 'NONE',  ( -15.72974639402197994, 15.80617190586746368, 90.62390960531436690 ) ) ;
#80902 = CARTESIAN_POINT ( 'NONE',  ( 21.53943276465977519, 0.05219959533937863772, 56.25109039468568284 ) ) ;
#80903 = CARTESIAN_POINT ( 'NONE',  ( -13.89961937509977652, 13.97604488694528158, 25.62390960531434558 ) ) ;
#80904 = CARTESIAN_POINT ( 'NONE',  ( -19.03943276465977164, 0.05219959533909376836, 86.24890960531436690 ) ) ;
#80905 = CARTESIAN_POINT ( 'NONE',  ( 4.483927247898790824, -16.52544592524335698, 80.20942372801901854 ) ) ;
#80906 = CARTESIAN_POINT ( 'NONE',  ( -14.29746914071049879, 8.314922557960819915, 105.8322429386476955 ) ) ;
#80907 = CARTESIAN_POINT ( 'NONE',  ( -13.97604488694527625, -13.89961937509977652, 101.8739096053143811 ) ) ;
#80908 = CARTESIAN_POINT ( 'NONE',  ( 16.55341960407611168, 4.379528057220329451, 58.95724293864770971 ) ) ;
#80909 = CARTESIAN_POINT ( 'NONE',  ( -14.34966873604960291, -8.224510206698953496, 26.66557627198103475 ) ) ;
#80910 = CARTESIAN_POINT ( 'NONE',  ( -16.51473224551069308, -9.474510206698971260, 51.66557627198102409 ) ) ;
#80911 = CARTESIAN_POINT ( 'NONE',  ( 5.153800228976335163, 19.02544592524342804, 34.79057627198102409 ) ) ;
#80912 = CARTESIAN_POINT ( 'NONE',  ( 5.823673210054125526, 21.52544592524343514, 44.79057627198103120 ) ) ;
#80913 = CARTESIAN_POINT ( 'NONE',  ( -19.03943276465977164, -0.05219959533935918106, 23.75109039468566152 ) ) ;
#80915 = CARTESIAN_POINT ( 'NONE',  ( 14.34966873604960469, 8.224510206698951720, 34.16557627198102409 ) ) ;
#80914 = DIRECTION ( 'NONE',  ( 1.000000000000000000, 0.000000000000000000, 3.709348145883536076E-20 ) ) ;
#80916 = VECTOR ( 'NONE', #181939, 1000.000000000000000 ) ;
#80917 = CARTESIAN_POINT ( 'NONE',  ( 15.80617190586769283, -15.72974639402175789, 45.62609039468567573 ) ) ;
#80918 = DIRECTION ( 'NONE',  ( 0.9930308165857338887, 0.1178549842436482642, 0.000000000000000000 ) ) ;
#80919 = CARTESIAN_POINT ( 'NONE',  ( 16.52544592524335698, 4.483927247898782831, 56.45942372801902565 ) ) ;
#80920 = CARTESIAN_POINT ( 'NONE',  ( 5.153800228976615827, -19.02544592524334988, 60.20942372801899012 ) ) ;
#80921 = CARTESIAN_POINT ( 'NONE',  ( -16.52544592524342804, 4.483927247898546575, 31.04057627198102409 ) ) ;
#80922 = CARTESIAN_POINT ( 'NONE',  ( -12.14591786802326823, 12.06949235617739902, 108.1260903946856757 ) ) ;
#80923 = CARTESIAN_POINT ( 'NONE',  ( 13.89961937509977652, -13.97604488694527269, 33.12390960531434558 ) ) ;
#80924 = CARTESIAN_POINT ( 'NONE',  ( 9.564922557960805705, 16.46253265017160317, 64.58224293864769550 ) ) ;
#80925 = CARTESIAN_POINT ( 'NONE',  ( -0.05219959533909027116, -19.03943276465977164, 32.49890960531435979 ) ) ;
#80926 = CARTESIAN_POINT ( 'NONE',  ( -21.52544592524334988, -5.823673210054445271, 28.95942372801902209 ) ) ;
#80927 = CARTESIAN_POINT ( 'NONE',  ( -19.05341960407611168, -5.049401038298163336, 46.45724293864768129 ) ) ;
#80928 = CARTESIAN_POINT ( 'NONE',  ( -3.962867913677101228, -5.961113794123787279, -62.32090908991690981 ) ) ;
#80929 = CARTESIAN_POINT ( 'NONE',  ( -9.474510206698964154, 16.51473224551069663, 40.41557627198103120 ) ) ;
#80930 = EDGE_CURVE ( 'NONE', #127622, #56210, #85071, .T. ) ;
#80931 = CARTESIAN_POINT ( 'NONE',  ( 5.719274019375991003, -21.55341960407610458, 27.70724293864769905 ) ) ;
#80933 = CARTESIAN_POINT ( 'NONE',  ( 8.314922557960818139, 14.29746914071049879, 104.5822429386477097 ) ) ;
#80932 = CARTESIAN_POINT ( 'NONE',  ( -15.72974639402176322, -15.80617190586768395, 64.37609039468568994 ) ) ;
#80934 = CARTESIAN_POINT ( 'NONE',  ( -13.89961937509977652, 13.97604488694528158, 115.6239096053143669 ) ) ;
#80935 = CARTESIAN_POINT ( 'NONE',  ( 16.52544592524335698, 4.483927247898782831, 81.45942372801900433 ) ) ;
#80936 = CARTESIAN_POINT ( 'NONE',  ( -15.72974639402176322, -15.80617190586768395, 89.37609039468568994 ) ) ;
#80937 = CARTESIAN_POINT ( 'NONE',  ( 4.379528057220092307, 16.55341960407617563, 52.29275706135236135 ) ) ;
#80938 = CARTESIAN_POINT ( 'NONE',  ( 9.564922557960805705, 16.46253265017160317, 89.58224293864769550 ) ) ;
#80939 = EDGE_CURVE ( 'NONE', #45831, #29612, #180474, .T. ) ;
#80940 = CARTESIAN_POINT ( 'NONE',  ( 0.05219959533934541429, -16.53943276465976808, 35.00109039468568284 ) ) ;
#80941 = CARTESIAN_POINT ( 'NONE',  ( 0.05219959533934541429, -16.53943276465976808, 30.00109039468568284 ) ) ;
#80942 = CARTESIAN_POINT ( 'NONE',  ( 0.05219959533934541429, -16.53943276465976808, 95.00109039468568994 ) ) ;
#80943 = CARTESIAN_POINT ( 'NONE',  ( -9.474510206698720793, -16.51473224551083518, 104.5844237280190043 ) ) ;
#80944 = CARTESIAN_POINT ( 'NONE',  ( 15.80617190586746368, 15.72974639402197994, 99.37390960531436690 ) ) ;
#80946 = CARTESIAN_POINT ( 'NONE',  ( 5.153800228976615827, -19.02544592524334988, 100.2094237280190043 ) ) ;
#80945 = CARTESIAN_POINT ( 'NONE',  ( -16.55341960407611168, -4.379528057220339221, 101.4572429386476955 ) ) ;
#80947 = CARTESIAN_POINT ( 'NONE',  ( -16.55341960407617563, 4.379528057220093196, 73.54275706135234714 ) ) ;
#80948 = CARTESIAN_POINT ( 'NONE',  ( 22.65770943308888263, 11.99324031494455589, 167.9410816520763206 ) ) ;
#80949 = CARTESIAN_POINT ( 'NONE',  ( 16.51473224551083163, -9.474510206698727899, 75.83442372801900433 ) ) ;
#80950 = CARTESIAN_POINT ( 'NONE',  ( -16.55341960407611168, -4.379528057220339221, 51.45724293864770260 ) ) ;
#80951 = CARTESIAN_POINT ( 'NONE',  ( 14.34966873604960469, 8.224510206698951720, 29.16557627198103120 ) ) ;
#80952 = CARTESIAN_POINT ( 'NONE',  ( -16.55341960407611168, -4.379528057220339221, 91.45724293864769550 ) ) ;
#80954 = CARTESIAN_POINT ( 'NONE',  ( -16.88567814943162659, 6.947325034625692730, 88.70998877347416567 ) ) ;
#80953 = CARTESIAN_POINT ( 'NONE',  ( -5.049401038297874678, -19.05341960407617918, 39.79275706135232582 ) ) ;
#80955 = CARTESIAN_POINT ( 'NONE',  ( 21.55341960407619695, -5.719274019375665929, 36.04275706135234714 ) ) ;
#80956 = CARTESIAN_POINT ( 'NONE',  ( -19.05341960407617563, 5.049401038297882671, 93.54275706135234714 ) ) ;
#80957 = DIRECTION ( 'NONE',  ( 0.7071067811865483499, 0.000000000000000000, 0.7071067811865465735 ) ) ;
#80958 = CARTESIAN_POINT ( 'NONE',  ( 16.46253265017160672, -9.564922557960803928, 88.33224293864769550 ) ) ;
#80959 = CARTESIAN_POINT ( 'NONE',  ( 9.564922557960805705, 16.46253265017160317, 94.58224293864769550 ) ) ;
#80960 = CARTESIAN_POINT ( 'NONE',  ( -15.72974639402197994, 15.80617190586746368, 55.62390960531436690 ) ) ;
#80961 = CARTESIAN_POINT ( 'NONE',  ( 8.314922557960818139, 14.29746914071049879, 89.58224293864768129 ) ) ;
#80962 = CARTESIAN_POINT ( 'NONE',  ( 0.05219959533909260263, 19.03943276465977164, 74.99890960531435269 ) ) ;
#80963 = CARTESIAN_POINT ( 'NONE',  ( -13.89961937509977652, 13.97604488694528158, 30.62390960531435269 ) ) ;
#80964 = CARTESIAN_POINT ( 'NONE',  ( 18.62759615963255655, 10.81492255796105972, 36.66775706135234714 ) ) ;
#80965 = CARTESIAN_POINT ( 'NONE',  ( -10.72451020669870658, -18.67979575497194134, 74.58442372801901854 ) ) ;
#80966 = CARTESIAN_POINT ( 'NONE',  ( -13.97604488694527625, -13.89961937509977652, 61.87390960531435979 ) ) ;
#80967 = CARTESIAN_POINT ( 'NONE',  ( 16.53943276465976808, 0.05219959533934440121, 76.25109039468568994 ) ) ;
#80968 = CARTESIAN_POINT ( 'NONE',  ( -10.81492255796105439, 18.62759615963255655, 32.91775706135234714 ) ) ;
#80969 = CARTESIAN_POINT ( 'NONE',  ( 10.81492255796106328, -18.62759615963255655, 20.41775706135234714 ) ) ;
#80971 = CARTESIAN_POINT ( 'NONE',  ( 9.474510206698971260, -16.51473224551069308, 77.91557627198103830 ) ) ;
#80970 = CARTESIAN_POINT ( 'NONE',  ( -16.51473224551082808, 9.474510206698731452, 48.33442372801900433 ) ) ;
#80972 = CARTESIAN_POINT ( 'NONE',  ( 13.89961937509957401, 13.97604488694547697, 36.87609039468565442 ) ) ;
#80973 = CARTESIAN_POINT ( 'NONE',  ( -5.823673210054431948, 21.52544592524334988, 87.70942372801901854 ) ) ;
#80974 = EDGE_CURVE ( 'NONE', #127568, #150038, #147962, .T. ) ;
#80975 = CARTESIAN_POINT ( 'NONE',  ( 0.05219959533907565091, 21.53943276465977519, 69.99890960531435269 ) ) ;
#80976 = CARTESIAN_POINT ( 'NONE',  ( -14.34966873604960291, -8.224510206698953496, 51.66557627198102409 ) ) ;
#80978 = CARTESIAN_POINT ( 'NONE',  ( 16.46253265017146816, 9.564922557961045513, 26.66775706135234003 ) ) ;
#80977 = CARTESIAN_POINT ( 'NONE',  ( 18.62759615963255655, 10.81492255796105972, 96.66775706135234714 ) ) ;
#80979 = CARTESIAN_POINT ( 'NONE',  ( 12.06949235617757843, -12.14591786802309237, 68.12390960531436690 ) ) ;
#80980 = CARTESIAN_POINT ( 'NONE',  ( -16.51473224551069308, -9.474510206698971260, 26.66557627198103120 ) ) ;
#80981 = CARTESIAN_POINT ( 'NONE',  ( -5.049401038297874678, -19.05341960407617918, 74.79275706135231871 ) ) ;
#80982 = CARTESIAN_POINT ( 'NONE',  ( -0.05219959533910754901, -16.53943276465976808, 32.49890960531435979 ) ) ;
#80983 = CARTESIAN_POINT ( 'NONE',  ( -0.05219959533937732626, 21.53943276465977519, 82.50109039468568994 ) ) ;
#80984 = CARTESIAN_POINT ( 'NONE',  ( 19.05341960407611168, 5.049401038298154454, 73.95724293864768129 ) ) ;
#80985 = CARTESIAN_POINT ( 'NONE',  ( -13.97604488694547697, 13.89961937509957934, 53.12609039468565442 ) ) ;
#80986 = CARTESIAN_POINT ( 'NONE',  ( 18.62759615963271287, -10.81492255796078972, 53.33224293864769550 ) ) ;
#80987 = CARTESIAN_POINT ( 'NONE',  ( 10.81492255796078972, 18.62759615963270932, 109.5822429386476955 ) ) ;
#80988 = CARTESIAN_POINT ( 'NONE',  ( -13.97604488694547697, 13.89961937509957934, 108.1260903946856331 ) ) ;
#80989 = CARTESIAN_POINT ( 'NONE',  ( -16.53943276465976808, -0.05219959533934237506, 68.75109039468568994 ) ) ;
#80991 = CARTESIAN_POINT ( 'NONE',  ( -15.72974639402197994, 15.80617190586746368, 105.6239096053143669 ) ) ;
#80990 = CARTESIAN_POINT ( 'NONE',  ( -6.791538853603066528, 3.181980515339468241, 1.110912703473986074 ) ) ;
#80992 = CARTESIAN_POINT ( 'NONE',  ( -0.05219959533910754901, -16.53943276465976808, 102.4989096053143811 ) ) ;
#80993 = CARTESIAN_POINT ( 'NONE',  ( -17.49999999999999645, -3.189878218039150504, 30.12948562571235556 ) ) ;
#80994 = CARTESIAN_POINT ( 'NONE',  ( 12.06949235617739724, 12.14591786802326823, 31.87609039468567929 ) ) ;
#80995 = CARTESIAN_POINT ( 'NONE',  ( -0.05219959533907301413, -21.53943276465977519, 67.49890960531436690 ) ) ;
#80996 = CARTESIAN_POINT ( 'NONE',  ( 12.14591786802327356, -12.06949235617739191, 100.6260903946857184 ) ) ;
#80997 = CARTESIAN_POINT ( 'NONE',  ( -16.46253265017160317, 9.564922557960807481, 35.83224293864768839 ) ) ;
#80998 = B_SPLINE_CURVE_WITH_KNOTS ( 'NONE', 3,
 ( #16262, #97048, #156762, #77913, #1065, #63751, #124420, #187121, #32420, #96067, #79909, #158730, #20220, #141580, #111239, #142571, #143559, #5042, #123413, #70736, #8048, #86893, #191077, #117232, #102066, #162735 ),
 .UNSPECIFIED., .F., .F.,
 ( 4, 2, 2, 2, 2, 2, 2, 2, 2, 2, 2, 2, 4 ),
 ( 1.971390914159136004E-07, 0.0002963316798228975667, 0.0005924662205543791650, 0.0008886007612858607633, 0.001184735302017342470, 0.001777004383480305667, 0.002369273464943269080, 0.002665408005674750787, 0.002961542546406232494, 0.003257677087137714200, 0.003553811627869195473, 0.004146080709332164091, 0.004738349790795131841 ),
 .UNSPECIFIED. ) ;
#80999 = CARTESIAN_POINT ( 'NONE',  ( 4.483927247898790824, -16.52544592524335698, 65.20942372801901854 ) ) ;
#81000 = CARTESIAN_POINT ( 'NONE',  ( 0.05219959533936267826, -19.03943276465977164, 65.00109039468567573 ) ) ;
#81001 = CARTESIAN_POINT ( 'NONE',  ( 21.52544592524334988, 5.823673210054432836, 46.45942372801901854 ) ) ;
#81002 = CARTESIAN_POINT ( 'NONE',  ( 21.53943276465977519, -0.05219959533907433946, 53.74890960531437401 ) ) ;
#81003 = CARTESIAN_POINT ( 'NONE',  ( -14.29746914071037622, -8.314922557961029526, 99.16775706135234714 ) ) ;
#81004 = CARTESIAN_POINT ( 'NONE',  ( 21.52544592524334988, 5.823673210054432836, 81.45942372801900433 ) ) ;
#81005 = CARTESIAN_POINT ( 'NONE',  ( 5.823673210054125526, 21.52544592524343514, 49.79057627198102409 ) ) ;
#81006 = CARTESIAN_POINT ( 'NONE',  ( 15.80617190586746368, 15.72974639402197994, 29.37390960531435269 ) ) ;
#81007 = CARTESIAN_POINT ( 'NONE',  ( -16.52544592524335698, -4.483927247898792601, 73.95942372801901854 ) ) ;
#81008 = CARTESIAN_POINT ( 'NONE',  ( -0.05219959533907301413, -21.53943276465977519, 42.49890960531435979 ) ) ;
#81009 = ORIENTED_EDGE ( 'NONE', *, *, #85538, .F. ) ;
#81010 = CARTESIAN_POINT ( 'NONE',  ( -19.05341960407611168, -5.049401038298163336, 101.4572429386476955 ) ) ;
#81011 = DIRECTION ( 'NONE',  ( -0.000000000000000000, -0.000000000000000000, 1.000000000000000000 ) ) ;
#81012 = CARTESIAN_POINT ( 'NONE',  ( -9.474510206698964154, 16.51473224551069663, 25.41557627198103120 ) ) ;
#81013 = CARTESIAN_POINT ( 'NONE',  ( 15.80617190586746368, 15.72974639402197994, 64.37390960531435269 ) ) ;
#81014 = CARTESIAN_POINT ( 'NONE',  ( 16.53943276465976808, 0.05219959533934440121, 86.25109039468568994 ) ) ;
#81015 = CARTESIAN_POINT ( 'NONE',  ( -0.05219959533937732626, 21.53943276465977519, 42.50109039468567573 ) ) ;
#81016 = CARTESIAN_POINT ( 'NONE',  ( 0.05219959533936267826, -19.03943276465977164, 110.0010903946856757 ) ) ;
#81017 = CARTESIAN_POINT ( 'NONE',  ( 14.34966873604960469, 8.224510206698951720, 99.16557627198100988 ) ) ;
#81018 = CARTESIAN_POINT ( 'NONE',  ( 19.05341960407617918, -5.049401038297876454, 111.0427570613523329 ) ) ;
#81019 = CARTESIAN_POINT ( 'NONE',  ( -19.02544592524342804, 5.153800228976336051, 41.04057627198103120 ) ) ;
#81020 = CARTESIAN_POINT ( 'NONE',  ( 15.57446157010957855, -1.455575599910922557, -61.81477736546833768 ) ) ;
#81021 = CARTESIAN_POINT ( 'NONE',  ( -13.89961937509977652, 13.97604488694528158, 90.62390960531432427 ) ) ;
#81022 = CARTESIAN_POINT ( 'NONE',  ( 4.379528057220092307, 16.55341960407617563, 72.29275706135236135 ) ) ;
#81023 = CARTESIAN_POINT ( 'NONE',  ( -15.72974639402176322, -15.80617190586768395, 104.3760903946856899 ) ) ;
#81024 = CARTESIAN_POINT ( 'NONE',  ( 21.52544592524344225, -5.823673210054117533, 68.54057627198103830 ) ) ;
#81025 = CARTESIAN_POINT ( 'NONE',  ( 12.14591786802327356, -12.06949235617739191, 85.62609039468568994 ) ) ;
#81026 = CARTESIAN_POINT ( 'NONE',  ( 0.05219959533936267826, -19.03943276465977164, 85.00109039468567573 ) ) ;
#81027 = CARTESIAN_POINT ( 'NONE',  ( -19.02544592524342804, 5.153800228976336051, 36.04057627198100988 ) ) ;
#81028 = CARTESIAN_POINT ( 'NONE',  ( -16.46253265017160317, 9.564922557960807481, 75.83224293864769550 ) ) ;
#81029 = CARTESIAN_POINT ( 'NONE',  ( -19.05341960407611168, -5.049401038298163336, 36.45724293864766707 ) ) ;
#81030 = CARTESIAN_POINT ( 'NONE',  ( -0.05219959533936034679, 19.03943276465977164, 77.50109039468566152 ) ) ;
#81031 = CARTESIAN_POINT ( 'NONE',  ( 25.34721418589261432, -10.09305078451928317, 170.5222919391072764 ) ) ;
#81032 = CARTESIAN_POINT ( 'NONE',  ( -9.474510206698964154, 16.51473224551069663, 95.41557627198102409 ) ) ;
#81033 = CARTESIAN_POINT ( 'NONE',  ( -4.379528057220328563, 16.55341960407611168, 55.20724293864770260 ) ) ;
#81034 = CARTESIAN_POINT ( 'NONE',  ( -10.81492255796078084, -18.62759615963271287, 67.08224293864770971 ) ) ;
#81035 = CARTESIAN_POINT ( 'NONE',  ( -17.49999999999998579, 3.512728167236896848, 105.2280999518112168 ) ) ;
#81036 = CARTESIAN_POINT ( 'NONE',  ( 13.97604488694548053, -13.89961937509957401, 25.62609039468566507 ) ) ;
#81037 = FILL_AREA_STYLE_COLOUR ( '', #170318 ) ;
#81039 = CARTESIAN_POINT ( 'NONE',  ( 16.46253265017160672, -9.564922557960803928, 73.33224293864769550 ) ) ;
#81038 = CARTESIAN_POINT ( 'NONE',  ( 19.05341960407611168, 5.049401038298154454, 68.95724293864769550 ) ) ;
#81040 = CARTESIAN_POINT ( 'NONE',  ( -16.53943276465976808, -0.05219959533934237506, 38.75109039468567573 ) ) ;
#81041 = CARTESIAN_POINT ( 'NONE',  ( -33.78625674316659655, -2.758724085166798456, 99.76151011743466768 ) ) ;
#81042 = CARTESIAN_POINT ( 'NONE',  ( 23.88380138457669588, -7.642903512909267505, 172.4262750319489612 ) ) ;
#81043 = CARTESIAN_POINT ( 'NONE',  ( 16.55341960407618274, -4.379528057220086978, 81.04275706135236135 ) ) ;
#81045 = CARTESIAN_POINT ( 'NONE',  ( -15.72974639402197994, 15.80617190586746368, 90.62390960531436690 ) ) ;
#81044 = CARTESIAN_POINT ( 'NONE',  ( 16.55341960407618274, -4.379528057220086978, 71.04275706135234714 ) ) ;
#81046 = CARTESIAN_POINT ( 'NONE',  ( 14.34966873604972726, -8.224510206698740333, 40.83442372801901854 ) ) ;
#81048 = DIRECTION ( 'NONE',  ( -0.8437662581494459468, -0.5367108174878556515, 0.000000000000000000 ) ) ;
#81047 = CARTESIAN_POINT ( 'NONE',  ( 19.05341960407611168, 5.049401038298154454, 43.95724293864769550 ) ) ;
#81049 = CARTESIAN_POINT ( 'NONE',  ( -21.53943276465977519, -0.05219959533937600094, 48.75109039468568284 ) ) ;
#81050 = CARTESIAN_POINT ( 'NONE',  ( 5.049401038297881783, 19.05341960407617563, 57.29275706135231871 ) ) ;
#81051 = CARTESIAN_POINT ( 'NONE',  ( 21.55341960407619695, -5.719274019375665929, 91.04275706135236135 ) ) ;
#81052 = CARTESIAN_POINT ( 'NONE',  ( -19.05341960407611168, -5.049401038298163336, 31.45724293864769550 ) ) ;
#81053 = CARTESIAN_POINT ( 'NONE',  ( -0.8613000766924595597, -7.878827036337484380, 3.431593142121016626 ) ) ;
#81054 = CARTESIAN_POINT ( 'NONE',  ( 10.81492255796078972, 18.62759615963270932, 54.58224293864769550 ) ) ;
#81055 = CARTESIAN_POINT ( 'NONE',  ( -9.474510206698964154, 16.51473224551069663, 100.4155762719810241 ) ) ;
#81056 = CARTESIAN_POINT ( 'NONE',  ( 4.379528057220339221, -16.55341960407611168, 107.7072429386476955 ) ) ;
#81057 = CARTESIAN_POINT ( 'NONE',  ( -14.29746914071037622, -8.314922557961029526, 34.16775706135234714 ) ) ;
#81058 = CARTESIAN_POINT ( 'NONE',  ( -4.483927247898782831, 16.52544592524335698, 107.7094237280190328 ) ) ;
#81059 = ORIENTED_EDGE ( 'NONE', *, *, #105844, .T. ) ;
#81060 = CARTESIAN_POINT ( 'NONE',  ( -5.719274019375978568, 21.55341960407610458, 105.2072429386477097 ) ) ;
#81061 = CARTESIAN_POINT ( 'NONE',  ( 4.483927247898545687, 16.52544592524342804, 44.79057627198103120 ) ) ;
#81062 = CARTESIAN_POINT ( 'NONE',  ( 13.89961937509957401, 13.97604488694547697, 96.87609039468566152 ) ) ;
#81063 = CARTESIAN_POINT ( 'NONE',  ( -19.02544592524334988, -5.153800228976617603, 28.95942372801900433 ) ) ;
#81064 = CARTESIAN_POINT ( 'NONE',  ( 4.483927247898545687, 16.52544592524342804, 24.79057627198103120 ) ) ;
#81065 = CARTESIAN_POINT ( 'NONE',  ( -0.05219959533907301413, -21.53943276465977519, 92.49890960531436690 ) ) ;
#81066 = CARTESIAN_POINT ( 'NONE',  ( -18.62759615963270932, 10.81492255796079327, 50.83224293864770971 ) ) ;
#81067 = CARTESIAN_POINT ( 'NONE',  ( 0.05219959533909260263, 19.03943276465977164, 59.99890960531436690 ) ) ;
#81068 = CARTESIAN_POINT ( 'NONE',  ( -16.53943276465976808, 0.05219959533911058130, 41.24890960531435269 ) ) ;
#81069 = CARTESIAN_POINT ( 'NONE',  ( -13.89961937509977652, 13.97604488694528158, 95.62390960531436690 ) ) ;
#81070 = DIRECTION ( 'NONE',  ( -0.000000000000000000, -0.000000000000000000, 1.000000000000000000 ) ) ;
#81071 = CARTESIAN_POINT ( 'NONE',  ( 19.05341960407617918, -5.049401038297876454, 41.04275706135233293 ) ) ;
#81072 = CARTESIAN_POINT ( 'NONE',  ( -15.72974639402197994, 15.80617190586746368, 75.62390960531439532 ) ) ;
#81073 = CARTESIAN_POINT ( 'NONE',  ( -4.379528057220328563, 16.55341960407611168, 100.2072429386476955 ) ) ;
#81074 = CARTESIAN_POINT ( 'NONE',  ( -21.55341960407619339, 5.719274019375674811, 43.54275706135235424 ) ) ;
#81075 = CARTESIAN_POINT ( 'NONE',  ( -17.14385361876520264, -23.59649016807271593, 139.1750000027311955 ) ) ;
#81076 = CARTESIAN_POINT ( 'NONE',  ( 14.34966873604972726, -8.224510206698740333, 110.8344237280190043 ) ) ;
#81077 = CARTESIAN_POINT ( 'NONE',  ( 5.153800228976335163, 19.02544592524342804, 34.79057627198102409 ) ) ;
#81078 = CARTESIAN_POINT ( 'NONE',  ( 19.02544592524343514, -5.153800228976328945, 88.54057627198102409 ) ) ;
#81079 = CARTESIAN_POINT ( 'NONE',  ( 17.14385361876520264, 23.59649016807275856, 140.1750000027311955 ) ) ;
#81080 = CARTESIAN_POINT ( 'NONE',  ( -16.46253265017160317, 9.564922557960807481, 30.83224293864769550 ) ) ;
#81081 = CARTESIAN_POINT ( 'NONE',  ( 8.314922557960818139, 14.29746914071049879, 39.58224293864769550 ) ) ;
#81082 = ADVANCED_FACE ( 'NONE', ( #147775 ), #9262, .T. ) ;
#81083 = CARTESIAN_POINT ( 'NONE',  ( 0.05219959533937995610, -21.53943276465977519, 80.00109039468568994 ) ) ;
#81085 = CARTESIAN_POINT ( 'NONE',  ( -16.55341960407617563, 4.379528057220093196, 73.54275706135234714 ) ) ;
#81084 = CARTESIAN_POINT ( 'NONE',  ( 24.94166821950292956, -28.00113106726958989, -18.51304999530601947 ) ) ;
#81086 = CARTESIAN_POINT ( 'NONE',  ( -5.049401038298153566, 19.05341960407611168, 60.20724293864768129 ) ) ;
#81087 = CARTESIAN_POINT ( 'NONE',  ( 19.02544592524343514, -5.153800228976328945, 68.54057627198103830 ) ) ;
#81088 = ORIENTED_EDGE ( 'NONE', *, *, #32424, .F. ) ;
#81089 = CARTESIAN_POINT ( 'NONE',  ( -10.81492255796105439, 18.62759615963255655, 112.9177570613523329 ) ) ;
#81090 = CARTESIAN_POINT ( 'NONE',  ( 4.379528057220092307, 16.55341960407617563, 72.29275706135236135 ) ) ;
#81091 = CARTESIAN_POINT ( 'NONE',  ( 5.823673210054444382, -21.52544592524334988, 105.2094237280190328 ) ) ;
#81092 = CARTESIAN_POINT ( 'NONE',  ( 13.97604488694527802, 13.89961937509977652, 64.37390960531436690 ) ) ;
#81093 = CARTESIAN_POINT ( 'NONE',  ( 5.823673210054125526, 21.52544592524343514, 39.79057627198103830 ) ) ;
#81094 = CARTESIAN_POINT ( 'NONE',  ( -16.46253265017146816, -9.564922557961047289, 109.1677570613523471 ) ) ;
#81095 = CARTESIAN_POINT ( 'NONE',  ( -15.80617190586768217, 15.72974639402176855, 63.12609039468568994 ) ) ;
#81096 = CARTESIAN_POINT ( 'NONE',  ( -12.06949235617739369, -12.14591786802326823, 54.37609039468568994 ) ) ;
#81097 = CARTESIAN_POINT ( 'NONE',  ( -18.62759615963270932, 10.81492255796079327, 95.83224293864770971 ) ) ;
#81098 = CARTESIAN_POINT ( 'NONE',  ( -13.97604488694547697, 13.89961937509957934, 93.12609039468566152 ) ) ;
#81099 = CARTESIAN_POINT ( 'NONE',  ( -9.474510206698964154, 16.51473224551069663, 80.41557627198103830 ) ) ;
#81100 = CARTESIAN_POINT ( 'NONE',  ( 9.474510206698729675, 16.51473224551082808, 107.0844237280190043 ) ) ;
#81101 = CARTESIAN_POINT ( 'NONE',  ( 19.05341960407617918, -5.049401038297876454, 96.04275706135231871 ) ) ;
#81102 = CARTESIAN_POINT ( 'NONE',  ( 0.05219959533910956823, 16.53943276465976808, 59.99890960531436690 ) ) ;
#81103 = CARTESIAN_POINT ( 'NONE',  ( -8.314922557961024197, 14.29746914071037800, 77.91775706135231871 ) ) ;
#81105 = CARTESIAN_POINT ( 'NONE',  ( 9.474510206698971260, -16.51473224551069308, 52.91557627198102409 ) ) ;
#81104 = CARTESIAN_POINT ( 'NONE',  ( -10.72451020669898014, 18.67979575497178502, 110.4155762719810383 ) ) ;
#81106 = CARTESIAN_POINT ( 'NONE',  ( -5.049401038298153566, 19.05341960407611168, 60.20724293864768129 ) ) ;
#81107 = CARTESIAN_POINT ( 'NONE',  ( -16.53943276465976808, -0.05219959533934237506, 68.75109039468568994 ) ) ;
#81108 = ORIENTED_EDGE ( 'NONE', *, *, #119454, .T. ) ;
#81109 = CARTESIAN_POINT ( 'NONE',  ( 13.89961937509957401, 13.97604488694547697, 21.87609039468566152 ) ) ;
#81110 = CARTESIAN_POINT ( 'NONE',  ( -16.46253265017160317, 9.564922557960807481, 30.83224293864769550 ) ) ;
#81111 = ORIENTED_EDGE ( 'NONE', *, *, #114259, .T. ) ;
#81112 = CARTESIAN_POINT ( 'NONE',  ( -0.05219959533936034679, 19.03943276465977164, 107.5010903946856615 ) ) ;
#81114 = CARTESIAN_POINT ( 'NONE',  ( -4.379528057220086978, -16.55341960407618274, 29.79275706135234358 ) ) ;
#81113 = CARTESIAN_POINT ( 'NONE',  ( 19.02544592524334988, 5.153800228976608722, 46.45942372801899012 ) ) ;
#81115 = CARTESIAN_POINT ( 'NONE',  ( 13.89961937509977652, -13.97604488694527269, 38.12390960531436690 ) ) ;
#81116 = CARTESIAN_POINT ( 'NONE',  ( 9.564922557960805705, 16.46253265017160317, 64.58224293864769550 ) ) ;
#81117 = CARTESIAN_POINT ( 'NONE',  ( -15.72974639402197994, 15.80617190586746368, 90.62390960531436690 ) ) ;
#81118 = CARTESIAN_POINT ( 'NONE',  ( 19.03943276465977164, -0.05219959533909143690, 113.7489096053143669 ) ) ;
#81119 = CARTESIAN_POINT ( 'NONE',  ( 16.46253265017160672, -9.564922557960803928, 48.33224293864769550 ) ) ;
#81120 = DIRECTION ( 'NONE',  ( 6.938893903907222461E-16, -1.000000000000000000, 0.000000000000000000 ) ) ;
#81121 = CARTESIAN_POINT ( 'NONE',  ( -9.564922557961040184, 16.46253265017147172, 102.9177570613523329 ) ) ;
#81122 = CARTESIAN_POINT ( 'NONE',  ( 8.224510206698953496, -14.34966873604960469, 67.91557627198102409 ) ) ;
#81123 = CARTESIAN_POINT ( 'NONE',  ( -0.05219959533936034679, 19.03943276465977164, 22.50109039468566152 ) ) ;
#81124 = CARTESIAN_POINT ( 'NONE',  ( -8.314922557960811034, -14.29746914071050412, 67.08224293864770971 ) ) ;
#81125 = CARTESIAN_POINT ( 'NONE',  ( 15.72974639402176855, 15.80617190586768217, 81.87609039468568994 ) ) ;
#81126 = CARTESIAN_POINT ( 'NONE',  ( -9.474510206698964154, 16.51473224551069663, 25.41557627198103120 ) ) ;
#81127 = CARTESIAN_POINT ( 'NONE',  ( -10.72451020669870658, -18.67979575497194134, 84.58442372801903275 ) ) ;
#81129 = CARTESIAN_POINT ( 'NONE',  ( 10.81492255796106328, -18.62759615963255655, 75.41775706135233293 ) ) ;
#81128 = CARTESIAN_POINT ( 'NONE',  ( 14.29746914071049879, -8.314922557960816363, 28.33224293864769550 ) ) ;
#81130 = CARTESIAN_POINT ( 'NONE',  ( 19.02544592524343514, -5.153800228976328945, 78.54057627198099567 ) ) ;
#81131 = CARTESIAN_POINT ( 'NONE',  ( -15.80617190586768217, 15.72974639402176855, 38.12609039468567573 ) ) ;
#81132 = CARTESIAN_POINT ( 'NONE',  ( -5.153800228976328057, -19.02544592524343514, 87.29057627198103830 ) ) ;
#81133 = CARTESIAN_POINT ( 'NONE',  ( 4.483927247898545687, 16.52544592524342804, 99.79057627198103830 ) ) ;
#81134 = CARTESIAN_POINT ( 'NONE',  ( -12.14591786802309592, -12.06949235617757132, 56.87390960531436690 ) ) ;
#81135 = CARTESIAN_POINT ( 'NONE',  ( -18.67979575497178146, -10.72451020669898902, 66.66557627198102409 ) ) ;
#81136 = CARTESIAN_POINT ( 'NONE',  ( 19.05341960407611168, 5.049401038298154454, 78.95724293864769550 ) ) ;
#81137 = CARTESIAN_POINT ( 'NONE',  ( 15.80617190586746368, 15.72974639402197994, 84.37390960531438111 ) ) ;
#81138 = CARTESIAN_POINT ( 'NONE',  ( 9.564922557961047289, -16.46253265017146816, 70.41775706135233293 ) ) ;
#81140 = CARTESIAN_POINT ( 'NONE',  ( -16.52544592524342804, 4.483927247898546575, 76.04057627198102409 ) ) ;
#81139 = CARTESIAN_POINT ( 'NONE',  ( -13.97604488694547520, 13.89961937509957934, 33.12609039468566152 ) ) ;
#81141 = CARTESIAN_POINT ( 'NONE',  ( 21.52544592524344225, -5.823673210054117533, 48.54057627198103120 ) ) ;
#81142 = DIRECTION ( 'NONE',  ( -1.000000000000000000, 6.391086490440865492E-16, 0.000000000000000000 ) ) ;
#81144 = CARTESIAN_POINT ( 'NONE',  ( -17.14385361876520975, 23.59649016807275856, 145.0750000027311444 ) ) ;
#81143 = CARTESIAN_POINT ( 'NONE',  ( -14.34966873604972548, 8.224510206698743886, 103.3344237280190043 ) ) ;
#81145 = CARTESIAN_POINT ( 'NONE',  ( -0.05219959533936034679, 19.03943276465977164, 97.50109039468567573 ) ) ;
#81146 = CARTESIAN_POINT ( 'NONE',  ( 12.06949235617757843, -12.14591786802309237, 63.12390960531435979 ) ) ;
#81147 = CARTESIAN_POINT ( 'NONE',  ( -17.50000000000002132, 3.237210098469563313, 34.71236987379540295 ) ) ;
#81148 = CARTESIAN_POINT ( 'NONE',  ( -9.474510206698964154, 16.51473224551069663, 60.41557627198102409 ) ) ;
#81149 = CARTESIAN_POINT ( 'NONE',  ( 16.53943276465976808, -0.05219959533910856209, 53.74890960531437401 ) ) ;
#81150 = CARTESIAN_POINT ( 'NONE',  ( -16.51473224551069308, -9.474510206698971260, 101.6655762719810241 ) ) ;
#81152 = CARTESIAN_POINT ( 'NONE',  ( -19.02544592524342804, 5.153800228976336051, 71.04057627198099567 ) ) ;
#81151 = CARTESIAN_POINT ( 'NONE',  ( -19.02544592524334988, -5.153800228976617603, 78.95942372801900433 ) ) ;
#81153 = CARTESIAN_POINT ( 'NONE',  ( 16.51473224551069308, 9.474510206698969483, 79.16557627198103830 ) ) ;
#81154 = CARTESIAN_POINT ( 'NONE',  ( -19.02544592524342804, 5.153800228976336051, 86.04057627198103830 ) ) ;
#81155 = CARTESIAN_POINT ( 'NONE',  ( -5.719274019375978568, 21.55341960407610458, 65.20724293864768129 ) ) ;
#81156 = CARTESIAN_POINT ( 'NONE',  ( 8.224510206698742110, 14.34966873604972548, 52.08442372801901854 ) ) ;
#81157 = CARTESIAN_POINT ( 'NONE',  ( -5.153800228976607833, 19.02544592524335343, 102.7094237280189901 ) ) ;
#81158 = CARTESIAN_POINT ( 'NONE',  ( 16.46253265017160672, -9.564922557960803928, 48.33224293864769550 ) ) ;
#81159 = CARTESIAN_POINT ( 'NONE',  ( -15.80617190586745835, -15.72974639402198527, 56.87390960531436690 ) ) ;
#81160 = CARTESIAN_POINT ( 'NONE',  ( 9.564922557961047289, -16.46253265017146816, 100.4177570613523329 ) ) ;
#81162 = CARTESIAN_POINT ( 'NONE',  ( 18.62759615963255655, 10.81492255796105972, 41.66775706135235424 ) ) ;
#81161 = CARTESIAN_POINT ( 'NONE',  ( -8.224510206698948167, 14.34966873604960824, 25.41557627198103120 ) ) ;
#81163 = CARTESIAN_POINT ( 'NONE',  ( 13.89961937509957401, 13.97604488694547697, 41.87609039468566152 ) ) ;
#81165 = CARTESIAN_POINT ( 'NONE',  ( 8.314922557961029526, -14.29746914071037800, 100.4177570613523471 ) ) ;
#81164 = CARTESIAN_POINT ( 'NONE',  ( 16.55341960407618274, -4.379528057220086978, 61.04275706135234714 ) ) ;
#81166 = CARTESIAN_POINT ( 'NONE',  ( -3.573655867282028392E-15, 12.39993551617566681, 167.9999999999999716 ) ) ;
#81167 = CARTESIAN_POINT ( 'NONE',  ( 8.314922557961029526, -14.29746914071037800, 85.41775706135236135 ) ) ;
#81168 = CARTESIAN_POINT ( 'NONE',  ( -14.29746914071037622, -8.314922557961029526, 34.16775706135234714 ) ) ;
#81169 = CARTESIAN_POINT ( 'NONE',  ( 9.474510206698971260, -16.51473224551069308, 47.91557627198102409 ) ) ;
#81170 = CARTESIAN_POINT ( 'NONE',  ( -5.049401038298153566, 19.05341960407611168, 45.20724293864769550 ) ) ;
#81171 = CARTESIAN_POINT ( 'NONE',  ( -9.474510206698964154, 16.51473224551069663, 65.41557627198102409 ) ) ;
#81172 = CARTESIAN_POINT ( 'NONE',  ( -10.81492255796105439, 18.62759615963255655, 57.91775706135234714 ) ) ;
#81173 = CARTESIAN_POINT ( 'NONE',  ( -16.55341960407617563, 4.379528057220093196, 53.54275706135234714 ) ) ;
#81174 = CARTESIAN_POINT ( 'NONE',  ( 4.483927247898790824, -16.52544592524335698, 110.2094237280190185 ) ) ;
#81175 = CARTESIAN_POINT ( 'NONE',  ( -16.51473224551069308, -9.474510206698971260, 26.66557627198103120 ) ) ;
#81176 = CARTESIAN_POINT ( 'NONE',  ( 10.81492255796106328, -18.62759615963255655, 110.4177570613523756 ) ) ;
#81177 = CARTESIAN_POINT ( 'NONE',  ( 5.153800228976615827, -19.02544592524334988, 105.2094237280190185 ) ) ;
#81178 = CARTESIAN_POINT ( 'NONE',  ( -13.89961937509957401, -13.97604488694547875, 79.37609039468567573 ) ) ;
#81179 = CARTESIAN_POINT ( 'NONE',  ( -12.14591786802309592, -12.06949235617757132, 86.87390960531438111 ) ) ;
#81180 = CARTESIAN_POINT ( 'NONE',  ( -9.564922557960796823, -16.46253265017161027, 42.08224293864769550 ) ) ;
#81182 = CARTESIAN_POINT ( 'NONE',  ( 2.500000000000000000, -1.178949249685218970, -2.041999999999998039 ) ) ;
#81181 = CARTESIAN_POINT ( 'NONE',  ( -19.02544592524334988, -5.153800228976617603, 68.95942372801896170 ) ) ;
#81183 = CARTESIAN_POINT ( 'NONE',  ( 15.72974639402176855, 15.80617190586768217, 81.87609039468568994 ) ) ;
#81184 = CARTESIAN_POINT ( 'NONE',  ( -8.224510206698735004, -14.34966873604973081, 44.58442372801901854 ) ) ;
#81185 = CARTESIAN_POINT ( 'NONE',  ( -17.49999999999999645, 3.189878218039151392, 24.87051437428774747 ) ) ;
#81186 = CARTESIAN_POINT ( 'NONE',  ( 15.80617190586746368, 15.72974639402197994, 39.37390960531436690 ) ) ;
#81187 = CARTESIAN_POINT ( 'NONE',  ( -16.52544592524335698, -4.483927247898792601, 28.95942372801902209 ) ) ;
#81188 = CARTESIAN_POINT ( 'NONE',  ( 9.564922557960805705, 16.46253265017160317, 24.58224293864769194 ) ) ;
#81189 = CARTESIAN_POINT ( 'NONE',  ( 9.564922557961047289, -16.46253265017146816, 25.41775706135234003 ) ) ;
#81190 = CARTESIAN_POINT ( 'NONE',  ( 2.400000000000000799, 2.449293598294705428E-16, -1.999999999999999112 ) ) ;
#81191 = CARTESIAN_POINT ( 'NONE',  ( 9.474510206698971260, -16.51473224551069308, 42.91557627198103120 ) ) ;
#81192 = CARTESIAN_POINT ( 'NONE',  ( 17.58332526062528345, 7.635886036038587399, 56.57665040441533932 ) ) ;
#81193 = CARTESIAN_POINT ( 'NONE',  ( -19.03943276465977164, 0.05219959533909376836, 76.24890960531435269 ) ) ;
#81194 = CARTESIAN_POINT ( 'NONE',  ( 17.49999999999999645, -4.013004640162573189, 112.9460572099440725 ) ) ;
#81195 = CARTESIAN_POINT ( 'NONE',  ( 5.823673210054444382, -21.52544592524334988, 110.2094237280190185 ) ) ;
#81196 = CARTESIAN_POINT ( 'NONE',  ( -16.52544592524342804, 4.483927247898546575, 36.04057627198102409 ) ) ;
#81197 = CARTESIAN_POINT ( 'NONE',  ( 16.51473224551069308, 9.474510206698969483, 39.16557627198103120 ) ) ;
#81198 = CARTESIAN_POINT ( 'NONE',  ( -13.89961937509977652, 13.97604488694528158, 95.62390960531436690 ) ) ;
#81199 = CARTESIAN_POINT ( 'NONE',  ( -21.52544592524334988, -5.823673210054445271, 63.95942372801901854 ) ) ;
#81200 = CARTESIAN_POINT ( 'NONE',  ( -0.05219959533909027116, -19.03943276465977164, 52.49890960531436690 ) ) ;
#81201 = CARTESIAN_POINT ( 'NONE',  ( 5.823673210054444382, -21.52544592524334988, 60.20942372801902565 ) ) ;
#81202 = CARTESIAN_POINT ( 'NONE',  ( 18.67979575497178502, 10.72451020669898547, 29.16557627198103120 ) ) ;
#81203 = CARTESIAN_POINT ( 'NONE',  ( 9.564922557960805705, 16.46253265017160317, 29.58224293864769550 ) ) ;
#81204 = CARTESIAN_POINT ( 'NONE',  ( 21.53943276465977519, -0.05219959533907433946, 108.7489096053143669 ) ) ;
#81205 = CARTESIAN_POINT ( 'NONE',  ( 13.97604488694548053, -13.89961937509957401, 45.62609039468566863 ) ) ;
#81206 = CARTESIAN_POINT ( 'NONE',  ( 4.483927247898545687, 16.52544592524342804, 109.7905762719810383 ) ) ;
#81207 = CARTESIAN_POINT ( 'NONE',  ( -19.05341960407611168, -5.049401038298163336, 56.45724293864768129 ) ) ;
#81208 = CARTESIAN_POINT ( 'NONE',  ( 16.52544592524335698, 4.483927247898782831, 21.45942372801901499 ) ) ;
#81209 = CARTESIAN_POINT ( 'NONE',  ( -4.483927247898539470, -16.52544592524342804, 77.29057627198102409 ) ) ;
#81210 = CARTESIAN_POINT ( 'NONE',  ( -9.564922557960796823, -16.46253265017161027, 112.0822429386476955 ) ) ;
#81211 = CARTESIAN_POINT ( 'NONE',  ( -9.564922557961040184, 16.46253265017147172, 87.91775706135233293 ) ) ;
#81212 = CARTESIAN_POINT ( 'NONE',  ( -10.72451020669898014, 18.67979575497178502, 110.4155762719810383 ) ) ;
#81213 = CARTESIAN_POINT ( 'NONE',  ( -21.53943276465977519, -0.05219959533937600094, 53.75109039468568994 ) ) ;
#81214 = CARTESIAN_POINT ( 'NONE',  ( 0.05219959533934541429, -16.53943276465976808, 55.00109039468568284 ) ) ;
#81215 = CARTESIAN_POINT ( 'NONE',  ( 14.34966873604972726, -8.224510206698740333, 60.83442372801901854 ) ) ;
#81216 = CARTESIAN_POINT ( 'NONE',  ( 21.52544592524344225, -5.823673210054117533, 48.54057627198103120 ) ) ;
#81217 = CARTESIAN_POINT ( 'NONE',  ( -13.97604488694527625, -13.89961937509977652, 51.87390960531436690 ) ) ;
#81218 = CARTESIAN_POINT ( 'NONE',  ( 23.48529157249599919, 32.32473071737754111, -4.449999994537627401 ) ) ;
#81219 = CARTESIAN_POINT ( 'NONE',  ( -16.52544592524335698, -4.483927247898792601, 78.95942372801901854 ) ) ;
#81220 = CARTESIAN_POINT ( 'NONE',  ( 18.62759615963271287, -10.81492255796078972, 98.33224293864769550 ) ) ;
#81221 = CARTESIAN_POINT ( 'NONE',  ( -16.53943276465976808, 0.05219959533911058130, 56.24890960531436690 ) ) ;
#81222 = CARTESIAN_POINT ( 'NONE',  ( -19.03943276465977164, 0.05219959533909376836, 66.24890960531436690 ) ) ;
#81223 = CARTESIAN_POINT ( 'NONE',  ( 12.06949235617739724, 12.14591786802326823, 76.87609039468567573 ) ) ;
#81224 = CARTESIAN_POINT ( 'NONE',  ( 9.474510206698729675, 16.51473224551082808, 102.0844237280190043 ) ) ;
#81225 = CARTESIAN_POINT ( 'NONE',  ( -18.67979575497178146, -10.72451020669898902, 96.66557627198102409 ) ) ;
#81226 = CARTESIAN_POINT ( 'NONE',  ( 4.379528057220339221, -16.55341960407611168, 42.70724293864770260 ) ) ;
#81227 = ORIENTED_EDGE ( 'NONE', *, *, #51319, .T. ) ;
#81228 = CARTESIAN_POINT ( 'NONE',  ( -16.61371651742602396, 7.165104196376146817, 68.85415069992998838 ) ) ;
#81229 = CARTESIAN_POINT ( 'NONE',  ( 5.719274019375991003, -21.55341960407610458, 77.70724293864770971 ) ) ;
#81230 = CARTESIAN_POINT ( 'NONE',  ( -14.34966873604960291, -8.224510206698953496, 21.66557627198102409 ) ) ;
#81231 = EDGE_LOOP ( 'NONE', ( #3644, #102177, #173337, #161852, #116906 ) ) ;
#81232 = CARTESIAN_POINT ( 'NONE',  ( -16.38665767535054485, -7.295008042176057472, 54.73599135785457293 ) ) ;
#81233 = CARTESIAN_POINT ( 'NONE',  ( 10.72451020669898902, -18.67979575497178502, 107.9155762719810241 ) ) ;
#81234 = CARTESIAN_POINT ( 'NONE',  ( 5.823673210054444382, -21.52544592524334988, 25.20942372801901854 ) ) ;
#81235 = CARTESIAN_POINT ( 'NONE',  ( 16.53943276465976808, -0.05219959533910856209, 43.74890960531435979 ) ) ;
#81236 = CARTESIAN_POINT ( 'NONE',  ( -8.314922557961024197, 14.29746914071037800, 52.91775706135235424 ) ) ;
#81237 = CARTESIAN_POINT ( 'NONE',  ( -19.05341960407611168, -5.049401038298163336, 51.45724293864770260 ) ) ;
#81238 = CARTESIAN_POINT ( 'NONE',  ( -19.02544592524342804, 5.153800228976336051, 76.04057627198102409 ) ) ;
#81239 = ORIENTED_EDGE ( 'NONE', *, *, #76155, .F. ) ;
#81240 = CARTESIAN_POINT ( 'NONE',  ( -21.55341960407610458, -5.719274019375992779, 31.45724293864769550 ) ) ;
#81241 = CARTESIAN_POINT ( 'NONE',  ( -33.60028042027822437, -17.96933036163185449, -21.71044752825889290 ) ) ;
#81242 = CARTESIAN_POINT ( 'NONE',  ( 12.06949235617739724, 12.14591786802326823, 26.87609039468567218 ) ) ;
#81243 = CARTESIAN_POINT ( 'NONE',  ( -19.05341960407617563, 5.049401038297882671, 48.54275706135233293 ) ) ;
#81244 = CARTESIAN_POINT ( 'NONE',  ( 15.72974639402199770, -15.80617190586745480, 103.1239096053143811 ) ) ;
#81245 = CARTESIAN_POINT ( 'NONE',  ( 0.05219959533910956823, 16.53943276465976808, 39.99890960531436690 ) ) ;
#81246 = CARTESIAN_POINT ( 'NONE',  ( 9.474510206698971260, -16.51473224551069308, 72.91557627198102409 ) ) ;
#81247 = CARTESIAN_POINT ( 'NONE',  ( 5.823673210054125526, 21.52544592524343514, 64.79057627198103830 ) ) ;
#81249 = CARTESIAN_POINT ( 'NONE',  ( 14.34966873604972726, -8.224510206698740333, 30.83442372801902209 ) ) ;
#81248 = CARTESIAN_POINT ( 'NONE',  ( 18.67979575497178502, 10.72451020669898547, 99.16557627198100988 ) ) ;
#81250 = CARTESIAN_POINT ( 'NONE',  ( 5.153800228976335163, 19.02544592524342804, 114.7905762719810241 ) ) ;
#81251 = CARTESIAN_POINT ( 'NONE',  ( -21.52544592524334988, -5.823673210054445271, 83.95942372801900433 ) ) ;
#81252 = CARTESIAN_POINT ( 'NONE',  ( -9.474510206698964154, 16.51473224551069663, 80.41557627198103830 ) ) ;
#81253 = CARTESIAN_POINT ( 'NONE',  ( 13.97604488694527802, 13.89961937509977652, 24.37390960531435624 ) ) ;
#81254 = CARTESIAN_POINT ( 'NONE',  ( -0.05219959533909027116, -19.03943276465977164, 87.49890960531436690 ) ) ;
#81255 = CARTESIAN_POINT ( 'NONE',  ( -16.52544592524342804, 4.483927247898546575, 106.0405762719810525 ) ) ;
#81256 = B_SPLINE_CURVE_WITH_KNOTS ( 'NONE', 3,
 ( #51259, #174614, #20914, #190772, #52247, #175602, #191762, #130063, #113904, #114922, #38090, #99745, #171284, #65083, #80247, #142909, #77272, #4391, #19585, #63095, #81228, #127741, #172269, #97387, #47949, #2418, #93427, #17601, #66075, #170284, #16607, #46947 ),
 .UNSPECIFIED., .F., .F.,
 ( 4, 2, 2, 2, 2, 2, 2, 2, 2, 2, 2, 2, 2, 2, 2, 4 ),
 ( 2.367436813247751133E-17, 0.0003712461730036969152, 0.0007424923460073700864, 0.001113738519011043312, 0.001484984692014716537, 0.002227477038022056266, 0.002598723211025725805, 0.002969969384029395344, 0.003341215557033064450, 0.003712461730036733989, 0.004083707903040402661, 0.004454954076044071766, 0.004826200249047740871, 0.005197446422051409977, 0.005568692595055079950, 0.005939938768058749055 ),
 .UNSPECIFIED. ) ;
#81257 = CARTESIAN_POINT ( 'NONE',  ( -5.049401038297874678, -19.05341960407617918, 99.79275706135234714 ) ) ;
#81258 = CARTESIAN_POINT ( 'NONE',  ( 17.50000000000000000, 5.500000000000001776, 33.78230962303567253 ) ) ;
#81259 = CARTESIAN_POINT ( 'NONE',  ( 5.049401038298161559, -19.05341960407611168, 77.70724293864765286 ) ) ;
#81261 = CARTESIAN_POINT ( 'NONE',  ( 5.823673210054125526, 21.52544592524343514, 24.79057627198103120 ) ) ;
#81260 = CARTESIAN_POINT ( 'NONE',  ( 0.05219959533937995610, -21.53943276465977519, 95.00109039468568994 ) ) ;
#81262 = CARTESIAN_POINT ( 'NONE',  ( 16.55341960407618274, -4.379528057220086978, 96.04275706135236135 ) ) ;
#81263 = CARTESIAN_POINT ( 'NONE',  ( -29.34370184275724114, 1.069973119863280697, -49.12095057784389951 ) ) ;
#81264 = CARTESIAN_POINT ( 'NONE',  ( -19.02544592524334988, -5.153800228976617603, 58.95942372801900433 ) ) ;
#81265 = CARTESIAN_POINT ( 'NONE',  ( -13.89961937509957401, -13.97604488694547875, 19.37609039468566507 ) ) ;
#81266 = CARTESIAN_POINT ( 'NONE',  ( 0.000000000000000000, 0.000000000000000000, -58.85720012050612837 ) ) ;
#81267 = CARTESIAN_POINT ( 'NONE',  ( -0.05219959533909027116, -19.03943276465977164, 22.49890960531436690 ) ) ;
#81268 = CARTESIAN_POINT ( 'NONE',  ( -12.06949235617756955, 12.14591786802309770, 25.62390960531435624 ) ) ;
#81269 = CARTESIAN_POINT ( 'NONE',  ( -35.24470855014510562, -4.955302550156636343, 39.34877664276075393 ) ) ;
#81270 = CARTESIAN_POINT ( 'NONE',  ( 4.379528057220092307, 16.55341960407617563, 107.2927570613523471 ) ) ;
#81271 = CARTESIAN_POINT ( 'NONE',  ( 6.874011537017776341, -5.570717421327670671, -64.00967186878696680 ) ) ;
#81272 = CARTESIAN_POINT ( 'NONE',  ( -8.314922557961024197, 14.29746914071037800, 82.91775706135234714 ) ) ;
#81273 = CARTESIAN_POINT ( 'NONE',  ( -19.05341960407611168, -5.049401038298163336, 26.45724293864769550 ) ) ;
#81274 = CARTESIAN_POINT ( 'NONE',  ( -10.72451020669870658, -18.67979575497194134, 99.58442372801900433 ) ) ;
#81275 = CARTESIAN_POINT ( 'NONE',  ( -13.97604488694547697, 13.89961937509957934, 103.1260903946856473 ) ) ;
#81276 = CARTESIAN_POINT ( 'NONE',  ( 5.823673210054444382, -21.52544592524334988, 65.20942372801901854 ) ) ;
#81277 = CARTESIAN_POINT ( 'NONE',  ( 5.153800228976615827, -19.02544592524334988, 35.20942372801899722 ) ) ;
#81278 = CARTESIAN_POINT ( 'NONE',  ( 19.03943276465977164, -0.05219959533909143690, 83.74890960531436690 ) ) ;
#81279 = CARTESIAN_POINT ( 'NONE',  ( -0.05219959533909027116, -19.03943276465977164, 72.49890960531435269 ) ) ;
#81280 = CARTESIAN_POINT ( 'NONE',  ( 17.44270441346519362, 5.991230190322990978, 73.86335079264227943 ) ) ;
#81281 = CARTESIAN_POINT ( 'NONE',  ( 15.80617190586746368, 15.72974639402197994, 49.37390960531436690 ) ) ;
#81282 = CARTESIAN_POINT ( 'NONE',  ( -9.474510206698964154, 16.51473224551069663, 45.41557627198103120 ) ) ;
#81284 = CARTESIAN_POINT ( 'NONE',  ( 12.06949235617739724, 12.14591786802326823, 81.87609039468568994 ) ) ;
#81283 = CARTESIAN_POINT ( 'NONE',  ( 18.67979575497178502, 10.72451020669898547, 84.16557627198103830 ) ) ;
#81285 = ORIENTED_EDGE ( 'NONE', *, *, #47103, .F. ) ;
#81287 = CARTESIAN_POINT ( 'NONE',  ( 11.40812507854755253, -35.11059874428192273, -4.024999997268814411 ) ) ;
#81286 = CARTESIAN_POINT ( 'NONE',  ( -14.29746914071049879, 8.314922557960819915, 85.83224293864768129 ) ) ;
#81288 = CARTESIAN_POINT ( 'NONE',  ( -8.314922557961024197, 14.29746914071037800, 42.91775706135235424 ) ) ;
#81289 = CARTESIAN_POINT ( 'NONE',  ( -19.03943276465977164, 0.05219959533909376836, 21.24890960531436335 ) ) ;
#81290 = CARTESIAN_POINT ( 'NONE',  ( 9.564922557961047289, -16.46253265017146816, 70.41775706135233293 ) ) ;
#81291 = CARTESIAN_POINT ( 'NONE',  ( 14.29746914071049879, -8.314922557960816363, 73.33224293864769550 ) ) ;
#81292 = CARTESIAN_POINT ( 'NONE',  ( -0.05219959533937732626, 21.53943276465977519, 42.50109039468567573 ) ) ;
#81294 = CARTESIAN_POINT ( 'NONE',  ( -18.62759615963270932, 10.81492255796079327, 85.83224293864768129 ) ) ;
#81293 = DIRECTION ( 'NONE',  ( 0.000000000000000000, 0.000000000000000000, -1.000000000000000000 ) ) ;
#81295 = CARTESIAN_POINT ( 'NONE',  ( -19.03943276465977164, 0.05219959533909376836, 116.2489096053143669 ) ) ;
#81296 = CARTESIAN_POINT ( 'NONE',  ( 12.14591786802309770, 12.06949235617756955, 69.37390960531436690 ) ) ;
#81297 = CARTESIAN_POINT ( 'NONE',  ( 23.74378949185148358, -32.05510596162020676, -22.01707947879874538 ) ) ;
#81298 = CARTESIAN_POINT ( 'NONE',  ( 19.05341960407611168, 5.049401038298154454, 48.95724293864768129 ) ) ;
#81299 = CARTESIAN_POINT ( 'NONE',  ( 3.556970738554034288E-15, -38.81732327939057114, -6.124999997268812280 ) ) ;
#81300 = CARTESIAN_POINT ( 'NONE',  ( 13.97604488694548053, -13.89961937509957401, 75.62609039468564731 ) ) ;
#81301 = CARTESIAN_POINT ( 'NONE',  ( 18.62759615963255655, 10.81492255796105972, 26.66775706135235424 ) ) ;
#81302 = CARTESIAN_POINT ( 'NONE',  ( -19.03943276465977164, 0.05219959533909376836, 76.24890960531435269 ) ) ;
#81303 = CARTESIAN_POINT ( 'NONE',  ( 13.97604488694548053, -13.89961937509957401, 50.62609039468566152 ) ) ;
#81304 = CARTESIAN_POINT ( 'NONE',  ( 5.153800228976335163, 19.02544592524342804, 49.79057627198100988 ) ) ;
#81305 = CARTESIAN_POINT ( 'NONE',  ( -16.55341960407611168, -4.379528057220339221, 61.45724293864770260 ) ) ;
#81306 = CARTESIAN_POINT ( 'NONE',  ( 16.55341960407611168, 4.379528057220329451, 48.95724293864770971 ) ) ;
#81307 = CARTESIAN_POINT ( 'NONE',  ( 16.46253265017160672, -9.564922557960803928, 78.33224293864769550 ) ) ;
#81308 = CARTESIAN_POINT ( 'NONE',  ( -15.72974639402197994, 15.80617190586746368, 85.62390960531436690 ) ) ;
#81309 = CARTESIAN_POINT ( 'NONE',  ( 5.049401038298161559, -19.05341960407611168, 67.70724293864769550 ) ) ;
#81310 = CARTESIAN_POINT ( 'NONE',  ( 21.55341960407610458, 5.719274019375980345, 73.95724293864769550 ) ) ;
#81311 = ADVANCED_FACE ( 'NONE', ( #83076 ), #117425, .F. ) ;
#81312 = CARTESIAN_POINT ( 'NONE',  ( 19.03943276465977164, 0.05219959533936151252, 21.25109039468565797 ) ) ;
#81315 = CARTESIAN_POINT ( 'NONE',  ( 16.55341960407611168, 4.379528057220329451, 98.95724293864770971 ) ) ;
#81314 = CARTESIAN_POINT ( 'NONE',  ( -4.483927247898782831, 16.52544592524335698, 107.7094237280190328 ) ) ;
#81313 = CARTESIAN_POINT ( 'NONE',  ( 16.51473224551069308, 9.474510206698969483, 29.16557627198103475 ) ) ;
#81316 = CARTESIAN_POINT ( 'NONE',  ( 13.89961937509957401, 13.97604488694547697, 101.8760903946856331 ) ) ;
#81317 = ORIENTED_EDGE ( 'NONE', *, *, #21840, .F. ) ;
#81318 = CARTESIAN_POINT ( 'NONE',  ( -10.81492255796105439, 18.62759615963255655, 27.91775706135234358 ) ) ;
#81319 = CARTESIAN_POINT ( 'NONE',  ( -0.05219959533936034679, 19.03943276465977164, 52.50109039468566863 ) ) ;
#81320 = CARTESIAN_POINT ( 'NONE',  ( 12.14591786802309770, 12.06949235617756955, 24.37390960531435979 ) ) ;
#81321 = CARTESIAN_POINT ( 'NONE',  ( 21.53943276465977519, -0.05219959533907433946, 73.74890960531433848 ) ) ;
#81322 = CARTESIAN_POINT ( 'NONE',  ( -13.97604488694527625, -13.89961937509977652, 96.87390960531433848 ) ) ;
#81323 = CARTESIAN_POINT ( 'NONE',  ( -0.05219959533910754901, -16.53943276465976808, 62.49890960531436690 ) ) ;
#81324 = CYLINDRICAL_SURFACE ( 'NONE', #41278, 9.100000000000001421 ) ;
#81325 = CARTESIAN_POINT ( 'NONE',  ( 16.46253265017160672, -9.564922557960803928, 38.33224293864768839 ) ) ;
#81326 = CARTESIAN_POINT ( 'NONE',  ( -21.53943276465977519, -0.05219959533937600094, 113.7510903946856757 ) ) ;
#81327 = CARTESIAN_POINT ( 'NONE',  ( 16.53943276465976808, 0.05219959533934440121, 86.25109039468568994 ) ) ;
#81328 = CARTESIAN_POINT ( 'NONE',  ( 21.53943276465977519, 0.05219959533937863772, 46.25109039468567573 ) ) ;
#81329 = CARTESIAN_POINT ( 'NONE',  ( -8.224510206698735004, -14.34966873604973081, 39.58442372801901143 ) ) ;
#81330 = CARTESIAN_POINT ( 'NONE',  ( -13.89961937509977652, 13.97604488694528158, 115.6239096053143669 ) ) ;
#81331 = CARTESIAN_POINT ( 'NONE',  ( -5.049401038298153566, 19.05341960407611168, 60.20724293864768129 ) ) ;
#81332 = CARTESIAN_POINT ( 'NONE',  ( -5.153800228976328057, -19.02544592524343514, 67.29057627198102409 ) ) ;
#81333 = CARTESIAN_POINT ( 'NONE',  ( -16.53943276465976808, -0.05219959533934237506, 63.75109039468568284 ) ) ;
#81334 = CARTESIAN_POINT ( 'NONE',  ( -14.29746914071049879, 8.314922557960819915, 110.8322429386476955 ) ) ;
#81335 = CARTESIAN_POINT ( 'NONE',  ( -16.55341960407611168, -4.379528057220339221, 21.45724293864769550 ) ) ;
#81336 = FACE_OUTER_BOUND ( 'NONE', #114177, .T. ) ;
#81339 = CARTESIAN_POINT ( 'NONE',  ( 19.03943276465977164, -0.05219959533909143690, 78.74890960531436690 ) ) ;
#81338 = CARTESIAN_POINT ( 'NONE',  ( -13.97604488694527625, -13.89961937509977652, 96.87390960531433848 ) ) ;
#81337 = CARTESIAN_POINT ( 'NONE',  ( 18.67979575497194134, -10.72451020669871369, 60.83442372801901854 ) ) ;
#81340 = CARTESIAN_POINT ( 'NONE',  ( 13.97604488694527802, 13.89961937509977652, 114.3739096053143669 ) ) ;
#81341 = CARTESIAN_POINT ( 'NONE',  ( -4.483927247898539470, -16.52544592524342804, 42.29057627198103120 ) ) ;
#81342 = CARTESIAN_POINT ( 'NONE',  ( -4.483927247898782831, 16.52544592524335698, 112.7094237280190328 ) ) ;
#81343 = CARTESIAN_POINT ( 'NONE',  ( 0.05219959533910956823, 16.53943276465976808, 39.99890960531436690 ) ) ;
#81344 = CARTESIAN_POINT ( 'NONE',  ( -25.62086810090349687, 2.114847725256050184E-14, 167.9999999999999716 ) ) ;
#81345 = CARTESIAN_POINT ( 'NONE',  ( -19.03943276465977164, -0.05219959533935918106, 43.75109039468566863 ) ) ;
#81346 = CARTESIAN_POINT ( 'NONE',  ( 0.05219959533909260263, 19.03943276465977164, 79.99890960531436690 ) ) ;
#81347 = CARTESIAN_POINT ( 'NONE',  ( 9.474510206698729675, 16.51473224551082808, 47.08442372801900433 ) ) ;
#81348 = CARTESIAN_POINT ( 'NONE',  ( 36.91746824999999887, 11.99521256947799053, -3.524999997268813079 ) ) ;
#81349 = CARTESIAN_POINT ( 'NONE',  ( 17.58332526062526568, -7.635886036038552760, 68.42334959558466778 ) ) ;
#81351 = CARTESIAN_POINT ( 'NONE',  ( -4.483927247898782831, 16.52544592524335698, 67.70942372801901854 ) ) ;
#81350 = CARTESIAN_POINT ( 'NONE',  ( -16.46253265017146816, -9.564922557961047289, 89.16775706135234714 ) ) ;
#81352 = DIRECTION ( 'NONE',  ( -0.000000000000000000, -0.000000000000000000, -1.000000000000000000 ) ) ;
#81353 = CARTESIAN_POINT ( 'NONE',  ( 16.46253265017160672, -9.564922557960803928, 98.33224293864769550 ) ) ;
#81354 = CARTESIAN_POINT ( 'NONE',  ( -5.719274019375665041, -21.55341960407619695, 34.79275706135235424 ) ) ;
#81355 = CARTESIAN_POINT ( 'NONE',  ( -19.05341960407617563, 5.049401038297882671, 93.54275706135234714 ) ) ;
#81357 = CARTESIAN_POINT ( 'NONE',  ( -9.474510206698964154, 16.51473224551069663, 50.41557627198102409 ) ) ;
#81356 = CARTESIAN_POINT ( 'NONE',  ( 17.13100169013300089, 6.664070546373171311, 86.73210164300154190 ) ) ;
#81358 = CARTESIAN_POINT ( 'NONE',  ( -9.474510206698964154, 16.51473224551069663, 95.41557627198102409 ) ) ;
#81360 = CARTESIAN_POINT ( 'NONE',  ( 19.03943276465977164, -0.05219959533909143690, 43.74890960531435979 ) ) ;
#81359 = CARTESIAN_POINT ( 'NONE',  ( -8.314922557960811034, -14.29746914071050412, 52.08224293864768839 ) ) ;
#81361 = CARTESIAN_POINT ( 'NONE',  ( -19.03943276465977164, -0.05219959533935918106, 63.75109039468566863 ) ) ;
#81362 = CARTESIAN_POINT ( 'NONE',  ( 16.51473224551083163, -9.474510206698727899, 30.83442372801900433 ) ) ;
#81363 = CARTESIAN_POINT ( 'NONE',  ( -5.153800228976328057, -19.02544592524343514, 67.29057627198102409 ) ) ;
#81364 = CARTESIAN_POINT ( 'NONE',  ( -21.52544592524343514, 5.823673210054127303, 61.04057627198103120 ) ) ;
#81366 = CARTESIAN_POINT ( 'NONE',  ( -5.823673210054431948, 21.52544592524334988, 112.7094237280190328 ) ) ;
#81365 = CARTESIAN_POINT ( 'NONE',  ( 4.379528057220339221, -16.55341960407611168, 67.70724293864769550 ) ) ;
#81367 = CARTESIAN_POINT ( 'NONE',  ( -3.735172737399431091E-16, -6.100000000000006750, -64.53213882399991519 ) ) ;
#81368 = CARTESIAN_POINT ( 'NONE',  ( -19.03943276465977164, 0.05219959533909376836, 116.2489096053143669 ) ) ;
#81369 = CARTESIAN_POINT ( 'NONE',  ( 9.564922557960805705, 16.46253265017160317, 59.58224293864769550 ) ) ;
#81370 = CARTESIAN_POINT ( 'NONE',  ( 0.05219959533909260263, 19.03943276465977164, 39.99890960531436690 ) ) ;
#81371 = CARTESIAN_POINT ( 'NONE',  ( -8.314922557960811034, -14.29746914071050412, 97.08224293864770971 ) ) ;
#81372 = CARTESIAN_POINT ( 'NONE',  ( -18.62759615963270932, 10.81492255796079327, 110.8322429386476955 ) ) ;
#81373 = CARTESIAN_POINT ( 'NONE',  ( -5.049401038298153566, 19.05341960407611168, 115.2072429386477097 ) ) ;
#81374 = CARTESIAN_POINT ( 'NONE',  ( -10.72451020669870658, -18.67979575497194134, 29.58442372801901854 ) ) ;
#81375 = CARTESIAN_POINT ( 'NONE',  ( -0.05219959533910754901, -16.53943276465976808, 112.4989096053143669 ) ) ;
#81376 = CARTESIAN_POINT ( 'NONE',  ( 10.72451020669871369, 18.67979575497193778, 77.08442372801901854 ) ) ;
#81377 = CARTESIAN_POINT ( 'NONE',  ( -18.67979575497178146, -10.72451020669898902, 86.66557627198102409 ) ) ;
#81378 = CARTESIAN_POINT ( 'NONE',  ( -16.51473224551082808, 9.474510206698731452, 33.33442372801899722 ) ) ;
#81379 = CARTESIAN_POINT ( 'NONE',  ( 19.05341960407611168, 5.049401038298154454, 23.95724293864769194 ) ) ;
#81380 = CARTESIAN_POINT ( 'NONE',  ( 19.52837319214027900, -5.499999999999890754, 77.10471352585537375 ) ) ;
#81381 = CARTESIAN_POINT ( 'NONE',  ( 29.39134536520995766, -1.114265510929745240, -52.10946600208646373 ) ) ;
#81382 = CARTESIAN_POINT ( 'NONE',  ( -0.05219959533934338120, 16.53943276465976808, 52.50109039468567573 ) ) ;
#81383 = CARTESIAN_POINT ( 'NONE',  ( 16.52544592524342804, -4.483927247898539470, 103.5405762719810383 ) ) ;
#81384 = CARTESIAN_POINT ( 'NONE',  ( 33.68492599513092500, -4.777136547582187198, 97.74919260172212887 ) ) ;
#81385 = CARTESIAN_POINT ( 'NONE',  ( 19.02544592524343514, -5.153800228976328945, 78.54057627198099567 ) ) ;
#81386 = CARTESIAN_POINT ( 'NONE',  ( 0.05219959533910956823, 16.53943276465976808, 99.99890960531436690 ) ) ;
#81387 = CARTESIAN_POINT ( 'NONE',  ( -5.823673210054116645, -21.52544592524344225, 47.29057627198103120 ) ) ;
#81388 = CARTESIAN_POINT ( 'NONE',  ( -8.224510206698948167, 14.34966873604960824, 60.41557627198102409 ) ) ;
#81389 = CARTESIAN_POINT ( 'NONE',  ( -14.34966873604972548, 8.224510206698743886, 38.33442372801900433 ) ) ;
#81390 = CARTESIAN_POINT ( 'NONE',  ( 0.05219959533937995610, -21.53943276465977519, 85.00109039468568994 ) ) ;
#81391 = CARTESIAN_POINT ( 'NONE',  ( 16.62475595723696031, -7.163666690055368491, 78.02713351810469078 ) ) ;
#81392 = CARTESIAN_POINT ( 'NONE',  ( 16.53943276465976808, 0.05219959533934440121, 101.2510903946856757 ) ) ;
#81393 = CARTESIAN_POINT ( 'NONE',  ( -14.29746914071049879, 8.314922557960819915, 40.83224293864769550 ) ) ;
#81394 = CARTESIAN_POINT ( 'NONE',  ( -16.46253265017160317, 9.564922557960807481, 35.83224293864768839 ) ) ;
#81395 = CARTESIAN_POINT ( 'NONE',  ( 5.823673210054444382, -21.52544592524334988, 100.2094237280190043 ) ) ;
#81396 = CARTESIAN_POINT ( 'NONE',  ( 18.67979575497178502, 10.72451020669898547, 104.1655762719810241 ) ) ;
#81397 = CARTESIAN_POINT ( 'NONE',  ( -21.53943276465977519, -0.05219959533937600094, 63.75109039468568284 ) ) ;
#81398 = CARTESIAN_POINT ( 'NONE',  ( 0.05219959533934541429, -16.53943276465976808, 45.00109039468568284 ) ) ;
#81400 = CARTESIAN_POINT ( 'NONE',  ( -5.719274019375665041, -21.55341960407619695, 84.79275706135234714 ) ) ;
#81399 = CARTESIAN_POINT ( 'NONE',  ( 16.55341960407611168, 4.379528057220329451, 63.95724293864770260 ) ) ;
#81401 = CARTESIAN_POINT ( 'NONE',  ( -8.314922557961024197, 14.29746914071037800, 97.91775706135236135 ) ) ;
#81402 = CARTESIAN_POINT ( 'NONE',  ( 16.36317988757058473, 7.306389748694950725, 28.40210391636777487 ) ) ;
#81403 = DIRECTION ( 'NONE',  ( -0.000000000000000000, -0.000000000000000000, 1.000000000000000000 ) ) ;
#81404 = CARTESIAN_POINT ( 'NONE',  ( 8.314922557960818139, 14.29746914071049879, 34.58224293864770260 ) ) ;
#81405 = CARTESIAN_POINT ( 'NONE',  ( 12.14591786802327356, -12.06949235617739191, 70.62609039468567573 ) ) ;
#81406 = CARTESIAN_POINT ( 'NONE',  ( -16.46253265017160317, 9.564922557960807481, 90.83224293864769550 ) ) ;
#81407 = CARTESIAN_POINT ( 'NONE',  ( 19.02544592524343514, -5.153800228976328945, 98.54057627198100988 ) ) ;
#81408 = CARTESIAN_POINT ( 'NONE',  ( 15.72974639402176855, 15.80617190586768217, 86.87609039468568994 ) ) ;
#81409 = CARTESIAN_POINT ( 'NONE',  ( -4.483927247898782831, 16.52544592524335698, 82.70942372801900433 ) ) ;
#81410 = CARTESIAN_POINT ( 'NONE',  ( 0.05219959533910956823, 16.53943276465976808, 59.99890960531436690 ) ) ;
#81411 = CARTESIAN_POINT ( 'NONE',  ( -9.474510206698964154, 16.51473224551069663, 70.41557627198102409 ) ) ;
#81412 = VERTEX_POINT ( 'NONE', #102262 ) ;
#81413 = CARTESIAN_POINT ( 'NONE',  ( 8.314922557961029526, -14.29746914071037800, 30.41775706135234358 ) ) ;
#81414 = CARTESIAN_POINT ( 'NONE',  ( 0.05219959533909260263, 19.03943276465977164, 34.99890960531435979 ) ) ;
#81415 = CARTESIAN_POINT ( 'NONE',  ( -19.02544592524342804, 5.153800228976336051, 76.04057627198102409 ) ) ;
#81417 = CARTESIAN_POINT ( 'NONE',  ( -29.86685920354755197, -21.69954338932560134, -8.424999997268812990 ) ) ;
#81416 = CARTESIAN_POINT ( 'NONE',  ( -12.06949235617739369, -12.14591786802326823, 19.37609039468568639 ) ) ;
#81418 = CARTESIAN_POINT ( 'NONE',  ( 16.46253265017146816, 9.564922557961045513, 26.66775706135234003 ) ) ;
#81419 = CARTESIAN_POINT ( 'NONE',  ( -16.55341960407617563, 4.379528057220093196, 78.54275706135236135 ) ) ;
#81420 = CARTESIAN_POINT ( 'NONE',  ( 9.564922557961047289, -16.46253265017146816, 100.4177570613523329 ) ) ;
#81421 = CARTESIAN_POINT ( 'NONE',  ( -13.97604488694527625, -13.89961937509977652, 21.87390960531435979 ) ) ;
#81422 = CARTESIAN_POINT ( 'NONE',  ( -14.29746914071037622, -8.314922557961029526, 64.16775706135234714 ) ) ;
#81423 = CARTESIAN_POINT ( 'NONE',  ( 4.483927247898790824, -16.52544592524335698, 50.20942372801901854 ) ) ;
#81424 = CARTESIAN_POINT ( 'NONE',  ( 37.99999999999999289, 2.893978650043524126E-14, -4.749999994537627224 ) ) ;
#81425 = CARTESIAN_POINT ( 'NONE',  ( 16.51473224551083163, -9.474510206698727899, 70.83442372801900433 ) ) ;
#81426 = CARTESIAN_POINT ( 'NONE',  ( 9.564922557961047289, -16.46253265017146816, 20.41775706135233293 ) ) ;
#81427 = CARTESIAN_POINT ( 'NONE',  ( -19.02544592524342804, 5.153800228976336051, 46.04057627198101699 ) ) ;
#81428 = CARTESIAN_POINT ( 'NONE',  ( -9.474510206698964154, 16.51473224551069663, 80.41557627198103830 ) ) ;
#81429 = CARTESIAN_POINT ( 'NONE',  ( -14.34966873604960291, -8.224510206698953496, 76.66557627198103830 ) ) ;
#81430 = CARTESIAN_POINT ( 'NONE',  ( 16.51473224551083163, -9.474510206698727899, 40.83442372801900433 ) ) ;
#81431 = CARTESIAN_POINT ( 'NONE',  ( 5.823673210054125526, 21.52544592524343514, 34.79057627198103120 ) ) ;
#81432 = CARTESIAN_POINT ( 'NONE',  ( 21.55341960407619695, -5.719274019375665929, 111.0427570613523613 ) ) ;
#81433 = CARTESIAN_POINT ( 'NONE',  ( 19.05341960407611168, 5.049401038298154454, 88.95724293864769550 ) ) ;
#81434 = CARTESIAN_POINT ( 'NONE',  ( 5.719274019375673035, 21.55341960407619339, 107.2927570613523471 ) ) ;
#81435 = CARTESIAN_POINT ( 'NONE',  ( 21.53943276465977519, -0.05219959533907433946, 63.74890960531435979 ) ) ;
#81436 = CARTESIAN_POINT ( 'NONE',  ( -9.474510206698964154, 16.51473224551069663, 90.41557627198103830 ) ) ;
#81437 = CARTESIAN_POINT ( 'NONE',  ( -16.46253265017146816, -9.564922557961047289, 84.16775706135233293 ) ) ;
#81438 = CARTESIAN_POINT ( 'NONE',  ( 9.474510206698971260, -16.51473224551069308, 102.9155762719810241 ) ) ;
#81439 = CARTESIAN_POINT ( 'NONE',  ( 13.89961937509957401, 13.97604488694547697, 101.8760903946856331 ) ) ;
#81440 = CARTESIAN_POINT ( 'NONE',  ( -19.03943276465977164, 0.05219959533909376836, 26.24890960531435624 ) ) ;
#81441 = CARTESIAN_POINT ( 'NONE',  ( -9.474510206698964154, 16.51473224551069663, 90.41557627198103830 ) ) ;
#81442 = CARTESIAN_POINT ( 'NONE',  ( -10.81492255796078084, -18.62759615963271287, 57.08224293864769550 ) ) ;
#81443 = CARTESIAN_POINT ( 'NONE',  ( -4.379528057220086978, -16.55341960407618274, 39.79275706135235424 ) ) ;
#81444 = CARTESIAN_POINT ( 'NONE',  ( -0.05219959533937732626, 21.53943276465977519, 52.50109039468567573 ) ) ;
#81445 = CARTESIAN_POINT ( 'NONE',  ( 21.52544592524334988, 5.823673210054432836, 91.45942372801901854 ) ) ;
#81446 = CARTESIAN_POINT ( 'NONE',  ( -12.06949235617739369, -12.14591786802326823, 94.37609039468568994 ) ) ;
#81447 = CARTESIAN_POINT ( 'NONE',  ( 19.03943276465977164, -0.05219959533909143690, 83.74890960531436690 ) ) ;
#81448 = CARTESIAN_POINT ( 'NONE',  ( -4.379528057220328563, 16.55341960407611168, 95.20724293864769550 ) ) ;
#81449 = CARTESIAN_POINT ( 'NONE',  ( -0.05219959533910754901, -16.53943276465976808, 22.49890960531436335 ) ) ;
#81450 = CARTESIAN_POINT ( 'NONE',  ( 9.564922557961047289, -16.46253265017146816, 65.41775706135233293 ) ) ;
#81451 = ADVANCED_FACE ( 'NONE', ( #163950 ), #143754, .F. ) ;
#81452 = CARTESIAN_POINT ( 'NONE',  ( -5.719274019375665041, -21.55341960407619695, 39.79275706135235424 ) ) ;
#81453 = CARTESIAN_POINT ( 'NONE',  ( 8.224510206698953496, -14.34966873604960469, 97.91557627198103830 ) ) ;
#81454 = CARTESIAN_POINT ( 'NONE',  ( 13.97604488694527802, 13.89961937509977652, 114.3739096053143669 ) ) ;
#81455 = CARTESIAN_POINT ( 'NONE',  ( -14.34966873604972548, 8.224510206698743886, 113.3344237280190328 ) ) ;
#81456 = CARTESIAN_POINT ( 'NONE',  ( 18.62759615963255655, 10.81492255796105972, 91.66775706135234714 ) ) ;
#81457 = CARTESIAN_POINT ( 'NONE',  ( -12.14591786802326823, 12.06949235617739902, 63.12609039468568994 ) ) ;
#81458 = CARTESIAN_POINT ( 'NONE',  ( 15.72974639402176855, 15.80617190586768217, 46.87609039468568994 ) ) ;
#81459 = EDGE_LOOP ( 'NONE', ( #106495, #27835, #99592, #161714 ) ) ;
#81460 = CARTESIAN_POINT ( 'NONE',  ( -15.72974639402176322, -15.80617190586768395, 29.37609039468568284 ) ) ;
#81461 = CARTESIAN_POINT ( 'NONE',  ( -8.314922557960811034, -14.29746914071050412, 107.0822429386476955 ) ) ;
#81462 = CARTESIAN_POINT ( 'NONE',  ( 19.50973618000806198, 5.499999999999992895, 37.50000000000000000 ) ) ;
#81463 = CARTESIAN_POINT ( 'NONE',  ( -8.314922557960811034, -14.29746914071050412, 67.08224293864770971 ) ) ;
#81464 = CARTESIAN_POINT ( 'NONE',  ( 16.46253265017160672, -9.564922557960803928, 53.33224293864768839 ) ) ;
#81465 = CARTESIAN_POINT ( 'NONE',  ( -14.29746914071037622, -8.314922557961029526, 104.1677570613523471 ) ) ;
#81466 = CARTESIAN_POINT ( 'NONE',  ( 13.97604488694527802, 13.89961937509977652, 34.37390960531436690 ) ) ;
#81467 = CARTESIAN_POINT ( 'NONE',  ( -18.62759615963270932, 10.81492255796079327, 40.83224293864769550 ) ) ;
#81468 = CARTESIAN_POINT ( 'NONE',  ( 12.06949235617757843, -12.14591786802309237, 78.12390960531436690 ) ) ;
#81469 = CARTESIAN_POINT ( 'NONE',  ( -15.72974639402197994, 15.80617190586746368, 95.62390960531436690 ) ) ;
#81470 = CARTESIAN_POINT ( 'NONE',  ( 19.05341960407611168, 5.049401038298154454, 88.95724293864769550 ) ) ;
#81472 = CARTESIAN_POINT ( 'NONE',  ( -9.564922557961040184, 16.46253265017147172, 97.91775706135233293 ) ) ;
#81471 = CARTESIAN_POINT ( 'NONE',  ( 9.474510206698971260, -16.51473224551069308, 57.91557627198103120 ) ) ;
#81473 = CARTESIAN_POINT ( 'NONE',  ( -18.67979575497178146, -10.72451020669898902, 41.66557627198103120 ) ) ;
#81474 = CARTESIAN_POINT ( 'NONE',  ( -15.72974639402176322, -15.80617190586768395, 64.37609039468568994 ) ) ;
#81475 = CARTESIAN_POINT ( 'NONE',  ( 13.97604488694527802, 13.89961937509977652, 49.37390960531434558 ) ) ;
#81476 = CARTESIAN_POINT ( 'NONE',  ( 16.46253265017160672, -9.564922557960803928, 88.33224293864769550 ) ) ;
#81477 = VERTEX_POINT ( 'NONE', #1785 ) ;
#81478 = CARTESIAN_POINT ( 'NONE',  ( 16.53943276465976808, 0.05219959533934440121, 66.25109039468567573 ) ) ;
#81479 = CARTESIAN_POINT ( 'NONE',  ( -5.823673210054431948, 21.52544592524334988, 37.70942372801900433 ) ) ;
#81480 = CARTESIAN_POINT ( 'NONE',  ( -21.53943276465977519, -0.05219959533937600094, 68.75109039468568994 ) ) ;
#81481 = CARTESIAN_POINT ( 'NONE',  ( 18.62759615963271287, -10.81492255796078972, 28.33224293864769550 ) ) ;
#81482 = CARTESIAN_POINT ( 'NONE',  ( 10.72451020669898902, -18.67979575497178502, 102.9155762719810383 ) ) ;
#81484 = CARTESIAN_POINT ( 'NONE',  ( -0.05219959533934338120, 16.53943276465976808, 67.50109039468568994 ) ) ;
#81483 = CARTESIAN_POINT ( 'NONE',  ( -21.52544592524334988, -5.823673210054445271, 33.95942372801901143 ) ) ;
#81485 = CARTESIAN_POINT ( 'NONE',  ( -21.55341960407610458, -5.719274019375992779, 66.45724293864768129 ) ) ;
#81486 = CARTESIAN_POINT ( 'NONE',  ( -9.564922557961040184, 16.46253265017147172, 32.91775706135233293 ) ) ;
#81488 = CARTESIAN_POINT ( 'NONE',  ( 16.55341960407618274, -4.379528057220086978, 106.0427570613523471 ) ) ;
#81487 = CARTESIAN_POINT ( 'NONE',  ( 13.89961937509977652, -13.97604488694527269, 73.12390960531436690 ) ) ;
#81489 = CARTESIAN_POINT ( 'NONE',  ( -17.50000000000014566, -3.292511757969676101, 104.9347972978947183 ) ) ;
#81490 = CARTESIAN_POINT ( 'NONE',  ( -19.05341960407611168, -5.049401038298163336, 101.4572429386476955 ) ) ;
#81491 = CARTESIAN_POINT ( 'NONE',  ( 17.50000000000000000, 5.499999999999992895, 81.70309617465829888 ) ) ;
#81492 = CARTESIAN_POINT ( 'NONE',  ( 19.03943276465977164, 0.05219959533936151252, 76.25109039468566152 ) ) ;
#81493 = CARTESIAN_POINT ( 'NONE',  ( -15.72974639402197994, 15.80617190586746368, 60.62390960531437401 ) ) ;
#81494 = CARTESIAN_POINT ( 'NONE',  ( 8.224510206698953496, -14.34966873604960469, 32.91557627198102409 ) ) ;
#81495 = CARTESIAN_POINT ( 'NONE',  ( -13.89961937509957401, -13.97604488694547875, 94.37609039468566152 ) ) ;
#81496 = CARTESIAN_POINT ( 'NONE',  ( -5.153800228976328057, -19.02544592524343514, 22.29057627198102765 ) ) ;
#81497 = CARTESIAN_POINT ( 'NONE',  ( -0.05219959533936034679, 19.03943276465977164, 112.5010903946856757 ) ) ;
#81499 = CARTESIAN_POINT ( 'NONE',  ( -5.049401038297874678, -19.05341960407617918, 59.79275706135231871 ) ) ;
#81498 = CARTESIAN_POINT ( 'NONE',  ( -21.53943276465977519, 0.05219959533907696930, 86.24890960531436690 ) ) ;
#81500 = CARTESIAN_POINT ( 'NONE',  ( -16.52544592524335698, -4.483927247898792601, 83.95942372801900433 ) ) ;
#81501 = CARTESIAN_POINT ( 'NONE',  ( 16.51473224551069308, 9.474510206698969483, 64.16557627198102409 ) ) ;
#81502 = CARTESIAN_POINT ( 'NONE',  ( 14.29746914071049879, -8.314922557960816363, 63.33224293864770260 ) ) ;
#81503 = CARTESIAN_POINT ( 'NONE',  ( -5.153800228976328057, -19.02544592524343514, 52.29057627198100988 ) ) ;
#81504 = CARTESIAN_POINT ( 'NONE',  ( 16.53943276465976808, -0.05219959533910856209, 48.74890960531435979 ) ) ;
#81505 = CARTESIAN_POINT ( 'NONE',  ( 13.89961937509977652, -13.97604488694527269, 23.12390960531436335 ) ) ;
#81506 = CARTESIAN_POINT ( 'NONE',  ( 31.79921067246704780, -6.362367971534556688, 91.02144216243110009 ) ) ;
#81507 = CARTESIAN_POINT ( 'NONE',  ( 16.53943276465976808, -0.05219959533910856209, 33.74890960531436690 ) ) ;
#81508 = CARTESIAN_POINT ( 'NONE',  ( 16.51473224551069308, 9.474510206698969483, 79.16557627198103830 ) ) ;
#81509 = CARTESIAN_POINT ( 'NONE',  ( 37.99999999999999289, 2.893978650043524126E-14, -9.000000000000001776 ) ) ;
#81510 = CARTESIAN_POINT ( 'NONE',  ( 13.89961937509957401, 13.97604488694547697, 36.87609039468565442 ) ) ;
#81511 = CARTESIAN_POINT ( 'NONE',  ( -4.379528057220086978, -16.55341960407618274, 44.79275706135234714 ) ) ;
#81512 = CARTESIAN_POINT ( 'NONE',  ( 18.67979575497178502, 10.72451020669898547, 49.16557627198102409 ) ) ;
#81513 = CARTESIAN_POINT ( 'NONE',  ( 21.52544592524334988, 5.823673210054432836, 101.4594237280190185 ) ) ;
#81514 = CARTESIAN_POINT ( 'NONE',  ( 16.51473224551069308, 9.474510206698969483, 74.16557627198103830 ) ) ;
#81515 = CARTESIAN_POINT ( 'NONE',  ( 19.03943276465977164, -0.05219959533909143690, 113.7489096053143669 ) ) ;
#81516 = CARTESIAN_POINT ( 'NONE',  ( 19.03943276465977164, -0.05219959533909143690, 108.7489096053143527 ) ) ;
#81517 = CARTESIAN_POINT ( 'NONE',  ( -5.823673210054431948, 21.52544592524334988, 42.70942372801901854 ) ) ;
#81518 = CARTESIAN_POINT ( 'NONE',  ( 16.53943276465976808, -0.05219959533910856209, 98.74890960531438111 ) ) ;
#81519 = EDGE_CURVE ( 'NONE', #53380, #128521, #4249, .T. ) ;
#81522 = ORIENTED_EDGE ( 'NONE', *, *, #195610, .F. ) ;
#81521 = CARTESIAN_POINT ( 'NONE',  ( -13.97604488694527625, -13.89961937509977652, 86.87390960531436690 ) ) ;
#81520 = CARTESIAN_POINT ( 'NONE',  ( 18.62759615963271287, -10.81492255796078972, 88.33224293864769550 ) ) ;
#81523 = CARTESIAN_POINT ( 'NONE',  ( 21.52544592524334988, 5.823673210054432836, 21.45942372801901499 ) ) ;
#81524 = ORIENTED_EDGE ( 'NONE', *, *, #137185, .F. ) ;
#81525 = CARTESIAN_POINT ( 'NONE',  ( -16.46253265017160317, 9.564922557960807481, 90.83224293864769550 ) ) ;
#81526 = CARTESIAN_POINT ( 'NONE',  ( 18.22780087662122384, -5.500000000000022204, 81.01540105326105845 ) ) ;
#81528 = CARTESIAN_POINT ( 'NONE',  ( -0.05219959533909027116, -19.03943276465977164, 32.49890960531435979 ) ) ;
#81527 = CARTESIAN_POINT ( 'NONE',  ( 19.05341960407611168, 5.049401038298154454, 28.95724293864769550 ) ) ;
#81529 = CARTESIAN_POINT ( 'NONE',  ( 9.474510206698729675, 16.51473224551082808, 112.0844237280190043 ) ) ;
#81530 = CARTESIAN_POINT ( 'NONE',  ( -29.86685920354755197, -21.69954338932560134, -8.924999997268812990 ) ) ;
#81531 = CARTESIAN_POINT ( 'NONE',  ( -14.34966873604960291, -8.224510206698953496, 106.6655762719810383 ) ) ;
#81532 = CARTESIAN_POINT ( 'NONE',  ( -10.72451020669870658, -18.67979575497194134, 84.58442372801903275 ) ) ;
#81534 = CARTESIAN_POINT ( 'NONE',  ( -18.62759615963255300, -10.81492255796106328, 34.16775706135234714 ) ) ;
#81533 = CARTESIAN_POINT ( 'NONE',  ( 16.46253265017160672, -9.564922557960803928, 63.33224293864769550 ) ) ;
#81535 = CARTESIAN_POINT ( 'NONE',  ( 21.53943276465977519, 0.05219959533937863772, 31.25109039468568639 ) ) ;
#81536 = CARTESIAN_POINT ( 'NONE',  ( 1.993301997531345292E-15, -30.30510711980685912, 146.5000000000000000 ) ) ;
#81537 = CARTESIAN_POINT ( 'NONE',  ( 5.153800228976335163, 19.02544592524342804, 79.79057627198102409 ) ) ;
#81538 = DIRECTION ( 'NONE',  ( 0.000000000000000000, 0.000000000000000000, 1.000000000000000000 ) ) ;
#81540 = CARTESIAN_POINT ( 'NONE',  ( 10.81492255796078972, 18.62759615963270932, 44.58224293864769550 ) ) ;
#81539 = CARTESIAN_POINT ( 'NONE',  ( 14.34966873604972726, -8.224510206698740333, 20.83442372801901143 ) ) ;
#81541 = CARTESIAN_POINT ( 'NONE',  ( -18.62759615963255300, -10.81492255796106328, 64.16775706135234714 ) ) ;
#81542 = CARTESIAN_POINT ( 'NONE',  ( 19.02544592524343514, -5.153800228976328945, 103.5405762719809957 ) ) ;
#81543 =( BOUNDED_CURVE ( )  B_SPLINE_CURVE ( 2, ( #43740, #13398, #123529, #76047, #199407, #45718, #77039, #107371, #185223, #108377, #46714 ),
 .UNSPECIFIED., .F., .T. ) 
 B_SPLINE_CURVE_WITH_KNOTS ( ( 3, 2, 2, 2, 2, 3 ),
 ( 0.6000000000000000888, 0.6200000000000001066, 0.6400000000000001243, 0.6600000000000002531, 0.6800000000000002709, 0.7000000000000001776 ),
 .UNSPECIFIED. ) 
 CURVE ( )  GEOMETRIC_REPRESENTATION_ITEM ( )  RATIONAL_B_SPLINE_CURVE ( ( 0.9999999999999997780, 0.9510565162951537532, 1.000000000000000000, 0.9510565162951535312, 1.000000000000000000, 0.9510565162951535312, 1.000000000000000000, 0.9510565162951535312, 1.000000000000000000, 0.9510565162951529761, 1.000000000000000444 ) ) 
 REPRESENTATION_ITEM ( '' )  );
#81544 = CARTESIAN_POINT ( 'NONE',  ( -9.564922557961040184, 16.46253265017147172, 92.91775706135233293 ) ) ;
#81545 = CARTESIAN_POINT ( 'NONE',  ( -19.05341960407611168, -5.049401038298163336, 56.45724293864768129 ) ) ;
#81546 = CARTESIAN_POINT ( 'NONE',  ( 0.05219959533909260263, 19.03943276465977164, 89.99890960531436690 ) ) ;
#81547 = CARTESIAN_POINT ( 'NONE',  ( 16.53943276465976808, -0.05219959533910856209, 93.74890960531436690 ) ) ;
#81548 = CARTESIAN_POINT ( 'NONE',  ( 0.05219959533910956823, 16.53943276465976808, 109.9989096053143527 ) ) ;
#81549 = CARTESIAN_POINT ( 'NONE',  ( -5.823673210054116645, -21.52544592524344225, 22.29057627198102765 ) ) ;
#81551 = CARTESIAN_POINT ( 'NONE',  ( -19.02544592524342804, 5.153800228976336051, 46.04057627198101699 ) ) ;
#81550 = CARTESIAN_POINT ( 'NONE',  ( -0.05219959533910754901, -16.53943276465976808, 52.49890960531435979 ) ) ;
#81552 = CARTESIAN_POINT ( 'NONE',  ( -18.62759615963255300, -10.81492255796106328, 74.16775706135231871 ) ) ;
#81553 = CARTESIAN_POINT ( 'NONE',  ( 19.03943276465977164, 0.05219959533936151252, 96.25109039468567573 ) ) ;
#81554 = CARTESIAN_POINT ( 'NONE',  ( 14.29746914071049879, -8.314922557960816363, 58.33224293864768839 ) ) ;
#81555 = CARTESIAN_POINT ( 'NONE',  ( -5.719274019375978568, 21.55341960407610458, 115.2072429386476955 ) ) ;
#81556 = CARTESIAN_POINT ( 'NONE',  ( -10.81492255796078084, -18.62759615963271287, 42.08224293864769550 ) ) ;
#81557 = CARTESIAN_POINT ( 'NONE',  ( 13.97604488694527802, 13.89961937509977652, 114.3739096053143669 ) ) ;
#81558 = CARTESIAN_POINT ( 'NONE',  ( 8.571926809382597767, 26.38167802310806209, 148.2750000027311899 ) ) ;
#81559 = CARTESIAN_POINT ( 'NONE',  ( -16.46253265017160317, 9.564922557960807481, 65.83224293864769550 ) ) ;
#81560 = CARTESIAN_POINT ( 'NONE',  ( -8.224510206698948167, 14.34966873604960824, 35.41557627198102409 ) ) ;
#81561 = CARTESIAN_POINT ( 'NONE',  ( -16.55341960407617563, 4.379528057220093196, 108.5427570613523756 ) ) ;
#81562 = CARTESIAN_POINT ( 'NONE',  ( -4.379528057220086978, -16.55341960407618274, 79.79275706135236135 ) ) ;
#81563 = CARTESIAN_POINT ( 'NONE',  ( 19.02544592524334988, 5.153800228976608722, 41.45942372801900433 ) ) ;
#81564 = CARTESIAN_POINT ( 'NONE',  ( -23.71437922609632665, 10.61260870832700931, 165.9744018657351887 ) ) ;
#81565 = CARTESIAN_POINT ( 'NONE',  ( 9.564922557960805705, 16.46253265017160317, 89.58224293864769550 ) ) ;
#81566 = CARTESIAN_POINT ( 'NONE',  ( -13.89961937509977652, 13.97604488694528158, 50.62390960531435979 ) ) ;
#81567 = CARTESIAN_POINT ( 'NONE',  ( 0.05219959533910956823, 16.53943276465976808, 54.99890960531435269 ) ) ;
#81569 = CARTESIAN_POINT ( 'NONE',  ( 15.80617190586746368, 15.72974639402197994, 24.37390960531435979 ) ) ;
#81568 = CARTESIAN_POINT ( 'NONE',  ( -15.49999999999999822, 7.499999999999998224, 118.0000000000000142 ) ) ;
#81570 = CARTESIAN_POINT ( 'NONE',  ( -15.80617190586745835, -15.72974639402198527, 56.87390960531436690 ) ) ;
#81571 = CARTESIAN_POINT ( 'NONE',  ( 14.34966873604960469, 8.224510206698951720, 84.16557627198103830 ) ) ;
#81572 = CARTESIAN_POINT ( 'NONE',  ( 12.06949235617739724, 12.14591786802326823, 36.87609039468568994 ) ) ;
#81573 = AXIS2_PLACEMENT_3D ( 'NONE', #23486, #132659, #85135 ) ;
#81574 = CARTESIAN_POINT ( 'NONE',  ( 16.52544592524342804, -4.483927247898539470, 73.54057627198102409 ) ) ;
#81575 = CARTESIAN_POINT ( 'NONE',  ( 21.23184647844211881, -181.1785498424364675, -25.00000000000000000 ) ) ;
#81576 = CARTESIAN_POINT ( 'NONE',  ( 16.51473224551083163, -9.474510206698727899, 80.83442372801899012 ) ) ;
#81577 = CARTESIAN_POINT ( 'NONE',  ( -13.97604488694527625, -13.89961937509977652, 111.8739096053143243 ) ) ;
#81578 = CARTESIAN_POINT ( 'NONE',  ( -36.91746825000001309, 11.99521256947798342, -5.224999997268811924 ) ) ;
#81579 = CARTESIAN_POINT ( 'NONE',  ( -17.81289503416611097, -24.51734667627696496, 142.2999999999999829 ) ) ;
#81581 = CARTESIAN_POINT ( 'NONE',  ( 16.55341960407618274, -4.379528057220086978, 106.0427570613523471 ) ) ;
#81580 = CARTESIAN_POINT ( 'NONE',  ( 0.05219959533934541429, -16.53943276465976808, 25.00109039468567218 ) ) ;
#81582 = CARTESIAN_POINT ( 'NONE',  ( -9.564922557961040184, 16.46253265017147172, 77.91775706135234714 ) ) ;
#81583 = CARTESIAN_POINT ( 'NONE',  ( -21.52544592524343514, 5.823673210054127303, 46.04057627198103830 ) ) ;
#81584 = CARTESIAN_POINT ( 'NONE',  ( 10.72451020669871369, 18.67979575497193778, 72.08442372801899012 ) ) ;
#81585 = FACE_OUTER_BOUND ( 'NONE', #106624, .T. ) ;
#81586 = CARTESIAN_POINT ( 'NONE',  ( -0.05219959533934338120, 16.53943276465976808, 37.50109039468568284 ) ) ;
#81588 = CARTESIAN_POINT ( 'NONE',  ( -9.474510206698964154, 16.51473224551069663, 85.41557627198102409 ) ) ;
#81587 = CARTESIAN_POINT ( 'NONE',  ( -9.564922557960796823, -16.46253265017161027, 22.08224293864768839 ) ) ;
#81589 = CARTESIAN_POINT ( 'NONE',  ( -0.05219959533909027116, -19.03943276465977164, 22.49890960531436690 ) ) ;
#81590 = CARTESIAN_POINT ( 'NONE',  ( 16.53943276465976808, -0.05219959533910856209, 98.74890960531438111 ) ) ;
#81591 = CONTEXT_DEPENDENT_SHAPE_REPRESENTATION ( #178536, #30753 ) ;
#81592 = CARTESIAN_POINT ( 'NONE',  ( -0.05219959533909027116, -19.03943276465977164, 107.4989096053143527 ) ) ;
#81593 = EDGE_LOOP ( 'NONE', ( #76799, #13396, #147113, #43043, #43588, #154879, #115421, #47823 ) ) ;
#81594 = CARTESIAN_POINT ( 'NONE',  ( 14.29746914071037800, 8.314922557961029526, 61.66775706135235424 ) ) ;
#81595 = CARTESIAN_POINT ( 'NONE',  ( -5.049401038297874678, -19.05341960407617918, 104.7927570613523471 ) ) ;
#81596 = CARTESIAN_POINT ( 'NONE',  ( 10.72451020669898902, -18.67979575497178502, 72.91557627198103830 ) ) ;
#81597 = CARTESIAN_POINT ( 'NONE',  ( 5.153800228976335163, 19.02544592524342804, 39.79057627198100988 ) ) ;
#81599 = CARTESIAN_POINT ( 'NONE',  ( 18.67979575497194134, -10.72451020669871369, 20.83442372801901143 ) ) ;
#81598 = CARTESIAN_POINT ( 'NONE',  ( 19.03943276465977164, 0.05219959533936151252, 66.25109039468567573 ) ) ;
#81600 = CARTESIAN_POINT ( 'NONE',  ( -9.474510206698964154, 16.51473224551069663, 65.41557627198102409 ) ) ;
#81601 = CARTESIAN_POINT ( 'NONE',  ( -5.153800228976328057, -19.02544592524343514, 112.2905762719810099 ) ) ;
#81602 = ORIENTED_EDGE ( 'NONE', *, *, #28979, .T. ) ;
#81603 = CARTESIAN_POINT ( 'NONE',  ( 14.34966873604972726, -8.224510206698740333, 30.83442372801902209 ) ) ;
#81604 = CARTESIAN_POINT ( 'NONE',  ( 5.823673210054125526, 21.52544592524343514, 99.79057627198103830 ) ) ;
#81607 = CARTESIAN_POINT ( 'NONE',  ( 9.564922557961047289, -16.46253265017146816, 80.41775706135234714 ) ) ;
#81606 = CARTESIAN_POINT ( 'NONE',  ( 9.474510206698971260, -16.51473224551069308, 92.91557627198103830 ) ) ;
#81605 = CARTESIAN_POINT ( 'NONE',  ( 14.29746914071049879, -8.314922557960816363, 103.3322429386476955 ) ) ;
#81608 = CARTESIAN_POINT ( 'NONE',  ( 5.823673210054125526, 21.52544592524343514, 84.79057627198102409 ) ) ;
#81609 = CARTESIAN_POINT ( 'NONE',  ( 14.34966873604960469, 8.224510206698951720, 44.16557627198103120 ) ) ;
#81610 = CARTESIAN_POINT ( 'NONE',  ( -15.80617190586768217, 15.72974639402176855, 113.1260903946856899 ) ) ;
#81611 = CARTESIAN_POINT ( 'NONE',  ( 16.55341960407618274, -4.379528057220086978, 71.04275706135234714 ) ) ;
#81613 = ORIENTED_EDGE ( 'NONE', *, *, #164879, .T. ) ;
#81612 = CARTESIAN_POINT ( 'NONE',  ( 13.97604488694527802, 13.89961937509977652, 99.37390960531436690 ) ) ;
#81614 = CARTESIAN_POINT ( 'NONE',  ( -9.474510206698964154, 16.51473224551069663, 45.41557627198103120 ) ) ;
#81615 = CARTESIAN_POINT ( 'NONE',  ( -21.55341960407619339, 5.719274019375674811, 58.54275706135235424 ) ) ;
#81616 = CARTESIAN_POINT ( 'NONE',  ( -18.67979575497193778, 10.72451020669871902, 73.33442372801901854 ) ) ;
#81617 = CARTESIAN_POINT ( 'NONE',  ( 9.474510206698971260, -16.51473224551069308, 67.91557627198102409 ) ) ;
#81618 = CARTESIAN_POINT ( 'NONE',  ( -10.81492255796105439, 18.62759615963255655, 37.91775706135235424 ) ) ;
#81619 = CARTESIAN_POINT ( 'NONE',  ( -19.05341960407617563, 5.049401038297882671, 73.54275706135233293 ) ) ;
#81620 = CARTESIAN_POINT ( 'NONE',  ( -5.049401038298153566, 19.05341960407611168, 35.20724293864768839 ) ) ;
#81621 = CARTESIAN_POINT ( 'NONE',  ( 8.314922557961029526, -14.29746914071037800, 85.41775706135236135 ) ) ;
#81622 = CARTESIAN_POINT ( 'NONE',  ( 19.02544592524343514, -5.153800228976328945, 58.54057627198102409 ) ) ;
#81623 = CARTESIAN_POINT ( 'NONE',  ( -13.89961937509977652, 13.97604488694528158, 110.6239096053143243 ) ) ;
#81624 = CARTESIAN_POINT ( 'NONE',  ( 9.564922557960805705, 16.46253265017160317, 34.58224293864770260 ) ) ;
#81625 = CARTESIAN_POINT ( 'NONE',  ( 18.62759615963271287, -10.81492255796078972, 88.33224293864769550 ) ) ;
#81626 = CARTESIAN_POINT ( 'NONE',  ( 16.53943276465976808, 0.05219959533934440121, 71.25109039468568994 ) ) ;
#81627 = FACE_OUTER_BOUND ( 'NONE', #13644, .T. ) ;
#81628 = CARTESIAN_POINT ( 'NONE',  ( -9.474510206698720793, -16.51473224551083518, 34.58442372801899722 ) ) ;
#81629 = CARTESIAN_POINT ( 'NONE',  ( 19.05341960407611168, 5.049401038298154454, 58.95724293864768129 ) ) ;
#81630 = CARTESIAN_POINT ( 'NONE',  ( 14.34966873604960469, 8.224510206698951720, 44.16557627198103120 ) ) ;
#81631 = CARTESIAN_POINT ( 'NONE',  ( -4.379528057220328563, 16.55341960407611168, 85.20724293864770971 ) ) ;
#81632 = CARTESIAN_POINT ( 'NONE',  ( 9.564922557960805705, 16.46253265017160317, 99.58224293864770971 ) ) ;
#81633 = CARTESIAN_POINT ( 'NONE',  ( 16.46253265017160672, -9.564922557960803928, 83.33224293864768129 ) ) ;
#81634 = CARTESIAN_POINT ( 'NONE',  ( 5.823673210054444382, -21.52544592524334988, 50.20942372801901854 ) ) ;
#81635 = CARTESIAN_POINT ( 'NONE',  ( 5.049401038298161559, -19.05341960407611168, 92.70724293864769550 ) ) ;
#81636 =( REPRESENTATION_RELATIONSHIP ('NONE','NONE', #154205, #125845 ) REPRESENTATION_RELATIONSHIP_WITH_TRANSFORMATION ( #190799 )SHAPE_REPRESENTATION_RELATIONSHIP( ) );
#81637 = CARTESIAN_POINT ( 'NONE',  ( 5.823673210054444382, -21.52544592524334988, 105.2094237280190328 ) ) ;
#81638 = CARTESIAN_POINT ( 'NONE',  ( -16.55341960407617563, 4.379528057220093196, 83.54275706135234714 ) ) ;
#81639 = CARTESIAN_POINT ( 'NONE',  ( -18.62759615963255300, -10.81492255796106328, 29.16775706135234003 ) ) ;
#81640 = CARTESIAN_POINT ( 'NONE',  ( -15.80617190586745835, -15.72974639402198527, 101.8739096053143811 ) ) ;
#81641 = CARTESIAN_POINT ( 'NONE',  ( -8.224510206698948167, 14.34966873604960824, 55.41557627198102409 ) ) ;
#81642 = CARTESIAN_POINT ( 'NONE',  ( 9.564922557960805705, 16.46253265017160317, 39.58224293864768839 ) ) ;
#81643 = CARTESIAN_POINT ( 'NONE',  ( 4.379528057220339221, -16.55341960407611168, 72.70724293864769550 ) ) ;
#81644 = CARTESIAN_POINT ( 'NONE',  ( 0.05219959533907565091, 21.53943276465977519, 24.99890960531435624 ) ) ;
#81645 = CARTESIAN_POINT ( 'NONE',  ( 5.049401038297881783, 19.05341960407617563, 27.29275706135232937 ) ) ;
#81646 = CARTESIAN_POINT ( 'NONE',  ( -16.51473224551069308, -9.474510206698971260, 21.66557627198102765 ) ) ;
#81647 = VERTEX_POINT ( 'NONE', #47312 ) ;
#81648 = CARTESIAN_POINT ( 'NONE',  ( -14.34966873604972548, 8.224510206698743886, 73.33442372801901854 ) ) ;
#81649 = CARTESIAN_POINT ( 'NONE',  ( 0.05219959533909260263, 19.03943276465977164, 69.99890960531435269 ) ) ;
#81650 = CARTESIAN_POINT ( 'NONE',  ( 8.571926809382603096, -26.38167802310801235, 139.4750000027311785 ) ) ;
#81651 = CARTESIAN_POINT ( 'NONE',  ( 4.379528057220339221, -16.55341960407611168, 87.70724293864769550 ) ) ;
#81652 = CARTESIAN_POINT ( 'NONE',  ( -10.81492255796078084, -18.62759615963271287, 32.08224293864769550 ) ) ;
#81653 = ORIENTED_EDGE ( 'NONE', *, *, #41383, .T. ) ;
#81654 = CARTESIAN_POINT ( 'NONE',  ( 4.379528057220092307, 16.55341960407617563, 92.29275706135236135 ) ) ;
#81655 = CARTESIAN_POINT ( 'NONE',  ( 9.474510206698729675, 16.51473224551082808, 112.0844237280190043 ) ) ;
#81656 = CARTESIAN_POINT ( 'NONE',  ( -15.80617190586768217, 15.72974639402176855, 83.12609039468568994 ) ) ;
#81657 = CARTESIAN_POINT ( 'NONE',  ( 19.02544592524343514, -5.153800228976328945, 93.54057627198102409 ) ) ;
#81658 = CARTESIAN_POINT ( 'NONE',  ( -21.55341960407610458, -5.719274019375992779, 106.4572429386477097 ) ) ;
#81659 = CARTESIAN_POINT ( 'NONE',  ( 16.53943276465976808, 0.05219959533934440121, 51.25109039468568994 ) ) ;
#81660 = CARTESIAN_POINT ( 'NONE',  ( -5.153800228976328057, -19.02544592524343514, 32.29057627198102409 ) ) ;
#81661 = CARTESIAN_POINT ( 'NONE',  ( -4.483927247898782831, 16.52544592524335698, 22.70942372801901499 ) ) ;
#81662 = CARTESIAN_POINT ( 'NONE',  ( 5.049401038297881783, 19.05341960407617563, 92.29275706135234714 ) ) ;
#81663 = CARTESIAN_POINT ( 'NONE',  ( -15.80617190586745835, -15.72974639402198527, 86.87390960531438111 ) ) ;
#81664 = CARTESIAN_POINT ( 'NONE',  ( 16.46253265017146816, 9.564922557961045513, 51.66775706135233293 ) ) ;
#81665 = CARTESIAN_POINT ( 'NONE',  ( 19.52217212775660826, -5.499999999999907629, 87.43993709005259518 ) ) ;
#81666 = CARTESIAN_POINT ( 'NONE',  ( 21.52544592524344225, -5.823673210054117533, 98.54057627198105251 ) ) ;
#81667 = CARTESIAN_POINT ( 'NONE',  ( 19.49401214000076976, 12.39993551617566681, 164.9999999999999716 ) ) ;
#81668 = CARTESIAN_POINT ( 'NONE',  ( 19.05341960407611168, 5.049401038298154454, 83.95724293864766707 ) ) ;
#81669 = LINE ( 'NONE', #68515, #114286 ) ;
#81670 = CARTESIAN_POINT ( 'NONE',  ( -16.52544592524335698, -4.483927247898792601, 38.95942372801901854 ) ) ;
#81671 = CARTESIAN_POINT ( 'NONE',  ( 13.16545937439093272, -37.77263716084178213, -11.88623523016686967 ) ) ;
#81673 = CARTESIAN_POINT ( 'NONE',  ( 4.483927247898545687, 16.52544592524342804, 59.79057627198103120 ) ) ;
#81672 = CARTESIAN_POINT ( 'NONE',  ( -5.719274019375978568, 21.55341960407610458, 110.2072429386477239 ) ) ;
#81674 = CARTESIAN_POINT ( 'NONE',  ( -19.05341960407611168, -5.049401038298163336, 76.45724293864769550 ) ) ;
#81676 = CARTESIAN_POINT ( 'NONE',  ( 0.05219959533936267826, -19.03943276465977164, 45.00109039468566863 ) ) ;
#81675 = CARTESIAN_POINT ( 'NONE',  ( -4.379528057220086978, -16.55341960407618274, 34.79275706135235424 ) ) ;
#81677 = CARTESIAN_POINT ( 'NONE',  ( -15.72974639402176322, -15.80617190586768395, 49.37609039468569705 ) ) ;
#81678 = CARTESIAN_POINT ( 'NONE',  ( -0.05219959533936034679, 19.03943276465977164, 112.5010903946856757 ) ) ;
#81680 = EDGE_CURVE ( 'NONE', #151905, #29984, #41443, .T. ) ;
#81679 = CARTESIAN_POINT ( 'NONE',  ( 19.02544592524343514, -5.153800228976328945, 53.54057627198102409 ) ) ;
#81681 = CARTESIAN_POINT ( 'NONE',  ( -9.564922557961040184, 16.46253265017147172, 87.91775706135233293 ) ) ;
#81682 = CARTESIAN_POINT ( 'NONE',  ( -21.53943276465977519, -0.05219959533937600094, 83.75109039468568994 ) ) ;
#81683 = CARTESIAN_POINT ( 'NONE',  ( 5.153800228976615827, -19.02544592524334988, 60.20942372801899012 ) ) ;
#81684 = CARTESIAN_POINT ( 'NONE',  ( -5.049401038298153566, 19.05341960407611168, 40.20724293864768839 ) ) ;
#81685 = CARTESIAN_POINT ( 'NONE',  ( -18.67979575497178146, -10.72451020669898902, 61.66557627198103120 ) ) ;
#81686 = CARTESIAN_POINT ( 'NONE',  ( 4.379528057220339221, -16.55341960407611168, 57.70724293864770260 ) ) ;
#81687 = CARTESIAN_POINT ( 'NONE',  ( 21.96985492114658811, 8.492568044003455441, 171.8755390570805730 ) ) ;
#81688 = CARTESIAN_POINT ( 'NONE',  ( 5.049401038297881783, 19.05341960407617563, 32.29275706135233293 ) ) ;
#81689 = CARTESIAN_POINT ( 'NONE',  ( 16.53943276465976808, 0.05219959533934440121, 101.2510903946856757 ) ) ;
#81690 = CARTESIAN_POINT ( 'NONE',  ( 8.314922557960818139, 14.29746914071049879, 54.58224293864769550 ) ) ;
#81691 = CARTESIAN_POINT ( 'NONE',  ( 5.719274019375673035, 21.55341960407619339, 92.29275706135236135 ) ) ;
#81692 = CARTESIAN_POINT ( 'NONE',  ( 5.823673210054444382, -21.52544592524334988, 85.20942372801901854 ) ) ;
#81693 = CARTESIAN_POINT ( 'NONE',  ( -21.55341960407610458, -5.719274019375992779, 91.45724293864769550 ) ) ;
#81694 = CARTESIAN_POINT ( 'NONE',  ( -5.153800228976328057, -19.02544592524343514, 52.29057627198100988 ) ) ;
#81695 = CARTESIAN_POINT ( 'NONE',  ( 21.53943276465977519, 0.05219959533937863772, 76.25109039468568994 ) ) ;
#81696 = CARTESIAN_POINT ( 'NONE',  ( 19.05341960407611168, 5.049401038298154454, 53.95724293864770260 ) ) ;
#81697 = EDGE_LOOP ( 'NONE', ( #145815, #193197, #171709 ) ) ;
#81698 = CARTESIAN_POINT ( 'NONE',  ( -19.05341960407611168, -5.049401038298163336, 61.45724293864769550 ) ) ;
#81699 = CARTESIAN_POINT ( 'NONE',  ( 8.224510206698953496, -14.34966873604960469, 107.9155762719810241 ) ) ;
#81700 = CARTESIAN_POINT ( 'NONE',  ( 5.153800228976335163, 19.02544592524342804, 114.7905762719810241 ) ) ;
#81701 = CARTESIAN_POINT ( 'NONE',  ( 8.224510206698953496, -14.34966873604960469, 52.91557627198103830 ) ) ;
#81702 = CARTESIAN_POINT ( 'NONE',  ( -0.05219959533909027116, -19.03943276465977164, 22.49890960531436690 ) ) ;
#81703 = CARTESIAN_POINT ( 'NONE',  ( 14.29746914071049879, -8.314922557960816363, 68.33224293864769550 ) ) ;
#81704 = CARTESIAN_POINT ( 'NONE',  ( 21.53943276465977519, -0.05219959533907433946, 83.74890960531435269 ) ) ;
#81705 = CARTESIAN_POINT ( 'NONE',  ( 5.823673210054444382, -21.52544592524334988, 35.20942372801901854 ) ) ;
#81706 = DIRECTION ( 'NONE',  ( -1.000000000000000000, 0.000000000000000000, -0.000000000000000000 ) ) ;
#81707 = CARTESIAN_POINT ( 'NONE',  ( -4.483927247898782831, 16.52544592524335698, 37.70942372801900433 ) ) ;
#81708 = CARTESIAN_POINT ( 'NONE',  ( 18.62759615963271287, -10.81492255796078972, 88.33224293864769550 ) ) ;
#81709 = CARTESIAN_POINT ( 'NONE',  ( -5.823673210054431948, 21.52544592524334988, 107.7094237280190328 ) ) ;
#81710 = CARTESIAN_POINT ( 'NONE',  ( 19.05341960407611168, 5.049401038298154454, 98.95724293864766707 ) ) ;
#81711 = CARTESIAN_POINT ( 'NONE',  ( 5.719274019375673035, 21.55341960407619339, 47.29275706135234003 ) ) ;
#81712 = AXIS2_PLACEMENT_3D ( 'NONE', #24749, #134918, #119736 ) ;
#81713 = CARTESIAN_POINT ( 'NONE',  ( 21.53943276465977519, -0.05219959533907433946, 23.74890960531435269 ) ) ;
#81714 = CARTESIAN_POINT ( 'NONE',  ( 14.29746914071037800, 8.314922557961029526, 101.6677570613523613 ) ) ;
#81716 = CARTESIAN_POINT ( 'NONE',  ( -5.823673210054431948, 21.52544592524334988, 82.70942372801900433 ) ) ;
#81715 = CARTESIAN_POINT ( 'NONE',  ( -5.719274019375665041, -21.55341960407619695, 49.79275706135234714 ) ) ;
#81717 = CARTESIAN_POINT ( 'NONE',  ( -9.564922557961040184, 16.46253265017147172, 22.91775706135233648 ) ) ;
#81718 = CARTESIAN_POINT ( 'NONE',  ( 16.55341960407618274, -4.379528057220086978, 71.04275706135234714 ) ) ;
#81719 = CARTESIAN_POINT ( 'NONE',  ( -5.719274019375665041, -21.55341960407619695, 44.79275706135234714 ) ) ;
#81720 = CARTESIAN_POINT ( 'NONE',  ( 19.02544592524343514, -5.153800228976328945, 33.54057627198102409 ) ) ;
#81721 = CARTESIAN_POINT ( 'NONE',  ( -10.81492255796105439, 18.62759615963255655, 102.9177570613523756 ) ) ;
#81722 = CARTESIAN_POINT ( 'NONE',  ( -13.89961937509977652, 13.97604488694528158, 100.6239096053143669 ) ) ;
#81724 = CARTESIAN_POINT ( 'NONE',  ( 18.62759615963271287, -10.81492255796078972, 103.3322429386476955 ) ) ;
#81723 = B_SPLINE_CURVE_WITH_KNOTS ( 'NONE', 3,
 ( #146172, #176540, #5665, #114846, #129002, #86510, #55177, #37002, #193708, #190700, #100669, #22847, #163365, #175527 ),
 .UNSPECIFIED., .F., .F.,
 ( 4, 2, 2, 2, 2, 2, 4 ),
 ( 0.002427643230453600375, 0.002603325520439084273, 0.002779007810424568171, 0.003130372390395535533, 0.003833101550337468522, 0.004535830710279402378, 0.005238559870221335367 ),
 .UNSPECIFIED. ) ;
#81726 = CARTESIAN_POINT ( 'NONE',  ( 18.62759615963271287, -10.81492255796078972, 68.33224293864769550 ) ) ;
#81725 = CARTESIAN_POINT ( 'NONE',  ( 17.60728821187776205, -5.500000000000032863, 88.36690927743606494 ) ) ;
#81728 = CARTESIAN_POINT ( 'NONE',  ( 14.34966873604960469, 8.224510206698951720, 44.16557627198103120 ) ) ;
#81727 = CARTESIAN_POINT ( 'NONE',  ( -0.05219959533934338120, 16.53943276465976808, 52.50109039468567573 ) ) ;
#81729 = CARTESIAN_POINT ( 'NONE',  ( 10.59477242850415024, -90.60836494048558620, 0.000000000000000000 ) ) ;
#81730 = CARTESIAN_POINT ( 'NONE',  ( 19.02544592524334988, 5.153800228976608722, 86.45942372801900433 ) ) ;
#81731 = CARTESIAN_POINT ( 'NONE',  ( -24.30000000000002913, 0.1121107154833756725, -54.21489346206829651 ) ) ;
#81732 = CARTESIAN_POINT ( 'NONE',  ( -16.55341960407617563, 4.379528057220093196, 28.54275706135234358 ) ) ;
#81733 = CARTESIAN_POINT ( 'NONE',  ( -21.52544592524343514, 5.823673210054127303, 101.0405762719810383 ) ) ;
#81734 = CARTESIAN_POINT ( 'NONE',  ( 18.67979575497178502, 10.72451020669898547, 79.16557627198103830 ) ) ;
#81735 = CARTESIAN_POINT ( 'NONE',  ( 16.46253265017160672, -9.564922557960803928, 113.3322429386476955 ) ) ;
#81736 = CARTESIAN_POINT ( 'NONE',  ( -16.55341960407617563, 4.379528057220093196, 48.54275706135234714 ) ) ;
#81737 = CARTESIAN_POINT ( 'NONE',  ( -5.049401038298153566, 19.05341960407611168, 75.20724293864769550 ) ) ;
#81739 = CARTESIAN_POINT ( 'NONE',  ( -16.46253265017146816, -9.564922557961047289, 94.16775706135233293 ) ) ;
#81738 = CARTESIAN_POINT ( 'NONE',  ( -15.72974639402176322, -15.80617190586768395, 24.37609039468567573 ) ) ;
#81740 = CARTESIAN_POINT ( 'NONE',  ( -16.46253265017160317, 9.564922557960807481, 110.8322429386476955 ) ) ;
#81741 = CARTESIAN_POINT ( 'NONE',  ( 0.05219959533909260263, 19.03943276465977164, 89.99890960531436690 ) ) ;
#81742 = CARTESIAN_POINT ( 'NONE',  ( -21.55341960407610458, -5.719274019375992779, 86.45724293864770971 ) ) ;
#81743 = CARTESIAN_POINT ( 'NONE',  ( 9.474510206698971260, -16.51473224551069308, 57.91557627198103120 ) ) ;
#81744 = CARTESIAN_POINT ( 'NONE',  ( 23.48529157249599564, 32.32473071737754111, -0.6999999999999997335 ) ) ;
#81745 = CARTESIAN_POINT ( 'NONE',  ( 14.29746914071049879, -8.314922557960816363, 68.33224293864769550 ) ) ;
#81746 = CARTESIAN_POINT ( 'NONE',  ( -10.81492255796078084, -18.62759615963271287, 22.08224293864769194 ) ) ;
#81747 = CARTESIAN_POINT ( 'NONE',  ( -29.85394078251578520, 1.399641368456010060, -51.58569050288880931 ) ) ;
#81748 = CARTESIAN_POINT ( 'NONE',  ( -5.823673210054116645, -21.52544592524344225, 97.29057627198105251 ) ) ;
#81749 = CARTESIAN_POINT ( 'NONE',  ( -16.46253265017146816, -9.564922557961047289, 64.16775706135233293 ) ) ;
#81750 = CARTESIAN_POINT ( 'NONE',  ( 0.05219959533909260263, 19.03943276465977164, 114.9989096053143669 ) ) ;
#81751 = FILL_AREA_STYLE_COLOUR ( '', #56542 ) ;
#81752 = CARTESIAN_POINT ( 'NONE',  ( -21.55341960407610458, -5.719274019375992779, 56.45724293864768839 ) ) ;
#81753 = CARTESIAN_POINT ( 'NONE',  ( -5.153800228976328057, -19.02544592524343514, 82.29057627198103830 ) ) ;
#81754 = CARTESIAN_POINT ( 'NONE',  ( -18.67979575497193778, 10.72451020669871902, 83.33442372801903275 ) ) ;
#81755 = CARTESIAN_POINT ( 'NONE',  ( 0.05219959533909260263, 19.03943276465977164, 44.99890960531435979 ) ) ;
#81756 = EDGE_CURVE ( 'NONE', #56919, #120176, #86286, .T. ) ;
#81757 = CARTESIAN_POINT ( 'NONE',  ( 16.52544592524342804, -4.483927247898539470, 93.54057627198103830 ) ) ;
#81758 = CARTESIAN_POINT ( 'NONE',  ( -8.314922557961024197, 14.29746914071037800, 32.91775706135234714 ) ) ;
#81759 = CARTESIAN_POINT ( 'NONE',  ( 0.05219959533937995610, -21.53943276465977519, 65.00109039468568994 ) ) ;
#81760 = ORIENTED_EDGE ( 'NONE', *, *, #113163, .F. ) ;
#81761 = CARTESIAN_POINT ( 'NONE',  ( -9.474510206698720793, -16.51473224551083518, 19.58442372801899722 ) ) ;
#81762 = CARTESIAN_POINT ( 'NONE',  ( 13.89961937509957401, 13.97604488694547697, 76.87609039468566152 ) ) ;
#81763 = CARTESIAN_POINT ( 'NONE',  ( 28.92784451463930040, -27.23096741515436392, -20.32502560054408747 ) ) ;
#81764 = CARTESIAN_POINT ( 'NONE',  ( 21.52544592524334988, 5.823673210054432836, 41.45942372801901143 ) ) ;
#81765 = CARTESIAN_POINT ( 'NONE',  ( -11.74264578624799782, -36.14014761921581709, -3.349999994537626868 ) ) ;
#81766 = CARTESIAN_POINT ( 'NONE',  ( -19.02544592524334988, -5.153800228976617603, 28.95942372801900433 ) ) ;
#81767 = CARTESIAN_POINT ( 'NONE',  ( 16.46253265017160672, -9.564922557960803928, 53.33224293864768839 ) ) ;
#81768 = CARTESIAN_POINT ( 'NONE',  ( -16.51473224551082808, 9.474510206698731452, 33.33442372801899722 ) ) ;
#81769 = CARTESIAN_POINT ( 'NONE',  ( -8.314922557961024197, 14.29746914071037800, 97.91775706135236135 ) ) ;
#81771 = CARTESIAN_POINT ( 'NONE',  ( -18.62759615963255300, -10.81492255796106328, 74.16775706135231871 ) ) ;
#81770 = CARTESIAN_POINT ( 'NONE',  ( 16.46253265017160672, -9.564922557960803928, 103.3322429386476955 ) ) ;
#81772 = CARTESIAN_POINT ( 'NONE',  ( 22.81625015709509441, 31.40387420917330275, -7.324999997268812457 ) ) ;
#81773 = DIRECTION ( 'NONE',  ( 0.000000000000000000, 0.000000000000000000, -1.000000000000000000 ) ) ;
#81774 = CARTESIAN_POINT ( 'NONE',  ( -21.55341960407619339, 5.719274019375674811, 83.54275706135234714 ) ) ;
#81775 = AXIS2_PLACEMENT_3D ( 'NONE', #169591, #120106, #181796 ) ;
#81776 = DIRECTION ( 'NONE',  ( 1.000000000000000000, 0.000000000000000000, 0.000000000000000000 ) ) ;
#81777 = CARTESIAN_POINT ( 'NONE',  ( -19.03943276465977164, 0.05219959533909376836, 101.2489096053143669 ) ) ;
#81778 = CARTESIAN_POINT ( 'NONE',  ( -13.89961937509957401, -13.97604488694547875, 19.37609039468566507 ) ) ;
#81779 = CARTESIAN_POINT ( 'NONE',  ( 26.42731554605158095, -26.90581007260905366, -20.33945912742372286 ) ) ;
#81780 = CARTESIAN_POINT ( 'NONE',  ( -0.05219959533909027116, -19.03943276465977164, 32.49890960531435979 ) ) ;
#81781 = CARTESIAN_POINT ( 'NONE',  ( 18.67979575497178502, 10.72451020669898547, 59.16557627198103120 ) ) ;
#81782 = CARTESIAN_POINT ( 'NONE',  ( 4.483927247898545687, 16.52544592524342804, 24.79057627198103120 ) ) ;
#81784 = CARTESIAN_POINT ( 'NONE',  ( -16.46253265017160317, 9.564922557960807481, 75.83224293864769550 ) ) ;
#81783 = CARTESIAN_POINT ( 'NONE',  ( -4.379528057220328563, 16.55341960407611168, 100.2072429386476955 ) ) ;
#81785 = CARTESIAN_POINT ( 'NONE',  ( 16.46253265017146816, 9.564922557961045513, 26.66775706135234003 ) ) ;
#81786 = CARTESIAN_POINT ( 'NONE',  ( -19.05341960407611168, -5.049401038298163336, 41.45724293864769550 ) ) ;
#81787 = CARTESIAN_POINT ( 'NONE',  ( 16.52544592524342804, -4.483927247898539470, 108.5405762719810241 ) ) ;
#81788 = CARTESIAN_POINT ( 'NONE',  ( -10.72451020669870658, -18.67979575497194134, 59.58442372801901854 ) ) ;
#81789 = CARTESIAN_POINT ( 'NONE',  ( -18.62759615963270932, 10.81492255796079327, 90.83224293864769550 ) ) ;
#81790 = CARTESIAN_POINT ( 'NONE',  ( 0.05219959533936267826, -19.03943276465977164, 60.00109039468566863 ) ) ;
#81791 = CARTESIAN_POINT ( 'NONE',  ( -20.43538597629143538, -20.43538597629106945, -49.67367017693150189 ) ) ;
#81792 = CARTESIAN_POINT ( 'NONE',  ( -13.89961937509977652, 13.97604488694528158, 110.6239096053143243 ) ) ;
#81793 = CARTESIAN_POINT ( 'NONE',  ( -14.29746914071049879, 8.314922557960819915, 80.83224293864769550 ) ) ;
#81794 = CARTESIAN_POINT ( 'NONE',  ( -5.153800228976607833, 19.02544592524334988, 42.70942372801901143 ) ) ;
#81795 = CARTESIAN_POINT ( 'NONE',  ( -5.049401038298153566, 19.05341960407611168, 65.20724293864765286 ) ) ;
#81796 = CARTESIAN_POINT ( 'NONE',  ( 4.379528057220339221, -16.55341960407611168, 57.70724293864770260 ) ) ;
#81797 = CARTESIAN_POINT ( 'NONE',  ( 16.51473224551083163, -9.474510206698727899, 75.83442372801900433 ) ) ;
#81798 = FACE_OUTER_BOUND ( 'NONE', #41869, .T. ) ;
#81799 = CARTESIAN_POINT ( 'NONE',  ( -15.80617190586745835, -15.72974639402198527, 36.87390960531435979 ) ) ;
#81800 = EDGE_LOOP ( 'NONE', ( #5769, #171157, #186714, #29673 ) ) ;
#81801 = CARTESIAN_POINT ( 'NONE',  ( -14.34966873604960291, -8.224510206698953496, 106.6655762719810383 ) ) ;
#81802 = CARTESIAN_POINT ( 'NONE',  ( -3.573655867282028392E-15, 2.428612866367529932E-14, 0.000000000000000000 ) ) ;
#81804 = CARTESIAN_POINT ( 'NONE',  ( -21.52544592524343514, 5.823673210054127303, 56.04057627198102409 ) ) ;
#81803 = CARTESIAN_POINT ( 'NONE',  ( -0.05219959533909027116, -19.03943276465977164, 52.49890960531436690 ) ) ;
#81805 = CARTESIAN_POINT ( 'NONE',  ( -9.474510206698964154, 16.51473224551069663, 35.41557627198102409 ) ) ;
#81807 = CARTESIAN_POINT ( 'NONE',  ( -5.153800228976328057, -19.02544592524343514, 77.29057627198099567 ) ) ;
#81806 = CARTESIAN_POINT ( 'NONE',  ( -14.29746914071037622, -8.314922557961029526, 84.16775706135234714 ) ) ;
#81808 = CARTESIAN_POINT ( 'NONE',  ( -0.05219959533936034679, 19.03943276465977164, 57.50109039468566863 ) ) ;
#81809 = CARTESIAN_POINT ( 'NONE',  ( -10.81492255796105439, 18.62759615963255655, 62.91775706135236135 ) ) ;
#81810 = CARTESIAN_POINT ( 'NONE',  ( 10.81492255796078972, 18.62759615963270932, 54.58224293864769550 ) ) ;
#81811 = CARTESIAN_POINT ( 'NONE',  ( -4.379528057220328563, 16.55341960407611168, 115.2072429386476955 ) ) ;
#81812 = CARTESIAN_POINT ( 'NONE',  ( 16.52544592524335698, 4.483927247898782831, 86.45942372801901854 ) ) ;
#81813 = CARTESIAN_POINT ( 'NONE',  ( 9.564922557961047289, -16.46253265017146816, 110.4177570613523471 ) ) ;
#81814 = CARTESIAN_POINT ( 'NONE',  ( -36.91746825000000598, 2.428612866367529932E-14, -1.124999997268813390 ) ) ;
#81815 = CARTESIAN_POINT ( 'NONE',  ( 19.49671883438228548, 5.499999999999968914, 77.39279849105680853 ) ) ;
#81816 = CARTESIAN_POINT ( 'NONE',  ( -10.81492255796105439, 18.62759615963255655, 92.91775706135236135 ) ) ;
#81817 = EDGE_LOOP ( 'NONE', ( #116867, #87482, #89768, #108079 ) ) ;
#81818 = CARTESIAN_POINT ( 'NONE',  ( -14.29746914071049879, 8.314922557960819915, 40.83224293864769550 ) ) ;
#81819 = CARTESIAN_POINT ( 'NONE',  ( -0.05219959533910754901, -16.53943276465976808, 57.49890960531435979 ) ) ;
#81820 = CARTESIAN_POINT ( 'NONE',  ( -18.62759615963270932, 10.81492255796079327, 95.83224293864770971 ) ) ;
#81821 = CARTESIAN_POINT ( 'NONE',  ( 15.80617190586746368, 15.72974639402197994, 94.37390960531436690 ) ) ;
#81822 = CARTESIAN_POINT ( 'NONE',  ( -1.359215367441039879, -31.05479031690790492, -46.85916094508147012 ) ) ;
#81823 = CARTESIAN_POINT ( 'NONE',  ( -21.53943276465977519, 0.05219959533907696930, 26.24890960531435624 ) ) ;
#81824 = CARTESIAN_POINT ( 'NONE',  ( 8.224510206698742110, 14.34966873604972548, 62.08442372801901143 ) ) ;
#81825 = CARTESIAN_POINT ( 'NONE',  ( -8.224510206698948167, 14.34966873604960824, 80.41557627198103830 ) ) ;
#81826 = CARTESIAN_POINT ( 'NONE',  ( 16.46253265017160672, -9.564922557960803928, 43.33224293864769550 ) ) ;
#81827 = CARTESIAN_POINT ( 'NONE',  ( 34.78522506798721992, -0.4968532545621706098, 52.50000000000000711 ) ) ;
#81828 = CARTESIAN_POINT ( 'NONE',  ( -12.06949235617739369, -12.14591786802326823, 94.37609039468568994 ) ) ;
#81829 = CARTESIAN_POINT ( 'NONE',  ( 21.55341960407619695, -5.719274019375665929, 21.04275706135234714 ) ) ;
#81830 = CARTESIAN_POINT ( 'NONE',  ( -16.51473224551069308, -9.474510206698971260, 86.66557627198102409 ) ) ;
#81831 = CARTESIAN_POINT ( 'NONE',  ( -15.72974639402176322, -15.80617190586768395, 54.37609039468568994 ) ) ;
#81832 = CARTESIAN_POINT ( 'NONE',  ( 19.05341960407611168, 5.049401038298154454, 103.9572429386476671 ) ) ;
#81833 = CARTESIAN_POINT ( 'NONE',  ( -17.67029085834473889, -36.01944455193051908, -22.64778610421867100 ) ) ;
#81834 = ORIENTED_EDGE ( 'NONE', *, *, #41647, .T. ) ;
#81835 = CARTESIAN_POINT ( 'NONE',  ( -18.62759615963255300, -10.81492255796106328, 49.16775706135234003 ) ) ;
#81837 = CARTESIAN_POINT ( 'NONE',  ( 1.300000000000000044, -1.443375672974063884, -3.691112476943992763E-18 ) ) ;
#81836 = CARTESIAN_POINT ( 'NONE',  ( 19.02544592524343514, -5.153800228976328945, 43.54057627198103120 ) ) ;
#81838 = CARTESIAN_POINT ( 'NONE',  ( 19.05341960407617918, -5.049401038297876454, 56.04275706135234714 ) ) ;
#81839 = CARTESIAN_POINT ( 'NONE',  ( -15.80617190586768217, 15.72974639402176855, 33.12609039468569705 ) ) ;
#81840 = CARTESIAN_POINT ( 'NONE',  ( 5.049401038297881783, 19.05341960407617563, 57.29275706135231871 ) ) ;
#81841 = CARTESIAN_POINT ( 'NONE',  ( 0.05219959533909260263, 19.03943276465977164, 29.99890960531435979 ) ) ;
#81842 = CARTESIAN_POINT ( 'NONE',  ( -4.483927247898782831, 16.52544592524335698, 87.70942372801901854 ) ) ;
#81843 = CARTESIAN_POINT ( 'NONE',  ( -16.51473224551082808, 9.474510206698731452, 58.33442372801900433 ) ) ;
#81844 = CARTESIAN_POINT ( 'NONE',  ( -12.06949235617739369, -12.14591786802326823, 99.37609039468568994 ) ) ;
#81846 = ORIENTED_EDGE ( 'NONE', *, *, #64444, .F. ) ;
#81845 = DIRECTION ( 'NONE',  ( -1.000000000000000000, -0.000000000000000000, -0.000000000000000000 ) ) ;
#81847 = CARTESIAN_POINT ( 'NONE',  ( 16.46253265017160672, -9.564922557960803928, 88.33224293864769550 ) ) ;
#81848 = CARTESIAN_POINT ( 'NONE',  ( 10.81492255796106328, -18.62759615963255655, 90.41775706135236135 ) ) ;
#81849 = CARTESIAN_POINT ( 'NONE',  ( -21.53943276465977519, -0.05219959533937600094, 108.7510903946857042 ) ) ;
#81850 = CARTESIAN_POINT ( 'NONE',  ( -18.22780087662124160, -5.499999999999927169, 88.98236817873107896 ) ) ;
#81851 = CARTESIAN_POINT ( 'NONE',  ( 10.72451020669871369, 18.67979575497193778, 72.08442372801899012 ) ) ;
#81852 = CARTESIAN_POINT ( 'NONE',  ( 16.55341960407618274, -4.379528057220086978, 36.04275706135234714 ) ) ;
#81853 = CARTESIAN_POINT ( 'NONE',  ( 19.03943276465977164, -0.05219959533909143690, 78.74890960531436690 ) ) ;
#81855 = EDGE_CURVE ( 'NONE', #147696, #108375, #199920, .T. ) ;
#81854 = CARTESIAN_POINT ( 'NONE',  ( 10.72451020669898902, -18.67979575497178502, 27.91557627198103830 ) ) ;
#81856 = AXIS2_PLACEMENT_3D ( 'NONE', #9000, #118171, #179862 ) ;
#81857 = CARTESIAN_POINT ( 'NONE',  ( -8.571926809382601320, -26.38167802310801591, 139.2750000027311899 ) ) ;
#81858 = CARTESIAN_POINT ( 'NONE',  ( -5.049401038298153566, 19.05341960407611168, 60.20724293864768129 ) ) ;
#81859 = CARTESIAN_POINT ( 'NONE',  ( -14.34966873604972548, 8.224510206698743886, 113.3344237280190328 ) ) ;
#81860 = CARTESIAN_POINT ( 'NONE',  ( -17.44270441346520784, 5.991230190322873739, 98.63664920735773478 ) ) ;
#81861 = CARTESIAN_POINT ( 'NONE',  ( -5.153800228976607833, 19.02544592524334988, 72.70942372801900433 ) ) ;
#81862 = CARTESIAN_POINT ( 'NONE',  ( -9.564922557960796823, -16.46253265017161027, 102.0822429386477097 ) ) ;
#81863 = CARTESIAN_POINT ( 'NONE',  ( -21.53943276465977519, -0.05219959533937600094, 98.75109039468568994 ) ) ;
#81864 = CARTESIAN_POINT ( 'NONE',  ( -14.34966873604960291, -8.224510206698953496, 91.66557627198103830 ) ) ;
#81865 = CARTESIAN_POINT ( 'NONE',  ( -21.55341960407610458, -5.719274019375992779, 51.45724293864770260 ) ) ;
#81866 = CARTESIAN_POINT ( 'NONE',  ( -10.81492255796078084, -18.62759615963271287, 37.08224293864768129 ) ) ;
#81867 = CARTESIAN_POINT ( 'NONE',  ( 16.52544592524342804, -4.483927247898539470, 103.5405762719810383 ) ) ;
#81868 = CARTESIAN_POINT ( 'NONE',  ( -14.30340603398753885, 1.218621689577188416, -62.33590500446655369 ) ) ;
#81869 = CARTESIAN_POINT ( 'NONE',  ( -19.02544592524334988, -5.153800228976617603, 58.95942372801900433 ) ) ;
#81870 = CARTESIAN_POINT ( 'NONE',  ( 12.14591786802309770, 12.06949235617756955, 24.37390960531435979 ) ) ;
#81871 = CARTESIAN_POINT ( 'NONE',  ( 19.05341960407611168, 5.049401038298154454, 103.9572429386476671 ) ) ;
#81872 = CARTESIAN_POINT ( 'NONE',  ( -15.72974639402176322, -15.80617190586768395, 69.37609039468567573 ) ) ;
#81873 = CARTESIAN_POINT ( 'NONE',  ( -5.823673210054116645, -21.52544592524344225, 62.29057627198102409 ) ) ;
#81874 = CARTESIAN_POINT ( 'NONE',  ( 21.55341960407619695, -5.719274019375665929, 46.04275706135234714 ) ) ;
#81875 = CARTESIAN_POINT ( 'NONE',  ( 10.72451020669898902, -18.67979575497178502, 102.9155762719810383 ) ) ;
#81876 = CARTESIAN_POINT ( 'NONE',  ( 21.53943276465977519, 0.05219959533937863772, 36.25109039468567573 ) ) ;
#81877 = CARTESIAN_POINT ( 'NONE',  ( -5.049401038298153566, 19.05341960407611168, 30.20724293864768839 ) ) ;
#81878 = CARTESIAN_POINT ( 'NONE',  ( 5.049401038297881783, 19.05341960407617563, 67.29275706135234714 ) ) ;
#81879 = CARTESIAN_POINT ( 'NONE',  ( 16.53943276465976808, -0.05219959533910856209, 98.74890960531438111 ) ) ;
#81880 = CARTESIAN_POINT ( 'NONE',  ( 19.02544592524343514, -5.153800228976328945, 108.5405762719810383 ) ) ;
#81881 = CARTESIAN_POINT ( 'NONE',  ( -12.06949235617756955, 12.14591786802309770, 55.62390960531436690 ) ) ;
#81882 = CARTESIAN_POINT ( 'NONE',  ( 8.314922557961029526, -14.29746914071037800, 110.4177570613523756 ) ) ;
#81883 = CARTESIAN_POINT ( 'NONE',  ( -5.153800228976328057, -19.02544592524343514, 52.29057627198100988 ) ) ;
#81884 = CARTESIAN_POINT ( 'NONE',  ( 0.05219959533910956823, 16.53943276465976808, 114.9989096053143669 ) ) ;
#81885 = CARTESIAN_POINT ( 'NONE',  ( 18.67979575497178502, 10.72451020669898547, 29.16557627198103120 ) ) ;
#81886 = CARTESIAN_POINT ( 'NONE',  ( -13.89961937509957401, -13.97604488694547875, 19.37609039468566507 ) ) ;
#81888 = CARTESIAN_POINT ( 'NONE',  ( 12.14591786802309770, 12.06949235617756955, 34.37390960531435979 ) ) ;
#81887 = CARTESIAN_POINT ( 'NONE',  ( 18.09867054820434262, 5.499999999999818812, 51.48393025253587751 ) ) ;
#81889 = CARTESIAN_POINT ( 'NONE',  ( -15.80617190586768217, 15.72974639402176855, 53.12609039468568284 ) ) ;
#81890 = CARTESIAN_POINT ( 'NONE',  ( -9.349452323154864075, -36.27485578735121408, -31.39434858484993640 ) ) ;
#81891 = CARTESIAN_POINT ( 'NONE',  ( -16.53943276465976808, -0.05219959533934237506, 63.75109039468568284 ) ) ;
#81892 = CARTESIAN_POINT ( 'NONE',  ( -5.153800228976607833, 19.02544592524334988, 62.70942372801899722 ) ) ;
#81893 = CARTESIAN_POINT ( 'NONE',  ( -16.55341960407611168, -4.379528057220339221, 31.45724293864769550 ) ) ;
#81894 = CARTESIAN_POINT ( 'NONE',  ( -0.05219959533934338120, 16.53943276465976808, 112.5010903946857042 ) ) ;
#81895 = CARTESIAN_POINT ( 'NONE',  ( 19.05341960407611168, 5.049401038298154454, 43.95724293864769550 ) ) ;
#81896 = CARTESIAN_POINT ( 'NONE',  ( 13.89961937509977652, -13.97604488694527269, 63.12390960531435979 ) ) ;
#81897 = CARTESIAN_POINT ( 'NONE',  ( 16.46253265017160672, -9.564922557960803928, 28.33224293864769550 ) ) ;
#81898 = CARTESIAN_POINT ( 'NONE',  ( -15.80617190586768217, 15.72974639402176855, 33.12609039468569705 ) ) ;
#81899 = CARTESIAN_POINT ( 'NONE',  ( 16.51473224551069308, 9.474510206698969483, 39.16557627198103120 ) ) ;
#81900 = CARTESIAN_POINT ( 'NONE',  ( -5.069580672095056251, -6.850104167616680506, -62.03238449839263069 ) ) ;
#81901 = CARTESIAN_POINT ( 'NONE',  ( -19.05341960407611168, -5.049401038298163336, 36.45724293864766707 ) ) ;
#81902 = CARTESIAN_POINT ( 'NONE',  ( -5.719274019375978568, 21.55341960407610458, 25.20724293864769550 ) ) ;
#81904 = CARTESIAN_POINT ( 'NONE',  ( -16.55341960407611168, -4.379528057220339221, 106.4572429386477097 ) ) ;
#81903 = CARTESIAN_POINT ( 'NONE',  ( 0.05219959533937995610, -21.53943276465977519, 60.00109039468568284 ) ) ;
#81905 = CARTESIAN_POINT ( 'NONE',  ( 13.97604488694527802, 13.89961937509977652, 109.3739096053143669 ) ) ;
#81906 = CARTESIAN_POINT ( 'NONE',  ( -12.14591786802326823, 12.06949235617739902, 78.12609039468570415 ) ) ;
#81907 = CARTESIAN_POINT ( 'NONE',  ( -10.72451020669870658, -18.67979575497194134, 89.58442372801901854 ) ) ;
#81908 = CARTESIAN_POINT ( 'NONE',  ( 12.06949235617739724, 12.14591786802326823, 51.87609039468568284 ) ) ;
#81909 = CARTESIAN_POINT ( 'NONE',  ( -16.51473224551069308, -9.474510206698971260, 96.66557627198102409 ) ) ;
#81910 = CARTESIAN_POINT ( 'NONE',  ( -16.55341960407617563, 4.379528057220093196, 38.54275706135234714 ) ) ;
#81911 = CARTESIAN_POINT ( 'NONE',  ( -14.34966873604972548, 8.224510206698743886, 33.33442372801900433 ) ) ;
#81912 = CARTESIAN_POINT ( 'NONE',  ( 8.224510206698742110, 14.34966873604972548, 82.08442372801901854 ) ) ;
#81913 = CARTESIAN_POINT ( 'NONE',  ( 16.46253265017146816, 9.564922557961045513, 111.6677570613523329 ) ) ;
#81914 = CARTESIAN_POINT ( 'NONE',  ( 15.72974639402199770, -15.80617190586745480, 103.1239096053143811 ) ) ;
#81916 = CARTESIAN_POINT ( 'NONE',  ( -13.89961937509957401, -13.97604488694547875, 104.3760903946856757 ) ) ;
#81915 = CARTESIAN_POINT ( 'NONE',  ( 16.53943276465976808, -0.05219959533910856209, 98.74890960531438111 ) ) ;
#81917 = CARTESIAN_POINT ( 'NONE',  ( 16.53943276465976808, 0.05219959533934440121, 76.25109039468568994 ) ) ;
#81918 = DIRECTION ( 'NONE',  ( 0.000000000000000000, 0.000000000000000000, -1.000000000000000000 ) ) ;
#81919 = CARTESIAN_POINT ( 'NONE',  ( 5.049401038297881783, 19.05341960407617563, 67.29275706135234714 ) ) ;
#81920 = CARTESIAN_POINT ( 'NONE',  ( 16.53943276465976808, -0.05219959533910856209, 48.74890960531435979 ) ) ;
#81921 = CARTESIAN_POINT ( 'NONE',  ( -4.379528057220328563, 16.55341960407611168, 35.20724293864768839 ) ) ;
#81922 = CARTESIAN_POINT ( 'NONE',  ( 14.34966873604960469, 8.224510206698951720, 99.16557627198100988 ) ) ;
#81924 =( NAMED_UNIT ( * ) PLANE_ANGLE_UNIT ( ) SI_UNIT ( $, .RADIAN. ) );
#81923 = CARTESIAN_POINT ( 'NONE',  ( -13.97604488694547697, 13.89961937509957934, 33.12609039468566863 ) ) ;
#81925 = CARTESIAN_POINT ( 'NONE',  ( -18.62759615963255300, -10.81492255796106328, 39.16775706135235424 ) ) ;
#81926 = CARTESIAN_POINT ( 'NONE',  ( 9.474510206698729675, 16.51473224551082808, 92.08442372801900433 ) ) ;
#81927 = CARTESIAN_POINT ( 'NONE',  ( 0.05219959533909260263, 19.03943276465977164, 109.9989096053143669 ) ) ;
#81928 = CARTESIAN_POINT ( 'NONE',  ( 9.474510206698971260, -16.51473224551069308, 97.91557627198102409 ) ) ;
#81929 = CARTESIAN_POINT ( 'NONE',  ( -19.02544592524342804, 5.153800228976336051, 86.04057627198103830 ) ) ;
#81930 = CARTESIAN_POINT ( 'NONE',  ( -0.05219959533907301413, -21.53943276465977519, 57.49890960531435979 ) ) ;
#81931 = CARTESIAN_POINT ( 'NONE',  ( -16.53943276465976808, 0.05219959533911058130, 91.24890960531436690 ) ) ;
#81932 = CARTESIAN_POINT ( 'NONE',  ( -9.564922557960796823, -16.46253265017161027, 72.08224293864770971 ) ) ;
#81933 = CARTESIAN_POINT ( 'NONE',  ( -0.05219959533910754901, -16.53943276465976808, 112.4989096053143669 ) ) ;
#81934 = CIRCLE ( 'NONE', #78795, 10.00000000000000178 ) ;
#81935 = CARTESIAN_POINT ( 'NONE',  ( -5.719274019375665041, -21.55341960407619695, 39.79275706135235424 ) ) ;
#81936 = CARTESIAN_POINT ( 'NONE',  ( -15.80617190586768217, 15.72974639402176855, 78.12609039468570415 ) ) ;
#81937 = CARTESIAN_POINT ( 'NONE',  ( 16.46253265017160672, -9.564922557960803928, 58.33224293864769550 ) ) ;
#81938 = CARTESIAN_POINT ( 'NONE',  ( 4.483927247898790824, -16.52544592524335698, 80.20942372801901854 ) ) ;
#81939 = ADVANCED_FACE ( 'NONE', ( #10262 ), #62452, .F. ) ;
#81940 = CARTESIAN_POINT ( 'NONE',  ( -18.67979575497193778, 10.72451020669871902, 28.33442372801902209 ) ) ;
#81941 = CARTESIAN_POINT ( 'NONE',  ( 21.52544592524334988, 5.823673210054432836, 26.45942372801901854 ) ) ;
#81943 = CARTESIAN_POINT ( 'NONE',  ( 5.153800228976335163, 19.02544592524342804, 84.79057627198099567 ) ) ;
#81942 = CARTESIAN_POINT ( 'NONE',  ( 13.89961937509957401, 13.97604488694547697, 51.87609039468566863 ) ) ;
#81944 = CARTESIAN_POINT ( 'NONE',  ( 9.474510206698729675, 16.51473224551082808, 27.08442372801900433 ) ) ;
#81945 = CARTESIAN_POINT ( 'NONE',  ( 5.823673210054444382, -21.52544592524334988, 90.20942372801903275 ) ) ;
#81946 = CARTESIAN_POINT ( 'NONE',  ( -10.72451020669898014, 18.67979575497178502, 65.41557627198102409 ) ) ;
#81947 = CARTESIAN_POINT ( 'NONE',  ( 16.53943276465976808, -0.05219959533910856209, 53.74890960531437401 ) ) ;
#81949 = CARTESIAN_POINT ( 'NONE',  ( 16.51473224551083163, -9.474510206698727899, 30.83442372801900433 ) ) ;
#81948 = CARTESIAN_POINT ( 'NONE',  ( 10.72451020669871369, 18.67979575497193778, 87.08442372801901854 ) ) ;
#81950 = CARTESIAN_POINT ( 'NONE',  ( -14.34966873604960291, -8.224510206698953496, 71.66557627198100988 ) ) ;
#81951 = CARTESIAN_POINT ( 'NONE',  ( 19.03943276465977164, -0.05219959533909143690, 28.74890960531435624 ) ) ;
#81952 = CARTESIAN_POINT ( 'NONE',  ( -13.97604488694547697, 13.89961937509957934, 63.12609039468566152 ) ) ;
#81953 = CARTESIAN_POINT ( 'NONE',  ( -4.483927247898539470, -16.52544592524342804, 32.29057627198102409 ) ) ;
#81954 = CARTESIAN_POINT ( 'NONE',  ( -21.53943276465977519, -0.05219959533937600094, 78.75109039468568994 ) ) ;
#81955 = CARTESIAN_POINT ( 'NONE',  ( -19.02544592524342804, 5.153800228976336051, 81.04057627198103830 ) ) ;
#81956 = CARTESIAN_POINT ( 'NONE',  ( 16.46253265017146816, 9.564922557961045513, 51.66775706135233293 ) ) ;
#81957 = CARTESIAN_POINT ( 'NONE',  ( 18.62759615963271287, -10.81492255796078972, 48.33224293864770260 ) ) ;
#81958 = CARTESIAN_POINT ( 'NONE',  ( 18.62759615963255655, 10.81492255796105972, 41.66775706135235424 ) ) ;
#81959 = CARTESIAN_POINT ( 'NONE',  ( 10.72451020669898902, -18.67979575497178502, 97.91557627198103830 ) ) ;
#81960 = CARTESIAN_POINT ( 'NONE',  ( 13.97604488694548053, -13.89961937509957401, 95.62609039468563310 ) ) ;
#81961 = CARTESIAN_POINT ( 'NONE',  ( -4.483927247898782831, 16.52544592524335698, 62.70942372801902565 ) ) ;
#81963 = CARTESIAN_POINT ( 'NONE',  ( -21.55341960407610458, -5.719274019375992779, 101.4572429386476955 ) ) ;
#81962 = DIRECTION ( 'NONE',  ( -0.000000000000000000, 0.000000000000000000, 1.000000000000000000 ) ) ;
#81964 = CARTESIAN_POINT ( 'NONE',  ( 4.379528057220339221, -16.55341960407611168, 107.7072429386476955 ) ) ;
#81965 = CARTESIAN_POINT ( 'NONE',  ( -17.50000000000011724, -3.292511757969963870, 29.93479729789457977 ) ) ;
#81966 = CARTESIAN_POINT ( 'NONE',  ( -12.14591786802326823, 12.06949235617739902, 33.12609039468569705 ) ) ;
#81967 = PRODUCT_RELATED_PRODUCT_CATEGORY ( 'part', '', ( #159611 ) ) ;
#81968 = CARTESIAN_POINT ( 'NONE',  ( -10.81492255796078084, -18.62759615963271287, 62.08224293864769550 ) ) ;
#81969 = CARTESIAN_POINT ( 'NONE',  ( 16.55341960407618274, -4.379528057220086978, 106.0427570613523471 ) ) ;
#81970 = CARTESIAN_POINT ( 'NONE',  ( 19.05341960407611168, 5.049401038298154454, 28.95724293864769550 ) ) ;
#81971 = CARTESIAN_POINT ( 'NONE',  ( 16.52544592524335698, 4.483927247898782831, 61.45942372801901854 ) ) ;
#81972 = CARTESIAN_POINT ( 'NONE',  ( -5.049401038297874678, -19.05341960407617918, 59.79275706135231871 ) ) ;
#81973 = CARTESIAN_POINT ( 'NONE',  ( 18.67979575497194134, -10.72451020669871369, 35.83442372801901143 ) ) ;
#81974 = CARTESIAN_POINT ( 'NONE',  ( 5.719274019375991003, -21.55341960407610458, 52.70724293864769550 ) ) ;
#81975 = CARTESIAN_POINT ( 'NONE',  ( -0.05219959533934338120, 16.53943276465976808, 92.50109039468567573 ) ) ;
#81976 = CARTESIAN_POINT ( 'NONE',  ( -15.72974639402176322, -15.80617190586768395, 74.37609039468568994 ) ) ;
#81977 = CARTESIAN_POINT ( 'NONE',  ( 0.05219959533907565091, 21.53943276465977519, 49.99890960531437401 ) ) ;
#81978 = CARTESIAN_POINT ( 'NONE',  ( 15.80617190586746368, 15.72974639402197994, 39.37390960531436690 ) ) ;
#81979 = EDGE_LOOP ( 'NONE', ( #3982, #157724, #70324, #80863 ) ) ;
#81980 = CARTESIAN_POINT ( 'NONE',  ( -4.483927247898782831, 16.52544592524335698, 72.70942372801901854 ) ) ;
#81981 = CARTESIAN_POINT ( 'NONE',  ( 5.719274019375991003, -21.55341960407610458, 27.70724293864769905 ) ) ;
#81982 = ORIENTED_EDGE ( 'NONE', *, *, #2501, .F. ) ;
#81983 = CARTESIAN_POINT ( 'NONE',  ( 16.46253265017160672, -9.564922557960803928, 103.3322429386476955 ) ) ;
#81984 = CARTESIAN_POINT ( 'NONE',  ( -8.314922557961024197, 14.29746914071037800, 107.9177570613523471 ) ) ;
#81985 = CARTESIAN_POINT ( 'NONE',  ( -24.43795752428855650, -7.704305290315005550, 171.8420761435737916 ) ) ;
#81986 = CARTESIAN_POINT ( 'NONE',  ( 16.52544592524342804, -4.483927247898539470, 103.5405762719810383 ) ) ;
#81987 = CARTESIAN_POINT ( 'NONE',  ( 21.55341960407610458, 5.719274019375980345, 58.95724293864770971 ) ) ;
#81988 = CARTESIAN_POINT ( 'NONE',  ( 4.483927247898790824, -16.52544592524335698, 90.20942372801903275 ) ) ;
#81989 = CARTESIAN_POINT ( 'NONE',  ( 0.05219959533937995610, -21.53943276465977519, 50.00109039468568994 ) ) ;
#81990 = CARTESIAN_POINT ( 'NONE',  ( 13.89961937509957401, 13.97604488694547697, 106.8760903946856757 ) ) ;
#81991 = CARTESIAN_POINT ( 'NONE',  ( -12.06949235617756955, 12.14591786802309770, 100.6239096053143811 ) ) ;
#81992 = CARTESIAN_POINT ( 'NONE',  ( 13.89961937509977652, -13.97604488694527269, 48.12390960531435979 ) ) ;
#81993 = CARTESIAN_POINT ( 'NONE',  ( 5.049401038298161559, -19.05341960407611168, 32.70724293864768129 ) ) ;
#81994 = CARTESIAN_POINT ( 'NONE',  ( 17.50000000000000355, -5.624438216177593652, 38.31670344914644488 ) ) ;
#81995 = CARTESIAN_POINT ( 'NONE',  ( -19.05341960407611168, -5.049401038298163336, 86.45724293864769550 ) ) ;
#81996 = CARTESIAN_POINT ( 'NONE',  ( -16.52544592524335698, -4.483927247898792601, 73.95942372801901854 ) ) ;
#81997 = CARTESIAN_POINT ( 'NONE',  ( 10.72451020669871369, 18.67979575497193778, 112.0844237280190185 ) ) ;
#81998 = CARTESIAN_POINT ( 'NONE',  ( 15.80617190586746368, 15.72974639402197994, 49.37390960531436690 ) ) ;
#81999 = CARTESIAN_POINT ( 'NONE',  ( 8.224510206698742110, 14.34966873604972548, 67.08442372801901854 ) ) ;
#82000 = CARTESIAN_POINT ( 'NONE',  ( -13.97604488694547697, 13.89961937509957934, 83.12609039468564731 ) ) ;
#82001 = EDGE_LOOP ( 'NONE', ( #144397, #36269, #115118, #138705 ) ) ;
#82002 = CARTESIAN_POINT ( 'NONE',  ( -5.153800228976328057, -19.02544592524343514, 37.29057627198102409 ) ) ;
#82003 = CARTESIAN_POINT ( 'NONE',  ( -16.51473224551069308, -9.474510206698971260, 81.66557627198103830 ) ) ;
#82004 = CARTESIAN_POINT ( 'NONE',  ( -9.564922557960796823, -16.46253265017161027, 37.08224293864768839 ) ) ;
#82005 = CARTESIAN_POINT ( 'NONE',  ( 5.049401038297881783, 19.05341960407617563, 72.29275706135234714 ) ) ;
#82006 = CARTESIAN_POINT ( 'NONE',  ( 21.94905633995417915, -8.886455535323333876, 171.4390084046505365 ) ) ;
#82007 = CARTESIAN_POINT ( 'NONE',  ( 16.51473224551069308, 9.474510206698969483, 99.16557627198102409 ) ) ;
#82008 = CARTESIAN_POINT ( 'NONE',  ( 16.55341960407611168, 4.379528057220329451, 53.95724293864770260 ) ) ;
#82009 = CARTESIAN_POINT ( 'NONE',  ( -5.823673210054116645, -21.52544592524344225, 62.29057627198102409 ) ) ;
#82010 = CARTESIAN_POINT ( 'NONE',  ( -17.50000000000000000, 3.345213924137368622, 104.5876862309435182 ) ) ;
#82011 = CARTESIAN_POINT ( 'NONE',  ( -0.05219959533936034679, 19.03943276465977164, 32.50109039468566863 ) ) ;
#82012 = CARTESIAN_POINT ( 'NONE',  ( 0.000000000000000000, 0.000000000000000000, -15.00000000000000000 ) ) ;
#82014 = CARTESIAN_POINT ( 'NONE',  ( 5.049401038298161559, -19.05341960407611168, 57.70724293864769550 ) ) ;
#82013 = CARTESIAN_POINT ( 'NONE',  ( 13.89961937509977652, -13.97604488694527269, 48.12390960531435979 ) ) ;
#82015 = CARTESIAN_POINT ( 'NONE',  ( -4.379528057220086978, -16.55341960407618274, 39.79275706135235424 ) ) ;
#82016 = CARTESIAN_POINT ( 'NONE',  ( -33.67956615508440876, -5.223713096473153961, 96.75862529643663379 ) ) ;
#82017 = CARTESIAN_POINT ( 'NONE',  ( -16.52216118717207038, 7.221426719304506747, 108.9240097895301318 ) ) ;
#82018 = CARTESIAN_POINT ( 'NONE',  ( -4.379528057220086978, -16.55341960407618274, 74.79275706135234714 ) ) ;
#82019 = CARTESIAN_POINT ( 'NONE',  ( -5.823673210054116645, -21.52544592524344225, 97.29057627198105251 ) ) ;
#82020 = CIRCLE ( 'NONE', #159989, 40.00000000000000000 ) ;
#82021 = CARTESIAN_POINT ( 'NONE',  ( 12.14591786802327356, -12.06949235617739191, 40.62609039468567573 ) ) ;
#82022 = CARTESIAN_POINT ( 'NONE',  ( 16.51473224551069308, 9.474510206698969483, 39.16557627198103120 ) ) ;
#82023 = CARTESIAN_POINT ( 'NONE',  ( 15.72974639402176855, 15.80617190586768217, 51.87609039468568284 ) ) ;
#82024 = CARTESIAN_POINT ( 'NONE',  ( -5.049401038297874678, -19.05341960407617918, 64.79275706135233293 ) ) ;
#82025 = CARTESIAN_POINT ( 'NONE',  ( -15.72974639402176322, -15.80617190586768395, 99.37609039468568994 ) ) ;
#82026 = CARTESIAN_POINT ( 'NONE',  ( 5.049401038298161559, -19.05341960407611168, 22.70724293864769194 ) ) ;
#82027 = CARTESIAN_POINT ( 'NONE',  ( -12.14591786802309592, -12.06949235617757132, 41.87390960531435979 ) ) ;
#82028 = CARTESIAN_POINT ( 'NONE',  ( 19.39720447994797325, 5.499999999999973355, 42.16317477297180005 ) ) ;
#82029 = CARTESIAN_POINT ( 'NONE',  ( 18.67979575497178502, 10.72451020669898547, 59.16557627198103120 ) ) ;
#82030 = CARTESIAN_POINT ( 'NONE',  ( -8.571926809382608425, 26.38167802310805854, 142.4750000027312069 ) ) ;
#82031 = CARTESIAN_POINT ( 'NONE',  ( -9.564922557960796823, -16.46253265017161027, 97.08224293864769550 ) ) ;
#82032 = CARTESIAN_POINT ( 'NONE',  ( 16.55341960407611168, 4.379528057220329451, 98.95724293864770971 ) ) ;
#82033 = CARTESIAN_POINT ( 'NONE',  ( 12.14591786802327356, -12.06949235617739191, 20.62609039468568639 ) ) ;
#82034 = CARTESIAN_POINT ( 'NONE',  ( 8.314922557961029526, -14.29746914071037800, 105.4177570613523613 ) ) ;
#82035 = VERTEX_POINT ( 'NONE', #92793 ) ;
#82036 = CIRCLE ( 'NONE', #95345, 38.00000000000000000 ) ;
#82037 = CARTESIAN_POINT ( 'NONE',  ( 10.81492255796078972, 18.62759615963270932, 104.5822429386477097 ) ) ;
#82039 = CARTESIAN_POINT ( 'NONE',  ( 13.97604488694527802, 13.89961937509977652, 114.3739096053143669 ) ) ;
#82038 = CARTESIAN_POINT ( 'NONE',  ( 4.483927247898545687, 16.52544592524342804, 24.79057627198103120 ) ) ;
#82040 = CARTESIAN_POINT ( 'NONE',  ( 5.049401038297881783, 19.05341960407617563, 87.29275706135234714 ) ) ;
#82041 = CARTESIAN_POINT ( 'NONE',  ( -5.719274019375665041, -21.55341960407619695, 104.7927570613523898 ) ) ;
#82042 = CARTESIAN_POINT ( 'NONE',  ( 8.314922557960818139, 14.29746914071049879, 24.58224293864768839 ) ) ;
#82044 = EDGE_CURVE ( 'NONE', #191474, #185826, #156105, .T. ) ;
#82043 = CARTESIAN_POINT ( 'NONE',  ( -0.05219959533907301413, -21.53943276465977519, 87.49890960531436690 ) ) ;
#82045 = CARTESIAN_POINT ( 'NONE',  ( -5.719274019375978568, 21.55341960407610458, 55.20724293864770260 ) ) ;
#82046 = VECTOR ( 'NONE', #60912, 1000.000000000000000 ) ;
#82047 = CARTESIAN_POINT ( 'NONE',  ( 19.03943276465977164, -0.05219959533909143690, 58.74890960531435979 ) ) ;
#82048 = CARTESIAN_POINT ( 'NONE',  ( 16.55341960407611168, 4.379528057220329451, 28.95724293864769905 ) ) ;
#82049 = CARTESIAN_POINT ( 'NONE',  ( 5.153800228976335163, 19.02544592524342804, 79.79057627198102409 ) ) ;
#82050 = CARTESIAN_POINT ( 'NONE',  ( 19.48894818550245844, -5.499999999999921840, 62.60307310435241135 ) ) ;
#82051 = CARTESIAN_POINT ( 'NONE',  ( 9.564922557961047289, -16.46253265017146816, 40.41775706135234003 ) ) ;
#82052 = CARTESIAN_POINT ( 'NONE',  ( -21.55341960407610458, -5.719274019375992779, 81.45724293864769550 ) ) ;
#82053 = CARTESIAN_POINT ( 'NONE',  ( 12.14591786802309770, 12.06949235617756955, 89.37390960531435269 ) ) ;
#82054 = AXIS2_PLACEMENT_3D ( 'NONE', #82060, #99242, #83075 ) ;
#82055 = CARTESIAN_POINT ( 'NONE',  ( -18.67979575497193778, 10.72451020669871902, 38.33442372801900433 ) ) ;
#82056 = CARTESIAN_POINT ( 'NONE',  ( 27.73933785331498569, 2.768321779492822058E-14, 139.8750000027311842 ) ) ;
#82057 = CARTESIAN_POINT ( 'NONE',  ( 12.06949235617739724, 12.14591786802326823, 106.8760903946856899 ) ) ;
#82058 = CARTESIAN_POINT ( 'NONE',  ( 19.02544592524343514, -5.153800228976328945, 38.54057627198103120 ) ) ;
#82059 = CARTESIAN_POINT ( 'NONE',  ( -9.564922557960796823, -16.46253265017161027, 87.08224293864769550 ) ) ;
#82060 = CARTESIAN_POINT ( 'NONE',  ( 0.000000000000000000, 0.000000000000000000, 0.000000000000000000 ) ) ;
#82061 = CARTESIAN_POINT ( 'NONE',  ( -9.474510206698964154, 16.51473224551069663, 35.41557627198102409 ) ) ;
#82062 = CARTESIAN_POINT ( 'NONE',  ( 4.379528057220339221, -16.55341960407611168, 47.70724293864770260 ) ) ;
#82063 = CARTESIAN_POINT ( 'NONE',  ( -18.67979575497193778, 10.72451020669871902, 73.33442372801901854 ) ) ;
#82065 = CARTESIAN_POINT ( 'NONE',  ( 0.05219959533934541429, -16.53943276465976808, 65.00109039468568994 ) ) ;
#82064 = CARTESIAN_POINT ( 'NONE',  ( 33.17841651222155974, -18.64421535753841397, -21.40882326905910560 ) ) ;
#82066 = CARTESIAN_POINT ( 'NONE',  ( -19.05341960407611168, -5.049401038298163336, 41.45724293864769550 ) ) ;
#82067 = CARTESIAN_POINT ( 'NONE',  ( -19.02544592524342804, 5.153800228976336051, 56.04057627198100988 ) ) ;
#82068 = ORIENTED_EDGE ( 'NONE', *, *, #181804, .T. ) ;
#82069 = CARTESIAN_POINT ( 'NONE',  ( -5.823673210054431948, 21.52544592524334988, 112.7094237280190328 ) ) ;
#82070 = CARTESIAN_POINT ( 'NONE',  ( 14.34966873604972726, -8.224510206698740333, 55.83442372801901854 ) ) ;
#82071 = CARTESIAN_POINT ( 'NONE',  ( 0.05219959533937995610, -21.53943276465977519, 100.0010903946857042 ) ) ;
#82072 = CARTESIAN_POINT ( 'NONE',  ( -21.53943276465977519, 0.05219959533907696930, 41.24890960531435269 ) ) ;
#82073 = CARTESIAN_POINT ( 'NONE',  ( 16.51473224551083163, -9.474510206698727899, 105.8344237280190043 ) ) ;
#82074 = CARTESIAN_POINT ( 'NONE',  ( 18.62759615963255655, 10.81492255796105972, 66.66775706135234714 ) ) ;
#82075 = CARTESIAN_POINT ( 'NONE',  ( 12.06949235617739724, 12.14591786802326823, 31.87609039468567929 ) ) ;
#82076 = CARTESIAN_POINT ( 'NONE',  ( 5.823673210054125526, 21.52544592524343514, 104.7905762719810241 ) ) ;
#82077 = CARTESIAN_POINT ( 'NONE',  ( 9.564922557961047289, -16.46253265017146816, 95.41775706135233293 ) ) ;
#82078 = CARTESIAN_POINT ( 'NONE',  ( -16.51473224551069308, -9.474510206698971260, 71.66557627198102409 ) ) ;
#82079 = CARTESIAN_POINT ( 'NONE',  ( 16.51473224551083163, -9.474510206698727899, 110.8344237280190043 ) ) ;
#82080 = AXIS2_PLACEMENT_3D ( 'NONE', #194047, #192022, #24193 ) ;
#82081 = CARTESIAN_POINT ( 'NONE',  ( 9.474510206698729675, 16.51473224551082808, 102.0844237280190043 ) ) ;
#82082 = CARTESIAN_POINT ( 'NONE',  ( 12.06949235617757843, -12.14591786802309237, 63.12390960531435979 ) ) ;
#82083 = CARTESIAN_POINT ( 'NONE',  ( -12.14591786802326823, 12.06949235617739902, 73.12609039468567573 ) ) ;
#82085 = CARTESIAN_POINT ( 'NONE',  ( 9.474510206698971260, -16.51473224551069308, 57.91557627198103120 ) ) ;
#82084 = CARTESIAN_POINT ( 'NONE',  ( 21.55341960407619695, -5.719274019375665929, 21.04275706135234714 ) ) ;
#82086 = CARTESIAN_POINT ( 'NONE',  ( -0.05219959533909027116, -19.03943276465977164, 52.49890960531436690 ) ) ;
#82087 = CARTESIAN_POINT ( 'NONE',  ( 4.379528057220092307, 16.55341960407617563, 67.29275706135234714 ) ) ;
#82088 = CARTESIAN_POINT ( 'NONE',  ( 27.73933785331498214, 9.013057229001095294, 142.4750000027311785 ) ) ;
#82089 = EDGE_CURVE ( 'NONE', #166090, #17663, #167461, .T. ) ;
#82090 = CARTESIAN_POINT ( 'NONE',  ( -28.82186960331499037, 2.428612866367529932E-14, 148.2500000054623683 ) ) ;
#82091 = ORIENTED_EDGE ( 'NONE', *, *, #14309, .T. ) ;
#82092 = CARTESIAN_POINT ( 'NONE',  ( 10.72451020669871369, 18.67979575497193778, 112.0844237280190185 ) ) ;
#82093 = CARTESIAN_POINT ( 'NONE',  ( -19.03943276465977164, 0.05219959533909376836, 21.24890960531436335 ) ) ;
#82094 = ORIENTED_EDGE ( 'NONE', *, *, #131324, .F. ) ;
#82095 = CARTESIAN_POINT ( 'NONE',  ( -19.03943276465977164, -0.05219959533935918106, 113.7510903946856757 ) ) ;
#82096 = CARTESIAN_POINT ( 'NONE',  ( -21.52544592524343514, 5.823673210054127303, 46.04057627198103830 ) ) ;
#82098 = CARTESIAN_POINT ( 'NONE',  ( -12.06949235617739369, -12.14591786802326823, 34.37609039468568284 ) ) ;
#82097 = CARTESIAN_POINT ( 'NONE',  ( -19.02544592524334988, -5.153800228976617603, 48.95942372801900433 ) ) ;
#82099 = CARTESIAN_POINT ( 'NONE',  ( -13.89961937509977652, 13.97604488694528158, 40.62390960531435979 ) ) ;
#82100 = CARTESIAN_POINT ( 'NONE',  ( -19.05341960407611168, -5.049401038298163336, 46.45724293864768129 ) ) ;
#82101 = CARTESIAN_POINT ( 'NONE',  ( -21.52544592524343514, 5.823673210054127303, 81.04057627198102409 ) ) ;
#82102 = LINE ( 'NONE', #97273, #14909 ) ;
#82103 = CARTESIAN_POINT ( 'NONE',  ( -0.05219959533909027116, -19.03943276465977164, 52.49890960531436690 ) ) ;
#82104 = CARTESIAN_POINT ( 'NONE',  ( -17.14385361876520975, 23.59649016807275856, 149.0750000027312012 ) ) ;
#82105 = CARTESIAN_POINT ( 'NONE',  ( 16.46253265017146816, 9.564922557961045513, 91.66775706135234714 ) ) ;
#82106 = CARTESIAN_POINT ( 'NONE',  ( -14.29746914071049879, 8.314922557960819915, 60.83224293864769550 ) ) ;
#82107 = CARTESIAN_POINT ( 'NONE',  ( -5.153800228976607833, 19.02544592524334988, 27.70942372801899722 ) ) ;
#82108 = TOROIDAL_SURFACE ( 'NONE', #40149, 2.700000000000000622, 0.2000000000000000111 ) ;
#82109 = CARTESIAN_POINT ( 'NONE',  ( 5.719274019375991003, -21.55341960407610458, 92.70724293864770971 ) ) ;
#82110 = CARTESIAN_POINT ( 'NONE',  ( -21.55341960407619339, 5.719274019375674811, 83.54275706135234714 ) ) ;
#82111 = CARTESIAN_POINT ( 'NONE',  ( 19.02544592524343514, -5.153800228976328945, 23.54057627198102054 ) ) ;
#82112 = CARTESIAN_POINT ( 'NONE',  ( -21.52544592524334988, -5.823673210054445271, 83.95942372801900433 ) ) ;
#82114 = CARTESIAN_POINT ( 'NONE',  ( -10.72451020669870658, -18.67979575497194134, 74.58442372801901854 ) ) ;
#82113 = CARTESIAN_POINT ( 'NONE',  ( -16.55341960407611168, -4.379528057220339221, 21.45724293864769550 ) ) ;
#82115 = CARTESIAN_POINT ( 'NONE',  ( -0.05219959533909027116, -19.03943276465977164, 67.49890960531436690 ) ) ;
#82116 = CARTESIAN_POINT ( 'NONE',  ( 21.55341960407619695, -5.719274019375665929, 41.04275706135236135 ) ) ;
#82117 = CARTESIAN_POINT ( 'NONE',  ( -19.05341960407611168, -5.049401038298163336, 81.45724293864769550 ) ) ;
#82118 = CARTESIAN_POINT ( 'NONE',  ( 4.379528057220339221, -16.55341960407611168, 92.70724293864770971 ) ) ;
#82119 = CARTESIAN_POINT ( 'NONE',  ( -16.55341960407611168, -4.379528057220339221, 56.45724293864768839 ) ) ;
#82120 = CARTESIAN_POINT ( 'NONE',  ( 15.72974639402199770, -15.80617190586745480, 68.12390960531436690 ) ) ;
#82121 = CARTESIAN_POINT ( 'NONE',  ( 5.153800228976335163, 19.02544592524342804, 54.79057627198103120 ) ) ;
#82122 = CARTESIAN_POINT ( 'NONE',  ( -18.62759615963270932, 10.81492255796079327, 90.83224293864769550 ) ) ;
#82123 = CARTESIAN_POINT ( 'NONE',  ( 19.05341960407617918, -5.049401038297876454, 61.04275706135232582 ) ) ;
#82125 = CARTESIAN_POINT ( 'NONE',  ( -16.55341960407611168, -4.379528057220339221, 81.45724293864769550 ) ) ;
#82124 = CARTESIAN_POINT ( 'NONE',  ( 13.97604488694548053, -13.89961937509957401, 30.62609039468566863 ) ) ;
#82126 = CARTESIAN_POINT ( 'NONE',  ( -21.53943276465977519, 0.05219959533907696930, 56.24890960531436690 ) ) ;
#82127 = CARTESIAN_POINT ( 'NONE',  ( 17.40805194822031510, 6.112264579159339739, 101.6662872748938895 ) ) ;
#82129 = CARTESIAN_POINT ( 'NONE',  ( 17.14385361876520264, -23.59649016807270883, 148.0750000027312012 ) ) ;
#82128 = CARTESIAN_POINT ( 'NONE',  ( 8.314922557961029526, -14.29746914071037800, 95.41775706135234714 ) ) ;
#82130 = CARTESIAN_POINT ( 'NONE',  ( 19.05341960407617918, -5.049401038297876454, 96.04275706135231871 ) ) ;
#82131 = CARTESIAN_POINT ( 'NONE',  ( -0.05219959533910754901, -16.53943276465976808, 67.49890960531436690 ) ) ;
#82132 = DIRECTION ( 'NONE',  ( 0.000000000000000000, 0.000000000000000000, -1.000000000000000000 ) ) ;
#82133 = CARTESIAN_POINT ( 'NONE',  ( -13.97604488694527625, -13.89961937509977652, 56.87390960531434558 ) ) ;
#82134 = CARTESIAN_POINT ( 'NONE',  ( -12.06949235617756955, 12.14591786802309770, 55.62390960531436690 ) ) ;
#82135 = CARTESIAN_POINT ( 'NONE',  ( 0.05219959533909260263, 19.03943276465977164, 99.99890960531436690 ) ) ;
#82137 = CARTESIAN_POINT ( 'NONE',  ( 9.474510206698971260, -16.51473224551069308, 67.91557627198102409 ) ) ;
#82136 = CARTESIAN_POINT ( 'NONE',  ( -9.564922557961040184, 16.46253265017147172, 72.91775706135233293 ) ) ;
#82138 = CARTESIAN_POINT ( 'NONE',  ( -16.46253265017160317, 9.564922557960807481, 85.83224293864769550 ) ) ;
#82139 = CARTESIAN_POINT ( 'NONE',  ( 19.02544592524343514, -5.153800228976328945, 83.54057627198100988 ) ) ;
#82140 = CARTESIAN_POINT ( 'NONE',  ( -21.55341960407610458, -5.719274019375992779, 56.45724293864768839 ) ) ;
#82141 = CARTESIAN_POINT ( 'NONE',  ( -16.53943276465976808, -0.05219959533934237506, 53.75109039468568994 ) ) ;
#82142 = CARTESIAN_POINT ( 'NONE',  ( -5.049401038298153566, 19.05341960407611168, 45.20724293864769550 ) ) ;
#82143 = CARTESIAN_POINT ( 'NONE',  ( -15.72974639402197994, 15.80617190586746368, 50.62390960531435979 ) ) ;
#82144 = CARTESIAN_POINT ( 'NONE',  ( 9.564922557961047289, -16.46253265017146816, 95.41775706135233293 ) ) ;
#82146 = CARTESIAN_POINT ( 'NONE',  ( -10.72451020669870658, -18.67979575497194134, 34.58442372801900433 ) ) ;
#82145 = CARTESIAN_POINT ( 'NONE',  ( -8.314922557960811034, -14.29746914071050412, 22.08224293864769194 ) ) ;
#82147 = CARTESIAN_POINT ( 'NONE',  ( -9.564922557961040184, 16.46253265017147172, 32.91775706135233293 ) ) ;
#82149 = CARTESIAN_POINT ( 'NONE',  ( -14.29746914071037622, -8.314922557961029526, 89.16775706135236135 ) ) ;
#82148 = CARTESIAN_POINT ( 'NONE',  ( 12.06949235617739724, 12.14591786802326823, 56.87609039468568994 ) ) ;
#82150 = CARTESIAN_POINT ( 'NONE',  ( 19.36337904590693881, -5.499999999999945821, 42.91494137495619299 ) ) ;
#82151 = CARTESIAN_POINT ( 'NONE',  ( -14.34966873604972548, 8.224510206698743886, 83.33442372801903275 ) ) ;
#82153 = CARTESIAN_POINT ( 'NONE',  ( 8.224510206698742110, 14.34966873604972548, 37.08442372801901143 ) ) ;
#82152 = CARTESIAN_POINT ( 'NONE',  ( -10.81492255796078084, -18.62759615963271287, 22.08224293864769194 ) ) ;
#82154 = CARTESIAN_POINT ( 'NONE',  ( -5.049401038298153566, 19.05341960407611168, 50.20724293864770260 ) ) ;
#82155 = CARTESIAN_POINT ( 'NONE',  ( 9.564922557960805705, 16.46253265017160317, 44.58224293864769550 ) ) ;
#82156 = CARTESIAN_POINT ( 'NONE',  ( 9.474510206698971260, -16.51473224551069308, 62.91557627198102409 ) ) ;
#82157 = CARTESIAN_POINT ( 'NONE',  ( 10.81492255796106328, -18.62759615963255655, 45.41775706135234003 ) ) ;
#82158 = CARTESIAN_POINT ( 'NONE',  ( -12.14591786802326823, 12.06949235617739902, 48.12609039468568284 ) ) ;
#82159 = CARTESIAN_POINT ( 'NONE',  ( 14.29746914071037800, 8.314922557961029526, 106.6677570613523756 ) ) ;
#82160 = CARTESIAN_POINT ( 'NONE',  ( -0.05219959533909027116, -19.03943276465977164, 27.49890960531435624 ) ) ;
#82161 = CARTESIAN_POINT ( 'NONE',  ( -9.474510206698720793, -16.51473224551083518, 24.58442372801900078 ) ) ;
#82162 = CARTESIAN_POINT ( 'NONE',  ( -9.474510206698720793, -16.51473224551083518, 109.5844237280190043 ) ) ;
#82163 = CARTESIAN_POINT ( 'NONE',  ( 9.564922557961047289, -16.46253265017146816, 65.41775706135233293 ) ) ;
#82164 = CARTESIAN_POINT ( 'NONE',  ( -12.14591786802309592, -12.06949235617757132, 71.87390960531438111 ) ) ;
#82165 = CARTESIAN_POINT ( 'NONE',  ( 0.05219959533909260263, 19.03943276465977164, 34.99890960531435979 ) ) ;
#82167 = CARTESIAN_POINT ( 'NONE',  ( 16.38665767535053064, 7.295008042176054808, 77.23599135785458714 ) ) ;
#82166 = CARTESIAN_POINT ( 'NONE',  ( -19.02544592524334988, -5.153800228976617603, 78.95942372801900433 ) ) ;
#82168 = CARTESIAN_POINT ( 'NONE',  ( -21.52544592524334988, -5.823673210054445271, 73.95942372801901854 ) ) ;
#82169 = CARTESIAN_POINT ( 'NONE',  ( -4.379528057220086978, -16.55341960407618274, 39.79275706135235424 ) ) ;
#82170 = CARTESIAN_POINT ( 'NONE',  ( -17.50000000000012434, 3.417042746627156014, 25.17380396232484685 ) ) ;
#82171 = CARTESIAN_POINT ( 'NONE',  ( 10.72451020669898902, -18.67979575497178502, 37.91557627198102409 ) ) ;
#82172 = CARTESIAN_POINT ( 'NONE',  ( 4.483927247898790824, -16.52544592524335698, 30.20942372801902565 ) ) ;
#82173 = CARTESIAN_POINT ( 'NONE',  ( -5.049401038298153566, 19.05341960407611168, 25.20724293864768839 ) ) ;
#82174 = CARTESIAN_POINT ( 'NONE',  ( -19.03943276465977164, -0.05219959533935918106, 23.75109039468566152 ) ) ;
#82175 = DIRECTION ( 'NONE',  ( 0.000000000000000000, 0.000000000000000000, -1.000000000000000000 ) ) ;
#82176 = CARTESIAN_POINT ( 'NONE',  ( 13.97604488694527802, 13.89961937509977652, 39.37390960531435269 ) ) ;
#82177 = DIRECTION ( 'NONE',  ( 0.000000000000000000, 0.000000000000000000, -1.000000000000000000 ) ) ;
#82178 = CARTESIAN_POINT ( 'NONE',  ( 13.97604488694527802, 13.89961937509977652, 59.37390960531434558 ) ) ;
#82179 = CARTESIAN_POINT ( 'NONE',  ( 17.49999999999999289, -4.640572885337564735, 113.1378816454884344 ) ) ;
#82180 = CARTESIAN_POINT ( 'NONE',  ( 16.46253265017146816, 9.564922557961045513, 26.66775706135234003 ) ) ;
#82181 = CARTESIAN_POINT ( 'NONE',  ( 8.314922557960818139, 14.29746914071049879, 24.58224293864768839 ) ) ;
#82182 = CARTESIAN_POINT ( 'NONE',  ( 9.474510206698971260, -16.51473224551069308, 27.91557627198103120 ) ) ;
#82183 = EDGE_CURVE ( 'NONE', #114473, #119772, #146425, .T. ) ;
#82184 = VECTOR ( 'NONE', #150798, 1000.000000000000000 ) ;
#82185 = CARTESIAN_POINT ( 'NONE',  ( -16.46253265017160317, 9.564922557960807481, 90.83224293864769550 ) ) ;
#82186 = CARTESIAN_POINT ( 'NONE',  ( -21.55341960407619339, 5.719274019375674811, 63.54275706135234003 ) ) ;
#82187 = CARTESIAN_POINT ( 'NONE',  ( 19.02544592524343514, -5.153800228976328945, 33.54057627198102409 ) ) ;
#82188 = CARTESIAN_POINT ( 'NONE',  ( -0.05219959533937732626, 21.53943276465977519, 67.50109039468568994 ) ) ;
#82190 = CARTESIAN_POINT ( 'NONE',  ( 10.72451020669898902, -18.67979575497178502, 27.91557627198103830 ) ) ;
#82189 = CARTESIAN_POINT ( 'NONE',  ( -19.02544592524334988, -5.153800228976617603, 98.95942372801900433 ) ) ;
#82191 = CARTESIAN_POINT ( 'NONE',  ( -9.564922557960796823, -16.46253265017161027, 32.08224293864769550 ) ) ;
#82192 = CARTESIAN_POINT ( 'NONE',  ( -10.72451020669898014, 18.67979575497178502, 115.4155762719810241 ) ) ;
#82193 = CARTESIAN_POINT ( 'NONE',  ( -19.03943276465977164, -0.05219959533935918106, 33.75109039468566863 ) ) ;
#82194 = CARTESIAN_POINT ( 'NONE',  ( -16.53943276465976808, 0.05219959533911058130, 116.2489096053143669 ) ) ;
#82195 = CARTESIAN_POINT ( 'NONE',  ( 19.03943276465977164, -0.05219959533909143690, 68.74890960531436690 ) ) ;
#82197 = MECHANICAL_DESIGN_GEOMETRIC_PRESENTATION_REPRESENTATION (  '', ( #179109 ), #33882 ) ;
#82196 = CARTESIAN_POINT ( 'NONE',  ( -16.51473224551082808, 9.474510206698731452, 113.3344237280190043 ) ) ;
#82198 = CARTESIAN_POINT ( 'NONE',  ( -14.34966873604960291, -8.224510206698953496, 81.66557627198103830 ) ) ;
#82199 = CARTESIAN_POINT ( 'NONE',  ( -0.05219959533907301413, -21.53943276465977519, 22.49890960531436335 ) ) ;
#82200 = CARTESIAN_POINT ( 'NONE',  ( -16.51473224551082808, 9.474510206698731452, 83.33442372801899012 ) ) ;
#82201 = CARTESIAN_POINT ( 'NONE',  ( 10.81492255796078972, 18.62759615963270932, 89.58224293864768129 ) ) ;
#82202 = CARTESIAN_POINT ( 'NONE',  ( 21.53943276465977519, 0.05219959533937863772, 46.25109039468567573 ) ) ;
#82203 = CARTESIAN_POINT ( 'NONE',  ( 16.52544592524335698, 4.483927247898782831, 56.45942372801902565 ) ) ;
#82205 = CARTESIAN_POINT ( 'NONE',  ( -10.72451020669870658, -18.67979575497194134, 44.58442372801901854 ) ) ;
#82204 = CARTESIAN_POINT ( 'NONE',  ( 12.06949235617739724, 12.14591786802326823, 51.87609039468568284 ) ) ;
#82206 = CARTESIAN_POINT ( 'NONE',  ( 21.55341960407610458, 5.719274019375980345, 48.95724293864770971 ) ) ;
#82207 = STYLED_ITEM ( 'NONE', ( #178881 ), #51975 ) ;
#82208 = CARTESIAN_POINT ( 'NONE',  ( 9.474510206698971260, -16.51473224551069308, 47.91557627198102409 ) ) ;
#82209 = CARTESIAN_POINT ( 'NONE',  ( 37.99999999999999289, 2.893978650043524126E-14, -2.749999994537626780 ) ) ;
#82210 = CARTESIAN_POINT ( 'NONE',  ( 0.05219959533934541429, -16.53943276465976808, 80.00109039468568994 ) ) ;
#82211 = CARTESIAN_POINT ( 'NONE',  ( 15.80617190586746368, 15.72974639402197994, 104.3739096053143669 ) ) ;
#82212 = CARTESIAN_POINT ( 'NONE',  ( 12.06949235617757843, -12.14591786802309237, 48.12390960531436690 ) ) ;
#82213 = CARTESIAN_POINT ( 'NONE',  ( -14.34966873604972548, 8.224510206698743886, 68.33442372801900433 ) ) ;
#82214 = CARTESIAN_POINT ( 'NONE',  ( 5.153800228976615827, -19.02544592524334988, 105.2094237280190185 ) ) ;
#82215 = CARTESIAN_POINT ( 'NONE',  ( -18.62759615963270932, 10.81492255796079327, 100.8322429386477097 ) ) ;
#82216 = CARTESIAN_POINT ( 'NONE',  ( 4.379528057220339221, -16.55341960407611168, 47.70724293864770260 ) ) ;
#82217 = EDGE_CURVE ( 'NONE', #2480, #69839, #35108, .T. ) ;
#82218 = ORIENTED_EDGE ( 'NONE', *, *, #3863, .F. ) ;
#82219 = PLANE ( 'NONE',  #176125 ) ;
#82220 = CARTESIAN_POINT ( 'NONE',  ( 21.52544592524344225, -5.823673210054117533, 78.54057627198103830 ) ) ;
#82221 = CARTESIAN_POINT ( 'NONE',  ( 16.55341960407611168, 4.379528057220329451, 28.95724293864769905 ) ) ;
#82222 = ORIENTED_EDGE ( 'NONE', *, *, #178686, .T. ) ;
#82223 = CARTESIAN_POINT ( 'NONE',  ( -16.52216118717207038, -7.221426719304521846, 56.07599021046991083 ) ) ;
#82224 = CARTESIAN_POINT ( 'NONE',  ( -18.62759615963270932, 10.81492255796079327, 105.8322429386476955 ) ) ;
#82225 = CARTESIAN_POINT ( 'NONE',  ( -21.53943276465977519, 0.05219959533907696930, 111.2489096053143669 ) ) ;
#82226 = CARTESIAN_POINT ( 'NONE',  ( -16.53943276465976808, 0.05219959533911058130, 41.24890960531435269 ) ) ;
#82228 = CARTESIAN_POINT ( 'NONE',  ( 16.53943276465976808, 0.05219959533934440121, 51.25109039468568994 ) ) ;
#82227 = AXIS2_PLACEMENT_3D ( 'NONE', #101966, #59434, #150480 ) ;
#82229 = CARTESIAN_POINT ( 'NONE',  ( 13.97604488694527802, 13.89961937509977652, 44.37390960531435269 ) ) ;
#82230 = CARTESIAN_POINT ( 'NONE',  ( 13.89961937509977652, -13.97604488694527269, 73.12390960531436690 ) ) ;
#82231 = ORIENTED_EDGE ( 'NONE', *, *, #114246, .F. ) ;
#82232 = CARTESIAN_POINT ( 'NONE',  ( 10.81492255796078972, 18.62759615963270932, 39.58224293864769550 ) ) ;
#82233 = CARTESIAN_POINT ( 'NONE',  ( -26.63963442026891570, -26.88931099783081180, -16.54750829168120418 ) ) ;
#82234 = CARTESIAN_POINT ( 'NONE',  ( -19.02544592524334988, -5.153800228976617603, 108.9594237280189759 ) ) ;
#82235 = CARTESIAN_POINT ( 'NONE',  ( 13.97604488694548053, -13.89961937509957401, 45.62609039468566863 ) ) ;
#82236 = CARTESIAN_POINT ( 'NONE',  ( -21.52544592524343514, 5.823673210054127303, 106.0405762719810525 ) ) ;
#82237 = CARTESIAN_POINT ( 'NONE',  ( -16.55341960407611168, -4.379528057220339221, 31.45724293864769550 ) ) ;
#82238 = CARTESIAN_POINT ( 'NONE',  ( -5.049401038298153566, 19.05341960407611168, 80.20724293864769550 ) ) ;
#82239 = CARTESIAN_POINT ( 'NONE',  ( 10.81492255796078972, 18.62759615963270932, 49.58224293864769550 ) ) ;
#82241 = CARTESIAN_POINT ( 'NONE',  ( 4.379528057220092307, 16.55341960407617563, 22.29275706135235069 ) ) ;
#82240 = CARTESIAN_POINT ( 'NONE',  ( 15.80617190586746368, 15.72974639402197994, 84.37390960531438111 ) ) ;
#82242 = CARTESIAN_POINT ( 'NONE',  ( -21.55341960407610458, -5.719274019375992779, 21.45724293864769550 ) ) ;
#82243 = CARTESIAN_POINT ( 'NONE',  ( -18.67979575497193778, 10.72451020669871902, 78.33442372801901854 ) ) ;
#82244 = CARTESIAN_POINT ( 'NONE',  ( 19.03943276465977164, -0.05219959533909143690, 68.74890960531436690 ) ) ;
#82245 = CARTESIAN_POINT ( 'NONE',  ( -0.05219959533909027116, -19.03943276465977164, 32.49890960531435979 ) ) ;
#82246 = CARTESIAN_POINT ( 'NONE',  ( -5.049401038298153566, 19.05341960407611168, 80.20724293864769550 ) ) ;
#82247 = CARTESIAN_POINT ( 'NONE',  ( -8.314922557960811034, -14.29746914071050412, 97.08224293864770971 ) ) ;
#82248 = ORIENTED_EDGE ( 'NONE', *, *, #50678, .F. ) ;
#82249 = CARTESIAN_POINT ( 'NONE',  ( 13.89961937509957401, 13.97604488694547697, 106.8760903946856757 ) ) ;
#82250 = CARTESIAN_POINT ( 'NONE',  ( 17.49999999999999645, -5.500000000000031086, 83.29690382534172954 ) ) ;
#82251 = CARTESIAN_POINT ( 'NONE',  ( -19.05341960407611168, -5.049401038298163336, 71.45724293864766707 ) ) ;
#82253 = CARTESIAN_POINT ( 'NONE',  ( -9.564922557960796823, -16.46253265017161027, 112.0822429386476955 ) ) ;
#82252 = CARTESIAN_POINT ( 'NONE',  ( 0.05219959533937995610, -21.53943276465977519, 85.00109039468568994 ) ) ;
#82254 = CARTESIAN_POINT ( 'NONE',  ( -0.05219959533934338120, 16.53943276465976808, 77.50109039468567573 ) ) ;
#82255 = CARTESIAN_POINT ( 'NONE',  ( -17.05116617787826527, -6.768360034955819948, 76.34324446740801307 ) ) ;
#82256 = CARTESIAN_POINT ( 'NONE',  ( -16.46253265017146816, -9.564922557961047289, 54.16775706135234003 ) ) ;
#82257 = CARTESIAN_POINT ( 'NONE',  ( 15.80617190586769283, -15.72974639402175789, 110.6260903946857042 ) ) ;
#82258 = DIRECTION ( 'NONE',  ( -0.8437662581494472791, 0.5367108174878539861, 0.000000000000000000 ) ) ;
#82259 = LINE ( 'NONE', #5431, #179029 ) ;
#82260 = CARTESIAN_POINT ( 'NONE',  ( 36.91746824999999177, 2.880721459617395097E-14, -6.124999997268813168 ) ) ;
#82261 = CARTESIAN_POINT ( 'NONE',  ( -0.05219959533910754901, -16.53943276465976808, 27.49890960531435269 ) ) ;
#82262 = FACE_OUTER_BOUND ( 'NONE', #76152, .T. ) ;
#82263 = CARTESIAN_POINT ( 'NONE',  ( 12.06949235617739724, 12.14591786802326823, 101.8760903946857042 ) ) ;
#82264 = CARTESIAN_POINT ( 'NONE',  ( 30.66720998790079022, -25.69103205420833902, -17.62974664729441798 ) ) ;
#82265 = CARTESIAN_POINT ( 'NONE',  ( 8.224510206698742110, 14.34966873604972548, 82.08442372801901854 ) ) ;
#82266 = CARTESIAN_POINT ( 'NONE',  ( 5.823673210054444382, -21.52544592524334988, 95.20942372801903275 ) ) ;
#82267 = CARTESIAN_POINT ( 'NONE',  ( -16.46253265017146816, -9.564922557961047289, 104.1677570613523329 ) ) ;
#82268 = CARTESIAN_POINT ( 'NONE',  ( 18.62759615963255655, 10.81492255796105972, 61.66775706135235424 ) ) ;
#82269 = CARTESIAN_POINT ( 'NONE',  ( 19.05341960407617918, -5.049401038297876454, 41.04275706135233293 ) ) ;
#82270 = CARTESIAN_POINT ( 'NONE',  ( 9.564922557960805705, 16.46253265017160317, 79.58224293864769550 ) ) ;
#82271 = CARTESIAN_POINT ( 'NONE',  ( 5.153800228976335163, 19.02544592524342804, 59.79057627198100988 ) ) ;
#82272 = CARTESIAN_POINT ( 'NONE',  ( -13.97604488694527625, -13.89961937509977830, 86.87390960531436690 ) ) ;
#82273 = CARTESIAN_POINT ( 'NONE',  ( 15.72974639402199770, -15.80617190586745480, 93.12390960531436690 ) ) ;
#82274 = CARTESIAN_POINT ( 'NONE',  ( 5.719274019375991003, -21.55341960407610458, 47.70724293864770260 ) ) ;
#82275 = CARTESIAN_POINT ( 'NONE',  ( -16.46253265017160317, 9.564922557960807481, 45.83224293864769550 ) ) ;
#82276 = CARTESIAN_POINT ( 'NONE',  ( -16.55341960407617563, 4.379528057220093196, 63.54275706135234003 ) ) ;
#82277 = UNCERTAINTY_MEASURE_WITH_UNIT (LENGTH_MEASURE( 1.000000000000000082E-05 ), #175872, 'distance_accuracy_value', 'NONE');
#82278 = ORIENTED_EDGE ( 'NONE', *, *, #110488, .T. ) ;
#82279 = CARTESIAN_POINT ( 'NONE',  ( 18.62759615963255655, 10.81492255796105972, 46.66775706135234714 ) ) ;
#82280 = AXIS2_PLACEMENT_3D ( 'NONE', #164983, #26478, #197311 ) ;
#82282 = CARTESIAN_POINT ( 'NONE',  ( -36.91746825000001309, -11.99521256947794789, -2.524999997268813523 ) ) ;
#82281 = CARTESIAN_POINT ( 'NONE',  ( 0.05219959533910956823, 16.53943276465976808, 79.99890960531435269 ) ) ;
#82283 = CARTESIAN_POINT ( 'NONE',  ( -14.29746914071037622, -8.314922557961029526, 44.16775706135234714 ) ) ;
#82284 = CARTESIAN_POINT ( 'NONE',  ( -14.34966873604960291, -8.224510206698953496, 101.6655762719810383 ) ) ;
#82285 = CARTESIAN_POINT ( 'NONE',  ( -16.51473224551082808, 9.474510206698731452, 53.33442372801900433 ) ) ;
#82286 = CARTESIAN_POINT ( 'NONE',  ( -16.53943276465976808, 0.05219959533911058130, 66.24890960531436690 ) ) ;
#82288 = EDGE_CURVE ( 'NONE', #6627, #145279, #115764, .T. ) ;
#82287 = CARTESIAN_POINT ( 'NONE',  ( 15.72974639402176855, 15.80617190586768217, 36.87609039468568994 ) ) ;
#82290 = CARTESIAN_POINT ( 'NONE',  ( -15.72974639402197994, 15.80617190586746368, 85.62390960531436690 ) ) ;
#82289 = CARTESIAN_POINT ( 'NONE',  ( -9.474510206698964154, 16.51473224551069663, 25.41557627198103120 ) ) ;
#82291 = CARTESIAN_POINT ( 'NONE',  ( 5.049401038298161559, -19.05341960407611168, 102.7072429386476955 ) ) ;
#82292 = CARTESIAN_POINT ( 'NONE',  ( 16.53943276465976808, -0.05219959533910856209, 68.74890960531435269 ) ) ;
#82293 = CARTESIAN_POINT ( 'NONE',  ( 23.17010908000658631, -32.51358278116848055, -22.50838357033831727 ) ) ;
#82294 = CARTESIAN_POINT ( 'NONE',  ( -5.950531402560715689E-15, 38.81732327939063509, -1.124999997268813168 ) ) ;
#82295 = CARTESIAN_POINT ( 'NONE',  ( 5.153800228976615827, -19.02544592524334988, 80.20942372801901854 ) ) ;
#82296 = CARTESIAN_POINT ( 'NONE',  ( 10.81492255796078972, 18.62759615963270932, 114.5822429386477097 ) ) ;
#82297 = CARTESIAN_POINT ( 'NONE',  ( 16.51473224551069308, 9.474510206698969483, 69.16557627198102409 ) ) ;
#82298 = CARTESIAN_POINT ( 'NONE',  ( 16.46253265017146816, 9.564922557961045513, 61.66775706135234003 ) ) ;
#82299 = CARTESIAN_POINT ( 'NONE',  ( -9.474510206698964154, 16.51473224551069663, 45.41557627198103120 ) ) ;
#82300 = CARTESIAN_POINT ( 'NONE',  ( -4.483927247898539470, -16.52544592524342804, 62.29057627198102409 ) ) ;
#82301 = EDGE_CURVE ( 'NONE', #68796, #138021, #21572, .T. ) ;
#82302 = CARTESIAN_POINT ( 'NONE',  ( 14.34966873604960469, 8.224510206698951720, 49.16557627198102409 ) ) ;
#82303 = CARTESIAN_POINT ( 'NONE',  ( 19.03943276465977164, -0.05219959533909143690, 73.74890960531435269 ) ) ;
#82304 = CARTESIAN_POINT ( 'NONE',  ( 21.55341960407610458, 5.719274019375980345, 88.95724293864769550 ) ) ;
#82305 = CARTESIAN_POINT ( 'NONE',  ( -5.153800228976328057, -19.02544592524343514, 67.29057627198102409 ) ) ;
#82306 = CARTESIAN_POINT ( 'NONE',  ( 18.67979575497178502, 10.72451020669898547, 79.16557627198103830 ) ) ;
#82307 = CARTESIAN_POINT ( 'NONE',  ( 21.52544592524334988, 5.823673210054432836, 111.4594237280190328 ) ) ;
#82310 = CARTESIAN_POINT ( 'NONE',  ( 12.06949235617757843, -12.14591786802309237, 98.12390960531436690 ) ) ;
#82309 = CARTESIAN_POINT ( 'NONE',  ( -8.224510206698735004, -14.34966873604973081, 109.5844237280190328 ) ) ;
#82308 = PLANE ( 'NONE',  #96088 ) ;
#82311 = CARTESIAN_POINT ( 'NONE',  ( -19.05341960407617563, 5.049401038297882671, 103.5427570613523329 ) ) ;
#82312 = VERTEX_POINT ( 'NONE', #53260 ) ;
#82313 = CARTESIAN_POINT ( 'NONE',  ( -15.80617190586768217, 15.72974639402176855, 23.12609039468567573 ) ) ;
#82314 = CARTESIAN_POINT ( 'NONE',  ( -13.97604488694547697, 13.89961937509957934, 58.12609039468566863 ) ) ;
#82315 = CARTESIAN_POINT ( 'NONE',  ( 4.379528057220092307, 16.55341960407617563, 102.2927570613523613 ) ) ;
#82316 = CARTESIAN_POINT ( 'NONE',  ( 16.46253265017146816, 9.564922557961045513, 41.66775706135234003 ) ) ;
#82317 = CARTESIAN_POINT ( 'NONE',  ( -19.05341960407611168, -5.049401038298163336, 101.4572429386476955 ) ) ;
#82318 = CARTESIAN_POINT ( 'NONE',  ( 8.224510206698953496, -14.34966873604960469, 52.91557627198103830 ) ) ;
#82319 = CARTESIAN_POINT ( 'NONE',  ( -19.49149378614655959, 5.499999999999766409, 49.43757513605356024 ) ) ;
#82320 = CARTESIAN_POINT ( 'NONE',  ( 0.05219959533909260263, 19.03943276465977164, 34.99890960531435979 ) ) ;
#82321 = CARTESIAN_POINT ( 'NONE',  ( -21.52544592524334988, -5.823673210054445271, 108.9594237280190185 ) ) ;
#82322 = CARTESIAN_POINT ( 'NONE',  ( 16.53943276465976808, 0.05219959533934440121, 91.25109039468568994 ) ) ;
#82323 = CARTESIAN_POINT ( 'NONE',  ( 0.05219959533937995610, -21.53943276465977519, 40.00109039468567573 ) ) ;
#82324 = CARTESIAN_POINT ( 'NONE',  ( -14.34966873604972548, 8.224510206698743886, 38.33442372801900433 ) ) ;
#82325 = CARTESIAN_POINT ( 'NONE',  ( -9.564922557960796823, -16.46253265017161027, 107.0822429386476955 ) ) ;
#82326 = CARTESIAN_POINT ( 'NONE',  ( -0.05219959533909027116, -19.03943276465977164, 47.49890960531435979 ) ) ;
#82327 = CARTESIAN_POINT ( 'NONE',  ( -19.03943276465977164, 0.05219959533909376836, 66.24890960531436690 ) ) ;
#82328 = AXIS2_PLACEMENT_3D ( 'NONE', #53195, #22871, #84518 ) ;
#82329 = CARTESIAN_POINT ( 'NONE',  ( -0.05219959533934338120, 16.53943276465976808, 47.50109039468568994 ) ) ;
#82330 = CARTESIAN_POINT ( 'NONE',  ( -16.55341960407611168, -4.379528057220339221, 111.4572429386476813 ) ) ;
#82331 = CARTESIAN_POINT ( 'NONE',  ( -16.55341960407611168, -4.379528057220339221, 26.45724293864768839 ) ) ;
#82332 = DIRECTION ( 'NONE',  ( 0.000000000000000000, 0.8164965809277221487, -0.5773502691896313932 ) ) ;
#82335 = CARTESIAN_POINT ( 'NONE',  ( 5.049401038298161559, -19.05341960407611168, 77.70724293864765286 ) ) ;
#82334 = CARTESIAN_POINT ( 'NONE',  ( 19.05341960407611168, 5.049401038298154454, 88.95724293864769550 ) ) ;
#82333 = CARTESIAN_POINT ( 'NONE',  ( 21.53943276465977519, 0.05219959533937863772, 61.25109039468567573 ) ) ;
#82336 = CARTESIAN_POINT ( 'NONE',  ( 9.564922557960805705, 16.46253265017160317, 94.58224293864769550 ) ) ;
#82337 = CARTESIAN_POINT ( 'NONE',  ( 4.483927247898545687, 16.52544592524342804, 39.79057627198103830 ) ) ;
#82338 = CARTESIAN_POINT ( 'NONE',  ( -12.14591786802309592, -12.06949235617757132, 21.87390960531436690 ) ) ;
#82339 = CARTESIAN_POINT ( 'NONE',  ( 16.55341960407611168, 4.379528057220329451, 38.95724293864768839 ) ) ;
#82340 = ORIENTED_EDGE ( 'NONE', *, *, #195934, .F. ) ;
#82342 = VECTOR ( 'NONE', #122973, 1000.000000000000000 ) ;
#82341 = CARTESIAN_POINT ( 'NONE',  ( 18.22780087662126647, 5.499999999999818812, 56.48236817873107185 ) ) ;
#82343 = CARTESIAN_POINT ( 'NONE',  ( 9.474510206698971260, -16.51473224551069308, 67.91557627198102409 ) ) ;
#82344 = CARTESIAN_POINT ( 'NONE',  ( 5.049401038297881783, 19.05341960407617563, 57.29275706135231871 ) ) ;
#82345 = CARTESIAN_POINT ( 'NONE',  ( 11.40812507854755253, -35.11059874428192273, -10.52499999726881263 ) ) ;
#82346 = CARTESIAN_POINT ( 'NONE',  ( -3.573655867282028392E-15, 2.428612866367529932E-14, 150.0000000000000000 ) ) ;
#82348 = CARTESIAN_POINT ( 'NONE',  ( 8.314922557961029526, -14.29746914071037800, 65.41775706135234714 ) ) ;
#82347 = CARTESIAN_POINT ( 'NONE',  ( -5.049401038297874678, -19.05341960407617918, 84.79275706135233293 ) ) ;
#82350 = CARTESIAN_POINT ( 'NONE',  ( 17.26172910966779384, 6.454744622555852018, 91.69353091350777163 ) ) ;
#82349 = PRODUCT_DEFINITION_FORMATION_WITH_SPECIFIED_SOURCE ( 'ANY', '', #184101, .NOT_KNOWN. ) ;
#82351 = CARTESIAN_POINT ( 'NONE',  ( -5.049401038298153566, 19.05341960407611168, 85.20724293864766707 ) ) ;
#82352 = CARTESIAN_POINT ( 'NONE',  ( 10.81492255796106328, -18.62759615963255655, 25.41775706135235779 ) ) ;
#82353 = CARTESIAN_POINT ( 'NONE',  ( 0.05219959533936267826, -19.03943276465977164, 90.00109039468567573 ) ) ;
#82355 = CARTESIAN_POINT ( 'NONE',  ( -0.05219959533909027116, -19.03943276465977164, 42.49890960531435269 ) ) ;
#82354 = CARTESIAN_POINT ( 'NONE',  ( 16.21995358207305316, 7.366697692864115687, 87.56448998487846325 ) ) ;
#82356 = CARTESIAN_POINT ( 'NONE',  ( -16.46253265017160317, 9.564922557960807481, 85.83224293864769550 ) ) ;
#82358 = CARTESIAN_POINT ( 'NONE',  ( -0.05219959533909027116, -19.03943276465977164, 47.49890960531435979 ) ) ;
#82357 = CARTESIAN_POINT ( 'NONE',  ( -14.34966873604960291, -8.224510206698953496, 51.66557627198102409 ) ) ;
#82359 = CARTESIAN_POINT ( 'NONE',  ( -13.97604488694547697, 13.89961937509957934, 63.12609039468566152 ) ) ;
#82360 = CARTESIAN_POINT ( 'NONE',  ( 4.483927247898545687, 16.52544592524342804, 84.79057627198102409 ) ) ;
#82361 = CARTESIAN_POINT ( 'NONE',  ( 13.97604488694548053, -13.89961937509957401, 35.62609039468567573 ) ) ;
#82362 = CARTESIAN_POINT ( 'NONE',  ( 13.89961937509977652, -13.97604488694527269, 63.12390960531435979 ) ) ;
#82363 =( BOUNDED_CURVE ( )  B_SPLINE_CURVE ( 2, ( #172455, #17787, #141113, #125947, #77453, #49116, #139124, #601, #54091, #111770, #113742 ),
 .UNSPECIFIED., .F., .F. ) 
 B_SPLINE_CURVE_WITH_KNOTS ( ( 3, 2, 2, 2, 2, 3 ),
 ( 0.7000000000000033973, 0.7200000000000034150, 0.7400000000000034328, 0.7600000000000035616, 0.7800000000000035794, 0.8000000000000035971 ),
 .UNSPECIFIED. ) 
 CURVE ( )  GEOMETRIC_REPRESENTATION_ITEM ( )  RATIONAL_B_SPLINE_CURVE ( ( 0.9999999999999915623, 0.9510565162951619689, 1.000000000000000000, 0.9510565162951535312, 1.000000000000000000, 0.9510565162951535312, 1.000000000000000000, 0.9510565162951535312, 1.000000000000000000, 0.9510565162951448714, 1.000000000000008660 ) ) 
 REPRESENTATION_ITEM ( '' )  );
#82364 = CARTESIAN_POINT ( 'NONE',  ( 10.72451020669898902, -18.67979575497178502, 62.91557627198102409 ) ) ;
#82366 = CARTESIAN_POINT ( 'NONE',  ( -19.02544592524334988, -5.153800228976617603, 18.95942372801899722 ) ) ;
#82365 = CARTESIAN_POINT ( 'NONE',  ( 4.379528057220339221, -16.55341960407611168, 62.70724293864769550 ) ) ;
#82367 = CARTESIAN_POINT ( 'NONE',  ( -19.03943276465977164, 0.05219959533909376836, 106.2489096053143669 ) ) ;
#82368 = CARTESIAN_POINT ( 'NONE',  ( 21.55341960407610458, 5.719274019375980345, 28.95724293864769905 ) ) ;
#82369 = CARTESIAN_POINT ( 'NONE',  ( -5.153800228976328057, -19.02544592524343514, 52.29057627198100988 ) ) ;
#82370 = CARTESIAN_POINT ( 'NONE',  ( 9.474510206698971260, -16.51473224551069308, 32.91557627198102409 ) ) ;
#82371 = CARTESIAN_POINT ( 'NONE',  ( -16.52544592524342804, 4.483927247898546575, 96.04057627198102409 ) ) ;
#82372 = CIRCLE ( 'NONE', #40412, 5.000000000000000888 ) ;
#82373 = CARTESIAN_POINT ( 'NONE',  ( 5.719274019375991003, -21.55341960407610458, 112.7072429386476955 ) ) ;
#82374 = CARTESIAN_POINT ( 'NONE',  ( 16.46253265017160672, -9.564922557960803928, 113.3322429386476955 ) ) ;
#82375 = CARTESIAN_POINT ( 'NONE',  ( -21.53943276465977519, -0.05219959533937600094, 23.75109039468567929 ) ) ;
#82376 = CARTESIAN_POINT ( 'NONE',  ( -9.564922557960796823, -16.46253265017161027, 107.0822429386476955 ) ) ;
#82377 = CARTESIAN_POINT ( 'NONE',  ( -14.34966873604960291, -8.224510206698953496, 111.6655762719810525 ) ) ;
#82378 = CARTESIAN_POINT ( 'NONE',  ( 15.72974639402176855, 15.80617190586768217, 81.87609039468568994 ) ) ;
#82379 = CARTESIAN_POINT ( 'NONE',  ( 18.62759615963271287, -10.81492255796078972, 93.33224293864769550 ) ) ;
#82380 = DIRECTION ( 'NONE',  ( -0.000000000000000000, -0.000000000000000000, -1.000000000000000000 ) ) ;
#82381 = CARTESIAN_POINT ( 'NONE',  ( -9.564922557960796823, -16.46253265017161027, 52.08224293864768839 ) ) ;
#82382 = CARTESIAN_POINT ( 'NONE',  ( 31.82351365011403743, -0.4884129450683361018, -49.22894560581804058 ) ) ;
#82383 = CARTESIAN_POINT ( 'NONE',  ( 4.379528057220092307, 16.55341960407617563, 42.29275706135235424 ) ) ;
#82384 = CARTESIAN_POINT ( 'NONE',  ( -8.314922557960811034, -14.29746914071050412, 102.0822429386476955 ) ) ;
#82385 = CARTESIAN_POINT ( 'NONE',  ( 33.67973855159210217, -4.949490125723492007, 97.42538428767439029 ) ) ;
#82386 = CARTESIAN_POINT ( 'NONE',  ( -16.46253265017160317, 9.564922557960807481, 55.83224293864769550 ) ) ;
#82387 = CARTESIAN_POINT ( 'NONE',  ( 4.483927247898545687, 16.52544592524342804, 89.79057627198103830 ) ) ;
#82388 = CARTESIAN_POINT ( 'NONE',  ( 18.67979575497178502, 10.72451020669898547, 44.16557627198103120 ) ) ;
#82389 = CARTESIAN_POINT ( 'NONE',  ( 16.55341960407611168, 4.379528057220329451, 58.95724293864770971 ) ) ;
#82390 = CARTESIAN_POINT ( 'NONE',  ( -16.52544592524335698, -4.483927247898792601, 23.95942372801901143 ) ) ;
#82391 = CARTESIAN_POINT ( 'NONE',  ( 0.05219959533937995610, -21.53943276465977519, 90.00109039468567573 ) ) ;
#82392 = CARTESIAN_POINT ( 'NONE',  ( 17.31747979337950838, -6.344076630960993946, 76.12055131934818064 ) ) ;
#82393 = CARTESIAN_POINT ( 'NONE',  ( -14.34966873604972548, 8.224510206698743886, 103.3344237280190043 ) ) ;
#82394 = CARTESIAN_POINT ( 'NONE',  ( -0.05219959533910754901, -16.53943276465976808, 37.49890960531436690 ) ) ;
#82395 = CARTESIAN_POINT ( 'NONE',  ( -5.153800228976328057, -19.02544592524343514, 32.29057627198102409 ) ) ;
#82396 = CARTESIAN_POINT ( 'NONE',  ( 16.51473224551069308, 9.474510206698969483, 94.16557627198103830 ) ) ;
#82397 = CARTESIAN_POINT ( 'NONE',  ( 0.05219959533907565091, 21.53943276465977519, 89.99890960531438111 ) ) ;
#82398 = CARTESIAN_POINT ( 'NONE',  ( -14.34966873604972548, 8.224510206698743886, 43.33442372801901143 ) ) ;
#82400 = CARTESIAN_POINT ( 'NONE',  ( -5.719274019375665041, -21.55341960407619695, 79.79275706135236135 ) ) ;
#82399 = CARTESIAN_POINT ( 'NONE',  ( 0.05219959533910956823, 16.53943276465976808, 64.99890960531435269 ) ) ;
#82401 = CARTESIAN_POINT ( 'NONE',  ( 12.06949235617739724, 12.14591786802326823, 96.87609039468568994 ) ) ;
#82402 = CARTESIAN_POINT ( 'NONE',  ( 16.62475595723696387, 7.163666690055258357, 26.97286648189535185 ) ) ;
#82403 = CARTESIAN_POINT ( 'NONE',  ( -18.22780087662121673, -5.500000000000063061, 66.48459894673892734 ) ) ;
#82404 = CARTESIAN_POINT ( 'NONE',  ( 4.483927247898545687, 16.52544592524342804, 24.79057627198103120 ) ) ;
#82405 = CARTESIAN_POINT ( 'NONE',  ( -12.06949235617739369, -12.14591786802326823, 69.37609039468567573 ) ) ;
#82406 = CARTESIAN_POINT ( 'NONE',  ( 19.05341960407611168, 5.049401038298154454, 83.95724293864766707 ) ) ;
#82407 = CARTESIAN_POINT ( 'NONE',  ( 13.97604488694527802, 13.89961937509977652, 99.37390960531436690 ) ) ;
#82408 = CARTESIAN_POINT ( 'NONE',  ( -15.72974639402176322, -15.80617190586768395, 89.37609039468568994 ) ) ;
#82409 = CARTESIAN_POINT ( 'NONE',  ( -0.05219959533934338120, 16.53943276465976808, 92.50109039468567573 ) ) ;
#82410 = CARTESIAN_POINT ( 'NONE',  ( -14.29746914071049879, 8.314922557960819915, 55.83224293864770260 ) ) ;
#82411 = CARTESIAN_POINT ( 'NONE',  ( 19.02544592524343514, -5.153800228976328945, 63.54057627198103830 ) ) ;
#82412 = EDGE_LOOP ( 'NONE', ( #108595, #88475, #31396, #163957, #91192, #127283, #157629, #79806, #26971, #106148, #109218, #173862 ) ) ;
#82413 = CARTESIAN_POINT ( 'NONE',  ( 5.153800228976615827, -19.02544592524334988, 105.2094237280190185 ) ) ;
#82414 = CARTESIAN_POINT ( 'NONE',  ( -4.379528057220328563, 16.55341960407611168, 115.2072429386476955 ) ) ;
#82415 = CARTESIAN_POINT ( 'NONE',  ( 5.049401038298161559, -19.05341960407611168, 77.70724293864765286 ) ) ;
#82417 = CARTESIAN_POINT ( 'NONE',  ( 36.91746824999999887, 11.99521256947799053, -9.524999997268812635 ) ) ;
#82416 = CARTESIAN_POINT ( 'NONE',  ( 4.379528057220092307, 16.55341960407617563, 22.29275706135235069 ) ) ;
#82418 = CARTESIAN_POINT ( 'NONE',  ( -9.474510206698720793, -16.51473224551083518, 24.58442372801900078 ) ) ;
#82419 = CARTESIAN_POINT ( 'NONE',  ( -12.06949235617739369, -12.14591786802326823, 84.37609039468570415 ) ) ;
#82420 = CARTESIAN_POINT ( 'NONE',  ( -5.153800228976607833, 19.02544592524334988, 112.7094237280190043 ) ) ;
#82421 = CARTESIAN_POINT ( 'NONE',  ( -16.53943276465976808, 0.05219959533911058130, 111.2489096053143669 ) ) ;
#82422 = CARTESIAN_POINT ( 'NONE',  ( 16.55341960407618274, -4.379528057220086978, 71.04275706135234714 ) ) ;
#82423 = CARTESIAN_POINT ( 'NONE',  ( -8.224510206698735004, -14.34966873604973081, 49.58442372801901143 ) ) ;
#82424 = CARTESIAN_POINT ( 'NONE',  ( -19.05341960407611168, -5.049401038298163336, 21.45724293864768839 ) ) ;
#82425 = CARTESIAN_POINT ( 'NONE',  ( 0.05219959533936267826, -19.03943276465977164, 65.00109039468567573 ) ) ;
#82426 = CIRCLE ( 'NONE', #43633, 6.100000000000006750 ) ;
#82427 = CARTESIAN_POINT ( 'NONE',  ( -21.52544592524334988, -5.823673210054445271, 108.9594237280190185 ) ) ;
#82428 = CARTESIAN_POINT ( 'NONE',  ( 16.51473224551069308, 9.474510206698969483, 39.16557627198103120 ) ) ;
#82429 = CARTESIAN_POINT ( 'NONE',  ( 5.049401038298161559, -19.05341960407611168, 77.70724293864765286 ) ) ;
#82430 = CARTESIAN_POINT ( 'NONE',  ( -14.29746914071049879, 8.314922557960819915, 65.83224293864769550 ) ) ;
#82431 = CARTESIAN_POINT ( 'NONE',  ( 9.564922557961047289, -16.46253265017146816, 35.41775706135233293 ) ) ;
#82432 = CARTESIAN_POINT ( 'NONE',  ( 15.80617190586746368, 15.72974639402197994, 34.37390960531435979 ) ) ;
#82433 = CARTESIAN_POINT ( 'NONE',  ( -0.05219959533937732626, 21.53943276465977519, 107.5010903946856899 ) ) ;
#82434 = CARTESIAN_POINT ( 'NONE',  ( -16.51473224551069308, -9.474510206698971260, 86.66557627198102409 ) ) ;
#82435 = CARTESIAN_POINT ( 'NONE',  ( -18.62759615963255300, -10.81492255796106328, 104.1677570613523471 ) ) ;
#82436 = CARTESIAN_POINT ( 'NONE',  ( -18.67979575497178146, -10.72451020669898902, 66.66557627198102409 ) ) ;
#82437 = CARTESIAN_POINT ( 'NONE',  ( -16.51473224551069308, -9.474510206698971260, 96.66557627198102409 ) ) ;
#82438 = CARTESIAN_POINT ( 'NONE',  ( 5.153800228976615827, -19.02544592524334988, 75.20942372801896170 ) ) ;
#82439 = CARTESIAN_POINT ( 'NONE',  ( 16.46253265017160672, -9.564922557960803928, 108.3322429386476955 ) ) ;
#82440 = CARTESIAN_POINT ( 'NONE',  ( 9.474510206698729675, 16.51473224551082808, 92.08442372801900433 ) ) ;
#82441 = CARTESIAN_POINT ( 'NONE',  ( 8.224510206698742110, 14.34966873604972548, 62.08442372801901143 ) ) ;
#82442 = CARTESIAN_POINT ( 'NONE',  ( 12.06949235617757843, -12.14591786802309237, 113.1239096053143953 ) ) ;
#82443 = CARTESIAN_POINT ( 'NONE',  ( -5.049401038298153566, 19.05341960407611168, 85.20724293864766707 ) ) ;
#82444 = CARTESIAN_POINT ( 'NONE',  ( 18.67979575497178502, 10.72451020669898547, 64.16557627198102409 ) ) ;
#82445 = CARTESIAN_POINT ( 'NONE',  ( -16.53943276465976808, -0.05219959533934237506, 28.75109039468567929 ) ) ;
#82446 = CARTESIAN_POINT ( 'NONE',  ( 21.52544592524334988, 5.823673210054432836, 31.45942372801901854 ) ) ;
#82447 = CARTESIAN_POINT ( 'NONE',  ( 21.53943276465977519, 0.05219959533937863772, 101.2510903946856757 ) ) ;
#82448 = CARTESIAN_POINT ( 'NONE',  ( -16.52544592524335698, -4.483927247898792601, 98.95942372801903275 ) ) ;
#82449 = CARTESIAN_POINT ( 'NONE',  ( -13.97604488694527625, -13.89961937509977652, 81.87390960531436690 ) ) ;
#82450 = CARTESIAN_POINT ( 'NONE',  ( 14.29746914071049879, -8.314922557960816363, 83.33224293864769550 ) ) ;
#82451 = CARTESIAN_POINT ( 'NONE',  ( 8.224510206698953496, -14.34966873604960469, 22.91557627198102765 ) ) ;
#82452 = CARTESIAN_POINT ( 'NONE',  ( 5.049401038297881783, 19.05341960407617563, 67.29275706135234714 ) ) ;
#82453 = CARTESIAN_POINT ( 'NONE',  ( 5.719274019375673035, 21.55341960407619339, 47.29275706135234003 ) ) ;
#82454 = CARTESIAN_POINT ( 'NONE',  ( -16.55341960407611168, -4.379528057220339221, 96.45724293864770971 ) ) ;
#82455 = CARTESIAN_POINT ( 'NONE',  ( 9.564922557960805705, 16.46253265017160317, 109.5822429386476955 ) ) ;
#82456 = CARTESIAN_POINT ( 'NONE',  ( 8.314922557961029526, -14.29746914071037800, 105.4177570613523613 ) ) ;
#82457 = CARTESIAN_POINT ( 'NONE',  ( -5.719274019375665041, -21.55341960407619695, 89.79275706135236135 ) ) ;
#82458 = CARTESIAN_POINT ( 'NONE',  ( 14.34966873604972726, -8.224510206698740333, 50.83442372801901143 ) ) ;
#82459 = CARTESIAN_POINT ( 'NONE',  ( 0.05219959533937995610, -21.53943276465977519, 45.00109039468568284 ) ) ;
#82460 = EDGE_CURVE ( 'NONE', #107482, #188641, #158449, .T. ) ;
#82461 = EDGE_LOOP ( 'NONE', ( #143675, #197422 ) ) ;
#82462 = CARTESIAN_POINT ( 'NONE',  ( -18.67979575497178146, -10.72451020669898902, 111.6655762719810525 ) ) ;
#82463 = CARTESIAN_POINT ( 'NONE',  ( -16.53943276465976808, 0.05219959533911058130, 96.24890960531435269 ) ) ;
#82464 = DIRECTION ( 'NONE',  ( 0.000000000000000000, 0.000000000000000000, -1.000000000000000000 ) ) ;
#82465 = CARTESIAN_POINT ( 'NONE',  ( 8.314922557960818139, 14.29746914071049879, 64.58224293864769550 ) ) ;
#82466 = CARTESIAN_POINT ( 'NONE',  ( -16.55341960407617563, 4.379528057220093196, 108.5427570613523756 ) ) ;
#82467 = CARTESIAN_POINT ( 'NONE',  ( 0.05219959533909260263, 19.03943276465977164, 34.99890960531435979 ) ) ;
#82468 = CARTESIAN_POINT ( 'NONE',  ( -15.80617190586745835, -15.72974639402198527, 46.87390960531435979 ) ) ;
#82469 = CARTESIAN_POINT ( 'NONE',  ( -14.34966873604960291, -8.224510206698953496, 76.66557627198103830 ) ) ;
#82470 = CIRCLE ( 'NONE', #198707, 5.000000000000000888 ) ;
#82471 = CARTESIAN_POINT ( 'NONE',  ( 5.823673210054125526, 21.52544592524343514, 84.79057627198102409 ) ) ;
#82472 = CARTESIAN_POINT ( 'NONE',  ( -13.97604488694527625, -13.89961937509977652, 86.87390960531436690 ) ) ;
#82474 = CARTESIAN_POINT ( 'NONE',  ( -16.51473224551082808, 9.474510206698731452, 88.33442372801900433 ) ) ;
#82473 = CARTESIAN_POINT ( 'NONE',  ( -0.05219959533909027116, -19.03943276465977164, 42.49890960531435269 ) ) ;
#82475 = CARTESIAN_POINT ( 'NONE',  ( -18.62759615963270932, 10.81492255796079327, 30.83224293864770260 ) ) ;
#82476 = CARTESIAN_POINT ( 'NONE',  ( -15.80617190586768217, 15.72974639402176855, 63.12609039468568994 ) ) ;
#82477 = B_SPLINE_CURVE_WITH_KNOTS ( 'NONE', 3,
 ( #170203, #49840, #94340, #185372, #111504, #18517, #19502, #186387, #20482, #138861, #173190, #95334, #62009, #125684, #1331, #47864, #341, #46863, #141836, #123674 ),
 .UNSPECIFIED., .F., .F.,
 ( 4, 2, 2, 2, 2, 2, 2, 2, 2, 4 ),
 ( 0.000000000000000000, 0.0004987090165372711848, 0.0009974180330745423696, 0.001246772541343177908, 0.001496127049611813446, 0.001994836066149084739, 0.002493545082686355815, 0.002742899590954988968, 0.002992254099223622121, 0.003989672132298143457 ),
 .UNSPECIFIED. ) ;
#82478 = CARTESIAN_POINT ( 'NONE',  ( 19.02544592524343514, -5.153800228976328945, 48.54057627198103120 ) ) ;
#82479 = CARTESIAN_POINT ( 'NONE',  ( -13.89961937509977652, 13.97604488694528158, 85.62390960531433848 ) ) ;
#82480 = ORIENTED_EDGE ( 'NONE', *, *, #98256, .T. ) ;
#82481 = CARTESIAN_POINT ( 'NONE',  ( -14.29746914071037622, -8.314922557961029526, 69.16775706135234714 ) ) ;
#82482 = CARTESIAN_POINT ( 'NONE',  ( -5.719274019375665041, -21.55341960407619695, 44.79275706135234714 ) ) ;
#82483 = CARTESIAN_POINT ( 'NONE',  ( 21.53943276465977519, 0.05219959533937863772, 71.25109039468568994 ) ) ;
#82484 = CARTESIAN_POINT ( 'NONE',  ( 21.53943276465977519, -0.05219959533907433946, 23.74890960531435269 ) ) ;
#82485 = CARTESIAN_POINT ( 'NONE',  ( -0.05219959533907301413, -21.53943276465977519, 97.49890960531436690 ) ) ;
#82487 = CARTESIAN_POINT ( 'NONE',  ( -4.379528057220086978, -16.55341960407618274, 59.79275706135234714 ) ) ;
#82486 = CARTESIAN_POINT ( 'NONE',  ( -18.62759615963255300, -10.81492255796106328, 19.16775706135234714 ) ) ;
#82488 = CARTESIAN_POINT ( 'NONE',  ( -21.53943276465977519, 0.05219959533907696930, 66.24890960531436690 ) ) ;
#82489 = CARTESIAN_POINT ( 'NONE',  ( 5.049401038297881783, 19.05341960407617563, 22.29275706135233648 ) ) ;
#82490 = VECTOR ( 'NONE', #87793, 1000.000000000000000 ) ;
#82492 = CARTESIAN_POINT ( 'NONE',  ( 14.29746914071037800, 8.314922557961029526, 106.6677570613523756 ) ) ;
#82491 = CARTESIAN_POINT ( 'NONE',  ( 9.564922557960805705, 16.46253265017160317, 69.58224293864770971 ) ) ;
#82493 = CARTESIAN_POINT ( 'NONE',  ( -17.50000000000147793, -3.254303733634544837, 104.9760410692860688 ) ) ;
#82494 = CARTESIAN_POINT ( 'NONE',  ( 5.153800228976335163, 19.02544592524342804, 89.79057627198102409 ) ) ;
#82495 = CARTESIAN_POINT ( 'NONE',  ( -8.314922557961024197, 14.29746914071037800, 37.91775706135235424 ) ) ;
#82496 = CARTESIAN_POINT ( 'NONE',  ( 21.42625476241836679, 22.99713674769907001, -46.35568673344853607 ) ) ;
#82497 = CARTESIAN_POINT ( 'NONE',  ( -5.153800228976607833, 19.02544592524334988, 87.70942372801897591 ) ) ;
#82498 = AXIS2_PLACEMENT_3D ( 'NONE', #82529, #144211, #8454 ) ;
#82499 = CARTESIAN_POINT ( 'NONE',  ( -5.823673210054116645, -21.52544592524344225, 62.29057627198102409 ) ) ;
#82500 = CARTESIAN_POINT ( 'NONE',  ( 14.29746914071049879, -8.314922557960816363, 23.33224293864769194 ) ) ;
#82501 = CARTESIAN_POINT ( 'NONE',  ( 5.153800228976615827, -19.02544592524334988, 95.20942372801897591 ) ) ;
#82502 = DIRECTION ( 'NONE',  ( 0.000000000000000000, 0.000000000000000000, -1.000000000000000000 ) ) ;
#82503 = CARTESIAN_POINT ( 'NONE',  ( -19.05341960407617563, 5.049401038297882671, 93.54275706135234714 ) ) ;
#82505 = CARTESIAN_POINT ( 'NONE',  ( -9.474510206698720793, -16.51473224551083518, 54.58442372801899722 ) ) ;
#82504 = CARTESIAN_POINT ( 'NONE',  ( 21.55341960407610458, 5.719274019375980345, 83.95724293864770971 ) ) ;
#82506 = CARTESIAN_POINT ( 'NONE',  ( 24.37407968765134569, -13.84118768211351735, 165.9040744261181430 ) ) ;
#82507 = CARTESIAN_POINT ( 'NONE',  ( -5.049401038298153566, 19.05341960407611168, 70.20724293864769550 ) ) ;
#82508 = CARTESIAN_POINT ( 'NONE',  ( -4.483927247898539470, -16.52544592524342804, 62.29057627198102409 ) ) ;
#82509 = CARTESIAN_POINT ( 'NONE',  ( 13.89961937509977652, -13.97604488694527269, 53.12390960531434558 ) ) ;
#82510 = CARTESIAN_POINT ( 'NONE',  ( -4.379528057220328563, 16.55341960407611168, 50.20724293864769550 ) ) ;
#82511 = DIRECTION ( 'NONE',  ( 1.000000000000000000, -4.336808689942018352E-17, 0.000000000000000000 ) ) ;
#82512 = CARTESIAN_POINT ( 'NONE',  ( 31.56677620984796917, -3.765895691706358850, 101.5045925518948593 ) ) ;
#82513 = CARTESIAN_POINT ( 'NONE',  ( 12.14591786802309770, 12.06949235617756955, 24.37390960531435979 ) ) ;
#82514 = CARTESIAN_POINT ( 'NONE',  ( 19.03943276465977164, -0.05219959533909143690, 63.74890960531435979 ) ) ;
#82515 = CARTESIAN_POINT ( 'NONE',  ( -17.59860650958993844, 7.585241751806885979, 73.42337014262493256 ) ) ;
#82516 = CARTESIAN_POINT ( 'NONE',  ( -0.05219959533936034679, 19.03943276465977164, 32.50109039468566863 ) ) ;
#82517 = CARTESIAN_POINT ( 'NONE',  ( -14.34966873604972548, 8.224510206698743886, 53.33442372801901854 ) ) ;
#82518 = CARTESIAN_POINT ( 'NONE',  ( 21.53943276465977519, -0.05219959533907433946, 53.74890960531437401 ) ) ;
#82519 = CARTESIAN_POINT ( 'NONE',  ( -18.67979575497193778, 10.72451020669871902, 103.3344237280190043 ) ) ;
#82520 = CARTESIAN_POINT ( 'NONE',  ( -13.97604488694527625, -13.89961937509977652, 71.87390960531433848 ) ) ;
#82521 = CARTESIAN_POINT ( 'NONE',  ( 9.474510206698971260, -16.51473224551069308, 112.9155762719810383 ) ) ;
#82522 = CARTESIAN_POINT ( 'NONE',  ( 16.46253265017160672, -9.564922557960803928, 108.3322429386476955 ) ) ;
#82523 = CARTESIAN_POINT ( 'NONE',  ( -36.91746825000000598, 11.99521256947798520, -2.724999997268813701 ) ) ;
#82524 = CARTESIAN_POINT ( 'NONE',  ( -15.72974639402176322, -15.80617190586768395, 34.37609039468568284 ) ) ;
#82526 = CARTESIAN_POINT ( 'NONE',  ( 14.29746914071049879, -8.314922557960816363, 88.33224293864769550 ) ) ;
#82525 = PRODUCT_DEFINITION_SHAPE ( 'NONE', 'NONE',  #200199 ) ;
#82529 = CARTESIAN_POINT ( 'NONE',  ( 7.992609269207028790E-30, -165.0000000000000000, -15.00000000000000000 ) ) ;
#82528 = CARTESIAN_POINT ( 'NONE',  ( -19.05341960407611168, -5.049401038298163336, 76.45724293864769550 ) ) ;
#82527 = CARTESIAN_POINT ( 'NONE',  ( -18.67979575497178146, -10.72451020669898902, 86.66557627198102409 ) ) ;
#82530 = CARTESIAN_POINT ( 'NONE',  ( -13.89961937509977652, 13.97604488694528158, 80.62390960531436690 ) ) ;
#82531 = CARTESIAN_POINT ( 'NONE',  ( -10.72451020669870658, -18.67979575497194134, 19.58442372801901143 ) ) ;
#82532 = ORIENTED_EDGE ( 'NONE', *, *, #78822, .F. ) ;
#82533 = CARTESIAN_POINT ( 'NONE',  ( -9.474510206698964154, 16.51473224551069663, 75.41557627198103830 ) ) ;
#82534 = CARTESIAN_POINT ( 'NONE',  ( 19.52217212775660116, -5.499999999999906741, 97.43993709005258097 ) ) ;
#82536 = CARTESIAN_POINT ( 'NONE',  ( 9.564922557960805705, 16.46253265017160317, 34.58224293864770260 ) ) ;
#82535 = CARTESIAN_POINT ( 'NONE',  ( -19.05341960407611168, -5.049401038298163336, 26.45724293864769550 ) ) ;
#82537 = CARTESIAN_POINT ( 'NONE',  ( 13.89961937509957401, 13.97604488694547697, 111.8760903946856757 ) ) ;
#82538 = CARTESIAN_POINT ( 'NONE',  ( -5.950531402560715689E-15, 38.81732327939063509, -9.624999997268815832 ) ) ;
#82539 = CARTESIAN_POINT ( 'NONE',  ( -4.379528057220328563, 16.55341960407611168, 110.2072429386477239 ) ) ;
#82540 = CARTESIAN_POINT ( 'NONE',  ( -10.81492255796105439, 18.62759615963255655, 77.91775706135231871 ) ) ;
#82542 = CARTESIAN_POINT ( 'NONE',  ( -10.81492255796105439, 18.62759615963255655, 37.91775706135235424 ) ) ;
#82541 = CARTESIAN_POINT ( 'NONE',  ( 0.05219959533909260263, 19.03943276465977164, 59.99890960531436690 ) ) ;
#82543 = CARTESIAN_POINT ( 'NONE',  ( -18.67979575497178146, -10.72451020669898902, 111.6655762719810525 ) ) ;
#82544 = CARTESIAN_POINT ( 'NONE',  ( 17.14385361876520264, -23.59649016807271238, 140.0750000027311728 ) ) ;
#82545 = CARTESIAN_POINT ( 'NONE',  ( -13.89961937509977652, 13.97604488694528158, 80.62390960531436690 ) ) ;
#82546 = CARTESIAN_POINT ( 'NONE',  ( 10.20000000000000107, 0.000000000000000000, 0.000000000000000000 ) ) ;
#82548 = CARTESIAN_POINT ( 'NONE',  ( 0.05219959533907565091, 21.53943276465977519, 39.99890960531436690 ) ) ;
#82547 = CARTESIAN_POINT ( 'NONE',  ( -8.314922557961024197, 14.29746914071037800, 32.91775706135234714 ) ) ;
#82549 = CARTESIAN_POINT ( 'NONE',  ( -10.81492255796105439, 18.62759615963255655, 67.91775706135234714 ) ) ;
#82550 = CARTESIAN_POINT ( 'NONE',  ( -0.05219959533909027116, -19.03943276465977164, 112.4989096053143669 ) ) ;
#82551 = CARTESIAN_POINT ( 'NONE',  ( 16.51473224551083163, -9.474510206698727899, 90.83442372801900433 ) ) ;
#82552 = CARTESIAN_POINT ( 'NONE',  ( -19.02544592524342804, 5.153800228976336051, 46.04057627198101699 ) ) ;
#82553 = CARTESIAN_POINT ( 'NONE',  ( -19.05341960407611168, -5.049401038298163336, 86.45724293864769550 ) ) ;
#82554 = CARTESIAN_POINT ( 'NONE',  ( 16.55341960407611168, 4.379528057220329451, 93.95724293864770971 ) ) ;
#82555 = CARTESIAN_POINT ( 'NONE',  ( -16.52544592524342804, 4.483927247898546575, 96.04057627198102409 ) ) ;
#82556 = CARTESIAN_POINT ( 'NONE',  ( 9.474510206698971260, -16.51473224551069308, 112.9155762719810383 ) ) ;
#82558 = CARTESIAN_POINT ( 'NONE',  ( -16.51473224551069308, -9.474510206698971260, 41.66557627198103120 ) ) ;
#82557 = CARTESIAN_POINT ( 'NONE',  ( 12.06949235617757843, -12.14591786802309237, 58.12390960531435979 ) ) ;
#82559 = CARTESIAN_POINT ( 'NONE',  ( -21.53943276465977519, -0.05219959533937600094, 63.75109039468568284 ) ) ;
#82560 = CARTESIAN_POINT ( 'NONE',  ( 16.46253265017146816, 9.564922557961045513, 91.66775706135234714 ) ) ;
#82561 = CARTESIAN_POINT ( 'NONE',  ( 16.55341960407611168, 4.379528057220329451, 63.95724293864770260 ) ) ;
#82562 = CARTESIAN_POINT ( 'NONE',  ( -21.52544592524343514, 5.823673210054127303, 111.0405762719810525 ) ) ;
#82563 = CARTESIAN_POINT ( 'NONE',  ( -15.72974639402197994, 15.80617190586746368, 40.62390960531435269 ) ) ;
#82565 = CARTESIAN_POINT ( 'NONE',  ( -13.97604488694527625, -13.89961937509977652, 106.8739096053143669 ) ) ;
#82564 = AXIS2_PLACEMENT_3D ( 'NONE', #163038, #37689, #71036 ) ;
#82566 = CARTESIAN_POINT ( 'NONE',  ( -5.429308488886486681E-15, 30.30510711980690175, 141.7500000054623683 ) ) ;
#82567 = CARTESIAN_POINT ( 'NONE',  ( -19.02544592524342804, 5.153800228976336051, 61.04057627198103120 ) ) ;
#82568 = CARTESIAN_POINT ( 'NONE',  ( 4.379528057220339221, -16.55341960407611168, 37.70724293864769550 ) ) ;
#82569 = CARTESIAN_POINT ( 'NONE',  ( -16.52544592524335698, -4.483927247898792601, 98.95942372801903275 ) ) ;
#82570 = CARTESIAN_POINT ( 'NONE',  ( 8.314922557961029526, -14.29746914071037800, 90.41775706135236135 ) ) ;
#82571 = CARTESIAN_POINT ( 'NONE',  ( 9.564922557961047289, -16.46253265017146816, 35.41775706135233293 ) ) ;
#82572 = CARTESIAN_POINT ( 'NONE',  ( -21.98685479826779954, 13.98560643873834408, 165.5209445330007441 ) ) ;
#82573 = CARTESIAN_POINT ( 'NONE',  ( 16.51473224551069308, 9.474510206698969483, 94.16557627198103830 ) ) ;
#82574 = CARTESIAN_POINT ( 'NONE',  ( -13.97604488694527625, -13.89961937509977652, 51.87390960531436690 ) ) ;
#82575 = CARTESIAN_POINT ( 'NONE',  ( -16.55341960407611168, -4.379528057220339221, 56.45724293864768839 ) ) ;
#82577 = CARTESIAN_POINT ( 'NONE',  ( 10.81492255796078972, 18.62759615963270932, 24.58224293864768839 ) ) ;
#82576 = CARTESIAN_POINT ( 'NONE',  ( 17.26172910966780094, -6.454744622555852018, 103.3064690864922426 ) ) ;
#82578 = CARTESIAN_POINT ( 'NONE',  ( -10.81492255796078084, -18.62759615963271287, 42.08224293864769550 ) ) ;
#82579 = CARTESIAN_POINT ( 'NONE',  ( 4.379528057220339221, -16.55341960407611168, 87.70724293864769550 ) ) ;
#82580 = CARTESIAN_POINT ( 'NONE',  ( -14.34966873604972548, 8.224510206698743886, 33.33442372801900433 ) ) ;
#82581 = CARTESIAN_POINT ( 'NONE',  ( 14.29746914071049879, -8.314922557960816363, 73.33224293864769550 ) ) ;
#82582 = CARTESIAN_POINT ( 'NONE',  ( -18.39443945427638738, 5.500000000000031086, 63.51745347608650150 ) ) ;
#82583 = CARTESIAN_POINT ( 'NONE',  ( -5.153800228976607833, 19.02544592524334988, 72.70942372801900433 ) ) ;
#82584 = CARTESIAN_POINT ( 'NONE',  ( -19.03943276465977164, 0.05219959533909376836, 111.2489096053143669 ) ) ;
#82585 = CARTESIAN_POINT ( 'NONE',  ( -22.81625015709510507, 31.40387420917330275, -5.424999997268812990 ) ) ;
#82586 = CARTESIAN_POINT ( 'NONE',  ( -22.92260996908694892, 21.00373069265135584, -50.16862556671883056 ) ) ;
#82588 = CARTESIAN_POINT ( 'NONE',  ( -4.483927247898539470, -16.52544592524342804, 22.29057627198102765 ) ) ;
#82587 = CARTESIAN_POINT ( 'NONE',  ( -12.14591786802326823, 12.06949235617739902, 23.12609039468567573 ) ) ;
#82589 = CARTESIAN_POINT ( 'NONE',  ( -16.51473224551082808, 9.474510206698731452, 73.33442372801900433 ) ) ;
#82590 = CARTESIAN_POINT ( 'NONE',  ( 5.823673210054125526, 21.52544592524343514, 49.79057627198102409 ) ) ;
#82591 = CARTESIAN_POINT ( 'NONE',  ( -5.823673210054431948, 21.52544592524334988, 67.70942372801901854 ) ) ;
#82592 = CARTESIAN_POINT ( 'NONE',  ( 16.53943276465976808, 0.05219959533934440121, 36.25109039468567573 ) ) ;
#82594 = CARTESIAN_POINT ( 'NONE',  ( 9.474510206698971260, -16.51473224551069308, 82.91557627198103830 ) ) ;
#82593 = CARTESIAN_POINT ( 'NONE',  ( 16.46253265017160672, -9.564922557960803928, 28.33224293864769550 ) ) ;
#82595 = CARTESIAN_POINT ( 'NONE',  ( 16.24235425892372930, 17.62966412709566910, -57.02231465076383898 ) ) ;
#82596 = CARTESIAN_POINT ( 'NONE',  ( -8.224510206698948167, 14.34966873604960824, 85.41557627198102409 ) ) ;
#82597 = PRODUCT_CONTEXT ( 'NONE', #161685, 'mechanical' ) ;
#82598 = CARTESIAN_POINT ( 'NONE',  ( -19.03943276465977164, 0.05219959533909376836, 96.24890960531436690 ) ) ;
#82599 = VERTEX_POINT ( 'NONE', #173639 ) ;
#82600 = CARTESIAN_POINT ( 'NONE',  ( -5.049401038297874678, -19.05341960407617918, 109.7927570613523187 ) ) ;
#82601 = CARTESIAN_POINT ( 'NONE',  ( 21.52544592524344225, -5.823673210054117533, 78.54057627198103830 ) ) ;
#82602 = CARTESIAN_POINT ( 'NONE',  ( 0.05219959533909260263, 19.03943276465977164, 39.99890960531436690 ) ) ;
#82604 = CARTESIAN_POINT ( 'NONE',  ( 15.72974639402199770, -15.80617190586745480, 113.1239096053143953 ) ) ;
#82603 = CARTESIAN_POINT ( 'NONE',  ( -19.02544592524334988, -5.153800228976617603, 73.95942372801900433 ) ) ;
#82605 = CARTESIAN_POINT ( 'NONE',  ( -19.03943276465977164, 0.05219959533909376836, 66.24890960531436690 ) ) ;
#82606 = CARTESIAN_POINT ( 'NONE',  ( -0.05219959533909027116, -19.03943276465977164, 112.4989096053143669 ) ) ;
#82607 = ORIENTED_EDGE ( 'NONE', *, *, #195188, .T. ) ;
#82608 = CARTESIAN_POINT ( 'NONE',  ( 8.314922557961029526, -14.29746914071037800, 30.41775706135234358 ) ) ;
#82609 = CARTESIAN_POINT ( 'NONE',  ( -5.823673210054116645, -21.52544592524344225, 102.2905762719810383 ) ) ;
#82612 = CARTESIAN_POINT ( 'NONE',  ( 13.97604488694548053, -13.89961937509957401, 55.62609039468566863 ) ) ;
#82611 = CARTESIAN_POINT ( 'NONE',  ( -16.46253265017160317, 9.564922557960807481, 95.83224293864769550 ) ) ;
#82610 = CARTESIAN_POINT ( 'NONE',  ( 12.14591786802309770, 12.06949235617756955, 104.3739096053143669 ) ) ;
#82613 = CARTESIAN_POINT ( 'NONE',  ( -5.823673210054116645, -21.52544592524344225, 87.29057627198103830 ) ) ;
#82614 = CARTESIAN_POINT ( 'NONE',  ( 14.29746914071049879, -8.314922557960816363, 48.33224293864770260 ) ) ;
#82615 = CARTESIAN_POINT ( 'NONE',  ( 5.049401038297881783, 19.05341960407617563, 27.29275706135232937 ) ) ;
#82616 = CARTESIAN_POINT ( 'NONE',  ( -16.52544592524335698, -4.483927247898792601, 58.95942372801902565 ) ) ;
#82617 = CARTESIAN_POINT ( 'NONE',  ( 13.89961937509977652, -13.97604488694527269, 88.12390960531438111 ) ) ;
#82618 = CARTESIAN_POINT ( 'NONE',  ( -19.05341960407611168, -5.049401038298163336, 41.45724293864769550 ) ) ;
#82619 = CARTESIAN_POINT ( 'NONE',  ( 5.719274019375673035, 21.55341960407619339, 47.29275706135234003 ) ) ;
#82620 = CARTESIAN_POINT ( 'NONE',  ( -5.823673210054431948, 21.52544592524334988, 62.70942372801902565 ) ) ;
#82621 = CARTESIAN_POINT ( 'NONE',  ( 19.02544592524343514, -5.153800228976328945, 63.54057627198103830 ) ) ;
#82622 = CARTESIAN_POINT ( 'NONE',  ( 21.55341960407619695, -5.719274019375665929, 31.04275706135234714 ) ) ;
#82623 = CARTESIAN_POINT ( 'NONE',  ( -16.51473224551082808, 9.474510206698731452, 68.33442372801900433 ) ) ;
#82624 = CARTESIAN_POINT ( 'NONE',  ( -9.564922557961040184, 16.46253265017147172, 72.91775706135233293 ) ) ;
#82625 = CARTESIAN_POINT ( 'NONE',  ( 5.049401038298161559, -19.05341960407611168, 42.70724293864767418 ) ) ;
#82626 = CARTESIAN_POINT ( 'NONE',  ( -12.14591786802326823, 12.06949235617739902, 88.12609039468570415 ) ) ;
#82627 = CARTESIAN_POINT ( 'NONE',  ( 13.89961937509977652, -13.97604488694527269, 48.12390960531435979 ) ) ;
#82628 = CARTESIAN_POINT ( 'NONE',  ( -13.97604488694527625, -13.89961937509977652, 26.87390960531434558 ) ) ;
#82629 = CARTESIAN_POINT ( 'NONE',  ( 16.51473224551069308, 9.474510206698969483, 104.1655762719810241 ) ) ;
#82630 = CARTESIAN_POINT ( 'NONE',  ( -5.153800228976328057, -19.02544592524343514, 37.29057627198102409 ) ) ;
#82631 = CARTESIAN_POINT ( 'NONE',  ( -21.52544592524343514, 5.823673210054127303, 86.04057627198102409 ) ) ;
#82632 = CARTESIAN_POINT ( 'NONE',  ( -8.314922557961024197, 14.29746914071037800, 57.91775706135234714 ) ) ;
#82633 = CARTESIAN_POINT ( 'NONE',  ( -0.05219959533936034679, 19.03943276465977164, 37.50109039468567573 ) ) ;
#82634 = CARTESIAN_POINT ( 'NONE',  ( -19.02544592524342804, 5.153800228976336051, 51.04057627198103120 ) ) ;
#82635 = CARTESIAN_POINT ( 'NONE',  ( -14.29746914071049879, 8.314922557960819915, 45.83224293864769550 ) ) ;
#82636 = CARTESIAN_POINT ( 'NONE',  ( 4.483927247898545687, 16.52544592524342804, 84.79057627198102409 ) ) ;
#82637 = CARTESIAN_POINT ( 'NONE',  ( 19.03943276465977164, -0.05219959533909143690, 98.74890960531436690 ) ) ;
#82638 = CARTESIAN_POINT ( 'NONE',  ( -5.049401038298153566, 19.05341960407611168, 85.20724293864766707 ) ) ;
#82639 = CARTESIAN_POINT ( 'NONE',  ( -18.62759615963255300, -10.81492255796106328, 39.16775706135235424 ) ) ;
#82640 = CARTESIAN_POINT ( 'NONE',  ( 16.46253265017160672, -9.564922557960803928, 88.33224293864769550 ) ) ;
#82641 = CARTESIAN_POINT ( 'NONE',  ( -15.80617190586768217, 15.72974639402176855, 93.12609039468568994 ) ) ;
#82642 = CARTESIAN_POINT ( 'NONE',  ( -8.314922557961024197, 14.29746914071037800, 82.91775706135234714 ) ) ;
#82643 = CARTESIAN_POINT ( 'NONE',  ( -10.81492255796105439, 18.62759615963255655, 22.91775706135235069 ) ) ;
#82644 = CARTESIAN_POINT ( 'NONE',  ( -15.80617190586745835, -15.72974639402198527, 91.87390960531436690 ) ) ;
#82645 = CARTESIAN_POINT ( 'NONE',  ( 12.06949235617757843, -12.14591786802309237, 53.12390960531436690 ) ) ;
#82646 = CARTESIAN_POINT ( 'NONE',  ( 13.89961937509977652, -13.97604488694527269, 43.12390960531434558 ) ) ;
#82647 = CARTESIAN_POINT ( 'NONE',  ( -16.55341960407611168, -4.379528057220339221, 71.45724293864769550 ) ) ;
#82648 = B_SPLINE_CURVE_WITH_KNOTS ( 'NONE', 3,
 ( #130502, #38517, #117349, #83999, #23349, #56688 ),
 .UNSPECIFIED., .F., .F.,
 ( 4, 2, 4 ),
 ( 0.000000000000000000, 0.0003837532665635236652, 0.0007675065331270473305 ),
 .UNSPECIFIED. ) ;
#82649 = CARTESIAN_POINT ( 'NONE',  ( -10.81492255796078084, -18.62759615963271287, 27.08224293864769550 ) ) ;
#82650 = CARTESIAN_POINT ( 'NONE',  ( 16.46253265017146816, 9.564922557961045513, 36.66775706135233293 ) ) ;
#82651 = CARTESIAN_POINT ( 'NONE',  ( 12.06949235617757843, -12.14591786802309237, 103.1239096053143811 ) ) ;
#82652 = ORIENTED_EDGE ( 'NONE', *, *, #38347, .T. ) ;
#82653 = CARTESIAN_POINT ( 'NONE',  ( 4.379528057220092307, 16.55341960407617563, 57.29275706135234714 ) ) ;
#82654 = CARTESIAN_POINT ( 'NONE',  ( 0.05219959533909260263, 19.03943276465977164, 74.99890960531435269 ) ) ;
#82655 = CARTESIAN_POINT ( 'NONE',  ( -17.15575107149451028, -6.384131856062659871, 21.29645598401388895 ) ) ;
#82656 = CARTESIAN_POINT ( 'NONE',  ( 21.53943276465977519, -0.05219959533907433946, 43.74890960531435979 ) ) ;
#82657 = CARTESIAN_POINT ( 'NONE',  ( -12.06949235617739369, -12.14591786802326823, 94.37609039468568994 ) ) ;
#82658 = CARTESIAN_POINT ( 'NONE',  ( -5.153800228976607833, 19.02544592524334988, 107.7094237280189759 ) ) ;
#82659 = CARTESIAN_POINT ( 'NONE',  ( 21.53943276465977519, 0.05219959533937863772, 81.25109039468568994 ) ) ;
#82660 = CARTESIAN_POINT ( 'NONE',  ( -13.89961937509977652, 13.97604488694528158, 80.62390960531436690 ) ) ;
#82661 = CARTESIAN_POINT ( 'NONE',  ( -18.67979575497178146, -10.72451020669898902, 106.6655762719810383 ) ) ;
#82662 = CARTESIAN_POINT ( 'NONE',  ( -16.55341960407617563, 4.379528057220093196, 53.54275706135234714 ) ) ;
#82663 = CARTESIAN_POINT ( 'NONE',  ( -16.53943276465976808, 0.05219959533911058130, 111.2489096053143669 ) ) ;
#82664 = CIRCLE ( 'NONE', #198894, 2.500000000000000000 ) ;
#82665 = CARTESIAN_POINT ( 'NONE',  ( -16.55341960407617563, 4.379528057220093196, 23.54275706135235424 ) ) ;
#82666 = CARTESIAN_POINT ( 'NONE',  ( -9.474510206698720793, -16.51473224551083518, 79.58442372801899012 ) ) ;
#82667 = CARTESIAN_POINT ( 'NONE',  ( 10.72451020669898902, -18.67979575497178502, 82.91557627198103830 ) ) ;
#82668 = CARTESIAN_POINT ( 'NONE',  ( -16.46253265017146816, -9.564922557961047289, 59.16775706135233293 ) ) ;
#82669 = CARTESIAN_POINT ( 'NONE',  ( 30.00000000000000000, -5.499999999999992895, 102.5000000000000142 ) ) ;
#82670 = CARTESIAN_POINT ( 'NONE',  ( -21.52544592524343514, 5.823673210054127303, 106.0405762719810525 ) ) ;
#82671 = CARTESIAN_POINT ( 'NONE',  ( 1.993301997531345686E-15, -30.30510711980685556, 148.5000000000000000 ) ) ;
#82672 = CARTESIAN_POINT ( 'NONE',  ( 13.89961937509977652, -13.97604488694527269, 78.12390960531433848 ) ) ;
#82673 = CARTESIAN_POINT ( 'NONE',  ( -11.14892969833547198, -12.20117655778085819, -59.21778057892716163 ) ) ;
#82674 = CARTESIAN_POINT ( 'NONE',  ( -4.483927247898782831, 16.52544592524335698, 27.70942372801901854 ) ) ;
#82675 = CARTESIAN_POINT ( 'NONE',  ( 36.89607807516674143, -1.430951785632629036, 50.32279621992266527 ) ) ;
#82677 = CARTESIAN_POINT ( 'NONE',  ( -0.05219959533910754901, -16.53943276465976808, 62.49890960531436690 ) ) ;
#82676 = CARTESIAN_POINT ( 'NONE',  ( 21.53943276465977519, -0.05219959533907433946, 108.7489096053143669 ) ) ;
#82678 = CARTESIAN_POINT ( 'NONE',  ( 16.46253265017160672, -9.564922557960803928, 63.33224293864769550 ) ) ;
#82679 = CARTESIAN_POINT ( 'NONE',  ( 18.62759615963255655, 10.81492255796105972, 86.66775706135234714 ) ) ;
#82681 = CARTESIAN_POINT ( 'NONE',  ( 19.03943276465977164, 0.05219959533936151252, 46.25109039468566863 ) ) ;
#82680 = CARTESIAN_POINT ( 'NONE',  ( -0.05219959533934338120, 16.53943276465976808, 42.50109039468567573 ) ) ;
#82682 = CARTESIAN_POINT ( 'NONE',  ( 10.81492255796106328, -18.62759615963255655, 50.41775706135235424 ) ) ;
#82683 = CARTESIAN_POINT ( 'NONE',  ( 18.62759615963271287, -10.81492255796078972, 63.33224293864770260 ) ) ;
#82684 = CARTESIAN_POINT ( 'NONE',  ( 19.02544592524334988, 5.153800228976608722, 106.4594237280190185 ) ) ;
#82685 = CARTESIAN_POINT ( 'NONE',  ( -9.474510206698964154, 16.51473224551069663, 50.41557627198102409 ) ) ;
#82686 = CARTESIAN_POINT ( 'NONE',  ( -5.049401038297874678, -19.05341960407617918, 64.79275706135233293 ) ) ;
#82687 = CARTESIAN_POINT ( 'NONE',  ( -15.72974639402176322, -15.80617190586768395, 79.37609039468567573 ) ) ;
#82688 = CARTESIAN_POINT ( 'NONE',  ( -19.03943276465977164, -0.05219959533935918106, 53.75109039468566863 ) ) ;
#82689 = CARTESIAN_POINT ( 'NONE',  ( -19.03943276465977164, 0.05219959533909376836, 31.24890960531435979 ) ) ;
#82690 = CARTESIAN_POINT ( 'NONE',  ( 10.72451020669898902, -18.67979575497178502, 52.91557627198103830 ) ) ;
#82691 = CARTESIAN_POINT ( 'NONE',  ( -14.34966873604960291, -8.224510206698953496, 56.66557627198103830 ) ) ;
#82692 = DIRECTION ( 'NONE',  ( 1.000000000000000000, 0.000000000000000000, 0.000000000000000000 ) ) ;
#82693 = CARTESIAN_POINT ( 'NONE',  ( 19.02544592524334988, 5.153800228976608722, 26.45942372801899722 ) ) ;
#82694 = CARTESIAN_POINT ( 'NONE',  ( 8.314922557961029526, -14.29746914071037800, 85.41775706135236135 ) ) ;
#82695 = CARTESIAN_POINT ( 'NONE',  ( 12.14591786802309770, 12.06949235617756955, 59.37390960531436690 ) ) ;
#82696 = CARTESIAN_POINT ( 'NONE',  ( -10.72451020669870658, -18.67979575497194134, 84.58442372801903275 ) ) ;
#82697 = CARTESIAN_POINT ( 'NONE',  ( 21.52544592524334988, 5.823673210054432836, 76.45942372801901854 ) ) ;
#82698 = CARTESIAN_POINT ( 'NONE',  ( 15.72974639402199770, -15.80617190586745480, 93.12390960531436690 ) ) ;
#82699 = EDGE_CURVE ( 'NONE', #193525, #26587, #96759, .T. ) ;
#82700 = CARTESIAN_POINT ( 'NONE',  ( -9.564922557960796823, -16.46253265017161027, 47.08224293864769550 ) ) ;
#82701 = CARTESIAN_POINT ( 'NONE',  ( 5.719274019375673035, 21.55341960407619339, 62.29275706135236845 ) ) ;
#82702 = CARTESIAN_POINT ( 'NONE',  ( -13.97604488694527625, -13.89961937509977652, 36.87390960531436690 ) ) ;
#82703 = ORIENTED_EDGE ( 'NONE', *, *, #138326, .F. ) ;
#82704 = CARTESIAN_POINT ( 'NONE',  ( -13.97604488694527625, -13.89961937509977652, 46.87390960531435979 ) ) ;
#82705 = CARTESIAN_POINT ( 'NONE',  ( -12.06949235617756955, 12.14591786802309770, 100.6239096053143811 ) ) ;
#82706 = CARTESIAN_POINT ( 'NONE',  ( 9.474510206698971260, -16.51473224551069308, 102.9155762719810241 ) ) ;
#82707 = AXIS2_PLACEMENT_3D ( 'NONE', #97453, #3475, #65152 ) ;
#82708 = CARTESIAN_POINT ( 'NONE',  ( 14.34966873604960469, 8.224510206698951720, 59.16557627198103120 ) ) ;
#82709 = CARTESIAN_POINT ( 'NONE',  ( 12.06949235617757843, -12.14591786802309237, 113.1239096053143953 ) ) ;
#82710 = CARTESIAN_POINT ( 'NONE',  ( 21.53943276465977519, -0.05219959533907433946, 78.74890960531436690 ) ) ;
#82711 = CARTESIAN_POINT ( 'NONE',  ( 21.52544592524344225, -5.823673210054117533, 113.5405762719810383 ) ) ;
#82712 = CARTESIAN_POINT ( 'NONE',  ( -15.06137443927351072, 15.06137443927345210, -56.46919128290398504 ) ) ;
#82713 = CARTESIAN_POINT ( 'NONE',  ( -8.314922557961024197, 14.29746914071037800, 32.91775706135234714 ) ) ;
#82714 = ORIENTED_EDGE ( 'NONE', *, *, #30441, .T. ) ;
#82715 = CARTESIAN_POINT ( 'NONE',  ( 10.72451020669898902, -18.67979575497178502, 82.91557627198103830 ) ) ;
#82717 = CARTESIAN_POINT ( 'NONE',  ( 0.05219959533937995610, -21.53943276465977519, 110.0010903946856757 ) ) ;
#82716 = PRODUCT_DEFINITION_CONTEXT ( 'detailed design', #57191, 'design' ) ;
#82718 = CARTESIAN_POINT ( 'NONE',  ( 19.02544592524343514, -5.153800228976328945, 98.54057627198100988 ) ) ;
#82719 = CARTESIAN_POINT ( 'NONE',  ( -18.62759615963255300, -10.81492255796106328, 29.16775706135234003 ) ) ;
#82720 = B_SPLINE_CURVE_WITH_KNOTS ( 'NONE', 3,
 ( #149053, #23707, #56030, #10541, #150047, #89359, #135873, #57043, #59012, #165220, #70210, #40868, #26715, #100530, #134890, #85355 ),
 .UNSPECIFIED., .F., .F.,
 ( 4, 2, 2, 2, 2, 2, 2, 4 ),
 ( 2.788292365851994434E-07, 0.0004449923513095699877, 0.0008897058733825547209, 0.001779132917528529392, 0.002223846439601516890, 0.002668559961674504388, 0.003113273483747491886, 0.003557987005820478950 ),
 .UNSPECIFIED. ) ;
#82721 = CARTESIAN_POINT ( 'NONE',  ( -0.05219959533907301413, -21.53943276465977519, 32.49890960531435979 ) ) ;
#82722 = CARTESIAN_POINT ( 'NONE',  ( -12.14591786802326823, 12.06949235617739902, 98.12609039468570415 ) ) ;
#82724 = CARTESIAN_POINT ( 'NONE',  ( 21.53943276465977519, 0.05219959533937863772, 86.25109039468568994 ) ) ;
#82723 = CARTESIAN_POINT ( 'NONE',  ( -5.823673210054431948, 21.52544592524334988, 47.70942372801902565 ) ) ;
#82725 = CARTESIAN_POINT ( 'NONE',  ( -10.81492255796105439, 18.62759615963255655, 107.9177570613523471 ) ) ;
#82726 = CARTESIAN_POINT ( 'NONE',  ( -0.05219959533934338120, 16.53943276465976808, 72.50109039468568994 ) ) ;
#82727 = CARTESIAN_POINT ( 'NONE',  ( -5.823673210054431948, 21.52544592524334988, 37.70942372801900433 ) ) ;
#82728 = CARTESIAN_POINT ( 'NONE',  ( -13.97604488694527625, -13.89961937509977652, 31.87390960531435979 ) ) ;
#82729 = CARTESIAN_POINT ( 'NONE',  ( -18.62759615963255300, -10.81492255796106328, 104.1677570613523471 ) ) ;
#82730 = CARTESIAN_POINT ( 'NONE',  ( 0.05219959533909260263, 19.03943276465977164, 109.9989096053143669 ) ) ;
#82731 = CARTESIAN_POINT ( 'NONE',  ( -15.72974639402197994, 15.80617190586746368, 105.6239096053143669 ) ) ;
#82733 = CARTESIAN_POINT ( 'NONE',  ( 0.05219959533907565091, 21.53943276465977519, 64.99890960531435269 ) ) ;
#82732 = CARTESIAN_POINT ( 'NONE',  ( -5.985463302383371875, -36.83348364107523309, -32.36600886826531109 ) ) ;
#82735 = CARTESIAN_POINT ( 'NONE',  ( -12.06949235617756955, 12.14591786802309770, 45.62390960531436690 ) ) ;
#82734 = CARTESIAN_POINT ( 'NONE',  ( 14.34966873604972726, -8.224510206698740333, 55.83442372801901854 ) ) ;
#82736 = CARTESIAN_POINT ( 'NONE',  ( 21.38418241377623019, 7.427326039334300134, 174.4773576836617224 ) ) ;
#82737 = CARTESIAN_POINT ( 'NONE',  ( -13.97604488694547697, 13.89961937509957934, 88.12609039468563310 ) ) ;
#82738 =( BOUNDED_SURFACE ( )  B_SPLINE_SURFACE ( 3, 2, ( 
 ( #197980, #59450, #154903, #80048, #126542, #141717, #138733, #15404, #79048, #17392, #173069, #63893, #139717, #45741, #95215, #107393, #140722, #60893, #1205, #184259, #33553, #77061, #62882, #64881, #169066, #125564, #16402, #213, #47738, #108399, #2212, #122569, #188241, #124563, #187261, #123552, #171071, #49716, #196720, #172066, #30572, #109391, #3207, #157894, #111381, #92223, #153909, #94215, #34546, #78048, #31567, #96205, #110384, #61882, #73372, #185247, #186260, #155894, #32561, #93218, #46738, #156901, #48730, #135044, #170076, #18397, #5183, #114358, #52694, #127538, #190221, #38541, #130526, #193224, #54698, #176063, #65866, #66864, #174068, #116371, #178059, #6185, #82007, #39527, #99193, #128527, #101187, #112376, #84023, #83025, #19383, #37530, #50718, #192223, #175055, #189240, #53705, #160881, #100197, #22372, #81032, #35537, #115382, #51700, #4187, #97184, #177070, #158870, #8196, #20359, #68867, #159876, #143701, #191220, #113363, #145701, #36519, #69871, #67865, #7183, #98174, #161879, #131540, #142708, #23373, #21367, #85018, #146699, #144699, #129520, #117371, #132543, #181064, #121343, #103208, #118382, #198201, #197221, #163897, #59671, #70876, #88023, #42539, #149711, #180076, #194232, #120350, #57711, #183036, #148720, #40537, #10208, #119381, #196242, #55698, #133536, #182045, #73879, #136520, #44519, #104202, #9209, #71868, #179068, #162876, #24384, #11210, #25393, #86035, #165883, #195228, #147722, #102208, #27380, #26384, #87035, #89026, #56709, #135549, #41545, #164890, #58683, #150717, #43528, #12216, #72885, #134554, #105193, #166880, #28381, #90019, #151702, #13195, #74858, #186020, #75832, #139487, #141487, #93982, #969, #188008, #152675, #200180, #155662, #17158, #64650, #90988, #153671, #184023, #62645, #45505, #2970, #138498, #106175, #169838, #185010, #110153, #156665, #171831, #168831, #107160, #109158, #47502, #126312, #78811, #31332, #137510, #125331, #199191, #170837, #14164, #92983, #60658, #63658, #30336, #154668, #122331, #140490, #76827, #29358, #1978, #167858, #18160, #79816, #91977, #16164, #108156, #15168, #61649, #123317, #77818, #46495, #187028, #124322, #32329, #48499, #33319, #94980, #52450, #50479, #34310, #82775, #53450, #144456, #65631, #38290, #157657, #160631, #173831, #114107, #189985, #127291, #189004, #112139, #35296, #37283, #96952, #176818, #98940, #99944, #83772, #128287, #67617, #5941, #175810, #66623, #161630, #69623, #23124, #4939, #174811, #111141, #97931, #131289, #49478, #22122, #129278, #172831, #36276, #158632, #20123, #21119, #81767, #143454, #84769, #51459, #113121, #19146, #115125, #142474, #145452, #191964, #159624, #95973, #80796, #146447, #3952, #6934, #7940, #190973, #68613, #130269, #181802, #10958, #74616, #134307, #54456, #150474, #116126, #103957, #85785, #196977, #27134, #193988, #147471, #165636, #163640, #177815, #39285, #55450, #12951, #56457, #180818, #26135, #135305, #100942, #8961, #70629, #28138, #72632, #42297, #162626, #57466, #24133, #118136, #192977, #120112, #132296, #119138, #88781, #178815, #117121, #40285, #58444, #11969, #179825, #89778, #149463, #101959, #73634, #148469, #25142, #43281, #195993, #104950, #166636, #86784, #9962, #151463, #71622, #133288, #194978, #41295, #102956, #164640, #87778, #105936, #169596, #171593, #124072, #31094, #17918, #182795, #30097, #185773, #47260, #94737, #121101, #183784, #13925, #92742, #75592, #33081, #168597, #136282, #199949, #14930, #140242, #186785, #1734, #198953, #137271, #139254, #77582, #156417, #108917, #61413, #167621, #155425, #29117, #730, #44278, #123084, #90756, #93744, #60420, #184770, #125087, #152439, #170597, #76590, #122093, #107911, #91737, #62402, #45270, #48255, #46256, #32087, #106924, #154430, #109909, #59427, #16915, #153432, #15924, #63412, #197958, #138266, #78568, #49243, #97695, #38055, #19890, #35058, #114887, #113871 ),
 ( #65393, #174581, #112887, #187773, #50245, #98704, #190740, #53209, #176581, #36046, #126077, #127054, #34073, #99711, #161395, #66390, #142231, #79573, #159386, #188761, #141242, #172587, #67382, #20881, #21887, #64408, #95731, #157417, #2731, #82539, #129039, #110901, #144221, #18911, #4700, #80556, #6698, #3716, #5705, #52214, #111901, #173589, #96713, #145216, #158401, #175568, #81531, #143218, #37045, #128052, #191727, #189754, #51226, #160398, #83537, #68376, #130028, #40042, #148233, #54222, #103727, #147230, #115893, #133055, #193748, #104715, #25904, #23891, #7698, #56217, #26900, #117899, #39050, #11736, #131050, #134067, #8722, #87549, #163406, #100708, #162388, #85544, #70391, #10727, #132059, #150241, #72391, #73403, #57231, #101716, #41060, #179588, #149236, #24902, #135074, #43049, #196750, #178577, #9727, #84533, #71391, #22887, #146210, #195757, #102723, #69381, #194745, #55216, #116885, #164412, #86549, #118905, #58217, #180589, #42063, #192740, #88543, #177583, #165407, #119886, #181571, #12719, #74385, #31846, #136050, #139010, #93497, #16674, #46015, #154193, #155184, #184535, #48015, #107671, #27901, #123827, #89544, #77344, #59191, #170354, #490, #167390, #120860, #62163, #137029, #151230, #197725, #28886, #186542, #29861, #185525, #45034, #169348, #122847, #92504, #183548, #78323, #166406, #139996, #121856, #91498, #182560, #14688, #30857, #1485, #106692, #44043, #60186, #15683, #47017, #124842, #105703, #13692, #90526, #108676, #152208, #63163, #198719, #75359, #153185, #168365, #76350, #138027, #199710, #61175, #49001, #112643, #50983, #6452, #97451, #173344, #79329, #128799, #140999, #174335, #94490, #34815, #17671, #67141, #110657, #96470, #98457, #2487, #159137, #49992, #33826, #81291, #141985, #35805, #156172, #160150, #158158, #20634, #157172, #4452, #21642, #32840, #5459, #64168, #142975, #175325, #191481, #36791, #125833, #187536, #127805, #68133, #111657, #65150, #144971, #143978, #172337, #129784, #95486, #19650, #189509, #66142, #126807, #18666, #190498, #82286, #109671, #80312, #3473, #188515, #51971, #113630, #83295, #171351, #72141, #164165, #26652, #88295, #86304, #99467, #38811, #7452, #149983, #11489, #39797, #115650, #73160, #132812, #100469, #134830, #145970, #117648, #116644, #52959, #9482, #84291, #25663, #8471, #161147, #87308, #194498, #133817, #114635, #180346, #70146, #178334, #176334, #101461, #37805, #163152, #195508, #55971, #22644, #24655, #177340, #162148, #147993, #85292, #23644, #41814, #131816, #146984, #69136, #56981, #130803, #40808, #118655, #193495, #192494, #53978, #103482, #54974, #148991, #165160, #71146, #179345, #102478, #10481, #14440, #78084, #137778, #57979, #153945, #119651, #107429, #89300, #249, #30608, #197487, #150992, #169101, #167147, #181333, #42812, #58954, #16435, #59943, #184295, #29618, #138768, #104474, #12484, #74145, #31603, #76103, #45777, #166159, #60931, #27660, #121611, #196509, #123588, #135817, #122605, #92261, #182318, #120622, #43798, #61918, #105461, #15440, #28646, #90282, #77099, #93252, #108433, #170109, #151966, #183306, #198472, #13454, #154938, #75118, #44788, #136786, #185282, #106441, #168122, #91250, #152941, #199464, #46774, #140756, #124598, #173104, #143739, #34581, #155931, #128562, #47773, #50751, #63927, #142742, #80081, #17426, #79083, #2244, #125596, #127574, #187293, #66899, #189275, #190257, #174101, #18431, #157926, #96238, #65900, #156934, #51734, #162660, #116158, #109426, #112409, #35570, #48764, #1239, #110419, #5218, #172100, #97218, #33586, #62918, #158904, #39316, #177848, #100976, #24166, #64914, #141750, #171105, #139752, #3240, #126575, #32598, #20395, #95249, #94251, #49749, #188276, #186293, #4222, #111418, #19416, #81064, #82042, #119168, #101992, #74649, #194020, #197012, #9994, #88814, #26168, #163673, #25175, #148504, #86817, #73666, #71654, #12986, #135338 ),
 ( #180852, #165668, #150507, #136315, #41327, #132329, #179857, #58477, #120144, #44310, #70662, #133321, #195011, #42328, #56488, #121134, #118166, #85817, #149495, #164673, #89813, #197990, #151494, #102987, #87809, #12005, #27167, #182828, #181835, #10992, #55483, #104982, #117153, #43315, #178849, #72664, #40315, #166669, #134340, #196024, #59461, #57499, #28171, #103989, #105969, #167654, #147504, #8994, #13957, #17952, #77617, #93777, #76621, #124108, #79605, #152471, #125122, #122126, #62435, #94770, #110933, #156453, #183814, #198984, #60452, #186819, #185808, #64440, #14961, #106955, #138299, #47294, #108951, #137303, #199980, #48289, #140276, #2764, #126111, #170631, #75624, #61446, #45304, #187806, #49275, #15957, #91770, #29150, #32120, #123117, #90787, #168628, #155458, #92776, #30128, #16948, #153464, #1768, #184802, #46288, #63446, #78602, #109945, #171626, #107945, #169631, #33114, #31127, #154465, #139287, #141275, #764, #82570, #52245, #142264, #5737, #113902, #175600, #22919, #128082, #18944, #66421, #21919, #160429, #131081, #157450, #19920, #50276, #129069, #111934, #7729, #4732, #172620, #36077, #51257, #176613, #84565, #38088, #35090, #173621, #37077, #98736, #69415, #83570, #97726, #3747, #191760, #65424, #145249, #80589, #159416, #127085, #130061, #96743, #20912, #161427, #188794, #6730, #112917, #158433, #144251, #189786, #68408, #81562, #146243, #67414, #53243, #143248, #190770, #192770, #95764, #114920, #174612, #99743, #54254, #34107, #43080, #70424, #85577, #134101, #74417, #56249, #71421, #151262, #150273, #116916, #12752, #23922, #41092, #195791, #102756, #133085, #177615, #162420, #178609, #136083, #179620, #103759, #149267, #58249, #100739, #132090, #8753, #197757, #57263, #165438, #147263, #180622, #193779, #164443, #115925, #104747, #55248, #42094, #88575, #101750, #39083, #40072, #181603, #163438, #26933, #86581, #24935, #11769, #148264, #27933, #89576, #9757, #25937, #117931, #194775, #87580, #10759, #72423, #118937, #196781, #73434, #135105, #119917, #166438, #141036, #62197, #60219, #44077, #92538, #63199, #154227, #75392, #48051, #167423, #170389, #183582, #123861, #199742, #137064, #198754, #121889, #45067, #47053, #106725, #186578, #108710, #109707, #93534, #138061, #77377, #15717, #185559, #76384, #171389, #79365, #32876, #14724, #184568, #120893, #107704, #17708, #122880, #78358, #31880, #182593, #46049, #168399, #29894, #30891, #91532, #153219, #94526, #61208, #169383, #28919, #124879, #152241, #155219, #1521, #139045, #105736, #90559, #156208, #13726, #16708, #59224, #525, #140032, #190534, #191521, #20670, #84329, #144014, #64203, #160188, #125870, #113667, #95523, #6490, #36829, #3511, #157209, #175361, #173382, #52008, #99505, #114676, #176372, #2523, #127842, #4490, #33863, #37845, #19687, #189548, #18703, #83332, #126846, #80350, #112681, #34852, #187570, #5495, #65187, #49038, #35843, #68170, #97489, #142022, #52998, #110693, #98495, #188552, #67178, #143012, #50030, #111695, #96507, #158197, #21678, #81329, #129822, #145009, #161186, #22682, #66180, #82324, #159175, #128835, #51020, #172373, #174373, #73198, #101501, #71185, #7491, #194537, #104513, #9519, #165197, #149031, #69176, #132849, #8508, #55011, #117686, #178371, #70186, #134868, #24694, #39835, #115690, #150023, #38850, #133856, #88332, #131854, #192533, #54016, #11528, #177378, #118693, #196546, #58016, #25700, #195546, #119686, #164202, #27695, #87345, #130842, #103521, #100507, #57020, #162186, #181369, #180385, #147024, #23684, #41855, #116681, #85332, #193537, #163190, #166194, #56008, #26692, #179383, #42848, #86343, #148030, #40845, #146008, #10519, #102519, #72182, #153983, #58991, #14478, #109460, #16470, #197523, #15480, #61956, #75155, #151028, #90318, #154974, #105498, #138806, #59981, #12519, #152979, #168159, #93289, #139788, #78119, #152004, #28683, #92299, #30646 ),
 ( #1276, #182356, #287, #29656, #13490, #60968, #121648, #77137, #74183, #62953, #137818, #123623, #136826, #184332, #124633, #135853, #185318, #43834, #122642, #186328, #171143, #47810, #167184, #120658, #107465, #89336, #91288, #44825, #198510, #46809, #183343, #106480, #76140, #199502, #169141, #45814, #108468, #170145, #31640, #127608, #67931, #18464, #110454, #80115, #189307, #65936, #140790, #3277, #51765, #143770, #6252, #129585, #50784, #79118, #141783, #187329, #191281, #52756, #19450, #95284, #114425, #112444, #64949, #32632, #125631, #97250, #96273, #94286, #174133, #63962, #5251, #188310, #2279, #66932, #35604, #113426, #158938, #155964, #48800, #128595, #126608, #17461, #172135, #190289, #33621, #142776, #20427, #156967, #82077, #175118, #36586, #83091, #49787, #111453, #173139, #98241, #159944, #34614, #157959, #81098, #4257, #21431, #144767, #11281, #8265, #176127, #9278, #192293, #164958, #84088, #87103, #100264, #179138, #116441, #53772, #115446, #38608, #177137, #163965, #161945, #103278, #25463, #26451, #10277, #54767, #194300, #132611, #102277, #193293, #88093, #196308, #149779, #131608, #101256, #37597, #24452, #134624, #39597, #195299, #40607, #99259, #162945, #23440, #85087, #147792, #69944, #146771, #72955, #178130, #86101, #145767, #180144, #68934, #148788, #118453, #70943, #22439, #7249, #41613, #130596, #71936, #57778, #160946, #55766, #133606, #117440, #56781, #1041, #60729, #181133, #76896, #42607, #30406, #12281, #123388, #153742, #120418, #73946, #92052, #90085, #104271, #165953, #182109, #139557, #183105, #107229, #152743, #61720, #27453, #135615, #197286, #154741, #137579, #168900, #89095, #184093, #150786, #44586, #119448, #46569, #58749, #45576, #15237, #105260, #43594, #166946, #185080, #28449, #138567, #151767, #13260, #45, #16237, #31403, #93054, #74923, #106243, #121412, #136586, #77889, #198266, #167925, #59742, #108230, #29425, #91056, #14233, #75904, #199262, #122403, #169911, #47573, #96044, #66698, #50553, #157731, #5016, #109225, #17227, #155729, #98005, #80870, #112213, #170904, #127368, #32396, #188080, #82852, #190058, #94051, #189080, #35372, #48568, #124396, #63726, #128362, #78879, #173903, #33390, #186091, #97024, #159699, #174886, #36352, #144531, #49551, #62714, #158705, #19220, #140558, #95049, #81840, #20194, #21196, #2047, #142546, #125401, #110221, #187098, #171902, #156738, #111214, #18232, #79886, #4024, #141556, #3045, #64721, #143528, #126383, #172906, #65702, #34384, #51534, #113197, #52522, #178895, #85861, #86865, #24212, #67696, #22198, #40363, #176895, #191049, #114183, #163721, #83847, #116205, #147550, #175887, #39364, #9038, #70707, #56536, #161708, #37358, #100021, #55529, #194068, #164719, #99016, #53525, #145529, #162707, #7008, #41371, #38366, #6017, #69699, #84847, #10040, #118214, #71700, #68690, #130345, #132375, #117203, #103037, #102038, #131366, #160707, #25223, #192044, #148549, #115203, #193055, #23204, #133367, #146525, #54532, #195058, #8016, #179905, #177894, #101022, #26214, #87853, #129354, #72712, #183861, #28217, #57543, #137346, #150550, #180897, #151540, #135385, #17746, #182873, #27211, #134384, #74695, #60495, #136360, #42372, #45348, #196070, #29196, #88857, #44354, #43358, #104035, #165714, #12049, #73713, #106013, #197055, #122171, #167699, #107000, #152514, #181879, #59504, #198036, #90830, #120189, #168673, #156244, #32911, #58523, #166713, #11036, #89857, #149541, #121179, #94565, #14002, #105029, #75669, #13029, #199026, #119212, #162357, #192705, #118874, #8688, #23858, #99678, #134033, #22853, #117866, #72359, #54188, #176546, #38022, #195726, #161362, #102692, #57199, #180558, #9694, #179556, #42032, #148201, #11705, #71359, #191693, #87517, #53176, #41026, #84500, #103696, #164380, #131015, #146178, #25873, #100675, #114852, #7663, #115861, #150208, #193714, #149205, #163371, #165375, #69347 ),
 ( #85509, #26869, #10696, #177551, #88512, #39020, #55183, #133023, #116852, #147197, #70358, #129993, #24868, #132025, #178543, #40009, #101682, #86517, #194713, #56182, #189993, #176828, #116136, #115136, #69633, #38300, #6943, #159632, #147481, #84779, #25152, #68622, #163650, #71632, #24143, #23134, #97939, #160640, #8971, #100952, #86794, #148481, #146457, #36284, #175818, #144464, #9972, #51468, #99954, #52458, #113129, #131299, #37291, #174819, #82783, #54466, #53460, #21128, #7950, #5949, #162636, #145461, #67626, #85795, #192988, #70640, #177825, #129286, #190981, #132306, #22131, #114115, #98950, #193998, #83782, #161640, #39295, #130278, #55460, #117131, #178824, #40295, #191973, #101969, #27144, #182805, #121111, #91747, #118144, #180828, #10967, #89788, #72641, #168607, #165646, #133298, #196988, #11979, #137281, #183794, #198963, #196002, #134316, #136292, #74626, #30107, #44288, #58454, #102965, #152449, #164650, #197968, #179834, #120122, #41304, #90766, #57475, #181813, #122104, #26145, #105946, #73644, #119147, #104960, #88791, #59438, #87787, #45281, #43291, #167631, #42306, #28148, #106934, #56466, #29128, #149472, #166646, #60430, #14940, #153442, #103967, #150484, #151473, #194988, #135315, #12962, #13935, #75602, #187783, #169607, #80566, #110911, #77594, #31105, #49253, #47271, #138276, #123095, #139265, #96723, #140253, #64418, #109921, #18921, #61424, #92753, #154441, #111911, #94748, #126087, #184781, #141252, #46267, #1745, #158411, #3726, #107922, #2741, #172597, #62413, #65403, #35068, #199959, #156428, #34083, #108928, #15935, #95741, #173599, #188771, #50255, #76600, #155436, #142241, #741, #63423, #93755, #125098, #124083, #157427, #185784, #170608, #186796, #32098, #16926, #79583, #78579, #48267, #171604, #127064, #33092, #17929, #8732, #128062, #131060, #144231, #22897, #160408, #97705, #36056, #82549, #159396, #7708, #5715, #147240, #69391, #70401, #54232, #98714, #38065, #176591, #146220, #37055, #132069, #40051, #193758, #175578, #145226, #81541, #68386, #178587, #83547, #39060, #84543, #143228, #6708, #67392, #129049, #191737, #52224, #190750, #55226, #21897, #113881, #189764, #23901, #112897, #192749, #162398, #130038, #66400, #51236, #85554, #174591, #115903, #116895, #101727, #99721, #177593, #19900, #161405, #4710, #100718, #20891, #53219, #114897, #121866, #43059, #10737, #45044, #56227, #27911, #26910, #198730, #119896, #194755, #74395, #118915, #9737, #136060, #104725, #44053, #181581, #24912, #179598, #197735, #134077, #148243, #71401, #120870, #41070, #73413, #166417, #133065, #196760, #89554, #151240, #13702, #180599, #117909, #57241, #12729, #59201, #183558, #102733, #72401, #164422, #182570, #25915, #60196, #195767, #163416, #88553, #42073, #167400, #75369, #28896, #87559, #149246, #105713, #90536, #86559, #152218, #150252, #103737, #137039, #165417, #11746, #135084, #58227, #14699, #64178, #46025, #31856, #95496, #199719, #156183, #47028, #30868, #78334, #139021, #109682, #91508, #157182, #155195, #171363, #154203, #1496, #18676, #29871, #2497, #61185, #140007, #172347, #188525, #33836, #122857, #76361, #124853, #65160, #108686, #62173, #141995, #17682, #106702, #93509, #32851, #16684, #186553, #63174, #123837, #138038, #125843, #48025, #3483, #185535, #80322, #168375, #141010, #94501, #184545, #77354, #187545, #79340, #126819, #153195, #49012, #107681, #92514, #169358, #15693, #501, #110667, #170364, #19660, #68142, #8480, #190507, #5468, #85301, #99476, #50002, #36801, #176343, #175334, #129793, #98466, #67150, #81301, #7461, #144981, #146993, #128808, #23653, #131825, #84300, #83304, #158168, #20643, #69145, #161157, #70155, #111667, #6461, #96480, #35815, #4463, #173354, #34825, #160160, #112654, #142985, #191490, #97461, #66152, #127815, #114645, #113639, #189520, #52968, #50993, #22653, #51981, #174345, #145979, #37815, #130812 ),
 ( #192503, #53987, #100478, #21651, #159147, #143987, #115660, #177350, #82296, #38820, #162157, #71155, #149992, #132821, #28656, #25672, #193506, #56990, #72150, #197496, #43807, #58963, #55980, #194507, #196518, #134839, #90291, #181342, #118664, #163161, #12493, #24664, #57989, #178343, #180355, #101471, #151002, #117657, #41824, #182328, #86313, #42821, #133826, #179354, #165169, #87317, #119660, #39805, #105470, #103491, #104484, #40817, #88304, #167156, #116652, #89309, #148002, #26662, #120631, #75127, #151975, #74155, #166168, #13463, #54983, #11498, #9492, #102487, #164174, #149001, #10490, #73169, #195517, #27669, #135826, #184305, #18439, #29627, #1248, #259, #172109, #93262, #168131, #47782, #92270, #183315, #109434, #16444, #17435, #154948, #198481, #152950, #171116, #107438, #121620, #44797, #94259, #14449, #46783, #78093, #106452, #170118, #139762, #62927, #187302, #153954, #91259, #30617, #186302, #124607, #95259, #76112, #45786, #137789, #32606, #199473, #33595, #169110, #136795, #61928, #15450, #140764, #48773, #2253, #60940, #122615, #155939, #79091, #156942, #63935, #123597, #77108, #125604, #138778, #110428, #185291, #108442, #31612, #59953, #19425, #5226, #71662, #173113, #129561, #20404, #4231, #51743, #112418, #83067, #64923, #133329, #128571, #144742, #127583, #175094, #195020, #3250, #178857, #34589, #113404, #148512, #164682, #10002, #96246, #49759, #98218, #41335, #82052, #35580, #118174, #194028, #80090, #66908, #6229, #190266, #159921, #36563, #97226, #111427, #40323, #21410, #179865, #158913, #56496, #141758, #117161, #67908, #188285, #50761, #55491, #102996, #126583, #101999, #157934, #163681, #81072, #142751, #65910, #189283, #174110, #25184, #143747, #86826, #181843, #61455, #75633, #26176, #12994, #152479, #151502, #105977, #74657, #43323, #196031, #183822, #121142, #123125, #104990, #199988, #107953, #60460, #59469, #134349, #197020, #45312, #137311, #184810, #46296, #182836, #72672, #12013, #180861, #87817, #149503, #136324, #88822, #11000, #167662, #73674, #57507, #119176, #90795, #89821, #42337, #44318, #103998, #198992, #166678, #165676, #122135, #29158, #106962, #13966, #27175, #150515, #168636, #58486, #135346, #120153, #30136, #28179, #197999, #91779, #153473, #14969, #76629, #138307, #19929, #125131, #15965, #63454, #18951, #157457, #128090, #154473, #16956, #47303, #126118, #108960, #4740, #1776, #169640, #33121, #48297, #173629, #81570, #35099, #32128, #170639, #172626, #110940, #66429, #80597, #94778, #139295, #188801, #772, #34114, #77625, #156460, #62442, #127092, #93785, #17959, #158441, #124116, #142272, #109953, #155466, #141282, #186828, #95771, #185816, #143256, #79613, #3754, #78610, #50284, #65431, #189794, #51265, #2772, #140284, #171633, #64448, #31136, #92784, #187813, #49282, #111942, #96751, #160437, #194784, #5746, #177624, #176622, #148274, #69424, #144259, #23930, #68416, #159424, #85585, #192779, #193787, #131091, #174620, #129077, #147271, #83578, #97735, #20920, #70431, #190778, #22928, #54262, #82578, #146252, #115934, #39092, #163446, #130069, #67422, #6738, #162429, #100748, #71430, #52253, #21927, #8762, #191768, #53251, #113910, #116924, #175609, #132097, #55256, #37085, #98744, #145257, #178617, #114929, #40080, #101758, #24943, #86591, #9766, #133094, #112925, #36085, #38097, #99752, #161436, #84574, #7738, #149275, #60229, #90568, #57271, #10768, #28928, #26942, #117940, #102765, #118946, #76394, #119927, #44087, #89585, #198763, #41100, #72432, #134110, #91541, #74426, #105745, #164452, #120902, #25946, #181612, #138070, #183591, #87589, #182602, #152250, #42104, #45076, #14733, #179629, #136092, #167432, #88584, #195799, #13735, #153229, #168408, #29903, #56257, #135114, #121898, #180631, #43090, #73443, #104757, #103768, #165447, #106734, #150282, #11779, #197767, #196790, #58258, #166447, #27943, #75402, #151271, #12761 ),
 ( #59233, #137073, #124891, #30901, #80362, #123871, #92548, #109718, #170400, #81340, #2535, #535, #184577, #32888, #3523, #94538, #15727, #188564, #107713, #110705, #185569, #64216, #140043, #77387, #139055, #62207, #47063, #187582, #108723, #126858, #49050, #50043, #33876, #78369, #17720, #156220, #125882, #16719, #111707, #19698, #173393, #155230, #186590, #61217, #48062, #158208, #63211, #18715, #172385, #122889, #171401, #31891, #93545, #1532, #79378, #141049, #95535, #157222, #142035, #169392, #65199, #154237, #34863, #96518, #199751, #46058, #51031, #8519, #112692, #115700, #70197, #193548, #22693, #130852, #131864, #161197, #24705, #84340, #4501, #100517, #66192, #54027, #35854, #147035, #177389, #144026, #97500, #38860, #113678, #127854, #189559, #5507, #163201, #6501, #192544, #176383, #85342, #174384, #159186, #20681, #178381, #146019, #162196, #55021, #82336, #23694, #67189, #37857, #116691, #143023, #39845, #128846, #190545, #7502, #101511, #83343, #98505, #52019, #175372, #36840, #129833, #69186, #68181, #160200, #191532, #21690, #145020, #53009, #99516, #114688, #165207, #59990, #168168, #120667, #119696, #194547, #57031, #105508, #197533, #121658, #183352, #181379, #132859, #72192, #40856, #44835, #106490, #73208, #149041, #86354, #166203, #133866, #148040, #179393, #151038, #150033, #9529, #42857, #117696, #59001, #41866, #56018, #182365, #27704, #167195, #104522, #71195, #102530, #43843, #118704, #164213, #25710, #28692, #87355, #196555, #89347, #10529, #12528, #74193, #135862, #136836, #103532, #195557, #180395, #90328, #152013, #13499, #26702, #88342, #75164, #198519, #11540, #134879, #58026, #29665, #93298, #108478, #33630, #80123, #95292, #92309, #169151, #32641, #171153, #126616, #17471, #154984, #199511, #48808, #60977, #94295, #14487, #16479, #137828, #187338, #30655, #78129, #18473, #122653, #79127, #170156, #153992, #1286, #61965, #155974, #76149, #141792, #139797, #140800, #77146, #124643, #15489, #156976, #2289, #3286, #63971, #31649, #47820, #186338, #125641, #46818, #64957, #49796, #188318, #185328, #62962, #91297, #109469, #111462, #110462, #172143, #152988, #184341, #45823, #138816, #297, #123632, #107474, #66943, #7257, #51775, #128605, #142784, #177145, #65945, #160954, #115455, #97258, #19459, #81106, #38616, #4265, #145776, #100274, #23449, #52766, #22448, #161953, #191290, #54777, #114435, #34622, #130606, #96281, #84097, #127616, #85096, #68942, #174141, #189316, #192301, #143779, #157967, #50793, #35613, #193302, #36595, #53780, #6261, #146782, #112452, #158946, #20435, #8275, #176136, #69953, #82086, #37605, #5260, #98251, #173147, #131618, #190298, #99268, #113435, #175128, #159953, #21441, #83101, #144777, #67941, #129594, #39606, #165962, #13269, #28458, #90094, #198275, #195310, #182118, #101265, #41624, #133617, #103288, #147802, #197295, #40616, #9287, #26461, #87112, #116451, #119458, #117449, #162955, #149789, #120427, #11293, #132622, #105269, #24461, #27463, #102286, #181142, #56791, #194309, #55776, #179148, #163975, #104280, #25472, #89105, #148798, #43604, #150795, #166956, #12291, #118463, #134634, #72965, #42616, #180155, #151776, #136595, #74932, #71946, #164968, #178140, #88104, #86111, #196319, #135624, #73956, #70952, #57788, #10288, #58758, #184103, #15246, #153751, #94060, #138576, #76905, #29434, #63735, #152752, #47581, #2057, #45585, #106252, #167935, #125410, #91065, #32405, #187107, #110230, #139565, #109233, #48577, #77898, #141565, #1049, #121422, #17236, #183114, #170912, #14242, #171911, #155739, #60739, #75914, #78888, #30415, #44597, #137588, #122413, #79895, #123397, #140567, #93062, #33400, #199271, #107238, #168909, #95058, #62722, #156748, #92063, #124406, #56, #185089, #59752, #18242, #61729, #186099, #46578, #108239, #169919, #31411, #154749, #16246, #52531, #173913, #126392, #114192, #100032, #115212, #176905 ) ),
 .UNSPECIFIED., .T., .F., .T. ) 
 B_SPLINE_SURFACE_WITH_KNOTS ( ( 4, 3, 4 ),
 ( 3, 2, 2, 2, 2, 2, 2, 2, 2, 2, 2, 2, 2, 2, 2, 2, 2, 2, 2, 2, 2, 2, 2, 2, 2, 2, 2, 2, 2, 2, 2, 2, 2, 2, 2, 2, 2, 2, 2, 2, 2, 2, 2, 2, 2, 2, 2, 2, 2, 2, 2, 2, 2, 2, 2, 2, 2, 2, 2, 2, 2, 2, 2, 2, 2, 2, 2, 2, 2, 2, 2, 2, 2, 2, 2, 2, 2, 2, 2, 2, 2, 2, 2, 2, 2, 2, 2, 2, 2, 2, 2, 2, 2, 2, 2, 2, 2, 2, 2, 2, 2, 2, 2, 2, 2, 2, 2, 2, 2, 2, 2, 2, 2, 2, 2, 2, 2, 2, 2, 2, 2, 2, 2, 2, 2, 2, 2, 2, 2, 2, 2, 2, 2, 2, 2, 2, 2, 2, 2, 2, 2, 2, 2, 2, 2, 2, 2, 2, 2, 2, 2, 2, 2, 2, 2, 2, 2, 2, 2, 2, 2, 2, 2, 2, 2, 2, 2, 2, 2, 2, 2, 2, 2, 2, 2, 2, 2, 2, 2, 2, 2, 2, 2, 2, 2, 2, 2, 2, 2, 2, 2, 2, 2, 2, 2, 2, 2, 2, 2, 2, 2, 2, 2, 2, 2, 2, 2, 2, 2, 2, 2, 2, 2, 2, 2, 2, 2, 2, 2, 2, 2, 2, 2, 2, 2, 2, 2, 2, 3 ),
 ( 0.000000000000000000, 0.5000000000000000000, 1.000000000000000000 ),
 ( 0.000000000000000000, 0.004385964912280701511, 0.008771929824561403022, 0.01315789473684210453, 0.01754385964912280604, 0.02192982456140350755, 0.02631578947368420907, 0.03070175438596491058, 0.03508771929824561209, 0.03947368421052631360, 0.04385964912280701511, 0.04824561403508771662, 0.05263157894736841813, 0.05701754385964911964, 0.06140350877192982115, 0.06578947368421052266, 0.07017543859649122417, 0.07456140350877192569, 0.07894736842105262720, 0.08333333333333332871, 0.08771929824561403022, 0.09210526315789473173, 0.09649122807017543324, 0.1008771929824561348, 0.1052631578947368363, 0.1096491228070175378, 0.1140350877192982393, 0.1184210526315789408, 0.1228070175438596423, 0.1271929824561403577, 0.1315789473684210453, 0.1359649122807017607, 0.1403508771929824483, 0.1447368421052631637, 0.1491228070175438514, 0.1535087719298245668, 0.1578947368421052544, 0.1622807017543859698, 0.1666666666666666574, 0.1710526315789473728, 0.1754385964912280604, 0.1798245614035087758, 0.1842105263157894635, 0.1885964912280701788, 0.1929824561403508665, 0.1973684210526315819, 0.2017543859649122695, 0.2061403508771929849, 0.2105263157894736725, 0.2149122807017543879, 0.2192982456140350755, 0.2236842105263157909, 0.2280701754385964786, 0.2324561403508771940, 0.2368421052631578816, 0.2412280701754385970, 0.2456140350877192846, 0.2500000000000000000, 0.2543859649122807154, 0.2587719298245614308, 0.2631578947368420907, 0.2675438596491228060, 0.2719298245614035214, 0.2763157894736842368, 0.2807017543859648967, 0.2850877192982456121, 0.2894736842105263275, 0.2938596491228070429, 0.2982456140350877027, 0.3026315789473684181, 0.3070175438596491335, 0.3114035087719298489, 0.3157894736842105088, 0.3201754385964912242, 0.3245614035087719396, 0.3289473684210526550, 0.3333333333333333148, 0.3377192982456140302, 0.3421052631578947456, 0.3464912280701754610, 0.3508771929824561209, 0.3552631578947368363, 0.3596491228070175517, 0.3640350877192982670, 0.3684210526315789269, 0.3728070175438596423, 0.3771929824561403577, 0.3815789473684210731, 0.3859649122807017330, 0.3903508771929824483, 0.3947368421052631637, 0.3991228070175438791, 0.4035087719298245390, 0.4078947368421052544, 0.4122807017543859698, 0.4166666666666666852, 0.4210526315789473450, 0.4254385964912280604, 0.4298245614035087758, 0.4342105263157894912, 0.4385964912280701511, 0.4429824561403508665, 0.4473684210526315819, 0.4517543859649122973, 0.4561403508771929571, 0.4605263157894736725, 0.4649122807017543879, 0.4692982456140351033, 0.4736842105263157632, 0.4780701754385964786, 0.4824561403508771940, 0.4868421052631579093, 0.4912280701754385692, 0.4956140350877192846, 0.5000000000000000000, 0.5043859649122807154, 0.5087719298245614308, 0.5131578947368421462, 0.5175438596491228616, 0.5219298245614034659, 0.5263157894736841813, 0.5307017543859648967, 0.5350877192982456121, 0.5394736842105263275, 0.5438596491228070429, 0.5482456140350877583, 0.5526315789473684736, 0.5570175438596490780, 0.5614035087719297934, 0.5657894736842105088, 0.5701754385964912242, 0.5745614035087719396, 0.5789473684210526550, 0.5833333333333333703, 0.5877192982456140857, 0.5921052631578946901, 0.5964912280701754055, 0.6008771929824561209, 0.6052631578947368363, 0.6096491228070175517, 0.6140350877192982670, 0.6184210526315789824, 0.6228070175438596978, 0.6271929824561403022, 0.6315789473684210176, 0.6359649122807017330, 0.6403508771929824483, 0.6447368421052631637, 0.6491228070175438791, 0.6535087719298245945, 0.6578947368421053099, 0.6622807017543859143, 0.6666666666666666297, 0.6710526315789473450, 0.6754385964912280604, 0.6798245614035087758, 0.6842105263157894912, 0.6885964912280702066, 0.6929824561403509220, 0.6973684210526315264, 0.7017543859649122417, 0.7061403508771929571, 0.7105263157894736725, 0.7149122807017543879, 0.7192982456140351033, 0.7236842105263158187, 0.7280701754385965341, 0.7324561403508771384, 0.7368421052631578538, 0.7412280701754385692, 0.7456140350877192846, 0.7500000000000000000, 0.7543859649122807154, 0.7587719298245614308, 0.7631578947368421462, 0.7675438596491228616, 0.7719298245614034659, 0.7763157894736841813, 0.7807017543859648967, 0.7850877192982456121, 0.7894736842105263275, 0.7938596491228070429, 0.7982456140350877583, 0.8026315789473684736, 0.8070175438596490780, 0.8114035087719297934, 0.8157894736842105088, 0.8201754385964912242, 0.8245614035087719396, 0.8289473684210526550, 0.8333333333333333703, 0.8377192982456140857, 0.8421052631578946901, 0.8464912280701754055, 0.8508771929824561209, 0.8552631578947368363, 0.8596491228070175517, 0.8640350877192982670, 0.8684210526315789824, 0.8728070175438596978, 0.8771929824561403022, 0.8815789473684210176, 0.8859649122807017330, 0.8903508771929824483, 0.8947368421052631637, 0.8991228070175438791, 0.9035087719298245945, 0.9078947368421053099, 0.9122807017543859143, 0.9166666666666666297, 0.9210526315789473450, 0.9254385964912280604, 0.9298245614035087758, 0.9342105263157894912, 0.9385964912280702066, 0.9429824561403509220, 0.9473684210526315264, 0.9517543859649122417, 0.9561403508771929571, 0.9605263157894736725, 0.9649122807017543879, 0.9692982456140351033, 0.9736842105263158187, 0.9780701754385965341, 0.9824561403508771384, 0.9868421052631578538, 0.9912280701754385692, 0.9956140350877192846, 1.000000000000000000 ),
 .UNSPECIFIED. ) 
 GEOMETRIC_REPRESENTATION_ITEM ( )  RATIONAL_B_SPLINE_SURFACE ( (
 ( 1.000000000000000000, 0.9659258262890683122, 1.000000000000000000, 0.9659258262890683122, 1.000000000000000000, 0.9659258262890683122, 1.000000000000000000, 0.9659258262890683122, 1.000000000000000000, 0.9659258262890683122, 1.000000000000000000, 0.9659258262890683122, 1.000000000000000000, 0.9659258262890683122, 1.000000000000000000, 0.9659258262890683122, 1.000000000000000000, 0.9659258262890683122, 1.000000000000000000, 0.9659258262890683122, 1.000000000000000000, 0.9659258262890683122, 1.000000000000000000, 0.9659258262890683122, 1.000000000000000000, 0.9659258262890683122, 1.000000000000000000, 0.9659258262890683122, 1.000000000000000000, 0.9659258262890683122, 1.000000000000000000, 0.9659258262890683122, 1.000000000000000000, 0.9659258262890683122, 1.000000000000000000, 0.9659258262890683122, 1.000000000000000000, 0.9659258262890683122, 1.000000000000000000, 0.9659258262890683122, 1.000000000000000000, 0.9659258262890683122, 1.000000000000000000, 0.9659258262890683122, 1.000000000000000000, 0.9659258262890683122, 1.000000000000000000, 0.9659258262890683122, 1.000000000000000000, 0.9659258262890683122, 1.000000000000000000, 0.9659258262890683122, 1.000000000000000000, 0.9659258262890683122, 1.000000000000000000, 0.9659258262890683122, 1.000000000000000000, 0.9659258262890683122, 1.000000000000000000, 0.9659258262890683122, 1.000000000000000000, 0.9659258262890683122, 1.000000000000000000, 0.9659258262890683122, 1.000000000000000000, 0.9659258262890683122, 1.000000000000000000, 0.9659258262890683122, 1.000000000000000000, 0.9659258262890683122, 1.000000000000000000, 0.9659258262890683122, 1.000000000000000000, 0.9659258262890683122, 1.000000000000000000, 0.9659258262890683122, 1.000000000000000000, 0.9659258262890683122, 1.000000000000000000, 0.9659258262890683122, 1.000000000000000000, 0.9659258262890683122, 1.000000000000000000, 0.9659258262890683122, 1.000000000000000000, 0.9659258262890683122, 1.000000000000000000, 0.9659258262890683122, 1.000000000000000000, 0.9659258262890683122, 1.000000000000000000, 0.9659258262890683122, 1.000000000000000000, 0.9659258262890683122, 1.000000000000000000, 0.9659258262890683122, 1.000000000000000000, 0.9659258262890683122, 1.000000000000000000, 0.9659258262890683122, 1.000000000000000000, 0.9659258262890683122, 1.000000000000000000, 0.9659258262890683122, 1.000000000000000000, 0.9659258262890683122, 1.000000000000000000, 0.9659258262890683122, 1.000000000000000000, 0.9659258262890683122, 1.000000000000000000, 0.9659258262890683122, 1.000000000000000000, 0.9659258262890683122, 1.000000000000000000, 0.9659258262890683122, 1.000000000000000000, 0.9659258262890683122, 1.000000000000000000, 0.9659258262890683122, 1.000000000000000000, 0.9659258262890683122, 1.000000000000000000, 0.9659258262890683122, 1.000000000000000000, 0.9659258262890683122, 1.000000000000000000, 0.9659258262890683122, 1.000000000000000000, 0.9659258262890683122, 1.000000000000000000, 0.9659258262890683122, 1.000000000000000000, 0.9659258262890683122, 1.000000000000000000, 0.9659258262890683122, 1.000000000000000000, 0.9659258262890683122, 1.000000000000000000, 0.9659258262890683122, 1.000000000000000000, 0.9659258262890683122, 1.000000000000000000, 0.9659258262890683122, 1.000000000000000000, 0.9659258262890683122, 1.000000000000000000, 0.9659258262890683122, 1.000000000000000000, 0.9659258262890683122, 1.000000000000000000, 0.9659258262890683122, 1.000000000000000000, 0.9659258262890683122, 1.000000000000000000, 0.9659258262890683122, 1.000000000000000000, 0.9659258262890683122, 1.000000000000000000, 0.9659258262890683122, 1.000000000000000000, 0.9659258262890683122, 1.000000000000000000, 0.9659258262890683122, 1.000000000000000000, 0.9659258262890683122, 1.000000000000000000, 0.9659258262890683122, 1.000000000000000000, 0.9659258262890683122, 1.000000000000000000, 0.9659258262890683122, 1.000000000000000000, 0.9659258262890683122, 1.000000000000000000, 0.9659258262890683122, 1.000000000000000000, 0.9659258262890683122, 1.000000000000000000, 0.9659258262890683122, 1.000000000000000000, 0.9659258262890683122, 1.000000000000000000, 0.9659258262890683122, 1.000000000000000000, 0.9659258262890683122, 1.000000000000000000, 0.9659258262890683122, 1.000000000000000000, 0.9659258262890683122, 1.000000000000000000, 0.9659258262890683122, 1.000000000000000000, 0.9659258262890683122, 1.000000000000000000, 0.9659258262890683122, 1.000000000000000000, 0.9659258262890683122, 1.000000000000000000, 0.9659258262890683122, 1.000000000000000000, 0.9659258262890683122, 1.000000000000000000, 0.9659258262890683122, 1.000000000000000000, 0.9659258262890683122, 1.000000000000000000, 0.9659258262890683122, 1.000000000000000000, 0.9659258262890683122, 1.000000000000000000, 0.9659258262890683122, 1.000000000000000000, 0.9659258262890683122, 1.000000000000000000, 0.9659258262890683122, 1.000000000000000000, 0.9659258262890683122, 1.000000000000000000, 0.9659258262890683122, 1.000000000000000000, 0.9659258262890683122, 1.000000000000000000, 0.9659258262890683122, 1.000000000000000000, 0.9659258262890683122, 1.000000000000000000, 0.9659258262890683122, 1.000000000000000000, 0.9659258262890683122, 1.000000000000000000, 0.9659258262890683122, 1.000000000000000000, 0.9659258262890683122, 1.000000000000000000, 0.9659258262890683122, 1.000000000000000000, 0.9659258262890683122, 1.000000000000000000, 0.9659258262890683122, 1.000000000000000000, 0.9659258262890683122, 1.000000000000000000, 0.9659258262890683122, 1.000000000000000000, 0.9659258262890683122, 1.000000000000000000, 0.9659258262890683122, 1.000000000000000000, 0.9659258262890683122, 1.000000000000000000, 0.9659258262890683122, 1.000000000000000000, 0.9659258262890683122, 1.000000000000000000, 0.9659258262890683122, 1.000000000000000000, 0.9659258262890683122, 1.000000000000000000, 0.9659258262890683122, 1.000000000000000000, 0.9659258262890683122, 1.000000000000000000, 0.9659258262890683122, 1.000000000000000000, 0.9659258262890683122, 1.000000000000000000, 0.9659258262890683122, 1.000000000000000000, 0.9659258262890683122, 1.000000000000000000, 0.9659258262890683122, 1.000000000000000000, 0.9659258262890683122, 1.000000000000000000, 0.9659258262890683122, 1.000000000000000000, 0.9659258262890683122, 1.000000000000000000, 0.9659258262890683122, 1.000000000000000000, 0.9659258262890683122, 1.000000000000000000, 0.9659258262890683122, 1.000000000000000000, 0.9659258262890683122, 1.000000000000000000, 0.9659258262890683122, 1.000000000000000000, 0.9659258262890683122, 1.000000000000000000, 0.9659258262890683122, 1.000000000000000000, 0.9659258262890683122, 1.000000000000000000, 0.9659258262890683122, 1.000000000000000000, 0.9659258262890683122, 1.000000000000000000, 0.9659258262890683122, 1.000000000000000000, 0.9659258262890683122, 1.000000000000000000, 0.9659258262890683122, 1.000000000000000000, 0.9659258262890683122, 1.000000000000000000, 0.9659258262890683122, 1.000000000000000000, 0.9659258262890683122, 1.000000000000000000, 0.9659258262890683122, 1.000000000000000000, 0.9659258262890683122, 1.000000000000000000, 0.9659258262890683122, 1.000000000000000000, 0.9659258262890683122, 1.000000000000000000, 0.9659258262890683122, 1.000000000000000000, 0.9659258262890683122, 1.000000000000000000, 0.9659258262890683122, 1.000000000000000000, 0.9659258262890683122, 1.000000000000000000, 0.9659258262890683122, 1.000000000000000000, 0.9659258262890683122, 1.000000000000000000, 0.9659258262890683122, 1.000000000000000000, 0.9659258262890683122, 1.000000000000000000, 0.9659258262890683122, 1.000000000000000000, 0.9659258262890683122, 1.000000000000000000, 0.9659258262890683122, 1.000000000000000000, 0.9659258262890683122, 1.000000000000000000, 0.9659258262890683122, 1.000000000000000000, 0.9659258262890683122, 1.000000000000000000, 0.9659258262890683122, 1.000000000000000000, 0.9659258262890683122, 1.000000000000000000, 0.9659258262890683122, 1.000000000000000000, 0.9659258262890683122, 1.000000000000000000, 0.9659258262890683122, 1.000000000000000000, 0.9659258262890683122, 1.000000000000000000, 0.9659258262890683122, 1.000000000000000000, 0.9659258262890683122, 1.000000000000000000, 0.9659258262890683122, 1.000000000000000000, 0.9659258262890683122, 1.000000000000000000, 0.9659258262890683122, 1.000000000000000000, 0.9659258262890683122, 1.000000000000000000, 0.9659258262890683122, 1.000000000000000000, 0.9659258262890683122, 1.000000000000000000, 0.9659258262890683122, 1.000000000000000000, 0.9659258262890683122, 1.000000000000000000, 0.9659258262890683122, 1.000000000000000000, 0.9659258262890683122, 1.000000000000000000, 0.9659258262890683122, 1.000000000000000000, 0.9659258262890683122, 1.000000000000000000, 0.9659258262890683122, 1.000000000000000000, 0.9659258262890683122, 1.000000000000000000, 0.9659258262890683122, 1.000000000000000000, 0.9659258262890683122, 1.000000000000000000, 0.9659258262890683122, 1.000000000000000000, 0.9659258262890683122, 1.000000000000000000, 0.9659258262890683122, 1.000000000000000000, 0.9659258262890683122, 1.000000000000000000, 0.9659258262890683122, 1.000000000000000000, 0.9659258262890683122, 1.000000000000000000, 0.9659258262890683122, 1.000000000000000000, 0.9659258262890683122, 1.000000000000000000, 0.9659258262890683122, 1.000000000000000000, 0.9659258262890683122, 1.000000000000000000, 0.9659258262890683122, 1.000000000000000000, 0.9659258262890683122, 1.000000000000000000, 0.9659258262890683122, 1.000000000000000000, 0.9659258262890683122, 1.000000000000000000, 0.9659258262890683122, 1.000000000000000000, 0.9659258262890683122, 1.000000000000000000, 0.9659258262890683122, 1.000000000000000000, 0.9659258262890683122, 1.000000000000000000, 0.9659258262890683122, 1.000000000000000000, 0.9659258262890683122, 1.000000000000000000, 0.9659258262890683122, 1.000000000000000000, 0.9659258262890683122, 1.000000000000000000, 0.9659258262890683122, 1.000000000000000000, 0.9659258262890683122, 1.000000000000000000, 0.9659258262890683122, 1.000000000000000000, 0.9659258262890683122, 1.000000000000000000, 0.9659258262890683122, 1.000000000000000000, 0.9659258262890683122, 1.000000000000000000, 0.9659258262890683122, 1.000000000000000000, 0.9659258262890683122, 1.000000000000000000, 0.9659258262890683122, 1.000000000000000000),
 ( 0.3333333333333333703, 0.3219752754296894559, 0.3333333333333333703, 0.3219752754296894559, 0.3333333333333333703, 0.3219752754296894559, 0.3333333333333333703, 0.3219752754296894559, 0.3333333333333333703, 0.3219752754296894559, 0.3333333333333333703, 0.3219752754296894559, 0.3333333333333333703, 0.3219752754296894559, 0.3333333333333333703, 0.3219752754296894559, 0.3333333333333333703, 0.3219752754296894559, 0.3333333333333333703, 0.3219752754296894559, 0.3333333333333333703, 0.3219752754296894559, 0.3333333333333333703, 0.3219752754296894559, 0.3333333333333333703, 0.3219752754296894559, 0.3333333333333333703, 0.3219752754296894559, 0.3333333333333333703, 0.3219752754296894559, 0.3333333333333333703, 0.3219752754296894559, 0.3333333333333333703, 0.3219752754296894559, 0.3333333333333333703, 0.3219752754296894559, 0.3333333333333333703, 0.3219752754296894559, 0.3333333333333333703, 0.3219752754296894559, 0.3333333333333333703, 0.3219752754296894559, 0.3333333333333333703, 0.3219752754296894559, 0.3333333333333333703, 0.3219752754296894559, 0.3333333333333333703, 0.3219752754296894559, 0.3333333333333333703, 0.3219752754296894559, 0.3333333333333333703, 0.3219752754296894559, 0.3333333333333333703, 0.3219752754296894559, 0.3333333333333333703, 0.3219752754296894559, 0.3333333333333333703, 0.3219752754296894559, 0.3333333333333333703, 0.3219752754296894559, 0.3333333333333333703, 0.3219752754296894559, 0.3333333333333333703, 0.3219752754296894559, 0.3333333333333333703, 0.3219752754296894559, 0.3333333333333333703, 0.3219752754296894559, 0.3333333333333333703, 0.3219752754296894559, 0.3333333333333333703, 0.3219752754296894559, 0.3333333333333333703, 0.3219752754296894559, 0.3333333333333333703, 0.3219752754296894559, 0.3333333333333333703, 0.3219752754296894559, 0.3333333333333333703, 0.3219752754296894559, 0.3333333333333333703, 0.3219752754296894559, 0.3333333333333333703, 0.3219752754296894559, 0.3333333333333333703, 0.3219752754296894559, 0.3333333333333333703, 0.3219752754296894559, 0.3333333333333333703, 0.3219752754296894559, 0.3333333333333333703, 0.3219752754296894559, 0.3333333333333333703, 0.3219752754296894559, 0.3333333333333333703, 0.3219752754296894559, 0.3333333333333333703, 0.3219752754296894559, 0.3333333333333333703, 0.3219752754296894559, 0.3333333333333333703, 0.3219752754296894559, 0.3333333333333333703, 0.3219752754296894559, 0.3333333333333333703, 0.3219752754296894559, 0.3333333333333333703, 0.3219752754296894559, 0.3333333333333333703, 0.3219752754296894559, 0.3333333333333333703, 0.3219752754296894559, 0.3333333333333333703, 0.3219752754296894559, 0.3333333333333333703, 0.3219752754296894559, 0.3333333333333333703, 0.3219752754296894559, 0.3333333333333333703, 0.3219752754296894559, 0.3333333333333333703, 0.3219752754296894559, 0.3333333333333333703, 0.3219752754296894559, 0.3333333333333333703, 0.3219752754296894559, 0.3333333333333333703, 0.3219752754296894559, 0.3333333333333333703, 0.3219752754296894559, 0.3333333333333333703, 0.3219752754296894559, 0.3333333333333333703, 0.3219752754296894559, 0.3333333333333333703, 0.3219752754296894559, 0.3333333333333333703, 0.3219752754296894559, 0.3333333333333333703, 0.3219752754296894559, 0.3333333333333333703, 0.3219752754296894559, 0.3333333333333333703, 0.3219752754296894559, 0.3333333333333333703, 0.3219752754296894559, 0.3333333333333333703, 0.3219752754296894559, 0.3333333333333333703, 0.3219752754296894559, 0.3333333333333333703, 0.3219752754296894559, 0.3333333333333333703, 0.3219752754296894559, 0.3333333333333333703, 0.3219752754296894559, 0.3333333333333333703, 0.3219752754296894559, 0.3333333333333333703, 0.3219752754296894559, 0.3333333333333333703, 0.3219752754296894559, 0.3333333333333333703, 0.3219752754296894559, 0.3333333333333333703, 0.3219752754296894559, 0.3333333333333333703, 0.3219752754296894559, 0.3333333333333333703, 0.3219752754296894559, 0.3333333333333333703, 0.3219752754296894559, 0.3333333333333333703, 0.3219752754296894559, 0.3333333333333333703, 0.3219752754296894559, 0.3333333333333333703, 0.3219752754296894559, 0.3333333333333333703, 0.3219752754296894559, 0.3333333333333333703, 0.3219752754296894559, 0.3333333333333333703, 0.3219752754296894559, 0.3333333333333333703, 0.3219752754296894559, 0.3333333333333333703, 0.3219752754296894559, 0.3333333333333333703, 0.3219752754296894559, 0.3333333333333333703, 0.3219752754296894559, 0.3333333333333333703, 0.3219752754296894559, 0.3333333333333333703, 0.3219752754296894559, 0.3333333333333333703, 0.3219752754296894559, 0.3333333333333333703, 0.3219752754296894559, 0.3333333333333333703, 0.3219752754296894559, 0.3333333333333333703, 0.3219752754296894559, 0.3333333333333333703, 0.3219752754296894559, 0.3333333333333333703, 0.3219752754296894559, 0.3333333333333333703, 0.3219752754296894559, 0.3333333333333333703, 0.3219752754296894559, 0.3333333333333333703, 0.3219752754296894559, 0.3333333333333333703, 0.3219752754296894559, 0.3333333333333333703, 0.3219752754296894559, 0.3333333333333333703, 0.3219752754296894559, 0.3333333333333333703, 0.3219752754296894559, 0.3333333333333333703, 0.3219752754296894559, 0.3333333333333333703, 0.3219752754296894559, 0.3333333333333333703, 0.3219752754296894559, 0.3333333333333333703, 0.3219752754296894559, 0.3333333333333333703, 0.3219752754296894559, 0.3333333333333333703, 0.3219752754296894559, 0.3333333333333333703, 0.3219752754296894559, 0.3333333333333333703, 0.3219752754296894559, 0.3333333333333333703, 0.3219752754296894559, 0.3333333333333333703, 0.3219752754296894559, 0.3333333333333333703, 0.3219752754296894559, 0.3333333333333333703, 0.3219752754296894559, 0.3333333333333333703, 0.3219752754296894559, 0.3333333333333333703, 0.3219752754296894559, 0.3333333333333333703, 0.3219752754296894559, 0.3333333333333333703, 0.3219752754296894559, 0.3333333333333333703, 0.3219752754296894559, 0.3333333333333333703, 0.3219752754296894559, 0.3333333333333333703, 0.3219752754296894559, 0.3333333333333333703, 0.3219752754296894559, 0.3333333333333333703, 0.3219752754296894559, 0.3333333333333333703, 0.3219752754296894559, 0.3333333333333333703, 0.3219752754296894559, 0.3333333333333333703, 0.3219752754296894559, 0.3333333333333333703, 0.3219752754296894559, 0.3333333333333333703, 0.3219752754296894559, 0.3333333333333333703, 0.3219752754296894559, 0.3333333333333333703, 0.3219752754296894559, 0.3333333333333333703, 0.3219752754296894559, 0.3333333333333333703, 0.3219752754296894559, 0.3333333333333333703, 0.3219752754296894559, 0.3333333333333333703, 0.3219752754296894559, 0.3333333333333333703, 0.3219752754296894559, 0.3333333333333333703, 0.3219752754296894559, 0.3333333333333333703, 0.3219752754296894559, 0.3333333333333333703, 0.3219752754296894559, 0.3333333333333333703, 0.3219752754296894559, 0.3333333333333333703, 0.3219752754296894559, 0.3333333333333333703, 0.3219752754296894559, 0.3333333333333333703, 0.3219752754296894559, 0.3333333333333333703, 0.3219752754296894559, 0.3333333333333333703, 0.3219752754296894559, 0.3333333333333333703, 0.3219752754296894559, 0.3333333333333333703, 0.3219752754296894559, 0.3333333333333333703, 0.3219752754296894559, 0.3333333333333333703, 0.3219752754296894559, 0.3333333333333333703, 0.3219752754296894559, 0.3333333333333333703, 0.3219752754296894559, 0.3333333333333333703, 0.3219752754296894559, 0.3333333333333333703, 0.3219752754296894559, 0.3333333333333333703, 0.3219752754296894559, 0.3333333333333333703, 0.3219752754296894559, 0.3333333333333333703, 0.3219752754296894559, 0.3333333333333333703, 0.3219752754296894559, 0.3333333333333333703, 0.3219752754296894559, 0.3333333333333333703, 0.3219752754296894559, 0.3333333333333333703, 0.3219752754296894559, 0.3333333333333333703, 0.3219752754296894559, 0.3333333333333333703, 0.3219752754296894559, 0.3333333333333333703, 0.3219752754296894559, 0.3333333333333333703, 0.3219752754296894559, 0.3333333333333333703, 0.3219752754296894559, 0.3333333333333333703, 0.3219752754296894559, 0.3333333333333333703, 0.3219752754296894559, 0.3333333333333333703, 0.3219752754296894559, 0.3333333333333333703, 0.3219752754296894559, 0.3333333333333333703, 0.3219752754296894559, 0.3333333333333333703, 0.3219752754296894559, 0.3333333333333333703, 0.3219752754296894559, 0.3333333333333333703, 0.3219752754296894559, 0.3333333333333333703, 0.3219752754296894559, 0.3333333333333333703, 0.3219752754296894559, 0.3333333333333333703, 0.3219752754296894559, 0.3333333333333333703, 0.3219752754296894559, 0.3333333333333333703, 0.3219752754296894559, 0.3333333333333333703, 0.3219752754296894559, 0.3333333333333333703, 0.3219752754296894559, 0.3333333333333333703, 0.3219752754296894559, 0.3333333333333333703, 0.3219752754296894559, 0.3333333333333333703, 0.3219752754296894559, 0.3333333333333333703, 0.3219752754296894559, 0.3333333333333333703, 0.3219752754296894559, 0.3333333333333333703, 0.3219752754296894559, 0.3333333333333333703, 0.3219752754296894559, 0.3333333333333333703, 0.3219752754296894559, 0.3333333333333333703, 0.3219752754296894559, 0.3333333333333333703, 0.3219752754296894559, 0.3333333333333333703, 0.3219752754296894559, 0.3333333333333333703, 0.3219752754296894559, 0.3333333333333333703, 0.3219752754296894559, 0.3333333333333333703, 0.3219752754296894559, 0.3333333333333333703, 0.3219752754296894559, 0.3333333333333333703, 0.3219752754296894559, 0.3333333333333333703, 0.3219752754296894559, 0.3333333333333333703, 0.3219752754296894559, 0.3333333333333333703, 0.3219752754296894559, 0.3333333333333333703, 0.3219752754296894559, 0.3333333333333333703, 0.3219752754296894559, 0.3333333333333333703, 0.3219752754296894559, 0.3333333333333333703, 0.3219752754296894559, 0.3333333333333333703, 0.3219752754296894559, 0.3333333333333333703, 0.3219752754296894559, 0.3333333333333333703, 0.3219752754296894559, 0.3333333333333333703, 0.3219752754296894559, 0.3333333333333333703, 0.3219752754296894559, 0.3333333333333333703, 0.3219752754296894559, 0.3333333333333333703, 0.3219752754296894559, 0.3333333333333333703, 0.3219752754296894559, 0.3333333333333333703, 0.3219752754296894559, 0.3333333333333333703, 0.3219752754296894559, 0.3333333333333333703, 0.3219752754296894559, 0.3333333333333333703, 0.3219752754296894559, 0.3333333333333333703, 0.3219752754296894559, 0.3333333333333333703, 0.3219752754296894559, 0.3333333333333333703, 0.3219752754296894559, 0.3333333333333333703, 0.3219752754296894559, 0.3333333333333333703, 0.3219752754296894559, 0.3333333333333333703),
 ( 0.3333333333333333703, 0.3219752754296894559, 0.3333333333333333703, 0.3219752754296894559, 0.3333333333333333703, 0.3219752754296894559, 0.3333333333333333703, 0.3219752754296894559, 0.3333333333333333703, 0.3219752754296894559, 0.3333333333333333703, 0.3219752754296894559, 0.3333333333333333703, 0.3219752754296894559, 0.3333333333333333703, 0.3219752754296894559, 0.3333333333333333703, 0.3219752754296894559, 0.3333333333333333703, 0.3219752754296894559, 0.3333333333333333703, 0.3219752754296894559, 0.3333333333333333703, 0.3219752754296894559, 0.3333333333333333703, 0.3219752754296894559, 0.3333333333333333703, 0.3219752754296894559, 0.3333333333333333703, 0.3219752754296894559, 0.3333333333333333703, 0.3219752754296894559, 0.3333333333333333703, 0.3219752754296894559, 0.3333333333333333703, 0.3219752754296894559, 0.3333333333333333703, 0.3219752754296894559, 0.3333333333333333703, 0.3219752754296894559, 0.3333333333333333703, 0.3219752754296894559, 0.3333333333333333703, 0.3219752754296894559, 0.3333333333333333703, 0.3219752754296894559, 0.3333333333333333703, 0.3219752754296894559, 0.3333333333333333703, 0.3219752754296894559, 0.3333333333333333703, 0.3219752754296894559, 0.3333333333333333703, 0.3219752754296894559, 0.3333333333333333703, 0.3219752754296894559, 0.3333333333333333703, 0.3219752754296894559, 0.3333333333333333703, 0.3219752754296894559, 0.3333333333333333703, 0.3219752754296894559, 0.3333333333333333703, 0.3219752754296894559, 0.3333333333333333703, 0.3219752754296894559, 0.3333333333333333703, 0.3219752754296894559, 0.3333333333333333703, 0.3219752754296894559, 0.3333333333333333703, 0.3219752754296894559, 0.3333333333333333703, 0.3219752754296894559, 0.3333333333333333703, 0.3219752754296894559, 0.3333333333333333703, 0.3219752754296894559, 0.3333333333333333703, 0.3219752754296894559, 0.3333333333333333703, 0.3219752754296894559, 0.3333333333333333703, 0.3219752754296894559, 0.3333333333333333703, 0.3219752754296894559, 0.3333333333333333703, 0.3219752754296894559, 0.3333333333333333703, 0.3219752754296894559, 0.3333333333333333703, 0.3219752754296894559, 0.3333333333333333703, 0.3219752754296894559, 0.3333333333333333703, 0.3219752754296894559, 0.3333333333333333703, 0.3219752754296894559, 0.3333333333333333703, 0.3219752754296894559, 0.3333333333333333703, 0.3219752754296894559, 0.3333333333333333703, 0.3219752754296894559, 0.3333333333333333703, 0.3219752754296894559, 0.3333333333333333703, 0.3219752754296894559, 0.3333333333333333703, 0.3219752754296894559, 0.3333333333333333703, 0.3219752754296894559, 0.3333333333333333703, 0.3219752754296894559, 0.3333333333333333703, 0.3219752754296894559, 0.3333333333333333703, 0.3219752754296894559, 0.3333333333333333703, 0.3219752754296894559, 0.3333333333333333703, 0.3219752754296894559, 0.3333333333333333703, 0.3219752754296894559, 0.3333333333333333703, 0.3219752754296894559, 0.3333333333333333703, 0.3219752754296894559, 0.3333333333333333703, 0.3219752754296894559, 0.3333333333333333703, 0.3219752754296894559, 0.3333333333333333703, 0.3219752754296894559, 0.3333333333333333703, 0.3219752754296894559, 0.3333333333333333703, 0.3219752754296894559, 0.3333333333333333703, 0.3219752754296894559, 0.3333333333333333703, 0.3219752754296894559, 0.3333333333333333703, 0.3219752754296894559, 0.3333333333333333703, 0.3219752754296894559, 0.3333333333333333703, 0.3219752754296894559, 0.3333333333333333703, 0.3219752754296894559, 0.3333333333333333703, 0.3219752754296894559, 0.3333333333333333703, 0.3219752754296894559, 0.3333333333333333703, 0.3219752754296894559, 0.3333333333333333703, 0.3219752754296894559, 0.3333333333333333703, 0.3219752754296894559, 0.3333333333333333703, 0.3219752754296894559, 0.3333333333333333703, 0.3219752754296894559, 0.3333333333333333703, 0.3219752754296894559, 0.3333333333333333703, 0.3219752754296894559, 0.3333333333333333703, 0.3219752754296894559, 0.3333333333333333703, 0.3219752754296894559, 0.3333333333333333703, 0.3219752754296894559, 0.3333333333333333703, 0.3219752754296894559, 0.3333333333333333703, 0.3219752754296894559, 0.3333333333333333703, 0.3219752754296894559, 0.3333333333333333703, 0.3219752754296894559, 0.3333333333333333703, 0.3219752754296894559, 0.3333333333333333703, 0.3219752754296894559, 0.3333333333333333703, 0.3219752754296894559, 0.3333333333333333703, 0.3219752754296894559, 0.3333333333333333703, 0.3219752754296894559, 0.3333333333333333703, 0.3219752754296894559, 0.3333333333333333703, 0.3219752754296894559, 0.3333333333333333703, 0.3219752754296894559, 0.3333333333333333703, 0.3219752754296894559, 0.3333333333333333703, 0.3219752754296894559, 0.3333333333333333703, 0.3219752754296894559, 0.3333333333333333703, 0.3219752754296894559, 0.3333333333333333703, 0.3219752754296894559, 0.3333333333333333703, 0.3219752754296894559, 0.3333333333333333703, 0.3219752754296894559, 0.3333333333333333703, 0.3219752754296894559, 0.3333333333333333703, 0.3219752754296894559, 0.3333333333333333703, 0.3219752754296894559, 0.3333333333333333703, 0.3219752754296894559, 0.3333333333333333703, 0.3219752754296894559, 0.3333333333333333703, 0.3219752754296894559, 0.3333333333333333703, 0.3219752754296894559, 0.3333333333333333703, 0.3219752754296894559, 0.3333333333333333703, 0.3219752754296894559, 0.3333333333333333703, 0.3219752754296894559, 0.3333333333333333703, 0.3219752754296894559, 0.3333333333333333703, 0.3219752754296894559, 0.3333333333333333703, 0.3219752754296894559, 0.3333333333333333703, 0.3219752754296894559, 0.3333333333333333703, 0.3219752754296894559, 0.3333333333333333703, 0.3219752754296894559, 0.3333333333333333703, 0.3219752754296894559, 0.3333333333333333703, 0.3219752754296894559, 0.3333333333333333703, 0.3219752754296894559, 0.3333333333333333703, 0.3219752754296894559, 0.3333333333333333703, 0.3219752754296894559, 0.3333333333333333703, 0.3219752754296894559, 0.3333333333333333703, 0.3219752754296894559, 0.3333333333333333703, 0.3219752754296894559, 0.3333333333333333703, 0.3219752754296894559, 0.3333333333333333703, 0.3219752754296894559, 0.3333333333333333703, 0.3219752754296894559, 0.3333333333333333703, 0.3219752754296894559, 0.3333333333333333703, 0.3219752754296894559, 0.3333333333333333703, 0.3219752754296894559, 0.3333333333333333703, 0.3219752754296894559, 0.3333333333333333703, 0.3219752754296894559, 0.3333333333333333703, 0.3219752754296894559, 0.3333333333333333703, 0.3219752754296894559, 0.3333333333333333703, 0.3219752754296894559, 0.3333333333333333703, 0.3219752754296894559, 0.3333333333333333703, 0.3219752754296894559, 0.3333333333333333703, 0.3219752754296894559, 0.3333333333333333703, 0.3219752754296894559, 0.3333333333333333703, 0.3219752754296894559, 0.3333333333333333703, 0.3219752754296894559, 0.3333333333333333703, 0.3219752754296894559, 0.3333333333333333703, 0.3219752754296894559, 0.3333333333333333703, 0.3219752754296894559, 0.3333333333333333703, 0.3219752754296894559, 0.3333333333333333703, 0.3219752754296894559, 0.3333333333333333703, 0.3219752754296894559, 0.3333333333333333703, 0.3219752754296894559, 0.3333333333333333703, 0.3219752754296894559, 0.3333333333333333703, 0.3219752754296894559, 0.3333333333333333703, 0.3219752754296894559, 0.3333333333333333703, 0.3219752754296894559, 0.3333333333333333703, 0.3219752754296894559, 0.3333333333333333703, 0.3219752754296894559, 0.3333333333333333703, 0.3219752754296894559, 0.3333333333333333703, 0.3219752754296894559, 0.3333333333333333703, 0.3219752754296894559, 0.3333333333333333703, 0.3219752754296894559, 0.3333333333333333703, 0.3219752754296894559, 0.3333333333333333703, 0.3219752754296894559, 0.3333333333333333703, 0.3219752754296894559, 0.3333333333333333703, 0.3219752754296894559, 0.3333333333333333703, 0.3219752754296894559, 0.3333333333333333703, 0.3219752754296894559, 0.3333333333333333703, 0.3219752754296894559, 0.3333333333333333703, 0.3219752754296894559, 0.3333333333333333703, 0.3219752754296894559, 0.3333333333333333703, 0.3219752754296894559, 0.3333333333333333703, 0.3219752754296894559, 0.3333333333333333703, 0.3219752754296894559, 0.3333333333333333703, 0.3219752754296894559, 0.3333333333333333703, 0.3219752754296894559, 0.3333333333333333703, 0.3219752754296894559, 0.3333333333333333703, 0.3219752754296894559, 0.3333333333333333703, 0.3219752754296894559, 0.3333333333333333703, 0.3219752754296894559, 0.3333333333333333703, 0.3219752754296894559, 0.3333333333333333703, 0.3219752754296894559, 0.3333333333333333703, 0.3219752754296894559, 0.3333333333333333703, 0.3219752754296894559, 0.3333333333333333703, 0.3219752754296894559, 0.3333333333333333703, 0.3219752754296894559, 0.3333333333333333703, 0.3219752754296894559, 0.3333333333333333703, 0.3219752754296894559, 0.3333333333333333703, 0.3219752754296894559, 0.3333333333333333703, 0.3219752754296894559, 0.3333333333333333703, 0.3219752754296894559, 0.3333333333333333703, 0.3219752754296894559, 0.3333333333333333703, 0.3219752754296894559, 0.3333333333333333703, 0.3219752754296894559, 0.3333333333333333703, 0.3219752754296894559, 0.3333333333333333703, 0.3219752754296894559, 0.3333333333333333703, 0.3219752754296894559, 0.3333333333333333703, 0.3219752754296894559, 0.3333333333333333703, 0.3219752754296894559, 0.3333333333333333703, 0.3219752754296894559, 0.3333333333333333703, 0.3219752754296894559, 0.3333333333333333703, 0.3219752754296894559, 0.3333333333333333703, 0.3219752754296894559, 0.3333333333333333703, 0.3219752754296894559, 0.3333333333333333703, 0.3219752754296894559, 0.3333333333333333703, 0.3219752754296894559, 0.3333333333333333703, 0.3219752754296894559, 0.3333333333333333703, 0.3219752754296894559, 0.3333333333333333703, 0.3219752754296894559, 0.3333333333333333703, 0.3219752754296894559, 0.3333333333333333703, 0.3219752754296894559, 0.3333333333333333703, 0.3219752754296894559, 0.3333333333333333703, 0.3219752754296894559, 0.3333333333333333703, 0.3219752754296894559, 0.3333333333333333703, 0.3219752754296894559, 0.3333333333333333703, 0.3219752754296894559, 0.3333333333333333703, 0.3219752754296894559, 0.3333333333333333703, 0.3219752754296894559, 0.3333333333333333703, 0.3219752754296894559, 0.3333333333333333703, 0.3219752754296894559, 0.3333333333333333703, 0.3219752754296894559, 0.3333333333333333703, 0.3219752754296894559, 0.3333333333333333703, 0.3219752754296894559, 0.3333333333333333703, 0.3219752754296894559, 0.3333333333333333703, 0.3219752754296894559, 0.3333333333333333703, 0.3219752754296894559, 0.3333333333333333703),
 ( 1.000000000000000000, 0.9659258262890683122, 1.000000000000000000, 0.9659258262890683122, 1.000000000000000000, 0.9659258262890683122, 1.000000000000000000, 0.9659258262890683122, 1.000000000000000000, 0.9659258262890683122, 1.000000000000000000, 0.9659258262890683122, 1.000000000000000000, 0.9659258262890683122, 1.000000000000000000, 0.9659258262890683122, 1.000000000000000000, 0.9659258262890683122, 1.000000000000000000, 0.9659258262890683122, 1.000000000000000000, 0.9659258262890683122, 1.000000000000000000, 0.9659258262890683122, 1.000000000000000000, 0.9659258262890683122, 1.000000000000000000, 0.9659258262890683122, 1.000000000000000000, 0.9659258262890683122, 1.000000000000000000, 0.9659258262890683122, 1.000000000000000000, 0.9659258262890683122, 1.000000000000000000, 0.9659258262890683122, 1.000000000000000000, 0.9659258262890683122, 1.000000000000000000, 0.9659258262890683122, 1.000000000000000000, 0.9659258262890683122, 1.000000000000000000, 0.9659258262890683122, 1.000000000000000000, 0.9659258262890683122, 1.000000000000000000, 0.9659258262890683122, 1.000000000000000000, 0.9659258262890683122, 1.000000000000000000, 0.9659258262890683122, 1.000000000000000000, 0.9659258262890683122, 1.000000000000000000, 0.9659258262890683122, 1.000000000000000000, 0.9659258262890683122, 1.000000000000000000, 0.9659258262890683122, 1.000000000000000000, 0.9659258262890683122, 1.000000000000000000, 0.9659258262890683122, 1.000000000000000000, 0.9659258262890683122, 1.000000000000000000, 0.9659258262890683122, 1.000000000000000000, 0.9659258262890683122, 1.000000000000000000, 0.9659258262890683122, 1.000000000000000000, 0.9659258262890683122, 1.000000000000000000, 0.9659258262890683122, 1.000000000000000000, 0.9659258262890683122, 1.000000000000000000, 0.9659258262890683122, 1.000000000000000000, 0.9659258262890683122, 1.000000000000000000, 0.9659258262890683122, 1.000000000000000000, 0.9659258262890683122, 1.000000000000000000, 0.9659258262890683122, 1.000000000000000000, 0.9659258262890683122, 1.000000000000000000, 0.9659258262890683122, 1.000000000000000000, 0.9659258262890683122, 1.000000000000000000, 0.9659258262890683122, 1.000000000000000000, 0.9659258262890683122, 1.000000000000000000, 0.9659258262890683122, 1.000000000000000000, 0.9659258262890683122, 1.000000000000000000, 0.9659258262890683122, 1.000000000000000000, 0.9659258262890683122, 1.000000000000000000, 0.9659258262890683122, 1.000000000000000000, 0.9659258262890683122, 1.000000000000000000, 0.9659258262890683122, 1.000000000000000000, 0.9659258262890683122, 1.000000000000000000, 0.9659258262890683122, 1.000000000000000000, 0.9659258262890683122, 1.000000000000000000, 0.9659258262890683122, 1.000000000000000000, 0.9659258262890683122, 1.000000000000000000, 0.9659258262890683122, 1.000000000000000000, 0.9659258262890683122, 1.000000000000000000, 0.9659258262890683122, 1.000000000000000000, 0.9659258262890683122, 1.000000000000000000, 0.9659258262890683122, 1.000000000000000000, 0.9659258262890683122, 1.000000000000000000, 0.9659258262890683122, 1.000000000000000000, 0.9659258262890683122, 1.000000000000000000, 0.9659258262890683122, 1.000000000000000000, 0.9659258262890683122, 1.000000000000000000, 0.9659258262890683122, 1.000000000000000000, 0.9659258262890683122, 1.000000000000000000, 0.9659258262890683122, 1.000000000000000000, 0.9659258262890683122, 1.000000000000000000, 0.9659258262890683122, 1.000000000000000000, 0.9659258262890683122, 1.000000000000000000, 0.9659258262890683122, 1.000000000000000000, 0.9659258262890683122, 1.000000000000000000, 0.9659258262890683122, 1.000000000000000000, 0.9659258262890683122, 1.000000000000000000, 0.9659258262890683122, 1.000000000000000000, 0.9659258262890683122, 1.000000000000000000, 0.9659258262890683122, 1.000000000000000000, 0.9659258262890683122, 1.000000000000000000, 0.9659258262890683122, 1.000000000000000000, 0.9659258262890683122, 1.000000000000000000, 0.9659258262890683122, 1.000000000000000000, 0.9659258262890683122, 1.000000000000000000, 0.9659258262890683122, 1.000000000000000000, 0.9659258262890683122, 1.000000000000000000, 0.9659258262890683122, 1.000000000000000000, 0.9659258262890683122, 1.000000000000000000, 0.9659258262890683122, 1.000000000000000000, 0.9659258262890683122, 1.000000000000000000, 0.9659258262890683122, 1.000000000000000000, 0.9659258262890683122, 1.000000000000000000, 0.9659258262890683122, 1.000000000000000000, 0.9659258262890683122, 1.000000000000000000, 0.9659258262890683122, 1.000000000000000000, 0.9659258262890683122, 1.000000000000000000, 0.9659258262890683122, 1.000000000000000000, 0.9659258262890683122, 1.000000000000000000, 0.9659258262890683122, 1.000000000000000000, 0.9659258262890683122, 1.000000000000000000, 0.9659258262890683122, 1.000000000000000000, 0.9659258262890683122, 1.000000000000000000, 0.9659258262890683122, 1.000000000000000000, 0.9659258262890683122, 1.000000000000000000, 0.9659258262890683122, 1.000000000000000000, 0.9659258262890683122, 1.000000000000000000, 0.9659258262890683122, 1.000000000000000000, 0.9659258262890683122, 1.000000000000000000, 0.9659258262890683122, 1.000000000000000000, 0.9659258262890683122, 1.000000000000000000, 0.9659258262890683122, 1.000000000000000000, 0.9659258262890683122, 1.000000000000000000, 0.9659258262890683122, 1.000000000000000000, 0.9659258262890683122, 1.000000000000000000, 0.9659258262890683122, 1.000000000000000000, 0.9659258262890683122, 1.000000000000000000, 0.9659258262890683122, 1.000000000000000000, 0.9659258262890683122, 1.000000000000000000, 0.9659258262890683122, 1.000000000000000000, 0.9659258262890683122, 1.000000000000000000, 0.9659258262890683122, 1.000000000000000000, 0.9659258262890683122, 1.000000000000000000, 0.9659258262890683122, 1.000000000000000000, 0.9659258262890683122, 1.000000000000000000, 0.9659258262890683122, 1.000000000000000000, 0.9659258262890683122, 1.000000000000000000, 0.9659258262890683122, 1.000000000000000000, 0.9659258262890683122, 1.000000000000000000, 0.9659258262890683122, 1.000000000000000000, 0.9659258262890683122, 1.000000000000000000, 0.9659258262890683122, 1.000000000000000000, 0.9659258262890683122, 1.000000000000000000, 0.9659258262890683122, 1.000000000000000000, 0.9659258262890683122, 1.000000000000000000, 0.9659258262890683122, 1.000000000000000000, 0.9659258262890683122, 1.000000000000000000, 0.9659258262890683122, 1.000000000000000000, 0.9659258262890683122, 1.000000000000000000, 0.9659258262890683122, 1.000000000000000000, 0.9659258262890683122, 1.000000000000000000, 0.9659258262890683122, 1.000000000000000000, 0.9659258262890683122, 1.000000000000000000, 0.9659258262890683122, 1.000000000000000000, 0.9659258262890683122, 1.000000000000000000, 0.9659258262890683122, 1.000000000000000000, 0.9659258262890683122, 1.000000000000000000, 0.9659258262890683122, 1.000000000000000000, 0.9659258262890683122, 1.000000000000000000, 0.9659258262890683122, 1.000000000000000000, 0.9659258262890683122, 1.000000000000000000, 0.9659258262890683122, 1.000000000000000000, 0.9659258262890683122, 1.000000000000000000, 0.9659258262890683122, 1.000000000000000000, 0.9659258262890683122, 1.000000000000000000, 0.9659258262890683122, 1.000000000000000000, 0.9659258262890683122, 1.000000000000000000, 0.9659258262890683122, 1.000000000000000000, 0.9659258262890683122, 1.000000000000000000, 0.9659258262890683122, 1.000000000000000000, 0.9659258262890683122, 1.000000000000000000, 0.9659258262890683122, 1.000000000000000000, 0.9659258262890683122, 1.000000000000000000, 0.9659258262890683122, 1.000000000000000000, 0.9659258262890683122, 1.000000000000000000, 0.9659258262890683122, 1.000000000000000000, 0.9659258262890683122, 1.000000000000000000, 0.9659258262890683122, 1.000000000000000000, 0.9659258262890683122, 1.000000000000000000, 0.9659258262890683122, 1.000000000000000000, 0.9659258262890683122, 1.000000000000000000, 0.9659258262890683122, 1.000000000000000000, 0.9659258262890683122, 1.000000000000000000, 0.9659258262890683122, 1.000000000000000000, 0.9659258262890683122, 1.000000000000000000, 0.9659258262890683122, 1.000000000000000000, 0.9659258262890683122, 1.000000000000000000, 0.9659258262890683122, 1.000000000000000000, 0.9659258262890683122, 1.000000000000000000, 0.9659258262890683122, 1.000000000000000000, 0.9659258262890683122, 1.000000000000000000, 0.9659258262890683122, 1.000000000000000000, 0.9659258262890683122, 1.000000000000000000, 0.9659258262890683122, 1.000000000000000000, 0.9659258262890683122, 1.000000000000000000, 0.9659258262890683122, 1.000000000000000000, 0.9659258262890683122, 1.000000000000000000, 0.9659258262890683122, 1.000000000000000000, 0.9659258262890683122, 1.000000000000000000, 0.9659258262890683122, 1.000000000000000000, 0.9659258262890683122, 1.000000000000000000, 0.9659258262890683122, 1.000000000000000000, 0.9659258262890683122, 1.000000000000000000, 0.9659258262890683122, 1.000000000000000000, 0.9659258262890683122, 1.000000000000000000, 0.9659258262890683122, 1.000000000000000000, 0.9659258262890683122, 1.000000000000000000, 0.9659258262890683122, 1.000000000000000000, 0.9659258262890683122, 1.000000000000000000, 0.9659258262890683122, 1.000000000000000000, 0.9659258262890683122, 1.000000000000000000, 0.9659258262890683122, 1.000000000000000000, 0.9659258262890683122, 1.000000000000000000, 0.9659258262890683122, 1.000000000000000000, 0.9659258262890683122, 1.000000000000000000, 0.9659258262890683122, 1.000000000000000000, 0.9659258262890683122, 1.000000000000000000, 0.9659258262890683122, 1.000000000000000000, 0.9659258262890683122, 1.000000000000000000, 0.9659258262890683122, 1.000000000000000000, 0.9659258262890683122, 1.000000000000000000, 0.9659258262890683122, 1.000000000000000000, 0.9659258262890683122, 1.000000000000000000, 0.9659258262890683122, 1.000000000000000000, 0.9659258262890683122, 1.000000000000000000, 0.9659258262890683122, 1.000000000000000000, 0.9659258262890683122, 1.000000000000000000, 0.9659258262890683122, 1.000000000000000000, 0.9659258262890683122, 1.000000000000000000, 0.9659258262890683122, 1.000000000000000000, 0.9659258262890683122, 1.000000000000000000, 0.9659258262890683122, 1.000000000000000000, 0.9659258262890683122, 1.000000000000000000, 0.9659258262890683122, 1.000000000000000000),
 ( 0.3333333333333333703, 0.3219752754296894559, 0.3333333333333333703, 0.3219752754296894559, 0.3333333333333333703, 0.3219752754296894559, 0.3333333333333333703, 0.3219752754296894559, 0.3333333333333333703, 0.3219752754296894559, 0.3333333333333333703, 0.3219752754296894559, 0.3333333333333333703, 0.3219752754296894559, 0.3333333333333333703, 0.3219752754296894559, 0.3333333333333333703, 0.3219752754296894559, 0.3333333333333333703, 0.3219752754296894559, 0.3333333333333333703, 0.3219752754296894559, 0.3333333333333333703, 0.3219752754296894559, 0.3333333333333333703, 0.3219752754296894559, 0.3333333333333333703, 0.3219752754296894559, 0.3333333333333333703, 0.3219752754296894559, 0.3333333333333333703, 0.3219752754296894559, 0.3333333333333333703, 0.3219752754296894559, 0.3333333333333333703, 0.3219752754296894559, 0.3333333333333333703, 0.3219752754296894559, 0.3333333333333333703, 0.3219752754296894559, 0.3333333333333333703, 0.3219752754296894559, 0.3333333333333333703, 0.3219752754296894559, 0.3333333333333333703, 0.3219752754296894559, 0.3333333333333333703, 0.3219752754296894559, 0.3333333333333333703, 0.3219752754296894559, 0.3333333333333333703, 0.3219752754296894559, 0.3333333333333333703, 0.3219752754296894559, 0.3333333333333333703, 0.3219752754296894559, 0.3333333333333333703, 0.3219752754296894559, 0.3333333333333333703, 0.3219752754296894559, 0.3333333333333333703, 0.3219752754296894559, 0.3333333333333333703, 0.3219752754296894559, 0.3333333333333333703, 0.3219752754296894559, 0.3333333333333333703, 0.3219752754296894559, 0.3333333333333333703, 0.3219752754296894559, 0.3333333333333333703, 0.3219752754296894559, 0.3333333333333333703, 0.3219752754296894559, 0.3333333333333333703, 0.3219752754296894559, 0.3333333333333333703, 0.3219752754296894559, 0.3333333333333333703, 0.3219752754296894559, 0.3333333333333333703, 0.3219752754296894559, 0.3333333333333333703, 0.3219752754296894559, 0.3333333333333333703, 0.3219752754296894559, 0.3333333333333333703, 0.3219752754296894559, 0.3333333333333333703, 0.3219752754296894559, 0.3333333333333333703, 0.3219752754296894559, 0.3333333333333333703, 0.3219752754296894559, 0.3333333333333333703, 0.3219752754296894559, 0.3333333333333333703, 0.3219752754296894559, 0.3333333333333333703, 0.3219752754296894559, 0.3333333333333333703, 0.3219752754296894559, 0.3333333333333333703, 0.3219752754296894559, 0.3333333333333333703, 0.3219752754296894559, 0.3333333333333333703, 0.3219752754296894559, 0.3333333333333333703, 0.3219752754296894559, 0.3333333333333333703, 0.3219752754296894559, 0.3333333333333333703, 0.3219752754296894559, 0.3333333333333333703, 0.3219752754296894559, 0.3333333333333333703, 0.3219752754296894559, 0.3333333333333333703, 0.3219752754296894559, 0.3333333333333333703, 0.3219752754296894559, 0.3333333333333333703, 0.3219752754296894559, 0.3333333333333333703, 0.3219752754296894559, 0.3333333333333333703, 0.3219752754296894559, 0.3333333333333333703, 0.3219752754296894559, 0.3333333333333333703, 0.3219752754296894559, 0.3333333333333333703, 0.3219752754296894559, 0.3333333333333333703, 0.3219752754296894559, 0.3333333333333333703, 0.3219752754296894559, 0.3333333333333333703, 0.3219752754296894559, 0.3333333333333333703, 0.3219752754296894559, 0.3333333333333333703, 0.3219752754296894559, 0.3333333333333333703, 0.3219752754296894559, 0.3333333333333333703, 0.3219752754296894559, 0.3333333333333333703, 0.3219752754296894559, 0.3333333333333333703, 0.3219752754296894559, 0.3333333333333333703, 0.3219752754296894559, 0.3333333333333333703, 0.3219752754296894559, 0.3333333333333333703, 0.3219752754296894559, 0.3333333333333333703, 0.3219752754296894559, 0.3333333333333333703, 0.3219752754296894559, 0.3333333333333333703, 0.3219752754296894559, 0.3333333333333333703, 0.3219752754296894559, 0.3333333333333333703, 0.3219752754296894559, 0.3333333333333333703, 0.3219752754296894559, 0.3333333333333333703, 0.3219752754296894559, 0.3333333333333333703, 0.3219752754296894559, 0.3333333333333333703, 0.3219752754296894559, 0.3333333333333333703, 0.3219752754296894559, 0.3333333333333333703, 0.3219752754296894559, 0.3333333333333333703, 0.3219752754296894559, 0.3333333333333333703, 0.3219752754296894559, 0.3333333333333333703, 0.3219752754296894559, 0.3333333333333333703, 0.3219752754296894559, 0.3333333333333333703, 0.3219752754296894559, 0.3333333333333333703, 0.3219752754296894559, 0.3333333333333333703, 0.3219752754296894559, 0.3333333333333333703, 0.3219752754296894559, 0.3333333333333333703, 0.3219752754296894559, 0.3333333333333333703, 0.3219752754296894559, 0.3333333333333333703, 0.3219752754296894559, 0.3333333333333333703, 0.3219752754296894559, 0.3333333333333333703, 0.3219752754296894559, 0.3333333333333333703, 0.3219752754296894559, 0.3333333333333333703, 0.3219752754296894559, 0.3333333333333333703, 0.3219752754296894559, 0.3333333333333333703, 0.3219752754296894559, 0.3333333333333333703, 0.3219752754296894559, 0.3333333333333333703, 0.3219752754296894559, 0.3333333333333333703, 0.3219752754296894559, 0.3333333333333333703, 0.3219752754296894559, 0.3333333333333333703, 0.3219752754296894559, 0.3333333333333333703, 0.3219752754296894559, 0.3333333333333333703, 0.3219752754296894559, 0.3333333333333333703, 0.3219752754296894559, 0.3333333333333333703, 0.3219752754296894559, 0.3333333333333333703, 0.3219752754296894559, 0.3333333333333333703, 0.3219752754296894559, 0.3333333333333333703, 0.3219752754296894559, 0.3333333333333333703, 0.3219752754296894559, 0.3333333333333333703, 0.3219752754296894559, 0.3333333333333333703, 0.3219752754296894559, 0.3333333333333333703, 0.3219752754296894559, 0.3333333333333333703, 0.3219752754296894559, 0.3333333333333333703, 0.3219752754296894559, 0.3333333333333333703, 0.3219752754296894559, 0.3333333333333333703, 0.3219752754296894559, 0.3333333333333333703, 0.3219752754296894559, 0.3333333333333333703, 0.3219752754296894559, 0.3333333333333333703, 0.3219752754296894559, 0.3333333333333333703, 0.3219752754296894559, 0.3333333333333333703, 0.3219752754296894559, 0.3333333333333333703, 0.3219752754296894559, 0.3333333333333333703, 0.3219752754296894559, 0.3333333333333333703, 0.3219752754296894559, 0.3333333333333333703, 0.3219752754296894559, 0.3333333333333333703, 0.3219752754296894559, 0.3333333333333333703, 0.3219752754296894559, 0.3333333333333333703, 0.3219752754296894559, 0.3333333333333333703, 0.3219752754296894559, 0.3333333333333333703, 0.3219752754296894559, 0.3333333333333333703, 0.3219752754296894559, 0.3333333333333333703, 0.3219752754296894559, 0.3333333333333333703, 0.3219752754296894559, 0.3333333333333333703, 0.3219752754296894559, 0.3333333333333333703, 0.3219752754296894559, 0.3333333333333333703, 0.3219752754296894559, 0.3333333333333333703, 0.3219752754296894559, 0.3333333333333333703, 0.3219752754296894559, 0.3333333333333333703, 0.3219752754296894559, 0.3333333333333333703, 0.3219752754296894559, 0.3333333333333333703, 0.3219752754296894559, 0.3333333333333333703, 0.3219752754296894559, 0.3333333333333333703, 0.3219752754296894559, 0.3333333333333333703, 0.3219752754296894559, 0.3333333333333333703, 0.3219752754296894559, 0.3333333333333333703, 0.3219752754296894559, 0.3333333333333333703, 0.3219752754296894559, 0.3333333333333333703, 0.3219752754296894559, 0.3333333333333333703, 0.3219752754296894559, 0.3333333333333333703, 0.3219752754296894559, 0.3333333333333333703, 0.3219752754296894559, 0.3333333333333333703, 0.3219752754296894559, 0.3333333333333333703, 0.3219752754296894559, 0.3333333333333333703, 0.3219752754296894559, 0.3333333333333333703, 0.3219752754296894559, 0.3333333333333333703, 0.3219752754296894559, 0.3333333333333333703, 0.3219752754296894559, 0.3333333333333333703, 0.3219752754296894559, 0.3333333333333333703, 0.3219752754296894559, 0.3333333333333333703, 0.3219752754296894559, 0.3333333333333333703, 0.3219752754296894559, 0.3333333333333333703, 0.3219752754296894559, 0.3333333333333333703, 0.3219752754296894559, 0.3333333333333333703, 0.3219752754296894559, 0.3333333333333333703, 0.3219752754296894559, 0.3333333333333333703, 0.3219752754296894559, 0.3333333333333333703, 0.3219752754296894559, 0.3333333333333333703, 0.3219752754296894559, 0.3333333333333333703, 0.3219752754296894559, 0.3333333333333333703, 0.3219752754296894559, 0.3333333333333333703, 0.3219752754296894559, 0.3333333333333333703, 0.3219752754296894559, 0.3333333333333333703, 0.3219752754296894559, 0.3333333333333333703, 0.3219752754296894559, 0.3333333333333333703, 0.3219752754296894559, 0.3333333333333333703, 0.3219752754296894559, 0.3333333333333333703, 0.3219752754296894559, 0.3333333333333333703, 0.3219752754296894559, 0.3333333333333333703, 0.3219752754296894559, 0.3333333333333333703, 0.3219752754296894559, 0.3333333333333333703, 0.3219752754296894559, 0.3333333333333333703, 0.3219752754296894559, 0.3333333333333333703, 0.3219752754296894559, 0.3333333333333333703, 0.3219752754296894559, 0.3333333333333333703, 0.3219752754296894559, 0.3333333333333333703, 0.3219752754296894559, 0.3333333333333333703, 0.3219752754296894559, 0.3333333333333333703, 0.3219752754296894559, 0.3333333333333333703, 0.3219752754296894559, 0.3333333333333333703, 0.3219752754296894559, 0.3333333333333333703, 0.3219752754296894559, 0.3333333333333333703, 0.3219752754296894559, 0.3333333333333333703, 0.3219752754296894559, 0.3333333333333333703, 0.3219752754296894559, 0.3333333333333333703, 0.3219752754296894559, 0.3333333333333333703, 0.3219752754296894559, 0.3333333333333333703, 0.3219752754296894559, 0.3333333333333333703, 0.3219752754296894559, 0.3333333333333333703, 0.3219752754296894559, 0.3333333333333333703, 0.3219752754296894559, 0.3333333333333333703, 0.3219752754296894559, 0.3333333333333333703, 0.3219752754296894559, 0.3333333333333333703, 0.3219752754296894559, 0.3333333333333333703, 0.3219752754296894559, 0.3333333333333333703, 0.3219752754296894559, 0.3333333333333333703, 0.3219752754296894559, 0.3333333333333333703, 0.3219752754296894559, 0.3333333333333333703, 0.3219752754296894559, 0.3333333333333333703, 0.3219752754296894559, 0.3333333333333333703, 0.3219752754296894559, 0.3333333333333333703, 0.3219752754296894559, 0.3333333333333333703, 0.3219752754296894559, 0.3333333333333333703, 0.3219752754296894559, 0.3333333333333333703, 0.3219752754296894559, 0.3333333333333333703, 0.3219752754296894559, 0.3333333333333333703, 0.3219752754296894559, 0.3333333333333333703, 0.3219752754296894559, 0.3333333333333333703),
 ( 0.3333333333333333703, 0.3219752754296894559, 0.3333333333333333703, 0.3219752754296894559, 0.3333333333333333703, 0.3219752754296894559, 0.3333333333333333703, 0.3219752754296894559, 0.3333333333333333703, 0.3219752754296894559, 0.3333333333333333703, 0.3219752754296894559, 0.3333333333333333703, 0.3219752754296894559, 0.3333333333333333703, 0.3219752754296894559, 0.3333333333333333703, 0.3219752754296894559, 0.3333333333333333703, 0.3219752754296894559, 0.3333333333333333703, 0.3219752754296894559, 0.3333333333333333703, 0.3219752754296894559, 0.3333333333333333703, 0.3219752754296894559, 0.3333333333333333703, 0.3219752754296894559, 0.3333333333333333703, 0.3219752754296894559, 0.3333333333333333703, 0.3219752754296894559, 0.3333333333333333703, 0.3219752754296894559, 0.3333333333333333703, 0.3219752754296894559, 0.3333333333333333703, 0.3219752754296894559, 0.3333333333333333703, 0.3219752754296894559, 0.3333333333333333703, 0.3219752754296894559, 0.3333333333333333703, 0.3219752754296894559, 0.3333333333333333703, 0.3219752754296894559, 0.3333333333333333703, 0.3219752754296894559, 0.3333333333333333703, 0.3219752754296894559, 0.3333333333333333703, 0.3219752754296894559, 0.3333333333333333703, 0.3219752754296894559, 0.3333333333333333703, 0.3219752754296894559, 0.3333333333333333703, 0.3219752754296894559, 0.3333333333333333703, 0.3219752754296894559, 0.3333333333333333703, 0.3219752754296894559, 0.3333333333333333703, 0.3219752754296894559, 0.3333333333333333703, 0.3219752754296894559, 0.3333333333333333703, 0.3219752754296894559, 0.3333333333333333703, 0.3219752754296894559, 0.3333333333333333703, 0.3219752754296894559, 0.3333333333333333703, 0.3219752754296894559, 0.3333333333333333703, 0.3219752754296894559, 0.3333333333333333703, 0.3219752754296894559, 0.3333333333333333703, 0.3219752754296894559, 0.3333333333333333703, 0.3219752754296894559, 0.3333333333333333703, 0.3219752754296894559, 0.3333333333333333703, 0.3219752754296894559, 0.3333333333333333703, 0.3219752754296894559, 0.3333333333333333703, 0.3219752754296894559, 0.3333333333333333703, 0.3219752754296894559, 0.3333333333333333703, 0.3219752754296894559, 0.3333333333333333703, 0.3219752754296894559, 0.3333333333333333703, 0.3219752754296894559, 0.3333333333333333703, 0.3219752754296894559, 0.3333333333333333703, 0.3219752754296894559, 0.3333333333333333703, 0.3219752754296894559, 0.3333333333333333703, 0.3219752754296894559, 0.3333333333333333703, 0.3219752754296894559, 0.3333333333333333703, 0.3219752754296894559, 0.3333333333333333703, 0.3219752754296894559, 0.3333333333333333703, 0.3219752754296894559, 0.3333333333333333703, 0.3219752754296894559, 0.3333333333333333703, 0.3219752754296894559, 0.3333333333333333703, 0.3219752754296894559, 0.3333333333333333703, 0.3219752754296894559, 0.3333333333333333703, 0.3219752754296894559, 0.3333333333333333703, 0.3219752754296894559, 0.3333333333333333703, 0.3219752754296894559, 0.3333333333333333703, 0.3219752754296894559, 0.3333333333333333703, 0.3219752754296894559, 0.3333333333333333703, 0.3219752754296894559, 0.3333333333333333703, 0.3219752754296894559, 0.3333333333333333703, 0.3219752754296894559, 0.3333333333333333703, 0.3219752754296894559, 0.3333333333333333703, 0.3219752754296894559, 0.3333333333333333703, 0.3219752754296894559, 0.3333333333333333703, 0.3219752754296894559, 0.3333333333333333703, 0.3219752754296894559, 0.3333333333333333703, 0.3219752754296894559, 0.3333333333333333703, 0.3219752754296894559, 0.3333333333333333703, 0.3219752754296894559, 0.3333333333333333703, 0.3219752754296894559, 0.3333333333333333703, 0.3219752754296894559, 0.3333333333333333703, 0.3219752754296894559, 0.3333333333333333703, 0.3219752754296894559, 0.3333333333333333703, 0.3219752754296894559, 0.3333333333333333703, 0.3219752754296894559, 0.3333333333333333703, 0.3219752754296894559, 0.3333333333333333703, 0.3219752754296894559, 0.3333333333333333703, 0.3219752754296894559, 0.3333333333333333703, 0.3219752754296894559, 0.3333333333333333703, 0.3219752754296894559, 0.3333333333333333703, 0.3219752754296894559, 0.3333333333333333703, 0.3219752754296894559, 0.3333333333333333703, 0.3219752754296894559, 0.3333333333333333703, 0.3219752754296894559, 0.3333333333333333703, 0.3219752754296894559, 0.3333333333333333703, 0.3219752754296894559, 0.3333333333333333703, 0.3219752754296894559, 0.3333333333333333703, 0.3219752754296894559, 0.3333333333333333703, 0.3219752754296894559, 0.3333333333333333703, 0.3219752754296894559, 0.3333333333333333703, 0.3219752754296894559, 0.3333333333333333703, 0.3219752754296894559, 0.3333333333333333703, 0.3219752754296894559, 0.3333333333333333703, 0.3219752754296894559, 0.3333333333333333703, 0.3219752754296894559, 0.3333333333333333703, 0.3219752754296894559, 0.3333333333333333703, 0.3219752754296894559, 0.3333333333333333703, 0.3219752754296894559, 0.3333333333333333703, 0.3219752754296894559, 0.3333333333333333703, 0.3219752754296894559, 0.3333333333333333703, 0.3219752754296894559, 0.3333333333333333703, 0.3219752754296894559, 0.3333333333333333703, 0.3219752754296894559, 0.3333333333333333703, 0.3219752754296894559, 0.3333333333333333703, 0.3219752754296894559, 0.3333333333333333703, 0.3219752754296894559, 0.3333333333333333703, 0.3219752754296894559, 0.3333333333333333703, 0.3219752754296894559, 0.3333333333333333703, 0.3219752754296894559, 0.3333333333333333703, 0.3219752754296894559, 0.3333333333333333703, 0.3219752754296894559, 0.3333333333333333703, 0.3219752754296894559, 0.3333333333333333703, 0.3219752754296894559, 0.3333333333333333703, 0.3219752754296894559, 0.3333333333333333703, 0.3219752754296894559, 0.3333333333333333703, 0.3219752754296894559, 0.3333333333333333703, 0.3219752754296894559, 0.3333333333333333703, 0.3219752754296894559, 0.3333333333333333703, 0.3219752754296894559, 0.3333333333333333703, 0.3219752754296894559, 0.3333333333333333703, 0.3219752754296894559, 0.3333333333333333703, 0.3219752754296894559, 0.3333333333333333703, 0.3219752754296894559, 0.3333333333333333703, 0.3219752754296894559, 0.3333333333333333703, 0.3219752754296894559, 0.3333333333333333703, 0.3219752754296894559, 0.3333333333333333703, 0.3219752754296894559, 0.3333333333333333703, 0.3219752754296894559, 0.3333333333333333703, 0.3219752754296894559, 0.3333333333333333703, 0.3219752754296894559, 0.3333333333333333703, 0.3219752754296894559, 0.3333333333333333703, 0.3219752754296894559, 0.3333333333333333703, 0.3219752754296894559, 0.3333333333333333703, 0.3219752754296894559, 0.3333333333333333703, 0.3219752754296894559, 0.3333333333333333703, 0.3219752754296894559, 0.3333333333333333703, 0.3219752754296894559, 0.3333333333333333703, 0.3219752754296894559, 0.3333333333333333703, 0.3219752754296894559, 0.3333333333333333703, 0.3219752754296894559, 0.3333333333333333703, 0.3219752754296894559, 0.3333333333333333703, 0.3219752754296894559, 0.3333333333333333703, 0.3219752754296894559, 0.3333333333333333703, 0.3219752754296894559, 0.3333333333333333703, 0.3219752754296894559, 0.3333333333333333703, 0.3219752754296894559, 0.3333333333333333703, 0.3219752754296894559, 0.3333333333333333703, 0.3219752754296894559, 0.3333333333333333703, 0.3219752754296894559, 0.3333333333333333703, 0.3219752754296894559, 0.3333333333333333703, 0.3219752754296894559, 0.3333333333333333703, 0.3219752754296894559, 0.3333333333333333703, 0.3219752754296894559, 0.3333333333333333703, 0.3219752754296894559, 0.3333333333333333703, 0.3219752754296894559, 0.3333333333333333703, 0.3219752754296894559, 0.3333333333333333703, 0.3219752754296894559, 0.3333333333333333703, 0.3219752754296894559, 0.3333333333333333703, 0.3219752754296894559, 0.3333333333333333703, 0.3219752754296894559, 0.3333333333333333703, 0.3219752754296894559, 0.3333333333333333703, 0.3219752754296894559, 0.3333333333333333703, 0.3219752754296894559, 0.3333333333333333703, 0.3219752754296894559, 0.3333333333333333703, 0.3219752754296894559, 0.3333333333333333703, 0.3219752754296894559, 0.3333333333333333703, 0.3219752754296894559, 0.3333333333333333703, 0.3219752754296894559, 0.3333333333333333703, 0.3219752754296894559, 0.3333333333333333703, 0.3219752754296894559, 0.3333333333333333703, 0.3219752754296894559, 0.3333333333333333703, 0.3219752754296894559, 0.3333333333333333703, 0.3219752754296894559, 0.3333333333333333703, 0.3219752754296894559, 0.3333333333333333703, 0.3219752754296894559, 0.3333333333333333703, 0.3219752754296894559, 0.3333333333333333703, 0.3219752754296894559, 0.3333333333333333703, 0.3219752754296894559, 0.3333333333333333703, 0.3219752754296894559, 0.3333333333333333703, 0.3219752754296894559, 0.3333333333333333703, 0.3219752754296894559, 0.3333333333333333703, 0.3219752754296894559, 0.3333333333333333703, 0.3219752754296894559, 0.3333333333333333703, 0.3219752754296894559, 0.3333333333333333703, 0.3219752754296894559, 0.3333333333333333703, 0.3219752754296894559, 0.3333333333333333703, 0.3219752754296894559, 0.3333333333333333703, 0.3219752754296894559, 0.3333333333333333703, 0.3219752754296894559, 0.3333333333333333703, 0.3219752754296894559, 0.3333333333333333703, 0.3219752754296894559, 0.3333333333333333703, 0.3219752754296894559, 0.3333333333333333703, 0.3219752754296894559, 0.3333333333333333703, 0.3219752754296894559, 0.3333333333333333703, 0.3219752754296894559, 0.3333333333333333703, 0.3219752754296894559, 0.3333333333333333703, 0.3219752754296894559, 0.3333333333333333703, 0.3219752754296894559, 0.3333333333333333703, 0.3219752754296894559, 0.3333333333333333703, 0.3219752754296894559, 0.3333333333333333703, 0.3219752754296894559, 0.3333333333333333703, 0.3219752754296894559, 0.3333333333333333703, 0.3219752754296894559, 0.3333333333333333703, 0.3219752754296894559, 0.3333333333333333703, 0.3219752754296894559, 0.3333333333333333703, 0.3219752754296894559, 0.3333333333333333703, 0.3219752754296894559, 0.3333333333333333703, 0.3219752754296894559, 0.3333333333333333703, 0.3219752754296894559, 0.3333333333333333703, 0.3219752754296894559, 0.3333333333333333703, 0.3219752754296894559, 0.3333333333333333703, 0.3219752754296894559, 0.3333333333333333703, 0.3219752754296894559, 0.3333333333333333703, 0.3219752754296894559, 0.3333333333333333703, 0.3219752754296894559, 0.3333333333333333703, 0.3219752754296894559, 0.3333333333333333703, 0.3219752754296894559, 0.3333333333333333703, 0.3219752754296894559, 0.3333333333333333703, 0.3219752754296894559, 0.3333333333333333703, 0.3219752754296894559, 0.3333333333333333703),
 ( 1.000000000000000000, 0.9659258262890683122, 1.000000000000000000, 0.9659258262890683122, 1.000000000000000000, 0.9659258262890683122, 1.000000000000000000, 0.9659258262890683122, 1.000000000000000000, 0.9659258262890683122, 1.000000000000000000, 0.9659258262890683122, 1.000000000000000000, 0.9659258262890683122, 1.000000000000000000, 0.9659258262890683122, 1.000000000000000000, 0.9659258262890683122, 1.000000000000000000, 0.9659258262890683122, 1.000000000000000000, 0.9659258262890683122, 1.000000000000000000, 0.9659258262890683122, 1.000000000000000000, 0.9659258262890683122, 1.000000000000000000, 0.9659258262890683122, 1.000000000000000000, 0.9659258262890683122, 1.000000000000000000, 0.9659258262890683122, 1.000000000000000000, 0.9659258262890683122, 1.000000000000000000, 0.9659258262890683122, 1.000000000000000000, 0.9659258262890683122, 1.000000000000000000, 0.9659258262890683122, 1.000000000000000000, 0.9659258262890683122, 1.000000000000000000, 0.9659258262890683122, 1.000000000000000000, 0.9659258262890683122, 1.000000000000000000, 0.9659258262890683122, 1.000000000000000000, 0.9659258262890683122, 1.000000000000000000, 0.9659258262890683122, 1.000000000000000000, 0.9659258262890683122, 1.000000000000000000, 0.9659258262890683122, 1.000000000000000000, 0.9659258262890683122, 1.000000000000000000, 0.9659258262890683122, 1.000000000000000000, 0.9659258262890683122, 1.000000000000000000, 0.9659258262890683122, 1.000000000000000000, 0.9659258262890683122, 1.000000000000000000, 0.9659258262890683122, 1.000000000000000000, 0.9659258262890683122, 1.000000000000000000, 0.9659258262890683122, 1.000000000000000000, 0.9659258262890683122, 1.000000000000000000, 0.9659258262890683122, 1.000000000000000000, 0.9659258262890683122, 1.000000000000000000, 0.9659258262890683122, 1.000000000000000000, 0.9659258262890683122, 1.000000000000000000, 0.9659258262890683122, 1.000000000000000000, 0.9659258262890683122, 1.000000000000000000, 0.9659258262890683122, 1.000000000000000000, 0.9659258262890683122, 1.000000000000000000, 0.9659258262890683122, 1.000000000000000000, 0.9659258262890683122, 1.000000000000000000, 0.9659258262890683122, 1.000000000000000000, 0.9659258262890683122, 1.000000000000000000, 0.9659258262890683122, 1.000000000000000000, 0.9659258262890683122, 1.000000000000000000, 0.9659258262890683122, 1.000000000000000000, 0.9659258262890683122, 1.000000000000000000, 0.9659258262890683122, 1.000000000000000000, 0.9659258262890683122, 1.000000000000000000, 0.9659258262890683122, 1.000000000000000000, 0.9659258262890683122, 1.000000000000000000, 0.9659258262890683122, 1.000000000000000000, 0.9659258262890683122, 1.000000000000000000, 0.9659258262890683122, 1.000000000000000000, 0.9659258262890683122, 1.000000000000000000, 0.9659258262890683122, 1.000000000000000000, 0.9659258262890683122, 1.000000000000000000, 0.9659258262890683122, 1.000000000000000000, 0.9659258262890683122, 1.000000000000000000, 0.9659258262890683122, 1.000000000000000000, 0.9659258262890683122, 1.000000000000000000, 0.9659258262890683122, 1.000000000000000000, 0.9659258262890683122, 1.000000000000000000, 0.9659258262890683122, 1.000000000000000000, 0.9659258262890683122, 1.000000000000000000, 0.9659258262890683122, 1.000000000000000000, 0.9659258262890683122, 1.000000000000000000, 0.9659258262890683122, 1.000000000000000000, 0.9659258262890683122, 1.000000000000000000, 0.9659258262890683122, 1.000000000000000000, 0.9659258262890683122, 1.000000000000000000, 0.9659258262890683122, 1.000000000000000000, 0.9659258262890683122, 1.000000000000000000, 0.9659258262890683122, 1.000000000000000000, 0.9659258262890683122, 1.000000000000000000, 0.9659258262890683122, 1.000000000000000000, 0.9659258262890683122, 1.000000000000000000, 0.9659258262890683122, 1.000000000000000000, 0.9659258262890683122, 1.000000000000000000, 0.9659258262890683122, 1.000000000000000000, 0.9659258262890683122, 1.000000000000000000, 0.9659258262890683122, 1.000000000000000000, 0.9659258262890683122, 1.000000000000000000, 0.9659258262890683122, 1.000000000000000000, 0.9659258262890683122, 1.000000000000000000, 0.9659258262890683122, 1.000000000000000000, 0.9659258262890683122, 1.000000000000000000, 0.9659258262890683122, 1.000000000000000000, 0.9659258262890683122, 1.000000000000000000, 0.9659258262890683122, 1.000000000000000000, 0.9659258262890683122, 1.000000000000000000, 0.9659258262890683122, 1.000000000000000000, 0.9659258262890683122, 1.000000000000000000, 0.9659258262890683122, 1.000000000000000000, 0.9659258262890683122, 1.000000000000000000, 0.9659258262890683122, 1.000000000000000000, 0.9659258262890683122, 1.000000000000000000, 0.9659258262890683122, 1.000000000000000000, 0.9659258262890683122, 1.000000000000000000, 0.9659258262890683122, 1.000000000000000000, 0.9659258262890683122, 1.000000000000000000, 0.9659258262890683122, 1.000000000000000000, 0.9659258262890683122, 1.000000000000000000, 0.9659258262890683122, 1.000000000000000000, 0.9659258262890683122, 1.000000000000000000, 0.9659258262890683122, 1.000000000000000000, 0.9659258262890683122, 1.000000000000000000, 0.9659258262890683122, 1.000000000000000000, 0.9659258262890683122, 1.000000000000000000, 0.9659258262890683122, 1.000000000000000000, 0.9659258262890683122, 1.000000000000000000, 0.9659258262890683122, 1.000000000000000000, 0.9659258262890683122, 1.000000000000000000, 0.9659258262890683122, 1.000000000000000000, 0.9659258262890683122, 1.000000000000000000, 0.9659258262890683122, 1.000000000000000000, 0.9659258262890683122, 1.000000000000000000, 0.9659258262890683122, 1.000000000000000000, 0.9659258262890683122, 1.000000000000000000, 0.9659258262890683122, 1.000000000000000000, 0.9659258262890683122, 1.000000000000000000, 0.9659258262890683122, 1.000000000000000000, 0.9659258262890683122, 1.000000000000000000, 0.9659258262890683122, 1.000000000000000000, 0.9659258262890683122, 1.000000000000000000, 0.9659258262890683122, 1.000000000000000000, 0.9659258262890683122, 1.000000000000000000, 0.9659258262890683122, 1.000000000000000000, 0.9659258262890683122, 1.000000000000000000, 0.9659258262890683122, 1.000000000000000000, 0.9659258262890683122, 1.000000000000000000, 0.9659258262890683122, 1.000000000000000000, 0.9659258262890683122, 1.000000000000000000, 0.9659258262890683122, 1.000000000000000000, 0.9659258262890683122, 1.000000000000000000, 0.9659258262890683122, 1.000000000000000000, 0.9659258262890683122, 1.000000000000000000, 0.9659258262890683122, 1.000000000000000000, 0.9659258262890683122, 1.000000000000000000, 0.9659258262890683122, 1.000000000000000000, 0.9659258262890683122, 1.000000000000000000, 0.9659258262890683122, 1.000000000000000000, 0.9659258262890683122, 1.000000000000000000, 0.9659258262890683122, 1.000000000000000000, 0.9659258262890683122, 1.000000000000000000, 0.9659258262890683122, 1.000000000000000000, 0.9659258262890683122, 1.000000000000000000, 0.9659258262890683122, 1.000000000000000000, 0.9659258262890683122, 1.000000000000000000, 0.9659258262890683122, 1.000000000000000000, 0.9659258262890683122, 1.000000000000000000, 0.9659258262890683122, 1.000000000000000000, 0.9659258262890683122, 1.000000000000000000, 0.9659258262890683122, 1.000000000000000000, 0.9659258262890683122, 1.000000000000000000, 0.9659258262890683122, 1.000000000000000000, 0.9659258262890683122, 1.000000000000000000, 0.9659258262890683122, 1.000000000000000000, 0.9659258262890683122, 1.000000000000000000, 0.9659258262890683122, 1.000000000000000000, 0.9659258262890683122, 1.000000000000000000, 0.9659258262890683122, 1.000000000000000000, 0.9659258262890683122, 1.000000000000000000, 0.9659258262890683122, 1.000000000000000000, 0.9659258262890683122, 1.000000000000000000, 0.9659258262890683122, 1.000000000000000000, 0.9659258262890683122, 1.000000000000000000, 0.9659258262890683122, 1.000000000000000000, 0.9659258262890683122, 1.000000000000000000, 0.9659258262890683122, 1.000000000000000000, 0.9659258262890683122, 1.000000000000000000, 0.9659258262890683122, 1.000000000000000000, 0.9659258262890683122, 1.000000000000000000, 0.9659258262890683122, 1.000000000000000000, 0.9659258262890683122, 1.000000000000000000, 0.9659258262890683122, 1.000000000000000000, 0.9659258262890683122, 1.000000000000000000, 0.9659258262890683122, 1.000000000000000000, 0.9659258262890683122, 1.000000000000000000, 0.9659258262890683122, 1.000000000000000000, 0.9659258262890683122, 1.000000000000000000, 0.9659258262890683122, 1.000000000000000000, 0.9659258262890683122, 1.000000000000000000, 0.9659258262890683122, 1.000000000000000000, 0.9659258262890683122, 1.000000000000000000, 0.9659258262890683122, 1.000000000000000000, 0.9659258262890683122, 1.000000000000000000, 0.9659258262890683122, 1.000000000000000000, 0.9659258262890683122, 1.000000000000000000, 0.9659258262890683122, 1.000000000000000000, 0.9659258262890683122, 1.000000000000000000, 0.9659258262890683122, 1.000000000000000000, 0.9659258262890683122, 1.000000000000000000, 0.9659258262890683122, 1.000000000000000000, 0.9659258262890683122, 1.000000000000000000, 0.9659258262890683122, 1.000000000000000000, 0.9659258262890683122, 1.000000000000000000, 0.9659258262890683122, 1.000000000000000000, 0.9659258262890683122, 1.000000000000000000, 0.9659258262890683122, 1.000000000000000000, 0.9659258262890683122, 1.000000000000000000, 0.9659258262890683122, 1.000000000000000000, 0.9659258262890683122, 1.000000000000000000, 0.9659258262890683122, 1.000000000000000000, 0.9659258262890683122, 1.000000000000000000, 0.9659258262890683122, 1.000000000000000000, 0.9659258262890683122, 1.000000000000000000, 0.9659258262890683122, 1.000000000000000000, 0.9659258262890683122, 1.000000000000000000, 0.9659258262890683122, 1.000000000000000000, 0.9659258262890683122, 1.000000000000000000, 0.9659258262890683122, 1.000000000000000000, 0.9659258262890683122, 1.000000000000000000, 0.9659258262890683122, 1.000000000000000000, 0.9659258262890683122, 1.000000000000000000, 0.9659258262890683122, 1.000000000000000000, 0.9659258262890683122, 1.000000000000000000, 0.9659258262890683122, 1.000000000000000000, 0.9659258262890683122, 1.000000000000000000, 0.9659258262890683122, 1.000000000000000000, 0.9659258262890683122, 1.000000000000000000, 0.9659258262890683122, 1.000000000000000000) ) ) 
 REPRESENTATION_ITEM ( '' )  SURFACE ( )  );
#82739 = DIRECTION ( 'NONE',  ( 0.000000000000000000, 0.000000000000000000, 1.000000000000000000 ) ) ;
#82740 = CARTESIAN_POINT ( 'NONE',  ( -12.06949235617739369, -12.14591786802326823, 24.37609039468567573 ) ) ;
#82741 = CARTESIAN_POINT ( 'NONE',  ( 15.80617190586746368, 15.72974639402197994, 94.37390960531436690 ) ) ;
#82742 = CARTESIAN_POINT ( 'NONE',  ( 5.823673210054125526, 21.52544592524343514, 69.79057627198102409 ) ) ;
#82743 = CARTESIAN_POINT ( 'NONE',  ( 10.72451020669898902, -18.67979575497178502, 22.91557627198102765 ) ) ;
#82744 = CARTESIAN_POINT ( 'NONE',  ( -12.06949235617739369, -12.14591786802326823, 39.37609039468567573 ) ) ;
#82745 = CARTESIAN_POINT ( 'NONE',  ( 0.05219959533909260263, 19.03943276465977164, 54.99890960531435979 ) ) ;
#82747 = CARTESIAN_POINT ( 'NONE',  ( -9.564922557961040184, 16.46253265017147172, 97.91775706135233293 ) ) ;
#82746 = CARTESIAN_POINT ( 'NONE',  ( -5.823673210054431948, 21.52544592524334988, 32.70942372801900433 ) ) ;
#82748 = CARTESIAN_POINT ( 'NONE',  ( 5.049401038298161559, -19.05341960407611168, 112.7072429386476813 ) ) ;
#82749 = CARTESIAN_POINT ( 'NONE',  ( -0.05219959533909027116, -19.03943276465977164, 92.49890960531436690 ) ) ;
#82750 = CARTESIAN_POINT ( 'NONE',  ( -21.53943276465977519, 0.05219959533907696930, 96.24890960531435269 ) ) ;
#82751 = CARTESIAN_POINT ( 'NONE',  ( 13.97604488694527802, 13.89961937509977652, 59.37390960531434558 ) ) ;
#82752 = CARTESIAN_POINT ( 'NONE',  ( -17.48847506799967277, -5.747544572773808369, 59.17302562156722701 ) ) ;
#82753 = CARTESIAN_POINT ( 'NONE',  ( -8.224510206698948167, 14.34966873604960824, 70.41557627198102409 ) ) ;
#82754 = CARTESIAN_POINT ( 'NONE',  ( 19.03943276465977164, -0.05219959533909143690, 103.7489096053143669 ) ) ;
#82755 = DIRECTION ( 'NONE',  ( 0.000000000000000000, 0.000000000000000000, -1.000000000000000000 ) ) ;
#82756 = CARTESIAN_POINT ( 'NONE',  ( -5.153800228976607833, 19.02544592524334988, 77.70942372801900433 ) ) ;
#82757 = CARTESIAN_POINT ( 'NONE',  ( -5.823673210054116645, -21.52544592524344225, 87.29057627198103830 ) ) ;
#82758 = CARTESIAN_POINT ( 'NONE',  ( 9.474510206698729675, 16.51473224551082808, 47.08442372801900433 ) ) ;
#82759 = CARTESIAN_POINT ( 'NONE',  ( -10.81492255796078084, -18.62759615963271287, 22.08224293864769194 ) ) ;
#82760 = DIRECTION ( 'NONE',  ( -1.000000000000000000, 0.000000000000000000, 0.000000000000000000 ) ) ;
#82761 = CARTESIAN_POINT ( 'NONE',  ( -15.72974639402197994, 15.80617190586746368, 55.62390960531436690 ) ) ;
#82762 = CARTESIAN_POINT ( 'NONE',  ( -19.05341960407611168, -5.049401038298163336, 91.45724293864766707 ) ) ;
#82763 = CARTESIAN_POINT ( 'NONE',  ( -5.719274019375665041, -21.55341960407619695, 79.79275706135236135 ) ) ;
#82764 = CARTESIAN_POINT ( 'NONE',  ( 19.05341960407611168, 5.049401038298154454, 43.95724293864769550 ) ) ;
#82765 = CARTESIAN_POINT ( 'NONE',  ( 16.52544592524342804, -4.483927247898539470, 78.54057627198103830 ) ) ;
#82766 = CARTESIAN_POINT ( 'NONE',  ( -8.224510206698735004, -14.34966873604973081, 19.58442372801901143 ) ) ;
#82767 = CARTESIAN_POINT ( 'NONE',  ( -0.05219959533937732626, 21.53943276465977519, 62.50109039468568284 ) ) ;
#82768 = ORIENTED_EDGE ( 'NONE', *, *, #52659, .F. ) ;
#82769 = CARTESIAN_POINT ( 'NONE',  ( 0.05219959533936267826, -19.03943276465977164, 20.00109039468567218 ) ) ;
#82770 = CARTESIAN_POINT ( 'NONE',  ( 9.474510206698729675, 16.51473224551082808, 82.08442372801899012 ) ) ;
#82771 = CARTESIAN_POINT ( 'NONE',  ( 30.65641173115121276, -25.45263461537905769, -21.37460845010012989 ) ) ;
#82772 = CARTESIAN_POINT ( 'NONE',  ( 10.72451020669871369, 18.67979575497193778, 27.08442372801901854 ) ) ;
#82773 = DIRECTION ( 'NONE',  ( 3.491481338843133750E-15, 1.000000000000000000, -0.000000000000000000 ) ) ;
#82774 = CARTESIAN_POINT ( 'NONE',  ( 0.05219959533936267826, -19.03943276465977164, 20.00109039468567218 ) ) ;
#82775 = CARTESIAN_POINT ( 'NONE',  ( -13.97604488694527625, -13.89961937509977652, 61.87390960531435979 ) ) ;
#82776 = CARTESIAN_POINT ( 'NONE',  ( -5.153800228976607833, 19.02544592524334988, 27.70942372801899722 ) ) ;
#82777 = CARTESIAN_POINT ( 'NONE',  ( -0.05219959533934338120, 16.53943276465976808, 102.5010903946856899 ) ) ;
#82779 = CARTESIAN_POINT ( 'NONE',  ( -5.823673210054431948, 21.52544592524334988, 72.70942372801901854 ) ) ;
#82778 = CARTESIAN_POINT ( 'NONE',  ( -5.153800228976328057, -19.02544592524343514, 97.29057627198099567 ) ) ;
#82780 = CARTESIAN_POINT ( 'NONE',  ( -11.40812507854755609, 35.11059874428196537, -5.024999997268813523 ) ) ;
#82781 = CARTESIAN_POINT ( 'NONE',  ( -17.49999999999995737, -3.565345528328239588, 35.57505513193538604 ) ) ;
#82782 = CARTESIAN_POINT ( 'NONE',  ( -15.80617190586768217, 15.72974639402176855, 88.12609039468570415 ) ) ;
#82783 = CARTESIAN_POINT ( 'NONE',  ( -0.05219959533937732626, 21.53943276465977519, 102.5010903946856899 ) ) ;
#82784 = DIRECTION ( 'NONE',  ( -1.000000000000000000, -0.000000000000000000, -0.000000000000000000 ) ) ;
#82785 = CARTESIAN_POINT ( 'NONE',  ( 13.97604488694527802, 13.89961937509977652, 99.37390960531436690 ) ) ;
#82786 = CARTESIAN_POINT ( 'NONE',  ( 13.97604488694548053, -13.89961937509957401, 20.62609039468567573 ) ) ;
#82787 = CARTESIAN_POINT ( 'NONE',  ( 25.05471026796681500, -28.22563722313803325, -20.55515279800749795 ) ) ;
#82788 = CARTESIAN_POINT ( 'NONE',  ( 19.03943276465977164, -0.05219959533909143690, 43.74890960531435979 ) ) ;
#82789 = CARTESIAN_POINT ( 'NONE',  ( 21.55341960407610458, 5.719274019375980345, 58.95724293864770971 ) ) ;
#82790 = CARTESIAN_POINT ( 'NONE',  ( 12.06949235617739724, 12.14591786802326823, 106.8760903946856899 ) ) ;
#82792 = CARTESIAN_POINT ( 'NONE',  ( 5.153800228976335163, 19.02544592524342804, 74.79057627198103830 ) ) ;
#82791 = CARTESIAN_POINT ( 'NONE',  ( -16.53943276465976808, 0.05219959533911058130, 96.24890960531435269 ) ) ;
#82793 = CARTESIAN_POINT ( 'NONE',  ( -15.80617190586768217, 15.72974639402176855, 108.1260903946856757 ) ) ;
#82794 = CARTESIAN_POINT ( 'NONE',  ( -13.97604488694527625, -13.89961937509977652, 36.87390960531436690 ) ) ;
#82795 = CARTESIAN_POINT ( 'NONE',  ( 4.483927247898545687, 16.52544592524342804, 99.79057627198103830 ) ) ;
#82796 = CARTESIAN_POINT ( 'NONE',  ( -5.823673210054431948, 21.52544592524334988, 57.70942372801901143 ) ) ;
#82797 = CARTESIAN_POINT ( 'NONE',  ( 21.53943276465977519, -0.05219959533907433946, 83.74890960531435269 ) ) ;
#82798 = CARTESIAN_POINT ( 'NONE',  ( 19.03943276465977164, 0.05219959533936151252, 51.25109039468567573 ) ) ;
#82799 = DIRECTION ( 'NONE',  ( -1.000000000000000000, 0.000000000000000000, 0.000000000000000000 ) ) ;
#82800 = CARTESIAN_POINT ( 'NONE',  ( 19.02544592524343514, -5.153800228976328945, 98.54057627198100988 ) ) ;
#82801 = CARTESIAN_POINT ( 'NONE',  ( -16.55341960407611168, -4.379528057220339221, 81.45724293864769550 ) ) ;
#82803 = CARTESIAN_POINT ( 'NONE',  ( -5.049401038297874678, -19.05341960407617918, 39.79275706135232582 ) ) ;
#82802 = CIRCLE ( 'NONE', #66651, 40.00000000000000000 ) ;
#82804 = CARTESIAN_POINT ( 'NONE',  ( -19.02544592524342804, 5.153800228976336051, 61.04057627198103120 ) ) ;
#82805 = CARTESIAN_POINT ( 'NONE',  ( -8.314922557960811034, -14.29746914071050412, 52.08224293864768839 ) ) ;
#82806 = CARTESIAN_POINT ( 'NONE',  ( 0.05219959533936267826, -19.03943276465977164, 80.00109039468567573 ) ) ;
#82807 = CARTESIAN_POINT ( 'NONE',  ( 6.791538853603062975, 3.181980515339470905, 8.889087296526001936 ) ) ;
#82808 = CARTESIAN_POINT ( 'NONE',  ( 10.72451020669898902, -18.67979575497178502, 37.91557627198102409 ) ) ;
#82809 = CARTESIAN_POINT ( 'NONE',  ( 16.53943276465976808, -0.05219959533910856209, 103.7489096053143669 ) ) ;
#82810 = CARTESIAN_POINT ( 'NONE',  ( -28.90000000000004476, 2.980639576201346218E-13, -52.65483682830183199 ) ) ;
#82812 = CARTESIAN_POINT ( 'NONE',  ( -15.72974639402197994, 15.80617190586746368, 60.62390960531437401 ) ) ;
#82811 = CARTESIAN_POINT ( 'NONE',  ( -9.474510206698964154, 16.51473224551069663, 60.41557627198102409 ) ) ;
#82813 = CARTESIAN_POINT ( 'NONE',  ( 13.97604488694527802, 13.89961937509977652, 24.37390960531435624 ) ) ;
#82815 = CARTESIAN_POINT ( 'NONE',  ( -13.97604488694527625, -13.89961937509977652, 56.87390960531434558 ) ) ;
#82814 = CARTESIAN_POINT ( 'NONE',  ( -12.14591786802326823, 12.06949235617739902, 83.12609039468568994 ) ) ;
#82816 = CARTESIAN_POINT ( 'NONE',  ( -19.05341960407617563, 5.049401038297882671, 48.54275706135233293 ) ) ;
#82817 = CARTESIAN_POINT ( 'NONE',  ( -21.55341960407619339, 5.719274019375674811, 68.54275706135234714 ) ) ;
#82818 = VERTEX_POINT ( 'NONE', #143264 ) ;
#82819 = CARTESIAN_POINT ( 'NONE',  ( -21.52544592524343514, 5.823673210054127303, 56.04057627198102409 ) ) ;
#82820 = CARTESIAN_POINT ( 'NONE',  ( 19.03943276465977164, -0.05219959533909143690, 23.74890960531435269 ) ) ;
#82821 = CARTESIAN_POINT ( 'NONE',  ( -4.379528057220086978, -16.55341960407618274, 84.79275706135234714 ) ) ;
#82822 = CARTESIAN_POINT ( 'NONE',  ( -5.049401038297874678, -19.05341960407617918, 109.7927570613523187 ) ) ;
#82823 = CARTESIAN_POINT ( 'NONE',  ( -11.40812507854755609, 35.11059874428196537, -1.524999997268813301 ) ) ;
#82825 = CARTESIAN_POINT ( 'NONE',  ( -21.55341960407610458, -5.719274019375992779, 56.45724293864768839 ) ) ;
#82824 = CARTESIAN_POINT ( 'NONE',  ( 19.20446147854521968, 5.500000000000081712, 76.88999695167670723 ) ) ;
#82826 = CARTESIAN_POINT ( 'NONE',  ( -10.81492255796105439, 18.62759615963255655, 102.9177570613523756 ) ) ;
#82827 = CARTESIAN_POINT ( 'NONE',  ( 16.53943276465976808, -0.05219959533910856209, 48.74890960531435979 ) ) ;
#82828 = CARTESIAN_POINT ( 'NONE',  ( 4.379528057220339221, -16.55341960407611168, 52.70724293864769550 ) ) ;
#82829 = CARTESIAN_POINT ( 'NONE',  ( -10.81492255796078084, -18.62759615963271287, 82.08224293864768129 ) ) ;
#82830 = CARTESIAN_POINT ( 'NONE',  ( 21.52544592524344225, -5.823673210054117533, 93.54057627198103830 ) ) ;
#82831 = CARTESIAN_POINT ( 'NONE',  ( -40.00200000000003087, -5.510910596163089556E-15, 37.50000000000000000 ) ) ;
#82833 = EDGE_CURVE ( 'NONE', #34604, #3755, #163292, .T. ) ;
#82832 = CARTESIAN_POINT ( 'NONE',  ( -0.05219959533907301413, -21.53943276465977519, 27.49890960531435269 ) ) ;
#82834 = CARTESIAN_POINT ( 'NONE',  ( -4.379528057220086978, -16.55341960407618274, 69.79275706135234714 ) ) ;
#82835 = CARTESIAN_POINT ( 'NONE',  ( 16.52544592524342804, -4.483927247898539470, 73.54057627198102409 ) ) ;
#82836 = CARTESIAN_POINT ( 'NONE',  ( -5.153800228976328057, -19.02544592524343514, 37.29057627198102409 ) ) ;
#82837 =( LENGTH_UNIT ( ) NAMED_UNIT ( * ) SI_UNIT ( .MILLI., .METRE. ) );
#82838 = CARTESIAN_POINT ( 'NONE',  ( 28.82186960331498327, 2.428612866367529932E-14, 150.0000000000000000 ) ) ;
#82839 = EDGE_CURVE ( 'NONE', #169831, #84227, #8600, .T. ) ;
#82840 = CARTESIAN_POINT ( 'NONE',  ( 8.224510206698742110, 14.34966873604972548, 97.08442372801904696 ) ) ;
#82841 = CARTESIAN_POINT ( 'NONE',  ( -0.05219959533907301413, -21.53943276465977519, 112.4989096053143669 ) ) ;
#82842 = CARTESIAN_POINT ( 'NONE',  ( -19.03943276465977164, 0.05219959533909376836, 81.24890960531436690 ) ) ;
#82843 = CARTESIAN_POINT ( 'NONE',  ( 10.81492255796106328, -18.62759615963255655, 60.41775706135235424 ) ) ;
#82844 = CARTESIAN_POINT ( 'NONE',  ( 19.05341960407611168, 5.049401038298154454, 108.9572429386477097 ) ) ;
#82845 = CARTESIAN_POINT ( 'NONE',  ( -11.70497261680383261, -44.13276428439564825, -23.15274968897044516 ) ) ;
#82846 = EDGE_LOOP ( 'NONE', ( #9710, #16090, #190668, #133038 ) ) ;
#82847 = CARTESIAN_POINT ( 'NONE',  ( -21.55341960407619339, 5.719274019375674811, 43.54275706135235424 ) ) ;
#82849 = CARTESIAN_POINT ( 'NONE',  ( 16.46253265017160672, -9.564922557960803928, 98.33224293864769550 ) ) ;
#82848 = CARTESIAN_POINT ( 'NONE',  ( 9.564922557960805705, 16.46253265017160317, 34.58224293864770260 ) ) ;
#82850 = CARTESIAN_POINT ( 'NONE',  ( -9.564922557961040184, 16.46253265017147172, 52.91775706135233293 ) ) ;
#82851 = CARTESIAN_POINT ( 'NONE',  ( 10.81492255796106328, -18.62759615963255655, 25.41775706135235779 ) ) ;
#82852 = CARTESIAN_POINT ( 'NONE',  ( 5.049401038297881783, 19.05341960407617563, 62.29275706135234003 ) ) ;
#82853 = CARTESIAN_POINT ( 'NONE',  ( 28.82186960331477010, -9.364793116373819615, 140.9000000000000057 ) ) ;
#82854 = CARTESIAN_POINT ( 'NONE',  ( 16.52544592524335698, 4.483927247898782831, 91.45942372801901854 ) ) ;
#82855 = CARTESIAN_POINT ( 'NONE',  ( -19.03943276465977164, -0.05219959533935918106, 63.75109039468566863 ) ) ;
#82856 = CARTESIAN_POINT ( 'NONE',  ( 16.55341960407618274, -4.379528057220086978, 101.0427570613523756 ) ) ;
#82858 = VERTEX_POINT ( 'NONE', #11787 ) ;
#82857 = CARTESIAN_POINT ( 'NONE',  ( -19.49401214000074489, -12.39993551617566503, 169.9999999999999716 ) ) ;
#82859 = CARTESIAN_POINT ( 'NONE',  ( 9.564922557960805705, 16.46253265017160317, 84.58224293864769550 ) ) ;
#82860 = CIRCLE ( 'NONE', #108714, 2.500000000000000000 ) ;
#82861 = CARTESIAN_POINT ( 'NONE',  ( 15.80617190586769283, -15.72974639402175789, 95.62609039468568994 ) ) ;
#82862 = CARTESIAN_POINT ( 'NONE',  ( 5.719274019375673035, 21.55341960407619339, 112.2927570613523471 ) ) ;
#82863 = CARTESIAN_POINT ( 'NONE',  ( 11.74149087413294268, 36.13659316521247433, -4.602157773949822506 ) ) ;
#82864 = CARTESIAN_POINT ( 'NONE',  ( 5.153800228976335163, 19.02544592524342804, 94.79057627198103830 ) ) ;
#82865 = CARTESIAN_POINT ( 'NONE',  ( 0.05219959533937995610, -21.53943276465977519, 80.00109039468568994 ) ) ;
#82866 = CARTESIAN_POINT ( 'NONE',  ( 12.14591786802327356, -12.06949235617739191, 25.62609039468567929 ) ) ;
#82867 = CARTESIAN_POINT ( 'NONE',  ( 13.97604488694527802, 13.89961937509977652, 79.37390960531435269 ) ) ;
#82868 = CARTESIAN_POINT ( 'NONE',  ( -15.72974639402197994, 15.80617190586746368, 35.62390960531437401 ) ) ;
#82869 = CARTESIAN_POINT ( 'NONE',  ( -5.049401038298153566, 19.05341960407611168, 95.20724293864770971 ) ) ;
#82870 = DIRECTION ( 'NONE',  ( 1.000000000000000000, -0.000000000000000000, -0.000000000000000000 ) ) ;
#82871 = CARTESIAN_POINT ( 'NONE',  ( 5.153800228976335163, 19.02544592524342804, 74.79057627198103830 ) ) ;
#82872 = CARTESIAN_POINT ( 'NONE',  ( -9.474510206698964154, 16.51473224551069663, 65.41557627198102409 ) ) ;
#82873 = CARTESIAN_POINT ( 'NONE',  ( 0.05219959533910956823, 16.53943276465976808, 24.99890960531435624 ) ) ;
#82874 = CARTESIAN_POINT ( 'NONE',  ( 0.000000000000000000, -165.0000000000000000, 12.00000000000000355 ) ) ;
#82875 = CARTESIAN_POINT ( 'NONE',  ( 19.03943276465977164, 0.05219959533936151252, 71.25109039468566152 ) ) ;
#82876 = CARTESIAN_POINT ( 'NONE',  ( -5.153800228976328057, -19.02544592524343514, 97.29057627198099567 ) ) ;
#82877 = CARTESIAN_POINT ( 'NONE',  ( 16.52544592524342804, -4.483927247898539470, 83.54057627198102409 ) ) ;
#82878 = CARTESIAN_POINT ( 'NONE',  ( -18.67979575497178146, -10.72451020669898902, 41.66557627198103120 ) ) ;
#82879 = CARTESIAN_POINT ( 'NONE',  ( -18.67979575497178146, -10.72451020669898902, 26.66557627198103475 ) ) ;
#82880 = CARTESIAN_POINT ( 'NONE',  ( 0.05219959533910956823, 16.53943276465976808, 99.99890960531436690 ) ) ;
#82881 = CARTESIAN_POINT ( 'NONE',  ( -32.00000000000000000, -5.510910596163089556E-15, 45.00000000000000000 ) ) ;
#82882 = CARTESIAN_POINT ( 'NONE',  ( -19.03943276465977164, -0.05219959533935918106, 43.75109039468566863 ) ) ;
#82883 = CARTESIAN_POINT ( 'NONE',  ( 4.483927247898545687, 16.52544592524342804, 24.79057627198103120 ) ) ;
#82884 = CARTESIAN_POINT ( 'NONE',  ( -9.474510206698964154, 16.51473224551069663, 105.4155762719810383 ) ) ;
#82885 = CARTESIAN_POINT ( 'NONE',  ( 21.55341960407619695, -5.719274019375665929, 61.04275706135234714 ) ) ;
#82886 = CARTESIAN_POINT ( 'NONE',  ( 18.62759615963271287, -10.81492255796078972, 63.33224293864770260 ) ) ;
#82887 = CARTESIAN_POINT ( 'NONE',  ( 15.72974639402176855, 15.80617190586768217, 51.87609039468568284 ) ) ;
#82888 = CARTESIAN_POINT ( 'NONE',  ( 5.719274019375991003, -21.55341960407610458, 77.70724293864770971 ) ) ;
#82889 = CARTESIAN_POINT ( 'NONE',  ( 5.719274019375673035, 21.55341960407619339, 42.29275706135235424 ) ) ;
#82890 = CARTESIAN_POINT ( 'NONE',  ( 16.55341960407611168, 4.379528057220329451, 108.9572429386476955 ) ) ;
#82891 = CARTESIAN_POINT ( 'NONE',  ( -5.049401038297874678, -19.05341960407617918, 64.79275706135233293 ) ) ;
#82892 = CARTESIAN_POINT ( 'NONE',  ( -19.02544592524342804, 5.153800228976336051, 46.04057627198101699 ) ) ;
#82893 = CARTESIAN_POINT ( 'NONE',  ( 0.05219959533910956823, 16.53943276465976808, 104.9989096053143669 ) ) ;
#82894 = CARTESIAN_POINT ( 'NONE',  ( 0.05219959533909260263, 19.03943276465977164, 104.9989096053143669 ) ) ;
#82895 = CARTESIAN_POINT ( 'NONE',  ( 16.53943276465976808, -0.05219959533910856209, 43.74890960531435979 ) ) ;
#82896 = CARTESIAN_POINT ( 'NONE',  ( -14.29746914071037622, -8.314922557961029526, 104.1677570613523471 ) ) ;
#82897 = CARTESIAN_POINT ( 'NONE',  ( -13.89961937509977652, 13.97604488694528158, 55.62390960531434558 ) ) ;
#82898 = CARTESIAN_POINT ( 'NONE',  ( -0.05219959533910754901, -16.53943276465976808, 112.4989096053143669 ) ) ;
#82899 = CARTESIAN_POINT ( 'NONE',  ( -16.46253265017146816, -9.564922557961047289, 24.16775706135233648 ) ) ;
#82901 = CARTESIAN_POINT ( 'NONE',  ( -8.224510206698948167, 14.34966873604960824, 40.41557627198103120 ) ) ;
#82900 = CARTESIAN_POINT ( 'NONE',  ( -9.564922557960796823, -16.46253265017161027, 112.0822429386476955 ) ) ;
#82902 = CARTESIAN_POINT ( 'NONE',  ( 21.52544592524334988, 5.823673210054432836, 46.45942372801901854 ) ) ;
#82903 = CARTESIAN_POINT ( 'NONE',  ( -19.02544592524342804, 5.153800228976336051, 116.0405762719810383 ) ) ;
#82904 = CARTESIAN_POINT ( 'NONE',  ( -8.314922557961024197, 14.29746914071037800, 57.91775706135234714 ) ) ;
#82905 = EDGE_CURVE ( 'NONE', #47253, #60866, #34561, .T. ) ;
#82906 = CARTESIAN_POINT ( 'NONE',  ( 8.224510206698953496, -14.34966873604960469, 27.91557627198103830 ) ) ;
#82907 = CARTESIAN_POINT ( 'NONE',  ( 14.29746914071037800, 8.314922557961029526, 106.6677570613523756 ) ) ;
#82908 = CARTESIAN_POINT ( 'NONE',  ( -14.29746914071037622, -8.314922557961029526, 24.16775706135235424 ) ) ;
#82909 = CARTESIAN_POINT ( 'NONE',  ( -19.05341960407611168, -5.049401038298163336, 51.45724293864770260 ) ) ;
#82910 = CARTESIAN_POINT ( 'NONE',  ( 16.55341960407611168, 4.379528057220329451, 108.9572429386476955 ) ) ;
#82911 = CARTESIAN_POINT ( 'NONE',  ( -21.52544592524334988, -5.823673210054445271, 23.95942372801901143 ) ) ;
#82912 = CARTESIAN_POINT ( 'NONE',  ( -5.049401038298153566, 19.05341960407611168, 40.20724293864768839 ) ) ;
#82913 = CARTESIAN_POINT ( 'NONE',  ( 9.474510206698971260, -16.51473224551069308, 112.9155762719810383 ) ) ;
#82914 = CARTESIAN_POINT ( 'NONE',  ( 16.46253265017160672, -9.564922557960803928, 28.33224293864769550 ) ) ;
#82915 = CARTESIAN_POINT ( 'NONE',  ( 19.05341960407611168, 5.049401038298154454, 113.9572429386477097 ) ) ;
#82916 = CARTESIAN_POINT ( 'NONE',  ( -17.26058549869092573, -6.457015423128558140, 36.37745837476068544 ) ) ;
#82917 = EDGE_CURVE ( 'NONE', #54470, #169095, #67249, .T. ) ;
#82918 = CARTESIAN_POINT ( 'NONE',  ( -9.564922557960796823, -16.46253265017161027, 102.0822429386477097 ) ) ;
#82920 = CARTESIAN_POINT ( 'NONE',  ( -12.14591786802309592, -12.06949235617757132, 106.8739096053143811 ) ) ;
#82919 = CARTESIAN_POINT ( 'NONE',  ( -21.55341960407619339, 5.719274019375674811, 48.54275706135234714 ) ) ;
#82921 = CARTESIAN_POINT ( 'NONE',  ( 19.05341960407611168, 5.049401038298154454, 108.9572429386477097 ) ) ;
#82922 = CARTESIAN_POINT ( 'NONE',  ( 0.05219959533936267826, -19.03943276465977164, 70.00109039468566152 ) ) ;
#82923 = CARTESIAN_POINT ( 'NONE',  ( 8.314922557961029526, -14.29746914071037800, 75.41775706135233293 ) ) ;
#82924 = CARTESIAN_POINT ( 'NONE',  ( -15.80617190586768217, 15.72974639402176855, 93.12609039468568994 ) ) ;
#82925 = CARTESIAN_POINT ( 'NONE',  ( 4.379528057220092307, 16.55341960407617563, 57.29275706135234714 ) ) ;
#82926 = CARTESIAN_POINT ( 'NONE',  ( -9.564922557960796823, -16.46253265017161027, 97.08224293864769550 ) ) ;
#82927 = CARTESIAN_POINT ( 'NONE',  ( 14.29746914071037800, 8.314922557961029526, 41.66775706135235424 ) ) ;
#82928 = CARTESIAN_POINT ( 'NONE',  ( -0.05219959533934338120, 16.53943276465976808, 32.50109039468568284 ) ) ;
#82929 = CARTESIAN_POINT ( 'NONE',  ( -4.483927247898782831, 16.52544592524335698, 77.70942372801900433 ) ) ;
#82930 = CARTESIAN_POINT ( 'NONE',  ( -0.05219959533936034679, 19.03943276465977164, 107.5010903946856615 ) ) ;
#82931 = CARTESIAN_POINT ( 'NONE',  ( 9.474510206698971260, -16.51473224551069308, 77.91557627198103830 ) ) ;
#82932 = CARTESIAN_POINT ( 'NONE',  ( -5.823673210054116645, -21.52544592524344225, 92.29057627198103830 ) ) ;
#82934 = CARTESIAN_POINT ( 'NONE',  ( -13.89961937509957401, -13.97604488694547875, 109.3760903946856331 ) ) ;
#82933 = CARTESIAN_POINT ( 'NONE',  ( -8.224510206698948167, 14.34966873604960824, 105.4155762719810383 ) ) ;
#82935 = CARTESIAN_POINT ( 'NONE',  ( -4.379528057220086978, -16.55341960407618274, 69.79275706135234714 ) ) ;
#82936 = CARTESIAN_POINT ( 'NONE',  ( -16.52216118717247895, 7.221426719304377073, 43.92400978952973389 ) ) ;
#82937 = CARTESIAN_POINT ( 'NONE',  ( -16.46253265017146816, -9.564922557961047289, 69.16775706135233293 ) ) ;
#82938 = CARTESIAN_POINT ( 'NONE',  ( -8.224510206698948167, 14.34966873604960824, 50.41557627198103120 ) ) ;
#82939 = CARTESIAN_POINT ( 'NONE',  ( 14.29746914071049879, -8.314922557960816363, 93.33224293864769550 ) ) ;
#82941 = CARTESIAN_POINT ( 'NONE',  ( -16.52216118717206683, 7.221426719304492536, 88.92400978953007495 ) ) ;
#82940 = CARTESIAN_POINT ( 'NONE',  ( -13.89961937509957401, -13.97604488694547875, 39.37609039468566152 ) ) ;
#82942 = CARTESIAN_POINT ( 'NONE',  ( -10.72451020669870658, -18.67979575497194134, 34.58442372801900433 ) ) ;
#82943 = CARTESIAN_POINT ( 'NONE',  ( 5.153800228976615827, -19.02544592524334988, 95.20942372801897591 ) ) ;
#82944 = CARTESIAN_POINT ( 'NONE',  ( -9.564922557960796823, -16.46253265017161027, 112.0822429386476955 ) ) ;
#82945 = CARTESIAN_POINT ( 'NONE',  ( -16.46253265017160317, 9.564922557960807481, 95.83224293864769550 ) ) ;
#82946 = CARTESIAN_POINT ( 'NONE',  ( 10.72451020669871369, 18.67979575497193778, 107.0844237280190043 ) ) ;
#82947 = CARTESIAN_POINT ( 'NONE',  ( 5.049401038298161559, -19.05341960407611168, 77.70724293864765286 ) ) ;
#82948 = CARTESIAN_POINT ( 'NONE',  ( 0.05219959533907565091, 21.53943276465977519, 44.99890960531435979 ) ) ;
#82949 = CARTESIAN_POINT ( 'NONE',  ( -4.483927247898539470, -16.52544592524342804, 97.29057627198105251 ) ) ;
#82950 = CARTESIAN_POINT ( 'NONE',  ( 5.049401038298161559, -19.05341960407611168, 57.70724293864769550 ) ) ;
#82951 = CARTESIAN_POINT ( 'NONE',  ( -14.29746914071049879, 8.314922557960819915, 110.8322429386476955 ) ) ;
#82952 = VECTOR ( 'NONE', #142044, 1000.000000000000000 ) ;
#82953 = CARTESIAN_POINT ( 'NONE',  ( 15.80617190586769283, -15.72974639402175789, 20.62609039468568639 ) ) ;
#82954 = CARTESIAN_POINT ( 'NONE',  ( 10.72451020669871369, 18.67979575497193778, 82.08442372801901854 ) ) ;
#82955 = CARTESIAN_POINT ( 'NONE',  ( 19.02544592524343514, -5.153800228976328945, 48.54057627198103120 ) ) ;
#82956 = CARTESIAN_POINT ( 'NONE',  ( -16.52544592524335698, -4.483927247898792601, 78.95942372801901854 ) ) ;
#82957 = CARTESIAN_POINT ( 'NONE',  ( -21.52544592524343514, 5.823673210054127303, 116.0405762719810383 ) ) ;
#82958 = ORIENTED_EDGE ( 'NONE', *, *, #46060, .F. ) ;
#82959 = CARTESIAN_POINT ( 'NONE',  ( 21.52544592524334988, 5.823673210054432836, 31.45942372801901854 ) ) ;
#82961 = CARTESIAN_POINT ( 'NONE',  ( 16.46253265017160672, -9.564922557960803928, 63.33224293864769550 ) ) ;
#82960 = CARTESIAN_POINT ( 'NONE',  ( -16.51473224551082808, 9.474510206698731452, 58.33442372801900433 ) ) ;
#82962 = CARTESIAN_POINT ( 'NONE',  ( 9.564922557961047289, -16.46253265017146816, 35.41775706135233293 ) ) ;
#82963 = CARTESIAN_POINT ( 'NONE',  ( 10.81492255796106328, -18.62759615963255655, 65.41775706135234714 ) ) ;
#82964 = CARTESIAN_POINT ( 'NONE',  ( -10.72451020669898014, 18.67979575497178502, 75.41557627198102409 ) ) ;
#82965 = CARTESIAN_POINT ( 'NONE',  ( -4.379528057220328563, 16.55341960407611168, 55.20724293864770260 ) ) ;
#82967 = CARTESIAN_POINT ( 'NONE',  ( -5.153800228976607833, 19.02544592524334988, 32.70942372801899722 ) ) ;
#82966 = CARTESIAN_POINT ( 'NONE',  ( 15.72974639402176855, 15.80617190586768217, 86.87609039468568994 ) ) ;
#82968 = CARTESIAN_POINT ( 'NONE',  ( -8.314922557960811034, -14.29746914071050412, 77.08224293864769550 ) ) ;
#82969 = CARTESIAN_POINT ( 'NONE',  ( -12.06949235617756955, 12.14591786802309770, 115.6239096053143669 ) ) ;
#82970 = CARTESIAN_POINT ( 'NONE',  ( 16.51473224551083163, -9.474510206698727899, 60.83442372801900433 ) ) ;
#82971 = CARTESIAN_POINT ( 'NONE',  ( 8.224510206698953496, -14.34966873604960469, 27.91557627198103830 ) ) ;
#82972 = VECTOR ( 'NONE', #162351, 1000.000000000000000 ) ;
#82973 = CARTESIAN_POINT ( 'NONE',  ( 5.719274019375673035, 21.55341960407619339, 77.29275706135234714 ) ) ;
#82974 = CARTESIAN_POINT ( 'NONE',  ( -0.05219959533909027116, -19.03943276465977164, 77.49890960531435269 ) ) ;
#82975 = CARTESIAN_POINT ( 'NONE',  ( -16.51473224551082808, 9.474510206698731452, 48.33442372801900433 ) ) ;
#82976 = CARTESIAN_POINT ( 'NONE',  ( -21.55341960407610458, -5.719274019375992779, 51.45724293864770260 ) ) ;
#82977 = CARTESIAN_POINT ( 'NONE',  ( -10.72451020669870658, -18.67979575497194134, 44.58442372801901854 ) ) ;
#82978 = CARTESIAN_POINT ( 'NONE',  ( 10.72451020669898902, -18.67979575497178502, 102.9155762719810383 ) ) ;
#82979 = CARTESIAN_POINT ( 'NONE',  ( -5.153800228976607833, 19.02544592524334988, 92.70942372801901854 ) ) ;
#82980 = CARTESIAN_POINT ( 'NONE',  ( 0.05219959533934541429, -16.53943276465976808, 60.00109039468568284 ) ) ;
#82982 = CARTESIAN_POINT ( 'NONE',  ( 10.72451020669898902, -18.67979575497178502, 107.9155762719810241 ) ) ;
#82981 = DIRECTION ( 'NONE',  ( 0.000000000000000000, 0.000000000000000000, 1.000000000000000000 ) ) ;
#82983 = CARTESIAN_POINT ( 'NONE',  ( 16.55341960407611168, 4.379528057220329451, 88.95724293864769550 ) ) ;
#82984 = CARTESIAN_POINT ( 'NONE',  ( -17.49999999999999289, -3.471454075611644541, 30.51667418855634395 ) ) ;
#82985 = CARTESIAN_POINT ( 'NONE',  ( 8.224510206698742110, 14.34966873604972548, 37.08442372801901143 ) ) ;
#82986 = CARTESIAN_POINT ( 'NONE',  ( 21.55341960407610458, 5.719274019375980345, 43.95724293864769550 ) ) ;
#82987 = CARTESIAN_POINT ( 'NONE',  ( -16.53943276465976808, -0.05219959533934237506, 93.75109039468567573 ) ) ;
#82988 = CARTESIAN_POINT ( 'NONE',  ( -19.03943276465977164, 0.05219959533909376836, 26.24890960531435624 ) ) ;
#82989 = CARTESIAN_POINT ( 'NONE',  ( 0.05219959533934541429, -16.53943276465976808, 60.00109039468568284 ) ) ;
#82990 = CARTESIAN_POINT ( 'NONE',  ( -21.55341960407619339, 5.719274019375674811, 38.54275706135234714 ) ) ;
#82991 = CARTESIAN_POINT ( 'NONE',  ( -10.81492255796078084, -18.62759615963271287, 52.08224293864768839 ) ) ;
#82992 = CARTESIAN_POINT ( 'NONE',  ( -8.224510206698735004, -14.34966873604973081, 84.58442372801903275 ) ) ;
#82993 = CARTESIAN_POINT ( 'NONE',  ( 10.72451020669871369, 18.67979575497193778, 67.08442372801901854 ) ) ;
#82994 = CARTESIAN_POINT ( 'NONE',  ( -5.719274019375978568, 21.55341960407610458, 50.20724293864769550 ) ) ;
#82995 = CARTESIAN_POINT ( 'NONE',  ( -0.05219959533907301413, -21.53943276465977519, 37.49890960531436690 ) ) ;
#82996 = ORIENTED_EDGE ( 'NONE', *, *, #34762, .T. ) ;
#82997 = CARTESIAN_POINT ( 'NONE',  ( 16.55341960407618274, -4.379528057220086978, 61.04275706135234714 ) ) ;
#82998 = CARTESIAN_POINT ( 'NONE',  ( 10.72451020669898902, -18.67979575497178502, 37.91557627198102409 ) ) ;
#82999 = VERTEX_POINT ( 'NONE', #161444 ) ;
#83000 = CARTESIAN_POINT ( 'NONE',  ( 13.97604488694527802, 13.89961937509977652, 94.37390960531436690 ) ) ;
#83001 = CARTESIAN_POINT ( 'NONE',  ( 16.55341960407611168, 4.379528057220329451, 23.95724293864769550 ) ) ;
#83002 = DIRECTION ( 'NONE',  ( -0.000000000000000000, -0.000000000000000000, 1.000000000000000000 ) ) ;
#83003 = CARTESIAN_POINT ( 'NONE',  ( 4.483927247898545687, 16.52544592524342804, 114.7905762719810383 ) ) ;
#83004 = CARTESIAN_POINT ( 'NONE',  ( -15.72974639402197994, 15.80617190586746368, 60.62390960531437401 ) ) ;
#83005 = CARTESIAN_POINT ( 'NONE',  ( 16.51473224551069308, 9.474510206698969483, 39.16557627198103120 ) ) ;
#83006 = CARTESIAN_POINT ( 'NONE',  ( -12.06949235617739369, -12.14591786802326823, 89.37609039468568994 ) ) ;
#83007 = CARTESIAN_POINT ( 'NONE',  ( -5.719274019375665041, -21.55341960407619695, 29.79275706135234358 ) ) ;
#83008 = CARTESIAN_POINT ( 'NONE',  ( 5.049401038297881783, 19.05341960407617563, 87.29275706135234714 ) ) ;
#83009 = CARTESIAN_POINT ( 'NONE',  ( 12.06949235617757843, -12.14591786802309237, 98.12390960531436690 ) ) ;
#83010 = CARTESIAN_POINT ( 'NONE',  ( -0.05219959533909027116, -19.03943276465977164, 47.49890960531435979 ) ) ;
#83011 = CARTESIAN_POINT ( 'NONE',  ( -19.03943276465977164, 0.05219959533909376836, 21.24890960531436335 ) ) ;
#83012 = DIRECTION ( 'NONE',  ( 0.000000000000000000, -1.000000000000000000, 0.000000000000000000 ) ) ;
#83013 = CARTESIAN_POINT ( 'NONE',  ( -19.05341960407611168, -5.049401038298163336, 76.45724293864769550 ) ) ;
#83014 = CARTESIAN_POINT ( 'NONE',  ( 4.379528057220092307, 16.55341960407617563, 62.29275706135236845 ) ) ;
#83015 = CARTESIAN_POINT ( 'NONE',  ( 15.80617190586769283, -15.72974639402175789, 105.6260903946856899 ) ) ;
#83016 = CARTESIAN_POINT ( 'NONE',  ( -5.719274019375978568, 21.55341960407610458, 45.20724293864769550 ) ) ;
#83017 = ADVANCED_FACE ( 'NONE', ( #8770 ), #103077, .T. ) ;
#83018 = CARTESIAN_POINT ( 'NONE',  ( -8.314922557961024197, 14.29746914071037800, 72.91775706135234714 ) ) ;
#83019 = CARTESIAN_POINT ( 'NONE',  ( 16.51473224551083163, -9.474510206698727899, 65.83442372801900433 ) ) ;
#83020 = CARTESIAN_POINT ( 'NONE',  ( -18.62759615963255300, -10.81492255796106328, 59.16775706135234714 ) ) ;
#83021 = CARTESIAN_POINT ( 'NONE',  ( 5.049401038298161559, -19.05341960407611168, 72.70724293864768129 ) ) ;
#83022 = CARTESIAN_POINT ( 'NONE',  ( 13.89961937509977652, -13.97604488694527269, 33.12390960531434558 ) ) ;
#83023 = CARTESIAN_POINT ( 'NONE',  ( 19.05341960407617918, -5.049401038297876454, 56.04275706135234714 ) ) ;
#83024 = CARTESIAN_POINT ( 'NONE',  ( -5.049401038298153566, 19.05341960407611168, 110.2072429386476671 ) ) ;
#83025 = CARTESIAN_POINT ( 'NONE',  ( 5.049401038298161559, -19.05341960407611168, 97.70724293864766707 ) ) ;
#83026 = CARTESIAN_POINT ( 'NONE',  ( 8.314922557960818139, 14.29746914071049879, 49.58224293864769550 ) ) ;
#83027 = CARTESIAN_POINT ( 'NONE',  ( 18.62759615963271287, -10.81492255796078972, 53.33224293864769550 ) ) ;
#83028 = FACE_OUTER_BOUND ( 'NONE', #114384, .T. ) ;
#83029 = CARTESIAN_POINT ( 'NONE',  ( 19.03943276465977164, 0.05219959533936151252, 26.25109039468566507 ) ) ;
#83030 = CARTESIAN_POINT ( 'NONE',  ( -17.05116617787825462, -6.768360034955808402, 81.34324446740802728 ) ) ;
#83031 = CARTESIAN_POINT ( 'NONE',  ( 9.564922557960805705, 16.46253265017160317, 54.58224293864769550 ) ) ;
#83032 = CARTESIAN_POINT ( 'NONE',  ( 16.52544592524335698, 4.483927247898782831, 41.45942372801901143 ) ) ;
#83033 = CARTESIAN_POINT ( 'NONE',  ( 193.3062444957835453, -155.7167183371837496, -15.00000000000000000 ) ) ;
#83034 = DIRECTION ( 'NONE',  ( -1.000000000000000000, -0.000000000000000000, -0.000000000000000000 ) ) ;
#83035 = CARTESIAN_POINT ( 'NONE',  ( 12.14591786802327356, -12.06949235617739191, 75.62609039468567573 ) ) ;
#83036 = CARTESIAN_POINT ( 'NONE',  ( -15.80617190586745835, -15.72974639402198527, 101.8739096053143811 ) ) ;
#83038 = FACE_OUTER_BOUND ( 'NONE', #141773, .T. ) ;
#83037 = CARTESIAN_POINT ( 'NONE',  ( -19.02544592524342804, 5.153800228976336051, 36.04057627198100988 ) ) ;
#83039 = CARTESIAN_POINT ( 'NONE',  ( 10.81492255796106328, -18.62759615963255655, 40.41775706135234714 ) ) ;
#83040 = CARTESIAN_POINT ( 'NONE',  ( -5.049401038297874678, -19.05341960407617918, 44.79275706135232582 ) ) ;
#83041 = CARTESIAN_POINT ( 'NONE',  ( 19.02544592524343514, -5.153800228976328945, 48.54057627198103120 ) ) ;
#83042 = CARTESIAN_POINT ( 'NONE',  ( 5.719274019375673035, 21.55341960407619339, 92.29275706135236135 ) ) ;
#83043 = CARTESIAN_POINT ( 'NONE',  ( 17.31728774477274868, 6.344390552232392899, 96.68093348310684121 ) ) ;
#83044 = CARTESIAN_POINT ( 'NONE',  ( 0.05219959533910956823, 16.53943276465976808, 34.99890960531435979 ) ) ;
#83045 = DIRECTION ( 'NONE',  ( -1.000000000000000000, 0.000000000000000000, -0.000000000000000000 ) ) ;
#83046 = CARTESIAN_POINT ( 'NONE',  ( -15.72974639402197994, 15.80617190586746368, 50.62390960531435979 ) ) ;
#83047 = B_SPLINE_CURVE_WITH_KNOTS ( 'NONE', 3,
 ( #84749, #80775, #19125, #142453, #190952, #68592, #20103, #83752, #176797, #146427, #52429, #38270, #188984, #4920, #112119, #81747, #157636, #99924, #143434, #145431, #7917, #69601, #66603, #51440, #54435, #113100, #97910, #159601 ),
 .UNSPECIFIED., .F., .F.,
 ( 4, 2, 2, 2, 2, 2, 2, 2, 2, 2, 2, 2, 2, 4 ),
 ( 1.961533960614312002E-07, 0.0003775868847195944732, 0.0007549776160431275265, 0.001132368347366660742, 0.001509759078690194175, 0.002264540541337254752, 0.003019322003984315113, 0.003774103466631376341, 0.004151494197954899365, 0.004528884929278421956, 0.004906275660601946281, 0.005283666391925468872, 0.005661057123248991463, 0.006038447854572514054 ),
 .UNSPECIFIED. ) ;
#83048 = CARTESIAN_POINT ( 'NONE',  ( -22.44159573604009950, -16.30477369853688430, 143.0750000027311728 ) ) ;
#83049 = CARTESIAN_POINT ( 'NONE',  ( 16.51473224551069308, 9.474510206698969483, 99.16557627198102409 ) ) ;
#83050 = CARTESIAN_POINT ( 'NONE',  ( -16.55341960407611168, -4.379528057220339221, 106.4572429386477097 ) ) ;
#83051 = CARTESIAN_POINT ( 'NONE',  ( 4.483927247898790824, -16.52544592524335698, 20.20942372801900788 ) ) ;
#83052 = CARTESIAN_POINT ( 'NONE',  ( -12.06949235617739369, -12.14591786802326823, 104.3760903946856899 ) ) ;
#83053 = EDGE_LOOP ( 'NONE', ( #163427, #130261, #89087, #150693 ) ) ;
#83055 = CARTESIAN_POINT ( 'NONE',  ( -18.67979575497178146, -10.72451020669898902, 101.6655762719810383 ) ) ;
#83054 = CARTESIAN_POINT ( 'NONE',  ( -9.564922557960796823, -16.46253265017161027, 102.0822429386477097 ) ) ;
#83057 = CARTESIAN_POINT ( 'NONE',  ( 13.89961937509977652, -13.97604488694527269, 103.1239096053143527 ) ) ;
#83056 = CARTESIAN_POINT ( 'NONE',  ( -14.34966873604960291, -8.224510206698953496, 26.66557627198103475 ) ) ;
#83058 = CARTESIAN_POINT ( 'NONE',  ( -13.97604488694547697, 13.89961937509957934, 98.12609039468566152 ) ) ;
#83059 = CARTESIAN_POINT ( 'NONE',  ( -5.719274019375665041, -21.55341960407619695, 109.7927570613523613 ) ) ;
#83060 = CARTESIAN_POINT ( 'NONE',  ( -15.80617190586745835, -15.72974639402198527, 91.87390960531436690 ) ) ;
#83061 = CARTESIAN_POINT ( 'NONE',  ( -10.72451020669898014, 18.67979575497178502, 55.41557627198102409 ) ) ;
#83062 = CARTESIAN_POINT ( 'NONE',  ( -19.05341960407611168, -5.049401038298163336, 66.45724293864769550 ) ) ;
#83063 = CARTESIAN_POINT ( 'NONE',  ( -16.52544592524342804, 4.483927247898546575, 36.04057627198102409 ) ) ;
#83064 = CARTESIAN_POINT ( 'NONE',  ( -9.474510206698964154, 16.51473224551069663, 80.41557627198103830 ) ) ;
#83065 = CARTESIAN_POINT ( 'NONE',  ( 19.20446147854530139, 5.499999999999904965, 56.88999695167677828 ) ) ;
#83066 = CARTESIAN_POINT ( 'NONE',  ( 19.03943276465977164, 0.05219959533936151252, 36.25109039468567573 ) ) ;
#83067 = CARTESIAN_POINT ( 'NONE',  ( -10.72451020669898014, 18.67979575497178502, 85.41557627198102409 ) ) ;
#83068 = CARTESIAN_POINT ( 'NONE',  ( -12.06949235617756955, 12.14591786802309770, 80.62390960531438111 ) ) ;
#83069 = CARTESIAN_POINT ( 'NONE',  ( -0.05219959533937732626, 21.53943276465977519, 37.50109039468568284 ) ) ;
#83070 = CARTESIAN_POINT ( 'NONE',  ( -27.73933785331498925, 2.428612866367529932E-14, 147.3750000027311842 ) ) ;
#83071 = EDGE_CURVE ( 'NONE', #52978, #112132, #192285, .T. ) ;
#83072 = CARTESIAN_POINT ( 'NONE',  ( 0.05219959533934541429, -16.53943276465976808, 105.0010903946856757 ) ) ;
#83073 = CARTESIAN_POINT ( 'NONE',  ( -19.03943276465977164, 0.05219959533909376836, 26.24890960531435624 ) ) ;
#83074 = CARTESIAN_POINT ( 'NONE',  ( 19.03943276465977164, -0.05219959533909143690, 83.74890960531436690 ) ) ;
#83075 = DIRECTION ( 'NONE',  ( 1.000000000000000000, 0.000000000000000000, 0.000000000000000000 ) ) ;
#83076 = FACE_OUTER_BOUND ( 'NONE', #102499, .T. ) ;
#83077 = CARTESIAN_POINT ( 'NONE',  ( 14.34966873604960469, 8.224510206698951720, 39.16557627198102409 ) ) ;
#83078 = CARTESIAN_POINT ( 'NONE',  ( -21.55341960407619339, 5.719274019375674811, 63.54275706135234003 ) ) ;
#83079 = CARTESIAN_POINT ( 'NONE',  ( 29.30938409335578854, -24.40035533028643755, -16.80062434859663512 ) ) ;
#83080 = CARTESIAN_POINT ( 'NONE',  ( 5.153800228976335163, 19.02544592524342804, 39.79057627198100988 ) ) ;
#83081 = CARTESIAN_POINT ( 'NONE',  ( -9.564922557960796823, -16.46253265017161027, 57.08224293864769550 ) ) ;
#83082 = ORIENTED_EDGE ( 'NONE', *, *, #65754, .F. ) ;
#83083 = CARTESIAN_POINT ( 'NONE',  ( 18.62759615963255655, 10.81492255796105972, 111.6677570613523613 ) ) ;
#83084 = CARTESIAN_POINT ( 'NONE',  ( -12.06949235617739369, -12.14591786802326823, 59.37609039468568284 ) ) ;
#83085 = CARTESIAN_POINT ( 'NONE',  ( -18.67979575497193778, 10.72451020669871902, 88.33442372801901854 ) ) ;
#83086 = CARTESIAN_POINT ( 'NONE',  ( 5.823673210054125526, 21.52544592524343514, 24.79057627198103120 ) ) ;
#83087 = CARTESIAN_POINT ( 'NONE',  ( -19.03943276465977164, -0.05219959533935918106, 98.75109039468567573 ) ) ;
#83088 = CARTESIAN_POINT ( 'NONE',  ( 5.719274019375673035, 21.55341960407619339, 72.29275706135236135 ) ) ;
#83089 = CARTESIAN_POINT ( 'NONE',  ( 0.05219959533934541429, -16.53943276465976808, 30.00109039468568284 ) ) ;
#83090 = CARTESIAN_POINT ( 'NONE',  ( 10.72451020669898902, -18.67979575497178502, 82.91557627198103830 ) ) ;
#83091 = CARTESIAN_POINT ( 'NONE',  ( -5.049401038297874678, -19.05341960407617918, 94.79275706135230450 ) ) ;
#83092 = CARTESIAN_POINT ( 'NONE',  ( -5.049401038298153566, 19.05341960407611168, 60.20724293864768129 ) ) ;
#83093 = CARTESIAN_POINT ( 'NONE',  ( -16.53943276465976808, -0.05219959533934237506, 18.75109039468568639 ) ) ;
#83094 = CIRCLE ( 'NONE', #73481, 21.30000000000002913 ) ;
#83095 = CARTESIAN_POINT ( 'NONE',  ( 16.46253265017146816, 9.564922557961045513, 101.6677570613523329 ) ) ;
#83096 = CARTESIAN_POINT ( 'NONE',  ( 4.483927247898545687, 16.52544592524342804, 49.79057627198102409 ) ) ;
#83097 = CARTESIAN_POINT ( 'NONE',  ( -16.46253265017146816, -9.564922557961047289, 74.16775706135234714 ) ) ;
#83098 = CARTESIAN_POINT ( 'NONE',  ( 4.379528057220092307, 16.55341960407617563, 62.29275706135236845 ) ) ;
#83100 = CARTESIAN_POINT ( 'NONE',  ( 9.474510206698971260, -16.51473224551069308, 42.91557627198103120 ) ) ;
#83099 = CARTESIAN_POINT ( 'NONE',  ( -0.05219959533937732626, 21.53943276465977519, 22.50109039468567573 ) ) ;
#83102 = EDGE_CURVE ( 'NONE', #188707, #149684, #21097, .T. ) ;
#83101 = CARTESIAN_POINT ( 'NONE',  ( 0.05219959533909260263, 19.03943276465977164, 49.99890960531435979 ) ) ;
#83103 = CARTESIAN_POINT ( 'NONE',  ( -14.34966873604972548, 8.224510206698743886, 53.33442372801901854 ) ) ;
#83104 = FACE_OUTER_BOUND ( 'NONE', #32644, .T. ) ;
#83105 = CARTESIAN_POINT ( 'NONE',  ( 23.31738231874054890, -16.94106989632523508, 145.0500000054623513 ) ) ;
#83106 = CARTESIAN_POINT ( 'NONE',  ( -16.46253265017160317, 9.564922557960807481, 110.8322429386476955 ) ) ;
#83107 = DIRECTION ( 'NONE',  ( 0.000000000000000000, 0.04175967627138096189, 0.9991276842514722478 ) ) ;
#83108 = ORIENTED_EDGE ( 'NONE', *, *, #99422, .T. ) ;
#83109 = CARTESIAN_POINT ( 'NONE',  ( -12.06949235617739369, -12.14591786802326823, 19.37609039468568639 ) ) ;
#83110 = CARTESIAN_POINT ( 'NONE',  ( 5.719274019375991003, -21.55341960407610458, 42.70724293864770260 ) ) ;
#83112 = CARTESIAN_POINT ( 'NONE',  ( -8.224510206698735004, -14.34966873604973081, 29.58442372801901854 ) ) ;
#83111 = CARTESIAN_POINT ( 'NONE',  ( -0.05219959533936034679, 19.03943276465977164, 47.50109039468566863 ) ) ;
#83113 = CARTESIAN_POINT ( 'NONE',  ( 13.97604488694527802, 13.89961937509977652, 24.37390960531435624 ) ) ;
#83114 = CARTESIAN_POINT ( 'NONE',  ( 9.564922557960805705, 16.46253265017160317, 49.58224293864770260 ) ) ;
#83115 = CARTESIAN_POINT ( 'NONE',  ( -10.81492255796078084, -18.62759615963271287, 87.08224293864769550 ) ) ;
#83116 = CARTESIAN_POINT ( 'NONE',  ( -9.474510206698964154, 16.51473224551069663, 105.4155762719810383 ) ) ;
#83117 = CARTESIAN_POINT ( 'NONE',  ( 13.97604488694527802, 13.89961937509977652, 49.37390960531434558 ) ) ;
#83118 = CARTESIAN_POINT ( 'NONE',  ( 22.44159573604009239, 16.30477369853692693, 146.5750000027312012 ) ) ;
#83119 = CARTESIAN_POINT ( 'NONE',  ( 0.05219959533936267826, -19.03943276465977164, 85.00109039468567573 ) ) ;
#83121 = VECTOR ( 'NONE', #134560, 1000.000000000000000 ) ;
#83120 = CARTESIAN_POINT ( 'NONE',  ( 16.55341960407611168, 4.379528057220329451, 63.95724293864770260 ) ) ;
#83122 = CARTESIAN_POINT ( 'NONE',  ( -5.719274019375665041, -21.55341960407619695, 104.7927570613523898 ) ) ;
#83123 = CARTESIAN_POINT ( 'NONE',  ( -21.55341960407610458, -5.719274019375992779, 96.45724293864770971 ) ) ;
#83124 = CARTESIAN_POINT ( 'NONE',  ( -15.72974639402176322, -15.80617190586768395, 89.37609039468568994 ) ) ;
#83125 = CARTESIAN_POINT ( 'NONE',  ( 10.72451020669871369, 18.67979575497193778, 82.08442372801901854 ) ) ;
#83126 = CARTESIAN_POINT ( 'NONE',  ( 19.03943276465977164, -0.05219959533909143690, 103.7489096053143669 ) ) ;
#83128 = CARTESIAN_POINT ( 'NONE',  ( 21.52544592524334988, 5.823673210054432836, 76.45942372801901854 ) ) ;
#83127 = CARTESIAN_POINT ( 'NONE',  ( 16.52544592524335698, 4.483927247898782831, 106.4594237280190328 ) ) ;
#83129 = CARTESIAN_POINT ( 'NONE',  ( -16.51473224551069308, -9.474510206698971260, 61.66557627198103120 ) ) ;
#83130 = CARTESIAN_POINT ( 'NONE',  ( -18.67979575497193778, 10.72451020669871902, 48.33442372801902565 ) ) ;
#83131 = CARTESIAN_POINT ( 'NONE',  ( -9.474510206698964154, 16.51473224551069663, 85.41557627198102409 ) ) ;
#83132 = CARTESIAN_POINT ( 'NONE',  ( -16.55341960407611168, -4.379528057220339221, 81.45724293864769550 ) ) ;
#83133 = CARTESIAN_POINT ( 'NONE',  ( 4.483927247898545687, 16.52544592524342804, 54.79057627198104541 ) ) ;
#83134 = CARTESIAN_POINT ( 'NONE',  ( 10.81492255796078972, 18.62759615963270932, 64.58224293864769550 ) ) ;
#83135 = CARTESIAN_POINT ( 'NONE',  ( 16.51473224551069308, 9.474510206698969483, 59.16557627198102409 ) ) ;
#83136 = CARTESIAN_POINT ( 'NONE',  ( 18.67979575497178502, 10.72451020669898547, 74.16557627198102409 ) ) ;
#83137 = CARTESIAN_POINT ( 'NONE',  ( -16.46253265017146816, -9.564922557961047289, 59.16775706135233293 ) ) ;
#83139 = CARTESIAN_POINT ( 'NONE',  ( 16.52544592524342804, -4.483927247898539470, 73.54057627198102409 ) ) ;
#83138 = CARTESIAN_POINT ( 'NONE',  ( -9.474510206698720793, -16.51473224551083518, 34.58442372801899722 ) ) ;
#83140 = AXIS2_PLACEMENT_3D ( 'NONE', #125701, #140861, #29727 ) ;
#83141 = CARTESIAN_POINT ( 'NONE',  ( -18.67979575497178146, -10.72451020669898902, 51.66557627198102409 ) ) ;
#83142 = CARTESIAN_POINT ( 'NONE',  ( 17.18269478283314911, 17.18269478283310647, -56.77278709839600879 ) ) ;
#83144 = CARTESIAN_POINT ( 'NONE',  ( 1.784210473542230573E-15, -29.16686587814331588, 145.8750000027311557 ) ) ;
#83143 = CARTESIAN_POINT ( 'NONE',  ( 4.483927247898790824, -16.52544592524335698, 105.2094237280190328 ) ) ;
#83145 = EDGE_CURVE ( 'NONE', #91305, #50923, #187665, .T. ) ;
#83146 = CARTESIAN_POINT ( 'NONE',  ( -5.049401038297874678, -19.05341960407617918, 99.79275706135234714 ) ) ;
#83147 = CARTESIAN_POINT ( 'NONE',  ( -16.52544592524342804, 4.483927247898546575, 66.04057627198103830 ) ) ;
#83148 = CARTESIAN_POINT ( 'NONE',  ( -20.96320343559654020, -21.46320343559631638, 4.646446609406719830 ) ) ;
#83149 = CARTESIAN_POINT ( 'NONE',  ( -16.51473224551069308, -9.474510206698971260, 66.66557627198102409 ) ) ;
#83150 = CARTESIAN_POINT ( 'NONE',  ( 14.34966873604960469, 8.224510206698951720, 59.16557627198103120 ) ) ;
#83151 = CARTESIAN_POINT ( 'NONE',  ( -13.89961937509977652, 13.97604488694528158, 90.62390960531432427 ) ) ;
#83153 = CARTESIAN_POINT ( 'NONE',  ( 16.51473224551069308, 9.474510206698969483, 69.16557627198102409 ) ) ;
#83152 = CARTESIAN_POINT ( 'NONE',  ( 19.05341960407617918, -5.049401038297876454, 81.04275706135231871 ) ) ;
#83154 = CARTESIAN_POINT ( 'NONE',  ( -19.05341960407611168, -5.049401038298163336, 86.45724293864769550 ) ) ;
#83155 = CARTESIAN_POINT ( 'NONE',  ( 5.049401038298161559, -19.05341960407611168, 72.70724293864768129 ) ) ;
#83156 = CARTESIAN_POINT ( 'NONE',  ( 15.72974639402199770, -15.80617190586745480, 63.12390960531435979 ) ) ;
#83157 = CARTESIAN_POINT ( 'NONE',  ( 8.314922557961029526, -14.29746914071037800, 55.41775706135234714 ) ) ;
#83158 = CARTESIAN_POINT ( 'NONE',  ( -19.02544592524335343, -5.153800228976618492, 103.9594237280190043 ) ) ;
#83159 = CARTESIAN_POINT ( 'NONE',  ( -19.03943276465977164, 0.05219959533909376836, 51.24890960531436690 ) ) ;
#83160 = CARTESIAN_POINT ( 'NONE',  ( 5.823673210054125526, 21.52544592524343514, 54.79057627198104541 ) ) ;
#83161 = CARTESIAN_POINT ( 'NONE',  ( 5.049401038297881783, 19.05341960407617563, 87.29275706135234714 ) ) ;
#83162 = CARTESIAN_POINT ( 'NONE',  ( 12.14591786802309770, 12.06949235617756955, 29.37390960531435269 ) ) ;
#83163 = CARTESIAN_POINT ( 'NONE',  ( 16.46253265017146816, 9.564922557961045513, 41.66775706135234003 ) ) ;
#83165 = CARTESIAN_POINT ( 'NONE',  ( -4.483927247898782831, 16.52544592524335698, 92.70942372801901854 ) ) ;
#83164 = CARTESIAN_POINT ( 'NONE',  ( 4.379528057220092307, 16.55341960407617563, 62.29275706135236845 ) ) ;
#83166 = CARTESIAN_POINT ( 'NONE',  ( -5.000000000000000888, -130.0000000000000000, 15.50000000000000000 ) ) ;
#83167 = CARTESIAN_POINT ( 'NONE',  ( 16.53943276465976808, 0.05219959533934440121, 86.25109039468568994 ) ) ;
#83169 = CARTESIAN_POINT ( 'NONE',  ( 4.379528057220092307, 16.55341960407617563, 37.29275706135235424 ) ) ;
#83168 = CARTESIAN_POINT ( 'NONE',  ( -21.52544592524343514, 5.823673210054127303, 31.04057627198102409 ) ) ;
#83170 = CARTESIAN_POINT ( 'NONE',  ( -19.03943276465977164, 0.05219959533909376836, 41.24890960531435269 ) ) ;
#83171 = CARTESIAN_POINT ( 'NONE',  ( -16.51473224551069308, -9.474510206698971260, 51.66557627198102409 ) ) ;
#83172 = CARTESIAN_POINT ( 'NONE',  ( -13.97604488694527625, -13.89961937509977652, 41.87390960531435979 ) ) ;
#83173 = CARTESIAN_POINT ( 'NONE',  ( -18.62759615963255300, -10.81492255796106328, 39.16775706135235424 ) ) ;
#83174 = CARTESIAN_POINT ( 'NONE',  ( -4.379528057220086978, -16.55341960407618274, 49.79275706135234714 ) ) ;
#83175 = CARTESIAN_POINT ( 'NONE',  ( -16.52544592524335698, -4.483927247898792601, 108.9594237280190185 ) ) ;
#83176 = CARTESIAN_POINT ( 'NONE',  ( -9.564922557960796823, -16.46253265017161027, 27.08224293864769550 ) ) ;
#83177 = CARTESIAN_POINT ( 'NONE',  ( 0.05219959533937995610, -21.53943276465977519, 110.0010903946856757 ) ) ;
#83178 = CARTESIAN_POINT ( 'NONE',  ( -16.52544592524335698, -4.483927247898792601, 18.95942372801901143 ) ) ;
#83179 = CARTESIAN_POINT ( 'NONE',  ( -0.05219959533936034679, 19.03943276465977164, 62.50109039468566863 ) ) ;
#83180 = CARTESIAN_POINT ( 'NONE',  ( -8.314922557960811034, -14.29746914071050412, 72.08224293864769550 ) ) ;
#83181 = CARTESIAN_POINT ( 'NONE',  ( -13.89961937509977652, 13.97604488694528158, 40.62390960531435979 ) ) ;
#83183 = CARTESIAN_POINT ( 'NONE',  ( 17.05116617787825106, -6.768360034955811955, 91.15675553259201536 ) ) ;
#83182 = CARTESIAN_POINT ( 'NONE',  ( 9.474510206698729675, 16.51473224551082808, 72.08442372801900433 ) ) ;
#83184 = CARTESIAN_POINT ( 'NONE',  ( 0.05219959533937995610, -21.53943276465977519, 80.00109039468568994 ) ) ;
#83185 = CARTESIAN_POINT ( 'NONE',  ( 8.224510206698742110, 14.34966873604972548, 42.08442372801901854 ) ) ;
#83186 = CARTESIAN_POINT ( 'NONE',  ( 28.79475375365586132, 2.781246896534039337E-14, 150.0000000000000000 ) ) ;
#83187 = CARTESIAN_POINT ( 'NONE',  ( 15.72974639402199770, -15.80617190586745480, 38.12390960531436690 ) ) ;
#83188 = CARTESIAN_POINT ( 'NONE',  ( -4.379528057220086978, -16.55341960407618274, 29.79275706135234358 ) ) ;
#83189 = CARTESIAN_POINT ( 'NONE',  ( 17.49999999999999645, 5.500000000000010658, 88.78230962303567253 ) ) ;
#83190 = CARTESIAN_POINT ( 'NONE',  ( 21.52544592524334988, 5.823673210054432836, 106.4594237280190328 ) ) ;
#83191 = CARTESIAN_POINT ( 'NONE',  ( -21.75836449082843060, 9.620754668593672676, 170.8405250346329467 ) ) ;
#83192 = CARTESIAN_POINT ( 'NONE',  ( 9.564922557960805705, 16.46253265017160317, 44.58224293864769550 ) ) ;
#83193 = CARTESIAN_POINT ( 'NONE',  ( -17.79613651744293890, -24.49428055684528260, 142.5656553485623590 ) ) ;
#83194 = CARTESIAN_POINT ( 'NONE',  ( 13.97604488694527802, 13.89961937509977652, 54.37390960531435979 ) ) ;
#83195 = CARTESIAN_POINT ( 'NONE',  ( 21.52544592524334988, 5.823673210054432836, 71.45942372801901854 ) ) ;
#83196 = CARTESIAN_POINT ( 'NONE',  ( 15.72974639402176855, 15.80617190586768217, 111.8760903946856615 ) ) ;
#83197 = CARTESIAN_POINT ( 'NONE',  ( -16.55341960407611168, -4.379528057220339221, 21.45724293864769550 ) ) ;
#83198 = CARTESIAN_POINT ( 'NONE',  ( -16.46253265017160317, 9.564922557960807481, 25.83224293864769194 ) ) ;
#83199 = CARTESIAN_POINT ( 'NONE',  ( 19.03943276465977164, -0.05219959533909143690, 88.74890960531436690 ) ) ;
#83200 = CARTESIAN_POINT ( 'NONE',  ( 5.823673210054444382, -21.52544592524334988, 55.20942372801902565 ) ) ;
#83201 = CARTESIAN_POINT ( 'NONE',  ( 9.564922557960805705, 16.46253265017160317, 39.58224293864768839 ) ) ;
#83202 = CARTESIAN_POINT ( 'NONE',  ( 5.719274019375673035, 21.55341960407619339, 67.29275706135234714 ) ) ;
#83204 = CARTESIAN_POINT ( 'NONE',  ( -9.564922557960796823, -16.46253265017161027, 112.0822429386476955 ) ) ;
#83203 = CARTESIAN_POINT ( 'NONE',  ( 13.89961937509957401, 13.97604488694547697, 91.87609039468567573 ) ) ;
#83205 = CARTESIAN_POINT ( 'NONE',  ( -13.89961937509977652, 13.97604488694528158, 35.62390960531435269 ) ) ;
#83206 = CARTESIAN_POINT ( 'NONE',  ( 21.53943276465977519, -0.05219959533907433946, 103.7489096053143669 ) ) ;
#83207 = CARTESIAN_POINT ( 'NONE',  ( -16.46253265017146816, -9.564922557961047289, 34.16775706135233293 ) ) ;
#83208 = CARTESIAN_POINT ( 'NONE',  ( -14.29746914071049879, 8.314922557960819915, 115.8322429386477097 ) ) ;
#83209 = CARTESIAN_POINT ( 'NONE',  ( 0.05219959533909260263, 19.03943276465977164, 59.99890960531436690 ) ) ;
#83210 = CARTESIAN_POINT ( 'NONE',  ( 19.05341960407617918, -5.049401038297876454, 96.04275706135231871 ) ) ;
#83211 = CARTESIAN_POINT ( 'NONE',  ( -16.52544592524342804, 4.483927247898546575, 61.04057627198103120 ) ) ;
#83212 = CARTESIAN_POINT ( 'NONE',  ( 18.67979575497178502, 10.72451020669898547, 29.16557627198103120 ) ) ;
#83213 = CARTESIAN_POINT ( 'NONE',  ( -19.03943276465977164, -0.05219959533935918106, 88.75109039468567573 ) ) ;
#83214 = CARTESIAN_POINT ( 'NONE',  ( -21.52544592524343514, 5.823673210054127303, 86.04057627198102409 ) ) ;
#83215 = CARTESIAN_POINT ( 'NONE',  ( -15.72974639402176322, -15.80617190586768395, 49.37609039468569705 ) ) ;
#83216 = CARTESIAN_POINT ( 'NONE',  ( -16.53943276465976808, -0.05219959533934237506, 38.75109039468567573 ) ) ;
#83218 = CARTESIAN_POINT ( 'NONE',  ( 21.55341960407619695, -5.719274019375665929, 46.04275706135234714 ) ) ;
#83217 = CARTESIAN_POINT ( 'NONE',  ( -4.483927247898782831, 16.52544592524335698, 42.70942372801901854 ) ) ;
#83219 = CARTESIAN_POINT ( 'NONE',  ( 18.67979575497178502, 10.72451020669898547, 54.16557627198103120 ) ) ;
#83220 = CARTESIAN_POINT ( 'NONE',  ( -19.02544592524342804, 5.153800228976336051, 41.04057627198103120 ) ) ;
#83221 = CARTESIAN_POINT ( 'NONE',  ( -30.74264578624800492, 22.33583958711400186, -5.949999994537626513 ) ) ;
#83222 = CARTESIAN_POINT ( 'NONE',  ( 14.34966873604972726, -8.224510206698740333, 70.83442372801901854 ) ) ;
#83223 = CARTESIAN_POINT ( 'NONE',  ( -5.823673210054116645, -21.52544592524344225, 107.2905762719810525 ) ) ;
#83224 = CARTESIAN_POINT ( 'NONE',  ( 8.224510206698953496, -14.34966873604960469, 42.91557627198103120 ) ) ;
#83225 = CARTESIAN_POINT ( 'NONE',  ( 16.52544592524335698, 4.483927247898782831, 56.45942372801902565 ) ) ;
#83226 = CARTESIAN_POINT ( 'NONE',  ( 13.89961937509957401, 13.97604488694547697, 101.8760903946856331 ) ) ;
#83227 = CARTESIAN_POINT ( 'NONE',  ( -5.823673210054116645, -21.52544592524344225, 102.2905762719810383 ) ) ;
#83228 = CARTESIAN_POINT ( 'NONE',  ( 12.06949235617757843, -12.14591786802309237, 28.12390960531435979 ) ) ;
#83229 = ORIENTED_EDGE ( 'NONE', *, *, #87285, .T. ) ;
#83230 = CARTESIAN_POINT ( 'NONE',  ( -14.34966873604972548, 8.224510206698743886, 83.33442372801903275 ) ) ;
#83231 = CARTESIAN_POINT ( 'NONE',  ( 21.04946095171257525, 10.86023174791543866, 170.2405914574444239 ) ) ;
#83232 = CARTESIAN_POINT ( 'NONE',  ( 10.81492255796078972, 18.62759615963270932, 79.58224293864769550 ) ) ;
#83233 = CARTESIAN_POINT ( 'NONE',  ( -14.29746914071037622, -8.314922557961029526, 104.1677570613523471 ) ) ;
#83234 = CARTESIAN_POINT ( 'NONE',  ( -17.05116617787826527, -6.768360034955705373, 56.34324446740804149 ) ) ;
#83235 = CARTESIAN_POINT ( 'NONE',  ( 0.05219959533907565091, 21.53943276465977519, 104.9989096053143669 ) ) ;
#83236 = CARTESIAN_POINT ( 'NONE',  ( -10.81492255796078084, -18.62759615963271287, 107.0822429386476955 ) ) ;
#83237 = CARTESIAN_POINT ( 'NONE',  ( 16.55341960407611168, 4.379528057220329451, 38.95724293864768839 ) ) ;
#83238 = CARTESIAN_POINT ( 'NONE',  ( 8.314922557961029526, -14.29746914071037800, 50.41775706135235424 ) ) ;
#83239 = CIRCLE ( 'NONE', #15429, 27.91311885011353766 ) ;
#83240 = CARTESIAN_POINT ( 'NONE',  ( -5.153800228976328057, -19.02544592524343514, 42.29057627198101699 ) ) ;
#83241 = CARTESIAN_POINT ( 'NONE',  ( -5.153800228976328057, -19.02544592524343514, 62.29057627198100988 ) ) ;
#83242 = CARTESIAN_POINT ( 'NONE',  ( -19.03943276465977164, 0.05219959533909376836, 116.2489096053143669 ) ) ;
#83243 = CARTESIAN_POINT ( 'NONE',  ( -16.46253265017160317, 9.564922557960807481, 65.83224293864769550 ) ) ;
#83244 = CARTESIAN_POINT ( 'NONE',  ( 16.46253265017146816, 9.564922557961045513, 106.6677570613523471 ) ) ;
#83245 = CARTESIAN_POINT ( 'NONE',  ( 9.474510206698729675, 16.51473224551082808, 47.08442372801900433 ) ) ;
#83246 = CARTESIAN_POINT ( 'NONE',  ( -21.55341960407610458, -5.719274019375992779, 86.45724293864770971 ) ) ;
#83247 = ADVANCED_FACE ( 'NONE', ( #129507 ), #154446, .F. ) ;
#83248 = CARTESIAN_POINT ( 'NONE',  ( 16.53943276465976808, -0.05219959533910856209, 23.74890960531435269 ) ) ;
#83249 = CARTESIAN_POINT ( 'NONE',  ( -9.564922557960796823, -16.46253265017161027, 82.08224293864768129 ) ) ;
#83250 = CARTESIAN_POINT ( 'NONE',  ( 10.72451020669898902, -18.67979575497178502, 47.91557627198102409 ) ) ;
#83252 = CARTESIAN_POINT ( 'NONE',  ( 0.05219959533934541429, -16.53943276465976808, 30.00109039468568284 ) ) ;
#83251 = CARTESIAN_POINT ( 'NONE',  ( -10.72451020669898014, 18.67979575497178502, 85.41557627198102409 ) ) ;
#83253 = CARTESIAN_POINT ( 'NONE',  ( -15.80617190586745835, -15.72974639402198527, 26.87390960531435979 ) ) ;
#83254 = CARTESIAN_POINT ( 'NONE',  ( 0.05219959533937995610, -21.53943276465977519, 80.00109039468568994 ) ) ;
#83255 = CARTESIAN_POINT ( 'NONE',  ( 13.97604488694527802, 13.89961937509977652, 74.37390960531436690 ) ) ;
#83256 = CARTESIAN_POINT ( 'NONE',  ( 31.45250202946434825, 4.971043627493195949, 100.6372900316468986 ) ) ;
#83257 = CARTESIAN_POINT ( 'NONE',  ( 13.97604488694527802, 13.89961937509977652, 74.37390960531436690 ) ) ;
#83258 = CARTESIAN_POINT ( 'NONE',  ( -16.52544592524342804, 4.483927247898546575, 91.04057627198103830 ) ) ;
#83259 = ORIENTED_EDGE ( 'NONE', *, *, #139684, .T. ) ;
#83260 = CARTESIAN_POINT ( 'NONE',  ( -19.05341960407617563, 5.049401038297882671, 108.5427570613523187 ) ) ;
#83261 = DIRECTION ( 'NONE',  ( 0.06104853953485701173, 0.000000000000000000, -0.9981347984218670311 ) ) ;
#83262 = CARTESIAN_POINT ( 'NONE',  ( -5.049401038298153566, 19.05341960407611168, 75.20724293864769550 ) ) ;
#83263 = AXIS2_PLACEMENT_3D ( 'NONE', #146458, #7951, #69634 ) ;
#83265 = CARTESIAN_POINT ( 'NONE',  ( -5.153800228976328057, -19.02544592524343514, 97.29057627198099567 ) ) ;
#83264 = CARTESIAN_POINT ( 'NONE',  ( -5.719274019375665041, -21.55341960407619695, 79.79275706135236135 ) ) ;
#83266 = CARTESIAN_POINT ( 'NONE',  ( -4.379528057220086978, -16.55341960407618274, 74.79275706135234714 ) ) ;
#83267 = CARTESIAN_POINT ( 'NONE',  ( -28.90000000000003411, 0.1353689087806527469, -49.67367017693149478 ) ) ;
#83268 = CARTESIAN_POINT ( 'NONE',  ( -19.05341960407617563, 5.049401038297882671, 53.54275706135231871 ) ) ;
#83269 = CARTESIAN_POINT ( 'NONE',  ( -18.67979575497193778, 10.72451020669871902, 113.3344237280190328 ) ) ;
#83270 = LINE ( 'NONE', #145945, #130864 ) ;
#83271 = LINE ( 'NONE', #9458, #4618 ) ;
#83272 = CARTESIAN_POINT ( 'NONE',  ( 3.556970738554033499E-15, -38.81732327939057825, -6.624999997268814056 ) ) ;
#83273 = CARTESIAN_POINT ( 'NONE',  ( -0.05219959533934338120, 16.53943276465976808, 112.5010903946857042 ) ) ;
#83274 = CARTESIAN_POINT ( 'NONE',  ( -35.63774670715083204, -1.952809719854284198, 37.74170157406051374 ) ) ;
#83275 = CARTESIAN_POINT ( 'NONE',  ( -0.05219959533934338120, 16.53943276465976808, 112.5010903946857042 ) ) ;
#83276 = CARTESIAN_POINT ( 'NONE',  ( 12.06949235617739724, 12.14591786802326823, 86.87609039468568994 ) ) ;
#83277 = CARTESIAN_POINT ( 'NONE',  ( 18.67979575497194134, -10.72451020669871369, 75.83442372801900433 ) ) ;
#83278 = CARTESIAN_POINT ( 'NONE',  ( -5.153800228976607833, 19.02544592524334988, 82.70942372801897591 ) ) ;
#83279 = CARTESIAN_POINT ( 'NONE',  ( -15.72974639402176322, -15.80617190586768395, 69.37609039468567573 ) ) ;
#83280 = CARTESIAN_POINT ( 'NONE',  ( 16.46253265017146816, 9.564922557961045513, 41.66775706135234003 ) ) ;
#83281 = CARTESIAN_POINT ( 'NONE',  ( 19.05341960407611168, 5.049401038298154454, 78.95724293864769550 ) ) ;
#83282 = CARTESIAN_POINT ( 'NONE',  ( -9.474510206698964154, 16.51473224551069663, 55.41557627198103120 ) ) ;
#83283 = CARTESIAN_POINT ( 'NONE',  ( -5.153800228976328057, -19.02544592524343514, 87.29057627198102409 ) ) ;
#83284 = CARTESIAN_POINT ( 'NONE',  ( -5.719274019375978568, 21.55341960407610458, 90.20724293864770971 ) ) ;
#83285 = CARTESIAN_POINT ( 'NONE',  ( -21.52544592524343514, 5.823673210054127303, 46.04057627198103830 ) ) ;
#83286 = CARTESIAN_POINT ( 'NONE',  ( 13.89961937509977652, -13.97604488694527269, 48.12390960531435979 ) ) ;
#83287 = CARTESIAN_POINT ( 'NONE',  ( -16.55341960407617563, 4.379528057220093196, 58.54275706135235424 ) ) ;
#83288 = ORIENTED_EDGE ( 'NONE', *, *, #63230, .T. ) ;
#83289 = CARTESIAN_POINT ( 'NONE',  ( -18.67979575497193778, 10.72451020669871902, 48.33442372801902565 ) ) ;
#83291 = CARTESIAN_POINT ( 'NONE',  ( 3.556970738554033499E-15, -38.81732327939057825, -10.12499999726881228 ) ) ;
#83290 = CARTESIAN_POINT ( 'NONE',  ( 16.55341960407611168, 4.379528057220329451, 68.95724293864769550 ) ) ;
#83292 = CARTESIAN_POINT ( 'NONE',  ( -14.34966873604972548, 8.224510206698743886, 38.33442372801900433 ) ) ;
#83293 = CARTESIAN_POINT ( 'NONE',  ( -4.483927247898539470, -16.52544592524342804, 97.29057627198105251 ) ) ;
#83294 = CARTESIAN_POINT ( 'NONE',  ( 9.474510206698729675, 16.51473224551082808, 47.08442372801900433 ) ) ;
#83295 = CARTESIAN_POINT ( 'NONE',  ( 4.483927247898545687, 16.52544592524342804, 64.79057627198103830 ) ) ;
#83296 = CARTESIAN_POINT ( 'NONE',  ( 15.80617190586769283, -15.72974639402175789, 25.62609039468567929 ) ) ;
#83298 = CARTESIAN_POINT ( 'NONE',  ( 0.05219959533907565091, 21.53943276465977519, 94.99890960531436690 ) ) ;
#83297 = CARTESIAN_POINT ( 'NONE',  ( 9.474510206698971260, -16.51473224551069308, 27.91557627198103120 ) ) ;
#83299 = CARTESIAN_POINT ( 'NONE',  ( -19.02544592524342804, 5.153800228976336051, 101.0405762719810241 ) ) ;
#83300 = CARTESIAN_POINT ( 'NONE',  ( -14.34966873604960291, -8.224510206698953496, 76.66557627198103830 ) ) ;
#83301 = CARTESIAN_POINT ( 'NONE',  ( 30.85002141291950295, -24.92539791875765331, -19.32025355660333688 ) ) ;
#83302 = CARTESIAN_POINT ( 'NONE',  ( 11.40812507854755253, -35.11059874428192273, -6.024999997268814411 ) ) ;
#83303 = CARTESIAN_POINT ( 'NONE',  ( -16.51473224551082808, 9.474510206698731452, 78.33442372801900433 ) ) ;
#83304 = CARTESIAN_POINT ( 'NONE',  ( 0.05219959533937995610, -21.53943276465977519, 25.00109039468567218 ) ) ;
#83305 = CARTESIAN_POINT ( 'NONE',  ( 19.05341960407611168, 5.049401038298154454, 68.95724293864769550 ) ) ;
#83306 = CARTESIAN_POINT ( 'NONE',  ( -0.05219959533936034679, 19.03943276465977164, 52.50109039468566863 ) ) ;
#83307 = CARTESIAN_POINT ( 'NONE',  ( 19.02544592524343514, -5.153800228976328945, 33.54057627198102409 ) ) ;
#83308 = CARTESIAN_POINT ( 'NONE',  ( 14.34966873604960469, 8.224510206698951720, 69.16557627198102409 ) ) ;
#83309 = CARTESIAN_POINT ( 'NONE',  ( -14.29746914071049879, 8.314922557960819915, 55.83224293864770260 ) ) ;
#83310 = CARTESIAN_POINT ( 'NONE',  ( 5.049401038298161559, -19.05341960407611168, 67.70724293864769550 ) ) ;
#83311 = CARTESIAN_POINT ( 'NONE',  ( 18.62759615963271287, -10.81492255796078972, 83.33224293864769550 ) ) ;
#83312 = CARTESIAN_POINT ( 'NONE',  ( 5.153800228976335163, 19.02544592524342804, 54.79057627198103120 ) ) ;
#83313 = VERTEX_POINT ( 'NONE', #48716 ) ;
#83314 = CARTESIAN_POINT ( 'NONE',  ( -10.81492255796078084, -18.62759615963271287, 77.08224293864769550 ) ) ;
#83315 = CARTESIAN_POINT ( 'NONE',  ( 21.52544592524334988, 5.823673210054432836, 101.4594237280190185 ) ) ;
#83318 = CARTESIAN_POINT ( 'NONE',  ( 8.224510206698953496, -14.34966873604960469, 92.91557627198103830 ) ) ;
#83317 = CARTESIAN_POINT ( 'NONE',  ( -14.34966873604960291, -8.224510206698953496, 21.66557627198102409 ) ) ;
#83316 = CARTESIAN_POINT ( 'NONE',  ( -9.564922557960796823, -16.46253265017161027, 22.08224293864768839 ) ) ;
#83319 = CARTESIAN_POINT ( 'NONE',  ( -19.03943276465977164, -0.05219959533935918106, 88.75109039468567573 ) ) ;
#83320 = VERTEX_POINT ( 'NONE', #174055 ) ;
#83321 = CARTESIAN_POINT ( 'NONE',  ( -21.53943276465977519, -0.05219959533937600094, 18.75109039468568639 ) ) ;
#83322 = CARTESIAN_POINT ( 'NONE',  ( -9.564922557961040184, 16.46253265017147172, 52.91775706135233293 ) ) ;
#83323 = CARTESIAN_POINT ( 'NONE',  ( -8.314922557961024197, 14.29746914071037800, 102.9177570613523756 ) ) ;
#83324 = CARTESIAN_POINT ( 'NONE',  ( 9.564922557961047289, -16.46253265017146816, 25.41775706135234003 ) ) ;
#83325 = CARTESIAN_POINT ( 'NONE',  ( 13.97604488694527802, 13.89961937509977652, 99.37390960531436690 ) ) ;
#83326 = CARTESIAN_POINT ( 'NONE',  ( -5.719274019375978568, 21.55341960407610458, 65.20724293864768129 ) ) ;
#83327 = DIRECTION ( 'NONE',  ( -1.000000000000000000, -0.000000000000000000, -0.000000000000000000 ) ) ;
#83328 = CARTESIAN_POINT ( 'NONE',  ( 5.153800228976335163, 19.02544592524342804, 29.79057627198102409 ) ) ;
#83329 = CARTESIAN_POINT ( 'NONE',  ( -5.049401038297874678, -19.05341960407617918, 19.79275706135233293 ) ) ;
#83330 = CARTESIAN_POINT ( 'NONE',  ( -16.53943276465976808, -0.05219959533934237506, 73.75109039468567573 ) ) ;
#83331 = CARTESIAN_POINT ( 'NONE',  ( 21.55341960407619695, -5.719274019375665929, 26.04275706135235779 ) ) ;
#83332 = CARTESIAN_POINT ( 'NONE',  ( -8.224510206698735004, -14.34966873604973081, 44.58442372801901854 ) ) ;
#83333 = CARTESIAN_POINT ( 'NONE',  ( -16.51473224551069308, -9.474510206698971260, 106.6655762719810383 ) ) ;
#83334 = CARTESIAN_POINT ( 'NONE',  ( 9.564922557960805705, 16.46253265017160317, 54.58224293864769550 ) ) ;
#83335 = CARTESIAN_POINT ( 'NONE',  ( -19.02544592524342804, 5.153800228976336051, 66.04057627198103830 ) ) ;
#83336 = CARTESIAN_POINT ( 'NONE',  ( 16.53943276465976808, 0.05219959533934440121, 41.25109039468568284 ) ) ;
#83337 = CARTESIAN_POINT ( 'NONE',  ( 16.55341960407611168, 4.379528057220329451, 93.95724293864770971 ) ) ;
#83338 = CARTESIAN_POINT ( 'NONE',  ( -14.34966873604972548, 8.224510206698743886, 113.3344237280190328 ) ) ;
#83339 = CARTESIAN_POINT ( 'NONE',  ( 0.05219959533909260263, 19.03943276465977164, 49.99890960531435979 ) ) ;
#83342 = CARTESIAN_POINT ( 'NONE',  ( 19.02544592524343514, -5.153800228976328945, 63.54057627198103830 ) ) ;
#83341 = CARTESIAN_POINT ( 'NONE',  ( 19.03943276465977164, -0.05219959533909143690, 83.74890960531436690 ) ) ;
#83340 = CARTESIAN_POINT ( 'NONE',  ( 18.62759615963255655, 10.81492255796105972, 56.66775706135235424 ) ) ;
#83344 = EDGE_CURVE ( 'NONE', #38038, #149173, #189948, .T. ) ;
#83343 = CARTESIAN_POINT ( 'NONE',  ( -5.153800228976328057, -19.02544592524343514, 92.29057627198099567 ) ) ;
#83345 = CARTESIAN_POINT ( 'NONE',  ( 4.379528057220339221, -16.55341960407611168, 42.70724293864770260 ) ) ;
#83346 = CARTESIAN_POINT ( 'NONE',  ( -12.06949235617739369, -12.14591786802326823, 94.37609039468568994 ) ) ;
#83347 = CARTESIAN_POINT ( 'NONE',  ( -4.379528057220328563, 16.55341960407611168, 40.20724293864769550 ) ) ;
#83348 = ORIENTED_EDGE ( 'NONE', *, *, #7609, .F. ) ;
#83349 = CARTESIAN_POINT ( 'NONE',  ( -16.46253265017146816, -9.564922557961047289, 44.16775706135232582 ) ) ;
#83350 = CARTESIAN_POINT ( 'NONE',  ( -14.93657930744004148, -17.05128149819693917, -55.49887180089014294 ) ) ;
#83351 = CARTESIAN_POINT ( 'NONE',  ( -9.474510206698964154, 16.51473224551069663, 60.41557627198102409 ) ) ;
#83352 = CARTESIAN_POINT ( 'NONE',  ( 16.51473224551083163, -9.474510206698727899, 35.83442372801899722 ) ) ;
#83353 = CARTESIAN_POINT ( 'NONE',  ( 3.556970738554033499E-15, -38.81732327939057825, -2.124999997268813612 ) ) ;
#83354 = DIRECTION ( 'NONE',  ( 0.000000000000000000, 0.000000000000000000, 1.000000000000000000 ) ) ;
#83356 = CARTESIAN_POINT ( 'NONE',  ( -14.29746914071037622, -8.314922557961029526, 74.16775706135231871 ) ) ;
#83355 = CARTESIAN_POINT ( 'NONE',  ( -5.153800228976607833, 19.02544592524334988, 87.70942372801897591 ) ) ;
#83357 = CARTESIAN_POINT ( 'NONE',  ( 17.48847506799968698, 5.747544572773784388, 91.67302562156724832 ) ) ;
#83358 = CARTESIAN_POINT ( 'NONE',  ( 19.05341960407611168, 5.049401038298154454, 88.95724293864769550 ) ) ;
#83359 = CARTESIAN_POINT ( 'NONE',  ( -21.53943276465977519, -0.05219959533937600094, 33.75109039468568284 ) ) ;
#83360 = CARTESIAN_POINT ( 'NONE',  ( 19.02544592524334988, 5.153800228976608722, 71.45942372801900433 ) ) ;
#83362 = CARTESIAN_POINT ( 'NONE',  ( -16.51473224551069308, -9.474510206698971260, 51.66557627198102409 ) ) ;
#83361 = CARTESIAN_POINT ( 'NONE',  ( -9.474510206698964154, 16.51473224551069663, 115.4155762719810241 ) ) ;
#83363 = CARTESIAN_POINT ( 'NONE',  ( -19.02544592524342804, 5.153800228976336051, 96.04057627198103830 ) ) ;
#83365 = CARTESIAN_POINT ( 'NONE',  ( 0.05219959533909260263, 19.03943276465977164, 49.99890960531435979 ) ) ;
#83364 = CARTESIAN_POINT ( 'NONE',  ( 12.14591786802309770, 12.06949235617756955, 44.37390960531435979 ) ) ;
#83366 = CARTESIAN_POINT ( 'NONE',  ( 19.03943276465977164, 0.05219959533936151252, 51.25109039468567573 ) ) ;
#83367 = CARTESIAN_POINT ( 'NONE',  ( -16.52544592524342804, 4.483927247898546575, 91.04057627198103830 ) ) ;
#83368 = CARTESIAN_POINT ( 'NONE',  ( 13.89961937509957401, 13.97604488694547697, 26.87609039468566507 ) ) ;
#83369 = CARTESIAN_POINT ( 'NONE',  ( 13.97604488694527802, 13.89961937509977652, 69.37390960531436690 ) ) ;
#83370 = CARTESIAN_POINT ( 'NONE',  ( 5.719274019375991003, -21.55341960407610458, 67.70724293864769550 ) ) ;
#83372 = CARTESIAN_POINT ( 'NONE',  ( 13.89961937509957401, 13.97604488694547697, 26.87609039468566507 ) ) ;
#83371 = CARTESIAN_POINT ( 'NONE',  ( 8.314922557960818139, 14.29746914071049879, 69.58224293864769550 ) ) ;
#83373 = CARTESIAN_POINT ( 'NONE',  ( -9.474510206698964154, 16.51473224551069663, 105.4155762719810383 ) ) ;
#83374 = CARTESIAN_POINT ( 'NONE',  ( -5.719274019375978568, 21.55341960407610458, 30.20724293864769550 ) ) ;
#83375 = CARTESIAN_POINT ( 'NONE',  ( 13.89961937509977652, -13.97604488694527269, 53.12390960531434558 ) ) ;
#83376 = CARTESIAN_POINT ( 'NONE',  ( 16.46253265017160672, -9.564922557960803928, 38.33224293864768839 ) ) ;
#83377 = CARTESIAN_POINT ( 'NONE',  ( 16.55341960407611168, 4.379528057220329451, 98.95724293864770971 ) ) ;
#83378 = CARTESIAN_POINT ( 'NONE',  ( 21.52544592524344225, -5.823673210054117533, 108.5405762719810241 ) ) ;
#83379 = CARTESIAN_POINT ( 'NONE',  ( -5.049401038298153566, 19.05341960407611168, 105.2072429386476671 ) ) ;
#83380 = CARTESIAN_POINT ( 'NONE',  ( -21.55341960407610458, -5.719274019375992779, 111.4572429386476813 ) ) ;
#83381 = CARTESIAN_POINT ( 'NONE',  ( 13.97604488694527802, 13.89961937509977652, 109.3739096053143669 ) ) ;
#83382 = CARTESIAN_POINT ( 'NONE',  ( 13.97604488694527802, 13.89961937509977652, 24.37390960531435624 ) ) ;
#83383 = CARTESIAN_POINT ( 'NONE',  ( 21.52544592524334988, 5.823673210054432836, 81.45942372801900433 ) ) ;
#83384 = CARTESIAN_POINT ( 'NONE',  ( -21.55341960407610458, -5.719274019375992779, 91.45724293864769550 ) ) ;
#83385 = CARTESIAN_POINT ( 'NONE',  ( 16.29526858892874941, -7.335722546920139031, 106.7032940219979196 ) ) ;
#83386 = DIRECTION ( 'NONE',  ( -1.000000000000000000, 0.000000000000000000, 0.000000000000000000 ) ) ;
#83387 = CARTESIAN_POINT ( 'NONE',  ( 29.12650189376885024, -0.8004727011104447731, -52.40478149256041007 ) ) ;
#83388 = CARTESIAN_POINT ( 'NONE',  ( -14.29746914071037622, -8.314922557961029526, 44.16775706135234714 ) ) ;
#83389 = CARTESIAN_POINT ( 'NONE',  ( 0.05219959533910956823, 16.53943276465976808, 109.9989096053143527 ) ) ;
#83390 = CARTESIAN_POINT ( 'NONE',  ( -17.50000000000000355, -3.512728167236954580, 109.7719000481887690 ) ) ;
#83391 = CARTESIAN_POINT ( 'NONE',  ( 19.02544592524343514, -5.153800228976328945, 63.54057627198103830 ) ) ;
#83392 = CARTESIAN_POINT ( 'NONE',  ( -0.05219959533910754901, -16.53943276465976808, 92.49890960531436690 ) ) ;
#83393 = CARTESIAN_POINT ( 'NONE',  ( 21.53943276465977519, -0.05219959533907433946, 43.74890960531435979 ) ) ;
#83394 = CARTESIAN_POINT ( 'NONE',  ( -0.05219959533910754901, -16.53943276465976808, 62.49890960531436690 ) ) ;
#83395 = CARTESIAN_POINT ( 'NONE',  ( 4.483927247898790824, -16.52544592524335698, 20.20942372801900788 ) ) ;
#83396 = CARTESIAN_POINT ( 'NONE',  ( -5.719274019375665041, -21.55341960407619695, 74.79275706135234714 ) ) ;
#83397 = CARTESIAN_POINT ( 'NONE',  ( -12.14591786802326823, 12.06949235617739902, 103.1260903946856757 ) ) ;
#83398 = CARTESIAN_POINT ( 'NONE',  ( 14.34966873604960469, 8.224510206698951720, 44.16557627198103120 ) ) ;
#83399 = CARTESIAN_POINT ( 'NONE',  ( 13.89961937509977652, -13.97604488694527269, 33.12390960531434558 ) ) ;
#83400 = CARTESIAN_POINT ( 'NONE',  ( 19.05341960407611168, 5.049401038298154454, 83.95724293864766707 ) ) ;
#83401 = CARTESIAN_POINT ( 'NONE',  ( 15.80617190586746368, 15.72974639402197994, 99.37390960531436690 ) ) ;
#83402 = CARTESIAN_POINT ( 'NONE',  ( 0.05219959533934541429, -16.53943276465976808, 20.00109039468568639 ) ) ;
#83404 = CARTESIAN_POINT ( 'NONE',  ( -0.05219959533937732626, 21.53943276465977519, 72.50109039468568994 ) ) ;
#83403 = CARTESIAN_POINT ( 'NONE',  ( -14.34966873604960291, -8.224510206698953496, 66.66557627198102409 ) ) ;
#83405 = AXIS2_PLACEMENT_3D ( 'NONE', #37089, #96755, #98748 ) ;
#83406 = CARTESIAN_POINT ( 'NONE',  ( -0.05219959533934338120, 16.53943276465976808, 97.50109039468567573 ) ) ;
#83407 = CARTESIAN_POINT ( 'NONE',  ( 17.49999999999999645, 5.624438216177604311, 26.68329655085357288 ) ) ;
#83408 = CARTESIAN_POINT ( 'NONE',  ( -19.20446147854528007, -5.499999999999907629, 64.38999695167679249 ) ) ;
#83409 = CARTESIAN_POINT ( 'NONE',  ( -4.483927247898539470, -16.52544592524342804, 32.29057627198102409 ) ) ;
#83410 = CARTESIAN_POINT ( 'NONE',  ( 16.53943276465976808, 0.05219959533934440121, 76.25109039468568994 ) ) ;
#83411 = CARTESIAN_POINT ( 'NONE',  ( 16.51473224551069308, 9.474510206698969483, 89.16557627198103830 ) ) ;
#83412 = CARTESIAN_POINT ( 'NONE',  ( 0.05219959533909260263, 19.03943276465977164, 99.99890960531436690 ) ) ;
#83413 = CARTESIAN_POINT ( 'NONE',  ( 21.53943276465977519, 0.05219959533937863772, 86.25109039468568994 ) ) ;
#83414 = CARTESIAN_POINT ( 'NONE',  ( 12.14591786802327356, -12.06949235617739191, 85.62609039468568994 ) ) ;
#83415 = CARTESIAN_POINT ( 'NONE',  ( 8.224510206698953496, -14.34966873604960469, 62.91557627198102409 ) ) ;
#83416 = CARTESIAN_POINT ( 'NONE',  ( 9.564922557960805705, 16.46253265017160317, 69.58224293864770971 ) ) ;
#83417 = VERTEX_POINT ( 'NONE', #160868 ) ;
#83418 = CARTESIAN_POINT ( 'NONE',  ( -16.53943276465976808, -0.05219959533934237506, 18.75109039468568639 ) ) ;
#83419 = CARTESIAN_POINT ( 'NONE',  ( -4.483927247898539470, -16.52544592524342804, 112.2905762719810241 ) ) ;
#83420 = CARTESIAN_POINT ( 'NONE',  ( -9.474510206698964154, 16.51473224551069663, 75.41557627198103830 ) ) ;
#83422 = CARTESIAN_POINT ( 'NONE',  ( 30.74264578624799782, 22.33583958711400541, -0.7999999999999999334 ) ) ;
#83421 = CARTESIAN_POINT ( 'NONE',  ( -9.564922557961040184, 16.46253265017147172, 112.9177570613523329 ) ) ;
#83423 = CARTESIAN_POINT ( 'NONE',  ( 18.62759615963255655, 10.81492255796105972, 111.6677570613523613 ) ) ;
#83424 = CARTESIAN_POINT ( 'NONE',  ( -4.379528057220086978, -16.55341960407618274, 79.79275706135236135 ) ) ;
#83425 = CARTESIAN_POINT ( 'NONE',  ( 5.049401038297881783, 19.05341960407617563, 92.29275706135234714 ) ) ;
#83426 = CARTESIAN_POINT ( 'NONE',  ( 8.314922557960818139, 14.29746914071049879, 114.5822429386477097 ) ) ;
#83427 = CARTESIAN_POINT ( 'NONE',  ( 8.224510206698742110, 14.34966873604972548, 72.08442372801899012 ) ) ;
#83428 = CARTESIAN_POINT ( 'NONE',  ( -0.05219959533934338120, 16.53943276465976808, 47.50109039468568994 ) ) ;
#83429 = CARTESIAN_POINT ( 'NONE',  ( 16.51473224551069308, 9.474510206698969483, 24.16557627198102765 ) ) ;
#83430 = CARTESIAN_POINT ( 'NONE',  ( 13.97604488694548053, -13.89961937509957401, 65.62609039468567573 ) ) ;
#83431 = CARTESIAN_POINT ( 'NONE',  ( 15.80617190586769283, -15.72974639402175789, 100.6260903946857184 ) ) ;
#83432 = CARTESIAN_POINT ( 'NONE',  ( 19.02544592524343514, -5.153800228976328945, 33.54057627198102409 ) ) ;
#83433 = CARTESIAN_POINT ( 'NONE',  ( 16.51473224551069308, 9.474510206698969483, 84.16557627198102409 ) ) ;
#83434 = CARTESIAN_POINT ( 'NONE',  ( 14.34966873604960469, 8.224510206698951720, 69.16557627198102409 ) ) ;
#83435 = CARTESIAN_POINT ( 'NONE',  ( -5.719274019375665041, -21.55341960407619695, 94.79275706135234714 ) ) ;
#83436 = CARTESIAN_POINT ( 'NONE',  ( 9.564922557961047289, -16.46253265017146816, 40.41775706135234003 ) ) ;
#83437 = CARTESIAN_POINT ( 'NONE',  ( 15.72974639402199770, -15.80617190586745480, 33.12390960531435979 ) ) ;
#83438 = CARTESIAN_POINT ( 'NONE',  ( 21.53943276465977519, 0.05219959533937863772, 111.2510903946856899 ) ) ;
#83439 = CARTESIAN_POINT ( 'NONE',  ( 9.564922557960805705, 16.46253265017160317, 74.58224293864769550 ) ) ;
#83440 = CARTESIAN_POINT ( 'NONE',  ( 21.53943276465977519, 0.05219959533937863772, 106.2510903946856757 ) ) ;
#83441 = CARTESIAN_POINT ( 'NONE',  ( 21.55341960407610458, 5.719274019375980345, 48.95724293864770971 ) ) ;
#83442 = CARTESIAN_POINT ( 'NONE',  ( -19.03943276465977164, 0.05219959533909376836, 96.24890960531436690 ) ) ;
#83443 = CARTESIAN_POINT ( 'NONE',  ( 5.153800228976615827, -19.02544592524334988, 70.20942372801899012 ) ) ;
#83444 = CARTESIAN_POINT ( 'NONE',  ( -5.153800228976328057, -19.02544592524343514, 107.2905762719810383 ) ) ;
#83445 = ADVANCED_FACE ( 'NONE', ( #6172, #7170, #189228 ), #191207, .F. ) ;
#83446 = CARTESIAN_POINT ( 'NONE',  ( -9.474510206698720793, -16.51473224551083518, 89.58442372801900433 ) ) ;
#83447 = CARTESIAN_POINT ( 'NONE',  ( 14.29746914071037800, 8.314922557961029526, 41.66775706135235424 ) ) ;
#83448 = CARTESIAN_POINT ( 'NONE',  ( -12.06949235617756955, 12.14591786802309770, 115.6239096053143669 ) ) ;
#83449 = CARTESIAN_POINT ( 'NONE',  ( 19.02544592524343514, -5.153800228976328945, 78.54057627198099567 ) ) ;
#83450 = CARTESIAN_POINT ( 'NONE',  ( 5.823673210054125526, 21.52544592524343514, 59.79057627198103120 ) ) ;
#83451 = CARTESIAN_POINT ( 'NONE',  ( 14.29746914071037800, 8.314922557961029526, 26.66775706135235424 ) ) ;
#83452 = CARTESIAN_POINT ( 'NONE',  ( -15.72974639402176322, -15.80617190586768395, 29.37609039468568284 ) ) ;
#83453 = CARTESIAN_POINT ( 'NONE',  ( -18.67979575497193778, 10.72451020669871902, 78.33442372801901854 ) ) ;
#83454 = CARTESIAN_POINT ( 'NONE',  ( 4.483927247898790824, -16.52544592524335698, 85.20942372801901854 ) ) ;
#83455 = CARTESIAN_POINT ( 'NONE',  ( -16.46253265017160317, 9.564922557960807481, 90.83224293864769550 ) ) ;
#83456 = CARTESIAN_POINT ( 'NONE',  ( 4.379528057220339221, -16.55341960407611168, 72.70724293864769550 ) ) ;
#83457 = CARTESIAN_POINT ( 'NONE',  ( 14.34966873604972726, -8.224510206698740333, 110.8344237280190043 ) ) ;
#83458 = CARTESIAN_POINT ( 'NONE',  ( -9.474510206698720793, -16.51473224551083518, 54.58442372801899722 ) ) ;
#83459 = CARTESIAN_POINT ( 'NONE',  ( -21.55341960407619339, 5.719274019375674811, 43.54275706135235424 ) ) ;
#83460 = ADVANCED_FACE ( 'NONE', ( #4175 ), #128514, .T. ) ;
#83461 = CARTESIAN_POINT ( 'NONE',  ( 0.05219959533910956823, 16.53943276465976808, 84.99890960531436690 ) ) ;
#83462 = CARTESIAN_POINT ( 'NONE',  ( 5.153800228976335163, 19.02544592524342804, 109.7905762719810099 ) ) ;
#83463 = CARTESIAN_POINT ( 'NONE',  ( 4.379528057220092307, 16.55341960407617563, 97.29275706135234714 ) ) ;
#83464 = CARTESIAN_POINT ( 'NONE',  ( -10.72451020669870658, -18.67979575497194134, 89.58442372801901854 ) ) ;
#83465 = CARTESIAN_POINT ( 'NONE',  ( 16.52544592524335698, 4.483927247898782831, 41.45942372801901143 ) ) ;
#83466 = CARTESIAN_POINT ( 'NONE',  ( 0.05219959533937995610, -21.53943276465977519, 40.00109039468567573 ) ) ;
#83467 = ORIENTED_EDGE ( 'NONE', *, *, #139917, .F. ) ;
#83468 = CARTESIAN_POINT ( 'NONE',  ( -21.53943276465977519, -0.05219959533937600094, 18.75109039468568639 ) ) ;
#83469 = CARTESIAN_POINT ( 'NONE',  ( -12.14591786802309592, -12.06949235617757132, 86.87390960531438111 ) ) ;
#83470 = CARTESIAN_POINT ( 'NONE',  ( 17.50000000000001066, -3.237210098469561093, 27.21236987379542782 ) ) ;
#83471 = CARTESIAN_POINT ( 'NONE',  ( -14.34966873604960291, -8.224510206698953496, 66.66557627198102409 ) ) ;
#83472 = CARTESIAN_POINT ( 'NONE',  ( 14.29746914071037800, 8.314922557961029526, 96.66775706135234714 ) ) ;
#83473 = CARTESIAN_POINT ( 'NONE',  ( 16.51473224551069308, 9.474510206698969483, 44.16557627198103120 ) ) ;
#83474 = CARTESIAN_POINT ( 'NONE',  ( 10.72451020669898902, -18.67979575497178502, 47.91557627198102409 ) ) ;
#83475 = CARTESIAN_POINT ( 'NONE',  ( -12.06949235617756955, 12.14591786802309770, 80.62390960531438111 ) ) ;
#83476 = CARTESIAN_POINT ( 'NONE',  ( -15.80617190586745835, -15.72974639402198527, 76.87390960531439532 ) ) ;
#83477 = CARTESIAN_POINT ( 'NONE',  ( 16.46253265017160672, -9.564922557960803928, 83.33224293864768129 ) ) ;
#83479 = CARTESIAN_POINT ( 'NONE',  ( -9.474510206698720793, -16.51473224551083518, 89.58442372801900433 ) ) ;
#83478 = CARTESIAN_POINT ( 'NONE',  ( -0.05219959533909027116, -19.03943276465977164, 37.49890960531436690 ) ) ;
#83480 = CARTESIAN_POINT ( 'NONE',  ( 10.81492255796078972, 18.62759615963270932, 34.58224293864770260 ) ) ;
#83481 = CARTESIAN_POINT ( 'NONE',  ( 10.72451020669871369, 18.67979575497193778, 52.08442372801901854 ) ) ;
#83482 = CARTESIAN_POINT ( 'NONE',  ( 19.02544592524343514, -5.153800228976328945, 58.54057627198102409 ) ) ;
#83483 = CARTESIAN_POINT ( 'NONE',  ( 9.474510206698971260, -16.51473224551069308, 82.91557627198103830 ) ) ;
#83484 = VERTEX_POINT ( 'NONE', #52682 ) ;
#83485 = CARTESIAN_POINT ( 'NONE',  ( -12.06949235617739369, -12.14591786802326823, 44.37609039468567573 ) ) ;
#83486 = CARTESIAN_POINT ( 'NONE',  ( 10.81492255796106328, -18.62759615963255655, 35.41775706135234003 ) ) ;
#83487 = ADVANCED_FACE ( 'NONE', ( #99179 ), #112364, .F. ) ;
#83488 = CARTESIAN_POINT ( 'NONE',  ( -5.823673210054431948, 21.52544592524334988, 77.70942372801900433 ) ) ;
#83489 = CARTESIAN_POINT ( 'NONE',  ( 10.72451020669898902, -18.67979575497178502, 27.91557627198103830 ) ) ;
#83490 = CARTESIAN_POINT ( 'NONE',  ( -21.52544592524343514, 5.823673210054127303, 91.04057627198103830 ) ) ;
#83492 = CARTESIAN_POINT ( 'NONE',  ( 8.314922557961029526, -14.29746914071037800, 70.41775706135236135 ) ) ;
#83491 = CARTESIAN_POINT ( 'NONE',  ( 10.72451020669871369, 18.67979575497193778, 22.08442372801901143 ) ) ;
#83493 = CARTESIAN_POINT ( 'NONE',  ( 21.55341960407610458, 5.719274019375980345, 68.95724293864769550 ) ) ;
#83494 = CARTESIAN_POINT ( 'NONE',  ( 19.02544592524334988, 5.153800228976608722, 21.45942372801899012 ) ) ;
#83495 = CARTESIAN_POINT ( 'NONE',  ( 5.153800228976335163, 19.02544592524342804, 64.79057627198100988 ) ) ;
#83496 = DIRECTION ( 'NONE',  ( 0.000000000000000000, -0.7071067811865485719, 0.7071067811865465735 ) ) ;
#83497 = CARTESIAN_POINT ( 'NONE',  ( 16.46253265017160672, -9.564922557960803928, 83.33224293864768129 ) ) ;
#83498 = CARTESIAN_POINT ( 'NONE',  ( 17.58332526062528345, 7.635886036038587399, 51.57665040441534643 ) ) ;
#83499 = CARTESIAN_POINT ( 'NONE',  ( 9.474510206698729675, 16.51473224551082808, 77.08442372801900433 ) ) ;
#83500 = CARTESIAN_POINT ( 'NONE',  ( 15.72974639402199770, -15.80617190586745480, 48.12390960531436690 ) ) ;
#83501 = CARTESIAN_POINT ( 'NONE',  ( 12.06949235617739724, 12.14591786802326823, 111.8760903946856615 ) ) ;
#83502 = CARTESIAN_POINT ( 'NONE',  ( 5.049401038297881783, 19.05341960407617563, 97.29275706135233293 ) ) ;
#83503 = CARTESIAN_POINT ( 'NONE',  ( 5.153800228976335163, 19.02544592524342804, 39.79057627198102409 ) ) ;
#83504 = CARTESIAN_POINT ( 'NONE',  ( -19.02544592524334988, -5.153800228976617603, 98.95942372801900433 ) ) ;
#83506 = CARTESIAN_POINT ( 'NONE',  ( 9.474510206698729675, 16.51473224551082808, 57.08442372801900433 ) ) ;
#83505 = CARTESIAN_POINT ( 'NONE',  ( 10.81492255796078972, 18.62759615963270932, 84.58224293864769550 ) ) ;
#83507 = PLANE ( 'NONE',  #36888 ) ;
#83508 = CARTESIAN_POINT ( 'NONE',  ( 19.05341960407611168, 5.049401038298154454, 53.95724293864770260 ) ) ;
#83509 = CARTESIAN_POINT ( 'NONE',  ( 4.379528057220339221, -16.55341960407611168, 67.70724293864769550 ) ) ;
#83510 = CARTESIAN_POINT ( 'NONE',  ( 19.05341960407611168, 5.049401038298154454, 43.95724293864769550 ) ) ;
#83511 = CARTESIAN_POINT ( 'NONE',  ( 8.314922557960818139, 14.29746914071049879, 59.58224293864770260 ) ) ;
#83512 = CARTESIAN_POINT ( 'NONE',  ( -22.78725946537530334, -32.81619059092837887, -22.84582334174709928 ) ) ;
#83513 = CARTESIAN_POINT ( 'NONE',  ( 32.36699822888682121, -3.753862658156253751, 88.50241378327223174 ) ) ;
#83514 = CARTESIAN_POINT ( 'NONE',  ( -0.05219959533910754901, -16.53943276465976808, 27.49890960531435269 ) ) ;
#83515 = CARTESIAN_POINT ( 'NONE',  ( 9.474510206698971260, -16.51473224551069308, 62.91557627198102409 ) ) ;
#83516 = DIRECTION ( 'NONE',  ( 0.5000000000000037748, 0.4999999999999950040, 0.7071067811865483499 ) ) ;
#83517 = CARTESIAN_POINT ( 'NONE',  ( -9.564922557961040184, 16.46253265017147172, 37.91775706135233293 ) ) ;
#83518 = CARTESIAN_POINT ( 'NONE',  ( -12.14591786802326823, 12.06949235617739902, 53.12609039468568284 ) ) ;
#83519 = CARTESIAN_POINT ( 'NONE',  ( 0.05219959533907565091, 21.53943276465977519, 54.99890960531435269 ) ) ;
#83520 = CARTESIAN_POINT ( 'NONE',  ( 21.53943276465977519, 0.05219959533937863772, 101.2510903946856757 ) ) ;
#83521 = CARTESIAN_POINT ( 'NONE',  ( 19.05341960407611168, 5.049401038298154454, 63.95724293864769550 ) ) ;
#83522 = DIRECTION ( 'NONE',  ( 0.000000000000000000, 0.000000000000000000, -1.000000000000000000 ) ) ;
#83523 = CARTESIAN_POINT ( 'NONE',  ( -9.474510206698964154, 16.51473224551069663, 100.4155762719810241 ) ) ;
#83524 = CARTESIAN_POINT ( 'NONE',  ( -5.950531402560715689E-15, 38.81732327939063509, -5.124999997268813168 ) ) ;
#83525 = CARTESIAN_POINT ( 'NONE',  ( -21.55341960407619339, 5.719274019375674811, 28.54275706135234358 ) ) ;
#83526 = CARTESIAN_POINT ( 'NONE',  ( 4.483927247898545687, 16.52544592524342804, 94.79057627198105251 ) ) ;
#83528 = CARTESIAN_POINT ( 'NONE',  ( 9.474510206698971260, -16.51473224551069308, 77.91557627198103830 ) ) ;
#83527 = CARTESIAN_POINT ( 'NONE',  ( 15.80617190586746368, 15.72974639402197994, 89.37390960531435269 ) ) ;
#83529 = CARTESIAN_POINT ( 'NONE',  ( 5.153800228976335163, 19.02544592524342804, 84.79057627198099567 ) ) ;
#83530 = CARTESIAN_POINT ( 'NONE',  ( 10.81492255796078972, 18.62759615963270932, 109.5822429386476955 ) ) ;
#83531 = EDGE_LOOP ( 'NONE', ( #31652, #83082, #131510, #66836 ) ) ;
#83532 = CARTESIAN_POINT ( 'NONE',  ( 5.153800228976335163, 19.02544592524342804, 69.79057627198103830 ) ) ;
#83533 = CARTESIAN_POINT ( 'NONE',  ( -28.79475375365606737, 9.355982642738961630, 147.8843446568999980 ) ) ;
#83535 = CARTESIAN_POINT ( 'NONE',  ( 19.05341960407611168, 5.049401038298154454, 28.95724293864769550 ) ) ;
#83534 = CARTESIAN_POINT ( 'NONE',  ( -16.52544592524342804, 4.483927247898546575, 101.0405762719810383 ) ) ;
#83536 = CARTESIAN_POINT ( 'NONE',  ( -13.97604488694547697, 13.89961937509957934, 98.12609039468566152 ) ) ;
#83537 = CARTESIAN_POINT ( 'NONE',  ( 0.05219959533910956823, 16.53943276465976808, 104.9989096053143669 ) ) ;
#83538 = CARTESIAN_POINT ( 'NONE',  ( 15.72974639402176855, 15.80617190586768217, 66.87609039468568994 ) ) ;
#83540 = CARTESIAN_POINT ( 'NONE',  ( -21.55341960407619339, 5.719274019375674811, 38.54275706135234714 ) ) ;
#83539 = CARTESIAN_POINT ( 'NONE',  ( -13.89961937509977652, 13.97604488694528158, 60.62390960531436690 ) ) ;
#83541 = CARTESIAN_POINT ( 'NONE',  ( -15.72974639402197994, 15.80617190586746368, 105.6239096053143669 ) ) ;
#83542 = CARTESIAN_POINT ( 'NONE',  ( -17.81289503416611097, -24.51734667627696496, 140.2999999999999545 ) ) ;
#83543 = CARTESIAN_POINT ( 'NONE',  ( 19.05341960407611168, 5.049401038298154454, 73.95724293864768129 ) ) ;
#83544 = CARTESIAN_POINT ( 'NONE',  ( 25.64061671795035124, 10.58440545630783269, 139.9999999999999716 ) ) ;
#83546 = CARTESIAN_POINT ( 'NONE',  ( 15.72974639402199770, -15.80617190586745480, 28.12390960531435979 ) ) ;
#83545 = CARTESIAN_POINT ( 'NONE',  ( -0.05219959533934338120, 16.53943276465976808, 32.50109039468568284 ) ) ;
#83547 = CARTESIAN_POINT ( 'NONE',  ( -21.55341960407619339, 5.719274019375674811, 63.54275706135234003 ) ) ;
#83548 = CARTESIAN_POINT ( 'NONE',  ( -5.153800228976328057, -19.02544592524343514, 112.2905762719810099 ) ) ;
#83549 = CARTESIAN_POINT ( 'NONE',  ( 19.05341960407617918, -5.049401038297876454, 101.0427570613523045 ) ) ;
#83550 = CARTESIAN_POINT ( 'NONE',  ( 19.02544592524343514, -5.153800228976328945, 43.54057627198103120 ) ) ;
#83551 = CARTESIAN_POINT ( 'NONE',  ( 16.46253265017160672, -9.564922557960803928, 73.33224293864769550 ) ) ;
#83552 = CARTESIAN_POINT ( 'NONE',  ( 16.53943276465976808, -0.05219959533910856209, 98.74890960531438111 ) ) ;
#83553 = CARTESIAN_POINT ( 'NONE',  ( 13.89961937509977652, -13.97604488694527269, 113.1239096053143527 ) ) ;
#83554 = CARTESIAN_POINT ( 'NONE',  ( -12.14591786802309592, -12.06949235617757132, 91.87390960531436690 ) ) ;
#83555 = CARTESIAN_POINT ( 'NONE',  ( -19.03943276465977164, 0.05219959533909376836, 96.24890960531436690 ) ) ;
#83558 = CARTESIAN_POINT ( 'NONE',  ( -0.05219959533909027116, -19.03943276465977164, 47.49890960531435979 ) ) ;
#83557 =( BOUNDED_CURVE ( )  B_SPLINE_CURVE ( 3, ( #99442, #53952, #131792, #69111 ),
 .UNSPECIFIED., .F., .T. ) 
 B_SPLINE_CURVE_WITH_KNOTS ( ( 4, 4 ),
 ( 5.150538010968860547, 5.257537365396776075 ),
 .UNSPECIFIED. ) 
 CURVE ( )  GEOMETRIC_REPRESENTATION_ITEM ( )  RATIONAL_B_SPLINE_CURVE ( ( 1.000000000000000000, 0.9990461557208837329, 0.9990461557208837329, 1.000000000000000000 ) ) 
 REPRESENTATION_ITEM ( '' )  );
#83556 = CARTESIAN_POINT ( 'NONE',  ( 14.34966873604960469, 8.224510206698951720, 59.16557627198103120 ) ) ;
#83559 = CARTESIAN_POINT ( 'NONE',  ( 21.55341960407619695, -5.719274019375665929, 56.04275706135235424 ) ) ;
#83560 = CARTESIAN_POINT ( 'NONE',  ( -9.474510206698720793, -16.51473224551083518, 99.58442372801900433 ) ) ;
#83561 = CARTESIAN_POINT ( 'NONE',  ( 0.05219959533910956823, 16.53943276465976808, 49.99890960531437401 ) ) ;
#83562 = CARTESIAN_POINT ( 'NONE',  ( 21.55341960407610458, 5.719274019375980345, 113.9572429386477239 ) ) ;
#83563 = CARTESIAN_POINT ( 'NONE',  ( 18.62759615963271287, -10.81492255796078972, 43.33224293864769550 ) ) ;
#83565 = CARTESIAN_POINT ( 'NONE',  ( 0.05219959533910956823, 16.53943276465976808, 79.99890960531435269 ) ) ;
#83564 = CARTESIAN_POINT ( 'NONE',  ( -13.97604488694527625, -13.89961937509977652, 111.8739096053143243 ) ) ;
#83566 = CARTESIAN_POINT ( 'NONE',  ( -5.429308488886486681E-15, 30.30510711980690175, 139.7500000054623683 ) ) ;
#83567 = CARTESIAN_POINT ( 'NONE',  ( -5.049401038298153566, 19.05341960407611168, 50.20724293864770260 ) ) ;
#83568 = CARTESIAN_POINT ( 'NONE',  ( 16.53943276465976808, 0.05219959533934440121, 111.2510903946856899 ) ) ;
#83569 = CARTESIAN_POINT ( 'NONE',  ( 12.06949235617739724, 12.14591786802326823, 106.8760903946856899 ) ) ;
#83570 = CARTESIAN_POINT ( 'NONE',  ( -16.52544592524335698, -4.483927247898792601, 83.95942372801900433 ) ) ;
#83571 = CARTESIAN_POINT ( 'NONE',  ( -19.02544592524334988, -5.153800228976617603, 43.95942372801899012 ) ) ;
#83572 = CARTESIAN_POINT ( 'NONE',  ( 0.000000000000000000, -165.0000000000000000, 7.000000000000003553 ) ) ;
#83573 = CARTESIAN_POINT ( 'NONE',  ( 13.89961937509977652, -13.97604488694527269, 93.12390960531436690 ) ) ;
#83574 = CARTESIAN_POINT ( 'NONE',  ( 13.89961937509977652, -13.97604488694527269, 53.12390960531434558 ) ) ;
#83575 = CARTESIAN_POINT ( 'NONE',  ( 14.34966873604960469, 8.224510206698951720, 64.16557627198102409 ) ) ;
#83577 = CARTESIAN_POINT ( 'NONE',  ( 5.049401038298161559, -19.05341960407611168, 107.7072429386476955 ) ) ;
#83576 = CARTESIAN_POINT ( 'NONE',  ( -9.474510206698964154, 16.51473224551069663, 25.41557627198103120 ) ) ;
#83578 = CARTESIAN_POINT ( 'NONE',  ( 21.52544592524344225, -5.823673210054117533, 43.54057627198103830 ) ) ;
#83579 = CARTESIAN_POINT ( 'NONE',  ( 16.53943276465976808, -0.05219959533910856209, 88.74890960531436690 ) ) ;
#83580 = CARTESIAN_POINT ( 'NONE',  ( 4.483927247898790824, -16.52544592524335698, 35.20942372801901854 ) ) ;
#83581 = CARTESIAN_POINT ( 'NONE',  ( -8.224510206698948167, 14.34966873604960824, 80.41557627198103830 ) ) ;
#83582 = CARTESIAN_POINT ( 'NONE',  ( 21.98685479826779243, 13.98560643873834231, 165.5209445330007441 ) ) ;
#83583 = CARTESIAN_POINT ( 'NONE',  ( -9.474510206698720793, -16.51473224551083518, 74.58442372801900433 ) ) ;
#83584 = CARTESIAN_POINT ( 'NONE',  ( 9.564922557960805705, 16.46253265017160317, 104.5822429386476955 ) ) ;
#83585 = CARTESIAN_POINT ( 'NONE',  ( -16.46253265017146816, -9.564922557961047289, 74.16775706135234714 ) ) ;
#83586 = CARTESIAN_POINT ( 'NONE',  ( -5.153800228976328057, -19.02544592524343514, 42.29057627198102409 ) ) ;
#83588 = CARTESIAN_POINT ( 'NONE',  ( 16.53943276465976808, 0.05219959533934440121, 106.2510903946856757 ) ) ;
#83587 = CARTESIAN_POINT ( 'NONE',  ( 4.483927247898790824, -16.52544592524335698, 30.20942372801902565 ) ) ;
#83589 = CARTESIAN_POINT ( 'NONE',  ( 19.03943276465977164, 0.05219959533936151252, 76.25109039468566152 ) ) ;
#83590 = CARTESIAN_POINT ( 'NONE',  ( 0.05219959533907565091, 21.53943276465977519, 39.99890960531436690 ) ) ;
#83591 = CARTESIAN_POINT ( 'NONE',  ( 10.81492255796106328, -18.62759615963255655, 70.41775706135236135 ) ) ;
#83592 = CARTESIAN_POINT ( 'NONE',  ( 18.85284094683695244, 5.500000000000118128, 38.82762727607044440 ) ) ;
#83593 = CARTESIAN_POINT ( 'NONE',  ( 8.314922557961029526, -14.29746914071037800, 40.41775706135234714 ) ) ;
#83595 = CARTESIAN_POINT ( 'NONE',  ( 9.474510206698971260, -16.51473224551069308, 92.91557627198103830 ) ) ;
#83594 = CARTESIAN_POINT ( 'NONE',  ( 9.474510206698971260, -16.51473224551069308, 27.91557627198103120 ) ) ;
#83596 = CARTESIAN_POINT ( 'NONE',  ( -13.89961937509977652, 13.97604488694528158, 25.62390960531434558 ) ) ;
#83597 = CARTESIAN_POINT ( 'NONE',  ( 16.55341960407611168, 4.379528057220329451, 93.95724293864770971 ) ) ;
#83598 = ITEM_DEFINED_TRANSFORMATION ( 'NONE', 'NONE', #40243,  #82054 ) ;
#83599 = CARTESIAN_POINT ( 'NONE',  ( -16.51473224551069308, -9.474510206698971260, 86.66557627198102409 ) ) ;
#83600 = ORIENTED_EDGE ( 'NONE', *, *, #163734, .T. ) ;
#83601 = CARTESIAN_POINT ( 'NONE',  ( 13.97604488694548053, -13.89961937509957401, 105.6260903946856757 ) ) ;
#83602 = CARTESIAN_POINT ( 'NONE',  ( 21.53943276465977519, -0.05219959533907433946, 83.74890960531435269 ) ) ;
#83603 = CARTESIAN_POINT ( 'NONE',  ( -5.049401038298153566, 19.05341960407611168, 45.20724293864769550 ) ) ;
#83605 = CARTESIAN_POINT ( 'NONE',  ( -21.53943276465977519, -0.05219959533937600094, 18.75109039468568639 ) ) ;
#83604 = CARTESIAN_POINT ( 'NONE',  ( -9.474510206698720793, -16.51473224551083518, 69.58442372801901854 ) ) ;
#83606 = CARTESIAN_POINT ( 'NONE',  ( -13.89961937509977652, 13.97604488694528158, 75.62390960531438111 ) ) ;
#83608 = EDGE_CURVE ( 'NONE', #160325, #179909, #66925, .T. ) ;
#83607 = CARTESIAN_POINT ( 'NONE',  ( 19.02544592524343514, -5.153800228976328945, 103.5405762719809957 ) ) ;
#83609 = ORIENTED_EDGE ( 'NONE', *, *, #97135, .T. ) ;
#83610 = CARTESIAN_POINT ( 'NONE',  ( -8.224510206698735004, -14.34966873604973081, 39.58442372801901143 ) ) ;
#83611 = CARTESIAN_POINT ( 'NONE',  ( 21.52544592524344225, -5.823673210054117533, 103.5405762719810383 ) ) ;
#83614 = CARTESIAN_POINT ( 'NONE',  ( -19.05341960407617563, 5.049401038297882671, 63.54275706135234003 ) ) ;
#83613 = CARTESIAN_POINT ( 'NONE',  ( 19.02544592524343514, -5.153800228976328945, 88.54057627198102409 ) ) ;
#83612 = CARTESIAN_POINT ( 'NONE',  ( -8.314922557960811034, -14.29746914071050412, 112.0822429386477097 ) ) ;
#83615 = CARTESIAN_POINT ( 'NONE',  ( -21.52544592524343514, 5.823673210054127303, 91.04057627198103830 ) ) ;
#83616 = CARTESIAN_POINT ( 'NONE',  ( -5.823673210054116645, -21.52544592524344225, 77.29057627198102409 ) ) ;
#83617 = CARTESIAN_POINT ( 'NONE',  ( 16.55341960407611168, 4.379528057220329451, 43.95724293864769550 ) ) ;
#83618 = CARTESIAN_POINT ( 'NONE',  ( -5.049401038297874678, -19.05341960407617918, 24.79275706135233648 ) ) ;
#83619 = CARTESIAN_POINT ( 'NONE',  ( 14.29746914071037800, 8.314922557961029526, 61.66775706135235424 ) ) ;
#83620 = EDGE_CURVE ( 'NONE', #182074, #171133, #75897, .T. ) ;
#83621 = CARTESIAN_POINT ( 'NONE',  ( -19.02544592524342804, 5.153800228976336051, 91.04057627198100988 ) ) ;
#83622 = CARTESIAN_POINT ( 'NONE',  ( -16.51473224551069308, -9.474510206698971260, 41.66557627198103120 ) ) ;
#83623 = CARTESIAN_POINT ( 'NONE',  ( -10.72451020669870658, -18.67979575497194134, 54.58442372801901143 ) ) ;
#83624 = CARTESIAN_POINT ( 'NONE',  ( -21.53943276465977519, -0.05219959533937600094, 68.75109039468568994 ) ) ;
#83625 = CARTESIAN_POINT ( 'NONE',  ( -5.153800228976328057, -19.02544592524343514, 57.29057627198103120 ) ) ;
#83626 = CARTESIAN_POINT ( 'NONE',  ( 10.81492255796106328, -18.62759615963255655, 40.41775706135234714 ) ) ;
#83627 = CARTESIAN_POINT ( 'NONE',  ( -19.05341960407617563, 5.049401038297882671, 78.54275706135233293 ) ) ;
#83628 = CARTESIAN_POINT ( 'NONE',  ( 5.153800228976615827, -19.02544592524334988, 70.20942372801899012 ) ) ;
#83629 = CARTESIAN_POINT ( 'NONE',  ( -13.89961937509977652, 13.97604488694528158, 35.62390960531435269 ) ) ;
#83630 = CARTESIAN_POINT ( 'NONE',  ( 12.06949235617739724, 12.14591786802326823, 81.87609039468568994 ) ) ;
#83631 = CARTESIAN_POINT ( 'NONE',  ( 19.03943276465977164, -0.05219959533909143690, 58.74890960531435979 ) ) ;
#83632 = CARTESIAN_POINT ( 'NONE',  ( 24.79447686064953160, -6.332871904612202840, 168.1804317516249512 ) ) ;
#83633 = CARTESIAN_POINT ( 'NONE',  ( 0.05219959533909260263, 19.03943276465977164, 94.99890960531436690 ) ) ;
#83634 = CARTESIAN_POINT ( 'NONE',  ( 19.02544592524343514, -5.153800228976328945, 43.54057627198103120 ) ) ;
#83635 = CARTESIAN_POINT ( 'NONE',  ( -15.80617190586745835, -15.72974639402198527, 81.87390960531435269 ) ) ;
#83636 = CARTESIAN_POINT ( 'NONE',  ( -14.29746914071037622, -8.314922557961029526, 64.16775706135234714 ) ) ;
#83637 = CARTESIAN_POINT ( 'NONE',  ( 10.72451020669871369, 18.67979575497193778, 112.0844237280190185 ) ) ;
#83638 = CARTESIAN_POINT ( 'NONE',  ( 9.564922557960805705, 16.46253265017160317, 49.58224293864770260 ) ) ;
#83639 = CARTESIAN_POINT ( 'NONE',  ( 16.52544592524342804, -4.483927247898539470, 48.54057627198103120 ) ) ;
#83640 = CARTESIAN_POINT ( 'NONE',  ( -4.379528057220328563, 16.55341960407611168, 80.20724293864769550 ) ) ;
#83641 = AXIS2_PLACEMENT_3D ( 'NONE', #171074, #155897, #17395 ) ;
#83642 = CARTESIAN_POINT ( 'NONE',  ( 9.474510206698971260, -16.51473224551069308, 72.91557627198102409 ) ) ;
#83643 = CARTESIAN_POINT ( 'NONE',  ( -21.55341960407619339, 5.719274019375674811, 43.54275706135235424 ) ) ;
#83644 = CARTESIAN_POINT ( 'NONE',  ( -19.03943276465977164, 0.05219959533909376836, 91.24890960531436690 ) ) ;
#83645 = CARTESIAN_POINT ( 'NONE',  ( 10.81492255796106328, -18.62759615963255655, 95.41775706135234714 ) ) ;
#83646 = CARTESIAN_POINT ( 'NONE',  ( -12.14591786802326823, 12.06949235617739902, 73.12609039468567573 ) ) ;
#83647 = CARTESIAN_POINT ( 'NONE',  ( -10.72451020669870658, -18.67979575497194134, 29.58442372801901854 ) ) ;
#83648 = CARTESIAN_POINT ( 'NONE',  ( 9.474510206698971260, -16.51473224551069308, 112.9155762719810383 ) ) ;
#83649 = CARTESIAN_POINT ( 'NONE',  ( 18.67979575497178502, 10.72451020669898547, 94.16557627198103830 ) ) ;
#83650 = CARTESIAN_POINT ( 'NONE',  ( -16.55341960407611168, -4.379528057220339221, 41.45724293864769550 ) ) ;
#83651 = CARTESIAN_POINT ( 'NONE',  ( 19.05341960407611168, 5.049401038298154454, 43.95724293864769550 ) ) ;
#83652 = CARTESIAN_POINT ( 'NONE',  ( 0.05219959533910956823, 16.53943276465976808, 69.99890960531435269 ) ) ;
#83653 = CARTESIAN_POINT ( 'NONE',  ( 5.823673210054125526, 21.52544592524343514, 34.79057627198103120 ) ) ;
#83654 = CARTESIAN_POINT ( 'NONE',  ( 19.02544592524334988, 5.153800228976608722, 36.45942372801900433 ) ) ;
#83655 = CARTESIAN_POINT ( 'NONE',  ( 12.14591786802309770, 12.06949235617756955, 99.37390960531436690 ) ) ;
#83656 = CARTESIAN_POINT ( 'NONE',  ( -19.02544592524342804, 5.153800228976336051, 106.0405762719810241 ) ) ;
#83657 = ORIENTED_EDGE ( 'NONE', *, *, #179822, .T. ) ;
#83658 = CARTESIAN_POINT ( 'NONE',  ( -4.483927247898782831, 16.52544592524335698, 52.70942372801902565 ) ) ;
#83659 = CARTESIAN_POINT ( 'NONE',  ( 5.153800228976335163, 19.02544592524342804, 59.79057627198100988 ) ) ;
#83660 = CARTESIAN_POINT ( 'NONE',  ( 0.2500000000000002220, 0.000000000000000000, 4.000000000000000000 ) ) ;
#83661 = CARTESIAN_POINT ( 'NONE',  ( -16.53943276465976808, -0.05219959533934237506, 98.75109039468568994 ) ) ;
#83662 = CARTESIAN_POINT ( 'NONE',  ( 19.03943276465977164, 0.05219959533936151252, 106.2510903946856615 ) ) ;
#83663 = CARTESIAN_POINT ( 'NONE',  ( -0.05219959533937732626, 21.53943276465977519, 77.50109039468567573 ) ) ;
#83664 = CARTESIAN_POINT ( 'NONE',  ( -19.03943276465977164, 0.05219959533909376836, 71.24890960531435269 ) ) ;
#83665 = CARTESIAN_POINT ( 'NONE',  ( 21.52544592524344225, -5.823673210054117533, 103.5405762719810383 ) ) ;
#83666 = CARTESIAN_POINT ( 'NONE',  ( 16.55341960407618274, -4.379528057220086978, 61.04275706135234714 ) ) ;
#83667 = CARTESIAN_POINT ( 'NONE',  ( 8.224510206698953496, -14.34966873604960469, 112.9155762719810383 ) ) ;
#83668 = CARTESIAN_POINT ( 'NONE',  ( -19.03943276465977164, -0.05219959533935918106, 113.7510903946856757 ) ) ;
#83669 = CARTESIAN_POINT ( 'NONE',  ( -9.564922557961040184, 16.46253265017147172, 87.91775706135233293 ) ) ;
#83670 = CARTESIAN_POINT ( 'NONE',  ( -0.05219959533907301413, -21.53943276465977519, 77.49890960531433848 ) ) ;
#83671 = CARTESIAN_POINT ( 'NONE',  ( 13.97604488694548053, -13.89961937509957401, 60.62609039468564731 ) ) ;
#83672 = LINE ( 'NONE', #22020, #99579 ) ;
#83673 = CARTESIAN_POINT ( 'NONE',  ( 10.72451020669898902, -18.67979575497178502, 107.9155762719810241 ) ) ;
#83674 = CARTESIAN_POINT ( 'NONE',  ( 17.50000000000002842, 3.805241302050184515, 27.12647527217411536 ) ) ;
#83675 = CARTESIAN_POINT ( 'NONE',  ( 9.564922557960805705, 16.46253265017160317, 64.58224293864769550 ) ) ;
#83676 = FACE_BOUND ( 'NONE', #142403, .T. ) ;
#83677 = CARTESIAN_POINT ( 'NONE',  ( -12.06949235617739369, -12.14591786802326823, 19.37609039468568639 ) ) ;
#83678 = CARTESIAN_POINT ( 'NONE',  ( 22.40074995931641766, 13.33491940220945793, 165.5209445330007441 ) ) ;
#83679 = CARTESIAN_POINT ( 'NONE',  ( -21.55341960407619339, 5.719274019375674811, 48.54275706135234714 ) ) ;
#83681 = CARTESIAN_POINT ( 'NONE',  ( 4.483927247898545687, 16.52544592524342804, 69.79057627198102409 ) ) ;
#83680 = CARTESIAN_POINT ( 'NONE',  ( -10.72451020669898014, 18.67979575497178502, 100.4155762719810241 ) ) ;
#83682 = CARTESIAN_POINT ( 'NONE',  ( 9.474510206698971260, -16.51473224551069308, 67.91557627198102409 ) ) ;
#83683 = CARTESIAN_POINT ( 'NONE',  ( -18.67979575497193778, 10.72451020669871902, 68.33442372801900433 ) ) ;
#83685 = CARTESIAN_POINT ( 'NONE',  ( 0.05219959533936267826, -19.03943276465977164, 30.00109039468566863 ) ) ;
#83684 = CARTESIAN_POINT ( 'NONE',  ( 14.34966873604972726, -8.224510206698740333, 25.83442372801901499 ) ) ;
#83686 = CARTESIAN_POINT ( 'NONE',  ( -5.823673210054431948, 21.52544592524334988, 47.70942372801902565 ) ) ;
#83687 = CARTESIAN_POINT ( 'NONE',  ( 15.72974639402199770, -15.80617190586745480, 113.1239096053143953 ) ) ;
#83688 = CARTESIAN_POINT ( 'NONE',  ( 18.67979575497178502, 10.72451020669898547, 59.16557627198103120 ) ) ;
#83689 = CARTESIAN_POINT ( 'NONE',  ( -9.474510206698720793, -16.51473224551083518, 99.58442372801900433 ) ) ;
#83690 = CARTESIAN_POINT ( 'NONE',  ( -5.049401038297874678, -19.05341960407617918, 74.79275706135231871 ) ) ;
#83691 = CARTESIAN_POINT ( 'NONE',  ( 21.53943276465977519, 0.05219959533937863772, 81.25109039468568994 ) ) ;
#83692 = CARTESIAN_POINT ( 'NONE',  ( 5.049401038297881783, 19.05341960407617563, 47.29275706135231161 ) ) ;
#83693 = CARTESIAN_POINT ( 'NONE',  ( 19.02544592524343514, -5.153800228976328945, 33.54057627198102409 ) ) ;
#83694 = CARTESIAN_POINT ( 'NONE',  ( 15.80617190586746368, 15.72974639402197994, 54.37390960531435979 ) ) ;
#83695 = CARTESIAN_POINT ( 'NONE',  ( 0.05219959533910956823, 16.53943276465976808, 49.99890960531437401 ) ) ;
#83696 = CARTESIAN_POINT ( 'NONE',  ( -19.36337904590692105, 5.499999999999949374, 95.41494137495622851 ) ) ;
#83697 = CARTESIAN_POINT ( 'NONE',  ( -13.89961937509957401, -13.97604488694547875, 29.37609039468565797 ) ) ;
#83698 = CARTESIAN_POINT ( 'NONE',  ( -16.55341960407617563, 4.379528057220093196, 83.54275706135234714 ) ) ;
#83699 = CARTESIAN_POINT ( 'NONE',  ( 16.55341960407611168, 4.379528057220329451, 58.95724293864770971 ) ) ;
#83700 = CARTESIAN_POINT ( 'NONE',  ( -15.80617190586768217, 15.72974639402176855, 83.12609039468568994 ) ) ;
#83701 = CARTESIAN_POINT ( 'NONE',  ( 21.55341960407619695, -5.719274019375665929, 86.04275706135236135 ) ) ;
#83702 = CARTESIAN_POINT ( 'NONE',  ( -18.62759615963270932, 10.81492255796079327, 75.83224293864769550 ) ) ;
#83703 = CARTESIAN_POINT ( 'NONE',  ( 9.564922557960805705, 16.46253265017160317, 39.58224293864768839 ) ) ;
#83704 = CARTESIAN_POINT ( 'NONE',  ( 18.62759615963255655, 10.81492255796105972, 51.66775706135234714 ) ) ;
#83705 = CARTESIAN_POINT ( 'NONE',  ( -13.97604488694527625, -13.89961937509977652, 41.87390960531435979 ) ) ;
#83706 = CARTESIAN_POINT ( 'NONE',  ( 16.46253265017160672, -9.564922557960803928, 48.33224293864769550 ) ) ;
#83707 = CARTESIAN_POINT ( 'NONE',  ( -0.05219959533910754901, -16.53943276465976808, 102.4989096053143811 ) ) ;
#83708 = CARTESIAN_POINT ( 'NONE',  ( 19.02544592524343514, -5.153800228976328945, 103.5405762719809957 ) ) ;
#83709 = CARTESIAN_POINT ( 'NONE',  ( 8.314922557960818139, 14.29746914071049879, 39.58224293864769550 ) ) ;
#83710 = CARTESIAN_POINT ( 'NONE',  ( -14.29746914071049879, 8.314922557960819915, 105.8322429386476955 ) ) ;
#83711 = CARTESIAN_POINT ( 'NONE',  ( -5.719274019375978568, 21.55341960407610458, 80.20724293864769550 ) ) ;
#83712 = CARTESIAN_POINT ( 'NONE',  ( -10.72451020669870658, -18.67979575497194134, 24.58442372801901499 ) ) ;
#83713 = CARTESIAN_POINT ( 'NONE',  ( -7.500000000000000000, 0.000000000000000000, 10.00000000000000000 ) ) ;
#83714 = CARTESIAN_POINT ( 'NONE',  ( -16.52544592524335698, -4.483927247898792601, 33.95942372801901143 ) ) ;
#83715 = ORIENTED_EDGE ( 'NONE', *, *, #28639, .F. ) ;
#83716 = CARTESIAN_POINT ( 'NONE',  ( -21.55341960407610458, -5.719274019375992779, 66.45724293864768129 ) ) ;
#83717 = CARTESIAN_POINT ( 'NONE',  ( -21.53943276465977519, -0.05219959533937600094, 88.75109039468567573 ) ) ;
#83718 = CARTESIAN_POINT ( 'NONE',  ( -9.474510206698964154, 16.51473224551069663, 90.41557627198103830 ) ) ;
#83719 = CARTESIAN_POINT ( 'NONE',  ( 18.67979575497194134, -10.72451020669871369, 25.83442372801901499 ) ) ;
#83720 = CARTESIAN_POINT ( 'NONE',  ( 18.62759615963271287, -10.81492255796078972, 33.33224293864769550 ) ) ;
#83721 = CARTESIAN_POINT ( 'NONE',  ( 16.55341960407618274, -4.379528057220086978, 96.04275706135236135 ) ) ;
#83722 = CARTESIAN_POINT ( 'NONE',  ( 0.05219959533937995610, -21.53943276465977519, 80.00109039468568994 ) ) ;
#83723 = CARTESIAN_POINT ( 'NONE',  ( -9.474510206698720793, -16.51473224551083518, 24.58442372801900078 ) ) ;
#83724 = CARTESIAN_POINT ( 'NONE',  ( -14.34966873604972548, 8.224510206698743886, 68.33442372801900433 ) ) ;
#83725 = CARTESIAN_POINT ( 'NONE',  ( 5.823673210054444382, -21.52544592524334988, 25.20942372801901854 ) ) ;
#83726 = CARTESIAN_POINT ( 'NONE',  ( -19.02544592524342804, 5.153800228976336051, 31.04057627198102409 ) ) ;
#83727 = CARTESIAN_POINT ( 'NONE',  ( -0.05219959533937732626, 21.53943276465977519, 107.5010903946856899 ) ) ;
#83728 = CARTESIAN_POINT ( 'NONE',  ( -5.049401038298153566, 19.05341960407611168, 105.2072429386476671 ) ) ;
#83729 = CARTESIAN_POINT ( 'NONE',  ( 5.823673210054125526, 21.52544592524343514, 99.79057627198103830 ) ) ;
#83731 = CARTESIAN_POINT ( 'NONE',  ( -5.719274019375978568, 21.55341960407610458, 70.20724293864769550 ) ) ;
#83730 = CARTESIAN_POINT ( 'NONE',  ( -6.020883695541781933, -38.43099163646787986, -23.90977630326744929 ) ) ;
#83733 = CARTESIAN_POINT ( 'NONE',  ( 0.05219959533910956823, 16.53943276465976808, 54.99890960531435269 ) ) ;
#83732 = CARTESIAN_POINT ( 'NONE',  ( 4.483927247898790824, -16.52544592524335698, 50.20942372801901854 ) ) ;
#83734 = CARTESIAN_POINT ( 'NONE',  ( -7.500000000000000000, 0.000000000000000000, 5.707106781186540800 ) ) ;
#83735 = CARTESIAN_POINT ( 'NONE',  ( 13.89961937509957401, 13.97604488694547697, 76.87609039468566152 ) ) ;
#83736 = CARTESIAN_POINT ( 'NONE',  ( -0.7813480796679098672, -13.90353822939981754, -62.49831333862088911 ) ) ;
#83737 = CARTESIAN_POINT ( 'NONE',  ( 4.379528057220092307, 16.55341960407617563, 32.29275706135235424 ) ) ;
#83738 = CARTESIAN_POINT ( 'NONE',  ( -10.72451020669898014, 18.67979575497178502, 100.4155762719810241 ) ) ;
#83739 = CARTESIAN_POINT ( 'NONE',  ( -4.379528057220328563, 16.55341960407611168, 60.20724293864768839 ) ) ;
#83740 = CARTESIAN_POINT ( 'NONE',  ( -16.46253265017160317, 9.564922557960807481, 100.8322429386477097 ) ) ;
#83741 = CARTESIAN_POINT ( 'NONE',  ( -4.483927247898782831, 16.52544592524335698, 37.70942372801900433 ) ) ;
#83742 = CARTESIAN_POINT ( 'NONE',  ( 9.474510206698971260, -16.51473224551069308, 62.91557627198102409 ) ) ;
#83744 = CARTESIAN_POINT ( 'NONE',  ( -0.05219959533936034679, 19.03943276465977164, 102.5010903946856757 ) ) ;
#83743 = CARTESIAN_POINT ( 'NONE',  ( -15.80617190586768217, 15.72974639402176855, 28.12609039468568284 ) ) ;
#83745 = CARTESIAN_POINT ( 'NONE',  ( 16.46253265017160672, -9.564922557960803928, 98.33224293864769550 ) ) ;
#83746 = CARTESIAN_POINT ( 'NONE',  ( -0.05219959533909027116, -19.03943276465977164, 87.49890960531436690 ) ) ;
#83747 = CARTESIAN_POINT ( 'NONE',  ( 5.719274019375991003, -21.55341960407610458, 87.70724293864769550 ) ) ;
#83748 = CARTESIAN_POINT ( 'NONE',  ( -0.05219959533909027116, -19.03943276465977164, 42.49890960531435269 ) ) ;
#83749 = CARTESIAN_POINT ( 'NONE',  ( -38.00000000000000711, 2.428612866367529932E-14, 0.000000000000000000 ) ) ;
#83750 = CARTESIAN_POINT ( 'NONE',  ( 4.379528057220339221, -16.55341960407611168, 67.70724293864769550 ) ) ;
#83751 = CARTESIAN_POINT ( 'NONE',  ( 9.474510206698971260, -16.51473224551069308, 97.91557627198102409 ) ) ;
#83752 = CARTESIAN_POINT ( 'NONE',  ( -31.49504140153648635, 1.029908246020472040, -49.63772645510943704 ) ) ;
#83753 = CARTESIAN_POINT ( 'NONE',  ( -19.03943276465977164, -0.05219959533935918106, 78.75109039468567573 ) ) ;
#83754 = CARTESIAN_POINT ( 'NONE',  ( -15.72974639402197994, 15.80617190586746368, 90.62390960531436690 ) ) ;
#83755 = CARTESIAN_POINT ( 'NONE',  ( -13.89961937509957401, -13.97604488694547875, 44.37609039468566863 ) ) ;
#83756 = CARTESIAN_POINT ( 'NONE',  ( -5.823673210054116645, -21.52544592524344225, 22.29057627198102765 ) ) ;
#83757 = CARTESIAN_POINT ( 'NONE',  ( -2.973862142520662832, -93.04182470242767522, -15.00000000000000000 ) ) ;
#83758 = CARTESIAN_POINT ( 'NONE',  ( -10.72451020669898014, 18.67979575497178502, 35.41557627198102409 ) ) ;
#83759 = CARTESIAN_POINT ( 'NONE',  ( -0.05219959533909027116, -19.03943276465977164, 87.49890960531436690 ) ) ;
#83760 = CARTESIAN_POINT ( 'NONE',  ( 18.62759615963255655, 10.81492255796105972, 66.66775706135234714 ) ) ;
#83761 = CARTESIAN_POINT ( 'NONE',  ( -19.02544592524342804, 5.153800228976336051, 36.04057627198100988 ) ) ;
#83762 = CARTESIAN_POINT ( 'NONE',  ( -12.06949235617756955, 12.14591786802309770, 70.62390960531436690 ) ) ;
#83763 = CARTESIAN_POINT ( 'NONE',  ( 12.14591786802327356, -12.06949235617739191, 25.62609039468567929 ) ) ;
#83764 = CARTESIAN_POINT ( 'NONE',  ( 10.72451020669871369, 18.67979575497193778, 47.08442372801901854 ) ) ;
#83765 = ORIENTED_EDGE ( 'NONE', *, *, #145712, .T. ) ;
#83766 = CARTESIAN_POINT ( 'NONE',  ( -28.53458682541353042, -3.706052286928735562, 140.0000000000000568 ) ) ;
#83767 = CARTESIAN_POINT ( 'NONE',  ( 19.02544592524334988, 5.153800228976608722, 86.45942372801900433 ) ) ;
#83768 = CARTESIAN_POINT ( 'NONE',  ( 17.50000000000000000, 5.499999999999992895, 46.70309617465829888 ) ) ;
#83769 = CARTESIAN_POINT ( 'NONE',  ( -18.62759615963255300, -10.81492255796106328, 19.16775706135234714 ) ) ;
#83770 = CARTESIAN_POINT ( 'NONE',  ( -19.20446147854529784, -5.499999999999912070, 44.38999695167677118 ) ) ;
#83771 = CARTESIAN_POINT ( 'NONE',  ( 16.51473224551083163, -9.474510206698727899, 20.83442372801899722 ) ) ;
#83772 = CARTESIAN_POINT ( 'NONE',  ( 9.474510206698971260, -16.51473224551069308, 57.91557627198103120 ) ) ;
#83773 = CARTESIAN_POINT ( 'NONE',  ( 16.46253265017146816, 9.564922557961045513, 21.66775706135233648 ) ) ;
#83774 = CARTESIAN_POINT ( 'NONE',  ( -4.483927247898782831, 16.52544592524335698, 102.7094237280190185 ) ) ;
#83776 = CARTESIAN_POINT ( 'NONE',  ( -5.719274019375665041, -21.55341960407619695, 69.79275706135234714 ) ) ;
#83775 = CARTESIAN_POINT ( 'NONE',  ( 5.049401038298161559, -19.05341960407611168, 107.7072429386476955 ) ) ;
#83777 = AXIS2_PLACEMENT_3D ( 'NONE', #197342, #11338, #137633 ) ;
#83778 = CARTESIAN_POINT ( 'NONE',  ( -29.86685920354755197, -21.69954338932560134, -8.424999997268812990 ) ) ;
#83779 = CARTESIAN_POINT ( 'NONE',  ( -33.72265478998904342, 5.501106843017430137, 95.34580731367213957 ) ) ;
#83780 = CARTESIAN_POINT ( 'NONE',  ( -40.00000000000002842, 1.938754146708588393E-14, 0.000000000000000000 ) ) ;
#83781 = CARTESIAN_POINT ( 'NONE',  ( -15.72974639402176322, -15.80617190586768395, 74.37609039468568994 ) ) ;
#83782 = CARTESIAN_POINT ( 'NONE',  ( -18.67979575497193778, 10.72451020669871902, 98.33442372801901854 ) ) ;
#83783 = FACE_OUTER_BOUND ( 'NONE', #130737, .T. ) ;
#83784 = CARTESIAN_POINT ( 'NONE',  ( -13.89961937509977652, 13.97604488694528158, 85.62390960531433848 ) ) ;
#83785 = CARTESIAN_POINT ( 'NONE',  ( -19.03943276465977164, -0.05219959533935918106, 28.75109039468566507 ) ) ;
#83786 = CARTESIAN_POINT ( 'NONE',  ( -0.5954834035867282438, -31.78116016545939360, -49.28208245900471240 ) ) ;
#83787 = CARTESIAN_POINT ( 'NONE',  ( -0.05219959533909027116, -19.03943276465977164, 37.49890960531436690 ) ) ;
#83788 = CARTESIAN_POINT ( 'NONE',  ( 15.72974639402199770, -15.80617190586745480, 58.12390960531435979 ) ) ;
#83789 = CARTESIAN_POINT ( 'NONE',  ( 16.55341960407618274, -4.379528057220086978, 101.0427570613523756 ) ) ;
#83791 = CARTESIAN_POINT ( 'NONE',  ( 19.05341960407611168, 5.049401038298154454, 83.95724293864766707 ) ) ;
#83790 = CARTESIAN_POINT ( 'NONE',  ( 12.06949235617757843, -12.14591786802309237, 93.12390960531436690 ) ) ;
#83792 = CARTESIAN_POINT ( 'NONE',  ( -5.823673210054431948, 21.52544592524334988, 102.7094237280190185 ) ) ;
#83793 = CARTESIAN_POINT ( 'NONE',  ( -19.03943276465977164, 0.05219959533909376836, 41.24890960531435269 ) ) ;
#83794 = CARTESIAN_POINT ( 'NONE',  ( -16.55341960407611168, -4.379528057220339221, 91.45724293864769550 ) ) ;
#83795 = CARTESIAN_POINT ( 'NONE',  ( -15.80617190586768217, 15.72974639402176855, 58.12609039468568994 ) ) ;
#83796 = CARTESIAN_POINT ( 'NONE',  ( 10.72451020669898902, -18.67979575497178502, 92.91557627198103830 ) ) ;
#83797 = CARTESIAN_POINT ( 'NONE',  ( 19.02544592524334988, 5.153800228976608722, 46.45942372801899012 ) ) ;
#83798 = CARTESIAN_POINT ( 'NONE',  ( -15.49999999999999822, 5.499999999999997335, 120.0000000000000142 ) ) ;
#83799 = CARTESIAN_POINT ( 'NONE',  ( 5.049401038298161559, -19.05341960407611168, 92.70724293864769550 ) ) ;
#83800 = CARTESIAN_POINT ( 'NONE',  ( 14.29746914071049879, -8.314922557960816363, 58.33224293864768839 ) ) ;
#83801 = CARTESIAN_POINT ( 'NONE',  ( 19.05341960407617918, -5.049401038297876454, 41.04275706135233293 ) ) ;
#83803 = VECTOR ( 'NONE', #106833, 1000.000000000000114 ) ;
#83802 = CARTESIAN_POINT ( 'NONE',  ( -0.05219959533909027116, -19.03943276465977164, 67.49890960531436690 ) ) ;
#83804 = CARTESIAN_POINT ( 'NONE',  ( 14.29746914071049879, -8.314922557960816363, 43.33224293864769550 ) ) ;
#83805 = CARTESIAN_POINT ( 'NONE',  ( 0.05219959533936267826, -19.03943276465977164, 85.00109039468567573 ) ) ;
#83806 = DIRECTION ( 'NONE',  ( 0.000000000000000000, 0.000000000000000000, 1.000000000000000000 ) ) ;
#83807 = CARTESIAN_POINT ( 'NONE',  ( 18.67979575497178502, 10.72451020669898547, 39.16557627198102409 ) ) ;
#83808 = CARTESIAN_POINT ( 'NONE',  ( -14.34966873604960291, -8.224510206698953496, 96.66557627198102409 ) ) ;
#83809 = DIRECTION ( 'NONE',  ( -0.000000000000000000, 1.000000000000000000, -0.000000000000000000 ) ) ;
#83811 = CARTESIAN_POINT ( 'NONE',  ( 10.72451020669898902, -18.67979575497178502, 57.91557627198103120 ) ) ;
#83810 = CARTESIAN_POINT ( 'NONE',  ( 9.474510206698971260, -16.51473224551069308, 57.91557627198103120 ) ) ;
#83812 = CARTESIAN_POINT ( 'NONE',  ( -13.89961937509977652, 13.97604488694528158, 25.62390960531434558 ) ) ;
#83814 = CARTESIAN_POINT ( 'NONE',  ( 19.02544592524343514, -5.153800228976328945, 63.54057627198103830 ) ) ;
#83813 = CARTESIAN_POINT ( 'NONE',  ( 12.14591786802327356, -12.06949235617739191, 80.62609039468567573 ) ) ;
#83815 = CARTESIAN_POINT ( 'NONE',  ( 5.049401038297881783, 19.05341960407617563, 37.29275706135232582 ) ) ;
#83816 = CARTESIAN_POINT ( 'NONE',  ( 5.719274019375673035, 21.55341960407619339, 72.29275706135236135 ) ) ;
#83817 = CARTESIAN_POINT ( 'NONE',  ( 21.55341960407610458, 5.719274019375980345, 53.95724293864770260 ) ) ;
#83818 = CARTESIAN_POINT ( 'NONE',  ( -5.049401038298153566, 19.05341960407611168, 30.20724293864768839 ) ) ;
#83819 = CARTESIAN_POINT ( 'NONE',  ( 13.97604488694548053, -13.89961937509957401, 110.6260903946856615 ) ) ;
#83820 = CARTESIAN_POINT ( 'NONE',  ( -5.049401038298153566, 19.05341960407611168, 25.20724293864768484 ) ) ;
#83822 = CARTESIAN_POINT ( 'NONE',  ( 10.81492255796078972, 18.62759615963270932, 44.58224293864769550 ) ) ;
#83821 = CARTESIAN_POINT ( 'NONE',  ( -1.044764468832696025, -23.88070017481513929, -57.07230391339724918 ) ) ;
#83823 = CARTESIAN_POINT ( 'NONE',  ( 5.823673210054444382, -21.52544592524334988, 85.20942372801901854 ) ) ;
#83824 = CARTESIAN_POINT ( 'NONE',  ( 8.224510206698953496, -14.34966873604960469, 42.91557627198103120 ) ) ;
#83825 = CARTESIAN_POINT ( 'NONE',  ( 8.224510206698953496, -14.34966873604960469, 62.91557627198102409 ) ) ;
#83826 = CARTESIAN_POINT ( 'NONE',  ( -18.62759615963270932, 10.81492255796079327, 80.83224293864769550 ) ) ;
#83827 = CARTESIAN_POINT ( 'NONE',  ( 10.72451020669898902, -18.67979575497178502, 72.91557627198103830 ) ) ;
#83828 = DIRECTION ( 'NONE',  ( 0.000000000000000000, 0.000000000000000000, 1.000000000000000000 ) ) ;
#83829 = CARTESIAN_POINT ( 'NONE',  ( 21.52544592524344225, -5.823673210054117533, 38.54057627198103120 ) ) ;
#83830 = CARTESIAN_POINT ( 'NONE',  ( -16.53943276465976808, -0.05219959533934237506, 48.75109039468568284 ) ) ;
#83831 = CARTESIAN_POINT ( 'NONE',  ( -14.34966873604960291, -8.224510206698953496, 81.66557627198103830 ) ) ;
#83832 = CARTESIAN_POINT ( 'NONE',  ( 5.049401038298161559, -19.05341960407611168, 27.70724293864769550 ) ) ;
#83833 = CARTESIAN_POINT ( 'NONE',  ( 0.000000000000000000, 0.000000000000000000, -58.85720012050612837 ) ) ;
#83834 = CARTESIAN_POINT ( 'NONE',  ( -16.52544592524335698, -4.483927247898792601, 83.95942372801900433 ) ) ;
#83835 = CARTESIAN_POINT ( 'NONE',  ( -10.72451020669870658, -18.67979575497194134, 24.58442372801901499 ) ) ;
#83836 = CARTESIAN_POINT ( 'NONE',  ( 13.97604488694527802, 13.89961937509977652, 89.37390960531436690 ) ) ;
#83837 = CARTESIAN_POINT ( 'NONE',  ( 21.53943276465977519, 0.05219959533937863772, 51.25109039468568994 ) ) ;
#83838 = CARTESIAN_POINT ( 'NONE',  ( 16.51473224551069308, 9.474510206698969483, 104.1655762719810241 ) ) ;
#83840 = EDGE_CURVE ( 'NONE', #98984, #132746, #118962, .T. ) ;
#83839 = CARTESIAN_POINT ( 'NONE',  ( -4.576660509524040243, -38.96431129323312348, -32.99999999890196989 ) ) ;
#83841 = VERTEX_POINT ( 'NONE', #29166 ) ;
#83842 = CARTESIAN_POINT ( 'NONE',  ( -21.53943276465977519, -0.05219959533937600094, 43.75109039468568284 ) ) ;
#83844 = CARTESIAN_POINT ( 'NONE',  ( 13.89961937509977652, -13.97604488694527269, 108.1239096053143669 ) ) ;
#83843 = CARTESIAN_POINT ( 'NONE',  ( 19.02544592524343514, -5.153800228976328945, 38.54057627198103120 ) ) ;
#83845 = CARTESIAN_POINT ( 'NONE',  ( 5.153800228976615827, -19.02544592524334988, 60.20942372801899012 ) ) ;
#83846 = CARTESIAN_POINT ( 'NONE',  ( 15.72974639402176855, 15.80617190586768217, 26.87609039468567218 ) ) ;
#83847 = CARTESIAN_POINT ( 'NONE',  ( -5.049401038297874678, -19.05341960407617918, 49.79275706135231871 ) ) ;
#83848 = CARTESIAN_POINT ( 'NONE',  ( -19.02544592524342804, 5.153800228976336051, 31.04057627198102409 ) ) ;
#83849 = CARTESIAN_POINT ( 'NONE',  ( -16.55341960407617563, 4.379528057220093196, 88.54275706135236135 ) ) ;
#83850 = CARTESIAN_POINT ( 'NONE',  ( 13.97604488694548053, -13.89961937509957401, 65.62609039468567573 ) ) ;
#83851 = CARTESIAN_POINT ( 'NONE',  ( -12.06949235617739369, -12.14591786802326823, 109.3760903946857042 ) ) ;
#83853 = VERTEX_POINT ( 'NONE', #136331 ) ;
#83852 = DIRECTION ( 'NONE',  ( -0.000000000000000000, -0.000000000000000000, -1.000000000000000000 ) ) ;
#83854 = CARTESIAN_POINT ( 'NONE',  ( -19.02544592524342804, 5.153800228976336051, 86.04057627198103830 ) ) ;
#83855 = CARTESIAN_POINT ( 'NONE',  ( 21.52544592524334988, 5.823673210054432836, 91.45942372801901854 ) ) ;
#83856 = CARTESIAN_POINT ( 'NONE',  ( 21.55341960407619695, -5.719274019375665929, 101.0427570613523756 ) ) ;
#83857 = CARTESIAN_POINT ( 'NONE',  ( 25.04568634023502582, -21.46320343559646560, 8.240304736541396835 ) ) ;
#83858 = CARTESIAN_POINT ( 'NONE',  ( -9.474510206698964154, 16.51473224551069663, 105.4155762719810383 ) ) ;
#83859 = CARTESIAN_POINT ( 'NONE',  ( 10.81492255796106328, -18.62759615963255655, 75.41775706135233293 ) ) ;
#83860 = CARTESIAN_POINT ( 'NONE',  ( 16.51473224551083163, -9.474510206698727899, 110.8344237280190043 ) ) ;
#83861 = CARTESIAN_POINT ( 'NONE',  ( -0.05219959533909027116, -19.03943276465977164, 82.49890960531436690 ) ) ;
#83862 = CARTESIAN_POINT ( 'NONE',  ( -15.80617190586745835, -15.72974639402198527, 36.87390960531435979 ) ) ;
#83863 = CARTESIAN_POINT ( 'NONE',  ( 13.97604488694527802, 13.89961937509977652, 89.37390960531436690 ) ) ;
#83864 = DIRECTION ( 'NONE',  ( 1.000000000000000000, 0.000000000000000000, 0.000000000000000000 ) ) ;
#83865 = CARTESIAN_POINT ( 'NONE',  ( 19.05341960407611168, 5.049401038298154454, 73.95724293864768129 ) ) ;
#83866 = CARTESIAN_POINT ( 'NONE',  ( -13.89961937509977652, 13.97604488694528158, 60.62390960531436690 ) ) ;
#83867 = CARTESIAN_POINT ( 'NONE',  ( 8.224510206698742110, 14.34966873604972548, 102.0844237280190185 ) ) ;
#83868 = CARTESIAN_POINT ( 'NONE',  ( -16.21995358207276539, 7.366697692864274671, 99.93551001512065568 ) ) ;
#83869 = CARTESIAN_POINT ( 'NONE',  ( -5.153800228976607833, 19.02544592524334988, 77.70942372801900433 ) ) ;
#83870 = CARTESIAN_POINT ( 'NONE',  ( 19.02544592524343514, -5.153800228976328945, 88.54057627198102409 ) ) ;
#83871 = CARTESIAN_POINT ( 'NONE',  ( 0.05219959533910956823, 16.53943276465976808, 84.99890960531436690 ) ) ;
#83872 = CARTESIAN_POINT ( 'NONE',  ( 15.80617190586746368, 15.72974639402197994, 29.37390960531435269 ) ) ;
#83873 = CARTESIAN_POINT ( 'NONE',  ( 21.55341960407610458, 5.719274019375980345, 23.95724293864769550 ) ) ;
#83874 = CARTESIAN_POINT ( 'NONE',  ( -8.314922557960811034, -14.29746914071050412, 97.08224293864770971 ) ) ;
#83875 = DIRECTION ( 'NONE',  ( 1.000000000000000000, 0.000000000000000000, 0.000000000000000000 ) ) ;
#83876 = CARTESIAN_POINT ( 'NONE',  ( -0.05219959533936034679, 19.03943276465977164, 47.50109039468566863 ) ) ;
#83877 = CARTESIAN_POINT ( 'NONE',  ( -0.05219959533910754901, -16.53943276465976808, 27.49890960531435269 ) ) ;
#83878 = CARTESIAN_POINT ( 'NONE',  ( -0.05219959533909027116, -19.03943276465977164, 107.4989096053143527 ) ) ;
#83879 = CARTESIAN_POINT ( 'NONE',  ( 10.81492255796106328, -18.62759615963255655, 65.41775706135234714 ) ) ;
#83880 = CARTESIAN_POINT ( 'NONE',  ( -21.55341960407610458, -5.719274019375992779, 61.45724293864770260 ) ) ;
#83881 = CARTESIAN_POINT ( 'NONE',  ( -18.62759615963255300, -10.81492255796106328, 34.16775706135234714 ) ) ;
#83882 = CARTESIAN_POINT ( 'NONE',  ( 10.72451020669898902, -18.67979575497178502, 82.91557627198103830 ) ) ;
#83883 = CARTESIAN_POINT ( 'NONE',  ( -0.05219959533937732626, 21.53943276465977519, 42.50109039468567573 ) ) ;
#83884 = CARTESIAN_POINT ( 'NONE',  ( 4.483927247898545687, 16.52544592524342804, 114.7905762719810383 ) ) ;
#83885 = CARTESIAN_POINT ( 'NONE',  ( 19.05341960407617918, -5.049401038297876454, 71.04275706135234714 ) ) ;
#83886 = CARTESIAN_POINT ( 'NONE',  ( 0.05219959533909260263, 19.03943276465977164, 39.99890960531436690 ) ) ;
#83888 = CARTESIAN_POINT ( 'NONE',  ( 19.05341960407611168, 5.049401038298154454, 93.95724293864769550 ) ) ;
#83887 = CARTESIAN_POINT ( 'NONE',  ( -4.379528057220328563, 16.55341960407611168, 85.20724293864770971 ) ) ;
#83889 = CARTESIAN_POINT ( 'NONE',  ( -16.51473224551069308, -9.474510206698971260, 91.66557627198103830 ) ) ;
#83890 = CARTESIAN_POINT ( 'NONE',  ( 14.29746914071049879, -8.314922557960816363, 108.3322429386477097 ) ) ;
#83891 = CARTESIAN_POINT ( 'NONE',  ( -8.314922557960811034, -14.29746914071050412, 37.08224293864768129 ) ) ;
#83892 = CARTESIAN_POINT ( 'NONE',  ( -8.314922557961024197, 14.29746914071037800, 97.91775706135236135 ) ) ;
#83893 = CARTESIAN_POINT ( 'NONE',  ( 19.02544592524343514, -5.153800228976328945, 48.54057627198103120 ) ) ;
#83894 = CARTESIAN_POINT ( 'NONE',  ( -9.564922557960796823, -16.46253265017161027, 27.08224293864769550 ) ) ;
#83895 = CARTESIAN_POINT ( 'NONE',  ( -19.02544592524334988, -5.153800228976617603, 28.95942372801900433 ) ) ;
#83897 = CARTESIAN_POINT ( 'NONE',  ( 8.224510206698742110, 14.34966873604972548, 112.0844237280190185 ) ) ;
#83896 = CARTESIAN_POINT ( 'NONE',  ( -16.46253265017160317, 9.564922557960807481, 115.8322429386477097 ) ) ;
#83898 = CARTESIAN_POINT ( 'NONE',  ( 18.62759615963255655, 10.81492255796105972, 51.66775706135234714 ) ) ;
#83899 = CARTESIAN_POINT ( 'NONE',  ( 22.54345066063599035, -5.578190839439335136, 172.9373910537578354 ) ) ;
#83900 = CARTESIAN_POINT ( 'NONE',  ( 8.224510206698742110, 14.34966873604972548, 52.08442372801901854 ) ) ;
#83901 = CARTESIAN_POINT ( 'NONE',  ( -12.06949235617756955, 12.14591786802309770, 30.62390960531436335 ) ) ;
#83902 = CARTESIAN_POINT ( 'NONE',  ( 9.564922557960805705, 16.46253265017160317, 49.58224293864770260 ) ) ;
#83903 = CARTESIAN_POINT ( 'NONE',  ( -8.224510206698735004, -14.34966873604973081, 99.58442372801900433 ) ) ;
#83904 = CARTESIAN_POINT ( 'NONE',  ( 4.483927247898790824, -16.52544592524335698, 20.20942372801900788 ) ) ;
#83905 = CARTESIAN_POINT ( 'NONE',  ( -0.05219959533909027116, -19.03943276465977164, 47.49890960531435979 ) ) ;
#83906 = CARTESIAN_POINT ( 'NONE',  ( 4.379528057220339221, -16.55341960407611168, 112.7072429386476955 ) ) ;
#83907 = CARTESIAN_POINT ( 'NONE',  ( -10.81492255796078084, -18.62759615963271287, 112.0822429386477097 ) ) ;
#83908 = CARTESIAN_POINT ( 'NONE',  ( -19.05341960407611168, -5.049401038298163336, 41.45724293864769550 ) ) ;
#83909 = CARTESIAN_POINT ( 'NONE',  ( 19.02544592524343514, -5.153800228976328945, 103.5405762719809957 ) ) ;
#83910 = CARTESIAN_POINT ( 'NONE',  ( -9.474510206698964154, 16.51473224551069663, 35.41557627198102409 ) ) ;
#83911 = CARTESIAN_POINT ( 'NONE',  ( 9.474510206698971260, -16.51473224551069308, 107.9155762719810383 ) ) ;
#83912 = DIRECTION ( 'NONE',  ( 0.000000000000000000, 0.000000000000000000, 1.000000000000000000 ) ) ;
#83913 = VECTOR ( 'NONE', #135052, 1000.000000000000227 ) ;
#83914 = CARTESIAN_POINT ( 'NONE',  ( -0.05219959533909027116, -19.03943276465977164, 92.49890960531436690 ) ) ;
#83916 = CARTESIAN_POINT ( 'NONE',  ( 16.55341960407611168, 4.379528057220329451, 108.9572429386476955 ) ) ;
#83915 = CARTESIAN_POINT ( 'NONE',  ( 21.55341960407619695, -5.719274019375665929, 51.04275706135234714 ) ) ;
#83917 = CARTESIAN_POINT ( 'NONE',  ( 5.153800228976335163, 19.02544592524342804, 109.7905762719810099 ) ) ;
#83918 = CARTESIAN_POINT ( 'NONE',  ( -9.474510206698720793, -16.51473224551083518, 69.58442372801901854 ) ) ;
#83920 =( BOUNDED_CURVE ( )  B_SPLINE_CURVE ( 3, ( #50847, #113490, #5316, #35666 ),
 .UNSPECIFIED., .F., .T. ) 
 B_SPLINE_CURVE_WITH_KNOTS ( ( 4, 4 ),
 ( 2.008945357379067875, 2.115944711806982070 ),
 .UNSPECIFIED. ) 
 CURVE ( )  GEOMETRIC_REPRESENTATION_ITEM ( )  RATIONAL_B_SPLINE_CURVE ( ( 1.000000000000000000, 0.9990461557208837329, 0.9990461557208837329, 1.000000000000000000 ) ) 
 REPRESENTATION_ITEM ( '' )  );
#83919 = CARTESIAN_POINT ( 'NONE',  ( 12.06949235617739724, 12.14591786802326823, 61.87609039468568284 ) ) ;
#83921 = CARTESIAN_POINT ( 'NONE',  ( -15.80617190586768217, 15.72974639402176855, 88.12609039468570415 ) ) ;
#83922 = CARTESIAN_POINT ( 'NONE',  ( 8.314922557961029526, -14.29746914071037800, 60.41775706135235424 ) ) ;
#83923 = CARTESIAN_POINT ( 'NONE',  ( -0.05219959533909027116, -19.03943276465977164, 82.49890960531436690 ) ) ;
#83924 = CARTESIAN_POINT ( 'NONE',  ( -12.14591786802326823, 12.06949235617739902, 38.12609039468567573 ) ) ;
#83925 = CARTESIAN_POINT ( 'NONE',  ( -9.474510206698720793, -16.51473224551083518, 104.5844237280190043 ) ) ;
#83926 = CARTESIAN_POINT ( 'NONE',  ( -4.483927247898782831, 16.52544592524335698, 82.70942372801900433 ) ) ;
#83927 = CARTESIAN_POINT ( 'NONE',  ( -16.46253265017146816, -9.564922557961047289, 99.16775706135233293 ) ) ;
#83928 = CARTESIAN_POINT ( 'NONE',  ( -19.02544592524342804, 5.153800228976336051, 81.04057627198103830 ) ) ;
#83929 = CARTESIAN_POINT ( 'NONE',  ( -21.52544592524343514, 5.823673210054127303, 101.0405762719810383 ) ) ;
#83931 = CARTESIAN_POINT ( 'NONE',  ( 13.97604488694548053, -13.89961937509957401, 110.6260903946856615 ) ) ;
#83930 = CARTESIAN_POINT ( 'NONE',  ( -16.52544592524342804, 4.483927247898546575, 86.04057627198102409 ) ) ;
#83932 = CARTESIAN_POINT ( 'NONE',  ( -12.06949235617739369, -12.14591786802326823, 74.37609039468568994 ) ) ;
#83933 = CARTESIAN_POINT ( 'NONE',  ( 19.83802472612599743, 12.02135855755798133, 167.9999999999999716 ) ) ;
#83934 = CARTESIAN_POINT ( 'NONE',  ( 0.05219959533936267826, -19.03943276465977164, 75.00109039468566152 ) ) ;
#83935 = CARTESIAN_POINT ( 'NONE',  ( -12.06949235617756955, 12.14591786802309770, 30.62390960531436335 ) ) ;
#83936 = CARTESIAN_POINT ( 'NONE',  ( 4.483927247898545687, 16.52544592524342804, 89.79057627198103830 ) ) ;
#83938 = CARTESIAN_POINT ( 'NONE',  ( -16.19135201231366139, 7.376712067591927990, 89.81319145947971094 ) ) ;
#83937 = CARTESIAN_POINT ( 'NONE',  ( -9.564922557961040184, 16.46253265017147172, 32.91775706135233293 ) ) ;
#83939 = CARTESIAN_POINT ( 'NONE',  ( 18.62759615963255655, 10.81492255796105972, 21.66775706135235069 ) ) ;
#83940 = CARTESIAN_POINT ( 'NONE',  ( 16.46253265017146816, 9.564922557961045513, 96.66775706135233293 ) ) ;
#83941 = CARTESIAN_POINT ( 'NONE',  ( -5.049401038298153566, 19.05341960407611168, 110.2072429386476671 ) ) ;
#83942 = CARTESIAN_POINT ( 'NONE',  ( 9.564922557960805705, 16.46253265017160317, 94.58224293864769550 ) ) ;
#83943 = CARTESIAN_POINT ( 'NONE',  ( 18.62759615963255655, 10.81492255796105972, 96.66775706135234714 ) ) ;
#83944 = CARTESIAN_POINT ( 'NONE',  ( -13.97604488694527625, -13.89961937509977652, 71.87390960531433848 ) ) ;
#83945 = CARTESIAN_POINT ( 'NONE',  ( -18.62759615963270932, 10.81492255796079327, 40.83224293864769550 ) ) ;
#83946 = CARTESIAN_POINT ( 'NONE',  ( -14.29746914071049879, 8.314922557960819915, 90.83224293864769550 ) ) ;
#83947 = CARTESIAN_POINT ( 'NONE',  ( -13.89961937509977652, 13.97604488694528158, 50.62390960531435979 ) ) ;
#83948 = CARTESIAN_POINT ( 'NONE',  ( 8.224510206698953496, -14.34966873604960469, 112.9155762719810383 ) ) ;
#83949 = CARTESIAN_POINT ( 'NONE',  ( -5.719274019375665041, -21.55341960407619695, 24.79275706135235779 ) ) ;
#83950 = CARTESIAN_POINT ( 'NONE',  ( -21.53943276465977519, -0.05219959533937600094, 58.75109039468568994 ) ) ;
#83951 = CARTESIAN_POINT ( 'NONE',  ( 5.153800228976335163, 19.02544592524342804, 44.79057627198103830 ) ) ;
#83952 = CARTESIAN_POINT ( 'NONE',  ( -16.53943276465976808, -0.05219959533934237506, 83.75109039468568994 ) ) ;
#83953 = CARTESIAN_POINT ( 'NONE',  ( -10.81492255796105439, 18.62759615963255655, 22.91775706135235069 ) ) ;
#83954 = ORIENTED_EDGE ( 'NONE', *, *, #59210, .T. ) ;
#83955 = CARTESIAN_POINT ( 'NONE',  ( 5.823673210054125526, 21.52544592524343514, 114.7905762719810383 ) ) ;
#83957 = CARTESIAN_POINT ( 'NONE',  ( 9.474510206698971260, -16.51473224551069308, 67.91557627198102409 ) ) ;
#83956 = CARTESIAN_POINT ( 'NONE',  ( 13.97604488694548053, -13.89961937509957401, 50.62609039468566152 ) ) ;
#83958 = CARTESIAN_POINT ( 'NONE',  ( -19.05341960407617563, 5.049401038297882671, 33.54275706135231871 ) ) ;
#83959 = CARTESIAN_POINT ( 'NONE',  ( -15.72974639402176322, -15.80617190586768395, 64.37609039468568994 ) ) ;
#83960 = CARTESIAN_POINT ( 'NONE',  ( -15.72974639402197994, 15.80617190586746368, 70.62390960531436690 ) ) ;
#83961 = CARTESIAN_POINT ( 'NONE',  ( -8.314922557960811034, -14.29746914071050412, 47.08224293864770260 ) ) ;
#83963 = CARTESIAN_POINT ( 'NONE',  ( -19.02544592524334988, -5.153800228976617603, 23.95942372801900078 ) ) ;
#83962 = CARTESIAN_POINT ( 'NONE',  ( 5.823673210054444382, -21.52544592524334988, 95.20942372801903275 ) ) ;
#83964 = CARTESIAN_POINT ( 'NONE',  ( -12.06949235617756955, 12.14591786802309770, 65.62390960531436690 ) ) ;
#83965 = CARTESIAN_POINT ( 'NONE',  ( -12.06949235617756955, 12.14591786802309770, 100.6239096053143811 ) ) ;
#83966 = CARTESIAN_POINT ( 'NONE',  ( -9.474510206698720793, -16.51473224551083518, 54.58442372801899722 ) ) ;
#83967 = CARTESIAN_POINT ( 'NONE',  ( -4.483927247898539470, -16.52544592524342804, 22.29057627198102765 ) ) ;
#83968 = CARTESIAN_POINT ( 'NONE',  ( 5.823673210054444382, -21.52544592524334988, 75.20942372801901854 ) ) ;
#83969 = CARTESIAN_POINT ( 'NONE',  ( -9.474510206698720793, -16.51473224551083518, 54.58442372801899722 ) ) ;
#83970 = CARTESIAN_POINT ( 'NONE',  ( 18.62759615963271287, -10.81492255796078972, 58.33224293864768839 ) ) ;
#83971 = CARTESIAN_POINT ( 'NONE',  ( -15.72974639402176322, -15.80617190586768395, 49.37609039468569705 ) ) ;
#83972 = CARTESIAN_POINT ( 'NONE',  ( -21.53943276465977519, 0.05219959533907696930, 106.2489096053143811 ) ) ;
#83973 = CARTESIAN_POINT ( 'NONE',  ( -16.46253265017146816, -9.564922557961047289, 104.1677570613523329 ) ) ;
#83974 = CARTESIAN_POINT ( 'NONE',  ( 12.14591786802327356, -12.06949235617739191, 65.62609039468568994 ) ) ;
#83976 = CARTESIAN_POINT ( 'NONE',  ( 5.719274019375991003, -21.55341960407610458, 102.7072429386476955 ) ) ;
#83975 = CARTESIAN_POINT ( 'NONE',  ( -17.60728821186567927, 5.500000000000037303, 55.86690927743004664 ) ) ;
#83977 = CARTESIAN_POINT ( 'NONE',  ( -12.06949235617756955, 12.14591786802309770, 85.62390960531436690 ) ) ;
#83978 = CARTESIAN_POINT ( 'NONE',  ( -16.62475595723698873, -7.163666690055323194, 99.47286648189528080 ) ) ;
#83979 = CARTESIAN_POINT ( 'NONE',  ( 4.483927247898790824, -16.52544592524335698, 25.20942372801901854 ) ) ;
#83980 = ADVANCED_FACE ( 'NONE', ( #199993 ), #61460, .F. ) ;
#83981 = CARTESIAN_POINT ( 'NONE',  ( 21.53943276465977519, -0.05219959533907433946, 48.74890960531435979 ) ) ;
#83982 = CARTESIAN_POINT ( 'NONE',  ( 14.34966873604972726, -8.224510206698740333, 85.83442372801901854 ) ) ;
#83983 = CARTESIAN_POINT ( 'NONE',  ( 34.12434206616184440, 14.08647367304311260, -8.000000000000001776 ) ) ;
#83984 = CARTESIAN_POINT ( 'NONE',  ( 14.29746914071037800, 8.314922557961029526, 66.66775706135234714 ) ) ;
#83985 = CARTESIAN_POINT ( 'NONE',  ( 21.52544592524334988, 5.823673210054432836, 36.45942372801901143 ) ) ;
#83986 = CARTESIAN_POINT ( 'NONE',  ( 21.52544592524344225, -5.823673210054117533, 53.54057627198103120 ) ) ;
#83987 = CARTESIAN_POINT ( 'NONE',  ( 14.34966873604972726, -8.224510206698740333, 85.83442372801901854 ) ) ;
#83988 = CARTESIAN_POINT ( 'NONE',  ( 19.02544592524343514, -5.153800228976328945, 93.54057627198102409 ) ) ;
#83989 = CARTESIAN_POINT ( 'NONE',  ( -18.67979575497193778, 10.72451020669871902, 73.33442372801901854 ) ) ;
#83990 = CARTESIAN_POINT ( 'NONE',  ( -0.05219959533907301413, -21.53943276465977519, 47.49890960531435979 ) ) ;
#83991 = CARTESIAN_POINT ( 'NONE',  ( 5.719274019375991003, -21.55341960407610458, 32.70724293864770260 ) ) ;
#83992 = ORIENTED_EDGE ( 'NONE', *, *, #141591, .F. ) ;
#83993 = CARTESIAN_POINT ( 'NONE',  ( -5.153800228976607833, 19.02544592524334988, 47.70942372801900433 ) ) ;
#83994 = CARTESIAN_POINT ( 'NONE',  ( 12.06949235617739724, 12.14591786802326823, 66.87609039468568994 ) ) ;
#83995 = CARTESIAN_POINT ( 'NONE',  ( -5.719274019375978568, 21.55341960407610458, 30.20724293864769550 ) ) ;
#83996 = VERTEX_POINT ( 'NONE', #63459 ) ;
#83997 = CARTESIAN_POINT ( 'NONE',  ( -9.474510206698964154, 16.51473224551069663, 100.4155762719810241 ) ) ;
#83998 = CARTESIAN_POINT ( 'NONE',  ( 14.29746914071049879, -8.314922557960816363, 23.33224293864769194 ) ) ;
#83999 = CARTESIAN_POINT ( 'NONE',  ( -17.72517630440434644, 5.499999999999979572, 85.92175719257211597 ) ) ;
#84000 = CARTESIAN_POINT ( 'NONE',  ( -16.55341960407611168, -4.379528057220339221, 111.4572429386476813 ) ) ;
#84001 = CARTESIAN_POINT ( 'NONE',  ( -21.52544592524343514, 5.823673210054127303, 51.04057627198103120 ) ) ;
#84002 = CARTESIAN_POINT ( 'NONE',  ( 19.03943276465977164, -0.05219959533909143690, 38.74890960531436690 ) ) ;
#84003 = EDGE_CURVE ( 'NONE', #62967, #15377, #123131, .T. ) ;
#84004 = CARTESIAN_POINT ( 'NONE',  ( 14.34966873604972726, -8.224510206698740333, 95.83442372801903275 ) ) ;
#84005 = CARTESIAN_POINT ( 'NONE',  ( -5.719274019375665041, -21.55341960407619695, 34.79275706135235424 ) ) ;
#84006 = CARTESIAN_POINT ( 'NONE',  ( -19.05341960407617563, 5.049401038297882671, 88.54275706135230450 ) ) ;
#84007 = CARTESIAN_POINT ( 'NONE',  ( -16.53943276465976808, 0.05219959533911058130, 106.2489096053143811 ) ) ;
#84008 = CARTESIAN_POINT ( 'NONE',  ( -13.97604488694527625, -13.89961937509977652, 51.87390960531436690 ) ) ;
#84009 = CARTESIAN_POINT ( 'NONE',  ( -9.564922557960796823, -16.46253265017161027, 27.08224293864769550 ) ) ;
#84010 = CARTESIAN_POINT ( 'NONE',  ( 0.8197377589650296503, 24.06023304481832170, -54.40145518167209104 ) ) ;
#84011 = CARTESIAN_POINT ( 'NONE',  ( -13.89961937509977652, 13.97604488694528158, 75.62390960531438111 ) ) ;
#84012 = CARTESIAN_POINT ( 'NONE',  ( -12.06949235617739369, -12.14591786802326823, 59.37609039468568284 ) ) ;
#84013 = CARTESIAN_POINT ( 'NONE',  ( 0.05219959533937995610, -21.53943276465977519, 110.0010903946856757 ) ) ;
#84014 = CARTESIAN_POINT ( 'NONE',  ( 5.823673210054125526, 21.52544592524343514, 44.79057627198103120 ) ) ;
#84015 = CARTESIAN_POINT ( 'NONE',  ( -16.52544592524335698, -4.483927247898792601, 73.95942372801901854 ) ) ;
#84016 = CARTESIAN_POINT ( 'NONE',  ( -16.51473224551082808, 9.474510206698731452, 48.33442372801900433 ) ) ;
#84017 = CARTESIAN_POINT ( 'NONE',  ( 19.02544592524334988, 5.153800228976608722, 61.45942372801900433 ) ) ;
#84018 = CARTESIAN_POINT ( 'NONE',  ( -10.72451020669870658, -18.67979575497194134, 64.58442372801900433 ) ) ;
#84019 = CARTESIAN_POINT ( 'NONE',  ( -19.02544592524342804, 5.153800228976336051, 61.04057627198103120 ) ) ;
#84020 = CARTESIAN_POINT ( 'NONE',  ( -19.03943276465977164, 0.05219959533909376836, 31.24890960531435979 ) ) ;
#84021 = CARTESIAN_POINT ( 'NONE',  ( -9.564922557961040184, 16.46253265017147172, 62.91775706135233293 ) ) ;
#84022 = CARTESIAN_POINT ( 'NONE',  ( 9.474510206698971260, -16.51473224551069308, 107.9155762719810383 ) ) ;
#84023 = CARTESIAN_POINT ( 'NONE',  ( 9.474510206698971260, -16.51473224551069308, 97.91557627198102409 ) ) ;
#84024 = CARTESIAN_POINT ( 'NONE',  ( 8.224510206698953496, -14.34966873604960469, 52.91557627198103830 ) ) ;
#84025 = CARTESIAN_POINT ( 'NONE',  ( -5.719274019375978568, 21.55341960407610458, 45.20724293864769550 ) ) ;
#84026 = CARTESIAN_POINT ( 'NONE',  ( -17.50000000000000000, 3.305555262949662954, 104.6251715215659459 ) ) ;
#84027 = CARTESIAN_POINT ( 'NONE',  ( 5.823673210054444382, -21.52544592524334988, 105.2094237280190328 ) ) ;
#84028 = FACE_BOUND ( 'NONE', #57034, .T. ) ;
#84029 = CARTESIAN_POINT ( 'NONE',  ( -16.51473224551069308, -9.474510206698971260, 56.66557627198103120 ) ) ;
#84030 = CARTESIAN_POINT ( 'NONE',  ( 29.64655366937556380, -26.74020568361524752, -17.07338589137926022 ) ) ;
#84031 = DIRECTION ( 'NONE',  ( 1.000000000000000000, 0.000000000000000000, 0.000000000000000000 ) ) ;
#84032 = CARTESIAN_POINT ( 'NONE',  ( 8.224510206698742110, 14.34966873604972548, 72.08442372801899012 ) ) ;
#84033 = CARTESIAN_POINT ( 'NONE',  ( 10.81492255796078972, 18.62759615963270932, 94.58224293864769550 ) ) ;
#84034 = CARTESIAN_POINT ( 'NONE',  ( 8.314922557960818139, 14.29746914071049879, 49.58224293864769550 ) ) ;
#84036 = CARTESIAN_POINT ( 'NONE',  ( -9.474510206698964154, 16.51473224551069663, 115.4155762719810241 ) ) ;
#84035 = CARTESIAN_POINT ( 'NONE',  ( -16.46253265017160317, 9.564922557960807481, 35.83224293864768839 ) ) ;
#84037 = CARTESIAN_POINT ( 'NONE',  ( -10.72451020669870658, -18.67979575497194134, 39.58442372801901143 ) ) ;
#84038 = CARTESIAN_POINT ( 'NONE',  ( -19.02544592524334988, -5.153800228976617603, 48.95942372801900433 ) ) ;
#84039 = CARTESIAN_POINT ( 'NONE',  ( 13.89961937509977652, -13.97604488694527269, 43.12390960531434558 ) ) ;
#84040 = CARTESIAN_POINT ( 'NONE',  ( 15.80617190586769283, -15.72974639402175789, 90.62609039468567573 ) ) ;
#84041 = CARTESIAN_POINT ( 'NONE',  ( 17.40861289039002457, 6.110651285853315073, 98.87232470827433417 ) ) ;
#84042 = VERTEX_POINT ( 'NONE', #171637 ) ;
#84043 = CARTESIAN_POINT ( 'NONE',  ( -14.34966873604960291, -8.224510206698953496, 46.66557627198102409 ) ) ;
#84044 = CARTESIAN_POINT ( 'NONE',  ( -13.74275686049844403, 0.4100021152178338069, -60.42614020214175241 ) ) ;
#84045 = CARTESIAN_POINT ( 'NONE',  ( 10.72451020669898902, -18.67979575497178502, 42.91557627198103120 ) ) ;
#84046 = CARTESIAN_POINT ( 'NONE',  ( 22.44159573604009239, 16.30477369853692693, 144.0750000027311728 ) ) ;
#84047 = CARTESIAN_POINT ( 'NONE',  ( -19.05341960407611168, -5.049401038298163336, 106.4572429386476955 ) ) ;
#84048 = CARTESIAN_POINT ( 'NONE',  ( -16.55341960407611168, -4.379528057220339221, 86.45724293864770971 ) ) ;
#84049 = CARTESIAN_POINT ( 'NONE',  ( -8.314922557961024197, 14.29746914071037800, 27.91775706135234358 ) ) ;
#84050 = EDGE_CURVE ( 'NONE', #98984, #133568, #12455, .T. ) ;
#84051 = CARTESIAN_POINT ( 'NONE',  ( -16.55341960407611168, -4.379528057220339221, 21.45724293864769550 ) ) ;
#84052 = ORIENTED_EDGE ( 'NONE', *, *, #68000, .T. ) ;
#84054 = CARTESIAN_POINT ( 'NONE',  ( 21.53943276465977519, -0.05219959533907433946, 98.74890960531438111 ) ) ;
#84053 = CARTESIAN_POINT ( 'NONE',  ( -0.05219959533909027116, -19.03943276465977164, 102.4989096053143669 ) ) ;
#84056 = CARTESIAN_POINT ( 'NONE',  ( -9.474510206698964154, 16.51473224551069663, 95.41557627198102409 ) ) ;
#84055 = CARTESIAN_POINT ( 'NONE',  ( -14.29746914071049879, 8.314922557960819915, 25.83224293864769194 ) ) ;
#84057 = CARTESIAN_POINT ( 'NONE',  ( -13.89961937509957401, -13.97604488694547875, 99.37609039468567573 ) ) ;
#84058 = CARTESIAN_POINT ( 'NONE',  ( -15.80617190586768217, 15.72974639402176855, 113.1260903946856899 ) ) ;
#84059 = CARTESIAN_POINT ( 'NONE',  ( 5.823673210054125526, 21.52544592524343514, 94.79057627198105251 ) ) ;
#84060 = CARTESIAN_POINT ( 'NONE',  ( 10.81492255796078972, 18.62759615963270932, 44.58224293864769550 ) ) ;
#84061 = CARTESIAN_POINT ( 'NONE',  ( 9.474510206698971260, -16.51473224551069308, 57.91557627198103120 ) ) ;
#84062 = CARTESIAN_POINT ( 'NONE',  ( 8.224510206698953496, -14.34966873604960469, 32.91557627198102409 ) ) ;
#84063 = CARTESIAN_POINT ( 'NONE',  ( 5.049401038298161559, -19.05341960407611168, 82.70724293864770971 ) ) ;
#84064 = CARTESIAN_POINT ( 'NONE',  ( -32.64453336272028139, 2.028832619897439204E-14, 87.50000000000000000 ) ) ;
#84065 = CARTESIAN_POINT ( 'NONE',  ( -0.05219959533936034679, 19.03943276465977164, 32.50109039468566863 ) ) ;
#84066 = CARTESIAN_POINT ( 'NONE',  ( 8.224510206698953496, -14.34966873604960469, 92.91557627198103830 ) ) ;
#84067 = CARTESIAN_POINT ( 'NONE',  ( 21.53943276465977519, 0.05219959533937863772, 21.25109039468567218 ) ) ;
#84068 = CARTESIAN_POINT ( 'NONE',  ( -17.14385361876520619, 23.59649016807275856, 143.0750000027311444 ) ) ;
#84069 = CARTESIAN_POINT ( 'NONE',  ( 0.05219959533934541429, -16.53943276465976808, 110.0010903946856757 ) ) ;
#84070 = CARTESIAN_POINT ( 'NONE',  ( 16.51473224551069308, 9.474510206698969483, 24.16557627198102765 ) ) ;
#84071 = CARTESIAN_POINT ( 'NONE',  ( 16.46253265017160672, -9.564922557960803928, 78.33224293864769550 ) ) ;
#84072 = CARTESIAN_POINT ( 'NONE',  ( -6.020228577223754586E-15, 39.95556452105416412, -10.24999999453762456 ) ) ;
#84073 = CARTESIAN_POINT ( 'NONE',  ( -14.34966873604960291, -8.224510206698953496, 46.66557627198102409 ) ) ;
#84074 = CARTESIAN_POINT ( 'NONE',  ( -21.53943276465977519, -0.05219959533937600094, 53.75109039468568994 ) ) ;
#84075 = CARTESIAN_POINT ( 'NONE',  ( 3.424326230466315568, -6.677994727576229472, 8.646741581399133736 ) ) ;
#84076 = CARTESIAN_POINT ( 'NONE',  ( -18.67979575497193778, 10.72451020669871902, 88.33442372801901854 ) ) ;
#84077 = CARTESIAN_POINT ( 'NONE',  ( 19.02544592524343514, -5.153800228976328945, 48.54057627198103120 ) ) ;
#84078 = CARTESIAN_POINT ( 'NONE',  ( -0.05219959533909027116, -19.03943276465977164, 52.49890960531436690 ) ) ;
#84079 = ORIENTED_EDGE ( 'NONE', *, *, #72341, .F. ) ;
#84080 = CARTESIAN_POINT ( 'NONE',  ( -15.72974639402176322, -15.80617190586768395, 89.37609039468568994 ) ) ;
#84081 = CARTESIAN_POINT ( 'NONE',  ( 16.55341960407618274, -4.379528057220086978, 56.04275706135235424 ) ) ;
#84082 = CARTESIAN_POINT ( 'NONE',  ( 5.823673210054444382, -21.52544592524334988, 80.20942372801901854 ) ) ;
#84083 = CARTESIAN_POINT ( 'NONE',  ( 5.153800228976335163, 19.02544592524342804, 114.7905762719810241 ) ) ;
#84084 = CARTESIAN_POINT ( 'NONE',  ( -9.474510206698720793, -16.51473224551083518, 89.58442372801900433 ) ) ;
#84085 = CARTESIAN_POINT ( 'NONE',  ( 15.80617190586769283, -15.72974639402175789, 70.62609039468567573 ) ) ;
#84086 = CARTESIAN_POINT ( 'NONE',  ( -0.05219959533934338120, 16.53943276465976808, 37.50109039468568284 ) ) ;
#84087 = CARTESIAN_POINT ( 'NONE',  ( -21.55341960407610458, -5.719274019375992779, 86.45724293864770971 ) ) ;
#84088 = CARTESIAN_POINT ( 'NONE',  ( 19.05341960407617918, -5.049401038297876454, 91.04275706135234714 ) ) ;
#84089 = CARTESIAN_POINT ( 'NONE',  ( -9.564922557960796823, -16.46253265017161027, 67.08224293864769550 ) ) ;
#84090 = CARTESIAN_POINT ( 'NONE',  ( -19.02544592524334988, -5.153800228976617603, 98.95942372801900433 ) ) ;
#84091 = AXIS2_PLACEMENT_3D ( 'NONE', #59065, #183417, #167259 ) ;
#84092 = CARTESIAN_POINT ( 'NONE',  ( -9.564922557961040184, 16.46253265017147172, 107.9177570613523471 ) ) ;
#84093 = CARTESIAN_POINT ( 'NONE',  ( -4.483927247898539470, -16.52544592524342804, 52.29057627198102409 ) ) ;
#84094 = CARTESIAN_POINT ( 'NONE',  ( 13.89961937509957401, 13.97604488694547697, 76.87609039468566152 ) ) ;
#84095 = CARTESIAN_POINT ( 'NONE',  ( 4.483927247898790824, -16.52544592524335698, 55.20942372801902565 ) ) ;
#84096 = CARTESIAN_POINT ( 'NONE',  ( -5.153800228976328057, -19.02544592524343514, 42.29057627198101699 ) ) ;
#84097 = CARTESIAN_POINT ( 'NONE',  ( -9.564922557960796823, -16.46253265017161027, 57.08224293864769550 ) ) ;
#84098 = CARTESIAN_POINT ( 'NONE',  ( 16.53943276465976808, 0.05219959533934440121, 61.25109039468567573 ) ) ;
#84099 = CARTESIAN_POINT ( 'NONE',  ( -17.14385361876520619, 23.59649016807275856, 141.0750000027311728 ) ) ;
#84100 = CARTESIAN_POINT ( 'NONE',  ( 1.993301997531345292E-15, -30.30510711980685912, 138.7500000054623683 ) ) ;
#84101 = CARTESIAN_POINT ( 'NONE',  ( -9.474510206698964154, 16.51473224551069663, 110.4155762719810383 ) ) ;
#84102 = CARTESIAN_POINT ( 'NONE',  ( -3.573655867282028392E-15, 2.428612866367529932E-14, -25.00000000000000000 ) ) ;
#84103 = EDGE_LOOP ( 'NONE', ( #190428, #31418, #167975 ) ) ;
#84104 = CARTESIAN_POINT ( 'NONE',  ( 13.89961937509957401, 13.97604488694547697, 111.8760903946856757 ) ) ;
#84105 = CARTESIAN_POINT ( 'NONE',  ( -21.53943276465977519, 0.05219959533907696930, 36.24890960531435979 ) ) ;
#84107 = CARTESIAN_POINT ( 'NONE',  ( -4.379528057220086978, -16.55341960407618274, 24.79275706135235779 ) ) ;
#84106 = CARTESIAN_POINT ( 'NONE',  ( 5.049401038297881783, 19.05341960407617563, 37.29275706135232582 ) ) ;
#84108 = CARTESIAN_POINT ( 'NONE',  ( 13.89961937509977652, -13.97604488694527269, 28.12390960531435624 ) ) ;
#84109 = CARTESIAN_POINT ( 'NONE',  ( -13.89961937509977652, 13.97604488694528158, 55.62390960531434558 ) ) ;
#84110 = CARTESIAN_POINT ( 'NONE',  ( -15.72974639402197994, 15.80617190586746368, 80.62390960531438111 ) ) ;
#84111 = CARTESIAN_POINT ( 'NONE',  ( 9.474510206698971260, -16.51473224551069308, 97.91557627198102409 ) ) ;
#84112 = CARTESIAN_POINT ( 'NONE',  ( -5.049401038298153566, 19.05341960407611168, 50.20724293864770260 ) ) ;
#84113 = CARTESIAN_POINT ( 'NONE',  ( 27.73933785331498569, 2.768321779492822058E-14, 146.3750000027311842 ) ) ;
#84114 = CARTESIAN_POINT ( 'NONE',  ( 19.03943276465977164, 0.05219959533936151252, 86.25109039468567573 ) ) ;
#84115 = CARTESIAN_POINT ( 'NONE',  ( -12.14591786802309592, -12.06949235617757132, 71.87390960531438111 ) ) ;
#84116 = CARTESIAN_POINT ( 'NONE',  ( 5.719274019375991003, -21.55341960407610458, 52.70724293864769550 ) ) ;
#84117 = CARTESIAN_POINT ( 'NONE',  ( -15.80617190586768217, 15.72974639402176855, 113.1260903946856899 ) ) ;
#84118 = CARTESIAN_POINT ( 'NONE',  ( -21.52544592524343514, 5.823673210054127303, 91.04057627198103830 ) ) ;
#84119 = CARTESIAN_POINT ( 'NONE',  ( 5.823673210054444382, -21.52544592524334988, 75.20942372801901854 ) ) ;
#84120 = CARTESIAN_POINT ( 'NONE',  ( 18.62759615963255655, 10.81492255796105972, 81.66775706135236135 ) ) ;
#84121 = CARTESIAN_POINT ( 'NONE',  ( -13.97604488694527625, -13.89961937509977652, 111.8739096053143243 ) ) ;
#84123 = CARTESIAN_POINT ( 'NONE',  ( -21.55341960407619339, 5.719274019375674811, 78.54275706135236135 ) ) ;
#84122 = CARTESIAN_POINT ( 'NONE',  ( -16.55341960407617563, 4.379528057220093196, 103.5427570613523613 ) ) ;
#84124 = CARTESIAN_POINT ( 'NONE',  ( -5.153800228976328057, -19.02544592524343514, 72.29057627198102409 ) ) ;
#84125 = CARTESIAN_POINT ( 'NONE',  ( -5.823673210054431948, 21.52544592524334988, 32.70942372801900433 ) ) ;
#84126 = CARTESIAN_POINT ( 'NONE',  ( -5.153800228976328057, -19.02544592524343514, 67.29057627198102409 ) ) ;
#84127 = CARTESIAN_POINT ( 'NONE',  ( 4.483927247898545687, 16.52544592524342804, 74.79057627198105251 ) ) ;
#84128 = CARTESIAN_POINT ( 'NONE',  ( 4.483927247898545687, 16.52544592524342804, 44.79057627198103120 ) ) ;
#84129 = CARTESIAN_POINT ( 'NONE',  ( 18.67979575497178502, 10.72451020669898547, 54.16557627198103120 ) ) ;
#84130 = CARTESIAN_POINT ( 'NONE',  ( -5.153800228976328057, -19.02544592524343514, 67.29057627198102409 ) ) ;
#84131 = CARTESIAN_POINT ( 'NONE',  ( -18.62759615963270932, 10.81492255796079327, 65.83224293864769550 ) ) ;
#84132 = CARTESIAN_POINT ( 'NONE',  ( -5.049401038297874678, -19.05341960407617918, 64.79275706135233293 ) ) ;
#84134 = CARTESIAN_POINT ( 'NONE',  ( -8.224510206698948167, 14.34966873604960824, 60.41557627198102409 ) ) ;
#84133 = CARTESIAN_POINT ( 'NONE',  ( 0.05219959533936267826, -19.03943276465977164, 20.00109039468567218 ) ) ;
#84135 = CARTESIAN_POINT ( 'NONE',  ( 5.823673210054125526, 21.52544592524343514, 49.79057627198102409 ) ) ;
#84136 = ORIENTED_EDGE ( 'NONE', *, *, #113277, .T. ) ;
#84137 = CARTESIAN_POINT ( 'NONE',  ( -22.00000000000000000, -1.163414459189985801E-14, 97.50000000000000000 ) ) ;
#84139 = CARTESIAN_POINT ( 'NONE',  ( -8.571926809382608425, 26.38167802310805854, 148.4750000027311785 ) ) ;
#84138 = CARTESIAN_POINT ( 'NONE',  ( -16.55341960407617563, 4.379528057220093196, 103.5427570613523613 ) ) ;
#84140 = CARTESIAN_POINT ( 'NONE',  ( 0.05219959533936267826, -19.03943276465977164, 85.00109039468567573 ) ) ;
#84141 = CARTESIAN_POINT ( 'NONE',  ( -4.379528057220328563, 16.55341960407611168, 70.20724293864769550 ) ) ;
#84142 = CARTESIAN_POINT ( 'NONE',  ( 37.99626262588765258, 2.893932880411085066E-14, 6.432029388270255055E-14 ) ) ;
#84143 = CARTESIAN_POINT ( 'NONE',  ( 0.05219959533909260263, 19.03943276465977164, 59.99890960531436690 ) ) ;
#84144 = CARTESIAN_POINT ( 'NONE',  ( -0.05219959533910754901, -16.53943276465976808, 52.49890960531435979 ) ) ;
#84145 = CARTESIAN_POINT ( 'NONE',  ( 16.46253265017160672, -9.564922557960803928, 83.33224293864768129 ) ) ;
#84147 = CARTESIAN_POINT ( 'NONE',  ( -19.02544592524342804, 5.153800228976336051, 56.04057627198100988 ) ) ;
#84146 = CARTESIAN_POINT ( 'NONE',  ( -9.474510206698720793, -16.51473224551083518, 74.58442372801900433 ) ) ;
#84148 = CARTESIAN_POINT ( 'NONE',  ( -19.05341960407611168, -5.049401038298163336, 81.45724293864769550 ) ) ;
#84149 = CARTESIAN_POINT ( 'NONE',  ( -13.97604488694527625, -13.89961937509977652, 66.87390960531436690 ) ) ;
#84150 = CARTESIAN_POINT ( 'NONE',  ( 15.80617190586746368, 15.72974639402197994, 64.37390960531435269 ) ) ;
#84151 = CARTESIAN_POINT ( 'NONE',  ( -6.856101608890801443E-16, -64.85304063214812231, -22.99999966871703094 ) ) ;
#84152 = CARTESIAN_POINT ( 'NONE',  ( -13.97604488694527625, -13.89961937509977652, 46.87390960531435979 ) ) ;
#84153 = CARTESIAN_POINT ( 'NONE',  ( -5.823673210054116645, -21.52544592524344225, 57.29057627198103120 ) ) ;
#84154 = CARTESIAN_POINT ( 'NONE',  ( -9.474510206698720793, -16.51473224551083518, 84.58442372801900433 ) ) ;
#84155 = CARTESIAN_POINT ( 'NONE',  ( -16.53943276465976808, -0.05219959533934237506, 113.7510903946856757 ) ) ;
#84156 = CARTESIAN_POINT ( 'NONE',  ( -16.51473224551082808, 9.474510206698731452, 33.33442372801899722 ) ) ;
#84158 = CARTESIAN_POINT ( 'NONE',  ( -0.05219959533934338120, 16.53943276465976808, 87.50109039468568994 ) ) ;
#84157 = CARTESIAN_POINT ( 'NONE',  ( 12.14591786802327356, -12.06949235617739191, 60.62609039468567573 ) ) ;
#84159 = CARTESIAN_POINT ( 'NONE',  ( -28.79475375365585066, 2.428612866367529932E-14, 148.2656553485623760 ) ) ;
#84160 = CARTESIAN_POINT ( 'NONE',  ( 8.224510206698742110, 14.34966873604972548, 87.08442372801901854 ) ) ;
#84161 = CARTESIAN_POINT ( 'NONE',  ( -9.474510206698964154, 16.51473224551069663, 115.4155762719810241 ) ) ;
#84162 = CARTESIAN_POINT ( 'NONE',  ( 5.049401038298161559, -19.05341960407611168, 37.70724293864768839 ) ) ;
#84163 = CARTESIAN_POINT ( 'NONE',  ( -4.379528057220086978, -16.55341960407618274, 34.79275706135235424 ) ) ;
#84164 = CARTESIAN_POINT ( 'NONE',  ( 5.153800228976335163, 19.02544592524342804, 49.79057627198100988 ) ) ;
#84165 = CARTESIAN_POINT ( 'NONE',  ( 18.67979575497194134, -10.72451020669871369, 40.83442372801901854 ) ) ;
#84166 = CARTESIAN_POINT ( 'NONE',  ( 8.314922557961029526, -14.29746914071037800, 55.41775706135234714 ) ) ;
#84167 = CARTESIAN_POINT ( 'NONE',  ( -16.53943276465976808, -0.05219959533934237506, 108.7510903946857042 ) ) ;
#84168 = CARTESIAN_POINT ( 'NONE',  ( -13.97604488694527625, -13.89961937509977652, 26.87390960531434558 ) ) ;
#84169 = CARTESIAN_POINT ( 'NONE',  ( 19.03943276465977164, 0.05219959533936151252, 21.25109039468565797 ) ) ;
#84170 = CARTESIAN_POINT ( 'NONE',  ( -0.05219959533936034679, 19.03943276465977164, 112.5010903946856757 ) ) ;
#84171 = CARTESIAN_POINT ( 'NONE',  ( 16.46253265017146816, 9.564922557961045513, 71.66775706135233293 ) ) ;
#84172 = CARTESIAN_POINT ( 'NONE',  ( 4.483927247898545687, 16.52544592524342804, 69.79057627198102409 ) ) ;
#84173 = CARTESIAN_POINT ( 'NONE',  ( -16.51473224551069308, -9.474510206698971260, 36.66557627198102409 ) ) ;
#84175 = CARTESIAN_POINT ( 'NONE',  ( 17.31747979337948706, -6.344076630961054342, 91.12055131934815222 ) ) ;
#84174 = CARTESIAN_POINT ( 'NONE',  ( 16.51473224551083163, -9.474510206698727899, 70.83442372801900433 ) ) ;
#84176 = CARTESIAN_POINT ( 'NONE',  ( -21.53943276465977519, -0.05219959533937600094, 83.75109039468568994 ) ) ;
#84177 = CARTESIAN_POINT ( 'NONE',  ( -12.06949235617739369, -12.14591786802326823, 39.37609039468567573 ) ) ;
#84178 = CARTESIAN_POINT ( 'NONE',  ( -29.82770300773734107, -26.65766548392525692, -16.82146946961924527 ) ) ;
#84179 = CARTESIAN_POINT ( 'NONE',  ( 15.80617190586746368, 15.72974639402197994, 34.37390960531435979 ) ) ;
#84180 = CARTESIAN_POINT ( 'NONE',  ( -12.14591786802326823, 12.06949235617739902, 23.12609039468567573 ) ) ;
#84181 = CARTESIAN_POINT ( 'NONE',  ( -5.049401038298153566, 19.05341960407611168, 115.2072429386477097 ) ) ;
#84182 = FACE_OUTER_BOUND ( 'NONE', #113390, .T. ) ;
#84183 = CARTESIAN_POINT ( 'NONE',  ( 13.97604488694527802, 13.89961937509977652, 34.37390960531436690 ) ) ;
#84184 = CARTESIAN_POINT ( 'NONE',  ( -20.00321537600460431, -21.32363904033505975, -52.29808436870553123 ) ) ;
#84185 = CARTESIAN_POINT ( 'NONE',  ( -13.89961937509977652, 13.97604488694528158, 55.62390960531434558 ) ) ;
#84186 = CARTESIAN_POINT ( 'NONE',  ( 15.80617190586769283, -15.72974639402175789, 60.62609039468567573 ) ) ;
#84187 = CARTESIAN_POINT ( 'NONE',  ( 15.80617190586769283, -15.72974639402175789, 105.6260903946856899 ) ) ;
#84188 = CARTESIAN_POINT ( 'NONE',  ( -0.05219959533910754901, -16.53943276465976808, 22.49890960531436335 ) ) ;
#84189 = CARTESIAN_POINT ( 'NONE',  ( 19.05341960407611168, 5.049401038298154454, 33.95724293864769550 ) ) ;
#84190 = CARTESIAN_POINT ( 'NONE',  ( -9.474510206698964154, 16.51473224551069663, 95.41557627198102409 ) ) ;
#84191 = CARTESIAN_POINT ( 'NONE',  ( -5.719274019375665041, -21.55341960407619695, 54.79275706135235424 ) ) ;
#84192 = CARTESIAN_POINT ( 'NONE',  ( -0.05219959533909027116, -19.03943276465977164, 42.49890960531435269 ) ) ;
#84193 = CARTESIAN_POINT ( 'NONE',  ( 5.823673210054444382, -21.52544592524334988, 65.20942372801901854 ) ) ;
#84195 = CARTESIAN_POINT ( 'NONE',  ( -13.89961937509977652, 13.97604488694528158, 110.6239096053143243 ) ) ;
#84194 = CARTESIAN_POINT ( 'NONE',  ( -9.474510206698720793, -16.51473224551083518, 94.58442372801900433 ) ) ;
#84196 = CARTESIAN_POINT ( 'NONE',  ( 19.05341960407611168, 5.049401038298154454, 28.95724293864769550 ) ) ;
#84197 = CARTESIAN_POINT ( 'NONE',  ( 5.719274019375991003, -21.55341960407610458, 107.7072429386476955 ) ) ;
#84198 = CARTESIAN_POINT ( 'NONE',  ( 9.564922557961047289, -16.46253265017146816, 30.41775706135232937 ) ) ;
#84199 = CARTESIAN_POINT ( 'NONE',  ( -4.379528057220328563, 16.55341960407611168, 105.2072429386477097 ) ) ;
#84200 = CARTESIAN_POINT ( 'NONE',  ( -13.89961937509977652, 13.97604488694528158, 60.62390960531436690 ) ) ;
#84201 = CARTESIAN_POINT ( 'NONE',  ( -16.46253265017146816, -9.564922557961047289, 94.16775706135233293 ) ) ;
#84202 = CARTESIAN_POINT ( 'NONE',  ( -16.53943276465976808, 0.05219959533911058130, 61.24890960531435979 ) ) ;
#84203 = CARTESIAN_POINT ( 'NONE',  ( 19.05341960407617918, -5.049401038297876454, 21.04275706135232582 ) ) ;
#84204 = CARTESIAN_POINT ( 'NONE',  ( 16.46253265017160672, -9.564922557960803928, 113.3322429386476955 ) ) ;
#84205 = CARTESIAN_POINT ( 'NONE',  ( -5.153800228976607833, 19.02544592524334988, 87.70942372801897591 ) ) ;
#84206 = CARTESIAN_POINT ( 'NONE',  ( -5.823673210054116645, -21.52544592524344225, 97.29057627198105251 ) ) ;
#84207 = CARTESIAN_POINT ( 'NONE',  ( 5.823673210054444382, -21.52544592524334988, 40.20942372801901854 ) ) ;
#84208 = CARTESIAN_POINT ( 'NONE',  ( -4.379528057220086978, -16.55341960407618274, 44.79275706135234714 ) ) ;
#84209 = CARTESIAN_POINT ( 'NONE',  ( 16.55341960407618274, -4.379528057220086978, 111.0427570613523613 ) ) ;
#84211 = CARTESIAN_POINT ( 'NONE',  ( -15.80617190586768217, 15.72974639402176855, 48.12609039468568284 ) ) ;
#84210 = CARTESIAN_POINT ( 'NONE',  ( 8.314922557961029526, -14.29746914071037800, 35.41775706135234003 ) ) ;
#84212 = CARTESIAN_POINT ( 'NONE',  ( -18.67979575497178146, -10.72451020669898902, 51.66557627198102409 ) ) ;
#84213 = CARTESIAN_POINT ( 'NONE',  ( 19.05341960407611168, 5.049401038298154454, 28.95724293864769550 ) ) ;
#84214 = CARTESIAN_POINT ( 'NONE',  ( 30.74264578624800137, -22.33583958711395212, -4.949999994537626513 ) ) ;
#84215 = CARTESIAN_POINT ( 'NONE',  ( 14.29746914071037800, 8.314922557961029526, 76.66775706135234714 ) ) ;
#84216 = EDGE_CURVE ( 'NONE', #134048, #103535, #35073, .T. ) ;
#84217 = CARTESIAN_POINT ( 'NONE',  ( 21.53943276465977519, -0.05219959533907433946, 93.74890960531436690 ) ) ;
#84218 = CARTESIAN_POINT ( 'NONE',  ( 16.55341960407611168, 4.379528057220329451, 33.95724293864769550 ) ) ;
#84219 = CARTESIAN_POINT ( 'NONE',  ( -16.52544592524335698, -4.483927247898792601, 68.95942372801901854 ) ) ;
#84220 = CARTESIAN_POINT ( 'NONE',  ( -9.474510206698720793, -16.51473224551083518, 104.5844237280190043 ) ) ;
#84221 = CARTESIAN_POINT ( 'NONE',  ( -21.55341960407610458, -5.719274019375992779, 101.4572429386476955 ) ) ;
#84222 = CARTESIAN_POINT ( 'NONE',  ( -12.06949235617756955, 12.14591786802309770, 35.62390960531437401 ) ) ;
#84223 = ORIENTED_EDGE ( 'NONE', *, *, #150915, .T. ) ;
#84224 = CARTESIAN_POINT ( 'NONE',  ( -14.29746914071037622, -8.314922557961029526, 84.16775706135234714 ) ) ;
#84225 = CARTESIAN_POINT ( 'NONE',  ( 26.70292545465260048, 6.820347898102890660, 168.5277281069536741 ) ) ;
#84226 = CARTESIAN_POINT ( 'NONE',  ( 5.823673210054125526, 21.52544592524343514, 74.79057627198105251 ) ) ;
#84227 = VERTEX_POINT ( 'NONE', #152485 ) ;
#84228 = CARTESIAN_POINT ( 'NONE',  ( 12.06949235617739724, 12.14591786802326823, 101.8760903946857042 ) ) ;
#84229 = VERTEX_POINT ( 'NONE', #198998 ) ;
#84230 = DIRECTION ( 'NONE',  ( 0.8660254037844410391, -0.000000000000000000, -0.4999999999999958367 ) ) ;
#84231 = CARTESIAN_POINT ( 'NONE',  ( 0.05219959533907565091, 21.53943276465977519, 89.99890960531438111 ) ) ;
#84232 = CARTESIAN_POINT ( 'NONE',  ( -18.67979575497178146, -10.72451020669898902, 106.6655762719810383 ) ) ;
#84233 = CARTESIAN_POINT ( 'NONE',  ( 16.52544592524342804, -4.483927247898539470, 38.54057627198103120 ) ) ;
#84234 = CARTESIAN_POINT ( 'NONE',  ( 0.05219959533934541429, -16.53943276465976808, 30.00109039468568284 ) ) ;
#84235 = CARTESIAN_POINT ( 'NONE',  ( -13.89961937509977652, 13.97604488694528158, 45.62390960531433848 ) ) ;
#84236 = CARTESIAN_POINT ( 'NONE',  ( -9.474510206698964154, 16.51473224551069663, 70.41557627198102409 ) ) ;
#84237 = VERTEX_POINT ( 'NONE', #13972 ) ;
#84238 = CARTESIAN_POINT ( 'NONE',  ( -10.81492255796078084, -18.62759615963271287, 27.08224293864769550 ) ) ;
#84239 = CARTESIAN_POINT ( 'NONE',  ( -0.05219959533909027116, -19.03943276465977164, 112.4989096053143669 ) ) ;
#84240 = CARTESIAN_POINT ( 'NONE',  ( -13.89961937509957401, -13.97604488694547875, 99.37609039468567573 ) ) ;
#84241 = CARTESIAN_POINT ( 'NONE',  ( 19.03943276465977164, 0.05219959533936151252, 51.25109039468567573 ) ) ;
#84242 = CARTESIAN_POINT ( 'NONE',  ( -18.62759615963270932, 10.81492255796079327, 90.83224293864769550 ) ) ;
#84243 = CARTESIAN_POINT ( 'NONE',  ( -8.314922557961024197, 14.29746914071037800, 107.9177570613523471 ) ) ;
#84244 = CARTESIAN_POINT ( 'NONE',  ( -18.62759615963270932, 10.81492255796079327, 50.83224293864770971 ) ) ;
#84246 = CARTESIAN_POINT ( 'NONE',  ( 9.564922557961047289, -16.46253265017146816, 100.4177570613523329 ) ) ;
#84245 = CARTESIAN_POINT ( 'NONE',  ( -18.62759615963270932, 10.81492255796079327, 75.83224293864769550 ) ) ;
#84247 = CARTESIAN_POINT ( 'NONE',  ( 16.51473224551069308, 9.474510206698969483, 104.1655762719810241 ) ) ;
#84248 = CARTESIAN_POINT ( 'NONE',  ( 5.823673210054444382, -21.52544592524334988, 70.20942372801904696 ) ) ;
#84249 = CARTESIAN_POINT ( 'NONE',  ( 13.97604488694527802, 13.89961937509977652, 69.37390960531436690 ) ) ;
#84250 = CARTESIAN_POINT ( 'NONE',  ( 31.25711108810727623, 6.845500155895383187, 98.07395821223764187 ) ) ;
#84251 = CARTESIAN_POINT ( 'NONE',  ( -16.51473224551069308, -9.474510206698971260, 66.66557627198102409 ) ) ;
#84252 = CARTESIAN_POINT ( 'NONE',  ( 16.52544592524342804, -4.483927247898539470, 93.54057627198103830 ) ) ;
#84253 = ORIENTED_EDGE ( 'NONE', *, *, #45012, .F. ) ;
#84254 = CARTESIAN_POINT ( 'NONE',  ( -16.51473224551082808, 9.474510206698731452, 108.3344237280190043 ) ) ;
#84255 = CARTESIAN_POINT ( 'NONE',  ( 16.62475595723694965, -7.163666690055372044, 83.02713351810466236 ) ) ;
#84256 = CARTESIAN_POINT ( 'NONE',  ( 5.153800228976335163, 19.02544592524342804, 74.79057627198103830 ) ) ;
#84258 = CARTESIAN_POINT ( 'NONE',  ( 19.03943276465977164, -0.05219959533909143690, 93.74890960531435269 ) ) ;
#84257 = CARTESIAN_POINT ( 'NONE',  ( -21.55341960407619339, 5.719274019375674811, 78.54275706135236135 ) ) ;
#84259 = CARTESIAN_POINT ( 'NONE',  ( 16.52544592524335698, 4.483927247898782831, 71.45942372801901854 ) ) ;
#84260 = CARTESIAN_POINT ( 'NONE',  ( -16.20579543436678094, -7.371946100355095233, 75.56520834171877254 ) ) ;
#84261 = B_SPLINE_CURVE_WITH_KNOTS ( 'NONE', 3,
 ( #10453, #28619, #58927, #56955, #182290, #43770, #26625, #105434, #88268, #167119, #109400, #61891, #1214, #31576 ),
 .UNSPECIFIED., .F., .F.,
 ( 4, 2, 2, 2, 2, 2, 4 ),
 ( 0.000000000000000000, 0.05072380597786840806, 0.1014476119557368161, 0.2028952239114668876, 0.4057904478229276135, 0.6086856717343883671, 0.8115808956458491208 ),
 .UNSPECIFIED. ) ;
#84262 = CARTESIAN_POINT ( 'NONE',  ( 16.51473224551083163, -9.474510206698727899, 50.83442372801899722 ) ) ;
#84263 = CARTESIAN_POINT ( 'NONE',  ( 5.153800228976615827, -19.02544592524334988, 20.20942372801899722 ) ) ;
#84264 = DIRECTION ( 'NONE',  ( 1.000000000000000000, 0.000000000000000000, 0.000000000000000000 ) ) ;
#84265 = CARTESIAN_POINT ( 'NONE',  ( -38.00000000000000711, 2.428612866367529932E-14, -7.749999994537626336 ) ) ;
#84266 = CARTESIAN_POINT ( 'NONE',  ( 36.91746824999999177, 2.880721459617395097E-14, -2.124999997268813168 ) ) ;
#84267 = CARTESIAN_POINT ( 'NONE',  ( 8.224510206698953496, -14.34966873604960469, 22.91557627198102765 ) ) ;
#84268 = CARTESIAN_POINT ( 'NONE',  ( -34.38809498607734838, -6.739667044264582074, 48.29962152465627412 ) ) ;
#84269 = CARTESIAN_POINT ( 'NONE',  ( 12.14591786802327356, -12.06949235617739191, 90.62609039468567573 ) ) ;
#84270 = CARTESIAN_POINT ( 'NONE',  ( -35.99626262588765968, 2.428612866367529932E-14, 2.000000000000000000 ) ) ;
#84271 = CARTESIAN_POINT ( 'NONE',  ( -0.05219959533934338120, 16.53943276465976808, 62.50109039468568284 ) ) ;
#84272 = CARTESIAN_POINT ( 'NONE',  ( -5.719274019375665041, -21.55341960407619695, 74.79275706135234714 ) ) ;
#84273 = CARTESIAN_POINT ( 'NONE',  ( 16.46253265017146816, 9.564922557961045513, 86.66775706135233293 ) ) ;
#84274 = CARTESIAN_POINT ( 'NONE',  ( 9.474510206698729675, 16.51473224551082808, 37.08442372801899722 ) ) ;
#84275 = CARTESIAN_POINT ( 'NONE',  ( 16.51473224551069308, 9.474510206698969483, 84.16557627198102409 ) ) ;
#84276 = CARTESIAN_POINT ( 'NONE',  ( 13.97604488694527802, 13.89961937509977652, 54.37390960531435979 ) ) ;
#84277 = CARTESIAN_POINT ( 'NONE',  ( 5.049401038298163336, -19.05341960407611168, 87.70724293864769550 ) ) ;
#84278 = CARTESIAN_POINT ( 'NONE',  ( -5.823673210054116645, -21.52544592524344225, 87.29057627198103830 ) ) ;
#84279 = CARTESIAN_POINT ( 'NONE',  ( 21.53943276465977519, -0.05219959533907433946, 48.74890960531435979 ) ) ;
#84280 = CARTESIAN_POINT ( 'NONE',  ( 16.46253265017160672, -9.564922557960803928, 33.33224293864770260 ) ) ;
#84281 = CARTESIAN_POINT ( 'NONE',  ( -4.483927247898782831, 16.52544592524335698, 57.70942372801901143 ) ) ;
#84282 = ADVANCED_FACE ( 'NONE', ( #75639 ), #45318, .T. ) ;
#84283 = UNCERTAINTY_MEASURE_WITH_UNIT (LENGTH_MEASURE( 1.000000000000000082E-05 ), #177880, 'distance_accuracy_value', 'NONE');
#84284 = ORIENTED_EDGE ( 'NONE', *, *, #117196, .T. ) ;
#84285 = CARTESIAN_POINT ( 'NONE',  ( 18.67979575497194134, -10.72451020669871369, 50.83442372801901143 ) ) ;
#84287 = CARTESIAN_POINT ( 'NONE',  ( 30.74264578624800137, -22.33583958711395212, -1.200000000000000178 ) ) ;
#84286 = CARTESIAN_POINT ( 'NONE',  ( 0.05219959533910956823, 16.53943276465976808, 59.99890960531436690 ) ) ;
#84288 = CARTESIAN_POINT ( 'NONE',  ( -0.05219959533934338120, 16.53943276465976808, 42.50109039468567573 ) ) ;
#84289 = CARTESIAN_POINT ( 'NONE',  ( -16.53943276465976808, 0.05219959533911058130, 106.2489096053143811 ) ) ;
#84290 = CARTESIAN_POINT ( 'NONE',  ( -13.97604488694547697, 13.89961937509957934, 48.12609039468566863 ) ) ;
#84291 = CARTESIAN_POINT ( 'NONE',  ( 0.05219959533910956823, 16.53943276465976808, 59.99890960531436690 ) ) ;
#84292 = CARTESIAN_POINT ( 'NONE',  ( -5.823673210054431948, 21.52544592524334988, 27.70942372801901854 ) ) ;
#84294 = CARTESIAN_POINT ( 'NONE',  ( -18.62759615963270932, 10.81492255796079327, 90.83224293864769550 ) ) ;
#84293 = CARTESIAN_POINT ( 'NONE',  ( -16.51473224551069308, -9.474510206698971260, 26.66557627198103120 ) ) ;
#84295 = CARTESIAN_POINT ( 'NONE',  ( -16.46253265017160317, 9.564922557960807481, 105.8322429386476955 ) ) ;
#84296 = CARTESIAN_POINT ( 'NONE',  ( 0.05219959533910956823, 16.53943276465976808, 74.99890960531435269 ) ) ;
#84297 = CARTESIAN_POINT ( 'NONE',  ( -19.05341960407611168, -5.049401038298163336, 111.4572429386476671 ) ) ;
#84298 = CARTESIAN_POINT ( 'NONE',  ( -11.40812507854754720, -35.11059874428192273, -2.224999997268813701 ) ) ;
#84299 = CARTESIAN_POINT ( 'NONE',  ( 9.474510206698729675, 16.51473224551082808, 82.08442372801899012 ) ) ;
#84300 = CARTESIAN_POINT ( 'NONE',  ( 5.823673210054444382, -21.52544592524334988, 25.20942372801901854 ) ) ;
#84301 = CARTESIAN_POINT ( 'NONE',  ( -19.03943276465977164, 0.05219959533909376836, 71.24890960531435269 ) ) ;
#84302 = CARTESIAN_POINT ( 'NONE',  ( -16.51473224551082808, 9.474510206698731452, 58.33442372801900433 ) ) ;
#84303 = CARTESIAN_POINT ( 'NONE',  ( -0.05219959533909027116, -19.03943276465977164, 32.49890960531435979 ) ) ;
#84304 = CARTESIAN_POINT ( 'NONE',  ( 10.72451020669871369, 18.67979575497193778, 62.08442372801901143 ) ) ;
#84305 = FACE_OUTER_BOUND ( 'NONE', #174388, .T. ) ;
#84306 = CARTESIAN_POINT ( 'NONE',  ( 4.379528057220339221, -16.55341960407611168, 52.70724293864769550 ) ) ;
#84307 = CARTESIAN_POINT ( 'NONE',  ( -13.89961937509977652, 13.97604488694528158, 60.62390960531436690 ) ) ;
#84308 = CARTESIAN_POINT ( 'NONE',  ( 18.67979575497178502, 10.72451020669898547, 94.16557627198103830 ) ) ;
#84309 = CARTESIAN_POINT ( 'NONE',  ( 5.049401038298161559, -19.05341960407611168, 52.70724293864767418 ) ) ;
#84310 = VERTEX_POINT ( 'NONE', #91784 ) ;
#84311 = CARTESIAN_POINT ( 'NONE',  ( -21.53943276465977519, 0.05219959533907696930, 86.24890960531436690 ) ) ;
#84312 = CARTESIAN_POINT ( 'NONE',  ( 10.72451020669871369, 18.67979575497193778, 97.08442372801904696 ) ) ;
#84315 = CARTESIAN_POINT ( 'NONE',  ( -16.52544592524342804, 4.483927247898546575, 96.04057627198102409 ) ) ;
#84314 = CARTESIAN_POINT ( 'NONE',  ( -0.05219959533934338120, 16.53943276465976808, 102.5010903946856899 ) ) ;
#84313 = CARTESIAN_POINT ( 'NONE',  ( 19.05341960407611168, 5.049401038298154454, 23.95724293864769194 ) ) ;
#84316 = CARTESIAN_POINT ( 'NONE',  ( 5.049401038297881783, 19.05341960407617563, 92.29275706135234714 ) ) ;
#84317 = ORIENTED_EDGE ( 'NONE', *, *, #95584, .T. ) ;
#84318 = CARTESIAN_POINT ( 'NONE',  ( -15.72974639402176322, -15.80617190586768395, 19.37609039468568639 ) ) ;
#84319 = CARTESIAN_POINT ( 'NONE',  ( 5.153800228976615827, -19.02544592524334988, 35.20942372801899722 ) ) ;
#84320 = CARTESIAN_POINT ( 'NONE',  ( 16.55341960407618274, -4.379528057220086978, 101.0427570613523756 ) ) ;
#84321 = CARTESIAN_POINT ( 'NONE',  ( 0.05219959533936267826, -19.03943276465977164, 25.00109039468566152 ) ) ;
#84322 = CARTESIAN_POINT ( 'NONE',  ( 19.02544592524343514, -5.153800228976328945, 103.5405762719809957 ) ) ;
#84323 = CARTESIAN_POINT ( 'NONE',  ( -10.81492255796078084, -18.62759615963271287, 67.08224293864770971 ) ) ;
#84324 = LINE ( 'NONE', #191516, #66935 ) ;
#84325 = CARTESIAN_POINT ( 'NONE',  ( 16.55341960407611168, 4.379528057220329451, 113.9572429386477239 ) ) ;
#84326 = CARTESIAN_POINT ( 'NONE',  ( -15.80617190586768217, 15.72974639402176855, 108.1260903946856757 ) ) ;
#84327 = CARTESIAN_POINT ( 'NONE',  ( -14.34966873604972548, 8.224510206698743886, 73.33442372801901854 ) ) ;
#84328 = CARTESIAN_POINT ( 'NONE',  ( -18.67979575497193778, 10.72451020669871902, 23.33442372801901499 ) ) ;
#84329 = CARTESIAN_POINT ( 'NONE',  ( -4.379528057220086978, -16.55341960407618274, 49.79275706135234714 ) ) ;
#84330 = CARTESIAN_POINT ( 'NONE',  ( 13.97604488694527802, 13.89961937509977652, 99.37390960531436690 ) ) ;
#84331 = CARTESIAN_POINT ( 'NONE',  ( -19.05341960407611168, -5.049401038298163336, 46.45724293864768129 ) ) ;
#84332 = CARTESIAN_POINT ( 'NONE',  ( -9.474510206698964154, 16.51473224551069663, 65.41557627198102409 ) ) ;
#84333 = CARTESIAN_POINT ( 'NONE',  ( -14.34966873604972548, 8.224510206698743886, 48.33442372801902565 ) ) ;
#84334 = CARTESIAN_POINT ( 'NONE',  ( 8.224510206698953496, -14.34966873604960469, 92.91557627198103830 ) ) ;
#84335 = CARTESIAN_POINT ( 'NONE',  ( 8.224510206698742110, 14.34966873604972548, 97.08442372801904696 ) ) ;
#84336 = CARTESIAN_POINT ( 'NONE',  ( 17.59860650958989936, 7.585241751807028088, 49.07662985737507455 ) ) ;
#84339 = CARTESIAN_POINT ( 'NONE',  ( -5.049401038298153566, 19.05341960407611168, 65.20724293864765286 ) ) ;
#84338 = CARTESIAN_POINT ( 'NONE',  ( 19.05341960407611168, 5.049401038298154454, 73.95724293864768129 ) ) ;
#84337 = CARTESIAN_POINT ( 'NONE',  ( 5.719274019375673035, 21.55341960407619339, 52.29275706135236135 ) ) ;
#84340 = CARTESIAN_POINT ( 'NONE',  ( -5.049401038298153566, 19.05341960407611168, 100.2072429386476955 ) ) ;
#84341 = CARTESIAN_POINT ( 'NONE',  ( 8.314922557960818139, 14.29746914071049879, 44.58224293864769550 ) ) ;
#84342 = CARTESIAN_POINT ( 'NONE',  ( -8.314922557961024197, 14.29746914071037800, 102.9177570613523756 ) ) ;
#84343 = CARTESIAN_POINT ( 'NONE',  ( -0.05219959533910754901, -16.53943276465976808, 27.49890960531435269 ) ) ;
#84344 = EDGE_LOOP ( 'NONE', ( #160083, #87947, #35564, #146092 ) ) ;
#84345 = CARTESIAN_POINT ( 'NONE',  ( -13.97604488694547697, 13.89961937509957934, 48.12609039468566863 ) ) ;
#84346 = CARTESIAN_POINT ( 'NONE',  ( -5.049401038298153566, 19.05341960407611168, 110.2072429386476671 ) ) ;
#84347 = CARTESIAN_POINT ( 'NONE',  ( -13.89961937509977652, 13.97604488694528158, 60.62390960531436690 ) ) ;
#84348 = CARTESIAN_POINT ( 'NONE',  ( -13.97604488694547697, 13.89961937509957934, 33.12609039468566863 ) ) ;
#84349 = CARTESIAN_POINT ( 'NONE',  ( 36.91746824999999887, 11.99521256947799053, -5.524999997268812635 ) ) ;
#84350 = CARTESIAN_POINT ( 'NONE',  ( 18.22780087662122384, -5.500000000000022204, 71.01540105326107266 ) ) ;
#84352 = CARTESIAN_POINT ( 'NONE',  ( 4.483927247898790824, -16.52544592524335698, 70.20942372801904696 ) ) ;
#84351 = CARTESIAN_POINT ( 'NONE',  ( -13.89961937509957401, -13.97604488694547875, 69.37609039468564731 ) ) ;
#84353 = DIRECTION ( 'NONE',  ( 0.4999999999999978906, -0.5000000000000033307, 0.7071067811865466846 ) ) ;
#84354 = CARTESIAN_POINT ( 'NONE',  ( -13.89961937509977652, 13.97604488694528158, 85.62390960531433848 ) ) ;
#84355 = CARTESIAN_POINT ( 'NONE',  ( 21.52544592524334988, 5.823673210054432836, 31.45942372801901854 ) ) ;
#84356 = CARTESIAN_POINT ( 'NONE',  ( 16.51473224551083163, -9.474510206698727899, 80.83442372801899012 ) ) ;
#84358 = CARTESIAN_POINT ( 'NONE',  ( 13.97604488694527802, 13.89961937509977652, 29.37390960531435979 ) ) ;
#84357 = CARTESIAN_POINT ( 'NONE',  ( -5.049401038298153566, 19.05341960407611168, 115.2072429386477097 ) ) ;
#84359 = CARTESIAN_POINT ( 'NONE',  ( 5.153800228976335163, 19.02544592524342804, 89.79057627198102409 ) ) ;
#84361 = CARTESIAN_POINT ( 'NONE',  ( -0.05219959533909027116, -19.03943276465977164, 37.49890960531436690 ) ) ;
#84360 = CARTESIAN_POINT ( 'NONE',  ( 14.34966873604960469, 8.224510206698951720, 44.16557627198103120 ) ) ;
#84362 = CARTESIAN_POINT ( 'NONE',  ( -16.51473224551082808, 9.474510206698731452, 48.33442372801900433 ) ) ;
#84363 = ORIENTED_EDGE ( 'NONE', *, *, #180435, .F. ) ;
#84364 = CARTESIAN_POINT ( 'NONE',  ( -12.14591786802309592, -12.06949235617757132, 81.87390960531435269 ) ) ;
#84365 = CARTESIAN_POINT ( 'NONE',  ( 13.89961937509957401, 13.97604488694547697, 31.87609039468566863 ) ) ;
#84366 = CARTESIAN_POINT ( 'NONE',  ( -19.05341960407611168, -5.049401038298163336, 56.45724293864768129 ) ) ;
#84367 = CARTESIAN_POINT ( 'NONE',  ( 0.05219959533907565091, 21.53943276465977519, 64.99890960531435269 ) ) ;
#84369 = CARTESIAN_POINT ( 'NONE',  ( 21.55341960407619695, -5.719274019375665929, 111.0427570613523613 ) ) ;
#84368 = CARTESIAN_POINT ( 'NONE',  ( 8.314922557960818139, 14.29746914071049879, 59.58224293864770260 ) ) ;
#84370 = CARTESIAN_POINT ( 'NONE',  ( 13.89961937509977652, -13.97604488694527269, 108.1239096053143669 ) ) ;
#84371 = CARTESIAN_POINT ( 'NONE',  ( 10.81492255796078972, 18.62759615963270932, 24.58224293864768839 ) ) ;
#84372 = CARTESIAN_POINT ( 'NONE',  ( 9.474510206698971260, -16.51473224551069308, 52.91557627198102409 ) ) ;
#84373 = CARTESIAN_POINT ( 'NONE',  ( -19.05341960407611168, -5.049401038298163336, 26.45724293864769550 ) ) ;
#84374 = CARTESIAN_POINT ( 'NONE',  ( 0.05219959533910956823, 16.53943276465976808, 89.99890960531438111 ) ) ;
#84375 = CARTESIAN_POINT ( 'NONE',  ( -18.62759615963270932, 10.81492255796079327, 95.83224293864770971 ) ) ;
#84376 = CARTESIAN_POINT ( 'NONE',  ( -19.05341960407611168, -5.049401038298163336, 96.45724293864769550 ) ) ;
#84377 = CARTESIAN_POINT ( 'NONE',  ( -10.72451020669898014, 18.67979575497178502, 105.4155762719810383 ) ) ;
#84378 = CARTESIAN_POINT ( 'NONE',  ( 13.97604488694527802, 13.89961937509977652, 104.3739096053143385 ) ) ;
#84379 = CARTESIAN_POINT ( 'NONE',  ( 0.05219959533909260263, 19.03943276465977164, 24.99890960531435269 ) ) ;
#84380 = CARTESIAN_POINT ( 'NONE',  ( -10.81492255796105439, 18.62759615963255655, 82.91775706135234714 ) ) ;
#84381 = CARTESIAN_POINT ( 'NONE',  ( 5.823673210054125526, 21.52544592524343514, 94.79057627198105251 ) ) ;
#84382 = CARTESIAN_POINT ( 'NONE',  ( 16.79531203550646978, -7.028104445595627858, 106.2475501177955977 ) ) ;
#84383 = CARTESIAN_POINT ( 'NONE',  ( -17.59860650958989936, -7.585241751807033417, 51.57662985737508876 ) ) ;
#84384 = CARTESIAN_POINT ( 'NONE',  ( 30.26186088262144835, -1.502453648625374116, -51.11561252063852834 ) ) ;
#84385 = CARTESIAN_POINT ( 'NONE',  ( -4.483927247898782831, 16.52544592524335698, 37.70942372801900433 ) ) ;
#84386 = CARTESIAN_POINT ( 'NONE',  ( -12.14591786802309592, -12.06949235617757132, 111.8739096053143669 ) ) ;
#84387 = DIRECTION ( 'NONE',  ( -0.000000000000000000, -0.000000000000000000, 1.000000000000000000 ) ) ;
#84388 = CARTESIAN_POINT ( 'NONE',  ( -19.02544592524342804, 5.153800228976336051, 61.04057627198103120 ) ) ;
#84390 = EDGE_CURVE ( 'NONE', #76158, #16157, #183613, .T. ) ;
#84389 = CARTESIAN_POINT ( 'NONE',  ( -16.53943276465976808, 0.05219959533911058130, 91.24890960531436690 ) ) ;
#84391 = CARTESIAN_POINT ( 'NONE',  ( 15.72974639402199770, -15.80617190586745480, 38.12390960531436690 ) ) ;
#84392 = CARTESIAN_POINT ( 'NONE',  ( -16.52544592524342804, 4.483927247898546575, 61.04057627198103120 ) ) ;
#84393 = CARTESIAN_POINT ( 'NONE',  ( -4.483927247898782831, 16.52544592524335698, 22.70942372801901499 ) ) ;
#84394 = CARTESIAN_POINT ( 'NONE',  ( -5.823673210054431948, 21.52544592524334988, 67.70942372801901854 ) ) ;
#84395 = CARTESIAN_POINT ( 'NONE',  ( -4.429638872090642462E-30, -165.0000000000000000, -13.00000000000000000 ) ) ;
#84396 = CARTESIAN_POINT ( 'NONE',  ( -13.89961937509977652, 13.97604488694528158, 115.6239096053143669 ) ) ;
#84397 = CARTESIAN_POINT ( 'NONE',  ( 16.52544592524335698, 4.483927247898782831, 91.45942372801901854 ) ) ;
#84398 = CARTESIAN_POINT ( 'NONE',  ( -16.51473224551069308, -9.474510206698971260, 36.66557627198102409 ) ) ;
#84399 = CARTESIAN_POINT ( 'NONE',  ( -5.049401038298153566, 19.05341960407611168, 95.20724293864770971 ) ) ;
#84400 = CARTESIAN_POINT ( 'NONE',  ( 5.719274019375991003, -21.55341960407610458, 97.70724293864772392 ) ) ;
#84401 = CARTESIAN_POINT ( 'NONE',  ( -0.05219959533934338120, 16.53943276465976808, 22.50109039468567573 ) ) ;
#84403 = CARTESIAN_POINT ( 'NONE',  ( -10.72451020669870658, -18.67979575497194134, 74.58442372801901854 ) ) ;
#84402 = CARTESIAN_POINT ( 'NONE',  ( 12.06949235617757843, -12.14591786802309237, 68.12390960531436690 ) ) ;
#84404 = CARTESIAN_POINT ( 'NONE',  ( -8.224510206698735004, -14.34966873604973081, 104.5844237280190185 ) ) ;
#84405 = CARTESIAN_POINT ( 'NONE',  ( 17.31728774477273092, 6.344390552232404445, 26.68093348310682345 ) ) ;
#84406 = CARTESIAN_POINT ( 'NONE',  ( 1.300000000000000044, -1.443375672974063884, -3.691112476943992763E-18 ) ) ;
#84407 = CARTESIAN_POINT ( 'NONE',  ( -0.05219959533910754901, -16.53943276465976808, 32.49890960531435979 ) ) ;
#84408 = CARTESIAN_POINT ( 'NONE',  ( 14.34966873604972726, -8.224510206698740333, 70.83442372801901854 ) ) ;
#84409 = CARTESIAN_POINT ( 'NONE',  ( 0.05219959533909260263, 19.03943276465977164, 89.99890960531436690 ) ) ;
#84410 = CARTESIAN_POINT ( 'NONE',  ( -9.564922557960796823, -16.46253265017161027, 87.08224293864769550 ) ) ;
#84411 = CARTESIAN_POINT ( 'NONE',  ( 5.823673210054444382, -21.52544592524334988, 85.20942372801901854 ) ) ;
#84412 = CARTESIAN_POINT ( 'NONE',  ( 4.379528057220092307, 16.55341960407617563, 87.29275706135236135 ) ) ;
#84413 = CARTESIAN_POINT ( 'NONE',  ( 4.483927247898545687, 16.52544592524342804, 59.79057627198103120 ) ) ;
#84414 = CARTESIAN_POINT ( 'NONE',  ( -13.97604488694527625, -13.89961937509977652, 61.87390960531435979 ) ) ;
#84415 = ORIENTED_EDGE ( 'NONE', *, *, #110780, .T. ) ;
#84416 = CARTESIAN_POINT ( 'NONE',  ( -16.46253265017146816, -9.564922557961047289, 104.1677570613523329 ) ) ;
#84417 = CARTESIAN_POINT ( 'NONE',  ( 16.53943276465976808, -0.05219959533910856209, 103.7489096053143669 ) ) ;
#84418 = CARTESIAN_POINT ( 'NONE',  ( 19.02544592524343514, -5.153800228976328945, 83.54057627198100988 ) ) ;
#84420 = CARTESIAN_POINT ( 'NONE',  ( 36.91746825000000598, -11.99521256947793546, -7.724999997268812812 ) ) ;
#84419 = CARTESIAN_POINT ( 'NONE',  ( -16.51473224551082808, 9.474510206698731452, 108.3344237280190043 ) ) ;
#84421 = CARTESIAN_POINT ( 'NONE',  ( -9.564922557961040184, 16.46253265017147172, 22.91775706135233648 ) ) ;
#84422 = CARTESIAN_POINT ( 'NONE',  ( -14.29746914071037622, -8.314922557961029526, 84.16775706135234714 ) ) ;
#84423 = CARTESIAN_POINT ( 'NONE',  ( -13.89961937509957401, -13.97604488694547875, 89.37609039468563310 ) ) ;
#84424 = CARTESIAN_POINT ( 'NONE',  ( -0.05219959533909027116, -19.03943276465977164, 22.49890960531436690 ) ) ;
#84425 = CARTESIAN_POINT ( 'NONE',  ( -8.314922557961024197, 14.29746914071037800, 62.91775706135236135 ) ) ;
#84426 = DIRECTION ( 'NONE',  ( 0.000000000000000000, 0.000000000000000000, 1.000000000000000000 ) ) ;
#84427 = CARTESIAN_POINT ( 'NONE',  ( -16.51473224551082808, 9.474510206698731452, 58.33442372801900433 ) ) ;
#84428 = CARTESIAN_POINT ( 'NONE',  ( -18.62759615963255300, -10.81492255796106328, 99.16775706135234714 ) ) ;
#84429 = CARTESIAN_POINT ( 'NONE',  ( -19.05341960407611168, -5.049401038298163336, 36.45724293864766707 ) ) ;
#84430 = CARTESIAN_POINT ( 'NONE',  ( 19.03943276465977164, -0.05219959533909143690, 83.74890960531436690 ) ) ;
#84431 = CARTESIAN_POINT ( 'NONE',  ( 16.52544592524342804, -4.483927247898539470, 73.54057627198102409 ) ) ;
#84432 = CARTESIAN_POINT ( 'NONE',  ( -5.719274019375665041, -21.55341960407619695, 84.79275706135234714 ) ) ;
#84433 = CARTESIAN_POINT ( 'NONE',  ( 5.153800228976615827, -19.02544592524334988, 55.20942372801899722 ) ) ;
#84434 = CARTESIAN_POINT ( 'NONE',  ( -13.97604488694547697, 13.89961937509957934, 38.12609039468566152 ) ) ;
#84435 = CARTESIAN_POINT ( 'NONE',  ( -10.81492255796078084, -18.62759615963271287, 32.08224293864769550 ) ) ;
#84436 = CARTESIAN_POINT ( 'NONE',  ( -10.81492255796105439, 18.62759615963255655, 97.91775706135236135 ) ) ;
#84437 = CARTESIAN_POINT ( 'NONE',  ( -0.05219959533909027116, -19.03943276465977164, 82.49890960531436690 ) ) ;
#84438 = CARTESIAN_POINT ( 'NONE',  ( 15.72974639402176855, 15.80617190586768217, 106.8760903946856899 ) ) ;
#84439 = CARTESIAN_POINT ( 'NONE',  ( -15.80617190586745835, -15.72974639402198527, 46.87390960531435979 ) ) ;
#84440 = CARTESIAN_POINT ( 'NONE',  ( 19.05341960407611168, 5.049401038298154454, 93.95724293864769550 ) ) ;
#84441 = CARTESIAN_POINT ( 'NONE',  ( -13.97604488694547697, 13.89961937509957934, 73.12609039468568994 ) ) ;
#84442 = CARTESIAN_POINT ( 'NONE',  ( -19.02544592524342804, 5.153800228976336051, 101.0405762719810241 ) ) ;
#84443 = CARTESIAN_POINT ( 'NONE',  ( 16.46253265017146816, 9.564922557961045513, 96.66775706135233293 ) ) ;
#84444 = CARTESIAN_POINT ( 'NONE',  ( -4.483927247898782831, 16.52544592524335698, 37.70942372801900433 ) ) ;
#84445 = CARTESIAN_POINT ( 'NONE',  ( 8.314922557960818139, 14.29746914071049879, 99.58224293864770971 ) ) ;
#84446 = CARTESIAN_POINT ( 'NONE',  ( 13.97604488694527802, 13.89961937509977652, 79.37390960531435269 ) ) ;
#84447 = CARTESIAN_POINT ( 'NONE',  ( -5.719274019375978568, 21.55341960407610458, 60.20724293864768839 ) ) ;
#84448 = CARTESIAN_POINT ( 'NONE',  ( -14.34966873604972548, 8.224510206698743886, 33.33442372801900433 ) ) ;
#84449 = CARTESIAN_POINT ( 'NONE',  ( -10.72451020669870658, -18.67979575497194134, 39.58442372801901143 ) ) ;
#84450 = CARTESIAN_POINT ( 'NONE',  ( -18.62759615963255300, -10.81492255796106328, 84.16775706135234714 ) ) ;
#84451 = CARTESIAN_POINT ( 'NONE',  ( 16.52544592524335698, 4.483927247898782831, 81.45942372801900433 ) ) ;
#84452 = CARTESIAN_POINT ( 'NONE',  ( -16.46253265017160317, 9.564922557960807481, 80.83224293864769550 ) ) ;
#84453 = CARTESIAN_POINT ( 'NONE',  ( 16.53943276465976808, -0.05219959533910856209, 73.74890960531433848 ) ) ;
#84454 = CARTESIAN_POINT ( 'NONE',  ( 8.314922557961029526, -14.29746914071037800, 110.4177570613523756 ) ) ;
#84455 = CARTESIAN_POINT ( 'NONE',  ( -16.46253265017146816, -9.564922557961047289, 59.16775706135233293 ) ) ;
#84456 = CARTESIAN_POINT ( 'NONE',  ( 18.67979575497194134, -10.72451020669871369, 35.83442372801901143 ) ) ;
#84457 = CARTESIAN_POINT ( 'NONE',  ( 4.379528057220339221, -16.55341960407611168, 82.70724293864770971 ) ) ;
#84458 = CARTESIAN_POINT ( 'NONE',  ( 19.02544592524343514, -5.153800228976328945, 93.54057627198102409 ) ) ;
#84459 = CARTESIAN_POINT ( 'NONE',  ( -8.224510206698735004, -14.34966873604973081, 104.5844237280190185 ) ) ;
#84460 = CARTESIAN_POINT ( 'NONE',  ( 21.55341960407619695, -5.719274019375665929, 71.04275706135234714 ) ) ;
#84461 = CARTESIAN_POINT ( 'NONE',  ( -16.52544592524335698, -4.483927247898792601, 38.95942372801901854 ) ) ;
#84462 = CARTESIAN_POINT ( 'NONE',  ( 0.05219959533937995610, -21.53943276465977519, 35.00109039468568284 ) ) ;
#84463 = VERTEX_POINT ( 'NONE', #111946 ) ;
#84464 = CARTESIAN_POINT ( 'NONE',  ( -5.823673210054116645, -21.52544592524344225, 112.2905762719810241 ) ) ;
#84465 = CARTESIAN_POINT ( 'NONE',  ( -14.34966873604960291, -8.224510206698953496, 86.66557627198102409 ) ) ;
#84466 = CARTESIAN_POINT ( 'NONE',  ( -30.00000000000000000, -5.510910596163089556E-15, 45.00000000000000000 ) ) ;
#84467 = CARTESIAN_POINT ( 'NONE',  ( -4.483927247898539470, -16.52544592524342804, 52.29057627198102409 ) ) ;
#84468 = CARTESIAN_POINT ( 'NONE',  ( -5.153800228976328057, -19.02544592524343514, 22.29057627198102765 ) ) ;
#84469 = CARTESIAN_POINT ( 'NONE',  ( 15.72974639402199770, -15.80617190586745480, 43.12390960531435269 ) ) ;
#84470 = CARTESIAN_POINT ( 'NONE',  ( -8.314922557960811034, -14.29746914071050412, 77.08224293864769550 ) ) ;
#84471 = CARTESIAN_POINT ( 'NONE',  ( 0.05219959533907565091, 21.53943276465977519, 79.99890960531435269 ) ) ;
#84472 = CARTESIAN_POINT ( 'NONE',  ( -9.564922557960796823, -16.46253265017161027, 87.08224293864769550 ) ) ;
#84474 = CARTESIAN_POINT ( 'NONE',  ( 16.51473224551083163, -9.474510206698727899, 80.83442372801899012 ) ) ;
#84473 = CARTESIAN_POINT ( 'NONE',  ( -16.51473224551069308, -9.474510206698971260, 41.66557627198103120 ) ) ;
#84475 = EDGE_CURVE ( 'NONE', #107664, #139693, #42987, .T. ) ;
#84476 = CARTESIAN_POINT ( 'NONE',  ( -18.62759615963270932, 10.81492255796079327, 25.83224293864769194 ) ) ;
#84478 = CARTESIAN_POINT ( 'NONE',  ( -10.81492255796078084, -18.62759615963271287, 62.08224293864769550 ) ) ;
#84477 = CARTESIAN_POINT ( 'NONE',  ( -10.81492255796105439, 18.62759615963255655, 57.91775706135234714 ) ) ;
#84479 = CARTESIAN_POINT ( 'NONE',  ( -13.89961937509977652, 13.97604488694528158, 35.62390960531435269 ) ) ;
#84480 = CARTESIAN_POINT ( 'NONE',  ( 9.474510206698971260, -16.51473224551069308, 77.91557627198103830 ) ) ;
#84481 = ORIENTED_EDGE ( 'NONE', *, *, #171107, .T. ) ;
#84482 = CARTESIAN_POINT ( 'NONE',  ( -16.52544592524335698, -4.483927247898792601, 43.95942372801902565 ) ) ;
#84483 = CARTESIAN_POINT ( 'NONE',  ( 21.55341960407619695, -5.719274019375665929, 36.04275706135234714 ) ) ;
#84484 = CARTESIAN_POINT ( 'NONE',  ( 18.62759615963255655, 10.81492255796105972, 76.66775706135234714 ) ) ;
#84485 = CARTESIAN_POINT ( 'NONE',  ( -19.03943276465977164, 0.05219959533909376836, 116.2489096053143669 ) ) ;
#84486 = CARTESIAN_POINT ( 'NONE',  ( 5.719274019375991003, -21.55341960407610458, 92.70724293864770971 ) ) ;
#84488 = CARTESIAN_POINT ( 'NONE',  ( -4.379528057220086978, -16.55341960407618274, 49.79275706135234714 ) ) ;
#84487 = CARTESIAN_POINT ( 'NONE',  ( 5.719274019375673035, 21.55341960407619339, 27.29275706135234358 ) ) ;
#84489 = CARTESIAN_POINT ( 'NONE',  ( 5.823673210054125526, 21.52544592524343514, 64.79057627198103830 ) ) ;
#84490 = CARTESIAN_POINT ( 'NONE',  ( 21.55341960407619695, -5.719274019375665929, 111.0427570613523613 ) ) ;
#84491 = CARTESIAN_POINT ( 'NONE',  ( 19.05341960407611168, 5.049401038298154454, 58.95724293864768129 ) ) ;
#84492 = CARTESIAN_POINT ( 'NONE',  ( -19.02544592524342804, 5.153800228976336051, 111.0405762719810099 ) ) ;
#84493 = CARTESIAN_POINT ( 'NONE',  ( -0.05219959533909027116, -19.03943276465977164, 92.49890960531436690 ) ) ;
#84494 = CARTESIAN_POINT ( 'NONE',  ( 1.820000000000000062, -3.800000000000000266, -4.653657836759940757E-16 ) ) ;
#84495 = CARTESIAN_POINT ( 'NONE',  ( 19.03943276465977164, 0.05219959533936151252, 71.25109039468566152 ) ) ;
#84496 = CARTESIAN_POINT ( 'NONE',  ( -18.62759615963270932, 10.81492255796079327, 50.83224293864770971 ) ) ;
#84497 = CARTESIAN_POINT ( 'NONE',  ( -16.55341960407611168, -4.379528057220339221, 31.45724293864769550 ) ) ;
#84498 = CARTESIAN_POINT ( 'NONE',  ( -5.153800228976607833, 19.02544592524334988, 97.70942372801900433 ) ) ;
#84499 = CARTESIAN_POINT ( 'NONE',  ( -19.03943276465977164, 0.05219959533909376836, 21.24890960531436335 ) ) ;
#84500 = CARTESIAN_POINT ( 'NONE',  ( 13.89961937509957401, 13.97604488694547697, 21.87609039468566152 ) ) ;
#84501 = CARTESIAN_POINT ( 'NONE',  ( -16.46253265017146816, -9.564922557961047289, 94.16775706135233293 ) ) ;
#84503 = CARTESIAN_POINT ( 'NONE',  ( -19.05341960407617563, 5.049401038297882671, 58.54275706135234003 ) ) ;
#84502 = CARTESIAN_POINT ( 'NONE',  ( 5.719274019375991003, -21.55341960407610458, 82.70724293864770971 ) ) ;
#84504 = CARTESIAN_POINT ( 'NONE',  ( 16.62475595723699584, 7.163666690055298325, 106.9728664818953519 ) ) ;
#84505 = CARTESIAN_POINT ( 'NONE',  ( 0.05219959533909260263, 19.03943276465977164, 54.99890960531435979 ) ) ;
#84506 = CARTESIAN_POINT ( 'NONE',  ( 0.05219959533910956823, 16.53943276465976808, 59.99890960531436690 ) ) ;
#84507 = CARTESIAN_POINT ( 'NONE',  ( -19.02544592524342804, 5.153800228976336051, 51.04057627198103120 ) ) ;
#84508 = CARTESIAN_POINT ( 'NONE',  ( -12.14591786802309592, -12.06949235617757132, 51.87390960531437401 ) ) ;
#84509 = CARTESIAN_POINT ( 'NONE',  ( 30.73962218707677252, 22.33364281372847060, -6.547842220587804185 ) ) ;
#84510 = CARTESIAN_POINT ( 'NONE',  ( -16.55341960407611168, -4.379528057220339221, 26.45724293864768839 ) ) ;
#84511 = CARTESIAN_POINT ( 'NONE',  ( 16.51473224551069308, 9.474510206698969483, 59.16557627198102409 ) ) ;
#84512 = CARTESIAN_POINT ( 'NONE',  ( 9.474510206698729675, 16.51473224551082808, 32.08442372801900433 ) ) ;
#84513 = CARTESIAN_POINT ( 'NONE',  ( -16.53943276465976808, -0.05219959533934237506, 28.75109039468567929 ) ) ;
#84514 = CARTESIAN_POINT ( 'NONE',  ( -5.823673210054116645, -21.52544592524344225, 52.29057627198102409 ) ) ;
#84516 = EDGE_LOOP ( 'NONE', ( #5420, #74084, #155981, #198406, #112581 ) ) ;
#84515 = CARTESIAN_POINT ( 'NONE',  ( 21.53943276465977519, 0.05219959533937863772, 106.2510903946856757 ) ) ;
#84517 = CARTESIAN_POINT ( 'NONE',  ( 19.02544592524343514, -5.153800228976328945, 58.54057627198102409 ) ) ;
#84518 = DIRECTION ( 'NONE',  ( 0.8164965809277243691, 0.000000000000000000, -0.5773502691896280625 ) ) ;
#84519 = CARTESIAN_POINT ( 'NONE',  ( -16.51473224551069308, -9.474510206698971260, 91.66557627198103830 ) ) ;
#84520 = DIRECTION ( 'NONE',  ( 0.000000000000000000, 0.000000000000000000, -1.000000000000000000 ) ) ;
#84521 = CARTESIAN_POINT ( 'NONE',  ( -0.05219959533937732626, 21.53943276465977519, 27.50109039468567929 ) ) ;
#84522 = CARTESIAN_POINT ( 'NONE',  ( -14.34966873604960291, -8.224510206698953496, 96.66557627198102409 ) ) ;
#84524 = CARTESIAN_POINT ( 'NONE',  ( -19.02544592524342804, 5.153800228976336051, 71.04057627198099567 ) ) ;
#84523 = CARTESIAN_POINT ( 'NONE',  ( -15.72974639402197994, 15.80617190586746368, 85.62390960531436690 ) ) ;
#84525 = CARTESIAN_POINT ( 'NONE',  ( -19.03943276465977164, 0.05219959533909376836, 76.24890960531435269 ) ) ;
#84526 = CARTESIAN_POINT ( 'NONE',  ( 10.81492255796078972, 18.62759615963270932, 104.5822429386477097 ) ) ;
#84527 = ORIENTED_EDGE ( 'NONE', *, *, #49302, .T. ) ;
#84528 = CARTESIAN_POINT ( 'NONE',  ( -5.049401038298153566, 19.05341960407611168, 75.20724293864769550 ) ) ;
#84529 = CARTESIAN_POINT ( 'NONE',  ( 19.53037848336980176, -5.499999999999991118, 97.35532783611445495 ) ) ;
#84531 = CARTESIAN_POINT ( 'NONE',  ( 28.86264817322070542, -27.69526727176378245, -15.91384944864139861 ) ) ;
#84530 = CARTESIAN_POINT ( 'NONE',  ( -4.483927247898539470, -16.52544592524342804, 112.2905762719810241 ) ) ;
#84532 = CARTESIAN_POINT ( 'NONE',  ( -9.474510206698720793, -16.51473224551083518, 89.58442372801900433 ) ) ;
#84533 = CARTESIAN_POINT ( 'NONE',  ( -12.06949235617756955, 12.14591786802309770, 95.62390960531436690 ) ) ;
#84534 = CARTESIAN_POINT ( 'NONE',  ( 15.72974639402176855, 15.80617190586768217, 71.87609039468568994 ) ) ;
#84536 = CARTESIAN_POINT ( 'NONE',  ( -5.719274019375665041, -21.55341960407619695, 39.79275706135235424 ) ) ;
#84535 = CARTESIAN_POINT ( 'NONE',  ( -0.05219959533909027116, -19.03943276465977164, 62.49890960531435979 ) ) ;
#84537 = CARTESIAN_POINT ( 'NONE',  ( 10.81492255796078972, 18.62759615963270932, 114.5822429386477097 ) ) ;
#84538 = CARTESIAN_POINT ( 'NONE',  ( 1.993301997531345292E-15, -30.30510711980685912, 140.5000000000000000 ) ) ;
#84539 = CARTESIAN_POINT ( 'NONE',  ( 9.474510206698971260, -16.51473224551069308, 72.91557627198102409 ) ) ;
#84540 = DIRECTION ( 'NONE',  ( -1.000000000000000000, -0.000000000000000000, 0.000000000000000000 ) ) ;
#84542 = CARTESIAN_POINT ( 'NONE',  ( -15.72974639402197994, 15.80617190586746368, 30.62390960531436335 ) ) ;
#84541 = CARTESIAN_POINT ( 'NONE',  ( -14.29746914071037622, -8.314922557961029526, 29.16775706135234003 ) ) ;
#84543 = CARTESIAN_POINT ( 'NONE',  ( -15.80617190586768217, 15.72974639402176855, 63.12609039468568994 ) ) ;
#84544 = CARTESIAN_POINT ( 'NONE',  ( 9.564922557960805705, 16.46253265017160317, 109.5822429386476955 ) ) ;
#84545 = CARTESIAN_POINT ( 'NONE',  ( 5.049401038297881783, 19.05341960407617563, 97.29275706135233293 ) ) ;
#84546 = CARTESIAN_POINT ( 'NONE',  ( 19.02544592524343514, -5.153800228976328945, 53.54057627198102409 ) ) ;
#84547 = CARTESIAN_POINT ( 'NONE',  ( 16.51473224551069308, 9.474510206698969483, 74.16557627198103830 ) ) ;
#84548 = CARTESIAN_POINT ( 'NONE',  ( 4.379528057220339221, -16.55341960407611168, 97.70724293864772392 ) ) ;
#84549 = CARTESIAN_POINT ( 'NONE',  ( -5.049401038298153566, 19.05341960407611168, 105.2072429386476671 ) ) ;
#84550 = CARTESIAN_POINT ( 'NONE',  ( -16.55341960407611168, -4.379528057220339221, 91.45724293864769550 ) ) ;
#84551 = CARTESIAN_POINT ( 'NONE',  ( -0.05219959533909027116, -19.03943276465977164, 92.49890960531436690 ) ) ;
#84553 = CARTESIAN_POINT ( 'NONE',  ( -5.049401038298153566, 19.05341960407611168, 45.20724293864769550 ) ) ;
#84552 = CARTESIAN_POINT ( 'NONE',  ( -8.314922557960811034, -14.29746914071050412, 47.08224293864770260 ) ) ;
#84554 = CARTESIAN_POINT ( 'NONE',  ( 18.62759615963255655, 10.81492255796105972, 56.66775706135235424 ) ) ;
#84555 = CARTESIAN_POINT ( 'NONE',  ( -0.05219959533936034679, 19.03943276465977164, 97.50109039468567573 ) ) ;
#84556 = CARTESIAN_POINT ( 'NONE',  ( 8.314922557960818139, 14.29746914071049879, 54.58224293864769550 ) ) ;
#84557 = CARTESIAN_POINT ( 'NONE',  ( 21.53943276465977519, -0.05219959533907433946, 103.7489096053143669 ) ) ;
#84558 = CARTESIAN_POINT ( 'NONE',  ( -21.53943276465977519, 0.05219959533907696930, 51.24890960531436690 ) ) ;
#84560 = CARTESIAN_POINT ( 'NONE',  ( 14.29746914071049879, -8.314922557960816363, 83.33224293864769550 ) ) ;
#84559 = CARTESIAN_POINT ( 'NONE',  ( 19.03943276465977164, -0.05219959533909143690, 108.7489096053143527 ) ) ;
#84561 = CARTESIAN_POINT ( 'NONE',  ( 22.44159573604009594, -16.30477369853687364, 143.6750000027311671 ) ) ;
#84562 = CARTESIAN_POINT ( 'NONE',  ( 5.049401038298161559, -19.05341960407611168, 62.70724293864769550 ) ) ;
#84563 = CARTESIAN_POINT ( 'NONE',  ( 8.224510206698953496, -14.34966873604960469, 27.91557627198103830 ) ) ;
#84564 = CARTESIAN_POINT ( 'NONE',  ( 14.34966873604972726, -8.224510206698740333, 105.8344237280190328 ) ) ;
#84565 = CARTESIAN_POINT ( 'NONE',  ( 8.314922557961029526, -14.29746914071037800, 85.41775706135236135 ) ) ;
#84566 = CARTESIAN_POINT ( 'NONE',  ( -5.153800228976607833, 19.02544592524334988, 37.70942372801899722 ) ) ;
#84568 = CARTESIAN_POINT ( 'NONE',  ( -16.51473224551069308, -9.474510206698971260, 106.6655762719810383 ) ) ;
#84567 = CARTESIAN_POINT ( 'NONE',  ( -28.82186960331499037, 2.428612866367529932E-14, 144.2500000054623683 ) ) ;
#84569 = CARTESIAN_POINT ( 'NONE',  ( -19.05341960407611168, -5.049401038298163336, 81.45724293864769550 ) ) ;
#84570 = CARTESIAN_POINT ( 'NONE',  ( 9.564922557960805705, 16.46253265017160317, 39.58224293864768839 ) ) ;
#84571 = CARTESIAN_POINT ( 'NONE',  ( -12.06949235617756955, 12.14591786802309770, 45.62390960531436690 ) ) ;
#84573 = CARTESIAN_POINT ( 'NONE',  ( 16.46253265017160672, -9.564922557960803928, 108.3322429386476955 ) ) ;
#84572 = CARTESIAN_POINT ( 'NONE',  ( -19.03943276465977164, 0.05219959533909376836, 116.2489096053143669 ) ) ;
#84574 = CARTESIAN_POINT ( 'NONE',  ( 15.80617190586746368, 15.72974639402197994, 34.37390960531435979 ) ) ;
#84575 = CARTESIAN_POINT ( 'NONE',  ( 16.55341960407611168, 4.379528057220329451, 88.95724293864769550 ) ) ;
#84576 = CARTESIAN_POINT ( 'NONE',  ( 16.52544592524335698, 4.483927247898782831, 36.45942372801901143 ) ) ;
#84577 = CARTESIAN_POINT ( 'NONE',  ( -16.52544592524342804, 4.483927247898546575, 71.04057627198103830 ) ) ;
#84578 = CARTESIAN_POINT ( 'NONE',  ( 17.50000000000018119, -3.417042746626921534, 32.67380396232485396 ) ) ;
#84579 = CARTESIAN_POINT ( 'NONE',  ( -5.049401038297874678, -19.05341960407617918, 64.79275706135233293 ) ) ;
#84580 = CARTESIAN_POINT ( 'NONE',  ( -13.89961937509977652, 13.97604488694528158, 105.6239096053143527 ) ) ;
#84581 = CARTESIAN_POINT ( 'NONE',  ( 16.46253265017146816, 9.564922557961045513, 76.66775706135234714 ) ) ;
#84582 = CARTESIAN_POINT ( 'NONE',  ( 5.153800228976617603, -19.02544592524335343, 40.20942372801899012 ) ) ;
#84584 = CARTESIAN_POINT ( 'NONE',  ( 8.314922557961029526, -14.29746914071037800, 105.4177570613523613 ) ) ;
#84583 = CARTESIAN_POINT ( 'NONE',  ( -0.05219959533934338120, 16.53943276465976808, 32.50109039468568284 ) ) ;
#84585 = CARTESIAN_POINT ( 'NONE',  ( 19.05341960407617918, -5.049401038297876454, 76.04275706135230450 ) ) ;
#84586 = CARTESIAN_POINT ( 'NONE',  ( 21.55341960407610458, 5.719274019375980345, 38.95724293864768839 ) ) ;
#84587 = CARTESIAN_POINT ( 'NONE',  ( 21.55341960407619695, -5.719274019375665929, 66.04275706135236135 ) ) ;
#84588 = CARTESIAN_POINT ( 'NONE',  ( 19.43099193148526638, 5.500000000000092371, 38.23279185469454688 ) ) ;
#84589 = CARTESIAN_POINT ( 'NONE',  ( -4.483927247898782831, 16.52544592524335698, 27.70942372801901854 ) ) ;
#84591 = CARTESIAN_POINT ( 'NONE',  ( -9.564922557960796823, -16.46253265017161027, 92.08224293864769550 ) ) ;
#84590 = CARTESIAN_POINT ( 'NONE',  ( 30.00000000000000355, 3.889087296526017479, 8.181980515339454030 ) ) ;
#84592 = CARTESIAN_POINT ( 'NONE',  ( 14.98335265924517579, 15.13939621930179058, -58.85720012050614969 ) ) ;
#84595 = ADVANCED_FACE ( 'NONE', ( #191773 ), #68422, .T. ) ;
#84594 = CARTESIAN_POINT ( 'NONE',  ( 16.51473224551069308, 9.474510206698969483, 74.16557627198103830 ) ) ;
#84593 = CARTESIAN_POINT ( 'NONE',  ( 16.53943276465976808, -0.05219959533910856209, 88.74890960531436690 ) ) ;
#84596 = PRODUCT_CONTEXT ( 'NONE', #151378, 'mechanical' ) ;
#84597 = CARTESIAN_POINT ( 'NONE',  ( -5.153800228976328057, -19.02544592524343514, 87.29057627198103830 ) ) ;
#84598 = ORIENTED_EDGE ( 'NONE', *, *, #156164, .T. ) ;
#84599 = CARTESIAN_POINT ( 'NONE',  ( 19.03943276465977164, 0.05219959533936151252, 91.25109039468566152 ) ) ;
#84600 = CARTESIAN_POINT ( 'NONE',  ( 5.719274019375991003, -21.55341960407610458, 82.70724293864770971 ) ) ;
#84601 = CARTESIAN_POINT ( 'NONE',  ( -13.89961937509977652, 13.97604488694528158, 30.62390960531435269 ) ) ;
#84603 = CARTESIAN_POINT ( 'NONE',  ( 10.81492255796078972, 18.62759615963270932, 109.5822429386476955 ) ) ;
#84602 = CARTESIAN_POINT ( 'NONE',  ( 16.46253265017146816, 9.564922557961045513, 66.66775706135233293 ) ) ;
#84604 = CARTESIAN_POINT ( 'NONE',  ( -19.02544592524342804, 5.153800228976336051, 76.04057627198102409 ) ) ;
#84605 = CARTESIAN_POINT ( 'NONE',  ( -5.153800228976328057, -19.02544592524343514, 107.2905762719810383 ) ) ;
#84606 = ORIENTED_EDGE ( 'NONE', *, *, #168074, .T. ) ;
#84607 = CARTESIAN_POINT ( 'NONE',  ( -10.81492255796078084, -18.62759615963271287, 107.0822429386476955 ) ) ;
#84610 = CARTESIAN_POINT ( 'NONE',  ( 16.51473224551083163, -9.474510206698727899, 60.83442372801900433 ) ) ;
#84609 = CARTESIAN_POINT ( 'NONE',  ( -13.89961937509977652, 13.97604488694528158, 80.62390960531436690 ) ) ;
#84608 = CARTESIAN_POINT ( 'NONE',  ( 16.55341960407611168, 4.379528057220329451, 88.95724293864769550 ) ) ;
#84611 = CARTESIAN_POINT ( 'NONE',  ( 10.81492255796078972, 18.62759615963270932, 84.58224293864769550 ) ) ;
#84612 = CARTESIAN_POINT ( 'NONE',  ( 10.72451020669898902, -18.67979575497178502, 67.91557627198102409 ) ) ;
#84613 = CARTESIAN_POINT ( 'NONE',  ( -4.379528057220328563, 16.55341960407611168, 50.20724293864769550 ) ) ;
#84614 = CARTESIAN_POINT ( 'NONE',  ( -21.52544592524334988, -5.823673210054445271, 98.95942372801903275 ) ) ;
#84615 = CARTESIAN_POINT ( 'NONE',  ( -12.14591786802326823, 12.06949235617739902, 63.12609039468568994 ) ) ;
#84616 = CARTESIAN_POINT ( 'NONE',  ( 13.89961937509977652, -13.97604488694527269, 98.12390960531433848 ) ) ;
#84617 = CARTESIAN_POINT ( 'NONE',  ( -9.564922557960796823, -16.46253265017161027, 52.08224293864768839 ) ) ;
#84618 = CARTESIAN_POINT ( 'NONE',  ( -15.80617190586768217, 15.72974639402176855, 48.12609039468568284 ) ) ;
#84619 = CARTESIAN_POINT ( 'NONE',  ( -10.81492255796105439, 18.62759615963255655, 47.91775706135234714 ) ) ;
#84620 = CARTESIAN_POINT ( 'NONE',  ( -5.153800228976328057, -19.02544592524343514, 67.29057627198102409 ) ) ;
#84621 = CARTESIAN_POINT ( 'NONE',  ( 21.53943276465977519, 0.05219959533937863772, 36.25109039468567573 ) ) ;
#84622 = CARTESIAN_POINT ( 'NONE',  ( 19.05341960407617918, -5.049401038297876454, 71.04275706135234714 ) ) ;
#84624 = CARTESIAN_POINT ( 'NONE',  ( 9.474510206698729675, 16.51473224551082808, 77.08442372801900433 ) ) ;
#84623 = B_SPLINE_CURVE_WITH_KNOTS ( 'NONE', 3,
 ( #154628, #45465, #106134, #136480, #198160, #93942, #59630, #29317, #60615, #169796, #140445, #16123, #17117, #46452, #28341, #90947, #200139, #152634, #109116, #928, #122290, #78768, #77778, #76787 ),
 .UNSPECIFIED., .F., .F.,
 ( 4, 2, 2, 2, 2, 2, 2, 2, 2, 2, 2, 4 ),
 ( 2.775519118949223281E-07, 0.0003993838752237342609, 0.0007984901985355736219, 0.001596702845159247899, 0.002394915491782921742, 0.003193128138406596019, 0.003991340785030269428, 0.004789553431653943705, 0.005188659754965783445, 0.005587766078277624920, 0.005986872401589464661, 0.006385978724901306136 ),
 .UNSPECIFIED. ) ;
#84625 = CARTESIAN_POINT ( 'NONE',  ( 16.51473224551069308, 9.474510206698969483, 34.16557627198102409 ) ) ;
#84626 = CARTESIAN_POINT ( 'NONE',  ( 8.224510206698742110, 14.34966873604972548, 87.08442372801901854 ) ) ;
#84627 = CARTESIAN_POINT ( 'NONE',  ( -13.97604488694527625, -13.89961937509977652, 56.87390960531434558 ) ) ;
#84628 = CARTESIAN_POINT ( 'NONE',  ( 23.03120525563227972, -11.22467059994892935, 168.0473679553712429 ) ) ;
#84629 = CARTESIAN_POINT ( 'NONE',  ( -9.564922557960796823, -16.46253265017161027, 102.0822429386477097 ) ) ;
#84631 = EDGE_CURVE ( 'NONE', #100015, #76158, #79619, .T. ) ;
#84630 = CARTESIAN_POINT ( 'NONE',  ( 13.89961937509977652, -13.97604488694527269, 33.12390960531434558 ) ) ;
#84632 = CARTESIAN_POINT ( 'NONE',  ( 15.80617190586746368, 15.72974639402197994, 69.37390960531436690 ) ) ;
#84633 = CARTESIAN_POINT ( 'NONE',  ( 4.483927247898790824, -16.52544592524335698, 60.20942372801902565 ) ) ;
#84634 = CARTESIAN_POINT ( 'NONE',  ( -0.05219959533936034679, 19.03943276465977164, 22.50109039468566152 ) ) ;
#84635 = CARTESIAN_POINT ( 'NONE',  ( 9.564922557960805705, 16.46253265017160317, 59.58224293864769550 ) ) ;
#84636 = CARTESIAN_POINT ( 'NONE',  ( -14.34966873604960291, -8.224510206698953496, 41.66557627198103120 ) ) ;
#84637 = CARTESIAN_POINT ( 'NONE',  ( -8.314922557960811034, -14.29746914071050412, 77.08224293864769550 ) ) ;
#84638 = CARTESIAN_POINT ( 'NONE',  ( -0.05219959533909027116, -19.03943276465977164, 82.49890960531436690 ) ) ;
#84639 = CARTESIAN_POINT ( 'NONE',  ( 10.81492255796106328, -18.62759615963255655, 30.41775706135234358 ) ) ;
#84640 = CARTESIAN_POINT ( 'NONE',  ( 19.02544592524343514, -5.153800228976328945, 88.54057627198102409 ) ) ;
#84641 = CARTESIAN_POINT ( 'NONE',  ( 18.67979575497194134, -10.72451020669871369, 100.8344237280190185 ) ) ;
#84642 = CARTESIAN_POINT ( 'NONE',  ( 14.34966873604972726, -8.224510206698740333, 65.83442372801900433 ) ) ;
#84643 = CARTESIAN_POINT ( 'NONE',  ( -0.05219959533937732626, 21.53943276465977519, 32.50109039468568284 ) ) ;
#84644 = CARTESIAN_POINT ( 'NONE',  ( 16.51473224551069308, 9.474510206698969483, 104.1655762719810241 ) ) ;
#84645 = CARTESIAN_POINT ( 'NONE',  ( -15.72974639402197994, 15.80617190586746368, 90.62390960531436690 ) ) ;
#84646 = CARTESIAN_POINT ( 'NONE',  ( -12.14591786802309592, -12.06949235617757132, 41.87390960531435979 ) ) ;
#84647 = CARTESIAN_POINT ( 'NONE',  ( 19.05341960407611168, 5.049401038298154454, 38.95724293864767418 ) ) ;
#84648 = CARTESIAN_POINT ( 'NONE',  ( 16.53943276465976808, -0.05219959533910856209, 73.74890960531433848 ) ) ;
#84649 = CARTESIAN_POINT ( 'NONE',  ( -21.55341960407610458, -5.719274019375992779, 31.45724293864769550 ) ) ;
#84650 = CARTESIAN_POINT ( 'NONE',  ( 9.474510206698729675, 16.51473224551082808, 27.08442372801900433 ) ) ;
#84651 = CARTESIAN_POINT ( 'NONE',  ( 14.29746914071049879, -8.314922557960816363, 98.33224293864769550 ) ) ;
#84652 = CARTESIAN_POINT ( 'NONE',  ( -13.89961937509977652, 13.97604488694528158, 110.6239096053143243 ) ) ;
#84653 = VERTEX_POINT ( 'NONE', #83582 ) ;
#84654 = CARTESIAN_POINT ( 'NONE',  ( -4.379528057220086978, -16.55341960407618274, 59.79275706135234714 ) ) ;
#84655 = CARTESIAN_POINT ( 'NONE',  ( 13.97604488694527802, 13.89961937509977652, 49.37390960531434558 ) ) ;
#84656 = CARTESIAN_POINT ( 'NONE',  ( 27.73933785331498925, -9.013057229001034898, 139.7750000027311899 ) ) ;
#84657 = CARTESIAN_POINT ( 'NONE',  ( 16.52544592524335698, 4.483927247898782831, 96.45942372801901854 ) ) ;
#84658 = CARTESIAN_POINT ( 'NONE',  ( 16.51473224551083163, -9.474510206698727899, 95.83442372801900433 ) ) ;
#84659 = CARTESIAN_POINT ( 'NONE',  ( 5.719274019375673035, 21.55341960407619339, 67.29275706135234714 ) ) ;
#84660 = CARTESIAN_POINT ( 'NONE',  ( 13.89961937509977652, -13.97604488694527269, 78.12390960531433848 ) ) ;
#84661 = CARTESIAN_POINT ( 'NONE',  ( -15.80617190586745835, -15.72974639402198527, 86.87390960531438111 ) ) ;
#84662 = CARTESIAN_POINT ( 'NONE',  ( 4.379528057220092307, 16.55341960407617563, 47.29275706135234003 ) ) ;
#84663 = CARTESIAN_POINT ( 'NONE',  ( 0.05219959533910956823, 16.53943276465976808, 109.9989096053143527 ) ) ;
#84664 = CARTESIAN_POINT ( 'NONE',  ( 5.049401038297881783, 19.05341960407617563, 87.29275706135234714 ) ) ;
#84665 = CARTESIAN_POINT ( 'NONE',  ( -15.80617190586745835, -15.72974639402198527, 76.87390960531439532 ) ) ;
#84666 = CARTESIAN_POINT ( 'NONE',  ( 0.05219959533936267826, -19.03943276465977164, 45.00109039468566863 ) ) ;
#84667 = FACE_BOUND ( 'NONE', #146672, .T. ) ;
#84668 = CARTESIAN_POINT ( 'NONE',  ( 5.823673210054125526, 21.52544592524343514, 94.79057627198105251 ) ) ;
#84669 = CARTESIAN_POINT ( 'NONE',  ( 17.50000000000000000, -5.500000000000000888, 120.0000000000000142 ) ) ;
#84670 = CARTESIAN_POINT ( 'NONE',  ( -19.05341960407611168, -5.049401038298163336, 61.45724293864769550 ) ) ;
#84671 = CARTESIAN_POINT ( 'NONE',  ( 1.300000000000000044, 1.443375672974065216, 7.017607234860990640E-28 ) ) ;
#84672 = CARTESIAN_POINT ( 'NONE',  ( -13.97604488694547697, 13.89961937509957934, 113.1260903946856757 ) ) ;
#84673 = CARTESIAN_POINT ( 'NONE',  ( 15.76494486619527180, -36.76728419955058058, -10.58017208825962818 ) ) ;
#84674 = CARTESIAN_POINT ( 'NONE',  ( 13.97604488694527802, 13.89961937509977652, 44.37390960531435269 ) ) ;
#84676 = CARTESIAN_POINT ( 'NONE',  ( -14.34966873604960291, -8.224510206698953496, 51.66557627198102409 ) ) ;
#84675 = CARTESIAN_POINT ( 'NONE',  ( 18.62759615963271287, -10.81492255796078972, 108.3322429386477097 ) ) ;
#84677 = CARTESIAN_POINT ( 'NONE',  ( 19.05341960407611168, 5.049401038298154454, 58.95724293864768129 ) ) ;
#84678 = CARTESIAN_POINT ( 'NONE',  ( -5.823673210054431948, 21.52544592524334988, 77.70942372801900433 ) ) ;
#84680 = CARTESIAN_POINT ( 'NONE',  ( -16.51473224551082808, 9.474510206698731452, 33.33442372801899722 ) ) ;
#84679 = CARTESIAN_POINT ( 'NONE',  ( 0.05219959533934541429, -16.53943276465976808, 25.00109039468567218 ) ) ;
#84681 = CARTESIAN_POINT ( 'NONE',  ( 5.823673210054444382, -21.52544592524334988, 45.20942372801901854 ) ) ;
#84682 = CARTESIAN_POINT ( 'NONE',  ( 21.55341960407619695, -5.719274019375665929, 21.04275706135234714 ) ) ;
#84683 = CARTESIAN_POINT ( 'NONE',  ( 15.80617190586746368, 15.72974639402197994, 54.37390960531435979 ) ) ;
#84684 = CARTESIAN_POINT ( 'NONE',  ( 16.46253265017146816, 9.564922557961045513, 101.6677570613523329 ) ) ;
#84685 = CARTESIAN_POINT ( 'NONE',  ( -9.564922557961040184, 16.46253265017147172, 67.91775706135233293 ) ) ;
#84686 = CARTESIAN_POINT ( 'NONE',  ( -21.52544592524334988, -5.823673210054445271, 78.95942372801901854 ) ) ;
#84687 = CARTESIAN_POINT ( 'NONE',  ( 13.89961937509957401, 13.97604488694547697, 46.87609039468565442 ) ) ;
#84688 = CARTESIAN_POINT ( 'NONE',  ( 19.02544592524343514, -5.153800228976328945, 28.54057627198102409 ) ) ;
#84689 = CARTESIAN_POINT ( 'NONE',  ( -15.80617190586745835, -15.72974639402198527, 61.87390960531436690 ) ) ;
#84690 = CARTESIAN_POINT ( 'NONE',  ( -16.55341960407611168, -4.379528057220339221, 51.45724293864770260 ) ) ;
#84691 = CARTESIAN_POINT ( 'NONE',  ( -19.48894818550246200, 5.499999999999919176, 95.10307310435240424 ) ) ;
#84692 = CARTESIAN_POINT ( 'NONE',  ( 16.46253265017146816, 9.564922557961045513, 21.66775706135233648 ) ) ;
#84693 = CARTESIAN_POINT ( 'NONE',  ( -12.06949235617739369, -12.14591786802326823, 84.37609039468570415 ) ) ;
#84694 = CARTESIAN_POINT ( 'NONE',  ( -4.379528057220328563, 16.55341960407611168, 40.20724293864769550 ) ) ;
#84695 = CARTESIAN_POINT ( 'NONE',  ( -18.62759615963255300, -10.81492255796106328, 74.16775706135231871 ) ) ;
#84696 = CARTESIAN_POINT ( 'NONE',  ( -21.52544592524334988, -5.823673210054445271, 78.95942372801901854 ) ) ;
#84697 = CARTESIAN_POINT ( 'NONE',  ( -18.62759615963270932, 10.81492255796079327, 85.83224293864768129 ) ) ;
#84698 = CARTESIAN_POINT ( 'NONE',  ( -16.46253265017160317, 9.564922557960807481, 35.83224293864768839 ) ) ;
#84699 = CARTESIAN_POINT ( 'NONE',  ( -18.67979575497193778, 10.72451020669871902, 63.33442372801900433 ) ) ;
#84700 = CARTESIAN_POINT ( 'NONE',  ( 0.05219959533909260263, 19.03943276465977164, 29.99890960531435979 ) ) ;
#84701 = ORIENTED_EDGE ( 'NONE', *, *, #90984, .F. ) ;
#84702 = CARTESIAN_POINT ( 'NONE',  ( 19.03943276465977164, -0.05219959533909143690, 48.74890960531435979 ) ) ;
#84703 = CARTESIAN_POINT ( 'NONE',  ( 4.483927247898545687, 16.52544592524342804, 89.79057627198103830 ) ) ;
#84704 = CARTESIAN_POINT ( 'NONE',  ( 16.51473224551069308, 9.474510206698969483, 99.16557627198102409 ) ) ;
#84705 = CARTESIAN_POINT ( 'NONE',  ( -16.52544592524342804, 4.483927247898546575, 36.04057627198102409 ) ) ;
#84706 = CARTESIAN_POINT ( 'NONE',  ( -14.29746914071049879, 8.314922557960819915, 110.8322429386476955 ) ) ;
#84707 = CARTESIAN_POINT ( 'NONE',  ( 5.719274019375991003, -21.55341960407610458, 82.70724293864770971 ) ) ;
#84708 = CARTESIAN_POINT ( 'NONE',  ( -18.62759615963255300, -10.81492255796106328, 19.16775706135234714 ) ) ;
#84709 = LINE ( 'NONE', #143389, #46840 ) ;
#84710 = CARTESIAN_POINT ( 'NONE',  ( 0.05219959533934541429, -16.53943276465976808, 40.00109039468567573 ) ) ;
#84711 = EDGE_CURVE ( 'NONE', #167341, #99125, #28615, .T. ) ;
#84712 = CARTESIAN_POINT ( 'NONE',  ( -18.62759615963270932, 10.81492255796079327, 65.83224293864769550 ) ) ;
#84713 = CARTESIAN_POINT ( 'NONE',  ( -0.05219959533937732626, 21.53943276465977519, 97.50109039468567573 ) ) ;
#84714 = CARTESIAN_POINT ( 'NONE',  ( 5.153800228976335163, 19.02544592524342804, 94.79057627198103830 ) ) ;
#84715 = CARTESIAN_POINT ( 'NONE',  ( -5.719274019375665041, -21.55341960407619695, 24.79275706135235779 ) ) ;
#84716 = CARTESIAN_POINT ( 'NONE',  ( -9.474510206698964154, 16.51473224551069663, 105.4155762719810383 ) ) ;
#84717 = CARTESIAN_POINT ( 'NONE',  ( -4.379528057220086978, -16.55341960407618274, 94.79275706135234714 ) ) ;
#84718 = CARTESIAN_POINT ( 'NONE',  ( -0.05219959533937732626, 21.53943276465977519, 67.50109039468568994 ) ) ;
#84719 = CARTESIAN_POINT ( 'NONE',  ( -5.823673210054431948, 21.52544592524334988, 107.7094237280190328 ) ) ;
#84720 = CARTESIAN_POINT ( 'NONE',  ( 8.314922557961029526, -14.29746914071037800, 75.41775706135233293 ) ) ;
#84721 = CARTESIAN_POINT ( 'NONE',  ( -0.05219959533937732626, 21.53943276465977519, 27.50109039468567929 ) ) ;
#84722 = CARTESIAN_POINT ( 'NONE',  ( -9.564922557960796823, -16.46253265017161027, 27.08224293864769550 ) ) ;
#84723 = CARTESIAN_POINT ( 'NONE',  ( 5.719274019375673035, 21.55341960407619339, 92.29275706135236135 ) ) ;
#84724 = CARTESIAN_POINT ( 'NONE',  ( -9.474510206698964154, 16.51473224551069663, 110.4155762719810383 ) ) ;
#84725 = CARTESIAN_POINT ( 'NONE',  ( -15.80617190586745835, -15.72974639402198527, 96.87390960531436690 ) ) ;
#84727 = CARTESIAN_POINT ( 'NONE',  ( 18.67979575497178502, 10.72451020669898547, 54.16557627198103120 ) ) ;
#84726 = CARTESIAN_POINT ( 'NONE',  ( 18.22780087662122739, 5.500000000000000888, 81.48236817873103632 ) ) ;
#84729 = CARTESIAN_POINT ( 'NONE',  ( -16.52544592524342804, 4.483927247898546575, 46.04057627198103830 ) ) ;
#84728 = CARTESIAN_POINT ( 'NONE',  ( 19.02544592524343514, -5.153800228976328945, 98.54057627198100988 ) ) ;
#84730 = CARTESIAN_POINT ( 'NONE',  ( 21.38418241377623019, 5.438282248597753110, 174.2683007571264113 ) ) ;
#84731 = CARTESIAN_POINT ( 'NONE',  ( 9.564922557961047289, -16.46253265017146816, 75.41775706135234714 ) ) ;
#84732 = CARTESIAN_POINT ( 'NONE',  ( -16.61371651742600974, 7.165104196376165469, 103.8541506999300026 ) ) ;
#84733 = CARTESIAN_POINT ( 'NONE',  ( -8.224510206698735004, -14.34966873604973081, 19.58442372801901143 ) ) ;
#84734 = CARTESIAN_POINT ( 'NONE',  ( -18.67979575497178146, -10.72451020669898902, 91.66557627198103830 ) ) ;
#84735 = CARTESIAN_POINT ( 'NONE',  ( -8.314922557960811034, -14.29746914071050412, 62.08224293864769550 ) ) ;
#84736 = CARTESIAN_POINT ( 'NONE',  ( 5.049401038298161559, -19.05341960407611168, 97.70724293864766707 ) ) ;
#84737 = CARTESIAN_POINT ( 'NONE',  ( -4.483927247898782831, 16.52544592524335698, 42.70942372801901854 ) ) ;
#84738 = CARTESIAN_POINT ( 'NONE',  ( -9.564922557960796823, -16.46253265017161027, 52.08224293864768839 ) ) ;
#84740 = CARTESIAN_POINT ( 'NONE',  ( -19.05341960407617563, 5.049401038297882671, 103.5427570613523329 ) ) ;
#84739 = CARTESIAN_POINT ( 'NONE',  ( -18.62759615963255300, -10.81492255796106328, 34.16775706135234714 ) ) ;
#84741 = EDGE_CURVE ( 'NONE', #197513, #89826, #65436, .T. ) ;
#84742 = CARTESIAN_POINT ( 'NONE',  ( 13.89961937509977652, -13.97604488694527269, 93.12390960531436690 ) ) ;
#84743 =( BOUNDED_SURFACE ( )  B_SPLINE_SURFACE ( 1, 2, ( 
 ( #82090, #4268, #140802, #126619, #157969, #2291, #114438, #188320, #141794, #111464, #112455, #158949, #63973, #5264, #187340, #94298, #143782, #175131, #142786, #6264, #155976, #67944, #21444, #173149, #129597, #156978, #18475, #125643, #51778, #159957, #174144, #110464, #83105, #48811, #144781, #50796, #96283, #19462, #34624, #172146, #95294, #65947, #127619, #189319, #35616, #20438, #80125, #66946, #128608, #190301, #113438, #36598, #98254, #149792, #119461, #11296, #164971, #193306, #72968, #100277, #161956, #196323, #195313, #103291, #117452, #53783, #26465, #7260, #88108, #194313, #39609, #101268, #85099, #177148, #40619, #134637, #131621, #86114, #55780, #116455, #37609, #9290, #54780, #178143, #133620, #102289, #70956, #115459, #57791, #160958, #162958, #99271, #87115, #38620, #22451, #84100, #145779, #163978, #23452, #179151, #24464 ),
 ( #146785, #68945, #130608, #8278, #147805, #69956, #192304, #25475, #132625, #148802, #10291, #71949, #56794, #118466, #180158, #41627, #58762, #92067, #14246, #74936, #182124, #169923, #27467, #165965, #89109, #29438, #15251, #185094, #122416, #1054, #167939, #75918, #138580, #73960, #151780, #120432, #43608, #42619, #76909, #105273, #60743, #137593, #104285, #166960, #60, #61733, #136599, #91070, #152757, #28462, #197299, #199275, #150799, #59757, #184108, #153755, #108244, #31415, #45589, #93067, #30419, #168914, #12295, #121425, #90098, #154753, #16250, #13273, #107243, #198279, #77902, #123401, #135628, #46582, #183118, #44601, #139569, #62727, #106256, #181145, #2061, #35387, #157745, #18246, #125414, #113214, #170917, #109238, #32409, #172920, #158719, #128378, #65717, #144548, #111228, #19236, #81857, #17241, #95063, #63740, #187111 ) ),
 .UNSPECIFIED., .F., .F., .T. ) 
 B_SPLINE_SURFACE_WITH_KNOTS ( ( 2, 2 ),
 ( 3, 2, 2, 2, 2, 2, 2, 2, 2, 2, 2, 2, 2, 2, 2, 2, 2, 2, 2, 2, 2, 2, 2, 2, 2, 2, 2, 2, 2, 2, 2, 2, 2, 2, 2, 2, 2, 2, 2, 2, 2, 2, 2, 2, 2, 2, 2, 2, 2, 2, 3 ),
 ( 0.000000000000000000, 1.000000000000000000 ),
 ( 0.000000000000000000, 0.02000000000000000042, 0.04000000000000000083, 0.05999999999999999778, 0.08000000000000000167, 0.1000000000000000056, 0.1199999999999999956, 0.1400000000000000133, 0.1600000000000000033, 0.1799999999999999933, 0.2000000000000000111, 0.2200000000000000011, 0.2399999999999999911, 0.2600000000000000089, 0.2800000000000000266, 0.2999999999999999889, 0.3200000000000000067, 0.3400000000000000244, 0.3599999999999999867, 0.3800000000000000044, 0.4000000000000000222, 0.4199999999999999845, 0.4400000000000000022, 0.4600000000000000200, 0.4799999999999999822, 0.5000000000000000000, 0.5200000000000000178, 0.5400000000000000355, 0.5600000000000000533, 0.5799999999999999600, 0.5999999999999999778, 0.6199999999999999956, 0.6400000000000000133, 0.6600000000000000311, 0.6800000000000000488, 0.6999999999999999556, 0.7199999999999999734, 0.7399999999999999911, 0.7600000000000000089, 0.7800000000000000266, 0.8000000000000000444, 0.8199999999999999512, 0.8399999999999999689, 0.8599999999999999867, 0.8800000000000000044, 0.9000000000000000222, 0.9200000000000000400, 0.9399999999999999467, 0.9599999999999999645, 0.9799999999999999822, 1.000000000000000000 ),
 .UNSPECIFIED. ) 
 GEOMETRIC_REPRESENTATION_ITEM ( )  RATIONAL_B_SPLINE_SURFACE ( (
 ( 1.000000000000000000, 0.9510565162951535312, 1.000000000000000000, 0.9510565162951535312, 1.000000000000000000, 0.9510565162951535312, 1.000000000000000000, 0.9510565162951535312, 1.000000000000000000, 0.9510565162951535312, 1.000000000000000000, 0.9510565162951535312, 1.000000000000000000, 0.9510565162951535312, 1.000000000000000000, 0.9510565162951535312, 1.000000000000000000, 0.9510565162951535312, 1.000000000000000000, 0.9510565162951535312, 1.000000000000000000, 0.9510565162951535312, 1.000000000000000000, 0.9510565162951535312, 1.000000000000000000, 0.9510565162951535312, 1.000000000000000000, 0.9510565162951535312, 1.000000000000000000, 0.9510565162951535312, 1.000000000000000000, 0.9510565162951535312, 1.000000000000000000, 0.9510565162951535312, 1.000000000000000000, 0.9510565162951535312, 1.000000000000000000, 0.9510565162951535312, 1.000000000000000000, 0.9510565162951535312, 1.000000000000000000, 0.9510565162951535312, 1.000000000000000000, 0.9510565162951535312, 1.000000000000000000, 0.9510565162951535312, 1.000000000000000000, 0.9510565162951535312, 1.000000000000000000, 0.9510565162951535312, 1.000000000000000000, 0.9510565162951535312, 1.000000000000000000, 0.9510565162951535312, 1.000000000000000000, 0.9510565162951535312, 1.000000000000000000, 0.9510565162951535312, 1.000000000000000000, 0.9510565162951535312, 1.000000000000000000, 0.9510565162951535312, 1.000000000000000000, 0.9510565162951535312, 1.000000000000000000, 0.9510565162951535312, 1.000000000000000000, 0.9510565162951535312, 1.000000000000000000, 0.9510565162951535312, 1.000000000000000000, 0.9510565162951535312, 1.000000000000000000, 0.9510565162951535312, 1.000000000000000000, 0.9510565162951535312, 1.000000000000000000, 0.9510565162951535312, 1.000000000000000000, 0.9510565162951535312, 1.000000000000000000, 0.9510565162951535312, 1.000000000000000000, 0.9510565162951535312, 1.000000000000000000, 0.9510565162951535312, 1.000000000000000000, 0.9510565162951535312, 1.000000000000000000, 0.9510565162951535312, 1.000000000000000000, 0.9510565162951535312, 1.000000000000000000, 0.9510565162951535312, 1.000000000000000000, 0.9510565162951535312, 1.000000000000000000, 0.9510565162951535312, 1.000000000000000000, 0.9510565162951535312, 1.000000000000000000),
 ( 1.000000000000000000, 0.9510565162951535312, 1.000000000000000000, 0.9510565162951535312, 1.000000000000000000, 0.9510565162951535312, 1.000000000000000000, 0.9510565162951535312, 1.000000000000000000, 0.9510565162951535312, 1.000000000000000000, 0.9510565162951535312, 1.000000000000000000, 0.9510565162951535312, 1.000000000000000000, 0.9510565162951535312, 1.000000000000000000, 0.9510565162951535312, 1.000000000000000000, 0.9510565162951535312, 1.000000000000000000, 0.9510565162951535312, 1.000000000000000000, 0.9510565162951535312, 1.000000000000000000, 0.9510565162951535312, 1.000000000000000000, 0.9510565162951535312, 1.000000000000000000, 0.9510565162951535312, 1.000000000000000000, 0.9510565162951535312, 1.000000000000000000, 0.9510565162951535312, 1.000000000000000000, 0.9510565162951535312, 1.000000000000000000, 0.9510565162951535312, 1.000000000000000000, 0.9510565162951535312, 1.000000000000000000, 0.9510565162951535312, 1.000000000000000000, 0.9510565162951535312, 1.000000000000000000, 0.9510565162951535312, 1.000000000000000000, 0.9510565162951535312, 1.000000000000000000, 0.9510565162951535312, 1.000000000000000000, 0.9510565162951535312, 1.000000000000000000, 0.9510565162951535312, 1.000000000000000000, 0.9510565162951535312, 1.000000000000000000, 0.9510565162951535312, 1.000000000000000000, 0.9510565162951535312, 1.000000000000000000, 0.9510565162951535312, 1.000000000000000000, 0.9510565162951535312, 1.000000000000000000, 0.9510565162951535312, 1.000000000000000000, 0.9510565162951535312, 1.000000000000000000, 0.9510565162951535312, 1.000000000000000000, 0.9510565162951535312, 1.000000000000000000, 0.9510565162951535312, 1.000000000000000000, 0.9510565162951535312, 1.000000000000000000, 0.9510565162951535312, 1.000000000000000000, 0.9510565162951535312, 1.000000000000000000, 0.9510565162951535312, 1.000000000000000000, 0.9510565162951535312, 1.000000000000000000, 0.9510565162951535312, 1.000000000000000000, 0.9510565162951535312, 1.000000000000000000, 0.9510565162951535312, 1.000000000000000000, 0.9510565162951535312, 1.000000000000000000, 0.9510565162951535312, 1.000000000000000000, 0.9510565162951535312, 1.000000000000000000, 0.9510565162951535312, 1.000000000000000000, 0.9510565162951535312, 1.000000000000000000) ) ) 
 REPRESENTATION_ITEM ( '' )  SURFACE ( )  );
#84744 = CARTESIAN_POINT ( 'NONE',  ( -5.049401038298153566, 19.05341960407611168, 85.20724293864766707 ) ) ;
#84745 = CARTESIAN_POINT ( 'NONE',  ( 18.62759615963271287, -10.81492255796078972, 93.33224293864769550 ) ) ;
#84746 = CARTESIAN_POINT ( 'NONE',  ( -19.02544592524342804, 5.153800228976336051, 46.04057627198101699 ) ) ;
#84747 = CARTESIAN_POINT ( 'NONE',  ( -0.05219959533910754901, -16.53943276465976808, 72.49890960531435269 ) ) ;
#84748 = CARTESIAN_POINT ( 'NONE',  ( 19.02544592524343514, -5.153800228976328945, 108.5405762719810383 ) ) ;
#84749 = CARTESIAN_POINT ( 'NONE',  ( -31.90000000000003411, 3.219216299777112361E-13, -49.13275782002545355 ) ) ;
#84750 = CARTESIAN_POINT ( 'NONE',  ( 5.153800228976615827, -19.02544592524334988, 60.20942372801899012 ) ) ;
#84751 = CARTESIAN_POINT ( 'NONE',  ( 21.55341960407610458, 5.719274019375980345, 93.95724293864770971 ) ) ;
#84752 = CARTESIAN_POINT ( 'NONE',  ( 16.51473224551083163, -9.474510206698727899, 50.83442372801899722 ) ) ;
#84753 = CARTESIAN_POINT ( 'NONE',  ( 9.474510206698971260, -16.51473224551069308, 97.91557627198102409 ) ) ;
#84754 = CARTESIAN_POINT ( 'NONE',  ( -6.434671708797603529, 6.434671708797564449, -63.95112321872120731 ) ) ;
#84755 = CARTESIAN_POINT ( 'NONE',  ( 10.72451020669898902, -18.67979575497178502, 47.91557627198102409 ) ) ;
#84756 = CARTESIAN_POINT ( 'NONE',  ( -9.564922557960796823, -16.46253265017161027, 87.08224293864769550 ) ) ;
#84757 = CARTESIAN_POINT ( 'NONE',  ( -0.05219959533937732626, 21.53943276465977519, 67.50109039468568994 ) ) ;
#84758 = CARTESIAN_POINT ( 'NONE',  ( -13.97604488694527625, -13.89961937509977652, 31.87390960531435979 ) ) ;
#84759 = CARTESIAN_POINT ( 'NONE',  ( -4.379528057220328563, 16.55341960407611168, 80.20724293864769550 ) ) ;
#84760 = CARTESIAN_POINT ( 'NONE',  ( -14.29746914071037622, -8.314922557961029526, 29.16775706135234003 ) ) ;
#84761 = CARTESIAN_POINT ( 'NONE',  ( -15.80617190586768217, 15.72974639402176855, 53.12609039468568284 ) ) ;
#84762 = ORIENTED_EDGE ( 'NONE', *, *, #32808, .F. ) ;
#84763 = CARTESIAN_POINT ( 'NONE',  ( -27.66235494655239791, -7.573861383418037718, 139.9999999999999716 ) ) ;
#84764 = CARTESIAN_POINT ( 'NONE',  ( -16.51473224551082808, 9.474510206698731452, 68.33442372801900433 ) ) ;
#84765 = FACE_OUTER_BOUND ( 'NONE', #134673, .T. ) ;
#84766 = CARTESIAN_POINT ( 'NONE',  ( 10.72451020669871369, 18.67979575497193778, 22.08442372801901143 ) ) ;
#84767 = CARTESIAN_POINT ( 'NONE',  ( -6.020228577223754586E-15, 39.95556452105416412, -6.249999994537626336 ) ) ;
#84768 = CARTESIAN_POINT ( 'NONE',  ( 16.46253265017146816, 9.564922557961045513, 21.66775706135233648 ) ) ;
#84769 = CARTESIAN_POINT ( 'NONE',  ( 9.474510206698971260, -16.51473224551069308, 52.91557627198102409 ) ) ;
#84770 = CARTESIAN_POINT ( 'NONE',  ( 0.05219959533937995610, -21.53943276465977519, 110.0010903946856757 ) ) ;
#84771 = CARTESIAN_POINT ( 'NONE',  ( -14.29746914071037622, -8.314922557961029526, 104.1677570613523471 ) ) ;
#84773 = CARTESIAN_POINT ( 'NONE',  ( 10.81492255796106328, -18.62759615963255655, 75.41775706135233293 ) ) ;
#84772 = CARTESIAN_POINT ( 'NONE',  ( 19.02544592524343514, -5.153800228976328945, 103.5405762719809957 ) ) ;
#84774 = CARTESIAN_POINT ( 'NONE',  ( 27.73933785331498214, 9.013057229001095294, 148.4750000027311785 ) ) ;
#84775 = CARTESIAN_POINT ( 'NONE',  ( 13.97604488694527802, 13.89961937509977652, 109.3739096053143669 ) ) ;
#84776 = DIRECTION ( 'NONE',  ( -0.000000000000000000, -0.000000000000000000, 1.000000000000000000 ) ) ;
#84778 = CARTESIAN_POINT ( 'NONE',  ( -21.55341960407619339, 5.719274019375674811, 73.54275706135234714 ) ) ;
#84777 = CARTESIAN_POINT ( 'NONE',  ( -14.29746914071037622, -8.314922557961029526, 64.16775706135234714 ) ) ;
#84779 = CARTESIAN_POINT ( 'NONE',  ( -5.823673210054431948, 21.52544592524334988, 107.7094237280190328 ) ) ;
#84780 = DIRECTION ( 'NONE',  ( -0.000000000000000000, -0.000000000000000000, 1.000000000000000000 ) ) ;
#84781 = CARTESIAN_POINT ( 'NONE',  ( -19.05341960407611168, -5.049401038298163336, 81.45724293864769550 ) ) ;
#84782 = CARTESIAN_POINT ( 'NONE',  ( -9.474510206698964154, 16.51473224551069663, 105.4155762719810383 ) ) ;
#84783 = ORIENTED_EDGE ( 'NONE', *, *, #71047, .F. ) ;
#84784 = CARTESIAN_POINT ( 'NONE',  ( -1.046637022530759076, -29.32058373238551852, -52.18867397238358308 ) ) ;
#84785 = CARTESIAN_POINT ( 'NONE',  ( 0.05219959533909260263, 19.03943276465977164, 39.99890960531436690 ) ) ;
#84786 = CARTESIAN_POINT ( 'NONE',  ( 0.05219959533907565091, 21.53943276465977519, 44.99890960531435979 ) ) ;
#84787 = CARTESIAN_POINT ( 'NONE',  ( 0.05219959533934541429, -16.53943276465976808, 100.0010903946857042 ) ) ;
#84789 = CARTESIAN_POINT ( 'NONE',  ( -13.89961937509977652, 13.97604488694528158, 85.62390960531433848 ) ) ;
#84788 = CARTESIAN_POINT ( 'NONE',  ( 4.379528057220339221, -16.55341960407611168, 102.7072429386476955 ) ) ;
#84790 = CARTESIAN_POINT ( 'NONE',  ( -10.81492255796105439, 18.62759615963255655, 102.9177570613523756 ) ) ;
#84791 = CARTESIAN_POINT ( 'NONE',  ( -16.46253265017160317, 9.564922557960807481, 40.83224293864769550 ) ) ;
#84792 = CARTESIAN_POINT ( 'NONE',  ( -4.483927247898539470, -16.52544592524342804, 87.29057627198103830 ) ) ;
#84793 = CARTESIAN_POINT ( 'NONE',  ( 21.55341960407619695, -5.719274019375665929, 36.04275706135234714 ) ) ;
#84794 = CARTESIAN_POINT ( 'NONE',  ( 21.55341960407610458, 5.719274019375980345, 83.95724293864770971 ) ) ;
#84795 = CARTESIAN_POINT ( 'NONE',  ( 0.05219959533936267826, -19.03943276465977164, 50.00109039468566863 ) ) ;
#84796 = CARTESIAN_POINT ( 'NONE',  ( -4.500000000000000000, 5.510910596163088569E-16, -20.00000000000000000 ) ) ;
#84797 = CARTESIAN_POINT ( 'NONE',  ( -5.049401038298153566, 19.05341960407611168, 100.2072429386476955 ) ) ;
#84798 = CARTESIAN_POINT ( 'NONE',  ( -8.314922557960811034, -14.29746914071050412, 62.08224293864769550 ) ) ;
#84799 = CARTESIAN_POINT ( 'NONE',  ( -9.564922557961040184, 16.46253265017147172, 42.91775706135234003 ) ) ;
#84800 = CARTESIAN_POINT ( 'NONE',  ( -4.483927247898539470, -16.52544592524342804, 47.29057627198103120 ) ) ;
#84801 = CARTESIAN_POINT ( 'NONE',  ( 13.97604488694548053, -13.89961937509957401, 80.62609039468567573 ) ) ;
#84802 = CYLINDRICAL_SURFACE ( 'NONE', #189261, 59.99999999999998579 ) ;
#84803 = CARTESIAN_POINT ( 'NONE',  ( 18.62759615963271287, -10.81492255796078972, 33.33224293864769550 ) ) ;
#84804 = CARTESIAN_POINT ( 'NONE',  ( 14.34966873604960469, 8.224510206698951720, 94.16557627198103830 ) ) ;
#84805 = CARTESIAN_POINT ( 'NONE',  ( 2.995967610389833449E-15, -78.62686331009497565, -14.99999901254159873 ) ) ;
#84807 = CARTESIAN_POINT ( 'NONE',  ( -21.53943276465977519, 0.05219959533907696930, 51.24890960531436690 ) ) ;
#84806 = CARTESIAN_POINT ( 'NONE',  ( -9.564922557960796823, -16.46253265017161027, 52.08224293864768839 ) ) ;
#84808 = CARTESIAN_POINT ( 'NONE',  ( 13.97604488694527802, 13.89961937509977652, 34.37390960531436690 ) ) ;
#84810 = CARTESIAN_POINT ( 'NONE',  ( -19.03943276465977164, 0.05219959533909376836, 56.24890960531435979 ) ) ;
#84809 = CARTESIAN_POINT ( 'NONE',  ( 14.34966873604972726, -8.224510206698740333, 80.83442372801901854 ) ) ;
#84811 = CARTESIAN_POINT ( 'NONE',  ( -13.89961937509957401, -13.97604488694547875, 44.37609039468566863 ) ) ;
#84812 = CARTESIAN_POINT ( 'NONE',  ( 15.80617190586769283, -15.72974639402175789, 70.62609039468567573 ) ) ;
#84813 = CARTESIAN_POINT ( 'NONE',  ( -21.53943276465977519, 0.05219959533907696930, 51.24890960531436690 ) ) ;
#84814 = CARTESIAN_POINT ( 'NONE',  ( -14.29746914071049879, 8.314922557960819915, 115.8322429386477097 ) ) ;
#84815 = EDGE_CURVE ( 'NONE', #114713, #20950, #188806, .T. ) ;
#84816 = CARTESIAN_POINT ( 'NONE',  ( -9.564922557961040184, 16.46253265017147172, 97.91775706135233293 ) ) ;
#84817 = CARTESIAN_POINT ( 'NONE',  ( 29.86685920354754487, 21.69954338932564752, -7.924999997268814766 ) ) ;
#84819 = CARTESIAN_POINT ( 'NONE',  ( -0.05219959533907301413, -21.53943276465977519, 47.49890960531435979 ) ) ;
#84818 = DIRECTION ( 'NONE',  ( 1.000000000000000000, 0.000000000000000000, 0.000000000000000000 ) ) ;
#84820 = CARTESIAN_POINT ( 'NONE',  ( -19.05341960407611168, -5.049401038298163336, 26.45724293864769550 ) ) ;
#84821 = CARTESIAN_POINT ( 'NONE',  ( -0.05219959533937732626, 21.53943276465977519, 77.50109039468567573 ) ) ;
#84822 = CARTESIAN_POINT ( 'NONE',  ( -4.483927247898539470, -16.52544592524342804, 42.29057627198103120 ) ) ;
#84823 = CARTESIAN_POINT ( 'NONE',  ( -8.224510206698948167, 14.34966873604960824, 60.41557627198102409 ) ) ;
#84824 = CARTESIAN_POINT ( 'NONE',  ( -21.55341960407610458, -5.719274019375992779, 76.45724293864769550 ) ) ;
#84825 = CARTESIAN_POINT ( 'NONE',  ( 21.52544592524344225, -5.823673210054117533, 78.54057627198103830 ) ) ;
#84826 = CARTESIAN_POINT ( 'NONE',  ( -0.9155518048963315891, -29.20736712825161874, -49.29216761470102881 ) ) ;
#84827 = CARTESIAN_POINT ( 'NONE',  ( -15.80617190586745835, -15.72974639402198527, 36.87390960531435979 ) ) ;
#84828 = CARTESIAN_POINT ( 'NONE',  ( -8.314922557961024197, 14.29746914071037800, 47.91775706135234714 ) ) ;
#84829 = CARTESIAN_POINT ( 'NONE',  ( 4.483927247898545687, 16.52544592524342804, 79.79057627198102409 ) ) ;
#84830 = CARTESIAN_POINT ( 'NONE',  ( -19.02544592524342804, 5.153800228976336051, 56.04057627198100988 ) ) ;
#84831 = CARTESIAN_POINT ( 'NONE',  ( -0.05219959533909027116, -19.03943276465977164, 37.49890960531436690 ) ) ;
#84832 = FILL_AREA_STYLE_COLOUR ( '', #8045 ) ;
#84833 = CARTESIAN_POINT ( 'NONE',  ( 25.22509938781154304, -6.326560822155840924, 165.8168946714177991 ) ) ;
#84834 = ORIENTED_EDGE ( 'NONE', *, *, #17351, .F. ) ;
#84835 = CARTESIAN_POINT ( 'NONE',  ( 8.224510206698742110, 14.34966873604972548, 77.08442372801901854 ) ) ;
#84836 = CARTESIAN_POINT ( 'NONE',  ( -15.72974639402176322, -15.80617190586768395, 19.37609039468568639 ) ) ;
#84837 = CARTESIAN_POINT ( 'NONE',  ( 5.153800228976335163, 19.02544592524342804, 69.79057627198103830 ) ) ;
#84838 = CARTESIAN_POINT ( 'NONE',  ( 21.53943276465977519, 0.05219959533937863772, 56.25109039468568284 ) ) ;
#84839 = CARTESIAN_POINT ( 'NONE',  ( 13.97604488694527802, 13.89961937509977652, 114.3739096053143669 ) ) ;
#84840 = CARTESIAN_POINT ( 'NONE',  ( 0.000000000000000000, 0.000000000000000000, -18.00000000000000000 ) ) ;
#84841 = ORIENTED_EDGE ( 'NONE', *, *, #10071, .T. ) ;
#84842 = CARTESIAN_POINT ( 'NONE',  ( -10.72451020669870658, -18.67979575497194134, 49.58442372801901143 ) ) ;
#84844 = CARTESIAN_POINT ( 'NONE',  ( -16.51473224551069308, -9.474510206698971260, 106.6655762719810383 ) ) ;
#84843 = FACE_OUTER_BOUND ( 'NONE', #168286, .T. ) ;
#84845 = CARTESIAN_POINT ( 'NONE',  ( -9.564922557961040184, 16.46253265017147172, 57.91775706135233293 ) ) ;
#84846 = CARTESIAN_POINT ( 'NONE',  ( 10.81492255796078972, 18.62759615963270932, 114.5822429386477097 ) ) ;
#84847 = CARTESIAN_POINT ( 'NONE',  ( 0.05219959533936267826, -19.03943276465977164, 45.00109039468566863 ) ) ;
#84848 = CARTESIAN_POINT ( 'NONE',  ( 9.564922557960805705, 16.46253265017160317, 24.58224293864769194 ) ) ;
#84849 = CARTESIAN_POINT ( 'NONE',  ( 0.05219959533934541429, -16.53943276465976808, 90.00109039468567573 ) ) ;
#84850 = CARTESIAN_POINT ( 'NONE',  ( 19.02544592524334988, 5.153800228976608722, 56.45942372801898301 ) ) ;
#84851 = CARTESIAN_POINT ( 'NONE',  ( 16.52544592524335698, 4.483927247898782831, 111.4594237280190328 ) ) ;
#84852 = CARTESIAN_POINT ( 'NONE',  ( 9.687362902255726382, 9.687362902255699737, -62.58071313852362039 ) ) ;
#84853 = CARTESIAN_POINT ( 'NONE',  ( -19.02544592524342804, 5.153800228976336051, 81.04057627198103830 ) ) ;
#84854 = CARTESIAN_POINT ( 'NONE',  ( -15.80617190586768217, 15.72974639402176855, 98.12609039468570415 ) ) ;
#84855 = CARTESIAN_POINT ( 'NONE',  ( 21.52544592524334988, 5.823673210054432836, 96.45942372801901854 ) ) ;
#84856 = CARTESIAN_POINT ( 'NONE',  ( 17.50000000000000000, 5.499999999999992895, 66.70309617465828467 ) ) ;
#84857 = CARTESIAN_POINT ( 'NONE',  ( 19.05341960407611168, 5.049401038298154454, 98.95724293864766707 ) ) ;
#84858 = CARTESIAN_POINT ( 'NONE',  ( 18.62759615963255655, 10.81492255796105972, 81.66775706135236135 ) ) ;
#84859 = CARTESIAN_POINT ( 'NONE',  ( -19.05341960407617563, 5.049401038297882671, 113.5427570613523471 ) ) ;
#84860 = CARTESIAN_POINT ( 'NONE',  ( -13.89961937509977652, 13.97604488694528158, 85.62390960531433848 ) ) ;
#84861 = CARTESIAN_POINT ( 'NONE',  ( -15.80617190586745835, -15.72974639402198527, 26.87390960531435979 ) ) ;
#84862 = CARTESIAN_POINT ( 'NONE',  ( -9.474510206698964154, 16.51473224551069663, 90.41557627198103830 ) ) ;
#84863 = CARTESIAN_POINT ( 'NONE',  ( -16.29526858892876362, -7.335722546920120379, 90.79670597800210885 ) ) ;
#84864 = CARTESIAN_POINT ( 'NONE',  ( -19.03943276465977164, 0.05219959533909376836, 81.24890960531436690 ) ) ;
#84865 = CARTESIAN_POINT ( 'NONE',  ( -13.89961937509977652, 13.97604488694528158, 65.62390960531436690 ) ) ;
#84866 = CARTESIAN_POINT ( 'NONE',  ( -0.05219959533934338120, 16.53943276465976808, 102.5010903946856899 ) ) ;
#84867 = CYLINDRICAL_SURFACE ( 'NONE', #8128, 13.70000000000001528 ) ;
#84868 = CARTESIAN_POINT ( 'NONE',  ( -13.97604488694547697, 13.89961937509957934, 53.12609039468565442 ) ) ;
#84869 = CARTESIAN_POINT ( 'NONE',  ( -5.049401038298153566, 19.05341960407611168, 95.20724293864770971 ) ) ;
#84870 = CARTESIAN_POINT ( 'NONE',  ( 14.34966873604960469, 8.224510206698951720, 89.16557627198102409 ) ) ;
#84871 = CARTESIAN_POINT ( 'NONE',  ( -5.719274019375978568, 21.55341960407610458, 35.20724293864768839 ) ) ;
#84872 = CARTESIAN_POINT ( 'NONE',  ( 5.049401038298161559, -19.05341960407611168, 112.7072429386476813 ) ) ;
#84873 = VECTOR ( 'NONE', #184532, 1000.000000000000000 ) ;
#84874 = CARTESIAN_POINT ( 'NONE',  ( 4.483927247898545687, 16.52544592524342804, 94.79057627198105251 ) ) ;
#84875 = CARTESIAN_POINT ( 'NONE',  ( 0.000000000000000000, 0.000000000000000000, -64.92179855667829713 ) ) ;
#84876 = CARTESIAN_POINT ( 'NONE',  ( -5.153800228976607833, 19.02544592524334988, 42.70942372801901143 ) ) ;
#84877 = CARTESIAN_POINT ( 'NONE',  ( -8.224510206698735004, -14.34966873604973081, 109.5844237280190328 ) ) ;
#84878 = CARTESIAN_POINT ( 'NONE',  ( -16.46253265017160317, 9.564922557960807481, 90.83224293864769550 ) ) ;
#84879 = CARTESIAN_POINT ( 'NONE',  ( 5.719274019375673035, 21.55341960407619339, 72.29275706135236135 ) ) ;
#84880 = CARTESIAN_POINT ( 'NONE',  ( -15.72974639402197994, 15.80617190586746368, 60.62390960531437401 ) ) ;
#84881 = CARTESIAN_POINT ( 'NONE',  ( -0.05219959533937732626, 21.53943276465977519, 27.50109039468567929 ) ) ;
#84882 = CARTESIAN_POINT ( 'NONE',  ( -5.719274019375978568, 21.55341960407610458, 85.20724293864770971 ) ) ;
#84883 = CARTESIAN_POINT ( 'NONE',  ( -0.05219959533937732626, 21.53943276465977519, 37.50109039468568284 ) ) ;
#84884 = CARTESIAN_POINT ( 'NONE',  ( -8.224510206698948167, 14.34966873604960824, 105.4155762719810383 ) ) ;
#84885 = CARTESIAN_POINT ( 'NONE',  ( 9.564922557961047289, -16.46253265017146816, 65.41775706135233293 ) ) ;
#84886 = CARTESIAN_POINT ( 'NONE',  ( -5.049401038298153566, 19.05341960407611168, 50.20724293864770260 ) ) ;
#84888 = CARTESIAN_POINT ( 'NONE',  ( -9.564922557960796823, -16.46253265017161027, 97.08224293864769550 ) ) ;
#84887 = CARTESIAN_POINT ( 'NONE',  ( 4.483927247898545687, 16.52544592524342804, 89.79057627198103830 ) ) ;
#84889 = CARTESIAN_POINT ( 'NONE',  ( 19.02544592524343514, -5.153800228976328945, 98.54057627198100988 ) ) ;
#84890 = CARTESIAN_POINT ( 'NONE',  ( -0.05219959533910754901, -16.53943276465976808, 112.4989096053143669 ) ) ;
#84891 = CARTESIAN_POINT ( 'NONE',  ( 8.224510206698953496, -14.34966873604960469, 42.91557627198103120 ) ) ;
#84892 = CARTESIAN_POINT ( 'NONE',  ( -5.049401038298153566, 19.05341960407611168, 50.20724293864770260 ) ) ;
#84893 = CARTESIAN_POINT ( 'NONE',  ( 16.46253265017160672, -9.564922557960803928, 23.33224293864769194 ) ) ;
#84894 = CARTESIAN_POINT ( 'NONE',  ( 13.97604488694548053, -13.89961937509957401, 30.62609039468566863 ) ) ;
#84896 = CARTESIAN_POINT ( 'NONE',  ( -16.53943276465976808, 0.05219959533911058130, 26.24890960531435624 ) ) ;
#84895 = CARTESIAN_POINT ( 'NONE',  ( -19.03943276465977164, 0.05219959533909376836, 111.2489096053143669 ) ) ;
#84897 = CARTESIAN_POINT ( 'NONE',  ( -0.05219959533937732626, 21.53943276465977519, 37.50109039468568284 ) ) ;
#84898 = CARTESIAN_POINT ( 'NONE',  ( -16.46253265017160317, 9.564922557960807481, 110.8322429386476955 ) ) ;
#84899 = CARTESIAN_POINT ( 'NONE',  ( 8.224510206698742110, 14.34966873604972548, 42.08442372801901854 ) ) ;
#84900 = CARTESIAN_POINT ( 'NONE',  ( -16.53943276465976808, -0.05219959533934237506, 103.7510903946857042 ) ) ;
#84901 = CARTESIAN_POINT ( 'NONE',  ( 12.14591786802327356, -12.06949235617739191, 90.62609039468567573 ) ) ;
#84902 = CARTESIAN_POINT ( 'NONE',  ( -4.379528057220086978, -16.55341960407618274, 29.79275706135234358 ) ) ;
#84903 = CARTESIAN_POINT ( 'NONE',  ( -5.153800228976328057, -19.02544592524343514, 47.29057627198102409 ) ) ;
#84904 = AXIS2_PLACEMENT_3D ( 'NONE', #179185, #25508, #40653 ) ;
#84905 = CARTESIAN_POINT ( 'NONE',  ( 12.14591786802309770, 12.06949235617756955, 114.3739096053143527 ) ) ;
#84906 = CARTESIAN_POINT ( 'NONE',  ( -21.53943276465977519, -0.05219959533937600094, 18.75109039468568639 ) ) ;
#84907 = CARTESIAN_POINT ( 'NONE',  ( -9.564922557960796823, -16.46253265017161027, 37.08224293864768839 ) ) ;
#84908 = CARTESIAN_POINT ( 'NONE',  ( 16.46253265017160672, -9.564922557960803928, 108.3322429386476955 ) ) ;
#84909 = CARTESIAN_POINT ( 'NONE',  ( 9.474510206698971260, -16.51473224551069308, 37.91557627198102409 ) ) ;
#84910 = CARTESIAN_POINT ( 'NONE',  ( 19.05341960407611168, 5.049401038298154454, 98.95724293864766707 ) ) ;
#84911 = DIRECTION ( 'NONE',  ( -0.000000000000000000, -0.000000000000000000, 1.000000000000000000 ) ) ;
#84912 = CARTESIAN_POINT ( 'NONE',  ( 5.049401038298161559, -19.05341960407611168, 92.70724293864769550 ) ) ;
#84914 = CARTESIAN_POINT ( 'NONE',  ( -4.379528057220328563, 16.55341960407611168, 105.2072429386477097 ) ) ;
#84913 = CARTESIAN_POINT ( 'NONE',  ( 15.72974639402176855, 15.80617190586768217, 41.87609039468568284 ) ) ;
#84915 = CARTESIAN_POINT ( 'NONE',  ( 5.049401038298161559, -19.05341960407611168, 112.7072429386476813 ) ) ;
#84916 = CARTESIAN_POINT ( 'NONE',  ( 7.284589286804261654, -1.784589286804270980, 8.181980515339454030 ) ) ;
#84917 = CARTESIAN_POINT ( 'NONE',  ( -12.14591786802326823, 12.06949235617739902, 58.12609039468568994 ) ) ;
#84918 = CARTESIAN_POINT ( 'NONE',  ( -18.67979575497193778, 10.72451020669871902, 78.33442372801901854 ) ) ;
#84919 = CARTESIAN_POINT ( 'NONE',  ( -8.224510206698735004, -14.34966873604973081, 39.58442372801901143 ) ) ;
#84920 = CARTESIAN_POINT ( 'NONE',  ( -5.153800228976328057, -19.02544592524343514, 87.29057627198103830 ) ) ;
#84921 = CARTESIAN_POINT ( 'NONE',  ( -19.03943276465977164, -0.05219959533935918106, 113.7510903946856757 ) ) ;
#84922 = CARTESIAN_POINT ( 'NONE',  ( -8.314922557961024197, 14.29746914071037800, 82.91775706135234714 ) ) ;
#84923 = CARTESIAN_POINT ( 'NONE',  ( -5.049401038297874678, -19.05341960407617918, 89.79275706135230450 ) ) ;
#84924 = CARTESIAN_POINT ( 'NONE',  ( 16.46253265017160672, -9.564922557960803928, 68.33224293864770971 ) ) ;
#84925 = CARTESIAN_POINT ( 'NONE',  ( -5.719274019375978568, 21.55341960407610458, 95.20724293864769550 ) ) ;
#84927 = CARTESIAN_POINT ( 'NONE',  ( -9.474510206698720793, -16.51473224551083518, 84.58442372801900433 ) ) ;
#84926 = CARTESIAN_POINT ( 'NONE',  ( 16.53943276465976808, -0.05219959533910856209, 83.74890960531435269 ) ) ;
#84928 = CARTESIAN_POINT ( 'NONE',  ( 8.224510206698742110, 14.34966873604972548, 62.08442372801901143 ) ) ;
#84929 = CARTESIAN_POINT ( 'NONE',  ( 24.24393946303100122, 5.863316274095517144, 172.4343578713345551 ) ) ;
#84930 = CARTESIAN_POINT ( 'NONE',  ( 16.46253265017146816, 9.564922557961045513, 76.66775706135234714 ) ) ;
#84931 = CARTESIAN_POINT ( 'NONE',  ( -0.05219959533910754901, -16.53943276465976808, 32.49890960531435979 ) ) ;
#84932 = CARTESIAN_POINT ( 'NONE',  ( 8.314922557960818139, 14.29746914071049879, 74.58224293864768129 ) ) ;
#84934 = CARTESIAN_POINT ( 'NONE',  ( -16.62475595723610411, 7.163666690055884523, 40.52713351810402287 ) ) ;
#84933 = CARTESIAN_POINT ( 'NONE',  ( 19.02544592524334988, 5.153800228976608722, 26.45942372801899722 ) ) ;
#84935 = CARTESIAN_POINT ( 'NONE',  ( -10.72451020669870658, -18.67979575497194134, 29.58442372801901854 ) ) ;
#84936 = CARTESIAN_POINT ( 'NONE',  ( 19.02544592524343514, -5.153800228976328945, 108.5405762719810383 ) ) ;
#84937 = CARTESIAN_POINT ( 'NONE',  ( 13.97604488694527802, 13.89961937509977652, 84.37390960531433848 ) ) ;
#84938 = CARTESIAN_POINT ( 'NONE',  ( 5.719274019375673035, 21.55341960407619339, 102.2927570613523613 ) ) ;
#84939 = CARTESIAN_POINT ( 'NONE',  ( 0.05219959533909260263, 19.03943276465977164, 69.99890960531435269 ) ) ;
#84940 = CARTESIAN_POINT ( 'NONE',  ( -21.53943276465977519, 0.05219959533907696930, 46.24890960531435979 ) ) ;
#84941 = CARTESIAN_POINT ( 'NONE',  ( -4.379528057220328563, 16.55341960407611168, 80.20724293864769550 ) ) ;
#84942 = CARTESIAN_POINT ( 'NONE',  ( 16.46253265017160672, -9.564922557960803928, 58.33224293864769550 ) ) ;
#84943 = CARTESIAN_POINT ( 'NONE',  ( -16.55341960407611168, -4.379528057220339221, 106.4572429386477097 ) ) ;
#84944 = CARTESIAN_POINT ( 'NONE',  ( -10.81492255796105439, 18.62759615963255655, 22.91775706135235069 ) ) ;
#84945 = CARTESIAN_POINT ( 'NONE',  ( 18.62759615963255655, 10.81492255796105972, 56.66775706135235424 ) ) ;
#84946 = CARTESIAN_POINT ( 'NONE',  ( 19.05341960407611168, 5.049401038298154454, 48.95724293864768129 ) ) ;
#84947 = CARTESIAN_POINT ( 'NONE',  ( -14.34966873604972548, 8.224510206698743886, 73.33442372801901854 ) ) ;
#84948 = CARTESIAN_POINT ( 'NONE',  ( 5.719274019375991003, -21.55341960407610458, 107.7072429386476955 ) ) ;
#84949 = CARTESIAN_POINT ( 'NONE',  ( -10.72451020669870658, -18.67979575497194134, 19.58442372801901143 ) ) ;
#84951 = CARTESIAN_POINT ( 'NONE',  ( -9.564922557960796823, -16.46253265017161027, 62.08224293864769550 ) ) ;
#84950 = CARTESIAN_POINT ( 'NONE',  ( 13.97604488694548053, -13.89961937509957401, 35.62609039468567573 ) ) ;
#84952 = CARTESIAN_POINT ( 'NONE',  ( -19.03943276465977164, -0.05219959533935918106, 33.75109039468566863 ) ) ;
#84953 = CARTESIAN_POINT ( 'NONE',  ( -15.72974639402176322, -15.80617190586768395, 69.37609039468567573 ) ) ;
#84954 = CARTESIAN_POINT ( 'NONE',  ( 21.52544592524344225, -5.823673210054117533, 63.54057627198103830 ) ) ;
#84955 = CARTESIAN_POINT ( 'NONE',  ( -16.53943276465976808, 0.05219959533911058130, 41.24890960531435269 ) ) ;
#84957 = CARTESIAN_POINT ( 'NONE',  ( 0.05219959533936267826, -19.03943276465977164, 20.00109039468567218 ) ) ;
#84956 = CARTESIAN_POINT ( 'NONE',  ( 15.72974639402176855, 15.80617190586768217, 91.87609039468568994 ) ) ;
#84958 = CARTESIAN_POINT ( 'NONE',  ( -14.34966873604960291, -8.224510206698953496, 56.66557627198103830 ) ) ;
#84959 = CARTESIAN_POINT ( 'NONE',  ( -14.34966873604960291, -8.224510206698953496, 101.6655762719810383 ) ) ;
#84960 = CARTESIAN_POINT ( 'NONE',  ( 16.51473224551083163, -9.474510206698727899, 55.83442372801899722 ) ) ;
#84961 = CARTESIAN_POINT ( 'NONE',  ( 14.29746914071049879, -8.314922557960816363, 23.33224293864769194 ) ) ;
#84962 = CARTESIAN_POINT ( 'NONE',  ( -18.67979575497193778, 10.72451020669871902, 63.33442372801900433 ) ) ;
#84963 = CARTESIAN_POINT ( 'NONE',  ( -19.02544592524342804, 5.153800228976336051, 76.04057627198102409 ) ) ;
#84964 = CARTESIAN_POINT ( 'NONE',  ( -9.564922557961040184, 16.46253265017147172, 42.91775706135234003 ) ) ;
#84965 = CARTESIAN_POINT ( 'NONE',  ( 15.72974639402199770, -15.80617190586745480, 58.12390960531435979 ) ) ;
#84966 = CARTESIAN_POINT ( 'NONE',  ( 10.81492255796106328, -18.62759615963255655, 45.41775706135234003 ) ) ;
#84967 = CARTESIAN_POINT ( 'NONE',  ( 18.62759615963271287, -10.81492255796078972, 103.3322429386476955 ) ) ;
#84968 = CARTESIAN_POINT ( 'NONE',  ( 19.02544592524334988, 5.153800228976608722, 96.45942372801897591 ) ) ;
#84969 = CARTESIAN_POINT ( 'NONE',  ( -16.55341960407617563, 4.379528057220093196, 63.54275706135234003 ) ) ;
#84970 = CARTESIAN_POINT ( 'NONE',  ( -18.62759615963270932, 10.81492255796079327, 110.8322429386476955 ) ) ;
#84971 = CARTESIAN_POINT ( 'NONE',  ( -12.14591786802309592, -12.06949235617757132, 86.87390960531438111 ) ) ;
#84972 = CARTESIAN_POINT ( 'NONE',  ( -17.40861289039002457, -6.110651285853315962, 101.3723247082743200 ) ) ;
#84973 = CARTESIAN_POINT ( 'NONE',  ( 12.14591786802327356, -12.06949235617739191, 20.62609039468568639 ) ) ;
#84974 = AXIS2_PLACEMENT_3D ( 'NONE', #42536, #56706, #134550 ) ;
#84975 = CARTESIAN_POINT ( 'NONE',  ( 21.55341960407610458, 5.719274019375980345, 48.95724293864770971 ) ) ;
#84976 = CARTESIAN_POINT ( 'NONE',  ( -8.314922557961024197, 14.29746914071037800, 87.91775706135234714 ) ) ;
#84977 = CARTESIAN_POINT ( 'NONE',  ( 31.37807670187659070, -19.48766232597224501, -7.999999999999996447 ) ) ;
#84978 = CARTESIAN_POINT ( 'NONE',  ( 12.06949235617739724, 12.14591786802326823, 71.87609039468568994 ) ) ;
#84979 = CARTESIAN_POINT ( 'NONE',  ( -15.72974639402176322, -15.80617190586768395, 29.37609039468568284 ) ) ;
#84980 = CARTESIAN_POINT ( 'NONE',  ( 5.823673210054125526, 21.52544592524343514, 39.79057627198103830 ) ) ;
#84981 = CARTESIAN_POINT ( 'NONE',  ( -8.314922557961024197, 14.29746914071037800, 82.91775706135234714 ) ) ;
#84982 = CARTESIAN_POINT ( 'NONE',  ( -19.05341960407611168, -5.049401038298163336, 96.45724293864769550 ) ) ;
#84983 = CARTESIAN_POINT ( 'NONE',  ( -15.72974639402176322, -15.80617190586768395, 64.37609039468568994 ) ) ;
#84984 = ADVANCED_FACE ( 'NONE', ( #53255 ), #145261, .F. ) ;
#84985 = CARTESIAN_POINT ( 'NONE',  ( -21.53943276465977519, 0.05219959533907696930, 46.24890960531435979 ) ) ;
#84986 = CARTESIAN_POINT ( 'NONE',  ( 21.55341960407610458, 5.719274019375980345, 38.95724293864768839 ) ) ;
#84987 = VERTEX_POINT ( 'NONE', #141287 ) ;
#84988 = CARTESIAN_POINT ( 'NONE',  ( 5.153800228976615827, -19.02544592524334988, 50.20942372801897591 ) ) ;
#84989 = CARTESIAN_POINT ( 'NONE',  ( 12.06949235617739724, 12.14591786802326823, 71.87609039468568994 ) ) ;
#84990 = CARTESIAN_POINT ( 'NONE',  ( 21.52544592524344225, -5.823673210054117533, 28.54057627198103120 ) ) ;
#84991 = ORIENTED_EDGE ( 'NONE', *, *, #66645, .F. ) ;
#84992 = CARTESIAN_POINT ( 'NONE',  ( 16.46253265017160672, -9.564922557960803928, 83.33224293864768129 ) ) ;
#84993 = CARTESIAN_POINT ( 'NONE',  ( -12.06949235617756955, 12.14591786802309770, 25.62390960531435624 ) ) ;
#84994 = CARTESIAN_POINT ( 'NONE',  ( 0.000000000000000000, 0.000000000000000000, -64.53213882399991519 ) ) ;
#84995 = CARTESIAN_POINT ( 'NONE',  ( -16.52544592524342804, 4.483927247898546575, 106.0405762719810525 ) ) ;
#84996 = CARTESIAN_POINT ( 'NONE',  ( -0.05219959533907301413, -21.53943276465977519, 47.49890960531435979 ) ) ;
#84997 = CARTESIAN_POINT ( 'NONE',  ( 5.049401038298161559, -19.05341960407611168, 47.70724293864770260 ) ) ;
#84998 = CARTESIAN_POINT ( 'NONE',  ( -4.379528057220086978, -16.55341960407618274, 74.79275706135234714 ) ) ;
#84999 = CARTESIAN_POINT ( 'NONE',  ( -10.81492255796105439, 18.62759615963255655, 37.91775706135235424 ) ) ;
#85000 = CARTESIAN_POINT ( 'NONE',  ( -19.02544592524334988, -5.153800228976617603, 88.95942372801897591 ) ) ;
#85001 = CARTESIAN_POINT ( 'NONE',  ( 12.14591786802309770, 12.06949235617756955, 94.37390960531436690 ) ) ;
#85002 = CARTESIAN_POINT ( 'NONE',  ( -9.474510206698964154, 16.51473224551069663, 50.41557627198102409 ) ) ;
#85003 = CARTESIAN_POINT ( 'NONE',  ( 16.46253265017160672, -9.564922557960803928, 33.33224293864770260 ) ) ;
#85004 = CARTESIAN_POINT ( 'NONE',  ( -5.823673210054431948, 21.52544592524334988, 102.7094237280190185 ) ) ;
#85005 = CARTESIAN_POINT ( 'NONE',  ( -16.46253265017160317, 9.564922557960807481, 75.83224293864769550 ) ) ;
#85007 = B_SPLINE_CURVE_WITH_KNOTS ( 'NONE', 3,
 ( #174817, #34316, #65637, #173837, #79821, #190979, #95979, #2976, #158638, #127297, #128293, #189010, #21125, #50485, #189991, #52456, #82781, #112145, #22128, #156670, #144462, #35303 ),
 .UNSPECIFIED., .F., .F.,
 ( 4, 2, 2, 2, 2, 2, 2, 2, 2, 2, 4 ),
 ( 2.776912483567713316E-17, 0.001309639967555412338, 0.001964459951333103437, 0.002291869943221948227, 0.002455574939166377344, 0.002619279935110806028, 0.002782984931055234711, 0.002946689926999664262, 0.003274099918888506884, 0.003928919902666203404, 0.005238559870221597310 ),
 .UNSPECIFIED. ) ;
#85006 = CARTESIAN_POINT ( 'NONE',  ( -4.483927247898782831, 16.52544592524335698, 62.70942372801902565 ) ) ;
#85008 = CARTESIAN_POINT ( 'NONE',  ( -21.53943276465977519, -0.05219959533937600094, 88.75109039468567573 ) ) ;
#85009 = CARTESIAN_POINT ( 'NONE',  ( 10.81492255796078972, 18.62759615963270932, 49.58224293864769550 ) ) ;
#85010 = CARTESIAN_POINT ( 'NONE',  ( 4.483927247898790824, -16.52544592524335698, 80.20942372801901854 ) ) ;
#85011 = CARTESIAN_POINT ( 'NONE',  ( -9.564922557961040184, 16.46253265017147172, 47.91775706135233293 ) ) ;
#85012 = CARTESIAN_POINT ( 'NONE',  ( 16.46253265017146816, 9.564922557961045513, 66.66775706135233293 ) ) ;
#85013 = CARTESIAN_POINT ( 'NONE',  ( 10.72451020669871369, 18.67979575497193778, 62.08442372801901143 ) ) ;
#85014 = CARTESIAN_POINT ( 'NONE',  ( -19.05341960407611168, -5.049401038298163336, 71.45724293864766707 ) ) ;
#85015 = CARTESIAN_POINT ( 'NONE',  ( -19.05341960407611168, -5.049401038298163336, 21.45724293864768839 ) ) ;
#85016 = CARTESIAN_POINT ( 'NONE',  ( -9.474510206698720793, -16.51473224551083518, 54.58442372801899722 ) ) ;
#85017 = CARTESIAN_POINT ( 'NONE',  ( -26.03370437638687918, 6.875205692009823011, 160.5968874236874910 ) ) ;
#85018 = CARTESIAN_POINT ( 'NONE',  ( 0.05219959533909260263, 19.03943276465977164, 89.99890960531436690 ) ) ;
#85019 = CARTESIAN_POINT ( 'NONE',  ( -12.06949235617756955, 12.14591786802309770, 50.62390960531435979 ) ) ;
#85020 = CARTESIAN_POINT ( 'NONE',  ( -5.823673210054116645, -21.52544592524344225, 52.29057627198102409 ) ) ;
#85021 = B_SPLINE_CURVE_WITH_KNOTS ( 'NONE', 3,
 ( #105134, #11147, #72821, #74797, #136459, #85967 ),
 .UNSPECIFIED., .F., .F.,
 ( 4, 2, 4 ),
 ( 0.003239945802372281181, 0.003620412082092138578, 0.004000878361811996409 ),
 .UNSPECIFIED. ) ;
#85022 = DIRECTION ( 'NONE',  ( 0.000000000000000000, 0.000000000000000000, 1.000000000000000000 ) ) ;
#85023 = CARTESIAN_POINT ( 'NONE',  ( -18.67979575497193778, 10.72451020669871902, 108.3344237280190185 ) ) ;
#85024 = CARTESIAN_POINT ( 'NONE',  ( -17.31747979337951548, -6.344076630960987728, 81.37944868065184778 ) ) ;
#85025 = CARTESIAN_POINT ( 'NONE',  ( -16.46253265017160317, 9.564922557960807481, 45.83224293864769550 ) ) ;
#85026 = CARTESIAN_POINT ( 'NONE',  ( -5.049401038298153566, 19.05341960407611168, 85.20724293864769550 ) ) ;
#85027 = CARTESIAN_POINT ( 'NONE',  ( -17.49999999999999289, 5.500000000000037303, 80.79690382534172954 ) ) ;
#85028 = CARTESIAN_POINT ( 'NONE',  ( -17.31747979337947640, 6.344076630961060559, 108.6205513193481664 ) ) ;
#85029 = CARTESIAN_POINT ( 'NONE',  ( 12.14591786802327356, -12.06949235617739191, 60.62609039468567573 ) ) ;
#85030 = CARTESIAN_POINT ( 'NONE',  ( 21.55341960407610458, 5.719274019375980345, 78.95724293864769550 ) ) ;
#85031 = CARTESIAN_POINT ( 'NONE',  ( -0.05219959533910754901, -16.53943276465976808, 57.49890960531435979 ) ) ;
#85033 = CARTESIAN_POINT ( 'NONE',  ( -19.03943276465977164, 0.05219959533909376836, 116.2489096053143669 ) ) ;
#85032 = CARTESIAN_POINT ( 'NONE',  ( -9.564922557960796823, -16.46253265017161027, 47.08224293864769550 ) ) ;
#85034 = CARTESIAN_POINT ( 'NONE',  ( -0.05219959533937732626, 21.53943276465977519, 37.50109039468568284 ) ) ;
#85035 = CARTESIAN_POINT ( 'NONE',  ( -0.05219959533936034679, 19.03943276465977164, 47.50109039468566863 ) ) ;
#85036 = CARTESIAN_POINT ( 'NONE',  ( 16.46253265017160672, -9.564922557960803928, 33.33224293864770260 ) ) ;
#85037 = CARTESIAN_POINT ( 'NONE',  ( -21.55341960407619339, 5.719274019375674811, 98.54275706135234714 ) ) ;
#85038 = CARTESIAN_POINT ( 'NONE',  ( -18.22780087662114212, 5.499999999999995559, 48.51540105326107266 ) ) ;
#85039 = CARTESIAN_POINT ( 'NONE',  ( -16.55341960407611168, -4.379528057220339221, 46.45724293864769550 ) ) ;
#85040 = CARTESIAN_POINT ( 'NONE',  ( -16.70000000000002061, 1.759457951533292443E-13, -59.13370768023891344 ) ) ;
#85041 = CARTESIAN_POINT ( 'NONE',  ( 5.719274019375991003, -21.55341960407610458, 37.70724293864769550 ) ) ;
#85042 = CARTESIAN_POINT ( 'NONE',  ( 27.73933785331498569, 2.768321779492822058E-14, 141.8750000027311842 ) ) ;
#85043 = CARTESIAN_POINT ( 'NONE',  ( 16.46253265017160672, -9.564922557960803928, 83.33224293864768129 ) ) ;
#85044 = CARTESIAN_POINT ( 'NONE',  ( -12.14591786802309592, -12.06949235617757132, 86.87390960531438111 ) ) ;
#85045 = CARTESIAN_POINT ( 'NONE',  ( 16.52544592524335698, 4.483927247898782831, 21.45942372801901499 ) ) ;
#85046 = CARTESIAN_POINT ( 'NONE',  ( 16.53943276465976808, 0.05219959533934440121, 111.2510903946856899 ) ) ;
#85047 = VERTEX_POINT ( 'NONE', #158445 ) ;
#85048 = CARTESIAN_POINT ( 'NONE',  ( -19.03943276465977164, 0.05219959533909376836, 46.24890960531435979 ) ) ;
#85050 = CARTESIAN_POINT ( 'NONE',  ( -18.62759615963270932, 10.81492255796079327, 95.83224293864770971 ) ) ;
#85049 = CARTESIAN_POINT ( 'NONE',  ( 16.51473224551069308, 9.474510206698969483, 84.16557627198102409 ) ) ;
#85051 = AXIS2_PLACEMENT_3D ( 'NONE', #167235, #166244, #179434 ) ;
#85053 = CARTESIAN_POINT ( 'NONE',  ( 9.564922557960805705, 16.46253265017160317, 104.5822429386476955 ) ) ;
#85052 = CARTESIAN_POINT ( 'NONE',  ( 16.53943276465976808, -0.05219959533910856209, 28.74890960531435624 ) ) ;
#85054 = CARTESIAN_POINT ( 'NONE',  ( 0.05219959533936267826, -19.03943276465977164, 75.00109039468566152 ) ) ;
#85055 = CARTESIAN_POINT ( 'NONE',  ( -10.72451020669870658, -18.67979575497194134, 104.5844237280190185 ) ) ;
#85056 = CARTESIAN_POINT ( 'NONE',  ( 18.62759615963271287, -10.81492255796078972, 83.33224293864769550 ) ) ;
#85057 = CARTESIAN_POINT ( 'NONE',  ( 21.52544592524344225, -5.823673210054117533, 43.54057627198103830 ) ) ;
#85058 = CARTESIAN_POINT ( 'NONE',  ( -0.05219959533909027116, -19.03943276465977164, 67.49890960531436690 ) ) ;
#85059 = CARTESIAN_POINT ( 'NONE',  ( -8.224510206698948167, 14.34966873604960824, 30.41557627198101699 ) ) ;
#85060 = CARTESIAN_POINT ( 'NONE',  ( -19.03943276465977164, 0.05219959533909376836, 81.24890960531436690 ) ) ;
#85061 = VERTEX_POINT ( 'NONE', #6743 ) ;
#85062 = CARTESIAN_POINT ( 'NONE',  ( -32.42844225013699599, -3.321486864536487893, 88.27111922316775861 ) ) ;
#85063 = CARTESIAN_POINT ( 'NONE',  ( -9.474510206698720793, -16.51473224551083518, 34.58442372801899722 ) ) ;
#85064 = CARTESIAN_POINT ( 'NONE',  ( -0.05219959533910754901, -16.53943276465976808, 82.49890960531436690 ) ) ;
#85065 = CARTESIAN_POINT ( 'NONE',  ( 21.55341960407619695, -5.719274019375665929, 26.04275706135235779 ) ) ;
#85066 = CARTESIAN_POINT ( 'NONE',  ( -8.571926809382601320, -26.38167802310801591, 143.7750000027311899 ) ) ;
#85067 = CARTESIAN_POINT ( 'NONE',  ( -15.72974639402197994, 15.80617190586746368, 75.62390960531439532 ) ) ;
#85068 = CARTESIAN_POINT ( 'NONE',  ( -12.14591786802326823, 12.06949235617739902, 98.12609039468570415 ) ) ;
#85069 = CARTESIAN_POINT ( 'NONE',  ( -16.52544592524342804, 4.483927247898546575, 116.0405762719810383 ) ) ;
#85070 = CARTESIAN_POINT ( 'NONE',  ( -16.46253265017160317, 9.564922557960807481, 75.83224293864769550 ) ) ;
#85071 = LINE ( 'NONE', #193277, #164134 ) ;
#85072 = CARTESIAN_POINT ( 'NONE',  ( 16.52544592524342804, -4.483927247898539470, 28.54057627198103120 ) ) ;
#85073 = CARTESIAN_POINT ( 'NONE',  ( -10.81492255796105439, 18.62759615963255655, 57.91775706135234714 ) ) ;
#85074 = CARTESIAN_POINT ( 'NONE',  ( 26.63963442026837214, -26.88931099783062351, -16.54750829168370529 ) ) ;
#85075 = CARTESIAN_POINT ( 'NONE',  ( 15.72974639402176855, 15.80617190586768217, 91.87609039468568994 ) ) ;
#85076 = CARTESIAN_POINT ( 'NONE',  ( -9.474510206698964154, 16.51473224551069663, 40.41557627198103120 ) ) ;
#85077 = CARTESIAN_POINT ( 'NONE',  ( -13.97604488694527625, -13.89961937509977652, 46.87390960531435979 ) ) ;
#85078 = VERTEX_POINT ( 'NONE', #126123 ) ;
#85079 = CARTESIAN_POINT ( 'NONE',  ( 15.80617190586769283, -15.72974639402175789, 95.62609039468568994 ) ) ;
#85080 = CARTESIAN_POINT ( 'NONE',  ( 16.52544592524335698, 4.483927247898782831, 61.45942372801901854 ) ) ;
#85081 = CARTESIAN_POINT ( 'NONE',  ( -10.72451020669870658, -18.67979575497194134, 79.58442372801903275 ) ) ;
#85082 = CARTESIAN_POINT ( 'NONE',  ( -0.05219959533907301413, -21.53943276465977519, 22.49890960531436335 ) ) ;
#85083 = CARTESIAN_POINT ( 'NONE',  ( 13.89961937509957401, 13.97604488694547697, 96.87609039468566152 ) ) ;
#85084 = CARTESIAN_POINT ( 'NONE',  ( -18.62759615963255300, -10.81492255796106328, 54.16775706135235424 ) ) ;
#85085 = CARTESIAN_POINT ( 'NONE',  ( -12.06949235617739369, -12.14591786802326823, 34.37609039468568284 ) ) ;
#85086 = CARTESIAN_POINT ( 'NONE',  ( -21.53943276465977519, 0.05219959533907696930, 86.24890960531436690 ) ) ;
#85087 = CARTESIAN_POINT ( 'NONE',  ( -19.02544592524334988, -5.153800228976617603, 83.95942372801901854 ) ) ;
#85088 = CARTESIAN_POINT ( 'NONE',  ( 13.89961937509977652, -13.97604488694527269, 68.12390960531436690 ) ) ;
#85089 = CARTESIAN_POINT ( 'NONE',  ( 5.153800228976615827, -19.02544592524334988, 95.20942372801897591 ) ) ;
#85090 = CARTESIAN_POINT ( 'NONE',  ( -19.05341960407617563, 5.049401038297882671, 103.5427570613523329 ) ) ;
#85091 = CARTESIAN_POINT ( 'NONE',  ( 16.55341960407611168, 4.379528057220329451, 53.95724293864770260 ) ) ;
#85092 = CARTESIAN_POINT ( 'NONE',  ( 9.564922557961047289, -16.46253265017146816, 75.41775706135234714 ) ) ;
#85093 = CARTESIAN_POINT ( 'NONE',  ( -4.379528057220086978, -16.55341960407618274, 54.79275706135235424 ) ) ;
#85094 = CARTESIAN_POINT ( 'NONE',  ( -16.46253265017146816, -9.564922557961047289, 39.16775706135234003 ) ) ;
#85095 = CARTESIAN_POINT ( 'NONE',  ( 5.153800228976335163, 19.02544592524342804, 39.79057627198100988 ) ) ;
#85096 = CARTESIAN_POINT ( 'NONE',  ( -16.51473224551069308, -9.474510206698971260, 56.66557627198103120 ) ) ;
#85097 = CARTESIAN_POINT ( 'NONE',  ( -16.55341960407617563, 4.379528057220093196, 58.54275706135235424 ) ) ;
#85098 = CARTESIAN_POINT ( 'NONE',  ( 8.571926809382603096, -26.38167802310801235, 141.9750000027312069 ) ) ;
#85099 = CARTESIAN_POINT ( 'NONE',  ( 23.31738231874054890, -16.94106989632523508, 141.0500000054623513 ) ) ;
#85100 = CARTESIAN_POINT ( 'NONE',  ( -19.02544592524342804, 5.153800228976336051, 106.0405762719810241 ) ) ;
#85101 = CARTESIAN_POINT ( 'NONE',  ( 5.153800228976335163, 19.02544592524342804, 24.79057627198102765 ) ) ;
#85102 = VERTEX_POINT ( 'NONE', #144263 ) ;
#85103 = CARTESIAN_POINT ( 'NONE',  ( -19.02544592524334988, -5.153800228976617603, 103.9594237280190043 ) ) ;
#85104 = CARTESIAN_POINT ( 'NONE',  ( -21.53943276465977519, 0.05219959533907696930, 31.24890960531435979 ) ) ;
#85106 = CARTESIAN_POINT ( 'NONE',  ( -16.52544592524335698, -4.483927247898792601, 18.95942372801901143 ) ) ;
#85105 = CARTESIAN_POINT ( 'NONE',  ( 16.51473224551083163, -9.474510206698727899, 35.83442372801899722 ) ) ;
#85107 = CARTESIAN_POINT ( 'NONE',  ( -5.049401038298153566, 19.05341960407611168, 35.20724293864768839 ) ) ;
#85108 = CARTESIAN_POINT ( 'NONE',  ( 19.05341960407611168, 5.049401038298154454, 48.95724293864768129 ) ) ;
#85109 = CARTESIAN_POINT ( 'NONE',  ( 5.719274019375991003, -21.55341960407610458, 67.70724293864769550 ) ) ;
#85110 = CARTESIAN_POINT ( 'NONE',  ( -19.03943276465977164, 0.05219959533909376836, 101.2489096053143669 ) ) ;
#85111 = CIRCLE ( 'NONE', #130418, 4.000000000000000888 ) ;
#85112 = EDGE_CURVE ( 'NONE', #190052, #93673, #182636, .T. ) ;
#85113 = CARTESIAN_POINT ( 'NONE',  ( 19.05341960407611168, 5.049401038298154454, 38.95724293864767418 ) ) ;
#85114 = CARTESIAN_POINT ( 'NONE',  ( 17.14385361876520264, 23.59649016807275856, 146.6750000027311671 ) ) ;
#85115 = CARTESIAN_POINT ( 'NONE',  ( 19.05341960407617918, -5.049401038297876454, 81.04275706135231871 ) ) ;
#85116 = CARTESIAN_POINT ( 'NONE',  ( 14.29746914071049879, -8.314922557960816363, 63.33224293864770260 ) ) ;
#85117 = CARTESIAN_POINT ( 'NONE',  ( -15.80617190586745835, -15.72974639402198527, 46.87390960531435979 ) ) ;
#85118 = CARTESIAN_POINT ( 'NONE',  ( -5.719274019375665041, -21.55341960407619695, 109.7927570613523613 ) ) ;
#85119 = CARTESIAN_POINT ( 'NONE',  ( -21.52544592524343514, 5.823673210054127303, 101.0405762719810383 ) ) ;
#85120 = CARTESIAN_POINT ( 'NONE',  ( 5.719274019375673035, 21.55341960407619339, 67.29275706135234714 ) ) ;
#85121 = CARTESIAN_POINT ( 'NONE',  ( -0.05219959533937732626, 21.53943276465977519, 82.50109039468568994 ) ) ;
#85122 = CARTESIAN_POINT ( 'NONE',  ( -19.02544592524342804, 5.153800228976336051, 116.0405762719810383 ) ) ;
#85124 = CARTESIAN_POINT ( 'NONE',  ( -21.53943276465977519, -0.05219959533937600094, 73.75109039468567573 ) ) ;
#85123 = CARTESIAN_POINT ( 'NONE',  ( -4.379528057220086978, -16.55341960407618274, 104.7927570613523898 ) ) ;
#85125 = CARTESIAN_POINT ( 'NONE',  ( 5.153800228976335163, 19.02544592524342804, 64.79057627198100988 ) ) ;
#85126 = CARTESIAN_POINT ( 'NONE',  ( 13.97604488694548053, -13.89961937509957401, 30.62609039468566863 ) ) ;
#85127 = CARTESIAN_POINT ( 'NONE',  ( 21.53943276465977519, 0.05219959533937863772, 36.25109039468567573 ) ) ;
#85128 = CARTESIAN_POINT ( 'NONE',  ( 16.51473224551069308, 9.474510206698969483, 64.16557627198102409 ) ) ;
#85129 = CARTESIAN_POINT ( 'NONE',  ( -4.379528057220328563, 16.55341960407611168, 80.20724293864769550 ) ) ;
#85130 = CARTESIAN_POINT ( 'NONE',  ( -8.314922557960811034, -14.29746914071050412, 42.08224293864769550 ) ) ;
#85131 = CARTESIAN_POINT ( 'NONE',  ( -15.80617190586745835, -15.72974639402198527, 61.87390960531436690 ) ) ;
#85132 = CARTESIAN_POINT ( 'NONE',  ( 13.89961937509977652, -13.97604488694527269, 58.12390960531436690 ) ) ;
#85133 = CARTESIAN_POINT ( 'NONE',  ( -21.53943276465977519, 0.05219959533907696930, 76.24890960531435269 ) ) ;
#85134 = CARTESIAN_POINT ( 'NONE',  ( 5.153800228976615827, -19.02544592524334988, 70.20942372801899012 ) ) ;
#85136 = CARTESIAN_POINT ( 'NONE',  ( 16.55341960407611168, 4.379528057220329451, 68.95724293864769550 ) ) ;
#85135 = DIRECTION ( 'NONE',  ( 1.000000000000000000, 0.000000000000000000, 0.000000000000000000 ) ) ;
#85137 = CARTESIAN_POINT ( 'NONE',  ( -21.55341960407610458, -5.719274019375992779, 41.45724293864769550 ) ) ;
#85138 = ORIENTED_EDGE ( 'NONE', *, *, #59660, .T. ) ;
#85139 = CARTESIAN_POINT ( 'NONE',  ( 30.00000000000000711, -1.071565949253934124E-14, 102.5000000000000142 ) ) ;
#85141 = CARTESIAN_POINT ( 'NONE',  ( 22.44159573604009239, 16.30477369853692693, 148.0750000027312012 ) ) ;
#85140 = CARTESIAN_POINT ( 'NONE',  ( -4.379528057220086978, -16.55341960407618274, 84.79275706135234714 ) ) ;
#85142 = CARTESIAN_POINT ( 'NONE',  ( 19.03943276465977164, 0.05219959533936151252, 91.25109039468566152 ) ) ;
#85143 = CARTESIAN_POINT ( 'NONE',  ( 16.52544592524342804, -4.483927247898539470, 58.54057627198103120 ) ) ;
#85144 = CARTESIAN_POINT ( 'NONE',  ( -16.51473224551069308, -9.474510206698971260, 51.66557627198102409 ) ) ;
#85145 = CARTESIAN_POINT ( 'NONE',  ( 4.379528057220339221, -16.55341960407611168, 37.70724293864769550 ) ) ;
#85146 = CARTESIAN_POINT ( 'NONE',  ( 5.049401038298161559, -19.05341960407611168, 82.70724293864770971 ) ) ;
#85148 = CARTESIAN_POINT ( 'NONE',  ( 5.049401038298161559, -19.05341960407611168, 47.70724293864770260 ) ) ;
#85147 = CARTESIAN_POINT ( 'NONE',  ( -19.03943276465977164, -0.05219959533935918106, 73.75109039468566152 ) ) ;
#85149 = CARTESIAN_POINT ( 'NONE',  ( 10.81492255796106328, -18.62759615963255655, 65.41775706135234714 ) ) ;
#85150 = CARTESIAN_POINT ( 'NONE',  ( 0.05219959533909260263, 19.03943276465977164, 69.99890960531435269 ) ) ;
#85151 = CARTESIAN_POINT ( 'NONE',  ( 9.564922557960805705, 16.46253265017160317, 29.58224293864769550 ) ) ;
#85152 = CARTESIAN_POINT ( 'NONE',  ( -5.049401038298153566, 19.05341960407611168, 75.20724293864769550 ) ) ;
#85153 = CARTESIAN_POINT ( 'NONE',  ( -21.55341960407610458, -5.719274019375992779, 51.45724293864770260 ) ) ;
#85154 = CARTESIAN_POINT ( 'NONE',  ( 13.89961937509977652, -13.97604488694527269, 43.12390960531434558 ) ) ;
#85155 = CARTESIAN_POINT ( 'NONE',  ( -15.72974639402197994, 15.80617190586746368, 60.62390960531437401 ) ) ;
#85156 = CARTESIAN_POINT ( 'NONE',  ( -13.97604488694547697, 13.89961937509957934, 83.12609039468564731 ) ) ;
#85157 = CARTESIAN_POINT ( 'NONE',  ( 8.314922557961029526, -14.29746914071037800, 105.4177570613523613 ) ) ;
#85158 = CARTESIAN_POINT ( 'NONE',  ( -5.049401038297874678, -19.05341960407617918, 39.79275706135232582 ) ) ;
#85160 = CARTESIAN_POINT ( 'NONE',  ( 12.06949235617739724, 12.14591786802326823, 81.87609039468568994 ) ) ;
#85159 = CARTESIAN_POINT ( 'NONE',  ( -8.224510206698735004, -14.34966873604973081, 54.58442372801901143 ) ) ;
#85161 = CARTESIAN_POINT ( 'NONE',  ( -12.06949235617739369, -12.14591786802326823, 69.37609039468567573 ) ) ;
#85162 = CARTESIAN_POINT ( 'NONE',  ( -21.55341960407610458, -5.719274019375992779, 21.45724293864769550 ) ) ;
#85163 = CARTESIAN_POINT ( 'NONE',  ( -5.049401038298153566, 19.05341960407611168, 35.20724293864768839 ) ) ;
#85164 = CARTESIAN_POINT ( 'NONE',  ( 0.05219959533934541429, -16.53943276465976808, 40.00109039468567573 ) ) ;
#85165 = CARTESIAN_POINT ( 'NONE',  ( 9.474510206698971260, -16.51473224551069308, 52.91557627198102409 ) ) ;
#85166 = CARTESIAN_POINT ( 'NONE',  ( -21.52544592524334988, -5.823673210054445271, 43.95942372801902565 ) ) ;
#85167 = CARTESIAN_POINT ( 'NONE',  ( -4.379528057220086978, -16.55341960407618274, 34.79275706135235424 ) ) ;
#85168 = CARTESIAN_POINT ( 'NONE',  ( -4.483927247898782831, 16.52544592524335698, 112.7094237280190328 ) ) ;
#85169 = CARTESIAN_POINT ( 'NONE',  ( -25.90238458237723052, -6.509645158105411333, 161.8463118039487085 ) ) ;
#85170 = CARTESIAN_POINT ( 'NONE',  ( 16.51473224551083163, -9.474510206698727899, 20.83442372801899722 ) ) ;
#85171 = CARTESIAN_POINT ( 'NONE',  ( 13.89961937509957401, 13.97604488694547697, 106.8760903946856757 ) ) ;
#85172 = CARTESIAN_POINT ( 'NONE',  ( 5.049401038297881783, 19.05341960407617563, 67.29275706135234714 ) ) ;
#85173 = CARTESIAN_POINT ( 'NONE',  ( -14.34966873604960291, -8.224510206698953496, 71.66557627198100988 ) ) ;
#85174 = CARTESIAN_POINT ( 'NONE',  ( 5.153800228976335163, 19.02544592524342804, 44.79057627198103830 ) ) ;
#85176 = DIRECTION ( 'NONE',  ( 0.000000000000000000, 4.336808689942013792E-16, 1.000000000000000000 ) ) ;
#85175 = CARTESIAN_POINT ( 'NONE',  ( -13.89961937509957401, -13.97604488694547875, 54.37609039468565442 ) ) ;
#85177 = CARTESIAN_POINT ( 'NONE',  ( -10.72451020669870658, -18.67979575497194134, 59.58442372801901854 ) ) ;
#85178 = CARTESIAN_POINT ( 'NONE',  ( -16.55341960407617563, 4.379528057220093196, 43.54275706135235424 ) ) ;
#85179 = CARTESIAN_POINT ( 'NONE',  ( 18.56453257813361546, -5.500000000000034639, 58.49000423690687711 ) ) ;
#85180 = CARTESIAN_POINT ( 'NONE',  ( -10.72451020669898014, 18.67979575497178502, 25.41557627198103120 ) ) ;
#85181 = CARTESIAN_POINT ( 'NONE',  ( 16.55341960407618274, -4.379528057220086978, 26.04275706135235779 ) ) ;
#85182 = CARTESIAN_POINT ( 'NONE',  ( -9.564922557960796823, -16.46253265017161027, 112.0822429386476955 ) ) ;
#85183 = CARTESIAN_POINT ( 'NONE',  ( -23.64874990377915509, 15.04272038711346049, 165.8682408883346397 ) ) ;
#85184 = CARTESIAN_POINT ( 'NONE',  ( -16.51473224551069308, -9.474510206698971260, 31.66557627198102054 ) ) ;
#85185 = CARTESIAN_POINT ( 'NONE',  ( -15.72974639402176322, -15.80617190586768395, 104.3760903946856899 ) ) ;
#85186 = CARTESIAN_POINT ( 'NONE',  ( 5.153800228976335163, 19.02544592524342804, 54.79057627198103120 ) ) ;
#85187 = CARTESIAN_POINT ( 'NONE',  ( -5.719274019375665041, -21.55341960407619695, 64.79275706135234714 ) ) ;
#85188 = EDGE_CURVE ( 'NONE', #4644, #171283, #95949, .T. ) ;
#85189 = CARTESIAN_POINT ( 'NONE',  ( -5.823673210054431948, 21.52544592524334988, 97.70942372801904696 ) ) ;
#85190 = CARTESIAN_POINT ( 'NONE',  ( -8.314922557961024197, 14.29746914071037800, 112.9177570613523329 ) ) ;
#85191 = CARTESIAN_POINT ( 'NONE',  ( -19.05341960407611168, -5.049401038298163336, 26.45724293864769550 ) ) ;
#85192 = CARTESIAN_POINT ( 'NONE',  ( 19.02544592524343514, -5.153800228976328945, 98.54057627198100988 ) ) ;
#85193 = CARTESIAN_POINT ( 'NONE',  ( 21.52544592524334988, 5.823673210054432836, 61.45942372801901854 ) ) ;
#85194 = CARTESIAN_POINT ( 'NONE',  ( -19.03943276465977164, 0.05219959533909376836, 41.24890960531435269 ) ) ;
#85195 = AXIS2_PLACEMENT_3D ( 'NONE', #143036, #65211, #68194 ) ;
#85196 = CARTESIAN_POINT ( 'NONE',  ( 18.62759615963255655, 10.81492255796105972, 51.66775706135234714 ) ) ;
#85198 = CARTESIAN_POINT ( 'NONE',  ( 0.05219959533909260263, 19.03943276465977164, 104.9989096053143669 ) ) ;
#85197 = CARTESIAN_POINT ( 'NONE',  ( 5.153800228976615827, -19.02544592524334988, 85.20942372801900433 ) ) ;
#85199 = CARTESIAN_POINT ( 'NONE',  ( 16.52544592524342804, -4.483927247898539470, 113.5405762719810383 ) ) ;
#85200 = CARTESIAN_POINT ( 'NONE',  ( 18.67979575497178502, 10.72451020669898547, 109.1655762719810383 ) ) ;
#85201 = CARTESIAN_POINT ( 'NONE',  ( 19.03943276465977164, 0.05219959533936151252, 41.25109039468566152 ) ) ;
#85202 = CARTESIAN_POINT ( 'NONE',  ( 4.483927247898545687, 16.52544592524342804, 94.79057627198105251 ) ) ;
#85203 = CARTESIAN_POINT ( 'NONE',  ( -5.049401038298153566, 19.05341960407611168, 50.20724293864770260 ) ) ;
#85204 = CARTESIAN_POINT ( 'NONE',  ( -9.564922557961040184, 16.46253265017147172, 97.91775706135233293 ) ) ;
#85205 = CARTESIAN_POINT ( 'NONE',  ( -16.55341960407611168, -4.379528057220339221, 66.45724293864768129 ) ) ;
#85206 = CARTESIAN_POINT ( 'NONE',  ( 0.05219959533937995610, -21.53943276465977519, 105.0010903946856757 ) ) ;
#85207 = CARTESIAN_POINT ( 'NONE',  ( -0.05219959533909027116, -19.03943276465977164, 112.4989096053143669 ) ) ;
#85208 = CARTESIAN_POINT ( 'NONE',  ( -13.89961937509957401, -13.97604488694547875, 94.37609039468566152 ) ) ;
#85209 = CARTESIAN_POINT ( 'NONE',  ( 15.72974639402199770, -15.80617190586745480, 98.12390960531436690 ) ) ;
#85210 = CARTESIAN_POINT ( 'NONE',  ( 18.62759615963255655, 10.81492255796105972, 46.66775706135234714 ) ) ;
#85211 = CARTESIAN_POINT ( 'NONE',  ( -12.06949235617739369, -12.14591786802326823, 44.37609039468567573 ) ) ;
#85212 = CARTESIAN_POINT ( 'NONE',  ( 14.29746914071037800, 8.314922557961029526, 111.6677570613523613 ) ) ;
#85214 = CARTESIAN_POINT ( 'NONE',  ( 0.05219959533937995610, -21.53943276465977519, 50.00109039468568994 ) ) ;
#85213 = CARTESIAN_POINT ( 'NONE',  ( -12.06949235617739369, -12.14591786802326823, 44.37609039468567573 ) ) ;
#85215 = CARTESIAN_POINT ( 'NONE',  ( -5.719274019375978568, 21.55341960407610458, 40.20724293864769550 ) ) ;
#85216 = CARTESIAN_POINT ( 'NONE',  ( 9.564922557960805705, 16.46253265017160317, 39.58224293864768839 ) ) ;
#85217 = CARTESIAN_POINT ( 'NONE',  ( -23.48529157249599919, -32.32473071737750558, -7.449999994537624737 ) ) ;
#85218 = CARTESIAN_POINT ( 'NONE',  ( 12.06949235617739724, 12.14591786802326823, 61.87609039468568284 ) ) ;
#85219 = CARTESIAN_POINT ( 'NONE',  ( -21.53943276465977519, 0.05219959533907696930, 86.24890960531436690 ) ) ;
#85220 = CARTESIAN_POINT ( 'NONE',  ( 12.14591786802309770, 12.06949235617756955, 44.37390960531435979 ) ) ;
#85221 = CARTESIAN_POINT ( 'NONE',  ( -8.314922557961024197, 14.29746914071037800, 62.91775706135236135 ) ) ;
#85222 = CARTESIAN_POINT ( 'NONE',  ( 13.89961937509977652, -13.97604488694527269, 53.12390960531434558 ) ) ;
#85223 = CARTESIAN_POINT ( 'NONE',  ( -9.564922557961040184, 16.46253265017147172, 102.9177570613523329 ) ) ;
#85224 = CARTESIAN_POINT ( 'NONE',  ( -18.67979575497178146, -10.72451020669898902, 91.66557627198103830 ) ) ;
#85225 = CARTESIAN_POINT ( 'NONE',  ( -14.34966873604960291, -8.224510206698953496, 36.66557627198103120 ) ) ;
#85226 = VERTEX_POINT ( 'NONE', #99756 ) ;
#85227 = CARTESIAN_POINT ( 'NONE',  ( 0.05219959533934541429, -16.53943276465976808, 85.00109039468568994 ) ) ;
#85228 = CARTESIAN_POINT ( 'NONE',  ( 25.47140278216034304, 9.703455644539843661, 170.7619267275324262 ) ) ;
#85229 = CARTESIAN_POINT ( 'NONE',  ( 10.72451020669898902, -18.67979575497178502, 77.91557627198102409 ) ) ;
#85230 = ORIENTED_EDGE ( 'NONE', *, *, #178148, .F. ) ;
#85231 = CARTESIAN_POINT ( 'NONE',  ( 16.55341960407618274, -4.379528057220086978, 111.0427570613523613 ) ) ;
#85232 = ORIENTED_EDGE ( 'NONE', *, *, #53585, .F. ) ;
#85233 = CARTESIAN_POINT ( 'NONE',  ( -38.00000000000000711, -12.34694845685042708, -3.899999999999999911 ) ) ;
#85234 = CARTESIAN_POINT ( 'NONE',  ( 5.719274019375991003, -21.55341960407610458, 82.70724293864770971 ) ) ;
#85235 = CARTESIAN_POINT ( 'NONE',  ( 21.55341960407610458, 5.719274019375980345, 113.9572429386477239 ) ) ;
#85236 = CARTESIAN_POINT ( 'NONE',  ( 16.53943276465976808, -0.05219959533910856209, 33.74890960531436690 ) ) ;
#85237 = CARTESIAN_POINT ( 'NONE',  ( -16.52544592524335698, -4.483927247898792601, 28.95942372801902209 ) ) ;
#85238 = CARTESIAN_POINT ( 'NONE',  ( -19.02544592524342804, 5.153800228976336051, 36.04057627198100988 ) ) ;
#85239 = CARTESIAN_POINT ( 'NONE',  ( 0.05219959533909260263, 19.03943276465977164, 64.99890960531436690 ) ) ;
#85240 = CARTESIAN_POINT ( 'NONE',  ( -17.14385361876520264, -23.59649016807271593, 139.6750000027311955 ) ) ;
#85241 = CARTESIAN_POINT ( 'NONE',  ( 5.049401038298161559, -19.05341960407611168, 112.7072429386476813 ) ) ;
#85242 = CARTESIAN_POINT ( 'NONE',  ( 1.037572752228153927, 29.31194926455886929, -52.19832300604669229 ) ) ;
#85243 = CARTESIAN_POINT ( 'NONE',  ( 5.153800228976615827, -19.02544592524334988, 100.2094237280190043 ) ) ;
#85244 = CARTESIAN_POINT ( 'NONE',  ( -16.51473224551082808, 9.474510206698731452, 43.33442372801900433 ) ) ;
#85245 = CARTESIAN_POINT ( 'NONE',  ( 5.719274019375991003, -21.55341960407610458, 87.70724293864769550 ) ) ;
#85246 = CARTESIAN_POINT ( 'NONE',  ( -4.379528057220328563, 16.55341960407611168, 25.20724293864769550 ) ) ;
#85247 = CARTESIAN_POINT ( 'NONE',  ( -5.719274019375978568, 21.55341960407610458, 50.20724293864769550 ) ) ;
#85249 = CARTESIAN_POINT ( 'NONE',  ( 19.03943276465977164, 0.05219959533936151252, 106.2510903946856615 ) ) ;
#85248 = CARTESIAN_POINT ( 'NONE',  ( 5.823673210054125526, 21.52544592524343514, 79.79057627198102409 ) ) ;
#85250 = CARTESIAN_POINT ( 'NONE',  ( 13.97604488694527802, 13.89961937509977652, 99.37390960531436690 ) ) ;
#85251 = CARTESIAN_POINT ( 'NONE',  ( 18.67979575497194134, -10.72451020669871369, 70.83442372801901854 ) ) ;
#85252 = CARTESIAN_POINT ( 'NONE',  ( -0.05219959533909027116, -19.03943276465977164, 67.49890960531436690 ) ) ;
#85253 = CARTESIAN_POINT ( 'NONE',  ( -4.483927247898539470, -16.52544592524342804, 102.2905762719810383 ) ) ;
#85254 = CARTESIAN_POINT ( 'NONE',  ( 31.91717023173579193, 5.953136853522610572, 90.41250038490909446 ) ) ;
#85255 = CARTESIAN_POINT ( 'NONE',  ( -16.51473224551069308, -9.474510206698971260, 76.66557627198103830 ) ) ;
#85256 = CARTESIAN_POINT ( 'NONE',  ( -12.06949235617756955, 12.14591786802309770, 90.62390960531436690 ) ) ;
#85257 = ORIENTED_EDGE ( 'NONE', *, *, #185806, .F. ) ;
#85258 = CARTESIAN_POINT ( 'NONE',  ( 0.05219959533936267826, -19.03943276465977164, 105.0010903946856615 ) ) ;
#85259 = AXIS2_PLACEMENT_3D ( 'NONE', #5204, #36539, #97205 ) ;
#85260 = LINE ( 'NONE', #115618, #195745 ) ;
#85261 = CARTESIAN_POINT ( 'NONE',  ( 9.564922557960805705, 16.46253265017160317, 54.58224293864769550 ) ) ;
#85263 = CARTESIAN_POINT ( 'NONE',  ( -13.89961937509977652, 13.97604488694528158, 100.6239096053143669 ) ) ;
#85262 = CARTESIAN_POINT ( 'NONE',  ( 21.52544592524334988, 5.823673210054432836, 81.45942372801900433 ) ) ;
#85264 = CARTESIAN_POINT ( 'NONE',  ( -16.53943276465976808, -0.05219959533934237506, 83.75109039468568994 ) ) ;
#85265 = CARTESIAN_POINT ( 'NONE',  ( -16.29526858892875651, -7.335722546920120379, 75.79670597800210885 ) ) ;
#85266 = CARTESIAN_POINT ( 'NONE',  ( -19.03943276465977164, -0.05219959533935918106, 53.75109039468566863 ) ) ;
#85267 = CARTESIAN_POINT ( 'NONE',  ( 15.72974639402176855, 15.80617190586768217, 101.8760903946857042 ) ) ;
#85268 = CARTESIAN_POINT ( 'NONE',  ( 37.52489844900623694, 1.772207303729227856, 39.79021962610334384 ) ) ;
#85269 = CARTESIAN_POINT ( 'NONE',  ( 37.99999999999999289, 2.893978650043524126E-14, -6.749999994537627224 ) ) ;
#85270 = CARTESIAN_POINT ( 'NONE',  ( -16.53943276465976808, 0.05219959533911058130, 26.24890960531435624 ) ) ;
#85271 = CARTESIAN_POINT ( 'NONE',  ( -34.72618186072388369, -2.417897188208103731, 52.10384489098235861 ) ) ;
#85272 = CARTESIAN_POINT ( 'NONE',  ( -16.55341960407617563, 4.379528057220093196, 88.54275706135236135 ) ) ;
#85273 = CARTESIAN_POINT ( 'NONE',  ( 0.000000000000000000, -105.0000000000000000, -23.00000000000000000 ) ) ;
#85274 = CARTESIAN_POINT ( 'NONE',  ( 8.224510206698742110, 14.34966873604972548, 67.08442372801901854 ) ) ;
#85275 = CARTESIAN_POINT ( 'NONE',  ( 18.67979575497194134, -10.72451020669871369, 80.83442372801901854 ) ) ;
#85276 = CARTESIAN_POINT ( 'NONE',  ( -13.97604488694547697, 13.89961937509957934, 88.12609039468563310 ) ) ;
#85277 = CARTESIAN_POINT ( 'NONE',  ( 19.03943276465977164, 0.05219959533936151252, 46.25109039468566863 ) ) ;
#85278 = CARTESIAN_POINT ( 'NONE',  ( -9.564922557960796823, -16.46253265017161027, 67.08224293864769550 ) ) ;
#85279 = CARTESIAN_POINT ( 'NONE',  ( 9.474510206698971260, -16.51473224551069308, 62.91557627198102409 ) ) ;
#85280 = CARTESIAN_POINT ( 'NONE',  ( 16.46253265017160672, -9.564922557960803928, 88.33224293864769550 ) ) ;
#85281 = CARTESIAN_POINT ( 'NONE',  ( -10.81492255796078084, -18.62759615963271287, 77.08224293864769550 ) ) ;
#85282 = VECTOR ( 'NONE', #96853, 1000.000000000000000 ) ;
#85283 = CARTESIAN_POINT ( 'NONE',  ( -10.72451020669898014, 18.67979575497178502, 50.41557627198103120 ) ) ;
#85284 = CARTESIAN_POINT ( 'NONE',  ( -9.474510206698964154, 16.51473224551069663, 30.41557627198102054 ) ) ;
#85285 = CARTESIAN_POINT ( 'NONE',  ( 12.06949235617739724, 12.14591786802326823, 66.87609039468568994 ) ) ;
#85286 = EDGE_LOOP ( 'NONE', ( #136633, #155954 ) ) ;
#85287 = CARTESIAN_POINT ( 'NONE',  ( 10.81492255796106328, -18.62759615963255655, 35.41775706135234003 ) ) ;
#85289 = CARTESIAN_POINT ( 'NONE',  ( -30.74264578624800492, 22.33583958711400186, -2.200000000000000178 ) ) ;
#85288 = CARTESIAN_POINT ( 'NONE',  ( 12.14591786802309770, 12.06949235617756955, 69.37390960531436690 ) ) ;
#85290 = CARTESIAN_POINT ( 'NONE',  ( 8.314922557961029526, -14.29746914071037800, 25.41775706135235779 ) ) ;
#85291 = CARTESIAN_POINT ( 'NONE',  ( 9.474510206698729675, 16.51473224551082808, 57.08442372801900433 ) ) ;
#85292 = CARTESIAN_POINT ( 'NONE',  ( -8.224510206698948167, 14.34966873604960824, 55.41557627198102409 ) ) ;
#85293 = CARTESIAN_POINT ( 'NONE',  ( -21.52544592524334988, -5.823673210054445271, 33.95942372801901143 ) ) ;
#85295 = CARTESIAN_POINT ( 'NONE',  ( -18.67979575497178146, -10.72451020669898902, 76.66557627198103830 ) ) ;
#85294 = DIRECTION ( 'NONE',  ( 0.000000000000000000, 0.000000000000000000, 1.000000000000000000 ) ) ;
#85296 = CARTESIAN_POINT ( 'NONE',  ( -19.05341960407611168, -5.049401038298163336, 101.4572429386476955 ) ) ;
#85297 = CARTESIAN_POINT ( 'NONE',  ( -0.05219959533910754901, -16.53943276465976808, 72.49890960531435269 ) ) ;
#85298 = CARTESIAN_POINT ( 'NONE',  ( 35.08666314276448617, -21.80769648729754806, -18.77091308353056576 ) ) ;
#85299 = CARTESIAN_POINT ( 'NONE',  ( -37.54602941011386008, 1.427078192699135162, 39.68530545529164755 ) ) ;
#85300 = CARTESIAN_POINT ( 'NONE',  ( -19.03943276465977164, -0.05219959533935918106, 73.75109039468566152 ) ) ;
#85301 = CARTESIAN_POINT ( 'NONE',  ( -21.55341960407619339, 5.719274019375674811, 28.54275706135234358 ) ) ;
#85302 = CARTESIAN_POINT ( 'NONE',  ( -5.153800228976328057, -19.02544592524343514, 52.29057627198100988 ) ) ;
#85303 = CARTESIAN_POINT ( 'NONE',  ( -16.46253265017146816, -9.564922557961047289, 49.16775706135233293 ) ) ;
#85304 = CARTESIAN_POINT ( 'NONE',  ( -19.02544592524342804, 5.153800228976336051, 26.04057627198103120 ) ) ;
#85305 = CARTESIAN_POINT ( 'NONE',  ( -10.81492255796105439, 18.62759615963255655, 62.91775706135236135 ) ) ;
#85306 = EDGE_CURVE ( 'NONE', #65144, #133811, #57303, .T. ) ;
#85307 = CARTESIAN_POINT ( 'NONE',  ( -17.31728774477272736, -6.344390552232369807, 69.18093348310679858 ) ) ;
#85308 = CARTESIAN_POINT ( 'NONE',  ( 4.379528057220339221, -16.55341960407611168, 37.70724293864769550 ) ) ;
#85310 = AXIS2_PLACEMENT_3D ( 'NONE', #132024, #68342, #129992 ) ;
#85309 = CARTESIAN_POINT ( 'NONE',  ( 5.049401038298161559, -19.05341960407611168, 57.70724293864769550 ) ) ;
#85311 = CARTESIAN_POINT ( 'NONE',  ( -10.81492255796078084, -18.62759615963271287, 92.08224293864769550 ) ) ;
#85312 = CARTESIAN_POINT ( 'NONE',  ( -9.474510206698964154, 16.51473224551069663, 60.41557627198102409 ) ) ;
#85313 = VERTEX_POINT ( 'NONE', #131095 ) ;
#85314 = CARTESIAN_POINT ( 'NONE',  ( 15.80617190586746368, 15.72974639402197994, 69.37390960531436690 ) ) ;
#85315 = CARTESIAN_POINT ( 'NONE',  ( 21.53943276465977519, 0.05219959533937863772, 101.2510903946856757 ) ) ;
#85318 = CARTESIAN_POINT ( 'NONE',  ( 8.314922557960818139, 14.29746914071049879, 79.58224293864769550 ) ) ;
#85317 = CARTESIAN_POINT ( 'NONE',  ( 16.55341960407618274, -4.379528057220086978, 96.04275706135236135 ) ) ;
#85316 = CARTESIAN_POINT ( 'NONE',  ( 0.05219959533909260263, 19.03943276465977164, 24.99890960531435269 ) ) ;
#85319 = CARTESIAN_POINT ( 'NONE',  ( -16.46253265017146816, -9.564922557961047289, 94.16775706135233293 ) ) ;
#85320 = ORIENTED_EDGE ( 'NONE', *, *, #178569, .T. ) ;
#85321 = CARTESIAN_POINT ( 'NONE',  ( -21.53943276465977519, 0.05219959533907696930, 111.2489096053143669 ) ) ;
#85322 = CARTESIAN_POINT ( 'NONE',  ( 19.02544592524334988, 5.153800228976608722, 41.45942372801900433 ) ) ;
#85323 = CARTESIAN_POINT ( 'NONE',  ( -16.53943276465976808, -0.05219959533934237506, 103.7510903946857042 ) ) ;
#85324 = CARTESIAN_POINT ( 'NONE',  ( -13.89961937509957401, -13.97604488694547875, 34.37609039468566863 ) ) ;
#85325 = CARTESIAN_POINT ( 'NONE',  ( -5.049401038298153566, 19.05341960407611168, 95.20724293864770971 ) ) ;
#85326 = CARTESIAN_POINT ( 'NONE',  ( 10.81492255796078972, 18.62759615963270932, 59.58224293864770260 ) ) ;
#85327 = LINE ( 'NONE', #21673, #41140 ) ;
#85328 = CARTESIAN_POINT ( 'NONE',  ( -9.564922557960796823, -16.46253265017161027, 22.08224293864768839 ) ) ;
#85329 = CARTESIAN_POINT ( 'NONE',  ( 5.153800228976615827, -19.02544592524334988, 20.20942372801899722 ) ) ;
#85330 = CARTESIAN_POINT ( 'NONE',  ( -0.05219959533934338120, 16.53943276465976808, 82.50109039468568994 ) ) ;
#85331 = CARTESIAN_POINT ( 'NONE',  ( 18.62759615963255655, 10.81492255796105972, 26.66775706135235424 ) ) ;
#85332 = CARTESIAN_POINT ( 'NONE',  ( 12.06949235617739724, 12.14591786802326823, 26.87609039468567218 ) ) ;
#85333 = CARTESIAN_POINT ( 'NONE',  ( 5.153800228976335163, 19.02544592524342804, 99.79057627198102409 ) ) ;
#85334 = CARTESIAN_POINT ( 'NONE',  ( 19.03943276465977164, -0.05219959533909143690, 43.74890960531435979 ) ) ;
#85335 = CARTESIAN_POINT ( 'NONE',  ( 19.05341960407611168, 5.049401038298154454, 63.95724293864769550 ) ) ;
#85336 = CARTESIAN_POINT ( 'NONE',  ( 14.34966873604972726, -8.224510206698740333, 45.83442372801901854 ) ) ;
#85337 = CARTESIAN_POINT ( 'NONE',  ( 12.14591786802309770, 12.06949235617756955, 94.37390960531436690 ) ) ;
#85338 = CARTESIAN_POINT ( 'NONE',  ( 8.314922557961029526, -14.29746914071037800, 95.41775706135234714 ) ) ;
#85341 = CARTESIAN_POINT ( 'NONE',  ( -5.049401038298153566, 19.05341960407611168, 70.20724293864769550 ) ) ;
#85340 = CARTESIAN_POINT ( 'NONE',  ( 9.474510206698971260, -16.51473224551069308, 72.91557627198102409 ) ) ;
#85339 = CARTESIAN_POINT ( 'NONE',  ( 0.05219959533937995610, -21.53943276465977519, 40.00109039468567573 ) ) ;
#85342 = CARTESIAN_POINT ( 'NONE',  ( -19.03943276465977164, 0.05219959533909376836, 96.24890960531436690 ) ) ;
#85343 = CARTESIAN_POINT ( 'NONE',  ( 0.05219959533910956823, 16.53943276465976808, 34.99890960531435979 ) ) ;
#85344 = CARTESIAN_POINT ( 'NONE',  ( -8.314922557961024197, 14.29746914071037800, 92.91775706135236135 ) ) ;
#85345 = ORIENTED_EDGE ( 'NONE', *, *, #177190, .F. ) ;
#85346 = CARTESIAN_POINT ( 'NONE',  ( -9.474510206698720793, -16.51473224551083518, 39.58442372801899722 ) ) ;
#85347 = CARTESIAN_POINT ( 'NONE',  ( 5.153800228976335163, 19.02544592524342804, 109.7905762719810099 ) ) ;
#85348 = CARTESIAN_POINT ( 'NONE',  ( -19.02544592524342804, 5.153800228976336051, 66.04057627198103830 ) ) ;
#85349 = CARTESIAN_POINT ( 'NONE',  ( 13.97604488694548053, -13.89961937509957401, 40.62609039468564731 ) ) ;
#85350 = CARTESIAN_POINT ( 'NONE',  ( 22.81625015709510151, -31.40387420917324590, -9.924999997268814766 ) ) ;
#85351 = CARTESIAN_POINT ( 'NONE',  ( 19.49149378614663064, -5.499999999999580780, 71.93757513605363840 ) ) ;
#85352 = CARTESIAN_POINT ( 'NONE',  ( -14.34966873604972548, 8.224510206698743886, 58.33442372801901143 ) ) ;
#85354 = CARTESIAN_POINT ( 'NONE',  ( -14.29746914071037622, -8.314922557961029526, 54.16775706135235424 ) ) ;
#85353 = CARTESIAN_POINT ( 'NONE',  ( -0.05219959533936034679, 19.03943276465977164, 67.50109039468566152 ) ) ;
#85355 = CARTESIAN_POINT ( 'NONE',  ( 6.874011537017776341, -5.374011537017756801, -64.03675147074802965 ) ) ;
#85356 = CARTESIAN_POINT ( 'NONE',  ( -0.05219959533909027116, -19.03943276465977164, 87.49890960531436690 ) ) ;
#85357 = CARTESIAN_POINT ( 'NONE',  ( -15.72974639402176322, -15.80617190586768395, 19.37609039468568639 ) ) ;
#85358 = CARTESIAN_POINT ( 'NONE',  ( 13.89961937509957401, 13.97604488694547697, 81.87609039468564731 ) ) ;
#85360 = CARTESIAN_POINT ( 'NONE',  ( -5.049401038298153566, 19.05341960407611168, 30.20724293864768839 ) ) ;
#85359 = CARTESIAN_POINT ( 'NONE',  ( -16.51473224551069308, -9.474510206698971260, 111.6655762719810383 ) ) ;
#85361 = EDGE_CURVE ( 'NONE', #115644, #50694, #128574, .T. ) ;
#85362 = CARTESIAN_POINT ( 'NONE',  ( -5.049401038298153566, 19.05341960407611168, 80.20724293864769550 ) ) ;
#85364 = CARTESIAN_POINT ( 'NONE',  ( 9.474510206698971260, -16.51473224551069308, 32.91557627198102409 ) ) ;
#85363 = CARTESIAN_POINT ( 'NONE',  ( 8.314922557960818139, 14.29746914071049879, 54.58224293864769550 ) ) ;
#85365 = CARTESIAN_POINT ( 'NONE',  ( 16.46253265017146816, 9.564922557961045513, 51.66775706135233293 ) ) ;
#85366 = CARTESIAN_POINT ( 'NONE',  ( -16.53943276465976808, 0.05219959533911058130, 91.24890960531436690 ) ) ;
#85367 = CARTESIAN_POINT ( 'NONE',  ( -16.46253265017146816, -9.564922557961047289, 19.16775706135233293 ) ) ;
#85368 = CARTESIAN_POINT ( 'NONE',  ( 0.05219959533909260263, 19.03943276465977164, 49.99890960531435979 ) ) ;
#85369 = AXIS2_PLACEMENT_3D ( 'NONE', #3673, #175525, #126036 ) ;
#85370 = CARTESIAN_POINT ( 'NONE',  ( -10.81492255796078084, -18.62759615963271287, 47.08224293864770260 ) ) ;
#85372 = CARTESIAN_POINT ( 'NONE',  ( 13.89961937509957401, 13.97604488694547697, 21.87609039468566152 ) ) ;
#85371 = CARTESIAN_POINT ( 'NONE',  ( 4.379528057220339221, -16.55341960407611168, 47.70724293864770260 ) ) ;
#85373 = CARTESIAN_POINT ( 'NONE',  ( -0.05219959533909027116, -19.03943276465977164, 107.4989096053143527 ) ) ;
#85374 = CARTESIAN_POINT ( 'NONE',  ( 19.02544592524343514, -5.153800228976328945, 103.5405762719809957 ) ) ;
#85375 = CARTESIAN_POINT ( 'NONE',  ( -19.02544592524342804, 5.153800228976336051, 36.04057627198100988 ) ) ;
#85376 = CARTESIAN_POINT ( 'NONE',  ( -14.29746914071049879, 8.314922557960819915, 115.8322429386477097 ) ) ;
#85377 = CARTESIAN_POINT ( 'NONE',  ( -14.29746914071049879, 8.314922557960819915, 90.83224293864769550 ) ) ;
#85378 = CARTESIAN_POINT ( 'NONE',  ( 21.55341960407610458, 5.719274019375980345, 98.95724293864770971 ) ) ;
#85379 = CARTESIAN_POINT ( 'NONE',  ( -19.02544592524342804, 5.153800228976336051, 101.0405762719810241 ) ) ;
#85380 = CARTESIAN_POINT ( 'NONE',  ( -18.62759615963270932, 10.81492255796079327, 115.8322429386477097 ) ) ;
#85381 = CARTESIAN_POINT ( 'NONE',  ( 5.153800228976335163, 19.02544592524342804, 99.79057627198102409 ) ) ;
#85383 = CARTESIAN_POINT ( 'NONE',  ( -12.14591786802309592, -12.06949235617757132, 101.8739096053143811 ) ) ;
#85382 = DIRECTION ( 'NONE',  ( -0.000000000000000000, -0.000000000000000000, -1.000000000000000000 ) ) ;
#85384 = CARTESIAN_POINT ( 'NONE',  ( -5.049401038298153566, 19.05341960407611168, 65.20724293864765286 ) ) ;
#85385 = CARTESIAN_POINT ( 'NONE',  ( -5.719274019375978568, 21.55341960407610458, 85.20724293864770971 ) ) ;
#85386 = CARTESIAN_POINT ( 'NONE',  ( 17.48853670773245028, -5.747243402303111814, 106.1667129974999142 ) ) ;
#85387 = CARTESIAN_POINT ( 'NONE',  ( 4.500000000000000888, -126.1226662136678556, 8.481152457036394310 ) ) ;
#85389 = CARTESIAN_POINT ( 'NONE',  ( 18.87075004821571511, -5.499999999999891642, 66.17408112101047379 ) ) ;
#85388 = CARTESIAN_POINT ( 'NONE',  ( -15.80617190586745835, -15.72974639402198527, 31.87390960531435979 ) ) ;
#85390 = CARTESIAN_POINT ( 'NONE',  ( 8.224510206698742110, 14.34966873604972548, 27.08442372801901854 ) ) ;
#85392 = MECHANICAL_DESIGN_GEOMETRIC_PRESENTATION_REPRESENTATION (  '', ( #101560 ), #133915 ) ;
#85391 = CARTESIAN_POINT ( 'NONE',  ( -16.52544592524342804, 4.483927247898546575, 106.0405762719810525 ) ) ;
#85393 = CARTESIAN_POINT ( 'NONE',  ( -17.50000000000002132, -4.658240926743155264, 111.0552958218319901 ) ) ;
#85394 = CARTESIAN_POINT ( 'NONE',  ( -0.05219959533909027116, -19.03943276465977164, 62.49890960531435979 ) ) ;
#85395 = CARTESIAN_POINT ( 'NONE',  ( -4.483927247898539470, -16.52544592524342804, 82.29057627198103830 ) ) ;
#85396 = CARTESIAN_POINT ( 'NONE',  ( 10.81492255796078972, 18.62759615963270932, 29.58224293864769905 ) ) ;
#85397 = CARTESIAN_POINT ( 'NONE',  ( -8.224510206698948167, 14.34966873604960824, 65.41557627198102409 ) ) ;
#85398 = CARTESIAN_POINT ( 'NONE',  ( -12.06949235617739369, -12.14591786802326823, 19.37609039468568639 ) ) ;
#85399 = CARTESIAN_POINT ( 'NONE',  ( 21.52544592524334988, 5.823673210054432836, 76.45942372801901854 ) ) ;
#85400 = AXIS2_PLACEMENT_3D ( 'NONE', #69885, #145715, #113377 ) ;
#85401 = CARTESIAN_POINT ( 'NONE',  ( 16.88567814943163015, -6.947325034625693618, 76.20998877347416567 ) ) ;
#85402 = CARTESIAN_POINT ( 'NONE',  ( -19.05341960407611168, -5.049401038298163336, 106.4572429386476955 ) ) ;
#85403 = CARTESIAN_POINT ( 'NONE',  ( -16.53943276465976808, -0.05219959533934237506, 88.75109039468567573 ) ) ;
#85404 = CARTESIAN_POINT ( 'NONE',  ( 0.05219959533909260263, 19.03943276465977164, 44.99890960531435979 ) ) ;
#85405 = CARTESIAN_POINT ( 'NONE',  ( 19.05341960407611168, 5.049401038298154454, 93.95724293864769550 ) ) ;
#85406 = CARTESIAN_POINT ( 'NONE',  ( 5.719274019375991003, -21.55341960407610458, 92.70724293864770971 ) ) ;
#85407 = CARTESIAN_POINT ( 'NONE',  ( -8.314922557961024197, 14.29746914071037800, 22.91775706135235069 ) ) ;
#85409 = CARTESIAN_POINT ( 'NONE',  ( 21.53943276465977519, 0.05219959533937863772, 66.25109039468567573 ) ) ;
#85408 = CARTESIAN_POINT ( 'NONE',  ( -8.224510206698948167, 14.34966873604960824, 45.41557627198103830 ) ) ;
#85410 = CARTESIAN_POINT ( 'NONE',  ( -14.29746914071037622, -8.314922557961029526, 99.16775706135234714 ) ) ;
#85411 = CARTESIAN_POINT ( 'NONE',  ( 25.41627434887081805, 11.65185368830120893, 166.2643564577823270 ) ) ;
#85412 = CARTESIAN_POINT ( 'NONE',  ( -17.40805194822031154, 6.112264579159342404, 80.83371272510612471 ) ) ;
#85413 = CARTESIAN_POINT ( 'NONE',  ( 14.34966873604960469, 8.224510206698951720, 34.16557627198102409 ) ) ;
#85414 = CARTESIAN_POINT ( 'NONE',  ( -14.29746914071037622, -8.314922557961029526, 59.16775706135234714 ) ) ;
#85416 = ORIENTED_EDGE ( 'NONE', *, *, #65731, .F. ) ;
#85415 = CARTESIAN_POINT ( 'NONE',  ( 9.474510206698971260, -16.51473224551069308, 67.91557627198102409 ) ) ;
#85417 = CARTESIAN_POINT ( 'NONE',  ( -9.474510206698964154, 16.51473224551069663, 85.41557627198102409 ) ) ;
#85418 = CARTESIAN_POINT ( 'NONE',  ( -10.81492255796105439, 18.62759615963255655, 67.91775706135234714 ) ) ;
#85419 = CARTESIAN_POINT ( 'NONE',  ( 14.29746914071037800, 8.314922557961029526, 71.66775706135234714 ) ) ;
#85420 = CARTESIAN_POINT ( 'NONE',  ( 14.34966873604960469, 8.224510206698951720, 64.16557627198102409 ) ) ;
#85421 = CARTESIAN_POINT ( 'NONE',  ( -5.153800228976328057, -19.02544592524343514, 67.29057627198102409 ) ) ;
#85422 = EDGE_LOOP ( 'NONE', ( #31538, #190304, #73522, #195984 ) ) ;
#85423 = CARTESIAN_POINT ( 'NONE',  ( -0.05219959533936034679, 19.03943276465977164, 107.5010903946856615 ) ) ;
#85424 = CARTESIAN_POINT ( 'NONE',  ( 4.379528057220339221, -16.55341960407611168, 112.7072429386476955 ) ) ;
#85425 = CARTESIAN_POINT ( 'NONE',  ( 16.46253265017160672, -9.564922557960803928, 83.33224293864768129 ) ) ;
#85427 = CARTESIAN_POINT ( 'NONE',  ( 36.91746824999999887, 11.99521256947799053, -5.524999997268812635 ) ) ;
#85426 = CARTESIAN_POINT ( 'NONE',  ( -8.224510206698735004, -14.34966873604973081, 24.58442372801901499 ) ) ;
#85428 = CARTESIAN_POINT ( 'NONE',  ( -21.52544592524334988, -5.823673210054445271, 103.9594237280190185 ) ) ;
#85429 = CARTESIAN_POINT ( 'NONE',  ( -16.53943276465976808, -0.05219959533934237506, 83.75109039468568994 ) ) ;
#85430 = CARTESIAN_POINT ( 'NONE',  ( 9.564922557961047289, -16.46253265017146816, 95.41775706135233293 ) ) ;
#85431 = CARTESIAN_POINT ( 'NONE',  ( 16.53943276465976808, -0.05219959533910856209, 108.7489096053143669 ) ) ;
#85432 = CARTESIAN_POINT ( 'NONE',  ( 16.53943276465976808, 0.05219959533934440121, 66.25109039468567573 ) ) ;
#85433 = CARTESIAN_POINT ( 'NONE',  ( 1.300000000000000044, -0.7216878364870319418, 1.249999999999999778 ) ) ;
#85434 = CARTESIAN_POINT ( 'NONE',  ( 19.02544592524334988, 5.153800228976608722, 56.45942372801898301 ) ) ;
#85435 = CARTESIAN_POINT ( 'NONE',  ( -10.72451020669870658, -18.67979575497194134, 94.58442372801901854 ) ) ;
#85436 = CARTESIAN_POINT ( 'NONE',  ( 19.03943276465977164, -0.05219959533909143690, 33.74890960531435979 ) ) ;
#85437 = CARTESIAN_POINT ( 'NONE',  ( 9.564922557960805705, 16.46253265017160317, 79.58224293864769550 ) ) ;
#85438 = CARTESIAN_POINT ( 'NONE',  ( 8.224510206698953496, -14.34966873604960469, 72.91557627198103830 ) ) ;
#85439 = CARTESIAN_POINT ( 'NONE',  ( 0.05219959533937995610, -21.53943276465977519, 90.00109039468567573 ) ) ;
#85440 = ADVANCED_FACE ( 'NONE', ( #116929 ), #193792, .T. ) ;
#85441 = CARTESIAN_POINT ( 'NONE',  ( 19.03943276465977164, 0.05219959533936151252, 41.25109039468566152 ) ) ;
#85442 = CARTESIAN_POINT ( 'NONE',  ( -9.564922557961040184, 16.46253265017147172, 42.91775706135234003 ) ) ;
#85443 = CARTESIAN_POINT ( 'NONE',  ( 15.72974639402199770, -15.80617190586745480, 38.12390960531436690 ) ) ;
#85444 = CARTESIAN_POINT ( 'NONE',  ( 18.62759615963255655, 10.81492255796105972, 91.66775706135234714 ) ) ;
#85445 = CARTESIAN_POINT ( 'NONE',  ( 13.89961937509977652, -13.97604488694527269, 83.12390960531436690 ) ) ;
#85446 = CARTESIAN_POINT ( 'NONE',  ( -18.67979575497193778, 10.72451020669871902, 93.33442372801901854 ) ) ;
#85447 = CARTESIAN_POINT ( 'NONE',  ( 10.81492255796078972, 18.62759615963270932, 44.58224293864769550 ) ) ;
#85448 = CARTESIAN_POINT ( 'NONE',  ( 5.049401038298161559, -19.05341960407611168, 87.70724293864769550 ) ) ;
#85449 = CARTESIAN_POINT ( 'NONE',  ( 19.03943276465977164, 0.05219959533936151252, 76.25109039468566152 ) ) ;
#85450 = CARTESIAN_POINT ( 'NONE',  ( -9.474510206698964154, 16.51473224551069663, 95.41557627198102409 ) ) ;
#85451 = CARTESIAN_POINT ( 'NONE',  ( -13.97604488694547697, 13.89961937509957934, 93.12609039468566152 ) ) ;
#85452 = CARTESIAN_POINT ( 'NONE',  ( 8.224510206698742110, 14.34966873604972548, 37.08442372801901143 ) ) ;
#85453 = CARTESIAN_POINT ( 'NONE',  ( -4.483927247898539470, -16.52544592524342804, 107.2905762719810525 ) ) ;
#85454 = CARTESIAN_POINT ( 'NONE',  ( -19.02544592524342804, 5.153800228976336051, 76.04057627198102409 ) ) ;
#85455 = EDGE_CURVE ( 'NONE', #45202, #163628, #178622, .T. ) ;
#85456 = CARTESIAN_POINT ( 'NONE',  ( -21.55341960407610458, -5.719274019375992779, 66.45724293864768129 ) ) ;
#85457 = CARTESIAN_POINT ( 'NONE',  ( 4.379528057220092307, 16.55341960407617563, 32.29275706135235424 ) ) ;
#85458 = CARTESIAN_POINT ( 'NONE',  ( 21.52544592524334988, 5.823673210054432836, 36.45942372801901143 ) ) ;
#85459 = CARTESIAN_POINT ( 'NONE',  ( -21.52544592524334988, -5.823673210054445271, 78.95942372801901854 ) ) ;
#85460 = CARTESIAN_POINT ( 'NONE',  ( 14.29746914071037800, 8.314922557961029526, 86.66775706135234714 ) ) ;
#85461 = CARTESIAN_POINT ( 'NONE',  ( 19.03943276465977164, -0.05219959533909143690, 68.74890960531436690 ) ) ;
#85462 = CARTESIAN_POINT ( 'NONE',  ( -8.224510206698948167, 14.34966873604960824, 80.41557627198103830 ) ) ;
#85463 = CARTESIAN_POINT ( 'NONE',  ( 14.34966873604972726, -8.224510206698740333, 100.8344237280190185 ) ) ;
#85464 = CARTESIAN_POINT ( 'NONE',  ( -5.049401038297874678, -19.05341960407617918, 49.79275706135231871 ) ) ;
#85465 = CARTESIAN_POINT ( 'NONE',  ( -5.823673210054431948, 21.52544592524334988, 27.70942372801901854 ) ) ;
#85466 = CARTESIAN_POINT ( 'NONE',  ( 12.14591786802309770, 12.06949235617756955, 74.37390960531436690 ) ) ;
#85467 = CARTESIAN_POINT ( 'NONE',  ( 13.89961937509977652, -13.97604488694527269, 103.1239096053143527 ) ) ;
#85468 = CARTESIAN_POINT ( 'NONE',  ( -16.55341960407617563, 4.379528057220093196, 98.54275706135234714 ) ) ;
#85469 = CARTESIAN_POINT ( 'NONE',  ( 0.05219959533937995610, -21.53943276465977519, 75.00109039468568994 ) ) ;
#85470 = CARTESIAN_POINT ( 'NONE',  ( 12.14591786802327356, -12.06949235617739191, 50.62609039468568994 ) ) ;
#85471 = CARTESIAN_POINT ( 'NONE',  ( 21.53943276465977519, 0.05219959533937863772, 46.25109039468567573 ) ) ;
#85472 = CARTESIAN_POINT ( 'NONE',  ( 16.55341960407611168, 4.379528057220329451, 73.95724293864769550 ) ) ;
#85473 = ORIENTED_EDGE ( 'NONE', *, *, #140308, .F. ) ;
#85474 = CARTESIAN_POINT ( 'NONE',  ( 21.55341960407619695, -5.719274019375665929, 21.04275706135234714 ) ) ;
#85475 = CARTESIAN_POINT ( 'NONE',  ( 17.49999999999996803, -3.805241302050390573, 27.87352472782592017 ) ) ;
#85476 = CARTESIAN_POINT ( 'NONE',  ( -4.483927247898539470, -16.52544592524342804, 47.29057627198103120 ) ) ;
#85477 = CARTESIAN_POINT ( 'NONE',  ( 5.153800228976335163, 19.02544592524342804, 24.79057627198102765 ) ) ;
#85478 = CARTESIAN_POINT ( 'NONE',  ( 15.80617190586746368, 15.72974639402197994, 39.37390960531436690 ) ) ;
#85479 = CARTESIAN_POINT ( 'NONE',  ( -4.379528057220328563, 16.55341960407611168, 75.20724293864769550 ) ) ;
#85480 = CARTESIAN_POINT ( 'NONE',  ( 0.05219959533907565091, 21.53943276465977519, 84.99890960531436690 ) ) ;
#85481 = CARTESIAN_POINT ( 'NONE',  ( -9.474510206698964154, 16.51473224551069663, 90.41557627198103830 ) ) ;
#85483 = CARTESIAN_POINT ( 'NONE',  ( -13.89961937509957401, -13.97604488694547875, 74.37609039468566152 ) ) ;
#85482 = CARTESIAN_POINT ( 'NONE',  ( 9.564922557960805705, 16.46253265017160317, 34.58224293864770260 ) ) ;
#85485 = CARTESIAN_POINT ( 'NONE',  ( -0.05219959533907301413, -21.53943276465977519, 67.49890960531436690 ) ) ;
#85484 = CARTESIAN_POINT ( 'NONE',  ( 5.823673210054444382, -21.52544592524334988, 55.20942372801902565 ) ) ;
#85486 = CARTESIAN_POINT ( 'NONE',  ( 19.03943276465977164, -0.05219959533909143690, 33.74890960531435979 ) ) ;
#85487 = CARTESIAN_POINT ( 'NONE',  ( 19.03943276465977164, -0.05219959533909143690, 68.74890960531436690 ) ) ;
#85488 = ORIENTED_EDGE ( 'NONE', *, *, #34560, .F. ) ;
#85489 = CARTESIAN_POINT ( 'NONE',  ( -14.29746914071037622, -8.314922557961029526, 54.16775706135235424 ) ) ;
#85490 = CARTESIAN_POINT ( 'NONE',  ( 18.62759615963255655, 10.81492255796105972, 26.66775706135235424 ) ) ;
#85491 = AXIS2_PLACEMENT_3D ( 'NONE', #20454, #141808, #2307 ) ;
#85492 = CARTESIAN_POINT ( 'NONE',  ( 18.62759615963255655, 10.81492255796105972, 61.66775706135235424 ) ) ;
#85493 = CARTESIAN_POINT ( 'NONE',  ( -5.049401038298153566, 19.05341960407611168, 110.2072429386476671 ) ) ;
#85494 = CARTESIAN_POINT ( 'NONE',  ( -5.823673210054116645, -21.52544592524344225, 92.29057627198103830 ) ) ;
#85496 = CARTESIAN_POINT ( 'NONE',  ( 16.55341960407618274, -4.379528057220086978, 46.04275706135234714 ) ) ;
#85495 = CARTESIAN_POINT ( 'NONE',  ( -15.72974639402176322, -15.80617190586768395, 24.37609039468567573 ) ) ;
#85497 = CARTESIAN_POINT ( 'NONE',  ( 21.53943276465977519, -0.05219959533907433946, 53.74890960531437401 ) ) ;
#85498 = CARTESIAN_POINT ( 'NONE',  ( 0.05219959533936267826, -19.03943276465977164, 25.00109039468566152 ) ) ;
#85499 = CARTESIAN_POINT ( 'NONE',  ( -13.89961937509977652, 13.97604488694528158, 55.62390960531434558 ) ) ;
#85500 = CARTESIAN_POINT ( 'NONE',  ( 13.89961937509977652, -13.97604488694527269, 88.12390960531438111 ) ) ;
#85501 =( REPRESENTATION_RELATIONSHIP ('NONE','NONE', #154205, #9542 ) REPRESENTATION_RELATIONSHIP_WITH_TRANSFORMATION ( #147293 )SHAPE_REPRESENTATION_RELATIONSHIP( ) );
#85502 = CARTESIAN_POINT ( 'NONE',  ( 21.15706064682975196, 22.96834507599301034, -46.65423976109394033 ) ) ;
#85503 = CARTESIAN_POINT ( 'NONE',  ( 9.564922557961047289, -16.46253265017146816, 65.41775706135233293 ) ) ;
#85504 = CARTESIAN_POINT ( 'NONE',  ( 10.81492255796078972, 18.62759615963270932, 39.58224293864769550 ) ) ;
#85505 = CARTESIAN_POINT ( 'NONE',  ( -16.53943276465976808, 0.05219959533911058130, 21.24890960531436690 ) ) ;
#85506 = CARTESIAN_POINT ( 'NONE',  ( 9.474510206698729675, 16.51473224551082808, 97.08442372801900433 ) ) ;
#85507 = FACE_OUTER_BOUND ( 'NONE', #175109, .T. ) ;
#85508 = VECTOR ( 'NONE', #138879, 1000.000000000000000 ) ;
#85509 = CARTESIAN_POINT ( 'NONE',  ( -21.53943276465977519, -0.05219959533937600094, 113.7510903946856757 ) ) ;
#85510 = CARTESIAN_POINT ( 'NONE',  ( -13.89961937509957401, -13.97604488694547875, 94.37609039468566152 ) ) ;
#85511 = CARTESIAN_POINT ( 'NONE',  ( -13.97604488694547697, 13.89961937509957934, 43.12609039468566152 ) ) ;
#85512 = CARTESIAN_POINT ( 'NONE',  ( 16.29526858892874941, 7.335722546920133702, 108.2967059780021231 ) ) ;
#85513 = CARTESIAN_POINT ( 'NONE',  ( 0.05219959533909260263, 19.03943276465977164, 59.99890960531436690 ) ) ;
#85514 = CARTESIAN_POINT ( 'NONE',  ( 16.55341960407611168, 4.379528057220329451, 58.95724293864770971 ) ) ;
#85515 = CARTESIAN_POINT ( 'NONE',  ( -19.03943276465977164, 0.05219959533909376836, 31.24890960531435979 ) ) ;
#85516 = CARTESIAN_POINT ( 'NONE',  ( 14.29746914071049879, -8.314922557960816363, 43.33224293864769550 ) ) ;
#85517 = CARTESIAN_POINT ( 'NONE',  ( 0.000000000000000000, 0.000000000000000000, -56.46919128290398504 ) ) ;
#85518 = CARTESIAN_POINT ( 'NONE',  ( -16.55341960407611168, -4.379528057220339221, 21.45724293864769550 ) ) ;
#85519 = CARTESIAN_POINT ( 'NONE',  ( 5.153800228976335163, 19.02544592524342804, 59.79057627198100988 ) ) ;
#85520 = CARTESIAN_POINT ( 'NONE',  ( 0.05219959533936267826, -19.03943276465977164, 25.00109039468566152 ) ) ;
#85521 = CARTESIAN_POINT ( 'NONE',  ( -4.379528057220086978, -16.55341960407618274, 34.79275706135235424 ) ) ;
#85522 = CARTESIAN_POINT ( 'NONE',  ( -5.823673210054116645, -21.52544592524344225, 57.29057627198103120 ) ) ;
#85524 = EDGE_LOOP ( 'NONE', ( #23178, #49451 ) ) ;
#85523 = CARTESIAN_POINT ( 'NONE',  ( -18.62759615963255300, -10.81492255796106328, 104.1677570613523471 ) ) ;
#85525 = CARTESIAN_POINT ( 'NONE',  ( 16.46253265017160672, -9.564922557960803928, 58.33224293864769550 ) ) ;
#85526 = CARTESIAN_POINT ( 'NONE',  ( 19.03943276465977164, -0.05219959533909143690, 108.7489096053143527 ) ) ;
#85527 = CARTESIAN_POINT ( 'NONE',  ( 16.46253265017160672, -9.564922557960803928, 103.3322429386476955 ) ) ;
#85528 = CARTESIAN_POINT ( 'NONE',  ( 22.81625015709510151, -31.40387420917324590, -3.924999997268812102 ) ) ;
#85529 = CARTESIAN_POINT ( 'NONE',  ( 21.52544592524334988, 5.823673210054432836, 21.45942372801901499 ) ) ;
#85530 = VECTOR ( 'NONE', #180629, 1000.000000000000000 ) ;
#85531 = CARTESIAN_POINT ( 'NONE',  ( -4.379528057220328563, 16.55341960407611168, 90.20724293864770971 ) ) ;
#85533 = CARTESIAN_POINT ( 'NONE',  ( 13.89961937509977652, -13.97604488694527269, 63.12390960531435979 ) ) ;
#85532 = CARTESIAN_POINT ( 'NONE',  ( -21.52544592524343514, 5.823673210054127303, 91.04057627198103830 ) ) ;
#85534 = CARTESIAN_POINT ( 'NONE',  ( -13.97604488694527625, -13.89961937509977652, 71.87390960531433848 ) ) ;
#85535 = CARTESIAN_POINT ( 'NONE',  ( 15.80617190586746368, 15.72974639402197994, 109.3739096053143811 ) ) ;
#85536 = ORIENTED_EDGE ( 'NONE', *, *, #123690, .F. ) ;
#85537 = CARTESIAN_POINT ( 'NONE',  ( 0.05219959533909260263, 19.03943276465977164, 69.99890960531435269 ) ) ;
#85538 = EDGE_CURVE ( 'NONE', #53136, #107603, #117944, .T. ) ;
#85539 = CARTESIAN_POINT ( 'NONE',  ( -30.44363203418366481, -22.74636568843913409, -19.69742113251491489 ) ) ;
#85541 = CARTESIAN_POINT ( 'NONE',  ( -9.564922557960796823, -16.46253265017161027, 22.08224293864768839 ) ) ;
#85540 = CARTESIAN_POINT ( 'NONE',  ( 8.314922557960818139, 14.29746914071049879, 99.58224293864770971 ) ) ;
#85542 = CARTESIAN_POINT ( 'NONE',  ( -16.46253265017146816, -9.564922557961047289, 94.16775706135233293 ) ) ;
#85543 = VECTOR ( 'NONE', #191850, 1000.000000000000000 ) ;
#85544 = CARTESIAN_POINT ( 'NONE',  ( 12.14591786802309770, 12.06949235617756955, 99.37390960531436690 ) ) ;
#85545 = CARTESIAN_POINT ( 'NONE',  ( 5.823673210054444382, -21.52544592524334988, 70.20942372801904696 ) ) ;
#85547 = CARTESIAN_POINT ( 'NONE',  ( 10.81492255796106328, -18.62759615963255655, 35.41775706135234003 ) ) ;
#85546 = CARTESIAN_POINT ( 'NONE',  ( 19.05341960407611168, 5.049401038298154454, 68.95724293864769550 ) ) ;
#85548 = CARTESIAN_POINT ( 'NONE',  ( -18.62759615963255300, -10.81492255796106328, 19.16775706135234714 ) ) ;
#85549 = CARTESIAN_POINT ( 'NONE',  ( -9.564922557960796823, -16.46253265017161027, 67.08224293864769550 ) ) ;
#85550 = AXIS2_PLACEMENT_3D ( 'NONE', #46507, #136529, #124332 ) ;
#85551 = DIRECTION ( 'NONE',  ( -0.000000000000000000, 0.000000000000000000, 1.000000000000000000 ) ) ;
#85553 = CARTESIAN_POINT ( 'NONE',  ( 15.72974639402199770, -15.80617190586745480, 33.12390960531435979 ) ) ;
#85552 = CARTESIAN_POINT ( 'NONE',  ( 19.03943276465977164, 0.05219959533936151252, 111.2510903946856757 ) ) ;
#85554 = CARTESIAN_POINT ( 'NONE',  ( -18.62759615963255300, -10.81492255796106328, 59.16775706135234714 ) ) ;
#85555 =( GEOMETRIC_REPRESENTATION_CONTEXT ( 3 ) GLOBAL_UNCERTAINTY_ASSIGNED_CONTEXT ( ( #84283 ) ) GLOBAL_UNIT_ASSIGNED_CONTEXT ( ( #177880, #157716, #118199 ) ) REPRESENTATION_CONTEXT ( 'NONE', 'WORKASPACE' ) );
#85556 = CARTESIAN_POINT ( 'NONE',  ( -9.564922557960796823, -16.46253265017161027, 92.08224293864769550 ) ) ;
#85557 = CARTESIAN_POINT ( 'NONE',  ( -9.564922557961040184, 16.46253265017147172, 87.91775706135233293 ) ) ;
#85558 = CARTESIAN_POINT ( 'NONE',  ( 19.02544592524343514, -5.153800228976328945, 48.54057627198103120 ) ) ;
#85559 = CARTESIAN_POINT ( 'NONE',  ( -5.049401038298153566, 19.05341960407611168, 75.20724293864769550 ) ) ;
#85560 = CARTESIAN_POINT ( 'NONE',  ( -12.06949235617756955, 12.14591786802309770, 90.62390960531436690 ) ) ;
#85561 = CARTESIAN_POINT ( 'NONE',  ( -19.03943276465977164, 0.05219959533909376836, 106.2489096053143669 ) ) ;
#85562 = CARTESIAN_POINT ( 'NONE',  ( -0.05219959533910754901, -16.53943276465976808, 87.49890960531436690 ) ) ;
#85563 = CARTESIAN_POINT ( 'NONE',  ( -5.153800228976328057, -19.02544592524343514, 97.29057627198099567 ) ) ;
#85565 = CARTESIAN_POINT ( 'NONE',  ( 9.564922557960805705, 16.46253265017160317, 29.58224293864769550 ) ) ;
#85564 = CARTESIAN_POINT ( 'NONE',  ( 14.29746914071049879, -8.314922557960816363, 38.33224293864768839 ) ) ;
#85566 = ORIENTED_EDGE ( 'NONE', *, *, #87955, .F. ) ;
#85567 = CARTESIAN_POINT ( 'NONE',  ( 21.53943276465977519, 0.05219959533937863772, 61.25109039468567573 ) ) ;
#85568 = CARTESIAN_POINT ( 'NONE',  ( -16.46253265017146816, -9.564922557961047289, 79.16775706135234714 ) ) ;
#85569 = CARTESIAN_POINT ( 'NONE',  ( 12.14591786802309770, 12.06949235617756955, 54.37390960531435979 ) ) ;
#85570 = CARTESIAN_POINT ( 'NONE',  ( 0.05219959533907565091, 21.53943276465977519, 104.9989096053143669 ) ) ;
#85571 = CARTESIAN_POINT ( 'NONE',  ( 10.81492255796078972, 18.62759615963270932, 34.58224293864770260 ) ) ;
#85572 = CARTESIAN_POINT ( 'NONE',  ( -8.314922557960811034, -14.29746914071050412, 77.08224293864769550 ) ) ;
#85573 = CARTESIAN_POINT ( 'NONE',  ( -16.51473224551069308, -9.474510206698971260, 61.66557627198103120 ) ) ;
#85574 = CARTESIAN_POINT ( 'NONE',  ( 4.483927247898545687, 16.52544592524342804, 24.79057627198103120 ) ) ;
#85575 = AXIS2_PLACEMENT_3D ( 'NONE', #145949, #132790, #103460 ) ;
#85576 = CARTESIAN_POINT ( 'NONE',  ( -4.379528057220086978, -16.55341960407618274, 104.7927570613523898 ) ) ;
#85577 = CARTESIAN_POINT ( 'NONE',  ( 14.29746914071037800, 8.314922557961029526, 76.66775706135234714 ) ) ;
#85578 = CARTESIAN_POINT ( 'NONE',  ( 13.97604488694548053, -13.89961937509957401, 30.62609039468566863 ) ) ;
#85579 = CARTESIAN_POINT ( 'NONE',  ( -16.46253265017160317, 9.564922557960807481, 105.8322429386476955 ) ) ;
#85580 = CARTESIAN_POINT ( 'NONE',  ( 16.51473224551069308, 9.474510206698969483, 79.16557627198103830 ) ) ;
#85581 = CARTESIAN_POINT ( 'NONE',  ( -19.05341960407611168, -5.049401038298163336, 36.45724293864766707 ) ) ;
#85582 = CARTESIAN_POINT ( 'NONE',  ( 16.52544592524342804, -4.483927247898539470, 53.54057627198103120 ) ) ;
#85584 = CARTESIAN_POINT ( 'NONE',  ( -5.153800228976328057, -19.02544592524343514, 102.2905762719810383 ) ) ;
#85583 = CARTESIAN_POINT ( 'NONE',  ( -28.82186960331499037, 2.781578969918950771E-14, 139.9999999999999716 ) ) ;
#85585 = CARTESIAN_POINT ( 'NONE',  ( 0.05219959533907565091, 21.53943276465977519, 44.99890960531435979 ) ) ;
#85586 = CARTESIAN_POINT ( 'NONE',  ( -12.14591786802309592, -12.06949235617757132, 91.87390960531436690 ) ) ;
#85587 = CARTESIAN_POINT ( 'NONE',  ( 12.14591786802327356, -12.06949235617739191, 30.62609039468567929 ) ) ;
#85588 = CARTESIAN_POINT ( 'NONE',  ( -16.55341960407611168, -4.379528057220339221, 66.45724293864768129 ) ) ;
#85589 = DIRECTION ( 'NONE',  ( 0.000000000000000000, -0.7071067811865466846, 0.7071067811865484609 ) ) ;
#85590 = CARTESIAN_POINT ( 'NONE',  ( -5.153800228976607833, 19.02544592524334988, 67.70942372801900433 ) ) ;
#85591 = CARTESIAN_POINT ( 'NONE',  ( -19.03943276465977164, 0.05219959533909376836, 106.2489096053143669 ) ) ;
#85592 = CARTESIAN_POINT ( 'NONE',  ( -9.564922557961040184, 16.46253265017147172, 82.91775706135233293 ) ) ;
#85593 = CARTESIAN_POINT ( 'NONE',  ( 17.59860650958994555, -7.585241751806880650, 40.92337014262493966 ) ) ;
#85595 = CARTESIAN_POINT ( 'NONE',  ( -0.05219959533934338120, 16.53943276465976808, 107.5010903946856899 ) ) ;
#85594 = CARTESIAN_POINT ( 'NONE',  ( 4.379528057220092307, 16.55341960407617563, 22.29275706135235069 ) ) ;
#85596 = CARTESIAN_POINT ( 'NONE',  ( 5.153800228976615827, -19.02544592524334988, 70.20942372801899012 ) ) ;
#85597 = CARTESIAN_POINT ( 'NONE',  ( 5.719274019375991003, -21.55341960407610458, 37.70724293864769550 ) ) ;
#85598 = CARTESIAN_POINT ( 'NONE',  ( 10.81492255796106328, -18.62759615963255655, 50.41775706135235424 ) ) ;
#85599 = CARTESIAN_POINT ( 'NONE',  ( -21.70479006154309687, -8.695791278452020379, 169.0563666577075423 ) ) ;
#85600 = CARTESIAN_POINT ( 'NONE',  ( -4.379528057220086978, -16.55341960407618274, 19.79275706135235069 ) ) ;
#85602 = CARTESIAN_POINT ( 'NONE',  ( -5.049401038298153566, 19.05341960407611168, 75.20724293864769550 ) ) ;
#85601 = CARTESIAN_POINT ( 'NONE',  ( 17.49999999999998934, 3.258235366253115384, 22.47418410639502184 ) ) ;
#85603 = EDGE_CURVE ( 'NONE', #78316, #20950, #176626, .T. ) ;
#85604 = CARTESIAN_POINT ( 'NONE',  ( 15.19424636789221417, 17.31426855362213146, -57.70166256124680615 ) ) ;
#85606 = CARTESIAN_POINT ( 'NONE',  ( -5.049401038298153566, 19.05341960407611168, 80.20724293864769550 ) ) ;
#85605 = CARTESIAN_POINT ( 'NONE',  ( -14.34966873604960291, -8.224510206698953496, 91.66557627198103830 ) ) ;
#85607 = CARTESIAN_POINT ( 'NONE',  ( 13.97604488694527802, 13.89961937509977652, 94.37390960531436690 ) ) ;
#85608 = ORIENTED_EDGE ( 'NONE', *, *, #182123, .T. ) ;
#85609 = CARTESIAN_POINT ( 'NONE',  ( -0.05219959533936034679, 19.03943276465977164, 97.50109039468567573 ) ) ;
#85610 = CARTESIAN_POINT ( 'NONE',  ( 15.72974639402199770, -15.80617190586745480, 73.12390960531436690 ) ) ;
#85611 = CARTESIAN_POINT ( 'NONE',  ( -19.03943276465977164, 0.05219959533909376836, 31.24890960531435979 ) ) ;
#85612 = CARTESIAN_POINT ( 'NONE',  ( 5.153800228976615827, -19.02544592524334988, 55.20942372801899722 ) ) ;
#85613 = CARTESIAN_POINT ( 'NONE',  ( 13.89961937509977652, -13.97604488694527269, 53.12390960531434558 ) ) ;
#85614 = CARTESIAN_POINT ( 'NONE',  ( -16.46253265017160317, 9.564922557960807481, 95.83224293864769550 ) ) ;
#85615 = EDGE_LOOP ( 'NONE', ( #15998, #72164, #195272, #9445 ) ) ;
#85616 = CARTESIAN_POINT ( 'NONE',  ( -15.80617190586745835, -15.72974639402198527, 101.8739096053143811 ) ) ;
#85619 = CARTESIAN_POINT ( 'NONE',  ( -9.474510206698720793, -16.51473224551083518, 59.58442372801900433 ) ) ;
#85618 = CARTESIAN_POINT ( 'NONE',  ( -16.51473224551069308, -9.474510206698971260, 86.66557627198102409 ) ) ;
#85617 = CARTESIAN_POINT ( 'NONE',  ( -4.379528057220328563, 16.55341960407611168, 100.2072429386476955 ) ) ;
#85620 = CARTESIAN_POINT ( 'NONE',  ( 15.80617190586746368, 15.72974639402197994, 94.37390960531436690 ) ) ;
#85621 = CARTESIAN_POINT ( 'NONE',  ( -18.62759615963270932, 10.81492255796079327, 70.83224293864770971 ) ) ;
#85622 = VECTOR ( 'NONE', #88236, 999.9999999999998863 ) ;
#85623 = CARTESIAN_POINT ( 'NONE',  ( 14.34966873604960469, 8.224510206698951720, 34.16557627198102409 ) ) ;
#85624 = CARTESIAN_POINT ( 'NONE',  ( -21.53943276465977519, -0.05219959533937600094, 98.75109039468568994 ) ) ;
#85625 = CARTESIAN_POINT ( 'NONE',  ( -4.379528057220086978, -16.55341960407618274, 59.79275706135234714 ) ) ;
#85626 = CARTESIAN_POINT ( 'NONE',  ( -16.51473224551069308, -9.474510206698971260, 91.66557627198103830 ) ) ;
#85627 = CARTESIAN_POINT ( 'NONE',  ( 16.46253265017160672, -9.564922557960803928, 28.33224293864769550 ) ) ;
#85628 = CARTESIAN_POINT ( 'NONE',  ( 18.62759615963255655, 10.81492255796105972, 36.66775706135234714 ) ) ;
#85629 = CARTESIAN_POINT ( 'NONE',  ( 10.81492255796106328, -18.62759615963255655, 55.41775706135234714 ) ) ;
#85630 = CARTESIAN_POINT ( 'NONE',  ( -0.05219959533909027116, -19.03943276465977164, 42.49890960531435269 ) ) ;
#85631 = CARTESIAN_POINT ( 'NONE',  ( 15.72974639402176855, 15.80617190586768217, 36.87609039468568994 ) ) ;
#85632 = CARTESIAN_POINT ( 'NONE',  ( 19.02544592524334988, 5.153800228976608722, 71.45942372801900433 ) ) ;
#85633 = EDGE_CURVE ( 'NONE', #38745, #146788, #194818, .T. ) ;
#85634 = CARTESIAN_POINT ( 'NONE',  ( -5.153800228976607833, 19.02544592524334988, 67.70942372801900433 ) ) ;
#85635 = CARTESIAN_POINT ( 'NONE',  ( -13.97604488694527625, -13.89961937509977652, 26.87390960531434558 ) ) ;
#85636 = CARTESIAN_POINT ( 'NONE',  ( 16.55341960407618274, -4.379528057220086978, 76.04275706135237556 ) ) ;
#85637 = CARTESIAN_POINT ( 'NONE',  ( -5.049401038298153566, 19.05341960407611168, 55.20724293864769550 ) ) ;
#85638 = CARTESIAN_POINT ( 'NONE',  ( 24.10180676228338825, -9.559744493756877404, 166.3058469464611449 ) ) ;
#85639 = CARTESIAN_POINT ( 'NONE',  ( -16.46253265017160317, 9.564922557960807481, 100.8322429386477097 ) ) ;
#85640 = CARTESIAN_POINT ( 'NONE',  ( -16.51473224551069308, -9.474510206698971260, 36.66557627198102409 ) ) ;
#85641 = VECTOR ( 'NONE', #154276, 1000.000000000000000 ) ;
#85642 = CARTESIAN_POINT ( 'NONE',  ( -0.05219959533907301413, -21.53943276465977519, 67.49890960531436690 ) ) ;
#85643 = CARTESIAN_POINT ( 'NONE',  ( -12.14591786802326823, 12.06949235617739902, 58.12609039468568994 ) ) ;
#85644 = CARTESIAN_POINT ( 'NONE',  ( -16.46253265017146816, -9.564922557961047289, 24.16775706135233648 ) ) ;
#85645 = CARTESIAN_POINT ( 'NONE',  ( -9.474510206698964154, 16.51473224551069663, 50.41557627198102409 ) ) ;
#85646 = CARTESIAN_POINT ( 'NONE',  ( -4.483927247898539470, -16.52544592524342804, 42.29057627198103120 ) ) ;
#85647 = CARTESIAN_POINT ( 'NONE',  ( 8.224510206698953496, -14.34966873604960469, 62.91557627198102409 ) ) ;
#85648 = CARTESIAN_POINT ( 'NONE',  ( -5.153800228976328057, -19.02544592524343514, 77.29057627198099567 ) ) ;
#85649 = CARTESIAN_POINT ( 'NONE',  ( 18.62759615963255655, 10.81492255796105972, 36.66775706135234714 ) ) ;
#85650 = CARTESIAN_POINT ( 'NONE',  ( -16.51473224551069308, -9.474510206698971260, 96.66557627198102409 ) ) ;
#85651 = CARTESIAN_POINT ( 'NONE',  ( 15.80617190586769283, -15.72974639402175789, 100.6260903946857184 ) ) ;
#85652 = CARTESIAN_POINT ( 'NONE',  ( -8.314922557961024197, 14.29746914071037800, 67.91775706135234714 ) ) ;
#85653 = CARTESIAN_POINT ( 'NONE',  ( 0.05219959533909260263, 19.03943276465977164, 104.9989096053143669 ) ) ;
#85654 = CARTESIAN_POINT ( 'NONE',  ( -10.72451020669898014, 18.67979575497178502, 85.41557627198102409 ) ) ;
#85655 = CARTESIAN_POINT ( 'NONE',  ( 14.29746914071049879, -8.314922557960816363, 48.33224293864770260 ) ) ;
#85656 = CARTESIAN_POINT ( 'NONE',  ( -5.153800228976328057, -19.02544592524343514, 47.29057627198102409 ) ) ;
#85657 = CARTESIAN_POINT ( 'NONE',  ( -4.483927247898782831, 16.52544592524335698, 57.70942372801901143 ) ) ;
#85658 = CARTESIAN_POINT ( 'NONE',  ( -14.34966873604960291, -8.224510206698953496, 66.66557627198102409 ) ) ;
#85659 = CARTESIAN_POINT ( 'NONE',  ( 9.474510206698971260, -16.51473224551069308, 107.9155762719810383 ) ) ;
#85660 = CARTESIAN_POINT ( 'NONE',  ( 18.62759615963271287, -10.81492255796078972, 28.33224293864769550 ) ) ;
#85661 = CARTESIAN_POINT ( 'NONE',  ( -9.564922557961040184, 16.46253265017147172, 32.91775706135233293 ) ) ;
#85662 = CARTESIAN_POINT ( 'NONE',  ( -16.52544592524342804, 4.483927247898546575, 101.0405762719810383 ) ) ;
#85663 = CARTESIAN_POINT ( 'NONE',  ( 9.474510206698971260, -16.51473224551069308, 112.9155762719810383 ) ) ;
#85664 = ORIENTED_EDGE ( 'NONE', *, *, #177312, .F. ) ;
#85665 = CARTESIAN_POINT ( 'NONE',  ( -12.06949235617739369, -12.14591786802326823, 59.37609039468568284 ) ) ;
#85666 = CARTESIAN_POINT ( 'NONE',  ( 9.564922557960805705, 16.46253265017160317, 59.58224293864769550 ) ) ;
#85667 = CARTESIAN_POINT ( 'NONE',  ( 4.336808689942017736E-16, -0.7216878364870318308, 1.249999999999999778 ) ) ;
#85668 = CARTESIAN_POINT ( 'NONE',  ( -16.51473224551082808, 9.474510206698731452, 43.33442372801900433 ) ) ;
#85669 = CARTESIAN_POINT ( 'NONE',  ( 12.06949235617739724, 12.14591786802326823, 91.87609039468568994 ) ) ;
#85670 = CARTESIAN_POINT ( 'NONE',  ( 5.153800228976615827, -19.02544592524334988, 90.20942372801900433 ) ) ;
#85671 = CARTESIAN_POINT ( 'NONE',  ( -10.81492255796105439, 18.62759615963255655, 62.91775706135236135 ) ) ;
#85672 = CARTESIAN_POINT ( 'NONE',  ( 16.46253265017160672, -9.564922557960803928, 73.33224293864769550 ) ) ;
#85673 = CARTESIAN_POINT ( 'NONE',  ( -5.823673210054116645, -21.52544592524344225, 97.29057627198105251 ) ) ;
#85674 = CARTESIAN_POINT ( 'NONE',  ( -12.14591786802309592, -12.06949235617757132, 111.8739096053143669 ) ) ;
#85675 = CARTESIAN_POINT ( 'NONE',  ( -5.153800228976607833, 19.02544592524334988, 87.70942372801897591 ) ) ;
#85676 = CARTESIAN_POINT ( 'NONE',  ( -15.80617190586745835, -15.72974639402198527, 81.87390960531435269 ) ) ;
#85677 = CARTESIAN_POINT ( 'NONE',  ( 16.51473224551083163, -9.474510206698727899, 40.83442372801900433 ) ) ;
#85678 = CARTESIAN_POINT ( 'NONE',  ( 19.39720447994795194, 5.500000000000020428, 97.16317477297175742 ) ) ;
#85679 = CARTESIAN_POINT ( 'NONE',  ( 10.72451020669898902, -18.67979575497178502, 87.91557627198103830 ) ) ;
#85680 = DIRECTION ( 'NONE',  ( -1.000000000000000000, -0.000000000000000000, -0.000000000000000000 ) ) ;
#85681 = CARTESIAN_POINT ( 'NONE',  ( -19.02544592524342804, 5.153800228976336051, 66.04057627198103830 ) ) ;
#85682 = DIRECTION ( 'NONE',  ( -0.000000000000000000, -0.000000000000000000, 1.000000000000000000 ) ) ;
#85683 = CARTESIAN_POINT ( 'NONE',  ( 16.55341960407618274, -4.379528057220086978, 21.04275706135234714 ) ) ;
#85684 = CARTESIAN_POINT ( 'NONE',  ( 36.76875311564133142, -5.017346702420294235, 47.26027925686761932 ) ) ;
#85685 = CARTESIAN_POINT ( 'NONE',  ( -19.05341960407611168, -5.049401038298163336, 51.45724293864770260 ) ) ;
#85686 = CARTESIAN_POINT ( 'NONE',  ( -16.46253265017160317, 9.564922557960807481, 115.8322429386477097 ) ) ;
#85688 = CARTESIAN_POINT ( 'NONE',  ( -14.34966873604960291, -8.224510206698953496, 46.66557627198102409 ) ) ;
#85687 = CARTESIAN_POINT ( 'NONE',  ( 21.55341960407610458, 5.719274019375980345, 98.95724293864770971 ) ) ;
#85689 = CARTESIAN_POINT ( 'NONE',  ( 0.05219959533937995610, -21.53943276465977519, 80.00109039468568994 ) ) ;
#85692 = CARTESIAN_POINT ( 'NONE',  ( -16.46253265017146816, -9.564922557961047289, 24.16775706135233648 ) ) ;
#85691 = CARTESIAN_POINT ( 'NONE',  ( -4.379528057220086978, -16.55341960407618274, 29.79275706135234358 ) ) ;
#85690 = SHAPE_REPRESENTATION ( 'front house', ( #82054 ), #50057 ) ;
#85693 = CARTESIAN_POINT ( 'NONE',  ( -16.52544592524342804, 4.483927247898546575, 26.04057627198103475 ) ) ;
#85694 = CARTESIAN_POINT ( 'NONE',  ( -18.67979575497193778, 10.72451020669871902, 33.33442372801900433 ) ) ;
#85695 = CARTESIAN_POINT ( 'NONE',  ( -5.719274019375665041, -21.55341960407619695, 19.79275706135235069 ) ) ;
#85696 = CARTESIAN_POINT ( 'NONE',  ( 21.52544592524344225, -5.823673210054117533, 58.54057627198103120 ) ) ;
#85697 = CARTESIAN_POINT ( 'NONE',  ( 19.02544592524334988, 5.153800228976608722, 96.45942372801897591 ) ) ;
#85698 = CARTESIAN_POINT ( 'NONE',  ( 19.02544592524334988, 5.153800228976608722, 71.45942372801900433 ) ) ;
#85699 = AXIS2_PLACEMENT_3D ( 'NONE', #157909, #77081, #189257 ) ;
#85700 = CARTESIAN_POINT ( 'NONE',  ( -15.72974639402176322, -15.80617190586768395, 74.37609039468568994 ) ) ;
#85701 = CARTESIAN_POINT ( 'NONE',  ( 16.51473224551083163, -9.474510206698727899, 50.83442372801899722 ) ) ;
#85702 = CARTESIAN_POINT ( 'NONE',  ( -5.153800228976328057, -19.02544592524343514, 22.29057627198102765 ) ) ;
#85703 = CARTESIAN_POINT ( 'NONE',  ( 10.72451020669898902, -18.67979575497178502, 42.91557627198103120 ) ) ;
#85704 = CARTESIAN_POINT ( 'NONE',  ( 16.55341960407611168, 4.379528057220329451, 53.95724293864770260 ) ) ;
#85705 = CARTESIAN_POINT ( 'NONE',  ( -16.52216118717209881, -7.221426719304473885, 26.07599021046994281 ) ) ;
#85706 = CARTESIAN_POINT ( 'NONE',  ( -15.80617190586768217, 15.72974639402176855, 108.1260903946856757 ) ) ;
#85707 = CARTESIAN_POINT ( 'NONE',  ( 12.14591786802327356, -12.06949235617739191, 80.62609039468567573 ) ) ;
#85708 = CARTESIAN_POINT ( 'NONE',  ( -12.14591786802309592, -12.06949235617757132, 46.87390960531435979 ) ) ;
#85709 = CARTESIAN_POINT ( 'NONE',  ( 0.05219959533937995610, -21.53943276465977519, 70.00109039468568994 ) ) ;
#85710 = CARTESIAN_POINT ( 'NONE',  ( -15.80617190586768217, 15.72974639402176855, 78.12609039468570415 ) ) ;
#85711 = CARTESIAN_POINT ( 'NONE',  ( -5.823673210054116645, -21.52544592524344225, 82.29057627198103830 ) ) ;
#85712 = CARTESIAN_POINT ( 'NONE',  ( 5.153800228976335163, 19.02544592524342804, 44.79057627198103830 ) ) ;
#85713 = CARTESIAN_POINT ( 'NONE',  ( -5.823673210054431948, 21.52544592524334988, 57.70942372801901143 ) ) ;
#85714 = CARTESIAN_POINT ( 'NONE',  ( -9.564922557960796823, -16.46253265017161027, 37.08224293864768839 ) ) ;
#85715 = CARTESIAN_POINT ( 'NONE',  ( 19.05341960407611168, 5.049401038298154454, 48.95724293864768129 ) ) ;
#85716 = CARTESIAN_POINT ( 'NONE',  ( -14.29746914071049879, 8.314922557960819915, 95.83224293864770971 ) ) ;
#85717 = CARTESIAN_POINT ( 'NONE',  ( -9.474510206698964154, 16.51473224551069663, 95.41557627198102409 ) ) ;
#85718 = CARTESIAN_POINT ( 'NONE',  ( 0.05219959533910956823, 16.53943276465976808, 34.99890960531435979 ) ) ;
#85719 = CARTESIAN_POINT ( 'NONE',  ( -16.52544592524342804, 4.483927247898546575, 116.0405762719810383 ) ) ;
#85720 = CARTESIAN_POINT ( 'NONE',  ( -10.81492255796078084, -18.62759615963271287, 77.08224293864769550 ) ) ;
#85721 = CARTESIAN_POINT ( 'NONE',  ( 5.719274019375673035, 21.55341960407619339, 27.29275706135234358 ) ) ;
#85722 = DIRECTION ( 'NONE',  ( -0.000000000000000000, -0.000000000000000000, 1.000000000000000000 ) ) ;
#85723 = CARTESIAN_POINT ( 'NONE',  ( -16.53943276465976808, -0.05219959533934237506, 28.75109039468567929 ) ) ;
#85724 = CARTESIAN_POINT ( 'NONE',  ( 15.72974639402199770, -15.80617190586745480, 68.12390960531436690 ) ) ;
#85725 = CARTESIAN_POINT ( 'NONE',  ( 21.52544592524334988, 5.823673210054432836, 91.45942372801901854 ) ) ;
#85726 = CARTESIAN_POINT ( 'NONE',  ( -19.03943276465977164, 0.05219959533909376836, 86.24890960531436690 ) ) ;
#85727 = CARTESIAN_POINT ( 'NONE',  ( -5.719274019375665041, -21.55341960407619695, 29.79275706135234358 ) ) ;
#85728 = CARTESIAN_POINT ( 'NONE',  ( -19.02544592524342804, 5.153800228976336051, 111.0405762719810099 ) ) ;
#85729 = CARTESIAN_POINT ( 'NONE',  ( 8.314922557961029526, -14.29746914071037800, 90.41775706135236135 ) ) ;
#85730 = CARTESIAN_POINT ( 'NONE',  ( 10.72451020669871369, 18.67979575497193778, 67.08442372801901854 ) ) ;
#85731 = B_SPLINE_CURVE_WITH_KNOTS ( 'NONE', 3,
 ( #133382, #175904, #8034, #195073, #56552, #41387, #26229, #87868, #149556, #37376, #99033, #160723, #23220, #115220, #176912, #100039, #22215, #84863, #7024, #68706, #130363, #192060, #69715, #131382, #198051, #123176, #92836, #105044, #135400, #166728, #11052, #73727 ),
 .UNSPECIFIED., .F., .F.,
 ( 4, 2, 2, 2, 2, 2, 2, 2, 2, 2, 2, 2, 2, 2, 2, 4 ),
 ( 3.469446951953614189E-18, 0.0003712461730036830374, 0.0007424923460073626054, 0.001113738519011042011, 0.001484984692014721741, 0.002227477038022078817, 0.002598723211025754428, 0.002969969384029430039, 0.003341215557033105649, 0.003712461730036781260, 0.004083707903040456437, 0.004454954076044132481, 0.004826200249047807658, 0.005197446422051483703, 0.005568692595055158880, 0.005939938768058834057 ),
 .UNSPECIFIED. ) ;
#85732 = CARTESIAN_POINT ( 'NONE',  ( 0.05219959533936267826, -19.03943276465977164, 20.00109039468567218 ) ) ;
#85733 = CARTESIAN_POINT ( 'NONE',  ( -16.55341960407617563, 4.379528057220093196, 73.54275706135234714 ) ) ;
#85734 = CARTESIAN_POINT ( 'NONE',  ( -21.55341960407619339, 5.719274019375674811, 28.54275706135234358 ) ) ;
#85735 = CARTESIAN_POINT ( 'NONE',  ( -16.46253265017160317, 9.564922557960807481, 25.83224293864769194 ) ) ;
#85736 = CARTESIAN_POINT ( 'NONE',  ( -21.55341960407619339, 5.719274019375674811, 93.54275706135234714 ) ) ;
#85737 = CARTESIAN_POINT ( 'NONE',  ( 16.46253265017160672, -9.564922557960803928, 88.33224293864769550 ) ) ;
#85738 = CARTESIAN_POINT ( 'NONE',  ( -21.52544592524343514, 5.823673210054127303, 86.04057627198102409 ) ) ;
#85739 = CARTESIAN_POINT ( 'NONE',  ( -19.03943276465977164, -0.05219959533935918106, 53.75109039468566863 ) ) ;
#85741 = CARTESIAN_POINT ( 'NONE',  ( 18.62759615963271287, -10.81492255796078972, 48.33224293864770260 ) ) ;
#85740 = CARTESIAN_POINT ( 'NONE',  ( 18.22780087662123805, -5.499999999999976019, 88.51763182126893525 ) ) ;
#85743 = CARTESIAN_POINT ( 'NONE',  ( -8.224510206698948167, 14.34966873604960824, 55.41557627198102409 ) ) ;
#85742 = CARTESIAN_POINT ( 'NONE',  ( -9.474510206698964154, 16.51473224551069663, 90.41557627198103830 ) ) ;
#85744 = CARTESIAN_POINT ( 'NONE',  ( 10.34110108248005133, -9.296341836507240330, -62.50551787159913886 ) ) ;
#85745 = CARTESIAN_POINT ( 'NONE',  ( 19.03943276465977164, 0.05219959533936151252, 81.25109039468567573 ) ) ;
#85746 = CARTESIAN_POINT ( 'NONE',  ( -1.022580077288041090E-15, -16.70000000000002061, -61.34707691135562868 ) ) ;
#85747 = CARTESIAN_POINT ( 'NONE',  ( -9.564922557961040184, 16.46253265017147172, 102.9177570613523329 ) ) ;
#85748 = CARTESIAN_POINT ( 'NONE',  ( -21.52544592524343514, 5.823673210054127303, 86.04057627198102409 ) ) ;
#85749 = CARTESIAN_POINT ( 'NONE',  ( 12.14591786802309770, 12.06949235617756955, 69.37390960531436690 ) ) ;
#85750 = CARTESIAN_POINT ( 'NONE',  ( -13.89961937509977652, 13.97604488694528158, 105.6239096053143527 ) ) ;
#85751 = CARTESIAN_POINT ( 'NONE',  ( -4.379528057220086978, -16.55341960407618274, 49.79275706135234714 ) ) ;
#85752 = CARTESIAN_POINT ( 'NONE',  ( 16.51473224551069308, 9.474510206698969483, 59.16557627198102409 ) ) ;
#85754 = CARTESIAN_POINT ( 'NONE',  ( 9.564922557961047289, -16.46253265017146816, 95.41775706135233293 ) ) ;
#85753 = CARTESIAN_POINT ( 'NONE',  ( -21.53943276465977519, 0.05219959533907696930, 111.2489096053143669 ) ) ;
#85755 = CARTESIAN_POINT ( 'NONE',  ( 19.02544592524343514, -5.153800228976328945, 93.54057627198102409 ) ) ;
#85756 = CARTESIAN_POINT ( 'NONE',  ( -9.564922557960796823, -16.46253265017161027, 77.08224293864769550 ) ) ;
#85757 = CARTESIAN_POINT ( 'NONE',  ( -21.55341960407610458, -5.719274019375992779, 71.45724293864769550 ) ) ;
#85758 = CARTESIAN_POINT ( 'NONE',  ( -19.03943276465977164, 0.05219959533909376836, 46.24890960531435979 ) ) ;
#85759 = CARTESIAN_POINT ( 'NONE',  ( 24.68382089499486653, 27.82722013636965031, -8.000000000000003553 ) ) ;
#85760 = CARTESIAN_POINT ( 'NONE',  ( -12.06949235617756955, 12.14591786802309770, 60.62390960531437401 ) ) ;
#85761 = CARTESIAN_POINT ( 'NONE',  ( 5.153800228976335163, 19.02544592524342804, 99.79057627198102409 ) ) ;
#85762 = CARTESIAN_POINT ( 'NONE',  ( 28.82186960331486958, -9.364793116373689941, 144.9000000000000057 ) ) ;
#85763 = CARTESIAN_POINT ( 'NONE',  ( 9.564922557961047289, -16.46253265017146816, 65.41775706135233293 ) ) ;
#85764 = AXIS2_PLACEMENT_3D ( 'NONE', #172993, #126470, #62803 ) ;
#85765 = CARTESIAN_POINT ( 'NONE',  ( 18.62759615963271287, -10.81492255796078972, 88.33224293864769550 ) ) ;
#85766 = CARTESIAN_POINT ( 'NONE',  ( -16.51473224551082808, 9.474510206698731452, 53.33442372801900433 ) ) ;
#85767 = CARTESIAN_POINT ( 'NONE',  ( -9.474510206698964154, 16.51473224551069663, 95.41557627198102409 ) ) ;
#85768 = CARTESIAN_POINT ( 'NONE',  ( -21.53943276465977519, 0.05219959533907696930, 36.24890960531435979 ) ) ;
#85769 = CARTESIAN_POINT ( 'NONE',  ( -19.05341960407611168, -5.049401038298163336, 71.45724293864766707 ) ) ;
#85770 = CARTESIAN_POINT ( 'NONE',  ( -21.55341960407619339, 5.719274019375674811, 68.54275706135234714 ) ) ;
#85771 = CARTESIAN_POINT ( 'NONE',  ( 0.05219959533909260263, 19.03943276465977164, 39.99890960531436690 ) ) ;
#85773 = ORIENTED_EDGE ( 'NONE', *, *, #168827, .T. ) ;
#85772 = CARTESIAN_POINT ( 'NONE',  ( 16.55341960407611168, 4.379528057220329451, 78.95724293864769550 ) ) ;
#85774 = CARTESIAN_POINT ( 'NONE',  ( 14.34966873604972726, -8.224510206698740333, 20.83442372801901143 ) ) ;
#85775 = CARTESIAN_POINT ( 'NONE',  ( -21.52544592524334988, -5.823673210054445271, 58.95942372801902565 ) ) ;
#85776 = ORIENTED_EDGE ( 'NONE', *, *, #117794, .F. ) ;
#85777 = CARTESIAN_POINT ( 'NONE',  ( -9.474510206698964154, 16.51473224551069663, 110.4155762719810383 ) ) ;
#85779 = ADVANCED_FACE ( 'NONE', ( #77392 ), #166452, .F. ) ;
#85778 = CARTESIAN_POINT ( 'NONE',  ( 19.02544592524334988, 5.153800228976608722, 66.45942372801899012 ) ) ;
#85780 = DIRECTION ( 'NONE',  ( 0.000000000000000000, 0.000000000000000000, -1.000000000000000000 ) ) ;
#85781 = CARTESIAN_POINT ( 'NONE',  ( 15.80617190586769283, -15.72974639402175789, 25.62609039468567929 ) ) ;
#85782 = CARTESIAN_POINT ( 'NONE',  ( 9.564922557960805705, 16.46253265017160317, 54.58224293864769550 ) ) ;
#85783 = CARTESIAN_POINT ( 'NONE',  ( 11.74264578624800315, -36.14014761921581709, -7.149999994537626691 ) ) ;
#85784 = CARTESIAN_POINT ( 'NONE',  ( 9.474510206698729675, 16.51473224551082808, 22.08442372801899722 ) ) ;
#85785 = CARTESIAN_POINT ( 'NONE',  ( -0.05219959533909027116, -19.03943276465977164, 47.49890960531435979 ) ) ;
#85786 = CARTESIAN_POINT ( 'NONE',  ( 10.72451020669871369, 18.67979575497193778, 112.0844237280190185 ) ) ;
#85787 = CARTESIAN_POINT ( 'NONE',  ( -0.05219959533934338120, 16.53943276465976808, 92.50109039468567573 ) ) ;
#85789 = CARTESIAN_POINT ( 'NONE',  ( -18.62759615963255300, -10.81492255796106328, 69.16775706135234714 ) ) ;
#85788 = CARTESIAN_POINT ( 'NONE',  ( 9.564922557960805705, 16.46253265017160317, 99.58224293864770971 ) ) ;
#85790 = CARTESIAN_POINT ( 'NONE',  ( 4.419823376501902601, -4.206879353973994817, -62.50719930893271226 ) ) ;
#85791 = CARTESIAN_POINT ( 'NONE',  ( -19.02544592524342804, 5.153800228976336051, 111.0405762719810099 ) ) ;
#85792 = FACE_OUTER_BOUND ( 'NONE', #187529, .T. ) ;
#85794 = CARTESIAN_POINT ( 'NONE',  ( -10.81492255796105439, 18.62759615963255655, 72.91775706135234714 ) ) ;
#85793 = CARTESIAN_POINT ( 'NONE',  ( -16.53943276465976808, -0.05219959533934237506, 68.75109039468568994 ) ) ;
#85795 = CARTESIAN_POINT ( 'NONE',  ( 15.80617190586769283, -15.72974639402175789, 100.6260903946857184 ) ) ;
#85796 = CARTESIAN_POINT ( 'NONE',  ( -3.573655867282028392E-15, 2.428612866367529932E-14, -25.00000000000000000 ) ) ;
#85797 = CARTESIAN_POINT ( 'NONE',  ( -12.06949235617739369, -12.14591786802326823, 39.37609039468567573 ) ) ;
#85798 = CARTESIAN_POINT ( 'NONE',  ( -16.46253265017160317, 9.564922557960807481, 85.83224293864769550 ) ) ;
#85799 = CARTESIAN_POINT ( 'NONE',  ( 5.153800228976335163, 19.02544592524342804, 109.7905762719810099 ) ) ;
#85800 = VERTEX_POINT ( 'NONE', #89590 ) ;
#85801 = CARTESIAN_POINT ( 'NONE',  ( 17.12812012977024168, 6.668231424566063659, 43.85948759323144230 ) ) ;
#85802 = CARTESIAN_POINT ( 'NONE',  ( 5.049401038298161559, -19.05341960407611168, 37.70724293864768839 ) ) ;
#85803 = CARTESIAN_POINT ( 'NONE',  ( 21.53943276465977519, -0.05219959533907433946, 43.74890960531435979 ) ) ;
#85804 = CARTESIAN_POINT ( 'NONE',  ( 14.29746914071037800, 8.314922557961029526, 106.6677570613523756 ) ) ;
#85806 = CARTESIAN_POINT ( 'NONE',  ( -19.03943276465977164, 0.05219959533909376836, 81.24890960531436690 ) ) ;
#85805 = CARTESIAN_POINT ( 'NONE',  ( 16.52544592524342804, -4.483927247898539470, 83.54057627198102409 ) ) ;
#85807 = CARTESIAN_POINT ( 'NONE',  ( -21.52544592524334988, -5.823673210054445271, 103.9594237280190185 ) ) ;
#85808 = CARTESIAN_POINT ( 'NONE',  ( 14.34966873604972726, -8.224510206698740333, 20.83442372801901143 ) ) ;
#85809 = CARTESIAN_POINT ( 'NONE',  ( 12.14591786802309770, 12.06949235617756955, 94.37390960531436690 ) ) ;
#85810 = CARTESIAN_POINT ( 'NONE',  ( 10.72451020669871369, 18.67979575497193778, 47.08442372801901854 ) ) ;
#85811 = CARTESIAN_POINT ( 'NONE',  ( -21.55341960407610458, -5.719274019375992779, 81.45724293864769550 ) ) ;
#85812 = CARTESIAN_POINT ( 'NONE',  ( -9.564922557961040184, 16.46253265017147172, 52.91775706135233293 ) ) ;
#85813 = CARTESIAN_POINT ( 'NONE',  ( -16.46253265017160317, 9.564922557960807481, 45.83224293864769550 ) ) ;
#85814 = CARTESIAN_POINT ( 'NONE',  ( 16.51473224551069308, 9.474510206698969483, 94.16557627198103830 ) ) ;
#85815 = CARTESIAN_POINT ( 'NONE',  ( 0.05219959533910956823, 16.53943276465976808, 69.99890960531435269 ) ) ;
#85816 = CARTESIAN_POINT ( 'NONE',  ( -16.53943276465976808, 0.05219959533911058130, 46.24890960531435979 ) ) ;
#85817 = CARTESIAN_POINT ( 'NONE',  ( 4.483927247898790824, -16.52544592524335698, 110.2094237280190185 ) ) ;
#85818 = CARTESIAN_POINT ( 'NONE',  ( 9.564922557961047289, -16.46253265017146816, 60.41775706135233293 ) ) ;
#85819 = CARTESIAN_POINT ( 'NONE',  ( -19.52217212775661181, 5.499999999999920064, 84.93993709005259518 ) ) ;
#85820 = CARTESIAN_POINT ( 'NONE',  ( 0.05219959533907565091, 21.53943276465977519, 24.99890960531435624 ) ) ;
#85821 = CARTESIAN_POINT ( 'NONE',  ( 14.29746914071049879, -8.314922557960816363, 93.33224293864769550 ) ) ;
#85822 = DIRECTION ( 'NONE',  ( 1.000000000000000000, 0.000000000000000000, -0.000000000000000000 ) ) ;
#85824 = CARTESIAN_POINT ( 'NONE',  ( 5.823673210054125526, 21.52544592524343514, 54.79057627198104541 ) ) ;
#85823 = CARTESIAN_POINT ( 'NONE',  ( 9.474510206698971260, -16.51473224551069308, 42.91557627198103120 ) ) ;
#85825 = CARTESIAN_POINT ( 'NONE',  ( -13.97604488694527625, -13.89961937509977652, 26.87390960531434558 ) ) ;
#85827 = CARTESIAN_POINT ( 'NONE',  ( 16.51473224551069308, 9.474510206698969483, 64.16557627198102409 ) ) ;
#85826 = CARTESIAN_POINT ( 'NONE',  ( -16.55341960407617563, 4.379528057220093196, 83.54275706135234714 ) ) ;
#85828 = CARTESIAN_POINT ( 'NONE',  ( -16.51473224551082808, 9.474510206698731452, 43.33442372801900433 ) ) ;
#85829 = CARTESIAN_POINT ( 'NONE',  ( 10.81492255796106328, -18.62759615963255655, 50.41775706135235424 ) ) ;
#85830 = CARTESIAN_POINT ( 'NONE',  ( 15.80617190586746368, 15.72974639402197994, 39.37390960531436690 ) ) ;
#85831 = CARTESIAN_POINT ( 'NONE',  ( 4.483927247898545687, 16.52544592524342804, 104.7905762719810241 ) ) ;
#85832 = CARTESIAN_POINT ( 'NONE',  ( -0.05219959533936034679, 19.03943276465977164, 97.50109039468567573 ) ) ;
#85833 = CARTESIAN_POINT ( 'NONE',  ( 36.91746824999999887, -11.99521256947793546, -6.224999997268814589 ) ) ;
#85835 = CARTESIAN_POINT ( 'NONE',  ( 15.80617190586746368, 15.72974639402197994, 49.37390960531436690 ) ) ;
#85834 = CARTESIAN_POINT ( 'NONE',  ( 17.49999999999999645, 3.242565516156353134, 37.49999999998637179 ) ) ;
#85836 = CARTESIAN_POINT ( 'NONE',  ( -19.03943276465977164, 0.05219959533909376836, 21.24890960531436335 ) ) ;
#85837 = CARTESIAN_POINT ( 'NONE',  ( -15.80617190586768217, 15.72974639402176855, 83.12609039468568994 ) ) ;
#85838 = CARTESIAN_POINT ( 'NONE',  ( 12.06949235617757843, -12.14591786802309237, 43.12390960531435269 ) ) ;
#85840 = CARTESIAN_POINT ( 'NONE',  ( 12.14591786802309770, 12.06949235617756955, 59.37390960531436690 ) ) ;
#85839 = CARTESIAN_POINT ( 'NONE',  ( -4.483927247898782831, 16.52544592524335698, 57.70942372801901143 ) ) ;
#85841 = CARTESIAN_POINT ( 'NONE',  ( 10.81492255796078972, 18.62759615963270932, 79.58224293864769550 ) ) ;
#85842 = CARTESIAN_POINT ( 'NONE',  ( 21.52544592524344225, -5.823673210054117533, 73.54057627198102409 ) ) ;
#85843 = CARTESIAN_POINT ( 'NONE',  ( -0.5143648618586742494, -28.98522958361497359, -49.56847006845431736 ) ) ;
#85844 = CARTESIAN_POINT ( 'NONE',  ( -19.02544592524342804, 5.153800228976336051, 116.0405762719810383 ) ) ;
#85845 = CARTESIAN_POINT ( 'NONE',  ( 13.89961937509977652, -13.97604488694527269, 68.12390960531436690 ) ) ;
#85846 = CARTESIAN_POINT ( 'NONE',  ( -13.89961937509977652, 13.97604488694528158, 35.62390960531435269 ) ) ;
#85847 = CARTESIAN_POINT ( 'NONE',  ( -4.313351365237961588, 4.313351365237934942, -64.53213882399992940 ) ) ;
#85848 = VERTEX_POINT ( 'NONE', #151277 ) ;
#85849 = CARTESIAN_POINT ( 'NONE',  ( -12.06949235617739369, -12.14591786802326823, 79.37609039468567573 ) ) ;
#85850 = CARTESIAN_POINT ( 'NONE',  ( -21.55341960407619339, 5.719274019375674811, 23.54275706135235424 ) ) ;
#85851 = CARTESIAN_POINT ( 'NONE',  ( -9.474510206698964154, 16.51473224551069663, 70.41557627198102409 ) ) ;
#85852 = CARTESIAN_POINT ( 'NONE',  ( -15.80617190586768217, 15.72974639402176855, 58.12609039468568994 ) ) ;
#85853 = CARTESIAN_POINT ( 'NONE',  ( 19.02544592524343514, -5.153800228976328945, 113.5405762719810241 ) ) ;
#85854 = CARTESIAN_POINT ( 'NONE',  ( -23.69010019206611872, -31.82897765507213705, -19.48018210901399883 ) ) ;
#85855 = ORIENTED_EDGE ( 'NONE', *, *, #85188, .F. ) ;
#85856 = CARTESIAN_POINT ( 'NONE',  ( -5.719274019375665041, -21.55341960407619695, 44.79275706135234714 ) ) ;
#85858 = CARTESIAN_POINT ( 'NONE',  ( 13.97604488694527802, 13.89961937509977652, 104.3739096053143385 ) ) ;
#85857 = CARTESIAN_POINT ( 'NONE',  ( 9.474510206698971260, -16.51473224551069308, 22.91557627198102765 ) ) ;
#85859 = CARTESIAN_POINT ( 'NONE',  ( 13.97604488694548053, -13.89961937509957401, 55.62609039468566863 ) ) ;
#85860 = CARTESIAN_POINT ( 'NONE',  ( 15.80617190586746368, 15.72974639402197994, 109.3739096053143811 ) ) ;
#85861 = CARTESIAN_POINT ( 'NONE',  ( 13.89961937509957401, 13.97604488694547697, 51.87609039468566863 ) ) ;
#85862 = CARTESIAN_POINT ( 'NONE',  ( -13.89961937509957401, -13.97604488694547875, 49.37609039468567573 ) ) ;
#85864 = ORIENTED_EDGE ( 'NONE', *, *, #29949, .T. ) ;
#85863 = CARTESIAN_POINT ( 'NONE',  ( 12.14591786802327356, -12.06949235617739191, 110.6260903946857042 ) ) ;
#85866 = ORIENTED_EDGE ( 'NONE', *, *, #85994, .F. ) ;
#85865 = DIRECTION ( 'NONE',  ( -0.000000000000000000, -0.000000000000000000, 1.000000000000000000 ) ) ;
#85867 = CARTESIAN_POINT ( 'NONE',  ( -9.564922557960796823, -16.46253265017161027, 77.08224293864769550 ) ) ;
#85868 = TOROIDAL_SURFACE ( 'NONE', #137534, 69.99999999999998579, 8.000000000000000000 ) ;
#85869 = CARTESIAN_POINT ( 'NONE',  ( -21.55341960407619339, 5.719274019375674811, 78.54275706135236135 ) ) ;
#85870 = CARTESIAN_POINT ( 'NONE',  ( -21.55341960407619339, 5.719274019375674811, 98.54275706135234714 ) ) ;
#85871 = CARTESIAN_POINT ( 'NONE',  ( -17.18269478283316332, 17.18269478283309226, -56.77278709839600879 ) ) ;
#85872 = CARTESIAN_POINT ( 'NONE',  ( -9.474510206698964154, 16.51473224551069663, 100.4155762719810241 ) ) ;
#85873 = CARTESIAN_POINT ( 'NONE',  ( 10.72451020669871369, 18.67979575497193778, 77.08442372801901854 ) ) ;
#85874 = CARTESIAN_POINT ( 'NONE',  ( 12.06949235617739724, 12.14591786802326823, 21.87609039468567573 ) ) ;
#85875 = EDGE_CURVE ( 'NONE', #166568, #160624, #132132, .T. ) ;
#85876 = CARTESIAN_POINT ( 'NONE',  ( -9.564922557960796823, -16.46253265017161027, 77.08224293864769550 ) ) ;
#85877 = CARTESIAN_POINT ( 'NONE',  ( 10.72451020669898902, -18.67979575497178502, 22.91557627198102765 ) ) ;
#85878 = CARTESIAN_POINT ( 'NONE',  ( 19.05341960407611168, 5.049401038298154454, 88.95724293864769550 ) ) ;
#85879 = CARTESIAN_POINT ( 'NONE',  ( -16.51473224551082808, 9.474510206698731452, 88.33442372801900433 ) ) ;
#85880 = CARTESIAN_POINT ( 'NONE',  ( 0.05219959533909260263, 19.03943276465977164, 79.99890960531436690 ) ) ;
#85881 = CARTESIAN_POINT ( 'NONE',  ( -19.05341960407611168, -5.049401038298163336, 61.45724293864769550 ) ) ;
#85882 = CARTESIAN_POINT ( 'NONE',  ( 5.719274019375991003, -21.55341960407610458, 107.7072429386476955 ) ) ;
#85883 = CARTESIAN_POINT ( 'NONE',  ( -12.14591786802326823, 12.06949235617739902, 103.1260903946856757 ) ) ;
#85884 = CARTESIAN_POINT ( 'NONE',  ( 23.96320343559640165, -18.46320343559646560, 8.181980515339454030 ) ) ;
#85885 = CARTESIAN_POINT ( 'NONE',  ( -19.02544592524334988, -5.153800228976617603, 63.95942372801899012 ) ) ;
#85886 = CARTESIAN_POINT ( 'NONE',  ( -0.05219959533909027116, -19.03943276465977164, 87.49890960531436690 ) ) ;
#85887 = CARTESIAN_POINT ( 'NONE',  ( 12.14591786802309770, 12.06949235617756955, 84.37390960531438111 ) ) ;
#85888 = CARTESIAN_POINT ( 'NONE',  ( -13.89961937509977652, 13.97604488694528158, 30.62390960531435269 ) ) ;
#85889 = CARTESIAN_POINT ( 'NONE',  ( -0.05219959533907301413, -21.53943276465977519, 32.49890960531435979 ) ) ;
#85890 = CARTESIAN_POINT ( 'NONE',  ( 5.719274019375991003, -21.55341960407610458, 27.70724293864769905 ) ) ;
#85891 = CARTESIAN_POINT ( 'NONE',  ( 8.224510206698953496, -14.34966873604960469, 87.91557627198103830 ) ) ;
#85892 = CARTESIAN_POINT ( 'NONE',  ( -16.81555441253551564, 7.025013491695475842, 55.63685445334254354 ) ) ;
#85893 = CARTESIAN_POINT ( 'NONE',  ( -19.02544592524334988, -5.153800228976617603, 48.95942372801900433 ) ) ;
#85894 = CARTESIAN_POINT ( 'NONE',  ( -4.483927247898782831, 16.52544592524335698, 112.7094237280190328 ) ) ;
#85895 = CARTESIAN_POINT ( 'NONE',  ( 13.97604488694527802, 13.89961937509977652, 94.37390960531436690 ) ) ;
#85896 = CARTESIAN_POINT ( 'NONE',  ( 21.52544592524334988, 5.823673210054432836, 66.45942372801903275 ) ) ;
#85897 = CARTESIAN_POINT ( 'NONE',  ( -15.72974639402197994, 15.80617190586746368, 45.62390960531436690 ) ) ;
#85899 = ORIENTED_EDGE ( 'NONE', *, *, #24537, .F. ) ;
#85898 = CARTESIAN_POINT ( 'NONE',  ( 10.72451020669871369, 18.67979575497193778, 27.08442372801901854 ) ) ;
#85900 = CARTESIAN_POINT ( 'NONE',  ( 0.05219959533907565091, 21.53943276465977519, 84.99890960531436690 ) ) ;
#85901 = CARTESIAN_POINT ( 'NONE',  ( -16.55341960407611168, -4.379528057220339221, 106.4572429386477097 ) ) ;
#85902 = CARTESIAN_POINT ( 'NONE',  ( 19.03943276465977164, 0.05219959533936151252, 76.25109039468566152 ) ) ;
#85903 = CARTESIAN_POINT ( 'NONE',  ( -0.05219959533909027116, -19.03943276465977164, 47.49890960531435979 ) ) ;
#85904 = CARTESIAN_POINT ( 'NONE',  ( -16.51473224551069308, -9.474510206698971260, 91.66557627198103830 ) ) ;
#85905 = CARTESIAN_POINT ( 'NONE',  ( -5.049401038298153566, 19.05341960407611168, 100.2072429386476955 ) ) ;
#85906 = CARTESIAN_POINT ( 'NONE',  ( -16.52544592524342804, 4.483927247898546575, 116.0405762719810383 ) ) ;
#85907 = CIRCLE ( 'NONE', #131222, 40.00000000000002132 ) ;
#85908 = CARTESIAN_POINT ( 'NONE',  ( -12.14591786802309592, -12.06949235617757132, 41.87390960531435979 ) ) ;
#85909 = CARTESIAN_POINT ( 'NONE',  ( -12.06949235617739369, -12.14591786802326823, 39.37609039468567573 ) ) ;
#85910 = CARTESIAN_POINT ( 'NONE',  ( 5.823673210054444382, -21.52544592524334988, 110.2094237280190185 ) ) ;
#85911 = CARTESIAN_POINT ( 'NONE',  ( -0.05219959533910754901, -16.53943276465976808, 27.49890960531435269 ) ) ;
#85912 = CARTESIAN_POINT ( 'NONE',  ( 10.72451020669871369, 18.67979575497193778, 27.08442372801901854 ) ) ;
#85913 = CARTESIAN_POINT ( 'NONE',  ( 5.049401038298161559, -19.05341960407611168, 107.7072429386476955 ) ) ;
#85914 = CARTESIAN_POINT ( 'NONE',  ( 14.34966873604972726, -8.224510206698740333, 100.8344237280190185 ) ) ;
#85915 = CARTESIAN_POINT ( 'NONE',  ( -12.06949235617739369, -12.14591786802326823, 94.37609039468568994 ) ) ;
#85916 = CARTESIAN_POINT ( 'NONE',  ( 14.34966873604972726, -8.224510206698740333, 30.83442372801902209 ) ) ;
#85917 = CARTESIAN_POINT ( 'NONE',  ( 9.564922557960805705, 16.46253265017160317, 44.58224293864769550 ) ) ;
#85918 = CARTESIAN_POINT ( 'NONE',  ( -16.52544592524342804, 4.483927247898546575, 111.0405762719810525 ) ) ;
#85919 = CARTESIAN_POINT ( 'NONE',  ( -18.67979575497193778, 10.72451020669871902, 23.33442372801901499 ) ) ;
#85920 = CARTESIAN_POINT ( 'NONE',  ( -9.474510206698964154, 16.51473224551069663, 30.41557627198102054 ) ) ;
#85921 = CARTESIAN_POINT ( 'NONE',  ( 19.03943276465977164, -0.05219959533909143690, 103.7489096053143669 ) ) ;
#85922 = CARTESIAN_POINT ( 'NONE',  ( 10.72451020669871369, 18.67979575497193778, 27.08442372801901854 ) ) ;
#85923 = CARTESIAN_POINT ( 'NONE',  ( 9.564922557960805705, 16.46253265017160317, 29.58224293864769550 ) ) ;
#85924 = CARTESIAN_POINT ( 'NONE',  ( 13.89961937509977652, -13.97604488694527269, 108.1239096053143669 ) ) ;
#85925 = CARTESIAN_POINT ( 'NONE',  ( -16.19135201231363652, -7.376712067592051447, 35.18680854052033169 ) ) ;
#85926 = CARTESIAN_POINT ( 'NONE',  ( 19.03943276465977164, -0.05219959533909143690, 103.7489096053143669 ) ) ;
#85928 = CARTESIAN_POINT ( 'NONE',  ( 8.224510206698953496, -14.34966873604960469, 92.91557627198103830 ) ) ;
#85927 = CARTESIAN_POINT ( 'NONE',  ( 18.62759615963255655, 10.81492255796105972, 41.66775706135235424 ) ) ;
#85929 = CARTESIAN_POINT ( 'NONE',  ( -5.049401038298153566, 19.05341960407611168, 95.20724293864770971 ) ) ;
#85930 = CARTESIAN_POINT ( 'NONE',  ( 17.72696623605161292, -5.499999999999952038, 96.09811031808415294 ) ) ;
#85931 = CARTESIAN_POINT ( 'NONE',  ( -14.29746914071037622, -8.314922557961029526, 69.16775706135234714 ) ) ;
#85932 = CARTESIAN_POINT ( 'NONE',  ( 21.55341960407619695, -5.719274019375665929, 81.04275706135236135 ) ) ;
#85933 = CARTESIAN_POINT ( 'NONE',  ( -16.55341960407617563, 4.379528057220093196, 43.54275706135235424 ) ) ;
#85934 = CARTESIAN_POINT ( 'NONE',  ( 16.46253265017160672, -9.564922557960803928, 78.33224293864769550 ) ) ;
#85935 = CARTESIAN_POINT ( 'NONE',  ( 4.483927247898790824, -16.52544592524335698, 20.20942372801900788 ) ) ;
#85936 = CARTESIAN_POINT ( 'NONE',  ( 16.52544592524335698, 4.483927247898782831, 86.45942372801901854 ) ) ;
#85937 = CARTESIAN_POINT ( 'NONE',  ( 5.153800228976615827, -19.02544592524334988, 90.20942372801900433 ) ) ;
#85938 = CARTESIAN_POINT ( 'NONE',  ( 19.05341960407611168, 5.049401038298154454, 68.95724293864769550 ) ) ;
#85939 = CARTESIAN_POINT ( 'NONE',  ( -15.72974639402197994, 15.80617190586746368, 85.62390960531436690 ) ) ;
#85941 = CARTESIAN_POINT ( 'NONE',  ( 0.05219959533936267826, -19.03943276465977164, 95.00109039468567573 ) ) ;
#85940 = CARTESIAN_POINT ( 'NONE',  ( -8.224510206698948167, 14.34966873604960824, 90.41557627198103830 ) ) ;
#85942 = CARTESIAN_POINT ( 'NONE',  ( -12.06949235617739369, -12.14591786802326823, 54.37609039468568994 ) ) ;
#85943 = CARTESIAN_POINT ( 'NONE',  ( -18.39443945427638738, 5.500000000000032863, 78.51745347608651571 ) ) ;
#85944 = CARTESIAN_POINT ( 'NONE',  ( -19.05341960407617563, 5.049401038297882671, 53.54275706135231871 ) ) ;
#85945 = CARTESIAN_POINT ( 'NONE',  ( 0.05219959533910956823, 16.53943276465976808, 34.99890960531435979 ) ) ;
#85946 = CARTESIAN_POINT ( 'NONE',  ( -0.05219959533910754901, -16.53943276465976808, 77.49890960531433848 ) ) ;
#85948 = CARTESIAN_POINT ( 'NONE',  ( -19.52217212775660471, 5.499999999999917399, 89.93993709005258097 ) ) ;
#85947 = CARTESIAN_POINT ( 'NONE',  ( 5.153800228976615827, -19.02544592524334988, 25.20942372801900433 ) ) ;
#85949 = CARTESIAN_POINT ( 'NONE',  ( -0.05219959533937732626, 21.53943276465977519, 27.50109039468567929 ) ) ;
#85950 =( BOUNDED_SURFACE ( )  B_SPLINE_SURFACE ( 3, 2, ( 
 ( #120360, #168840, #90998, #31341, #105201, #139495, #14173, #182053, #108165, #977, #62653, #138507, #151710, #200189, #124330, #13203, #45514, #121352, #74866, #184032, #61658, #75842, #152684, #104210, #166888, #123326, #89034, #165891, #122341, #185020, #136528, #46505, #186028, #150725, #59680, #137519, #12224, #29367, #199200, #60668, #73887, #198209, #43536, #183045, #107169, #189013, #3961, #2979, #144466, #110161, #94988, #158641, #113131, #78819, #64658, #1986, #63666, #67628, #142483, #19156, #50488, #189995, #48507, #36286, #5951, #174821, #97942, #20132, #96961, #49488, #111150, #129288, #81777, #143463, #159634, #21130, #188017, #171840, #80805, #4948, #79824, #82785, #35306, #66632, #47510, #33327, #140498, #125339, #170846, #141495, #112148, #109166, #65641, #128296, #187037, #32337, #93990, #155670, #17166, #156673, #18168, #126320, #173840, #172840, #127300, #51470, #34319, #95982, #157666, #114118, #175820, #37293, #98952, #25155, #100955, #146459, #145463, #147484, #102968, #148484, #9975, #133301, #194992, #101972, #160642, #6945, #178828, #164653, #130281, #71635, #162640, #161642, #179837, #190983, #69635, #24146, #38302, #10971, #8974, #22133, #68624, #55463, #177828, #118147, #191975, #41307, #85798, #83784, #56469, #26148, #87790, #117134, #176830, #86797, #72644, #99956, #132309, #7952, #23136, #70643, #149475, #194001, #39298, #52460, #53462, #40298, #115138, #84781, #163653, #131301, #192990, #54468, #116138, #183797, #89791, #105949, #60433, #74629, #167634, #121114, #14943, #58457, #73647, #196005, #181816, #75605, #90769, #151475, #31108, #196991, #43295, #45284, #199962, #165649, #12965, #88794, #150487, #154444, #29131, #152453, #137284, #76603, #135318, #123098, #92756, #61427, #184784, #106937, #168610, #136295, #197971, #15938, #30110, #91750, #46270, #107925, #59441, #120125, #13938, #153445, #166650, #169610, #122107, #138280, #134319, #104963, #27147, #11982, #182808, #44291, #198966, #57478, #119150, #180832, #28151, #42309, #103970, #4714, #2744, #141255, #155439, #97708, #19903, #174594, #64421, #188775, #157430, #80569, #142244, #62416, #33095, #108931, #77597, #16929, #65406, #159399, #189767, #126090, #66403, #36059, #3729, #744, #156432, #78582, #127067, #50258, #124088, #128065, #94751, #139268, #49256, #51239, #170611, #186799, #185787, #111914, #47274, #140256, #173602, #35071, #112900, #109925, #32101, #96726, #93758, #158414, #48270, #81545, #171607, #1748, #143231, #63426, #17932, #172600, #125101, #187786, #79586, #110914, #34086, #95745, #18924, #84546, #21900, #54235, #101731, #114900, #116898, #176594, #6711, #144234, #53224, #52227, #24916, #130041, #99724, #115906, #70404, #23904, #68389, #7711, #161408, #86562, #98717, #146224, #178591, #85558, #132072, #147243, #129052, #190753, #5718, #37058, #193761, #191740, #38068, #22900, #160411, #82552, #177596, #55229, #69395, #40054, #131063, #192752, #20894, #163419, #39064, #67396, #100721, #83550, #113883, #162402, #8735, #175581, #145229, #51880, #32746, #18575, #156079, #17575, #21545, #96381, #173248, #142884, #143884, #2393, #190404, #160058, #67049, #113539, #112552, #50894, #3384, #65059, #98359, #174247, #97362, #128707, #175233, #141893, #125742, #34723, #159048, #33732, #36698, #189419, #35715, #83205, #187442, #94398, #79236, #124750, #95393, #4366, #1390, #158068, #20542, #140907, #63071, #186446, #47922, #109576, #171259, #64072, #82191, #111564, #157079, #48910, #19559, #110564, #5365, #172245, #80222, #126716, #188420, #49897, #81203, #66049, #127717, #84196, #102384, #54879, #115560, #133718, #144880, #23551, #178242, #192403, #165064, #101366, #68042, #99372, #9387, #131722, #72044, #145876, #195410, #116553, #37710, #148897, #56888, #118562, #71053, #130709, #40715, #26558, #53885, #86211, #162055, #177247, #24562, #179249, #39703, #193404, #6362, #7359, #132719 ),
 ( #163055, #161055, #52868, #87215, #180252, #38719, #147901, #100377, #194407, #41722, #146887, #103386, #8379, #85199, #10387, #55877, #114539, #22550, #117550, #129694, #69044, #164072, #25571, #70054, #191391, #176239, #167051, #121517, #135722, #108335, #44693, #11391, #42716, #152850, #75026, #15345, #89202, #77001, #198373, #181240, #92160, #138673, #153, #14344, #74051, #184199, #170015, #197393, #29528, #105364, #58858, #168031, #122509, #59850, #136691, #88201, #150895, #76010, #73061, #149885, #106347, #137685, #12389, #30509, #61822, #199370, #43702, #183212, #60834, #28552, #91161, #45681, #169005, #120525, #27562, #134733, #182218, #107332, #153847, #90189, #185185, #151872, #13362, #123492, #46675, #119557, #196415, #104378, #166061, #57885, #3631, #156334, #33000, #35963, #172503, #2650, #97610, #78484, #187692, #66306, #50158, #81448, #34978, #185683, #47173, #62315, #155344, #19807, #48171, #94654, #186700, #16833, #139168, #18829, #143135, #171511, #158319, #49162, #17834, #174496, #111817, #33990, #127966, #141161, #108832, #15839, #32002, #110821, #170512, #93659, #189669, #79492, #64327, #95646, #80474, #51142, #125994, #109828, #157334, #142147, #4614, #65310, #126970, #188678, #173505, #96631, #645, #112803, #140157, #77498, #1649, #123985, #63327, #125005, #22807, #150897, #58861, #162311, #82450, #37973, #160314, #8639, #23812, #144138, #12391, #176497, #120527, #130967, #74053, #190658, #68296, #182220, #85462, #5620, #21804, #147151, #70311, #135724, #191647, #197395, #131980, #52134, #193665, #129947, #55136, #53126, #20795, #166063, #43704, #99631, #54140, #116806, #146131, #113791, #67299, #104380, #159299, #114804, #192657, #145134, #178498, #128958, #161313, #175486, #84453, #7617, #36958, #69301, #98620, #83456, #115814, #177504, #42718, #38973, #100630, #6617, #27564, #89204, #187203, #168033, #77003, #155836, #139659, #171014, #124505, #75028, #136694, #151874, #44695, #109332, #137687, #122511, #76012, #106349, #28554, #108337, #32505, #60836, #47682, #138675, #107334, #63833, #1147, #123494, #17333, #30511, #198375, #125506, #121519, #155, #59852, #183214, #78989, #45683, #169007, #61824, #170018, #140663, #92163, #199372, #46678, #184201, #94157, #153849, #15347, #29530, #105366, #2155, #167053, #185187, #91163, #31508, #90191, #62822, #13364, #186200, #152852, #14347, #93161, #154846, #16343, #77992, #65809, #19328, #49657, #172007, #51639, #114300, #4130, #191162, #20299, #50656, #7121, #82965, #66804, #160822, #174007, #18337, #68803, #64825, #81947, #141660, #3152, #99132, #189183, #112317, #143639, #113303, #22310, #35478, #80976, #190163, #127478, #176002, #97127, #158811, #126487, #130462, #52635, #145641, #5122, #159813, #128467, #174994, #36459, #33495, #98116, #79992, #48674, #188185, #21308, #110326, #83961, #144642, #37471, #95154, #6125, #156842, #67808, #111321, #129463, #173011, #34490, #96148, #157837, #142651, #163830, #42480, #23311, #101126, #150659, #118322, #177009, #54634, #180015, #41482, #165825, #24321, #27322, #56649, #84955, #103147, #162812, #195168, #85970, #53640, #196180, #88969, #70814, #86973, #164828, #179005, #146637, #100135, #134493, #12157, #147660, #25332, #177998, #26324, #73822, #194172, #104143, #55636, #9147, #115317, #132483, #8130, #192160, #117309, #40473, #87964, #102145, #148660, #38478, #10148, #71808, #161816, #69808, #149652, #11150, #131475, #116309, #193162, #39465, #133476, #72824, #57652, #119318, #181005, #108095, #28324, #197162, #170779, #58628, #120294, #181987, #43469, #169780, #45449, #90931, #89963, #91921, #47444, #92924, #154610, #77763, #139429, #46436, #105137, #151643, #123260, #109100, #74800, #16105, #107103, #106117, #124264, #135492, #14108, #168773, #182979, #155604, #153613, #166823, #13138, #200123, #122274, #62586, #136463, #185959, #30275, #198143, #912, #32269, #93926, #61592 ),
 ( #184952, #59613, #121286, #15109, #31273, #44463, #17100, #167801, #29301, #152617, #76770, #75775, #137453, #138442, #183962, #199132, #60599, #18104, #140429, #126258, #20070, #35243, #34257, #175753, #141429, #187955, #189932, #144403, #110098, #95916, #33265, #94924, #98887, #173777, #156609, #96897, #52397, #50428, #67565, #37230, #5889, #129223, #51407, #128235, #80741, #142419, #160581, #113067, #174759, #190920, #114056, #19092, #2916, #112087, #36225, #111086, #78752, #64594, #81714, #157601, #49425, #158581, #97877, #143399, #127237, #1919, #172776, #4888, #63598, #125274, #66570, #159568, #3898, #21066, #186971, #82722, #65578, #48441, #171776, #188951, #79758, #8904, #102903, #146395, #161578, #83721, #69570, #163585, #178761, #177762, #119087, #84717, #131236, #133233, #87725, #53396, #39231, #176766, #38238, #42244, #117065, #99893, #40226, #195940, #193932, #10906, #180769, #149410, #72579, #194925, #71568, #24074, #85729, #103905, #56400, #118082, #134253, #57414, #162571, #7884, #55395, #179772, #54402, #22070, #9908, #41241, #145400, #192924, #115074, #23071, #6882, #116074, #25086, #68560, #101903, #164587, #100887, #130217, #191912, #147417, #70572, #132240, #86728, #26081, #148413, #121049, #120062, #122043, #77529, #123032, #184718, #107856, #169541, #76539, #135256, #181750, #153376, #139201, #104898, #46202, #75542, #136233, #154377, #165586, #44229, #198903, #12901, #185714, #183733, #88730, #43232, #30045, #152389, #92689, #166587, #15871, #137216, #58396, #31040, #676, #62347, #91686, #151413, #61361, #182744, #196928, #27084, #28087, #14878, #47205, #124017, #29067, #150425, #11920, #168547, #73584, #105886, #89727, #138215, #199897, #74565, #197907, #167573, #59377, #60371, #90706, #13875, #45219, #106874, #35006, #93691, #171541, #96661, #158348, #82481, #141191, #144165, #173537, #1680, #19837, #79521, #111847, #2680, #170543, #112833, #5650, #187722, #3662, #81478, #95679, #63358, #16863, #51173, #67327, #64357, #80505, #94684, #143165, #128989, #110851, #159328, #172535, #126026, #32034, #49193, #125035, #190687, #34021, #157365, #4645, #18859, #142178, #108864, #65340, #127000, #155374, #33029, #188708, #20824, #66336, #174525, #127997, #78514, #140188, #186731, #48202, #35992, #50190, #189700, #97639, #109856, #156363, #17866, #117845, #7645, #194694, #23840, #54170, #10675, #86498, #70340, #164359, #177532, #21833, #72339, #68325, #85489, #145163, #6647, #102674, #192687, #115843, #147178, #55163, #25854, #39001, #22835, #193694, #69329, #179538, #100657, #162339, #129975, #134014, #56164, #149186, #8667, #163353, #132007, #116833, #178524, #36988, #53155, #41007, #39991, #191675, #87498, #52162, #113819, #101662, #38004, #148182, #175514, #99659, #24849, #130995, #161343, #9676, #71341, #133004, #98650, #160344, #114834, #83485, #176528, #84482, #146159, #44980, #119837, #137973, #169296, #106640, #151182, #167338, #121803, #136003, #28835, #182508, #76295, #181522, #135025, #57178, #43001, #136979, #152158, #12670, #92451, #58170, #104668, #168313, #61121, #26849, #74337, #150185, #11686, #15631, #90476, #73352, #13641, #30802, #75308, #184485, #154139, #122795, #45964, #29809, #91445, #197674, #59139, #77288, #153133, #14636, #107618, #195706, #120809, #166353, #198668, #199655, #27851, #118855, #183496, #180538, #42012, #89492, #88490, #196700, #103676, #43988, #60135, #165355, #105649, #111606, #31794, #437, #174285, #62112, #123775, #185474, #46964, #173291, #48950, #94439, #93443, #95435, #50935, #96422, #158108, #81242, #142923, #49941, #108623, #155130, #126757, #112593, #78271, #19600, #110603, #109617, #127756, #138958, #17619, #172285, #186489, #159087, #157119, #170301, #16623, #3423, #125782, #66090, #34765, #4405, #189457, #139944, #1434, #63112, #124790, #35755, #171301, #156120, #32787, #47965, #79278, #141932, #97400, #140948, #20582 ),
 ( #2435, #64117, #187484, #33775, #18615, #80262, #65099, #188460, #194449, #39747, #101410, #24606, #86254, #193447, #51920, #36739, #70096, #55920, #21586, #163102, #192445, #52909, #71095, #82234, #161097, #115602, #129735, #102429, #38761, #5405, #98403, #146934, #69086, #9430, #83244, #132762, #53927, #175273, #147944, #117595, #179296, #8424, #68083, #178284, #164116, #191432, #23596, #99415, #114585, #162100, #116595, #177291, #130753, #143924, #144920, #131765, #67089, #128748, #100419, #54923, #6402, #40760, #190445, #113579, #37754, #85243, #160099, #22592, #176282, #84240, #145919, #7402, #165112, #87258, #73110, #167097, #182267, #181286, #122559, #88247, #134780, #136738, #91206, #56935, #42764, #180299, #41767, #45731, #120573, #103432, #43750, #199418, #197440, #14393, #184249, #152896, #76059, #198422, #151919, #166109, #58906, #12437, #106396, #149932, #26604, #148943, #196462, #28598, #105413, #104426, #107383, #11439, #57932, #59897, #137734, #118609, #27611, #119603, #89251, #25614, #90236, #150943, #13408, #60882, #75072, #10433, #72091, #133765, #195460, #121565, #183259, #74099, #135769, #44740, #168078, #29575, #37263, #98921, #109380, #93208, #2201, #67599, #1194, #22103, #159602, #21100, #6915, #154893, #203, #185235, #92213, #62871, #110372, #160613, #140711, #144436, #61872, #30562, #68593, #153899, #15394, #77051, #138722, #5922, #79036, #124552, #123542, #125553, #83753, #129258, #190953, #114088, #175789, #82756, #46727, #108389, #52430, #145432, #170066, #130249, #63882, #139707, #191944, #169055, #47727, #187250, #16391, #53429, #48719, #31557, #78038, #33541, #155883, #186249, #171060, #32550, #172054, #94203, #17380, #97911, #27114, #41272, #100920, #10937, #135284, #162605, #56434, #132274, #24109, #194957, #149441, #86763, #163618, #115106, #177794, #102934, #38271, #176798, #133266, #164619, #39264, #57444, #88760, #26113, #70607, #148446, #55428, #117099, #9941, #118114, #150453, #178794, #85763, #179803, #193965, #42277, #40263, #101936, #192957, #196956, #119117, #11949, #25119, #87756, #72610, #134284, #195972, #99925, #71600, #146428, #161610, #54436, #180798, #23104, #73613, #103935, #165615, #84750, #7918, #69602, #131269, #116106, #147450, #8938, #43260, #108896, #75570, #16894, #30074, #170575, #89755, #167599, #78545, #184749, #104928, #121078, #46234, #107888, #32066, #90733, #93722, #123063, #151441, #169575, #29094, #61391, #152416, #120091, #62380, #155404, #137246, #153409, #31072, #45249, #12928, #166614, #708, #140220, #13904, #91715, #44256, #92720, #58424, #60399, #181779, #122071, #198931, #28117, #183763, #74592, #136260, #106903, #168576, #154409, #14907, #76569, #197935, #138244, #199928, #59404, #182772, #15903, #105913, #77561, #124050, #139233, #185749, #47237, #48233, #141221, #5684, #34053, #18891, #172567, #2712, #125066, #4678, #67360, #157398, #144198, #173569, #3694, #160376, #36024, #19870, #113851, #127033, #171572, #21867, #17898, #35038, #94716, #156394, #52193, #64389, #190720, #111879, #79552, #129019, #175547, #37022, #128030, #187754, #97673, #83517, #49224, #143197, #80537, #110882, #81510, #159362, #96692, #50225, #1713, #126057, #189732, #186763, #63389, #66370, #51205, #95710, #98683, #109888, #112866, #142211, #158381, #174557, #65373, #20859, #188740, #82516, #33061, #84512, #6677, #192717, #86528, #101693, #100686, #42043, #7675, #54201, #56194, #10707, #176559, #162368, #99690, #161374, #165387, #40020, #22865, #163382, #118885, #116863, #134044, #103707, #72370, #195737, #117877, #194724, #147208, #8699, #26880, #179567, #41037, #57210, #180569, #85520, #69359, #178554, #102703, #177562, #145194, #133034, #164391, #68355, #131028, #38034, #146190, #130006, #39031, #148212, #191705, #24879, #25884, #115873, #53189, #114864, #23869, #70369, #132037, #193726, #87529, #55194, #9706, #71370, #149216, #469 ),
 ( #73383, #44022, #119867, #88523, #27881, #76328, #108655, #62143, #152189, #77322, #185505, #91478, #90507, #60166, #153166, #123807, #28867, #59172, #29841, #105683, #15663, #13673, #75340, #166385, #170333, #30835, #150219, #167370, #122827, #11716, #14667, #138005, #135055, #137010, #181552, #196731, #89523, #199689, #58199, #46996, #198700, #138990, #43031, #61154, #104697, #121835, #151212, #184516, #45996, #12700, #74366, #183529, #136032, #45013, #197706, #120841, #182540, #106672, #107651, #168345, #169328, #92483, #154172, #5438, #64149, #67122, #96453, #124822, #81274, #2467, #34798, #125813, #93476, #35788, #128780, #110637, #126789, #142956, #18648, #186522, #139976, #174318, #190480, #187516, #3455, #17650, #158140, #51952, #33807, #82266, #95467, #48982, #155163, #172318, #47996, #113612, #157153, #80294, #19632, #141966, #65132, #31826, #188495, #49974, #16655, #94471, #111638, #143958, #66124, #97435, #50967, #1465, #63143, #78303, #171332, #159120, #173323, #4436, #127789, #32820, #109650, #189489, #20616, #112626, #156152, #79310, #140979, #133799, #9466, #193479, #87291, #100451, #144952, #195490, #191463, #8455, #68115, #129767, #25646, #115634, #161129, #178317, #72125, #177323, #148975, #38794, #145953, #98437, #192476, #52941, #56965, #130784, #162131, #163135, #23627, #53959, #175306, #131800, #85275, #36772, #37785, #146966, #10464, #71129, #40792, #194482, #6433, #114615, #21620, #176315, #179328, #7434, #70128, #69118, #99449, #160132, #39780, #102461, #54956, #117630, #116628, #101444, #83277, #132795, #24638, #22625, #86287, #84272, #147977, #55954, #164149, #11472, #73143, #169085, #58937, #120606, #90266, #121594, #92243, #182300, #89283, #59926, #74129, #45760, #43780, #105445, #196493, #138751, #60913, #180330, #197471, #152924, #233, #183289, #44771, #103465, #135800, #149966, #118638, #57963, #106424, #41798, #30591, #167129, #107412, #15423, #168105, #165144, #28629, #119634, #29602, #91234, #26635, #153929, #151949, #77082, #13438, #88278, #134813, #27643, #181317, #14421, #42796, #104458, #76085, #137761, #166141, #150974, #12468, #199445, #75102, #122589, #136769, #184277, #198455, #123571, #65883, #158886, #140739, #156918, #173086, #48748, #16419, #170092, #4205, #35553, #32580, #33570, #80064, #111401, #186277, #127557, #97200, #34565, #17409, #95232, #188259, #2228, #18415, #110401, #142725, #47756, #1223, #185266, #109410, #3224, #141734, #79066, #20376, #124581, #171089, #96221, #189258, #93236, #63910, #78066, #139734, #82023, #64898, #62901, #126559, #143719, #49733, #50734, #61900, #112393, #174084, #157910, #19400, #125580, #187278, #46758, #81049, #108416, #31586, #154921, #172083, #94233, #155914, #101201, #37543, #55715, #193240, #54713, #40555, #129533, #36533, #21380, #128541, #99207, #146715, #132559, #177084, #178075, #98189, #66880, #102224, #190238, #51715, #113378, #175068, #39542, #115396, #160895, #159892, #161892, #117387, #162891, #24400, #147738, #9225, #116385, #83039, #144714, #86049, #114371, #84037, #70892, #23388, #176075, #194248, #5198, #145716, #38555, #52707, #25409, #85034, #6200, #67880, #69886, #192239, #179086, #191233, #163913, #100212, #22387, #87051, #7197, #68881, #131555, #130541, #53719, #8211, #149727, #120367, #119397, #11228, #58697, #151717, #12232, #89042, #148736, #72902, #105209, #133554, #71884, #28396, #43543, #195245, #106191, #181080, #152691, #73894, #167875, #180093, #134571, #14180, #166896, #56729, #196258, #90035, #13210, #29374, #57727, #91005, #74873, #41561, #136535, #42555, #182060, #104218, #10224, #118399, #103224, #197236, #198216, #44536, #59688, #165899, #27397, #164906, #26400, #135564, #121359, #150732, #183052, #88039, #131200, #179737, #192890, #99860, #52361, #146362, #22035, #149376, #84682, #116040, #117031, #69536, #7849, #10872, #85695, #177729, #129187, #191877, #100854, #41207 ),
 ( #132206, #194890, #54368, #71533, #162536, #39198, #87691, #163551, #147381, #102868, #24040, #98851, #190885, #145365, #8870, #83687, #6847, #164553, #70537, #193897, #55361, #178726, #26046, #40188, #161544, #101868, #25051, #56364, #86694, #148378, #68526, #114018, #133199, #175715, #9873, #118047, #37194, #160546, #130181, #53361, #115038, #176731, #38204, #23037, #60337, #92657, #184687, #136199, #61330, #169508, #75509, #195905, #151379, #73550, #12869, #89693, #154346, #29035, #59342, #72542, #135223, #44194, #123001, #106843, #138183, #91654, #42211, #103871, #119053, #11887, #76507, #104864, #74534, #43197, #196895, #57380, #137182, #199866, #28052, #14844, #105853, #197874, #31008, #168518, #90675, #46171, #121011, #165552, #134219, #88695, #167540, #27049, #150391, #107824, #182709, #152357, #13842, #198870, #180735, #122011, #166553, #183702, #45189, #58362, #30016, #153343, #120029, #181714, #176844, #36299, #5963, #99970, #83796, #97954, #116151, #127314, #67641, #160654, #174834, #147497, #145476, #50499, #81789, #191987, #114131, #54481, #128308, #177842, #37305, #20144, #131314, #39310, #100969, #53474, #113144, #23150, #8988, #159646, #68637, #144479, #21142, #6957, #161654, #98964, #175832, #189025, #190008, #115151, #112163, #173852, #130293, #38315, #51482, #69648, #162654, #84794, #82797, #22146, #146473, #129300, #7965, #193004, #24160, #190996, #66646, #35318, #52472, #85811, #96972, #158653, #143476, #4960, #118160, #181829, #136309, #101986, #87803, #25169, #86811, #90781, #165662, #89806, #40310, #163667, #117147, #9988, #74643, #102981, #149489, #41321, #71648, #194014, #73660, #197984, #26162, #12979, #42322, #72658, #29144, #104976, #88807, #182822, #196017, #148497, #152465, #133315, #103983, #195004, #56482, #121127, #10985, #134333, #27160, #135332, #44304, #57493, #164666, #11997, #119162, #59454, #180845, #105963, #120138, #70656, #167648, #132322, #150500, #166663, #55477, #197005, #58471, #178842, #43308, #179850, #28164, #151488, #1761, #34100, #126104, #77610, #2758, #110927, #16942, #137296, #92769, #14955, #63439, #78596, #198978, #64434, #31121, #172613, #185800, #187800, #45297, #123111, #95758, #140269, #60445, #76615, #125115, #186813, #49269, #46282, #13951, #48283, #106949, #109938, #184796, #171620, #107938, #75617, #17945, #122120, #154459, #108944, #33108, #758, #168622, #183809, #156446, #30122, #169624, #47288, #199974, #94764, #91763, #15951, #153457, #139281, #62429, #138293, #124101, #61439, #170625, #32114, #93771, #79599, #155452, #141268, #177609, #113896, #144245, #39077, #19914, #129063, #7723, #191753, #22912, #80583, #51251, #98729, #84558, #190764, #130053, #50270, #18938, #192764, #142257, #3741, #65418, #127079, #53236, #67408, #112911, #111928, #175594, #69409, #114912, #176606, #99736, #161420, #21912, #96737, #5729, #6723, #66414, #36071, #38080, #37070, #128076, #146236, #157443, #97720, #52239, #4725, #188787, #160423, #173614, #35084, #83563, #145242, #131075, #158426, #54247, #68401, #81556, #115919, #143242, #189779, #174605, #159410, #20905, #82563, #86575, #42090, #117925, #148259, #180617, #135101, #72418, #149262, #100734, #163432, #26929, #23917, #162415, #118932, #150269, #24930, #43076, #74413, #11763, #56244, #134095, #88571, #41087, #195785, #87575, #181599, #9752, #40067, #85571, #71416, #103755, #57258, #179614, #197753, #133080, #194770, #73430, #166434, #132085, #102750, #55243, #116911, #120889, #165434, #178604, #196777, #136079, #58245, #89572, #59220, #27929, #151258, #119913, #104743, #164438, #25932, #182588, #12748, #147257, #8748, #70418, #10754, #193774, #101744, #140027, #76379, #94520, #31875, #93529, #79359, #168394, #75387, #60214, #109701, #199737, #186572, #15712, #46044, #2517, #78353, #62192, #156202, #169378, #13721, #64197, #121884, #77372, #137059, #198749, #17702, #184563, #107699, #139040 ),
 ( #153214, #122875, #16703, #520, #14719, #32870, #44071, #30886, #123856, #91527, #125864, #185554, #167418, #183577, #108705, #92533, #171383, #45062, #141030, #154222, #106720, #48045, #105731, #28914, #170384, #29889, #1516, #90554, #138056, #47048, #61203, #155214, #63193, #124873, #152236, #35836, #187564, #50023, #113660, #110686, #49031, #5488, #36822, #111688, #129815, #161179, #98488, #143005, #159168, #175354, #127835, #20663, #174366, #68163, #173375, #126839, #172366, #34845, #128828, #144007, #4483, #84322, #96500, #158190, #160181, #52991, #18696, #66173, #142015, #3504, #7484, #82317, #65180, #67171, #22675, #190527, #176365, #146001, #114669, #37838, #21671, #83325, #189541, #51013, #69168, #145002, #6483, #99498, #33856, #112674, #19680, #52001, #191514, #81322, #95516, #157202, #80343, #188545, #97482, #164195, #23677, #85325, #181364, #71178, #132842, #102511, #133849, #104508, #194530, #101494, #72175, #86336, #58011, #56001, #119681, #180378, #130835, #42843, #192526, #9512, #165191, #12514, #195539, #57013, #115683, #148023, #162179, #54009, #70179, #118686, #151023, #166189, #117679, #27690, #89331, #41848, #177371, #179376, #131847, #103515, #26686, #38843, #100500, #40838, #147017, #25693, #8502, #193530, #39828, #55004, #88326, #116674, #178364, #150017, #11522, #163183, #24687, #87338, #73192, #149024, #134863, #10512, #196541, #168153, #135848, #78113, #171137, #152973, #169135, #185312, #60962, #28677, #182350, #16464, #47804, #44819, #45808, #59975, #77131, #32626, #76134, #124627, #137812, #106474, #197517, #91282, #167178, #94280, #29650, #122636, #61950, #14472, #199496, #155958, #30640, #184326, #74178, #136820, #107459, #186322, #108462, #139782, #93283, #43828, #105492, #120652, #13484, #1270, #92293, #153977, #15474, #75149, #58985, #138800, #62947, #281, #109454, #123617, #46803, #90312, #170139, #31634, #151998, #154968, #198504, #121642, #183337, #117185, #80109, #64943, #131351, #85845, #48794, #34608, #172129, #33615, #40346, #115187, #95278, #38350, #194051, #192026, #9023, #178879, #147535, #70692, #193039, #69684, #19444, #81092, #102021, #54517, #116189, #132359, #55514, #157953, #141777, #53510, #177878, #49781, #17455, #8000, #39346, #79111, #3271, #110448, #156961, #140784, #111446, #161692, #2273, #176880, #101005, #18458, #63956, #125625, #187323, #126602, #188304, #173133, #162689, #130329, #96267, #142770, #100005, #4251, #24195, #65930, #23187, #84830, #146510, #103019, #150533, #13013, #72693, #42356, #136344, #120172, #134368, #152497, #163704, #104018, #197039, #11020, #183842, #181863, #86848, #118196, #28199, #12033, #90814, #164702, #13985, #73696, #56518, #167682, #75651, #137329, #89841, #149524, #59488, #45331, #196052, #105012, #180881, #57527, #43342, #198019, #135368, #58506, #25206, #26198, #151522, #148533, #10024, #166696, #74677, #87837, #105995, #199010, #121163, #119196, #182856, #44338, #165697, #29178, #60478, #122153, #27195, #88841, #71684, #133350, #195041, #179888, #41355, #138327, #123145, #30155, #793, #48318, #34133, #78631, #79634, #200008, #168655, #142294, #91798, #153492, #14988, #76649, #141303, #16977, #62465, #61474, #63475, #18971, #64471, #126138, #49303, #110961, #171653, #46318, #93806, #156479, #15987, #185837, #2792, #125150, #77645, #95792, #106981, #47324, #140306, #154492, #127114, #186849, #184832, #107973, #33142, #155485, #157479, #169660, #80617, #1797, #31156, #172645, #3774, #65451, #94800, #92805, #187833, #188820, #139314, #109973, #124138, #108980, #17980, #170660, #32148, #98762, #50303, #112945, #176640, #173650, #111960, #68436, #99770, #174638, #192798, #23949, #161455, #5765, #21947, #38116, #190797, #83596, #37103, #131110, #36103, #189813, #35118, #97755, #191788, #6757, #67440, #147290, #159443, #20938, #22946, #115953, #81589, #129097, #4759, #66447, #70450, #145276, #128108 ) ),
 .UNSPECIFIED., .T., .F., .T. ) 
 B_SPLINE_SURFACE_WITH_KNOTS ( ( 4, 3, 4 ),
 ( 3, 2, 2, 2, 2, 2, 2, 2, 2, 2, 2, 2, 2, 2, 2, 2, 2, 2, 2, 2, 2, 2, 2, 2, 2, 2, 2, 2, 2, 2, 2, 2, 2, 2, 2, 2, 2, 2, 2, 2, 2, 2, 2, 2, 2, 2, 2, 2, 2, 2, 2, 2, 2, 2, 2, 2, 2, 2, 2, 2, 2, 2, 2, 2, 2, 2, 2, 2, 2, 2, 2, 2, 2, 2, 2, 2, 2, 2, 2, 2, 2, 2, 2, 2, 2, 2, 2, 2, 2, 2, 2, 2, 2, 2, 2, 2, 2, 2, 2, 2, 2, 2, 2, 2, 2, 2, 2, 2, 2, 2, 2, 2, 2, 2, 2, 2, 2, 2, 2, 2, 2, 2, 2, 2, 2, 2, 2, 2, 2, 2, 2, 2, 2, 2, 2, 2, 2, 2, 2, 2, 2, 2, 2, 2, 2, 2, 2, 2, 2, 2, 2, 2, 2, 2, 2, 2, 2, 2, 2, 2, 2, 2, 2, 2, 2, 2, 2, 2, 2, 2, 2, 2, 2, 2, 2, 2, 2, 2, 2, 2, 2, 2, 2, 2, 2, 2, 2, 2, 2, 2, 2, 2, 2, 2, 2, 2, 2, 2, 2, 2, 2, 2, 2, 2, 2, 2, 2, 2, 2, 2, 2, 2, 2, 2, 2, 2, 2, 2, 2, 2, 2, 2, 2, 2, 2, 2, 2, 2, 3 ),
 ( 0.000000000000000000, 0.5000000000000000000, 1.000000000000000000 ),
 ( 0.000000000000000000, 0.004385964912280701511, 0.008771929824561403022, 0.01315789473684210453, 0.01754385964912280604, 0.02192982456140350755, 0.02631578947368420907, 0.03070175438596491058, 0.03508771929824561209, 0.03947368421052631360, 0.04385964912280701511, 0.04824561403508771662, 0.05263157894736841813, 0.05701754385964911964, 0.06140350877192982115, 0.06578947368421052266, 0.07017543859649122417, 0.07456140350877192569, 0.07894736842105262720, 0.08333333333333332871, 0.08771929824561403022, 0.09210526315789473173, 0.09649122807017543324, 0.1008771929824561348, 0.1052631578947368363, 0.1096491228070175378, 0.1140350877192982393, 0.1184210526315789408, 0.1228070175438596423, 0.1271929824561403577, 0.1315789473684210453, 0.1359649122807017607, 0.1403508771929824483, 0.1447368421052631637, 0.1491228070175438514, 0.1535087719298245668, 0.1578947368421052544, 0.1622807017543859698, 0.1666666666666666574, 0.1710526315789473728, 0.1754385964912280604, 0.1798245614035087758, 0.1842105263157894635, 0.1885964912280701788, 0.1929824561403508665, 0.1973684210526315819, 0.2017543859649122695, 0.2061403508771929849, 0.2105263157894736725, 0.2149122807017543879, 0.2192982456140350755, 0.2236842105263157909, 0.2280701754385964786, 0.2324561403508771940, 0.2368421052631578816, 0.2412280701754385970, 0.2456140350877192846, 0.2500000000000000000, 0.2543859649122807154, 0.2587719298245614308, 0.2631578947368420907, 0.2675438596491228060, 0.2719298245614035214, 0.2763157894736842368, 0.2807017543859648967, 0.2850877192982456121, 0.2894736842105263275, 0.2938596491228070429, 0.2982456140350877027, 0.3026315789473684181, 0.3070175438596491335, 0.3114035087719298489, 0.3157894736842105088, 0.3201754385964912242, 0.3245614035087719396, 0.3289473684210526550, 0.3333333333333333148, 0.3377192982456140302, 0.3421052631578947456, 0.3464912280701754610, 0.3508771929824561209, 0.3552631578947368363, 0.3596491228070175517, 0.3640350877192982670, 0.3684210526315789269, 0.3728070175438596423, 0.3771929824561403577, 0.3815789473684210731, 0.3859649122807017330, 0.3903508771929824483, 0.3947368421052631637, 0.3991228070175438791, 0.4035087719298245390, 0.4078947368421052544, 0.4122807017543859698, 0.4166666666666666852, 0.4210526315789473450, 0.4254385964912280604, 0.4298245614035087758, 0.4342105263157894912, 0.4385964912280701511, 0.4429824561403508665, 0.4473684210526315819, 0.4517543859649122973, 0.4561403508771929571, 0.4605263157894736725, 0.4649122807017543879, 0.4692982456140351033, 0.4736842105263157632, 0.4780701754385964786, 0.4824561403508771940, 0.4868421052631579093, 0.4912280701754385692, 0.4956140350877192846, 0.5000000000000000000, 0.5043859649122807154, 0.5087719298245614308, 0.5131578947368421462, 0.5175438596491228616, 0.5219298245614034659, 0.5263157894736841813, 0.5307017543859648967, 0.5350877192982456121, 0.5394736842105263275, 0.5438596491228070429, 0.5482456140350877583, 0.5526315789473684736, 0.5570175438596490780, 0.5614035087719297934, 0.5657894736842105088, 0.5701754385964912242, 0.5745614035087719396, 0.5789473684210526550, 0.5833333333333333703, 0.5877192982456140857, 0.5921052631578946901, 0.5964912280701754055, 0.6008771929824561209, 0.6052631578947368363, 0.6096491228070175517, 0.6140350877192982670, 0.6184210526315789824, 0.6228070175438596978, 0.6271929824561403022, 0.6315789473684210176, 0.6359649122807017330, 0.6403508771929824483, 0.6447368421052631637, 0.6491228070175438791, 0.6535087719298245945, 0.6578947368421053099, 0.6622807017543859143, 0.6666666666666666297, 0.6710526315789473450, 0.6754385964912280604, 0.6798245614035087758, 0.6842105263157894912, 0.6885964912280702066, 0.6929824561403509220, 0.6973684210526315264, 0.7017543859649122417, 0.7061403508771929571, 0.7105263157894736725, 0.7149122807017543879, 0.7192982456140351033, 0.7236842105263158187, 0.7280701754385965341, 0.7324561403508771384, 0.7368421052631578538, 0.7412280701754385692, 0.7456140350877192846, 0.7500000000000000000, 0.7543859649122807154, 0.7587719298245614308, 0.7631578947368421462, 0.7675438596491228616, 0.7719298245614034659, 0.7763157894736841813, 0.7807017543859648967, 0.7850877192982456121, 0.7894736842105263275, 0.7938596491228070429, 0.7982456140350877583, 0.8026315789473684736, 0.8070175438596490780, 0.8114035087719297934, 0.8157894736842105088, 0.8201754385964912242, 0.8245614035087719396, 0.8289473684210526550, 0.8333333333333333703, 0.8377192982456140857, 0.8421052631578946901, 0.8464912280701754055, 0.8508771929824561209, 0.8552631578947368363, 0.8596491228070175517, 0.8640350877192982670, 0.8684210526315789824, 0.8728070175438596978, 0.8771929824561403022, 0.8815789473684210176, 0.8859649122807017330, 0.8903508771929824483, 0.8947368421052631637, 0.8991228070175438791, 0.9035087719298245945, 0.9078947368421053099, 0.9122807017543859143, 0.9166666666666666297, 0.9210526315789473450, 0.9254385964912280604, 0.9298245614035087758, 0.9342105263157894912, 0.9385964912280702066, 0.9429824561403509220, 0.9473684210526315264, 0.9517543859649122417, 0.9561403508771929571, 0.9605263157894736725, 0.9649122807017543879, 0.9692982456140351033, 0.9736842105263158187, 0.9780701754385965341, 0.9824561403508771384, 0.9868421052631578538, 0.9912280701754385692, 0.9956140350877192846, 1.000000000000000000 ),
 .UNSPECIFIED. ) 
 GEOMETRIC_REPRESENTATION_ITEM ( )  RATIONAL_B_SPLINE_SURFACE ( (
 ( 1.000000000000000000, 0.9659258262890683122, 1.000000000000000000, 0.9659258262890683122, 1.000000000000000000, 0.9659258262890683122, 1.000000000000000000, 0.9659258262890683122, 1.000000000000000000, 0.9659258262890683122, 1.000000000000000000, 0.9659258262890683122, 1.000000000000000000, 0.9659258262890683122, 1.000000000000000000, 0.9659258262890683122, 1.000000000000000000, 0.9659258262890683122, 1.000000000000000000, 0.9659258262890683122, 1.000000000000000000, 0.9659258262890683122, 1.000000000000000000, 0.9659258262890683122, 1.000000000000000000, 0.9659258262890683122, 1.000000000000000000, 0.9659258262890683122, 1.000000000000000000, 0.9659258262890683122, 1.000000000000000000, 0.9659258262890683122, 1.000000000000000000, 0.9659258262890683122, 1.000000000000000000, 0.9659258262890683122, 1.000000000000000000, 0.9659258262890683122, 1.000000000000000000, 0.9659258262890683122, 1.000000000000000000, 0.9659258262890683122, 1.000000000000000000, 0.9659258262890683122, 1.000000000000000000, 0.9659258262890683122, 1.000000000000000000, 0.9659258262890683122, 1.000000000000000000, 0.9659258262890683122, 1.000000000000000000, 0.9659258262890683122, 1.000000000000000000, 0.9659258262890683122, 1.000000000000000000, 0.9659258262890683122, 1.000000000000000000, 0.9659258262890683122, 1.000000000000000000, 0.9659258262890683122, 1.000000000000000000, 0.9659258262890683122, 1.000000000000000000, 0.9659258262890683122, 1.000000000000000000, 0.9659258262890683122, 1.000000000000000000, 0.9659258262890683122, 1.000000000000000000, 0.9659258262890683122, 1.000000000000000000, 0.9659258262890683122, 1.000000000000000000, 0.9659258262890683122, 1.000000000000000000, 0.9659258262890683122, 1.000000000000000000, 0.9659258262890683122, 1.000000000000000000, 0.9659258262890683122, 1.000000000000000000, 0.9659258262890683122, 1.000000000000000000, 0.9659258262890683122, 1.000000000000000000, 0.9659258262890683122, 1.000000000000000000, 0.9659258262890683122, 1.000000000000000000, 0.9659258262890683122, 1.000000000000000000, 0.9659258262890683122, 1.000000000000000000, 0.9659258262890683122, 1.000000000000000000, 0.9659258262890683122, 1.000000000000000000, 0.9659258262890683122, 1.000000000000000000, 0.9659258262890683122, 1.000000000000000000, 0.9659258262890683122, 1.000000000000000000, 0.9659258262890683122, 1.000000000000000000, 0.9659258262890683122, 1.000000000000000000, 0.9659258262890683122, 1.000000000000000000, 0.9659258262890683122, 1.000000000000000000, 0.9659258262890683122, 1.000000000000000000, 0.9659258262890683122, 1.000000000000000000, 0.9659258262890683122, 1.000000000000000000, 0.9659258262890683122, 1.000000000000000000, 0.9659258262890683122, 1.000000000000000000, 0.9659258262890683122, 1.000000000000000000, 0.9659258262890683122, 1.000000000000000000, 0.9659258262890683122, 1.000000000000000000, 0.9659258262890683122, 1.000000000000000000, 0.9659258262890683122, 1.000000000000000000, 0.9659258262890683122, 1.000000000000000000, 0.9659258262890683122, 1.000000000000000000, 0.9659258262890683122, 1.000000000000000000, 0.9659258262890683122, 1.000000000000000000, 0.9659258262890683122, 1.000000000000000000, 0.9659258262890683122, 1.000000000000000000, 0.9659258262890683122, 1.000000000000000000, 0.9659258262890683122, 1.000000000000000000, 0.9659258262890683122, 1.000000000000000000, 0.9659258262890683122, 1.000000000000000000, 0.9659258262890683122, 1.000000000000000000, 0.9659258262890683122, 1.000000000000000000, 0.9659258262890683122, 1.000000000000000000, 0.9659258262890683122, 1.000000000000000000, 0.9659258262890683122, 1.000000000000000000, 0.9659258262890683122, 1.000000000000000000, 0.9659258262890683122, 1.000000000000000000, 0.9659258262890683122, 1.000000000000000000, 0.9659258262890683122, 1.000000000000000000, 0.9659258262890683122, 1.000000000000000000, 0.9659258262890683122, 1.000000000000000000, 0.9659258262890683122, 1.000000000000000000, 0.9659258262890683122, 1.000000000000000000, 0.9659258262890683122, 1.000000000000000000, 0.9659258262890683122, 1.000000000000000000, 0.9659258262890683122, 1.000000000000000000, 0.9659258262890683122, 1.000000000000000000, 0.9659258262890683122, 1.000000000000000000, 0.9659258262890683122, 1.000000000000000000, 0.9659258262890683122, 1.000000000000000000, 0.9659258262890683122, 1.000000000000000000, 0.9659258262890683122, 1.000000000000000000, 0.9659258262890683122, 1.000000000000000000, 0.9659258262890683122, 1.000000000000000000, 0.9659258262890683122, 1.000000000000000000, 0.9659258262890683122, 1.000000000000000000, 0.9659258262890683122, 1.000000000000000000, 0.9659258262890683122, 1.000000000000000000, 0.9659258262890683122, 1.000000000000000000, 0.9659258262890683122, 1.000000000000000000, 0.9659258262890683122, 1.000000000000000000, 0.9659258262890683122, 1.000000000000000000, 0.9659258262890683122, 1.000000000000000000, 0.9659258262890683122, 1.000000000000000000, 0.9659258262890683122, 1.000000000000000000, 0.9659258262890683122, 1.000000000000000000, 0.9659258262890683122, 1.000000000000000000, 0.9659258262890683122, 1.000000000000000000, 0.9659258262890683122, 1.000000000000000000, 0.9659258262890683122, 1.000000000000000000, 0.9659258262890683122, 1.000000000000000000, 0.9659258262890683122, 1.000000000000000000, 0.9659258262890683122, 1.000000000000000000, 0.9659258262890683122, 1.000000000000000000, 0.9659258262890683122, 1.000000000000000000, 0.9659258262890683122, 1.000000000000000000, 0.9659258262890683122, 1.000000000000000000, 0.9659258262890683122, 1.000000000000000000, 0.9659258262890683122, 1.000000000000000000, 0.9659258262890683122, 1.000000000000000000, 0.9659258262890683122, 1.000000000000000000, 0.9659258262890683122, 1.000000000000000000, 0.9659258262890683122, 1.000000000000000000, 0.9659258262890683122, 1.000000000000000000, 0.9659258262890683122, 1.000000000000000000, 0.9659258262890683122, 1.000000000000000000, 0.9659258262890683122, 1.000000000000000000, 0.9659258262890683122, 1.000000000000000000, 0.9659258262890683122, 1.000000000000000000, 0.9659258262890683122, 1.000000000000000000, 0.9659258262890683122, 1.000000000000000000, 0.9659258262890683122, 1.000000000000000000, 0.9659258262890683122, 1.000000000000000000, 0.9659258262890683122, 1.000000000000000000, 0.9659258262890683122, 1.000000000000000000, 0.9659258262890683122, 1.000000000000000000, 0.9659258262890683122, 1.000000000000000000, 0.9659258262890683122, 1.000000000000000000, 0.9659258262890683122, 1.000000000000000000, 0.9659258262890683122, 1.000000000000000000, 0.9659258262890683122, 1.000000000000000000, 0.9659258262890683122, 1.000000000000000000, 0.9659258262890683122, 1.000000000000000000, 0.9659258262890683122, 1.000000000000000000, 0.9659258262890683122, 1.000000000000000000, 0.9659258262890683122, 1.000000000000000000, 0.9659258262890683122, 1.000000000000000000, 0.9659258262890683122, 1.000000000000000000, 0.9659258262890683122, 1.000000000000000000, 0.9659258262890683122, 1.000000000000000000, 0.9659258262890683122, 1.000000000000000000, 0.9659258262890683122, 1.000000000000000000, 0.9659258262890683122, 1.000000000000000000, 0.9659258262890683122, 1.000000000000000000, 0.9659258262890683122, 1.000000000000000000, 0.9659258262890683122, 1.000000000000000000, 0.9659258262890683122, 1.000000000000000000, 0.9659258262890683122, 1.000000000000000000, 0.9659258262890683122, 1.000000000000000000, 0.9659258262890683122, 1.000000000000000000, 0.9659258262890683122, 1.000000000000000000, 0.9659258262890683122, 1.000000000000000000, 0.9659258262890683122, 1.000000000000000000, 0.9659258262890683122, 1.000000000000000000, 0.9659258262890683122, 1.000000000000000000, 0.9659258262890683122, 1.000000000000000000, 0.9659258262890683122, 1.000000000000000000, 0.9659258262890683122, 1.000000000000000000, 0.9659258262890683122, 1.000000000000000000, 0.9659258262890683122, 1.000000000000000000, 0.9659258262890683122, 1.000000000000000000, 0.9659258262890683122, 1.000000000000000000, 0.9659258262890683122, 1.000000000000000000, 0.9659258262890683122, 1.000000000000000000, 0.9659258262890683122, 1.000000000000000000, 0.9659258262890683122, 1.000000000000000000, 0.9659258262890683122, 1.000000000000000000, 0.9659258262890683122, 1.000000000000000000, 0.9659258262890683122, 1.000000000000000000, 0.9659258262890683122, 1.000000000000000000, 0.9659258262890683122, 1.000000000000000000, 0.9659258262890683122, 1.000000000000000000, 0.9659258262890683122, 1.000000000000000000, 0.9659258262890683122, 1.000000000000000000, 0.9659258262890683122, 1.000000000000000000, 0.9659258262890683122, 1.000000000000000000, 0.9659258262890683122, 1.000000000000000000, 0.9659258262890683122, 1.000000000000000000, 0.9659258262890683122, 1.000000000000000000, 0.9659258262890683122, 1.000000000000000000, 0.9659258262890683122, 1.000000000000000000, 0.9659258262890683122, 1.000000000000000000, 0.9659258262890683122, 1.000000000000000000, 0.9659258262890683122, 1.000000000000000000, 0.9659258262890683122, 1.000000000000000000, 0.9659258262890683122, 1.000000000000000000, 0.9659258262890683122, 1.000000000000000000, 0.9659258262890683122, 1.000000000000000000, 0.9659258262890683122, 1.000000000000000000, 0.9659258262890683122, 1.000000000000000000, 0.9659258262890683122, 1.000000000000000000, 0.9659258262890683122, 1.000000000000000000, 0.9659258262890683122, 1.000000000000000000, 0.9659258262890683122, 1.000000000000000000, 0.9659258262890683122, 1.000000000000000000, 0.9659258262890683122, 1.000000000000000000, 0.9659258262890683122, 1.000000000000000000, 0.9659258262890683122, 1.000000000000000000, 0.9659258262890683122, 1.000000000000000000, 0.9659258262890683122, 1.000000000000000000, 0.9659258262890683122, 1.000000000000000000, 0.9659258262890683122, 1.000000000000000000, 0.9659258262890683122, 1.000000000000000000, 0.9659258262890683122, 1.000000000000000000, 0.9659258262890683122, 1.000000000000000000, 0.9659258262890683122, 1.000000000000000000, 0.9659258262890683122, 1.000000000000000000, 0.9659258262890683122, 1.000000000000000000, 0.9659258262890683122, 1.000000000000000000, 0.9659258262890683122, 1.000000000000000000, 0.9659258262890683122, 1.000000000000000000, 0.9659258262890683122, 1.000000000000000000, 0.9659258262890683122, 1.000000000000000000),
 ( 0.3333333333333333703, 0.3219752754296894559, 0.3333333333333333703, 0.3219752754296894559, 0.3333333333333333703, 0.3219752754296894559, 0.3333333333333333703, 0.3219752754296894559, 0.3333333333333333703, 0.3219752754296894559, 0.3333333333333333703, 0.3219752754296894559, 0.3333333333333333703, 0.3219752754296894559, 0.3333333333333333703, 0.3219752754296894559, 0.3333333333333333703, 0.3219752754296894559, 0.3333333333333333703, 0.3219752754296894559, 0.3333333333333333703, 0.3219752754296894559, 0.3333333333333333703, 0.3219752754296894559, 0.3333333333333333703, 0.3219752754296894559, 0.3333333333333333703, 0.3219752754296894559, 0.3333333333333333703, 0.3219752754296894559, 0.3333333333333333703, 0.3219752754296894559, 0.3333333333333333703, 0.3219752754296894559, 0.3333333333333333703, 0.3219752754296894559, 0.3333333333333333703, 0.3219752754296894559, 0.3333333333333333703, 0.3219752754296894559, 0.3333333333333333703, 0.3219752754296894559, 0.3333333333333333703, 0.3219752754296894559, 0.3333333333333333703, 0.3219752754296894559, 0.3333333333333333703, 0.3219752754296894559, 0.3333333333333333703, 0.3219752754296894559, 0.3333333333333333703, 0.3219752754296894559, 0.3333333333333333703, 0.3219752754296894559, 0.3333333333333333703, 0.3219752754296894559, 0.3333333333333333703, 0.3219752754296894559, 0.3333333333333333703, 0.3219752754296894559, 0.3333333333333333703, 0.3219752754296894559, 0.3333333333333333703, 0.3219752754296894559, 0.3333333333333333703, 0.3219752754296894559, 0.3333333333333333703, 0.3219752754296894559, 0.3333333333333333703, 0.3219752754296894559, 0.3333333333333333703, 0.3219752754296894559, 0.3333333333333333703, 0.3219752754296894559, 0.3333333333333333703, 0.3219752754296894559, 0.3333333333333333703, 0.3219752754296894559, 0.3333333333333333703, 0.3219752754296894559, 0.3333333333333333703, 0.3219752754296894559, 0.3333333333333333703, 0.3219752754296894559, 0.3333333333333333703, 0.3219752754296894559, 0.3333333333333333703, 0.3219752754296894559, 0.3333333333333333703, 0.3219752754296894559, 0.3333333333333333703, 0.3219752754296894559, 0.3333333333333333703, 0.3219752754296894559, 0.3333333333333333703, 0.3219752754296894559, 0.3333333333333333703, 0.3219752754296894559, 0.3333333333333333703, 0.3219752754296894559, 0.3333333333333333703, 0.3219752754296894559, 0.3333333333333333703, 0.3219752754296894559, 0.3333333333333333703, 0.3219752754296894559, 0.3333333333333333703, 0.3219752754296894559, 0.3333333333333333703, 0.3219752754296894559, 0.3333333333333333703, 0.3219752754296894559, 0.3333333333333333703, 0.3219752754296894559, 0.3333333333333333703, 0.3219752754296894559, 0.3333333333333333703, 0.3219752754296894559, 0.3333333333333333703, 0.3219752754296894559, 0.3333333333333333703, 0.3219752754296894559, 0.3333333333333333703, 0.3219752754296894559, 0.3333333333333333703, 0.3219752754296894559, 0.3333333333333333703, 0.3219752754296894559, 0.3333333333333333703, 0.3219752754296894559, 0.3333333333333333703, 0.3219752754296894559, 0.3333333333333333703, 0.3219752754296894559, 0.3333333333333333703, 0.3219752754296894559, 0.3333333333333333703, 0.3219752754296894559, 0.3333333333333333703, 0.3219752754296894559, 0.3333333333333333703, 0.3219752754296894559, 0.3333333333333333703, 0.3219752754296894559, 0.3333333333333333703, 0.3219752754296894559, 0.3333333333333333703, 0.3219752754296894559, 0.3333333333333333703, 0.3219752754296894559, 0.3333333333333333703, 0.3219752754296894559, 0.3333333333333333703, 0.3219752754296894559, 0.3333333333333333703, 0.3219752754296894559, 0.3333333333333333703, 0.3219752754296894559, 0.3333333333333333703, 0.3219752754296894559, 0.3333333333333333703, 0.3219752754296894559, 0.3333333333333333703, 0.3219752754296894559, 0.3333333333333333703, 0.3219752754296894559, 0.3333333333333333703, 0.3219752754296894559, 0.3333333333333333703, 0.3219752754296894559, 0.3333333333333333703, 0.3219752754296894559, 0.3333333333333333703, 0.3219752754296894559, 0.3333333333333333703, 0.3219752754296894559, 0.3333333333333333703, 0.3219752754296894559, 0.3333333333333333703, 0.3219752754296894559, 0.3333333333333333703, 0.3219752754296894559, 0.3333333333333333703, 0.3219752754296894559, 0.3333333333333333703, 0.3219752754296894559, 0.3333333333333333703, 0.3219752754296894559, 0.3333333333333333703, 0.3219752754296894559, 0.3333333333333333703, 0.3219752754296894559, 0.3333333333333333703, 0.3219752754296894559, 0.3333333333333333703, 0.3219752754296894559, 0.3333333333333333703, 0.3219752754296894559, 0.3333333333333333703, 0.3219752754296894559, 0.3333333333333333703, 0.3219752754296894559, 0.3333333333333333703, 0.3219752754296894559, 0.3333333333333333703, 0.3219752754296894559, 0.3333333333333333703, 0.3219752754296894559, 0.3333333333333333703, 0.3219752754296894559, 0.3333333333333333703, 0.3219752754296894559, 0.3333333333333333703, 0.3219752754296894559, 0.3333333333333333703, 0.3219752754296894559, 0.3333333333333333703, 0.3219752754296894559, 0.3333333333333333703, 0.3219752754296894559, 0.3333333333333333703, 0.3219752754296894559, 0.3333333333333333703, 0.3219752754296894559, 0.3333333333333333703, 0.3219752754296894559, 0.3333333333333333703, 0.3219752754296894559, 0.3333333333333333703, 0.3219752754296894559, 0.3333333333333333703, 0.3219752754296894559, 0.3333333333333333703, 0.3219752754296894559, 0.3333333333333333703, 0.3219752754296894559, 0.3333333333333333703, 0.3219752754296894559, 0.3333333333333333703, 0.3219752754296894559, 0.3333333333333333703, 0.3219752754296894559, 0.3333333333333333703, 0.3219752754296894559, 0.3333333333333333703, 0.3219752754296894559, 0.3333333333333333703, 0.3219752754296894559, 0.3333333333333333703, 0.3219752754296894559, 0.3333333333333333703, 0.3219752754296894559, 0.3333333333333333703, 0.3219752754296894559, 0.3333333333333333703, 0.3219752754296894559, 0.3333333333333333703, 0.3219752754296894559, 0.3333333333333333703, 0.3219752754296894559, 0.3333333333333333703, 0.3219752754296894559, 0.3333333333333333703, 0.3219752754296894559, 0.3333333333333333703, 0.3219752754296894559, 0.3333333333333333703, 0.3219752754296894559, 0.3333333333333333703, 0.3219752754296894559, 0.3333333333333333703, 0.3219752754296894559, 0.3333333333333333703, 0.3219752754296894559, 0.3333333333333333703, 0.3219752754296894559, 0.3333333333333333703, 0.3219752754296894559, 0.3333333333333333703, 0.3219752754296894559, 0.3333333333333333703, 0.3219752754296894559, 0.3333333333333333703, 0.3219752754296894559, 0.3333333333333333703, 0.3219752754296894559, 0.3333333333333333703, 0.3219752754296894559, 0.3333333333333333703, 0.3219752754296894559, 0.3333333333333333703, 0.3219752754296894559, 0.3333333333333333703, 0.3219752754296894559, 0.3333333333333333703, 0.3219752754296894559, 0.3333333333333333703, 0.3219752754296894559, 0.3333333333333333703, 0.3219752754296894559, 0.3333333333333333703, 0.3219752754296894559, 0.3333333333333333703, 0.3219752754296894559, 0.3333333333333333703, 0.3219752754296894559, 0.3333333333333333703, 0.3219752754296894559, 0.3333333333333333703, 0.3219752754296894559, 0.3333333333333333703, 0.3219752754296894559, 0.3333333333333333703, 0.3219752754296894559, 0.3333333333333333703, 0.3219752754296894559, 0.3333333333333333703, 0.3219752754296894559, 0.3333333333333333703, 0.3219752754296894559, 0.3333333333333333703, 0.3219752754296894559, 0.3333333333333333703, 0.3219752754296894559, 0.3333333333333333703, 0.3219752754296894559, 0.3333333333333333703, 0.3219752754296894559, 0.3333333333333333703, 0.3219752754296894559, 0.3333333333333333703, 0.3219752754296894559, 0.3333333333333333703, 0.3219752754296894559, 0.3333333333333333703, 0.3219752754296894559, 0.3333333333333333703, 0.3219752754296894559, 0.3333333333333333703, 0.3219752754296894559, 0.3333333333333333703, 0.3219752754296894559, 0.3333333333333333703, 0.3219752754296894559, 0.3333333333333333703, 0.3219752754296894559, 0.3333333333333333703, 0.3219752754296894559, 0.3333333333333333703, 0.3219752754296894559, 0.3333333333333333703, 0.3219752754296894559, 0.3333333333333333703, 0.3219752754296894559, 0.3333333333333333703, 0.3219752754296894559, 0.3333333333333333703, 0.3219752754296894559, 0.3333333333333333703, 0.3219752754296894559, 0.3333333333333333703, 0.3219752754296894559, 0.3333333333333333703, 0.3219752754296894559, 0.3333333333333333703, 0.3219752754296894559, 0.3333333333333333703, 0.3219752754296894559, 0.3333333333333333703, 0.3219752754296894559, 0.3333333333333333703, 0.3219752754296894559, 0.3333333333333333703, 0.3219752754296894559, 0.3333333333333333703, 0.3219752754296894559, 0.3333333333333333703, 0.3219752754296894559, 0.3333333333333333703, 0.3219752754296894559, 0.3333333333333333703, 0.3219752754296894559, 0.3333333333333333703, 0.3219752754296894559, 0.3333333333333333703, 0.3219752754296894559, 0.3333333333333333703, 0.3219752754296894559, 0.3333333333333333703, 0.3219752754296894559, 0.3333333333333333703, 0.3219752754296894559, 0.3333333333333333703, 0.3219752754296894559, 0.3333333333333333703, 0.3219752754296894559, 0.3333333333333333703, 0.3219752754296894559, 0.3333333333333333703, 0.3219752754296894559, 0.3333333333333333703, 0.3219752754296894559, 0.3333333333333333703, 0.3219752754296894559, 0.3333333333333333703, 0.3219752754296894559, 0.3333333333333333703, 0.3219752754296894559, 0.3333333333333333703, 0.3219752754296894559, 0.3333333333333333703, 0.3219752754296894559, 0.3333333333333333703, 0.3219752754296894559, 0.3333333333333333703, 0.3219752754296894559, 0.3333333333333333703, 0.3219752754296894559, 0.3333333333333333703, 0.3219752754296894559, 0.3333333333333333703, 0.3219752754296894559, 0.3333333333333333703, 0.3219752754296894559, 0.3333333333333333703, 0.3219752754296894559, 0.3333333333333333703, 0.3219752754296894559, 0.3333333333333333703, 0.3219752754296894559, 0.3333333333333333703, 0.3219752754296894559, 0.3333333333333333703, 0.3219752754296894559, 0.3333333333333333703, 0.3219752754296894559, 0.3333333333333333703, 0.3219752754296894559, 0.3333333333333333703, 0.3219752754296894559, 0.3333333333333333703, 0.3219752754296894559, 0.3333333333333333703, 0.3219752754296894559, 0.3333333333333333703, 0.3219752754296894559, 0.3333333333333333703, 0.3219752754296894559, 0.3333333333333333703, 0.3219752754296894559, 0.3333333333333333703, 0.3219752754296894559, 0.3333333333333333703, 0.3219752754296894559, 0.3333333333333333703, 0.3219752754296894559, 0.3333333333333333703),
 ( 0.3333333333333333703, 0.3219752754296894559, 0.3333333333333333703, 0.3219752754296894559, 0.3333333333333333703, 0.3219752754296894559, 0.3333333333333333703, 0.3219752754296894559, 0.3333333333333333703, 0.3219752754296894559, 0.3333333333333333703, 0.3219752754296894559, 0.3333333333333333703, 0.3219752754296894559, 0.3333333333333333703, 0.3219752754296894559, 0.3333333333333333703, 0.3219752754296894559, 0.3333333333333333703, 0.3219752754296894559, 0.3333333333333333703, 0.3219752754296894559, 0.3333333333333333703, 0.3219752754296894559, 0.3333333333333333703, 0.3219752754296894559, 0.3333333333333333703, 0.3219752754296894559, 0.3333333333333333703, 0.3219752754296894559, 0.3333333333333333703, 0.3219752754296894559, 0.3333333333333333703, 0.3219752754296894559, 0.3333333333333333703, 0.3219752754296894559, 0.3333333333333333703, 0.3219752754296894559, 0.3333333333333333703, 0.3219752754296894559, 0.3333333333333333703, 0.3219752754296894559, 0.3333333333333333703, 0.3219752754296894559, 0.3333333333333333703, 0.3219752754296894559, 0.3333333333333333703, 0.3219752754296894559, 0.3333333333333333703, 0.3219752754296894559, 0.3333333333333333703, 0.3219752754296894559, 0.3333333333333333703, 0.3219752754296894559, 0.3333333333333333703, 0.3219752754296894559, 0.3333333333333333703, 0.3219752754296894559, 0.3333333333333333703, 0.3219752754296894559, 0.3333333333333333703, 0.3219752754296894559, 0.3333333333333333703, 0.3219752754296894559, 0.3333333333333333703, 0.3219752754296894559, 0.3333333333333333703, 0.3219752754296894559, 0.3333333333333333703, 0.3219752754296894559, 0.3333333333333333703, 0.3219752754296894559, 0.3333333333333333703, 0.3219752754296894559, 0.3333333333333333703, 0.3219752754296894559, 0.3333333333333333703, 0.3219752754296894559, 0.3333333333333333703, 0.3219752754296894559, 0.3333333333333333703, 0.3219752754296894559, 0.3333333333333333703, 0.3219752754296894559, 0.3333333333333333703, 0.3219752754296894559, 0.3333333333333333703, 0.3219752754296894559, 0.3333333333333333703, 0.3219752754296894559, 0.3333333333333333703, 0.3219752754296894559, 0.3333333333333333703, 0.3219752754296894559, 0.3333333333333333703, 0.3219752754296894559, 0.3333333333333333703, 0.3219752754296894559, 0.3333333333333333703, 0.3219752754296894559, 0.3333333333333333703, 0.3219752754296894559, 0.3333333333333333703, 0.3219752754296894559, 0.3333333333333333703, 0.3219752754296894559, 0.3333333333333333703, 0.3219752754296894559, 0.3333333333333333703, 0.3219752754296894559, 0.3333333333333333703, 0.3219752754296894559, 0.3333333333333333703, 0.3219752754296894559, 0.3333333333333333703, 0.3219752754296894559, 0.3333333333333333703, 0.3219752754296894559, 0.3333333333333333703, 0.3219752754296894559, 0.3333333333333333703, 0.3219752754296894559, 0.3333333333333333703, 0.3219752754296894559, 0.3333333333333333703, 0.3219752754296894559, 0.3333333333333333703, 0.3219752754296894559, 0.3333333333333333703, 0.3219752754296894559, 0.3333333333333333703, 0.3219752754296894559, 0.3333333333333333703, 0.3219752754296894559, 0.3333333333333333703, 0.3219752754296894559, 0.3333333333333333703, 0.3219752754296894559, 0.3333333333333333703, 0.3219752754296894559, 0.3333333333333333703, 0.3219752754296894559, 0.3333333333333333703, 0.3219752754296894559, 0.3333333333333333703, 0.3219752754296894559, 0.3333333333333333703, 0.3219752754296894559, 0.3333333333333333703, 0.3219752754296894559, 0.3333333333333333703, 0.3219752754296894559, 0.3333333333333333703, 0.3219752754296894559, 0.3333333333333333703, 0.3219752754296894559, 0.3333333333333333703, 0.3219752754296894559, 0.3333333333333333703, 0.3219752754296894559, 0.3333333333333333703, 0.3219752754296894559, 0.3333333333333333703, 0.3219752754296894559, 0.3333333333333333703, 0.3219752754296894559, 0.3333333333333333703, 0.3219752754296894559, 0.3333333333333333703, 0.3219752754296894559, 0.3333333333333333703, 0.3219752754296894559, 0.3333333333333333703, 0.3219752754296894559, 0.3333333333333333703, 0.3219752754296894559, 0.3333333333333333703, 0.3219752754296894559, 0.3333333333333333703, 0.3219752754296894559, 0.3333333333333333703, 0.3219752754296894559, 0.3333333333333333703, 0.3219752754296894559, 0.3333333333333333703, 0.3219752754296894559, 0.3333333333333333703, 0.3219752754296894559, 0.3333333333333333703, 0.3219752754296894559, 0.3333333333333333703, 0.3219752754296894559, 0.3333333333333333703, 0.3219752754296894559, 0.3333333333333333703, 0.3219752754296894559, 0.3333333333333333703, 0.3219752754296894559, 0.3333333333333333703, 0.3219752754296894559, 0.3333333333333333703, 0.3219752754296894559, 0.3333333333333333703, 0.3219752754296894559, 0.3333333333333333703, 0.3219752754296894559, 0.3333333333333333703, 0.3219752754296894559, 0.3333333333333333703, 0.3219752754296894559, 0.3333333333333333703, 0.3219752754296894559, 0.3333333333333333703, 0.3219752754296894559, 0.3333333333333333703, 0.3219752754296894559, 0.3333333333333333703, 0.3219752754296894559, 0.3333333333333333703, 0.3219752754296894559, 0.3333333333333333703, 0.3219752754296894559, 0.3333333333333333703, 0.3219752754296894559, 0.3333333333333333703, 0.3219752754296894559, 0.3333333333333333703, 0.3219752754296894559, 0.3333333333333333703, 0.3219752754296894559, 0.3333333333333333703, 0.3219752754296894559, 0.3333333333333333703, 0.3219752754296894559, 0.3333333333333333703, 0.3219752754296894559, 0.3333333333333333703, 0.3219752754296894559, 0.3333333333333333703, 0.3219752754296894559, 0.3333333333333333703, 0.3219752754296894559, 0.3333333333333333703, 0.3219752754296894559, 0.3333333333333333703, 0.3219752754296894559, 0.3333333333333333703, 0.3219752754296894559, 0.3333333333333333703, 0.3219752754296894559, 0.3333333333333333703, 0.3219752754296894559, 0.3333333333333333703, 0.3219752754296894559, 0.3333333333333333703, 0.3219752754296894559, 0.3333333333333333703, 0.3219752754296894559, 0.3333333333333333703, 0.3219752754296894559, 0.3333333333333333703, 0.3219752754296894559, 0.3333333333333333703, 0.3219752754296894559, 0.3333333333333333703, 0.3219752754296894559, 0.3333333333333333703, 0.3219752754296894559, 0.3333333333333333703, 0.3219752754296894559, 0.3333333333333333703, 0.3219752754296894559, 0.3333333333333333703, 0.3219752754296894559, 0.3333333333333333703, 0.3219752754296894559, 0.3333333333333333703, 0.3219752754296894559, 0.3333333333333333703, 0.3219752754296894559, 0.3333333333333333703, 0.3219752754296894559, 0.3333333333333333703, 0.3219752754296894559, 0.3333333333333333703, 0.3219752754296894559, 0.3333333333333333703, 0.3219752754296894559, 0.3333333333333333703, 0.3219752754296894559, 0.3333333333333333703, 0.3219752754296894559, 0.3333333333333333703, 0.3219752754296894559, 0.3333333333333333703, 0.3219752754296894559, 0.3333333333333333703, 0.3219752754296894559, 0.3333333333333333703, 0.3219752754296894559, 0.3333333333333333703, 0.3219752754296894559, 0.3333333333333333703, 0.3219752754296894559, 0.3333333333333333703, 0.3219752754296894559, 0.3333333333333333703, 0.3219752754296894559, 0.3333333333333333703, 0.3219752754296894559, 0.3333333333333333703, 0.3219752754296894559, 0.3333333333333333703, 0.3219752754296894559, 0.3333333333333333703, 0.3219752754296894559, 0.3333333333333333703, 0.3219752754296894559, 0.3333333333333333703, 0.3219752754296894559, 0.3333333333333333703, 0.3219752754296894559, 0.3333333333333333703, 0.3219752754296894559, 0.3333333333333333703, 0.3219752754296894559, 0.3333333333333333703, 0.3219752754296894559, 0.3333333333333333703, 0.3219752754296894559, 0.3333333333333333703, 0.3219752754296894559, 0.3333333333333333703, 0.3219752754296894559, 0.3333333333333333703, 0.3219752754296894559, 0.3333333333333333703, 0.3219752754296894559, 0.3333333333333333703, 0.3219752754296894559, 0.3333333333333333703, 0.3219752754296894559, 0.3333333333333333703, 0.3219752754296894559, 0.3333333333333333703, 0.3219752754296894559, 0.3333333333333333703, 0.3219752754296894559, 0.3333333333333333703, 0.3219752754296894559, 0.3333333333333333703, 0.3219752754296894559, 0.3333333333333333703, 0.3219752754296894559, 0.3333333333333333703, 0.3219752754296894559, 0.3333333333333333703, 0.3219752754296894559, 0.3333333333333333703, 0.3219752754296894559, 0.3333333333333333703, 0.3219752754296894559, 0.3333333333333333703, 0.3219752754296894559, 0.3333333333333333703, 0.3219752754296894559, 0.3333333333333333703, 0.3219752754296894559, 0.3333333333333333703, 0.3219752754296894559, 0.3333333333333333703, 0.3219752754296894559, 0.3333333333333333703, 0.3219752754296894559, 0.3333333333333333703, 0.3219752754296894559, 0.3333333333333333703, 0.3219752754296894559, 0.3333333333333333703, 0.3219752754296894559, 0.3333333333333333703, 0.3219752754296894559, 0.3333333333333333703, 0.3219752754296894559, 0.3333333333333333703, 0.3219752754296894559, 0.3333333333333333703, 0.3219752754296894559, 0.3333333333333333703, 0.3219752754296894559, 0.3333333333333333703, 0.3219752754296894559, 0.3333333333333333703, 0.3219752754296894559, 0.3333333333333333703, 0.3219752754296894559, 0.3333333333333333703, 0.3219752754296894559, 0.3333333333333333703, 0.3219752754296894559, 0.3333333333333333703, 0.3219752754296894559, 0.3333333333333333703, 0.3219752754296894559, 0.3333333333333333703, 0.3219752754296894559, 0.3333333333333333703, 0.3219752754296894559, 0.3333333333333333703, 0.3219752754296894559, 0.3333333333333333703, 0.3219752754296894559, 0.3333333333333333703, 0.3219752754296894559, 0.3333333333333333703, 0.3219752754296894559, 0.3333333333333333703, 0.3219752754296894559, 0.3333333333333333703, 0.3219752754296894559, 0.3333333333333333703, 0.3219752754296894559, 0.3333333333333333703, 0.3219752754296894559, 0.3333333333333333703, 0.3219752754296894559, 0.3333333333333333703, 0.3219752754296894559, 0.3333333333333333703, 0.3219752754296894559, 0.3333333333333333703, 0.3219752754296894559, 0.3333333333333333703, 0.3219752754296894559, 0.3333333333333333703, 0.3219752754296894559, 0.3333333333333333703, 0.3219752754296894559, 0.3333333333333333703, 0.3219752754296894559, 0.3333333333333333703, 0.3219752754296894559, 0.3333333333333333703, 0.3219752754296894559, 0.3333333333333333703, 0.3219752754296894559, 0.3333333333333333703, 0.3219752754296894559, 0.3333333333333333703, 0.3219752754296894559, 0.3333333333333333703, 0.3219752754296894559, 0.3333333333333333703, 0.3219752754296894559, 0.3333333333333333703, 0.3219752754296894559, 0.3333333333333333703),
 ( 1.000000000000000000, 0.9659258262890683122, 1.000000000000000000, 0.9659258262890683122, 1.000000000000000000, 0.9659258262890683122, 1.000000000000000000, 0.9659258262890683122, 1.000000000000000000, 0.9659258262890683122, 1.000000000000000000, 0.9659258262890683122, 1.000000000000000000, 0.9659258262890683122, 1.000000000000000000, 0.9659258262890683122, 1.000000000000000000, 0.9659258262890683122, 1.000000000000000000, 0.9659258262890683122, 1.000000000000000000, 0.9659258262890683122, 1.000000000000000000, 0.9659258262890683122, 1.000000000000000000, 0.9659258262890683122, 1.000000000000000000, 0.9659258262890683122, 1.000000000000000000, 0.9659258262890683122, 1.000000000000000000, 0.9659258262890683122, 1.000000000000000000, 0.9659258262890683122, 1.000000000000000000, 0.9659258262890683122, 1.000000000000000000, 0.9659258262890683122, 1.000000000000000000, 0.9659258262890683122, 1.000000000000000000, 0.9659258262890683122, 1.000000000000000000, 0.9659258262890683122, 1.000000000000000000, 0.9659258262890683122, 1.000000000000000000, 0.9659258262890683122, 1.000000000000000000, 0.9659258262890683122, 1.000000000000000000, 0.9659258262890683122, 1.000000000000000000, 0.9659258262890683122, 1.000000000000000000, 0.9659258262890683122, 1.000000000000000000, 0.9659258262890683122, 1.000000000000000000, 0.9659258262890683122, 1.000000000000000000, 0.9659258262890683122, 1.000000000000000000, 0.9659258262890683122, 1.000000000000000000, 0.9659258262890683122, 1.000000000000000000, 0.9659258262890683122, 1.000000000000000000, 0.9659258262890683122, 1.000000000000000000, 0.9659258262890683122, 1.000000000000000000, 0.9659258262890683122, 1.000000000000000000, 0.9659258262890683122, 1.000000000000000000, 0.9659258262890683122, 1.000000000000000000, 0.9659258262890683122, 1.000000000000000000, 0.9659258262890683122, 1.000000000000000000, 0.9659258262890683122, 1.000000000000000000, 0.9659258262890683122, 1.000000000000000000, 0.9659258262890683122, 1.000000000000000000, 0.9659258262890683122, 1.000000000000000000, 0.9659258262890683122, 1.000000000000000000, 0.9659258262890683122, 1.000000000000000000, 0.9659258262890683122, 1.000000000000000000, 0.9659258262890683122, 1.000000000000000000, 0.9659258262890683122, 1.000000000000000000, 0.9659258262890683122, 1.000000000000000000, 0.9659258262890683122, 1.000000000000000000, 0.9659258262890683122, 1.000000000000000000, 0.9659258262890683122, 1.000000000000000000, 0.9659258262890683122, 1.000000000000000000, 0.9659258262890683122, 1.000000000000000000, 0.9659258262890683122, 1.000000000000000000, 0.9659258262890683122, 1.000000000000000000, 0.9659258262890683122, 1.000000000000000000, 0.9659258262890683122, 1.000000000000000000, 0.9659258262890683122, 1.000000000000000000, 0.9659258262890683122, 1.000000000000000000, 0.9659258262890683122, 1.000000000000000000, 0.9659258262890683122, 1.000000000000000000, 0.9659258262890683122, 1.000000000000000000, 0.9659258262890683122, 1.000000000000000000, 0.9659258262890683122, 1.000000000000000000, 0.9659258262890683122, 1.000000000000000000, 0.9659258262890683122, 1.000000000000000000, 0.9659258262890683122, 1.000000000000000000, 0.9659258262890683122, 1.000000000000000000, 0.9659258262890683122, 1.000000000000000000, 0.9659258262890683122, 1.000000000000000000, 0.9659258262890683122, 1.000000000000000000, 0.9659258262890683122, 1.000000000000000000, 0.9659258262890683122, 1.000000000000000000, 0.9659258262890683122, 1.000000000000000000, 0.9659258262890683122, 1.000000000000000000, 0.9659258262890683122, 1.000000000000000000, 0.9659258262890683122, 1.000000000000000000, 0.9659258262890683122, 1.000000000000000000, 0.9659258262890683122, 1.000000000000000000, 0.9659258262890683122, 1.000000000000000000, 0.9659258262890683122, 1.000000000000000000, 0.9659258262890683122, 1.000000000000000000, 0.9659258262890683122, 1.000000000000000000, 0.9659258262890683122, 1.000000000000000000, 0.9659258262890683122, 1.000000000000000000, 0.9659258262890683122, 1.000000000000000000, 0.9659258262890683122, 1.000000000000000000, 0.9659258262890683122, 1.000000000000000000, 0.9659258262890683122, 1.000000000000000000, 0.9659258262890683122, 1.000000000000000000, 0.9659258262890683122, 1.000000000000000000, 0.9659258262890683122, 1.000000000000000000, 0.9659258262890683122, 1.000000000000000000, 0.9659258262890683122, 1.000000000000000000, 0.9659258262890683122, 1.000000000000000000, 0.9659258262890683122, 1.000000000000000000, 0.9659258262890683122, 1.000000000000000000, 0.9659258262890683122, 1.000000000000000000, 0.9659258262890683122, 1.000000000000000000, 0.9659258262890683122, 1.000000000000000000, 0.9659258262890683122, 1.000000000000000000, 0.9659258262890683122, 1.000000000000000000, 0.9659258262890683122, 1.000000000000000000, 0.9659258262890683122, 1.000000000000000000, 0.9659258262890683122, 1.000000000000000000, 0.9659258262890683122, 1.000000000000000000, 0.9659258262890683122, 1.000000000000000000, 0.9659258262890683122, 1.000000000000000000, 0.9659258262890683122, 1.000000000000000000, 0.9659258262890683122, 1.000000000000000000, 0.9659258262890683122, 1.000000000000000000, 0.9659258262890683122, 1.000000000000000000, 0.9659258262890683122, 1.000000000000000000, 0.9659258262890683122, 1.000000000000000000, 0.9659258262890683122, 1.000000000000000000, 0.9659258262890683122, 1.000000000000000000, 0.9659258262890683122, 1.000000000000000000, 0.9659258262890683122, 1.000000000000000000, 0.9659258262890683122, 1.000000000000000000, 0.9659258262890683122, 1.000000000000000000, 0.9659258262890683122, 1.000000000000000000, 0.9659258262890683122, 1.000000000000000000, 0.9659258262890683122, 1.000000000000000000, 0.9659258262890683122, 1.000000000000000000, 0.9659258262890683122, 1.000000000000000000, 0.9659258262890683122, 1.000000000000000000, 0.9659258262890683122, 1.000000000000000000, 0.9659258262890683122, 1.000000000000000000, 0.9659258262890683122, 1.000000000000000000, 0.9659258262890683122, 1.000000000000000000, 0.9659258262890683122, 1.000000000000000000, 0.9659258262890683122, 1.000000000000000000, 0.9659258262890683122, 1.000000000000000000, 0.9659258262890683122, 1.000000000000000000, 0.9659258262890683122, 1.000000000000000000, 0.9659258262890683122, 1.000000000000000000, 0.9659258262890683122, 1.000000000000000000, 0.9659258262890683122, 1.000000000000000000, 0.9659258262890683122, 1.000000000000000000, 0.9659258262890683122, 1.000000000000000000, 0.9659258262890683122, 1.000000000000000000, 0.9659258262890683122, 1.000000000000000000, 0.9659258262890683122, 1.000000000000000000, 0.9659258262890683122, 1.000000000000000000, 0.9659258262890683122, 1.000000000000000000, 0.9659258262890683122, 1.000000000000000000, 0.9659258262890683122, 1.000000000000000000, 0.9659258262890683122, 1.000000000000000000, 0.9659258262890683122, 1.000000000000000000, 0.9659258262890683122, 1.000000000000000000, 0.9659258262890683122, 1.000000000000000000, 0.9659258262890683122, 1.000000000000000000, 0.9659258262890683122, 1.000000000000000000, 0.9659258262890683122, 1.000000000000000000, 0.9659258262890683122, 1.000000000000000000, 0.9659258262890683122, 1.000000000000000000, 0.9659258262890683122, 1.000000000000000000, 0.9659258262890683122, 1.000000000000000000, 0.9659258262890683122, 1.000000000000000000, 0.9659258262890683122, 1.000000000000000000, 0.9659258262890683122, 1.000000000000000000, 0.9659258262890683122, 1.000000000000000000, 0.9659258262890683122, 1.000000000000000000, 0.9659258262890683122, 1.000000000000000000, 0.9659258262890683122, 1.000000000000000000, 0.9659258262890683122, 1.000000000000000000, 0.9659258262890683122, 1.000000000000000000, 0.9659258262890683122, 1.000000000000000000, 0.9659258262890683122, 1.000000000000000000, 0.9659258262890683122, 1.000000000000000000, 0.9659258262890683122, 1.000000000000000000, 0.9659258262890683122, 1.000000000000000000, 0.9659258262890683122, 1.000000000000000000, 0.9659258262890683122, 1.000000000000000000, 0.9659258262890683122, 1.000000000000000000, 0.9659258262890683122, 1.000000000000000000, 0.9659258262890683122, 1.000000000000000000, 0.9659258262890683122, 1.000000000000000000, 0.9659258262890683122, 1.000000000000000000, 0.9659258262890683122, 1.000000000000000000, 0.9659258262890683122, 1.000000000000000000, 0.9659258262890683122, 1.000000000000000000, 0.9659258262890683122, 1.000000000000000000, 0.9659258262890683122, 1.000000000000000000, 0.9659258262890683122, 1.000000000000000000, 0.9659258262890683122, 1.000000000000000000, 0.9659258262890683122, 1.000000000000000000, 0.9659258262890683122, 1.000000000000000000, 0.9659258262890683122, 1.000000000000000000, 0.9659258262890683122, 1.000000000000000000, 0.9659258262890683122, 1.000000000000000000, 0.9659258262890683122, 1.000000000000000000, 0.9659258262890683122, 1.000000000000000000, 0.9659258262890683122, 1.000000000000000000, 0.9659258262890683122, 1.000000000000000000, 0.9659258262890683122, 1.000000000000000000, 0.9659258262890683122, 1.000000000000000000, 0.9659258262890683122, 1.000000000000000000, 0.9659258262890683122, 1.000000000000000000, 0.9659258262890683122, 1.000000000000000000, 0.9659258262890683122, 1.000000000000000000, 0.9659258262890683122, 1.000000000000000000, 0.9659258262890683122, 1.000000000000000000, 0.9659258262890683122, 1.000000000000000000, 0.9659258262890683122, 1.000000000000000000, 0.9659258262890683122, 1.000000000000000000, 0.9659258262890683122, 1.000000000000000000, 0.9659258262890683122, 1.000000000000000000, 0.9659258262890683122, 1.000000000000000000, 0.9659258262890683122, 1.000000000000000000, 0.9659258262890683122, 1.000000000000000000, 0.9659258262890683122, 1.000000000000000000, 0.9659258262890683122, 1.000000000000000000, 0.9659258262890683122, 1.000000000000000000, 0.9659258262890683122, 1.000000000000000000, 0.9659258262890683122, 1.000000000000000000, 0.9659258262890683122, 1.000000000000000000, 0.9659258262890683122, 1.000000000000000000, 0.9659258262890683122, 1.000000000000000000, 0.9659258262890683122, 1.000000000000000000, 0.9659258262890683122, 1.000000000000000000, 0.9659258262890683122, 1.000000000000000000, 0.9659258262890683122, 1.000000000000000000, 0.9659258262890683122, 1.000000000000000000, 0.9659258262890683122, 1.000000000000000000),
 ( 0.3333333333333333703, 0.3219752754296894559, 0.3333333333333333703, 0.3219752754296894559, 0.3333333333333333703, 0.3219752754296894559, 0.3333333333333333703, 0.3219752754296894559, 0.3333333333333333703, 0.3219752754296894559, 0.3333333333333333703, 0.3219752754296894559, 0.3333333333333333703, 0.3219752754296894559, 0.3333333333333333703, 0.3219752754296894559, 0.3333333333333333703, 0.3219752754296894559, 0.3333333333333333703, 0.3219752754296894559, 0.3333333333333333703, 0.3219752754296894559, 0.3333333333333333703, 0.3219752754296894559, 0.3333333333333333703, 0.3219752754296894559, 0.3333333333333333703, 0.3219752754296894559, 0.3333333333333333703, 0.3219752754296894559, 0.3333333333333333703, 0.3219752754296894559, 0.3333333333333333703, 0.3219752754296894559, 0.3333333333333333703, 0.3219752754296894559, 0.3333333333333333703, 0.3219752754296894559, 0.3333333333333333703, 0.3219752754296894559, 0.3333333333333333703, 0.3219752754296894559, 0.3333333333333333703, 0.3219752754296894559, 0.3333333333333333703, 0.3219752754296894559, 0.3333333333333333703, 0.3219752754296894559, 0.3333333333333333703, 0.3219752754296894559, 0.3333333333333333703, 0.3219752754296894559, 0.3333333333333333703, 0.3219752754296894559, 0.3333333333333333703, 0.3219752754296894559, 0.3333333333333333703, 0.3219752754296894559, 0.3333333333333333703, 0.3219752754296894559, 0.3333333333333333703, 0.3219752754296894559, 0.3333333333333333703, 0.3219752754296894559, 0.3333333333333333703, 0.3219752754296894559, 0.3333333333333333703, 0.3219752754296894559, 0.3333333333333333703, 0.3219752754296894559, 0.3333333333333333703, 0.3219752754296894559, 0.3333333333333333703, 0.3219752754296894559, 0.3333333333333333703, 0.3219752754296894559, 0.3333333333333333703, 0.3219752754296894559, 0.3333333333333333703, 0.3219752754296894559, 0.3333333333333333703, 0.3219752754296894559, 0.3333333333333333703, 0.3219752754296894559, 0.3333333333333333703, 0.3219752754296894559, 0.3333333333333333703, 0.3219752754296894559, 0.3333333333333333703, 0.3219752754296894559, 0.3333333333333333703, 0.3219752754296894559, 0.3333333333333333703, 0.3219752754296894559, 0.3333333333333333703, 0.3219752754296894559, 0.3333333333333333703, 0.3219752754296894559, 0.3333333333333333703, 0.3219752754296894559, 0.3333333333333333703, 0.3219752754296894559, 0.3333333333333333703, 0.3219752754296894559, 0.3333333333333333703, 0.3219752754296894559, 0.3333333333333333703, 0.3219752754296894559, 0.3333333333333333703, 0.3219752754296894559, 0.3333333333333333703, 0.3219752754296894559, 0.3333333333333333703, 0.3219752754296894559, 0.3333333333333333703, 0.3219752754296894559, 0.3333333333333333703, 0.3219752754296894559, 0.3333333333333333703, 0.3219752754296894559, 0.3333333333333333703, 0.3219752754296894559, 0.3333333333333333703, 0.3219752754296894559, 0.3333333333333333703, 0.3219752754296894559, 0.3333333333333333703, 0.3219752754296894559, 0.3333333333333333703, 0.3219752754296894559, 0.3333333333333333703, 0.3219752754296894559, 0.3333333333333333703, 0.3219752754296894559, 0.3333333333333333703, 0.3219752754296894559, 0.3333333333333333703, 0.3219752754296894559, 0.3333333333333333703, 0.3219752754296894559, 0.3333333333333333703, 0.3219752754296894559, 0.3333333333333333703, 0.3219752754296894559, 0.3333333333333333703, 0.3219752754296894559, 0.3333333333333333703, 0.3219752754296894559, 0.3333333333333333703, 0.3219752754296894559, 0.3333333333333333703, 0.3219752754296894559, 0.3333333333333333703, 0.3219752754296894559, 0.3333333333333333703, 0.3219752754296894559, 0.3333333333333333703, 0.3219752754296894559, 0.3333333333333333703, 0.3219752754296894559, 0.3333333333333333703, 0.3219752754296894559, 0.3333333333333333703, 0.3219752754296894559, 0.3333333333333333703, 0.3219752754296894559, 0.3333333333333333703, 0.3219752754296894559, 0.3333333333333333703, 0.3219752754296894559, 0.3333333333333333703, 0.3219752754296894559, 0.3333333333333333703, 0.3219752754296894559, 0.3333333333333333703, 0.3219752754296894559, 0.3333333333333333703, 0.3219752754296894559, 0.3333333333333333703, 0.3219752754296894559, 0.3333333333333333703, 0.3219752754296894559, 0.3333333333333333703, 0.3219752754296894559, 0.3333333333333333703, 0.3219752754296894559, 0.3333333333333333703, 0.3219752754296894559, 0.3333333333333333703, 0.3219752754296894559, 0.3333333333333333703, 0.3219752754296894559, 0.3333333333333333703, 0.3219752754296894559, 0.3333333333333333703, 0.3219752754296894559, 0.3333333333333333703, 0.3219752754296894559, 0.3333333333333333703, 0.3219752754296894559, 0.3333333333333333703, 0.3219752754296894559, 0.3333333333333333703, 0.3219752754296894559, 0.3333333333333333703, 0.3219752754296894559, 0.3333333333333333703, 0.3219752754296894559, 0.3333333333333333703, 0.3219752754296894559, 0.3333333333333333703, 0.3219752754296894559, 0.3333333333333333703, 0.3219752754296894559, 0.3333333333333333703, 0.3219752754296894559, 0.3333333333333333703, 0.3219752754296894559, 0.3333333333333333703, 0.3219752754296894559, 0.3333333333333333703, 0.3219752754296894559, 0.3333333333333333703, 0.3219752754296894559, 0.3333333333333333703, 0.3219752754296894559, 0.3333333333333333703, 0.3219752754296894559, 0.3333333333333333703, 0.3219752754296894559, 0.3333333333333333703, 0.3219752754296894559, 0.3333333333333333703, 0.3219752754296894559, 0.3333333333333333703, 0.3219752754296894559, 0.3333333333333333703, 0.3219752754296894559, 0.3333333333333333703, 0.3219752754296894559, 0.3333333333333333703, 0.3219752754296894559, 0.3333333333333333703, 0.3219752754296894559, 0.3333333333333333703, 0.3219752754296894559, 0.3333333333333333703, 0.3219752754296894559, 0.3333333333333333703, 0.3219752754296894559, 0.3333333333333333703, 0.3219752754296894559, 0.3333333333333333703, 0.3219752754296894559, 0.3333333333333333703, 0.3219752754296894559, 0.3333333333333333703, 0.3219752754296894559, 0.3333333333333333703, 0.3219752754296894559, 0.3333333333333333703, 0.3219752754296894559, 0.3333333333333333703, 0.3219752754296894559, 0.3333333333333333703, 0.3219752754296894559, 0.3333333333333333703, 0.3219752754296894559, 0.3333333333333333703, 0.3219752754296894559, 0.3333333333333333703, 0.3219752754296894559, 0.3333333333333333703, 0.3219752754296894559, 0.3333333333333333703, 0.3219752754296894559, 0.3333333333333333703, 0.3219752754296894559, 0.3333333333333333703, 0.3219752754296894559, 0.3333333333333333703, 0.3219752754296894559, 0.3333333333333333703, 0.3219752754296894559, 0.3333333333333333703, 0.3219752754296894559, 0.3333333333333333703, 0.3219752754296894559, 0.3333333333333333703, 0.3219752754296894559, 0.3333333333333333703, 0.3219752754296894559, 0.3333333333333333703, 0.3219752754296894559, 0.3333333333333333703, 0.3219752754296894559, 0.3333333333333333703, 0.3219752754296894559, 0.3333333333333333703, 0.3219752754296894559, 0.3333333333333333703, 0.3219752754296894559, 0.3333333333333333703, 0.3219752754296894559, 0.3333333333333333703, 0.3219752754296894559, 0.3333333333333333703, 0.3219752754296894559, 0.3333333333333333703, 0.3219752754296894559, 0.3333333333333333703, 0.3219752754296894559, 0.3333333333333333703, 0.3219752754296894559, 0.3333333333333333703, 0.3219752754296894559, 0.3333333333333333703, 0.3219752754296894559, 0.3333333333333333703, 0.3219752754296894559, 0.3333333333333333703, 0.3219752754296894559, 0.3333333333333333703, 0.3219752754296894559, 0.3333333333333333703, 0.3219752754296894559, 0.3333333333333333703, 0.3219752754296894559, 0.3333333333333333703, 0.3219752754296894559, 0.3333333333333333703, 0.3219752754296894559, 0.3333333333333333703, 0.3219752754296894559, 0.3333333333333333703, 0.3219752754296894559, 0.3333333333333333703, 0.3219752754296894559, 0.3333333333333333703, 0.3219752754296894559, 0.3333333333333333703, 0.3219752754296894559, 0.3333333333333333703, 0.3219752754296894559, 0.3333333333333333703, 0.3219752754296894559, 0.3333333333333333703, 0.3219752754296894559, 0.3333333333333333703, 0.3219752754296894559, 0.3333333333333333703, 0.3219752754296894559, 0.3333333333333333703, 0.3219752754296894559, 0.3333333333333333703, 0.3219752754296894559, 0.3333333333333333703, 0.3219752754296894559, 0.3333333333333333703, 0.3219752754296894559, 0.3333333333333333703, 0.3219752754296894559, 0.3333333333333333703, 0.3219752754296894559, 0.3333333333333333703, 0.3219752754296894559, 0.3333333333333333703, 0.3219752754296894559, 0.3333333333333333703, 0.3219752754296894559, 0.3333333333333333703, 0.3219752754296894559, 0.3333333333333333703, 0.3219752754296894559, 0.3333333333333333703, 0.3219752754296894559, 0.3333333333333333703, 0.3219752754296894559, 0.3333333333333333703, 0.3219752754296894559, 0.3333333333333333703, 0.3219752754296894559, 0.3333333333333333703, 0.3219752754296894559, 0.3333333333333333703, 0.3219752754296894559, 0.3333333333333333703, 0.3219752754296894559, 0.3333333333333333703, 0.3219752754296894559, 0.3333333333333333703, 0.3219752754296894559, 0.3333333333333333703, 0.3219752754296894559, 0.3333333333333333703, 0.3219752754296894559, 0.3333333333333333703, 0.3219752754296894559, 0.3333333333333333703, 0.3219752754296894559, 0.3333333333333333703, 0.3219752754296894559, 0.3333333333333333703, 0.3219752754296894559, 0.3333333333333333703, 0.3219752754296894559, 0.3333333333333333703, 0.3219752754296894559, 0.3333333333333333703, 0.3219752754296894559, 0.3333333333333333703, 0.3219752754296894559, 0.3333333333333333703, 0.3219752754296894559, 0.3333333333333333703, 0.3219752754296894559, 0.3333333333333333703, 0.3219752754296894559, 0.3333333333333333703, 0.3219752754296894559, 0.3333333333333333703, 0.3219752754296894559, 0.3333333333333333703, 0.3219752754296894559, 0.3333333333333333703, 0.3219752754296894559, 0.3333333333333333703, 0.3219752754296894559, 0.3333333333333333703, 0.3219752754296894559, 0.3333333333333333703, 0.3219752754296894559, 0.3333333333333333703, 0.3219752754296894559, 0.3333333333333333703, 0.3219752754296894559, 0.3333333333333333703, 0.3219752754296894559, 0.3333333333333333703, 0.3219752754296894559, 0.3333333333333333703, 0.3219752754296894559, 0.3333333333333333703, 0.3219752754296894559, 0.3333333333333333703, 0.3219752754296894559, 0.3333333333333333703, 0.3219752754296894559, 0.3333333333333333703, 0.3219752754296894559, 0.3333333333333333703, 0.3219752754296894559, 0.3333333333333333703, 0.3219752754296894559, 0.3333333333333333703, 0.3219752754296894559, 0.3333333333333333703),
 ( 0.3333333333333333703, 0.3219752754296894559, 0.3333333333333333703, 0.3219752754296894559, 0.3333333333333333703, 0.3219752754296894559, 0.3333333333333333703, 0.3219752754296894559, 0.3333333333333333703, 0.3219752754296894559, 0.3333333333333333703, 0.3219752754296894559, 0.3333333333333333703, 0.3219752754296894559, 0.3333333333333333703, 0.3219752754296894559, 0.3333333333333333703, 0.3219752754296894559, 0.3333333333333333703, 0.3219752754296894559, 0.3333333333333333703, 0.3219752754296894559, 0.3333333333333333703, 0.3219752754296894559, 0.3333333333333333703, 0.3219752754296894559, 0.3333333333333333703, 0.3219752754296894559, 0.3333333333333333703, 0.3219752754296894559, 0.3333333333333333703, 0.3219752754296894559, 0.3333333333333333703, 0.3219752754296894559, 0.3333333333333333703, 0.3219752754296894559, 0.3333333333333333703, 0.3219752754296894559, 0.3333333333333333703, 0.3219752754296894559, 0.3333333333333333703, 0.3219752754296894559, 0.3333333333333333703, 0.3219752754296894559, 0.3333333333333333703, 0.3219752754296894559, 0.3333333333333333703, 0.3219752754296894559, 0.3333333333333333703, 0.3219752754296894559, 0.3333333333333333703, 0.3219752754296894559, 0.3333333333333333703, 0.3219752754296894559, 0.3333333333333333703, 0.3219752754296894559, 0.3333333333333333703, 0.3219752754296894559, 0.3333333333333333703, 0.3219752754296894559, 0.3333333333333333703, 0.3219752754296894559, 0.3333333333333333703, 0.3219752754296894559, 0.3333333333333333703, 0.3219752754296894559, 0.3333333333333333703, 0.3219752754296894559, 0.3333333333333333703, 0.3219752754296894559, 0.3333333333333333703, 0.3219752754296894559, 0.3333333333333333703, 0.3219752754296894559, 0.3333333333333333703, 0.3219752754296894559, 0.3333333333333333703, 0.3219752754296894559, 0.3333333333333333703, 0.3219752754296894559, 0.3333333333333333703, 0.3219752754296894559, 0.3333333333333333703, 0.3219752754296894559, 0.3333333333333333703, 0.3219752754296894559, 0.3333333333333333703, 0.3219752754296894559, 0.3333333333333333703, 0.3219752754296894559, 0.3333333333333333703, 0.3219752754296894559, 0.3333333333333333703, 0.3219752754296894559, 0.3333333333333333703, 0.3219752754296894559, 0.3333333333333333703, 0.3219752754296894559, 0.3333333333333333703, 0.3219752754296894559, 0.3333333333333333703, 0.3219752754296894559, 0.3333333333333333703, 0.3219752754296894559, 0.3333333333333333703, 0.3219752754296894559, 0.3333333333333333703, 0.3219752754296894559, 0.3333333333333333703, 0.3219752754296894559, 0.3333333333333333703, 0.3219752754296894559, 0.3333333333333333703, 0.3219752754296894559, 0.3333333333333333703, 0.3219752754296894559, 0.3333333333333333703, 0.3219752754296894559, 0.3333333333333333703, 0.3219752754296894559, 0.3333333333333333703, 0.3219752754296894559, 0.3333333333333333703, 0.3219752754296894559, 0.3333333333333333703, 0.3219752754296894559, 0.3333333333333333703, 0.3219752754296894559, 0.3333333333333333703, 0.3219752754296894559, 0.3333333333333333703, 0.3219752754296894559, 0.3333333333333333703, 0.3219752754296894559, 0.3333333333333333703, 0.3219752754296894559, 0.3333333333333333703, 0.3219752754296894559, 0.3333333333333333703, 0.3219752754296894559, 0.3333333333333333703, 0.3219752754296894559, 0.3333333333333333703, 0.3219752754296894559, 0.3333333333333333703, 0.3219752754296894559, 0.3333333333333333703, 0.3219752754296894559, 0.3333333333333333703, 0.3219752754296894559, 0.3333333333333333703, 0.3219752754296894559, 0.3333333333333333703, 0.3219752754296894559, 0.3333333333333333703, 0.3219752754296894559, 0.3333333333333333703, 0.3219752754296894559, 0.3333333333333333703, 0.3219752754296894559, 0.3333333333333333703, 0.3219752754296894559, 0.3333333333333333703, 0.3219752754296894559, 0.3333333333333333703, 0.3219752754296894559, 0.3333333333333333703, 0.3219752754296894559, 0.3333333333333333703, 0.3219752754296894559, 0.3333333333333333703, 0.3219752754296894559, 0.3333333333333333703, 0.3219752754296894559, 0.3333333333333333703, 0.3219752754296894559, 0.3333333333333333703, 0.3219752754296894559, 0.3333333333333333703, 0.3219752754296894559, 0.3333333333333333703, 0.3219752754296894559, 0.3333333333333333703, 0.3219752754296894559, 0.3333333333333333703, 0.3219752754296894559, 0.3333333333333333703, 0.3219752754296894559, 0.3333333333333333703, 0.3219752754296894559, 0.3333333333333333703, 0.3219752754296894559, 0.3333333333333333703, 0.3219752754296894559, 0.3333333333333333703, 0.3219752754296894559, 0.3333333333333333703, 0.3219752754296894559, 0.3333333333333333703, 0.3219752754296894559, 0.3333333333333333703, 0.3219752754296894559, 0.3333333333333333703, 0.3219752754296894559, 0.3333333333333333703, 0.3219752754296894559, 0.3333333333333333703, 0.3219752754296894559, 0.3333333333333333703, 0.3219752754296894559, 0.3333333333333333703, 0.3219752754296894559, 0.3333333333333333703, 0.3219752754296894559, 0.3333333333333333703, 0.3219752754296894559, 0.3333333333333333703, 0.3219752754296894559, 0.3333333333333333703, 0.3219752754296894559, 0.3333333333333333703, 0.3219752754296894559, 0.3333333333333333703, 0.3219752754296894559, 0.3333333333333333703, 0.3219752754296894559, 0.3333333333333333703, 0.3219752754296894559, 0.3333333333333333703, 0.3219752754296894559, 0.3333333333333333703, 0.3219752754296894559, 0.3333333333333333703, 0.3219752754296894559, 0.3333333333333333703, 0.3219752754296894559, 0.3333333333333333703, 0.3219752754296894559, 0.3333333333333333703, 0.3219752754296894559, 0.3333333333333333703, 0.3219752754296894559, 0.3333333333333333703, 0.3219752754296894559, 0.3333333333333333703, 0.3219752754296894559, 0.3333333333333333703, 0.3219752754296894559, 0.3333333333333333703, 0.3219752754296894559, 0.3333333333333333703, 0.3219752754296894559, 0.3333333333333333703, 0.3219752754296894559, 0.3333333333333333703, 0.3219752754296894559, 0.3333333333333333703, 0.3219752754296894559, 0.3333333333333333703, 0.3219752754296894559, 0.3333333333333333703, 0.3219752754296894559, 0.3333333333333333703, 0.3219752754296894559, 0.3333333333333333703, 0.3219752754296894559, 0.3333333333333333703, 0.3219752754296894559, 0.3333333333333333703, 0.3219752754296894559, 0.3333333333333333703, 0.3219752754296894559, 0.3333333333333333703, 0.3219752754296894559, 0.3333333333333333703, 0.3219752754296894559, 0.3333333333333333703, 0.3219752754296894559, 0.3333333333333333703, 0.3219752754296894559, 0.3333333333333333703, 0.3219752754296894559, 0.3333333333333333703, 0.3219752754296894559, 0.3333333333333333703, 0.3219752754296894559, 0.3333333333333333703, 0.3219752754296894559, 0.3333333333333333703, 0.3219752754296894559, 0.3333333333333333703, 0.3219752754296894559, 0.3333333333333333703, 0.3219752754296894559, 0.3333333333333333703, 0.3219752754296894559, 0.3333333333333333703, 0.3219752754296894559, 0.3333333333333333703, 0.3219752754296894559, 0.3333333333333333703, 0.3219752754296894559, 0.3333333333333333703, 0.3219752754296894559, 0.3333333333333333703, 0.3219752754296894559, 0.3333333333333333703, 0.3219752754296894559, 0.3333333333333333703, 0.3219752754296894559, 0.3333333333333333703, 0.3219752754296894559, 0.3333333333333333703, 0.3219752754296894559, 0.3333333333333333703, 0.3219752754296894559, 0.3333333333333333703, 0.3219752754296894559, 0.3333333333333333703, 0.3219752754296894559, 0.3333333333333333703, 0.3219752754296894559, 0.3333333333333333703, 0.3219752754296894559, 0.3333333333333333703, 0.3219752754296894559, 0.3333333333333333703, 0.3219752754296894559, 0.3333333333333333703, 0.3219752754296894559, 0.3333333333333333703, 0.3219752754296894559, 0.3333333333333333703, 0.3219752754296894559, 0.3333333333333333703, 0.3219752754296894559, 0.3333333333333333703, 0.3219752754296894559, 0.3333333333333333703, 0.3219752754296894559, 0.3333333333333333703, 0.3219752754296894559, 0.3333333333333333703, 0.3219752754296894559, 0.3333333333333333703, 0.3219752754296894559, 0.3333333333333333703, 0.3219752754296894559, 0.3333333333333333703, 0.3219752754296894559, 0.3333333333333333703, 0.3219752754296894559, 0.3333333333333333703, 0.3219752754296894559, 0.3333333333333333703, 0.3219752754296894559, 0.3333333333333333703, 0.3219752754296894559, 0.3333333333333333703, 0.3219752754296894559, 0.3333333333333333703, 0.3219752754296894559, 0.3333333333333333703, 0.3219752754296894559, 0.3333333333333333703, 0.3219752754296894559, 0.3333333333333333703, 0.3219752754296894559, 0.3333333333333333703, 0.3219752754296894559, 0.3333333333333333703, 0.3219752754296894559, 0.3333333333333333703, 0.3219752754296894559, 0.3333333333333333703, 0.3219752754296894559, 0.3333333333333333703, 0.3219752754296894559, 0.3333333333333333703, 0.3219752754296894559, 0.3333333333333333703, 0.3219752754296894559, 0.3333333333333333703, 0.3219752754296894559, 0.3333333333333333703, 0.3219752754296894559, 0.3333333333333333703, 0.3219752754296894559, 0.3333333333333333703, 0.3219752754296894559, 0.3333333333333333703, 0.3219752754296894559, 0.3333333333333333703, 0.3219752754296894559, 0.3333333333333333703, 0.3219752754296894559, 0.3333333333333333703, 0.3219752754296894559, 0.3333333333333333703, 0.3219752754296894559, 0.3333333333333333703, 0.3219752754296894559, 0.3333333333333333703, 0.3219752754296894559, 0.3333333333333333703, 0.3219752754296894559, 0.3333333333333333703, 0.3219752754296894559, 0.3333333333333333703, 0.3219752754296894559, 0.3333333333333333703, 0.3219752754296894559, 0.3333333333333333703, 0.3219752754296894559, 0.3333333333333333703, 0.3219752754296894559, 0.3333333333333333703, 0.3219752754296894559, 0.3333333333333333703, 0.3219752754296894559, 0.3333333333333333703, 0.3219752754296894559, 0.3333333333333333703, 0.3219752754296894559, 0.3333333333333333703, 0.3219752754296894559, 0.3333333333333333703, 0.3219752754296894559, 0.3333333333333333703, 0.3219752754296894559, 0.3333333333333333703, 0.3219752754296894559, 0.3333333333333333703, 0.3219752754296894559, 0.3333333333333333703, 0.3219752754296894559, 0.3333333333333333703, 0.3219752754296894559, 0.3333333333333333703, 0.3219752754296894559, 0.3333333333333333703, 0.3219752754296894559, 0.3333333333333333703, 0.3219752754296894559, 0.3333333333333333703, 0.3219752754296894559, 0.3333333333333333703, 0.3219752754296894559, 0.3333333333333333703, 0.3219752754296894559, 0.3333333333333333703, 0.3219752754296894559, 0.3333333333333333703, 0.3219752754296894559, 0.3333333333333333703, 0.3219752754296894559, 0.3333333333333333703),
 ( 1.000000000000000000, 0.9659258262890683122, 1.000000000000000000, 0.9659258262890683122, 1.000000000000000000, 0.9659258262890683122, 1.000000000000000000, 0.9659258262890683122, 1.000000000000000000, 0.9659258262890683122, 1.000000000000000000, 0.9659258262890683122, 1.000000000000000000, 0.9659258262890683122, 1.000000000000000000, 0.9659258262890683122, 1.000000000000000000, 0.9659258262890683122, 1.000000000000000000, 0.9659258262890683122, 1.000000000000000000, 0.9659258262890683122, 1.000000000000000000, 0.9659258262890683122, 1.000000000000000000, 0.9659258262890683122, 1.000000000000000000, 0.9659258262890683122, 1.000000000000000000, 0.9659258262890683122, 1.000000000000000000, 0.9659258262890683122, 1.000000000000000000, 0.9659258262890683122, 1.000000000000000000, 0.9659258262890683122, 1.000000000000000000, 0.9659258262890683122, 1.000000000000000000, 0.9659258262890683122, 1.000000000000000000, 0.9659258262890683122, 1.000000000000000000, 0.9659258262890683122, 1.000000000000000000, 0.9659258262890683122, 1.000000000000000000, 0.9659258262890683122, 1.000000000000000000, 0.9659258262890683122, 1.000000000000000000, 0.9659258262890683122, 1.000000000000000000, 0.9659258262890683122, 1.000000000000000000, 0.9659258262890683122, 1.000000000000000000, 0.9659258262890683122, 1.000000000000000000, 0.9659258262890683122, 1.000000000000000000, 0.9659258262890683122, 1.000000000000000000, 0.9659258262890683122, 1.000000000000000000, 0.9659258262890683122, 1.000000000000000000, 0.9659258262890683122, 1.000000000000000000, 0.9659258262890683122, 1.000000000000000000, 0.9659258262890683122, 1.000000000000000000, 0.9659258262890683122, 1.000000000000000000, 0.9659258262890683122, 1.000000000000000000, 0.9659258262890683122, 1.000000000000000000, 0.9659258262890683122, 1.000000000000000000, 0.9659258262890683122, 1.000000000000000000, 0.9659258262890683122, 1.000000000000000000, 0.9659258262890683122, 1.000000000000000000, 0.9659258262890683122, 1.000000000000000000, 0.9659258262890683122, 1.000000000000000000, 0.9659258262890683122, 1.000000000000000000, 0.9659258262890683122, 1.000000000000000000, 0.9659258262890683122, 1.000000000000000000, 0.9659258262890683122, 1.000000000000000000, 0.9659258262890683122, 1.000000000000000000, 0.9659258262890683122, 1.000000000000000000, 0.9659258262890683122, 1.000000000000000000, 0.9659258262890683122, 1.000000000000000000, 0.9659258262890683122, 1.000000000000000000, 0.9659258262890683122, 1.000000000000000000, 0.9659258262890683122, 1.000000000000000000, 0.9659258262890683122, 1.000000000000000000, 0.9659258262890683122, 1.000000000000000000, 0.9659258262890683122, 1.000000000000000000, 0.9659258262890683122, 1.000000000000000000, 0.9659258262890683122, 1.000000000000000000, 0.9659258262890683122, 1.000000000000000000, 0.9659258262890683122, 1.000000000000000000, 0.9659258262890683122, 1.000000000000000000, 0.9659258262890683122, 1.000000000000000000, 0.9659258262890683122, 1.000000000000000000, 0.9659258262890683122, 1.000000000000000000, 0.9659258262890683122, 1.000000000000000000, 0.9659258262890683122, 1.000000000000000000, 0.9659258262890683122, 1.000000000000000000, 0.9659258262890683122, 1.000000000000000000, 0.9659258262890683122, 1.000000000000000000, 0.9659258262890683122, 1.000000000000000000, 0.9659258262890683122, 1.000000000000000000, 0.9659258262890683122, 1.000000000000000000, 0.9659258262890683122, 1.000000000000000000, 0.9659258262890683122, 1.000000000000000000, 0.9659258262890683122, 1.000000000000000000, 0.9659258262890683122, 1.000000000000000000, 0.9659258262890683122, 1.000000000000000000, 0.9659258262890683122, 1.000000000000000000, 0.9659258262890683122, 1.000000000000000000, 0.9659258262890683122, 1.000000000000000000, 0.9659258262890683122, 1.000000000000000000, 0.9659258262890683122, 1.000000000000000000, 0.9659258262890683122, 1.000000000000000000, 0.9659258262890683122, 1.000000000000000000, 0.9659258262890683122, 1.000000000000000000, 0.9659258262890683122, 1.000000000000000000, 0.9659258262890683122, 1.000000000000000000, 0.9659258262890683122, 1.000000000000000000, 0.9659258262890683122, 1.000000000000000000, 0.9659258262890683122, 1.000000000000000000, 0.9659258262890683122, 1.000000000000000000, 0.9659258262890683122, 1.000000000000000000, 0.9659258262890683122, 1.000000000000000000, 0.9659258262890683122, 1.000000000000000000, 0.9659258262890683122, 1.000000000000000000, 0.9659258262890683122, 1.000000000000000000, 0.9659258262890683122, 1.000000000000000000, 0.9659258262890683122, 1.000000000000000000, 0.9659258262890683122, 1.000000000000000000, 0.9659258262890683122, 1.000000000000000000, 0.9659258262890683122, 1.000000000000000000, 0.9659258262890683122, 1.000000000000000000, 0.9659258262890683122, 1.000000000000000000, 0.9659258262890683122, 1.000000000000000000, 0.9659258262890683122, 1.000000000000000000, 0.9659258262890683122, 1.000000000000000000, 0.9659258262890683122, 1.000000000000000000, 0.9659258262890683122, 1.000000000000000000, 0.9659258262890683122, 1.000000000000000000, 0.9659258262890683122, 1.000000000000000000, 0.9659258262890683122, 1.000000000000000000, 0.9659258262890683122, 1.000000000000000000, 0.9659258262890683122, 1.000000000000000000, 0.9659258262890683122, 1.000000000000000000, 0.9659258262890683122, 1.000000000000000000, 0.9659258262890683122, 1.000000000000000000, 0.9659258262890683122, 1.000000000000000000, 0.9659258262890683122, 1.000000000000000000, 0.9659258262890683122, 1.000000000000000000, 0.9659258262890683122, 1.000000000000000000, 0.9659258262890683122, 1.000000000000000000, 0.9659258262890683122, 1.000000000000000000, 0.9659258262890683122, 1.000000000000000000, 0.9659258262890683122, 1.000000000000000000, 0.9659258262890683122, 1.000000000000000000, 0.9659258262890683122, 1.000000000000000000, 0.9659258262890683122, 1.000000000000000000, 0.9659258262890683122, 1.000000000000000000, 0.9659258262890683122, 1.000000000000000000, 0.9659258262890683122, 1.000000000000000000, 0.9659258262890683122, 1.000000000000000000, 0.9659258262890683122, 1.000000000000000000, 0.9659258262890683122, 1.000000000000000000, 0.9659258262890683122, 1.000000000000000000, 0.9659258262890683122, 1.000000000000000000, 0.9659258262890683122, 1.000000000000000000, 0.9659258262890683122, 1.000000000000000000, 0.9659258262890683122, 1.000000000000000000, 0.9659258262890683122, 1.000000000000000000, 0.9659258262890683122, 1.000000000000000000, 0.9659258262890683122, 1.000000000000000000, 0.9659258262890683122, 1.000000000000000000, 0.9659258262890683122, 1.000000000000000000, 0.9659258262890683122, 1.000000000000000000, 0.9659258262890683122, 1.000000000000000000, 0.9659258262890683122, 1.000000000000000000, 0.9659258262890683122, 1.000000000000000000, 0.9659258262890683122, 1.000000000000000000, 0.9659258262890683122, 1.000000000000000000, 0.9659258262890683122, 1.000000000000000000, 0.9659258262890683122, 1.000000000000000000, 0.9659258262890683122, 1.000000000000000000, 0.9659258262890683122, 1.000000000000000000, 0.9659258262890683122, 1.000000000000000000, 0.9659258262890683122, 1.000000000000000000, 0.9659258262890683122, 1.000000000000000000, 0.9659258262890683122, 1.000000000000000000, 0.9659258262890683122, 1.000000000000000000, 0.9659258262890683122, 1.000000000000000000, 0.9659258262890683122, 1.000000000000000000, 0.9659258262890683122, 1.000000000000000000, 0.9659258262890683122, 1.000000000000000000, 0.9659258262890683122, 1.000000000000000000, 0.9659258262890683122, 1.000000000000000000, 0.9659258262890683122, 1.000000000000000000, 0.9659258262890683122, 1.000000000000000000, 0.9659258262890683122, 1.000000000000000000, 0.9659258262890683122, 1.000000000000000000, 0.9659258262890683122, 1.000000000000000000, 0.9659258262890683122, 1.000000000000000000, 0.9659258262890683122, 1.000000000000000000, 0.9659258262890683122, 1.000000000000000000, 0.9659258262890683122, 1.000000000000000000, 0.9659258262890683122, 1.000000000000000000, 0.9659258262890683122, 1.000000000000000000, 0.9659258262890683122, 1.000000000000000000, 0.9659258262890683122, 1.000000000000000000, 0.9659258262890683122, 1.000000000000000000, 0.9659258262890683122, 1.000000000000000000, 0.9659258262890683122, 1.000000000000000000, 0.9659258262890683122, 1.000000000000000000, 0.9659258262890683122, 1.000000000000000000, 0.9659258262890683122, 1.000000000000000000, 0.9659258262890683122, 1.000000000000000000, 0.9659258262890683122, 1.000000000000000000, 0.9659258262890683122, 1.000000000000000000, 0.9659258262890683122, 1.000000000000000000, 0.9659258262890683122, 1.000000000000000000, 0.9659258262890683122, 1.000000000000000000, 0.9659258262890683122, 1.000000000000000000, 0.9659258262890683122, 1.000000000000000000, 0.9659258262890683122, 1.000000000000000000, 0.9659258262890683122, 1.000000000000000000, 0.9659258262890683122, 1.000000000000000000, 0.9659258262890683122, 1.000000000000000000, 0.9659258262890683122, 1.000000000000000000, 0.9659258262890683122, 1.000000000000000000, 0.9659258262890683122, 1.000000000000000000, 0.9659258262890683122, 1.000000000000000000, 0.9659258262890683122, 1.000000000000000000, 0.9659258262890683122, 1.000000000000000000, 0.9659258262890683122, 1.000000000000000000, 0.9659258262890683122, 1.000000000000000000, 0.9659258262890683122, 1.000000000000000000, 0.9659258262890683122, 1.000000000000000000, 0.9659258262890683122, 1.000000000000000000, 0.9659258262890683122, 1.000000000000000000, 0.9659258262890683122, 1.000000000000000000, 0.9659258262890683122, 1.000000000000000000, 0.9659258262890683122, 1.000000000000000000, 0.9659258262890683122, 1.000000000000000000, 0.9659258262890683122, 1.000000000000000000, 0.9659258262890683122, 1.000000000000000000, 0.9659258262890683122, 1.000000000000000000, 0.9659258262890683122, 1.000000000000000000, 0.9659258262890683122, 1.000000000000000000, 0.9659258262890683122, 1.000000000000000000, 0.9659258262890683122, 1.000000000000000000, 0.9659258262890683122, 1.000000000000000000, 0.9659258262890683122, 1.000000000000000000, 0.9659258262890683122, 1.000000000000000000, 0.9659258262890683122, 1.000000000000000000, 0.9659258262890683122, 1.000000000000000000, 0.9659258262890683122, 1.000000000000000000, 0.9659258262890683122, 1.000000000000000000) ) ) 
 REPRESENTATION_ITEM ( '' )  SURFACE ( )  );
#85951 = DIRECTION ( 'NONE',  ( -1.000000000000000000, 0.000000000000000000, 0.000000000000000000 ) ) ;
#85952 = CARTESIAN_POINT ( 'NONE',  ( 9.474510206698971260, -16.51473224551069308, 82.91557627198103830 ) ) ;
#85953 = CARTESIAN_POINT ( 'NONE',  ( -18.67979575497193778, 10.72451020669871902, 98.33442372801901854 ) ) ;
#85954 = CARTESIAN_POINT ( 'NONE',  ( -5.049401038298153566, 19.05341960407611168, 75.20724293864769550 ) ) ;
#85955 = CARTESIAN_POINT ( 'NONE',  ( -15.80617190586745835, -15.72974639402198527, 46.87390960531435979 ) ) ;
#85956 = CARTESIAN_POINT ( 'NONE',  ( -8.314922557960811034, -14.29746914071050412, 77.08224293864769550 ) ) ;
#85957 = CARTESIAN_POINT ( 'NONE',  ( -0.05219959533909027116, -19.03943276465977164, 62.49890960531435979 ) ) ;
#85958 = CARTESIAN_POINT ( 'NONE',  ( 4.379528057220339221, -16.55341960407611168, 112.7072429386476955 ) ) ;
#85959 = CARTESIAN_POINT ( 'NONE',  ( 21.53943276465977519, 0.05219959533937863772, 21.25109039468567218 ) ) ;
#85960 = CARTESIAN_POINT ( 'NONE',  ( -21.52544592524334988, -5.823673210054445271, 63.95942372801901854 ) ) ;
#85961 = CARTESIAN_POINT ( 'NONE',  ( 19.03943276465977164, -0.05219959533909143690, 38.74890960531436690 ) ) ;
#85962 = CARTESIAN_POINT ( 'NONE',  ( -8.314922557961024197, 14.29746914071037800, 57.91775706135234714 ) ) ;
#85963 = CARTESIAN_POINT ( 'NONE',  ( -5.823673210054116645, -21.52544592524344225, 112.2905762719810241 ) ) ;
#85964 = CARTESIAN_POINT ( 'NONE',  ( -18.62759615963270932, 10.81492255796079327, 110.8322429386476955 ) ) ;
#85966 = CARTESIAN_POINT ( 'NONE',  ( 13.97604488694527802, 13.89961937509977652, 69.37390960531436690 ) ) ;
#85965 = CARTESIAN_POINT ( 'NONE',  ( -9.474510206698720793, -16.51473224551083518, 44.58442372801900433 ) ) ;
#85967 = CARTESIAN_POINT ( 'NONE',  ( -18.22780087662122028, 5.500000000000031086, 83.51540105326107266 ) ) ;
#85968 = CARTESIAN_POINT ( 'NONE',  ( -15.80617190586768217, 15.72974639402176855, 68.12609039468567573 ) ) ;
#85969 = CARTESIAN_POINT ( 'NONE',  ( -18.62759615963270932, 10.81492255796079327, 55.83224293864770260 ) ) ;
#85970 = CARTESIAN_POINT ( 'NONE',  ( -8.224510206698948167, 14.34966873604960824, 40.41557627198103120 ) ) ;
#85972 = CARTESIAN_POINT ( 'NONE',  ( -5.823673210054431948, 21.52544592524334988, 112.7094237280190328 ) ) ;
#85971 = CARTESIAN_POINT ( 'NONE',  ( 5.719274019375673035, 21.55341960407619339, 77.29275706135234714 ) ) ;
#85973 = CARTESIAN_POINT ( 'NONE',  ( 14.34966873604960469, 8.224510206698951720, 54.16557627198103120 ) ) ;
#85974 = CARTESIAN_POINT ( 'NONE',  ( 8.314922557960818139, 14.29746914071049879, 99.58224293864770971 ) ) ;
#85975 = CARTESIAN_POINT ( 'NONE',  ( -16.46253265017146816, -9.564922557961047289, 64.16775706135233293 ) ) ;
#85976 = CARTESIAN_POINT ( 'NONE',  ( -16.53943276465976808, 0.05219959533911058130, 26.24890960531435624 ) ) ;
#85978 = EDGE_CURVE ( 'NONE', #14496, #145279, #153236, .T. ) ;
#85977 = CARTESIAN_POINT ( 'NONE',  ( 5.719274019375673035, 21.55341960407619339, 62.29275706135236845 ) ) ;
#85979 = CARTESIAN_POINT ( 'NONE',  ( 9.474510206698971260, -16.51473224551069308, 67.91557627198102409 ) ) ;
#85980 = CARTESIAN_POINT ( 'NONE',  ( -19.02544592524334988, -5.153800228976617603, 28.95942372801900433 ) ) ;
#85981 = CARTESIAN_POINT ( 'NONE',  ( 5.719274019375991003, -21.55341960407610458, 32.70724293864770260 ) ) ;
#85982 = CARTESIAN_POINT ( 'NONE',  ( 5.823673210054444382, -21.52544592524334988, 35.20942372801901854 ) ) ;
#85983 = CARTESIAN_POINT ( 'NONE',  ( -18.62759615963270932, 10.81492255796079327, 105.8322429386476955 ) ) ;
#85984 = CARTESIAN_POINT ( 'NONE',  ( -16.51473224551082808, 9.474510206698731452, 98.33442372801900433 ) ) ;
#85985 = CARTESIAN_POINT ( 'NONE',  ( 4.379528057220092307, 16.55341960407617563, 52.29275706135236135 ) ) ;
#85987 = CARTESIAN_POINT ( 'NONE',  ( 10.81492255796078972, 18.62759615963270932, 99.58224293864770971 ) ) ;
#85986 = CARTESIAN_POINT ( 'NONE',  ( -17.49999999999999289, 5.500000000000034639, 55.79690382534172954 ) ) ;
#85988 = CARTESIAN_POINT ( 'NONE',  ( -4.483927247898539470, -16.52544592524342804, 87.29057627198103830 ) ) ;
#85989 = CARTESIAN_POINT ( 'NONE',  ( 0.2731799622684817352, 31.88037471264000544, -45.67814385241111808 ) ) ;
#85990 = CARTESIAN_POINT ( 'NONE',  ( 16.52544592524335698, 4.483927247898782831, 26.45942372801901854 ) ) ;
#85991 = CARTESIAN_POINT ( 'NONE',  ( -21.53943276465977519, 0.05219959533907696930, 51.24890960531436690 ) ) ;
#85992 = CARTESIAN_POINT ( 'NONE',  ( 4.483927247898790824, -16.52544592524335698, 95.20942372801903275 ) ) ;
#85993 = CARTESIAN_POINT ( 'NONE',  ( 24.42644823724867464, -27.78615197534793069, -8.000000000000001776 ) ) ;
#85994 = EDGE_CURVE ( 'NONE', #100015, #87857, #47940, .T. ) ;
#85995 = CARTESIAN_POINT ( 'NONE',  ( 0.05219959533934541429, -16.53943276465976808, 50.00109039468568994 ) ) ;
#85996 = CARTESIAN_POINT ( 'NONE',  ( -21.52544592524334988, -5.823673210054445271, 28.95942372801902209 ) ) ;
#85997 = CARTESIAN_POINT ( 'NONE',  ( 15.72974639402199770, -15.80617190586745480, 48.12390960531436690 ) ) ;
#85998 = CARTESIAN_POINT ( 'NONE',  ( -14.34966873604972548, 8.224510206698743886, 78.33442372801901854 ) ) ;
#85999 = CARTESIAN_POINT ( 'NONE',  ( 13.97604488694527802, 13.89961937509977652, 104.3739096053143385 ) ) ;
#86000 = CARTESIAN_POINT ( 'NONE',  ( -15.72974639402176322, -15.80617190586768395, 69.37609039468567573 ) ) ;
#86001 = CARTESIAN_POINT ( 'NONE',  ( 21.53943276465977519, -0.05219959533907433946, 33.74890960531436690 ) ) ;
#86002 = CARTESIAN_POINT ( 'NONE',  ( 10.81492255796078972, 18.62759615963270932, 24.58224293864768839 ) ) ;
#86003 = ORIENTED_EDGE ( 'NONE', *, *, #27064, .F. ) ;
#86004 = CARTESIAN_POINT ( 'NONE',  ( -19.03943276465977164, -0.05219959533935918106, 58.75109039468566863 ) ) ;
#86005 = CARTESIAN_POINT ( 'NONE',  ( -12.14591786802326823, 12.06949235617739902, 63.12609039468568994 ) ) ;
#86006 = CARTESIAN_POINT ( 'NONE',  ( -15.72974639402197994, 15.80617190586746368, 35.62390960531437401 ) ) ;
#86007 = ORIENTED_EDGE ( 'NONE', *, *, #173264, .F. ) ;
#86008 = CARTESIAN_POINT ( 'NONE',  ( -9.474510206698964154, 16.51473224551069663, 90.41557627198103830 ) ) ;
#86009 = CARTESIAN_POINT ( 'NONE',  ( -14.29746914071037622, -8.314922557961029526, 109.1677570613523613 ) ) ;
#86010 = CYLINDRICAL_SURFACE ( 'NONE', #34336, 4.000000000000000888 ) ;
#86011 = CARTESIAN_POINT ( 'NONE',  ( -12.14591786802309592, -12.06949235617757132, 106.8739096053143811 ) ) ;
#86012 = CARTESIAN_POINT ( 'NONE',  ( -5.719274019375978568, 21.55341960407610458, 45.20724293864769550 ) ) ;
#86013 = CARTESIAN_POINT ( 'NONE',  ( -13.97604488694527625, -13.89961937509977652, 41.87390960531435979 ) ) ;
#86014 = CARTESIAN_POINT ( 'NONE',  ( 0.05219959533934541429, -16.53943276465976808, 80.00109039468568994 ) ) ;
#86015 = CARTESIAN_POINT ( 'NONE',  ( 21.52544592524334988, 5.823673210054432836, 31.45942372801901854 ) ) ;
#86016 = CARTESIAN_POINT ( 'NONE',  ( 16.51473224551083163, -9.474510206698727899, 95.83442372801900433 ) ) ;
#86017 = CARTESIAN_POINT ( 'NONE',  ( -16.52544592524342804, 4.483927247898546575, 96.04057627198102409 ) ) ;
#86018 = CARTESIAN_POINT ( 'NONE',  ( -5.153800228976328057, -19.02544592524343514, 57.29057627198103120 ) ) ;
#86019 = VECTOR ( 'NONE', #30250, 1000.000000000000000 ) ;
#86020 = CARTESIAN_POINT ( 'NONE',  ( 13.97604488694527802, 13.89961937509977652, 29.37390960531435979 ) ) ;
#86021 = CARTESIAN_POINT ( 'NONE',  ( -18.62759615963255300, -10.81492255796106328, 109.1677570613523613 ) ) ;
#86022 = CARTESIAN_POINT ( 'NONE',  ( 19.03943276465977164, -0.05219959533909143690, 73.74890960531435269 ) ) ;
#86023 = CARTESIAN_POINT ( 'NONE',  ( -14.29746914071037622, -8.314922557961029526, 64.16775706135234714 ) ) ;
#86024 = CARTESIAN_POINT ( 'NONE',  ( 21.53943276465977519, 0.05219959533937863772, 96.25109039468568994 ) ) ;
#86025 = CARTESIAN_POINT ( 'NONE',  ( 16.55341960407618274, -4.379528057220086978, 71.04275706135234714 ) ) ;
#86026 = CARTESIAN_POINT ( 'NONE',  ( -16.51473224551082808, 9.474510206698731452, 58.33442372801900433 ) ) ;
#86027 = EDGE_CURVE ( 'NONE', #83484, #113002, #64099, .T. ) ;
#86028 = CARTESIAN_POINT ( 'NONE',  ( 19.05341960407617918, -5.049401038297876454, 66.04275706135233293 ) ) ;
#86029 = ORIENTED_EDGE ( 'NONE', *, *, #175799, .F. ) ;
#86030 = CARTESIAN_POINT ( 'NONE',  ( -21.53943276465977519, -0.05219959533937600094, 63.75109039468568284 ) ) ;
#86031 = CARTESIAN_POINT ( 'NONE',  ( 13.97604488694527802, 13.89961937509977652, 69.37390960531436690 ) ) ;
#86032 = CARTESIAN_POINT ( 'NONE',  ( -5.153800228976328057, -19.02544592524343514, 57.29057627198103120 ) ) ;
#86033 = CARTESIAN_POINT ( 'NONE',  ( 9.564922557961047289, -16.46253265017146816, 65.41775706135233293 ) ) ;
#86034 = CARTESIAN_POINT ( 'NONE',  ( -13.89961937509977652, 13.97604488694528158, 115.6239096053143669 ) ) ;
#86035 = CARTESIAN_POINT ( 'NONE',  ( -19.03943276465977164, 0.05219959533909376836, 81.24890960531436690 ) ) ;
#86036 = CARTESIAN_POINT ( 'NONE',  ( -0.05219959533910754901, -16.53943276465976808, 42.49890960531435979 ) ) ;
#86037 = CARTESIAN_POINT ( 'NONE',  ( -5.823673210054116645, -21.52544592524344225, 47.29057627198103120 ) ) ;
#86038 = CARTESIAN_POINT ( 'NONE',  ( 20.43538597629129328, 20.43538597629121156, -52.65483682830182488 ) ) ;
#86039 = CARTESIAN_POINT ( 'NONE',  ( 21.55341960407619695, -5.719274019375665929, 106.0427570613523471 ) ) ;
#86040 = CARTESIAN_POINT ( 'NONE',  ( -9.564922557960796823, -16.46253265017161027, 52.08224293864768839 ) ) ;
#86041 = DIRECTION ( 'NONE',  ( 0.06104853953485701173, 0.000000000000000000, -0.9981347984218670311 ) ) ;
#86042 = CARTESIAN_POINT ( 'NONE',  ( -33.76764775315835010, -5.498935319396523802, 94.62547034095167930 ) ) ;
#86043 = CARTESIAN_POINT ( 'NONE',  ( -17.50000000000001421, -5.499999999999956479, 26.28230962303566542 ) ) ;
#86044 = CARTESIAN_POINT ( 'NONE',  ( -4.483927247898782831, 16.52544592524335698, 57.70942372801901143 ) ) ;
#86045 = CARTESIAN_POINT ( 'NONE',  ( -21.55341960407610458, -5.719274019375992779, 76.45724293864769550 ) ) ;
#86046 = CARTESIAN_POINT ( 'NONE',  ( 12.14591786802309770, 12.06949235617756955, 59.37390960531436690 ) ) ;
#86048 = CARTESIAN_POINT ( 'NONE',  ( -16.46253265017160317, 9.564922557960807481, 115.8322429386477097 ) ) ;
#86047 = CARTESIAN_POINT ( 'NONE',  ( 5.153800228976335163, 19.02544592524342804, 24.79057627198102765 ) ) ;
#86049 = CARTESIAN_POINT ( 'NONE',  ( 0.05219959533937995610, -21.53943276465977519, 40.00109039468567573 ) ) ;
#86050 = CARTESIAN_POINT ( 'NONE',  ( 16.46253265017146816, 9.564922557961045513, 46.66775706135233293 ) ) ;
#86051 = CARTESIAN_POINT ( 'NONE',  ( -5.153800228976328057, -19.02544592524343514, 37.29057627198102409 ) ) ;
#86052 = CARTESIAN_POINT ( 'NONE',  ( 18.62759615963255655, 10.81492255796105972, 86.66775706135234714 ) ) ;
#86053 = CARTESIAN_POINT ( 'NONE',  ( 31.99999999999970868, 4.794320942884877174E-13, 42.30000000000021743 ) ) ;
#86054 = CARTESIAN_POINT ( 'NONE',  ( -16.52544592524342804, 4.483927247898546575, 36.04057627198102409 ) ) ;
#86055 = CARTESIAN_POINT ( 'NONE',  ( 17.49999999999999645, 5.076555817581245300, 113.6795149204977236 ) ) ;
#86056 = CARTESIAN_POINT ( 'NONE',  ( -15.80617190586745835, -15.72974639402198527, 46.87390960531435979 ) ) ;
#86057 = DIRECTION ( 'NONE',  ( -0.000000000000000000, -6.938893903907222856E-15, -1.000000000000000000 ) ) ;
#86058 = CARTESIAN_POINT ( 'NONE',  ( -13.89961937509977652, 13.97604488694528158, 85.62390960531433848 ) ) ;
#86059 = CARTESIAN_POINT ( 'NONE',  ( 8.314922557960818139, 14.29746914071049879, 94.58224293864769550 ) ) ;
#86060 = CARTESIAN_POINT ( 'NONE',  ( -4.483927247898782831, 16.52544592524335698, 22.70942372801901499 ) ) ;
#86061 = CARTESIAN_POINT ( 'NONE',  ( -21.52544592524343514, 5.823673210054127303, 61.04057627198103120 ) ) ;
#86062 = EDGE_LOOP ( 'NONE', ( #94788, #106290, #153550, #107477 ) ) ;
#86063 = CARTESIAN_POINT ( 'NONE',  ( 19.03943276465977164, -0.05219959533909143690, 33.74890960531435979 ) ) ;
#86065 = CARTESIAN_POINT ( 'NONE',  ( -10.72451020669898014, 18.67979575497178502, 95.41557627198102409 ) ) ;
#86064 = CARTESIAN_POINT ( 'NONE',  ( -16.51473224551069308, -9.474510206698971260, 86.66557627198102409 ) ) ;
#86067 = CARTESIAN_POINT ( 'NONE',  ( 5.049401038298161559, -19.05341960407611168, 97.70724293864766707 ) ) ;
#86066 = CARTESIAN_POINT ( 'NONE',  ( 4.379528057220092307, 16.55341960407617563, 112.2927570613523471 ) ) ;
#86068 = CARTESIAN_POINT ( 'NONE',  ( 9.564922557961047289, -16.46253265017146816, 85.41775706135233293 ) ) ;
#86069 = CARTESIAN_POINT ( 'NONE',  ( -15.80617190586768217, 15.72974639402176855, 103.1260903946856757 ) ) ;
#86070 = CARTESIAN_POINT ( 'NONE',  ( -10.72451020669898014, 18.67979575497178502, 70.41557627198102409 ) ) ;
#86071 = CARTESIAN_POINT ( 'NONE',  ( -15.72974639402197994, 15.80617190586746368, 35.62390960531437401 ) ) ;
#86072 = CARTESIAN_POINT ( 'NONE',  ( 9.564922557960805705, 16.46253265017160317, 54.58224293864769550 ) ) ;
#86073 = CARTESIAN_POINT ( 'NONE',  ( 12.14591786802309770, 12.06949235617756955, 24.37390960531435979 ) ) ;
#86074 = CARTESIAN_POINT ( 'NONE',  ( 19.05341960407611168, 5.049401038298154454, 73.95724293864768129 ) ) ;
#86075 = DIRECTION ( 'NONE',  ( 0.000000000000000000, 0.000000000000000000, 1.000000000000000000 ) ) ;
#86076 = CARTESIAN_POINT ( 'NONE',  ( 9.564922557961047289, -16.46253265017146816, 30.41775706135232937 ) ) ;
#86077 = CARTESIAN_POINT ( 'NONE',  ( -16.52544592524342804, 4.483927247898546575, 91.04057627198103830 ) ) ;
#86078 = CARTESIAN_POINT ( 'NONE',  ( 5.719274019375673035, 21.55341960407619339, 22.29275706135235069 ) ) ;
#86079 = CARTESIAN_POINT ( 'NONE',  ( 17.14385361876520264, 23.59649016807275856, 146.6750000027311671 ) ) ;
#86080 = CARTESIAN_POINT ( 'NONE',  ( 21.52544592524344225, -5.823673210054117533, 68.54057627198103830 ) ) ;
#86081 = CARTESIAN_POINT ( 'NONE',  ( -12.14591786802326823, 12.06949235617739902, 88.12609039468570415 ) ) ;
#86082 = CARTESIAN_POINT ( 'NONE',  ( -8.314922557960811034, -14.29746914071050412, 112.0822429386477097 ) ) ;
#86083 = CARTESIAN_POINT ( 'NONE',  ( 16.46253265017160672, -9.564922557960803928, 73.33224293864769550 ) ) ;
#86084 =( NAMED_UNIT ( * ) PLANE_ANGLE_UNIT ( ) SI_UNIT ( $, .RADIAN. ) );
#86085 = CARTESIAN_POINT ( 'NONE',  ( 11.74149087413295156, -36.13659316521243881, -5.147842220587802942 ) ) ;
#86086 = CARTESIAN_POINT ( 'NONE',  ( -0.05219959533910754901, -16.53943276465976808, 32.49890960531435979 ) ) ;
#86087 = CARTESIAN_POINT ( 'NONE',  ( -15.72974639402176322, -15.80617190586768395, 59.37609039468568284 ) ) ;
#86088 = CARTESIAN_POINT ( 'NONE',  ( -19.05341960407611168, -5.049401038298163336, 106.4572429386476955 ) ) ;
#86089 = CARTESIAN_POINT ( 'NONE',  ( -21.52544592524334988, -5.823673210054445271, 88.95942372801901854 ) ) ;
#86090 = CARTESIAN_POINT ( 'NONE',  ( 13.97604488694527802, 13.89961937509977652, 44.37390960531435269 ) ) ;
#86091 = CARTESIAN_POINT ( 'NONE',  ( -19.02544592524342804, 5.153800228976336051, 51.04057627198103120 ) ) ;
#86092 = EDGE_LOOP ( 'NONE', ( #137838, #150006 ) ) ;
#86093 = CARTESIAN_POINT ( 'NONE',  ( -10.72451020669870658, -18.67979575497194134, 99.58442372801900433 ) ) ;
#86094 = CARTESIAN_POINT ( 'NONE',  ( -12.06949235617739369, -12.14591786802326823, 64.37609039468568994 ) ) ;
#86095 = CARTESIAN_POINT ( 'NONE',  ( -15.80617190586768217, 15.72974639402176855, 83.12609039468568994 ) ) ;
#86096 = CARTESIAN_POINT ( 'NONE',  ( -10.72451020669898014, 18.67979575497178502, 25.41557627198103120 ) ) ;
#86097 = CARTESIAN_POINT ( 'NONE',  ( -13.89961937509957401, -13.97604488694547875, 94.37609039468566152 ) ) ;
#86098 = CARTESIAN_POINT ( 'NONE',  ( 15.72974639402176855, 15.80617190586768217, 56.87609039468568994 ) ) ;
#86099 = CARTESIAN_POINT ( 'NONE',  ( 4.379528057220092307, 16.55341960407617563, 42.29275706135235424 ) ) ;
#86100 = CARTESIAN_POINT ( 'NONE',  ( 0.05219959533907565091, 21.53943276465977519, 84.99890960531436690 ) ) ;
#86101 = CARTESIAN_POINT ( 'NONE',  ( -5.153800228976607833, 19.02544592524334988, 82.70942372801897591 ) ) ;
#86102 = CARTESIAN_POINT ( 'NONE',  ( -13.97604488694527625, -13.89961937509977652, 66.87390960531436690 ) ) ;
#86103 = CARTESIAN_POINT ( 'NONE',  ( 19.05341960407617918, -5.049401038297876454, 101.0427570613523045 ) ) ;
#86104 = CARTESIAN_POINT ( 'NONE',  ( -19.02544592524334988, -5.153800228976617603, 83.95942372801901854 ) ) ;
#86105 = CARTESIAN_POINT ( 'NONE',  ( 16.52544592524342804, -4.483927247898539470, 53.54057627198103120 ) ) ;
#86106 = ADVANCED_FACE ( 'NONE', ( #106739 ), #105750, .T. ) ;
#86107 = CARTESIAN_POINT ( 'NONE',  ( -13.89961937509957401, -13.97604488694547875, 79.37609039468567573 ) ) ;
#86108 = CARTESIAN_POINT ( 'NONE',  ( -14.29746914071037622, -8.314922557961029526, 59.16775706135234714 ) ) ;
#86109 = CARTESIAN_POINT ( 'NONE',  ( 13.97604488694548053, -13.89961937509957401, 35.62609039468567573 ) ) ;
#86110 = CARTESIAN_POINT ( 'NONE',  ( 5.049401038298161559, -19.05341960407611168, 42.70724293864767418 ) ) ;
#86111 = CARTESIAN_POINT ( 'NONE',  ( -0.05219959533909027116, -19.03943276465977164, 37.49890960531436690 ) ) ;
#86112 = CARTESIAN_POINT ( 'NONE',  ( -14.34966873604972548, 8.224510206698743886, 63.33442372801900433 ) ) ;
#86113 = DIRECTION ( 'NONE',  ( -0.4999999999999945599, 0.5000000000000066613, 0.7071067811865467956 ) ) ;
#86114 = CARTESIAN_POINT ( 'NONE',  ( -17.81289503416611097, -24.51734667627696496, 140.5500000054623513 ) ) ;
#86115 = CARTESIAN_POINT ( 'NONE',  ( 13.89961937509977652, -13.97604488694527269, 108.1239096053143669 ) ) ;
#86116 = CARTESIAN_POINT ( 'NONE',  ( -16.46253265017160317, 9.564922557960807481, 25.83224293864769194 ) ) ;
#86117 = ORIENTED_EDGE ( 'NONE', *, *, #125997, .T. ) ;
#86118 = CARTESIAN_POINT ( 'NONE',  ( 16.51473224551083163, -9.474510206698727899, 100.8344237280190043 ) ) ;
#86119 = CARTESIAN_POINT ( 'NONE',  ( -18.62759615963270932, 10.81492255796079327, 40.83224293864769550 ) ) ;
#86121 = CARTESIAN_POINT ( 'NONE',  ( 9.474510206698729675, 16.51473224551082808, 107.0844237280190043 ) ) ;
#86120 = CARTESIAN_POINT ( 'NONE',  ( 5.153800228976615827, -19.02544592524334988, 25.20942372801900433 ) ) ;
#86122 = CARTESIAN_POINT ( 'NONE',  ( -16.46253265017160317, 9.564922557960807481, 25.83224293864769194 ) ) ;
#86123 = CARTESIAN_POINT ( 'NONE',  ( 13.97604488694527802, 13.89961937509977652, 44.37390960531435269 ) ) ;
#86124 = CARTESIAN_POINT ( 'NONE',  ( 21.52544592524344225, -5.823673210054117533, 68.54057627198103830 ) ) ;
#86125 = CARTESIAN_POINT ( 'NONE',  ( 16.46253265017160672, -9.564922557960803928, 98.33224293864769550 ) ) ;
#86126 = CARTESIAN_POINT ( 'NONE',  ( -5.049401038298153566, 19.05341960407611168, 40.20724293864768839 ) ) ;
#86127 = CARTESIAN_POINT ( 'NONE',  ( -27.73933785331498925, 2.428612866367529932E-14, 143.3750000027311842 ) ) ;
#86128 = CARTESIAN_POINT ( 'NONE',  ( 9.564922557961047289, -16.46253265017146816, 90.41775706135234714 ) ) ;
#86129 = CARTESIAN_POINT ( 'NONE',  ( 14.34966873604960469, 8.224510206698951720, 49.16557627198102409 ) ) ;
#86130 = CARTESIAN_POINT ( 'NONE',  ( 21.55341960407610458, 5.719274019375980345, 33.95724293864769550 ) ) ;
#86131 = CARTESIAN_POINT ( 'NONE',  ( -21.53943276465977519, -0.05219959533937600094, 103.7510903946857042 ) ) ;
#86132 = CARTESIAN_POINT ( 'NONE',  ( 5.719274019375991003, -21.55341960407610458, 102.7072429386476955 ) ) ;
#86133 = CARTESIAN_POINT ( 'NONE',  ( -10.81492255796105439, 18.62759615963255655, 77.91775706135231871 ) ) ;
#86134 = CARTESIAN_POINT ( 'NONE',  ( -21.52544592524334988, -5.823673210054445271, 73.95942372801901854 ) ) ;
#86135 = EDGE_CURVE ( 'NONE', #165860, #41053, #186801, .T. ) ;
#86136 = CARTESIAN_POINT ( 'NONE',  ( 19.02544592524343514, -5.153800228976328945, 113.5405762719810241 ) ) ;
#86138 = CARTESIAN_POINT ( 'NONE',  ( -0.05219959533937732626, 21.53943276465977519, 57.50109039468568994 ) ) ;
#86137 = CARTESIAN_POINT ( 'NONE',  ( 4.379528057220092307, 16.55341960407617563, 112.2927570613523471 ) ) ;
#86139 = CARTESIAN_POINT ( 'NONE',  ( 19.03943276465977164, -0.05219959533909143690, 68.74890960531436690 ) ) ;
#86140 = CARTESIAN_POINT ( 'NONE',  ( 16.51473224551083163, -9.474510206698727899, 40.83442372801900433 ) ) ;
#86141 = CARTESIAN_POINT ( 'NONE',  ( 18.67979575497194134, -10.72451020669871369, 35.83442372801901143 ) ) ;
#86142 = CARTESIAN_POINT ( 'NONE',  ( -13.89961937509977652, 13.97604488694528158, 65.62390960531436690 ) ) ;
#86143 = CARTESIAN_POINT ( 'NONE',  ( 8.224510206698953496, -14.34966873604960469, 77.91557627198102409 ) ) ;
#86144 = CARTESIAN_POINT ( 'NONE',  ( -16.53943276465976808, 0.05219959533911058130, 41.24890960531435269 ) ) ;
#86145 = CARTESIAN_POINT ( 'NONE',  ( -18.62759615963270932, 10.81492255796079327, 50.83224293864770971 ) ) ;
#86146 = CARTESIAN_POINT ( 'NONE',  ( -9.564922557960796823, -16.46253265017161027, 57.08224293864769550 ) ) ;
#86147 = CARTESIAN_POINT ( 'NONE',  ( 21.52544592524344225, -5.823673210054117533, 78.54057627198103830 ) ) ;
#86148 = CARTESIAN_POINT ( 'NONE',  ( -5.049401038297874678, -19.05341960407617918, 44.79275706135232582 ) ) ;
#86151 = CARTESIAN_POINT ( 'NONE',  ( -12.14591786802309592, -12.06949235617757132, 56.87390960531436690 ) ) ;
#86150 = CARTESIAN_POINT ( 'NONE',  ( -5.049401038297874678, -19.05341960407618274, 19.79275706135233293 ) ) ;
#86149 = CIRCLE ( 'NONE', #40998, 0.5000000000000041078 ) ;
#86152 = CARTESIAN_POINT ( 'NONE',  ( -18.62759615963270932, 10.81492255796079327, 40.83224293864769550 ) ) ;
#86153 = ORIENTED_EDGE ( 'NONE', *, *, #64134, .F. ) ;
#86154 = DIRECTION ( 'NONE',  ( -0.000000000000000000, -0.000000000000000000, -1.000000000000000000 ) ) ;
#86156 = CARTESIAN_POINT ( 'NONE',  ( 27.73933785331498569, 9.013057229001093518, 147.9750000027311501 ) ) ;
#86155 = CARTESIAN_POINT ( 'NONE',  ( -0.05219959533934338120, 16.53943276465976808, 87.50109039468568994 ) ) ;
#86157 = CARTESIAN_POINT ( 'NONE',  ( 19.02544592524334988, 5.153800228976608722, 91.45942372801900433 ) ) ;
#86158 = CARTESIAN_POINT ( 'NONE',  ( 16.52544592524342804, -4.483927247898539470, 48.54057627198103120 ) ) ;
#86159 = CARTESIAN_POINT ( 'NONE',  ( -18.22780087662121673, -5.500000000000063061, 61.48459894673894155 ) ) ;
#86160 = CARTESIAN_POINT ( 'NONE',  ( 9.564922557960805705, 16.46253265017160317, 44.58224293864769550 ) ) ;
#86161 = CARTESIAN_POINT ( 'NONE',  ( 14.34966873604960469, 8.224510206698951720, 44.16557627198103120 ) ) ;
#86162 = CARTESIAN_POINT ( 'NONE',  ( 13.89961937509977652, -13.97604488694527269, 88.12390960531438111 ) ) ;
#86163 = CARTESIAN_POINT ( 'NONE',  ( -5.153800228976328057, -19.02544592524343514, 52.29057627198100988 ) ) ;
#86164 = CARTESIAN_POINT ( 'NONE',  ( -18.62759615963255300, -10.81492255796106328, 64.16775706135234714 ) ) ;
#86165 = CARTESIAN_POINT ( 'NONE',  ( -13.97604488694527625, -13.89961937509977652, 71.87390960531433848 ) ) ;
#86166 = CARTESIAN_POINT ( 'NONE',  ( 0.05219959533909260263, 19.03943276465977164, 29.99890960531435979 ) ) ;
#86167 = AXIS2_PLACEMENT_3D ( 'NONE', #116846, #23852, #145175 ) ;
#86168 = CARTESIAN_POINT ( 'NONE',  ( 13.89961937509977652, -13.97604488694527269, 78.12390960531433848 ) ) ;
#86169 = CARTESIAN_POINT ( 'NONE',  ( 5.823673210054125526, 21.52544592524343514, 44.79057627198103120 ) ) ;
#86170 = CARTESIAN_POINT ( 'NONE',  ( 16.51473224551069308, 9.474510206698969483, 34.16557627198102409 ) ) ;
#86171 = CARTESIAN_POINT ( 'NONE',  ( 10.81492255796078972, 18.62759615963270932, 44.58224293864769550 ) ) ;
#86172 = CARTESIAN_POINT ( 'NONE',  ( -16.53943276465976808, -0.05219959533934237506, 103.7510903946857042 ) ) ;
#86173 = CARTESIAN_POINT ( 'NONE',  ( 5.049401038297881783, 19.05341960407617563, 22.29275706135233648 ) ) ;
#86175 = CARTESIAN_POINT ( 'NONE',  ( -16.52544592524335698, -4.483927247898792601, 78.95942372801901854 ) ) ;
#86174 = CARTESIAN_POINT ( 'NONE',  ( -8.314922557961024197, 14.29746914071037800, 47.91775706135234714 ) ) ;
#86176 = DIRECTION ( 'NONE',  ( 0.000000000000000000, 0.000000000000000000, 1.000000000000000000 ) ) ;
#86177 = CARTESIAN_POINT ( 'NONE',  ( -16.53943276465976808, -0.05219959533934237506, 73.75109039468567573 ) ) ;
#86178 = CARTESIAN_POINT ( 'NONE',  ( -21.52544592524343514, 5.823673210054127303, 26.04057627198103475 ) ) ;
#86179 = CARTESIAN_POINT ( 'NONE',  ( 13.89961937509977652, -13.97604488694527269, 33.12390960531434558 ) ) ;
#86180 = CARTESIAN_POINT ( 'NONE',  ( 12.14591786802327356, -12.06949235617739191, 35.62609039468568994 ) ) ;
#86181 = CARTESIAN_POINT ( 'NONE',  ( -9.564922557960796823, -16.46253265017161027, 52.08224293864768839 ) ) ;
#86182 = CARTESIAN_POINT ( 'NONE',  ( 5.719274019375673035, 21.55341960407619339, 37.29275706135235424 ) ) ;
#86183 = CARTESIAN_POINT ( 'NONE',  ( 16.55341960407618274, -4.379528057220086978, 36.04275706135234714 ) ) ;
#86184 = CARTESIAN_POINT ( 'NONE',  ( -14.29746914071037622, -8.314922557961029526, 104.1677570613523471 ) ) ;
#86185 = FACE_OUTER_BOUND ( 'NONE', #113563, .T. ) ;
#86186 = CARTESIAN_POINT ( 'NONE',  ( 18.67979575497194134, -10.72451020669871369, 95.83442372801903275 ) ) ;
#86187 = CARTESIAN_POINT ( 'NONE',  ( 9.564922557961047289, -16.46253265017146816, 90.41775706135234714 ) ) ;
#86188 = CARTESIAN_POINT ( 'NONE',  ( -0.05219959533936034679, 19.03943276465977164, 52.50109039468566863 ) ) ;
#86189 = CARTESIAN_POINT ( 'NONE',  ( -16.55341960407611168, -4.379528057220339221, 66.45724293864768129 ) ) ;
#86190 = CARTESIAN_POINT ( 'NONE',  ( 4.483927247898545687, 16.52544592524342804, 114.7905762719810383 ) ) ;
#86192 = CARTESIAN_POINT ( 'NONE',  ( 17.48853670773247870, 5.747243402303063853, 78.83328700250008580 ) ) ;
#86191 = CARTESIAN_POINT ( 'NONE',  ( -5.049401038297874678, -19.05341960407617918, 59.79275706135231871 ) ) ;
#86193 = CARTESIAN_POINT ( 'NONE',  ( -5.823673210054431948, 21.52544592524334988, 62.70942372801902565 ) ) ;
#86194 = CARTESIAN_POINT ( 'NONE',  ( -16.52544592524335698, -4.483927247898792601, 33.95942372801901143 ) ) ;
#86195 = CARTESIAN_POINT ( 'NONE',  ( -17.49999999999998579, 5.500000000000031974, 90.79690382534171533 ) ) ;
#86196 = CARTESIAN_POINT ( 'NONE',  ( 0.05219959533907565091, 21.53943276465977519, 24.99890960531435624 ) ) ;
#86197 = CARTESIAN_POINT ( 'NONE',  ( -9.564922557961040184, 16.46253265017147172, 112.9177570613523329 ) ) ;
#86198 = CARTESIAN_POINT ( 'NONE',  ( -16.51473224551069308, -9.474510206698971260, 111.6655762719810383 ) ) ;
#86199 = CARTESIAN_POINT ( 'NONE',  ( -25.11239783071224707, 12.35465959875007336, 166.1131185557730987 ) ) ;
#86200 = CARTESIAN_POINT ( 'NONE',  ( -16.52544592524342804, 4.483927247898546575, 116.0405762719810383 ) ) ;
#86201 = CARTESIAN_POINT ( 'NONE',  ( -15.80617190586768217, 15.72974639402176855, 108.1260903946856757 ) ) ;
#86202 = CARTESIAN_POINT ( 'NONE',  ( -16.46253265017160317, 9.564922557960807481, 60.83224293864769550 ) ) ;
#86203 = CARTESIAN_POINT ( 'NONE',  ( -0.05219959533937732626, 21.53943276465977519, 67.50109039468568994 ) ) ;
#86204 = CARTESIAN_POINT ( 'NONE',  ( 15.80617190586769283, -15.72974639402175789, 95.62609039468568994 ) ) ;
#86205 = CARTESIAN_POINT ( 'NONE',  ( -4.483927247898539470, -16.52544592524342804, 22.29057627198102765 ) ) ;
#86206 = CARTESIAN_POINT ( 'NONE',  ( 16.51473224551069308, 9.474510206698969483, 79.16557627198103830 ) ) ;
#86207 = CARTESIAN_POINT ( 'NONE',  ( 15.72974639402176855, 15.80617190586768217, 61.87609039468568284 ) ) ;
#86208 = CARTESIAN_POINT ( 'NONE',  ( -15.72974639402176322, -15.80617190586768395, 49.37609039468569705 ) ) ;
#86210 = CARTESIAN_POINT ( 'NONE',  ( -19.02544592524342804, 5.153800228976336051, 111.0405762719810099 ) ) ;
#86209 = CARTESIAN_POINT ( 'NONE',  ( 16.46253265017146816, 9.564922557961045513, 76.66775706135234714 ) ) ;
#86211 = CARTESIAN_POINT ( 'NONE',  ( 13.89961937509977652, -13.97604488694527269, 23.12390960531436335 ) ) ;
#86212 = CARTESIAN_POINT ( 'NONE',  ( 10.72451020669898902, -18.67979575497178502, 102.9155762719810383 ) ) ;
#86213 = CARTESIAN_POINT ( 'NONE',  ( -9.564922557961040184, 16.46253265017147172, 37.91775706135233293 ) ) ;
#86214 = CARTESIAN_POINT ( 'NONE',  ( -14.29746914071049879, 8.314922557960819915, 90.83224293864769550 ) ) ;
#86215 = CARTESIAN_POINT ( 'NONE',  ( -9.474510206698964154, 16.51473224551069663, 45.41557627198103120 ) ) ;
#86216 = CARTESIAN_POINT ( 'NONE',  ( 5.049401038297881783, 19.05341960407617563, 102.2927570613523045 ) ) ;
#86217 = CARTESIAN_POINT ( 'NONE',  ( -16.52544592524342804, 4.483927247898546575, 56.04057627198102409 ) ) ;
#86218 = CARTESIAN_POINT ( 'NONE',  ( 15.72974639402176855, 15.80617190586768217, 106.8760903946856899 ) ) ;
#86219 = CARTESIAN_POINT ( 'NONE',  ( 13.97604488694527802, 13.89961937509977652, 99.37390960531436690 ) ) ;
#86220 = CARTESIAN_POINT ( 'NONE',  ( -9.474510206698720793, -16.51473224551083518, 74.58442372801900433 ) ) ;
#86221 = CARTESIAN_POINT ( 'NONE',  ( -21.53943276465977519, 0.05219959533907696930, 96.24890960531435269 ) ) ;
#86222 = CARTESIAN_POINT ( 'NONE',  ( 5.823673210054444382, -21.52544592524334988, 45.20942372801901854 ) ) ;
#86223 = CARTESIAN_POINT ( 'NONE',  ( 14.34966873604972726, -8.224510206698740333, 45.83442372801901854 ) ) ;
#86224 = CARTESIAN_POINT ( 'NONE',  ( -4.483927247898782831, 16.52544592524335698, 87.70942372801901854 ) ) ;
#86226 = CARTESIAN_POINT ( 'NONE',  ( -0.05219959533937732626, 21.53943276465977519, 32.50109039468568284 ) ) ;
#86225 = CARTESIAN_POINT ( 'NONE',  ( 16.53943276465976808, 0.05219959533934440121, 41.25109039468568284 ) ) ;
#86227 = CARTESIAN_POINT ( 'NONE',  ( 15.80617190586746368, 15.72974639402197994, 39.37390960531436690 ) ) ;
#86228 = CARTESIAN_POINT ( 'NONE',  ( -19.05341960407611168, -5.049401038298163336, 36.45724293864766707 ) ) ;
#86229 = CARTESIAN_POINT ( 'NONE',  ( -6.020228577223754586E-15, 39.95556452105416412, -10.24999999453762456 ) ) ;
#86230 = CARTESIAN_POINT ( 'NONE',  ( -16.55341960407617563, 4.379528057220093196, 58.54275706135235424 ) ) ;
#86231 = CARTESIAN_POINT ( 'NONE',  ( -10.72451020669898014, 18.67979575497178502, 95.41557627198102409 ) ) ;
#86232 = CARTESIAN_POINT ( 'NONE',  ( -4.483927247898539470, -16.52544592524342804, 32.29057627198102409 ) ) ;
#86233 = CARTESIAN_POINT ( 'NONE',  ( -8.314922557961024197, 14.29746914071037800, 67.91775706135234714 ) ) ;
#86234 = CARTESIAN_POINT ( 'NONE',  ( 19.05341960407611168, 5.049401038298154454, 63.95724293864769550 ) ) ;
#86235 = CARTESIAN_POINT ( 'NONE',  ( 13.97604488694548053, -13.89961937509957401, 85.62609039468568994 ) ) ;
#86236 = CARTESIAN_POINT ( 'NONE',  ( 18.67979575497178502, 10.72451020669898547, 79.16557627198103830 ) ) ;
#86237 = CARTESIAN_POINT ( 'NONE',  ( 12.14591786802309770, 12.06949235617756955, 29.37390960531435269 ) ) ;
#86238 = ORIENTED_EDGE ( 'NONE', *, *, #46300, .F. ) ;
#86239 = CARTESIAN_POINT ( 'NONE',  ( 26.62494319856311975, 7.396441074661496806, 168.1134502243650104 ) ) ;
#86240 = CARTESIAN_POINT ( 'NONE',  ( -21.55341960407610458, -5.719274019375992779, 66.45724293864768129 ) ) ;
#86241 = VERTEX_POINT ( 'NONE', #16726 ) ;
#86242 = CARTESIAN_POINT ( 'NONE',  ( -12.14591786802326823, 12.06949235617739902, 103.1260903946856757 ) ) ;
#86243 = ORIENTED_EDGE ( 'NONE', *, *, #175605, .T. ) ;
#86244 = CARTESIAN_POINT ( 'NONE',  ( 3.766062262543149401E-15, -39.95556452105413570, -3.499999999999999556 ) ) ;
#86245 = CARTESIAN_POINT ( 'NONE',  ( -10.81492255796078084, -18.62759615963271287, 92.08224293864769550 ) ) ;
#86246 = CARTESIAN_POINT ( 'NONE',  ( -16.55341960407611168, -4.379528057220339221, 21.45724293864769550 ) ) ;
#86247 = CARTESIAN_POINT ( 'NONE',  ( -14.29746914071037622, -8.314922557961029526, 34.16775706135234714 ) ) ;
#86248 = CARTESIAN_POINT ( 'NONE',  ( 0.05219959533909260263, 19.03943276465977164, 29.99890960531435979 ) ) ;
#86249 = CARTESIAN_POINT ( 'NONE',  ( -19.03943276465977164, 0.05219959533909376836, 66.24890960531436690 ) ) ;
#86250 = CARTESIAN_POINT ( 'NONE',  ( -23.31738231874055600, 16.94106989632528837, 145.7999999999999829 ) ) ;
#86251 = CARTESIAN_POINT ( 'NONE',  ( -0.05219959533907301413, -21.53943276465977519, 22.49890960531436335 ) ) ;
#86252 = CARTESIAN_POINT ( 'NONE',  ( 0.000000000000000000, 5.051668046482832750E-16, -4.000000000000000000 ) ) ;
#86253 = CARTESIAN_POINT ( 'NONE',  ( 16.55341960407618274, -4.379528057220086978, 101.0427570613523756 ) ) ;
#86254 = CARTESIAN_POINT ( 'NONE',  ( 19.03943276465977164, 0.05219959533936151252, 111.2510903946856757 ) ) ;
#86255 = CARTESIAN_POINT ( 'NONE',  ( 13.97604488694548053, -13.89961937509957401, 35.62609039468567573 ) ) ;
#86256 = CARTESIAN_POINT ( 'NONE',  ( -5.823673210054116645, -21.52544592524344225, 87.29057627198103830 ) ) ;
#86257 = CARTESIAN_POINT ( 'NONE',  ( -8.314922557960811034, -14.29746914071050412, 22.08224293864769194 ) ) ;
#86258 = CARTESIAN_POINT ( 'NONE',  ( -10.81492255796078084, -18.62759615963271287, 52.08224293864768839 ) ) ;
#86260 = CARTESIAN_POINT ( 'NONE',  ( 9.474510206698729675, 16.51473224551082808, 112.0844237280190043 ) ) ;
#86259 = CARTESIAN_POINT ( 'NONE',  ( 10.81492255796078972, 18.62759615963270932, 84.58224293864769550 ) ) ;
#86261 = CARTESIAN_POINT ( 'NONE',  ( 5.049401038298161559, -19.05341960407611168, 107.7072429386476955 ) ) ;
#86262 = CARTESIAN_POINT ( 'NONE',  ( -21.55341960407619339, 5.719274019375674811, 78.54275706135236135 ) ) ;
#86263 = CARTESIAN_POINT ( 'NONE',  ( 5.153800228976335163, 19.02544592524342804, 64.79057627198100988 ) ) ;
#86264 = CARTESIAN_POINT ( 'NONE',  ( -12.14591786802309592, -12.06949235617757132, 106.8739096053143811 ) ) ;
#86265 = CARTESIAN_POINT ( 'NONE',  ( 31.69373074887816344, 1.710217150889069782, 102.3065243757510956 ) ) ;
#86266 = CARTESIAN_POINT ( 'NONE',  ( 16.51473224551069308, 9.474510206698969483, 74.16557627198103830 ) ) ;
#86267 = CARTESIAN_POINT ( 'NONE',  ( 8.224510206698953496, -14.34966873604960469, 92.91557627198103830 ) ) ;
#86268 = ORIENTED_EDGE ( 'NONE', *, *, #52445, .F. ) ;
#86269 = CARTESIAN_POINT ( 'NONE',  ( 5.153800228976615827, -19.02544592524334988, 95.20942372801897591 ) ) ;
#86270 = CARTESIAN_POINT ( 'NONE',  ( 17.40861289039004944, -6.110651285853253789, 81.12767529172569425 ) ) ;
#86271 = CARTESIAN_POINT ( 'NONE',  ( -9.564922557960796823, -16.46253265017161027, 57.08224293864769550 ) ) ;
#86273 = CARTESIAN_POINT ( 'NONE',  ( -13.89961937509977652, 13.97604488694528158, 95.62390960531436690 ) ) ;
#86272 = CARTESIAN_POINT ( 'NONE',  ( -15.80617190586768217, 15.72974639402176855, 88.12609039468570415 ) ) ;
#86274 = CARTESIAN_POINT ( 'NONE',  ( -16.52544592524335698, -4.483927247898792601, 73.95942372801901854 ) ) ;
#86275 = CARTESIAN_POINT ( 'NONE',  ( -17.50000000000000711, -5.500000000000025757, 51.28230962303570095 ) ) ;
#86276 = CARTESIAN_POINT ( 'NONE',  ( -9.474510206698720793, -16.51473224551083518, 49.58442372801899722 ) ) ;
#86277 = CARTESIAN_POINT ( 'NONE',  ( -5.719274019375665041, -21.55341960407619695, 104.7927570613523898 ) ) ;
#86278 = CARTESIAN_POINT ( 'NONE',  ( 37.99999999999999289, 2.428612866367529932E-14, 0.000000000000000000 ) ) ;
#86279 = CARTESIAN_POINT ( 'NONE',  ( 15.06137443927351249, -15.06137443927345210, -58.85720012050613548 ) ) ;
#86280 = CARTESIAN_POINT ( 'NONE',  ( -4.483927247898782831, 16.52544592524335698, 102.7094237280190185 ) ) ;
#86281 = CARTESIAN_POINT ( 'NONE',  ( 16.16661445520356821, -1.151164073136631272, -59.37042179516131313 ) ) ;
#86282 = CARTESIAN_POINT ( 'NONE',  ( 4.379528057220092307, 16.55341960407617563, 87.29275706135236135 ) ) ;
#86283 = CARTESIAN_POINT ( 'NONE',  ( -69.65682714487590488, -71.74905178543390605, -25.00000000000000000 ) ) ;
#86284 = CARTESIAN_POINT ( 'NONE',  ( 4.483927247898790824, -16.52544592524335698, 70.20942372801904696 ) ) ;
#86285 = ORIENTED_EDGE ( 'NONE', *, *, #89035, .F. ) ;
#86286 = B_SPLINE_CURVE_WITH_KNOTS ( 'NONE', 3,
 ( #48305, #124126, #198010, #122144, #168646, #44330, #184821, #46306, #107962, #59480, #185825, #15974, #32136, #14978 ),
 .UNSPECIFIED., .F., .F.,
 ( 4, 2, 2, 2, 2, 2, 4 ),
 ( 1.971416326048476669E-07, 0.0002961152624844829405, 0.0005920333833363609737, 0.0008879515041882391152, 0.001183869625040117257, 0.001775705866743883081, 0.002367542108447648688 ),
 .UNSPECIFIED. ) ;
#86287 = CARTESIAN_POINT ( 'NONE',  ( 0.05219959533937995610, -21.53943276465977519, 75.00109039468568994 ) ) ;
#86288 = CARTESIAN_POINT ( 'NONE',  ( 0.05219959533936267826, -19.03943276465977164, 90.00109039468567573 ) ) ;
#86289 = CARTESIAN_POINT ( 'NONE',  ( 0.05219959533936267826, -19.03943276465977164, 30.00109039468566863 ) ) ;
#86290 = CARTESIAN_POINT ( 'NONE',  ( 13.97604488694527802, 13.89961937509977652, 69.37390960531436690 ) ) ;
#86291 = CARTESIAN_POINT ( 'NONE',  ( 16.51473224551069308, 9.474510206698969483, 59.16557627198102409 ) ) ;
#86292 = DIRECTION ( 'NONE',  ( 0.000000000000000000, 0.000000000000000000, -1.000000000000000000 ) ) ;
#86293 = CARTESIAN_POINT ( 'NONE',  ( 0.05219959533907565091, 21.53943276465977519, 74.99890960531435269 ) ) ;
#86294 = AXIS2_PLACEMENT_3D ( 'NONE', #155248, #156237, #90587 ) ;
#86295 = CARTESIAN_POINT ( 'NONE',  ( 15.72974639402199770, -15.80617190586745480, 33.12390960531435979 ) ) ;
#86296 = CARTESIAN_POINT ( 'NONE',  ( 13.89961937509977652, -13.97604488694527269, 33.12390960531434558 ) ) ;
#86297 = CARTESIAN_POINT ( 'NONE',  ( 14.34966873604972726, -8.224510206698740333, 65.83442372801900433 ) ) ;
#86298 = ORIENTED_EDGE ( 'NONE', *, *, #176519, .T. ) ;
#86299 = CARTESIAN_POINT ( 'NONE',  ( 18.67979575497194134, -10.72451020669871369, 30.83442372801902209 ) ) ;
#86301 = CARTESIAN_POINT ( 'NONE',  ( 11.40812507854755253, -35.11059874428192273, -8.024999997268814411 ) ) ;
#86300 = CARTESIAN_POINT ( 'NONE',  ( 8.224510206698953496, -14.34966873604960469, 67.91557627198102409 ) ) ;
#86302 = CARTESIAN_POINT ( 'NONE',  ( 16.55341960407618274, -4.379528057220086978, 21.04275706135234714 ) ) ;
#86303 = CARTESIAN_POINT ( 'NONE',  ( -16.46253265017146816, -9.564922557961047289, 59.16775706135233293 ) ) ;
#86304 = CARTESIAN_POINT ( 'NONE',  ( 16.52544592524342804, -4.483927247898539470, 63.54057627198103830 ) ) ;
#86305 = CARTESIAN_POINT ( 'NONE',  ( 5.823673210054444382, -21.52544592524334988, 30.20942372801902565 ) ) ;
#86307 = CARTESIAN_POINT ( 'NONE',  ( 15.72974639402199770, -15.80617190586745480, 78.12390960531436690 ) ) ;
#86306 = CARTESIAN_POINT ( 'NONE',  ( 24.95432927374997334, -3.806786798636382141, 190.0000000000000000 ) ) ;
#86308 = CARTESIAN_POINT ( 'NONE',  ( 19.02544592524343514, -5.153800228976328945, 98.54057627198100988 ) ) ;
#86309 = CARTESIAN_POINT ( 'NONE',  ( -12.14591786802309592, -12.06949235617757132, 61.87390960531436690 ) ) ;
#86310 = CARTESIAN_POINT ( 'NONE',  ( 34.63261191446840570, -20.08610687337147382, -21.92908410840965772 ) ) ;
#86311 = CARTESIAN_POINT ( 'NONE',  ( 29.86685920354754487, 21.69954338932564752, -7.424999997268813878 ) ) ;
#86312 = CARTESIAN_POINT ( 'NONE',  ( -16.51473224551082808, 9.474510206698731452, 63.33442372801900433 ) ) ;
#86313 = CARTESIAN_POINT ( 'NONE',  ( 10.72451020669898902, -18.67979575497178502, 107.9155762719810241 ) ) ;
#86314 = CARTESIAN_POINT ( 'NONE',  ( 5.049401038298161559, -19.05341960407611168, 57.70724293864769550 ) ) ;
#86315 = B_SPLINE_CURVE_WITH_KNOTS ( 'NONE', 3,
 ( #131704, #84178, #68023, #55859, #7340, #129674 ),
 .UNSPECIFIED., .F., .F.,
 ( 4, 2, 4 ),
 ( 0.02150008358963344246, 0.02352197444946371035, 0.02554386530929397825 ),
 .UNSPECIFIED. ) ;
#86316 = CARTESIAN_POINT ( 'NONE',  ( 5.153800228976615827, -19.02544592524334988, 40.20942372801898301 ) ) ;
#86317 = CARTESIAN_POINT ( 'NONE',  ( 19.02544592524343514, -5.153800228976328945, 28.54057627198102409 ) ) ;
#86318 = CARTESIAN_POINT ( 'NONE',  ( 21.52544592524334988, 5.823673210054432836, 66.45942372801903275 ) ) ;
#86319 = VECTOR ( 'NONE', #90025, 1000.000000000000000 ) ;
#86320 = CARTESIAN_POINT ( 'NONE',  ( -28.96383432292632776, 7.816291847812730786, 151.8521076810907005 ) ) ;
#86321 = CARTESIAN_POINT ( 'NONE',  ( -8.314922557960811034, -14.29746914071050412, 47.08224293864770260 ) ) ;
#86322 = CARTESIAN_POINT ( 'NONE',  ( -0.05219959533909027116, -19.03943276465977164, 67.49890960531436690 ) ) ;
#86323 = CARTESIAN_POINT ( 'NONE',  ( 5.823673210054125526, 21.52544592524343514, 79.79057627198102409 ) ) ;
#86324 = CARTESIAN_POINT ( 'NONE',  ( 13.97604488694527802, 13.89961937509977652, 64.37390960531436690 ) ) ;
#86325 = ORIENTED_EDGE ( 'NONE', *, *, #103239, .F. ) ;
#86326 = CARTESIAN_POINT ( 'NONE',  ( 15.72974639402199770, -15.80617190586745480, 63.12390960531435979 ) ) ;
#86327 = CARTESIAN_POINT ( 'NONE',  ( 15.80617190586769283, -15.72974639402175789, 95.62609039468568994 ) ) ;
#86330 = CARTESIAN_POINT ( 'NONE',  ( -14.34966873604960291, -8.224510206698953496, 76.66557627198103830 ) ) ;
#86329 = CARTESIAN_POINT ( 'NONE',  ( -4.379528057220086978, -16.55341960407618274, 89.79275706135236135 ) ) ;
#86328 = CARTESIAN_POINT ( 'NONE',  ( 3.620324696381902907, -38.95353743399085289, -23.38767721381919884 ) ) ;
#86331 = CARTESIAN_POINT ( 'NONE',  ( 9.474510206698729675, 16.51473224551082808, 97.08442372801900433 ) ) ;
#86332 = ORIENTED_EDGE ( 'NONE', *, *, #28653, .F. ) ;
#86333 = CARTESIAN_POINT ( 'NONE',  ( 13.97604488694548053, -13.89961937509957401, 35.62609039468567573 ) ) ;
#86334 = CARTESIAN_POINT ( 'NONE',  ( -12.14591786802326823, 12.06949235617739902, 108.1260903946856757 ) ) ;
#86335 = CARTESIAN_POINT ( 'NONE',  ( -13.89961937509957401, -13.97604488694547875, 29.37609039468565797 ) ) ;
#86336 = CARTESIAN_POINT ( 'NONE',  ( 13.89961937509977652, -13.97604488694527269, 93.12390960531436690 ) ) ;
#86337 = CARTESIAN_POINT ( 'NONE',  ( 5.823673210054125526, 21.52544592524343514, 59.79057627198103120 ) ) ;
#86338 = CARTESIAN_POINT ( 'NONE',  ( -21.71309667856399628, -34.72214947970702781, -18.33762378602112264 ) ) ;
#86339 = CARTESIAN_POINT ( 'NONE',  ( 16.53943276465976808, -0.05219959533910856209, 113.7489096053143527 ) ) ;
#86340 = CARTESIAN_POINT ( 'NONE',  ( 10.81492255796106328, -18.62759615963255655, 95.41775706135234714 ) ) ;
#86341 = CARTESIAN_POINT ( 'NONE',  ( 16.52544592524335698, 4.483927247898782831, 71.45942372801901854 ) ) ;
#86342 = CARTESIAN_POINT ( 'NONE',  ( -18.62759615963255300, -10.81492255796106328, 29.16775706135234003 ) ) ;
#86343 = CARTESIAN_POINT ( 'NONE',  ( 4.483927247898790824, -16.52544592524335698, 25.20942372801901854 ) ) ;
#86344 = CARTESIAN_POINT ( 'NONE',  ( -19.03943276465977164, 0.05219959533909376836, 111.2489096053143669 ) ) ;
#86345 = CARTESIAN_POINT ( 'NONE',  ( 9.564922557960805705, 16.46253265017160317, 39.58224293864768839 ) ) ;
#86346 = CARTESIAN_POINT ( 'NONE',  ( -0.05219959533909027116, -19.03943276465977164, 57.49890960531435979 ) ) ;
#86347 = AXIS2_PLACEMENT_3D ( 'NONE', #162604, #24108, #26112 ) ;
#86348 = CARTESIAN_POINT ( 'NONE',  ( 4.483927247898790824, -16.52544592524335698, 50.20942372801901854 ) ) ;
#86349 = CARTESIAN_POINT ( 'NONE',  ( -8.314922557960811034, -14.29746914071050412, 92.08224293864769550 ) ) ;
#86350 = CARTESIAN_POINT ( 'NONE',  ( 14.29746914071037800, 8.314922557961029526, 106.6677570613523756 ) ) ;
#86353 = CARTESIAN_POINT ( 'NONE',  ( -19.02544592524342804, 5.153800228976336051, 61.04057627198103120 ) ) ;
#86352 = CARTESIAN_POINT ( 'NONE',  ( 19.02544592524343514, -5.153800228976328945, 83.54057627198100988 ) ) ;
#86351 = CARTESIAN_POINT ( 'NONE',  ( -10.81492255796105439, 18.62759615963255655, 37.91775706135235424 ) ) ;
#86354 = CARTESIAN_POINT ( 'NONE',  ( -5.049401038298153566, 19.05341960407611168, 85.20724293864766707 ) ) ;
#86355 = CARTESIAN_POINT ( 'NONE',  ( 14.34966873604960469, 8.224510206698951720, 29.16557627198103120 ) ) ;
#86356 = CARTESIAN_POINT ( 'NONE',  ( -8.224510206698735004, -14.34966873604973081, 104.5844237280190185 ) ) ;
#86357 = EDGE_LOOP ( 'NONE', ( #105686, #15093, #145758, #61939 ) ) ;
#86358 = CARTESIAN_POINT ( 'NONE',  ( -13.89961937509957401, -13.97604488694547875, 49.37609039468567573 ) ) ;
#86359 = CARTESIAN_POINT ( 'NONE',  ( 19.05341960407611168, 5.049401038298154454, 113.9572429386477097 ) ) ;
#86360 = CARTESIAN_POINT ( 'NONE',  ( -16.51473224551069308, -9.474510206698971260, 56.66557627198103120 ) ) ;
#86361 = CARTESIAN_POINT ( 'NONE',  ( 9.564922557961047289, -16.46253265017146816, 45.41775706135232582 ) ) ;
#86362 = CARTESIAN_POINT ( 'NONE',  ( 36.91746825000000598, -11.99521256947793546, -5.724999997268813701 ) ) ;
#86363 = CARTESIAN_POINT ( 'NONE',  ( -16.53943276465976808, -0.05219959533934237506, 43.75109039468568284 ) ) ;
#86365 = CARTESIAN_POINT ( 'NONE',  ( 4.483927247898790824, -16.52544592524335698, 60.20942372801902565 ) ) ;
#86364 = CARTESIAN_POINT ( 'NONE',  ( 19.03943276465977164, 0.05219959533936151252, 76.25109039468566152 ) ) ;
#86366 = LINE ( 'NONE', #164225, #194923 ) ;
#86367 = CARTESIAN_POINT ( 'NONE',  ( -9.564922557960796823, -16.46253265017161027, 87.08224293864769550 ) ) ;
#86368 = CARTESIAN_POINT ( 'NONE',  ( -18.67979575497178146, -10.72451020669898902, 111.6655762719810525 ) ) ;
#86369 = CARTESIAN_POINT ( 'NONE',  ( -5.049401038297874678, -19.05341960407617918, 74.79275706135231871 ) ) ;
#86371 = CARTESIAN_POINT ( 'NONE',  ( -16.51473224551069308, -9.474510206698971260, 31.66557627198102054 ) ) ;
#86370 = CARTESIAN_POINT ( 'NONE',  ( -13.97604488694527625, -13.89961937509977652, 106.8739096053143669 ) ) ;
#86372 = CARTESIAN_POINT ( 'NONE',  ( 5.049401038298161559, -19.05341960407611168, 82.70724293864770971 ) ) ;
#86374 = CARTESIAN_POINT ( 'NONE',  ( -16.51473224551069308, -9.474510206698971260, 31.66557627198102054 ) ) ;
#86373 = CARTESIAN_POINT ( 'NONE',  ( -12.14591786802309592, -12.06949235617757132, 36.87390960531435979 ) ) ;
#86375 = CARTESIAN_POINT ( 'NONE',  ( 19.03943276465977164, 0.05219959533936151252, 56.25109039468566863 ) ) ;
#86376 = CARTESIAN_POINT ( 'NONE',  ( 16.55341960407611168, 4.379528057220329451, 93.95724293864770971 ) ) ;
#86377 = CARTESIAN_POINT ( 'NONE',  ( -10.72451020669870658, -18.67979575497194134, 109.5844237280190328 ) ) ;
#86378 = CARTESIAN_POINT ( 'NONE',  ( 13.97604488694527802, 13.89961937509977652, 54.37390960531435979 ) ) ;
#86379 = ADVANCED_FACE ( 'NONE', ( #90574 ), #46065, .F. ) ;
#86380 = CARTESIAN_POINT ( 'NONE',  ( 21.53943276465977519, -0.05219959533907433946, 48.74890960531435979 ) ) ;
#86382 = CARTESIAN_POINT ( 'NONE',  ( -0.05219959533937732626, 21.53943276465977519, 97.50109039468567573 ) ) ;
#86381 = CARTESIAN_POINT ( 'NONE',  ( 0.05219959533910956823, 16.53943276465976808, 59.99890960531436690 ) ) ;
#86383 = CARTESIAN_POINT ( 'NONE',  ( -13.97604488694527625, -13.89961937509977652, 111.8739096053143243 ) ) ;
#86384 = CARTESIAN_POINT ( 'NONE',  ( -13.97604488694527625, -13.89961937509977652, 101.8739096053143811 ) ) ;
#86385 = CARTESIAN_POINT ( 'NONE',  ( -16.46253265017160317, 9.564922557960807481, 45.83224293864769550 ) ) ;
#86386 = CARTESIAN_POINT ( 'NONE',  ( -0.05219959533909027116, -19.03943276465977164, 22.49890960531436690 ) ) ;
#86387 = CARTESIAN_POINT ( 'NONE',  ( 12.06949235617757843, -12.14591786802309237, 93.12390960531436690 ) ) ;
#86388 = CARTESIAN_POINT ( 'NONE',  ( -10.72451020669898014, 18.67979575497178502, 95.41557627198102409 ) ) ;
#86389 = CARTESIAN_POINT ( 'NONE',  ( -19.03943276465977164, 0.05219959533909376836, 96.24890960531436690 ) ) ;
#86390 = CARTESIAN_POINT ( 'NONE',  ( -18.62759615963255300, -10.81492255796106328, 19.16775706135234714 ) ) ;
#86391 = CARTESIAN_POINT ( 'NONE',  ( -19.05341960407611168, -5.049401038298163336, 101.4572429386476955 ) ) ;
#86393 = CARTESIAN_POINT ( 'NONE',  ( 8.314922557960818139, 14.29746914071049879, 99.58224293864770971 ) ) ;
#86392 = CARTESIAN_POINT ( 'NONE',  ( 12.99999999999999822, 0.000000000000000000, 0.000000000000000000 ) ) ;
#86394 = CARTESIAN_POINT ( 'NONE',  ( 5.153800228976335163, 19.02544592524342804, 74.79057627198103830 ) ) ;
#86395 = CARTESIAN_POINT ( 'NONE',  ( -21.55341960407610458, -5.719274019375992779, 76.45724293864769550 ) ) ;
#86396 = DIRECTION ( 'NONE',  ( 1.000000000000000000, 0.000000000000000000, 0.000000000000000000 ) ) ;
#86398 = CARTESIAN_POINT ( 'NONE',  ( 193.3062444957835453, -155.7167183371837496, -23.00000000000000000 ) ) ;
#86397 = CARTESIAN_POINT ( 'NONE',  ( 15.72974639402199770, -15.80617190586745480, 28.12390960531435979 ) ) ;
#86399 = CARTESIAN_POINT ( 'NONE',  ( -8.314922557961024197, 14.29746914071037800, 32.91775706135234714 ) ) ;
#86400 = CARTESIAN_POINT ( 'NONE',  ( -16.53943276465976808, 0.05219959533911058130, 96.24890960531435269 ) ) ;
#86401 = DIRECTION ( 'NONE',  ( 1.000000000000000000, 0.000000000000000000, 0.000000000000000000 ) ) ;
#86402 = CARTESIAN_POINT ( 'NONE',  ( -19.02544592524342804, 5.153800228976336051, 86.04057627198103830 ) ) ;
#86403 = CARTESIAN_POINT ( 'NONE',  ( 5.049401038298161559, -19.05341960407611168, 62.70724293864769550 ) ) ;
#86404 = CARTESIAN_POINT ( 'NONE',  ( 16.53943276465976808, -0.05219959533910856209, 78.74890960531436690 ) ) ;
#86405 = CARTESIAN_POINT ( 'NONE',  ( 21.52544592524344225, -5.823673210054117533, 33.54057627198102409 ) ) ;
#86406 = CARTESIAN_POINT ( 'NONE',  ( 16.53943276465976808, -0.05219959533910856209, 58.74890960531436690 ) ) ;
#86407 = CARTESIAN_POINT ( 'NONE',  ( 12.14591786802327356, -12.06949235617739191, 25.62609039468567929 ) ) ;
#86408 = CARTESIAN_POINT ( 'NONE',  ( 21.52544592524334988, 5.823673210054432836, 71.45942372801901854 ) ) ;
#86409 = CARTESIAN_POINT ( 'NONE',  ( -17.14385361876520975, 23.59649016807275856, 148.5750000027311728 ) ) ;
#86410 = CARTESIAN_POINT ( 'NONE',  ( -9.474510206698964154, 16.51473224551069663, 115.4155762719810241 ) ) ;
#86411 = CARTESIAN_POINT ( 'NONE',  ( -4.379528057220086978, -16.55341960407618274, 89.79275706135236135 ) ) ;
#86412 = CARTESIAN_POINT ( 'NONE',  ( -13.97604488694527625, -13.89961937509977652, 26.87390960531434558 ) ) ;
#86413 = CARTESIAN_POINT ( 'NONE',  ( 16.51473224551069308, 9.474510206698969483, 84.16557627198102409 ) ) ;
#86414 = CARTESIAN_POINT ( 'NONE',  ( 21.53943276465977519, -0.05219959533907433946, 98.74890960531438111 ) ) ;
#86415 = CARTESIAN_POINT ( 'NONE',  ( 16.52544592524335698, 4.483927247898782831, 26.45942372801901854 ) ) ;
#86417 = CARTESIAN_POINT ( 'NONE',  ( -15.80617190586768217, 15.72974639402176855, 78.12609039468570415 ) ) ;
#86416 = CARTESIAN_POINT ( 'NONE',  ( -0.05219959533910754901, -16.53943276465976808, 52.49890960531435979 ) ) ;
#86419 = CARTESIAN_POINT ( 'NONE',  ( -5.049401038298153566, 19.05341960407611168, 115.2072429386477097 ) ) ;
#86418 = CARTESIAN_POINT ( 'NONE',  ( -4.379528057220086978, -16.55341960407618274, 89.79275706135236135 ) ) ;
#86420 = CARTESIAN_POINT ( 'NONE',  ( 17.26058549869090797, 6.457015423128630971, 28.87745837476070321 ) ) ;
#86421 = CARTESIAN_POINT ( 'NONE',  ( -16.19135201231366139, 7.376712067591925326, 79.81319145947969673 ) ) ;
#86422 = CARTESIAN_POINT ( 'NONE',  ( -8.224510206698735004, -14.34966873604973081, 109.5844237280190328 ) ) ;
#86423 = CARTESIAN_POINT ( 'NONE',  ( 4.379528057220092307, 16.55341960407617563, 62.29275706135236845 ) ) ;
#86424 = CARTESIAN_POINT ( 'NONE',  ( -16.51473224551069308, -9.474510206698971260, 66.66557627198102409 ) ) ;
#86425 = CARTESIAN_POINT ( 'NONE',  ( -13.89961937509977652, 13.97604488694528158, 80.62390960531436690 ) ) ;
#86426 = CARTESIAN_POINT ( 'NONE',  ( -21.52544592524334988, -5.823673210054445271, 68.95942372801901854 ) ) ;
#86427 = CARTESIAN_POINT ( 'NONE',  ( -16.55341960407617563, 4.379528057220093196, 73.54275706135234714 ) ) ;
#86428 = CARTESIAN_POINT ( 'NONE',  ( 16.55341960407611168, 4.379528057220329451, 48.95724293864770971 ) ) ;
#86429 = CARTESIAN_POINT ( 'NONE',  ( -19.02544592524342804, 5.153800228976336051, 61.04057627198103120 ) ) ;
#86430 = CARTESIAN_POINT ( 'NONE',  ( 13.97604488694527802, 13.89961937509977652, 54.37390960531435979 ) ) ;
#86431 = EDGE_LOOP ( 'NONE', ( #30629, #42750, #8497, #149741, #116878, #80437, #102238, #36723, #129348, #143098, #81524, #162174 ) ) ;
#86432 = CARTESIAN_POINT ( 'NONE',  ( -14.29746914071037622, -8.314922557961029526, 19.16775706135234714 ) ) ;
#86433 = CARTESIAN_POINT ( 'NONE',  ( 16.53943276465976808, -0.05219959533910856209, 108.7489096053143669 ) ) ;
#86434 = CARTESIAN_POINT ( 'NONE',  ( 9.474510206698971260, -16.51473224551069308, 62.91557627198102409 ) ) ;
#86436 = CARTESIAN_POINT ( 'NONE',  ( 23.48529157249599919, 32.32473071737754111, -4.699999999999999289 ) ) ;
#86435 = CARTESIAN_POINT ( 'NONE',  ( -13.89961937509957401, -13.97604488694547875, 99.37609039468567573 ) ) ;
#86437 = CARTESIAN_POINT ( 'NONE',  ( -10.81492255796105439, 18.62759615963255655, 97.91775706135236135 ) ) ;
#86438 = CARTESIAN_POINT ( 'NONE',  ( 16.55341960407618274, -4.379528057220086978, 66.04275706135236135 ) ) ;
#86439 = CARTESIAN_POINT ( 'NONE',  ( 5.153800228976615827, -19.02544592524334988, 95.20942372801897591 ) ) ;
#86440 = CARTESIAN_POINT ( 'NONE',  ( -18.67979575497178146, -10.72451020669898902, 61.66557627198103120 ) ) ;
#86441 = CARTESIAN_POINT ( 'NONE',  ( -16.52544592524335698, -4.483927247898792601, 58.95942372801902565 ) ) ;
#86442 = LINE ( 'NONE', #101605, #92638 ) ;
#86443 = CARTESIAN_POINT ( 'NONE',  ( -13.89961937509957401, -13.97604488694547875, 59.37609039468566863 ) ) ;
#86444 = CARTESIAN_POINT ( 'NONE',  ( -15.72974639402176322, -15.80617190586768395, 99.37609039468568994 ) ) ;
#86445 = CARTESIAN_POINT ( 'NONE',  ( 14.34966873604960469, 8.224510206698951720, 114.1655762719810383 ) ) ;
#86446 = CARTESIAN_POINT ( 'NONE',  ( 19.02544592524343514, -5.153800228976328945, 68.54057627198103830 ) ) ;
#86447 = CARTESIAN_POINT ( 'NONE',  ( 16.53943276465976808, -0.05219959533910856209, 58.74890960531436690 ) ) ;
#86448 = VECTOR ( 'NONE', #117671, 1000.000000000000000 ) ;
#86449 = CARTESIAN_POINT ( 'NONE',  ( 21.52544592524334988, 5.823673210054432836, 96.45942372801901854 ) ) ;
#86450 = CARTESIAN_POINT ( 'NONE',  ( -5.049401038297874678, -19.05341960407617918, 44.79275706135232582 ) ) ;
#86451 = CARTESIAN_POINT ( 'NONE',  ( -9.474510206698720793, -16.51473224551083518, 34.58442372801899722 ) ) ;
#86452 = CARTESIAN_POINT ( 'NONE',  ( 9.474510206698971260, -16.51473224551069308, 112.9155762719810383 ) ) ;
#86453 = CARTESIAN_POINT ( 'NONE',  ( -21.52544592524334988, -5.823673210054445271, 93.95942372801903275 ) ) ;
#86454 = CARTESIAN_POINT ( 'NONE',  ( 9.474510206698971260, -16.51473224551069308, 82.91557627198103830 ) ) ;
#86455 = CARTESIAN_POINT ( 'NONE',  ( 5.719274019375673035, 21.55341960407619339, 97.29275706135234714 ) ) ;
#86456 = CARTESIAN_POINT ( 'NONE',  ( -5.719274019375978568, 21.55341960407610458, 55.20724293864770260 ) ) ;
#86457 = CARTESIAN_POINT ( 'NONE',  ( -13.89961937509977652, 13.97604488694528158, 80.62390960531436690 ) ) ;
#86458 = CARTESIAN_POINT ( 'NONE',  ( 13.89961937509957401, 13.97604488694547697, 71.87609039468567573 ) ) ;
#86459 = CARTESIAN_POINT ( 'NONE',  ( -16.51473224551069308, -9.474510206698971260, 46.66557627198102409 ) ) ;
#86460 = CARTESIAN_POINT ( 'NONE',  ( 16.51473224551069308, 9.474510206698969483, 84.16557627198102409 ) ) ;
#86461 = CARTESIAN_POINT ( 'NONE',  ( 13.97604488694548053, -13.89961937509957401, 85.62609039468568994 ) ) ;
#86462 = CARTESIAN_POINT ( 'NONE',  ( 8.314922557961029526, -14.29746914071037800, 40.41775706135234714 ) ) ;
#86463 = CARTESIAN_POINT ( 'NONE',  ( 4.483927247898545687, 16.52544592524342804, 104.7905762719810241 ) ) ;
#86464 = CARTESIAN_POINT ( 'NONE',  ( -19.03943276465977164, 0.05219959533909376836, 76.24890960531435269 ) ) ;
#86465 = CARTESIAN_POINT ( 'NONE',  ( 5.719274019375991003, -21.55341960407610458, 47.70724293864770260 ) ) ;
#86466 = CARTESIAN_POINT ( 'NONE',  ( 8.224510206698742110, 14.34966873604972548, 32.08442372801901854 ) ) ;
#86467 = CARTESIAN_POINT ( 'NONE',  ( 18.67979575497194134, -10.72451020669871369, 35.83442372801901143 ) ) ;
#86468 = CARTESIAN_POINT ( 'NONE',  ( -18.62759615963255300, -10.81492255796106328, 89.16775706135236135 ) ) ;
#86469 = CARTESIAN_POINT ( 'NONE',  ( -4.379528057220086978, -16.55341960407618274, 84.79275706135234714 ) ) ;
#86470 = CARTESIAN_POINT ( 'NONE',  ( -19.03943276465977164, 0.05219959533909376836, 81.24890960531436690 ) ) ;
#86471 = CARTESIAN_POINT ( 'NONE',  ( -0.05219959533934338120, 16.53943276465976808, 102.5010903946856899 ) ) ;
#86472 = CARTESIAN_POINT ( 'NONE',  ( -19.02544592524334988, -5.153800228976617603, 53.95942372801898301 ) ) ;
#86473 = TOROIDAL_SURFACE ( 'NONE', #144602, 2.700000000000000622, 0.2000000000000000111 ) ;
#86474 = CARTESIAN_POINT ( 'NONE',  ( 21.55341960407619695, -5.719274019375665929, 36.04275706135234714 ) ) ;
#86475 = CARTESIAN_POINT ( 'NONE',  ( -12.06949235617756955, 12.14591786802309770, 75.62390960531439532 ) ) ;
#86476 = CARTESIAN_POINT ( 'NONE',  ( -19.02544592524342804, 5.153800228976336051, 101.0405762719810241 ) ) ;
#86477 = CARTESIAN_POINT ( 'NONE',  ( 12.06949235617739724, 12.14591786802326823, 106.8760903946856899 ) ) ;
#86478 = CARTESIAN_POINT ( 'NONE',  ( -18.67979575497193778, 10.72451020669871902, 73.33442372801901854 ) ) ;
#86479 = CARTESIAN_POINT ( 'NONE',  ( -14.34966873604972548, 8.224510206698743886, 43.33442372801901143 ) ) ;
#86480 = CARTESIAN_POINT ( 'NONE',  ( 5.823673210054444382, -21.52544592524334988, 30.20942372801902565 ) ) ;
#86481 = CARTESIAN_POINT ( 'NONE',  ( 14.34966873604960469, 8.224510206698951720, 69.16557627198102409 ) ) ;
#86482 = ORIENTED_EDGE ( 'NONE', *, *, #75962, .T. ) ;
#86483 = CARTESIAN_POINT ( 'NONE',  ( -5.823673210054431948, 21.52544592524334988, 22.70942372801901499 ) ) ;
#86484 = CARTESIAN_POINT ( 'NONE',  ( -16.53943276465976808, 0.05219959533911058130, 51.24890960531436690 ) ) ;
#86485 = CARTESIAN_POINT ( 'NONE',  ( -3.735172737399431091E-16, -6.100000000000006750, -62.50719930893269805 ) ) ;
#86486 = CARTESIAN_POINT ( 'NONE',  ( 15.72974639402199770, -15.80617190586745480, 28.12390960531435979 ) ) ;
#86487 = CARTESIAN_POINT ( 'NONE',  ( -21.52544592524334988, -5.823673210054445271, 53.95942372801900433 ) ) ;
#86488 = CARTESIAN_POINT ( 'NONE',  ( 8.224510206698953496, -14.34966873604960469, 62.91557627198102409 ) ) ;
#86489 = CARTESIAN_POINT ( 'NONE',  ( 18.67979575497178502, 10.72451020669898547, 74.16557627198102409 ) ) ;
#86490 = CARTESIAN_POINT ( 'NONE',  ( 9.564922557960805705, 16.46253265017160317, 79.58224293864769550 ) ) ;
#86492 = CARTESIAN_POINT ( 'NONE',  ( 5.153800228976615827, -19.02544592524334988, 75.20942372801896170 ) ) ;
#86491 = CARTESIAN_POINT ( 'NONE',  ( -19.05341960407611168, -5.049401038298163336, 36.45724293864766707 ) ) ;
#86494 = CARTESIAN_POINT ( 'NONE',  ( 10.81492255796078972, 18.62759615963270932, 64.58224293864769550 ) ) ;
#86493 = CARTESIAN_POINT ( 'NONE',  ( -18.67979575497193778, 10.72451020669871902, 53.33442372801901854 ) ) ;
#86495 = CARTESIAN_POINT ( 'NONE',  ( -9.564922557960796823, -16.46253265017161027, 42.08224293864769550 ) ) ;
#86496 = CARTESIAN_POINT ( 'NONE',  ( -9.564922557960796823, -16.46253265017161027, 67.08224293864769550 ) ) ;
#86497 = ORIENTED_EDGE ( 'NONE', *, *, #126426, .F. ) ;
#86498 = CARTESIAN_POINT ( 'NONE',  ( 12.14591786802327356, -12.06949235617739191, 55.62609039468568284 ) ) ;
#86499 = CARTESIAN_POINT ( 'NONE',  ( -21.55341960407619339, 5.719274019375674811, 28.54275706135234358 ) ) ;
#86500 = CARTESIAN_POINT ( 'NONE',  ( 18.67979575497194134, -10.72451020669871369, 55.83442372801901854 ) ) ;
#86501 = CARTESIAN_POINT ( 'NONE',  ( -19.03943276465977164, 0.05219959533909376836, 101.2489096053143669 ) ) ;
#86502 = CARTESIAN_POINT ( 'NONE',  ( 21.55341960407610458, 5.719274019375980345, 88.95724293864769550 ) ) ;
#86504 = CARTESIAN_POINT ( 'NONE',  ( -12.14591786802326823, 12.06949235617739902, 53.12609039468568284 ) ) ;
#86503 = CARTESIAN_POINT ( 'NONE',  ( -5.823673210054431948, 21.52544592524334988, 22.70942372801901499 ) ) ;
#86505 = CARTESIAN_POINT ( 'NONE',  ( 21.55341960407610458, 5.719274019375980345, 43.95724293864769550 ) ) ;
#86506 = CARTESIAN_POINT ( 'NONE',  ( 19.02544592524334988, 5.153800228976608722, 26.45942372801899722 ) ) ;
#86507 = CARTESIAN_POINT ( 'NONE',  ( -9.474510206698964154, 16.51473224551069663, 60.41557627198102409 ) ) ;
#86508 = CARTESIAN_POINT ( 'NONE',  ( -9.474510206698964154, 16.51473224551069663, 105.4155762719810383 ) ) ;
#86509 = CARTESIAN_POINT ( 'NONE',  ( -5.049401038298153566, 19.05341960407611168, 95.20724293864770971 ) ) ;
#86510 = CARTESIAN_POINT ( 'NONE',  ( 17.49999999999999645, 3.341627039121310982, 102.9223102399844976 ) ) ;
#86511 = EDGE_CURVE ( 'NONE', #85800, #199879, #153261, .T. ) ;
#86512 = CARTESIAN_POINT ( 'NONE',  ( 19.05341960407617918, -5.049401038297876454, 66.04275706135233293 ) ) ;
#86513 = CARTESIAN_POINT ( 'NONE',  ( -18.62759615963270932, 10.81492255796079327, 45.83224293864769550 ) ) ;
#86514 = CARTESIAN_POINT ( 'NONE',  ( 0.05219959533910956823, 16.53943276465976808, 29.99890960531435979 ) ) ;
#86515 = CARTESIAN_POINT ( 'NONE',  ( 13.97604488694548053, -13.89961937509957401, 80.62609039468567573 ) ) ;
#86516 = CARTESIAN_POINT ( 'NONE',  ( -17.49999999999998579, 5.500000000000032863, 60.79690382534172244 ) ) ;
#86517 = CARTESIAN_POINT ( 'NONE',  ( 5.823673210054444382, -21.52544592524334988, 110.2094237280190185 ) ) ;
#86518 = CARTESIAN_POINT ( 'NONE',  ( -9.564922557961040184, 16.46253265017147172, 77.91775706135234714 ) ) ;
#86519 = CARTESIAN_POINT ( 'NONE',  ( -19.03943276465977164, -0.05219959533935918106, 43.75109039468566863 ) ) ;
#86520 = CARTESIAN_POINT ( 'NONE',  ( 26.53518950525897679, -7.921153050709833998, 167.7791411921787699 ) ) ;
#86521 = CARTESIAN_POINT ( 'NONE',  ( -16.46253265017160317, 9.564922557960807481, 60.83224293864769550 ) ) ;
#86522 = CARTESIAN_POINT ( 'NONE',  ( 16.52544592524342804, -4.483927247898539470, 53.54057627198103120 ) ) ;
#86523 = CARTESIAN_POINT ( 'NONE',  ( -19.05341960407611168, -5.049401038298163336, 31.45724293864769550 ) ) ;
#86524 = CARTESIAN_POINT ( 'NONE',  ( -16.53943276465976808, 0.05219959533911058130, 46.24890960531435979 ) ) ;
#86525 = CARTESIAN_POINT ( 'NONE',  ( -19.03943276465977164, -1.327063459122257427E-13, 20.00000000000001776 ) ) ;
#86526 = CARTESIAN_POINT ( 'NONE',  ( -12.14591786802326823, 12.06949235617739902, 113.1260903946856899 ) ) ;
#86527 = CARTESIAN_POINT ( 'NONE',  ( 13.97604488694527802, 13.89961937509977652, 69.37390960531436690 ) ) ;
#86528 = CARTESIAN_POINT ( 'NONE',  ( 19.02544592524334988, 5.153800228976608722, 31.45942372801900433 ) ) ;
#86529 = CARTESIAN_POINT ( 'NONE',  ( -8.314922557961024197, 14.29746914071037800, 37.91775706135235424 ) ) ;
#86530 = CARTESIAN_POINT ( 'NONE',  ( -15.72974639402197994, 15.80617190586746368, 35.62390960531437401 ) ) ;
#86532 = ORIENTED_EDGE ( 'NONE', *, *, #31655, .F. ) ;
#86531 = CARTESIAN_POINT ( 'NONE',  ( 21.53943276465977519, 0.05219959533937863772, 86.25109039468568994 ) ) ;
#86533 = CARTESIAN_POINT ( 'NONE',  ( 19.02544592524343514, -5.153800228976328945, 63.54057627198103830 ) ) ;
#86534 = CARTESIAN_POINT ( 'NONE',  ( 16.51473224551069308, 9.474510206698969483, 104.1655762719810241 ) ) ;
#86535 = CARTESIAN_POINT ( 'NONE',  ( 19.05341960407611168, 5.049401038298154454, 98.95724293864766707 ) ) ;
#86536 = CARTESIAN_POINT ( 'NONE',  ( 36.91746824999999177, 11.99521256947799230, -1.524999997268813523 ) ) ;
#86537 = CARTESIAN_POINT ( 'NONE',  ( -21.55341960407619339, 5.719274019375674811, 23.54275706135235424 ) ) ;
#86538 = CARTESIAN_POINT ( 'NONE',  ( 12.14591786802309770, 12.06949235617756955, 79.37390960531436690 ) ) ;
#86540 = CARTESIAN_POINT ( 'NONE',  ( 19.05341960407611168, 5.049401038298154454, 73.95724293864768129 ) ) ;
#86539 = CARTESIAN_POINT ( 'NONE',  ( 18.67979575497178502, 10.72451020669898547, 79.16557627198103830 ) ) ;
#86541 = CARTESIAN_POINT ( 'NONE',  ( -13.89961937509977652, 13.97604488694528158, 75.62390960531438111 ) ) ;
#86542 = CARTESIAN_POINT ( 'NONE',  ( 15.72974639402199770, -15.80617190586745480, 108.1239096053143811 ) ) ;
#86543 = ORIENTED_EDGE ( 'NONE', *, *, #157461, .T. ) ;
#86544 = CARTESIAN_POINT ( 'NONE',  ( 9.564922557960805705, 16.46253265017160317, 74.58224293864769550 ) ) ;
#86546 = CARTESIAN_POINT ( 'NONE',  ( 16.46253265017160672, -9.564922557960803928, 23.33224293864769194 ) ) ;
#86545 = CARTESIAN_POINT ( 'NONE',  ( 12.14591786802309770, 12.06949235617756955, 104.3739096053143669 ) ) ;
#86547 = CARTESIAN_POINT ( 'NONE',  ( -16.51473224551069308, -9.474510206698971260, 61.66557627198103120 ) ) ;
#86548 = CARTESIAN_POINT ( 'NONE',  ( 5.153800228976615827, -19.02544592524334988, 90.20942372801900433 ) ) ;
#86549 = CARTESIAN_POINT ( 'NONE',  ( 14.29746914071049879, -8.314922557960816363, 93.33224293864769550 ) ) ;
#86550 = CARTESIAN_POINT ( 'NONE',  ( 18.62759615963255655, 10.81492255796105972, 76.66775706135234714 ) ) ;
#86552 = CARTESIAN_POINT ( 'NONE',  ( -15.80617190586745835, -15.72974639402198527, 111.8739096053143669 ) ) ;
#86551 = CARTESIAN_POINT ( 'NONE',  ( -16.46253265017160317, 9.564922557960807481, 50.83224293864770260 ) ) ;
#86553 = CARTESIAN_POINT ( 'NONE',  ( 15.72974639402199770, -15.80617190586745480, 108.1239096053143811 ) ) ;
#86554 = CARTESIAN_POINT ( 'NONE',  ( -23.31738231874055245, -16.94106989632524574, 144.1999999999999886 ) ) ;
#86555 = CARTESIAN_POINT ( 'NONE',  ( 0.05219959533909260263, 19.03943276465977164, 69.99890960531435269 ) ) ;
#86556 = CARTESIAN_POINT ( 'NONE',  ( 1.993301997531345686E-15, -30.30510711980685556, 138.7500000054623683 ) ) ;
#86558 = CARTESIAN_POINT ( 'NONE',  ( 21.52544592524344225, -5.823673210054117533, 28.54057627198103120 ) ) ;
#86557 = CARTESIAN_POINT ( 'NONE',  ( 13.89961937509957401, 13.97604488694547697, 106.8760903946856757 ) ) ;
#86559 = CARTESIAN_POINT ( 'NONE',  ( -5.719274019375665041, -21.55341960407619695, 44.79275706135234714 ) ) ;
#86560 = CARTESIAN_POINT ( 'NONE',  ( 19.02544592524343514, -5.153800228976328945, 93.54057627198102409 ) ) ;
#86561 = CARTESIAN_POINT ( 'NONE',  ( -16.46253265017146816, -9.564922557961047289, 84.16775706135233293 ) ) ;
#86562 = CARTESIAN_POINT ( 'NONE',  ( 13.97604488694527802, 13.89961937509977652, 49.37390960531434558 ) ) ;
#86563 = CARTESIAN_POINT ( 'NONE',  ( 9.474510206698971260, -16.51473224551069308, 72.91557627198102409 ) ) ;
#86564 = CARTESIAN_POINT ( 'NONE',  ( -8.224510206698948167, 14.34966873604960824, 85.41557627198102409 ) ) ;
#86565 = CARTESIAN_POINT ( 'NONE',  ( 13.97604488694527802, 13.89961937509977652, 104.3739096053143385 ) ) ;
#86566 = CARTESIAN_POINT ( 'NONE',  ( 16.53943276465976808, -0.05219959533910856209, 93.74890960531436690 ) ) ;
#86567 = CARTESIAN_POINT ( 'NONE',  ( -0.05219959533909027116, -19.03943276465977164, 102.4989096053143669 ) ) ;
#86569 = CARTESIAN_POINT ( 'NONE',  ( -13.97604488694527625, -13.89961937509977652, 21.87390960531435979 ) ) ;
#86568 = CARTESIAN_POINT ( 'NONE',  ( 14.34966873604960469, 8.224510206698951720, 39.16557627198102409 ) ) ;
#86570 = ORIENTED_EDGE ( 'NONE', *, *, #147245, .F. ) ;
#86571 = CARTESIAN_POINT ( 'NONE',  ( 5.719274019375673035, 21.55341960407619339, 52.29275706135236135 ) ) ;
#86572 = CARTESIAN_POINT ( 'NONE',  ( 19.03943276465977164, 0.05219959533936151252, 86.25109039468567573 ) ) ;
#86573 = CARTESIAN_POINT ( 'NONE',  ( -0.05219959533910754901, -16.53943276465976808, 42.49890960531435979 ) ) ;
#86574 = CARTESIAN_POINT ( 'NONE',  ( 5.823673210054125526, 21.52544592524343514, 99.79057627198103830 ) ) ;
#86575 = CARTESIAN_POINT ( 'NONE',  ( -10.72451020669898014, 18.67979575497178502, 40.41557627198103120 ) ) ;
#86576 = CARTESIAN_POINT ( 'NONE',  ( -4.379528057220328563, 16.55341960407611168, 85.20724293864770971 ) ) ;
#86577 = CARTESIAN_POINT ( 'NONE',  ( 19.03943276465977164, -0.05219959533909143690, 58.74890960531435979 ) ) ;
#86578 = CARTESIAN_POINT ( 'NONE',  ( 4.379528057220339221, -16.55341960407611168, 22.70724293864769194 ) ) ;
#86579 = AXIS2_PLACEMENT_3D ( 'NONE', #91940, #89983, #153633 ) ;
#86580 = CARTESIAN_POINT ( 'NONE',  ( -8.224510206698735004, -14.34966873604973081, 99.58442372801900433 ) ) ;
#86581 = CARTESIAN_POINT ( 'NONE',  ( -4.483927247898782831, 16.52544592524335698, 67.70942372801901854 ) ) ;
#86582 = CARTESIAN_POINT ( 'NONE',  ( 19.02544592524334988, 5.153800228976608722, 31.45942372801900433 ) ) ;
#86583 = CARTESIAN_POINT ( 'NONE',  ( 19.02544592524343514, -5.153800228976328945, 93.54057627198102409 ) ) ;
#86584 = CARTESIAN_POINT ( 'NONE',  ( 0.05219959533909260263, 19.03943276465977164, 79.99890960531436690 ) ) ;
#86585 = CARTESIAN_POINT ( 'NONE',  ( -4.483927247898782831, 16.52544592524335698, 82.70942372801900433 ) ) ;
#86586 = CARTESIAN_POINT ( 'NONE',  ( 9.474510206698971260, -16.51473224551069308, 32.91557627198102409 ) ) ;
#86587 = EDGE_CURVE ( 'NONE', #17186, #166399, #148103, .T. ) ;
#86588 = CARTESIAN_POINT ( 'NONE',  ( -0.05219959533910754901, -16.53943276465976808, 42.49890960531435979 ) ) ;
#86590 = CARTESIAN_POINT ( 'NONE',  ( -16.46253265017160317, 9.564922557960807481, 105.8322429386476955 ) ) ;
#86589 = PRESENTATION_STYLE_ASSIGNMENT (( #161434 ) ) ;
#86591 = CARTESIAN_POINT ( 'NONE',  ( -21.52544592524343514, 5.823673210054127303, 36.04057627198102409 ) ) ;
#86592 = CARTESIAN_POINT ( 'NONE',  ( -16.55341960407611168, -4.379528057220339221, 66.45724293864768129 ) ) ;
#86593 = CARTESIAN_POINT ( 'NONE',  ( 0.05219959533934541429, -16.53943276465976808, 20.00109039468568639 ) ) ;
#86594 = CARTESIAN_POINT ( 'NONE',  ( -4.483927247898539470, -16.52544592524342804, 62.29057627198102409 ) ) ;
#86595 = CARTESIAN_POINT ( 'NONE',  ( 31.77050690183225257, -0.6194686979412523664, -45.83912112027729080 ) ) ;
#86596 = CARTESIAN_POINT ( 'NONE',  ( -9.474510206698720793, -16.51473224551083518, 59.58442372801900433 ) ) ;
#86597 = CARTESIAN_POINT ( 'NONE',  ( 13.97604488694527802, 13.89961937509977652, 99.37390960531436690 ) ) ;
#86598 = CARTESIAN_POINT ( 'NONE',  ( 9.564922557961047289, -16.46253265017146816, 75.41775706135234714 ) ) ;
#86599 = CARTESIAN_POINT ( 'NONE',  ( -17.14385361876520264, -23.59649016807271593, 147.6750000027311671 ) ) ;
#86601 = CARTESIAN_POINT ( 'NONE',  ( 16.53943276465976808, 0.05219959533934440121, 91.25109039468568994 ) ) ;
#86600 = CARTESIAN_POINT ( 'NONE',  ( -19.05341960407617563, 5.049401038297882671, 108.5427570613523187 ) ) ;
#86602 = CARTESIAN_POINT ( 'NONE',  ( -19.05341960407611168, -5.049401038298163336, 36.45724293864766707 ) ) ;
#86603 = CARTESIAN_POINT ( 'NONE',  ( -18.67979575497178146, -10.72451020669898902, 36.66557627198103120 ) ) ;
#86604 = CARTESIAN_POINT ( 'NONE',  ( -21.52544592524334988, -5.823673210054445271, 48.95942372801902565 ) ) ;
#86605 = CARTESIAN_POINT ( 'NONE',  ( -12.06949235617739369, -12.14591786802326823, 19.37609039468568639 ) ) ;
#86607 = CARTESIAN_POINT ( 'NONE',  ( 16.46253265017160672, -9.564922557960803928, 68.33224293864770971 ) ) ;
#86606 = CARTESIAN_POINT ( 'NONE',  ( 17.50000000000001421, 3.235083232844117251, 22.78281610344516039 ) ) ;
#86608 = CARTESIAN_POINT ( 'NONE',  ( 11.74149087413294268, 36.13659316521247433, -0.6021577739498229498 ) ) ;
#86610 = CARTESIAN_POINT ( 'NONE',  ( -19.03943276465977164, 0.05219959533909376836, 81.24890960531436690 ) ) ;
#86609 = CARTESIAN_POINT ( 'NONE',  ( 12.14591786802309770, 12.06949235617756955, 94.37390960531436690 ) ) ;
#86611 = CARTESIAN_POINT ( 'NONE',  ( -16.46253265017160317, 9.564922557960807481, 85.83224293864769550 ) ) ;
#86612 = ORIENTED_EDGE ( 'NONE', *, *, #83102, .T. ) ;
#86613 = CARTESIAN_POINT ( 'NONE',  ( -19.03943276465977164, -0.05219959533935918106, 88.75109039468567573 ) ) ;
#86614 = CARTESIAN_POINT ( 'NONE',  ( 10.72451020669898902, -18.67979575497178502, 67.91557627198102409 ) ) ;
#86615 = CARTESIAN_POINT ( 'NONE',  ( 16.46253265017160672, -9.564922557960803928, 23.33224293864769194 ) ) ;
#86616 = CARTESIAN_POINT ( 'NONE',  ( 9.564922557961047289, -16.46253265017146816, 50.41775706135233293 ) ) ;
#86617 = CARTESIAN_POINT ( 'NONE',  ( 13.97604488694527802, 13.89961937509977652, 54.37390960531435979 ) ) ;
#86618 = CARTESIAN_POINT ( 'NONE',  ( 5.049401038298161559, -19.05341960407611168, 87.70724293864769550 ) ) ;
#86619 = VERTEX_POINT ( 'NONE', #61224 ) ;
#86620 = CARTESIAN_POINT ( 'NONE',  ( 18.62759615963271287, -10.81492255796078972, 88.33224293864769550 ) ) ;
#86622 = CARTESIAN_POINT ( 'NONE',  ( -5.153800228976607833, 19.02544592524334988, 67.70942372801900433 ) ) ;
#86621 = CARTESIAN_POINT ( 'NONE',  ( -4.379528057220328563, 16.55341960407611168, 90.20724293864770971 ) ) ;
#86623 = CARTESIAN_POINT ( 'NONE',  ( 18.67979575497178502, 10.72451020669898547, 89.16557627198102409 ) ) ;
#86624 = CARTESIAN_POINT ( 'NONE',  ( 15.72974639402199770, -15.80617190586745480, 78.12390960531436690 ) ) ;
#86625 = CARTESIAN_POINT ( 'NONE',  ( -12.14591786802309592, -12.06949235617757132, 26.87390960531435979 ) ) ;
#86626 = CARTESIAN_POINT ( 'NONE',  ( 15.80617190586769283, -15.72974639402175789, 105.6260903946856899 ) ) ;
#86627 = CARTESIAN_POINT ( 'NONE',  ( 4.379528057220092307, 16.55341960407617563, 52.29275706135236135 ) ) ;
#86628 = CARTESIAN_POINT ( 'NONE',  ( 19.02544592524343514, -5.153800228976328945, 83.54057627198100988 ) ) ;
#86629 = CARTESIAN_POINT ( 'NONE',  ( -19.05341960407611168, -5.049401038298163336, 36.45724293864766707 ) ) ;
#86630 = CARTESIAN_POINT ( 'NONE',  ( 18.62759615963255655, 10.81492255796105972, 41.66775706135235424 ) ) ;
#86631 = CARTESIAN_POINT ( 'NONE',  ( -15.72974639402176322, -15.80617190586768395, 59.37609039468568284 ) ) ;
#86632 = CARTESIAN_POINT ( 'NONE',  ( -13.97604488694527625, -13.89961937509977652, 46.87390960531435979 ) ) ;
#86633 = CARTESIAN_POINT ( 'NONE',  ( 0.05219959533937995610, -21.53943276465977519, 25.00109039468567218 ) ) ;
#86634 = CARTESIAN_POINT ( 'NONE',  ( 13.89961937509957401, 13.97604488694547697, 56.87609039468564731 ) ) ;
#86635 = CARTESIAN_POINT ( 'NONE',  ( 19.02544592524334988, 5.153800228976608722, 76.45942372801897591 ) ) ;
#86636 = CARTESIAN_POINT ( 'NONE',  ( 0.05219959533934541429, -16.53943276465976808, 30.00109039468568284 ) ) ;
#86637 = CARTESIAN_POINT ( 'NONE',  ( 13.97604488694527802, 13.89961937509977652, 29.37390960531435979 ) ) ;
#86638 = CARTESIAN_POINT ( 'NONE',  ( -12.06949235617739369, -12.14591786802326823, 69.37609039468567573 ) ) ;
#86639 = CARTESIAN_POINT ( 'NONE',  ( -16.46253265017160317, 9.564922557960807481, 40.83224293864769550 ) ) ;
#86640 = CARTESIAN_POINT ( 'NONE',  ( 24.85901545656367873, -5.346793810781269585, 169.1018111888375870 ) ) ;
#86641 = CARTESIAN_POINT ( 'NONE',  ( 19.02544592524343514, -5.153800228976328945, 93.54057627198102409 ) ) ;
#86642 = CARTESIAN_POINT ( 'NONE',  ( 16.51473224551069308, 9.474510206698969483, 24.16557627198102765 ) ) ;
#86643 = CARTESIAN_POINT ( 'NONE',  ( 15.80617190586746368, 15.72974639402197994, 79.37390960531436690 ) ) ;
#86644 = CARTESIAN_POINT ( 'NONE',  ( -8.224510206698735004, -14.34966873604973081, 54.58442372801901143 ) ) ;
#86645 = CARTESIAN_POINT ( 'NONE',  ( 16.51473224551083163, -9.474510206698727899, 20.83442372801899722 ) ) ;
#86646 = CARTESIAN_POINT ( 'NONE',  ( -19.03943276465977164, 0.05219959533909376836, 46.24890960531435979 ) ) ;
#86647 = CARTESIAN_POINT ( 'NONE',  ( -4.379528057220328563, 16.55341960407611168, 30.20724293864769550 ) ) ;
#86648 = CARTESIAN_POINT ( 'NONE',  ( -12.14591786802309592, -12.06949235617757132, 66.87390960531436690 ) ) ;
#86649 = CARTESIAN_POINT ( 'NONE',  ( -16.51473224551069308, -9.474510206698971260, 71.66557627198102409 ) ) ;
#86650 = CARTESIAN_POINT ( 'NONE',  ( -18.67979575497193778, 10.72451020669871902, 38.33442372801900433 ) ) ;
#86651 = CARTESIAN_POINT ( 'NONE',  ( 19.03943276465977164, -0.05219959533909143690, 78.74890960531436690 ) ) ;
#86652 = CARTESIAN_POINT ( 'NONE',  ( 15.80617190586769283, -15.72974639402175789, 90.62609039468567573 ) ) ;
#86653 = CARTESIAN_POINT ( 'NONE',  ( 12.06949235617739724, 12.14591786802326823, 71.87609039468568994 ) ) ;
#86654 = CARTESIAN_POINT ( 'NONE',  ( -9.474510206698964154, 16.51473224551069663, 105.4155762719810383 ) ) ;
#86655 = CARTESIAN_POINT ( 'NONE',  ( -14.29746914071049879, 8.314922557960819915, 50.83224293864770971 ) ) ;
#86656 = CARTESIAN_POINT ( 'NONE',  ( 19.02544592524343514, -5.153800228976328945, 28.54057627198102409 ) ) ;
#86657 = CARTESIAN_POINT ( 'NONE',  ( -0.05219959533934338120, 16.53943276465976808, 52.50109039468567573 ) ) ;
#86658 = CARTESIAN_POINT ( 'NONE',  ( -14.29746914071049879, 8.314922557960819915, 50.83224293864770971 ) ) ;
#86659 = CARTESIAN_POINT ( 'NONE',  ( -9.564922557960796823, -16.46253265017161027, 107.0822429386476955 ) ) ;
#86660 = CARTESIAN_POINT ( 'NONE',  ( -21.55341960407610458, -5.719274019375992779, 36.45724293864768839 ) ) ;
#86661 = CARTESIAN_POINT ( 'NONE',  ( 19.02544592524334988, 5.153800228976608722, 21.45942372801899012 ) ) ;
#86662 = CARTESIAN_POINT ( 'NONE',  ( -12.14591786802309592, -12.06949235617757132, 96.87390960531436690 ) ) ;
#86663 = CARTESIAN_POINT ( 'NONE',  ( -16.51473224551069308, -9.474510206698971260, 91.66557627198103830 ) ) ;
#86664 = ORIENTED_EDGE ( 'NONE', *, *, #12763, .T. ) ;
#86665 = EDGE_LOOP ( 'NONE', ( #39990, #157482, #111442, #81009 ) ) ;
#86666 = CARTESIAN_POINT ( 'NONE',  ( -16.55341960407617563, 4.379528057220093196, 53.54275706135234714 ) ) ;
#86667 = CARTESIAN_POINT ( 'NONE',  ( -0.05219959533909027116, -19.03943276465977164, 52.49890960531436690 ) ) ;
#86668 = CARTESIAN_POINT ( 'NONE',  ( 17.72566875460849189, 5.499999999999970690, 101.5781329180409642 ) ) ;
#86669 = CARTESIAN_POINT ( 'NONE',  ( -13.97604488694547697, 13.89961937509957934, 43.12609039468566152 ) ) ;
#86670 = CARTESIAN_POINT ( 'NONE',  ( -12.06949235617739369, -12.14591786802326823, 79.37609039468567573 ) ) ;
#86671 = CARTESIAN_POINT ( 'NONE',  ( 19.02544592524334988, 5.153800228976608722, 91.45942372801900433 ) ) ;
#86672 = CARTESIAN_POINT ( 'NONE',  ( -15.80617190586768217, 15.72974639402176855, 73.12609039468567573 ) ) ;
#86673 = CARTESIAN_POINT ( 'NONE',  ( 9.474510206698971260, -16.51473224551069308, 77.91557627198103830 ) ) ;
#86674 = CARTESIAN_POINT ( 'NONE',  ( -15.80617190586745835, -15.72974639402198527, 91.87390960531436690 ) ) ;
#86675 = CARTESIAN_POINT ( 'NONE',  ( 4.483927247898545687, 16.52544592524342804, 94.79057627198105251 ) ) ;
#86676 = CARTESIAN_POINT ( 'NONE',  ( 19.02544592524334988, 5.153800228976608722, 76.45942372801897591 ) ) ;
#86677 = CARTESIAN_POINT ( 'NONE',  ( -5.719274019375978568, 21.55341960407610458, 75.20724293864769550 ) ) ;
#86678 = CARTESIAN_POINT ( 'NONE',  ( -16.46253265017146816, -9.564922557961047289, 44.16775706135232582 ) ) ;
#86679 = FACE_BOUND ( 'NONE', #119871, .T. ) ;
#86680 = CARTESIAN_POINT ( 'NONE',  ( 5.823673210054125526, 21.52544592524343514, 89.79057627198103830 ) ) ;
#86681 = CARTESIAN_POINT ( 'NONE',  ( -17.13100169013299379, 6.664070546373142889, 85.76789835699847231 ) ) ;
#86682 = CARTESIAN_POINT ( 'NONE',  ( -9.474510206698964154, 16.51473224551069663, 70.41557627198102409 ) ) ;
#86683 = CARTESIAN_POINT ( 'NONE',  ( -6.791538853603066528, 3.181980515339468241, 1.110912703473986074 ) ) ;
#86684 = CARTESIAN_POINT ( 'NONE',  ( -4.379528057220086978, -16.55341960407618274, 19.79275706135235069 ) ) ;
#86685 = CARTESIAN_POINT ( 'NONE',  ( 37.36625173109577958, -3.353228347065799309, 40.62582701645503391 ) ) ;
#86686 = CARTESIAN_POINT ( 'NONE',  ( -13.89961937509977652, 13.97604488694528158, 40.62390960531435979 ) ) ;
#86687 = CARTESIAN_POINT ( 'NONE',  ( 19.02544592524343514, -5.153800228976328945, 108.5405762719810383 ) ) ;
#86689 = CARTESIAN_POINT ( 'NONE',  ( -8.314922557960811034, -14.29746914071050412, 52.08224293864768839 ) ) ;
#86688 = CARTESIAN_POINT ( 'NONE',  ( 0.05219959533907565091, 21.53943276465977519, 89.99890960531438111 ) ) ;
#86690 = CARTESIAN_POINT ( 'NONE',  ( 21.53943276465977519, 0.05219959533937863772, 71.25109039468568994 ) ) ;
#86692 = CARTESIAN_POINT ( 'NONE',  ( 5.049401038297881783, 19.05341960407617563, 32.29275706135233293 ) ) ;
#86691 = CARTESIAN_POINT ( 'NONE',  ( -12.06949235617739369, -12.14591786802326823, 24.37609039468567573 ) ) ;
#86693 = CARTESIAN_POINT ( 'NONE',  ( -16.55341960407611168, -4.379528057220339221, 31.45724293864769550 ) ) ;
#86694 = CARTESIAN_POINT ( 'NONE',  ( -10.72451020669898014, 18.67979575497178502, 110.4155762719810383 ) ) ;
#86695 = CARTESIAN_POINT ( 'NONE',  ( -12.06949235617756955, 12.14591786802309770, 55.62390960531436690 ) ) ;
#86696 = CARTESIAN_POINT ( 'NONE',  ( 19.05341960407617918, -5.049401038297876454, 91.04275706135234714 ) ) ;
#86697 = CARTESIAN_POINT ( 'NONE',  ( 19.05341960407617918, -5.049401038297876454, 71.04275706135234714 ) ) ;
#86698 = CARTESIAN_POINT ( 'NONE',  ( -5.719274019375665041, -21.55341960407619695, 69.79275706135234714 ) ) ;
#86699 = CARTESIAN_POINT ( 'NONE',  ( -9.564922557961040184, 16.46253265017147172, 57.91775706135233293 ) ) ;
#86700 = CARTESIAN_POINT ( 'NONE',  ( 12.06949235617757843, -12.14591786802309237, 113.1239096053143953 ) ) ;
#86701 = CARTESIAN_POINT ( 'NONE',  ( 0.05219959533907565091, 21.53943276465977519, 44.99890960531435979 ) ) ;
#86702 = CARTESIAN_POINT ( 'NONE',  ( 8.314922557960818139, 14.29746914071049879, 44.58224293864769550 ) ) ;
#86703 = CARTESIAN_POINT ( 'NONE',  ( -18.87075004821569024, 5.499999999999995559, 93.67408112101048800 ) ) ;
#86704 = CARTESIAN_POINT ( 'NONE',  ( 9.564922557961047289, -16.46253265017146816, 20.41775706135233293 ) ) ;
#86705 = CARTESIAN_POINT ( 'NONE',  ( -16.53943276465976808, -0.05219959533934237506, 78.75109039468568994 ) ) ;
#86706 = CARTESIAN_POINT ( 'NONE',  ( 16.53943276465976808, -0.05219959533910856209, 38.74890960531435979 ) ) ;
#86707 = CARTESIAN_POINT ( 'NONE',  ( -21.55341960407619339, 5.719274019375674811, 78.54275706135236135 ) ) ;
#86708 = CARTESIAN_POINT ( 'NONE',  ( 5.823673210054444382, -21.52544592524334988, 65.20942372801901854 ) ) ;
#86709 = CARTESIAN_POINT ( 'NONE',  ( 21.55341960407610458, 5.719274019375980345, 78.95724293864769550 ) ) ;
#86710 = CARTESIAN_POINT ( 'NONE',  ( 19.02544592524343514, -5.153800228976328945, 38.54057627198103120 ) ) ;
#86711 = CARTESIAN_POINT ( 'NONE',  ( -21.52544592524334988, -5.823673210054445271, 53.95942372801900433 ) ) ;
#86712 = CARTESIAN_POINT ( 'NONE',  ( -5.049401038298153566, 19.05341960407611168, 40.20724293864768839 ) ) ;
#86713 = CARTESIAN_POINT ( 'NONE',  ( -9.564922557960796823, -16.46253265017161027, 52.08224293864768839 ) ) ;
#86714 = CARTESIAN_POINT ( 'NONE',  ( 12.06949235617757843, -12.14591786802309237, 98.12390960531436690 ) ) ;
#86715 = CARTESIAN_POINT ( 'NONE',  ( 9.564922557960805705, 16.46253265017160317, 79.58224293864769550 ) ) ;
#86716 = CARTESIAN_POINT ( 'NONE',  ( -12.06949235617756955, 12.14591786802309770, 45.62390960531436690 ) ) ;
#86717 = CARTESIAN_POINT ( 'NONE',  ( -14.29746914071049879, 8.314922557960819915, 95.83224293864770971 ) ) ;
#86718 = CARTESIAN_POINT ( 'NONE',  ( 5.719274019375991003, -21.55341960407610458, 67.70724293864769550 ) ) ;
#86719 = CARTESIAN_POINT ( 'NONE',  ( -15.80617190586768217, 15.72974639402176855, 23.12609039468567573 ) ) ;
#86720 = CARTESIAN_POINT ( 'NONE',  ( 16.12203461105333702, -16.12203461105326951, -64.92279855667830191 ) ) ;
#86722 = CARTESIAN_POINT ( 'NONE',  ( -9.564922557961040184, 16.46253265017147172, 112.9177570613523329 ) ) ;
#86721 = CARTESIAN_POINT ( 'NONE',  ( 19.05341960407611168, 5.049401038298154454, 78.95724293864769550 ) ) ;
#86723 = CARTESIAN_POINT ( 'NONE',  ( -5.719274019375978568, 21.55341960407610458, 65.20724293864768129 ) ) ;
#86724 = CARTESIAN_POINT ( 'NONE',  ( -0.05219959533937732626, 21.53943276465977519, 92.50109039468567573 ) ) ;
#86725 = CARTESIAN_POINT ( 'NONE',  ( 9.474510206698971260, -16.51473224551069308, 77.91557627198103830 ) ) ;
#86726 = CARTESIAN_POINT ( 'NONE',  ( -10.81492255796105439, 18.62759615963255655, 27.91775706135234358 ) ) ;
#86727 = CARTESIAN_POINT ( 'NONE',  ( 19.05341960407611168, 5.049401038298154454, 108.9572429386477097 ) ) ;
#86728 = CARTESIAN_POINT ( 'NONE',  ( -14.29746914071037622, -8.314922557961029526, 84.16775706135234714 ) ) ;
#86729 = CARTESIAN_POINT ( 'NONE',  ( -18.67979575497193778, 10.72451020669871902, 73.33442372801901854 ) ) ;
#86730 = CARTESIAN_POINT ( 'NONE',  ( -15.72974639402176322, -15.80617190586768395, 94.37609039468568994 ) ) ;
#86731 = CARTESIAN_POINT ( 'NONE',  ( 8.224510206698742110, 14.34966873604972548, 57.08442372801901854 ) ) ;
#86732 = CARTESIAN_POINT ( 'NONE',  ( 5.719274019375673035, 21.55341960407619339, 22.29275706135235069 ) ) ;
#86733 = CARTESIAN_POINT ( 'NONE',  ( -13.89961937509977652, 13.97604488694528158, 115.6239096053143669 ) ) ;
#86734 = CARTESIAN_POINT ( 'NONE',  ( -21.52544592524334988, -5.823673210054445271, 93.95942372801903275 ) ) ;
#86735 = CARTESIAN_POINT ( 'NONE',  ( 19.05341960407611168, 5.049401038298154454, 98.95724293864766707 ) ) ;
#86736 = CARTESIAN_POINT ( 'NONE',  ( 21.52544592524344225, -5.823673210054117533, 93.54057627198103830 ) ) ;
#86737 = CARTESIAN_POINT ( 'NONE',  ( 16.51473224551083163, -9.474510206698727899, 55.83442372801899722 ) ) ;
#86739 = CARTESIAN_POINT ( 'NONE',  ( 5.823673210054125526, 21.52544592524343514, 59.79057627198103120 ) ) ;
#86738 = CARTESIAN_POINT ( 'NONE',  ( -22.30909568229876072, -31.30078617544283048, -17.06157116626747694 ) ) ;
#86741 = CARTESIAN_POINT ( 'NONE',  ( 16.55341960407611168, 4.379528057220329451, 38.95724293864768839 ) ) ;
#86740 = CARTESIAN_POINT ( 'NONE',  ( -16.46253265017160317, 9.564922557960807481, 100.8322429386477097 ) ) ;
#86742 = CARTESIAN_POINT ( 'NONE',  ( 21.72193145969975703, 8.667250440200810147, 169.0624054586918987 ) ) ;
#86743 = CARTESIAN_POINT ( 'NONE',  ( -0.05219959533936034679, 19.03943276465977164, 72.50109039468566152 ) ) ;
#86744 = VECTOR ( 'NONE', #36846, 1000.000000000000000 ) ;
#86745 = CARTESIAN_POINT ( 'NONE',  ( -0.9460486868805269012, -16.38029848613151174, -61.48057501744756337 ) ) ;
#86746 = ADVANCED_FACE ( 'NONE', ( #92554 ), #95539, .T. ) ;
#86747 = CARTESIAN_POINT ( 'NONE',  ( -16.51473224551082808, 9.474510206698731452, 113.3344237280190043 ) ) ;
#86748 = CARTESIAN_POINT ( 'NONE',  ( 21.52544592524344225, -5.823673210054117533, 83.54057627198102409 ) ) ;
#86749 = CARTESIAN_POINT ( 'NONE',  ( 4.483927247898545687, 16.52544592524342804, 59.79057627198103120 ) ) ;
#86750 = CARTESIAN_POINT ( 'NONE',  ( -13.97604488694527625, -13.89961937509977652, 101.8739096053143811 ) ) ;
#86751 = CARTESIAN_POINT ( 'NONE',  ( -0.05219959533934338120, 16.53943276465976808, 32.50109039468568284 ) ) ;
#86752 = CARTESIAN_POINT ( 'NONE',  ( -9.564922557960796823, -16.46253265017161027, 62.08224293864769550 ) ) ;
#86754 = CARTESIAN_POINT ( 'NONE',  ( -9.474510206698720793, -16.51473224551083518, 84.58442372801900433 ) ) ;
#86753 = CARTESIAN_POINT ( 'NONE',  ( -5.823673210054116645, -21.52544592524344225, 112.2905762719810241 ) ) ;
#86755 = CARTESIAN_POINT ( 'NONE',  ( 5.153800228976335163, 19.02544592524342804, 99.79057627198102409 ) ) ;
#86756 = CARTESIAN_POINT ( 'NONE',  ( -0.05219959533909027116, -19.03943276465977164, 72.49890960531435269 ) ) ;
#86757 = CARTESIAN_POINT ( 'NONE',  ( 10.81492255796078972, 18.62759615963270932, 79.58224293864769550 ) ) ;
#86758 = CARTESIAN_POINT ( 'NONE',  ( -9.474510206698964154, 16.51473224551069663, 50.41557627198102409 ) ) ;
#86759 = CARTESIAN_POINT ( 'NONE',  ( -20.62648400444483343, 31.81274089240160308, -7.999999999999996447 ) ) ;
#86760 = CARTESIAN_POINT ( 'NONE',  ( 16.52544592524342804, -4.483927247898539470, 58.54057627198103120 ) ) ;
#86761 = CARTESIAN_POINT ( 'NONE',  ( 16.46253265017160672, -9.564922557960803928, 103.3322429386476955 ) ) ;
#86762 = DIRECTION ( 'NONE',  ( 0.000000000000000000, 0.000000000000000000, 1.000000000000000000 ) ) ;
#86763 = CARTESIAN_POINT ( 'NONE',  ( -5.049401038297874678, -19.05341960407617918, 69.79275706135233293 ) ) ;
#86764 = CARTESIAN_POINT ( 'NONE',  ( 10.72451020669898902, -18.67979575497178502, 82.91557627198103830 ) ) ;
#86765 = CARTESIAN_POINT ( 'NONE',  ( 9.564922557961047289, -16.46253265017146816, 50.41775706135233293 ) ) ;
#86766 = CARTESIAN_POINT ( 'NONE',  ( 0.05219959533909260263, 19.03943276465977164, 104.9989096053143669 ) ) ;
#86767 = DIRECTION ( 'NONE',  ( 0.000000000000000000, 0.000000000000000000, -1.000000000000000000 ) ) ;
#86768 = CARTESIAN_POINT ( 'NONE',  ( -15.80617190586745835, -15.72974639402198527, 46.87390960531435979 ) ) ;
#86769 = CARTESIAN_POINT ( 'NONE',  ( 13.89961937509977652, -13.97604488694527269, 68.12390960531436690 ) ) ;
#86770 = CARTESIAN_POINT ( 'NONE',  ( 21.53943276465977519, 0.05219959533937863772, 66.25109039468567573 ) ) ;
#86771 = CARTESIAN_POINT ( 'NONE',  ( 13.89961937509977652, -13.97604488694527269, 33.12390960531434558 ) ) ;
#86773 = VERTEX_POINT ( 'NONE', #21696 ) ;
#86772 = CARTESIAN_POINT ( 'NONE',  ( -10.72451020669870658, -18.67979575497194134, 19.58442372801901143 ) ) ;
#86774 = CARTESIAN_POINT ( 'NONE',  ( -5.719274019375665041, -21.55341960407619695, 54.79275706135235424 ) ) ;
#86775 = ORIENTED_EDGE ( 'NONE', *, *, #172493, .T. ) ;
#86776 = CARTESIAN_POINT ( 'NONE',  ( 17.50000000000000355, 5.499999999999998224, 20.00000000000000000 ) ) ;
#86777 = CARTESIAN_POINT ( 'NONE',  ( 0.05219959533936267826, -19.03943276465977164, 70.00109039468566152 ) ) ;
#86778 = CARTESIAN_POINT ( 'NONE',  ( -37.99626262588766679, 2.428612866367529932E-14, -5.747842220587803475 ) ) ;
#86779 = CARTESIAN_POINT ( 'NONE',  ( 21.55341960407619695, -5.719274019375665929, 26.04275706135235779 ) ) ;
#86780 = CARTESIAN_POINT ( 'NONE',  ( 19.03943276465977164, -0.05219959533909143690, 53.74890960531436690 ) ) ;
#86781 = CARTESIAN_POINT ( 'NONE',  ( -12.14591786802326823, 12.06949235617739902, 38.12609039468567573 ) ) ;
#86782 = CARTESIAN_POINT ( 'NONE',  ( -23.48529157249600985, 32.32473071737754111, -8.049999994537627046 ) ) ;
#86783 = CARTESIAN_POINT ( 'NONE',  ( 21.52544592524334988, 5.823673210054432836, 111.4594237280190328 ) ) ;
#86784 = CARTESIAN_POINT ( 'NONE',  ( 9.474510206698971260, -16.51473224551069308, 37.91557627198102409 ) ) ;
#86785 = CARTESIAN_POINT ( 'NONE',  ( 21.53943276465977519, 0.05219959533937863772, 111.2510903946856899 ) ) ;
#86786 = CARTESIAN_POINT ( 'NONE',  ( 12.06949235617739724, 12.14591786802326823, 91.87609039468568994 ) ) ;
#86788 = CARTESIAN_POINT ( 'NONE',  ( -5.823673210054431948, 21.52544592524334988, 57.70942372801901143 ) ) ;
#86787 = CARTESIAN_POINT ( 'NONE',  ( 13.97604488694527802, 13.89961937509977652, 84.37390960531433848 ) ) ;
#86789 = CARTESIAN_POINT ( 'NONE',  ( 30.00000000000000000, -5.510910596163089556E-15, 42.49999999999999289 ) ) ;
#86790 = DIRECTION ( 'NONE',  ( -0.000000000000000000, -0.000000000000000000, -1.000000000000000000 ) ) ;
#86791 = DIRECTION ( 'NONE',  ( 1.000000000000000000, -5.392603844284257652E-33, 0.000000000000000000 ) ) ;
#86793 = CARTESIAN_POINT ( 'NONE',  ( -15.80617190586768217, 15.72974639402176855, 73.12609039468567573 ) ) ;
#86792 = CARTESIAN_POINT ( 'NONE',  ( -12.06949235617739369, -12.14591786802326823, 54.37609039468568994 ) ) ;
#86794 = CARTESIAN_POINT ( 'NONE',  ( 10.81492255796106328, -18.62759615963255655, 105.4177570613523613 ) ) ;
#86795 = CARTESIAN_POINT ( 'NONE',  ( -11.67169337655814410, 9.562403590618668403, -59.87610203618464766 ) ) ;
#86796 = CARTESIAN_POINT ( 'NONE',  ( -8.314922557961024197, 14.29746914071037800, 32.91775706135234714 ) ) ;
#86797 = CARTESIAN_POINT ( 'NONE',  ( 13.97604488694527802, 13.89961937509977652, 84.37390960531433848 ) ) ;
#86798 = CARTESIAN_POINT ( 'NONE',  ( -16.51473224551069308, -9.474510206698971260, 111.6655762719810383 ) ) ;
#86799 = ORIENTED_EDGE ( 'NONE', *, *, #88864, .T. ) ;
#86800 = CARTESIAN_POINT ( 'NONE',  ( -35.00000000000000000, 3.889087296526014814, 1.818019484660534424 ) ) ;
#86801 = B_SPLINE_CURVE_WITH_KNOTS ( 'NONE', 3,
 ( #100441, #191453, #162121, #99438, #37774, #173312, #5427, #97423, #159109, #35776, #23618, #20603, #66113, #36761, #98424, #161118, #84260, #85265, #142944, #144941, #6423, #146956, #38784, #82255, #143947, #68104, #52930, #19621, #145942, #51941, #53948, #112615 ),
 .UNSPECIFIED., .F., .F.,
 ( 4, 2, 2, 2, 2, 2, 2, 2, 2, 2, 2, 2, 2, 2, 2, 4 ),
 ( 4.336808689942017736E-18, 0.0003712461730036848806, 0.0007424923460073654244, 0.001113738519011045914, 0.001484984692014726512, 0.002227477038022087491, 0.002598723211025768306, 0.002969969384029448687, 0.003341215557033129068, 0.003712461730036809883, 0.004083707903040490264, 0.004454954076044170645, 0.004826200249047851026, 0.005197446422051532275, 0.005568692595055212656, 0.005939938768058893037 ),
 .UNSPECIFIED. ) ;
#86802 = CARTESIAN_POINT ( 'NONE',  ( -5.153800228976328057, -19.02544592524343514, 27.29057627198103120 ) ) ;
#86803 = CARTESIAN_POINT ( 'NONE',  ( 10.81492255796078972, 18.62759615963270932, 44.58224293864769550 ) ) ;
#86804 = CARTESIAN_POINT ( 'NONE',  ( -4.379528057220086978, -16.55341960407618274, 104.7927570613523898 ) ) ;
#86806 = CARTESIAN_POINT ( 'NONE',  ( 9.474510206698971260, -16.51473224551069308, 67.91557627198102409 ) ) ;
#86805 = CARTESIAN_POINT ( 'NONE',  ( 14.34966873604960469, 8.224510206698951720, 84.16557627198103830 ) ) ;
#86807 = CARTESIAN_POINT ( 'NONE',  ( 10.72451020669871369, 18.67979575497193778, 92.08442372801901854 ) ) ;
#86808 = CARTESIAN_POINT ( 'NONE',  ( -14.34966873604972548, 8.224510206698743886, 28.33442372801902209 ) ) ;
#86809 = CARTESIAN_POINT ( 'NONE',  ( -12.14591786802309592, -12.06949235617757132, 91.87390960531436690 ) ) ;
#86810 = CARTESIAN_POINT ( 'NONE',  ( 10.72451020669871369, 18.67979575497193778, 42.08442372801901854 ) ) ;
#86811 = CARTESIAN_POINT ( 'NONE',  ( 18.67979575497178502, 10.72451020669898547, 79.16557627198103830 ) ) ;
#86812 = CARTESIAN_POINT ( 'NONE',  ( 16.46253265017146816, 9.564922557961045513, 56.66775706135233293 ) ) ;
#86813 = CARTESIAN_POINT ( 'NONE',  ( -34.52932710190716392, 5.142084072295503461, 50.46524955901336540 ) ) ;
#86814 = CARTESIAN_POINT ( 'NONE',  ( 13.97604488694527802, 13.89961937509977652, 99.37390960531436690 ) ) ;
#86815 = CARTESIAN_POINT ( 'NONE',  ( -0.05219959533910754901, -16.53943276465976808, 67.49890960531436690 ) ) ;
#86816 = CARTESIAN_POINT ( 'NONE',  ( 16.52544592524342804, -4.483927247898539470, 53.54057627198103120 ) ) ;
#86817 = CARTESIAN_POINT ( 'NONE',  ( -8.314922557960811034, -14.29746914071050412, 22.08224293864769194 ) ) ;
#86818 = CARTESIAN_POINT ( 'NONE',  ( -19.03943276465977164, -0.05219959533935918106, 63.75109039468566863 ) ) ;
#86819 = CARTESIAN_POINT ( 'NONE',  ( 9.564922557961047289, -16.46253265017146816, 90.41775706135234714 ) ) ;
#86820 = CARTESIAN_POINT ( 'NONE',  ( 19.02544592524343514, -5.153800228976328945, 113.5405762719810241 ) ) ;
#86821 = EDGE_CURVE ( 'NONE', #56776, #188843, #37941, .T. ) ;
#86822 = CARTESIAN_POINT ( 'NONE',  ( 8.224510206698953496, -14.34966873604960469, 82.91557627198103830 ) ) ;
#86823 = LINE ( 'NONE', #180858, #184009 ) ;
#86825 = CARTESIAN_POINT ( 'NONE',  ( -0.05219959533907301413, -21.53943276465977519, 52.49890960531435979 ) ) ;
#86824 = CARTESIAN_POINT ( 'NONE',  ( -5.049401038298153566, 19.05341960407611168, 50.20724293864770260 ) ) ;
#86826 = CARTESIAN_POINT ( 'NONE',  ( 18.67979575497178502, 10.72451020669898547, 74.16557627198102409 ) ) ;
#86827 = CARTESIAN_POINT ( 'NONE',  ( 8.224510206698953496, -14.34966873604960469, 112.9155762719810383 ) ) ;
#86829 = CARTESIAN_POINT ( 'NONE',  ( 13.89961937509977652, -13.97604488694527269, 43.12390960531434558 ) ) ;
#86828 = CARTESIAN_POINT ( 'NONE',  ( 4.379528057220092307, 16.55341960407617563, 67.29275706135234714 ) ) ;
#86830 = CARTESIAN_POINT ( 'NONE',  ( -9.474510206698720793, -16.51473224551083518, 34.58442372801899722 ) ) ;
#86831 = CARTESIAN_POINT ( 'NONE',  ( -0.05219959533937732626, 21.53943276465977519, 57.50109039468568994 ) ) ;
#86832 = CARTESIAN_POINT ( 'NONE',  ( 12.06949235617757843, -12.14591786802309237, 103.1239096053143811 ) ) ;
#86833 = CARTESIAN_POINT ( 'NONE',  ( 16.51473224551083163, -9.474510206698727899, 85.83442372801900433 ) ) ;
#86834 = CARTESIAN_POINT ( 'NONE',  ( -11.40812507854754720, -35.11059874428192273, -4.724999997268812812 ) ) ;
#86836 = CARTESIAN_POINT ( 'NONE',  ( -10.72451020669898014, 18.67979575497178502, 50.41557627198103120 ) ) ;
#86835 = CARTESIAN_POINT ( 'NONE',  ( 17.50000000000004263, 3.647616755428117585, 37.20330205721256078 ) ) ;
#86837 = CARTESIAN_POINT ( 'NONE',  ( -9.564922557960796823, -16.46253265017161027, 27.08224293864769550 ) ) ;
#86838 = CARTESIAN_POINT ( 'NONE',  ( 18.67979575497194134, -10.72451020669871369, 80.83442372801901854 ) ) ;
#86839 = VECTOR ( 'NONE', #173072, 1000.000000000000000 ) ;
#86840 = CARTESIAN_POINT ( 'NONE',  ( 16.52544592524342804, -4.483927247898539470, 38.54057627198103120 ) ) ;
#86842 = CARTESIAN_POINT ( 'NONE',  ( 16.55341960407611168, 4.379528057220329451, 38.95724293864768839 ) ) ;
#86841 = CARTESIAN_POINT ( 'NONE',  ( -12.14591786802326823, 12.06949235617739902, 53.12609039468568284 ) ) ;
#86843 = CARTESIAN_POINT ( 'NONE',  ( 18.62759615963271287, -10.81492255796078972, 88.33224293864769550 ) ) ;
#86844 = CARTESIAN_POINT ( 'NONE',  ( 18.62759615963271287, -10.81492255796078972, 78.33224293864770971 ) ) ;
#86845 = CARTESIAN_POINT ( 'NONE',  ( -26.46959431505283789, -27.26463967846487435, -15.00000000000000178 ) ) ;
#86847 = CARTESIAN_POINT ( 'NONE',  ( 16.51473224551069308, 9.474510206698969483, 114.1655762719810241 ) ) ;
#86846 = CARTESIAN_POINT ( 'NONE',  ( -0.05219959533936034679, 19.03943276465977164, 77.50109039468566152 ) ) ;
#86848 = CARTESIAN_POINT ( 'NONE',  ( -0.05219959533909027116, -19.03943276465977164, 52.49890960531436690 ) ) ;
#86849 = CARTESIAN_POINT ( 'NONE',  ( 19.03943276465977164, -0.05219959533909143690, 33.74890960531435979 ) ) ;
#86850 = SURFACE_STYLE_FILL_AREA ( #149526 ) ;
#86851 = DIRECTION ( 'NONE',  ( 0.000000000000000000, 0.000000000000000000, -1.000000000000000000 ) ) ;
#86852 = VERTEX_POINT ( 'NONE', #128851 ) ;
#86853 = CARTESIAN_POINT ( 'NONE',  ( -12.14591786802326823, 12.06949235617739902, 83.12609039468568994 ) ) ;
#86854 = CARTESIAN_POINT ( 'NONE',  ( 21.53943276465977519, -0.05219959533907433946, 103.7489096053143669 ) ) ;
#86855 = CARTESIAN_POINT ( 'NONE',  ( -19.05341960407611168, -5.049401038298163336, 71.45724293864766707 ) ) ;
#86856 = CARTESIAN_POINT ( 'NONE',  ( -15.72974639402176322, -15.80617190586768395, 44.37609039468567573 ) ) ;
#86857 = CARTESIAN_POINT ( 'NONE',  ( 13.89961937509977652, -13.97604488694527269, 93.12390960531436690 ) ) ;
#86858 = CARTESIAN_POINT ( 'NONE',  ( -28.30573922537829290, -27.84595035627394921, -20.14355118861611516 ) ) ;
#86859 = VERTEX_POINT ( 'NONE', #188569 ) ;
#86860 = CARTESIAN_POINT ( 'NONE',  ( -21.53943276465977519, -0.05219959533937600094, 38.75109039468567573 ) ) ;
#86862 = CARTESIAN_POINT ( 'NONE',  ( 13.97604488694527802, 13.89961937509977652, 109.3739096053143669 ) ) ;
#86861 = CARTESIAN_POINT ( 'NONE',  ( 5.049401038298161559, -19.05341960407611168, 27.70724293864769550 ) ) ;
#86863 = CARTESIAN_POINT ( 'NONE',  ( -5.153800228976607833, 19.02544592524334988, 42.70942372801901143 ) ) ;
#86864 = CARTESIAN_POINT ( 'NONE',  ( -21.53943276465977519, 0.05219959533907696930, 111.2489096053143669 ) ) ;
#86865 = CARTESIAN_POINT ( 'NONE',  ( 16.46253265017146816, 9.564922557961045513, 51.66775706135233293 ) ) ;
#86866 = CARTESIAN_POINT ( 'NONE',  ( -5.049401038297874678, -19.05341960407617918, 44.79275706135232582 ) ) ;
#86867 = CARTESIAN_POINT ( 'NONE',  ( 8.314922557961029526, -14.29746914071037800, 85.41775706135236135 ) ) ;
#86868 = CARTESIAN_POINT ( 'NONE',  ( 8.898068258721473001, -27.38543819252872069, 146.5843446569000150 ) ) ;
#86869 = CARTESIAN_POINT ( 'NONE',  ( -19.03943276465977164, 0.05219959533909376836, 76.24890960531435269 ) ) ;
#86870 = CARTESIAN_POINT ( 'NONE',  ( -10.81492255796105439, 18.62759615963255655, 77.91775706135231871 ) ) ;
#86871 = CARTESIAN_POINT ( 'NONE',  ( -21.52544592524334988, -5.823673210054445271, 93.95942372801903275 ) ) ;
#86872 = CARTESIAN_POINT ( 'NONE',  ( 21.46320343559639454, -20.96320343559646915, 4.646446609406721606 ) ) ;
#86873 = CARTESIAN_POINT ( 'NONE',  ( -13.89961937509977652, 13.97604488694528158, 90.62390960531432427 ) ) ;
#86874 = CARTESIAN_POINT ( 'NONE',  ( 21.52544592524334988, 5.823673210054432836, 66.45942372801903275 ) ) ;
#86875 = CARTESIAN_POINT ( 'NONE',  ( 13.97604488694548053, -13.89961937509957401, 95.62609039468563310 ) ) ;
#86876 = CARTESIAN_POINT ( 'NONE',  ( -5.049401038298153566, 19.05341960407611168, 70.20724293864769550 ) ) ;
#86877 = CARTESIAN_POINT ( 'NONE',  ( 19.03943276465977164, -0.05219959533909143690, 108.7489096053143527 ) ) ;
#86878 = CARTESIAN_POINT ( 'NONE',  ( -19.03943276465977164, 0.05219959533909376836, 86.24890960531436690 ) ) ;
#86879 = CARTESIAN_POINT ( 'NONE',  ( -28.28060372831499336, 2.428612866367529932E-14, 149.6875000013656063 ) ) ;
#86880 = CARTESIAN_POINT ( 'NONE',  ( 19.03943276465977164, -0.05219959533909143690, 63.74890960531435979 ) ) ;
#86881 = CARTESIAN_POINT ( 'NONE',  ( 13.89961937509977652, -13.97604488694527269, 53.12390960531434558 ) ) ;
#86882 = CARTESIAN_POINT ( 'NONE',  ( 21.52544592524344225, -5.823673210054117533, 108.5405762719810241 ) ) ;
#86883 = CARTESIAN_POINT ( 'NONE',  ( -8.314922557961024197, 14.29746914071037800, 102.9177570613523756 ) ) ;
#86884 = CARTESIAN_POINT ( 'NONE',  ( 0.1032920037969625171, 16.70000000000001705, -61.34707691135563579 ) ) ;
#86885 = CARTESIAN_POINT ( 'NONE',  ( 5.049401038297881783, 19.05341960407617563, 57.29275706135231871 ) ) ;
#86886 = CARTESIAN_POINT ( 'NONE',  ( -13.89961937509977652, 13.97604488694528158, 90.62390960531432427 ) ) ;
#86887 = CARTESIAN_POINT ( 'NONE',  ( 4.379528057220339221, -16.55341960407611168, 72.70724293864769550 ) ) ;
#86888 = CARTESIAN_POINT ( 'NONE',  ( 14.29746914071049879, -8.314922557960816363, 108.3322429386477097 ) ) ;
#86889 = CARTESIAN_POINT ( 'NONE',  ( 18.62759615963271287, -10.81492255796078972, 28.33224293864769550 ) ) ;
#86890 =( BOUNDED_CURVE ( )  B_SPLINE_CURVE ( 2, ( #67338, #64367, #141201, #172546, #96672, #174536, #111858, #65351, #171551, #20836, #33040 ),
 .UNSPECIFIED., .F., .T. ) 
 B_SPLINE_CURVE_WITH_KNOTS ( ( 3, 2, 2, 2, 2, 3 ),
 ( 0.5000000000000000000, 0.5200000000000000178, 0.5400000000000000355, 0.5600000000000001643, 0.5800000000000000711, 0.6000000000000000888 ),
 .UNSPECIFIED. ) 
 CURVE ( )  GEOMETRIC_REPRESENTATION_ITEM ( )  RATIONAL_B_SPLINE_CURVE ( ( 1.000000000000000000, 0.9510565162951535312, 1.000000000000000000, 0.9510565162951535312, 1.000000000000000000, 0.9510565162951535312, 1.000000000000000000, 0.9510565162951535312, 1.000000000000000000, 0.9510565162951533091, 1.000000000000000222 ) ) 
 REPRESENTATION_ITEM ( '' )  );
#86891 = CARTESIAN_POINT ( 'NONE',  ( -18.62759615963270932, 10.81492255796079327, 25.83224293864769194 ) ) ;
#86892 = CARTESIAN_POINT ( 'NONE',  ( 4.483927247898545687, 16.52544592524342804, 89.79057627198103830 ) ) ;
#86893 = CARTESIAN_POINT ( 'NONE',  ( -0.9277198534072325087, -6.404810000729023400, -62.44539631020980863 ) ) ;
#86894 = CARTESIAN_POINT ( 'NONE',  ( 16.46253265017146816, 9.564922557961045513, 31.66775706135232937 ) ) ;
#86895 = CARTESIAN_POINT ( 'NONE',  ( -16.52544592524335698, -4.483927247898792601, 108.9594237280190185 ) ) ;
#86896 = CARTESIAN_POINT ( 'NONE',  ( 19.02544592524343514, -5.153800228976328945, 93.54057627198102409 ) ) ;
#86897 = CARTESIAN_POINT ( 'NONE',  ( -21.52544592524334988, -5.823673210054445271, 48.95942372801902565 ) ) ;
#86898 = CARTESIAN_POINT ( 'NONE',  ( -5.719274019375978568, 21.55341960407610458, 50.20724293864769550 ) ) ;
#86900 = VERTEX_POINT ( 'NONE', #63216 ) ;
#86899 = CARTESIAN_POINT ( 'NONE',  ( 10.81492255796106328, -18.62759615963255655, 35.41775706135234003 ) ) ;
#86901 = CARTESIAN_POINT ( 'NONE',  ( 10.81492255796078972, 18.62759615963270932, 79.58224293864769550 ) ) ;
#86902 = CARTESIAN_POINT ( 'NONE',  ( -8.314922557960811034, -14.29746914071050412, 102.0822429386476955 ) ) ;
#86903 = CARTESIAN_POINT ( 'NONE',  ( 5.153800228976615827, -19.02544592524334988, 60.20942372801899012 ) ) ;
#86904 = CARTESIAN_POINT ( 'NONE',  ( -0.05219959533909027116, -19.03943276465977164, 42.49890960531435269 ) ) ;
#86905 = CARTESIAN_POINT ( 'NONE',  ( -5.049401038298153566, 19.05341960407611168, 100.2072429386476955 ) ) ;
#86906 = CARTESIAN_POINT ( 'NONE',  ( -13.97604488694527625, -13.89961937509977652, 96.87390960531433848 ) ) ;
#86907 = CARTESIAN_POINT ( 'NONE',  ( 8.314922557960818139, 14.29746914071049879, 114.5822429386477097 ) ) ;
#86908 = CARTESIAN_POINT ( 'NONE',  ( 16.55341960407611168, 4.379528057220329451, 38.95724293864768839 ) ) ;
#86909 = CARTESIAN_POINT ( 'NONE',  ( 14.29746914071037800, 8.314922557961029526, 36.66775706135234714 ) ) ;
#86910 = CARTESIAN_POINT ( 'NONE',  ( -5.823673210054431948, 21.52544592524334988, 112.7094237280190328 ) ) ;
#86912 = CARTESIAN_POINT ( 'NONE',  ( 12.14591786802309770, 12.06949235617756955, 24.37390960531435979 ) ) ;
#86911 = CARTESIAN_POINT ( 'NONE',  ( -5.374011537017813644, -5.374011537017721274, -64.92279855667830191 ) ) ;
#86913 = CARTESIAN_POINT ( 'NONE',  ( 5.719274019375673035, 21.55341960407619339, 27.29275706135234358 ) ) ;
#86914 = CARTESIAN_POINT ( 'NONE',  ( -19.05341960407611168, -5.049401038298163336, 111.4572429386476671 ) ) ;
#86915 = CARTESIAN_POINT ( 'NONE',  ( -0.05219959533934338120, 16.53943276465976808, 52.50109039468567573 ) ) ;
#86916 = CARTESIAN_POINT ( 'NONE',  ( -12.14591786802326823, 12.06949235617739902, 113.1260903946856899 ) ) ;
#86917 = CARTESIAN_POINT ( 'NONE',  ( 8.224510206698742110, 14.34966873604972548, 92.08442372801901854 ) ) ;
#86918 = CARTESIAN_POINT ( 'NONE',  ( 8.224510206698742110, 14.34966873604972548, 22.08442372801901143 ) ) ;
#86919 = ADVANCED_FACE ( 'NONE', ( #20687 ), #171407, .T. ) ;
#86920 = CARTESIAN_POINT ( 'NONE',  ( 19.03943276465977164, -0.05219959533909143690, 53.74890960531436690 ) ) ;
#86921 = CARTESIAN_POINT ( 'NONE',  ( -14.34966873604960291, -8.224510206698953496, 101.6655762719810383 ) ) ;
#86922 = CARTESIAN_POINT ( 'NONE',  ( 21.55341960407610458, 5.719274019375980345, 113.9572429386477239 ) ) ;
#86923 = CARTESIAN_POINT ( 'NONE',  ( -16.46253265017160317, 9.564922557960807481, 35.83224293864768839 ) ) ;
#86924 = CARTESIAN_POINT ( 'NONE',  ( 13.89961937509977652, -13.97604488694527269, 108.1239096053143669 ) ) ;
#86925 = CARTESIAN_POINT ( 'NONE',  ( -18.62759615963255300, -10.81492255796106328, 39.16775706135235424 ) ) ;
#86926 = CARTESIAN_POINT ( 'NONE',  ( 5.153800228976335163, 19.02544592524342804, 24.79057627198102765 ) ) ;
#86927 = CARTESIAN_POINT ( 'NONE',  ( 0.05219959533909260263, 19.03943276465977164, 109.9989096053143669 ) ) ;
#86928 = CARTESIAN_POINT ( 'NONE',  ( -17.49999999999998579, -5.499999999999973355, 101.2823096230356583 ) ) ;
#86929 = CARTESIAN_POINT ( 'NONE',  ( -16.51473224551069308, -9.474510206698971260, 96.66557627198102409 ) ) ;
#86931 = CARTESIAN_POINT ( 'NONE',  ( 8.224510206698953496, -14.34966873604960469, 87.91557627198103830 ) ) ;
#86930 = CARTESIAN_POINT ( 'NONE',  ( 21.52544592524334988, 5.823673210054432836, 46.45942372801901854 ) ) ;
#86932 = CARTESIAN_POINT ( 'NONE',  ( 19.02544592524343514, -5.153800228976328945, 98.54057627198100988 ) ) ;
#86933 = CARTESIAN_POINT ( 'NONE',  ( -27.07824611089070999, -7.738748529344896987, 165.1039267699996458 ) ) ;
#86934 = CARTESIAN_POINT ( 'NONE',  ( -12.14591786802326823, 12.06949235617739902, 63.12609039468568994 ) ) ;
#86935 = CARTESIAN_POINT ( 'NONE',  ( -10.72451020669870658, -18.67979575497194134, 74.58442372801901854 ) ) ;
#86936 = CARTESIAN_POINT ( 'NONE',  ( -8.224510206698735004, -14.34966873604973081, 34.58442372801900433 ) ) ;
#86937 = CARTESIAN_POINT ( 'NONE',  ( 5.049401038298161559, -19.05341960407611168, 87.70724293864769550 ) ) ;
#86938 = CARTESIAN_POINT ( 'NONE',  ( -19.02544592524334988, -5.153800228976617603, 103.9594237280190043 ) ) ;
#86939 = CARTESIAN_POINT ( 'NONE',  ( 8.314922557961029526, -14.29746914071037800, 70.41775706135236135 ) ) ;
#86940 = CARTESIAN_POINT ( 'NONE',  ( 9.474510206698729675, 16.51473224551082808, 22.08442372801899722 ) ) ;
#86941 = CARTESIAN_POINT ( 'NONE',  ( 5.049401038297881783, 19.05341960407617563, 92.29275706135234714 ) ) ;
#86942 = CARTESIAN_POINT ( 'NONE',  ( 13.97604488694527802, 13.89961937509977652, 59.37390960531434558 ) ) ;
#86943 = CARTESIAN_POINT ( 'NONE',  ( 10.72451020669898902, -18.67979575497178502, 87.91557627198103830 ) ) ;
#86945 = CARTESIAN_POINT ( 'NONE',  ( 5.049401038297881783, 19.05341960407617563, 87.29275706135234714 ) ) ;
#86944 = CARTESIAN_POINT ( 'NONE',  ( 14.34966873604960469, 8.224510206698951720, 89.16557627198102409 ) ) ;
#86946 = CARTESIAN_POINT ( 'NONE',  ( -12.06949235617739369, -12.14591786802326823, 59.37609039468568284 ) ) ;
#86947 = CARTESIAN_POINT ( 'NONE',  ( 24.50238749460113752, 2.981321037229033521, 173.3223451563238200 ) ) ;
#86948 = CARTESIAN_POINT ( 'NONE',  ( 19.02544592524334988, 5.153800228976608722, 56.45942372801898301 ) ) ;
#86949 = CARTESIAN_POINT ( 'NONE',  ( -16.52544592524342804, 4.483927247898546575, 31.04057627198102409 ) ) ;
#86950 = CARTESIAN_POINT ( 'NONE',  ( 14.34966873604960469, 8.224510206698951720, 84.16557627198103830 ) ) ;
#86952 = CARTESIAN_POINT ( 'NONE',  ( -16.19135201231351218, 7.376712067592062994, 39.81319145947881566 ) ) ;
#86951 = CARTESIAN_POINT ( 'NONE',  ( 16.46253265017146816, 9.564922557961045513, 26.66775706135234003 ) ) ;
#86953 = CARTESIAN_POINT ( 'NONE',  ( 15.72974639402176855, 15.80617190586768217, 21.87609039468567573 ) ) ;
#86954 = CARTESIAN_POINT ( 'NONE',  ( -19.02544592524342804, 5.153800228976336051, 106.0405762719810241 ) ) ;
#86955 = CARTESIAN_POINT ( 'NONE',  ( -19.03943276465977164, 0.05219959533909376836, 81.24890960531436690 ) ) ;
#86956 = CARTESIAN_POINT ( 'NONE',  ( -21.52544592524334988, -5.823673210054445271, 98.95942372801903275 ) ) ;
#86957 = CARTESIAN_POINT ( 'NONE',  ( 0.05219959533909260263, 19.03943276465977164, 79.99890960531436690 ) ) ;
#86958 = CARTESIAN_POINT ( 'NONE',  ( 21.52544592524344225, -5.823673210054117533, 38.54057627198103120 ) ) ;
#86959 = CARTESIAN_POINT ( 'NONE',  ( -8.224510206698948167, 14.34966873604960824, 85.41557627198102409 ) ) ;
#86960 = CARTESIAN_POINT ( 'NONE',  ( -13.97604488694527625, -13.89961937509977652, 56.87390960531434558 ) ) ;
#86961 = CARTESIAN_POINT ( 'NONE',  ( 14.34966873604960469, 8.224510206698951720, 104.1655762719810241 ) ) ;
#86962 = CARTESIAN_POINT ( 'NONE',  ( -18.67979575497193778, 10.72451020669871902, 28.33442372801902209 ) ) ;
#86963 = CARTESIAN_POINT ( 'NONE',  ( 15.80617190586769283, -15.72974639402175789, 65.62609039468568994 ) ) ;
#86964 = CARTESIAN_POINT ( 'NONE',  ( -9.564922557960796823, -16.46253265017161027, 37.08224293864768839 ) ) ;
#86965 = CARTESIAN_POINT ( 'NONE',  ( -0.05219959533934338120, 16.53943276465976808, 57.50109039468568994 ) ) ;
#86966 = CARTESIAN_POINT ( 'NONE',  ( 5.719274019375673035, 21.55341960407619339, 22.29275706135235069 ) ) ;
#86967 = CARTESIAN_POINT ( 'NONE',  ( 21.53943276465977519, -0.05219959533907433946, 108.7489096053143669 ) ) ;
#86969 = CARTESIAN_POINT ( 'NONE',  ( -16.51473224551069308, -9.474510206698971260, 51.66557627198102409 ) ) ;
#86968 = CARTESIAN_POINT ( 'NONE',  ( 16.46253265017146816, 9.564922557961045513, 41.66775706135234003 ) ) ;
#86970 = CARTESIAN_POINT ( 'NONE',  ( -30.00000000000000355, 3.889087296526015258, 1.818019484660534646 ) ) ;
#86971 = CARTESIAN_POINT ( 'NONE',  ( -21.55341960407619339, 5.719274019375674811, 73.54275706135234714 ) ) ;
#86972 = CARTESIAN_POINT ( 'NONE',  ( -0.05219959533907301413, -21.53943276465977519, 52.49890960531435979 ) ) ;
#86973 = CARTESIAN_POINT ( 'NONE',  ( 12.14591786802309770, 12.06949235617756955, 39.37390960531436690 ) ) ;
#86975 = CARTESIAN_POINT ( 'NONE',  ( 5.719274019375673035, 21.55341960407619339, 107.2927570613523471 ) ) ;
#86974 = CARTESIAN_POINT ( 'NONE',  ( 10.81492255796106328, -18.62759615963255655, 70.41775706135236135 ) ) ;
#86976 = CARTESIAN_POINT ( 'NONE',  ( 4.379528057220339221, -16.55341960407611168, 62.70724293864769550 ) ) ;
#86977 = CARTESIAN_POINT ( 'NONE',  ( 14.29746914071049879, -8.314922557960816363, 98.33224293864769550 ) ) ;
#86978 = CARTESIAN_POINT ( 'NONE',  ( 13.97604488694548053, -13.89961937509957401, 50.62609039468566152 ) ) ;
#86979 = CARTESIAN_POINT ( 'NONE',  ( 12.14591786802327356, -12.06949235617739191, 110.6260903946857042 ) ) ;
#86980 = CARTESIAN_POINT ( 'NONE',  ( -10.72451020669870658, -18.67979575497194134, 74.58442372801901854 ) ) ;
#86981 = CARTESIAN_POINT ( 'NONE',  ( -13.97604488694527625, -13.89961937509977652, 61.87390960531435979 ) ) ;
#86982 = CARTESIAN_POINT ( 'NONE',  ( -19.05341960407617563, 5.049401038297882671, 38.54275706135233293 ) ) ;
#86983 = CARTESIAN_POINT ( 'NONE',  ( 10.81492255796078972, 18.62759615963270932, 39.58224293864769550 ) ) ;
#86984 = CARTESIAN_POINT ( 'NONE',  ( -10.72451020669870658, -18.67979575497194134, 34.58442372801900433 ) ) ;
#86985 = CARTESIAN_POINT ( 'NONE',  ( 21.55341960407610458, 5.719274019375980345, 83.95724293864770971 ) ) ;
#86986 = CARTESIAN_POINT ( 'NONE',  ( 19.05341960407617918, -5.049401038297876454, 86.04275706135233293 ) ) ;
#86987 = CARTESIAN_POINT ( 'NONE',  ( -14.34966873604972548, 8.224510206698743886, 53.33442372801901854 ) ) ;
#86989 = CARTESIAN_POINT ( 'NONE',  ( 21.55341960407610458, 5.719274019375980345, 98.95724293864770971 ) ) ;
#86988 = DIRECTION ( 'NONE',  ( -0.000000000000000000, -0.000000000000000000, 1.000000000000000000 ) ) ;
#86990 = CARTESIAN_POINT ( 'NONE',  ( -0.05219959533910754901, -16.53943276465976808, 92.49890960531436690 ) ) ;
#86991 = CARTESIAN_POINT ( 'NONE',  ( 17.72560187377285601, 5.500000000000050626, 41.57814504131319211 ) ) ;
#86992 = CARTESIAN_POINT ( 'NONE',  ( 4.379528057220092307, 16.55341960407617563, 22.29275706135235069 ) ) ;
#86993 = CARTESIAN_POINT ( 'NONE',  ( -15.80617190586745835, -15.72974639402198527, 46.87390960531435979 ) ) ;
#86994 = CARTESIAN_POINT ( 'NONE',  ( 8.224510206698742110, 14.34966873604972548, 77.08442372801901854 ) ) ;
#86995 = CARTESIAN_POINT ( 'NONE',  ( -30.00000000000000000, 5.499999999999992895, 37.50000000000000000 ) ) ;
#86996 = CARTESIAN_POINT ( 'NONE',  ( -4.379528057220086978, -16.55341960407618274, 54.79275706135235424 ) ) ;
#86997 = CARTESIAN_POINT ( 'NONE',  ( -0.05219959533937732626, 21.53943276465977519, 22.50109039468567573 ) ) ;
#86998 = CARTESIAN_POINT ( 'NONE',  ( 0.05219959533907565091, 21.53943276465977519, 49.99890960531437401 ) ) ;
#86999 = CARTESIAN_POINT ( 'NONE',  ( 14.29746914071037800, 8.314922557961029526, 81.66775706135236135 ) ) ;
#87000 = CARTESIAN_POINT ( 'NONE',  ( -16.46253265017160317, 9.564922557960807481, 95.83224293864769550 ) ) ;
#87002 = CARTESIAN_POINT ( 'NONE',  ( 5.153800228976335163, 19.02544592524342804, 24.79057627198102765 ) ) ;
#87001 = CARTESIAN_POINT ( 'NONE',  ( -21.52544592524334988, -5.823673210054445271, 58.95942372801902565 ) ) ;
#87003 = CARTESIAN_POINT ( 'NONE',  ( 0.05219959533907565091, 21.53943276465977519, 39.99890960531436690 ) ) ;
#87004 = CARTESIAN_POINT ( 'NONE',  ( -5.719274019375978568, 21.55341960407610458, 25.20724293864769550 ) ) ;
#87005 = ORIENTED_EDGE ( 'NONE', *, *, #190360, .F. ) ;
#87006 = CARTESIAN_POINT ( 'NONE',  ( 16.46253265017146816, 9.564922557961045513, 41.66775706135234003 ) ) ;
#87007 = CARTESIAN_POINT ( 'NONE',  ( -8.314922557961024197, 14.29746914071037800, 62.91775706135236135 ) ) ;
#87008 = CARTESIAN_POINT ( 'NONE',  ( -5.823673210054116645, -21.52544592524344225, 22.29057627198102765 ) ) ;
#87009 = ORIENTED_EDGE ( 'NONE', *, *, #98272, .T. ) ;
#87010 = EDGE_CURVE ( 'NONE', #145773, #188324, #18719, .T. ) ;
#87011 = CARTESIAN_POINT ( 'NONE',  ( 5.049401038298161559, -19.05341960407611168, 92.70724293864769550 ) ) ;
#87012 = CARTESIAN_POINT ( 'NONE',  ( 8.314922557961029526, -14.29746914071037800, 95.41775706135234714 ) ) ;
#87013 = CARTESIAN_POINT ( 'NONE',  ( -18.22780087662124160, -5.499999999999927169, 78.98236817873106475 ) ) ;
#87014 = CARTESIAN_POINT ( 'NONE',  ( 16.53943276465976808, -0.05219959533910856209, 93.74890960531436690 ) ) ;
#87015 = CARTESIAN_POINT ( 'NONE',  ( 18.67979575497178502, 10.72451020669898547, 44.16557627198103120 ) ) ;
#87016 = CARTESIAN_POINT ( 'NONE',  ( -9.474510206698964154, 16.51473224551069663, 30.41557627198102054 ) ) ;
#87017 = CARTESIAN_POINT ( 'NONE',  ( 4.379528057220092307, 16.55341960407617563, 77.29275706135234714 ) ) ;
#87018 = CARTESIAN_POINT ( 'NONE',  ( 5.719274019375673035, 21.55341960407619339, 32.29275706135235424 ) ) ;
#87019 = CARTESIAN_POINT ( 'NONE',  ( -5.153800228976607833, 19.02544592524334988, 92.70942372801901854 ) ) ;
#87020 = CARTESIAN_POINT ( 'NONE',  ( -16.51473224551069308, -9.474510206698971260, 41.66557627198103120 ) ) ;
#87021 = CARTESIAN_POINT ( 'NONE',  ( 5.049401038298161559, -19.05341960407611168, 107.7072429386476955 ) ) ;
#87022 = CARTESIAN_POINT ( 'NONE',  ( 10.81492255796106328, -18.62759615963255655, 110.4177570613523756 ) ) ;
#87023 = CARTESIAN_POINT ( 'NONE',  ( 19.02544592524343514, -5.153800228976328945, 83.54057627198100988 ) ) ;
#87024 = EDGE_CURVE ( 'NONE', #45951, #10420, #98511, .T. ) ;
#87025 = CARTESIAN_POINT ( 'NONE',  ( 14.34966873604972726, -8.224510206698740333, 65.83442372801900433 ) ) ;
#87026 = CARTESIAN_POINT ( 'NONE',  ( -21.52544592524334988, -5.823673210054445271, 98.95942372801903275 ) ) ;
#87027 = CARTESIAN_POINT ( 'NONE',  ( 13.97604488694548053, -13.89961937509957401, 50.62609039468566152 ) ) ;
#87028 = CARTESIAN_POINT ( 'NONE',  ( -9.474510206698720793, -16.51473224551083518, 64.58442372801900433 ) ) ;
#87029 = EDGE_LOOP ( 'NONE', ( #20401, #28497, #155691, #197144 ) ) ;
#87030 = CARTESIAN_POINT ( 'NONE',  ( -10.81492255796105439, 18.62759615963255655, 67.91775706135234714 ) ) ;
#87031 = CARTESIAN_POINT ( 'NONE',  ( 19.05341960407611168, 5.049401038298154454, 63.95724293864769550 ) ) ;
#87032 = CARTESIAN_POINT ( 'NONE',  ( 16.46253265017160672, -9.564922557960803928, 58.33224293864769550 ) ) ;
#87033 = CARTESIAN_POINT ( 'NONE',  ( -5.049401038297874678, -19.05341960407617918, 59.79275706135231871 ) ) ;
#87034 = CARTESIAN_POINT ( 'NONE',  ( 5.049401038298161559, -19.05341960407611168, 112.7072429386476813 ) ) ;
#87035 = CARTESIAN_POINT ( 'NONE',  ( 5.153800228976335163, 19.02544592524342804, 79.79057627198102409 ) ) ;
#87036 = CARTESIAN_POINT ( 'NONE',  ( 12.14591786802309770, 12.06949235617756955, 44.37390960531435979 ) ) ;
#87037 = CARTESIAN_POINT ( 'NONE',  ( -18.62759615963270932, 10.81492255796079327, 35.83224293864768839 ) ) ;
#87038 = CARTESIAN_POINT ( 'NONE',  ( -17.97214573761833378, -5.499999999999959144, 96.46970049038655759 ) ) ;
#87039 = CARTESIAN_POINT ( 'NONE',  ( -21.55341960407619339, 5.719274019375674811, 113.5427570613523756 ) ) ;
#87040 = CARTESIAN_POINT ( 'NONE',  ( -27.96813078753325144, 7.160245613316167379, 161.0900052257269692 ) ) ;
#87041 = CARTESIAN_POINT ( 'NONE',  ( -13.97604488694527625, -13.89961937509977652, 36.87390960531436690 ) ) ;
#87042 = CARTESIAN_POINT ( 'NONE',  ( -18.22780087662123805, 5.499999999999981348, 86.01763182126894947 ) ) ;
#87043 = CARTESIAN_POINT ( 'NONE',  ( -34.11707783341799427, -4.368959606072635005, 91.63974055655047835 ) ) ;
#87044 = CARTESIAN_POINT ( 'NONE',  ( -21.52544592524334988, -5.823673210054445271, 68.95942372801901854 ) ) ;
#87045 = LINE ( 'NONE', #41555, #159879 ) ;
#87046 = CARTESIAN_POINT ( 'NONE',  ( -4.379528057220086978, -16.55341960407618274, 64.79275706135234714 ) ) ;
#87047 = CARTESIAN_POINT ( 'NONE',  ( 21.55341960407610458, 5.719274019375980345, 83.95724293864770971 ) ) ;
#87048 = CARTESIAN_POINT ( 'NONE',  ( -16.52544592524342804, 4.483927247898546575, 51.04057627198103120 ) ) ;
#87050 = CARTESIAN_POINT ( 'NONE',  ( -5.049401038298153566, 19.05341960407611168, 105.2072429386476671 ) ) ;
#87049 = CARTESIAN_POINT ( 'NONE',  ( 19.03943276465977164, -0.05219959533909143690, 23.74890960531435269 ) ) ;
#87051 = CARTESIAN_POINT ( 'NONE',  ( 10.81492255796106328, -18.62759615963255655, 35.41775706135234003 ) ) ;
#87052 = CARTESIAN_POINT ( 'NONE',  ( 5.153800228976615827, -19.02544592524334988, 50.20942372801897591 ) ) ;
#87053 = CARTESIAN_POINT ( 'NONE',  ( 19.02544592524343514, -5.153800228976328945, 38.54057627198103120 ) ) ;
#87054 = CARTESIAN_POINT ( 'NONE',  ( -5.719274019375665041, -21.55341960407619695, 79.79275706135236135 ) ) ;
#87055 = CARTESIAN_POINT ( 'NONE',  ( 17.05116617787827948, -6.768360034955673399, 31.15675553259201180 ) ) ;
#87056 = CARTESIAN_POINT ( 'NONE',  ( 0.05219959533910956823, 16.53943276465976808, 29.99890960531435979 ) ) ;
#87057 = CARTESIAN_POINT ( 'NONE',  ( 17.50000000000002487, 4.658240926743192567, 113.5552958218319901 ) ) ;
#87058 = CARTESIAN_POINT ( 'NONE',  ( -10.81492255796078084, -18.62759615963271287, 47.08224293864770260 ) ) ;
#87059 = DIRECTION ( 'NONE',  ( 0.000000000000000000, 0.000000000000000000, 1.000000000000000000 ) ) ;
#87060 = CARTESIAN_POINT ( 'NONE',  ( -19.03943276465977164, 0.05219959533909376836, 96.24890960531436690 ) ) ;
#87061 = CARTESIAN_POINT ( 'NONE',  ( -8.224510206698948167, 14.34966873604960824, 90.41557627198103830 ) ) ;
#87062 = CARTESIAN_POINT ( 'NONE',  ( 16.51473224551083163, -9.474510206698727899, 100.8344237280190043 ) ) ;
#87063 = CARTESIAN_POINT ( 'NONE',  ( -18.67979575497178146, -10.72451020669898902, 56.66557627198103830 ) ) ;
#87064 = ORIENTED_EDGE ( 'NONE', *, *, #15340, .T. ) ;
#87065 = CARTESIAN_POINT ( 'NONE',  ( -13.89961937509977652, 13.97604488694528158, 30.62390960531435269 ) ) ;
#87067 = CARTESIAN_POINT ( 'NONE',  ( 10.72451020669898902, -18.67979575497178502, 87.91557627198103830 ) ) ;
#87066 = CARTESIAN_POINT ( 'NONE',  ( -9.564922557960796823, -16.46253265017161027, 87.08224293864769550 ) ) ;
#87069 = CARTESIAN_POINT ( 'NONE',  ( -19.02544592524342804, 5.153800228976336051, 101.0405762719810241 ) ) ;
#87068 = CARTESIAN_POINT ( 'NONE',  ( 4.379528057220092307, 16.55341960407617563, 107.2927570613523471 ) ) ;
#87070 = CARTESIAN_POINT ( 'NONE',  ( -16.51473224551082808, 9.474510206698731452, 83.33442372801899012 ) ) ;
#87071 = CARTESIAN_POINT ( 'NONE',  ( 10.81492255796106328, -18.62759615963255655, 95.41775706135234714 ) ) ;
#87072 = CARTESIAN_POINT ( 'NONE',  ( -18.62759615963270932, 10.81492255796079327, 75.83224293864769550 ) ) ;
#87073 = CARTESIAN_POINT ( 'NONE',  ( 15.72974639402199770, -15.80617190586745480, 43.12390960531435269 ) ) ;
#87074 = CARTESIAN_POINT ( 'NONE',  ( 5.153800228976335163, 19.02544592524342804, 54.79057627198103120 ) ) ;
#87075 = CARTESIAN_POINT ( 'NONE',  ( -16.53943276465976808, -0.05219959533934237506, 108.7510903946857042 ) ) ;
#87076 = CARTESIAN_POINT ( 'NONE',  ( 5.153800228976335163, 19.02544592524342804, 69.79057627198103830 ) ) ;
#87077 = ORIENTED_EDGE ( 'NONE', *, *, #49174, .F. ) ;
#87078 = CARTESIAN_POINT ( 'NONE',  ( 18.22780087662121673, 5.500000000000056843, 38.98459894673893444 ) ) ;
#87079 = CARTESIAN_POINT ( 'NONE',  ( -16.51473224551082808, 9.474510206698731452, 28.33442372801900433 ) ) ;
#87080 = CARTESIAN_POINT ( 'NONE',  ( 8.224510206698953496, -14.34966873604960469, 77.91557627198102409 ) ) ;
#87081 = CARTESIAN_POINT ( 'NONE',  ( 21.55341960407619695, -5.719274019375665929, 21.04275706135234714 ) ) ;
#87082 = CARTESIAN_POINT ( 'NONE',  ( -22.44159573604009950, -16.30477369853688430, 145.5750000027311728 ) ) ;
#87083 = CARTESIAN_POINT ( 'NONE',  ( -10.72451020669898014, 18.67979575497178502, 65.41557627198102409 ) ) ;
#87084 = CARTESIAN_POINT ( 'NONE',  ( 4.483927247898790824, -16.52544592524335698, 90.20942372801903275 ) ) ;
#87085 = CARTESIAN_POINT ( 'NONE',  ( 16.51473224551069308, 9.474510206698969483, 29.16557627198103475 ) ) ;
#87086 = CARTESIAN_POINT ( 'NONE',  ( -19.05341960407611168, -5.049401038298163336, 71.45724293864766707 ) ) ;
#87087 = CARTESIAN_POINT ( 'NONE',  ( 3.765340386950246872E-15, -39.95163481335715971, -7.247842220587804363 ) ) ;
#87088 = CARTESIAN_POINT ( 'NONE',  ( -12.06949235617756955, 12.14591786802309770, 35.62390960531437401 ) ) ;
#87089 = ORIENTED_EDGE ( 'NONE', *, *, #152778, .T. ) ;
#87090 = CARTESIAN_POINT ( 'NONE',  ( -0.05219959533937732626, 21.53943276465977519, 57.50109039468568994 ) ) ;
#87091 = CARTESIAN_POINT ( 'NONE',  ( 9.564922557960805705, 16.46253265017160317, 114.5822429386476955 ) ) ;
#87092 = CARTESIAN_POINT ( 'NONE',  ( 0.05219959533937995610, -21.53943276465977519, 100.0010903946857042 ) ) ;
#87093 = CARTESIAN_POINT ( 'NONE',  ( -5.049401038298153566, 19.05341960407611168, 30.20724293864768839 ) ) ;
#87094 = CARTESIAN_POINT ( 'NONE',  ( 9.474510206698971260, -16.51473224551069308, 32.91557627198102409 ) ) ;
#87095 = ORIENTED_EDGE ( 'NONE', *, *, #182320, .T. ) ;
#87096 = CARTESIAN_POINT ( 'NONE',  ( -18.62759615963255300, -10.81492255796106328, 99.16775706135234714 ) ) ;
#87097 = CARTESIAN_POINT ( 'NONE',  ( 8.224510206698742110, 14.34966873604972548, 47.08442372801901854 ) ) ;
#87098 = CARTESIAN_POINT ( 'NONE',  ( 18.67979575497194134, -10.72451020669871369, 80.83442372801901854 ) ) ;
#87099 = CARTESIAN_POINT ( 'NONE',  ( 13.97604488694527802, 13.89961937509977652, 99.37390960531436690 ) ) ;
#87100 = CARTESIAN_POINT ( 'NONE',  ( -19.03943276465977164, -0.05219959533935918106, 88.75109039468567573 ) ) ;
#87101 = CARTESIAN_POINT ( 'NONE',  ( 10.72451020669871369, 18.67979575497193778, 57.08442372801901854 ) ) ;
#87102 = CARTESIAN_POINT ( 'NONE',  ( -5.153800228976607833, 19.02544592524334988, 112.7094237280190043 ) ) ;
#87103 = CARTESIAN_POINT ( 'NONE',  ( 16.51473224551083163, -9.474510206698727899, 90.83442372801900433 ) ) ;
#87104 = CARTESIAN_POINT ( 'NONE',  ( -9.564922557960796823, -16.46253265017161027, 47.08224293864769550 ) ) ;
#87105 = CARTESIAN_POINT ( 'NONE',  ( -19.05341960407617563, 5.049401038297882671, 93.54275706135234714 ) ) ;
#87106 = CARTESIAN_POINT ( 'NONE',  ( 9.564922557961047289, -16.46253265017146816, 90.41775706135234714 ) ) ;
#87107 = CARTESIAN_POINT ( 'NONE',  ( 8.314922557960818139, 14.29746914071049879, 49.58224293864769550 ) ) ;
#87108 = CARTESIAN_POINT ( 'NONE',  ( -16.46253265017146816, -9.564922557961047289, 69.16775706135233293 ) ) ;
#87109 = CARTESIAN_POINT ( 'NONE',  ( 4.379528057220092307, 16.55341960407617563, 67.29275706135234714 ) ) ;
#87110 = CARTESIAN_POINT ( 'NONE',  ( -16.46253265017146816, -9.564922557961047289, 24.16775706135233648 ) ) ;
#87111 = CARTESIAN_POINT ( 'NONE',  ( 13.97604488694527802, 13.89961937509977652, 39.37390960531435269 ) ) ;
#87112 = CARTESIAN_POINT ( 'NONE',  ( -13.89961937509977652, 13.97604488694528158, 45.62390960531433848 ) ) ;
#87113 = CARTESIAN_POINT ( 'NONE',  ( -8.314922557961024197, 14.29746914071037800, 57.91775706135234714 ) ) ;
#87114 = CARTESIAN_POINT ( 'NONE',  ( 3.885274725274726393, -8.673617379884035472E-16, 0.000000000000000000 ) ) ;
#87115 = CARTESIAN_POINT ( 'NONE',  ( 23.31738231874054890, -16.94106989632523508, 139.0500000054623513 ) ) ;
#87116 = CARTESIAN_POINT ( 'NONE',  ( -13.97604488694527625, -13.89961937509977652, 101.8739096053143811 ) ) ;
#87117 = EDGE_CURVE ( 'NONE', #26126, #36918, #173940, .T. ) ;
#87118 = CARTESIAN_POINT ( 'NONE',  ( 17.50000000000000000, -5.500000000000000888, 120.0000000000000142 ) ) ;
#87119 = VERTEX_POINT ( 'NONE', #3527 ) ;
#87120 = CARTESIAN_POINT ( 'NONE',  ( 5.049401038297881783, 19.05341960407617563, 102.2927570613523045 ) ) ;
#87122 = CARTESIAN_POINT ( 'NONE',  ( -5.719274019375978568, 21.55341960407610458, 40.20724293864769550 ) ) ;
#87121 = CIRCLE ( 'NONE', #106605, 2.000000000000001776 ) ;
#87124 = CARTESIAN_POINT ( 'NONE',  ( 16.55341960407618274, -4.379528057220086978, 21.04275706135234714 ) ) ;
#87123 = CARTESIAN_POINT ( 'NONE',  ( 9.474510206698729675, 16.51473224551082808, 37.08442372801899722 ) ) ;
#87125 = CARTESIAN_POINT ( 'NONE',  ( -9.564922557960796823, -16.46253265017161027, 32.08224293864769550 ) ) ;
#87126 = CARTESIAN_POINT ( 'NONE',  ( -19.02544592524342804, 5.153800228976336051, 31.04057627198102409 ) ) ;
#87127 = CARTESIAN_POINT ( 'NONE',  ( 15.72974639402199770, -15.80617190586745480, 78.12390960531436690 ) ) ;
#87128 = CARTESIAN_POINT ( 'NONE',  ( -13.89961937509977652, 13.97604488694528158, 40.62390960531435979 ) ) ;
#87129 = CARTESIAN_POINT ( 'NONE',  ( 27.73933785331498569, 9.013057229001093518, 142.4750000027312069 ) ) ;
#87130 = CARTESIAN_POINT ( 'NONE',  ( -5.153800228976607833, 19.02544592524334988, 82.70942372801897591 ) ) ;
#87131 = CARTESIAN_POINT ( 'NONE',  ( -8.224510206698948167, 14.34966873604960824, 50.41557627198103120 ) ) ;
#87132 = CARTESIAN_POINT ( 'NONE',  ( -10.72451020669898014, 18.67979575497178502, 30.41557627198101699 ) ) ;
#87133 = CARTESIAN_POINT ( 'NONE',  ( -0.05219959533937732626, 21.53943276465977519, 102.5010903946856899 ) ) ;
#87134 = EDGE_CURVE ( 'NONE', #13627, #36918, #173397, .T. ) ;
#87135 = CARTESIAN_POINT ( 'NONE',  ( 15.72974639402199770, -15.80617190586745480, 88.12390960531436690 ) ) ;
#87136 = CARTESIAN_POINT ( 'NONE',  ( -18.62759615963255300, -10.81492255796106328, 69.16775706135234714 ) ) ;
#87137 = CARTESIAN_POINT ( 'NONE',  ( 10.81492255796106328, -18.62759615963255655, 60.41775706135235424 ) ) ;
#87138 = CARTESIAN_POINT ( 'NONE',  ( 9.564922557960805705, 16.46253265017160317, 104.5822429386476955 ) ) ;
#87140 = CARTESIAN_POINT ( 'NONE',  ( 15.80617190586769283, -15.72974639402175789, 65.62609039468568994 ) ) ;
#87139 = CARTESIAN_POINT ( 'NONE',  ( 16.52544592524335698, 4.483927247898782831, 101.4594237280190185 ) ) ;
#87141 = CARTESIAN_POINT ( 'NONE',  ( 0.05219959533909260263, 19.03943276465977164, 54.99890960531435979 ) ) ;
#87142 =( BOUNDED_SURFACE ( )  B_SPLINE_SURFACE ( 3, 2, ( 
 ( #8012, #101018, #69695, #148545, #131362, #162703, #10036, #54528, #116201, #39360, #71696, #24208, #133363, #200021, #106009, #167695, #154505, #105025, #152509, #182869, #166709, #184847, #47338, #137342, #124152, #153505, #89853, #61489, #185851, #123159, #151536, #807, #77659, #13998, #32162, #169673, #31169, #16992, #29192, #13025, #91813, #90826, #75665, #139328, #108993, #15002, #16001, #74690, #136356, #106996, #199022, #46331, #170674, #107986, #138341, #60491, #93819, #122167, #183857, #92819, #62480, #155499, #78646, #140321, #1811, #121175, #168669, #63489, #181875, #43354, #28213, #198032, #45344, #59500, #44350, #30169, #76662, #171668, #97771, #49317, #156494, #17996, #142310, #33157, #95808, #2807, #36119, #158476, #79649, #129114, #175644, #37118, #109988, #94816, #173668, #159458, #64485, #3790, #82611, #160471, #4776, #20954, #96787, #35135, #141318, #19964, #65467, #126152, #186864, #143290, #174654, #110977, #81606, #187848, #128126, #66464, #157494, #189828, #67456, #144292, #111976, #5782, #172662, #34149, #48333, #18987, #51300, #112961, #80633, #21962, #127130, #188836, #50321, #83613, #190813, #52288, #113945, #98777, #145291, #125165, #6774, #23963, #85618, #55287, #132129, #116959, #70464, #193822, #147305, #162462, #69458, #131125, #22961, #38133, #191803, #177655, #8794, #39124, #53284, #178650, #68453, #146288, #130107, #114963, #176656, #99786, #192813, #7775, #161472, #100779, #115967, #84609, #54295, #20599, #21604, #141951, #18632, #174303, #19617, #128765, #176298, #51937, #5423, #158125, #114601, #81259, #142940, #160117, #6419, #68100, #191449, #52926, #113597, #188479, #35772, #98420, #175291, #83262, #144937, #84256, #4422, #37770, #48967, #127774, #95452, #157137, #129752, #173308, #80279, #3440, #66108, #65116, #189474, #126774, #99432, #82251, #49959, #161114, #22610, #145938, #33792, #111623, #97419, #7419, #34782, #50952, #69103, #130769, #190464, #110621, #143942, #159105, #96438, #67106, #112611, #36757, #172303, #10448, #41783, #116613, #40776, #38780, #195474, #72108, #24623, #133781, #134797, #103450, #179312, #73128, #178301, #131783, #53944, #39765, #56950, #148959, #147961, #89268, #54941, #101429, #146952, #27628, #102445, #118624, #87274, #164132, #149951, #192461, #25630, #165128, #26620, #150959, #181302, #12453, #57948, #42780, #88263, #11456, #194466, #55937, #163120, #193464, #117614, #196478, #86271, #180315, #119619, #74115, #9448, #104442, #166126, #115619, #177308, #100436, #162117, #23614, #85261, #71113, #132779, #8440, #70113, #133191, #194882, #56356, #11880, #87684, #73543, #162528, #69526, #148370, #24031, #85685, #195898, #165545, #9865, #10865, #131191, #7840, #163543, #8861, #118038, #27042, #41199, #179729, #147372, #103864, #70528, #132197, #149369, #57373, #119046, #180728, #42204, #102861, #177720, #25043, #72535, #164546, #134211, #88688, #135216, #193888, #150384, #38196, #117023, #84674, #146353, #196888, #55353, #192881, #54359, #178718, #116031, #40180, #39188, #58355, #71524, #100846, #120022, #99852, #161536, #23029, #101859, #86686, #26039, #59334, #198863, #139159, #16824, #61322, #15829, #153335, #30008, #89686, #76499, #122004, #151371, #43188, #199856, #30999, #105846, #91646, #28045, #184679, #122993, #13835, #46162, #123976, #92648, #168510, #62306, #167533, #121004, #104857, #29028, #107816, #138175, #137175, #78475, #44187, #90668, #136192, #140148, #14836, #169500, #154337, #77489, #636, #181707, #197867, #12862, #185674, #155335, #152350, #47164, #75501, #108823, #1640, #183695, #31992, #60330, #170502, #93650, #74527, #63317, #166546, #45181, #182702, #106835, #126961, #128949, #187684, #81440, #111809, #6609, #49154, #96622, #175478, #159290, #190650, #34970, #127958, #98612, #143126, #110812, #172495, #97602, #48162, #158311, #174488, #52126, #109820, #113782, #80465, #67291, #19799, #20787 ),
 ( #33982, #36950, #160306, #83448, #4606, #186692, #66298, #142139, #21796, #50150, #145125, #35955, #124997, #171503, #32992, #82442, #144130, #94646, #189661, #51134, #156326, #3623, #95638, #112794, #5612, #17826, #79484, #141153, #2642, #157326, #65302, #64318, #125986, #18821, #188670, #173497, #132969, #54132, #53118, #114796, #116798, #102640, #146123, #85453, #25818, #103643, #148148, #164325, #39956, #178489, #176489, #163316, #8631, #37965, #129939, #86463, #117810, #192649, #101627, #99623, #71306, #9639, #100621, #194659, #10641, #179503, #55128, #56128, #161304, #40969, #38965, #22799, #24814, #150149, #26813, #7607, #72302, #165321, #87464, #149151, #84445, #69293, #133980, #41976, #162303, #195671, #115805, #57142, #88453, #70303, #118818, #23803, #180504, #68288, #130959, #191638, #177495, #147143, #131972, #193656, #13607, #15595, #74301, #168278, #198634, #93408, #135970, #183461, #62074, #45929, #77253, #121768, #14602, #185438, #29775, #197641, #59107, #184449, #134987, #44947, #61087, #138921, #196665, #402, #167304, #154101, #106602, #107584, #120772, #31759, #92415, #123739, #136945, #181488, #11650, #137936, #91410, #153098, #58134, #46928, #60100, #182473, #108588, #170265, #73316, #76258, #119803, #199620, #28800, #42966, #122759, #104629, #169262, #166318, #27815, #89456, #30768, #151145, #12636, #43954, #105616, #90439, #152125, #75275, #111570, #173254, #82198, #159054, #97368, #158074, #125748, #95399, #34729, #127723, #126722, #124756, #141899, #157085, #186452, #80228, #19565, #49904, #17582, #96387, #51886, #36704, #171265, #81209, #139907, #79242, #142890, #35721, #109582, #20548, #67055, #18581, #3390, #64078, #94404, #63077, #4372, #143890, #66056, #47928, #174253, #189425, #50900, #112558, #128713, #5371, #190410, #140913, #32753, #65065, #2399, #187448, #113545, #175239, #188426, #155094, #156085, #48916, #16588, #110570, #78236, #1397, #172251, #33739, #7365, #164078, #69050, #192409, #9393, #55883, #117556, #40721, #102390, #163062, #37716, #85205, #147907, #101372, #71059, #194413, #133724, #130716, #87221, #98366, #177253, #144886, #6368, #132725, #22556, #129700, #191397, #115566, #68048, #53891, #176245, #179256, #131728, #25577, #148903, #52874, #84202, #83211, #114546, #146894, #10393, #99378, #38725, #72050, #195416, #178248, #56894, #70060, #8385, #161061, #193410, #100383, #145882, #160064, #116559, #118568, #162061, #54885, #23557, #24568, #39709, #86217, #180258, #21551, #91168, #28559, #122516, #166068, #181246, #103392, #89209, #183219, #198380, #197400, #138680, #104385, #150902, #196421, #77008, #90196, #44700, #136699, #151879, #199377, #41728, #13369, #152857, #76017, #161, #30516, #61829, #107339, #92168, #14352, #137692, #121524, #184206, #60841, #75033, #45688, #27570, #42723, #165070, #12396, #106354, #59857, #58866, #123499, #74058, #135729, #57891, #26564, #168038, #29535, #169012, #153854, #15352, #88207, #149891, #11398, #73067, #134739, #119563, #120532, #182225, #43710, #105371, #167058, #187208, #48679, #94162, #124510, #93166, #64831, #127484, #126493, #154851, #4136, #79998, #141666, #3158, #158817, #34496, #20305, #109337, #16349, #95160, #171019, #32510, #142657, #112323, #156848, #157843, #77997, #139664, #110331, #155841, #188191, #174013, #49663, #111327, #17338, #50662, #78994, #140668, #96154, #65815, #189189, #35484, #97133, #173017, #186205, #172012, #19334, #80982, #81953, #143645, #5128, #2160, #66810, #185192, #63838, #31513, #1152, #46683, #125511, #62827, #47687, #33501, #18343, #108342, #170023, #39471, #161822, #132489, #70820, #82971, #114306, #113309, #175000, #177015, #162818, #6131, #145647, #85976, #163836, #8136, #24327, #100141, #38484, #36465, #23317, #68809, #98122, #190169, #146643, #178004, #52641, #84961, #159819, #131481, #69814, #160828, #83967, #193168, #147666, #21314, #54640, #25338 ),
 ( #130468, #192166, #37477, #67814, #144648, #116315, #194178, #101132, #129469, #9154, #55642, #117315, #179011, #102151, #40479, #86979, #176008, #191168, #148666, #99138, #22316, #10154, #128473, #51645, #7127, #53646, #115323, #197166, #42485, #151647, #199136, #74804, #28328, #181011, #137457, #104148, #165830, #182983, #29305, #90935, #14112, #75779, #136467, #11156, #58632, #121290, #198147, #44467, #167805, #107107, #27327, #60603, #71814, #150663, #118328, #180021, #106121, #196186, #103153, #164834, #88973, #41488, #12161, #149658, #152621, #105141, #122278, #183966, #26330, #57658, #56655, #87970, #120298, #45453, #72830, #73826, #168777, #30279, #13142, #91925, #43473, #181991, #134500, #166827, #135496, #119324, #133482, #89967, #153617, #59617, #195174, #61596, #18108, #33269, #47448, #94928, #157605, #64598, #1923, #95920, #139434, #154614, #76774, #62590, #156613, #171781, #170783, #112091, #77767, #186975, #138446, #79762, #32273, #142423, #140433, #3902, #126262, #15113, #127241, #200127, #172780, #187959, #173781, #141433, #2920, #123265, #93930, #124268, #49429, #111090, #65582, #19096, #80745, #34261, #185963, #155609, #188955, #50432, #48445, #184956, #63602, #17104, #46440, #125278, #35248, #110102, #916, #96901, #108099, #169784, #31277, #92928, #16109, #109104, #78756, #39234, #113071, #100890, #70575, #23075, #51411, #7887, #129227, #143403, #130220, #40229, #117068, #97881, #162574, #193935, #191915, #145403, #174763, #66574, #24077, #132243, #190924, #53399, #144407, #161581, #55398, #160584, #8907, #114060, #84720, #192927, #36229, #146398, #178764, #52401, #176769, #54405, #22073, #85733, #21070, #115077, #6885, #158585, #82726, #38241, #20074, #116077, #147420, #68563, #69573, #81718, #99896, #5893, #67569, #131239, #4892, #177765, #128239, #189936, #159572, #175757, #37234, #98890, #83724, #430, #149413, #124783, #185467, #16616, #27087, #71571, #186481, #28090, #11923, #43235, #25089, #31787, #88733, #10909, #46957, #155122, #63105, #196931, #58399, #120065, #78264, #154130, #139936, #26084, #133236, #73587, #87728, #72582, #62104, #93436, #135259, #77281, #194928, #56403, #150428, #134256, #181753, #1426, #104901, #166590, #195943, #170293, #57417, #119090, #15624, #123767, #108616, #101906, #163588, #92444, #41244, #138950, #86731, #148416, #9911, #118085, #179775, #180772, #102906, #164590, #42247, #103908, #165589, #20575, #172279, #79270, #140941, #65092, #94432, #18608, #125775, #159081, #81236, #51914, #190438, #2428, #33768, #32780, #156113, #96415, #82228, #187475, #126751, #5399, #83238, #127750, #143918, #19593, #158101, #17611, #142917, #188453, #64108, #109609, #66084, #97395, #95428, #4399, #48944, #50928, #189451, #80256, #112586, #113573, #67082, #34756, #128742, #157112, #110597, #171293, #141926, #174280, #35749, #3417, #144914, #49934, #111599, #173283, #6397, #175267, #36733, #98396, #160094, #21580, #47958, #68076, #129730, #25607, #26596, #180291, #149924, #56926, #41759, #102421, #40753, #193441, #54917, #100413, #130748, #99408, #71088, #133757, #132755, #161091, #10425, #164108, #178278, #72083, #115596, #192440, #52903, #38756, #194442, #147937, #146928, #88239, #53922, #162094, #145912, #11431, #39741, #55913, #86247, #101403, #148935, #191427, #163097, #87251, #195452, #73101, #103424, #114579, #118601, #165103, #176277, #37748, #116589, #24600, #23589, #177285, #22586, #117587, #84234, #179288, #7397, #69081, #9423, #85237, #8418, #70090, #131759, #170058, #58898, #166101, #44733, #120564, #182258, #92206, #61865, #106389, #107376, #27603, #104418, #59890, #105405, #14385, #123534, #137727, #91199, #43743, #196, #167090, #28591, #45723, #153890, #15387, #77044, #138715, #199411, #74091, #121556, #184242, #60875, #169048, #30554, #31549, #90228, #185228, #134771, #13401, #181278, #42755, #46719, #151912, #89242, #150935, #75065 ),
 ( #12428, #136731, #108382, #93201, #76051, #154886, #168070, #183252, #135761, #29568, #198413, #197432, #196454, #152889, #16384, #122552, #57924, #119595, #81016, #96189, #110365, #157878, #20341, #3191, #47720, #98157, #4171, #188225, #19367, #1186, #5164, #64864, #187242, #81990, #128510, #36503, #49698, #139700, #142691, #33534, #66847, #126526, #190205, #127519, #78031, #51684, #62863, #35520, #189223, #159857, #65849, #50701, #124545, #95196, #125546, #34529, #112360, #113346, #143683, #175038, #174051, #48712, #18379, #97168, #158853, #111363, #109371, #173052, #80031, #171053, #186242, #32543, #94196, #140703, #155876, #17373, #79028, #2193, #63875, #172047, #156882, #141700, #102190, #176044, #163878, #133522, #86016, #114341, #70858, #192204, #6168, #193206, #103193, #180061, #160864, #25377, #56694, #54679, #8176, #37512, #129503, #87019, #195214, #53686, #116353, #7166, #24365, #118368, #23355, #71853, #177053, #147705, #55681, #99174, #9193, #41530, #115363, #39510, #117355, #85000, #148705, #84006, #178042, #69852, #21350, #145684, #101170, #83008, #179051, #10193, #131520, #132527, #144683, #162858, #68849, #130508, #194216, #67848, #40519, #191203, #38523, #100179, #52678, #22354, #161861, #146681, #74841, #150702, #89011, #122315, #91961, #120334, #107144, #136504, #60641, #12200, #184993, #45489, #76811, #90004, #134539, #46477, #90972, #198184, #106160, #88009, #153654, #151686, #73865, #168814, #15149, #123301, #59654, #26369, #167842, #182029, #138482, #13178, #200163, #14149, #164874, #61633, #149697, #184006, #75816, #11195, #29343, #152659, #72870, #43512, #135534, #121328, #183020, #196227, #30318, #57697, #137494, #197205, #105178, #44504, #199174, #119365, #181049, #42524, #166864, #104187, #165869, #27365, #58668, #28366, #126293, #4923, #189967, #124303, #34292, #92965, #170818, #95953, #188987, #62625, #50462, #20105, #172812, #950, #157638, #78791, #154651, #79795, #108137, #66605, #47482, #112121, #143436, #141468, #94961, #186000, #16146, #173813, #81749, #140469, #2952, #93964, #111122, #128269, #110135, #158615, #63637, #19127, #142455, #109139, #80777, #169821, #1958, #187990, #3933, #171814, #35278, #32310, #64631, #156646, #31312, #155644, #49460, #77801, #65613, #96933, #18141, #127273, #139470, #17139, #125313, #187009, #48479, #33302, #148448, #117101, #99927, #97913, #178796, #69605, #147452, #53432, #55430, #114090, #7920, #38273, #133268, #175791, #23106, #101939, #85766, #40265, #161612, #54438, #25121, #131271, #37265, #98923, #24111, #174793, #9943, #163620, #84752, #159604, #86765, #6917, #193967, #146430, #8940, #160615, #71602, #132276, #51442, #176800, #21103, #113102, #177796, #192959, #116108, #36259, #82758, #39266, #22105, #144438, #5924, #67601, #100922, #129260, #162607, #68595, #190955, #70609, #52432, #83755, #145434, #130251, #191946, #115108, #105916, #153412, #197938, #59407, #179805, #150456, #42279, #151444, #12931, #122074, #198935, #137249, #121081, #165617, #135286, #74595, #167602, #166617, #164621, #181781, #196958, #26115, #120093, #182776, #89758, #57446, #136263, #91718, #76572, #10939, #44259, #41274, #119119, #29097, #75573, #149443, #60402, #106906, #90736, #87758, #152419, #27116, #102936, #28119, #194959, #14911, #134287, #183766, #30077, #13907, #43262, #72612, #195974, #45252, #168579, #88763, #56436, #180800, #118117, #103937, #58426, #11951, #73615, #104930, #172570, #31076, #2715, #35041, #32069, #169578, #92723, #155407, #184752, #108899, #15906, #49227, #171575, #142214, #80540, #154412, #124053, #123066, #46237, #186766, #34056, #77564, #16897, #95714, #173572, #17901, #157401, #109891, #48236, #107891, #33064, #78548, #139236, #199931, #156397, #187757, #62383, #94719, #711, #141224, #79556, #170578, #64392, #3697, #110885, #125069, #18894, #185752, #47241, #61394, #93725, #126060, #65376, #140223, #96695 ),
 ( #158384, #127036, #19873, #188743, #50228, #111882, #138247, #1716, #63392, #190723, #20862, #189735, #161377, #23872, #22868, #51208, #100689, #115876, #66373, #52196, #67363, #131031, #116866, #5687, #112869, #191708, #129022, #113854, #39034, #8702, #53192, #54204, #174560, #36027, #6680, #175550, #84515, #70372, #146193, #38037, #37025, #147211, #98686, #160379, #192720, #162371, #85523, #132040, #193729, #7678, #82519, #68358, #177565, #69362, #55197, #178557, #40023, #21870, #101696, #81513, #83520, #128033, #97676, #163385, #145197, #143200, #4681, #159365, #144201, #130009, #114867, #176562, #99693, #74369, #60168, #149219, #56197, #135058, #10710, #72373, #182542, #152191, #196734, #197709, #117880, #194727, #150222, #195740, #104700, #13675, #27884, #181555, #134047, #90509, #57213, #118888, #136035, #44024, #105685, #167372, #28869, #89526, #164394, #11719, #59175, #151215, #120843, #75342, #121837, #180572, #137012, #24882, #103710, #71373, #133037, #198702, #42046, #179570, #41040, #165390, #102706, #26883, #25887, #183531, #58202, #45015, #106674, #87532, #88526, #9709, #73386, #119870, #86531, #43034, #166388, #148215, #12703, #47998, #2469, #139978, #16657, #76330, #63145, #108657, #138007, #29843, #186524, #17652, #92485, #78305, #14669, #171334, #109652, #471, #32822, #110639, #79312, #155165, #48984, #154174, #107653, #91480, #15665, #94473, #124824, #123809, #65134, #30837, #77324, #122829, #3457, #1467, #156154, #140981, #64151, #125815, #168347, #187518, #172320, #33809, #126791, #157155, #188497, #95469, #18650, #80296, #141968, #170335, #31828, #138992, #169330, #199691, #49976, #153168, #61156, #184518, #45998, #62145, #185507, #46998, #93478, #163906, #175308, #179077, #174320, #118392, #102217, #71877, #128782, #19634, #180086, #70885, #113614, #83279, #34800, #87044, #190482, #35790, #25402, #10217, #56721, #36774, #173325, #147731, #20618, #148729, #51954, #133547, #132553, #111640, #96455, #158142, #195237, #81276, #142958, #40548, #4438, #189491, #98439, #160134, #55708, #117380, #66126, #127791, #50969, #112628, #9218, #194241, #97437, #159122, #82268, #21622, #143960, #5440, #67124, #17301, #156812, #187171, #154811, #110294, #191869, #176723, #108303, #18304, #76970, #16309, #79960, #172978, #46643, #37185, #6839, #141629, #185153, #3119, #62788, #138641, #63802, #92129, #53352, #31474, #98843, #130172, #125475, #78955, #169983, #122, #160538, #68518, #124469, #48642, #77959, #95122, #115030, #94124, #145357, #47648, #64794, #126455, #93126, #188153, #153816, #186166, #171976, #49626, #155803, #22027, #139626, #33464, #140630, #15311, #1114, #111288, #61791, #83679, #123461, #2120, #109299, #170978, #32471, #113328, #3176, #64849, #129487, #81001, #188209, #49681, #174032, #126511, #127502, #34514, #67831, #190189, #160845, #99156, #111345, #142675, #141685, #173036, #5148, #191185, #96172, #35503, #114323, #192184, #36484, #52661, #128494, #66830, #157862, #51664, #97153, #19352, #18363, #175021, #6151, #4154, #98140, #65833, #159838, #21332, #189207, #82990, #22334, #176025, #143666, #37494, #50684, #112342, #80016, #158836, #144666, #83985, #20324, #53665, #81973, #145664, #7145, #115343, #68829, #130488, #177033, #38503, #156867, #100159, #148684, #11174, #134519, #135515, #88991, #58650, #165849, #150682, #72849, #149676, #102169, #163857, #9172, #39490, #8156, #180040, #56673, #146661, #10172, #161841, #196205, #84979, #70839, #85996, #57677, #197186, #24345, #131499, #71832, #147685, #132507, #119345, #27345, #133501, #181029, #193186, #69832, #25356, #194196, #41509, #12180, #103172, #118346, #55661, #73844, #117335, #179030, #42503, #104167, #120316, #182010, #23335, #164852, #101150, #86997, #54659, #26348, #116333, #178022, #162837, #40497, #195193, #87988, #122295, #200144, #199154, #140449, #106140, #90952, #198165, #78773, #30299, #184973 ),
 ( #93946, #77782, #109121, #153635, #46458, #17121, #61614, #1939, #183985, #45470, #59635, #63619, #170799, #91942, #89985, #32291, #60621, #185981, #15130, #139451, #152639, #125295, #124284, #155625, #168795, #13160, #43492, #169801, #76792, #108118, #166845, #105159, #138463, #14129, #47464, #28347, #151666, #123282, #74824, #31294, #107124, #136485, #92946, #121309, #154632, #183001, #44485, #167823, #932, #16127, #29322, #62606, #75796, #137474, #142439, #34276, #143419, #4906, #114073, #190938, #129242, #189951, #157621, #127257, #66589, #159587, #158599, #156628, #173796, #188970, #18123, #112105, #51425, #81733, #49443, #128253, #83738, #68578, #2935, #113085, #171796, #111106, #174777, #67584, #141450, #52415, #98905, #36243, #79778, #97896, #19111, #33284, #20089, #186991, #145417, #126277, #175774, #22088, #21084, #35262, #64615, #94944, #37248, #160598, #80761, #82741, #172795, #144421, #95935, #5907, #6899, #48461, #187974, #110118, #3917, #65597, #50446, #96917, #84734, #72596, #42261, #194943, #23089, #179789, #100905, #115091, #101921, #11935, #88746, #69587, #134270, #165601, #163603, #117084, #146412, #38256, #195957, #103921, #162589, #25104, #116091, #133251, #27100, #132259, #180784, #85748, #56419, #164605, #7903, #118099, #150439, #24094, #148431, #26099, #193950, #57430, #192942, #86748, #178779, #130234, #54421, #9926, #191930, #87742, #119103, #40247, #41258, #53414, #71585, #176783, #8923, #55413, #131254, #99910, #161595, #102920, #177779, #39249, #147435, #70591, #149427, #10923, #121063, #93705, #154391, #185731, #198915, #43246, #155387, #199911, #183748, #14892, #196942, #691, #60384, #182757, #15886, #124032, #32048, #45234, #135270, #76553, #29079, #62363, #122056, #47220, #123046, #73598, #108879, #58410, #31055, #184732, #120077, #138229, #61375, #181765, #90718, #44241, #30059, #91700, #170558, #77544, #139216, #46217, #105898, #13888, #153394, #107870, #106888, #104914, #168561, #75555, #166601, #169558, #92703, #28101, #89740, #151426, #12913, #74577, #152401, #136245, #197921, #167584, #59389, #137231, #66352, #144181, #188723, #189715, #109870, #186746, #142194, #187736, #96676, #5667, #19853, #173552, #126040, #82499, #49207, #110865, #128013, #174540, #36007, #159345, #20841, #81493, #156376, #3677, #51188, #143180, #112849, #97656, #52176, #172550, #67343, #16877, #95693, #63372, #125049, #129004, #141205, #48216, #171554, #34036, #33044, #157381, #94699, #190703, #50208, #113834, #175530, #17881, #2695, #1696, #79535, #65355, #37004, #64372, #18874, #98665, #78528, #158364, #140202, #111862, #127016, #80520, #35021, #4660, #68339, #21849, #178539, #9690, #84496, #8683, #6661, #163367, #40005, #192701, #101677, #102688, #71355, #147193, #41022, #146174, #99674, #83500, #7659, #24863, #116848, #115857, #57195, #22849, #69343, #114848, #195722, #70354, #86513, #55179, #132021, #117861, #160359, #193710, #133019, #194709, #118870, #149201, #180554, #25869, #10691, #56178, #179552, #162353, #23854, #131010, #161358, #129989, #148197, #164376, #191689, #87513, #42028, #72355, #145177, #134029, #177547, #53171, #85504, #176542, #38018, #54184, #39016, #100671, #61141, #14654, #62130, #106659, #168332, #88507, #59157, #151198, #60152, #121821, #30822, #107638, #45983, #29828, #74352, #44007, #183516, #76314, #75326, #73368, #90493, #105669, #135040, #28853, #91465, #198685, #166370, #44999, #455, #185492, #119853, #153152, #150203, #27867, #137992, #184503, #58185, #169315, #15650, #199675, #196716, #122813, #136018, #11701, #136996, #103692, #123794, #43016, #92470, #138977, #154159, #152175, #181537, #104683, #77308, #165371, #197692, #26865, #89508, #12686, #120826, #167355, #182526, #13658, #49961, #81261, #139963, #111625, #143944, #140966, #65118, #142942, #48969, #50954, #109636, #3442, #33794, #128767, #171319, #18635, #97421, #4424, #112613 ),
 ( #2454, #189476, #80281, #157139, #188481, #173310, #186509, #159107, #172305, #16642, #67109, #34785, #141953, #96440, #170320, #174305, #95454, #156139, #35774, #20601, #82253, #64136, #158127, #66110, #1452, #19619, #5425, #125800, #126776, #127776, #110623, #46982, #32806, #108642, #31812, #93463, #94458, #155149, #78289, #63130, #124809, #47983, #17637, #79297, #187502, #148962, #69105, #192463, #6421, #87277, #55940, #38782, #36759, #117617, #145940, #132782, #162119, #100438, #131786, #54943, #129754, #102448, #115622, #160119, #10451, #116615, #23616, #193466, #113599, #179315, #177310, #99435, #194469, #40779, #72111, #85263, #51939, #178303, #7421, #164136, #146954, #25633, #39767, #190466, #175293, #98422, #147964, #101431, #21606, #163122, #24625, #83265, #130771, #37772, #8442, #70115, #144939, #68102, #191451, #86273, #161116, #53946, #9451, #71116, #52928, #114603, #176300, #22612, #84258, #58925, #198442, #28617, #196481, #151937, #30579, #15411, #149954, #59914, #118627, #57951, #121582, #14410, #88266, #76074, #45748, #183277, #26623, #44758, #104445, #180318, #105432, #133784, #92230, #73131, #137750, #169073, #167115, #120593, #11459, #41786, #199434, #107400, #166129, #90254, #119622, #136757, #153916, #135788, #195477, #75090, #89271, #60902, #182288, #122576, #106413, #56953, #103453, #165131, #91223, #168094, #134800, #29592, #152914, #181305, #150962, #42783, #13426, #184266, #27631, #12457, #74117, #197459, #43768, #17399, #33559, #49723, #48737, #46747, #63900, #79056, #108406, #2218, #141724, #172073, #139723, #95222, #174075, #158877, #93225, #3214, #61889, #1212, #64888, #157901, #31574, #19390, #189247, #126549, #170082, #188249, #47745, #123559, #110391, #77069, #35544, #16408, #81039, #112383, #156908, #125570, #154910, #185254, #142715, #50725, #109398, #18405, #62890, #80054, #97191, #140729, #127547, #32569, #111390, #173076, #78054, #34553, #138739, #171078, #96212, #4195, #187268, #65873, #124570, #220, #186266, #94222, #155902, #194974, #73630, #57461, #88777, #133284, #26131, #196973, #41291, #181798, #101954, #25138, #39282, #120108, #150470, #71618, #69620, #11965, #178811, #165632, #56453, #118132, #164636, #87774, #162623, #135300, #148465, #192974, #43277, #149459, #179820, #10954, #143710, #58440, #9958, #132292, #27130, #104946, #20366, #102952, #119134, #7937, #193984, #8958, #72628, #82014, #147468, #54453, #55446, #180814, #103953, #134303, #131286, #195989, #42293, #116123, #177812, #100939, #117117, #24129, #85782, #70626, #40281, #163636, #86780, #75588, #60417, #77579, #124068, #185770, #108914, #170594, #31091, #105932, #153429, #15921, #169593, #139251, #62399, #1731, #137267, #155422, #166632, #45267, #12947, #74612, #727, #90752, #197954, #59423, #183781, #136278, #198950, #44274, #47257, #199946, #32084, #93741, #121097, #152435, #151459, #182791, #14927, #16912, #167617, #106921, #78565, #63409, #46253, #140238, #138263, #76587, #29113, #61410, #168594, #13921, #28134, #184767, #125084, #122090, #123081, #30094, #92739, #107907, #91733, #154427, #186782, #48252, #89774, #190738, #34070, #49240, #171590, #157414, #51223, #66387, #65390, #6696, #172583, #18908, #64405, #145214, #96710, #112884, #4696, #158398, #67379, #109906, #19887, #20878, #144218, #68374, #98702, #130026, #175566, #160396, #82536, #159383, #111898, #173586, #80553, #110898, #17915, #189751, #128049, #156413, #81528, #33078, #174578, #36043, #37042, #113869, #52212, #97692, #142228, #50242, #5702, #129037, #143215, #79570, #21885, #35055, #141239, #83535, #191725, #94734, #95728, #2728, #126074, #187770, #3713, #127051, #188757, #115891, #179585, #134063, #7696, #195754, #165404, #117895, #146208, #102720, #23889, #38053, #24899, #135071, #11733, #192738, #57228, #88540, #86546, #40039, #69378, #161393, #118902, #26897, #85541, #148230, #39048, #56214, #150237 ) ),
 .UNSPECIFIED., .T., .F., .F. ) 
 B_SPLINE_SURFACE_WITH_KNOTS ( ( 4, 3, 4 ),
 ( 3, 2, 2, 2, 2, 2, 2, 2, 2, 2, 2, 2, 2, 2, 2, 2, 2, 2, 2, 2, 2, 2, 2, 2, 2, 2, 2, 2, 2, 2, 2, 2, 2, 2, 2, 2, 2, 2, 2, 2, 2, 2, 2, 2, 2, 2, 2, 2, 2, 2, 2, 2, 2, 2, 2, 2, 2, 2, 2, 2, 2, 2, 2, 2, 2, 2, 2, 2, 2, 2, 2, 2, 2, 2, 2, 2, 2, 2, 2, 2, 2, 2, 2, 2, 2, 2, 2, 2, 2, 2, 2, 2, 2, 2, 2, 2, 2, 2, 2, 2, 2, 2, 2, 2, 2, 2, 2, 2, 2, 2, 2, 2, 2, 2, 2, 2, 2, 2, 2, 2, 2, 2, 2, 2, 2, 2, 2, 2, 2, 2, 2, 2, 2, 2, 2, 2, 2, 2, 2, 2, 2, 2, 2, 2, 2, 2, 2, 2, 2, 2, 2, 2, 2, 2, 2, 2, 2, 2, 2, 2, 2, 2, 2, 2, 2, 2, 2, 2, 2, 2, 2, 2, 2, 2, 2, 2, 2, 2, 2, 2, 2, 2, 2, 2, 2, 2, 2, 2, 2, 2, 2, 2, 2, 2, 2, 2, 2, 2, 2, 2, 2, 2, 2, 2, 2, 2, 2, 2, 2, 2, 2, 2, 2, 2, 2, 2, 2, 2, 2, 2, 2, 2, 2, 2, 2, 2, 2, 2, 3 ),
 ( 0.000000000000000000, 0.5000000000000000000, 1.000000000000000000 ),
 ( 0.000000000000000000, 0.004385964912280701511, 0.008771929824561403022, 0.01315789473684210453, 0.01754385964912280604, 0.02192982456140350755, 0.02631578947368420907, 0.03070175438596491058, 0.03508771929824561209, 0.03947368421052631360, 0.04385964912280701511, 0.04824561403508771662, 0.05263157894736841813, 0.05701754385964911964, 0.06140350877192982115, 0.06578947368421052266, 0.07017543859649122417, 0.07456140350877192569, 0.07894736842105262720, 0.08333333333333332871, 0.08771929824561403022, 0.09210526315789473173, 0.09649122807017543324, 0.1008771929824561348, 0.1052631578947368363, 0.1096491228070175378, 0.1140350877192982393, 0.1184210526315789408, 0.1228070175438596423, 0.1271929824561403577, 0.1315789473684210453, 0.1359649122807017607, 0.1403508771929824483, 0.1447368421052631637, 0.1491228070175438514, 0.1535087719298245668, 0.1578947368421052544, 0.1622807017543859698, 0.1666666666666666574, 0.1710526315789473728, 0.1754385964912280604, 0.1798245614035087758, 0.1842105263157894635, 0.1885964912280701788, 0.1929824561403508665, 0.1973684210526315819, 0.2017543859649122695, 0.2061403508771929849, 0.2105263157894736725, 0.2149122807017543879, 0.2192982456140350755, 0.2236842105263157909, 0.2280701754385964786, 0.2324561403508771940, 0.2368421052631578816, 0.2412280701754385970, 0.2456140350877192846, 0.2500000000000000000, 0.2543859649122807154, 0.2587719298245614308, 0.2631578947368420907, 0.2675438596491228060, 0.2719298245614035214, 0.2763157894736842368, 0.2807017543859648967, 0.2850877192982456121, 0.2894736842105263275, 0.2938596491228070429, 0.2982456140350877027, 0.3026315789473684181, 0.3070175438596491335, 0.3114035087719298489, 0.3157894736842105088, 0.3201754385964912242, 0.3245614035087719396, 0.3289473684210526550, 0.3333333333333333148, 0.3377192982456140302, 0.3421052631578947456, 0.3464912280701754610, 0.3508771929824561209, 0.3552631578947368363, 0.3596491228070175517, 0.3640350877192982670, 0.3684210526315789269, 0.3728070175438596423, 0.3771929824561403577, 0.3815789473684210731, 0.3859649122807017330, 0.3903508771929824483, 0.3947368421052631637, 0.3991228070175438791, 0.4035087719298245390, 0.4078947368421052544, 0.4122807017543859698, 0.4166666666666666852, 0.4210526315789473450, 0.4254385964912280604, 0.4298245614035087758, 0.4342105263157894912, 0.4385964912280701511, 0.4429824561403508665, 0.4473684210526315819, 0.4517543859649122973, 0.4561403508771929571, 0.4605263157894736725, 0.4649122807017543879, 0.4692982456140351033, 0.4736842105263157632, 0.4780701754385964786, 0.4824561403508771940, 0.4868421052631579093, 0.4912280701754385692, 0.4956140350877192846, 0.5000000000000000000, 0.5043859649122807154, 0.5087719298245614308, 0.5131578947368421462, 0.5175438596491228616, 0.5219298245614034659, 0.5263157894736841813, 0.5307017543859648967, 0.5350877192982456121, 0.5394736842105263275, 0.5438596491228070429, 0.5482456140350877583, 0.5526315789473684736, 0.5570175438596490780, 0.5614035087719297934, 0.5657894736842105088, 0.5701754385964912242, 0.5745614035087719396, 0.5789473684210526550, 0.5833333333333333703, 0.5877192982456140857, 0.5921052631578946901, 0.5964912280701754055, 0.6008771929824561209, 0.6052631578947368363, 0.6096491228070175517, 0.6140350877192982670, 0.6184210526315789824, 0.6228070175438596978, 0.6271929824561403022, 0.6315789473684210176, 0.6359649122807017330, 0.6403508771929824483, 0.6447368421052631637, 0.6491228070175438791, 0.6535087719298245945, 0.6578947368421053099, 0.6622807017543859143, 0.6666666666666666297, 0.6710526315789473450, 0.6754385964912280604, 0.6798245614035087758, 0.6842105263157894912, 0.6885964912280702066, 0.6929824561403509220, 0.6973684210526315264, 0.7017543859649122417, 0.7061403508771929571, 0.7105263157894736725, 0.7149122807017543879, 0.7192982456140351033, 0.7236842105263158187, 0.7280701754385965341, 0.7324561403508771384, 0.7368421052631578538, 0.7412280701754385692, 0.7456140350877192846, 0.7500000000000000000, 0.7543859649122807154, 0.7587719298245614308, 0.7631578947368421462, 0.7675438596491228616, 0.7719298245614034659, 0.7763157894736841813, 0.7807017543859648967, 0.7850877192982456121, 0.7894736842105263275, 0.7938596491228070429, 0.7982456140350877583, 0.8026315789473684736, 0.8070175438596490780, 0.8114035087719297934, 0.8157894736842105088, 0.8201754385964912242, 0.8245614035087719396, 0.8289473684210526550, 0.8333333333333333703, 0.8377192982456140857, 0.8421052631578946901, 0.8464912280701754055, 0.8508771929824561209, 0.8552631578947368363, 0.8596491228070175517, 0.8640350877192982670, 0.8684210526315789824, 0.8728070175438596978, 0.8771929824561403022, 0.8815789473684210176, 0.8859649122807017330, 0.8903508771929824483, 0.8947368421052631637, 0.8991228070175438791, 0.9035087719298245945, 0.9078947368421053099, 0.9122807017543859143, 0.9166666666666666297, 0.9210526315789473450, 0.9254385964912280604, 0.9298245614035087758, 0.9342105263157894912, 0.9385964912280702066, 0.9429824561403509220, 0.9473684210526315264, 0.9517543859649122417, 0.9561403508771929571, 0.9605263157894736725, 0.9649122807017543879, 0.9692982456140351033, 0.9736842105263158187, 0.9780701754385965341, 0.9824561403508771384, 0.9868421052631578538, 0.9912280701754385692, 0.9956140350877192846, 1.000000000000000000 ),
 .UNSPECIFIED. ) 
 GEOMETRIC_REPRESENTATION_ITEM ( )  RATIONAL_B_SPLINE_SURFACE ( (
 ( 1.000000000000000000, 0.9659258262890683122, 1.000000000000000000, 0.9659258262890683122, 1.000000000000000000, 0.9659258262890683122, 1.000000000000000000, 0.9659258262890683122, 1.000000000000000000, 0.9659258262890683122, 1.000000000000000000, 0.9659258262890683122, 1.000000000000000000, 0.9659258262890683122, 1.000000000000000000, 0.9659258262890683122, 1.000000000000000000, 0.9659258262890683122, 1.000000000000000000, 0.9659258262890683122, 1.000000000000000000, 0.9659258262890683122, 1.000000000000000000, 0.9659258262890683122, 1.000000000000000000, 0.9659258262890683122, 1.000000000000000000, 0.9659258262890683122, 1.000000000000000000, 0.9659258262890683122, 1.000000000000000000, 0.9659258262890683122, 1.000000000000000000, 0.9659258262890683122, 1.000000000000000000, 0.9659258262890683122, 1.000000000000000000, 0.9659258262890683122, 1.000000000000000000, 0.9659258262890683122, 1.000000000000000000, 0.9659258262890683122, 1.000000000000000000, 0.9659258262890683122, 1.000000000000000000, 0.9659258262890683122, 1.000000000000000000, 0.9659258262890683122, 1.000000000000000000, 0.9659258262890683122, 1.000000000000000000, 0.9659258262890683122, 1.000000000000000000, 0.9659258262890683122, 1.000000000000000000, 0.9659258262890683122, 1.000000000000000000, 0.9659258262890683122, 1.000000000000000000, 0.9659258262890683122, 1.000000000000000000, 0.9659258262890683122, 1.000000000000000000, 0.9659258262890683122, 1.000000000000000000, 0.9659258262890683122, 1.000000000000000000, 0.9659258262890683122, 1.000000000000000000, 0.9659258262890683122, 1.000000000000000000, 0.9659258262890683122, 1.000000000000000000, 0.9659258262890683122, 1.000000000000000000, 0.9659258262890683122, 1.000000000000000000, 0.9659258262890683122, 1.000000000000000000, 0.9659258262890683122, 1.000000000000000000, 0.9659258262890683122, 1.000000000000000000, 0.9659258262890683122, 1.000000000000000000, 0.9659258262890683122, 1.000000000000000000, 0.9659258262890683122, 1.000000000000000000, 0.9659258262890683122, 1.000000000000000000, 0.9659258262890683122, 1.000000000000000000, 0.9659258262890683122, 1.000000000000000000, 0.9659258262890683122, 1.000000000000000000, 0.9659258262890683122, 1.000000000000000000, 0.9659258262890683122, 1.000000000000000000, 0.9659258262890683122, 1.000000000000000000, 0.9659258262890683122, 1.000000000000000000, 0.9659258262890683122, 1.000000000000000000, 0.9659258262890683122, 1.000000000000000000, 0.9659258262890683122, 1.000000000000000000, 0.9659258262890683122, 1.000000000000000000, 0.9659258262890683122, 1.000000000000000000, 0.9659258262890683122, 1.000000000000000000, 0.9659258262890683122, 1.000000000000000000, 0.9659258262890683122, 1.000000000000000000, 0.9659258262890683122, 1.000000000000000000, 0.9659258262890683122, 1.000000000000000000, 0.9659258262890683122, 1.000000000000000000, 0.9659258262890683122, 1.000000000000000000, 0.9659258262890683122, 1.000000000000000000, 0.9659258262890683122, 1.000000000000000000, 0.9659258262890683122, 1.000000000000000000, 0.9659258262890683122, 1.000000000000000000, 0.9659258262890683122, 1.000000000000000000, 0.9659258262890683122, 1.000000000000000000, 0.9659258262890683122, 1.000000000000000000, 0.9659258262890683122, 1.000000000000000000, 0.9659258262890683122, 1.000000000000000000, 0.9659258262890683122, 1.000000000000000000, 0.9659258262890683122, 1.000000000000000000, 0.9659258262890683122, 1.000000000000000000, 0.9659258262890683122, 1.000000000000000000, 0.9659258262890683122, 1.000000000000000000, 0.9659258262890683122, 1.000000000000000000, 0.9659258262890683122, 1.000000000000000000, 0.9659258262890683122, 1.000000000000000000, 0.9659258262890683122, 1.000000000000000000, 0.9659258262890683122, 1.000000000000000000, 0.9659258262890683122, 1.000000000000000000, 0.9659258262890683122, 1.000000000000000000, 0.9659258262890683122, 1.000000000000000000, 0.9659258262890683122, 1.000000000000000000, 0.9659258262890683122, 1.000000000000000000, 0.9659258262890683122, 1.000000000000000000, 0.9659258262890683122, 1.000000000000000000, 0.9659258262890683122, 1.000000000000000000, 0.9659258262890683122, 1.000000000000000000, 0.9659258262890683122, 1.000000000000000000, 0.9659258262890683122, 1.000000000000000000, 0.9659258262890683122, 1.000000000000000000, 0.9659258262890683122, 1.000000000000000000, 0.9659258262890683122, 1.000000000000000000, 0.9659258262890683122, 1.000000000000000000, 0.9659258262890683122, 1.000000000000000000, 0.9659258262890683122, 1.000000000000000000, 0.9659258262890683122, 1.000000000000000000, 0.9659258262890683122, 1.000000000000000000, 0.9659258262890683122, 1.000000000000000000, 0.9659258262890683122, 1.000000000000000000, 0.9659258262890683122, 1.000000000000000000, 0.9659258262890683122, 1.000000000000000000, 0.9659258262890683122, 1.000000000000000000, 0.9659258262890683122, 1.000000000000000000, 0.9659258262890683122, 1.000000000000000000, 0.9659258262890683122, 1.000000000000000000, 0.9659258262890683122, 1.000000000000000000, 0.9659258262890683122, 1.000000000000000000, 0.9659258262890683122, 1.000000000000000000, 0.9659258262890683122, 1.000000000000000000, 0.9659258262890683122, 1.000000000000000000, 0.9659258262890683122, 1.000000000000000000, 0.9659258262890683122, 1.000000000000000000, 0.9659258262890683122, 1.000000000000000000, 0.9659258262890683122, 1.000000000000000000, 0.9659258262890683122, 1.000000000000000000, 0.9659258262890683122, 1.000000000000000000, 0.9659258262890683122, 1.000000000000000000, 0.9659258262890683122, 1.000000000000000000, 0.9659258262890683122, 1.000000000000000000, 0.9659258262890683122, 1.000000000000000000, 0.9659258262890683122, 1.000000000000000000, 0.9659258262890683122, 1.000000000000000000, 0.9659258262890683122, 1.000000000000000000, 0.9659258262890683122, 1.000000000000000000, 0.9659258262890683122, 1.000000000000000000, 0.9659258262890683122, 1.000000000000000000, 0.9659258262890683122, 1.000000000000000000, 0.9659258262890683122, 1.000000000000000000, 0.9659258262890683122, 1.000000000000000000, 0.9659258262890683122, 1.000000000000000000, 0.9659258262890683122, 1.000000000000000000, 0.9659258262890683122, 1.000000000000000000, 0.9659258262890683122, 1.000000000000000000, 0.9659258262890683122, 1.000000000000000000, 0.9659258262890683122, 1.000000000000000000, 0.9659258262890683122, 1.000000000000000000, 0.9659258262890683122, 1.000000000000000000, 0.9659258262890683122, 1.000000000000000000, 0.9659258262890683122, 1.000000000000000000, 0.9659258262890683122, 1.000000000000000000, 0.9659258262890683122, 1.000000000000000000, 0.9659258262890683122, 1.000000000000000000, 0.9659258262890683122, 1.000000000000000000, 0.9659258262890683122, 1.000000000000000000, 0.9659258262890683122, 1.000000000000000000, 0.9659258262890683122, 1.000000000000000000, 0.9659258262890683122, 1.000000000000000000, 0.9659258262890683122, 1.000000000000000000, 0.9659258262890683122, 1.000000000000000000, 0.9659258262890683122, 1.000000000000000000, 0.9659258262890683122, 1.000000000000000000, 0.9659258262890683122, 1.000000000000000000, 0.9659258262890683122, 1.000000000000000000, 0.9659258262890683122, 1.000000000000000000, 0.9659258262890683122, 1.000000000000000000, 0.9659258262890683122, 1.000000000000000000, 0.9659258262890683122, 1.000000000000000000, 0.9659258262890683122, 1.000000000000000000, 0.9659258262890683122, 1.000000000000000000, 0.9659258262890683122, 1.000000000000000000, 0.9659258262890683122, 1.000000000000000000, 0.9659258262890683122, 1.000000000000000000, 0.9659258262890683122, 1.000000000000000000, 0.9659258262890683122, 1.000000000000000000, 0.9659258262890683122, 1.000000000000000000, 0.9659258262890683122, 1.000000000000000000, 0.9659258262890683122, 1.000000000000000000, 0.9659258262890683122, 1.000000000000000000, 0.9659258262890683122, 1.000000000000000000, 0.9659258262890683122, 1.000000000000000000, 0.9659258262890683122, 1.000000000000000000, 0.9659258262890683122, 1.000000000000000000, 0.9659258262890683122, 1.000000000000000000, 0.9659258262890683122, 1.000000000000000000, 0.9659258262890683122, 1.000000000000000000, 0.9659258262890683122, 1.000000000000000000, 0.9659258262890683122, 1.000000000000000000, 0.9659258262890683122, 1.000000000000000000, 0.9659258262890683122, 1.000000000000000000, 0.9659258262890683122, 1.000000000000000000, 0.9659258262890683122, 1.000000000000000000, 0.9659258262890683122, 1.000000000000000000, 0.9659258262890683122, 1.000000000000000000, 0.9659258262890683122, 1.000000000000000000, 0.9659258262890683122, 1.000000000000000000, 0.9659258262890683122, 1.000000000000000000, 0.9659258262890683122, 1.000000000000000000, 0.9659258262890683122, 1.000000000000000000, 0.9659258262890683122, 1.000000000000000000, 0.9659258262890683122, 1.000000000000000000, 0.9659258262890683122, 1.000000000000000000, 0.9659258262890683122, 1.000000000000000000, 0.9659258262890683122, 1.000000000000000000, 0.9659258262890683122, 1.000000000000000000, 0.9659258262890683122, 1.000000000000000000, 0.9659258262890683122, 1.000000000000000000, 0.9659258262890683122, 1.000000000000000000, 0.9659258262890683122, 1.000000000000000000, 0.9659258262890683122, 1.000000000000000000, 0.9659258262890683122, 1.000000000000000000, 0.9659258262890683122, 1.000000000000000000, 0.9659258262890683122, 1.000000000000000000, 0.9659258262890683122, 1.000000000000000000, 0.9659258262890683122, 1.000000000000000000, 0.9659258262890683122, 1.000000000000000000, 0.9659258262890683122, 1.000000000000000000, 0.9659258262890683122, 1.000000000000000000, 0.9659258262890683122, 1.000000000000000000, 0.9659258262890683122, 1.000000000000000000, 0.9659258262890683122, 1.000000000000000000, 0.9659258262890683122, 1.000000000000000000, 0.9659258262890683122, 1.000000000000000000, 0.9659258262890683122, 1.000000000000000000, 0.9659258262890683122, 1.000000000000000000, 0.9659258262890683122, 1.000000000000000000, 0.9659258262890683122, 1.000000000000000000, 0.9659258262890683122, 1.000000000000000000, 0.9659258262890683122, 1.000000000000000000, 0.9659258262890683122, 1.000000000000000000, 0.9659258262890683122, 1.000000000000000000, 0.9659258262890683122, 1.000000000000000000, 0.9659258262890683122, 1.000000000000000000, 0.9659258262890683122, 1.000000000000000000),
 ( 0.3333333333333333703, 0.3219752754296894559, 0.3333333333333333703, 0.3219752754296894559, 0.3333333333333333703, 0.3219752754296894559, 0.3333333333333333703, 0.3219752754296894559, 0.3333333333333333703, 0.3219752754296894559, 0.3333333333333333703, 0.3219752754296894559, 0.3333333333333333703, 0.3219752754296894559, 0.3333333333333333703, 0.3219752754296894559, 0.3333333333333333703, 0.3219752754296894559, 0.3333333333333333703, 0.3219752754296894559, 0.3333333333333333703, 0.3219752754296894559, 0.3333333333333333703, 0.3219752754296894559, 0.3333333333333333703, 0.3219752754296894559, 0.3333333333333333703, 0.3219752754296894559, 0.3333333333333333703, 0.3219752754296894559, 0.3333333333333333703, 0.3219752754296894559, 0.3333333333333333703, 0.3219752754296894559, 0.3333333333333333703, 0.3219752754296894559, 0.3333333333333333703, 0.3219752754296894559, 0.3333333333333333703, 0.3219752754296894559, 0.3333333333333333703, 0.3219752754296894559, 0.3333333333333333703, 0.3219752754296894559, 0.3333333333333333703, 0.3219752754296894559, 0.3333333333333333703, 0.3219752754296894559, 0.3333333333333333703, 0.3219752754296894559, 0.3333333333333333703, 0.3219752754296894559, 0.3333333333333333703, 0.3219752754296894559, 0.3333333333333333703, 0.3219752754296894559, 0.3333333333333333703, 0.3219752754296894559, 0.3333333333333333703, 0.3219752754296894559, 0.3333333333333333703, 0.3219752754296894559, 0.3333333333333333703, 0.3219752754296894559, 0.3333333333333333703, 0.3219752754296894559, 0.3333333333333333703, 0.3219752754296894559, 0.3333333333333333703, 0.3219752754296894559, 0.3333333333333333703, 0.3219752754296894559, 0.3333333333333333703, 0.3219752754296894559, 0.3333333333333333703, 0.3219752754296894559, 0.3333333333333333703, 0.3219752754296894559, 0.3333333333333333703, 0.3219752754296894559, 0.3333333333333333703, 0.3219752754296894559, 0.3333333333333333703, 0.3219752754296894559, 0.3333333333333333703, 0.3219752754296894559, 0.3333333333333333703, 0.3219752754296894559, 0.3333333333333333703, 0.3219752754296894559, 0.3333333333333333703, 0.3219752754296894559, 0.3333333333333333703, 0.3219752754296894559, 0.3333333333333333703, 0.3219752754296894559, 0.3333333333333333703, 0.3219752754296894559, 0.3333333333333333703, 0.3219752754296894559, 0.3333333333333333703, 0.3219752754296894559, 0.3333333333333333703, 0.3219752754296894559, 0.3333333333333333703, 0.3219752754296894559, 0.3333333333333333703, 0.3219752754296894559, 0.3333333333333333703, 0.3219752754296894559, 0.3333333333333333703, 0.3219752754296894559, 0.3333333333333333703, 0.3219752754296894559, 0.3333333333333333703, 0.3219752754296894559, 0.3333333333333333703, 0.3219752754296894559, 0.3333333333333333703, 0.3219752754296894559, 0.3333333333333333703, 0.3219752754296894559, 0.3333333333333333703, 0.3219752754296894559, 0.3333333333333333703, 0.3219752754296894559, 0.3333333333333333703, 0.3219752754296894559, 0.3333333333333333703, 0.3219752754296894559, 0.3333333333333333703, 0.3219752754296894559, 0.3333333333333333703, 0.3219752754296894559, 0.3333333333333333703, 0.3219752754296894559, 0.3333333333333333703, 0.3219752754296894559, 0.3333333333333333703, 0.3219752754296894559, 0.3333333333333333703, 0.3219752754296894559, 0.3333333333333333703, 0.3219752754296894559, 0.3333333333333333703, 0.3219752754296894559, 0.3333333333333333703, 0.3219752754296894559, 0.3333333333333333703, 0.3219752754296894559, 0.3333333333333333703, 0.3219752754296894559, 0.3333333333333333703, 0.3219752754296894559, 0.3333333333333333703, 0.3219752754296894559, 0.3333333333333333703, 0.3219752754296894559, 0.3333333333333333703, 0.3219752754296894559, 0.3333333333333333703, 0.3219752754296894559, 0.3333333333333333703, 0.3219752754296894559, 0.3333333333333333703, 0.3219752754296894559, 0.3333333333333333703, 0.3219752754296894559, 0.3333333333333333703, 0.3219752754296894559, 0.3333333333333333703, 0.3219752754296894559, 0.3333333333333333703, 0.3219752754296894559, 0.3333333333333333703, 0.3219752754296894559, 0.3333333333333333703, 0.3219752754296894559, 0.3333333333333333703, 0.3219752754296894559, 0.3333333333333333703, 0.3219752754296894559, 0.3333333333333333703, 0.3219752754296894559, 0.3333333333333333703, 0.3219752754296894559, 0.3333333333333333703, 0.3219752754296894559, 0.3333333333333333703, 0.3219752754296894559, 0.3333333333333333703, 0.3219752754296894559, 0.3333333333333333703, 0.3219752754296894559, 0.3333333333333333703, 0.3219752754296894559, 0.3333333333333333703, 0.3219752754296894559, 0.3333333333333333703, 0.3219752754296894559, 0.3333333333333333703, 0.3219752754296894559, 0.3333333333333333703, 0.3219752754296894559, 0.3333333333333333703, 0.3219752754296894559, 0.3333333333333333703, 0.3219752754296894559, 0.3333333333333333703, 0.3219752754296894559, 0.3333333333333333703, 0.3219752754296894559, 0.3333333333333333703, 0.3219752754296894559, 0.3333333333333333703, 0.3219752754296894559, 0.3333333333333333703, 0.3219752754296894559, 0.3333333333333333703, 0.3219752754296894559, 0.3333333333333333703, 0.3219752754296894559, 0.3333333333333333703, 0.3219752754296894559, 0.3333333333333333703, 0.3219752754296894559, 0.3333333333333333703, 0.3219752754296894559, 0.3333333333333333703, 0.3219752754296894559, 0.3333333333333333703, 0.3219752754296894559, 0.3333333333333333703, 0.3219752754296894559, 0.3333333333333333703, 0.3219752754296894559, 0.3333333333333333703, 0.3219752754296894559, 0.3333333333333333703, 0.3219752754296894559, 0.3333333333333333703, 0.3219752754296894559, 0.3333333333333333703, 0.3219752754296894559, 0.3333333333333333703, 0.3219752754296894559, 0.3333333333333333703, 0.3219752754296894559, 0.3333333333333333703, 0.3219752754296894559, 0.3333333333333333703, 0.3219752754296894559, 0.3333333333333333703, 0.3219752754296894559, 0.3333333333333333703, 0.3219752754296894559, 0.3333333333333333703, 0.3219752754296894559, 0.3333333333333333703, 0.3219752754296894559, 0.3333333333333333703, 0.3219752754296894559, 0.3333333333333333703, 0.3219752754296894559, 0.3333333333333333703, 0.3219752754296894559, 0.3333333333333333703, 0.3219752754296894559, 0.3333333333333333703, 0.3219752754296894559, 0.3333333333333333703, 0.3219752754296894559, 0.3333333333333333703, 0.3219752754296894559, 0.3333333333333333703, 0.3219752754296894559, 0.3333333333333333703, 0.3219752754296894559, 0.3333333333333333703, 0.3219752754296894559, 0.3333333333333333703, 0.3219752754296894559, 0.3333333333333333703, 0.3219752754296894559, 0.3333333333333333703, 0.3219752754296894559, 0.3333333333333333703, 0.3219752754296894559, 0.3333333333333333703, 0.3219752754296894559, 0.3333333333333333703, 0.3219752754296894559, 0.3333333333333333703, 0.3219752754296894559, 0.3333333333333333703, 0.3219752754296894559, 0.3333333333333333703, 0.3219752754296894559, 0.3333333333333333703, 0.3219752754296894559, 0.3333333333333333703, 0.3219752754296894559, 0.3333333333333333703, 0.3219752754296894559, 0.3333333333333333703, 0.3219752754296894559, 0.3333333333333333703, 0.3219752754296894559, 0.3333333333333333703, 0.3219752754296894559, 0.3333333333333333703, 0.3219752754296894559, 0.3333333333333333703, 0.3219752754296894559, 0.3333333333333333703, 0.3219752754296894559, 0.3333333333333333703, 0.3219752754296894559, 0.3333333333333333703, 0.3219752754296894559, 0.3333333333333333703, 0.3219752754296894559, 0.3333333333333333703, 0.3219752754296894559, 0.3333333333333333703, 0.3219752754296894559, 0.3333333333333333703, 0.3219752754296894559, 0.3333333333333333703, 0.3219752754296894559, 0.3333333333333333703, 0.3219752754296894559, 0.3333333333333333703, 0.3219752754296894559, 0.3333333333333333703, 0.3219752754296894559, 0.3333333333333333703, 0.3219752754296894559, 0.3333333333333333703, 0.3219752754296894559, 0.3333333333333333703, 0.3219752754296894559, 0.3333333333333333703, 0.3219752754296894559, 0.3333333333333333703, 0.3219752754296894559, 0.3333333333333333703, 0.3219752754296894559, 0.3333333333333333703, 0.3219752754296894559, 0.3333333333333333703, 0.3219752754296894559, 0.3333333333333333703, 0.3219752754296894559, 0.3333333333333333703, 0.3219752754296894559, 0.3333333333333333703, 0.3219752754296894559, 0.3333333333333333703, 0.3219752754296894559, 0.3333333333333333703, 0.3219752754296894559, 0.3333333333333333703, 0.3219752754296894559, 0.3333333333333333703, 0.3219752754296894559, 0.3333333333333333703, 0.3219752754296894559, 0.3333333333333333703, 0.3219752754296894559, 0.3333333333333333703, 0.3219752754296894559, 0.3333333333333333703, 0.3219752754296894559, 0.3333333333333333703, 0.3219752754296894559, 0.3333333333333333703, 0.3219752754296894559, 0.3333333333333333703, 0.3219752754296894559, 0.3333333333333333703, 0.3219752754296894559, 0.3333333333333333703, 0.3219752754296894559, 0.3333333333333333703, 0.3219752754296894559, 0.3333333333333333703, 0.3219752754296894559, 0.3333333333333333703, 0.3219752754296894559, 0.3333333333333333703, 0.3219752754296894559, 0.3333333333333333703, 0.3219752754296894559, 0.3333333333333333703, 0.3219752754296894559, 0.3333333333333333703, 0.3219752754296894559, 0.3333333333333333703, 0.3219752754296894559, 0.3333333333333333703, 0.3219752754296894559, 0.3333333333333333703, 0.3219752754296894559, 0.3333333333333333703, 0.3219752754296894559, 0.3333333333333333703, 0.3219752754296894559, 0.3333333333333333703, 0.3219752754296894559, 0.3333333333333333703, 0.3219752754296894559, 0.3333333333333333703, 0.3219752754296894559, 0.3333333333333333703, 0.3219752754296894559, 0.3333333333333333703, 0.3219752754296894559, 0.3333333333333333703, 0.3219752754296894559, 0.3333333333333333703, 0.3219752754296894559, 0.3333333333333333703, 0.3219752754296894559, 0.3333333333333333703, 0.3219752754296894559, 0.3333333333333333703, 0.3219752754296894559, 0.3333333333333333703, 0.3219752754296894559, 0.3333333333333333703, 0.3219752754296894559, 0.3333333333333333703, 0.3219752754296894559, 0.3333333333333333703, 0.3219752754296894559, 0.3333333333333333703, 0.3219752754296894559, 0.3333333333333333703, 0.3219752754296894559, 0.3333333333333333703, 0.3219752754296894559, 0.3333333333333333703, 0.3219752754296894559, 0.3333333333333333703, 0.3219752754296894559, 0.3333333333333333703, 0.3219752754296894559, 0.3333333333333333703, 0.3219752754296894559, 0.3333333333333333703, 0.3219752754296894559, 0.3333333333333333703, 0.3219752754296894559, 0.3333333333333333703, 0.3219752754296894559, 0.3333333333333333703),
 ( 0.3333333333333333703, 0.3219752754296894559, 0.3333333333333333703, 0.3219752754296894559, 0.3333333333333333703, 0.3219752754296894559, 0.3333333333333333703, 0.3219752754296894559, 0.3333333333333333703, 0.3219752754296894559, 0.3333333333333333703, 0.3219752754296894559, 0.3333333333333333703, 0.3219752754296894559, 0.3333333333333333703, 0.3219752754296894559, 0.3333333333333333703, 0.3219752754296894559, 0.3333333333333333703, 0.3219752754296894559, 0.3333333333333333703, 0.3219752754296894559, 0.3333333333333333703, 0.3219752754296894559, 0.3333333333333333703, 0.3219752754296894559, 0.3333333333333333703, 0.3219752754296894559, 0.3333333333333333703, 0.3219752754296894559, 0.3333333333333333703, 0.3219752754296894559, 0.3333333333333333703, 0.3219752754296894559, 0.3333333333333333703, 0.3219752754296894559, 0.3333333333333333703, 0.3219752754296894559, 0.3333333333333333703, 0.3219752754296894559, 0.3333333333333333703, 0.3219752754296894559, 0.3333333333333333703, 0.3219752754296894559, 0.3333333333333333703, 0.3219752754296894559, 0.3333333333333333703, 0.3219752754296894559, 0.3333333333333333703, 0.3219752754296894559, 0.3333333333333333703, 0.3219752754296894559, 0.3333333333333333703, 0.3219752754296894559, 0.3333333333333333703, 0.3219752754296894559, 0.3333333333333333703, 0.3219752754296894559, 0.3333333333333333703, 0.3219752754296894559, 0.3333333333333333703, 0.3219752754296894559, 0.3333333333333333703, 0.3219752754296894559, 0.3333333333333333703, 0.3219752754296894559, 0.3333333333333333703, 0.3219752754296894559, 0.3333333333333333703, 0.3219752754296894559, 0.3333333333333333703, 0.3219752754296894559, 0.3333333333333333703, 0.3219752754296894559, 0.3333333333333333703, 0.3219752754296894559, 0.3333333333333333703, 0.3219752754296894559, 0.3333333333333333703, 0.3219752754296894559, 0.3333333333333333703, 0.3219752754296894559, 0.3333333333333333703, 0.3219752754296894559, 0.3333333333333333703, 0.3219752754296894559, 0.3333333333333333703, 0.3219752754296894559, 0.3333333333333333703, 0.3219752754296894559, 0.3333333333333333703, 0.3219752754296894559, 0.3333333333333333703, 0.3219752754296894559, 0.3333333333333333703, 0.3219752754296894559, 0.3333333333333333703, 0.3219752754296894559, 0.3333333333333333703, 0.3219752754296894559, 0.3333333333333333703, 0.3219752754296894559, 0.3333333333333333703, 0.3219752754296894559, 0.3333333333333333703, 0.3219752754296894559, 0.3333333333333333703, 0.3219752754296894559, 0.3333333333333333703, 0.3219752754296894559, 0.3333333333333333703, 0.3219752754296894559, 0.3333333333333333703, 0.3219752754296894559, 0.3333333333333333703, 0.3219752754296894559, 0.3333333333333333703, 0.3219752754296894559, 0.3333333333333333703, 0.3219752754296894559, 0.3333333333333333703, 0.3219752754296894559, 0.3333333333333333703, 0.3219752754296894559, 0.3333333333333333703, 0.3219752754296894559, 0.3333333333333333703, 0.3219752754296894559, 0.3333333333333333703, 0.3219752754296894559, 0.3333333333333333703, 0.3219752754296894559, 0.3333333333333333703, 0.3219752754296894559, 0.3333333333333333703, 0.3219752754296894559, 0.3333333333333333703, 0.3219752754296894559, 0.3333333333333333703, 0.3219752754296894559, 0.3333333333333333703, 0.3219752754296894559, 0.3333333333333333703, 0.3219752754296894559, 0.3333333333333333703, 0.3219752754296894559, 0.3333333333333333703, 0.3219752754296894559, 0.3333333333333333703, 0.3219752754296894559, 0.3333333333333333703, 0.3219752754296894559, 0.3333333333333333703, 0.3219752754296894559, 0.3333333333333333703, 0.3219752754296894559, 0.3333333333333333703, 0.3219752754296894559, 0.3333333333333333703, 0.3219752754296894559, 0.3333333333333333703, 0.3219752754296894559, 0.3333333333333333703, 0.3219752754296894559, 0.3333333333333333703, 0.3219752754296894559, 0.3333333333333333703, 0.3219752754296894559, 0.3333333333333333703, 0.3219752754296894559, 0.3333333333333333703, 0.3219752754296894559, 0.3333333333333333703, 0.3219752754296894559, 0.3333333333333333703, 0.3219752754296894559, 0.3333333333333333703, 0.3219752754296894559, 0.3333333333333333703, 0.3219752754296894559, 0.3333333333333333703, 0.3219752754296894559, 0.3333333333333333703, 0.3219752754296894559, 0.3333333333333333703, 0.3219752754296894559, 0.3333333333333333703, 0.3219752754296894559, 0.3333333333333333703, 0.3219752754296894559, 0.3333333333333333703, 0.3219752754296894559, 0.3333333333333333703, 0.3219752754296894559, 0.3333333333333333703, 0.3219752754296894559, 0.3333333333333333703, 0.3219752754296894559, 0.3333333333333333703, 0.3219752754296894559, 0.3333333333333333703, 0.3219752754296894559, 0.3333333333333333703, 0.3219752754296894559, 0.3333333333333333703, 0.3219752754296894559, 0.3333333333333333703, 0.3219752754296894559, 0.3333333333333333703, 0.3219752754296894559, 0.3333333333333333703, 0.3219752754296894559, 0.3333333333333333703, 0.3219752754296894559, 0.3333333333333333703, 0.3219752754296894559, 0.3333333333333333703, 0.3219752754296894559, 0.3333333333333333703, 0.3219752754296894559, 0.3333333333333333703, 0.3219752754296894559, 0.3333333333333333703, 0.3219752754296894559, 0.3333333333333333703, 0.3219752754296894559, 0.3333333333333333703, 0.3219752754296894559, 0.3333333333333333703, 0.3219752754296894559, 0.3333333333333333703, 0.3219752754296894559, 0.3333333333333333703, 0.3219752754296894559, 0.3333333333333333703, 0.3219752754296894559, 0.3333333333333333703, 0.3219752754296894559, 0.3333333333333333703, 0.3219752754296894559, 0.3333333333333333703, 0.3219752754296894559, 0.3333333333333333703, 0.3219752754296894559, 0.3333333333333333703, 0.3219752754296894559, 0.3333333333333333703, 0.3219752754296894559, 0.3333333333333333703, 0.3219752754296894559, 0.3333333333333333703, 0.3219752754296894559, 0.3333333333333333703, 0.3219752754296894559, 0.3333333333333333703, 0.3219752754296894559, 0.3333333333333333703, 0.3219752754296894559, 0.3333333333333333703, 0.3219752754296894559, 0.3333333333333333703, 0.3219752754296894559, 0.3333333333333333703, 0.3219752754296894559, 0.3333333333333333703, 0.3219752754296894559, 0.3333333333333333703, 0.3219752754296894559, 0.3333333333333333703, 0.3219752754296894559, 0.3333333333333333703, 0.3219752754296894559, 0.3333333333333333703, 0.3219752754296894559, 0.3333333333333333703, 0.3219752754296894559, 0.3333333333333333703, 0.3219752754296894559, 0.3333333333333333703, 0.3219752754296894559, 0.3333333333333333703, 0.3219752754296894559, 0.3333333333333333703, 0.3219752754296894559, 0.3333333333333333703, 0.3219752754296894559, 0.3333333333333333703, 0.3219752754296894559, 0.3333333333333333703, 0.3219752754296894559, 0.3333333333333333703, 0.3219752754296894559, 0.3333333333333333703, 0.3219752754296894559, 0.3333333333333333703, 0.3219752754296894559, 0.3333333333333333703, 0.3219752754296894559, 0.3333333333333333703, 0.3219752754296894559, 0.3333333333333333703, 0.3219752754296894559, 0.3333333333333333703, 0.3219752754296894559, 0.3333333333333333703, 0.3219752754296894559, 0.3333333333333333703, 0.3219752754296894559, 0.3333333333333333703, 0.3219752754296894559, 0.3333333333333333703, 0.3219752754296894559, 0.3333333333333333703, 0.3219752754296894559, 0.3333333333333333703, 0.3219752754296894559, 0.3333333333333333703, 0.3219752754296894559, 0.3333333333333333703, 0.3219752754296894559, 0.3333333333333333703, 0.3219752754296894559, 0.3333333333333333703, 0.3219752754296894559, 0.3333333333333333703, 0.3219752754296894559, 0.3333333333333333703, 0.3219752754296894559, 0.3333333333333333703, 0.3219752754296894559, 0.3333333333333333703, 0.3219752754296894559, 0.3333333333333333703, 0.3219752754296894559, 0.3333333333333333703, 0.3219752754296894559, 0.3333333333333333703, 0.3219752754296894559, 0.3333333333333333703, 0.3219752754296894559, 0.3333333333333333703, 0.3219752754296894559, 0.3333333333333333703, 0.3219752754296894559, 0.3333333333333333703, 0.3219752754296894559, 0.3333333333333333703, 0.3219752754296894559, 0.3333333333333333703, 0.3219752754296894559, 0.3333333333333333703, 0.3219752754296894559, 0.3333333333333333703, 0.3219752754296894559, 0.3333333333333333703, 0.3219752754296894559, 0.3333333333333333703, 0.3219752754296894559, 0.3333333333333333703, 0.3219752754296894559, 0.3333333333333333703, 0.3219752754296894559, 0.3333333333333333703, 0.3219752754296894559, 0.3333333333333333703, 0.3219752754296894559, 0.3333333333333333703, 0.3219752754296894559, 0.3333333333333333703, 0.3219752754296894559, 0.3333333333333333703, 0.3219752754296894559, 0.3333333333333333703, 0.3219752754296894559, 0.3333333333333333703, 0.3219752754296894559, 0.3333333333333333703, 0.3219752754296894559, 0.3333333333333333703, 0.3219752754296894559, 0.3333333333333333703, 0.3219752754296894559, 0.3333333333333333703, 0.3219752754296894559, 0.3333333333333333703, 0.3219752754296894559, 0.3333333333333333703, 0.3219752754296894559, 0.3333333333333333703, 0.3219752754296894559, 0.3333333333333333703, 0.3219752754296894559, 0.3333333333333333703, 0.3219752754296894559, 0.3333333333333333703, 0.3219752754296894559, 0.3333333333333333703, 0.3219752754296894559, 0.3333333333333333703, 0.3219752754296894559, 0.3333333333333333703, 0.3219752754296894559, 0.3333333333333333703, 0.3219752754296894559, 0.3333333333333333703, 0.3219752754296894559, 0.3333333333333333703, 0.3219752754296894559, 0.3333333333333333703, 0.3219752754296894559, 0.3333333333333333703, 0.3219752754296894559, 0.3333333333333333703, 0.3219752754296894559, 0.3333333333333333703, 0.3219752754296894559, 0.3333333333333333703, 0.3219752754296894559, 0.3333333333333333703, 0.3219752754296894559, 0.3333333333333333703, 0.3219752754296894559, 0.3333333333333333703, 0.3219752754296894559, 0.3333333333333333703, 0.3219752754296894559, 0.3333333333333333703, 0.3219752754296894559, 0.3333333333333333703, 0.3219752754296894559, 0.3333333333333333703, 0.3219752754296894559, 0.3333333333333333703, 0.3219752754296894559, 0.3333333333333333703, 0.3219752754296894559, 0.3333333333333333703, 0.3219752754296894559, 0.3333333333333333703, 0.3219752754296894559, 0.3333333333333333703, 0.3219752754296894559, 0.3333333333333333703, 0.3219752754296894559, 0.3333333333333333703, 0.3219752754296894559, 0.3333333333333333703, 0.3219752754296894559, 0.3333333333333333703, 0.3219752754296894559, 0.3333333333333333703, 0.3219752754296894559, 0.3333333333333333703, 0.3219752754296894559, 0.3333333333333333703, 0.3219752754296894559, 0.3333333333333333703),
 ( 1.000000000000000000, 0.9659258262890683122, 1.000000000000000000, 0.9659258262890683122, 1.000000000000000000, 0.9659258262890683122, 1.000000000000000000, 0.9659258262890683122, 1.000000000000000000, 0.9659258262890683122, 1.000000000000000000, 0.9659258262890683122, 1.000000000000000000, 0.9659258262890683122, 1.000000000000000000, 0.9659258262890683122, 1.000000000000000000, 0.9659258262890683122, 1.000000000000000000, 0.9659258262890683122, 1.000000000000000000, 0.9659258262890683122, 1.000000000000000000, 0.9659258262890683122, 1.000000000000000000, 0.9659258262890683122, 1.000000000000000000, 0.9659258262890683122, 1.000000000000000000, 0.9659258262890683122, 1.000000000000000000, 0.9659258262890683122, 1.000000000000000000, 0.9659258262890683122, 1.000000000000000000, 0.9659258262890683122, 1.000000000000000000, 0.9659258262890683122, 1.000000000000000000, 0.9659258262890683122, 1.000000000000000000, 0.9659258262890683122, 1.000000000000000000, 0.9659258262890683122, 1.000000000000000000, 0.9659258262890683122, 1.000000000000000000, 0.9659258262890683122, 1.000000000000000000, 0.9659258262890683122, 1.000000000000000000, 0.9659258262890683122, 1.000000000000000000, 0.9659258262890683122, 1.000000000000000000, 0.9659258262890683122, 1.000000000000000000, 0.9659258262890683122, 1.000000000000000000, 0.9659258262890683122, 1.000000000000000000, 0.9659258262890683122, 1.000000000000000000, 0.9659258262890683122, 1.000000000000000000, 0.9659258262890683122, 1.000000000000000000, 0.9659258262890683122, 1.000000000000000000, 0.9659258262890683122, 1.000000000000000000, 0.9659258262890683122, 1.000000000000000000, 0.9659258262890683122, 1.000000000000000000, 0.9659258262890683122, 1.000000000000000000, 0.9659258262890683122, 1.000000000000000000, 0.9659258262890683122, 1.000000000000000000, 0.9659258262890683122, 1.000000000000000000, 0.9659258262890683122, 1.000000000000000000, 0.9659258262890683122, 1.000000000000000000, 0.9659258262890683122, 1.000000000000000000, 0.9659258262890683122, 1.000000000000000000, 0.9659258262890683122, 1.000000000000000000, 0.9659258262890683122, 1.000000000000000000, 0.9659258262890683122, 1.000000000000000000, 0.9659258262890683122, 1.000000000000000000, 0.9659258262890683122, 1.000000000000000000, 0.9659258262890683122, 1.000000000000000000, 0.9659258262890683122, 1.000000000000000000, 0.9659258262890683122, 1.000000000000000000, 0.9659258262890683122, 1.000000000000000000, 0.9659258262890683122, 1.000000000000000000, 0.9659258262890683122, 1.000000000000000000, 0.9659258262890683122, 1.000000000000000000, 0.9659258262890683122, 1.000000000000000000, 0.9659258262890683122, 1.000000000000000000, 0.9659258262890683122, 1.000000000000000000, 0.9659258262890683122, 1.000000000000000000, 0.9659258262890683122, 1.000000000000000000, 0.9659258262890683122, 1.000000000000000000, 0.9659258262890683122, 1.000000000000000000, 0.9659258262890683122, 1.000000000000000000, 0.9659258262890683122, 1.000000000000000000, 0.9659258262890683122, 1.000000000000000000, 0.9659258262890683122, 1.000000000000000000, 0.9659258262890683122, 1.000000000000000000, 0.9659258262890683122, 1.000000000000000000, 0.9659258262890683122, 1.000000000000000000, 0.9659258262890683122, 1.000000000000000000, 0.9659258262890683122, 1.000000000000000000, 0.9659258262890683122, 1.000000000000000000, 0.9659258262890683122, 1.000000000000000000, 0.9659258262890683122, 1.000000000000000000, 0.9659258262890683122, 1.000000000000000000, 0.9659258262890683122, 1.000000000000000000, 0.9659258262890683122, 1.000000000000000000, 0.9659258262890683122, 1.000000000000000000, 0.9659258262890683122, 1.000000000000000000, 0.9659258262890683122, 1.000000000000000000, 0.9659258262890683122, 1.000000000000000000, 0.9659258262890683122, 1.000000000000000000, 0.9659258262890683122, 1.000000000000000000, 0.9659258262890683122, 1.000000000000000000, 0.9659258262890683122, 1.000000000000000000, 0.9659258262890683122, 1.000000000000000000, 0.9659258262890683122, 1.000000000000000000, 0.9659258262890683122, 1.000000000000000000, 0.9659258262890683122, 1.000000000000000000, 0.9659258262890683122, 1.000000000000000000, 0.9659258262890683122, 1.000000000000000000, 0.9659258262890683122, 1.000000000000000000, 0.9659258262890683122, 1.000000000000000000, 0.9659258262890683122, 1.000000000000000000, 0.9659258262890683122, 1.000000000000000000, 0.9659258262890683122, 1.000000000000000000, 0.9659258262890683122, 1.000000000000000000, 0.9659258262890683122, 1.000000000000000000, 0.9659258262890683122, 1.000000000000000000, 0.9659258262890683122, 1.000000000000000000, 0.9659258262890683122, 1.000000000000000000, 0.9659258262890683122, 1.000000000000000000, 0.9659258262890683122, 1.000000000000000000, 0.9659258262890683122, 1.000000000000000000, 0.9659258262890683122, 1.000000000000000000, 0.9659258262890683122, 1.000000000000000000, 0.9659258262890683122, 1.000000000000000000, 0.9659258262890683122, 1.000000000000000000, 0.9659258262890683122, 1.000000000000000000, 0.9659258262890683122, 1.000000000000000000, 0.9659258262890683122, 1.000000000000000000, 0.9659258262890683122, 1.000000000000000000, 0.9659258262890683122, 1.000000000000000000, 0.9659258262890683122, 1.000000000000000000, 0.9659258262890683122, 1.000000000000000000, 0.9659258262890683122, 1.000000000000000000, 0.9659258262890683122, 1.000000000000000000, 0.9659258262890683122, 1.000000000000000000, 0.9659258262890683122, 1.000000000000000000, 0.9659258262890683122, 1.000000000000000000, 0.9659258262890683122, 1.000000000000000000, 0.9659258262890683122, 1.000000000000000000, 0.9659258262890683122, 1.000000000000000000, 0.9659258262890683122, 1.000000000000000000, 0.9659258262890683122, 1.000000000000000000, 0.9659258262890683122, 1.000000000000000000, 0.9659258262890683122, 1.000000000000000000, 0.9659258262890683122, 1.000000000000000000, 0.9659258262890683122, 1.000000000000000000, 0.9659258262890683122, 1.000000000000000000, 0.9659258262890683122, 1.000000000000000000, 0.9659258262890683122, 1.000000000000000000, 0.9659258262890683122, 1.000000000000000000, 0.9659258262890683122, 1.000000000000000000, 0.9659258262890683122, 1.000000000000000000, 0.9659258262890683122, 1.000000000000000000, 0.9659258262890683122, 1.000000000000000000, 0.9659258262890683122, 1.000000000000000000, 0.9659258262890683122, 1.000000000000000000, 0.9659258262890683122, 1.000000000000000000, 0.9659258262890683122, 1.000000000000000000, 0.9659258262890683122, 1.000000000000000000, 0.9659258262890683122, 1.000000000000000000, 0.9659258262890683122, 1.000000000000000000, 0.9659258262890683122, 1.000000000000000000, 0.9659258262890683122, 1.000000000000000000, 0.9659258262890683122, 1.000000000000000000, 0.9659258262890683122, 1.000000000000000000, 0.9659258262890683122, 1.000000000000000000, 0.9659258262890683122, 1.000000000000000000, 0.9659258262890683122, 1.000000000000000000, 0.9659258262890683122, 1.000000000000000000, 0.9659258262890683122, 1.000000000000000000, 0.9659258262890683122, 1.000000000000000000, 0.9659258262890683122, 1.000000000000000000, 0.9659258262890683122, 1.000000000000000000, 0.9659258262890683122, 1.000000000000000000, 0.9659258262890683122, 1.000000000000000000, 0.9659258262890683122, 1.000000000000000000, 0.9659258262890683122, 1.000000000000000000, 0.9659258262890683122, 1.000000000000000000, 0.9659258262890683122, 1.000000000000000000, 0.9659258262890683122, 1.000000000000000000, 0.9659258262890683122, 1.000000000000000000, 0.9659258262890683122, 1.000000000000000000, 0.9659258262890683122, 1.000000000000000000, 0.9659258262890683122, 1.000000000000000000, 0.9659258262890683122, 1.000000000000000000, 0.9659258262890683122, 1.000000000000000000, 0.9659258262890683122, 1.000000000000000000, 0.9659258262890683122, 1.000000000000000000, 0.9659258262890683122, 1.000000000000000000, 0.9659258262890683122, 1.000000000000000000, 0.9659258262890683122, 1.000000000000000000, 0.9659258262890683122, 1.000000000000000000, 0.9659258262890683122, 1.000000000000000000, 0.9659258262890683122, 1.000000000000000000, 0.9659258262890683122, 1.000000000000000000, 0.9659258262890683122, 1.000000000000000000, 0.9659258262890683122, 1.000000000000000000, 0.9659258262890683122, 1.000000000000000000, 0.9659258262890683122, 1.000000000000000000, 0.9659258262890683122, 1.000000000000000000, 0.9659258262890683122, 1.000000000000000000, 0.9659258262890683122, 1.000000000000000000, 0.9659258262890683122, 1.000000000000000000, 0.9659258262890683122, 1.000000000000000000, 0.9659258262890683122, 1.000000000000000000, 0.9659258262890683122, 1.000000000000000000, 0.9659258262890683122, 1.000000000000000000, 0.9659258262890683122, 1.000000000000000000, 0.9659258262890683122, 1.000000000000000000, 0.9659258262890683122, 1.000000000000000000, 0.9659258262890683122, 1.000000000000000000, 0.9659258262890683122, 1.000000000000000000, 0.9659258262890683122, 1.000000000000000000, 0.9659258262890683122, 1.000000000000000000, 0.9659258262890683122, 1.000000000000000000, 0.9659258262890683122, 1.000000000000000000, 0.9659258262890683122, 1.000000000000000000, 0.9659258262890683122, 1.000000000000000000, 0.9659258262890683122, 1.000000000000000000, 0.9659258262890683122, 1.000000000000000000, 0.9659258262890683122, 1.000000000000000000, 0.9659258262890683122, 1.000000000000000000, 0.9659258262890683122, 1.000000000000000000, 0.9659258262890683122, 1.000000000000000000, 0.9659258262890683122, 1.000000000000000000, 0.9659258262890683122, 1.000000000000000000, 0.9659258262890683122, 1.000000000000000000, 0.9659258262890683122, 1.000000000000000000, 0.9659258262890683122, 1.000000000000000000, 0.9659258262890683122, 1.000000000000000000, 0.9659258262890683122, 1.000000000000000000, 0.9659258262890683122, 1.000000000000000000, 0.9659258262890683122, 1.000000000000000000, 0.9659258262890683122, 1.000000000000000000, 0.9659258262890683122, 1.000000000000000000, 0.9659258262890683122, 1.000000000000000000, 0.9659258262890683122, 1.000000000000000000, 0.9659258262890683122, 1.000000000000000000, 0.9659258262890683122, 1.000000000000000000, 0.9659258262890683122, 1.000000000000000000, 0.9659258262890683122, 1.000000000000000000, 0.9659258262890683122, 1.000000000000000000, 0.9659258262890683122, 1.000000000000000000),
 ( 0.3333333333333333703, 0.3219752754296894559, 0.3333333333333333703, 0.3219752754296894559, 0.3333333333333333703, 0.3219752754296894559, 0.3333333333333333703, 0.3219752754296894559, 0.3333333333333333703, 0.3219752754296894559, 0.3333333333333333703, 0.3219752754296894559, 0.3333333333333333703, 0.3219752754296894559, 0.3333333333333333703, 0.3219752754296894559, 0.3333333333333333703, 0.3219752754296894559, 0.3333333333333333703, 0.3219752754296894559, 0.3333333333333333703, 0.3219752754296894559, 0.3333333333333333703, 0.3219752754296894559, 0.3333333333333333703, 0.3219752754296894559, 0.3333333333333333703, 0.3219752754296894559, 0.3333333333333333703, 0.3219752754296894559, 0.3333333333333333703, 0.3219752754296894559, 0.3333333333333333703, 0.3219752754296894559, 0.3333333333333333703, 0.3219752754296894559, 0.3333333333333333703, 0.3219752754296894559, 0.3333333333333333703, 0.3219752754296894559, 0.3333333333333333703, 0.3219752754296894559, 0.3333333333333333703, 0.3219752754296894559, 0.3333333333333333703, 0.3219752754296894559, 0.3333333333333333703, 0.3219752754296894559, 0.3333333333333333703, 0.3219752754296894559, 0.3333333333333333703, 0.3219752754296894559, 0.3333333333333333703, 0.3219752754296894559, 0.3333333333333333703, 0.3219752754296894559, 0.3333333333333333703, 0.3219752754296894559, 0.3333333333333333703, 0.3219752754296894559, 0.3333333333333333703, 0.3219752754296894559, 0.3333333333333333703, 0.3219752754296894559, 0.3333333333333333703, 0.3219752754296894559, 0.3333333333333333703, 0.3219752754296894559, 0.3333333333333333703, 0.3219752754296894559, 0.3333333333333333703, 0.3219752754296894559, 0.3333333333333333703, 0.3219752754296894559, 0.3333333333333333703, 0.3219752754296894559, 0.3333333333333333703, 0.3219752754296894559, 0.3333333333333333703, 0.3219752754296894559, 0.3333333333333333703, 0.3219752754296894559, 0.3333333333333333703, 0.3219752754296894559, 0.3333333333333333703, 0.3219752754296894559, 0.3333333333333333703, 0.3219752754296894559, 0.3333333333333333703, 0.3219752754296894559, 0.3333333333333333703, 0.3219752754296894559, 0.3333333333333333703, 0.3219752754296894559, 0.3333333333333333703, 0.3219752754296894559, 0.3333333333333333703, 0.3219752754296894559, 0.3333333333333333703, 0.3219752754296894559, 0.3333333333333333703, 0.3219752754296894559, 0.3333333333333333703, 0.3219752754296894559, 0.3333333333333333703, 0.3219752754296894559, 0.3333333333333333703, 0.3219752754296894559, 0.3333333333333333703, 0.3219752754296894559, 0.3333333333333333703, 0.3219752754296894559, 0.3333333333333333703, 0.3219752754296894559, 0.3333333333333333703, 0.3219752754296894559, 0.3333333333333333703, 0.3219752754296894559, 0.3333333333333333703, 0.3219752754296894559, 0.3333333333333333703, 0.3219752754296894559, 0.3333333333333333703, 0.3219752754296894559, 0.3333333333333333703, 0.3219752754296894559, 0.3333333333333333703, 0.3219752754296894559, 0.3333333333333333703, 0.3219752754296894559, 0.3333333333333333703, 0.3219752754296894559, 0.3333333333333333703, 0.3219752754296894559, 0.3333333333333333703, 0.3219752754296894559, 0.3333333333333333703, 0.3219752754296894559, 0.3333333333333333703, 0.3219752754296894559, 0.3333333333333333703, 0.3219752754296894559, 0.3333333333333333703, 0.3219752754296894559, 0.3333333333333333703, 0.3219752754296894559, 0.3333333333333333703, 0.3219752754296894559, 0.3333333333333333703, 0.3219752754296894559, 0.3333333333333333703, 0.3219752754296894559, 0.3333333333333333703, 0.3219752754296894559, 0.3333333333333333703, 0.3219752754296894559, 0.3333333333333333703, 0.3219752754296894559, 0.3333333333333333703, 0.3219752754296894559, 0.3333333333333333703, 0.3219752754296894559, 0.3333333333333333703, 0.3219752754296894559, 0.3333333333333333703, 0.3219752754296894559, 0.3333333333333333703, 0.3219752754296894559, 0.3333333333333333703, 0.3219752754296894559, 0.3333333333333333703, 0.3219752754296894559, 0.3333333333333333703, 0.3219752754296894559, 0.3333333333333333703, 0.3219752754296894559, 0.3333333333333333703, 0.3219752754296894559, 0.3333333333333333703, 0.3219752754296894559, 0.3333333333333333703, 0.3219752754296894559, 0.3333333333333333703, 0.3219752754296894559, 0.3333333333333333703, 0.3219752754296894559, 0.3333333333333333703, 0.3219752754296894559, 0.3333333333333333703, 0.3219752754296894559, 0.3333333333333333703, 0.3219752754296894559, 0.3333333333333333703, 0.3219752754296894559, 0.3333333333333333703, 0.3219752754296894559, 0.3333333333333333703, 0.3219752754296894559, 0.3333333333333333703, 0.3219752754296894559, 0.3333333333333333703, 0.3219752754296894559, 0.3333333333333333703, 0.3219752754296894559, 0.3333333333333333703, 0.3219752754296894559, 0.3333333333333333703, 0.3219752754296894559, 0.3333333333333333703, 0.3219752754296894559, 0.3333333333333333703, 0.3219752754296894559, 0.3333333333333333703, 0.3219752754296894559, 0.3333333333333333703, 0.3219752754296894559, 0.3333333333333333703, 0.3219752754296894559, 0.3333333333333333703, 0.3219752754296894559, 0.3333333333333333703, 0.3219752754296894559, 0.3333333333333333703, 0.3219752754296894559, 0.3333333333333333703, 0.3219752754296894559, 0.3333333333333333703, 0.3219752754296894559, 0.3333333333333333703, 0.3219752754296894559, 0.3333333333333333703, 0.3219752754296894559, 0.3333333333333333703, 0.3219752754296894559, 0.3333333333333333703, 0.3219752754296894559, 0.3333333333333333703, 0.3219752754296894559, 0.3333333333333333703, 0.3219752754296894559, 0.3333333333333333703, 0.3219752754296894559, 0.3333333333333333703, 0.3219752754296894559, 0.3333333333333333703, 0.3219752754296894559, 0.3333333333333333703, 0.3219752754296894559, 0.3333333333333333703, 0.3219752754296894559, 0.3333333333333333703, 0.3219752754296894559, 0.3333333333333333703, 0.3219752754296894559, 0.3333333333333333703, 0.3219752754296894559, 0.3333333333333333703, 0.3219752754296894559, 0.3333333333333333703, 0.3219752754296894559, 0.3333333333333333703, 0.3219752754296894559, 0.3333333333333333703, 0.3219752754296894559, 0.3333333333333333703, 0.3219752754296894559, 0.3333333333333333703, 0.3219752754296894559, 0.3333333333333333703, 0.3219752754296894559, 0.3333333333333333703, 0.3219752754296894559, 0.3333333333333333703, 0.3219752754296894559, 0.3333333333333333703, 0.3219752754296894559, 0.3333333333333333703, 0.3219752754296894559, 0.3333333333333333703, 0.3219752754296894559, 0.3333333333333333703, 0.3219752754296894559, 0.3333333333333333703, 0.3219752754296894559, 0.3333333333333333703, 0.3219752754296894559, 0.3333333333333333703, 0.3219752754296894559, 0.3333333333333333703, 0.3219752754296894559, 0.3333333333333333703, 0.3219752754296894559, 0.3333333333333333703, 0.3219752754296894559, 0.3333333333333333703, 0.3219752754296894559, 0.3333333333333333703, 0.3219752754296894559, 0.3333333333333333703, 0.3219752754296894559, 0.3333333333333333703, 0.3219752754296894559, 0.3333333333333333703, 0.3219752754296894559, 0.3333333333333333703, 0.3219752754296894559, 0.3333333333333333703, 0.3219752754296894559, 0.3333333333333333703, 0.3219752754296894559, 0.3333333333333333703, 0.3219752754296894559, 0.3333333333333333703, 0.3219752754296894559, 0.3333333333333333703, 0.3219752754296894559, 0.3333333333333333703, 0.3219752754296894559, 0.3333333333333333703, 0.3219752754296894559, 0.3333333333333333703, 0.3219752754296894559, 0.3333333333333333703, 0.3219752754296894559, 0.3333333333333333703, 0.3219752754296894559, 0.3333333333333333703, 0.3219752754296894559, 0.3333333333333333703, 0.3219752754296894559, 0.3333333333333333703, 0.3219752754296894559, 0.3333333333333333703, 0.3219752754296894559, 0.3333333333333333703, 0.3219752754296894559, 0.3333333333333333703, 0.3219752754296894559, 0.3333333333333333703, 0.3219752754296894559, 0.3333333333333333703, 0.3219752754296894559, 0.3333333333333333703, 0.3219752754296894559, 0.3333333333333333703, 0.3219752754296894559, 0.3333333333333333703, 0.3219752754296894559, 0.3333333333333333703, 0.3219752754296894559, 0.3333333333333333703, 0.3219752754296894559, 0.3333333333333333703, 0.3219752754296894559, 0.3333333333333333703, 0.3219752754296894559, 0.3333333333333333703, 0.3219752754296894559, 0.3333333333333333703, 0.3219752754296894559, 0.3333333333333333703, 0.3219752754296894559, 0.3333333333333333703, 0.3219752754296894559, 0.3333333333333333703, 0.3219752754296894559, 0.3333333333333333703, 0.3219752754296894559, 0.3333333333333333703, 0.3219752754296894559, 0.3333333333333333703, 0.3219752754296894559, 0.3333333333333333703, 0.3219752754296894559, 0.3333333333333333703, 0.3219752754296894559, 0.3333333333333333703, 0.3219752754296894559, 0.3333333333333333703, 0.3219752754296894559, 0.3333333333333333703, 0.3219752754296894559, 0.3333333333333333703, 0.3219752754296894559, 0.3333333333333333703, 0.3219752754296894559, 0.3333333333333333703, 0.3219752754296894559, 0.3333333333333333703, 0.3219752754296894559, 0.3333333333333333703, 0.3219752754296894559, 0.3333333333333333703, 0.3219752754296894559, 0.3333333333333333703, 0.3219752754296894559, 0.3333333333333333703, 0.3219752754296894559, 0.3333333333333333703, 0.3219752754296894559, 0.3333333333333333703, 0.3219752754296894559, 0.3333333333333333703, 0.3219752754296894559, 0.3333333333333333703, 0.3219752754296894559, 0.3333333333333333703, 0.3219752754296894559, 0.3333333333333333703, 0.3219752754296894559, 0.3333333333333333703, 0.3219752754296894559, 0.3333333333333333703, 0.3219752754296894559, 0.3333333333333333703, 0.3219752754296894559, 0.3333333333333333703, 0.3219752754296894559, 0.3333333333333333703, 0.3219752754296894559, 0.3333333333333333703, 0.3219752754296894559, 0.3333333333333333703, 0.3219752754296894559, 0.3333333333333333703, 0.3219752754296894559, 0.3333333333333333703, 0.3219752754296894559, 0.3333333333333333703, 0.3219752754296894559, 0.3333333333333333703, 0.3219752754296894559, 0.3333333333333333703, 0.3219752754296894559, 0.3333333333333333703, 0.3219752754296894559, 0.3333333333333333703, 0.3219752754296894559, 0.3333333333333333703, 0.3219752754296894559, 0.3333333333333333703, 0.3219752754296894559, 0.3333333333333333703, 0.3219752754296894559, 0.3333333333333333703, 0.3219752754296894559, 0.3333333333333333703, 0.3219752754296894559, 0.3333333333333333703, 0.3219752754296894559, 0.3333333333333333703, 0.3219752754296894559, 0.3333333333333333703, 0.3219752754296894559, 0.3333333333333333703, 0.3219752754296894559, 0.3333333333333333703),
 ( 0.3333333333333333703, 0.3219752754296894559, 0.3333333333333333703, 0.3219752754296894559, 0.3333333333333333703, 0.3219752754296894559, 0.3333333333333333703, 0.3219752754296894559, 0.3333333333333333703, 0.3219752754296894559, 0.3333333333333333703, 0.3219752754296894559, 0.3333333333333333703, 0.3219752754296894559, 0.3333333333333333703, 0.3219752754296894559, 0.3333333333333333703, 0.3219752754296894559, 0.3333333333333333703, 0.3219752754296894559, 0.3333333333333333703, 0.3219752754296894559, 0.3333333333333333703, 0.3219752754296894559, 0.3333333333333333703, 0.3219752754296894559, 0.3333333333333333703, 0.3219752754296894559, 0.3333333333333333703, 0.3219752754296894559, 0.3333333333333333703, 0.3219752754296894559, 0.3333333333333333703, 0.3219752754296894559, 0.3333333333333333703, 0.3219752754296894559, 0.3333333333333333703, 0.3219752754296894559, 0.3333333333333333703, 0.3219752754296894559, 0.3333333333333333703, 0.3219752754296894559, 0.3333333333333333703, 0.3219752754296894559, 0.3333333333333333703, 0.3219752754296894559, 0.3333333333333333703, 0.3219752754296894559, 0.3333333333333333703, 0.3219752754296894559, 0.3333333333333333703, 0.3219752754296894559, 0.3333333333333333703, 0.3219752754296894559, 0.3333333333333333703, 0.3219752754296894559, 0.3333333333333333703, 0.3219752754296894559, 0.3333333333333333703, 0.3219752754296894559, 0.3333333333333333703, 0.3219752754296894559, 0.3333333333333333703, 0.3219752754296894559, 0.3333333333333333703, 0.3219752754296894559, 0.3333333333333333703, 0.3219752754296894559, 0.3333333333333333703, 0.3219752754296894559, 0.3333333333333333703, 0.3219752754296894559, 0.3333333333333333703, 0.3219752754296894559, 0.3333333333333333703, 0.3219752754296894559, 0.3333333333333333703, 0.3219752754296894559, 0.3333333333333333703, 0.3219752754296894559, 0.3333333333333333703, 0.3219752754296894559, 0.3333333333333333703, 0.3219752754296894559, 0.3333333333333333703, 0.3219752754296894559, 0.3333333333333333703, 0.3219752754296894559, 0.3333333333333333703, 0.3219752754296894559, 0.3333333333333333703, 0.3219752754296894559, 0.3333333333333333703, 0.3219752754296894559, 0.3333333333333333703, 0.3219752754296894559, 0.3333333333333333703, 0.3219752754296894559, 0.3333333333333333703, 0.3219752754296894559, 0.3333333333333333703, 0.3219752754296894559, 0.3333333333333333703, 0.3219752754296894559, 0.3333333333333333703, 0.3219752754296894559, 0.3333333333333333703, 0.3219752754296894559, 0.3333333333333333703, 0.3219752754296894559, 0.3333333333333333703, 0.3219752754296894559, 0.3333333333333333703, 0.3219752754296894559, 0.3333333333333333703, 0.3219752754296894559, 0.3333333333333333703, 0.3219752754296894559, 0.3333333333333333703, 0.3219752754296894559, 0.3333333333333333703, 0.3219752754296894559, 0.3333333333333333703, 0.3219752754296894559, 0.3333333333333333703, 0.3219752754296894559, 0.3333333333333333703, 0.3219752754296894559, 0.3333333333333333703, 0.3219752754296894559, 0.3333333333333333703, 0.3219752754296894559, 0.3333333333333333703, 0.3219752754296894559, 0.3333333333333333703, 0.3219752754296894559, 0.3333333333333333703, 0.3219752754296894559, 0.3333333333333333703, 0.3219752754296894559, 0.3333333333333333703, 0.3219752754296894559, 0.3333333333333333703, 0.3219752754296894559, 0.3333333333333333703, 0.3219752754296894559, 0.3333333333333333703, 0.3219752754296894559, 0.3333333333333333703, 0.3219752754296894559, 0.3333333333333333703, 0.3219752754296894559, 0.3333333333333333703, 0.3219752754296894559, 0.3333333333333333703, 0.3219752754296894559, 0.3333333333333333703, 0.3219752754296894559, 0.3333333333333333703, 0.3219752754296894559, 0.3333333333333333703, 0.3219752754296894559, 0.3333333333333333703, 0.3219752754296894559, 0.3333333333333333703, 0.3219752754296894559, 0.3333333333333333703, 0.3219752754296894559, 0.3333333333333333703, 0.3219752754296894559, 0.3333333333333333703, 0.3219752754296894559, 0.3333333333333333703, 0.3219752754296894559, 0.3333333333333333703, 0.3219752754296894559, 0.3333333333333333703, 0.3219752754296894559, 0.3333333333333333703, 0.3219752754296894559, 0.3333333333333333703, 0.3219752754296894559, 0.3333333333333333703, 0.3219752754296894559, 0.3333333333333333703, 0.3219752754296894559, 0.3333333333333333703, 0.3219752754296894559, 0.3333333333333333703, 0.3219752754296894559, 0.3333333333333333703, 0.3219752754296894559, 0.3333333333333333703, 0.3219752754296894559, 0.3333333333333333703, 0.3219752754296894559, 0.3333333333333333703, 0.3219752754296894559, 0.3333333333333333703, 0.3219752754296894559, 0.3333333333333333703, 0.3219752754296894559, 0.3333333333333333703, 0.3219752754296894559, 0.3333333333333333703, 0.3219752754296894559, 0.3333333333333333703, 0.3219752754296894559, 0.3333333333333333703, 0.3219752754296894559, 0.3333333333333333703, 0.3219752754296894559, 0.3333333333333333703, 0.3219752754296894559, 0.3333333333333333703, 0.3219752754296894559, 0.3333333333333333703, 0.3219752754296894559, 0.3333333333333333703, 0.3219752754296894559, 0.3333333333333333703, 0.3219752754296894559, 0.3333333333333333703, 0.3219752754296894559, 0.3333333333333333703, 0.3219752754296894559, 0.3333333333333333703, 0.3219752754296894559, 0.3333333333333333703, 0.3219752754296894559, 0.3333333333333333703, 0.3219752754296894559, 0.3333333333333333703, 0.3219752754296894559, 0.3333333333333333703, 0.3219752754296894559, 0.3333333333333333703, 0.3219752754296894559, 0.3333333333333333703, 0.3219752754296894559, 0.3333333333333333703, 0.3219752754296894559, 0.3333333333333333703, 0.3219752754296894559, 0.3333333333333333703, 0.3219752754296894559, 0.3333333333333333703, 0.3219752754296894559, 0.3333333333333333703, 0.3219752754296894559, 0.3333333333333333703, 0.3219752754296894559, 0.3333333333333333703, 0.3219752754296894559, 0.3333333333333333703, 0.3219752754296894559, 0.3333333333333333703, 0.3219752754296894559, 0.3333333333333333703, 0.3219752754296894559, 0.3333333333333333703, 0.3219752754296894559, 0.3333333333333333703, 0.3219752754296894559, 0.3333333333333333703, 0.3219752754296894559, 0.3333333333333333703, 0.3219752754296894559, 0.3333333333333333703, 0.3219752754296894559, 0.3333333333333333703, 0.3219752754296894559, 0.3333333333333333703, 0.3219752754296894559, 0.3333333333333333703, 0.3219752754296894559, 0.3333333333333333703, 0.3219752754296894559, 0.3333333333333333703, 0.3219752754296894559, 0.3333333333333333703, 0.3219752754296894559, 0.3333333333333333703, 0.3219752754296894559, 0.3333333333333333703, 0.3219752754296894559, 0.3333333333333333703, 0.3219752754296894559, 0.3333333333333333703, 0.3219752754296894559, 0.3333333333333333703, 0.3219752754296894559, 0.3333333333333333703, 0.3219752754296894559, 0.3333333333333333703, 0.3219752754296894559, 0.3333333333333333703, 0.3219752754296894559, 0.3333333333333333703, 0.3219752754296894559, 0.3333333333333333703, 0.3219752754296894559, 0.3333333333333333703, 0.3219752754296894559, 0.3333333333333333703, 0.3219752754296894559, 0.3333333333333333703, 0.3219752754296894559, 0.3333333333333333703, 0.3219752754296894559, 0.3333333333333333703, 0.3219752754296894559, 0.3333333333333333703, 0.3219752754296894559, 0.3333333333333333703, 0.3219752754296894559, 0.3333333333333333703, 0.3219752754296894559, 0.3333333333333333703, 0.3219752754296894559, 0.3333333333333333703, 0.3219752754296894559, 0.3333333333333333703, 0.3219752754296894559, 0.3333333333333333703, 0.3219752754296894559, 0.3333333333333333703, 0.3219752754296894559, 0.3333333333333333703, 0.3219752754296894559, 0.3333333333333333703, 0.3219752754296894559, 0.3333333333333333703, 0.3219752754296894559, 0.3333333333333333703, 0.3219752754296894559, 0.3333333333333333703, 0.3219752754296894559, 0.3333333333333333703, 0.3219752754296894559, 0.3333333333333333703, 0.3219752754296894559, 0.3333333333333333703, 0.3219752754296894559, 0.3333333333333333703, 0.3219752754296894559, 0.3333333333333333703, 0.3219752754296894559, 0.3333333333333333703, 0.3219752754296894559, 0.3333333333333333703, 0.3219752754296894559, 0.3333333333333333703, 0.3219752754296894559, 0.3333333333333333703, 0.3219752754296894559, 0.3333333333333333703, 0.3219752754296894559, 0.3333333333333333703, 0.3219752754296894559, 0.3333333333333333703, 0.3219752754296894559, 0.3333333333333333703, 0.3219752754296894559, 0.3333333333333333703, 0.3219752754296894559, 0.3333333333333333703, 0.3219752754296894559, 0.3333333333333333703, 0.3219752754296894559, 0.3333333333333333703, 0.3219752754296894559, 0.3333333333333333703, 0.3219752754296894559, 0.3333333333333333703, 0.3219752754296894559, 0.3333333333333333703, 0.3219752754296894559, 0.3333333333333333703, 0.3219752754296894559, 0.3333333333333333703, 0.3219752754296894559, 0.3333333333333333703, 0.3219752754296894559, 0.3333333333333333703, 0.3219752754296894559, 0.3333333333333333703, 0.3219752754296894559, 0.3333333333333333703, 0.3219752754296894559, 0.3333333333333333703, 0.3219752754296894559, 0.3333333333333333703, 0.3219752754296894559, 0.3333333333333333703, 0.3219752754296894559, 0.3333333333333333703, 0.3219752754296894559, 0.3333333333333333703, 0.3219752754296894559, 0.3333333333333333703, 0.3219752754296894559, 0.3333333333333333703, 0.3219752754296894559, 0.3333333333333333703, 0.3219752754296894559, 0.3333333333333333703, 0.3219752754296894559, 0.3333333333333333703, 0.3219752754296894559, 0.3333333333333333703, 0.3219752754296894559, 0.3333333333333333703, 0.3219752754296894559, 0.3333333333333333703, 0.3219752754296894559, 0.3333333333333333703, 0.3219752754296894559, 0.3333333333333333703, 0.3219752754296894559, 0.3333333333333333703, 0.3219752754296894559, 0.3333333333333333703, 0.3219752754296894559, 0.3333333333333333703, 0.3219752754296894559, 0.3333333333333333703, 0.3219752754296894559, 0.3333333333333333703, 0.3219752754296894559, 0.3333333333333333703, 0.3219752754296894559, 0.3333333333333333703, 0.3219752754296894559, 0.3333333333333333703, 0.3219752754296894559, 0.3333333333333333703, 0.3219752754296894559, 0.3333333333333333703, 0.3219752754296894559, 0.3333333333333333703, 0.3219752754296894559, 0.3333333333333333703, 0.3219752754296894559, 0.3333333333333333703, 0.3219752754296894559, 0.3333333333333333703, 0.3219752754296894559, 0.3333333333333333703, 0.3219752754296894559, 0.3333333333333333703, 0.3219752754296894559, 0.3333333333333333703, 0.3219752754296894559, 0.3333333333333333703, 0.3219752754296894559, 0.3333333333333333703),
 ( 1.000000000000000000, 0.9659258262890683122, 1.000000000000000000, 0.9659258262890683122, 1.000000000000000000, 0.9659258262890683122, 1.000000000000000000, 0.9659258262890683122, 1.000000000000000000, 0.9659258262890683122, 1.000000000000000000, 0.9659258262890683122, 1.000000000000000000, 0.9659258262890683122, 1.000000000000000000, 0.9659258262890683122, 1.000000000000000000, 0.9659258262890683122, 1.000000000000000000, 0.9659258262890683122, 1.000000000000000000, 0.9659258262890683122, 1.000000000000000000, 0.9659258262890683122, 1.000000000000000000, 0.9659258262890683122, 1.000000000000000000, 0.9659258262890683122, 1.000000000000000000, 0.9659258262890683122, 1.000000000000000000, 0.9659258262890683122, 1.000000000000000000, 0.9659258262890683122, 1.000000000000000000, 0.9659258262890683122, 1.000000000000000000, 0.9659258262890683122, 1.000000000000000000, 0.9659258262890683122, 1.000000000000000000, 0.9659258262890683122, 1.000000000000000000, 0.9659258262890683122, 1.000000000000000000, 0.9659258262890683122, 1.000000000000000000, 0.9659258262890683122, 1.000000000000000000, 0.9659258262890683122, 1.000000000000000000, 0.9659258262890683122, 1.000000000000000000, 0.9659258262890683122, 1.000000000000000000, 0.9659258262890683122, 1.000000000000000000, 0.9659258262890683122, 1.000000000000000000, 0.9659258262890683122, 1.000000000000000000, 0.9659258262890683122, 1.000000000000000000, 0.9659258262890683122, 1.000000000000000000, 0.9659258262890683122, 1.000000000000000000, 0.9659258262890683122, 1.000000000000000000, 0.9659258262890683122, 1.000000000000000000, 0.9659258262890683122, 1.000000000000000000, 0.9659258262890683122, 1.000000000000000000, 0.9659258262890683122, 1.000000000000000000, 0.9659258262890683122, 1.000000000000000000, 0.9659258262890683122, 1.000000000000000000, 0.9659258262890683122, 1.000000000000000000, 0.9659258262890683122, 1.000000000000000000, 0.9659258262890683122, 1.000000000000000000, 0.9659258262890683122, 1.000000000000000000, 0.9659258262890683122, 1.000000000000000000, 0.9659258262890683122, 1.000000000000000000, 0.9659258262890683122, 1.000000000000000000, 0.9659258262890683122, 1.000000000000000000, 0.9659258262890683122, 1.000000000000000000, 0.9659258262890683122, 1.000000000000000000, 0.9659258262890683122, 1.000000000000000000, 0.9659258262890683122, 1.000000000000000000, 0.9659258262890683122, 1.000000000000000000, 0.9659258262890683122, 1.000000000000000000, 0.9659258262890683122, 1.000000000000000000, 0.9659258262890683122, 1.000000000000000000, 0.9659258262890683122, 1.000000000000000000, 0.9659258262890683122, 1.000000000000000000, 0.9659258262890683122, 1.000000000000000000, 0.9659258262890683122, 1.000000000000000000, 0.9659258262890683122, 1.000000000000000000, 0.9659258262890683122, 1.000000000000000000, 0.9659258262890683122, 1.000000000000000000, 0.9659258262890683122, 1.000000000000000000, 0.9659258262890683122, 1.000000000000000000, 0.9659258262890683122, 1.000000000000000000, 0.9659258262890683122, 1.000000000000000000, 0.9659258262890683122, 1.000000000000000000, 0.9659258262890683122, 1.000000000000000000, 0.9659258262890683122, 1.000000000000000000, 0.9659258262890683122, 1.000000000000000000, 0.9659258262890683122, 1.000000000000000000, 0.9659258262890683122, 1.000000000000000000, 0.9659258262890683122, 1.000000000000000000, 0.9659258262890683122, 1.000000000000000000, 0.9659258262890683122, 1.000000000000000000, 0.9659258262890683122, 1.000000000000000000, 0.9659258262890683122, 1.000000000000000000, 0.9659258262890683122, 1.000000000000000000, 0.9659258262890683122, 1.000000000000000000, 0.9659258262890683122, 1.000000000000000000, 0.9659258262890683122, 1.000000000000000000, 0.9659258262890683122, 1.000000000000000000, 0.9659258262890683122, 1.000000000000000000, 0.9659258262890683122, 1.000000000000000000, 0.9659258262890683122, 1.000000000000000000, 0.9659258262890683122, 1.000000000000000000, 0.9659258262890683122, 1.000000000000000000, 0.9659258262890683122, 1.000000000000000000, 0.9659258262890683122, 1.000000000000000000, 0.9659258262890683122, 1.000000000000000000, 0.9659258262890683122, 1.000000000000000000, 0.9659258262890683122, 1.000000000000000000, 0.9659258262890683122, 1.000000000000000000, 0.9659258262890683122, 1.000000000000000000, 0.9659258262890683122, 1.000000000000000000, 0.9659258262890683122, 1.000000000000000000, 0.9659258262890683122, 1.000000000000000000, 0.9659258262890683122, 1.000000000000000000, 0.9659258262890683122, 1.000000000000000000, 0.9659258262890683122, 1.000000000000000000, 0.9659258262890683122, 1.000000000000000000, 0.9659258262890683122, 1.000000000000000000, 0.9659258262890683122, 1.000000000000000000, 0.9659258262890683122, 1.000000000000000000, 0.9659258262890683122, 1.000000000000000000, 0.9659258262890683122, 1.000000000000000000, 0.9659258262890683122, 1.000000000000000000, 0.9659258262890683122, 1.000000000000000000, 0.9659258262890683122, 1.000000000000000000, 0.9659258262890683122, 1.000000000000000000, 0.9659258262890683122, 1.000000000000000000, 0.9659258262890683122, 1.000000000000000000, 0.9659258262890683122, 1.000000000000000000, 0.9659258262890683122, 1.000000000000000000, 0.9659258262890683122, 1.000000000000000000, 0.9659258262890683122, 1.000000000000000000, 0.9659258262890683122, 1.000000000000000000, 0.9659258262890683122, 1.000000000000000000, 0.9659258262890683122, 1.000000000000000000, 0.9659258262890683122, 1.000000000000000000, 0.9659258262890683122, 1.000000000000000000, 0.9659258262890683122, 1.000000000000000000, 0.9659258262890683122, 1.000000000000000000, 0.9659258262890683122, 1.000000000000000000, 0.9659258262890683122, 1.000000000000000000, 0.9659258262890683122, 1.000000000000000000, 0.9659258262890683122, 1.000000000000000000, 0.9659258262890683122, 1.000000000000000000, 0.9659258262890683122, 1.000000000000000000, 0.9659258262890683122, 1.000000000000000000, 0.9659258262890683122, 1.000000000000000000, 0.9659258262890683122, 1.000000000000000000, 0.9659258262890683122, 1.000000000000000000, 0.9659258262890683122, 1.000000000000000000, 0.9659258262890683122, 1.000000000000000000, 0.9659258262890683122, 1.000000000000000000, 0.9659258262890683122, 1.000000000000000000, 0.9659258262890683122, 1.000000000000000000, 0.9659258262890683122, 1.000000000000000000, 0.9659258262890683122, 1.000000000000000000, 0.9659258262890683122, 1.000000000000000000, 0.9659258262890683122, 1.000000000000000000, 0.9659258262890683122, 1.000000000000000000, 0.9659258262890683122, 1.000000000000000000, 0.9659258262890683122, 1.000000000000000000, 0.9659258262890683122, 1.000000000000000000, 0.9659258262890683122, 1.000000000000000000, 0.9659258262890683122, 1.000000000000000000, 0.9659258262890683122, 1.000000000000000000, 0.9659258262890683122, 1.000000000000000000, 0.9659258262890683122, 1.000000000000000000, 0.9659258262890683122, 1.000000000000000000, 0.9659258262890683122, 1.000000000000000000, 0.9659258262890683122, 1.000000000000000000, 0.9659258262890683122, 1.000000000000000000, 0.9659258262890683122, 1.000000000000000000, 0.9659258262890683122, 1.000000000000000000, 0.9659258262890683122, 1.000000000000000000, 0.9659258262890683122, 1.000000000000000000, 0.9659258262890683122, 1.000000000000000000, 0.9659258262890683122, 1.000000000000000000, 0.9659258262890683122, 1.000000000000000000, 0.9659258262890683122, 1.000000000000000000, 0.9659258262890683122, 1.000000000000000000, 0.9659258262890683122, 1.000000000000000000, 0.9659258262890683122, 1.000000000000000000, 0.9659258262890683122, 1.000000000000000000, 0.9659258262890683122, 1.000000000000000000, 0.9659258262890683122, 1.000000000000000000, 0.9659258262890683122, 1.000000000000000000, 0.9659258262890683122, 1.000000000000000000, 0.9659258262890683122, 1.000000000000000000, 0.9659258262890683122, 1.000000000000000000, 0.9659258262890683122, 1.000000000000000000, 0.9659258262890683122, 1.000000000000000000, 0.9659258262890683122, 1.000000000000000000, 0.9659258262890683122, 1.000000000000000000, 0.9659258262890683122, 1.000000000000000000, 0.9659258262890683122, 1.000000000000000000, 0.9659258262890683122, 1.000000000000000000, 0.9659258262890683122, 1.000000000000000000, 0.9659258262890683122, 1.000000000000000000, 0.9659258262890683122, 1.000000000000000000, 0.9659258262890683122, 1.000000000000000000, 0.9659258262890683122, 1.000000000000000000, 0.9659258262890683122, 1.000000000000000000, 0.9659258262890683122, 1.000000000000000000, 0.9659258262890683122, 1.000000000000000000, 0.9659258262890683122, 1.000000000000000000, 0.9659258262890683122, 1.000000000000000000, 0.9659258262890683122, 1.000000000000000000, 0.9659258262890683122, 1.000000000000000000, 0.9659258262890683122, 1.000000000000000000, 0.9659258262890683122, 1.000000000000000000, 0.9659258262890683122, 1.000000000000000000, 0.9659258262890683122, 1.000000000000000000, 0.9659258262890683122, 1.000000000000000000, 0.9659258262890683122, 1.000000000000000000, 0.9659258262890683122, 1.000000000000000000, 0.9659258262890683122, 1.000000000000000000, 0.9659258262890683122, 1.000000000000000000, 0.9659258262890683122, 1.000000000000000000, 0.9659258262890683122, 1.000000000000000000, 0.9659258262890683122, 1.000000000000000000, 0.9659258262890683122, 1.000000000000000000, 0.9659258262890683122, 1.000000000000000000, 0.9659258262890683122, 1.000000000000000000, 0.9659258262890683122, 1.000000000000000000, 0.9659258262890683122, 1.000000000000000000, 0.9659258262890683122, 1.000000000000000000, 0.9659258262890683122, 1.000000000000000000, 0.9659258262890683122, 1.000000000000000000, 0.9659258262890683122, 1.000000000000000000, 0.9659258262890683122, 1.000000000000000000, 0.9659258262890683122, 1.000000000000000000, 0.9659258262890683122, 1.000000000000000000, 0.9659258262890683122, 1.000000000000000000, 0.9659258262890683122, 1.000000000000000000, 0.9659258262890683122, 1.000000000000000000, 0.9659258262890683122, 1.000000000000000000, 0.9659258262890683122, 1.000000000000000000, 0.9659258262890683122, 1.000000000000000000, 0.9659258262890683122, 1.000000000000000000, 0.9659258262890683122, 1.000000000000000000, 0.9659258262890683122, 1.000000000000000000, 0.9659258262890683122, 1.000000000000000000, 0.9659258262890683122, 1.000000000000000000) ) ) 
 REPRESENTATION_ITEM ( '' )  SURFACE ( )  );
#87143 = CARTESIAN_POINT ( 'NONE',  ( -9.474510206698720793, -16.51473224551083518, 34.58442372801899722 ) ) ;
#87144 = CARTESIAN_POINT ( 'NONE',  ( 10.81492255796106328, -18.62759615963255655, 25.41775706135235779 ) ) ;
#87145 = CARTESIAN_POINT ( 'NONE',  ( 13.97604488694527802, 13.89961937509977652, 74.37390960531436690 ) ) ;
#87146 = CARTESIAN_POINT ( 'NONE',  ( -0.05219959533910754901, -16.53943276465976808, 82.49890960531436690 ) ) ;
#87147 = CARTESIAN_POINT ( 'NONE',  ( -8.314922557960811034, -14.29746914071050412, 47.08224293864770260 ) ) ;
#87148 = CARTESIAN_POINT ( 'NONE',  ( -18.67979575497178146, -10.72451020669898902, 61.66557627198103120 ) ) ;
#87149 = CARTESIAN_POINT ( 'NONE',  ( -16.46253265017160317, 9.564922557960807481, 45.83224293864769550 ) ) ;
#87150 = CARTESIAN_POINT ( 'NONE',  ( -18.67979575497178146, -10.72451020669898902, 66.66557627198102409 ) ) ;
#87151 = CARTESIAN_POINT ( 'NONE',  ( 5.049401038297881783, 19.05341960407617563, 52.29275706135234003 ) ) ;
#87153 = CARTESIAN_POINT ( 'NONE',  ( 4.379528057220339221, -16.55341960407611168, 67.70724293864769550 ) ) ;
#87152 = CARTESIAN_POINT ( 'NONE',  ( 9.474510206698729675, 16.51473224551082808, 27.08442372801900433 ) ) ;
#87155 = AXIS2_PLACEMENT_3D ( 'NONE', #197996, #72669, #178854 ) ;
#87154 = CARTESIAN_POINT ( 'NONE',  ( 15.72974639402199770, -15.80617190586745480, 43.12390960531435269 ) ) ;
#87156 = ORIENTED_EDGE ( 'NONE', *, *, #32194, .T. ) ;
#87157 = CARTESIAN_POINT ( 'NONE',  ( 17.05587630539788080, 6.762274262135703928, 101.7581969096269177 ) ) ;
#87159 = CARTESIAN_POINT ( 'NONE',  ( 8.571926809382603096, -26.38167802310801235, 141.9750000027312069 ) ) ;
#87158 = CARTESIAN_POINT ( 'NONE',  ( -14.34966873604972548, 8.224510206698743886, 88.33442372801901854 ) ) ;
#87160 = CARTESIAN_POINT ( 'NONE',  ( -19.05341960407617563, 5.049401038297882671, 88.54275706135230450 ) ) ;
#87161 = CARTESIAN_POINT ( 'NONE',  ( -12.06949235617756955, 12.14591786802309770, 55.62390960531436690 ) ) ;
#87162 = CARTESIAN_POINT ( 'NONE',  ( 16.31925111598461342, -7.325300261831395154, 52.66424538967255842 ) ) ;
#87163 = CARTESIAN_POINT ( 'NONE',  ( 16.46253265017160672, -9.564922557960803928, 53.33224293864768839 ) ) ;
#87164 = CARTESIAN_POINT ( 'NONE',  ( -0.05219959533910754901, -16.53943276465976808, 42.49890960531435979 ) ) ;
#87165 = EDGE_CURVE ( 'NONE', #167693, #174271, #96522, .T. ) ;
#87166 = CARTESIAN_POINT ( 'NONE',  ( 16.46253265017160672, -9.564922557960803928, 88.33224293864769550 ) ) ;
#87167 = CARTESIAN_POINT ( 'NONE',  ( 19.02544592524343514, -5.153800228976328945, 53.54057627198102409 ) ) ;
#87168 = CARTESIAN_POINT ( 'NONE',  ( 5.823673210054444382, -21.52544592524334988, 60.20942372801902565 ) ) ;
#87169 = CARTESIAN_POINT ( 'NONE',  ( 19.03943276465977164, -0.05219959533909143690, 73.74890960531435269 ) ) ;
#87170 = CARTESIAN_POINT ( 'NONE',  ( 19.05341960407611168, 5.049401038298154454, 28.95724293864769550 ) ) ;
#87171 = CARTESIAN_POINT ( 'NONE',  ( 16.51473224551069308, 9.474510206698969483, 74.16557627198103830 ) ) ;
#87172 = CARTESIAN_POINT ( 'NONE',  ( 15.80617190586746368, 15.72974639402197994, 44.37390960531435979 ) ) ;
#87173 = CARTESIAN_POINT ( 'NONE',  ( -13.89961937509977652, 13.97604488694528158, 30.62390960531435269 ) ) ;
#87174 = CARTESIAN_POINT ( 'NONE',  ( 0.05219959533907565091, 21.53943276465977519, 44.99890960531435979 ) ) ;
#87175 = CARTESIAN_POINT ( 'NONE',  ( 8.314922557961029526, -14.29746914071037800, 110.4177570613523756 ) ) ;
#87176 = CARTESIAN_POINT ( 'NONE',  ( 9.474510206698729675, 16.51473224551082808, 27.08442372801900433 ) ) ;
#87178 = CARTESIAN_POINT ( 'NONE',  ( -16.52544592524335698, -4.483927247898792601, 83.95942372801900433 ) ) ;
#87177 = CARTESIAN_POINT ( 'NONE',  ( 14.29746914071037800, 8.314922557961029526, 41.66775706135235424 ) ) ;
#87179 = CARTESIAN_POINT ( 'NONE',  ( -17.97058386085787163, -5.500000000000017764, 94.00390968646219392 ) ) ;
#87180 = CARTESIAN_POINT ( 'NONE',  ( 4.379528057220092307, 16.55341960407617563, 72.29275706135236135 ) ) ;
#87181 = CARTESIAN_POINT ( 'NONE',  ( -0.05219959533934338120, 16.53943276465976808, 57.50109039468568994 ) ) ;
#87182 = CARTESIAN_POINT ( 'NONE',  ( -16.46253265017160317, 9.564922557960807481, 110.8322429386476955 ) ) ;
#87183 = CARTESIAN_POINT ( 'NONE',  ( 19.02544592524343514, -5.153800228976328945, 33.54057627198102409 ) ) ;
#87184 = CARTESIAN_POINT ( 'NONE',  ( 16.52544592524335698, 4.483927247898782831, 41.45942372801901143 ) ) ;
#87185 = CARTESIAN_POINT ( 'NONE',  ( 19.05341960407611168, 5.049401038298154454, 48.95724293864768129 ) ) ;
#87186 = CARTESIAN_POINT ( 'NONE',  ( -21.55341960407619339, 5.719274019375674811, 23.54275706135235424 ) ) ;
#87187 = CARTESIAN_POINT ( 'NONE',  ( -8.314922557961024197, 14.29746914071037800, 37.91775706135235424 ) ) ;
#87188 = CARTESIAN_POINT ( 'NONE',  ( -14.29746914071037622, -8.314922557961029526, 94.16775706135237556 ) ) ;
#87189 = DIRECTION ( 'NONE',  ( 0.000000000000000000, -0.8164965809277233699, -0.5773502691896295058 ) ) ;
#87190 = CARTESIAN_POINT ( 'NONE',  ( 0.05219959533937995610, -21.53943276465977519, 100.0010903946857042 ) ) ;
#87191 = CARTESIAN_POINT ( 'NONE',  ( -19.05341960407617563, 5.049401038297882671, 103.5427570613523329 ) ) ;
#87192 = CARTESIAN_POINT ( 'NONE',  ( 9.564922557961047289, -16.46253265017146816, 50.41775706135233293 ) ) ;
#87193 = CARTESIAN_POINT ( 'NONE',  ( 4.379528057220339221, -16.55341960407611168, 52.70724293864769550 ) ) ;
#87194 = CARTESIAN_POINT ( 'NONE',  ( 16.51473224551069308, 9.474510206698969483, 24.16557627198102765 ) ) ;
#87196 = CARTESIAN_POINT ( 'NONE',  ( 17.40861289039003523, 6.110651285853276882, 78.87232470827434838 ) ) ;
#87195 = CARTESIAN_POINT ( 'NONE',  ( 19.05341960407617918, -5.049401038297876454, 56.04275706135234714 ) ) ;
#87197 = CARTESIAN_POINT ( 'NONE',  ( -21.52544592524334988, -5.823673210054445271, 68.95942372801901854 ) ) ;
#87198 = CARTESIAN_POINT ( 'NONE',  ( -4.379528057220086978, -16.55341960407618274, 29.79275706135234358 ) ) ;
#87199 = CARTESIAN_POINT ( 'NONE',  ( 19.36337904590692105, -5.499999999999940492, 57.91494137495621430 ) ) ;
#87200 = CARTESIAN_POINT ( 'NONE',  ( -19.03943276465977164, 0.05219959533909376836, 116.2489096053143669 ) ) ;
#87201 = CARTESIAN_POINT ( 'NONE',  ( -9.474510206698720793, -16.51473224551083518, 104.5844237280190043 ) ) ;
#87202 = CARTESIAN_POINT ( 'NONE',  ( 0.05219959533909260263, 19.03943276465977164, 109.9989096053143669 ) ) ;
#87203 = CARTESIAN_POINT ( 'NONE',  ( -24.54404792736085739, 12.06373989673656943, 169.8487138613016896 ) ) ;
#87204 = CARTESIAN_POINT ( 'NONE',  ( -19.02544592524342804, 5.153800228976336051, 31.04057627198102409 ) ) ;
#87205 = CARTESIAN_POINT ( 'NONE',  ( 18.62759615963255655, 10.81492255796105972, 106.6677570613523756 ) ) ;
#87206 = CARTESIAN_POINT ( 'NONE',  ( -0.05219959533909027116, -19.03943276465977164, 37.49890960531436690 ) ) ;
#87207 = CARTESIAN_POINT ( 'NONE',  ( 15.72974639402176855, 15.80617190586768217, 61.87609039468568284 ) ) ;
#87208 = CARTESIAN_POINT ( 'NONE',  ( -21.55341960407619339, 5.719274019375674811, 108.5427570613523756 ) ) ;
#87209 = CARTESIAN_POINT ( 'NONE',  ( 8.314922557961029526, -14.29746914071037800, 105.4177570613523613 ) ) ;
#87210 = CARTESIAN_POINT ( 'NONE',  ( 19.03943276465977164, -0.05219959533909143690, 78.74890960531436690 ) ) ;
#87211 = CARTESIAN_POINT ( 'NONE',  ( -18.62759615963255300, -10.81492255796106328, 54.16775706135235424 ) ) ;
#87212 = CARTESIAN_POINT ( 'NONE',  ( 15.72974639402176855, 15.80617190586768217, 46.87609039468568994 ) ) ;
#87214 = CARTESIAN_POINT ( 'NONE',  ( 13.89961937509977652, -13.97604488694527269, 108.1239096053143669 ) ) ;
#87213 = CARTESIAN_POINT ( 'NONE',  ( -5.153800228976607833, 19.02544592524334988, 82.70942372801897591 ) ) ;
#87215 = CARTESIAN_POINT ( 'NONE',  ( -12.06949235617756955, 12.14591786802309770, 115.6239096053143669 ) ) ;
#87216 = CARTESIAN_POINT ( 'NONE',  ( -18.67979575497178146, -10.72451020669898902, 91.66557627198103830 ) ) ;
#87217 = CARTESIAN_POINT ( 'NONE',  ( -9.474510206698720793, -16.51473224551083518, 19.58442372801899722 ) ) ;
#87218 = CARTESIAN_POINT ( 'NONE',  ( 4.379528057220339221, -16.55341960407611168, 102.7072429386476955 ) ) ;
#87219 = CARTESIAN_POINT ( 'NONE',  ( -9.474510206698964154, 16.51473224551069663, 55.41557627198103120 ) ) ;
#87220 = CARTESIAN_POINT ( 'NONE',  ( -5.153800228976607833, 19.02544592524334988, 92.70942372801901854 ) ) ;
#87221 = CARTESIAN_POINT ( 'NONE',  ( 0.05219959533910956823, 16.53943276465976808, 64.99890960531435269 ) ) ;
#87222 = CARTESIAN_POINT ( 'NONE',  ( -15.72974639402176322, -15.80617190586768395, 109.3760903946857042 ) ) ;
#87223 = CARTESIAN_POINT ( 'NONE',  ( -9.474510206698964154, 16.51473224551069663, 105.4155762719810383 ) ) ;
#87224 = CARTESIAN_POINT ( 'NONE',  ( -19.03943276465977164, -0.05219959533935918106, 78.75109039468567573 ) ) ;
#87225 = CARTESIAN_POINT ( 'NONE',  ( -5.823673210054116645, -21.52544592524344225, 77.29057627198102409 ) ) ;
#87226 = CARTESIAN_POINT ( 'NONE',  ( 21.52544592524334988, 5.823673210054432836, 31.45942372801901854 ) ) ;
#87227 = CARTESIAN_POINT ( 'NONE',  ( -8.224510206698735004, -14.34966873604973081, 24.58442372801901499 ) ) ;
#87228 = CARTESIAN_POINT ( 'NONE',  ( 4.379528057220092307, 16.55341960407617563, 92.29275706135236135 ) ) ;
#87230 = CARTESIAN_POINT ( 'NONE',  ( -18.62759615963255300, -10.81492255796106328, 39.16775706135235424 ) ) ;
#87229 = CARTESIAN_POINT ( 'NONE',  ( -12.14591786802326823, 12.06949235617739902, 48.12609039468568284 ) ) ;
#87231 = CARTESIAN_POINT ( 'NONE',  ( 21.52544592524344225, -5.823673210054117533, 38.54057627198103120 ) ) ;
#87232 = CARTESIAN_POINT ( 'NONE',  ( -19.05341960407611168, -5.049401038298163336, 31.45724293864769550 ) ) ;
#87233 = CARTESIAN_POINT ( 'NONE',  ( 37.99999999999999289, 2.893978650043524126E-14, -10.74999999453762811 ) ) ;
#87234 = CARTESIAN_POINT ( 'NONE',  ( 8.314922557961029526, -14.29746914071037800, 65.41775706135234714 ) ) ;
#87235 = CARTESIAN_POINT ( 'NONE',  ( 21.55341960407610458, 5.719274019375980345, 83.95724293864770971 ) ) ;
#87236 = CARTESIAN_POINT ( 'NONE',  ( -16.52544592524342804, 4.483927247898546575, 36.04057627198102409 ) ) ;
#87237 = CARTESIAN_POINT ( 'NONE',  ( -16.55341960407617563, 4.379528057220093196, 48.54275706135234714 ) ) ;
#87238 = CARTESIAN_POINT ( 'NONE',  ( -5.049401038298153566, 19.05341960407611168, 55.20724293864769550 ) ) ;
#87239 = CARTESIAN_POINT ( 'NONE',  ( -16.52544592524335698, -4.483927247898792601, 93.95942372801903275 ) ) ;
#87240 = CARTESIAN_POINT ( 'NONE',  ( -13.89961937509957401, -13.97604488694547875, 84.37609039468567573 ) ) ;
#87241 = CARTESIAN_POINT ( 'NONE',  ( 5.719274019375991003, -21.55341960407610458, 87.70724293864769550 ) ) ;
#87242 = CARTESIAN_POINT ( 'NONE',  ( 8.224510206698953496, -14.34966873604960469, 27.91557627198103830 ) ) ;
#87243 = VERTEX_POINT ( 'NONE', #51035 ) ;
#87244 = DIRECTION ( 'NONE',  ( -1.000000000000000000, -0.000000000000000000, -0.000000000000000000 ) ) ;
#87245 = CARTESIAN_POINT ( 'NONE',  ( 10.81492255796078972, 18.62759615963270932, 59.58224293864770260 ) ) ;
#87246 = CARTESIAN_POINT ( 'NONE',  ( 8.314922557961029526, -14.29746914071037800, 100.4177570613523471 ) ) ;
#87247 = ORIENTED_EDGE ( 'NONE', *, *, #189313, .F. ) ;
#87248 = CARTESIAN_POINT ( 'NONE',  ( 17.50000000000001421, -3.385507783985830521, 102.6446170133486930 ) ) ;
#87249 = CARTESIAN_POINT ( 'NONE',  ( 21.52544592524344225, -5.823673210054117533, 83.54057627198102409 ) ) ;
#87250 = CARTESIAN_POINT ( 'NONE',  ( -12.14591786802326823, 12.06949235617739902, 113.1260903946856899 ) ) ;
#87251 = CARTESIAN_POINT ( 'NONE',  ( -12.14591786802326823, 12.06949235617739902, 33.12609039468569705 ) ) ;
#87252 = CARTESIAN_POINT ( 'NONE',  ( -19.03943276465977164, 0.05219959533909376836, 31.24890960531435979 ) ) ;
#87253 = CARTESIAN_POINT ( 'NONE',  ( 19.03943276465977164, -0.05219959533909143690, 48.74890960531435979 ) ) ;
#87254 = CARTESIAN_POINT ( 'NONE',  ( 27.73933785331498925, -9.013057229001033122, 140.2750000027311330 ) ) ;
#87255 = CARTESIAN_POINT ( 'NONE',  ( 9.564922557960805705, 16.46253265017160317, 114.5822429386476955 ) ) ;
#87256 = CARTESIAN_POINT ( 'NONE',  ( -9.444051989377744150, -10.00006765622181604, -62.56086220006871912 ) ) ;
#87257 = CARTESIAN_POINT ( 'NONE',  ( -4.483927247898782831, 16.52544592524335698, 97.70942372801904696 ) ) ;
#87258 = CARTESIAN_POINT ( 'NONE',  ( -19.05341960407617563, 5.049401038297882671, 98.54275706135233293 ) ) ;
#87259 = CARTESIAN_POINT ( 'NONE',  ( -19.05341960407617563, 5.049401038297882671, 38.54275706135233293 ) ) ;
#87260 = CARTESIAN_POINT ( 'NONE',  ( 21.55341960407610458, 5.719274019375980345, 83.95724293864770971 ) ) ;
#87261 = CARTESIAN_POINT ( 'NONE',  ( 4.483927247898790824, -16.52544592524335698, 110.2094237280190185 ) ) ;
#87262 = CARTESIAN_POINT ( 'NONE',  ( -18.62759615963270932, 10.81492255796079327, 30.83224293864770260 ) ) ;
#87263 = CARTESIAN_POINT ( 'NONE',  ( -5.153800228976607833, 19.02544592524334988, 107.7094237280189759 ) ) ;
#87264 = CARTESIAN_POINT ( 'NONE',  ( 9.564922557960805705, 16.46253265017160317, 104.5822429386476955 ) ) ;
#87265 = CARTESIAN_POINT ( 'NONE',  ( -5.823673210054431948, 21.52544592524334988, 67.70942372801901854 ) ) ;
#87266 = CARTESIAN_POINT ( 'NONE',  ( 19.03943276465977164, -0.05219959533909143690, 58.74890960531435979 ) ) ;
#87267 = AXIS2_PLACEMENT_3D ( 'NONE', #37783, #177321, #115632 ) ;
#87268 = CARTESIAN_POINT ( 'NONE',  ( -14.34966873604960291, -8.224510206698953496, 106.6655762719810383 ) ) ;
#87269 = DIRECTION ( 'NONE',  ( 0.000000000000000000, 0.000000000000000000, -1.000000000000000000 ) ) ;
#87270 = CARTESIAN_POINT ( 'NONE',  ( 19.02544592524343514, -5.153800228976328945, 68.54057627198103830 ) ) ;
#87271 = CARTESIAN_POINT ( 'NONE',  ( -4.483927247898539470, -16.52544592524342804, 72.29057627198102409 ) ) ;
#87272 = ORIENTED_EDGE ( 'NONE', *, *, #155178, .F. ) ;
#87273 = CARTESIAN_POINT ( 'NONE',  ( -16.46253265017146816, -9.564922557961047289, 94.16775706135233293 ) ) ;
#87274 = CARTESIAN_POINT ( 'NONE',  ( -19.03943276465977164, 0.05219959533909376836, 61.24890960531436690 ) ) ;
#87275 = CARTESIAN_POINT ( 'NONE',  ( 1.304248841091933035E-15, 21.30000000000002913, -56.46919128290398504 ) ) ;
#87277 = CARTESIAN_POINT ( 'NONE',  ( -19.02544592524342804, 5.153800228976336051, 106.0405762719810241 ) ) ;
#87276 = CARTESIAN_POINT ( 'NONE',  ( -16.46253265017160317, 9.564922557960807481, 70.83224293864770971 ) ) ;
#87278 = CARTESIAN_POINT ( 'NONE',  ( -14.29746914071037622, -8.314922557961029526, 59.16775706135234714 ) ) ;
#87279 = CARTESIAN_POINT ( 'NONE',  ( -23.46320343559652954, -18.96320343559629507, 1.110912703473986074 ) ) ;
#87280 = CARTESIAN_POINT ( 'NONE',  ( -13.97604488694547697, 13.89961937509957934, 43.12609039468566152 ) ) ;
#87281 = CARTESIAN_POINT ( 'NONE',  ( 10.72451020669871369, 18.67979575497193778, 102.0844237280190185 ) ) ;
#87282 = DIRECTION ( 'NONE',  ( 1.000000000000000000, 6.391086490440868450E-16, 0.000000000000000000 ) ) ;
#87283 = CARTESIAN_POINT ( 'NONE',  ( 9.474510206698971260, -16.51473224551069308, 107.9155762719810383 ) ) ;
#87284 = CARTESIAN_POINT ( 'NONE',  ( 14.29746914071037800, 8.314922557961029526, 96.66775706135234714 ) ) ;
#87285 = EDGE_CURVE ( 'NONE', #94244, #44638, #153592, .T. ) ;
#87286 = CARTESIAN_POINT ( 'NONE',  ( 9.564922557961047289, -16.46253265017146816, 75.41775706135234714 ) ) ;
#87287 = CARTESIAN_POINT ( 'NONE',  ( -0.05219959533934338120, 16.53943276465976808, 92.50109039468567573 ) ) ;
#87288 = CARTESIAN_POINT ( 'NONE',  ( -17.05116617787826527, 6.768360034955678728, 28.65675553259198693 ) ) ;
#87289 = CARTESIAN_POINT ( 'NONE',  ( 14.29746914071037800, 8.314922557961029526, 61.66775706135235424 ) ) ;
#87290 = ORIENTED_EDGE ( 'NONE', *, *, #117570, .T. ) ;
#87291 = CARTESIAN_POINT ( 'NONE',  ( 18.62759615963255655, 10.81492255796105972, 86.66775706135234714 ) ) ;
#87292 = CARTESIAN_POINT ( 'NONE',  ( 5.049401038297881783, 19.05341960407617563, 92.29275706135234714 ) ) ;
#87293 = CARTESIAN_POINT ( 'NONE',  ( -13.89961937509957401, -13.97604488694547875, 24.37609039468565442 ) ) ;
#87294 = CARTESIAN_POINT ( 'NONE',  ( -19.03943276465977164, 0.05219959533909376836, 61.24890960531436690 ) ) ;
#87295 = CARTESIAN_POINT ( 'NONE',  ( -0.05219959533909027116, -19.03943276465977164, 47.49890960531435979 ) ) ;
#87296 = CARTESIAN_POINT ( 'NONE',  ( -14.06429661546934184, -37.45132032961591761, -11.50520302883531087 ) ) ;
#87297 = CARTESIAN_POINT ( 'NONE',  ( -18.67979575497178146, -10.72451020669898902, 86.66557627198102409 ) ) ;
#87298 = CIRCLE ( 'NONE', #113106, 4.000000000000000888 ) ;
#87299 = CARTESIAN_POINT ( 'NONE',  ( 0.05219959533907565091, 21.53943276465977519, 34.99890960531435979 ) ) ;
#87300 = CARTESIAN_POINT ( 'NONE',  ( -19.02544592524342804, 5.153800228976336051, 36.04057627198100988 ) ) ;
#87301 = CARTESIAN_POINT ( 'NONE',  ( -8.224510206698735004, -14.34966873604973081, 49.58442372801901143 ) ) ;
#87302 = ORIENTED_EDGE ( 'NONE', *, *, #131670, .T. ) ;
#87303 = CARTESIAN_POINT ( 'NONE',  ( 18.62759615963255655, 10.81492255796105972, 31.66775706135234358 ) ) ;
#87305 = CARTESIAN_POINT ( 'NONE',  ( -11.40812507854755609, 35.11059874428196537, -9.024999997268814411 ) ) ;
#87304 = CARTESIAN_POINT ( 'NONE',  ( -16.52544592524342804, 4.483927247898546575, 61.04057627198103120 ) ) ;
#87306 = CARTESIAN_POINT ( 'NONE',  ( -12.06949235617739369, -12.14591786802326823, 19.37609039468568639 ) ) ;
#87307 = CARTESIAN_POINT ( 'NONE',  ( -19.03943276465977164, -0.05219959533935918106, 43.75109039468566863 ) ) ;
#87308 = CARTESIAN_POINT ( 'NONE',  ( 14.34966873604960469, 8.224510206698951720, 59.16557627198103120 ) ) ;
#87309 = CARTESIAN_POINT ( 'NONE',  ( -15.72974639402197994, 15.80617190586746368, 115.6239096053143669 ) ) ;
#87311 = CARTESIAN_POINT ( 'NONE',  ( 21.52544592524344225, -5.823673210054117533, 83.54057627198102409 ) ) ;
#87310 = CARTESIAN_POINT ( 'NONE',  ( 0.4053451330847814282, 16.64779159201958691, -59.15694982147774539 ) ) ;
#87312 = CARTESIAN_POINT ( 'NONE',  ( 16.51473224551069308, 9.474510206698969483, 84.16557627198102409 ) ) ;
#87313 = CARTESIAN_POINT ( 'NONE',  ( -16.52544592524342804, 4.483927247898546575, 56.04057627198102409 ) ) ;
#87314 = CARTESIAN_POINT ( 'NONE',  ( 19.05341960407611168, 5.049401038298154454, 113.9572429386477097 ) ) ;
#87315 = DIRECTION ( 'NONE',  ( -0.000000000000000000, -0.000000000000000000, 1.000000000000000000 ) ) ;
#87316 = CARTESIAN_POINT ( 'NONE',  ( -0.05219959533936034679, 19.03943276465977164, 67.50109039468566152 ) ) ;
#87317 = CARTESIAN_POINT ( 'NONE',  ( -15.80617190586745835, -15.72974639402198527, 106.8739096053143811 ) ) ;
#87318 = CARTESIAN_POINT ( 'NONE',  ( -5.049401038298153566, 19.05341960407611168, 55.20724293864769550 ) ) ;
#87319 = CARTESIAN_POINT ( 'NONE',  ( 5.049401038297881783, 19.05341960407617563, 42.29275706135234003 ) ) ;
#87320 = CARTESIAN_POINT ( 'NONE',  ( 16.46253265017160672, -9.564922557960803928, 33.33224293864770260 ) ) ;
#87321 = CARTESIAN_POINT ( 'NONE',  ( 5.719274019375673035, 21.55341960407619339, 62.29275706135236845 ) ) ;
#87322 = CARTESIAN_POINT ( 'NONE',  ( -17.13100169013299734, -6.664070546373136672, 69.23210164300149927 ) ) ;
#87323 = CARTESIAN_POINT ( 'NONE',  ( 4.379528057220339221, -16.55341960407611168, 42.70724293864770260 ) ) ;
#87324 = CARTESIAN_POINT ( 'NONE',  ( 19.02544592524343514, -5.153800228976328945, 63.54057627198103830 ) ) ;
#87325 = CARTESIAN_POINT ( 'NONE',  ( 21.52544592524344225, -5.823673210054117533, 68.54057627198103830 ) ) ;
#87326 = CARTESIAN_POINT ( 'NONE',  ( 16.46253265017160672, -9.564922557960803928, 53.33224293864768839 ) ) ;
#87327 = ORIENTED_EDGE ( 'NONE', *, *, #5408, .F. ) ;
#87328 = CARTESIAN_POINT ( 'NONE',  ( -21.52544592524343514, 5.823673210054127303, 61.04057627198103120 ) ) ;
#87329 = CARTESIAN_POINT ( 'NONE',  ( 21.53943276465977519, 0.05219959533937863772, 106.2510903946856757 ) ) ;
#87332 = CARTESIAN_POINT ( 'NONE',  ( 4.483927247898545687, 16.52544592524342804, 84.79057627198102409 ) ) ;
#87331 = CARTESIAN_POINT ( 'NONE',  ( 14.29746914071037800, 8.314922557961029526, 96.66775706135234714 ) ) ;
#87330 = CARTESIAN_POINT ( 'NONE',  ( 5.985463302384318673, -36.83348364107504835, -32.36600886826526136 ) ) ;
#87333 = CARTESIAN_POINT ( 'NONE',  ( -19.05341960407611168, -5.049401038298163336, 66.45724293864769550 ) ) ;
#87334 = ORIENTED_EDGE ( 'NONE', *, *, #168981, .F. ) ;
#87335 = CARTESIAN_POINT ( 'NONE',  ( 19.02544592524334988, 5.153800228976608722, 36.45942372801900433 ) ) ;
#87336 = CARTESIAN_POINT ( 'NONE',  ( -14.34966873604972548, 8.224510206698743886, 83.33442372801903275 ) ) ;
#87337 = CARTESIAN_POINT ( 'NONE',  ( 9.564922557961047289, -16.46253265017146816, 30.41775706135232937 ) ) ;
#87338 = CARTESIAN_POINT ( 'NONE',  ( 19.02544592524343514, -5.153800228976328945, 83.54057627198100988 ) ) ;
#87339 = CARTESIAN_POINT ( 'NONE',  ( -5.719274019375978568, 21.55341960407610458, 60.20724293864768839 ) ) ;
#87340 = CARTESIAN_POINT ( 'NONE',  ( 27.32543223595603266, -4.845308524273388429, 167.4404622590848817 ) ) ;
#87341 = CARTESIAN_POINT ( 'NONE',  ( 19.05341960407611168, 5.049401038298154454, 23.95724293864769194 ) ) ;
#87342 = CARTESIAN_POINT ( 'NONE',  ( 21.55341960407619695, -5.719274019375665929, 96.04275706135236135 ) ) ;
#87343 = CARTESIAN_POINT ( 'NONE',  ( -4.483927247898782831, 16.52544592524335698, 62.70942372801902565 ) ) ;
#87344 = CARTESIAN_POINT ( 'NONE',  ( -18.62759615963255300, -10.81492255796106328, 34.16775706135234714 ) ) ;
#87345 = CARTESIAN_POINT ( 'NONE',  ( -12.06949235617739369, -12.14591786802326823, 29.37609039468568284 ) ) ;
#87346 = CARTESIAN_POINT ( 'NONE',  ( -9.564922557960796823, -16.46253265017161027, 97.08224293864769550 ) ) ;
#87347 = CARTESIAN_POINT ( 'NONE',  ( 0.05219959533909260263, 19.03943276465977164, 44.99890960531435979 ) ) ;
#87348 = CARTESIAN_POINT ( 'NONE',  ( -9.474510206698964154, 16.51473224551069663, 55.41557627198103120 ) ) ;
#87349 = CARTESIAN_POINT ( 'NONE',  ( 4.483927247898790824, -16.52544592524335698, 35.20942372801901854 ) ) ;
#87350 = CARTESIAN_POINT ( 'NONE',  ( 0.05219959533910956823, 16.53943276465976808, 89.99890960531438111 ) ) ;
#87351 = CARTESIAN_POINT ( 'NONE',  ( -4.483927247898782831, 16.52544592524335698, 102.7094237280190185 ) ) ;
#87354 = CARTESIAN_POINT ( 'NONE',  ( 13.89961937509977652, -13.97604488694527269, 58.12390960531436690 ) ) ;
#87353 = CARTESIAN_POINT ( 'NONE',  ( 13.97604488694527802, 13.89961937509977652, 79.37390960531435269 ) ) ;
#87352 = CARTESIAN_POINT ( 'NONE',  ( -0.05219959533937732626, 21.53943276465977519, 47.50109039468568994 ) ) ;
#87355 = CARTESIAN_POINT ( 'NONE',  ( -5.049401038298153566, 19.05341960407611168, 80.20724293864769550 ) ) ;
#87356 = CARTESIAN_POINT ( 'NONE',  ( -4.483927247898539470, -16.52544592524342804, 37.29057627198102409 ) ) ;
#87357 = CARTESIAN_POINT ( 'NONE',  ( -14.29746914071037622, -8.314922557961029526, 104.1677570613523471 ) ) ;
#87358 = VERTEX_POINT ( 'NONE', #124896 ) ;
#87359 = CARTESIAN_POINT ( 'NONE',  ( 19.05341960407617918, -5.049401038297876454, 46.04275706135233293 ) ) ;
#87360 = CARTESIAN_POINT ( 'NONE',  ( -3.573655867282028392E-15, 2.428612866367529932E-14, 164.9999999999999716 ) ) ;
#87361 = VECTOR ( 'NONE', #42031, 1000.000000000000114 ) ;
#87362 = CARTESIAN_POINT ( 'NONE',  ( 13.97604488694527802, 13.89961937509977652, 44.37390960531435269 ) ) ;
#87363 = CARTESIAN_POINT ( 'NONE',  ( -9.474510206698720793, -16.51473224551083518, 44.58442372801900433 ) ) ;
#87364 = CARTESIAN_POINT ( 'NONE',  ( -29.86685920354755197, -21.69954338932560134, -6.424999997268812990 ) ) ;
#87365 = CARTESIAN_POINT ( 'NONE',  ( -8.314922557961024197, 14.29746914071037800, 47.91775706135234714 ) ) ;
#87367 = CARTESIAN_POINT ( 'NONE',  ( -16.53943276465976808, -0.05219959533934237506, 58.75109039468568994 ) ) ;
#87366 = CARTESIAN_POINT ( 'NONE',  ( -19.03943276465977164, -0.05219959533935918106, 73.75109039468566152 ) ) ;
#87368 = CARTESIAN_POINT ( 'NONE',  ( -18.22780087662123805, 5.499999999999981348, 71.01763182126894947 ) ) ;
#87369 = CARTESIAN_POINT ( 'NONE',  ( 9.474510206698971260, -16.51473224551069308, 82.91557627198103830 ) ) ;
#87370 = CARTESIAN_POINT ( 'NONE',  ( 15.72974639402199770, -15.80617190586745480, 113.1239096053143953 ) ) ;
#87371 = CARTESIAN_POINT ( 'NONE',  ( -0.05219959533936034679, 19.03943276465977164, 72.50109039468566152 ) ) ;
#87373 = CARTESIAN_POINT ( 'NONE',  ( 16.46253265017160672, -9.564922557960803928, 38.33224293864768839 ) ) ;
#87372 = CARTESIAN_POINT ( 'NONE',  ( 9.474510206698971260, -16.51473224551069308, 107.9155762719810383 ) ) ;
#87374 = CARTESIAN_POINT ( 'NONE',  ( -19.05341960407611168, -5.049401038298163336, 76.45724293864769550 ) ) ;
#87376 = CARTESIAN_POINT ( 'NONE',  ( -13.89961937509977652, 13.97604488694528158, 30.62390960531435269 ) ) ;
#87375 = CARTESIAN_POINT ( 'NONE',  ( 14.34966873604960469, 8.224510206698951720, 29.16557627198103120 ) ) ;
#87377 = CARTESIAN_POINT ( 'NONE',  ( -5.049401038297874678, -19.05341960407617918, 49.79275706135231871 ) ) ;
#87378 = CARTESIAN_POINT ( 'NONE',  ( 4.379528057220339221, -16.55341960407611168, 67.70724293864769550 ) ) ;
#87379 = CARTESIAN_POINT ( 'NONE',  ( -5.049401038297874678, -19.05341960407617918, 19.79275706135233293 ) ) ;
#87380 = CARTESIAN_POINT ( 'NONE',  ( 5.049401038298161559, -19.05341960407611168, 57.70724293864769550 ) ) ;
#87381 = CARTESIAN_POINT ( 'NONE',  ( 10.81492255796078972, 18.62759615963270932, 44.58224293864769550 ) ) ;
#87383 = CARTESIAN_POINT ( 'NONE',  ( 10.72451020669871369, 18.67979575497193778, 107.0844237280190043 ) ) ;
#87382 = CARTESIAN_POINT ( 'NONE',  ( 16.55341960407611168, 4.379528057220329451, 58.95724293864770971 ) ) ;
#87384 = CARTESIAN_POINT ( 'NONE',  ( 16.46253265017160672, -9.564922557960803928, 98.33224293864769550 ) ) ;
#87385 = CARTESIAN_POINT ( 'NONE',  ( 5.153800228976335163, 19.02544592524342804, 104.7905762719809957 ) ) ;
#87386 = CARTESIAN_POINT ( 'NONE',  ( 13.89961937509977652, -13.97604488694527269, 43.12390960531434558 ) ) ;
#87387 = CARTESIAN_POINT ( 'NONE',  ( -9.564922557960796823, -16.46253265017161027, 27.08224293864769550 ) ) ;
#87388 = CARTESIAN_POINT ( 'NONE',  ( 16.53943276465976808, -0.05219959533910856209, 88.74890960531436690 ) ) ;
#87389 = CARTESIAN_POINT ( 'NONE',  ( 15.80617190586746368, 15.72974639402197994, 99.37390960531436690 ) ) ;
#87390 = CARTESIAN_POINT ( 'NONE',  ( 9.564922557960805705, 16.46253265017160317, 104.5822429386476955 ) ) ;
#87391 = CARTESIAN_POINT ( 'NONE',  ( 21.55341960407610458, 5.719274019375980345, 113.9572429386477239 ) ) ;
#87392 = CARTESIAN_POINT ( 'NONE',  ( -19.03943276465977164, 0.05219959533909376836, 96.24890960531436690 ) ) ;
#87394 = CARTESIAN_POINT ( 'NONE',  ( 14.29746914071049879, -8.314922557960816363, 108.3322429386477097 ) ) ;
#87393 = DIRECTION ( 'NONE',  ( -0.000000000000000000, -0.000000000000000000, 1.000000000000000000 ) ) ;
#87395 = CARTESIAN_POINT ( 'NONE',  ( -13.89961937509977652, 13.97604488694528158, 70.62390960531432427 ) ) ;
#87396 = CARTESIAN_POINT ( 'NONE',  ( 15.80617190586746368, 15.72974639402197994, 79.37390960531436690 ) ) ;
#87397 = DIRECTION ( 'NONE',  ( -0.000000000000000000, -0.000000000000000000, 1.000000000000000000 ) ) ;
#87398 = FACE_OUTER_BOUND ( 'NONE', #97759, .T. ) ;
#87400 = DIRECTION ( 'NONE',  ( 0.000000000000000000, 0.000000000000000000, -1.000000000000000000 ) ) ;
#87399 = CARTESIAN_POINT ( 'NONE',  ( 21.53943276465977519, -0.05219959533907433946, 23.74890960531435269 ) ) ;
#87401 = CARTESIAN_POINT ( 'NONE',  ( -12.06949235617739369, -12.14591786802326823, 34.37609039468568284 ) ) ;
#87402 = CARTESIAN_POINT ( 'NONE',  ( 14.29746914071049879, -8.314922557960816363, 88.33224293864769550 ) ) ;
#87403 = CARTESIAN_POINT ( 'NONE',  ( -17.49999999999997868, -4.640572885337623354, 109.3621183545115798 ) ) ;
#87404 = CARTESIAN_POINT ( 'NONE',  ( 19.05341960407611168, 5.049401038298154454, 83.95724293864766707 ) ) ;
#87405 = CARTESIAN_POINT ( 'NONE',  ( -0.05219959533909027116, -19.03943276465977164, 42.49890960531435269 ) ) ;
#87406 = CARTESIAN_POINT ( 'NONE',  ( -16.55341960407611168, -4.379528057220339221, 76.45724293864769550 ) ) ;
#87407 = CARTESIAN_POINT ( 'NONE',  ( -21.55341960407610458, -5.719274019375992779, 26.45724293864768839 ) ) ;
#87408 = CARTESIAN_POINT ( 'NONE',  ( -4.379528057220328563, 16.55341960407611168, 50.20724293864769550 ) ) ;
#87409 = CARTESIAN_POINT ( 'NONE',  ( 19.03943276465977164, 0.05219959533936151252, 101.2510903946856757 ) ) ;
#87410 = CARTESIAN_POINT ( 'NONE',  ( -10.81492255796105439, 18.62759615963255655, 77.91775706135231871 ) ) ;
#87411 = CARTESIAN_POINT ( 'NONE',  ( -27.73933785331498925, 9.013057229001088189, 148.7750000027311899 ) ) ;
#87412 = CARTESIAN_POINT ( 'NONE',  ( 0.05219959533909260263, 19.03943276465977164, 109.9989096053143669 ) ) ;
#87413 = CARTESIAN_POINT ( 'NONE',  ( -4.379528057220086978, -16.55341960407618274, 84.79275706135234714 ) ) ;
#87414 = DIRECTION ( 'NONE',  ( -0.000000000000000000, 1.000000000000000000, -0.000000000000000000 ) ) ;
#87415 = CARTESIAN_POINT ( 'NONE',  ( -13.97604488694527625, -13.89961937509977652, 81.87390960531436690 ) ) ;
#87416 = CARTESIAN_POINT ( 'NONE',  ( 0.05219959533907565091, 21.53943276465977519, 84.99890960531436690 ) ) ;
#87417 = CARTESIAN_POINT ( 'NONE',  ( -4.379528057220086978, -16.55341960407618274, 24.79275706135235779 ) ) ;
#87419 = CARTESIAN_POINT ( 'NONE',  ( -5.823673210054431948, 21.52544592524334988, 72.70942372801901854 ) ) ;
#87418 = CARTESIAN_POINT ( 'NONE',  ( 16.53943276465976808, -0.05219959533910856209, 53.74890960531437401 ) ) ;
#87421 = CARTESIAN_POINT ( 'NONE',  ( 18.67979575497178502, 10.72451020669898547, 29.16557627198103120 ) ) ;
#87420 = CARTESIAN_POINT ( 'NONE',  ( 16.53943276465976808, 0.05219959533934440121, 86.25109039468568994 ) ) ;
#87422 = CARTESIAN_POINT ( 'NONE',  ( 9.564922557960805705, 16.46253265017160317, 109.5822429386476955 ) ) ;
#87423 = CARTESIAN_POINT ( 'NONE',  ( 31.72709406046299918, -1.071565338629617092E-14, 102.5000000000000142 ) ) ;
#87424 = CARTESIAN_POINT ( 'NONE',  ( -14.34966873604972548, 8.224510206698743886, 103.3344237280190043 ) ) ;
#87425 = CARTESIAN_POINT ( 'NONE',  ( -4.483927247898782831, 16.52544592524335698, 57.70942372801901143 ) ) ;
#87426 = CARTESIAN_POINT ( 'NONE',  ( 19.02544592524343514, -5.153800228976328945, 73.54057627198103830 ) ) ;
#87427 = CARTESIAN_POINT ( 'NONE',  ( -5.049401038298153566, 19.05341960407611168, 90.20724293864766707 ) ) ;
#87428 = CARTESIAN_POINT ( 'NONE',  ( 10.72451020669871369, 18.67979575497193778, 72.08442372801899012 ) ) ;
#87429 = CARTESIAN_POINT ( 'NONE',  ( -0.05219959533934338120, 16.53943276465976808, 82.50109039468568994 ) ) ;
#87430 = CARTESIAN_POINT ( 'NONE',  ( -12.06949235617756955, 12.14591786802309770, 45.62390960531436690 ) ) ;
#87431 = CARTESIAN_POINT ( 'NONE',  ( 9.564922557960805705, 16.46253265017160317, 59.58224293864769550 ) ) ;
#87432 = CARTESIAN_POINT ( 'NONE',  ( -0.05219959533909027116, -19.03943276465977164, 42.49890960531435269 ) ) ;
#87433 = VERTEX_POINT ( 'NONE', #81344 ) ;
#87434 = CARTESIAN_POINT ( 'NONE',  ( -5.153800228976607833, 19.02544592524334988, 92.70942372801901854 ) ) ;
#87435 = CARTESIAN_POINT ( 'NONE',  ( 4.379528057220339221, -16.55341960407611168, 92.70724293864770971 ) ) ;
#87436 = CARTESIAN_POINT ( 'NONE',  ( -5.049401038298153566, 19.05341960407611168, 60.20724293864768129 ) ) ;
#87438 = CARTESIAN_POINT ( 'NONE',  ( -30.74264578624800492, 22.33583958711400186, -4.200000000000000178 ) ) ;
#87437 = CARTESIAN_POINT ( 'NONE',  ( 5.153800228976615827, -19.02544592524334988, 100.2094237280190043 ) ) ;
#87439 = CARTESIAN_POINT ( 'NONE',  ( -5.719274019375665041, -21.55341960407619695, 104.7927570613523898 ) ) ;
#87440 = CARTESIAN_POINT ( 'NONE',  ( 4.483927247898790824, -16.52544592524335698, 65.20942372801901854 ) ) ;
#87441 = CARTESIAN_POINT ( 'NONE',  ( -13.97604488694547697, 13.89961937509957934, 88.12609039468563310 ) ) ;
#87442 = CARTESIAN_POINT ( 'NONE',  ( 5.719274019375991003, -21.55341960407610458, 67.70724293864769550 ) ) ;
#87443 = CARTESIAN_POINT ( 'NONE',  ( -8.224510206698735004, -14.34966873604973081, 59.58442372801901854 ) ) ;
#87444 = CARTESIAN_POINT ( 'NONE',  ( 8.695259559498534685, -39.05792023227123622, -15.00000000000000178 ) ) ;
#87445 = CARTESIAN_POINT ( 'NONE',  ( -16.46253265017146816, -9.564922557961047289, 59.16775706135233293 ) ) ;
#87446 = CARTESIAN_POINT ( 'NONE',  ( 10.72451020669871369, 18.67979575497193778, 102.0844237280190185 ) ) ;
#87447 = CARTESIAN_POINT ( 'NONE',  ( 8.314922557960818139, 14.29746914071049879, 114.5822429386477097 ) ) ;
#87448 = CARTESIAN_POINT ( 'NONE',  ( -19.03943276465977164, 0.05219959533909376836, 66.24890960531436690 ) ) ;
#87449 = CARTESIAN_POINT ( 'NONE',  ( 14.34966873604960469, 8.224510206698951720, 59.16557627198103120 ) ) ;
#87450 = CARTESIAN_POINT ( 'NONE',  ( -21.53943276465977519, -0.05219959533937600094, 88.75109039468567573 ) ) ;
#87451 = CARTESIAN_POINT ( 'NONE',  ( 9.474510206698729675, 16.51473224551082808, 42.08442372801900433 ) ) ;
#87452 = CARTESIAN_POINT ( 'NONE',  ( -9.564922557961040184, 16.46253265017147172, 22.91775706135233648 ) ) ;
#87453 = CARTESIAN_POINT ( 'NONE',  ( -0.05219959533909027116, -19.03943276465977164, 112.4989096053143669 ) ) ;
#87454 = CARTESIAN_POINT ( 'NONE',  ( -21.55341960407619339, 5.719274019375674811, 98.54275706135234714 ) ) ;
#87455 = CARTESIAN_POINT ( 'NONE',  ( -19.03943276465977164, 0.05219959533909376836, 81.24890960531436690 ) ) ;
#87456 = CARTESIAN_POINT ( 'NONE',  ( 21.55341960407619695, -5.719274019375665929, 96.04275706135236135 ) ) ;
#87457 = CARTESIAN_POINT ( 'NONE',  ( -0.05219959533907301413, -21.53943276465977519, 47.49890960531435979 ) ) ;
#87458 = CARTESIAN_POINT ( 'NONE',  ( 19.03943276465977164, -0.05219959533909143690, 78.74890960531436690 ) ) ;
#87459 = CARTESIAN_POINT ( 'NONE',  ( 16.46253265017146816, 9.564922557961045513, 66.66775706135233293 ) ) ;
#87460 = CARTESIAN_POINT ( 'NONE',  ( -13.89961937509977652, 13.97604488694528158, 45.62390960531433848 ) ) ;
#87461 = CARTESIAN_POINT ( 'NONE',  ( -19.03943276465977164, 0.05219959533909376836, 86.24890960531436690 ) ) ;
#87462 = CARTESIAN_POINT ( 'NONE',  ( 13.89961937509957401, 13.97604488694547697, 86.87609039468567573 ) ) ;
#87463 = CARTESIAN_POINT ( 'NONE',  ( -12.06949235617739369, -12.14591786802326823, 39.37609039468567573 ) ) ;
#87464 = CARTESIAN_POINT ( 'NONE',  ( 0.05219959533910956823, 16.53943276465976808, 99.99890960531436690 ) ) ;
#87465 = CARTESIAN_POINT ( 'NONE',  ( 13.89961937509977652, -13.97604488694527269, 73.12390960531436690 ) ) ;
#87466 = CARTESIAN_POINT ( 'NONE',  ( 21.55341960407610458, 5.719274019375980345, 43.95724293864769550 ) ) ;
#87467 = CARTESIAN_POINT ( 'NONE',  ( -19.05341960407617563, 5.049401038297882671, 113.5427570613523471 ) ) ;
#87468 = CARTESIAN_POINT ( 'NONE',  ( 0.05219959533907565091, 21.53943276465977519, 114.9989096053143669 ) ) ;
#87469 = CARTESIAN_POINT ( 'NONE',  ( -18.67979575497193778, 10.72451020669871902, 88.33442372801901854 ) ) ;
#87470 = CARTESIAN_POINT ( 'NONE',  ( -14.34966873604972548, 8.224510206698743886, 78.33442372801901854 ) ) ;
#87471 = CARTESIAN_POINT ( 'NONE',  ( -5.049401038298153566, 19.05341960407611168, 80.20724293864769550 ) ) ;
#87472 = CARTESIAN_POINT ( 'NONE',  ( 16.55341960407618274, -4.379528057220086978, 106.0427570613523471 ) ) ;
#87473 = CARTESIAN_POINT ( 'NONE',  ( 5.049401038297881783, 19.05341960407617563, 57.29275706135231871 ) ) ;
#87474 = CARTESIAN_POINT ( 'NONE',  ( -18.62759615963255300, -10.81492255796106328, 34.16775706135234714 ) ) ;
#87475 = CARTESIAN_POINT ( 'NONE',  ( -12.14591786802309592, -12.06949235617757132, 81.87390960531435269 ) ) ;
#87476 = CARTESIAN_POINT ( 'NONE',  ( -5.049401038298153566, 19.05341960407611168, 100.2072429386476955 ) ) ;
#87477 = CARTESIAN_POINT ( 'NONE',  ( -14.29746914071037622, -8.314922557961029526, 84.16775706135234714 ) ) ;
#87478 = CARTESIAN_POINT ( 'NONE',  ( 5.823673210054444382, -21.52544592524334988, 70.20942372801904696 ) ) ;
#87479 = CARTESIAN_POINT ( 'NONE',  ( 8.224510206698742110, 14.34966873604972548, 32.08442372801901854 ) ) ;
#87480 = CARTESIAN_POINT ( 'NONE',  ( -15.80617190586768217, 15.72974639402176855, 28.12609039468568284 ) ) ;
#87481 = CARTESIAN_POINT ( 'NONE',  ( 8.224510206698953496, -14.34966873604960469, 77.91557627198102409 ) ) ;
#87482 = ORIENTED_EDGE ( 'NONE', *, *, #144540, .T. ) ;
#87483 = CARTESIAN_POINT ( 'NONE',  ( -15.80617190586745835, -15.72974639402198527, 96.87390960531436690 ) ) ;
#87484 = CARTESIAN_POINT ( 'NONE',  ( 12.06949235617757843, -12.14591786802309237, 58.12390960531435979 ) ) ;
#87485 = ORIENTED_EDGE ( 'NONE', *, *, #174158, .T. ) ;
#87486 = CARTESIAN_POINT ( 'NONE',  ( 16.51473224551069308, 9.474510206698969483, 24.16557627198102765 ) ) ;
#87487 = CARTESIAN_POINT ( 'NONE',  ( 18.62759615963271287, -10.81492255796078972, 23.33224293864769194 ) ) ;
#87488 = CARTESIAN_POINT ( 'NONE',  ( 21.55341960407619695, -5.719274019375665929, 51.04275706135234714 ) ) ;
#87489 = CARTESIAN_POINT ( 'NONE',  ( -16.53943276465976808, 0.05219959533911058130, 71.24890960531435269 ) ) ;
#87490 = CARTESIAN_POINT ( 'NONE',  ( -21.55341960407610458, -5.719274019375992779, 61.45724293864770260 ) ) ;
#87491 = CARTESIAN_POINT ( 'NONE',  ( 13.89961937509977652, -13.97604488694527269, 68.12390960531436690 ) ) ;
#87493 = CARTESIAN_POINT ( 'NONE',  ( -5.153800228976607833, 19.02544592524334988, 77.70942372801900433 ) ) ;
#87492 = CARTESIAN_POINT ( 'NONE',  ( 13.97604488694527802, 13.89961937509977652, 29.37390960531435979 ) ) ;
#87494 = CARTESIAN_POINT ( 'NONE',  ( 15.72974639402199770, -15.80617190586745480, 68.12390960531436690 ) ) ;
#87495 = CARTESIAN_POINT ( 'NONE',  ( 19.02544592524343514, -5.153800228976328945, 38.54057627198103120 ) ) ;
#87496 = CARTESIAN_POINT ( 'NONE',  ( -19.03943276465977164, 0.05219959533909376836, 66.24890960531436690 ) ) ;
#87497 = ORIENTED_EDGE ( 'NONE', *, *, #183262, .T. ) ;
#87498 = CARTESIAN_POINT ( 'NONE',  ( -8.314922557961024197, 14.29746914071037800, 47.91775706135234714 ) ) ;
#87499 = CARTESIAN_POINT ( 'NONE',  ( 5.823673210054444382, -21.52544592524334988, 30.20942372801902565 ) ) ;
#87500 = CARTESIAN_POINT ( 'NONE',  ( -15.72974639402176322, -15.80617190586768395, 54.37609039468568994 ) ) ;
#87501 = CARTESIAN_POINT ( 'NONE',  ( 13.97604488694527802, 13.89961937509977652, 99.37390960531436690 ) ) ;
#87502 = CARTESIAN_POINT ( 'NONE',  ( -21.55341960407610458, -5.719274019375992779, 91.45724293864769550 ) ) ;
#87504 = CARTESIAN_POINT ( 'NONE',  ( 16.52544592524335698, 4.483927247898782831, 56.45942372801902565 ) ) ;
#87503 = CARTESIAN_POINT ( 'NONE',  ( 5.823673210054125526, 21.52544592524343514, 109.7905762719810383 ) ) ;
#87505 = CARTESIAN_POINT ( 'NONE',  ( -21.52544592524343514, 5.823673210054127303, 51.04057627198103120 ) ) ;
#87506 = CARTESIAN_POINT ( 'NONE',  ( -10.72451020669870658, -18.67979575497194134, 99.58442372801900433 ) ) ;
#87507 = CARTESIAN_POINT ( 'NONE',  ( 16.51473224551069308, 9.474510206698969483, 49.16557627198102409 ) ) ;
#87508 = CARTESIAN_POINT ( 'NONE',  ( -5.049401038298153566, 19.05341960407611168, 105.2072429386476671 ) ) ;
#87509 = CARTESIAN_POINT ( 'NONE',  ( 9.564922557960805705, 16.46253265017160317, 79.58224293864769550 ) ) ;
#87510 = CARTESIAN_POINT ( 'NONE',  ( -9.979912183652590585, -44.24332767168411351, -21.75883150241363495 ) ) ;
#87511 = CARTESIAN_POINT ( 'NONE',  ( -0.05219959533936034679, 19.03943276465977164, 72.50109039468566152 ) ) ;
#87513 = CARTESIAN_POINT ( 'NONE',  ( -21.52544592524343514, 5.823673210054127303, 41.04057627198103120 ) ) ;
#87512 = CARTESIAN_POINT ( 'NONE',  ( 21.53943276465977519, 0.05219959533937863772, 111.2510903946856899 ) ) ;
#87514 = CARTESIAN_POINT ( 'NONE',  ( 16.55341960407618274, -4.379528057220086978, 111.0427570613523613 ) ) ;
#87515 = CARTESIAN_POINT ( 'NONE',  ( 9.564922557961047289, -16.46253265017146816, 90.41775706135234714 ) ) ;
#87516 = FACE_OUTER_BOUND ( 'NONE', #193193, .T. ) ;
#87517 = CARTESIAN_POINT ( 'NONE',  ( -0.05219959533936034679, 19.03943276465977164, 22.50109039468566152 ) ) ;
#87518 = CARTESIAN_POINT ( 'NONE',  ( -5.153800228976607833, 19.02544592524334988, 87.70942372801897591 ) ) ;
#87519 = CARTESIAN_POINT ( 'NONE',  ( -13.97604488694547697, 13.89961937509957934, 38.12609039468566152 ) ) ;
#87520 = CARTESIAN_POINT ( 'NONE',  ( -17.49999999999999645, -5.499999999999992895, 44.20309617465829888 ) ) ;
#87521 = CARTESIAN_POINT ( 'NONE',  ( -5.049401038298153566, 19.05341960407611168, 60.20724293864768129 ) ) ;
#87522 = CARTESIAN_POINT ( 'NONE',  ( 14.34966873604960469, 8.224510206698951720, 44.16557627198103120 ) ) ;
#87523 = EDGE_CURVE ( 'NONE', #133568, #60209, #17726, .T. ) ;
#87524 = CARTESIAN_POINT ( 'NONE',  ( 19.05341960407611168, 5.049401038298154454, 28.95724293864769550 ) ) ;
#87525 = CARTESIAN_POINT ( 'NONE',  ( -4.379528057220328563, 16.55341960407611168, 40.20724293864769550 ) ) ;
#87526 = CARTESIAN_POINT ( 'NONE',  ( -33.78191506369886810, -21.41920200728862511, -24.99999999999999289 ) ) ;
#87527 = CARTESIAN_POINT ( 'NONE',  ( -14.29746914071037622, -8.314922557961029526, 109.1677570613523613 ) ) ;
#87528 = CARTESIAN_POINT ( 'NONE',  ( -5.153800228976328057, -19.02544592524343514, 52.29057627198100988 ) ) ;
#87529 = CARTESIAN_POINT ( 'NONE',  ( -5.049401038297874678, -19.05341960407617918, 19.79275706135233293 ) ) ;
#87530 = CARTESIAN_POINT ( 'NONE',  ( 16.55341960407618274, -4.379528057220086978, 31.04275706135234714 ) ) ;
#87531 = CARTESIAN_POINT ( 'NONE',  ( 21.55341960407610458, 5.719274019375980345, 38.95724293864768839 ) ) ;
#87533 = ORIENTED_EDGE ( 'NONE', *, *, #97920, .F. ) ;
#87532 = CARTESIAN_POINT ( 'NONE',  ( 5.719274019375673035, 21.55341960407619339, 87.29275706135236135 ) ) ;
#87534 = CARTESIAN_POINT ( 'NONE',  ( -19.05341960407611168, -5.049401038298163336, 101.4572429386476955 ) ) ;
#87535 = CARTESIAN_POINT ( 'NONE',  ( -5.153800228976328057, -19.02544592524343514, 102.2905762719810383 ) ) ;
#87536 = CARTESIAN_POINT ( 'NONE',  ( -22.81625015709510507, 31.40387420917330275, -6.924999997268812990 ) ) ;
#87537 = CARTESIAN_POINT ( 'NONE',  ( -18.67979575497193778, 10.72451020669871902, 28.33442372801902209 ) ) ;
#87538 = CARTESIAN_POINT ( 'NONE',  ( 4.483927247898545687, 16.52544592524342804, 79.79057627198102409 ) ) ;
#87540 = CARTESIAN_POINT ( 'NONE',  ( 9.564922557960805705, 16.46253265017160317, 74.58224293864769550 ) ) ;
#87539 = CARTESIAN_POINT ( 'NONE',  ( 0.05219959533907565091, 21.53943276465977519, 69.99890960531435269 ) ) ;
#87541 = CARTESIAN_POINT ( 'NONE',  ( 19.03943276465977164, -0.05219959533909143690, 78.74890960531436690 ) ) ;
#87542 = CARTESIAN_POINT ( 'NONE',  ( -0.05219959533907301413, -21.53943276465977519, 107.4989096053143669 ) ) ;
#87543 = ORIENTED_EDGE ( 'NONE', *, *, #117399, .T. ) ;
#87544 = CARTESIAN_POINT ( 'NONE',  ( 19.02544592524343514, -5.153800228976328945, 63.54057627198103830 ) ) ;
#87546 = DIRECTION ( 'NONE',  ( -7.709882115452493155E-15, 0.000000000000000000, 1.000000000000000000 ) ) ;
#87545 = CARTESIAN_POINT ( 'NONE',  ( 14.34966873604960469, 8.224510206698951720, 104.1655762719810241 ) ) ;
#87547 = CARTESIAN_POINT ( 'NONE',  ( 19.02544592524343514, -5.153800228976328945, 58.54057627198102409 ) ) ;
#87548 = CARTESIAN_POINT ( 'NONE',  ( -13.97604488694547697, 13.89961937509957934, 88.12609039468563310 ) ) ;
#87549 = CARTESIAN_POINT ( 'NONE',  ( -4.379528057220328563, 16.55341960407611168, 100.2072429386476955 ) ) ;
#87550 = CARTESIAN_POINT ( 'NONE',  ( 0.05219959533937995610, -21.53943276465977519, 60.00109039468568284 ) ) ;
#87552 = CARTESIAN_POINT ( 'NONE',  ( -21.55341960407610458, -5.719274019375992779, 111.4572429386476813 ) ) ;
#87551 = CARTESIAN_POINT ( 'NONE',  ( 5.049401038298161559, -19.05341960407611168, 42.70724293864767418 ) ) ;
#87553 = CARTESIAN_POINT ( 'NONE',  ( 16.52544592524342804, -4.483927247898539470, 103.5405762719810383 ) ) ;
#87554 = CARTESIAN_POINT ( 'NONE',  ( 17.81289503416610742, 24.51734667627700404, 141.2999999999999829 ) ) ;
#87555 = CARTESIAN_POINT ( 'NONE',  ( -19.02544592524342804, 5.153800228976336051, 71.04057627198099567 ) ) ;
#87556 = CARTESIAN_POINT ( 'NONE',  ( -28.82186960331499037, 2.428612866367529932E-14, 144.2500000054623683 ) ) ;
#87558 = CARTESIAN_POINT ( 'NONE',  ( 10.72451020669898902, -18.67979575497178502, 27.91557627198103830 ) ) ;
#87557 = CARTESIAN_POINT ( 'NONE',  ( -19.02544592524334988, -5.153800228976617603, 108.9594237280189759 ) ) ;
#87559 = CARTESIAN_POINT ( 'NONE',  ( 15.80617190586769283, -15.72974639402175789, 45.62609039468567573 ) ) ;
#87560 = CARTESIAN_POINT ( 'NONE',  ( -19.05341960407611168, -5.049401038298163336, 96.45724293864769550 ) ) ;
#87561 = CARTESIAN_POINT ( 'NONE',  ( 0.05219959533936267826, -19.03943276465977164, 85.00109039468567573 ) ) ;
#87562 = CARTESIAN_POINT ( 'NONE',  ( 19.02544592524343514, -5.153800228976328945, 73.54057627198103830 ) ) ;
#87563 = CARTESIAN_POINT ( 'NONE',  ( -0.05219959533910754901, -16.53943276465976808, 87.49890960531436690 ) ) ;
#87564 = CARTESIAN_POINT ( 'NONE',  ( 19.02544592524343514, -5.153800228976328945, 103.5405762719809957 ) ) ;
#87565 = CARTESIAN_POINT ( 'NONE',  ( -14.34966873604960291, -8.224510206698953496, 76.66557627198103830 ) ) ;
#87566 = CARTESIAN_POINT ( 'NONE',  ( -5.153800228976328057, -19.02544592524343514, 92.29057627198099567 ) ) ;
#87569 = CARTESIAN_POINT ( 'NONE',  ( 19.03943276465977164, -0.05219959533909143690, 28.74890960531435624 ) ) ;
#87568 = CARTESIAN_POINT ( 'NONE',  ( -16.52544592524342804, 4.483927247898546575, 41.04057627198103120 ) ) ;
#87567 = CARTESIAN_POINT ( 'NONE',  ( 5.049401038298161559, -19.05341960407611168, 47.70724293864770260 ) ) ;
#87570 = ORIENTED_EDGE ( 'NONE', *, *, #179632, .F. ) ;
#87571 = CARTESIAN_POINT ( 'NONE',  ( -18.67979575497193778, 10.72451020669871902, 48.33442372801902565 ) ) ;
#87572 = CARTESIAN_POINT ( 'NONE',  ( -16.51473224551082808, 9.474510206698731452, 78.33442372801900433 ) ) ;
#87573 = CARTESIAN_POINT ( 'NONE',  ( -8.224510206698948167, 14.34966873604960824, 55.41557627198102409 ) ) ;
#87574 = CARTESIAN_POINT ( 'NONE',  ( 18.62759615963271287, -10.81492255796078972, 103.3322429386476955 ) ) ;
#87575 = CARTESIAN_POINT ( 'NONE',  ( -10.72451020669898014, 18.67979575497178502, 35.41557627198102409 ) ) ;
#87576 = CARTESIAN_POINT ( 'NONE',  ( 16.55341960407611168, 4.379528057220329451, 88.95724293864769550 ) ) ;
#87577 = CARTESIAN_POINT ( 'NONE',  ( 5.049401038298161559, -19.05341960407611168, 47.70724293864770260 ) ) ;
#87578 = CARTESIAN_POINT ( 'NONE',  ( 16.52544592524342804, -4.483927247898539470, 23.54057627198102765 ) ) ;
#87579 = CARTESIAN_POINT ( 'NONE',  ( -16.53943276465976808, -0.05219959533934237506, 88.75109039468567573 ) ) ;
#87580 = CARTESIAN_POINT ( 'NONE',  ( 12.14591786802327356, -12.06949235617739191, 65.62609039468568994 ) ) ;
#87581 = CARTESIAN_POINT ( 'NONE',  ( -9.474510206698720793, -16.51473224551083518, 24.58442372801900078 ) ) ;
#87582 = CARTESIAN_POINT ( 'NONE',  ( 9.564922557960805705, 16.46253265017160317, 89.58224293864769550 ) ) ;
#87583 = CARTESIAN_POINT ( 'NONE',  ( -5.049401038298153566, 19.05341960407611168, 75.20724293864769550 ) ) ;
#87584 = CARTESIAN_POINT ( 'NONE',  ( 12.06949235617739724, 12.14591786802326823, 76.87609039468567573 ) ) ;
#87585 = CARTESIAN_POINT ( 'NONE',  ( -9.474510206698964154, 16.51473224551069663, 40.41557627198103120 ) ) ;
#87586 = CARTESIAN_POINT ( 'NONE',  ( -16.52544592524342804, 4.483927247898546575, 46.04057627198103830 ) ) ;
#87588 = CARTESIAN_POINT ( 'NONE',  ( 5.153800228976335163, 19.02544592524342804, 104.7905762719809957 ) ) ;
#87587 = FILL_AREA_STYLE_COLOUR ( '', #27553 ) ;
#87589 = CARTESIAN_POINT ( 'NONE',  ( 18.62759615963271287, -10.81492255796078972, 28.33224293864769550 ) ) ;
#87590 = CARTESIAN_POINT ( 'NONE',  ( 16.53943276465976808, -0.05219959533910856209, 68.74890960531435269 ) ) ;
#87591 = CARTESIAN_POINT ( 'NONE',  ( -4.483927247898539470, -16.52544592524342804, 67.29057627198103830 ) ) ;
#87592 = CARTESIAN_POINT ( 'NONE',  ( 17.50000000000001421, -3.189878218039136293, 32.37051437428772260 ) ) ;
#87593 = CARTESIAN_POINT ( 'NONE',  ( -5.049401038297874678, -19.05341960407617918, 69.79275706135233293 ) ) ;
#87594 = CARTESIAN_POINT ( 'NONE',  ( 13.89961937509977652, -13.97604488694527269, 88.12390960531438111 ) ) ;
#87595 = CARTESIAN_POINT ( 'NONE',  ( -19.03943276465977164, -0.05219959533935918106, 78.75109039468567573 ) ) ;
#87596 = CARTESIAN_POINT ( 'NONE',  ( 22.44159573604009239, 16.30477369853692693, 148.5750000027312012 ) ) ;
#87598 = CARTESIAN_POINT ( 'NONE',  ( 4.379528057220092307, 16.55341960407617563, 102.2927570613523613 ) ) ;
#87597 = CARTESIAN_POINT ( 'NONE',  ( 5.153800228976615827, -19.02544592524334988, 105.2094237280190185 ) ) ;
#87599 = CARTESIAN_POINT ( 'NONE',  ( 13.89961937509977652, -13.97604488694527269, 33.12390960531434558 ) ) ;
#87600 = CARTESIAN_POINT ( 'NONE',  ( 15.80617190586746368, 15.72974639402197994, 39.37390960531436690 ) ) ;
#87601 = CARTESIAN_POINT ( 'NONE',  ( 21.53943276465977519, 0.05219959533937863772, 61.25109039468567573 ) ) ;
#87602 = CARTESIAN_POINT ( 'NONE',  ( -12.14591786802326823, 12.06949235617739902, 28.12609039468568284 ) ) ;
#87604 = CARTESIAN_POINT ( 'NONE',  ( 19.05341960407611168, 5.049401038298154454, 78.95724293864769550 ) ) ;
#87603 = CARTESIAN_POINT ( 'NONE',  ( -35.00000000000000000, 3.181980515339468241, 1.110912703473986074 ) ) ;
#87605 = CARTESIAN_POINT ( 'NONE',  ( -23.48298174826590667, 32.32155151706776053, -0.3021577739498228499 ) ) ;
#87607 = CARTESIAN_POINT ( 'NONE',  ( -9.564922557960796823, -16.46253265017161027, 77.08224293864769550 ) ) ;
#87606 = CARTESIAN_POINT ( 'NONE',  ( 16.52544592524342804, -4.483927247898539470, 68.54057627198103830 ) ) ;
#87608 = CARTESIAN_POINT ( 'NONE',  ( 19.03943276465977164, -0.05219959533909143690, 78.74890960531436690 ) ) ;
#87609 = ORIENTED_EDGE ( 'NONE', *, *, #189313, .T. ) ;
#87610 = CARTESIAN_POINT ( 'NONE',  ( -13.97604488694547697, 13.89961937509957934, 93.12609039468566152 ) ) ;
#87611 = CARTESIAN_POINT ( 'NONE',  ( 15.72974639402199770, -15.80617190586745480, 58.12390960531435979 ) ) ;
#87612 = CARTESIAN_POINT ( 'NONE',  ( -0.05219959533909027116, -19.03943276465977164, 32.49890960531435979 ) ) ;
#87613 = CARTESIAN_POINT ( 'NONE',  ( 5.153800228976615827, -19.02544592524334988, 60.20942372801899012 ) ) ;
#87614 = CARTESIAN_POINT ( 'NONE',  ( 9.474510206698971260, -16.51473224551069308, 57.91557627198103120 ) ) ;
#87615 = CARTESIAN_POINT ( 'NONE',  ( 16.46253265017160672, -9.564922557960803928, 93.33224293864769550 ) ) ;
#87616 = VERTEX_POINT ( 'NONE', #143028 ) ;
#87617 = CARTESIAN_POINT ( 'NONE',  ( 21.53943276465977519, -0.05219959533907433946, 88.74890960531436690 ) ) ;
#87619 = CARTESIAN_POINT ( 'NONE',  ( -16.46253265017146816, -9.564922557961047289, 44.16775706135232582 ) ) ;
#87618 = CARTESIAN_POINT ( 'NONE',  ( -0.05219959533910754901, -16.53943276465976808, 92.49890960531436690 ) ) ;
#87620 = CARTESIAN_POINT ( 'NONE',  ( 0.05219959533907565091, 21.53943276465977519, 89.99890960531438111 ) ) ;
#87621 = CARTESIAN_POINT ( 'NONE',  ( -21.52544592524343514, 5.823673210054127303, 76.04057627198102409 ) ) ;
#87622 = CARTESIAN_POINT ( 'NONE',  ( -8.314922557960811034, -14.29746914071050412, 32.08224293864769550 ) ) ;
#87623 = CARTESIAN_POINT ( 'NONE',  ( 15.80617190586769283, -15.72974639402175789, 100.6260903946857184 ) ) ;
#87624 = CARTESIAN_POINT ( 'NONE',  ( 16.51473224551069308, 9.474510206698969483, 74.16557627198103830 ) ) ;
#87625 = CARTESIAN_POINT ( 'NONE',  ( 5.049401038298161559, -19.05341960407611168, 32.70724293864768129 ) ) ;
#87626 = CARTESIAN_POINT ( 'NONE',  ( -5.823673210054431948, 21.52544592524334988, 42.70942372801901854 ) ) ;
#87627 = CARTESIAN_POINT ( 'NONE',  ( 18.62759615963255655, 10.81492255796105972, 51.66775706135234714 ) ) ;
#87628 = CARTESIAN_POINT ( 'NONE',  ( 19.05341960407611168, 5.049401038298154454, 48.95724293864768129 ) ) ;
#87629 = CARTESIAN_POINT ( 'NONE',  ( 21.55341960407610458, 5.719274019375980345, 113.9572429386477239 ) ) ;
#87630 = CARTESIAN_POINT ( 'NONE',  ( -5.049401038297874678, -19.05341960407617918, 59.79275706135231871 ) ) ;
#87631 = CARTESIAN_POINT ( 'NONE',  ( -5.153800228976328057, -19.02544592524343514, 37.29057627198102409 ) ) ;
#87632 = CARTESIAN_POINT ( 'NONE',  ( -12.06949235617739369, -12.14591786802326823, 24.37609039468567573 ) ) ;
#87633 = CARTESIAN_POINT ( 'NONE',  ( 13.89961937509977652, -13.97604488694527269, 23.12390960531436335 ) ) ;
#87634 = CARTESIAN_POINT ( 'NONE',  ( 4.483927247898790824, -16.52544592524335698, 75.20942372801901854 ) ) ;
#87635 = CARTESIAN_POINT ( 'NONE',  ( -13.89961937509977652, 13.97604488694528158, 35.62390960531435269 ) ) ;
#87636 = CARTESIAN_POINT ( 'NONE',  ( 23.97133246043717136, -5.390759101651049434, 174.7603932261090733 ) ) ;
#87637 = CARTESIAN_POINT ( 'NONE',  ( 19.02544592524343514, -5.153800228976328945, 83.54057627198100988 ) ) ;
#87638 = CARTESIAN_POINT ( 'NONE',  ( 9.564922557960805705, 16.46253265017160317, 29.58224293864769550 ) ) ;
#87639 = CARTESIAN_POINT ( 'NONE',  ( -18.62759615963270932, 10.81492255796079327, 70.83224293864770971 ) ) ;
#87640 = CARTESIAN_POINT ( 'NONE',  ( 4.483927247898790824, -16.52544592524335698, 45.20942372801901854 ) ) ;
#87641 = CARTESIAN_POINT ( 'NONE',  ( 21.55341960407619695, -5.719274019375665929, 111.0427570613523613 ) ) ;
#87642 = CARTESIAN_POINT ( 'NONE',  ( 13.97604488694527802, 13.89961937509977652, 34.37390960531436690 ) ) ;
#87643 = CARTESIAN_POINT ( 'NONE',  ( 12.06949235617757843, -12.14591786802309237, 28.12390960531435979 ) ) ;
#87644 = CARTESIAN_POINT ( 'NONE',  ( 8.224510206698953496, -14.34966873604960469, 72.91557627198103830 ) ) ;
#87645 = CARTESIAN_POINT ( 'NONE',  ( -19.03943276465977164, 0.05219959533909376836, 61.24890960531436690 ) ) ;
#87646 = CARTESIAN_POINT ( 'NONE',  ( -19.03943276465977164, -0.05219959533935918106, 18.75109039468567218 ) ) ;
#87647 = CARTESIAN_POINT ( 'NONE',  ( -21.53943276465977519, -0.05219959533937600094, 18.75109039468568639 ) ) ;
#87648 = CARTESIAN_POINT ( 'NONE',  ( -16.46253265017160317, 9.564922557960807481, 85.83224293864769550 ) ) ;
#87649 = CARTESIAN_POINT ( 'NONE',  ( -5.719274019375665041, -21.55341960407619695, 79.79275706135236135 ) ) ;
#87650 = CARTESIAN_POINT ( 'NONE',  ( 14.29746914071037800, 8.314922557961029526, 61.66775706135235424 ) ) ;
#87651 = EDGE_CURVE ( 'NONE', #99459, #9532, #127859, .T. ) ;
#87652 = CARTESIAN_POINT ( 'NONE',  ( 13.97604488694527802, 13.89961937509977652, 104.3739096053143385 ) ) ;
#87653 = CARTESIAN_POINT ( 'NONE',  ( -14.34966873604960291, -8.224510206698953496, 31.66557627198102054 ) ) ;
#87654 = CARTESIAN_POINT ( 'NONE',  ( 5.049401038298161559, -19.05341960407611168, 27.70724293864769550 ) ) ;
#87655 = CARTESIAN_POINT ( 'NONE',  ( -4.379528057220086978, -16.55341960407618274, 49.79275706135234714 ) ) ;
#87656 = CARTESIAN_POINT ( 'NONE',  ( -16.52544592524342804, 4.483927247898546575, 51.04057627198103120 ) ) ;
#87657 = CARTESIAN_POINT ( 'NONE',  ( -12.06949235617739369, -12.14591786802326823, 99.37609039468568994 ) ) ;
#87658 = CARTESIAN_POINT ( 'NONE',  ( -9.564922557960796823, -16.46253265017161027, 112.0822429386476955 ) ) ;
#87659 = CARTESIAN_POINT ( 'NONE',  ( 15.80617190586746368, 15.72974639402197994, 34.37390960531435979 ) ) ;
#87660 = CARTESIAN_POINT ( 'NONE',  ( 18.62759615963255655, 10.81492255796105972, 111.6677570613523613 ) ) ;
#87661 = CARTESIAN_POINT ( 'NONE',  ( -16.53943276465976808, 0.05219959533911058130, 86.24890960531436690 ) ) ;
#87662 = CARTESIAN_POINT ( 'NONE',  ( -9.474510206698964154, 16.51473224551069663, 90.41557627198103830 ) ) ;
#87663 = ORIENTED_EDGE ( 'NONE', *, *, #34170, .F. ) ;
#87664 = CARTESIAN_POINT ( 'NONE',  ( -12.06949235617739369, -12.14591786802326823, 44.37609039468567573 ) ) ;
#87665 = CARTESIAN_POINT ( 'NONE',  ( 5.049401038298161559, -19.05341960407611168, 57.70724293864769550 ) ) ;
#87666 = PRESENTATION_STYLE_ASSIGNMENT (( #73526 ) ) ;
#87667 = CARTESIAN_POINT ( 'NONE',  ( 5.153800228976615827, -19.02544592524334988, 50.20942372801897591 ) ) ;
#87668 = CARTESIAN_POINT ( 'NONE',  ( 16.51473224551069308, 9.474510206698969483, 44.16557627198103120 ) ) ;
#87669 = CARTESIAN_POINT ( 'NONE',  ( 8.314922557961029526, -14.29746914071037800, 75.41775706135233293 ) ) ;
#87670 = CARTESIAN_POINT ( 'NONE',  ( -13.89961937509957401, -13.97604488694547875, 99.37609039468567573 ) ) ;
#87671 = CARTESIAN_POINT ( 'NONE',  ( -18.67979575497193778, 10.72451020669871902, 68.33442372801900433 ) ) ;
#87672 = CARTESIAN_POINT ( 'NONE',  ( 16.46253265017160672, -9.564922557960803928, 63.33224293864769550 ) ) ;
#87673 = CARTESIAN_POINT ( 'NONE',  ( -21.55341960407610458, -5.719274019375992779, 91.45724293864769550 ) ) ;
#87674 = CARTESIAN_POINT ( 'NONE',  ( 12.14591786802309770, 12.06949235617756955, 99.37390960531436690 ) ) ;
#87675 = CARTESIAN_POINT ( 'NONE',  ( -19.02544592524334988, -5.153800228976617603, 68.95942372801896170 ) ) ;
#87676 = CARTESIAN_POINT ( 'NONE',  ( -21.52544592524343514, 5.823673210054127303, 61.04057627198103120 ) ) ;
#87677 = CARTESIAN_POINT ( 'NONE',  ( 13.89961937509957401, 13.97604488694547697, 41.87609039468566152 ) ) ;
#87678 = CARTESIAN_POINT ( 'NONE',  ( 9.474510206698971260, -16.51473224551069308, 112.9155762719810383 ) ) ;
#87679 = CARTESIAN_POINT ( 'NONE',  ( -15.80617190586745835, -15.72974639402198527, 96.87390960531436690 ) ) ;
#87680 = CARTESIAN_POINT ( 'NONE',  ( -16.31925111598455658, 7.325300261831604764, 85.16424538967253000 ) ) ;
#87681 = CARTESIAN_POINT ( 'NONE',  ( 13.89961937509957401, 13.97604488694547697, 101.8760903946856331 ) ) ;
#87682 = CARTESIAN_POINT ( 'NONE',  ( 13.89961937509957579, 13.97604488694547520, 96.87609039468567573 ) ) ;
#87683 = CARTESIAN_POINT ( 'NONE',  ( -16.53943276465976808, -0.05219959533934237506, 23.75109039468567929 ) ) ;
#87684 = CARTESIAN_POINT ( 'NONE',  ( 5.049401038298161559, -19.05341960407611168, 52.70724293864767418 ) ) ;
#87685 = CARTESIAN_POINT ( 'NONE',  ( 13.97604488694527802, 13.89961937509977652, 104.3739096053143385 ) ) ;
#87686 = CARTESIAN_POINT ( 'NONE',  ( -5.719274019375978568, 21.55341960407610458, 90.20724293864770971 ) ) ;
#87687 = CARTESIAN_POINT ( 'NONE',  ( -21.55341960407619339, 5.719274019375674811, 73.54275706135234714 ) ) ;
#87689 = CARTESIAN_POINT ( 'NONE',  ( 19.02544592524334988, 5.153800228976608722, 26.45942372801899722 ) ) ;
#87688 = CARTESIAN_POINT ( 'NONE',  ( 16.55341960407618274, -4.379528057220086978, 26.04275706135235779 ) ) ;
#87690 = CARTESIAN_POINT ( 'NONE',  ( -14.29746914071049879, 8.314922557960819915, 30.83224293864770260 ) ) ;
#87691 = CARTESIAN_POINT ( 'NONE',  ( 0.05219959533907565091, 21.53943276465977519, 114.9989096053143669 ) ) ;
#87692 = CARTESIAN_POINT ( 'NONE',  ( -12.14591786802309592, -12.06949235617757132, 51.87390960531437401 ) ) ;
#87693 = CARTESIAN_POINT ( 'NONE',  ( 0.05219959533936267826, -19.03943276465977164, 95.00109039468567573 ) ) ;
#87694 = CARTESIAN_POINT ( 'NONE',  ( 19.02544592524334988, 5.153800228976608722, 61.45942372801900433 ) ) ;
#87695 = CARTESIAN_POINT ( 'NONE',  ( -10.72451020669870658, -18.67979575497194134, 64.58442372801900433 ) ) ;
#87696 = CARTESIAN_POINT ( 'NONE',  ( 16.51473224551083163, -9.474510206698727899, 45.83442372801900433 ) ) ;
#87697 = CARTESIAN_POINT ( 'NONE',  ( 19.02544592524343514, -5.153800228976328945, 23.54057627198102054 ) ) ;
#87698 = CARTESIAN_POINT ( 'NONE',  ( 5.719274019375991003, -21.55341960407610458, 37.70724293864769550 ) ) ;
#87699 = CARTESIAN_POINT ( 'NONE',  ( -4.379528057220328563, 16.55341960407611168, 55.20724293864770260 ) ) ;
#87700 = CARTESIAN_POINT ( 'NONE',  ( -16.46253265017146816, -9.564922557961047289, 19.16775706135233293 ) ) ;
#87701 = CARTESIAN_POINT ( 'NONE',  ( 12.14591786802327356, -12.06949235617739191, 70.62609039468567573 ) ) ;
#87702 = CARTESIAN_POINT ( 'NONE',  ( -16.53943276465976808, 0.05219959533911058130, 36.24890960531435979 ) ) ;
#87703 = CARTESIAN_POINT ( 'NONE',  ( -21.55341960407619339, 5.719274019375674811, 73.54275706135234714 ) ) ;
#87704 = CARTESIAN_POINT ( 'NONE',  ( -15.72974639402176322, -15.80617190586768395, 64.37609039468568994 ) ) ;
#87705 = CARTESIAN_POINT ( 'NONE',  ( -15.80617190586745835, -15.72974639402198527, 81.87390960531435269 ) ) ;
#87706 = CARTESIAN_POINT ( 'NONE',  ( -5.049401038298153566, 19.05341960407611168, 35.20724293864768839 ) ) ;
#87707 = CARTESIAN_POINT ( 'NONE',  ( 0.05219959533937995610, -21.53943276465977519, 45.00109039468568284 ) ) ;
#87708 = CARTESIAN_POINT ( 'NONE',  ( 9.474510206698971260, -16.51473224551069308, 22.91557627198102765 ) ) ;
#87709 = CARTESIAN_POINT ( 'NONE',  ( -13.89961937509977652, 13.97604488694528158, 35.62390960531435269 ) ) ;
#87710 = CARTESIAN_POINT ( 'NONE',  ( 8.224510206698953496, -14.34966873604960469, 97.91557627198103830 ) ) ;
#87711 = CARTESIAN_POINT ( 'NONE',  ( 16.51473224551069308, 9.474510206698969483, 79.16557627198103830 ) ) ;
#87712 = CARTESIAN_POINT ( 'NONE',  ( -14.34966873604960291, -8.224510206698953496, 36.66557627198103120 ) ) ;
#87713 = CARTESIAN_POINT ( 'NONE',  ( -12.06949235617756955, 12.14591786802309770, 95.62390960531436690 ) ) ;
#87714 = CARTESIAN_POINT ( 'NONE',  ( 10.81492255796078972, 18.62759615963270932, 64.58224293864769550 ) ) ;
#87715 = CARTESIAN_POINT ( 'NONE',  ( 18.67979575497178502, 10.72451020669898547, 109.1655762719810383 ) ) ;
#87716 = CARTESIAN_POINT ( 'NONE',  ( 5.153800228976335163, 19.02544592524342804, 114.7905762719810241 ) ) ;
#87717 = ADVANCED_FACE ( 'NONE', ( #35859 ), #173931, .T. ) ;
#87719 = CARTESIAN_POINT ( 'NONE',  ( -14.29746914071037622, -8.314922557961029526, 29.16775706135234003 ) ) ;
#87718 = CARTESIAN_POINT ( 'NONE',  ( -5.049401038298153566, 19.05341960407611168, 60.20724293864768129 ) ) ;
#87720 = CARTESIAN_POINT ( 'NONE',  ( 21.55341960407610458, 5.719274019375980345, 68.95724293864769550 ) ) ;
#87721 = CARTESIAN_POINT ( 'NONE',  ( -5.719274019375665041, -21.55341960407619695, 89.79275706135236135 ) ) ;
#87722 = CARTESIAN_POINT ( 'NONE',  ( -16.46253265017160317, 9.564922557960807481, 85.83224293864769550 ) ) ;
#87723 = CARTESIAN_POINT ( 'NONE',  ( -18.62759615963270932, 10.81492255796079327, 115.8322429386477097 ) ) ;
#87724 = CARTESIAN_POINT ( 'NONE',  ( -5.153800228976328057, -19.02544592524343514, 107.2905762719810383 ) ) ;
#87725 = CARTESIAN_POINT ( 'NONE',  ( -14.29746914071037622, -8.314922557961029526, 94.16775706135237556 ) ) ;
#87726 = CARTESIAN_POINT ( 'NONE',  ( 5.823673210054444382, -21.52544592524334988, 70.20942372801904696 ) ) ;
#87727 = CARTESIAN_POINT ( 'NONE',  ( 5.823673210054444382, -21.52544592524334988, 100.2094237280190043 ) ) ;
#87728 = CARTESIAN_POINT ( 'NONE',  ( -0.05219959533934338120, 16.53943276465976808, 62.50109039468568284 ) ) ;
#87729 = CARTESIAN_POINT ( 'NONE',  ( 15.80617190586769283, -15.72974639402175789, 30.62609039468567929 ) ) ;
#87730 = CARTESIAN_POINT ( 'NONE',  ( -13.97604488694527625, -13.89961937509977652, 111.8739096053143243 ) ) ;
#87731 = CARTESIAN_POINT ( 'NONE',  ( 10.72451020669871369, 18.67979575497193778, 87.08442372801901854 ) ) ;
#87732 = CARTESIAN_POINT ( 'NONE',  ( 0.05219959533909260263, 19.03943276465977164, 94.99890960531436690 ) ) ;
#87733 = CARTESIAN_POINT ( 'NONE',  ( 5.823673210054125526, 21.52544592524343514, 94.79057627198105251 ) ) ;
#87734 = CARTESIAN_POINT ( 'NONE',  ( 16.46253265017146816, 9.564922557961045513, 61.66775706135234003 ) ) ;
#87735 = CARTESIAN_POINT ( 'NONE',  ( 10.81492255796078972, 18.62759615963270932, 49.58224293864769550 ) ) ;
#87737 = CARTESIAN_POINT ( 'NONE',  ( 16.52544592524342804, -4.483927247898539470, 33.54057627198102409 ) ) ;
#87736 = CARTESIAN_POINT ( 'NONE',  ( 9.474510206698971260, -16.51473224551069308, 97.91557627198102409 ) ) ;
#87738 = CARTESIAN_POINT ( 'NONE',  ( 0.000000000000000000, 2.357898499370431722, -2.818925648462311528E-15 ) ) ;
#87739 = CARTESIAN_POINT ( 'NONE',  ( -5.153800228976607833, 19.02544592524334988, 77.70942372801900433 ) ) ;
#87740 = FACE_OUTER_BOUND ( 'NONE', #154124, .T. ) ;
#87741 = CARTESIAN_POINT ( 'NONE',  ( -9.474510206698720793, -16.51473224551083518, 109.5844237280190043 ) ) ;
#87742 = CARTESIAN_POINT ( 'NONE',  ( -5.823673210054116645, -21.52544592524344225, 82.29057627198103830 ) ) ;
#87743 = CARTESIAN_POINT ( 'NONE',  ( -14.34966873604960291, -8.224510206698953496, 66.66557627198102409 ) ) ;
#87744 = CARTESIAN_POINT ( 'NONE',  ( -16.53943276465976808, -0.05219959533934237506, 28.75109039468567929 ) ) ;
#87745 = CARTESIAN_POINT ( 'NONE',  ( -9.564922557960796823, -16.46253265017161027, 42.08224293864769550 ) ) ;
#87747 = CARTESIAN_POINT ( 'NONE',  ( 19.05341960407617918, -5.049401038297876454, 86.04275706135233293 ) ) ;
#87746 = CARTESIAN_POINT ( 'NONE',  ( -10.72451020669898014, 18.67979575497178502, 115.4155762719810241 ) ) ;
#87748 = CARTESIAN_POINT ( 'NONE',  ( 13.97604488694527802, 13.89961937509977652, 89.37390960531436690 ) ) ;
#87749 = CARTESIAN_POINT ( 'NONE',  ( 16.46253265017160672, -9.564922557960803928, 78.33224293864769550 ) ) ;
#87750 = CARTESIAN_POINT ( 'NONE',  ( -21.52544592524343514, 5.823673210054127303, 76.04057627198102409 ) ) ;
#87751 = CARTESIAN_POINT ( 'NONE',  ( -19.03943276465977164, 0.05219959533909376836, 51.24890960531436690 ) ) ;
#87752 = CARTESIAN_POINT ( 'NONE',  ( -24.35524355471601510, 29.14552502360113095, -7.999999999999998224 ) ) ;
#87753 = CARTESIAN_POINT ( 'NONE',  ( 12.06949235617757843, -12.14591786802309237, 58.12390960531435979 ) ) ;
#87754 = CARTESIAN_POINT ( 'NONE',  ( -16.46253265017160317, 9.564922557960807481, 85.83224293864769550 ) ) ;
#87755 = DIRECTION ( 'NONE',  ( 0.000000000000000000, 0.000000000000000000, -1.000000000000000000 ) ) ;
#87756 = CARTESIAN_POINT ( 'NONE',  ( -13.97604488694547697, 13.89961937509957934, 63.12609039468566152 ) ) ;
#87757 = CARTESIAN_POINT ( 'NONE',  ( -0.05219959533907301413, -21.53943276465977519, 72.49890960531435269 ) ) ;
#87758 = CARTESIAN_POINT ( 'NONE',  ( 5.153800228976615827, -19.02544592524334988, 35.20942372801899722 ) ) ;
#87759 = CARTESIAN_POINT ( 'NONE',  ( 19.02544592524343514, -5.153800228976328945, 103.5405762719809957 ) ) ;
#87760 = DIRECTION ( 'NONE',  ( -1.000000000000000000, 5.392603844284257652E-33, 0.000000000000000000 ) ) ;
#87761 = CARTESIAN_POINT ( 'NONE',  ( 21.53943276465977519, -0.05219959533907433946, 43.74890960531435979 ) ) ;
#87762 = CARTESIAN_POINT ( 'NONE',  ( 13.89961937509977652, -13.97604488694527269, 78.12390960531433848 ) ) ;
#87763 = CARTESIAN_POINT ( 'NONE',  ( 15.72974639402176855, 15.80617190586768217, 66.87609039468568994 ) ) ;
#87764 = CARTESIAN_POINT ( 'NONE',  ( 0.05219959533909260263, 19.03943276465977164, 24.99890960531435269 ) ) ;
#87766 = ORIENTED_EDGE ( 'NONE', *, *, #43996, .F. ) ;
#87765 = CARTESIAN_POINT ( 'NONE',  ( 21.53943276465977519, -0.05219959533907433946, 113.7489096053143527 ) ) ;
#87767 = CARTESIAN_POINT ( 'NONE',  ( 21.55341960407619695, -5.719274019375665929, 56.04275706135235424 ) ) ;
#87768 = ORIENTED_EDGE ( 'NONE', *, *, #111598, .F. ) ;
#87769 = DIRECTION ( 'NONE',  ( 1.000000000000000000, -0.000000000000000000, -0.000000000000000000 ) ) ;
#87770 = CARTESIAN_POINT ( 'NONE',  ( -9.474510206698720793, -16.51473224551083518, 69.58442372801901854 ) ) ;
#87771 = CIRCLE ( 'NONE', #123261, 23.10356920737165254 ) ;
#87772 = DIRECTION ( 'NONE',  ( 0.000000000000000000, 0.000000000000000000, -1.000000000000000000 ) ) ;
#87773 = CARTESIAN_POINT ( 'NONE',  ( 21.55341960407610458, 5.719274019375980345, 103.9572429386476813 ) ) ;
#87774 = CARTESIAN_POINT ( 'NONE',  ( -5.153800228976328057, -19.02544592524343514, 62.29057627198100988 ) ) ;
#87775 = CARTESIAN_POINT ( 'NONE',  ( 16.53943276465976808, 0.05219959533934440121, 36.25109039468567573 ) ) ;
#87776 = CARTESIAN_POINT ( 'NONE',  ( -30.74264578624800492, 22.33583958711400186, -9.949999994537627401 ) ) ;
#87777 = CARTESIAN_POINT ( 'NONE',  ( -0.05219959533937732626, 21.53943276465977519, 97.50109039468567573 ) ) ;
#87778 = CARTESIAN_POINT ( 'NONE',  ( -19.02544592524342804, 5.153800228976336051, 36.04057627198100988 ) ) ;
#87779 = CARTESIAN_POINT ( 'NONE',  ( 10.72451020669871369, 18.67979575497193778, 107.0844237280190043 ) ) ;
#87781 = CARTESIAN_POINT ( 'NONE',  ( -15.80617190586768217, 15.72974639402176855, 63.12609039468568994 ) ) ;
#87780 = CARTESIAN_POINT ( 'NONE',  ( 16.46253265017160672, -9.564922557960803928, 83.33224293864768129 ) ) ;
#87782 = CARTESIAN_POINT ( 'NONE',  ( -5.359611314223446995E-15, 29.16686587814335496, 148.8750000027311842 ) ) ;
#87783 = CARTESIAN_POINT ( 'NONE',  ( 13.89961937509977652, -13.97604488694527269, 108.1239096053143669 ) ) ;
#87784 = CARTESIAN_POINT ( 'NONE',  ( 22.99604614807110181, -21.49604614807103786, -46.28618945597792589 ) ) ;
#87786 = CARTESIAN_POINT ( 'NONE',  ( 21.53943276465977519, 0.05219959533937863772, 76.25109039468568994 ) ) ;
#87785 = CARTESIAN_POINT ( 'NONE',  ( 4.379528057220092307, 16.55341960407617563, 47.29275706135234003 ) ) ;
#87787 = CARTESIAN_POINT ( 'NONE',  ( -0.05219959533937732626, 21.53943276465977519, 87.50109039468568994 ) ) ;
#87788 = DIRECTION ( 'NONE',  ( 0.000000000000000000, 0.000000000000000000, -1.000000000000000000 ) ) ;
#87789 = CARTESIAN_POINT ( 'NONE',  ( 4.379528057220092307, 16.55341960407617563, 22.29275706135235069 ) ) ;
#87790 = CARTESIAN_POINT ( 'NONE',  ( 0.05219959533909260263, 19.03943276465977164, 84.99890960531436690 ) ) ;
#87791 = CARTESIAN_POINT ( 'NONE',  ( 5.049401038298161559, -19.05341960407611168, 112.7072429386476813 ) ) ;
#87792 = EDGE_LOOP ( 'NONE', ( #90131, #126341, #105868, #28880 ) ) ;
#87793 = DIRECTION ( 'NONE',  ( -0.000000000000000000, -0.000000000000000000, 1.000000000000000000 ) ) ;
#87794 = CARTESIAN_POINT ( 'NONE',  ( 0.05219959533910956823, 16.53943276465976808, 114.9989096053143669 ) ) ;
#87795 = CARTESIAN_POINT ( 'NONE',  ( -21.55341960407610458, -5.719274019375992779, 46.45724293864769550 ) ) ;
#87796 = CARTESIAN_POINT ( 'NONE',  ( 16.52544592524335698, 4.483927247898782831, 96.45942372801901854 ) ) ;
#87798 = CARTESIAN_POINT ( 'NONE',  ( -9.474510206698964154, 16.51473224551069663, 70.41557627198102409 ) ) ;
#87797 = CARTESIAN_POINT ( 'NONE',  ( -4.379528057220328563, 16.55341960407611168, 80.20724293864769550 ) ) ;
#87799 = CARTESIAN_POINT ( 'NONE',  ( -10.72451020669870658, -18.67979575497194134, 89.58442372801901854 ) ) ;
#87800 = CARTESIAN_POINT ( 'NONE',  ( -16.52544592524335698, -4.483927247898792601, 18.95942372801901143 ) ) ;
#87801 = CARTESIAN_POINT ( 'NONE',  ( 4.379528057220339221, -16.55341960407611168, 87.70724293864769550 ) ) ;
#87802 = CARTESIAN_POINT ( 'NONE',  ( -0.05219959533937732626, 21.53943276465977519, 42.50109039468567573 ) ) ;
#87803 = CARTESIAN_POINT ( 'NONE',  ( 10.81492255796078972, 18.62759615963270932, 79.58224293864769550 ) ) ;
#87804 = CARTESIAN_POINT ( 'NONE',  ( 19.05341960407617918, -5.049401038297876454, 41.04275706135233293 ) ) ;
#87805 = CARTESIAN_POINT ( 'NONE',  ( -5.049401038298153566, 19.05341960407611168, 45.20724293864769550 ) ) ;
#87806 = CARTESIAN_POINT ( 'NONE',  ( 16.51473224551069308, 9.474510206698969483, 79.16557627198103830 ) ) ;
#87807 = CARTESIAN_POINT ( 'NONE',  ( 4.483927247898545687, 16.52544592524342804, 59.79057627198103120 ) ) ;
#87808 = CARTESIAN_POINT ( 'NONE',  ( 8.224510206698953496, -14.34966873604960469, 37.91557627198102409 ) ) ;
#87809 = CARTESIAN_POINT ( 'NONE',  ( -16.53943276465976808, -0.05219959533934237506, 108.7510903946857042 ) ) ;
#87810 = CARTESIAN_POINT ( 'NONE',  ( 13.89961937509957401, 13.97604488694547697, 61.87609039468566863 ) ) ;
#87811 = CARTESIAN_POINT ( 'NONE',  ( 19.52851543214742946, 5.500000000000025757, 52.89357721762586095 ) ) ;
#87812 = CARTESIAN_POINT ( 'NONE',  ( 10.72451020669898902, -18.67979575497178502, 27.91557627198103830 ) ) ;
#87813 = CARTESIAN_POINT ( 'NONE',  ( -16.55341960407611168, -4.379528057220339221, 81.45724293864769550 ) ) ;
#87814 = CARTESIAN_POINT ( 'NONE',  ( 18.22780087662119897, -5.500000000000146549, 38.51763182126893525 ) ) ;
#87816 = CARTESIAN_POINT ( 'NONE',  ( -5.823673210054116645, -21.52544592524344225, 52.29057627198102409 ) ) ;
#87815 = CARTESIAN_POINT ( 'NONE',  ( -5.049401038298153566, 19.05341960407611168, 45.20724293864769550 ) ) ;
#87817 = CARTESIAN_POINT ( 'NONE',  ( 10.72451020669898902, -18.67979575497178502, 67.91557627198102409 ) ) ;
#87818 = CARTESIAN_POINT ( 'NONE',  ( -4.483927247898539470, -16.52544592524342804, 107.2905762719810525 ) ) ;
#87820 = CARTESIAN_POINT ( 'NONE',  ( -19.03943276465977164, 0.05219959533909376836, 41.24890960531435269 ) ) ;
#87819 = CARTESIAN_POINT ( 'NONE',  ( 8.314922557961029526, -14.29746914071037800, 60.41775706135235424 ) ) ;
#87821 = CARTESIAN_POINT ( 'NONE',  ( -18.62759615963255300, -10.81492255796106328, 59.16775706135234714 ) ) ;
#87822 = CARTESIAN_POINT ( 'NONE',  ( 8.224510206698953496, -14.34966873604960469, 107.9155762719810241 ) ) ;
#87823 = CARTESIAN_POINT ( 'NONE',  ( -13.89961937509957401, -13.97604488694547875, 84.37609039468567573 ) ) ;
#87824 = CARTESIAN_POINT ( 'NONE',  ( -29.86685920354755552, 21.69954338932564397, -7.324999997268814234 ) ) ;
#87826 = CARTESIAN_POINT ( 'NONE',  ( 21.52544592524344225, -5.823673210054117533, 43.54057627198103830 ) ) ;
#87825 = CARTESIAN_POINT ( 'NONE',  ( -23.64874990377915509, 15.04272038711346049, 165.8682408883346397 ) ) ;
#87827 = CARTESIAN_POINT ( 'NONE',  ( 19.02544592524343514, -5.153800228976328945, 28.54057627198102409 ) ) ;
#87828 = CARTESIAN_POINT ( 'NONE',  ( 0.05219959533937995610, -21.53943276465977519, 85.00109039468568994 ) ) ;
#87829 = CARTESIAN_POINT ( 'NONE',  ( 16.53943276465976808, -0.05219959533910856209, 33.74890960531436690 ) ) ;
#87831 = CARTESIAN_POINT ( 'NONE',  ( -16.53943276465976808, 0.05219959533911058130, 46.24890960531435979 ) ) ;
#87830 = CARTESIAN_POINT ( 'NONE',  ( 14.34966873604972726, -8.224510206698740333, 50.83442372801901143 ) ) ;
#87832 = CARTESIAN_POINT ( 'NONE',  ( 18.62759615963271287, -10.81492255796078972, 73.33224293864769550 ) ) ;
#87833 = CARTESIAN_POINT ( 'NONE',  ( -10.72451020669898014, 18.67979575497178502, 80.41557627198103830 ) ) ;
#87834 = CARTESIAN_POINT ( 'NONE',  ( 31.22300027783691334, -21.66299953960490043, -21.91126201009245023 ) ) ;
#87836 = CARTESIAN_POINT ( 'NONE',  ( -19.03943276465977164, 0.05219959533909376836, 116.2489096053143669 ) ) ;
#87835 = CARTESIAN_POINT ( 'NONE',  ( -5.049401038297874678, -19.05341960407617918, 89.79275706135230450 ) ) ;
#87837 = CARTESIAN_POINT ( 'NONE',  ( -19.02544592524342804, 5.153800228976336051, 46.04057627198101699 ) ) ;
#87838 = CARTESIAN_POINT ( 'NONE',  ( -4.379528057220328563, 16.55341960407611168, 115.2072429386476955 ) ) ;
#87839 = CARTESIAN_POINT ( 'NONE',  ( -3.573655867282028392E-15, 12.39993551617566681, 169.9999999999999716 ) ) ;
#87840 = ORIENTED_EDGE ( 'NONE', *, *, #134567, .T. ) ;
#87841 = CARTESIAN_POINT ( 'NONE',  ( 0.05219959533934541429, -16.53943276465976808, 80.00109039468568994 ) ) ;
#87842 = CARTESIAN_POINT ( 'NONE',  ( -5.719274019375978568, 21.55341960407610458, 110.2072429386477239 ) ) ;
#87843 = CARTESIAN_POINT ( 'NONE',  ( -0.05219959533909027116, -19.03943276465977164, 72.49890960531435269 ) ) ;
#87844 = CARTESIAN_POINT ( 'NONE',  ( -5.719274019375665041, -21.55341960407619695, 34.79275706135235424 ) ) ;
#87845 = CARTESIAN_POINT ( 'NONE',  ( -19.03943276465977164, 0.05219959533909376836, 101.2489096053143669 ) ) ;
#87846 = CARTESIAN_POINT ( 'NONE',  ( -21.53686564358551792, -33.52628202223520759, -20.57266355564332727 ) ) ;
#87847 = ORIENTED_EDGE ( 'NONE', *, *, #85455, .F. ) ;
#87848 = CARTESIAN_POINT ( 'NONE',  ( 18.62759615963255655, 10.81492255796105972, 26.66775706135235424 ) ) ;
#87850 = CARTESIAN_POINT ( 'NONE',  ( 5.049401038297881783, 19.05341960407617563, 87.29275706135234714 ) ) ;
#87849 = CARTESIAN_POINT ( 'NONE',  ( -5.049401038298153566, 19.05341960407611168, 25.20724293864768484 ) ) ;
#87851 = CARTESIAN_POINT ( 'NONE',  ( -19.05341960407617563, 5.049401038297882671, 38.54275706135233293 ) ) ;
#87852 = CARTESIAN_POINT ( 'NONE',  ( 21.52544592524344225, -5.823673210054117533, 108.5405762719810241 ) ) ;
#87853 = CARTESIAN_POINT ( 'NONE',  ( -13.89961937509957401, -13.97604488694547875, 39.37609039468566152 ) ) ;
#87854 = CARTESIAN_POINT ( 'NONE',  ( -5.049401038297874678, -19.05341960407617918, 49.79275706135231871 ) ) ;
#87855 = CARTESIAN_POINT ( 'NONE',  ( 12.06949235617739724, 12.14591786802326823, 91.87609039468568994 ) ) ;
#87857 = VERTEX_POINT ( 'NONE', #164218 ) ;
#87856 = LINE ( 'NONE', #74698, #60362 ) ;
#87858 = CARTESIAN_POINT ( 'NONE',  ( 19.05341960407611168, 5.049401038298154454, 68.95724293864769550 ) ) ;
#87859 = CARTESIAN_POINT ( 'NONE',  ( 5.823673210054444382, -21.52544592524334988, 75.20942372801901854 ) ) ;
#87860 = CARTESIAN_POINT ( 'NONE',  ( -21.55341960407619339, 5.719274019375674811, 93.54275706135234714 ) ) ;
#87861 = CARTESIAN_POINT ( 'NONE',  ( 17.50000000000000000, -5.499999999999992895, 66.21769037696435589 ) ) ;
#87862 = CARTESIAN_POINT ( 'NONE',  ( 19.05341960407611168, 5.049401038298154454, 88.95724293864769550 ) ) ;
#87863 = CARTESIAN_POINT ( 'NONE',  ( 0.05219959533937995610, -21.53943276465977519, 65.00109039468568994 ) ) ;
#87864 = CARTESIAN_POINT ( 'NONE',  ( 19.03943276465977164, 0.05219959533936151252, 96.25109039468567573 ) ) ;
#87865 = CARTESIAN_POINT ( 'NONE',  ( -16.46253265017160317, 9.564922557960807481, 60.83224293864769550 ) ) ;
#87866 = CARTESIAN_POINT ( 'NONE',  ( 5.049401038298161559, -19.05341960407611168, 112.7072429386476813 ) ) ;
#87867 = CARTESIAN_POINT ( 'NONE',  ( -9.474510206698964154, 16.51473224551069663, 75.41557627198103830 ) ) ;
#87868 = CARTESIAN_POINT ( 'NONE',  ( -17.13100169013300444, -6.664070546373141113, 89.23210164300155611 ) ) ;
#87869 = CARTESIAN_POINT ( 'NONE',  ( -9.474510206698964154, 16.51473224551069663, 65.41557627198102409 ) ) ;
#87870 = CARTESIAN_POINT ( 'NONE',  ( -0.05219959533909027116, -19.03943276465977164, 47.49890960531435979 ) ) ;
#87871 = CARTESIAN_POINT ( 'NONE',  ( 21.53943276465977519, 0.05219959533937863772, 21.25109039468567218 ) ) ;
#87872 = CARTESIAN_POINT ( 'NONE',  ( 8.224510206698742110, 14.34966873604972548, 97.08442372801904696 ) ) ;
#87873 = PLANE ( 'NONE',  #121146 ) ;
#87874 = DIRECTION ( 'NONE',  ( -0.5000000000000037748, -0.4999999999999950040, -0.7071067811865484609 ) ) ;
#87875 = CARTESIAN_POINT ( 'NONE',  ( -13.89961937509957401, -13.97604488694547875, 59.37609039468566863 ) ) ;
#87876 = CARTESIAN_POINT ( 'NONE',  ( 13.97604488694527802, 13.89961937509977652, 79.37390960531435269 ) ) ;
#87877 = CARTESIAN_POINT ( 'NONE',  ( 4.483927247898545687, 16.52544592524342804, 74.79057627198105251 ) ) ;
#87878 = CARTESIAN_POINT ( 'NONE',  ( 8.224510206698953496, -14.34966873604960469, 112.9155762719810383 ) ) ;
#87879 = CARTESIAN_POINT ( 'NONE',  ( -21.55341960407610458, -5.719274019375992779, 31.45724293864769550 ) ) ;
#87880 = CARTESIAN_POINT ( 'NONE',  ( 16.51473224551069308, 9.474510206698969483, 104.1655762719810241 ) ) ;
#87881 = CARTESIAN_POINT ( 'NONE',  ( 16.55341960407611168, 4.379528057220329451, 93.95724293864770971 ) ) ;
#87882 = CARTESIAN_POINT ( 'NONE',  ( 5.049401038298163336, -19.05341960407611168, 82.70724293864769550 ) ) ;
#87883 = CARTESIAN_POINT ( 'NONE',  ( 0.05219959533936267826, -19.03943276465977164, 30.00109039468566863 ) ) ;
#87884 = CARTESIAN_POINT ( 'NONE',  ( 8.224510206698742110, 14.34966873604972548, 112.0844237280190185 ) ) ;
#87886 = EDGE_CURVE ( 'NONE', #19028, #197049, #71136, .T. ) ;
#87885 = CARTESIAN_POINT ( 'NONE',  ( -13.97604488694527625, -13.89961937509977652, 86.87390960531436690 ) ) ;
#87887 = CARTESIAN_POINT ( 'NONE',  ( 10.72451020669871369, 18.67979575497193778, 47.08442372801901854 ) ) ;
#87888 = CARTESIAN_POINT ( 'NONE',  ( 15.72974639402199770, -15.80617190586745480, 38.12390960531436690 ) ) ;
#87890 = ORIENTED_EDGE ( 'NONE', *, *, #89537, .F. ) ;
#87889 = CARTESIAN_POINT ( 'NONE',  ( 18.67979575497194134, -10.72451020669871369, 25.83442372801901499 ) ) ;
#87891 = CARTESIAN_POINT ( 'NONE',  ( -10.72451020669898014, 18.67979575497178502, 65.41557627198102409 ) ) ;
#87892 = CARTESIAN_POINT ( 'NONE',  ( -14.34966873604960291, -8.224510206698953496, 91.66557627198103830 ) ) ;
#87893 = CARTESIAN_POINT ( 'NONE',  ( -5.049401038297874678, -19.05341960407617918, 54.79275706135234003 ) ) ;
#87894 = CARTESIAN_POINT ( 'NONE',  ( 13.89961937509977652, -13.97604488694527269, 33.12390960531434558 ) ) ;
#87895 = CARTESIAN_POINT ( 'NONE',  ( 9.474510206698971260, -16.51473224551069308, 97.91557627198102409 ) ) ;
#87896 = CARTESIAN_POINT ( 'NONE',  ( 13.97604488694527802, 13.89961937509977652, 94.37390960531436690 ) ) ;
#87897 = CARTESIAN_POINT ( 'NONE',  ( 5.153800228976335163, 19.02544592524342804, 24.79057627198102765 ) ) ;
#87898 = CARTESIAN_POINT ( 'NONE',  ( 14.34966873604960469, 8.224510206698951720, 29.16557627198103120 ) ) ;
#87899 = CARTESIAN_POINT ( 'NONE',  ( -8.224510206698735004, -14.34966873604973081, 39.58442372801901143 ) ) ;
#87900 = CARTESIAN_POINT ( 'NONE',  ( -21.53943276465977519, -0.05219959533937600094, 108.7510903946857042 ) ) ;
#87902 = CARTESIAN_POINT ( 'NONE',  ( 4.379528057220339221, -16.55341960407611168, 27.70724293864769905 ) ) ;
#87901 = CARTESIAN_POINT ( 'NONE',  ( -16.51473224551069308, -9.474510206698971260, 96.66557627198102409 ) ) ;
#87903 = CARTESIAN_POINT ( 'NONE',  ( 21.52544592524334988, 5.823673210054432836, 31.45942372801901854 ) ) ;
#87904 = CARTESIAN_POINT ( 'NONE',  ( 16.46253265017160672, -9.564922557960803928, 48.33224293864769550 ) ) ;
#87905 = CARTESIAN_POINT ( 'NONE',  ( -14.34966873604972548, 8.224510206698743886, 48.33442372801902565 ) ) ;
#87906 = CARTESIAN_POINT ( 'NONE',  ( -4.379528057220086978, -16.55341960407618274, 104.7927570613523898 ) ) ;
#87907 = CARTESIAN_POINT ( 'NONE',  ( 16.53943276465976808, 0.05219959533934440121, 96.25109039468568994 ) ) ;
#87908 = B_SPLINE_CURVE_WITH_KNOTS ( 'NONE', 3,
 ( #100449, #82264, #116625, #143956, #159118, #71126, #147974, #162129, #53957, #22623, #23625, #7432, #67120, #128778 ),
 .UNSPECIFIED., .F., .F.,
 ( 4, 2, 2, 2, 2, 2, 4 ),
 ( 6.009258394948636926E-18, 0.002470145813542335908, 0.004940291627084665745, 0.007410437440626995581, 0.008645510347398159198, 0.009263046800783741874, 0.009880583254169324550 ),
 .UNSPECIFIED. ) ;
#87909 = CARTESIAN_POINT ( 'NONE',  ( -13.89961937509957401, -13.97604488694547875, 109.3760903946856331 ) ) ;
#87910 = CARTESIAN_POINT ( 'NONE',  ( -13.97604488694527625, -13.89961937509977652, 36.87390960531436690 ) ) ;
#87911 = CARTESIAN_POINT ( 'NONE',  ( -16.53943276465976808, 0.05219959533911058130, 96.24890960531435269 ) ) ;
#87912 = CARTESIAN_POINT ( 'NONE',  ( 10.72451020669898902, -18.67979575497178502, 107.9155762719810241 ) ) ;
#87913 = CARTESIAN_POINT ( 'NONE',  ( -9.474510206698964154, 16.51473224551069663, 35.41557627198102409 ) ) ;
#87914 = CARTESIAN_POINT ( 'NONE',  ( 5.049401038298161559, -19.05341960407611168, 107.7072429386476955 ) ) ;
#87915 = CARTESIAN_POINT ( 'NONE',  ( 21.53943276465977519, 0.05219959533937863772, 31.25109039468568639 ) ) ;
#87916 = CARTESIAN_POINT ( 'NONE',  ( 193.3062444957835453, -155.7167183371837496, -23.00000000000000000 ) ) ;
#87917 = CARTESIAN_POINT ( 'NONE',  ( -9.564922557960796823, -16.46253265017161027, 102.0822429386477097 ) ) ;
#87918 = LINE ( 'NONE', #179968, #132615 ) ;
#87919 = CARTESIAN_POINT ( 'NONE',  ( -16.46253265017160317, 9.564922557960807481, 80.83224293864769550 ) ) ;
#87921 = CARTESIAN_POINT ( 'NONE',  ( -16.55341960407611168, -4.379528057220339221, 96.45724293864770971 ) ) ;
#87920 = CARTESIAN_POINT ( 'NONE',  ( 15.72974639402176855, 15.80617190586768217, 36.87609039468568994 ) ) ;
#87922 = CARTESIAN_POINT ( 'NONE',  ( 9.564922557960805705, 16.46253265017160317, 94.58224293864769550 ) ) ;
#87923 = CARTESIAN_POINT ( 'NONE',  ( 9.564922557961047289, -16.46253265017146816, 20.41775706135233293 ) ) ;
#87924 = CARTESIAN_POINT ( 'NONE',  ( -4.379528057220086978, -16.55341960407618274, 59.79275706135234714 ) ) ;
#87925 = CARTESIAN_POINT ( 'NONE',  ( -15.80617190586768217, 15.72974639402176855, 83.12609039468568994 ) ) ;
#87926 = CARTESIAN_POINT ( 'NONE',  ( 12.14591786802327356, -12.06949235617739191, 35.62609039468568994 ) ) ;
#87927 = CARTESIAN_POINT ( 'NONE',  ( 0.05219959533909260263, 19.03943276465977164, 79.99890960531436690 ) ) ;
#87928 = CARTESIAN_POINT ( 'NONE',  ( -13.97604488694547697, 13.89961937509957934, 98.12609039468566152 ) ) ;
#87929 = CARTESIAN_POINT ( 'NONE',  ( 4.483927247898790824, -16.52544592524335698, 75.20942372801901854 ) ) ;
#87930 = CARTESIAN_POINT ( 'NONE',  ( -18.67979575497193778, 10.72451020669871902, 113.3344237280190328 ) ) ;
#87931 = CARTESIAN_POINT ( 'NONE',  ( 13.89961937509957401, 13.97604488694547697, 91.87609039468567573 ) ) ;
#87932 = CARTESIAN_POINT ( 'NONE',  ( -16.51473224551069308, -9.474510206698971260, 61.66557627198103120 ) ) ;
#87933 = CARTESIAN_POINT ( 'NONE',  ( 18.62759615963271287, -10.81492255796078972, 83.33224293864769550 ) ) ;
#87935 = CARTESIAN_POINT ( 'NONE',  ( -5.049401038297874678, -19.05341960407617918, 89.79275706135230450 ) ) ;
#87934 = CARTESIAN_POINT ( 'NONE',  ( 12.14591786802309770, 12.06949235617756955, 89.37390960531435269 ) ) ;
#87936 = CARTESIAN_POINT ( 'NONE',  ( -12.14591786802326823, 12.06949235617739902, 58.12609039468568994 ) ) ;
#87937 = CARTESIAN_POINT ( 'NONE',  ( -18.56453257813363678, 5.500000000000053291, 80.99000423690688422 ) ) ;
#87938 = CARTESIAN_POINT ( 'NONE',  ( 16.46253265017146816, 9.564922557961045513, 61.66775706135234003 ) ) ;
#87939 = CARTESIAN_POINT ( 'NONE',  ( 0.05219959533910956823, 16.53943276465976808, 29.99890960531435979 ) ) ;
#87940 = CARTESIAN_POINT ( 'NONE',  ( -12.06949235617756955, 12.14591786802309770, 80.62390960531438111 ) ) ;
#87941 = CARTESIAN_POINT ( 'NONE',  ( 16.46253265017146816, 9.564922557961045513, 21.66775706135233648 ) ) ;
#87942 = CARTESIAN_POINT ( 'NONE',  ( -10.81492255796105439, 18.62759615963255655, 22.91775706135235069 ) ) ;
#87943 = CARTESIAN_POINT ( 'NONE',  ( -19.03943276465977164, 0.05219959533909376836, 96.24890960531436690 ) ) ;
#87944 = CARTESIAN_POINT ( 'NONE',  ( -19.02544592524342804, 5.153800228976336051, 76.04057627198102409 ) ) ;
#87945 = CARTESIAN_POINT ( 'NONE',  ( 15.80617190586769283, -15.72974639402175789, 90.62609039468567573 ) ) ;
#87946 = CARTESIAN_POINT ( 'NONE',  ( -13.89961937509977652, 13.97604488694528158, 60.62390960531436690 ) ) ;
#87947 = ORIENTED_EDGE ( 'NONE', *, *, #131422, .F. ) ;
#87948 = CARTESIAN_POINT ( 'NONE',  ( -15.80617190586745835, -15.72974639402198527, 31.87390960531435979 ) ) ;
#87949 = CARTESIAN_POINT ( 'NONE',  ( -16.55341960407611168, -4.379528057220339221, 81.45724293864769550 ) ) ;
#87950 = CARTESIAN_POINT ( 'NONE',  ( 19.03943276465977164, -0.05219959533909143690, 43.74890960531435979 ) ) ;
#87951 = CARTESIAN_POINT ( 'NONE',  ( 16.55341960407611168, 4.379528057220329451, 93.95724293864770971 ) ) ;
#87952 = CARTESIAN_POINT ( 'NONE',  ( -10.81492255796078084, -18.62759615963271287, 112.0822429386477097 ) ) ;
#87953 = CARTESIAN_POINT ( 'NONE',  ( 10.81492255796106328, -18.62759615963255655, 65.41775706135234714 ) ) ;
#87954 = CARTESIAN_POINT ( 'NONE',  ( -16.51473224551069308, -9.474510206698971260, 26.66557627198103120 ) ) ;
#87955 = EDGE_CURVE ( 'NONE', #133509, #101645, #192549, .T. ) ;
#87956 = CARTESIAN_POINT ( 'NONE',  ( -14.34966873604972548, 8.224510206698743886, 63.33442372801900433 ) ) ;
#87957 = CARTESIAN_POINT ( 'NONE',  ( 0.05219959533907565091, 21.53943276465977519, 99.99890960531436690 ) ) ;
#87958 = CARTESIAN_POINT ( 'NONE',  ( -15.72974639402176322, -15.80617190586768395, 19.37609039468568639 ) ) ;
#87960 = CARTESIAN_POINT ( 'NONE',  ( 13.89961937509977652, -13.97604488694527269, 48.12390960531435979 ) ) ;
#87959 = CARTESIAN_POINT ( 'NONE',  ( -19.03943276465977164, -0.05219959533935918106, 43.75109039468566863 ) ) ;
#87961 = CARTESIAN_POINT ( 'NONE',  ( -9.474510206698964154, 16.51473224551069663, 115.4155762719810241 ) ) ;
#87962 = CARTESIAN_POINT ( 'NONE',  ( 18.67979575497194134, -10.72451020669871369, 55.83442372801901854 ) ) ;
#87963 = CARTESIAN_POINT ( 'NONE',  ( -5.823673210054116645, -21.52544592524344225, 57.29057627198103120 ) ) ;
#87964 = CARTESIAN_POINT ( 'NONE',  ( 4.483927247898545687, 16.52544592524342804, 34.79057627198103120 ) ) ;
#87966 = CARTESIAN_POINT ( 'NONE',  ( -15.72974639402176322, -15.80617190586768395, 104.3760903946856899 ) ) ;
#87965 = CARTESIAN_POINT ( 'NONE',  ( 0.05219959533937995610, -21.53943276465977519, 80.00109039468568994 ) ) ;
#87967 = CARTESIAN_POINT ( 'NONE',  ( 14.34966873604960469, 8.224510206698951720, 59.16557627198103120 ) ) ;
#87968 = CARTESIAN_POINT ( 'NONE',  ( -4.379528057220328563, 16.55341960407611168, 105.2072429386477097 ) ) ;
#87969 = CARTESIAN_POINT ( 'NONE',  ( 0.05219959533936267826, -19.03943276465977164, 40.00109039468566152 ) ) ;
#87970 = CARTESIAN_POINT ( 'NONE',  ( -16.52544592524335698, -4.483927247898792601, 98.95942372801903275 ) ) ;
#87971 = CARTESIAN_POINT ( 'NONE',  ( 21.55341960407619695, -5.719274019375665929, 66.04275706135236135 ) ) ;
#87972 = CARTESIAN_POINT ( 'NONE',  ( -5.049401038298153566, 19.05341960407611168, 65.20724293864765286 ) ) ;
#87973 = CARTESIAN_POINT ( 'NONE',  ( 19.05341960407617918, -5.049401038297876454, 36.04275706135234003 ) ) ;
#87974 = CARTESIAN_POINT ( 'NONE',  ( 18.67979575497178502, 10.72451020669898547, 34.16557627198102409 ) ) ;
#87975 = CARTESIAN_POINT ( 'NONE',  ( 5.719274019375673035, 21.55341960407619339, 32.29275706135235424 ) ) ;
#87976 = CARTESIAN_POINT ( 'NONE',  ( 18.67979575497178502, 10.72451020669898547, 94.16557627198103830 ) ) ;
#87977 = CARTESIAN_POINT ( 'NONE',  ( 0.05219959533936267826, -19.03943276465977164, 85.00109039468567573 ) ) ;
#87978 = CARTESIAN_POINT ( 'NONE',  ( 12.14591786802327356, -12.06949235617739191, 55.62609039468568284 ) ) ;
#87980 = CARTESIAN_POINT ( 'NONE',  ( -10.81492255796078084, -18.62759615963271287, 97.08224293864770971 ) ) ;
#87979 = CARTESIAN_POINT ( 'NONE',  ( -7.500000000000000000, 0.000000000000000000, 0.000000000000000000 ) ) ;
#87981 = CARTESIAN_POINT ( 'NONE',  ( 12.14591786802309770, 12.06949235617756955, 79.37390960531436690 ) ) ;
#87982 = CARTESIAN_POINT ( 'NONE',  ( 1.499999999999985123, 30.56208168264224412, -47.53402626646857954 ) ) ;
#87983 = CARTESIAN_POINT ( 'NONE',  ( -4.483927247898782831, 16.52544592524335698, 27.70942372801901854 ) ) ;
#87984 = CARTESIAN_POINT ( 'NONE',  ( -18.67979575497178146, -10.72451020669898902, 41.66557627198103120 ) ) ;
#87985 = CARTESIAN_POINT ( 'NONE',  ( -12.06949235617739369, -12.14591786802326823, 79.37609039468567573 ) ) ;
#87986 = DIRECTION ( 'NONE',  ( -0.000000000000000000, -0.000000000000000000, -1.000000000000000000 ) ) ;
#87987 = CARTESIAN_POINT ( 'NONE',  ( -4.483927247898782831, 16.52544592524335698, 52.70942372801902565 ) ) ;
#87988 = CARTESIAN_POINT ( 'NONE',  ( 18.67979575497194134, -10.72451020669871369, 20.83442372801901143 ) ) ;
#87989 = CARTESIAN_POINT ( 'NONE',  ( -5.823673210054116645, -21.52544592524344225, 47.29057627198103120 ) ) ;
#87990 = CARTESIAN_POINT ( 'NONE',  ( 8.224510206698742110, 14.34966873604972548, 77.08442372801901854 ) ) ;
#87991 = CARTESIAN_POINT ( 'NONE',  ( 16.51473224551069308, 9.474510206698969483, 84.16557627198102409 ) ) ;
#87993 = CARTESIAN_POINT ( 'NONE',  ( 9.564922557960805705, 16.46253265017160317, 24.58224293864769194 ) ) ;
#87992 = CARTESIAN_POINT ( 'NONE',  ( 21.53943276465977519, 0.05219959533937863772, 51.25109039468568994 ) ) ;
#87994 = CARTESIAN_POINT ( 'NONE',  ( 21.52544592524344225, -5.823673210054117533, 38.54057627198103120 ) ) ;
#87995 = CARTESIAN_POINT ( 'NONE',  ( 5.719274019375991003, -21.55341960407610458, 22.70724293864769194 ) ) ;
#87996 = EDGE_LOOP ( 'NONE', ( #62706, #169589, #103661, #38623, #199402, #155209, #69693, #49053 ) ) ;
#87997 = CARTESIAN_POINT ( 'NONE',  ( -5.153800228976607833, 19.02544592524334988, 37.70942372801899722 ) ) ;
#87998 = CARTESIAN_POINT ( 'NONE',  ( -8.224510206698735004, -14.34966873604973081, 49.58442372801901143 ) ) ;
#87999 = CARTESIAN_POINT ( 'NONE',  ( 19.02544592524343514, -5.153800228976328945, 108.5405762719810383 ) ) ;
#88000 = ORIENTED_EDGE ( 'NONE', *, *, #69759, .F. ) ;
#88001 = CARTESIAN_POINT ( 'NONE',  ( -16.46253265017160317, 9.564922557960807481, 90.83224293864769550 ) ) ;
#88002 = CARTESIAN_POINT ( 'NONE',  ( 12.06949235617739724, 12.14591786802326823, 101.8760903946857042 ) ) ;
#88003 = SPHERICAL_SURFACE ( 'NONE', #44030, 8.000000000000000000 ) ;
#88004 = CARTESIAN_POINT ( 'NONE',  ( 16.55341960407611168, 4.379528057220329451, 88.95724293864769550 ) ) ;
#88005 = CARTESIAN_POINT ( 'NONE',  ( -18.67979575497178146, -10.72451020669898902, 51.66557627198102409 ) ) ;
#88006 = CARTESIAN_POINT ( 'NONE',  ( 13.89961937509977652, -13.97604488694527269, 28.12390960531435624 ) ) ;
#88007 = CARTESIAN_POINT ( 'NONE',  ( -16.53943276465976808, -0.05219959533934237506, 73.75109039468567573 ) ) ;
#88008 = CARTESIAN_POINT ( 'NONE',  ( -15.72974639402197994, 15.80617190586746368, 115.6239096053143669 ) ) ;
#88009 = CARTESIAN_POINT ( 'NONE',  ( -13.89961937509957401, -13.97604488694547875, 79.37609039468567573 ) ) ;
#88010 = CARTESIAN_POINT ( 'NONE',  ( 9.564922557960805705, 16.46253265017160317, 34.58224293864770260 ) ) ;
#88011 = CARTESIAN_POINT ( 'NONE',  ( -16.46253265017160317, 9.564922557960807481, 110.8322429386476955 ) ) ;
#88012 = CARTESIAN_POINT ( 'NONE',  ( -15.80617190586768217, 15.72974639402176855, 108.1260903946856757 ) ) ;
#88013 = CARTESIAN_POINT ( 'NONE',  ( -13.89961937509977652, 13.97604488694528158, 70.62390960531432427 ) ) ;
#88014 = CARTESIAN_POINT ( 'NONE',  ( 0.05219959533934541429, -16.53943276465976808, 50.00109039468568994 ) ) ;
#88015 = CARTESIAN_POINT ( 'NONE',  ( -18.67979575497193778, 10.72451020669871902, 88.33442372801901854 ) ) ;
#88016 = CARTESIAN_POINT ( 'NONE',  ( -5.153800228976607833, 19.02544592524334988, 47.70942372801900433 ) ) ;
#88017 = CARTESIAN_POINT ( 'NONE',  ( -16.51473224551082808, 9.474510206698731452, 58.33442372801900433 ) ) ;
#88018 = ORIENTED_EDGE ( 'NONE', *, *, #66474, .F. ) ;
#88019 = CARTESIAN_POINT ( 'NONE',  ( -5.719274019375665041, -21.55341960407619695, 54.79275706135235424 ) ) ;
#88020 = CARTESIAN_POINT ( 'NONE',  ( -19.03943276465977164, 0.05219959533909376836, 21.24890960531436335 ) ) ;
#88021 = CARTESIAN_POINT ( 'NONE',  ( -16.46253265017146816, -9.564922557961047289, 44.16775706135232582 ) ) ;
#88022 = CARTESIAN_POINT ( 'NONE',  ( -16.46253265017160317, 9.564922557960807481, 95.83224293864769550 ) ) ;
#88023 = CARTESIAN_POINT ( 'NONE',  ( -13.97604488694527625, -13.89961937509977652, 86.87390960531436690 ) ) ;
#88024 = CARTESIAN_POINT ( 'NONE',  ( -8.314922557960811034, -14.29746914071050412, 42.08224293864769550 ) ) ;
#88025 = CARTESIAN_POINT ( 'NONE',  ( -21.55341960407610458, -5.719274019375992779, 31.45724293864769550 ) ) ;
#88026 = CARTESIAN_POINT ( 'NONE',  ( -22.94331271462295163, 0.000000000000000000, 190.0000000000000000 ) ) ;
#88027 = CARTESIAN_POINT ( 'NONE',  ( 22.55670631985092811, 22.55670631985084640, -49.13275782002545355 ) ) ;
#88028 = CARTESIAN_POINT ( 'NONE',  ( 5.719274019375673035, 21.55341960407619339, 107.2927570613523471 ) ) ;
#88029 = LINE ( 'NONE', #149717, #115475 ) ;
#88030 = CARTESIAN_POINT ( 'NONE',  ( 16.51473224551069308, 9.474510206698969483, 39.16557627198103120 ) ) ;
#88031 = CARTESIAN_POINT ( 'NONE',  ( -9.474510206698964154, 16.51473224551069663, 85.41557627198102409 ) ) ;
#88032 = CARTESIAN_POINT ( 'NONE',  ( -17.60728821186568283, 5.500000000000041744, 80.86690927743008217 ) ) ;
#88033 = CARTESIAN_POINT ( 'NONE',  ( -25.76063610039751595, -27.36442781147108150, -7.999999999999992895 ) ) ;
#88034 = CARTESIAN_POINT ( 'NONE',  ( -8.224510206698735004, -14.34966873604973081, 59.58442372801901854 ) ) ;
#88035 = CARTESIAN_POINT ( 'NONE',  ( 15.80617190586746368, 15.72974639402197994, 89.37390960531435269 ) ) ;
#88036 = CARTESIAN_POINT ( 'NONE',  ( -14.34966873604960291, -8.224510206698953496, 56.66557627198103830 ) ) ;
#88038 = CARTESIAN_POINT ( 'NONE',  ( -0.05219959533909027116, -19.03943276465977164, 112.4989096053143669 ) ) ;
#88037 = CARTESIAN_POINT ( 'NONE',  ( -9.564922557960796823, -16.46253265017161027, 22.08224293864768839 ) ) ;
#88039 = CARTESIAN_POINT ( 'NONE',  ( -10.81492255796105439, 18.62759615963255655, 22.91775706135235069 ) ) ;
#88040 = CARTESIAN_POINT ( 'NONE',  ( 13.89961937509957401, 13.97604488694547697, 36.87609039468565442 ) ) ;
#88041 = CARTESIAN_POINT ( 'NONE',  ( 19.03943276465977164, -0.05219959533909143690, 38.74890960531436690 ) ) ;
#88042 = CARTESIAN_POINT ( 'NONE',  ( -21.53943276465977519, -0.05219959533937600094, 78.75109039468568994 ) ) ;
#88043 = CARTESIAN_POINT ( 'NONE',  ( 16.29526858892873165, -7.335722546920260712, 31.70329402199793734 ) ) ;
#88044 = CARTESIAN_POINT ( 'NONE',  ( 14.34966873604960469, 8.224510206698951720, 24.16557627198103120 ) ) ;
#88045 = CARTESIAN_POINT ( 'NONE',  ( 17.50000000000000000, -5.499999999999992895, 101.2176903769643559 ) ) ;
#88046 = CARTESIAN_POINT ( 'NONE',  ( -18.67979575497178146, -10.72451020669898902, 46.66557627198102409 ) ) ;
#88047 = CARTESIAN_POINT ( 'NONE',  ( -16.53943276465976808, 0.05219959533911058130, 101.2489096053143669 ) ) ;
#88048 = CARTESIAN_POINT ( 'NONE',  ( -18.09867054820433907, -5.499999999999827693, 38.98393025253586330 ) ) ;
#88049 = CARTESIAN_POINT ( 'NONE',  ( -9.474510206698964154, 16.51473224551069663, 85.41557627198102409 ) ) ;
#88050 = CARTESIAN_POINT ( 'NONE',  ( 16.53943276465976808, -0.05219959533910856209, 73.74890960531433848 ) ) ;
#88051 = CARTESIAN_POINT ( 'NONE',  ( -9.564922557961040184, 16.46253265017147172, 107.9177570613523471 ) ) ;
#88052 = CARTESIAN_POINT ( 'NONE',  ( 21.53943276465977519, -0.05219959533907433946, 58.74890960531436690 ) ) ;
#88053 = ORIENTED_EDGE ( 'NONE', *, *, #42790, .F. ) ;
#88054 = CARTESIAN_POINT ( 'NONE',  ( -0.05219959533909027116, -19.03943276465977164, 32.49890960531435979 ) ) ;
#88055 = ADVANCED_FACE ( 'NONE', ( #149046 ), #893, .T. ) ;
#88057 = CARTESIAN_POINT ( 'NONE',  ( 21.55341960407610458, 5.719274019375980345, 88.95724293864769550 ) ) ;
#88056 = CARTESIAN_POINT ( 'NONE',  ( -13.97604488694527625, -13.89961937509977652, 91.87390960531432427 ) ) ;
#88059 = CARTESIAN_POINT ( 'NONE',  ( 19.03943276465977164, -0.05219959533909143690, 93.74890960531435269 ) ) ;
#88058 = CARTESIAN_POINT ( 'NONE',  ( -0.05219959533934338120, 16.53943276465976808, 102.5010903946856899 ) ) ;
#88060 = CARTESIAN_POINT ( 'NONE',  ( -16.46253265017146816, -9.564922557961047289, 84.16775706135233293 ) ) ;
#88061 = CARTESIAN_POINT ( 'NONE',  ( 5.823673210054444382, -21.52544592524334988, 100.2094237280190043 ) ) ;
#88062 = CARTESIAN_POINT ( 'NONE',  ( 21.53943276465977519, -0.05219959533907433946, 73.74890960531433848 ) ) ;
#88063 = CARTESIAN_POINT ( 'NONE',  ( 5.719274019375991003, -21.55341960407610458, 42.70724293864770260 ) ) ;
#88064 = CARTESIAN_POINT ( 'NONE',  ( 9.564922557960805705, 16.46253265017160317, 44.58224293864769550 ) ) ;
#88065 = CARTESIAN_POINT ( 'NONE',  ( -4.483927247898539470, -16.52544592524342804, 22.29057627198102765 ) ) ;
#88066 = CARTESIAN_POINT ( 'NONE',  ( 5.049401038298161559, -19.05341960407611168, 62.70724293864769550 ) ) ;
#88067 = ORIENTED_EDGE ( 'NONE', *, *, #95479, .T. ) ;
#88068 = CARTESIAN_POINT ( 'NONE',  ( -31.33613174426653458, -7.485780765379336010, 94.47638157584334806 ) ) ;
#88069 = CARTESIAN_POINT ( 'NONE',  ( -19.03943276465977164, -0.05219959533935918106, 33.75109039468566863 ) ) ;
#88070 = CARTESIAN_POINT ( 'NONE',  ( 0.05219959533910956823, 16.53943276465976808, 74.99890960531435269 ) ) ;
#88071 =( BOUNDED_CURVE ( )  B_SPLINE_CURVE ( 2, ( #8680, #113832, #98663, #70352, #189713, #160357, #21847, #101675, #131007, #54182, #132019, #83498, #115855 ),
 .UNSPECIFIED., .F., .F. ) 
 B_SPLINE_CURVE_WITH_KNOTS ( ( 3, 2, 2, 2, 2, 2, 3 ),
 ( 0.6340550636175563692, 0.6359649122807017330, 0.6403508771929824483, 0.6447368421052631637, 0.6491228070175438791, 0.6535087719298245945, 0.6554643004150603192 ),
 .UNSPECIFIED. ) 
 CURVE ( )  GEOMETRIC_REPRESENTATION_ITEM ( )  RATIONAL_B_SPLINE_CURVE ( ( 0.9832469066685285419, 0.9851625545550100060, 1.000000000000000000, 0.9659258262890683122, 1.000000000000000000, 0.9659258262890683122, 1.000000000000000000, 0.9659258262890683122, 1.000000000000000000, 0.9659258262890683122, 1.000000000000000000, 0.9848076720550078544, 0.9831626618144001517 ) ) 
 REPRESENTATION_ITEM ( '' )  );
#88072 = CARTESIAN_POINT ( 'NONE',  ( -15.72974639402176322, -15.80617190586768395, 29.37609039468568284 ) ) ;
#88073 = CARTESIAN_POINT ( 'NONE',  ( -6.863278975470372245, 5.170161995863669979, -64.06628402976478753 ) ) ;
#88074 = CARTESIAN_POINT ( 'NONE',  ( 18.62759615963271287, -10.81492255796078972, 53.33224293864769550 ) ) ;
#88075 = CARTESIAN_POINT ( 'NONE',  ( -16.53943276465976808, -0.05219959533934237506, 98.75109039468568994 ) ) ;
#88076 = CARTESIAN_POINT ( 'NONE',  ( -12.14591786802309592, -12.06949235617757132, 101.8739096053143811 ) ) ;
#88077 = CARTESIAN_POINT ( 'NONE',  ( 9.474510206698971260, -16.51473224551069308, 67.91557627198102409 ) ) ;
#88078 = SURFACE_STYLE_FILL_AREA ( #91043 ) ;
#88079 = CARTESIAN_POINT ( 'NONE',  ( 16.55341960407611168, 4.379528057220329451, 23.95724293864769550 ) ) ;
#88080 = CARTESIAN_POINT ( 'NONE',  ( -0.05219959533937732626, 21.53943276465977519, 47.50109039468568994 ) ) ;
#88081 = CARTESIAN_POINT ( 'NONE',  ( 13.97604488694527802, 13.89961937509977652, 114.3739096053143669 ) ) ;
#88082 = CARTESIAN_POINT ( 'NONE',  ( -5.719274019375665041, -21.55341960407619695, 74.79275706135234714 ) ) ;
#88083 = CARTESIAN_POINT ( 'NONE',  ( -0.05219959533909027116, -19.03943276465977164, 32.49890960531435979 ) ) ;
#88084 = CARTESIAN_POINT ( 'NONE',  ( -9.564922557960796823, -16.46253265017161027, 37.08224293864768839 ) ) ;
#88085 = VERTEX_POINT ( 'NONE', #80842 ) ;
#88086 = CARTESIAN_POINT ( 'NONE',  ( 18.67979575497194134, -10.72451020669871369, 95.83442372801903275 ) ) ;
#88087 = CARTESIAN_POINT ( 'NONE',  ( -8.224510206698735004, -14.34966873604973081, 49.58442372801901143 ) ) ;
#88088 = CARTESIAN_POINT ( 'NONE',  ( 5.719274019375673035, 21.55341960407619339, 72.29275706135236135 ) ) ;
#88089 = CARTESIAN_POINT ( 'NONE',  ( -0.05219959533909027116, -19.03943276465977164, 97.49890960531436690 ) ) ;
#88090 = CARTESIAN_POINT ( 'NONE',  ( -19.02544592524334988, -5.153800228976617603, 78.95942372801900433 ) ) ;
#88091 = CARTESIAN_POINT ( 'NONE',  ( -10.81492255796105439, 18.62759615963255655, 52.91775706135235424 ) ) ;
#88092 = CARTESIAN_POINT ( 'NONE',  ( 16.46253265017146816, 9.564922557961045513, 111.6677570613523329 ) ) ;
#88093 = CARTESIAN_POINT ( 'NONE',  ( 13.89961937509957401, 13.97604488694547697, 86.87609039468567573 ) ) ;
#88094 = CARTESIAN_POINT ( 'NONE',  ( 19.03943276465977164, -0.05219959533909143690, 53.74890960531436690 ) ) ;
#88095 = CARTESIAN_POINT ( 'NONE',  ( -9.564922557961040184, 16.46253265017147172, 77.91775706135234714 ) ) ;
#88096 = CARTESIAN_POINT ( 'NONE',  ( 16.53943276465976808, -0.05219959533910856209, 28.74890960531435624 ) ) ;
#88097 = CARTESIAN_POINT ( 'NONE',  ( 19.02544592524334988, 5.153800228976608722, 91.45942372801900433 ) ) ;
#88098 = CARTESIAN_POINT ( 'NONE',  ( -16.55341960407611168, -4.379528057220339221, 41.45724293864769550 ) ) ;
#88100 = B_SPLINE_CURVE_WITH_KNOTS ( 'NONE', 3,
 ( #138542, #135591, #120394, #107205, #198244, #76872, #185056, #59717, #121389, #183081, #106219, #167903, #29403, #199237, #169885, #108204, #91033, #14210, #109201, #51509, #2022, #21168, #191022, #3019, #33363, #64696, #170880, #171874, #95022, #67669, #66673, #174859 ),
 .UNSPECIFIED., .F., .F.,
 ( 4, 2, 2, 2, 2, 2, 2, 2, 2, 2, 2, 2, 2, 2, 2, 4 ),
 ( 2.539163526713095107E-17, 0.0003712461730036967526, 0.0007424923460073681349, 0.001113738519011039626, 0.001484984692014710899, 0.002227477038022051929, 0.002598723211025729708, 0.002969969384029407054, 0.003341215557033084399, 0.003712461730036761744, 0.004083707903040438222, 0.004454954076044116001, 0.004826200249047792913, 0.005197446422051470692, 0.005568692595055147604, 0.005939938768058825383 ),
 .UNSPECIFIED. ) ;
#88099 = CARTESIAN_POINT ( 'NONE',  ( -5.153800228976607833, 19.02544592524334988, 62.70942372801899722 ) ) ;
#88101 = CARTESIAN_POINT ( 'NONE',  ( -16.53943276465976808, -0.05219959533934237506, 53.75109039468568994 ) ) ;
#88102 = CARTESIAN_POINT ( 'NONE',  ( -13.97604488694547697, 13.89961937509957934, 23.12609039468565442 ) ) ;
#88103 = CARTESIAN_POINT ( 'NONE',  ( 16.46253265017160672, -9.564922557960803928, 23.33224293864769194 ) ) ;
#88104 = CARTESIAN_POINT ( 'NONE',  ( 5.049401038298161559, -19.05341960407611168, 37.70724293864768839 ) ) ;
#88105 = CARTESIAN_POINT ( 'NONE',  ( -12.06949235617739369, -12.14591786802326823, 49.37609039468569705 ) ) ;
#88106 = CARTESIAN_POINT ( 'NONE',  ( 17.50000000000000000, 5.499999999999995559, 113.7823096230356583 ) ) ;
#88107 = VECTOR ( 'NONE', #46615, 1000.000000000000000 ) ;
#88108 = CARTESIAN_POINT ( 'NONE',  ( 23.31738231874054534, 16.94106989632529192, 141.4500000054623854 ) ) ;
#88109 = CARTESIAN_POINT ( 'NONE',  ( 13.97604488694527802, 13.89961937509977652, 89.37390960531436690 ) ) ;
#88110 = CARTESIAN_POINT ( 'NONE',  ( 17.69326672847916271, 2.167987141922683492, 102.5000000000000284 ) ) ;
#88111 = VERTEX_POINT ( 'NONE', #22170 ) ;
#88112 = CARTESIAN_POINT ( 'NONE',  ( -5.049401038297874678, -19.05341960407617918, 94.79275706135230450 ) ) ;
#88113 = CARTESIAN_POINT ( 'NONE',  ( 19.03943276465977164, -0.05219959533909143690, 113.7489096053143669 ) ) ;
#88115 = CARTESIAN_POINT ( 'NONE',  ( 14.34966873604972726, -8.224510206698740333, 20.83442372801901143 ) ) ;
#88114 = CARTESIAN_POINT ( 'NONE',  ( 13.97604488694548053, -13.89961937509957401, 30.62609039468566863 ) ) ;
#88116 = CARTESIAN_POINT ( 'NONE',  ( -4.379528057220328563, 16.55341960407611168, 105.2072429386477097 ) ) ;
#88117 = CARTESIAN_POINT ( 'NONE',  ( 16.51473224551069308, 9.474510206698969483, 34.16557627198102409 ) ) ;
#88118 = CARTESIAN_POINT ( 'NONE',  ( 5.823673210054125526, 21.52544592524343514, 74.79057627198105251 ) ) ;
#88119 = CARTESIAN_POINT ( 'NONE',  ( 9.564922557960805705, 16.46253265017160317, 39.58224293864768839 ) ) ;
#88120 = CARTESIAN_POINT ( 'NONE',  ( -27.05641397906351742, -3.631740835637518927, 169.9999999999999716 ) ) ;
#88121 = CARTESIAN_POINT ( 'NONE',  ( 0.05219959533936267826, -19.03943276465977164, 75.00109039468566152 ) ) ;
#88122 = CARTESIAN_POINT ( 'NONE',  ( -4.379528057220328563, 16.55341960407611168, 55.20724293864770260 ) ) ;
#88123 = CARTESIAN_POINT ( 'NONE',  ( 21.53943276465977519, -0.05219959533907433946, 38.74890960531435979 ) ) ;
#88124 = CARTESIAN_POINT ( 'NONE',  ( -0.05219959533937732626, 21.53943276465977519, 92.50109039468567573 ) ) ;
#88125 = CARTESIAN_POINT ( 'NONE',  ( -18.62759615963270932, 10.81492255796079327, 85.83224293864768129 ) ) ;
#88126 = CARTESIAN_POINT ( 'NONE',  ( -18.62759615963255300, -10.81492255796106328, 74.16775706135231871 ) ) ;
#88127 = CARTESIAN_POINT ( 'NONE',  ( -21.55341960407619339, 5.719274019375674811, 58.54275706135235424 ) ) ;
#88128 = CARTESIAN_POINT ( 'NONE',  ( 5.049401038298161559, -19.05341960407611168, 97.70724293864766707 ) ) ;
#88130 = CARTESIAN_POINT ( 'NONE',  ( -15.80617190586768217, 15.72974639402176855, 63.12609039468568994 ) ) ;
#88129 = CARTESIAN_POINT ( 'NONE',  ( -8.224510206698735004, -14.34966873604973081, 94.58442372801901854 ) ) ;
#88131 = CARTESIAN_POINT ( 'NONE',  ( -19.02544592524342804, 5.153800228976336051, 51.04057627198103120 ) ) ;
#88132 = CARTESIAN_POINT ( 'NONE',  ( 10.81492255796106328, -18.62759615963255655, 30.41775706135234358 ) ) ;
#88133 = CARTESIAN_POINT ( 'NONE',  ( 5.153800228976335163, 19.02544592524342804, 74.79057627198103830 ) ) ;
#88134 = CARTESIAN_POINT ( 'NONE',  ( -12.14591786802309592, -12.06949235617757132, 66.87390960531436690 ) ) ;
#88135 = CARTESIAN_POINT ( 'NONE',  ( 8.224510206698953496, -14.34966873604960469, 47.91557627198102409 ) ) ;
#88136 = CARTESIAN_POINT ( 'NONE',  ( -21.55341960407610458, -5.719274019375992779, 56.45724293864768839 ) ) ;
#88137 = CARTESIAN_POINT ( 'NONE',  ( -13.97604488694527625, -13.89961937509977652, 41.87390960531435979 ) ) ;
#88138 = CARTESIAN_POINT ( 'NONE',  ( 21.52544592524344225, -5.823673210054117533, 53.54057627198103120 ) ) ;
#88139 = CARTESIAN_POINT ( 'NONE',  ( 19.02544592524334988, 5.153800228976608722, 46.45942372801899012 ) ) ;
#88141 = CARTESIAN_POINT ( 'NONE',  ( 8.314922557960818139, 14.29746914071049879, 64.58224293864769550 ) ) ;
#88140 = CARTESIAN_POINT ( 'NONE',  ( -13.89961937509957401, -13.97604488694547697, 24.37609039468565797 ) ) ;
#88142 = CARTESIAN_POINT ( 'NONE',  ( 21.55341960407610458, 5.719274019375980345, 33.95724293864769550 ) ) ;
#88143 = ORIENTED_EDGE ( 'NONE', *, *, #1107, .T. ) ;
#88144 = DIRECTION ( 'NONE',  ( -0.000000000000000000, -0.000000000000000000, 1.000000000000000000 ) ) ;
#88145 = CARTESIAN_POINT ( 'NONE',  ( -14.34966873604972548, 8.224510206698743886, 83.33442372801903275 ) ) ;
#88146 = CARTESIAN_POINT ( 'NONE',  ( -13.97604488694547697, 13.89961937509957934, 88.12609039468563310 ) ) ;
#88147 = EDGE_CURVE ( 'NONE', #17083, #121093, #138951, .T. ) ;
#88148 = CARTESIAN_POINT ( 'NONE',  ( 14.34966873604960469, 8.224510206698951720, 54.16557627198103120 ) ) ;
#88149 = DIRECTION ( 'NONE',  ( -0.5367108174878562066, -0.8437662581494459468, 0.000000000000000000 ) ) ;
#88150 = CARTESIAN_POINT ( 'NONE',  ( -16.46253265017160317, 9.564922557960807481, 45.83224293864769550 ) ) ;
#88151 = CARTESIAN_POINT ( 'NONE',  ( 16.55341960407611168, 4.379528057220329451, 38.95724293864768839 ) ) ;
#88152 = CARTESIAN_POINT ( 'NONE',  ( -19.02544592524342804, 5.153800228976336051, 51.04057627198103120 ) ) ;
#88153 = CARTESIAN_POINT ( 'NONE',  ( -9.564922557960796823, -16.46253265017161027, 72.08224293864770971 ) ) ;
#88154 = CARTESIAN_POINT ( 'NONE',  ( 19.05341960407611168, 5.049401038298154454, 48.95724293864768129 ) ) ;
#88155 = CARTESIAN_POINT ( 'NONE',  ( -10.81492255796105439, 18.62759615963255655, 57.91775706135234714 ) ) ;
#88156 = CARTESIAN_POINT ( 'NONE',  ( 5.153800228976335163, 19.02544592524342804, 69.79057627198103830 ) ) ;
#88157 = CARTESIAN_POINT ( 'NONE',  ( -0.05219959533909027116, -19.03943276465977164, 32.49890960531435979 ) ) ;
#88158 = CARTESIAN_POINT ( 'NONE',  ( -16.46253265017160317, 9.564922557960807481, 60.83224293864769550 ) ) ;
#88159 = CARTESIAN_POINT ( 'NONE',  ( -18.67979575497178146, -10.72451020669898902, 51.66557627198102409 ) ) ;
#88160 = CARTESIAN_POINT ( 'NONE',  ( -5.153800228976328057, -19.02544592524343514, 37.29057627198102409 ) ) ;
#88161 = CARTESIAN_POINT ( 'NONE',  ( -10.72451020669898014, 18.67979575497178502, 35.41557627198102409 ) ) ;
#88162 = APPLICATION_CONTEXT ( 'automotive_design' ) ;
#88163 = CARTESIAN_POINT ( 'NONE',  ( 16.53943276465976808, 0.05219959533934440121, 106.2510903946856757 ) ) ;
#88164 = CARTESIAN_POINT ( 'NONE',  ( -9.474510206698720793, -16.51473224551083518, 24.58442372801900078 ) ) ;
#88166 = CARTESIAN_POINT ( 'NONE',  ( 8.314922557961029526, -14.29746914071037800, 75.41775706135233293 ) ) ;
#88165 = CARTESIAN_POINT ( 'NONE',  ( 8.314922557961029526, -14.29746914071037800, 40.41775706135234714 ) ) ;
#88167 = PLANE ( 'NONE',  #75844 ) ;
#88168 = CARTESIAN_POINT ( 'NONE',  ( -4.483927247898782831, 16.52544592524335698, 72.70942372801901854 ) ) ;
#88169 = CARTESIAN_POINT ( 'NONE',  ( -8.314922557961024197, 14.29746914071037800, 52.91775706135235424 ) ) ;
#88170 = CARTESIAN_POINT ( 'NONE',  ( 5.049401038298161559, -19.05341960407611168, 107.7072429386476955 ) ) ;
#88171 = CARTESIAN_POINT ( 'NONE',  ( 4.483927247898790824, -16.52544592524335698, 40.20942372801901854 ) ) ;
#88172 = CARTESIAN_POINT ( 'NONE',  ( 0.05219959533909260263, 19.03943276465977164, 39.99890960531436690 ) ) ;
#88173 = CARTESIAN_POINT ( 'NONE',  ( -21.52544592524334988, -5.823673210054445271, 28.95942372801902209 ) ) ;
#88174 = CARTESIAN_POINT ( 'NONE',  ( 14.29746914071037800, 8.314922557961029526, 31.66775706135234358 ) ) ;
#88175 = CARTESIAN_POINT ( 'NONE',  ( -16.52544592524335698, -4.483927247898792601, 103.9594237280190185 ) ) ;
#88176 = CARTESIAN_POINT ( 'NONE',  ( 26.99873734152944138, 22.49873734152883387, 1.110912703473986074 ) ) ;
#88177 = CARTESIAN_POINT ( 'NONE',  ( 10.81492255796106328, -18.62759615963255655, 100.4177570613523471 ) ) ;
#88178 = CARTESIAN_POINT ( 'NONE',  ( -5.153800228976607833, 19.02544592524334988, 97.70942372801900433 ) ) ;
#88179 = CARTESIAN_POINT ( 'NONE',  ( 12.06949235617757843, -12.14591786802309237, 53.12390960531436690 ) ) ;
#88180 = CARTESIAN_POINT ( 'NONE',  ( -0.05219959533909027116, -19.03943276465977164, 27.49890960531435624 ) ) ;
#88182 = CARTESIAN_POINT ( 'NONE',  ( 17.05116617787824040, 6.768360034955837712, 78.84324446740806991 ) ) ;
#88181 = CARTESIAN_POINT ( 'NONE',  ( -13.97604488694547697, 13.89961937509957934, 58.12609039468566863 ) ) ;
#88183 = CARTESIAN_POINT ( 'NONE',  ( 15.80617190586769283, -15.72974639402175789, 65.62609039468568994 ) ) ;
#88184 = CARTESIAN_POINT ( 'NONE',  ( 12.06949235617739724, 12.14591786802326823, 21.87609039468567573 ) ) ;
#88185 = LINE ( 'NONE', #75993, #89094 ) ;
#88186 = CARTESIAN_POINT ( 'NONE',  ( 5.719274019375991003, -21.55341960407610458, 22.70724293864769194 ) ) ;
#88187 = CARTESIAN_POINT ( 'NONE',  ( -0.05219959533936034679, 19.03943276465977164, 112.5010903946856757 ) ) ;
#88188 = LINE ( 'NONE', #73047, #24839 ) ;
#88189 = CARTESIAN_POINT ( 'NONE',  ( 0.05219959533936267826, -19.03943276465977164, 50.00109039468566863 ) ) ;
#88190 = CARTESIAN_POINT ( 'NONE',  ( 5.049401038298161559, -19.05341960407611168, 27.70724293864769550 ) ) ;
#88191 = CARTESIAN_POINT ( 'NONE',  ( 0.05219959533937995610, -21.53943276465977519, 105.0010903946856757 ) ) ;
#88192 = CARTESIAN_POINT ( 'NONE',  ( -16.51473224551069308, -9.474510206698971260, 46.66557627198102409 ) ) ;
#88193 = CARTESIAN_POINT ( 'NONE',  ( -0.05219959533937732626, 21.53943276465977519, 52.50109039468567573 ) ) ;
#88194 = CARTESIAN_POINT ( 'NONE',  ( -15.72974639402176322, -15.80617190586768395, 104.3760903946856899 ) ) ;
#88195 = CARTESIAN_POINT ( 'NONE',  ( 0.05219959533934541429, -16.53943276465976808, 110.0010903946856757 ) ) ;
#88196 = CARTESIAN_POINT ( 'NONE',  ( 19.02544592524343514, -5.153800228976328945, 83.54057627198100988 ) ) ;
#88197 = CARTESIAN_POINT ( 'NONE',  ( -21.52544592524334988, -5.823673210054445271, 38.95942372801901854 ) ) ;
#88198 = CARTESIAN_POINT ( 'NONE',  ( 10.72451020669871369, 18.67979575497193778, 47.08442372801901854 ) ) ;
#88200 = CARTESIAN_POINT ( 'NONE',  ( -9.564922557960796823, -16.46253265017161027, 92.08224293864769550 ) ) ;
#88199 = CARTESIAN_POINT ( 'NONE',  ( -5.049401038297874678, -19.05341960407617918, 79.79275706135233293 ) ) ;
#88201 = CARTESIAN_POINT ( 'NONE',  ( 4.483927247898545687, 16.52544592524342804, 104.7905762719810241 ) ) ;
#88202 = CARTESIAN_POINT ( 'NONE',  ( -18.62759615963270932, 10.81492255796079327, 90.83224293864769550 ) ) ;
#88203 = CARTESIAN_POINT ( 'NONE',  ( 0.05219959533936267826, -19.03943276465977164, 25.00109039468566152 ) ) ;
#88204 = CARTESIAN_POINT ( 'NONE',  ( 12.06949235617757843, -12.14591786802309237, 98.12390960531436690 ) ) ;
#88205 = CARTESIAN_POINT ( 'NONE',  ( 0.05219959533909260263, 19.03943276465977164, 54.99890960531435979 ) ) ;
#88206 = CARTESIAN_POINT ( 'NONE',  ( -13.97604488694547697, 13.89961937509957934, 78.12609039468567573 ) ) ;
#88207 = CARTESIAN_POINT ( 'NONE',  ( 12.14591786802309770, 12.06949235617756955, 44.37390960531435979 ) ) ;
#88208 = CARTESIAN_POINT ( 'NONE',  ( -5.823673210054431948, 21.52544592524334988, 102.7094237280190185 ) ) ;
#88209 = CARTESIAN_POINT ( 'NONE',  ( -16.51473224551069308, -9.474510206698971260, 111.6655762719810383 ) ) ;
#88210 = CARTESIAN_POINT ( 'NONE',  ( -13.97604488694547697, 13.89961937509957934, 73.12609039468568994 ) ) ;
#88211 = CARTESIAN_POINT ( 'NONE',  ( 5.823673210054125526, 21.52544592524343514, 74.79057627198105251 ) ) ;
#88212 = CARTESIAN_POINT ( 'NONE',  ( -21.52544592524334988, -5.823673210054445271, 28.95942372801902209 ) ) ;
#88213 = CARTESIAN_POINT ( 'NONE',  ( 16.53943276465976808, 0.05219959533934440121, 31.25109039468568639 ) ) ;
#88214 = CARTESIAN_POINT ( 'NONE',  ( -16.53943276465976808, -0.05219959533934237506, 98.75109039468568994 ) ) ;
#88216 = CARTESIAN_POINT ( 'NONE',  ( -18.62759615963255300, -10.81492255796106328, 34.16775706135234714 ) ) ;
#88215 = CARTESIAN_POINT ( 'NONE',  ( -19.05341960407611168, -5.049401038298163336, 31.45724293864769550 ) ) ;
#88217 = CARTESIAN_POINT ( 'NONE',  ( -10.81492255796078084, -18.62759615963271287, 37.08224293864768129 ) ) ;
#88218 = CARTESIAN_POINT ( 'NONE',  ( -16.51473224551069308, -9.474510206698971260, 26.66557627198103120 ) ) ;
#88219 = CARTESIAN_POINT ( 'NONE',  ( -36.91746825000001309, -11.99521256947794789, -3.024999997268812635 ) ) ;
#88220 = CARTESIAN_POINT ( 'NONE',  ( -8.224510206698735004, -14.34966873604973081, 59.58442372801901854 ) ) ;
#88221 = CARTESIAN_POINT ( 'NONE',  ( 16.52544592524342804, -4.483927247898539470, 93.54057627198103830 ) ) ;
#88222 = CARTESIAN_POINT ( 'NONE',  ( 18.67979575497178502, 10.72451020669898547, 84.16557627198103830 ) ) ;
#88223 = CARTESIAN_POINT ( 'NONE',  ( 4.379528057220092307, 16.55341960407617563, 112.2927570613523471 ) ) ;
#88224 = CARTESIAN_POINT ( 'NONE',  ( 16.52544592524335698, 4.483927247898782831, 51.45942372801901854 ) ) ;
#88225 = CARTESIAN_POINT ( 'NONE',  ( 19.02544592524343514, -5.153800228976328945, 63.54057627198103830 ) ) ;
#88226 = CARTESIAN_POINT ( 'NONE',  ( 16.52544592524335698, 4.483927247898782831, 91.45942372801901854 ) ) ;
#88227 = CARTESIAN_POINT ( 'NONE',  ( 19.03943276465977164, 0.05219959533936151252, 86.25109039468567573 ) ) ;
#88228 = CARTESIAN_POINT ( 'NONE',  ( 21.55341960407610458, 5.719274019375980345, 83.95724293864770971 ) ) ;
#88229 = CARTESIAN_POINT ( 'NONE',  ( -16.55341960407611168, -4.379528057220339221, 21.45724293864769550 ) ) ;
#88230 = ORIENTED_EDGE ( 'NONE', *, *, #72705, .F. ) ;
#88231 = CARTESIAN_POINT ( 'NONE',  ( -5.049401038298153566, 19.05341960407611168, 115.2072429386477097 ) ) ;
#88232 = CARTESIAN_POINT ( 'NONE',  ( -18.67979575497178146, -10.72451020669898902, 66.66557627198102409 ) ) ;
#88233 = CARTESIAN_POINT ( 'NONE',  ( -14.29746914071037622, -8.314922557961029526, 94.16775706135237556 ) ) ;
#88234 = ORIENTED_EDGE ( 'NONE', *, *, #10475, .T. ) ;
#88235 = CARTESIAN_POINT ( 'NONE',  ( -10.81492255796078084, -18.62759615963271287, 27.08224293864769550 ) ) ;
#88236 = DIRECTION ( 'NONE',  ( 0.7071067811865512365, 0.7071067811865439090, -0.000000000000000000 ) ) ;
#88237 = CARTESIAN_POINT ( 'NONE',  ( 0.05219959533907565091, 21.53943276465977519, 94.99890960531436690 ) ) ;
#88238 = CARTESIAN_POINT ( 'NONE',  ( 12.06949235617757843, -12.14591786802309237, 23.12390960531436335 ) ) ;
#88239 = CARTESIAN_POINT ( 'NONE',  ( 12.14591786802327356, -12.06949235617739191, 35.62609039468568994 ) ) ;
#88240 = CARTESIAN_POINT ( 'NONE',  ( 16.46253265017160672, -9.564922557960803928, 28.33224293864769550 ) ) ;
#88241 = CARTESIAN_POINT ( 'NONE',  ( -14.34966873604972548, 8.224510206698743886, 33.33442372801900433 ) ) ;
#88242 = CARTESIAN_POINT ( 'NONE',  ( -0.05219959533909027116, -19.03943276465977164, 57.49890960531435979 ) ) ;
#88243 = CARTESIAN_POINT ( 'NONE',  ( 17.81289503416610742, 24.51734667627700404, 147.2999999999999545 ) ) ;
#88244 = CARTESIAN_POINT ( 'NONE',  ( 19.03943276465977164, -0.05219959533909143690, 108.7489096053143527 ) ) ;
#88245 = CARTESIAN_POINT ( 'NONE',  ( -9.285263851164359039, -10.36200767871436490, -62.50269714056246073 ) ) ;
#88246 = CARTESIAN_POINT ( 'NONE',  ( 16.53943276465976808, 0.05219959533934440121, 106.2510903946856757 ) ) ;
#88247 = CARTESIAN_POINT ( 'NONE',  ( 5.049401038297881783, 19.05341960407617563, 97.29275706135233293 ) ) ;
#88248 = CARTESIAN_POINT ( 'NONE',  ( -13.89961937509957401, -13.97604488694547875, 34.37609039468566863 ) ) ;
#88249 = CARTESIAN_POINT ( 'NONE',  ( -21.55341960407610458, -5.719274019375992779, 81.45724293864769550 ) ) ;
#88250 = CARTESIAN_POINT ( 'NONE',  ( 14.34966873604972726, -8.224510206698740333, 105.8344237280190328 ) ) ;
#88251 = CARTESIAN_POINT ( 'NONE',  ( -21.55341960407610458, -5.719274019375992779, 36.45724293864768839 ) ) ;
#88252 = CARTESIAN_POINT ( 'NONE',  ( -16.46253265017146816, -9.564922557961047289, 104.1677570613523329 ) ) ;
#88253 = CARTESIAN_POINT ( 'NONE',  ( 13.97604488694527802, 13.89961937509977652, 104.3739096053143385 ) ) ;
#88254 = CARTESIAN_POINT ( 'NONE',  ( 18.62759615963255655, 10.81492255796105972, 66.66775706135234714 ) ) ;
#88255 = CARTESIAN_POINT ( 'NONE',  ( 19.02544592524343514, -5.153800228976328945, 63.54057627198103830 ) ) ;
#88256 = CARTESIAN_POINT ( 'NONE',  ( 8.314922557960818139, 14.29746914071049879, 94.58224293864769550 ) ) ;
#88257 = CARTESIAN_POINT ( 'NONE',  ( -16.38665767535050577, -7.295008042176168495, 84.73599135785454450 ) ) ;
#88258 = CARTESIAN_POINT ( 'NONE',  ( -8.224510206698948167, 14.34966873604960824, 80.41557627198103830 ) ) ;
#88259 = CARTESIAN_POINT ( 'NONE',  ( 15.80617190586746368, 15.72974639402197994, 69.37390960531436690 ) ) ;
#88260 = VERTEX_POINT ( 'NONE', #113170 ) ;
#88261 = CARTESIAN_POINT ( 'NONE',  ( 9.564922557961047289, -16.46253265017146816, 90.41775706135234714 ) ) ;
#88262 = CARTESIAN_POINT ( 'NONE',  ( 69.65682714487590488, -71.74905178543389184, -15.00000000000000178 ) ) ;
#88263 = CARTESIAN_POINT ( 'NONE',  ( 19.03943276465977164, -0.05219959533909143690, 58.74890960531435979 ) ) ;
#88264 = CARTESIAN_POINT ( 'NONE',  ( 17.48853670773243962, -5.747243402303062076, 71.16671299749988577 ) ) ;
#88266 = CARTESIAN_POINT ( 'NONE',  ( -16.46253265017160317, 9.564922557960807481, 90.83224293864769550 ) ) ;
#88265 = CARTESIAN_POINT ( 'NONE',  ( 0.05219959533909260263, 19.03943276465977164, 79.99890960531436690 ) ) ;
#88267 = CARTESIAN_POINT ( 'NONE',  ( 14.34966873604972726, -8.224510206698740333, 65.83442372801900433 ) ) ;
#88268 = CARTESIAN_POINT ( 'NONE',  ( -23.48258780958832048, 5.709364865862125882, 171.6892424014284018 ) ) ;
#88269 = CARTESIAN_POINT ( 'NONE',  ( 5.153800228976615827, -19.02544592524334988, 45.20942372801901143 ) ) ;
#88270 = CARTESIAN_POINT ( 'NONE',  ( 36.91128768240056246, 2.428612879436746321E-14, 50.50000000000002842 ) ) ;
#88271 = CARTESIAN_POINT ( 'NONE',  ( 13.89961937509977652, -13.97604488694527269, 108.1239096053143669 ) ) ;
#88272 = CARTESIAN_POINT ( 'NONE',  ( 0.05219959533934541429, -16.53943276465976808, 105.0010903946856757 ) ) ;
#88273 = CARTESIAN_POINT ( 'NONE',  ( -34.41611627805855278, -6.381310488372556655, 48.94841969467692877 ) ) ;
#88274 = CARTESIAN_POINT ( 'NONE',  ( -16.55341960407617563, 4.379528057220093196, 98.54275706135234714 ) ) ;
#88275 = CARTESIAN_POINT ( 'NONE',  ( -17.12812012977024168, 6.668231424566044119, 28.64051240676857191 ) ) ;
#88276 = CARTESIAN_POINT ( 'NONE',  ( -12.06949235617739369, -12.14591786802326823, 64.37609039468568994 ) ) ;
#88277 = CARTESIAN_POINT ( 'NONE',  ( 12.24802307403555446, -10.74802307403551715, -64.92279855667830191 ) ) ;
#88278 = CARTESIAN_POINT ( 'NONE',  ( -15.72974639402176322, -15.80617190586768395, 64.37609039468568994 ) ) ;
#88279 = CARTESIAN_POINT ( 'NONE',  ( 13.89961937509957401, 13.97604488694547697, 71.87609039468567573 ) ) ;
#88280 = CARTESIAN_POINT ( 'NONE',  ( -19.03943276465977164, -0.05219959533935918106, 28.75109039468566507 ) ) ;
#88281 = CARTESIAN_POINT ( 'NONE',  ( 0.05219959533909260263, 19.03943276465977164, 64.99890960531436690 ) ) ;
#88282 = CARTESIAN_POINT ( 'NONE',  ( 5.049401038298161559, -19.05341960407611168, 42.70724293864767418 ) ) ;
#88283 = CARTESIAN_POINT ( 'NONE',  ( 67.00000000000000000, -1.163414459189985801E-14, 95.00000000000000000 ) ) ;
#88284 = CARTESIAN_POINT ( 'NONE',  ( 18.67979575497178502, 10.72451020669898547, 79.16557627198103830 ) ) ;
#88285 = CARTESIAN_POINT ( 'NONE',  ( -18.62759615963270932, 10.81492255796079327, 30.83224293864770260 ) ) ;
#88286 = CARTESIAN_POINT ( 'NONE',  ( -0.05219959533909027116, -19.03943276465977164, 27.49890960531435624 ) ) ;
#88287 = CARTESIAN_POINT ( 'NONE',  ( -4.379528057220086978, -16.55341960407618274, 49.79275706135234714 ) ) ;
#88288 = ORIENTED_EDGE ( 'NONE', *, *, #126225, .T. ) ;
#88289 = EDGE_CURVE ( 'NONE', #62156, #107790, #143910, .T. ) ;
#88290 = CARTESIAN_POINT ( 'NONE',  ( -0.05219959533937732626, 21.53943276465977519, 37.50109039468568284 ) ) ;
#88292 = CARTESIAN_POINT ( 'NONE',  ( -38.00000000000000711, 2.428612866367529932E-14, -4.000000000000000000 ) ) ;
#88291 = CARTESIAN_POINT ( 'NONE',  ( 16.55341960407611168, 4.379528057220329451, 53.95724293864770260 ) ) ;
#88293 = CARTESIAN_POINT ( 'NONE',  ( 4.483927247898790824, -16.52544592524335698, 25.20942372801901854 ) ) ;
#88294 = CARTESIAN_POINT ( 'NONE',  ( -5.049401038297874678, -19.05341960407617918, 44.79275706135232582 ) ) ;
#88295 = CARTESIAN_POINT ( 'NONE',  ( 16.53943276465976808, -0.05219959533910856209, 63.74890960531435979 ) ) ;
#88296 = CARTESIAN_POINT ( 'NONE',  ( -5.823673210054116645, -21.52544592524344225, 112.2905762719810241 ) ) ;
#88298 = CARTESIAN_POINT ( 'NONE',  ( -5.823673210054116645, -21.52544592524344225, 72.29057627198102409 ) ) ;
#88297 = CARTESIAN_POINT ( 'NONE',  ( 0.9489761088441257542, 16.37794455013558093, -59.27687827943704946 ) ) ;
#88299 = CARTESIAN_POINT ( 'NONE',  ( -16.51473224551069308, -9.474510206698971260, 96.66557627198102409 ) ) ;
#88300 = CARTESIAN_POINT ( 'NONE',  ( 8.224510206698953496, -14.34966873604960469, 67.91557627198102409 ) ) ;
#88301 = CARTESIAN_POINT ( 'NONE',  ( 0.05219959533909260263, 19.03943276465977164, 99.99890960531436690 ) ) ;
#88302 = CARTESIAN_POINT ( 'NONE',  ( -18.22780087662114212, 5.499999999999995559, 48.51540105326107266 ) ) ;
#88303 = CARTESIAN_POINT ( 'NONE',  ( 9.474510206698729675, 16.51473224551082808, 62.08442372801899722 ) ) ;
#88304 = CARTESIAN_POINT ( 'NONE',  ( -10.72451020669898014, 18.67979575497178502, 105.4155762719810383 ) ) ;
#88305 = CARTESIAN_POINT ( 'NONE',  ( -16.51473224551069308, -9.474510206698971260, 56.66557627198103120 ) ) ;
#88306 = CARTESIAN_POINT ( 'NONE',  ( 0.05219959533936267826, -19.03943276465977164, 45.00109039468566863 ) ) ;
#88307 = CARTESIAN_POINT ( 'NONE',  ( -12.06949235617756955, 12.14591786802309770, 110.6239096053143669 ) ) ;
#88308 = CARTESIAN_POINT ( 'NONE',  ( -21.52544592524334988, -5.823673210054445271, 58.95942372801902565 ) ) ;
#88309 = CARTESIAN_POINT ( 'NONE',  ( -16.79531203550649820, -7.028104445595611871, 71.25244988220447340 ) ) ;
#88310 = CARTESIAN_POINT ( 'NONE',  ( -4.379528057220328563, 16.55341960407611168, 45.20724293864769550 ) ) ;
#88311 = CARTESIAN_POINT ( 'NONE',  ( -19.03943276465977164, 0.05219959533909376836, 51.24890960531436690 ) ) ;
#88312 = CARTESIAN_POINT ( 'NONE',  ( 5.049401038298161559, -19.05341960407611168, 112.7072429386476813 ) ) ;
#88313 = CARTESIAN_POINT ( 'NONE',  ( 21.52544592524344225, -5.823673210054117533, 78.54057627198103830 ) ) ;
#88314 = CARTESIAN_POINT ( 'NONE',  ( -27.73933785331498925, -9.013057229001049109, 144.9750000027312069 ) ) ;
#88315 = CARTESIAN_POINT ( 'NONE',  ( 5.049401038298161559, -19.05341960407611168, 47.70724293864770260 ) ) ;
#88316 = CARTESIAN_POINT ( 'NONE',  ( -10.81492255796078084, -18.62759615963271287, 62.08224293864769550 ) ) ;
#88317 = CARTESIAN_POINT ( 'NONE',  ( -15.80617190586768217, 15.72974639402176855, 83.12609039468568994 ) ) ;
#88320 = CARTESIAN_POINT ( 'NONE',  ( -12.14591786802309592, -12.06949235617757132, 81.87390960531435269 ) ) ;
#88319 = CARTESIAN_POINT ( 'NONE',  ( -14.29746914071037622, -8.314922557961029526, 94.16775706135237556 ) ) ;
#88318 = CARTESIAN_POINT ( 'NONE',  ( 7.840974544913427380, -46.02298249793697948, -22.40017284086515303 ) ) ;
#88321 = CARTESIAN_POINT ( 'NONE',  ( 16.51473224551069308, 9.474510206698969483, 64.16557627198102409 ) ) ;
#88322 = ORIENTED_EDGE ( 'NONE', *, *, #97283, .T. ) ;
#88323 = CARTESIAN_POINT ( 'NONE',  ( 5.153800228976615827, -19.02544592524334988, 45.20942372801901143 ) ) ;
#88324 = CARTESIAN_POINT ( 'NONE',  ( 8.314922557961029526, -14.29746914071037800, 85.41775706135236135 ) ) ;
#88325 = CARTESIAN_POINT ( 'NONE',  ( 13.89961937509957401, 13.97604488694547697, 21.87609039468566152 ) ) ;
#88326 = CARTESIAN_POINT ( 'NONE',  ( 0.05219959533909260263, 19.03943276465977164, 84.99890960531436690 ) ) ;
#88327 = CARTESIAN_POINT ( 'NONE',  ( -10.72451020669898014, 18.67979575497178502, 50.41557627198103120 ) ) ;
#88328 = DIRECTION ( 'NONE',  ( 0.000000000000000000, 0.000000000000000000, 1.000000000000000000 ) ) ;
#88329 = CARTESIAN_POINT ( 'NONE',  ( 10.72451020669871369, 18.67979575497193778, 102.0844237280190185 ) ) ;
#88330 = CARTESIAN_POINT ( 'NONE',  ( -12.06949235617739369, -12.14591786802326823, 59.37609039468568284 ) ) ;
#88331 = CARTESIAN_POINT ( 'NONE',  ( 15.80617190586769283, -15.72974639402175789, 20.62609039468568639 ) ) ;
#88332 = CARTESIAN_POINT ( 'NONE',  ( 4.379528057220092307, 16.55341960407617563, 32.29275706135235424 ) ) ;
#88333 = CARTESIAN_POINT ( 'NONE',  ( 9.474510206698971260, -16.51473224551069308, 92.91557627198103830 ) ) ;
#88334 = CARTESIAN_POINT ( 'NONE',  ( 19.03943276465977164, -0.05219959533909143690, 38.74890960531436690 ) ) ;
#88335 = CARTESIAN_POINT ( 'NONE',  ( 16.46253265017160672, -9.564922557960803928, 58.33224293864769550 ) ) ;
#88336 = CARTESIAN_POINT ( 'NONE',  ( 4.379528057220092307, 16.55341960407617563, 32.29275706135235424 ) ) ;
#88337 = CARTESIAN_POINT ( 'NONE',  ( -4.379528057220328563, 16.55341960407611168, 75.20724293864769550 ) ) ;
#88338 = CARTESIAN_POINT ( 'NONE',  ( 16.53943276465976808, 0.05219959533934440121, 81.25109039468568994 ) ) ;
#88341 = CARTESIAN_POINT ( 'NONE',  ( -5.049401038298153566, 19.05341960407611168, 55.20724293864769550 ) ) ;
#88340 = CARTESIAN_POINT ( 'NONE',  ( 5.049401038298161559, -19.05341960407611168, 62.70724293864769550 ) ) ;
#88339 = CARTESIAN_POINT ( 'NONE',  ( -21.55341960407619339, 5.719274019375674811, 43.54275706135235424 ) ) ;
#88342 = CARTESIAN_POINT ( 'NONE',  ( -9.564922557960796823, -16.46253265017161027, 77.08224293864769550 ) ) ;
#88343 = CARTESIAN_POINT ( 'NONE',  ( -8.314922557960811034, -14.29746914071050412, 32.08224293864769550 ) ) ;
#88344 = CARTESIAN_POINT ( 'NONE',  ( -16.52544592524335698, -4.483927247898792601, 83.95942372801900433 ) ) ;
#88345 = ORIENTED_EDGE ( 'NONE', *, *, #191015, .T. ) ;
#88346 = CARTESIAN_POINT ( 'NONE',  ( 9.474510206698729675, 16.51473224551082808, 27.08442372801900433 ) ) ;
#88347 = CARTESIAN_POINT ( 'NONE',  ( -19.02544592524342804, 5.153800228976336051, 106.0405762719810241 ) ) ;
#88348 = CARTESIAN_POINT ( 'NONE',  ( -5.153800228976328057, -19.02544592524343514, 52.29057627198100988 ) ) ;
#88349 = CARTESIAN_POINT ( 'NONE',  ( -5.049401038297874678, -19.05341960407617918, 24.79275706135233648 ) ) ;
#88350 = CARTESIAN_POINT ( 'NONE',  ( -36.91746825000000598, 2.428612866367529932E-14, -6.624999997268814056 ) ) ;
#88351 = CARTESIAN_POINT ( 'NONE',  ( 4.379528057220092307, 16.55341960407617563, 42.29275706135235424 ) ) ;
#88353 = CARTESIAN_POINT ( 'NONE',  ( -12.06949235617739369, -12.14591786802326823, 54.37609039468568994 ) ) ;
#88352 = CARTESIAN_POINT ( 'NONE',  ( 16.46253265017146816, 9.564922557961045513, 66.66775706135233293 ) ) ;
#88354 = CARTESIAN_POINT ( 'NONE',  ( -19.03943276465977164, 0.05219959533909376836, 116.2489096053143669 ) ) ;
#88355 = CARTESIAN_POINT ( 'NONE',  ( 16.46253265017160672, -9.564922557960803928, 73.33224293864769550 ) ) ;
#88356 = CARTESIAN_POINT ( 'NONE',  ( -0.05219959533907301413, -21.53943276465977519, 112.4989096053143669 ) ) ;
#88357 = CARTESIAN_POINT ( 'NONE',  ( -16.46253265017146816, -9.564922557961047289, 69.16775706135233293 ) ) ;
#88359 = CARTESIAN_POINT ( 'NONE',  ( -16.51473224551069308, -9.474510206698971260, 36.66557627198102409 ) ) ;
#88358 = CARTESIAN_POINT ( 'NONE',  ( 13.89961937509977652, -13.97604488694527269, 103.1239096053143527 ) ) ;
#88360 = CARTESIAN_POINT ( 'NONE',  ( -19.05341960407611168, -5.049401038298163336, 81.45724293864769550 ) ) ;
#88362 = CARTESIAN_POINT ( 'NONE',  ( 13.89961937509977652, -13.97604488694527269, 38.12390960531436690 ) ) ;
#88361 = CARTESIAN_POINT ( 'NONE',  ( -4.379528057220328563, 16.55341960407611168, 40.20724293864769550 ) ) ;
#88363 = CARTESIAN_POINT ( 'NONE',  ( -16.51473224551082808, 9.474510206698731452, 33.33442372801899722 ) ) ;
#88364 = CARTESIAN_POINT ( 'NONE',  ( 8.224510206698953496, -14.34966873604960469, 72.91557627198103830 ) ) ;
#88365 = CARTESIAN_POINT ( 'NONE',  ( 9.564922557961047289, -16.46253265017146816, 20.41775706135233293 ) ) ;
#88366 = CARTESIAN_POINT ( 'NONE',  ( -9.564922557960796823, -16.46253265017161027, 52.08224293864768839 ) ) ;
#88368 = CARTESIAN_POINT ( 'NONE',  ( -5.823673210054431948, 21.52544592524334988, 102.7094237280190185 ) ) ;
#88367 = CARTESIAN_POINT ( 'NONE',  ( 4.483927247898545687, 16.52544592524342804, 49.79057627198102409 ) ) ;
#88369 = CARTESIAN_POINT ( 'NONE',  ( 13.97604488694527802, 13.89961937509977652, 89.37390960531436690 ) ) ;
#88370 = CARTESIAN_POINT ( 'NONE',  ( 19.03943276465977164, -0.05219959533909143690, 113.7489096053143669 ) ) ;
#88371 = CARTESIAN_POINT ( 'NONE',  ( 19.02544592524343514, -5.153800228976328945, 38.54057627198103120 ) ) ;
#88372 = CARTESIAN_POINT ( 'NONE',  ( -16.51473224551069308, -9.474510206698971260, 21.66557627198102765 ) ) ;
#88373 = CARTESIAN_POINT ( 'NONE',  ( 8.314922557960818139, 14.29746914071049879, 84.58224293864769550 ) ) ;
#88374 = CARTESIAN_POINT ( 'NONE',  ( -15.72974639402197994, 15.80617190586746368, 95.62390960531436690 ) ) ;
#88375 = CARTESIAN_POINT ( 'NONE',  ( -19.05341960407611168, -5.049401038298163336, 81.45724293864769550 ) ) ;
#88376 = CARTESIAN_POINT ( 'NONE',  ( -10.72451020669898014, 18.67979575497178502, 100.4155762719810241 ) ) ;
#88377 = CARTESIAN_POINT ( 'NONE',  ( -5.049401038298153566, 19.05341960407611168, 85.20724293864766707 ) ) ;
#88379 = CARTESIAN_POINT ( 'NONE',  ( 14.29746914071049879, -8.314922557960816363, 103.3322429386476955 ) ) ;
#88378 = LINE ( 'NONE', #150072, #23600 ) ;
#88380 = CARTESIAN_POINT ( 'NONE',  ( -0.05219959533909027116, -19.03943276465977164, 77.49890960531435269 ) ) ;
#88381 = CARTESIAN_POINT ( 'NONE',  ( -15.80617190586745835, -15.72974639402198527, 76.87390960531439532 ) ) ;
#88382 = CARTESIAN_POINT ( 'NONE',  ( 8.906447517083057264, -27.41122689804191026, 146.5999999999999943 ) ) ;
#88384 = CARTESIAN_POINT ( 'NONE',  ( 3.424326230466405718, 6.677994727576183287, 1.353258418600855606 ) ) ;
#88383 = CARTESIAN_POINT ( 'NONE',  ( -15.80617190586745835, -15.72974639402198527, 26.87390960531435979 ) ) ;
#88385 = CARTESIAN_POINT ( 'NONE',  ( -16.52544592524335698, -4.483927247898792601, 28.95942372801902209 ) ) ;
#88386 = EDGE_CURVE ( 'NONE', #164159, #133568, #135807, .T. ) ;
#88387 = CARTESIAN_POINT ( 'NONE',  ( -12.06949235617756955, 12.14591786802309770, 90.62390960531436690 ) ) ;
#88388 = CARTESIAN_POINT ( 'NONE',  ( -16.81555441253550853, -7.025013491695485612, 94.36314554665744936 ) ) ;
#88389 = CARTESIAN_POINT ( 'NONE',  ( 19.03943276465977164, -0.05219959533909143690, 88.74890960531436690 ) ) ;
#88390 = CARTESIAN_POINT ( 'NONE',  ( 0.05219959533909260263, 19.03943276465977164, 39.99890960531436690 ) ) ;
#88391 = CARTESIAN_POINT ( 'NONE',  ( 16.53943276465976808, -0.05219959533910856209, 83.74890960531435269 ) ) ;
#88392 = TOROIDAL_SURFACE ( 'NONE', #188567, 206.0437394197456911, 10.00000000000000000 ) ;
#88393 = CARTESIAN_POINT ( 'NONE',  ( 0.05219959533907565091, 21.53943276465977519, 34.99890960531435979 ) ) ;
#88394 = CARTESIAN_POINT ( 'NONE',  ( 8.314922557960818139, 14.29746914071049879, 49.58224293864769550 ) ) ;
#88395 = CARTESIAN_POINT ( 'NONE',  ( -19.03943276465977164, -0.05219959533935918106, 108.7510903946856615 ) ) ;
#88396 = CARTESIAN_POINT ( 'NONE',  ( 10.81492255796106328, -18.62759615963255655, 65.41775706135234714 ) ) ;
#88397 = CARTESIAN_POINT ( 'NONE',  ( -17.14385361876520975, 23.59649016807275856, 146.5750000027311728 ) ) ;
#88398 = CARTESIAN_POINT ( 'NONE',  ( 9.474510206698971260, -16.51473224551069308, 102.9155762719810241 ) ) ;
#88399 = CARTESIAN_POINT ( 'NONE',  ( -14.29746914071037622, -8.314922557961029526, 84.16775706135234714 ) ) ;
#88400 = CARTESIAN_POINT ( 'NONE',  ( -9.564922557960796823, -16.46253265017161027, 27.08224293864769550 ) ) ;
#88401 = CARTESIAN_POINT ( 'NONE',  ( -16.51473224551069308, -9.474510206698971260, 81.66557627198103830 ) ) ;
#88402 = CARTESIAN_POINT ( 'NONE',  ( 10.72451020669898902, -18.67979575497178502, 87.91557627198103830 ) ) ;
#88403 = CARTESIAN_POINT ( 'NONE',  ( -19.05341960407617563, 5.049401038297882671, 108.5427570613523187 ) ) ;
#88405 = CARTESIAN_POINT ( 'NONE',  ( -21.53943276465977519, -0.05219959533937600094, 63.75109039468568284 ) ) ;
#88404 = CARTESIAN_POINT ( 'NONE',  ( -8.224510206698948167, 14.34966873604960824, 50.41557627198103120 ) ) ;
#88407 = CARTESIAN_POINT ( 'NONE',  ( -19.02544592524342804, 5.153800228976336051, 116.0405762719810383 ) ) ;
#88406 = CARTESIAN_POINT ( 'NONE',  ( -4.483927247898782831, 16.52544592524335698, 92.70942372801901854 ) ) ;
#88408 = CARTESIAN_POINT ( 'NONE',  ( 13.97604488694527802, 13.89961937509977830, 114.3739096053143669 ) ) ;
#88409 = CARTESIAN_POINT ( 'NONE',  ( -24.95432927374998044, -3.806786798636382585, 190.0000000000000000 ) ) ;
#88410 = CARTESIAN_POINT ( 'NONE',  ( 14.34966873604972726, -8.224510206698740333, 110.8344237280190043 ) ) ;
#88411 = CARTESIAN_POINT ( 'NONE',  ( 16.52544592524335698, 4.483927247898782831, 61.45942372801901854 ) ) ;
#88413 = ORIENTED_EDGE ( 'NONE', *, *, #110272, .F. ) ;
#88412 = CARTESIAN_POINT ( 'NONE',  ( 19.05341960407611168, 5.049401038298154454, 73.95724293864768129 ) ) ;
#88414 = CARTESIAN_POINT ( 'NONE',  ( 9.564922557960805705, 16.46253265017160317, 84.58224293864769550 ) ) ;
#88415 = CARTESIAN_POINT ( 'NONE',  ( -21.55341960407619339, 5.719274019375674811, 68.54275706135234714 ) ) ;
#88416 = ADVANCED_FACE ( 'NONE', ( #128335 ), #189051, .F. ) ;
#88417 = CARTESIAN_POINT ( 'NONE',  ( 16.52544592524335698, 4.483927247898782831, 76.45942372801901854 ) ) ;
#88418 = CARTESIAN_POINT ( 'NONE',  ( -12.06949235617756955, 12.14591786802309770, 50.62390960531435979 ) ) ;
#88419 = CARTESIAN_POINT ( 'NONE',  ( -0.05219959533909027116, -19.03943276465977164, 57.49890960531435979 ) ) ;
#88420 = CARTESIAN_POINT ( 'NONE',  ( -16.51473224551069308, -9.474510206698971260, 51.66557627198102409 ) ) ;
#88422 = ORIENTED_EDGE ( 'NONE', *, *, #7520, .F. ) ;
#88421 = CARTESIAN_POINT ( 'NONE',  ( -16.53943276465976808, -0.05219959533934237506, 38.75109039468567573 ) ) ;
#88423 = CARTESIAN_POINT ( 'NONE',  ( 13.97604488694548053, -13.89961937509957401, 95.62609039468563310 ) ) ;
#88424 = CARTESIAN_POINT ( 'NONE',  ( -12.06949235617756955, 12.14591786802309770, 100.6239096053143811 ) ) ;
#88425 = CARTESIAN_POINT ( 'NONE',  ( -5.153800228976328057, -19.02544592524343514, 62.29057627198100988 ) ) ;
#88427 = CARTESIAN_POINT ( 'NONE',  ( -38.00000000000001421, 12.34694845685046438, -2.099999999999999645 ) ) ;
#88426 = CARTESIAN_POINT ( 'NONE',  ( 13.89961937509957401, 13.97604488694547697, 106.8760903946856757 ) ) ;
#88428 = CARTESIAN_POINT ( 'NONE',  ( -15.80617190586768217, 15.72974639402176855, 108.1260903946856757 ) ) ;
#88429 = CARTESIAN_POINT ( 'NONE',  ( -8.224510206698735004, -14.34966873604973081, 69.58442372801900433 ) ) ;
#88430 = CARTESIAN_POINT ( 'NONE',  ( 5.000000000000000888, -130.0000000000000000, 12.49999999999999645 ) ) ;
#88431 = CARTESIAN_POINT ( 'NONE',  ( 15.80617190586746368, 15.72974639402197994, 69.37390960531436690 ) ) ;
#88432 = CARTESIAN_POINT ( 'NONE',  ( -8.224510206698735004, -14.34966873604973081, 49.58442372801901143 ) ) ;
#88433 = DIRECTION ( 'NONE',  ( -1.047444401652940164E-14, -1.000000000000000000, -0.000000000000000000 ) ) ;
#88434 = CARTESIAN_POINT ( 'NONE',  ( -16.51473224551082808, 9.474510206698731452, 53.33442372801900433 ) ) ;
#88435 = CARTESIAN_POINT ( 'NONE',  ( 13.97604488694527802, 13.89961937509977652, 94.37390960531436690 ) ) ;
#88436 = CARTESIAN_POINT ( 'NONE',  ( -16.53943276465976808, 0.05219959533911058130, 116.2489096053143669 ) ) ;
#88437 = CARTESIAN_POINT ( 'NONE',  ( 16.51473224551069308, 9.474510206698969483, 59.16557627198102409 ) ) ;
#88438 = CARTESIAN_POINT ( 'NONE',  ( -0.05219959533910754901, -16.53943276465976808, 52.49890960531435979 ) ) ;
#88439 = CARTESIAN_POINT ( 'NONE',  ( -21.53943276465977519, -0.05219959533937600094, 73.75109039468567573 ) ) ;
#88440 = CARTESIAN_POINT ( 'NONE',  ( 0.05219959533936267826, -19.03943276465977164, 50.00109039468566863 ) ) ;
#88441 = CARTESIAN_POINT ( 'NONE',  ( 13.97604488694548053, -13.89961937509957401, 30.62609039468566863 ) ) ;
#88442 = CARTESIAN_POINT ( 'NONE',  ( -13.97604488694527625, -13.89961937509977652, 51.87390960531436690 ) ) ;
#88443 = CARTESIAN_POINT ( 'NONE',  ( 18.67979575497178502, 10.72451020669898547, 29.16557627198103120 ) ) ;
#88444 = CARTESIAN_POINT ( 'NONE',  ( 5.823673210054444382, -21.52544592524334988, 90.20942372801903275 ) ) ;
#88445 = CARTESIAN_POINT ( 'NONE',  ( 13.89961937509977652, -13.97604488694527269, 68.12390960531436690 ) ) ;
#88446 = CARTESIAN_POINT ( 'NONE',  ( -10.72451020669870658, -18.67979575497194134, 89.58442372801901854 ) ) ;
#88447 = CARTESIAN_POINT ( 'NONE',  ( 5.823673210054125526, 21.52544592524343514, 39.79057627198103830 ) ) ;
#88448 = CARTESIAN_POINT ( 'NONE',  ( 16.51473224551069308, 9.474510206698969483, 89.16557627198103830 ) ) ;
#88449 = CARTESIAN_POINT ( 'NONE',  ( 0.05219959533936267826, -19.03943276465977164, 65.00109039468567573 ) ) ;
#88450 = CARTESIAN_POINT ( 'NONE',  ( 5.049401038298161559, -19.05341960407611168, 37.70724293864768839 ) ) ;
#88451 = CARTESIAN_POINT ( 'NONE',  ( 19.05341960407611168, 5.049401038298154454, 93.95724293864769550 ) ) ;
#88452 = CARTESIAN_POINT ( 'NONE',  ( -4.483927247898782831, 16.52544592524335698, 32.70942372801900433 ) ) ;
#88453 = CARTESIAN_POINT ( 'NONE',  ( 8.224510206698953496, -14.34966873604960469, 97.91557627198103830 ) ) ;
#88454 = CARTESIAN_POINT ( 'NONE',  ( -16.46253265017160317, 9.564922557960807481, 75.83224293864769550 ) ) ;
#88455 = CARTESIAN_POINT ( 'NONE',  ( -0.05219959533907301413, -21.53943276465977519, 47.49890960531435979 ) ) ;
#88456 = CARTESIAN_POINT ( 'NONE',  ( -13.89961937509957401, -13.97604488694547875, 109.3760903946856331 ) ) ;
#88457 = CARTESIAN_POINT ( 'NONE',  ( 5.823673210054444382, -21.52544592524334988, 25.20942372801901854 ) ) ;
#88458 = CARTESIAN_POINT ( 'NONE',  ( -10.72451020669870658, -18.67979575497194134, 64.58442372801900433 ) ) ;
#88459 = CARTESIAN_POINT ( 'NONE',  ( 0.05219959533934541429, -16.53943276465976808, 65.00109039468568994 ) ) ;
#88460 = VECTOR ( 'NONE', #60918, 1000.000000000000000 ) ;
#88461 = CARTESIAN_POINT ( 'NONE',  ( -13.89961937509977652, 13.97604488694528158, 70.62390960531432427 ) ) ;
#88462 = CARTESIAN_POINT ( 'NONE',  ( -12.14591786802326823, 12.06949235617739902, 98.12609039468570415 ) ) ;
#88463 = CARTESIAN_POINT ( 'NONE',  ( -13.97604488694547697, 13.89961937509957934, 38.12609039468566152 ) ) ;
#88464 = CARTESIAN_POINT ( 'NONE',  ( -0.05219959533937732626, 21.53943276465977519, 32.50109039468568284 ) ) ;
#88465 = CARTESIAN_POINT ( 'NONE',  ( 12.06949235617757843, -12.14591786802309237, 63.12390960531435979 ) ) ;
#88466 = CARTESIAN_POINT ( 'NONE',  ( 5.049401038298161559, -19.05341960407611168, 102.7072429386476955 ) ) ;
#88467 = CARTESIAN_POINT ( 'NONE',  ( -12.06949235617739369, -12.14591786802326823, 84.37609039468570415 ) ) ;
#88468 = CARTESIAN_POINT ( 'NONE',  ( 21.52544592524334988, 5.823673210054432836, 66.45942372801903275 ) ) ;
#88469 = CARTESIAN_POINT ( 'NONE',  ( 12.06949235617739724, 12.14591786802326823, 26.87609039468567218 ) ) ;
#88470 = CARTESIAN_POINT ( 'NONE',  ( 18.67979575497194134, -10.72451020669871369, 25.83442372801901499 ) ) ;
#88471 = CARTESIAN_POINT ( 'NONE',  ( 12.06949235617757843, -12.14591786802309237, 63.12390960531435979 ) ) ;
#88472 = VERTEX_POINT ( 'NONE', #96997 ) ;
#88473 = CARTESIAN_POINT ( 'NONE',  ( 21.52544592524344225, -5.823673210054117533, 103.5405762719810383 ) ) ;
#88474 = CARTESIAN_POINT ( 'NONE',  ( 16.55341960407611168, 4.379528057220329451, 38.95724293864768839 ) ) ;
#88475 = ORIENTED_EDGE ( 'NONE', *, *, #55774, .T. ) ;
#88476 = CARTESIAN_POINT ( 'NONE',  ( -19.02544592524342804, 5.153800228976336051, 31.04057627198102409 ) ) ;
#88477 = CARTESIAN_POINT ( 'NONE',  ( 10.81492255796078972, 18.62759615963270932, 24.58224293864768839 ) ) ;
#88478 = CARTESIAN_POINT ( 'NONE',  ( -21.52544592524334988, -5.823673210054445271, 33.95942372801901143 ) ) ;
#88479 = CARTESIAN_POINT ( 'NONE',  ( -0.05219959533910754901, -16.53943276465976808, 67.49890960531436690 ) ) ;
#88480 = CIRCLE ( 'NONE', #56440, 61.99999999999998579 ) ;
#88481 = CARTESIAN_POINT ( 'NONE',  ( -21.53943276465977519, 0.05219959533907696930, 61.24890960531435979 ) ) ;
#88482 = CARTESIAN_POINT ( 'NONE',  ( -13.89961937509977652, 13.97604488694528158, 75.62390960531438111 ) ) ;
#88483 = B_SPLINE_CURVE_WITH_KNOTS ( 'NONE', 3,
 ( #192501, #133824, #115658, #196516, #85299, #180353, #41822, #103489, #12491, #74153, #54981, #165167, #149990, #11496, #100476, #73167, #162155, #57987, #194505, #55978, #119658, #42819, #104482, #166166, #183313, #75125, #138776, #32604, #29625, #184303, #92268, #136793, #90289, #59951, #78091, #152948, #31610, #257, #107436, #13461, #94257, #93260 ),
 .UNSPECIFIED., .F., .F.,
 ( 4, 2, 2, 2, 2, 2, 2, 2, 2, 2, 2, 2, 2, 2, 2, 2, 2, 2, 2, 2, 4 ),
 ( 0.004226304204691694322, 0.005303825792898751723, 0.005842586587002280424, 0.006381347381105809992, 0.007458868969312869128, 0.008536390557519929131, 0.009613912145726988268, 0.01069143373393404740, 0.01123019452803758825, 0.01176895532214112562, 0.01284647691034820384, 0.01392399849855528206, 0.01446275929265882290, 0.01500152008676236375, 0.01607904167496944370, 0.01715656326317651845, 0.01823408485138360013, 0.01877284564548713924, 0.01931160643959067488, 0.02038912802779774616, 0.02146664961600481397 ),
 .UNSPECIFIED. ) ;
#88485 = CARTESIAN_POINT ( 'NONE',  ( -16.51473224551082808, 9.474510206698731452, 73.33442372801900433 ) ) ;
#88484 = CARTESIAN_POINT ( 'NONE',  ( -16.46253265017160317, 9.564922557960807481, 25.83224293864769194 ) ) ;
#88486 = CARTESIAN_POINT ( 'NONE',  ( -21.52544592524343514, 5.823673210054127303, 51.04057627198103120 ) ) ;
#88487 = CARTESIAN_POINT ( 'NONE',  ( 16.46253265017160672, -9.564922557960803928, 43.33224293864769550 ) ) ;
#88488 = CARTESIAN_POINT ( 'NONE',  ( 19.05341960407611168, 5.049401038298154454, 68.95724293864769550 ) ) ;
#88489 = ORIENTED_EDGE ( 'NONE', *, *, #160927, .T. ) ;
#88490 = CARTESIAN_POINT ( 'NONE',  ( 14.29746914071037800, 8.314922557961029526, 31.66775706135234358 ) ) ;
#88491 = CARTESIAN_POINT ( 'NONE',  ( 10.81492255796106328, -18.62759615963255655, 20.41775706135234714 ) ) ;
#88492 = CARTESIAN_POINT ( 'NONE',  ( -0.05219959533910754901, -16.53943276465976808, 42.49890960531435979 ) ) ;
#88493 = CARTESIAN_POINT ( 'NONE',  ( 21.52544592524334988, 5.823673210054432836, 61.45942372801901854 ) ) ;
#88494 = CARTESIAN_POINT ( 'NONE',  ( 19.02544592524343514, -5.153800228976328945, 103.5405762719809957 ) ) ;
#88495 = CARTESIAN_POINT ( 'NONE',  ( 5.719274019375991003, -21.55341960407610458, 72.70724293864769550 ) ) ;
#88497 = CARTESIAN_POINT ( 'NONE',  ( -8.224510206698735004, -14.34966873604973081, 49.58442372801901143 ) ) ;
#88496 = CARTESIAN_POINT ( 'NONE',  ( 10.72451020669898902, -18.67979575497178502, 112.9155762719810383 ) ) ;
#88498 = EDGE_CURVE ( 'NONE', #82858, #191214, #45302, .T. ) ;
#88499 = CARTESIAN_POINT ( 'NONE',  ( 10.81492255796078972, 18.62759615963270932, 49.58224293864769550 ) ) ;
#88500 = CARTESIAN_POINT ( 'NONE',  ( 10.72451020669871369, 18.67979575497193778, 107.0844237280190043 ) ) ;
#88501 = CARTESIAN_POINT ( 'NONE',  ( 0.05219959533909260263, 19.03943276465977164, 49.99890960531435979 ) ) ;
#88502 = CARTESIAN_POINT ( 'NONE',  ( -19.03943276465977164, 0.05219959533909376836, 96.24890960531436690 ) ) ;
#88503 = CARTESIAN_POINT ( 'NONE',  ( -19.03943276465977164, 0.05219959533909376836, 81.24890960531436690 ) ) ;
#88504 = CARTESIAN_POINT ( 'NONE',  ( -27.93585545099111656, -25.65867777193844645, -16.61539413803384946 ) ) ;
#88505 = CARTESIAN_POINT ( 'NONE',  ( -13.97604488694547697, 13.89961937509957934, 73.12609039468568994 ) ) ;
#88507 = CARTESIAN_POINT ( 'NONE',  ( -5.823673210054116645, -21.52544592524344225, 37.29057627198102409 ) ) ;
#88506 = CARTESIAN_POINT ( 'NONE',  ( 13.89961937509957401, 13.97604488694547697, 21.87609039468566152 ) ) ;
#88509 = EDGE_CURVE ( 'NONE', #19675, #74853, #6197, .T. ) ;
#88508 = CARTESIAN_POINT ( 'NONE',  ( 0.05219959533934541429, -16.53943276465976808, 105.0010903946856757 ) ) ;
#88510 = CARTESIAN_POINT ( 'NONE',  ( -19.05341960407617563, 5.049401038297882671, 88.54275706135230450 ) ) ;
#88511 = CARTESIAN_POINT ( 'NONE',  ( -17.05116617787826172, 6.768360034955673399, 58.65675553259200115 ) ) ;
#88512 = CARTESIAN_POINT ( 'NONE',  ( -10.81492255796105439, 18.62759615963255655, 112.9177570613523329 ) ) ;
#88513 = CARTESIAN_POINT ( 'NONE',  ( 9.564922557961047289, -16.46253265017146816, 85.41775706135233293 ) ) ;
#88514 = CARTESIAN_POINT ( 'NONE',  ( 5.153800228976615827, -19.02544592524334988, 50.20942372801897591 ) ) ;
#88515 = CARTESIAN_POINT ( 'NONE',  ( 193.3062444957835453, -155.7167183371837496, -4.999999999999999112 ) ) ;
#88516 = CARTESIAN_POINT ( 'NONE',  ( 13.97604488694527802, 13.89961937509977652, 44.37390960531435269 ) ) ;
#88517 = CARTESIAN_POINT ( 'NONE',  ( 0.05219959533910956823, 16.53943276465976808, 49.99890960531437401 ) ) ;
#88518 = CARTESIAN_POINT ( 'NONE',  ( 0.05219959533909260263, 19.03943276465977164, 29.99890960531435979 ) ) ;
#88519 = CARTESIAN_POINT ( 'NONE',  ( 4.379528057220339221, -16.55341960407611168, 37.70724293864769550 ) ) ;
#88520 = CARTESIAN_POINT ( 'NONE',  ( -17.49999999999999645, -5.500000000000000888, 120.0000000000000142 ) ) ;
#88521 = CARTESIAN_POINT ( 'NONE',  ( 16.53943276465976808, 0.05219959533934440121, 106.2510903946856757 ) ) ;
#88522 = CARTESIAN_POINT ( 'NONE',  ( -16.46253265017160317, 9.564922557960807481, 55.83224293864769550 ) ) ;
#88523 = CARTESIAN_POINT ( 'NONE',  ( -15.80617190586768217, 15.72974639402176855, 113.1260903946856899 ) ) ;
#88524 = CARTESIAN_POINT ( 'NONE',  ( -14.34966873604972548, 8.224510206698743886, 33.33442372801900433 ) ) ;
#88525 = CARTESIAN_POINT ( 'NONE',  ( 21.55341960407610458, 5.719274019375980345, 43.95724293864769550 ) ) ;
#88527 = ORIENTED_EDGE ( 'NONE', *, *, #141815, .T. ) ;
#88526 = CARTESIAN_POINT ( 'NONE',  ( 10.72451020669871369, 18.67979575497193778, 87.08442372801901854 ) ) ;
#88528 = CARTESIAN_POINT ( 'NONE',  ( -9.474510206698964154, 16.51473224551069663, 100.4155762719810241 ) ) ;
#88529 = CARTESIAN_POINT ( 'NONE',  ( -16.51473224551069308, -9.474510206698971260, 86.66557627198102409 ) ) ;
#88530 = CARTESIAN_POINT ( 'NONE',  ( -30.66585169841567193, -25.69259602932061881, -17.62843888640922785 ) ) ;
#88531 = CARTESIAN_POINT ( 'NONE',  ( -15.72974639402197994, 15.80617190586746368, 110.6239096053143669 ) ) ;
#88532 = CARTESIAN_POINT ( 'NONE',  ( 0.05219959533910956823, 16.53943276465976808, 79.99890960531435269 ) ) ;
#88534 = CARTESIAN_POINT ( 'NONE',  ( 13.89961937509977652, -13.97604488694527269, 73.12390960531436690 ) ) ;
#88533 = CARTESIAN_POINT ( 'NONE',  ( 18.67979575497178502, 10.72451020669898547, 69.16557627198102409 ) ) ;
#88535 = CARTESIAN_POINT ( 'NONE',  ( 0.05219959533909260263, 19.03943276465977164, 74.99890960531435269 ) ) ;
#88536 = CARTESIAN_POINT ( 'NONE',  ( 21.55341960407610458, 5.719274019375980345, 93.95724293864770971 ) ) ;
#88537 = EDGE_LOOP ( 'NONE', ( #25645, #176271, #76669, #64102, #170590, #176458, #187765, #195446 ) ) ;
#88538 = CARTESIAN_POINT ( 'NONE',  ( 16.51473224551069308, 9.474510206698969483, 54.16557627198103120 ) ) ;
#88540 = CARTESIAN_POINT ( 'NONE',  ( 19.02544592524343514, -5.153800228976328945, 23.54057627198102054 ) ) ;
#88539 = CARTESIAN_POINT ( 'NONE',  ( 16.55341960407611168, 4.379528057220329451, 93.95724293864770971 ) ) ;
#88541 = CARTESIAN_POINT ( 'NONE',  ( -13.89961937509977652, 13.97604488694528158, 65.62390960531436690 ) ) ;
#88542 = CARTESIAN_POINT ( 'NONE',  ( 19.05341960407617918, -5.049401038297876454, 76.04275706135230450 ) ) ;
#88543 = CARTESIAN_POINT ( 'NONE',  ( -8.314922557960811034, -14.29746914071050412, 92.08224293864769550 ) ) ;
#88544 = CARTESIAN_POINT ( 'NONE',  ( -21.53943276465977519, -0.05219959533937600094, 58.75109039468568994 ) ) ;
#88546 = CARTESIAN_POINT ( 'NONE',  ( -18.62759615963270932, 10.81492255796079327, 115.8322429386477097 ) ) ;
#88545 = CARTESIAN_POINT ( 'NONE',  ( 19.03943276465977164, -0.05219959533909143690, 48.74890960531435979 ) ) ;
#88547 = CARTESIAN_POINT ( 'NONE',  ( -0.05219959533910754901, -16.53943276465976808, 97.49890960531436690 ) ) ;
#88548 = CARTESIAN_POINT ( 'NONE',  ( 7.095528360788435407, -39.96100899395969464, -25.59277598899998196 ) ) ;
#88549 = CARTESIAN_POINT ( 'NONE',  ( -13.89961937509977652, 13.97604488694528158, 55.62390960531434558 ) ) ;
#88550 = CARTESIAN_POINT ( 'NONE',  ( -5.429308488886486681E-15, 30.30510711980690175, 143.7500000054623399 ) ) ;
#88552 = CARTESIAN_POINT ( 'NONE',  ( 13.89961937509977652, -13.97604488694527269, 113.1239096053143527 ) ) ;
#88551 = CARTESIAN_POINT ( 'NONE',  ( 16.51473224551083163, -9.474510206698727899, 105.8344237280190043 ) ) ;
#88553 = CARTESIAN_POINT ( 'NONE',  ( 18.62759615963255655, 10.81492255796105972, 46.66775706135234714 ) ) ;
#88554 = CARTESIAN_POINT ( 'NONE',  ( 19.02544592524343514, -5.153800228976328945, 98.54057627198100988 ) ) ;
#88555 = CARTESIAN_POINT ( 'NONE',  ( -9.474510206698720793, -16.51473224551083518, 84.58442372801900433 ) ) ;
#88556 = CARTESIAN_POINT ( 'NONE',  ( -0.05219959533909027116, -19.03943276465977164, 57.49890960531435979 ) ) ;
#88557 = CARTESIAN_POINT ( 'NONE',  ( 16.53943276465976808, -0.05219959533910856209, 78.74890960531436690 ) ) ;
#88558 = CARTESIAN_POINT ( 'NONE',  ( 16.46253265017160672, -9.564922557960803928, 83.33224293864768129 ) ) ;
#88559 = CARTESIAN_POINT ( 'NONE',  ( -14.29746914071049879, 8.314922557960819915, 75.83224293864769550 ) ) ;
#88560 = CARTESIAN_POINT ( 'NONE',  ( -9.564922557960796823, -16.46253265017161027, 87.08224293864769550 ) ) ;
#88561 = VECTOR ( 'NONE', #15882, 1000.000000000000000 ) ;
#88562 = CARTESIAN_POINT ( 'NONE',  ( -13.89961937509957401, -13.97604488694547875, 44.37609039468566863 ) ) ;
#88565 = CARTESIAN_POINT ( 'NONE',  ( 16.46253265017160672, -9.564922557960803928, 28.33224293864769550 ) ) ;
#88564 = CARTESIAN_POINT ( 'NONE',  ( 16.52544592524342804, -4.483927247898539470, 38.54057627198103120 ) ) ;
#88563 = CARTESIAN_POINT ( 'NONE',  ( 13.97604488694527802, 13.89961937509977652, 44.37390960531435269 ) ) ;
#88566 = ORIENTED_EDGE ( 'NONE', *, *, #11536, .T. ) ;
#88567 = CARTESIAN_POINT ( 'NONE',  ( -15.80617190586768217, 15.72974639402176855, 43.12609039468568284 ) ) ;
#88568 = CARTESIAN_POINT ( 'NONE',  ( 19.03943276465977164, 0.05219959533936151252, 76.25109039468566152 ) ) ;
#88569 = CARTESIAN_POINT ( 'NONE',  ( 12.14591786802309770, 12.06949235617756955, 34.37390960531435979 ) ) ;
#88570 = CARTESIAN_POINT ( 'NONE',  ( 10.81492255796078972, 18.62759615963270932, 99.58224293864770971 ) ) ;
#88571 = CARTESIAN_POINT ( 'NONE',  ( -21.52544592524343514, 5.823673210054127303, 36.04057627198102409 ) ) ;
#88572 = CARTESIAN_POINT ( 'NONE',  ( -16.55341960407611168, -4.379528057220339221, 76.45724293864769550 ) ) ;
#88573 = CARTESIAN_POINT ( 'NONE',  ( -0.05219959533909027116, -19.03943276465977164, 42.49890960531435269 ) ) ;
#88574 = CARTESIAN_POINT ( 'NONE',  ( 0.05219959533934541429, -16.53943276465976808, 100.0010903946857042 ) ) ;
#88575 = CARTESIAN_POINT ( 'NONE',  ( -14.29746914071037622, -8.314922557961029526, 69.16775706135234714 ) ) ;
#88576 = CARTESIAN_POINT ( 'NONE',  ( -19.02544592524334988, -5.153800228976617603, 23.95942372801900078 ) ) ;
#88577 = CARTESIAN_POINT ( 'NONE',  ( 5.049401038298161559, -19.05341960407611168, 92.70724293864769550 ) ) ;
#88578 = CARTESIAN_POINT ( 'NONE',  ( 16.46253265017160672, -9.564922557960803928, 83.33224293864768129 ) ) ;
#88579 = CARTESIAN_POINT ( 'NONE',  ( -16.52544592524335698, -4.483927247898792601, 73.95942372801901854 ) ) ;
#88580 = CARTESIAN_POINT ( 'NONE',  ( 19.03943276465977164, -0.05219959533909143690, 33.74890960531435979 ) ) ;
#88581 = CARTESIAN_POINT ( 'NONE',  ( 16.52544592524342804, -4.483927247898539470, 43.54057627198103830 ) ) ;
#88583 = CARTESIAN_POINT ( 'NONE',  ( -16.46253265017160317, 9.564922557960807481, 90.83224293864769550 ) ) ;
#88582 = CARTESIAN_POINT ( 'NONE',  ( -13.97604488694527625, -13.89961937509977652, 101.8739096053143811 ) ) ;
#88584 = CARTESIAN_POINT ( 'NONE',  ( -21.55341960407610458, -5.719274019375992779, 26.45724293864768839 ) ) ;
#88585 = CARTESIAN_POINT ( 'NONE',  ( -12.06949235617756955, 12.14591786802309770, 70.62390960531436690 ) ) ;
#88586 = VERTEX_POINT ( 'NONE', #45319 ) ;
#88587 = CARTESIAN_POINT ( 'NONE',  ( -14.29746914071049879, 8.314922557960819915, 65.83224293864769550 ) ) ;
#88590 = AXIS2_PLACEMENT_3D ( 'NONE', #16173, #167867, #92992 ) ;
#88589 = CARTESIAN_POINT ( 'NONE',  ( 17.49999999999999645, -3.237210098469573971, 32.21236987379557348 ) ) ;
#88588 = CARTESIAN_POINT ( 'NONE',  ( 4.379528057220092307, 16.55341960407617563, 52.29275706135236135 ) ) ;
#88591 = CARTESIAN_POINT ( 'NONE',  ( -19.02544592524334988, -5.153800228976617603, 68.95942372801896170 ) ) ;
#88592 = CARTESIAN_POINT ( 'NONE',  ( 5.153800228976335163, 19.02544592524342804, 84.79057627198099567 ) ) ;
#88593 = CARTESIAN_POINT ( 'NONE',  ( 9.474510206698729675, 16.51473224551082808, 62.08442372801899722 ) ) ;
#88594 = CARTESIAN_POINT ( 'NONE',  ( 22.44159573604009594, -16.30477369853687364, 148.1750000027311671 ) ) ;
#88596 = CARTESIAN_POINT ( 'NONE',  ( -12.14591786802326823, 12.06949235617739902, 98.12609039468570415 ) ) ;
#88595 = CARTESIAN_POINT ( 'NONE',  ( -14.29746914071037622, -8.314922557961029526, 19.16775706135234714 ) ) ;
#88598 = CARTESIAN_POINT ( 'NONE',  ( -5.153800228976328057, -19.02544592524343514, 42.29057627198101699 ) ) ;
#88597 = MECHANICAL_DESIGN_GEOMETRIC_PRESENTATION_REPRESENTATION (  '', ( #149949 ), #198437 ) ;
#88599 = CARTESIAN_POINT ( 'NONE',  ( 18.62759615963271287, -10.81492255796078972, 28.33224293864769550 ) ) ;
#88600 = CARTESIAN_POINT ( 'NONE',  ( -10.81492255796105439, 18.62759615963255655, 57.91775706135234714 ) ) ;
#88601 = CARTESIAN_POINT ( 'NONE',  ( -9.564922557961040184, 16.46253265017147172, 102.9177570613523329 ) ) ;
#88603 = CARTESIAN_POINT ( 'NONE',  ( 19.05341960407611168, 5.049401038298154454, 73.95724293864768129 ) ) ;
#88602 = CARTESIAN_POINT ( 'NONE',  ( -9.297033629063200522E-15, -64.87124026077283645, -24.99999901254159695 ) ) ;
#88604 = DIRECTION ( 'NONE',  ( 1.000000000000000000, 0.000000000000000000, 0.000000000000000000 ) ) ;
#88606 = CARTESIAN_POINT ( 'NONE',  ( -16.51473224551069308, -9.474510206698971260, 76.66557627198103830 ) ) ;
#88605 = CARTESIAN_POINT ( 'NONE',  ( 8.224510206698953496, -14.34966873604960469, 77.91557627198102409 ) ) ;
#88607 = CARTESIAN_POINT ( 'NONE',  ( -19.02544592524342804, 5.153800228976336051, 76.04057627198102409 ) ) ;
#88608 = CARTESIAN_POINT ( 'NONE',  ( 9.564922557961047289, -16.46253265017146816, 85.41775706135233293 ) ) ;
#88609 = CARTESIAN_POINT ( 'NONE',  ( 21.52544592524344225, -5.823673210054117533, 63.54057627198103830 ) ) ;
#88610 = CARTESIAN_POINT ( 'NONE',  ( 19.03943276465977164, -0.05219959533909143690, 33.74890960531435979 ) ) ;
#88611 = CARTESIAN_POINT ( 'NONE',  ( 19.03943276465977164, 0.05219959533936151252, 61.25109039468566863 ) ) ;
#88612 = CARTESIAN_POINT ( 'NONE',  ( -13.97604488694527625, -13.89961937509977652, 51.87390960531436690 ) ) ;
#88613 = CARTESIAN_POINT ( 'NONE',  ( 9.474510206698971260, -16.51473224551069308, 87.91557627198102409 ) ) ;
#88614 = ORIENTED_EDGE ( 'NONE', *, *, #68093, .F. ) ;
#88615 = CARTESIAN_POINT ( 'NONE',  ( -5.823673210054116645, -21.52544592524344225, 92.29057627198103830 ) ) ;
#88617 = CARTESIAN_POINT ( 'NONE',  ( -16.51473224551082808, 9.474510206698731452, 48.33442372801900433 ) ) ;
#88616 = CARTESIAN_POINT ( 'NONE',  ( 12.06949235617757843, -12.14591786802309237, 93.12390960531436690 ) ) ;
#88618 = CARTESIAN_POINT ( 'NONE',  ( 5.823673210054125526, 21.52544592524343514, 79.79057627198102409 ) ) ;
#88619 = CARTESIAN_POINT ( 'NONE',  ( 10.81492255796078972, 18.62759615963270932, 54.58224293864769550 ) ) ;
#88620 = CARTESIAN_POINT ( 'NONE',  ( 16.52544592524342804, -4.483927247898539470, 28.54057627198103120 ) ) ;
#88621 = CARTESIAN_POINT ( 'NONE',  ( -21.55341960407619339, 5.719274019375674811, 103.5427570613523613 ) ) ;
#88622 = CARTESIAN_POINT ( 'NONE',  ( 13.89961937509977652, -13.97604488694527269, 73.12390960531436690 ) ) ;
#88623 = CARTESIAN_POINT ( 'NONE',  ( -19.03943276465977164, 0.05219959533909376836, 36.24890960531436690 ) ) ;
#88624 = AXIS2_PLACEMENT_3D ( 'NONE', #48582, #82870, #94064 ) ;
#88625 = CARTESIAN_POINT ( 'NONE',  ( 10.81492255796106328, -18.62759615963255655, 35.41775706135234003 ) ) ;
#88626 = EDGE_CURVE ( 'NONE', #45948, #135096, #71751, .T. ) ;
#88627 = CARTESIAN_POINT ( 'NONE',  ( -21.52544592524334988, -5.823673210054445271, 58.95942372801902565 ) ) ;
#88628 = CARTESIAN_POINT ( 'NONE',  ( 13.97604488694527802, 13.89961937509977652, 49.37390960531434558 ) ) ;
#88629 = CARTESIAN_POINT ( 'NONE',  ( -10.81492255796105439, 18.62759615963255655, 27.91775706135234358 ) ) ;
#88630 = CARTESIAN_POINT ( 'NONE',  ( 9.474510206698729675, 16.51473224551082808, 62.08442372801899722 ) ) ;
#88631 = CARTESIAN_POINT ( 'NONE',  ( -16.51473224551069308, -9.474510206698971260, 31.66557627198102054 ) ) ;
#88632 = CARTESIAN_POINT ( 'NONE',  ( -8.224510206698735004, -14.34966873604973081, 34.58442372801900433 ) ) ;
#88633 = CARTESIAN_POINT ( 'NONE',  ( -13.97604488694527625, -13.89961937509977652, 31.87390960531435979 ) ) ;
#88634 = CARTESIAN_POINT ( 'NONE',  ( -14.34966873604972548, 8.224510206698743886, 78.33442372801901854 ) ) ;
#88635 = CARTESIAN_POINT ( 'NONE',  ( -19.02544592524342804, 5.153800228976336051, 36.04057627198100988 ) ) ;
#88636 = CARTESIAN_POINT ( 'NONE',  ( -26.70292545465317247, -6.820347898097931072, 168.5277281069577953 ) ) ;
#88637 = CARTESIAN_POINT ( 'NONE',  ( -16.51473224551069308, -9.474510206698971260, 91.66557627198103830 ) ) ;
#88638 = CARTESIAN_POINT ( 'NONE',  ( 5.153800228976335163, 19.02544592524342804, 24.79057627198102765 ) ) ;
#88639 = CARTESIAN_POINT ( 'NONE',  ( 5.823673210054125526, 21.52544592524343514, 69.79057627198102409 ) ) ;
#88640 = CARTESIAN_POINT ( 'NONE',  ( -4.379528057220086978, -16.55341960407618274, 49.79275706135234714 ) ) ;
#88641 = CARTESIAN_POINT ( 'NONE',  ( -5.823673210054431948, 21.52544592524334988, 102.7094237280190185 ) ) ;
#88642 = CARTESIAN_POINT ( 'NONE',  ( 19.02544592524343514, -5.153800228976328945, 43.54057627198103120 ) ) ;
#88643 = CARTESIAN_POINT ( 'NONE',  ( -4.483927247898539470, -16.52544592524342804, 27.29057627198103120 ) ) ;
#88644 = CARTESIAN_POINT ( 'NONE',  ( 0.05219959533910956823, 16.53943276465976808, 64.99890960531435269 ) ) ;
#88645 = CARTESIAN_POINT ( 'NONE',  ( -13.97604488694527625, -13.89961937509977652, 66.87390960531436690 ) ) ;
#88646 = CARTESIAN_POINT ( 'NONE',  ( -0.05219959533937732626, 21.53943276465977519, 107.5010903946856899 ) ) ;
#88647 = CARTESIAN_POINT ( 'NONE',  ( -21.55341960407619339, 5.719274019375674811, 23.54275706135235424 ) ) ;
#88648 = CARTESIAN_POINT ( 'NONE',  ( 5.049401038298161559, -19.05341960407611168, 82.70724293864770971 ) ) ;
#88649 = CARTESIAN_POINT ( 'NONE',  ( -5.719274019375665041, -21.55341960407619695, 89.79275706135236135 ) ) ;
#88650 = CARTESIAN_POINT ( 'NONE',  ( -4.379528057220086978, -16.55341960407618274, 69.79275706135234714 ) ) ;
#88651 = CARTESIAN_POINT ( 'NONE',  ( 8.314922557961029526, -14.29746914071037800, 35.41775706135234003 ) ) ;
#88653 = CARTESIAN_POINT ( 'NONE',  ( 10.81492255796106328, -18.62759615963255655, 105.4177570613523613 ) ) ;
#88652 = CARTESIAN_POINT ( 'NONE',  ( -16.55341960407611168, -4.379528057220339221, 96.45724293864770971 ) ) ;
#88654 = CARTESIAN_POINT ( 'NONE',  ( 8.314922557960818139, 14.29746914071049879, 34.58224293864770260 ) ) ;
#88655 = CARTESIAN_POINT ( 'NONE',  ( -19.05341960407611168, -5.049401038298163336, 31.45724293864769550 ) ) ;
#88656 = CARTESIAN_POINT ( 'NONE',  ( 14.34966873604972726, -8.224510206698740333, 50.83442372801901143 ) ) ;
#88657 = CARTESIAN_POINT ( 'NONE',  ( 8.314922557960818139, 14.29746914071049879, 49.58224293864769550 ) ) ;
#88658 = CARTESIAN_POINT ( 'NONE',  ( -16.53943276465976808, -0.05219959533934237506, 98.75109039468568994 ) ) ;
#88659 = CARTESIAN_POINT ( 'NONE',  ( 15.72974639402199770, -15.80617190586745480, 23.12390960531436335 ) ) ;
#88660 = CARTESIAN_POINT ( 'NONE',  ( -18.67979575497178146, -10.72451020669898902, 36.66557627198103120 ) ) ;
#88661 = CARTESIAN_POINT ( 'NONE',  ( -21.53943276465977519, -0.05219959533937600094, 108.7510903946857042 ) ) ;
#88662 = ADVANCED_FACE ( 'NONE', ( #127920 ), #191598, .F. ) ;
#88663 = CARTESIAN_POINT ( 'NONE',  ( -8.224510206698948167, 14.34966873604960824, 80.41557627198103830 ) ) ;
#88664 = CARTESIAN_POINT ( 'NONE',  ( 13.89961937509977652, -13.97604488694527269, 93.12390960531436690 ) ) ;
#88665 = ORIENTED_EDGE ( 'NONE', *, *, #62849, .F. ) ;
#88666 = CARTESIAN_POINT ( 'NONE',  ( 8.314922557961029526, -14.29746914071037800, 45.41775706135234003 ) ) ;
#88667 = CARTESIAN_POINT ( 'NONE',  ( -13.97604488694527625, -13.89961937509977652, 36.87390960531436690 ) ) ;
#88669 = DIRECTION ( 'NONE',  ( 0.000000000000000000, 0.000000000000000000, -1.000000000000000000 ) ) ;
#88668 = CARTESIAN_POINT ( 'NONE',  ( -16.52544592524335698, -4.483927247898792601, 38.95942372801901854 ) ) ;
#88670 = CARTESIAN_POINT ( 'NONE',  ( 5.153800228976615827, -19.02544592524334988, 55.20942372801899722 ) ) ;
#88671 = CARTESIAN_POINT ( 'NONE',  ( -13.97604488694527625, -13.89961937509977652, 51.87390960531436690 ) ) ;
#88672 = CARTESIAN_POINT ( 'NONE',  ( -8.224510206698735004, -14.34966873604973081, 74.58442372801901854 ) ) ;
#88673 = CARTESIAN_POINT ( 'NONE',  ( 13.97604488694548053, -13.89961937509957401, 100.6260903946856615 ) ) ;
#88674 = CARTESIAN_POINT ( 'NONE',  ( -5.153800228976607833, 19.02544592524334988, 32.70942372801899722 ) ) ;
#88675 = CARTESIAN_POINT ( 'NONE',  ( -19.03943276465977164, 0.05219959533909376836, 66.24890960531436690 ) ) ;
#88676 = ADVANCED_FACE ( 'NONE', ( #160266 ), #144091, .F. ) ;
#88677 = CARTESIAN_POINT ( 'NONE',  ( 16.53943276465976808, -0.05219959533910856209, 93.74890960531436690 ) ) ;
#88678 = CARTESIAN_POINT ( 'NONE',  ( 5.153800228976615827, -19.02544592524334988, 65.20942372801900433 ) ) ;
#88679 = CARTESIAN_POINT ( 'NONE',  ( 15.72974639402199770, -15.80617190586745480, 68.12390960531436690 ) ) ;
#88680 = CARTESIAN_POINT ( 'NONE',  ( 9.564922557961047289, -16.46253265017146816, 35.41775706135233293 ) ) ;
#88681 = CARTESIAN_POINT ( 'NONE',  ( -5.049401038298153566, 19.05341960407611168, 110.2072429386476671 ) ) ;
#88682 = CIRCLE ( 'NONE', #140340, 7.500000000000000000 ) ;
#88683 = CARTESIAN_POINT ( 'NONE',  ( 0.05219959533907565091, 21.53943276465977519, 84.99890960531436690 ) ) ;
#88684 = CARTESIAN_POINT ( 'NONE',  ( -16.61371651742600619, 7.165104196376140600, 83.85415069992994574 ) ) ;
#88685 = CARTESIAN_POINT ( 'NONE',  ( -19.05341960407617563, 5.049401038297882671, 98.54275706135233293 ) ) ;
#88686 = LINE ( 'NONE', #154335, #83803 ) ;
#88687 = CARTESIAN_POINT ( 'NONE',  ( 4.379528057220092307, 16.55341960407617563, 27.29275706135234358 ) ) ;
#88688 = CARTESIAN_POINT ( 'NONE',  ( -13.89961937509977652, 13.97604488694528158, 45.62390960531433848 ) ) ;
#88689 = CARTESIAN_POINT ( 'NONE',  ( -15.80617190586745835, -15.72974639402198527, 21.87390960531436690 ) ) ;
#88690 = CARTESIAN_POINT ( 'NONE',  ( 5.719274019375991003, -21.55341960407610458, 92.70724293864770971 ) ) ;
#88691 = CARTESIAN_POINT ( 'NONE',  ( 5.823673210054444382, -21.52544592524334988, 65.20942372801901854 ) ) ;
#88693 = CARTESIAN_POINT ( 'NONE',  ( 18.67979575497194134, -10.72451020669871369, 105.8344237280190328 ) ) ;
#88692 = CARTESIAN_POINT ( 'NONE',  ( -0.05219959533936034679, 19.03943276465977164, 112.5010903946856757 ) ) ;
#88694 = CARTESIAN_POINT ( 'NONE',  ( -16.55341960407611168, -4.379528057220339221, 21.45724293864769550 ) ) ;
#88695 = CARTESIAN_POINT ( 'NONE',  ( 5.719274019375991003, -21.55341960407610458, 97.70724293864772392 ) ) ;
#88696 = CARTESIAN_POINT ( 'NONE',  ( -16.53943276465976808, 0.05219959533911058130, 56.24890960531436690 ) ) ;
#88697 = CARTESIAN_POINT ( 'NONE',  ( -9.564922557961040184, 16.46253265017147172, 82.91775706135233293 ) ) ;
#88698 = CARTESIAN_POINT ( 'NONE',  ( 19.03943276465977164, 0.05219959533936151252, 56.25109039468566863 ) ) ;
#88699 = CARTESIAN_POINT ( 'NONE',  ( 15.72974639402176855, 15.80617190586768217, 66.87609039468568994 ) ) ;
#88700 = CARTESIAN_POINT ( 'NONE',  ( 9.564922557961047289, -16.46253265017146816, 35.41775706135233293 ) ) ;
#88701 = CARTESIAN_POINT ( 'NONE',  ( -0.05219959533909027116, -19.03943276465977164, 22.49890960531436690 ) ) ;
#88702 = CARTESIAN_POINT ( 'NONE',  ( -15.80617190586745835, -15.72974639402198527, 41.87390960531435979 ) ) ;
#88703 = CARTESIAN_POINT ( 'NONE',  ( -16.52544592524342804, 4.483927247898546575, 36.04057627198102409 ) ) ;
#88704 = CARTESIAN_POINT ( 'NONE',  ( 10.72451020669871369, 18.67979575497193778, 107.0844237280190043 ) ) ;
#88705 = CARTESIAN_POINT ( 'NONE',  ( -0.05219959533934338120, 16.53943276465976808, 67.50109039468568994 ) ) ;
#88706 = CARTESIAN_POINT ( 'NONE',  ( 8.224510206698953496, -14.34966873604960469, 42.91557627198103120 ) ) ;
#88707 = CARTESIAN_POINT ( 'NONE',  ( 5.719274019375673035, 21.55341960407619339, 62.29275706135236845 ) ) ;
#88708 = CARTESIAN_POINT ( 'NONE',  ( 10.72451020669871369, 18.67979575497193778, 72.08442372801899012 ) ) ;
#88709 = CARTESIAN_POINT ( 'NONE',  ( 21.52544592524344225, -5.823673210054117533, 68.54057627198103830 ) ) ;
#88710 = AXIS2_PLACEMENT_3D ( 'NONE', #81667, #112041, #143350 ) ;
#88711 = EDGE_LOOP ( 'NONE', ( #166525, #80338 ) ) ;
#88712 = CARTESIAN_POINT ( 'NONE',  ( -19.03943276465977164, 0.05219959533909376836, 21.24890960531436335 ) ) ;
#88713 = CARTESIAN_POINT ( 'NONE',  ( 5.719274019375673035, 21.55341960407619339, 37.29275706135235424 ) ) ;
#88714 = CARTESIAN_POINT ( 'NONE',  ( -8.314922557960811034, -14.29746914071050412, 112.0822429386477097 ) ) ;
#88715 = CARTESIAN_POINT ( 'NONE',  ( 13.89961937509977652, -13.97604488694527269, 33.12390960531434558 ) ) ;
#88716 = CARTESIAN_POINT ( 'NONE',  ( -0.05219959533910754901, -16.53943276465976808, 87.49890960531436690 ) ) ;
#88717 = CARTESIAN_POINT ( 'NONE',  ( 5.153800228976335163, 19.02544592524342804, 89.79057627198102409 ) ) ;
#88718 = CARTESIAN_POINT ( 'NONE',  ( -4.483927247898539470, -16.52544592524342804, 22.29057627198102765 ) ) ;
#88719 = CARTESIAN_POINT ( 'NONE',  ( 8.224510206698953496, -14.34966873604960469, 97.91557627198103830 ) ) ;
#88720 = CARTESIAN_POINT ( 'NONE',  ( -15.80617190586745835, -15.72974639402198527, 71.87390960531438111 ) ) ;
#88721 = CARTESIAN_POINT ( 'NONE',  ( 18.67979575497178502, 10.72451020669898547, 104.1655762719810241 ) ) ;
#88722 = CARTESIAN_POINT ( 'NONE',  ( -17.45991095687933026, 16.83259678516729707, -54.25516819912629529 ) ) ;
#88724 = CARTESIAN_POINT ( 'NONE',  ( 16.52544592524335698, 4.483927247898782831, 26.45942372801901854 ) ) ;
#88723 = CARTESIAN_POINT ( 'NONE',  ( -13.97604488694527625, -13.89961937509977652, 66.87390960531436690 ) ) ;
#88725 = CARTESIAN_POINT ( 'NONE',  ( 10.81492255796078972, 18.62759615963270932, 54.58224293864769550 ) ) ;
#88726 = CIRCLE ( 'NONE', #98352, 2.699999999999993960 ) ;
#88727 = CARTESIAN_POINT ( 'NONE',  ( 5.719274019375673035, 21.55341960407619339, 87.29275706135236135 ) ) ;
#88728 = CARTESIAN_POINT ( 'NONE',  ( 13.89961937509977652, -13.97604488694527269, 83.12390960531436690 ) ) ;
#88729 = CARTESIAN_POINT ( 'NONE',  ( -19.03943276465977164, 0.05219959533909376836, 106.2489096053143669 ) ) ;
#88730 = CARTESIAN_POINT ( 'NONE',  ( -16.55341960407617563, 4.379528057220093196, 78.54275706135236135 ) ) ;
#88731 = CARTESIAN_POINT ( 'NONE',  ( 10.81492255796106328, -18.62759615963255655, 75.41775706135233293 ) ) ;
#88732 = CARTESIAN_POINT ( 'NONE',  ( 18.67979575497194134, -10.72451020669871369, 105.8344237280190328 ) ) ;
#88733 = CARTESIAN_POINT ( 'NONE',  ( 8.314922557961029526, -14.29746914071037800, 65.41775706135234714 ) ) ;
#88734 = CARTESIAN_POINT ( 'NONE',  ( -18.67979575497178146, -10.72451020669898902, 111.6655762719810525 ) ) ;
#88735 = AXIS2_PLACEMENT_3D ( 'NONE', #32685, #153032, #156016 ) ;
#88736 = CARTESIAN_POINT ( 'NONE',  ( -0.05219959533909027116, -19.03943276465977164, 112.4989096053143669 ) ) ;
#88737 = CARTESIAN_POINT ( 'NONE',  ( -0.05219959533907301413, -21.53943276465977519, 87.49890960531436690 ) ) ;
#88738 = CARTESIAN_POINT ( 'NONE',  ( 13.97604488694548053, -13.89961937509957401, 50.62609039468566152 ) ) ;
#88739 = CARTESIAN_POINT ( 'NONE',  ( 15.72974639402199770, -15.80617190586745480, 48.12390960531436690 ) ) ;
#88741 = CARTESIAN_POINT ( 'NONE',  ( -8.314922557960811034, -14.29746914071050412, 37.08224293864768129 ) ) ;
#88740 = CARTESIAN_POINT ( 'NONE',  ( -19.05341960407611168, -5.049401038298163336, 91.45724293864766707 ) ) ;
#88742 = CARTESIAN_POINT ( 'NONE',  ( 19.49401214000076621, 12.39993551617566681, 167.9999999999999716 ) ) ;
#88743 = STYLED_ITEM ( 'NONE', ( #22183 ), #15828 ) ;
#88744 = LINE ( 'NONE', #120074, #183167 ) ;
#88745 = CARTESIAN_POINT ( 'NONE',  ( 19.05341960407617918, -5.049401038297876454, 111.0427570613523329 ) ) ;
#88746 = CARTESIAN_POINT ( 'NONE',  ( 10.81492255796078972, 18.62759615963270932, 89.58224293864768129 ) ) ;
#88747 = CARTESIAN_POINT ( 'NONE',  ( -12.06949235617756955, 12.14591786802309770, 45.62390960531436690 ) ) ;
#88748 = CARTESIAN_POINT ( 'NONE',  ( -16.55341960407617563, 4.379528057220093196, 33.54275706135234714 ) ) ;
#88749 = CARTESIAN_POINT ( 'NONE',  ( -16.46253265017160317, 9.564922557960807481, 45.83224293864769550 ) ) ;
#88751 = CARTESIAN_POINT ( 'NONE',  ( 19.05341960407617918, -5.049401038297876454, 91.04275706135234714 ) ) ;
#88750 = CARTESIAN_POINT ( 'NONE',  ( 21.53943276465977519, -0.05219959533907433946, 108.7489096053143669 ) ) ;
#88752 = CARTESIAN_POINT ( 'NONE',  ( -9.564922557960796823, -16.46253265017161027, 82.08224293864768129 ) ) ;
#88753 = CARTESIAN_POINT ( 'NONE',  ( -9.474510206698964154, 16.51473224551069663, 75.41557627198103830 ) ) ;
#88754 = CARTESIAN_POINT ( 'NONE',  ( -0.05219959533907301413, -21.53943276465977519, 82.49890960531436690 ) ) ;
#88755 = CARTESIAN_POINT ( 'NONE',  ( 9.474510206698971260, -16.51473224551069308, 37.91557627198102409 ) ) ;
#88756 = CARTESIAN_POINT ( 'NONE',  ( -3.417157638698077982, 37.49351071327306784, -7.999999999999996447 ) ) ;
#88757 = CARTESIAN_POINT ( 'NONE',  ( -14.34966873604960291, -8.224510206698953496, 61.66557627198103120 ) ) ;
#88758 = CARTESIAN_POINT ( 'NONE',  ( 16.51473224551069308, 9.474510206698969483, 84.16557627198102409 ) ) ;
#88759 = DIRECTION ( 'NONE',  ( -1.000000000000000000, 0.000000000000000000, 0.000000000000000000 ) ) ;
#88760 = CARTESIAN_POINT ( 'NONE',  ( -0.05219959533936034679, 19.03943276465977164, 67.50109039468566152 ) ) ;
#88761 = CARTESIAN_POINT ( 'NONE',  ( -21.55341960407610458, -5.719274019375992779, 51.45724293864770260 ) ) ;
#88762 = CARTESIAN_POINT ( 'NONE',  ( 0.05219959533907565091, 21.53943276465977519, 74.99890960531435269 ) ) ;
#88763 = CARTESIAN_POINT ( 'NONE',  ( 13.89961937509957401, 13.97604488694547697, 31.87609039468566863 ) ) ;
#88764 = CARTESIAN_POINT ( 'NONE',  ( -19.02544592524342804, 5.153800228976336051, 101.0405762719810241 ) ) ;
#88765 = CARTESIAN_POINT ( 'NONE',  ( -4.500000000000001776, -126.2936762853306902, 8.011306146643438097 ) ) ;
#88766 = CARTESIAN_POINT ( 'NONE',  ( -18.67979575497178146, -10.72451020669898902, 31.66557627198102054 ) ) ;
#88767 = CARTESIAN_POINT ( 'NONE',  ( 5.049401038298161559, -19.05341960407611168, 77.70724293864765286 ) ) ;
#88768 = CARTESIAN_POINT ( 'NONE',  ( -21.52544592524334988, -5.823673210054445271, 48.95942372801902565 ) ) ;
#88769 = CARTESIAN_POINT ( 'NONE',  ( 16.51473224551069308, 9.474510206698969483, 29.16557627198103475 ) ) ;
#88771 = ORIENTED_EDGE ( 'NONE', *, *, #162970, .F. ) ;
#88770 = CARTESIAN_POINT ( 'NONE',  ( 5.823673210054125526, 21.52544592524343514, 114.7905762719810383 ) ) ;
#88772 = CARTESIAN_POINT ( 'NONE',  ( -15.72974639402176322, -15.80617190586768395, 39.37609039468567573 ) ) ;
#88773 = VERTEX_POINT ( 'NONE', #146083 ) ;
#88774 = CARTESIAN_POINT ( 'NONE',  ( 19.03943276465977164, -0.05219959533909143690, 98.74890960531436690 ) ) ;
#88775 = DIRECTION ( 'NONE',  ( -0.000000000000000000, 0.000000000000000000, 1.000000000000000000 ) ) ;
#88776 = CARTESIAN_POINT ( 'NONE',  ( 21.52544592524344225, -5.823673210054117533, 113.5405762719810383 ) ) ;
#88777 = CARTESIAN_POINT ( 'NONE',  ( -19.03943276465977164, 0.05219959533909376836, 66.24890960531436690 ) ) ;
#88778 = CARTESIAN_POINT ( 'NONE',  ( 4.483927247898790824, -16.52544592524335698, 20.20942372801900788 ) ) ;
#88779 = CARTESIAN_POINT ( 'NONE',  ( -23.48529157249600985, 32.32473071737754111, -6.049999994537625270 ) ) ;
#88780 = CARTESIAN_POINT ( 'NONE',  ( 5.719274019375673035, 21.55341960407619339, 107.2927570613523471 ) ) ;
#88781 = CARTESIAN_POINT ( 'NONE',  ( -19.05341960407611168, -5.049401038298163336, 41.45724293864769550 ) ) ;
#88782 = CARTESIAN_POINT ( 'NONE',  ( -21.53943276465977519, -0.05219959533937600094, 98.75109039468568994 ) ) ;
#88784 = CARTESIAN_POINT ( 'NONE',  ( -21.55341960407619339, 5.719274019375674811, 53.54275706135234714 ) ) ;
#88783 = CARTESIAN_POINT ( 'NONE',  ( 9.564922557960805705, 16.46253265017160317, 89.58224293864769550 ) ) ;
#88785 = CARTESIAN_POINT ( 'NONE',  ( 22.44159573604009594, -16.30477369853687364, 148.1750000027311671 ) ) ;
#88786 = CARTESIAN_POINT ( 'NONE',  ( -5.049401038298153566, 19.05341960407611168, 115.2072429386477097 ) ) ;
#88787 = CARTESIAN_POINT ( 'NONE',  ( -2.552343178074577779, 7.052343178074668373, 1.110912703473986074 ) ) ;
#88790 = CARTESIAN_POINT ( 'NONE',  ( -5.823673210054431948, 21.52544592524334988, 62.70942372801902565 ) ) ;
#88789 = CARTESIAN_POINT ( 'NONE',  ( -12.06949235617739369, -12.14591786802326823, 64.37609039468568994 ) ) ;
#88788 = CARTESIAN_POINT ( 'NONE',  ( -16.52544592524335698, -4.483927247898792601, 58.95942372801902565 ) ) ;
#88791 = CARTESIAN_POINT ( 'NONE',  ( -10.81492255796105439, 18.62759615963255655, 87.91775706135234714 ) ) ;
#88792 = CARTESIAN_POINT ( 'NONE',  ( -10.01085954718718440, 9.437681514439628216, -60.42207423661104571 ) ) ;
#88793 = CARTESIAN_POINT ( 'NONE',  ( 8.224510206698742110, 14.34966873604972548, 32.08442372801901854 ) ) ;
#88794 = CARTESIAN_POINT ( 'NONE',  ( -13.89961937509977652, 13.97604488694528158, 75.62390960531438111 ) ) ;
#88795 = CARTESIAN_POINT ( 'NONE',  ( 9.474510206698971260, -16.51473224551069308, 112.9155762719810383 ) ) ;
#88796 = CARTESIAN_POINT ( 'NONE',  ( 16.38665767535054130, 7.295008042176048590, 42.23599135785459424 ) ) ;
#88797 = CARTESIAN_POINT ( 'NONE',  ( 19.05341960407611168, 5.049401038298154454, 23.95724293864769194 ) ) ;
#88798 = CARTESIAN_POINT ( 'NONE',  ( 21.52544592524344225, -5.823673210054117533, 38.54057627198103120 ) ) ;
#88799 = CARTESIAN_POINT ( 'NONE',  ( 14.34966873604972726, -8.224510206698740333, 90.83442372801901854 ) ) ;
#88801 = CARTESIAN_POINT ( 'NONE',  ( 0.05219959533909260263, 19.03943276465977164, 64.99890960531436690 ) ) ;
#88800 = CARTESIAN_POINT ( 'NONE',  ( -8.314922557960811034, -14.29746914071050412, 77.08224293864769550 ) ) ;
#88802 = CARTESIAN_POINT ( 'NONE',  ( -18.62759615963255300, -10.81492255796106328, 89.16775706135236135 ) ) ;
#88803 = CARTESIAN_POINT ( 'NONE',  ( 28.79475375365586132, 2.781246896534039337E-14, 145.2656553485623760 ) ) ;
#88804 = CARTESIAN_POINT ( 'NONE',  ( -4.379528057220086978, -16.55341960407618274, 24.79275706135235779 ) ) ;
#88805 = CARTESIAN_POINT ( 'NONE',  ( -8.224510206698948167, 14.34966873604960824, 70.41557627198102409 ) ) ;
#88806 = CARTESIAN_POINT ( 'NONE',  ( 5.719274019375673035, 21.55341960407619339, 37.29275706135235424 ) ) ;
#88807 = CARTESIAN_POINT ( 'NONE',  ( 10.81492255796078972, 18.62759615963270932, 74.58224293864768129 ) ) ;
#88809 = CARTESIAN_POINT ( 'NONE',  ( -19.02544592524334988, -5.153800228976617603, 33.95942372801897591 ) ) ;
#88808 = VECTOR ( 'NONE', #48939, 1000.000000000000000 ) ;
#88810 = DIRECTION ( 'NONE',  ( 1.000000000000000000, 0.000000000000000000, 0.000000000000000000 ) ) ;
#88811 = CARTESIAN_POINT ( 'NONE',  ( -5.153800228976328057, -19.02544592524343514, 77.29057627198099567 ) ) ;
#88812 = CARTESIAN_POINT ( 'NONE',  ( -14.29746914071049879, 8.314922557960819915, 45.83224293864769550 ) ) ;
#88813 = CARTESIAN_POINT ( 'NONE',  ( -8.224510206698948167, 14.34966873604960824, 40.41557627198103120 ) ) ;
#88814 = CARTESIAN_POINT ( 'NONE',  ( 12.06949235617757843, -12.14591786802309237, 23.12390960531436335 ) ) ;
#88815 = CARTESIAN_POINT ( 'NONE',  ( 13.97604488694548053, -13.89961937509957401, 65.62609039468567573 ) ) ;
#88816 = CARTESIAN_POINT ( 'NONE',  ( 17.05587630539784882, 6.762274262135711922, 46.75819690962689634 ) ) ;
#88817 = CARTESIAN_POINT ( 'NONE',  ( 21.52544592524344225, -5.823673210054117533, 28.54057627198103120 ) ) ;
#88818 = CARTESIAN_POINT ( 'NONE',  ( -12.06949235617756955, 12.14591786802309770, 85.62390960531436690 ) ) ;
#88819 = LINE ( 'NONE', #90792, #146539 ) ;
#88821 = CARTESIAN_POINT ( 'NONE',  ( -10.72451020669898014, 18.67979575497178502, 35.41557627198102409 ) ) ;
#88820 = CARTESIAN_POINT ( 'NONE',  ( 5.153800228976335163, 19.02544592524342804, 39.79057627198100988 ) ) ;
#88822 = CARTESIAN_POINT ( 'NONE',  ( -5.823673210054116645, -21.52544592524344225, 67.29057627198103830 ) ) ;
#88823 = CARTESIAN_POINT ( 'NONE',  ( -8.224510206698948167, 14.34966873604960824, 105.4155762719810383 ) ) ;
#88825 = CARTESIAN_POINT ( 'NONE',  ( 19.05341960407611168, 5.049401038298154454, 53.95724293864770260 ) ) ;
#88824 = CARTESIAN_POINT ( 'NONE',  ( -4.483927247898782831, 16.52544592524335698, 67.70942372801901854 ) ) ;
#88826 = CARTESIAN_POINT ( 'NONE',  ( -21.52544592524334988, -5.823673210054445271, 58.95942372801902565 ) ) ;
#88827 = CARTESIAN_POINT ( 'NONE',  ( 16.52544592524342804, -4.483927247898539470, 103.5405762719810383 ) ) ;
#88828 = CARTESIAN_POINT ( 'NONE',  ( 19.05341960407617918, -5.049401038297876454, 91.04275706135234714 ) ) ;
#88829 = CARTESIAN_POINT ( 'NONE',  ( -36.91746825000000598, -11.99521256947794789, -7.024999997268812635 ) ) ;
#88831 = CARTESIAN_POINT ( 'NONE',  ( 10.72451020669898902, -18.67979575497178502, 37.91557627198102409 ) ) ;
#88830 = CARTESIAN_POINT ( 'NONE',  ( -0.4315818942737878472, -21.35939100396077706, -58.81718527612537883 ) ) ;
#88832 = CARTESIAN_POINT ( 'NONE',  ( -29.86685920354755552, 21.69954338932564397, -1.324999997268813345 ) ) ;
#88833 = CARTESIAN_POINT ( 'NONE',  ( 15.80617190586769283, -15.72974639402175789, 65.62609039468568994 ) ) ;
#88835 = CARTESIAN_POINT ( 'NONE',  ( 12.14591786802309770, 12.06949235617756955, 49.37390960531436690 ) ) ;
#88834 = CARTESIAN_POINT ( 'NONE',  ( -16.52544592524335698, -4.483927247898792601, 58.95942372801902565 ) ) ;
#88836 = CARTESIAN_POINT ( 'NONE',  ( 5.719274019375991003, -21.55341960407610458, 62.70724293864769550 ) ) ;
#88837 = CARTESIAN_POINT ( 'NONE',  ( -5.719274019375978568, 21.55341960407610458, 65.20724293864768129 ) ) ;
#88838 = CARTESIAN_POINT ( 'NONE',  ( -19.49401214000074489, -12.39993551617566503, 169.9999999999999716 ) ) ;
#88840 = CARTESIAN_POINT ( 'NONE',  ( -19.03943276465977164, 0.05219959533909376836, 111.2489096053143669 ) ) ;
#88839 = CARTESIAN_POINT ( 'NONE',  ( -9.474510206698720793, -16.51473224551083518, 89.58442372801900433 ) ) ;
#88841 = CARTESIAN_POINT ( 'NONE',  ( 19.02544592524343514, -5.153800228976328945, 43.54057627198103120 ) ) ;
#88842 = CARTESIAN_POINT ( 'NONE',  ( -19.02544592524342804, 5.153800228976336051, 26.04057627198103120 ) ) ;
#88843 = CARTESIAN_POINT ( 'NONE',  ( 9.474510206698971260, -16.51473224551069308, 112.9155762719810383 ) ) ;
#88844 = EDGE_LOOP ( 'NONE', ( #166757, #170165, #152935, #87570 ) ) ;
#88845 = CARTESIAN_POINT ( 'NONE',  ( -12.14591786802326823, 12.06949235617739902, 73.12609039468567573 ) ) ;
#88846 = CARTESIAN_POINT ( 'NONE',  ( 18.62759615963271287, -10.81492255796078972, 98.33224293864769550 ) ) ;
#88847 = CARTESIAN_POINT ( 'NONE',  ( 9.564922557960805705, 16.46253265017160317, 74.58224293864769550 ) ) ;
#88848 = CARTESIAN_POINT ( 'NONE',  ( 21.53943276465977519, 0.05219959533937863772, 36.25109039468567573 ) ) ;
#88849 = CARTESIAN_POINT ( 'NONE',  ( -19.02544592524342804, 5.153800228976336051, 96.04057627198103830 ) ) ;
#88850 = CARTESIAN_POINT ( 'NONE',  ( -31.47347929072011397, -24.22385046035113731, -19.66336643902676329 ) ) ;
#88851 = ORIENTED_EDGE ( 'NONE', *, *, #66871, .T. ) ;
#88852 = CARTESIAN_POINT ( 'NONE',  ( 21.55341960407619695, -5.719274019375665929, 36.04275706135234714 ) ) ;
#88854 = CARTESIAN_POINT ( 'NONE',  ( -19.03943276465977164, -0.05219959533935918106, 88.75109039468567573 ) ) ;
#88853 = CARTESIAN_POINT ( 'NONE',  ( -16.46253265017160317, 9.564922557960807481, 25.83224293864769194 ) ) ;
#88855 = CARTESIAN_POINT ( 'NONE',  ( -16.46253265017146816, -9.564922557961047289, 39.16775706135234003 ) ) ;
#88856 = CARTESIAN_POINT ( 'NONE',  ( 15.80617190586746368, 15.72974639402197994, 114.3739096053143527 ) ) ;
#88857 = CARTESIAN_POINT ( 'NONE',  ( -5.049401038297874678, -19.05341960407617918, 34.79275706135233293 ) ) ;
#88858 = CARTESIAN_POINT ( 'NONE',  ( 9.474510206698729675, 16.51473224551082808, 52.08442372801900433 ) ) ;
#88859 = CARTESIAN_POINT ( 'NONE',  ( 16.52544592524335698, 4.483927247898782831, 96.45942372801901854 ) ) ;
#88860 = CARTESIAN_POINT ( 'NONE',  ( -23.29544513554940721, -16.92513159979223403, 146.1843446569000093 ) ) ;
#88861 = CARTESIAN_POINT ( 'NONE',  ( -9.564922557960796823, -16.46253265017161027, 67.08224293864769550 ) ) ;
#88862 = STYLED_ITEM ( 'NONE', ( #86589 ), #142731 ) ;
#88863 = CARTESIAN_POINT ( 'NONE',  ( -15.80617190586768217, 15.72974639402176855, 83.12609039468568994 ) ) ;
#88864 = EDGE_CURVE ( 'NONE', #43345, #171283, #129898, .T. ) ;
#88865 = CARTESIAN_POINT ( 'NONE',  ( -21.53943276465977519, -0.05219959533937600094, 93.75109039468567573 ) ) ;
#88866 = CARTESIAN_POINT ( 'NONE',  ( -0.4877194249720437358, -9.021937450273805226, -63.96635223026897421 ) ) ;
#88867 = CARTESIAN_POINT ( 'NONE',  ( 13.97604488694527802, 13.89961937509977652, 89.37390960531436690 ) ) ;
#88868 = CARTESIAN_POINT ( 'NONE',  ( 15.72974639402176855, 15.80617190586768217, 56.87609039468568994 ) ) ;
#88869 = CARTESIAN_POINT ( 'NONE',  ( -9.564922557961040184, 16.46253265017147172, 102.9177570613523329 ) ) ;
#88870 = CARTESIAN_POINT ( 'NONE',  ( 16.51473224551069308, 9.474510206698969483, 64.16557627198102409 ) ) ;
#88871 = CARTESIAN_POINT ( 'NONE',  ( -16.51473224551069308, -9.474510206698971260, 111.6655762719810383 ) ) ;
#88872 = CARTESIAN_POINT ( 'NONE',  ( 19.02544592524343514, -5.153800228976328945, 78.54057627198099567 ) ) ;
#88873 = CARTESIAN_POINT ( 'NONE',  ( 17.50000000000001776, -3.252092809005011187, 22.52397829382482897 ) ) ;
#88874 = CARTESIAN_POINT ( 'NONE',  ( -16.51473224551069308, -9.474510206698971260, 71.66557627198102409 ) ) ;
#88875 = CARTESIAN_POINT ( 'NONE',  ( 19.02544592524343514, -5.153800228976328945, 48.54057627198103120 ) ) ;
#88876 = CARTESIAN_POINT ( 'NONE',  ( 10.81492255796078972, 18.62759615963270932, 114.5822429386477097 ) ) ;
#88877 = CARTESIAN_POINT ( 'NONE',  ( -4.379528057220086978, -16.55341960407618274, 89.79275706135236135 ) ) ;
#88878 = AXIS2_PLACEMENT_3D ( 'NONE', #53331, #24011, #132178 ) ;
#88879 = DIRECTION ( 'NONE',  ( 0.000000000000000000, 0.000000000000000000, 1.000000000000000000 ) ) ;
#88880 = CARTESIAN_POINT ( 'NONE',  ( 13.89961937509957401, 13.97604488694547697, 61.87609039468566863 ) ) ;
#88881 = CARTESIAN_POINT ( 'NONE',  ( 5.049401038298161559, -19.05341960407611168, 77.70724293864765286 ) ) ;
#88882 = CARTESIAN_POINT ( 'NONE',  ( -4.379528057220328563, 16.55341960407611168, 70.20724293864769550 ) ) ;
#88883 = CARTESIAN_POINT ( 'NONE',  ( 14.34966873604960469, 8.224510206698951720, 114.1655762719810383 ) ) ;
#88884 = CARTESIAN_POINT ( 'NONE',  ( 13.97604488694527802, 13.89961937509977652, 114.3739096053143669 ) ) ;
#88885 = CARTESIAN_POINT ( 'NONE',  ( -19.02544592524342804, 5.153800228976336051, 111.0405762719810099 ) ) ;
#88886 = CARTESIAN_POINT ( 'NONE',  ( -0.05219959533910754901, -16.53943276465976808, 77.49890960531433848 ) ) ;
#88887 = FACE_OUTER_BOUND ( 'NONE', #87996, .T. ) ;
#88888 = CARTESIAN_POINT ( 'NONE',  ( 13.89961937509957401, 13.97604488694547697, 31.87609039468566863 ) ) ;
#88889 = CARTESIAN_POINT ( 'NONE',  ( 8.314922557961029526, -14.29746914071037800, 110.4177570613523756 ) ) ;
#88890 = CARTESIAN_POINT ( 'NONE',  ( 13.89961937509977652, -13.97604488694527269, 88.12390960531438111 ) ) ;
#88891 = CARTESIAN_POINT ( 'NONE',  ( -5.823673210054431948, 21.52544592524334988, 57.70942372801901143 ) ) ;
#88892 = CARTESIAN_POINT ( 'NONE',  ( -21.52544592524343514, 5.823673210054127303, 46.04057627198103830 ) ) ;
#88893 = CARTESIAN_POINT ( 'NONE',  ( -5.719274019375665041, -21.55341960407619695, 24.79275706135235779 ) ) ;
#88894 = CARTESIAN_POINT ( 'NONE',  ( 18.67979575497178502, 10.72451020669898547, 64.16557627198102409 ) ) ;
#88895 = CARTESIAN_POINT ( 'NONE',  ( -14.29746914071049879, 8.314922557960819915, 100.8322429386477097 ) ) ;
#88896 = CARTESIAN_POINT ( 'NONE',  ( -5.153800228976607833, 19.02544592524334988, 62.70942372801899722 ) ) ;
#88897 = EDGE_CURVE ( 'NONE', #51904, #144525, #74465, .T. ) ;
#88898 = CARTESIAN_POINT ( 'NONE',  ( -19.03943276465977164, 0.05219959533909376836, 26.24890960531435624 ) ) ;
#88899 =( BOUNDED_SURFACE ( )  B_SPLINE_SURFACE ( 3, 2, ( 
 ( #88354, #116704, #71208, #11553, #72205, #131877, #39858, #133879, #178394, #163215, #132871, #195570, #117708, #179404, #102542, #119707, #181390, #78142, #169164, #139810, #122665, #92321, #136848, #107486, #105521, #199523, #30668, #93313, #47832, #171167, #309, #32654, #108491, #13511, #184353, #61977, #182378, #1298, #43856, #154006, #109484, #183366, #44848, #75176, #60004, #185340, #170170, #120679, #62976, #168181, #167206, #124656, #90340, #186352, #94308, #155986, #15502, #152025, #154997, #138829, #31663, #28704, #46831, #198533, #91309, #45835, #140811, #16493, #121671, #2301, #153001, #123643, #29677, #77159, #106504, #17483, #79140, #14500, #76162, #137842, #60991, #36367, #148563, #177909, #38382, #131381, #129369, #39377, #51549, #9051, #23219, #191065, #159715, #176911, #37375, #100038, #98020, #193070, #21212, #53541, #128377, #82869, #66716, #190073, #175903, #68705, #99032, #147566, #101036, #113213, #160722, #144547, #54545, #161724, #6032, #194082, #116218, #117217, #162722, #8033, #67711, #52538, #69714, #22214, #84862, #146540, #55545, #114199, #24227, #83863, #132389, #85878, #70722, #174902, #7023, #178911, #145545, #130362, #40378, #102052, #163737, #192059, #115219, #25237, #86878, #107013, #198050, #14015, #12064, #73726, #133381, #74710, #195072, #135399, #118228, #10053, #119226, #56551, #168686, #121193, #179919, #27224, #166727, #197070, #167713, #182886, #181893, #26228, #41386, #103051, #45361, #60509, #183876, #58537, #122184, #164733, #43371, #75681, #91829, #105043, #44369, #88872, #150565, #28231, #151553, #104048, #137360, #30187, #120203, #106026, #89871, #13043, #42385, #71713, #136373, #59516, #87867, #149555, #11051, #29209, #72726, #134399, #90843, #196086, #152528, #57556, #199039, #180910, #165728, #127145, #186879, #93834, #18011, #138356, #154520, #822, #173683, #49332, #78661, #17009, #35150, #185869, #110003, #187863, #31184, #79665, #110993, #172678, #140336, #77674, #184863, #126168, #33173, #34163, #171684, #188852, #3805, #169689, #47355, #125183, #153522, #62496, #200038, #48349, #94832, #95824, #32178, #109010, #15019, #76680, #157509, #108003, #92835, #156510, #16017, #124167, #141336, #2823, #50336, #139343, #1826, #65483, #170689, #19003, #63508, #142325, #61506, #111993, #64501, #123175, #80649, #46346, #155514, #98795, #68470, #112977, #83631, #81622, #175661, #6791, #69477, #23981, #147324, #176674, #8812, #84627, #189843, #160489, #38150, #158492, #54312, #19979, #145308, #85637, #159476, #20970, #51316, #36135, #161490, #146305, #96806, #177673, #144309, #143305, #39141, #66481, #115984, #100796, #162479, #130125, #128143, #131143, #114981, #7794, #4791, #22978, #174670, #67472, #21979, #116976, #192831, #97787, #178668, #129131, #99804, #5799, #191822, #82627, #70481, #53302, #132147, #193840, #190829, #55304, #52305, #113962, #37135, #11826, #104806, #102814, #12809, #24995, #182651, #196837, #164499, #133143, #150331, #10815, #73491, #71478, #166495, #194834, #26990, #101809, #9817, #40131, #163497, #149321, #42154, #72485, #120952, #74476, #86639, #134158, #56307, #27993, #135164, #117989, #167480, #89632, #90617, #136141, #181658, #179679, #43137, #28975, #44135, #152299, #151320, #41151, #103814, #197817, #148322, #59282, #25992, #88635, #13783, #87635, #195846, #57319, #118995, #105794, #75450, #180678, #137124, #165494, #58305, #198811, #119972, #60276, #121949, #49096, #31937, #153282, #156266, #1582, #32932, #91592, #48105, #14783, #154285, #47109, #3566, #17767, #183642, #65244, #15775, #124937, #30948, #108768, #46107, #79423, #155277, #109761, #94587, #76443, #157265, #138120, #45124, #141094, #16766, #171445, #107761, #2581, #168457, #125927, #140090, #169446, #199801, #93591, #77434, #78414, #61268, #64261, #122938, #170446, #106782, #184625, #29954, #92595, #139106, #185619, #580, #187626, #110753, #62251, #123920 ),
 ( #63257, #172434, #186634, #33923, #95580, #18761, #80408, #142080, #98553, #100562, #189602, #113723, #177435, #51075, #192590, #175419, #115747, #50091, #162242, #37904, #23742, #84386, #36887, #146063, #128890, #160247, #143068, #21737, #111751, #5553, #83389, #99563, #54073, #38905, #6547, #147085, #161244, #126904, #8569, #159232, #68226, #174429, #190590, #112736, #22738, #145066, #191578, #176430, #19742, #85391, #96564, #188610, #7547, #129879, #53056, #35899, #69233, #173439, #130900, #114736, #97545, #81383, #34908, #20727, #158252, #4546, #66240, #127900, #82384, #144072, #67232, #52066, #131912, #179438, #72238, #40904, #151080, #104566, #55068, #102577, #101559, #134922, #180441, #163251, #197577, #58070, #120710, #166249, #11585, #39892, #73252, #59044, #12571, #193596, #74237, #24753, #86400, #196599, #9576, #117743, #150080, #41913, #43890, #132906, #57078, #182410, #194593, #135906, #118752, #105553, #116738, #167239, #181423, #28737, #27749, #103579, #89392, #133914, #165254, #148085, #26748, #178428, #149087, #88387, #42901, #90374, #152059, #119740, #70244, #71242, #56064, #195605, #164261, #25756, #87402, #10576, #62008, #2333, #76195, #137874, #106537, #153034, #78172, #63010, #13544, #94339, #61024, #60037, #156018, #183398, #32688, #171198, #79173, #123673, #44881, #186385, #31695, #124689, #121705, #139841, #168214, #184385, #77191, #1330, #30702, #140844, #17515, #64014, #95333, #154038, #125683, #14534, #199555, #187381, #170202, #47863, #107519, #91343, #16525, #155030, #110505, #109516, #48850, #15533, #138860, #136881, #172186, #198567, #340, #29711, #75210, #122696, #45866, #33671, #169195, #92352, #185371, #93344, #46862, #108523, #129637, #128648, #173189, #126658, #141835, #192346, #7303, #130652, #143825, #68988, #49839, #190343, #22494, #38664, #51819, #67983, #35655, #174187, #113479, #98296, #50836, #84141, #53828, #20481, #191333, #175173, #36639, #189359, #157018, #159998, #5305, #115503, #3327, #65000, #82131, #177191, #188362, #144821, #18516, #21486, #34665, #83147, #52811, #80163, #111503, #6305, #97303, #114478, #96323, #158010, #4307, #19501, #176181, #66989, #37651, #81146, #112493, #99316, #161000, #142827, #145820, #65990, #127659, #158989, #24507, #131666, #73008, #180199, #181185, #118509, #73999, #150839, #116498, #194356, #71990, #120472, #147848, #85143, #133664, #195354, #134677, #179193, #55823, #100319, #193348, #103332, #132668, #56834, #41668, #89150, #163001, #87161, #135669, #146828, #8322, #164020, #12335, #69998, #88148, #197341, #165011, #178186, #26505, #11337, #58804, #182164, #149833, #40661, #196363, #54824, #101312, #9334, #161998, #57831, #25516, #148843, #23494, #117496, #119504, #42662, #39651, #104324, #166009, #27509, #10334, #86158, #71000, #102330, #123437, #124448, #61769, #17279, #94103, #59796, #137632, #15289, #63780, #91109, #28501, #76949, #138618, #77938, #122455, #199318, #43649, #136637, #46621, #75958, #100, #185130, #32450, #106294, #108282, #60784, #109277, #62767, #186144, #125452, #184148, #47623, #183158, #44642, #170956, #169960, #31452, #45629, #121466, #93105, #154790, #140609, #16288, #155782, #107281, #168952, #166999, #139605, #90135, #30458, #151820, #105312, #152798, #13309, #2099, #1091, #74975, #92106, #78933, #153794, #198319, #167980, #29478, #14290, #156790, #171954, #22252, #37413, #160762, #173955, #99072, #79938, #20245, #52577, #68743, #158756, #98056, #65755, #4077, #81893, #128413, #80921, #114237, #83901, #50604, #21251, #143586, #5069, #19274, #187148, #66752, #48621, #159756, #190109, #51584, #49603, #82906, #33442, #129406, #113249, #111266, #141608, #97075, #157784, #174939, #18283, #36402, #3095, #35422, #110273, #64772, #95101, #126434, #96095, #189132, #142597, #67748, #144584, #188132, #127424, #172957, #6070, #191103, #34435, #175943, #145584, #7062, #112263, #71750 ),
 ( #23257, #133420, #162756, #86916, #10091, #119262, #193106, #195109, #147602, #196122, #149593, #72767, #14819, #70757, #11090, #69750, #131419, #134437, #148599, #56592, #24265, #8074, #118266, #179956, #29991, #41423, #57592, #132425, #194117, #53581, #103089, #115258, #55580, #38421, #130401, #39411, #176951, #91630, #164770, #100077, #9089, #26265, #117254, #87906, #183678, #102088, #146579, #161762, #84900, #168493, #45163, #106819, #178946, #153318, #54580, #163773, #192099, #116253, #25274, #177944, #40417, #101071, #85914, #17804, #170483, #142117, #173475, #140127, #110791, #32970, #94624, #108804, #158289, #156303, #63294, #111787, #122975, #139141, #49133, #48141, #184662, #124974, #34948, #46144, #107798, #1618, #126940, #169482, #64297, #96600, #79461, #92630, #141130, #187662, #50127, #76480, #109798, #16803, #2620, #61305, #77471, #123956, #138157, #172472, #186671, #171481, #199838, #31973, #125964, #33959, #154321, #95617, #157302, #18799, #80444, #618, #30982, #3602, #65281, #188648, #15810, #62288, #185654, #47146, #93629, #155314, #78453, #67268, #4584, #53093, #114771, #54108, #98588, #113759, #19778, #112772, #22774, #52102, #176465, #99599, #8607, #82419, #84422, #36926, #85429, #38940, #162279, #101601, #160282, #100597, #159268, #20764, #23779, #37938, #146099, #175455, #97580, #7583, #161279, #116774, #69269, #147120, #21773, #83424, #143105, #130935, #66277, #145101, #127936, #81419, #128926, #189638, #178465, #192626, #51113, #6584, #115782, #68263, #177471, #70280, #191614, #35934, #174465, #144108, #55104, #131948, #193632, #129914, #39932, #5588, #190627, #28774, #44919, #134962, #74276, #41952, #180481, #196640, #104605, #57118, #90412, #60074, #26787, #197616, #119779, #135946, #181463, #12612, #71280, #27789, #132945, #133954, #88429, #183434, #59081, #163289, #24790, #195645, #166293, #10616, #150123, #25794, #149125, #182447, #136919, #72277, #56103, #198606, #194633, #86438, #120748, #58109, #89431, #87440, #43927, #148124, #105589, #42941, #118792, #117784, #73292, #103618, #151120, #179478, #167275, #40943, #11624, #9615, #102615, #164301, #165294, #152097, #13581, #75248, #121742, #140883, #91383, #15570, #137912, #171236, #16563, #199594, #33711, #94377, #157058, #2373, #47901, #76232, #109555, #95373, #48890, #29748, #110545, #61061, #122733, #32725, #45904, #154076, #186425, #78210, #80203, #169235, #93382, #18555, #30741, #172226, #155068, #141874, #153072, #3365, #17554, #65040, #64053, #139880, #125723, #108562, #1369, #184424, #63048, #14574, #185411, #124727, #79214, #126696, #188400, #156057, #106575, #187422, #107557, #170240, #168252, #92389, #77228, #138897, #377, #62049, #123714, #46902, #31734, #189397, #114518, #99353, #49878, #130689, #97342, #96361, #192383, #19539, #69024, #7339, #115540, #98338, #81184, #113519, #100357, #158049, #37688, #85178, #191371, #66030, #52847, #161036, #23532, #146867, #83185, #190384, #176219, #34704, #50874, #159028, #70034, #145857, #175213, #36678, #131703, #82169, #6342, #84177, #127697, #22530, #53866, #177228, #160037, #174226, #142866, #38700, #129673, #162036, #68022, #8359, #111543, #112532, #143865, #21524, #173228, #20521, #4345, #144859, #35695, #5344, #128687, #67028, #51859, #86194, #196398, #25554, #149868, #73043, #182198, #55858, #57867, #10370, #58840, #12370, #135704, #75008, #133700, #74033, #132702, #194391, #197375, #11373, #119539, #87198, #71035, #181222, #134715, #90170, #42698, #120507, #195392, #56870, #116534, #104359, #178222, #118545, #101348, #193384, #102366, #39686, #151853, #166043, #163037, #72027, #27543, #180235, #150876, #89184, #165047, #9370, #24544, #147884, #28534, #43683, #167032, #41704, #105345, #117532, #26540, #13344, #54860, #88184, #179230, #103369, #40696, #164055, #148879, #30492, #2135, #33478, #136, #170992, #93140, #155817, #32485, #92143, #183193 ),
 ( #61805, #123475, #156825, #168988, #154825, #94138, #14327, #62802, #17315, #78970, #185167, #60817, #168014, #109313, #16323, #140645, #77973, #110308, #187185, #152833, #153830, #108317, #18318, #184182, #121499, #169997, #31488, #63815, #15325, #76984, #136673, #29510, #139640, #138655, #1128, #124484, #125488, #199352, #186180, #46658, #48656, #171990, #95136, #198355, #47662, #59829, #75992, #137665, #44675, #106328, #91144, #122491, #45664, #107315, #51618, #160801, #36438, #129442, #173988, #35457, #3133, #113283, #64808, #97108, #126469, #79975, #4110, #188167, #22289, #159791, #49640, #112298, #128446, #158791, #144621, #21286, #143618, #34470, #111303, #172992, #99109, #175980, #83940, #20280, #37448, #96129, #5102, #191141, #141643, #82943, #157818, #174974, #190142, #6104, #52614, #66784, #19308, #80956, #98093, #142631, #114276, #65789, #127458, #67785, #81926, #189164, #50636, #106976, #168650, #124131, #110954, #30150, #48311, #95785, #1790, #76642, #63468, #171645, #34126, #172638, #157471, #47317, #18964, #153486, #93798, #126131, #142287, #32141, #33135, #139307, #77638, #155478, #125143, #154485, #187826, #80610, #185830, #94793, #16970, #79627, #156472, #15979, #91792, #108972, #60472, #14982, #138320, #170653, #122148, #200002, #109966, #183837, #186842, #61468, #17973, #141295, #45326, #123139, #78624, #786, #2785, #184825, #46311, #107966, #169653, #64464, #140299, #49295, #31149, #92797, #62458, #38108, #81582, #130082, #99763, #161448, #67433, #128101, #35111, #176633, #83589, #84585, #21938, #177636, #54273, #19941, #97748, #175622, #23942, #51277, #188813, #37096, #98755, #22939, #82589, #159436, #3767, #96763, #6750, #36096, #160448, #145269, #192791, #66440, #68429, #20931, #69435, #146265, #7750, #85596, #144270, #131103, #143268, #4751, #115946, #191781, #53263, #5757, #189805, #114940, #39103, #100759, #162441, #65444, #129090, #190790, #127106, #50296, #111953, #52264, #173642, #158452, #112938, #174631, #113922, #155686, #124349, #17181, #109182, #60683, #141511, #108183, #107184, #2996, #30360, #79841, #77844, #126336, #64674, #188033, #142499, #994, #49503, #200192, #61674, #111166, #78835, #187053, #154694, #138522, #63681, #2003, #157682, #48523, #172856, #62668, #186044, #184047, #125356, #45530, #47526, #168855, #122358, #169864, #92003, #19172, #110177, #170861, #140513, #34337, #32352, #18185, #33344, #94005, #76851, #153697, #15192, #95997, #80821, #123343, #171856, #185036, #46523, #95003, #31357, #93008, #156691, #16189, #139511, #21148, #175837, #145482, #97959, #72409, #103746, #67647, #38320, #160659, #23156, #99975, #159651, #50505, #191001, #42081, #112168, #173857, #129305, #57249, #35323, #191992, #165425, #6962, #20149, #68642, #115157, #180608, #26919, #37311, #144484, #130298, #189031, #4966, #51487, #88562, #161659, #52477, #114136, #3977, #36304, #22151, #84799, #81794, #53479, #146478, #10745, #98969, #128313, #96977, #176849, #83801, #134086, #195776, #65657, #118923, #143481, #82803, #127319, #158658, #113149, #66652, #190014, #174839, #5968, #28905, #44062, #150260, #43067, #153205, #182579, #106711, #29880, #139031, #12738, #14710, #92524, #31865, #90545, #30877, #89563, #151249, #154213, #168385, #76370, #105722, #27920, #138047, #91518, #47038, #199728, #15703, #152227, #13712, #73421, #61194, #135092, #75378, #58236, #11754, #59211, #196768, #108695, #122866, #198740, #184554, #77363, #137050, #107690, #46035, #121875, #166425, #119904, #181590, #185544, #510, #123846, #60205, #62182, #104734, #183568, #170374, #74404, #45053, #169369, #136070, #167409, #197744, #120880, #187554, #159158, #190517, #157192, #127825, #50013, #112664, #189531, #49021, #140017, #80333, #128818, #1506, #63183, #18686, #143997, #124863, #81312, #51991, #34835, #109691, #96490, #4473, #67161, #113650, #126829, #33846, #158180, #78343, #94510 ),
 ( #186562, #19670, #3494, #48035, #20653, #142995, #5478, #51003, #66163, #171373, #174356, #82307, #35826, #16693, #97472, #32860, #156192, #175344, #17692, #141020, #173365, #65170, #93519, #79349, #142005, #155204, #2507, #64187, #188535, #125854, #110676, #172356, #95506, #111678, #21661, #72165, #87329, #10503, #23667, #149015, #129805, #70169, #102502, #118677, #8492, #148014, #115673, #53999, #131837, #178355, #130825, #164186, #133840, #100490, #71169, #193520, #55992, #132833, #192516, #83315, #85315, #195530, #144992, #6473, #162169, #57004, #68153, #24678, #36812, #39819, #52980, #101485, #9503, #98478, #160171, #54995, #177361, #163174, #191504, #37828, #84312, #114659, #194520, #147007, #116664, #176355, #69158, #86327, #117670, #99488, #179367, #40829, #25684, #161168, #22665, #145991, #7474, #38832, #60953, #198495, #153967, #30630, #196532, #74169, #151989, #271, #27681, #165182, #13476, #75140, #14462, #58976, #135839, #180369, #73183, #183328, #12505, #136811, #59966, #169125, #42834, #44809, #197508, #45798, #199486, #122627, #61940, #120643, #184317, #119672, #181355, #107450, #121633, #106464, #182341, #58002, #168143, #29640, #77121, #91272, #92283, #43819, #105483, #103506, #152963, #26677, #167169, #88317, #41838, #89322, #150007, #138790, #76124, #28668, #137802, #15464, #90303, #11513, #134854, #104499, #166180, #151014, #81083, #96258, #95269, #139773, #93274, #108453, #158924, #174119, #97236, #110439, #35590, #16455, #156952, #189293, #5237, #18449, #34599, #2264, #140775, #80100, #64934, #141768, #65921, #126593, #171128, #187314, #186313, #109445, #142761, #20413, #32617, #78104, #82063, #154959, #123608, #157944, #3261, #188295, #47795, #19435, #170130, #127594, #49772, #94271, #1261, #33606, #155949, #111437, #62938, #173124, #124618, #172120, #185303, #17446, #46794, #31624, #79102, #125616, #63947, #4241, #50770, #48785, #112430, #143756, #131594, #177123, #98228, #194287, #54753, #117427, #101242, #8250, #36573, #69930, #55753, #9264, #190276, #70930, #21418, #83078, #193279, #6239, #114411, #146756, #38594, #40593, #129571, #53758, #179125, #191268, #132597, #115432, #102264, #51752, #163952, #178115, #25450, #24438, #100250, #86087, #68920, #161931, #144754, #23426, #113413, #145753, #85073, #39583, #87090, #148775, #116427, #66918, #162931, #159931, #130582, #147778, #128582, #175104, #67918, #52743, #176112, #37583, #99245, #160933, #192277, #22424, #84074, #7235, #45564, #56766, #118438, #73934, #60717, #180131, #198255, #107217, #151756, #26438, #13249, #121400, #184080, #168888, #43583, #150774, #74912, #195285, #11268, #57765, #30393, #106231, #135603, #197274, #92040, #42594, #166935, #44575, #88080, #136575, #167914, #29414, #58737, #134611, #41600, #183094, #90073, #91045, #28438, #10264, #122391, #149766, #104257, #182099, #71923, #119435, #103265, #105249, #59731, #152732, #89082, #165940, #133593, #164945, #14222, #27440, #75892, #137567, #199250, #72941, #196295, #12269, #181120, #120406, #96032, #35361, #94039, #34372, #93041, #154728, #157719, #110209, #79875, #47560, #31391, #156726, #95035, #50541, #141544, #19208, #155717, #17214, #76884, #18219, #138555, #78866, #61706, #153729, #62700, #33, #112202, #3033, #2034, #171890, #80858, #140546, #111201, #126371, #125389, #169898, #123376, #185068, #189069, #4013, #127356, #63714, #65691, #46556, #187086, #142534, #15225, #48556, #64709, #32384, #170892, #173892, #188068, #108218, #49539, #16224, #33377, #172893, #77876, #139543, #1028, #109213, #124383, #186078, #39352, #51523, #113186, #100010, #36341, #144520, #176884, #68679, #70696, #159687, #83835, #147539, #21185, #162695, #145517, #85850, #20183, #132364, #8005, #194057, #54521, #6997, #116194, #99005, #130334, #174875, #192032, #81829, #175875, #53514, #69688, #24201, #9027, #38355, #55518, #84836, #190048, #160696, #161696 ),
 ( #6005, #143516, #101011, #66688, #177883, #117191, #178884, #115192, #128350, #131355, #23193, #146515, #5005, #193044, #97994, #67685, #22187, #97013, #82841, #158694, #129343, #191038, #52511, #114172, #37347, #103026, #26203, #59493, #13991, #87842, #133356, #75658, #10029, #122159, #151529, #12038, #105018, #164708, #13018, #25212, #182862, #197044, #149530, #195046, #150538, #11025, #73702, #71689, #166702, #56525, #27200, #102027, #118203, #40352, #163709, #72700, #42361, #134373, #121168, #74683, #86854, #196059, #179894, #28205, #135374, #41360, #167688, #89846, #90819, #136349, #181868, #57532, #43347, #29185, #198025, #119201, #180886, #44343, #106001, #137335, #152502, #199015, #104024, #165703, #148538, #60484, #88846, #58512, #120178, #183848, #92811, #168661, #80623, #48324, #32154, #1802, #187839, #108985, #141309, #156485, #155491, #200013, #153497, #30161, #18977, #34139, #157484, #170666, #95798, #76654, #16983, #49308, #65457, #78637, #94806, #62472, #799, #142300, #17987, #14994, #186855, #3780, #47330, #79640, #140312, #2798, #64476, #139319, #91805, #93811, #45336, #138333, #61480, #63480, #106988, #123151, #171659, #184839, #125156, #46324, #109979, #126143, #107978, #169666, #33148, #124144, #110967, #31161, #154498, #15993, #77651, #172651, #185843, #190803, #147297, #159448, #83602, #161462, #4766, #53275, #22952, #84600, #52277, #51290, #158466, #99777, #6764, #7766, #145281, #100771, #177647, #143280, #20944, #98767, #8786, #174644, #111966, #160461, #21952, #146279, #5771, #82601, #127120, #19954, #130097, #144282, #68443, #191794, #115959, #189818, #114954, #67446, #192805, #69449, #131116, #188826, #129104, #54287, #66453, #128115, #39115, #176647, #96777, #38123, #162454, #23955, #50310, #85610, #81596, #112951, #173658, #36109, #97761, #35125, #113935, #175634, #37108, #57293, #120928, #194807, #136117, #118970, #59259, #193814, #105770, #181634, #167457, #27968, #180653, #89608, #72459, #42129, #86614, #103790, #55279, #149297, #165470, #43114, #197793, #182627, #150305, #44112, #58280, #163471, #134133, #11802, #132121, #151297, #116950, #26966, #28953, #133118, #56281, #88609, #195822, #73466, #135139, #70456, #12786, #117963, #178642, #74451, #40105, #90594, #152276, #101783, #196813, #24968, #104782, #119949, #166470, #148297, #9791, #71453, #41124, #179654, #102788, #164474, #25968, #87611, #10791, #155255, #61244, #77412, #76420, #199777, #35622, #190307, #122916, #106759, #51783, #183619, #98260, #127624, #185598, #78393, #138096, #189324, #198788, #158955, #170424, #184604, #168434, #123899, #46085, #47087, #45102, #140069, #29930, #560, #75428, #91569, #13760, #137102, #107740, #15753, #169421, #97267, #50801, #60254, #30926, #153257, #1560, #108748, #14759, #143788, #65953, #66952, #112459, #16744, #113443, #92574, #121925, #174151, #31916, #20445, #154262, #82096, #139082, #5271, #93570, #62231, #128614, #175136, #36603, #193311, #191298, #24469, #52774, #146790, #21449, #129602, #159962, #83110, #68950, #161961, #130613, #40624, #194318, #144787, #192309, #114443, #86119, #69961, #176144, #87122, #147810, #10297, #55786, #101273, #37614, #162963, #148807, #102294, #6270, #163983, #99276, #160963, #9296, #22457, #7266, #39614, #131627, #133627, #84105, #8283, #71954, #145784, #25480, #54785, #195319, #67948, #56799, #70962, #118472, #117457, #116460, #179156, #23457, #178149, #53789, #132630, #115464, #38626, #180162, #41632, #177153, #100283, #85104, #153761, #91075, #196328, #166965, #44606, #164976, #60748, #26471, #151786, #92072, #165970, #27472, #198284, #28467, #59762, #13277, #103297, #184113, #150803, #149797, #45595, #72973, #122421, #107248, #168919, #74941, #134642, #75923, #121430, #152762, #11303, #167945, #57796, #73965, #90102, #123405, #119467, #136604, #183123, #30425, #106261, #12299, #29443, #89115, #135634, #15256, #76914, #197304 ),
 ( #138585, #14252, #58768, #137598, #120436, #182129, #66, #61737, #43613, #181150, #185098, #42625, #88113, #199281, #104289, #105277, #109242, #19241, #31420, #189099, #3062, #170922, #139573, #156756, #17245, #79903, #77906, #111233, #1058, #33409, #108248, #16255, #46587, #169928, #155747, #48586, #78897, #127389, #80888, #93072, #140575, #62732, #172924, #18250, #124414, #173922, #34403, #97042, #142565, #188097, #186108, #49570, #35391, #50572, #154757, #112232, #47589, #32413, #96061, #94068, #2065, #126401, #141574, #20214, #63744, #95068, #158724, #125418, #81862, #64739, #143551, #187114, #5036, #157749, #66722, #4044, #65721, #128383, #110238, #171919, #6039, #176918, #174909, #68712, #100045, #162730, #117225, #40387, #69722, #102060, #177917, #82876, #53548, #131389, #51555, #147574, #113219, #38389, #178919, #52545, #114206, #84869, #115226, #146547, #161731, #190079, #70730, #37382, #36373, #132397, #159723, #9060, #194090, #55552, #23226, #21220, #24236, #193078, #163745, #175911, #54553, #7030, #25245, #86886, #148571, #71721, #130369, #10061, #129375, #191072, #98027, #8041, #116226, #83870, #67718, #39385, #101044, #144554, #85886, #99039, #192066, #160729, #22221, #145552, #118237, #197078, #41395, #133390, #42394, #179928, #30194, #198058, #181901, #151562, #137367, #58545, #90850, #106033, #105051, #149564, #103060, #164742, #168693, #183883, #107021, #120211, #45368, #26237, #166735, #199046, #15026, #28239, #44377, #12072, #150573, #91836, #167719, #87876, #136381, #153529, #43379, #29217, #89879, #152535, #14022, #88881, #11060, #13051, #195081, #72736, #134409, #74718, #56561, #196095, #121201, #57565, #59524, #119235, #182893, #75688, #180919, #104057, #60516, #73734, #122191, #165737, #27232, #135407, #96813, #172686, #1833, #140345, #158499, #109017, #33180, #111000, #154527, #2830, #34171, #95832, #63515, #830, #108011, #49338, #156519, #157516, #94839, #50343, #127152, #92842, #170696, #48356, #76687, #124175, #61513, #110010, #171691, #19010, #155521, #32185, #138363, #169696, #79672, #93842, #18019, #80656, #141343, #185876, #125190, #139350, #62504, #142332, #112002, #47362, #31190, #173691, #46353, #200044, #187870, #64508, #126175, #17016, #3812, #123182, #65490, #188860, #78669, #16024, #186886, #35158, #184871, #77682, #84635, #51324, #6799, #81629, #189851, #19986, #143312, #129139, #21986, #190836, #100804, #54319, #4799, #52312, #131150, #8819, #97795, #192839, #99811, #162487, #38157, #193847, #70488, #36143, #113970, #191829, #40139, #67480, #66488, #53310, #114988, #115991, #98802, #175668, #128151, #112985, #22987, #37143, #176682, #161497, #132154, #82634, #146312, #160496, #85645, #39148, #23988, #101816, #83638, #147331, #159483, #20977, #55312, #7801, #69485, #145316, #144317, #177680, #116983, #178676, #174678, #5806, #68477, #130132, #86646, #28000, #148329, #26997, #71485, #163504, #72492, #9824, #60283, #89640, #11834, #181665, #167488, #88642, #120959, #136148, #135171, #179686, #133151, #194841, #198818, #13791, #137131, #150338, #75457, #56315, #196844, #28983, #45132, #58311, #74483, #42161, #180685, #121956, #197824, #117997, #103821, #90624, #182658, #105801, #25002, #165501, #44142, #102821, #164506, #152306, #119979, #151328, #57326, #41158, #166502, #104813, #183649, #12816, #26000, #73499, #43144, #87642, #59290, #149328, #10822, #134166, #195854, #119002, #91599, #3574, #171453, #155285, #124945, #110762, #31945, #64269, #79431, #78424, #122946, #76450, #153289, #142088, #157273, #80416, #93599, #18769, #199808, #140099, #172443, #188618, #1590, #17776, #185626, #123928, #65252, #141102, #138127, #109769, #126912, #170454, #2589, #63265, #125935, #187634, #62260, #14790, #16775, #106790, #61275, #184634, #186642, #168464, #46115, #94596, #29962, #48113, #107768, #32941, #49104, #169453, #30955, #156275, #47117, #33931, #92602 ) ),
 .UNSPECIFIED., .T., .F., .F. ) 
 B_SPLINE_SURFACE_WITH_KNOTS ( ( 4, 3, 4 ),
 ( 3, 2, 2, 2, 2, 2, 2, 2, 2, 2, 2, 2, 2, 2, 2, 2, 2, 2, 2, 2, 2, 2, 2, 2, 2, 2, 2, 2, 2, 2, 2, 2, 2, 2, 2, 2, 2, 2, 2, 2, 2, 2, 2, 2, 2, 2, 2, 2, 2, 2, 2, 2, 2, 2, 2, 2, 2, 2, 2, 2, 2, 2, 2, 2, 2, 2, 2, 2, 2, 2, 2, 2, 2, 2, 2, 2, 2, 2, 2, 2, 2, 2, 2, 2, 2, 2, 2, 2, 2, 2, 2, 2, 2, 2, 2, 2, 2, 2, 2, 2, 2, 2, 2, 2, 2, 2, 2, 2, 2, 2, 2, 2, 2, 2, 2, 2, 2, 2, 2, 2, 2, 2, 2, 2, 2, 2, 2, 2, 2, 2, 2, 2, 2, 2, 2, 2, 2, 2, 2, 2, 2, 2, 2, 2, 2, 2, 2, 2, 2, 2, 2, 2, 2, 2, 2, 2, 2, 2, 2, 2, 2, 2, 2, 2, 2, 2, 2, 2, 2, 2, 2, 2, 2, 2, 2, 2, 2, 2, 2, 2, 2, 2, 2, 2, 2, 2, 2, 2, 2, 2, 2, 2, 2, 2, 2, 2, 2, 2, 2, 2, 2, 2, 2, 2, 2, 2, 2, 2, 2, 2, 2, 2, 2, 2, 2, 2, 2, 2, 2, 2, 2, 2, 2, 2, 2, 2, 2, 2, 3 ),
 ( 0.000000000000000000, 0.5000000000000000000, 1.000000000000000000 ),
 ( 0.000000000000000000, 0.004385964912280701511, 0.008771929824561403022, 0.01315789473684210453, 0.01754385964912280604, 0.02192982456140350755, 0.02631578947368420907, 0.03070175438596491058, 0.03508771929824561209, 0.03947368421052631360, 0.04385964912280701511, 0.04824561403508771662, 0.05263157894736841813, 0.05701754385964911964, 0.06140350877192982115, 0.06578947368421052266, 0.07017543859649122417, 0.07456140350877192569, 0.07894736842105262720, 0.08333333333333332871, 0.08771929824561403022, 0.09210526315789473173, 0.09649122807017543324, 0.1008771929824561348, 0.1052631578947368363, 0.1096491228070175378, 0.1140350877192982393, 0.1184210526315789408, 0.1228070175438596423, 0.1271929824561403577, 0.1315789473684210453, 0.1359649122807017607, 0.1403508771929824483, 0.1447368421052631637, 0.1491228070175438514, 0.1535087719298245668, 0.1578947368421052544, 0.1622807017543859698, 0.1666666666666666574, 0.1710526315789473728, 0.1754385964912280604, 0.1798245614035087758, 0.1842105263157894635, 0.1885964912280701788, 0.1929824561403508665, 0.1973684210526315819, 0.2017543859649122695, 0.2061403508771929849, 0.2105263157894736725, 0.2149122807017543879, 0.2192982456140350755, 0.2236842105263157909, 0.2280701754385964786, 0.2324561403508771940, 0.2368421052631578816, 0.2412280701754385970, 0.2456140350877192846, 0.2500000000000000000, 0.2543859649122807154, 0.2587719298245614308, 0.2631578947368420907, 0.2675438596491228060, 0.2719298245614035214, 0.2763157894736842368, 0.2807017543859648967, 0.2850877192982456121, 0.2894736842105263275, 0.2938596491228070429, 0.2982456140350877027, 0.3026315789473684181, 0.3070175438596491335, 0.3114035087719298489, 0.3157894736842105088, 0.3201754385964912242, 0.3245614035087719396, 0.3289473684210526550, 0.3333333333333333148, 0.3377192982456140302, 0.3421052631578947456, 0.3464912280701754610, 0.3508771929824561209, 0.3552631578947368363, 0.3596491228070175517, 0.3640350877192982670, 0.3684210526315789269, 0.3728070175438596423, 0.3771929824561403577, 0.3815789473684210731, 0.3859649122807017330, 0.3903508771929824483, 0.3947368421052631637, 0.3991228070175438791, 0.4035087719298245390, 0.4078947368421052544, 0.4122807017543859698, 0.4166666666666666852, 0.4210526315789473450, 0.4254385964912280604, 0.4298245614035087758, 0.4342105263157894912, 0.4385964912280701511, 0.4429824561403508665, 0.4473684210526315819, 0.4517543859649122973, 0.4561403508771929571, 0.4605263157894736725, 0.4649122807017543879, 0.4692982456140351033, 0.4736842105263157632, 0.4780701754385964786, 0.4824561403508771940, 0.4868421052631579093, 0.4912280701754385692, 0.4956140350877192846, 0.5000000000000000000, 0.5043859649122807154, 0.5087719298245614308, 0.5131578947368421462, 0.5175438596491228616, 0.5219298245614034659, 0.5263157894736841813, 0.5307017543859648967, 0.5350877192982456121, 0.5394736842105263275, 0.5438596491228070429, 0.5482456140350877583, 0.5526315789473684736, 0.5570175438596490780, 0.5614035087719297934, 0.5657894736842105088, 0.5701754385964912242, 0.5745614035087719396, 0.5789473684210526550, 0.5833333333333333703, 0.5877192982456140857, 0.5921052631578946901, 0.5964912280701754055, 0.6008771929824561209, 0.6052631578947368363, 0.6096491228070175517, 0.6140350877192982670, 0.6184210526315789824, 0.6228070175438596978, 0.6271929824561403022, 0.6315789473684210176, 0.6359649122807017330, 0.6403508771929824483, 0.6447368421052631637, 0.6491228070175438791, 0.6535087719298245945, 0.6578947368421053099, 0.6622807017543859143, 0.6666666666666666297, 0.6710526315789473450, 0.6754385964912280604, 0.6798245614035087758, 0.6842105263157894912, 0.6885964912280702066, 0.6929824561403509220, 0.6973684210526315264, 0.7017543859649122417, 0.7061403508771929571, 0.7105263157894736725, 0.7149122807017543879, 0.7192982456140351033, 0.7236842105263158187, 0.7280701754385965341, 0.7324561403508771384, 0.7368421052631578538, 0.7412280701754385692, 0.7456140350877192846, 0.7500000000000000000, 0.7543859649122807154, 0.7587719298245614308, 0.7631578947368421462, 0.7675438596491228616, 0.7719298245614034659, 0.7763157894736841813, 0.7807017543859648967, 0.7850877192982456121, 0.7894736842105263275, 0.7938596491228070429, 0.7982456140350877583, 0.8026315789473684736, 0.8070175438596490780, 0.8114035087719297934, 0.8157894736842105088, 0.8201754385964912242, 0.8245614035087719396, 0.8289473684210526550, 0.8333333333333333703, 0.8377192982456140857, 0.8421052631578946901, 0.8464912280701754055, 0.8508771929824561209, 0.8552631578947368363, 0.8596491228070175517, 0.8640350877192982670, 0.8684210526315789824, 0.8728070175438596978, 0.8771929824561403022, 0.8815789473684210176, 0.8859649122807017330, 0.8903508771929824483, 0.8947368421052631637, 0.8991228070175438791, 0.9035087719298245945, 0.9078947368421053099, 0.9122807017543859143, 0.9166666666666666297, 0.9210526315789473450, 0.9254385964912280604, 0.9298245614035087758, 0.9342105263157894912, 0.9385964912280702066, 0.9429824561403509220, 0.9473684210526315264, 0.9517543859649122417, 0.9561403508771929571, 0.9605263157894736725, 0.9649122807017543879, 0.9692982456140351033, 0.9736842105263158187, 0.9780701754385965341, 0.9824561403508771384, 0.9868421052631578538, 0.9912280701754385692, 0.9956140350877192846, 1.000000000000000000 ),
 .UNSPECIFIED. ) 
 GEOMETRIC_REPRESENTATION_ITEM ( )  RATIONAL_B_SPLINE_SURFACE ( (
 ( 1.000000000000000000, 0.9659258262890683122, 1.000000000000000000, 0.9659258262890683122, 1.000000000000000000, 0.9659258262890683122, 1.000000000000000000, 0.9659258262890683122, 1.000000000000000000, 0.9659258262890683122, 1.000000000000000000, 0.9659258262890683122, 1.000000000000000000, 0.9659258262890683122, 1.000000000000000000, 0.9659258262890683122, 1.000000000000000000, 0.9659258262890683122, 1.000000000000000000, 0.9659258262890683122, 1.000000000000000000, 0.9659258262890683122, 1.000000000000000000, 0.9659258262890683122, 1.000000000000000000, 0.9659258262890683122, 1.000000000000000000, 0.9659258262890683122, 1.000000000000000000, 0.9659258262890683122, 1.000000000000000000, 0.9659258262890683122, 1.000000000000000000, 0.9659258262890683122, 1.000000000000000000, 0.9659258262890683122, 1.000000000000000000, 0.9659258262890683122, 1.000000000000000000, 0.9659258262890683122, 1.000000000000000000, 0.9659258262890683122, 1.000000000000000000, 0.9659258262890683122, 1.000000000000000000, 0.9659258262890683122, 1.000000000000000000, 0.9659258262890683122, 1.000000000000000000, 0.9659258262890683122, 1.000000000000000000, 0.9659258262890683122, 1.000000000000000000, 0.9659258262890683122, 1.000000000000000000, 0.9659258262890683122, 1.000000000000000000, 0.9659258262890683122, 1.000000000000000000, 0.9659258262890683122, 1.000000000000000000, 0.9659258262890683122, 1.000000000000000000, 0.9659258262890683122, 1.000000000000000000, 0.9659258262890683122, 1.000000000000000000, 0.9659258262890683122, 1.000000000000000000, 0.9659258262890683122, 1.000000000000000000, 0.9659258262890683122, 1.000000000000000000, 0.9659258262890683122, 1.000000000000000000, 0.9659258262890683122, 1.000000000000000000, 0.9659258262890683122, 1.000000000000000000, 0.9659258262890683122, 1.000000000000000000, 0.9659258262890683122, 1.000000000000000000, 0.9659258262890683122, 1.000000000000000000, 0.9659258262890683122, 1.000000000000000000, 0.9659258262890683122, 1.000000000000000000, 0.9659258262890683122, 1.000000000000000000, 0.9659258262890683122, 1.000000000000000000, 0.9659258262890683122, 1.000000000000000000, 0.9659258262890683122, 1.000000000000000000, 0.9659258262890683122, 1.000000000000000000, 0.9659258262890683122, 1.000000000000000000, 0.9659258262890683122, 1.000000000000000000, 0.9659258262890683122, 1.000000000000000000, 0.9659258262890683122, 1.000000000000000000, 0.9659258262890683122, 1.000000000000000000, 0.9659258262890683122, 1.000000000000000000, 0.9659258262890683122, 1.000000000000000000, 0.9659258262890683122, 1.000000000000000000, 0.9659258262890683122, 1.000000000000000000, 0.9659258262890683122, 1.000000000000000000, 0.9659258262890683122, 1.000000000000000000, 0.9659258262890683122, 1.000000000000000000, 0.9659258262890683122, 1.000000000000000000, 0.9659258262890683122, 1.000000000000000000, 0.9659258262890683122, 1.000000000000000000, 0.9659258262890683122, 1.000000000000000000, 0.9659258262890683122, 1.000000000000000000, 0.9659258262890683122, 1.000000000000000000, 0.9659258262890683122, 1.000000000000000000, 0.9659258262890683122, 1.000000000000000000, 0.9659258262890683122, 1.000000000000000000, 0.9659258262890683122, 1.000000000000000000, 0.9659258262890683122, 1.000000000000000000, 0.9659258262890683122, 1.000000000000000000, 0.9659258262890683122, 1.000000000000000000, 0.9659258262890683122, 1.000000000000000000, 0.9659258262890683122, 1.000000000000000000, 0.9659258262890683122, 1.000000000000000000, 0.9659258262890683122, 1.000000000000000000, 0.9659258262890683122, 1.000000000000000000, 0.9659258262890683122, 1.000000000000000000, 0.9659258262890683122, 1.000000000000000000, 0.9659258262890683122, 1.000000000000000000, 0.9659258262890683122, 1.000000000000000000, 0.9659258262890683122, 1.000000000000000000, 0.9659258262890683122, 1.000000000000000000, 0.9659258262890683122, 1.000000000000000000, 0.9659258262890683122, 1.000000000000000000, 0.9659258262890683122, 1.000000000000000000, 0.9659258262890683122, 1.000000000000000000, 0.9659258262890683122, 1.000000000000000000, 0.9659258262890683122, 1.000000000000000000, 0.9659258262890683122, 1.000000000000000000, 0.9659258262890683122, 1.000000000000000000, 0.9659258262890683122, 1.000000000000000000, 0.9659258262890683122, 1.000000000000000000, 0.9659258262890683122, 1.000000000000000000, 0.9659258262890683122, 1.000000000000000000, 0.9659258262890683122, 1.000000000000000000, 0.9659258262890683122, 1.000000000000000000, 0.9659258262890683122, 1.000000000000000000, 0.9659258262890683122, 1.000000000000000000, 0.9659258262890683122, 1.000000000000000000, 0.9659258262890683122, 1.000000000000000000, 0.9659258262890683122, 1.000000000000000000, 0.9659258262890683122, 1.000000000000000000, 0.9659258262890683122, 1.000000000000000000, 0.9659258262890683122, 1.000000000000000000, 0.9659258262890683122, 1.000000000000000000, 0.9659258262890683122, 1.000000000000000000, 0.9659258262890683122, 1.000000000000000000, 0.9659258262890683122, 1.000000000000000000, 0.9659258262890683122, 1.000000000000000000, 0.9659258262890683122, 1.000000000000000000, 0.9659258262890683122, 1.000000000000000000, 0.9659258262890683122, 1.000000000000000000, 0.9659258262890683122, 1.000000000000000000, 0.9659258262890683122, 1.000000000000000000, 0.9659258262890683122, 1.000000000000000000, 0.9659258262890683122, 1.000000000000000000, 0.9659258262890683122, 1.000000000000000000, 0.9659258262890683122, 1.000000000000000000, 0.9659258262890683122, 1.000000000000000000, 0.9659258262890683122, 1.000000000000000000, 0.9659258262890683122, 1.000000000000000000, 0.9659258262890683122, 1.000000000000000000, 0.9659258262890683122, 1.000000000000000000, 0.9659258262890683122, 1.000000000000000000, 0.9659258262890683122, 1.000000000000000000, 0.9659258262890683122, 1.000000000000000000, 0.9659258262890683122, 1.000000000000000000, 0.9659258262890683122, 1.000000000000000000, 0.9659258262890683122, 1.000000000000000000, 0.9659258262890683122, 1.000000000000000000, 0.9659258262890683122, 1.000000000000000000, 0.9659258262890683122, 1.000000000000000000, 0.9659258262890683122, 1.000000000000000000, 0.9659258262890683122, 1.000000000000000000, 0.9659258262890683122, 1.000000000000000000, 0.9659258262890683122, 1.000000000000000000, 0.9659258262890683122, 1.000000000000000000, 0.9659258262890683122, 1.000000000000000000, 0.9659258262890683122, 1.000000000000000000, 0.9659258262890683122, 1.000000000000000000, 0.9659258262890683122, 1.000000000000000000, 0.9659258262890683122, 1.000000000000000000, 0.9659258262890683122, 1.000000000000000000, 0.9659258262890683122, 1.000000000000000000, 0.9659258262890683122, 1.000000000000000000, 0.9659258262890683122, 1.000000000000000000, 0.9659258262890683122, 1.000000000000000000, 0.9659258262890683122, 1.000000000000000000, 0.9659258262890683122, 1.000000000000000000, 0.9659258262890683122, 1.000000000000000000, 0.9659258262890683122, 1.000000000000000000, 0.9659258262890683122, 1.000000000000000000, 0.9659258262890683122, 1.000000000000000000, 0.9659258262890683122, 1.000000000000000000, 0.9659258262890683122, 1.000000000000000000, 0.9659258262890683122, 1.000000000000000000, 0.9659258262890683122, 1.000000000000000000, 0.9659258262890683122, 1.000000000000000000, 0.9659258262890683122, 1.000000000000000000, 0.9659258262890683122, 1.000000000000000000, 0.9659258262890683122, 1.000000000000000000, 0.9659258262890683122, 1.000000000000000000, 0.9659258262890683122, 1.000000000000000000, 0.9659258262890683122, 1.000000000000000000, 0.9659258262890683122, 1.000000000000000000, 0.9659258262890683122, 1.000000000000000000, 0.9659258262890683122, 1.000000000000000000, 0.9659258262890683122, 1.000000000000000000, 0.9659258262890683122, 1.000000000000000000, 0.9659258262890683122, 1.000000000000000000, 0.9659258262890683122, 1.000000000000000000, 0.9659258262890683122, 1.000000000000000000, 0.9659258262890683122, 1.000000000000000000, 0.9659258262890683122, 1.000000000000000000, 0.9659258262890683122, 1.000000000000000000, 0.9659258262890683122, 1.000000000000000000, 0.9659258262890683122, 1.000000000000000000, 0.9659258262890683122, 1.000000000000000000, 0.9659258262890683122, 1.000000000000000000, 0.9659258262890683122, 1.000000000000000000, 0.9659258262890683122, 1.000000000000000000, 0.9659258262890683122, 1.000000000000000000, 0.9659258262890683122, 1.000000000000000000, 0.9659258262890683122, 1.000000000000000000, 0.9659258262890683122, 1.000000000000000000, 0.9659258262890683122, 1.000000000000000000, 0.9659258262890683122, 1.000000000000000000, 0.9659258262890683122, 1.000000000000000000, 0.9659258262890683122, 1.000000000000000000, 0.9659258262890683122, 1.000000000000000000, 0.9659258262890683122, 1.000000000000000000, 0.9659258262890683122, 1.000000000000000000, 0.9659258262890683122, 1.000000000000000000, 0.9659258262890683122, 1.000000000000000000, 0.9659258262890683122, 1.000000000000000000, 0.9659258262890683122, 1.000000000000000000, 0.9659258262890683122, 1.000000000000000000, 0.9659258262890683122, 1.000000000000000000, 0.9659258262890683122, 1.000000000000000000, 0.9659258262890683122, 1.000000000000000000, 0.9659258262890683122, 1.000000000000000000, 0.9659258262890683122, 1.000000000000000000, 0.9659258262890683122, 1.000000000000000000, 0.9659258262890683122, 1.000000000000000000, 0.9659258262890683122, 1.000000000000000000, 0.9659258262890683122, 1.000000000000000000, 0.9659258262890683122, 1.000000000000000000, 0.9659258262890683122, 1.000000000000000000, 0.9659258262890683122, 1.000000000000000000, 0.9659258262890683122, 1.000000000000000000, 0.9659258262890683122, 1.000000000000000000, 0.9659258262890683122, 1.000000000000000000, 0.9659258262890683122, 1.000000000000000000, 0.9659258262890683122, 1.000000000000000000, 0.9659258262890683122, 1.000000000000000000, 0.9659258262890683122, 1.000000000000000000, 0.9659258262890683122, 1.000000000000000000, 0.9659258262890683122, 1.000000000000000000, 0.9659258262890683122, 1.000000000000000000, 0.9659258262890683122, 1.000000000000000000, 0.9659258262890683122, 1.000000000000000000, 0.9659258262890683122, 1.000000000000000000, 0.9659258262890683122, 1.000000000000000000, 0.9659258262890683122, 1.000000000000000000, 0.9659258262890683122, 1.000000000000000000),
 ( 0.3333333333333333703, 0.3219752754296894559, 0.3333333333333333703, 0.3219752754296894559, 0.3333333333333333703, 0.3219752754296894559, 0.3333333333333333703, 0.3219752754296894559, 0.3333333333333333703, 0.3219752754296894559, 0.3333333333333333703, 0.3219752754296894559, 0.3333333333333333703, 0.3219752754296894559, 0.3333333333333333703, 0.3219752754296894559, 0.3333333333333333703, 0.3219752754296894559, 0.3333333333333333703, 0.3219752754296894559, 0.3333333333333333703, 0.3219752754296894559, 0.3333333333333333703, 0.3219752754296894559, 0.3333333333333333703, 0.3219752754296894559, 0.3333333333333333703, 0.3219752754296894559, 0.3333333333333333703, 0.3219752754296894559, 0.3333333333333333703, 0.3219752754296894559, 0.3333333333333333703, 0.3219752754296894559, 0.3333333333333333703, 0.3219752754296894559, 0.3333333333333333703, 0.3219752754296894559, 0.3333333333333333703, 0.3219752754296894559, 0.3333333333333333703, 0.3219752754296894559, 0.3333333333333333703, 0.3219752754296894559, 0.3333333333333333703, 0.3219752754296894559, 0.3333333333333333703, 0.3219752754296894559, 0.3333333333333333703, 0.3219752754296894559, 0.3333333333333333703, 0.3219752754296894559, 0.3333333333333333703, 0.3219752754296894559, 0.3333333333333333703, 0.3219752754296894559, 0.3333333333333333703, 0.3219752754296894559, 0.3333333333333333703, 0.3219752754296894559, 0.3333333333333333703, 0.3219752754296894559, 0.3333333333333333703, 0.3219752754296894559, 0.3333333333333333703, 0.3219752754296894559, 0.3333333333333333703, 0.3219752754296894559, 0.3333333333333333703, 0.3219752754296894559, 0.3333333333333333703, 0.3219752754296894559, 0.3333333333333333703, 0.3219752754296894559, 0.3333333333333333703, 0.3219752754296894559, 0.3333333333333333703, 0.3219752754296894559, 0.3333333333333333703, 0.3219752754296894559, 0.3333333333333333703, 0.3219752754296894559, 0.3333333333333333703, 0.3219752754296894559, 0.3333333333333333703, 0.3219752754296894559, 0.3333333333333333703, 0.3219752754296894559, 0.3333333333333333703, 0.3219752754296894559, 0.3333333333333333703, 0.3219752754296894559, 0.3333333333333333703, 0.3219752754296894559, 0.3333333333333333703, 0.3219752754296894559, 0.3333333333333333703, 0.3219752754296894559, 0.3333333333333333703, 0.3219752754296894559, 0.3333333333333333703, 0.3219752754296894559, 0.3333333333333333703, 0.3219752754296894559, 0.3333333333333333703, 0.3219752754296894559, 0.3333333333333333703, 0.3219752754296894559, 0.3333333333333333703, 0.3219752754296894559, 0.3333333333333333703, 0.3219752754296894559, 0.3333333333333333703, 0.3219752754296894559, 0.3333333333333333703, 0.3219752754296894559, 0.3333333333333333703, 0.3219752754296894559, 0.3333333333333333703, 0.3219752754296894559, 0.3333333333333333703, 0.3219752754296894559, 0.3333333333333333703, 0.3219752754296894559, 0.3333333333333333703, 0.3219752754296894559, 0.3333333333333333703, 0.3219752754296894559, 0.3333333333333333703, 0.3219752754296894559, 0.3333333333333333703, 0.3219752754296894559, 0.3333333333333333703, 0.3219752754296894559, 0.3333333333333333703, 0.3219752754296894559, 0.3333333333333333703, 0.3219752754296894559, 0.3333333333333333703, 0.3219752754296894559, 0.3333333333333333703, 0.3219752754296894559, 0.3333333333333333703, 0.3219752754296894559, 0.3333333333333333703, 0.3219752754296894559, 0.3333333333333333703, 0.3219752754296894559, 0.3333333333333333703, 0.3219752754296894559, 0.3333333333333333703, 0.3219752754296894559, 0.3333333333333333703, 0.3219752754296894559, 0.3333333333333333703, 0.3219752754296894559, 0.3333333333333333703, 0.3219752754296894559, 0.3333333333333333703, 0.3219752754296894559, 0.3333333333333333703, 0.3219752754296894559, 0.3333333333333333703, 0.3219752754296894559, 0.3333333333333333703, 0.3219752754296894559, 0.3333333333333333703, 0.3219752754296894559, 0.3333333333333333703, 0.3219752754296894559, 0.3333333333333333703, 0.3219752754296894559, 0.3333333333333333703, 0.3219752754296894559, 0.3333333333333333703, 0.3219752754296894559, 0.3333333333333333703, 0.3219752754296894559, 0.3333333333333333703, 0.3219752754296894559, 0.3333333333333333703, 0.3219752754296894559, 0.3333333333333333703, 0.3219752754296894559, 0.3333333333333333703, 0.3219752754296894559, 0.3333333333333333703, 0.3219752754296894559, 0.3333333333333333703, 0.3219752754296894559, 0.3333333333333333703, 0.3219752754296894559, 0.3333333333333333703, 0.3219752754296894559, 0.3333333333333333703, 0.3219752754296894559, 0.3333333333333333703, 0.3219752754296894559, 0.3333333333333333703, 0.3219752754296894559, 0.3333333333333333703, 0.3219752754296894559, 0.3333333333333333703, 0.3219752754296894559, 0.3333333333333333703, 0.3219752754296894559, 0.3333333333333333703, 0.3219752754296894559, 0.3333333333333333703, 0.3219752754296894559, 0.3333333333333333703, 0.3219752754296894559, 0.3333333333333333703, 0.3219752754296894559, 0.3333333333333333703, 0.3219752754296894559, 0.3333333333333333703, 0.3219752754296894559, 0.3333333333333333703, 0.3219752754296894559, 0.3333333333333333703, 0.3219752754296894559, 0.3333333333333333703, 0.3219752754296894559, 0.3333333333333333703, 0.3219752754296894559, 0.3333333333333333703, 0.3219752754296894559, 0.3333333333333333703, 0.3219752754296894559, 0.3333333333333333703, 0.3219752754296894559, 0.3333333333333333703, 0.3219752754296894559, 0.3333333333333333703, 0.3219752754296894559, 0.3333333333333333703, 0.3219752754296894559, 0.3333333333333333703, 0.3219752754296894559, 0.3333333333333333703, 0.3219752754296894559, 0.3333333333333333703, 0.3219752754296894559, 0.3333333333333333703, 0.3219752754296894559, 0.3333333333333333703, 0.3219752754296894559, 0.3333333333333333703, 0.3219752754296894559, 0.3333333333333333703, 0.3219752754296894559, 0.3333333333333333703, 0.3219752754296894559, 0.3333333333333333703, 0.3219752754296894559, 0.3333333333333333703, 0.3219752754296894559, 0.3333333333333333703, 0.3219752754296894559, 0.3333333333333333703, 0.3219752754296894559, 0.3333333333333333703, 0.3219752754296894559, 0.3333333333333333703, 0.3219752754296894559, 0.3333333333333333703, 0.3219752754296894559, 0.3333333333333333703, 0.3219752754296894559, 0.3333333333333333703, 0.3219752754296894559, 0.3333333333333333703, 0.3219752754296894559, 0.3333333333333333703, 0.3219752754296894559, 0.3333333333333333703, 0.3219752754296894559, 0.3333333333333333703, 0.3219752754296894559, 0.3333333333333333703, 0.3219752754296894559, 0.3333333333333333703, 0.3219752754296894559, 0.3333333333333333703, 0.3219752754296894559, 0.3333333333333333703, 0.3219752754296894559, 0.3333333333333333703, 0.3219752754296894559, 0.3333333333333333703, 0.3219752754296894559, 0.3333333333333333703, 0.3219752754296894559, 0.3333333333333333703, 0.3219752754296894559, 0.3333333333333333703, 0.3219752754296894559, 0.3333333333333333703, 0.3219752754296894559, 0.3333333333333333703, 0.3219752754296894559, 0.3333333333333333703, 0.3219752754296894559, 0.3333333333333333703, 0.3219752754296894559, 0.3333333333333333703, 0.3219752754296894559, 0.3333333333333333703, 0.3219752754296894559, 0.3333333333333333703, 0.3219752754296894559, 0.3333333333333333703, 0.3219752754296894559, 0.3333333333333333703, 0.3219752754296894559, 0.3333333333333333703, 0.3219752754296894559, 0.3333333333333333703, 0.3219752754296894559, 0.3333333333333333703, 0.3219752754296894559, 0.3333333333333333703, 0.3219752754296894559, 0.3333333333333333703, 0.3219752754296894559, 0.3333333333333333703, 0.3219752754296894559, 0.3333333333333333703, 0.3219752754296894559, 0.3333333333333333703, 0.3219752754296894559, 0.3333333333333333703, 0.3219752754296894559, 0.3333333333333333703, 0.3219752754296894559, 0.3333333333333333703, 0.3219752754296894559, 0.3333333333333333703, 0.3219752754296894559, 0.3333333333333333703, 0.3219752754296894559, 0.3333333333333333703, 0.3219752754296894559, 0.3333333333333333703, 0.3219752754296894559, 0.3333333333333333703, 0.3219752754296894559, 0.3333333333333333703, 0.3219752754296894559, 0.3333333333333333703, 0.3219752754296894559, 0.3333333333333333703, 0.3219752754296894559, 0.3333333333333333703, 0.3219752754296894559, 0.3333333333333333703, 0.3219752754296894559, 0.3333333333333333703, 0.3219752754296894559, 0.3333333333333333703, 0.3219752754296894559, 0.3333333333333333703, 0.3219752754296894559, 0.3333333333333333703, 0.3219752754296894559, 0.3333333333333333703, 0.3219752754296894559, 0.3333333333333333703, 0.3219752754296894559, 0.3333333333333333703, 0.3219752754296894559, 0.3333333333333333703, 0.3219752754296894559, 0.3333333333333333703, 0.3219752754296894559, 0.3333333333333333703, 0.3219752754296894559, 0.3333333333333333703, 0.3219752754296894559, 0.3333333333333333703, 0.3219752754296894559, 0.3333333333333333703, 0.3219752754296894559, 0.3333333333333333703, 0.3219752754296894559, 0.3333333333333333703, 0.3219752754296894559, 0.3333333333333333703, 0.3219752754296894559, 0.3333333333333333703, 0.3219752754296894559, 0.3333333333333333703, 0.3219752754296894559, 0.3333333333333333703, 0.3219752754296894559, 0.3333333333333333703, 0.3219752754296894559, 0.3333333333333333703, 0.3219752754296894559, 0.3333333333333333703, 0.3219752754296894559, 0.3333333333333333703, 0.3219752754296894559, 0.3333333333333333703, 0.3219752754296894559, 0.3333333333333333703, 0.3219752754296894559, 0.3333333333333333703, 0.3219752754296894559, 0.3333333333333333703, 0.3219752754296894559, 0.3333333333333333703, 0.3219752754296894559, 0.3333333333333333703, 0.3219752754296894559, 0.3333333333333333703, 0.3219752754296894559, 0.3333333333333333703, 0.3219752754296894559, 0.3333333333333333703, 0.3219752754296894559, 0.3333333333333333703, 0.3219752754296894559, 0.3333333333333333703, 0.3219752754296894559, 0.3333333333333333703, 0.3219752754296894559, 0.3333333333333333703, 0.3219752754296894559, 0.3333333333333333703, 0.3219752754296894559, 0.3333333333333333703, 0.3219752754296894559, 0.3333333333333333703, 0.3219752754296894559, 0.3333333333333333703, 0.3219752754296894559, 0.3333333333333333703, 0.3219752754296894559, 0.3333333333333333703, 0.3219752754296894559, 0.3333333333333333703, 0.3219752754296894559, 0.3333333333333333703, 0.3219752754296894559, 0.3333333333333333703, 0.3219752754296894559, 0.3333333333333333703, 0.3219752754296894559, 0.3333333333333333703, 0.3219752754296894559, 0.3333333333333333703, 0.3219752754296894559, 0.3333333333333333703, 0.3219752754296894559, 0.3333333333333333703),
 ( 0.3333333333333333703, 0.3219752754296894559, 0.3333333333333333703, 0.3219752754296894559, 0.3333333333333333703, 0.3219752754296894559, 0.3333333333333333703, 0.3219752754296894559, 0.3333333333333333703, 0.3219752754296894559, 0.3333333333333333703, 0.3219752754296894559, 0.3333333333333333703, 0.3219752754296894559, 0.3333333333333333703, 0.3219752754296894559, 0.3333333333333333703, 0.3219752754296894559, 0.3333333333333333703, 0.3219752754296894559, 0.3333333333333333703, 0.3219752754296894559, 0.3333333333333333703, 0.3219752754296894559, 0.3333333333333333703, 0.3219752754296894559, 0.3333333333333333703, 0.3219752754296894559, 0.3333333333333333703, 0.3219752754296894559, 0.3333333333333333703, 0.3219752754296894559, 0.3333333333333333703, 0.3219752754296894559, 0.3333333333333333703, 0.3219752754296894559, 0.3333333333333333703, 0.3219752754296894559, 0.3333333333333333703, 0.3219752754296894559, 0.3333333333333333703, 0.3219752754296894559, 0.3333333333333333703, 0.3219752754296894559, 0.3333333333333333703, 0.3219752754296894559, 0.3333333333333333703, 0.3219752754296894559, 0.3333333333333333703, 0.3219752754296894559, 0.3333333333333333703, 0.3219752754296894559, 0.3333333333333333703, 0.3219752754296894559, 0.3333333333333333703, 0.3219752754296894559, 0.3333333333333333703, 0.3219752754296894559, 0.3333333333333333703, 0.3219752754296894559, 0.3333333333333333703, 0.3219752754296894559, 0.3333333333333333703, 0.3219752754296894559, 0.3333333333333333703, 0.3219752754296894559, 0.3333333333333333703, 0.3219752754296894559, 0.3333333333333333703, 0.3219752754296894559, 0.3333333333333333703, 0.3219752754296894559, 0.3333333333333333703, 0.3219752754296894559, 0.3333333333333333703, 0.3219752754296894559, 0.3333333333333333703, 0.3219752754296894559, 0.3333333333333333703, 0.3219752754296894559, 0.3333333333333333703, 0.3219752754296894559, 0.3333333333333333703, 0.3219752754296894559, 0.3333333333333333703, 0.3219752754296894559, 0.3333333333333333703, 0.3219752754296894559, 0.3333333333333333703, 0.3219752754296894559, 0.3333333333333333703, 0.3219752754296894559, 0.3333333333333333703, 0.3219752754296894559, 0.3333333333333333703, 0.3219752754296894559, 0.3333333333333333703, 0.3219752754296894559, 0.3333333333333333703, 0.3219752754296894559, 0.3333333333333333703, 0.3219752754296894559, 0.3333333333333333703, 0.3219752754296894559, 0.3333333333333333703, 0.3219752754296894559, 0.3333333333333333703, 0.3219752754296894559, 0.3333333333333333703, 0.3219752754296894559, 0.3333333333333333703, 0.3219752754296894559, 0.3333333333333333703, 0.3219752754296894559, 0.3333333333333333703, 0.3219752754296894559, 0.3333333333333333703, 0.3219752754296894559, 0.3333333333333333703, 0.3219752754296894559, 0.3333333333333333703, 0.3219752754296894559, 0.3333333333333333703, 0.3219752754296894559, 0.3333333333333333703, 0.3219752754296894559, 0.3333333333333333703, 0.3219752754296894559, 0.3333333333333333703, 0.3219752754296894559, 0.3333333333333333703, 0.3219752754296894559, 0.3333333333333333703, 0.3219752754296894559, 0.3333333333333333703, 0.3219752754296894559, 0.3333333333333333703, 0.3219752754296894559, 0.3333333333333333703, 0.3219752754296894559, 0.3333333333333333703, 0.3219752754296894559, 0.3333333333333333703, 0.3219752754296894559, 0.3333333333333333703, 0.3219752754296894559, 0.3333333333333333703, 0.3219752754296894559, 0.3333333333333333703, 0.3219752754296894559, 0.3333333333333333703, 0.3219752754296894559, 0.3333333333333333703, 0.3219752754296894559, 0.3333333333333333703, 0.3219752754296894559, 0.3333333333333333703, 0.3219752754296894559, 0.3333333333333333703, 0.3219752754296894559, 0.3333333333333333703, 0.3219752754296894559, 0.3333333333333333703, 0.3219752754296894559, 0.3333333333333333703, 0.3219752754296894559, 0.3333333333333333703, 0.3219752754296894559, 0.3333333333333333703, 0.3219752754296894559, 0.3333333333333333703, 0.3219752754296894559, 0.3333333333333333703, 0.3219752754296894559, 0.3333333333333333703, 0.3219752754296894559, 0.3333333333333333703, 0.3219752754296894559, 0.3333333333333333703, 0.3219752754296894559, 0.3333333333333333703, 0.3219752754296894559, 0.3333333333333333703, 0.3219752754296894559, 0.3333333333333333703, 0.3219752754296894559, 0.3333333333333333703, 0.3219752754296894559, 0.3333333333333333703, 0.3219752754296894559, 0.3333333333333333703, 0.3219752754296894559, 0.3333333333333333703, 0.3219752754296894559, 0.3333333333333333703, 0.3219752754296894559, 0.3333333333333333703, 0.3219752754296894559, 0.3333333333333333703, 0.3219752754296894559, 0.3333333333333333703, 0.3219752754296894559, 0.3333333333333333703, 0.3219752754296894559, 0.3333333333333333703, 0.3219752754296894559, 0.3333333333333333703, 0.3219752754296894559, 0.3333333333333333703, 0.3219752754296894559, 0.3333333333333333703, 0.3219752754296894559, 0.3333333333333333703, 0.3219752754296894559, 0.3333333333333333703, 0.3219752754296894559, 0.3333333333333333703, 0.3219752754296894559, 0.3333333333333333703, 0.3219752754296894559, 0.3333333333333333703, 0.3219752754296894559, 0.3333333333333333703, 0.3219752754296894559, 0.3333333333333333703, 0.3219752754296894559, 0.3333333333333333703, 0.3219752754296894559, 0.3333333333333333703, 0.3219752754296894559, 0.3333333333333333703, 0.3219752754296894559, 0.3333333333333333703, 0.3219752754296894559, 0.3333333333333333703, 0.3219752754296894559, 0.3333333333333333703, 0.3219752754296894559, 0.3333333333333333703, 0.3219752754296894559, 0.3333333333333333703, 0.3219752754296894559, 0.3333333333333333703, 0.3219752754296894559, 0.3333333333333333703, 0.3219752754296894559, 0.3333333333333333703, 0.3219752754296894559, 0.3333333333333333703, 0.3219752754296894559, 0.3333333333333333703, 0.3219752754296894559, 0.3333333333333333703, 0.3219752754296894559, 0.3333333333333333703, 0.3219752754296894559, 0.3333333333333333703, 0.3219752754296894559, 0.3333333333333333703, 0.3219752754296894559, 0.3333333333333333703, 0.3219752754296894559, 0.3333333333333333703, 0.3219752754296894559, 0.3333333333333333703, 0.3219752754296894559, 0.3333333333333333703, 0.3219752754296894559, 0.3333333333333333703, 0.3219752754296894559, 0.3333333333333333703, 0.3219752754296894559, 0.3333333333333333703, 0.3219752754296894559, 0.3333333333333333703, 0.3219752754296894559, 0.3333333333333333703, 0.3219752754296894559, 0.3333333333333333703, 0.3219752754296894559, 0.3333333333333333703, 0.3219752754296894559, 0.3333333333333333703, 0.3219752754296894559, 0.3333333333333333703, 0.3219752754296894559, 0.3333333333333333703, 0.3219752754296894559, 0.3333333333333333703, 0.3219752754296894559, 0.3333333333333333703, 0.3219752754296894559, 0.3333333333333333703, 0.3219752754296894559, 0.3333333333333333703, 0.3219752754296894559, 0.3333333333333333703, 0.3219752754296894559, 0.3333333333333333703, 0.3219752754296894559, 0.3333333333333333703, 0.3219752754296894559, 0.3333333333333333703, 0.3219752754296894559, 0.3333333333333333703, 0.3219752754296894559, 0.3333333333333333703, 0.3219752754296894559, 0.3333333333333333703, 0.3219752754296894559, 0.3333333333333333703, 0.3219752754296894559, 0.3333333333333333703, 0.3219752754296894559, 0.3333333333333333703, 0.3219752754296894559, 0.3333333333333333703, 0.3219752754296894559, 0.3333333333333333703, 0.3219752754296894559, 0.3333333333333333703, 0.3219752754296894559, 0.3333333333333333703, 0.3219752754296894559, 0.3333333333333333703, 0.3219752754296894559, 0.3333333333333333703, 0.3219752754296894559, 0.3333333333333333703, 0.3219752754296894559, 0.3333333333333333703, 0.3219752754296894559, 0.3333333333333333703, 0.3219752754296894559, 0.3333333333333333703, 0.3219752754296894559, 0.3333333333333333703, 0.3219752754296894559, 0.3333333333333333703, 0.3219752754296894559, 0.3333333333333333703, 0.3219752754296894559, 0.3333333333333333703, 0.3219752754296894559, 0.3333333333333333703, 0.3219752754296894559, 0.3333333333333333703, 0.3219752754296894559, 0.3333333333333333703, 0.3219752754296894559, 0.3333333333333333703, 0.3219752754296894559, 0.3333333333333333703, 0.3219752754296894559, 0.3333333333333333703, 0.3219752754296894559, 0.3333333333333333703, 0.3219752754296894559, 0.3333333333333333703, 0.3219752754296894559, 0.3333333333333333703, 0.3219752754296894559, 0.3333333333333333703, 0.3219752754296894559, 0.3333333333333333703, 0.3219752754296894559, 0.3333333333333333703, 0.3219752754296894559, 0.3333333333333333703, 0.3219752754296894559, 0.3333333333333333703, 0.3219752754296894559, 0.3333333333333333703, 0.3219752754296894559, 0.3333333333333333703, 0.3219752754296894559, 0.3333333333333333703, 0.3219752754296894559, 0.3333333333333333703, 0.3219752754296894559, 0.3333333333333333703, 0.3219752754296894559, 0.3333333333333333703, 0.3219752754296894559, 0.3333333333333333703, 0.3219752754296894559, 0.3333333333333333703, 0.3219752754296894559, 0.3333333333333333703, 0.3219752754296894559, 0.3333333333333333703, 0.3219752754296894559, 0.3333333333333333703, 0.3219752754296894559, 0.3333333333333333703, 0.3219752754296894559, 0.3333333333333333703, 0.3219752754296894559, 0.3333333333333333703, 0.3219752754296894559, 0.3333333333333333703, 0.3219752754296894559, 0.3333333333333333703, 0.3219752754296894559, 0.3333333333333333703, 0.3219752754296894559, 0.3333333333333333703, 0.3219752754296894559, 0.3333333333333333703, 0.3219752754296894559, 0.3333333333333333703, 0.3219752754296894559, 0.3333333333333333703, 0.3219752754296894559, 0.3333333333333333703, 0.3219752754296894559, 0.3333333333333333703, 0.3219752754296894559, 0.3333333333333333703, 0.3219752754296894559, 0.3333333333333333703, 0.3219752754296894559, 0.3333333333333333703, 0.3219752754296894559, 0.3333333333333333703, 0.3219752754296894559, 0.3333333333333333703, 0.3219752754296894559, 0.3333333333333333703, 0.3219752754296894559, 0.3333333333333333703, 0.3219752754296894559, 0.3333333333333333703, 0.3219752754296894559, 0.3333333333333333703, 0.3219752754296894559, 0.3333333333333333703, 0.3219752754296894559, 0.3333333333333333703, 0.3219752754296894559, 0.3333333333333333703, 0.3219752754296894559, 0.3333333333333333703, 0.3219752754296894559, 0.3333333333333333703, 0.3219752754296894559, 0.3333333333333333703, 0.3219752754296894559, 0.3333333333333333703, 0.3219752754296894559, 0.3333333333333333703, 0.3219752754296894559, 0.3333333333333333703, 0.3219752754296894559, 0.3333333333333333703, 0.3219752754296894559, 0.3333333333333333703),
 ( 1.000000000000000000, 0.9659258262890683122, 1.000000000000000000, 0.9659258262890683122, 1.000000000000000000, 0.9659258262890683122, 1.000000000000000000, 0.9659258262890683122, 1.000000000000000000, 0.9659258262890683122, 1.000000000000000000, 0.9659258262890683122, 1.000000000000000000, 0.9659258262890683122, 1.000000000000000000, 0.9659258262890683122, 1.000000000000000000, 0.9659258262890683122, 1.000000000000000000, 0.9659258262890683122, 1.000000000000000000, 0.9659258262890683122, 1.000000000000000000, 0.9659258262890683122, 1.000000000000000000, 0.9659258262890683122, 1.000000000000000000, 0.9659258262890683122, 1.000000000000000000, 0.9659258262890683122, 1.000000000000000000, 0.9659258262890683122, 1.000000000000000000, 0.9659258262890683122, 1.000000000000000000, 0.9659258262890683122, 1.000000000000000000, 0.9659258262890683122, 1.000000000000000000, 0.9659258262890683122, 1.000000000000000000, 0.9659258262890683122, 1.000000000000000000, 0.9659258262890683122, 1.000000000000000000, 0.9659258262890683122, 1.000000000000000000, 0.9659258262890683122, 1.000000000000000000, 0.9659258262890683122, 1.000000000000000000, 0.9659258262890683122, 1.000000000000000000, 0.9659258262890683122, 1.000000000000000000, 0.9659258262890683122, 1.000000000000000000, 0.9659258262890683122, 1.000000000000000000, 0.9659258262890683122, 1.000000000000000000, 0.9659258262890683122, 1.000000000000000000, 0.9659258262890683122, 1.000000000000000000, 0.9659258262890683122, 1.000000000000000000, 0.9659258262890683122, 1.000000000000000000, 0.9659258262890683122, 1.000000000000000000, 0.9659258262890683122, 1.000000000000000000, 0.9659258262890683122, 1.000000000000000000, 0.9659258262890683122, 1.000000000000000000, 0.9659258262890683122, 1.000000000000000000, 0.9659258262890683122, 1.000000000000000000, 0.9659258262890683122, 1.000000000000000000, 0.9659258262890683122, 1.000000000000000000, 0.9659258262890683122, 1.000000000000000000, 0.9659258262890683122, 1.000000000000000000, 0.9659258262890683122, 1.000000000000000000, 0.9659258262890683122, 1.000000000000000000, 0.9659258262890683122, 1.000000000000000000, 0.9659258262890683122, 1.000000000000000000, 0.9659258262890683122, 1.000000000000000000, 0.9659258262890683122, 1.000000000000000000, 0.9659258262890683122, 1.000000000000000000, 0.9659258262890683122, 1.000000000000000000, 0.9659258262890683122, 1.000000000000000000, 0.9659258262890683122, 1.000000000000000000, 0.9659258262890683122, 1.000000000000000000, 0.9659258262890683122, 1.000000000000000000, 0.9659258262890683122, 1.000000000000000000, 0.9659258262890683122, 1.000000000000000000, 0.9659258262890683122, 1.000000000000000000, 0.9659258262890683122, 1.000000000000000000, 0.9659258262890683122, 1.000000000000000000, 0.9659258262890683122, 1.000000000000000000, 0.9659258262890683122, 1.000000000000000000, 0.9659258262890683122, 1.000000000000000000, 0.9659258262890683122, 1.000000000000000000, 0.9659258262890683122, 1.000000000000000000, 0.9659258262890683122, 1.000000000000000000, 0.9659258262890683122, 1.000000000000000000, 0.9659258262890683122, 1.000000000000000000, 0.9659258262890683122, 1.000000000000000000, 0.9659258262890683122, 1.000000000000000000, 0.9659258262890683122, 1.000000000000000000, 0.9659258262890683122, 1.000000000000000000, 0.9659258262890683122, 1.000000000000000000, 0.9659258262890683122, 1.000000000000000000, 0.9659258262890683122, 1.000000000000000000, 0.9659258262890683122, 1.000000000000000000, 0.9659258262890683122, 1.000000000000000000, 0.9659258262890683122, 1.000000000000000000, 0.9659258262890683122, 1.000000000000000000, 0.9659258262890683122, 1.000000000000000000, 0.9659258262890683122, 1.000000000000000000, 0.9659258262890683122, 1.000000000000000000, 0.9659258262890683122, 1.000000000000000000, 0.9659258262890683122, 1.000000000000000000, 0.9659258262890683122, 1.000000000000000000, 0.9659258262890683122, 1.000000000000000000, 0.9659258262890683122, 1.000000000000000000, 0.9659258262890683122, 1.000000000000000000, 0.9659258262890683122, 1.000000000000000000, 0.9659258262890683122, 1.000000000000000000, 0.9659258262890683122, 1.000000000000000000, 0.9659258262890683122, 1.000000000000000000, 0.9659258262890683122, 1.000000000000000000, 0.9659258262890683122, 1.000000000000000000, 0.9659258262890683122, 1.000000000000000000, 0.9659258262890683122, 1.000000000000000000, 0.9659258262890683122, 1.000000000000000000, 0.9659258262890683122, 1.000000000000000000, 0.9659258262890683122, 1.000000000000000000, 0.9659258262890683122, 1.000000000000000000, 0.9659258262890683122, 1.000000000000000000, 0.9659258262890683122, 1.000000000000000000, 0.9659258262890683122, 1.000000000000000000, 0.9659258262890683122, 1.000000000000000000, 0.9659258262890683122, 1.000000000000000000, 0.9659258262890683122, 1.000000000000000000, 0.9659258262890683122, 1.000000000000000000, 0.9659258262890683122, 1.000000000000000000, 0.9659258262890683122, 1.000000000000000000, 0.9659258262890683122, 1.000000000000000000, 0.9659258262890683122, 1.000000000000000000, 0.9659258262890683122, 1.000000000000000000, 0.9659258262890683122, 1.000000000000000000, 0.9659258262890683122, 1.000000000000000000, 0.9659258262890683122, 1.000000000000000000, 0.9659258262890683122, 1.000000000000000000, 0.9659258262890683122, 1.000000000000000000, 0.9659258262890683122, 1.000000000000000000, 0.9659258262890683122, 1.000000000000000000, 0.9659258262890683122, 1.000000000000000000, 0.9659258262890683122, 1.000000000000000000, 0.9659258262890683122, 1.000000000000000000, 0.9659258262890683122, 1.000000000000000000, 0.9659258262890683122, 1.000000000000000000, 0.9659258262890683122, 1.000000000000000000, 0.9659258262890683122, 1.000000000000000000, 0.9659258262890683122, 1.000000000000000000, 0.9659258262890683122, 1.000000000000000000, 0.9659258262890683122, 1.000000000000000000, 0.9659258262890683122, 1.000000000000000000, 0.9659258262890683122, 1.000000000000000000, 0.9659258262890683122, 1.000000000000000000, 0.9659258262890683122, 1.000000000000000000, 0.9659258262890683122, 1.000000000000000000, 0.9659258262890683122, 1.000000000000000000, 0.9659258262890683122, 1.000000000000000000, 0.9659258262890683122, 1.000000000000000000, 0.9659258262890683122, 1.000000000000000000, 0.9659258262890683122, 1.000000000000000000, 0.9659258262890683122, 1.000000000000000000, 0.9659258262890683122, 1.000000000000000000, 0.9659258262890683122, 1.000000000000000000, 0.9659258262890683122, 1.000000000000000000, 0.9659258262890683122, 1.000000000000000000, 0.9659258262890683122, 1.000000000000000000, 0.9659258262890683122, 1.000000000000000000, 0.9659258262890683122, 1.000000000000000000, 0.9659258262890683122, 1.000000000000000000, 0.9659258262890683122, 1.000000000000000000, 0.9659258262890683122, 1.000000000000000000, 0.9659258262890683122, 1.000000000000000000, 0.9659258262890683122, 1.000000000000000000, 0.9659258262890683122, 1.000000000000000000, 0.9659258262890683122, 1.000000000000000000, 0.9659258262890683122, 1.000000000000000000, 0.9659258262890683122, 1.000000000000000000, 0.9659258262890683122, 1.000000000000000000, 0.9659258262890683122, 1.000000000000000000, 0.9659258262890683122, 1.000000000000000000, 0.9659258262890683122, 1.000000000000000000, 0.9659258262890683122, 1.000000000000000000, 0.9659258262890683122, 1.000000000000000000, 0.9659258262890683122, 1.000000000000000000, 0.9659258262890683122, 1.000000000000000000, 0.9659258262890683122, 1.000000000000000000, 0.9659258262890683122, 1.000000000000000000, 0.9659258262890683122, 1.000000000000000000, 0.9659258262890683122, 1.000000000000000000, 0.9659258262890683122, 1.000000000000000000, 0.9659258262890683122, 1.000000000000000000, 0.9659258262890683122, 1.000000000000000000, 0.9659258262890683122, 1.000000000000000000, 0.9659258262890683122, 1.000000000000000000, 0.9659258262890683122, 1.000000000000000000, 0.9659258262890683122, 1.000000000000000000, 0.9659258262890683122, 1.000000000000000000, 0.9659258262890683122, 1.000000000000000000, 0.9659258262890683122, 1.000000000000000000, 0.9659258262890683122, 1.000000000000000000, 0.9659258262890683122, 1.000000000000000000, 0.9659258262890683122, 1.000000000000000000, 0.9659258262890683122, 1.000000000000000000, 0.9659258262890683122, 1.000000000000000000, 0.9659258262890683122, 1.000000000000000000, 0.9659258262890683122, 1.000000000000000000, 0.9659258262890683122, 1.000000000000000000, 0.9659258262890683122, 1.000000000000000000, 0.9659258262890683122, 1.000000000000000000, 0.9659258262890683122, 1.000000000000000000, 0.9659258262890683122, 1.000000000000000000, 0.9659258262890683122, 1.000000000000000000, 0.9659258262890683122, 1.000000000000000000, 0.9659258262890683122, 1.000000000000000000, 0.9659258262890683122, 1.000000000000000000, 0.9659258262890683122, 1.000000000000000000, 0.9659258262890683122, 1.000000000000000000, 0.9659258262890683122, 1.000000000000000000, 0.9659258262890683122, 1.000000000000000000, 0.9659258262890683122, 1.000000000000000000, 0.9659258262890683122, 1.000000000000000000, 0.9659258262890683122, 1.000000000000000000, 0.9659258262890683122, 1.000000000000000000, 0.9659258262890683122, 1.000000000000000000, 0.9659258262890683122, 1.000000000000000000, 0.9659258262890683122, 1.000000000000000000, 0.9659258262890683122, 1.000000000000000000, 0.9659258262890683122, 1.000000000000000000, 0.9659258262890683122, 1.000000000000000000, 0.9659258262890683122, 1.000000000000000000, 0.9659258262890683122, 1.000000000000000000, 0.9659258262890683122, 1.000000000000000000, 0.9659258262890683122, 1.000000000000000000, 0.9659258262890683122, 1.000000000000000000, 0.9659258262890683122, 1.000000000000000000, 0.9659258262890683122, 1.000000000000000000, 0.9659258262890683122, 1.000000000000000000, 0.9659258262890683122, 1.000000000000000000, 0.9659258262890683122, 1.000000000000000000, 0.9659258262890683122, 1.000000000000000000, 0.9659258262890683122, 1.000000000000000000, 0.9659258262890683122, 1.000000000000000000, 0.9659258262890683122, 1.000000000000000000, 0.9659258262890683122, 1.000000000000000000, 0.9659258262890683122, 1.000000000000000000, 0.9659258262890683122, 1.000000000000000000, 0.9659258262890683122, 1.000000000000000000, 0.9659258262890683122, 1.000000000000000000),
 ( 0.3333333333333333703, 0.3219752754296894559, 0.3333333333333333703, 0.3219752754296894559, 0.3333333333333333703, 0.3219752754296894559, 0.3333333333333333703, 0.3219752754296894559, 0.3333333333333333703, 0.3219752754296894559, 0.3333333333333333703, 0.3219752754296894559, 0.3333333333333333703, 0.3219752754296894559, 0.3333333333333333703, 0.3219752754296894559, 0.3333333333333333703, 0.3219752754296894559, 0.3333333333333333703, 0.3219752754296894559, 0.3333333333333333703, 0.3219752754296894559, 0.3333333333333333703, 0.3219752754296894559, 0.3333333333333333703, 0.3219752754296894559, 0.3333333333333333703, 0.3219752754296894559, 0.3333333333333333703, 0.3219752754296894559, 0.3333333333333333703, 0.3219752754296894559, 0.3333333333333333703, 0.3219752754296894559, 0.3333333333333333703, 0.3219752754296894559, 0.3333333333333333703, 0.3219752754296894559, 0.3333333333333333703, 0.3219752754296894559, 0.3333333333333333703, 0.3219752754296894559, 0.3333333333333333703, 0.3219752754296894559, 0.3333333333333333703, 0.3219752754296894559, 0.3333333333333333703, 0.3219752754296894559, 0.3333333333333333703, 0.3219752754296894559, 0.3333333333333333703, 0.3219752754296894559, 0.3333333333333333703, 0.3219752754296894559, 0.3333333333333333703, 0.3219752754296894559, 0.3333333333333333703, 0.3219752754296894559, 0.3333333333333333703, 0.3219752754296894559, 0.3333333333333333703, 0.3219752754296894559, 0.3333333333333333703, 0.3219752754296894559, 0.3333333333333333703, 0.3219752754296894559, 0.3333333333333333703, 0.3219752754296894559, 0.3333333333333333703, 0.3219752754296894559, 0.3333333333333333703, 0.3219752754296894559, 0.3333333333333333703, 0.3219752754296894559, 0.3333333333333333703, 0.3219752754296894559, 0.3333333333333333703, 0.3219752754296894559, 0.3333333333333333703, 0.3219752754296894559, 0.3333333333333333703, 0.3219752754296894559, 0.3333333333333333703, 0.3219752754296894559, 0.3333333333333333703, 0.3219752754296894559, 0.3333333333333333703, 0.3219752754296894559, 0.3333333333333333703, 0.3219752754296894559, 0.3333333333333333703, 0.3219752754296894559, 0.3333333333333333703, 0.3219752754296894559, 0.3333333333333333703, 0.3219752754296894559, 0.3333333333333333703, 0.3219752754296894559, 0.3333333333333333703, 0.3219752754296894559, 0.3333333333333333703, 0.3219752754296894559, 0.3333333333333333703, 0.3219752754296894559, 0.3333333333333333703, 0.3219752754296894559, 0.3333333333333333703, 0.3219752754296894559, 0.3333333333333333703, 0.3219752754296894559, 0.3333333333333333703, 0.3219752754296894559, 0.3333333333333333703, 0.3219752754296894559, 0.3333333333333333703, 0.3219752754296894559, 0.3333333333333333703, 0.3219752754296894559, 0.3333333333333333703, 0.3219752754296894559, 0.3333333333333333703, 0.3219752754296894559, 0.3333333333333333703, 0.3219752754296894559, 0.3333333333333333703, 0.3219752754296894559, 0.3333333333333333703, 0.3219752754296894559, 0.3333333333333333703, 0.3219752754296894559, 0.3333333333333333703, 0.3219752754296894559, 0.3333333333333333703, 0.3219752754296894559, 0.3333333333333333703, 0.3219752754296894559, 0.3333333333333333703, 0.3219752754296894559, 0.3333333333333333703, 0.3219752754296894559, 0.3333333333333333703, 0.3219752754296894559, 0.3333333333333333703, 0.3219752754296894559, 0.3333333333333333703, 0.3219752754296894559, 0.3333333333333333703, 0.3219752754296894559, 0.3333333333333333703, 0.3219752754296894559, 0.3333333333333333703, 0.3219752754296894559, 0.3333333333333333703, 0.3219752754296894559, 0.3333333333333333703, 0.3219752754296894559, 0.3333333333333333703, 0.3219752754296894559, 0.3333333333333333703, 0.3219752754296894559, 0.3333333333333333703, 0.3219752754296894559, 0.3333333333333333703, 0.3219752754296894559, 0.3333333333333333703, 0.3219752754296894559, 0.3333333333333333703, 0.3219752754296894559, 0.3333333333333333703, 0.3219752754296894559, 0.3333333333333333703, 0.3219752754296894559, 0.3333333333333333703, 0.3219752754296894559, 0.3333333333333333703, 0.3219752754296894559, 0.3333333333333333703, 0.3219752754296894559, 0.3333333333333333703, 0.3219752754296894559, 0.3333333333333333703, 0.3219752754296894559, 0.3333333333333333703, 0.3219752754296894559, 0.3333333333333333703, 0.3219752754296894559, 0.3333333333333333703, 0.3219752754296894559, 0.3333333333333333703, 0.3219752754296894559, 0.3333333333333333703, 0.3219752754296894559, 0.3333333333333333703, 0.3219752754296894559, 0.3333333333333333703, 0.3219752754296894559, 0.3333333333333333703, 0.3219752754296894559, 0.3333333333333333703, 0.3219752754296894559, 0.3333333333333333703, 0.3219752754296894559, 0.3333333333333333703, 0.3219752754296894559, 0.3333333333333333703, 0.3219752754296894559, 0.3333333333333333703, 0.3219752754296894559, 0.3333333333333333703, 0.3219752754296894559, 0.3333333333333333703, 0.3219752754296894559, 0.3333333333333333703, 0.3219752754296894559, 0.3333333333333333703, 0.3219752754296894559, 0.3333333333333333703, 0.3219752754296894559, 0.3333333333333333703, 0.3219752754296894559, 0.3333333333333333703, 0.3219752754296894559, 0.3333333333333333703, 0.3219752754296894559, 0.3333333333333333703, 0.3219752754296894559, 0.3333333333333333703, 0.3219752754296894559, 0.3333333333333333703, 0.3219752754296894559, 0.3333333333333333703, 0.3219752754296894559, 0.3333333333333333703, 0.3219752754296894559, 0.3333333333333333703, 0.3219752754296894559, 0.3333333333333333703, 0.3219752754296894559, 0.3333333333333333703, 0.3219752754296894559, 0.3333333333333333703, 0.3219752754296894559, 0.3333333333333333703, 0.3219752754296894559, 0.3333333333333333703, 0.3219752754296894559, 0.3333333333333333703, 0.3219752754296894559, 0.3333333333333333703, 0.3219752754296894559, 0.3333333333333333703, 0.3219752754296894559, 0.3333333333333333703, 0.3219752754296894559, 0.3333333333333333703, 0.3219752754296894559, 0.3333333333333333703, 0.3219752754296894559, 0.3333333333333333703, 0.3219752754296894559, 0.3333333333333333703, 0.3219752754296894559, 0.3333333333333333703, 0.3219752754296894559, 0.3333333333333333703, 0.3219752754296894559, 0.3333333333333333703, 0.3219752754296894559, 0.3333333333333333703, 0.3219752754296894559, 0.3333333333333333703, 0.3219752754296894559, 0.3333333333333333703, 0.3219752754296894559, 0.3333333333333333703, 0.3219752754296894559, 0.3333333333333333703, 0.3219752754296894559, 0.3333333333333333703, 0.3219752754296894559, 0.3333333333333333703, 0.3219752754296894559, 0.3333333333333333703, 0.3219752754296894559, 0.3333333333333333703, 0.3219752754296894559, 0.3333333333333333703, 0.3219752754296894559, 0.3333333333333333703, 0.3219752754296894559, 0.3333333333333333703, 0.3219752754296894559, 0.3333333333333333703, 0.3219752754296894559, 0.3333333333333333703, 0.3219752754296894559, 0.3333333333333333703, 0.3219752754296894559, 0.3333333333333333703, 0.3219752754296894559, 0.3333333333333333703, 0.3219752754296894559, 0.3333333333333333703, 0.3219752754296894559, 0.3333333333333333703, 0.3219752754296894559, 0.3333333333333333703, 0.3219752754296894559, 0.3333333333333333703, 0.3219752754296894559, 0.3333333333333333703, 0.3219752754296894559, 0.3333333333333333703, 0.3219752754296894559, 0.3333333333333333703, 0.3219752754296894559, 0.3333333333333333703, 0.3219752754296894559, 0.3333333333333333703, 0.3219752754296894559, 0.3333333333333333703, 0.3219752754296894559, 0.3333333333333333703, 0.3219752754296894559, 0.3333333333333333703, 0.3219752754296894559, 0.3333333333333333703, 0.3219752754296894559, 0.3333333333333333703, 0.3219752754296894559, 0.3333333333333333703, 0.3219752754296894559, 0.3333333333333333703, 0.3219752754296894559, 0.3333333333333333703, 0.3219752754296894559, 0.3333333333333333703, 0.3219752754296894559, 0.3333333333333333703, 0.3219752754296894559, 0.3333333333333333703, 0.3219752754296894559, 0.3333333333333333703, 0.3219752754296894559, 0.3333333333333333703, 0.3219752754296894559, 0.3333333333333333703, 0.3219752754296894559, 0.3333333333333333703, 0.3219752754296894559, 0.3333333333333333703, 0.3219752754296894559, 0.3333333333333333703, 0.3219752754296894559, 0.3333333333333333703, 0.3219752754296894559, 0.3333333333333333703, 0.3219752754296894559, 0.3333333333333333703, 0.3219752754296894559, 0.3333333333333333703, 0.3219752754296894559, 0.3333333333333333703, 0.3219752754296894559, 0.3333333333333333703, 0.3219752754296894559, 0.3333333333333333703, 0.3219752754296894559, 0.3333333333333333703, 0.3219752754296894559, 0.3333333333333333703, 0.3219752754296894559, 0.3333333333333333703, 0.3219752754296894559, 0.3333333333333333703, 0.3219752754296894559, 0.3333333333333333703, 0.3219752754296894559, 0.3333333333333333703, 0.3219752754296894559, 0.3333333333333333703, 0.3219752754296894559, 0.3333333333333333703, 0.3219752754296894559, 0.3333333333333333703, 0.3219752754296894559, 0.3333333333333333703, 0.3219752754296894559, 0.3333333333333333703, 0.3219752754296894559, 0.3333333333333333703, 0.3219752754296894559, 0.3333333333333333703, 0.3219752754296894559, 0.3333333333333333703, 0.3219752754296894559, 0.3333333333333333703, 0.3219752754296894559, 0.3333333333333333703, 0.3219752754296894559, 0.3333333333333333703, 0.3219752754296894559, 0.3333333333333333703, 0.3219752754296894559, 0.3333333333333333703, 0.3219752754296894559, 0.3333333333333333703, 0.3219752754296894559, 0.3333333333333333703, 0.3219752754296894559, 0.3333333333333333703, 0.3219752754296894559, 0.3333333333333333703, 0.3219752754296894559, 0.3333333333333333703, 0.3219752754296894559, 0.3333333333333333703, 0.3219752754296894559, 0.3333333333333333703, 0.3219752754296894559, 0.3333333333333333703, 0.3219752754296894559, 0.3333333333333333703, 0.3219752754296894559, 0.3333333333333333703, 0.3219752754296894559, 0.3333333333333333703, 0.3219752754296894559, 0.3333333333333333703, 0.3219752754296894559, 0.3333333333333333703, 0.3219752754296894559, 0.3333333333333333703, 0.3219752754296894559, 0.3333333333333333703, 0.3219752754296894559, 0.3333333333333333703, 0.3219752754296894559, 0.3333333333333333703, 0.3219752754296894559, 0.3333333333333333703, 0.3219752754296894559, 0.3333333333333333703, 0.3219752754296894559, 0.3333333333333333703, 0.3219752754296894559, 0.3333333333333333703, 0.3219752754296894559, 0.3333333333333333703, 0.3219752754296894559, 0.3333333333333333703, 0.3219752754296894559, 0.3333333333333333703, 0.3219752754296894559, 0.3333333333333333703, 0.3219752754296894559, 0.3333333333333333703),
 ( 0.3333333333333333703, 0.3219752754296894559, 0.3333333333333333703, 0.3219752754296894559, 0.3333333333333333703, 0.3219752754296894559, 0.3333333333333333703, 0.3219752754296894559, 0.3333333333333333703, 0.3219752754296894559, 0.3333333333333333703, 0.3219752754296894559, 0.3333333333333333703, 0.3219752754296894559, 0.3333333333333333703, 0.3219752754296894559, 0.3333333333333333703, 0.3219752754296894559, 0.3333333333333333703, 0.3219752754296894559, 0.3333333333333333703, 0.3219752754296894559, 0.3333333333333333703, 0.3219752754296894559, 0.3333333333333333703, 0.3219752754296894559, 0.3333333333333333703, 0.3219752754296894559, 0.3333333333333333703, 0.3219752754296894559, 0.3333333333333333703, 0.3219752754296894559, 0.3333333333333333703, 0.3219752754296894559, 0.3333333333333333703, 0.3219752754296894559, 0.3333333333333333703, 0.3219752754296894559, 0.3333333333333333703, 0.3219752754296894559, 0.3333333333333333703, 0.3219752754296894559, 0.3333333333333333703, 0.3219752754296894559, 0.3333333333333333703, 0.3219752754296894559, 0.3333333333333333703, 0.3219752754296894559, 0.3333333333333333703, 0.3219752754296894559, 0.3333333333333333703, 0.3219752754296894559, 0.3333333333333333703, 0.3219752754296894559, 0.3333333333333333703, 0.3219752754296894559, 0.3333333333333333703, 0.3219752754296894559, 0.3333333333333333703, 0.3219752754296894559, 0.3333333333333333703, 0.3219752754296894559, 0.3333333333333333703, 0.3219752754296894559, 0.3333333333333333703, 0.3219752754296894559, 0.3333333333333333703, 0.3219752754296894559, 0.3333333333333333703, 0.3219752754296894559, 0.3333333333333333703, 0.3219752754296894559, 0.3333333333333333703, 0.3219752754296894559, 0.3333333333333333703, 0.3219752754296894559, 0.3333333333333333703, 0.3219752754296894559, 0.3333333333333333703, 0.3219752754296894559, 0.3333333333333333703, 0.3219752754296894559, 0.3333333333333333703, 0.3219752754296894559, 0.3333333333333333703, 0.3219752754296894559, 0.3333333333333333703, 0.3219752754296894559, 0.3333333333333333703, 0.3219752754296894559, 0.3333333333333333703, 0.3219752754296894559, 0.3333333333333333703, 0.3219752754296894559, 0.3333333333333333703, 0.3219752754296894559, 0.3333333333333333703, 0.3219752754296894559, 0.3333333333333333703, 0.3219752754296894559, 0.3333333333333333703, 0.3219752754296894559, 0.3333333333333333703, 0.3219752754296894559, 0.3333333333333333703, 0.3219752754296894559, 0.3333333333333333703, 0.3219752754296894559, 0.3333333333333333703, 0.3219752754296894559, 0.3333333333333333703, 0.3219752754296894559, 0.3333333333333333703, 0.3219752754296894559, 0.3333333333333333703, 0.3219752754296894559, 0.3333333333333333703, 0.3219752754296894559, 0.3333333333333333703, 0.3219752754296894559, 0.3333333333333333703, 0.3219752754296894559, 0.3333333333333333703, 0.3219752754296894559, 0.3333333333333333703, 0.3219752754296894559, 0.3333333333333333703, 0.3219752754296894559, 0.3333333333333333703, 0.3219752754296894559, 0.3333333333333333703, 0.3219752754296894559, 0.3333333333333333703, 0.3219752754296894559, 0.3333333333333333703, 0.3219752754296894559, 0.3333333333333333703, 0.3219752754296894559, 0.3333333333333333703, 0.3219752754296894559, 0.3333333333333333703, 0.3219752754296894559, 0.3333333333333333703, 0.3219752754296894559, 0.3333333333333333703, 0.3219752754296894559, 0.3333333333333333703, 0.3219752754296894559, 0.3333333333333333703, 0.3219752754296894559, 0.3333333333333333703, 0.3219752754296894559, 0.3333333333333333703, 0.3219752754296894559, 0.3333333333333333703, 0.3219752754296894559, 0.3333333333333333703, 0.3219752754296894559, 0.3333333333333333703, 0.3219752754296894559, 0.3333333333333333703, 0.3219752754296894559, 0.3333333333333333703, 0.3219752754296894559, 0.3333333333333333703, 0.3219752754296894559, 0.3333333333333333703, 0.3219752754296894559, 0.3333333333333333703, 0.3219752754296894559, 0.3333333333333333703, 0.3219752754296894559, 0.3333333333333333703, 0.3219752754296894559, 0.3333333333333333703, 0.3219752754296894559, 0.3333333333333333703, 0.3219752754296894559, 0.3333333333333333703, 0.3219752754296894559, 0.3333333333333333703, 0.3219752754296894559, 0.3333333333333333703, 0.3219752754296894559, 0.3333333333333333703, 0.3219752754296894559, 0.3333333333333333703, 0.3219752754296894559, 0.3333333333333333703, 0.3219752754296894559, 0.3333333333333333703, 0.3219752754296894559, 0.3333333333333333703, 0.3219752754296894559, 0.3333333333333333703, 0.3219752754296894559, 0.3333333333333333703, 0.3219752754296894559, 0.3333333333333333703, 0.3219752754296894559, 0.3333333333333333703, 0.3219752754296894559, 0.3333333333333333703, 0.3219752754296894559, 0.3333333333333333703, 0.3219752754296894559, 0.3333333333333333703, 0.3219752754296894559, 0.3333333333333333703, 0.3219752754296894559, 0.3333333333333333703, 0.3219752754296894559, 0.3333333333333333703, 0.3219752754296894559, 0.3333333333333333703, 0.3219752754296894559, 0.3333333333333333703, 0.3219752754296894559, 0.3333333333333333703, 0.3219752754296894559, 0.3333333333333333703, 0.3219752754296894559, 0.3333333333333333703, 0.3219752754296894559, 0.3333333333333333703, 0.3219752754296894559, 0.3333333333333333703, 0.3219752754296894559, 0.3333333333333333703, 0.3219752754296894559, 0.3333333333333333703, 0.3219752754296894559, 0.3333333333333333703, 0.3219752754296894559, 0.3333333333333333703, 0.3219752754296894559, 0.3333333333333333703, 0.3219752754296894559, 0.3333333333333333703, 0.3219752754296894559, 0.3333333333333333703, 0.3219752754296894559, 0.3333333333333333703, 0.3219752754296894559, 0.3333333333333333703, 0.3219752754296894559, 0.3333333333333333703, 0.3219752754296894559, 0.3333333333333333703, 0.3219752754296894559, 0.3333333333333333703, 0.3219752754296894559, 0.3333333333333333703, 0.3219752754296894559, 0.3333333333333333703, 0.3219752754296894559, 0.3333333333333333703, 0.3219752754296894559, 0.3333333333333333703, 0.3219752754296894559, 0.3333333333333333703, 0.3219752754296894559, 0.3333333333333333703, 0.3219752754296894559, 0.3333333333333333703, 0.3219752754296894559, 0.3333333333333333703, 0.3219752754296894559, 0.3333333333333333703, 0.3219752754296894559, 0.3333333333333333703, 0.3219752754296894559, 0.3333333333333333703, 0.3219752754296894559, 0.3333333333333333703, 0.3219752754296894559, 0.3333333333333333703, 0.3219752754296894559, 0.3333333333333333703, 0.3219752754296894559, 0.3333333333333333703, 0.3219752754296894559, 0.3333333333333333703, 0.3219752754296894559, 0.3333333333333333703, 0.3219752754296894559, 0.3333333333333333703, 0.3219752754296894559, 0.3333333333333333703, 0.3219752754296894559, 0.3333333333333333703, 0.3219752754296894559, 0.3333333333333333703, 0.3219752754296894559, 0.3333333333333333703, 0.3219752754296894559, 0.3333333333333333703, 0.3219752754296894559, 0.3333333333333333703, 0.3219752754296894559, 0.3333333333333333703, 0.3219752754296894559, 0.3333333333333333703, 0.3219752754296894559, 0.3333333333333333703, 0.3219752754296894559, 0.3333333333333333703, 0.3219752754296894559, 0.3333333333333333703, 0.3219752754296894559, 0.3333333333333333703, 0.3219752754296894559, 0.3333333333333333703, 0.3219752754296894559, 0.3333333333333333703, 0.3219752754296894559, 0.3333333333333333703, 0.3219752754296894559, 0.3333333333333333703, 0.3219752754296894559, 0.3333333333333333703, 0.3219752754296894559, 0.3333333333333333703, 0.3219752754296894559, 0.3333333333333333703, 0.3219752754296894559, 0.3333333333333333703, 0.3219752754296894559, 0.3333333333333333703, 0.3219752754296894559, 0.3333333333333333703, 0.3219752754296894559, 0.3333333333333333703, 0.3219752754296894559, 0.3333333333333333703, 0.3219752754296894559, 0.3333333333333333703, 0.3219752754296894559, 0.3333333333333333703, 0.3219752754296894559, 0.3333333333333333703, 0.3219752754296894559, 0.3333333333333333703, 0.3219752754296894559, 0.3333333333333333703, 0.3219752754296894559, 0.3333333333333333703, 0.3219752754296894559, 0.3333333333333333703, 0.3219752754296894559, 0.3333333333333333703, 0.3219752754296894559, 0.3333333333333333703, 0.3219752754296894559, 0.3333333333333333703, 0.3219752754296894559, 0.3333333333333333703, 0.3219752754296894559, 0.3333333333333333703, 0.3219752754296894559, 0.3333333333333333703, 0.3219752754296894559, 0.3333333333333333703, 0.3219752754296894559, 0.3333333333333333703, 0.3219752754296894559, 0.3333333333333333703, 0.3219752754296894559, 0.3333333333333333703, 0.3219752754296894559, 0.3333333333333333703, 0.3219752754296894559, 0.3333333333333333703, 0.3219752754296894559, 0.3333333333333333703, 0.3219752754296894559, 0.3333333333333333703, 0.3219752754296894559, 0.3333333333333333703, 0.3219752754296894559, 0.3333333333333333703, 0.3219752754296894559, 0.3333333333333333703, 0.3219752754296894559, 0.3333333333333333703, 0.3219752754296894559, 0.3333333333333333703, 0.3219752754296894559, 0.3333333333333333703, 0.3219752754296894559, 0.3333333333333333703, 0.3219752754296894559, 0.3333333333333333703, 0.3219752754296894559, 0.3333333333333333703, 0.3219752754296894559, 0.3333333333333333703, 0.3219752754296894559, 0.3333333333333333703, 0.3219752754296894559, 0.3333333333333333703, 0.3219752754296894559, 0.3333333333333333703, 0.3219752754296894559, 0.3333333333333333703, 0.3219752754296894559, 0.3333333333333333703, 0.3219752754296894559, 0.3333333333333333703, 0.3219752754296894559, 0.3333333333333333703, 0.3219752754296894559, 0.3333333333333333703, 0.3219752754296894559, 0.3333333333333333703, 0.3219752754296894559, 0.3333333333333333703, 0.3219752754296894559, 0.3333333333333333703, 0.3219752754296894559, 0.3333333333333333703, 0.3219752754296894559, 0.3333333333333333703, 0.3219752754296894559, 0.3333333333333333703, 0.3219752754296894559, 0.3333333333333333703, 0.3219752754296894559, 0.3333333333333333703, 0.3219752754296894559, 0.3333333333333333703, 0.3219752754296894559, 0.3333333333333333703, 0.3219752754296894559, 0.3333333333333333703, 0.3219752754296894559, 0.3333333333333333703, 0.3219752754296894559, 0.3333333333333333703, 0.3219752754296894559, 0.3333333333333333703, 0.3219752754296894559, 0.3333333333333333703, 0.3219752754296894559, 0.3333333333333333703, 0.3219752754296894559, 0.3333333333333333703, 0.3219752754296894559, 0.3333333333333333703, 0.3219752754296894559, 0.3333333333333333703, 0.3219752754296894559, 0.3333333333333333703, 0.3219752754296894559, 0.3333333333333333703, 0.3219752754296894559, 0.3333333333333333703),
 ( 1.000000000000000000, 0.9659258262890683122, 1.000000000000000000, 0.9659258262890683122, 1.000000000000000000, 0.9659258262890683122, 1.000000000000000000, 0.9659258262890683122, 1.000000000000000000, 0.9659258262890683122, 1.000000000000000000, 0.9659258262890683122, 1.000000000000000000, 0.9659258262890683122, 1.000000000000000000, 0.9659258262890683122, 1.000000000000000000, 0.9659258262890683122, 1.000000000000000000, 0.9659258262890683122, 1.000000000000000000, 0.9659258262890683122, 1.000000000000000000, 0.9659258262890683122, 1.000000000000000000, 0.9659258262890683122, 1.000000000000000000, 0.9659258262890683122, 1.000000000000000000, 0.9659258262890683122, 1.000000000000000000, 0.9659258262890683122, 1.000000000000000000, 0.9659258262890683122, 1.000000000000000000, 0.9659258262890683122, 1.000000000000000000, 0.9659258262890683122, 1.000000000000000000, 0.9659258262890683122, 1.000000000000000000, 0.9659258262890683122, 1.000000000000000000, 0.9659258262890683122, 1.000000000000000000, 0.9659258262890683122, 1.000000000000000000, 0.9659258262890683122, 1.000000000000000000, 0.9659258262890683122, 1.000000000000000000, 0.9659258262890683122, 1.000000000000000000, 0.9659258262890683122, 1.000000000000000000, 0.9659258262890683122, 1.000000000000000000, 0.9659258262890683122, 1.000000000000000000, 0.9659258262890683122, 1.000000000000000000, 0.9659258262890683122, 1.000000000000000000, 0.9659258262890683122, 1.000000000000000000, 0.9659258262890683122, 1.000000000000000000, 0.9659258262890683122, 1.000000000000000000, 0.9659258262890683122, 1.000000000000000000, 0.9659258262890683122, 1.000000000000000000, 0.9659258262890683122, 1.000000000000000000, 0.9659258262890683122, 1.000000000000000000, 0.9659258262890683122, 1.000000000000000000, 0.9659258262890683122, 1.000000000000000000, 0.9659258262890683122, 1.000000000000000000, 0.9659258262890683122, 1.000000000000000000, 0.9659258262890683122, 1.000000000000000000, 0.9659258262890683122, 1.000000000000000000, 0.9659258262890683122, 1.000000000000000000, 0.9659258262890683122, 1.000000000000000000, 0.9659258262890683122, 1.000000000000000000, 0.9659258262890683122, 1.000000000000000000, 0.9659258262890683122, 1.000000000000000000, 0.9659258262890683122, 1.000000000000000000, 0.9659258262890683122, 1.000000000000000000, 0.9659258262890683122, 1.000000000000000000, 0.9659258262890683122, 1.000000000000000000, 0.9659258262890683122, 1.000000000000000000, 0.9659258262890683122, 1.000000000000000000, 0.9659258262890683122, 1.000000000000000000, 0.9659258262890683122, 1.000000000000000000, 0.9659258262890683122, 1.000000000000000000, 0.9659258262890683122, 1.000000000000000000, 0.9659258262890683122, 1.000000000000000000, 0.9659258262890683122, 1.000000000000000000, 0.9659258262890683122, 1.000000000000000000, 0.9659258262890683122, 1.000000000000000000, 0.9659258262890683122, 1.000000000000000000, 0.9659258262890683122, 1.000000000000000000, 0.9659258262890683122, 1.000000000000000000, 0.9659258262890683122, 1.000000000000000000, 0.9659258262890683122, 1.000000000000000000, 0.9659258262890683122, 1.000000000000000000, 0.9659258262890683122, 1.000000000000000000, 0.9659258262890683122, 1.000000000000000000, 0.9659258262890683122, 1.000000000000000000, 0.9659258262890683122, 1.000000000000000000, 0.9659258262890683122, 1.000000000000000000, 0.9659258262890683122, 1.000000000000000000, 0.9659258262890683122, 1.000000000000000000, 0.9659258262890683122, 1.000000000000000000, 0.9659258262890683122, 1.000000000000000000, 0.9659258262890683122, 1.000000000000000000, 0.9659258262890683122, 1.000000000000000000, 0.9659258262890683122, 1.000000000000000000, 0.9659258262890683122, 1.000000000000000000, 0.9659258262890683122, 1.000000000000000000, 0.9659258262890683122, 1.000000000000000000, 0.9659258262890683122, 1.000000000000000000, 0.9659258262890683122, 1.000000000000000000, 0.9659258262890683122, 1.000000000000000000, 0.9659258262890683122, 1.000000000000000000, 0.9659258262890683122, 1.000000000000000000, 0.9659258262890683122, 1.000000000000000000, 0.9659258262890683122, 1.000000000000000000, 0.9659258262890683122, 1.000000000000000000, 0.9659258262890683122, 1.000000000000000000, 0.9659258262890683122, 1.000000000000000000, 0.9659258262890683122, 1.000000000000000000, 0.9659258262890683122, 1.000000000000000000, 0.9659258262890683122, 1.000000000000000000, 0.9659258262890683122, 1.000000000000000000, 0.9659258262890683122, 1.000000000000000000, 0.9659258262890683122, 1.000000000000000000, 0.9659258262890683122, 1.000000000000000000, 0.9659258262890683122, 1.000000000000000000, 0.9659258262890683122, 1.000000000000000000, 0.9659258262890683122, 1.000000000000000000, 0.9659258262890683122, 1.000000000000000000, 0.9659258262890683122, 1.000000000000000000, 0.9659258262890683122, 1.000000000000000000, 0.9659258262890683122, 1.000000000000000000, 0.9659258262890683122, 1.000000000000000000, 0.9659258262890683122, 1.000000000000000000, 0.9659258262890683122, 1.000000000000000000, 0.9659258262890683122, 1.000000000000000000, 0.9659258262890683122, 1.000000000000000000, 0.9659258262890683122, 1.000000000000000000, 0.9659258262890683122, 1.000000000000000000, 0.9659258262890683122, 1.000000000000000000, 0.9659258262890683122, 1.000000000000000000, 0.9659258262890683122, 1.000000000000000000, 0.9659258262890683122, 1.000000000000000000, 0.9659258262890683122, 1.000000000000000000, 0.9659258262890683122, 1.000000000000000000, 0.9659258262890683122, 1.000000000000000000, 0.9659258262890683122, 1.000000000000000000, 0.9659258262890683122, 1.000000000000000000, 0.9659258262890683122, 1.000000000000000000, 0.9659258262890683122, 1.000000000000000000, 0.9659258262890683122, 1.000000000000000000, 0.9659258262890683122, 1.000000000000000000, 0.9659258262890683122, 1.000000000000000000, 0.9659258262890683122, 1.000000000000000000, 0.9659258262890683122, 1.000000000000000000, 0.9659258262890683122, 1.000000000000000000, 0.9659258262890683122, 1.000000000000000000, 0.9659258262890683122, 1.000000000000000000, 0.9659258262890683122, 1.000000000000000000, 0.9659258262890683122, 1.000000000000000000, 0.9659258262890683122, 1.000000000000000000, 0.9659258262890683122, 1.000000000000000000, 0.9659258262890683122, 1.000000000000000000, 0.9659258262890683122, 1.000000000000000000, 0.9659258262890683122, 1.000000000000000000, 0.9659258262890683122, 1.000000000000000000, 0.9659258262890683122, 1.000000000000000000, 0.9659258262890683122, 1.000000000000000000, 0.9659258262890683122, 1.000000000000000000, 0.9659258262890683122, 1.000000000000000000, 0.9659258262890683122, 1.000000000000000000, 0.9659258262890683122, 1.000000000000000000, 0.9659258262890683122, 1.000000000000000000, 0.9659258262890683122, 1.000000000000000000, 0.9659258262890683122, 1.000000000000000000, 0.9659258262890683122, 1.000000000000000000, 0.9659258262890683122, 1.000000000000000000, 0.9659258262890683122, 1.000000000000000000, 0.9659258262890683122, 1.000000000000000000, 0.9659258262890683122, 1.000000000000000000, 0.9659258262890683122, 1.000000000000000000, 0.9659258262890683122, 1.000000000000000000, 0.9659258262890683122, 1.000000000000000000, 0.9659258262890683122, 1.000000000000000000, 0.9659258262890683122, 1.000000000000000000, 0.9659258262890683122, 1.000000000000000000, 0.9659258262890683122, 1.000000000000000000, 0.9659258262890683122, 1.000000000000000000, 0.9659258262890683122, 1.000000000000000000, 0.9659258262890683122, 1.000000000000000000, 0.9659258262890683122, 1.000000000000000000, 0.9659258262890683122, 1.000000000000000000, 0.9659258262890683122, 1.000000000000000000, 0.9659258262890683122, 1.000000000000000000, 0.9659258262890683122, 1.000000000000000000, 0.9659258262890683122, 1.000000000000000000, 0.9659258262890683122, 1.000000000000000000, 0.9659258262890683122, 1.000000000000000000, 0.9659258262890683122, 1.000000000000000000, 0.9659258262890683122, 1.000000000000000000, 0.9659258262890683122, 1.000000000000000000, 0.9659258262890683122, 1.000000000000000000, 0.9659258262890683122, 1.000000000000000000, 0.9659258262890683122, 1.000000000000000000, 0.9659258262890683122, 1.000000000000000000, 0.9659258262890683122, 1.000000000000000000, 0.9659258262890683122, 1.000000000000000000, 0.9659258262890683122, 1.000000000000000000, 0.9659258262890683122, 1.000000000000000000, 0.9659258262890683122, 1.000000000000000000, 0.9659258262890683122, 1.000000000000000000, 0.9659258262890683122, 1.000000000000000000, 0.9659258262890683122, 1.000000000000000000, 0.9659258262890683122, 1.000000000000000000, 0.9659258262890683122, 1.000000000000000000, 0.9659258262890683122, 1.000000000000000000, 0.9659258262890683122, 1.000000000000000000, 0.9659258262890683122, 1.000000000000000000, 0.9659258262890683122, 1.000000000000000000, 0.9659258262890683122, 1.000000000000000000, 0.9659258262890683122, 1.000000000000000000, 0.9659258262890683122, 1.000000000000000000, 0.9659258262890683122, 1.000000000000000000, 0.9659258262890683122, 1.000000000000000000, 0.9659258262890683122, 1.000000000000000000, 0.9659258262890683122, 1.000000000000000000, 0.9659258262890683122, 1.000000000000000000, 0.9659258262890683122, 1.000000000000000000, 0.9659258262890683122, 1.000000000000000000, 0.9659258262890683122, 1.000000000000000000, 0.9659258262890683122, 1.000000000000000000, 0.9659258262890683122, 1.000000000000000000, 0.9659258262890683122, 1.000000000000000000, 0.9659258262890683122, 1.000000000000000000, 0.9659258262890683122, 1.000000000000000000, 0.9659258262890683122, 1.000000000000000000, 0.9659258262890683122, 1.000000000000000000, 0.9659258262890683122, 1.000000000000000000, 0.9659258262890683122, 1.000000000000000000, 0.9659258262890683122, 1.000000000000000000, 0.9659258262890683122, 1.000000000000000000, 0.9659258262890683122, 1.000000000000000000, 0.9659258262890683122, 1.000000000000000000, 0.9659258262890683122, 1.000000000000000000, 0.9659258262890683122, 1.000000000000000000, 0.9659258262890683122, 1.000000000000000000, 0.9659258262890683122, 1.000000000000000000, 0.9659258262890683122, 1.000000000000000000, 0.9659258262890683122, 1.000000000000000000, 0.9659258262890683122, 1.000000000000000000, 0.9659258262890683122, 1.000000000000000000, 0.9659258262890683122, 1.000000000000000000) ) ) 
 REPRESENTATION_ITEM ( '' )  SURFACE ( )  );
#88900 = CARTESIAN_POINT ( 'NONE',  ( -19.02544592524342804, 5.153800228976336051, 86.04057627198103830 ) ) ;
#88901 = CARTESIAN_POINT ( 'NONE',  ( 0.05219959533909260263, 19.03943276465977164, 79.99890960531436690 ) ) ;
#88902 = CARTESIAN_POINT ( 'NONE',  ( -14.29746914071049879, 8.314922557960819915, 105.8322429386476955 ) ) ;
#88903 = ORIENTED_EDGE ( 'NONE', *, *, #61218, .F. ) ;
#88904 = CARTESIAN_POINT ( 'NONE',  ( 8.224510206698953496, -14.34966873604960469, 32.91557627198102409 ) ) ;
#88905 = CARTESIAN_POINT ( 'NONE',  ( 4.483927247898790824, -16.52544592524335698, 45.20942372801901854 ) ) ;
#88906 = CARTESIAN_POINT ( 'NONE',  ( -0.05219959533937732626, 21.53943276465977519, 107.5010903946856899 ) ) ;
#88907 = CARTESIAN_POINT ( 'NONE',  ( -5.153800228976328057, -19.02544592524343514, 97.29057627198099567 ) ) ;
#88908 = CARTESIAN_POINT ( 'NONE',  ( 21.52544592524334988, 5.823673210054432836, 36.45942372801901143 ) ) ;
#88909 = CARTESIAN_POINT ( 'NONE',  ( 19.02544592524343514, -5.153800228976328945, 43.54057627198103120 ) ) ;
#88910 = CARTESIAN_POINT ( 'NONE',  ( 0.05219959533934541429, -16.53943276465976808, 50.00109039468568994 ) ) ;
#88911 = CARTESIAN_POINT ( 'NONE',  ( 4.379528057220092307, 16.55341960407617563, 82.29275706135234714 ) ) ;
#88912 = CARTESIAN_POINT ( 'NONE',  ( 19.02544592524334988, 5.153800228976608722, 106.4594237280190185 ) ) ;
#88913 = CARTESIAN_POINT ( 'NONE',  ( -19.05341960407611168, -5.049401038298163336, 31.45724293864769550 ) ) ;
#88914 = CARTESIAN_POINT ( 'NONE',  ( -12.06949235617756955, 12.14591786802309770, 95.62390960531436690 ) ) ;
#88915 = CARTESIAN_POINT ( 'NONE',  ( -5.823673210054116645, -21.52544592524344225, 97.29057627198105251 ) ) ;
#88916 = CARTESIAN_POINT ( 'NONE',  ( -0.05219959533936034679, 19.03943276465977164, 82.50109039468567573 ) ) ;
#88917 = CARTESIAN_POINT ( 'NONE',  ( 9.564922557960805705, 16.46253265017160317, 29.58224293864769550 ) ) ;
#88918 = CARTESIAN_POINT ( 'NONE',  ( 19.03943276465977164, -0.05219959533909143690, 88.74890960531436690 ) ) ;
#88919 = CARTESIAN_POINT ( 'NONE',  ( -10.81492255796105439, 18.62759615963255655, 32.91775706135234714 ) ) ;
#88920 = CARTESIAN_POINT ( 'NONE',  ( -30.73962218707678318, 22.33364281372846705, -3.947842220587803208 ) ) ;
#88921 = CARTESIAN_POINT ( 'NONE',  ( 9.564922557960805705, 16.46253265017160317, 94.58224293864769550 ) ) ;
#88922 = DIRECTION ( 'NONE',  ( -0.000000000000000000, -0.000000000000000000, -1.000000000000000000 ) ) ;
#88923 = CARTESIAN_POINT ( 'NONE',  ( 19.03943276465977164, -0.05219959533909143690, 88.74890960531436690 ) ) ;
#88925 = CARTESIAN_POINT ( 'NONE',  ( 4.379528057220339221, -16.55341960407611168, 92.70724293864770971 ) ) ;
#88924 = CARTESIAN_POINT ( 'NONE',  ( -15.72974639402176322, -15.80617190586768395, 34.37609039468568284 ) ) ;
#88926 = CARTESIAN_POINT ( 'NONE',  ( -13.97604488694527625, -13.89961937509977652, 101.8739096053143811 ) ) ;
#88927 = CARTESIAN_POINT ( 'NONE',  ( 19.02544592524334988, 5.153800228976608722, 21.45942372801899012 ) ) ;
#88928 = CARTESIAN_POINT ( 'NONE',  ( -14.29746914071037622, -8.314922557961029526, 54.16775706135235424 ) ) ;
#88929 = CARTESIAN_POINT ( 'NONE',  ( -15.72974639402176322, -15.80617190586768395, 84.37609039468570415 ) ) ;
#88930 = CARTESIAN_POINT ( 'NONE',  ( -14.29746914071037622, -8.314922557961029526, 44.16775706135234714 ) ) ;
#88931 = CARTESIAN_POINT ( 'NONE',  ( 5.153800228976335163, 19.02544592524342804, 69.79057627198103830 ) ) ;
#88932 = CARTESIAN_POINT ( 'NONE',  ( -16.51473224551082808, 9.474510206698731452, 93.33442372801900433 ) ) ;
#88933 = CARTESIAN_POINT ( 'NONE',  ( 12.14591786802327356, -12.06949235617739191, 70.62609039468567573 ) ) ;
#88935 = B_SPLINE_CURVE_WITH_KNOTS ( 'NONE', 3,
 ( #41057, #54220, #73400, #178574, #84531, #53207, #164409, #163403 ),
 .UNSPECIFIED., .F., .F.,
 ( 4, 2, 2, 4 ),
 ( -3.098386792788301083E-05, 0.0009765746000771589885, 0.001984133068082204274, 0.003999250004092276198 ),
 .UNSPECIFIED. ) ;
#88934 = CARTESIAN_POINT ( 'NONE',  ( -18.67979575497193778, 10.72451020669871902, 108.3344237280190185 ) ) ;
#88936 = CARTESIAN_POINT ( 'NONE',  ( 9.564922557961047289, -16.46253265017146816, 85.41775706135233293 ) ) ;
#88937 = CARTESIAN_POINT ( 'NONE',  ( 13.89961937509977652, -13.97604488694527269, 63.12390960531435979 ) ) ;
#88938 = CARTESIAN_POINT ( 'NONE',  ( -21.55341960407610458, -5.719274019375992779, 86.45724293864770971 ) ) ;
#88940 = CARTESIAN_POINT ( 'NONE',  ( -19.02544592524334988, -5.153800228976617603, 83.95942372801901854 ) ) ;
#88939 = CARTESIAN_POINT ( 'NONE',  ( 4.379528057220339221, -16.55341960407611168, 82.70724293864770971 ) ) ;
#88941 = CARTESIAN_POINT ( 'NONE',  ( 24.22576942085165896, 7.195495839727253262, 170.3116806589316354 ) ) ;
#88942 = CARTESIAN_POINT ( 'NONE',  ( 5.049401038297881783, 19.05341960407617563, 52.29275706135234003 ) ) ;
#88943 = CARTESIAN_POINT ( 'NONE',  ( 14.29746914071037800, 8.314922557961029526, 111.6677570613523613 ) ) ;
#88944 = CARTESIAN_POINT ( 'NONE',  ( -8.224510206698948167, 14.34966873604960824, 80.41557627198103830 ) ) ;
#88946 = CARTESIAN_POINT ( 'NONE',  ( -16.29526858892907271, 7.335722546920045772, 39.20329402199734403 ) ) ;
#88945 = CARTESIAN_POINT ( 'NONE',  ( -0.05219959533936034679, 19.03943276465977164, 22.50109039468566152 ) ) ;
#88947 = CARTESIAN_POINT ( 'NONE',  ( 21.55341960407610458, 5.719274019375980345, 103.9572429386476813 ) ) ;
#88948 = CARTESIAN_POINT ( 'NONE',  ( -16.51473224551069308, -9.474510206698971260, 106.6655762719810383 ) ) ;
#88949 = CARTESIAN_POINT ( 'NONE',  ( 9.564922557960805705, 16.46253265017160317, 84.58224293864769550 ) ) ;
#88950 = CARTESIAN_POINT ( 'NONE',  ( 21.55341960407619695, -5.719274019375665929, 86.04275706135236135 ) ) ;
#88951 = CARTESIAN_POINT ( 'NONE',  ( 13.97604488694527802, 13.89961937509977652, 59.37390960531434558 ) ) ;
#88952 = CARTESIAN_POINT ( 'NONE',  ( -16.46253265017160317, 9.564922557960807481, 40.83224293864769550 ) ) ;
#88953 = CARTESIAN_POINT ( 'NONE',  ( -18.62759615963270932, 10.81492255796079327, 25.83224293864769194 ) ) ;
#88954 = AXIS2_PLACEMENT_3D ( 'NONE', #2188, #4166, #17368 ) ;
#88955 = CARTESIAN_POINT ( 'NONE',  ( -0.05219959533910754901, -16.53943276465976808, 77.49890960531433848 ) ) ;
#88956 = CARTESIAN_POINT ( 'NONE',  ( -9.564922557960796823, -16.46253265017161027, 47.08224293864769550 ) ) ;
#88957 = CARTESIAN_POINT ( 'NONE',  ( 16.53943276465976808, -0.05219959533910856209, 98.74890960531438111 ) ) ;
#88958 = CARTESIAN_POINT ( 'NONE',  ( -10.72451020669898014, 18.67979575497178502, 115.4155762719810241 ) ) ;
#88959 = CARTESIAN_POINT ( 'NONE',  ( 5.823673210054444382, -21.52544592524334988, 50.20942372801901854 ) ) ;
#88960 = CARTESIAN_POINT ( 'NONE',  ( 5.153800228976335163, 19.02544592524342804, 24.79057627198102765 ) ) ;
#88961 = CARTESIAN_POINT ( 'NONE',  ( 16.53943276465976808, 0.05219959533934440121, 66.25109039468567573 ) ) ;
#88962 = CARTESIAN_POINT ( 'NONE',  ( -18.62759615963270932, 10.81492255796079327, 100.8322429386477097 ) ) ;
#88963 = CARTESIAN_POINT ( 'NONE',  ( 18.67979575497178502, 10.72451020669898547, 104.1655762719810241 ) ) ;
#88965 = CARTESIAN_POINT ( 'NONE',  ( -13.97604488694527625, -13.89961937509977652, 46.87390960531435979 ) ) ;
#88964 = CARTESIAN_POINT ( 'NONE',  ( -19.05341960407617563, 5.049401038297882671, 43.54275706135232582 ) ) ;
#88966 = CARTESIAN_POINT ( 'NONE',  ( 13.97604488694527802, 13.89961937509977652, 114.3739096053143669 ) ) ;
#88967 = CARTESIAN_POINT ( 'NONE',  ( 18.62759615963255655, 10.81492255796105972, 61.66775706135235424 ) ) ;
#88968 = CARTESIAN_POINT ( 'NONE',  ( -21.55341960407610458, -5.719274019375992779, 56.45724293864768839 ) ) ;
#88969 = CARTESIAN_POINT ( 'NONE',  ( 4.483927247898545687, 16.52544592524342804, 39.79057627198103830 ) ) ;
#88971 = CARTESIAN_POINT ( 'NONE',  ( -15.80617190586768217, 15.72974639402176855, 113.1260903946856899 ) ) ;
#88970 = CARTESIAN_POINT ( 'NONE',  ( 18.67979575497194134, -10.72451020669871369, 75.83442372801900433 ) ) ;
#88972 = CARTESIAN_POINT ( 'NONE',  ( -5.049401038297874678, -19.05341960407617918, 44.79275706135232582 ) ) ;
#88973 = CARTESIAN_POINT ( 'NONE',  ( 16.53943276465976808, 0.05219959533934440121, 101.2510903946856757 ) ) ;
#88974 = CARTESIAN_POINT ( 'NONE',  ( 15.72974639402176855, 15.80617190586768217, 56.87609039468568994 ) ) ;
#88975 = CARTESIAN_POINT ( 'NONE',  ( -19.05341960407611168, -5.049401038298163336, 56.45724293864768129 ) ) ;
#88976 = CARTESIAN_POINT ( 'NONE',  ( -0.05219959533936034679, 19.03943276465977164, 37.50109039468567573 ) ) ;
#88977 = CARTESIAN_POINT ( 'NONE',  ( 5.823673210054125526, 21.52544592524343514, 39.79057627198103830 ) ) ;
#88978 = CARTESIAN_POINT ( 'NONE',  ( 0.05219959533937995610, -21.53943276465977519, 30.00109039468568284 ) ) ;
#88979 = CARTESIAN_POINT ( 'NONE',  ( 21.55341960407610458, 5.719274019375980345, 88.95724293864769550 ) ) ;
#88980 = CARTESIAN_POINT ( 'NONE',  ( -19.05341960407617563, 5.049401038297882671, 88.54275706135230450 ) ) ;
#88981 = CARTESIAN_POINT ( 'NONE',  ( 16.53943276465976808, 0.05219959533934440121, 51.25109039468568994 ) ) ;
#88983 = CARTESIAN_POINT ( 'NONE',  ( -10.81492255796078084, -18.62759615963271287, 92.08224293864769550 ) ) ;
#88982 = DIRECTION ( 'NONE',  ( 1.000000000000000000, -5.392603844284257652E-33, 0.000000000000000000 ) ) ;
#88985 = CARTESIAN_POINT ( 'NONE',  ( -8.314922557960811034, -14.29746914071050412, 82.08224293864768129 ) ) ;
#88984 = CARTESIAN_POINT ( 'NONE',  ( -16.52544592524335698, -4.483927247898792601, 73.95942372801901854 ) ) ;
#88986 = CARTESIAN_POINT ( 'NONE',  ( -24.75282386541777413, -28.51018972888603642, -20.68147073028497118 ) ) ;
#88987 = CARTESIAN_POINT ( 'NONE',  ( 0.05219959533936267826, -19.03943276465977164, 100.0010903946856757 ) ) ;
#88988 = CARTESIAN_POINT ( 'NONE',  ( -18.62759615963270932, 10.81492255796079327, 30.83224293864770260 ) ) ;
#88989 = DIRECTION ( 'NONE',  ( 1.000000000000000000, -0.000000000000000000, -0.000000000000000000 ) ) ;
#88990 = CARTESIAN_POINT ( 'NONE',  ( 4.483927247898790824, -16.52544592524335698, 55.20942372801902565 ) ) ;
#88991 = CARTESIAN_POINT ( 'NONE',  ( -10.81492255796105439, 18.62759615963255655, 32.91775706135234714 ) ) ;
#88992 = CARTESIAN_POINT ( 'NONE',  ( -5.719274019375978568, 21.55341960407610458, 50.20724293864769550 ) ) ;
#88993 = CARTESIAN_POINT ( 'NONE',  ( 4.483927247898790824, -16.52544592524335698, 70.20942372801904696 ) ) ;
#88994 = CARTESIAN_POINT ( 'NONE',  ( 5.153800228976335163, 19.02544592524342804, 79.79057627198102409 ) ) ;
#88996 = CARTESIAN_POINT ( 'NONE',  ( -16.46253265017160317, 9.564922557960807481, 25.83224293864769194 ) ) ;
#88995 = CARTESIAN_POINT ( 'NONE',  ( 21.53943276465977519, 0.05219959533937863772, 61.25109039468567573 ) ) ;
#88997 = CARTESIAN_POINT ( 'NONE',  ( 18.62759615963271287, -10.81492255796078972, 23.33224293864769194 ) ) ;
#88998 = VERTEX_POINT ( 'NONE', #52086 ) ;
#88999 = CARTESIAN_POINT ( 'NONE',  ( -5.049401038297874678, -19.05341960407617918, 39.79275706135232582 ) ) ;
#89000 = CARTESIAN_POINT ( 'NONE',  ( 4.379528057220092307, 16.55341960407617563, 57.29275706135234714 ) ) ;
#89001 = CARTESIAN_POINT ( 'NONE',  ( -5.049401038298153566, 19.05341960407611168, 115.2072429386477097 ) ) ;
#89002 = EDGE_LOOP ( 'NONE', ( #50932, #92528, #39975, #35183, #146978 ) ) ;
#89003 = CARTESIAN_POINT ( 'NONE',  ( 13.97604488694527802, 13.89961937509977652, 89.37390960531436690 ) ) ;
#89004 = CARTESIAN_POINT ( 'NONE',  ( 12.06949235617739724, 12.14591786802326823, 96.87609039468568994 ) ) ;
#89005 = CARTESIAN_POINT ( 'NONE',  ( -28.79475375365586842, 2.428612866367529932E-14, 142.2656553485623760 ) ) ;
#89006 = CARTESIAN_POINT ( 'NONE',  ( -16.53943276465976808, 0.05219959533911058130, 101.2489096053143669 ) ) ;
#89007 = CARTESIAN_POINT ( 'NONE',  ( 10.72451020669898902, -18.67979575497178502, 32.91557627198102409 ) ) ;
#89008 = CARTESIAN_POINT ( 'NONE',  ( -5.153800228976328057, -19.02544592524343514, 37.29057627198102409 ) ) ;
#89009 = CARTESIAN_POINT ( 'NONE',  ( 14.29746914071037800, 8.314922557961029526, 76.66775706135234714 ) ) ;
#89010 = CARTESIAN_POINT ( 'NONE',  ( 0.05219959533937995610, -21.53943276465977519, 20.00109039468568639 ) ) ;
#89011 = CARTESIAN_POINT ( 'NONE',  ( -9.564922557961040184, 16.46253265017147172, 82.91775706135233293 ) ) ;
#89012 = CARTESIAN_POINT ( 'NONE',  ( -19.02544592524342804, 5.153800228976336051, 46.04057627198101699 ) ) ;
#89013 = AXIS2_PLACEMENT_3D ( 'NONE', #27401, #150736, #185030 ) ;
#89014 = DIRECTION ( 'NONE',  ( 0.000000000000000000, 0.8164965809277253683, -0.5773502691896269523 ) ) ;
#89015 = CARTESIAN_POINT ( 'NONE',  ( 10.72451020669871369, 18.67979575497193778, 107.0844237280190043 ) ) ;
#89016 = CARTESIAN_POINT ( 'NONE',  ( 13.97604488694527802, 13.89961937509977652, 59.37390960531434558 ) ) ;
#89017 = CARTESIAN_POINT ( 'NONE',  ( 12.14591786802327356, -12.06949235617739191, 45.62609039468567573 ) ) ;
#89018 = CARTESIAN_POINT ( 'NONE',  ( 0.05219959533937995610, -21.53943276465977519, 95.00109039468568994 ) ) ;
#89019 = CARTESIAN_POINT ( 'NONE',  ( -19.05341960407617563, 5.049401038297882671, 43.54275706135232582 ) ) ;
#89020 = CARTESIAN_POINT ( 'NONE',  ( 9.474510206698729675, 16.51473224551082808, 47.08442372801900433 ) ) ;
#89021 = ORIENTED_EDGE ( 'NONE', *, *, #175399, .F. ) ;
#89022 = CARTESIAN_POINT ( 'NONE',  ( -10.72451020669870658, -18.67979575497194134, 44.58442372801901854 ) ) ;
#89023 = CARTESIAN_POINT ( 'NONE',  ( -13.89961937509977652, 13.97604488694528158, 25.62390960531434558 ) ) ;
#89024 = CARTESIAN_POINT ( 'NONE',  ( 9.564922557961047289, -16.46253265017146816, 45.41775706135232582 ) ) ;
#89025 = CARTESIAN_POINT ( 'NONE',  ( 5.049401038298161559, -19.05341960407611168, 102.7072429386476955 ) ) ;
#89026 = CARTESIAN_POINT ( 'NONE',  ( 9.564922557960805705, 16.46253265017160317, 79.58224293864769550 ) ) ;
#89027 = CARTESIAN_POINT ( 'NONE',  ( 12.06949235617757843, -12.14591786802309237, 38.12390960531436690 ) ) ;
#89028 = CARTESIAN_POINT ( 'NONE',  ( -0.05219959533907301413, -21.53943276465977519, 32.49890960531435979 ) ) ;
#89029 = CARTESIAN_POINT ( 'NONE',  ( -36.91746825000000598, 2.428612866367529932E-14, -1.124999997268813390 ) ) ;
#89030 = DIRECTION ( 'NONE',  ( 0.000000000000000000, 0.000000000000000000, 1.000000000000000000 ) ) ;
#89031 = CARTESIAN_POINT ( 'NONE',  ( 5.823673210054444382, -21.52544592524334988, 95.20942372801903275 ) ) ;
#89032 = CARTESIAN_POINT ( 'NONE',  ( -27.91697786073761023, 6.847065636290214918, 161.8035115693297712 ) ) ;
#89033 = CARTESIAN_POINT ( 'NONE',  ( 5.049401038298161559, -19.05341960407611168, 37.70724293864768839 ) ) ;
#89034 = CARTESIAN_POINT ( 'NONE',  ( -16.46253265017160317, 9.564922557960807481, 110.8322429386476955 ) ) ;
#89035 = EDGE_CURVE ( 'NONE', #86900, #128850, #146580, .T. ) ;
#89036 = CARTESIAN_POINT ( 'NONE',  ( -34.37111623004060590, -2.754365613946270219, 90.23597232697538573 ) ) ;
#89037 = CARTESIAN_POINT ( 'NONE',  ( -14.29746914071037622, -8.314922557961029526, 64.16775706135234714 ) ) ;
#89038 = CARTESIAN_POINT ( 'NONE',  ( 15.72974639402199770, -15.80617190586745480, 83.12390960531436690 ) ) ;
#89039 = CARTESIAN_POINT ( 'NONE',  ( 8.224510206698953496, -14.34966873604960469, 37.91557627198102409 ) ) ;
#89041 = CARTESIAN_POINT ( 'NONE',  ( 19.05341960407611168, 5.049401038298154454, 113.9572429386477097 ) ) ;
#89040 = CARTESIAN_POINT ( 'NONE',  ( 19.05341960407611168, 5.049401038298154454, 33.95724293864769550 ) ) ;
#89042 = CARTESIAN_POINT ( 'NONE',  ( -0.05219959533937732626, 21.53943276465977519, 32.50109039468568284 ) ) ;
#89043 = CARTESIAN_POINT ( 'NONE',  ( 5.153800228976615827, -19.02544592524334988, 40.20942372801898301 ) ) ;
#89044 = CARTESIAN_POINT ( 'NONE',  ( 16.46253265017160672, -9.564922557960803928, 38.33224293864768839 ) ) ;
#89045 = CARTESIAN_POINT ( 'NONE',  ( 0.05219959533937995610, -21.53943276465977519, 85.00109039468568994 ) ) ;
#89046 = CARTESIAN_POINT ( 'NONE',  ( 17.50000000000000000, -5.500000000000000888, 33.29690382534174375 ) ) ;
#89047 = CARTESIAN_POINT ( 'NONE',  ( 8.224510206698953496, -14.34966873604960469, 22.91557627198102765 ) ) ;
#89048 = CARTESIAN_POINT ( 'NONE',  ( -11.40812507854755609, 35.11059874428196537, -3.524999997268813523 ) ) ;
#89049 = CARTESIAN_POINT ( 'NONE',  ( 15.80617190586746368, 15.72974639402197994, 24.37390960531435979 ) ) ;
#89050 = CARTESIAN_POINT ( 'NONE',  ( 14.29746914071049879, -8.314922557960816363, 98.33224293864769550 ) ) ;
#89052 = CARTESIAN_POINT ( 'NONE',  ( 17.50000000000000000, 5.499999999999995559, 108.7823096230356867 ) ) ;
#89051 = AXIS2_PLACEMENT_3D ( 'NONE', #193982, #132290, #55444 ) ;
#89053 = CARTESIAN_POINT ( 'NONE',  ( 0.05219959533909260263, 19.03943276465977164, 89.99890960531436690 ) ) ;
#89054 = CARTESIAN_POINT ( 'NONE',  ( -4.483927247898539470, -16.52544592524342804, 77.29057627198102409 ) ) ;
#89055 = CARTESIAN_POINT ( 'NONE',  ( -16.46253265017146816, -9.564922557961047289, 109.1677570613523471 ) ) ;
#89056 = CARTESIAN_POINT ( 'NONE',  ( 10.72451020669898902, -18.67979575497178502, 62.91557627198102409 ) ) ;
#89057 = VERTEX_POINT ( 'NONE', #189622 ) ;
#89058 = CARTESIAN_POINT ( 'NONE',  ( -9.474510206698964154, 16.51473224551069663, 30.41557627198102054 ) ) ;
#89060 = CARTESIAN_POINT ( 'NONE',  ( 18.67979575497178502, 10.72451020669898547, 89.16557627198102409 ) ) ;
#89059 = CARTESIAN_POINT ( 'NONE',  ( -19.02544592524342804, 5.153800228976336051, 81.04057627198103830 ) ) ;
#89062 = CARTESIAN_POINT ( 'NONE',  ( -16.51473224551069308, -9.474510206698971260, 86.66557627198102409 ) ) ;
#89061 = CARTESIAN_POINT ( 'NONE',  ( -8.224510206698735004, -14.34966873604973081, 99.58442372801900433 ) ) ;
#89063 = CARTESIAN_POINT ( 'NONE',  ( 13.97604488694548053, -13.89961937509957401, 85.62609039468568994 ) ) ;
#89064 = CARTESIAN_POINT ( 'NONE',  ( 21.52544592524334988, 5.823673210054432836, 91.45942372801901854 ) ) ;
#89065 = CARTESIAN_POINT ( 'NONE',  ( -15.72974639402197994, 15.80617190586746368, 75.62390960531439532 ) ) ;
#89066 = CARTESIAN_POINT ( 'NONE',  ( -21.52544592524343514, 5.823673210054127303, 31.04057627198102409 ) ) ;
#89067 = CARTESIAN_POINT ( 'NONE',  ( -0.05219959533909027116, -19.03943276465977164, 47.49890960531435979 ) ) ;
#89068 = CARTESIAN_POINT ( 'NONE',  ( -16.53943276465976808, -0.05219959533934237506, 113.7510903946856757 ) ) ;
#89069 = CARTESIAN_POINT ( 'NONE',  ( 19.03943276465977164, -0.05219959533909143690, 63.74890960531435979 ) ) ;
#89070 = CARTESIAN_POINT ( 'NONE',  ( 1.500000000000008216, 22.80000000000002913, -65.00100000000003320 ) ) ;
#89071 = CARTESIAN_POINT ( 'NONE',  ( 21.52544592524334988, 5.823673210054432836, 106.4594237280190328 ) ) ;
#89072 = CARTESIAN_POINT ( 'NONE',  ( 8.314922557960818139, 14.29746914071049879, 69.58224293864769550 ) ) ;
#89073 = CARTESIAN_POINT ( 'NONE',  ( -18.62759615963270932, 10.81492255796079327, 105.8322429386476955 ) ) ;
#89074 = CARTESIAN_POINT ( 'NONE',  ( 10.81492255796078972, 18.62759615963270932, 109.5822429386476955 ) ) ;
#89075 = CARTESIAN_POINT ( 'NONE',  ( -5.000000000000000000, -130.0000000000000000, 13.99999999999999822 ) ) ;
#89076 = CARTESIAN_POINT ( 'NONE',  ( 5.719274019375991003, -21.55341960407610458, 57.70724293864770260 ) ) ;
#89077 = CARTESIAN_POINT ( 'NONE',  ( 0.05219959533934541429, -16.53943276465976808, 90.00109039468567573 ) ) ;
#89078 = CARTESIAN_POINT ( 'NONE',  ( 16.53943276465976808, -0.05219959533910856209, 103.7489096053143669 ) ) ;
#89079 = CARTESIAN_POINT ( 'NONE',  ( -13.89961937509977652, 13.97604488694528158, 55.62390960531434558 ) ) ;
#89080 =( LENGTH_UNIT ( ) NAMED_UNIT ( * ) SI_UNIT ( .MILLI., .METRE. ) );
#89081 = CARTESIAN_POINT ( 'NONE',  ( 16.55341960407611168, 4.379528057220329451, 28.95724293864769905 ) ) ;
#89082 = CARTESIAN_POINT ( 'NONE',  ( -10.81492255796105439, 18.62759615963255655, 42.91775706135235424 ) ) ;
#89083 = CARTESIAN_POINT ( 'NONE',  ( 16.51473224551069308, 9.474510206698969483, 104.1655762719810241 ) ) ;
#89084 = CARTESIAN_POINT ( 'NONE',  ( 0.05219959533937995610, -21.53943276465977519, 75.00109039468568994 ) ) ;
#89085 = CARTESIAN_POINT ( 'NONE',  ( -16.46253265017160317, 9.564922557960807481, 30.83224293864769550 ) ) ;
#89086 = CARTESIAN_POINT ( 'NONE',  ( 16.51473224551069308, 9.474510206698969483, 44.16557627198103120 ) ) ;
#89087 = ORIENTED_EDGE ( 'NONE', *, *, #4758, .T. ) ;
#89088 = CARTESIAN_POINT ( 'NONE',  ( -15.80617190586768217, 15.72974639402176855, 78.12609039468570415 ) ) ;
#89089 = CARTESIAN_POINT ( 'NONE',  ( -18.67979575497193778, 10.72451020669871902, 78.33442372801901854 ) ) ;
#89090 = CARTESIAN_POINT ( 'NONE',  ( -13.89961937509977652, 13.97604488694528158, 105.6239096053143527 ) ) ;
#89091 = CARTESIAN_POINT ( 'NONE',  ( 13.89961937509957401, 13.97604488694547697, 76.87609039468566152 ) ) ;
#89092 = CARTESIAN_POINT ( 'NONE',  ( -21.53943276465977519, -0.05219959533937600094, 53.75109039468568994 ) ) ;
#89093 = CARTESIAN_POINT ( 'NONE',  ( -4.379528057220086978, -16.55341960407618274, 19.79275706135235069 ) ) ;
#89094 = VECTOR ( 'NONE', #107316, 1000.000000000000000 ) ;
#89095 = CARTESIAN_POINT ( 'NONE',  ( -16.51473224551082808, 9.474510206698731452, 73.33442372801900433 ) ) ;
#89096 = CARTESIAN_POINT ( 'NONE',  ( 5.049401038298161559, -19.05341960407611168, 52.70724293864767418 ) ) ;
#89097 = CARTESIAN_POINT ( 'NONE',  ( 19.05341960407617918, -5.049401038297876454, 81.04275706135231871 ) ) ;
#89098 = CARTESIAN_POINT ( 'NONE',  ( 14.34966873604960469, 8.224510206698951720, 24.16557627198103120 ) ) ;
#89099 = CARTESIAN_POINT ( 'NONE',  ( 5.153800228976615827, -19.02544592524334988, 95.20942372801897591 ) ) ;
#89100 = CARTESIAN_POINT ( 'NONE',  ( 12.14591786802309770, 12.06949235617756955, 39.37390960531436690 ) ) ;
#89101 = CARTESIAN_POINT ( 'NONE',  ( 16.51473224551083163, -9.474510206698727899, 65.83442372801900433 ) ) ;
#89102 = CARTESIAN_POINT ( 'NONE',  ( 14.29746914071037800, 8.314922557961029526, 51.66775706135234714 ) ) ;
#89103 = CARTESIAN_POINT ( 'NONE',  ( -9.474510206698720793, -16.51473224551083518, 19.58442372801899722 ) ) ;
#89104 = EDGE_CURVE ( 'NONE', #150360, #84987, #22757, .T. ) ;
#89105 = CARTESIAN_POINT ( 'NONE',  ( -19.03943276465977164, 0.05219959533909376836, 41.24890960531435269 ) ) ;
#89106 = CARTESIAN_POINT ( 'NONE',  ( 18.56453257813364033, -5.500000000000045297, 73.49000423690687001 ) ) ;
#89107 = CARTESIAN_POINT ( 'NONE',  ( 16.52544592524335698, 4.483927247898782831, 51.45942372801901854 ) ) ;
#89108 = DIRECTION ( 'NONE',  ( -0.7071067811865466846, 2.468850131082262977E-15, 0.7071067811865484609 ) ) ;
#89109 = CARTESIAN_POINT ( 'NONE',  ( -8.571926809382608425, 26.38167802310805854, 146.4750000027311785 ) ) ;
#89110 = CARTESIAN_POINT ( 'NONE',  ( -0.05219959533909027116, -19.03943276465977164, 97.49890960531436690 ) ) ;
#89111 = DIRECTION ( 'NONE',  ( 0.000000000000000000, 0.000000000000000000, -1.000000000000000000 ) ) ;
#89112 = VERTEX_POINT ( 'NONE', #68247 ) ;
#89113 = CARTESIAN_POINT ( 'NONE',  ( 13.97604488694548053, -13.89961937509957401, 95.62609039468563310 ) ) ;
#89114 = ADVANCED_FACE ( 'NONE', ( #173459 ), #175439, .T. ) ;
#89115 = CARTESIAN_POINT ( 'NONE',  ( -10.81492255796078084, -18.62759615963271287, 22.08224293864769194 ) ) ;
#89117 = CARTESIAN_POINT ( 'NONE',  ( -5.153800228976607833, 19.02544592524334988, 112.7094237280190043 ) ) ;
#89116 = CARTESIAN_POINT ( 'NONE',  ( -0.05219959533937732626, 21.53943276465977519, 107.5010903946856899 ) ) ;
#89118 = CARTESIAN_POINT ( 'NONE',  ( 5.049401038298161559, -19.05341960407611168, 22.70724293864769194 ) ) ;
#89119 = CARTESIAN_POINT ( 'NONE',  ( -9.564922557960796823, -16.46253265017161027, 32.08224293864769550 ) ) ;
#89120 = CARTESIAN_POINT ( 'NONE',  ( -18.62759615963270932, 10.81492255796079327, 55.83224293864770260 ) ) ;
#89121 = CARTESIAN_POINT ( 'NONE',  ( 13.97604488694527802, 13.89961937509977652, 39.37390960531435269 ) ) ;
#89122 = CARTESIAN_POINT ( 'NONE',  ( -27.86473085795038429, -130.0000000000000000, -13.99999999999999822 ) ) ;
#89123 = CARTESIAN_POINT ( 'NONE',  ( -0.05219959533936034679, 19.03943276465977164, 77.50109039468566152 ) ) ;
#89124 = CARTESIAN_POINT ( 'NONE',  ( -4.379528057220328563, 16.55341960407611168, 50.20724293864769550 ) ) ;
#89125 = CARTESIAN_POINT ( 'NONE',  ( 5.823673210054125526, 21.52544592524343514, 29.79057627198102409 ) ) ;
#89126 = CARTESIAN_POINT ( 'NONE',  ( 15.72974639402176855, 15.80617190586768217, 91.87609039468568994 ) ) ;
#89127 = CARTESIAN_POINT ( 'NONE',  ( -0.05219959533907301413, -21.53943276465977519, 87.49890960531436690 ) ) ;
#89128 = CARTESIAN_POINT ( 'NONE',  ( 5.823673210054444382, -21.52544592524334988, 60.20942372801902565 ) ) ;
#89129 = CARTESIAN_POINT ( 'NONE',  ( 5.823673210054444382, -21.52544592524334988, 70.20942372801904696 ) ) ;
#89130 = CARTESIAN_POINT ( 'NONE',  ( 9.474510206698971260, -16.51473224551069308, 92.91557627198103830 ) ) ;
#89132 = CARTESIAN_POINT ( 'NONE',  ( 5.823673210054444382, -21.52544592524334988, 60.20942372801902565 ) ) ;
#89131 = CARTESIAN_POINT ( 'NONE',  ( 4.379528057220092307, 16.55341960407617563, 87.29275706135236135 ) ) ;
#89133 = CARTESIAN_POINT ( 'NONE',  ( 13.89961937509977652, -13.97604488694527269, 58.12390960531436690 ) ) ;
#89134 = CARTESIAN_POINT ( 'NONE',  ( 13.97604488694527802, 13.89961937509977652, 24.37390960531435624 ) ) ;
#89135 = CARTESIAN_POINT ( 'NONE',  ( -16.51473224551069308, -9.474510206698971260, 56.66557627198103120 ) ) ;
#89136 = CARTESIAN_POINT ( 'NONE',  ( 14.29746914071049879, -8.314922557960816363, 63.33224293864770260 ) ) ;
#89137 = CARTESIAN_POINT ( 'NONE',  ( -12.06949235617756955, 12.14591786802309770, 35.62390960531437401 ) ) ;
#89138 = CARTESIAN_POINT ( 'NONE',  ( -10.81492255796078084, -18.62759615963271287, 42.08224293864769550 ) ) ;
#89139 = CARTESIAN_POINT ( 'NONE',  ( 13.89961937509977652, -13.97604488694527269, 53.12390960531434558 ) ) ;
#89140 = CARTESIAN_POINT ( 'NONE',  ( 10.72451020669898902, -18.67979575497178502, 62.91557627198102409 ) ) ;
#89141 = CARTESIAN_POINT ( 'NONE',  ( 5.153800228976615827, -19.02544592524334988, 50.20942372801897591 ) ) ;
#89143 = CARTESIAN_POINT ( 'NONE',  ( -16.55341960407611168, -4.379528057220339221, 56.45724293864768839 ) ) ;
#89142 = CARTESIAN_POINT ( 'NONE',  ( 0.000000000000000000, -105.0000000000000000, 12.00000000000000355 ) ) ;
#89144 = CARTESIAN_POINT ( 'NONE',  ( 5.823673210054125526, 21.52544592524343514, 44.79057627198103120 ) ) ;
#89145 = ORIENTED_EDGE ( 'NONE', *, *, #76779, .F. ) ;
#89146 = ORIENTED_EDGE ( 'NONE', *, *, #25866, .T. ) ;
#89147 = CARTESIAN_POINT ( 'NONE',  ( -20.43538597629128262, 20.43538597629122222, -65.00100000000003320 ) ) ;
#89148 = CARTESIAN_POINT ( 'NONE',  ( -8.224510206698735004, -14.34966873604973081, 89.58442372801901854 ) ) ;
#89149 = CARTESIAN_POINT ( 'NONE',  ( 19.05341960407617918, -5.049401038297876454, 71.04275706135234714 ) ) ;
#89150 = CARTESIAN_POINT ( 'NONE',  ( -16.52544592524342804, 4.483927247898546575, 56.04057627198102409 ) ) ;
#89151 = CARTESIAN_POINT ( 'NONE',  ( -19.49190055781009789, -5.500000000000056843, 60.56116087098778422 ) ) ;
#89152 = CARTESIAN_POINT ( 'NONE',  ( -4.379528057220328563, 16.55341960407611168, 35.20724293864768839 ) ) ;
#89153 = CARTESIAN_POINT ( 'NONE',  ( 13.89961937509977652, -13.97604488694527269, 48.12390960531435979 ) ) ;
#89154 = CARTESIAN_POINT ( 'NONE',  ( 19.03943276465977164, -0.05219959533909143690, 68.74890960531436690 ) ) ;
#89155 = CARTESIAN_POINT ( 'NONE',  ( -16.46253265017160317, 9.564922557960807481, 40.83224293864769550 ) ) ;
#89156 = CARTESIAN_POINT ( 'NONE',  ( 15.72974639402176855, 15.80617190586768217, 51.87609039468568284 ) ) ;
#89157 = CARTESIAN_POINT ( 'NONE',  ( 9.474510206698971260, -16.51473224551069308, 77.91557627198103830 ) ) ;
#89158 = CARTESIAN_POINT ( 'NONE',  ( -0.05219959533909027116, -19.03943276465977164, 27.49890960531435624 ) ) ;
#89159 = CARTESIAN_POINT ( 'NONE',  ( -13.97604488694527625, -13.89961937509977652, 61.87390960531435979 ) ) ;
#89160 = CARTESIAN_POINT ( 'NONE',  ( -15.80617190586745835, -15.72974639402198527, 46.87390960531435979 ) ) ;
#89161 = CARTESIAN_POINT ( 'NONE',  ( 13.97604488694527802, 13.89961937509977652, 34.37390960531436690 ) ) ;
#89162 = CARTESIAN_POINT ( 'NONE',  ( -5.823673210054116645, -21.52544592524344225, 47.29057627198103120 ) ) ;
#89163 = CARTESIAN_POINT ( 'NONE',  ( -4.379528057220086978, -16.55341960407618274, 104.7927570613523898 ) ) ;
#89164 = CARTESIAN_POINT ( 'NONE',  ( 19.05341960407617918, -5.049401038297876454, 26.04275706135233293 ) ) ;
#89166 = CARTESIAN_POINT ( 'NONE',  ( 12.06949235617739724, 12.14591786802326823, 86.87609039468568994 ) ) ;
#89165 = CARTESIAN_POINT ( 'NONE',  ( -8.224510206698735004, -14.34966873604973081, 49.58442372801901143 ) ) ;
#89167 = CARTESIAN_POINT ( 'NONE',  ( -9.687362902255793884, -9.687362902255632235, -62.58071313852362039 ) ) ;
#89168 = CARTESIAN_POINT ( 'NONE',  ( -4.483927247898782831, 16.52544592524335698, 62.70942372801902565 ) ) ;
#89169 = CARTESIAN_POINT ( 'NONE',  ( 14.29746914071037800, 8.314922557961029526, 46.66775706135234714 ) ) ;
#89170 = CARTESIAN_POINT ( 'NONE',  ( -16.51473224551069308, -9.474510206698971260, 101.6655762719810241 ) ) ;
#89171 = CARTESIAN_POINT ( 'NONE',  ( 0.05219959533934541429, -16.53943276465976808, 30.00109039468568284 ) ) ;
#89172 = CARTESIAN_POINT ( 'NONE',  ( 13.97604488694527802, 13.89961937509977652, 39.37390960531435269 ) ) ;
#89173 = CARTESIAN_POINT ( 'NONE',  ( -18.67979575497193778, 10.72451020669871902, 28.33442372801902209 ) ) ;
#89174 = CARTESIAN_POINT ( 'NONE',  ( -12.14591786802326823, 12.06949235617739902, 38.12609039468567573 ) ) ;
#89175 = CARTESIAN_POINT ( 'NONE',  ( -16.52544592524335698, -4.483927247898792601, 98.95942372801903275 ) ) ;
#89176 = FACE_OUTER_BOUND ( 'NONE', #107455, .T. ) ;
#89177 = CARTESIAN_POINT ( 'NONE',  ( -18.62759615963255300, -10.81492255796106328, 99.16775706135234714 ) ) ;
#89178 = CARTESIAN_POINT ( 'NONE',  ( 16.46253265017146816, 9.564922557961045513, 101.6677570613523329 ) ) ;
#89179 = CARTESIAN_POINT ( 'NONE',  ( -4.379528057220328563, 16.55341960407611168, 55.20724293864770260 ) ) ;
#89180 = CARTESIAN_POINT ( 'NONE',  ( -13.89961937509977652, 13.97604488694528158, 30.62390960531435269 ) ) ;
#89182 = CARTESIAN_POINT ( 'NONE',  ( 23.48529157249600630, -32.32473071737748427, -3.049999994537627046 ) ) ;
#89181 = CARTESIAN_POINT ( 'NONE',  ( 5.153800228976615827, -19.02544592524334988, 65.20942372801900433 ) ) ;
#89183 = CARTESIAN_POINT ( 'NONE',  ( 5.719274019375673035, 21.55341960407619339, 52.29275706135236135 ) ) ;
#89184 = CARTESIAN_POINT ( 'NONE',  ( -4.379528057220086978, -16.55341960407618274, 24.79275706135235779 ) ) ;
#89185 = CARTESIAN_POINT ( 'NONE',  ( 17.48853670773247515, 5.747243402303061188, 83.83328700250011423 ) ) ;
#89186 = CARTESIAN_POINT ( 'NONE',  ( 18.67979575497178502, 10.72451020669898547, 29.16557627198103120 ) ) ;
#89187 = CARTESIAN_POINT ( 'NONE',  ( 5.719274019375991003, -21.55341960407610458, 67.70724293864769550 ) ) ;
#89188 = CARTESIAN_POINT ( 'NONE',  ( -14.29746914071037622, -8.314922557961029526, 19.16775706135234714 ) ) ;
#89189 = CARTESIAN_POINT ( 'NONE',  ( 13.89961937509977652, -13.97604488694527269, 103.1239096053143527 ) ) ;
#89190 = CARTESIAN_POINT ( 'NONE',  ( 5.049401038298161559, -19.05341960407611168, 22.70724293864769194 ) ) ;
#89191 = CARTESIAN_POINT ( 'NONE',  ( -21.53943276465977519, -0.05219959533937600094, 113.7510903946856757 ) ) ;
#89192 = CARTESIAN_POINT ( 'NONE',  ( 13.97604488694527802, 13.89961937509977652, 44.37390960531435269 ) ) ;
#89193 = VECTOR ( 'NONE', #17635, 1000.000000000000000 ) ;
#89194 = CARTESIAN_POINT ( 'NONE',  ( -18.62759615963255300, -10.81492255796106328, 49.16775706135234003 ) ) ;
#89195 = CARTESIAN_POINT ( 'NONE',  ( 21.55341960407619695, -5.719274019375665929, 91.04275706135236135 ) ) ;
#89196 = CARTESIAN_POINT ( 'NONE',  ( 12.06949235617739724, 12.14591786802326823, 101.8760903946857042 ) ) ;
#89197 = CARTESIAN_POINT ( 'NONE',  ( -19.05341960407611168, -5.049401038298163336, 76.45724293864769550 ) ) ;
#89198 = CARTESIAN_POINT ( 'NONE',  ( 21.52544592524334988, 5.823673210054432836, 46.45942372801901854 ) ) ;
#89199 = CARTESIAN_POINT ( 'NONE',  ( 0.05219959533937995610, -21.53943276465977519, 40.00109039468567573 ) ) ;
#89201 = CARTESIAN_POINT ( 'NONE',  ( 19.02544592524343514, -5.153800228976328945, 93.54057627198102409 ) ) ;
#89200 = CARTESIAN_POINT ( 'NONE',  ( -19.05341960407617563, 5.049401038297882671, 73.54275706135233293 ) ) ;
#89202 = CARTESIAN_POINT ( 'NONE',  ( 16.53943276465976808, -0.05219959533910856209, 108.7489096053143669 ) ) ;
#89203 = CARTESIAN_POINT ( 'NONE',  ( -10.81492255796078084, -18.62759615963271287, 102.0822429386476955 ) ) ;
#89204 = CARTESIAN_POINT ( 'NONE',  ( -16.52544592524342804, 4.483927247898546575, 71.04057627198103830 ) ) ;
#89205 = CARTESIAN_POINT ( 'NONE',  ( 21.53943276465977519, 0.05219959533937863772, 111.2510903946856899 ) ) ;
#89206 = CARTESIAN_POINT ( 'NONE',  ( -16.53943276465976808, 0.05219959533911058130, 101.2489096053143669 ) ) ;
#89207 = CARTESIAN_POINT ( 'NONE',  ( 16.51473224551069308, 9.474510206698969483, 49.16557627198102409 ) ) ;
#89208 = CARTESIAN_POINT ( 'NONE',  ( 19.03943276465977164, 0.05219959533936151252, 91.25109039468566152 ) ) ;
#89209 = CARTESIAN_POINT ( 'NONE',  ( 14.34966873604960469, 8.224510206698951720, 54.16557627198103120 ) ) ;
#89210 = CARTESIAN_POINT ( 'NONE',  ( -21.55341960407619339, 5.719274019375674811, 103.5427570613523613 ) ) ;
#89211 = CARTESIAN_POINT ( 'NONE',  ( -19.05341960407611168, -5.049401038298163336, 101.4572429386476955 ) ) ;
#89212 = CARTESIAN_POINT ( 'NONE',  ( -16.46253265017146816, -9.564922557961047289, 69.16775706135233293 ) ) ;
#89213 = CARTESIAN_POINT ( 'NONE',  ( -21.55341960407610458, -5.719274019375992779, 76.45724293864769550 ) ) ;
#89214 = CARTESIAN_POINT ( 'NONE',  ( 18.67979575497194134, -10.72451020669871369, 30.83442372801902209 ) ) ;
#89215 = CARTESIAN_POINT ( 'NONE',  ( -12.06949235617739369, -12.14591786802326823, 24.37609039468567573 ) ) ;
#89216 = CARTESIAN_POINT ( 'NONE',  ( 8.224510206698742110, 14.34966873604972548, 92.08442372801901854 ) ) ;
#89218 = CARTESIAN_POINT ( 'NONE',  ( -5.719274019375665041, -21.55341960407619695, 29.79275706135234358 ) ) ;
#89217 = CARTESIAN_POINT ( 'NONE',  ( 17.05587630539785238, 6.762274262135715475, 61.75819690962688924 ) ) ;
#89219 = CARTESIAN_POINT ( 'NONE',  ( -4.379528057220328563, 16.55341960407611168, 110.2072429386477239 ) ) ;
#89220 = CARTESIAN_POINT ( 'NONE',  ( -38.00000000000001421, 12.34694845685046438, -9.849999994537625980 ) ) ;
#89221 = CARTESIAN_POINT ( 'NONE',  ( -4.483927247898782831, 16.52544592524335698, 62.70942372801902565 ) ) ;
#89222 = CARTESIAN_POINT ( 'NONE',  ( -12.06949235617756955, 12.14591786802309770, 80.62390960531438111 ) ) ;
#89223 = CARTESIAN_POINT ( 'NONE',  ( 5.823673210054125526, 21.52544592524343514, 74.79057627198105251 ) ) ;
#89224 = CARTESIAN_POINT ( 'NONE',  ( 8.224510206698953496, -14.34966873604960469, 22.91557627198102765 ) ) ;
#89225 = CARTESIAN_POINT ( 'NONE',  ( 8.224510206698742110, 14.34966873604972548, 47.08442372801901854 ) ) ;
#89226 = CARTESIAN_POINT ( 'NONE',  ( 16.51473224551069308, 9.474510206698969483, 49.16557627198102409 ) ) ;
#89227 = CARTESIAN_POINT ( 'NONE',  ( -16.53943276465976808, -0.05219959533934237506, 98.75109039468568994 ) ) ;
#89228 = CARTESIAN_POINT ( 'NONE',  ( -13.97604488694547697, 13.89961937509957934, 88.12609039468563310 ) ) ;
#89229 = CARTESIAN_POINT ( 'NONE',  ( 10.81492255796078972, 18.62759615963270932, 89.58224293864768129 ) ) ;
#89230 = CARTESIAN_POINT ( 'NONE',  ( 16.55341960407611168, 4.379528057220329451, 23.95724293864769550 ) ) ;
#89231 = ORIENTED_EDGE ( 'NONE', *, *, #114658, .F. ) ;
#89232 = CARTESIAN_POINT ( 'NONE',  ( 26.26139018963107574, 3.005588016160658071, 174.9127113745526572 ) ) ;
#89233 = CARTESIAN_POINT ( 'NONE',  ( -0.05219959533907301413, -21.53943276465977519, 62.49890960531436690 ) ) ;
#89234 = ORIENTED_EDGE ( 'NONE', *, *, #94263, .T. ) ;
#89235 = CARTESIAN_POINT ( 'NONE',  ( 4.379528057220092307, 16.55341960407617563, 87.29275706135236135 ) ) ;
#89236 = VERTEX_POINT ( 'NONE', #34931 ) ;
#89237 = CARTESIAN_POINT ( 'NONE',  ( 10.81492255796078972, 18.62759615963270932, 29.58224293864769905 ) ) ;
#89238 = CARTESIAN_POINT ( 'NONE',  ( -19.01533133064924641, 5.499999999999450218, 73.76586590595742621 ) ) ;
#89239 = CARTESIAN_POINT ( 'NONE',  ( 5.823673210054125526, 21.52544592524343514, 79.79057627198102409 ) ) ;
#89240 = AXIS2_PLACEMENT_3D ( 'NONE', #69655, #67652, #6966 ) ;
#89241 = CARTESIAN_POINT ( 'NONE',  ( -12.14591786802309592, -12.06949235617757132, 26.87390960531435979 ) ) ;
#89242 = CARTESIAN_POINT ( 'NONE',  ( -14.29746914071037622, -8.314922557961029526, 19.16775706135234714 ) ) ;
#89243 = CARTESIAN_POINT ( 'NONE',  ( 16.46253265017160672, -9.564922557960803928, 33.33224293864770260 ) ) ;
#89244 = CARTESIAN_POINT ( 'NONE',  ( -12.06949235617739369, -12.14591786802326823, 34.37609039468568284 ) ) ;
#89245 = AXIS2_PLACEMENT_3D ( 'NONE', #43805, #62925, #186300 ) ;
#89246 = CARTESIAN_POINT ( 'NONE',  ( -16.46253265017160317, 9.564922557960807481, 50.83224293864770260 ) ) ;
#89247 = CARTESIAN_POINT ( 'NONE',  ( -17.81289503416611097, -24.51734667627696496, 148.2999999999999545 ) ) ;
#89248 = CARTESIAN_POINT ( 'NONE',  ( -5.049401038298153566, 19.05341960407611168, 110.2072429386476671 ) ) ;
#89249 = CARTESIAN_POINT ( 'NONE',  ( 9.474510206698971260, -16.51473224551069308, 102.9155762719810241 ) ) ;
#89250 = CARTESIAN_POINT ( 'NONE',  ( -8.224510206698735004, -14.34966873604973081, 94.58442372801901854 ) ) ;
#89251 = CARTESIAN_POINT ( 'NONE',  ( -16.46253265017146816, -9.564922557961047289, 89.16775706135234714 ) ) ;
#89252 = CARTESIAN_POINT ( 'NONE',  ( -0.05219959533936034679, 19.03943276465977164, 32.50109039468566863 ) ) ;
#89253 = CARTESIAN_POINT ( 'NONE',  ( 5.823673210054125526, 21.52544592524343514, 69.79057627198102409 ) ) ;
#89254 = CARTESIAN_POINT ( 'NONE',  ( 4.379528057220092307, 16.55341960407617563, 97.29275706135234714 ) ) ;
#89255 = CARTESIAN_POINT ( 'NONE',  ( -5.823673210054116645, -21.52544592524344225, 32.29057627198102409 ) ) ;
#89256 = CARTESIAN_POINT ( 'NONE',  ( -16.51473224551082808, 9.474510206698731452, 93.33442372801900433 ) ) ;
#89257 = CARTESIAN_POINT ( 'NONE',  ( 5.049401038298161559, -19.05341960407611168, 47.70724293864770260 ) ) ;
#89258 = CARTESIAN_POINT ( 'NONE',  ( -9.564922557960796823, -16.46253265017161027, 87.08224293864769550 ) ) ;
#89259 = CARTESIAN_POINT ( 'NONE',  ( -10.81492255796105439, 18.62759615963255655, 62.91775706135236135 ) ) ;
#89260 = CARTESIAN_POINT ( 'NONE',  ( 9.564922557960805705, 16.46253265017160317, 64.58224293864769550 ) ) ;
#89261 = CARTESIAN_POINT ( 'NONE',  ( 14.34966873604960469, 8.224510206698951720, 104.1655762719810241 ) ) ;
#89262 = CARTESIAN_POINT ( 'NONE',  ( 23.35043118190389677, -14.19381810411683809, 169.8796877288295093 ) ) ;
#89263 = CARTESIAN_POINT ( 'NONE',  ( -8.314922557960811034, -14.29746914071050412, 77.08224293864769550 ) ) ;
#89264 = CARTESIAN_POINT ( 'NONE',  ( -21.52544592524343514, 5.823673210054127303, 71.04057627198103830 ) ) ;
#89265 = CARTESIAN_POINT ( 'NONE',  ( -5.153800228976607833, 19.02544592524334988, 92.70942372801901854 ) ) ;
#89266 =( BOUNDED_CURVE ( )  B_SPLINE_CURVE ( 2, ( #186859, #167692, #75662, #47334, #94810, #90823, #1806, #171663, #60488, #2802, #122163 ),
 .UNSPECIFIED., .F., .F. ) 
 B_SPLINE_CURVE_WITH_KNOTS ( ( 3, 2, 2, 2, 2, 3 ),
 ( 0.5000000000000004441, 0.5200000000000004619, 0.5400000000000004796, 0.5600000000000006084, 0.5800000000000006262, 0.6000000000000005329 ),
 .UNSPECIFIED. ) 
 CURVE ( )  GEOMETRIC_REPRESENTATION_ITEM ( )  RATIONAL_B_SPLINE_CURVE ( ( 0.9999999999999988898, 0.9510565162951546414, 1.000000000000000000, 0.9510565162951535312, 1.000000000000000000, 0.9510565162951535312, 1.000000000000000000, 0.9510565162951535312, 1.000000000000000000, 0.9510565162951521989, 1.000000000000001332 ) ) 
 REPRESENTATION_ITEM ( '' )  );
#89267 = CARTESIAN_POINT ( 'NONE',  ( 18.22780087662122384, 5.500000000000018652, 93.98459894673892734 ) ) ;
#89268 = CARTESIAN_POINT ( 'NONE',  ( 5.049401038298161559, -19.05341960407611168, 62.70724293864769550 ) ) ;
#89269 = CARTESIAN_POINT ( 'NONE',  ( 31.72709406046299208, -0.4963711039037253525, 102.5000000000000284 ) ) ;
#89271 = CARTESIAN_POINT ( 'NONE',  ( 0.05219959533909260263, 19.03943276465977164, 84.99890960531436690 ) ) ;
#89270 = CARTESIAN_POINT ( 'NONE',  ( -9.564922557960796823, -16.46253265017161027, 82.08224293864768129 ) ) ;
#89272 = EDGE_CURVE ( 'NONE', #192686, #142224, #58294, .T. ) ;
#89273 = CARTESIAN_POINT ( 'NONE',  ( -16.55341960407617563, 4.379528057220093196, 68.54275706135234714 ) ) ;
#89274 = CARTESIAN_POINT ( 'NONE',  ( -17.26058549869088665, -6.457015423128631859, 51.37745837476068544 ) ) ;
#89275 = CARTESIAN_POINT ( 'NONE',  ( -19.03943276465977164, -0.05219959533935918106, 48.75109039468566863 ) ) ;
#89276 = CARTESIAN_POINT ( 'NONE',  ( 36.88729982035407318, 1.776435236410516039, 50.21758054017369233 ) ) ;
#89277 = CARTESIAN_POINT ( 'NONE',  ( -13.89961937509977652, 13.97604488694528158, 115.6239096053143669 ) ) ;
#89278 = CARTESIAN_POINT ( 'NONE',  ( -4.483927247898782831, 16.52544592524335698, 97.70942372801904696 ) ) ;
#89279 = CARTESIAN_POINT ( 'NONE',  ( -1.374935097489159874, -23.51385019162033174, -54.82293943248599533 ) ) ;
#89280 = CARTESIAN_POINT ( 'NONE',  ( 12.06949235617739724, 12.14591786802326823, 81.87609039468568994 ) ) ;
#89281 = CARTESIAN_POINT ( 'NONE',  ( -4.999999999999999112, -140.0000000000000000, -12.99999999999999645 ) ) ;
#89282 = CARTESIAN_POINT ( 'NONE',  ( -4.379528057220086978, -16.55341960407618274, 49.79275706135234714 ) ) ;
#89283 = CARTESIAN_POINT ( 'NONE',  ( 10.72451020669871369, 18.67979575497193778, 72.08442372801899012 ) ) ;
#89284 = CARTESIAN_POINT ( 'NONE',  ( 19.05341960407617918, -5.049401038297876454, 71.04275706135234714 ) ) ;
#89285 = CARTESIAN_POINT ( 'NONE',  ( 13.89961937509957401, 13.97604488694547697, 31.87609039468566863 ) ) ;
#89286 = CARTESIAN_POINT ( 'NONE',  ( -13.97604488694527625, -13.89961937509977652, 61.87390960531435979 ) ) ;
#89287 = CARTESIAN_POINT ( 'NONE',  ( 9.474510206698971260, -16.51473224551069308, 47.91557627198102409 ) ) ;
#89288 = DIRECTION ( 'NONE',  ( 0.000000000000000000, 0.000000000000000000, -1.000000000000000000 ) ) ;
#89289 = CARTESIAN_POINT ( 'NONE',  ( -10.72451020669898014, 18.67979575497178502, 65.41557627198102409 ) ) ;
#89290 = CARTESIAN_POINT ( 'NONE',  ( 21.55341960407610458, 5.719274019375980345, 38.95724293864768839 ) ) ;
#89291 = CARTESIAN_POINT ( 'NONE',  ( -4.379528057220328563, 16.55341960407611168, 115.2072429386476955 ) ) ;
#89292 = CARTESIAN_POINT ( 'NONE',  ( 16.52544592524335698, 4.483927247898782831, 46.45942372801901854 ) ) ;
#89293 = EDGE_CURVE ( 'NONE', #9747, #58678, #148648, .T. ) ;
#89294 = ORIENTED_EDGE ( 'NONE', *, *, #57363, .T. ) ;
#89295 = CARTESIAN_POINT ( 'NONE',  ( -0.05219959533937732626, 21.53943276465977519, 32.50109039468568284 ) ) ;
#89297 = CARTESIAN_POINT ( 'NONE',  ( 11.74264578624799427, 36.14014761921585972, -4.599999999999999645 ) ) ;
#89296 = CARTESIAN_POINT ( 'NONE',  ( -8.224510206698948167, 14.34966873604960824, 55.41557627198102409 ) ) ;
#89298 = CARTESIAN_POINT ( 'NONE',  ( -16.55341960407617563, 4.379528057220093196, 28.54275706135234358 ) ) ;
#89299 = CARTESIAN_POINT ( 'NONE',  ( 19.02544592524334988, 5.153800228976608722, 46.45942372801899012 ) ) ;
#89300 = CARTESIAN_POINT ( 'NONE',  ( 8.314922557960818139, 14.29746914071049879, 49.58224293864769550 ) ) ;
#89301 = CARTESIAN_POINT ( 'NONE',  ( -5.719274019375978568, 21.55341960407610458, 115.2072429386476955 ) ) ;
#89303 = CARTESIAN_POINT ( 'NONE',  ( -0.05219959533907301413, -21.53943276465977519, 77.49890960531433848 ) ) ;
#89302 = CARTESIAN_POINT ( 'NONE',  ( 1.429357700123697894, 15.66473995800721575, -59.59166688515647792 ) ) ;
#89304 = CARTESIAN_POINT ( 'NONE',  ( -9.474510206698964154, 16.51473224551069663, 95.41557627198102409 ) ) ;
#89305 = CARTESIAN_POINT ( 'NONE',  ( -4.379528057220328563, 16.55341960407611168, 60.20724293864768839 ) ) ;
#89306 = CARTESIAN_POINT ( 'NONE',  ( -0.05219959533909027116, -19.03943276465977164, 107.4989096053143527 ) ) ;
#89307 = CARTESIAN_POINT ( 'NONE',  ( 22.81625015709509441, 31.40387420917330275, -7.324999997268812457 ) ) ;
#89308 = CARTESIAN_POINT ( 'NONE',  ( 13.97604488694548053, -13.89961937509957401, 70.62609039468567573 ) ) ;
#89309 = CARTESIAN_POINT ( 'NONE',  ( 5.823673210054125526, 21.52544592524343514, 104.7905762719810241 ) ) ;
#89310 = CARTESIAN_POINT ( 'NONE',  ( -13.97604488694527625, -13.89961937509977652, 56.87390960531434558 ) ) ;
#89311 = CARTESIAN_POINT ( 'NONE',  ( -14.34966873604960291, -8.224510206698953496, 111.6655762719810525 ) ) ;
#89312 = CARTESIAN_POINT ( 'NONE',  ( 0.05219959533937995610, -21.53943276465977519, 50.00109039468568994 ) ) ;
#89313 = CARTESIAN_POINT ( 'NONE',  ( 8.571926809382597767, 26.38167802310806209, 144.2750000027311899 ) ) ;
#89314 = CARTESIAN_POINT ( 'NONE',  ( 8.224510206698953496, -14.34966873604960469, 42.91557627198103120 ) ) ;
#89315 = CARTESIAN_POINT ( 'NONE',  ( 16.51473224551069308, 9.474510206698969483, 44.16557627198103120 ) ) ;
#89316 = CARTESIAN_POINT ( 'NONE',  ( 13.89961937509977652, -13.97604488694527269, 98.12390960531433848 ) ) ;
#89317 = CARTESIAN_POINT ( 'NONE',  ( 10.81492255796078972, 18.62759615963270932, 74.58224293864768129 ) ) ;
#89318 = CARTESIAN_POINT ( 'NONE',  ( -17.14385361876520619, 23.59649016807275856, 144.5750000027312012 ) ) ;
#89319 = CARTESIAN_POINT ( 'NONE',  ( -19.02544592524342804, 5.153800228976336051, 41.04057627198103120 ) ) ;
#89320 = ORIENTED_EDGE ( 'NONE', *, *, #163734, .F. ) ;
#89321 = CARTESIAN_POINT ( 'NONE',  ( 15.80617190586746368, 15.72974639402197994, 64.37390960531435269 ) ) ;
#89322 = CARTESIAN_POINT ( 'NONE',  ( -5.823673210054431948, 21.52544592524334988, 82.70942372801900433 ) ) ;
#89325 = CARTESIAN_POINT ( 'NONE',  ( -8.314922557960811034, -14.29746914071050412, 87.08224293864769550 ) ) ;
#89324 = CARTESIAN_POINT ( 'NONE',  ( -12.06949235617739369, -12.14591786802326823, 84.37609039468570415 ) ) ;
#89323 = CARTESIAN_POINT ( 'NONE',  ( 15.50000000000000178, 5.499999999999998224, 118.0000000000000142 ) ) ;
#89326 = CARTESIAN_POINT ( 'NONE',  ( -16.46253265017160317, 9.564922557960807481, 65.83224293864769550 ) ) ;
#89327 = ORIENTED_EDGE ( 'NONE', *, *, #141481, .F. ) ;
#89328 = CARTESIAN_POINT ( 'NONE',  ( 5.153800228976615827, -19.02544592524334988, 20.20942372801899722 ) ) ;
#89329 = CARTESIAN_POINT ( 'NONE',  ( -4.379528057220086978, -16.55341960407618274, 89.79275706135236135 ) ) ;
#89330 = CARTESIAN_POINT ( 'NONE',  ( 18.62759615963255655, 10.81492255796105972, 106.6677570613523756 ) ) ;
#89331 = CARTESIAN_POINT ( 'NONE',  ( 16.46253265017160672, -9.564922557960803928, 88.33224293864769550 ) ) ;
#89332 = CARTESIAN_POINT ( 'NONE',  ( 10.81492255796078972, 18.62759615963270932, 49.58224293864769550 ) ) ;
#89333 = CARTESIAN_POINT ( 'NONE',  ( 5.719274019375673035, 21.55341960407619339, 97.29275706135234714 ) ) ;
#89334 = CARTESIAN_POINT ( 'NONE',  ( 12.06949235617739724, 12.14591786802326823, 56.87609039468568994 ) ) ;
#89335 = CARTESIAN_POINT ( 'NONE',  ( -5.719274019375665041, -21.55341960407619695, 19.79275706135235069 ) ) ;
#89336 = CARTESIAN_POINT ( 'NONE',  ( -19.05341960407617563, 5.049401038297882671, 108.5427570613523187 ) ) ;
#89337 = CARTESIAN_POINT ( 'NONE',  ( -5.049401038298153566, 19.05341960407611168, 90.20724293864766707 ) ) ;
#89338 = CARTESIAN_POINT ( 'NONE',  ( -16.53943276465976808, -0.05219959533934237506, 33.75109039468568284 ) ) ;
#89339 = CARTESIAN_POINT ( 'NONE',  ( 5.049401038298161559, -19.05341960407611168, 57.70724293864769550 ) ) ;
#89340 = AXIS2_PLACEMENT_3D ( 'NONE', #2889, #21039, #186944 ) ;
#89341 = CARTESIAN_POINT ( 'NONE',  ( -4.379528057220086978, -16.55341960407618274, 39.79275706135235424 ) ) ;
#89342 = CARTESIAN_POINT ( 'NONE',  ( -0.05219959533910754901, -16.53943276465976808, 82.49890960531436690 ) ) ;
#89343 = CARTESIAN_POINT ( 'NONE',  ( 8.314922557961029526, -14.29746914071037800, 85.41775706135236135 ) ) ;
#89344 = EDGE_CURVE ( 'NONE', #72946, #56681, #171294, .T. ) ;
#89346 = CARTESIAN_POINT ( 'NONE',  ( -5.153800228976328057, -19.02544592524343514, 62.29057627198100988 ) ) ;
#89345 = CARTESIAN_POINT ( 'NONE',  ( 21.55341960407619695, -5.719274019375665929, 41.04275706135236135 ) ) ;
#89347 = CARTESIAN_POINT ( 'NONE',  ( 5.153800228976335163, 19.02544592524342804, 79.79057627198102409 ) ) ;
#89348 = CARTESIAN_POINT ( 'NONE',  ( 12.06949235617757843, -12.14591786802309237, 28.12390960531435979 ) ) ;
#89349 = CARTESIAN_POINT ( 'NONE',  ( 14.29746914071037800, 8.314922557961029526, 86.66775706135234714 ) ) ;
#89350 = DIRECTION ( 'NONE',  ( 1.000000000000000000, 0.000000000000000000, 0.000000000000000000 ) ) ;
#89351 = ORIENTED_EDGE ( 'NONE', *, *, #6212, .F. ) ;
#89352 = CARTESIAN_POINT ( 'NONE',  ( -9.474510206698720793, -16.51473224551083518, 24.58442372801900078 ) ) ;
#89353 = CARTESIAN_POINT ( 'NONE',  ( 0.05219959533909260263, 19.03943276465977164, 104.9989096053143669 ) ) ;
#89354 = CARTESIAN_POINT ( 'NONE',  ( -13.97604488694527625, -13.89961937509977652, 51.87390960531436690 ) ) ;
#89355 = CARTESIAN_POINT ( 'NONE',  ( 0.2065856650645460646, 13.70000000000002061, -62.58071313852362039 ) ) ;
#89356 = CARTESIAN_POINT ( 'NONE',  ( 0.05219959533934541429, -16.53943276465976808, 40.00109039468567573 ) ) ;
#89358 = CARTESIAN_POINT ( 'NONE',  ( 14.34966873604972726, -8.224510206698740333, 50.83442372801901143 ) ) ;
#89357 = CARTESIAN_POINT ( 'NONE',  ( -5.049401038297874678, -19.05341960407617918, 64.79275706135233293 ) ) ;
#89359 = CARTESIAN_POINT ( 'NONE',  ( 5.379963195099918494, -3.845052905827775369, -64.45073299057952454 ) ) ;
#89360 = CARTESIAN_POINT ( 'NONE',  ( -0.05219959533909027116, -19.03943276465977164, 72.49890960531435269 ) ) ;
#89361 = CARTESIAN_POINT ( 'NONE',  ( 10.81492255796078972, 18.62759615963270932, 114.5822429386477097 ) ) ;
#89362 = CARTESIAN_POINT ( 'NONE',  ( -5.153800228976607833, 19.02544592524334988, 62.70942372801899722 ) ) ;
#89364 = FACE_OUTER_BOUND ( 'NONE', #92070, .T. ) ;
#89363 = CARTESIAN_POINT ( 'NONE',  ( 13.97604488694527802, 13.89961937509977652, 109.3739096053143669 ) ) ;
#89365 = CARTESIAN_POINT ( 'NONE',  ( -0.05219959533909027116, -19.03943276465977164, 72.49890960531435269 ) ) ;
#89367 = CARTESIAN_POINT ( 'NONE',  ( 37.99999999999999289, 2.428612866367529932E-14, -25.00000000000000000 ) ) ;
#89366 = CARTESIAN_POINT ( 'NONE',  ( -4.379528057220328563, 16.55341960407611168, 35.20724293864768839 ) ) ;
#89368 = CARTESIAN_POINT ( 'NONE',  ( -13.97604488694547697, 13.89961937509957934, 33.12609039468566863 ) ) ;
#89369 = CARTESIAN_POINT ( 'NONE',  ( -0.05219959533910754901, -16.53943276465976808, 72.49890960531435269 ) ) ;
#89370 = CARTESIAN_POINT ( 'NONE',  ( -15.80617190586768217, 15.72974639402176855, 113.1260903946856899 ) ) ;
#89371 = CARTESIAN_POINT ( 'NONE',  ( -16.51473224551069308, -9.474510206698971260, 41.66557627198103120 ) ) ;
#89373 = CARTESIAN_POINT ( 'NONE',  ( -21.52544592524334988, -5.823673210054445271, 103.9594237280190185 ) ) ;
#89372 = CARTESIAN_POINT ( 'NONE',  ( 14.34966873604960469, 8.224510206698951720, 44.16557627198103120 ) ) ;
#89374 = CARTESIAN_POINT ( 'NONE',  ( 5.049401038298161559, -19.05341960407611168, 87.70724293864769550 ) ) ;
#89375 = CARTESIAN_POINT ( 'NONE',  ( 19.02544592524343514, -5.153800228976328945, 108.5405762719810383 ) ) ;
#89376 = CARTESIAN_POINT ( 'NONE',  ( 0.05219959533909260263, 19.03943276465977164, 44.99890960531435979 ) ) ;
#89377 = CARTESIAN_POINT ( 'NONE',  ( 4.483927247898545687, 16.52544592524342804, 109.7905762719810383 ) ) ;
#89378 = CARTESIAN_POINT ( 'NONE',  ( 12.14591786802309770, 12.06949235617756955, 79.37390960531436690 ) ) ;
#89379 = CARTESIAN_POINT ( 'NONE',  ( 10.81492255796078972, 18.62759615963270932, 89.58224293864768129 ) ) ;
#89380 = CARTESIAN_POINT ( 'NONE',  ( 5.049401038298161559, -19.05341960407611168, 82.70724293864770971 ) ) ;
#89381 = CARTESIAN_POINT ( 'NONE',  ( 21.52544592524344225, -5.823673210054117533, 103.5405762719810383 ) ) ;
#89382 = CARTESIAN_POINT ( 'NONE',  ( 9.564922557960805705, 16.46253265017160317, 84.58224293864769550 ) ) ;
#89384 = CARTESIAN_POINT ( 'NONE',  ( 4.483927247898545687, 16.52544592524342804, 109.7905762719810383 ) ) ;
#89383 = CARTESIAN_POINT ( 'NONE',  ( -18.56101223717332260, -5.500000000000064837, 91.44978406935680937 ) ) ;
#89386 = CARTESIAN_POINT ( 'NONE',  ( 16.46253265017160672, -9.564922557960803928, 73.33224293864769550 ) ) ;
#89385 = AXIS2_PLACEMENT_3D ( 'NONE', #144022, #4497, #111703 ) ;
#89387 = CARTESIAN_POINT ( 'NONE',  ( -10.81492255796078084, -18.62759615963271287, 82.08224293864768129 ) ) ;
#89388 = CARTESIAN_POINT ( 'NONE',  ( -20.96339774546121504, -10.39907118706507561, 168.2889211417202944 ) ) ;
#89390 = CARTESIAN_POINT ( 'NONE',  ( 4.999999999999999112, 11.45643923738960090, -18.00000000000000000 ) ) ;
#89389 = CARTESIAN_POINT ( 'NONE',  ( -10.81492255796078084, -18.62759615963271287, 27.08224293864769550 ) ) ;
#89391 = CARTESIAN_POINT ( 'NONE',  ( 16.53943276465976808, 0.05219959533934440121, 21.25109039468567218 ) ) ;
#89392 = CARTESIAN_POINT ( 'NONE',  ( -8.314922557960811034, -14.29746914071050412, 92.08224293864769550 ) ) ;
#89393 = CARTESIAN_POINT ( 'NONE',  ( -16.20579543436678449, -7.371946100355106779, 95.56520834171877254 ) ) ;
#89394 = CARTESIAN_POINT ( 'NONE',  ( -5.049401038298153566, 19.05341960407611168, 90.20724293864766707 ) ) ;
#89395 = CARTESIAN_POINT ( 'NONE',  ( 19.05341960407611168, 5.049401038298154454, 43.95724293864769550 ) ) ;
#89396 = CARTESIAN_POINT ( 'NONE',  ( -16.53943276465976808, 0.05219959533911058130, 86.24890960531436690 ) ) ;
#89397 = CARTESIAN_POINT ( 'NONE',  ( -0.05219959533907301413, -21.53943276465977519, 22.49890960531436335 ) ) ;
#89398 = CARTESIAN_POINT ( 'NONE',  ( 12.14591786802309770, 12.06949235617756955, 49.37390960531436690 ) ) ;
#89399 = CARTESIAN_POINT ( 'NONE',  ( -0.05219959533936034679, 19.03943276465977164, 102.5010903946856757 ) ) ;
#89400 = CARTESIAN_POINT ( 'NONE',  ( -10.72451020669870658, -18.67979575497194134, 59.58442372801901854 ) ) ;
#89401 = CARTESIAN_POINT ( 'NONE',  ( 27.73933785331498569, 2.768321779492822058E-14, 147.8750000027311842 ) ) ;
#89402 = CARTESIAN_POINT ( 'NONE',  ( 19.05341960407611168, 5.049401038298154454, 103.9572429386476671 ) ) ;
#89403 = CARTESIAN_POINT ( 'NONE',  ( 10.72451020669898902, -18.67979575497178502, 92.91557627198103830 ) ) ;
#89404 = CARTESIAN_POINT ( 'NONE',  ( 0.05219959533934541429, -16.53943276465976808, 85.00109039468568994 ) ) ;
#89405 = CARTESIAN_POINT ( 'NONE',  ( 13.97604488694527802, 13.89961937509977652, 24.37390960531435624 ) ) ;
#89406 = CARTESIAN_POINT ( 'NONE',  ( 0.05219959533909260263, 19.03943276465977164, 79.99890960531436690 ) ) ;
#89407 = CARTESIAN_POINT ( 'NONE',  ( 21.52544592524344225, -5.823673210054117533, 78.54057627198103830 ) ) ;
#89408 = CARTESIAN_POINT ( 'NONE',  ( 13.97604488694548053, -13.89961937509957401, 105.6260903946856757 ) ) ;
#89410 = CARTESIAN_POINT ( 'NONE',  ( 0.05219959533937995610, -21.53943276465977519, 55.00109039468568284 ) ) ;
#89409 = CARTESIAN_POINT ( 'NONE',  ( 8.224510206698953496, -14.34966873604960469, 47.91557627198102409 ) ) ;
#89412 = CARTESIAN_POINT ( 'NONE',  ( 16.51473224551069308, 9.474510206698969483, 114.1655762719810241 ) ) ;
#89411 = CARTESIAN_POINT ( 'NONE',  ( 4.379528057220092307, 16.55341960407617563, 87.29275706135236135 ) ) ;
#89413 = CARTESIAN_POINT ( 'NONE',  ( -13.89961937509977830, 13.97604488694528158, 110.6239096053143527 ) ) ;
#89414 = CARTESIAN_POINT ( 'NONE',  ( 28.79475375365586132, 2.781246896534039337E-14, 147.2656553485624045 ) ) ;
#89415 = CARTESIAN_POINT ( 'NONE',  ( -12.06949235617739369, -12.14591786802326823, 104.3760903946856899 ) ) ;
#89416 = CARTESIAN_POINT ( 'NONE',  ( 14.29746914071037800, 8.314922557961029526, 56.66775706135235424 ) ) ;
#89417 = CARTESIAN_POINT ( 'NONE',  ( 16.46253265017160672, -9.564922557960803928, 68.33224293864770971 ) ) ;
#89418 = CARTESIAN_POINT ( 'NONE',  ( 0.05219959533909260263, 19.03943276465977164, 79.99890960531436690 ) ) ;
#89419 = CARTESIAN_POINT ( 'NONE',  ( -12.06949235617739369, -12.14591786802326823, 74.37609039468568994 ) ) ;
#89420 = CARTESIAN_POINT ( 'NONE',  ( -16.53943276465976808, 0.05219959533911058130, 46.24890960531435979 ) ) ;
#89421 = CARTESIAN_POINT ( 'NONE',  ( 16.46253265017160672, -9.564922557960803928, 58.33224293864769550 ) ) ;
#89422 = CARTESIAN_POINT ( 'NONE',  ( -9.474510206698964154, 16.51473224551069663, 45.41557627198103120 ) ) ;
#89424 = ORIENTED_EDGE ( 'NONE', *, *, #49003, .T. ) ;
#89423 = CARTESIAN_POINT ( 'NONE',  ( -4.483927247898782831, 16.52544592524335698, 42.70942372801901854 ) ) ;
#89425 = CARTESIAN_POINT ( 'NONE',  ( -16.46253265017146816, -9.564922557961047289, 94.16775706135233293 ) ) ;
#89426 = CARTESIAN_POINT ( 'NONE',  ( 8.224510206698953496, -14.34966873604960469, 97.91557627198103830 ) ) ;
#89427 = CARTESIAN_POINT ( 'NONE',  ( -5.049401038298153566, 19.05341960407611168, 65.20724293864765286 ) ) ;
#89429 = CARTESIAN_POINT ( 'NONE',  ( -11.74264578624799782, -36.14014761921581709, -3.600000000000000533 ) ) ;
#89428 = CARTESIAN_POINT ( 'NONE',  ( -9.474510206698720793, -16.51473224551083518, 94.58442372801900433 ) ) ;
#89430 = CARTESIAN_POINT ( 'NONE',  ( -21.55341960407619339, 5.719274019375674811, 98.54275706135234714 ) ) ;
#89431 = CARTESIAN_POINT ( 'NONE',  ( 8.314922557961029526, -14.29746914071037800, 65.41775706135234714 ) ) ;
#89432 = DIRECTION ( 'NONE',  ( -0.000000000000000000, -0.000000000000000000, 1.000000000000000000 ) ) ;
#89433 = CARTESIAN_POINT ( 'NONE',  ( -18.62759615963270932, 10.81492255796079327, 60.83224293864769550 ) ) ;
#89434 = CARTESIAN_POINT ( 'NONE',  ( 14.34966873604972726, -8.224510206698740333, 50.83442372801901143 ) ) ;
#89435 = DIRECTION ( 'NONE',  ( -1.000000000000000000, 0.000000000000000000, 0.000000000000000000 ) ) ;
#89436 = CARTESIAN_POINT ( 'NONE',  ( -13.89961937509957401, -13.97604488694547875, 39.37609039468566152 ) ) ;
#89437 = CARTESIAN_POINT ( 'NONE',  ( -13.97604488694527625, -13.89961937509977652, 91.87390960531432427 ) ) ;
#89438 = CARTESIAN_POINT ( 'NONE',  ( 16.53943276465976808, -0.05219959533910856209, 113.7489096053143527 ) ) ;
#89439 = CARTESIAN_POINT ( 'NONE',  ( 19.02544592524343514, -5.153800228976328945, 63.54057627198103830 ) ) ;
#89440 = CARTESIAN_POINT ( 'NONE',  ( -5.823673210054431948, 21.52544592524334988, 82.70942372801900433 ) ) ;
#89441 = CARTESIAN_POINT ( 'NONE',  ( -16.46253265017146816, -9.564922557961047289, 44.16775706135232582 ) ) ;
#89442 = CARTESIAN_POINT ( 'NONE',  ( -5.153800228976607833, 19.02544592524334988, 32.70942372801899722 ) ) ;
#89443 = CARTESIAN_POINT ( 'NONE',  ( -13.97604488694527625, -13.89961937509977652, 56.87390960531434558 ) ) ;
#89444 = CARTESIAN_POINT ( 'NONE',  ( 19.03943276465977164, -0.05219959533909143690, 113.7489096053143669 ) ) ;
#89445 = CARTESIAN_POINT ( 'NONE',  ( -10.72451020669870658, -18.67979575497194134, 89.58442372801901854 ) ) ;
#89446 = CARTESIAN_POINT ( 'NONE',  ( -9.564922557960796823, -16.46253265017161027, 67.08224293864769550 ) ) ;
#89447 = EDGE_CURVE ( 'NONE', #1233, #171664, #187476, .T. ) ;
#89448 = CARTESIAN_POINT ( 'NONE',  ( 18.67979575497194134, -10.72451020669871369, 95.83442372801903275 ) ) ;
#89449 = CARTESIAN_POINT ( 'NONE',  ( 5.719274019375991003, -21.55341960407610458, 32.70724293864770260 ) ) ;
#89450 = CARTESIAN_POINT ( 'NONE',  ( 9.474510206698971260, -16.51473224551069308, 77.91557627198103830 ) ) ;
#89451 = CARTESIAN_POINT ( 'NONE',  ( -21.52544592524334988, -5.823673210054445271, 38.95942372801901854 ) ) ;
#89452 = CARTESIAN_POINT ( 'NONE',  ( -19.02544592524334988, -5.153800228976617603, 58.95942372801900433 ) ) ;
#89453 = CARTESIAN_POINT ( 'NONE',  ( -0.05219959533909027116, -19.03943276465977164, 47.49890960531435979 ) ) ;
#89454 = CARTESIAN_POINT ( 'NONE',  ( -16.51473224551069308, -9.474510206698971260, 86.66557627198102409 ) ) ;
#89455 = CARTESIAN_POINT ( 'NONE',  ( -12.06949235617739369, -12.14591786802326823, 24.37609039468567573 ) ) ;
#89456 = CARTESIAN_POINT ( 'NONE',  ( 16.55341960407611168, 4.379528057220329451, 83.95724293864770971 ) ) ;
#89457 = CARTESIAN_POINT ( 'NONE',  ( 19.02544592524343514, -5.153800228976328945, 73.54057627198103830 ) ) ;
#89459 = B_SPLINE_CURVE_WITH_KNOTS ( 'NONE', 3,
 ( #4821, #20007, #113005, #161518, #55335, #8842, #37164, #143334, #66509, #129160, #69506, #175689, #174699, #131172, #192862, #51345, #21000, #190857, #82655, #54341, #98823, #58337, #134192, #102843 ),
 .UNSPECIFIED., .F., .F.,
 ( 4, 2, 2, 2, 2, 2, 2, 2, 2, 2, 2, 4 ),
 ( 3.849469143858236616E-15, 0.0003995125125255656411, 0.0007990250250472818224, 0.0009987812813081384765, 0.001198537537568994914, 0.001398293793829851351, 0.001598050050090707788, 0.001797806306351564225, 0.001997562562612420229, 0.002397075075134141777, 0.002796587587655863325, 0.003196100100177584440 ),
 .UNSPECIFIED. ) ;
#89458 = CARTESIAN_POINT ( 'NONE',  ( -21.55341960407610458, -5.719274019375992779, 46.45724293864769550 ) ) ;
#89460 = CARTESIAN_POINT ( 'NONE',  ( 19.02544592524334988, 5.153800228976608722, 111.4594237280190043 ) ) ;
#89461 = CARTESIAN_POINT ( 'NONE',  ( 21.53943276465977519, 0.05219959533937863772, 26.25109039468567573 ) ) ;
#89462 = CARTESIAN_POINT ( 'NONE',  ( 0.05219959533937995610, -21.53943276465977519, 75.00109039468568994 ) ) ;
#89463 = CARTESIAN_POINT ( 'NONE',  ( -14.29746914071037622, -8.314922557961029526, 64.16775706135234714 ) ) ;
#89464 = CARTESIAN_POINT ( 'NONE',  ( -16.53943276465976808, -0.05219959533934237506, 63.75109039468568284 ) ) ;
#89465 = CARTESIAN_POINT ( 'NONE',  ( 0.05219959533909260263, 19.03943276465977164, 64.99890960531436690 ) ) ;
#89466 = CARTESIAN_POINT ( 'NONE',  ( -16.53943276465976808, -0.05219959533934237506, 103.7510903946857042 ) ) ;
#89467 = CARTESIAN_POINT ( 'NONE',  ( 16.46253265017146816, 9.564922557961045513, 46.66775706135233293 ) ) ;
#89468 = CARTESIAN_POINT ( 'NONE',  ( -5.719274019375978568, 21.55341960407610458, 115.2072429386476955 ) ) ;
#89469 = CARTESIAN_POINT ( 'NONE',  ( -14.29746914071049879, 8.314922557960819915, 60.83224293864769550 ) ) ;
#89470 = CARTESIAN_POINT ( 'NONE',  ( -0.05219959533909027116, -19.03943276465977164, 87.49890960531436690 ) ) ;
#89471 = CARTESIAN_POINT ( 'NONE',  ( -8.314922557961024197, 14.29746914071037800, 82.91775706135234714 ) ) ;
#89472 = CARTESIAN_POINT ( 'NONE',  ( 5.823673210054444382, -21.52544592524334988, 65.20942372801901854 ) ) ;
#89473 = CARTESIAN_POINT ( 'NONE',  ( -4.483927247898782831, 16.52544592524335698, 37.70942372801900433 ) ) ;
#89474 = CARTESIAN_POINT ( 'NONE',  ( 21.52544592524334988, 5.823673210054432836, 21.45942372801901499 ) ) ;
#89475 = CARTESIAN_POINT ( 'NONE',  ( -16.52544592524342804, 4.483927247898546575, 61.04057627198103120 ) ) ;
#89476 = ORIENTED_EDGE ( 'NONE', *, *, #139684, .F. ) ;
#89477 = CARTESIAN_POINT ( 'NONE',  ( -10.81492255796078084, -18.62759615963271287, 107.0822429386476955 ) ) ;
#89478 = CARTESIAN_POINT ( 'NONE',  ( -0.05219959533910754901, -16.53943276465976808, 42.49890960531435979 ) ) ;
#89479 = ORIENTED_EDGE ( 'NONE', *, *, #2987, .T. ) ;
#89480 = CARTESIAN_POINT ( 'NONE',  ( 35.70266437024451278, 0.2453497911276426302, 37.50000000000002132 ) ) ;
#89481 = CARTESIAN_POINT ( 'NONE',  ( 10.81492255796078972, 18.62759615963270932, 29.58224293864769905 ) ) ;
#89482 = CARTESIAN_POINT ( 'NONE',  ( -15.72974639402176322, -15.80617190586768395, 39.37609039468567573 ) ) ;
#89483 = CARTESIAN_POINT ( 'NONE',  ( -4.483927247898539470, -16.52544592524342804, 67.29057627198103830 ) ) ;
#89484 = CIRCLE ( 'NONE', #111984, 4.000000000000000000 ) ;
#89485 = CARTESIAN_POINT ( 'NONE',  ( 10.72451020669898902, -18.67979575497178502, 72.91557627198103830 ) ) ;
#89486 = CARTESIAN_POINT ( 'NONE',  ( -16.51473224551069308, -9.474510206698971260, 71.66557627198102409 ) ) ;
#89488 = CARTESIAN_POINT ( 'NONE',  ( -0.05219959533936034679, 19.03943276465977164, 62.50109039468566863 ) ) ;
#89487 = CARTESIAN_POINT ( 'NONE',  ( 5.049401038298161559, -19.05341960407611168, 27.70724293864769550 ) ) ;
#89489 = CARTESIAN_POINT ( 'NONE',  ( -15.72974639402197994, 15.80617190586746368, 50.62390960531435979 ) ) ;
#89490 = CARTESIAN_POINT ( 'NONE',  ( 13.97604488694527802, 13.89961937509977652, 59.37390960531434558 ) ) ;
#89491 = ORIENTED_EDGE ( 'NONE', *, *, #54770, .T. ) ;
#89492 = CARTESIAN_POINT ( 'NONE',  ( 12.06949235617739724, 12.14591786802326823, 31.87609039468567929 ) ) ;
#89493 = CARTESIAN_POINT ( 'NONE',  ( -18.67979575497178146, -10.72451020669898902, 111.6655762719810525 ) ) ;
#89494 = CARTESIAN_POINT ( 'NONE',  ( 16.52544592524342804, -4.483927247898539470, 53.54057627198103120 ) ) ;
#89495 = CARTESIAN_POINT ( 'NONE',  ( 5.049401038298161559, -19.05341960407611168, 97.70724293864766707 ) ) ;
#89496 = CARTESIAN_POINT ( 'NONE',  ( -5.719274019375978568, 21.55341960407610458, 70.20724293864769550 ) ) ;
#89498 = CARTESIAN_POINT ( 'NONE',  ( -8.224510206698735004, -14.34966873604973081, 34.58442372801900433 ) ) ;
#89497 = CARTESIAN_POINT ( 'NONE',  ( 10.81492255796078972, 18.62759615963270932, 109.5822429386476955 ) ) ;
#89499 = VECTOR ( 'NONE', #77542, 1000.000000000000000 ) ;
#89500 = CARTESIAN_POINT ( 'NONE',  ( -5.719274019375978568, 21.55341960407610458, 35.20724293864768839 ) ) ;
#89501 = CARTESIAN_POINT ( 'NONE',  ( 18.62759615963255655, 10.81492255796105972, 96.66775706135234714 ) ) ;
#89502 = CARTESIAN_POINT ( 'NONE',  ( 0.05219959533909260263, 19.03943276465977164, 39.99890960531436690 ) ) ;
#89503 = CARTESIAN_POINT ( 'NONE',  ( 19.05341960407611168, 5.049401038298154454, 98.95724293864766707 ) ) ;
#89504 = CARTESIAN_POINT ( 'NONE',  ( 19.02544592524343514, -5.153800228976328945, 73.54057627198103830 ) ) ;
#89505 = FACE_BOUND ( 'NONE', #101247, .T. ) ;
#89506 = CARTESIAN_POINT ( 'NONE',  ( 5.049401038297881783, 19.05341960407617563, 52.29275706135234003 ) ) ;
#89508 = CARTESIAN_POINT ( 'NONE',  ( -21.53943276465977519, 0.05219959533907696930, 26.24890960531435624 ) ) ;
#89507 = CARTESIAN_POINT ( 'NONE',  ( 21.52544592524334988, 5.823673210054432836, 106.4594237280190328 ) ) ;
#89509 = CARTESIAN_POINT ( 'NONE',  ( 14.34966873604972726, -8.224510206698740333, 110.8344237280190043 ) ) ;
#89510 = CARTESIAN_POINT ( 'NONE',  ( -5.049401038297874678, -19.05341960407617918, 79.79275706135233293 ) ) ;
#89511 = PLANE ( 'NONE',  #160 ) ;
#89512 = CARTESIAN_POINT ( 'NONE',  ( 19.02544592524334988, 5.153800228976608722, 86.45942372801900433 ) ) ;
#89513 = CARTESIAN_POINT ( 'NONE',  ( 19.05341960407617918, -5.049401038297876454, 41.04275706135233293 ) ) ;
#89514 = CARTESIAN_POINT ( 'NONE',  ( -17.49999999999999645, -5.624438216177608751, 44.18329655085357643 ) ) ;
#89515 = CARTESIAN_POINT ( 'NONE',  ( -13.97604488694527625, -13.89961937509977652, 41.87390960531435979 ) ) ;
#89516 = CARTESIAN_POINT ( 'NONE',  ( -4.379528057220328563, 16.55341960407611168, 55.20724293864770260 ) ) ;
#89517 = CARTESIAN_POINT ( 'NONE',  ( -13.89961937509977652, 13.97604488694528158, 30.62390960531435269 ) ) ;
#89518 = CARTESIAN_POINT ( 'NONE',  ( 14.34966873604960469, 8.224510206698951720, 39.16557627198102409 ) ) ;
#89519 = CARTESIAN_POINT ( 'NONE',  ( 17.50000000000000000, -7.500000000000000888, 118.0000000000000142 ) ) ;
#89520 = CARTESIAN_POINT ( 'NONE',  ( -16.52544592524335698, -4.483927247898792601, 103.9594237280190185 ) ) ;
#89521 = CARTESIAN_POINT ( 'NONE',  ( 16.46253265017160672, -9.564922557960803928, 53.33224293864768839 ) ) ;
#89522 = EDGE_CURVE ( 'NONE', #100170, #126623, #158273, .T. ) ;
#89523 = CARTESIAN_POINT ( 'NONE',  ( 21.53943276465977519, 0.05219959533937863772, 106.2510903946856757 ) ) ;
#89524 = CARTESIAN_POINT ( 'NONE',  ( 12.06949235617739724, 12.14591786802326823, 21.87609039468567573 ) ) ;
#89525 = CARTESIAN_POINT ( 'NONE',  ( -18.67979575497178146, -10.72451020669898902, 41.66557627198103120 ) ) ;
#89527 = VERTEX_POINT ( 'NONE', #162263 ) ;
#89526 = CARTESIAN_POINT ( 'NONE',  ( -5.823673210054431948, 21.52544592524334988, 92.70942372801901854 ) ) ;
#89528 = CARTESIAN_POINT ( 'NONE',  ( 9.564922557960805705, 16.46253265017160317, 99.58224293864770971 ) ) ;
#89529 = CARTESIAN_POINT ( 'NONE',  ( 5.049401038298161559, -19.05341960407611168, 87.70724293864769550 ) ) ;
#89530 = CARTESIAN_POINT ( 'NONE',  ( -31.74953202133205110, -24.33172034662469940, -19.41189923848662247 ) ) ;
#89531 = CARTESIAN_POINT ( 'NONE',  ( 0.05219959533907565091, 21.53943276465977519, 104.9989096053143669 ) ) ;
#89532 = AXIS2_PLACEMENT_3D ( 'NONE', #27113, #165614, #39263 ) ;
#89533 = CARTESIAN_POINT ( 'NONE',  ( 8.224510206698953496, -14.34966873604960469, 77.91557627198102409 ) ) ;
#89534 = CARTESIAN_POINT ( 'NONE',  ( -10.72451020669898014, 18.67979575497178502, 70.41557627198102409 ) ) ;
#89535 = CARTESIAN_POINT ( 'NONE',  ( -19.03943276465977164, 0.05219959533909376836, 56.24890960531435979 ) ) ;
#89536 = CARTESIAN_POINT ( 'NONE',  ( -21.55341960407610458, -5.719274019375992779, 96.45724293864770971 ) ) ;
#89537 = EDGE_CURVE ( 'NONE', #45261, #165759, #9807, .T. ) ;
#89538 = ORIENTED_EDGE ( 'NONE', *, *, #185853, .T. ) ;
#89539 = CARTESIAN_POINT ( 'NONE',  ( 5.153800228976335163, 19.02544592524342804, 64.79057627198100988 ) ) ;
#89541 = CARTESIAN_POINT ( 'NONE',  ( -4.000000000000000888, -105.0000000000000000, 12.00000000000000355 ) ) ;
#89540 = CARTESIAN_POINT ( 'NONE',  ( 4.379528057220339221, -16.55341960407611168, 87.70724293864769550 ) ) ;
#89542 = CARTESIAN_POINT ( 'NONE',  ( -16.46253265017160317, 9.564922557960807481, 65.83224293864769550 ) ) ;
#89543 = CARTESIAN_POINT ( 'NONE',  ( -13.89961937509957401, -13.97604488694547875, 84.37609039468567573 ) ) ;
#89544 = CARTESIAN_POINT ( 'NONE',  ( 8.224510206698953496, -14.34966873604960469, 87.91557627198103830 ) ) ;
#89545 = CARTESIAN_POINT ( 'NONE',  ( -10.81492255796105439, 18.62759615963255655, 52.91775706135235424 ) ) ;
#89547 = CARTESIAN_POINT ( 'NONE',  ( -18.62759615963255300, -10.81492255796106328, 19.16775706135234714 ) ) ;
#89546 = CARTESIAN_POINT ( 'NONE',  ( 16.46253265017160672, -9.564922557960803928, 53.33224293864768839 ) ) ;
#89548 = CARTESIAN_POINT ( 'NONE',  ( -16.53943276465976808, 0.05219959533911058130, 106.2489096053143811 ) ) ;
#89549 = CARTESIAN_POINT ( 'NONE',  ( 11.23063180226361091, -38.81524874329667796, -25.08899775095413531 ) ) ;
#89550 = CARTESIAN_POINT ( 'NONE',  ( -5.153800228976328057, -19.02544592524343514, 62.29057627198100988 ) ) ;
#89551 = LINE ( 'NONE', #58224, #134099 ) ;
#89553 = CARTESIAN_POINT ( 'NONE',  ( -5.049401038298153566, 19.05341960407611168, 115.2072429386477097 ) ) ;
#89552 = CARTESIAN_POINT ( 'NONE',  ( 19.05341960407617918, -5.049401038297876454, 111.0427570613523329 ) ) ;
#89554 = CARTESIAN_POINT ( 'NONE',  ( 5.823673210054444382, -21.52544592524334988, 50.20942372801901854 ) ) ;
#89555 = CARTESIAN_POINT ( 'NONE',  ( -16.51473224551069308, -9.474510206698971260, 101.6655762719810241 ) ) ;
#89556 = CARTESIAN_POINT ( 'NONE',  ( 5.153800228976615827, -19.02544592524334988, 80.20942372801901854 ) ) ;
#89557 = CARTESIAN_POINT ( 'NONE',  ( 13.97604488694527802, 13.89961937509977652, 64.37390960531436690 ) ) ;
#89558 = CARTESIAN_POINT ( 'NONE',  ( 16.53943276465976808, -0.05219959533910856209, 73.74890960531433848 ) ) ;
#89559 = CARTESIAN_POINT ( 'NONE',  ( -14.29746914071049879, 8.314922557960819915, 80.83224293864769550 ) ) ;
#89560 = CARTESIAN_POINT ( 'NONE',  ( -13.89961937509977652, 13.97604488694528158, 95.62390960531436690 ) ) ;
#89561 = CARTESIAN_POINT ( 'NONE',  ( -4.379528057220328563, 16.55341960407611168, 75.20724293864769550 ) ) ;
#89562 = CARTESIAN_POINT ( 'NONE',  ( 9.474510206698971260, -16.51473224551069308, 82.91557627198103830 ) ) ;
#89563 = CARTESIAN_POINT ( 'NONE',  ( 0.05219959533936267826, -19.03943276465977164, 35.00109039468566863 ) ) ;
#89566 = CARTESIAN_POINT ( 'NONE',  ( 19.02544592524343514, -5.153800228976328945, 28.54057627198102409 ) ) ;
#89565 = CARTESIAN_POINT ( 'NONE',  ( -0.05219959533910754901, -16.53943276465976808, 32.49890960531435979 ) ) ;
#89564 = CARTESIAN_POINT ( 'NONE',  ( -16.46253265017160317, 9.564922557960807481, 55.83224293864769550 ) ) ;
#89567 = EDGE_LOOP ( 'NONE', ( #4402, #31658, #116340, #51756 ) ) ;
#89568 = CARTESIAN_POINT ( 'NONE',  ( 15.80617190586769283, -15.72974639402175789, 50.62609039468568994 ) ) ;
#89569 = CARTESIAN_POINT ( 'NONE',  ( 9.564922557961047289, -16.46253265017146816, 85.41775706135233293 ) ) ;
#89570 = CARTESIAN_POINT ( 'NONE',  ( 8.224510206698953496, -14.34966873604960469, 37.91557627198102409 ) ) ;
#89571 = CARTESIAN_POINT ( 'NONE',  ( -5.823673210054116645, -21.52544592524344225, 92.29057627198103830 ) ) ;
#89572 = CARTESIAN_POINT ( 'NONE',  ( -10.72451020669898014, 18.67979575497178502, 30.41557627198101699 ) ) ;
#89573 = CARTESIAN_POINT ( 'NONE',  ( 4.483927247898545687, 16.52544592524342804, 64.79057627198103830 ) ) ;
#89574 = CARTESIAN_POINT ( 'NONE',  ( 13.97604488694527802, 13.89961937509977652, 44.37390960531435269 ) ) ;
#89575 = CARTESIAN_POINT ( 'NONE',  ( -8.224510206698735004, -14.34966873604973081, 104.5844237280190185 ) ) ;
#89576 = CARTESIAN_POINT ( 'NONE',  ( 14.29746914071037800, 8.314922557961029526, 66.66775706135234714 ) ) ;
#89577 = CARTESIAN_POINT ( 'NONE',  ( 0.05219959533907565091, 21.53943276465977519, 34.99890960531435979 ) ) ;
#89578 = CARTESIAN_POINT ( 'NONE',  ( 13.97604488694548053, -13.89961937509957401, 20.62609039468567573 ) ) ;
#89579 = CARTESIAN_POINT ( 'NONE',  ( 5.153800228976335163, 19.02544592524342804, 89.79057627198102409 ) ) ;
#89580 = CARTESIAN_POINT ( 'NONE',  ( 14.34966873604972726, -8.224510206698740333, 70.83442372801901854 ) ) ;
#89581 = CARTESIAN_POINT ( 'NONE',  ( -9.564922557960796823, -16.46253265017161027, 22.08224293864768839 ) ) ;
#89582 = CARTESIAN_POINT ( 'NONE',  ( -14.29746914071049879, 8.314922557960819915, 35.83224293864768839 ) ) ;
#89584 = CARTESIAN_POINT ( 'NONE',  ( -9.564922557960796823, -16.46253265017161027, 92.08224293864769550 ) ) ;
#89583 = CARTESIAN_POINT ( 'NONE',  ( 5.049401038298161559, -19.05341960407611168, 107.7072429386476955 ) ) ;
#89585 = CARTESIAN_POINT ( 'NONE',  ( -21.53943276465977519, 0.05219959533907696930, 31.24890960531435979 ) ) ;
#89586 = CARTESIAN_POINT ( 'NONE',  ( -4.483927247898539470, -16.52544592524342804, 77.29057627198102409 ) ) ;
#89587 = VERTEX_POINT ( 'NONE', #39916 ) ;
#89588 = CARTESIAN_POINT ( 'NONE',  ( 12.06949235617757843, -12.14591786802309237, 53.12390960531436690 ) ) ;
#89590 = CARTESIAN_POINT ( 'NONE',  ( -7.052343178074647945, -2.552343178074588437, 1.110912703473986074 ) ) ;
#89589 = CARTESIAN_POINT ( 'NONE',  ( -8.314922557961024197, 14.29746914071037800, 57.91775706135234714 ) ) ;
#89591 = CARTESIAN_POINT ( 'NONE',  ( -19.05341960407617563, 5.049401038297882671, 53.54275706135231871 ) ) ;
#89592 = CARTESIAN_POINT ( 'NONE',  ( 13.97604488694527802, 13.89961937509977652, 94.37390960531436690 ) ) ;
#89593 = CARTESIAN_POINT ( 'NONE',  ( -19.03943276465977164, -0.05219959533935918106, 68.75109039468566152 ) ) ;
#89594 = CARTESIAN_POINT ( 'NONE',  ( -8.571926809382601320, -26.38167802310801591, 141.7750000027311899 ) ) ;
#89596 = CARTESIAN_POINT ( 'NONE',  ( 14.34966873604972726, -8.224510206698740333, 90.83442372801901854 ) ) ;
#89595 = CARTESIAN_POINT ( 'NONE',  ( 19.03943276465977164, 0.05219959533936151252, 111.2510903946856757 ) ) ;
#89597 = CARTESIAN_POINT ( 'NONE',  ( 19.02544592524343514, -5.153800228976328945, 33.54057627198102409 ) ) ;
#89598 = CARTESIAN_POINT ( 'NONE',  ( 16.51473224551069308, 9.474510206698969483, 114.1655762719810241 ) ) ;
#89599 = CARTESIAN_POINT ( 'NONE',  ( -5.823673210054431948, 21.52544592524334988, 52.70942372801902565 ) ) ;
#89600 = CARTESIAN_POINT ( 'NONE',  ( -13.89961937509957401, -13.97604488694547875, 99.37609039468567573 ) ) ;
#89602 = CARTESIAN_POINT ( 'NONE',  ( -19.05341960407611168, -5.049401038298163336, 71.45724293864766707 ) ) ;
#89601 = CARTESIAN_POINT ( 'NONE',  ( 17.50000000000000711, 4.034393320798373317, 22.04839310049790413 ) ) ;
#89603 = CARTESIAN_POINT ( 'NONE',  ( -24.99873734152895466, 24.49873734152938454, 4.646446609406721606 ) ) ;
#89605 = CARTESIAN_POINT ( 'NONE',  ( 0.05219959533909260263, 19.03943276465977164, 64.99890960531436690 ) ) ;
#89604 = CARTESIAN_POINT ( 'NONE',  ( -12.14591786802309592, -12.06949235617757132, 76.87390960531439532 ) ) ;
#89606 = CARTESIAN_POINT ( 'NONE',  ( 5.153800228976335163, 19.02544592524342804, 79.79057627198102409 ) ) ;
#89607 = CARTESIAN_POINT ( 'NONE',  ( -5.153800228976607833, 19.02544592524334988, 72.70942372801900433 ) ) ;
#89608 = CARTESIAN_POINT ( 'NONE',  ( 21.52544592524344225, -5.823673210054117533, 68.54057627198103830 ) ) ;
#89609 = CARTESIAN_POINT ( 'NONE',  ( -12.14591786802309592, -12.06949235617757132, 111.8739096053143669 ) ) ;
#89610 = CARTESIAN_POINT ( 'NONE',  ( -0.05219959533936034679, 19.03943276465977164, 52.50109039468566863 ) ) ;
#89611 = CARTESIAN_POINT ( 'NONE',  ( 19.02544592524343514, -5.153800228976328945, 58.54057627198102409 ) ) ;
#89612 = CARTESIAN_POINT ( 'NONE',  ( -13.89961937509977652, 13.97604488694528158, 95.62390960531436690 ) ) ;
#89613 = CARTESIAN_POINT ( 'NONE',  ( 0.05219959533907565091, 21.53943276465977519, 94.99890960531436690 ) ) ;
#89615 = CARTESIAN_POINT ( 'NONE',  ( -13.97604488694547697, 13.89961937509957934, 43.12609039468566152 ) ) ;
#89614 = CARTESIAN_POINT ( 'NONE',  ( 4.483927247898545687, 16.52544592524342804, 84.79057627198102409 ) ) ;
#89616 = CARTESIAN_POINT ( 'NONE',  ( 5.719274019375991003, -21.55341960407610458, 82.70724293864770971 ) ) ;
#89617 = CARTESIAN_POINT ( 'NONE',  ( -21.53943276465977519, 0.05219959533907696930, 61.24890960531435979 ) ) ;
#89618 = CARTESIAN_POINT ( 'NONE',  ( 4.379528057220339221, -16.55341960407611168, 27.70724293864769905 ) ) ;
#89619 = CARTESIAN_POINT ( 'NONE',  ( -21.52544592524334988, -5.823673210054445271, 93.95942372801903275 ) ) ;
#89620 = CARTESIAN_POINT ( 'NONE',  ( 9.474510206698971260, -16.51473224551069308, 82.91557627198103830 ) ) ;
#89621 = CARTESIAN_POINT ( 'NONE',  ( 13.97604488694527802, 13.89961937509977652, 34.37390960531436690 ) ) ;
#89622 = AXIS2_PLACEMENT_3D ( 'NONE', #3037, #93045, #154732 ) ;
#89623 = CARTESIAN_POINT ( 'NONE',  ( 21.53943276465977519, 0.05219959533937863772, 41.25109039468568284 ) ) ;
#89624 = CARTESIAN_POINT ( 'NONE',  ( 21.52544592524334988, 5.823673210054432836, 46.45942372801901854 ) ) ;
#89625 = CARTESIAN_POINT ( 'NONE',  ( -16.51473224551069308, -9.474510206698971260, 51.66557627198102409 ) ) ;
#89626 = CARTESIAN_POINT ( 'NONE',  ( 15.72974639402176855, 15.80617190586768217, 21.87609039468567573 ) ) ;
#89627 = CARTESIAN_POINT ( 'NONE',  ( 13.89961937509957401, 13.97604488694547697, 66.87609039468567573 ) ) ;
#89628 = CARTESIAN_POINT ( 'NONE',  ( 9.474510206698971260, -16.51473224551069308, 42.91557627198103120 ) ) ;
#89629 = CARTESIAN_POINT ( 'NONE',  ( -4.483927247898782831, 16.52544592524335698, 22.70942372801901499 ) ) ;
#89630 = CARTESIAN_POINT ( 'NONE',  ( 37.66961640367472341, -4.999999999999976019, -15.00000000000000000 ) ) ;
#89631 = CARTESIAN_POINT ( 'NONE',  ( -16.52544592524335698, -4.483927247898792601, 68.95942372801901854 ) ) ;
#89632 = CARTESIAN_POINT ( 'NONE',  ( 13.97604488694527802, 13.89961937509977652, 39.37390960531435269 ) ) ;
#89633 = CARTESIAN_POINT ( 'NONE',  ( -26.38458505201405657, -8.641005086744426578, 167.3773361139123779 ) ) ;
#89634 = CARTESIAN_POINT ( 'NONE',  ( -13.89961937509977652, 13.97604488694528158, 90.62390960531432427 ) ) ;
#89635 = CARTESIAN_POINT ( 'NONE',  ( -19.03943276465977164, 0.05219959533909376836, 31.24890960531435979 ) ) ;
#89636 = CARTESIAN_POINT ( 'NONE',  ( 5.823673210054125526, 21.52544592524343514, 59.79057627198103120 ) ) ;
#89637 = CARTESIAN_POINT ( 'NONE',  ( 8.224510206698742110, 14.34966873604972548, 42.08442372801901854 ) ) ;
#89638 = CARTESIAN_POINT ( 'NONE',  ( -5.719274019375665041, -21.55341960407619695, 94.79275706135234714 ) ) ;
#89639 = ADVANCED_FACE ( 'NONE', ( #23763, #101584 ), #26769, .T. ) ;
#89640 = CARTESIAN_POINT ( 'NONE',  ( 13.97604488694527802, 13.89961937509977652, 44.37390960531435269 ) ) ;
#89641 = CARTESIAN_POINT ( 'NONE',  ( -16.52544592524342804, 4.483927247898546575, 36.04057627198102409 ) ) ;
#89642 = CARTESIAN_POINT ( 'NONE',  ( 16.53943276465976808, -0.05219959533910856209, 68.74890960531435269 ) ) ;
#89643 = CARTESIAN_POINT ( 'NONE',  ( 16.51473224551069308, 9.474510206698969483, 69.16557627198102409 ) ) ;
#89644 = CARTESIAN_POINT ( 'NONE',  ( -15.72974639402176322, -15.80617190586768395, 109.3760903946857042 ) ) ;
#89645 = CARTESIAN_POINT ( 'NONE',  ( -18.62759615963255300, -10.81492255796106328, 24.16775706135235424 ) ) ;
#89646 = CARTESIAN_POINT ( 'NONE',  ( 13.97604488694527802, 13.89961937509977652, 84.37390960531433848 ) ) ;
#89647 = CARTESIAN_POINT ( 'NONE',  ( 0.05219959533937995610, -21.53943276465977519, 85.00109039468568994 ) ) ;
#89648 = CARTESIAN_POINT ( 'NONE',  ( 12.06949235617739724, 12.14591786802326823, 51.87609039468568284 ) ) ;
#89649 = CARTESIAN_POINT ( 'NONE',  ( -14.29746914071037622, -8.314922557961029526, 29.16775706135234003 ) ) ;
#89651 = CARTESIAN_POINT ( 'NONE',  ( -5.719274019375665041, -21.55341960407619695, 99.79275706135234714 ) ) ;
#89650 = CARTESIAN_POINT ( 'NONE',  ( -12.14591786802309592, -12.06949235617757132, 86.87390960531438111 ) ) ;
#89652 = MECHANICAL_DESIGN_GEOMETRIC_PRESENTATION_REPRESENTATION (  '', ( #5623 ), #189672 ) ;
#89653 = ADVANCED_FACE ( 'NONE', ( #147104, #8589 ), #73274, .F. ) ;
#89654 = CARTESIAN_POINT ( 'NONE',  ( -16.55341960407611168, -4.379528057220339221, 36.45724293864768839 ) ) ;
#89655 = CARTESIAN_POINT ( 'NONE',  ( 9.564922557960805705, 16.46253265017160317, 24.58224293864769194 ) ) ;
#89656 = CARTESIAN_POINT ( 'NONE',  ( -8.224510206698735004, -14.34966873604973081, 49.58442372801901143 ) ) ;
#89657 = CARTESIAN_POINT ( 'NONE',  ( -4.483927247898539470, -16.52544592524342804, 57.29057627198103120 ) ) ;
#89658 = CARTESIAN_POINT ( 'NONE',  ( 14.29746914071037800, 8.314922557961029526, 96.66775706135234714 ) ) ;
#89659 = CARTESIAN_POINT ( 'NONE',  ( 0.05219959533909260263, 19.03943276465977164, 114.9989096053143669 ) ) ;
#89660 = CARTESIAN_POINT ( 'NONE',  ( 21.53943276465977519, -0.05219959533907433946, 23.74890960531435269 ) ) ;
#89661 = CARTESIAN_POINT ( 'NONE',  ( 21.52544592524334988, 5.823673210054432836, 111.4594237280190328 ) ) ;
#89662 = CARTESIAN_POINT ( 'NONE',  ( -0.05219959533910754901, -16.53943276465976808, 92.49890960531436690 ) ) ;
#89663 = CARTESIAN_POINT ( 'NONE',  ( -19.03943276465977164, 0.05219959533909376836, 101.2489096053143669 ) ) ;
#89664 = VERTEX_POINT ( 'NONE', #148107 ) ;
#89665 = CARTESIAN_POINT ( 'NONE',  ( -16.53943276465976808, -0.05219959533934237506, 33.75109039468568284 ) ) ;
#89666 = CARTESIAN_POINT ( 'NONE',  ( 5.049401038298161559, -19.05341960407611168, 37.70724293864768839 ) ) ;
#89667 = CARTESIAN_POINT ( 'NONE',  ( 12.14591786802327356, -12.06949235617739191, 45.62609039468567573 ) ) ;
#89668 = CARTESIAN_POINT ( 'NONE',  ( -5.049401038297874678, -19.05341960407617918, 44.79275706135232582 ) ) ;
#89669 = CARTESIAN_POINT ( 'NONE',  ( -9.564922557960796823, -16.46253265017161027, 47.08224293864769550 ) ) ;
#89670 = CARTESIAN_POINT ( 'NONE',  ( 12.14591786802327356, -12.06949235617739191, 85.62609039468568994 ) ) ;
#89671 = CARTESIAN_POINT ( 'NONE',  ( 19.02544592524334988, 5.153800228976608722, 76.45942372801897591 ) ) ;
#89672 = CARTESIAN_POINT ( 'NONE',  ( 5.153800228976615827, -19.02544592524334988, 25.20942372801900433 ) ) ;
#89673 = CARTESIAN_POINT ( 'NONE',  ( 13.89961937509977652, -13.97604488694527269, 58.12390960531436690 ) ) ;
#89674 = CARTESIAN_POINT ( 'NONE',  ( -16.52544592524342804, 4.483927247898546575, 96.04057627198102409 ) ) ;
#89675 = VECTOR ( 'NONE', #47233, 1000.000000000000114 ) ;
#89676 = CARTESIAN_POINT ( 'NONE',  ( 16.46253265017146816, 9.564922557961045513, 66.66775706135233293 ) ) ;
#89677 = CARTESIAN_POINT ( 'NONE',  ( -21.55341960407610458, -5.719274019375992779, 66.45724293864768129 ) ) ;
#89678 = CARTESIAN_POINT ( 'NONE',  ( -0.05219959533936034679, 19.03943276465977164, 22.50109039468566152 ) ) ;
#89679 = CARTESIAN_POINT ( 'NONE',  ( 16.46253265017160672, -9.564922557960803928, 98.33224293864769550 ) ) ;
#89680 = EDGE_CURVE ( 'NONE', #199732, #122026, #48616, .T. ) ;
#89681 = CARTESIAN_POINT ( 'NONE',  ( -21.52544592524343514, 5.823673210054127303, 81.04057627198102409 ) ) ;
#89682 = CARTESIAN_POINT ( 'NONE',  ( -26.63278688795740834, 27.10001173645601114, -8.000000000000000000 ) ) ;
#89683 = CARTESIAN_POINT ( 'NONE',  ( 9.474510206698729675, 16.51473224551082808, 107.0844237280190043 ) ) ;
#89684 = CARTESIAN_POINT ( 'NONE',  ( -1.304248841091933035E-15, -21.30000000000002913, -58.85720012050612837 ) ) ;
#89685 = CARTESIAN_POINT ( 'NONE',  ( -12.14591786802326823, 12.06949235617739902, 33.12609039468569705 ) ) ;
#89686 = CARTESIAN_POINT ( 'NONE',  ( 19.02544592524343514, -5.153800228976328945, 38.54057627198103120 ) ) ;
#89687 = CARTESIAN_POINT ( 'NONE',  ( -9.474510206698964154, 16.51473224551069663, 105.4155762719810383 ) ) ;
#89688 = CARTESIAN_POINT ( 'NONE',  ( 10.81492255796078972, 18.62759615963270932, 89.58224293864768129 ) ) ;
#89689 = CARTESIAN_POINT ( 'NONE',  ( 15.72974639402176855, 15.80617190586768217, 56.87609039468568994 ) ) ;
#89691 = CARTESIAN_POINT ( 'NONE',  ( 9.564922557961047289, -16.46253265017146816, 20.41775706135233293 ) ) ;
#89690 = CARTESIAN_POINT ( 'NONE',  ( -19.02544592524334988, -5.153800228976617603, 108.9594237280189759 ) ) ;
#89692 = CARTESIAN_POINT ( 'NONE',  ( 4.379528057220092307, 16.55341960407617563, 107.2927570613523471 ) ) ;
#89693 = CARTESIAN_POINT ( 'NONE',  ( 5.823673210054125526, 21.52544592524343514, 104.7905762719810241 ) ) ;
#89694 = CARTESIAN_POINT ( 'NONE',  ( 16.55341960407611168, 4.379528057220329451, 43.95724293864769550 ) ) ;
#89695 = CARTESIAN_POINT ( 'NONE',  ( 9.474510206698729675, 16.51473224551082808, 77.08442372801900433 ) ) ;
#89696 = CARTESIAN_POINT ( 'NONE',  ( -13.89961937509957401, -13.97604488694547875, 59.37609039468566863 ) ) ;
#89697 = CARTESIAN_POINT ( 'NONE',  ( -15.80617190586768217, 15.72974639402176855, 68.12609039468567573 ) ) ;
#89698 = CARTESIAN_POINT ( 'NONE',  ( 13.97604488694548053, -13.89961937509957401, 35.62609039468567573 ) ) ;
#89699 = CARTESIAN_POINT ( 'NONE',  ( 16.53943276465976808, -0.05219959533910856209, 108.7489096053143669 ) ) ;
#89700 = CARTESIAN_POINT ( 'NONE',  ( 0.05219959533907565091, 21.53943276465977519, 39.99890960531436690 ) ) ;
#89701 = CARTESIAN_POINT ( 'NONE',  ( 4.379528057220339221, -16.55341960407611168, 37.70724293864769550 ) ) ;
#89702 = CARTESIAN_POINT ( 'NONE',  ( -18.62759615963255300, -10.81492255796106328, 94.16775706135237556 ) ) ;
#89703 = CARTESIAN_POINT ( 'NONE',  ( -16.55341960407617563, 4.379528057220093196, 68.54275706135234714 ) ) ;
#89704 = CARTESIAN_POINT ( 'NONE',  ( 4.379528057220339221, -16.55341960407611168, 22.70724293864769194 ) ) ;
#89705 = CARTESIAN_POINT ( 'NONE',  ( -15.80617190586768217, 15.72974639402176855, 58.12609039468568994 ) ) ;
#89706 = CARTESIAN_POINT ( 'NONE',  ( 15.72974639402176855, 15.80617190586768217, 66.87609039468568994 ) ) ;
#89707 = CARTESIAN_POINT ( 'NONE',  ( 15.80617190586746368, 15.72974639402197994, 64.37390960531435269 ) ) ;
#89708 = ORIENTED_EDGE ( 'NONE', *, *, #155738, .F. ) ;
#89709 = VERTEX_POINT ( 'NONE', #58091 ) ;
#89710 = CARTESIAN_POINT ( 'NONE',  ( -9.474510206698964154, 16.51473224551069663, 30.41557627198102054 ) ) ;
#89711 = CARTESIAN_POINT ( 'NONE',  ( -21.53943276465977519, -0.05219959533937600094, 48.75109039468568284 ) ) ;
#89712 = CARTESIAN_POINT ( 'NONE',  ( 16.51473224551069308, 9.474510206698969483, 24.16557627198102765 ) ) ;
#89713 = CARTESIAN_POINT ( 'NONE',  ( 16.51473224551069308, 9.474510206698969483, 34.16557627198102409 ) ) ;
#89714 = CARTESIAN_POINT ( 'NONE',  ( 16.52544592524342804, -4.483927247898539470, 73.54057627198102409 ) ) ;
#89715 = CARTESIAN_POINT ( 'NONE',  ( 19.05341960407611168, 5.049401038298154454, 83.95724293864766707 ) ) ;
#89716 = CARTESIAN_POINT ( 'NONE',  ( -16.55341960407611168, -4.379528057220339221, 21.45724293864769550 ) ) ;
#89717 = CARTESIAN_POINT ( 'NONE',  ( 16.53943276465976808, -0.05219959533910856209, 98.74890960531438111 ) ) ;
#89718 = CARTESIAN_POINT ( 'NONE',  ( 21.55341960407610458, 5.719274019375980345, 73.95724293864769550 ) ) ;
#89719 = CARTESIAN_POINT ( 'NONE',  ( -15.72974639402197994, 15.80617190586746368, 100.6239096053143811 ) ) ;
#89720 = CARTESIAN_POINT ( 'NONE',  ( -16.93990830356624855, 14.81572341150380012, -55.62237631978509711 ) ) ;
#89722 = CARTESIAN_POINT ( 'NONE',  ( 4.483927247898790824, -16.52544592524335698, 30.20942372801902565 ) ) ;
#89721 = CARTESIAN_POINT ( 'NONE',  ( -9.474510206698964154, 16.51473224551069663, 70.41557627198102409 ) ) ;
#89723 = CARTESIAN_POINT ( 'NONE',  ( -10.81492255796078084, -18.62759615963271287, 62.08224293864769550 ) ) ;
#89724 = CARTESIAN_POINT ( 'NONE',  ( 5.719274019375673035, 21.55341960407619339, 77.29275706135234714 ) ) ;
#89725 = CARTESIAN_POINT ( 'NONE',  ( 13.97604488694527802, 13.89961937509977652, 69.37390960531436690 ) ) ;
#89726 = CARTESIAN_POINT ( 'NONE',  ( -16.51473224551069308, -9.474510206698971260, 101.6655762719810241 ) ) ;
#89727 = CARTESIAN_POINT ( 'NONE',  ( -4.483927247898782831, 16.52544592524335698, 72.70942372801901854 ) ) ;
#89728 = CARTESIAN_POINT ( 'NONE',  ( -21.53943276465977519, -0.05219959533937600094, 63.75109039468568284 ) ) ;
#89729 = CARTESIAN_POINT ( 'NONE',  ( 21.52544592524334988, 5.823673210054432836, 96.45942372801901854 ) ) ;
#89730 = CARTESIAN_POINT ( 'NONE',  ( 0.05219959533937995610, -21.53943276465977519, 20.00109039468568639 ) ) ;
#89731 = CARTESIAN_POINT ( 'NONE',  ( -9.564922557960796823, -16.46253265017161027, 22.08224293864768839 ) ) ;
#89732 = CARTESIAN_POINT ( 'NONE',  ( -5.823673210054116645, -21.52544592524344225, 87.29057627198103830 ) ) ;
#89733 = CARTESIAN_POINT ( 'NONE',  ( -16.46253265017146816, -9.564922557961047289, 44.16775706135232582 ) ) ;
#89734 = CARTESIAN_POINT ( 'NONE',  ( 18.62759615963271287, -10.81492255796078972, 38.33224293864768839 ) ) ;
#89736 = CARTESIAN_POINT ( 'NONE',  ( -12.14591786802309592, -12.06949235617757132, 31.87390960531435979 ) ) ;
#89735 = CARTESIAN_POINT ( 'NONE',  ( 9.474510206698971260, -16.51473224551069308, 77.91557627198103830 ) ) ;
#89737 = CARTESIAN_POINT ( 'NONE',  ( -17.49999999999998934, 5.624438216177590988, 65.81670344914645909 ) ) ;
#89738 = CARTESIAN_POINT ( 'NONE',  ( -19.99604614807126524, -21.49604614807088154, -64.92279855667830191 ) ) ;
#89739 = CARTESIAN_POINT ( 'NONE',  ( 16.46253265017146816, 9.564922557961045513, 101.6677570613523329 ) ) ;
#89740 = CARTESIAN_POINT ( 'NONE',  ( -10.81492255796078084, -18.62759615963271287, 67.08224293864770971 ) ) ;
#89741 = CARTESIAN_POINT ( 'NONE',  ( 12.06949235617757843, -12.14591786802309237, 48.12390960531436690 ) ) ;
#89742 = CARTESIAN_POINT ( 'NONE',  ( -12.06949235617739369, -12.14591786802326823, 29.37609039468568284 ) ) ;
#89743 = CARTESIAN_POINT ( 'NONE',  ( 16.51473224551069308, 9.474510206698969483, 44.16557627198103120 ) ) ;
#89745 = CARTESIAN_POINT ( 'NONE',  ( -13.97604488694547697, 13.89961937509957934, 88.12609039468563310 ) ) ;
#89744 = CARTESIAN_POINT ( 'NONE',  ( 21.52544592524344225, -5.823673210054117533, 108.5405762719810241 ) ) ;
#89746 = CARTESIAN_POINT ( 'NONE',  ( -19.03943276465977164, 0.05219959533909376836, 76.24890960531435269 ) ) ;
#89747 = CARTESIAN_POINT ( 'NONE',  ( 14.29746914071049879, -8.314922557960816363, 93.33224293864769550 ) ) ;
#89748 = CARTESIAN_POINT ( 'NONE',  ( 9.564922557960805705, 16.46253265017160317, 79.58224293864769550 ) ) ;
#89749 = CARTESIAN_POINT ( 'NONE',  ( 0.05219959533907565091, 21.53943276465977519, 74.99890960531435269 ) ) ;
#89750 = CARTESIAN_POINT ( 'NONE',  ( -5.153800228976328057, -19.02544592524343514, 32.29057627198102409 ) ) ;
#89751 = CARTESIAN_POINT ( 'NONE',  ( 6.465454559173637428, 36.91613723712380590, -7.999999999999996447 ) ) ;
#89752 = CARTESIAN_POINT ( 'NONE',  ( 14.34966873604960469, 8.224510206698951720, 59.16557627198103120 ) ) ;
#89753 = CARTESIAN_POINT ( 'NONE',  ( -5.049401038298153566, 19.05341960407611168, 90.20724293864766707 ) ) ;
#89754 = LINE ( 'NONE', #195971, #163881 ) ;
#89755 = CARTESIAN_POINT ( 'NONE',  ( -0.05219959533936034679, 19.03943276465977164, 57.50109039468566863 ) ) ;
#89756 = CARTESIAN_POINT ( 'NONE',  ( 14.29746914071037800, 8.314922557961029526, 66.66775706135234714 ) ) ;
#89757 = CARTESIAN_POINT ( 'NONE',  ( 10.81492255796078972, 18.62759615963270932, 74.58224293864768129 ) ) ;
#89758 = CARTESIAN_POINT ( 'NONE',  ( -16.51473224551082808, 9.474510206698731452, 38.33442372801899722 ) ) ;
#89759 = CARTESIAN_POINT ( 'NONE',  ( 19.03943276465977164, -0.05219959533909143690, 88.74890960531436690 ) ) ;
#89760 = DIRECTION ( 'NONE',  ( -1.000000000000000000, 0.000000000000000000, 0.000000000000000000 ) ) ;
#89761 = CARTESIAN_POINT ( 'NONE',  ( -18.62759615963270932, 10.81492255796079327, 30.83224293864770260 ) ) ;
#89762 = CIRCLE ( 'NONE', #12284, 2.700000000000001066 ) ;
#89763 = CARTESIAN_POINT ( 'NONE',  ( 9.474510206698971260, -16.51473224551069308, 72.91557627198102409 ) ) ;
#89764 = CARTESIAN_POINT ( 'NONE',  ( 21.53943276465977519, 0.05219959533937863772, 46.25109039468567573 ) ) ;
#89765 = CARTESIAN_POINT ( 'NONE',  ( -19.02544592524342804, 5.153800228976336051, 26.04057627198103120 ) ) ;
#89768 = ORIENTED_EDGE ( 'NONE', *, *, #134940, .T. ) ;
#89767 = CARTESIAN_POINT ( 'NONE',  ( -16.51473224551069308, -9.474510206698971260, 91.66557627198103830 ) ) ;
#89766 = CARTESIAN_POINT ( 'NONE',  ( 10.72451020669871369, 18.67979575497193778, 22.08442372801901143 ) ) ;
#89769 = CARTESIAN_POINT ( 'NONE',  ( 10.81492255796106328, -18.62759615963255655, 40.41775706135234714 ) ) ;
#89770 = VERTEX_POINT ( 'NONE', #165275 ) ;
#89771 = CARTESIAN_POINT ( 'NONE',  ( -16.46253265017160317, 9.564922557960807481, 105.8322429386476955 ) ) ;
#89772 = CYLINDRICAL_SURFACE ( 'NONE', #121368, 1.499999999999996225 ) ;
#89773 = CARTESIAN_POINT ( 'NONE',  ( -5.719274019375978568, 21.55341960407610458, 110.2072429386477239 ) ) ;
#89774 = CARTESIAN_POINT ( 'NONE',  ( -9.474510206698964154, 16.51473224551069663, 40.41557627198103120 ) ) ;
#89775 = CARTESIAN_POINT ( 'NONE',  ( -12.06949235617739369, -12.14591786802326823, 29.37609039468568284 ) ) ;
#89776 = CARTESIAN_POINT ( 'NONE',  ( -11.40812507854755609, 35.11059874428196537, -3.524999997268813523 ) ) ;
#89777 = CARTESIAN_POINT ( 'NONE',  ( 10.72451020669871369, 18.67979575497193778, 107.0844237280190043 ) ) ;
#89778 = CARTESIAN_POINT ( 'NONE',  ( 0.05219959533909260263, 19.03943276465977164, 39.99890960531436690 ) ) ;
#89779 = CARTESIAN_POINT ( 'NONE',  ( -21.55341960407619339, 5.719274019375674811, 93.54275706135234714 ) ) ;
#89781 = CARTESIAN_POINT ( 'NONE',  ( -21.52544592524334988, -5.823673210054445271, 63.95942372801901854 ) ) ;
#89780 = CARTESIAN_POINT ( 'NONE',  ( -16.51473224551069308, -9.474510206698971260, 86.66557627198102409 ) ) ;
#89782 = CARTESIAN_POINT ( 'NONE',  ( 27.73933785331498214, 9.013057229001095294, 144.4750000027311501 ) ) ;
#89783 = CARTESIAN_POINT ( 'NONE',  ( -5.049401038298153566, 19.05341960407611168, 105.2072429386476671 ) ) ;
#89784 = DIRECTION ( 'NONE',  ( 0.000000000000000000, 0.000000000000000000, 1.000000000000000000 ) ) ;
#89787 = CARTESIAN_POINT ( 'NONE',  ( 18.62759615963255655, 10.81492255796105972, 56.66775706135235424 ) ) ;
#89786 = CARTESIAN_POINT ( 'NONE',  ( -8.314922557961024197, 14.29746914071037800, 67.91775706135234714 ) ) ;
#89785 = CARTESIAN_POINT ( 'NONE',  ( -8.314922557961024197, 14.29746914071037800, 57.91775706135234714 ) ) ;
#89788 = CARTESIAN_POINT ( 'NONE',  ( -5.719274019375665041, -21.55341960407619695, 94.79275706135234714 ) ) ;
#89789 = DIRECTION ( 'NONE',  ( 0.000000000000000000, 0.000000000000000000, -1.000000000000000000 ) ) ;
#89790 = CARTESIAN_POINT ( 'NONE',  ( 4.483927247898790824, -16.52544592524335698, 25.20942372801901854 ) ) ;
#89791 = CARTESIAN_POINT ( 'NONE',  ( 0.05219959533909260263, 19.03943276465977164, 79.99890960531436690 ) ) ;
#89792 = CARTESIAN_POINT ( 'NONE',  ( -16.51473224551069308, -9.474510206698971260, 96.66557627198102409 ) ) ;
#89793 = CIRCLE ( 'NONE', #76790, 0.5000000000000005551 ) ;
#89794 = CARTESIAN_POINT ( 'NONE',  ( -16.51473224551069308, -9.474510206698971260, 111.6655762719810383 ) ) ;
#89795 = CARTESIAN_POINT ( 'NONE',  ( -5.153800228976328057, -19.02544592524343514, 32.29057627198102409 ) ) ;
#89797 = ADVANCED_FACE ( 'NONE', ( #194614 ), #13127, .T. ) ;
#89796 = CARTESIAN_POINT ( 'NONE',  ( -10.81492255796078084, -18.62759615963271287, 27.08224293864769550 ) ) ;
#89798 = CARTESIAN_POINT ( 'NONE',  ( 4.483927247898790824, -16.52544592524335698, 95.20942372801903275 ) ) ;
#89800 = CARTESIAN_POINT ( 'NONE',  ( 19.05341960407611168, 5.049401038298154454, 68.95724293864769550 ) ) ;
#89799 = CARTESIAN_POINT ( 'NONE',  ( -16.52544592524342804, 4.483927247898546575, 81.04057627198102409 ) ) ;
#89801 = CARTESIAN_POINT ( 'NONE',  ( -18.67979575497193778, 10.72451020669871902, 88.33442372801901854 ) ) ;
#89802 = DIRECTION ( 'NONE',  ( 1.000000000000000000, 0.000000000000000000, 0.000000000000000000 ) ) ;
#89803 = CARTESIAN_POINT ( 'NONE',  ( -16.55341960407617563, 4.379528057220093196, 28.54275706135234358 ) ) ;
#89804 = CARTESIAN_POINT ( 'NONE',  ( 4.483927247898545687, 16.52544592524342804, 69.79057627198102409 ) ) ;
#89805 = CARTESIAN_POINT ( 'NONE',  ( -5.823673210054431948, 21.52544592524334988, 32.70942372801900433 ) ) ;
#89806 = CARTESIAN_POINT ( 'NONE',  ( 21.52544592524344225, -5.823673210054117533, 78.54057627198103830 ) ) ;
#89807 = CARTESIAN_POINT ( 'NONE',  ( -0.05219959533936034679, 19.03943276465977164, 37.50109039468567573 ) ) ;
#89808 = CARTESIAN_POINT ( 'NONE',  ( -18.22780087662119897, 5.500000000000102141, 46.01763182126894947 ) ) ;
#89809 = CARTESIAN_POINT ( 'NONE',  ( 19.02544592524343514, -5.153800228976328945, 83.54057627198100988 ) ) ;
#89810 = CARTESIAN_POINT ( 'NONE',  ( 12.14591786802309770, 12.06949235617756955, 44.37390960531435979 ) ) ;
#89811 = EDGE_CURVE ( 'NONE', #126623, #10845, #76266, .T. ) ;
#89812 = CARTESIAN_POINT ( 'NONE',  ( -16.53943276465976808, 0.05219959533911058130, 31.24890960531435979 ) ) ;
#89813 = CARTESIAN_POINT ( 'NONE',  ( -8.224510206698735004, -14.34966873604973081, 109.5844237280190328 ) ) ;
#89814 = CARTESIAN_POINT ( 'NONE',  ( 19.05341960407617918, -5.049401038297876454, 71.04275706135234714 ) ) ;
#89815 = DIRECTION ( 'NONE',  ( -1.000000000000000000, 0.000000000000000000, 0.000000000000000000 ) ) ;
#89816 = CARTESIAN_POINT ( 'NONE',  ( 5.153800228976335163, 19.02544592524342804, 114.7905762719810241 ) ) ;
#89817 = CARTESIAN_POINT ( 'NONE',  ( -16.52544592524342804, 4.483927247898546575, 71.04057627198103830 ) ) ;
#89818 = CARTESIAN_POINT ( 'NONE',  ( -17.72696623605163424, 5.499999999999873879, 58.59811031808418846 ) ) ;
#89820 = CARTESIAN_POINT ( 'NONE',  ( -21.52544592524343514, 5.823673210054127303, 31.04057627198102409 ) ) ;
#89819 = CARTESIAN_POINT ( 'NONE',  ( 9.474510206698971260, -16.51473224551069308, 27.91557627198103120 ) ) ;
#89821 = CARTESIAN_POINT ( 'NONE',  ( -18.62759615963270932, 10.81492255796079327, 65.83224293864769550 ) ) ;
#89822 = CARTESIAN_POINT ( 'NONE',  ( -16.52544592524342804, 4.483927247898546575, 111.0405762719810525 ) ) ;
#89824 = CARTESIAN_POINT ( 'NONE',  ( -13.97604488694527625, -13.89961937509977652, 46.87390960531435979 ) ) ;
#89823 = CARTESIAN_POINT ( 'NONE',  ( 16.53943276465976808, 0.05219959533934440121, 66.25109039468567573 ) ) ;
#89825 = CARTESIAN_POINT ( 'NONE',  ( -5.719274019375665041, -21.55341960407619695, 54.79275706135235424 ) ) ;
#89826 = VERTEX_POINT ( 'NONE', #164284 ) ;
#89827 = CARTESIAN_POINT ( 'NONE',  ( -12.06949235617756955, 12.14591786802309770, 100.6239096053143811 ) ) ;
#89828 = CARTESIAN_POINT ( 'NONE',  ( 17.50000000000000000, -5.499999999999992895, 36.21769037696435589 ) ) ;
#89829 = CARTESIAN_POINT ( 'NONE',  ( 36.91746824999999177, 2.880721459617395097E-14, -8.124999997268814056 ) ) ;
#89831 = CARTESIAN_POINT ( 'NONE',  ( -10.81492255796078084, -18.62759615963271287, 37.08224293864768129 ) ) ;
#89830 = CARTESIAN_POINT ( 'NONE',  ( 5.000000000000000000, -139.5000000000000000, 13.35010376910484275 ) ) ;
#89832 = DIRECTION ( 'NONE',  ( 0.000000000000000000, 0.8660254037844380415, -0.5000000000000011102 ) ) ;
#89833 = CARTESIAN_POINT ( 'NONE',  ( -18.62759615963255300, -10.81492255796106328, 69.16775706135234714 ) ) ;
#89835 = CARTESIAN_POINT ( 'NONE',  ( 4.379528057220339221, -16.55341960407611168, 47.70724293864770260 ) ) ;
#89834 = CARTESIAN_POINT ( 'NONE',  ( -8.224510206698735004, -14.34966873604973081, 54.58442372801901143 ) ) ;
#89836 = CARTESIAN_POINT ( 'NONE',  ( 21.52544592524344225, -5.823673210054117533, 63.54057627198103830 ) ) ;
#89837 = CARTESIAN_POINT ( 'NONE',  ( -5.719274019375978568, 21.55341960407610458, 60.20724293864768839 ) ) ;
#89838 = CARTESIAN_POINT ( 'NONE',  ( -21.16473053983486352, -10.71450305990368790, 170.2845851188454560 ) ) ;
#89840 = CARTESIAN_POINT ( 'NONE',  ( -19.02544592524342804, 5.153800228976336051, 111.0405762719810099 ) ) ;
#89839 = CARTESIAN_POINT ( 'NONE',  ( 13.97604488694548053, -13.89961937509957401, 80.62609039468567573 ) ) ;
#89841 = CARTESIAN_POINT ( 'NONE',  ( 0.05219959533909260263, 19.03943276465977164, 49.99890960531435979 ) ) ;
#89842 = CARTESIAN_POINT ( 'NONE',  ( 5.049401038298161559, -19.05341960407611168, 22.70724293864769194 ) ) ;
#89843 = FACE_BOUND ( 'NONE', #47936, .T. ) ;
#89844 = ORIENTED_EDGE ( 'NONE', *, *, #52535, .F. ) ;
#89845 = CARTESIAN_POINT ( 'NONE',  ( -12.06949235617739369, -12.14591786802326823, 64.37609039468568994 ) ) ;
#89846 = CARTESIAN_POINT ( 'NONE',  ( -5.823673210054116645, -21.52544592524344225, 102.2905762719810383 ) ) ;
#89847 = CARTESIAN_POINT ( 'NONE',  ( -19.05341960407611168, -5.049401038298163336, 61.45724293864769550 ) ) ;
#89848 = CARTESIAN_POINT ( 'NONE',  ( 15.72974639402176855, 15.80617190586768217, 41.87609039468568284 ) ) ;
#89849 = CARTESIAN_POINT ( 'NONE',  ( 19.03943276465977164, -0.05219959533909143690, 98.74890960531436690 ) ) ;
#89850 = CARTESIAN_POINT ( 'NONE',  ( -30.87493573979928385, -25.21320017017148984, -21.56479137964121406 ) ) ;
#89851 = ORIENTED_EDGE ( 'NONE', *, *, #16988, .F. ) ;
#89852 = CARTESIAN_POINT ( 'NONE',  ( -18.62759615963255300, -10.81492255796106328, 34.16775706135234714 ) ) ;
#89854 = CARTESIAN_POINT ( 'NONE',  ( -0.05219959533936034679, 19.03943276465977164, 82.50109039468567573 ) ) ;
#89853 = CARTESIAN_POINT ( 'NONE',  ( -16.46253265017160317, 9.564922557960807481, 110.8322429386476955 ) ) ;
#89855 = CARTESIAN_POINT ( 'NONE',  ( 9.564922557961047289, -16.46253265017146816, 45.41775706135232582 ) ) ;
#89856 = CARTESIAN_POINT ( 'NONE',  ( -21.52544592524343514, 5.823673210054127303, 96.04057627198102409 ) ) ;
#89857 = CARTESIAN_POINT ( 'NONE',  ( -5.049401038297874678, -19.05341960407617918, 29.79275706135232227 ) ) ;
#89858 = CARTESIAN_POINT ( 'NONE',  ( -13.89961937509957401, -13.97604488694547875, 44.37609039468566863 ) ) ;
#89859 = CARTESIAN_POINT ( 'NONE',  ( 8.224510206698742110, 14.34966873604972548, 97.08442372801904696 ) ) ;
#89861 = VERTEX_POINT ( 'NONE', #87423 ) ;
#89860 = CARTESIAN_POINT ( 'NONE',  ( 1.988064558232696151E-15, -30.27659582821216588, 146.4843446569000207 ) ) ;
#89862 = CARTESIAN_POINT ( 'NONE',  ( -16.46253265017160317, 9.564922557960807481, 70.83224293864770971 ) ) ;
#89863 = CARTESIAN_POINT ( 'NONE',  ( 21.55341960407619695, -5.719274019375665929, 76.04275706135237556 ) ) ;
#89864 = CARTESIAN_POINT ( 'NONE',  ( 21.55341960407619695, -5.719274019375665929, 76.04275706135237556 ) ) ;
#89865 = CARTESIAN_POINT ( 'NONE',  ( -17.72560187377285246, -5.500000000000057732, 54.07814504131319921 ) ) ;
#89866 = CARTESIAN_POINT ( 'NONE',  ( -16.51473224551069308, -9.474510206698971260, 91.66557627198103830 ) ) ;
#89867 = CARTESIAN_POINT ( 'NONE',  ( 21.53943276465977519, 0.05219959533937863772, 66.25109039468567573 ) ) ;
#89868 = CARTESIAN_POINT ( 'NONE',  ( -0.05219959533936034679, 19.03943276465977164, 107.5010903946856615 ) ) ;
#89869 = CARTESIAN_POINT ( 'NONE',  ( -9.474510206698964154, 16.51473224551069663, 65.41557627198102409 ) ) ;
#89870 = CARTESIAN_POINT ( 'NONE',  ( 9.474510206698971260, -16.51473224551069308, 107.9155762719810383 ) ) ;
#89871 = CARTESIAN_POINT ( 'NONE',  ( -16.51473224551069308, -9.474510206698971260, 76.66557627198103830 ) ) ;
#89872 = CARTESIAN_POINT ( 'NONE',  ( 17.50000000000003197, -3.228180402290367290, 22.22094556969252466 ) ) ;
#89873 = CARTESIAN_POINT ( 'NONE',  ( -19.03943276465977164, 0.05219959533909376836, 71.24890960531435269 ) ) ;
#89874 = CARTESIAN_POINT ( 'NONE',  ( -9.474510206698964154, 16.51473224551069663, 55.41557627198103120 ) ) ;
#89875 = CARTESIAN_POINT ( 'NONE',  ( 15.80617190586746368, 15.72974639402197994, 109.3739096053143811 ) ) ;
#89876 = CARTESIAN_POINT ( 'NONE',  ( -16.53943276465976808, -0.05219959533934237506, 88.75109039468567573 ) ) ;
#89877 = CARTESIAN_POINT ( 'NONE',  ( 6.853560127763690168, -1.304723572972866119, -64.38700459888464422 ) ) ;
#89878 = CARTESIAN_POINT ( 'NONE',  ( 9.564922557961047289, -16.46253265017146816, 45.41775706135232582 ) ) ;
#89879 = CARTESIAN_POINT ( 'NONE',  ( 16.46253265017160672, -9.564922557960803928, 78.33224293864769550 ) ) ;
#89880 = CARTESIAN_POINT ( 'NONE',  ( -14.29746914071049879, 8.314922557960819915, 70.83224293864770971 ) ) ;
#89881 = CARTESIAN_POINT ( 'NONE',  ( 16.53943276465976808, -0.05219959533910856209, 103.7489096053143669 ) ) ;
#89882 = CARTESIAN_POINT ( 'NONE',  ( -13.97604488694527625, -13.89961937509977652, 111.8739096053143243 ) ) ;
#89883 = CARTESIAN_POINT ( 'NONE',  ( -5.049401038298153566, 19.05341960407611168, 110.2072429386476671 ) ) ;
#89884 = CARTESIAN_POINT ( 'NONE',  ( -8.224510206698948167, 14.34966873604960824, 85.41557627198102409 ) ) ;
#89885 = CARTESIAN_POINT ( 'NONE',  ( 3.765340386950246872E-15, -39.95163481335715971, -3.502157773949823305 ) ) ;
#89886 = CARTESIAN_POINT ( 'NONE',  ( -9.564922557961040184, 16.46253265017147172, 27.91775706135232582 ) ) ;
#89887 = CARTESIAN_POINT ( 'NONE',  ( 14.34966873604972726, -8.224510206698740333, 90.83442372801901854 ) ) ;
#89888 = CARTESIAN_POINT ( 'NONE',  ( -0.05219959533909027116, -19.03943276465977164, 77.49890960531435269 ) ) ;
#89889 = CARTESIAN_POINT ( 'NONE',  ( 5.719274019375673035, 21.55341960407619339, 52.29275706135236135 ) ) ;
#89890 = CARTESIAN_POINT ( 'NONE',  ( 5.823673210054125526, 21.52544592524343514, 39.79057627198103830 ) ) ;
#89891 = CARTESIAN_POINT ( 'NONE',  ( -15.72974639402197994, 15.80617190586746368, 115.6239096053143669 ) ) ;
#89892 = CARTESIAN_POINT ( 'NONE',  ( -5.719274019375978568, 21.55341960407610458, 75.20724293864769550 ) ) ;
#89893 = CARTESIAN_POINT ( 'NONE',  ( 4.483927247898545687, 16.52544592524342804, 99.79057627198103830 ) ) ;
#89894 = CARTESIAN_POINT ( 'NONE',  ( 13.97604488694548053, -13.89961937509957401, 60.62609039468564731 ) ) ;
#89895 = CARTESIAN_POINT ( 'NONE',  ( 5.153800228976335163, 19.02544592524342804, 29.79057627198102409 ) ) ;
#89896 = CARTESIAN_POINT ( 'NONE',  ( -19.02544592524342804, 5.153800228976336051, 81.04057627198103830 ) ) ;
#89897 = CARTESIAN_POINT ( 'NONE',  ( 13.89961937509977652, -13.97604488694527269, 88.12390960531438111 ) ) ;
#89898 = CARTESIAN_POINT ( 'NONE',  ( 4.483927247898545687, 16.52544592524342804, 99.79057627198103830 ) ) ;
#89899 = CARTESIAN_POINT ( 'NONE',  ( 4.379528057220339221, -16.55341960407611168, 32.70724293864770260 ) ) ;
#89900 = CARTESIAN_POINT ( 'NONE',  ( -16.55341960407617563, 4.379528057220093196, 23.54275706135235424 ) ) ;
#89901 = CARTESIAN_POINT ( 'NONE',  ( -21.53943276465977519, -0.05219959533937600094, 103.7510903946857042 ) ) ;
#89902 = CARTESIAN_POINT ( 'NONE',  ( -19.02544592524342804, 5.153800228976336051, 106.0405762719810241 ) ) ;
#89903 = CARTESIAN_POINT ( 'NONE',  ( -5.719274019375665041, -21.55341960407619695, 19.79275706135235069 ) ) ;
#89904 = CARTESIAN_POINT ( 'NONE',  ( -19.03943276465977164, 0.05219959533909376836, 46.24890960531435979 ) ) ;
#89905 = CARTESIAN_POINT ( 'NONE',  ( 4.483927247898790824, -16.52544592524335698, 50.20942372801901854 ) ) ;
#89906 = CARTESIAN_POINT ( 'NONE',  ( -19.05341960407617563, 5.049401038297882671, 113.5427570613523471 ) ) ;
#89908 = B_SPLINE_CURVE_WITH_KNOTS ( 'NONE', 3,
 ( #121300, #29313, #166836, #133491, #195183, #120307, #58641, #164843, #26339, #152630, #182000, #89976, #151657, #14120, #104158, #165839, #199145, #197176, #73835, #59626, #122286, #135506, #43483, #183975, #45461, #105150 ),
 .UNSPECIFIED., .F., .F.,
 ( 4, 2, 2, 2, 2, 2, 2, 2, 2, 2, 2, 2, 4 ),
 ( 2.788259459799404871E-07, 0.0002964138711649451233, 0.0005925489163839094348, 0.0008886839616028737463, 0.001184819006821837733, 0.001777089097259766572, 0.002369359187697695195, 0.002665494232916662543, 0.002961629278135629890, 0.003257764323354597237, 0.003553899368573564151, 0.004146169459011502315, 0.004738439549449439611 ),
 .UNSPECIFIED. ) ;
#89907 = CARTESIAN_POINT ( 'NONE',  ( 19.02544592524343514, -5.153800228976328945, 38.54057627198103120 ) ) ;
#89909 = CARTESIAN_POINT ( 'NONE',  ( -14.29746914071049879, 8.314922557960819915, 95.83224293864770971 ) ) ;
#89910 = CARTESIAN_POINT ( 'NONE',  ( 10.81492255796078972, 18.62759615963270932, 99.58224293864770971 ) ) ;
#89911 = CARTESIAN_POINT ( 'NONE',  ( 9.564922557961047289, -16.46253265017146816, 75.41775706135234714 ) ) ;
#89912 =( NAMED_UNIT ( * ) SI_UNIT ( $, .STERADIAN. ) SOLID_ANGLE_UNIT ( ) );
#89913 = CARTESIAN_POINT ( 'NONE',  ( -9.564922557960796823, -16.46253265017161027, 87.08224293864769550 ) ) ;
#89914 = CARTESIAN_POINT ( 'NONE',  ( 21.53943276465977519, -0.05219959533907433946, 113.7489096053143527 ) ) ;
#89915 = CARTESIAN_POINT ( 'NONE',  ( 9.564922557960805705, 16.46253265017160317, 24.58224293864769194 ) ) ;
#89916 = CARTESIAN_POINT ( 'NONE',  ( -5.153800228976328057, -19.02544592524343514, 87.29057627198103830 ) ) ;
#89917 = CARTESIAN_POINT ( 'NONE',  ( 16.31925111598458500, -7.325300261831533710, 112.6642453896725726 ) ) ;
#89918 = CARTESIAN_POINT ( 'NONE',  ( 5.153800228976335163, 19.02544592524342804, 89.79057627198102409 ) ) ;
#89920 = CARTESIAN_POINT ( 'NONE',  ( 16.52544592524342804, -4.483927247898539470, 88.54057627198103830 ) ) ;
#89919 = CARTESIAN_POINT ( 'NONE',  ( 15.80617190586769283, -15.72974639402175789, 35.62609039468568994 ) ) ;
#89921 = CARTESIAN_POINT ( 'NONE',  ( -13.97604488694527625, -13.89961937509977652, 91.87390960531432427 ) ) ;
#89922 = CARTESIAN_POINT ( 'NONE',  ( -13.89961937509957401, -13.97604488694547875, 29.37609039468565797 ) ) ;
#89923 = CARTESIAN_POINT ( 'NONE',  ( 8.314922557961029526, -14.29746914071037800, 45.41775706135234003 ) ) ;
#89924 = CARTESIAN_POINT ( 'NONE',  ( 18.62759615963255655, 10.81492255796105972, 66.66775706135234714 ) ) ;
#89925 = AXIS2_PLACEMENT_3D ( 'NONE', #140294, #29170, #75643 ) ;
#89926 = CARTESIAN_POINT ( 'NONE',  ( 0.05219959533934541429, -16.53943276465976808, 25.00109039468567218 ) ) ;
#89927 = CARTESIAN_POINT ( 'NONE',  ( -5.049401038298153566, 19.05341960407611168, 75.20724293864769550 ) ) ;
#89928 = CARTESIAN_POINT ( 'NONE',  ( -16.46253265017146816, -9.564922557961047289, 94.16775706135233293 ) ) ;
#89929 = CARTESIAN_POINT ( 'NONE',  ( -0.05219959533934338120, 16.53943276465976808, 67.50109039468568994 ) ) ;
#89930 = CARTESIAN_POINT ( 'NONE',  ( -5.823673210054431948, 21.52544592524334988, 107.7094237280190328 ) ) ;
#89931 = CARTESIAN_POINT ( 'NONE',  ( 19.03943276465977164, 0.05219959533936151252, 76.25109039468566152 ) ) ;
#89932 = CARTESIAN_POINT ( 'NONE',  ( -13.89961937509977652, 13.97604488694528158, 55.62390960531434558 ) ) ;
#89933 = CARTESIAN_POINT ( 'NONE',  ( 5.823673210054125526, 21.52544592524343514, 84.79057627198102409 ) ) ;
#89935 = CARTESIAN_POINT ( 'NONE',  ( -13.89961937509957401, -13.97604488694547875, 79.37609039468567573 ) ) ;
#89934 = CARTESIAN_POINT ( 'NONE',  ( -0.05219959533910754901, -16.53943276465976808, 82.49890960531436690 ) ) ;
#89936 = CARTESIAN_POINT ( 'NONE',  ( -19.25918095147779496, -5.499999999999484857, 69.45284276293932635 ) ) ;
#89937 = CARTESIAN_POINT ( 'NONE',  ( 9.564922557961047289, -16.46253265017146816, 50.41775706135233293 ) ) ;
#89938 = CARTESIAN_POINT ( 'NONE',  ( 8.224510206698742110, 14.34966873604972548, 112.0844237280190185 ) ) ;
#89939 = CARTESIAN_POINT ( 'NONE',  ( -14.34966873604960291, -8.224510206698953496, 66.66557627198102409 ) ) ;
#89941 = CARTESIAN_POINT ( 'NONE',  ( -27.73933785331498925, 9.013057229001089965, 148.7750000027311899 ) ) ;
#89940 = CARTESIAN_POINT ( 'NONE',  ( -5.823673210054431948, 21.52544592524334988, 97.70942372801904696 ) ) ;
#89942 = CARTESIAN_POINT ( 'NONE',  ( -18.67979575497178146, -10.72451020669898902, 111.6655762719810525 ) ) ;
#89943 = CARTESIAN_POINT ( 'NONE',  ( 16.46253265017160672, -9.564922557960803928, 63.33224293864769550 ) ) ;
#89944 = CARTESIAN_POINT ( 'NONE',  ( -21.55341960407619339, 5.719274019375674811, 78.54275706135236135 ) ) ;
#89945 = CARTESIAN_POINT ( 'NONE',  ( -16.51473224551069308, -9.474510206698971260, 56.66557627198103120 ) ) ;
#89946 = EDGE_LOOP ( 'NONE', ( #182370, #180900, #197336, #78024, #85320, #199399, #88067, #19883 ) ) ;
#89947 = CARTESIAN_POINT ( 'NONE',  ( -5.153800228976328057, -19.02544592524343514, 27.29057627198103120 ) ) ;
#89948 = CARTESIAN_POINT ( 'NONE',  ( 21.55341960407610458, 5.719274019375980345, 23.95724293864769550 ) ) ;
#89949 = CARTESIAN_POINT ( 'NONE',  ( -14.29746914071049879, 8.314922557960819915, 70.83224293864770971 ) ) ;
#89950 = CARTESIAN_POINT ( 'NONE',  ( -13.97604488694527625, -13.89961937509977652, 46.87390960531435979 ) ) ;
#89951 = CARTESIAN_POINT ( 'NONE',  ( 14.34966873604960469, 8.224510206698951720, 94.16557627198103830 ) ) ;
#89952 = CARTESIAN_POINT ( 'NONE',  ( 15.80617190586746368, 15.72974639402197994, 114.3739096053143527 ) ) ;
#89953 = CARTESIAN_POINT ( 'NONE',  ( -21.53943276465977519, -0.05219959533937600094, 48.75109039468568284 ) ) ;
#89954 = CARTESIAN_POINT ( 'NONE',  ( -19.03943276465977164, 0.05219959533909376836, 26.24890960531435624 ) ) ;
#89955 = CARTESIAN_POINT ( 'NONE',  ( 16.53943276465976808, 0.05219959533934440121, 61.25109039468567573 ) ) ;
#89956 = CARTESIAN_POINT ( 'NONE',  ( -5.719274019375978568, 21.55341960407610458, 100.2072429386476955 ) ) ;
#89957 = CARTESIAN_POINT ( 'NONE',  ( 18.67979575497178502, 10.72451020669898547, 99.16557627198100988 ) ) ;
#89959 = CARTESIAN_POINT ( 'NONE',  ( -0.05219959533909027116, -19.03943276465977164, 57.49890960531435979 ) ) ;
#89958 = CARTESIAN_POINT ( 'NONE',  ( -5.049401038297874678, -19.05341960407617918, 29.79275706135232227 ) ) ;
#89960 = CARTESIAN_POINT ( 'NONE',  ( 18.22780087662123805, -5.499999999999976019, 73.51763182126894947 ) ) ;
#89961 = CARTESIAN_POINT ( 'NONE',  ( 21.52544592524334988, 5.823673210054432836, 61.45942372801901854 ) ) ;
#89962 = CARTESIAN_POINT ( 'NONE',  ( -15.80617190586745835, -15.72974639402198527, 51.87390960531437401 ) ) ;
#89963 = CARTESIAN_POINT ( 'NONE',  ( 16.52544592524342804, -4.483927247898539470, 28.54057627198103120 ) ) ;
#89965 = CARTESIAN_POINT ( 'NONE',  ( 10.72451020669871369, 18.67979575497193778, 102.0844237280190185 ) ) ;
#89964 = CARTESIAN_POINT ( 'NONE',  ( -0.05219959533937732626, 21.53943276465977519, 82.50109039468568994 ) ) ;
#89966 = CARTESIAN_POINT ( 'NONE',  ( -16.46253265017146816, -9.564922557961047289, 44.16775706135232582 ) ) ;
#89967 = CARTESIAN_POINT ( 'NONE',  ( 12.14591786802327356, -12.06949235617739191, 95.62609039468568994 ) ) ;
#89968 = CARTESIAN_POINT ( 'NONE',  ( -21.52544592524334988, -5.823673210054445271, 58.95942372801902565 ) ) ;
#89969 = CARTESIAN_POINT ( 'NONE',  ( 16.51473224551069308, 9.474510206698969483, 54.16557627198103120 ) ) ;
#89970 = CARTESIAN_POINT ( 'NONE',  ( -5.153800228976607833, 19.02544592524334988, 37.70942372801899722 ) ) ;
#89971 = CARTESIAN_POINT ( 'NONE',  ( 18.62759615963271287, -10.81492255796078972, 43.33224293864769550 ) ) ;
#89972 = CARTESIAN_POINT ( 'NONE',  ( -0.05219959533937732626, 21.53943276465977519, 27.50109039468567929 ) ) ;
#89973 = CARTESIAN_POINT ( 'NONE',  ( 5.823673210054125526, 21.52544592524343514, 84.79057627198102409 ) ) ;
#89974 = CARTESIAN_POINT ( 'NONE',  ( 13.89961937509957401, 13.97604488694547697, 86.87609039468567573 ) ) ;
#89975 = CARTESIAN_POINT ( 'NONE',  ( -12.14591786802326823, 12.06949235617739902, 58.12609039468568994 ) ) ;
#89977 = CARTESIAN_POINT ( 'NONE',  ( 5.719274019375991003, -21.55341960407610458, 97.70724293864772392 ) ) ;
#89976 = CARTESIAN_POINT ( 'NONE',  ( -6.132035242901182848, 4.065169771515680708, -62.28151743970310861 ) ) ;
#89979 = CARTESIAN_POINT ( 'NONE',  ( -0.05219959533910754901, -16.53943276465976808, 82.49890960531436690 ) ) ;
#89978 = CARTESIAN_POINT ( 'NONE',  ( 8.314922557961029526, -14.29746914071037800, 80.41775706135234714 ) ) ;
#89980 = CARTESIAN_POINT ( 'NONE',  ( -37.99626262588766679, 2.428612866367529932E-14, -8.000000000000000000 ) ) ;
#89981 = CARTESIAN_POINT ( 'NONE',  ( 13.97604488694548053, -13.89961937509957401, 100.6260903946856615 ) ) ;
#89982 = CARTESIAN_POINT ( 'NONE',  ( 18.62759615963271287, -10.81492255796078972, 38.33224293864768839 ) ) ;
#89983 = DIRECTION ( 'NONE',  ( -0.000000000000000000, -0.000000000000000000, 1.000000000000000000 ) ) ;
#89984 = CARTESIAN_POINT ( 'NONE',  ( -16.55341960407617563, 4.379528057220093196, 38.54275706135234714 ) ) ;
#89985 = CARTESIAN_POINT ( 'NONE',  ( 18.62759615963271287, -10.81492255796078972, 113.3322429386476955 ) ) ;
#89986 = CARTESIAN_POINT ( 'NONE',  ( 5.823673210054125526, 21.52544592524343514, 34.79057627198103120 ) ) ;
#89987 = CARTESIAN_POINT ( 'NONE',  ( -8.314922557961024197, 14.29746914071037800, 72.91775706135234714 ) ) ;
#89988 = CARTESIAN_POINT ( 'NONE',  ( -9.564922557960796823, -16.46253265017161027, 82.08224293864768129 ) ) ;
#89990 = CARTESIAN_POINT ( 'NONE',  ( 19.03943276465977164, -0.05219959533909143690, 23.74890960531435269 ) ) ;
#89989 = CARTESIAN_POINT ( 'NONE',  ( 5.719274019375673035, 21.55341960407619339, 57.29275706135234714 ) ) ;
#89991 = CARTESIAN_POINT ( 'NONE',  ( 5.719274019375991003, -21.55341960407610458, 22.70724293864769194 ) ) ;
#89992 = VERTEX_POINT ( 'NONE', #150105 ) ;
#89993 = CARTESIAN_POINT ( 'NONE',  ( 5.153800228976615827, -19.02544592524334988, 35.20942372801899722 ) ) ;
#89994 = CARTESIAN_POINT ( 'NONE',  ( 4.379528057220092307, 16.55341960407617563, 52.29275706135236135 ) ) ;
#89995 = CARTESIAN_POINT ( 'NONE',  ( -19.02544592524342804, 5.153800228976336051, 111.0405762719810099 ) ) ;
#89996 = CARTESIAN_POINT ( 'NONE',  ( -13.97604488694527625, -13.89961937509977652, 71.87390960531433848 ) ) ;
#89997 = CARTESIAN_POINT ( 'NONE',  ( -4.483927247898782831, 16.52544592524335698, 102.7094237280190185 ) ) ;
#89998 = FACE_OUTER_BOUND ( 'NONE', #62187, .T. ) ;
#89999 = CARTESIAN_POINT ( 'NONE',  ( 4.379528057220339221, -16.55341960407611168, 92.70724293864770971 ) ) ;
#90000 = CARTESIAN_POINT ( 'NONE',  ( 15.80617190586746368, 15.72974639402197994, 29.37390960531435269 ) ) ;
#90001 = CARTESIAN_POINT ( 'NONE',  ( 16.46253265017160672, -9.564922557960803928, 33.33224293864770260 ) ) ;
#90002 = CARTESIAN_POINT ( 'NONE',  ( -8.224510206698735004, -14.34966873604973081, 69.58442372801900433 ) ) ;
#90003 = CARTESIAN_POINT ( 'NONE',  ( 21.52544592524334988, 5.823673210054432836, 26.45942372801901854 ) ) ;
#90004 = CARTESIAN_POINT ( 'NONE',  ( 13.97604488694548053, -13.89961937509957401, 80.62609039468567573 ) ) ;
#90005 = CARTESIAN_POINT ( 'NONE',  ( -13.97604488694527625, -13.89961937509977652, 41.87390960531435979 ) ) ;
#90006 = CARTESIAN_POINT ( 'NONE',  ( 21.53943276465977519, -0.05219959533907433946, 73.74890960531433848 ) ) ;
#90007 = CARTESIAN_POINT ( 'NONE',  ( 13.89961937509977652, -13.97604488694527269, 113.1239096053143527 ) ) ;
#90008 = CARTESIAN_POINT ( 'NONE',  ( -10.72451020669870658, -18.67979575497194134, 94.58442372801901854 ) ) ;
#90009 = CARTESIAN_POINT ( 'NONE',  ( 16.51473224551069308, 9.474510206698969483, 69.16557627198102409 ) ) ;
#90010 = CARTESIAN_POINT ( 'NONE',  ( -8.224510206698735004, -14.34966873604973081, 54.58442372801901143 ) ) ;
#90011 = CARTESIAN_POINT ( 'NONE',  ( 21.53943276465977519, 0.05219959533937863772, 81.25109039468568994 ) ) ;
#90012 = CARTESIAN_POINT ( 'NONE',  ( 5.153800228976615827, -19.02544592524334988, 35.20942372801899722 ) ) ;
#90013 = CARTESIAN_POINT ( 'NONE',  ( -19.05341960407617563, 5.049401038297882671, 53.54275706135231871 ) ) ;
#90014 = EDGE_LOOP ( 'NONE', ( #188540, #84317, #92195, #142356 ) ) ;
#90015 = CARTESIAN_POINT ( 'NONE',  ( -15.72974639402176322, -15.80617190586768395, 49.37609039468569705 ) ) ;
#90016 = CARTESIAN_POINT ( 'NONE',  ( -7.215019197202725110, 1.452998035947277833, -62.28058590214430268 ) ) ;
#90017 = CARTESIAN_POINT ( 'NONE',  ( -9.564922557961040184, 16.46253265017147172, 42.91775706135234003 ) ) ;
#90018 = CARTESIAN_POINT ( 'NONE',  ( 13.97604488694527802, 13.89961937509977652, 94.37390960531436690 ) ) ;
#90019 = CARTESIAN_POINT ( 'NONE',  ( -16.51473224551069308, -9.474510206698971260, 76.66557627198103830 ) ) ;
#90020 = CARTESIAN_POINT ( 'NONE',  ( -16.55341960407611168, -4.379528057220339221, 41.45724293864769550 ) ) ;
#90021 = CARTESIAN_POINT ( 'NONE',  ( 18.67979575497178502, 10.72451020669898547, 34.16557627198102409 ) ) ;
#90022 = CARTESIAN_POINT ( 'NONE',  ( -36.91746825000000598, 2.428612866367529932E-14, -7.124999997268813168 ) ) ;
#90023 = DIRECTION ( 'NONE',  ( 1.000000000000000000, 0.000000000000000000, 0.000000000000000000 ) ) ;
#90024 = CARTESIAN_POINT ( 'NONE',  ( -10.72451020669870658, -18.67979575497194134, 104.5844237280190185 ) ) ;
#90025 = DIRECTION ( 'NONE',  ( -1.000000000000000000, -0.000000000000000000, -0.000000000000000000 ) ) ;
#90026 = CARTESIAN_POINT ( 'NONE',  ( -0.05219959533909027116, -19.03943276465977164, 37.49890960531436690 ) ) ;
#90027 = CARTESIAN_POINT ( 'NONE',  ( 2.500000000000000000, 1.768423874527822459, -1.021000000000002794 ) ) ;
#90028 = CARTESIAN_POINT ( 'NONE',  ( -28.91127206596838306, -24.07972945715490809, -8.000000000000003553 ) ) ;
#90029 = CARTESIAN_POINT ( 'NONE',  ( 12.14591786802327356, -12.06949235617739191, 50.62609039468568994 ) ) ;
#90031 = EDGE_CURVE ( 'NONE', #42534, #157648, #10598, .T. ) ;
#90030 = CARTESIAN_POINT ( 'NONE',  ( -18.62759615963270932, 10.81492255796079327, 70.83224293864770971 ) ) ;
#90032 = CARTESIAN_POINT ( 'NONE',  ( -16.55341960407611168, -4.379528057220339221, 41.45724293864769550 ) ) ;
#90034 = CARTESIAN_POINT ( 'NONE',  ( 16.51473224551069308, 9.474510206698969483, 104.1655762719810241 ) ) ;
#90033 = CARTESIAN_POINT ( 'NONE',  ( 9.564922557960805705, 16.46253265017160317, 34.58224293864770260 ) ) ;
#90035 = CARTESIAN_POINT ( 'NONE',  ( -18.67979575497193778, 10.72451020669871902, 28.33442372801902209 ) ) ;
#90036 = CARTESIAN_POINT ( 'NONE',  ( 19.03943276465977164, 0.05219959533936151252, 36.25109039468567573 ) ) ;
#90037 = CARTESIAN_POINT ( 'NONE',  ( 14.34966873604960469, 8.224510206698951720, 114.1655762719810383 ) ) ;
#90038 = CARTESIAN_POINT ( 'NONE',  ( 21.55341960407619695, -5.719274019375665929, 76.04275706135237556 ) ) ;
#90039 = CARTESIAN_POINT ( 'NONE',  ( 0.000000000000000000, 0.000000000000000000, -65.00100000000003320 ) ) ;
#90040 = CARTESIAN_POINT ( 'NONE',  ( -8.224510206698948167, 14.34966873604960824, 30.41557627198101699 ) ) ;
#90041 = DIRECTION ( 'NONE',  ( -1.000000000000000000, -0.000000000000000000, -0.000000000000000000 ) ) ;
#90042 = CARTESIAN_POINT ( 'NONE',  ( 0.05219959533907565091, 21.53943276465977519, 24.99890960531435624 ) ) ;
#90043 = CARTESIAN_POINT ( 'NONE',  ( 12.06949235617757843, -12.14591786802309237, 93.12390960531436690 ) ) ;
#90044 = CARTESIAN_POINT ( 'NONE',  ( -4.288219549287815902, -6.449757054545090185, -64.24412156979190058 ) ) ;
#90045 = CARTESIAN_POINT ( 'NONE',  ( -0.05219959533909027116, -19.03943276465977164, 82.49890960531436690 ) ) ;
#90046 = CARTESIAN_POINT ( 'NONE',  ( -16.55341960407611168, -4.379528057220339221, 76.45724293864769550 ) ) ;
#90047 = CARTESIAN_POINT ( 'NONE',  ( 19.05341960407617918, -5.049401038297876454, 106.0427570613523471 ) ) ;
#90048 = CARTESIAN_POINT ( 'NONE',  ( 21.55341960407610458, 5.719274019375980345, 68.95724293864769550 ) ) ;
#90049 = VERTEX_POINT ( 'NONE', #89414 ) ;
#90050 = CARTESIAN_POINT ( 'NONE',  ( -9.474510206698964154, 16.51473224551069663, 35.41557627198102409 ) ) ;
#90052 = CARTESIAN_POINT ( 'NONE',  ( -5.719274019375978568, 21.55341960407610458, 70.20724293864769550 ) ) ;
#90051 = CARTESIAN_POINT ( 'NONE',  ( -16.46253265017160317, 9.564922557960807481, 65.83224293864769550 ) ) ;
#90054 = CARTESIAN_POINT ( 'NONE',  ( 9.474510206698971260, -16.51473224551069308, 87.91557627198102409 ) ) ;
#90053 = CARTESIAN_POINT ( 'NONE',  ( -12.06949235617739369, -12.14591786802326823, 104.3760903946856899 ) ) ;
#90055 = CARTESIAN_POINT ( 'NONE',  ( -5.049401038297874678, -19.05341960407617918, 69.79275706135233293 ) ) ;
#90056 = CARTESIAN_POINT ( 'NONE',  ( -5.823673210054431948, 21.52544592524334988, 97.70942372801904696 ) ) ;
#90057 = CARTESIAN_POINT ( 'NONE',  ( 21.52544592524344225, -5.823673210054117533, 78.54057627198103830 ) ) ;
#90058 = CARTESIAN_POINT ( 'NONE',  ( -21.55341960407610458, -5.719274019375992779, 26.45724293864768839 ) ) ;
#90059 = CARTESIAN_POINT ( 'NONE',  ( 19.05341960407611168, 5.049401038298154454, 43.95724293864769550 ) ) ;
#90060 = CARTESIAN_POINT ( 'NONE',  ( 16.55341960407618274, -4.379528057220086978, 111.0427570613523613 ) ) ;
#90061 = CARTESIAN_POINT ( 'NONE',  ( -9.564922557960796823, -16.46253265017161027, 67.08224293864769550 ) ) ;
#90062 = CARTESIAN_POINT ( 'NONE',  ( -0.05219959533936034679, 19.03943276465977164, 82.50109039468567573 ) ) ;
#90063 = CARTESIAN_POINT ( 'NONE',  ( -18.62759615963255300, -10.81492255796106328, 109.1677570613523613 ) ) ;
#90064 = CARTESIAN_POINT ( 'NONE',  ( -4.483927247898539470, -16.52544592524342804, 72.29057627198102409 ) ) ;
#90065 = CARTESIAN_POINT ( 'NONE',  ( 0.05219959533907565091, 21.53943276465977519, 109.9989096053143527 ) ) ;
#90066 = CARTESIAN_POINT ( 'NONE',  ( 5.823673210054125526, 21.52544592524343514, 99.79057627198103830 ) ) ;
#90067 = CARTESIAN_POINT ( 'NONE',  ( 27.73933785331498569, 2.768321779492822058E-14, 140.3750000027311842 ) ) ;
#90068 = CARTESIAN_POINT ( 'NONE',  ( 21.53943276465977519, -0.05219959533907433946, 63.74890960531435979 ) ) ;
#90069 = CARTESIAN_POINT ( 'NONE',  ( -0.05219959533934338120, 16.53943276465976808, 82.50109039468568994 ) ) ;
#90070 = CARTESIAN_POINT ( 'NONE',  ( 16.55341960407611168, 4.379528057220329451, 103.9572429386476813 ) ) ;
#90071 = CARTESIAN_POINT ( 'NONE',  ( 16.51473224551069308, 9.474510206698969483, 64.16557627198102409 ) ) ;
#90072 = CARTESIAN_POINT ( 'NONE',  ( 4.379528057220092307, 16.55341960407617563, 112.2927570613523471 ) ) ;
#90073 = CARTESIAN_POINT ( 'NONE',  ( 18.67979575497194134, -10.72451020669871369, 45.83442372801901854 ) ) ;
#90074 = CARTESIAN_POINT ( 'NONE',  ( 9.474510206698971260, -16.51473224551069308, 112.9155762719810383 ) ) ;
#90075 = CARTESIAN_POINT ( 'NONE',  ( -0.05219959533937732626, 21.53943276465977519, 87.50109039468568994 ) ) ;
#90076 = CARTESIAN_POINT ( 'NONE',  ( 5.049401038298161559, -19.05341960407611168, 32.70724293864768129 ) ) ;
#90077 = CARTESIAN_POINT ( 'NONE',  ( 13.97604488694527802, 13.89961937509977652, 39.37390960531435269 ) ) ;
#90078 =( BOUNDED_CURVE ( )  B_SPLINE_CURVE ( 2, ( #168838, #30343, #93989, #18167, #61656, #187036, #123324, #31339, #79823, #185018, #157665 ),
 .UNSPECIFIED., .F., .F. ) 
 B_SPLINE_CURVE_WITH_KNOTS ( ( 3, 2, 2, 2, 2, 3 ),
 ( 0.09999999999999997780, 0.1199999999999999678, 0.1399999999999999856, 0.1600000000000000033, 0.1799999999999999933, 0.2000000000000000111 ),
 .UNSPECIFIED. ) 
 CURVE ( )  GEOMETRIC_REPRESENTATION_ITEM ( )  RATIONAL_B_SPLINE_CURVE ( ( 1.000000000000000000, 0.9510565162951533091, 1.000000000000000000, 0.9510565162951535312, 1.000000000000000000, 0.9510565162951535312, 1.000000000000000000, 0.9510565162951535312, 1.000000000000000000, 0.9510565162951535312, 1.000000000000000000 ) ) 
 REPRESENTATION_ITEM ( '' )  );
#90079 = EDGE_LOOP ( 'NONE', ( #61343, #32622 ) ) ;
#90080 = CARTESIAN_POINT ( 'NONE',  ( 21.55341960407619695, -5.719274019375665929, 66.04275706135236135 ) ) ;
#90081 = CARTESIAN_POINT ( 'NONE',  ( 19.03943276465977164, -0.05219959533909143690, 103.7489096053143669 ) ) ;
#90082 = CARTESIAN_POINT ( 'NONE',  ( 13.97604488694548053, -13.89961937509957401, 75.62609039468564731 ) ) ;
#90083 = CARTESIAN_POINT ( 'NONE',  ( 18.67979575497194134, -10.72451020669871369, 40.83442372801901854 ) ) ;
#90084 = CARTESIAN_POINT ( 'NONE',  ( 4.483927247898790824, -16.52544592524335698, 20.20942372801900788 ) ) ;
#90085 = CARTESIAN_POINT ( 'NONE',  ( 19.02544592524334988, 5.153800228976608722, 76.45942372801897591 ) ) ;
#90086 = CARTESIAN_POINT ( 'NONE',  ( 5.049401038298161559, -19.05341960407611168, 57.70724293864769550 ) ) ;
#90087 = CARTESIAN_POINT ( 'NONE',  ( 16.46253265017146816, 9.564922557961045513, 81.66775706135233293 ) ) ;
#90088 = CARTESIAN_POINT ( 'NONE',  ( 12.06949235617757843, -12.14591786802309237, 28.12390960531435979 ) ) ;
#90089 = CARTESIAN_POINT ( 'NONE',  ( 13.97604488694548053, -13.89961937509957401, 95.62609039468563310 ) ) ;
#90090 = CARTESIAN_POINT ( 'NONE',  ( 4.483927247898545687, 16.52544592524342804, 39.79057627198103830 ) ) ;
#90091 = CARTESIAN_POINT ( 'NONE',  ( 19.02544592524334988, 5.153800228976608722, 61.45942372801900433 ) ) ;
#90092 = CARTESIAN_POINT ( 'NONE',  ( 14.29746914071037800, 8.314922557961029526, 41.66775706135235424 ) ) ;
#90093 = CARTESIAN_POINT ( 'NONE',  ( 9.564922557961047289, -16.46253265017146816, 20.41775706135233293 ) ) ;
#90094 = CARTESIAN_POINT ( 'NONE',  ( 16.46253265017160672, -9.564922557960803928, 48.33224293864769550 ) ) ;
#90095 = CARTESIAN_POINT ( 'NONE',  ( -16.62475595723694255, -7.163666690055256581, 64.47286648189536606 ) ) ;
#90096 = CARTESIAN_POINT ( 'NONE',  ( -16.52544592524335698, -4.483927247898792601, 48.95942372801902565 ) ) ;
#90097 = DIRECTION ( 'NONE',  ( -0.000000000000000000, -0.000000000000000000, 1.000000000000000000 ) ) ;
#90098 = CARTESIAN_POINT ( 'NONE',  ( -8.571926809382608425, 26.38167802310805854, 142.4750000027312069 ) ) ;
#90099 = CARTESIAN_POINT ( 'NONE',  ( 16.51473224551069308, 9.474510206698969483, 94.16557627198103830 ) ) ;
#90100 = DIRECTION ( 'NONE',  ( 0.000000000000000000, 0.000000000000000000, 1.000000000000000000 ) ) ;
#90101 = CARTESIAN_POINT ( 'NONE',  ( 19.03943276465977164, 0.05219959533936151252, 86.25109039468567573 ) ) ;
#90102 = CARTESIAN_POINT ( 'NONE',  ( 21.55341960407610458, 5.719274019375980345, 23.95724293864769550 ) ) ;
#90104 = CARTESIAN_POINT ( 'NONE',  ( 13.97604488694548053, -13.89961937509957401, 100.6260903946856615 ) ) ;
#90103 = CARTESIAN_POINT ( 'NONE',  ( 21.55341960407619695, -5.719274019375665929, 111.0427570613523613 ) ) ;
#90105 = CARTESIAN_POINT ( 'NONE',  ( 4.483927247898545687, 16.52544592524342804, 109.7905762719810383 ) ) ;
#90106 = CARTESIAN_POINT ( 'NONE',  ( 19.03943276465977164, -0.05219959533909143690, 33.74890960531435979 ) ) ;
#90107 = CARTESIAN_POINT ( 'NONE',  ( 21.53943276465977519, -0.05219959533907433946, 53.74890960531437401 ) ) ;
#90108 = CARTESIAN_POINT ( 'NONE',  ( -19.05341960407611168, -5.049401038298163336, 26.45724293864769550 ) ) ;
#90109 = CARTESIAN_POINT ( 'NONE',  ( 17.50000000000000000, 5.499999999999992895, 101.7030961746583131 ) ) ;
#90110 = CARTESIAN_POINT ( 'NONE',  ( -19.02544592524334988, -5.153800228976617603, 73.95942372801900433 ) ) ;
#90111 = CARTESIAN_POINT ( 'NONE',  ( -4.483927247898539470, -16.52544592524342804, 52.29057627198102409 ) ) ;
#90112 = CARTESIAN_POINT ( 'NONE',  ( 5.823673210054125526, 21.52544592524343514, 34.79057627198103120 ) ) ;
#90113 = CARTESIAN_POINT ( 'NONE',  ( -18.62759615963255300, -10.81492255796106328, 94.16775706135237556 ) ) ;
#90114 = CARTESIAN_POINT ( 'NONE',  ( 0.05219959533907565091, 21.53943276465977519, 89.99890960531438111 ) ) ;
#90115 = CARTESIAN_POINT ( 'NONE',  ( -21.55341960407619339, 5.719274019375674811, 58.54275706135235424 ) ) ;
#90116 = CARTESIAN_POINT ( 'NONE',  ( -5.823673210054431948, 21.52544592524334988, 67.70942372801901854 ) ) ;
#90117 = CARTESIAN_POINT ( 'NONE',  ( 0.05219959533909260263, 19.03943276465977164, 99.99890960531436690 ) ) ;
#90119 = CARTESIAN_POINT ( 'NONE',  ( 10.72451020669871369, 18.67979575497193778, 62.08442372801901143 ) ) ;
#90118 = CARTESIAN_POINT ( 'NONE',  ( 8.224510206698742110, 14.34966873604972548, 97.08442372801904696 ) ) ;
#90120 = CARTESIAN_POINT ( 'NONE',  ( -4.379528057220328563, 16.55341960407611168, 115.2072429386476955 ) ) ;
#90121 = CARTESIAN_POINT ( 'NONE',  ( -12.14591786802309592, -12.06949235617757132, 61.87390960531436690 ) ) ;
#90122 = CARTESIAN_POINT ( 'NONE',  ( -16.52544592524342804, 4.483927247898546575, 31.04057627198102409 ) ) ;
#90123 = CARTESIAN_POINT ( 'NONE',  ( 21.55341960407610458, 5.719274019375980345, 43.95724293864769550 ) ) ;
#90124 = CARTESIAN_POINT ( 'NONE',  ( -19.03943276465977164, 0.05219959533909376836, 51.24890960531436690 ) ) ;
#90125 = CARTESIAN_POINT ( 'NONE',  ( -18.67979575497178146, -10.72451020669898902, 61.66557627198103120 ) ) ;
#90126 = CARTESIAN_POINT ( 'NONE',  ( 19.03943276465977164, 0.05219959533936151252, 51.25109039468567573 ) ) ;
#90128 = CARTESIAN_POINT ( 'NONE',  ( 16.52544592524342804, -4.483927247898539470, 43.54057627198103830 ) ) ;
#90127 = CARTESIAN_POINT ( 'NONE',  ( -3.573655867282028392E-15, 2.428612866367529932E-14, 139.9999999999999716 ) ) ;
#90129 = CARTESIAN_POINT ( 'NONE',  ( 18.62759615963271287, -10.81492255796078972, 28.33224293864769550 ) ) ;
#90130 = ORIENTED_EDGE ( 'NONE', *, *, #3863, .T. ) ;
#90131 = ORIENTED_EDGE ( 'NONE', *, *, #7790, .F. ) ;
#90132 = CARTESIAN_POINT ( 'NONE',  ( 17.78954161113920307, 0.5375896797884988088, 37.50000000000000711 ) ) ;
#90133 = CARTESIAN_POINT ( 'NONE',  ( 14.34966873604972726, -8.224510206698740333, 70.83442372801901854 ) ) ;
#90134 = CARTESIAN_POINT ( 'NONE',  ( -5.049401038297874678, -19.05341960407617918, 79.79275706135233293 ) ) ;
#90135 = CARTESIAN_POINT ( 'NONE',  ( 8.224510206698953496, -14.34966873604960469, 37.91557627198102409 ) ) ;
#90136 = CARTESIAN_POINT ( 'NONE',  ( -19.39720447994794839, -5.499999999999978684, 59.66317477297175742 ) ) ;
#90137 = CARTESIAN_POINT ( 'NONE',  ( -16.53943276465976808, 0.05219959533911058130, 26.24890960531435624 ) ) ;
#90138 = CARTESIAN_POINT ( 'NONE',  ( -16.46253265017160317, 9.564922557960807481, 45.83224293864769550 ) ) ;
#90139 = CARTESIAN_POINT ( 'NONE',  ( -13.89961937509977652, 13.97604488694528158, 70.62390960531432427 ) ) ;
#90140 = CARTESIAN_POINT ( 'NONE',  ( 5.049401038298161559, -19.05341960407611168, 37.70724293864768839 ) ) ;
#90141 = CARTESIAN_POINT ( 'NONE',  ( 18.62759615963255655, 10.81492255796105972, 51.66775706135234714 ) ) ;
#90142 = CARTESIAN_POINT ( 'NONE',  ( 9.564922557960805705, 16.46253265017160317, 59.58224293864769550 ) ) ;
#90143 = CARTESIAN_POINT ( 'NONE',  ( -24.95432927374998755, 4.974562764236792667, 189.9999999999999716 ) ) ;
#90144 = CARTESIAN_POINT ( 'NONE',  ( 0.05219959533909260263, 19.03943276465977164, 59.99890960531436690 ) ) ;
#90145 = CARTESIAN_POINT ( 'NONE',  ( -21.55341960407610458, -5.719274019375992779, 41.45724293864769550 ) ) ;
#90146 = AXIS2_PLACEMENT_3D ( 'NONE', #30575, #92226, #153912 ) ;
#90147 = CARTESIAN_POINT ( 'NONE',  ( -19.02544592524342804, 5.153800228976336051, 36.04057627198100988 ) ) ;
#90148 = CARTESIAN_POINT ( 'NONE',  ( -21.55341960407610458, -5.719274019375992779, 36.45724293864768839 ) ) ;
#90149 = CARTESIAN_POINT ( 'NONE',  ( 4.483927247898790824, -16.52544592524335698, 90.20942372801903275 ) ) ;
#90150 = EDGE_CURVE ( 'NONE', #12274, #143427, #70263, .T. ) ;
#90151 = CARTESIAN_POINT ( 'NONE',  ( 19.03943276465977164, 0.05219959533936151252, 26.25109039468566507 ) ) ;
#90152 = CARTESIAN_POINT ( 'NONE',  ( -14.34966873604972548, 8.224510206698743886, 68.33442372801900433 ) ) ;
#90153 = CARTESIAN_POINT ( 'NONE',  ( -5.049401038298153566, 19.05341960407611168, 115.2072429386477097 ) ) ;
#90154 = CARTESIAN_POINT ( 'NONE',  ( 16.55341960407618274, -4.379528057220086978, 56.04275706135235424 ) ) ;
#90155 = CARTESIAN_POINT ( 'NONE',  ( 14.34966873604972726, -8.224510206698740333, 45.83442372801901854 ) ) ;
#90156 = CARTESIAN_POINT ( 'NONE',  ( 13.97604488694527802, 13.89961937509977652, 114.3739096053143669 ) ) ;
#90157 = CARTESIAN_POINT ( 'NONE',  ( -16.52544592524335698, -4.483927247898792601, 23.95942372801901143 ) ) ;
#90158 = CARTESIAN_POINT ( 'NONE',  ( 9.474510206698971260, -16.51473224551069308, 32.91557627198102409 ) ) ;
#90159 = CARTESIAN_POINT ( 'NONE',  ( 5.719274019375673035, 21.55341960407619339, 22.29275706135235069 ) ) ;
#90160 = CARTESIAN_POINT ( 'NONE',  ( 0.05219959533934541429, -16.53943276465976808, 25.00109039468567218 ) ) ;
#90161 = CARTESIAN_POINT ( 'NONE',  ( -14.34966873604972548, 8.224510206698743886, 103.3344237280190043 ) ) ;
#90162 = CARTESIAN_POINT ( 'NONE',  ( -38.00000000000000711, 2.428612866367529932E-14, -3.749999994537626780 ) ) ;
#90163 = CARTESIAN_POINT ( 'NONE',  ( -5.719274019375665041, -21.55341960407619695, 104.7927570613523898 ) ) ;
#90164 = CARTESIAN_POINT ( 'NONE',  ( -5.049401038297874678, -19.05341960407617918, 94.79275706135230450 ) ) ;
#90165 = CARTESIAN_POINT ( 'NONE',  ( 16.53943276465976808, -0.05219959533910856209, 53.74890960531437401 ) ) ;
#90166 = CARTESIAN_POINT ( 'NONE',  ( 16.46253265017160672, -9.564922557960803928, 28.33224293864769550 ) ) ;
#90168 = CARTESIAN_POINT ( 'NONE',  ( -6.853560127763669740, 1.304723572972908086, -64.38700459888461580 ) ) ;
#90167 = CARTESIAN_POINT ( 'NONE',  ( -0.05219959533936034679, 19.03943276465977164, 52.50109039468566863 ) ) ;
#90169 = CARTESIAN_POINT ( 'NONE',  ( 18.67979575497194134, -10.72451020669871369, 45.83442372801901854 ) ) ;
#90170 = CARTESIAN_POINT ( 'NONE',  ( -16.52544592524335698, -4.483927247898792601, 28.95942372801902209 ) ) ;
#90171 = CARTESIAN_POINT ( 'NONE',  ( 16.18388926212236711, 7.379444403734555458, 82.93953151366150678 ) ) ;
#90172 = CARTESIAN_POINT ( 'NONE',  ( 5.049401038298161559, -19.05341960407611168, 107.7072429386476955 ) ) ;
#90173 = CARTESIAN_POINT ( 'NONE',  ( -5.823673210054116645, -21.52544592524344225, 67.29057627198103830 ) ) ;
#90174 = CARTESIAN_POINT ( 'NONE',  ( 13.97604488694548053, -13.89961937509957401, 100.6260903946856615 ) ) ;
#90175 = CARTESIAN_POINT ( 'NONE',  ( 13.97604488694527802, 13.89961937509977652, 109.3739096053143669 ) ) ;
#90176 = CARTESIAN_POINT ( 'NONE',  ( -26.45763050569055252, 3.219288925403916313, 173.6696415116524861 ) ) ;
#90177 = CARTESIAN_POINT ( 'NONE',  ( 16.53943276465976808, -0.05219959533910856209, 108.7489096053143669 ) ) ;
#90178 = CARTESIAN_POINT ( 'NONE',  ( -5.823673210054431948, 21.52544592524334988, 92.70942372801901854 ) ) ;
#90179 = CARTESIAN_POINT ( 'NONE',  ( -19.03943276465977164, 0.05219959533909376836, 46.24890960531435979 ) ) ;
#90180 = CARTESIAN_POINT ( 'NONE',  ( 18.62759615963255655, 10.81492255796105972, 56.66775706135235424 ) ) ;
#90181 = AXIS2_PLACEMENT_3D ( 'NONE', #139386, #95874, #108050 ) ;
#90182 = CARTESIAN_POINT ( 'NONE',  ( 10.81492255796106328, -18.62759615963255655, 90.41775706135236135 ) ) ;
#90183 = CARTESIAN_POINT ( 'NONE',  ( -12.06949235617739369, -12.14591786802326823, 109.3760903946857042 ) ) ;
#90184 = CARTESIAN_POINT ( 'NONE',  ( 5.153800228976335163, 19.02544592524342804, 74.79057627198103830 ) ) ;
#90185 = CARTESIAN_POINT ( 'NONE',  ( -0.05219959533937732626, 21.53943276465977519, 47.50109039468568994 ) ) ;
#90186 = CARTESIAN_POINT ( 'NONE',  ( -15.72974639402176322, -15.80617190586768395, 34.37609039468568284 ) ) ;
#90188 = CARTESIAN_POINT ( 'NONE',  ( -16.46253265017160317, 9.564922557960807481, 85.83224293864769550 ) ) ;
#90187 = CARTESIAN_POINT ( 'NONE',  ( -9.474510206698720793, -16.51473224551083518, 64.58442372801900433 ) ) ;
#90189 = CARTESIAN_POINT ( 'NONE',  ( 4.483927247898545687, 16.52544592524342804, 99.79057627198103830 ) ) ;
#90190 = CARTESIAN_POINT ( 'NONE',  ( -10.81492255796078084, -18.62759615963271287, 92.08224293864769550 ) ) ;
#90191 = CARTESIAN_POINT ( 'NONE',  ( 8.314922557960818139, 14.29746914071049879, 59.58224293864770260 ) ) ;
#90192 = CARTESIAN_POINT ( 'NONE',  ( 9.564922557961047289, -16.46253265017146816, 25.41775706135234003 ) ) ;
#90193 = CARTESIAN_POINT ( 'NONE',  ( -0.05219959533910754901, -16.53943276465976808, 82.49890960531436690 ) ) ;
#90194 = CARTESIAN_POINT ( 'NONE',  ( -16.46253265017160317, 9.564922557960807481, 30.83224293864769550 ) ) ;
#90195 = CARTESIAN_POINT ( 'NONE',  ( 9.564922557961047289, -16.46253265017146816, 85.41775706135233293 ) ) ;
#90196 = CARTESIAN_POINT ( 'NONE',  ( -4.483927247898539470, -16.52544592524342804, 52.29057627198102409 ) ) ;
#90197 = CARTESIAN_POINT ( 'NONE',  ( 5.823673210054444382, -21.52544592524334988, 100.2094237280190043 ) ) ;
#90198 = CARTESIAN_POINT ( 'NONE',  ( -16.51473224551069308, -9.474510206698971260, 96.66557627198102409 ) ) ;
#90199 = CARTESIAN_POINT ( 'NONE',  ( 0.05219959533936267826, -19.03943276465977164, 75.00109039468566152 ) ) ;
#90200 = CARTESIAN_POINT ( 'NONE',  ( -15.72974639402197994, 15.80617190586746368, 80.62390960531438111 ) ) ;
#90201 = CARTESIAN_POINT ( 'NONE',  ( -10.81492255796105439, 18.62759615963255655, 27.91775706135234358 ) ) ;
#90202 = CARTESIAN_POINT ( 'NONE',  ( -4.483927247898782831, 16.52544592524335698, 27.70942372801901854 ) ) ;
#90203 = CARTESIAN_POINT ( 'NONE',  ( 14.29746914071037800, 8.314922557961029526, 91.66775706135234714 ) ) ;
#90205 = CARTESIAN_POINT ( 'NONE',  ( 15.80617190586769283, -15.72974639402175789, 40.62609039468567573 ) ) ;
#90204 = CARTESIAN_POINT ( 'NONE',  ( -19.03943276465977164, 0.05219959533909376836, 31.24890960531435979 ) ) ;
#90206 = CARTESIAN_POINT ( 'NONE',  ( 12.06949235617757843, -12.14591786802309237, 113.1239096053143953 ) ) ;
#90207 = CARTESIAN_POINT ( 'NONE',  ( -23.48529157249599919, -32.32473071737750558, -11.44999999453762385 ) ) ;
#90208 = CARTESIAN_POINT ( 'NONE',  ( 12.06949235617739724, 12.14591786802326823, 51.87609039468568284 ) ) ;
#90209 = CARTESIAN_POINT ( 'NONE',  ( 4.379528057220339221, -16.55341960407611168, 77.70724293864770971 ) ) ;
#90210 = CARTESIAN_POINT ( 'NONE',  ( 5.823673210054125526, 21.52544592524343514, 69.79057627198102409 ) ) ;
#90211 = CARTESIAN_POINT ( 'NONE',  ( 4.483927247898545687, 16.52544592524342804, 24.79057627198103120 ) ) ;
#90212 = CARTESIAN_POINT ( 'NONE',  ( 4.379528057220092307, 16.55341960407617563, 52.29275706135236135 ) ) ;
#90213 = CARTESIAN_POINT ( 'NONE',  ( -19.02544592524342804, 5.153800228976336051, 41.04057627198103120 ) ) ;
#90214 = CARTESIAN_POINT ( 'NONE',  ( 12.14591786802327356, -12.06949235617739191, 90.62609039468567573 ) ) ;
#90215 = CARTESIAN_POINT ( 'NONE',  ( -0.05219959533936034679, 19.03943276465977164, 82.50109039468567573 ) ) ;
#90216 = CARTESIAN_POINT ( 'NONE',  ( -15.80617190586745835, -15.72974639402198527, 71.87390960531438111 ) ) ;
#90217 = CARTESIAN_POINT ( 'NONE',  ( 4.483927247898790824, -16.52544592524335698, 110.2094237280190185 ) ) ;
#90218 = EDGE_LOOP ( 'NONE', ( #156982, #20686, #64097, #133304, #4692, #46946 ) ) ;
#90219 = CARTESIAN_POINT ( 'NONE',  ( 9.564922557960805705, 16.46253265017160317, 114.5822429386476955 ) ) ;
#90220 = CARTESIAN_POINT ( 'NONE',  ( -5.823673210054116645, -21.52544592524344225, 62.29057627198102409 ) ) ;
#90221 = ORIENTED_EDGE ( 'NONE', *, *, #66504, .T. ) ;
#90222 = CARTESIAN_POINT ( 'NONE',  ( -12.14591786802326823, 12.06949235617739902, 93.12609039468568994 ) ) ;
#90223 = ORIENTED_EDGE ( 'NONE', *, *, #11874, .F. ) ;
#90224 = CARTESIAN_POINT ( 'NONE',  ( -9.474510206698964154, 16.51473224551069663, 110.4155762719810383 ) ) ;
#90225 = CARTESIAN_POINT ( 'NONE',  ( -18.39443945427639449, 5.500000000000031974, 73.51745347608654413 ) ) ;
#90226 = CARTESIAN_POINT ( 'NONE',  ( -18.62759615963270932, 10.81492255796079327, 70.83224293864770971 ) ) ;
#90227 = CARTESIAN_POINT ( 'NONE',  ( -4.483927247898782831, 16.52544592524335698, 97.70942372801904696 ) ) ;
#90228 = CARTESIAN_POINT ( 'NONE',  ( 14.34966873604972726, -8.224510206698740333, 20.83442372801901143 ) ) ;
#90229 = CARTESIAN_POINT ( 'NONE',  ( 13.89961937509977652, -13.97604488694527269, 23.12390960531436335 ) ) ;
#90230 = CARTESIAN_POINT ( 'NONE',  ( 16.53943276465976808, 0.05219959533934440121, 31.25109039468568639 ) ) ;
#90231 = CARTESIAN_POINT ( 'NONE',  ( -19.05341960407611168, -5.049401038298163336, 51.45724293864770260 ) ) ;
#90232 = ADVANCED_FACE ( 'NONE', ( #131932 ), #174476, .T. ) ;
#90233 = CARTESIAN_POINT ( 'NONE',  ( 28.82186960331498327, 9.364793116373570925, 143.0999999999999659 ) ) ;
#90234 = CARTESIAN_POINT ( 'NONE',  ( 19.03943276465977164, -0.05219959533909143690, 108.7489096053143527 ) ) ;
#90235 = CARTESIAN_POINT ( 'NONE',  ( 16.52544592524335698, 4.483927247898782831, 91.45942372801901854 ) ) ;
#90236 = CARTESIAN_POINT ( 'NONE',  ( -19.03943276465977164, -0.05219959533935918106, 88.75109039468567573 ) ) ;
#90237 = CARTESIAN_POINT ( 'NONE',  ( -19.03943276465977164, -0.05219959533935918106, 23.75109039468566152 ) ) ;
#90238 = CARTESIAN_POINT ( 'NONE',  ( -5.823673210054116645, -21.52544592524344225, 72.29057627198102409 ) ) ;
#90239 = CARTESIAN_POINT ( 'NONE',  ( 16.53943276465976808, 0.05219959533934440121, 101.2510903946856757 ) ) ;
#90240 = CARTESIAN_POINT ( 'NONE',  ( -13.89961937509957401, -13.97604488694547875, 94.37609039468566152 ) ) ;
#90241 = CARTESIAN_POINT ( 'NONE',  ( 19.05341960407611168, 5.049401038298154454, 43.95724293864769550 ) ) ;
#90242 = CARTESIAN_POINT ( 'NONE',  ( -19.02544592524342804, 5.153800228976336051, 96.04057627198103830 ) ) ;
#90243 = CARTESIAN_POINT ( 'NONE',  ( 15.72974639402176855, 15.80617190586768217, 56.87609039468568994 ) ) ;
#90244 = CARTESIAN_POINT ( 'NONE',  ( 13.89961937509977652, -13.97604488694527269, 63.12390960531435979 ) ) ;
#90245 = CARTESIAN_POINT ( 'NONE',  ( -14.29746914071049879, 8.314922557960819915, 90.83224293864769550 ) ) ;
#90246 = CARTESIAN_POINT ( 'NONE',  ( 1.300000000000000044, 0.000000000000000000, 1.249999999999999778 ) ) ;
#90247 = CARTESIAN_POINT ( 'NONE',  ( 16.53943276465976808, -0.05219959533910856209, 78.74890960531436690 ) ) ;
#90248 = CARTESIAN_POINT ( 'NONE',  ( 0.05219959533907565091, 21.53943276465977519, 69.99890960531435269 ) ) ;
#90249 = CARTESIAN_POINT ( 'NONE',  ( -9.474510206698720793, -16.51473224551083518, 94.58442372801900433 ) ) ;
#90250 = DIRECTION ( 'NONE',  ( -0.5000000000000051070, 1.060575238724903217E-16, -0.8660254037844355990 ) ) ;
#90251 = CARTESIAN_POINT ( 'NONE',  ( -0.05219959533936034679, 19.03943276465977164, 42.50109039468566152 ) ) ;
#90252 = CARTESIAN_POINT ( 'NONE',  ( 31.72709406046299918, -1.071565338629617092E-14, 102.5000000000000142 ) ) ;
#90254 = CARTESIAN_POINT ( 'NONE',  ( -19.05341960407611168, -5.049401038298163336, 86.45724293864769550 ) ) ;
#90253 = CARTESIAN_POINT ( 'NONE',  ( -5.153800228976328057, -19.02544592524343514, 82.29057627198103830 ) ) ;
#90255 = CARTESIAN_POINT ( 'NONE',  ( 4.483927247898790824, -16.52544592524335698, 60.20942372801902565 ) ) ;
#90256 = CARTESIAN_POINT ( 'NONE',  ( -17.44270441346514033, -5.991230190323107330, 51.36335079264230785 ) ) ;
#90257 = CARTESIAN_POINT ( 'NONE',  ( 16.46253265017146816, 9.564922557961045513, 46.66775706135233293 ) ) ;
#90258 = CARTESIAN_POINT ( 'NONE',  ( 15.61223984149541799, -14.70183385125136333, -58.76599187376303490 ) ) ;
#90259 = CARTESIAN_POINT ( 'NONE',  ( -16.46253265017160317, 9.564922557960807481, 105.8322429386476955 ) ) ;
#90260 = CARTESIAN_POINT ( 'NONE',  ( -8.314922557961024197, 14.29746914071037800, 107.9177570613523471 ) ) ;
#90261 = CARTESIAN_POINT ( 'NONE',  ( 14.02111363790003828, -0.9482109960935805049, -60.30654223653039736 ) ) ;
#90262 = CARTESIAN_POINT ( 'NONE',  ( -16.52544592524335698, -4.483927247898792601, 83.95942372801900433 ) ) ;
#90263 = CARTESIAN_POINT ( 'NONE',  ( 39.99999999999999289, 2.428612866367529932E-14, 0.000000000000000000 ) ) ;
#90264 = CARTESIAN_POINT ( 'NONE',  ( -16.55341960407617563, 4.379528057220093196, 48.54275706135234714 ) ) ;
#90265 = DIRECTION ( 'NONE',  ( 0.000000000000000000, 0.000000000000000000, -1.000000000000000000 ) ) ;
#90266 = CARTESIAN_POINT ( 'NONE',  ( -10.81492255796105439, 18.62759615963255655, 72.91775706135234714 ) ) ;
#90267 = CARTESIAN_POINT ( 'NONE',  ( 5.153800228976615827, -19.02544592524334988, 70.20942372801899012 ) ) ;
#90268 = CARTESIAN_POINT ( 'NONE',  ( 9.474510206698729675, 16.51473224551082808, 22.08442372801899722 ) ) ;
#90269 = CARTESIAN_POINT ( 'NONE',  ( 16.51473224551069308, 9.474510206698969483, 54.16557627198103120 ) ) ;
#90270 = CARTESIAN_POINT ( 'NONE',  ( -5.153800228976328057, -19.02544592524343514, 42.29057627198101699 ) ) ;
#90271 = CARTESIAN_POINT ( 'NONE',  ( -19.78838472062539822, -34.76237422906578445, -6.192482694737989846 ) ) ;
#90272 = CARTESIAN_POINT ( 'NONE',  ( 0.05219959533907565091, 21.53943276465977519, 64.99890960531435269 ) ) ;
#90273 = CARTESIAN_POINT ( 'NONE',  ( -19.03943276465977164, 0.05219959533909376836, 111.2489096053143669 ) ) ;
#90274 = CARTESIAN_POINT ( 'NONE',  ( -13.97604488694527625, -13.89961937509977652, 21.87390960531435979 ) ) ;
#90275 = CARTESIAN_POINT ( 'NONE',  ( -4.483927247898782831, 16.52544592524335698, 47.70942372801902565 ) ) ;
#90276 = ORIENTED_EDGE ( 'NONE', *, *, #150999, .F. ) ;
#90277 = CARTESIAN_POINT ( 'NONE',  ( -15.80617190586745835, -15.72974639402198527, 111.8739096053143669 ) ) ;
#90279 = CARTESIAN_POINT ( 'NONE',  ( 3.766062262543149401E-15, -39.95556452105413570, -7.500000000000000888 ) ) ;
#90278 = CARTESIAN_POINT ( 'NONE',  ( 16.53943276465976808, -0.05219959533910856209, 53.74890960531437401 ) ) ;
#90280 = CARTESIAN_POINT ( 'NONE',  ( 9.564922557961047289, -16.46253265017146816, 110.4177570613523471 ) ) ;
#90281 = CARTESIAN_POINT ( 'NONE',  ( -13.97604488694547697, 13.89961937509957934, 43.12609039468566152 ) ) ;
#90282 = CARTESIAN_POINT ( 'NONE',  ( -12.14591786802309592, -12.06949235617757132, 41.87390960531435979 ) ) ;
#90283 = CARTESIAN_POINT ( 'NONE',  ( 0.05219959533907565091, 21.53943276465977519, 114.9989096053143669 ) ) ;
#90285 = CARTESIAN_POINT ( 'NONE',  ( -0.05219959533907301413, -21.53943276465977519, 67.49890960531436690 ) ) ;
#90284 = CARTESIAN_POINT ( 'NONE',  ( 16.52216118717206328, 7.221426719304519182, 33.57599021046992505 ) ) ;
#90286 = CARTESIAN_POINT ( 'NONE',  ( 16.46253265017160672, -9.564922557960803928, 88.33224293864769550 ) ) ;
#90287 = CARTESIAN_POINT ( 'NONE',  ( 4.379528057220339221, -16.55341960407611168, 62.70724293864769550 ) ) ;
#90288 = CARTESIAN_POINT ( 'NONE',  ( -9.474510206698964154, 16.51473224551069663, 105.4155762719810383 ) ) ;
#90289 = CARTESIAN_POINT ( 'NONE',  ( -36.82860559483759033, 3.362349505172651298, 49.36759404993757983 ) ) ;
#90290 = CARTESIAN_POINT ( 'NONE',  ( 19.03943276465977164, 0.05219959533936151252, 61.25109039468566863 ) ) ;
#90291 = CARTESIAN_POINT ( 'NONE',  ( -18.62759615963270932, 10.81492255796079327, 110.8322429386476955 ) ) ;
#90292 = CARTESIAN_POINT ( 'NONE',  ( 9.474510206698971260, -16.51473224551069308, 47.91557627198102409 ) ) ;
#90293 = CARTESIAN_POINT ( 'NONE',  ( -8.224510206698948167, 14.34966873604960824, 110.4155762719810383 ) ) ;
#90294 = CARTESIAN_POINT ( 'NONE',  ( 21.53943276465977519, 0.05219959533937863772, 56.25109039468568284 ) ) ;
#90295 = CARTESIAN_POINT ( 'NONE',  ( 22.44159573604009239, 16.30477369853692693, 144.0750000027311728 ) ) ;
#90296 = CARTESIAN_POINT ( 'NONE',  ( -0.05219959533910754901, -16.53943276465976808, 32.49890960531435979 ) ) ;
#90297 = CARTESIAN_POINT ( 'NONE',  ( 16.46253265017160672, -9.564922557960803928, 43.33224293864769550 ) ) ;
#90298 = CARTESIAN_POINT ( 'NONE',  ( -5.049401038298153566, 19.05341960407611168, 105.2072429386476671 ) ) ;
#90299 = CARTESIAN_POINT ( 'NONE',  ( -21.53943276465977519, 0.05219959533907696930, 76.24890960531435269 ) ) ;
#90300 = CARTESIAN_POINT ( 'NONE',  ( 27.73933785331498569, 2.768321779492822058E-14, 141.8750000027311842 ) ) ;
#90301 = CARTESIAN_POINT ( 'NONE',  ( 5.049401038298161559, -19.05341960407611168, 42.70724293864767418 ) ) ;
#90302 = CARTESIAN_POINT ( 'NONE',  ( 15.72974639402199770, -15.80617190586745480, 48.12390960531436690 ) ) ;
#90303 = CARTESIAN_POINT ( 'NONE',  ( 21.53943276465977519, 0.05219959533937863772, 81.25109039468568994 ) ) ;
#90306 = CARTESIAN_POINT ( 'NONE',  ( 4.379528057220339221, -16.55341960407611168, 72.70724293864769550 ) ) ;
#90305 = CARTESIAN_POINT ( 'NONE',  ( -16.52544592524335698, -4.483927247898792601, 78.95942372801901854 ) ) ;
#90304 = CARTESIAN_POINT ( 'NONE',  ( -26.99873734152928506, -22.49873734152901861, 1.110912703473986074 ) ) ;
#90307 = CARTESIAN_POINT ( 'NONE',  ( -19.05341960407611168, -5.049401038298163336, 71.45724293864766707 ) ) ;
#90308 = ORIENTED_EDGE ( 'NONE', *, *, #169114, .T. ) ;
#90309 = CARTESIAN_POINT ( 'NONE',  ( -5.049401038297874678, -19.05341960407617918, 24.79275706135233648 ) ) ;
#90310 = CARTESIAN_POINT ( 'NONE',  ( 0.05219959533934541429, -16.53943276465976808, 90.00109039468567573 ) ) ;
#90311 = CARTESIAN_POINT ( 'NONE',  ( -5.823673210054431948, 21.52544592524334988, 112.7094237280190328 ) ) ;
#90312 = CARTESIAN_POINT ( 'NONE',  ( -13.89961937509977652, 13.97604488694528158, 70.62390960531432427 ) ) ;
#90313 = CARTESIAN_POINT ( 'NONE',  ( 21.53943276465977519, -0.05219959533907433946, 53.74890960531437401 ) ) ;
#90314 = CARTESIAN_POINT ( 'NONE',  ( -16.52544592524335698, -4.483927247898792601, 18.95942372801901143 ) ) ;
#90315 = CARTESIAN_POINT ( 'NONE',  ( 0.05219959533937995610, -21.53943276465977519, 95.00109039468568994 ) ) ;
#90316 = CARTESIAN_POINT ( 'NONE',  ( 4.483927247898790824, -16.52544592524335698, 65.20942372801901854 ) ) ;
#90317 = CARTESIAN_POINT ( 'NONE',  ( 15.80617190586746368, 15.72974639402197994, 109.3739096053143811 ) ) ;
#90318 = CARTESIAN_POINT ( 'NONE',  ( 14.29746914071037800, 8.314922557961029526, 21.66775706135235069 ) ) ;
#90319 = CARTESIAN_POINT ( 'NONE',  ( 16.46253265017160672, -9.564922557960803928, 88.33224293864769550 ) ) ;
#90320 = CARTESIAN_POINT ( 'NONE',  ( 4.379528057220092307, 16.55341960407617563, 22.29275706135235069 ) ) ;
#90321 = CARTESIAN_POINT ( 'NONE',  ( -5.153800228976328057, -19.02544592524343514, 52.29057627198100988 ) ) ;
#90322 = VECTOR ( 'NONE', #51417, 999.9999999999998863 ) ;
#90323 = CARTESIAN_POINT ( 'NONE',  ( -4.483927247898782831, 16.52544592524335698, 37.70942372801900433 ) ) ;
#90324 = CARTESIAN_POINT ( 'NONE',  ( -8.314922557960811034, -14.29746914071050412, 77.08224293864769550 ) ) ;
#90325 = CARTESIAN_POINT ( 'NONE',  ( 16.55341960407618274, -4.379528057220086978, 91.04275706135236135 ) ) ;
#90327 = CARTESIAN_POINT ( 'NONE',  ( -16.46253265017160317, 9.564922557960807481, 70.83224293864770971 ) ) ;
#90326 = CARTESIAN_POINT ( 'NONE',  ( 21.52544592524334988, 5.823673210054432836, 36.45942372801901143 ) ) ;
#90328 = CARTESIAN_POINT ( 'NONE',  ( 9.474510206698971260, -16.51473224551069308, 77.91557627198103830 ) ) ;
#90329 = CARTESIAN_POINT ( 'NONE',  ( -12.06949235617739369, -12.14591786802326823, 89.37609039468568994 ) ) ;
#90331 = ORIENTED_EDGE ( 'NONE', *, *, #32497, .T. ) ;
#90330 = CARTESIAN_POINT ( 'NONE',  ( -21.97054992548789087, -7.027819292989581967, 170.5066066589220100 ) ) ;
#90332 = ORIENTED_EDGE ( 'NONE', *, *, #7594, .T. ) ;
#90333 = CARTESIAN_POINT ( 'NONE',  ( -16.51473224551082808, 9.474510206698731452, 33.33442372801899722 ) ) ;
#90334 = CARTESIAN_POINT ( 'NONE',  ( 13.89961937509977652, -13.97604488694527269, 93.12390960531436690 ) ) ;
#90335 = CARTESIAN_POINT ( 'NONE',  ( -9.474510206698964154, 16.51473224551069663, 45.41557627198103120 ) ) ;
#90336 = CARTESIAN_POINT ( 'NONE',  ( -9.474510206698964154, 16.51473224551069663, 115.4155762719810241 ) ) ;
#90337 = CARTESIAN_POINT ( 'NONE',  ( 16.53943276465976808, 0.05219959533934440121, 46.25109039468567573 ) ) ;
#90339 = CARTESIAN_POINT ( 'NONE',  ( 14.29746914071037800, 8.314922557961029526, 41.66775706135235424 ) ) ;
#90338 = CARTESIAN_POINT ( 'NONE',  ( 16.46253265017146816, 9.564922557961045513, 56.66775706135233293 ) ) ;
#90340 = CARTESIAN_POINT ( 'NONE',  ( -9.474510206698964154, 16.51473224551069663, 105.4155762719810383 ) ) ;
#90341 = CARTESIAN_POINT ( 'NONE',  ( -9.474510206698964154, 16.51473224551069663, 75.41557627198103830 ) ) ;
#90342 = CARTESIAN_POINT ( 'NONE',  ( -10.81492255796078084, -18.62759615963271287, 97.08224293864770971 ) ) ;
#90343 = CARTESIAN_POINT ( 'NONE',  ( -5.153800228976607833, 19.02544592524334988, 67.70942372801900433 ) ) ;
#90345 = CARTESIAN_POINT ( 'NONE',  ( 27.86273085795036408, -28.69962071417356242, -4.999999999999999112 ) ) ;
#90344 = CARTESIAN_POINT ( 'NONE',  ( -9.564922557960796823, -16.46253265017161027, 87.08224293864769550 ) ) ;
#90346 = CARTESIAN_POINT ( 'NONE',  ( -5.049401038298153566, 19.05341960407611168, 70.20724293864769550 ) ) ;
#90348 = CARTESIAN_POINT ( 'NONE',  ( 18.22780087662121673, 5.500000000000056843, 68.98459894673892734 ) ) ;
#90347 = CARTESIAN_POINT ( 'NONE',  ( 14.29746914071049879, -8.314922557960816363, 33.33224293864769550 ) ) ;
#90349 = EDGE_CURVE ( 'NONE', #21815, #72076, #91067, .T. ) ;
#90350 = CARTESIAN_POINT ( 'NONE',  ( 9.564922557961047289, -16.46253265017146816, 40.41775706135234003 ) ) ;
#90351 = CARTESIAN_POINT ( 'NONE',  ( 16.53943276465976808, -0.05219959533910856209, 78.74890960531436690 ) ) ;
#90352 = CARTESIAN_POINT ( 'NONE',  ( -15.80617190586768217, 15.72974639402176855, 98.12609039468570415 ) ) ;
#90353 = CARTESIAN_POINT ( 'NONE',  ( 9.564922557960805705, 16.46253265017160317, 34.58224293864770260 ) ) ;
#90354 = CARTESIAN_POINT ( 'NONE',  ( 14.34966873604972726, -8.224510206698740333, 55.83442372801901854 ) ) ;
#90356 = CARTESIAN_POINT ( 'NONE',  ( 5.823673210054444382, -21.52544592524334988, 105.2094237280190328 ) ) ;
#90355 = CARTESIAN_POINT ( 'NONE',  ( -8.314922557960811034, -14.29746914071050412, 42.08224293864769550 ) ) ;
#90357 = CARTESIAN_POINT ( 'NONE',  ( 5.049401038298161559, -19.05341960407611168, 97.70724293864766707 ) ) ;
#90358 = CARTESIAN_POINT ( 'NONE',  ( 19.02544592524343514, -5.153800228976328945, 88.54057627198102409 ) ) ;
#90359 = CARTESIAN_POINT ( 'NONE',  ( 9.564922557960805705, 16.46253265017160317, 24.58224293864769194 ) ) ;
#90360 = CARTESIAN_POINT ( 'NONE',  ( 16.55341960407611168, 4.379528057220329451, 108.9572429386476955 ) ) ;
#90361 = CARTESIAN_POINT ( 'NONE',  ( -16.53943276465976808, 0.05219959533911058130, 71.24890960531435269 ) ) ;
#90362 = CARTESIAN_POINT ( 'NONE',  ( 5.719274019375991003, -21.55341960407610458, 82.70724293864770971 ) ) ;
#90363 = CARTESIAN_POINT ( 'NONE',  ( 19.02544592524343514, -5.153800228976328945, 83.54057627198100988 ) ) ;
#90364 = CARTESIAN_POINT ( 'NONE',  ( -21.52544592524343514, 5.823673210054127303, 96.04057627198102409 ) ) ;
#90365 = CARTESIAN_POINT ( 'NONE',  ( -13.89961937509977652, 13.97604488694528158, 95.62390960531436690 ) ) ;
#90367 = CARTESIAN_POINT ( 'NONE',  ( 14.29746914071049879, -8.314922557960816363, 93.33224293864769550 ) ) ;
#90366 = CARTESIAN_POINT ( 'NONE',  ( 19.52217212775657984, -5.500000000000105693, 47.43993709005262360 ) ) ;
#90368 = CARTESIAN_POINT ( 'NONE',  ( 5.153800228976335163, 19.02544592524342804, 64.79057627198100988 ) ) ;
#90369 = CARTESIAN_POINT ( 'NONE',  ( -18.67979575497178146, -10.72451020669898902, 66.66557627198102409 ) ) ;
#90370 = DIRECTION ( 'NONE',  ( 0.5150380749100522682, 1.049727191138620051E-16, 0.8571673007021134438 ) ) ;
#90372 = PRESENTATION_STYLE_ASSIGNMENT (( #59042 ) ) ;
#90371 = CARTESIAN_POINT ( 'NONE',  ( 14.34966873604972726, -8.224510206698740333, 110.8344237280190043 ) ) ;
#90373 = CARTESIAN_POINT ( 'NONE',  ( 4.483927247898790824, -16.52544592524335698, 20.20942372801900788 ) ) ;
#90374 = CARTESIAN_POINT ( 'NONE',  ( -4.379528057220328563, 16.55341960407611168, 90.20724293864770971 ) ) ;
#90375 = CARTESIAN_POINT ( 'NONE',  ( -16.88567814943165502, -6.947325034625643880, 96.29001122652589117 ) ) ;
#90376 = CARTESIAN_POINT ( 'NONE',  ( -16.51473224551069308, -9.474510206698971260, 81.66557627198103830 ) ) ;
#90377 = CARTESIAN_POINT ( 'NONE',  ( -9.564922557960796823, -16.46253265017161027, 42.08224293864769550 ) ) ;
#90378 = CARTESIAN_POINT ( 'NONE',  ( -16.53943276465976808, 0.05219959533911058130, 61.24890960531435979 ) ) ;
#90379 = CARTESIAN_POINT ( 'NONE',  ( 16.46253265017160672, -9.564922557960803928, 108.3322429386476955 ) ) ;
#90380 = CARTESIAN_POINT ( 'NONE',  ( 13.89961937509957401, 13.97604488694547697, 101.8760903946856331 ) ) ;
#90381 = CARTESIAN_POINT ( 'NONE',  ( -21.53943276465977519, -0.05219959533937600094, 58.75109039468568994 ) ) ;
#90382 = CARTESIAN_POINT ( 'NONE',  ( 19.05341960407611168, 5.049401038298154454, 93.95724293864769550 ) ) ;
#90383 = CARTESIAN_POINT ( 'NONE',  ( -10.81492255796078084, -18.62759615963271287, 77.08224293864769550 ) ) ;
#90384 = CARTESIAN_POINT ( 'NONE',  ( -8.224510206698735004, -14.34966873604973081, 64.58442372801900433 ) ) ;
#90385 = CARTESIAN_POINT ( 'NONE',  ( 0.000000000000000000, 1.443375672974065216, 7.017607234860990640E-28 ) ) ;
#90386 = CARTESIAN_POINT ( 'NONE',  ( -16.46253265017160317, 9.564922557960807481, 70.83224293864770971 ) ) ;
#90387 = CARTESIAN_POINT ( 'NONE',  ( -21.53943276465977519, 0.05219959533907696930, 76.24890960531435269 ) ) ;
#90388 = CARTESIAN_POINT ( 'NONE',  ( -5.049401038297874678, -19.05341960407617918, 104.7927570613523471 ) ) ;
#90390 = CARTESIAN_POINT ( 'NONE',  ( 21.55341960407619695, -5.719274019375665929, 66.04275706135236135 ) ) ;
#90389 = CARTESIAN_POINT ( 'NONE',  ( 16.55341960407611168, 4.379528057220329451, 43.95724293864769550 ) ) ;
#90391 = EDGE_CURVE ( 'NONE', #71084, #74970, #126109, .T. ) ;
#90393 = CARTESIAN_POINT ( 'NONE',  ( 21.53943276465977519, -0.05219959533907433946, 23.74890960531435269 ) ) ;
#90392 = CARTESIAN_POINT ( 'NONE',  ( 14.29746914071037800, 8.314922557961029526, 86.66775706135234714 ) ) ;
#90394 = CARTESIAN_POINT ( 'NONE',  ( -5.153800228976328057, -19.02544592524343514, 107.2905762719810383 ) ) ;
#90395 = CARTESIAN_POINT ( 'NONE',  ( 17.49999999999999645, -5.500000000000031974, 93.29690382534172954 ) ) ;
#90396 = CARTESIAN_POINT ( 'NONE',  ( 16.53943276465976808, 0.05219959533934440121, 111.2510903946856899 ) ) ;
#90397 = CARTESIAN_POINT ( 'NONE',  ( -8.314922557961024197, 14.29746914071037800, 42.91775706135235424 ) ) ;
#90398 = CARTESIAN_POINT ( 'NONE',  ( 16.51473224551069308, 9.474510206698969483, 59.16557627198102409 ) ) ;
#90399 = CARTESIAN_POINT ( 'NONE',  ( 5.049401038298161559, -19.05341960407611168, 67.70724293864769550 ) ) ;
#90400 = CARTESIAN_POINT ( 'NONE',  ( -8.224510206698735004, -14.34966873604973081, 64.58442372801900433 ) ) ;
#90401 = CARTESIAN_POINT ( 'NONE',  ( 8.314922557960818139, 14.29746914071049879, 44.58224293864769550 ) ) ;
#90402 = CARTESIAN_POINT ( 'NONE',  ( 5.153800228976335163, 19.02544592524342804, 59.79057627198100988 ) ) ;
#90403 = CARTESIAN_POINT ( 'NONE',  ( -16.51473224551069308, -9.474510206698971260, 46.66557627198102409 ) ) ;
#90405 = VERTEX_POINT ( 'NONE', #90395 ) ;
#90404 = CARTESIAN_POINT ( 'NONE',  ( -8.224510206698735004, -14.34966873604973081, 44.58442372801901854 ) ) ;
#90406 = CARTESIAN_POINT ( 'NONE',  ( -5.153800228976607833, 19.02544592524334988, 97.70942372801900433 ) ) ;
#90407 = CARTESIAN_POINT ( 'NONE',  ( 8.224510206698953496, -14.34966873604960469, 92.91557627198103830 ) ) ;
#90408 = CARTESIAN_POINT ( 'NONE',  ( -19.05341960407611168, -5.049401038298163336, 71.45724293864766707 ) ) ;
#90410 = CARTESIAN_POINT ( 'NONE',  ( -23.96320343559652599, -18.46320343559629507, 1.818019484660534424 ) ) ;
#90409 = CARTESIAN_POINT ( 'NONE',  ( 19.03943276465977164, 0.05219959533936151252, 96.25109039468567573 ) ) ;
#90411 = CARTESIAN_POINT ( 'NONE',  ( 21.53943276465977519, 0.05219959533937863772, 96.25109039468568994 ) ) ;
#90412 = CARTESIAN_POINT ( 'NONE',  ( 8.224510206698742110, 14.34966873604972548, 72.08442372801899012 ) ) ;
#90413 = DIRECTION ( 'NONE',  ( 0.000000000000000000, 0.000000000000000000, -1.000000000000000000 ) ) ;
#90414 = CARTESIAN_POINT ( 'NONE',  ( 21.53943276465977519, -0.05219959533907433946, 58.74890960531436690 ) ) ;
#90415 = CARTESIAN_POINT ( 'NONE',  ( 8.224510206698742110, 14.34966873604972548, 47.08442372801901854 ) ) ;
#90416 = CARTESIAN_POINT ( 'NONE',  ( -19.03943276465977164, 0.05219959533909376836, 31.24890960531435979 ) ) ;
#90417 = CARTESIAN_POINT ( 'NONE',  ( -13.97604488694547697, 13.89961937509957934, 43.12609039468566152 ) ) ;
#90418 = CARTESIAN_POINT ( 'NONE',  ( 9.564922557960805705, 16.46253265017160317, 89.58224293864769550 ) ) ;
#90419 = CARTESIAN_POINT ( 'NONE',  ( -16.51473224551069308, -9.474510206698971260, 26.66557627198103120 ) ) ;
#90420 = CARTESIAN_POINT ( 'NONE',  ( 5.049401038298161559, -19.05341960407611168, 62.70724293864769550 ) ) ;
#90421 = CARTESIAN_POINT ( 'NONE',  ( 14.98214168267148949, 15.14060719587546622, -56.46919128290397794 ) ) ;
#90422 = CARTESIAN_POINT ( 'NONE',  ( -21.55341960407619339, 5.719274019375674811, 73.54275706135234714 ) ) ;
#90423 = CARTESIAN_POINT ( 'NONE',  ( -17.72560187377287022, -5.499999999999974243, 89.07814504131324895 ) ) ;
#90424 = CARTESIAN_POINT ( 'NONE',  ( -5.049401038297874678, -19.05341960407617918, 29.79275706135232227 ) ) ;
#90425 = CARTESIAN_POINT ( 'NONE',  ( 9.564922557961047289, -16.46253265017146816, 30.41775706135232937 ) ) ;
#90426 = CARTESIAN_POINT ( 'NONE',  ( 8.314922557960818139, 14.29746914071049879, 54.58224293864769550 ) ) ;
#90427 = CARTESIAN_POINT ( 'NONE',  ( 13.97604488694527802, 13.89961937509977652, 59.37390960531434558 ) ) ;
#90428 = CARTESIAN_POINT ( 'NONE',  ( 21.52544592524344225, -5.823673210054117533, 28.54057627198103120 ) ) ;
#90429 = CARTESIAN_POINT ( 'NONE',  ( -5.719274019375665041, -21.55341960407619695, 79.79275706135236135 ) ) ;
#90430 = CARTESIAN_POINT ( 'NONE',  ( -13.97604488694527625, -13.89961937509977652, 61.87390960531435979 ) ) ;
#90431 = CARTESIAN_POINT ( 'NONE',  ( -15.80617190586768217, 15.72974639402176855, 78.12609039468570415 ) ) ;
#90432 = CARTESIAN_POINT ( 'NONE',  ( 21.53943276465977519, -0.05219959533907433946, 38.74890960531435979 ) ) ;
#90433 = CARTESIAN_POINT ( 'NONE',  ( -13.89961937509977652, 13.97604488694528158, 65.62390960531436690 ) ) ;
#90434 = CARTESIAN_POINT ( 'NONE',  ( -0.05219959533937732626, 21.53943276465977519, 37.50109039468568284 ) ) ;
#90435 = CARTESIAN_POINT ( 'NONE',  ( -5.153800228976607833, 19.02544592524334988, 57.70942372801899012 ) ) ;
#90436 = CARTESIAN_POINT ( 'NONE',  ( 19.03943276465977164, -0.05219959533909143690, 48.74890960531435979 ) ) ;
#90437 = CARTESIAN_POINT ( 'NONE',  ( 13.89961937509977652, -13.97604488694527269, 78.12390960531433848 ) ) ;
#90438 = CARTESIAN_POINT ( 'NONE',  ( -8.314922557961024197, 14.29746914071037800, 27.91775706135234358 ) ) ;
#90439 = CARTESIAN_POINT ( 'NONE',  ( 4.379528057220339221, -16.55341960407611168, 82.70724293864770971 ) ) ;
#90440 = CARTESIAN_POINT ( 'NONE',  ( 9.474510206698971260, -16.51473224551069308, 52.91557627198102409 ) ) ;
#90441 = CARTESIAN_POINT ( 'NONE',  ( -10.81492255796078084, -18.62759615963271287, 47.08224293864770260 ) ) ;
#90442 = VECTOR ( 'NONE', #61151, 1000.000000000000000 ) ;
#90443 = CARTESIAN_POINT ( 'NONE',  ( -0.05219959533936034679, 19.03943276465977164, 112.5010903946856757 ) ) ;
#90444 = CARTESIAN_POINT ( 'NONE',  ( 15.72974639402176855, 15.80617190586768217, 21.87609039468567573 ) ) ;
#90445 = CARTESIAN_POINT ( 'NONE',  ( 18.62759615963255655, 10.81492255796105972, 76.66775706135234714 ) ) ;
#90446 = CARTESIAN_POINT ( 'NONE',  ( -0.05219959533934338120, 16.53943276465976808, 67.50109039468568994 ) ) ;
#90447 = CARTESIAN_POINT ( 'NONE',  ( 16.52544592524335698, 4.483927247898782831, 71.45942372801901854 ) ) ;
#90448 =( BOUNDED_CURVE ( )  B_SPLINE_CURVE ( 3, ( #53820, #195346, #118501, #180191 ),
 .UNSPECIFIED., .F., .F. ) 
 B_SPLINE_CURVE_WITH_KNOTS ( ( 4, 4 ),
 ( 1.132647296210725241, 2.115944711806983847 ),
 .UNSPECIFIED. ) 
 CURVE ( )  GEOMETRIC_REPRESENTATION_ITEM ( )  RATIONAL_B_SPLINE_CURVE ( ( 1.000000000000000000, 0.9210371567966659789, 0.9210371567966659789, 1.000000000000000000 ) ) 
 REPRESENTATION_ITEM ( '' )  );
#90449 = CARTESIAN_POINT ( 'NONE',  ( 16.46253265017160672, -9.564922557960803928, 63.33224293864769550 ) ) ;
#90450 = CARTESIAN_POINT ( 'NONE',  ( -4.379528057220086978, -16.55341960407618274, 94.79275706135234714 ) ) ;
#90451 = CARTESIAN_POINT ( 'NONE',  ( 0.05219959533936267826, -19.03943276465977164, 40.00109039468566152 ) ) ;
#90452 = CARTESIAN_POINT ( 'NONE',  ( -15.72974639402176322, -15.80617190586768395, 24.37609039468567573 ) ) ;
#90453 = CARTESIAN_POINT ( 'NONE',  ( 16.55341960407611168, 4.379528057220329451, 68.95724293864769550 ) ) ;
#90454 = CARTESIAN_POINT ( 'NONE',  ( 5.153800228976335163, 19.02544592524342804, 89.79057627198102409 ) ) ;
#90455 = CARTESIAN_POINT ( 'NONE',  ( -12.14591786802326823, 12.06949235617739902, 93.12609039468568994 ) ) ;
#90456 = CARTESIAN_POINT ( 'NONE',  ( -21.52544592524334988, -5.823673210054445271, 53.95942372801900433 ) ) ;
#90457 = CARTESIAN_POINT ( 'NONE',  ( -8.224510206698735004, -14.34966873604973081, 29.58442372801901854 ) ) ;
#90458 = CARTESIAN_POINT ( 'NONE',  ( 5.719274019375673035, 21.55341960407619339, 32.29275706135235424 ) ) ;
#90459 = CARTESIAN_POINT ( 'NONE',  ( 12.14591786802309770, 12.06949235617756955, 54.37390960531435979 ) ) ;
#90460 = ORIENTED_EDGE ( 'NONE', *, *, #158042, .T. ) ;
#90461 = CARTESIAN_POINT ( 'NONE',  ( -21.52544592524343514, 5.823673210054127303, 96.04057627198102409 ) ) ;
#90462 = CARTESIAN_POINT ( 'NONE',  ( 4.379528057220339221, -16.55341960407611168, 42.70724293864770260 ) ) ;
#90463 = ORIENTED_EDGE ( 'NONE', *, *, #196878, .T. ) ;
#90464 = CARTESIAN_POINT ( 'NONE',  ( -12.49999999999997691, -89.99999999999997158, -15.00000000000000000 ) ) ;
#90465 = CARTESIAN_POINT ( 'NONE',  ( -21.53943276465977519, 0.05219959533907696930, 26.24890960531435624 ) ) ;
#90466 = CARTESIAN_POINT ( 'NONE',  ( -18.67979575497193778, 10.72451020669871902, 38.33442372801900433 ) ) ;
#90467 = CARTESIAN_POINT ( 'NONE',  ( 16.55341960407611168, 4.379528057220329451, 68.95724293864769550 ) ) ;
#90468 = AXIS2_PLACEMENT_3D ( 'NONE', #15297, #13317, #105320 ) ;
#90469 = CARTESIAN_POINT ( 'NONE',  ( -9.564922557960796823, -16.46253265017161027, 67.08224293864769550 ) ) ;
#90471 = CARTESIAN_POINT ( 'NONE',  ( -16.46253265017146816, -9.564922557961047289, 64.16775706135233293 ) ) ;
#90470 = CARTESIAN_POINT ( 'NONE',  ( -13.97604488694527625, -13.89961937509977652, 21.87390960531435979 ) ) ;
#90472 = EDGE_CURVE ( 'NONE', #167085, #16610, #180992, .T. ) ;
#90473 = CARTESIAN_POINT ( 'NONE',  ( 18.62759615963271287, -10.81492255796078972, 43.33224293864769550 ) ) ;
#90474 = CARTESIAN_POINT ( 'NONE',  ( -23.57492084471414628, -29.96337447969917633, -16.79025860371109502 ) ) ;
#90475 = CARTESIAN_POINT ( 'NONE',  ( 5.153800228976335163, 19.02544592524342804, 54.79057627198103120 ) ) ;
#90476 = CARTESIAN_POINT ( 'NONE',  ( -0.05219959533934338120, 16.53943276465976808, 37.50109039468568284 ) ) ;
#90477 = CARTESIAN_POINT ( 'NONE',  ( 5.823673210054125526, 21.52544592524343514, 114.7905762719810383 ) ) ;
#90478 = CARTESIAN_POINT ( 'NONE',  ( -8.314922557960811034, -14.29746914071050412, 47.08224293864770260 ) ) ;
#90479 = ORIENTED_EDGE ( 'NONE', *, *, #44009, .T. ) ;
#90480 = CARTESIAN_POINT ( 'NONE',  ( 9.474510206698971260, -16.51473224551069308, 92.91557627198103830 ) ) ;
#90481 = CARTESIAN_POINT ( 'NONE',  ( 10.81492255796078972, 18.62759615963270932, 74.58224293864768129 ) ) ;
#90483 = CARTESIAN_POINT ( 'NONE',  ( -14.34966873604972548, 8.224510206698743886, 43.33442372801901143 ) ) ;
#90482 = CARTESIAN_POINT ( 'NONE',  ( -5.823673210054116645, -21.52544592524344225, 112.2905762719810241 ) ) ;
#90484 = CARTESIAN_POINT ( 'NONE',  ( 15.72974639402199770, -15.80617190586745480, 43.12390960531435269 ) ) ;
#90485 = CARTESIAN_POINT ( 'NONE',  ( 21.52544592524334988, 5.823673210054432836, 106.4594237280190328 ) ) ;
#90486 = CARTESIAN_POINT ( 'NONE',  ( -13.97604488694527625, -13.89961937509977652, 96.87390960531433848 ) ) ;
#90487 = CARTESIAN_POINT ( 'NONE',  ( -16.51473224551069308, -9.474510206698971260, 46.66557627198102409 ) ) ;
#90488 = CARTESIAN_POINT ( 'NONE',  ( -19.05341960407611168, -5.049401038298163336, 96.45724293864769550 ) ) ;
#90489 = CARTESIAN_POINT ( 'NONE',  ( -9.564922557960796823, -16.46253265017161027, 82.08224293864768129 ) ) ;
#90490 = CARTESIAN_POINT ( 'NONE',  ( 16.81555441253471983, -7.025013491696154411, 88.13685445334212432 ) ) ;
#90491 = CARTESIAN_POINT ( 'NONE',  ( 19.02544592524334988, 5.153800228976608722, 61.45942372801900433 ) ) ;
#90493 = CARTESIAN_POINT ( 'NONE',  ( 18.67979575497178502, 10.72451020669898547, 34.16557627198102409 ) ) ;
#90492 = CARTESIAN_POINT ( 'NONE',  ( 18.67979575497194134, -10.72451020669871369, 105.8344237280190328 ) ) ;
#90494 = CARTESIAN_POINT ( 'NONE',  ( -0.05219959533934338120, 16.53943276465976808, 107.5010903946856899 ) ) ;
#90495 = CARTESIAN_POINT ( 'NONE',  ( 16.46253265017146816, 9.564922557961045513, 81.66775706135233293 ) ) ;
#90496 = CARTESIAN_POINT ( 'NONE',  ( 18.22780087662121673, 5.500000000000056843, 38.98459894673893444 ) ) ;
#90497 = CARTESIAN_POINT ( 'NONE',  ( -0.05219959533936034679, 19.03943276465977164, 87.50109039468567573 ) ) ;
#90498 = CARTESIAN_POINT ( 'NONE',  ( 13.89961937509957401, 13.97604488694547697, 36.87609039468565442 ) ) ;
#90499 = CARTESIAN_POINT ( 'NONE',  ( -16.29526858892878849, -7.335722546920001363, 45.79670597800205201 ) ) ;
#90500 = CARTESIAN_POINT ( 'NONE',  ( -19.03943276465977164, 0.05219959533909376836, 46.24890960531435979 ) ) ;
#90501 = CARTESIAN_POINT ( 'NONE',  ( -14.29746914071049879, 8.314922557960819915, 50.83224293864770971 ) ) ;
#90502 = CARTESIAN_POINT ( 'NONE',  ( -5.049401038298153566, 19.05341960407611168, 25.20724293864768484 ) ) ;
#90503 = CARTESIAN_POINT ( 'NONE',  ( -16.52544592524342804, 4.483927247898546575, 26.04057627198103475 ) ) ;
#90504 = DIRECTION ( 'NONE',  ( 0.000000000000000000, -0.7071067811865483499, 0.7071067811865465735 ) ) ;
#90505 = CARTESIAN_POINT ( 'NONE',  ( -16.52544592524335698, -4.483927247898792601, 88.95942372801901854 ) ) ;
#90506 = CARTESIAN_POINT ( 'NONE',  ( 0.05219959533909260263, 19.03943276465977164, 44.99890960531435979 ) ) ;
#90507 = CARTESIAN_POINT ( 'NONE',  ( 21.53943276465977519, 0.05219959533937863772, 111.2510903946856899 ) ) ;
#90508 = CARTESIAN_POINT ( 'NONE',  ( 16.55341960407618274, -4.379528057220086978, 26.04275706135235779 ) ) ;
#90510 = ORIENTED_EDGE ( 'NONE', *, *, #18810, .T. ) ;
#90509 = CARTESIAN_POINT ( 'NONE',  ( -15.72974639402176322, -15.80617190586768395, 94.37609039468568994 ) ) ;
#90511 = CARTESIAN_POINT ( 'NONE',  ( -5.153800228976328057, -19.02544592524343514, 92.29057627198099567 ) ) ;
#90512 = CARTESIAN_POINT ( 'NONE',  ( 9.474510206698971260, -16.51473224551069308, 77.91557627198103830 ) ) ;
#90513 = CARTESIAN_POINT ( 'NONE',  ( -5.950531402560715689E-15, 38.81732327939063509, -7.124999997268814056 ) ) ;
#90514 = CARTESIAN_POINT ( 'NONE',  ( -18.62759615963270932, 10.81492255796079327, 115.8322429386477097 ) ) ;
#90515 = CARTESIAN_POINT ( 'NONE',  ( 16.55341960407611168, 4.379528057220329451, 73.95724293864769550 ) ) ;
#90516 = CARTESIAN_POINT ( 'NONE',  ( 21.53943276465977519, -0.05219959533907433946, 68.74890960531435269 ) ) ;
#90517 = CARTESIAN_POINT ( 'NONE',  ( 9.564922557960805705, 16.46253265017160317, 54.58224293864769550 ) ) ;
#90519 = CARTESIAN_POINT ( 'NONE',  ( -12.06949235617739369, -12.14591786802326823, 94.37609039468568994 ) ) ;
#90518 = CARTESIAN_POINT ( 'NONE',  ( 5.719274019375991003, -21.55341960407610458, 97.70724293864772392 ) ) ;
#90520 = EDGE_LOOP ( 'NONE', ( #12191, #161221, #105072, #76889 ) ) ;
#90521 = CARTESIAN_POINT ( 'NONE',  ( -9.474510206698964154, 16.51473224551069663, 60.41557627198102409 ) ) ;
#90523 = LINE ( 'NONE', #152205, #72064 ) ;
#90522 = CARTESIAN_POINT ( 'NONE',  ( -16.55341960407611168, -4.379528057220339221, 86.45724293864770971 ) ) ;
#90524 = CARTESIAN_POINT ( 'NONE',  ( 13.97604488694527802, 13.89961937509977652, 69.37390960531436690 ) ) ;
#90525 = CARTESIAN_POINT ( 'NONE',  ( -19.02544592524334988, -5.153800228976617603, 83.95942372801901854 ) ) ;
#90526 = CARTESIAN_POINT ( 'NONE',  ( -4.379528057220328563, 16.55341960407611168, 80.20724293864769550 ) ) ;
#90527 = CARTESIAN_POINT ( 'NONE',  ( -5.719274019375665041, -21.55341960407619695, 64.79275706135234714 ) ) ;
#90529 = CARTESIAN_POINT ( 'NONE',  ( 21.52544592524344225, -5.823673210054117533, 113.5405762719810383 ) ) ;
#90528 = CARTESIAN_POINT ( 'NONE',  ( -16.51473224551069308, -9.474510206698971260, 41.66557627198103120 ) ) ;
#90530 = CARTESIAN_POINT ( 'NONE',  ( -8.314922557960811034, -14.29746914071050412, 107.0822429386476955 ) ) ;
#90531 = CARTESIAN_POINT ( 'NONE',  ( 4.755560754627824238, -48.37114524149939854, -25.00000000000000000 ) ) ;
#90532 = CARTESIAN_POINT ( 'NONE',  ( 9.474510206698971260, -16.51473224551069308, 62.91557627198102409 ) ) ;
#90533 = CARTESIAN_POINT ( 'NONE',  ( 17.12812012977027010, 6.668231424565983723, 113.8594875932314636 ) ) ;
#90535 = CARTESIAN_POINT ( 'NONE',  ( 19.03943276465977164, -0.05219959533909143690, 108.7489096053143527 ) ) ;
#90534 = CARTESIAN_POINT ( 'NONE',  ( -5.153800228976607833, 19.02544592524334988, 92.70942372801901854 ) ) ;
#90536 = CARTESIAN_POINT ( 'NONE',  ( 0.05219959533937995610, -21.53943276465977519, 45.00109039468568284 ) ) ;
#90537 = CARTESIAN_POINT ( 'NONE',  ( 13.97604488694527802, 13.89961937509977652, 84.37390960531433848 ) ) ;
#90538 = CARTESIAN_POINT ( 'NONE',  ( 5.049401038297881783, 19.05341960407617563, 72.29275706135234714 ) ) ;
#90539 = CARTESIAN_POINT ( 'NONE',  ( -13.89961937509977652, 13.97604488694528158, 60.62390960531436690 ) ) ;
#90540 = CARTESIAN_POINT ( 'NONE',  ( -4.483927247898539470, -16.52544592524342804, 77.29057627198102409 ) ) ;
#90541 = CARTESIAN_POINT ( 'NONE',  ( 4.483927247898545687, 16.52544592524342804, 79.79057627198102409 ) ) ;
#90542 = CARTESIAN_POINT ( 'NONE',  ( -19.02544592524342804, 5.153800228976336051, 86.04057627198103830 ) ) ;
#90543 = CARTESIAN_POINT ( 'NONE',  ( -14.34966873604960291, -8.224510206698953496, 81.66557627198103830 ) ) ;
#90544 = CARTESIAN_POINT ( 'NONE',  ( 5.049401038298161559, -19.05341960407611168, 87.70724293864769550 ) ) ;
#90545 = CARTESIAN_POINT ( 'NONE',  ( 9.564922557961047289, -16.46253265017146816, 35.41775706135233293 ) ) ;
#90548 = CARTESIAN_POINT ( 'NONE',  ( 14.29746914071049879, -8.314922557960816363, 113.3322429386476955 ) ) ;
#90547 = CARTESIAN_POINT ( 'NONE',  ( -12.06949235617756955, 12.14591786802309770, 30.62390960531436335 ) ) ;
#90546 = CARTESIAN_POINT ( 'NONE',  ( 5.153800228976335163, 19.02544592524342804, 54.79057627198103120 ) ) ;
#90549 = ORIENTED_EDGE ( 'NONE', *, *, #142462, .T. ) ;
#90550 = CARTESIAN_POINT ( 'NONE',  ( -15.80617190586768217, 15.72974639402176855, 48.12609039468568284 ) ) ;
#90551 = CARTESIAN_POINT ( 'NONE',  ( -16.51473224551082808, 9.474510206698731452, 63.33442372801900433 ) ) ;
#90552 = CARTESIAN_POINT ( 'NONE',  ( -16.52544592524342804, 4.483927247898546575, 36.04057627198102409 ) ) ;
#90553 = CARTESIAN_POINT ( 'NONE',  ( -5.823673210054116645, -21.52544592524344225, 87.29057627198103830 ) ) ;
#90554 = CARTESIAN_POINT ( 'NONE',  ( -13.89961937509977652, 13.97604488694528158, 110.6239096053143243 ) ) ;
#90555 = CARTESIAN_POINT ( 'NONE',  ( -4.379528057220328563, 16.55341960407611168, 65.20724293864768129 ) ) ;
#90556 = CARTESIAN_POINT ( 'NONE',  ( -16.51473224551069308, -9.474510206698971260, 41.66557627198103120 ) ) ;
#90557 = CARTESIAN_POINT ( 'NONE',  ( -9.474510206698720793, -16.51473224551083518, 44.58442372801900433 ) ) ;
#90558 = CARTESIAN_POINT ( 'NONE',  ( -12.06949235617739369, -12.14591786802326823, 104.3760903946856899 ) ) ;
#90559 = CARTESIAN_POINT ( 'NONE',  ( 12.06949235617739724, 12.14591786802326823, 51.87609039468568284 ) ) ;
#90560 = CARTESIAN_POINT ( 'NONE',  ( 18.62759615963271287, -10.81492255796078972, 33.33224293864769550 ) ) ;
#90561 = CARTESIAN_POINT ( 'NONE',  ( -5.719274019375665041, -21.55341960407619695, 104.7927570613523898 ) ) ;
#90562 = CARTESIAN_POINT ( 'NONE',  ( -19.05341960407611168, -5.049401038298163336, 86.45724293864769550 ) ) ;
#90563 = CARTESIAN_POINT ( 'NONE',  ( 4.483927247898790824, -16.52544592524335698, 80.20942372801901854 ) ) ;
#90564 = CARTESIAN_POINT ( 'NONE',  ( 14.29746914071049879, -8.314922557960816363, 113.3322429386476955 ) ) ;
#90565 = CARTESIAN_POINT ( 'NONE',  ( 4.483927247898545687, 16.52544592524342804, 29.79057627198102409 ) ) ;
#90567 = CARTESIAN_POINT ( 'NONE',  ( 19.03943276465977164, -0.05219959533909143690, 88.74890960531436690 ) ) ;
#90566 = CARTESIAN_POINT ( 'NONE',  ( 16.46253265017160672, -9.564922557960803928, 108.3322429386476955 ) ) ;
#90568 = CARTESIAN_POINT ( 'NONE',  ( 21.52544592524344225, -5.823673210054117533, 33.54057627198102409 ) ) ;
#90569 = CARTESIAN_POINT ( 'NONE',  ( 8.224510206698953496, -14.34966873604960469, 67.91557627198102409 ) ) ;
#90570 = EDGE_CURVE ( 'NONE', #182913, #161515, #122788, .T. ) ;
#90571 = CARTESIAN_POINT ( 'NONE',  ( 14.29746914071049879, -8.314922557960816363, 53.33224293864769550 ) ) ;
#90572 = VERTEX_POINT ( 'NONE', #13564 ) ;
#90574 = FACE_OUTER_BOUND ( 'NONE', #163655, .T. ) ;
#90573 = CARTESIAN_POINT ( 'NONE',  ( -12.14591786802326823, 12.06949235617739902, 58.12609039468568994 ) ) ;
#90575 = CARTESIAN_POINT ( 'NONE',  ( -9.474510206698720793, -16.51473224551083518, 49.58442372801899722 ) ) ;
#90576 = CARTESIAN_POINT ( 'NONE',  ( -0.05219959533909027116, -19.03943276465977164, 92.49890960531436690 ) ) ;
#90577 = CARTESIAN_POINT ( 'NONE',  ( -13.97604488694547697, 13.89961937509957934, 63.12609039468566152 ) ) ;
#90578 = CARTESIAN_POINT ( 'NONE',  ( -8.571926809382601320, -26.38167802310801591, 145.7750000027311899 ) ) ;
#90579 = CARTESIAN_POINT ( 'NONE',  ( -13.97604488694547697, 13.89961937509957934, 53.12609039468565442 ) ) ;
#90581 = CARTESIAN_POINT ( 'NONE',  ( 8.224510206698742110, 14.34966873604972548, 102.0844237280190185 ) ) ;
#90580 = CARTESIAN_POINT ( 'NONE',  ( 9.564922557961047289, -16.46253265017146816, 100.4177570613523329 ) ) ;
#90582 = CARTESIAN_POINT ( 'NONE',  ( 27.73933785331498214, 9.013057229001095294, 144.4750000027311501 ) ) ;
#90583 = CARTESIAN_POINT ( 'NONE',  ( 19.03943276465977164, -0.05219959533909143690, 28.74890960531435624 ) ) ;
#90584 = CARTESIAN_POINT ( 'NONE',  ( 21.53943276465977519, -0.05219959533907433946, 28.74890960531435624 ) ) ;
#90585 = CARTESIAN_POINT ( 'NONE',  ( 18.62759615963255655, 10.81492255796105972, 46.66775706135234714 ) ) ;
#90586 = CARTESIAN_POINT ( 'NONE',  ( 5.049401038297881783, 19.05341960407617563, 102.2927570613523045 ) ) ;
#90588 = CARTESIAN_POINT ( 'NONE',  ( -5.049401038298153566, 19.05341960407611168, 65.20724293864765286 ) ) ;
#90587 = DIRECTION ( 'NONE',  ( 0.000000000000000000, 0.000000000000000000, 1.000000000000000000 ) ) ;
#90589 = DIRECTION ( 'NONE',  ( 0.000000000000000000, 0.000000000000000000, 1.000000000000000000 ) ) ;
#90591 = CARTESIAN_POINT ( 'NONE',  ( -19.05341960407611168, -5.049401038298163336, 66.45724293864769550 ) ) ;
#90590 = CARTESIAN_POINT ( 'NONE',  ( 12.14591786802309770, 12.06949235617756955, 79.37390960531436690 ) ) ;
#90592 = CARTESIAN_POINT ( 'NONE',  ( -13.97604488694527625, -13.89961937509977652, 71.87390960531433848 ) ) ;
#90593 = CARTESIAN_POINT ( 'NONE',  ( 19.05341960407617918, -5.049401038297876454, 81.04275706135231871 ) ) ;
#90594 = CARTESIAN_POINT ( 'NONE',  ( -21.55341960407610458, -5.719274019375992779, 61.45724293864770260 ) ) ;
#90595 = CARTESIAN_POINT ( 'NONE',  ( 16.52544592524342804, -4.483927247898539470, 108.5405762719810241 ) ) ;
#90596 = CARTESIAN_POINT ( 'NONE',  ( -13.89961937509957401, -13.97604488694547875, 44.37609039468566863 ) ) ;
#90597 = CARTESIAN_POINT ( 'NONE',  ( 19.03943276465977164, -0.05219959533909143690, 78.74890960531436690 ) ) ;
#90598 = CARTESIAN_POINT ( 'NONE',  ( 10.81492255796078972, 18.62759615963270932, 84.58224293864769550 ) ) ;
#90600 = CARTESIAN_POINT ( 'NONE',  ( -13.89961937509957401, -13.97604488694547875, 49.37609039468567573 ) ) ;
#90599 = CARTESIAN_POINT ( 'NONE',  ( 0.05219959533910956823, 16.53943276465976808, 74.99890960531435269 ) ) ;
#90601 = CARTESIAN_POINT ( 'NONE',  ( -21.52544592524343514, 5.823673210054127303, 76.04057627198102409 ) ) ;
#90602 = CARTESIAN_POINT ( 'NONE',  ( 18.67979575497178502, 10.72451020669898547, 59.16557627198103120 ) ) ;
#90603 = CARTESIAN_POINT ( 'NONE',  ( -18.67979575497178146, -10.72451020669898902, 41.66557627198103120 ) ) ;
#90604 = CARTESIAN_POINT ( 'NONE',  ( 21.52544592524334988, 5.823673210054432836, 86.45942372801901854 ) ) ;
#90605 = CARTESIAN_POINT ( 'NONE',  ( 13.89961937509977652, -13.97604488694527269, 68.12390960531436690 ) ) ;
#90606 = CARTESIAN_POINT ( 'NONE',  ( 16.52544592524342804, -4.483927247898539470, 113.5405762719810383 ) ) ;
#90607 = VECTOR ( 'NONE', #119761, 1000.000000000000000 ) ;
#90608 = CARTESIAN_POINT ( 'NONE',  ( -21.55341960407619339, 5.719274019375674811, 23.54275706135235424 ) ) ;
#90609 = CARTESIAN_POINT ( 'NONE',  ( -5.719274019375665041, -21.55341960407619695, 34.79275706135235424 ) ) ;
#90610 = CARTESIAN_POINT ( 'NONE',  ( 0.05219959533909260263, 19.03943276465977164, 34.99890960531435979 ) ) ;
#90611 = CARTESIAN_POINT ( 'NONE',  ( 21.52544592524344225, -5.823673210054117533, 108.5405762719810241 ) ) ;
#90612 = CARTESIAN_POINT ( 'NONE',  ( 19.05341960407617918, -5.049401038297876454, 61.04275706135232582 ) ) ;
#90613 = CARTESIAN_POINT ( 'NONE',  ( -9.564922557960796823, -16.46253265017161027, 37.08224293864768839 ) ) ;
#90614 = CARTESIAN_POINT ( 'NONE',  ( -16.55341960407617563, 4.379528057220093196, 33.54275706135234714 ) ) ;
#90615 = CARTESIAN_POINT ( 'NONE',  ( 16.20063489777861676, -7.373262058553140541, 22.00000000000000711 ) ) ;
#90616 = CARTESIAN_POINT ( 'NONE',  ( 14.29746914071037800, 8.314922557961029526, 56.66775706135235424 ) ) ;
#90617 = CARTESIAN_POINT ( 'NONE',  ( 16.51473224551069308, 9.474510206698969483, 39.16557627198103120 ) ) ;
#90618 = CARTESIAN_POINT ( 'NONE',  ( -26.73207562759412070, -6.543912086054805677, 168.7462576975848378 ) ) ;
#90619 = CARTESIAN_POINT ( 'NONE',  ( -0.05219959533909027116, -19.03943276465977164, 87.49890960531436690 ) ) ;
#90620 = CARTESIAN_POINT ( 'NONE',  ( -19.05341960407611168, -5.049401038298163336, 21.45724293864768839 ) ) ;
#90621 = CARTESIAN_POINT ( 'NONE',  ( -5.719274019375978568, 21.55341960407610458, 55.20724293864770260 ) ) ;
#90622 = CARTESIAN_POINT ( 'NONE',  ( -8.314922557961024197, 14.29746914071037800, 47.91775706135234714 ) ) ;
#90623 = CARTESIAN_POINT ( 'NONE',  ( 21.52544592524334988, 5.823673210054432836, 106.4594237280190328 ) ) ;
#90624 = CARTESIAN_POINT ( 'NONE',  ( 19.02544592524343514, -5.153800228976328945, 38.54057627198103120 ) ) ;
#90625 = CARTESIAN_POINT ( 'NONE',  ( -14.29746914071049879, 8.314922557960819915, 25.83224293864769194 ) ) ;
#90626 = CARTESIAN_POINT ( 'NONE',  ( -8.314922557960811034, -14.29746914071050412, 57.08224293864769550 ) ) ;
#90627 = CARTESIAN_POINT ( 'NONE',  ( 19.03943276465977164, -0.05219959533909143690, 58.74890960531435979 ) ) ;
#90628 = CARTESIAN_POINT ( 'NONE',  ( 5.719274019375673035, 21.55341960407619339, 112.2927570613523471 ) ) ;
#90629 = CARTESIAN_POINT ( 'NONE',  ( -21.53943276465977519, 0.05219959533907696930, 116.2489096053143669 ) ) ;
#90630 = CARTESIAN_POINT ( 'NONE',  ( 21.52544592524334988, 5.823673210054432836, 81.45942372801900433 ) ) ;
#90631 = CARTESIAN_POINT ( 'NONE',  ( 4.379528057220092307, 16.55341960407617563, 52.29275706135236135 ) ) ;
#90632 = CARTESIAN_POINT ( 'NONE',  ( -12.14591786802326823, 12.06949235617739902, 28.12609039468568284 ) ) ;
#90634 = CARTESIAN_POINT ( 'NONE',  ( -21.55341960407619339, 5.719274019375674811, 103.5427570613523613 ) ) ;
#90633 = CARTESIAN_POINT ( 'NONE',  ( 4.379528057220339221, -16.55341960407611168, 87.70724293864769550 ) ) ;
#90635 = CARTESIAN_POINT ( 'NONE',  ( 16.53943276465976808, -0.05219959533910856209, 33.74890960531436690 ) ) ;
#90636 = CARTESIAN_POINT ( 'NONE',  ( -16.51473224551069308, -9.474510206698971260, 31.66557627198102054 ) ) ;
#90637 = CARTESIAN_POINT ( 'NONE',  ( 16.52544592524335698, 4.483927247898782831, 41.45942372801901143 ) ) ;
#90638 = CARTESIAN_POINT ( 'NONE',  ( -4.379528057220328563, 16.55341960407611168, 55.20724293864770260 ) ) ;
#90639 = CARTESIAN_POINT ( 'NONE',  ( 4.483927247898790824, -16.52544592524335698, 90.20942372801903275 ) ) ;
#90640 = CARTESIAN_POINT ( 'NONE',  ( 0.05219959533909260263, 19.03943276465977164, 104.9989096053143669 ) ) ;
#90641 = CARTESIAN_POINT ( 'NONE',  ( 16.51473224551069308, 9.474510206698969483, 114.1655762719810241 ) ) ;
#90642 = CARTESIAN_POINT ( 'NONE',  ( 5.719274019375673035, 21.55341960407619339, 112.2927570613523471 ) ) ;
#90643 = CARTESIAN_POINT ( 'NONE',  ( -4.379528057220328563, 16.55341960407611168, 90.20724293864770971 ) ) ;
#90644 = CARTESIAN_POINT ( 'NONE',  ( 13.97604488694527802, 13.89961937509977652, 99.37390960531436690 ) ) ;
#90645 = VERTEX_POINT ( 'NONE', #75231 ) ;
#90646 = CARTESIAN_POINT ( 'NONE',  ( -14.34966873604972548, 8.224510206698743886, 38.33442372801900433 ) ) ;
#90647 = CARTESIAN_POINT ( 'NONE',  ( 13.89961937509977652, -13.97604488694527269, 48.12390960531435979 ) ) ;
#90648 = CARTESIAN_POINT ( 'NONE',  ( -9.564922557960796823, -16.46253265017161027, 102.0822429386477097 ) ) ;
#90650 = FILL_AREA_STYLE ('',( #119028 ) ) ;
#90649 = CARTESIAN_POINT ( 'NONE',  ( 14.29746914071037800, 8.314922557961029526, 41.66775706135235424 ) ) ;
#90651 = CARTESIAN_POINT ( 'NONE',  ( 5.153800228976615827, -19.02544592524334988, 40.20942372801898301 ) ) ;
#90652 = CARTESIAN_POINT ( 'NONE',  ( -13.97604488694527625, -13.89961937509977652, 46.87390960531435979 ) ) ;
#90653 = CARTESIAN_POINT ( 'NONE',  ( 4.379528057220092307, 16.55341960407617563, 77.29275706135234714 ) ) ;
#90654 = CARTESIAN_POINT ( 'NONE',  ( -13.89961937509957401, -13.97604488694547875, 79.37609039468567573 ) ) ;
#90655 = CARTESIAN_POINT ( 'NONE',  ( 16.46253265017146816, 9.564922557961045513, 26.66775706135234003 ) ) ;
#90656 = CARTESIAN_POINT ( 'NONE',  ( -16.51473224551069308, -9.474510206698971260, 66.66557627198102409 ) ) ;
#90657 = CARTESIAN_POINT ( 'NONE',  ( 8.314922557960818139, 14.29746914071049879, 104.5822429386477097 ) ) ;
#90658 = EDGE_CURVE ( 'NONE', #102786, #4269, #98436, .T. ) ;
#90659 = CARTESIAN_POINT ( 'NONE',  ( -19.05341960407617563, 5.049401038297882671, 73.54275706135233293 ) ) ;
#90660 = CARTESIAN_POINT ( 'NONE',  ( 15.80617190586746368, 15.72974639402197994, 59.37390960531436690 ) ) ;
#90661 = CARTESIAN_POINT ( 'NONE',  ( -19.03943276465977164, -0.05219959533935918106, 23.75109039468566152 ) ) ;
#90662 = CARTESIAN_POINT ( 'NONE',  ( -9.564922557960796823, -16.46253265017161027, 102.0822429386477097 ) ) ;
#90663 = CARTESIAN_POINT ( 'NONE',  ( 10.81492255796078972, 18.62759615963270932, 74.58224293864768129 ) ) ;
#90664 = CARTESIAN_POINT ( 'NONE',  ( -37.99626262588766679, 2.428612866367529932E-14, -7.747842220587803475 ) ) ;
#90665 = CARTESIAN_POINT ( 'NONE',  ( -13.89961937509957401, -13.97604488694547875, 104.3760903946856757 ) ) ;
#90666 = CARTESIAN_POINT ( 'NONE',  ( -19.53037848336981241, 5.499999999999902300, 59.85532783611444785 ) ) ;
#90667 = CARTESIAN_POINT ( 'NONE',  ( 14.34966873604972726, -8.224510206698740333, 25.83442372801901499 ) ) ;
#90668 = CARTESIAN_POINT ( 'NONE',  ( 9.474510206698971260, -16.51473224551069308, 32.91557627198102409 ) ) ;
#90669 = CARTESIAN_POINT ( 'NONE',  ( -13.89961937509977652, 13.97604488694528158, 100.6239096053143669 ) ) ;
#90670 = CARTESIAN_POINT ( 'NONE',  ( -18.62759615963270932, 10.81492255796079327, 95.83224293864770971 ) ) ;
#90671 = CARTESIAN_POINT ( 'NONE',  ( -5.719274019375665041, -21.55341960407619695, 64.79275706135234714 ) ) ;
#90673 = CARTESIAN_POINT ( 'NONE',  ( -19.02544592524334988, -5.153800228976617603, 18.95942372801899722 ) ) ;
#90672 = CARTESIAN_POINT ( 'NONE',  ( -9.474510206698720793, -16.51473224551083518, 104.5844237280190043 ) ) ;
#90674 = CARTESIAN_POINT ( 'NONE',  ( -12.14591786802326823, 12.06949235617739902, 103.1260903946856757 ) ) ;
#90675 = CARTESIAN_POINT ( 'NONE',  ( 21.53943276465977519, -0.05219959533907433946, 98.74890960531438111 ) ) ;
#90676 = CARTESIAN_POINT ( 'NONE',  ( 14.34966873604960469, 8.224510206698951720, 34.16557627198102409 ) ) ;
#90677 = CARTESIAN_POINT ( 'NONE',  ( -19.03943276465977164, -0.05219959533935918106, 88.75109039468567573 ) ) ;
#90678 = CARTESIAN_POINT ( 'NONE',  ( -19.02544592524334988, -5.153800228976617603, 58.95942372801900433 ) ) ;
#90679 = CARTESIAN_POINT ( 'NONE',  ( -21.53943276465977519, -0.05219959533937600094, 63.75109039468568284 ) ) ;
#90680 = CARTESIAN_POINT ( 'NONE',  ( -9.564922557961040184, 16.46253265017147172, 42.91775706135234003 ) ) ;
#90681 = CARTESIAN_POINT ( 'NONE',  ( -4.483927247898539470, -16.52544592524342804, 107.2905762719810525 ) ) ;
#90682 = CARTESIAN_POINT ( 'NONE',  ( -18.67979575497178146, -10.72451020669898902, 36.66557627198103120 ) ) ;
#90683 = CARTESIAN_POINT ( 'NONE',  ( 0.05219959533910956823, 16.53943276465976808, 39.99890960531436690 ) ) ;
#90684 = CARTESIAN_POINT ( 'NONE',  ( -18.67979575497193778, 10.72451020669871902, 93.33442372801901854 ) ) ;
#90685 = CARTESIAN_POINT ( 'NONE',  ( 4.379528057220092307, 16.55341960407617563, 72.29275706135236135 ) ) ;
#90686 = CARTESIAN_POINT ( 'NONE',  ( -16.53943276465976808, 0.05219959533911058130, 21.24890960531436690 ) ) ;
#90687 = CARTESIAN_POINT ( 'NONE',  ( -5.823673210054431948, 21.52544592524334988, 62.70942372801902565 ) ) ;
#90688 = CARTESIAN_POINT ( 'NONE',  ( 18.62759615963255655, 10.81492255796105972, 61.66775706135235424 ) ) ;
#90689 = CARTESIAN_POINT ( 'NONE',  ( 21.55341960407610458, 5.719274019375980345, 63.95724293864770260 ) ) ;
#90690 = CARTESIAN_POINT ( 'NONE',  ( -19.05341960407611168, -5.049401038298163336, 31.45724293864769550 ) ) ;
#90691 = CARTESIAN_POINT ( 'NONE',  ( 21.53943276465977519, 0.05219959533937863772, 41.25109039468568284 ) ) ;
#90692 = CARTESIAN_POINT ( 'NONE',  ( -0.05219959533909027116, -19.03943276465977164, 22.49890960531436690 ) ) ;
#90693 = CARTESIAN_POINT ( 'NONE',  ( -19.05341960407611168, -5.049401038298163336, 36.45724293864766707 ) ) ;
#90694 = CARTESIAN_POINT ( 'NONE',  ( -0.05219959533910754901, -16.53943276465976808, 77.49890960531433848 ) ) ;
#90695 = CARTESIAN_POINT ( 'NONE',  ( -13.89961937509977652, 13.97604488694528158, 85.62390960531433848 ) ) ;
#90696 = CARTESIAN_POINT ( 'NONE',  ( -16.52544592524342804, 4.483927247898546575, 31.04057627198102409 ) ) ;
#90697 = CARTESIAN_POINT ( 'NONE',  ( 10.81492255796078972, 18.62759615963270932, 74.58224293864768129 ) ) ;
#90698 = CARTESIAN_POINT ( 'NONE',  ( -21.55341960407610458, -5.719274019375992779, 111.4572429386476813 ) ) ;
#90699 = DIRECTION ( 'NONE',  ( 1.000000000000000000, 0.000000000000000000, 0.000000000000000000 ) ) ;
#90701 = CARTESIAN_POINT ( 'NONE',  ( 13.89961937509957401, 13.97604488694547697, 106.8760903946856757 ) ) ;
#90700 = CARTESIAN_POINT ( 'NONE',  ( -16.46253265017160317, 9.564922557960807481, 65.83224293864769550 ) ) ;
#90702 = CARTESIAN_POINT ( 'NONE',  ( -18.62759615963270932, 10.81492255796079327, 55.83224293864770260 ) ) ;
#90703 = CARTESIAN_POINT ( 'NONE',  ( -15.80617190586768217, 15.72974639402176855, 88.12609039468570415 ) ) ;
#90704 = CARTESIAN_POINT ( 'NONE',  ( 13.97604488694527802, 13.89961937509977652, 64.37390960531436690 ) ) ;
#90705 = CARTESIAN_POINT ( 'NONE',  ( 9.564922557960805705, 16.46253265017160317, 94.58224293864769550 ) ) ;
#90706 = CARTESIAN_POINT ( 'NONE',  ( 16.55341960407618274, -4.379528057220086978, 71.04275706135234714 ) ) ;
#90707 = CARTESIAN_POINT ( 'NONE',  ( -21.52544592524334988, -5.823673210054445271, 63.95942372801901854 ) ) ;
#90708 = CARTESIAN_POINT ( 'NONE',  ( 18.62759615963255655, 10.81492255796105972, 96.66775706135234714 ) ) ;
#90709 = CARTESIAN_POINT ( 'NONE',  ( -18.62759615963270932, 10.81492255796079327, 115.8322429386477097 ) ) ;
#90710 = CARTESIAN_POINT ( 'NONE',  ( -0.05219959533907301413, -21.53943276465977519, 72.49890960531435269 ) ) ;
#90711 = CARTESIAN_POINT ( 'NONE',  ( 0.05219959533936267826, -19.03943276465977164, 50.00109039468566863 ) ) ;
#90712 = CARTESIAN_POINT ( 'NONE',  ( -15.80617190586745835, -15.72974639402198527, 36.87390960531435979 ) ) ;
#90714 = CARTESIAN_POINT ( 'NONE',  ( -12.14591786802309592, -12.06949235617757132, 36.87390960531435979 ) ) ;
#90713 = CARTESIAN_POINT ( 'NONE',  ( -16.51473224551069308, -9.474510206698971260, 86.66557627198102409 ) ) ;
#90715 = CARTESIAN_POINT ( 'NONE',  ( -3.573655867282028392E-15, 2.428612866367529932E-14, -8.000000000000000000 ) ) ;
#90716 = CARTESIAN_POINT ( 'NONE',  ( 2.500000000000000000, -1.178949249685214307, 2.042000000000002036 ) ) ;
#90717 = CARTESIAN_POINT ( 'NONE',  ( -19.02544592524334988, -5.153800228976617603, 98.95942372801900433 ) ) ;
#90718 = CARTESIAN_POINT ( 'NONE',  ( -21.53943276465977519, 0.05219959533907696930, 71.24890960531435269 ) ) ;
#90719 = CARTESIAN_POINT ( 'NONE',  ( 12.14591786802309770, 12.06949235617756955, 49.37390960531436690 ) ) ;
#90720 = CARTESIAN_POINT ( 'NONE',  ( 4.483927247898790824, -16.52544592524335698, 35.20942372801901854 ) ) ;
#90721 = CARTESIAN_POINT ( 'NONE',  ( -5.153800228976328057, -19.02544592524343514, 47.29057627198102409 ) ) ;
#90723 = CARTESIAN_POINT ( 'NONE',  ( 9.564922557961047289, -16.46253265017146816, 85.41775706135233293 ) ) ;
#90722 = CARTESIAN_POINT ( 'NONE',  ( 10.81492255796078972, 18.62759615963270932, 94.58224293864769550 ) ) ;
#90724 = CARTESIAN_POINT ( 'NONE',  ( -5.153800228976328057, -19.02544592524343514, 77.29057627198099567 ) ) ;
#90725 = CARTESIAN_POINT ( 'NONE',  ( -12.14591786802309592, -12.06949235617757132, 86.87390960531438111 ) ) ;
#90726 = CARTESIAN_POINT ( 'NONE',  ( 19.03943276465977164, -0.05219959533909143690, 63.74890960531435979 ) ) ;
#90727 = CARTESIAN_POINT ( 'NONE',  ( -12.14591786802309592, -12.06949235617757132, 66.87390960531436690 ) ) ;
#90728 = CARTESIAN_POINT ( 'NONE',  ( 16.46253265017160672, -9.564922557960803928, 38.33224293864768839 ) ) ;
#90729 = CARTESIAN_POINT ( 'NONE',  ( 28.82186960331498327, 2.428612866367529932E-14, 139.9999999999999716 ) ) ;
#90730 = CARTESIAN_POINT ( 'NONE',  ( -12.06949235617756955, 12.14591786802309770, 35.62390960531437401 ) ) ;
#90731 = CARTESIAN_POINT ( 'NONE',  ( 5.049401038298161559, -19.05341960407611168, 87.70724293864769550 ) ) ;
#90732 = CARTESIAN_POINT ( 'NONE',  ( -0.9482109960935514170, -14.02111363790006138, -60.30654223653038315 ) ) ;
#90733 = CARTESIAN_POINT ( 'NONE',  ( 13.97604488694548053, -13.89961937509957401, 55.62609039468566863 ) ) ;
#90734 = CARTESIAN_POINT ( 'NONE',  ( -16.53943276465976808, -0.05219959533934237506, 53.75109039468568994 ) ) ;
#90735 = CARTESIAN_POINT ( 'NONE',  ( 18.67979575497178502, 10.72451020669898547, 74.16557627198102409 ) ) ;
#90736 = CARTESIAN_POINT ( 'NONE',  ( 9.564922557961047289, -16.46253265017146816, 35.41775706135233293 ) ) ;
#90737 = CARTESIAN_POINT ( 'NONE',  ( 19.05341960407611168, 5.049401038298154454, 88.95724293864769550 ) ) ;
#90738 = CARTESIAN_POINT ( 'NONE',  ( 9.909549000311971056, -9.465176804199456839, -60.44446360152741704 ) ) ;
#90739 = CARTESIAN_POINT ( 'NONE',  ( 10.72451020669898902, -18.67979575497178502, 22.91557627198102765 ) ) ;
#90740 = CARTESIAN_POINT ( 'NONE',  ( 9.564922557960805705, 16.46253265017160317, 59.58224293864769550 ) ) ;
#90741 = CARTESIAN_POINT ( 'NONE',  ( 0.05219959533937995610, -21.53943276465977519, 55.00109039468568284 ) ) ;
#90742 = CARTESIAN_POINT ( 'NONE',  ( -9.474510206698964154, 16.51473224551069663, 25.41557627198103120 ) ) ;
#90745 = EDGE_LOOP ( 'NONE', ( #187287, #198196, #44550, #40859 ) ) ;
#90744 = CARTESIAN_POINT ( 'NONE',  ( 5.049401038298161559, -19.05341960407611168, 92.70724293864769550 ) ) ;
#90743 = CARTESIAN_POINT ( 'NONE',  ( -18.62759615963255300, -10.81492255796106328, 19.16775706135234714 ) ) ;
#90746 = CARTESIAN_POINT ( 'NONE',  ( 5.719274019375673035, 21.55341960407619339, 37.29275706135235424 ) ) ;
#90747 = ORIENTED_EDGE ( 'NONE', *, *, #198087, .T. ) ;
#90748 = CARTESIAN_POINT ( 'NONE',  ( 9.564922557960805705, 16.46253265017160317, 99.58224293864770971 ) ) ;
#90749 = FACE_BOUND ( 'NONE', #93809, .T. ) ;
#90750 = B_SPLINE_CURVE_WITH_KNOTS ( 'NONE', 3,
 ( #101037, #147567, #67712, #10054 ),
 .UNSPECIFIED., .F., .F.,
 ( 4, 4 ),
 ( -3.069853556319535759E-05, 0.003328242942582103868 ),
 .UNSPECIFIED. ) ;
#90751 = CARTESIAN_POINT ( 'NONE',  ( -21.55341960407610458, -5.719274019375992779, 111.4572429386476813 ) ) ;
#90752 = CARTESIAN_POINT ( 'NONE',  ( 19.05341960407611168, 5.049401038298154454, 48.95724293864768129 ) ) ;
#90753 = CARTESIAN_POINT ( 'NONE',  ( 8.314922557961029526, -14.29746914071037800, 30.41775706135234358 ) ) ;
#90754 = CARTESIAN_POINT ( 'NONE',  ( 11.74264578624800315, -36.14014761921581709, -11.14999999453762669 ) ) ;
#90755 = CARTESIAN_POINT ( 'NONE',  ( -21.52544592524334988, -5.823673210054445271, 98.95942372801903275 ) ) ;
#90756 = CARTESIAN_POINT ( 'NONE',  ( 13.89961937509977652, -13.97604488694527269, 28.12390960531435624 ) ) ;
#90757 = CARTESIAN_POINT ( 'NONE',  ( 18.62759615963255655, 10.81492255796105972, 96.66775706135234714 ) ) ;
#90759 = CARTESIAN_POINT ( 'NONE',  ( 21.52544592524334988, 5.823673210054432836, 56.45942372801902565 ) ) ;
#90758 = CARTESIAN_POINT ( 'NONE',  ( -5.153800228976328057, -19.02544592524343514, 87.29057627198103830 ) ) ;
#90760 = CARTESIAN_POINT ( 'NONE',  ( -5.359611314223446995E-15, 29.16686587814335496, 146.8750000027311273 ) ) ;
#90761 = CARTESIAN_POINT ( 'NONE',  ( -5.049401038298153566, 19.05341960407611168, 95.20724293864770971 ) ) ;
#90762 = CARTESIAN_POINT ( 'NONE',  ( -17.50000000000000000, 5.076555817581215102, 28.82048507950227290 ) ) ;
#90765 = CARTESIAN_POINT ( 'NONE',  ( -18.62759615963255300, -10.81492255796106328, 59.16775706135234714 ) ) ;
#90764 = CARTESIAN_POINT ( 'NONE',  ( 8.314922557961029526, -14.29746914071037800, 65.41775706135234714 ) ) ;
#90763 = CARTESIAN_POINT ( 'NONE',  ( 16.52544592524335698, 4.483927247898782831, 56.45942372801902565 ) ) ;
#90766 = CARTESIAN_POINT ( 'NONE',  ( -5.719274019375665041, -21.55341960407619695, 89.79275706135236135 ) ) ;
#90767 = CARTESIAN_POINT ( 'NONE',  ( 32.00000000000000000, -1.163414459189985801E-14, 95.00000000000000000 ) ) ;
#90768 = CARTESIAN_POINT ( 'NONE',  ( -4.379528057220086978, -16.55341960407618274, 29.79275706135234358 ) ) ;
#90769 = CARTESIAN_POINT ( 'NONE',  ( -0.05219959533909027116, -19.03943276465977164, 77.49890960531435269 ) ) ;
#90770 = CARTESIAN_POINT ( 'NONE',  ( 13.97604488694527802, 13.89961937509977652, 104.3739096053143385 ) ) ;
#90771 = CARTESIAN_POINT ( 'NONE',  ( -9.564922557960796823, -16.46253265017161027, 32.08224293864769550 ) ) ;
#90772 = CARTESIAN_POINT ( 'NONE',  ( 5.719274019375991003, -21.55341960407610458, 32.70724293864770260 ) ) ;
#90773 = CARTESIAN_POINT ( 'NONE',  ( -4.483927247898782831, 16.52544592524335698, 97.70942372801904696 ) ) ;
#90775 = CARTESIAN_POINT ( 'NONE',  ( -5.153800228976328057, -19.02544592524343514, 67.29057627198102409 ) ) ;
#90774 = CARTESIAN_POINT ( 'NONE',  ( -16.55341960407611168, -4.379528057220339221, 66.45724293864768129 ) ) ;
#90776 = CARTESIAN_POINT ( 'NONE',  ( 15.80617190586769283, -15.72974639402175789, 90.62609039468567573 ) ) ;
#90777 = CARTESIAN_POINT ( 'NONE',  ( -23.29544513554940721, -16.92513159979223758, 144.4656553485623647 ) ) ;
#90778 = CARTESIAN_POINT ( 'NONE',  ( 16.51473224551083163, -9.474510206698727899, 110.8344237280190043 ) ) ;
#90779 = CARTESIAN_POINT ( 'NONE',  ( -14.34966873604960291, -8.224510206698953496, 81.66557627198103830 ) ) ;
#90780 = CARTESIAN_POINT ( 'NONE',  ( -15.72974639402176322, -15.80617190586768395, 34.37609039468568284 ) ) ;
#90781 = CARTESIAN_POINT ( 'NONE',  ( 21.55341960407610458, 5.719274019375980345, 78.95724293864769550 ) ) ;
#90782 = CARTESIAN_POINT ( 'NONE',  ( 9.474510206698729675, 16.51473224551082808, 32.08442372801900433 ) ) ;
#90783 = CARTESIAN_POINT ( 'NONE',  ( 17.81289503416611453, -24.51734667627695785, 146.9500000054623570 ) ) ;
#90784 = CARTESIAN_POINT ( 'NONE',  ( 16.46253265017160672, -9.564922557960803928, 88.33224293864769550 ) ) ;
#90785 = CARTESIAN_POINT ( 'NONE',  ( 12.14591786802309770, 12.06949235617756955, 54.37390960531435979 ) ) ;
#90786 = CARTESIAN_POINT ( 'NONE',  ( -16.52544592524342804, 4.483927247898546575, 31.04057627198102409 ) ) ;
#90787 = CARTESIAN_POINT ( 'NONE',  ( 0.05219959533934541429, -16.53943276465976808, 95.00109039468568994 ) ) ;
#90788 = CARTESIAN_POINT ( 'NONE',  ( 19.03943276465977164, 0.05219959533936151252, 56.25109039468566863 ) ) ;
#90789 = CARTESIAN_POINT ( 'NONE',  ( 17.50000000000000000, 5.499999999999992895, 46.70309617465829888 ) ) ;
#90790 = CARTESIAN_POINT ( 'NONE',  ( 13.97604488694527802, 13.89961937509977652, 104.3739096053143385 ) ) ;
#90791 = CARTESIAN_POINT ( 'NONE',  ( 16.55341960407611168, 4.379528057220329451, 78.95724293864769550 ) ) ;
#90792 = CARTESIAN_POINT ( 'NONE',  ( 17.50000000000000000, 5.499999999999997335, 120.0000000000000142 ) ) ;
#90794 = CARTESIAN_POINT ( 'NONE',  ( 10.81492255796078972, 18.62759615963270932, 29.58224293864769905 ) ) ;
#90793 = CARTESIAN_POINT ( 'NONE',  ( -19.05341960407611168, -5.049401038298163336, 36.45724293864766707 ) ) ;
#90795 = CARTESIAN_POINT ( 'NONE',  ( -21.52544592524343514, 5.823673210054127303, 66.04057627198103830 ) ) ;
#90796 = CARTESIAN_POINT ( 'NONE',  ( 5.049401038298161559, -19.05341960407611168, 22.70724293864769194 ) ) ;
#90798 = CARTESIAN_POINT ( 'NONE',  ( -5.049401038298153566, 19.05341960407611168, 45.20724293864769550 ) ) ;
#90797 = CARTESIAN_POINT ( 'NONE',  ( -4.379528057220086978, -16.55341960407618274, 69.79275706135234714 ) ) ;
#90799 = EDGE_CURVE ( 'NONE', #88111, #10027, #61044, .T. ) ;
#90800 = CARTESIAN_POINT ( 'NONE',  ( 15.80617190586769283, -15.72974639402175789, 35.62609039468568994 ) ) ;
#90801 = CARTESIAN_POINT ( 'NONE',  ( -4.379528057220328563, 16.55341960407611168, 95.20724293864769550 ) ) ;
#90802 = DIRECTION ( 'NONE',  ( 0.000000000000000000, 0.000000000000000000, 1.000000000000000000 ) ) ;
#90803 = CARTESIAN_POINT ( 'NONE',  ( -16.20579543436674896, 7.371946100355232900, 49.43479165828122035 ) ) ;
#90804 = CARTESIAN_POINT ( 'NONE',  ( -21.55341960407610458, -5.719274019375992779, 31.45724293864769550 ) ) ;
#90805 = CARTESIAN_POINT ( 'NONE',  ( 1.300000000000000044, 0.7216878364870328300, -1.250000000000000000 ) ) ;
#90806 = CARTESIAN_POINT ( 'NONE',  ( 0.1105433493105908715, 24.30000000000003268, -56.77278709839600879 ) ) ;
#90808 = CARTESIAN_POINT ( 'NONE',  ( -8.224510206698948167, 14.34966873604960824, 45.41557627198103830 ) ) ;
#90807 = CARTESIAN_POINT ( 'NONE',  ( -14.34966873604972548, 8.224510206698743886, 48.33442372801902565 ) ) ;
#90809 = CARTESIAN_POINT ( 'NONE',  ( 15.72974639402199770, -15.80617190586745480, 68.12390960531436690 ) ) ;
#90810 = CARTESIAN_POINT ( 'NONE',  ( -15.80617190586745835, -15.72974639402198527, 56.87390960531436690 ) ) ;
#90811 = PLANE ( 'NONE',  #182307 ) ;
#90813 = CARTESIAN_POINT ( 'NONE',  ( 5.049401038298161559, -19.05341960407611168, 97.70724293864766707 ) ) ;
#90812 = CARTESIAN_POINT ( 'NONE',  ( -5.153800228976607833, 19.02544592524334988, 77.70942372801900433 ) ) ;
#90814 = CARTESIAN_POINT ( 'NONE',  ( -16.51473224551069308, -9.474510206698971260, 51.66557627198102409 ) ) ;
#90815 = CARTESIAN_POINT ( 'NONE',  ( -16.55341960407611168, -4.379528057220339221, 111.4572429386476813 ) ) ;
#90816 = SHAPE_DEFINITION_REPRESENTATION ( #7926, #154205 ) ;
#90817 = EDGE_LOOP ( 'NONE', ( #3289, #133837, #22392, #184844 ) ) ;
#90818 = CARTESIAN_POINT ( 'NONE',  ( -14.34966873604972548, 8.224510206698743886, 68.33442372801900433 ) ) ;
#90819 = CARTESIAN_POINT ( 'NONE',  ( -10.81492255796078084, -18.62759615963271287, 102.0822429386476955 ) ) ;
#90820 = CARTESIAN_POINT ( 'NONE',  ( 0.05219959533909260263, 19.03943276465977164, 49.99890960531435979 ) ) ;
#90821 = CARTESIAN_POINT ( 'NONE',  ( -0.05219959533937732626, 21.53943276465977519, 47.50109039468568994 ) ) ;
#90822 = CARTESIAN_POINT ( 'NONE',  ( -13.97604488694527625, -13.89961937509977652, 76.87390960531433848 ) ) ;
#90823 = CARTESIAN_POINT ( 'NONE',  ( -5.427562675786936573E-15, 30.27659582821221207, 145.4843446568999639 ) ) ;
#90824 = EDGE_LOOP ( 'NONE', ( #43402, #152144, #159960, #149453 ) ) ;
#90825 = CARTESIAN_POINT ( 'NONE',  ( -15.80617190586768217, 15.72974639402176855, 28.12609039468568284 ) ) ;
#90827 = CARTESIAN_POINT ( 'NONE',  ( -9.474510206698720793, -16.51473224551083518, 94.58442372801900433 ) ) ;
#90826 = CARTESIAN_POINT ( 'NONE',  ( 5.049401038298161559, -19.05341960407611168, 107.7072429386476955 ) ) ;
#90828 = CARTESIAN_POINT ( 'NONE',  ( 13.89961937509957401, 13.97604488694547697, 46.87609039468565442 ) ) ;
#90829 = CARTESIAN_POINT ( 'NONE',  ( 5.823673210054125526, 21.52544592524343514, 99.79057627198103830 ) ) ;
#90830 = CARTESIAN_POINT ( 'NONE',  ( 19.02544592524334988, 5.153800228976608722, 31.45942372801900433 ) ) ;
#90831 = CARTESIAN_POINT ( 'NONE',  ( -9.474510206698720793, -16.51473224551083518, 34.58442372801899722 ) ) ;
#90832 = CARTESIAN_POINT ( 'NONE',  ( -16.55341960407617563, 4.379528057220093196, 98.54275706135234714 ) ) ;
#90833 = CARTESIAN_POINT ( 'NONE',  ( 13.89961937509977652, -13.97604488694527269, 113.1239096053143527 ) ) ;
#90834 = CARTESIAN_POINT ( 'NONE',  ( -16.46253265017160317, 9.564922557960807481, 55.83224293864769550 ) ) ;
#90835 = CARTESIAN_POINT ( 'NONE',  ( -21.55341960407619339, 5.719274019375674811, 68.54275706135234714 ) ) ;
#90836 = CARTESIAN_POINT ( 'NONE',  ( -15.80617190586768217, 15.72974639402176855, 78.12609039468570415 ) ) ;
#90837 = FACE_OUTER_BOUND ( 'NONE', #112349, .T. ) ;
#90838 = CARTESIAN_POINT ( 'NONE',  ( 19.02544592524343514, -5.153800228976328945, 83.54057627198100988 ) ) ;
#90839 = CARTESIAN_POINT ( 'NONE',  ( 15.80617190586769283, -15.72974639402175789, 65.62609039468568994 ) ) ;
#90840 = CARTESIAN_POINT ( 'NONE',  ( -5.049401038297874678, -19.05341960407617918, 99.79275706135234714 ) ) ;
#90841 = CARTESIAN_POINT ( 'NONE',  ( 5.153800228976335163, 19.02544592524342804, 69.79057627198103830 ) ) ;
#90842 = CARTESIAN_POINT ( 'NONE',  ( 13.89961937509977652, -13.97604488694527269, 98.12390960531433848 ) ) ;
#90843 = CARTESIAN_POINT ( 'NONE',  ( 16.51473224551069308, 9.474510206698969483, 74.16557627198103830 ) ) ;
#90844 = CARTESIAN_POINT ( 'NONE',  ( 5.049401038298163336, -19.05341960407611168, 77.70724293864768129 ) ) ;
#90845 = CARTESIAN_POINT ( 'NONE',  ( -19.02544592524342804, 5.153800228976336051, 61.04057627198103120 ) ) ;
#90846 = CARTESIAN_POINT ( 'NONE',  ( -21.53943276465977519, 0.05219959533907696930, 96.24890960531435269 ) ) ;
#90847 = CARTESIAN_POINT ( 'NONE',  ( 16.53943276465976808, 0.05219959533934440121, 86.25109039468568994 ) ) ;
#90848 = DIRECTION ( 'NONE',  ( -1.000000000000000000, -0.000000000000000000, -0.000000000000000000 ) ) ;
#90849 = CARTESIAN_POINT ( 'NONE',  ( 19.03943276465977164, 0.05219959533936151252, 41.25109039468566152 ) ) ;
#90850 = CARTESIAN_POINT ( 'NONE',  ( 19.03943276465977164, -0.05219959533909143690, 83.74890960531436690 ) ) ;
#90851 = CARTESIAN_POINT ( 'NONE',  ( 0.05219959533910956823, 16.53943276465976808, 69.99890960531435269 ) ) ;
#90852 = CARTESIAN_POINT ( 'NONE',  ( 16.53943276465976808, -0.05219959533910856209, 113.7489096053143527 ) ) ;
#90853 = CARTESIAN_POINT ( 'NONE',  ( 16.46253265017160672, -9.564922557960803928, 108.3322429386476955 ) ) ;
#90854 = CARTESIAN_POINT ( 'NONE',  ( 13.97604488694527802, 13.89961937509977652, 109.3739096053143669 ) ) ;
#90855 = CARTESIAN_POINT ( 'NONE',  ( -5.153800228976328057, -19.02544592524343514, 82.29057627198102409 ) ) ;
#90856 = CARTESIAN_POINT ( 'NONE',  ( 5.049401038297881783, 19.05341960407617563, 37.29275706135232582 ) ) ;
#90857 = CARTESIAN_POINT ( 'NONE',  ( -4.379528057220086978, -16.55341960407618274, 89.79275706135236135 ) ) ;
#90858 = CARTESIAN_POINT ( 'NONE',  ( -16.51473224551069308, -9.474510206698971260, 71.66557627198102409 ) ) ;
#90859 = CARTESIAN_POINT ( 'NONE',  ( 18.67979575497194134, -10.72451020669871369, 55.83442372801901854 ) ) ;
#90860 = CARTESIAN_POINT ( 'NONE',  ( 21.52544592524344225, -5.823673210054117533, 28.54057627198103120 ) ) ;
#90861 = CARTESIAN_POINT ( 'NONE',  ( 0.05219959533907565091, 21.53943276465977519, 114.9989096053143669 ) ) ;
#90862 = CARTESIAN_POINT ( 'NONE',  ( -18.67979575497178146, -10.72451020669898902, 76.66557627198103830 ) ) ;
#90863 = CARTESIAN_POINT ( 'NONE',  ( -8.224510206698948167, 14.34966873604960824, 90.41557627198103830 ) ) ;
#90864 = CARTESIAN_POINT ( 'NONE',  ( 9.564922557961047289, -16.46253265017146816, 55.41775706135234003 ) ) ;
#90865 = CARTESIAN_POINT ( 'NONE',  ( 16.46253265017160672, -9.564922557960803928, 33.33224293864770260 ) ) ;
#90866 = CARTESIAN_POINT ( 'NONE',  ( 16.51473224551069308, 9.474510206698969483, 89.16557627198103830 ) ) ;
#90867 = CARTESIAN_POINT ( 'NONE',  ( 13.97604488694527802, 13.89961937509977652, 84.37390960531433848 ) ) ;
#90868 = CARTESIAN_POINT ( 'NONE',  ( 3.735172737399431091E-16, 6.100000000000006750, -64.53213882399991519 ) ) ;
#90869 = CARTESIAN_POINT ( 'NONE',  ( -12.06949235617756955, 12.14591786802309770, 105.6239096053143669 ) ) ;
#90870 = VERTEX_POINT ( 'NONE', #74259 ) ;
#90871 = CARTESIAN_POINT ( 'NONE',  ( 12.14591786802309770, 12.06949235617756955, 29.37390960531435269 ) ) ;
#90872 = CARTESIAN_POINT ( 'NONE',  ( 0.05219959533934541429, -16.53943276465976808, 25.00109039468567218 ) ) ;
#90873 = CARTESIAN_POINT ( 'NONE',  ( 21.52544592524334988, 5.823673210054432836, 91.45942372801901854 ) ) ;
#90874 = CARTESIAN_POINT ( 'NONE',  ( -13.89961937509977652, 13.97604488694528158, 105.6239096053143527 ) ) ;
#90875 = CARTESIAN_POINT ( 'NONE',  ( -0.05219959533937732626, 21.53943276465977519, 22.50109039468567573 ) ) ;
#90876 = CARTESIAN_POINT ( 'NONE',  ( -5.153800228976328057, -19.02544592524343514, 42.29057627198101699 ) ) ;
#90877 = CARTESIAN_POINT ( 'NONE',  ( 16.55341960407618274, -4.379528057220086978, 41.04275706135236135 ) ) ;
#90878 = ADVANCED_FACE ( 'NONE', ( #120732 ), #186407, .F. ) ;
#90879 = CARTESIAN_POINT ( 'NONE',  ( -19.03943276465977164, -0.05219959533935918106, 113.7510903946856757 ) ) ;
#90880 = CARTESIAN_POINT ( 'NONE',  ( 5.153800228976335163, 19.02544592524342804, 39.79057627198100988 ) ) ;
#90881 = CARTESIAN_POINT ( 'NONE',  ( -12.14591786802309592, -12.06949235617757132, 91.87390960531436690 ) ) ;
#90882 = CARTESIAN_POINT ( 'NONE',  ( -0.05219959533907301413, -21.53943276465977519, 102.4989096053143811 ) ) ;
#90883 = CARTESIAN_POINT ( 'NONE',  ( -13.89961937509957401, -13.97604488694547875, 74.37609039468566152 ) ) ;
#90884 = CARTESIAN_POINT ( 'NONE',  ( 0.05219959533937995610, -21.53943276465977519, 25.00109039468567218 ) ) ;
#90885 = CARTESIAN_POINT ( 'NONE',  ( 5.153800228976335163, 19.02544592524342804, 94.79057627198103830 ) ) ;
#90886 = CARTESIAN_POINT ( 'NONE',  ( -8.898068258721467672, -27.38543819252872069, 142.3843446568999980 ) ) ;
#90887 = CARTESIAN_POINT ( 'NONE',  ( 5.049401038298161559, -19.05341960407611168, 82.70724293864770971 ) ) ;
#90889 = CARTESIAN_POINT ( 'NONE',  ( -8.224510206698948167, 14.34966873604960824, 80.41557627198103830 ) ) ;
#90888 = CARTESIAN_POINT ( 'NONE',  ( -10.72451020669870658, -18.67979575497194134, 34.58442372801900433 ) ) ;
#90890 = CARTESIAN_POINT ( 'NONE',  ( -9.564922557960796823, -16.46253265017161027, 77.08224293864769550 ) ) ;
#90892 = CARTESIAN_POINT ( 'NONE',  ( 19.02544592524334988, 5.153800228976608722, 51.45942372801900433 ) ) ;
#90891 = CARTESIAN_POINT ( 'NONE',  ( -16.55341960407617563, 4.379528057220093196, 48.54275706135234714 ) ) ;
#90893 = CARTESIAN_POINT ( 'NONE',  ( -5.823673210054431948, 21.52544592524334988, 67.70942372801901854 ) ) ;
#90894 = CARTESIAN_POINT ( 'NONE',  ( -14.29746914071037622, -8.314922557961029526, 29.16775706135234003 ) ) ;
#90895 = CARTESIAN_POINT ( 'NONE',  ( -13.97604488694527625, -13.89961937509977652, 66.87390960531436690 ) ) ;
#90896 = CARTESIAN_POINT ( 'NONE',  ( -0.05219959533936034679, 19.03943276465977164, 97.50109039468567573 ) ) ;
#90897 = CARTESIAN_POINT ( 'NONE',  ( 8.314922557961029526, -14.29746914071037800, 50.41775706135235424 ) ) ;
#90898 = CARTESIAN_POINT ( 'NONE',  ( 18.62759615963255655, 10.81492255796105972, 101.6677570613523613 ) ) ;
#90899 = CARTESIAN_POINT ( 'NONE',  ( -16.51473224551082808, 9.474510206698731452, 78.33442372801900433 ) ) ;
#90900 = CARTESIAN_POINT ( 'NONE',  ( -19.03943276465977164, 0.05219959533909376836, 56.24890960531435979 ) ) ;
#90901 = CARTESIAN_POINT ( 'NONE',  ( 5.823673210054125526, 21.52544592524343514, 64.79057627198103830 ) ) ;
#90903 = CARTESIAN_POINT ( 'NONE',  ( 16.46253265017146816, 9.564922557961045513, 71.66775706135233293 ) ) ;
#90902 = CARTESIAN_POINT ( 'NONE',  ( 14.29746914071049879, -8.314922557960816363, 78.33224293864770971 ) ) ;
#90904 = CARTESIAN_POINT ( 'NONE',  ( 16.79531203550644136, -7.028104445595666050, 61.24755011779559055 ) ) ;
#90906 = ADVANCED_FACE ( 'NONE', ( #76215 ), #107540, .T. ) ;
#90905 = CARTESIAN_POINT ( 'NONE',  ( -0.05219959533936034679, 19.03943276465977164, 47.50109039468566863 ) ) ;
#90907 = CARTESIAN_POINT ( 'NONE',  ( 4.483927247898790824, -16.52544592524335698, 105.2094237280190328 ) ) ;
#90908 = CARTESIAN_POINT ( 'NONE',  ( -14.29746914071049879, 8.314922557960819915, 65.83224293864769550 ) ) ;
#90910 = CARTESIAN_POINT ( 'NONE',  ( -27.73933785331498925, 2.428612866367529932E-14, 144.8750000027311842 ) ) ;
#90909 = CARTESIAN_POINT ( 'NONE',  ( 10.72451020669871369, 18.67979575497193778, 97.08442372801904696 ) ) ;
#90911 = CARTESIAN_POINT ( 'NONE',  ( -21.52544592524343514, 5.823673210054127303, 111.0405762719810525 ) ) ;
#90912 = CARTESIAN_POINT ( 'NONE',  ( -9.474510206698964154, 16.51473224551069663, 65.41557627198102409 ) ) ;
#90913 = CARTESIAN_POINT ( 'NONE',  ( -5.823673210054431948, 21.52544592524334988, 77.70942372801900433 ) ) ;
#90914 = CARTESIAN_POINT ( 'NONE',  ( -9.564922557960796823, -16.46253265017161027, 62.08224293864769550 ) ) ;
#90915 = CARTESIAN_POINT ( 'NONE',  ( 16.52544592524342804, -4.483927247898539470, 113.5405762719810383 ) ) ;
#90916 = CARTESIAN_POINT ( 'NONE',  ( 21.52544592524344225, -5.823673210054117533, 33.54057627198102409 ) ) ;
#90917 = CARTESIAN_POINT ( 'NONE',  ( -14.34966873604960291, -8.224510206698953496, 61.66557627198103120 ) ) ;
#90918 = CARTESIAN_POINT ( 'NONE',  ( 19.05341960407611168, 5.049401038298154454, 48.95724293864768129 ) ) ;
#90919 = CARTESIAN_POINT ( 'NONE',  ( 14.29746914071049879, -8.314922557960816363, 98.33224293864769550 ) ) ;
#90920 = CARTESIAN_POINT ( 'NONE',  ( -18.67979575497178146, -10.72451020669898902, 106.6655762719810383 ) ) ;
#90921 = CARTESIAN_POINT ( 'NONE',  ( -15.80617190586768217, 15.72974639402176855, 48.12609039468568284 ) ) ;
#90922 = CARTESIAN_POINT ( 'NONE',  ( -16.46253265017160317, 9.564922557960807481, 30.83224293864769550 ) ) ;
#90923 = CARTESIAN_POINT ( 'NONE',  ( 16.53943276465976808, 0.05219959533934440121, 56.25109039468568284 ) ) ;
#90924 = CARTESIAN_POINT ( 'NONE',  ( -21.55341960407610458, -5.719274019375992779, 106.4572429386477097 ) ) ;
#90925 = CARTESIAN_POINT ( 'NONE',  ( -21.52544592524343514, 5.823673210054127303, 91.04057627198103830 ) ) ;
#90927 = CARTESIAN_POINT ( 'NONE',  ( -19.05341960407611168, -5.049401038298163336, 51.45724293864770260 ) ) ;
#90926 = CARTESIAN_POINT ( 'NONE',  ( -19.02544592524334988, -5.153800228976617603, 28.95942372801900433 ) ) ;
#90928 = CARTESIAN_POINT ( 'NONE',  ( 19.02544592524343514, -5.153800228976328945, 103.5405762719809957 ) ) ;
#90929 = CARTESIAN_POINT ( 'NONE',  ( 10.72451020669871369, 18.67979575497193778, 52.08442372801901854 ) ) ;
#90930 = CARTESIAN_POINT ( 'NONE',  ( -18.62759615963270932, 10.81492255796079327, 45.83224293864769550 ) ) ;
#90931 = CARTESIAN_POINT ( 'NONE',  ( 16.53943276465976808, -0.05219959533910856209, 28.74890960531435624 ) ) ;
#90933 = CARTESIAN_POINT ( 'NONE',  ( -5.719274019375665041, -21.55341960407619695, 94.79275706135234714 ) ) ;
#90932 = CARTESIAN_POINT ( 'NONE',  ( -21.53943276465977519, -0.05219959533937600094, 68.75109039468568994 ) ) ;
#90934 = CARTESIAN_POINT ( 'NONE',  ( 5.153800228976615827, -19.02544592524334988, 45.20942372801901143 ) ) ;
#90935 = CARTESIAN_POINT ( 'NONE',  ( 12.14591786802327356, -12.06949235617739191, 105.6260903946856899 ) ) ;
#90936 = CARTESIAN_POINT ( 'NONE',  ( -5.719274019375665041, -21.55341960407619695, 49.79275706135234714 ) ) ;
#90937 = CARTESIAN_POINT ( 'NONE',  ( -9.474510206698964154, 16.51473224551069663, 65.41557627198102409 ) ) ;
#90938 = CARTESIAN_POINT ( 'NONE',  ( -13.97604488694547697, 13.89961937509957934, 23.12609039468565442 ) ) ;
#90939 = CARTESIAN_POINT ( 'NONE',  ( -18.67979575497178146, -10.72451020669898902, 21.66557627198102409 ) ) ;
#90940 = CARTESIAN_POINT ( 'NONE',  ( 18.67979575497178502, 10.72451020669898547, 114.1655762719810383 ) ) ;
#90941 = CARTESIAN_POINT ( 'NONE',  ( -18.67979575497178146, -10.72451020669898902, 91.66557627198103830 ) ) ;
#90942 = CARTESIAN_POINT ( 'NONE',  ( 16.53943276465976808, 0.05219959533934440121, 36.25109039468567573 ) ) ;
#90944 = CARTESIAN_POINT ( 'NONE',  ( -18.62759615963270932, 10.81492255796079327, 75.83224293864769550 ) ) ;
#90943 = CARTESIAN_POINT ( 'NONE',  ( 37.99999999999999289, 2.893978650043524126E-14, -7.000000000000000000 ) ) ;
#90946 = CARTESIAN_POINT ( 'NONE',  ( 4.483927247898545687, 16.52544592524342804, 79.79057627198102409 ) ) ;
#90945 = CARTESIAN_POINT ( 'NONE',  ( -16.53943276465976808, -0.05219959533934237506, 58.75109039468568994 ) ) ;
#90947 = CARTESIAN_POINT ( 'NONE',  ( -22.99713674769915173, 21.42625476241829219, -46.35568673344857160 ) ) ;
#90948 = CARTESIAN_POINT ( 'NONE',  ( -19.03943276465977164, -0.05219959533935918106, 108.7510903946856615 ) ) ;
#90949 = CARTESIAN_POINT ( 'NONE',  ( -5.823673210054116645, -21.52544592524344225, 32.29057627198102409 ) ) ;
#90950 = CARTESIAN_POINT ( 'NONE',  ( -28.82186960331499037, 2.428612866367529932E-14, 150.0000000000000000 ) ) ;
#90951 = CARTESIAN_POINT ( 'NONE',  ( -8.314922557961024197, 14.29746914071037800, 37.91775706135235424 ) ) ;
#90952 = CARTESIAN_POINT ( 'NONE',  ( -10.72451020669870658, -18.67979575497194134, 19.58442372801901143 ) ) ;
#90953 = CARTESIAN_POINT ( 'NONE',  ( -15.72974639402197994, 15.80617190586746368, 35.62390960531437401 ) ) ;
#90954 = CARTESIAN_POINT ( 'NONE',  ( -4.379528057220086978, -16.55341960407618274, 74.79275706135234714 ) ) ;
#90955 = CARTESIAN_POINT ( 'NONE',  ( -16.46253265017160317, 9.564922557960807481, 80.83224293864769550 ) ) ;
#90957 = CARTESIAN_POINT ( 'NONE',  ( 16.51473224551069308, 9.474510206698969483, 24.16557627198102765 ) ) ;
#90956 = CARTESIAN_POINT ( 'NONE',  ( 5.823673210054444382, -21.52544592524334988, 60.20942372801902565 ) ) ;
#90958 = CARTESIAN_POINT ( 'NONE',  ( -21.55341960407610458, -5.719274019375992779, 26.45724293864768839 ) ) ;
#90959 = VERTEX_POINT ( 'NONE', #169216 ) ;
#90960 = CARTESIAN_POINT ( 'NONE',  ( -13.89961937509957401, -13.97604488694547875, 39.37609039468566152 ) ) ;
#90961 = CARTESIAN_POINT ( 'NONE',  ( -12.14591786802326823, 12.06949235617739902, 58.12609039468568994 ) ) ;
#90962 = CARTESIAN_POINT ( 'NONE',  ( 21.53943276465977519, -0.05219959533907433946, 23.74890960531435269 ) ) ;
#90963 = CARTESIAN_POINT ( 'NONE',  ( 15.80617190586746368, 15.72974639402197994, 104.3739096053143669 ) ) ;
#90964 = CARTESIAN_POINT ( 'NONE',  ( 13.97604488694527802, 13.89961937509977652, 79.37390960531435269 ) ) ;
#90965 = CARTESIAN_POINT ( 'NONE',  ( -15.49999999999999822, -5.500000000000000888, 118.0000000000000142 ) ) ;
#90966 = DIRECTION ( 'NONE',  ( 0.000000000000000000, 1.000000000000000000, 0.000000000000000000 ) ) ;
#90967 = CARTESIAN_POINT ( 'NONE',  ( -12.14591786802309592, -12.06949235617757132, 101.8739096053143811 ) ) ;
#90968 = CARTESIAN_POINT ( 'NONE',  ( -5.719274019375978568, 21.55341960407610458, 30.20724293864769550 ) ) ;
#90969 = CARTESIAN_POINT ( 'NONE',  ( -16.29526858892872454, 7.335722546920266041, 34.20329402199793378 ) ) ;
#90970 = CARTESIAN_POINT ( 'NONE',  ( 16.53943276465976808, 0.05219959533934440121, 66.25109039468567573 ) ) ;
#90971 = CARTESIAN_POINT ( 'NONE',  ( 5.719274019375673035, 21.55341960407619339, 22.29275706135235069 ) ) ;
#90972 = CARTESIAN_POINT ( 'NONE',  ( 0.05219959533936267826, -19.03943276465977164, 80.00109039468567573 ) ) ;
#90973 = CARTESIAN_POINT ( 'NONE',  ( -0.05219959533909027116, -19.03943276465977164, 37.49890960531436690 ) ) ;
#90974 = CARTESIAN_POINT ( 'NONE',  ( 10.81492255796078972, 18.62759615963270932, 64.58224293864769550 ) ) ;
#90975 = CARTESIAN_POINT ( 'NONE',  ( 9.564922557960805705, 16.46253265017160317, 109.5822429386476955 ) ) ;
#90976 = CARTESIAN_POINT ( 'NONE',  ( 21.55341960407619695, -5.719274019375665929, 86.04275706135236135 ) ) ;
#90977 = CARTESIAN_POINT ( 'NONE',  ( -19.05341960407611168, -5.049401038298163336, 61.45724293864769550 ) ) ;
#90978 = CARTESIAN_POINT ( 'NONE',  ( -8.224510206698735004, -14.34966873604973081, 44.58442372801901854 ) ) ;
#90979 = CARTESIAN_POINT ( 'NONE',  ( 5.153800228976335163, 19.02544592524342804, 59.79057627198100988 ) ) ;
#90980 = CARTESIAN_POINT ( 'NONE',  ( -21.55341960407619339, 5.719274019375674811, 78.54275706135236135 ) ) ;
#90981 = CARTESIAN_POINT ( 'NONE',  ( 9.564922557961047289, -16.46253265017146816, 45.41775706135232582 ) ) ;
#90982 = CARTESIAN_POINT ( 'NONE',  ( -19.02544592524334988, -5.153800228976617603, 58.95942372801900433 ) ) ;
#90983 = CARTESIAN_POINT ( 'NONE',  ( 18.67979575497194134, -10.72451020669871369, 50.83442372801901143 ) ) ;
#90984 = EDGE_CURVE ( 'NONE', #723, #17186, #154058, .T. ) ;
#90985 = CARTESIAN_POINT ( 'NONE',  ( -9.021779378622673207, 0.4881926659582808137, -61.91041879129566183 ) ) ;
#90986 = CARTESIAN_POINT ( 'NONE',  ( -16.51473224551082808, 9.474510206698731452, 48.33442372801900433 ) ) ;
#90987 = CARTESIAN_POINT ( 'NONE',  ( 13.97604488694527802, 13.89961937509977652, 99.37390960531436690 ) ) ;
#90988 = CARTESIAN_POINT ( 'NONE',  ( 16.46253265017160672, -9.564922557960803928, 73.33224293864769550 ) ) ;
#90989 = CARTESIAN_POINT ( 'NONE',  ( -4.483927247898782831, 16.52544592524335698, 112.7094237280190328 ) ) ;
#90991 = CARTESIAN_POINT ( 'NONE',  ( -21.53943276465977519, -0.05219959533937600094, 103.7510903946857042 ) ) ;
#90990 = CARTESIAN_POINT ( 'NONE',  ( 21.52544592524344225, -5.823673210054117533, 38.54057627198103120 ) ) ;
#90992 = CARTESIAN_POINT ( 'NONE',  ( 22.81625015709510151, -31.40387420917324590, -1.924999997268813434 ) ) ;
#90993 = CARTESIAN_POINT ( 'NONE',  ( -34.37139930337508531, 2.751904643975403797, 90.23455903727463578 ) ) ;
#90994 =( BOUNDED_SURFACE ( )  B_SPLINE_SURFACE ( 1, 2, ( 
 ( #33317, #160629, #142472, #98938, #188006, #190971, #128285, #79814, #49476, #172829, #4937, #52448, #34308, #157655, #20121, #114105, #81765, #80794, #66621, #37281, #145450, #189002, #50477, #143452, #165634, #25140, #103955, #70627, #56455, #150472, #27132, #69621, #118134, #147469, #148467, #100940, #40283, #196975, #24131, #23122, #38288, #119136, #134305, #88779, #9960, #84767, #11967, #73632, #8959, #55448, #135303, #7938, #54454, #179823, #85783, #146445, #101957, #178813, #131287, #115123, #192975, #161628, #117119, #86782, #177813, #180816, #71620, #176816, #194976, #132294, #193986, #99942, #116124, #39283, #162624, #133286, #72630, #163638, #41293, #102954, #164638, #26133, #87776, #149461, #10956, #195991, #57464, #42295, #198952, #43279, #729, #123083, #140240, #153431, #90754, #139253, #61412, #152437, #76589, #13923, #138265 ),
 ( #155424, #62401, #124071, #58442, #197956, #75590, #184769, #77581, #74614, #166634, #185772, #120110, #28136, #122092, #104948, #45269, #16914, #47259, #181800, #183783, #106923, #78567, #108916, #154429, #89776, #151461, #107909, #15923, #170596, #168596, #12949, #137269, #30096, #136280, #14929, #59425, #60419, #91735, #32086, #199948, #46255, #169595, #31093, #92741, #93743, #121099, #182793, #44276, #105934, #167619, #29115, #142230, #143217, #18910, #19889, #158400, #112886, #109908, #144220, #4698, #187772, #95730, #35057, #173588, #96712, #49242, #65392, #36045, #33080, #3715, #110900, #157416, #141241, #172585, #127053, #125086, #63411, #34072, #81530, #66389, #174580, #80555, #5704, #188759, #50244, #82538, #111900, #156415, #128051, #189753, #51225, #97694, #159385, #20880, #67381, #1733, #186784, #2730, #48254, #171592, #94736 ) ),
 .UNSPECIFIED., .F., .F., .F. ) 
 B_SPLINE_SURFACE_WITH_KNOTS ( ( 2, 2 ),
 ( 3, 2, 2, 2, 2, 2, 2, 2, 2, 2, 2, 2, 2, 2, 2, 2, 2, 2, 2, 2, 2, 2, 2, 2, 2, 2, 2, 2, 2, 2, 2, 2, 2, 2, 2, 2, 2, 2, 2, 2, 2, 2, 2, 2, 2, 2, 2, 2, 2, 2, 3 ),
 ( 0.000000000000000000, 1.000000000000000000 ),
 ( 0.000000000000000000, 0.02000000000000000042, 0.04000000000000000083, 0.05999999999999999778, 0.08000000000000000167, 0.1000000000000000056, 0.1199999999999999956, 0.1400000000000000133, 0.1600000000000000033, 0.1799999999999999933, 0.2000000000000000111, 0.2200000000000000011, 0.2399999999999999911, 0.2600000000000000089, 0.2800000000000000266, 0.2999999999999999889, 0.3200000000000000067, 0.3400000000000000244, 0.3599999999999999867, 0.3800000000000000044, 0.4000000000000000222, 0.4199999999999999845, 0.4400000000000000022, 0.4600000000000000200, 0.4799999999999999822, 0.5000000000000000000, 0.5200000000000000178, 0.5400000000000000355, 0.5600000000000000533, 0.5799999999999999600, 0.5999999999999999778, 0.6199999999999999956, 0.6400000000000000133, 0.6600000000000000311, 0.6800000000000000488, 0.6999999999999999556, 0.7199999999999999734, 0.7399999999999999911, 0.7600000000000000089, 0.7800000000000000266, 0.8000000000000000444, 0.8199999999999999512, 0.8399999999999999689, 0.8599999999999999867, 0.8800000000000000044, 0.9000000000000000222, 0.9200000000000000400, 0.9399999999999999467, 0.9599999999999999645, 0.9799999999999999822, 1.000000000000000000 ),
 .UNSPECIFIED. ) 
 GEOMETRIC_REPRESENTATION_ITEM ( )  RATIONAL_B_SPLINE_SURFACE ( (
 ( 1.000000000000000000, 0.9510565162951535312, 1.000000000000000000, 0.9510565162951535312, 1.000000000000000000, 0.9510565162951535312, 1.000000000000000000, 0.9510565162951535312, 1.000000000000000000, 0.9510565162951535312, 1.000000000000000000, 0.9510565162951535312, 1.000000000000000000, 0.9510565162951535312, 1.000000000000000000, 0.9510565162951535312, 1.000000000000000000, 0.9510565162951535312, 1.000000000000000000, 0.9510565162951535312, 1.000000000000000000, 0.9510565162951535312, 1.000000000000000000, 0.9510565162951535312, 1.000000000000000000, 0.9510565162951535312, 1.000000000000000000, 0.9510565162951535312, 1.000000000000000000, 0.9510565162951535312, 1.000000000000000000, 0.9510565162951535312, 1.000000000000000000, 0.9510565162951535312, 1.000000000000000000, 0.9510565162951535312, 1.000000000000000000, 0.9510565162951535312, 1.000000000000000000, 0.9510565162951535312, 1.000000000000000000, 0.9510565162951535312, 1.000000000000000000, 0.9510565162951535312, 1.000000000000000000, 0.9510565162951535312, 1.000000000000000000, 0.9510565162951535312, 1.000000000000000000, 0.9510565162951535312, 1.000000000000000000, 0.9510565162951535312, 1.000000000000000000, 0.9510565162951535312, 1.000000000000000000, 0.9510565162951535312, 1.000000000000000000, 0.9510565162951535312, 1.000000000000000000, 0.9510565162951535312, 1.000000000000000000, 0.9510565162951535312, 1.000000000000000000, 0.9510565162951535312, 1.000000000000000000, 0.9510565162951535312, 1.000000000000000000, 0.9510565162951535312, 1.000000000000000000, 0.9510565162951535312, 1.000000000000000000, 0.9510565162951535312, 1.000000000000000000, 0.9510565162951535312, 1.000000000000000000, 0.9510565162951535312, 1.000000000000000000, 0.9510565162951535312, 1.000000000000000000, 0.9510565162951535312, 1.000000000000000000, 0.9510565162951535312, 1.000000000000000000, 0.9510565162951535312, 1.000000000000000000, 0.9510565162951535312, 1.000000000000000000, 0.9510565162951535312, 1.000000000000000000, 0.9510565162951535312, 1.000000000000000000, 0.9510565162951535312, 1.000000000000000000, 0.9510565162951535312, 1.000000000000000000, 0.9510565162951535312, 1.000000000000000000, 0.9510565162951535312, 1.000000000000000000, 0.9510565162951535312, 1.000000000000000000),
 ( 1.000000000000000000, 0.9510565162951535312, 1.000000000000000000, 0.9510565162951535312, 1.000000000000000000, 0.9510565162951535312, 1.000000000000000000, 0.9510565162951535312, 1.000000000000000000, 0.9510565162951535312, 1.000000000000000000, 0.9510565162951535312, 1.000000000000000000, 0.9510565162951535312, 1.000000000000000000, 0.9510565162951535312, 1.000000000000000000, 0.9510565162951535312, 1.000000000000000000, 0.9510565162951535312, 1.000000000000000000, 0.9510565162951535312, 1.000000000000000000, 0.9510565162951535312, 1.000000000000000000, 0.9510565162951535312, 1.000000000000000000, 0.9510565162951535312, 1.000000000000000000, 0.9510565162951535312, 1.000000000000000000, 0.9510565162951535312, 1.000000000000000000, 0.9510565162951535312, 1.000000000000000000, 0.9510565162951535312, 1.000000000000000000, 0.9510565162951535312, 1.000000000000000000, 0.9510565162951535312, 1.000000000000000000, 0.9510565162951535312, 1.000000000000000000, 0.9510565162951535312, 1.000000000000000000, 0.9510565162951535312, 1.000000000000000000, 0.9510565162951535312, 1.000000000000000000, 0.9510565162951535312, 1.000000000000000000, 0.9510565162951535312, 1.000000000000000000, 0.9510565162951535312, 1.000000000000000000, 0.9510565162951535312, 1.000000000000000000, 0.9510565162951535312, 1.000000000000000000, 0.9510565162951535312, 1.000000000000000000, 0.9510565162951535312, 1.000000000000000000, 0.9510565162951535312, 1.000000000000000000, 0.9510565162951535312, 1.000000000000000000, 0.9510565162951535312, 1.000000000000000000, 0.9510565162951535312, 1.000000000000000000, 0.9510565162951535312, 1.000000000000000000, 0.9510565162951535312, 1.000000000000000000, 0.9510565162951535312, 1.000000000000000000, 0.9510565162951535312, 1.000000000000000000, 0.9510565162951535312, 1.000000000000000000, 0.9510565162951535312, 1.000000000000000000, 0.9510565162951535312, 1.000000000000000000, 0.9510565162951535312, 1.000000000000000000, 0.9510565162951535312, 1.000000000000000000, 0.9510565162951535312, 1.000000000000000000, 0.9510565162951535312, 1.000000000000000000, 0.9510565162951535312, 1.000000000000000000, 0.9510565162951535312, 1.000000000000000000, 0.9510565162951535312, 1.000000000000000000, 0.9510565162951535312, 1.000000000000000000) ) ) 
 REPRESENTATION_ITEM ( '' )  SURFACE ( )  );
#90995 = CARTESIAN_POINT ( 'NONE',  ( 18.62759615963255655, 10.81492255796105972, 91.66775706135234714 ) ) ;
#90996 = DIRECTION ( 'NONE',  ( 0.000000000000000000, 0.000000000000000000, 1.000000000000000000 ) ) ;
#90997 = CARTESIAN_POINT ( 'NONE',  ( 0.05219959533910956823, 16.53943276465976808, 114.9989096053143669 ) ) ;
#90998 = CARTESIAN_POINT ( 'NONE',  ( -16.46253265017160317, 9.564922557960807481, 115.8322429386477097 ) ) ;
#90999 = CARTESIAN_POINT ( 'NONE',  ( 33.85315667487628133, 2.428612866512670557E-14, 100.5000000000010232 ) ) ;
#91000 = CARTESIAN_POINT ( 'NONE',  ( -4.483927247898782831, 16.52544592524335698, 52.70942372801902565 ) ) ;
#91001 = CARTESIAN_POINT ( 'NONE',  ( -18.67979575497178146, -10.72451020669898902, 71.66557627198100988 ) ) ;
#91002 = CARTESIAN_POINT ( 'NONE',  ( -4.483927247898539470, -16.52544592524342804, 42.29057627198103120 ) ) ;
#91004 = CARTESIAN_POINT ( 'NONE',  ( -19.03943276465977164, 0.05219959533909376836, 106.2489096053143669 ) ) ;
#91003 = CARTESIAN_POINT ( 'NONE',  ( -8.314922557960811034, -14.29746914071050412, 107.0822429386476955 ) ) ;
#91005 = CARTESIAN_POINT ( 'NONE',  ( -0.05219959533937732626, 21.53943276465977519, 27.50109039468567929 ) ) ;
#91006 = CARTESIAN_POINT ( 'NONE',  ( -19.03943276465977164, -0.05219959533935918106, 38.75109039468566152 ) ) ;
#91007 = CARTESIAN_POINT ( 'NONE',  ( -0.05219959533910754901, -16.53943276465976808, 112.4989096053143669 ) ) ;
#91008 = CARTESIAN_POINT ( 'NONE',  ( 5.719274019375673035, 21.55341960407619339, 72.29275706135236135 ) ) ;
#91009 = CARTESIAN_POINT ( 'NONE',  ( 16.20579543436675252, -7.371946100355225795, 31.93479165828123811 ) ) ;
#91010 = CARTESIAN_POINT ( 'NONE',  ( 4.483927247898545687, 16.52544592524342804, 29.79057627198102409 ) ) ;
#91011 = CARTESIAN_POINT ( 'NONE',  ( -11.40812507854755609, 35.11059874428196537, -5.524999997268813523 ) ) ;
#91012 = CARTESIAN_POINT ( 'NONE',  ( 5.719274019375991003, -21.55341960407610458, 32.70724293864770260 ) ) ;
#91013 = CARTESIAN_POINT ( 'NONE',  ( 16.52544592524342804, -4.483927247898539470, 93.54057627198103830 ) ) ;
#91014 = CARTESIAN_POINT ( 'NONE',  ( -3.874011537017660434, -5.521060904931721858, -64.42755313133395134 ) ) ;
#91015 = CARTESIAN_POINT ( 'NONE',  ( -19.03943276465977164, 0.05219959533909376836, 76.24890960531435269 ) ) ;
#91016 = CARTESIAN_POINT ( 'NONE',  ( -8.314922557960811034, -14.29746914071050412, 72.08224293864769550 ) ) ;
#91017 = CARTESIAN_POINT ( 'NONE',  ( -13.89961937509957401, -13.97604488694547875, 109.3760903946856331 ) ) ;
#91018 = CARTESIAN_POINT ( 'NONE',  ( 0.05219959533907565091, 21.53943276465977519, 44.99890960531435979 ) ) ;
#91019 = ORIENTED_EDGE ( 'NONE', *, *, #50162, .F. ) ;
#91020 = CARTESIAN_POINT ( 'NONE',  ( 8.314922557960818139, 14.29746914071049879, 114.5822429386477097 ) ) ;
#91022 = CARTESIAN_POINT ( 'NONE',  ( 5.719274019375991003, -21.55341960407610458, 72.70724293864769550 ) ) ;
#91021 = CARTESIAN_POINT ( 'NONE',  ( 19.02544592524343514, -5.153800228976328945, 68.54057627198103830 ) ) ;
#91024 = CARTESIAN_POINT ( 'NONE',  ( 5.153800228976335163, 19.02544592524342804, 84.79057627198099567 ) ) ;
#91023 = CARTESIAN_POINT ( 'NONE',  ( -14.29746914071037622, -8.314922557961029526, 109.1677570613523613 ) ) ;
#91025 = CARTESIAN_POINT ( 'NONE',  ( 19.05341960407617918, -5.049401038297876454, 71.04275706135234714 ) ) ;
#91026 = CARTESIAN_POINT ( 'NONE',  ( 5.719274019375673035, 21.55341960407619339, 92.29275706135236135 ) ) ;
#91027 = CARTESIAN_POINT ( 'NONE',  ( 21.52544592524344225, -5.823673210054117533, 63.54057627198103830 ) ) ;
#91028 = CARTESIAN_POINT ( 'NONE',  ( 10.72451020669898902, -18.67979575497178502, 27.91557627198103830 ) ) ;
#91029 = CARTESIAN_POINT ( 'NONE',  ( -13.97604488694527625, -13.89961937509977652, 31.87390960531435979 ) ) ;
#91030 = CARTESIAN_POINT ( 'NONE',  ( 12.14591786802327356, -12.06949235617739191, 105.6260903946856899 ) ) ;
#91031 = CARTESIAN_POINT ( 'NONE',  ( 19.05341960407611168, 5.049401038298154454, 68.95724293864769550 ) ) ;
#91032 = CARTESIAN_POINT ( 'NONE',  ( -0.05219959533934338120, 16.53943276465976808, 27.50109039468567929 ) ) ;
#91033 = CARTESIAN_POINT ( 'NONE',  ( 16.20579543436681647, 7.371946100354975329, 53.06520834171878676 ) ) ;
#91034 = CARTESIAN_POINT ( 'NONE',  ( 21.53943276465977519, 0.05219959533937863772, 111.2510903946856899 ) ) ;
#91035 = CARTESIAN_POINT ( 'NONE',  ( 16.53943276465976808, -0.05219959533910856209, 73.74890960531433848 ) ) ;
#91036 = CARTESIAN_POINT ( 'NONE',  ( 18.67979575497178502, 10.72451020669898547, 104.1655762719810241 ) ) ;
#91037 = CARTESIAN_POINT ( 'NONE',  ( -15.80617190586745835, -15.72974639402198527, 96.87390960531436690 ) ) ;
#91038 = CARTESIAN_POINT ( 'NONE',  ( -6.686840650406351116, 6.126184129041750914, -63.95889547717843726 ) ) ;
#91039 = CARTESIAN_POINT ( 'NONE',  ( -21.52544592524343514, 5.823673210054127303, 41.04057627198103120 ) ) ;
#91040 = CARTESIAN_POINT ( 'NONE',  ( -8.224510206698735004, -14.34966873604973081, 84.58442372801903275 ) ) ;
#91041 = CARTESIAN_POINT ( 'NONE',  ( 0.05219959533910956823, 16.53943276465976808, 109.9989096053143527 ) ) ;
#91042 = CARTESIAN_POINT ( 'NONE',  ( -19.02544592524342804, 5.153800228976336051, 61.04057627198103120 ) ) ;
#91043 = FILL_AREA_STYLE ('',( #135601 ) ) ;
#91044 = CARTESIAN_POINT ( 'NONE',  ( 14.29746914071037800, 8.314922557961029526, 106.6677570613523756 ) ) ;
#91045 = CARTESIAN_POINT ( 'NONE',  ( 15.80617190586769283, -15.72974639402175789, 45.62609039468567573 ) ) ;
#91046 = CARTESIAN_POINT ( 'NONE',  ( -13.89961937509977652, 13.97604488694528158, 95.62390960531436690 ) ) ;
#91047 = CARTESIAN_POINT ( 'NONE',  ( -18.67979575497193778, 10.72451020669871902, 78.33442372801901854 ) ) ;
#91048 = CARTESIAN_POINT ( 'NONE',  ( 5.153800228976335163, 19.02544592524342804, 29.79057627198102409 ) ) ;
#91049 = CARTESIAN_POINT ( 'NONE',  ( -19.02544592524342804, 5.153800228976336051, 36.04057627198100988 ) ) ;
#91050 = ORIENTED_EDGE ( 'NONE', *, *, #3703, .T. ) ;
#91051 = CARTESIAN_POINT ( 'NONE',  ( -5.823673210054431948, 21.52544592524334988, 72.70942372801901854 ) ) ;
#91052 = CARTESIAN_POINT ( 'NONE',  ( -13.97604488694527625, -13.89961937509977652, 101.8739096053143811 ) ) ;
#91053 = CARTESIAN_POINT ( 'NONE',  ( -13.97604488694547697, 13.89961937509957934, 83.12609039468564731 ) ) ;
#91054 = CARTESIAN_POINT ( 'NONE',  ( -0.05219959533937732626, 21.53943276465977519, 37.50109039468568284 ) ) ;
#91055 = CARTESIAN_POINT ( 'NONE',  ( -4.483927247898782831, 16.52544592524335698, 22.70942372801901499 ) ) ;
#91056 = CARTESIAN_POINT ( 'NONE',  ( 13.89961937509957401, 13.97604488694547697, 66.87609039468567573 ) ) ;
#91057 = CARTESIAN_POINT ( 'NONE',  ( 16.46253265017160672, -9.564922557960803928, 58.33224293864769550 ) ) ;
#91058 = CARTESIAN_POINT ( 'NONE',  ( -16.46253265017146816, -9.564922557961047289, 79.16775706135234714 ) ) ;
#91059 = CARTESIAN_POINT ( 'NONE',  ( 8.224510206698953496, -14.34966873604960469, 27.91557627198103830 ) ) ;
#91060 = CARTESIAN_POINT ( 'NONE',  ( -19.03943276465977164, -0.05219959533935918106, 78.75109039468567573 ) ) ;
#91061 = CARTESIAN_POINT ( 'NONE',  ( 16.52544592524342804, -4.483927247898539470, 38.54057627198103120 ) ) ;
#91062 = CARTESIAN_POINT ( 'NONE',  ( 9.474510206698729675, 16.51473224551082808, 62.08442372801899722 ) ) ;
#91063 = CARTESIAN_POINT ( 'NONE',  ( 16.53943276465976808, 0.05219959533934440121, 46.25109039468567573 ) ) ;
#91064 = CARTESIAN_POINT ( 'NONE',  ( 10.72451020669871369, 18.67979575497193778, 112.0844237280190185 ) ) ;
#91065 = CARTESIAN_POINT ( 'NONE',  ( 5.049401038298161559, -19.05341960407611168, 32.70724293864768129 ) ) ;
#91066 = CARTESIAN_POINT ( 'NONE',  ( -17.40805194822029378, -6.112264579159361055, 64.16628727489388950 ) ) ;
#91067 = B_SPLINE_CURVE_WITH_KNOTS ( 'NONE', 3,
 ( #177454, #130919, #133937, #38924, #85412, #118774, #180462, #24774, #193615, #103600, #166273, #27771, #55087, #163272, #86421, #40925, #94360, #135929, #43911, #44901, #137894, #108544, #138880, #29731, #105573, #171219, #168235, #122716, #30725, #92372, #106558, #156039 ),
 .UNSPECIFIED., .F., .F.,
 ( 4, 2, 2, 2, 2, 2, 2, 2, 2, 2, 2, 2, 2, 2, 2, 4 ),
 ( 2.711112516444420852E-17, 0.0003712461730036987042, 0.0007424923460073703033, 0.001113738519011041794, 0.001484984692014713501, 0.002227477038022075348, 0.002598723211025741851, 0.002969969384029408355, 0.003341215557033074424, 0.003712461730036740928, 0.004083707903040406997, 0.004454954076044073501, 0.004826200249047739137, 0.005197446422051405640, 0.005568692595055072143, 0.005939938768058737779 ),
 .UNSPECIFIED. ) ;
#91068 = CARTESIAN_POINT ( 'NONE',  ( 14.34966873604972726, -8.224510206698740333, 50.83442372801901143 ) ) ;
#91069 = CARTESIAN_POINT ( 'NONE',  ( 11.30153831258471797, -180.0000000000000000, -15.00000000000000178 ) ) ;
#91070 = CARTESIAN_POINT ( 'NONE',  ( 17.14385361876520264, 23.59649016807275856, 144.1750000027311671 ) ) ;
#91071 = CARTESIAN_POINT ( 'NONE',  ( 19.03943276465977164, -0.05219959533909143690, 88.74890960531436690 ) ) ;
#91072 = CARTESIAN_POINT ( 'NONE',  ( 0.000000000000000000, 0.000000000000000000, 0.000000000000000000 ) ) ;
#91073 = ORIENTED_EDGE ( 'NONE', *, *, #103944, .T. ) ;
#91074 = CARTESIAN_POINT ( 'NONE',  ( 19.03943276465977164, 0.05219959533936151252, 81.25109039468567573 ) ) ;
#91075 = CARTESIAN_POINT ( 'NONE',  ( -18.62759615963270932, 10.81492255796079327, 30.83224293864770260 ) ) ;
#91077 = CARTESIAN_POINT ( 'NONE',  ( -9.564922557961040184, 16.46253265017147172, 97.91775706135233293 ) ) ;
#91076 = CARTESIAN_POINT ( 'NONE',  ( -10.81492255796105439, 18.62759615963255655, 112.9177570613523329 ) ) ;
#91078 = CARTESIAN_POINT ( 'NONE',  ( -0.05219959533910754901, -16.53943276465976808, 107.4989096053143669 ) ) ;
#91079 = CARTESIAN_POINT ( 'NONE',  ( -13.97604488694527625, -13.89961937509977652, 31.87390960531435979 ) ) ;
#91080 = CARTESIAN_POINT ( 'NONE',  ( 21.52544592524344225, -5.823673210054117533, 63.54057627198103830 ) ) ;
#91081 = CARTESIAN_POINT ( 'NONE',  ( 15.72974639402199770, -15.80617190586745480, 53.12390960531436690 ) ) ;
#91082 = CARTESIAN_POINT ( 'NONE',  ( -13.97604488694527625, -13.89961937509977652, 21.87390960531435979 ) ) ;
#91083 = DIRECTION ( 'NONE',  ( 0.000000000000000000, 1.000000000000000000, 0.000000000000000000 ) ) ;
#91084 = CARTESIAN_POINT ( 'NONE',  ( 16.51473224551083163, -9.474510206698727899, 65.83442372801900433 ) ) ;
#91085 = CARTESIAN_POINT ( 'NONE',  ( 4.379528057220339221, -16.55341960407611168, 42.70724293864770260 ) ) ;
#91086 = CARTESIAN_POINT ( 'NONE',  ( -18.67979575497178146, -10.72451020669898902, 26.66557627198103475 ) ) ;
#91087 = CARTESIAN_POINT ( 'NONE',  ( 21.55341960407619695, -5.719274019375665929, 91.04275706135236135 ) ) ;
#91088 = CARTESIAN_POINT ( 'NONE',  ( -21.55341960407610458, -5.719274019375992779, 81.45724293864769550 ) ) ;
#91089 = CARTESIAN_POINT ( 'NONE',  ( 18.67979575497194134, -10.72451020669871369, 60.83442372801901854 ) ) ;
#91090 = CARTESIAN_POINT ( 'NONE',  ( -21.53943276465977519, -0.05219959533937600094, 68.75109039468568994 ) ) ;
#91091 = CARTESIAN_POINT ( 'NONE',  ( -16.46253265017160317, 9.564922557960807481, 90.83224293864769550 ) ) ;
#91093 = CARTESIAN_POINT ( 'NONE',  ( 5.719274019375673035, 21.55341960407619339, 47.29275706135234003 ) ) ;
#91092 = CARTESIAN_POINT ( 'NONE',  ( -8.224510206698735004, -14.34966873604973081, 99.58442372801900433 ) ) ;
#91094 = CARTESIAN_POINT ( 'NONE',  ( 16.46253265017160672, -9.564922557960803928, 28.33224293864769550 ) ) ;
#91095 = CARTESIAN_POINT ( 'NONE',  ( -32.36630342937671401, 3.758454152357579403, 88.50505952879542804 ) ) ;
#91096 = CARTESIAN_POINT ( 'NONE',  ( -16.55341960407611168, -4.379528057220339221, 66.45724293864768129 ) ) ;
#91097 = CARTESIAN_POINT ( 'NONE',  ( 8.224510206698953496, -14.34966873604960469, 32.91557627198102409 ) ) ;
#91098 = CARTESIAN_POINT ( 'NONE',  ( 15.72974639402199770, -15.80617190586745480, 48.12390960531436690 ) ) ;
#91099 = CARTESIAN_POINT ( 'NONE',  ( 5.049401038298161559, -19.05341960407611168, 72.70724293864768129 ) ) ;
#91100 = CARTESIAN_POINT ( 'NONE',  ( -16.51473224551069308, -9.474510206698971260, 51.66557627198102409 ) ) ;
#91101 = CARTESIAN_POINT ( 'NONE',  ( 10.72451020669898902, -18.67979575497178502, 57.91557627198103120 ) ) ;
#91102 = CARTESIAN_POINT ( 'NONE',  ( 16.51473224551083163, -9.474510206698727899, 40.83442372801900433 ) ) ;
#91104 = CARTESIAN_POINT ( 'NONE',  ( 14.34966873604960469, 8.224510206698951720, 54.16557627198103120 ) ) ;
#91103 = DIRECTION ( 'NONE',  ( 0.000000000000000000, 0.000000000000000000, -1.000000000000000000 ) ) ;
#91105 = CARTESIAN_POINT ( 'NONE',  ( 21.52544592524344225, -5.823673210054117533, 23.54057627198102765 ) ) ;
#91106 = ORIENTED_EDGE ( 'NONE', *, *, #42468, .T. ) ;
#91107 = CARTESIAN_POINT ( 'NONE',  ( -8.314922557961024197, 14.29746914071037800, 67.91775706135234714 ) ) ;
#91108 = CARTESIAN_POINT ( 'NONE',  ( -0.05219959533936034679, 19.03943276465977164, 72.50109039468566152 ) ) ;
#91109 = CARTESIAN_POINT ( 'NONE',  ( -16.52544592524342804, 4.483927247898546575, 46.04057627198103830 ) ) ;
#91110 = CARTESIAN_POINT ( 'NONE',  ( 19.49401214000073068, -12.39993551617567391, 164.9999999999999716 ) ) ;
#91111 = CARTESIAN_POINT ( 'NONE',  ( 12.06949235617757843, -12.14591786802309237, 28.12390960531435979 ) ) ;
#91112 = CARTESIAN_POINT ( 'NONE',  ( 9.474510206698971260, -16.51473224551069308, 57.91557627198103120 ) ) ;
#91113 = CARTESIAN_POINT ( 'NONE',  ( -19.02544592524342804, 5.153800228976336051, 76.04057627198102409 ) ) ;
#91114 = CARTESIAN_POINT ( 'NONE',  ( 13.89961937509977652, -13.97604488694527269, 43.12390960531434558 ) ) ;
#91115 = CARTESIAN_POINT ( 'NONE',  ( -5.719274019375665041, -21.55341960407619695, 49.79275706135234714 ) ) ;
#91116 = CARTESIAN_POINT ( 'NONE',  ( -9.474510206698964154, 16.51473224551069663, 65.41557627198102409 ) ) ;
#91117 = B_SPLINE_CURVE_WITH_KNOTS ( 'NONE', 3,
 ( #19549, #2384, #82179, #81194, #48900, #141884, #190394, #1380, #80213, #142875, #188410, #94388, #64063, #140896, #4355, #49887, #187432, #125733, #67038, #139891, #78220, #111553 ),
 .UNSPECIFIED., .F., .F.,
 ( 4, 2, 2, 2, 2, 2, 2, 2, 2, 2, 4 ),
 ( 2.602085213965210642E-18, 0.001309639967555351406, 0.001964459951333025808, 0.002291869943221863659, 0.002455574939166268490, 0.002619279935110673321, 0.002782984931055078152, 0.002946689926999482550, 0.003274099918888319100, 0.003928919902665989165, 0.005238559870221329295 ),
 .UNSPECIFIED. ) ;
#91118 = DIRECTION ( 'NONE',  ( -0.8437662581494473901, -0.5367108174878535420, 0.000000000000000000 ) ) ;
#91119 = CARTESIAN_POINT ( 'NONE',  ( 16.51473224551069308, 9.474510206698969483, 59.16557627198102409 ) ) ;
#91120 = CARTESIAN_POINT ( 'NONE',  ( -15.80617190586745835, -15.72974639402198527, 36.87390960531435979 ) ) ;
#91121 = CARTESIAN_POINT ( 'NONE',  ( -16.46253265017160317, 9.564922557960807481, 25.83224293864769194 ) ) ;
#91122 = CARTESIAN_POINT ( 'NONE',  ( 5.823673210054125526, 21.52544592524343514, 29.79057627198102409 ) ) ;
#91123 = CARTESIAN_POINT ( 'NONE',  ( 12.14591786802327356, -12.06949235617739191, 85.62609039468568994 ) ) ;
#91124 = CARTESIAN_POINT ( 'NONE',  ( -15.72974639402176322, -15.80617190586768395, 109.3760903946857042 ) ) ;
#91125 = CARTESIAN_POINT ( 'NONE',  ( -16.55341960407617563, 4.379528057220093196, 63.54275706135234003 ) ) ;
#91126 = CARTESIAN_POINT ( 'NONE',  ( 19.02544592524343514, -5.153800228976328945, 113.5405762719810241 ) ) ;
#91127 = CARTESIAN_POINT ( 'NONE',  ( -16.52544592524335698, -4.483927247898792601, 58.95942372801902565 ) ) ;
#91128 = CARTESIAN_POINT ( 'NONE',  ( 16.55341960407618274, -4.379528057220086978, 46.04275706135234714 ) ) ;
#91129 = CARTESIAN_POINT ( 'NONE',  ( 9.564922557960805705, 16.46253265017160317, 114.5822429386476955 ) ) ;
#91130 = CARTESIAN_POINT ( 'NONE',  ( -4.483927247898782831, 16.52544592524335698, 27.70942372801901854 ) ) ;
#91131 = CARTESIAN_POINT ( 'NONE',  ( -13.97604488694527625, -13.89961937509977652, 31.87390960531435979 ) ) ;
#91132 = CARTESIAN_POINT ( 'NONE',  ( 10.81492255796106328, -18.62759615963255655, 25.41775706135235779 ) ) ;
#91133 = CARTESIAN_POINT ( 'NONE',  ( 16.53943276465976808, 0.05219959533934440121, 26.25109039468567573 ) ) ;
#91134 = CARTESIAN_POINT ( 'NONE',  ( -4.483927247898782831, 16.52544592524335698, 82.70942372801900433 ) ) ;
#91135 = CYLINDRICAL_SURFACE ( 'NONE', #176516, 0.5000000000000004441 ) ;
#91136 = CARTESIAN_POINT ( 'NONE',  ( -10.72451020669870658, -18.67979575497194134, 84.58442372801903275 ) ) ;
#91138 = EDGE_CURVE ( 'NONE', #45079, #22766, #142128, .T. ) ;
#91137 = CARTESIAN_POINT ( 'NONE',  ( 5.049401038297881783, 19.05341960407617563, 82.29275706135229029 ) ) ;
#91139 = CARTESIAN_POINT ( 'NONE',  ( 14.29746914071049879, -8.314922557960816363, 58.33224293864768839 ) ) ;
#91140 = CARTESIAN_POINT ( 'NONE',  ( -4.379528057220328563, 16.55341960407611168, 110.2072429386477239 ) ) ;
#91142 = CARTESIAN_POINT ( 'NONE',  ( 17.97161686093728150, -5.500000000000001776, 53.49637206859166128 ) ) ;
#91141 = CARTESIAN_POINT ( 'NONE',  ( 19.02544592524334988, 5.153800228976608722, 51.45942372801900433 ) ) ;
#91143 = CARTESIAN_POINT ( 'NONE',  ( -5.719274019375665041, -21.55341960407619695, 49.79275706135234714 ) ) ;
#91144 = CARTESIAN_POINT ( 'NONE',  ( -16.51473224551082808, 9.474510206698731452, 103.3344237280190043 ) ) ;
#91145 = CARTESIAN_POINT ( 'NONE',  ( 16.88567814943161238, 6.947325034625710494, 83.79001122652586275 ) ) ;
#91146 = CARTESIAN_POINT ( 'NONE',  ( 5.153800228976335163, 19.02544592524342804, 104.7905762719809957 ) ) ;
#91147 = CARTESIAN_POINT ( 'NONE',  ( -21.55341960407610458, -5.719274019375992779, 76.45724293864769550 ) ) ;
#91148 = CARTESIAN_POINT ( 'NONE',  ( 16.51473224551083163, -9.474510206698727899, 90.83442372801900433 ) ) ;
#91149 = CARTESIAN_POINT ( 'NONE',  ( 9.564922557960805705, 16.46253265017160317, 99.58224293864770971 ) ) ;
#91150 = CARTESIAN_POINT ( 'NONE',  ( -21.47376810973062433, 7.452933495370294814, 174.2084625793499981 ) ) ;
#91151 = CARTESIAN_POINT ( 'NONE',  ( -8.314922557960811034, -14.29746914071050412, 112.0822429386477097 ) ) ;
#91152 = CARTESIAN_POINT ( 'NONE',  ( -5.719274019375665041, -21.55341960407619695, 94.79275706135234714 ) ) ;
#91153 = CARTESIAN_POINT ( 'NONE',  ( 16.46253265017160672, -9.564922557960803928, 38.33224293864768839 ) ) ;
#91154 = CARTESIAN_POINT ( 'NONE',  ( -18.67979575497193778, 10.72451020669871902, 58.33442372801901143 ) ) ;
#91155 = CARTESIAN_POINT ( 'NONE',  ( 5.719274019375673035, 21.55341960407619339, 82.29275706135234714 ) ) ;
#91156 = CARTESIAN_POINT ( 'NONE',  ( -16.55341960407617563, 4.379528057220093196, 108.5427570613523756 ) ) ;
#91157 = CARTESIAN_POINT ( 'NONE',  ( -15.72974639402176322, -15.80617190586768395, 39.37609039468567573 ) ) ;
#91158 = CARTESIAN_POINT ( 'NONE',  ( 18.67979575497194134, -10.72451020669871369, 40.83442372801901854 ) ) ;
#91160 = CARTESIAN_POINT ( 'NONE',  ( 5.153800228976335163, 19.02544592524342804, 89.79057627198102409 ) ) ;
#91159 = CARTESIAN_POINT ( 'NONE',  ( -13.97604488694547697, 13.89961937509957934, 63.12609039468566152 ) ) ;
#91161 = CARTESIAN_POINT ( 'NONE',  ( -14.34966873604960291, -8.224510206698953496, 101.6655762719810383 ) ) ;
#91162 = CARTESIAN_POINT ( 'NONE',  ( -10.81492255796078084, -18.62759615963271287, 87.08224293864769550 ) ) ;
#91163 = CARTESIAN_POINT ( 'NONE',  ( 0.05219959533910956823, 16.53943276465976808, 59.99890960531436690 ) ) ;
#91164 = CARTESIAN_POINT ( 'NONE',  ( 10.72451020669871369, 18.67979575497193778, 102.0844237280190185 ) ) ;
#91165 = CARTESIAN_POINT ( 'NONE',  ( -16.52544592524342804, 4.483927247898546575, 81.04057627198102409 ) ) ;
#91166 = CARTESIAN_POINT ( 'NONE',  ( 5.153800228976335163, 19.02544592524342804, 29.79057627198102409 ) ) ;
#91167 = CARTESIAN_POINT ( 'NONE',  ( -9.564922557961040184, 16.46253265017147172, 82.91775706135233293 ) ) ;
#91168 = CARTESIAN_POINT ( 'NONE',  ( -8.224510206698948167, 14.34966873604960824, 55.41557627198102409 ) ) ;
#91169 = CARTESIAN_POINT ( 'NONE',  ( 10.81492255796106328, -18.62759615963255655, 100.4177570613523471 ) ) ;
#91170 = CARTESIAN_POINT ( 'NONE',  ( -13.97604488694527625, -13.89961937509977652, 96.87390960531433848 ) ) ;
#91171 = CARTESIAN_POINT ( 'NONE',  ( 19.05341960407617918, -5.049401038297876454, 61.04275706135232582 ) ) ;
#91172 = CARTESIAN_POINT ( 'NONE',  ( -18.67979575497178146, -10.72451020669898902, 81.66557627198103830 ) ) ;
#91173 = CARTESIAN_POINT ( 'NONE',  ( -21.53943276465977519, -0.05219959533937600094, 28.75109039468567929 ) ) ;
#91174 = CARTESIAN_POINT ( 'NONE',  ( -8.314922557961024197, 14.29746914071037800, 32.91775706135234714 ) ) ;
#91175 = CARTESIAN_POINT ( 'NONE',  ( -12.14591786802326823, 12.06949235617739902, 78.12609039468570415 ) ) ;
#91177 = CARTESIAN_POINT ( 'NONE',  ( 0.05219959533907565091, 21.53943276465977519, 114.9989096053143669 ) ) ;
#91176 = CARTESIAN_POINT ( 'NONE',  ( -5.153800228976328057, -19.02544592524343514, 27.29057627198103120 ) ) ;
#91178 = CARTESIAN_POINT ( 'NONE',  ( 8.224510206698953496, -14.34966873604960469, 112.9155762719810383 ) ) ;
#91179 = CARTESIAN_POINT ( 'NONE',  ( -36.91746825000000598, 2.428612866367529932E-14, -5.124999997268813168 ) ) ;
#91180 = CARTESIAN_POINT ( 'NONE',  ( -4.483927247898782831, 16.52544592524335698, 42.70942372801901854 ) ) ;
#91181 = CARTESIAN_POINT ( 'NONE',  ( -16.53943276465976808, 0.05219959533911058130, 81.24890960531436690 ) ) ;
#91182 = CARTESIAN_POINT ( 'NONE',  ( -5.719274019375978568, 21.55341960407610458, 75.20724293864769550 ) ) ;
#91183 = CARTESIAN_POINT ( 'NONE',  ( 8.224510206698953496, -14.34966873604960469, 27.91557627198103830 ) ) ;
#91184 = CARTESIAN_POINT ( 'NONE',  ( 8.314922557961029526, -14.29746914071037800, 45.41775706135234003 ) ) ;
#91185 = CARTESIAN_POINT ( 'NONE',  ( -19.03943276465977164, 0.05219959533909376836, 41.24890960531435269 ) ) ;
#91186 = CARTESIAN_POINT ( 'NONE',  ( 8.224510206698742110, 14.34966873604972548, 77.08442372801901854 ) ) ;
#91187 = CARTESIAN_POINT ( 'NONE',  ( 19.02544592524334988, 5.153800228976608722, 76.45942372801897591 ) ) ;
#91188 = CARTESIAN_POINT ( 'NONE',  ( -18.67979575497178146, -10.72451020669898902, 66.66557627198102409 ) ) ;
#91189 = CARTESIAN_POINT ( 'NONE',  ( 0.05219959533934541429, -16.53943276465976808, 110.0010903946856757 ) ) ;
#91190 = ORIENTED_EDGE ( 'NONE', *, *, #188483, .F. ) ;
#91191 = CARTESIAN_POINT ( 'NONE',  ( -21.53943276465977519, 0.05219959533907696930, 46.24890960531435979 ) ) ;
#91192 = ORIENTED_EDGE ( 'NONE', *, *, #72915, .T. ) ;
#91193 = CARTESIAN_POINT ( 'NONE',  ( -8.224510206698735004, -14.34966873604973081, 89.58442372801901854 ) ) ;
#91194 = ORIENTED_EDGE ( 'NONE', *, *, #177334, .T. ) ;
#91195 = CARTESIAN_POINT ( 'NONE',  ( -13.89961937509977652, 13.97604488694528158, 115.6239096053143669 ) ) ;
#91196 = CARTESIAN_POINT ( 'NONE',  ( 28.82186960331498327, 2.428612866367529932E-14, 139.9999999999999716 ) ) ;
#91197 = CARTESIAN_POINT ( 'NONE',  ( 15.80617190586746368, 15.72974639402197994, 79.37390960531436690 ) ) ;
#91198 = CARTESIAN_POINT ( 'NONE',  ( -8.314922557961024197, 14.29746914071037800, 107.9177570613523471 ) ) ;
#91199 = CARTESIAN_POINT ( 'NONE',  ( -8.224510206698735004, -14.34966873604973081, 24.58442372801901499 ) ) ;
#91200 = CARTESIAN_POINT ( 'NONE',  ( -13.97604488694527625, -13.89961937509977652, 21.87390960531435979 ) ) ;
#91201 = CARTESIAN_POINT ( 'NONE',  ( 14.29746914071037800, 8.314922557961029526, 31.66775706135234358 ) ) ;
#91202 = CARTESIAN_POINT ( 'NONE',  ( 5.153800228976335163, 19.02544592524342804, 54.79057627198103120 ) ) ;
#91203 = CARTESIAN_POINT ( 'NONE',  ( 8.906447517083057264, -27.41122689804191026, 142.5999999999999943 ) ) ;
#91204 = CARTESIAN_POINT ( 'NONE',  ( 16.46253265017160672, -9.564922557960803928, 98.33224293864769550 ) ) ;
#91205 = CARTESIAN_POINT ( 'NONE',  ( -12.06949235617739369, -12.14591786802326823, 89.37609039468568994 ) ) ;
#91206 = CARTESIAN_POINT ( 'NONE',  ( 16.46253265017146816, 9.564922557961045513, 96.66775706135233293 ) ) ;
#91207 = CARTESIAN_POINT ( 'NONE',  ( 13.97604488694548053, -13.89961937509957401, 25.62609039468566507 ) ) ;
#91208 = CARTESIAN_POINT ( 'NONE',  ( 15.72974639402199770, -15.80617190586745480, 73.12390960531436690 ) ) ;
#91209 = CARTESIAN_POINT ( 'NONE',  ( 12.14591786802327356, -12.06949235617739191, 100.6260903946857184 ) ) ;
#91210 = CARTESIAN_POINT ( 'NONE',  ( -19.03943276465977164, -0.05219959533935918106, 98.75109039468567573 ) ) ;
#91211 = CARTESIAN_POINT ( 'NONE',  ( -16.46253265017160317, 9.564922557960807481, 55.83224293864769550 ) ) ;
#91212 = CARTESIAN_POINT ( 'NONE',  ( 19.05341960407611168, 5.049401038298154454, 88.95724293864769550 ) ) ;
#91213 = CARTESIAN_POINT ( 'NONE',  ( 10.72451020669871369, 18.67979575497193778, 67.08442372801901854 ) ) ;
#91214 = CARTESIAN_POINT ( 'NONE',  ( 0.05219959533909260263, 19.03943276465977164, 49.99890960531435979 ) ) ;
#91215 = CARTESIAN_POINT ( 'NONE',  ( -17.50000000000000355, -5.624438216177585659, 84.18329655085358354 ) ) ;
#91216 = CARTESIAN_POINT ( 'NONE',  ( -16.53943276465976808, 0.05219959533911058130, 81.24890960531436690 ) ) ;
#91217 = CARTESIAN_POINT ( 'NONE',  ( -15.72974639402197994, 15.80617190586746368, 75.62390960531439532 ) ) ;
#91218 = CARTESIAN_POINT ( 'NONE',  ( 20.28939339942064279, -0.9295024462021991285, 102.5000000000000284 ) ) ;
#91219 = CARTESIAN_POINT ( 'NONE',  ( -23.48529157249600985, 32.32473071737754111, -6.049999994537626158 ) ) ;
#91220 = CARTESIAN_POINT ( 'NONE',  ( -19.03943276465977164, -0.05219959533935918106, 48.75109039468566863 ) ) ;
#91221 = FACE_OUTER_BOUND ( 'NONE', #127374, .T. ) ;
#91223 = CARTESIAN_POINT ( 'NONE',  ( 16.46253265017160672, -9.564922557960803928, 83.33224293864768129 ) ) ;
#91222 = CARTESIAN_POINT ( 'NONE',  ( 5.049401038298161559, -19.05341960407611168, 82.70724293864770971 ) ) ;
#91224 = CARTESIAN_POINT ( 'NONE',  ( 4.379528057220092307, 16.55341960407617563, 62.29275706135236845 ) ) ;
#91225 = CARTESIAN_POINT ( 'NONE',  ( -17.50000000000000355, -5.500000000000022204, 66.28230962303567253 ) ) ;
#91226 = CARTESIAN_POINT ( 'NONE',  ( 9.564922557961047289, -16.46253265017146816, 25.41775706135234003 ) ) ;
#91227 = CARTESIAN_POINT ( 'NONE',  ( 4.500000000000000888, -130.0000000000000000, 12.99999999999999822 ) ) ;
#91228 = CARTESIAN_POINT ( 'NONE',  ( -16.52544592524335698, -4.483927247898792601, 83.95942372801900433 ) ) ;
#91229 = CARTESIAN_POINT ( 'NONE',  ( -0.4346045811322798991, -24.23981148858511503, -54.26183423998840993 ) ) ;
#91230 = CARTESIAN_POINT ( 'NONE',  ( 8.224510206698742110, 14.34966873604972548, 77.08442372801901854 ) ) ;
#91231 =( BOUNDED_CURVE ( )  B_SPLINE_CURVE ( 2, ( #120867, #182567, #162395, #196757, #25912, #86556, #193755, #132066, #195764, #72398, #135081 ),
 .UNSPECIFIED., .F., .F. ) 
 B_SPLINE_CURVE_WITH_KNOTS ( ( 3, 2, 2, 2, 2, 3 ),
 ( 0.9000000000000007994, 0.9200000000000007061, 0.9400000000000003908, 0.9600000000000002975, 0.9800000000000002043, 1.000000000000000000 ),
 .UNSPECIFIED. ) 
 CURVE ( )  GEOMETRIC_REPRESENTATION_ITEM ( )  RATIONAL_B_SPLINE_CURVE ( ( 0.9999999999999981126, 0.9510565162951554186, 1.000000000000000000, 0.9510565162951535312, 1.000000000000000000, 0.9510565162951535312, 1.000000000000000000, 0.9510565162951535312, 1.000000000000000000, 0.9510565162951535312, 1.000000000000000000 ) ) 
 REPRESENTATION_ITEM ( '' )  );
#91232 = CARTESIAN_POINT ( 'NONE',  ( 14.29746914071037800, 8.314922557961029526, 56.66775706135235424 ) ) ;
#91233 = CARTESIAN_POINT ( 'NONE',  ( 21.46320343559668231, 20.96320343559617072, 5.353553390593269512 ) ) ;
#91234 = CARTESIAN_POINT ( 'NONE',  ( 15.80617190586769283, -15.72974639402175789, 65.62609039468568994 ) ) ;
#91235 = CARTESIAN_POINT ( 'NONE',  ( 19.02544592524334988, 5.153800228976608722, 81.45942372801897591 ) ) ;
#91236 = CARTESIAN_POINT ( 'NONE',  ( 10.72451020669871369, 18.67979575497193778, 102.0844237280190185 ) ) ;
#91237 = CARTESIAN_POINT ( 'NONE',  ( -5.153800228976328057, -19.02544592524343514, 52.29057627198100988 ) ) ;
#91238 = CARTESIAN_POINT ( 'NONE',  ( 13.89961937509977652, -13.97604488694527269, 38.12390960531436690 ) ) ;
#91239 = LINE ( 'NONE', #137766, #88460 ) ;
#91240 = CARTESIAN_POINT ( 'NONE',  ( 21.55341960407610458, 5.719274019375980345, 63.95724293864770260 ) ) ;
#91241 = CARTESIAN_POINT ( 'NONE',  ( 16.51473224551069308, 9.474510206698969483, 114.1655762719810241 ) ) ;
#91242 = CARTESIAN_POINT ( 'NONE',  ( -16.51473224551069308, -9.474510206698971260, 26.66557627198103120 ) ) ;
#91243 = CARTESIAN_POINT ( 'NONE',  ( 8.224510206698742110, 14.34966873604972548, 52.08442372801901854 ) ) ;
#91244 = VERTEX_POINT ( 'NONE', #139863 ) ;
#91245 = CARTESIAN_POINT ( 'NONE',  ( -18.62759615963270932, 10.81492255796079327, 110.8322429386476955 ) ) ;
#91247 = CARTESIAN_POINT ( 'NONE',  ( -30.74264578624800492, 22.33583958711400186, -4.200000000000000178 ) ) ;
#91246 = CARTESIAN_POINT ( 'NONE',  ( 14.34966873604960469, 8.224510206698951720, 49.16557627198102409 ) ) ;
#91248 = CARTESIAN_POINT ( 'NONE',  ( -0.05219959533936034679, 19.03943276465977164, 112.5010903946856757 ) ) ;
#91249 = CARTESIAN_POINT ( 'NONE',  ( 19.03943276465977164, 0.05219959533936151252, 41.25109039468566152 ) ) ;
#91250 = CARTESIAN_POINT ( 'NONE',  ( 16.52544592524342804, -4.483927247898539470, 38.54057627198103120 ) ) ;
#91251 = CARTESIAN_POINT ( 'NONE',  ( -5.719274019375665041, -21.55341960407619695, 19.79275706135235069 ) ) ;
#91253 = CARTESIAN_POINT ( 'NONE',  ( -5.823673210054116645, -21.52544592524344225, 62.29057627198102409 ) ) ;
#91252 = CARTESIAN_POINT ( 'NONE',  ( 16.21995358207305316, 7.366697692864111247, 32.56448998487844193 ) ) ;
#91254 = CARTESIAN_POINT ( 'NONE',  ( -5.049401038298153566, 19.05341960407611168, 85.20724293864766707 ) ) ;
#91255 = CARTESIAN_POINT ( 'NONE',  ( 4.379528057220339221, -16.55341960407611168, 52.70724293864769550 ) ) ;
#91256 = CARTESIAN_POINT ( 'NONE',  ( -9.564922557960796823, -16.46253265017161027, 107.0822429386476955 ) ) ;
#91257 = DIRECTION ( 'NONE',  ( 0.000000000000000000, 0.000000000000000000, -1.000000000000000000 ) ) ;
#91258 = CARTESIAN_POINT ( 'NONE',  ( 16.51473224551083163, -9.474510206698727899, 55.83442372801899722 ) ) ;
#91259 = CARTESIAN_POINT ( 'NONE',  ( 18.67979575497178502, 10.72451020669898547, 94.16557627198103830 ) ) ;
#91260 = CARTESIAN_POINT ( 'NONE',  ( 9.474510206698971260, -16.51473224551069308, 37.91557627198102409 ) ) ;
#91261 = CARTESIAN_POINT ( 'NONE',  ( 19.03943276465977164, -0.05219959533909143690, 23.74890960531435269 ) ) ;
#91262 = ADVANCED_FACE ( 'NONE', ( #1352 ), #40428, .T. ) ;
#91263 = CARTESIAN_POINT ( 'NONE',  ( 5.823673210054444382, -21.52544592524334988, 55.20942372801902565 ) ) ;
#91264 = CARTESIAN_POINT ( 'NONE',  ( -22.44159573604010305, 16.30477369853692338, 148.6750000027311671 ) ) ;
#91265 = CARTESIAN_POINT ( 'NONE',  ( 12.14591786802309770, 12.06949235617756955, 29.37390960531435269 ) ) ;
#91266 = CARTESIAN_POINT ( 'NONE',  ( 19.02544592524343514, -5.153800228976328945, 53.54057627198102409 ) ) ;
#91267 = CARTESIAN_POINT ( 'NONE',  ( -19.03943276465977164, 0.05219959533909376836, 96.24890960531436690 ) ) ;
#91268 = CARTESIAN_POINT ( 'NONE',  ( 21.53943276465977519, -0.05219959533907433946, 58.74890960531436690 ) ) ;
#91269 = CARTESIAN_POINT ( 'NONE',  ( -22.44159573604010305, 16.30477369853692338, 146.6750000027311671 ) ) ;
#91270 = CARTESIAN_POINT ( 'NONE',  ( 19.03943276465977164, -0.05219959533909143690, 43.74890960531435979 ) ) ;
#91271 = CARTESIAN_POINT ( 'NONE',  ( 18.62759615963271287, -10.81492255796078972, 58.33224293864768839 ) ) ;
#91272 = CARTESIAN_POINT ( 'NONE',  ( -5.719274019375665041, -21.55341960407619695, 84.79275706135234714 ) ) ;
#91275 = CARTESIAN_POINT ( 'NONE',  ( -4.379528057220328563, 16.55341960407611168, 70.20724293864769550 ) ) ;
#91274 = CARTESIAN_POINT ( 'NONE',  ( -0.05219959533934338120, 16.53943276465976808, 87.50109039468568994 ) ) ;
#91273 = CARTESIAN_POINT ( 'NONE',  ( 7.213464565009756413, -38.12638803158730383, -24.00445952849677056 ) ) ;
#91276 = CARTESIAN_POINT ( 'NONE',  ( 0.05219959533934541429, -16.53943276465976808, 90.00109039468567573 ) ) ;
#91277 = CARTESIAN_POINT ( 'NONE',  ( 13.97604488694527802, 13.89961937509977652, 69.37390960531436690 ) ) ;
#91278 = ORIENTED_EDGE ( 'NONE', *, *, #98059, .T. ) ;
#91279 = CARTESIAN_POINT ( 'NONE',  ( -0.05219959533936034679, 19.03943276465977164, 27.50109039468566507 ) ) ;
#91280 = CARTESIAN_POINT ( 'NONE',  ( -14.29746914071037622, -8.314922557961029526, 84.16775706135234714 ) ) ;
#91281 = CARTESIAN_POINT ( 'NONE',  ( 9.474510206698729675, 16.51473224551082808, 22.08442372801899722 ) ) ;
#91282 = CARTESIAN_POINT ( 'NONE',  ( 5.049401038298161559, -19.05341960407611168, 77.70724293864765286 ) ) ;
#91283 = CARTESIAN_POINT ( 'NONE',  ( -21.53943276465977519, 0.05219959533907696930, 51.24890960531436690 ) ) ;
#91284 = CARTESIAN_POINT ( 'NONE',  ( 8.224510206698742110, 14.34966873604972548, 22.08442372801901143 ) ) ;
#91285 = CARTESIAN_POINT ( 'NONE',  ( -10.81492255796105439, 18.62759615963255655, 77.91775706135231871 ) ) ;
#91286 = CARTESIAN_POINT ( 'NONE',  ( -16.52544592524335698, -4.483927247898792601, 63.95942372801901854 ) ) ;
#91287 = CARTESIAN_POINT ( 'NONE',  ( 21.52544592524334988, 5.823673210054432836, 21.45942372801901499 ) ) ;
#91288 = CARTESIAN_POINT ( 'NONE',  ( -16.51473224551082808, 9.474510206698731452, 108.3344237280190043 ) ) ;
#91289 = CARTESIAN_POINT ( 'NONE',  ( 5.049401038298161559, -19.05341960407611168, 87.70724293864769550 ) ) ;
#91290 = CARTESIAN_POINT ( 'NONE',  ( 12.06949235617739724, 12.14591786802326823, 21.87609039468567573 ) ) ;
#91291 = CARTESIAN_POINT ( 'NONE',  ( 19.05341960407611168, 5.049401038298154454, 43.95724293864769550 ) ) ;
#91292 = CARTESIAN_POINT ( 'NONE',  ( 14.34966873604972726, -8.224510206698740333, 30.83442372801902209 ) ) ;
#91293 = CARTESIAN_POINT ( 'NONE',  ( 16.53943276465976808, -0.05219959533910856209, 83.74890960531435269 ) ) ;
#91294 = CARTESIAN_POINT ( 'NONE',  ( 4.483927247898790824, -16.52544592524335698, 90.20942372801903275 ) ) ;
#91296 = CARTESIAN_POINT ( 'NONE',  ( -16.46253265017160317, 9.564922557960807481, 65.83224293864769550 ) ) ;
#91295 = CARTESIAN_POINT ( 'NONE',  ( -21.52544592524334988, -5.823673210054445271, 23.95942372801901143 ) ) ;
#91297 = CARTESIAN_POINT ( 'NONE',  ( 0.05219959533909260263, 19.03943276465977164, 64.99890960531436690 ) ) ;
#91298 = CARTESIAN_POINT ( 'NONE',  ( 12.06949235617739724, 12.14591786802326823, 81.87609039468568994 ) ) ;
#91300 = ORIENTED_EDGE ( 'NONE', *, *, #5739, .F. ) ;
#91299 = CARTESIAN_POINT ( 'NONE',  ( -24.81886791266594017, -6.075537473407860212, 168.3989613422462241 ) ) ;
#91301 = ORIENTED_EDGE ( 'NONE', *, *, #192849, .F. ) ;
#91302 = CARTESIAN_POINT ( 'NONE',  ( 0.05219959533936267826, -19.03943276465977164, 30.00109039468566863 ) ) ;
#91303 = CARTESIAN_POINT ( 'NONE',  ( 9.564922557960805705, 16.46253265017160317, 49.58224293864770260 ) ) ;
#91305 = VERTEX_POINT ( 'NONE', #101081 ) ;
#91304 = CARTESIAN_POINT ( 'NONE',  ( -16.51473224551069308, -9.474510206698971260, 111.6655762719810383 ) ) ;
#91306 = CARTESIAN_POINT ( 'NONE',  ( -16.53943276465976808, -0.05219959533934237506, 23.75109039468567929 ) ) ;
#91308 = CARTESIAN_POINT ( 'NONE',  ( 0.05219959533934541429, -16.53943276465976808, 45.00109039468568284 ) ) ;
#91307 = CARTESIAN_POINT ( 'NONE',  ( -19.03943276465977164, -0.05219959533935918106, 63.75109039468566863 ) ) ;
#91309 = CARTESIAN_POINT ( 'NONE',  ( 9.474510206698971260, -16.51473224551069308, 102.9155762719810241 ) ) ;
#91310 = CARTESIAN_POINT ( 'NONE',  ( 5.049401038298161559, -19.05341960407611168, 82.70724293864770971 ) ) ;
#91311 = CARTESIAN_POINT ( 'NONE',  ( -18.62759615963270932, 10.81492255796079327, 95.83224293864770971 ) ) ;
#91312 = CARTESIAN_POINT ( 'NONE',  ( -5.049401038297874678, -19.05341960407617918, 64.79275706135233293 ) ) ;
#91314 = CARTESIAN_POINT ( 'NONE',  ( 13.89961937509977652, -13.97604488694527269, 23.12390960531436335 ) ) ;
#91313 = CARTESIAN_POINT ( 'NONE',  ( -19.05341960407611168, -5.049401038298163336, 91.45724293864766707 ) ) ;
#91315 = EDGE_CURVE ( 'NONE', #138197, #164346, #87298, .T. ) ;
#91316 = CARTESIAN_POINT ( 'NONE',  ( -0.05219959533909027116, -19.03943276465977164, 57.49890960531435979 ) ) ;
#91318 = CARTESIAN_POINT ( 'NONE',  ( -5.153800228976328057, -19.02544592524343514, 27.29057627198103120 ) ) ;
#91317 = CARTESIAN_POINT ( 'NONE',  ( -14.34966873604972548, 8.224510206698743886, 108.3344237280190185 ) ) ;
#91319 = CARTESIAN_POINT ( 'NONE',  ( 19.02544592524334988, 5.153800228976608722, 36.45942372801900433 ) ) ;
#91320 = CARTESIAN_POINT ( 'NONE',  ( 16.55341960407611168, 4.379528057220329451, 78.95724293864769550 ) ) ;
#91321 = CARTESIAN_POINT ( 'NONE',  ( -21.55341960407619339, 5.719274019375674811, 93.54275706135234714 ) ) ;
#91322 = CARTESIAN_POINT ( 'NONE',  ( 19.03943276465977164, -0.05219959533909143690, 38.74890960531436690 ) ) ;
#91323 = CARTESIAN_POINT ( 'NONE',  ( -12.14591786802326823, 12.06949235617739902, 53.12609039468568284 ) ) ;
#91325 = CARTESIAN_POINT ( 'NONE',  ( 5.823673210054444382, -21.52544592524334988, 90.20942372801903275 ) ) ;
#91324 = CARTESIAN_POINT ( 'NONE',  ( -12.14591786802309592, -12.06949235617757132, 41.87390960531435979 ) ) ;
#91326 = CARTESIAN_POINT ( 'NONE',  ( 16.51473224551069308, 9.474510206698969483, 89.16557627198103830 ) ) ;
#91327 = CARTESIAN_POINT ( 'NONE',  ( -5.049401038298153566, 19.05341960407611168, 100.2072429386476955 ) ) ;
#91328 = CARTESIAN_POINT ( 'NONE',  ( -16.53943276465976808, 0.05219959533911058130, 111.2489096053143669 ) ) ;
#91329 = CARTESIAN_POINT ( 'NONE',  ( -14.34966873604960291, -8.224510206698953496, 71.66557627198100988 ) ) ;
#91330 = CARTESIAN_POINT ( 'NONE',  ( 15.72974639402199770, -15.80617190586745480, 78.12390960531436690 ) ) ;
#91331 = CARTESIAN_POINT ( 'NONE',  ( -0.05219959533909027116, -19.03943276465977164, 82.49890960531436690 ) ) ;
#91332 = CARTESIAN_POINT ( 'NONE',  ( -18.62759615963270932, 10.81492255796079327, 100.8322429386477097 ) ) ;
#91333 = CARTESIAN_POINT ( 'NONE',  ( -16.51473224551069308, -9.474510206698971260, 86.66557627198102409 ) ) ;
#91335 = CARTESIAN_POINT ( 'NONE',  ( 16.52544592524342804, -4.483927247898539470, 93.54057627198103830 ) ) ;
#91334 = CARTESIAN_POINT ( 'NONE',  ( 19.01533133064927128, -5.499999999999451106, 46.26586590595743331 ) ) ;
#91336 = CARTESIAN_POINT ( 'NONE',  ( 19.05341960407611168, 5.049401038298154454, 53.95724293864770260 ) ) ;
#91337 = CARTESIAN_POINT ( 'NONE',  ( -10.72451020669898014, 18.67979575497178502, 60.41557627198102409 ) ) ;
#91338 = ADVANCED_FACE ( 'NONE', ( #24276 ), #187404, .F. ) ;
#91339 = CARTESIAN_POINT ( 'NONE',  ( 17.31747979337950483, -6.344076630960993946, 26.12055131934816998 ) ) ;
#91341 = DIRECTION ( 'NONE',  ( -0.000000000000000000, -0.000000000000000000, 1.000000000000000000 ) ) ;
#91340 = CARTESIAN_POINT ( 'NONE',  ( -0.05219959533910754901, -16.53943276465976808, 22.49890960531436335 ) ) ;
#91342 = CARTESIAN_POINT ( 'NONE',  ( 0.05219959533934541429, -16.53943276465976808, 25.00109039468567218 ) ) ;
#91343 = CARTESIAN_POINT ( 'NONE',  ( 12.14591786802309770, 12.06949235617756955, 79.37390960531436690 ) ) ;
#91344 = CARTESIAN_POINT ( 'NONE',  ( -16.61371651742605238, -7.165104196376108625, 96.14584930007005426 ) ) ;
#91345 = CARTESIAN_POINT ( 'NONE',  ( -16.51473224551069308, -9.474510206698971260, 71.66557627198102409 ) ) ;
#91346 = CARTESIAN_POINT ( 'NONE',  ( 16.51473224551069308, 9.474510206698969483, 39.16557627198103120 ) ) ;
#91347 = CARTESIAN_POINT ( 'NONE',  ( 12.14591786802309770, 12.06949235617756955, 69.37390960531436690 ) ) ;
#91348 = CARTESIAN_POINT ( 'NONE',  ( -9.474510206698964154, 16.51473224551069663, 115.4155762719810241 ) ) ;
#91349 = CARTESIAN_POINT ( 'NONE',  ( -9.564922557961040184, 16.46253265017147172, 107.9177570613523471 ) ) ;
#91350 = CARTESIAN_POINT ( 'NONE',  ( 5.153800228976335163, 19.02544592524342804, 104.7905762719809957 ) ) ;
#91351 = CARTESIAN_POINT ( 'NONE',  ( -10.81492255796078084, -18.62759615963271287, 72.08224293864769550 ) ) ;
#91352 = CARTESIAN_POINT ( 'NONE',  ( 14.34966873604972726, -8.224510206698740333, 75.83442372801900433 ) ) ;
#91353 = CARTESIAN_POINT ( 'NONE',  ( -16.19135201231352639, 7.376712067591987498, 94.81319145947880145 ) ) ;
#91354 = CARTESIAN_POINT ( 'NONE',  ( 19.05341960407611168, 5.049401038298154454, 63.95724293864769550 ) ) ;
#91355 = CARTESIAN_POINT ( 'NONE',  ( -10.81492255796078084, -18.62759615963271287, 87.08224293864769550 ) ) ;
#91356 = CARTESIAN_POINT ( 'NONE',  ( -16.51473224551082808, 9.474510206698731452, 103.3344237280190043 ) ) ;
#91357 = VECTOR ( 'NONE', #105001, 1000.000000000000000 ) ;
#91359 = CARTESIAN_POINT ( 'NONE',  ( 21.52544592524334988, 5.823673210054432836, 61.45942372801901854 ) ) ;
#91358 = CARTESIAN_POINT ( 'NONE',  ( -8.314922557960811034, -14.29746914071050412, 42.08224293864769550 ) ) ;
#91360 = CARTESIAN_POINT ( 'NONE',  ( 17.49999999999999289, 5.500000000000007994, 83.78230962303564411 ) ) ;
#91362 = CARTESIAN_POINT ( 'NONE',  ( -19.02544592524342804, 5.153800228976336051, 111.0405762719810099 ) ) ;
#91361 = CARTESIAN_POINT ( 'NONE',  ( -8.314922557961024197, 14.29746914071037800, 72.91775706135234714 ) ) ;
#91363 = CARTESIAN_POINT ( 'NONE',  ( -13.97604488694527625, -13.89961937509977830, 106.8739096053143669 ) ) ;
#91364 = DIRECTION ( 'NONE',  ( 1.000000000000000000, 0.000000000000000000, 0.000000000000000000 ) ) ;
#91365 = CARTESIAN_POINT ( 'NONE',  ( -0.05219959533934338120, 16.53943276465976808, 92.50109039468567573 ) ) ;
#91366 = CARTESIAN_POINT ( 'NONE',  ( -4.483927247898782831, 16.52544592524335698, 42.70942372801901854 ) ) ;
#91367 = CARTESIAN_POINT ( 'NONE',  ( 16.46253265017160672, -9.564922557960803928, 63.33224293864769550 ) ) ;
#91368 = CARTESIAN_POINT ( 'NONE',  ( 13.89961937509977652, -13.97604488694527269, 73.12390960531436690 ) ) ;
#91369 = CARTESIAN_POINT ( 'NONE',  ( -15.80617190586768217, 15.72974639402176855, 68.12609039468567573 ) ) ;
#91370 = CARTESIAN_POINT ( 'NONE',  ( 14.29746914071037800, 8.314922557961029526, 56.66775706135235424 ) ) ;
#91371 = CARTESIAN_POINT ( 'NONE',  ( -8.314922557960811034, -14.29746914071050412, 37.08224293864768129 ) ) ;
#91372 = CARTESIAN_POINT ( 'NONE',  ( -19.02544592524342804, 5.153800228976336051, 41.04057627198103120 ) ) ;
#91373 = CARTESIAN_POINT ( 'NONE',  ( 0.05219959533909260263, 19.03943276465977164, 34.99890960531435979 ) ) ;
#91376 = EDGE_CURVE ( 'NONE', #45713, #26126, #192111, .T. ) ;
#91375 = ORIENTED_EDGE ( 'NONE', *, *, #121465, .T. ) ;
#91374 = CARTESIAN_POINT ( 'NONE',  ( 12.14591786802327356, -12.06949235617739191, 40.62609039468567573 ) ) ;
#91377 = CARTESIAN_POINT ( 'NONE',  ( -19.02544592524334988, -5.153800228976617603, 88.95942372801897591 ) ) ;
#91378 = CARTESIAN_POINT ( 'NONE',  ( 16.55341960407611168, 4.379528057220329451, 98.95724293864770971 ) ) ;
#91379 = CARTESIAN_POINT ( 'NONE',  ( -19.05341960407611168, -5.049401038298163336, 51.45724293864770260 ) ) ;
#91381 = CARTESIAN_POINT ( 'NONE',  ( 30.74264578624800137, -22.33583958711395212, -9.199999999999999289 ) ) ;
#91380 = CARTESIAN_POINT ( 'NONE',  ( -9.564922557961040184, 16.46253265017147172, 87.91775706135233293 ) ) ;
#91382 = CARTESIAN_POINT ( 'NONE',  ( 18.67979575497194134, -10.72451020669871369, 85.83442372801901854 ) ) ;
#91383 = CARTESIAN_POINT ( 'NONE',  ( 8.314922557961029526, -14.29746914071037800, 60.41775706135235424 ) ) ;
#91384 = FACE_OUTER_BOUND ( 'NONE', #76281, .T. ) ;
#91385 = CARTESIAN_POINT ( 'NONE',  ( -10.81492255796078084, -18.62759615963271287, 47.08224293864770260 ) ) ;
#91386 = CARTESIAN_POINT ( 'NONE',  ( -8.314922557961024197, 14.29746914071037800, 42.91775706135235424 ) ) ;
#91387 = CARTESIAN_POINT ( 'NONE',  ( 5.049401038298163336, -19.05341960407611168, 37.70724293864768839 ) ) ;
#91388 = CARTESIAN_POINT ( 'NONE',  ( -5.153800228976607833, 19.02544592524334988, 42.70942372801901143 ) ) ;
#91389 = CARTESIAN_POINT ( 'NONE',  ( 5.153800228976335163, 19.02544592524342804, 84.79057627198099567 ) ) ;
#91390 = CARTESIAN_POINT ( 'NONE',  ( -16.53943276465976808, 0.05219959533911058130, 101.2489096053143669 ) ) ;
#91391 = CARTESIAN_POINT ( 'NONE',  ( 13.97604488694527802, 13.89961937509977652, 54.37390960531435979 ) ) ;
#91392 = CARTESIAN_POINT ( 'NONE',  ( -22.55670631985108443, -22.55670631985069008, -49.13275782002545355 ) ) ;
#91393 = CARTESIAN_POINT ( 'NONE',  ( 15.72974639402176855, 15.80617190586768217, 81.87609039468568994 ) ) ;
#91394 = CARTESIAN_POINT ( 'NONE',  ( -17.49999999999999645, -5.499999999999992895, 89.20309617465829888 ) ) ;
#91395 = CARTESIAN_POINT ( 'NONE',  ( -9.564922557961040184, 16.46253265017147172, 27.91775706135232582 ) ) ;
#91396 = CARTESIAN_POINT ( 'NONE',  ( -10.81492255796105439, 18.62759615963255655, 112.9177570613523329 ) ) ;
#91397 = CARTESIAN_POINT ( 'NONE',  ( 16.52544592524342804, -4.483927247898539470, 53.54057627198103120 ) ) ;
#91398 = CARTESIAN_POINT ( 'NONE',  ( 5.049401038298161559, -19.05341960407611168, 62.70724293864769550 ) ) ;
#91399 = CARTESIAN_POINT ( 'NONE',  ( -16.51473224551069308, -9.474510206698971260, 111.6655762719810383 ) ) ;
#91400 = CARTESIAN_POINT ( 'NONE',  ( 5.719274019375673035, 21.55341960407619339, 82.29275706135234714 ) ) ;
#91401 = CARTESIAN_POINT ( 'NONE',  ( -19.03943276465977164, 0.05219959533909376836, 61.24890960531436690 ) ) ;
#91402 = VECTOR ( 'NONE', #142591, 1000.000000000000000 ) ;
#91403 = CARTESIAN_POINT ( 'NONE',  ( 21.52544592524334988, 5.823673210054432836, 86.45942372801901854 ) ) ;
#91404 = CARTESIAN_POINT ( 'NONE',  ( -10.81492255796078084, -18.62759615963271287, 42.08224293864769550 ) ) ;
#91405 = CARTESIAN_POINT ( 'NONE',  ( -15.72974639402176322, -15.80617190586768395, 34.37609039468568284 ) ) ;
#91406 = CARTESIAN_POINT ( 'NONE',  ( 19.02544592524334988, 5.153800228976608722, 56.45942372801898301 ) ) ;
#91407 = CARTESIAN_POINT ( 'NONE',  ( 9.474510206698971260, -16.51473224551069308, 27.91557627198103120 ) ) ;
#91408 = CARTESIAN_POINT ( 'NONE',  ( -16.51473224551069308, -9.474510206698971260, 71.66557627198102409 ) ) ;
#91409 = CARTESIAN_POINT ( 'NONE',  ( -16.52544592524335698, -4.483927247898792601, 23.95942372801901143 ) ) ;
#91410 = CARTESIAN_POINT ( 'NONE',  ( 8.224510206698953496, -14.34966873604960469, 87.91557627198103830 ) ) ;
#91411 = CARTESIAN_POINT ( 'NONE',  ( -5.049401038298153566, 19.05341960407611168, 60.20724293864768129 ) ) ;
#91412 = CARTESIAN_POINT ( 'NONE',  ( 18.62759615963271287, -10.81492255796078972, 43.33224293864769550 ) ) ;
#91413 = B_SPLINE_CURVE_WITH_KNOTS ( 'NONE', 3,
 ( #49441, #109119, #139449, #930, #170797, #155623 ),
 .UNSPECIFIED., .F., .F.,
 ( 4, 2, 4 ),
 ( 0.003562460574610347517, 0.004150450062026994624, 0.004738439549443641298 ),
 .UNSPECIFIED. ) ;
#91414 = CARTESIAN_POINT ( 'NONE',  ( 13.89961937509957401, 13.97604488694547697, 111.8760903946856757 ) ) ;
#91415 = CARTESIAN_POINT ( 'NONE',  ( 21.52544592524334988, 5.823673210054432836, 21.45942372801901499 ) ) ;
#91416 = CARTESIAN_POINT ( 'NONE',  ( 15.80617190586769283, -15.72974639402175789, 75.62609039468567573 ) ) ;
#91417 = CARTESIAN_POINT ( 'NONE',  ( 16.55341960407618274, -4.379528057220086978, 76.04275706135237556 ) ) ;
#91418 = CARTESIAN_POINT ( 'NONE',  ( 16.55341960407618274, -4.379528057220086978, 71.04275706135234714 ) ) ;
#91419 = CARTESIAN_POINT ( 'NONE',  ( 19.05341960407611168, 5.049401038298154454, 63.95724293864769550 ) ) ;
#91420 = CARTESIAN_POINT ( 'NONE',  ( -4.483927247898782831, 16.52544592524335698, 87.70942372801901854 ) ) ;
#91421 = CARTESIAN_POINT ( 'NONE',  ( -13.97604488694547697, 13.89961937509957934, 43.12609039468566152 ) ) ;
#91422 = CARTESIAN_POINT ( 'NONE',  ( 21.52544592524344225, -5.823673210054117533, 113.5405762719810383 ) ) ;
#91423 = CARTESIAN_POINT ( 'NONE',  ( 16.55341960407611168, 4.379528057220329451, 63.95724293864770260 ) ) ;
#91424 = CARTESIAN_POINT ( 'NONE',  ( -5.049401038298153566, 19.05341960407611168, 85.20724293864766707 ) ) ;
#91425 = CARTESIAN_POINT ( 'NONE',  ( 14.34966873604972726, -8.224510206698740333, 85.83442372801901854 ) ) ;
#91426 = CARTESIAN_POINT ( 'NONE',  ( 5.823673210054444382, -21.52544592524334988, 60.20942372801902565 ) ) ;
#91427 = CARTESIAN_POINT ( 'NONE',  ( 12.06949235617739724, 12.14591786802326823, 36.87609039468568994 ) ) ;
#91428 = CARTESIAN_POINT ( 'NONE',  ( 0.05219959533937995610, -21.53943276465977519, 20.00109039468568639 ) ) ;
#91429 = CARTESIAN_POINT ( 'NONE',  ( 4.483927247898545687, 16.52544592524342804, 59.79057627198103120 ) ) ;
#91430 = EDGE_LOOP ( 'NONE', ( #107694, #9658, #111603, #10949 ) ) ;
#91431 = CARTESIAN_POINT ( 'NONE',  ( 21.55341960407610458, 5.719274019375980345, 103.9572429386476813 ) ) ;
#91432 = CARTESIAN_POINT ( 'NONE',  ( 0.05219959533910956823, 16.53943276465976808, 34.99890960531435979 ) ) ;
#91433 = ORIENTED_EDGE ( 'NONE', *, *, #33819, .T. ) ;
#91434 = CARTESIAN_POINT ( 'NONE',  ( 35.09778042078743709, 5.635567127521242448, 40.04523299337174080 ) ) ;
#91435 = CARTESIAN_POINT ( 'NONE',  ( -18.67979575497178146, -10.72451020669898902, 111.6655762719810525 ) ) ;
#91436 = CARTESIAN_POINT ( 'NONE',  ( -9.564922557960796823, -16.46253265017161027, 107.0822429386476955 ) ) ;
#91437 = CARTESIAN_POINT ( 'NONE',  ( 5.719274019375673035, 21.55341960407619339, 37.29275706135235424 ) ) ;
#91438 = CARTESIAN_POINT ( 'NONE',  ( -12.14591786802309592, -12.06949235617757132, 56.87390960531436690 ) ) ;
#91439 = CARTESIAN_POINT ( 'NONE',  ( -19.02544592524342804, 5.153800228976336051, 61.04057627198103120 ) ) ;
#91440 = CARTESIAN_POINT ( 'NONE',  ( 5.153800228976615827, -19.02544592524334988, 70.20942372801899012 ) ) ;
#91441 = CARTESIAN_POINT ( 'NONE',  ( -16.51473224551069308, -9.474510206698971260, 91.66557627198103830 ) ) ;
#91442 = CARTESIAN_POINT ( 'NONE',  ( 10.72451020669898902, -18.67979575497178502, 47.91557627198102409 ) ) ;
#91443 = CARTESIAN_POINT ( 'NONE',  ( -20.47606263883548294, -31.78721852327825914, -20.08103504831861130 ) ) ;
#91444 = CARTESIAN_POINT ( 'NONE',  ( 9.474510206698971260, -16.51473224551069308, 52.91557627198102409 ) ) ;
#91445 = CARTESIAN_POINT ( 'NONE',  ( 8.314922557961029526, -14.29746914071037800, 35.41775706135234003 ) ) ;
#91446 = CARTESIAN_POINT ( 'NONE',  ( -9.474510206698720793, -16.51473224551083518, 59.58442372801900433 ) ) ;
#91447 = CARTESIAN_POINT ( 'NONE',  ( 10.72451020669898902, -18.67979575497178502, 112.9155762719810383 ) ) ;
#91448 = CARTESIAN_POINT ( 'NONE',  ( -4.379528057220328563, 16.55341960407611168, 45.20724293864769550 ) ) ;
#91449 = VERTEX_POINT ( 'NONE', #116263 ) ;
#91450 = CARTESIAN_POINT ( 'NONE',  ( -13.89961937509977652, 13.97604488694528158, 85.62390960531433848 ) ) ;
#91451 = CARTESIAN_POINT ( 'NONE',  ( -21.55341960407610458, -5.719274019375992779, 66.45724293864768129 ) ) ;
#91453 = CARTESIAN_POINT ( 'NONE',  ( 4.483927247898790824, -16.52544592524335698, 40.20942372801901854 ) ) ;
#91452 = CARTESIAN_POINT ( 'NONE',  ( -15.72974639402197994, 15.80617190586746368, 110.6239096053143669 ) ) ;
#91454 = CARTESIAN_POINT ( 'NONE',  ( -5.823673210054116645, -21.52544592524344225, 32.29057627198102409 ) ) ;
#91455 = CARTESIAN_POINT ( 'NONE',  ( -21.55341960407619339, 5.719274019375674811, 103.5427570613523613 ) ) ;
#91456 = CARTESIAN_POINT ( 'NONE',  ( 0.05219959533909260263, 19.03943276465977164, 84.99890960531436690 ) ) ;
#91457 = CARTESIAN_POINT ( 'NONE',  ( 13.89961937509977652, -13.97604488694527269, 38.12390960531436690 ) ) ;
#91458 = CARTESIAN_POINT ( 'NONE',  ( 5.153800228976335163, 19.02544592524342804, 94.79057627198103830 ) ) ;
#91459 = CARTESIAN_POINT ( 'NONE',  ( -0.05219959533909027116, -19.03943276465977164, 72.49890960531435269 ) ) ;
#91460 = CARTESIAN_POINT ( 'NONE',  ( -16.55341960407617563, 4.379528057220093196, 23.54275706135235424 ) ) ;
#91461 = AXIS2_PLACEMENT_3D ( 'NONE', #170248, #78218, #79224 ) ;
#91462 = CARTESIAN_POINT ( 'NONE',  ( 17.48847506799950935, -5.747544572775296068, 88.32697437843289379 ) ) ;
#91463 = CARTESIAN_POINT ( 'NONE',  ( -9.474510206698720793, -16.51473224551083518, 54.58442372801899722 ) ) ;
#91465 = CARTESIAN_POINT ( 'NONE',  ( 18.62759615963271287, -10.81492255796078972, 33.33224293864769550 ) ) ;
#91464 = CARTESIAN_POINT ( 'NONE',  ( 5.049401038297881783, 19.05341960407617563, 22.29275706135233648 ) ) ;
#91466 = CARTESIAN_POINT ( 'NONE',  ( 8.314922557961029526, -14.29746914071037800, 100.4177570613523471 ) ) ;
#91467 = CARTESIAN_POINT ( 'NONE',  ( 20.76286210753433181, -20.18345802296806113, -49.60777730575491518 ) ) ;
#91468 = CARTESIAN_POINT ( 'NONE',  ( -5.049401038297874678, -19.05341960407617918, 64.79275706135233293 ) ) ;
#91469 = CARTESIAN_POINT ( 'NONE',  ( -0.05219959533936034679, 19.03943276465977164, 37.50109039468567573 ) ) ;
#91470 = CARTESIAN_POINT ( 'NONE',  ( 17.12812012977026654, 6.668231424565999710, 108.8594875932314494 ) ) ;
#91471 = CARTESIAN_POINT ( 'NONE',  ( -16.46253265017160317, 9.564922557960807481, 35.83224293864768839 ) ) ;
#91472 = CARTESIAN_POINT ( 'NONE',  ( 16.52544592524342804, -4.483927247898539470, 38.54057627198103120 ) ) ;
#91473 = CARTESIAN_POINT ( 'NONE',  ( -13.97604488694527625, -13.89961937509977652, 26.87390960531434558 ) ) ;
#91474 = CARTESIAN_POINT ( 'NONE',  ( -14.34966873604960291, -8.224510206698953496, 26.66557627198103475 ) ) ;
#91475 = FACE_OUTER_BOUND ( 'NONE', #29441, .T. ) ;
#91476 = CARTESIAN_POINT ( 'NONE',  ( -8.314922557961024197, 14.29746914071037800, 97.91775706135236135 ) ) ;
#91477 = CARTESIAN_POINT ( 'NONE',  ( -0.05219959533909027116, -19.03943276465977164, 52.49890960531436690 ) ) ;
#91478 = CARTESIAN_POINT ( 'NONE',  ( 21.52544592524334988, 5.823673210054432836, 111.4594237280190328 ) ) ;
#91479 = CARTESIAN_POINT ( 'NONE',  ( 16.52544592524335698, 4.483927247898782831, 26.45942372801901854 ) ) ;
#91481 = ORIENTED_EDGE ( 'NONE', *, *, #16720, .F. ) ;
#91480 = CARTESIAN_POINT ( 'NONE',  ( 5.823673210054444382, -21.52544592524334988, 80.20942372801901854 ) ) ;
#91482 = CARTESIAN_POINT ( 'NONE',  ( 16.51473224551083163, -9.474510206698727899, 60.83442372801900433 ) ) ;
#91483 = CARTESIAN_POINT ( 'NONE',  ( -16.46253265017160317, 9.564922557960807481, 85.83224293864769550 ) ) ;
#91484 = CARTESIAN_POINT ( 'NONE',  ( -5.049401038298153566, 19.05341960407611168, 80.20724293864769550 ) ) ;
#91485 = CARTESIAN_POINT ( 'NONE',  ( -5.950531402560715689E-15, 38.81732327939063509, -9.124999997268814056 ) ) ;
#91486 = CARTESIAN_POINT ( 'NONE',  ( -21.52544592524343514, 5.823673210054127303, 111.0405762719810525 ) ) ;
#91487 = CARTESIAN_POINT ( 'NONE',  ( -4.483927247898539470, -16.52544592524342804, 72.29057627198102409 ) ) ;
#91488 = CARTESIAN_POINT ( 'NONE',  ( -21.52544592524343514, 5.823673210054127303, 66.04057627198103830 ) ) ;
#91489 = CARTESIAN_POINT ( 'NONE',  ( -0.05219959533909027116, -19.03943276465977164, 62.49890960531435979 ) ) ;
#91491 = CARTESIAN_POINT ( 'NONE',  ( 16.52544592524335698, 4.483927247898782831, 91.45942372801901854 ) ) ;
#91490 = CARTESIAN_POINT ( 'NONE',  ( -18.67979575497178146, -10.72451020669898902, 101.6655762719810383 ) ) ;
#91492 = VERTEX_POINT ( 'NONE', #68755 ) ;
#91493 = CARTESIAN_POINT ( 'NONE',  ( -5.049401038298153566, 19.05341960407611168, 65.20724293864765286 ) ) ;
#91495 = DIRECTION ( 'NONE',  ( 0.000000000000000000, 0.000000000000000000, 1.000000000000000000 ) ) ;
#91494 = CARTESIAN_POINT ( 'NONE',  ( 16.53943276465976808, -0.05219959533910856209, 93.74890960531436690 ) ) ;
#91496 = CARTESIAN_POINT ( 'NONE',  ( -19.03943276465977164, 0.05219959533909376836, 56.24890960531435979 ) ) ;
#91497 = CARTESIAN_POINT ( 'NONE',  ( 13.97604488694548053, -13.89961937509957401, 85.62609039468568994 ) ) ;
#91498 = CARTESIAN_POINT ( 'NONE',  ( 8.224510206698953496, -14.34966873604960469, 82.91557627198103830 ) ) ;
#91499 = CARTESIAN_POINT ( 'NONE',  ( -21.55341960407619339, 5.719274019375674811, 58.54275706135235424 ) ) ;
#91501 = CARTESIAN_POINT ( 'NONE',  ( -15.80617190586745835, -15.72974639402198527, 106.8739096053143811 ) ) ;
#91500 = CARTESIAN_POINT ( 'NONE',  ( -13.89961937509977652, 13.97604488694528158, 40.62390960531435979 ) ) ;
#91502 = CARTESIAN_POINT ( 'NONE',  ( 4.379528057220339221, -16.55341960407611168, 107.7072429386476955 ) ) ;
#91503 = CARTESIAN_POINT ( 'NONE',  ( 17.81289503416610742, 24.51734667627700404, 147.5500000054623513 ) ) ;
#91504 = CARTESIAN_POINT ( 'NONE',  ( -19.02544592524342804, 5.153800228976336051, 61.04057627198103120 ) ) ;
#91505 = CARTESIAN_POINT ( 'NONE',  ( -10.41657218803457674, -12.21822558928538172, -61.63650692604122838 ) ) ;
#91507 = CARTESIAN_POINT ( 'NONE',  ( 16.46253265017160672, -9.564922557960803928, 108.3322429386476955 ) ) ;
#91506 = CARTESIAN_POINT ( 'NONE',  ( -13.89961937509957401, -13.97604488694547875, 99.37609039468567573 ) ) ;
#91508 = CARTESIAN_POINT ( 'NONE',  ( 10.81492255796106328, -18.62759615963255655, 40.41775706135234714 ) ) ;
#91509 = CARTESIAN_POINT ( 'NONE',  ( -19.05341960407611168, -5.049401038298163336, 81.45724293864769550 ) ) ;
#91510 = CARTESIAN_POINT ( 'NONE',  ( 19.05341960407617918, -5.049401038297876454, 66.04275706135233293 ) ) ;
#91511 = CARTESIAN_POINT ( 'NONE',  ( -19.03943276465977164, 0.05219959533909376836, 56.24890960531435979 ) ) ;
#91512 = EDGE_CURVE ( 'NONE', #172040, #167830, #17536, .T. ) ;
#91513 = CARTESIAN_POINT ( 'NONE',  ( 4.379528057220339221, -16.55341960407611168, 82.70724293864770971 ) ) ;
#91514 = CARTESIAN_POINT ( 'NONE',  ( 14.34966873604960469, 8.224510206698951720, 64.16557627198102409 ) ) ;
#91515 = CARTESIAN_POINT ( 'NONE',  ( -16.46253265017160317, 9.564922557960807481, 95.83224293864769550 ) ) ;
#91516 = CARTESIAN_POINT ( 'NONE',  ( 16.52544592524342804, -4.483927247898539470, 78.54057627198103830 ) ) ;
#91517 = CARTESIAN_POINT ( 'NONE',  ( 13.97604488694527802, 13.89961937509977652, 84.37390960531433848 ) ) ;
#91518 = CARTESIAN_POINT ( 'NONE',  ( -16.51473224551082808, 9.474510206698731452, 33.33442372801899722 ) ) ;
#91521 = CARTESIAN_POINT ( 'NONE',  ( -12.06949235617756955, 12.14591786802309770, 105.6239096053143669 ) ) ;
#91520 = CARTESIAN_POINT ( 'NONE',  ( 4.379528057220339221, -16.55341960407611168, 32.70724293864770260 ) ) ;
#91519 = CARTESIAN_POINT ( 'NONE',  ( 9.564922557960805705, 16.46253265017160317, 49.58224293864770260 ) ) ;
#91522 = ORIENTED_EDGE ( 'NONE', *, *, #91752, .T. ) ;
#91523 = CARTESIAN_POINT ( 'NONE',  ( -18.62759615963255300, -10.81492255796106328, 44.16775706135234714 ) ) ;
#91524 = CARTESIAN_POINT ( 'NONE',  ( 16.46253265017146816, 9.564922557961045513, 61.66775706135234003 ) ) ;
#91525 = CARTESIAN_POINT ( 'NONE',  ( -14.34966873604960291, -8.224510206698953496, 41.66557627198103120 ) ) ;
#91526 = CARTESIAN_POINT ( 'NONE',  ( -21.53943276465977519, 0.05219959533907696930, 81.24890960531436690 ) ) ;
#91527 = CARTESIAN_POINT ( 'NONE',  ( 13.97604488694527802, 13.89961937509977652, 114.3739096053143669 ) ) ;
#91528 = CARTESIAN_POINT ( 'NONE',  ( 16.55341960407611168, 4.379528057220329451, 68.95724293864769550 ) ) ;
#91529 = CARTESIAN_POINT ( 'NONE',  ( -0.05219959533909027116, -19.03943276465977164, 47.49890960531435979 ) ) ;
#91530 = CARTESIAN_POINT ( 'NONE',  ( 16.46253265017146816, 9.564922557961045513, 26.66775706135234003 ) ) ;
#91531 = CARTESIAN_POINT ( 'NONE',  ( -12.14591786802326823, 12.06949235617739902, 103.1260903946856757 ) ) ;
#91532 = CARTESIAN_POINT ( 'NONE',  ( -12.06949235617739369, -12.14591786802326823, 54.37609039468568994 ) ) ;
#91533 = CARTESIAN_POINT ( 'NONE',  ( -21.53943276465977519, 0.05219959533907696930, 41.24890960531435269 ) ) ;
#91534 = CARTESIAN_POINT ( 'NONE',  ( 21.52544592524334988, 5.823673210054432836, 106.4594237280190328 ) ) ;
#91535 = CARTESIAN_POINT ( 'NONE',  ( -9.474510206698964154, 16.51473224551069663, 85.41557627198102409 ) ) ;
#91536 = CARTESIAN_POINT ( 'NONE',  ( -16.53943276465976808, -0.05219959533934237506, 68.75109039468568994 ) ) ;
#91537 = CARTESIAN_POINT ( 'NONE',  ( -5.049401038298153566, 19.05341960407611168, 30.20724293864768839 ) ) ;
#91538 = CARTESIAN_POINT ( 'NONE',  ( 4.483927247898545687, 16.52544592524342804, 39.79057627198103830 ) ) ;
#91540 = CARTESIAN_POINT ( 'NONE',  ( 9.474510206698971260, -16.51473224551069308, 92.91557627198103830 ) ) ;
#91539 = CARTESIAN_POINT ( 'NONE',  ( 9.474510206698971260, -16.51473224551069308, 107.9155762719810383 ) ) ;
#91541 = CARTESIAN_POINT ( 'NONE',  ( -5.719274019375978568, 21.55341960407610458, 30.20724293864769550 ) ) ;
#91542 = CARTESIAN_POINT ( 'NONE',  ( 12.14591786802309770, 12.06949235617756955, 54.37390960531435979 ) ) ;
#91543 = CARTESIAN_POINT ( 'NONE',  ( 8.224510206698953496, -14.34966873604960469, 37.91557627198102409 ) ) ;
#91544 = VECTOR ( 'NONE', #69994, 1000.000000000000000 ) ;
#91545 = ORIENTED_EDGE ( 'NONE', *, *, #31222, .F. ) ;
#91546 = CARTESIAN_POINT ( 'NONE',  ( -12.06949235617756955, 12.14591786802309770, 45.62390960531436690 ) ) ;
#91547 = ORIENTED_EDGE ( 'NONE', *, *, #9668, .F. ) ;
#91549 = CARTESIAN_POINT ( 'NONE',  ( 0.05219959533936267826, -19.03943276465977164, 60.00109039468566863 ) ) ;
#91548 = CARTESIAN_POINT ( 'NONE',  ( 8.314922557961029526, -14.29746914071037800, 40.41775706135234714 ) ) ;
#91550 = CARTESIAN_POINT ( 'NONE',  ( -5.153800228976607833, 19.02544592524334988, 47.70942372801900433 ) ) ;
#91551 = CARTESIAN_POINT ( 'NONE',  ( -13.89961937509977652, 13.97604488694528158, 90.62390960531432427 ) ) ;
#91552 = CARTESIAN_POINT ( 'NONE',  ( 5.049401038297881783, 19.05341960407617563, 62.29275706135234003 ) ) ;
#91553 = CARTESIAN_POINT ( 'NONE',  ( -27.73933785331498925, 9.013057229001089965, 145.2750000027311899 ) ) ;
#91554 = CARTESIAN_POINT ( 'NONE',  ( 19.02544592524334988, 5.153800228976608722, 56.45942372801898301 ) ) ;
#91556 = CARTESIAN_POINT ( 'NONE',  ( 8.224510206698742110, 14.34966873604972548, 77.08442372801901854 ) ) ;
#91555 = CARTESIAN_POINT ( 'NONE',  ( -19.05341960407617563, 5.049401038297882671, 98.54275706135233293 ) ) ;
#91557 = CARTESIAN_POINT ( 'NONE',  ( 1.784210473542230573E-15, -29.16686587814331588, 147.8750000027311273 ) ) ;
#91558 = CARTESIAN_POINT ( 'NONE',  ( -0.05219959533909027116, -19.03943276465977164, 22.49890960531436690 ) ) ;
#91559 = CARTESIAN_POINT ( 'NONE',  ( -21.55341960407610458, -5.719274019375992779, 21.45724293864769550 ) ) ;
#91560 = CARTESIAN_POINT ( 'NONE',  ( -21.52544592524334988, -5.823673210054445271, 38.95942372801901854 ) ) ;
#91561 = CARTESIAN_POINT ( 'NONE',  ( -19.02544592524334988, -5.153800228976617603, 108.9594237280189759 ) ) ;
#91563 = CARTESIAN_POINT ( 'NONE',  ( 9.474510206698971260, -16.51473224551069308, 62.91557627198102409 ) ) ;
#91562 = CARTESIAN_POINT ( 'NONE',  ( 17.50000000000147793, -3.202012800152252758, 107.4282241602726629 ) ) ;
#91564 = CARTESIAN_POINT ( 'NONE',  ( 16.46253265017160672, -9.564922557960803928, 103.3322429386476955 ) ) ;
#91566 = CARTESIAN_POINT ( 'NONE',  ( -19.02544592524342804, 5.153800228976336051, 66.04057627198103830 ) ) ;
#91565 = CARTESIAN_POINT ( 'NONE',  ( 14.34966873604960469, 8.224510206698951720, 69.16557627198102409 ) ) ;
#91567 = CARTESIAN_POINT ( 'NONE',  ( 16.51473224551069308, 9.474510206698969483, 79.16557627198103830 ) ) ;
#91568 = CARTESIAN_POINT ( 'NONE',  ( -16.51473224551082808, 9.474510206698731452, 78.33442372801900433 ) ) ;
#91569 = CARTESIAN_POINT ( 'NONE',  ( -21.55341960407610458, -5.719274019375992779, 51.45724293864770260 ) ) ;
#91570 = CARTESIAN_POINT ( 'NONE',  ( 8.224510206698953496, -14.34966873604960469, 112.9155762719810383 ) ) ;
#91571 = CARTESIAN_POINT ( 'NONE',  ( 13.89961937509957401, 13.97604488694547697, 36.87609039468565442 ) ) ;
#91572 = CARTESIAN_POINT ( 'NONE',  ( -9.474510206698964154, 16.51473224551069663, 85.41557627198102409 ) ) ;
#91573 = CARTESIAN_POINT ( 'NONE',  ( 0.05219959533907565091, 21.53943276465977519, 74.99890960531435269 ) ) ;
#91575 = CARTESIAN_POINT ( 'NONE',  ( 9.564922557961047289, -16.46253265017146816, 45.41775706135232582 ) ) ;
#91574 = CARTESIAN_POINT ( 'NONE',  ( -4.483927247898539470, -16.52544592524342804, 77.29057627198102409 ) ) ;
#91576 = CARTESIAN_POINT ( 'NONE',  ( 21.52544592524344225, -5.823673210054117533, 73.54057627198102409 ) ) ;
#91577 = CARTESIAN_POINT ( 'NONE',  ( 10.72451020669898902, -18.67979575497178502, 62.91557627198102409 ) ) ;
#91578 = CARTESIAN_POINT ( 'NONE',  ( 18.62759615963271287, -10.81492255796078972, 43.33224293864769550 ) ) ;
#91579 = CARTESIAN_POINT ( 'NONE',  ( -10.72451020669870658, -18.67979575497194134, 89.58442372801901854 ) ) ;
#91580 = CARTESIAN_POINT ( 'NONE',  ( 13.89961937509977652, -13.97604488694527269, 63.12390960531435979 ) ) ;
#91581 = CARTESIAN_POINT ( 'NONE',  ( -5.153800228976328057, -19.02544592524343514, 22.29057627198102765 ) ) ;
#91582 = CARTESIAN_POINT ( 'NONE',  ( 15.80617190586769283, -15.72974639402175789, 30.62609039468567929 ) ) ;
#91583 = CARTESIAN_POINT ( 'NONE',  ( -18.67979575497193778, 10.72451020669871902, 43.33442372801901143 ) ) ;
#91584 = CARTESIAN_POINT ( 'NONE',  ( -9.474510206698964154, 16.51473224551069663, 35.41557627198102409 ) ) ;
#91585 = CARTESIAN_POINT ( 'NONE',  ( 0.05219959533907565091, 21.53943276465977519, 104.9989096053143669 ) ) ;
#91586 = EDGE_CURVE ( 'NONE', #169038, #114713, #156262, .T. ) ;
#91587 = CARTESIAN_POINT ( 'NONE',  ( 9.474510206698729675, 16.51473224551082808, 52.08442372801900433 ) ) ;
#91588 = CARTESIAN_POINT ( 'NONE',  ( -9.564922557960796823, -16.46253265017161027, 32.08224293864769550 ) ) ;
#91589 = CARTESIAN_POINT ( 'NONE',  ( -20.96320343559653665, -21.46320343559631638, 4.646446609406719830 ) ) ;
#91590 = CARTESIAN_POINT ( 'NONE',  ( 17.49999999999998934, -5.500000000000023981, 78.29690382534170112 ) ) ;
#91591 = CARTESIAN_POINT ( 'NONE',  ( -16.55341960407617563, 4.379528057220093196, 63.54275706135234003 ) ) ;
#91592 = CARTESIAN_POINT ( 'NONE',  ( -19.05341960407611168, -5.049401038298163336, 31.45724293864769550 ) ) ;
#91593 = CARTESIAN_POINT ( 'NONE',  ( -26.78465914369777678, -5.761000505272561689, 169.4491075441772807 ) ) ;
#91594 = CARTESIAN_POINT ( 'NONE',  ( 13.89961937509977652, -13.97604488694527269, 83.12390960531436690 ) ) ;
#91595 = CARTESIAN_POINT ( 'NONE',  ( 14.29746914071049879, -8.314922557960816363, 113.3322429386476955 ) ) ;
#91596 = CARTESIAN_POINT ( 'NONE',  ( 21.52544592524344225, -5.823673210054117533, 53.54057627198103120 ) ) ;
#91597 = CARTESIAN_POINT ( 'NONE',  ( 0.05219959533934541429, -16.53943276465976808, 50.00109039468568994 ) ) ;
#91598 = CARTESIAN_POINT ( 'NONE',  ( 21.53943276465977519, 0.05219959533937863772, 101.2510903946856757 ) ) ;
#91599 = CARTESIAN_POINT ( 'NONE',  ( 9.474510206698971260, -16.51473224551069308, 32.91557627198102409 ) ) ;
#91600 = ADVANCED_FACE ( 'NONE', ( #37423 ), #99083, .F. ) ;
#91601 = CARTESIAN_POINT ( 'NONE',  ( -8.224510206698735004, -14.34966873604973081, 104.5844237280190185 ) ) ;
#91602 = CARTESIAN_POINT ( 'NONE',  ( -12.14591786802309592, -12.06949235617757132, 51.87390960531437401 ) ) ;
#91603 = CARTESIAN_POINT ( 'NONE',  ( 9.474510206698971260, -16.51473224551069308, 57.91557627198103120 ) ) ;
#91604 = CARTESIAN_POINT ( 'NONE',  ( -9.474510206698720793, -16.51473224551083518, 19.58442372801899722 ) ) ;
#91605 = CARTESIAN_POINT ( 'NONE',  ( 18.67979575497194134, -10.72451020669871369, 25.83442372801901499 ) ) ;
#91606 = AXIS2_PLACEMENT_3D ( 'NONE', #172234, #95381, #157067 ) ;
#91607 = CARTESIAN_POINT ( 'NONE',  ( 5.823673210054444382, -21.52544592524334988, 70.20942372801904696 ) ) ;
#91608 = CARTESIAN_POINT ( 'NONE',  ( -12.14591786802326823, 12.06949235617739902, 58.12609039468568994 ) ) ;
#91609 = CARTESIAN_POINT ( 'NONE',  ( 4.379528057220092307, 16.55341960407617563, 27.29275706135234358 ) ) ;
#91611 = CARTESIAN_POINT ( 'NONE',  ( 21.55341960407619695, -5.719274019375665929, 101.0427570613523756 ) ) ;
#91610 = CARTESIAN_POINT ( 'NONE',  ( -12.14591786802309592, -12.06949235617757132, 76.87390960531439532 ) ) ;
#91612 = CARTESIAN_POINT ( 'NONE',  ( -14.34966873604960291, -8.224510206698953496, 36.66557627198103120 ) ) ;
#91613 = CARTESIAN_POINT ( 'NONE',  ( -17.44270441346515810, 5.991230190323032723, 113.6366492073577490 ) ) ;
#91614 = CARTESIAN_POINT ( 'NONE',  ( 8.224510206698742110, 14.34966873604972548, 37.08442372801901143 ) ) ;
#91615 = CARTESIAN_POINT ( 'NONE',  ( -4.483927247898539470, -16.52544592524342804, 42.29057627198103120 ) ) ;
#91616 = CARTESIAN_POINT ( 'NONE',  ( 16.55341960407618274, -4.379528057220086978, 91.04275706135236135 ) ) ;
#91617 = CARTESIAN_POINT ( 'NONE',  ( 5.049401038298161559, -19.05341960407611168, 92.70724293864769550 ) ) ;
#91618 = CARTESIAN_POINT ( 'NONE',  ( 5.823673210054125526, 21.52544592524343514, 24.79057627198103120 ) ) ;
#91619 = CARTESIAN_POINT ( 'NONE',  ( 0.05219959533937995610, -21.53943276465977519, 100.0010903946857042 ) ) ;
#91620 = CARTESIAN_POINT ( 'NONE',  ( -14.29746914071037622, -8.314922557961029526, 99.16775706135234714 ) ) ;
#91621 = CARTESIAN_POINT ( 'NONE',  ( -14.29746914071049879, 8.314922557960819915, 75.83224293864769550 ) ) ;
#91622 = CARTESIAN_POINT ( 'NONE',  ( -13.89961937509977652, 13.97604488694528158, 85.62390960531433848 ) ) ;
#91623 = ORIENTED_EDGE ( 'NONE', *, *, #52789, .F. ) ;
#91624 = CARTESIAN_POINT ( 'NONE',  ( -8.224510206698735004, -14.34966873604973081, 44.58442372801901854 ) ) ;
#91625 = CARTESIAN_POINT ( 'NONE',  ( 13.89961937509977652, -13.97604488694527269, 38.12390960531436690 ) ) ;
#91626 = CARTESIAN_POINT ( 'NONE',  ( -13.89961937509977652, 13.97604488694528158, 100.6239096053143669 ) ) ;
#91628 = LINE ( 'NONE', #156301, #8039 ) ;
#91627 = CARTESIAN_POINT ( 'NONE',  ( -16.55341960407617563, 4.379528057220093196, 33.54275706135234714 ) ) ;
#91629 = CARTESIAN_POINT ( 'NONE',  ( -13.89961937509957401, -13.97604488694547875, 29.37609039468565797 ) ) ;
#91630 = CARTESIAN_POINT ( 'NONE',  ( 16.55341960407618274, -4.379528057220086978, 106.0427570613523471 ) ) ;
#91631 = CARTESIAN_POINT ( 'NONE',  ( 16.51473224551069308, 9.474510206698969483, 34.16557627198102409 ) ) ;
#91632 = CARTESIAN_POINT ( 'NONE',  ( 16.53943276465976808, 0.05219959533934440121, 71.25109039468568994 ) ) ;
#91633 = CARTESIAN_POINT ( 'NONE',  ( 19.02544592524334988, 5.153800228976608722, 81.45942372801897591 ) ) ;
#91634 = CARTESIAN_POINT ( 'NONE',  ( 5.153800228976615827, -19.02544592524334988, 35.20942372801899722 ) ) ;
#91635 = CARTESIAN_POINT ( 'NONE',  ( -19.05341960407611168, -5.049401038298163336, 61.45724293864769550 ) ) ;
#91636 = CARTESIAN_POINT ( 'NONE',  ( -12.06949235617756955, 12.14591786802309770, 80.62390960531438111 ) ) ;
#91637 = CARTESIAN_POINT ( 'NONE',  ( 0.05219959533936267826, -19.03943276465977164, 55.00109039468566863 ) ) ;
#91638 = CARTESIAN_POINT ( 'NONE',  ( 18.62759615963271287, -10.81492255796078972, 68.33224293864769550 ) ) ;
#91639 = CARTESIAN_POINT ( 'NONE',  ( -5.049401038297874678, -19.05341960407617918, 24.79275706135233648 ) ) ;
#91640 = CARTESIAN_POINT ( 'NONE',  ( -13.97604488694527625, -13.89961937509977652, 101.8739096053143811 ) ) ;
#91641 = CARTESIAN_POINT ( 'NONE',  ( -18.62759615963270932, 10.81492255796079327, 70.83224293864770971 ) ) ;
#91642 = CARTESIAN_POINT ( 'NONE',  ( 19.02544592524343514, -5.153800228976328945, 108.5405762719810383 ) ) ;
#91643 = CARTESIAN_POINT ( 'NONE',  ( 19.02544592524334988, 5.153800228976608722, 101.4594237280189759 ) ) ;
#91644 = CARTESIAN_POINT ( 'NONE',  ( 19.02544592524343514, -5.153800228976328945, 113.5405762719810241 ) ) ;
#91645 = CARTESIAN_POINT ( 'NONE',  ( 8.314922557961029526, -14.29746914071037800, 30.41775706135234358 ) ) ;
#91646 = CARTESIAN_POINT ( 'NONE',  ( -13.97604488694527625, -13.89961937509977652, 36.87390960531436690 ) ) ;
#91647 = CARTESIAN_POINT ( 'NONE',  ( -13.97604488694527625, -13.89961937509977652, 96.87390960531433848 ) ) ;
#91648 = CARTESIAN_POINT ( 'NONE',  ( 21.52544592524344225, -5.823673210054117533, 78.54057627198103830 ) ) ;
#91649 = CARTESIAN_POINT ( 'NONE',  ( 8.314922557961029526, -14.29746914071037800, 65.41775706135234714 ) ) ;
#91650 = CARTESIAN_POINT ( 'NONE',  ( 10.72451020669871369, 18.67979575497193778, 62.08442372801901143 ) ) ;
#91652 = CARTESIAN_POINT ( 'NONE',  ( 16.51473224551083163, -9.474510206698727899, 20.83442372801899722 ) ) ;
#91651 = CARTESIAN_POINT ( 'NONE',  ( 16.51473224551083163, -9.474510206698727899, 100.8344237280190043 ) ) ;
#91653 = CARTESIAN_POINT ( 'NONE',  ( -4.483927247898782831, 16.52544592524335698, 107.7094237280190328 ) ) ;
#91654 = CARTESIAN_POINT ( 'NONE',  ( 5.719274019375991003, -21.55341960407610458, 102.7072429386476955 ) ) ;
#91655 = CARTESIAN_POINT ( 'NONE',  ( -14.29746914071049879, 8.314922557960819915, 40.83224293864769550 ) ) ;
#91656 = CARTESIAN_POINT ( 'NONE',  ( -5.153800228976607833, 19.02544592524334988, 77.70942372801900433 ) ) ;
#91657 = CARTESIAN_POINT ( 'NONE',  ( -5.823673210054431948, 21.52544592524334988, 52.70942372801902565 ) ) ;
#91658 = CARTESIAN_POINT ( 'NONE',  ( -5.049401038297874678, -19.05341960407617918, 44.79275706135232582 ) ) ;
#91659 = CARTESIAN_POINT ( 'NONE',  ( 4.379528057220339221, -16.55341960407611168, 102.7072429386476955 ) ) ;
#91660 = CARTESIAN_POINT ( 'NONE',  ( -10.81492255796078084, -18.62759615963271287, 27.08224293864769550 ) ) ;
#91661 = CARTESIAN_POINT ( 'NONE',  ( -12.14591786802309592, -12.06949235617757132, 31.87390960531435979 ) ) ;
#91662 = CARTESIAN_POINT ( 'NONE',  ( 5.719274019375673035, 21.55341960407619339, 102.2927570613523613 ) ) ;
#91663 = CARTESIAN_POINT ( 'NONE',  ( -16.53943276465976808, -0.05219959533934237506, 73.75109039468567573 ) ) ;
#91664 = CARTESIAN_POINT ( 'NONE',  ( 16.55341960407611168, 4.379528057220329451, 23.95724293864769550 ) ) ;
#91665 = CARTESIAN_POINT ( 'NONE',  ( 21.52544592524334988, 5.823673210054432836, 61.45942372801901854 ) ) ;
#91666 = CARTESIAN_POINT ( 'NONE',  ( 10.81492255796106328, -18.62759615963255655, 60.41775706135235424 ) ) ;
#91667 = CARTESIAN_POINT ( 'NONE',  ( -9.564922557960796823, -16.46253265017161027, 27.08224293864769550 ) ) ;
#91668 = CARTESIAN_POINT ( 'NONE',  ( -15.72974639402176322, -15.80617190586768395, 39.37609039468567573 ) ) ;
#91669 = CARTESIAN_POINT ( 'NONE',  ( -0.05219959533910754901, -16.53943276465976808, 112.4989096053143669 ) ) ;
#91670 = CARTESIAN_POINT ( 'NONE',  ( 0.05219959533909260263, 19.03943276465977164, 44.99890960531435979 ) ) ;
#91671 = CARTESIAN_POINT ( 'NONE',  ( -16.53943276465976808, 0.05219959533911058130, 76.24890960531435269 ) ) ;
#91672 = CARTESIAN_POINT ( 'NONE',  ( 19.02544592524343514, -5.153800228976328945, 73.54057627198103830 ) ) ;
#91673 = CARTESIAN_POINT ( 'NONE',  ( -8.224510206698948167, 14.34966873604960824, 30.41557627198101699 ) ) ;
#91674 = CARTESIAN_POINT ( 'NONE',  ( -21.52544592524343514, 5.823673210054127303, 61.04057627198103120 ) ) ;
#91675 = CARTESIAN_POINT ( 'NONE',  ( 8.224510206698953496, -14.34966873604960469, 97.91557627198103830 ) ) ;
#91676 = CARTESIAN_POINT ( 'NONE',  ( 15.80617190586746368, 15.72974639402197994, 104.3739096053143669 ) ) ;
#91677 = CARTESIAN_POINT ( 'NONE',  ( -13.89961937509977652, 13.97604488694528158, 105.6239096053143527 ) ) ;
#91679 = CARTESIAN_POINT ( 'NONE',  ( 19.02544592524334988, 5.153800228976608722, 111.4594237280190043 ) ) ;
#91678 = CARTESIAN_POINT ( 'NONE',  ( -9.564922557960796823, -16.46253265017161027, 62.08224293864769550 ) ) ;
#91680 = CARTESIAN_POINT ( 'NONE',  ( -5.823673210054116645, -21.52544592524344225, 52.29057627198102409 ) ) ;
#91681 = CARTESIAN_POINT ( 'NONE',  ( -15.72974639402176322, -15.80617190586768395, 79.37609039468567573 ) ) ;
#91682 = CARTESIAN_POINT ( 'NONE',  ( -5.153800228976328057, -19.02544592524343514, 67.29057627198102409 ) ) ;
#91683 = EDGE_CURVE ( 'NONE', #152430, #1611, #145595, .T. ) ;
#91684 = VECTOR ( 'NONE', #153190, 1000.000000000000000 ) ;
#91685 = CARTESIAN_POINT ( 'NONE',  ( 5.153800228976335163, 19.02544592524342804, 94.79057627198103830 ) ) ;
#91686 = CARTESIAN_POINT ( 'NONE',  ( 16.55341960407618274, -4.379528057220086978, 76.04275706135237556 ) ) ;
#91687 = CARTESIAN_POINT ( 'NONE',  ( -21.55341960407619339, 5.719274019375674811, 63.54275706135234003 ) ) ;
#91688 = CARTESIAN_POINT ( 'NONE',  ( -21.53943276465977519, -0.05219959533937600094, 83.75109039468568994 ) ) ;
#91689 = CARTESIAN_POINT ( 'NONE',  ( 18.62759615963271287, -10.81492255796078972, 108.3322429386477097 ) ) ;
#91690 = CARTESIAN_POINT ( 'NONE',  ( -14.34966873604972548, 8.224510206698743886, 78.33442372801901854 ) ) ;
#91691 = CARTESIAN_POINT ( 'NONE',  ( -15.72974639402197994, 15.80617190586746368, 80.62390960531438111 ) ) ;
#91692 = CARTESIAN_POINT ( 'NONE',  ( 16.46253265017146816, 9.564922557961045513, 46.66775706135233293 ) ) ;
#91693 = CARTESIAN_POINT ( 'NONE',  ( -21.53943276465977519, 0.05219959533907696930, 46.24890960531435979 ) ) ;
#91695 = CARTESIAN_POINT ( 'NONE',  ( -16.55341960407611168, -4.379528057220339221, 26.45724293864768839 ) ) ;
#91694 = CARTESIAN_POINT ( 'NONE',  ( -5.153800228976328057, -19.02544592524343514, 77.29057627198099567 ) ) ;
#91696 = CARTESIAN_POINT ( 'NONE',  ( 22.55670631985092456, -22.55670631985084995, -45.64921306006598201 ) ) ;
#91697 = CARTESIAN_POINT ( 'NONE',  ( 21.53943276465977519, -0.05219959533907433946, 23.74890960531435269 ) ) ;
#91698 = LINE ( 'NONE', #153391, #63203 ) ;
#91699 = CARTESIAN_POINT ( 'NONE',  ( 19.02544592524334988, 5.153800228976608722, 96.45942372801897591 ) ) ;
#91700 = CARTESIAN_POINT ( 'NONE',  ( -15.72974639402197994, 15.80617190586746368, 70.62390960531436690 ) ) ;
#91701 = CARTESIAN_POINT ( 'NONE',  ( -16.53943276465976808, 0.05219959533911058130, 51.24890960531436690 ) ) ;
#91702 = CARTESIAN_POINT ( 'NONE',  ( 19.02544592524334988, 5.153800228976608722, 106.4594237280190185 ) ) ;
#91703 = CARTESIAN_POINT ( 'NONE',  ( -13.89961937509977652, 13.97604488694528158, 50.62390960531435979 ) ) ;
#91705 = CARTESIAN_POINT ( 'NONE',  ( 19.03943276465977164, 0.05219959533936151252, 76.25109039468566152 ) ) ;
#91704 = CARTESIAN_POINT ( 'NONE',  ( -0.05219959533907301413, -21.53943276465977519, 102.4989096053143811 ) ) ;
#91706 = CARTESIAN_POINT ( 'NONE',  ( -5.153800228976328057, -19.02544592524343514, 82.29057627198103830 ) ) ;
#91707 = CARTESIAN_POINT ( 'NONE',  ( -0.05219959533910754901, -16.53943276465976808, 92.49890960531436690 ) ) ;
#91708 = CARTESIAN_POINT ( 'NONE',  ( -16.46253265017160317, 9.564922557960807481, 60.83224293864769550 ) ) ;
#91709 = CARTESIAN_POINT ( 'NONE',  ( -16.52544592524342804, 4.483927247898546575, 61.04057627198103120 ) ) ;
#91710 = CARTESIAN_POINT ( 'NONE',  ( -9.474510206698964154, 16.51473224551069663, 35.41557627198102409 ) ) ;
#91711 = CARTESIAN_POINT ( 'NONE',  ( -37.06950394710835184, -4.940869137700751423, 42.55762898535584071 ) ) ;
#91712 = CARTESIAN_POINT ( 'NONE',  ( -8.224510206698948167, 14.34966873604960824, 45.41557627198103830 ) ) ;
#91713 = CARTESIAN_POINT ( 'NONE',  ( -0.05219959533909027116, -19.03943276465977164, 92.49890960531436690 ) ) ;
#91714 = CARTESIAN_POINT ( 'NONE',  ( -28.79475375365586842, 2.428612866367529932E-14, 144.2656553485623760 ) ) ;
#91715 = CARTESIAN_POINT ( 'NONE',  ( 19.02544592524334988, 5.153800228976608722, 51.45942372801900433 ) ) ;
#91716 = CARTESIAN_POINT ( 'NONE',  ( 4.379528057220092307, 16.55341960407617563, 62.29275706135236845 ) ) ;
#91717 = CARTESIAN_POINT ( 'NONE',  ( -18.62759615963270932, 10.81492255796079327, 60.83224293864769550 ) ) ;
#91718 = CARTESIAN_POINT ( 'NONE',  ( -5.153800228976607833, 19.02544592524334988, 37.70942372801899722 ) ) ;
#91719 = CARTESIAN_POINT ( 'NONE',  ( 19.03943276465977164, -0.05219959533909143690, 83.74890960531436690 ) ) ;
#91720 = CARTESIAN_POINT ( 'NONE',  ( 0.4308872995781310444, 21.35919609616788506, -58.81731666137213210 ) ) ;
#91721 = CARTESIAN_POINT ( 'NONE',  ( 15.80617190586746368, 15.72974639402197994, 34.37390960531435979 ) ) ;
#91722 = CARTESIAN_POINT ( 'NONE',  ( -13.97604488694527625, -13.89961937509977652, 61.87390960531435979 ) ) ;
#91723 = CARTESIAN_POINT ( 'NONE',  ( 15.80617190586769283, -15.72974639402175789, 45.62609039468567573 ) ) ;
#91724 = CARTESIAN_POINT ( 'NONE',  ( 5.153800228976335163, 19.02544592524342804, 29.79057627198102409 ) ) ;
#91727 = ORIENTED_EDGE ( 'NONE', *, *, #89344, .T. ) ;
#91726 = CARTESIAN_POINT ( 'NONE',  ( -9.474510206698964154, 16.51473224551069663, 100.4155762719810241 ) ) ;
#91725 = CARTESIAN_POINT ( 'NONE',  ( 5.719274019375991003, -21.55341960407610458, 102.7072429386476955 ) ) ;
#91728 = CARTESIAN_POINT ( 'NONE',  ( -15.80617190586768217, 15.72974639402176855, 38.12609039468567573 ) ) ;
#91729 = EDGE_LOOP ( 'NONE', ( #72105, #199161, #73397, #13502, #7240 ) ) ;
#91730 = CARTESIAN_POINT ( 'NONE',  ( -16.46253265017160317, 9.564922557960807481, 100.8322429386477097 ) ) ;
#91731 = DIRECTION ( 'NONE',  ( -1.000000000000000000, 0.000000000000000000, 0.000000000000000000 ) ) ;
#91732 = CARTESIAN_POINT ( 'NONE',  ( -21.53943276465977519, 0.05219959533907696930, 106.2489096053143811 ) ) ;
#91733 = CARTESIAN_POINT ( 'NONE',  ( -19.03943276465977164, 0.05219959533909376836, 41.24890960531435269 ) ) ;
#91734 = CARTESIAN_POINT ( 'NONE',  ( -12.06949235617739369, -12.14591786802326823, 24.37609039468567573 ) ) ;
#91735 = CARTESIAN_POINT ( 'NONE',  ( -22.81625015709509441, -31.40387420917324590, -4.824999997268813345 ) ) ;
#91736 = AXIS2_PLACEMENT_3D ( 'NONE', #70127, #131799, #150973 ) ;
#91737 = CARTESIAN_POINT ( 'NONE',  ( -19.02544592524342804, 5.153800228976336051, 26.04057627198103120 ) ) ;
#91738 = CARTESIAN_POINT ( 'NONE',  ( 21.52544592524334988, 5.823673210054432836, 96.45942372801901854 ) ) ;
#91740 = CARTESIAN_POINT ( 'NONE',  ( 21.53943276465977519, 0.05219959533937863772, 51.25109039468568994 ) ) ;
#91739 = CARTESIAN_POINT ( 'NONE',  ( -19.02544592524342804, 5.153800228976336051, 76.04057627198102409 ) ) ;
#91741 = CARTESIAN_POINT ( 'NONE',  ( 22.44159573604009594, -16.30477369853687364, 146.1750000027311671 ) ) ;
#91742 = CARTESIAN_POINT ( 'NONE',  ( -13.89961937509977652, 13.97604488694528158, 105.6239096053143527 ) ) ;
#91743 = CARTESIAN_POINT ( 'NONE',  ( 19.20446147854529073, 5.499999999999903189, 61.88999695167678539 ) ) ;
#91746 = CARTESIAN_POINT ( 'NONE',  ( 21.53943276465977519, 0.05219959533937863772, 56.25109039468568284 ) ) ;
#91745 = CARTESIAN_POINT ( 'NONE',  ( -8.224510206698735004, -14.34966873604973081, 74.58442372801901854 ) ) ;
#91744 = CARTESIAN_POINT ( 'NONE',  ( -16.52544592524335698, -4.483927247898792601, 38.95942372801901854 ) ) ;
#91747 = CARTESIAN_POINT ( 'NONE',  ( 15.80617190586769283, -15.72974639402175789, 95.62609039468568994 ) ) ;
#91748 = CARTESIAN_POINT ( 'NONE',  ( 12.21174782391248392, -11.13111847464308468, -59.22005018971564283 ) ) ;
#91749 = CARTESIAN_POINT ( 'NONE',  ( -9.474510206698720793, -16.51473224551083518, 104.5844237280190043 ) ) ;
#91750 = CARTESIAN_POINT ( 'NONE',  ( -13.97604488694527625, -13.89961937509977652, 71.87390960531433848 ) ) ;
#91751 = CARTESIAN_POINT ( 'NONE',  ( 5.049401038298161559, -19.05341960407611168, 102.7072429386476955 ) ) ;
#91752 = EDGE_CURVE ( 'NONE', #25387, #38805, #38431, .T. ) ;
#91753 = CARTESIAN_POINT ( 'NONE',  ( 8.314922557960818139, 14.29746914071049879, 109.5822429386476955 ) ) ;
#91754 = CARTESIAN_POINT ( 'NONE',  ( 21.53943276465977519, -0.05219959533907433946, 28.74890960531435624 ) ) ;
#91755 = CARTESIAN_POINT ( 'NONE',  ( 4.379528057220092307, 16.55341960407617563, 97.29275706135234714 ) ) ;
#91757 = CARTESIAN_POINT ( 'NONE',  ( 9.474510206698971260, -16.51473224551069308, 52.91557627198102409 ) ) ;
#91756 = CARTESIAN_POINT ( 'NONE',  ( -8.224510206698948167, 14.34966873604960824, 75.41557627198102409 ) ) ;
#91758 = CARTESIAN_POINT ( 'NONE',  ( 0.05219959533937995610, -21.53943276465977519, 75.00109039468568994 ) ) ;
#91759 = CARTESIAN_POINT ( 'NONE',  ( -21.31248648291600389, 0.2211803504531069942, -58.84879416108404371 ) ) ;
#91760 = CARTESIAN_POINT ( 'NONE',  ( 19.02544592524334988, 5.153800228976608722, 101.4594237280189759 ) ) ;
#91761 = CARTESIAN_POINT ( 'NONE',  ( 14.29746914071049879, -8.314922557960816363, 78.33224293864770971 ) ) ;
#91762 = CARTESIAN_POINT ( 'NONE',  ( -5.719274019375665041, -21.55341960407619695, 29.79275706135234358 ) ) ;
#91763 = CARTESIAN_POINT ( 'NONE',  ( -18.67979575497178146, -10.72451020669898902, 56.66557627198103830 ) ) ;
#91764 = CARTESIAN_POINT ( 'NONE',  ( -16.18388926212238843, -7.379444403734516378, 105.4395315136615636 ) ) ;
#91765 = CARTESIAN_POINT ( 'NONE',  ( 28.82186960331498327, 2.781578969918950771E-14, 147.2500000054623683 ) ) ;
#91766 = CARTESIAN_POINT ( 'NONE',  ( 0.05219959533909260263, 19.03943276465977164, 79.99890960531436690 ) ) ;
#91767 = CARTESIAN_POINT ( 'NONE',  ( 0.05219959533910956823, 16.53943276465976808, 49.99890960531437401 ) ) ;
#91768 = AXIS2_PLACEMENT_3D ( 'NONE', #173884, #78859, #80850 ) ;
#91769 = CARTESIAN_POINT ( 'NONE',  ( -14.29746914071049879, 8.314922557960819915, 35.83224293864768839 ) ) ;
#91770 = CARTESIAN_POINT ( 'NONE',  ( 14.34966873604972726, -8.224510206698740333, 95.83442372801903275 ) ) ;
#91771 = CARTESIAN_POINT ( 'NONE',  ( 5.049401038297881783, 19.05341960407617563, 47.29275706135231161 ) ) ;
#91772 = CARTESIAN_POINT ( 'NONE',  ( 1.300000000000000044, 0.000000000000000000, 0.000000000000000000 ) ) ;
#91773 = CARTESIAN_POINT ( 'NONE',  ( 19.03943276465977164, -0.05219959533909143690, 98.74890960531436690 ) ) ;
#91774 = EDGE_CURVE ( 'NONE', #53443, #176653, #170814, .T. ) ;
#91775 = CARTESIAN_POINT ( 'NONE',  ( 14.29746914071049879, -8.314922557960816363, 68.33224293864769550 ) ) ;
#91776 = CARTESIAN_POINT ( 'NONE',  ( -9.474510206698720793, -16.51473224551083518, 39.58442372801899722 ) ) ;
#91778 = CARTESIAN_POINT ( 'NONE',  ( 18.67979575497178502, 10.72451020669898547, 39.16557627198102409 ) ) ;
#91777 = CARTESIAN_POINT ( 'NONE',  ( 19.05341960407611168, 5.049401038298154454, 38.95724293864767418 ) ) ;
#91779 = CARTESIAN_POINT ( 'NONE',  ( -18.67979575497178146, -10.72451020669898902, 61.66557627198103120 ) ) ;
#91780 = CARTESIAN_POINT ( 'NONE',  ( -4.483927247898539470, -16.52544592524342804, 97.29057627198105251 ) ) ;
#91781 = CARTESIAN_POINT ( 'NONE',  ( 0.05219959533934541429, -16.53943276465976808, 50.00109039468568994 ) ) ;
#91782 = CARTESIAN_POINT ( 'NONE',  ( 10.72451020669871369, 18.67979575497193778, 42.08442372801901854 ) ) ;
#91783 = CARTESIAN_POINT ( 'NONE',  ( 16.53943276465976808, -0.05219959533910856209, 98.74890960531438111 ) ) ;
#91784 = CARTESIAN_POINT ( 'NONE',  ( -3.503282210674363295, -48.86437366581481001, -25.00000000000000000 ) ) ;
#91785 = CARTESIAN_POINT ( 'NONE',  ( -16.29526858892872099, 7.335722546920265152, 49.20329402199791247 ) ) ;
#91786 = CARTESIAN_POINT ( 'NONE',  ( 15.80617190586746368, 15.72974639402197994, 34.37390960531435979 ) ) ;
#91787 = DIRECTION ( 'NONE',  ( -0.000000000000000000, 0.000000000000000000, 1.000000000000000000 ) ) ;
#91788 = CARTESIAN_POINT ( 'NONE',  ( 28.82186960331498327, 2.781578969918950771E-14, 143.0000000000000000 ) ) ;
#91790 = CARTESIAN_POINT ( 'NONE',  ( -4.483927247898539470, -16.52544592524342804, 32.29057627198102409 ) ) ;
#91789 = CARTESIAN_POINT ( 'NONE',  ( -8.224510206698735004, -14.34966873604973081, 44.58442372801901854 ) ) ;
#91791 = CARTESIAN_POINT ( 'NONE',  ( -10.72451020669898014, 18.67979575497178502, 65.41557627198102409 ) ) ;
#91792 = CARTESIAN_POINT ( 'NONE',  ( -16.46253265017146816, -9.564922557961047289, 84.16775706135233293 ) ) ;
#91793 = CARTESIAN_POINT ( 'NONE',  ( 15.80617190586746368, 15.72974639402197994, 64.37390960531435269 ) ) ;
#91794 = CARTESIAN_POINT ( 'NONE',  ( -21.76481224609945642, -7.725237430229303648, 173.1951747752679580 ) ) ;
#91795 = CARTESIAN_POINT ( 'NONE',  ( -12.06949235617739369, -12.14591786802326823, 54.37609039468568994 ) ) ;
#91797 = CARTESIAN_POINT ( 'NONE',  ( -16.46253265017160317, 9.564922557960807481, 95.83224293864769550 ) ) ;
#91796 = CARTESIAN_POINT ( 'NONE',  ( 5.153800228976335163, 19.02544592524342804, 34.79057627198102409 ) ) ;
#91798 = CARTESIAN_POINT ( 'NONE',  ( 0.05219959533909260263, 19.03943276465977164, 39.99890960531436690 ) ) ;
#91799 = CARTESIAN_POINT ( 'NONE',  ( -13.97604488694527625, -13.89961937509977652, 21.87390960531435979 ) ) ;
#91800 = DIRECTION ( 'NONE',  ( 0.000000000000000000, 0.000000000000000000, 1.000000000000000000 ) ) ;
#91801 = CARTESIAN_POINT ( 'NONE',  ( 19.03943276465977164, -0.05219959533909143690, 108.7489096053143527 ) ) ;
#91802 = AXIS2_PLACEMENT_3D ( 'NONE', #67115, #37778, #7427 ) ;
#91803 = ORIENTED_EDGE ( 'NONE', *, *, #51319, .F. ) ;
#91804 = CARTESIAN_POINT ( 'NONE',  ( 14.34966873604972726, -8.224510206698740333, 75.83442372801900433 ) ) ;
#91805 = CARTESIAN_POINT ( 'NONE',  ( 10.81492255796078972, 18.62759615963270932, 89.58224293864768129 ) ) ;
#91806 = CARTESIAN_POINT ( 'NONE',  ( 9.474510206698971260, -16.51473224551069308, 57.91557627198103120 ) ) ;
#91807 = CARTESIAN_POINT ( 'NONE',  ( -18.67979575497193778, 10.72451020669871902, 23.33442372801901499 ) ) ;
#91808 = CARTESIAN_POINT ( 'NONE',  ( 16.46253265017160672, -9.564922557960803928, 83.33224293864768129 ) ) ;
#91809 = CARTESIAN_POINT ( 'NONE',  ( 19.05341960407611168, 5.049401038298154454, 113.9572429386477097 ) ) ;
#91810 = ORIENTED_EDGE ( 'NONE', *, *, #116810, .F. ) ;
#91811 = CARTESIAN_POINT ( 'NONE',  ( -21.55341960407619339, 5.719274019375674811, 23.54275706135235424 ) ) ;
#91814 = CARTESIAN_POINT ( 'NONE',  ( 5.049401038297881783, 19.05341960407617563, 92.29275706135234714 ) ) ;
#91813 = CARTESIAN_POINT ( 'NONE',  ( 9.474510206698971260, -16.51473224551069308, 107.9155762719810383 ) ) ;
#91812 = CARTESIAN_POINT ( 'NONE',  ( 16.51473224551069308, 9.474510206698969483, 29.16557627198103475 ) ) ;
#91815 = CARTESIAN_POINT ( 'NONE',  ( -13.89961937509957401, -13.97604488694547875, 29.37609039468565797 ) ) ;
#91816 = CARTESIAN_POINT ( 'NONE',  ( 21.53943276465977519, -0.05219959533907433946, 93.74890960531436690 ) ) ;
#91817 = CARTESIAN_POINT ( 'NONE',  ( -5.049401038297874678, -19.05341960407617918, 29.79275706135232227 ) ) ;
#91818 = CARTESIAN_POINT ( 'NONE',  ( -14.29746914071037622, -8.314922557961029526, 84.16775706135234714 ) ) ;
#91819 = CARTESIAN_POINT ( 'NONE',  ( -9.474510206698964154, 16.51473224551069663, 100.4155762719810241 ) ) ;
#91820 = CARTESIAN_POINT ( 'NONE',  ( 5.153800228976335163, 19.02544592524342804, 54.79057627198103120 ) ) ;
#91821 = CARTESIAN_POINT ( 'NONE',  ( 21.52544592524334988, 5.823673210054432836, 71.45942372801901854 ) ) ;
#91822 = CARTESIAN_POINT ( 'NONE',  ( -15.72974639402176322, -15.80617190586768395, 84.37609039468570415 ) ) ;
#91823 = CARTESIAN_POINT ( 'NONE',  ( -19.03943276465977164, 0.05219959533909376836, 116.2489096053143669 ) ) ;
#91824 = CARTESIAN_POINT ( 'NONE',  ( 16.46253265017160672, -9.564922557960803928, 73.33224293864769550 ) ) ;
#91825 = CARTESIAN_POINT ( 'NONE',  ( -5.823673210054431948, 21.52544592524334988, 52.70942372801902565 ) ) ;
#91826 = CARTESIAN_POINT ( 'NONE',  ( 19.03943276465977164, 0.05219959533936151252, 81.25109039468567573 ) ) ;
#91827 = CARTESIAN_POINT ( 'NONE',  ( -9.564922557960796823, -16.46253265017161027, 57.08224293864769550 ) ) ;
#91828 = CARTESIAN_POINT ( 'NONE',  ( 16.46253265017160672, -9.564922557960803928, 93.33224293864769550 ) ) ;
#91829 = CARTESIAN_POINT ( 'NONE',  ( 16.51473224551069308, 9.474510206698969483, 79.16557627198103830 ) ) ;
#91830 = CARTESIAN_POINT ( 'NONE',  ( 17.50000000000003553, -4.509153483536745277, 23.09479828858030359 ) ) ;
#91831 = CARTESIAN_POINT ( 'NONE',  ( -19.03943276465977164, 0.05219959533909376836, 51.24890960531436690 ) ) ;
#91832 = CARTESIAN_POINT ( 'NONE',  ( 10.81492255796078972, 18.62759615963270932, 104.5822429386477097 ) ) ;
#91833 = CARTESIAN_POINT ( 'NONE',  ( 4.379528057220092307, 16.55341960407617563, 87.29275706135236135 ) ) ;
#91834 = DIRECTION ( 'NONE',  ( 0.000000000000000000, -3.469446951953611033E-15, 1.000000000000000000 ) ) ;
#91835 = CARTESIAN_POINT ( 'NONE',  ( 5.049401038297881783, 19.05341960407617563, 42.29275706135234003 ) ) ;
#91836 = CARTESIAN_POINT ( 'NONE',  ( 5.153800228976335163, 19.02544592524342804, 79.79057627198102409 ) ) ;
#91837 = CARTESIAN_POINT ( 'NONE',  ( -16.55341960407611168, -4.379528057220339221, 56.45724293864768839 ) ) ;
#91838 = CARTESIAN_POINT ( 'NONE',  ( 14.34966873604960469, 8.224510206698951720, 94.16557627198103830 ) ) ;
#91839 = CARTESIAN_POINT ( 'NONE',  ( 13.89961937509977652, -13.97604488694527269, 113.1239096053143527 ) ) ;
#91840 = CARTESIAN_POINT ( 'NONE',  ( -19.02544592524342804, 5.153800228976336051, 106.0405762719810241 ) ) ;
#91841 = CARTESIAN_POINT ( 'NONE',  ( 19.03943276465977164, -0.05219959533909143690, 113.7489096053143669 ) ) ;
#91842 = CARTESIAN_POINT ( 'NONE',  ( -13.89961937509957401, -13.97604488694547875, 19.37609039468566507 ) ) ;
#91843 = CARTESIAN_POINT ( 'NONE',  ( 8.314922557961029526, -14.29746914071037800, 90.41775706135236135 ) ) ;
#91844 = CARTESIAN_POINT ( 'NONE',  ( -5.049401038298153566, 19.05341960407611168, 75.20724293864769550 ) ) ;
#91845 = CARTESIAN_POINT ( 'NONE',  ( 21.52544592524334988, 5.823673210054432836, 36.45942372801901143 ) ) ;
#91846 = CARTESIAN_POINT ( 'NONE',  ( -21.53943276465977519, 0.05219959533907696930, 31.24890960531435979 ) ) ;
#91848 = VERTEX_POINT ( 'NONE', #86928 ) ;
#91847 = CARTESIAN_POINT ( 'NONE',  ( -5.823673210054116645, -21.52544592524344225, 112.2905762719810241 ) ) ;
#91849 = CARTESIAN_POINT ( 'NONE',  ( -18.62759615963270932, 10.81492255796079327, 65.83224293864769550 ) ) ;
#91850 = CARTESIAN_POINT ( 'NONE',  ( -0.05219959533910754901, -16.53943276465976808, 92.49890960531436690 ) ) ;
#91851 = CARTESIAN_POINT ( 'NONE',  ( 16.51473224551083163, -9.474510206698727899, 45.83442372801900433 ) ) ;
#91852 = CIRCLE ( 'NONE', #182249, 2.999999999999998668 ) ;
#91853 = CARTESIAN_POINT ( 'NONE',  ( -5.153800228976328057, -19.02544592524343514, 37.29057627198102409 ) ) ;
#91854 = CARTESIAN_POINT ( 'NONE',  ( 5.153800228976335163, 19.02544592524342804, 84.79057627198099567 ) ) ;
#91855 = CARTESIAN_POINT ( 'NONE',  ( 19.03943276465977164, -0.05219959533909143690, 78.74890960531436690 ) ) ;
#91856 = CARTESIAN_POINT ( 'NONE',  ( 22.44159573604009239, 16.30477369853692693, 142.0750000027311728 ) ) ;
#91857 = CARTESIAN_POINT ( 'NONE',  ( -16.53943276465976808, 0.05219959533911058130, 101.2489096053143669 ) ) ;
#91858 = CARTESIAN_POINT ( 'NONE',  ( -16.52544592524342804, 4.483927247898546575, 31.04057627198102409 ) ) ;
#91859 = CARTESIAN_POINT ( 'NONE',  ( 14.34966873604972726, -8.224510206698740333, 20.83442372801901143 ) ) ;
#91860 = CARTESIAN_POINT ( 'NONE',  ( -5.823673210054431948, 21.52544592524334988, 87.70942372801901854 ) ) ;
#91861 = CARTESIAN_POINT ( 'NONE',  ( 16.51473224551069308, 9.474510206698969483, 104.1655762719810241 ) ) ;
#91862 = CARTESIAN_POINT ( 'NONE',  ( 15.80617190586746368, 15.72974639402197994, 114.3739096053143527 ) ) ;
#91863 = CARTESIAN_POINT ( 'NONE',  ( -13.89961937509977652, 13.97604488694528158, 40.62390960531435979 ) ) ;
#91864 = CARTESIAN_POINT ( 'NONE',  ( 16.52544592524335698, 4.483927247898782831, 46.45942372801901854 ) ) ;
#91865 = CIRCLE ( 'NONE', #4691, 30.82560697742735556 ) ;
#91866 = CARTESIAN_POINT ( 'NONE',  ( 9.474510206698729675, 16.51473224551082808, 107.0844237280190043 ) ) ;
#91867 = CARTESIAN_POINT ( 'NONE',  ( -5.823673210054116645, -21.52544592524344225, 102.2905762719810383 ) ) ;
#91868 = CARTESIAN_POINT ( 'NONE',  ( 19.02544592524334988, 5.153800228976608722, 61.45942372801900433 ) ) ;
#91869 = CARTESIAN_POINT ( 'NONE',  ( 5.153800228976335163, 19.02544592524342804, 24.79057627198102765 ) ) ;
#91870 = CARTESIAN_POINT ( 'NONE',  ( -21.53943276465977519, 0.05219959533907696930, 111.2489096053143669 ) ) ;
#91871 = CARTESIAN_POINT ( 'NONE',  ( -28.82186960331483760, 9.364793116373787640, 142.1500000054624024 ) ) ;
#91872 = CARTESIAN_POINT ( 'NONE',  ( -9.564922557960796823, -16.46253265017161027, 97.08224293864769550 ) ) ;
#91873 = VECTOR ( 'NONE', #10785, 1000.000000000000114 ) ;
#91874 = CARTESIAN_POINT ( 'NONE',  ( -30.73962218707678673, 22.33364281372846705, -6.202157773949823927 ) ) ;
#91875 = CARTESIAN_POINT ( 'NONE',  ( -19.05341960407611168, -5.049401038298163336, 86.45724293864769550 ) ) ;
#91877 = CARTESIAN_POINT ( 'NONE',  ( 4.483927247898545687, 16.52544592524342804, 74.79057627198105251 ) ) ;
#91876 = CARTESIAN_POINT ( 'NONE',  ( 18.62759615963255655, 10.81492255796105972, 31.66775706135234358 ) ) ;
#91878 = CARTESIAN_POINT ( 'NONE',  ( 19.03943276465977164, -0.05219959533909143690, 83.74890960531436690 ) ) ;
#91879 = STYLED_ITEM ( 'NONE', ( #114169 ), #189513 ) ;
#91881 = CARTESIAN_POINT ( 'NONE',  ( 13.89961937509957401, 13.97604488694547697, 56.87609039468564731 ) ) ;
#91880 = CARTESIAN_POINT ( 'NONE',  ( 8.224510206698742110, 14.34966873604972548, 47.08442372801901854 ) ) ;
#91882 = CARTESIAN_POINT ( 'NONE',  ( -10.72451020669870658, -18.67979575497194134, 64.58442372801900433 ) ) ;
#91883 = CARTESIAN_POINT ( 'NONE',  ( -16.55341960407617563, 4.379528057220093196, 23.54275706135235424 ) ) ;
#91884 = CARTESIAN_POINT ( 'NONE',  ( -9.474510206698964154, 16.51473224551069663, 70.41557627198102409 ) ) ;
#91885 = CARTESIAN_POINT ( 'NONE',  ( 13.89961937509957401, 13.97604488694547697, 91.87609039468567573 ) ) ;
#91886 = CARTESIAN_POINT ( 'NONE',  ( -0.05219959533934338120, 16.53943276465976808, 52.50109039468567573 ) ) ;
#91887 = CARTESIAN_POINT ( 'NONE',  ( -10.72451020669870658, -18.67979575497194134, 94.58442372801901854 ) ) ;
#91888 = CARTESIAN_POINT ( 'NONE',  ( 19.05341960407617918, -5.049401038297876454, 81.04275706135231871 ) ) ;
#91889 = CARTESIAN_POINT ( 'NONE',  ( 16.51473224551069308, 9.474510206698969483, 44.16557627198103120 ) ) ;
#91890 = CARTESIAN_POINT ( 'NONE',  ( -5.823673210054116645, -21.52544592524344225, 77.29057627198102409 ) ) ;
#91892 = CARTESIAN_POINT ( 'NONE',  ( -5.153800228976607833, 19.02544592524334988, 82.70942372801897591 ) ) ;
#91891 = CARTESIAN_POINT ( 'NONE',  ( -12.14591786802309592, -12.06949235617757132, 81.87390960531435269 ) ) ;
#91893 = CARTESIAN_POINT ( 'NONE',  ( -18.39639308325438449, -5.499999999999988454, 71.48252246182195790 ) ) ;
#91894 = CARTESIAN_POINT ( 'NONE',  ( -16.46253265017146816, -9.564922557961047289, 39.16775706135234003 ) ) ;
#91895 = CARTESIAN_POINT ( 'NONE',  ( -14.29746914071037622, -8.314922557961029526, 109.1677570613523613 ) ) ;
#91896 = CARTESIAN_POINT ( 'NONE',  ( -12.06949235617756955, 12.14591786802309770, 60.62390960531437401 ) ) ;
#91898 = CARTESIAN_POINT ( 'NONE',  ( -27.73933785331498925, 9.013057229001089965, 142.7750000027311899 ) ) ;
#91897 = CARTESIAN_POINT ( 'NONE',  ( 21.55341960407619695, -5.719274019375665929, 101.0427570613523756 ) ) ;
#91899 = CARTESIAN_POINT ( 'NONE',  ( 5.719274019375991003, -21.55341960407610458, 112.7072429386476955 ) ) ;
#91900 = CARTESIAN_POINT ( 'NONE',  ( 13.97604488694527802, 13.89961937509977652, 69.37390960531436690 ) ) ;
#91901 = CARTESIAN_POINT ( 'NONE',  ( 15.80617190586769283, -15.72974639402175789, 85.62609039468568994 ) ) ;
#91902 = CARTESIAN_POINT ( 'NONE',  ( 19.05341960407611168, 5.049401038298154454, 63.95724293864769550 ) ) ;
#91903 = ORIENTED_EDGE ( 'NONE', *, *, #36961, .T. ) ;
#91904 = CARTESIAN_POINT ( 'NONE',  ( -8.224510206698948167, 14.34966873604960824, 115.4155762719810241 ) ) ;
#91905 = CARTESIAN_POINT ( 'NONE',  ( -21.52544592524343514, 5.823673210054127303, 36.04057627198102409 ) ) ;
#91906 = CARTESIAN_POINT ( 'NONE',  ( -16.52544592524342804, 4.483927247898546575, 61.04057627198103120 ) ) ;
#91907 = CARTESIAN_POINT ( 'NONE',  ( -5.049401038298153566, 19.05341960407611168, 40.20724293864768839 ) ) ;
#91908 = CARTESIAN_POINT ( 'NONE',  ( -4.379528057220328563, 16.55341960407611168, 90.20724293864770971 ) ) ;
#91909 = VECTOR ( 'NONE', #116219, 1000.000000000000000 ) ;
#91910 = CARTESIAN_POINT ( 'NONE',  ( 10.72451020669898902, -18.67979575497178502, 112.9155762719810383 ) ) ;
#91911 = CARTESIAN_POINT ( 'NONE',  ( 18.62759615963255655, 10.81492255796105972, 51.66775706135234714 ) ) ;
#91912 = CARTESIAN_POINT ( 'NONE',  ( 1.452840677238310674, 7.214434113892650657, -62.28070517238707282 ) ) ;
#91913 = CARTESIAN_POINT ( 'NONE',  ( 8.314922557961029526, -14.29746914071037800, 45.41775706135234003 ) ) ;
#91914 = CARTESIAN_POINT ( 'NONE',  ( -18.62759615963270932, 10.81492255796079327, 95.83224293864770971 ) ) ;
#91916 = CARTESIAN_POINT ( 'NONE',  ( 5.049401038298161559, -19.05341960407611168, 42.70724293864767418 ) ) ;
#91915 = CARTESIAN_POINT ( 'NONE',  ( -13.89961937509957401, -13.97604488694547875, 24.37609039468565442 ) ) ;
#91917 = CARTESIAN_POINT ( 'NONE',  ( -0.05219959533909027116, -19.03943276465977164, 102.4989096053143669 ) ) ;
#91918 = CARTESIAN_POINT ( 'NONE',  ( 15.72974639402176855, 15.80617190586768217, 61.87609039468568284 ) ) ;
#91919 = EDGE_CURVE ( 'NONE', #49306, #197846, #44416, .T. ) ;
#91920 = CARTESIAN_POINT ( 'NONE',  ( 5.823673210054125526, 21.52544592524343514, 44.79057627198103120 ) ) ;
#91921 = CARTESIAN_POINT ( 'NONE',  ( 14.29746914071049879, -8.314922557960816363, 28.33224293864769550 ) ) ;
#91923 = CARTESIAN_POINT ( 'NONE',  ( -0.05219959533937732626, 21.53943276465977519, 92.50109039468567573 ) ) ;
#91922 = CARTESIAN_POINT ( 'NONE',  ( -10.72451020669870658, -18.67979575497194134, 64.58442372801900433 ) ) ;
#91924 = CARTESIAN_POINT ( 'NONE',  ( -0.05219959533936034679, 19.03943276465977164, 37.50109039468567573 ) ) ;
#91925 = CARTESIAN_POINT ( 'NONE',  ( 4.379528057220092307, 16.55341960407617563, 97.29275706135234714 ) ) ;
#91926 = CARTESIAN_POINT ( 'NONE',  ( 15.80617190586769283, -15.72974639402175789, 55.62609039468568284 ) ) ;
#91927 = CARTESIAN_POINT ( 'NONE',  ( -13.97604488694527625, -13.89961937509977652, 46.87390960531435979 ) ) ;
#91928 = CARTESIAN_POINT ( 'NONE',  ( -18.67979575497193778, 10.72451020669871902, 113.3344237280190328 ) ) ;
#91929 = CARTESIAN_POINT ( 'NONE',  ( 16.51473224551069308, 9.474510206698969483, 114.1655762719810241 ) ) ;
#91930 = CARTESIAN_POINT ( 'NONE',  ( -5.719274019375665041, -21.55341960407619695, 19.79275706135235069 ) ) ;
#91931 = CARTESIAN_POINT ( 'NONE',  ( -15.72974639402197994, 15.80617190586746368, 70.62390960531436690 ) ) ;
#91932 = CARTESIAN_POINT ( 'NONE',  ( 0.05219959533934541429, -16.53943276465976808, 40.00109039468567573 ) ) ;
#91934 = CARTESIAN_POINT ( 'NONE',  ( -21.52544592524343514, 5.823673210054127303, 76.04057627198102409 ) ) ;
#91933 = CARTESIAN_POINT ( 'NONE',  ( 11.30153831258470731, -190.0000000000000000, -4.999999999999999112 ) ) ;
#91936 = CARTESIAN_POINT ( 'NONE',  ( -14.29746914071049879, 8.314922557960819915, 80.83224293864769550 ) ) ;
#91935 = CARTESIAN_POINT ( 'NONE',  ( -16.52544592524335698, -4.483927247898792601, 68.95942372801901854 ) ) ;
#91937 = CARTESIAN_POINT ( 'NONE',  ( -27.32543223595607884, -4.845308524273512774, 167.4404622590845690 ) ) ;
#91938 = CARTESIAN_POINT ( 'NONE',  ( 13.97604488694548053, -13.89961937509957401, 105.6260903946856757 ) ) ;
#91939 = CARTESIAN_POINT ( 'NONE',  ( 21.55341960407610458, 5.719274019375980345, 28.95724293864769905 ) ) ;
#91940 = CARTESIAN_POINT ( 'NONE',  ( -10.74802307403563084, -10.74802307403544077, -64.92279855667830191 ) ) ;
#91941 = CARTESIAN_POINT ( 'NONE',  ( -16.55341960407617563, 4.379528057220093196, 33.54275706135234714 ) ) ;
#91942 = CARTESIAN_POINT ( 'NONE',  ( 21.52544592524344225, -5.823673210054117533, 113.5405762719810383 ) ) ;
#91943 = CARTESIAN_POINT ( 'NONE',  ( -10.81492255796078084, -18.62759615963271287, 32.08224293864769550 ) ) ;
#91944 = CARTESIAN_POINT ( 'NONE',  ( 8.224510206698742110, 14.34966873604972548, 57.08442372801901854 ) ) ;
#91945 = CARTESIAN_POINT ( 'NONE',  ( 13.97604488694527802, 13.89961937509977652, 79.37390960531435269 ) ) ;
#91947 = CARTESIAN_POINT ( 'NONE',  ( 0.05219959533936267826, -19.03943276465977164, 110.0010903946856757 ) ) ;
#91946 = CARTESIAN_POINT ( 'NONE',  ( -21.53943276465977519, -0.05219959533937600094, 43.75109039468568284 ) ) ;
#91948 = CARTESIAN_POINT ( 'NONE',  ( -21.53943276465977519, 0.05219959533907696930, 26.24890960531435624 ) ) ;
#91949 = ORIENTED_EDGE ( 'NONE', *, *, #82460, .T. ) ;
#91950 = CARTESIAN_POINT ( 'NONE',  ( 5.049401038297881783, 19.05341960407617563, 27.29275706135232937 ) ) ;
#91951 = CARTESIAN_POINT ( 'NONE',  ( -4.483927247898782831, 16.52544592524335698, 42.70942372801901854 ) ) ;
#91952 = CARTESIAN_POINT ( 'NONE',  ( -16.51473224551069308, -9.474510206698971260, 106.6655762719810383 ) ) ;
#91953 = CARTESIAN_POINT ( 'NONE',  ( -15.80617190586745835, -15.72974639402198527, 101.8739096053143811 ) ) ;
#91954 = CARTESIAN_POINT ( 'NONE',  ( -13.97604488694527625, -13.89961937509977652, 66.87390960531436690 ) ) ;
#91955 = CARTESIAN_POINT ( 'NONE',  ( -17.12812012977024168, 6.668231424566045895, 23.64051240676857191 ) ) ;
#91956 = CARTESIAN_POINT ( 'NONE',  ( -8.224510206698948167, 14.34966873604960824, 85.41557627198102409 ) ) ;
#91957 = CARTESIAN_POINT ( 'NONE',  ( -18.67979575497178146, -10.72451020669898902, 31.66557627198102054 ) ) ;
#91958 = CARTESIAN_POINT ( 'NONE',  ( -17.48847506799968698, 5.747544572773787053, 35.82697437843280142 ) ) ;
#91959 = CARTESIAN_POINT ( 'NONE',  ( 14.29746914071037800, 8.314922557961029526, 66.66775706135234714 ) ) ;
#91960 = CARTESIAN_POINT ( 'NONE',  ( -10.81492255796078084, -18.62759615963271287, 112.0822429386477097 ) ) ;
#91961 = CARTESIAN_POINT ( 'NONE',  ( -0.05219959533936034679, 19.03943276465977164, 82.50109039468567573 ) ) ;
#91962 = CARTESIAN_POINT ( 'NONE',  ( -19.05341960407611168, -5.049401038298163336, 31.45724293864769550 ) ) ;
#91963 = CARTESIAN_POINT ( 'NONE',  ( -10.81492255796078084, -18.62759615963271287, 62.08224293864769550 ) ) ;
#91964 = CARTESIAN_POINT ( 'NONE',  ( 9.564922557960805705, 16.46253265017160317, 99.58224293864770971 ) ) ;
#91965 = CARTESIAN_POINT ( 'NONE',  ( 18.62759615963255655, 10.81492255796105972, 96.66775706135234714 ) ) ;
#91966 = CARTESIAN_POINT ( 'NONE',  ( 13.89961937509977652, -13.97604488694527269, 63.12390960531435979 ) ) ;
#91967 = CARTESIAN_POINT ( 'NONE',  ( 4.379528057220092307, 16.55341960407617563, 47.29275706135234003 ) ) ;
#91968 = CARTESIAN_POINT ( 'NONE',  ( -16.51473224551069308, -9.474510206698971260, 61.66557627198103120 ) ) ;
#91969 = CARTESIAN_POINT ( 'NONE',  ( 10.72451020669871369, 18.67979575497193778, 77.08442372801901854 ) ) ;
#91970 = EDGE_LOOP ( 'NONE', ( #177699, #19597 ) ) ;
#91971 = CARTESIAN_POINT ( 'NONE',  ( -19.03943276465977164, -0.05219959533935918106, 33.75109039468566863 ) ) ;
#91972 = CARTESIAN_POINT ( 'NONE',  ( -5.153800228976607833, 19.02544592524334988, 52.70942372801900433 ) ) ;
#91973 = CARTESIAN_POINT ( 'NONE',  ( 5.719274019375673035, 21.55341960407619339, 47.29275706135234003 ) ) ;
#91974 = CARTESIAN_POINT ( 'NONE',  ( -6.854124442541994711, 1.305043071815353395, -62.35408385982739077 ) ) ;
#91975 = CARTESIAN_POINT ( 'NONE',  ( -5.153800228976607833, 19.02544592524334988, 52.70942372801900433 ) ) ;
#91976 = CARTESIAN_POINT ( 'NONE',  ( -5.049401038298153566, 19.05341960407611168, 100.2072429386476955 ) ) ;
#91977 = CARTESIAN_POINT ( 'NONE',  ( -9.474510206698964154, 16.51473224551069663, 65.41557627198102409 ) ) ;
#91978 = CARTESIAN_POINT ( 'NONE',  ( -12.14591786802309592, -12.06949235617757132, 26.87390960531435979 ) ) ;
#91980 = CARTESIAN_POINT ( 'NONE',  ( -5.823673210054431948, 21.52544592524334988, 102.7094237280190185 ) ) ;
#91979 = CARTESIAN_POINT ( 'NONE',  ( 18.62759615963271287, -10.81492255796078972, 23.33224293864769194 ) ) ;
#91981 = CARTESIAN_POINT ( 'NONE',  ( 11.40812507854754365, 35.11059874428196537, -9.724999997268813701 ) ) ;
#91982 = CARTESIAN_POINT ( 'NONE',  ( -34.02686120844016671, 4.767814797156207263, 92.23495037107731775 ) ) ;
#91983 = CARTESIAN_POINT ( 'NONE',  ( -18.67979575497193778, 10.72451020669871902, 98.33442372801901854 ) ) ;
#91984 = CARTESIAN_POINT ( 'NONE',  ( 16.52216118717208460, -7.221426719304494313, 41.42400978953008206 ) ) ;
#91985 = CARTESIAN_POINT ( 'NONE',  ( -8.224510206698948167, 14.34966873604960824, 115.4155762719810241 ) ) ;
#91986 = CARTESIAN_POINT ( 'NONE',  ( -18.22780087662122028, 5.500000000000031086, 98.51540105326105845 ) ) ;
#91987 = CARTESIAN_POINT ( 'NONE',  ( -24.99788752995424446, -12.60079600866962579, 166.0698618172138197 ) ) ;
#91988 = CIRCLE ( 'NONE', #146850, 214.0437394197456342 ) ;
#91989 = CARTESIAN_POINT ( 'NONE',  ( -16.53943276465976808, -0.05219959533934237506, 48.75109039468568284 ) ) ;
#91990 = CARTESIAN_POINT ( 'NONE',  ( 5.719274019375991003, -21.55341960407610458, 72.70724293864769550 ) ) ;
#91991 = CARTESIAN_POINT ( 'NONE',  ( -12.06949235617756955, 12.14591786802309770, 45.62390960531436690 ) ) ;
#91993 = CARTESIAN_POINT ( 'NONE',  ( 13.97604488694527802, 13.89961937509977652, 94.37390960531436690 ) ) ;
#91992 = CARTESIAN_POINT ( 'NONE',  ( -8.224510206698948167, 14.34966873604960824, 105.4155762719810383 ) ) ;
#91994 = CARTESIAN_POINT ( 'NONE',  ( 9.564922557961047289, -16.46253265017146816, 40.41775706135234003 ) ) ;
#91995 = CARTESIAN_POINT ( 'NONE',  ( -4.483927247898539470, -16.52544592524342804, 112.2905762719810241 ) ) ;
#91996 = CARTESIAN_POINT ( 'NONE',  ( -10.81492255796105439, 18.62759615963255655, 72.91775706135234714 ) ) ;
#91997 = CARTESIAN_POINT ( 'NONE',  ( -0.05219959533909027116, -19.03943276465977164, 97.49890960531436690 ) ) ;
#91998 = CARTESIAN_POINT ( 'NONE',  ( 4.483927247898790824, -16.52544592524335698, 110.2094237280190185 ) ) ;
#91999 = CARTESIAN_POINT ( 'NONE',  ( 22.81625015709510151, -31.40387420917324590, -4.424999997268812990 ) ) ;
#92000 = CARTESIAN_POINT ( 'NONE',  ( 21.52544592524344225, -5.823673210054117533, 33.54057627198102409 ) ) ;
#92001 = CARTESIAN_POINT ( 'NONE',  ( -16.52544592524342804, 4.483927247898546575, 91.04057627198103830 ) ) ;
#92002 = CIRCLE ( 'NONE', #8023, 69.99999999999997158 ) ;
#92003 = CARTESIAN_POINT ( 'NONE',  ( 16.46253265017146816, 9.564922557961045513, 56.66775706135233293 ) ) ;
#92004 = CARTESIAN_POINT ( 'NONE',  ( 9.474510206698971260, -16.51473224551069308, 82.91557627198103830 ) ) ;
#92005 = CARTESIAN_POINT ( 'NONE',  ( 8.314922557960818139, 14.29746914071049879, 79.58224293864769550 ) ) ;
#92006 = CARTESIAN_POINT ( 'NONE',  ( 19.05341960407617918, -5.049401038297876454, 96.04275706135231871 ) ) ;
#92007 = CARTESIAN_POINT ( 'NONE',  ( 5.823673210054125526, 21.52544592524343514, 49.79057627198102409 ) ) ;
#92008 = EDGE_LOOP ( 'NONE', ( #170051, #137333, #179464, #104029 ) ) ;
#92009 = EDGE_CURVE ( 'NONE', #162114, #177366, #180830, .T. ) ;
#92010 = CARTESIAN_POINT ( 'NONE',  ( -5.153800228976328057, -19.02544592524343514, 22.29057627198102765 ) ) ;
#92011 = CARTESIAN_POINT ( 'NONE',  ( -16.88567814943164791, -6.947325034625600360, 31.29001122652585920 ) ) ;
#92013 = CARTESIAN_POINT ( 'NONE',  ( -21.53943276465977519, 0.05219959533907696930, 81.24890960531436690 ) ) ;
#92012 = CARTESIAN_POINT ( 'NONE',  ( 9.564922557960805705, 16.46253265017160317, 74.58224293864769550 ) ) ;
#92015 = CARTESIAN_POINT ( 'NONE',  ( 13.89961937509977652, -13.97604488694527269, 88.12390960531438111 ) ) ;
#92014 = CARTESIAN_POINT ( 'NONE',  ( -14.34966873604972548, 8.224510206698743886, 98.33442372801901854 ) ) ;
#92016 = CARTESIAN_POINT ( 'NONE',  ( 13.97604488694548053, -13.89961937509957401, 70.62609039468567573 ) ) ;
#92017 = CARTESIAN_POINT ( 'NONE',  ( 18.62759615963255655, 10.81492255796105972, 76.66775706135234714 ) ) ;
#92018 = CARTESIAN_POINT ( 'NONE',  ( 5.719274019375991003, -21.55341960407610458, 57.70724293864770260 ) ) ;
#92019 = CARTESIAN_POINT ( 'NONE',  ( 9.564922557960805705, 16.46253265017160317, 114.5822429386476955 ) ) ;
#92020 = VECTOR ( 'NONE', #186383, 1000.000000000000000 ) ;
#92021 = CARTESIAN_POINT ( 'NONE',  ( 19.02544592524343514, -5.153800228976328945, 33.54057627198102409 ) ) ;
#92022 = CARTESIAN_POINT ( 'NONE',  ( -8.224510206698735004, -14.34966873604973081, 99.58442372801900433 ) ) ;
#92023 = CARTESIAN_POINT ( 'NONE',  ( -19.02544592524342804, 5.153800228976336051, 51.04057627198103120 ) ) ;
#92024 = CARTESIAN_POINT ( 'NONE',  ( 16.53943276465976808, 0.05219959533934440121, 26.25109039468567573 ) ) ;
#92025 = CARTESIAN_POINT ( 'NONE',  ( -5.153800228976607833, 19.02544592524335343, 82.70942372801899012 ) ) ;
#92026 = CARTESIAN_POINT ( 'NONE',  ( 21.55341960407619695, -5.719274019375665929, 111.0427570613523613 ) ) ;
#92027 = CIRCLE ( 'NONE', #30713, 2.000000000000001776 ) ;
#92028 = CARTESIAN_POINT ( 'NONE',  ( 8.224510206698953496, -14.34966873604960469, 62.91557627198102409 ) ) ;
#92029 = CARTESIAN_POINT ( 'NONE',  ( -9.564922557960796823, -16.46253265017161027, 92.08224293864769550 ) ) ;
#92030 = CARTESIAN_POINT ( 'NONE',  ( 5.719274019375991003, -21.55341960407610458, 102.7072429386476955 ) ) ;
#92031 = CARTESIAN_POINT ( 'NONE',  ( -15.72974639402197994, 15.80617190586746368, 100.6239096053143811 ) ) ;
#92032 = DIRECTION ( 'NONE',  ( 0.000000000000000000, 0.000000000000000000, -1.000000000000000000 ) ) ;
#92033 = CARTESIAN_POINT ( 'NONE',  ( -21.52544592524343514, 5.823673210054127303, 46.04057627198103830 ) ) ;
#92034 = CARTESIAN_POINT ( 'NONE',  ( 14.34966873604972726, -8.224510206698740333, 75.83442372801900433 ) ) ;
#92035 = CARTESIAN_POINT ( 'NONE',  ( -8.314922557960811034, -14.29746914071050412, 87.08224293864769550 ) ) ;
#92036 = CARTESIAN_POINT ( 'NONE',  ( 9.564922557960805705, 16.46253265017160317, 59.58224293864769550 ) ) ;
#92037 = SHAPE_REPRESENTATION_RELATIONSHIP ( 'NONE' , 'NONE' ,  #125845, #107481 ) ;
#92038 = CARTESIAN_POINT ( 'NONE',  ( -15.49999999999999822, -7.500000000000000888, 22.00000000000000711 ) ) ;
#92039 = CARTESIAN_POINT ( 'NONE',  ( 12.14591786802327356, -12.06949235617739191, 110.6260903946857042 ) ) ;
#92040 = CARTESIAN_POINT ( 'NONE',  ( -18.67979575497193778, 10.72451020669871902, 48.33442372801902565 ) ) ;
#92041 = CARTESIAN_POINT ( 'NONE',  ( 13.89961937509977652, -13.97604488694527269, 93.12390960531436690 ) ) ;
#92042 = CARTESIAN_POINT ( 'NONE',  ( 18.62759615963255655, 10.81492255796105972, 71.66775706135234714 ) ) ;
#92043 = DIRECTION ( 'NONE',  ( 0.000000000000000000, 0.000000000000000000, -1.000000000000000000 ) ) ;
#92044 = CARTESIAN_POINT ( 'NONE',  ( -13.97604488694527625, -13.89961937509977652, 26.87390960531434558 ) ) ;
#92045 = VERTEX_POINT ( 'NONE', #164782 ) ;
#92046 = CARTESIAN_POINT ( 'NONE',  ( -5.823673210054431948, 21.52544592524334988, 77.70942372801900433 ) ) ;
#92047 = CARTESIAN_POINT ( 'NONE',  ( 16.46253265017160672, -9.564922557960803928, 48.33224293864769550 ) ) ;
#92048 = CARTESIAN_POINT ( 'NONE',  ( -5.153800228976328057, -19.02544592524343514, 92.29057627198099567 ) ) ;
#92049 = CARTESIAN_POINT ( 'NONE',  ( 5.049401038297881783, 19.05341960407617563, 77.29275706135231871 ) ) ;
#92050 = CARTESIAN_POINT ( 'NONE',  ( -15.80617190586768217, 15.72974639402176855, 43.12609039468568284 ) ) ;
#92051 = CARTESIAN_POINT ( 'NONE',  ( 13.89961937509957401, 13.97604488694547697, 101.8760903946856331 ) ) ;
#92052 = CARTESIAN_POINT ( 'NONE',  ( 16.46253265017146816, 9.564922557961045513, 76.66775706135234714 ) ) ;
#92053 = CARTESIAN_POINT ( 'NONE',  ( -16.51473224551069308, -9.474510206698971260, 41.66557627198103120 ) ) ;
#92054 = CARTESIAN_POINT ( 'NONE',  ( 13.89961937509957401, 13.97604488694547697, 81.87609039468564731 ) ) ;
#92055 = VECTOR ( 'NONE', #134313, 1000.000000000000000 ) ;
#92056 = CARTESIAN_POINT ( 'NONE',  ( -14.34966873604972548, 8.224510206698743886, 108.3344237280190185 ) ) ;
#92057 = CARTESIAN_POINT ( 'NONE',  ( -0.05219959533936034679, 19.03943276465977164, 72.50109039468566152 ) ) ;
#92058 = CARTESIAN_POINT ( 'NONE',  ( 0.05219959533910956823, 16.53943276465976808, 44.99890960531435979 ) ) ;
#92059 = CARTESIAN_POINT ( 'NONE',  ( -13.89961937509957401, -13.97604488694547875, 54.37609039468565442 ) ) ;
#92060 = CARTESIAN_POINT ( 'NONE',  ( -10.81492255796105439, 18.62759615963255655, 107.9177570613523471 ) ) ;
#92061 = PRODUCT ( 'Impeller Fan Blade Assembly', 'Impeller Fan Blade Assembly', '', ( #82597 ) ) ;
#92062 = CARTESIAN_POINT ( 'NONE',  ( -5.153800228976607833, 19.02544592524334988, 22.70942372801899012 ) ) ;
#92063 = CARTESIAN_POINT ( 'NONE',  ( -9.474510206698964154, 16.51473224551069663, 25.41557627198103120 ) ) ;
#92064 = CARTESIAN_POINT ( 'NONE',  ( 21.53943276465977519, 0.05219959533937863772, 86.25109039468568994 ) ) ;
#92065 = CARTESIAN_POINT ( 'NONE',  ( 14.29746914071037800, 8.314922557961029526, 51.66775706135234714 ) ) ;
#92066 = CARTESIAN_POINT ( 'NONE',  ( -19.02544592524342804, 5.153800228976336051, 91.04057627198100988 ) ) ;
#92067 = CARTESIAN_POINT ( 'NONE',  ( -17.14385361876520264, -23.59649016807271593, 147.1750000027311671 ) ) ;
#92068 = CARTESIAN_POINT ( 'NONE',  ( -16.46253265017160317, 9.564922557960807481, 90.83224293864769550 ) ) ;
#92069 = CARTESIAN_POINT ( 'NONE',  ( -17.13100169013222285, 6.664070546374236237, 100.7678983569982734 ) ) ;
#92070 = EDGE_LOOP ( 'NONE', ( #8438, #26124, #98109 ) ) ;
#92071 = CARTESIAN_POINT ( 'NONE',  ( 16.51473224551083163, -9.474510206698727899, 80.83442372801899012 ) ) ;
#92072 = CARTESIAN_POINT ( 'NONE',  ( 18.67979575497178502, 10.72451020669898547, 29.16557627198103120 ) ) ;
#92074 = CARTESIAN_POINT ( 'NONE',  ( -19.05341960407617563, 5.049401038297882671, 103.5427570613523329 ) ) ;
#92073 = CARTESIAN_POINT ( 'NONE',  ( -9.474510206698720793, -16.51473224551083518, 24.58442372801900078 ) ) ;
#92075 = CARTESIAN_POINT ( 'NONE',  ( -14.29746914071049879, 8.314922557960819915, 110.8322429386476955 ) ) ;
#92076 = CARTESIAN_POINT ( 'NONE',  ( -19.02544592524342804, 5.153800228976336051, 26.04057627198103120 ) ) ;
#92077 = CARTESIAN_POINT ( 'NONE',  ( -5.719274019375978568, 21.55341960407610458, 60.20724293864768839 ) ) ;
#92078 = CARTESIAN_POINT ( 'NONE',  ( -5.823673210054116645, -21.52544592524344225, 52.29057627198102409 ) ) ;
#92079 = CARTESIAN_POINT ( 'NONE',  ( -5.049401038298153566, 19.05341960407611168, 30.20724293864768839 ) ) ;
#92080 = CARTESIAN_POINT ( 'NONE',  ( -23.31738231874055245, -16.94106989632524574, 142.4500000054623854 ) ) ;
#92081 = CARTESIAN_POINT ( 'NONE',  ( 9.474510206698729675, 16.51473224551082808, 67.08442372801900433 ) ) ;
#92082 = CARTESIAN_POINT ( 'NONE',  ( -14.34966873604960291, -8.224510206698953496, 36.66557627198103120 ) ) ;
#92083 = CARTESIAN_POINT ( 'NONE',  ( 18.62759615963271287, -10.81492255796078972, 23.33224293864769194 ) ) ;
#92084 = CARTESIAN_POINT ( 'NONE',  ( 5.719274019375673035, 21.55341960407619339, 87.29275706135236135 ) ) ;
#92085 = CARTESIAN_POINT ( 'NONE',  ( 5.823673210054125526, 21.52544592524343514, 74.79057627198105251 ) ) ;
#92086 = CARTESIAN_POINT ( 'NONE',  ( -10.81492255796105439, 18.62759615963255655, 62.91775706135236135 ) ) ;
#92087 = CARTESIAN_POINT ( 'NONE',  ( 21.55341960407619695, -5.719274019375665929, 56.04275706135235424 ) ) ;
#92088 = CARTESIAN_POINT ( 'NONE',  ( -9.474510206698964154, 16.51473224551069663, 100.4155762719810241 ) ) ;
#92089 = CARTESIAN_POINT ( 'NONE',  ( 14.34966873604972726, -8.224510206698740333, 90.83442372801901854 ) ) ;
#92090 = CARTESIAN_POINT ( 'NONE',  ( 8.224510206698953496, -14.34966873604960469, 112.9155762719810383 ) ) ;
#92091 = CARTESIAN_POINT ( 'NONE',  ( -31.80025110837587832, 6.358902984670137037, 91.01589400111389239 ) ) ;
#92092 = VECTOR ( 'NONE', #152148, 1000.000000000000000 ) ;
#92093 = CARTESIAN_POINT ( 'NONE',  ( 16.53943276465976808, -0.05219959533910856209, 73.74890960531433848 ) ) ;
#92094 = CARTESIAN_POINT ( 'NONE',  ( -0.05219959533910754901, -16.53943276465976808, 37.49890960531436690 ) ) ;
#92095 = CARTESIAN_POINT ( 'NONE',  ( -13.97604488694527625, -13.89961937509977652, 61.87390960531435979 ) ) ;
#92096 = CARTESIAN_POINT ( 'NONE',  ( 9.564922557960805705, 16.46253265017160317, 39.58224293864768839 ) ) ;
#92097 = CARTESIAN_POINT ( 'NONE',  ( -5.719274019375978568, 21.55341960407610458, 55.20724293864770260 ) ) ;
#92098 = CARTESIAN_POINT ( 'NONE',  ( -13.97604488694547697, 13.89961937509957934, 33.12609039468566863 ) ) ;
#92100 = CARTESIAN_POINT ( 'NONE',  ( 16.52544592524342804, -4.483927247898539470, 53.54057627198103120 ) ) ;
#92099 = CARTESIAN_POINT ( 'NONE',  ( 0.000000000000000000, 0.000000000000000000, -56.46919128290398504 ) ) ;
#92101 = CARTESIAN_POINT ( 'NONE',  ( -21.53943276465977519, 0.05219959533907696930, 31.24890960531435979 ) ) ;
#92102 = VERTEX_POINT ( 'NONE', #166777 ) ;
#92103 = CARTESIAN_POINT ( 'NONE',  ( -17.79613651744293890, -24.49428055684527550, 140.2843446568999468 ) ) ;
#92104 = CARTESIAN_POINT ( 'NONE',  ( 14.34966873604972726, -8.224510206698740333, 75.83442372801900433 ) ) ;
#92105 = CARTESIAN_POINT ( 'NONE',  ( 16.51473224551083163, -9.474510206698727899, 70.83442372801900433 ) ) ;
#92106 = CARTESIAN_POINT ( 'NONE',  ( -16.52544592524342804, 4.483927247898546575, 36.04057627198102409 ) ) ;
#92107 = DIRECTION ( 'NONE',  ( 0.000000000000000000, 0.000000000000000000, -1.000000000000000000 ) ) ;
#92108 = CARTESIAN_POINT ( 'NONE',  ( 14.34966873604960469, 8.224510206698951720, 29.16557627198103120 ) ) ;
#92109 = CARTESIAN_POINT ( 'NONE',  ( 9.564922557960805705, 16.46253265017160317, 49.58224293864770260 ) ) ;
#92110 = CARTESIAN_POINT ( 'NONE',  ( 5.049401038298161559, -19.05341960407611168, 72.70724293864768129 ) ) ;
#92111 = CARTESIAN_POINT ( 'NONE',  ( 16.51473224551069308, 9.474510206698969483, 34.16557627198102409 ) ) ;
#92112 = CARTESIAN_POINT ( 'NONE',  ( 5.823673210054444382, -21.52544592524334988, 50.20942372801901854 ) ) ;
#92113 = CARTESIAN_POINT ( 'NONE',  ( -16.51473224551069308, -9.474510206698971260, 61.66557627198103120 ) ) ;
#92114 = FACE_OUTER_BOUND ( 'NONE', #26945, .T. ) ;
#92115 = CARTESIAN_POINT ( 'NONE',  ( -16.51473224551069308, -9.474510206698971260, 46.66557627198102409 ) ) ;
#92116 = EDGE_CURVE ( 'NONE', #139247, #122599, #87918, .T. ) ;
#92117 = CARTESIAN_POINT ( 'NONE',  ( 5.823673210054125526, 21.52544592524343514, 29.79057627198102409 ) ) ;
#92119 = CARTESIAN_POINT ( 'NONE',  ( -9.564922557960796823, -16.46253265017161027, 27.08224293864769550 ) ) ;
#92118 = CARTESIAN_POINT ( 'NONE',  ( 5.719274019375673035, 21.55341960407619339, 72.29275706135236135 ) ) ;
#92120 = CARTESIAN_POINT ( 'NONE',  ( -5.823673210054116645, -21.52544592524344225, 32.29057627198102409 ) ) ;
#92121 = CARTESIAN_POINT ( 'NONE',  ( -14.34966873604972548, 8.224510206698743886, 88.33442372801901854 ) ) ;
#92122 = CARTESIAN_POINT ( 'NONE',  ( 21.52544592524334988, 5.823673210054432836, 101.4594237280190185 ) ) ;
#92123 = CARTESIAN_POINT ( 'NONE',  ( 16.55341960407618274, -4.379528057220086978, 61.04275706135234714 ) ) ;
#92124 = CARTESIAN_POINT ( 'NONE',  ( 16.51473224551069308, 9.474510206698969483, 104.1655762719810241 ) ) ;
#92125 = EDGE_CURVE ( 'NONE', #38038, #118785, #72778, .T. ) ;
#92126 = CARTESIAN_POINT ( 'NONE',  ( -14.29746914071037622, -8.314922557961029526, 54.16775706135235424 ) ) ;
#92127 = CARTESIAN_POINT ( 'NONE',  ( -4.379528057220086978, -16.55341960407618274, 39.79275706135235424 ) ) ;
#92128 = CARTESIAN_POINT ( 'NONE',  ( 8.224510206698742110, 14.34966873604972548, 92.08442372801901854 ) ) ;
#92129 = CARTESIAN_POINT ( 'NONE',  ( 21.55341960407619695, -5.719274019375665929, 56.04275706135235424 ) ) ;
#92130 = CARTESIAN_POINT ( 'NONE',  ( 12.06949235617739724, 12.14591786802326823, 21.87609039468567573 ) ) ;
#92131 = CARTESIAN_POINT ( 'NONE',  ( -21.53943276465977519, 0.05219959533907696930, 116.2489096053143669 ) ) ;
#92132 = CARTESIAN_POINT ( 'NONE',  ( -9.564922557961040184, 16.46253265017147172, 112.9177570613523329 ) ) ;
#92133 = CARTESIAN_POINT ( 'NONE',  ( 14.34966873604972726, -8.224510206698740333, 80.83442372801901854 ) ) ;
#92134 = DIRECTION ( 'NONE',  ( -1.000000000000000000, 0.000000000000000000, 0.000000000000000000 ) ) ;
#92135 = CARTESIAN_POINT ( 'NONE',  ( -5.823673210054431948, 21.52544592524334988, 82.70942372801900433 ) ) ;
#92136 = CARTESIAN_POINT ( 'NONE',  ( -13.89961937509957401, -13.97604488694547875, 79.37609039468567573 ) ) ;
#92137 = CARTESIAN_POINT ( 'NONE',  ( -16.53943276465976808, 0.05219959533911058130, 61.24890960531435979 ) ) ;
#92138 = CARTESIAN_POINT ( 'NONE',  ( 0.05219959533910956823, 16.53943276465976808, 39.99890960531436690 ) ) ;
#92139 = CARTESIAN_POINT ( 'NONE',  ( -14.29746914071049879, 8.314922557960819915, 100.8322429386477097 ) ) ;
#92141 = CARTESIAN_POINT ( 'NONE',  ( -9.021937450273798120, 0.4877194249721380492, -63.96635223026897421 ) ) ;
#92140 = CARTESIAN_POINT ( 'NONE',  ( 16.51473224551083163, -9.474510206698727899, 40.83442372801900433 ) ) ;
#92142 = CARTESIAN_POINT ( 'NONE',  ( 21.55341960407619695, -5.719274019375665929, 51.04275706135234714 ) ) ;
#92143 = CARTESIAN_POINT ( 'NONE',  ( -16.52544592524335698, -4.483927247898792601, 18.95942372801901143 ) ) ;
#92144 = DIRECTION ( 'NONE',  ( 0.000000000000000000, 0.000000000000000000, 1.000000000000000000 ) ) ;
#92145 = CARTESIAN_POINT ( 'NONE',  ( 19.05341960407611168, 5.049401038298154454, 103.9572429386476671 ) ) ;
#92146 = CARTESIAN_POINT ( 'NONE',  ( -0.05219959533907301413, -21.53943276465977519, 77.49890960531433848 ) ) ;
#92147 = CARTESIAN_POINT ( 'NONE',  ( -19.02544592524334988, -5.153800228976617603, 93.95942372801900433 ) ) ;
#92148 = CARTESIAN_POINT ( 'NONE',  ( 19.02544592524343514, -5.153800228976328945, 108.5405762719810383 ) ) ;
#92149 = CARTESIAN_POINT ( 'NONE',  ( -26.36463166569313188, 3.076743934663749069, 174.2851114983683942 ) ) ;
#92150 = CARTESIAN_POINT ( 'NONE',  ( -4.483927247898539470, -16.52544592524342804, 112.2905762719810241 ) ) ;
#92151 = CARTESIAN_POINT ( 'NONE',  ( 0.05219959533937995610, -21.53943276465977519, 95.00109039468568994 ) ) ;
#92152 = CARTESIAN_POINT ( 'NONE',  ( -19.03943276465977164, 0.05219959533909376836, 31.24890960531435979 ) ) ;
#92153 = CARTESIAN_POINT ( 'NONE',  ( -5.823673210054431948, 21.52544592524334988, 47.70942372801902565 ) ) ;
#92154 = CARTESIAN_POINT ( 'NONE',  ( -10.72451020669870658, -18.67979575497194134, 84.58442372801903275 ) ) ;
#92155 = CARTESIAN_POINT ( 'NONE',  ( -8.314922557961024197, 14.29746914071037800, 87.91775706135234714 ) ) ;
#92156 = CARTESIAN_POINT ( 'NONE',  ( -15.80617190586768217, 15.72974639402176855, 43.12609039468568284 ) ) ;
#92157 = CARTESIAN_POINT ( 'NONE',  ( 0.05219959533937995610, -21.53943276465977519, 45.00109039468568284 ) ) ;
#92159 = CARTESIAN_POINT ( 'NONE',  ( -19.03943276465977164, 0.05219959533909376836, 96.24890960531436690 ) ) ;
#92158 = CARTESIAN_POINT ( 'NONE',  ( -16.51473224551082808, 9.474510206698731452, 68.33442372801900433 ) ) ;
#92160 = CARTESIAN_POINT ( 'NONE',  ( 8.224510206698953496, -14.34966873604960469, 107.9155762719810241 ) ) ;
#92161 = EDGE_CURVE ( 'NONE', #171158, #49922, #119273, .T. ) ;
#92162 = CARTESIAN_POINT ( 'NONE',  ( 21.55341960407610458, 5.719274019375980345, 78.95724293864769550 ) ) ;
#92163 = CARTESIAN_POINT ( 'NONE',  ( -0.05219959533910754901, -16.53943276465976808, 62.49890960531436690 ) ) ;
#92164 = CARTESIAN_POINT ( 'NONE',  ( 0.05219959533937995610, -21.53943276465977519, 100.0010903946857042 ) ) ;
#92165 = CARTESIAN_POINT ( 'NONE',  ( -0.05219959533910754901, -16.53943276465976808, 77.49890960531433848 ) ) ;
#92166 = CARTESIAN_POINT ( 'NONE',  ( 9.564922557960805705, 16.46253265017160317, 34.58224293864770260 ) ) ;
#92167 = CARTESIAN_POINT ( 'NONE',  ( 16.51473224551083163, -9.474510206698727899, 90.83442372801900433 ) ) ;
#92168 = CARTESIAN_POINT ( 'NONE',  ( 8.314922557960818139, 14.29746914071049879, 49.58224293864769550 ) ) ;
#92169 = CARTESIAN_POINT ( 'NONE',  ( 5.719274019375673035, 21.55341960407619339, 97.29275706135234714 ) ) ;
#92170 = CARTESIAN_POINT ( 'NONE',  ( 19.05341960407611168, 5.049401038298154454, 88.95724293864769550 ) ) ;
#92171 = CARTESIAN_POINT ( 'NONE',  ( 19.02544592524334988, 5.153800228976608722, 56.45942372801898301 ) ) ;
#92172 = CARTESIAN_POINT ( 'NONE',  ( 10.72451020669898902, -18.67979575497178502, 67.91557627198102409 ) ) ;
#92173 = AXIS2_PLACEMENT_3D ( 'NONE', #49542, #92043, #111204 ) ;
#92174 = CARTESIAN_POINT ( 'NONE',  ( 10.72451020669898902, -18.67979575497178502, 112.9155762719810383 ) ) ;
#92175 = CARTESIAN_POINT ( 'NONE',  ( 8.314922557961029526, -14.29746914071037800, 20.41775706135234714 ) ) ;
#92176 = CARTESIAN_POINT ( 'NONE',  ( -4.483927247898782831, 16.52544592524335698, 82.70942372801900433 ) ) ;
#92178 = CARTESIAN_POINT ( 'NONE',  ( 18.67979575497194134, -10.72451020669871369, 25.83442372801901499 ) ) ;
#92177 = CARTESIAN_POINT ( 'NONE',  ( 0.05219959533909260263, 19.03943276465977164, 24.99890960531435269 ) ) ;
#92179 = SHAPE_REPRESENTATION ( 'Rear Air Intake Grille & Cap', ( #82054 ), #24091 ) ;
#92180 = CARTESIAN_POINT ( 'NONE',  ( -19.03943276465977164, 0.05219959533909376836, 21.24890960531436335 ) ) ;
#92181 = CARTESIAN_POINT ( 'NONE',  ( 36.91746824999999177, 2.880721459617395097E-14, -8.124999997268814056 ) ) ;
#92182 = CARTESIAN_POINT ( 'NONE',  ( 14.34966873604972726, -8.224510206698740333, 50.83442372801901143 ) ) ;
#92183 = CARTESIAN_POINT ( 'NONE',  ( 8.314922557960818139, 14.29746914071049879, 84.58224293864769550 ) ) ;
#92184 = CARTESIAN_POINT ( 'NONE',  ( -21.55341960407610458, -5.719274019375992779, 76.45724293864769550 ) ) ;
#92185 = CARTESIAN_POINT ( 'NONE',  ( -16.55341960407617563, 4.379528057220093196, 113.5427570613523756 ) ) ;
#92186 = CARTESIAN_POINT ( 'NONE',  ( -14.29746914071037622, -8.314922557961029526, 34.16775706135234714 ) ) ;
#92187 = CARTESIAN_POINT ( 'NONE',  ( 9.564922557960805705, 16.46253265017160317, 39.58224293864768839 ) ) ;
#92188 = CARTESIAN_POINT ( 'NONE',  ( -8.224510206698735004, -14.34966873604973081, 74.58442372801901854 ) ) ;
#92189 = CARTESIAN_POINT ( 'NONE',  ( -9.474510206698720793, -16.51473224551083518, 74.58442372801900433 ) ) ;
#92190 = CARTESIAN_POINT ( 'NONE',  ( 5.719274019375991003, -21.55341960407610458, 67.70724293864769550 ) ) ;
#92191 = CARTESIAN_POINT ( 'NONE',  ( 8.224510206698742110, 14.34966873604972548, 107.0844237280190043 ) ) ;
#92192 = VERTEX_POINT ( 'NONE', #165779 ) ;
#92193 = CARTESIAN_POINT ( 'NONE',  ( -10.81492255796105439, 18.62759615963255655, 77.91775706135231871 ) ) ;
#92194 = CARTESIAN_POINT ( 'NONE',  ( -5.823673210054116645, -21.52544592524344225, 42.29057627198103120 ) ) ;
#92195 = ORIENTED_EDGE ( 'NONE', *, *, #68319, .F. ) ;
#92196 = ORIENTED_EDGE ( 'NONE', *, *, #188361, .T. ) ;
#92197 = CARTESIAN_POINT ( 'NONE',  ( -8.224510206698735004, -14.34966873604973081, 94.58442372801901854 ) ) ;
#92198 = CARTESIAN_POINT ( 'NONE',  ( -21.53943276465977519, 0.05219959533907696930, 41.24890960531435269 ) ) ;
#92199 = EDGE_LOOP ( 'NONE', ( #174803, #1902, #157346, #24593 ) ) ;
#92200 = CARTESIAN_POINT ( 'NONE',  ( -0.05219959533909027116, -19.03943276465977164, 107.4989096053143527 ) ) ;
#92201 = CARTESIAN_POINT ( 'NONE',  ( 17.49999999999999289, 3.237210098469622377, 107.7876301262046042 ) ) ;
#92202 = CARTESIAN_POINT ( 'NONE',  ( -5.049401038298153566, 19.05341960407611168, 30.20724293864768839 ) ) ;
#92203 = CARTESIAN_POINT ( 'NONE',  ( -0.05219959533907301413, -21.53943276465977519, 77.49890960531433848 ) ) ;
#92204 = CARTESIAN_POINT ( 'NONE',  ( -14.29746914071037622, -8.314922557961029526, 104.1677570613523471 ) ) ;
#92205 = CARTESIAN_POINT ( 'NONE',  ( -0.05219959533937732626, 21.53943276465977519, 62.50109039468568284 ) ) ;
#92206 = CARTESIAN_POINT ( 'NONE',  ( 12.06949235617739724, 12.14591786802326823, 26.87609039468567218 ) ) ;
#92207 = CARTESIAN_POINT ( 'NONE',  ( 16.46253265017160672, -9.564922557960803928, 23.33224293864769194 ) ) ;
#92208 = CARTESIAN_POINT ( 'NONE',  ( 4.483927247898790824, -16.52544592524335698, 20.20942372801900788 ) ) ;
#92209 = CARTESIAN_POINT ( 'NONE',  ( -19.05341960407611168, -5.049401038298163336, 36.45724293864766707 ) ) ;
#92210 = CARTESIAN_POINT ( 'NONE',  ( 23.31738231874054534, 16.94106989632529192, 143.1999999999999886 ) ) ;
#92211 = CARTESIAN_POINT ( 'NONE',  ( -9.474510206698964154, 16.51473224551069663, 110.4155762719810383 ) ) ;
#92212 = CARTESIAN_POINT ( 'NONE',  ( -14.29746914071037622, -8.314922557961029526, 84.16775706135234714 ) ) ;
#92213 = CARTESIAN_POINT ( 'NONE',  ( -0.05219959533936034679, 19.03943276465977164, 82.50109039468567573 ) ) ;
#92214 = CARTESIAN_POINT ( 'NONE',  ( -16.46253265017146816, -9.564922557961047289, 29.16775706135232937 ) ) ;
#92215 = CARTESIAN_POINT ( 'NONE',  ( 10.81492255796078972, 18.62759615963270932, 74.58224293864768129 ) ) ;
#92216 = CARTESIAN_POINT ( 'NONE',  ( -14.29746914071037622, -8.314922557961029526, 99.16775706135234714 ) ) ;
#92217 = CARTESIAN_POINT ( 'NONE',  ( 13.97604488694548053, -13.89961937509957401, 95.62609039468563310 ) ) ;
#92218 = CARTESIAN_POINT ( 'NONE',  ( 5.153800228976335163, 19.02544592524342804, 54.79057627198103120 ) ) ;
#92219 = CARTESIAN_POINT ( 'NONE',  ( 5.049401038298161559, -19.05341960407611168, 87.70724293864769550 ) ) ;
#92220 = CARTESIAN_POINT ( 'NONE',  ( -21.53943276465977519, -0.05219959533937600094, 48.75109039468568284 ) ) ;
#92221 = CARTESIAN_POINT ( 'NONE',  ( -16.46253265017160317, 9.564922557960807481, 50.83224293864770260 ) ) ;
#92222 = CARTESIAN_POINT ( 'NONE',  ( 26.79475375365586132, 2.756753960551091991E-14, 155.0000000000000000 ) ) ;
#92223 = CARTESIAN_POINT ( 'NONE',  ( -13.97604488694527625, -13.89961937509977652, 106.8739096053143669 ) ) ;
#92224 = CARTESIAN_POINT ( 'NONE',  ( -4.483927247898539470, -16.52544592524342804, 62.29057627198102409 ) ) ;
#92225 = CARTESIAN_POINT ( 'NONE',  ( 10.81492255796078972, 18.62759615963270932, 74.58224293864768129 ) ) ;
#92226 = DIRECTION ( 'NONE',  ( -0.000000000000000000, 0.000000000000000000, 1.000000000000000000 ) ) ;
#92227 = CARTESIAN_POINT ( 'NONE',  ( -16.51473224551082808, 9.474510206698731452, 48.33442372801900433 ) ) ;
#92228 = CARTESIAN_POINT ( 'NONE',  ( 16.19135201231354415, -7.376712067591905786, 72.31319145947880145 ) ) ;
#92230 = CARTESIAN_POINT ( 'NONE',  ( 19.03943276465977164, -0.05219959533909143690, 88.74890960531436690 ) ) ;
#92229 = CARTESIAN_POINT ( 'NONE',  ( -9.474510206698964154, 16.51473224551069663, 65.41557627198102409 ) ) ;
#92231 = B_SPLINE_CURVE_WITH_KNOTS ( 'NONE', 3,
 ( #93718, #1709, #153405, #152412, #16890, #46230, #170571, #15899, #183759, #154405, #77557, #78541, #199924, #704, #171568, #105909, #141217, #79548, #167595, #31068, #169571, #123059, #139229, #168572, #32062, #91711, #140216, #2708, #62376, #109884, #92716, #33057, #184745, #29090, #107884, #63385, #125062, #44252, #61387, #94712 ),
 .UNSPECIFIED., .F., .F.,
 ( 4, 2, 2, 2, 2, 2, 2, 2, 2, 2, 2, 2, 2, 2, 2, 2, 2, 2, 2, 4 ),
 ( 0.02146664961600481397, 0.02254346109514428556, 0.02362027257428375715, 0.02415867831385349468, 0.02469708405342323568, 0.02577389553256272461, 0.02685070701170221355, 0.02738911275127196149, 0.02792751849084170596, 0.02900432996998121224, 0.03008114144912071852, 0.03115795292826022828, 0.03223476440739973803, 0.03331157588653924778, 0.03438838736567875753, 0.03546519884481826035, 0.03600360458438801176, 0.03654201032395776316, 0.03761882180309726598, 0.03869563328223676879 ),
 .UNSPECIFIED. ) ;
#92232 = CARTESIAN_POINT ( 'NONE',  ( -12.14591786802326823, 12.06949235617739902, 48.12609039468568284 ) ) ;
#92233 = CARTESIAN_POINT ( 'NONE',  ( 28.90000000000004476, 0.000000000000000000, -52.65483682830183199 ) ) ;
#92234 = CARTESIAN_POINT ( 'NONE',  ( 0.05219959533936267826, -19.03943276465977164, 25.00109039468566152 ) ) ;
#92235 = CARTESIAN_POINT ( 'NONE',  ( 8.906447517083050158, 27.41122689804195645, 145.6500000054623740 ) ) ;
#92236 = CARTESIAN_POINT ( 'NONE',  ( 8.314922557961029526, -14.29746914071037800, 95.41775706135234714 ) ) ;
#92237 = DIRECTION ( 'NONE',  ( 0.000000000000000000, 0.000000000000000000, -1.000000000000000000 ) ) ;
#92238 = CARTESIAN_POINT ( 'NONE',  ( 12.14591786802327356, -12.06949235617739191, 80.62609039468567573 ) ) ;
#92239 = CARTESIAN_POINT ( 'NONE',  ( -8.314922557961024197, 14.29746914071037800, 52.91775706135235424 ) ) ;
#92240 = CARTESIAN_POINT ( 'NONE',  ( -18.67979575497193778, 10.72451020669871902, 113.3344237280190328 ) ) ;
#92242 = CARTESIAN_POINT ( 'NONE',  ( -17.49999999999999645, -5.499999999999992895, 59.20309617465829177 ) ) ;
#92241 = CARTESIAN_POINT ( 'NONE',  ( -19.03943276465977164, 0.05219959533909376836, 61.24890960531436690 ) ) ;
#92243 = CARTESIAN_POINT ( 'NONE',  ( -0.05219959533937732626, 21.53943276465977519, 72.50109039468568994 ) ) ;
#92244 = CARTESIAN_POINT ( 'NONE',  ( 16.46253265017146816, 9.564922557961045513, 81.66775706135233293 ) ) ;
#92245 = CARTESIAN_POINT ( 'NONE',  ( -15.72974639402176322, -15.80617190586768395, 104.3760903946856899 ) ) ;
#92246 = AXIS2_PLACEMENT_3D ( 'NONE', #159313, #144150, #162324 ) ;
#92247 = CARTESIAN_POINT ( 'NONE',  ( 13.97604488694527802, 13.89961937509977652, 24.37390960531435624 ) ) ;
#92248 = CARTESIAN_POINT ( 'NONE',  ( -37.99533089065118219, -0.2660902954431525469, -7.999999999999996447 ) ) ;
#92249 = CARTESIAN_POINT ( 'NONE',  ( -18.67979575497178146, -10.72451020669898902, 66.66557627198102409 ) ) ;
#92250 = EDGE_CURVE ( 'NONE', #164346, #515, #27274, .T. ) ;
#92251 = CARTESIAN_POINT ( 'NONE',  ( -15.72974639402197994, 15.80617190586746368, 25.62390960531435624 ) ) ;
#92252 = CARTESIAN_POINT ( 'NONE',  ( -16.55341960407611168, -4.379528057220339221, 111.4572429386476813 ) ) ;
#92253 = CARTESIAN_POINT ( 'NONE',  ( 12.14591786802327356, -12.06949235617739191, 35.62609039468568994 ) ) ;
#92254 = CARTESIAN_POINT ( 'NONE',  ( 12.14591786802309770, 12.06949235617756955, 34.37390960531435979 ) ) ;
#92255 = ORIENTED_EDGE ( 'NONE', *, *, #36295, .T. ) ;
#92256 = CARTESIAN_POINT ( 'NONE',  ( -5.823673210054116645, -21.52544592524344225, 112.2905762719810241 ) ) ;
#92258 = CARTESIAN_POINT ( 'NONE',  ( 37.99999999999999289, 2.893978650043524126E-14, -7.000000000000000000 ) ) ;
#92257 = CARTESIAN_POINT ( 'NONE',  ( 8.224510206698953496, -14.34966873604960469, 57.91557627198103120 ) ) ;
#92259 = CARTESIAN_POINT ( 'NONE',  ( -19.05341960407617563, 5.049401038297882671, 113.5427570613523471 ) ) ;
#92260 = CARTESIAN_POINT ( 'NONE',  ( -19.03943276465977164, -0.05219959533935918106, 28.75109039468566507 ) ) ;
#92261 = CARTESIAN_POINT ( 'NONE',  ( 16.52544592524342804, -4.483927247898539470, 43.54057627198103830 ) ) ;
#92262 = CARTESIAN_POINT ( 'NONE',  ( 21.52544592524344225, -5.823673210054117533, 108.5405762719810241 ) ) ;
#92264 = CARTESIAN_POINT ( 'NONE',  ( -18.62759615963270932, 10.81492255796079327, 65.83224293864769550 ) ) ;
#92263 = CYLINDRICAL_SURFACE ( 'NONE', #192437, 38.00000000000000000 ) ;
#92265 = CARTESIAN_POINT ( 'NONE',  ( -9.474510206698964154, 16.51473224551069663, 75.41557627198103830 ) ) ;
#92266 = CARTESIAN_POINT ( 'NONE',  ( -14.29746914071049879, 8.314922557960819915, 50.83224293864770971 ) ) ;
#92267 = CARTESIAN_POINT ( 'NONE',  ( 19.02544592524343514, -5.153800228976328945, 98.54057627198100988 ) ) ;
#92268 = CARTESIAN_POINT ( 'NONE',  ( -36.79349492566039714, 4.147684444183149743, 48.62988885745599532 ) ) ;
#92269 = CARTESIAN_POINT ( 'NONE',  ( 9.564922557961047289, -16.46253265017146816, 60.41775706135233293 ) ) ;
#92270 = CARTESIAN_POINT ( 'NONE',  ( 21.53943276465977519, -0.05219959533907433946, 98.74890960531438111 ) ) ;
#92271 = CARTESIAN_POINT ( 'NONE',  ( -5.049401038298153566, 19.05341960407611168, 45.20724293864769550 ) ) ;
#92272 = CARTESIAN_POINT ( 'NONE',  ( -16.53943276465976808, 0.05219959533911058130, 111.2489096053143669 ) ) ;
#92273 = CARTESIAN_POINT ( 'NONE',  ( 5.719274019375673035, 21.55341960407619339, 47.29275706135234003 ) ) ;
#92274 = CARTESIAN_POINT ( 'NONE',  ( 27.73933785331498569, 2.768321779492822058E-14, 147.8750000027311842 ) ) ;
#92275 = CARTESIAN_POINT ( 'NONE',  ( -12.06949235617756955, 12.14591786802309770, 30.62390960531436335 ) ) ;
#92276 = CARTESIAN_POINT ( 'NONE',  ( -19.05341960407611168, -5.049401038298163336, 46.45724293864768129 ) ) ;
#92277 = CARTESIAN_POINT ( 'NONE',  ( 9.474510206698971260, -16.51473224551069308, 102.9155762719810241 ) ) ;
#92278 = CARTESIAN_POINT ( 'NONE',  ( 5.823673210054125526, 21.52544592524343514, 64.79057627198103830 ) ) ;
#92279 = CARTESIAN_POINT ( 'NONE',  ( -19.49149378614658090, 5.499999999999782396, 44.43757513605364551 ) ) ;
#92280 = CARTESIAN_POINT ( 'NONE',  ( 5.153800228976335163, 19.02544592524342804, 39.79057627198100988 ) ) ;
#92281 = CARTESIAN_POINT ( 'NONE',  ( 10.72451020669898902, -18.67979575497178502, 57.91557627198103120 ) ) ;
#92282 = ADVANCED_FACE ( 'NONE', ( #58582, #79715 ), #123217, .F. ) ;
#92283 = CARTESIAN_POINT ( 'NONE',  ( -10.72451020669870658, -18.67979575497194134, 84.58442372801903275 ) ) ;
#92285 = CARTESIAN_POINT ( 'NONE',  ( 8.224510206698742110, 14.34966873604972548, 77.08442372801901854 ) ) ;
#92284 = CARTESIAN_POINT ( 'NONE',  ( 11.44429459766798729, -35.82063519324240275, -30.53178620540658983 ) ) ;
#92286 = CARTESIAN_POINT ( 'NONE',  ( -14.29746914071037622, -8.314922557961029526, 94.16775706135237556 ) ) ;
#92287 = CARTESIAN_POINT ( 'NONE',  ( -16.51473224551069308, -9.474510206698971260, 51.66557627198102409 ) ) ;
#92288 = CARTESIAN_POINT ( 'NONE',  ( -16.51473224551069308, -9.474510206698971260, 71.66557627198102409 ) ) ;
#92289 = ORIENTED_EDGE ( 'NONE', *, *, #163088, .F. ) ;
#92290 = CARTESIAN_POINT ( 'NONE',  ( 0.05219959533936267826, -19.03943276465977164, 25.00109039468566152 ) ) ;
#92291 = CARTESIAN_POINT ( 'NONE',  ( -4.379528057220086978, -16.55341960407618274, 79.79275706135236135 ) ) ;
#92292 = CARTESIAN_POINT ( 'NONE',  ( 15.80617190586769283, -15.72974639402175789, 110.6260903946857042 ) ) ;
#92293 = CARTESIAN_POINT ( 'NONE',  ( 9.474510206698971260, -16.51473224551069308, 72.91557627198102409 ) ) ;
#92294 = CARTESIAN_POINT ( 'NONE',  ( 5.823673210054125526, 21.52544592524343514, 54.79057627198104541 ) ) ;
#92295 = CARTESIAN_POINT ( 'NONE',  ( 8.314922557961029526, -14.29746914071037800, 30.41775706135234358 ) ) ;
#92296 = CARTESIAN_POINT ( 'NONE',  ( -10.72451020669870658, -18.67979575497194134, 84.58442372801903275 ) ) ;
#92297 = CARTESIAN_POINT ( 'NONE',  ( -4.379528057220086978, -16.55341960407618274, 44.79275706135234714 ) ) ;
#92298 = CARTESIAN_POINT ( 'NONE',  ( -0.05219959533907301413, -21.53943276465977519, 107.4989096053143669 ) ) ;
#92299 = CARTESIAN_POINT ( 'NONE',  ( -16.52544592524335698, -4.483927247898792601, 18.95942372801901143 ) ) ;
#92301 = EDGE_CURVE ( 'NONE', #129957, #68554, #106772, .T. ) ;
#92300 = CARTESIAN_POINT ( 'NONE',  ( -0.05219959533909027116, -19.03943276465977164, 82.49890960531436690 ) ) ;
#92302 = CARTESIAN_POINT ( 'NONE',  ( 14.34966873604972726, -8.224510206698740333, 30.83442372801902209 ) ) ;
#92303 = CARTESIAN_POINT ( 'NONE',  ( -19.02544592524342804, 5.153800228976336051, 46.04057627198101699 ) ) ;
#92304 = CARTESIAN_POINT ( 'NONE',  ( -16.52544592524335698, -4.483927247898792601, 23.95942372801901143 ) ) ;
#92305 = CARTESIAN_POINT ( 'NONE',  ( -16.52544592524342804, 4.483927247898546575, 76.04057627198102409 ) ) ;
#92306 = CARTESIAN_POINT ( 'NONE',  ( 14.29746914071037800, 8.314922557961029526, 81.66775706135236135 ) ) ;
#92308 = CARTESIAN_POINT ( 'NONE',  ( 0.05219959533909260263, 19.03943276465977164, 59.99890960531436690 ) ) ;
#92307 = CARTESIAN_POINT ( 'NONE',  ( -21.53943276465977519, -0.05219959533937600094, 28.75109039468567929 ) ) ;
#92309 = CARTESIAN_POINT ( 'NONE',  ( 9.564922557960805705, 16.46253265017160317, 74.58224293864769550 ) ) ;
#92310 = CARTESIAN_POINT ( 'NONE',  ( 14.34966873604972726, -8.224510206698740333, 85.83442372801901854 ) ) ;
#92312 = ORIENTED_EDGE ( 'NONE', *, *, #27194, .T. ) ;
#92311 = CARTESIAN_POINT ( 'NONE',  ( -24.79447686064995438, -6.332871904607631386, 168.1804317516292997 ) ) ;
#92313 = EDGE_LOOP ( 'NONE', ( #37743, #59971 ) ) ;
#92314 = CARTESIAN_POINT ( 'NONE',  ( 9.564922557961047289, -16.46253265017146816, 35.41775706135233293 ) ) ;
#92315 = CARTESIAN_POINT ( 'NONE',  ( -19.03943276465977164, 0.05219959533909376836, 41.24890960531435269 ) ) ;
#92317 = ORIENTED_EDGE ( 'NONE', *, *, #177190, .T. ) ;
#92316 = CARTESIAN_POINT ( 'NONE',  ( 19.02544592524343514, -5.153800228976328945, 113.5405762719810241 ) ) ;
#92318 = CARTESIAN_POINT ( 'NONE',  ( -12.14591786802326823, 12.06949235617739902, 23.12609039468567573 ) ) ;
#92320 = CARTESIAN_POINT ( 'NONE',  ( 16.55341960407618274, -4.379528057220086978, 41.04275706135236135 ) ) ;
#92319 = CARTESIAN_POINT ( 'NONE',  ( 16.51473224551083163, -9.474510206698727899, 55.83442372801899722 ) ) ;
#92321 = CARTESIAN_POINT ( 'NONE',  ( -13.97604488694527625, -13.89961937509977652, 111.8739096053143243 ) ) ;
#92322 = CARTESIAN_POINT ( 'NONE',  ( -16.51473224551069308, -9.474510206698971260, 66.66557627198102409 ) ) ;
#92323 = CARTESIAN_POINT ( 'NONE',  ( -5.719274019375978568, 21.55341960407610458, 105.2072429386477097 ) ) ;
#92325 = CARTESIAN_POINT ( 'NONE',  ( 9.474510206698971260, -16.51473224551069308, 22.91557627198102765 ) ) ;
#92324 = CARTESIAN_POINT ( 'NONE',  ( 19.02544592524343514, -5.153800228976328945, 98.54057627198100988 ) ) ;
#92326 = CARTESIAN_POINT ( 'NONE',  ( 9.474510206698971260, -16.51473224551069308, 67.91557627198102409 ) ) ;
#92328 = CARTESIAN_POINT ( 'NONE',  ( 9.564922557960805705, 16.46253265017160317, 29.58224293864769550 ) ) ;
#92327 = CARTESIAN_POINT ( 'NONE',  ( -16.53943276465976808, 0.05219959533911058130, 26.24890960531435624 ) ) ;
#92329 = CARTESIAN_POINT ( 'NONE',  ( -5.049401038297874678, -19.05341960407617918, 39.79275706135232582 ) ) ;
#92330 = CARTESIAN_POINT ( 'NONE',  ( -8.314922557960811034, -14.29746914071050412, 57.08224293864769550 ) ) ;
#92331 = CARTESIAN_POINT ( 'NONE',  ( -21.52544592524334988, -5.823673210054445271, 103.9594237280190185 ) ) ;
#92332 = CARTESIAN_POINT ( 'NONE',  ( 16.46253265017160672, -9.564922557960803928, 38.33224293864768839 ) ) ;
#92333 = CARTESIAN_POINT ( 'NONE',  ( 8.314922557961029526, -14.29746914071037800, 50.41775706135235424 ) ) ;
#92335 = CARTESIAN_POINT ( 'NONE',  ( 21.52544592524334988, 5.823673210054432836, 86.45942372801901854 ) ) ;
#92334 = CARTESIAN_POINT ( 'NONE',  ( 16.55341960407611168, 4.379528057220329451, 38.95724293864768839 ) ) ;
#92336 = CARTESIAN_POINT ( 'NONE',  ( 19.05341960407611168, 5.049401038298154454, 78.95724293864769550 ) ) ;
#92337 = CARTESIAN_POINT ( 'NONE',  ( -16.51473224551069308, -9.474510206698971260, 96.66557627198102409 ) ) ;
#92338 = CARTESIAN_POINT ( 'NONE',  ( 12.14591786802309770, 12.06949235617756955, 104.3739096053143669 ) ) ;
#92339 = CARTESIAN_POINT ( 'NONE',  ( 14.34966873604960469, 8.224510206698951720, 74.16557627198102409 ) ) ;
#92340 = CARTESIAN_POINT ( 'NONE',  ( -10.72451020669898014, 18.67979575497178502, 90.41557627198103830 ) ) ;
#92341 = CARTESIAN_POINT ( 'NONE',  ( 19.03943276465977164, -0.05219959533909143690, 88.74890960531436690 ) ) ;
#92342 = CARTESIAN_POINT ( 'NONE',  ( 21.53943276465977519, -0.05219959533907433946, 93.74890960531436690 ) ) ;
#92343 = CARTESIAN_POINT ( 'NONE',  ( 16.46253265017146816, 9.564922557961045513, 76.66775706135234714 ) ) ;
#92346 = CARTESIAN_POINT ( 'NONE',  ( 16.55341960407611168, 4.379528057220329451, 93.95724293864770971 ) ) ;
#92345 = CARTESIAN_POINT ( 'NONE',  ( -16.46253265017146816, -9.564922557961047289, 64.16775706135233293 ) ) ;
#92344 = CIRCLE ( 'NONE', #5167, 0.5000000000000004441 ) ;
#92347 = CARTESIAN_POINT ( 'NONE',  ( -16.51473224551069308, -9.474510206698971260, 51.66557627198102409 ) ) ;
#92348 = CARTESIAN_POINT ( 'NONE',  ( 5.823673210054125526, 21.52544592524343514, 69.79057627198102409 ) ) ;
#92349 = CARTESIAN_POINT ( 'NONE',  ( 17.50000000000000711, -5.622605283950868227, 26.18792689403890606 ) ) ;
#92350 = CARTESIAN_POINT ( 'NONE',  ( -16.55341960407617563, 4.379528057220093196, 113.5427570613523756 ) ) ;
#92351 = CARTESIAN_POINT ( 'NONE',  ( 14.34966873604972726, -8.224510206698740333, 20.83442372801901143 ) ) ;
#92352 = CARTESIAN_POINT ( 'NONE',  ( -12.06949235617756955, 12.14591786802309770, 75.62390960531439532 ) ) ;
#92353 = CARTESIAN_POINT ( 'NONE',  ( -9.656827144875922642, -71.74905178543390605, -15.00000000000000000 ) ) ;
#92354 = CARTESIAN_POINT ( 'NONE',  ( 16.46253265017160672, -9.564922557960803928, 68.33224293864770971 ) ) ;
#92355 = CARTESIAN_POINT ( 'NONE',  ( -0.05219959533909027116, -19.03943276465977164, 37.49890960531436690 ) ) ;
#92356 = CARTESIAN_POINT ( 'NONE',  ( 12.14591786802309770, 12.06949235617756955, 64.37390960531435269 ) ) ;
#92357 = CARTESIAN_POINT ( 'NONE',  ( -10.72451020669898014, 18.67979575497178502, 25.41557627198103120 ) ) ;
#92358 = CARTESIAN_POINT ( 'NONE',  ( -13.97604488694547697, 13.89961937509957934, 93.12609039468566152 ) ) ;
#92359 = CARTESIAN_POINT ( 'NONE',  ( 9.564922557960805705, 16.46253265017160317, 104.5822429386476955 ) ) ;
#92360 = CARTESIAN_POINT ( 'NONE',  ( -21.52544592524343514, 5.823673210054127303, 71.04057627198103830 ) ) ;
#92361 = CARTESIAN_POINT ( 'NONE',  ( 4.483927247898790824, -16.52544592524335698, 65.20942372801901854 ) ) ;
#92362 = CARTESIAN_POINT ( 'NONE',  ( -16.79531203550683927, 7.028104445595290350, 93.74755011779544134 ) ) ;
#92363 = CARTESIAN_POINT ( 'NONE',  ( 9.564922557960805705, 16.46253265017160317, 64.58224293864769550 ) ) ;
#92364 = CARTESIAN_POINT ( 'NONE',  ( -10.81492255796078084, -18.62759615963271287, 62.08224293864769550 ) ) ;
#92365 = CARTESIAN_POINT ( 'NONE',  ( -16.52544592524335698, -4.483927247898792601, 18.95942372801901143 ) ) ;
#92367 = CARTESIAN_POINT ( 'NONE',  ( 5.823673210054444382, -21.52544592524334988, 65.20942372801901854 ) ) ;
#92366 = CARTESIAN_POINT ( 'NONE',  ( -8.224510206698948167, 14.34966873604960824, 35.41557627198102409 ) ) ;
#92368 = CARTESIAN_POINT ( 'NONE',  ( -28.82186960331508985, -9.364793116373393289, 144.3500000054623627 ) ) ;
#92370 = CARTESIAN_POINT ( 'NONE',  ( -16.46253265017160317, 9.564922557960807481, 105.8322429386476955 ) ) ;
#92369 = CARTESIAN_POINT ( 'NONE',  ( 8.224510206698742110, 14.34966873604972548, 72.08442372801899012 ) ) ;
#92371 = CARTESIAN_POINT ( 'NONE',  ( 16.46253265017160672, -9.564922557960803928, 103.3322429386476955 ) ) ;
#92372 = CARTESIAN_POINT ( 'NONE',  ( -17.48853670773246449, 5.747243402303040760, 78.66671299749995683 ) ) ;
#92373 = CARTESIAN_POINT ( 'NONE',  ( -16.52544592524335698, -4.483927247898792601, 93.95942372801903275 ) ) ;
#92374 = CARTESIAN_POINT ( 'NONE',  ( -8.314922557961024197, 14.29746914071037800, 52.91775706135235424 ) ) ;
#92375 = CARTESIAN_POINT ( 'NONE',  ( 9.474510206698971260, -16.51473224551069308, 52.91557627198102409 ) ) ;
#92376 = CARTESIAN_POINT ( 'NONE',  ( -19.05341960407611168, -5.049401038298163336, 76.45724293864769550 ) ) ;
#92377 = CARTESIAN_POINT ( 'NONE',  ( 5.719274019375673035, 21.55341960407619339, 52.29275706135236135 ) ) ;
#92378 = CARTESIAN_POINT ( 'NONE',  ( 16.55341960407618274, -4.379528057220086978, 56.04275706135235424 ) ) ;
#92379 = CARTESIAN_POINT ( 'NONE',  ( 12.06949235617757843, -12.14591786802309237, 28.12390960531435979 ) ) ;
#92380 = CARTESIAN_POINT ( 'NONE',  ( -16.51473224551069308, -9.474510206698971260, 36.66557627198102409 ) ) ;
#92381 = CARTESIAN_POINT ( 'NONE',  ( -13.97604488694527625, -13.89961937509977652, 31.87390960531435979 ) ) ;
#92382 = CARTESIAN_POINT ( 'NONE',  ( -16.52544592524335698, -4.483927247898792601, 33.95942372801901143 ) ) ;
#92383 = CARTESIAN_POINT ( 'NONE',  ( 9.474510206698729675, 16.51473224551082808, 82.08442372801899012 ) ) ;
#92384 = CARTESIAN_POINT ( 'NONE',  ( 14.29746914071049879, -8.314922557960816363, 78.33224293864770971 ) ) ;
#92385 = CARTESIAN_POINT ( 'NONE',  ( -0.05219959533909027116, -19.03943276465977164, 47.49890960531435979 ) ) ;
#92387 = CARTESIAN_POINT ( 'NONE',  ( -3.573655867282028392E-15, 2.428612866367529932E-14, 2.000000000000000000 ) ) ;
#92386 = CARTESIAN_POINT ( 'NONE',  ( 19.03943276465977164, 0.05219959533936151252, 81.25109039468567573 ) ) ;
#92388 = CARTESIAN_POINT ( 'NONE',  ( -10.72451020669870658, -18.67979575497194134, 84.58442372801903275 ) ) ;
#92389 = CARTESIAN_POINT ( 'NONE',  ( -16.52544592524335698, -4.483927247898792601, 48.95942372801902565 ) ) ;
#92390 = CARTESIAN_POINT ( 'NONE',  ( -17.50000000000003197, 4.640572885337592268, 25.63788164548845572 ) ) ;
#92391 = CARTESIAN_POINT ( 'NONE',  ( 10.81492255796078972, 18.62759615963270932, 49.58224293864769550 ) ) ;
#92392 = CARTESIAN_POINT ( 'NONE',  ( -12.06949235617739369, -12.14591786802326823, 39.37609039468567573 ) ) ;
#92393 = CARTESIAN_POINT ( 'NONE',  ( -19.25663599770060941, 5.499999999999443112, 68.99419308057200340 ) ) ;
#92394 = CARTESIAN_POINT ( 'NONE',  ( 13.89961937509957401, 13.97604488694547697, 36.87609039468565442 ) ) ;
#92395 = CIRCLE ( 'NONE', #144056, 0.5000000000000004441 ) ;
#92396 = CARTESIAN_POINT ( 'NONE',  ( 5.049401038298161559, -19.05341960407611168, 92.70724293864769550 ) ) ;
#92397 = CARTESIAN_POINT ( 'NONE',  ( 13.89961937509977652, -13.97604488694527269, 48.12390960531435979 ) ) ;
#92398 = DIRECTION ( 'NONE',  ( 0.000000000000000000, 0.000000000000000000, -1.000000000000000000 ) ) ;
#92399 = CARTESIAN_POINT ( 'NONE',  ( 5.823673210054444382, -21.52544592524334988, 75.20942372801901854 ) ) ;
#92400 = CARTESIAN_POINT ( 'NONE',  ( 2.500000000000000000, -1.768423874527825124, -1.020999999999998575 ) ) ;
#92401 = CARTESIAN_POINT ( 'NONE',  ( 19.05341960407617918, -5.049401038297876454, 36.04275706135234003 ) ) ;
#92402 = CARTESIAN_POINT ( 'NONE',  ( 5.823673210054444382, -21.52544592524334988, 110.2094237280190185 ) ) ;
#92403 = CARTESIAN_POINT ( 'NONE',  ( 4.379528057220339221, -16.55341960407611168, 42.70724293864770260 ) ) ;
#92404 = CARTESIAN_POINT ( 'NONE',  ( -5.153800228976328057, -19.02544592524343514, 42.29057627198101699 ) ) ;
#92405 = CARTESIAN_POINT ( 'NONE',  ( 19.05341960407611168, 5.049401038298154454, 103.9572429386476671 ) ) ;
#92406 = CARTESIAN_POINT ( 'NONE',  ( 21.52544592524334988, 5.823673210054432836, 81.45942372801900433 ) ) ;
#92407 = CARTESIAN_POINT ( 'NONE',  ( 9.474510206698971260, -16.51473224551069308, 67.91557627198102409 ) ) ;
#92408 = CARTESIAN_POINT ( 'NONE',  ( -18.62759615963255300, -10.81492255796106328, 79.16775706135234714 ) ) ;
#92409 = CARTESIAN_POINT ( 'NONE',  ( 0.05219959533907565091, 21.53943276465977519, 34.99890960531435979 ) ) ;
#92410 = CARTESIAN_POINT ( 'NONE',  ( -10.72451020669870658, -18.67979575497194134, 24.58442372801901499 ) ) ;
#92411 = CARTESIAN_POINT ( 'NONE',  ( -5.049401038297874678, -19.05341960407617918, 44.79275706135232582 ) ) ;
#92412 = CARTESIAN_POINT ( 'NONE',  ( 19.02544592524343514, -5.153800228976328945, 23.54057627198102054 ) ) ;
#92413 = CARTESIAN_POINT ( 'NONE',  ( 5.153800228976335163, 19.02544592524342804, 69.79057627198103830 ) ) ;
#92414 = CARTESIAN_POINT ( 'NONE',  ( 14.29746914071037800, 8.314922557961029526, 26.66775706135235424 ) ) ;
#92415 = CARTESIAN_POINT ( 'NONE',  ( 14.34966873604960469, 8.224510206698951720, 89.16557627198102409 ) ) ;
#92416 = CARTESIAN_POINT ( 'NONE',  ( -0.05219959533909027116, -19.03943276465977164, 52.49890960531436690 ) ) ;
#92417 = CARTESIAN_POINT ( 'NONE',  ( -21.55341960407610458, -5.719274019375992779, 41.45724293864769550 ) ) ;
#92418 = CARTESIAN_POINT ( 'NONE',  ( 0.05219959533936267826, -19.03943276465977164, 105.0010903946856615 ) ) ;
#92419 = CARTESIAN_POINT ( 'NONE',  ( -21.53943276465977519, 0.05219959533907696930, 111.2489096053143669 ) ) ;
#92420 = CARTESIAN_POINT ( 'NONE',  ( 21.52544592524334988, 5.823673210054432836, 56.45942372801902565 ) ) ;
#92421 = CARTESIAN_POINT ( 'NONE',  ( 14.34966873604972726, -8.224510206698740333, 70.83442372801901854 ) ) ;
#92422 = CARTESIAN_POINT ( 'NONE',  ( -16.55341960407617563, 4.379528057220093196, 63.54275706135234003 ) ) ;
#92423 = ORIENTED_EDGE ( 'NONE', *, *, #153922, .F. ) ;
#92424 = CARTESIAN_POINT ( 'NONE',  ( -16.46253265017160317, 9.564922557960807481, 65.83224293864769550 ) ) ;
#92425 = CARTESIAN_POINT ( 'NONE',  ( -16.52544592524335698, -4.483927247898792601, 88.95942372801901854 ) ) ;
#92426 = CARTESIAN_POINT ( 'NONE',  ( -21.53943276465977519, -0.05219959533937600094, 18.75109039468568639 ) ) ;
#92427 = CARTESIAN_POINT ( 'NONE',  ( 0.05219959533910956823, 16.53943276465976808, 69.99890960531435269 ) ) ;
#92428 = CARTESIAN_POINT ( 'NONE',  ( 16.46253265017160672, -9.564922557960803928, 88.33224293864769550 ) ) ;
#92429 = CARTESIAN_POINT ( 'NONE',  ( 16.52544592524335698, 4.483927247898782831, 76.45942372801901854 ) ) ;
#92430 = CARTESIAN_POINT ( 'NONE',  ( 15.80617190586769283, -15.72974639402175789, 60.62609039468567573 ) ) ;
#92431 = CARTESIAN_POINT ( 'NONE',  ( 13.97604488694548053, -13.89961937509957401, 110.6260903946856615 ) ) ;
#92432 = CARTESIAN_POINT ( 'NONE',  ( 0.05219959533907565091, 21.53943276465977519, 114.9989096053143669 ) ) ;
#92433 = CARTESIAN_POINT ( 'NONE',  ( 12.14591786802309770, 12.06949235617756955, 59.37390960531436690 ) ) ;
#92434 = EDGE_LOOP ( 'NONE', ( #194625, #117206, #78635, #180537 ) ) ;
#92435 =( BOUNDED_CURVE ( )  B_SPLINE_CURVE ( 2, ( #8210, #176074, #22386, #68880, #116384, #129532, #147737, #158885, #37542, #53718, #6199 ),
 .UNSPECIFIED., .F., .T. ) 
 B_SPLINE_CURVE_WITH_KNOTS ( ( 3, 2, 2, 2, 2, 3 ),
 ( 0.3000000000000000444, 0.3200000000000000622, 0.3400000000000000799, 0.3599999999999999867, 0.3800000000000000044, 0.4000000000000000222 ),
 .UNSPECIFIED. ) 
 CURVE ( )  GEOMETRIC_REPRESENTATION_ITEM ( )  RATIONAL_B_SPLINE_CURVE ( ( 0.9999999999999998890, 0.9510565162951536422, 1.000000000000000000, 0.9510565162951535312, 1.000000000000000000, 0.9510565162951535312, 1.000000000000000000, 0.9510565162951535312, 1.000000000000000000, 0.9510565162951535312, 1.000000000000000000 ) ) 
 REPRESENTATION_ITEM ( '' )  );
#92436 = CARTESIAN_POINT ( 'NONE',  ( 5.719274019375991003, -21.55341960407610458, 87.70724293864769550 ) ) ;
#92437 = CARTESIAN_POINT ( 'NONE',  ( 14.29746914071049879, -8.314922557960816363, 38.33224293864768839 ) ) ;
#92438 = ORIENTED_EDGE ( 'NONE', *, *, #193497, .F. ) ;
#92439 = CARTESIAN_POINT ( 'NONE',  ( 35.52763170759349265, 3.100152895725894808, 38.16632899394347334 ) ) ;
#92440 = CARTESIAN_POINT ( 'NONE',  ( 18.67979575497194134, -10.72451020669871369, 20.83442372801901143 ) ) ;
#92441 = CARTESIAN_POINT ( 'NONE',  ( -0.05219959533907301413, -21.53943276465977519, 22.49890960531436335 ) ) ;
#92442 = CARTESIAN_POINT ( 'NONE',  ( 10.72451020669871369, 18.67979575497193778, 32.08442372801901854 ) ) ;
#92443 = CARTESIAN_POINT ( 'NONE',  ( 0.05219959533910956823, 16.53943276465976808, 44.99890960531435979 ) ) ;
#92444 = CARTESIAN_POINT ( 'NONE',  ( -4.483927247898782831, 16.52544592524335698, 57.70942372801901143 ) ) ;
#92445 = CARTESIAN_POINT ( 'NONE',  ( -19.03943276465977164, 0.05219959533909376836, 61.24890960531436690 ) ) ;
#92446 = CARTESIAN_POINT ( 'NONE',  ( 9.564922557961047289, -16.46253265017146816, 60.41775706135233293 ) ) ;
#92447 = CARTESIAN_POINT ( 'NONE',  ( -9.564922557960796823, -16.46253265017161027, 92.08224293864769550 ) ) ;
#92448 = CARTESIAN_POINT ( 'NONE',  ( 15.80617190586746368, 15.72974639402197994, 54.37390960531435979 ) ) ;
#92449 = CARTESIAN_POINT ( 'NONE',  ( -12.81081878835845522, -36.21111560917540828, -23.25335493477762583 ) ) ;
#92450 = CARTESIAN_POINT ( 'NONE',  ( -5.153800228976328057, -19.02544592524343514, 52.29057627198100988 ) ) ;
#92451 = CARTESIAN_POINT ( 'NONE',  ( -8.224510206698735004, -14.34966873604973081, 39.58442372801901143 ) ) ;
#92452 = CARTESIAN_POINT ( 'NONE',  ( -16.51473224551082808, 9.474510206698731452, 58.33442372801900433 ) ) ;
#92453 = CARTESIAN_POINT ( 'NONE',  ( 0.05219959533937995610, -21.53943276465977519, 20.00109039468568639 ) ) ;
#92454 = CARTESIAN_POINT ( 'NONE',  ( 12.06949235617757843, -12.14591786802309237, 43.12390960531435269 ) ) ;
#92455 = CARTESIAN_POINT ( 'NONE',  ( 13.97604488694527802, 13.89961937509977652, 84.37390960531433848 ) ) ;
#92456 = CARTESIAN_POINT ( 'NONE',  ( -10.72451020669898014, 18.67979575497178502, 60.41557627198102409 ) ) ;
#92458 = CARTESIAN_POINT ( 'NONE',  ( 14.29746914071037800, 8.314922557961029526, 41.66775706135235424 ) ) ;
#92457 = CARTESIAN_POINT ( 'NONE',  ( 21.55341960407610458, 5.719274019375980345, 93.95724293864770971 ) ) ;
#92459 = CARTESIAN_POINT ( 'NONE',  ( -10.72451020669898014, 18.67979575497178502, 35.41557627198102409 ) ) ;
#92460 = CARTESIAN_POINT ( 'NONE',  ( -21.52544592524334988, -5.823673210054445271, 88.95942372801901854 ) ) ;
#92461 = CARTESIAN_POINT ( 'NONE',  ( 9.564922557960805705, 16.46253265017160317, 84.58224293864769550 ) ) ;
#92462 = CARTESIAN_POINT ( 'NONE',  ( 19.02544592524343514, -5.153800228976328945, 38.54057627198103120 ) ) ;
#92463 = CARTESIAN_POINT ( 'NONE',  ( -5.153800228976328057, -19.02544592524343514, 92.29057627198099567 ) ) ;
#92464 = CARTESIAN_POINT ( 'NONE',  ( 0.05219959533910956823, 16.53943276465976808, 104.9989096053143669 ) ) ;
#92465 = CARTESIAN_POINT ( 'NONE',  ( 9.474510206698971260, -16.51473224551069308, 67.91557627198102409 ) ) ;
#92466 = CARTESIAN_POINT ( 'NONE',  ( -16.55341960407617563, 4.379528057220093196, 28.54275706135234358 ) ) ;
#92467 = CARTESIAN_POINT ( 'NONE',  ( -9.564922557961040184, 16.46253265017147172, 42.91775706135234003 ) ) ;
#92468 = CARTESIAN_POINT ( 'NONE',  ( -0.05219959533936034679, 19.03943276465977164, 57.50109039468566863 ) ) ;
#92470 = CARTESIAN_POINT ( 'NONE',  ( 18.62759615963271287, -10.81492255796078972, 28.33224293864769550 ) ) ;
#92469 = CARTESIAN_POINT ( 'NONE',  ( 18.62759615963255655, 10.81492255796105972, 101.6677570613523613 ) ) ;
#92471 = CARTESIAN_POINT ( 'NONE',  ( 0.05219959533934541429, -16.53943276465976808, 95.00109039468568994 ) ) ;
#92472 = FACE_OUTER_BOUND ( 'NONE', #163714, .T. ) ;
#92473 = CARTESIAN_POINT ( 'NONE',  ( 19.05341960407617918, -5.049401038297876454, 76.04275706135230450 ) ) ;
#92474 = CARTESIAN_POINT ( 'NONE',  ( 13.97604488694548053, -13.89961937509957401, 35.62609039468567573 ) ) ;
#92475 = DIRECTION ( 'NONE',  ( 0.7071067811865512365, 0.7071067811865439090, -0.000000000000000000 ) ) ;
#92476 = CARTESIAN_POINT ( 'NONE',  ( 5.049401038298161559, -19.05341960407611168, 27.70724293864769550 ) ) ;
#92477 = CARTESIAN_POINT ( 'NONE',  ( -0.05219959533910754901, -16.53943276465976808, 32.49890960531435979 ) ) ;
#92478 = CARTESIAN_POINT ( 'NONE',  ( 5.049401038298161559, -19.05341960407611168, 22.70724293864769194 ) ) ;
#92479 = CARTESIAN_POINT ( 'NONE',  ( -4.379528057220328563, 16.55341960407611168, 30.20724293864769550 ) ) ;
#92480 = CARTESIAN_POINT ( 'NONE',  ( 17.50000000000000000, -5.500000000000000888, 120.0000000000000142 ) ) ;
#92481 = CARTESIAN_POINT ( 'NONE',  ( -0.05219959533934338120, 16.53943276465976808, 97.50109039468567573 ) ) ;
#92482 = CARTESIAN_POINT ( 'NONE',  ( -16.46253265017160317, 9.564922557960807481, 40.83224293864769550 ) ) ;
#92483 = CARTESIAN_POINT ( 'NONE',  ( 21.55341960407619695, -5.719274019375665929, 101.0427570613523756 ) ) ;
#92484 = CARTESIAN_POINT ( 'NONE',  ( -8.224510206698735004, -14.34966873604973081, 24.58442372801901499 ) ) ;
#92485 = CARTESIAN_POINT ( 'NONE',  ( -10.81492255796105439, 18.62759615963255655, 82.91775706135234714 ) ) ;
#92486 = CARTESIAN_POINT ( 'NONE',  ( -19.02544592524334988, -5.153800228976617603, 58.95942372801900433 ) ) ;
#92487 = CARTESIAN_POINT ( 'NONE',  ( -16.51473224551069308, -9.474510206698971260, 96.66557627198102409 ) ) ;
#92488 = CARTESIAN_POINT ( 'NONE',  ( -13.97604488694527625, -13.89961937509977652, 86.87390960531436690 ) ) ;
#92489 = CARTESIAN_POINT ( 'NONE',  ( 17.40861289039004589, 6.110651285853279546, 73.87232470827433417 ) ) ;
#92490 = CARTESIAN_POINT ( 'NONE',  ( -15.80617190586745835, -15.72974639402198527, 111.8739096053143669 ) ) ;
#92491 = VECTOR ( 'NONE', #28526, 1000.000000000000000 ) ;
#92492 = CARTESIAN_POINT ( 'NONE',  ( -14.34966873604960291, -8.224510206698953496, 61.66557627198103120 ) ) ;
#92493 = CARTESIAN_POINT ( 'NONE',  ( 0.05219959533907565091, 21.53943276465977519, 59.99890960531436690 ) ) ;
#92494 = CARTESIAN_POINT ( 'NONE',  ( 0.05219959533909260263, 19.03943276465977164, 59.99890960531436690 ) ) ;
#92496 = CARTESIAN_POINT ( 'NONE',  ( -16.53943276465976808, -0.05219959533934237506, 93.75109039468567573 ) ) ;
#92495 = CARTESIAN_POINT ( 'NONE',  ( 15.72974639402199770, -15.80617190586745480, 103.1239096053143811 ) ) ;
#92497 = ORIENTED_EDGE ( 'NONE', *, *, #191495, .F. ) ;
#92498 = CARTESIAN_POINT ( 'NONE',  ( 5.049401038298161559, -19.05341960407611168, 47.70724293864770260 ) ) ;
#92500 = LINE ( 'NONE', #106689, #46214 ) ;
#92499 = CARTESIAN_POINT ( 'NONE',  ( 14.29746914071049879, -8.314922557960816363, 88.33224293864769550 ) ) ;
#92501 = CARTESIAN_POINT ( 'NONE',  ( -5.153800228976328057, -19.02544592524343514, 47.29057627198102409 ) ) ;
#92502 = CARTESIAN_POINT ( 'NONE',  ( 0.05219959533910956823, 16.53943276465976808, 114.9989096053143669 ) ) ;
#92503 = CARTESIAN_POINT ( 'NONE',  ( 5.153800228976615827, -19.02544592524334988, 85.20942372801900433 ) ) ;
#92504 = CARTESIAN_POINT ( 'NONE',  ( 14.34966873604960469, 8.224510206698951720, 84.16557627198103830 ) ) ;
#92505 = CARTESIAN_POINT ( 'NONE',  ( 15.80617190586769283, -15.72974639402175789, 50.62609039468568994 ) ) ;
#92507 = CARTESIAN_POINT ( 'NONE',  ( 21.55341960407610458, 5.719274019375980345, 108.9572429386476955 ) ) ;
#92506 = CARTESIAN_POINT ( 'NONE',  ( -19.05341960407611168, -5.049401038298163336, 31.45724293864769550 ) ) ;
#92508 = CARTESIAN_POINT ( 'NONE',  ( -14.34966873604960291, -8.224510206698953496, 91.66557627198103830 ) ) ;
#92509 = CARTESIAN_POINT ( 'NONE',  ( 2.919401842228637189, -40.72031138817901308, -24.99999999999999645 ) ) ;
#92510 = CARTESIAN_POINT ( 'NONE',  ( 19.02544592524343514, -5.153800228976328945, 58.54057627198102409 ) ) ;
#92511 = CARTESIAN_POINT ( 'NONE',  ( 18.39639308325437028, 5.500000000000037303, 48.98252246182195080 ) ) ;
#92513 = CARTESIAN_POINT ( 'NONE',  ( -16.46253265017160317, 9.564922557960807481, 105.8322429386476955 ) ) ;
#92512 = CARTESIAN_POINT ( 'NONE',  ( -19.02544592524334988, -5.153800228976617603, 93.95942372801900433 ) ) ;
#92514 = CARTESIAN_POINT ( 'NONE',  ( 18.67979575497194134, -10.72451020669871369, 30.83442372801902209 ) ) ;
#92515 = CARTESIAN_POINT ( 'NONE',  ( 9.474510206698971260, -16.51473224551069308, 77.91557627198103830 ) ) ;
#92516 = CARTESIAN_POINT ( 'NONE',  ( -16.51473224551082808, 9.474510206698731452, 68.33442372801900433 ) ) ;
#92517 = CARTESIAN_POINT ( 'NONE',  ( -0.05219959533909027116, -19.03943276465977164, 52.49890960531436690 ) ) ;
#92518 = CARTESIAN_POINT ( 'NONE',  ( 4.483927247898545687, 16.52544592524342804, 79.79057627198102409 ) ) ;
#92519 = CARTESIAN_POINT ( 'NONE',  ( -14.29746914071049879, 8.314922557960819915, 70.83224293864770971 ) ) ;
#92520 = CARTESIAN_POINT ( 'NONE',  ( 0.05219959533909260263, 19.03943276465977164, 94.99890960531436690 ) ) ;
#92521 = CARTESIAN_POINT ( 'NONE',  ( 15.80617190586746368, 15.72974639402197994, 104.3739096053143669 ) ) ;
#92522 = CARTESIAN_POINT ( 'NONE',  ( 19.03943276465977164, -0.05219959533909143690, 83.74890960531436690 ) ) ;
#92523 = EDGE_CURVE ( 'NONE', #183542, #94299, #158431, .T. ) ;
#92524 = CARTESIAN_POINT ( 'NONE',  ( 16.51473224551083163, -9.474510206698727899, 35.83442372801899722 ) ) ;
#92527 = CARTESIAN_POINT ( 'NONE',  ( -14.34966873604960291, -8.224510206698953496, 111.6655762719810525 ) ) ;
#92526 = CARTESIAN_POINT ( 'NONE',  ( -14.29746914071049879, 8.314922557960819915, 35.83224293864768839 ) ) ;
#92525 = CARTESIAN_POINT ( 'NONE',  ( -0.05219959533909027116, -19.03943276465977164, 37.49890960531436690 ) ) ;
#92528 = ORIENTED_EDGE ( 'NONE', *, *, #161100, .T. ) ;
#92529 = CARTESIAN_POINT ( 'NONE',  ( 21.53943276465977519, 0.05219959533937863772, 31.25109039468568639 ) ) ;
#92530 = CARTESIAN_POINT ( 'NONE',  ( -9.474510206698720793, -16.51473224551083518, 64.58442372801900433 ) ) ;
#92531 = CARTESIAN_POINT ( 'NONE',  ( -16.55341960407611168, -4.379528057220339221, 41.45724293864769550 ) ) ;
#92532 = CARTESIAN_POINT ( 'NONE',  ( 0.05219959533907565091, 21.53943276465977519, 84.99890960531436690 ) ) ;
#92533 = CARTESIAN_POINT ( 'NONE',  ( 13.89961937509977652, -13.97604488694527269, 113.1239096053143527 ) ) ;
#92534 = CARTESIAN_POINT ( 'NONE',  ( 12.06949235617757843, -12.14591786802309237, 73.12390960531436690 ) ) ;
#92535 = CARTESIAN_POINT ( 'NONE',  ( -5.049401038298153566, 19.05341960407611168, 25.20724293864768484 ) ) ;
#92536 = CARTESIAN_POINT ( 'NONE',  ( 13.89961937509957401, 13.97604488694547697, 21.87609039468566152 ) ) ;
#92537 = CARTESIAN_POINT ( 'NONE',  ( -12.14591786802326823, 12.06949235617739902, 108.1260903946856757 ) ) ;
#92538 = CARTESIAN_POINT ( 'NONE',  ( -8.314922557961024197, 14.29746914071037800, 62.91775706135236135 ) ) ;
#92539 = CARTESIAN_POINT ( 'NONE',  ( -21.53943276465977519, 0.05219959533907696930, 36.24890960531435979 ) ) ;
#92540 = CARTESIAN_POINT ( 'NONE',  ( 15.80617190586769283, -15.72974639402175789, 105.6260903946856899 ) ) ;
#92541 = CARTESIAN_POINT ( 'NONE',  ( 16.51473224551069308, 9.474510206698969483, 74.16557627198103830 ) ) ;
#92542 = AXIS2_PLACEMENT_3D ( 'NONE', #110196, #142520, #111187 ) ;
#92543 = CARTESIAN_POINT ( 'NONE',  ( 14.34966873604972726, -8.224510206698740333, 65.83442372801900433 ) ) ;
#92544 = CARTESIAN_POINT ( 'NONE',  ( 5.153800228976335163, 19.02544592524342804, 29.79057627198102409 ) ) ;
#92545 = CARTESIAN_POINT ( 'NONE',  ( -0.05219959533910754901, -16.53943276465976808, 37.49890960531436690 ) ) ;
#92547 = CARTESIAN_POINT ( 'NONE',  ( -0.05219959533909027116, -19.03943276465977164, 87.49890960531436690 ) ) ;
#92546 = CARTESIAN_POINT ( 'NONE',  ( -13.89961937509977652, 13.97604488694528158, 110.6239096053143243 ) ) ;
#92548 = CARTESIAN_POINT ( 'NONE',  ( 0.05219959533909260263, 19.03943276465977164, 114.9989096053143669 ) ) ;
#92549 = CARTESIAN_POINT ( 'NONE',  ( 8.224510206698953496, -14.34966873604960469, 62.91557627198102409 ) ) ;
#92550 = CARTESIAN_POINT ( 'NONE',  ( -14.29746914071049879, 8.314922557960819915, 35.83224293864768839 ) ) ;
#92551 = CARTESIAN_POINT ( 'NONE',  ( 4.379528057220339221, -16.55341960407611168, 52.70724293864769550 ) ) ;
#92552 = EDGE_LOOP ( 'NONE', ( #183300, #108372, #25966, #28909 ) ) ;
#92554 = FACE_OUTER_BOUND ( 'NONE', #110893, .T. ) ;
#92553 = CARTESIAN_POINT ( 'NONE',  ( -4.379528057220086978, -16.55341960407618274, 39.79275706135235424 ) ) ;
#92555 = CARTESIAN_POINT ( 'NONE',  ( -16.46253265017146816, -9.564922557961047289, 54.16775706135234003 ) ) ;
#92556 = CARTESIAN_POINT ( 'NONE',  ( -0.05219959533909027116, -19.03943276465977164, 77.49890960531435269 ) ) ;
#92557 = CARTESIAN_POINT ( 'NONE',  ( -16.46253265017146816, -9.564922557961047289, 69.16775706135233293 ) ) ;
#92558 = CARTESIAN_POINT ( 'NONE',  ( 1.784210473542230573E-15, -29.16686587814331588, 145.8750000027311273 ) ) ;
#92559 = CARTESIAN_POINT ( 'NONE',  ( -5.049401038297874678, -19.05341960407617918, 49.79275706135231871 ) ) ;
#92561 = CARTESIAN_POINT ( 'NONE',  ( 16.53943276465976808, 0.05219959533934440121, 76.25109039468568994 ) ) ;
#92560 = CARTESIAN_POINT ( 'NONE',  ( -19.03943276465977164, -0.05219959533935918106, 103.7510903946856757 ) ) ;
#92562 = CARTESIAN_POINT ( 'NONE',  ( 27.73933785331498569, 2.768321779492822058E-14, 144.3750000027311842 ) ) ;
#92563 = CARTESIAN_POINT ( 'NONE',  ( -10.74802307403563084, -10.74802307403544077, -64.92279855667830191 ) ) ;
#92564 = CARTESIAN_POINT ( 'NONE',  ( -13.89961937509977652, 13.97604488694528158, 115.6239096053143669 ) ) ;
#92565 = CARTESIAN_POINT ( 'NONE',  ( 5.719274019375673035, 21.55341960407619339, 47.29275706135234003 ) ) ;
#92566 = CARTESIAN_POINT ( 'NONE',  ( -19.03943276465977164, -0.05219959533935918106, 108.7510903946856615 ) ) ;
#92568 = CARTESIAN_POINT ( 'NONE',  ( -9.474510206698964154, 16.51473224551069663, 60.41557627198102409 ) ) ;
#92567 = DIRECTION ( 'NONE',  ( 8.673617379884035472E-16, 1.000000000000000000, 0.000000000000000000 ) ) ;
#92569 = CARTESIAN_POINT ( 'NONE',  ( -19.02544592524342804, 5.153800228976336051, 106.0405762719810241 ) ) ;
#92571 = CARTESIAN_POINT ( 'NONE',  ( -0.05219959533909027116, -19.03943276465977164, 57.49890960531435979 ) ) ;
#92570 = CARTESIAN_POINT ( 'NONE',  ( -4.379528057220328563, 16.55341960407611168, 60.20724293864768839 ) ) ;
#92572 = CARTESIAN_POINT ( 'NONE',  ( 16.46253265017160672, -9.564922557960803928, 58.33224293864769550 ) ) ;
#92573 = CARTESIAN_POINT ( 'NONE',  ( -9.474510206698720793, -16.51473224551083518, 74.58442372801900433 ) ) ;
#92574 = CARTESIAN_POINT ( 'NONE',  ( -5.823673210054116645, -21.52544592524344225, 47.29057627198103120 ) ) ;
#92575 = CARTESIAN_POINT ( 'NONE',  ( 16.52544592524342804, -4.483927247898539470, 113.5405762719810383 ) ) ;
#92576 = CARTESIAN_POINT ( 'NONE',  ( -19.02544592524334988, -5.153800228976617603, 48.95942372801900433 ) ) ;
#92577 = CARTESIAN_POINT ( 'NONE',  ( -9.474510206698964154, 16.51473224551069663, 80.41557627198103830 ) ) ;
#92578 = CARTESIAN_POINT ( 'NONE',  ( -21.55341960407610458, -5.719274019375992779, 76.45724293864769550 ) ) ;
#92580 = CARTESIAN_POINT ( 'NONE',  ( -16.51473224551082808, 9.474510206698731452, 38.33442372801899722 ) ) ;
#92579 = CARTESIAN_POINT ( 'NONE',  ( -4.483927247898539470, -16.52544592524342804, 82.29057627198103830 ) ) ;
#92581 = CARTESIAN_POINT ( 'NONE',  ( 21.55341960407610458, 5.719274019375980345, 63.95724293864770260 ) ) ;
#92582 = CARTESIAN_POINT ( 'NONE',  ( 18.67979575497178502, 10.72451020669898547, 34.16557627198102409 ) ) ;
#92583 = CARTESIAN_POINT ( 'NONE',  ( -18.62759615963255300, -10.81492255796106328, 89.16775706135236135 ) ) ;
#92584 = CARTESIAN_POINT ( 'NONE',  ( 5.153800228976335163, 19.02544592524342804, 64.79057627198100988 ) ) ;
#92585 = CARTESIAN_POINT ( 'NONE',  ( 16.46253265017160672, -9.564922557960803928, 23.33224293864769194 ) ) ;
#92586 = CARTESIAN_POINT ( 'NONE',  ( 5.823673210054444382, -21.52544592524334988, 25.20942372801901854 ) ) ;
#92587 = CARTESIAN_POINT ( 'NONE',  ( -17.97058386085787163, -5.500000000000059508, 49.00390968646215839 ) ) ;
#92588 = CARTESIAN_POINT ( 'NONE',  ( 0.05219959533937995610, -21.53943276465977519, 40.00109039468567573 ) ) ;
#92589 = CARTESIAN_POINT ( 'NONE',  ( 9.474510206698971260, -16.51473224551069308, 37.91557627198102409 ) ) ;
#92590 = CARTESIAN_POINT ( 'NONE',  ( -21.52544592524343514, 5.823673210054127303, 106.0405762719810525 ) ) ;
#92591 = CARTESIAN_POINT ( 'NONE',  ( 13.97604488694548053, -13.89961937509957401, 50.62609039468566152 ) ) ;
#92592 = CARTESIAN_POINT ( 'NONE',  ( -69.65682714487590488, -71.74905178543390605, -15.00000000000000178 ) ) ;
#92593 = DIRECTION ( 'NONE',  ( 0.4999999999999967248, -0.5000000000000019984, -0.7071067811865484609 ) ) ;
#92594 = CARTESIAN_POINT ( 'NONE',  ( 16.55341960407618274, -4.379528057220086978, 61.04275706135234714 ) ) ;
#92595 = CARTESIAN_POINT ( 'NONE',  ( 5.049401038298161559, -19.05341960407611168, 22.70724293864769194 ) ) ;
#92596 = DIRECTION ( 'NONE',  ( 0.000000000000000000, 0.000000000000000000, -1.000000000000000000 ) ) ;
#92597 = CARTESIAN_POINT ( 'NONE',  ( 16.46253265017160672, -9.564922557960803928, 78.33224293864769550 ) ) ;
#92598 = CARTESIAN_POINT ( 'NONE',  ( 12.06949235617757843, -12.14591786802309237, 108.1239096053143811 ) ) ;
#92599 = CARTESIAN_POINT ( 'NONE',  ( -18.67979575497178146, -10.72451020669898902, 56.66557627198103830 ) ) ;
#92600 = CARTESIAN_POINT ( 'NONE',  ( 12.06949235617739724, 12.14591786802326823, 36.87609039468568994 ) ) ;
#92601 = CARTESIAN_POINT ( 'NONE',  ( 18.62759615963255655, 10.81492255796105972, 101.6677570613523613 ) ) ;
#92602 = CARTESIAN_POINT ( 'NONE',  ( -19.03943276465977164, 0.05219959533909376836, 21.24890960531436335 ) ) ;
#92603 = CARTESIAN_POINT ( 'NONE',  ( -16.55341960407617563, 4.379528057220093196, 108.5427570613523756 ) ) ;
#92604 = CARTESIAN_POINT ( 'NONE',  ( 14.29746914071049879, -8.314922557960816363, 58.33224293864768839 ) ) ;
#92605 = CARTESIAN_POINT ( 'NONE',  ( -19.02544592524342804, 5.153800228976336051, 46.04057627198101699 ) ) ;
#92606 = CARTESIAN_POINT ( 'NONE',  ( -10.72451020669870658, -18.67979575497194134, 99.58442372801900433 ) ) ;
#92607 = CARTESIAN_POINT ( 'NONE',  ( -21.53943276465977519, 0.05219959533907696930, 106.2489096053143811 ) ) ;
#92608 = CARTESIAN_POINT ( 'NONE',  ( 21.53943276465977519, 0.05219959533937863772, 76.25109039468568994 ) ) ;
#92609 = CARTESIAN_POINT ( 'NONE',  ( -14.29746914071037622, -8.314922557961029526, 49.16775706135234003 ) ) ;
#92611 = CARTESIAN_POINT ( 'NONE',  ( -10.72451020669870658, -18.67979575497194134, 99.58442372801900433 ) ) ;
#92610 = CARTESIAN_POINT ( 'NONE',  ( -0.05219959533910754901, -16.53943276465976808, 77.49890960531433848 ) ) ;
#92612 = CARTESIAN_POINT ( 'NONE',  ( 16.52544592524335698, 4.483927247898782831, 111.4594237280190328 ) ) ;
#92613 = CARTESIAN_POINT ( 'NONE',  ( 17.50000000000000000, 5.499999999999992895, 71.70309617465829888 ) ) ;
#92614 = CARTESIAN_POINT ( 'NONE',  ( 8.224510206698742110, 14.34966873604972548, 42.08442372801901854 ) ) ;
#92615 = CARTESIAN_POINT ( 'NONE',  ( 4.483927247898545687, 16.52544592524342804, 44.79057627198103120 ) ) ;
#92616 = CARTESIAN_POINT ( 'NONE',  ( 16.53943276465976808, 0.05219959533934440121, 81.25109039468568994 ) ) ;
#92617 = CARTESIAN_POINT ( 'NONE',  ( -13.89961937509977652, 13.97604488694528158, 95.62390960531436690 ) ) ;
#92618 = CARTESIAN_POINT ( 'NONE',  ( -15.80617190586745835, -15.72974639402198527, 21.87390960531436690 ) ) ;
#92619 = CARTESIAN_POINT ( 'NONE',  ( -5.823673210054431948, 21.52544592524334988, 92.70942372801901854 ) ) ;
#92620 = CARTESIAN_POINT ( 'NONE',  ( 16.52544592524335698, 4.483927247898782831, 96.45942372801901854 ) ) ;
#92621 = CARTESIAN_POINT ( 'NONE',  ( -8.314922557960811034, -14.29746914071050412, 72.08224293864769550 ) ) ;
#92622 = CARTESIAN_POINT ( 'NONE',  ( -13.97604488694527625, -13.89961937509977652, 86.87390960531436690 ) ) ;
#92623 = ORIENTED_EDGE ( 'NONE', *, *, #177902, .F. ) ;
#92624 = CARTESIAN_POINT ( 'NONE',  ( -4.483927247898782831, 16.52544592524335698, 32.70942372801900433 ) ) ;
#92625 = CARTESIAN_POINT ( 'NONE',  ( 9.474510206698971260, -16.51473224551069308, 42.91557627198103120 ) ) ;
#92626 = CARTESIAN_POINT ( 'NONE',  ( 0.05219959533909260263, 19.03943276465977164, 89.99890960531436690 ) ) ;
#92628 = CARTESIAN_POINT ( 'NONE',  ( 36.91746824999999177, 2.880721459617395097E-14, -3.624999997268813168 ) ) ;
#92627 = CARTESIAN_POINT ( 'NONE',  ( -8.314922557961024197, 14.29746914071037800, 32.91775706135234714 ) ) ;
#92629 = CARTESIAN_POINT ( 'NONE',  ( -19.03943276465977164, -0.05219959533935918106, 28.75109039468566507 ) ) ;
#92630 = CARTESIAN_POINT ( 'NONE',  ( -4.379528057220086978, -16.55341960407618274, 94.79275706135234714 ) ) ;
#92631 = CARTESIAN_POINT ( 'NONE',  ( 19.03943276465977164, -0.05219959533909143690, 28.74890960531435624 ) ) ;
#92632 = CARTESIAN_POINT ( 'NONE',  ( 16.55341960407618274, -4.379528057220086978, 76.04275706135237556 ) ) ;
#92633 = CARTESIAN_POINT ( 'NONE',  ( -8.224510206698735004, -14.34966873604973081, 64.58442372801900433 ) ) ;
#92634 = CARTESIAN_POINT ( 'NONE',  ( -19.03943276465977164, -0.05219959533935918106, 88.75109039468567573 ) ) ;
#92635 = CARTESIAN_POINT ( 'NONE',  ( -13.89961937509957401, -13.97604488694547875, 34.37609039468566863 ) ) ;
#92636 = CARTESIAN_POINT ( 'NONE',  ( 13.97604488694527802, 13.89961937509977652, 49.37390960531434558 ) ) ;
#92637 = CARTESIAN_POINT ( 'NONE',  ( -12.14591786802309592, -12.06949235617757132, 91.87390960531436690 ) ) ;
#92638 = VECTOR ( 'NONE', #132949, 1000.000000000000000 ) ;
#92639 = CARTESIAN_POINT ( 'NONE',  ( 19.02544592524334988, 5.153800228976608722, 51.45942372801900433 ) ) ;
#92640 = CARTESIAN_POINT ( 'NONE',  ( 10.81492255796078972, 18.62759615963270932, 54.58224293864769550 ) ) ;
#92641 = CARTESIAN_POINT ( 'NONE',  ( -16.51473224551082808, 9.474510206698731452, 28.33442372801900433 ) ) ;
#92642 = CARTESIAN_POINT ( 'NONE',  ( 5.049401038298161559, -19.05341960407611168, 107.7072429386476955 ) ) ;
#92643 = CARTESIAN_POINT ( 'NONE',  ( 15.72974639402199770, -15.80617190586745480, 78.12390960531436690 ) ) ;
#92644 = CARTESIAN_POINT ( 'NONE',  ( 0.05219959533909260263, 19.03943276465977164, 114.9989096053143669 ) ) ;
#92645 = CARTESIAN_POINT ( 'NONE',  ( -9.564922557961040184, 16.46253265017147172, 92.91775706135233293 ) ) ;
#92646 = CARTESIAN_POINT ( 'NONE',  ( -17.50000000000001776, 4.658240926743198784, 108.9447041781680383 ) ) ;
#92647 = CARTESIAN_POINT ( 'NONE',  ( -19.02544592524334988, -5.153800228976617603, 108.9594237280189759 ) ) ;
#92648 = CARTESIAN_POINT ( 'NONE',  ( -9.474510206698964154, 16.51473224551069663, 35.41557627198102409 ) ) ;
#92649 = CARTESIAN_POINT ( 'NONE',  ( -0.05219959533909027116, -19.03943276465977164, 92.49890960531436690 ) ) ;
#92650 = CARTESIAN_POINT ( 'NONE',  ( 10.72451020669898902, -18.67979575497178502, 72.91557627198103830 ) ) ;
#92651 = CARTESIAN_POINT ( 'NONE',  ( 8.314922557961029526, -14.29746914071037800, 50.41775706135235424 ) ) ;
#92652 = CARTESIAN_POINT ( 'NONE',  ( -10.81492255796105439, 18.62759615963255655, 52.91775706135235424 ) ) ;
#92654 = CARTESIAN_POINT ( 'NONE',  ( 18.67979575497194134, -10.72451020669871369, 110.8344237280190043 ) ) ;
#92653 = CARTESIAN_POINT ( 'NONE',  ( -13.97604488694547697, 13.89961937509957934, 103.1260903946856473 ) ) ;
#92655 = CARTESIAN_POINT ( 'NONE',  ( -4.379528057220086978, -16.55341960407618274, 104.7927570613523898 ) ) ;
#92656 = CARTESIAN_POINT ( 'NONE',  ( 19.02544592524343514, -5.153800228976328945, 103.5405762719809957 ) ) ;
#92657 = CARTESIAN_POINT ( 'NONE',  ( -15.80617190586745835, -15.72974639402198527, 106.8739096053143811 ) ) ;
#92658 = CARTESIAN_POINT ( 'NONE',  ( 0.05219959533910956823, 16.53943276465976808, 29.99890960531435979 ) ) ;
#92659 = CARTESIAN_POINT ( 'NONE',  ( -19.05341960407617563, 5.049401038297882671, 83.54275706135233293 ) ) ;
#92660 = EDGE_CURVE ( 'NONE', #36339, #155869, #190145, .T. ) ;
#92661 = CARTESIAN_POINT ( 'NONE',  ( 10.72451020669871369, 18.67979575497193778, 52.08442372801901854 ) ) ;
#92662 = CARTESIAN_POINT ( 'NONE',  ( 19.02544592524334988, 5.153800228976608722, 31.45942372801900433 ) ) ;
#92663 = CARTESIAN_POINT ( 'NONE',  ( -0.05219959533910754901, -16.53943276465976808, 107.4989096053143669 ) ) ;
#92664 = CARTESIAN_POINT ( 'NONE',  ( 5.719274019375991003, -21.55341960407610458, 27.70724293864769905 ) ) ;
#92665 = CARTESIAN_POINT ( 'NONE',  ( 16.52544592524342804, -4.483927247898539470, 23.54057627198102765 ) ) ;
#92666 = CARTESIAN_POINT ( 'NONE',  ( 21.53943276465977519, 0.05219959533937863772, 101.2510903946856757 ) ) ;
#92667 = CARTESIAN_POINT ( 'NONE',  ( -16.55341960407617563, 4.379528057220093196, 63.54275706135234003 ) ) ;
#92668 = CARTESIAN_POINT ( 'NONE',  ( 14.29746914071049879, -8.314922557960816363, 33.33224293864769550 ) ) ;
#92669 = CARTESIAN_POINT ( 'NONE',  ( -0.05219959533937732626, 21.53943276465977519, 67.50109039468568994 ) ) ;
#92670 = CARTESIAN_POINT ( 'NONE',  ( 0.05219959533937995610, -21.53943276465977519, 50.00109039468568994 ) ) ;
#92671 = ORIENTED_EDGE ( 'NONE', *, *, #50546, .T. ) ;
#92672 = CARTESIAN_POINT ( 'NONE',  ( -9.474510206698964154, 16.51473224551069663, 25.41557627198103120 ) ) ;
#92673 = CARTESIAN_POINT ( 'NONE',  ( 21.53943276465977519, 0.05219959533937863772, 36.25109039468567573 ) ) ;
#92674 = CARTESIAN_POINT ( 'NONE',  ( -4.379528057220328563, 16.55341960407611168, 105.2072429386477097 ) ) ;
#92675 = CARTESIAN_POINT ( 'NONE',  ( 19.76836671444427651, 4.606730274327740737, 37.50000000000000711 ) ) ;
#92676 = CARTESIAN_POINT ( 'NONE',  ( -16.52544592524342804, 4.483927247898546575, 81.04057627198102409 ) ) ;
#92677 = CARTESIAN_POINT ( 'NONE',  ( 5.153800228976335163, 19.02544592524342804, 69.79057627198103830 ) ) ;
#92678 = CARTESIAN_POINT ( 'NONE',  ( -8.224510206698948167, 14.34966873604960824, 25.41557627198103120 ) ) ;
#92679 = CARTESIAN_POINT ( 'NONE',  ( -15.80617190586745835, -15.72974639402198527, 51.87390960531437401 ) ) ;
#92680 = CARTESIAN_POINT ( 'NONE',  ( 4.483927247898545687, 16.52544592524342804, 94.79057627198105251 ) ) ;
#92681 = CARTESIAN_POINT ( 'NONE',  ( -21.52544592524343514, 5.823673210054127303, 96.04057627198102409 ) ) ;
#92682 = CARTESIAN_POINT ( 'NONE',  ( -13.97604488694527625, -13.89961937509977652, 101.8739096053143811 ) ) ;
#92684 = CARTESIAN_POINT ( 'NONE',  ( -16.51473224551082808, 9.474510206698731452, 103.3344237280190043 ) ) ;
#92683 = CARTESIAN_POINT ( 'NONE',  ( -13.97604488694527625, -13.89961937509977652, 56.87390960531434558 ) ) ;
#92685 = CARTESIAN_POINT ( 'NONE',  ( -5.719274019375978568, 21.55341960407610458, 45.20724293864769550 ) ) ;
#92686 = CARTESIAN_POINT ( 'NONE',  ( 10.81492255796106328, -18.62759615963255655, 75.41775706135233293 ) ) ;
#92687 = CARTESIAN_POINT ( 'NONE',  ( 16.51473224551069308, 9.474510206698969483, 69.16557627198102409 ) ) ;
#92688 = CARTESIAN_POINT ( 'NONE',  ( 16.46253265017160672, -9.564922557960803928, 98.33224293864769550 ) ) ;
#92689 = CARTESIAN_POINT ( 'NONE',  ( -4.483927247898782831, 16.52544592524335698, 77.70942372801900433 ) ) ;
#92690 = CARTESIAN_POINT ( 'NONE',  ( -15.80617190586768217, 15.72974639402176855, 63.12609039468568994 ) ) ;
#92691 = CARTESIAN_POINT ( 'NONE',  ( 15.80617190586769283, -15.72974639402175789, 80.62609039468567573 ) ) ;
#92692 = CARTESIAN_POINT ( 'NONE',  ( -0.05219959533907301413, -21.53943276465977519, 107.4989096053143669 ) ) ;
#92693 = CARTESIAN_POINT ( 'NONE',  ( 0.05219959533934541429, -16.53943276465976808, 80.00109039468568994 ) ) ;
#92694 = CARTESIAN_POINT ( 'NONE',  ( -5.823673210054116645, -21.52544592524344225, 82.29057627198103830 ) ) ;
#92695 = CARTESIAN_POINT ( 'NONE',  ( 13.89961937509957401, 13.97604488694547697, 51.87609039468566863 ) ) ;
#92696 = CARTESIAN_POINT ( 'NONE',  ( -10.81492255796078084, -18.62759615963271287, 37.08224293864768129 ) ) ;
#92698 = CARTESIAN_POINT ( 'NONE',  ( 12.06949235617739724, 12.14591786802326823, 111.8760903946856615 ) ) ;
#92697 = CARTESIAN_POINT ( 'NONE',  ( 13.89961937509977652, -13.97604488694527269, 78.12390960531433848 ) ) ;
#92699 = CARTESIAN_POINT ( 'NONE',  ( -17.26058549869089731, 6.457015423128607878, 63.62254162523936429 ) ) ;
#92700 = CARTESIAN_POINT ( 'NONE',  ( -0.05219959533907301413, -21.53943276465977519, 22.49890960531436335 ) ) ;
#92701 = CARTESIAN_POINT ( 'NONE',  ( 4.500000000000000888, -130.0000000000000000, 13.99999999999999822 ) ) ;
#92702 = CARTESIAN_POINT ( 'NONE',  ( 5.153800228976615827, -19.02544592524334988, 100.2094237280190043 ) ) ;
#92703 = CARTESIAN_POINT ( 'NONE',  ( -0.05219959533907301413, -21.53943276465977519, 67.49890960531436690 ) ) ;
#92704 = CARTESIAN_POINT ( 'NONE',  ( -12.14591786802309592, -12.06949235617757132, 46.87390960531435979 ) ) ;
#92705 = CARTESIAN_POINT ( 'NONE',  ( -16.53943276465976808, -0.05219959533934237506, 18.75109039468568639 ) ) ;
#92706 = CARTESIAN_POINT ( 'NONE',  ( 0.05219959533909260263, 19.03943276465977164, 29.99890960531435979 ) ) ;
#92707 = CARTESIAN_POINT ( 'NONE',  ( 9.564922557961047289, -16.46253265017146816, 110.4177570613523471 ) ) ;
#92709 = CARTESIAN_POINT ( 'NONE',  ( 5.153800228976615827, -19.02544592524334988, 70.20942372801899012 ) ) ;
#92708 = CARTESIAN_POINT ( 'NONE',  ( 15.80617190586746368, 15.72974639402197994, 104.3739096053143669 ) ) ;
#92710 = CARTESIAN_POINT ( 'NONE',  ( -14.29746914071037622, -8.314922557961029526, 79.16775706135234714 ) ) ;
#92711 = CARTESIAN_POINT ( 'NONE',  ( -19.03943276465977164, 0.05219959533909376836, 86.24890960531436690 ) ) ;
#92712 = CARTESIAN_POINT ( 'NONE',  ( -16.53943276465976808, 0.05219959533911058130, 71.24890960531435269 ) ) ;
#92713 = CARTESIAN_POINT ( 'NONE',  ( -19.03943276465977164, 0.05219959533909376836, 66.24890960531436690 ) ) ;
#92714 = CARTESIAN_POINT ( 'NONE',  ( 12.06949235617757843, -12.14591786802309237, 68.12390960531436690 ) ) ;
#92715 = CARTESIAN_POINT ( 'NONE',  ( -13.97604488694527625, -13.89961937509977652, 26.87390960531434558 ) ) ;
#92716 = CARTESIAN_POINT ( 'NONE',  ( -37.36625173109578668, -3.353228347065801973, 40.62582701645504102 ) ) ;
#92717 = CARTESIAN_POINT ( 'NONE',  ( -16.52544592524342804, 4.483927247898546575, 41.04057627198103120 ) ) ;
#92718 = CARTESIAN_POINT ( 'NONE',  ( 9.474510206698971260, -16.51473224551069308, 77.91557627198103830 ) ) ;
#92719 = DIRECTION ( 'NONE',  ( -0.000000000000000000, -0.000000000000000000, 1.000000000000000000 ) ) ;
#92720 = CARTESIAN_POINT ( 'NONE',  ( 19.05341960407617918, -5.049401038297876454, 51.04275706135231871 ) ) ;
#92721 = CARTESIAN_POINT ( 'NONE',  ( -12.14591786802326823, 12.06949235617739902, 58.12609039468568994 ) ) ;
#92722 = CARTESIAN_POINT ( 'NONE',  ( 21.52544592524344225, -5.823673210054117533, 63.54057627198103830 ) ) ;
#92723 = CARTESIAN_POINT ( 'NONE',  ( -19.03943276465977164, -0.05219959533935918106, 28.75109039468566507 ) ) ;
#92724 = CARTESIAN_POINT ( 'NONE',  ( 16.51473224551069308, 9.474510206698969483, 84.16557627198102409 ) ) ;
#92725 = CARTESIAN_POINT ( 'NONE',  ( -20.02040504322455305, -21.79936378052101631, -48.83307992000326436 ) ) ;
#92726 = CARTESIAN_POINT ( 'NONE',  ( 21.52544592524344225, -5.823673210054117533, 33.54057627198102409 ) ) ;
#92727 = CARTESIAN_POINT ( 'NONE',  ( 19.05341960407611168, 5.049401038298154454, 63.95724293864769550 ) ) ;
#92728 = CARTESIAN_POINT ( 'NONE',  ( 5.719274019375673035, 21.55341960407619339, 57.29275706135234714 ) ) ;
#92729 = CARTESIAN_POINT ( 'NONE',  ( 12.06949235617757843, -12.14591786802309237, 103.1239096053143811 ) ) ;
#92730 = ADVANCED_FACE ( 'NONE', ( #127193, #17054, #126215, #32224 ), #125228, .T. ) ;
#92733 = VERTEX_POINT ( 'NONE', #184907 ) ;
#92732 = CARTESIAN_POINT ( 'NONE',  ( -16.46253265017160317, 9.564922557960807481, 100.8322429386477097 ) ) ;
#92731 = CARTESIAN_POINT ( 'NONE',  ( 10.72451020669898902, -18.67979575497178502, 97.91557627198103830 ) ) ;
#92734 = CARTESIAN_POINT ( 'NONE',  ( -10.81492255796105439, 18.62759615963255655, 37.91775706135235424 ) ) ;
#92735 = EDGE_LOOP ( 'NONE', ( #30399, #26780, #121791, #64939 ) ) ;
#92736 = CARTESIAN_POINT ( 'NONE',  ( 16.46253265017160672, -9.564922557960803928, 98.33224293864769550 ) ) ;
#92737 = DIRECTION ( 'NONE',  ( 3.709348145883536076E-20, 0.000000000000000000, -1.000000000000000000 ) ) ;
#92738 = CARTESIAN_POINT ( 'NONE',  ( -15.72974639402197994, 15.80617190586746368, 100.6239096053143811 ) ) ;
#92739 = CARTESIAN_POINT ( 'NONE',  ( -16.51473224551069308, -9.474510206698971260, 41.66557627198103120 ) ) ;
#92740 = CARTESIAN_POINT ( 'NONE',  ( -0.05219959533934338120, 16.53943276465976808, 22.50109039468567573 ) ) ;
#92741 = CARTESIAN_POINT ( 'NONE',  ( -22.81625015709510507, 31.40387420917330275, -5.424999997268812990 ) ) ;
#92742 = CARTESIAN_POINT ( 'NONE',  ( 9.474510206698971260, -16.51473224551069308, 32.91557627198102409 ) ) ;
#92743 = CARTESIAN_POINT ( 'NONE',  ( 5.823673210054444382, -21.52544592524334988, 80.20942372801901854 ) ) ;
#92745 = CARTESIAN_POINT ( 'NONE',  ( -10.81492255796105439, 18.62759615963255655, 42.91775706135235424 ) ) ;
#92744 = CARTESIAN_POINT ( 'NONE',  ( 13.97604488694527802, 13.89961937509977652, 74.37390960531436690 ) ) ;
#92746 = CARTESIAN_POINT ( 'NONE',  ( 18.62759615963255655, 10.81492255796105972, 31.66775706135234358 ) ) ;
#92747 = CARTESIAN_POINT ( 'NONE',  ( -17.14385361876520619, 23.59649016807275856, 145.0750000027311728 ) ) ;
#92748 = CARTESIAN_POINT ( 'NONE',  ( 19.03943276465977164, -0.05219959533909143690, 93.74890960531435269 ) ) ;
#92749 = CARTESIAN_POINT ( 'NONE',  ( 13.33220713530183765, 24.76230349490602833, 140.0000000000000853 ) ) ;
#92752 = CARTESIAN_POINT ( 'NONE',  ( -21.55341960407619339, 5.719274019375674811, 58.54275706135235424 ) ) ;
#92751 = CARTESIAN_POINT ( 'NONE',  ( -16.52544592524335698, -4.483927247898792601, 68.95942372801901854 ) ) ;
#92750 = CARTESIAN_POINT ( 'NONE',  ( -8.224510206698735004, -14.34966873604973081, 39.58442372801901143 ) ) ;
#92753 = CARTESIAN_POINT ( 'NONE',  ( -15.72974639402176322, -15.80617190586768395, 79.37609039468567573 ) ) ;
#92754 = CARTESIAN_POINT ( 'NONE',  ( 5.563226388833935943, 6.875118674992778622, -61.95704554880761350 ) ) ;
#92755 = CARTESIAN_POINT ( 'NONE',  ( 19.05341960407617918, -5.049401038297876454, 111.0427570613523329 ) ) ;
#92756 = CARTESIAN_POINT ( 'NONE',  ( 19.03943276465977164, -0.05219959533909143690, 73.74890960531435269 ) ) ;
#92757 = CARTESIAN_POINT ( 'NONE',  ( 13.97604488694527802, 13.89961937509977652, 99.37390960531436690 ) ) ;
#92758 = CARTESIAN_POINT ( 'NONE',  ( 16.53943276465976808, -0.05219959533910856209, 103.7489096053143669 ) ) ;
#92759 = CARTESIAN_POINT ( 'NONE',  ( 12.14591786802309770, 12.06949235617756955, 104.3739096053143669 ) ) ;
#92760 = CARTESIAN_POINT ( 'NONE',  ( -5.719274019375978568, 21.55341960407610458, 35.20724293864768839 ) ) ;
#92761 = CARTESIAN_POINT ( 'NONE',  ( -16.55341960407617563, 4.379528057220093196, 78.54275706135236135 ) ) ;
#92763 = CARTESIAN_POINT ( 'NONE',  ( -5.153800228976328057, -19.02544592524343514, 57.29057627198103120 ) ) ;
#92762 = CARTESIAN_POINT ( 'NONE',  ( -16.53943276465976808, 0.05219959533911058130, 71.24890960531435269 ) ) ;
#92764 = CARTESIAN_POINT ( 'NONE',  ( -10.81492255796105439, 18.62759615963255655, 72.91775706135234714 ) ) ;
#92765 = CARTESIAN_POINT ( 'NONE',  ( -10.81492255796105439, 18.62759615963255655, 72.91775706135234714 ) ) ;
#92766 = CARTESIAN_POINT ( 'NONE',  ( 0.05219959533936267826, -19.03943276465977164, 110.0010903946856757 ) ) ;
#92767 = CARTESIAN_POINT ( 'NONE',  ( 4.379528057220339221, -16.55341960407611168, 72.70724293864769550 ) ) ;
#92768 = CARTESIAN_POINT ( 'NONE',  ( -10.72451020669870658, -18.67979575497194134, 24.58442372801901499 ) ) ;
#92769 = CARTESIAN_POINT ( 'NONE',  ( -10.72451020669898014, 18.67979575497178502, 65.41557627198102409 ) ) ;
#92770 = CARTESIAN_POINT ( 'NONE',  ( -17.81289503416611097, -24.51734667627696496, 140.2999999999999545 ) ) ;
#92771 = CARTESIAN_POINT ( 'NONE',  ( -17.81289503416611808, 24.51734667627700404, 143.9500000054623854 ) ) ;
#92772 = CARTESIAN_POINT ( 'NONE',  ( -19.02544592524342804, 5.153800228976336051, 76.04057627198102409 ) ) ;
#92773 = CARTESIAN_POINT ( 'NONE',  ( -16.55341960407611168, -4.379528057220339221, 46.45724293864769550 ) ) ;
#92774 = CIRCLE ( 'NONE', #118645, 4.999999999999998224 ) ;
#92775 = CARTESIAN_POINT ( 'NONE',  ( -4.379528057220328563, 16.55341960407611168, 25.20724293864769550 ) ) ;
#92776 = CARTESIAN_POINT ( 'NONE',  ( -12.06949235617739369, -12.14591786802326823, 94.37609039468568994 ) ) ;
#92777 = CARTESIAN_POINT ( 'NONE',  ( -9.564922557961040184, 16.46253265017147172, 57.91775706135233293 ) ) ;
#92778 = CARTESIAN_POINT ( 'NONE',  ( 37.99999999999999289, 12.34694845685046793, -8.899999999999996803 ) ) ;
#92779 = CARTESIAN_POINT ( 'NONE',  ( -0.05219959533909027116, -19.03943276465977164, 107.4989096053143527 ) ) ;
#92780 = CARTESIAN_POINT ( 'NONE',  ( 14.34966873604960469, 8.224510206698951720, 79.16557627198103830 ) ) ;
#92781 = CARTESIAN_POINT ( 'NONE',  ( 9.474510206698729675, 16.51473224551082808, 47.08442372801900433 ) ) ;
#92783 = CARTESIAN_POINT ( 'NONE',  ( -10.81492255796078084, -18.62759615963271287, 37.08224293864768129 ) ) ;
#92782 = CARTESIAN_POINT ( 'NONE',  ( 0.05219959533909260263, 19.03943276465977164, 34.99890960531435979 ) ) ;
#92785 = ORIENTED_EDGE ( 'NONE', *, *, #8686, .F. ) ;
#92784 = CARTESIAN_POINT ( 'NONE',  ( 18.62759615963271287, -10.81492255796078972, 48.33224293864770260 ) ) ;
#92786 = CARTESIAN_POINT ( 'NONE',  ( 12.14591786802309770, 12.06949235617756955, 104.3739096053143669 ) ) ;
#92787 = CARTESIAN_POINT ( 'NONE',  ( 16.52544592524335698, 4.483927247898782831, 46.45942372801901854 ) ) ;
#92788 = CARTESIAN_POINT ( 'NONE',  ( -0.05219959533910754901, -16.53943276465976808, 97.49890960531436690 ) ) ;
#92789 = CARTESIAN_POINT ( 'NONE',  ( 17.50000000000000000, -5.622605283950865562, 36.18792689403888119 ) ) ;
#92790 = CARTESIAN_POINT ( 'NONE',  ( -17.13100169013300089, 6.664070546373151771, 50.76789835699851494 ) ) ;
#92791 = CARTESIAN_POINT ( 'NONE',  ( 5.823673210054125526, 21.52544592524343514, 39.79057627198103830 ) ) ;
#92792 = CARTESIAN_POINT ( 'NONE',  ( 17.72517630440433223, -5.499999999999963585, 78.42175719257211597 ) ) ;
#92793 = CARTESIAN_POINT ( 'NONE',  ( -11.30153831258470731, -190.0000000000000000, 0.000000000000000000 ) ) ;
#92795 = CARTESIAN_POINT ( 'NONE',  ( -4.379528057220328563, 16.55341960407611168, 25.20724293864769550 ) ) ;
#92794 = CARTESIAN_POINT ( 'NONE',  ( 8.314922557961029526, -14.29746914071037800, 45.41775706135234003 ) ) ;
#92796 = CARTESIAN_POINT ( 'NONE',  ( 21.53943276465977519, -0.05219959533907433946, 58.74890960531436690 ) ) ;
#92797 = CARTESIAN_POINT ( 'NONE',  ( -19.05341960407617563, 5.049401038297882671, 78.54275706135233293 ) ) ;
#92798 = CARTESIAN_POINT ( 'NONE',  ( 18.67979575497178502, 10.72451020669898547, 59.16557627198103120 ) ) ;
#92799 = CARTESIAN_POINT ( 'NONE',  ( -0.05219959533937732626, 21.53943276465977519, 77.50109039468567573 ) ) ;
#92800 = CARTESIAN_POINT ( 'NONE',  ( -10.97407593764241618, 9.252314257645080531, -62.33638803020407693 ) ) ;
#92801 = CARTESIAN_POINT ( 'NONE',  ( -4.483927247898782831, 16.52544592524335698, 42.70942372801901854 ) ) ;
#92803 = CARTESIAN_POINT ( 'NONE',  ( 9.474510206698971260, -16.51473224551069308, 102.9155762719810241 ) ) ;
#92802 = CARTESIAN_POINT ( 'NONE',  ( -19.03943276465977164, 0.05219959533909376836, 31.24890960531435979 ) ) ;
#92804 = CIRCLE ( 'NONE', #25011, 0.5000000000000004441 ) ;
#92805 = CARTESIAN_POINT ( 'NONE',  ( -19.02544592524342804, 5.153800228976336051, 31.04057627198102409 ) ) ;
#92806 = CARTESIAN_POINT ( 'NONE',  ( -12.14591786802309592, -12.06949235617757132, 96.87390960531436690 ) ) ;
#92807 = PRODUCT_CONTEXT ( 'NONE', #138369, 'mechanical' ) ;
#92808 = FACE_BOUND ( 'NONE', #200065, .T. ) ;
#92809 = ORIENTED_EDGE ( 'NONE', *, *, #72556, .T. ) ;
#92810 = CARTESIAN_POINT ( 'NONE',  ( -16.53943276465976808, -0.05219959533934237506, 68.75109039468568994 ) ) ;
#92811 = CARTESIAN_POINT ( 'NONE',  ( -0.05219959533907301413, -21.53943276465977519, 97.49890960531436690 ) ) ;
#92812 = CARTESIAN_POINT ( 'NONE',  ( -16.46253265017160317, 9.564922557960807481, 60.83224293864769550 ) ) ;
#92813 = CARTESIAN_POINT ( 'NONE',  ( 5.719274019375673035, 21.55341960407619339, 32.29275706135235424 ) ) ;
#92814 = CARTESIAN_POINT ( 'NONE',  ( 13.89961937509977652, -13.97604488694527269, 78.12390960531433848 ) ) ;
#92815 = CARTESIAN_POINT ( 'NONE',  ( -32.28837973138505646, -23.54499195901729180, -23.03346093386547722 ) ) ;
#92816 = ORIENTED_EDGE ( 'NONE', *, *, #16747, .F. ) ;
#92817 = CARTESIAN_POINT ( 'NONE',  ( -5.719274019375665041, -21.55341960407619695, 19.79275706135235069 ) ) ;
#92820 = CARTESIAN_POINT ( 'NONE',  ( -0.05219959533936034679, 19.03943276465977164, 72.50109039468566152 ) ) ;
#92819 = CARTESIAN_POINT ( 'NONE',  ( 19.05341960407611168, 5.049401038298154454, 103.9572429386476671 ) ) ;
#92818 = CARTESIAN_POINT ( 'NONE',  ( -5.049401038298153566, 19.05341960407611168, 25.20724293864768484 ) ) ;
#92821 = CARTESIAN_POINT ( 'NONE',  ( -19.03943276465977164, -0.05219959533935918106, 28.75109039468566507 ) ) ;
#92822 = CARTESIAN_POINT ( 'NONE',  ( -5.719274019375978568, 21.55341960407610458, 105.2072429386477097 ) ) ;
#92823 = CARTESIAN_POINT ( 'NONE',  ( -9.474510206698720793, -16.51473224551083518, 39.58442372801899722 ) ) ;
#92824 = CARTESIAN_POINT ( 'NONE',  ( -14.34966873604972548, 8.224510206698743886, 83.33442372801903275 ) ) ;
#92825 = CARTESIAN_POINT ( 'NONE',  ( -19.03943276465977164, 0.05219959533909376836, 106.2489096053143669 ) ) ;
#92826 = CARTESIAN_POINT ( 'NONE',  ( -5.049401038298153566, 19.05341960407611168, 65.20724293864765286 ) ) ;
#92827 = CIRCLE ( 'NONE', #2326, 216.0437394197456342 ) ;
#92828 = CARTESIAN_POINT ( 'NONE',  ( -18.67979575497193778, 10.72451020669871902, 63.33442372801900433 ) ) ;
#92829 = CARTESIAN_POINT ( 'NONE',  ( 15.72974639402176855, 15.80617190586768217, 76.87609039468567573 ) ) ;
#92830 = CARTESIAN_POINT ( 'NONE',  ( 5.153800228976335163, 19.02544592524342804, 74.79057627198103830 ) ) ;
#92831 = CARTESIAN_POINT ( 'NONE',  ( 0.05219959533937995610, -21.53943276465977519, 50.00109039468568994 ) ) ;
#92832 = CARTESIAN_POINT ( 'NONE',  ( -13.89961937509957401, -13.97604488694547875, 84.37609039468567573 ) ) ;
#92833 = CARTESIAN_POINT ( 'NONE',  ( 0.05219959533909260263, 19.03943276465977164, 49.99890960531435979 ) ) ;
#92834 = CARTESIAN_POINT ( 'NONE',  ( -5.153800228976328057, -19.02544592524343514, 92.29057627198099567 ) ) ;
#92835 = CARTESIAN_POINT ( 'NONE',  ( 19.03943276465977164, -0.05219959533909143690, 63.74890960531435979 ) ) ;
#92836 = CARTESIAN_POINT ( 'NONE',  ( -17.31747979337952259, -6.344076630960987728, 91.37944868065187620 ) ) ;
#92837 = CARTESIAN_POINT ( 'NONE',  ( -0.05219959533909027116, -19.03943276465977164, 47.49890960531435979 ) ) ;
#92838 = CARTESIAN_POINT ( 'NONE',  ( 21.53943276465977519, -0.05219959533907433946, 103.7489096053143669 ) ) ;
#92839 = CARTESIAN_POINT ( 'NONE',  ( -14.29746914071037622, -8.314922557961029526, 89.16775706135236135 ) ) ;
#92840 = CARTESIAN_POINT ( 'NONE',  ( -24.85901545656372491, 5.346793810781125700, 169.1018111888375870 ) ) ;
#92841 = CARTESIAN_POINT ( 'NONE',  ( -19.05341960407617563, 5.049401038297882671, 38.54275706135233293 ) ) ;
#92842 = CARTESIAN_POINT ( 'NONE',  ( 19.02544592524343514, -5.153800228976328945, 68.54057627198103830 ) ) ;
#92843 = CARTESIAN_POINT ( 'NONE',  ( -16.52544592524342804, 4.483927247898546575, 61.04057627198103120 ) ) ;
#92844 = CARTESIAN_POINT ( 'NONE',  ( -12.06949235617756955, 12.14591786802309770, 95.62390960531436690 ) ) ;
#92845 = CARTESIAN_POINT ( 'NONE',  ( -9.474510206698964154, 16.51473224551069663, 110.4155762719810383 ) ) ;
#92846 = CARTESIAN_POINT ( 'NONE',  ( 19.02544592524343514, -5.153800228976328945, 88.54057627198102409 ) ) ;
#92847 = CARTESIAN_POINT ( 'NONE',  ( -5.049401038298153566, 19.05341960407611168, 100.2072429386476955 ) ) ;
#92848 = CARTESIAN_POINT ( 'NONE',  ( -16.46253265017146816, -9.564922557961047289, 19.16775706135233293 ) ) ;
#92849 = CARTESIAN_POINT ( 'NONE',  ( -12.14591786802326823, 12.06949235617739902, 98.12609039468570415 ) ) ;
#92850 = CARTESIAN_POINT ( 'NONE',  ( 19.05341960407611168, 5.049401038298154454, 73.95724293864768129 ) ) ;
#92851 = CARTESIAN_POINT ( 'NONE',  ( 5.823673210054444382, -21.52544592524334988, 45.20942372801901854 ) ) ;
#92852 = CARTESIAN_POINT ( 'NONE',  ( -5.719274019375978568, 21.55341960407610458, 25.20724293864769550 ) ) ;
#92853 = CARTESIAN_POINT ( 'NONE',  ( 10.81492255796078972, 18.62759615963270932, 114.5822429386477097 ) ) ;
#92854 = CARTESIAN_POINT ( 'NONE',  ( -12.06949235617756955, 12.14591786802309770, 60.62390960531437401 ) ) ;
#92855 = CARTESIAN_POINT ( 'NONE',  ( 19.05341960407611168, 5.049401038298154454, 58.95724293864768129 ) ) ;
#92856 = CARTESIAN_POINT ( 'NONE',  ( -14.34966873604960291, -8.224510206698953496, 76.66557627198103830 ) ) ;
#92857 = CARTESIAN_POINT ( 'NONE',  ( 19.02544592524334988, 5.153800228976608722, 46.45942372801899012 ) ) ;
#92858 = CARTESIAN_POINT ( 'NONE',  ( -14.34966873604960291, -8.224510206698953496, 111.6655762719810525 ) ) ;
#92859 = CARTESIAN_POINT ( 'NONE',  ( -13.97604488694527625, -13.89961937509977652, 81.87390960531436690 ) ) ;
#92860 = CARTESIAN_POINT ( 'NONE',  ( -16.46253265017160317, 9.564922557960807481, 85.83224293864769550 ) ) ;
#92861 = CARTESIAN_POINT ( 'NONE',  ( -22.44159573604009950, -16.30477369853688430, 141.0750000027311728 ) ) ;
#92862 = CARTESIAN_POINT ( 'NONE',  ( -16.55341960407611168, -4.379528057220339221, 96.45724293864770971 ) ) ;
#92863 = VERTEX_POINT ( 'NONE', #49380 ) ;
#92864 = CARTESIAN_POINT ( 'NONE',  ( -14.29746914071037622, -8.314922557961029526, 104.1677570613523471 ) ) ;
#92865 = CARTESIAN_POINT ( 'NONE',  ( -4.483927247898782831, 16.52544592524335698, 27.70942372801901854 ) ) ;
#92866 = CARTESIAN_POINT ( 'NONE',  ( 18.62759615963255655, 10.81492255796105972, 91.66775706135234714 ) ) ;
#92867 = CARTESIAN_POINT ( 'NONE',  ( 16.51473224551069308, 9.474510206698969483, 84.16557627198102409 ) ) ;
#92868 = CARTESIAN_POINT ( 'NONE',  ( 15.80617190586769283, -15.72974639402175789, 20.62609039468568639 ) ) ;
#92869 = CARTESIAN_POINT ( 'NONE',  ( -19.03943276465977164, 0.05219959533909376836, 36.24890960531436690 ) ) ;
#92870 = CARTESIAN_POINT ( 'NONE',  ( -14.34966873604972548, 8.224510206698743886, 28.33442372801902209 ) ) ;
#92871 = CARTESIAN_POINT ( 'NONE',  ( -16.46253265017146816, -9.564922557961047289, 94.16775706135233293 ) ) ;
#92872 = CARTESIAN_POINT ( 'NONE',  ( -15.72974639402197994, 15.80617190586746368, 95.62390960531436690 ) ) ;
#92873 = CARTESIAN_POINT ( 'NONE',  ( 16.46253265017146816, 9.564922557961045513, 71.66775706135233293 ) ) ;
#92874 = CARTESIAN_POINT ( 'NONE',  ( 0.05219959533909260263, 19.03943276465977164, 24.99890960531435269 ) ) ;
#92875 = CARTESIAN_POINT ( 'NONE',  ( 0.05219959533907565091, 21.53943276465977519, 114.9989096053143669 ) ) ;
#92876 = CARTESIAN_POINT ( 'NONE',  ( 17.58332526062529411, -7.635886036038496805, 73.42334959558466778 ) ) ;
#92877 = CARTESIAN_POINT ( 'NONE',  ( -13.97604488694527625, -13.89961937509977652, 96.87390960531433848 ) ) ;
#92878 = CARTESIAN_POINT ( 'NONE',  ( 8.224510206698742110, 14.34966873604972548, 52.08442372801901854 ) ) ;
#92879 = CARTESIAN_POINT ( 'NONE',  ( 19.11401883044621286, -35.13836984581306666, -7.540766371346785846 ) ) ;
#92880 = CARTESIAN_POINT ( 'NONE',  ( -13.89961937509957401, -13.97604488694547875, 54.37609039468565442 ) ) ;
#92882 = CARTESIAN_POINT ( 'NONE',  ( 12.06949235617757843, -12.14591786802309237, 78.12390960531436690 ) ) ;
#92881 = CARTESIAN_POINT ( 'NONE',  ( -10.81492255796105439, 18.62759615963255655, 22.91775706135235069 ) ) ;
#92883 = CARTESIAN_POINT ( 'NONE',  ( 19.02544592524343514, -5.153800228976328945, 83.54057627198100988 ) ) ;
#92885 = CARTESIAN_POINT ( 'NONE',  ( 5.153800228976615827, -19.02544592524334988, 55.20942372801899722 ) ) ;
#92884 = CARTESIAN_POINT ( 'NONE',  ( -4.483927247898782831, 16.52544592524335698, 52.70942372801902565 ) ) ;
#92886 = CARTESIAN_POINT ( 'NONE',  ( -10.81492255796105439, 18.62759615963255655, 67.91775706135234714 ) ) ;
#92887 = CARTESIAN_POINT ( 'NONE',  ( 14.29746914071037800, 8.314922557961029526, 26.66775706135235424 ) ) ;
#92889 = EDGE_CURVE ( 'NONE', #191417, #60925, #110053, .T. ) ;
#92888 = CARTESIAN_POINT ( 'NONE',  ( 19.05341960407611168, 5.049401038298154454, 73.95724293864768129 ) ) ;
#92890 = CARTESIAN_POINT ( 'NONE',  ( 9.564922557961047289, -16.46253265017146816, 85.41775706135233293 ) ) ;
#92891 = CARTESIAN_POINT ( 'NONE',  ( -0.05219959533934338120, 16.53943276465976808, 57.50109039468568994 ) ) ;
#92892 = CARTESIAN_POINT ( 'NONE',  ( -5.719274019375665041, -21.55341960407619695, 99.79275706135234714 ) ) ;
#92893 = CARTESIAN_POINT ( 'NONE',  ( 19.02544592524334988, 5.153800228976608722, 76.45942372801897591 ) ) ;
#92894 = CARTESIAN_POINT ( 'NONE',  ( 13.97604488694527802, 13.89961937509977652, 44.37390960531435269 ) ) ;
#92895 = CARTESIAN_POINT ( 'NONE',  ( -10.72451020669898014, 18.67979575497178502, 65.41557627198102409 ) ) ;
#92897 = CARTESIAN_POINT ( 'NONE',  ( 0.05219959533936267826, -19.03943276465977164, 75.00109039468566152 ) ) ;
#92896 = CARTESIAN_POINT ( 'NONE',  ( 4.483927247898545687, 16.52544592524342804, 79.79057627198102409 ) ) ;
#92898 = CARTESIAN_POINT ( 'NONE',  ( 16.36317988757059894, -7.306389748694854802, 61.59789608363229974 ) ) ;
#92899 = CARTESIAN_POINT ( 'NONE',  ( -9.564922557961040184, 16.46253265017147172, 47.91775706135233293 ) ) ;
#92900 = CARTESIAN_POINT ( 'NONE',  ( -12.14591786802326823, 12.06949235617739902, 93.12609039468568994 ) ) ;
#92901 = CARTESIAN_POINT ( 'NONE',  ( 16.52544592524342804, -4.483927247898539470, 73.54057627198102409 ) ) ;
#92903 = CARTESIAN_POINT ( 'NONE',  ( 8.571926809382597767, 26.38167802310806209, 144.2750000027311899 ) ) ;
#92902 = CARTESIAN_POINT ( 'NONE',  ( 15.72974639402176855, 15.80617190586768217, 101.8760903946857042 ) ) ;
#92904 = CARTESIAN_POINT ( 'NONE',  ( 18.67979575497178502, 10.72451020669898547, 104.1655762719810241 ) ) ;
#92905 = CARTESIAN_POINT ( 'NONE',  ( 16.51473224551069308, 9.474510206698969483, 59.16557627198102409 ) ) ;
#92906 = CARTESIAN_POINT ( 'NONE',  ( 10.72451020669871369, 18.67979575497193778, 82.08442372801901854 ) ) ;
#92907 = CARTESIAN_POINT ( 'NONE',  ( -19.02544592524342804, 5.153800228976336051, 56.04057627198100988 ) ) ;
#92908 = ORIENTED_EDGE ( 'NONE', *, *, #120239, .T. ) ;
#92909 = CARTESIAN_POINT ( 'NONE',  ( -13.89961937509977652, 13.97604488694528158, 30.62390960531435269 ) ) ;
#92910 = CARTESIAN_POINT ( 'NONE',  ( -9.474510206698964154, 16.51473224551069663, 110.4155762719810383 ) ) ;
#92911 = CARTESIAN_POINT ( 'NONE',  ( 14.34966873604960469, 8.224510206698951720, 69.16557627198102409 ) ) ;
#92912 = CARTESIAN_POINT ( 'NONE',  ( -19.02544592524342804, 5.153800228976336051, 31.04057627198102409 ) ) ;
#92913 = CARTESIAN_POINT ( 'NONE',  ( 16.55341960407611168, 4.379528057220329451, 83.95724293864770971 ) ) ;
#92914 = VECTOR ( 'NONE', #134855, 1000.000000000000000 ) ;
#92915 = CARTESIAN_POINT ( 'NONE',  ( -21.55341960407610458, -5.719274019375992779, 91.45724293864769550 ) ) ;
#92916 = CARTESIAN_POINT ( 'NONE',  ( -5.823673210054431948, 21.52544592524334988, 42.70942372801901854 ) ) ;
#92917 = CARTESIAN_POINT ( 'NONE',  ( -19.05341960407611168, -5.049401038298163336, 21.45724293864768839 ) ) ;
#92918 = CARTESIAN_POINT ( 'NONE',  ( 8.314922557961029526, -14.29746914071037800, 50.41775706135235424 ) ) ;
#92919 = CARTESIAN_POINT ( 'NONE',  ( 21.52544592524344225, -5.823673210054117533, 98.54057627198105251 ) ) ;
#92920 = CARTESIAN_POINT ( 'NONE',  ( -16.51473224551082808, 9.474510206698731452, 28.33442372801900433 ) ) ;
#92921 = CARTESIAN_POINT ( 'NONE',  ( 9.474510206698971260, -16.51473224551069308, 112.9155762719810383 ) ) ;
#92922 = CARTESIAN_POINT ( 'NONE',  ( 5.823673210054444382, -21.52544592524334988, 45.20942372801901854 ) ) ;
#92923 = CARTESIAN_POINT ( 'NONE',  ( -5.823673210054116645, -21.52544592524344225, 42.29057627198103120 ) ) ;
#92924 = CARTESIAN_POINT ( 'NONE',  ( 8.224510206698953496, -14.34966873604960469, 27.91557627198103830 ) ) ;
#92926 = CARTESIAN_POINT ( 'NONE',  ( 21.55341960407619695, -5.719274019375665929, 101.0427570613523756 ) ) ;
#92925 = CARTESIAN_POINT ( 'NONE',  ( -21.55341960407619339, 5.719274019375674811, 68.54275706135234714 ) ) ;
#92927 = CARTESIAN_POINT ( 'NONE',  ( 19.02544592524334988, 5.153800228976608722, 26.45942372801899722 ) ) ;
#92928 = CARTESIAN_POINT ( 'NONE',  ( 4.379528057220092307, 16.55341960407617563, 82.29275706135234714 ) ) ;
#92929 = CARTESIAN_POINT ( 'NONE',  ( -10.72451020669870658, -18.67979575497194134, 54.58442372801901143 ) ) ;
#92930 = CARTESIAN_POINT ( 'NONE',  ( -16.46253265017160317, 9.564922557960807481, 40.83224293864769550 ) ) ;
#92931 = CARTESIAN_POINT ( 'NONE',  ( 16.51473224551083163, -9.474510206698727899, 20.83442372801899722 ) ) ;
#92932 = CARTESIAN_POINT ( 'NONE',  ( -15.80617190586745835, -15.72974639402198527, 26.87390960531435979 ) ) ;
#92933 = CARTESIAN_POINT ( 'NONE',  ( -15.72974639402197994, 15.80617190586746368, 115.6239096053143669 ) ) ;
#92934 = CARTESIAN_POINT ( 'NONE',  ( 18.62759615963271287, -10.81492255796078972, 73.33224293864769550 ) ) ;
#92935 = CARTESIAN_POINT ( 'NONE',  ( -16.55341960407617563, 4.379528057220093196, 43.54275706135235424 ) ) ;
#92937 = CARTESIAN_POINT ( 'NONE',  ( -21.52544592524343514, 5.823673210054127303, 86.04057627198102409 ) ) ;
#92936 = CARTESIAN_POINT ( 'NONE',  ( -5.000000000000003553, -4.999999999999996447, -18.00000000000000000 ) ) ;
#92939 = CARTESIAN_POINT ( 'NONE',  ( 14.29746914071049879, -8.314922557960816363, 68.33224293864769550 ) ) ;
#92938 = CARTESIAN_POINT ( 'NONE',  ( -8.224510206698735004, -14.34966873604973081, 64.58442372801900433 ) ) ;
#92940 = CARTESIAN_POINT ( 'NONE',  ( -4.647474457565486646E-15, 28.90000000000004476, -49.67367017693150189 ) ) ;
#92941 = CARTESIAN_POINT ( 'NONE',  ( -9.474510206698720793, -16.51473224551083518, 104.5844237280190043 ) ) ;
#92942 = CARTESIAN_POINT ( 'NONE',  ( 16.51473224551069308, 9.474510206698969483, 114.1655762719810241 ) ) ;
#92943 = VECTOR ( 'NONE', #2867, 1000.000000000000000 ) ;
#92944 = CARTESIAN_POINT ( 'NONE',  ( -22.62812085840268495, 1.500606516337707586, -55.49205433527804132 ) ) ;
#92945 = CARTESIAN_POINT ( 'NONE',  ( 4.379528057220092307, 16.55341960407617563, 42.29275706135235424 ) ) ;
#92946 = CARTESIAN_POINT ( 'NONE',  ( -0.05219959533907301413, -21.53943276465977519, 107.4989096053143669 ) ) ;
#92947 = CARTESIAN_POINT ( 'NONE',  ( -15.72974639402197994, 15.80617190586746368, 25.62390960531435624 ) ) ;
#92948 = CARTESIAN_POINT ( 'NONE',  ( 4.379528057220092307, 16.55341960407617563, 57.29275706135234714 ) ) ;
#92949 = CARTESIAN_POINT ( 'NONE',  ( -9.564922557960796823, -16.46253265017161027, 67.08224293864769550 ) ) ;
#92951 = CARTESIAN_POINT ( 'NONE',  ( 19.03943276465977164, 0.05219959533936151252, 106.2510903946856615 ) ) ;
#92950 = CARTESIAN_POINT ( 'NONE',  ( -15.80617190586768217, 15.72974639402176855, 48.12609039468568284 ) ) ;
#92952 = CARTESIAN_POINT ( 'NONE',  ( -21.53943276465977519, 0.05219959533907696930, 31.24890960531435979 ) ) ;
#92953 = ORIENTED_EDGE ( 'NONE', *, *, #30184, .F. ) ;
#92954 = CARTESIAN_POINT ( 'NONE',  ( 19.05341960407617918, -5.049401038297876454, 26.04275706135233293 ) ) ;
#92955 = CARTESIAN_POINT ( 'NONE',  ( 16.52544592524335698, 4.483927247898782831, 41.45942372801901143 ) ) ;
#92956 = CARTESIAN_POINT ( 'NONE',  ( 5.153800228976335163, 19.02544592524342804, 94.79057627198103830 ) ) ;
#92957 = CARTESIAN_POINT ( 'NONE',  ( -10.72451020669898014, 18.67979575497178502, 100.4155762719810241 ) ) ;
#92958 = CARTESIAN_POINT ( 'NONE',  ( 13.89961937509977652, -13.97604488694527269, 73.12390960531436690 ) ) ;
#92959 = CARTESIAN_POINT ( 'NONE',  ( -30.00000000000000000, 5.499999999999992895, 102.5000000000000142 ) ) ;
#92960 = CARTESIAN_POINT ( 'NONE',  ( -16.53943276465976808, 0.05219959533911058130, 86.24890960531436690 ) ) ;
#92961 = CARTESIAN_POINT ( 'NONE',  ( -21.53943276465977519, 0.05219959533907696930, 36.24890960531435979 ) ) ;
#92962 = CARTESIAN_POINT ( 'NONE',  ( 16.51473224551069308, 9.474510206698969483, 24.16557627198102765 ) ) ;
#92963 = CARTESIAN_POINT ( 'NONE',  ( -14.34966873604972548, 8.224510206698743886, 68.33442372801900433 ) ) ;
#92964 = CARTESIAN_POINT ( 'NONE',  ( -18.67979575497178146, -10.72451020669898902, 101.6655762719810383 ) ) ;
#92965 = CARTESIAN_POINT ( 'NONE',  ( -19.02544592524334988, -5.153800228976617603, 68.95942372801896170 ) ) ;
#92966 = CARTESIAN_POINT ( 'NONE',  ( 15.72974639402199770, -15.80617190586745480, 28.12390960531435979 ) ) ;
#92967 = CARTESIAN_POINT ( 'NONE',  ( -19.03943276465977164, 0.05219959533909376836, 21.24890960531436335 ) ) ;
#92968 = CARTESIAN_POINT ( 'NONE',  ( 21.53943276465977519, -0.05219959533907433946, 68.74890960531435269 ) ) ;
#92969 = CARTESIAN_POINT ( 'NONE',  ( 19.05341960407611168, 5.049401038298154454, 93.95724293864769550 ) ) ;
#92970 = CARTESIAN_POINT ( 'NONE',  ( -0.05219959533937732626, 21.53943276465977519, 92.50109039468567573 ) ) ;
#92971 = CARTESIAN_POINT ( 'NONE',  ( 19.05341960407611168, 5.049401038298154454, 48.95724293864768129 ) ) ;
#92972 = EDGE_CURVE ( 'NONE', #17604, #186287, #109056, .T. ) ;
#92973 = CARTESIAN_POINT ( 'NONE',  ( -16.52544592524335698, -4.483927247898792601, 38.95942372801901854 ) ) ;
#92974 = CARTESIAN_POINT ( 'NONE',  ( 19.05341960407611168, 5.049401038298154454, 53.95724293864770260 ) ) ;
#92975 = CARTESIAN_POINT ( 'NONE',  ( -0.05219959533937732626, 21.53943276465977519, 82.50109039468568994 ) ) ;
#92976 = ORIENTED_EDGE ( 'NONE', *, *, #151903, .F. ) ;
#92977 = CARTESIAN_POINT ( 'NONE',  ( 0.05219959533936267826, -19.03943276465977164, 40.00109039468566152 ) ) ;
#92978 = CARTESIAN_POINT ( 'NONE',  ( 19.05341960407617918, -5.049401038297876454, 36.04275706135234003 ) ) ;
#92979 = CARTESIAN_POINT ( 'NONE',  ( 21.52544592524334988, 5.823673210054432836, 31.45942372801901854 ) ) ;
#92980 = CARTESIAN_POINT ( 'NONE',  ( 27.86273085795036408, -28.69962071417356242, -15.00000000000000178 ) ) ;
#92981 = CARTESIAN_POINT ( 'NONE',  ( 9.474510206698729675, 16.51473224551082808, 27.08442372801900433 ) ) ;
#92982 = CARTESIAN_POINT ( 'NONE',  ( -9.474510206698964154, 16.51473224551069663, 90.41557627198103830 ) ) ;
#92983 = CARTESIAN_POINT ( 'NONE',  ( 13.89961937509977652, -13.97604488694527269, 68.12390960531436690 ) ) ;
#92984 = CARTESIAN_POINT ( 'NONE',  ( -4.483927247898539470, -16.52544592524342804, 27.29057627198103120 ) ) ;
#92986 = CARTESIAN_POINT ( 'NONE',  ( 21.53943276465977519, 0.05219959533937863772, 86.25109039468568994 ) ) ;
#92985 = CARTESIAN_POINT ( 'NONE',  ( -5.823673210054116645, -21.52544592524344225, 22.29057627198102765 ) ) ;
#92987 = CARTESIAN_POINT ( 'NONE',  ( 36.91746825000000598, -11.99521256947793546, -8.224999997268810148 ) ) ;
#92988 = CARTESIAN_POINT ( 'NONE',  ( 17.31728774477272736, 6.344390552232409775, 56.68093348310682700 ) ) ;
#92989 = CARTESIAN_POINT ( 'NONE',  ( -15.72974639402176322, -15.80617190586768395, 94.37609039468568994 ) ) ;
#92990 = CARTESIAN_POINT ( 'NONE',  ( 17.50000000000000000, -5.500000000000000888, 43.29690382534172244 ) ) ;
#92991 = CARTESIAN_POINT ( 'NONE',  ( 4.379528057220339221, -16.55341960407611168, 112.7072429386476955 ) ) ;
#92992 = DIRECTION ( 'NONE',  ( 0.000000000000000000, 0.000000000000000000, -1.000000000000000000 ) ) ;
#92993 = CARTESIAN_POINT ( 'NONE',  ( 33.81930014798969353, 1.942787237620516416, 100.1485738335251199 ) ) ;
#92994 = CARTESIAN_POINT ( 'NONE',  ( 14.29746914071037800, 8.314922557961029526, 46.66775706135234714 ) ) ;
#92995 = CARTESIAN_POINT ( 'NONE',  ( -10.72451020669898014, 18.67979575497178502, 70.41557627198102409 ) ) ;
#92996 = CARTESIAN_POINT ( 'NONE',  ( -12.06949235617756955, 12.14591786802309770, 40.62390960531435269 ) ) ;
#92998 = CARTESIAN_POINT ( 'NONE',  ( 9.564922557960805705, 16.46253265017160317, 89.58224293864769550 ) ) ;
#92997 = CARTESIAN_POINT ( 'NONE',  ( -0.05219959533910754901, -16.53943276465976808, 112.4989096053143669 ) ) ;
#92999 = CARTESIAN_POINT ( 'NONE',  ( -9.564922557961040184, 16.46253265017147172, 22.91775706135233648 ) ) ;
#93000 = CARTESIAN_POINT ( 'NONE',  ( -0.05219959533909027116, -19.03943276465977164, 22.49890960531436690 ) ) ;
#93001 = CARTESIAN_POINT ( 'NONE',  ( 5.719274019375673035, 21.55341960407619339, 67.29275706135234714 ) ) ;
#93002 = CARTESIAN_POINT ( 'NONE',  ( 17.58332526062529411, -7.635886036038496805, 98.42334959558466778 ) ) ;
#93003 = CARTESIAN_POINT ( 'NONE',  ( 12.14591786802327356, -12.06949235617739191, 100.6260903946857184 ) ) ;
#93004 = CARTESIAN_POINT ( 'NONE',  ( -19.03943276465977164, -0.05219959533935918106, 58.75109039468566863 ) ) ;
#93005 = CARTESIAN_POINT ( 'NONE',  ( 29.86685920354754842, -21.69954338932559068, -6.324999997268814234 ) ) ;
#93006 = CARTESIAN_POINT ( 'NONE',  ( 18.67979575497178502, 10.72451020669898547, 34.16557627198102409 ) ) ;
#93007 = CARTESIAN_POINT ( 'NONE',  ( -16.55341960407611168, -4.379528057220339221, 86.45724293864770971 ) ) ;
#93008 = CARTESIAN_POINT ( 'NONE',  ( 5.049401038297881783, 19.05341960407617563, 52.29275706135234003 ) ) ;
#93009 = CARTESIAN_POINT ( 'NONE',  ( -13.89961937509977652, 13.97604488694528158, 70.62390960531432427 ) ) ;
#93010 = CARTESIAN_POINT ( 'NONE',  ( 8.314922557960818139, 14.29746914071049879, 64.58224293864769550 ) ) ;
#93011 = CARTESIAN_POINT ( 'NONE',  ( 9.564922557961047289, -16.46253265017146816, 95.41775706135233293 ) ) ;
#93012 = CARTESIAN_POINT ( 'NONE',  ( 10.81492255796078972, 18.62759615963270932, 54.58224293864769550 ) ) ;
#93013 = VERTEX_POINT ( 'NONE', #171733 ) ;
#93014 = CARTESIAN_POINT ( 'NONE',  ( -8.314922557960811034, -14.29746914071050412, 112.0822429386477097 ) ) ;
#93015 = CARTESIAN_POINT ( 'NONE',  ( 17.59860650958994555, -7.585241751806880650, 100.9233701426249183 ) ) ;
#93017 = CARTESIAN_POINT ( 'NONE',  ( 15.72974639402199770, -15.80617190586745480, 78.12390960531436690 ) ) ;
#93016 = CARTESIAN_POINT ( 'NONE',  ( 5.153800228976335163, 19.02544592524342804, 74.79057627198103830 ) ) ;
#93019 = CARTESIAN_POINT ( 'NONE',  ( 9.564922557960805705, 16.46253265017160317, 79.58224293864769550 ) ) ;
#93018 = CARTESIAN_POINT ( 'NONE',  ( -8.314922557961024197, 14.29746914071037800, 87.91775706135234714 ) ) ;
#93020 = CARTESIAN_POINT ( 'NONE',  ( -16.51473224551082808, 9.474510206698731452, 73.33442372801900433 ) ) ;
#93021 = CARTESIAN_POINT ( 'NONE',  ( 15.80617190586769283, -15.72974639402175789, 85.62609039468568994 ) ) ;
#93022 = CARTESIAN_POINT ( 'NONE',  ( 10.72451020669898902, -18.67979575497178502, 62.91557627198102409 ) ) ;
#93023 = CARTESIAN_POINT ( 'NONE',  ( 16.51473224551069308, 9.474510206698969483, 114.1655762719810241 ) ) ;
#93024 = CARTESIAN_POINT ( 'NONE',  ( -19.05341960407611168, -5.049401038298163336, 31.45724293864769550 ) ) ;
#93025 = CARTESIAN_POINT ( 'NONE',  ( 16.55341960407618274, -4.379528057220086978, 106.0427570613523471 ) ) ;
#93026 = CARTESIAN_POINT ( 'NONE',  ( -13.89961937509977652, 13.97604488694528158, 55.62390960531434558 ) ) ;
#93027 = CARTESIAN_POINT ( 'NONE',  ( -4.379528057220086978, -16.55341960407618274, 24.79275706135235779 ) ) ;
#93028 = CARTESIAN_POINT ( 'NONE',  ( -31.60163464511078146, -3.334671618079672939, 101.7358725107059598 ) ) ;
#93029 = CARTESIAN_POINT ( 'NONE',  ( -18.67979575497193778, 10.72451020669871902, 113.3344237280190328 ) ) ;
#93030 = CARTESIAN_POINT ( 'NONE',  ( 4.483927247898545687, 16.52544592524342804, 54.79057627198104541 ) ) ;
#93031 = CARTESIAN_POINT ( 'NONE',  ( 15.72974639402199770, -15.80617190586745480, 98.12390960531436690 ) ) ;
#93032 = CARTESIAN_POINT ( 'NONE',  ( -21.52544592524343514, 5.823673210054127303, 96.04057627198102409 ) ) ;
#93033 = CARTESIAN_POINT ( 'NONE',  ( 16.36317988757059538, -7.306389748694917863, 96.59789608363225000 ) ) ;
#93034 = CARTESIAN_POINT ( 'NONE',  ( -18.67979575497178146, -10.72451020669898902, 46.66557627198102409 ) ) ;
#93035 = CARTESIAN_POINT ( 'NONE',  ( -16.55341960407617563, 4.379528057220093196, 78.54275706135236135 ) ) ;
#93036 = CARTESIAN_POINT ( 'NONE',  ( -12.14591786802309592, -12.06949235617757132, 91.87390960531436690 ) ) ;
#93037 = CARTESIAN_POINT ( 'NONE',  ( 19.03943276465977164, -0.05219959533909143690, 53.74890960531436690 ) ) ;
#93038 =( LENGTH_UNIT ( ) NAMED_UNIT ( * ) SI_UNIT ( .MILLI., .METRE. ) );
#93039 = CARTESIAN_POINT ( 'NONE',  ( -6.259396865588131575, -47.62116666102458851, -24.77619460540839569 ) ) ;
#93040 = CARTESIAN_POINT ( 'NONE',  ( -14.29746914071037622, -8.314922557961029526, 104.1677570613523471 ) ) ;
#93041 = CARTESIAN_POINT ( 'NONE',  ( -18.62759615963255300, -10.81492255796106328, 39.16775706135235424 ) ) ;
#93042 = CARTESIAN_POINT ( 'NONE',  ( 19.05341960407611168, 5.049401038298154454, 93.95724293864769550 ) ) ;
#93043 = CARTESIAN_POINT ( 'NONE',  ( -5.823673210054431948, 21.52544592524334988, 62.70942372801902565 ) ) ;
#93044 = DIRECTION ( 'NONE',  ( 0.000000000000000000, 0.000000000000000000, 1.000000000000000000 ) ) ;
#93045 = DIRECTION ( 'NONE',  ( 0.000000000000000000, 0.000000000000000000, 1.000000000000000000 ) ) ;
#93046 = ORIENTED_EDGE ( 'NONE', *, *, #111151, .F. ) ;
#93047 = CARTESIAN_POINT ( 'NONE',  ( 21.55341960407619695, -5.719274019375665929, 61.04275706135234714 ) ) ;
#93049 = CARTESIAN_POINT ( 'NONE',  ( 5.049401038298161559, -19.05341960407611168, 112.7072429386476813 ) ) ;
#93048 = CARTESIAN_POINT ( 'NONE',  ( 5.049401038298161559, -19.05341960407611168, 47.70724293864770260 ) ) ;
#93050 = CARTESIAN_POINT ( 'NONE',  ( -19.05341960407611168, -5.049401038298163336, 86.45724293864769550 ) ) ;
#93051 = CARTESIAN_POINT ( 'NONE',  ( 5.049401038297881783, 19.05341960407617563, 67.29275706135234714 ) ) ;
#93052 = CARTESIAN_POINT ( 'NONE',  ( -10.81492255796105439, 18.62759615963255655, 47.91775706135234714 ) ) ;
#93053 = CARTESIAN_POINT ( 'NONE',  ( -19.03943276465977164, -0.05219959533935918106, 98.75109039468567573 ) ) ;
#93054 = CARTESIAN_POINT ( 'NONE',  ( -16.46253265017146816, -9.564922557961047289, 69.16775706135233293 ) ) ;
#93055 = CARTESIAN_POINT ( 'NONE',  ( 19.05341960407611168, 5.049401038298154454, 38.95724293864767418 ) ) ;
#93056 = CARTESIAN_POINT ( 'NONE',  ( 0.05219959533934541429, -16.53943276465976808, 105.0010903946856757 ) ) ;
#93057 = CARTESIAN_POINT ( 'NONE',  ( 19.05341960407617918, -5.049401038297876454, 81.04275706135231871 ) ) ;
#93058 = CARTESIAN_POINT ( 'NONE',  ( 8.224510206698953496, -14.34966873604960469, 22.91557627198102765 ) ) ;
#93059 = CARTESIAN_POINT ( 'NONE',  ( 9.474510206698729675, 16.51473224551082808, 52.08442372801900433 ) ) ;
#93060 = CARTESIAN_POINT ( 'NONE',  ( -10.72451020669870658, -18.67979575497194134, 99.58442372801900433 ) ) ;
#93061 = CARTESIAN_POINT ( 'NONE',  ( 5.049401038297881783, 19.05341960407617563, 32.29275706135233293 ) ) ;
#93062 = CARTESIAN_POINT ( 'NONE',  ( -9.564922557960796823, -16.46253265017161027, 27.08224293864769550 ) ) ;
#93063 = CARTESIAN_POINT ( 'NONE',  ( -21.52544592524334988, -5.823673210054445271, 83.95942372801900433 ) ) ;
#93064 = CARTESIAN_POINT ( 'NONE',  ( 0.05219959533934541429, -16.53943276465976808, 30.00109039468568284 ) ) ;
#93065 = CARTESIAN_POINT ( 'NONE',  ( -0.05219959533909027116, -19.03943276465977164, 97.49890960531436690 ) ) ;
#93066 = EDGE_CURVE ( 'NONE', #146461, #84653, #77330, .T. ) ;
#93067 = CARTESIAN_POINT ( 'NONE',  ( -27.73933785331498925, -9.013057229001049109, 142.9750000027312069 ) ) ;
#93068 = CARTESIAN_POINT ( 'NONE',  ( 19.05341960407611168, 5.049401038298154454, 78.95724293864769550 ) ) ;
#93069 = CARTESIAN_POINT ( 'NONE',  ( -17.49999999999999289, 5.500000000000036415, 75.79690382534175797 ) ) ;
#93070 = VERTEX_POINT ( 'NONE', #30232 ) ;
#93071 = CARTESIAN_POINT ( 'NONE',  ( -13.97604488694547697, 13.89961937509957934, 88.12609039468563310 ) ) ;
#93072 = CARTESIAN_POINT ( 'NONE',  ( 13.89961937509977652, -13.97604488694527269, 108.1239096053143669 ) ) ;
#93073 = CARTESIAN_POINT ( 'NONE',  ( -18.62759615963255300, -10.81492255796106328, 109.1677570613523613 ) ) ;
#93074 = CARTESIAN_POINT ( 'NONE',  ( -4.483927247898539470, -16.52544592524342804, 92.29057627198103830 ) ) ;
#93075 = B_SPLINE_CURVE_WITH_KNOTS ( 'NONE', 3,
 ( #59463, #118168, #74651, #135340, #58479, #56490, #152473, #167656, #71656, #10994, #87811, #28173, #9996, #197992, #136317, #103991, #121136, #12988, #137305, #133323 ),
 .UNSPECIFIED., .F., .F.,
 ( 4, 2, 2, 2, 2, 2, 2, 2, 2, 4 ),
 ( 0.000000000000000000, 0.0004987090165372347556, 0.0009974180330744695112, 0.001246772541343097894, 0.001496127049611726059, 0.001994836066148982390, 0.002493545082686239155, 0.002742899590954876645, 0.002992254099223514568, 0.003989672132298030700 ),
 .UNSPECIFIED. ) ;
#93076 = CARTESIAN_POINT ( 'NONE',  ( 22.24685556490046068, -12.75834802357495157, 167.9013491530738520 ) ) ;
#93077 = CARTESIAN_POINT ( 'NONE',  ( 10.81492255796078972, 18.62759615963270932, 64.58224293864769550 ) ) ;
#93078 = CARTESIAN_POINT ( 'NONE',  ( -18.62759615963270932, 10.81492255796079327, 35.83224293864768839 ) ) ;
#93079 = CARTESIAN_POINT ( 'NONE',  ( 16.53943276465976808, -0.05219959533910856209, 113.7489096053143527 ) ) ;
#93080 = CARTESIAN_POINT ( 'NONE',  ( -14.01879992551667442, 0.9453496423220366651, -62.45159313300388959 ) ) ;
#93081 = CARTESIAN_POINT ( 'NONE',  ( -9.474510206698720793, -16.51473224551083518, 59.58442372801900433 ) ) ;
#93083 = VECTOR ( 'NONE', #162641, 1000.000000000000000 ) ;
#93082 = CARTESIAN_POINT ( 'NONE',  ( 4.483927247898545687, 16.52544592524342804, 44.79057627198103120 ) ) ;
#93084 = CARTESIAN_POINT ( 'NONE',  ( 5.153800228976335163, 19.02544592524342804, 114.7905762719810241 ) ) ;
#93085 = CARTESIAN_POINT ( 'NONE',  ( -5.719274019375665041, -21.55341960407619695, 84.79275706135234714 ) ) ;
#93086 = CARTESIAN_POINT ( 'NONE',  ( -18.62759615963270932, 10.81492255796079327, 75.83224293864769550 ) ) ;
#93087 = CARTESIAN_POINT ( 'NONE',  ( -0.05219959533937732626, 21.53943276465977519, 57.50109039468568994 ) ) ;
#93088 = CARTESIAN_POINT ( 'NONE',  ( -5.719274019375665041, -21.55341960407619695, 49.79275706135234714 ) ) ;
#93089 = CARTESIAN_POINT ( 'NONE',  ( 16.46253265017160672, -9.564922557960803928, 78.33224293864769550 ) ) ;
#93090 = CARTESIAN_POINT ( 'NONE',  ( -16.55341960407617563, 4.379528057220093196, 78.54275706135236135 ) ) ;
#93091 = CARTESIAN_POINT ( 'NONE',  ( -16.46253265017160317, 9.564922557960807481, 25.83224293864769194 ) ) ;
#93092 = CARTESIAN_POINT ( 'NONE',  ( -40.00200000000003087, -5.510910596163089556E-15, 37.50000000000000000 ) ) ;
#93093 = CARTESIAN_POINT ( 'NONE',  ( 14.29746914071049879, -8.314922557960816363, 48.33224293864770260 ) ) ;
#93094 = CARTESIAN_POINT ( 'NONE',  ( 14.29746914071049879, -8.314922557960816363, 28.33224293864769550 ) ) ;
#93095 = CARTESIAN_POINT ( 'NONE',  ( -9.474510206698964154, 16.51473224551069663, 65.41557627198102409 ) ) ;
#93096 = CARTESIAN_POINT ( 'NONE',  ( -16.51473224551069308, -9.474510206698971260, 31.66557627198102054 ) ) ;
#93097 = CARTESIAN_POINT ( 'NONE',  ( 21.55341960407610458, 5.719274019375980345, 38.95724293864768839 ) ) ;
#93098 = CARTESIAN_POINT ( 'NONE',  ( 19.02544592524334988, 5.153800228976608722, 36.45942372801900433 ) ) ;
#93100 = CARTESIAN_POINT ( 'NONE',  ( 4.379528057220339221, -16.55341960407611168, 52.70724293864769550 ) ) ;
#93099 = FACE_OUTER_BOUND ( 'NONE', #140285, .T. ) ;
#93101 = CARTESIAN_POINT ( 'NONE',  ( -19.02544592524342804, 5.153800228976336051, 116.0405762719810383 ) ) ;
#93102 = CARTESIAN_POINT ( 'NONE',  ( 17.79613651744294245, -24.49428055684527195, 140.6843446568999809 ) ) ;
#93103 = CARTESIAN_POINT ( 'NONE',  ( 12.06949235617739724, 12.14591786802326823, 76.87609039468567573 ) ) ;
#93104 = CARTESIAN_POINT ( 'NONE',  ( -5.153800228976607833, 19.02544592524334988, 72.70942372801900433 ) ) ;
#93105 = CARTESIAN_POINT ( 'NONE',  ( 4.483927247898545687, 16.52544592524342804, 39.79057627198103830 ) ) ;
#93106 = FACE_OUTER_BOUND ( 'NONE', #81697, .T. ) ;
#93107 = CARTESIAN_POINT ( 'NONE',  ( 8.224510206698953496, -14.34966873604960469, 32.91557627198102409 ) ) ;
#93108 = CARTESIAN_POINT ( 'NONE',  ( 9.474510206698971260, -16.51473224551069308, 42.91557627198103120 ) ) ;
#93109 = CARTESIAN_POINT ( 'NONE',  ( -16.46253265017160317, 9.564922557960807481, 60.83224293864769550 ) ) ;
#93110 = CARTESIAN_POINT ( 'NONE',  ( -9.564922557960796823, -16.46253265017161027, 42.08224293864769550 ) ) ;
#93111 = CARTESIAN_POINT ( 'NONE',  ( -18.67979575497193778, 10.72451020669871902, 28.33442372801902209 ) ) ;
#93112 = CARTESIAN_POINT ( 'NONE',  ( -5.153800228976328057, -19.02544592524343514, 57.29057627198103120 ) ) ;
#93113 = CARTESIAN_POINT ( 'NONE',  ( 35.99626262588764547, 2.869439944428138037E-14, 2.000000000000000000 ) ) ;
#93114 = CARTESIAN_POINT ( 'NONE',  ( -16.51473224551069308, -9.474510206698971260, 41.66557627198103120 ) ) ;
#93115 = CARTESIAN_POINT ( 'NONE',  ( -15.72974639402197994, 15.80617190586746368, 35.62390960531437401 ) ) ;
#93117 = CARTESIAN_POINT ( 'NONE',  ( 19.02544592524343514, -5.153800228976328945, 28.54057627198102409 ) ) ;
#93116 = CARTESIAN_POINT ( 'NONE',  ( -18.67979575497193778, 10.72451020669871902, 63.33442372801900433 ) ) ;
#93118 = CARTESIAN_POINT ( 'NONE',  ( 10.72451020669898902, -18.67979575497178502, 22.91557627198102765 ) ) ;
#93119 = CARTESIAN_POINT ( 'NONE',  ( 4.379528057220092307, 16.55341960407617563, 97.29275706135234714 ) ) ;
#93120 = CARTESIAN_POINT ( 'NONE',  ( -21.53943276465977519, -0.05219959533937600094, 103.7510903946857042 ) ) ;
#93121 = CARTESIAN_POINT ( 'NONE',  ( -4.483927247898782831, 16.52544592524335698, 67.70942372801901854 ) ) ;
#93122 = CARTESIAN_POINT ( 'NONE',  ( 13.89961937509977652, -13.97604488694527269, 108.1239096053143669 ) ) ;
#93123 = CARTESIAN_POINT ( 'NONE',  ( -8.224510206698735004, -14.34966873604973081, 49.58442372801901143 ) ) ;
#93124 = CARTESIAN_POINT ( 'NONE',  ( -12.06949235617739369, -12.14591786802326823, 44.37609039468567573 ) ) ;
#93125 = CARTESIAN_POINT ( 'NONE',  ( -0.05219959533934338120, 16.53943276465976808, 97.50109039468567573 ) ) ;
#93126 = CARTESIAN_POINT ( 'NONE',  ( 18.62759615963255655, 10.81492255796105972, 51.66775706135234714 ) ) ;
#93127 = CARTESIAN_POINT ( 'NONE',  ( 14.34966873604972726, -8.224510206698740333, 25.83442372801901499 ) ) ;
#93128 = CARTESIAN_POINT ( 'NONE',  ( 21.52544592524344225, -5.823673210054117533, 113.5405762719810383 ) ) ;
#93129 = CARTESIAN_POINT ( 'NONE',  ( -16.55341960407617563, 4.379528057220093196, 23.54275706135235424 ) ) ;
#93130 = CARTESIAN_POINT ( 'NONE',  ( 16.53943276465976808, 0.05219959533934440121, 91.25109039468568994 ) ) ;
#93131 = CARTESIAN_POINT ( 'NONE',  ( -16.31925111598407341, 7.325300261831848125, 45.16424538967171998 ) ) ;
#93132 = CARTESIAN_POINT ( 'NONE',  ( -21.52544592524334988, -5.823673210054445271, 93.95942372801903275 ) ) ;
#93133 = CARTESIAN_POINT ( 'NONE',  ( 13.89961937509957401, 13.97604488694547697, 81.87609039468564731 ) ) ;
#93134 = CARTESIAN_POINT ( 'NONE',  ( -8.224510206698948167, 14.34966873604960824, 65.41557627198102409 ) ) ;
#93135 = CARTESIAN_POINT ( 'NONE',  ( -16.55341960407611168, -4.379528057220339221, 46.45724293864769550 ) ) ;
#93136 = CARTESIAN_POINT ( 'NONE',  ( -16.55341960407611168, -4.379528057220339221, 111.4572429386476813 ) ) ;
#93138 = FACE_OUTER_BOUND ( 'NONE', #143331, .T. ) ;
#93137 = CARTESIAN_POINT ( 'NONE',  ( -5.153800228976607833, 19.02544592524334988, 47.70942372801900433 ) ) ;
#93139 = CARTESIAN_POINT ( 'NONE',  ( -21.52544592524334988, -5.823673210054445271, 43.95942372801902565 ) ) ;
#93140 = CARTESIAN_POINT ( 'NONE',  ( -8.224510206698735004, -14.34966873604973081, 19.58442372801901143 ) ) ;
#93141 = CARTESIAN_POINT ( 'NONE',  ( -17.49999999999999645, 7.499999999999998224, 120.0000000000000142 ) ) ;
#93142 = CARTESIAN_POINT ( 'NONE',  ( -13.97604488694527625, -13.89961937509977652, 101.8739096053143811 ) ) ;
#93143 = CARTESIAN_POINT ( 'NONE',  ( -15.80617190586745835, -15.72974639402198527, 66.87390960531436690 ) ) ;
#93144 = CARTESIAN_POINT ( 'NONE',  ( -9.474510206698720793, -16.51473224551083518, 99.58442372801900433 ) ) ;
#93145 = EDGE_CURVE ( 'NONE', #97386, #8281, #193801, .T. ) ;
#93146 = CARTESIAN_POINT ( 'NONE',  ( 19.02544592524343514, -5.153800228976328945, 98.54057627198100988 ) ) ;
#93147 = CARTESIAN_POINT ( 'NONE',  ( -21.52544592524343514, 5.823673210054127303, 61.04057627198103120 ) ) ;
#93148 = CARTESIAN_POINT ( 'NONE',  ( -4.379528057220328563, 16.55341960407611168, 110.2072429386477239 ) ) ;
#93149 = CARTESIAN_POINT ( 'NONE',  ( 15.80617190586769283, -15.72974639402175789, 95.62609039468568994 ) ) ;
#93150 = CARTESIAN_POINT ( 'NONE',  ( 19.03943276465977164, -0.05219959533909143690, 23.74890960531435269 ) ) ;
#93151 = CARTESIAN_POINT ( 'NONE',  ( 15.72974639402176855, 15.80617190586768217, 36.87609039468568994 ) ) ;
#93152 = CARTESIAN_POINT ( 'NONE',  ( -0.05219959533937732626, 21.53943276465977519, 87.50109039468568994 ) ) ;
#93153 = CARTESIAN_POINT ( 'NONE',  ( -12.06949235617739369, -12.14591786802326823, 84.37609039468570415 ) ) ;
#93154 = EDGE_CURVE ( 'NONE', #92045, #159210, #163663, .T. ) ;
#93155 = CARTESIAN_POINT ( 'NONE',  ( -10.72451020669870658, -18.67979575497194134, 29.58442372801901854 ) ) ;
#93156 = CARTESIAN_POINT ( 'NONE',  ( 21.53943276465977519, 0.05219959533937863772, 41.25109039468568284 ) ) ;
#93158 = CARTESIAN_POINT ( 'NONE',  ( -9.474510206698964154, 16.51473224551069663, 85.41557627198102409 ) ) ;
#93157 = CARTESIAN_POINT ( 'NONE',  ( 5.049401038297881783, 19.05341960407617563, 62.29275706135234003 ) ) ;
#93159 = CARTESIAN_POINT ( 'NONE',  ( 15.80617190586769283, -15.72974639402175789, 85.62609039468568994 ) ) ;
#93160 = CARTESIAN_POINT ( 'NONE',  ( 21.52544592524344225, -5.823673210054117533, 78.54057627198103830 ) ) ;
#93161 = CARTESIAN_POINT ( 'NONE',  ( 14.29746914071049879, -8.314922557960816363, 58.33224293864768839 ) ) ;
#93162 = CARTESIAN_POINT ( 'NONE',  ( 15.72974639402176855, 15.80617190586768217, 106.8760903946856899 ) ) ;
#93163 = CARTESIAN_POINT ( 'NONE',  ( -16.53943276465976808, 0.05219959533911058130, 81.24890960531436690 ) ) ;
#93164 = CARTESIAN_POINT ( 'NONE',  ( 16.46253265017160672, -9.564922557960803928, 38.33224293864768839 ) ) ;
#93165 = CARTESIAN_POINT ( 'NONE',  ( -5.153800228976607833, 19.02544592524334988, 77.70942372801900433 ) ) ;
#93166 = CARTESIAN_POINT ( 'NONE',  ( -16.53943276465976808, 0.05219959533911058130, 41.24890960531435269 ) ) ;
#93167 = CARTESIAN_POINT ( 'NONE',  ( 0.05219959533937995610, -21.53943276465977519, 100.0010903946857042 ) ) ;
#93168 = CARTESIAN_POINT ( 'NONE',  ( -16.46253265017160317, 9.564922557960807481, 90.83224293864769550 ) ) ;
#93169 = CARTESIAN_POINT ( 'NONE',  ( 16.46253265017146816, 9.564922557961045513, 66.66775706135233293 ) ) ;
#93170 = CARTESIAN_POINT ( 'NONE',  ( 21.53943276465977519, -0.05219959533907433946, 68.74890960531435269 ) ) ;
#93171 = CARTESIAN_POINT ( 'NONE',  ( -5.823673210054431948, 21.52544592524334988, 22.70942372801901499 ) ) ;
#93172 = CARTESIAN_POINT ( 'NONE',  ( -16.46253265017146816, -9.564922557961047289, 109.1677570613523471 ) ) ;
#93173 = CARTESIAN_POINT ( 'NONE',  ( -12.14591786802326823, 12.06949235617739902, 73.12609039468567573 ) ) ;
#93175 = CARTESIAN_POINT ( 'NONE',  ( 21.53943276465977519, 0.05219959533937863772, 26.25109039468567573 ) ) ;
#93174 = CARTESIAN_POINT ( 'NONE',  ( 16.21995358207306737, 7.366697692864131675, 62.56448998487839930 ) ) ;
#93176 = CARTESIAN_POINT ( 'NONE',  ( 0.05219959533910956823, 16.53943276465976808, 99.99890960531436690 ) ) ;
#93177 = CARTESIAN_POINT ( 'NONE',  ( -11.40812507854754720, -35.11059874428192273, -4.724999997268812812 ) ) ;
#93178 = CARTESIAN_POINT ( 'NONE',  ( -14.34966873604972548, 8.224510206698743886, 53.33442372801901854 ) ) ;
#93179 = CARTESIAN_POINT ( 'NONE',  ( 12.06949235617757843, -12.14591786802309237, 78.12390960531436690 ) ) ;
#93180 = CARTESIAN_POINT ( 'NONE',  ( 21.53943276465977519, -0.05219959533907433946, 73.74890960531433848 ) ) ;
#93181 = CARTESIAN_POINT ( 'NONE',  ( 0.05219959533934541429, -16.53943276465976808, 100.0010903946857042 ) ) ;
#93182 = CARTESIAN_POINT ( 'NONE',  ( 0.05219959533934541429, -16.53943276465976808, 40.00109039468567573 ) ) ;
#93183 = CARTESIAN_POINT ( 'NONE',  ( -19.05341960407611168, -5.049401038298163336, 41.45724293864769550 ) ) ;
#93184 = CARTESIAN_POINT ( 'NONE',  ( -16.52544592524335698, -4.483927247898792601, 73.95942372801901854 ) ) ;
#93185 = CARTESIAN_POINT ( 'NONE',  ( -0.05219959533936034679, 19.03943276465977164, 67.50109039468566152 ) ) ;
#93186 = CARTESIAN_POINT ( 'NONE',  ( 10.81492255796078972, 18.62759615963270932, 74.58224293864768129 ) ) ;
#93187 = CARTESIAN_POINT ( 'NONE',  ( 8.224510206698742110, 14.34966873604972548, 92.08442372801901854 ) ) ;
#93188 = CARTESIAN_POINT ( 'NONE',  ( -18.62759615963255300, -10.81492255796106328, 89.16775706135236135 ) ) ;
#93189 = CARTESIAN_POINT ( 'NONE',  ( -21.55341960407610458, -5.719274019375992779, 71.45724293864769550 ) ) ;
#93190 = CARTESIAN_POINT ( 'NONE',  ( -18.67979575497178146, -10.72451020669898902, 51.66557627198102409 ) ) ;
#93191 = VERTEX_POINT ( 'NONE', #174718 ) ;
#93192 = CARTESIAN_POINT ( 'NONE',  ( 14.29746914071037800, 8.314922557961029526, 81.66775706135236135 ) ) ;
#93193 = CARTESIAN_POINT ( 'NONE',  ( -21.52544592524343514, 5.823673210054127303, 51.04057627198103120 ) ) ;
#93194 = EDGE_LOOP ( 'NONE', ( #188218, #74139, #198885, #10789, #187345, #51917, #37500, #134296, #38599, #4818, #179524, #164864, #143939, #183777 ) ) ;
#93195 = CARTESIAN_POINT ( 'NONE',  ( 21.53943276465977519, -0.05219959533907433946, 23.74890960531435269 ) ) ;
#93196 = CARTESIAN_POINT ( 'NONE',  ( -22.19348515620997375, -7.491027558428858590, 173.8712782147084681 ) ) ;
#93197 = CARTESIAN_POINT ( 'NONE',  ( 19.03943276465977164, -0.05219959533909143690, 28.74890960531435624 ) ) ;
#93198 = CARTESIAN_POINT ( 'NONE',  ( 21.52544592524344225, -5.823673210054117533, 78.54057627198103830 ) ) ;
#93199 = CARTESIAN_POINT ( 'NONE',  ( 12.06949235617739724, 12.14591786802326823, 101.8760903946857042 ) ) ;
#93200 = CARTESIAN_POINT ( 'NONE',  ( 5.823673210054444382, -21.52544592524334988, 45.20942372801901854 ) ) ;
#93201 = CARTESIAN_POINT ( 'NONE',  ( -13.97604488694547697, 13.89961937509957934, 113.1260903946856757 ) ) ;
#93202 = CARTESIAN_POINT ( 'NONE',  ( -19.02544592524342804, 5.153800228976336051, 26.04057627198103120 ) ) ;
#93203 = CARTESIAN_POINT ( 'NONE',  ( -13.89961937509957401, -13.97604488694547875, 109.3760903946856331 ) ) ;
#93204 = CARTESIAN_POINT ( 'NONE',  ( -13.89961937509977652, 13.97604488694528158, 35.62390960531435269 ) ) ;
#93205 = CARTESIAN_POINT ( 'NONE',  ( 23.31738231874054534, 16.94106989632529192, 141.1999999999999886 ) ) ;
#93206 = CARTESIAN_POINT ( 'NONE',  ( 13.89961937509977652, -13.97604488694527269, 108.1239096053143669 ) ) ;
#93207 = CARTESIAN_POINT ( 'NONE',  ( -12.14591786802326823, 12.06949235617739902, 88.12609039468570415 ) ) ;
#93208 = CARTESIAN_POINT ( 'NONE',  ( -5.049401038297874678, -19.05341960407617918, 84.79275706135233293 ) ) ;
#93209 = CARTESIAN_POINT ( 'NONE',  ( 19.02544592524334988, 5.153800228976608722, 26.45942372801899722 ) ) ;
#93210 = CARTESIAN_POINT ( 'NONE',  ( 5.823673210054125526, 21.52544592524343514, 64.79057627198103830 ) ) ;
#93211 = CARTESIAN_POINT ( 'NONE',  ( -8.224510206698735004, -14.34966873604973081, 89.58442372801901854 ) ) ;
#93212 = CARTESIAN_POINT ( 'NONE',  ( 13.89961937509957401, 13.97604488694547697, 76.87609039468566152 ) ) ;
#93213 = CARTESIAN_POINT ( 'NONE',  ( 9.564922557960805705, 16.46253265017160317, 49.58224293864770260 ) ) ;
#93214 = CARTESIAN_POINT ( 'NONE',  ( -19.05341960407611168, -5.049401038298163336, 86.45724293864769550 ) ) ;
#93215 = CARTESIAN_POINT ( 'NONE',  ( 10.81492255796106328, -18.62759615963255655, 45.41775706135234003 ) ) ;
#93216 = CARTESIAN_POINT ( 'NONE',  ( -19.02544592524342804, 5.153800228976336051, 46.04057627198101699 ) ) ;
#93217 = CARTESIAN_POINT ( 'NONE',  ( 21.81230582904510840, -7.807068725607987147, 172.9985625539908085 ) ) ;
#93218 = CARTESIAN_POINT ( 'NONE',  ( 19.05341960407611168, 5.049401038298154454, 103.9572429386476671 ) ) ;
#93219 = CARTESIAN_POINT ( 'NONE',  ( 16.55341960407611168, 4.379528057220329451, 63.95724293864770260 ) ) ;
#93220 = CARTESIAN_POINT ( 'NONE',  ( 10.72451020669898902, -18.67979575497178502, 62.91557627198102409 ) ) ;
#93221 = CARTESIAN_POINT ( 'NONE',  ( 17.79613651744293534, 24.49428055684532524, 143.5656553485623590 ) ) ;
#93222 = CARTESIAN_POINT ( 'NONE',  ( 13.89961937509957401, 13.97604488694547697, 41.87609039468566152 ) ) ;
#93223 = CARTESIAN_POINT ( 'NONE',  ( 20.74358237093906254, -11.24271120488110043, 170.1279846108370180 ) ) ;
#93225 = CARTESIAN_POINT ( 'NONE',  ( -9.564922557960796823, -16.46253265017161027, 77.08224293864769550 ) ) ;
#93224 = CARTESIAN_POINT ( 'NONE',  ( -9.474510206698964154, 16.51473224551069663, 60.41557627198102409 ) ) ;
#93226 = CARTESIAN_POINT ( 'NONE',  ( 4.483927247898790824, -16.52544592524335698, 50.20942372801901854 ) ) ;
#93227 = CARTESIAN_POINT ( 'NONE',  ( -9.474510206698720793, -16.51473224551083518, 79.58442372801899012 ) ) ;
#93228 = CARTESIAN_POINT ( 'NONE',  ( -5.429308488886486681E-15, 30.30510711980690175, 145.7500000054623115 ) ) ;
#93229 = CARTESIAN_POINT ( 'NONE',  ( 12.06949235617739724, 12.14591786802326823, 91.87609039468568994 ) ) ;
#93230 = CARTESIAN_POINT ( 'NONE',  ( -0.7284999611695081034, -24.11542121825891627, -54.35861002160294930 ) ) ;
#93231 = CARTESIAN_POINT ( 'NONE',  ( 4.483927247898790824, -16.52544592524335698, 80.20942372801901854 ) ) ;
#93232 = CARTESIAN_POINT ( 'NONE',  ( -4.379528057220086978, -16.55341960407618274, 54.79275706135235424 ) ) ;
#93233 = CARTESIAN_POINT ( 'NONE',  ( 10.72451020669871369, 18.67979575497193778, 112.0844237280190185 ) ) ;
#93235 = FACE_BOUND ( 'NONE', #90817, .T. ) ;
#93234 = CARTESIAN_POINT ( 'NONE',  ( 13.97604488694527802, 13.89961937509977652, 49.37390960531434558 ) ) ;
#93236 = CARTESIAN_POINT ( 'NONE',  ( -5.823673210054431948, 21.52544592524334988, 52.70942372801902565 ) ) ;
#93237 = CARTESIAN_POINT ( 'NONE',  ( -19.03943276465977164, -0.05219959533935918106, 58.75109039468566863 ) ) ;
#93238 = CARTESIAN_POINT ( 'NONE',  ( -0.05219959533937732626, 21.53943276465977519, 112.5010903946857042 ) ) ;
#93239 = CARTESIAN_POINT ( 'NONE',  ( -5.153800228976328057, -19.02544592524343514, 27.29057627198103120 ) ) ;
#93240 = CARTESIAN_POINT ( 'NONE',  ( -15.40597107458654591, 14.79957802611868978, -58.81775317265829273 ) ) ;
#93241 = CARTESIAN_POINT ( 'NONE',  ( -5.719274019375978568, 21.55341960407610458, 65.20724293864768129 ) ) ;
#93242 = CARTESIAN_POINT ( 'NONE',  ( 19.03943276465977164, -0.05219959533909143690, 113.7489096053143669 ) ) ;
#93243 = CARTESIAN_POINT ( 'NONE',  ( -19.03943276465977164, 0.05219959533909376836, 26.24890960531435624 ) ) ;
#93244 = CARTESIAN_POINT ( 'NONE',  ( -0.05219959533934338120, 16.53943276465976808, 37.50109039468568284 ) ) ;
#93245 = CARTESIAN_POINT ( 'NONE',  ( 16.55341960407611168, 4.379528057220329451, 33.95724293864769550 ) ) ;
#93246 = ORIENTED_EDGE ( 'NONE', *, *, #72314, .F. ) ;
#93247 = CARTESIAN_POINT ( 'NONE',  ( 21.52544592524334988, 5.823673210054432836, 21.45942372801901499 ) ) ;
#93249 = CARTESIAN_POINT ( 'NONE',  ( 9.474510206698971260, -16.51473224551069308, 112.9155762719810383 ) ) ;
#93248 = CARTESIAN_POINT ( 'NONE',  ( -12.14591786802309592, -12.06949235617757132, 36.87390960531435979 ) ) ;
#93250 = CARTESIAN_POINT ( 'NONE',  ( -5.153800228976607833, 19.02544592524334988, 102.7094237280189759 ) ) ;
#93251 = CARTESIAN_POINT ( 'NONE',  ( 9.474510206698729675, 16.51473224551082808, 22.08442372801899722 ) ) ;
#93252 = CARTESIAN_POINT ( 'NONE',  ( -16.55341960407611168, -4.379528057220339221, 41.45724293864769550 ) ) ;
#93254 = EDGE_CURVE ( 'NONE', #30636, #75343, #35202, .T. ) ;
#93253 = CARTESIAN_POINT ( 'NONE',  ( 18.67979575497178502, 10.72451020669898547, 104.1655762719810241 ) ) ;
#93256 = CARTESIAN_POINT ( 'NONE',  ( -10.72451020669898014, 18.67979575497178502, 70.41557627198102409 ) ) ;
#93255 = DIRECTION ( 'NONE',  ( 0.000000000000000000, 0.000000000000000000, 1.000000000000000000 ) ) ;
#93257 = CARTESIAN_POINT ( 'NONE',  ( -19.03943276465977164, 0.05219959533909376836, 71.24890960531435269 ) ) ;
#93258 = CARTESIAN_POINT ( 'NONE',  ( 8.314922557960818139, 14.29746914071049879, 44.58224293864769550 ) ) ;
#93259 = CARTESIAN_POINT ( 'NONE',  ( -19.03943276465977164, 0.05219959533909376836, 86.24890960531436690 ) ) ;
#93260 = CARTESIAN_POINT ( 'NONE',  ( -36.91128768240056246, 1.976579976310101802E-14, 50.50000000000002842 ) ) ;
#93261 = CARTESIAN_POINT ( 'NONE',  ( 16.46253265017146816, 9.564922557961045513, 51.66775706135233293 ) ) ;
#93262 = CARTESIAN_POINT ( 'NONE',  ( 15.80617190586746368, 15.72974639402197994, 99.37390960531436690 ) ) ;
#93263 = CARTESIAN_POINT ( 'NONE',  ( -16.55341960407611168, -4.379528057220339221, 101.4572429386476955 ) ) ;
#93264 = CARTESIAN_POINT ( 'NONE',  ( 21.55341960407619695, -5.719274019375665929, 46.04275706135234714 ) ) ;
#93265 = CARTESIAN_POINT ( 'NONE',  ( 27.73933785331498925, -9.013057229001033122, 143.7750000027311614 ) ) ;
#93266 = EDGE_CURVE ( 'NONE', #102786, #186567, #160537, .T. ) ;
#93267 = CARTESIAN_POINT ( 'NONE',  ( 16.53943276465976808, -0.05219959533910856209, 28.74890960531435624 ) ) ;
#93268 = CARTESIAN_POINT ( 'NONE',  ( -19.03943276465977164, 0.05219959533909376836, 36.24890960531436690 ) ) ;
#93269 = CARTESIAN_POINT ( 'NONE',  ( 0.05219959533909260263, 19.03943276465977164, 104.9989096053143669 ) ) ;
#93270 = CARTESIAN_POINT ( 'NONE',  ( 15.80617190586746368, 15.72974639402197994, 54.37390960531435979 ) ) ;
#93271 = CARTESIAN_POINT ( 'NONE',  ( -19.35633801406906684, 5.499999999999782396, 44.13373818172762952 ) ) ;
#93272 = CARTESIAN_POINT ( 'NONE',  ( 19.05341960407611168, 5.049401038298154454, 28.95724293864769550 ) ) ;
#93273 = CARTESIAN_POINT ( 'NONE',  ( 5.823673210054125526, 21.52544592524343514, 54.79057627198104541 ) ) ;
#93274 = CARTESIAN_POINT ( 'NONE',  ( -18.62759615963255300, -10.81492255796106328, 79.16775706135234714 ) ) ;
#93276 = CARTESIAN_POINT ( 'NONE',  ( -14.29746914071037622, -8.314922557961029526, 89.16775706135236135 ) ) ;
#93275 = CARTESIAN_POINT ( 'NONE',  ( 16.98531384169471892, -34.11756901830160160, -21.70785296103238693 ) ) ;
#93277 = CARTESIAN_POINT ( 'NONE',  ( -9.474510206698964154, 16.51473224551069663, 60.41557627198102409 ) ) ;
#93278 = CARTESIAN_POINT ( 'NONE',  ( 19.03943276465977164, -0.05219959533909143690, 63.74890960531435979 ) ) ;
#93279 = ORIENTED_EDGE ( 'NONE', *, *, #33197, .T. ) ;
#93280 = CARTESIAN_POINT ( 'NONE',  ( -16.46253265017146816, -9.564922557961047289, 24.16775706135233648 ) ) ;
#93281 = CARTESIAN_POINT ( 'NONE',  ( 16.55341960407618274, -4.379528057220086978, 71.04275706135234714 ) ) ;
#93282 = CARTESIAN_POINT ( 'NONE',  ( -21.53943276465977519, -0.05219959533937600094, 103.7510903946857042 ) ) ;
#93283 = CARTESIAN_POINT ( 'NONE',  ( 16.51473224551069308, 9.474510206698969483, 74.16557627198103830 ) ) ;
#93284 = CARTESIAN_POINT ( 'NONE',  ( -15.80617190586745835, -15.72974639402198527, 31.87390960531435979 ) ) ;
#93285 = CARTESIAN_POINT ( 'NONE',  ( -9.564922557961040184, 16.46253265017147172, 107.9177570613523471 ) ) ;
#93286 = CARTESIAN_POINT ( 'NONE',  ( -0.05219959533937732626, 21.53943276465977519, 82.50109039468568994 ) ) ;
#93287 = CARTESIAN_POINT ( 'NONE',  ( 4.483927247898790824, -16.52544592524335698, 45.20942372801901854 ) ) ;
#93288 = CARTESIAN_POINT ( 'NONE',  ( -18.62759615963270932, 10.81492255796079327, 105.8322429386476955 ) ) ;
#93289 = CARTESIAN_POINT ( 'NONE',  ( 0.05219959533934541429, -16.53943276465976808, 20.00109039468568639 ) ) ;
#93290 = CARTESIAN_POINT ( 'NONE',  ( 9.474510206698971260, -16.51473224551069308, 72.91557627198102409 ) ) ;
#93291 = CARTESIAN_POINT ( 'NONE',  ( -8.314922557961024197, 14.29746914071037800, 22.91775706135235069 ) ) ;
#93292 = CARTESIAN_POINT ( 'NONE',  ( 0.05219959533909260263, 19.03943276465977164, 39.99890960531436690 ) ) ;
#93293 = CARTESIAN_POINT ( 'NONE',  ( 5.153800228976615827, -19.02544592524334988, 110.2094237280189901 ) ) ;
#93294 = CARTESIAN_POINT ( 'NONE',  ( 8.314922557960818139, 14.29746914071049879, 69.58224293864769550 ) ) ;
#93295 = CARTESIAN_POINT ( 'NONE',  ( 12.14591786802327356, -12.06949235617739191, 75.62609039468567573 ) ) ;
#93297 = CARTESIAN_POINT ( 'NONE',  ( 16.51473224551069308, 9.474510206698969483, 49.16557627198102409 ) ) ;
#93296 = CARTESIAN_POINT ( 'NONE',  ( -18.67979575497193778, 10.72451020669871902, 33.33442372801900433 ) ) ;
#93298 = CARTESIAN_POINT ( 'NONE',  ( -13.89961937509977652, 13.97604488694528158, 75.62390960531438111 ) ) ;
#93299 = CARTESIAN_POINT ( 'NONE',  ( -4.483927247898782831, 16.52544592524335698, 77.70942372801900433 ) ) ;
#93300 = EDGE_CURVE ( 'NONE', #71503, #189747, #38195, .T. ) ;
#93302 = ORIENTED_EDGE ( 'NONE', *, *, #161479, .T. ) ;
#93301 = DIRECTION ( 'NONE',  ( 1.000000000000000000, 0.000000000000000000, 0.000000000000000000 ) ) ;
#93303 = ORIENTED_EDGE ( 'NONE', *, *, #190368, .F. ) ;
#93304 = CARTESIAN_POINT ( 'NONE',  ( -5.823673210054431948, 21.52544592524334988, 107.7094237280190328 ) ) ;
#93305 = CARTESIAN_POINT ( 'NONE',  ( -9.474510206698964154, 16.51473224551069663, 40.41557627198103120 ) ) ;
#93307 = VERTEX_POINT ( 'NONE', #8860 ) ;
#93306 = CARTESIAN_POINT ( 'NONE',  ( 9.564922557960805705, 16.46253265017160317, 114.5822429386476955 ) ) ;
#93308 = CARTESIAN_POINT ( 'NONE',  ( -14.34966873604972548, 8.224510206698743886, 28.33442372801902209 ) ) ;
#93309 = CIRCLE ( 'NONE', #83641, 206.0437394197456911 ) ;
#93311 = CARTESIAN_POINT ( 'NONE',  ( 16.53943276465976808, 0.05219959533934440121, 46.25109039468567573 ) ) ;
#93310 = CARTESIAN_POINT ( 'NONE',  ( -13.89961937509957401, -13.97604488694547875, 59.37609039468566863 ) ) ;
#93312 = CARTESIAN_POINT ( 'NONE',  ( 9.564922557960805705, 16.46253265017160317, 39.58224293864768839 ) ) ;
#93313 = CARTESIAN_POINT ( 'NONE',  ( -13.89961937509977652, 13.97604488694528158, 110.6239096053143243 ) ) ;
#93314 = CARTESIAN_POINT ( 'NONE',  ( -16.51473224551069308, -9.474510206698971260, 61.66557627198103120 ) ) ;
#93315 = CARTESIAN_POINT ( 'NONE',  ( -0.05219959533907301413, -21.53943276465977519, 102.4989096053143811 ) ) ;
#93317 = CARTESIAN_POINT ( 'NONE',  ( -13.97604488694527625, -13.89961937509977652, 21.87390960531435979 ) ) ;
#93316 = CARTESIAN_POINT ( 'NONE',  ( 16.51473224551069308, 9.474510206698969483, 89.16557627198103830 ) ) ;
#93318 = CARTESIAN_POINT ( 'NONE',  ( -9.474510206698964154, 16.51473224551069663, 60.41557627198102409 ) ) ;
#93320 = CARTESIAN_POINT ( 'NONE',  ( -17.49999999999999645, -5.499999999999992895, 59.20309617465829177 ) ) ;
#93319 = CARTESIAN_POINT ( 'NONE',  ( -0.05219959533934338120, 16.53943276465976808, 107.5010903946856899 ) ) ;
#93321 = CARTESIAN_POINT ( 'NONE',  ( -19.05341960407617563, 5.049401038297882671, 98.54275706135233293 ) ) ;
#93322 = CARTESIAN_POINT ( 'NONE',  ( -19.02544592524334988, -5.153800228976617603, 28.95942372801900433 ) ) ;
#93323 = CARTESIAN_POINT ( 'NONE',  ( -16.52544592524342804, 4.483927247898546575, 56.04057627198102409 ) ) ;
#93324 = CARTESIAN_POINT ( 'NONE',  ( 5.719274019375673035, 21.55341960407619339, 102.2927570613523613 ) ) ;
#93325 = CARTESIAN_POINT ( 'NONE',  ( 13.97604488694527802, 13.89961937509977652, 34.37390960531436690 ) ) ;
#93327 = CARTESIAN_POINT ( 'NONE',  ( 21.53943276465977519, 0.05219959533937863772, 86.25109039468568994 ) ) ;
#93326 = CARTESIAN_POINT ( 'NONE',  ( -8.224510206698948167, 14.34966873604960824, 40.41557627198103120 ) ) ;
#93328 = CARTESIAN_POINT ( 'NONE',  ( -19.03943276465977164, 0.05219959533909376836, 86.24890960531436690 ) ) ;
#93329 = CARTESIAN_POINT ( 'NONE',  ( -9.474510206698964154, 16.51473224551069663, 100.4155762719810241 ) ) ;
#93330 = CARTESIAN_POINT ( 'NONE',  ( -8.314922557960811034, -14.29746914071050412, 107.0822429386476955 ) ) ;
#93331 = CARTESIAN_POINT ( 'NONE',  ( -14.29746914071049879, 8.314922557960819915, 70.83224293864770971 ) ) ;
#93332 = CARTESIAN_POINT ( 'NONE',  ( -10.81492255796078084, -18.62759615963271287, 82.08224293864768129 ) ) ;
#93333 = CARTESIAN_POINT ( 'NONE',  ( 9.474510206698971260, -16.51473224551069308, 77.91557627198103830 ) ) ;
#93334 = CARTESIAN_POINT ( 'NONE',  ( -10.81492255796078084, -18.62759615963271287, 82.08224293864768129 ) ) ;
#93335 = CARTESIAN_POINT ( 'NONE',  ( -13.89961937509957401, -13.97604488694547875, 84.37609039468567573 ) ) ;
#93337 = CARTESIAN_POINT ( 'NONE',  ( -16.53943276465976808, 0.05219959533911058130, 96.24890960531435269 ) ) ;
#93336 = CYLINDRICAL_SURFACE ( 'NONE', #104284, 1.000000000000000888 ) ;
#93338 = CARTESIAN_POINT ( 'NONE',  ( 19.02544592524343514, -5.153800228976328945, 58.54057627198102409 ) ) ;
#93339 = CARTESIAN_POINT ( 'NONE',  ( -15.72974639402197994, 15.80617190586746368, 65.62390960531436690 ) ) ;
#93340 = CYLINDRICAL_SURFACE ( 'NONE', #114054, 214.0437394197456342 ) ;
#93342 = CARTESIAN_POINT ( 'NONE',  ( -17.49999999999999645, 5.499999999999997335, 120.0000000000000142 ) ) ;
#93341 = CARTESIAN_POINT ( 'NONE',  ( -8.314922557961024197, 14.29746914071037800, 107.9177570613523471 ) ) ;
#93343 = CARTESIAN_POINT ( 'NONE',  ( 12.14591786802327356, -12.06949235617739191, 25.62609039468567929 ) ) ;
#93344 = CARTESIAN_POINT ( 'NONE',  ( -4.379528057220328563, 16.55341960407611168, 75.20724293864769550 ) ) ;
#93345 = CARTESIAN_POINT ( 'NONE',  ( 6.404810000729014519, -0.9277198534072479408, -62.44539631020982284 ) ) ;
#93346 = CARTESIAN_POINT ( 'NONE',  ( 19.02544592524343514, -5.153800228976328945, 78.54057627198099567 ) ) ;
#93347 = CARTESIAN_POINT ( 'NONE',  ( 19.03943276465977164, -0.05219959533909143690, 33.74890960531435979 ) ) ;
#93348 = CARTESIAN_POINT ( 'NONE',  ( 12.06949235617757843, -12.14591786802309237, 73.12390960531436690 ) ) ;
#93349 = CARTESIAN_POINT ( 'NONE',  ( -21.53943276465977519, 0.05219959533907696930, 21.24890960531436690 ) ) ;
#93351 = CARTESIAN_POINT ( 'NONE',  ( 19.03943276465977164, -0.05219959533909143690, 73.74890960531435269 ) ) ;
#93350 = CARTESIAN_POINT ( 'NONE',  ( 5.153800228976615827, -19.02544592524334988, 85.20942372801900433 ) ) ;
#93352 = CARTESIAN_POINT ( 'NONE',  ( -0.05219959533909027116, -19.03943276465977164, 82.49890960531436690 ) ) ;
#93353 = CARTESIAN_POINT ( 'NONE',  ( 18.67979575497178502, 10.72451020669898547, 79.16557627198103830 ) ) ;
#93354 = CARTESIAN_POINT ( 'NONE',  ( 8.224510206698742110, 14.34966873604972548, 77.08442372801901854 ) ) ;
#93355 = CARTESIAN_POINT ( 'NONE',  ( -17.40861289039008497, 6.110651285853112569, 93.62767529172570846 ) ) ;
#93356 = CARTESIAN_POINT ( 'NONE',  ( -9.564922557960796823, -16.46253265017161027, 57.08224293864769550 ) ) ;
#93357 = CARTESIAN_POINT ( 'NONE',  ( -10.81492255796078084, -18.62759615963271287, 67.08224293864770971 ) ) ;
#93358 = CARTESIAN_POINT ( 'NONE',  ( -0.05219959533936034679, 19.03943276465977164, 97.50109039468567573 ) ) ;
#93360 = CARTESIAN_POINT ( 'NONE',  ( 21.53943276465977519, 0.05219959533937863772, 51.25109039468568994 ) ) ;
#93359 = CARTESIAN_POINT ( 'NONE',  ( 12.14591786802309770, 12.06949235617756955, 39.37390960531436690 ) ) ;
#93362 = CARTESIAN_POINT ( 'NONE',  ( 13.97604488694527802, 13.89961937509977652, 104.3739096053143385 ) ) ;
#93361 = CARTESIAN_POINT ( 'NONE',  ( -4.483927247898782831, 16.52544592524335698, 77.70942372801900433 ) ) ;
#93363 = FACE_BOUND ( 'NONE', #13023, .T. ) ;
#93364 = CARTESIAN_POINT ( 'NONE',  ( 1.106442667531312596, 31.41700946213341794, -49.73385396542428794 ) ) ;
#93365 = CARTESIAN_POINT ( 'NONE',  ( -4.379528057220086978, -16.55341960407618274, 99.79275706135234714 ) ) ;
#93366 = CARTESIAN_POINT ( 'NONE',  ( -4.483927247898782831, 16.52544592524335698, 47.70942372801902565 ) ) ;
#93367 = CARTESIAN_POINT ( 'NONE',  ( -19.05341960407611168, -5.049401038298163336, 56.45724293864768129 ) ) ;
#93368 = CARTESIAN_POINT ( 'NONE',  ( 19.03943276465977164, -0.05219959533909143690, 68.74890960531436690 ) ) ;
#93369 = CARTESIAN_POINT ( 'NONE',  ( -21.55341960407619339, 5.719274019375674811, 58.54275706135235424 ) ) ;
#93370 = CARTESIAN_POINT ( 'NONE',  ( -4.483927247898782831, 16.52544592524335698, 62.70942372801902565 ) ) ;
#93371 = CARTESIAN_POINT ( 'NONE',  ( 16.52544592524342804, -4.483927247898539470, 33.54057627198102409 ) ) ;
#93372 = CARTESIAN_POINT ( 'NONE',  ( 13.89961937509977652, -13.97604488694527269, 38.12390960531436690 ) ) ;
#93373 = CARTESIAN_POINT ( 'NONE',  ( -19.03943276465977164, 0.05219959533909376836, 36.24890960531436690 ) ) ;
#93375 = ORIENTED_EDGE ( 'NONE', *, *, #36793, .F. ) ;
#93374 = CARTESIAN_POINT ( 'NONE',  ( -0.05219959533934338120, 16.53943276465976808, 22.50109039468567573 ) ) ;
#93376 = CARTESIAN_POINT ( 'NONE',  ( 19.02544592524334988, 5.153800228976608722, 86.45942372801900433 ) ) ;
#93377 = CARTESIAN_POINT ( 'NONE',  ( -16.52544592524342804, 4.483927247898546575, 86.04057627198102409 ) ) ;
#93378 = CARTESIAN_POINT ( 'NONE',  ( -16.51473224551069308, -9.474510206698971260, 51.66557627198102409 ) ) ;
#93380 = CARTESIAN_POINT ( 'NONE',  ( 11.74264578624800315, -36.14014761921581709, -9.400000000000000355 ) ) ;
#93379 = CARTESIAN_POINT ( 'NONE',  ( -16.51473224551082808, 9.474510206698731452, 88.33442372801900433 ) ) ;
#93381 = CARTESIAN_POINT ( 'NONE',  ( 15.72974639402176855, 15.80617190586768217, 96.87609039468568994 ) ) ;
#93382 = CARTESIAN_POINT ( 'NONE',  ( 0.05219959533934541429, -16.53943276465976808, 55.00109039468568284 ) ) ;
#93383 = CARTESIAN_POINT ( 'NONE',  ( -17.50000000000143530, 3.202012800152433059, 24.92822416027274457 ) ) ;
#93384 = CARTESIAN_POINT ( 'NONE',  ( -5.719274019375978568, 21.55341960407610458, 55.20724293864770260 ) ) ;
#93385 = CARTESIAN_POINT ( 'NONE',  ( 14.34966873604972726, -8.224510206698740333, 45.83442372801901854 ) ) ;
#93386 = CARTESIAN_POINT ( 'NONE',  ( -19.02130022317638236, 5.499999999999802824, 70.78188669246573284 ) ) ;
#93387 = CARTESIAN_POINT ( 'NONE',  ( 16.46253265017146816, 9.564922557961045513, 26.66775706135234003 ) ) ;
#93388 = CARTESIAN_POINT ( 'NONE',  ( 9.474510206698971260, -16.51473224551069308, 82.91557627198103830 ) ) ;
#93389 = CARTESIAN_POINT ( 'NONE',  ( -0.05219959533909027116, -19.03943276465977164, 52.49890960531436690 ) ) ;
#93390 = LINE ( 'NONE', #155076, #65768 ) ;
#93391 = CARTESIAN_POINT ( 'NONE',  ( 16.46253265017160672, -9.564922557960803928, 63.33224293864769550 ) ) ;
#93392 = CARTESIAN_POINT ( 'NONE',  ( -18.87255363501903460, -5.499999999999956479, 56.32513748171827928 ) ) ;
#93393 = CARTESIAN_POINT ( 'NONE',  ( -13.97604488694547697, 13.89961937509957934, 38.12609039468566152 ) ) ;
#93394 = CARTESIAN_POINT ( 'NONE',  ( -5.823673210054431948, 21.52544592524334988, 107.7094237280190328 ) ) ;
#93395 = CARTESIAN_POINT ( 'NONE',  ( -4.379528057220328563, 16.55341960407611168, 35.20724293864768839 ) ) ;
#93396 = CARTESIAN_POINT ( 'NONE',  ( 9.564922557960805705, 16.46253265017160317, 39.58224293864768839 ) ) ;
#93397 = EDGE_CURVE ( 'NONE', #84653, #148762, #26158, .T. ) ;
#93398 = CARTESIAN_POINT ( 'NONE',  ( -5.153800228976328057, -19.02544592524343514, 112.2905762719810099 ) ) ;
#93399 = CARTESIAN_POINT ( 'NONE',  ( -21.53943276465977519, -0.05219959533937600094, 78.75109039468568994 ) ) ;
#93400 = CARTESIAN_POINT ( 'NONE',  ( -5.153800228976328057, -19.02544592524343514, 47.29057627198102409 ) ) ;
#93401 = CARTESIAN_POINT ( 'NONE',  ( 15.72974639402176855, 15.80617190586768217, 76.87609039468567573 ) ) ;
#93402 = CARTESIAN_POINT ( 'NONE',  ( -18.67979575497178146, -10.72451020669898902, 21.66557627198102409 ) ) ;
#93403 = CARTESIAN_POINT ( 'NONE',  ( -15.72974639402176322, -15.80617190586768395, 19.37609039468568639 ) ) ;
#93404 = CARTESIAN_POINT ( 'NONE',  ( -19.03943276465977164, -0.05219959533935918106, 43.75109039468566863 ) ) ;
#93405 = CARTESIAN_POINT ( 'NONE',  ( 9.564922557960805705, 16.46253265017160317, 29.58224293864769550 ) ) ;
#93406 = CARTESIAN_POINT ( 'NONE',  ( -13.97604488694527625, -13.89961937509977652, 76.87390960531433848 ) ) ;
#93407 = CARTESIAN_POINT ( 'NONE',  ( 14.34966873604972726, -8.224510206698740333, 20.83442372801901143 ) ) ;
#93408 = CARTESIAN_POINT ( 'NONE',  ( 12.14591786802309770, 12.06949235617756955, 94.37390960531436690 ) ) ;
#93409 = CARTESIAN_POINT ( 'NONE',  ( -18.67979575497178146, -10.72451020669898902, 41.66557627198103120 ) ) ;
#93410 = CARTESIAN_POINT ( 'NONE',  ( 19.03943276465977164, 0.05219959533936151252, 101.2510903946856757 ) ) ;
#93411 = CARTESIAN_POINT ( 'NONE',  ( -5.719274019375978568, 21.55341960407610458, 100.2072429386476955 ) ) ;
#93412 = CARTESIAN_POINT ( 'NONE',  ( 21.53943276465977519, 0.05219959533937863772, 51.25109039468568994 ) ) ;
#93413 = CARTESIAN_POINT ( 'NONE',  ( -12.06949235617739369, -12.14591786802326823, 59.37609039468568284 ) ) ;
#93414 = CARTESIAN_POINT ( 'NONE',  ( 4.483927247898790824, -16.52544592524335698, 60.20942372801902565 ) ) ;
#93415 = CARTESIAN_POINT ( 'NONE',  ( -19.02544592524342804, 5.153800228976336051, 61.04057627198103120 ) ) ;
#93416 = CARTESIAN_POINT ( 'NONE',  ( 0.05219959533934541429, -16.53943276465976808, 95.00109039468568994 ) ) ;
#93417 = CARTESIAN_POINT ( 'NONE',  ( 21.55341960407610458, 5.719274019375980345, 113.9572429386477239 ) ) ;
#93418 = CARTESIAN_POINT ( 'NONE',  ( -16.53943276465976808, 0.05219959533911058130, 51.24890960531436690 ) ) ;
#93419 = CARTESIAN_POINT ( 'NONE',  ( -16.51473224551069308, -9.474510206698971260, 86.66557627198102409 ) ) ;
#93420 = CARTESIAN_POINT ( 'NONE',  ( 0.05219959533934541429, -16.53943276465976808, 70.00109039468568994 ) ) ;
#93421 = CARTESIAN_POINT ( 'NONE',  ( 10.81492255796106328, -18.62759615963255655, 65.41775706135234714 ) ) ;
#93422 = CARTESIAN_POINT ( 'NONE',  ( -13.97604488694547697, 13.89961937509957934, 108.1260903946856331 ) ) ;
#93423 = CARTESIAN_POINT ( 'NONE',  ( 21.53943276465977519, -0.05219959533907433946, 108.7489096053143669 ) ) ;
#93424 = CARTESIAN_POINT ( 'NONE',  ( -12.14591786802309592, -12.06949235617757132, 46.87390960531435979 ) ) ;
#93425 = EDGE_CURVE ( 'NONE', #68071, #184655, #62290, .T. ) ;
#93426 = EDGE_LOOP ( 'NONE', ( #103294, #191502, #120812, #75954 ) ) ;
#93427 = CARTESIAN_POINT ( 'NONE',  ( -17.31747979337950483, 6.344076630961001051, 68.62055131934820906 ) ) ;
#93428 = CARTESIAN_POINT ( 'NONE',  ( -18.67979575497178146, -10.72451020669898902, 81.66557627198103830 ) ) ;
#93429 = CARTESIAN_POINT ( 'NONE',  ( 12.06949235617757843, -12.14591786802309237, 28.12390960531435979 ) ) ;
#93430 = ORIENTED_EDGE ( 'NONE', *, *, #102515, .T. ) ;
#93431 = CARTESIAN_POINT ( 'NONE',  ( 34.52932710190714261, 5.142084072295515895, 50.46524955901335829 ) ) ;
#93432 = CARTESIAN_POINT ( 'NONE',  ( -15.80617190586745835, -15.72974639402198527, 111.8739096053143669 ) ) ;
#93433 = CARTESIAN_POINT ( 'NONE',  ( -19.03943276465977164, 0.05219959533909376836, 116.2489096053143669 ) ) ;
#93434 = CARTESIAN_POINT ( 'NONE',  ( -21.53943276465977519, -0.05219959533937600094, 28.75109039468567929 ) ) ;
#93435 = CARTESIAN_POINT ( 'NONE',  ( 14.34966873604960469, 8.224510206698951720, 54.16557627198103120 ) ) ;
#93436 = CARTESIAN_POINT ( 'NONE',  ( 12.06949235617739724, 12.14591786802326823, 61.87609039468568284 ) ) ;
#93437 = CARTESIAN_POINT ( 'NONE',  ( -9.474510206698964154, 16.51473224551069663, 65.41557627198102409 ) ) ;
#93438 = CARTESIAN_POINT ( 'NONE',  ( 19.02544592524334988, 5.153800228976608722, 71.45942372801900433 ) ) ;
#93439 = CARTESIAN_POINT ( 'NONE',  ( 5.153800228976335163, 19.02544592524342804, 74.79057627198103830 ) ) ;
#93440 = CARTESIAN_POINT ( 'NONE',  ( -21.52544592524343514, 5.823673210054127303, 41.04057627198103120 ) ) ;
#93441 = CARTESIAN_POINT ( 'NONE',  ( -22.01160362601145337, -30.88790364210668926, -22.63296439182591513 ) ) ;
#93442 = CARTESIAN_POINT ( 'NONE',  ( 0.05219959533909260263, 19.03943276465977164, 64.99890960531436690 ) ) ;
#93443 = CARTESIAN_POINT ( 'NONE',  ( -8.314922557961024197, 14.29746914071037800, 27.91775706135234358 ) ) ;
#93444 = CARTESIAN_POINT ( 'NONE',  ( -5.049401038297874678, -19.05341960407617918, 69.79275706135233293 ) ) ;
#93445 = CARTESIAN_POINT ( 'NONE',  ( -15.80617190586745835, -15.72974639402198527, 106.8739096053143811 ) ) ;
#93446 = CARTESIAN_POINT ( 'NONE',  ( -0.05219959533910754901, -16.53943276465976808, 32.49890960531435979 ) ) ;
#93447 = CARTESIAN_POINT ( 'NONE',  ( 19.02544592524343514, -5.153800228976328945, 88.54057627198102409 ) ) ;
#93448 = CARTESIAN_POINT ( 'NONE',  ( 15.80617190586746368, 15.72974639402197994, 59.37390960531436690 ) ) ;
#93450 = CARTESIAN_POINT ( 'NONE',  ( -8.224510206698735004, -14.34966873604973081, 44.58442372801901854 ) ) ;
#93449 = CARTESIAN_POINT ( 'NONE',  ( -10.81492255796078084, -18.62759615963271287, 92.08224293864769550 ) ) ;
#93451 = CARTESIAN_POINT ( 'NONE',  ( -5.823673210054116645, -21.52544592524344225, 42.29057627198103120 ) ) ;
#93452 = CARTESIAN_POINT ( 'NONE',  ( 5.719274019375673035, 21.55341960407619339, 87.29275706135236135 ) ) ;
#93453 = CARTESIAN_POINT ( 'NONE',  ( -9.474510206698964154, 16.51473224551069663, 85.41557627198102409 ) ) ;
#93454 = AXIS2_PLACEMENT_3D ( 'NONE', #107282, #180200, #119505 ) ;
#93455 = CARTESIAN_POINT ( 'NONE',  ( -5.049401038298153566, 19.05341960407611168, 45.20724293864769550 ) ) ;
#93456 = CARTESIAN_POINT ( 'NONE',  ( -19.03943276465977164, 0.05219959533909376836, 86.24890960531436690 ) ) ;
#93457 = CARTESIAN_POINT ( 'NONE',  ( 16.52544592524342804, -4.483927247898539470, 98.54057627198105251 ) ) ;
#93458 = B_SPLINE_CURVE_WITH_KNOTS ( 'NONE', 3,
 ( #191711, #159367, #189737, #5689, #18896, #173574, #99696 ),
 .UNSPECIFIED., .F., .F.,
 ( 4, 3, 4 ),
 ( 0.006877813788783031929, 0.01375562809188913063, 0.01380070845639008031 ),
 .UNSPECIFIED. ) ;
#93459 = CARTESIAN_POINT ( 'NONE',  ( 19.03943276465977164, -0.05219959533909143690, 68.74890960531436690 ) ) ;
#93460 = CARTESIAN_POINT ( 'NONE',  ( 16.52544592524335698, 4.483927247898782831, 26.45942372801901854 ) ) ;
#93461 = CARTESIAN_POINT ( 'NONE',  ( 13.89961937509957579, 13.97604488694547520, 41.87609039468566152 ) ) ;
#93463 = CARTESIAN_POINT ( 'NONE',  ( 19.05341960407611168, 5.049401038298154454, 108.9572429386477097 ) ) ;
#93462 = CARTESIAN_POINT ( 'NONE',  ( 21.52544592524334988, 5.823673210054432836, 96.45942372801901854 ) ) ;
#93464 = CARTESIAN_POINT ( 'NONE',  ( -16.52544592524335698, -4.483927247898792601, 88.95942372801901854 ) ) ;
#93465 = DIRECTION ( 'NONE',  ( -0.000000000000000000, 0.000000000000000000, 1.000000000000000000 ) ) ;
#93466 = CARTESIAN_POINT ( 'NONE',  ( 13.97604488694548053, -13.89961937509957401, 75.62609039468564731 ) ) ;
#93467 = CARTESIAN_POINT ( 'NONE',  ( -13.97604488694547697, 13.89961937509957934, 28.12609039468565797 ) ) ;
#93468 = CARTESIAN_POINT ( 'NONE',  ( -17.44270441346513678, -5.991230190323104665, 46.36335079264228654 ) ) ;
#93469 = CARTESIAN_POINT ( 'NONE',  ( 0.05219959533909260263, 19.03943276465977164, 24.99890960531435269 ) ) ;
#93470 = CARTESIAN_POINT ( 'NONE',  ( 16.53943276465976808, -0.05219959533910856209, 33.74890960531436690 ) ) ;
#93471 = CARTESIAN_POINT ( 'NONE',  ( -16.21995358207306026, -7.366697692864179636, 110.0644899848784206 ) ) ;
#93472 = CARTESIAN_POINT ( 'NONE',  ( -12.14591786802309592, -12.06949235617757132, 31.87390960531435979 ) ) ;
#93473 = CARTESIAN_POINT ( 'NONE',  ( 6.835613355214110953, -5.764477180739371320, -63.98825660581650254 ) ) ;
#93474 = CARTESIAN_POINT ( 'NONE',  ( -4.379528057220086978, -16.55341960407618274, 99.79275706135234714 ) ) ;
#93475 = CARTESIAN_POINT ( 'NONE',  ( -19.03943276465977164, 0.05219959533909376836, 36.24890960531436690 ) ) ;
#93476 = CARTESIAN_POINT ( 'NONE',  ( -21.53943276465977519, -0.05219959533937600094, 98.75109039468568994 ) ) ;
#93477 = CARTESIAN_POINT ( 'NONE',  ( 13.89961937509957401, 13.97604488694547697, 111.8760903946856757 ) ) ;
#93478 = CARTESIAN_POINT ( 'NONE',  ( 10.72451020669871369, 18.67979575497193778, 72.08442372801899012 ) ) ;
#93479 = CARTESIAN_POINT ( 'NONE',  ( 5.049401038297881783, 19.05341960407617563, 47.29275706135231161 ) ) ;
#93480 = CARTESIAN_POINT ( 'NONE',  ( 5.153800228976335163, 19.02544592524342804, 89.79057627198102409 ) ) ;
#93481 = CARTESIAN_POINT ( 'NONE',  ( -19.02544592524342804, 5.153800228976336051, 76.04057627198102409 ) ) ;
#93482 = CARTESIAN_POINT ( 'NONE',  ( 17.40805194822031865, 6.112264579159365496, 71.66628727489388950 ) ) ;
#93483 = CARTESIAN_POINT ( 'NONE',  ( -18.62759615963270932, 10.81492255796079327, 100.8322429386477097 ) ) ;
#93484 = AXIS2_PLACEMENT_3D ( 'NONE', #54650, #55652, #116324 ) ;
#93485 = CARTESIAN_POINT ( 'NONE',  ( 14.29746914071049879, -8.314922557960816363, 73.33224293864769550 ) ) ;
#93486 = CARTESIAN_POINT ( 'NONE',  ( 5.823673210054125526, 21.52544592524343514, 64.79057627198103830 ) ) ;
#93487 = CARTESIAN_POINT ( 'NONE',  ( 19.03943276465977164, -0.05219959533909143690, 58.74890960531435979 ) ) ;
#93489 = CARTESIAN_POINT ( 'NONE',  ( 8.224510206698742110, 14.34966873604972548, 82.08442372801901854 ) ) ;
#93488 = CARTESIAN_POINT ( 'NONE',  ( -5.719274019375978568, 21.55341960407610458, 80.20724293864769550 ) ) ;
#93490 = EDGE_LOOP ( 'NONE', ( #176088, #137628, #58007, #56797 ) ) ;
#93491 = CARTESIAN_POINT ( 'NONE',  ( -9.564922557960796823, -16.46253265017161027, 42.08224293864769550 ) ) ;
#93493 = LINE ( 'NONE', #30853, #7379 ) ;
#93492 = CARTESIAN_POINT ( 'NONE',  ( -8.224510206698948167, 14.34966873604960824, 80.41557627198103830 ) ) ;
#93494 = CARTESIAN_POINT ( 'NONE',  ( 19.02544592524343514, -5.153800228976328945, 48.54057627198103120 ) ) ;
#93495 = CARTESIAN_POINT ( 'NONE',  ( 13.97604488694527802, 13.89961937509977652, 24.37390960531435624 ) ) ;
#93496 = CARTESIAN_POINT ( 'NONE',  ( 5.153800228976615827, -19.02544592524334988, 60.20942372801899012 ) ) ;
#93497 = CARTESIAN_POINT ( 'NONE',  ( 0.05219959533910956823, 16.53943276465976808, 89.99890960531438111 ) ) ;
#93499 = EDGE_CURVE ( 'NONE', #4215, #11669, #187304, .T. ) ;
#93498 = CARTESIAN_POINT ( 'NONE',  ( -21.53943276465977519, -0.05219959533937600094, 43.75109039468568284 ) ) ;
#93501 = CARTESIAN_POINT ( 'NONE',  ( -10.81492255796078084, -18.62759615963271287, 107.0822429386476955 ) ) ;
#93500 = CARTESIAN_POINT ( 'NONE',  ( -9.564922557960796823, -16.46253265017161027, 42.08224293864769550 ) ) ;
#93502 = DIRECTION ( 'NONE',  ( 1.000000000000000000, 0.000000000000000000, 3.469446951953612217E-15 ) ) ;
#93503 = CARTESIAN_POINT ( 'NONE',  ( 4.379528057220339221, -16.55341960407611168, 92.70724293864770971 ) ) ;
#93504 = CARTESIAN_POINT ( 'NONE',  ( 15.53529872673065704, -37.10890965030476707, -23.64498726423094510 ) ) ;
#93505 = CARTESIAN_POINT ( 'NONE',  ( -9.564922557960796823, -16.46253265017161027, 47.08224293864769550 ) ) ;
#93506 = CARTESIAN_POINT ( 'NONE',  ( 19.53091890409951858, 5.500000000000029310, 47.56097431831422995 ) ) ;
#93508 = CARTESIAN_POINT ( 'NONE',  ( 16.51473224551069308, 9.474510206698969483, 99.16557627198102409 ) ) ;
#93507 = CARTESIAN_POINT ( 'NONE',  ( 5.153800228976615827, -19.02544592524334988, 90.20942372801900433 ) ) ;
#93509 = CARTESIAN_POINT ( 'NONE',  ( 15.80617190586769283, -15.72974639402175789, 35.62609039468568994 ) ) ;
#93510 = CARTESIAN_POINT ( 'NONE',  ( -13.97604488694527625, -13.89961937509977652, 86.87390960531436690 ) ) ;
#93511 = CARTESIAN_POINT ( 'NONE',  ( 5.153800228976615827, -19.02544592524334988, 75.20942372801896170 ) ) ;
#93512 = CARTESIAN_POINT ( 'NONE',  ( -13.97604488694527625, -13.89961937509977652, 46.87390960531435979 ) ) ;
#93513 = CARTESIAN_POINT ( 'NONE',  ( -16.55341960407611168, -4.379528057220339221, 71.45724293864769550 ) ) ;
#93514 = CARTESIAN_POINT ( 'NONE',  ( -16.55341960407611168, -4.379528057220339221, 71.45724293864769550 ) ) ;
#93515 = CARTESIAN_POINT ( 'NONE',  ( -16.51473224551069308, -9.474510206698971260, 81.66557627198103830 ) ) ;
#93516 = CARTESIAN_POINT ( 'NONE',  ( -5.719274019375978568, 21.55341960407610458, 105.2072429386477097 ) ) ;
#93517 = CARTESIAN_POINT ( 'NONE',  ( -16.51473224551069308, -9.474510206698971260, 71.66557627198102409 ) ) ;
#93518 = EDGE_CURVE ( 'NONE', #52144, #99274, #52617, .T. ) ;
#93519 = CARTESIAN_POINT ( 'NONE',  ( -18.62759615963255300, -10.81492255796106328, 109.1677570613523613 ) ) ;
#93522 = CARTESIAN_POINT ( 'NONE',  ( -4.483927247898539470, -16.52544592524342804, 112.2905762719810241 ) ) ;
#93521 = CARTESIAN_POINT ( 'NONE',  ( -8.224510206698948167, 14.34966873604960824, 30.41557627198101699 ) ) ;
#93520 = CARTESIAN_POINT ( 'NONE',  ( -19.02544592524342804, 5.153800228976336051, 36.04057627198100988 ) ) ;
#93523 = CARTESIAN_POINT ( 'NONE',  ( 13.89961937509957401, 13.97604488694547697, 111.8760903946856757 ) ) ;
#93524 = EDGE_LOOP ( 'NONE', ( #147843, #163476, #56286, #143145, #197889, #104178, #91903, #82091, #172330, #172649, #136492, #146285 ) ) ;
#93525 = CARTESIAN_POINT ( 'NONE',  ( -21.53943276465977519, -0.05219959533937600094, 33.75109039468568284 ) ) ;
#93526 = CARTESIAN_POINT ( 'NONE',  ( 19.05341960407617918, -5.049401038297876454, 66.04275706135233293 ) ) ;
#93527 = CARTESIAN_POINT ( 'NONE',  ( -16.55341960407611168, -4.379528057220339221, 21.45724293864769550 ) ) ;
#93528 = CARTESIAN_POINT ( 'NONE',  ( -18.62759615963270932, 10.81492255796079327, 85.83224293864768129 ) ) ;
#93529 = CARTESIAN_POINT ( 'NONE',  ( -21.53943276465977519, 0.05219959533907696930, 26.24890960531435624 ) ) ;
#93530 = CARTESIAN_POINT ( 'NONE',  ( 16.53943276465976808, -0.05219959533910856209, 58.74890960531436690 ) ) ;
#93531 = CARTESIAN_POINT ( 'NONE',  ( 19.05341960407611168, 5.049401038298154454, 28.95724293864769550 ) ) ;
#93532 = CARTESIAN_POINT ( 'NONE',  ( -9.474510206698720793, -16.51473224551083518, 24.58442372801900078 ) ) ;
#93533 = CARTESIAN_POINT ( 'NONE',  ( -16.52544592524335698, -4.483927247898792601, 93.95942372801903275 ) ) ;
#93534 = CARTESIAN_POINT ( 'NONE',  ( -16.52544592524335698, -4.483927247898792601, 58.95942372801902565 ) ) ;
#93535 = CARTESIAN_POINT ( 'NONE',  ( -15.80617190586745835, -15.72974639402198527, 21.87390960531436690 ) ) ;
#93536 = CARTESIAN_POINT ( 'NONE',  ( -16.46253265017146816, -9.564922557961047289, 19.16775706135233293 ) ) ;
#93537 = CARTESIAN_POINT ( 'NONE',  ( 16.51473224551069308, 9.474510206698969483, 79.16557627198103830 ) ) ;
#93538 = CARTESIAN_POINT ( 'NONE',  ( -12.06949235617739369, -12.14591786802326823, 54.37609039468568994 ) ) ;
#93539 = CARTESIAN_POINT ( 'NONE',  ( 13.89961937509977652, -13.97604488694527269, 23.12390960531436335 ) ) ;
#93540 = CARTESIAN_POINT ( 'NONE',  ( 4.379528057220339221, -16.55341960407611168, 37.70724293864769550 ) ) ;
#93541 = FACE_OUTER_BOUND ( 'NONE', #100408, .T. ) ;
#93544 = CARTESIAN_POINT ( 'NONE',  ( 19.02544592524343514, -5.153800228976328945, 73.54057627198103830 ) ) ;
#93543 = CARTESIAN_POINT ( 'NONE',  ( -9.474510206698964154, 16.51473224551069663, 90.41557627198103830 ) ) ;
#93542 = CARTESIAN_POINT ( 'NONE',  ( -0.05219959533937732626, 21.53943276465977519, 72.50109039468568994 ) ) ;
#93545 = CARTESIAN_POINT ( 'NONE',  ( -9.474510206698964154, 16.51473224551069663, 105.4155762719810383 ) ) ;
#93546 = CARTESIAN_POINT ( 'NONE',  ( -8.224510206698948167, 14.34966873604960824, 60.41557627198102409 ) ) ;
#93547 = CARTESIAN_POINT ( 'NONE',  ( -16.55341960407611168, -4.379528057220339221, 31.45724293864769550 ) ) ;
#93548 = CARTESIAN_POINT ( 'NONE',  ( 16.53943276465976808, -0.05219959533910856209, 48.74890960531435979 ) ) ;
#93550 = CARTESIAN_POINT ( 'NONE',  ( 30.00000000000000000, -5.499999999999992895, 102.5000000000000142 ) ) ;
#93549 = CARTESIAN_POINT ( 'NONE',  ( 14.29746914071037800, 8.314922557961029526, 36.66775706135234714 ) ) ;
#93551 = CARTESIAN_POINT ( 'NONE',  ( 5.153800228976615827, -19.02544592524334988, 45.20942372801901143 ) ) ;
#93552 = CARTESIAN_POINT ( 'NONE',  ( 0.05219959533909260263, 19.03943276465977164, 69.99890960531435269 ) ) ;
#93553 = CARTESIAN_POINT ( 'NONE',  ( 19.02544592524334988, 5.153800228976608722, 46.45942372801899012 ) ) ;
#93554 = CARTESIAN_POINT ( 'NONE',  ( 13.89961937509957401, 13.97604488694547697, 61.87609039468566863 ) ) ;
#93556 = CARTESIAN_POINT ( 'NONE',  ( 12.14591786802327356, -12.06949235617739191, 85.62609039468568994 ) ) ;
#93555 = CARTESIAN_POINT ( 'NONE',  ( 13.97604488694548053, -13.89961937509957401, 100.6260903946856615 ) ) ;
#93557 = CARTESIAN_POINT ( 'NONE',  ( -8.571926809382608425, 26.38167802310805854, 142.9750000027312069 ) ) ;
#93558 = DIRECTION ( 'NONE',  ( 0.000000000000000000, 0.000000000000000000, -1.000000000000000000 ) ) ;
#93559 = CARTESIAN_POINT ( 'NONE',  ( 5.153800228976335163, 19.02544592524342804, 104.7905762719809957 ) ) ;
#93560 = CARTESIAN_POINT ( 'NONE',  ( -10.81492255796105439, 18.62759615963255655, 37.91775706135235424 ) ) ;
#93561 = CARTESIAN_POINT ( 'NONE',  ( -5.049401038297874678, -19.05341960407617918, 84.79275706135233293 ) ) ;
#93563 = CARTESIAN_POINT ( 'NONE',  ( 5.049401038298161559, -19.05341960407611168, 67.70724293864769550 ) ) ;
#93562 = CARTESIAN_POINT ( 'NONE',  ( 38.00000000000001421, 12.34694845685043951, -2.900000000000000799 ) ) ;
#93564 = CARTESIAN_POINT ( 'NONE',  ( -5.153800228976328057, -19.02544592524343514, 102.2905762719810383 ) ) ;
#93566 = CARTESIAN_POINT ( 'NONE',  ( 19.03943276465977164, -0.05219959533909143690, 63.74890960531435979 ) ) ;
#93565 = CARTESIAN_POINT ( 'NONE',  ( 8.224510206698953496, -14.34966873604960469, 57.91557627198103120 ) ) ;
#93567 = CARTESIAN_POINT ( 'NONE',  ( -13.97604488694527625, -13.89961937509977652, 56.87390960531434558 ) ) ;
#93568 = CARTESIAN_POINT ( 'NONE',  ( -19.02544592524334988, -5.153800228976617603, 63.95942372801899012 ) ) ;
#93569 = B_SPLINE_CURVE_WITH_KNOTS ( 'NONE', 3,
 ( #33563, #138743, #46750, #141727, #2221, #31577, #63903, #48740, #172076, #95225, #3217, #156911, #44763, #128536, #97194, #49726, #143713, #19393, #146708, #82017, #113372, #4198, #144709, #100206, #98183, #115390, #85028, #192232, #177078, #37537, #176070, #190231 ),
 .UNSPECIFIED., .F., .F.,
 ( 4, 2, 2, 2, 2, 2, 2, 2, 2, 2, 2, 2, 2, 2, 2, 4 ),
 ( 1.734723475976807094E-18, 0.0003712461730036656360, 0.0007424923460073295373, 0.001113738519010993439, 0.001484984692014657340, 0.002227477038021991648, 0.002598723211025670294, 0.002969969384029348940, 0.003341215557033027587, 0.003712461730036706667, 0.004083707903040384446, 0.004454954076044063092, 0.004826200249047741739, 0.005197446422051420385, 0.005568692595055098164, 0.005939938768058776811 ),
 .UNSPECIFIED. ) ;
#93570 = CARTESIAN_POINT ( 'NONE',  ( -10.72451020669898014, 18.67979575497178502, 45.41557627198103830 ) ) ;
#93571 = CARTESIAN_POINT ( 'NONE',  ( -13.97604488694547697, 13.89961937509957934, 43.12609039468566152 ) ) ;
#93572 = CARTESIAN_POINT ( 'NONE',  ( -5.153800228976328057, -19.02544592524343514, 77.29057627198099567 ) ) ;
#93573 = CARTESIAN_POINT ( 'NONE',  ( -5.823673210054116645, -21.52544592524344225, 77.29057627198102409 ) ) ;
#93575 = CARTESIAN_POINT ( 'NONE',  ( -13.89961937509957401, -13.97604488694547875, 39.37609039468566152 ) ) ;
#93574 = CARTESIAN_POINT ( 'NONE',  ( 16.55341960407611168, 4.379528057220329451, 78.95724293864769550 ) ) ;
#93576 = CARTESIAN_POINT ( 'NONE',  ( -21.55341960407610458, -5.719274019375992779, 41.45724293864769550 ) ) ;
#93577 = CARTESIAN_POINT ( 'NONE',  ( -0.05219959533907301413, -21.53943276465977519, 42.49890960531435979 ) ) ;
#93578 = CARTESIAN_POINT ( 'NONE',  ( -13.97604488694527625, -13.89961937509977652, 66.87390960531436690 ) ) ;
#93579 = CARTESIAN_POINT ( 'NONE',  ( -0.05219959533909027116, -19.03943276465977164, 57.49890960531435979 ) ) ;
#93580 = CARTESIAN_POINT ( 'NONE',  ( -12.06949235617756955, 12.14591786802309770, 115.6239096053143669 ) ) ;
#93581 = CARTESIAN_POINT ( 'NONE',  ( 18.67979575497194134, -10.72451020669871369, 25.83442372801901499 ) ) ;
#93582 = CARTESIAN_POINT ( 'NONE',  ( -13.89961937509977652, 13.97604488694528158, 110.6239096053143243 ) ) ;
#93583 = CARTESIAN_POINT ( 'NONE',  ( 21.53943276465977519, 0.05219959533937863772, 36.25109039468567573 ) ) ;
#93584 = CARTESIAN_POINT ( 'NONE',  ( 19.05341960407611168, 5.049401038298154454, 38.95724293864767418 ) ) ;
#93585 = CARTESIAN_POINT ( 'NONE',  ( -18.62759615963270932, 10.81492255796079327, 110.8322429386476955 ) ) ;
#93586 = CARTESIAN_POINT ( 'NONE',  ( 16.46253265017146816, 9.564922557961045513, 51.66775706135233293 ) ) ;
#93587 = CARTESIAN_POINT ( 'NONE',  ( -3.573655867282028392E-15, 2.428612866367529932E-14, 167.9999999999999716 ) ) ;
#93588 = DIRECTION ( 'NONE',  ( -7.709882115452493155E-15, 0.000000000000000000, 1.000000000000000000 ) ) ;
#93589 = CARTESIAN_POINT ( 'NONE',  ( 16.26219239814447093, -7.340408916676126161, 21.79031256471339617 ) ) ;
#93590 = CARTESIAN_POINT ( 'NONE',  ( -0.05219959533934338120, 16.53943276465976808, 62.50109039468568284 ) ) ;
#93591 = CARTESIAN_POINT ( 'NONE',  ( 5.153800228976335163, 19.02544592524342804, 24.79057627198102765 ) ) ;
#93592 = CARTESIAN_POINT ( 'NONE',  ( -26.61723430050314221, -3.645106422947788083, 172.4622069319862305 ) ) ;
#93593 = CARTESIAN_POINT ( 'NONE',  ( 5.049401038298161559, -19.05341960407611168, 67.70724293864769550 ) ) ;
#93594 = CARTESIAN_POINT ( 'NONE',  ( 8.314922557960818139, 14.29746914071049879, 109.5822429386476955 ) ) ;
#93595 = CARTESIAN_POINT ( 'NONE',  ( 21.53943276465977519, -0.05219959533907433946, 58.74890960531436690 ) ) ;
#93596 = CARTESIAN_POINT ( 'NONE',  ( -16.52544592524342804, 4.483927247898546575, 81.04057627198102409 ) ) ;
#93597 = CARTESIAN_POINT ( 'NONE',  ( 8.224510206698742110, 14.34966873604972548, 32.08442372801901854 ) ) ;
#93598 = CARTESIAN_POINT ( 'NONE',  ( -21.53943276465977519, -0.05219959533937600094, 88.75109039468567573 ) ) ;
#93599 = CARTESIAN_POINT ( 'NONE',  ( 9.564922557960805705, 16.46253265017160317, 29.58224293864769550 ) ) ;
#93600 = CARTESIAN_POINT ( 'NONE',  ( 14.34966873604960469, 8.224510206698951720, 24.16557627198103120 ) ) ;
#93601 = CARTESIAN_POINT ( 'NONE',  ( 12.14591786802309770, 12.06949235617756955, 59.37390960531436690 ) ) ;
#93602 = AXIS2_PLACEMENT_3D ( 'NONE', #22862, #38031, #41034 ) ;
#93603 = CARTESIAN_POINT ( 'NONE',  ( -13.97604488694527625, -13.89961937509977652, 46.87390960531435979 ) ) ;
#93604 = CARTESIAN_POINT ( 'NONE',  ( 10.72451020669871369, 18.67979575497193778, 102.0844237280190185 ) ) ;
#93605 = CARTESIAN_POINT ( 'NONE',  ( 5.719274019375991003, -21.55341960407610458, 102.7072429386476955 ) ) ;
#93606 = CARTESIAN_POINT ( 'NONE',  ( -10.81492255796105439, 18.62759615963255655, 77.91775706135231871 ) ) ;
#93607 = CARTESIAN_POINT ( 'NONE',  ( 12.06949235617739724, 12.14591786802326823, 56.87609039468568994 ) ) ;
#93609 = CARTESIAN_POINT ( 'NONE',  ( -18.67979575497193778, 10.72451020669871902, 88.33442372801901854 ) ) ;
#93608 = CARTESIAN_POINT ( 'NONE',  ( 8.314922557960818139, 14.29746914071049879, 84.58224293864769550 ) ) ;
#93610 = CARTESIAN_POINT ( 'NONE',  ( -4.379528057220086978, -16.55341960407618274, 109.7927570613523613 ) ) ;
#93611 = CARTESIAN_POINT ( 'NONE',  ( -16.29526858892874586, 7.335722546920134590, 114.2032940219979906 ) ) ;
#93612 = CARTESIAN_POINT ( 'NONE',  ( 16.53943276465976808, 0.05219959533934440121, 41.25109039468568284 ) ) ;
#93613 = CARTESIAN_POINT ( 'NONE',  ( -4.379528057220328563, 16.55341960407611168, 45.20724293864769550 ) ) ;
#93614 = CARTESIAN_POINT ( 'NONE',  ( -14.29746914071037622, -8.314922557961029526, 84.16775706135234714 ) ) ;
#93615 = CARTESIAN_POINT ( 'NONE',  ( 13.97604488694527802, 13.89961937509977652, 104.3739096053143385 ) ) ;
#93616 = CARTESIAN_POINT ( 'NONE',  ( 16.46253265017160672, -9.564922557960803928, 108.3322429386476955 ) ) ;
#93617 = CARTESIAN_POINT ( 'NONE',  ( 10.72451020669871369, 18.67979575497193778, 97.08442372801904696 ) ) ;
#93618 = CARTESIAN_POINT ( 'NONE',  ( 4.379528057220092307, 16.55341960407617563, 102.2927570613523613 ) ) ;
#93619 = CARTESIAN_POINT ( 'NONE',  ( 8.224510206698953496, -14.34966873604960469, 77.91557627198102409 ) ) ;
#93620 = CARTESIAN_POINT ( 'NONE',  ( -13.97604488694527625, -13.89961937509977652, 76.87390960531433848 ) ) ;
#93621 = ORIENTED_EDGE ( 'NONE', *, *, #174158, .F. ) ;
#93623 = CARTESIAN_POINT ( 'NONE',  ( -8.314922557961024197, 14.29746914071037800, 32.91775706135234714 ) ) ;
#93622 =( BOUNDED_CURVE ( )  B_SPLINE_CURVE ( 2, ( #43610, #163980, #73962, #167941, #41629, #165967, #28464, #149794, #13275, #71951, #27469, #135630, #117454 ),
 .UNSPECIFIED., .F., .F. ) 
 B_SPLINE_CURVE_WITH_KNOTS ( ( 3, 2, 2, 2, 2, 2, 3 ),
 ( 0.2919498004596616791, 0.2938596491228070429, 0.2982456140350877027, 0.3026315789473684181, 0.3070175438596491335, 0.3114035087719298489, 0.3133590372571655180 ),
 .UNSPECIFIED. ) 
 CURVE ( )  GEOMETRIC_REPRESENTATION_ITEM ( )  RATIONAL_B_SPLINE_CURVE ( ( 0.9832469066685285419, 0.9851625545550100060, 1.000000000000000000, 0.9659258262890683122, 1.000000000000000000, 0.9659258262890683122, 1.000000000000000000, 0.9659258262890683122, 1.000000000000000000, 0.9659258262890683122, 1.000000000000000000, 0.9848076720550081875, 0.9831626618144004848 ) ) 
 REPRESENTATION_ITEM ( '' )  );
#93624 = CARTESIAN_POINT ( 'NONE',  ( -16.51473224551069308, -9.474510206698971260, 31.66557627198102054 ) ) ;
#93625 = CARTESIAN_POINT ( 'NONE',  ( -5.049401038298153566, 19.05341960407611168, 85.20724293864766707 ) ) ;
#93627 = CARTESIAN_POINT ( 'NONE',  ( -22.81625015709509441, -31.40387420917324590, -2.324999997268813789 ) ) ;
#93626 = CARTESIAN_POINT ( 'NONE',  ( 12.14591786802327356, -12.06949235617739191, 25.62609039468567929 ) ) ;
#93628 = CARTESIAN_POINT ( 'NONE',  ( -16.46253265017146816, -9.564922557961047289, 39.16775706135234003 ) ) ;
#93629 = CARTESIAN_POINT ( 'NONE',  ( -8.314922557961024197, 14.29746914071037800, 87.91775706135234714 ) ) ;
#93630 = CARTESIAN_POINT ( 'NONE',  ( -13.97604488694547697, 13.89961937509957934, 103.1260903946856473 ) ) ;
#93631 = CARTESIAN_POINT ( 'NONE',  ( 16.51473224551069308, 9.474510206698969483, 39.16557627198103120 ) ) ;
#93632 = CARTESIAN_POINT ( 'NONE',  ( 14.34966873604972726, -8.224510206698740333, 85.83442372801901854 ) ) ;
#93633 = CARTESIAN_POINT ( 'NONE',  ( -14.29746914071037622, -8.314922557961029526, 64.16775706135234714 ) ) ;
#93634 = CARTESIAN_POINT ( 'NONE',  ( -9.564922557961040184, 16.46253265017147172, 87.91775706135233293 ) ) ;
#93635 = CARTESIAN_POINT ( 'NONE',  ( -13.89961937509957401, -13.97604488694547875, 19.37609039468566507 ) ) ;
#93636 = CARTESIAN_POINT ( 'NONE',  ( -5.153800228976328057, -19.02544592524343514, 42.29057627198101699 ) ) ;
#93637 = CARTESIAN_POINT ( 'NONE',  ( 16.51473224551069308, 9.474510206698969483, 94.16557627198103830 ) ) ;
#93638 = CARTESIAN_POINT ( 'NONE',  ( 4.379528057220339221, -16.55341960407611168, 82.70724293864770971 ) ) ;
#93639 = VECTOR ( 'NONE', #60792, 1000.000000000000000 ) ;
#93640 = CARTESIAN_POINT ( 'NONE',  ( 5.049401038297881783, 19.05341960407617563, 52.29275706135234003 ) ) ;
#93641 = CARTESIAN_POINT ( 'NONE',  ( 18.67979575497178502, 10.72451020669898547, 44.16557627198103120 ) ) ;
#93642 = CARTESIAN_POINT ( 'NONE',  ( 16.46253265017146816, 9.564922557961045513, 26.66775706135234003 ) ) ;
#93643 = CARTESIAN_POINT ( 'NONE',  ( -16.46253265017160317, 9.564922557960807481, 90.83224293864769550 ) ) ;
#93644 = CARTESIAN_POINT ( 'NONE',  ( -19.02544592524334988, -5.153800228976617603, 28.95942372801900433 ) ) ;
#93645 = CARTESIAN_POINT ( 'NONE',  ( 21.53943276465977519, -0.05219959533907433946, 73.74890960531433848 ) ) ;
#93646 = CARTESIAN_POINT ( 'NONE',  ( 19.05341960407611168, 5.049401038298154454, 108.9572429386477097 ) ) ;
#93647 = CARTESIAN_POINT ( 'NONE',  ( 19.02544592524334988, 5.153800228976608722, 86.45942372801900433 ) ) ;
#93648 = CARTESIAN_POINT ( 'NONE',  ( -17.49999999999999645, 5.499999999999997335, 110.7969038253417295 ) ) ;
#93649 = CARTESIAN_POINT ( 'NONE',  ( 19.03943276465977164, 0.05219959533936151252, 106.2510903946856615 ) ) ;
#93650 = CARTESIAN_POINT ( 'NONE',  ( 16.46253265017160672, -9.564922557960803928, 28.33224293864769550 ) ) ;
#93651 = CARTESIAN_POINT ( 'NONE',  ( -13.89961937509977652, 13.97604488694528158, 95.62390960531436690 ) ) ;
#93652 = CARTESIAN_POINT ( 'NONE',  ( -21.53943276465977519, 0.05219959533907696930, 71.24890960531435269 ) ) ;
#93653 = CARTESIAN_POINT ( 'NONE',  ( 12.06949235617739724, 12.14591786802326823, 41.87609039468568284 ) ) ;
#93654 = CARTESIAN_POINT ( 'NONE',  ( -15.80617190586768217, 15.72974639402176855, 48.12609039468568284 ) ) ;
#93656 = CARTESIAN_POINT ( 'NONE',  ( -15.80617190586768217, 15.72974639402176855, 93.12609039468568994 ) ) ;
#93655 = CARTESIAN_POINT ( 'NONE',  ( -19.03943276465977164, -0.05219959533935918106, 93.75109039468566152 ) ) ;
#93657 = CARTESIAN_POINT ( 'NONE',  ( -12.06949235617739369, -12.14591786802326823, 99.37609039468568994 ) ) ;
#93658 = CARTESIAN_POINT ( 'NONE',  ( -5.049401038298153566, 19.05341960407611168, 100.2072429386476955 ) ) ;
#93659 = CARTESIAN_POINT ( 'NONE',  ( 12.14591786802309770, 12.06949235617756955, 89.37390960531435269 ) ) ;
#93660 = CARTESIAN_POINT ( 'NONE',  ( 16.55341960407611168, 4.379528057220329451, 33.95724293864769550 ) ) ;
#93661 = CARTESIAN_POINT ( 'NONE',  ( -0.05219959533936034679, 19.03943276465977164, 67.50109039468566152 ) ) ;
#93662 = CARTESIAN_POINT ( 'NONE',  ( 15.72974639402176855, 15.80617190586768217, 56.87609039468568994 ) ) ;
#93663 = CARTESIAN_POINT ( 'NONE',  ( 16.51473224551083163, -9.474510206698727899, 30.83442372801900433 ) ) ;
#93664 = CARTESIAN_POINT ( 'NONE',  ( -4.379528057220328563, 16.55341960407611168, 110.2072429386477239 ) ) ;
#93665 = CARTESIAN_POINT ( 'NONE',  ( -21.55341960407610458, -5.719274019375992779, 26.45724293864768839 ) ) ;
#93666 = CARTESIAN_POINT ( 'NONE',  ( 16.55341960407611168, 4.379528057220329451, 23.95724293864769550 ) ) ;
#93667 = CARTESIAN_POINT ( 'NONE',  ( 18.62759615963255655, 10.81492255796105972, 96.66775706135234714 ) ) ;
#93668 = CARTESIAN_POINT ( 'NONE',  ( 4.483927247898790824, -16.52544592524335698, 60.20942372801902565 ) ) ;
#93669 = CARTESIAN_POINT ( 'NONE',  ( 12.14591786802309770, 12.06949235617756955, 24.37390960531435979 ) ) ;
#93670 = CARTESIAN_POINT ( 'NONE',  ( 21.52544592524334988, 5.823673210054432836, 46.45942372801901854 ) ) ;
#93671 = CARTESIAN_POINT ( 'NONE',  ( -10.72451020669870658, -18.67979575497194134, 49.58442372801901143 ) ) ;
#93672 = EDGE_CURVE ( 'NONE', #121093, #78133, #25042, .T. ) ;
#93673 = VERTEX_POINT ( 'NONE', #40179 ) ;
#93674 = CARTESIAN_POINT ( 'NONE',  ( -38.00000000000001421, 12.34694845685046438, -1.849999994537626424 ) ) ;
#93675 = CARTESIAN_POINT ( 'NONE',  ( -21.55341960407619339, 5.719274019375674811, 23.54275706135235424 ) ) ;
#93676 = CARTESIAN_POINT ( 'NONE',  ( -14.34966873604960291, -8.224510206698953496, 106.6655762719810383 ) ) ;
#93677 = CARTESIAN_POINT ( 'NONE',  ( -16.51473224551069308, -9.474510206698971260, 26.66557627198103120 ) ) ;
#93678 = CARTESIAN_POINT ( 'NONE',  ( 14.34966873604960469, 8.224510206698951720, 79.16557627198103830 ) ) ;
#93679 = CARTESIAN_POINT ( 'NONE',  ( -5.049401038298153566, 19.05341960407611168, 75.20724293864769550 ) ) ;
#93680 = CARTESIAN_POINT ( 'NONE',  ( -8.224510206698735004, -14.34966873604973081, 104.5844237280190185 ) ) ;
#93681 = CARTESIAN_POINT ( 'NONE',  ( 21.55341960407610458, 5.719274019375980345, 58.95724293864770971 ) ) ;
#93682 = CARTESIAN_POINT ( 'NONE',  ( -8.314922557960811034, -14.29746914071050412, 87.08224293864769550 ) ) ;
#93683 = CARTESIAN_POINT ( 'NONE',  ( 0.05219959533907565091, 21.53943276465977519, 89.99890960531438111 ) ) ;
#93684 = CARTESIAN_POINT ( 'NONE',  ( 19.05341960407611168, 5.049401038298154454, 103.9572429386476671 ) ) ;
#93686 = CARTESIAN_POINT ( 'NONE',  ( 16.51473224551083163, -9.474510206698727899, 110.8344237280190043 ) ) ;
#93685 = CARTESIAN_POINT ( 'NONE',  ( -13.89961937509977652, 13.97604488694528158, 50.62390960531435979 ) ) ;
#93687 = CARTESIAN_POINT ( 'NONE',  ( 0.05219959533907565091, 21.53943276465977519, 39.99890960531436690 ) ) ;
#93688 = CARTESIAN_POINT ( 'NONE',  ( -10.81492255796105439, 18.62759615963255655, 62.91775706135236135 ) ) ;
#93689 = CARTESIAN_POINT ( 'NONE',  ( -5.153800228976328057, -19.02544592524343514, 62.29057627198100988 ) ) ;
#93690 = CARTESIAN_POINT ( 'NONE',  ( 16.51473224551069308, 9.474510206698969483, 94.16557627198103830 ) ) ;
#93691 = CARTESIAN_POINT ( 'NONE',  ( 0.05219959533934541429, -16.53943276465976808, 70.00109039468568994 ) ) ;
#93692 = CARTESIAN_POINT ( 'NONE',  ( -5.823673210054431948, 21.52544592524334988, 52.70942372801902565 ) ) ;
#93693 = CARTESIAN_POINT ( 'NONE',  ( 5.823673210054444382, -21.52544592524334988, 85.20942372801901854 ) ) ;
#93694 = CARTESIAN_POINT ( 'NONE',  ( -5.719274019375978568, 21.55341960407610458, 95.20724293864769550 ) ) ;
#93696 = CARTESIAN_POINT ( 'NONE',  ( -16.53943276465976808, -0.05219959533934237506, 73.75109039468567573 ) ) ;
#93695 = CARTESIAN_POINT ( 'NONE',  ( 18.62759615963255655, 10.81492255796105972, 36.66775706135234714 ) ) ;
#93697 = CARTESIAN_POINT ( 'NONE',  ( -15.80617190586745835, -15.72974639402198527, 76.87390960531439532 ) ) ;
#93698 = CARTESIAN_POINT ( 'NONE',  ( -9.474510206698720793, -16.51473224551083518, 39.58442372801899722 ) ) ;
#93700 = CARTESIAN_POINT ( 'NONE',  ( -16.53943276465976808, 0.05219959533911058130, 21.24890960531436690 ) ) ;
#93699 = CARTESIAN_POINT ( 'NONE',  ( -19.03943276465977164, 0.05219959533909376836, 81.24890960531436690 ) ) ;
#93701 = FACE_OUTER_BOUND ( 'NONE', #156544, .T. ) ;
#93702 = CARTESIAN_POINT ( 'NONE',  ( 16.51473224551069308, 9.474510206698969483, 109.1655762719810383 ) ) ;
#93703 = FACE_OUTER_BOUND ( 'NONE', #173110, .T. ) ;
#93704 = CARTESIAN_POINT ( 'NONE',  ( 13.97604488694548053, -13.89961937509957401, 95.62609039468563310 ) ) ;
#93705 = CARTESIAN_POINT ( 'NONE',  ( 15.72974639402199770, -15.80617190586745480, 78.12390960531436690 ) ) ;
#93706 = CARTESIAN_POINT ( 'NONE',  ( 16.53943276465976808, -0.05219959533910856209, 38.74890960531435979 ) ) ;
#93707 = CARTESIAN_POINT ( 'NONE',  ( 14.34966873604972726, -8.224510206698740333, 20.83442372801901143 ) ) ;
#93708 = CARTESIAN_POINT ( 'NONE',  ( -19.02544592524342804, 5.153800228976336051, 26.04057627198103120 ) ) ;
#93709 = CARTESIAN_POINT ( 'NONE',  ( -5.153800228976607833, 19.02544592524334988, 112.7094237280190043 ) ) ;
#93711 = CARTESIAN_POINT ( 'NONE',  ( 19.02544592524334988, 5.153800228976608722, 71.45942372801900433 ) ) ;
#93710 = CARTESIAN_POINT ( 'NONE',  ( -15.72974639402197994, 15.80617190586746368, 100.6239096053143811 ) ) ;
#93712 = CARTESIAN_POINT ( 'NONE',  ( 16.52544592524335698, 4.483927247898782831, 81.45942372801900433 ) ) ;
#93713 = CARTESIAN_POINT ( 'NONE',  ( -9.564922557960796823, -16.46253265017161027, 72.08224293864770971 ) ) ;
#93714 = CARTESIAN_POINT ( 'NONE',  ( 14.34966873604960469, 8.224510206698951720, 74.16557627198102409 ) ) ;
#93715 = CARTESIAN_POINT ( 'NONE',  ( 9.564922557960805705, 16.46253265017160317, 59.58224293864769550 ) ) ;
#93716 = CARTESIAN_POINT ( 'NONE',  ( 8.224510206698953496, -14.34966873604960469, 67.91557627198102409 ) ) ;
#93717 = CARTESIAN_POINT ( 'NONE',  ( -7.052343178074620411, 2.552343178074692354, 8.889087296526001936 ) ) ;
#93718 = CARTESIAN_POINT ( 'NONE',  ( -36.91128768240056246, 1.976579976310101802E-14, 50.50000000000002842 ) ) ;
#93719 = CARTESIAN_POINT ( 'NONE',  ( -16.55341960407611168, -4.379528057220339221, 41.45724293864769550 ) ) ;
#93720 = CARTESIAN_POINT ( 'NONE',  ( 9.474510206698971260, -16.51473224551069308, 82.91557627198103830 ) ) ;
#93721 = FACE_BOUND ( 'NONE', #24848, .T. ) ;
#93722 = CARTESIAN_POINT ( 'NONE',  ( 9.564922557961047289, -16.46253265017146816, 55.41775706135234003 ) ) ;
#93723 = CARTESIAN_POINT ( 'NONE',  ( 14.34966873604972726, -8.224510206698740333, 55.83442372801901854 ) ) ;
#93724 = CARTESIAN_POINT ( 'NONE',  ( -15.80617190586745835, -15.72974639402198527, 61.87390960531436690 ) ) ;
#93725 = CARTESIAN_POINT ( 'NONE',  ( -9.474510206698720793, -16.51473224551083518, 19.58442372801899722 ) ) ;
#93726 = CARTESIAN_POINT ( 'NONE',  ( -19.05341960407611168, -5.049401038298163336, 81.45724293864769550 ) ) ;
#93727 = CARTESIAN_POINT ( 'NONE',  ( 1.243777456120027214, 21.93922656192045650, -58.42410701432510223 ) ) ;
#93728 = CARTESIAN_POINT ( 'NONE',  ( -18.67979575497178146, -10.72451020669898902, 21.66557627198102409 ) ) ;
#93729 = CARTESIAN_POINT ( 'NONE',  ( 19.02544592524343514, -5.153800228976328945, 58.54057627198102409 ) ) ;
#93730 = CARTESIAN_POINT ( 'NONE',  ( -18.67979575497193778, 10.72451020669871902, 33.33442372801900433 ) ) ;
#93732 = CARTESIAN_POINT ( 'NONE',  ( 4.379528057220339221, -16.55341960407611168, 107.7072429386476955 ) ) ;
#93731 = PRODUCT_DEFINITION_SHAPE ( 'NONE', 'NONE',  #200193 ) ;
#93735 = VERTEX_POINT ( 'NONE', #89684 ) ;
#93734 = CARTESIAN_POINT ( 'NONE',  ( 16.46253265017160672, -9.564922557960803928, 98.33224293864769550 ) ) ;
#93733 = CARTESIAN_POINT ( 'NONE',  ( -0.05219959533907301413, -21.53943276465977519, 97.49890960531436690 ) ) ;
#93736 = CARTESIAN_POINT ( 'NONE',  ( 18.62759615963255655, 10.81492255796105972, 21.66775706135235069 ) ) ;
#93737 = ORIENTED_EDGE ( 'NONE', *, *, #195370, .F. ) ;
#93738 = CARTESIAN_POINT ( 'NONE',  ( -9.564922557960796823, -16.46253265017161027, 87.08224293864769550 ) ) ;
#93739 = DIRECTION ( 'NONE',  ( 1.000000000000000000, 0.000000000000000000, 0.000000000000000000 ) ) ;
#93740 = CARTESIAN_POINT ( 'NONE',  ( -21.52544592524343514, 5.823673210054127303, 91.04057627198103830 ) ) ;
#93741 = CARTESIAN_POINT ( 'NONE',  ( -13.97604488694527625, -13.89961937509977652, 46.87390960531435979 ) ) ;
#93742 = CARTESIAN_POINT ( 'NONE',  ( -16.51473224551082808, 9.474510206698731452, 103.3344237280190043 ) ) ;
#93743 = CARTESIAN_POINT ( 'NONE',  ( -11.40812507854755609, 35.11059874428196537, -5.524999997268813523 ) ) ;
#93744 = CARTESIAN_POINT ( 'NONE',  ( 9.474510206698971260, -16.51473224551069308, 27.91557627198103120 ) ) ;
#93745 = CARTESIAN_POINT ( 'NONE',  ( -5.719274019375665041, -21.55341960407619695, 89.79275706135236135 ) ) ;
#93747 = CARTESIAN_POINT ( 'NONE',  ( -15.72974639402176322, -15.80617190586768395, 49.37609039468569705 ) ) ;
#93746 = CARTESIAN_POINT ( 'NONE',  ( 16.46253265017160672, -9.564922557960803928, 78.33224293864769550 ) ) ;
#93748 = CARTESIAN_POINT ( 'NONE',  ( -21.55341960407619339, 5.719274019375674811, 23.54275706135235424 ) ) ;
#93749 = CARTESIAN_POINT ( 'NONE',  ( -27.73933785331498925, 2.428612866367529932E-14, 145.3750000027311842 ) ) ;
#93750 = CARTESIAN_POINT ( 'NONE',  ( -0.05219959533909027116, -19.03943276465977164, 97.49890960531436690 ) ) ;
#93751 = CARTESIAN_POINT ( 'NONE',  ( -17.53359108020402957, 22.79239813733060416, 139.9999999999999716 ) ) ;
#93754 = CARTESIAN_POINT ( 'NONE',  ( 18.67979575497194134, -10.72451020669871369, 40.83442372801901854 ) ) ;
#93753 = CARTESIAN_POINT ( 'NONE',  ( 10.81492255796078972, 18.62759615963270932, 49.58224293864769550 ) ) ;
#93752 = CARTESIAN_POINT ( 'NONE',  ( 12.06949235617739724, 12.14591786802326823, 36.87609039468568994 ) ) ;
#93755 = CARTESIAN_POINT ( 'NONE',  ( -10.81492255796105439, 18.62759615963255655, 72.91775706135234714 ) ) ;
#93756 = CARTESIAN_POINT ( 'NONE',  ( 3.873512393789732222, 5.284191517680363326, -62.43104308550748982 ) ) ;
#93757 = CARTESIAN_POINT ( 'NONE',  ( 0.05219959533934541429, -16.53943276465976808, 20.00109039468568639 ) ) ;
#93758 = CARTESIAN_POINT ( 'NONE',  ( -9.564922557960796823, -16.46253265017161027, 57.08224293864769550 ) ) ;
#93759 = CARTESIAN_POINT ( 'NONE',  ( 13.89961937509977652, -13.97604488694527269, 93.12390960531436690 ) ) ;
#93760 = CARTESIAN_POINT ( 'NONE',  ( 12.14591786802309770, 12.06949235617756955, 104.3739096053143669 ) ) ;
#93761 = CARTESIAN_POINT ( 'NONE',  ( 16.55341960407611168, 4.379528057220329451, 108.9572429386476955 ) ) ;
#93762 = CARTESIAN_POINT ( 'NONE',  ( -21.52544592524343514, 5.823673210054127303, 36.04057627198102409 ) ) ;
#93763 = CARTESIAN_POINT ( 'NONE',  ( 14.34966873604972726, -8.224510206698740333, 85.83442372801901854 ) ) ;
#93765 = CARTESIAN_POINT ( 'NONE',  ( 19.03943276465977164, -0.05219959533909143690, 53.74890960531436690 ) ) ;
#93764 = CARTESIAN_POINT ( 'NONE',  ( -12.06949235617756955, 12.14591786802309770, 65.62390960531436690 ) ) ;
#93766 = CARTESIAN_POINT ( 'NONE',  ( -21.52544592524334988, -5.823673210054445271, 73.95942372801901854 ) ) ;
#93767 = CARTESIAN_POINT ( 'NONE',  ( -21.55341960407619339, 5.719274019375674811, 73.54275706135234714 ) ) ;
#93768 = CARTESIAN_POINT ( 'NONE',  ( -19.02544592524334988, -5.153800228976617603, 103.9594237280190043 ) ) ;
#93769 = CARTESIAN_POINT ( 'NONE',  ( 4.483927247898545687, 16.52544592524342804, 64.79057627198103830 ) ) ;
#93770 = CARTESIAN_POINT ( 'NONE',  ( -21.52544592524334988, -5.823673210054445271, 23.95942372801901143 ) ) ;
#93771 = CARTESIAN_POINT ( 'NONE',  ( 10.81492255796078972, 18.62759615963270932, 54.58224293864769550 ) ) ;
#93772 = CARTESIAN_POINT ( 'NONE',  ( 18.22780087662121673, 5.500000000000056843, 73.98459894673894155 ) ) ;
#93773 = CARTESIAN_POINT ( 'NONE',  ( -17.81289503416611097, -24.51734667627696496, 146.5500000054623229 ) ) ;
#93774 = CARTESIAN_POINT ( 'NONE',  ( 13.97604488694527802, 13.89961937509977652, 64.37390960531436690 ) ) ;
#93775 = CARTESIAN_POINT ( 'NONE',  ( -8.314922557960811034, -14.29746914071050412, 37.08224293864768129 ) ) ;
#93776 = CARTESIAN_POINT ( 'NONE',  ( 16.53943276465976808, -0.05219959533910856209, 23.74890960531435269 ) ) ;
#93777 = CARTESIAN_POINT ( 'NONE',  ( -12.14591786802326823, 12.06949235617739902, 103.1260903946856757 ) ) ;
#93778 = CARTESIAN_POINT ( 'NONE',  ( 19.03943276465977164, 0.05219959533936151252, 51.25109039468567573 ) ) ;
#93779 = CARTESIAN_POINT ( 'NONE',  ( 30.74264578624799782, 22.33583958711400541, -8.800000000000000711 ) ) ;
#93780 = CARTESIAN_POINT ( 'NONE',  ( -5.049401038298153566, 19.05341960407611168, 105.2072429386476671 ) ) ;
#93781 = CARTESIAN_POINT ( 'NONE',  ( 14.34966873604960469, 8.224510206698951720, 74.16557627198102409 ) ) ;
#93782 = CARTESIAN_POINT ( 'NONE',  ( 5.153800228976615827, -19.02544592524334988, 40.20942372801898301 ) ) ;
#93784 = CARTESIAN_POINT ( 'NONE',  ( 21.53943276465977519, -0.05219959533907433946, 23.74890960531435269 ) ) ;
#93783 = CARTESIAN_POINT ( 'NONE',  ( -19.02544592524342804, 5.153800228976336051, 31.04057627198102409 ) ) ;
#93786 = ORIENTED_EDGE ( 'NONE', *, *, #168639, .F. ) ;
#93785 = CARTESIAN_POINT ( 'NONE',  ( 18.62759615963271287, -10.81492255796078972, 53.33224293864769550 ) ) ;
#93787 = CARTESIAN_POINT ( 'NONE',  ( -8.314922557960811034, -14.29746914071050412, 97.08224293864770971 ) ) ;
#93788 = CARTESIAN_POINT ( 'NONE',  ( -8.224510206698735004, -14.34966873604973081, 49.58442372801901143 ) ) ;
#93789 = CARTESIAN_POINT ( 'NONE',  ( 4.379528057220339221, -16.55341960407611168, 87.70724293864769550 ) ) ;
#93790 = CARTESIAN_POINT ( 'NONE',  ( -38.00000000000000711, 2.428612866367529932E-14, -11.74999999453762634 ) ) ;
#93791 = CARTESIAN_POINT ( 'NONE',  ( -17.31728774477273092, 6.344390552232386682, 50.81906651689320142 ) ) ;
#93792 = CARTESIAN_POINT ( 'NONE',  ( -16.46253265017160317, 9.564922557960807481, 110.8322429386476955 ) ) ;
#93793 = CARTESIAN_POINT ( 'NONE',  ( 36.91746824999999887, 11.99521256947799053, -6.024999997268811747 ) ) ;
#93794 = CARTESIAN_POINT ( 'NONE',  ( 0.5319425161145064918, 24.20639721642469411, -56.83990048018080188 ) ) ;
#93796 = CARTESIAN_POINT ( 'NONE',  ( 16.55341960407611168, 4.379528057220329451, 23.95724293864769550 ) ) ;
#93795 = CARTESIAN_POINT ( 'NONE',  ( 0.05219959533934541429, -16.53943276465976808, 45.00109039468568284 ) ) ;
#93797 = CARTESIAN_POINT ( 'NONE',  ( 15.80617190586746368, 15.72974639402197994, 54.37390960531435979 ) ) ;
#93798 = CARTESIAN_POINT ( 'NONE',  ( -9.564922557961040184, 16.46253265017147172, 87.91775706135233293 ) ) ;
#93799 = CARTESIAN_POINT ( 'NONE',  ( -15.72974639402197994, 15.80617190586746368, 50.62390960531435979 ) ) ;
#93800 = CARTESIAN_POINT ( 'NONE',  ( 21.52544592524334988, 5.823673210054432836, 76.45942372801901854 ) ) ;
#93801 = CARTESIAN_POINT ( 'NONE',  ( 16.49801837613234667, -34.15639402546909764, -27.41207208920353011 ) ) ;
#93802 = CARTESIAN_POINT ( 'NONE',  ( -16.52544592524335698, -4.483927247898792601, 53.95942372801900433 ) ) ;
#93805 = EDGE_CURVE ( 'NONE', #9238, #3778, #96651, .T. ) ;
#93804 = CARTESIAN_POINT ( 'NONE',  ( -13.97604488694527625, -13.89961937509977652, 101.8739096053143811 ) ) ;
#93803 = CARTESIAN_POINT ( 'NONE',  ( 13.97604488694527802, 13.89961937509977652, 39.37390960531435269 ) ) ;
#93806 = CARTESIAN_POINT ( 'NONE',  ( -16.51473224551069308, -9.474510206698971260, 36.66557627198102409 ) ) ;
#93807 = CARTESIAN_POINT ( 'NONE',  ( -8.314922557960811034, -14.29746914071050412, 102.0822429386476955 ) ) ;
#93808 = CARTESIAN_POINT ( 'NONE',  ( 13.89961937509977652, -13.97604488694527269, 98.12390960531433848 ) ) ;
#93809 = EDGE_LOOP ( 'NONE', ( #57826, #149012 ) ) ;
#93810 = CARTESIAN_POINT ( 'NONE',  ( 0.05219959533934541429, -16.53943276465976808, 55.00109039468568284 ) ) ;
#93811 = CARTESIAN_POINT ( 'NONE',  ( 15.80617190586746368, 15.72974639402197994, 89.37390960531435269 ) ) ;
#93812 = CARTESIAN_POINT ( 'NONE',  ( 19.05341960407611168, 5.049401038298154454, 53.95724293864770260 ) ) ;
#93813 = CARTESIAN_POINT ( 'NONE',  ( 15.72974639402176855, 15.80617190586768217, 31.87609039468567929 ) ) ;
#93814 = CARTESIAN_POINT ( 'NONE',  ( 5.049401038298161559, -19.05341960407611168, 82.70724293864770971 ) ) ;
#93815 = FACE_OUTER_BOUND ( 'NONE', #35739, .T. ) ;
#93816 = ORIENTED_EDGE ( 'NONE', *, *, #162015, .T. ) ;
#93817 = CARTESIAN_POINT ( 'NONE',  ( 5.823673210054444382, -21.52544592524334988, 25.20942372801901854 ) ) ;
#93820 = CARTESIAN_POINT ( 'NONE',  ( 9.564922557961047289, -16.46253265017146816, 70.41775706135233293 ) ) ;
#93819 = CARTESIAN_POINT ( 'NONE',  ( 9.564922557960805705, 16.46253265017160317, 104.5822429386476955 ) ) ;
#93818 = CARTESIAN_POINT ( 'NONE',  ( -19.02544592524342804, 5.153800228976336051, 26.04057627198103120 ) ) ;
#93821 = CARTESIAN_POINT ( 'NONE',  ( 5.049401038297881783, 19.05341960407617563, 32.29275706135233293 ) ) ;
#93822 = CARTESIAN_POINT ( 'NONE',  ( -18.62759615963270932, 10.81492255796079327, 105.8322429386476955 ) ) ;
#93823 = CARTESIAN_POINT ( 'NONE',  ( -13.89961937509957401, -13.97604488694547875, 34.37609039468566863 ) ) ;
#93824 = CARTESIAN_POINT ( 'NONE',  ( -16.55341960407617563, 4.379528057220093196, 78.54275706135236135 ) ) ;
#93825 = CARTESIAN_POINT ( 'NONE',  ( -19.03943276465977164, 0.05219959533909376836, 101.2489096053143669 ) ) ;
#93826 = CARTESIAN_POINT ( 'NONE',  ( -13.97604488694527625, -13.89961937509977652, 56.87390960531434558 ) ) ;
#93827 = CARTESIAN_POINT ( 'NONE',  ( -0.05219959533937732626, 21.53943276465977519, 72.50109039468568994 ) ) ;
#93828 = CARTESIAN_POINT ( 'NONE',  ( 5.823673210054444382, -21.52544592524334988, 80.20942372801901854 ) ) ;
#93829 = CARTESIAN_POINT ( 'NONE',  ( 13.89961937509977652, -13.97604488694527269, 73.12390960531436690 ) ) ;
#93830 = CARTESIAN_POINT ( 'NONE',  ( -21.53943276465977519, -0.05219959533937600094, 53.75109039468568994 ) ) ;
#93831 = CARTESIAN_POINT ( 'NONE',  ( 5.049401038297881783, 19.05341960407617563, 82.29275706135229029 ) ) ;
#93832 = CARTESIAN_POINT ( 'NONE',  ( 16.51473224551069308, 9.474510206698969483, 59.16557627198102409 ) ) ;
#93833 = CARTESIAN_POINT ( 'NONE',  ( -5.049401038298153566, 19.05341960407611168, 105.2072429386476671 ) ) ;
#93834 = CARTESIAN_POINT ( 'NONE',  ( -5.153800228976328057, -19.02544592524343514, 72.29057627198102409 ) ) ;
#93835 = CARTESIAN_POINT ( 'NONE',  ( -11.74149087413295511, 36.13659316521247433, -2.147842220587803830 ) ) ;
#93836 = CARTESIAN_POINT ( 'NONE',  ( -0.05219959533909027116, -19.03943276465977164, 57.49890960531435979 ) ) ;
#93837 = CARTESIAN_POINT ( 'NONE',  ( -10.81492255796078084, -18.62759615963271287, 97.08224293864770971 ) ) ;
#93838 = CARTESIAN_POINT ( 'NONE',  ( 14.29746914071037800, 8.314922557961029526, 76.66775706135234714 ) ) ;
#93839 = CIRCLE ( 'NONE', #58351, 8.000000000000001776 ) ;
#93840 = CARTESIAN_POINT ( 'NONE',  ( -20.56371838171435584, 11.04494471775268671, 168.1294998094271023 ) ) ;
#93841 = CARTESIAN_POINT ( 'NONE',  ( 19.05341960407617918, -5.049401038297876454, 46.04275706135233293 ) ) ;
#93842 = CARTESIAN_POINT ( 'NONE',  ( -13.89961937509977652, 13.97604488694528158, 65.62390960531436690 ) ) ;
#93843 = CARTESIAN_POINT ( 'NONE',  ( -4.379528057220328563, 16.55341960407611168, 55.20724293864770260 ) ) ;
#93844 = CARTESIAN_POINT ( 'NONE',  ( -14.29746914071049879, 8.314922557960819915, 90.83224293864769550 ) ) ;
#93845 = CARTESIAN_POINT ( 'NONE',  ( -5.049401038298153566, 19.05341960407611168, 105.2072429386476671 ) ) ;
#93846 = B_SPLINE_CURVE_WITH_KNOTS ( 'NONE', 3,
 ( #167529, #29024, #8856, #10861, #102857, #70523, #132192, #55348, #72530, #40175, #117018, #9860, #71519, #194877, #118033, #164543, #26035, #134207, #195894, #141148 ),
 .UNSPECIFIED., .F., .F.,
 ( 4, 2, 2, 2, 2, 2, 2, 2, 2, 4 ),
 ( 0.004000878361811913142, 0.004499404418915918698, 0.004997930476019923386, 0.005496456533123928942, 0.005994982590227933630, 0.006244245618779935975, 0.006493508647331939186, 0.006992034704435929997, 0.007490560761539919940, 0.007989086818643910751 ),
 .UNSPECIFIED. ) ;
#93847 = CARTESIAN_POINT ( 'NONE',  ( -13.89961937509977652, 13.97604488694528158, 90.62390960531432427 ) ) ;
#93848 = CARTESIAN_POINT ( 'NONE',  ( 9.564922557960805705, 16.46253265017160317, 99.58224293864770971 ) ) ;
#93849 = CARTESIAN_POINT ( 'NONE',  ( -19.03943276465977164, -0.05219959533935918106, 18.75109039468567218 ) ) ;
#93850 = CARTESIAN_POINT ( 'NONE',  ( 8.224510206698742110, 14.34966873604972548, 97.08442372801904696 ) ) ;
#93851 = CARTESIAN_POINT ( 'NONE',  ( 13.97604488694527802, 13.89961937509977652, 74.37390960531436690 ) ) ;
#93852 = CARTESIAN_POINT ( 'NONE',  ( -21.52544592524334988, -5.823673210054445271, 43.95942372801902565 ) ) ;
#93853 = CARTESIAN_POINT ( 'NONE',  ( 21.53943276465977519, -0.05219959533907433946, 33.74890960531436690 ) ) ;
#93854 = CARTESIAN_POINT ( 'NONE',  ( 18.62759615963271287, -10.81492255796078972, 98.33224293864769550 ) ) ;
#93855 = CARTESIAN_POINT ( 'NONE',  ( -16.53943276465976808, 0.05219959533911058130, 56.24890960531436690 ) ) ;
#93856 = CARTESIAN_POINT ( 'NONE',  ( -13.97604488694527625, -13.89961937509977652, 56.87390960531434558 ) ) ;
#93857 = CARTESIAN_POINT ( 'NONE',  ( -12.14591786802309592, -12.06949235617757132, 86.87390960531438111 ) ) ;
#93858 = CARTESIAN_POINT ( 'NONE',  ( -13.89961937509957401, -13.97604488694547875, 39.37609039468566152 ) ) ;
#93859 = CARTESIAN_POINT ( 'NONE',  ( 8.224510206698953496, -14.34966873604960469, 107.9155762719810241 ) ) ;
#93860 = VERTEX_POINT ( 'NONE', #59332 ) ;
#93861 = CARTESIAN_POINT ( 'NONE',  ( -0.05219959533934338120, 16.53943276465976808, 72.50109039468568994 ) ) ;
#93862 = CARTESIAN_POINT ( 'NONE',  ( 19.03943276465977164, -0.05219959533909143690, 73.74890960531435269 ) ) ;
#93863 = CARTESIAN_POINT ( 'NONE',  ( 17.14385361876520264, -23.59649016807270883, 145.5750000027311728 ) ) ;
#93864 = CARTESIAN_POINT ( 'NONE',  ( 14.29746914071049879, -8.314922557960816363, 93.33224293864769550 ) ) ;
#93865 = CARTESIAN_POINT ( 'NONE',  ( 5.719274019375991003, -21.55341960407610458, 37.70724293864769550 ) ) ;
#93866 = CARTESIAN_POINT ( 'NONE',  ( -0.05219959533934338120, 16.53943276465976808, 107.5010903946856899 ) ) ;
#93867 = CARTESIAN_POINT ( 'NONE',  ( 4.483927247898790824, -16.52544592524335698, 25.20942372801901854 ) ) ;
#93868 = CARTESIAN_POINT ( 'NONE',  ( -15.80617190586768217, 15.72974639402176855, 93.12609039468568994 ) ) ;
#93869 = CARTESIAN_POINT ( 'NONE',  ( 5.049401038298161559, -19.05341960407611168, 87.70724293864769550 ) ) ;
#93870 = CARTESIAN_POINT ( 'NONE',  ( -5.719274019375978568, 21.55341960407610458, 115.2072429386476955 ) ) ;
#93871 = CARTESIAN_POINT ( 'NONE',  ( 19.03943276465977164, -0.05219959533909143690, 28.74890960531435624 ) ) ;
#93872 = EDGE_CURVE ( 'NONE', #65322, #48812, #12576, .T. ) ;
#93873 = CARTESIAN_POINT ( 'NONE',  ( -8.224510206698735004, -14.34966873604973081, 29.58442372801901854 ) ) ;
#93874 = CARTESIAN_POINT ( 'NONE',  ( 19.02544592524334988, 5.153800228976608722, 91.45942372801900433 ) ) ;
#93875 = CARTESIAN_POINT ( 'NONE',  ( 18.67979575497178502, 10.72451020669898547, 84.16557627198103830 ) ) ;
#93876 = CARTESIAN_POINT ( 'NONE',  ( -19.05341960407617563, 5.049401038297882671, 68.54275706135230450 ) ) ;
#93877 = CARTESIAN_POINT ( 'NONE',  ( -9.474510206698964154, 16.51473224551069663, 25.41557627198103120 ) ) ;
#93878 = CARTESIAN_POINT ( 'NONE',  ( -21.53943276465977519, 0.05219959533907696930, 116.2489096053143669 ) ) ;
#93879 = CARTESIAN_POINT ( 'NONE',  ( 30.73962218707677252, 22.33364281372847060, -4.547842220587804185 ) ) ;
#93880 = CARTESIAN_POINT ( 'NONE',  ( -16.51473224551069308, -9.474510206698971260, 71.66557627198102409 ) ) ;
#93881 = CARTESIAN_POINT ( 'NONE',  ( -4.379528057220086978, -16.55341960407618274, 29.79275706135234358 ) ) ;
#93882 = DIRECTION ( 'NONE',  ( -1.000000000000000000, 0.000000000000000000, 0.000000000000000000 ) ) ;
#93883 = CARTESIAN_POINT ( 'NONE',  ( 13.97604488694548053, -13.89961937509957401, 60.62609039468564731 ) ) ;
#93885 = CARTESIAN_POINT ( 'NONE',  ( 8.224510206698953496, -14.34966873604960469, 82.91557627198103830 ) ) ;
#93884 = CARTESIAN_POINT ( 'NONE',  ( 0.05219959533937995610, -21.53943276465977519, 20.00109039468568639 ) ) ;
#93886 = CARTESIAN_POINT ( 'NONE',  ( -5.049401038298153566, 19.05341960407611168, 85.20724293864766707 ) ) ;
#93888 = CARTESIAN_POINT ( 'NONE',  ( 9.564922557961047289, -16.46253265017146816, 45.41775706135232582 ) ) ;
#93887 = CARTESIAN_POINT ( 'NONE',  ( -8.314922557961024197, 14.29746914071037800, 42.91775706135235424 ) ) ;
#93889 = CARTESIAN_POINT ( 'NONE',  ( 10.72451020669871369, 18.67979575497193778, 62.08442372801901143 ) ) ;
#93890 = CARTESIAN_POINT ( 'NONE',  ( -0.05219959533934338120, 16.53943276465976808, 32.50109039468568284 ) ) ;
#93891 = CARTESIAN_POINT ( 'NONE',  ( -16.51473224551069308, -9.474510206698971260, 61.66557627198103120 ) ) ;
#93892 = CARTESIAN_POINT ( 'NONE',  ( -5.153800228976607833, 19.02544592524334988, 77.70942372801900433 ) ) ;
#93893 = CARTESIAN_POINT ( 'NONE',  ( 14.29746914071037800, 8.314922557961029526, 51.66775706135234714 ) ) ;
#93894 = CARTESIAN_POINT ( 'NONE',  ( -21.52544592524334988, -5.823673210054445271, 98.95942372801903275 ) ) ;
#93895 = CARTESIAN_POINT ( 'NONE',  ( 16.46253265017146816, 9.564922557961045513, 66.66775706135233293 ) ) ;
#93896 = CARTESIAN_POINT ( 'NONE',  ( 0.05219959533909260263, 19.03943276465977164, 54.99890960531435979 ) ) ;
#93897 = CARTESIAN_POINT ( 'NONE',  ( -18.67979575497178146, -10.72451020669898902, 71.66557627198100988 ) ) ;
#93899 = CARTESIAN_POINT ( 'NONE',  ( 9.564922557961047289, -16.46253265017146816, 65.41775706135233293 ) ) ;
#93898 = CARTESIAN_POINT ( 'NONE',  ( -16.53943276465976808, 0.05219959533911058130, 61.24890960531435979 ) ) ;
#93900 = CARTESIAN_POINT ( 'NONE',  ( -19.19724070472094013, -5.500000000000084377, 71.06193348274381094 ) ) ;
#93901 = CARTESIAN_POINT ( 'NONE',  ( 0.05219959533936267826, -19.03943276465977164, 50.00109039468566863 ) ) ;
#93902 = CARTESIAN_POINT ( 'NONE',  ( -16.52544592524335698, -4.483927247898792601, 98.95942372801903275 ) ) ;
#93903 = CARTESIAN_POINT ( 'NONE',  ( -8.224510206698948167, 14.34966873604960824, 65.41557627198102409 ) ) ;
#93905 = CARTESIAN_POINT ( 'NONE',  ( 27.73933785331498214, 9.013057229001095294, 141.9750000027311501 ) ) ;
#93904 = CARTESIAN_POINT ( 'NONE',  ( 10.72451020669871369, 18.67979575497193778, 102.0844237280190185 ) ) ;
#93906 = CARTESIAN_POINT ( 'NONE',  ( 21.53943276465977519, -0.05219959533907433946, 88.74890960531436690 ) ) ;
#93907 = CARTESIAN_POINT ( 'NONE',  ( -5.153800228976328057, -19.02544592524343514, 67.29057627198102409 ) ) ;
#93908 = CARTESIAN_POINT ( 'NONE',  ( 10.81492255796106328, -18.62759615963255655, 65.41775706135234714 ) ) ;
#93909 = CARTESIAN_POINT ( 'NONE',  ( 5.153800228976335163, 19.02544592524342804, 44.79057627198103830 ) ) ;
#93910 = VERTEX_POINT ( 'NONE', #27040 ) ;
#93911 = CARTESIAN_POINT ( 'NONE',  ( -13.89961937509977652, 13.97604488694528158, 70.62390960531432427 ) ) ;
#93912 = CARTESIAN_POINT ( 'NONE',  ( -9.564922557960796823, -16.46253265017161027, 27.08224293864769550 ) ) ;
#93913 = CARTESIAN_POINT ( 'NONE',  ( -19.03943276465977164, 0.05219959533909376836, 111.2489096053143669 ) ) ;
#93914 = CARTESIAN_POINT ( 'NONE',  ( -0.05219959533910754901, -16.53943276465976808, 62.49890960531436690 ) ) ;
#93915 = CARTESIAN_POINT ( 'NONE',  ( -5.049401038298153566, 19.05341960407611168, 30.20724293864768839 ) ) ;
#93916 = CARTESIAN_POINT ( 'NONE',  ( -16.52544592524342804, 4.483927247898546575, 91.04057627198103830 ) ) ;
#93917 = CARTESIAN_POINT ( 'NONE',  ( 5.823673210054125526, 21.52544592524343514, 89.79057627198103830 ) ) ;
#93918 = CARTESIAN_POINT ( 'NONE',  ( -10.81492255796105439, 18.62759615963255655, 32.91775706135234714 ) ) ;
#93919 = CARTESIAN_POINT ( 'NONE',  ( 1.136082944010448514, 6.615573198874504790, -62.40258669366784972 ) ) ;
#93920 = CARTESIAN_POINT ( 'NONE',  ( -0.05219959533934338120, 16.53943276465976808, 47.50109039468568994 ) ) ;
#93921 = CARTESIAN_POINT ( 'NONE',  ( 10.72451020669898902, -18.67979575497178502, 77.91557627198102409 ) ) ;
#93922 = CARTESIAN_POINT ( 'NONE',  ( -19.03943276465977164, -0.05219959533935918106, 28.75109039468566507 ) ) ;
#93923 = CARTESIAN_POINT ( 'NONE',  ( -16.51473224551069308, -9.474510206698971260, 106.6655762719810383 ) ) ;
#93924 = CARTESIAN_POINT ( 'NONE',  ( -21.52544592524334988, -5.823673210054445271, 38.95942372801901854 ) ) ;
#93925 = CARTESIAN_POINT ( 'NONE',  ( 18.62759615963271287, -10.81492255796078972, 43.33224293864769550 ) ) ;
#93926 = CARTESIAN_POINT ( 'NONE',  ( -16.55341960407611168, -4.379528057220339221, 21.45724293864769550 ) ) ;
#93928 = CARTESIAN_POINT ( 'NONE',  ( -18.62759615963255300, -10.81492255796106328, 104.1677570613523471 ) ) ;
#93927 = CARTESIAN_POINT ( 'NONE',  ( -18.67979575497193778, 10.72451020669871902, 68.33442372801900433 ) ) ;
#93929 = CARTESIAN_POINT ( 'NONE',  ( 16.51473224551083163, -9.474510206698727899, 35.83442372801899722 ) ) ;
#93930 = CARTESIAN_POINT ( 'NONE',  ( -0.05219959533934338120, 16.53943276465976808, 87.50109039468568994 ) ) ;
#93931 = CARTESIAN_POINT ( 'NONE',  ( 5.823673210054444382, -21.52544592524334988, 45.20942372801901854 ) ) ;
#93932 = CARTESIAN_POINT ( 'NONE',  ( -9.564922557960796823, -16.46253265017161027, 52.08224293864768839 ) ) ;
#93933 = CARTESIAN_POINT ( 'NONE',  ( 21.53943276465977519, 0.05219959533937863772, 111.2510903946856899 ) ) ;
#93934 = CARTESIAN_POINT ( 'NONE',  ( 10.81492255796078972, 18.62759615963270932, 24.58224293864768839 ) ) ;
#93935 = CARTESIAN_POINT ( 'NONE',  ( 21.55341960407619695, -5.719274019375665929, 21.04275706135234714 ) ) ;
#93936 = CARTESIAN_POINT ( 'NONE',  ( 0.05219959533907565091, 21.53943276465977519, 74.99890960531435269 ) ) ;
#93937 = CARTESIAN_POINT ( 'NONE',  ( -4.379528057220086978, -16.55341960407618274, 39.79275706135235424 ) ) ;
#93939 = CARTESIAN_POINT ( 'NONE',  ( 5.823673210054125526, 21.52544592524343514, 84.79057627198102409 ) ) ;
#93938 = LINE ( 'NONE', #17113, #41859 ) ;
#93941 = CARTESIAN_POINT ( 'NONE',  ( 14.29746914071049879, -8.314922557960816363, 63.33224293864770260 ) ) ;
#93940 = CARTESIAN_POINT ( 'NONE',  ( 12.06949235617739724, 12.14591786802326823, 61.87609039468568284 ) ) ;
#93942 = CARTESIAN_POINT ( 'NONE',  ( -21.30378117525442860, 19.99074948409473862, -49.30207733784024526 ) ) ;
#93943 = CARTESIAN_POINT ( 'NONE',  ( 16.46253265017146816, 9.564922557961045513, 86.66775706135233293 ) ) ;
#93944 = CARTESIAN_POINT ( 'NONE',  ( -21.39623730026198700, 0.5392447798058846997, -56.39940532337661239 ) ) ;
#93945 = CARTESIAN_POINT ( 'NONE',  ( -12.06949235617739369, -12.14591786802326823, 34.37609039468568284 ) ) ;
#93946 = CARTESIAN_POINT ( 'NONE',  ( -21.53943276465977519, 0.05219959533907696930, 116.2489096053143669 ) ) ;
#93947 = B_SPLINE_CURVE_WITH_KNOTS ( 'NONE', 3,
 ( #98182, #19392, #38548, #3216, #158879, #68874, #99200, #81041, #161885, #65875, #127549, #22380, #50727, #159886, #21375, #82016, #143712, #130533, #53712, #103217, #165892, #86042, #25401, #178068, #196251, #56720, #193233, #87043, #162884, #117379, #57720, #148728, #89036, #9217, #39535, #164899, #10216, #70884, #101193, #119390 ),
 .UNSPECIFIED., .F., .F.,
 ( 4, 2, 2, 2, 2, 2, 2, 2, 2, 2, 2, 2, 2, 2, 2, 2, 2, 2, 2, 4 ),
 ( 0.02158449572284441495, 0.02266158837400312348, 0.02373868102516183201, 0.02427722735074119495, 0.02481577367632055789, 0.02589286632747930458, 0.02696995897863805128, 0.02804705162979680144, 0.02912414428095554814, 0.02966269060653492495, 0.03020123693211429483, 0.03127832958327309010, 0.03235542223443187149, 0.03343251488559066675, 0.03450960753674945508, 0.03558670018790824341, 0.03612524651348764104, 0.03666379283906703174, 0.03774088549022580619, 0.03881797814138458758 ),
 .UNSPECIFIED. ) ;
#93948 = CARTESIAN_POINT ( 'NONE',  ( -0.05219959533907301413, -21.53943276465977519, 72.49890960531435269 ) ) ;
#93949 = CARTESIAN_POINT ( 'NONE',  ( -5.823673210054116645, -21.52544592524344225, 32.29057627198102409 ) ) ;
#93950 = CARTESIAN_POINT ( 'NONE',  ( -4.379528057220086978, -16.55341960407618274, 59.79275706135234714 ) ) ;
#93951 = CARTESIAN_POINT ( 'NONE',  ( 19.02544592524343514, -5.153800228976328945, 68.54057627198103830 ) ) ;
#93953 = CARTESIAN_POINT ( 'NONE',  ( 16.52544592524335698, 4.483927247898782831, 21.45942372801901499 ) ) ;
#93952 = CARTESIAN_POINT ( 'NONE',  ( -18.62759615963255300, -10.81492255796106328, 49.16775706135234003 ) ) ;
#93954 = CARTESIAN_POINT ( 'NONE',  ( 19.05341960407611168, 5.049401038298154454, 108.9572429386477097 ) ) ;
#93955 = CARTESIAN_POINT ( 'NONE',  ( 19.02544592524334988, 5.153800228976608722, 21.45942372801899012 ) ) ;
#93956 = CARTESIAN_POINT ( 'NONE',  ( -16.55341960407617563, 4.379528057220093196, 43.54275706135235424 ) ) ;
#93957 = CARTESIAN_POINT ( 'NONE',  ( -13.89961937509977652, 13.97604488694528158, 100.6239096053143669 ) ) ;
#93958 = CARTESIAN_POINT ( 'NONE',  ( -15.72974639402197994, 15.80617190586746368, 100.6239096053143811 ) ) ;
#93959 = CARTESIAN_POINT ( 'NONE',  ( 5.153800228976335163, 19.02544592524342804, 74.79057627198103830 ) ) ;
#93960 = CARTESIAN_POINT ( 'NONE',  ( 16.53943276465976808, -0.05219959533910856209, 83.74890960531435269 ) ) ;
#93961 = CARTESIAN_POINT ( 'NONE',  ( -5.719274019375978568, 21.55341960407610458, 25.20724293864769550 ) ) ;
#93962 = CARTESIAN_POINT ( 'NONE',  ( 9.474510206698971260, -16.51473224551069308, 22.91557627198102765 ) ) ;
#93963 = CARTESIAN_POINT ( 'NONE',  ( 5.823673210054125526, 21.52544592524343514, 99.79057627198103830 ) ) ;
#93964 = CARTESIAN_POINT ( 'NONE',  ( -19.05341960407617563, 5.049401038297882671, 63.54275706135234003 ) ) ;
#93965 = CARTESIAN_POINT ( 'NONE',  ( 21.55341960407610458, 5.719274019375980345, 28.95724293864769905 ) ) ;
#93966 = CARTESIAN_POINT ( 'NONE',  ( -13.89961937509977652, 13.97604488694528158, 30.62390960531435269 ) ) ;
#93967 = CARTESIAN_POINT ( 'NONE',  ( -5.719274019375978568, 21.55341960407610458, 65.20724293864768129 ) ) ;
#93968 = CARTESIAN_POINT ( 'NONE',  ( 19.02544592524343514, -5.153800228976328945, 103.5405762719809957 ) ) ;
#93969 = CARTESIAN_POINT ( 'NONE',  ( -5.823673210054431948, 21.52544592524334988, 87.70942372801901854 ) ) ;
#93970 = CARTESIAN_POINT ( 'NONE',  ( -13.97604488694527625, -13.89961937509977652, 51.87390960531436690 ) ) ;
#93971 = CARTESIAN_POINT ( 'NONE',  ( 14.34966873604960469, 8.224510206698951720, 89.16557627198102409 ) ) ;
#93972 = CARTESIAN_POINT ( 'NONE',  ( 14.34966873604972726, -8.224510206698740333, 30.83442372801902209 ) ) ;
#93973 = CARTESIAN_POINT ( 'NONE',  ( -19.02544592524342804, 5.153800228976336051, 56.04057627198100988 ) ) ;
#93974 = CARTESIAN_POINT ( 'NONE',  ( 15.80617190586769283, -15.72974639402175789, 85.62609039468568994 ) ) ;
#93975 = ORIENTED_EDGE ( 'NONE', *, *, #42127, .T. ) ;
#93976 = CARTESIAN_POINT ( 'NONE',  ( 5.049401038297881783, 19.05341960407617563, 27.29275706135232937 ) ) ;
#93977 = CARTESIAN_POINT ( 'NONE',  ( 13.97604488694548053, -13.89961937509957401, 35.62609039468567573 ) ) ;
#93978 = CARTESIAN_POINT ( 'NONE',  ( 5.823673210054444382, -21.52544592524334988, 35.20942372801901854 ) ) ;
#93979 = DIRECTION ( 'NONE',  ( -0.000000000000000000, -0.000000000000000000, -1.000000000000000000 ) ) ;
#93980 = CARTESIAN_POINT ( 'NONE',  ( -16.51473224551082808, 9.474510206698731452, 28.33442372801900433 ) ) ;
#93981 = CARTESIAN_POINT ( 'NONE',  ( -19.02544592524342804, 5.153800228976336051, 81.04057627198103830 ) ) ;
#93982 = CARTESIAN_POINT ( 'NONE',  ( 0.05219959533909260263, 19.03943276465977164, 74.99890960531435269 ) ) ;
#93983 = CARTESIAN_POINT ( 'NONE',  ( 16.55341960407611168, 4.379528057220329451, 23.95724293864769550 ) ) ;
#93985 = CARTESIAN_POINT ( 'NONE',  ( -21.55341960407619339, 5.719274019375674811, 83.54275706135234714 ) ) ;
#93984 = CARTESIAN_POINT ( 'NONE',  ( 19.05341960407611168, 5.049401038298154454, 113.9572429386477097 ) ) ;
#93986 = CARTESIAN_POINT ( 'NONE',  ( -5.950531402560715689E-15, 38.81732327939063509, -7.624999997268814056 ) ) ;
#93987 = CARTESIAN_POINT ( 'NONE',  ( 19.97888994334919843, -34.65319547504301312, -10.00000000000000000 ) ) ;
#93988 = CARTESIAN_POINT ( 'NONE',  ( -21.53943276465977519, -0.05219959533937600094, 78.75109039468568994 ) ) ;
#93989 = CARTESIAN_POINT ( 'NONE',  ( 30.73962218707677607, -22.33364281372841376, -2.947842220587804096 ) ) ;
#93990 = CARTESIAN_POINT ( 'NONE',  ( -19.03943276465977164, 0.05219959533909376836, 96.24890960531436690 ) ) ;
#93991 = CARTESIAN_POINT ( 'NONE',  ( 33.67975787243658203, 4.948374891829404376, 97.42774497825463698 ) ) ;
#93992 = CARTESIAN_POINT ( 'NONE',  ( -21.52544592524343514, 5.823673210054127303, 71.04057627198103830 ) ) ;
#93993 = CARTESIAN_POINT ( 'NONE',  ( -12.14591786802309592, -12.06949235617757132, 26.87390960531435979 ) ) ;
#93995 = CARTESIAN_POINT ( 'NONE',  ( -16.46253265017160317, 9.564922557960807481, 100.8322429386477097 ) ) ;
#93994 = CARTESIAN_POINT ( 'NONE',  ( -12.14591786802309592, -12.06949235617757132, 111.8739096053143669 ) ) ;
#93996 = CARTESIAN_POINT ( 'NONE',  ( 9.474510206698729675, 16.51473224551082808, 27.08442372801900433 ) ) ;
#93997 = CARTESIAN_POINT ( 'NONE',  ( 5.153800228976335163, 19.02544592524342804, 24.79057627198102765 ) ) ;
#93998 = CARTESIAN_POINT ( 'NONE',  ( -21.52544592524334988, -5.823673210054445271, 63.95942372801901854 ) ) ;
#93999 = CARTESIAN_POINT ( 'NONE',  ( 9.564922557960805705, 16.46253265017160317, 109.5822429386476955 ) ) ;
#94000 = CARTESIAN_POINT ( 'NONE',  ( 16.53943276465976808, 0.05219959533934440121, 106.2510903946856757 ) ) ;
#94001 = CARTESIAN_POINT ( 'NONE',  ( 9.474510206698729675, 16.51473224551082808, 67.08442372801900433 ) ) ;
#94002 = CARTESIAN_POINT ( 'NONE',  ( 16.46253265017146816, 9.564922557961045513, 66.66775706135233293 ) ) ;
#94003 = CARTESIAN_POINT ( 'NONE',  ( 19.03943276465977164, -0.05219959533909143690, 108.7489096053143527 ) ) ;
#94004 = CARTESIAN_POINT ( 'NONE',  ( 4.483927247898545687, 16.52544592524342804, 89.79057627198103830 ) ) ;
#94005 = CARTESIAN_POINT ( 'NONE',  ( -5.049401038297874678, -19.05341960407617918, 54.79275706135234003 ) ) ;
#94006 = CARTESIAN_POINT ( 'NONE',  ( -9.564922557960796823, -16.46253265017161027, 77.08224293864769550 ) ) ;
#94007 = CARTESIAN_POINT ( 'NONE',  ( -12.06949235617756955, 12.14591786802309770, 65.62390960531436690 ) ) ;
#94008 = CARTESIAN_POINT ( 'NONE',  ( -13.89961937509957401, -13.97604488694547875, 89.37609039468563310 ) ) ;
#94009 = CARTESIAN_POINT ( 'NONE',  ( -18.62759615963270932, 10.81492255796079327, 55.83224293864770260 ) ) ;
#94010 = ORIENTED_EDGE ( 'NONE', *, *, #62627, .F. ) ;
#94011 = CARTESIAN_POINT ( 'NONE',  ( 0.05219959533910956823, 16.53943276465976808, 109.9989096053143527 ) ) ;
#94012 = DIRECTION ( 'NONE',  ( 1.000000000000000000, 0.000000000000000000, 0.000000000000000000 ) ) ;
#94014 = CARTESIAN_POINT ( 'NONE',  ( -21.55341960407610458, -5.719274019375992779, 81.45724293864769550 ) ) ;
#94013 = CARTESIAN_POINT ( 'NONE',  ( -16.51473224551069308, -9.474510206698971260, 66.66557627198102409 ) ) ;
#94016 = CARTESIAN_POINT ( 'NONE',  ( 19.05341960407611168, 5.049401038298154454, 78.95724293864769550 ) ) ;
#94015 = CARTESIAN_POINT ( 'NONE',  ( 16.53943276465976808, 0.05219959533934440121, 86.25109039468568994 ) ) ;
#94017 = CARTESIAN_POINT ( 'NONE',  ( 13.89961937509957401, 13.97604488694547697, 66.87609039468567573 ) ) ;
#94018 = CARTESIAN_POINT ( 'NONE',  ( 18.67979575497194134, -10.72451020669871369, 85.83442372801901854 ) ) ;
#94019 = CARTESIAN_POINT ( 'NONE',  ( -18.67979575497178146, -10.72451020669898902, 61.66557627198103120 ) ) ;
#94020 = CARTESIAN_POINT ( 'NONE',  ( 15.72974639402199770, -15.80617190586745480, 28.12390960531435979 ) ) ;
#94021 = CARTESIAN_POINT ( 'NONE',  ( -19.03943276465977164, 0.05219959533909376836, 36.24890960531436690 ) ) ;
#94022 = CARTESIAN_POINT ( 'NONE',  ( 14.34966873604972726, -8.224510206698740333, 100.8344237280190185 ) ) ;
#94023 = CARTESIAN_POINT ( 'NONE',  ( -16.52544592524335698, -4.483927247898792601, 28.95942372801902209 ) ) ;
#94024 = CARTESIAN_POINT ( 'NONE',  ( 19.49190055781010500, 5.500000000000053291, 78.06116087098780554 ) ) ;
#94025 = CARTESIAN_POINT ( 'NONE',  ( 21.52544592524334988, 5.823673210054432836, 101.4594237280190185 ) ) ;
#94026 = ORIENTED_EDGE ( 'NONE', *, *, #187948, .T. ) ;
#94027 = CARTESIAN_POINT ( 'NONE',  ( 8.314922557960818139, 14.29746914071049879, 54.58224293864769550 ) ) ;
#94028 = CARTESIAN_POINT ( 'NONE',  ( -0.05219959533907301413, -21.53943276465977519, 92.49890960531436690 ) ) ;
#94029 = CARTESIAN_POINT ( 'NONE',  ( 10.81492255796078972, 18.62759615963270932, 104.5822429386477097 ) ) ;
#94030 = CARTESIAN_POINT ( 'NONE',  ( -11.30153831258471975, -180.0000000000000000, -4.999999999999999112 ) ) ;
#94032 = EDGE_CURVE ( 'NONE', #46062, #126623, #88686, .T. ) ;
#94031 = CARTESIAN_POINT ( 'NONE',  ( -21.53943276465977519, 0.05219959533907696930, 41.24890960531435269 ) ) ;
#94033 = CARTESIAN_POINT ( 'NONE',  ( 12.06949235617739724, 12.14591786802326823, 76.87609039468567573 ) ) ;
#94034 = CARTESIAN_POINT ( 'NONE',  ( 0.05219959533910956823, 16.53943276465976808, 84.99890960531436690 ) ) ;
#94035 = CARTESIAN_POINT ( 'NONE',  ( -0.05219959533909027116, -19.03943276465977164, 42.49890960531435269 ) ) ;
#94036 = PRESENTATION_STYLE_ASSIGNMENT (( #16221 ) ) ;
#94037 = CARTESIAN_POINT ( 'NONE',  ( 34.77754859679603072, -0.9869066695168891012, 52.45091671276828293 ) ) ;
#94038 = CARTESIAN_POINT ( 'NONE',  ( -4.379528057220086978, -16.55341960407618274, 89.79275706135236135 ) ) ;
#94039 = CARTESIAN_POINT ( 'NONE',  ( -10.72451020669870658, -18.67979575497194134, 39.58442372801901143 ) ) ;
#94040 = CARTESIAN_POINT ( 'NONE',  ( 0.05219959533909260263, 19.03943276465977164, 89.99890960531436690 ) ) ;
#94041 = CARTESIAN_POINT ( 'NONE',  ( 0.05219959533937995610, -21.53943276465977519, 65.00109039468568994 ) ) ;
#94042 = CARTESIAN_POINT ( 'NONE',  ( -28.82186960331499037, 2.781578969918950771E-14, 139.9999999999999716 ) ) ;
#94043 = CARTESIAN_POINT ( 'NONE',  ( -5.049401038298153566, 19.05341960407611168, 25.20724293864768484 ) ) ;
#94044 = ORIENTED_EDGE ( 'NONE', *, *, #41146, .F. ) ;
#94045 = CARTESIAN_POINT ( 'NONE',  ( -0.05219959533937732626, 21.53943276465977519, 62.50109039468568284 ) ) ;
#94047 = CARTESIAN_POINT ( 'NONE',  ( 19.03943276465977164, -0.05219959533909143690, 23.74890960531435269 ) ) ;
#94046 = CARTESIAN_POINT ( 'NONE',  ( -19.03943276465977164, 0.05219959533909376836, 56.24890960531435979 ) ) ;
#94048 = CARTESIAN_POINT ( 'NONE',  ( 13.89961937509977652, -13.97604488694527269, 88.12390960531438111 ) ) ;
#94049 = CARTESIAN_POINT ( 'NONE',  ( -0.05219959533936034679, 19.03943276465977164, 62.50109039468566863 ) ) ;
#94050 = CARTESIAN_POINT ( 'NONE',  ( -0.05219959533937732626, 21.53943276465977519, 42.50109039468567573 ) ) ;
#94051 = CARTESIAN_POINT ( 'NONE',  ( 13.89961937509957401, 13.97604488694547697, 61.87609039468566863 ) ) ;
#94052 = CARTESIAN_POINT ( 'NONE',  ( 5.153800228976335163, 19.02544592524342804, 44.79057627198103830 ) ) ;
#94053 = CARTESIAN_POINT ( 'NONE',  ( 16.52544592524335698, 4.483927247898782831, 111.4594237280190328 ) ) ;
#94054 = CARTESIAN_POINT ( 'NONE',  ( 19.03943276465977164, 0.05219959533936151252, 76.25109039468566152 ) ) ;
#94055 = CARTESIAN_POINT ( 'NONE',  ( -4.483927247898539470, -16.52544592524342804, 22.29057627198102765 ) ) ;
#94056 = CARTESIAN_POINT ( 'NONE',  ( 0.05219959533936267826, -19.03943276465977164, 55.00109039468566863 ) ) ;
#94057 = CARTESIAN_POINT ( 'NONE',  ( -5.153800228976328057, -19.02544592524343514, 97.29057627198099567 ) ) ;
#94058 = CARTESIAN_POINT ( 'NONE',  ( 18.67979575497194134, -10.72451020669871369, 110.8344237280190043 ) ) ;
#94059 = CARTESIAN_POINT ( 'NONE',  ( 13.97604488694548053, -13.89961937509957401, 25.62609039468566507 ) ) ;
#94060 = CARTESIAN_POINT ( 'NONE',  ( -5.049401038298153566, 19.05341960407611168, 35.20724293864768839 ) ) ;
#94061 = CARTESIAN_POINT ( 'NONE',  ( 18.67979575497194134, -10.72451020669871369, 90.83442372801901854 ) ) ;
#94062 = CARTESIAN_POINT ( 'NONE',  ( 8.224510206698742110, 14.34966873604972548, 37.08442372801901143 ) ) ;
#94063 = CARTESIAN_POINT ( 'NONE',  ( -13.97604488694527625, -13.89961937509977652, 91.87390960531432427 ) ) ;
#94064 = DIRECTION ( 'NONE',  ( 0.000000000000000000, 0.000000000000000000, -1.000000000000000000 ) ) ;
#94065 = CARTESIAN_POINT ( 'NONE',  ( -16.46253265017160317, 9.564922557960807481, 75.83224293864769550 ) ) ;
#94066 = CARTESIAN_POINT ( 'NONE',  ( 0.05219959533936267826, -19.03943276465977164, 90.00109039468567573 ) ) ;
#94067 = B_SPLINE_CURVE_WITH_KNOTS ( 'NONE', 3,
 ( #28621, #198446, #105436, #90258, #12461, #135792, #165135, #149958, #147969, #197463, #133790, #120597, #167121, #180322 ),
 .UNSPECIFIED., .F., .F.,
 ( 4, 2, 2, 2, 2, 2, 4 ),
 ( 2.784816081883512217E-07, 0.0004992641294407349547, 0.0009982497772732814266, 0.001996221072938393019, 0.002994192368603504611, 0.003493178016436066045, 0.003992163664268632249 ),
 .UNSPECIFIED. ) ;
#94068 = CARTESIAN_POINT ( 'NONE',  ( 19.05341960407611168, 5.049401038298154454, 103.9572429386476671 ) ) ;
#94069 = CARTESIAN_POINT ( 'NONE',  ( 18.62759615963255655, 10.81492255796105972, 101.6677570613523613 ) ) ;
#94070 = CARTESIAN_POINT ( 'NONE',  ( -12.06949235617756955, 12.14591786802309770, 100.6239096053143811 ) ) ;
#94071 = CARTESIAN_POINT ( 'NONE',  ( 19.03943276465977164, -0.05219959533909143690, 23.74890960531435269 ) ) ;
#94072 = CARTESIAN_POINT ( 'NONE',  ( -0.05219959533907301413, -21.53943276465977519, 42.49890960531435979 ) ) ;
#94073 = CARTESIAN_POINT ( 'NONE',  ( -5.823673210054116645, -21.52544592524344225, 37.29057627198102409 ) ) ;
#94074 = CARTESIAN_POINT ( 'NONE',  ( 9.474510206698971260, -16.51473224551069308, 27.91557627198103120 ) ) ;
#94075 = LINE ( 'NONE', #188103, #159665 ) ;
#94076 = CARTESIAN_POINT ( 'NONE',  ( -19.02544592524334988, -5.153800228976617603, 63.95942372801899012 ) ) ;
#94077 = CARTESIAN_POINT ( 'NONE',  ( 8.314922557960818139, 14.29746914071049879, 44.58224293864769550 ) ) ;
#94078 = CARTESIAN_POINT ( 'NONE',  ( 13.89961937509977652, -13.97604488694527269, 113.1239096053143527 ) ) ;
#94079 = CARTESIAN_POINT ( 'NONE',  ( -15.72974639402176322, -15.80617190586768395, 84.37609039468570415 ) ) ;
#94080 = CARTESIAN_POINT ( 'NONE',  ( -18.67979575497178146, -10.72451020669898902, 71.66557627198100988 ) ) ;
#94081 = CARTESIAN_POINT ( 'NONE',  ( -15.72974639402176322, -15.80617190586768395, 49.37609039468569705 ) ) ;
#94082 = CARTESIAN_POINT ( 'NONE',  ( -21.53943276465977519, 0.05219959533907696930, 96.24890960531435269 ) ) ;
#94083 = CARTESIAN_POINT ( 'NONE',  ( 21.53943276465977519, 0.05219959533937863772, 51.25109039468568994 ) ) ;
#94084 = CARTESIAN_POINT ( 'NONE',  ( 0.05219959533909260263, 19.03943276465977164, 29.99890960531435979 ) ) ;
#94085 = CARTESIAN_POINT ( 'NONE',  ( -13.89961937509977652, 13.97604488694528158, 85.62390960531433848 ) ) ;
#94086 = CARTESIAN_POINT ( 'NONE',  ( 12.14591786802327356, -12.06949235617739191, 75.62609039468567573 ) ) ;
#94087 = CARTESIAN_POINT ( 'NONE',  ( -12.06949235617756955, 12.14591786802309770, 110.6239096053143669 ) ) ;
#94088 = CARTESIAN_POINT ( 'NONE',  ( -19.02544592524342804, 5.153800228976336051, 116.0405762719810383 ) ) ;
#94089 = CARTESIAN_POINT ( 'NONE',  ( -14.34966873604960291, -8.224510206698953496, 51.66557627198102409 ) ) ;
#94090 = CARTESIAN_POINT ( 'NONE',  ( 12.14591786802309770, 12.06949235617756955, 24.37390960531435979 ) ) ;
#94091 = CARTESIAN_POINT ( 'NONE',  ( -19.03943276465977164, 0.05219959533909376836, 71.24890960531435269 ) ) ;
#94092 = CARTESIAN_POINT ( 'NONE',  ( 9.564922557960805705, 16.46253265017160317, 29.58224293864769550 ) ) ;
#94093 = CARTESIAN_POINT ( 'NONE',  ( -18.67979575497178146, -10.72451020669898902, 46.66557627198102409 ) ) ;
#94094 = CARTESIAN_POINT ( 'NONE',  ( -5.153800228976607833, 19.02544592524334988, 37.70942372801899722 ) ) ;
#94096 = CARTESIAN_POINT ( 'NONE',  ( -12.14591786802309592, -12.06949235617757132, 36.87390960531435979 ) ) ;
#94095 = DIRECTION ( 'NONE',  ( 1.000000000000000000, 0.000000000000000000, 0.000000000000000000 ) ) ;
#94097 = CARTESIAN_POINT ( 'NONE',  ( 19.05341960407611168, 5.049401038298154454, 108.9572429386477097 ) ) ;
#94098 = CARTESIAN_POINT ( 'NONE',  ( 0.05219959533937995610, -21.53943276465977519, 60.00109039468568284 ) ) ;
#94099 = DIRECTION ( 'NONE',  ( -1.000000000000000000, -0.000000000000000000, 0.000000000000000000 ) ) ;
#94100 = CARTESIAN_POINT ( 'NONE',  ( 16.53943276465976808, 0.05219959533934440121, 71.25109039468568994 ) ) ;
#94101 = EDGE_CURVE ( 'NONE', #17363, #56096, #96914, .T. ) ;
#94102 = CARTESIAN_POINT ( 'NONE',  ( 5.049401038297881783, 19.05341960407617563, 62.29275706135234003 ) ) ;
#94103 = CARTESIAN_POINT ( 'NONE',  ( -8.314922557960811034, -14.29746914071050412, 47.08224293864770260 ) ) ;
#94104 = CARTESIAN_POINT ( 'NONE',  ( -18.56399227203343116, -5.499999999999928058, 73.97830131249904184 ) ) ;
#94105 = CARTESIAN_POINT ( 'NONE',  ( 16.53943276465976808, -0.05219959533910856209, 28.74890960531435624 ) ) ;
#94106 = CARTESIAN_POINT ( 'NONE',  ( -16.51473224551069308, -9.474510206698971260, 36.66557627198102409 ) ) ;
#94107 = CARTESIAN_POINT ( 'NONE',  ( 9.474510206698971260, -16.51473224551069308, 57.91557627198103120 ) ) ;
#94108 = CARTESIAN_POINT ( 'NONE',  ( 4.483927247898545687, 16.52544592524342804, 114.7905762719810383 ) ) ;
#94109 = CARTESIAN_POINT ( 'NONE',  ( -21.52544592524334988, -5.823673210054445271, 33.95942372801901143 ) ) ;
#94110 = CARTESIAN_POINT ( 'NONE',  ( 9.564922557960805705, 16.46253265017160317, 54.58224293864769550 ) ) ;
#94111 = CARTESIAN_POINT ( 'NONE',  ( -3.573655867282028392E-15, 2.428612866367529932E-14, 150.0000000000000000 ) ) ;
#94112 = CARTESIAN_POINT ( 'NONE',  ( -9.474510206698964154, 16.51473224551069663, 50.41557627198102409 ) ) ;
#94113 = CARTESIAN_POINT ( 'NONE',  ( -5.823673210054116645, -21.52544592524344225, 32.29057627198102409 ) ) ;
#94115 = CARTESIAN_POINT ( 'NONE',  ( -9.474510206698964154, 16.51473224551069663, 25.41557627198103120 ) ) ;
#94114 = CARTESIAN_POINT ( 'NONE',  ( -10.72451020669870658, -18.67979575497194134, 54.58442372801901143 ) ) ;
#94116 = CARTESIAN_POINT ( 'NONE',  ( 10.72451020669898902, -18.67979575497178502, 32.91557627198102409 ) ) ;
#94117 = CARTESIAN_POINT ( 'NONE',  ( 8.224510206698742110, 14.34966873604972548, 92.08442372801901854 ) ) ;
#94118 = CARTESIAN_POINT ( 'NONE',  ( 21.53943276465977519, 0.05219959533937863772, 106.2510903946856757 ) ) ;
#94119 = CARTESIAN_POINT ( 'NONE',  ( -16.55341960407617563, 4.379528057220093196, 73.54275706135234714 ) ) ;
#94120 = CARTESIAN_POINT ( 'NONE',  ( 16.46253265017160672, -9.564922557960803928, 108.3322429386476955 ) ) ;
#94121 = CARTESIAN_POINT ( 'NONE',  ( -16.55341960407617563, 4.379528057220093196, 53.54275706135234714 ) ) ;
#94122 = CARTESIAN_POINT ( 'NONE',  ( -8.224510206698735004, -14.34966873604973081, 29.58442372801901854 ) ) ;
#94123 = CARTESIAN_POINT ( 'NONE',  ( 4.379528057220092307, 16.55341960407617563, 102.2927570613523613 ) ) ;
#94124 = CARTESIAN_POINT ( 'NONE',  ( -5.823673210054431948, 21.52544592524334988, 52.70942372801902565 ) ) ;
#94125 = CARTESIAN_POINT ( 'NONE',  ( 19.02544592524334988, 5.153800228976608722, 106.4594237280190185 ) ) ;
#94126 = CARTESIAN_POINT ( 'NONE',  ( -15.72974639402197994, 15.80617190586746368, 110.6239096053143669 ) ) ;
#94127 = CARTESIAN_POINT ( 'NONE',  ( 8.314922557961029526, -14.29746914071037800, 25.41775706135235779 ) ) ;
#94128 = CARTESIAN_POINT ( 'NONE',  ( 4.483927247898790824, -16.52544592524335698, 80.20942372801901854 ) ) ;
#94129 = CARTESIAN_POINT ( 'NONE',  ( 0.000000000000000000, 1.443375672974065216, 7.017607234860990640E-28 ) ) ;
#94130 = CARTESIAN_POINT ( 'NONE',  ( -5.823673210054431948, 21.52544592524334988, 87.70942372801901854 ) ) ;
#94131 = CARTESIAN_POINT ( 'NONE',  ( 13.97604488694548053, -13.89961937509957401, 80.62609039468567573 ) ) ;
#94132 = CARTESIAN_POINT ( 'NONE',  ( -16.53943276465976808, 0.05219959533911058130, 46.24890960531435979 ) ) ;
#94133 = CARTESIAN_POINT ( 'NONE',  ( 8.224510206698953496, -14.34966873604960469, 37.91557627198102409 ) ) ;
#94134 = CARTESIAN_POINT ( 'NONE',  ( -4.379528057220328563, 16.55341960407611168, 105.2072429386477097 ) ) ;
#94136 = CARTESIAN_POINT ( 'NONE',  ( 18.22780087662123805, -5.499999999999989342, 53.51763182126895657 ) ) ;
#94135 = CARTESIAN_POINT ( 'NONE',  ( -19.02544592524334988, -5.153800228976617603, 43.95942372801899012 ) ) ;
#94137 = CARTESIAN_POINT ( 'NONE',  ( 15.80617190586769283, -15.72974639402175789, 40.62609039468567573 ) ) ;
#94138 = CARTESIAN_POINT ( 'NONE',  ( -5.153800228976607833, 19.02544592524334988, 112.7094237280190043 ) ) ;
#94139 = CARTESIAN_POINT ( 'NONE',  ( -15.38714178908729124, -36.74766143018473485, -28.97229394964855942 ) ) ;
#94140 = CARTESIAN_POINT ( 'NONE',  ( 19.03943276465977164, -0.05219959533909143690, 98.74890960531436690 ) ) ;
#94141 = CARTESIAN_POINT ( 'NONE',  ( 21.53943276465977519, -0.05219959533907433946, 53.74890960531437401 ) ) ;
#94142 = CARTESIAN_POINT ( 'NONE',  ( 9.564922557961047289, -16.46253265017146816, 100.4177570613523329 ) ) ;
#94143 = CARTESIAN_POINT ( 'NONE',  ( -0.05219959533909027116, -19.03943276465977164, 87.49890960531436690 ) ) ;
#94144 = CARTESIAN_POINT ( 'NONE',  ( 18.67979575497178502, 10.72451020669898547, 54.16557627198103120 ) ) ;
#94145 = CARTESIAN_POINT ( 'NONE',  ( 12.06949235617757843, -12.14591786802309237, 103.1239096053143811 ) ) ;
#94146 = CARTESIAN_POINT ( 'NONE',  ( 19.03943276465977164, -0.05219959533909143690, 63.74890960531435979 ) ) ;
#94147 = CARTESIAN_POINT ( 'NONE',  ( -16.46253265017160317, 9.564922557960807481, 35.83224293864768839 ) ) ;
#94148 = CARTESIAN_POINT ( 'NONE',  ( -15.80617190586768217, 15.72974639402176855, 33.12609039468569705 ) ) ;
#94149 = CARTESIAN_POINT ( 'NONE',  ( -10.72451020669870658, -18.67979575497194134, 79.58442372801903275 ) ) ;
#94150 = CARTESIAN_POINT ( 'NONE',  ( -12.06949235617739369, -12.14591786802326823, 94.37609039468568994 ) ) ;
#94151 = CARTESIAN_POINT ( 'NONE',  ( -10.72451020669870658, -18.67979575497194134, 24.58442372801901499 ) ) ;
#94152 = CARTESIAN_POINT ( 'NONE',  ( -18.62759615963255300, -10.81492255796106328, 24.16775706135235424 ) ) ;
#94154 = CARTESIAN_POINT ( 'NONE',  ( 19.02544592524343514, -5.153800228976328945, 83.54057627198100988 ) ) ;
#94153 = CARTESIAN_POINT ( 'NONE',  ( 19.03943276465977164, 0.05219959533936151252, 61.25109039468566863 ) ) ;
#94155 = CARTESIAN_POINT ( 'NONE',  ( -15.80617190586768217, 15.72974639402176855, 88.12609039468570415 ) ) ;
#94156 = CARTESIAN_POINT ( 'NONE',  ( 5.823673210054125526, 21.52544592524343514, 79.79057627198102409 ) ) ;
#94157 = CARTESIAN_POINT ( 'NONE',  ( -14.34966873604960291, -8.224510206698953496, 61.66557627198103120 ) ) ;
#94158 = CARTESIAN_POINT ( 'NONE',  ( -5.719274019375665041, -21.55341960407619695, 99.79275706135234714 ) ) ;
#94159 = CARTESIAN_POINT ( 'NONE',  ( 16.55341960407611168, 4.379528057220329451, 88.95724293864769550 ) ) ;
#94160 = CARTESIAN_POINT ( 'NONE',  ( -19.02544592524342804, 5.153800228976336051, 31.04057627198102409 ) ) ;
#94161 = CARTESIAN_POINT ( 'NONE',  ( -5.153800228976607833, 19.02544592524334988, 72.70942372801900433 ) ) ;
#94162 = CARTESIAN_POINT ( 'NONE',  ( -14.34966873604960291, -8.224510206698953496, 41.66557627198103120 ) ) ;
#94163 = CARTESIAN_POINT ( 'NONE',  ( -5.823673210054431948, 21.52544592524334988, 97.70942372801904696 ) ) ;
#94164 = CARTESIAN_POINT ( 'NONE',  ( 19.05341960407611168, 5.049401038298154454, 93.95724293864769550 ) ) ;
#94165 = CARTESIAN_POINT ( 'NONE',  ( -19.03943276465977164, -0.05219959533935918106, 58.75109039468566863 ) ) ;
#94166 = CARTESIAN_POINT ( 'NONE',  ( -21.53943276465977519, 0.05219959533907696930, 66.24890960531436690 ) ) ;
#94167 = CARTESIAN_POINT ( 'NONE',  ( -21.52544592524334988, -5.823673210054445271, 23.95942372801901143 ) ) ;
#94168 = CARTESIAN_POINT ( 'NONE',  ( 0.05219959533936267826, -19.03943276465977164, 105.0010903946856615 ) ) ;
#94169 = CARTESIAN_POINT ( 'NONE',  ( -8.224510206698735004, -14.34966873604973081, 79.58442372801903275 ) ) ;
#94171 = CARTESIAN_POINT ( 'NONE',  ( 21.52544592524334988, 5.823673210054432836, 26.45942372801901854 ) ) ;
#94170 = CARTESIAN_POINT ( 'NONE',  ( 6.856101608890750167E-16, -78.63162257080495010, -12.99999901186700946 ) ) ;
#94172 = CARTESIAN_POINT ( 'NONE',  ( 8.224510206698953496, -14.34966873604960469, 97.91557627198103830 ) ) ;
#94173 = CARTESIAN_POINT ( 'NONE',  ( 36.91746824999999887, 11.99521256947799053, -6.024999997268811747 ) ) ;
#94174 = CARTESIAN_POINT ( 'NONE',  ( -12.06949235617739369, -12.14591786802326823, 39.37609039468567573 ) ) ;
#94175 = CARTESIAN_POINT ( 'NONE',  ( 10.81492255796078972, 18.62759615963270932, 59.58224293864770260 ) ) ;
#94176 = CARTESIAN_POINT ( 'NONE',  ( 16.53943276465976808, 0.05219959533934440121, 101.2510903946856757 ) ) ;
#94177 = CARTESIAN_POINT ( 'NONE',  ( 14.29746914071037800, 8.314922557961029526, 41.66775706135235424 ) ) ;
#94178 = CARTESIAN_POINT ( 'NONE',  ( -0.05219959533909027116, -19.03943276465977164, 32.49890960531435979 ) ) ;
#94179 = CARTESIAN_POINT ( 'NONE',  ( -4.379528057220086978, -16.55341960407618274, 84.79275706135234714 ) ) ;
#94180 = CARTESIAN_POINT ( 'NONE',  ( -0.05219959533936034679, 19.03943276465977164, 72.50109039468566152 ) ) ;
#94181 = CARTESIAN_POINT ( 'NONE',  ( -5.823673210054116645, -21.52544592524344225, 67.29057627198103830 ) ) ;
#94182 = CARTESIAN_POINT ( 'NONE',  ( 0.05219959533934541429, -16.53943276465976808, 95.00109039468568994 ) ) ;
#94183 = CARTESIAN_POINT ( 'NONE',  ( 10.81492255796106328, -18.62759615963255655, 85.41775706135236135 ) ) ;
#94184 = CARTESIAN_POINT ( 'NONE',  ( -21.53943276465977519, 0.05219959533907696930, 66.24890960531436690 ) ) ;
#94185 = CARTESIAN_POINT ( 'NONE',  ( -0.05219959533907301413, -21.53943276465977519, 47.49890960531435979 ) ) ;
#94186 = ORIENTED_EDGE ( 'NONE', *, *, #20610, .T. ) ;
#94187 = CARTESIAN_POINT ( 'NONE',  ( -4.483927247898782831, 16.52544592524335698, 77.70942372801900433 ) ) ;
#94188 = CARTESIAN_POINT ( 'NONE',  ( -15.80617190586745835, -15.72974639402198527, 46.87390960531435979 ) ) ;
#94189 = VERTEX_POINT ( 'NONE', #79482 ) ;
#94190 = CARTESIAN_POINT ( 'NONE',  ( -9.474510206698964154, 16.51473224551069663, 115.4155762719810241 ) ) ;
#94191 = CARTESIAN_POINT ( 'NONE',  ( -22.03292204642282570, -7.478118144893485919, 173.9941030799742805 ) ) ;
#94192 = CARTESIAN_POINT ( 'NONE',  ( -8.224510206698948167, 14.34966873604960824, 115.4155762719810241 ) ) ;
#94193 = CARTESIAN_POINT ( 'NONE',  ( -18.67979575497178146, -10.72451020669898902, 56.66557627198103830 ) ) ;
#94194 = CARTESIAN_POINT ( 'NONE',  ( 16.53943276465976808, 0.05219959533934440121, 106.2510903946856757 ) ) ;
#94195 = CARTESIAN_POINT ( 'NONE',  ( -18.67979575497193778, 10.72451020669871902, 48.33442372801902565 ) ) ;
#94196 = CARTESIAN_POINT ( 'NONE',  ( -19.03943276465977164, -0.05219959533935918106, 98.75109039468567573 ) ) ;
#94197 = CARTESIAN_POINT ( 'NONE',  ( -16.55341960407611168, -4.379528057220339221, 111.4572429386476813 ) ) ;
#94198 = CARTESIAN_POINT ( 'NONE',  ( 16.46253265017146816, 9.564922557961045513, 106.6677570613523471 ) ) ;
#94199 = CARTESIAN_POINT ( 'NONE',  ( -9.564922557960796823, -16.46253265017161027, 42.08224293864769550 ) ) ;
#94200 = CARTESIAN_POINT ( 'NONE',  ( -8.906447517083053711, -27.41122689804191026, 144.4000000000000057 ) ) ;
#94201 = CARTESIAN_POINT ( 'NONE',  ( -19.02544592524342804, 5.153800228976336051, 91.04057627198100988 ) ) ;
#94202 = CARTESIAN_POINT ( 'NONE',  ( -12.06949235617739369, -12.14591786802326823, 79.37609039468567573 ) ) ;
#94203 = CARTESIAN_POINT ( 'NONE',  ( -5.153800228976607833, 19.02544592524334988, 72.70942372801900433 ) ) ;
#94204 = CARTESIAN_POINT ( 'NONE',  ( 9.474510206698729675, 16.51473224551082808, 27.08442372801900433 ) ) ;
#94205 = CARTESIAN_POINT ( 'NONE',  ( 5.719274019375991003, -21.55341960407610458, 57.70724293864770260 ) ) ;
#94206 = EDGE_CURVE ( 'NONE', #61533, #22005, #152564, .T. ) ;
#94207 = CARTESIAN_POINT ( 'NONE',  ( 16.55341960407618274, -4.379528057220086978, 81.04275706135236135 ) ) ;
#94208 = CARTESIAN_POINT ( 'NONE',  ( 13.97604488694548053, -13.89961937509957401, 75.62609039468564731 ) ) ;
#94209 = CARTESIAN_POINT ( 'NONE',  ( -13.97604488694527625, -13.89961937509977652, 41.87390960531435979 ) ) ;
#94210 = CARTESIAN_POINT ( 'NONE',  ( 16.46253265017160672, -9.564922557960803928, 83.33224293864768129 ) ) ;
#94211 = CARTESIAN_POINT ( 'NONE',  ( -15.72974639402176322, -15.80617190586768395, 49.37609039468569705 ) ) ;
#94212 = CARTESIAN_POINT ( 'NONE',  ( -19.03943276465977164, 0.05219959533909376836, 46.24890960531435979 ) ) ;
#94213 = CARTESIAN_POINT ( 'NONE',  ( 19.03943276465977164, 0.05219959533936151252, 76.25109039468566152 ) ) ;
#94214 = CARTESIAN_POINT ( 'NONE',  ( 24.42783677680755972, -12.30119602009776969, 169.8172178118632587 ) ) ;
#94215 = CARTESIAN_POINT ( 'NONE',  ( -19.05341960407611168, -5.049401038298163336, 106.4572429386476955 ) ) ;
#94216 = CARTESIAN_POINT ( 'NONE',  ( 14.34966873604960469, 8.224510206698951720, 59.16557627198103120 ) ) ;
#94217 = CARTESIAN_POINT ( 'NONE',  ( -21.52544592524343514, 5.823673210054127303, 61.04057627198103120 ) ) ;
#94218 = FACE_OUTER_BOUND ( 'NONE', #74408, .T. ) ;
#94219 = CARTESIAN_POINT ( 'NONE',  ( -9.474510206698720793, -16.51473224551083518, 49.58442372801899722 ) ) ;
#94220 = CARTESIAN_POINT ( 'NONE',  ( -17.97182807773871716, 5.500000000000055955, 88.53038844047284783 ) ) ;
#94222 = CARTESIAN_POINT ( 'NONE',  ( -5.153800228976328057, -19.02544592524343514, 67.29057627198102409 ) ) ;
#94221 = CARTESIAN_POINT ( 'NONE',  ( 16.46253265017160672, -9.564922557960803928, 68.33224293864770971 ) ) ;
#94223 = CARTESIAN_POINT ( 'NONE',  ( 4.483927247898790824, -16.52544592524335698, 55.20942372801902565 ) ) ;
#94224 = CARTESIAN_POINT ( 'NONE',  ( 17.81289503416610742, 24.51734667627700404, 143.2999999999999829 ) ) ;
#94225 = DIRECTION ( 'NONE',  ( 0.000000000000000000, 0.000000000000000000, -1.000000000000000000 ) ) ;
#94226 = CARTESIAN_POINT ( 'NONE',  ( 12.14591786802327356, -12.06949235617739191, 95.62609039468568994 ) ) ;
#94227 = CARTESIAN_POINT ( 'NONE',  ( 23.84755066337006113, 5.771293611162917614, 171.0999092862842019 ) ) ;
#94228 = CARTESIAN_POINT ( 'NONE',  ( -0.05219959533934338120, 16.53943276465976808, 72.50109039468568994 ) ) ;
#94229 = CARTESIAN_POINT ( 'NONE',  ( -0.05219959533934338120, 16.53943276465976808, 37.50109039468568284 ) ) ;
#94230 = CARTESIAN_POINT ( 'NONE',  ( -13.97604488694547697, 13.89961937509957934, 23.12609039468565442 ) ) ;
#94232 = FACE_BOUND ( 'NONE', #163939, .T. ) ;
#94231 = CARTESIAN_POINT ( 'NONE',  ( -16.51473224551069308, -9.474510206698971260, 56.66557627198103120 ) ) ;
#94233 = CARTESIAN_POINT ( 'NONE',  ( -5.823673210054431948, 21.52544592524334988, 47.70942372801902565 ) ) ;
#94234 = CARTESIAN_POINT ( 'NONE',  ( -19.03943276465977164, -0.05219959533935918106, 68.75109039468566152 ) ) ;
#94235 = CARTESIAN_POINT ( 'NONE',  ( -21.53943276465977519, -0.05219959533937600094, 103.7510903946857042 ) ) ;
#94236 = CARTESIAN_POINT ( 'NONE',  ( 5.153800228976335163, 19.02544592524342804, 29.79057627198102409 ) ) ;
#94237 = CARTESIAN_POINT ( 'NONE',  ( -17.61085972261891186, 15.85590801997748756, -57.22569728324523197 ) ) ;
#94238 = CARTESIAN_POINT ( 'NONE',  ( 0.05219959533907565091, 21.53943276465977519, 59.99890960531436690 ) ) ;
#94239 = ADVANCED_FACE ( 'NONE', ( #78472 ), #103448, .T. ) ;
#94240 = CARTESIAN_POINT ( 'NONE',  ( -18.67979575497178146, -10.72451020669898902, 21.66557627198102409 ) ) ;
#94241 = CARTESIAN_POINT ( 'NONE',  ( -14.34966873604960291, -8.224510206698953496, 96.66557627198102409 ) ) ;
#94242 = CARTESIAN_POINT ( 'NONE',  ( 8.314922557961029526, -14.29746914071037800, 40.41775706135234714 ) ) ;
#94243 = CARTESIAN_POINT ( 'NONE',  ( 12.14591786802309770, 12.06949235617756955, 29.37390960531435269 ) ) ;
#94244 = VERTEX_POINT ( 'NONE', #61837 ) ;
#94245 = CARTESIAN_POINT ( 'NONE',  ( 21.55341960407610458, 5.719274019375980345, 113.9572429386477239 ) ) ;
#94247 = CARTESIAN_POINT ( 'NONE',  ( 19.02544592524343514, -5.153800228976328945, 108.5405762719810383 ) ) ;
#94246 = CARTESIAN_POINT ( 'NONE',  ( 16.53943276465976808, -0.05219959533910856209, 33.74890960531436690 ) ) ;
#94248 = TOROIDAL_SURFACE ( 'NONE', #149144, 69.99999999999998579, 10.00000000000000000 ) ;
#94249 = CARTESIAN_POINT ( 'NONE',  ( 9.474510206698729675, 16.51473224551082808, 102.0844237280190043 ) ) ;
#94250 = CARTESIAN_POINT ( 'NONE',  ( 13.89961937509957401, 13.97604488694547697, 31.87609039468566863 ) ) ;
#94251 = CARTESIAN_POINT ( 'NONE',  ( -16.53943276465976808, 0.05219959533911058130, 26.24890960531435624 ) ) ;
#94252 = CARTESIAN_POINT ( 'NONE',  ( -15.80617190586745835, -15.72974639402198527, 106.8739096053143811 ) ) ;
#94253 = CARTESIAN_POINT ( 'NONE',  ( -5.719274019375978568, 21.55341960407610458, 70.20724293864769550 ) ) ;
#94254 = CARTESIAN_POINT ( 'NONE',  ( 5.049401038298161559, -19.05341960407611168, 82.70724293864770971 ) ) ;
#94255 = CARTESIAN_POINT ( 'NONE',  ( 16.53943276465976808, -0.05219959533910856209, 53.74890960531437401 ) ) ;
#94256 = CARTESIAN_POINT ( 'NONE',  ( -16.51473224551069308, -9.474510206698971260, 96.66557627198102409 ) ) ;
#94257 = CARTESIAN_POINT ( 'NONE',  ( -36.91128768240056246, 0.3596143131121838366, 50.50000000000001421 ) ) ;
#94258 = CARTESIAN_POINT ( 'NONE',  ( -0.05219959533936034679, 19.03943276465977164, 52.50109039468566863 ) ) ;
#94259 = CARTESIAN_POINT ( 'NONE',  ( -21.53943276465977519, 0.05219959533907696930, 96.24890960531435269 ) ) ;
#94260 = CARTESIAN_POINT ( 'NONE',  ( 16.53943276465976808, -0.05219959533910856209, 98.74890960531438111 ) ) ;
#94261 = CARTESIAN_POINT ( 'NONE',  ( -18.62759615963255300, -10.81492255796106328, 34.16775706135234714 ) ) ;
#94262 = CARTESIAN_POINT ( 'NONE',  ( -27.73933785331498925, -9.013057229001049109, 140.9750000027311501 ) ) ;
#94263 = EDGE_CURVE ( 'NONE', #141307, #53672, #184214, .T. ) ;
#94264 = CARTESIAN_POINT ( 'NONE',  ( -8.314922557960811034, -14.29746914071050412, 27.08224293864769550 ) ) ;
#94265 = CARTESIAN_POINT ( 'NONE',  ( -19.03943276465977164, 0.05219959533909376836, 31.24890960531435979 ) ) ;
#94266 = CARTESIAN_POINT ( 'NONE',  ( 9.564922557960805705, 16.46253265017160317, 84.58224293864769550 ) ) ;
#94267 = CARTESIAN_POINT ( 'NONE',  ( -10.72451020669898014, 18.67979575497178502, 60.41557627198102409 ) ) ;
#94268 = CARTESIAN_POINT ( 'NONE',  ( -25.63014048727048433, 6.600871414792726100, 163.2070037194167185 ) ) ;
#94269 = CARTESIAN_POINT ( 'NONE',  ( 16.51473224551069308, 9.474510206698969483, 34.16557627198102409 ) ) ;
#94270 = CARTESIAN_POINT ( 'NONE',  ( -15.72974639402197994, 15.80617190586746368, 55.62390960531436690 ) ) ;
#94271 = CARTESIAN_POINT ( 'NONE',  ( 21.55341960407619695, -5.719274019375665929, 71.04275706135234714 ) ) ;
#94273 = CARTESIAN_POINT ( 'NONE',  ( -12.06949235617739369, -12.14591786802326823, 74.37609039468568994 ) ) ;
#94272 = CARTESIAN_POINT ( 'NONE',  ( 21.54936698786741900, -30.95672727791841439, -19.59590204858815810 ) ) ;
#94274 = CARTESIAN_POINT ( 'NONE',  ( 13.89961937509977652, -13.97604488694527269, 63.12390960531435979 ) ) ;
#94275 = CARTESIAN_POINT ( 'NONE',  ( -16.46253265017160317, 9.564922557960807481, 65.83224293864769550 ) ) ;
#94276 = ORIENTED_EDGE ( 'NONE', *, *, #56725, .T. ) ;
#94277 = CARTESIAN_POINT ( 'NONE',  ( -21.52544592524334988, -5.823673210054445271, 108.9594237280190185 ) ) ;
#94278 = CARTESIAN_POINT ( 'NONE',  ( 12.14591786802327356, -12.06949235617739191, 80.62609039468567573 ) ) ;
#94279 = CARTESIAN_POINT ( 'NONE',  ( -5.823673210054431948, 21.52544592524334988, 92.70942372801901854 ) ) ;
#94280 = CARTESIAN_POINT ( 'NONE',  ( -5.153800228976328057, -19.02544592524343514, 77.29057627198099567 ) ) ;
#94281 = CARTESIAN_POINT ( 'NONE',  ( 0.05219959533907565091, 21.53943276465977519, 29.99890960531435979 ) ) ;
#94282 = CARTESIAN_POINT ( 'NONE',  ( -5.049401038297874678, -19.05341960407617918, 104.7927570613523471 ) ) ;
#94283 = CARTESIAN_POINT ( 'NONE',  ( -21.52544592524334988, -5.823673210054445271, 88.95942372801901854 ) ) ;
#94284 = CARTESIAN_POINT ( 'NONE',  ( 14.29746914071037800, 8.314922557961029526, 46.66775706135234714 ) ) ;
#94285 = CARTESIAN_POINT ( 'NONE',  ( 5.823673210054125526, 21.52544592524343514, 99.79057627198103830 ) ) ;
#94286 = CARTESIAN_POINT ( 'NONE',  ( -5.049401038297874678, -19.05341960407617918, 99.79275706135234714 ) ) ;
#94287 = CARTESIAN_POINT ( 'NONE',  ( 5.153800228976335163, 19.02544592524342804, 74.79057627198103830 ) ) ;
#94288 = CARTESIAN_POINT ( 'NONE',  ( 19.05341960407617918, -5.049401038297876454, 111.0427570613523329 ) ) ;
#94289 = CARTESIAN_POINT ( 'NONE',  ( -19.02544592524342804, 5.153800228976336051, 36.04057627198100988 ) ) ;
#94290 = CARTESIAN_POINT ( 'NONE',  ( -12.06949235617739369, -12.14591786802326823, 24.37609039468567573 ) ) ;
#94291 = CARTESIAN_POINT ( 'NONE',  ( 12.14591786802309770, 12.06949235617756955, 64.37390960531435269 ) ) ;
#94292 = CARTESIAN_POINT ( 'NONE',  ( -12.06949235617739369, -12.14591786802326823, 79.37609039468567573 ) ) ;
#94294 = CARTESIAN_POINT ( 'NONE',  ( -9.564922557960796823, -16.46253265017161027, 57.08224293864769550 ) ) ;
#94293 = CARTESIAN_POINT ( 'NONE',  ( 5.719274019375673035, 21.55341960407619339, 32.29275706135235424 ) ) ;
#94296 = EDGE_CURVE ( 'NONE', #76130, #149451, #169395, .T. ) ;
#94295 = CARTESIAN_POINT ( 'NONE',  ( -0.05219959533909027116, -19.03943276465977164, 72.49890960531435269 ) ) ;
#94297 = CARTESIAN_POINT ( 'NONE',  ( 16.55341960407618274, -4.379528057220086978, 71.04275706135234714 ) ) ;
#94298 = CARTESIAN_POINT ( 'NONE',  ( 1.993301997531345292E-15, -30.30510711980685912, 146.7500000054623683 ) ) ;
#94299 = VERTEX_POINT ( 'NONE', #173025 ) ;
#94300 = CARTESIAN_POINT ( 'NONE',  ( -21.55341960407619339, 5.719274019375674811, 113.5427570613523756 ) ) ;
#94301 = CARTESIAN_POINT ( 'NONE',  ( -19.03943276465977164, 0.05219959533909376836, 31.24890960531435979 ) ) ;
#94303 = ORIENTED_EDGE ( 'NONE', *, *, #165511, .F. ) ;
#94302 = CARTESIAN_POINT ( 'NONE',  ( -13.89961937509977652, 13.97604488694528158, 105.6239096053143527 ) ) ;
#94304 = CARTESIAN_POINT ( 'NONE',  ( -16.52544592524335698, -4.483927247898792601, 33.95942372801901143 ) ) ;
#94306 = CARTESIAN_POINT ( 'NONE',  ( -16.52544592524335698, -4.483927247898792601, 48.95942372801902565 ) ) ;
#94305 = CARTESIAN_POINT ( 'NONE',  ( 5.049401038297881783, 19.05341960407617563, 42.29275706135234003 ) ) ;
#94307 = CARTESIAN_POINT ( 'NONE',  ( 13.97604488694527802, 13.89961937509977652, 44.37390960531435269 ) ) ;
#94308 = CARTESIAN_POINT ( 'NONE',  ( 0.05219959533909260263, 19.03943276465977164, 104.9989096053143669 ) ) ;
#94309 = CARTESIAN_POINT ( 'NONE',  ( 16.46253265017160672, -9.564922557960803928, 58.33224293864769550 ) ) ;
#94310 = CARTESIAN_POINT ( 'NONE',  ( -5.719274019375978568, 21.55341960407610458, 100.2072429386476955 ) ) ;
#94312 = CARTESIAN_POINT ( 'NONE',  ( 5.049401038298161559, -19.05341960407611168, 112.7072429386476813 ) ) ;
#94311 = CARTESIAN_POINT ( 'NONE',  ( -5.049401038298153566, 19.05341960407611168, 90.20724293864766707 ) ) ;
#94313 = CARTESIAN_POINT ( 'NONE',  ( 13.97604488694527802, 13.89961937509977652, 64.37390960531436690 ) ) ;
#94315 = CARTESIAN_POINT ( 'NONE',  ( -27.73933785331498925, 2.428612866367529932E-14, 147.3750000027311842 ) ) ;
#94314 = CARTESIAN_POINT ( 'NONE',  ( 16.52544592524335698, 4.483927247898782831, 111.4594237280190328 ) ) ;
#94316 = CARTESIAN_POINT ( 'NONE',  ( -0.05219959533936034679, 19.03943276465977164, 102.5010903946856757 ) ) ;
#94317 = CARTESIAN_POINT ( 'NONE',  ( -13.89961937509957401, -13.97604488694547875, 24.37609039468565442 ) ) ;
#94318 = CARTESIAN_POINT ( 'NONE',  ( -4.379528057220328563, 16.55341960407611168, 60.20724293864768839 ) ) ;
#94319 = CARTESIAN_POINT ( 'NONE',  ( -21.52544592524334988, -5.823673210054445271, 78.95942372801901854 ) ) ;
#94320 = CARTESIAN_POINT ( 'NONE',  ( 16.51473224551069308, 9.474510206698969483, 24.16557627198102765 ) ) ;
#94322 = CARTESIAN_POINT ( 'NONE',  ( 15.72974639402176855, 15.80617190586768217, 96.87609039468568994 ) ) ;
#94321 = CARTESIAN_POINT ( 'NONE',  ( -4.483927247898539470, -16.52544592524342804, 32.29057627198102409 ) ) ;
#94323 = CARTESIAN_POINT ( 'NONE',  ( 16.51473224551069308, 9.474510206698969483, 79.16557627198103830 ) ) ;
#94324 = CARTESIAN_POINT ( 'NONE',  ( -0.05219959533937732626, 21.53943276465977519, 47.50109039468568994 ) ) ;
#94325 = CARTESIAN_POINT ( 'NONE',  ( -13.97604488694527625, -13.89961937509977652, 96.87390960531433848 ) ) ;
#94326 = CARTESIAN_POINT ( 'NONE',  ( 0.05219959533910956823, 16.53943276465976808, 94.99890960531436690 ) ) ;
#94327 = CARTESIAN_POINT ( 'NONE',  ( -16.52544592524342804, 4.483927247898546575, 66.04057627198103830 ) ) ;
#94328 = CARTESIAN_POINT ( 'NONE',  ( 21.52544592524344225, -5.823673210054117533, 73.54057627198102409 ) ) ;
#94329 = CARTESIAN_POINT ( 'NONE',  ( -16.51473224551069308, -9.474510206698971260, 76.66557627198103830 ) ) ;
#94330 = CARTESIAN_POINT ( 'NONE',  ( -21.55341960407610458, -5.719274019375992779, 81.45724293864769550 ) ) ;
#94331 = CARTESIAN_POINT ( 'NONE',  ( -5.049401038297874678, -19.05341960407617918, 79.79275706135233293 ) ) ;
#94333 = CARTESIAN_POINT ( 'NONE',  ( 4.483927247898545687, 16.52544592524342804, 84.79057627198102409 ) ) ;
#94332 = CARTESIAN_POINT ( 'NONE',  ( 19.05341960407618274, -5.049401038297876454, 31.04275706135232582 ) ) ;
#94334 = CARTESIAN_POINT ( 'NONE',  ( -19.03943276465977164, 0.05219959533909376836, 56.24890960531435979 ) ) ;
#94335 = CARTESIAN_POINT ( 'NONE',  ( 5.719274019375991003, -21.55341960407610458, 62.70724293864769550 ) ) ;
#94336 = CARTESIAN_POINT ( 'NONE',  ( 16.61371651742598843, -7.165104196376272938, 26.35415069992996706 ) ) ;
#94337 = CARTESIAN_POINT ( 'NONE',  ( -0.05219959533934338120, 16.53943276465976808, 107.5010903946856899 ) ) ;
#94338 = CARTESIAN_POINT ( 'NONE',  ( -5.153800228976607833, 19.02544592524334988, 102.7094237280189759 ) ) ;
#94339 = CARTESIAN_POINT ( 'NONE',  ( -16.52544592524342804, 4.483927247898546575, 86.04057627198102409 ) ) ;
#94340 = CARTESIAN_POINT ( 'NONE',  ( -18.56101223717332260, -5.500000000000006217, 96.44978406935675252 ) ) ;
#94341 = CARTESIAN_POINT ( 'NONE',  ( -5.049401038298153566, 19.05341960407611168, 75.20724293864769550 ) ) ;
#94342 = CARTESIAN_POINT ( 'NONE',  ( -19.05341960407611168, -5.049401038298163336, 36.45724293864766707 ) ) ;
#94343 = CARTESIAN_POINT ( 'NONE',  ( -4.379528057220328563, 16.55341960407611168, 70.20724293864769550 ) ) ;
#94344 = CARTESIAN_POINT ( 'NONE',  ( 5.049401038298161559, -19.05341960407611168, 97.70724293864766707 ) ) ;
#94346 = CARTESIAN_POINT ( 'NONE',  ( -9.564922557960796823, -16.46253265017161027, 62.08224293864769550 ) ) ;
#94345 = CARTESIAN_POINT ( 'NONE',  ( 9.474510206698729675, 16.51473224551082808, 92.08442372801900433 ) ) ;
#94347 = CARTESIAN_POINT ( 'NONE',  ( 19.03943276465977164, -0.05219959533909143690, 83.74890960531436690 ) ) ;
#94348 = CARTESIAN_POINT ( 'NONE',  ( -15.72974639402197994, 15.80617190586746368, 75.62390960531439532 ) ) ;
#94349 = CARTESIAN_POINT ( 'NONE',  ( 16.53943276465976808, 0.05219959533934440121, 71.25109039468568994 ) ) ;
#94350 = CARTESIAN_POINT ( 'NONE',  ( -17.44270441346520073, 5.991230190322872851, 93.63664920735774899 ) ) ;
#94351 = CARTESIAN_POINT ( 'NONE',  ( -5.049401038298153566, 19.05341960407611168, 60.20724293864768129 ) ) ;
#94352 = CARTESIAN_POINT ( 'NONE',  ( 5.719274019375991003, -21.55341960407610458, 72.70724293864769550 ) ) ;
#94353 = CARTESIAN_POINT ( 'NONE',  ( -13.89961937509957401, -13.97604488694547875, 89.37609039468563310 ) ) ;
#94355 = CARTESIAN_POINT ( 'NONE',  ( -15.72974639402176322, -15.80617190586768395, 49.37609039468569705 ) ) ;
#94354 = CARTESIAN_POINT ( 'NONE',  ( -8.224510206698948167, 14.34966873604960824, 40.41557627198103120 ) ) ;
#94356 = CARTESIAN_POINT ( 'NONE',  ( 9.474510206698729675, 16.51473224551082808, 72.08442372801900433 ) ) ;
#94358 = CARTESIAN_POINT ( 'NONE',  ( 19.05341960407611168, 5.049401038298154454, 108.9572429386477097 ) ) ;
#94357 = CARTESIAN_POINT ( 'NONE',  ( 4.379528057220092307, 16.55341960407617563, 77.29275706135234714 ) ) ;
#94359 = CARTESIAN_POINT ( 'NONE',  ( 19.02544592524343514, -5.153800228976328945, 103.5405762719810099 ) ) ;
#94360 = CARTESIAN_POINT ( 'NONE',  ( -16.20579543436678449, 7.371946100355091680, 79.43479165828127009 ) ) ;
#94361 = CARTESIAN_POINT ( 'NONE',  ( -14.29746914071037622, -8.314922557961029526, 89.16775706135236135 ) ) ;
#94362 = CARTESIAN_POINT ( 'NONE',  ( -16.53943276465976808, -0.05219959533934237506, 48.75109039468568284 ) ) ;
#94363 = CARTESIAN_POINT ( 'NONE',  ( 5.153800228976335163, 19.02544592524342804, 59.79057627198100988 ) ) ;
#94364 = CARTESIAN_POINT ( 'NONE',  ( 5.153800228976335163, 19.02544592524342804, 59.79057627198100988 ) ) ;
#94365 = CARTESIAN_POINT ( 'NONE',  ( 18.62759615963255655, 10.81492255796105972, 56.66775706135235424 ) ) ;
#94366 = CARTESIAN_POINT ( 'NONE',  ( 4.483927247898790824, -16.52544592524335698, 60.20942372801902565 ) ) ;
#94367 = CARTESIAN_POINT ( 'NONE',  ( -4.483927247898539470, -16.52544592524342804, 37.29057627198102409 ) ) ;
#94368 = CARTESIAN_POINT ( 'NONE',  ( -9.564922557960796823, -16.46253265017161027, 47.08224293864769550 ) ) ;
#94369 = CARTESIAN_POINT ( 'NONE',  ( 9.564922557960805705, 16.46253265017160317, 39.58224293864768839 ) ) ;
#94370 = CARTESIAN_POINT ( 'NONE',  ( -12.06949235617739369, -12.14591786802326823, 34.37609039468568284 ) ) ;
#94371 = CARTESIAN_POINT ( 'NONE',  ( 13.97604488694548053, -13.89961937509957401, 75.62609039468564731 ) ) ;
#94372 = CARTESIAN_POINT ( 'NONE',  ( -8.314922557960811034, -14.29746914071050412, 87.08224293864769550 ) ) ;
#94373 = CARTESIAN_POINT ( 'NONE',  ( 19.03943276465977164, -0.05219959533909143690, 48.74890960531435979 ) ) ;
#94375 = CARTESIAN_POINT ( 'NONE',  ( 30.74264578624799782, 22.33583958711400541, -8.800000000000000711 ) ) ;
#94374 = CARTESIAN_POINT ( 'NONE',  ( -13.97604488694547697, 13.89961937509957934, 83.12609039468564731 ) ) ;
#94376 = CARTESIAN_POINT ( 'NONE',  ( 5.719274019375673035, 21.55341960407619339, 92.29275706135236135 ) ) ;
#94377 = CARTESIAN_POINT ( 'NONE',  ( -16.52544592524335698, -4.483927247898792601, 58.95942372801902565 ) ) ;
#94378 = CARTESIAN_POINT ( 'NONE',  ( 17.12812012977024878, 6.668231424566068988, 38.85948759323144941 ) ) ;
#94379 = CARTESIAN_POINT ( 'NONE',  ( 18.62759615963271287, -10.81492255796078972, 48.33224293864770260 ) ) ;
#94380 = CARTESIAN_POINT ( 'NONE',  ( -8.224510206698735004, -14.34966873604973081, 39.58442372801901143 ) ) ;
#94381 = CARTESIAN_POINT ( 'NONE',  ( 18.22780087662121673, 5.500000000000056843, 88.98459894673892734 ) ) ;
#94382 = CARTESIAN_POINT ( 'NONE',  ( 0.05219959533936267826, -19.03943276465977164, 25.00109039468566152 ) ) ;
#94383 = CARTESIAN_POINT ( 'NONE',  ( -5.153800228976328057, -19.02544592524343514, 77.29057627198099567 ) ) ;
#94384 = CYLINDRICAL_SURFACE ( 'NONE', #39809, 28.79475375365586487 ) ;
#94385 = CARTESIAN_POINT ( 'NONE',  ( 13.89961937509977652, -13.97604488694527269, 53.12390960531434558 ) ) ;
#94386 = CARTESIAN_POINT ( 'NONE',  ( -20.38160892792488355, -22.50821459300682648, -51.03861378962740503 ) ) ;
#94387 = CARTESIAN_POINT ( 'NONE',  ( -0.05219959533909027116, -19.03943276465977164, 67.49890960531436690 ) ) ;
#94388 = CARTESIAN_POINT ( 'NONE',  ( 17.49999999999999645, -3.209263204892621513, 112.2619682560626444 ) ) ;
#94389 = CARTESIAN_POINT ( 'NONE',  ( 5.153800228976615827, -19.02544592524334988, 40.20942372801898301 ) ) ;
#94390 = CARTESIAN_POINT ( 'NONE',  ( 0.05219959533936267826, -19.03943276465977164, 20.00109039468567218 ) ) ;
#94391 = CARTESIAN_POINT ( 'NONE',  ( 16.53943276465976808, -0.05219959533910856209, 38.74890960531435979 ) ) ;
#94392 = CARTESIAN_POINT ( 'NONE',  ( -16.51473224551069308, -9.474510206698971260, 41.66557627198103120 ) ) ;
#94393 = CARTESIAN_POINT ( 'NONE',  ( -16.46253265017160317, 9.564922557960807481, 100.8322429386477097 ) ) ;
#94394 = CARTESIAN_POINT ( 'NONE',  ( 10.72451020669871369, 18.67979575497193778, 72.08442372801899012 ) ) ;
#94395 = CARTESIAN_POINT ( 'NONE',  ( -9.564922557960796823, -16.46253265017161027, 52.08224293864768839 ) ) ;
#94396 = CARTESIAN_POINT ( 'NONE',  ( 21.53943276465977519, 0.05219959533937863772, 86.25109039468568994 ) ) ;
#94397 = CARTESIAN_POINT ( 'NONE',  ( 16.46253265017160672, -9.564922557960803928, 113.3322429386476955 ) ) ;
#94398 = CARTESIAN_POINT ( 'NONE',  ( -5.049401038298153566, 19.05341960407611168, 35.20724293864768839 ) ) ;
#94399 = CARTESIAN_POINT ( 'NONE',  ( 5.719274019375673035, 21.55341960407619339, 27.29275706135234358 ) ) ;
#94400 = CARTESIAN_POINT ( 'NONE',  ( -19.03943276465977164, -0.05219959533935918106, 53.75109039468566863 ) ) ;
#94401 = CARTESIAN_POINT ( 'NONE',  ( 16.46253265017160672, -9.564922557960803928, 28.33224293864769550 ) ) ;
#94402 = CARTESIAN_POINT ( 'NONE',  ( 19.02544592524343514, -5.153800228976328945, 73.54057627198103830 ) ) ;
#94403 = CARTESIAN_POINT ( 'NONE',  ( 9.474510206698729675, 16.51473224551082808, 107.0844237280190043 ) ) ;
#94404 = CARTESIAN_POINT ( 'NONE',  ( 0.05219959533910956823, 16.53943276465976808, 74.99890960531435269 ) ) ;
#94405 = CARTESIAN_POINT ( 'NONE',  ( 15.72974639402199770, -15.80617190586745480, 33.12390960531435979 ) ) ;
#94406 = CARTESIAN_POINT ( 'NONE',  ( 5.153800228976615827, -19.02544592524334988, 100.2094237280190043 ) ) ;
#94407 = CARTESIAN_POINT ( 'NONE',  ( -0.05219959533907301413, -21.53943276465977519, 102.4989096053143811 ) ) ;
#94408 = CARTESIAN_POINT ( 'NONE',  ( 0.05219959533937995610, -21.53943276465977519, 60.00109039468568284 ) ) ;
#94409 = CARTESIAN_POINT ( 'NONE',  ( 12.14591786802327356, -12.06949235617739191, 50.62609039468568994 ) ) ;
#94410 = CARTESIAN_POINT ( 'NONE',  ( 16.55341960407618274, -4.379528057220086978, 51.04275706135234714 ) ) ;
#94411 = CARTESIAN_POINT ( 'NONE',  ( 15.80617190586746368, 15.72974639402197994, 69.37390960531436690 ) ) ;
#94412 = ORIENTED_EDGE ( 'NONE', *, *, #35307, .T. ) ;
#94413 = CARTESIAN_POINT ( 'NONE',  ( 13.97604488694527802, 13.89961937509977652, 44.37390960531435269 ) ) ;
#94414 = CARTESIAN_POINT ( 'NONE',  ( -4.483927247898782831, 16.52544592524335698, 82.70942372801900433 ) ) ;
#94415 = CARTESIAN_POINT ( 'NONE',  ( 18.62759615963271287, -10.81492255796078972, 108.3322429386477097 ) ) ;
#94416 = CARTESIAN_POINT ( 'NONE',  ( 16.52544592524342804, -4.483927247898539470, 48.54057627198103120 ) ) ;
#94417 = CARTESIAN_POINT ( 'NONE',  ( 16.51473224551069308, 9.474510206698969483, 79.16557627198103830 ) ) ;
#94418 = CARTESIAN_POINT ( 'NONE',  ( 4.379528057220092307, 16.55341960407617563, 72.29275706135236135 ) ) ;
#94419 = CARTESIAN_POINT ( 'NONE',  ( 0.05219959533934541429, -16.53943276465976808, 20.00109039468568639 ) ) ;
#94420 = CARTESIAN_POINT ( 'NONE',  ( 0.05219959533907565091, 21.53943276465977519, 109.9989096053143527 ) ) ;
#94421 = CARTESIAN_POINT ( 'NONE',  ( -14.34966873604960291, -8.224510206698953496, 41.66557627198103120 ) ) ;
#94422 = ORIENTED_EDGE ( 'NONE', *, *, #163088, .T. ) ;
#94423 = CARTESIAN_POINT ( 'NONE',  ( -16.29526858892874941, 7.335722546920117715, 74.20329402199800484 ) ) ;
#94424 = CARTESIAN_POINT ( 'NONE',  ( 21.52544592524344225, -5.823673210054117533, 88.54057627198103830 ) ) ;
#94425 = CARTESIAN_POINT ( 'NONE',  ( -14.34966873604960291, -8.224510206698953496, 31.66557627198102054 ) ) ;
#94426 = ORIENTED_EDGE ( 'NONE', *, *, #75553, .T. ) ;
#94427 = CARTESIAN_POINT ( 'NONE',  ( 35.00000000000000000, 3.889087296526017479, 8.181980515339454030 ) ) ;
#94428 = CARTESIAN_POINT ( 'NONE',  ( -21.53943276465977519, 0.05219959533907696930, 106.2489096053143811 ) ) ;
#94429 = CARTESIAN_POINT ( 'NONE',  ( -19.03943276465977164, 0.05219959533909376836, 111.2489096053143669 ) ) ;
#94430 = CARTESIAN_POINT ( 'NONE',  ( -21.55341960407619339, 5.719274019375674811, 23.54275706135235424 ) ) ;
#94431 = CARTESIAN_POINT ( 'NONE',  ( -0.05219959533910754901, -16.53943276465976808, 57.49890960531435979 ) ) ;
#94432 = CARTESIAN_POINT ( 'NONE',  ( -16.53943276465976808, -0.05219959533934237506, 53.75109039468568994 ) ) ;
#94433 = CARTESIAN_POINT ( 'NONE',  ( 9.564922557960805705, 16.46253265017160317, 59.58224293864769550 ) ) ;
#94434 = CARTESIAN_POINT ( 'NONE',  ( -13.97604488694547697, 13.89961937509957934, 48.12609039468566863 ) ) ;
#94435 = CARTESIAN_POINT ( 'NONE',  ( -9.474510206698964154, 16.51473224551069663, 85.41557627198102409 ) ) ;
#94436 = CARTESIAN_POINT ( 'NONE',  ( -21.53943276465977519, 0.05219959533907696930, 31.24890960531435979 ) ) ;
#94437 = CARTESIAN_POINT ( 'NONE',  ( -25.98457697381309472, -27.33515243881182144, -20.34861096990052332 ) ) ;
#94438 = CARTESIAN_POINT ( 'NONE',  ( -5.153800228976328057, -19.02544592524343514, 47.29057627198102409 ) ) ;
#94439 = CARTESIAN_POINT ( 'NONE',  ( -12.14591786802326823, 12.06949235617739902, 28.12609039468568284 ) ) ;
#94440 = CARTESIAN_POINT ( 'NONE',  ( -5.049401038297874678, -19.05341960407617918, 64.79275706135233293 ) ) ;
#94441 = CARTESIAN_POINT ( 'NONE',  ( -21.55341960407610458, -5.719274019375992779, 101.4572429386476955 ) ) ;
#94442 = EDGE_CURVE ( 'NONE', #68071, #33122, #63847, .T. ) ;
#94443 = CARTESIAN_POINT ( 'NONE',  ( 4.379528057220339221, -16.55341960407611168, 27.70724293864769905 ) ) ;
#94444 = CARTESIAN_POINT ( 'NONE',  ( 13.97604488694527802, 13.89961937509977652, 89.37390960531436690 ) ) ;
#94445 = CARTESIAN_POINT ( 'NONE',  ( -15.72974639402197994, 15.80617190586746368, 55.62390960531436690 ) ) ;
#94447 = CARTESIAN_POINT ( 'NONE',  ( 12.06949235617739724, 12.14591786802326823, 26.87609039468567218 ) ) ;
#94446 = CARTESIAN_POINT ( 'NONE',  ( -21.53943276465977519, 0.05219959533907696930, 91.24890960531436690 ) ) ;
#94448 = CARTESIAN_POINT ( 'NONE',  ( 5.823673210054125526, 21.52544592524343514, 29.79057627198102409 ) ) ;
#94449 = CARTESIAN_POINT ( 'NONE',  ( 5.719274019375673035, 21.55341960407619339, 92.29275706135236135 ) ) ;
#94450 = CARTESIAN_POINT ( 'NONE',  ( -0.05219959533909027116, -19.03943276465977164, 87.49890960531436690 ) ) ;
#94451 = CARTESIAN_POINT ( 'NONE',  ( 13.97604488694527802, 13.89961937509977652, 29.37390960531435979 ) ) ;
#94452 = CARTESIAN_POINT ( 'NONE',  ( 16.51473224551069308, 9.474510206698969483, 84.16557627198102409 ) ) ;
#94453 = CARTESIAN_POINT ( 'NONE',  ( -16.53943276465976808, 0.05219959533911058130, 101.2489096053143669 ) ) ;
#94454 = CARTESIAN_POINT ( 'NONE',  ( 5.049401038298161559, -19.05341960407611168, 67.70724293864769550 ) ) ;
#94455 = CARTESIAN_POINT ( 'NONE',  ( -19.03943276465977164, -0.05219959533935918106, 113.7510903946856757 ) ) ;
#94456 = DIRECTION ( 'NONE',  ( 0.000000000000000000, 0.000000000000000000, -1.000000000000000000 ) ) ;
#94458 = CARTESIAN_POINT ( 'NONE',  ( 19.03943276465977164, -0.05219959533909143690, 108.7489096053143527 ) ) ;
#94457 = CARTESIAN_POINT ( 'NONE',  ( -18.67979575497193778, 10.72451020669871902, 93.33442372801901854 ) ) ;
#94459 = CARTESIAN_POINT ( 'NONE',  ( 16.55341960407618274, -4.379528057220086978, 91.04275706135236135 ) ) ;
#94460 = CARTESIAN_POINT ( 'NONE',  ( 30.74264578624800137, -22.33583958711395212, -9.199999999999999289 ) ) ;
#94461 = CARTESIAN_POINT ( 'NONE',  ( -9.564922557961040184, 16.46253265017147172, 67.91775706135233293 ) ) ;
#94462 = CARTESIAN_POINT ( 'NONE',  ( 19.03943276465977164, 0.05219959533936151252, 26.25109039468566507 ) ) ;
#94463 = CARTESIAN_POINT ( 'NONE',  ( 26.85917411135797295, 7.165250986577666126, 139.9999999999999716 ) ) ;
#94464 = CARTESIAN_POINT ( 'NONE',  ( -5.153800228976328057, -19.02544592524343514, 22.29057627198102765 ) ) ;
#94465 = CARTESIAN_POINT ( 'NONE',  ( -4.379528057220328563, 16.55341960407611168, 30.20724293864769550 ) ) ;
#94466 = CARTESIAN_POINT ( 'NONE',  ( -9.564922557960796823, -16.46253265017161027, 22.08224293864768839 ) ) ;
#94467 = CARTESIAN_POINT ( 'NONE',  ( 4.379528057220092307, 16.55341960407617563, 112.2927570613523471 ) ) ;
#94468 = CARTESIAN_POINT ( 'NONE',  ( -18.56101223717332971, -5.500000000000068390, 86.44978406935680937 ) ) ;
#94469 = CARTESIAN_POINT ( 'NONE',  ( -16.53943276465976808, -0.05219959533934237506, 93.75109039468567573 ) ) ;
#94470 = CARTESIAN_POINT ( 'NONE',  ( 9.564922557960805705, 16.46253265017160317, 39.58224293864768839 ) ) ;
#94471 = CARTESIAN_POINT ( 'NONE',  ( 15.72974639402176855, 15.80617190586768217, 91.87609039468568994 ) ) ;
#94472 = CARTESIAN_POINT ( 'NONE',  ( 19.03943276465977164, 0.05219959533936151252, 106.2510903946856615 ) ) ;
#94473 = CARTESIAN_POINT ( 'NONE',  ( -5.719274019375665041, -21.55341960407619695, 79.79275706135236135 ) ) ;
#94474 = CARTESIAN_POINT ( 'NONE',  ( 5.049401038297881783, 19.05341960407617563, 52.29275706135234003 ) ) ;
#94475 = CARTESIAN_POINT ( 'NONE',  ( 13.97604488694527802, 13.89961937509977652, 89.37390960531436690 ) ) ;
#94476 = CARTESIAN_POINT ( 'NONE',  ( 0.05219959533909260263, 19.03943276465977164, 74.99890960531435269 ) ) ;
#94477 = CARTESIAN_POINT ( 'NONE',  ( 17.31728774477274158, 6.344390552232410663, 71.68093348310685542 ) ) ;
#94478 = CARTESIAN_POINT ( 'NONE',  ( 4.379528057220339221, -16.55341960407611168, 67.70724293864769550 ) ) ;
#94479 = CARTESIAN_POINT ( 'NONE',  ( 0.05219959533907565091, 21.53943276465977519, 54.99890960531435269 ) ) ;
#94480 = CARTESIAN_POINT ( 'NONE',  ( 19.05341960407611168, 5.049401038298154454, 48.95724293864768129 ) ) ;
#94482 = CARTESIAN_POINT ( 'NONE',  ( 16.52544592524335698, 4.483927247898782831, 76.45942372801901854 ) ) ;
#94481 = CARTESIAN_POINT ( 'NONE',  ( -5.823673210054116645, -21.52544592524344225, 82.29057627198103830 ) ) ;
#94483 = ORIENTED_EDGE ( 'NONE', *, *, #51286, .T. ) ;
#94484 = CARTESIAN_POINT ( 'NONE',  ( -19.05341960407611168, -5.049401038298163336, 46.45724293864768129 ) ) ;
#94486 = CARTESIAN_POINT ( 'NONE',  ( 29.86685920354754842, -21.69954338932559068, -5.824999997268813345 ) ) ;
#94485 = CARTESIAN_POINT ( 'NONE',  ( -8.224510206698948167, 14.34966873604960824, 75.41557627198102409 ) ) ;
#94487 = CARTESIAN_POINT ( 'NONE',  ( -9.474510206698964154, 16.51473224551069663, 55.41557627198103120 ) ) ;
#94488 = CARTESIAN_POINT ( 'NONE',  ( -5.153800228976328057, -19.02544592524343514, 27.29057627198103120 ) ) ;
#94489 = CARTESIAN_POINT ( 'NONE',  ( 9.474510206698729675, 16.51473224551082808, 67.08442372801900433 ) ) ;
#94490 = CARTESIAN_POINT ( 'NONE',  ( -12.06949235617756955, 12.14591786802309770, 75.62390960531439532 ) ) ;
#94491 = CARTESIAN_POINT ( 'NONE',  ( 18.62759615963255655, 10.81492255796105972, 51.66775706135234714 ) ) ;
#94493 = CARTESIAN_POINT ( 'NONE',  ( 21.53943276465977519, -0.05219959533907433946, 108.7489096053143669 ) ) ;
#94492 = CARTESIAN_POINT ( 'NONE',  ( -0.05219959533909027116, -19.03943276465977164, 37.49890960531436690 ) ) ;
#94494 = FACE_OUTER_BOUND ( 'NONE', #162410, .T. ) ;
#94495 = CARTESIAN_POINT ( 'NONE',  ( 0.05219959533910956823, 16.53943276465976808, 89.99890960531438111 ) ) ;
#94496 = CARTESIAN_POINT ( 'NONE',  ( 27.35218628822511278, -28.77384467243328459, -20.10380102095120947 ) ) ;
#94497 = CARTESIAN_POINT ( 'NONE',  ( 5.049401038298161559, -19.05341960407611168, 42.70724293864767418 ) ) ;
#94498 = CARTESIAN_POINT ( 'NONE',  ( -19.49401214000074489, -12.39993551617566325, 164.9999999999999716 ) ) ;
#94500 = CARTESIAN_POINT ( 'NONE',  ( 0.05219959533909260263, 19.03943276465977164, 104.9989096053143669 ) ) ;
#94499 = CARTESIAN_POINT ( 'NONE',  ( -9.474510206698720793, -16.51473224551083518, 94.58442372801900433 ) ) ;
#94501 = CARTESIAN_POINT ( 'NONE',  ( -5.823673210054431948, 21.52544592524334988, 32.70942372801900433 ) ) ;
#94502 = CARTESIAN_POINT ( 'NONE',  ( 5.049401038298161559, -19.05341960407611168, 77.70724293864765286 ) ) ;
#94503 = CARTESIAN_POINT ( 'NONE',  ( 19.03943276465977164, 0.05219959533936151252, 76.25109039468566152 ) ) ;
#94504 = CARTESIAN_POINT ( 'NONE',  ( -13.89961937509977652, 13.97604488694528158, 40.62390960531435979 ) ) ;
#94505 = CARTESIAN_POINT ( 'NONE',  ( -16.53943276465976808, 0.05219959533911058130, 66.24890960531436690 ) ) ;
#94506 = CARTESIAN_POINT ( 'NONE',  ( 14.29746914071049879, -8.314922557960816363, 63.33224293864770260 ) ) ;
#94507 = CARTESIAN_POINT ( 'NONE',  ( -5.049401038298153566, 19.05341960407611168, 75.20724293864769550 ) ) ;
#94508 = CARTESIAN_POINT ( 'NONE',  ( -10.72451020669898014, 18.67979575497178502, 105.4155762719810383 ) ) ;
#94509 = CARTESIAN_POINT ( 'NONE',  ( -9.474510206698964154, 16.51473224551069663, 65.41557627198102409 ) ) ;
#94510 = CARTESIAN_POINT ( 'NONE',  ( -19.03943276465977164, -0.05219959533935918106, 18.75109039468567218 ) ) ;
#94513 = CARTESIAN_POINT ( 'NONE',  ( -16.55341960407611168, -4.379528057220339221, 111.4572429386476813 ) ) ;
#94512 = CARTESIAN_POINT ( 'NONE',  ( 8.224510206698953496, -14.34966873604960469, 22.91557627198102765 ) ) ;
#94511 = CARTESIAN_POINT ( 'NONE',  ( 16.51473224551069308, 9.474510206698969483, 34.16557627198102409 ) ) ;
#94514 = CARTESIAN_POINT ( 'NONE',  ( 16.46253265017146816, 9.564922557961045513, 106.6677570613523471 ) ) ;
#94515 = EDGE_LOOP ( 'NONE', ( #29563, #38581, #38514, #57914 ) ) ;
#94516 = CARTESIAN_POINT ( 'NONE',  ( 15.72974639402176855, 15.80617190586768217, 26.87609039468567218 ) ) ;
#94517 = CARTESIAN_POINT ( 'NONE',  ( -16.46253265017146816, -9.564922557961047289, 69.16775706135233293 ) ) ;
#94518 = CARTESIAN_POINT ( 'NONE',  ( 16.55341960407618274, -4.379528057220086978, 111.0427570613523613 ) ) ;
#94519 = CARTESIAN_POINT ( 'NONE',  ( 21.52544592524344225, -5.823673210054117533, 78.54057627198103830 ) ) ;
#94520 = CARTESIAN_POINT ( 'NONE',  ( -18.67979575497178146, -10.72451020669898902, 26.66557627198103475 ) ) ;
#94521 = CARTESIAN_POINT ( 'NONE',  ( -14.29746914071049879, 8.314922557960819915, 50.83224293864770971 ) ) ;
#94522 = CARTESIAN_POINT ( 'NONE',  ( 19.02544592524343514, -5.153800228976328945, 33.54057627198102409 ) ) ;
#94523 = CARTESIAN_POINT ( 'NONE',  ( -9.474510206698964154, 16.51473224551069663, 35.41557627198102409 ) ) ;
#94524 = CARTESIAN_POINT ( 'NONE',  ( 16.51473224551083163, -9.474510206698727899, 25.83442372801900078 ) ) ;
#94525 = CARTESIAN_POINT ( 'NONE',  ( 4.379528057220092307, 16.55341960407617563, 92.29275706135236135 ) ) ;
#94526 = CARTESIAN_POINT ( 'NONE',  ( -16.52544592524335698, -4.483927247898792601, 53.95942372801900433 ) ) ;
#94527 = CARTESIAN_POINT ( 'NONE',  ( 18.62759615963271287, -10.81492255796078972, 23.33224293864769194 ) ) ;
#94529 = CARTESIAN_POINT ( 'NONE',  ( 5.719274019375673035, 21.55341960407619339, 107.2927570613523471 ) ) ;
#94528 = CARTESIAN_POINT ( 'NONE',  ( 13.97604488694527802, 13.89961937509977652, 54.37390960531435979 ) ) ;
#94530 = CARTESIAN_POINT ( 'NONE',  ( 19.02544592524343514, -5.153800228976328945, 83.54057627198100988 ) ) ;
#94531 = CARTESIAN_POINT ( 'NONE',  ( -12.14591786802326823, 12.06949235617739902, 58.12609039468568994 ) ) ;
#94532 = CARTESIAN_POINT ( 'NONE',  ( -16.52544592524342804, 4.483927247898546575, 111.0405762719810525 ) ) ;
#94533 = CARTESIAN_POINT ( 'NONE',  ( -16.52544592524342804, 4.483927247898546575, 26.04057627198103475 ) ) ;
#94534 = CARTESIAN_POINT ( 'NONE',  ( 5.000000000000001776, -120.0000000000000142, -13.00000000000000000 ) ) ;
#94537 = CARTESIAN_POINT ( 'NONE',  ( 19.05341960407611168, 5.049401038298154454, 73.95724293864768129 ) ) ;
#94536 = CARTESIAN_POINT ( 'NONE',  ( -5.153800228976328057, -19.02544592524343514, 87.29057627198103830 ) ) ;
#94535 = CARTESIAN_POINT ( 'NONE',  ( -21.53943276465977519, -0.05219959533937600094, 73.75109039468567573 ) ) ;
#94539 = EDGE_CURVE ( 'NONE', #46039, #138583, #131781, .T. ) ;
#94538 = CARTESIAN_POINT ( 'NONE',  ( 13.89961937509977652, -13.97604488694527269, 113.1239096053143527 ) ) ;
#94540 = CARTESIAN_POINT ( 'NONE',  ( -12.14591786802309592, -12.06949235617757132, 61.87390960531436690 ) ) ;
#94541 = CARTESIAN_POINT ( 'NONE',  ( -12.14591786802326823, 12.06949235617739902, 113.1260903946856899 ) ) ;
#94542 = ORIENTED_EDGE ( 'NONE', *, *, #32687, .F. ) ;
#94543 = CARTESIAN_POINT ( 'NONE',  ( 16.55341960407611168, 4.379528057220329451, 33.95724293864769550 ) ) ;
#94545 = DIRECTION ( 'NONE',  ( 0.000000000000000000, 0.4999999999999991118, -0.8660254037844391517 ) ) ;
#94544 = CARTESIAN_POINT ( 'NONE',  ( 16.55341960407618274, -4.379528057220086978, 41.04275706135236135 ) ) ;
#94546 = CARTESIAN_POINT ( 'NONE',  ( 13.89961937509957401, 13.97604488694547697, 36.87609039468565442 ) ) ;
#94547 = CARTESIAN_POINT ( 'NONE',  ( 16.51473224551069308, 9.474510206698969483, 79.16557627198103830 ) ) ;
#94548 = CARTESIAN_POINT ( 'NONE',  ( 0.05219959533936267826, -19.03943276465977164, 55.00109039468566863 ) ) ;
#94549 = CARTESIAN_POINT ( 'NONE',  ( 19.05341960407617918, -5.049401038297876454, 61.04275706135232582 ) ) ;
#94551 = CARTESIAN_POINT ( 'NONE',  ( 4.379528057220092307, 16.55341960407617563, 87.29275706135236135 ) ) ;
#94550 = CARTESIAN_POINT ( 'NONE',  ( -16.51473224551082808, 9.474510206698731452, 103.3344237280190043 ) ) ;
#94552 = CARTESIAN_POINT ( 'NONE',  ( -13.89961937509977652, 13.97604488694528158, 25.62390960531434558 ) ) ;
#94553 =( BOUNDED_SURFACE ( )  B_SPLINE_SURFACE ( 3, 2, ( 
 ( #4017, #6009, #53518 ),
 ( #83839, #127360, #38359 ),
 ( #189073, #114176, #8009 ),
 ( #115196, #69692, #173896 ),
 ( #35365, #159691, #193048 ),
 ( #5009, #19212, #131359 ),
 ( #145521, #67689, #39356 ),
 ( #129347, #177887, #175879 ),
 ( #21189, #100014, #54525 ),
 ( #97017, #99009, #82845 ),
 ( #160700, #101015, #7001 ),
 ( #128354, #50545, #191042 ),
 ( #144524, #68683, #130338 ),
 ( #80862, #65695, #158698 ),
 ( #23197, #22191, #176888 ),
 ( #20187, #81833, #143520 ),
 ( #52515, #192036, #66691 ),
 ( #51527, #113190, #174879 ),
 ( #36345, #178888, #197048 ),
 ( #41364, #87846, #163713 ),
 ( #181872, #44347, #166706 ),
 ( #196063, #162700, #42365 ),
 ( #24205, #151533, #103030 ),
 ( #120182, #85854, #150542 ),
 ( #71693, #73706, #132368 ),
 ( #26207, #117195, #70700 ),
 ( #195050, #119205, #147543 ),
 ( #9031, #74687, #194061 ),
 ( #56529, #40356, #135378 ),
 ( #121172, #55522, #104028 ),
 ( #11029, #165707, #148542 ),
 ( #28209, #118207, #102031 ),
 ( #43351, #182866, #25216 ),
 ( #86858, #12042, #59497 ),
 ( #180890, #10033, #133360 ),
 ( #149534, #58516, #27204 ),
 ( #179898, #105022, #164712 ),
 ( #72704, #134377, #57536 ),
 ( #89850, #88850, #13022 ),
 ( #136353, #198029, #62476 ),
 ( #92815, #170670, #125160 ),
 ( #126147, #123155, #15997 ),
 ( #803, #183852, #107982 ),
 ( #17991, #29189, #45340 ) ),
 .UNSPECIFIED., .F., .F., .F. ) 
 B_SPLINE_SURFACE_WITH_KNOTS ( ( 4, 2, 2, 2, 2, 2, 2, 2, 2, 2, 2, 2, 2, 2, 2, 2, 2, 2, 2, 2, 2, 4 ),
 ( 3, 3 ),
 ( 0.1334715276261017047, 0.1400397817209072804, 0.1416818452446086951, 0.1433239087683100821, 0.1466080358157128560, 0.1498921628631156300, 0.1531762899105184039, 0.1564604169579211779, 0.1597445440053239796, 0.1630286710527267813, 0.1646707345764281682, 0.1663127981001295552, 0.1679548616238309422, 0.1695969251475323292, 0.1712389886712337161, 0.1720600204330844096, 0.1728810521949351031, 0.1745231157186364901, 0.1761651792423378771, 0.1794493062897406788, 0.1827334333371434805, 0.1860175603845462544 ),
 ( 0.000000000000000000, 1.000000000000000000 ),
 .UNSPECIFIED. ) 
 GEOMETRIC_REPRESENTATION_ITEM ( )  RATIONAL_B_SPLINE_SURFACE ( (
 ( 1.000000000000000000, 0.7745966692414831822, 1.000000000000000000),
 ( 1.000000000000000000, 0.7873173169477361011, 1.000000000000000000),
 ( 1.000000000000000000, 0.8012080269090376961, 1.000000000000000000),
 ( 1.000000000000000000, 0.8197272276933634805, 1.000000000000000000),
 ( 1.000000000000000000, 0.8234885421913328285, 1.000000000000000000),
 ( 1.000000000000000000, 0.8311157573375301810, 1.000000000000000000),
 ( 1.000000000000000000, 0.8349728938256689714, 1.000000000000000000),
 ( 1.000000000000000000, 0.8465302108191189445, 1.000000000000000000),
 ( 1.000000000000000000, 0.8542644918356308015, 1.000000000000000000),
 ( 1.000000000000000000, 0.8696747091108885108, 1.000000000000000000),
 ( 1.000000000000000000, 0.8773507960692286112, 1.000000000000000000),
 ( 1.000000000000000000, 0.8925002889088409219, 1.000000000000000000),
 ( 1.000000000000000000, 0.8999891582780782384, 1.000000000000000000),
 ( 1.000000000000000000, 0.9145203485641840713, 1.000000000000000000),
 ( 1.000000000000000000, 0.9215166741120195404, 1.000000000000000000),
 ( 1.000000000000000000, 0.9348196634156171747, 1.000000000000000000),
 ( 1.000000000000000000, 0.9411264847295628400, 1.000000000000000000),
 ( 1.000000000000000000, 0.9528821887673051272, 1.000000000000000000),
 ( 1.000000000000000000, 0.9583320463343940609, 1.000000000000000000),
 ( 1.000000000000000000, 0.9657141226242619281, 1.000000000000000000),
 ( 1.000000000000000000, 0.9680424144921330187, 1.000000000000000000),
 ( 1.000000000000000000, 0.9724014971077669101, 1.000000000000000000),
 ( 1.000000000000000000, 0.9744334801158447412, 1.000000000000000000),
 ( 1.000000000000000000, 0.9781204877085358795, 1.000000000000000000),
 ( 1.000000000000000000, 0.9797809101336111270, 1.000000000000000000),
 ( 1.000000000000000000, 0.9826818083352576449, 1.000000000000000000),
 ( 1.000000000000000000, 0.9839230189806436044, 1.000000000000000000),
 ( 1.000000000000000000, 0.9859013487405714482, 1.000000000000000000),
 ( 1.000000000000000000, 0.9866146582094302842, 1.000000000000000000),
 ( 1.000000000000000000, 0.9872250220265940124, 1.000000000000000000),
 ( 1.000000000000000000, 0.9873522598263919647, 1.000000000000000000),
 ( 1.000000000000000000, 0.9874472609175171112, 1.000000000000000000),
 ( 1.000000000000000000, 0.9874138636738953867, 1.000000000000000000),
 ( 1.000000000000000000, 0.9870735186573816877, 1.000000000000000000),
 ( 1.000000000000000000, 0.9865315217161264583, 1.000000000000000000),
 ( 1.000000000000000000, 0.9848873008857174094, 1.000000000000000000),
 ( 1.000000000000000000, 0.9837743821442677117, 1.000000000000000000),
 ( 1.000000000000000000, 0.9797976954002749483, 1.000000000000000000),
 ( 1.000000000000000000, 0.9763000371664851684, 1.000000000000000000),
 ( 1.000000000000000000, 0.9680363503266700143, 1.000000000000000000),
 ( 1.000000000000000000, 0.9632464763793491258, 1.000000000000000000),
 ( 1.000000000000000000, 0.9526889542241591124, 1.000000000000000000),
 ( 1.000000000000000000, 0.9469283804590782339, 1.000000000000000000),
 ( 1.000000000000000000, 0.9407878411039237720, 1.000000000000000000) ) ) 
 REPRESENTATION_ITEM ( '' )  SURFACE ( )  );
#94554 = CARTESIAN_POINT ( 'NONE',  ( -19.03943276465977164, 0.05219959533909376836, 101.2489096053143669 ) ) ;
#94555 = CARTESIAN_POINT ( 'NONE',  ( -21.52544592524334988, -5.823673210054445271, 43.95942372801902565 ) ) ;
#94556 = CIRCLE ( 'NONE', #181762, 2.500000000000000000 ) ;
#94557 = CARTESIAN_POINT ( 'NONE',  ( -5.049401038297874678, -19.05341960407617918, 94.79275706135230450 ) ) ;
#94559 = CARTESIAN_POINT ( 'NONE',  ( -9.564922557960796823, -16.46253265017161027, 47.08224293864769550 ) ) ;
#94558 = CARTESIAN_POINT ( 'NONE',  ( -3.573655867282028392E-15, 2.428612866367529932E-14, 150.0000000000000000 ) ) ;
#94560 = CARTESIAN_POINT ( 'NONE',  ( 16.51473224551069308, 9.474510206698969483, 99.16557627198102409 ) ) ;
#94562 = CARTESIAN_POINT ( 'NONE',  ( -19.02544592524342804, 5.153800228976336051, 46.04057627198101699 ) ) ;
#94561 = CARTESIAN_POINT ( 'NONE',  ( -4.483927247898539470, -16.52544592524342804, 57.29057627198103120 ) ) ;
#94563 = CARTESIAN_POINT ( 'NONE',  ( 0.05219959533909260263, 19.03943276465977164, 64.99890960531436690 ) ) ;
#94564 = CARTESIAN_POINT ( 'NONE',  ( -19.05341960407617563, 5.049401038297882671, 58.54275706135234003 ) ) ;
#94565 = CARTESIAN_POINT ( 'NONE',  ( -16.46253265017146816, -9.564922557961047289, 29.16775706135232937 ) ) ;
#94566 = CARTESIAN_POINT ( 'NONE',  ( -19.02544592524334988, -5.153800228976617603, 43.95942372801899012 ) ) ;
#94568 = EDGE_CURVE ( 'NONE', #60209, #158522, #32170, .T. ) ;
#94567 = CARTESIAN_POINT ( 'NONE',  ( 19.05341960407611168, 5.049401038298154454, 83.95724293864766707 ) ) ;
#94569 = CARTESIAN_POINT ( 'NONE',  ( 15.80617190586746368, 15.72974639402197994, 74.37390960531436690 ) ) ;
#94571 = CARTESIAN_POINT ( 'NONE',  ( -5.153800228976607833, 19.02544592524334988, 37.70942372801899722 ) ) ;
#94570 = CARTESIAN_POINT ( 'NONE',  ( 14.29746914071049879, -8.314922557960816363, 63.33224293864770260 ) ) ;
#94572 = CARTESIAN_POINT ( 'NONE',  ( -5.823673210054116645, -21.52544592524344225, 52.29057627198102409 ) ) ;
#94573 = CARTESIAN_POINT ( 'NONE',  ( 18.67979575497178502, 10.72451020669898547, 39.16557627198102409 ) ) ;
#94574 = CARTESIAN_POINT ( 'NONE',  ( 13.97604488694527802, 13.89961937509977652, 69.37390960531436690 ) ) ;
#94575 = CARTESIAN_POINT ( 'NONE',  ( 9.564922557960805705, 16.46253265017160317, 39.58224293864768839 ) ) ;
#94576 = CARTESIAN_POINT ( 'NONE',  ( -14.29746914071049879, 8.314922557960819915, 115.8322429386477097 ) ) ;
#94577 = CARTESIAN_POINT ( 'NONE',  ( 5.823673210054125526, 21.52544592524343514, 104.7905762719810241 ) ) ;
#94578 = CARTESIAN_POINT ( 'NONE',  ( 13.97604488694527802, 13.89961937509977652, 109.3739096053143669 ) ) ;
#94579 = CARTESIAN_POINT ( 'NONE',  ( -0.05219959533937732626, 21.53943276465977519, 27.50109039468567929 ) ) ;
#94580 = CARTESIAN_POINT ( 'NONE',  ( -13.89961937509977652, 13.97604488694528158, 30.62390960531435269 ) ) ;
#94581 = CARTESIAN_POINT ( 'NONE',  ( 0.05219959533907565091, 21.53943276465977519, 99.99890960531436690 ) ) ;
#94582 = CARTESIAN_POINT ( 'NONE',  ( 13.89961937509957401, 13.97604488694547697, 51.87609039468566863 ) ) ;
#94583 = CARTESIAN_POINT ( 'NONE',  ( -13.97604488694527625, -13.89961937509977652, 21.87390960531435979 ) ) ;
#94584 = CARTESIAN_POINT ( 'NONE',  ( 5.153800228976335163, 19.02544592524342804, 29.79057627198102409 ) ) ;
#94585 = CARTESIAN_POINT ( 'NONE',  ( 12.24802307403557933, -10.74802307403627921, -61.53034260416801260 ) ) ;
#94586 = CARTESIAN_POINT ( 'NONE',  ( -4.483927247898782831, 16.52544592524335698, 62.70942372801902565 ) ) ;
#94587 = CARTESIAN_POINT ( 'NONE',  ( 9.474510206698971260, -16.51473224551069308, 27.91557627198103120 ) ) ;
#94588 = CARTESIAN_POINT ( 'NONE',  ( 33.70754165857146489, -5.457863348371952306, 95.70317755519533875 ) ) ;
#94589 = CARTESIAN_POINT ( 'NONE',  ( 5.049401038298161559, -19.05341960407611168, 72.70724293864768129 ) ) ;
#94590 = CARTESIAN_POINT ( 'NONE',  ( -12.06949235617756955, 12.14591786802309770, 105.6239096053143669 ) ) ;
#94591 = CIRCLE ( 'NONE', #172095, 5.000000000000000888 ) ;
#94592 = CARTESIAN_POINT ( 'NONE',  ( -21.55341960407610458, -5.719274019375992779, 41.45724293864769550 ) ) ;
#94593 = CARTESIAN_POINT ( 'NONE',  ( 16.53943276465976808, -0.05219959533910856209, 78.74890960531436690 ) ) ;
#94594 = CARTESIAN_POINT ( 'NONE',  ( 16.55341960407618274, -4.379528057220086978, 36.04275706135234714 ) ) ;
#94595 = CARTESIAN_POINT ( 'NONE',  ( 21.53943276465977519, 0.05219959533937863772, 81.25109039468568994 ) ) ;
#94596 = CARTESIAN_POINT ( 'NONE',  ( 19.02544592524343514, -5.153800228976328945, 23.54057627198102054 ) ) ;
#94597 = CARTESIAN_POINT ( 'NONE',  ( 14.29746914071049879, -8.314922557960816363, 23.33224293864769194 ) ) ;
#94598 = CARTESIAN_POINT ( 'NONE',  ( -16.52544592524342804, 4.483927247898546575, 56.04057627198102409 ) ) ;
#94599 = CARTESIAN_POINT ( 'NONE',  ( 0.05219959533909260263, 19.03943276465977164, 49.99890960531435979 ) ) ;
#94600 = CARTESIAN_POINT ( 'NONE',  ( -21.55341960407619339, 5.719274019375674811, 98.54275706135234714 ) ) ;
#94601 = CARTESIAN_POINT ( 'NONE',  ( -21.55341960407610458, -5.719274019375992779, 111.4572429386476813 ) ) ;
#94602 = CARTESIAN_POINT ( 'NONE',  ( -0.05219959533937732626, 21.53943276465977519, 72.50109039468568994 ) ) ;
#94603 = CARTESIAN_POINT ( 'NONE',  ( 14.34966873604972726, -8.224510206698740333, 35.83442372801901143 ) ) ;
#94605 = CARTESIAN_POINT ( 'NONE',  ( 21.55341960407619695, -5.719274019375665929, 81.04275706135236135 ) ) ;
#94604 = CARTESIAN_POINT ( 'NONE',  ( -16.52544592524342804, 4.483927247898546575, 76.04057627198102409 ) ) ;
#94606 = CARTESIAN_POINT ( 'NONE',  ( -16.55341960407617563, 4.379528057220093196, 108.5427570613523756 ) ) ;
#94607 = CARTESIAN_POINT ( 'NONE',  ( -16.31925111598458145, 7.325300261831528381, 115.1642453896725584 ) ) ;
#94608 = CARTESIAN_POINT ( 'NONE',  ( -0.05219959533934338120, 16.53943276465976808, 37.50109039468568284 ) ) ;
#94609 = CARTESIAN_POINT ( 'NONE',  ( 4.379528057220339221, -16.55341960407611168, 42.70724293864770260 ) ) ;
#94610 = CARTESIAN_POINT ( 'NONE',  ( -4.379528057220086978, -16.55341960407618274, 84.79275706135234714 ) ) ;
#94611 = CARTESIAN_POINT ( 'NONE',  ( -5.049401038298153566, 19.05341960407611168, 105.2072429386476671 ) ) ;
#94612 = CARTESIAN_POINT ( 'NONE',  ( 5.049401038298161559, -19.05341960407611168, 97.70724293864766707 ) ) ;
#94613 = CARTESIAN_POINT ( 'NONE',  ( -21.55341960407619339, 5.719274019375674811, 98.54275706135234714 ) ) ;
#94614 = CARTESIAN_POINT ( 'NONE',  ( 16.55341960407618274, -4.379528057220086978, 101.0427570613523756 ) ) ;
#94615 = CARTESIAN_POINT ( 'NONE',  ( -8.314922557960811034, -14.29746914071050412, 77.08224293864769550 ) ) ;
#94616 = CARTESIAN_POINT ( 'NONE',  ( -16.51473224551069308, -9.474510206698971260, 86.66557627198102409 ) ) ;
#94617 = ORIENTED_EDGE ( 'NONE', *, *, #17982, .F. ) ;
#94618 = CARTESIAN_POINT ( 'NONE',  ( 14.29746914071037800, 8.314922557961029526, 21.66775706135235069 ) ) ;
#94619 = CARTESIAN_POINT ( 'NONE',  ( -0.05219959533909027116, -19.03943276465977164, 22.49890960531436690 ) ) ;
#94620 = CARTESIAN_POINT ( 'NONE',  ( 19.05341960407611168, 5.049401038298154454, 93.95724293864769550 ) ) ;
#94622 = CARTESIAN_POINT ( 'NONE',  ( -11.40812507854754720, -35.11059874428192273, -2.224999997268813701 ) ) ;
#94621 = CARTESIAN_POINT ( 'NONE',  ( 16.55341960407618274, -4.379528057220086978, 31.04275706135234714 ) ) ;
#94623 = CARTESIAN_POINT ( 'NONE',  ( 16.46253265017146816, 9.564922557961045513, 31.66775706135232937 ) ) ;
#94624 = CARTESIAN_POINT ( 'NONE',  ( -14.29746914071037622, -8.314922557961029526, 99.16775706135234714 ) ) ;
#94625 = CARTESIAN_POINT ( 'NONE',  ( 16.51473224551083163, -9.474510206698727899, 105.8344237280190043 ) ) ;
#94626 = CARTESIAN_POINT ( 'NONE',  ( 19.05341960407611168, 5.049401038298154454, 33.95724293864769550 ) ) ;
#94627 = CARTESIAN_POINT ( 'NONE',  ( -4.379528057220086978, -16.55341960407618274, 79.79275706135236135 ) ) ;
#94628 = CARTESIAN_POINT ( 'NONE',  ( -12.14591786802326823, 12.06949235617739902, 68.12609039468567573 ) ) ;
#94629 = CARTESIAN_POINT ( 'NONE',  ( -9.474510206698964154, 16.51473224551069663, 30.41557627198102054 ) ) ;
#94630 = CARTESIAN_POINT ( 'NONE',  ( 5.153800228976615827, -19.02544592524334988, 70.20942372801899012 ) ) ;
#94631 = CARTESIAN_POINT ( 'NONE',  ( -5.823673210054431948, 21.52544592524334988, 107.7094237280190328 ) ) ;
#94632 = CARTESIAN_POINT ( 'NONE',  ( 19.02544592524343514, -5.153800228976328945, 53.54057627198102409 ) ) ;
#94633 = CARTESIAN_POINT ( 'NONE',  ( 5.049401038298161559, -19.05341960407611168, 92.70724293864769550 ) ) ;
#94634 = CARTESIAN_POINT ( 'NONE',  ( -16.52544592524342804, 4.483927247898546575, 86.04057627198102409 ) ) ;
#94635 = CARTESIAN_POINT ( 'NONE',  ( -16.46253265017146816, -9.564922557961047289, 59.16775706135233293 ) ) ;
#94636 = CARTESIAN_POINT ( 'NONE',  ( 0.05219959533907565091, 21.53943276465977519, 49.99890960531437401 ) ) ;
#94637 = CARTESIAN_POINT ( 'NONE',  ( 16.51473224551083163, -9.474510206698727899, 20.83442372801899722 ) ) ;
#94638 = CARTESIAN_POINT ( 'NONE',  ( -13.97604488694527625, -13.89961937509977652, 96.87390960531433848 ) ) ;
#94639 = CARTESIAN_POINT ( 'NONE',  ( -0.05219959533936034679, 19.03943276465977164, 27.50109039468566507 ) ) ;
#94640 = CARTESIAN_POINT ( 'NONE',  ( 21.55341960407610458, 5.719274019375980345, 63.95724293864770260 ) ) ;
#94641 = CARTESIAN_POINT ( 'NONE',  ( -13.97604488694527625, -13.89961937509977652, 106.8739096053143669 ) ) ;
#94642 = CARTESIAN_POINT ( 'NONE',  ( -13.97604488694547697, 13.89961937509957934, 83.12609039468564731 ) ) ;
#94643 = CARTESIAN_POINT ( 'NONE',  ( -13.89961937509977652, 13.97604488694528158, 115.6239096053143669 ) ) ;
#94644 = ADVANCED_FACE ( 'NONE', ( #47695 ), #174022, .F. ) ;
#94645 = CARTESIAN_POINT ( 'NONE',  ( 5.153800228976615827, -19.02544592524334988, 105.2094237280190185 ) ) ;
#94646 = CARTESIAN_POINT ( 'NONE',  ( 4.379528057220339221, -16.55341960407611168, 112.7072429386476955 ) ) ;
#94647 = CARTESIAN_POINT ( 'NONE',  ( -16.46253265017160317, 9.564922557960807481, 95.83224293864769550 ) ) ;
#94648 = CARTESIAN_POINT ( 'NONE',  ( 15.80617190586746368, 15.72974639402197994, 79.37390960531436690 ) ) ;
#94649 = CARTESIAN_POINT ( 'NONE',  ( -14.34966873604972548, 8.224510206698743886, 48.33442372801902565 ) ) ;
#94650 = CARTESIAN_POINT ( 'NONE',  ( -21.52544592524334988, -5.823673210054445271, 48.95942372801902565 ) ) ;
#94651 = CARTESIAN_POINT ( 'NONE',  ( -21.53943276465977519, -0.05219959533937600094, 98.75109039468568994 ) ) ;
#94652 = CARTESIAN_POINT ( 'NONE',  ( 12.14591786802327356, -12.06949235617739191, 95.62609039468568994 ) ) ;
#94653 = CARTESIAN_POINT ( 'NONE',  ( 9.564922557960805705, 16.46253265017160317, 84.58224293864769550 ) ) ;
#94654 = CARTESIAN_POINT ( 'NONE',  ( 16.52544592524342804, -4.483927247898539470, 93.54057627198103830 ) ) ;
#94655 = CARTESIAN_POINT ( 'NONE',  ( -16.55341960407611168, -4.379528057220339221, 31.45724293864769550 ) ) ;
#94656 = CARTESIAN_POINT ( 'NONE',  ( -9.474510206698720793, -16.51473224551083518, 64.58442372801900433 ) ) ;
#94657 = CARTESIAN_POINT ( 'NONE',  ( -5.719274019375665041, -21.55341960407619695, 59.79275706135234714 ) ) ;
#94659 = EDGE_CURVE ( 'NONE', #17478, #151987, #35493, .T. ) ;
#94658 = CARTESIAN_POINT ( 'NONE',  ( 0.05219959533936267826, -19.03943276465977164, 20.00109039468567218 ) ) ;
#94660 = CARTESIAN_POINT ( 'NONE',  ( -12.06949235617756955, 12.14591786802309770, 90.62390960531436690 ) ) ;
#94661 = CARTESIAN_POINT ( 'NONE',  ( -21.55341960407610458, -5.719274019375992779, 31.45724293864769550 ) ) ;
#94662 = CARTESIAN_POINT ( 'NONE',  ( 0.05219959533934541429, -16.53943276465976808, 110.0010903946856757 ) ) ;
#94663 = CARTESIAN_POINT ( 'NONE',  ( 0.05219959533937995610, -21.53943276465977519, 80.00109039468568994 ) ) ;
#94664 = CARTESIAN_POINT ( 'NONE',  ( -14.34966873604972548, 8.224510206698743886, 53.33442372801901854 ) ) ;
#94665 = CARTESIAN_POINT ( 'NONE',  ( 12.14591786802327356, -12.06949235617739191, 110.6260903946857042 ) ) ;
#94666 = CARTESIAN_POINT ( 'NONE',  ( -21.52544592524334988, -5.823673210054445271, 48.95942372801902565 ) ) ;
#94667 = VERTEX_POINT ( 'NONE', #170031 ) ;
#94668 = CARTESIAN_POINT ( 'NONE',  ( 5.719274019375673035, 21.55341960407619339, 32.29275706135235424 ) ) ;
#94669 = CARTESIAN_POINT ( 'NONE',  ( 12.14591786802309770, 12.06949235617756955, 104.3739096053143669 ) ) ;
#94670 = CARTESIAN_POINT ( 'NONE',  ( -5.153800228976328057, -19.02544592524343514, 22.29057627198102765 ) ) ;
#94671 = CARTESIAN_POINT ( 'NONE',  ( -8.224510206698948167, 14.34966873604960824, 70.41557627198102409 ) ) ;
#94672 = CARTESIAN_POINT ( 'NONE',  ( 19.02544592524343514, -5.153800228976328945, 78.54057627198099567 ) ) ;
#94673 = CARTESIAN_POINT ( 'NONE',  ( -4.483927247898782831, 16.52544592524335698, 102.7094237280190185 ) ) ;
#94674 = CARTESIAN_POINT ( 'NONE',  ( -15.72974639402197994, 15.80617190586746368, 60.62390960531437401 ) ) ;
#94675 = CARTESIAN_POINT ( 'NONE',  ( -14.34966873604960291, -8.224510206698953496, 96.66557627198102409 ) ) ;
#94676 = CARTESIAN_POINT ( 'NONE',  ( 21.53943276465977519, -0.05219959533907433946, 93.74890960531436690 ) ) ;
#94677 = CARTESIAN_POINT ( 'NONE',  ( -19.02544592524342804, 5.153800228976336051, 96.04057627198103830 ) ) ;
#94679 = CARTESIAN_POINT ( 'NONE',  ( 0.05219959533936267826, -19.03943276465977164, 110.0010903946856757 ) ) ;
#94678 = CARTESIAN_POINT ( 'NONE',  ( 5.049401038298161559, -19.05341960407611168, 52.70724293864767418 ) ) ;
#94680 = CARTESIAN_POINT ( 'NONE',  ( -21.52544592524343514, 5.823673210054127303, 46.04057627198103830 ) ) ;
#94681 = CARTESIAN_POINT ( 'NONE',  ( -0.05219959533937732626, 21.53943276465977519, 62.50109039468568284 ) ) ;
#94682 = CARTESIAN_POINT ( 'NONE',  ( 13.89961937509977652, -13.97604488694527269, 48.12390960531435979 ) ) ;
#94683 = CARTESIAN_POINT ( 'NONE',  ( -19.05341960407611168, -5.049401038298163336, 81.45724293864769550 ) ) ;
#94684 = CARTESIAN_POINT ( 'NONE',  ( -8.224510206698735004, -14.34966873604973081, 64.58442372801900433 ) ) ;
#94685 = CARTESIAN_POINT ( 'NONE',  ( 21.55341960407619695, -5.719274019375665929, 41.04275706135236135 ) ) ;
#94686 = EDGE_CURVE ( 'NONE', #153996, #138940, #177522, .T. ) ;
#94687 = CARTESIAN_POINT ( 'NONE',  ( -21.52544592524334988, -5.823673210054445271, 88.95942372801901854 ) ) ;
#94688 = CARTESIAN_POINT ( 'NONE',  ( 5.823673210054125526, 21.52544592524343514, 99.79057627198103830 ) ) ;
#94690 = CARTESIAN_POINT ( 'NONE',  ( -14.29746914071037622, -8.314922557961029526, 59.16775706135234714 ) ) ;
#94689 = CARTESIAN_POINT ( 'NONE',  ( -15.80617190586768217, 15.72974639402176855, 43.12609039468568284 ) ) ;
#94691 = CARTESIAN_POINT ( 'NONE',  ( 18.67979575497178502, 10.72451020669898547, 79.16557627198103830 ) ) ;
#94692 = CARTESIAN_POINT ( 'NONE',  ( -0.05219959533936034679, 19.03943276465977164, 37.50109039468567573 ) ) ;
#94694 = CARTESIAN_POINT ( 'NONE',  ( -12.14591786802326823, 12.06949235617739902, 113.1260903946856899 ) ) ;
#94693 = CARTESIAN_POINT ( 'NONE',  ( -13.89961937509977652, 13.97604488694528158, 65.62390960531436690 ) ) ;
#94695 = CARTESIAN_POINT ( 'NONE',  ( 17.49999999999999645, -5.500000000000031086, 83.29690382534172954 ) ) ;
#94696 = CARTESIAN_POINT ( 'NONE',  ( 19.02544592524343514, -5.153800228976328945, 98.54057627198100988 ) ) ;
#94697 = CARTESIAN_POINT ( 'NONE',  ( 5.000000000000000000, -130.0000000000000000, 13.99999999999999822 ) ) ;
#94698 = CARTESIAN_POINT ( 'NONE',  ( 19.02544592524334988, 5.153800228976608722, 86.45942372801900433 ) ) ;
#94699 = CARTESIAN_POINT ( 'NONE',  ( -21.53943276465977519, 0.05219959533907696930, 56.24890960531436690 ) ) ;
#94700 = CARTESIAN_POINT ( 'NONE',  ( -8.224510206698948167, 14.34966873604960824, 35.41557627198102409 ) ) ;
#94701 = CARTESIAN_POINT ( 'NONE',  ( -14.29746914071037622, -8.314922557961029526, 19.16775706135234714 ) ) ;
#94702 = CARTESIAN_POINT ( 'NONE',  ( -13.97604488694527625, -13.89961937509977652, 31.87390960531435979 ) ) ;
#94703 = CARTESIAN_POINT ( 'NONE',  ( 16.46253265017146816, 9.564922557961045513, 111.6677570613523329 ) ) ;
#94705 = CARTESIAN_POINT ( 'NONE',  ( -0.05219959533936034679, 19.03943276465977164, 77.50109039468566152 ) ) ;
#94704 = CARTESIAN_POINT ( 'NONE',  ( -15.72974639402197994, 15.80617190586746368, 95.62390960531436690 ) ) ;
#94706 = CARTESIAN_POINT ( 'NONE',  ( -14.34966873604972548, 8.224510206698743886, 78.33442372801901854 ) ) ;
#94707 = CARTESIAN_POINT ( 'NONE',  ( -5.153800228976328057, -19.02544592524343514, 72.29057627198102409 ) ) ;
#94708 = CARTESIAN_POINT ( 'NONE',  ( -14.29746914071049879, 8.314922557960819915, 80.83224293864769550 ) ) ;
#94709 = CARTESIAN_POINT ( 'NONE',  ( 16.46253265017160672, -9.564922557960803928, 58.33224293864769550 ) ) ;
#94710 = CARTESIAN_POINT ( 'NONE',  ( 12.14591786802309770, 12.06949235617756955, 69.37390960531436690 ) ) ;
#94711 = FACE_OUTER_BOUND ( 'NONE', #142791, .T. ) ;
#94712 = CARTESIAN_POINT ( 'NONE',  ( -37.58407650405589351, 1.968340676919130544E-14, 39.49999999999996447 ) ) ;
#94713 = CARTESIAN_POINT ( 'NONE',  ( 16.53943276465976808, -0.05219959533910856209, 43.74890960531435979 ) ) ;
#94714 = CARTESIAN_POINT ( 'NONE',  ( -19.02544592524342804, 5.153800228976336051, 71.04057627198099567 ) ) ;
#94715 = FACE_BOUND ( 'NONE', #103238, .T. ) ;
#94716 = CARTESIAN_POINT ( 'NONE',  ( 13.97604488694548053, -13.89961937509957401, 40.62609039468564731 ) ) ;
#94717 = CARTESIAN_POINT ( 'NONE',  ( 16.52544592524335698, 4.483927247898782831, 41.45942372801901143 ) ) ;
#94718 = CARTESIAN_POINT ( 'NONE',  ( -15.72974639402197994, 15.80617190586746368, 65.62390960531436690 ) ) ;
#94719 = CARTESIAN_POINT ( 'NONE',  ( 5.049401038297881783, 19.05341960407617563, 22.29275706135233648 ) ) ;
#94720 = CARTESIAN_POINT ( 'NONE',  ( 0.05219959533909260263, 19.03943276465977164, 79.99890960531436690 ) ) ;
#94721 = CARTESIAN_POINT ( 'NONE',  ( -20.56300917109736304, -22.67728815268617737, -47.51549809214670006 ) ) ;
#94722 = CARTESIAN_POINT ( 'NONE',  ( 5.153800228976335163, 19.02544592524342804, 109.7905762719810099 ) ) ;
#94723 = CARTESIAN_POINT ( 'NONE',  ( -0.05219959533937732626, 21.53943276465977519, 32.50109039468568284 ) ) ;
#94724 = CARTESIAN_POINT ( 'NONE',  ( -12.14591786802309592, -12.06949235617757132, 101.8739096053143811 ) ) ;
#94727 = EDGE_LOOP ( 'NONE', ( #190854, #54285, #188000, #66105 ) ) ;
#94726 = CARTESIAN_POINT ( 'NONE',  ( -19.03943276465977164, 0.05219959533909376836, 86.24890960531436690 ) ) ;
#94725 = CARTESIAN_POINT ( 'NONE',  ( 18.67979575497178502, 10.72451020669898547, 104.1655762719810241 ) ) ;
#94728 = CARTESIAN_POINT ( 'NONE',  ( 15.72974639402176855, 15.80617190586768217, 26.87609039468567218 ) ) ;
#94729 = ORIENTED_EDGE ( 'NONE', *, *, #194696, .F. ) ;
#94730 = CARTESIAN_POINT ( 'NONE',  ( -19.05341960407611168, -5.049401038298163336, 81.45724293864769550 ) ) ;
#94731 = AXIS2_PLACEMENT_3D ( 'NONE', #7544, #147081, #126901 ) ;
#94732 = CARTESIAN_POINT ( 'NONE',  ( -18.22780087662123094, -5.499999999999984901, 76.48459894673894155 ) ) ;
#94733 = CARTESIAN_POINT ( 'NONE',  ( 0.05219959533907565091, 21.53943276465977519, 94.99890960531436690 ) ) ;
#94734 = CARTESIAN_POINT ( 'NONE',  ( 19.02544592524343514, -5.153800228976328945, 28.54057627198102409 ) ) ;
#94735 = CARTESIAN_POINT ( 'NONE',  ( 9.564922557961047289, -16.46253265017146816, 100.4177570613523329 ) ) ;
#94736 = CARTESIAN_POINT ( 'NONE',  ( -36.91746825000000598, 2.428612866367529932E-14, -11.12499999726881228 ) ) ;
#94737 = CARTESIAN_POINT ( 'NONE',  ( 19.03943276465977164, -0.05219959533909143690, 33.74890960531435979 ) ) ;
#94738 = CARTESIAN_POINT ( 'NONE',  ( -0.05219959533937732626, 21.53943276465977519, 87.50109039468568994 ) ) ;
#94740 = CARTESIAN_POINT ( 'NONE',  ( -15.72974639402176322, -15.80617190586768395, 44.37609039468567573 ) ) ;
#94739 = CARTESIAN_POINT ( 'NONE',  ( -19.05341960407611168, -5.049401038298163336, 76.45724293864769550 ) ) ;
#94741 = CARTESIAN_POINT ( 'NONE',  ( 5.823673210054444382, -21.52544592524334988, 20.20942372801900788 ) ) ;
#94742 = CARTESIAN_POINT ( 'NONE',  ( 28.82186960331498327, 2.781578969918950771E-14, 149.0000000000000000 ) ) ;
#94743 = CARTESIAN_POINT ( 'NONE',  ( 5.153800228976335163, 19.02544592524342804, 89.79057627198102409 ) ) ;
#94744 = CARTESIAN_POINT ( 'NONE',  ( -8.492802586333358050, 27.26921223548736961, 140.0000000000000000 ) ) ;
#94747 = CARTESIAN_POINT ( 'NONE',  ( 21.55341960407619695, -5.719274019375665929, 51.04275706135234714 ) ) ;
#94746 = CARTESIAN_POINT ( 'NONE',  ( -0.05219959533907301413, -21.53943276465977519, 42.49890960531435979 ) ) ;
#94745 = CARTESIAN_POINT ( 'NONE',  ( 12.06949235617739724, 12.14591786802326823, 41.87609039468568284 ) ) ;
#94748 = CARTESIAN_POINT ( 'NONE',  ( -21.53943276465977519, -0.05219959533937600094, 78.75109039468568994 ) ) ;
#94749 = CARTESIAN_POINT ( 'NONE',  ( -35.00000000000000000, -3.181980515339470905, 8.889087296526001936 ) ) ;
#94750 = CARTESIAN_POINT ( 'NONE',  ( 14.34966873604972726, -8.224510206698740333, 20.83442372801901143 ) ) ;
#94751 = CARTESIAN_POINT ( 'NONE',  ( -9.474510206698964154, 16.51473224551069663, 60.41557627198102409 ) ) ;
#94752 = CARTESIAN_POINT ( 'NONE',  ( 13.97604488694527802, 13.89961937509977652, 79.37390960531435269 ) ) ;
#94753 = CARTESIAN_POINT ( 'NONE',  ( 16.55341960407611168, 4.379528057220329451, 108.9572429386476955 ) ) ;
#94754 = CARTESIAN_POINT ( 'NONE',  ( 12.14591786802309770, 12.06949235617756955, 109.3739096053143811 ) ) ;
#94755 = CARTESIAN_POINT ( 'NONE',  ( 13.97604488694527802, 13.89961937509977652, 109.3739096053143669 ) ) ;
#94756 = CARTESIAN_POINT ( 'NONE',  ( -16.53943276465976808, -0.05219959533934237506, 78.75109039468568994 ) ) ;
#94758 = CARTESIAN_POINT ( 'NONE',  ( 19.02544592524343514, -5.153800228976328945, 48.54057627198103120 ) ) ;
#94757 = CARTESIAN_POINT ( 'NONE',  ( 12.06949235617757843, -12.14591786802309237, 68.12390960531436690 ) ) ;
#94759 = CARTESIAN_POINT ( 'NONE',  ( -10.81492255796105439, 18.62759615963255655, 82.91775706135234714 ) ) ;
#94760 = CARTESIAN_POINT ( 'NONE',  ( -10.72451020669870658, -18.67979575497194134, 69.58442372801900433 ) ) ;
#94761 = CARTESIAN_POINT ( 'NONE',  ( -5.153800228976607833, 19.02544592524334988, 107.7094237280189759 ) ) ;
#94762 = CARTESIAN_POINT ( 'NONE',  ( 12.14591786802309770, 12.06949235617756955, 64.37390960531435269 ) ) ;
#94763 = CARTESIAN_POINT ( 'NONE',  ( 15.80617190586746368, 15.72974639402197994, 109.3739096053143811 ) ) ;
#94764 = CARTESIAN_POINT ( 'NONE',  ( -15.80617190586745835, -15.72974639402198527, 56.87390960531436690 ) ) ;
#94765 = CARTESIAN_POINT ( 'NONE',  ( -17.48847506799970120, -5.747544572773739979, 104.1730256215672341 ) ) ;
#94766 = CARTESIAN_POINT ( 'NONE',  ( 28.82186960331499392, -9.364793116373510529, 143.1500000054623740 ) ) ;
#94767 = CARTESIAN_POINT ( 'NONE',  ( -19.02544592524342804, 5.153800228976336051, 66.04057627198103830 ) ) ;
#94768 = CARTESIAN_POINT ( 'NONE',  ( 12.06949235617757843, -12.14591786802309237, 33.12390960531435979 ) ) ;
#94769 = CARTESIAN_POINT ( 'NONE',  ( 0.05219959533910956823, 16.53943276465976808, 24.99890960531435624 ) ) ;
#94770 = CARTESIAN_POINT ( 'NONE',  ( 16.52544592524335698, 4.483927247898782831, 101.4594237280190185 ) ) ;
#94772 = EDGE_CURVE ( 'NONE', #30159, #141361, #2998, .T. ) ;
#94771 = CARTESIAN_POINT ( 'NONE',  ( -19.02544592524334988, -5.153800228976617603, 58.95942372801900433 ) ) ;
#94773 = CARTESIAN_POINT ( 'NONE',  ( 17.49999999999999289, 5.500000000000006217, 48.78230962303565121 ) ) ;
#94774 = CARTESIAN_POINT ( 'NONE',  ( -19.05341960407611168, -5.049401038298163336, 101.4572429386476955 ) ) ;
#94775 = CARTESIAN_POINT ( 'NONE',  ( 12.06949235617757843, -12.14591786802309237, 63.12390960531435979 ) ) ;
#94777 = CARTESIAN_POINT ( 'NONE',  ( -9.564922557960796823, -16.46253265017161027, 112.0822429386476955 ) ) ;
#94776 = CARTESIAN_POINT ( 'NONE',  ( -5.153800228976328057, -19.02544592524343514, 22.29057627198102765 ) ) ;
#94779 = VERTEX_POINT ( 'NONE', #125519 ) ;
#94778 = CARTESIAN_POINT ( 'NONE',  ( -5.719274019375978568, 21.55341960407610458, 55.20724293864770260 ) ) ;
#94780 = CARTESIAN_POINT ( 'NONE',  ( -12.14591786802309592, -12.06949235617757132, 96.87390960531436690 ) ) ;
#94781 = CARTESIAN_POINT ( 'NONE',  ( 14.34966873604972726, -8.224510206698740333, 45.83442372801901854 ) ) ;
#94782 = CARTESIAN_POINT ( 'NONE',  ( -12.14591786802309592, -12.06949235617757132, 86.87390960531438111 ) ) ;
#94783 = CARTESIAN_POINT ( 'NONE',  ( -193.3062444957834884, -155.7167183371838064, -15.00000000000000178 ) ) ;
#94784 = CARTESIAN_POINT ( 'NONE',  ( 16.46253265017146816, 9.564922557961045513, 81.66775706135233293 ) ) ;
#94785 = CARTESIAN_POINT ( 'NONE',  ( 16.46253265017160672, -9.564922557960803928, 113.3322429386476955 ) ) ;
#94786 = CARTESIAN_POINT ( 'NONE',  ( -5.950531402560715689E-15, 38.81732327939063509, -7.624999997268814056 ) ) ;
#94787 = CARTESIAN_POINT ( 'NONE',  ( -18.22780087662121673, -5.500000000000062172, 41.48459894673893444 ) ) ;
#94788 = ORIENTED_EDGE ( 'NONE', *, *, #140094, .T. ) ;
#94790 = CARTESIAN_POINT ( 'NONE',  ( -0.05219959533910754901, -16.53943276465976808, 32.49890960531435979 ) ) ;
#94789 = CARTESIAN_POINT ( 'NONE',  ( 12.14591786802327356, -12.06949235617739191, 40.62609039468567573 ) ) ;
#94791 = CARTESIAN_POINT ( 'NONE',  ( -18.67979575497178146, -10.72451020669898902, 56.66557627198103830 ) ) ;
#94793 = CARTESIAN_POINT ( 'NONE',  ( 5.153800228976615827, -19.02544592524334988, 85.20942372801900433 ) ) ;
#94792 = VECTOR ( 'NONE', #37040, 1000.000000000000114 ) ;
#94794 = CARTESIAN_POINT ( 'NONE',  ( 0.05219959533907565091, 21.53943276465977519, 44.99890960531435979 ) ) ;
#94795 = CARTESIAN_POINT ( 'NONE',  ( 10.72451020669871369, 18.67979575497193778, 87.08442372801901854 ) ) ;
#94796 = CARTESIAN_POINT ( 'NONE',  ( 5.000000000000000000, -120.9970989573719038, 14.58956564881029294 ) ) ;
#94797 = CARTESIAN_POINT ( 'NONE',  ( 16.52544592524335698, 4.483927247898782831, 41.45942372801901143 ) ) ;
#94799 = CARTESIAN_POINT ( 'NONE',  ( -13.89961937509977652, 13.97604488694528158, 100.6239096053143669 ) ) ;
#94798 = CARTESIAN_POINT ( 'NONE',  ( 9.564922557960805705, 16.46253265017160317, 39.58224293864768839 ) ) ;
#94800 = CARTESIAN_POINT ( 'NONE',  ( -19.03943276465977164, 0.05219959533909376836, 31.24890960531435979 ) ) ;
#94801 = CARTESIAN_POINT ( 'NONE',  ( 0.05219959533910956823, 16.53943276465976808, 94.99890960531436690 ) ) ;
#94802 = DIRECTION ( 'NONE',  ( 1.000000000000000000, 0.000000000000000000, 0.000000000000000000 ) ) ;
#94803 = CARTESIAN_POINT ( 'NONE',  ( -19.05341960407611168, -5.049401038298163336, 106.4572429386476955 ) ) ;
#94804 = ORIENTED_EDGE ( 'NONE', *, *, #89811, .F. ) ;
#94805 = CARTESIAN_POINT ( 'NONE',  ( 14.29746914071037800, 8.314922557961029526, 56.66775706135235424 ) ) ;
#94806 = CARTESIAN_POINT ( 'NONE',  ( -0.05219959533907301413, -21.53943276465977519, 92.49890960531436690 ) ) ;
#94807 = CARTESIAN_POINT ( 'NONE',  ( 19.03943276465977164, -0.05219959533909143690, 43.74890960531435979 ) ) ;
#94808 = CARTESIAN_POINT ( 'NONE',  ( 21.53943276465977519, 0.05219959533937863772, 21.25109039468567218 ) ) ;
#94809 = CARTESIAN_POINT ( 'NONE',  ( 13.89961937509977652, -13.97604488694527269, 88.12390960531438111 ) ) ;
#94811 = EDGE_CURVE ( 'NONE', #20950, #129974, #62835, .T. ) ;
#94810 = CARTESIAN_POINT ( 'NONE',  ( 8.898068258721464119, 27.38543819252877398, 145.3843446568999980 ) ) ;
#94812 = ORIENTED_EDGE ( 'NONE', *, *, #15250, .F. ) ;
#94813 = CARTESIAN_POINT ( 'NONE',  ( 16.55341960407618274, -4.379528057220086978, 51.04275706135234714 ) ) ;
#94814 = CARTESIAN_POINT ( 'NONE',  ( -15.80617190586745835, -15.72974639402198527, 111.8739096053143669 ) ) ;
#94817 = CARTESIAN_POINT ( 'NONE',  ( 19.02544592524334988, 5.153800228976608722, 81.45942372801897591 ) ) ;
#94816 = CARTESIAN_POINT ( 'NONE',  ( -13.97604488694527625, -13.89961937509977652, 96.87390960531433848 ) ) ;
#94815 = CARTESIAN_POINT ( 'NONE',  ( 8.224510206698953496, -14.34966873604960469, 107.9155762719810241 ) ) ;
#94818 = CARTESIAN_POINT ( 'NONE',  ( -5.153800228976607833, 19.02544592524334988, 22.70942372801899012 ) ) ;
#94819 = CARTESIAN_POINT ( 'NONE',  ( 0.05219959533907565091, 21.53943276465977519, 89.99890960531438111 ) ) ;
#94820 = CARTESIAN_POINT ( 'NONE',  ( 16.51473224551083163, -9.474510206698727899, 30.83442372801900433 ) ) ;
#94821 = CARTESIAN_POINT ( 'NONE',  ( -14.29746914071037622, -8.314922557961029526, 79.16775706135234714 ) ) ;
#94823 = ORIENTED_EDGE ( 'NONE', *, *, #140691, .T. ) ;
#94822 = CARTESIAN_POINT ( 'NONE',  ( 19.02544592524343514, -5.153800228976328945, 103.5405762719809957 ) ) ;
#94824 = CARTESIAN_POINT ( 'NONE',  ( -19.05341960407611168, -5.049401038298163336, 56.45724293864768129 ) ) ;
#94825 = CARTESIAN_POINT ( 'NONE',  ( -5.823673210054431948, 21.52544592524334988, 72.70942372801901854 ) ) ;
#94826 = CARTESIAN_POINT ( 'NONE',  ( -21.52544592524334988, -5.823673210054445271, 63.95942372801901854 ) ) ;
#94827 = CARTESIAN_POINT ( 'NONE',  ( 9.564922557960805705, 16.46253265017160317, 74.58224293864769550 ) ) ;
#94828 = CARTESIAN_POINT ( 'NONE',  ( -21.52544592524334988, -5.823673210054445271, 43.95942372801902565 ) ) ;
#94829 = CARTESIAN_POINT ( 'NONE',  ( -16.51473224551082808, 9.474510206698731452, 93.33442372801900433 ) ) ;
#94830 = CARTESIAN_POINT ( 'NONE',  ( -5.049401038298153566, 19.05341960407611168, 50.20724293864770260 ) ) ;
#94831 = CARTESIAN_POINT ( 'NONE',  ( -19.02544592524342804, 5.153800228976336051, 96.04057627198103830 ) ) ;
#94832 = CARTESIAN_POINT ( 'NONE',  ( -9.474510206698964154, 16.51473224551069663, 65.41557627198102409 ) ) ;
#94833 = CARTESIAN_POINT ( 'NONE',  ( 17.50000000000000000, -5.500000000000000888, 113.2969038253417153 ) ) ;
#94834 = CARTESIAN_POINT ( 'NONE',  ( -19.02544592524342804, 5.153800228976336051, 51.04057627198103120 ) ) ;
#94835 = CARTESIAN_POINT ( 'NONE',  ( -21.52544592524343514, 5.823673210054127303, 96.04057627198102409 ) ) ;
#94836 = CARTESIAN_POINT ( 'NONE',  ( -16.52544592524335698, -4.483927247898792601, 73.95942372801901854 ) ) ;
#94837 = CARTESIAN_POINT ( 'NONE',  ( -23.75112013235324682, 10.51683317207909063, 166.0021274478078226 ) ) ;
#94838 = CARTESIAN_POINT ( 'NONE',  ( 5.153800228976615827, -19.02544592524334988, 30.20942372801900433 ) ) ;
#94839 = CARTESIAN_POINT ( 'NONE',  ( 16.51473224551069308, 9.474510206698969483, 69.16557627198102409 ) ) ;
#94840 = CARTESIAN_POINT ( 'NONE',  ( 16.52544592524342804, -4.483927247898539470, 58.54057627198103120 ) ) ;
#94841 = CARTESIAN_POINT ( 'NONE',  ( -4.379528057220328563, 16.55341960407611168, 95.20724293864769550 ) ) ;
#94842 = CARTESIAN_POINT ( 'NONE',  ( 13.89961937509977652, -13.97604488694527269, 103.1239096053143527 ) ) ;
#94843 = CARTESIAN_POINT ( 'NONE',  ( -5.049401038298153566, 19.05341960407611168, 95.20724293864770971 ) ) ;
#94844 = CARTESIAN_POINT ( 'NONE',  ( 10.81492255796106328, -18.62759615963255655, 45.41775706135234003 ) ) ;
#94845 = CARTESIAN_POINT ( 'NONE',  ( -16.51473224551069308, -9.474510206698971260, 111.6655762719810383 ) ) ;
#94846 = CARTESIAN_POINT ( 'NONE',  ( -21.53943276465977519, -0.05219959533937600094, 113.7510903946856757 ) ) ;
#94847 = CARTESIAN_POINT ( 'NONE',  ( 14.29746914071037800, 8.314922557961029526, 76.66775706135234714 ) ) ;
#94848 = CARTESIAN_POINT ( 'NONE',  ( 10.81492255796106328, -18.62759615963255655, 35.41775706135234003 ) ) ;
#94849 = CARTESIAN_POINT ( 'NONE',  ( -18.62759615963270932, 10.81492255796079327, 25.83224293864769194 ) ) ;
#94850 = CARTESIAN_POINT ( 'NONE',  ( -21.52544592524343514, 5.823673210054127303, 106.0405762719810525 ) ) ;
#94851 = CARTESIAN_POINT ( 'NONE',  ( -12.14591786802309592, -12.06949235617757132, 56.87390960531436690 ) ) ;
#94852 = CARTESIAN_POINT ( 'NONE',  ( -13.89961937509977652, 13.97604488694528158, 50.62390960531435979 ) ) ;
#94853 = CARTESIAN_POINT ( 'NONE',  ( 12.06949235617757843, -12.14591786802309237, 78.12390960531436690 ) ) ;
#94854 = CARTESIAN_POINT ( 'NONE',  ( 21.52544592524344225, -5.823673210054117533, 48.54057627198103120 ) ) ;
#94855 = CARTESIAN_POINT ( 'NONE',  ( -19.05341960407617563, 5.049401038297882671, 48.54275706135233293 ) ) ;
#94856 = CARTESIAN_POINT ( 'NONE',  ( 19.05341960407611168, 5.049401038298154454, 23.95724293864769194 ) ) ;
#94857 = ORIENTED_EDGE ( 'NONE', *, *, #191573, .T. ) ;
#94858 = CARTESIAN_POINT ( 'NONE',  ( -16.52544592524335698, -4.483927247898792601, 68.95942372801901854 ) ) ;
#94859 = CARTESIAN_POINT ( 'NONE',  ( -5.049401038298153566, 19.05341960407611168, 65.20724293864765286 ) ) ;
#94860 = CARTESIAN_POINT ( 'NONE',  ( -17.14385361876520264, -23.59649016807271238, 143.1750000027311671 ) ) ;
#94861 = CARTESIAN_POINT ( 'NONE',  ( 12.14591786802309770, 12.06949235617756955, 84.37390960531438111 ) ) ;
#94862 = CARTESIAN_POINT ( 'NONE',  ( 10.72451020669898902, -18.67979575497178502, 32.91557627198102409 ) ) ;
#94863 = ORIENTED_EDGE ( 'NONE', *, *, #162675, .F. ) ;
#94864 = CARTESIAN_POINT ( 'NONE',  ( 14.34966873604972726, -8.224510206698740333, 110.8344237280190043 ) ) ;
#94865 = CARTESIAN_POINT ( 'NONE',  ( -9.474510206698720793, -16.51473224551083518, 104.5844237280190043 ) ) ;
#94866 = CARTESIAN_POINT ( 'NONE',  ( 15.72974639402176855, 15.80617190586768217, 96.87609039468568994 ) ) ;
#94867 = CARTESIAN_POINT ( 'NONE',  ( 5.049401038298161559, -19.05341960407611168, 82.70724293864770971 ) ) ;
#94868 = CARTESIAN_POINT ( 'NONE',  ( -0.05219959533907301413, -21.53943276465977519, 102.4989096053143811 ) ) ;
#94869 = CARTESIAN_POINT ( 'NONE',  ( -4.483927247898782831, 16.52544592524335698, 57.70942372801901143 ) ) ;
#94870 = CARTESIAN_POINT ( 'NONE',  ( 19.03943276465977164, -0.05219959533909143690, 33.74890960531435979 ) ) ;
#94871 = CARTESIAN_POINT ( 'NONE',  ( -12.14591786802326823, 12.06949235617739902, 28.12609039468568284 ) ) ;
#94872 = CARTESIAN_POINT ( 'NONE',  ( -19.03943276465977164, -0.05219959533935918106, 88.75109039468567573 ) ) ;
#94873 = AXIS2_PLACEMENT_3D ( 'NONE', #177588, #39055, #100713 ) ;
#94874 = CARTESIAN_POINT ( 'NONE',  ( 0.05219959533907565091, 21.53943276465977519, 89.99890960531438111 ) ) ;
#94875 = CARTESIAN_POINT ( 'NONE',  ( -16.51473224551082808, 9.474510206698731452, 73.33442372801900433 ) ) ;
#94876 = CARTESIAN_POINT ( 'NONE',  ( 19.02130022317637525, -5.499999999999793943, 88.28188669246574705 ) ) ;
#94877 = CARTESIAN_POINT ( 'NONE',  ( -10.81492255796078084, -18.62759615963271287, 102.0822429386476955 ) ) ;
#94878 = CARTESIAN_POINT ( 'NONE',  ( 1.820000000000000062, 0.000000000000000000, 0.000000000000000000 ) ) ;
#94879 = CARTESIAN_POINT ( 'NONE',  ( 5.153800228976335163, 19.02544592524342804, 79.79057627198102409 ) ) ;
#94880 = CARTESIAN_POINT ( 'NONE',  ( -8.314922557961024197, 14.29746914071037800, 37.91775706135235424 ) ) ;
#94881 = DIRECTION ( 'NONE',  ( 0.000000000000000000, 0.000000000000000000, -1.000000000000000000 ) ) ;
#94882 = CARTESIAN_POINT ( 'NONE',  ( 13.89961937509957401, 13.97604488694547697, 56.87609039468564731 ) ) ;
#94884 = CARTESIAN_POINT ( 'NONE',  ( 16.52544592524342804, -4.483927247898539470, 58.54057627198103120 ) ) ;
#94883 = CARTESIAN_POINT ( 'NONE',  ( -21.52544592524334988, -5.823673210054445271, 18.95942372801901143 ) ) ;
#94885 = CARTESIAN_POINT ( 'NONE',  ( -16.46253265017160317, 9.564922557960807481, 80.83224293864769550 ) ) ;
#94887 = CARTESIAN_POINT ( 'NONE',  ( 16.51473224551083163, -9.474510206698727899, 40.83442372801900433 ) ) ;
#94886 = CARTESIAN_POINT ( 'NONE',  ( 4.379528057220092307, 16.55341960407617563, 32.29275706135235424 ) ) ;
#94888 = CARTESIAN_POINT ( 'NONE',  ( -0.05219959533937732626, 21.53943276465977519, 47.50109039468568994 ) ) ;
#94889 = CARTESIAN_POINT ( 'NONE',  ( -12.06949235617739369, -12.14591786802326823, 19.37609039468568639 ) ) ;
#94890 = CARTESIAN_POINT ( 'NONE',  ( -9.474510206698964154, 16.51473224551069663, 55.41557627198103120 ) ) ;
#94891 = CARTESIAN_POINT ( 'NONE',  ( 19.05341960407617918, -5.049401038297876454, 81.04275706135231871 ) ) ;
#94892 = CARTESIAN_POINT ( 'NONE',  ( -18.62759615963255300, -10.81492255796106328, 94.16775706135237556 ) ) ;
#94893 = CARTESIAN_POINT ( 'NONE',  ( -19.05341960407617563, 5.049401038297882671, 68.54275706135230450 ) ) ;
#94894 = CARTESIAN_POINT ( 'NONE',  ( -5.153800228976328057, -19.02544592524343514, 37.29057627198102409 ) ) ;
#94895 = CARTESIAN_POINT ( 'NONE',  ( -10.72451020669898014, 18.67979575497178502, 70.41557627198102409 ) ) ;
#94897 = CARTESIAN_POINT ( 'NONE',  ( -9.564922557961040184, 16.46253265017147172, 67.91775706135233293 ) ) ;
#94896 = CARTESIAN_POINT ( 'NONE',  ( -14.34966873604960291, -8.224510206698953496, 61.66557627198103120 ) ) ;
#94898 = CYLINDRICAL_SURFACE ( 'NONE', #111837, 12.50000000000000000 ) ;
#94899 = CARTESIAN_POINT ( 'NONE',  ( -19.02544592524334988, -5.153800228976617603, 48.95942372801900433 ) ) ;
#94900 = CARTESIAN_POINT ( 'NONE',  ( -8.314922557961024197, 14.29746914071037800, 92.91775706135236135 ) ) ;
#94901 = CARTESIAN_POINT ( 'NONE',  ( 8.224510206698953496, -14.34966873604960469, 57.91557627198103120 ) ) ;
#94903 = CARTESIAN_POINT ( 'NONE',  ( -27.73933785331498925, 9.013057229001089965, 149.2750000027311330 ) ) ;
#94902 = CARTESIAN_POINT ( 'NONE',  ( -21.52544592524334988, -5.823673210054445271, 83.95942372801900433 ) ) ;
#94904 = CARTESIAN_POINT ( 'NONE',  ( 5.823673210054125526, 21.52544592524343514, 94.79057627198105251 ) ) ;
#94905 = CARTESIAN_POINT ( 'NONE',  ( -5.049401038298153566, 19.05341960407611168, 50.20724293864770260 ) ) ;
#94906 = CARTESIAN_POINT ( 'NONE',  ( 21.55341960407619695, -5.719274019375665929, 66.04275706135236135 ) ) ;
#94907 = CARTESIAN_POINT ( 'NONE',  ( -0.05219959533909027116, -19.03943276465977164, 47.49890960531435979 ) ) ;
#94908 = CARTESIAN_POINT ( 'NONE',  ( 13.97604488694527802, 13.89961937509977652, 59.37390960531434558 ) ) ;
#94909 = CARTESIAN_POINT ( 'NONE',  ( -14.34966873604960291, -8.224510206698953496, 101.6655762719810383 ) ) ;
#94910 = CARTESIAN_POINT ( 'NONE',  ( -18.67979575497178146, -10.72451020669898902, 21.66557627198102409 ) ) ;
#94911 = CARTESIAN_POINT ( 'NONE',  ( 16.55341960407611168, 4.379528057220329451, 53.95724293864770260 ) ) ;
#94912 = CARTESIAN_POINT ( 'NONE',  ( -19.05341960407611168, -5.049401038298163336, 36.45724293864766707 ) ) ;
#94913 = CARTESIAN_POINT ( 'NONE',  ( 16.53943276465976808, -0.05219959533910856209, 78.74890960531436690 ) ) ;
#94914 = CARTESIAN_POINT ( 'NONE',  ( 0.05219959533907565091, 21.53943276465977519, 99.99890960531436690 ) ) ;
#94915 = CARTESIAN_POINT ( 'NONE',  ( -10.72451020669870658, -18.67979575497194134, 29.58442372801901854 ) ) ;
#94916 = CARTESIAN_POINT ( 'NONE',  ( 9.474510206698971260, -16.51473224551069308, 22.91557627198102765 ) ) ;
#94917 = CARTESIAN_POINT ( 'NONE',  ( -12.06949235617739369, -12.14591786802326823, 44.37609039468567573 ) ) ;
#94918 = CARTESIAN_POINT ( 'NONE',  ( 15.80617190586746368, 15.72974639402197994, 79.37390960531436690 ) ) ;
#94920 = CARTESIAN_POINT ( 'NONE',  ( 5.719274019375673035, 21.55341960407619339, 107.2927570613523471 ) ) ;
#94919 = PRODUCT_DEFINITION_CONTEXT ( 'detailed design', #88162, 'design' ) ;
#94921 = CARTESIAN_POINT ( 'NONE',  ( -0.05219959533909027116, -19.03943276465977164, 112.4989096053143669 ) ) ;
#94922 = CARTESIAN_POINT ( 'NONE',  ( 18.62759615963255655, 10.81492255796105972, 41.66775706135235424 ) ) ;
#94923 = CARTESIAN_POINT ( 'NONE',  ( -15.72974639402197994, 15.80617190586746368, 45.62390960531436690 ) ) ;
#94924 = CARTESIAN_POINT ( 'NONE',  ( 4.379528057220092307, 16.55341960407617563, 107.2927570613523471 ) ) ;
#94926 = CARTESIAN_POINT ( 'NONE',  ( 5.823673210054444382, -21.52544592524334988, 85.20942372801901854 ) ) ;
#94925 = CARTESIAN_POINT ( 'NONE',  ( -5.823673210054431948, 21.52544592524334988, 57.70942372801901143 ) ) ;
#94927 = CARTESIAN_POINT ( 'NONE',  ( 19.02544592524334988, 5.153800228976608722, 31.45942372801900433 ) ) ;
#94928 = CARTESIAN_POINT ( 'NONE',  ( -16.52544592524335698, -4.483927247898792601, 93.95942372801903275 ) ) ;
#94929 = CARTESIAN_POINT ( 'NONE',  ( -21.52544592524334988, -5.823673210054445271, 38.95942372801901854 ) ) ;
#94930 = CARTESIAN_POINT ( 'NONE',  ( -9.474510206698964154, 16.51473224551069663, 45.41557627198103120 ) ) ;
#94931 = CARTESIAN_POINT ( 'NONE',  ( -0.05219959533936034679, 19.03943276465977164, 22.50109039468566152 ) ) ;
#94932 = CARTESIAN_POINT ( 'NONE',  ( 15.72974639402199770, -15.80617190586745480, 28.12390960531435979 ) ) ;
#94933 = CARTESIAN_POINT ( 'NONE',  ( 21.53943276465977519, 0.05219959533937863772, 21.25109039468567218 ) ) ;
#94934 = CARTESIAN_POINT ( 'NONE',  ( -0.05219959533907301413, -21.53943276465977519, 77.49890960531433848 ) ) ;
#94936 = CARTESIAN_POINT ( 'NONE',  ( -10.72451020669898014, 18.67979575497178502, 60.41557627198102409 ) ) ;
#94935 = CARTESIAN_POINT ( 'NONE',  ( -17.49999999999998579, 5.500000000000032863, 60.79690382534172244 ) ) ;
#94938 = CARTESIAN_POINT ( 'NONE',  ( 12.14591786802309770, 12.06949235617756955, 64.37390960531435269 ) ) ;
#94937 = CARTESIAN_POINT ( 'NONE',  ( -12.14591786802326823, 12.06949235617739902, 63.12609039468568994 ) ) ;
#94939 = CARTESIAN_POINT ( 'NONE',  ( 9.687362902255733488, -9.687362902255692632, -62.58071313852362039 ) ) ;
#94940 = CARTESIAN_POINT ( 'NONE',  ( 19.05341960407617918, -5.049401038297876454, 91.04275706135234714 ) ) ;
#94941 = AXIS2_PLACEMENT_3D ( 'NONE', #129681, #125731, #188408 ) ;
#94942 = CARTESIAN_POINT ( 'NONE',  ( -21.30000000000002913, 2.244099063931684814E-13, -56.46919128290398504 ) ) ;
#94943 = CARTESIAN_POINT ( 'NONE',  ( -12.14591786802326823, 12.06949235617739902, 33.12609039468569705 ) ) ;
#94944 = CARTESIAN_POINT ( 'NONE',  ( -5.719274019375978568, 21.55341960407610458, 95.20724293864769550 ) ) ;
#94945 = CARTESIAN_POINT ( 'NONE',  ( 21.53943276465977519, -0.05219959533907433946, 78.74890960531436690 ) ) ;
#94946 = CARTESIAN_POINT ( 'NONE',  ( 21.55341960407610458, 5.719274019375980345, 23.95724293864769550 ) ) ;
#94947 = CARTESIAN_POINT ( 'NONE',  ( -12.14591786802326823, 12.06949235617739902, 53.12609039468568284 ) ) ;
#94948 = CARTESIAN_POINT ( 'NONE',  ( -19.02544592524342804, 5.153800228976336051, 66.04057627198103830 ) ) ;
#94950 = CARTESIAN_POINT ( 'NONE',  ( -4.483927247898782831, 16.52544592524335698, 22.70942372801901499 ) ) ;
#94949 = CARTESIAN_POINT ( 'NONE',  ( 21.53943276465977519, 0.05219959533937863772, 46.25109039468567573 ) ) ;
#94951 = CARTESIAN_POINT ( 'NONE',  ( 19.05341960407611168, 5.049401038298154454, 113.9572429386477097 ) ) ;
#94952 = CARTESIAN_POINT ( 'NONE',  ( 19.03943276465977164, 0.05219959533936151252, 21.25109039468565797 ) ) ;
#94953 = CARTESIAN_POINT ( 'NONE',  ( -19.05341960407611168, -5.049401038298163336, 101.4572429386476955 ) ) ;
#94954 = CARTESIAN_POINT ( 'NONE',  ( -21.55341960407610458, -5.719274019375992779, 106.4572429386477097 ) ) ;
#94955 = CARTESIAN_POINT ( 'NONE',  ( 0.05219959533909260263, 19.03943276465977164, 64.99890960531436690 ) ) ;
#94956 = CARTESIAN_POINT ( 'NONE',  ( -3.921756399366283397, -4.986025004891486923, -62.46690648838622906 ) ) ;
#94957 = CARTESIAN_POINT ( 'NONE',  ( 16.52544592524342804, -4.483927247898539470, 88.54057627198103830 ) ) ;
#94958 = CARTESIAN_POINT ( 'NONE',  ( 13.89961937509977652, -13.97604488694527269, 113.1239096053143527 ) ) ;
#94959 = CARTESIAN_POINT ( 'NONE',  ( -0.05219959533909027116, -19.03943276465977164, 22.49890960531436690 ) ) ;
#94960 = CARTESIAN_POINT ( 'NONE',  ( 21.52544592524344225, -5.823673210054117533, 103.5405762719810383 ) ) ;
#94961 = CARTESIAN_POINT ( 'NONE',  ( 0.05219959533936267826, -19.03943276465977164, 65.00109039468567573 ) ) ;
#94962 = CARTESIAN_POINT ( 'NONE',  ( 5.153800228976335163, 19.02544592524342804, 109.7905762719810099 ) ) ;
#94963 = CARTESIAN_POINT ( 'NONE',  ( 19.02544592524343514, -5.153800228976328945, 28.54057627198102409 ) ) ;
#94964 = CARTESIAN_POINT ( 'NONE',  ( -5.719274019375978568, 21.55341960407610458, 55.20724293864770260 ) ) ;
#94965 = VECTOR ( 'NONE', #71876, 1000.000000000000000 ) ;
#94966 = CARTESIAN_POINT ( 'NONE',  ( -5.049401038298153566, 19.05341960407611168, 100.2072429386476955 ) ) ;
#94967 = CARTESIAN_POINT ( 'NONE',  ( -18.67979575497193778, 10.72451020669871902, 73.33442372801901854 ) ) ;
#94968 = CARTESIAN_POINT ( 'NONE',  ( -13.89961937509977652, 13.97604488694528158, 45.62390960531433848 ) ) ;
#94969 = CARTESIAN_POINT ( 'NONE',  ( 14.29746914071049879, -8.314922557960816363, 93.33224293864769550 ) ) ;
#94970 = CARTESIAN_POINT ( 'NONE',  ( 8.224510206698742110, 14.34966873604972548, 37.08442372801901143 ) ) ;
#94971 = CARTESIAN_POINT ( 'NONE',  ( -5.823673210054431948, 21.52544592524334988, 62.70942372801902565 ) ) ;
#94972 = ORIENTED_EDGE ( 'NONE', *, *, #85361, .T. ) ;
#94973 = CARTESIAN_POINT ( 'NONE',  ( -16.51473224551082808, 9.474510206698731452, 28.33442372801900433 ) ) ;
#94974 = CARTESIAN_POINT ( 'NONE',  ( -16.51473224551082808, 9.474510206698731452, 73.33442372801900433 ) ) ;
#94975 = CARTESIAN_POINT ( 'NONE',  ( -19.02544592524334988, -5.153800228976617603, 38.95942372801900433 ) ) ;
#94976 = CARTESIAN_POINT ( 'NONE',  ( 33.78191506369888941, -21.41920200728860380, -24.99999999999997868 ) ) ;
#94977 = CARTESIAN_POINT ( 'NONE',  ( -21.53943276465977519, -0.05219959533937600094, 38.75109039468567573 ) ) ;
#94978 = CARTESIAN_POINT ( 'NONE',  ( -19.01529144963332385, -5.500000000000167866, 46.23431955728440101 ) ) ;
#94979 = CARTESIAN_POINT ( 'NONE',  ( -16.51473224551082808, 9.474510206698731452, 38.33442372801899722 ) ) ;
#94980 = CARTESIAN_POINT ( 'NONE',  ( 5.049401038298161559, -19.05341960407611168, 62.70724293864769550 ) ) ;
#94981 = CARTESIAN_POINT ( 'NONE',  ( -4.483927247898539470, -16.52544592524342804, 22.29057627198102765 ) ) ;
#94983 = CARTESIAN_POINT ( 'NONE',  ( -18.62759615963255300, -10.81492255796106328, 84.16775706135234714 ) ) ;
#94982 = CARTESIAN_POINT ( 'NONE',  ( 10.81492255796078972, 18.62759615963270932, 24.58224293864768839 ) ) ;
#94984 = CARTESIAN_POINT ( 'NONE',  ( -22.81625015709510507, 31.40387420917330275, -2.924999997268813434 ) ) ;
#94985 = CARTESIAN_POINT ( 'NONE',  ( -33.67975787243658203, 4.948374891829404376, 97.42774497825463698 ) ) ;
#94986 = CARTESIAN_POINT ( 'NONE',  ( -0.05219959533937732626, 21.53943276465977519, 82.50109039468568994 ) ) ;
#94987 = CARTESIAN_POINT ( 'NONE',  ( 16.79531203550645557, -7.028104445595743321, 41.24755011779557634 ) ) ;
#94988 = CARTESIAN_POINT ( 'NONE',  ( -16.46253265017160317, 9.564922557960807481, 105.8322429386476955 ) ) ;
#94989 = CARTESIAN_POINT ( 'NONE',  ( 34.52594549653173317, 2.428612888752089207E-14, 89.49999999999897682 ) ) ;
#94990 = CARTESIAN_POINT ( 'NONE',  ( -13.89961937509977652, 13.97604488694528158, 50.62390960531435979 ) ) ;
#94991 = CARTESIAN_POINT ( 'NONE',  ( 10.81492255796078972, 18.62759615963270932, 59.58224293864770260 ) ) ;
#94992 = CARTESIAN_POINT ( 'NONE',  ( -8.314922557961024197, 14.29746914071037800, 112.9177570613523329 ) ) ;
#94994 = CARTESIAN_POINT ( 'NONE',  ( 16.46253265017160672, -9.564922557960803928, 93.33224293864769550 ) ) ;
#94993 = CARTESIAN_POINT ( 'NONE',  ( 12.14591786802309770, 12.06949235617756955, 114.3739096053143527 ) ) ;
#94995 = CARTESIAN_POINT ( 'NONE',  ( -19.05341960407617563, 5.049401038297882671, 28.54275706135232937 ) ) ;
#94996 = CARTESIAN_POINT ( 'NONE',  ( 12.14591786802309770, 12.06949235617756955, 99.37390960531436690 ) ) ;
#94997 = CARTESIAN_POINT ( 'NONE',  ( -0.05219959533937732626, 21.53943276465977519, 72.50109039468568994 ) ) ;
#94998 = CARTESIAN_POINT ( 'NONE',  ( -19.02544592524342804, 5.153800228976336051, 116.0405762719810383 ) ) ;
#94999 = CARTESIAN_POINT ( 'NONE',  ( 14.34966873604972726, -8.224510206698740333, 110.8344237280190043 ) ) ;
#95000 = CARTESIAN_POINT ( 'NONE',  ( -5.049401038297874678, -19.05341960407617918, 69.79275706135233293 ) ) ;
#95001 = CARTESIAN_POINT ( 'NONE',  ( -16.46253265017160317, 9.564922557960807481, 115.8322429386477097 ) ) ;
#95002 = CARTESIAN_POINT ( 'NONE',  ( 16.55341960407611168, 4.379528057220329451, 78.95724293864769550 ) ) ;
#95003 = CARTESIAN_POINT ( 'NONE',  ( -5.153800228976607833, 19.02544592524334988, 52.70942372801900433 ) ) ;
#95004 = CARTESIAN_POINT ( 'NONE',  ( 13.97604488694527802, 13.89961937509977652, 69.37390960531436690 ) ) ;
#95005 = CARTESIAN_POINT ( 'NONE',  ( 16.52544592524342804, -4.483927247898539470, 58.54057627198103120 ) ) ;
#95006 = CARTESIAN_POINT ( 'NONE',  ( 0.05219959533936267826, -19.03943276465977164, 95.00109039468567573 ) ) ;
#95007 = CARTESIAN_POINT ( 'NONE',  ( -21.53943276465977519, 0.05219959533907696930, 56.24890960531436690 ) ) ;
#95008 = EDGE_LOOP ( 'NONE', ( #172912, #1511 ) ) ;
#95009 = CARTESIAN_POINT ( 'NONE',  ( 8.314922557960818139, 14.29746914071049879, 109.5822429386476955 ) ) ;
#95010 = CARTESIAN_POINT ( 'NONE',  ( -5.049401038297874678, -19.05341960407618274, 99.79275706135233293 ) ) ;
#95012 = CARTESIAN_POINT ( 'NONE',  ( 0.05219959533907565091, 21.53943276465977519, 59.99890960531436690 ) ) ;
#95011 = CARTESIAN_POINT ( 'NONE',  ( 16.51473224551069308, 9.474510206698969483, 54.16557627198103120 ) ) ;
#95014 = CARTESIAN_POINT ( 'NONE',  ( -16.46253265017160317, 9.564922557960807481, 70.83224293864770971 ) ) ;
#95013 = CARTESIAN_POINT ( 'NONE',  ( 8.314922557961029526, -14.29746914071037800, 95.41775706135234714 ) ) ;
#95015 = CARTESIAN_POINT ( 'NONE',  ( -19.05341960407617563, 5.049401038297882671, 58.54275706135234003 ) ) ;
#95016 = CARTESIAN_POINT ( 'NONE',  ( -21.55341960407619339, 5.719274019375674811, 83.54275706135234714 ) ) ;
#95017 = CARTESIAN_POINT ( 'NONE',  ( 10.72451020669898902, -18.67979575497178502, 67.91557627198102409 ) ) ;
#95018 = CARTESIAN_POINT ( 'NONE',  ( -5.049401038298153566, 19.05341960407611168, 110.2072429386476671 ) ) ;
#95019 = CARTESIAN_POINT ( 'NONE',  ( 13.89961937509977652, -13.97604488694527269, 38.12390960531436690 ) ) ;
#95020 = CARTESIAN_POINT ( 'NONE',  ( 16.55341960407618274, -4.379528057220086978, 96.04275706135236135 ) ) ;
#95021 = CARTESIAN_POINT ( 'NONE',  ( -5.153800228976607833, 19.02544592524334988, 112.7094237280190043 ) ) ;
#95022 = CARTESIAN_POINT ( 'NONE',  ( 17.44270441346514744, 5.991230190323102889, 53.86335079264230785 ) ) ;
#95023 = CARTESIAN_POINT ( 'NONE',  ( -21.55341960407619339, 5.719274019375674811, 98.54275706135234714 ) ) ;
#95024 = CARTESIAN_POINT ( 'NONE',  ( -8.224510206698948167, 14.34966873604960824, 65.41557627198102409 ) ) ;
#95025 = CARTESIAN_POINT ( 'NONE',  ( 8.224510206698953496, -14.34966873604960469, 67.91557627198102409 ) ) ;
#95026 = CARTESIAN_POINT ( 'NONE',  ( 21.53943276465977519, -0.05219959533907433946, 88.74890960531436690 ) ) ;
#95027 = CARTESIAN_POINT ( 'NONE',  ( -15.72974639402197994, 15.80617190586746368, 90.62390960531436690 ) ) ;
#95028 = CARTESIAN_POINT ( 'NONE',  ( 17.50000000000000000, -5.499999999999992895, 96.21769037696437010 ) ) ;
#95029 = CARTESIAN_POINT ( 'NONE',  ( -21.53943276465977519, 0.05219959533907696930, 51.24890960531436690 ) ) ;
#95030 = CARTESIAN_POINT ( 'NONE',  ( -14.29746914071037622, -8.314922557961029526, 64.16775706135234714 ) ) ;
#95031 = CARTESIAN_POINT ( 'NONE',  ( 8.314922557960818139, 14.29746914071049879, 94.58224293864769550 ) ) ;
#95032 = CARTESIAN_POINT ( 'NONE',  ( 16.51473224551069308, 9.474510206698969483, 49.16557627198102409 ) ) ;
#95033 = LINE ( 'NONE', #40348, #144578 ) ;
#95034 = CARTESIAN_POINT ( 'NONE',  ( -14.29746914071037622, -8.314922557961029526, 94.16775706135237556 ) ) ;
#95035 = CARTESIAN_POINT ( 'NONE',  ( -0.05219959533937732626, 21.53943276465977519, 37.50109039468568284 ) ) ;
#95036 = CARTESIAN_POINT ( 'NONE',  ( -5.049401038298153566, 19.05341960407611168, 100.2072429386476955 ) ) ;
#95037 = CARTESIAN_POINT ( 'NONE',  ( -10.81492255796105439, 18.62759615963255655, 72.91775706135234714 ) ) ;
#95038 = DIRECTION ( 'NONE',  ( 0.000000000000000000, -1.000000000000000000, 0.000000000000000000 ) ) ;
#95040 = EDGE_CURVE ( 'NONE', #141411, #27838, #121047, .T. ) ;
#95039 = CARTESIAN_POINT ( 'NONE',  ( 5.049401038298161559, -19.05341960407611168, 27.70724293864769550 ) ) ;
#95041 = VECTOR ( 'NONE', #64610, 1000.000000000000000 ) ;
#95042 = EDGE_LOOP ( 'NONE', ( #85664, #189454, #147460, #71637, #99412, #1969, #92908, #198642, #149220, #40062, #151170, #31539, #66316, #163336, #124127, #83288 ) ) ;
#95043 = CARTESIAN_POINT ( 'NONE',  ( 18.67979575497194134, -10.72451020669871369, 55.83442372801901854 ) ) ;
#95045 = CARTESIAN_POINT ( 'NONE',  ( -5.153800228976328057, -19.02544592524343514, 22.29057627198102765 ) ) ;
#95044 = CARTESIAN_POINT ( 'NONE',  ( 9.564922557960805705, 16.46253265017160317, 39.58224293864768839 ) ) ;
#95046 = CARTESIAN_POINT ( 'NONE',  ( -19.02544592524342804, 5.153800228976336051, 91.04057627198100988 ) ) ;
#95047 = CARTESIAN_POINT ( 'NONE',  ( -19.02544592524334988, -5.153800228976617603, 63.95942372801899012 ) ) ;
#95048 = CARTESIAN_POINT ( 'NONE',  ( 10.81492255796106328, -18.62759615963255655, 35.41775706135234003 ) ) ;
#95049 = CARTESIAN_POINT ( 'NONE',  ( -0.05219959533936034679, 19.03943276465977164, 57.50109039468566863 ) ) ;
#95050 = CARTESIAN_POINT ( 'NONE',  ( -19.03943276465977164, 0.05219959533909376836, 41.24890960531435269 ) ) ;
#95051 = CARTESIAN_POINT ( 'NONE',  ( 0.05219959533934541429, -16.53943276465976808, 100.0010903946857042 ) ) ;
#95052 = CARTESIAN_POINT ( 'NONE',  ( 19.05341960407617918, -5.049401038297876454, 76.04275706135230450 ) ) ;
#95053 = CARTESIAN_POINT ( 'NONE',  ( 16.53943276465976808, -0.05219959533910856209, 23.74890960531435269 ) ) ;
#95054 = CARTESIAN_POINT ( 'NONE',  ( 19.03943276465977164, 0.05219959533936151252, 56.25109039468566863 ) ) ;
#95055 = CARTESIAN_POINT ( 'NONE',  ( 19.02544592524343514, -5.153800228976328945, 98.54057627198100988 ) ) ;
#95056 = CARTESIAN_POINT ( 'NONE',  ( 18.62759615963255655, 10.81492255796105972, 101.6677570613523613 ) ) ;
#95057 = CARTESIAN_POINT ( 'NONE',  ( 5.823673210054444382, -21.52544592524334988, 105.2094237280190328 ) ) ;
#95058 = CARTESIAN_POINT ( 'NONE',  ( -19.02544592524342804, 5.153800228976336051, 26.04057627198103120 ) ) ;
#95059 = CARTESIAN_POINT ( 'NONE',  ( -15.72974639402176322, -15.80617190586768395, 89.37609039468568994 ) ) ;
#95060 = CARTESIAN_POINT ( 'NONE',  ( 16.53943276465976808, 0.05219959533934440121, 31.25109039468568639 ) ) ;
#95061 = VECTOR ( 'NONE', #21856, 1000.000000000000000 ) ;
#95062 = CARTESIAN_POINT ( 'NONE',  ( 5.153800228976335163, 19.02544592524342804, 94.79057627198103830 ) ) ;
#95063 = CARTESIAN_POINT ( 'NONE',  ( -22.44159573604009950, -16.30477369853688430, 139.0750000027311728 ) ) ;
#95064 = CARTESIAN_POINT ( 'NONE',  ( -13.97604488694527625, -13.89961937509977652, 76.87390960531433848 ) ) ;
#95065 = DIRECTION ( 'NONE',  ( -1.000000000000000000, 0.000000000000000000, 0.000000000000000000 ) ) ;
#95066 = AXIS2_PLACEMENT_3D ( 'NONE', #174427, #35897, #33921 ) ;
#95067 = CARTESIAN_POINT ( 'NONE',  ( 19.02544592524334988, 5.153800228976608722, 66.45942372801899012 ) ) ;
#95068 = CARTESIAN_POINT ( 'NONE',  ( 5.049401038298161559, -19.05341960407611168, 102.7072429386476955 ) ) ;
#95069 = CARTESIAN_POINT ( 'NONE',  ( 21.55341960407619695, -5.719274019375665929, 96.04275706135236135 ) ) ;
#95070 = CARTESIAN_POINT ( 'NONE',  ( -4.483927247898539470, -16.52544592524342804, 102.2905762719810383 ) ) ;
#95071 = CARTESIAN_POINT ( 'NONE',  ( 21.52544592524344225, -5.823673210054117533, 48.54057627198103120 ) ) ;
#95072 = CARTESIAN_POINT ( 'NONE',  ( 21.53943276465977519, -0.05219959533907433946, 33.74890960531436690 ) ) ;
#95073 = CARTESIAN_POINT ( 'NONE',  ( 4.379528057220339221, -16.55341960407611168, 102.7072429386476955 ) ) ;
#95074 = CARTESIAN_POINT ( 'NONE',  ( -13.70000000000001528, 1.443387660838688656E-13, -62.58071313852362039 ) ) ;
#95075 = CARTESIAN_POINT ( 'NONE',  ( 13.89961937509957401, 13.97604488694547697, 61.87609039468566863 ) ) ;
#95076 = CARTESIAN_POINT ( 'NONE',  ( -16.53943276465976808, 0.05219959533911058130, 36.24890960531435979 ) ) ;
#95077 = CARTESIAN_POINT ( 'NONE',  ( -5.049401038298153566, 19.05341960407611168, 110.2072429386476671 ) ) ;
#95078 = CARTESIAN_POINT ( 'NONE',  ( -5.719274019375665041, -21.55341960407619695, 79.79275706135236135 ) ) ;
#95079 = CARTESIAN_POINT ( 'NONE',  ( -21.55341960407610458, -5.719274019375992779, 71.45724293864769550 ) ) ;
#95080 = CARTESIAN_POINT ( 'NONE',  ( 18.62759615963255655, 10.81492255796105972, 46.66775706135234714 ) ) ;
#95081 = CARTESIAN_POINT ( 'NONE',  ( -21.52544592524343514, 5.823673210054127303, 101.0405762719810383 ) ) ;
#95082 = CARTESIAN_POINT ( 'NONE',  ( -10.81492255796105439, 18.62759615963255655, 52.91775706135235424 ) ) ;
#95083 = CARTESIAN_POINT ( 'NONE',  ( -19.03943276465977164, 0.05219959533909376836, 21.24890960531436335 ) ) ;
#95084 = CARTESIAN_POINT ( 'NONE',  ( 19.02544592524343514, -5.153800228976328945, 83.54057627198100988 ) ) ;
#95085 = CARTESIAN_POINT ( 'NONE',  ( -16.53943276465976808, -0.05219959533934237506, 83.75109039468568994 ) ) ;
#95086 = CARTESIAN_POINT ( 'NONE',  ( 16.53943276465976808, -0.05219959533910856209, 108.7489096053143669 ) ) ;
#95087 = CARTESIAN_POINT ( 'NONE',  ( -19.03943276465977164, 0.05219959533909376836, 106.2489096053143669 ) ) ;
#95088 = CARTESIAN_POINT ( 'NONE',  ( -0.05219959533910754901, -16.53943276465976808, 52.49890960531435979 ) ) ;
#95089 = CARTESIAN_POINT ( 'NONE',  ( -8.314922557961024197, 14.29746914071037800, 112.9177570613523329 ) ) ;
#95090 = CARTESIAN_POINT ( 'NONE',  ( -16.51473224551069308, -9.474510206698971260, 66.66557627198102409 ) ) ;
#95091 = CARTESIAN_POINT ( 'NONE',  ( 5.049401038298161559, -19.05341960407611168, 37.70724293864768839 ) ) ;
#95092 = CARTESIAN_POINT ( 'NONE',  ( 21.55341960407610458, 5.719274019375980345, 43.95724293864769550 ) ) ;
#95093 = CARTESIAN_POINT ( 'NONE',  ( 13.97604488694548053, -13.89961937509957401, 40.62609039468564731 ) ) ;
#95095 = CARTESIAN_POINT ( 'NONE',  ( -8.224510206698948167, 14.34966873604960824, 30.41557627198101699 ) ) ;
#95094 = CARTESIAN_POINT ( 'NONE',  ( -17.60779699588841751, -5.499999999999946709, 86.34981316670108242 ) ) ;
#95096 = CARTESIAN_POINT ( 'NONE',  ( -9.564922557960796823, -16.46253265017161027, 102.0822429386477097 ) ) ;
#95097 = CARTESIAN_POINT ( 'NONE',  ( -18.67979575497193778, 10.72451020669871902, 53.33442372801901854 ) ) ;
#95098 = CARTESIAN_POINT ( 'NONE',  ( 21.50819313649865805, -5.452397343345025682, 174.1340046013950200 ) ) ;
#95099 = CARTESIAN_POINT ( 'NONE',  ( 16.55341960407618274, -4.379528057220086978, 56.04275706135235424 ) ) ;
#95100 = CARTESIAN_POINT ( 'NONE',  ( 16.51473224551083163, -9.474510206698727899, 55.83442372801899722 ) ) ;
#95101 = CARTESIAN_POINT ( 'NONE',  ( 4.483927247898545687, 16.52544592524342804, 24.79057627198103120 ) ) ;
#95102 = CARTESIAN_POINT ( 'NONE',  ( 22.00000000000000000, -5.510910596163089556E-15, 45.00000000000000000 ) ) ;
#95103 = CARTESIAN_POINT ( 'NONE',  ( 12.06949235617739724, 12.14591786802326823, 111.8760903946856615 ) ) ;
#95104 = CARTESIAN_POINT ( 'NONE',  ( 16.51473224551069308, 9.474510206698969483, 39.16557627198103120 ) ) ;
#95105 = CARTESIAN_POINT ( 'NONE',  ( -19.03943276465977164, 0.05219959533909376836, 61.24890960531436690 ) ) ;
#95106 = CARTESIAN_POINT ( 'NONE',  ( 0.05219959533909260263, 19.03943276465977164, 24.99890960531435269 ) ) ;
#95107 = CARTESIAN_POINT ( 'NONE',  ( 15.72974639402176855, 15.80617190586768217, 36.87609039468568994 ) ) ;
#95108 = CARTESIAN_POINT ( 'NONE',  ( 19.02544592524343514, -5.153800228976328945, 43.54057627198103120 ) ) ;
#95109 = CARTESIAN_POINT ( 'NONE',  ( -19.03943276465977164, 0.05219959533909376836, 116.2489096053143669 ) ) ;
#95110 = CARTESIAN_POINT ( 'NONE',  ( 19.02544592524343514, -5.153800228976328945, 48.54057627198103120 ) ) ;
#95111 = CARTESIAN_POINT ( 'NONE',  ( -16.46253265017160317, 9.564922557960807481, 115.8322429386477097 ) ) ;
#95113 = CARTESIAN_POINT ( 'NONE',  ( -16.51473224551069308, -9.474510206698971260, 21.66557627198102765 ) ) ;
#95112 = CARTESIAN_POINT ( 'NONE',  ( 15.80617190586769283, -15.72974639402175789, 65.62609039468568994 ) ) ;
#95114 = CARTESIAN_POINT ( 'NONE',  ( -21.52544592524343514, 5.823673210054127303, 31.04057627198102409 ) ) ;
#95115 = CARTESIAN_POINT ( 'NONE',  ( 4.483927247898790824, -16.52544592524335698, 80.20942372801901854 ) ) ;
#95116 = CARTESIAN_POINT ( 'NONE',  ( 15.80617190586769283, -15.72974639402175789, 100.6260903946857184 ) ) ;
#95117 = CARTESIAN_POINT ( 'NONE',  ( 16.55341960407618274, -4.379528057220086978, 51.04275706135234714 ) ) ;
#95118 = CARTESIAN_POINT ( 'NONE',  ( 19.03943276465977164, -0.05219959533909143690, 93.74890960531435269 ) ) ;
#95119 = CARTESIAN_POINT ( 'NONE',  ( 16.52544592524335698, 4.483927247898782831, 36.45942372801901143 ) ) ;
#95120 = CARTESIAN_POINT ( 'NONE',  ( 14.34966873604972726, -8.224510206698740333, 25.83442372801901499 ) ) ;
#95121 = CARTESIAN_POINT ( 'NONE',  ( 16.55341960407618274, -4.379528057220086978, 96.04275706135236135 ) ) ;
#95122 = CARTESIAN_POINT ( 'NONE',  ( -15.80617190586768217, 15.72974639402176855, 53.12609039468568284 ) ) ;
#95123 = CARTESIAN_POINT ( 'NONE',  ( 0.05219959533936267826, -19.03943276465977164, 105.0010903946856615 ) ) ;
#95124 = CARTESIAN_POINT ( 'NONE',  ( -18.62759615963270932, 10.81492255796079327, 115.8322429386477097 ) ) ;
#95126 = CARTESIAN_POINT ( 'NONE',  ( -16.51473224551082808, 9.474510206698731452, 108.3344237280190043 ) ) ;
#95125 = CARTESIAN_POINT ( 'NONE',  ( 14.34966873604960469, 8.224510206698951720, 99.16557627198100988 ) ) ;
#95127 = CARTESIAN_POINT ( 'NONE',  ( -16.52544592524335698, -4.483927247898792601, 73.95942372801901854 ) ) ;
#95128 = CARTESIAN_POINT ( 'NONE',  ( -16.88567814943193568, 6.947325034625407625, 43.70998877347406619 ) ) ;
#95129 = CARTESIAN_POINT ( 'NONE',  ( -9.474510206698720793, -16.51473224551083518, 89.58442372801900433 ) ) ;
#95130 = CARTESIAN_POINT ( 'NONE',  ( -4.379528057220328563, 16.55341960407611168, 40.20724293864769550 ) ) ;
#95131 = CARTESIAN_POINT ( 'NONE',  ( -16.52544592524342804, 4.483927247898546575, 41.04057627198103120 ) ) ;
#95132 = CARTESIAN_POINT ( 'NONE',  ( 16.53943276465976808, -0.05219959533910856209, 103.7489096053143669 ) ) ;
#95134 = CARTESIAN_POINT ( 'NONE',  ( -17.49999999999999645, 5.499999999999992895, 93.71769037696437010 ) ) ;
#95133 = CARTESIAN_POINT ( 'NONE',  ( 5.153800228976615827, -19.02544592524334988, 40.20942372801898301 ) ) ;
#95135 = CARTESIAN_POINT ( 'NONE',  ( 21.55341960407619695, -5.719274019375665929, 31.04275706135234714 ) ) ;
#95136 = CARTESIAN_POINT ( 'NONE',  ( 0.05219959533936267826, -19.03943276465977164, 105.0010903946856615 ) ) ;
#95137 = CARTESIAN_POINT ( 'NONE',  ( -19.82991159619237820, -34.74521775907871302, -25.51696690232505915 ) ) ;
#95138 = CARTESIAN_POINT ( 'NONE',  ( 19.05341960407611168, 5.049401038298154454, 93.95724293864769550 ) ) ;
#95139 = CARTESIAN_POINT ( 'NONE',  ( -5.049401038298153566, 19.05341960407611168, 95.20724293864770971 ) ) ;
#95140 = CARTESIAN_POINT ( 'NONE',  ( 0.05219959533907565091, 21.53943276465977519, 54.99890960531435269 ) ) ;
#95141 = CARTESIAN_POINT ( 'NONE',  ( 8.224510206698953496, -14.34966873604960469, 97.91557627198103830 ) ) ;
#95142 = CARTESIAN_POINT ( 'NONE',  ( 16.46253265017160672, -9.564922557960803928, 68.33224293864770971 ) ) ;
#95143 = CARTESIAN_POINT ( 'NONE',  ( 0.05219959533909260263, 19.03943276465977164, 29.99890960531435979 ) ) ;
#95144 = CARTESIAN_POINT ( 'NONE',  ( 21.55341960407619695, -5.719274019375665929, 41.04275706135236135 ) ) ;
#95145 = CARTESIAN_POINT ( 'NONE',  ( 18.67979575497194134, -10.72451020669871369, 70.83442372801901854 ) ) ;
#95146 = CARTESIAN_POINT ( 'NONE',  ( -14.34966873604972548, 8.224510206698743886, 93.33442372801901854 ) ) ;
#95147 = CARTESIAN_POINT ( 'NONE',  ( 0.05219959533937995610, -21.53943276465977519, 35.00109039468568284 ) ) ;
#95148 = CARTESIAN_POINT ( 'NONE',  ( -10.81492255796105439, 18.62759615963255655, 27.91775706135234358 ) ) ;
#95150 = CARTESIAN_POINT ( 'NONE',  ( -13.97604488694527625, -13.89961937509977652, 81.87390960531436690 ) ) ;
#95149 = CARTESIAN_POINT ( 'NONE',  ( 13.89961937509957401, 13.97604488694547697, 56.87609039468564731 ) ) ;
#95151 = CARTESIAN_POINT ( 'NONE',  ( 15.72974639402176855, 15.80617190586768217, 81.87609039468568994 ) ) ;
#95152 = CIRCLE ( 'NONE', #130657, 206.0437394197456342 ) ;
#95153 = CARTESIAN_POINT ( 'NONE',  ( 18.67979575497178502, 10.72451020669898547, 84.16557627198103830 ) ) ;
#95154 = CARTESIAN_POINT ( 'NONE',  ( -16.55341960407611168, -4.379528057220339221, 46.45724293864769550 ) ) ;
#95156 = CARTESIAN_POINT ( 'NONE',  ( 19.03943276465977164, 0.05219959533936151252, 46.25109039468566863 ) ) ;
#95155 = CARTESIAN_POINT ( 'NONE',  ( -5.719274019375665041, -21.55341960407619695, 109.7927570613523613 ) ) ;
#95157 = CARTESIAN_POINT ( 'NONE',  ( -0.05219959533910754901, -16.53943276465976808, 72.49890960531435269 ) ) ;
#95158 = CARTESIAN_POINT ( 'NONE',  ( -5.049401038298153566, 19.05341960407611168, 25.20724293864768484 ) ) ;
#95159 = CARTESIAN_POINT ( 'NONE',  ( -19.05341960407617563, 5.049401038297882671, 73.54275706135233293 ) ) ;
#95160 = CARTESIAN_POINT ( 'NONE',  ( 14.29746914071049879, -8.314922557960816363, 38.33224293864768839 ) ) ;
#95161 = CARTESIAN_POINT ( 'NONE',  ( -10.72451020669870658, -18.67979575497194134, 79.58442372801903275 ) ) ;
#95162 = CARTESIAN_POINT ( 'NONE',  ( 0.05219959533909260263, 19.03943276465977164, 79.99890960531436690 ) ) ;
#95163 = CARTESIAN_POINT ( 'NONE',  ( -13.89961937509957401, -13.97604488694547875, 64.37609039468567573 ) ) ;
#95164 = CARTESIAN_POINT ( 'NONE',  ( -18.62759615963270932, 10.81492255796079327, 60.83224293864769550 ) ) ;
#95165 = CARTESIAN_POINT ( 'NONE',  ( -21.53943276465977519, 0.05219959533907696930, 116.2489096053143669 ) ) ;
#95166 = CARTESIAN_POINT ( 'NONE',  ( -12.06949235617739369, -12.14591786802326823, 19.37609039468568639 ) ) ;
#95167 = CARTESIAN_POINT ( 'NONE',  ( -8.314922557961024197, 14.29746914071037800, 82.91775706135234714 ) ) ;
#95169 = CARTESIAN_POINT ( 'NONE',  ( 21.55341960407619695, -5.719274019375665929, 26.04275706135235779 ) ) ;
#95168 = CARTESIAN_POINT ( 'NONE',  ( 17.12812012977025589, 6.668231424566066323, 63.85948759323147073 ) ) ;
#95170 = CARTESIAN_POINT ( 'NONE',  ( -4.379528057220328563, 16.55341960407611168, 100.2072429386476955 ) ) ;
#95171 = CARTESIAN_POINT ( 'NONE',  ( 29.86685920354754842, -21.69954338932559068, -4.324999997268814234 ) ) ;
#95172 = CARTESIAN_POINT ( 'NONE',  ( -8.314922557961024197, 14.29746914071037800, 37.91775706135235424 ) ) ;
#95173 = EDGE_CURVE ( 'NONE', #8281, #60180, #130197, .T. ) ;
#95174 = CARTESIAN_POINT ( 'NONE',  ( -5.719274019375978568, 21.55341960407610458, 60.20724293864768839 ) ) ;
#95175 = CARTESIAN_POINT ( 'NONE',  ( 14.34966873604972726, -8.224510206698740333, 105.8344237280190328 ) ) ;
#95176 = CARTESIAN_POINT ( 'NONE',  ( -8.314922557961024197, 14.29746914071037800, 37.91775706135235424 ) ) ;
#95177 = CARTESIAN_POINT ( 'NONE',  ( -13.97604488694527625, -13.89961937509977652, 31.87390960531435979 ) ) ;
#95178 = CARTESIAN_POINT ( 'NONE',  ( 16.55341960407618274, -4.379528057220086978, 86.04275706135236135 ) ) ;
#95179 = CARTESIAN_POINT ( 'NONE',  ( -0.05219959533936034679, 19.03943276465977164, 77.50109039468566152 ) ) ;
#95180 = ADVANCED_FACE ( 'NONE', ( #115333 ), #113318, .F. ) ;
#95181 = AXIS2_PLACEMENT_3D ( 'NONE', #16545, #78192, #122715 ) ;
#95182 = CARTESIAN_POINT ( 'NONE',  ( -10.81492255796078084, -18.62759615963271287, 57.08224293864769550 ) ) ;
#95183 = CARTESIAN_POINT ( 'NONE',  ( -16.52544592524335698, -4.483927247898792601, 103.9594237280190185 ) ) ;
#95184 = CARTESIAN_POINT ( 'NONE',  ( -0.05219959533937732626, 21.53943276465977519, 77.50109039468567573 ) ) ;
#95185 = CARTESIAN_POINT ( 'NONE',  ( -10.81492255796078084, -18.62759615963271287, 52.08224293864768839 ) ) ;
#95186 = CARTESIAN_POINT ( 'NONE',  ( 18.67979575497178502, 10.72451020669898547, 54.16557627198103120 ) ) ;
#95187 = CARTESIAN_POINT ( 'NONE',  ( 12.06949235617739724, 12.14591786802326823, 76.87609039468567573 ) ) ;
#95188 = CARTESIAN_POINT ( 'NONE',  ( -10.81492255796078084, -18.62759615963271287, 52.08224293864768839 ) ) ;
#95189 = ORIENTED_EDGE ( 'NONE', *, *, #26316, .T. ) ;
#95190 = CARTESIAN_POINT ( 'NONE',  ( 5.153800228976335163, 19.02544592524342804, 104.7905762719809957 ) ) ;
#95191 = CARTESIAN_POINT ( 'NONE',  ( -26.25049742697155253, 7.664248127782741449, 169.1476266185236454 ) ) ;
#95192 = CARTESIAN_POINT ( 'NONE',  ( -0.05219959533909027116, -19.03943276465977164, 32.49890960531435979 ) ) ;
#95193 = CARTESIAN_POINT ( 'NONE',  ( 10.72451020669898902, -18.67979575497178502, 57.91557627198103120 ) ) ;
#95194 = CARTESIAN_POINT ( 'NONE',  ( -12.06949235617739369, -12.14591786802326823, 94.37609039468568994 ) ) ;
#95195 = CARTESIAN_POINT ( 'NONE',  ( 10.81492255796106328, -18.62759615963255655, 50.41775706135235424 ) ) ;
#95196 = CARTESIAN_POINT ( 'NONE',  ( -5.153800228976607833, 19.02544592524334988, 102.7094237280189759 ) ) ;
#95197 = CARTESIAN_POINT ( 'NONE',  ( 16.52544592524342804, -4.483927247898539470, 108.5405762719810241 ) ) ;
#95198 = CARTESIAN_POINT ( 'NONE',  ( -13.89961937509957401, -13.97604488694547875, 104.3760903946856757 ) ) ;
#95199 = VECTOR ( 'NONE', #57448, 1000.000000000000000 ) ;
#95200 = CARTESIAN_POINT ( 'NONE',  ( 19.05341960407611168, 5.049401038298154454, 38.95724293864767418 ) ) ;
#95201 = CARTESIAN_POINT ( 'NONE',  ( 22.00000000000000000, -5.510910596163089556E-15, 45.00000000000000000 ) ) ;
#95202 = CARTESIAN_POINT ( 'NONE',  ( -9.474510206698964154, 16.51473224551069663, 85.41557627198102409 ) ) ;
#95203 = CARTESIAN_POINT ( 'NONE',  ( -4.483927247898782831, 16.52544592524335698, 77.70942372801900433 ) ) ;
#95204 = CARTESIAN_POINT ( 'NONE',  ( -15.80617190586768217, 15.72974639402176855, 108.1260903946856757 ) ) ;
#95205 = CARTESIAN_POINT ( 'NONE',  ( -15.80617190586745835, -15.72974639402198527, 66.87390960531436690 ) ) ;
#95206 = CARTESIAN_POINT ( 'NONE',  ( -14.29746914071037622, -8.314922557961029526, 89.16775706135236135 ) ) ;
#95207 = CARTESIAN_POINT ( 'NONE',  ( -9.474510206698720793, -16.51473224551083518, 74.58442372801900433 ) ) ;
#95208 = CARTESIAN_POINT ( 'NONE',  ( 5.049401038298161559, -19.05341960407611168, 42.70724293864767418 ) ) ;
#95210 = AXIS2_PLACEMENT_3D ( 'NONE', #19537, #113517, #191369 ) ;
#95209 = CARTESIAN_POINT ( 'NONE',  ( -19.05341960407611168, -5.049401038298163336, 76.45724293864769550 ) ) ;
#95211 = CARTESIAN_POINT ( 'NONE',  ( -5.719274019375665041, -21.55341960407619695, 44.79275706135234714 ) ) ;
#95212 = CARTESIAN_POINT ( 'NONE',  ( -19.05341960407611168, -5.049401038298163336, 51.45724293864770260 ) ) ;
#95213 = CARTESIAN_POINT ( 'NONE',  ( 13.89961937509957401, 13.97604488694547697, 76.87609039468566152 ) ) ;
#95214 = CARTESIAN_POINT ( 'NONE',  ( 24.54404792736082186, -12.06373989673630653, 169.8487138613017180 ) ) ;
#95215 = CARTESIAN_POINT ( 'NONE',  ( 16.46253265017160672, -9.564922557960803928, 113.3322429386476955 ) ) ;
#95216 = CARTESIAN_POINT ( 'NONE',  ( 14.29746914071049879, -8.314922557960816363, 68.33224293864769550 ) ) ;
#95217 = CARTESIAN_POINT ( 'NONE',  ( -21.53943276465977519, 0.05219959533907696930, 66.24890960531436690 ) ) ;
#95218 = DIRECTION ( 'NONE',  ( -1.000000000000000000, 0.000000000000000000, 0.000000000000000000 ) ) ;
#95219 = CARTESIAN_POINT ( 'NONE',  ( -16.51473224551082808, 9.474510206698731452, 23.33442372801900078 ) ) ;
#95220 = CARTESIAN_POINT ( 'NONE',  ( 0.2500000000000002220, 0.000000000000000000, 0.000000000000000000 ) ) ;
#95222 = CARTESIAN_POINT ( 'NONE',  ( 5.049401038298161559, -19.05341960407611168, 77.70724293864765286 ) ) ;
#95221 = CARTESIAN_POINT ( 'NONE',  ( -13.89961937509977652, 13.97604488694528158, 70.62390960531432427 ) ) ;
#95223 = CARTESIAN_POINT ( 'NONE',  ( 8.224510206698742110, 14.34966873604972548, 57.08442372801901854 ) ) ;
#95224 = CARTESIAN_POINT ( 'NONE',  ( 8.207766490800741721, -46.52841682978063886, -24.35011552986999916 ) ) ;
#95225 = CARTESIAN_POINT ( 'NONE',  ( -16.81555441253554051, 7.025013491695463408, 110.6368544533425791 ) ) ;
#95226 = CARTESIAN_POINT ( 'NONE',  ( 8.224510206698742110, 14.34966873604972548, 92.08442372801901854 ) ) ;
#95227 = CARTESIAN_POINT ( 'NONE',  ( 17.50000000000000711, 5.499999999999976907, 93.78230962303565832 ) ) ;
#95228 = CARTESIAN_POINT ( 'NONE',  ( -0.05219959533934338120, 16.53943276465976808, 67.50109039468568994 ) ) ;
#95229 = CARTESIAN_POINT ( 'NONE',  ( 0.05219959533934541429, -16.53943276465976808, 45.00109039468568284 ) ) ;
#95231 = CARTESIAN_POINT ( 'NONE',  ( -19.49401214000074489, -12.39993551617566148, 164.9999999999999716 ) ) ;
#95230 = CARTESIAN_POINT ( 'NONE',  ( 19.05341960407611168, 5.049401038298154454, 53.95724293864770260 ) ) ;
#95232 = CARTESIAN_POINT ( 'NONE',  ( 21.52544592524334988, 5.823673210054432836, 56.45942372801902565 ) ) ;
#95233 = CARTESIAN_POINT ( 'NONE',  ( -0.05219959533936034679, 19.03943276465977164, 57.50109039468566863 ) ) ;
#95234 = CARTESIAN_POINT ( 'NONE',  ( -10.81492255796105439, 18.62759615963255655, 112.9177570613523329 ) ) ;
#95235 = CARTESIAN_POINT ( 'NONE',  ( -13.89961937509977652, 13.97604488694528158, 30.62390960531435269 ) ) ;
#95236 = CARTESIAN_POINT ( 'NONE',  ( 16.23956094088878288, 7.360292434722755850, 22.49130789039435641 ) ) ;
#95237 = CARTESIAN_POINT ( 'NONE',  ( 10.72451020669898902, -18.67979575497178502, 47.91557627198102409 ) ) ;
#95238 = CARTESIAN_POINT ( 'NONE',  ( -13.89961937509977652, 13.97604488694528158, 105.6239096053143527 ) ) ;
#95239 = CARTESIAN_POINT ( 'NONE',  ( -0.05219959533910754901, -16.53943276465976808, 107.4989096053143669 ) ) ;
#95240 = CARTESIAN_POINT ( 'NONE',  ( -4.379528057220086978, -16.55341960407618274, 34.79275706135235424 ) ) ;
#95241 = EDGE_CURVE ( 'NONE', #3778, #9238, #54682, .T. ) ;
#95242 = CARTESIAN_POINT ( 'NONE',  ( -8.314922557960811034, -14.29746914071050412, 27.08224293864769550 ) ) ;
#95243 = ORIENTED_EDGE ( 'NONE', *, *, #93518, .T. ) ;
#95244 = CARTESIAN_POINT ( 'NONE',  ( -0.05219959533907301413, -21.53943276465977519, 97.49890960531436690 ) ) ;
#95246 = CARTESIAN_POINT ( 'NONE',  ( 16.51473224551069308, 9.474510206698969483, 114.1655762719810241 ) ) ;
#95245 = CARTESIAN_POINT ( 'NONE',  ( 8.224510206698953496, -14.34966873604960469, 32.91557627198102409 ) ) ;
#95247 = CARTESIAN_POINT ( 'NONE',  ( -0.05219959533936034679, 19.03943276465977164, 92.50109039468566152 ) ) ;
#95248 = CARTESIAN_POINT ( 'NONE',  ( -5.153800228976607833, 19.02544592524334988, 27.70942372801899722 ) ) ;
#95249 = CARTESIAN_POINT ( 'NONE',  ( -16.55341960407611168, -4.379528057220339221, 26.45724293864768839 ) ) ;
#95250 = CARTESIAN_POINT ( 'NONE',  ( -10.81492255796078084, -18.62759615963271287, 97.08224293864770971 ) ) ;
#95251 = CARTESIAN_POINT ( 'NONE',  ( -21.55341960407610458, -5.719274019375992779, 56.45724293864768839 ) ) ;
#95252 = CARTESIAN_POINT ( 'NONE',  ( 19.05341960407611168, 5.049401038298154454, 78.95724293864769550 ) ) ;
#95253 = CARTESIAN_POINT ( 'NONE',  ( 16.52544592524342804, -4.483927247898539470, 53.54057627198103120 ) ) ;
#95254 = CARTESIAN_POINT ( 'NONE',  ( 19.05341960407611168, 5.049401038298154454, 93.95724293864769550 ) ) ;
#95255 = EDGE_CURVE ( 'NONE', #34342, #127568, #130705, .T. ) ;
#95256 = ORIENTED_EDGE ( 'NONE', *, *, #84631, .T. ) ;
#95257 = CARTESIAN_POINT ( 'NONE',  ( 18.22780087662123805, -5.499999999999989342, 63.51763182126896368 ) ) ;
#95258 = CARTESIAN_POINT ( 'NONE',  ( -19.05341960407617563, 5.049401038297882671, 43.54275706135232582 ) ) ;
#95259 = CARTESIAN_POINT ( 'NONE',  ( 18.62759615963271287, -10.81492255796078972, 93.33224293864769550 ) ) ;
#95260 = CARTESIAN_POINT ( 'NONE',  ( 8.314922557960818139, 14.29746914071049879, 94.58224293864769550 ) ) ;
#95261 = CARTESIAN_POINT ( 'NONE',  ( 15.72974639402176855, 15.80617190586768217, 31.87609039468567929 ) ) ;
#95262 = CARTESIAN_POINT ( 'NONE',  ( -5.359611314223446995E-15, 29.16686587814335496, 142.3750000027311557 ) ) ;
#95263 = CARTESIAN_POINT ( 'NONE',  ( -8.314922557961024197, 14.29746914071037800, 102.9177570613523756 ) ) ;
#95264 = CARTESIAN_POINT ( 'NONE',  ( 9.474510206698971260, -16.51473224551069308, 37.91557627198102409 ) ) ;
#95265 = CARTESIAN_POINT ( 'NONE',  ( 0.05219959533909260263, 19.03943276465977164, 89.99890960531436690 ) ) ;
#95266 = CARTESIAN_POINT ( 'NONE',  ( -19.46398650005389541, 5.499999999999948486, 45.18269651486372851 ) ) ;
#95267 = CARTESIAN_POINT ( 'NONE',  ( 19.03943276465977164, -0.05219959533909143690, 28.74890960531435624 ) ) ;
#95268 = CARTESIAN_POINT ( 'NONE',  ( 8.224510206698953496, -14.34966873604960469, 37.91557627198102409 ) ) ;
#95269 = CARTESIAN_POINT ( 'NONE',  ( -10.72451020669870658, -18.67979575497194134, 79.58442372801903275 ) ) ;
#95271 = CARTESIAN_POINT ( 'NONE',  ( -0.05219959533934338120, 16.53943276465976808, 72.50109039468568994 ) ) ;
#95270 = CARTESIAN_POINT ( 'NONE',  ( 13.57915378923102523, -35.22819508409087064, -29.39033328706047854 ) ) ;
#95272 = CARTESIAN_POINT ( 'NONE',  ( -19.05341960407611168, -5.049401038298163336, 61.45724293864769550 ) ) ;
#95273 = CARTESIAN_POINT ( 'NONE',  ( -13.97604488694527625, -13.89961937509977652, 61.87390960531435979 ) ) ;
#95274 = ORIENTED_EDGE ( 'NONE', *, *, #14847, .T. ) ;
#95275 = CARTESIAN_POINT ( 'NONE',  ( -21.55341960407619339, 5.719274019375674811, 103.5427570613523613 ) ) ;
#95276 = CARTESIAN_POINT ( 'NONE',  ( -16.55341960407617563, 4.379528057220093196, 73.54275706135234714 ) ) ;
#95277 = CARTESIAN_POINT ( 'NONE',  ( -10.81492255796105439, 18.62759615963255655, 102.9177570613523756 ) ) ;
#95278 = CARTESIAN_POINT ( 'NONE',  ( -16.51473224551069308, -9.474510206698971260, 66.66557627198102409 ) ) ;
#95279 = CARTESIAN_POINT ( 'NONE',  ( -18.67979575497178146, -10.72451020669898902, 36.66557627198103120 ) ) ;
#95280 = CARTESIAN_POINT ( 'NONE',  ( 19.02544592524334988, 5.153800228976608722, 101.4594237280189759 ) ) ;
#95281 = CARTESIAN_POINT ( 'NONE',  ( -5.719274019375665041, -21.55341960407619695, 84.79275706135234714 ) ) ;
#95282 = CARTESIAN_POINT ( 'NONE',  ( -8.224510206698735004, -14.34966873604973081, 49.58442372801901143 ) ) ;
#95283 = CARTESIAN_POINT ( 'NONE',  ( -18.62759615963270932, 10.81492255796079327, 100.8322429386477097 ) ) ;
#95284 = CARTESIAN_POINT ( 'NONE',  ( 19.02544592524334988, 5.153800228976608722, 101.4594237280189759 ) ) ;
#95285 = CARTESIAN_POINT ( 'NONE',  ( -9.564922557960796823, -16.46253265017161027, 82.08224293864768129 ) ) ;
#95286 = CARTESIAN_POINT ( 'NONE',  ( 19.03943276465977164, 0.05219959533936151252, 106.2510903946856615 ) ) ;
#95287 = CARTESIAN_POINT ( 'NONE',  ( 14.34966873604972726, -8.224510206698740333, 25.83442372801901499 ) ) ;
#95288 = CARTESIAN_POINT ( 'NONE',  ( -14.34966873604960291, -8.224510206698953496, 71.66557627198100988 ) ) ;
#95289 = CARTESIAN_POINT ( 'NONE',  ( -14.34966873604972548, 8.224510206698743886, 68.33442372801900433 ) ) ;
#95291 = CARTESIAN_POINT ( 'NONE',  ( -0.05219959533909027116, -19.03943276465977164, 57.49890960531435979 ) ) ;
#95290 = CARTESIAN_POINT ( 'NONE',  ( 15.80617190586769283, -15.72974639402175789, 20.62609039468568639 ) ) ;
#95292 = CARTESIAN_POINT ( 'NONE',  ( 5.153800228976335163, 19.02544592524342804, 74.79057627198103830 ) ) ;
#95293 = CARTESIAN_POINT ( 'NONE',  ( -14.29746914071037622, -8.314922557961029526, 79.16775706135234714 ) ) ;
#95294 = CARTESIAN_POINT ( 'NONE',  ( -28.82186960331499037, 2.428612866367529932E-14, 144.2500000054623683 ) ) ;
#95295 = ORIENTED_EDGE ( 'NONE', *, *, #159341, .T. ) ;
#95296 = CARTESIAN_POINT ( 'NONE',  ( 21.52544592524334988, 5.823673210054432836, 106.4594237280190328 ) ) ;
#95297 = CARTESIAN_POINT ( 'NONE',  ( -9.564922557960796823, -16.46253265017161027, 42.08224293864769550 ) ) ;
#95298 = ORIENTED_EDGE ( 'NONE', *, *, #198923, .F. ) ;
#95299 = CARTESIAN_POINT ( 'NONE',  ( -0.05219959533934338120, 16.53943276465976808, 27.50109039468567929 ) ) ;
#95301 = CARTESIAN_POINT ( 'NONE',  ( -4.379528057220086978, -16.55341960407618274, 34.79275706135235424 ) ) ;
#95300 = CARTESIAN_POINT ( 'NONE',  ( -9.474510206698720793, -16.51473224551083518, 49.58442372801899722 ) ) ;
#95302 = CARTESIAN_POINT ( 'NONE',  ( 5.049401038298161559, -19.05341960407611168, 42.70724293864767418 ) ) ;
#95303 = CARTESIAN_POINT ( 'NONE',  ( -16.46253265017160317, 9.564922557960807481, 65.83224293864769550 ) ) ;
#95304 = CARTESIAN_POINT ( 'NONE',  ( 0.05219959533907565091, 21.53943276465977519, 89.99890960531438111 ) ) ;
#95305 = CARTESIAN_POINT ( 'NONE',  ( -19.05341960407611168, -5.049401038298163336, 106.4572429386476955 ) ) ;
#95306 = CARTESIAN_POINT ( 'NONE',  ( 9.474510206698971260, -16.51473224551069308, 47.91557627198102409 ) ) ;
#95307 = CARTESIAN_POINT ( 'NONE',  ( -8.571926809382608425, 26.38167802310805854, 146.9750000027311785 ) ) ;
#95308 = CARTESIAN_POINT ( 'NONE',  ( -5.049401038297874678, -19.05341960407617918, 94.79275706135230450 ) ) ;
#95309 = CARTESIAN_POINT ( 'NONE',  ( 21.55341960407610458, 5.719274019375980345, 73.95724293864769550 ) ) ;
#95310 = CARTESIAN_POINT ( 'NONE',  ( -21.53943276465977519, -0.05219959533937600094, 113.7510903946856757 ) ) ;
#95311 = CARTESIAN_POINT ( 'NONE',  ( -8.224510206698948167, 14.34966873604960824, 60.41557627198102409 ) ) ;
#95312 = CARTESIAN_POINT ( 'NONE',  ( 18.67979575497194134, -10.72451020669871369, 85.83442372801901854 ) ) ;
#95313 = CARTESIAN_POINT ( 'NONE',  ( 5.153800228976335163, 19.02544592524342804, 24.79057627198102765 ) ) ;
#95315 = CARTESIAN_POINT ( 'NONE',  ( -5.719274019375665041, -21.55341960407619695, 89.79275706135236135 ) ) ;
#95314 = CARTESIAN_POINT ( 'NONE',  ( 14.29746914071049879, -8.314922557960816363, 33.33224293864769550 ) ) ;
#95316 = CARTESIAN_POINT ( 'NONE',  ( 9.474510206698971260, -16.51473224551069308, 77.91557627198103830 ) ) ;
#95317 = CARTESIAN_POINT ( 'NONE',  ( 10.72451020669871369, 18.67979575497193778, 42.08442372801901854 ) ) ;
#95318 = CARTESIAN_POINT ( 'NONE',  ( -9.564922557960796823, -16.46253265017161027, 87.08224293864769550 ) ) ;
#95319 = CARTESIAN_POINT ( 'NONE',  ( 14.34966873604960469, 8.224510206698951720, 89.16557627198102409 ) ) ;
#95320 = CARTESIAN_POINT ( 'NONE',  ( 16.53943276465976808, -0.05219959533910856209, 63.74890960531435979 ) ) ;
#95321 = CARTESIAN_POINT ( 'NONE',  ( 0.05219959533907565091, 21.53943276465977519, 69.99890960531435269 ) ) ;
#95322 = CARTESIAN_POINT ( 'NONE',  ( -5.153800228976328057, -19.02544592524343514, 77.29057627198099567 ) ) ;
#95323 = CARTESIAN_POINT ( 'NONE',  ( 5.719274019375991003, -21.55341960407610458, 87.70724293864769550 ) ) ;
#95324 = AXIS2_PLACEMENT_3D ( 'NONE', #12933, #103939, #87760 ) ;
#95325 = CARTESIAN_POINT ( 'NONE',  ( 0.05219959533936267826, -19.03943276465977164, 75.00109039468566152 ) ) ;
#95327 = CARTESIAN_POINT ( 'NONE',  ( -4.379528057220328563, 16.55341960407611168, 70.20724293864769550 ) ) ;
#95326 = CARTESIAN_POINT ( 'NONE',  ( -19.03943276465977164, -0.05219959533935918106, 28.75109039468566507 ) ) ;
#95328 = CARTESIAN_POINT ( 'NONE',  ( 10.72451020669898902, -18.67979575497178502, 52.91557627198103830 ) ) ;
#95329 = CARTESIAN_POINT ( 'NONE',  ( -35.99626262588765968, 2.428612866367529932E-14, -8.000000000000000000 ) ) ;
#95331 = CARTESIAN_POINT ( 'NONE',  ( 17.14385361876520264, -23.59649016807270883, 146.0750000027311728 ) ) ;
#95330 = CARTESIAN_POINT ( 'NONE',  ( 8.314922557961029526, -14.29746914071037800, 100.4177570613523471 ) ) ;
#95332 = CARTESIAN_POINT ( 'NONE',  ( 9.564922557961047289, -16.46253265017146816, 100.4177570613523329 ) ) ;
#95333 = CARTESIAN_POINT ( 'NONE',  ( -16.53943276465976808, 0.05219959533911058130, 81.24890960531436690 ) ) ;
#95334 = CARTESIAN_POINT ( 'NONE',  ( -19.53091890409951858, -5.499999999999991118, 95.06097431831415179 ) ) ;
#95335 = CARTESIAN_POINT ( 'NONE',  ( 9.474510206698971260, -16.51473224551069308, 67.91557627198102409 ) ) ;
#95336 = CARTESIAN_POINT ( 'NONE',  ( -9.474510206698964154, 16.51473224551069663, 35.41557627198102409 ) ) ;
#95337 = CARTESIAN_POINT ( 'NONE',  ( 16.53943276465976808, -0.05219959533910856209, 48.74890960531435979 ) ) ;
#95338 = CARTESIAN_POINT ( 'NONE',  ( -9.474510206698964154, 16.51473224551069663, 105.4155762719810383 ) ) ;
#95340 = CARTESIAN_POINT ( 'NONE',  ( 13.89961937509977652, -13.97604488694527269, 63.12390960531435979 ) ) ;
#95339 = CARTESIAN_POINT ( 'NONE',  ( 9.474510206698729675, 16.51473224551082808, 87.08442372801900433 ) ) ;
#95341 = CARTESIAN_POINT ( 'NONE',  ( 8.224510206698742110, 14.34966873604972548, 32.08442372801901854 ) ) ;
#95342 = CARTESIAN_POINT ( 'NONE',  ( -19.05341960407611168, -5.049401038298163336, 86.45724293864769550 ) ) ;
#95343 = CARTESIAN_POINT ( 'NONE',  ( -15.72974639402197994, 15.80617190586746368, 60.62390960531437401 ) ) ;
#95344 = CARTESIAN_POINT ( 'NONE',  ( -14.29746914071037622, -8.314922557961029526, 59.16775706135234714 ) ) ;
#95345 = AXIS2_PLACEMENT_3D ( 'NONE', #186546, #171356, #79333 ) ;
#95346 = CARTESIAN_POINT ( 'NONE',  ( 19.03943276465977164, 0.05219959533936151252, 111.2510903946856757 ) ) ;
#95347 = CARTESIAN_POINT ( 'NONE',  ( 13.89961937509977652, -13.97604488694527269, 63.12390960531435979 ) ) ;
#95348 = CARTESIAN_POINT ( 'NONE',  ( 15.72974639402199770, -15.80617190586745480, 63.12390960531435979 ) ) ;
#95349 = CARTESIAN_POINT ( 'NONE',  ( -19.05341960407617563, 5.049401038297882671, 88.54275706135230450 ) ) ;
#95351 = CARTESIAN_POINT ( 'NONE',  ( 10.81492255796106328, -18.62759615963255655, 50.41775706135235424 ) ) ;
#95350 = CARTESIAN_POINT ( 'NONE',  ( -4.483927247898539470, -16.52544592524342804, 22.29057627198102765 ) ) ;
#95352 = CARTESIAN_POINT ( 'NONE',  ( -28.82186960331499037, 2.428612866367529932E-14, 144.2500000054623683 ) ) ;
#95354 = CARTESIAN_POINT ( 'NONE',  ( 0.05219959533934541429, -16.53943276465976808, 90.00109039468567573 ) ) ;
#95353 = CARTESIAN_POINT ( 'NONE',  ( -12.14591786802326823, 12.06949235617739902, 68.12609039468567573 ) ) ;
#95355 = CARTESIAN_POINT ( 'NONE',  ( -17.72696623605160227, 5.500000000000055955, 73.59811031808419557 ) ) ;
#95356 = CARTESIAN_POINT ( 'NONE',  ( -16.55341960407617563, 4.379528057220093196, 98.54275706135234714 ) ) ;
#95357 = CARTESIAN_POINT ( 'NONE',  ( 16.52544592524335698, 4.483927247898782831, 31.45942372801901854 ) ) ;
#95358 = CARTESIAN_POINT ( 'NONE',  ( -9.474510206698964154, 16.51473224551069663, 45.41557627198103120 ) ) ;
#95359 = CARTESIAN_POINT ( 'NONE',  ( -9.564922557960796823, -16.46253265017161027, 52.08224293864768839 ) ) ;
#95360 = CARTESIAN_POINT ( 'NONE',  ( 13.97604488694527802, 13.89961937509977652, 54.37390960531435979 ) ) ;
#95361 = CARTESIAN_POINT ( 'NONE',  ( 18.62759615963255655, 10.81492255796105972, 46.66775706135234714 ) ) ;
#95362 = CARTESIAN_POINT ( 'NONE',  ( 16.55341960407618274, -4.379528057220086978, 51.04275706135234714 ) ) ;
#95363 = CARTESIAN_POINT ( 'NONE',  ( -16.53943276465976808, 0.05219959533911058130, 31.24890960531435979 ) ) ;
#95364 = CARTESIAN_POINT ( 'NONE',  ( 5.049401038298161559, -19.05341960407611168, 47.70724293864770260 ) ) ;
#95365 = CARTESIAN_POINT ( 'NONE',  ( 19.02544592524343514, -5.153800228976328945, 33.54057627198102409 ) ) ;
#95366 = CARTESIAN_POINT ( 'NONE',  ( -14.34966873604972548, 8.224510206698743886, 33.33442372801900433 ) ) ;
#95367 = CARTESIAN_POINT ( 'NONE',  ( 5.153800228976615827, -19.02544592524334988, 85.20942372801900433 ) ) ;
#95368 = CARTESIAN_POINT ( 'NONE',  ( 0.05219959533910956823, 16.53943276465976808, 79.99890960531435269 ) ) ;
#95369 = CARTESIAN_POINT ( 'NONE',  ( 13.89961937509977652, -13.97604488694527269, 58.12390960531436690 ) ) ;
#95371 = DIRECTION ( 'NONE',  ( 0.000000000000000000, -0.5000000000000013323, -0.8660254037844380415 ) ) ;
#95370 = CARTESIAN_POINT ( 'NONE',  ( -9.564922557961040184, 16.46253265017147172, 92.91775706135233293 ) ) ;
#95372 = CARTESIAN_POINT ( 'NONE',  ( -18.67979575497193778, 10.72451020669871902, 83.33442372801903275 ) ) ;
#95373 = CARTESIAN_POINT ( 'NONE',  ( -4.483927247898782831, 16.52544592524335698, 57.70942372801901143 ) ) ;
#95374 = CARTESIAN_POINT ( 'NONE',  ( -17.49999999999998579, 3.345213924137300232, 24.58768623094359640 ) ) ;
#95375 = CARTESIAN_POINT ( 'NONE',  ( -21.55341960407610458, -5.719274019375992779, 46.45724293864769550 ) ) ;
#95376 = CARTESIAN_POINT ( 'NONE',  ( -16.53943276465976808, -0.05219959533934237506, 43.75109039468568284 ) ) ;
#95377 = CARTESIAN_POINT ( 'NONE',  ( -19.03943276465977164, 0.05219959533909376836, 26.24890960531435624 ) ) ;
#95378 = CARTESIAN_POINT ( 'NONE',  ( -9.564922557961040184, 16.46253265017147172, 22.91775706135233648 ) ) ;
#95379 = CARTESIAN_POINT ( 'NONE',  ( -38.00000000000000711, 2.428612866367529932E-14, -8.000000000000000000 ) ) ;
#95380 = CARTESIAN_POINT ( 'NONE',  ( -5.049401038298153566, 19.05341960407611168, 50.20724293864770260 ) ) ;
#95381 = DIRECTION ( 'NONE',  ( 1.000000000000000000, 9.445700745138859830E-17, -0.000000000000000000 ) ) ;
#95382 = CARTESIAN_POINT ( 'NONE',  ( -13.89961937509977652, 13.97604488694528158, 75.62390960531438111 ) ) ;
#95383 = CARTESIAN_POINT ( 'NONE',  ( -17.72517630440429315, 5.500000000000143885, 65.92175719257210176 ) ) ;
#95384 = PRODUCT ( 'tip', 'tip', '', ( #114950 ) ) ;
#95385 = CARTESIAN_POINT ( 'NONE',  ( -19.05341960407617563, 5.049401038297882671, 23.54275706135233648 ) ) ;
#95386 = CARTESIAN_POINT ( 'NONE',  ( -4.483927247898539470, -16.52544592524342804, 37.29057627198102409 ) ) ;
#95387 = CARTESIAN_POINT ( 'NONE',  ( 13.97604488694527802, 13.89961937509977652, 49.37390960531434558 ) ) ;
#95388 = CARTESIAN_POINT ( 'NONE',  ( 16.51473224551069308, 9.474510206698969483, 99.16557627198102409 ) ) ;
#95389 = CARTESIAN_POINT ( 'NONE',  ( -18.62759615963255300, -10.81492255796106328, 74.16775706135231871 ) ) ;
#95390 = CARTESIAN_POINT ( 'NONE',  ( -16.51473224551069308, -9.474510206698971260, 56.66557627198103120 ) ) ;
#95391 = CARTESIAN_POINT ( 'NONE',  ( -5.719274019375665041, -21.55341960407619695, 64.79275706135234714 ) ) ;
#95392 = CARTESIAN_POINT ( 'NONE',  ( 13.89961937509977652, -13.97604488694527269, 113.1239096053143527 ) ) ;
#95393 = CARTESIAN_POINT ( 'NONE',  ( 9.564922557960805705, 16.46253265017160317, 34.58224293864770260 ) ) ;
#95394 = CARTESIAN_POINT ( 'NONE',  ( -21.55341960407619339, 5.719274019375674811, 28.54275706135234358 ) ) ;
#95395 = CARTESIAN_POINT ( 'NONE',  ( 5.153800228976615827, -19.02544592524334988, 50.20942372801897591 ) ) ;
#95396 = CARTESIAN_POINT ( 'NONE',  ( 13.89961937509977652, -13.97604488694527269, 28.12390960531435624 ) ) ;
#95397 = CARTESIAN_POINT ( 'NONE',  ( 5.049401038298161559, -19.05341960407611168, 57.70724293864769550 ) ) ;
#95398 = CARTESIAN_POINT ( 'NONE',  ( 9.564922557961047289, -16.46253265017146816, 110.4177570613523471 ) ) ;
#95399 = CARTESIAN_POINT ( 'NONE',  ( -12.06949235617756955, 12.14591786802309770, 80.62390960531438111 ) ) ;
#95400 = CARTESIAN_POINT ( 'NONE',  ( -18.67979575497178146, -10.72451020669898902, 31.66557627198102054 ) ) ;
#95401 = CARTESIAN_POINT ( 'NONE',  ( -9.564922557961040184, 16.46253265017147172, 102.9177570613523329 ) ) ;
#95402 = CARTESIAN_POINT ( 'NONE',  ( -10.72451020669898014, 18.67979575497178502, 100.4155762719810241 ) ) ;
#95403 = CARTESIAN_POINT ( 'NONE',  ( 10.81492255796106328, -18.62759615963255655, 60.41775706135235424 ) ) ;
#95404 = CARTESIAN_POINT ( 'NONE',  ( 8.224510206698742110, 14.34966873604972548, 62.08442372801901143 ) ) ;
#95405 = CARTESIAN_POINT ( 'NONE',  ( -16.52544592524335698, -4.483927247898792601, 53.95942372801900433 ) ) ;
#95406 = CARTESIAN_POINT ( 'NONE',  ( 10.81492255796078972, 18.62759615963270932, 54.58224293864769550 ) ) ;
#95407 = CARTESIAN_POINT ( 'NONE',  ( -16.51473224551069308, -9.474510206698971260, 41.66557627198103120 ) ) ;
#95408 = CARTESIAN_POINT ( 'NONE',  ( 14.29746914071037800, 8.314922557961029526, 71.66775706135234714 ) ) ;
#95409 = EDGE_CURVE ( 'NONE', #171876, #41998, #109658, .T. ) ;
#95410 = CARTESIAN_POINT ( 'NONE',  ( 15.80617190586746368, 15.72974639402197994, 99.37390960531436690 ) ) ;
#95411 = CARTESIAN_POINT ( 'NONE',  ( -8.224510206698948167, 14.34966873604960824, 50.41557627198103120 ) ) ;
#95412 = CARTESIAN_POINT ( 'NONE',  ( 13.97604488694527802, 13.89961937509977652, 69.37390960531436690 ) ) ;
#95413 = CARTESIAN_POINT ( 'NONE',  ( 14.29746914071037800, 8.314922557961029526, 81.66775706135236135 ) ) ;
#95414 = CARTESIAN_POINT ( 'NONE',  ( 9.564922557961047289, -16.46253265017146816, 110.4177570613523471 ) ) ;
#95415 = CARTESIAN_POINT ( 'NONE',  ( 18.67979575497178502, 10.72451020669898547, 109.1655762719810383 ) ) ;
#95416 = CARTESIAN_POINT ( 'NONE',  ( -8.224510206698948167, 14.34966873604960824, 50.41557627198103120 ) ) ;
#95417 = ORIENTED_EDGE ( 'NONE', *, *, #171007, .F. ) ;
#95418 = CARTESIAN_POINT ( 'NONE',  ( 19.35633801406909171, -5.499999999999671374, 91.63373818172765084 ) ) ;
#95419 = CARTESIAN_POINT ( 'NONE',  ( -15.80617190586745835, -15.72974639402198527, 91.87390960531436690 ) ) ;
#95420 = ORIENTED_EDGE ( 'NONE', *, *, #154300, .F. ) ;
#95421 = CARTESIAN_POINT ( 'NONE',  ( -16.53943276465976808, 0.05219959533911058130, 26.24890960531435624 ) ) ;
#95422 = VERTEX_POINT ( 'NONE', #6140 ) ;
#95423 = CARTESIAN_POINT ( 'NONE',  ( 30.00000000000000355, -0.3535533905932703447, 5.353553390593268624 ) ) ;
#95424 = CARTESIAN_POINT ( 'NONE',  ( 21.55341960407610458, 5.719274019375980345, 103.9572429386476813 ) ) ;
#95425 = CARTESIAN_POINT ( 'NONE',  ( 19.05341960407611168, 5.049401038298154454, 108.9572429386477097 ) ) ;
#95426 = CARTESIAN_POINT ( 'NONE',  ( -21.53943276465977519, 0.05219959533907696930, 116.2489096053143669 ) ) ;
#95427 = CARTESIAN_POINT ( 'NONE',  ( -8.314922557960811034, -14.29746914071050412, 47.08224293864770260 ) ) ;
#95428 = CARTESIAN_POINT ( 'NONE',  ( -8.314922557961024197, 14.29746914071037800, 47.91775706135234714 ) ) ;
#95429 = CARTESIAN_POINT ( 'NONE',  ( 19.05341960407611168, 5.049401038298154454, 48.95724293864768129 ) ) ;
#95430 = CARTESIAN_POINT ( 'NONE',  ( -9.564922557961040184, 16.46253265017147172, 47.91775706135233293 ) ) ;
#95431 = CARTESIAN_POINT ( 'NONE',  ( 0.05219959533909260263, 19.03943276465977164, 84.99890960531436690 ) ) ;
#95432 = ADVANCED_FACE ( 'NONE', ( #162827 ), #146652, .T. ) ;
#95433 = CARTESIAN_POINT ( 'NONE',  ( -21.53943276465977519, 0.05219959533907696930, 36.24890960531435979 ) ) ;
#95434 = CARTESIAN_POINT ( 'NONE',  ( -27.86627820654446808, -25.72419401236984982, -16.61045157392797122 ) ) ;
#95435 = CARTESIAN_POINT ( 'NONE',  ( -4.483927247898782831, 16.52544592524335698, 27.70942372801901854 ) ) ;
#95436 = CARTESIAN_POINT ( 'NONE',  ( 13.89961937509957401, 13.97604488694547697, 66.87609039468567573 ) ) ;
#95437 = CARTESIAN_POINT ( 'NONE',  ( 10.72451020669898902, -18.67979575497178502, 102.9155762719810383 ) ) ;
#95438 = CARTESIAN_POINT ( 'NONE',  ( -12.14591786802309592, -12.06949235617757132, 36.87390960531435979 ) ) ;
#95439 = CARTESIAN_POINT ( 'NONE',  ( -16.51473224551069308, -9.474510206698971260, 76.66557627198103830 ) ) ;
#95440 = CARTESIAN_POINT ( 'NONE',  ( -18.67979575497178146, -10.72451020669898902, 56.66557627198103830 ) ) ;
#95442 = CARTESIAN_POINT ( 'NONE',  ( 0.05219959533934541429, -16.53943276465976808, 20.00109039468568639 ) ) ;
#95441 = CARTESIAN_POINT ( 'NONE',  ( -5.823673210054116645, -21.52544592524344225, 92.29057627198103830 ) ) ;
#95443 = CARTESIAN_POINT ( 'NONE',  ( 16.51473224551069308, 9.474510206698969483, 114.1655762719810241 ) ) ;
#95444 = CARTESIAN_POINT ( 'NONE',  ( -21.52544592524334988, -5.823673210054445271, 93.95942372801903275 ) ) ;
#95445 = CARTESIAN_POINT ( 'NONE',  ( -5.049401038298153566, 19.05341960407611168, 90.20724293864766707 ) ) ;
#95446 = CARTESIAN_POINT ( 'NONE',  ( -13.89961937509977652, 13.97604488694528158, 25.62390960531434558 ) ) ;
#95447 = CARTESIAN_POINT ( 'NONE',  ( -0.05219959533909027116, -19.03943276465977164, 77.49890960531435269 ) ) ;
#95448 = CARTESIAN_POINT ( 'NONE',  ( -12.14591786802309592, -12.06949235617757132, 106.8739096053143811 ) ) ;
#95449 = CARTESIAN_POINT ( 'NONE',  ( -5.049401038298153566, 19.05341960407611168, 60.20724293864768129 ) ) ;
#95450 = CARTESIAN_POINT ( 'NONE',  ( 16.55341960407618274, -4.379528057220086978, 26.04275706135235779 ) ) ;
#95451 = FACE_OUTER_BOUND ( 'NONE', #117455, .T. ) ;
#95452 = CARTESIAN_POINT ( 'NONE',  ( 19.03943276465977164, -0.05219959533909143690, 73.74890960531435269 ) ) ;
#95454 = CARTESIAN_POINT ( 'NONE',  ( 9.474510206698971260, -16.51473224551069308, 112.9155762719810383 ) ) ;
#95453 = CARTESIAN_POINT ( 'NONE',  ( -18.67979575497193778, 10.72451020669871902, 103.3344237280190043 ) ) ;
#95455 = CARTESIAN_POINT ( 'NONE',  ( -16.55341960407617563, 4.379528057220093196, 93.54275706135234714 ) ) ;
#95456 = CARTESIAN_POINT ( 'NONE',  ( 22.99604614807110181, -21.34824663401120759, -46.43544609871632645 ) ) ;
#95457 = CARTESIAN_POINT ( 'NONE',  ( 5.153800228976615827, -19.02544592524334988, 65.20942372801900433 ) ) ;
#95458 = CARTESIAN_POINT ( 'NONE',  ( -16.46253265017146816, -9.564922557961047289, 24.16775706135233648 ) ) ;
#95459 = LINE ( 'NONE', #141958, #72739 ) ;
#95460 = CARTESIAN_POINT ( 'NONE',  ( -0.05219959533909027116, -19.03943276465977164, 27.49890960531435624 ) ) ;
#95461 = CARTESIAN_POINT ( 'NONE',  ( -14.29746914071049879, 8.314922557960819915, 35.83224293864768839 ) ) ;
#95462 = CYLINDRICAL_SURFACE ( 'NONE', #20910, 24.30000000000003268 ) ;
#95463 = CARTESIAN_POINT ( 'NONE',  ( 0.05219959533934541429, -16.53943276465976808, 105.0010903946856757 ) ) ;
#95464 = CARTESIAN_POINT ( 'NONE',  ( 21.24746703654597724, -20.01434088805876144, -52.34924278636284356 ) ) ;
#95465 = CARTESIAN_POINT ( 'NONE',  ( 8.314922557961029526, -14.29746914071037800, 85.41775706135236135 ) ) ;
#95466 = CARTESIAN_POINT ( 'NONE',  ( -13.97604488694527625, -13.89961937509977652, 31.87390960531435979 ) ) ;
#95467 = CARTESIAN_POINT ( 'NONE',  ( 0.05219959533937995610, -21.53943276465977519, 95.00109039468568994 ) ) ;
#95468 = CARTESIAN_POINT ( 'NONE',  ( 19.02544592524334988, 5.153800228976608722, 96.45942372801897591 ) ) ;
#95469 = CARTESIAN_POINT ( 'NONE',  ( 15.80617190586769283, -15.72974639402175789, 75.62609039468567573 ) ) ;
#95470 = CARTESIAN_POINT ( 'NONE',  ( -13.89961937509957401, -13.97604488694547875, 54.37609039468565442 ) ) ;
#95471 = CARTESIAN_POINT ( 'NONE',  ( 13.97604488694527802, 13.89961937509977652, 74.37390960531436690 ) ) ;
#95472 = CARTESIAN_POINT ( 'NONE',  ( -19.03943276465977164, 0.05219959533909376836, 71.24890960531435269 ) ) ;
#95473 = CARTESIAN_POINT ( 'NONE',  ( 17.48853670773246449, 5.747243402303058524, 73.83328700250008580 ) ) ;
#95474 = CARTESIAN_POINT ( 'NONE',  ( -4.483927247898539470, -16.52544592524342804, 67.29057627198103830 ) ) ;
#95475 = CARTESIAN_POINT ( 'NONE',  ( 15.80617190586746368, 15.72974639402197994, 64.37390960531435269 ) ) ;
#95476 = CARTESIAN_POINT ( 'NONE',  ( -19.02544592524342804, 5.153800228976336051, 41.04057627198103120 ) ) ;
#95478 = CARTESIAN_POINT ( 'NONE',  ( -16.52544592524335698, -4.483927247898792601, 73.95942372801901854 ) ) ;
#95477 = CARTESIAN_POINT ( 'NONE',  ( -0.05219959533907301413, -21.53943276465977519, 82.49890960531436690 ) ) ;
#95479 = EDGE_CURVE ( 'NONE', #10184, #165187, #2864, .T. ) ;
#95480 = ORIENTED_EDGE ( 'NONE', *, *, #163889, .T. ) ;
#95482 = CARTESIAN_POINT ( 'NONE',  ( 22.81625015709510151, -31.40387420917324590, -1.924999997268813434 ) ) ;
#95481 = CARTESIAN_POINT ( 'NONE',  ( 14.34966873604960469, 8.224510206698951720, 84.16557627198103830 ) ) ;
#95483 = CARTESIAN_POINT ( 'NONE',  ( -8.314922557961024197, 14.29746914071037800, 37.91775706135235424 ) ) ;
#95484 = CARTESIAN_POINT ( 'NONE',  ( -14.34966873604960291, -8.224510206698953496, 111.6655762719810525 ) ) ;
#95485 = CARTESIAN_POINT ( 'NONE',  ( 19.05341960407617918, -5.049401038297876454, 71.04275706135234714 ) ) ;
#95486 = CARTESIAN_POINT ( 'NONE',  ( 4.379528057220339221, -16.55341960407611168, 67.70724293864769550 ) ) ;
#95487 = CARTESIAN_POINT ( 'NONE',  ( -10.72451020669870658, -18.67979575497194134, 39.58442372801901143 ) ) ;
#95489 = CARTESIAN_POINT ( 'NONE',  ( 5.719274019375991003, -21.55341960407610458, 107.7072429386476955 ) ) ;
#95488 = CARTESIAN_POINT ( 'NONE',  ( -5.153800228976328057, -19.02544592524343514, 22.29057627198102765 ) ) ;
#95490 = DIRECTION ( 'NONE',  ( 0.000000000000000000, -1.000000000000000000, 0.000000000000000000 ) ) ;
#95491 = CARTESIAN_POINT ( 'NONE',  ( -12.14591786802309592, -12.06949235617757132, 86.87390960531438111 ) ) ;
#95492 = CARTESIAN_POINT ( 'NONE',  ( 25.01910340989057246, -31.27285607038160364, -17.23782325461877107 ) ) ;
#95493 = CARTESIAN_POINT ( 'NONE',  ( -9.564922557960796823, -16.46253265017161027, 52.08224293864768839 ) ) ;
#95494 = CARTESIAN_POINT ( 'NONE',  ( 36.91746824999999177, 2.880721459617395097E-14, -5.624999997268813168 ) ) ;
#95495 = CARTESIAN_POINT ( 'NONE',  ( 13.97604488694548053, -13.89961937509957401, 80.62609039468567573 ) ) ;
#95496 = CARTESIAN_POINT ( 'NONE',  ( 10.72451020669871369, 18.67979575497193778, 42.08442372801901854 ) ) ;
#95497 = CARTESIAN_POINT ( 'NONE',  ( -5.049401038298153566, 19.05341960407611168, 75.20724293864769550 ) ) ;
#95498 = CARTESIAN_POINT ( 'NONE',  ( 13.97604488694548053, -13.89961937509957401, 60.62609039468564731 ) ) ;
#95499 = CARTESIAN_POINT ( 'NONE',  ( -16.46253265017160317, 9.564922557960807481, 45.83224293864769550 ) ) ;
#95500 = CARTESIAN_POINT ( 'NONE',  ( 16.55341960407611168, 4.379528057220329451, 58.95724293864770971 ) ) ;
#95501 = CARTESIAN_POINT ( 'NONE',  ( -16.52544592524342804, 4.483927247898546575, 61.04057627198103120 ) ) ;
#95502 = CARTESIAN_POINT ( 'NONE',  ( 19.02544592524343514, -5.153800228976328945, 78.54057627198099567 ) ) ;
#95503 = CARTESIAN_POINT ( 'NONE',  ( 15.72974639402199770, -15.80617190586745480, 103.1239096053143811 ) ) ;
#95504 = CARTESIAN_POINT ( 'NONE',  ( -9.564922557960796823, -16.46253265017161027, 72.08224293864770971 ) ) ;
#95505 = CARTESIAN_POINT ( 'NONE',  ( -15.72974639402197994, 15.80617190586746368, 85.62390960531436690 ) ) ;
#95506 = CARTESIAN_POINT ( 'NONE',  ( 10.72451020669871369, 18.67979575497193778, 107.0844237280190043 ) ) ;
#95509 = CARTESIAN_POINT ( 'NONE',  ( -14.34966873604960291, -8.224510206698953496, 91.66557627198103830 ) ) ;
#95508 = CARTESIAN_POINT ( 'NONE',  ( 0.05219959533934541429, -16.53943276465976808, 105.0010903946856757 ) ) ;
#95507 = CARTESIAN_POINT ( 'NONE',  ( -9.564922557960796823, -16.46253265017161027, 32.08224293864769550 ) ) ;
#95510 = CARTESIAN_POINT ( 'NONE',  ( 9.564922557961047289, -16.46253265017146816, 100.4177570613523329 ) ) ;
#95511 = ORIENTED_EDGE ( 'NONE', *, *, #112510, .F. ) ;
#95512 = CARTESIAN_POINT ( 'NONE',  ( -5.823673210054431948, 21.52544592524334988, 37.70942372801900433 ) ) ;
#95513 = CARTESIAN_POINT ( 'NONE',  ( 13.89961937509957401, 13.97604488694547697, 56.87609039468564731 ) ) ;
#95514 = CARTESIAN_POINT ( 'NONE',  ( -14.34966873604960291, -8.224510206698953496, 26.66557627198103475 ) ) ;
#95515 = CARTESIAN_POINT ( 'NONE',  ( -15.80617190586745835, -15.72974639402198527, 66.87390960531436690 ) ) ;
#95516 = CARTESIAN_POINT ( 'NONE',  ( -16.51473224551069308, -9.474510206698971260, 96.66557627198102409 ) ) ;
#95517 = CARTESIAN_POINT ( 'NONE',  ( -4.379528057220328563, 16.55341960407611168, 60.20724293864768839 ) ) ;
#95518 = CARTESIAN_POINT ( 'NONE',  ( 13.97604488694527802, 13.89961937509977652, 34.37390960531436690 ) ) ;
#95519 = CARTESIAN_POINT ( 'NONE',  ( -16.46253265017160317, 9.564922557960807481, 30.83224293864769550 ) ) ;
#95520 = CARTESIAN_POINT ( 'NONE',  ( -5.049401038297874678, -19.05341960407617918, 24.79275706135233648 ) ) ;
#95521 = CARTESIAN_POINT ( 'NONE',  ( 16.55341960407618274, -4.379528057220086978, 91.04275706135236135 ) ) ;
#95522 = CARTESIAN_POINT ( 'NONE',  ( -18.67979575497193778, 10.72451020669871902, 48.33442372801902565 ) ) ;
#95523 = CARTESIAN_POINT ( 'NONE',  ( -16.55341960407617563, 4.379528057220093196, 48.54275706135234714 ) ) ;
#95524 = CARTESIAN_POINT ( 'NONE',  ( -18.62759615963270932, 10.81492255796079327, 25.83224293864769194 ) ) ;
#95526 = CARTESIAN_POINT ( 'NONE',  ( 21.55341960407619695, -5.719274019375665929, 101.0427570613523756 ) ) ;
#95525 = CARTESIAN_POINT ( 'NONE',  ( -5.049401038298153566, 19.05341960407611168, 50.20724293864770260 ) ) ;
#95527 = CARTESIAN_POINT ( 'NONE',  ( 0.05219959533909260263, 19.03943276465977164, 79.99890960531436690 ) ) ;
#95528 = CARTESIAN_POINT ( 'NONE',  ( 8.314922557961029526, -14.29746914071037800, 65.41775706135234714 ) ) ;
#95529 = CARTESIAN_POINT ( 'NONE',  ( -12.14591786802309592, -12.06949235617757132, 101.8739096053143811 ) ) ;
#95530 = CARTESIAN_POINT ( 'NONE',  ( 8.224510206698742110, 14.34966873604972548, 112.0844237280190185 ) ) ;
#95531 = CARTESIAN_POINT ( 'NONE',  ( -17.97182807773875624, 5.499999999999873879, 38.53038844047286915 ) ) ;
#95534 = CARTESIAN_POINT ( 'NONE',  ( -0.05219959533909027116, -19.03943276465977164, 72.49890960531435269 ) ) ;
#95533 = CARTESIAN_POINT ( 'NONE',  ( -16.46253265017160317, 9.564922557960807481, 85.83224293864769550 ) ) ;
#95532 = CARTESIAN_POINT ( 'NONE',  ( 5.719274019375673035, 21.55341960407619339, 67.29275706135234714 ) ) ;
#95535 = CARTESIAN_POINT ( 'NONE',  ( 9.564922557960805705, 16.46253265017160317, 104.5822429386476955 ) ) ;
#95536 = CARTESIAN_POINT ( 'NONE',  ( -8.314922557960811034, -14.29746914071050412, 62.08224293864769550 ) ) ;
#95537 = CARTESIAN_POINT ( 'NONE',  ( 14.34966873604960469, 8.224510206698951720, 24.16557627198103120 ) ) ;
#95538 = CARTESIAN_POINT ( 'NONE',  ( -4.379528057220328563, 16.55341960407611168, 35.20724293864768839 ) ) ;
#95539 = CYLINDRICAL_SURFACE ( 'NONE', #112570, 37.99626262588765968 ) ;
#95540 = CARTESIAN_POINT ( 'NONE',  ( -16.51473224551082808, 9.474510206698731452, 33.33442372801899722 ) ) ;
#95541 = CARTESIAN_POINT ( 'NONE',  ( 16.46253265017160672, -9.564922557960803928, 73.33224293864769550 ) ) ;
#95542 = CARTESIAN_POINT ( 'NONE',  ( -5.049401038297874678, -19.05341960407617918, 54.79275706135234003 ) ) ;
#95543 = CARTESIAN_POINT ( 'NONE',  ( -5.950531402560715689E-15, 38.81732327939063509, -3.124999997268813168 ) ) ;
#95544 = CARTESIAN_POINT ( 'NONE',  ( -18.46320343559621691, 23.96320343559658994, 1.818019484660532870 ) ) ;
#95546 = CARTESIAN_POINT ( 'NONE',  ( -8.314922557961024197, 14.29746914071037800, 82.91775706135234714 ) ) ;
#95545 = CARTESIAN_POINT ( 'NONE',  ( 13.89961937509957401, 13.97604488694547697, 86.87609039468567573 ) ) ;
#95547 = CARTESIAN_POINT ( 'NONE',  ( 17.50000000000002132, 5.622605283950872668, 93.81207310596117566 ) ) ;
#95548 = CARTESIAN_POINT ( 'NONE',  ( 19.05341960407611168, 5.049401038298154454, 98.95724293864766707 ) ) ;
#95549 = CARTESIAN_POINT ( 'NONE',  ( -21.53943276465977519, -0.05219959533937600094, 28.75109039468567929 ) ) ;
#95550 = CARTESIAN_POINT ( 'NONE',  ( 9.564922557961047289, -16.46253265017146816, 90.41775706135234714 ) ) ;
#95552 = CARTESIAN_POINT ( 'NONE',  ( 19.02544592524343514, -5.153800228976328945, 48.54057627198103120 ) ) ;
#95551 = DIRECTION ( 'NONE',  ( -0.7071067811865463515, 0.7071067811865487940, -0.000000000000000000 ) ) ;
#95553 = CARTESIAN_POINT ( 'NONE',  ( -5.049401038298153566, 19.05341960407611168, 105.2072429386476671 ) ) ;
#95555 = CARTESIAN_POINT ( 'NONE',  ( 9.564922557960805705, 16.46253265017160317, 44.58224293864769550 ) ) ;
#95554 = CARTESIAN_POINT ( 'NONE',  ( -16.55341960407611168, -4.379528057220339221, 61.45724293864770260 ) ) ;
#95556 = CARTESIAN_POINT ( 'NONE',  ( 19.05341960407611168, 5.049401038298154454, 63.95724293864769550 ) ) ;
#95557 = CARTESIAN_POINT ( 'NONE',  ( 13.97604488694548053, -13.89961937509957401, 70.62609039468567573 ) ) ;
#95558 = CARTESIAN_POINT ( 'NONE',  ( -0.05219959533936034679, 19.03943276465977164, 27.50109039468566507 ) ) ;
#95559 = CARTESIAN_POINT ( 'NONE',  ( -19.03943276465977164, 0.05219959533909376836, 66.24890960531436690 ) ) ;
#95560 = CARTESIAN_POINT ( 'NONE',  ( 5.719274019375991003, -21.55341960407610458, 72.70724293864769550 ) ) ;
#95562 = CARTESIAN_POINT ( 'NONE',  ( 13.97604488694548053, -13.89961937509957401, 40.62609039468564731 ) ) ;
#95561 = CARTESIAN_POINT ( 'NONE',  ( 0.05219959533910956823, 16.53943276465976808, 64.99890960531435269 ) ) ;
#95563 = CARTESIAN_POINT ( 'NONE',  ( -1.135848680322148585, -6.615299585309119657, -64.43295106733368982 ) ) ;
#95564 = CARTESIAN_POINT ( 'NONE',  ( -21.53943276465977519, 0.05219959533907696930, 41.24890960531435269 ) ) ;
#95565 = CIRCLE ( 'NONE', #56924, 8.000000000000007105 ) ;
#95566 = CARTESIAN_POINT ( 'NONE',  ( -10.72451020669898014, 18.67979575497178502, 25.41557627198103120 ) ) ;
#95567 = CARTESIAN_POINT ( 'NONE',  ( -19.03943276465977164, 0.05219959533909376836, 56.24890960531435979 ) ) ;
#95568 = CARTESIAN_POINT ( 'NONE',  ( -9.474510206698964154, 16.51473224551069663, 40.41557627198103120 ) ) ;
#95569 = CARTESIAN_POINT ( 'NONE',  ( -14.34966873604960291, -8.224510206698953496, 106.6655762719810383 ) ) ;
#95570 = CARTESIAN_POINT ( 'NONE',  ( 21.55341960407610458, 5.719274019375980345, 113.9572429386477239 ) ) ;
#95571 = CARTESIAN_POINT ( 'NONE',  ( 0.05219959533909260263, 19.03943276465977164, 114.9989096053143669 ) ) ;
#95572 = CARTESIAN_POINT ( 'NONE',  ( 21.55341960407619695, -5.719274019375665929, 31.04275706135234714 ) ) ;
#95573 = CARTESIAN_POINT ( 'NONE',  ( 19.02544592524343514, -5.153800228976328945, 23.54057627198102054 ) ) ;
#95574 = CARTESIAN_POINT ( 'NONE',  ( -21.55341960407610458, -5.719274019375992779, 96.45724293864770971 ) ) ;
#95575 = CARTESIAN_POINT ( 'NONE',  ( -0.05219959533936034679, 19.03943276465977164, 42.50109039468566152 ) ) ;
#95576 = CARTESIAN_POINT ( 'NONE',  ( -0.05219959533909027116, -19.03943276465977164, 27.49890960531435624 ) ) ;
#95577 = CARTESIAN_POINT ( 'NONE',  ( 5.049401038298161559, -19.05341960407611168, 27.70724293864769550 ) ) ;
#95578 = CARTESIAN_POINT ( 'NONE',  ( 31.21487366219226445, -1.272595016298689430, -49.98150452412664180 ) ) ;
#95579 = CARTESIAN_POINT ( 'NONE',  ( 8.224510206698742110, 14.34966873604972548, 52.08442372801901854 ) ) ;
#95580 = CARTESIAN_POINT ( 'NONE',  ( -8.224510206698948167, 14.34966873604960824, 115.4155762719810241 ) ) ;
#95581 = CARTESIAN_POINT ( 'NONE',  ( 30.00000000000000000, -1.163414459189985801E-14, 92.50000000000000000 ) ) ;
#95582 = CARTESIAN_POINT ( 'NONE',  ( 16.46253265017160672, -9.564922557960803928, 68.33224293864770971 ) ) ;
#95584 = EDGE_CURVE ( 'NONE', #36546, #115704, #119367, .T. ) ;
#95583 = CARTESIAN_POINT ( 'NONE',  ( -16.52544592524342804, 4.483927247898546575, 111.0405762719810525 ) ) ;
#95585 = CARTESIAN_POINT ( 'NONE',  ( 0.05219959533907565091, 21.53943276465977519, 39.99890960531436690 ) ) ;
#95586 = CARTESIAN_POINT ( 'NONE',  ( 4.483927247898545687, 16.52544592524342804, 84.79057627198102409 ) ) ;
#95587 = CARTESIAN_POINT ( 'NONE',  ( 0.05219959533934541429, -16.53943276465976808, 40.00109039468567573 ) ) ;
#95588 = CARTESIAN_POINT ( 'NONE',  ( 5.823673210054444382, -21.52544592524334988, 85.20942372801901854 ) ) ;
#95589 = DIRECTION ( 'NONE',  ( -0.000000000000000000, 0.7071067811865467956, 0.7071067811865483499 ) ) ;
#95590 = CARTESIAN_POINT ( 'NONE',  ( 16.53943276465976808, 0.05219959533934440121, 106.2510903946856757 ) ) ;
#95591 = CARTESIAN_POINT ( 'NONE',  ( -4.379528057220328563, 16.55341960407611168, 45.20724293864769550 ) ) ;
#95592 = CARTESIAN_POINT ( 'NONE',  ( -19.03943276465977164, 0.05219959533909376836, 51.24890960531436690 ) ) ;
#95593 = CARTESIAN_POINT ( 'NONE',  ( -10.81492255796105439, 18.62759615963255655, 97.91775706135236135 ) ) ;
#95594 = CARTESIAN_POINT ( 'NONE',  ( -5.719274019375978568, 21.55341960407610458, 105.2072429386477097 ) ) ;
#95595 = CARTESIAN_POINT ( 'NONE',  ( -5.719274019375665041, -21.55341960407619695, 74.79275706135234714 ) ) ;
#95596 = CARTESIAN_POINT ( 'NONE',  ( -16.53943276465976808, -0.05219959533934237506, 38.75109039468567573 ) ) ;
#95598 = CARTESIAN_POINT ( 'NONE',  ( -0.05219959533937732626, 21.53943276465977519, 82.50109039468568994 ) ) ;
#95597 = CARTESIAN_POINT ( 'NONE',  ( 16.55341960407611168, 4.379528057220329451, 68.95724293864769550 ) ) ;
#95599 = CARTESIAN_POINT ( 'NONE',  ( -16.53943276465976808, -0.05219959533934237506, 113.7510903946856757 ) ) ;
#95600 = CARTESIAN_POINT ( 'NONE',  ( -16.81555441253555117, 7.025013491695454526, 115.6368544533426075 ) ) ;
#95601 = CARTESIAN_POINT ( 'NONE',  ( -3.573655867282028392E-15, 2.428612866367529932E-14, 139.9999999999999716 ) ) ;
#95602 = CARTESIAN_POINT ( 'NONE',  ( -16.55341960407611168, -4.379528057220339221, 41.45724293864769550 ) ) ;
#95603 = CARTESIAN_POINT ( 'NONE',  ( -8.224510206698735004, -14.34966873604973081, 79.58442372801903275 ) ) ;
#95604 = CARTESIAN_POINT ( 'NONE',  ( -5.153800228976328057, -19.02544592524343514, 82.29057627198103830 ) ) ;
#95605 = CARTESIAN_POINT ( 'NONE',  ( -9.474510206698964154, 16.51473224551069663, 105.4155762719810383 ) ) ;
#95606 = CARTESIAN_POINT ( 'NONE',  ( 10.81492255796106328, -18.62759615963255655, 105.4177570613523613 ) ) ;
#95607 = CARTESIAN_POINT ( 'NONE',  ( 14.29746914071037800, 8.314922557961029526, 101.6677570613523613 ) ) ;
#95608 = CARTESIAN_POINT ( 'NONE',  ( -4.483927247898539470, -16.52544592524342804, 67.29057627198103830 ) ) ;
#95609 = CARTESIAN_POINT ( 'NONE',  ( -9.474510206698964154, 16.51473224551069663, 85.41557627198102409 ) ) ;
#95610 = ORIENTED_EDGE ( 'NONE', *, *, #106006, .T. ) ;
#95611 = CARTESIAN_POINT ( 'NONE',  ( 12.14591786802327356, -12.06949235617739191, 25.62609039468567929 ) ) ;
#95612 = CARTESIAN_POINT ( 'NONE',  ( 19.02544592524343514, -5.153800228976328945, 23.54057627198102054 ) ) ;
#95613 = CARTESIAN_POINT ( 'NONE',  ( 5.049401038298161559, -19.05341960407611168, 92.70724293864769550 ) ) ;
#95615 = CARTESIAN_POINT ( 'NONE',  ( 36.91746825000000598, -11.99521256947793546, -1.724999997268813479 ) ) ;
#95614 = CARTESIAN_POINT ( 'NONE',  ( 4.379528057220092307, 16.55341960407617563, 27.29275706135234358 ) ) ;
#95616 = CARTESIAN_POINT ( 'NONE',  ( -9.474510206698720793, -16.51473224551083518, 19.58442372801899722 ) ) ;
#95617 = CARTESIAN_POINT ( 'NONE',  ( 12.14591786802327356, -12.06949235617739191, 90.62609039468567573 ) ) ;
#95618 = CARTESIAN_POINT ( 'NONE',  ( 16.46253265017146816, 9.564922557961045513, 101.6677570613523329 ) ) ;
#95619 = CARTESIAN_POINT ( 'NONE',  ( 9.474510206698971260, -16.51473224551069308, 32.91557627198102409 ) ) ;
#95620 = CARTESIAN_POINT ( 'NONE',  ( 0.05219959533934541429, -16.53943276465976808, 85.00109039468568994 ) ) ;
#95621 = CARTESIAN_POINT ( 'NONE',  ( -4.379528057220086978, -16.55341960407618274, 64.79275706135234714 ) ) ;
#95622 = CARTESIAN_POINT ( 'NONE',  ( 9.564922557960805705, 16.46253265017160317, 24.58224293864769194 ) ) ;
#95623 = CARTESIAN_POINT ( 'NONE',  ( -9.474510206698720793, -16.51473224551083518, 64.58442372801900433 ) ) ;
#95624 = CARTESIAN_POINT ( 'NONE',  ( 5.823673210054444382, -21.52544592524334988, 105.2094237280190328 ) ) ;
#95625 = CARTESIAN_POINT ( 'NONE',  ( 19.05341960407611168, 5.049401038298154454, 43.95724293864769550 ) ) ;
#95626 = CARTESIAN_POINT ( 'NONE',  ( -19.02544592524342804, 5.153800228976336051, 96.04057627198103830 ) ) ;
#95627 = CARTESIAN_POINT ( 'NONE',  ( -14.29746914071049879, 8.314922557960819915, 90.83224293864769550 ) ) ;
#95628 = CARTESIAN_POINT ( 'NONE',  ( -19.02544592524334988, -5.153800228976617603, 53.95942372801898301 ) ) ;
#95629 = CARTESIAN_POINT ( 'NONE',  ( 21.52544592524344225, -5.823673210054117533, 48.54057627198103120 ) ) ;
#95630 = CARTESIAN_POINT ( 'NONE',  ( 21.55341960407619695, -5.719274019375665929, 106.0427570613523471 ) ) ;
#95631 = CARTESIAN_POINT ( 'NONE',  ( 16.51473224551069308, 9.474510206698969483, 94.16557627198103830 ) ) ;
#95632 = CARTESIAN_POINT ( 'NONE',  ( 18.62759615963255655, 10.81492255796105972, 101.6677570613523613 ) ) ;
#95633 = CARTESIAN_POINT ( 'NONE',  ( 0.05219959533907565091, 21.53943276465977519, 64.99890960531435269 ) ) ;
#95634 = CARTESIAN_POINT ( 'NONE',  ( 9.474510206698971260, -16.51473224551069308, 97.91557627198102409 ) ) ;
#95635 = CARTESIAN_POINT ( 'NONE',  ( -19.02544592524334988, -5.153800228976617603, 93.95942372801900433 ) ) ;
#95636 = CARTESIAN_POINT ( 'NONE',  ( 16.46253265017160672, -9.564922557960803928, 113.3322429386476955 ) ) ;
#95637 = CARTESIAN_POINT ( 'NONE',  ( -16.46253265017146816, -9.564922557961047289, 109.1677570613523471 ) ) ;
#95638 = CARTESIAN_POINT ( 'NONE',  ( -14.34966873604960291, -8.224510206698953496, 111.6655762719810525 ) ) ;
#95639 = CARTESIAN_POINT ( 'NONE',  ( -9.564922557960796823, -16.46253265017161027, 82.08224293864768129 ) ) ;
#95640 = CARTESIAN_POINT ( 'NONE',  ( -5.823673210054116645, -21.52544592524344225, 77.29057627198102409 ) ) ;
#95641 = CARTESIAN_POINT ( 'NONE',  ( 4.379528057220092307, 16.55341960407617563, 52.29275706135236135 ) ) ;
#95642 = CARTESIAN_POINT ( 'NONE',  ( 21.52544592524334988, 5.823673210054432836, 46.45942372801901854 ) ) ;
#95643 = CARTESIAN_POINT ( 'NONE',  ( -21.55341960407619339, 5.719274019375674811, 98.54275706135234714 ) ) ;
#95644 = CARTESIAN_POINT ( 'NONE',  ( -8.314922557961024197, 14.29746914071037800, 92.91775706135236135 ) ) ;
#95645 = CARTESIAN_POINT ( 'NONE',  ( -5.153800228976328057, -19.02544592524343514, 82.29057627198103830 ) ) ;
#95646 = CARTESIAN_POINT ( 'NONE',  ( 16.52544592524342804, -4.483927247898539470, 88.54057627198103830 ) ) ;
#95647 = CARTESIAN_POINT ( 'NONE',  ( 16.52544592524342804, -4.483927247898539470, 28.54057627198103120 ) ) ;
#95648 = CARTESIAN_POINT ( 'NONE',  ( 19.05341960407617918, -5.049401038297876454, 66.04275706135233293 ) ) ;
#95649 = CARTESIAN_POINT ( 'NONE',  ( -15.72974639402176322, -15.80617190586768395, 44.37609039468567573 ) ) ;
#95650 = CARTESIAN_POINT ( 'NONE',  ( -19.03943276465977164, -0.05219959533935918106, 23.75109039468566152 ) ) ;
#95651 = CARTESIAN_POINT ( 'NONE',  ( 4.379528057220339221, -16.55341960407611168, 97.70724293864772392 ) ) ;
#95652 = CARTESIAN_POINT ( 'NONE',  ( -9.564922557960796823, -16.46253265017161027, 112.0822429386476955 ) ) ;
#95653 = CARTESIAN_POINT ( 'NONE',  ( -12.06949235617756955, 12.14591786802309770, 25.62390960531435624 ) ) ;
#95654 = CARTESIAN_POINT ( 'NONE',  ( -10.72451020669870658, -18.67979575497194134, 79.58442372801903275 ) ) ;
#95655 = CARTESIAN_POINT ( 'NONE',  ( -16.53943276465976808, -0.05219959533934237506, 53.75109039468568994 ) ) ;
#95656 = CARTESIAN_POINT ( 'NONE',  ( 12.14591786802327356, -12.06949235617739191, 100.6260903946857184 ) ) ;
#95657 = CARTESIAN_POINT ( 'NONE',  ( 15.72974639402176855, 15.80617190586768217, 56.87609039468568994 ) ) ;
#95658 = VERTEX_POINT ( 'NONE', #148675 ) ;
#95659 = CARTESIAN_POINT ( 'NONE',  ( -15.72974639402176322, -15.80617190586768395, 34.37609039468568284 ) ) ;
#95660 = CARTESIAN_POINT ( 'NONE',  ( 14.29746914071049879, -8.314922557960816363, 103.3322429386476955 ) ) ;
#95661 = EDGE_CURVE ( 'NONE', #4972, #90572, #129477, .T. ) ;
#95662 = CARTESIAN_POINT ( 'NONE',  ( 5.153800228976335163, 19.02544592524342804, 29.79057627198102409 ) ) ;
#95663 = CARTESIAN_POINT ( 'NONE',  ( 14.29746914071049879, -8.314922557960816363, 63.33224293864770260 ) ) ;
#95664 = CARTESIAN_POINT ( 'NONE',  ( -5.049401038298153566, 19.05341960407611168, 70.20724293864769550 ) ) ;
#95665 = CARTESIAN_POINT ( 'NONE',  ( -8.314922557961024197, 14.29746914071037800, 102.9177570613523756 ) ) ;
#95666 = CARTESIAN_POINT ( 'NONE',  ( 19.02544592524343514, -5.153800228976328945, 33.54057627198102409 ) ) ;
#95667 = CARTESIAN_POINT ( 'NONE',  ( 21.55341960407610458, 5.719274019375980345, 53.95724293864770260 ) ) ;
#95668 = CARTESIAN_POINT ( 'NONE',  ( -8.224510206698948167, 14.34966873604960824, 90.41557627198103830 ) ) ;
#95669 = AXIS2_PLACEMENT_3D ( 'NONE', #144376, #190895, #114028 ) ;
#95670 = CARTESIAN_POINT ( 'NONE',  ( -5.719274019375978568, 21.55341960407610458, 95.20724293864769550 ) ) ;
#95671 = CARTESIAN_POINT ( 'NONE',  ( 13.89961937509977652, -13.97604488694527269, 98.12390960531433848 ) ) ;
#95673 = CARTESIAN_POINT ( 'NONE',  ( 13.97604488694548053, -13.89961937509957401, 95.62609039468563310 ) ) ;
#95672 = CARTESIAN_POINT ( 'NONE',  ( 16.46253265017160672, -9.564922557960803928, 53.33224293864768839 ) ) ;
#95674 = EDGE_CURVE ( 'NONE', #39588, #126569, #42631, .T. ) ;
#95675 = CARTESIAN_POINT ( 'NONE',  ( -5.719274019375978568, 21.55341960407610458, 50.20724293864769550 ) ) ;
#95676 = CARTESIAN_POINT ( 'NONE',  ( -10.81492255796105439, 18.62759615963255655, 67.91775706135234714 ) ) ;
#95677 = CARTESIAN_POINT ( 'NONE',  ( -0.05219959533909027116, -19.03943276465977164, 52.49890960531436690 ) ) ;
#95678 = CARTESIAN_POINT ( 'NONE',  ( 16.51473224551069308, 9.474510206698969483, 89.16557627198103830 ) ) ;
#95679 = CARTESIAN_POINT ( 'NONE',  ( 16.55341960407618274, -4.379528057220086978, 66.04275706135236135 ) ) ;
#95680 = CARTESIAN_POINT ( 'NONE',  ( -21.55341960407619339, 5.719274019375674811, 38.54275706135234714 ) ) ;
#95681 = CARTESIAN_POINT ( 'NONE',  ( -21.52544592524334988, -5.823673210054445271, 83.95942372801900433 ) ) ;
#95682 = CARTESIAN_POINT ( 'NONE',  ( -18.62759615963270932, 10.81492255796079327, 95.83224293864770971 ) ) ;
#95684 = CARTESIAN_POINT ( 'NONE',  ( 8.224510206698742110, 14.34966873604972548, 67.08442372801901854 ) ) ;
#95683 = CARTESIAN_POINT ( 'NONE',  ( -21.52544592524334988, -5.823673210054445271, 38.95942372801901854 ) ) ;
#95685 = CARTESIAN_POINT ( 'NONE',  ( 18.67979575497178502, 10.72451020669898547, 64.16557627198102409 ) ) ;
#95686 = CARTESIAN_POINT ( 'NONE',  ( -13.89961937509957401, -13.97604488694547875, 29.37609039468565797 ) ) ;
#95688 = CARTESIAN_POINT ( 'NONE',  ( 16.55341960407611168, 4.379528057220329451, 28.95724293864769905 ) ) ;
#95687 = CARTESIAN_POINT ( 'NONE',  ( 13.89961937509977652, -13.97604488694527269, 63.12390960531435979 ) ) ;
#95689 = DIRECTION ( 'NONE',  ( -0.000000000000000000, -0.7071067811865466846, -0.7071067811865484609 ) ) ;
#95690 = CARTESIAN_POINT ( 'NONE',  ( -16.51473224551069308, -9.474510206698971260, 106.6655762719810383 ) ) ;
#95691 = LINE ( 'NONE', #80518, #89499 ) ;
#95692 = CARTESIAN_POINT ( 'NONE',  ( -13.97604488694547697, 13.89961937509957934, 78.12609039468567573 ) ) ;
#95693 = CARTESIAN_POINT ( 'NONE',  ( 18.62759615963271287, -10.81492255796078972, 58.33224293864768839 ) ) ;
#95694 = CARTESIAN_POINT ( 'NONE',  ( 4.483927247898545687, 16.52544592524342804, 39.79057627198103830 ) ) ;
#95695 = CARTESIAN_POINT ( 'NONE',  ( -19.05341960407617563, 5.049401038297882671, 113.5427570613523471 ) ) ;
#95696 = CARTESIAN_POINT ( 'NONE',  ( -5.153800228976328057, -19.02544592524343514, 32.29057627198102409 ) ) ;
#95697 = CARTESIAN_POINT ( 'NONE',  ( 16.46253265017146816, 9.564922557961045513, 106.6677570613523471 ) ) ;
#95699 = CARTESIAN_POINT ( 'NONE',  ( 16.46253265017146816, 9.564922557961045513, 66.66775706135233293 ) ) ;
#95698 = CARTESIAN_POINT ( 'NONE',  ( 18.62759615963271287, -10.81492255796078972, 93.33224293864769550 ) ) ;
#95700 = CARTESIAN_POINT ( 'NONE',  ( 8.224510206698742110, 14.34966873604972548, 82.08442372801901854 ) ) ;
#95701 = CARTESIAN_POINT ( 'NONE',  ( 19.03943276465977164, -0.05219959533909143690, 68.74890960531436690 ) ) ;
#95702 = CARTESIAN_POINT ( 'NONE',  ( 8.314922557960818139, 14.29746914071049879, 79.58224293864769550 ) ) ;
#95703 = CARTESIAN_POINT ( 'NONE',  ( -19.05341960407611168, -5.049401038298163336, 41.45724293864769550 ) ) ;
#95704 = CARTESIAN_POINT ( 'NONE',  ( 16.53943276465976808, -0.05219959533910856209, 53.74890960531437401 ) ) ;
#95705 = CARTESIAN_POINT ( 'NONE',  ( 11.74149087413294268, 36.13659316521247433, -6.347842220587802231 ) ) ;
#95706 = CARTESIAN_POINT ( 'NONE',  ( 0.2242313521320748737, 21.31285307430665554, -56.45988244333290851 ) ) ;
#95707 = CARTESIAN_POINT ( 'NONE',  ( 16.55341960407611168, 4.379528057220329451, 28.95724293864769905 ) ) ;
#95708 = CARTESIAN_POINT ( 'NONE',  ( -9.474510206698964154, 16.51473224551069663, 80.41557627198103830 ) ) ;
#95709 = CARTESIAN_POINT ( 'NONE',  ( 17.50000000000002132, 5.499999999999984013, 98.78230962303568674 ) ) ;
#95710 = CARTESIAN_POINT ( 'NONE',  ( -9.474510206698720793, -16.51473224551083518, 34.58442372801899722 ) ) ;
#95711 = CARTESIAN_POINT ( 'NONE',  ( 14.34966873604972726, -8.224510206698740333, 40.83442372801901854 ) ) ;
#95712 = VECTOR ( 'NONE', #34109, 1000.000000000000000 ) ;
#95713 = CARTESIAN_POINT ( 'NONE',  ( 5.719274019375991003, -21.55341960407610458, 67.70724293864769550 ) ) ;
#95714 = CARTESIAN_POINT ( 'NONE',  ( 5.153800228976615827, -19.02544592524334988, 25.20942372801900433 ) ) ;
#95715 = CARTESIAN_POINT ( 'NONE',  ( 16.51473224551069308, 9.474510206698969483, 79.16557627198103830 ) ) ;
#95716 = LINE ( 'NONE', #68361, #188892 ) ;
#95717 = CARTESIAN_POINT ( 'NONE',  ( 5.049401038298161559, -19.05341960407611168, 112.7072429386476813 ) ) ;
#95718 = CARTESIAN_POINT ( 'NONE',  ( 21.53943276465977519, 0.05219959533937863772, 36.25109039468567573 ) ) ;
#95719 = AXIS2_PLACEMENT_3D ( 'NONE', #1014, #27425, #122378 ) ;
#95720 = CARTESIAN_POINT ( 'NONE',  ( -16.52544592524342804, 4.483927247898546575, 106.0405762719810525 ) ) ;
#95723 = ORIENTED_EDGE ( 'NONE', *, *, #117641, .F. ) ;
#95722 = CARTESIAN_POINT ( 'NONE',  ( -13.89961937509977652, 13.97604488694528158, 75.62390960531438111 ) ) ;
#95721 = CARTESIAN_POINT ( 'NONE',  ( -10.72451020669898014, 18.67979575497178502, 100.4155762719810241 ) ) ;
#95724 = CARTESIAN_POINT ( 'NONE',  ( 18.67979575497194134, -10.72451020669871369, 25.83442372801901499 ) ) ;
#95725 = VERTEX_POINT ( 'NONE', #44475 ) ;
#95726 = CARTESIAN_POINT ( 'NONE',  ( -16.46253265017160317, 9.564922557960807481, 85.83224293864769550 ) ) ;
#95727 = CARTESIAN_POINT ( 'NONE',  ( -19.99999999999998224, -190.0000000000000000, -25.00000000000000000 ) ) ;
#95728 = CARTESIAN_POINT ( 'NONE',  ( 16.46253265017160672, -9.564922557960803928, 28.33224293864769550 ) ) ;
#95729 = CARTESIAN_POINT ( 'NONE',  ( -0.05219959533936034679, 19.03943276465977164, 112.5010903946856757 ) ) ;
#95730 = CARTESIAN_POINT ( 'NONE',  ( -36.91746825000001309, 11.99521256947798342, -7.224999997268814589 ) ) ;
#95731 = CARTESIAN_POINT ( 'NONE',  ( -14.29746914071049879, 8.314922557960819915, 110.8322429386476955 ) ) ;
#95732 = CARTESIAN_POINT ( 'NONE',  ( -21.55341960407619339, 5.719274019375674811, 88.54275706135236135 ) ) ;
#95734 = CARTESIAN_POINT ( 'NONE',  ( -21.53943276465977519, -0.05219959533937600094, 48.75109039468568284 ) ) ;
#95733 = CARTESIAN_POINT ( 'NONE',  ( 19.02544592524343514, -5.153800228976328945, 73.54057627198103830 ) ) ;
#95735 = CARTESIAN_POINT ( 'NONE',  ( -15.72974639402176322, -15.80617190586768395, 24.37609039468567573 ) ) ;
#95736 = CARTESIAN_POINT ( 'NONE',  ( 17.81289503416610742, 24.51734667627700404, 149.2999999999999545 ) ) ;
#95737 = CARTESIAN_POINT ( 'NONE',  ( 16.46253265017160672, -9.564922557960803928, 83.33224293864768129 ) ) ;
#95738 = CARTESIAN_POINT ( 'NONE',  ( 4.920875869067829811, 27.88293468337690229, 139.9999999999999147 ) ) ;
#95740 = CARTESIAN_POINT ( 'NONE',  ( -5.823673210054116645, -21.52544592524344225, 37.29057627198102409 ) ) ;
#95739 = CARTESIAN_POINT ( 'NONE',  ( 0.05219959533934541429, -16.53943276465976808, 45.00109039468568284 ) ) ;
#95741 = CARTESIAN_POINT ( 'NONE',  ( -5.719274019375665041, -21.55341960407619695, 74.79275706135234714 ) ) ;
#95742 = DIRECTION ( 'NONE',  ( -1.000000000000000000, 5.392603844284257652E-33, -0.000000000000000000 ) ) ;
#95743 =( BOUNDED_CURVE ( )  B_SPLINE_CURVE ( 2, ( #90664, #25038, #180724, #163538, #89682 ),
 .UNSPECIFIED., .F., .F. ) 
 B_SPLINE_CURVE_WITH_KNOTS ( ( 3, 2, 3 ),
 ( 0.6000000000000000888, 0.6199999999999999956, 0.6253070713679935722 ),
 .UNSPECIFIED. ) 
 CURVE ( )  GEOMETRIC_REPRESENTATION_ITEM ( )  RATIONAL_B_SPLINE_CURVE ( ( 0.9999999999999997780, 0.9510565162951537532, 1.000000000000000000, 0.9870126719490075473, 0.9809178115826312494 ) ) 
 REPRESENTATION_ITEM ( '' )  );
#95744 = CARTESIAN_POINT ( 'NONE',  ( 5.049401038297881783, 19.05341960407617563, 107.2927570613523187 ) ) ;
#95745 = CARTESIAN_POINT ( 'NONE',  ( 19.05341960407611168, 5.049401038298154454, 53.95724293864770260 ) ) ;
#95746 = CARTESIAN_POINT ( 'NONE',  ( 19.02544592524343514, -5.153800228976328945, 88.54057627198102409 ) ) ;
#95747 = CARTESIAN_POINT ( 'NONE',  ( -12.14591786802309592, -12.06949235617757132, 101.8739096053143811 ) ) ;
#95748 = CARTESIAN_POINT ( 'NONE',  ( -16.55341960407611168, -4.379528057220339221, 106.4572429386477097 ) ) ;
#95749 = CARTESIAN_POINT ( 'NONE',  ( -5.153800228976328057, -19.02544592524343514, 107.2905762719810383 ) ) ;
#95750 = CARTESIAN_POINT ( 'NONE',  ( -14.29746914071037622, -8.314922557961029526, 84.16775706135234714 ) ) ;
#95752 = CARTESIAN_POINT ( 'NONE',  ( 0.05219959533909260263, 19.03943276465977164, 59.99890960531436690 ) ) ;
#95751 = CARTESIAN_POINT ( 'NONE',  ( -12.06949235617756955, 12.14591786802309770, 60.62390960531437401 ) ) ;
#95753 = CARTESIAN_POINT ( 'NONE',  ( -15.80617190586768217, 15.72974639402176855, 83.12609039468568994 ) ) ;
#95754 = CARTESIAN_POINT ( 'NONE',  ( -21.53943276465977519, -0.05219959533937600094, 73.75109039468567573 ) ) ;
#95755 = CARTESIAN_POINT ( 'NONE',  ( 0.05219959533936267826, -19.03943276465977164, 95.00109039468567573 ) ) ;
#95756 = CARTESIAN_POINT ( 'NONE',  ( 16.52544592524342804, -4.483927247898539470, 58.54057627198103120 ) ) ;
#95757 = CARTESIAN_POINT ( 'NONE',  ( 18.67979575497178502, 10.72451020669898547, 109.1655762719810383 ) ) ;
#95758 = CARTESIAN_POINT ( 'NONE',  ( 10.72451020669898902, -18.67979575497178502, 62.91557627198102409 ) ) ;
#95759 = CARTESIAN_POINT ( 'NONE',  ( -19.97888994334924817, -34.65319547504297759, 0.000000000000000000 ) ) ;
#95760 = CARTESIAN_POINT ( 'NONE',  ( -8.906447517083060816, 27.41122689804195645, 141.8500000054623911 ) ) ;
#95761 = CARTESIAN_POINT ( 'NONE',  ( -16.46253265017160317, 9.564922557960807481, 70.83224293864770971 ) ) ;
#95762 = CARTESIAN_POINT ( 'NONE',  ( 4.379528057220339221, -16.55341960407611168, 42.70724293864770260 ) ) ;
#95763 = CARTESIAN_POINT ( 'NONE',  ( 16.55341960407611168, 4.379528057220329451, 23.95724293864769550 ) ) ;
#95764 = CARTESIAN_POINT ( 'NONE',  ( -14.34966873604972548, 8.224510206698743886, 78.33442372801901854 ) ) ;
#95765 = CARTESIAN_POINT ( 'NONE',  ( -13.97604488694547697, 13.89961937509957934, 43.12609039468566152 ) ) ;
#95766 = CARTESIAN_POINT ( 'NONE',  ( 37.99999999999999289, 2.893978650043524126E-14, -9.000000000000001776 ) ) ;
#95767 = CARTESIAN_POINT ( 'NONE',  ( 16.46253265017160672, -9.564922557960803928, 98.33224293864769550 ) ) ;
#95768 = CARTESIAN_POINT ( 'NONE',  ( 16.52544592524342804, -4.483927247898539470, 58.54057627198103120 ) ) ;
#95770 = CARTESIAN_POINT ( 'NONE',  ( -19.03943276465977164, 0.05219959533909376836, 111.2489096053143669 ) ) ;
#95769 = CARTESIAN_POINT ( 'NONE',  ( 16.19135201231366139, -7.376712067591918220, 102.3131914594797252 ) ) ;
#95772 = VERTEX_POINT ( 'NONE', #87979 ) ;
#95771 = CARTESIAN_POINT ( 'NONE',  ( -21.55341960407610458, -5.719274019375992779, 51.45724293864770260 ) ) ;
#95773 = CARTESIAN_POINT ( 'NONE',  ( 4.379528057220339221, -16.55341960407611168, 102.7072429386476955 ) ) ;
#95774 = CARTESIAN_POINT ( 'NONE',  ( -4.483927247898782831, 16.52544592524335698, 52.70942372801902565 ) ) ;
#95775 = CARTESIAN_POINT ( 'NONE',  ( -0.05219959533910754901, -16.53943276465976808, 77.49890960531433848 ) ) ;
#95776 = EDGE_CURVE ( 'NONE', #73688, #179909, #145398, .T. ) ;
#95777 = CARTESIAN_POINT ( 'NONE',  ( -19.46398650005389896, 5.499999999999950262, 65.18269651486376404 ) ) ;
#95778 = CARTESIAN_POINT ( 'NONE',  ( -0.05219959533936034679, 19.03943276465977164, 82.50109039468567573 ) ) ;
#95779 = CARTESIAN_POINT ( 'NONE',  ( -9.474510206698964154, 16.51473224551069663, 115.4155762719810241 ) ) ;
#95780 = CARTESIAN_POINT ( 'NONE',  ( -22.81625015709510507, 31.40387420917330275, -7.424999997268812990 ) ) ;
#95781 = CARTESIAN_POINT ( 'NONE',  ( -28.82186960331499037, 2.428612866367529932E-14, 142.0000000000000000 ) ) ;
#95783 = CARTESIAN_POINT ( 'NONE',  ( -14.34966873604960291, -8.224510206698953496, 26.66557627198103475 ) ) ;
#95782 = CARTESIAN_POINT ( 'NONE',  ( -12.14591786802326823, 12.06949235617739902, 28.12609039468568284 ) ) ;
#95784 = CARTESIAN_POINT ( 'NONE',  ( -5.823673210054116645, -21.52544592524344225, 52.29057627198102409 ) ) ;
#95785 = CARTESIAN_POINT ( 'NONE',  ( 5.153800228976615827, -19.02544592524334988, 90.20942372801900433 ) ) ;
#95786 = CARTESIAN_POINT ( 'NONE',  ( -5.823673210054116645, -21.52544592524344225, 42.29057627198103120 ) ) ;
#95787 = CARTESIAN_POINT ( 'NONE',  ( -15.80617190586768217, 15.72974639402176855, 88.12609039468570415 ) ) ;
#95788 = CARTESIAN_POINT ( 'NONE',  ( 9.349452323154965327, -36.27485578735120697, -31.39434858484990798 ) ) ;
#95789 = CARTESIAN_POINT ( 'NONE',  ( 14.29746914071037800, 8.314922557961029526, 36.66775706135234714 ) ) ;
#95791 = CARTESIAN_POINT ( 'NONE',  ( 16.51473224551069308, 9.474510206698969483, 84.16557627198102409 ) ) ;
#95790 = CARTESIAN_POINT ( 'NONE',  ( 13.89961937509977652, -13.97604488694527269, 43.12390960531434558 ) ) ;
#95792 = CARTESIAN_POINT ( 'NONE',  ( -5.049401038298153566, 19.05341960407611168, 35.20724293864768839 ) ) ;
#95794 = ADVANCED_FACE ( 'NONE', ( #107115 ), #75787, .F. ) ;
#95793 = CARTESIAN_POINT ( 'NONE',  ( 4.483927247898545687, 16.52544592524342804, 99.79057627198103830 ) ) ;
#95795 = CARTESIAN_POINT ( 'NONE',  ( -13.89961937509977652, 13.97604488694528158, 100.6239096053143669 ) ) ;
#95796 = ORIENTED_EDGE ( 'NONE', *, *, #45960, .F. ) ;
#95797 = CARTESIAN_POINT ( 'NONE',  ( 16.55341960407618274, -4.379528057220086978, 56.04275706135235424 ) ) ;
#95798 = CARTESIAN_POINT ( 'NONE',  ( 21.53943276465977519, -0.05219959533907433946, 93.74890960531436690 ) ) ;
#95799 = CARTESIAN_POINT ( 'NONE',  ( 13.89961937509977652, -13.97604488694527269, 38.12390960531436690 ) ) ;
#95801 = CARTESIAN_POINT ( 'NONE',  ( -10.72451020669870658, -18.67979575497194134, 29.58442372801901854 ) ) ;
#95800 = CARTESIAN_POINT ( 'NONE',  ( -16.51473224551082808, 9.474510206698731452, 73.33442372801900433 ) ) ;
#95802 = CARTESIAN_POINT ( 'NONE',  ( -13.89961937509977652, 13.97604488694528158, 65.62390960531436690 ) ) ;
#95803 = CARTESIAN_POINT ( 'NONE',  ( -19.05341960407611168, -5.049401038298163336, 101.4572429386476955 ) ) ;
#95804 = ORIENTED_EDGE ( 'NONE', *, *, #138549, .F. ) ;
#95805 = CARTESIAN_POINT ( 'NONE',  ( 16.52544592524335698, 4.483927247898782831, 36.45942372801901143 ) ) ;
#95806 = CARTESIAN_POINT ( 'NONE',  ( -10.81492255796105439, 18.62759615963255655, 22.91775706135235069 ) ) ;
#95809 = CARTESIAN_POINT ( 'NONE',  ( -19.03943276465977164, -0.05219959533935918106, 78.75109039468567573 ) ) ;
#95808 = CARTESIAN_POINT ( 'NONE',  ( 19.03943276465977164, -0.05219959533909143690, 98.74890960531436690 ) ) ;
#95807 = CARTESIAN_POINT ( 'NONE',  ( -8.224510206698948167, 14.34966873604960824, 110.4155762719810383 ) ) ;
#95810 = CARTESIAN_POINT ( 'NONE',  ( 15.72974639402199770, -15.80617190586745480, 88.12390960531436690 ) ) ;
#95811 = CARTESIAN_POINT ( 'NONE',  ( 0.05219959533910956823, 16.53943276465976808, 39.99890960531436690 ) ) ;
#95812 = CARTESIAN_POINT ( 'NONE',  ( 19.03943276465977164, 0.05219959533936151252, 21.25109039468565797 ) ) ;
#95813 = CARTESIAN_POINT ( 'NONE',  ( 16.55341960407618274, -4.379528057220086978, 76.04275706135237556 ) ) ;
#95814 = CARTESIAN_POINT ( 'NONE',  ( 5.153800228976335163, 19.02544592524342804, 99.79057627198102409 ) ) ;
#95815 = CARTESIAN_POINT ( 'NONE',  ( -0.05219959533909027116, -19.03943276465977164, 47.49890960531435979 ) ) ;
#95816 = AXIS2_PLACEMENT_3D ( 'NONE', #174230, #17558, #21528 ) ;
#95817 = CARTESIAN_POINT ( 'NONE',  ( 21.55341960407619695, -5.719274019375665929, 56.04275706135235424 ) ) ;
#95818 = CARTESIAN_POINT ( 'NONE',  ( 21.53943276465977519, 0.05219959533937863772, 66.25109039468567573 ) ) ;
#95819 = CARTESIAN_POINT ( 'NONE',  ( 19.02544592524343514, -5.153800228976328945, 68.54057627198103830 ) ) ;
#95820 = CARTESIAN_POINT ( 'NONE',  ( -15.80617190586768217, 15.72974639402176855, 48.12609039468568284 ) ) ;
#95821 = CARTESIAN_POINT ( 'NONE',  ( -9.564922557961040184, 16.46253265017147172, 87.91775706135233293 ) ) ;
#95822 = CARTESIAN_POINT ( 'NONE',  ( -9.564922557960796823, -16.46253265017161027, 47.08224293864769550 ) ) ;
#95823 = CARTESIAN_POINT ( 'NONE',  ( 0.05219959533934541429, -16.53943276465976808, 90.00109039468567573 ) ) ;
#95824 = CARTESIAN_POINT ( 'NONE',  ( -5.049401038298153566, 19.05341960407611168, 65.20724293864765286 ) ) ;
#95825 = CARTESIAN_POINT ( 'NONE',  ( -19.02544592524342804, 5.153800228976336051, 116.0405762719810383 ) ) ;
#95827 = EDGE_CURVE ( 'NONE', #149451, #199515, #29391, .T. ) ;
#95826 = CARTESIAN_POINT ( 'NONE',  ( -9.564922557960796823, -16.46253265017161027, 52.08224293864768839 ) ) ;
#95828 = CARTESIAN_POINT ( 'NONE',  ( -15.80617190586745835, -15.72974639402198527, 91.87390960531436690 ) ) ;
#95829 = CARTESIAN_POINT ( 'NONE',  ( -4.379528057220086978, -16.55341960407618274, 79.79275706135236135 ) ) ;
#95830 = CARTESIAN_POINT ( 'NONE',  ( -24.22576942085221674, 7.195495839727391818, 170.3116806589316354 ) ) ;
#95831 = CARTESIAN_POINT ( 'NONE',  ( -16.46253265017146816, -9.564922557961047289, 34.16775706135233293 ) ) ;
#95832 = CARTESIAN_POINT ( 'NONE',  ( -13.89961937509977652, 13.97604488694528158, 70.62390960531432427 ) ) ;
#95833 = CARTESIAN_POINT ( 'NONE',  ( -4.379528057220328563, 16.55341960407611168, 60.20724293864768839 ) ) ;
#95834 = CARTESIAN_POINT ( 'NONE',  ( 16.53943276465976808, -0.05219959533910856209, 93.74890960531436690 ) ) ;
#95835 = CARTESIAN_POINT ( 'NONE',  ( -9.474510206698964154, 16.51473224551069663, 105.4155762719810383 ) ) ;
#95836 = CARTESIAN_POINT ( 'NONE',  ( -13.89961937509977652, 13.97604488694528158, 95.62390960531436690 ) ) ;
#95837 = CARTESIAN_POINT ( 'NONE',  ( -21.52544592524334988, -5.823673210054445271, 43.95942372801902565 ) ) ;
#95838 = CARTESIAN_POINT ( 'NONE',  ( -9.474510206698964154, 16.51473224551069663, 110.4155762719810383 ) ) ;
#95839 = CARTESIAN_POINT ( 'NONE',  ( 18.67979575497194134, -10.72451020669871369, 110.8344237280190043 ) ) ;
#95840 = CARTESIAN_POINT ( 'NONE',  ( -12.06949235617739369, -12.14591786802326823, 79.37609039468567573 ) ) ;
#95841 = CARTESIAN_POINT ( 'NONE',  ( 5.823673210054444382, -21.52544592524334988, 40.20942372801901854 ) ) ;
#95842 = CARTESIAN_POINT ( 'NONE',  ( -9.474510206698964154, 16.51473224551069663, 110.4155762719810383 ) ) ;
#95843 = CARTESIAN_POINT ( 'NONE',  ( -5.823673210054116645, -21.52544592524344225, 97.29057627198105251 ) ) ;
#95844 = CARTESIAN_POINT ( 'NONE',  ( 4.379528057220339221, -16.55341960407611168, 57.70724293864770260 ) ) ;
#95845 = CARTESIAN_POINT ( 'NONE',  ( -13.89961937509977652, 13.97604488694528158, 55.62390960531434558 ) ) ;
#95846 = CARTESIAN_POINT ( 'NONE',  ( 16.53943276465976808, -0.05219959533910856209, 83.74890960531435269 ) ) ;
#95847 = CARTESIAN_POINT ( 'NONE',  ( -10.72451020669898014, 18.67979575497178502, 40.41557627198103120 ) ) ;
#95848 = CARTESIAN_POINT ( 'NONE',  ( 19.03943276465977164, 0.05219959533936151252, 46.25109039468566863 ) ) ;
#95849 = CARTESIAN_POINT ( 'NONE',  ( -5.153800228976328057, -19.02544592524343514, 22.29057627198102765 ) ) ;
#95850 = ORIENTED_EDGE ( 'NONE', *, *, #11874, .T. ) ;
#95851 = CARTESIAN_POINT ( 'NONE',  ( -4.483927247898782831, 16.52544592524335698, 67.70942372801901854 ) ) ;
#95852 = CARTESIAN_POINT ( 'NONE',  ( -5.049401038298153566, 19.05341960407611168, 70.20724293864769550 ) ) ;
#95853 = CARTESIAN_POINT ( 'NONE',  ( -8.571926809382601320, -26.38167802310801591, 141.2750000027311899 ) ) ;
#95854 = CARTESIAN_POINT ( 'NONE',  ( -12.06949235617756955, 12.14591786802309770, 85.62390960531436690 ) ) ;
#95855 = CARTESIAN_POINT ( 'NONE',  ( 18.62759615963271287, -10.81492255796078972, 43.33224293864769550 ) ) ;
#95856 = ORIENTED_EDGE ( 'NONE', *, *, #170997, .F. ) ;
#95857 = CARTESIAN_POINT ( 'NONE',  ( 8.224510206698742110, 14.34966873604972548, 112.0844237280190185 ) ) ;
#95858 = CARTESIAN_POINT ( 'NONE',  ( -4.379528057220086978, -16.55341960407618274, 19.79275706135235069 ) ) ;
#95859 = CARTESIAN_POINT ( 'NONE',  ( 5.823673210054444382, -21.52544592524334988, 80.20942372801901854 ) ) ;
#95860 = CARTESIAN_POINT ( 'NONE',  ( -9.474510206698964154, 16.51473224551069663, 85.41557627198102409 ) ) ;
#95861 = CARTESIAN_POINT ( 'NONE',  ( 15.80617190586746368, 15.72974639402197994, 99.37390960531436690 ) ) ;
#95862 = CARTESIAN_POINT ( 'NONE',  ( -8.224510206698735004, -14.34966873604973081, 49.58442372801901143 ) ) ;
#95863 = CARTESIAN_POINT ( 'NONE',  ( 13.89961937509977652, -13.97604488694527269, 33.12390960531434558 ) ) ;
#95864 = AXIS2_PLACEMENT_3D ( 'NONE', #9041, #85865, #8020 ) ;
#95865 = CARTESIAN_POINT ( 'NONE',  ( 4.379528057220092307, 16.55341960407617563, 37.29275706135235424 ) ) ;
#95866 = CARTESIAN_POINT ( 'NONE',  ( -13.89961937509957401, -13.97604488694547875, 99.37609039468567573 ) ) ;
#95867 = CARTESIAN_POINT ( 'NONE',  ( -10.81492255796078084, -18.62759615963271287, 87.08224293864769550 ) ) ;
#95868 = CARTESIAN_POINT ( 'NONE',  ( 5.153800228976615827, -19.02544592524334988, 60.20942372801899012 ) ) ;
#95869 = CARTESIAN_POINT ( 'NONE',  ( 19.52837319214027545, -5.499999999999890754, 87.10471352585537375 ) ) ;
#95870 = CARTESIAN_POINT ( 'NONE',  ( 18.62759615963271287, -10.81492255796078972, 98.33224293864769550 ) ) ;
#95871 = CARTESIAN_POINT ( 'NONE',  ( 25.64061671795035124, 10.58440545630783269, 139.9999999999999716 ) ) ;
#95872 = CARTESIAN_POINT ( 'NONE',  ( 13.89961937509977652, -13.97604488694527269, 73.12390960531436690 ) ) ;
#95873 = CARTESIAN_POINT ( 'NONE',  ( -4.379528057220086978, -16.55341960407618274, 39.79275706135235424 ) ) ;
#95874 = DIRECTION ( 'NONE',  ( -0.000000000000000000, -0.000000000000000000, -1.000000000000000000 ) ) ;
#95875 = CARTESIAN_POINT ( 'NONE',  ( -9.474510206698720793, -16.51473224551083518, 59.58442372801900433 ) ) ;
#95877 = CARTESIAN_POINT ( 'NONE',  ( 12.06949235617757843, -12.14591786802309237, 68.12390960531436690 ) ) ;
#95876 = CARTESIAN_POINT ( 'NONE',  ( -5.719274019375978568, 21.55341960407610458, 115.2072429386476955 ) ) ;
#95878 = CARTESIAN_POINT ( 'NONE',  ( 5.049401038298161559, -19.05341960407611168, 72.70724293864768129 ) ) ;
#95880 = CARTESIAN_POINT ( 'NONE',  ( 16.46253265017146816, 9.564922557961045513, 36.66775706135233293 ) ) ;
#95879 = CARTESIAN_POINT ( 'NONE',  ( 14.29746914071037800, 8.314922557961029526, 31.66775706135234358 ) ) ;
#95881 = CARTESIAN_POINT ( 'NONE',  ( -15.80617190586768217, 15.72974639402176855, 53.12609039468568284 ) ) ;
#95882 = CARTESIAN_POINT ( 'NONE',  ( 5.049401038297881783, 19.05341960407617563, 112.2927570613523471 ) ) ;
#95883 = CARTESIAN_POINT ( 'NONE',  ( -5.049401038298153566, 19.05341960407611168, 60.20724293864768129 ) ) ;
#95884 = CARTESIAN_POINT ( 'NONE',  ( 16.46253265017146816, 9.564922557961045513, 86.66775706135233293 ) ) ;
#95885 = CARTESIAN_POINT ( 'NONE',  ( 10.81492255796106328, -18.62759615963255655, 90.41775706135236135 ) ) ;
#95886 = CARTESIAN_POINT ( 'NONE',  ( 13.89961937509957401, 13.97604488694547697, 61.87609039468566863 ) ) ;
#95887 = CARTESIAN_POINT ( 'NONE',  ( -16.46253265017160317, 9.564922557960807481, 30.83224293864769550 ) ) ;
#95888 = CARTESIAN_POINT ( 'NONE',  ( 0.05219959533907565091, 21.53943276465977519, 54.99890960531435269 ) ) ;
#95890 = CARTESIAN_POINT ( 'NONE',  ( -16.51473224551082808, 9.474510206698731452, 68.33442372801900433 ) ) ;
#95889 = CARTESIAN_POINT ( 'NONE',  ( 4.483927247898545687, 16.52544592524342804, 64.79057627198103830 ) ) ;
#95891 = CARTESIAN_POINT ( 'NONE',  ( -18.09918380851993192, -5.500000000000014211, 101.4861830733561163 ) ) ;
#95892 = CARTESIAN_POINT ( 'NONE',  ( 13.97604488694548053, -13.89961937509957401, 30.62609039468566863 ) ) ;
#95893 = CARTESIAN_POINT ( 'NONE',  ( 0.05219959533934541429, -16.53943276465976808, 95.00109039468568994 ) ) ;
#95894 = CARTESIAN_POINT ( 'NONE',  ( 16.52544592524342804, -4.483927247898539470, 48.54057627198103120 ) ) ;
#95896 = CARTESIAN_POINT ( 'NONE',  ( -8.571926809382601320, -26.38167802310801591, 139.2750000027311899 ) ) ;
#95895 = CARTESIAN_POINT ( 'NONE',  ( -0.05219959533937732626, 21.53943276465977519, 92.50109039468567573 ) ) ;
#95897 = CARTESIAN_POINT ( 'NONE',  ( -18.67979575497178146, -10.72451020669898902, 91.66557627198103830 ) ) ;
#95898 = CARTESIAN_POINT ( 'NONE',  ( 5.153800228976335163, 19.02544592524342804, 49.79057627198100988 ) ) ;
#95899 = CARTESIAN_POINT ( 'NONE',  ( 18.67979575497194134, -10.72451020669871369, 65.83442372801900433 ) ) ;
#95900 = CARTESIAN_POINT ( 'NONE',  ( -9.564922557960796823, -16.46253265017161027, 47.08224293864769550 ) ) ;
#95901 = CARTESIAN_POINT ( 'NONE',  ( -16.46253265017160317, 9.564922557960807481, 65.83224293864769550 ) ) ;
#95902 = CARTESIAN_POINT ( 'NONE',  ( 16.53943276465976808, -0.05219959533910856209, 108.7489096053143669 ) ) ;
#95903 = CARTESIAN_POINT ( 'NONE',  ( 5.049401038298161559, -19.05341960407611168, 112.7072429386476813 ) ) ;
#95904 = CARTESIAN_POINT ( 'NONE',  ( -12.06949235617756955, 12.14591786802309770, 50.62390960531435979 ) ) ;
#95905 = CARTESIAN_POINT ( 'NONE',  ( -9.564922557960796823, -16.46253265017161027, 32.08224293864769550 ) ) ;
#95906 = CARTESIAN_POINT ( 'NONE',  ( -16.52544592524342804, 4.483927247898546575, 81.04057627198102409 ) ) ;
#95907 = CARTESIAN_POINT ( 'NONE',  ( -10.81492255796078084, -18.62759615963271287, 92.08224293864769550 ) ) ;
#95908 = CARTESIAN_POINT ( 'NONE',  ( -15.72974639402176322, -15.80617190586768395, 39.37609039468567573 ) ) ;
#95909 = CARTESIAN_POINT ( 'NONE',  ( 1.500000000004064082, 7.599999999999568878, -62.20201607440122871 ) ) ;
#95910 = CARTESIAN_POINT ( 'NONE',  ( 8.314922557961029526, -14.29746914071037800, 40.41775706135234714 ) ) ;
#95911 = CARTESIAN_POINT ( 'NONE',  ( -10.81492255796078084, -18.62759615963271287, 82.08224293864768129 ) ) ;
#95912 = CARTESIAN_POINT ( 'NONE',  ( -19.03943276465977164, -0.05219959533935918106, 18.75109039468567218 ) ) ;
#95913 = CARTESIAN_POINT ( 'NONE',  ( 0.05219959533909260263, 19.03943276465977164, 99.99890960531436690 ) ) ;
#95914 = CARTESIAN_POINT ( 'NONE',  ( 5.719274019375673035, 21.55341960407619339, 42.29275706135235424 ) ) ;
#95915 = CARTESIAN_POINT ( 'NONE',  ( -0.05219959533907301413, -21.53943276465977519, 27.49890960531435269 ) ) ;
#95916 = CARTESIAN_POINT ( 'NONE',  ( -4.483927247898782831, 16.52544592524335698, 107.7094237280190328 ) ) ;
#95918 = CARTESIAN_POINT ( 'NONE',  ( 5.719274019375673035, 21.55341960407619339, 82.29275706135234714 ) ) ;
#95917 = CARTESIAN_POINT ( 'NONE',  ( 15.80617190586769283, -15.72974639402175789, 55.62609039468568284 ) ) ;
#95919 = CARTESIAN_POINT ( 'NONE',  ( 16.51473224551083163, -9.474510206698727899, 25.83442372801900078 ) ) ;
#95920 = CARTESIAN_POINT ( 'NONE',  ( -12.14591786802326823, 12.06949235617739902, 93.12609039468568994 ) ) ;
#95921 = CARTESIAN_POINT ( 'NONE',  ( 18.62759615963255655, 10.81492255796105972, 36.66775706135234714 ) ) ;
#95922 = CARTESIAN_POINT ( 'NONE',  ( 9.564922557960805705, 16.46253265017160317, 49.58224293864770260 ) ) ;
#95923 = CARTESIAN_POINT ( 'NONE',  ( -10.72451020669870658, -18.67979575497194134, 104.5844237280190185 ) ) ;
#95924 = CARTESIAN_POINT ( 'NONE',  ( -16.51473224551069308, -9.474510206698971260, 111.6655762719810383 ) ) ;
#95925 = CARTESIAN_POINT ( 'NONE',  ( -10.81492255796078084, -18.62759615963271287, 107.0822429386476955 ) ) ;
#95926 = CARTESIAN_POINT ( 'NONE',  ( -15.72974639402197994, 15.80617190586746368, 55.62390960531436690 ) ) ;
#95928 = CARTESIAN_POINT ( 'NONE',  ( -10.72451020669898014, 18.67979575497178502, 70.41557627198102409 ) ) ;
#95927 = CARTESIAN_POINT ( 'NONE',  ( 11.30153831258473573, -180.0000000000000284, -4.999999999999999112 ) ) ;
#95930 = CARTESIAN_POINT ( 'NONE',  ( 12.06949235617757843, -12.14591786802309237, 68.12390960531436690 ) ) ;
#95929 = CARTESIAN_POINT ( 'NONE',  ( -4.379528057220086978, -16.55341960407618274, 49.79275706135234714 ) ) ;
#95931 = DIRECTION ( 'NONE',  ( 0.000000000000000000, 0.000000000000000000, -1.000000000000000000 ) ) ;
#95932 = CARTESIAN_POINT ( 'NONE',  ( -19.05341960407617563, 5.049401038297882671, 93.54275706135234714 ) ) ;
#95933 = DIRECTION ( 'NONE',  ( -0.1039620511844979445, 0.1039620511844979445, -0.9891328443778539814 ) ) ;
#95934 = CARTESIAN_POINT ( 'NONE',  ( -14.34966873604972548, 8.224510206698743886, 28.33442372801902209 ) ) ;
#95935 = CARTESIAN_POINT ( 'NONE',  ( 21.53943276465977519, -0.05219959533907433946, 93.74890960531436690 ) ) ;
#95936 = CARTESIAN_POINT ( 'NONE',  ( -5.719274019375978568, 21.55341960407610458, 75.20724293864769550 ) ) ;
#95937 = CARTESIAN_POINT ( 'NONE',  ( -5.049401038298153566, 19.05341960407611168, 115.2072429386477097 ) ) ;
#95938 = CARTESIAN_POINT ( 'NONE',  ( -8.314922557961024197, 14.29746914071037800, 62.91775706135236135 ) ) ;
#95939 = CARTESIAN_POINT ( 'NONE',  ( -19.02544592524342804, 5.153800228976336051, 71.04057627198099567 ) ) ;
#95941 = CARTESIAN_POINT ( 'NONE',  ( 9.564922557961047289, -16.46253265017146816, 105.4177570613523471 ) ) ;
#95940 = CARTESIAN_POINT ( 'NONE',  ( -10.81492255796105439, 18.62759615963255655, 37.91775706135235424 ) ) ;
#95942 = EDGE_CURVE ( 'NONE', #41053, #8238, #154836, .T. ) ;
#95943 = CARTESIAN_POINT ( 'NONE',  ( -13.97604488694527625, -13.89961937509977652, 101.8739096053143811 ) ) ;
#95944 = CARTESIAN_POINT ( 'NONE',  ( -13.89961937509977652, 13.97604488694528158, 90.62390960531432427 ) ) ;
#95945 = CARTESIAN_POINT ( 'NONE',  ( 0.05219959533907565091, 21.53943276465977519, 94.99890960531436690 ) ) ;
#95946 = CARTESIAN_POINT ( 'NONE',  ( 13.89961937509977652, -13.97604488694527269, 53.12390960531434558 ) ) ;
#95947 = PLANE ( 'NONE',  #95998 ) ;
#95949 = B_SPLINE_CURVE_WITH_KNOTS ( 'NONE', 3,
 ( #5750, #52257, #135120, #41104, #86595, #8766, #10773, #54266, #102768, #72437, #134114, #40084, #100752, #7742, #38101, #9771, #148278, #149278, #57275, #70435, #69428, #22932, #101763, #146258, #132101, #55260 ),
 .UNSPECIFIED., .F., .F.,
 ( 4, 2, 2, 2, 2, 2, 2, 2, 2, 2, 2, 2, 4 ),
 ( 1.969502666007334865E-07, 0.0004009345686709441360, 0.0008016721870752876794, 0.001603147423883954708, 0.002404622660692621629, 0.003206097897501288766, 0.004007573134309955903, 0.004408310752714287087, 0.004809048371118616536, 0.005209785989522947719, 0.005610523607927278902, 0.006011261226331608351, 0.006411998844735939534 ),
 .UNSPECIFIED. ) ;
#95948 = CARTESIAN_POINT ( 'NONE',  ( 14.29746914071049879, -8.314922557960816363, 73.33224293864769550 ) ) ;
#95950 = CARTESIAN_POINT ( 'NONE',  ( -19.03943276465977164, 0.05219959533909376836, 111.2489096053143669 ) ) ;
#95951 = CARTESIAN_POINT ( 'NONE',  ( 15.62200626734387754, -14.69813070946463718, -56.36792940895625748 ) ) ;
#95952 = CARTESIAN_POINT ( 'NONE',  ( 10.72451020669898902, -18.67979575497178502, 107.9155762719810241 ) ) ;
#95953 = CARTESIAN_POINT ( 'NONE',  ( -19.05341960407617563, 5.049401038297882671, 68.54275706135230450 ) ) ;
#95954 = CARTESIAN_POINT ( 'NONE',  ( 18.62759615963271287, -10.81492255796078972, 23.33224293864769194 ) ) ;
#95955 = CARTESIAN_POINT ( 'NONE',  ( -19.05341960407611168, -5.049401038298163336, 21.45724293864768839 ) ) ;
#95956 = CARTESIAN_POINT ( 'NONE',  ( 18.62759615963271287, -10.81492255796078972, 58.33224293864768839 ) ) ;
#95957 = AXIS2_PLACEMENT_3D ( 'NONE', #146270, #68434, #69440 ) ;
#95958 = CARTESIAN_POINT ( 'NONE',  ( -16.51473224551069308, -9.474510206698971260, 101.6655762719810241 ) ) ;
#95959 = CARTESIAN_POINT ( 'NONE',  ( 15.72974639402176855, 15.80617190586768217, 81.87609039468568994 ) ) ;
#95960 = CARTESIAN_POINT ( 'NONE',  ( -9.474510206698964154, 16.51473224551069663, 55.41557627198103120 ) ) ;
#95961 = CARTESIAN_POINT ( 'NONE',  ( -12.06949235617756955, 12.14591786802309770, 85.62390960531436690 ) ) ;
#95962 = CARTESIAN_POINT ( 'NONE',  ( 4.483927247898790824, -16.52544592524335698, 35.20942372801901854 ) ) ;
#95963 = CARTESIAN_POINT ( 'NONE',  ( 0.05219959533937995610, -21.53943276465977519, 60.00109039468568284 ) ) ;
#95964 = ORIENTED_EDGE ( 'NONE', *, *, #53248, .T. ) ;
#95965 = CARTESIAN_POINT ( 'NONE',  ( 19.05341960407617918, -5.049401038297876454, 26.04275706135233293 ) ) ;
#95966 = CARTESIAN_POINT ( 'NONE',  ( 16.51473224551083163, -9.474510206698727899, 80.83442372801899012 ) ) ;
#95967 = CARTESIAN_POINT ( 'NONE',  ( -16.46253265017146816, -9.564922557961047289, 44.16775706135232582 ) ) ;
#95968 = CARTESIAN_POINT ( 'NONE',  ( 18.22780087662121673, 5.500000000000056843, 88.98459894673892734 ) ) ;
#95969 = CARTESIAN_POINT ( 'NONE',  ( -18.62759615963255300, -10.81492255796106328, 34.16775706135234714 ) ) ;
#95970 = CIRCLE ( 'NONE', #137835, 1.000000000000000888 ) ;
#95971 = CARTESIAN_POINT ( 'NONE',  ( -19.49671883438229614, -5.499999999999982236, 44.89279849105685116 ) ) ;
#95972 = CARTESIAN_POINT ( 'NONE',  ( -9.474510206698720793, -16.51473224551083518, 29.58442372801900433 ) ) ;
#95973 = CARTESIAN_POINT ( 'NONE',  ( -19.02544592524342804, 5.153800228976336051, 51.04057627198103120 ) ) ;
#95974 = CARTESIAN_POINT ( 'NONE',  ( 16.46253265017146816, 9.564922557961045513, 31.66775706135232937 ) ) ;
#95975 = CARTESIAN_POINT ( 'NONE',  ( 4.483927247898790824, -16.52544592524335698, 105.2094237280190328 ) ) ;
#95977 = CARTESIAN_POINT ( 'NONE',  ( 21.53943276465977519, 0.05219959533937863772, 91.25109039468568994 ) ) ;
#95976 = CARTESIAN_POINT ( 'NONE',  ( -19.03943276465977164, 0.05219959533909376836, 111.2489096053143669 ) ) ;
#95978 = CARTESIAN_POINT ( 'NONE',  ( -5.950531402560715689E-15, 38.81732327939063509, -9.124999997268815832 ) ) ;
#95979 = CARTESIAN_POINT ( 'NONE',  ( -17.50000000000014921, -3.417042746626747896, 34.82619603767538052 ) ) ;
#95980 = CARTESIAN_POINT ( 'NONE',  ( -5.719274019375665041, -21.55341960407619695, 89.79275706135236135 ) ) ;
#95981 = CARTESIAN_POINT ( 'NONE',  ( 0.000000000000000000, -64.82615989628266107, -25.00000000000000000 ) ) ;
#95982 = CARTESIAN_POINT ( 'NONE',  ( 19.05341960407611168, 5.049401038298154454, 93.95724293864769550 ) ) ;
#95983 = CARTESIAN_POINT ( 'NONE',  ( -1.497147075633523894, -30.58708291193884676, -50.73425184351846440 ) ) ;
#95984 = CARTESIAN_POINT ( 'NONE',  ( -19.03943276465977164, 0.05219959533909376836, 56.24890960531435979 ) ) ;
#95985 = CARTESIAN_POINT ( 'NONE',  ( -18.67979575497178146, -10.72451020669898902, 56.66557627198103830 ) ) ;
#95986 = CARTESIAN_POINT ( 'NONE',  ( -14.34966873604972548, 8.224510206698743886, 113.3344237280190328 ) ) ;
#95988 = CARTESIAN_POINT ( 'NONE',  ( 0.05219959533909260263, 19.03943276465977164, 94.99890960531436690 ) ) ;
#95987 = CARTESIAN_POINT ( 'NONE',  ( 8.314922557960818139, 14.29746914071049879, 94.58224293864769550 ) ) ;
#95989 = CARTESIAN_POINT ( 'NONE',  ( 13.97604488694548053, -13.89961937509957401, 25.62609039468566507 ) ) ;
#95990 = CARTESIAN_POINT ( 'NONE',  ( 8.224510206698953496, -14.34966873604960469, 107.9155762719810241 ) ) ;
#95991 = CARTESIAN_POINT ( 'NONE',  ( 10.81492255796106328, -18.62759615963255655, 60.41775706135235424 ) ) ;
#95992 = CARTESIAN_POINT ( 'NONE',  ( -8.224510206698735004, -14.34966873604973081, 104.5844237280190185 ) ) ;
#95993 = CARTESIAN_POINT ( 'NONE',  ( 19.05341960407617918, -5.049401038297876454, 71.04275706135234714 ) ) ;
#95994 = DIRECTION ( 'NONE',  ( 0.000000000000000000, 0.7071067811865467956, 0.7071067811865483499 ) ) ;
#95995 = CARTESIAN_POINT ( 'NONE',  ( 19.03943276465977164, -0.05219959533909143690, 113.7489096053143669 ) ) ;
#95996 = CARTESIAN_POINT ( 'NONE',  ( -4.379528057220328563, 16.55341960407611168, 70.20724293864769550 ) ) ;
#95997 = CARTESIAN_POINT ( 'NONE',  ( -19.02544592524334988, -5.153800228976617603, 53.95942372801898301 ) ) ;
#95998 = AXIS2_PLACEMENT_3D ( 'NONE', #67595, #144432, #6911 ) ;
#95999 = CARTESIAN_POINT ( 'NONE',  ( -16.51473224551069308, -9.474510206698971260, 56.66557627198103120 ) ) ;
#96000 = CARTESIAN_POINT ( 'NONE',  ( -12.14591786802309592, -12.06949235617757132, 61.87390960531436690 ) ) ;
#96001 = CARTESIAN_POINT ( 'NONE',  ( 5.049401038297881783, 19.05341960407617563, 97.29275706135233293 ) ) ;
#96002 = CARTESIAN_POINT ( 'NONE',  ( -18.62759615963270932, 10.81492255796079327, 30.83224293864770260 ) ) ;
#96003 = ORIENTED_EDGE ( 'NONE', *, *, #20112, .F. ) ;
#96004 = CARTESIAN_POINT ( 'NONE',  ( -14.29746914071049879, 8.314922557960819915, 95.83224293864770971 ) ) ;
#96005 = CARTESIAN_POINT ( 'NONE',  ( -17.49999999999999645, -5.500000000000000888, 29.20309617465828467 ) ) ;
#96007 = CARTESIAN_POINT ( 'NONE',  ( 15.80617190586746368, 15.72974639402197994, 59.37390960531436690 ) ) ;
#96006 = CARTESIAN_POINT ( 'NONE',  ( -5.049401038298153566, 19.05341960407611168, 60.20724293864768129 ) ) ;
#96008 = CARTESIAN_POINT ( 'NONE',  ( 9.564922557960805705, 16.46253265017160317, 44.58224293864769550 ) ) ;
#96010 = CARTESIAN_POINT ( 'NONE',  ( 19.02544592524343514, -5.153800228976328945, 78.54057627198099567 ) ) ;
#96009 = CARTESIAN_POINT ( 'NONE',  ( -8.224510206698735004, -14.34966873604973081, 94.58442372801901854 ) ) ;
#96011 = CARTESIAN_POINT ( 'NONE',  ( -0.05219959533936034679, 19.03943276465977164, 47.50109039468566863 ) ) ;
#96012 = CARTESIAN_POINT ( 'NONE',  ( -0.05219959533937732626, 21.53943276465977519, 82.50109039468568994 ) ) ;
#96013 = CARTESIAN_POINT ( 'NONE',  ( 18.67979575497178502, 10.72451020669898547, 54.16557627198103120 ) ) ;
#96014 = CARTESIAN_POINT ( 'NONE',  ( 16.46253265017160672, -9.564922557960803928, 108.3322429386476955 ) ) ;
#96015 = CARTESIAN_POINT ( 'NONE',  ( -13.89961937509977652, 13.97604488694528158, 25.62390960531434558 ) ) ;
#96016 = CARTESIAN_POINT ( 'NONE',  ( -16.53943276465976808, -0.05219959533934237506, 93.75109039468567573 ) ) ;
#96017 = CARTESIAN_POINT ( 'NONE',  ( -5.049401038297874678, -19.05341960407617918, 104.7927570613523471 ) ) ;
#96018 = CARTESIAN_POINT ( 'NONE',  ( -16.51473224551069308, -9.474510206698971260, 21.66557627198102765 ) ) ;
#96019 = CARTESIAN_POINT ( 'NONE',  ( 19.39056639909674118, 5.500000000000052403, 78.28948781074343799 ) ) ;
#96020 = CARTESIAN_POINT ( 'NONE',  ( 18.62759615963255655, 10.81492255796105972, 101.6677570613523613 ) ) ;
#96021 = CARTESIAN_POINT ( 'NONE',  ( -12.14591786802309592, -12.06949235617757132, 56.87390960531436690 ) ) ;
#96022 = CARTESIAN_POINT ( 'NONE',  ( 4.483927247898545687, 16.52544592524342804, 64.79057627198103830 ) ) ;
#96023 = CARTESIAN_POINT ( 'NONE',  ( 21.53943276465977519, -0.05219959533907433946, 93.74890960531436690 ) ) ;
#96024 = CARTESIAN_POINT ( 'NONE',  ( 5.719274019375991003, -21.55341960407610458, 87.70724293864769550 ) ) ;
#96025 = CARTESIAN_POINT ( 'NONE',  ( 17.40805194822031865, -6.112264579159335298, 98.33371272510615313 ) ) ;
#96026 = CARTESIAN_POINT ( 'NONE',  ( -5.719274019375978568, 21.55341960407610458, 30.20724293864769550 ) ) ;
#96027 = CARTESIAN_POINT ( 'NONE',  ( -0.05219959533934338120, 16.53943276465976808, 62.50109039468568284 ) ) ;
#96028 = CARTESIAN_POINT ( 'NONE',  ( 4.483927247898545687, 16.52544592524342804, 84.79057627198102409 ) ) ;
#96029 = CARTESIAN_POINT ( 'NONE',  ( 19.05341960407611168, 5.049401038298154454, 43.95724293864769550 ) ) ;
#96030 = CARTESIAN_POINT ( 'NONE',  ( 34.87614885797842845, -6.488895056989331778, 41.23117619273099876 ) ) ;
#96031 = CARTESIAN_POINT ( 'NONE',  ( 16.55341960407618274, -4.379528057220086978, 91.04275706135236135 ) ) ;
#96032 = CARTESIAN_POINT ( 'NONE',  ( 0.05219959533937995610, -21.53943276465977519, 40.00109039468567573 ) ) ;
#96033 = CARTESIAN_POINT ( 'NONE',  ( 16.46253265017160672, -9.564922557960803928, 83.33224293864768129 ) ) ;
#96034 = CARTESIAN_POINT ( 'NONE',  ( -21.52544592524334988, -5.823673210054445271, 73.95942372801901854 ) ) ;
#96035 = DIRECTION ( 'NONE',  ( 0.000000000000000000, 0.000000000000000000, 1.000000000000000000 ) ) ;
#96036 = CARTESIAN_POINT ( 'NONE',  ( -13.89961937509977652, 13.97604488694528158, 25.62390960531434558 ) ) ;
#96037 = VERTEX_POINT ( 'NONE', #91933 ) ;
#96038 = CARTESIAN_POINT ( 'NONE',  ( 21.52544592524334988, 5.823673210054432836, 56.45942372801902565 ) ) ;
#96040 = CARTESIAN_POINT ( 'NONE',  ( 16.46253265017160672, -9.564922557960803928, 23.33224293864769194 ) ) ;
#96039 = CARTESIAN_POINT ( 'NONE',  ( -16.51473224551069308, -9.474510206698971260, 36.66557627198102409 ) ) ;
#96041 = CARTESIAN_POINT ( 'NONE',  ( 5.153800228976335163, 19.02544592524342804, 94.79057627198103830 ) ) ;
#96042 = CARTESIAN_POINT ( 'NONE',  ( -0.05219959533936034679, 19.03943276465977164, 72.50109039468566152 ) ) ;
#96043 = CARTESIAN_POINT ( 'NONE',  ( -15.80617190586768217, 15.72974639402176855, 23.12609039468567573 ) ) ;
#96044 = CARTESIAN_POINT ( 'NONE',  ( 9.564922557961047289, -16.46253265017146816, 65.41775706135233293 ) ) ;
#96045 = CARTESIAN_POINT ( 'NONE',  ( 19.02544592524343514, -5.153800228976328945, 43.54057627198103120 ) ) ;
#96046 = CARTESIAN_POINT ( 'NONE',  ( -14.29746914071037622, -8.314922557961029526, 104.1677570613523471 ) ) ;
#96047 = CARTESIAN_POINT ( 'NONE',  ( -9.474510206698720793, -16.51473224551083518, 64.58442372801900433 ) ) ;
#96048 = CARTESIAN_POINT ( 'NONE',  ( -8.314922557960811034, -14.29746914071050412, 32.08224293864769550 ) ) ;
#96049 = CARTESIAN_POINT ( 'NONE',  ( -16.46253265017146816, -9.564922557961047289, 49.16775706135233293 ) ) ;
#96050 = CARTESIAN_POINT ( 'NONE',  ( -13.97604488694527625, -13.89961937509977652, 81.87390960531436690 ) ) ;
#96051 = CARTESIAN_POINT ( 'NONE',  ( 10.81492255796106328, -18.62759615963255655, 95.41775706135234714 ) ) ;
#96052 = CARTESIAN_POINT ( 'NONE',  ( 18.62759615963255655, 10.81492255796105972, 101.6677570613523613 ) ) ;
#96053 = CARTESIAN_POINT ( 'NONE',  ( -26.99873734152897242, 22.49873734152939520, 8.889087296526001936 ) ) ;
#96054 = CARTESIAN_POINT ( 'NONE',  ( -0.05219959533937732626, 21.53943276465977519, 82.50109039468568994 ) ) ;
#96055 = CARTESIAN_POINT ( 'NONE',  ( 16.55341960407618274, -4.379528057220086978, 26.04275706135235779 ) ) ;
#96056 = CARTESIAN_POINT ( 'NONE',  ( 19.03943276465977164, -0.05219959533909143690, 88.74890960531436690 ) ) ;
#96057 = CARTESIAN_POINT ( 'NONE',  ( -30.00000000000000355, 0.3535533905932712884, 5.353553390593269512 ) ) ;
#96058 = CARTESIAN_POINT ( 'NONE',  ( 16.51473224551069308, 9.474510206698969483, 79.16557627198103830 ) ) ;
#96059 = CARTESIAN_POINT ( 'NONE',  ( -17.40861289039008497, 6.110651285853115233, 98.62767529172569425 ) ) ;
#96060 = CARTESIAN_POINT ( 'NONE',  ( -19.03943276465977164, -0.05219959533935918106, 68.75109039468566152 ) ) ;
#96061 = CARTESIAN_POINT ( 'NONE',  ( 16.51473224551069308, 9.474510206698969483, 104.1655762719810241 ) ) ;
#96062 = CARTESIAN_POINT ( 'NONE',  ( 10.81492255796106328, -18.62759615963255655, 100.4177570613523471 ) ) ;
#96063 = CARTESIAN_POINT ( 'NONE',  ( 4.483927247898545687, 16.52544592524342804, 104.7905762719810241 ) ) ;
#96064 = CARTESIAN_POINT ( 'NONE',  ( -10.72451020669898014, 18.67979575497178502, 50.41557627198103120 ) ) ;
#96065 = CARTESIAN_POINT ( 'NONE',  ( 15.72974639402199770, -15.80617190586745480, 43.12390960531435269 ) ) ;
#96066 = CARTESIAN_POINT ( 'NONE',  ( -8.224510206698948167, 14.34966873604960824, 110.4155762719810383 ) ) ;
#96067 = CARTESIAN_POINT ( 'NONE',  ( -1.203758653825231395, -8.516083024820099823, -62.01440738234572336 ) ) ;
#96068 = CARTESIAN_POINT ( 'NONE',  ( -9.564922557961040184, 16.46253265017147172, 57.91775706135233293 ) ) ;
#96069 = CARTESIAN_POINT ( 'NONE',  ( -14.34966873604960291, -8.224510206698953496, 26.66557627198103475 ) ) ;
#96070 = CARTESIAN_POINT ( 'NONE',  ( 16.51473224551069308, 9.474510206698969483, 104.1655762719810241 ) ) ;
#96071 = CARTESIAN_POINT ( 'NONE',  ( 21.55341960407619695, -5.719274019375665929, 81.04275706135236135 ) ) ;
#96072 = CARTESIAN_POINT ( 'NONE',  ( 0.05219959533907565091, 21.53943276465977519, 74.99890960531435269 ) ) ;
#96073 = B_SPLINE_CURVE_WITH_KNOTS ( 'NONE', 3,
 ( #51709, #20369, #111394, #66874, #81042, #126552, #175063, #36529 ),
 .UNSPECIFIED., .F., .F.,
 ( 4, 2, 2, 4 ),
 ( -1.451984513606386853E-05, 0.002415095736453700456, 0.003629903527248606616, 0.004844711318043512342 ),
 .UNSPECIFIED. ) ;
#96074 = CARTESIAN_POINT ( 'NONE',  ( -18.62759615963255300, -10.81492255796106328, 44.16775706135234714 ) ) ;
#96075 = CARTESIAN_POINT ( 'NONE',  ( -18.62759615963270932, 10.81492255796079327, 90.83224293864769550 ) ) ;
#96076 = CARTESIAN_POINT ( 'NONE',  ( -21.52544592524334988, -5.823673210054445271, 48.95942372801902565 ) ) ;
#96077 = CARTESIAN_POINT ( 'NONE',  ( 13.89961937509977652, -13.97604488694527269, 28.12390960531435624 ) ) ;
#96078 = CARTESIAN_POINT ( 'NONE',  ( 13.97604488694527802, 13.89961937509977652, 79.37390960531435269 ) ) ;
#96079 = CARTESIAN_POINT ( 'NONE',  ( -16.53943276465976808, -0.05219959533934237506, 78.75109039468568994 ) ) ;
#96080 = CARTESIAN_POINT ( 'NONE',  ( 16.55341960407611168, 4.379528057220329451, 108.9572429386476955 ) ) ;
#96081 = CARTESIAN_POINT ( 'NONE',  ( -0.05219959533909027116, -19.03943276465977164, 102.4989096053143669 ) ) ;
#96082 = CARTESIAN_POINT ( 'NONE',  ( 0.05219959533910956823, 16.53943276465976808, 49.99890960531437401 ) ) ;
#96083 = CARTESIAN_POINT ( 'NONE',  ( -16.52544592524335698, -4.483927247898792601, 108.9594237280190185 ) ) ;
#96084 = CARTESIAN_POINT ( 'NONE',  ( 13.97604488694527802, 13.89961937509977652, 49.37390960531434558 ) ) ;
#96085 = CARTESIAN_POINT ( 'NONE',  ( -5.049401038298153566, 19.05341960407611168, 30.20724293864768839 ) ) ;
#96086 = CARTESIAN_POINT ( 'NONE',  ( -15.72974639402197994, 15.80617190586746368, 40.62390960531435269 ) ) ;
#96087 = CARTESIAN_POINT ( 'NONE',  ( -13.89961937509957401, -13.97604488694547875, 29.37609039468565797 ) ) ;
#96090 = CARTESIAN_POINT ( 'NONE',  ( -16.53943276465976808, 0.05219959533911058130, 41.24890960531435269 ) ) ;
#96089 = CARTESIAN_POINT ( 'NONE',  ( -16.52216118717207394, -7.221426719304522734, 41.07599021046991794 ) ) ;
#96088 = AXIS2_PLACEMENT_3D ( 'NONE', #5479, #67162, #68154 ) ;
#96091 = CARTESIAN_POINT ( 'NONE',  ( -18.67979575497193778, 10.72451020669871902, 48.33442372801902565 ) ) ;
#96092 = CARTESIAN_POINT ( 'NONE',  ( 0.05219959533909260263, 19.03943276465977164, 114.9989096053143669 ) ) ;
#96093 = CARTESIAN_POINT ( 'NONE',  ( 12.14591786802327356, -12.06949235617739191, 60.62609039468567573 ) ) ;
#96094 = CARTESIAN_POINT ( 'NONE',  ( -13.97604488694547697, 13.89961937509957934, 68.12609039468563310 ) ) ;
#96095 = CARTESIAN_POINT ( 'NONE',  ( 12.14591786802309770, 12.06949235617756955, 24.37390960531435979 ) ) ;
#96096 = CARTESIAN_POINT ( 'NONE',  ( -4.483927247898782831, 16.52544592524335698, 112.7094237280190328 ) ) ;
#96097 = CARTESIAN_POINT ( 'NONE',  ( -19.05341960407611168, -5.049401038298163336, 41.45724293864769550 ) ) ;
#96098 = CARTESIAN_POINT ( 'NONE',  ( -16.46253265017160317, 9.564922557960807481, 65.83224293864769550 ) ) ;
#96099 = CARTESIAN_POINT ( 'NONE',  ( 0.05219959533909260263, 19.03943276465977164, 29.99890960531435979 ) ) ;
#96100 = CARTESIAN_POINT ( 'NONE',  ( -5.823673210054431948, 21.52544592524334988, 27.70942372801901854 ) ) ;
#96101 = CARTESIAN_POINT ( 'NONE',  ( 16.46253265017160672, -9.564922557960803928, 48.33224293864769550 ) ) ;
#96102 = CARTESIAN_POINT ( 'NONE',  ( -6.206452982517636663, -6.630588440586430821, -61.89901439314702003 ) ) ;
#96103 = CARTESIAN_POINT ( 'NONE',  ( -9.474510206698964154, 16.51473224551069663, 45.41557627198103120 ) ) ;
#96104 = CARTESIAN_POINT ( 'NONE',  ( -19.02544592524342804, 5.153800228976336051, 116.0405762719810383 ) ) ;
#96106 = CARTESIAN_POINT ( 'NONE',  ( -0.05219959533910754901, -16.53943276465976808, 107.4989096053143669 ) ) ;
#96105 = CARTESIAN_POINT ( 'NONE',  ( -5.823673210054431948, 21.52544592524334988, 62.70942372801902565 ) ) ;
#96107 = CARTESIAN_POINT ( 'NONE',  ( -9.474510206698964154, 16.51473224551069663, 110.4155762719810383 ) ) ;
#96108 = CARTESIAN_POINT ( 'NONE',  ( 14.34966873604972726, -8.224510206698740333, 80.83442372801901854 ) ) ;
#96109 = CARTESIAN_POINT ( 'NONE',  ( 15.80617190586769283, -15.72974639402175789, 90.62609039468567573 ) ) ;
#96110 = VECTOR ( 'NONE', #151594, 1000.000000000000000 ) ;
#96111 = CARTESIAN_POINT ( 'NONE',  ( -4.379528057220086978, -16.55341960407618274, 49.79275706135234714 ) ) ;
#96112 = CARTESIAN_POINT ( 'NONE',  ( -13.89961937509977652, 13.97604488694528158, 90.62390960531432427 ) ) ;
#96113 = CARTESIAN_POINT ( 'NONE',  ( -8.314922557961024197, 14.29746914071037800, 42.91775706135235424 ) ) ;
#96114 = CARTESIAN_POINT ( 'NONE',  ( 4.483927247898790824, -16.52544592524335698, 25.20942372801901854 ) ) ;
#96115 = CARTESIAN_POINT ( 'NONE',  ( 12.06949235617739724, 12.14591786802326823, 101.8760903946857042 ) ) ;
#96116 = CARTESIAN_POINT ( 'NONE',  ( 9.564922557961047289, -16.46253265017146816, 110.4177570613523471 ) ) ;
#96117 = CARTESIAN_POINT ( 'NONE',  ( -18.62759615963270932, 10.81492255796079327, 105.8322429386476955 ) ) ;
#96119 = CARTESIAN_POINT ( 'NONE',  ( 19.03943276465977164, 0.05219959533936151252, 101.2510903946856757 ) ) ;
#96118 = CARTESIAN_POINT ( 'NONE',  ( 8.224510206698953496, -14.34966873604960469, 107.9155762719810241 ) ) ;
#96120 = CARTESIAN_POINT ( 'NONE',  ( -16.53943276465976808, -0.05219959533934237506, 73.75109039468567573 ) ) ;
#96121 = CARTESIAN_POINT ( 'NONE',  ( 21.84611564451295962, 8.148379233837022895, 169.4346228884802485 ) ) ;
#96122 = CARTESIAN_POINT ( 'NONE',  ( 5.049401038297881783, 19.05341960407617563, 72.29275706135234714 ) ) ;
#96123 = CARTESIAN_POINT ( 'NONE',  ( 12.14591786802309770, 12.06949235617756955, 39.37390960531436690 ) ) ;
#96124 = CARTESIAN_POINT ( 'NONE',  ( 14.29746914071049879, -8.314922557960816363, 38.33224293864768839 ) ) ;
#96125 = CARTESIAN_POINT ( 'NONE',  ( 12.06949235617757843, -12.14591786802309237, 93.12390960531436690 ) ) ;
#96127 = CARTESIAN_POINT ( 'NONE',  ( -16.21995358207303894, 7.366697692864242697, 89.93551001512156517 ) ) ;
#96126 = CARTESIAN_POINT ( 'NONE',  ( 19.05341960407617918, -5.049401038297876454, 31.04275706135232227 ) ) ;
#96128 = CARTESIAN_POINT ( 'NONE',  ( -5.719274019375665041, -21.55341960407619695, 34.79275706135235424 ) ) ;
#96129 = CARTESIAN_POINT ( 'NONE',  ( 19.05341960407617918, -5.049401038297876454, 96.04275706135231871 ) ) ;
#96130 = CYLINDRICAL_SURFACE ( 'NONE', #43783, 61.99999999999998579 ) ;
#96131 = CARTESIAN_POINT ( 'NONE',  ( -9.564922557960796823, -16.46253265017161027, 92.08224293864769550 ) ) ;
#96132 = CARTESIAN_POINT ( 'NONE',  ( -19.03943276465977164, 0.05219959533909376836, 91.24890960531436690 ) ) ;
#96133 = CARTESIAN_POINT ( 'NONE',  ( -21.55341960407610458, -5.719274019375992779, 56.45724293864768839 ) ) ;
#96134 = CARTESIAN_POINT ( 'NONE',  ( 14.34966873604960469, 8.224510206698951720, 89.16557627198102409 ) ) ;
#96135 = CARTESIAN_POINT ( 'NONE',  ( -13.89961937509977652, 13.97604488694528158, 70.62390960531432427 ) ) ;
#96136 = CARTESIAN_POINT ( 'NONE',  ( -5.153800228976328057, -19.02544592524343514, 27.29057627198103120 ) ) ;
#96137 = CARTESIAN_POINT ( 'NONE',  ( -0.05219959533937732626, 21.53943276465977519, 42.50109039468567573 ) ) ;
#96138 = CARTESIAN_POINT ( 'NONE',  ( 18.62759615963255655, 10.81492255796105972, 81.66775706135236135 ) ) ;
#96139 = CARTESIAN_POINT ( 'NONE',  ( 5.153800228976335163, 19.02544592524342804, 59.79057627198100988 ) ) ;
#96140 = CARTESIAN_POINT ( 'NONE',  ( 4.483927247898790824, -16.52544592524335698, 85.20942372801901854 ) ) ;
#96141 = CARTESIAN_POINT ( 'NONE',  ( -18.62759615963255300, -10.81492255796106328, 34.16775706135234714 ) ) ;
#96142 = CARTESIAN_POINT ( 'NONE',  ( 18.62759615963255655, 10.81492255796105972, 31.66775706135234358 ) ) ;
#96144 = CARTESIAN_POINT ( 'NONE',  ( -13.89961937509977652, 13.97604488694528158, 85.62390960531433848 ) ) ;
#96143 = CARTESIAN_POINT ( 'NONE',  ( -13.89961937509957401, -13.97604488694547875, 49.37609039468567573 ) ) ;
#96145 = CARTESIAN_POINT ( 'NONE',  ( -9.564922557961040184, 16.46253265017147172, 32.91775706135233293 ) ) ;
#96146 = CARTESIAN_POINT ( 'NONE',  ( 15.72974639402176855, 15.80617190586768217, 86.87609039468568994 ) ) ;
#96147 = CARTESIAN_POINT ( 'NONE',  ( -21.53943276465977519, 0.05219959533907696930, 76.24890960531435269 ) ) ;
#96148 = CARTESIAN_POINT ( 'NONE',  ( 4.483927247898545687, 16.52544592524342804, 44.79057627198103120 ) ) ;
#96150 = CARTESIAN_POINT ( 'NONE',  ( 13.89961937509957401, 13.97604488694547697, 26.87609039468566507 ) ) ;
#96149 = CARTESIAN_POINT ( 'NONE',  ( -0.05219959533937732626, 21.53943276465977519, 92.50109039468567573 ) ) ;
#96151 = CARTESIAN_POINT ( 'NONE',  ( -12.14591786802309592, -12.06949235617757132, 71.87390960531438111 ) ) ;
#96152 = CARTESIAN_POINT ( 'NONE',  ( -13.89961937509977652, 13.97604488694528158, 25.62390960531434558 ) ) ;
#96153 = CARTESIAN_POINT ( 'NONE',  ( 9.474510206698729675, 16.51473224551082808, 67.08442372801900433 ) ) ;
#96154 = CARTESIAN_POINT ( 'NONE',  ( 12.14591786802309770, 12.06949235617756955, 34.37390960531435979 ) ) ;
#96155 = CARTESIAN_POINT ( 'NONE',  ( -18.67979575497193778, 10.72451020669871902, 83.33442372801903275 ) ) ;
#96156 = CARTESIAN_POINT ( 'NONE',  ( 9.564922557960805705, 16.46253265017160317, 74.58224293864769550 ) ) ;
#96157 = CARTESIAN_POINT ( 'NONE',  ( -5.049401038297874678, -19.05341960407617918, 49.79275706135231871 ) ) ;
#96158 = CARTESIAN_POINT ( 'NONE',  ( 15.72974639402199770, -15.80617190586745480, 48.12390960531436690 ) ) ;
#96159 = CARTESIAN_POINT ( 'NONE',  ( -10.81492255796105439, 18.62759615963255655, 22.91775706135235069 ) ) ;
#96160 = CARTESIAN_POINT ( 'NONE',  ( 19.02544592524334988, 5.153800228976608722, 106.4594237280190185 ) ) ;
#96161 = CARTESIAN_POINT ( 'NONE',  ( -4.379528057220086978, -16.55341960407618274, 69.79275706135234714 ) ) ;
#96163 = CARTESIAN_POINT ( 'NONE',  ( -15.80617190586745835, -15.72974639402198527, 106.8739096053143811 ) ) ;
#96162 = CARTESIAN_POINT ( 'NONE',  ( 16.61371651742603817, 7.165104196376034018, 63.64584930006999741 ) ) ;
#96164 = CARTESIAN_POINT ( 'NONE',  ( 12.14591786802309770, 12.06949235617756955, 109.3739096053143811 ) ) ;
#96165 = CARTESIAN_POINT ( 'NONE',  ( -17.50000000000149214, -3.254303733634606566, 29.97604106928586987 ) ) ;
#96166 = CARTESIAN_POINT ( 'NONE',  ( 4.379528057220092307, 16.55341960407617563, 37.29275706135235424 ) ) ;
#96167 = CARTESIAN_POINT ( 'NONE',  ( 21.52544592524344225, -5.823673210054117533, 63.54057627198103830 ) ) ;
#96168 = CARTESIAN_POINT ( 'NONE',  ( -8.314922557961024197, 14.29746914071037800, 102.9177570613523756 ) ) ;
#96169 = CARTESIAN_POINT ( 'NONE',  ( 19.03943276465977164, -0.05219959533909143690, 33.74890960531435979 ) ) ;
#96170 = CARTESIAN_POINT ( 'NONE',  ( -0.05219959533934338120, 16.53943276465976808, 72.50109039468568994 ) ) ;
#96171 = CARTESIAN_POINT ( 'NONE',  ( -19.05341960407617563, 5.049401038297882671, 63.54275706135234003 ) ) ;
#96172 = CARTESIAN_POINT ( 'NONE',  ( -10.81492255796105439, 18.62759615963255655, 42.91775706135235424 ) ) ;
#96173 = CARTESIAN_POINT ( 'NONE',  ( -18.62759615963270932, 10.81492255796079327, 60.83224293864769550 ) ) ;
#96174 = CARTESIAN_POINT ( 'NONE',  ( -8.314922557961024197, 14.29746914071037800, 102.9177570613523756 ) ) ;
#96175 = CARTESIAN_POINT ( 'NONE',  ( 10.72451020669871369, 18.67979575497193778, 87.08442372801901854 ) ) ;
#96176 = EDGE_CURVE ( 'NONE', #51904, #41517, #137465, .T. ) ;
#96177 = CARTESIAN_POINT ( 'NONE',  ( -15.72974639402197994, 15.80617190586746368, 50.62390960531435979 ) ) ;
#96178 = CARTESIAN_POINT ( 'NONE',  ( 10.72451020669898902, -18.67979575497178502, 32.91557627198102409 ) ) ;
#96179 = ORIENTED_EDGE ( 'NONE', *, *, #152995, .F. ) ;
#96180 = CARTESIAN_POINT ( 'NONE',  ( 4.379528057220092307, 16.55341960407617563, 82.29275706135234714 ) ) ;
#96181 = CARTESIAN_POINT ( 'NONE',  ( -18.62759615963270932, 10.81492255796079327, 45.83224293864769550 ) ) ;
#96182 = VERTEX_POINT ( 'NONE', #150672 ) ;
#96183 = CARTESIAN_POINT ( 'NONE',  ( 16.46253265017160672, -9.564922557960803928, 93.33224293864769550 ) ) ;
#96184 = CYLINDRICAL_SURFACE ( 'NONE', #150317, 21.30000000000002913 ) ;
#96185 = CARTESIAN_POINT ( 'NONE',  ( 13.97604488694527802, 13.89961937509977652, 29.37390960531435979 ) ) ;
#96186 = CARTESIAN_POINT ( 'NONE',  ( -18.67979575497178146, -10.72451020669898902, 66.66557627198102409 ) ) ;
#96187 = CARTESIAN_POINT ( 'NONE',  ( 14.29746914071037800, 8.314922557961029526, 86.66775706135234714 ) ) ;
#96188 = CARTESIAN_POINT ( 'NONE',  ( -5.719274019375665041, -21.55341960407619695, 49.79275706135234714 ) ) ;
#96189 = CARTESIAN_POINT ( 'NONE',  ( -5.049401038297874678, -19.05341960407617918, 109.7927570613523187 ) ) ;
#96190 = CARTESIAN_POINT ( 'NONE',  ( -0.05219959533910754901, -16.53943276465976808, 107.4989096053143669 ) ) ;
#96191 = CARTESIAN_POINT ( 'NONE',  ( 16.46253265017146816, 9.564922557961045513, 111.6677570613523329 ) ) ;
#96192 = CARTESIAN_POINT ( 'NONE',  ( 16.51473224551069308, 9.474510206698969483, 44.16557627198103120 ) ) ;
#96193 = CARTESIAN_POINT ( 'NONE',  ( 0.1123858161134816402, 24.30000000000003979, -54.21489346206829651 ) ) ;
#96194 = CARTESIAN_POINT ( 'NONE',  ( -16.51473224551069308, -9.474510206698971260, 91.66557627198103830 ) ) ;
#96195 = CARTESIAN_POINT ( 'NONE',  ( -12.14591786802326823, 12.06949235617739902, 78.12609039468570415 ) ) ;
#96196 = CARTESIAN_POINT ( 'NONE',  ( -15.72974639402176322, -15.80617190586768395, 109.3760903946857042 ) ) ;
#96197 = CARTESIAN_POINT ( 'NONE',  ( 21.53943276465977519, -0.05219959533907433946, 58.74890960531436690 ) ) ;
#96198 = CARTESIAN_POINT ( 'NONE',  ( -16.55341960407617563, 4.379528057220093196, 93.54275706135234714 ) ) ;
#96199 = CARTESIAN_POINT ( 'NONE',  ( -19.05341960407617563, 5.049401038297882671, 73.54275706135233293 ) ) ;
#96200 = CARTESIAN_POINT ( 'NONE',  ( -5.153800228976328057, -19.02544592524343514, 32.29057627198102409 ) ) ;
#96201 = CARTESIAN_POINT ( 'NONE',  ( 0.05219959533909260263, 19.03943276465977164, 79.99890960531436690 ) ) ;
#96202 = CARTESIAN_POINT ( 'NONE',  ( -16.51473224551069308, -9.474510206698971260, 31.66557627198102054 ) ) ;
#96203 = CARTESIAN_POINT ( 'NONE',  ( -19.05341960407617563, 5.049401038297882671, 68.54275706135230450 ) ) ;
#96204 = CARTESIAN_POINT ( 'NONE',  ( 26.78465914369787626, -5.761000505272217076, 169.4491075441770818 ) ) ;
#96205 = CARTESIAN_POINT ( 'NONE',  ( -13.89961937509977652, 13.97604488694528158, 105.6239096053143527 ) ) ;
#96206 = CARTESIAN_POINT ( 'NONE',  ( -12.06949235617756955, 12.14591786802309770, 60.62390960531437401 ) ) ;
#96207 = CARTESIAN_POINT ( 'NONE',  ( 18.67979575497178502, 10.72451020669898547, 64.16557627198102409 ) ) ;
#96208 = CARTESIAN_POINT ( 'NONE',  ( -17.49999999999998934, 4.640572885337569176, 105.6378816454884060 ) ) ;
#96209 = CARTESIAN_POINT ( 'NONE',  ( -5.049401038297874678, -19.05341960407617918, 34.79275706135233293 ) ) ;
#96210 = DIRECTION ( 'NONE',  ( 0.000000000000000000, -1.000000000000000000, 0.000000000000000000 ) ) ;
#96212 = CARTESIAN_POINT ( 'NONE',  ( 19.03943276465977164, -0.05219959533909143690, 68.74890960531436690 ) ) ;
#96211 = CARTESIAN_POINT ( 'NONE',  ( -5.153800228976328057, -19.02544592524343514, 67.29057627198102409 ) ) ;
#96213 = CARTESIAN_POINT ( 'NONE',  ( 16.55341960407618274, -4.379528057220086978, 46.04275706135234714 ) ) ;
#96214 = CARTESIAN_POINT ( 'NONE',  ( 27.99526582847387957, -28.30548820594174586, -16.92425894792105723 ) ) ;
#96215 = CARTESIAN_POINT ( 'NONE',  ( 11.33808637246520945, -35.21329618173263754, -8.000000000000000000 ) ) ;
#96216 = CARTESIAN_POINT ( 'NONE',  ( 12.06949235617739724, 12.14591786802326823, 81.87609039468568994 ) ) ;
#96217 = CARTESIAN_POINT ( 'NONE',  ( 14.34966873604972726, -8.224510206698740333, 60.83442372801901854 ) ) ;
#96218 = CARTESIAN_POINT ( 'NONE',  ( -12.14591786802326823, 12.06949235617739902, 38.12609039468567573 ) ) ;
#96220 = FACE_BOUND ( 'NONE', #118898, .T. ) ;
#96219 = CARTESIAN_POINT ( 'NONE',  ( -16.51473224551069308, -9.474510206698971260, 51.66557627198102409 ) ) ;
#96221 = CARTESIAN_POINT ( 'NONE',  ( -15.80617190586768217, 15.72974639402176855, 53.12609039468568284 ) ) ;
#96222 = CARTESIAN_POINT ( 'NONE',  ( 13.89961937509957401, 13.97604488694547697, 66.87609039468567573 ) ) ;
#96223 = CARTESIAN_POINT ( 'NONE',  ( -15.80617190586768217, 15.72974639402176855, 93.12609039468568994 ) ) ;
#96224 = CARTESIAN_POINT ( 'NONE',  ( 13.89961937509977652, -13.97604488694527269, 28.12390960531435624 ) ) ;
#96225 = CARTESIAN_POINT ( 'NONE',  ( 19.49671883438229614, 5.499999999999975131, 42.39279849105686537 ) ) ;
#96226 = CARTESIAN_POINT ( 'NONE',  ( 15.80617190586746368, 15.72974639402197994, 59.37390960531436690 ) ) ;
#96227 = AXIS2_PLACEMENT_3D ( 'NONE', #26346, #87986, #70837 ) ;
#96228 = CARTESIAN_POINT ( 'NONE',  ( -9.564922557960796823, -16.46253265017161027, 102.0822429386477097 ) ) ;
#96229 = CARTESIAN_POINT ( 'NONE',  ( -16.53943276465976808, 0.05219959533911058130, 106.2489096053143811 ) ) ;
#96230 = CARTESIAN_POINT ( 'NONE',  ( -8.224510206698735004, -14.34966873604973081, 34.58442372801900433 ) ) ;
#96231 = CARTESIAN_POINT ( 'NONE',  ( -16.55341960407617563, 4.379528057220093196, 113.5427570613523756 ) ) ;
#96232 = ORIENTED_EDGE ( 'NONE', *, *, #83620, .T. ) ;
#96233 = CARTESIAN_POINT ( 'NONE',  ( -10.81492255796078084, -18.62759615963271287, 107.0822429386476955 ) ) ;
#96235 = CARTESIAN_POINT ( 'NONE',  ( 19.02544592524343514, -5.153800228976328945, 113.5405762719810241 ) ) ;
#96234 = CARTESIAN_POINT ( 'NONE',  ( 4.379528057220339221, -16.55341960407611168, 32.70724293864770260 ) ) ;
#96236 = CARTESIAN_POINT ( 'NONE',  ( 13.89961937509957401, 13.97604488694547697, 91.87609039468567573 ) ) ;
#96237 = CARTESIAN_POINT ( 'NONE',  ( 0.05219959533936267826, -19.03943276465977164, 30.00109039468566863 ) ) ;
#96238 = CARTESIAN_POINT ( 'NONE',  ( 4.379528057220339221, -16.55341960407611168, 32.70724293864770260 ) ) ;
#96239 = CARTESIAN_POINT ( 'NONE',  ( 21.53943276465977519, -0.05219959533907433946, 88.74890960531436690 ) ) ;
#96240 = CARTESIAN_POINT ( 'NONE',  ( -21.55341960407610458, -5.719274019375992779, 46.45724293864769550 ) ) ;
#96241 = CARTESIAN_POINT ( 'NONE',  ( 16.46253265017160672, -9.564922557960803928, 83.33224293864768129 ) ) ;
#96242 = CARTESIAN_POINT ( 'NONE',  ( 4.483927247898545687, 16.52544592524342804, 39.79057627198103830 ) ) ;
#96243 = CARTESIAN_POINT ( 'NONE',  ( -16.51473224551069308, -9.474510206698971260, 86.66557627198102409 ) ) ;
#96244 = CARTESIAN_POINT ( 'NONE',  ( 19.39720447994797325, 5.499999999999975131, 57.16317477297181426 ) ) ;
#96245 = CARTESIAN_POINT ( 'NONE',  ( -5.049401038297874678, -19.05341960407617918, 44.79275706135232582 ) ) ;
#96246 = CARTESIAN_POINT ( 'NONE',  ( -5.823673210054116645, -21.52544592524344225, 82.29057627198103830 ) ) ;
#96247 = CARTESIAN_POINT ( 'NONE',  ( -16.55341960407611168, -4.379528057220339221, 106.4572429386477097 ) ) ;
#96248 = CARTESIAN_POINT ( 'NONE',  ( -18.62759615963255300, -10.81492255796106328, 39.16775706135235424 ) ) ;
#96249 = AXIS2_PLACEMENT_3D ( 'NONE', #114003, #116024, #69519 ) ;
#96250 = CARTESIAN_POINT ( 'NONE',  ( -17.14385361876520264, -23.59649016807271593, 141.1750000027311671 ) ) ;
#96251 = CARTESIAN_POINT ( 'NONE',  ( -14.34966873604972548, 8.224510206698743886, 103.3344237280190043 ) ) ;
#96252 = CARTESIAN_POINT ( 'NONE',  ( -5.049401038298153566, 19.05341960407611168, 40.20724293864768839 ) ) ;
#96253 = CARTESIAN_POINT ( 'NONE',  ( -9.564922557960796823, -16.46253265017161027, 92.08224293864769550 ) ) ;
#96254 = CARTESIAN_POINT ( 'NONE',  ( -31.99364916731038022, -1.163414459189985801E-14, 97.65000000000000568 ) ) ;
#96255 = CARTESIAN_POINT ( 'NONE',  ( -0.05219959533909027116, -19.03943276465977164, 32.49890960531435979 ) ) ;
#96256 = CARTESIAN_POINT ( 'NONE',  ( 16.53943276465976808, -0.05219959533910856209, 43.74890960531435979 ) ) ;
#96257 = VECTOR ( 'NONE', #132784, 1000.000000000000000 ) ;
#96258 = CARTESIAN_POINT ( 'NONE',  ( -5.719274019375665041, -21.55341960407619695, 79.79275706135236135 ) ) ;
#96260 = CARTESIAN_POINT ( 'NONE',  ( 8.314922557961029526, -14.29746914071037800, 75.41775706135233293 ) ) ;
#96259 = CARTESIAN_POINT ( 'NONE',  ( 30.67396074481323254, -22.36774236107039471, -23.13178788717692314 ) ) ;
#96261 = CARTESIAN_POINT ( 'NONE',  ( 9.564922557960805705, 16.46253265017160317, 54.58224293864769550 ) ) ;
#96262 = CARTESIAN_POINT ( 'NONE',  ( 5.153800228976335163, 19.02544592524342804, 64.79057627198100988 ) ) ;
#96263 = ORIENTED_EDGE ( 'NONE', *, *, #60352, .F. ) ;
#96264 = CARTESIAN_POINT ( 'NONE',  ( 5.823673210054444382, -21.52544592524334988, 105.2094237280190328 ) ) ;
#96265 = CARTESIAN_POINT ( 'NONE',  ( -4.483927247898782831, 16.52544592524335698, 72.70942372801901854 ) ) ;
#96266 = CARTESIAN_POINT ( 'NONE',  ( 0.05219959533937995610, -21.53943276465977519, 105.0010903946856757 ) ) ;
#96267 = CARTESIAN_POINT ( 'NONE',  ( -0.05219959533909027116, -19.03943276465977164, 57.49890960531435979 ) ) ;
#96268 = CARTESIAN_POINT ( 'NONE',  ( -18.67979575497178146, -10.72451020669898902, 31.66557627198102054 ) ) ;
#96269 = CARTESIAN_POINT ( 'NONE',  ( 9.474510206698729675, 16.51473224551082808, 107.0844237280190043 ) ) ;
#96270 = CARTESIAN_POINT ( 'NONE',  ( 15.72974639402176855, 15.80617190586768217, 66.87609039468568994 ) ) ;
#96271 = CARTESIAN_POINT ( 'NONE',  ( -4.483927247898782831, 16.52544592524335698, 52.70942372801902565 ) ) ;
#96272 = CARTESIAN_POINT ( 'NONE',  ( 15.80617190586746368, 15.72974639402197994, 99.37390960531436690 ) ) ;
#96273 = CARTESIAN_POINT ( 'NONE',  ( 0.05219959533936267826, -19.03943276465977164, 100.0010903946856757 ) ) ;
#96274 = CARTESIAN_POINT ( 'NONE',  ( 16.51473224551069308, 9.474510206698969483, 84.16557627198102409 ) ) ;
#96275 = CARTESIAN_POINT ( 'NONE',  ( 19.02544592524334988, 5.153800228976608722, 106.4594237280190185 ) ) ;
#96276 = CARTESIAN_POINT ( 'NONE',  ( 16.53943276465976808, 0.05219959533934440121, 26.25109039468567573 ) ) ;
#96277 = CARTESIAN_POINT ( 'NONE',  ( -12.06949235617756955, 12.14591786802309770, 65.62390960531436690 ) ) ;
#96278 = CARTESIAN_POINT ( 'NONE',  ( 8.314922557961029526, -14.29746914071037800, 80.41775706135234714 ) ) ;
#96280 = CARTESIAN_POINT ( 'NONE',  ( -16.51473224551069308, -9.474510206698971260, 51.66557627198102409 ) ) ;
#96279 = CARTESIAN_POINT ( 'NONE',  ( -0.05219959533907301413, -21.53943276465977519, 112.4989096053143669 ) ) ;
#96281 = CARTESIAN_POINT ( 'NONE',  ( -5.153800228976328057, -19.02544592524343514, 57.29057627198103120 ) ) ;
#96282 = CARTESIAN_POINT ( 'NONE',  ( -12.14591786802326823, 12.06949235617739902, 78.12609039468570415 ) ) ;
#96283 = CARTESIAN_POINT ( 'NONE',  ( -8.906447517083053711, -27.41122689804191026, 144.6500000054623740 ) ) ;
#96284 = ORIENTED_EDGE ( 'NONE', *, *, #116598, .F. ) ;
#96285 = CARTESIAN_POINT ( 'NONE',  ( -18.67979575497193778, 10.72451020669871902, 113.3344237280190328 ) ) ;
#96286 = CARTESIAN_POINT ( 'NONE',  ( 19.05341960407611168, 5.049401038298154454, 33.95724293864769550 ) ) ;
#96287 = ORIENTED_EDGE ( 'NONE', *, *, #167994, .T. ) ;
#96288 = CARTESIAN_POINT ( 'NONE',  ( 16.52544592524335698, 4.483927247898782831, 21.45942372801901499 ) ) ;
#96290 = CARTESIAN_POINT ( 'NONE',  ( 14.29746914071037800, 8.314922557961029526, 31.66775706135234358 ) ) ;
#96289 = CARTESIAN_POINT ( 'NONE',  ( 9.564922557961047289, -16.46253265017146816, 50.41775706135233293 ) ) ;
#96291 = CARTESIAN_POINT ( 'NONE',  ( -16.46253265017160317, 9.564922557960807481, 40.83224293864769550 ) ) ;
#96292 = CARTESIAN_POINT ( 'NONE',  ( -13.89961937509977652, 13.97604488694528158, 70.62390960531432427 ) ) ;
#96293 = CARTESIAN_POINT ( 'NONE',  ( -5.823673210054116645, -21.52544592524344225, 92.29057627198103830 ) ) ;
#96294 = CARTESIAN_POINT ( 'NONE',  ( -5.049401038298153566, 19.05341960407611168, 115.2072429386477097 ) ) ;
#96295 = EDGE_CURVE ( 'NONE', #50694, #190550, #89908, .T. ) ;
#96296 = CARTESIAN_POINT ( 'NONE',  ( 13.97604488694527802, 13.89961937509977652, 54.37390960531435979 ) ) ;
#96297 = CARTESIAN_POINT ( 'NONE',  ( -11.30153831258471442, -180.0000000000000000, -4.999999999999999112 ) ) ;
#96298 = CARTESIAN_POINT ( 'NONE',  ( 13.97604488694548053, -13.89961937509957401, 100.6260903946856615 ) ) ;
#96299 = CARTESIAN_POINT ( 'NONE',  ( 12.06949235617757843, -12.14591786802309237, 68.12390960531436690 ) ) ;
#96300 = CARTESIAN_POINT ( 'NONE',  ( -19.03943276465977164, -0.05219959533935918106, 28.75109039468566507 ) ) ;
#96301 = CARTESIAN_POINT ( 'NONE',  ( 16.52544592524342804, -4.483927247898539470, 63.54057627198103830 ) ) ;
#96302 = CARTESIAN_POINT ( 'NONE',  ( -18.62759615963255300, -10.81492255796106328, 89.16775706135236135 ) ) ;
#96303 = CARTESIAN_POINT ( 'NONE',  ( -13.97604488694527625, -13.89961937509977652, 26.87390960531434558 ) ) ;
#96304 = CARTESIAN_POINT ( 'NONE',  ( 15.72974639402176855, 15.80617190586768217, 86.87609039468568994 ) ) ;
#96306 = CARTESIAN_POINT ( 'NONE',  ( 21.53943276465977519, 0.05219959533937863772, 71.25109039468568994 ) ) ;
#96305 = CARTESIAN_POINT ( 'NONE',  ( -4.379528057220328563, 16.55341960407611168, 30.20724293864769550 ) ) ;
#96307 = CARTESIAN_POINT ( 'NONE',  ( 9.564922557960805705, 16.46253265017160317, 79.58224293864769550 ) ) ;
#96308 = CARTESIAN_POINT ( 'NONE',  ( -21.53943276465977519, -0.05219959533937600094, 38.75109039468567573 ) ) ;
#96309 = CARTESIAN_POINT ( 'NONE',  ( 16.46253265017160672, -9.564922557960803928, 83.33224293864768129 ) ) ;
#96310 = CARTESIAN_POINT ( 'NONE',  ( 14.34966873604960469, 8.224510206698951720, 99.16557627198100988 ) ) ;
#96311 = CARTESIAN_POINT ( 'NONE',  ( 16.55341960407611168, 4.379528057220329451, 63.95724293864770260 ) ) ;
#96312 = CARTESIAN_POINT ( 'NONE',  ( 10.72451020669898902, -18.67979575497178502, 67.91557627198102409 ) ) ;
#96313 = CARTESIAN_POINT ( 'NONE',  ( 13.97604488694527802, 13.89961937509977652, 79.37390960531435269 ) ) ;
#96314 = CARTESIAN_POINT ( 'NONE',  ( -18.62759615963270932, 10.81492255796079327, 80.83224293864769550 ) ) ;
#96315 = CARTESIAN_POINT ( 'NONE',  ( 9.474510206698729675, 16.51473224551082808, 62.08442372801899722 ) ) ;
#96317 = CARTESIAN_POINT ( 'NONE',  ( -14.29746914071049879, 8.314922557960819915, 75.83224293864769550 ) ) ;
#96316 = CARTESIAN_POINT ( 'NONE',  ( 5.049401038297881783, 19.05341960407617918, 37.29275706135232582 ) ) ;
#96318 = CARTESIAN_POINT ( 'NONE',  ( 21.52544592524344225, -5.823673210054117533, 53.54057627198103120 ) ) ;
#96319 = DIRECTION ( 'NONE',  ( 1.000000000000000000, 0.000000000000000000, 0.000000000000000000 ) ) ;
#96321 = CARTESIAN_POINT ( 'NONE',  ( -27.73933785331498925, -9.013057229001049109, 145.4750000027311785 ) ) ;
#96320 = CARTESIAN_POINT ( 'NONE',  ( -8.314922557961024197, 14.29746914071037800, 92.91775706135236135 ) ) ;
#96322 = CARTESIAN_POINT ( 'NONE',  ( 16.51473224551083163, -9.474510206698727899, 100.8344237280190043 ) ) ;
#96323 = CARTESIAN_POINT ( 'NONE',  ( 8.314922557960818139, 14.29746914071049879, 64.58224293864769550 ) ) ;
#96324 = CARTESIAN_POINT ( 'NONE',  ( 6.139906835403837526, -0.3968392070109495462, -62.49911542708241541 ) ) ;
#96325 = CARTESIAN_POINT ( 'NONE',  ( 13.97604488694527802, 13.89961937509977652, 64.37390960531436690 ) ) ;
#96326 = CARTESIAN_POINT ( 'NONE',  ( -4.379528057220328563, 16.55341960407611168, 60.20724293864768839 ) ) ;
#96327 = CARTESIAN_POINT ( 'NONE',  ( -19.03943276465977164, 0.05219959533909376836, 106.2489096053143669 ) ) ;
#96329 = CARTESIAN_POINT ( 'NONE',  ( 13.97604488694527802, 13.89961937509977652, 69.37390960531436690 ) ) ;
#96328 = CARTESIAN_POINT ( 'NONE',  ( 9.564922557961047289, -16.46253265017146816, 85.41775706135233293 ) ) ;
#96330 = CARTESIAN_POINT ( 'NONE',  ( 9.564922557960805705, 16.46253265017160317, 79.58224293864769550 ) ) ;
#96331 = CARTESIAN_POINT ( 'NONE',  ( -19.02544592524342804, 5.153800228976336051, 91.04057627198100988 ) ) ;
#96332 = CARTESIAN_POINT ( 'NONE',  ( 10.72451020669898902, -18.67979575497178502, 57.91557627198103120 ) ) ;
#96333 = CARTESIAN_POINT ( 'NONE',  ( -16.53943276465976808, -0.05219959533934237506, 63.75109039468568284 ) ) ;
#96334 = CARTESIAN_POINT ( 'NONE',  ( -19.03943276465977164, -0.05219959533935918106, 103.7510903946856757 ) ) ;
#96335 = CARTESIAN_POINT ( 'NONE',  ( -16.51473224551069308, -9.474510206698971260, 51.66557627198102409 ) ) ;
#96336 = CARTESIAN_POINT ( 'NONE',  ( 21.55341960407610458, 5.719274019375980345, 68.95724293864769550 ) ) ;
#96337 = CARTESIAN_POINT ( 'NONE',  ( 9.474510206698729675, 16.51473224551082808, 97.08442372801900433 ) ) ;
#96339 = CARTESIAN_POINT ( 'NONE',  ( -15.80617190586768217, 15.72974639402176855, 43.12609039468568284 ) ) ;
#96338 = CARTESIAN_POINT ( 'NONE',  ( 14.29746914071037800, 8.314922557961029526, 111.6677570613523613 ) ) ;
#96340 = CARTESIAN_POINT ( 'NONE',  ( -19.03943276465977164, -0.05219959533935918106, 38.75109039468566152 ) ) ;
#96342 = CARTESIAN_POINT ( 'NONE',  ( 14.34966873604972726, -8.224510206698740333, 95.83442372801903275 ) ) ;
#96341 = CARTESIAN_POINT ( 'NONE',  ( 14.34966873604972726, -8.224510206698740333, 55.83442372801901854 ) ) ;
#96343 = CARTESIAN_POINT ( 'NONE',  ( 1.300000000000000044, 0.7216878364870328300, 1.249999999999999778 ) ) ;
#96344 = CARTESIAN_POINT ( 'NONE',  ( 12.06949235617739724, 12.14591786802326823, 76.87609039468567573 ) ) ;
#96345 = CARTESIAN_POINT ( 'NONE',  ( -12.06949235617739369, -12.14591786802326823, 34.37609039468568284 ) ) ;
#96346 = CARTESIAN_POINT ( 'NONE',  ( -5.153800228976328057, -19.02544592524343514, 47.29057627198102409 ) ) ;
#96347 = CARTESIAN_POINT ( 'NONE',  ( 19.05341960407611168, 5.049401038298154454, 48.95724293864768129 ) ) ;
#96348 = CARTESIAN_POINT ( 'NONE',  ( 16.51473224551069308, 9.474510206698969483, 64.16557627198102409 ) ) ;
#96349 = CARTESIAN_POINT ( 'NONE',  ( 18.67979575497194134, -10.72451020669871369, 55.83442372801901854 ) ) ;
#96350 = CARTESIAN_POINT ( 'NONE',  ( 16.53943276465976808, 0.05219959533934440121, 51.25109039468568994 ) ) ;
#96351 = CARTESIAN_POINT ( 'NONE',  ( 16.53943276465976808, -0.05219959533910856209, 23.74890960531435269 ) ) ;
#96352 = CARTESIAN_POINT ( 'NONE',  ( -19.05341960407611168, -5.049401038298163336, 26.45724293864769550 ) ) ;
#96353 = CARTESIAN_POINT ( 'NONE',  ( -15.80617190586768217, 15.72974639402176855, 113.1260903946856899 ) ) ;
#96354 = CARTESIAN_POINT ( 'NONE',  ( -16.53943276465976808, -0.05219959533934237506, 23.75109039468567929 ) ) ;
#96355 = CARTESIAN_POINT ( 'NONE',  ( 13.89961937509957401, 13.97604488694547697, 86.87609039468567573 ) ) ;
#96356 = CARTESIAN_POINT ( 'NONE',  ( 16.53943276465976808, -0.05219959533910856209, 83.74890960531435269 ) ) ;
#96357 = CARTESIAN_POINT ( 'NONE',  ( 13.89961937509977652, -13.97604488694527269, 33.12390960531434558 ) ) ;
#96359 = CARTESIAN_POINT ( 'NONE',  ( 17.26172910966778673, 6.454744622555869782, 76.69353091350774321 ) ) ;
#96358 = CARTESIAN_POINT ( 'NONE',  ( -19.03943276465977164, -0.05219959533935918106, 73.75109039468566152 ) ) ;
#96360 = CARTESIAN_POINT ( 'NONE',  ( -5.719274019375665041, -21.55341960407619695, 74.79275706135234714 ) ) ;
#96361 = CARTESIAN_POINT ( 'NONE',  ( 16.55341960407618274, -4.379528057220086978, 46.04275706135234714 ) ) ;
#96362 = CARTESIAN_POINT ( 'NONE',  ( 16.19135201231368981, 7.376712067591805422, 37.68680854052031037 ) ) ;
#96363 = CARTESIAN_POINT ( 'NONE',  ( 5.823673210054125526, 21.52544592524343514, 34.79057627198103120 ) ) ;
#96364 = CARTESIAN_POINT ( 'NONE',  ( 4.379528057220092307, 16.55341960407617563, 32.29275706135235424 ) ) ;
#96365 = CARTESIAN_POINT ( 'NONE',  ( 16.46253265017160672, -9.564922557960803928, 28.33224293864769550 ) ) ;
#96366 = CARTESIAN_POINT ( 'NONE',  ( 5.049401038297881783, 19.05341960407617563, 27.29275706135232937 ) ) ;
#96367 = CARTESIAN_POINT ( 'NONE',  ( 9.250641775538104739, 10.87998047749157493, -60.21451611132644643 ) ) ;
#96368 = CARTESIAN_POINT ( 'NONE',  ( 5.153800228976335163, 19.02544592524342804, 44.79057627198103830 ) ) ;
#96369 = CARTESIAN_POINT ( 'NONE',  ( -19.99604614807122971, -21.41083295479474202, -52.23501749411500583 ) ) ;
#96370 = CARTESIAN_POINT ( 'NONE',  ( -19.05341960407611168, -5.049401038298163336, 71.45724293864766707 ) ) ;
#96371 = CARTESIAN_POINT ( 'NONE',  ( -19.49671883438229258, -5.499999999999978684, 54.89279849105684406 ) ) ;
#96372 = EDGE_CURVE ( 'NONE', #98417, #121093, #127249, .T. ) ;
#96373 = CARTESIAN_POINT ( 'NONE',  ( -13.89961937509957401, -13.97604488694547875, 24.37609039468565442 ) ) ;
#96374 = CARTESIAN_POINT ( 'NONE',  ( -8.314922557960811034, -14.29746914071050412, 37.08224293864768129 ) ) ;
#96375 = CARTESIAN_POINT ( 'NONE',  ( -19.03943276465977164, 0.05219959533909376836, 41.24890960531435269 ) ) ;
#96376 = CARTESIAN_POINT ( 'NONE',  ( -0.05219959533909027116, -19.03943276465977164, 92.49890960531436690 ) ) ;
#96377 = CARTESIAN_POINT ( 'NONE',  ( -15.72974639402176322, -15.80617190586768395, 64.37609039468568994 ) ) ;
#96378 = CARTESIAN_POINT ( 'NONE',  ( 13.97604488694527802, 13.89961937509977652, 49.37390960531434558 ) ) ;
#96379 = CARTESIAN_POINT ( 'NONE',  ( 15.80617190586769283, -15.72974639402175789, 60.62609039468567573 ) ) ;
#96380 = CARTESIAN_POINT ( 'NONE',  ( -21.53943276465977519, 0.05219959533907696930, 21.24890960531436690 ) ) ;
#96381 = CARTESIAN_POINT ( 'NONE',  ( -19.02544592524342804, 5.153800228976336051, 41.04057627198103120 ) ) ;
#96382 = CARTESIAN_POINT ( 'NONE',  ( 10.81492255796106328, -18.62759615963255655, 30.41775706135234358 ) ) ;
#96383 = CARTESIAN_POINT ( 'NONE',  ( 0.05219959533936267826, -19.03943276465977164, 45.00109039468566863 ) ) ;
#96384 = CARTESIAN_POINT ( 'NONE',  ( -12.14591786802309592, -12.06949235617757132, 111.8739096053143669 ) ) ;
#96385 = CARTESIAN_POINT ( 'NONE',  ( 16.46253265017160672, -9.564922557960803928, 58.33224293864769550 ) ) ;
#96386 = CARTESIAN_POINT ( 'NONE',  ( 19.02544592524334988, 5.153800228976608722, 106.4594237280190185 ) ) ;
#96387 = CARTESIAN_POINT ( 'NONE',  ( 12.06949235617757843, -12.14591786802309237, 78.12390960531436690 ) ) ;
#96388 = CARTESIAN_POINT ( 'NONE',  ( 19.03943276465977164, -0.05219959533909143690, 113.7489096053143669 ) ) ;
#96389 = CARTESIAN_POINT ( 'NONE',  ( -19.03943276465977164, -0.05219959533935918106, 98.75109039468567573 ) ) ;
#96390 = CARTESIAN_POINT ( 'NONE',  ( -5.823673210054116645, -21.52544592524344225, 102.2905762719810383 ) ) ;
#96391 = CARTESIAN_POINT ( 'NONE',  ( 21.52544592524334988, 5.823673210054432836, 61.45942372801901854 ) ) ;
#96392 = CARTESIAN_POINT ( 'NONE',  ( -16.53943276465976808, -0.05219959533934237506, 58.75109039468568994 ) ) ;
#96393 = CARTESIAN_POINT ( 'NONE',  ( 4.483927247898790824, -16.52544592524335698, 55.20942372801902565 ) ) ;
#96394 = CARTESIAN_POINT ( 'NONE',  ( -5.719274019375978568, 21.55341960407610458, 50.20724293864769550 ) ) ;
#96395 = CARTESIAN_POINT ( 'NONE',  ( 13.89961937509977652, -13.97604488694527269, 43.12390960531434558 ) ) ;
#96396 = CARTESIAN_POINT ( 'NONE',  ( 8.314922557961029526, -14.29746914071037800, 70.41775706135236135 ) ) ;
#96397 = AXIS2_PLACEMENT_3D ( 'NONE', #157882, #142695, #68853 ) ;
#96398 = CARTESIAN_POINT ( 'NONE',  ( 21.55341960407610458, 5.719274019375980345, 98.95724293864770971 ) ) ;
#96399 = CARTESIAN_POINT ( 'NONE',  ( 14.29746914071049879, -8.314922557960816363, 58.33224293864768839 ) ) ;
#96400 = CARTESIAN_POINT ( 'NONE',  ( 19.02544592524343514, -5.153800228976328945, 78.54057627198099567 ) ) ;
#96401 = CARTESIAN_POINT ( 'NONE',  ( -12.06949235617739369, -12.14591786802326823, 74.37609039468568994 ) ) ;
#96402 = CARTESIAN_POINT ( 'NONE',  ( -5.049401038297874678, -19.05341960407617918, 104.7927570613523471 ) ) ;
#96403 = CARTESIAN_POINT ( 'NONE',  ( 18.67979575497178502, 10.72451020669898547, 104.1655762719810241 ) ) ;
#96404 = CARTESIAN_POINT ( 'NONE',  ( 12.14591786802309770, 12.06949235617756955, 44.37390960531435979 ) ) ;
#96405 = ORIENTED_EDGE ( 'NONE', *, *, #81756, .F. ) ;
#96406 = CARTESIAN_POINT ( 'NONE',  ( -16.88567814943163015, 6.947325034625698947, 73.70998877347417988 ) ) ;
#96407 = CARTESIAN_POINT ( 'NONE',  ( 21.53943276465977519, -0.05219959533907433946, 83.74890960531435269 ) ) ;
#96408 = CARTESIAN_POINT ( 'NONE',  ( 12.14591786802309770, 12.06949235617756955, 24.37390960531435979 ) ) ;
#96409 = VERTEX_POINT ( 'NONE', #123273 ) ;
#96410 = DIRECTION ( 'NONE',  ( -1.000000000000000000, 5.392603844284257652E-33, 0.000000000000000000 ) ) ;
#96411 = CARTESIAN_POINT ( 'NONE',  ( -21.55341960407610458, -5.719274019375992779, 96.45724293864770971 ) ) ;
#96412 = CARTESIAN_POINT ( 'NONE',  ( 13.97604488694527802, 13.89961937509977652, 94.37390960531436690 ) ) ;
#96413 = CARTESIAN_POINT ( 'NONE',  ( -18.62759615963255300, -10.81492255796106328, 29.16775706135234003 ) ) ;
#96414 = CARTESIAN_POINT ( 'NONE',  ( 14.34966873604960469, 8.224510206698951720, 44.16557627198103120 ) ) ;
#96415 = CARTESIAN_POINT ( 'NONE',  ( 16.52544592524335698, 4.483927247898782831, 51.45942372801901854 ) ) ;
#96416 = CARTESIAN_POINT ( 'NONE',  ( -16.51473224551069308, -9.474510206698971260, 41.66557627198103120 ) ) ;
#96417 = CARTESIAN_POINT ( 'NONE',  ( 19.05341960407617918, -5.049401038297876454, 56.04275706135234714 ) ) ;
#96418 = CARTESIAN_POINT ( 'NONE',  ( -9.564922557960796823, -16.46253265017161027, 77.08224293864769550 ) ) ;
#96419 = ORIENTED_EDGE ( 'NONE', *, *, #110986, .F. ) ;
#96420 = CARTESIAN_POINT ( 'NONE',  ( 15.80617190586746368, 15.72974639402197994, 29.37390960531435269 ) ) ;
#96421 = CARTESIAN_POINT ( 'NONE',  ( -30.67396074481678525, -22.36774236106498748, -23.13178788717137024 ) ) ;
#96422 = CARTESIAN_POINT ( 'NONE',  ( 4.379528057220092307, 16.55341960407617563, 27.29275706135234358 ) ) ;
#96423 = CARTESIAN_POINT ( 'NONE',  ( 9.564922557961047289, -16.46253265017146816, 55.41775706135234003 ) ) ;
#96424 = CARTESIAN_POINT ( 'NONE',  ( -21.55341960407610458, -5.719274019375992779, 106.4572429386477097 ) ) ;
#96425 = CARTESIAN_POINT ( 'NONE',  ( 12.06949235617757843, -12.14591786802309237, 38.12390960531436690 ) ) ;
#96426 = CARTESIAN_POINT ( 'NONE',  ( -13.89961937509977652, 13.97604488694528158, 80.62390960531436690 ) ) ;
#96427 = CARTESIAN_POINT ( 'NONE',  ( 18.67979575497178502, 10.72451020669898547, 54.16557627198103120 ) ) ;
#96429 = CARTESIAN_POINT ( 'NONE',  ( -8.224510206698735004, -14.34966873604973081, 29.58442372801901854 ) ) ;
#96428 = CARTESIAN_POINT ( 'NONE',  ( 18.67979575497178502, 10.72451020669898547, 89.16557627198102409 ) ) ;
#96430 = CARTESIAN_POINT ( 'NONE',  ( 10.72451020669898902, -18.67979575497178502, 22.91557627198102765 ) ) ;
#96431 = CARTESIAN_POINT ( 'NONE',  ( -10.81492255796105439, 18.62759615963255655, 87.91775706135234714 ) ) ;
#96432 = CARTESIAN_POINT ( 'NONE',  ( -9.564922557960796823, -16.46253265017161027, 72.08224293864770971 ) ) ;
#96433 = CARTESIAN_POINT ( 'NONE',  ( 19.02544592524343514, -5.153800228976328945, 28.54057627198102409 ) ) ;
#96434 = CARTESIAN_POINT ( 'NONE',  ( 19.03943276465977164, -0.05219959533909143690, 83.74890960531436690 ) ) ;
#96435 = CARTESIAN_POINT ( 'NONE',  ( -0.05219959533910754901, -16.53943276465976808, 102.4989096053143811 ) ) ;
#96436 = CARTESIAN_POINT ( 'NONE',  ( 13.97604488694548053, -13.89961937509957401, 100.6260903946856615 ) ) ;
#96437 = FACE_OUTER_BOUND ( 'NONE', #158625, .T. ) ;
#96438 = CARTESIAN_POINT ( 'NONE',  ( 9.474510206698971260, -16.51473224551069308, 67.91557627198102409 ) ) ;
#96440 = CARTESIAN_POINT ( 'NONE',  ( 19.02544592524343514, -5.153800228976328945, 113.5405762719810241 ) ) ;
#96439 = CARTESIAN_POINT ( 'NONE',  ( 18.67979575497194134, -10.72451020669871369, 95.83442372801903275 ) ) ;
#96441 = CARTESIAN_POINT ( 'NONE',  ( 4.379528057220092307, 16.55341960407617563, 92.29275706135236135 ) ) ;
#96442 = CARTESIAN_POINT ( 'NONE',  ( -29.79829367730025425, 1.376802789501195168, -48.54110828511536369 ) ) ;
#96443 = CARTESIAN_POINT ( 'NONE',  ( -0.05219959533936034679, 19.03943276465977164, 62.50109039468566863 ) ) ;
#96444 = CARTESIAN_POINT ( 'NONE',  ( 19.03943276465977164, 0.05219959533936151252, 21.25109039468565797 ) ) ;
#96445 = CARTESIAN_POINT ( 'NONE',  ( -23.29544513554940721, -16.92513159979223403, 144.1843446569000093 ) ) ;
#96446 = CARTESIAN_POINT ( 'NONE',  ( -13.97604488694527625, -13.89961937509977652, 31.87390960531435979 ) ) ;
#96447 = CARTESIAN_POINT ( 'NONE',  ( 16.52544592524335698, 4.483927247898782831, 111.4594237280190328 ) ) ;
#96448 = DIRECTION ( 'NONE',  ( -1.000000000000000000, -0.000000000000000000, -0.000000000000000000 ) ) ;
#96449 = CARTESIAN_POINT ( 'NONE',  ( 14.34966873604972726, -8.224510206698740333, 105.8344237280190328 ) ) ;
#96450 = CARTESIAN_POINT ( 'NONE',  ( 21.32838159582145821, -20.00333696053909804, -52.29425578929144791 ) ) ;
#96451 = CARTESIAN_POINT ( 'NONE',  ( 8.224510206698742110, 14.34966873604972548, 77.08442372801901854 ) ) ;
#96452 = CARTESIAN_POINT ( 'NONE',  ( 5.049401038298161559, -19.05341960407611168, 37.70724293864768839 ) ) ;
#96453 = CARTESIAN_POINT ( 'NONE',  ( 0.05219959533937995610, -21.53943276465977519, 100.0010903946857042 ) ) ;
#96454 = CARTESIAN_POINT ( 'NONE',  ( 16.46253265017146816, 9.564922557961045513, 106.6677570613523471 ) ) ;
#96455 = CARTESIAN_POINT ( 'NONE',  ( 18.67979575497194134, -10.72451020669871369, 65.83442372801900433 ) ) ;
#96456 = CARTESIAN_POINT ( 'NONE',  ( -16.51473224551082808, 9.474510206698731452, 53.33442372801900433 ) ) ;
#96457 = CARTESIAN_POINT ( 'NONE',  ( -5.049401038298153566, 19.05341960407611168, 80.20724293864769550 ) ) ;
#96458 = CARTESIAN_POINT ( 'NONE',  ( -5.049401038298153566, 19.05341960407611168, 65.20724293864765286 ) ) ;
#96459 = CARTESIAN_POINT ( 'NONE',  ( 17.50000000000000000, 5.499999999999992895, 71.70309617465829888 ) ) ;
#96460 = CARTESIAN_POINT ( 'NONE',  ( -0.05219959533907301413, -21.53943276465977519, 42.49890960531435979 ) ) ;
#96461 = CARTESIAN_POINT ( 'NONE',  ( -13.89961937509977652, 13.97604488694528158, 40.62390960531435979 ) ) ;
#96463 = CARTESIAN_POINT ( 'NONE',  ( 16.55341960407618274, -4.379528057220086978, 76.04275706135237556 ) ) ;
#96462 = CARTESIAN_POINT ( 'NONE',  ( -18.62759615963270932, 10.81492255796079327, 80.83224293864769550 ) ) ;
#96464 = VERTEX_POINT ( 'NONE', #94935 ) ;
#96466 = CARTESIAN_POINT ( 'NONE',  ( 3.556970738554033499E-15, -38.81732327939057825, -2.124999997268813612 ) ) ;
#96465 = CARTESIAN_POINT ( 'NONE',  ( 12.14591786802309770, 12.06949235617756955, 74.37390960531436690 ) ) ;
#96467 = CARTESIAN_POINT ( 'NONE',  ( -14.29746914071037622, -8.314922557961029526, 34.16775706135234714 ) ) ;
#96468 = CARTESIAN_POINT ( 'NONE',  ( 13.89961937509977652, -13.97604488694527269, 23.12390960531436335 ) ) ;
#96469 = CARTESIAN_POINT ( 'NONE',  ( -13.97604488694547697, 13.89961937509957934, 63.12609039468566152 ) ) ;
#96470 = CARTESIAN_POINT ( 'NONE',  ( 8.314922557960818139, 14.29746914071049879, 74.58224293864768129 ) ) ;
#96471 = CARTESIAN_POINT ( 'NONE',  ( 10.72451020669871369, 18.67979575497193778, 47.08442372801901854 ) ) ;
#96473 = CARTESIAN_POINT ( 'NONE',  ( -10.81492255796078084, -18.62759615963271287, 92.08224293864769550 ) ) ;
#96472 = CARTESIAN_POINT ( 'NONE',  ( -13.97604488694527625, -13.89961937509977652, 21.87390960531435979 ) ) ;
#96474 = DIRECTION ( 'NONE',  ( -1.000000000000000000, -0.000000000000000000, -0.000000000000000000 ) ) ;
#96475 = CARTESIAN_POINT ( 'NONE',  ( -16.52544592524342804, 4.483927247898546575, 71.04057627198103830 ) ) ;
#96476 = CARTESIAN_POINT ( 'NONE',  ( 21.44681783661738095, -33.76292609718872484, -24.06782133912101074 ) ) ;
#96477 = CARTESIAN_POINT ( 'NONE',  ( 13.89961937509977652, -13.97604488694527269, 48.12390960531435979 ) ) ;
#96478 = CARTESIAN_POINT ( 'NONE',  ( 29.86685920354754842, -21.69954338932559068, -3.824999997268813345 ) ) ;
#96479 = CARTESIAN_POINT ( 'NONE',  ( 19.02544592524334988, 5.153800228976608722, 81.45942372801897591 ) ) ;
#96480 = CARTESIAN_POINT ( 'NONE',  ( -18.67979575497193778, 10.72451020669871902, 23.33442372801901499 ) ) ;
#96481 = CARTESIAN_POINT ( 'NONE',  ( 19.03943276465977164, -0.05219959533909143690, 73.74890960531435269 ) ) ;
#96482 = CARTESIAN_POINT ( 'NONE',  ( 16.51473224551083163, -9.474510206698727899, 50.83442372801899722 ) ) ;
#96483 = CARTESIAN_POINT ( 'NONE',  ( -19.02544592524342804, 5.153800228976336051, 41.04057627198103120 ) ) ;
#96484 = CARTESIAN_POINT ( 'NONE',  ( 14.34966873604960469, 8.224510206698951720, 64.16557627198102409 ) ) ;
#96485 = CARTESIAN_POINT ( 'NONE',  ( 0.05219959533910956823, 16.53943276465976808, 49.99890960531437401 ) ) ;
#96486 = CARTESIAN_POINT ( 'NONE',  ( -19.03943276465977164, 0.05219959533909376836, 76.24890960531435269 ) ) ;
#96487 = CARTESIAN_POINT ( 'NONE',  ( -10.81492255796078084, -18.62759615963271287, 102.0822429386476955 ) ) ;
#96488 = CARTESIAN_POINT ( 'NONE',  ( -16.46253265017160317, 9.564922557960807481, 75.83224293864769550 ) ) ;
#96489 = CARTESIAN_POINT ( 'NONE',  ( 0.05219959533907565091, 21.53943276465977519, 74.99890960531435269 ) ) ;
#96490 = CARTESIAN_POINT ( 'NONE',  ( 9.564922557961047289, -16.46253265017146816, 20.41775706135233293 ) ) ;
#96493 = CARTESIAN_POINT ( 'NONE',  ( 8.224510206698953496, -14.34966873604960469, 97.91557627198103830 ) ) ;
#96492 = CARTESIAN_POINT ( 'NONE',  ( -0.05219959533934338120, 16.53943276465976808, 112.5010903946857042 ) ) ;
#96491 = CARTESIAN_POINT ( 'NONE',  ( 5.153800228976335163, 19.02544592524342804, 24.79057627198102765 ) ) ;
#96494 = CARTESIAN_POINT ( 'NONE',  ( 9.564922557961047289, -16.46253265017146816, 105.4177570613523471 ) ) ;
#96495 = ORIENTED_EDGE ( 'NONE', *, *, #68610, .T. ) ;
#96496 = CARTESIAN_POINT ( 'NONE',  ( -21.55341960407619339, 5.719274019375674811, 28.54275706135234358 ) ) ;
#96497 = CARTESIAN_POINT ( 'NONE',  ( 16.46253265017146816, 9.564922557961045513, 46.66775706135233293 ) ) ;
#96498 = CARTESIAN_POINT ( 'NONE',  ( -12.14591786802309592, -12.06949235617757132, 21.87390960531436690 ) ) ;
#96499 = CARTESIAN_POINT ( 'NONE',  ( -21.55341960407610458, -5.719274019375992779, 71.45724293864769550 ) ) ;
#96500 = CARTESIAN_POINT ( 'NONE',  ( 16.46253265017160672, -9.564922557960803928, 103.3322429386476955 ) ) ;
#96501 = CARTESIAN_POINT ( 'NONE',  ( 14.34966873604960469, 8.224510206698951720, 59.16557627198103120 ) ) ;
#96502 = CARTESIAN_POINT ( 'NONE',  ( 0.05219959533909260263, 19.03943276465977164, 34.99890960531435979 ) ) ;
#96503 = CARTESIAN_POINT ( 'NONE',  ( 5.049401038298161559, -19.05341960407611168, 27.70724293864769550 ) ) ;
#96504 = CARTESIAN_POINT ( 'NONE',  ( 15.80617190586769283, -15.72974639402175789, 105.6260903946856899 ) ) ;
#96505 = CARTESIAN_POINT ( 'NONE',  ( 8.224510206698742110, 14.34966873604972548, 87.08442372801901854 ) ) ;
#96506 = CARTESIAN_POINT ( 'NONE',  ( -15.72974639402176322, -15.80617190586768395, 44.37609039468567573 ) ) ;
#96507 = CARTESIAN_POINT ( 'NONE',  ( 4.483927247898790824, -16.52544592524335698, 40.20942372801901854 ) ) ;
#96508 = CARTESIAN_POINT ( 'NONE',  ( -0.05219959533907301413, -21.53943276465977519, 22.49890960531436335 ) ) ;
#96509 = CARTESIAN_POINT ( 'NONE',  ( -13.97604488694527625, -13.89961937509977652, 51.87390960531436690 ) ) ;
#96510 = CARTESIAN_POINT ( 'NONE',  ( -13.97604488694527625, -13.89961937509977652, 66.87390960531436690 ) ) ;
#96511 = CARTESIAN_POINT ( 'NONE',  ( 16.53943276465976808, 0.05219959533934440121, 66.25109039468567573 ) ) ;
#96512 = CARTESIAN_POINT ( 'NONE',  ( 0.05219959533910956823, 16.53943276465976808, 99.99890960531436690 ) ) ;
#96513 = CARTESIAN_POINT ( 'NONE',  ( 8.314922557960818139, 14.29746914071049879, 24.58224293864768839 ) ) ;
#96514 = LINE ( 'NONE', #20677, #128181 ) ;
#96517 = CARTESIAN_POINT ( 'NONE',  ( 9.474510206698971260, -16.51473224551069308, 77.91557627198103830 ) ) ;
#96516 = CARTESIAN_POINT ( 'NONE',  ( -0.05219959533909027116, -19.03943276465977164, 92.49890960531436690 ) ) ;
#96515 = CARTESIAN_POINT ( 'NONE',  ( 5.823673210054444382, -21.52544592524334988, 60.20942372801902565 ) ) ;
#96518 = CARTESIAN_POINT ( 'NONE',  ( 13.89961937509977652, -13.97604488694527269, 103.1239096053143527 ) ) ;
#96519 = CARTESIAN_POINT ( 'NONE',  ( 12.06949235617757843, -12.14591786802309237, 43.12390960531435269 ) ) ;
#96520 = CARTESIAN_POINT ( 'NONE',  ( -16.53943276465976808, 0.05219959533911058130, 26.24890960531435624 ) ) ;
#96521 = CARTESIAN_POINT ( 'NONE',  ( 4.483927247898545687, 16.52544592524342804, 44.79057627198103120 ) ) ;
#96522 = LINE ( 'NONE', #158212, #86744 ) ;
#96523 = CARTESIAN_POINT ( 'NONE',  ( 9.474510206698729675, 16.51473224551082808, 32.08442372801900433 ) ) ;
#96524 = CARTESIAN_POINT ( 'NONE',  ( -5.049401038298153566, 19.05341960407611168, 80.20724293864769550 ) ) ;
#96525 = CARTESIAN_POINT ( 'NONE',  ( -5.049401038297874678, -19.05341960407617918, 49.79275706135231871 ) ) ;
#96526 = CARTESIAN_POINT ( 'NONE',  ( 22.81625015709509441, 31.40387420917330275, -9.824999997268811569 ) ) ;
#96527 = DIRECTION ( 'NONE',  ( -0.000000000000000000, -0.000000000000000000, -1.000000000000000000 ) ) ;
#96529 = CARTESIAN_POINT ( 'NONE',  ( -8.224510206698735004, -14.34966873604973081, 69.58442372801900433 ) ) ;
#96528 = CARTESIAN_POINT ( 'NONE',  ( -0.05219959533936034679, 19.03943276465977164, 87.50109039468567573 ) ) ;
#96530 = PLANE ( 'NONE',  #27082 ) ;
#96531 = CARTESIAN_POINT ( 'NONE',  ( -5.153800228976328057, -19.02544592524343514, 107.2905762719810383 ) ) ;
#96532 = CARTESIAN_POINT ( 'NONE',  ( -18.67979575497193778, 10.72451020669871902, 33.33442372801900433 ) ) ;
#96533 = CARTESIAN_POINT ( 'NONE',  ( 13.89961937509957401, 13.97604488694547697, 96.87609039468566152 ) ) ;
#96535 = CARTESIAN_POINT ( 'NONE',  ( 16.51473224551069308, 9.474510206698969483, 54.16557627198103120 ) ) ;
#96534 = CARTESIAN_POINT ( 'NONE',  ( 16.46253265017160672, -9.564922557960803928, 113.3322429386476955 ) ) ;
#96536 = EDGE_CURVE ( 'NONE', #44580, #199831, #44089, .T. ) ;
#96537 = CARTESIAN_POINT ( 'NONE',  ( -5.153800228976328057, -19.02544592524343514, 87.29057627198103830 ) ) ;
#96539 = CARTESIAN_POINT ( 'NONE',  ( 5.153800228976335163, 19.02544592524342804, 49.79057627198100988 ) ) ;
#96538 = CARTESIAN_POINT ( 'NONE',  ( 12.06949235617757843, -12.14591786802309237, 63.12390960531435979 ) ) ;
#96540 = CARTESIAN_POINT ( 'NONE',  ( 16.51473224551069308, 9.474510206698969483, 64.16557627198102409 ) ) ;
#96541 = CARTESIAN_POINT ( 'NONE',  ( 19.03943276465977164, 0.05219959533936151252, 66.25109039468567573 ) ) ;
#96542 = CARTESIAN_POINT ( 'NONE',  ( 9.564922557961047289, -16.46253265017146816, 35.41775706135233293 ) ) ;
#96543 = CARTESIAN_POINT ( 'NONE',  ( -0.05219959533909027116, -19.03943276465977164, 62.49890960531435979 ) ) ;
#96544 =( BOUNDED_SURFACE ( )  B_SPLINE_SURFACE ( 3, 2, ( 
 ( #101895, #163577, #103897, #194916, #9899, #121039, #152382, #87716, #150418, #102894, #151405, #72570, #182737, #195931, #181742, #118073, #136225, #29059, #43223, #137209, #134245, #135249, #74558, #119078, #44221, #41233, #105879, #165577, #198896, #164579, #196921, #149402, #26073, #180760, #27076, #11913, #73576, #167566, #104891, #166580, #76532, #126019, #157358, #187714, #108857, #106866, #62339, #107848, #199890, #63351, #49186, #91677, #79514, #110844, #139194, #60364, #32026, #15864, #169533, #93684, #669, #1673, #138208, #18852, #183726, #124009, #14871, #140180, #31033, #92682, #122036, #142171, #125028, #61354, #186724, #185707, #123025, #80498, #45212, #17858, #171534, #168540, #30038, #170536, #172528, #47197, #34014, #95671, #48195, #16856, #153369, #184710, #155367, #46195, #78507, #109849, #33022, #94677, #141184, #154370, #77522, #156356, #2673, #64350, #98641, #66328, #19829, #97631, #7637, #23831, #127989, #54162, #38993, #99650, #175506, #173528, #159320, #96653, #68316, #158340, #53146, #174517, #188700, #36980, #85481, #162330, #3655, #145155, #65333, #126993, #190678, #81470, #111839, #146150, #177524, #35984, #160336, #189692, #176518, #20815, #84472, #82472, #6638, #50182, #22826, #115835, #129967, #100649, #144157, #21825, #161334, #5642, #69321, #51164, #130987, #52154, #34998, #143156, #83477, #67319, #112825, #128980, #113811, #191667, #4637, #192679, #114825, #37995, #163345, #12664, #43982, #74332, #195698, #193687, #149180, #194686, #86490, #148175, #70332, #119831, #182502, #58164, #28828, #165348, #42005, #134007, #104662, #147170, #57170, #181516, #42995, #105643, #39982, #103670, #26842, #88482, #180531, #27845, #151176, #120802, #72332, #118848, #167332, #150178, #8659, #73344, #131999, #55155, #166347, #116825, #117837, #132995, #178516, #11679, #89486, #101653, #24841, #179530, #9667, #71333, #135998, #10668, #135017, #56156, #197669, #41000, #196694, #59134, #102667, #164352, #25848, #87491, #121797, #29803, #184478, #63106, #90469, #44974, #30796, #198663, #31788, #1427, #62105, #152152, #93437, #139937, #186483, #125776, #15625, #156114, #108617, #79271, #16617, #136974, #17612, #123768, #45957, #61115, #122789, #107612, #169290, #168306, #124784, #185468, #92445, #91439, #140942, #60129, #75302, #183490, #138952, #47959, #94433, #155124, #110598, #77282, #46958, #109610, #106633, #154132, #13635, #153127, #170295, #431, #14630, #78265, #171295, #76287, #137967, #199649, #32781, #172280, #2430, #64109, #187477, #48945, #188454, #141927, #176278, #7398, #4400, #5400, #19595, #6398, #189452, #52904, #22587, #112587, #33769, #67084, #50930, #81237, #128743, #174281, #175268, #111600, #192441, #157113, #35750, #49935, #113574, #66085, #142918, #95429, #115598, #98397, #173284, #36734, #159082, #34758, #53923, #18610, #191428, #144915, #80257, #130749, #143919, #161092, #20576, #84235, #145913, #21581, #190439, #3418, #65093, #82229, #158102, #97396, #51915, #68077, #160095, #114580, #127751, #126752, #129731, #83240, #37749, #99410, #96416, #69082, #71089, #181279, #197433, #101404, #27604, #12429, #73102, #148936, #146929, #132756, #70091, #41760, #131760, #26597, #147938, #42756, #23590, #162095, #164110, #58899, #118602, #177286, #38757, #25608, #193442, #85238, #119596, #150936, #9424, #10426, #163098, #149925, #194443, #57925, #55914, #180292, #100414, #196455, #89243, #103425, #74092, #117588, #195453, #134772, #179289, #104419, #39742, #166102, #87252, #135762, #8419, #56927, #40754, #24601, #86248, #102422, #72084, #54918, #116590, #178279, #165104, #133758, #88240, #11432, #186243, #169049, #167091, #122553, #168071, #59891, #123535, #109372, #151913, #93202, #45724, #185229, #15388, #183253, #136732, #14386, #124546, #140704, #44734, #171054, #155877, #16385, #92207, #90229, #76052, #13402, #46720, #75066, #170059, #91200, #47721, #28592, #105406 ),
 ( #77045, #79029, #121557, #43744, #154887, #17374, #31550, #2194, #138716, #197, #107377, #78032, #120565, #30555, #139701, #1187, #182259, #198414, #61866, #108383, #62864, #153891, #32544, #94197, #106390, #29569, #152890, #137728, #199412, #60876, #184243, #99175, #125547, #98158, #48713, #34530, #49699, #95197, #174052, #6169, #187243, #160865, #96190, #18380, #22355, #129504, #65850, #158854, #84007, #67849, #110366, #66848, #20342, #189224, #128511, #21351, #172048, #156883, #3192, #157879, #36504, #63876, #80032, #4172, #33535, #5165, #175039, #35521, #141701, #190206, #113347, #159858, #145685, #50702, #191204, #81991, #52679, #51685, #64865, #114342, #97169, #19368, #81017, #142692, #127520, #112361, #126527, #83009, #143684, #144684, #188226, #111364, #176045, #37513, #173053, #29086, #198922, #86017, #7167, #179052, #162859, #54680, #40520, #147706, #151433, #85001, #168568, #130509, #9194, #161862, #89747, #178043, #116354, #68850, #91707, #74584, #146682, #12920, #132528, #8177, #30066, #192205, #167591, #121070, #53687, #106895, #117356, #137238, #194217, #60391, #122063, #197928, #163879, #115364, #177054, #55682, #131521, #70859, #28108, #182764, #102191, #90725, #39511, #38524, #44248, #136252, #59396, #105905, #69853, #23356, #101171, #13895, #100180, #193207, #183755, #45241, #152408, #75562, #24366, #108888, #46226, #17890, #107879, #2704, #124041, #157390, #199919, #138236, #140211, #35030, #94708, #153401, #14899, #1705, #169567, #61383, #95702, #127025, #185740, #125058, #139225, #126049, #170567, #34045, #32057, #156385, #76560, #172559, #65364, #79544, #50217, #47229, #171563, #49216, #155396, #18883, #15895, #80529, #63381, #188732, #123055, #33053, #93714, #700, #77553, #62372, #16886, #111871, #110874, #142203, #141214, #31064, #3686, #173561, #184741, #186755, #92712, #78537, #48225, #154400, #109879, #64381, #187745, #53182, #55188, #97665, #19862, #69353, #132030, #7669, #178548, #114858, #191699, #83509, #54194, #96685, #145186, #131022, #192711, #193720, #189724, #176552, #38028, #99684, #129999, #177556, #100680, #70363, #21858, #6670, #116857, #161368, #158373, #22859, #81502, #143189, #115867, #4669, #67352, #82508, #128022, #68348, #39025, #66361, #51197, #129012, #112858, #174549, #162362, #98674, #84506, #36016, #23863, #159354, #146184, #85514, #147202, #8693, #20850, #144190, #5676, #190712, #52185, #113843, #175539, #37013, #160368, #148206, #181546, #151206, #11710, #40014, #43024, #89516, #136026, #75334, #165380, #105677, #58193, #28861, #166379, #86522, #167363, #73377, #195731, #10701, #72364, #57204, #134038, #117871, #12694, #135049, #118879, #41031, #90501, #9699, #24873, #71364, #88517, #74360, #44016, #104691, #60160, #26874, #196725, #197700, #133028, #180563, #101687, #194718, #119861, #42037, #163376, #27875, #59166, #164385, #25878, #120834, #182534, #103701, #150213, #152183, #179561, #56188, #13667, #137004, #87522, #102697, #198693, #121829, #149210, #107645, #33801, #18642, #79304, #155157, #153160, #138984, #76321, #47990, #137999, #32814, #154165, #187509, #29835, #168339, #170327, #65125, #124816, #183523, #45006, #31819, #199683, #91472, #125807, #157147, #15657, #16649, #169322, #156146, #462, #64143, #62137, #186516, #106666, #2461, #95461, #109643, #80288, #77316, #1459, #140973, #185499, #48976, #45990, #110631, #93470, #141960, #14661, #63137, #123801, #30829, #92477, #46990, #108649, #3449, #172312, #61148, #171326, #122820, #184510, #78296, #139970, #94465, #17644, #128775, #174312, #66118, #129762, #115629, #158134, #145948, #177318, #5433, #126783, #98430, #82261, #35782, #160127, #67117, #68110, #4430, #85270, #49968, #190474, #81268, #6428, #97429, #159115, #188489, #8449, #191458, #127783, #52936, #51947, #189483, #146961, #111632, #84267, #37780, #173317, #23622, #36767, #53953, #113607, #38789, #100446 ),
 ( #99444, #175301, #114610, #21615, #50961, #20609, #83273, #144947, #176308, #112620, #34792, #96447, #161124, #142949, #22620, #143953, #7429, #19626, #69113, #130779, #192471, #162126, #195484, #9459, #28623, #70122, #27637, #181311, #90260, #167123, #180324, #197465, #56959, #58931, #120599, #57957, #26629, #151943, #131793, #118633, #194476, #10458, #88272, #42789, #41792, #150968, #102455, #101438, #104452, #103459, #134807, #165137, #132789, #86280, #164143, #74123, #193473, #55948, #182294, #105438, #166135, #149960, #39774, #25640, #163129, #196487, #24632, #119628, #40786, #135794, #116622, #54950, #11466, #178311, #73137, #147971, #71123, #89278, #117624, #179322, #12463, #43774, #87284, #148969, #72119, #133792, #169078, #94226, #92236, #154914, #13432, #32573, #125574, #78059, #110395, #107405, #31578, #109402, #15416, #17403, #76079, #155907, #226, #187272, #95226, #93229, #184270, #199439, #137755, #60907, #122583, #172077, #171082, #79060, #16412, #29597, #140733, #33564, #2222, #61894, #59920, #77074, #45753, #152919, #139727, #63904, #44765, #48741, #75096, #153921, #136763, #185259, #30584, #198448, #123564, #46751, #121588, #106418, #138744, #183283, #168099, #170085, #108410, #91228, #1216, #62893, #124574, #186270, #14415, #47749, #112387, #5193, #66875, #96216, #173080, #143714, #37538, #81043, #157905, #18409, #4199, #98184, #113373, #115391, #19394, #80058, #129529, #192233, #67875, #38550, #175064, #51710, #128537, #114366, #156912, #190232, #191229, #52703, #53714, #49727, #36530, #159888, #21376, #83035, #99202, #160890, #130535, #82018, #144710, #177079, #6195, #141728, #176071, #3218, #64892, #22382, #126553, #127551, #142719, #188253, #84032, #145710, #111395, #34557, #189252, #65877, #50729, #7192, #158881, #68876, #174079, #35548, #97195, #20370, #56723, #25404, #164901, #57722, #23382, #131550, #39537, #194243, #72897, #100207, #54708, #40550, #8206, #41556, #11222, #71879, #161887, #103219, #149722, #196253, #135558, #87046, #165894, #118394, #89037, #26395, #146709, #27391, #133549, #55710, #70887, #132555, #117382, #179079, #178070, #134565, #195239, #102219, #101195, #150727, #69881, #85029, #193235, #148731, #119392, #104213, #88034, #116380, #181075, #180088, #10219, #42550, #12226, #162886, #24395, #86044, #163908, #73889, #147733, #9220, #197231, #58692, #120362, #182055, #107171, #43538, #76838, #123328, #169849, #124334, #122345, #77830, #153683, #139497, #195428, #151712, #16175, #168842, #75845, #91000, #152686, #137521, #14175, #59683, #185022, #30347, #199203, #183047, #979, #90029, #13205, #74868, #45516, #108168, #62655, #138509, #109168, #184034, #91989, #31343, #136530, #60670, #105204, #198211, #15179, #61660, #28391, #46508, #92994, #167869, #29369, #154680, #186030, #47512, #166891, #121354, #44531, #106186, #70020, #26527, #71021, #196385, #193370, #194377, #8345, #195379, #178208, #103356, #101334, #164041, #22516, #41691, #134702, #87184, #119526, #116520, #40682, #118532, #24529, #88171, #85164, #165034, #9356, #57854, #104346, #102352, #54846, #131689, #146852, #39672, #163023, #181209, #180221, #149855, #25540, #38687, #11360, #42685, #73030, #132689, #69009, #86180, #147870, #162022, #148865, #84163, #53852, #145843, #7325, #55844, #130675, #117518, #179216, #10356, #72013, #192369, #133686, #115526, #56857, #177214, #100343, #23518, #13330, #199339, #106315, #107301, #43670, #124470, #89171, #44662, #120494, #45650, #136660, #74995, #27530, #47649, #30478, #105332, #168973, #91130, #167020, #186167, #166030, #123462, #76971, #150863, #62789, #75979, #93127, #152820, #154812, #16310, #153817, #122477, #12357, #74020, #14314, #90157, #168001, #184168, #138642, #137652, #46644, #198341, #197362, #123, #60804, #92130, #15312, #28521, #182185, #59816, #169984, #135690, #151840, #77960, #1115, #61792, #185154, #58827, #121486, #183180, #108304 ),
 ( #31475, #29497, #139627, #170979, #156813, #50624, #65776, #67772, #110295, #32472, #81913, #144608, #20267, #191127, #127445, #4097, #96116, #66772, #109300, #157804, #143606, #5090, #6093, #2121, #189151, #112285, #173975, #142618, #190130, #113269, #82930, #34457, #19295, #129429, #35443, #94125, #97095, #155804, #17302, #128433, #78956, #79961, #95123, #140631, #80943, #51605, #63803, #174961, #36425, #125476, #187172, #158779, #98080, #159778, #21273, #48643, #171977, #33465, #18305, #141630, #3120, #64795, #126456, #188154, #49627, #111289, #172979, #37436, #23279, #38445, #83927, #162780, #195135, #114263, #102112, #11116, #145608, #160788, #118290, #54602, #147626, #72791, #56616, #175967, #55604, #9114, #177966, #117278, #10115, #99096, #7087, #192125, #146603, #25299, #52601, #68768, #193129, #22276, #194140, #163797, #24288, #130426, #178972, #86941, #148625, #87931, #39434, #179981, #70781, #41449, #40439, #53606, #103114, #85937, #8096, #84923, #69774, #131442, #116276, #115282, #71775, #132449, #101094, #176975, #164795, #100100, #161784, #133445, #26290, #149618, #134461, #137419, #16075, #182947, #29268, #153579, #88936, #166790, #57618, #165792, #152585, #28291, #119286, #14076, #45417, #120261, #181953, #15077, #76738, #151612, #44430, #106084, #135459, #12123, #150627, #75742, #74769, #91888, #180969, #43435, #199099, #60566, #154579, #197128, #42446, #168741, #31243, #107070, #77733, #122242, #90899, #167770, #138413, #196146, #183932, #104110, #200093, #108064, #30245, #92893, #89931, #61561, #123230, #198112, #184921, #58595, #46405, #169748, #27289, #73787, #105104, #13104, #136431, #59579, #121253, #63567, #97848, #96866, #4857, #19062, #155573, #66542, #36194, #128206, #187923, #185928, #141396, #186939, #78722, #142387, #126228, #189903, #159537, #170748, #18072, #139399, #111055, #94893, #48410, #172743, #79727, #80709, #17068, #21035, #62556, #2884, #93895, #3866, #110066, #171746, #881, #124232, #65545, #140398, #127204, #64563, #1886, #47413, #109069, #158550, #50396, #32237, #125241, #49392, #51378, #34224, #113039, #174731, #188918, #95886, #33235, #156577, #157569, #112056, #173744, #35213, #20040, #81683, #143365, #115044, #114024, #55366, #7854, #147387, #177734, #145370, #98856, #176736, #86699, #102873, #6852, #133204, #118052, #178731, #54373, #52367, #38209, #175721, #8875, #37200, #132211, #53366, #148384, #129193, #67535, #69541, #164558, #24045, #82688, #144372, #9878, #130186, #71538, #131205, #56369, #99865, #116045, #68531, #117036, #161549, #163556, #23042, #85701, #160551, #39203, #100859, #162541, #70543, #25056, #194895, #179742, #192896, #193902, #41212, #40194, #5859, #101874, #190891, #22041, #83692, #191882, #84687, #146367, #57385, #136204, #168522, #87696, #75514, #184691, #119058, #134225, #91658, #28057, #121016, #46175, #30020, #149381, #29040, #182714, #151384, #90680, #183707, #10877, #180740, #165557, #120034, #198875, #26052, #42216, #166558, #195910, #167545, #137188, #197879, #72547, #152362, #60342, #122016, #61334, #12874, #153347, #44199, #14849, #13847, #103877, #76511, #59348, #181720, #196900, #58367, #43202, #104869, #27054, #45193, #105858, #89698, #88700, #138187, #150396, #11892, #73555, #74539, #106847, #199870, #123005, #107828, #135228, #2654, #129701, #62319, #140161, #31012, #139172, #125999, #1653, #92662, #187696, #18833, #93663, #155348, #191398, #52875, #125009, #17838, #79496, #108836, #185687, #123989, #49166, #48176, #65314, #154350, #16837, #110825, #172507, #130717, #170517, #15843, #142152, #7366, #80478, #53892, #33994, #64331, #156338, #114547, #169512, #141165, #3636, #176246, #69051, #77502, #95650, #649, #157338, #47177, #32006, #37717, #78488, #99379, #161062, #145883, #63331, #22557, #186705, #84203, #109832, #192410, #171515, #33004, #94658, #134740, #27571, #180259, #12397, #9394, #133725 ),
 ( #39710, #74059, #73068, #181247, #195417, #131729, #42724, #135730, #104386, #164079, #162062, #117557, #163063, #54886, #118569, #102391, #166069, #197401, #146895, #194414, #115567, #87222, #71060, #24569, #148904, #55884, #56895, #193411, #177254, #38726, #179257, #70061, #41729, #86218, #147908, #100384, #23558, #103393, #116560, #165071, #40722, #178249, #85206, #8386, #196422, #26565, #101373, #132726, #25578, #89210, #10394, #150903, #72051, #88208, #149892, #11399, #57892, #119564, #183220, #199378, #15353, #31514, #30517, #139665, #91169, #90197, #93167, #184207, #123500, #153855, #121525, #75034, #152858, #62828, #78995, #44701, #109338, #94163, #154852, #92169, #28560, #14353, #151880, #185193, #13370, #108343, #29536, #124511, #105372, #162, #120533, #46684, #155842, #182226, #16350, #43711, #76018, #106355, #136700, #169013, #1153, #167059, #170024, #17339, #198381, #59858, #186206, #60842, #77009, #140669, #47688, #168039, #61830, #138681, #45689, #77998, #171020, #137693, #122517, #107340, #32511, #58867, #2161, #156849, #142658, #110332, #143646, #113310, #174014, #63839, #5129, #51646, #98123, #37478, #127485, #67815, #20306, #191169, #128474, #48680, #129470, #35485, #157844, #173018, #34497, #19335, #96155, #79999, #175001, #97134, #80983, #3159, #52642, #172013, #187209, #33502, #50664, #36466, #6132, #66812, #22317, #189190, #158818, #159820, #95161, #4137, #125512, #18344, #81954, #65816, #141667, #190170, #21315, #126494, #188192, #82973, #144649, #112324, #114307, #176009, #64832, #49664, #111328, #99140, #160829, #83968, #7128, #193169, #86980, #102152, #104149, #146644, #68810, #118329, #181012, #56656, #27328, #163837, #40480, #132490, #103154, #145648, #194179, #180022, #41489, #42486, #38485, #25339, #148667, #10155, #179012, #26331, #149659, #119325, #70821, #55643, #165831, #162819, #116316, #23318, #164835, #71815, #39472, #8137, #134501, #192167, #130469, #53647, #117316, #87971, #11157, #133483, #115325, #195175, #72831, #196187, #100142, #178005, #177016, #161823, #57659, #101133, #84962, #69815, #131482, #54641, #24328, #85977, #147667, #9155, #137458, #199137, #28329, #105142, #181992, #168778, #167806, #184957, #150664, #136468, #30280, #45454, #47449, #89968, #12162, #61597, #124269, #200128, #170784, #107108, #183967, #75780, #46441, #88974, #60604, #123266, #108100, #185964, #43474, #91926, #153618, #15114, #122279, #169785, #92929, #62591, #14113, #76775, #109105, #138447, #73827, #31278, #135497, #197167, #154615, #58633, #59618, #74805, #120299, #16110, #77768, #166828, #139435, #151648, #13143, #198148, #917, #90936, #121291, #182984, #44468, #106122, #29306, #152622, #157606, #96902, #189937, #155610, #63603, #171782, #126263, #4893, #32274, #186976, #172781, #140434, #173782, #143404, #3903, #93931, #35249, #81719, #128240, #67570, #19097, #97882, #50433, #21071, #158586, #78757, #159573, #65583, #187960, #2921, #64599, #17105, #80746, #156614, #34262, #188956, #66575, #127242, #113072, #49430, #125279, #51412, #142424, #20075, #112092, #94929, #48446, #111091, #36230, #52402, #18109, #82727, #129228, #174764, #144408, #1924, #95921, #110103, #5894, #33270, #190925, #114061, #79763, #141434, #160585, #162575, #57418, #117069, #175758, #37235, #179776, #23076, #41245, #24078, #149414, #146399, #147421, #161582, #148417, #131240, #56404, #54406, #178765, #98891, #194929, #87729, #40230, #72583, #69574, #193936, #71572, #177766, #102907, #38242, #118086, #85734, #10910, #22074, #55399, #7888, #84721, #99897, #192928, #116078, #134257, #133237, #164591, #101907, #191916, #26085, #195944, #83725, #8908, #145404, #39235, #100891, #115078, #163589, #70576, #6886, #68564, #130221, #132244, #53400, #25090, #86732, #9912, #176770, #59380, #60374, #196932, #77532, #42248, #197910, #73588, #198906, #89730, #166591, #180773, #679, #183736, #58400, #122046 ),
 ( #165590, #184721, #90709, #44232, #46205, #137219, #107859, #45222, #27088, #169544, #152392, #74568, #151416, #12904, #136236, #121052, #120066, #30048, #13878, #182747, #181754, #31043, #88734, #103909, #150429, #167576, #153379, #123035, #106877, #139204, #105889, #75545, #76542, #11924, #29070, #135260, #43236, #168550, #91689, #104902, #14881, #138218, #92692, #28091, #199900, #61364, #119091, #154380, #15874, #62350, #66340, #109859, #128002, #110854, #35996, #33032, #34024, #48205, #35010, #17869, #143169, #141194, #3666, #124020, #81482, #174529, #127004, #159332, #156366, #80509, #158352, #64360, #189704, #125038, #4649, #49196, #97643, #144169, #142182, #94688, #171544, #186734, #79524, #2683, #20829, #19841, #51177, #65344, #78517, #112837, #82485, #185717, #172539, #108867, #126029, #187725, #1683, #188712, #95682, #47208, #170546, #93694, #157369, #32037, #18863, #50195, #111851, #173541, #96665, #155377, #140191, #16866, #63361, #84486, #160348, #85494, #176532, #53160, #67331, #87502, #70344, #83490, #147182, #130999, #145167, #164363, #5655, #163357, #116838, #25858, #102678, #86502, #38008, #36993, #178528, #192691, #132011, #100661, #68329, #21837, #99663, #9680, #128993, #129979, #56168, #41011, #101667, #190691, #52166, #115847, #54174, #193698, #98654, #55167, #161348, #71345, #113823, #175518, #177536, #6651, #8671, #191679, #114838, #133008, #22839, #194699, #39006, #179542, #146163, #162343, #7649, #39995, #69333, #148186, #23844, #24853, #117849, #168318, #61127, #13646, #45969, #43005, #167343, #44986, #151186, #153139, #11690, #29815, #136007, #122800, #30807, #28840, #119841, #135029, #73356, #196704, #58174, #107623, #106646, #14641, #90481, #165360, #76301, #169301, #137979, #197679, #195710, #12674, #181526, #88495, #152163, #59144, #199661, #149190, #180542, #27856, #10679, #120814, #104672, #166358, #182514, #89496, #75313, #26854, #72344, #134018, #74341, #103681, #136984, #43993, #105655, #57182, #118859, #198673, #150192, #60140, #121807, #183503, #42016, #91451, #184490, #3428, #50940, #189462, #2440, #19605, #79283, #81247, #142929, #80267, #48955, #112598, #154144, #140953, #16629, #32792, #110608, #65104, #64122, #170306, #174290, #15636, #171306, #46969, #172291, #63117, #139949, #77293, #92456, #157124, #31799, #33780, #17624, #93448, #138964, #442, #49947, #126762, #62117, #123780, #125787, #4410, #187489, #66095, #127762, #141937, #95440, #185479, #108628, #18620, #78276, #94445, #188465, #111611, #173296, #34770, #124796, #155135, #96427, #158113, #1439, #186494, #47970, #109622, #156125, #39752, #55925, #160104, #86258, #71099, #131769, #194454, #20587, #145924, #84244, #100423, #128753, #85247, #6406, #101414, #82239, #143929, #22597, #117599, #177295, #35760, #97406, #163107, #83250, #24610, #7407, #9434, #68087, #69090, #21591, #8428, #191437, #116600, #114589, #38766, #159093, #54927, #147948, #162104, #132766, #129740, #53931, #193451, #37758, #5411, #98408, #178288, #130757, #67094, #190450, #115606, #52913, #144925, #176286, #99419, #161102, #51925, #113585, #175279, #23601, #36744, #192449, #146938, #70100, #27616, #25618, #181290, #26608, #118613, #182271, #166113, #170819, #78792, #10437, #57936, #179300, #150947, #134784, #88251, #12441, #119607, #120578, #72097, #154652, #104430, #46478, #74103, #41771, #195464, #73115, #186002, #1959, #103436, #32311, #17140, #77802, #140470, #164120, #89255, #135773, #108138, #133769, #31313, #149937, #47483, #87262, #148947, #197444, #63638, #169822, #40764, #102433, #109140, #11443, #93965, #58910, #155645, #196466, #92966, #165116, #16147, #42768, #62626, #139471, #951, #56939, #124304, #180303, #189968, #22106, #19128, #143437, #21104, #127274, #129261, #187991, #5925, #112122, #37266, #6918, #4924, #95954, #111123, #49461, #172813, #34293, #83756, #82759, #190956, #66606, #141469, #52433 ),
 ( #188988, #20106, #145435, #114091, #187010, #128270, #81750, #50463, #51443, #144439, #48480, #156647, #64632, #80778, #97914, #125314, #79796, #65614, #33303, #113103, #36260, #96934, #110136, #174794, #159605, #67602, #160616, #173814, #175792, #98924, #171815, #94962, #18143, #2953, #158616, #142456, #157639, #3934, #35279, #126294, #146431, #179806, #101940, #162608, #116109, #9944, #25122, #27117, #69606, #191947, #41275, #103938, #102937, #150457, #86766, #163621, #55431, #26116, #68596, #117102, #164622, #87759, #165618, #161613, #148449, #71603, #133269, #194960, #149444, #72613, #42280, #193968, #178797, #88764, #56437, #130252, #118118, #53433, #115109, #10940, #134288, #176801, #38274, #99928, #40266, #195975, #23107, #57447, #84753, #7921, #131272, #119120, #70610, #180801, #192960, #54439, #177797, #39267, #100923, #24112, #85767, #147453, #8941, #132277, #151445, #105917, #184753, #11952, #166618, #152420, #120094, #153413, #123067, #183767, #73616, #14912, #61395, #107892, #47242, #137250, #77565, #30078, #712, #138248, #58427, #139237, #45253, #167603, #182777, #44260, #29098, #90737, #89759, #46238, #106907, #13908, #12932, #62384, #181782, #196959, #43263, #60403, #169579, #15907, #76573, #32070, #198936, #168580, #31077, #104931, #75574, #74596, #136264, #135287, #92724, #28120, #91719, #154413, #197939, #59408, #124054, #185753, #122075, #199932, #108900, #121082, #170579, #93726, #35042, #34057, #51209, #16898, #3698, #65377, #94720, #171576, #48237, #96696, #95715, #112870, #78549, #2716, #158385, #111883, #113855, #156398, #140224, #128034, #190724, #66374, #37026, #173573, #50229, #142215, #174561, #155408, #127037, #189736, #36028, #52197, #109892, #19874, #81514, #143201, #188744, #97677, #159366, #129023, #80541, #4682, #175551, #20863, #1717, #82520, #63393, #125070, #144202, #5688, #186767, #33065, #17902, #67364, #79557, #141225, #64393, #126061, #187758, #49228, #110886, #157402, #172571, #18895, #9711, #98687, #193731, #147213, #39035, #55199, #24884, #21871, #130011, #176564, #7680, #40024, #160381, #38039, #177567, #191710, #116868, #163387, #8704, #83521, #178559, #86533, #71375, #164396, #162372, #117881, #101697, #179572, #148217, #53194, #56199, #70374, #115877, #131033, #192722, #100691, #54206, #99695, #133039, #132042, #23874, #22870, #41042, #114869, #161379, #84517, #85525, #194729, #102707, #145199, #6682, #68360, #146195, #69364, #172212, #49863, #157044, #18541, #140869, #113504, #2358, #97328, #128673, #3351, #65026, #98323, #160023, #34690, #21510, #111529, #110531, #51845, #4331, #143851, #174212, #141860, #95359, #173214, #83171, #99339, #126682, #129660, #114503, #175199, #37674, #64039, #189383, #127683, #5330, #33696, #190370, #96347, #144845, #125709, #187408, #66015, #161022, #20507, #79200, #48876, #6328, #188386, #68008, #50860, #52834, #158034, #112518, #19525, #36664, #81170, #191356, #142852, #82155, #80188, #176205, #35680, #67014, #159014, #57315, #27989, #89628, #152295, #75446, #76439, #134154, #136137, #197813, #59278, #74472, #121945, #45120, #14779, #166491, #151316, #138116, #182647, #102810, #167476, #199797, #164495, #120948, #105790, #122934, #25988, #72481, #12805, #183638, #87631, #90613, #61264, #195842, #149317, #106778, #43133, #44131, #41147, #168453, #10811, #28971, #13779, #137121, #198807, #60272, #118991, #180674, #42150, #135160, #29950, #103810, #165490, #181654, #26986, #91588, #153278, #88631, #150327, #11822, #73487, #196833, #58301, #119968, #104802, #2577, #173435, #110749, #30945, #50087, #156261, #140086, #155273, #16762, #1578, #78410, #62247, #95576, #17764, #143064, #185615, #107758, #157262, #19738, #18757, #66236, #64257, #96560, #170442, #576, #171441, #32928, #80404, #142076, #81379, #77431, #79420, #141090, #125924, #187622, #65240, #188606, #158248, #109757, #94583, #4542, #49092, #46103 ) ),
 .UNSPECIFIED., .T., .F., .F. ) 
 B_SPLINE_SURFACE_WITH_KNOTS ( ( 4, 3, 4 ),
 ( 3, 2, 2, 2, 2, 2, 2, 2, 2, 2, 2, 2, 2, 2, 2, 2, 2, 2, 2, 2, 2, 2, 2, 2, 2, 2, 2, 2, 2, 2, 2, 2, 2, 2, 2, 2, 2, 2, 2, 2, 2, 2, 2, 2, 2, 2, 2, 2, 2, 2, 2, 2, 2, 2, 2, 2, 2, 2, 2, 2, 2, 2, 2, 2, 2, 2, 2, 2, 2, 2, 2, 2, 2, 2, 2, 2, 2, 2, 2, 2, 2, 2, 2, 2, 2, 2, 2, 2, 2, 2, 2, 2, 2, 2, 2, 2, 2, 2, 2, 2, 2, 2, 2, 2, 2, 2, 2, 2, 2, 2, 2, 2, 2, 2, 2, 2, 2, 2, 2, 2, 2, 2, 2, 2, 2, 2, 2, 2, 2, 2, 2, 2, 2, 2, 2, 2, 2, 2, 2, 2, 2, 2, 2, 2, 2, 2, 2, 2, 2, 2, 2, 2, 2, 2, 2, 2, 2, 2, 2, 2, 2, 2, 2, 2, 2, 2, 2, 2, 2, 2, 2, 2, 2, 2, 2, 2, 2, 2, 2, 2, 2, 2, 2, 2, 2, 2, 2, 2, 2, 2, 2, 2, 2, 2, 2, 2, 2, 2, 2, 2, 2, 2, 2, 2, 2, 2, 2, 2, 2, 2, 2, 2, 2, 2, 2, 2, 2, 2, 2, 2, 2, 2, 2, 2, 2, 2, 2, 2, 3 ),
 ( 0.000000000000000000, 0.5000000000000000000, 1.000000000000000000 ),
 ( 0.000000000000000000, 0.004385964912280701511, 0.008771929824561403022, 0.01315789473684210453, 0.01754385964912280604, 0.02192982456140350755, 0.02631578947368420907, 0.03070175438596491058, 0.03508771929824561209, 0.03947368421052631360, 0.04385964912280701511, 0.04824561403508771662, 0.05263157894736841813, 0.05701754385964911964, 0.06140350877192982115, 0.06578947368421052266, 0.07017543859649122417, 0.07456140350877192569, 0.07894736842105262720, 0.08333333333333332871, 0.08771929824561403022, 0.09210526315789473173, 0.09649122807017543324, 0.1008771929824561348, 0.1052631578947368363, 0.1096491228070175378, 0.1140350877192982393, 0.1184210526315789408, 0.1228070175438596423, 0.1271929824561403577, 0.1315789473684210453, 0.1359649122807017607, 0.1403508771929824483, 0.1447368421052631637, 0.1491228070175438514, 0.1535087719298245668, 0.1578947368421052544, 0.1622807017543859698, 0.1666666666666666574, 0.1710526315789473728, 0.1754385964912280604, 0.1798245614035087758, 0.1842105263157894635, 0.1885964912280701788, 0.1929824561403508665, 0.1973684210526315819, 0.2017543859649122695, 0.2061403508771929849, 0.2105263157894736725, 0.2149122807017543879, 0.2192982456140350755, 0.2236842105263157909, 0.2280701754385964786, 0.2324561403508771940, 0.2368421052631578816, 0.2412280701754385970, 0.2456140350877192846, 0.2500000000000000000, 0.2543859649122807154, 0.2587719298245614308, 0.2631578947368420907, 0.2675438596491228060, 0.2719298245614035214, 0.2763157894736842368, 0.2807017543859648967, 0.2850877192982456121, 0.2894736842105263275, 0.2938596491228070429, 0.2982456140350877027, 0.3026315789473684181, 0.3070175438596491335, 0.3114035087719298489, 0.3157894736842105088, 0.3201754385964912242, 0.3245614035087719396, 0.3289473684210526550, 0.3333333333333333148, 0.3377192982456140302, 0.3421052631578947456, 0.3464912280701754610, 0.3508771929824561209, 0.3552631578947368363, 0.3596491228070175517, 0.3640350877192982670, 0.3684210526315789269, 0.3728070175438596423, 0.3771929824561403577, 0.3815789473684210731, 0.3859649122807017330, 0.3903508771929824483, 0.3947368421052631637, 0.3991228070175438791, 0.4035087719298245390, 0.4078947368421052544, 0.4122807017543859698, 0.4166666666666666852, 0.4210526315789473450, 0.4254385964912280604, 0.4298245614035087758, 0.4342105263157894912, 0.4385964912280701511, 0.4429824561403508665, 0.4473684210526315819, 0.4517543859649122973, 0.4561403508771929571, 0.4605263157894736725, 0.4649122807017543879, 0.4692982456140351033, 0.4736842105263157632, 0.4780701754385964786, 0.4824561403508771940, 0.4868421052631579093, 0.4912280701754385692, 0.4956140350877192846, 0.5000000000000000000, 0.5043859649122807154, 0.5087719298245614308, 0.5131578947368421462, 0.5175438596491228616, 0.5219298245614034659, 0.5263157894736841813, 0.5307017543859648967, 0.5350877192982456121, 0.5394736842105263275, 0.5438596491228070429, 0.5482456140350877583, 0.5526315789473684736, 0.5570175438596490780, 0.5614035087719297934, 0.5657894736842105088, 0.5701754385964912242, 0.5745614035087719396, 0.5789473684210526550, 0.5833333333333333703, 0.5877192982456140857, 0.5921052631578946901, 0.5964912280701754055, 0.6008771929824561209, 0.6052631578947368363, 0.6096491228070175517, 0.6140350877192982670, 0.6184210526315789824, 0.6228070175438596978, 0.6271929824561403022, 0.6315789473684210176, 0.6359649122807017330, 0.6403508771929824483, 0.6447368421052631637, 0.6491228070175438791, 0.6535087719298245945, 0.6578947368421053099, 0.6622807017543859143, 0.6666666666666666297, 0.6710526315789473450, 0.6754385964912280604, 0.6798245614035087758, 0.6842105263157894912, 0.6885964912280702066, 0.6929824561403509220, 0.6973684210526315264, 0.7017543859649122417, 0.7061403508771929571, 0.7105263157894736725, 0.7149122807017543879, 0.7192982456140351033, 0.7236842105263158187, 0.7280701754385965341, 0.7324561403508771384, 0.7368421052631578538, 0.7412280701754385692, 0.7456140350877192846, 0.7500000000000000000, 0.7543859649122807154, 0.7587719298245614308, 0.7631578947368421462, 0.7675438596491228616, 0.7719298245614034659, 0.7763157894736841813, 0.7807017543859648967, 0.7850877192982456121, 0.7894736842105263275, 0.7938596491228070429, 0.7982456140350877583, 0.8026315789473684736, 0.8070175438596490780, 0.8114035087719297934, 0.8157894736842105088, 0.8201754385964912242, 0.8245614035087719396, 0.8289473684210526550, 0.8333333333333333703, 0.8377192982456140857, 0.8421052631578946901, 0.8464912280701754055, 0.8508771929824561209, 0.8552631578947368363, 0.8596491228070175517, 0.8640350877192982670, 0.8684210526315789824, 0.8728070175438596978, 0.8771929824561403022, 0.8815789473684210176, 0.8859649122807017330, 0.8903508771929824483, 0.8947368421052631637, 0.8991228070175438791, 0.9035087719298245945, 0.9078947368421053099, 0.9122807017543859143, 0.9166666666666666297, 0.9210526315789473450, 0.9254385964912280604, 0.9298245614035087758, 0.9342105263157894912, 0.9385964912280702066, 0.9429824561403509220, 0.9473684210526315264, 0.9517543859649122417, 0.9561403508771929571, 0.9605263157894736725, 0.9649122807017543879, 0.9692982456140351033, 0.9736842105263158187, 0.9780701754385965341, 0.9824561403508771384, 0.9868421052631578538, 0.9912280701754385692, 0.9956140350877192846, 1.000000000000000000 ),
 .UNSPECIFIED. ) 
 GEOMETRIC_REPRESENTATION_ITEM ( )  RATIONAL_B_SPLINE_SURFACE ( (
 ( 1.000000000000000000, 0.9659258262890683122, 1.000000000000000000, 0.9659258262890683122, 1.000000000000000000, 0.9659258262890683122, 1.000000000000000000, 0.9659258262890683122, 1.000000000000000000, 0.9659258262890683122, 1.000000000000000000, 0.9659258262890683122, 1.000000000000000000, 0.9659258262890683122, 1.000000000000000000, 0.9659258262890683122, 1.000000000000000000, 0.9659258262890683122, 1.000000000000000000, 0.9659258262890683122, 1.000000000000000000, 0.9659258262890683122, 1.000000000000000000, 0.9659258262890683122, 1.000000000000000000, 0.9659258262890683122, 1.000000000000000000, 0.9659258262890683122, 1.000000000000000000, 0.9659258262890683122, 1.000000000000000000, 0.9659258262890683122, 1.000000000000000000, 0.9659258262890683122, 1.000000000000000000, 0.9659258262890683122, 1.000000000000000000, 0.9659258262890683122, 1.000000000000000000, 0.9659258262890683122, 1.000000000000000000, 0.9659258262890683122, 1.000000000000000000, 0.9659258262890683122, 1.000000000000000000, 0.9659258262890683122, 1.000000000000000000, 0.9659258262890683122, 1.000000000000000000, 0.9659258262890683122, 1.000000000000000000, 0.9659258262890683122, 1.000000000000000000, 0.9659258262890683122, 1.000000000000000000, 0.9659258262890683122, 1.000000000000000000, 0.9659258262890683122, 1.000000000000000000, 0.9659258262890683122, 1.000000000000000000, 0.9659258262890683122, 1.000000000000000000, 0.9659258262890683122, 1.000000000000000000, 0.9659258262890683122, 1.000000000000000000, 0.9659258262890683122, 1.000000000000000000, 0.9659258262890683122, 1.000000000000000000, 0.9659258262890683122, 1.000000000000000000, 0.9659258262890683122, 1.000000000000000000, 0.9659258262890683122, 1.000000000000000000, 0.9659258262890683122, 1.000000000000000000, 0.9659258262890683122, 1.000000000000000000, 0.9659258262890683122, 1.000000000000000000, 0.9659258262890683122, 1.000000000000000000, 0.9659258262890683122, 1.000000000000000000, 0.9659258262890683122, 1.000000000000000000, 0.9659258262890683122, 1.000000000000000000, 0.9659258262890683122, 1.000000000000000000, 0.9659258262890683122, 1.000000000000000000, 0.9659258262890683122, 1.000000000000000000, 0.9659258262890683122, 1.000000000000000000, 0.9659258262890683122, 1.000000000000000000, 0.9659258262890683122, 1.000000000000000000, 0.9659258262890683122, 1.000000000000000000, 0.9659258262890683122, 1.000000000000000000, 0.9659258262890683122, 1.000000000000000000, 0.9659258262890683122, 1.000000000000000000, 0.9659258262890683122, 1.000000000000000000, 0.9659258262890683122, 1.000000000000000000, 0.9659258262890683122, 1.000000000000000000, 0.9659258262890683122, 1.000000000000000000, 0.9659258262890683122, 1.000000000000000000, 0.9659258262890683122, 1.000000000000000000, 0.9659258262890683122, 1.000000000000000000, 0.9659258262890683122, 1.000000000000000000, 0.9659258262890683122, 1.000000000000000000, 0.9659258262890683122, 1.000000000000000000, 0.9659258262890683122, 1.000000000000000000, 0.9659258262890683122, 1.000000000000000000, 0.9659258262890683122, 1.000000000000000000, 0.9659258262890683122, 1.000000000000000000, 0.9659258262890683122, 1.000000000000000000, 0.9659258262890683122, 1.000000000000000000, 0.9659258262890683122, 1.000000000000000000, 0.9659258262890683122, 1.000000000000000000, 0.9659258262890683122, 1.000000000000000000, 0.9659258262890683122, 1.000000000000000000, 0.9659258262890683122, 1.000000000000000000, 0.9659258262890683122, 1.000000000000000000, 0.9659258262890683122, 1.000000000000000000, 0.9659258262890683122, 1.000000000000000000, 0.9659258262890683122, 1.000000000000000000, 0.9659258262890683122, 1.000000000000000000, 0.9659258262890683122, 1.000000000000000000, 0.9659258262890683122, 1.000000000000000000, 0.9659258262890683122, 1.000000000000000000, 0.9659258262890683122, 1.000000000000000000, 0.9659258262890683122, 1.000000000000000000, 0.9659258262890683122, 1.000000000000000000, 0.9659258262890683122, 1.000000000000000000, 0.9659258262890683122, 1.000000000000000000, 0.9659258262890683122, 1.000000000000000000, 0.9659258262890683122, 1.000000000000000000, 0.9659258262890683122, 1.000000000000000000, 0.9659258262890683122, 1.000000000000000000, 0.9659258262890683122, 1.000000000000000000, 0.9659258262890683122, 1.000000000000000000, 0.9659258262890683122, 1.000000000000000000, 0.9659258262890683122, 1.000000000000000000, 0.9659258262890683122, 1.000000000000000000, 0.9659258262890683122, 1.000000000000000000, 0.9659258262890683122, 1.000000000000000000, 0.9659258262890683122, 1.000000000000000000, 0.9659258262890683122, 1.000000000000000000, 0.9659258262890683122, 1.000000000000000000, 0.9659258262890683122, 1.000000000000000000, 0.9659258262890683122, 1.000000000000000000, 0.9659258262890683122, 1.000000000000000000, 0.9659258262890683122, 1.000000000000000000, 0.9659258262890683122, 1.000000000000000000, 0.9659258262890683122, 1.000000000000000000, 0.9659258262890683122, 1.000000000000000000, 0.9659258262890683122, 1.000000000000000000, 0.9659258262890683122, 1.000000000000000000, 0.9659258262890683122, 1.000000000000000000, 0.9659258262890683122, 1.000000000000000000, 0.9659258262890683122, 1.000000000000000000, 0.9659258262890683122, 1.000000000000000000, 0.9659258262890683122, 1.000000000000000000, 0.9659258262890683122, 1.000000000000000000, 0.9659258262890683122, 1.000000000000000000, 0.9659258262890683122, 1.000000000000000000, 0.9659258262890683122, 1.000000000000000000, 0.9659258262890683122, 1.000000000000000000, 0.9659258262890683122, 1.000000000000000000, 0.9659258262890683122, 1.000000000000000000, 0.9659258262890683122, 1.000000000000000000, 0.9659258262890683122, 1.000000000000000000, 0.9659258262890683122, 1.000000000000000000, 0.9659258262890683122, 1.000000000000000000, 0.9659258262890683122, 1.000000000000000000, 0.9659258262890683122, 1.000000000000000000, 0.9659258262890683122, 1.000000000000000000, 0.9659258262890683122, 1.000000000000000000, 0.9659258262890683122, 1.000000000000000000, 0.9659258262890683122, 1.000000000000000000, 0.9659258262890683122, 1.000000000000000000, 0.9659258262890683122, 1.000000000000000000, 0.9659258262890683122, 1.000000000000000000, 0.9659258262890683122, 1.000000000000000000, 0.9659258262890683122, 1.000000000000000000, 0.9659258262890683122, 1.000000000000000000, 0.9659258262890683122, 1.000000000000000000, 0.9659258262890683122, 1.000000000000000000, 0.9659258262890683122, 1.000000000000000000, 0.9659258262890683122, 1.000000000000000000, 0.9659258262890683122, 1.000000000000000000, 0.9659258262890683122, 1.000000000000000000, 0.9659258262890683122, 1.000000000000000000, 0.9659258262890683122, 1.000000000000000000, 0.9659258262890683122, 1.000000000000000000, 0.9659258262890683122, 1.000000000000000000, 0.9659258262890683122, 1.000000000000000000, 0.9659258262890683122, 1.000000000000000000, 0.9659258262890683122, 1.000000000000000000, 0.9659258262890683122, 1.000000000000000000, 0.9659258262890683122, 1.000000000000000000, 0.9659258262890683122, 1.000000000000000000, 0.9659258262890683122, 1.000000000000000000, 0.9659258262890683122, 1.000000000000000000, 0.9659258262890683122, 1.000000000000000000, 0.9659258262890683122, 1.000000000000000000, 0.9659258262890683122, 1.000000000000000000, 0.9659258262890683122, 1.000000000000000000, 0.9659258262890683122, 1.000000000000000000, 0.9659258262890683122, 1.000000000000000000, 0.9659258262890683122, 1.000000000000000000, 0.9659258262890683122, 1.000000000000000000, 0.9659258262890683122, 1.000000000000000000, 0.9659258262890683122, 1.000000000000000000, 0.9659258262890683122, 1.000000000000000000, 0.9659258262890683122, 1.000000000000000000, 0.9659258262890683122, 1.000000000000000000, 0.9659258262890683122, 1.000000000000000000, 0.9659258262890683122, 1.000000000000000000, 0.9659258262890683122, 1.000000000000000000, 0.9659258262890683122, 1.000000000000000000, 0.9659258262890683122, 1.000000000000000000, 0.9659258262890683122, 1.000000000000000000, 0.9659258262890683122, 1.000000000000000000, 0.9659258262890683122, 1.000000000000000000, 0.9659258262890683122, 1.000000000000000000, 0.9659258262890683122, 1.000000000000000000, 0.9659258262890683122, 1.000000000000000000, 0.9659258262890683122, 1.000000000000000000, 0.9659258262890683122, 1.000000000000000000, 0.9659258262890683122, 1.000000000000000000, 0.9659258262890683122, 1.000000000000000000, 0.9659258262890683122, 1.000000000000000000, 0.9659258262890683122, 1.000000000000000000, 0.9659258262890683122, 1.000000000000000000, 0.9659258262890683122, 1.000000000000000000, 0.9659258262890683122, 1.000000000000000000, 0.9659258262890683122, 1.000000000000000000, 0.9659258262890683122, 1.000000000000000000, 0.9659258262890683122, 1.000000000000000000, 0.9659258262890683122, 1.000000000000000000, 0.9659258262890683122, 1.000000000000000000, 0.9659258262890683122, 1.000000000000000000, 0.9659258262890683122, 1.000000000000000000, 0.9659258262890683122, 1.000000000000000000, 0.9659258262890683122, 1.000000000000000000, 0.9659258262890683122, 1.000000000000000000, 0.9659258262890683122, 1.000000000000000000, 0.9659258262890683122, 1.000000000000000000, 0.9659258262890683122, 1.000000000000000000, 0.9659258262890683122, 1.000000000000000000, 0.9659258262890683122, 1.000000000000000000, 0.9659258262890683122, 1.000000000000000000, 0.9659258262890683122, 1.000000000000000000, 0.9659258262890683122, 1.000000000000000000, 0.9659258262890683122, 1.000000000000000000, 0.9659258262890683122, 1.000000000000000000, 0.9659258262890683122, 1.000000000000000000, 0.9659258262890683122, 1.000000000000000000, 0.9659258262890683122, 1.000000000000000000, 0.9659258262890683122, 1.000000000000000000, 0.9659258262890683122, 1.000000000000000000, 0.9659258262890683122, 1.000000000000000000, 0.9659258262890683122, 1.000000000000000000, 0.9659258262890683122, 1.000000000000000000, 0.9659258262890683122, 1.000000000000000000, 0.9659258262890683122, 1.000000000000000000, 0.9659258262890683122, 1.000000000000000000, 0.9659258262890683122, 1.000000000000000000, 0.9659258262890683122, 1.000000000000000000, 0.9659258262890683122, 1.000000000000000000, 0.9659258262890683122, 1.000000000000000000, 0.9659258262890683122, 1.000000000000000000, 0.9659258262890683122, 1.000000000000000000),
 ( 0.3333333333333333703, 0.3219752754296894559, 0.3333333333333333703, 0.3219752754296894559, 0.3333333333333333703, 0.3219752754296894559, 0.3333333333333333703, 0.3219752754296894559, 0.3333333333333333703, 0.3219752754296894559, 0.3333333333333333703, 0.3219752754296894559, 0.3333333333333333703, 0.3219752754296894559, 0.3333333333333333703, 0.3219752754296894559, 0.3333333333333333703, 0.3219752754296894559, 0.3333333333333333703, 0.3219752754296894559, 0.3333333333333333703, 0.3219752754296894559, 0.3333333333333333703, 0.3219752754296894559, 0.3333333333333333703, 0.3219752754296894559, 0.3333333333333333703, 0.3219752754296894559, 0.3333333333333333703, 0.3219752754296894559, 0.3333333333333333703, 0.3219752754296894559, 0.3333333333333333703, 0.3219752754296894559, 0.3333333333333333703, 0.3219752754296894559, 0.3333333333333333703, 0.3219752754296894559, 0.3333333333333333703, 0.3219752754296894559, 0.3333333333333333703, 0.3219752754296894559, 0.3333333333333333703, 0.3219752754296894559, 0.3333333333333333703, 0.3219752754296894559, 0.3333333333333333703, 0.3219752754296894559, 0.3333333333333333703, 0.3219752754296894559, 0.3333333333333333703, 0.3219752754296894559, 0.3333333333333333703, 0.3219752754296894559, 0.3333333333333333703, 0.3219752754296894559, 0.3333333333333333703, 0.3219752754296894559, 0.3333333333333333703, 0.3219752754296894559, 0.3333333333333333703, 0.3219752754296894559, 0.3333333333333333703, 0.3219752754296894559, 0.3333333333333333703, 0.3219752754296894559, 0.3333333333333333703, 0.3219752754296894559, 0.3333333333333333703, 0.3219752754296894559, 0.3333333333333333703, 0.3219752754296894559, 0.3333333333333333703, 0.3219752754296894559, 0.3333333333333333703, 0.3219752754296894559, 0.3333333333333333703, 0.3219752754296894559, 0.3333333333333333703, 0.3219752754296894559, 0.3333333333333333703, 0.3219752754296894559, 0.3333333333333333703, 0.3219752754296894559, 0.3333333333333333703, 0.3219752754296894559, 0.3333333333333333703, 0.3219752754296894559, 0.3333333333333333703, 0.3219752754296894559, 0.3333333333333333703, 0.3219752754296894559, 0.3333333333333333703, 0.3219752754296894559, 0.3333333333333333703, 0.3219752754296894559, 0.3333333333333333703, 0.3219752754296894559, 0.3333333333333333703, 0.3219752754296894559, 0.3333333333333333703, 0.3219752754296894559, 0.3333333333333333703, 0.3219752754296894559, 0.3333333333333333703, 0.3219752754296894559, 0.3333333333333333703, 0.3219752754296894559, 0.3333333333333333703, 0.3219752754296894559, 0.3333333333333333703, 0.3219752754296894559, 0.3333333333333333703, 0.3219752754296894559, 0.3333333333333333703, 0.3219752754296894559, 0.3333333333333333703, 0.3219752754296894559, 0.3333333333333333703, 0.3219752754296894559, 0.3333333333333333703, 0.3219752754296894559, 0.3333333333333333703, 0.3219752754296894559, 0.3333333333333333703, 0.3219752754296894559, 0.3333333333333333703, 0.3219752754296894559, 0.3333333333333333703, 0.3219752754296894559, 0.3333333333333333703, 0.3219752754296894559, 0.3333333333333333703, 0.3219752754296894559, 0.3333333333333333703, 0.3219752754296894559, 0.3333333333333333703, 0.3219752754296894559, 0.3333333333333333703, 0.3219752754296894559, 0.3333333333333333703, 0.3219752754296894559, 0.3333333333333333703, 0.3219752754296894559, 0.3333333333333333703, 0.3219752754296894559, 0.3333333333333333703, 0.3219752754296894559, 0.3333333333333333703, 0.3219752754296894559, 0.3333333333333333703, 0.3219752754296894559, 0.3333333333333333703, 0.3219752754296894559, 0.3333333333333333703, 0.3219752754296894559, 0.3333333333333333703, 0.3219752754296894559, 0.3333333333333333703, 0.3219752754296894559, 0.3333333333333333703, 0.3219752754296894559, 0.3333333333333333703, 0.3219752754296894559, 0.3333333333333333703, 0.3219752754296894559, 0.3333333333333333703, 0.3219752754296894559, 0.3333333333333333703, 0.3219752754296894559, 0.3333333333333333703, 0.3219752754296894559, 0.3333333333333333703, 0.3219752754296894559, 0.3333333333333333703, 0.3219752754296894559, 0.3333333333333333703, 0.3219752754296894559, 0.3333333333333333703, 0.3219752754296894559, 0.3333333333333333703, 0.3219752754296894559, 0.3333333333333333703, 0.3219752754296894559, 0.3333333333333333703, 0.3219752754296894559, 0.3333333333333333703, 0.3219752754296894559, 0.3333333333333333703, 0.3219752754296894559, 0.3333333333333333703, 0.3219752754296894559, 0.3333333333333333703, 0.3219752754296894559, 0.3333333333333333703, 0.3219752754296894559, 0.3333333333333333703, 0.3219752754296894559, 0.3333333333333333703, 0.3219752754296894559, 0.3333333333333333703, 0.3219752754296894559, 0.3333333333333333703, 0.3219752754296894559, 0.3333333333333333703, 0.3219752754296894559, 0.3333333333333333703, 0.3219752754296894559, 0.3333333333333333703, 0.3219752754296894559, 0.3333333333333333703, 0.3219752754296894559, 0.3333333333333333703, 0.3219752754296894559, 0.3333333333333333703, 0.3219752754296894559, 0.3333333333333333703, 0.3219752754296894559, 0.3333333333333333703, 0.3219752754296894559, 0.3333333333333333703, 0.3219752754296894559, 0.3333333333333333703, 0.3219752754296894559, 0.3333333333333333703, 0.3219752754296894559, 0.3333333333333333703, 0.3219752754296894559, 0.3333333333333333703, 0.3219752754296894559, 0.3333333333333333703, 0.3219752754296894559, 0.3333333333333333703, 0.3219752754296894559, 0.3333333333333333703, 0.3219752754296894559, 0.3333333333333333703, 0.3219752754296894559, 0.3333333333333333703, 0.3219752754296894559, 0.3333333333333333703, 0.3219752754296894559, 0.3333333333333333703, 0.3219752754296894559, 0.3333333333333333703, 0.3219752754296894559, 0.3333333333333333703, 0.3219752754296894559, 0.3333333333333333703, 0.3219752754296894559, 0.3333333333333333703, 0.3219752754296894559, 0.3333333333333333703, 0.3219752754296894559, 0.3333333333333333703, 0.3219752754296894559, 0.3333333333333333703, 0.3219752754296894559, 0.3333333333333333703, 0.3219752754296894559, 0.3333333333333333703, 0.3219752754296894559, 0.3333333333333333703, 0.3219752754296894559, 0.3333333333333333703, 0.3219752754296894559, 0.3333333333333333703, 0.3219752754296894559, 0.3333333333333333703, 0.3219752754296894559, 0.3333333333333333703, 0.3219752754296894559, 0.3333333333333333703, 0.3219752754296894559, 0.3333333333333333703, 0.3219752754296894559, 0.3333333333333333703, 0.3219752754296894559, 0.3333333333333333703, 0.3219752754296894559, 0.3333333333333333703, 0.3219752754296894559, 0.3333333333333333703, 0.3219752754296894559, 0.3333333333333333703, 0.3219752754296894559, 0.3333333333333333703, 0.3219752754296894559, 0.3333333333333333703, 0.3219752754296894559, 0.3333333333333333703, 0.3219752754296894559, 0.3333333333333333703, 0.3219752754296894559, 0.3333333333333333703, 0.3219752754296894559, 0.3333333333333333703, 0.3219752754296894559, 0.3333333333333333703, 0.3219752754296894559, 0.3333333333333333703, 0.3219752754296894559, 0.3333333333333333703, 0.3219752754296894559, 0.3333333333333333703, 0.3219752754296894559, 0.3333333333333333703, 0.3219752754296894559, 0.3333333333333333703, 0.3219752754296894559, 0.3333333333333333703, 0.3219752754296894559, 0.3333333333333333703, 0.3219752754296894559, 0.3333333333333333703, 0.3219752754296894559, 0.3333333333333333703, 0.3219752754296894559, 0.3333333333333333703, 0.3219752754296894559, 0.3333333333333333703, 0.3219752754296894559, 0.3333333333333333703, 0.3219752754296894559, 0.3333333333333333703, 0.3219752754296894559, 0.3333333333333333703, 0.3219752754296894559, 0.3333333333333333703, 0.3219752754296894559, 0.3333333333333333703, 0.3219752754296894559, 0.3333333333333333703, 0.3219752754296894559, 0.3333333333333333703, 0.3219752754296894559, 0.3333333333333333703, 0.3219752754296894559, 0.3333333333333333703, 0.3219752754296894559, 0.3333333333333333703, 0.3219752754296894559, 0.3333333333333333703, 0.3219752754296894559, 0.3333333333333333703, 0.3219752754296894559, 0.3333333333333333703, 0.3219752754296894559, 0.3333333333333333703, 0.3219752754296894559, 0.3333333333333333703, 0.3219752754296894559, 0.3333333333333333703, 0.3219752754296894559, 0.3333333333333333703, 0.3219752754296894559, 0.3333333333333333703, 0.3219752754296894559, 0.3333333333333333703, 0.3219752754296894559, 0.3333333333333333703, 0.3219752754296894559, 0.3333333333333333703, 0.3219752754296894559, 0.3333333333333333703, 0.3219752754296894559, 0.3333333333333333703, 0.3219752754296894559, 0.3333333333333333703, 0.3219752754296894559, 0.3333333333333333703, 0.3219752754296894559, 0.3333333333333333703, 0.3219752754296894559, 0.3333333333333333703, 0.3219752754296894559, 0.3333333333333333703, 0.3219752754296894559, 0.3333333333333333703, 0.3219752754296894559, 0.3333333333333333703, 0.3219752754296894559, 0.3333333333333333703, 0.3219752754296894559, 0.3333333333333333703, 0.3219752754296894559, 0.3333333333333333703, 0.3219752754296894559, 0.3333333333333333703, 0.3219752754296894559, 0.3333333333333333703, 0.3219752754296894559, 0.3333333333333333703, 0.3219752754296894559, 0.3333333333333333703, 0.3219752754296894559, 0.3333333333333333703, 0.3219752754296894559, 0.3333333333333333703, 0.3219752754296894559, 0.3333333333333333703, 0.3219752754296894559, 0.3333333333333333703, 0.3219752754296894559, 0.3333333333333333703, 0.3219752754296894559, 0.3333333333333333703, 0.3219752754296894559, 0.3333333333333333703, 0.3219752754296894559, 0.3333333333333333703, 0.3219752754296894559, 0.3333333333333333703, 0.3219752754296894559, 0.3333333333333333703, 0.3219752754296894559, 0.3333333333333333703, 0.3219752754296894559, 0.3333333333333333703, 0.3219752754296894559, 0.3333333333333333703, 0.3219752754296894559, 0.3333333333333333703, 0.3219752754296894559, 0.3333333333333333703, 0.3219752754296894559, 0.3333333333333333703, 0.3219752754296894559, 0.3333333333333333703, 0.3219752754296894559, 0.3333333333333333703, 0.3219752754296894559, 0.3333333333333333703, 0.3219752754296894559, 0.3333333333333333703, 0.3219752754296894559, 0.3333333333333333703, 0.3219752754296894559, 0.3333333333333333703, 0.3219752754296894559, 0.3333333333333333703, 0.3219752754296894559, 0.3333333333333333703, 0.3219752754296894559, 0.3333333333333333703, 0.3219752754296894559, 0.3333333333333333703, 0.3219752754296894559, 0.3333333333333333703, 0.3219752754296894559, 0.3333333333333333703, 0.3219752754296894559, 0.3333333333333333703, 0.3219752754296894559, 0.3333333333333333703, 0.3219752754296894559, 0.3333333333333333703),
 ( 0.3333333333333333703, 0.3219752754296894559, 0.3333333333333333703, 0.3219752754296894559, 0.3333333333333333703, 0.3219752754296894559, 0.3333333333333333703, 0.3219752754296894559, 0.3333333333333333703, 0.3219752754296894559, 0.3333333333333333703, 0.3219752754296894559, 0.3333333333333333703, 0.3219752754296894559, 0.3333333333333333703, 0.3219752754296894559, 0.3333333333333333703, 0.3219752754296894559, 0.3333333333333333703, 0.3219752754296894559, 0.3333333333333333703, 0.3219752754296894559, 0.3333333333333333703, 0.3219752754296894559, 0.3333333333333333703, 0.3219752754296894559, 0.3333333333333333703, 0.3219752754296894559, 0.3333333333333333703, 0.3219752754296894559, 0.3333333333333333703, 0.3219752754296894559, 0.3333333333333333703, 0.3219752754296894559, 0.3333333333333333703, 0.3219752754296894559, 0.3333333333333333703, 0.3219752754296894559, 0.3333333333333333703, 0.3219752754296894559, 0.3333333333333333703, 0.3219752754296894559, 0.3333333333333333703, 0.3219752754296894559, 0.3333333333333333703, 0.3219752754296894559, 0.3333333333333333703, 0.3219752754296894559, 0.3333333333333333703, 0.3219752754296894559, 0.3333333333333333703, 0.3219752754296894559, 0.3333333333333333703, 0.3219752754296894559, 0.3333333333333333703, 0.3219752754296894559, 0.3333333333333333703, 0.3219752754296894559, 0.3333333333333333703, 0.3219752754296894559, 0.3333333333333333703, 0.3219752754296894559, 0.3333333333333333703, 0.3219752754296894559, 0.3333333333333333703, 0.3219752754296894559, 0.3333333333333333703, 0.3219752754296894559, 0.3333333333333333703, 0.3219752754296894559, 0.3333333333333333703, 0.3219752754296894559, 0.3333333333333333703, 0.3219752754296894559, 0.3333333333333333703, 0.3219752754296894559, 0.3333333333333333703, 0.3219752754296894559, 0.3333333333333333703, 0.3219752754296894559, 0.3333333333333333703, 0.3219752754296894559, 0.3333333333333333703, 0.3219752754296894559, 0.3333333333333333703, 0.3219752754296894559, 0.3333333333333333703, 0.3219752754296894559, 0.3333333333333333703, 0.3219752754296894559, 0.3333333333333333703, 0.3219752754296894559, 0.3333333333333333703, 0.3219752754296894559, 0.3333333333333333703, 0.3219752754296894559, 0.3333333333333333703, 0.3219752754296894559, 0.3333333333333333703, 0.3219752754296894559, 0.3333333333333333703, 0.3219752754296894559, 0.3333333333333333703, 0.3219752754296894559, 0.3333333333333333703, 0.3219752754296894559, 0.3333333333333333703, 0.3219752754296894559, 0.3333333333333333703, 0.3219752754296894559, 0.3333333333333333703, 0.3219752754296894559, 0.3333333333333333703, 0.3219752754296894559, 0.3333333333333333703, 0.3219752754296894559, 0.3333333333333333703, 0.3219752754296894559, 0.3333333333333333703, 0.3219752754296894559, 0.3333333333333333703, 0.3219752754296894559, 0.3333333333333333703, 0.3219752754296894559, 0.3333333333333333703, 0.3219752754296894559, 0.3333333333333333703, 0.3219752754296894559, 0.3333333333333333703, 0.3219752754296894559, 0.3333333333333333703, 0.3219752754296894559, 0.3333333333333333703, 0.3219752754296894559, 0.3333333333333333703, 0.3219752754296894559, 0.3333333333333333703, 0.3219752754296894559, 0.3333333333333333703, 0.3219752754296894559, 0.3333333333333333703, 0.3219752754296894559, 0.3333333333333333703, 0.3219752754296894559, 0.3333333333333333703, 0.3219752754296894559, 0.3333333333333333703, 0.3219752754296894559, 0.3333333333333333703, 0.3219752754296894559, 0.3333333333333333703, 0.3219752754296894559, 0.3333333333333333703, 0.3219752754296894559, 0.3333333333333333703, 0.3219752754296894559, 0.3333333333333333703, 0.3219752754296894559, 0.3333333333333333703, 0.3219752754296894559, 0.3333333333333333703, 0.3219752754296894559, 0.3333333333333333703, 0.3219752754296894559, 0.3333333333333333703, 0.3219752754296894559, 0.3333333333333333703, 0.3219752754296894559, 0.3333333333333333703, 0.3219752754296894559, 0.3333333333333333703, 0.3219752754296894559, 0.3333333333333333703, 0.3219752754296894559, 0.3333333333333333703, 0.3219752754296894559, 0.3333333333333333703, 0.3219752754296894559, 0.3333333333333333703, 0.3219752754296894559, 0.3333333333333333703, 0.3219752754296894559, 0.3333333333333333703, 0.3219752754296894559, 0.3333333333333333703, 0.3219752754296894559, 0.3333333333333333703, 0.3219752754296894559, 0.3333333333333333703, 0.3219752754296894559, 0.3333333333333333703, 0.3219752754296894559, 0.3333333333333333703, 0.3219752754296894559, 0.3333333333333333703, 0.3219752754296894559, 0.3333333333333333703, 0.3219752754296894559, 0.3333333333333333703, 0.3219752754296894559, 0.3333333333333333703, 0.3219752754296894559, 0.3333333333333333703, 0.3219752754296894559, 0.3333333333333333703, 0.3219752754296894559, 0.3333333333333333703, 0.3219752754296894559, 0.3333333333333333703, 0.3219752754296894559, 0.3333333333333333703, 0.3219752754296894559, 0.3333333333333333703, 0.3219752754296894559, 0.3333333333333333703, 0.3219752754296894559, 0.3333333333333333703, 0.3219752754296894559, 0.3333333333333333703, 0.3219752754296894559, 0.3333333333333333703, 0.3219752754296894559, 0.3333333333333333703, 0.3219752754296894559, 0.3333333333333333703, 0.3219752754296894559, 0.3333333333333333703, 0.3219752754296894559, 0.3333333333333333703, 0.3219752754296894559, 0.3333333333333333703, 0.3219752754296894559, 0.3333333333333333703, 0.3219752754296894559, 0.3333333333333333703, 0.3219752754296894559, 0.3333333333333333703, 0.3219752754296894559, 0.3333333333333333703, 0.3219752754296894559, 0.3333333333333333703, 0.3219752754296894559, 0.3333333333333333703, 0.3219752754296894559, 0.3333333333333333703, 0.3219752754296894559, 0.3333333333333333703, 0.3219752754296894559, 0.3333333333333333703, 0.3219752754296894559, 0.3333333333333333703, 0.3219752754296894559, 0.3333333333333333703, 0.3219752754296894559, 0.3333333333333333703, 0.3219752754296894559, 0.3333333333333333703, 0.3219752754296894559, 0.3333333333333333703, 0.3219752754296894559, 0.3333333333333333703, 0.3219752754296894559, 0.3333333333333333703, 0.3219752754296894559, 0.3333333333333333703, 0.3219752754296894559, 0.3333333333333333703, 0.3219752754296894559, 0.3333333333333333703, 0.3219752754296894559, 0.3333333333333333703, 0.3219752754296894559, 0.3333333333333333703, 0.3219752754296894559, 0.3333333333333333703, 0.3219752754296894559, 0.3333333333333333703, 0.3219752754296894559, 0.3333333333333333703, 0.3219752754296894559, 0.3333333333333333703, 0.3219752754296894559, 0.3333333333333333703, 0.3219752754296894559, 0.3333333333333333703, 0.3219752754296894559, 0.3333333333333333703, 0.3219752754296894559, 0.3333333333333333703, 0.3219752754296894559, 0.3333333333333333703, 0.3219752754296894559, 0.3333333333333333703, 0.3219752754296894559, 0.3333333333333333703, 0.3219752754296894559, 0.3333333333333333703, 0.3219752754296894559, 0.3333333333333333703, 0.3219752754296894559, 0.3333333333333333703, 0.3219752754296894559, 0.3333333333333333703, 0.3219752754296894559, 0.3333333333333333703, 0.3219752754296894559, 0.3333333333333333703, 0.3219752754296894559, 0.3333333333333333703, 0.3219752754296894559, 0.3333333333333333703, 0.3219752754296894559, 0.3333333333333333703, 0.3219752754296894559, 0.3333333333333333703, 0.3219752754296894559, 0.3333333333333333703, 0.3219752754296894559, 0.3333333333333333703, 0.3219752754296894559, 0.3333333333333333703, 0.3219752754296894559, 0.3333333333333333703, 0.3219752754296894559, 0.3333333333333333703, 0.3219752754296894559, 0.3333333333333333703, 0.3219752754296894559, 0.3333333333333333703, 0.3219752754296894559, 0.3333333333333333703, 0.3219752754296894559, 0.3333333333333333703, 0.3219752754296894559, 0.3333333333333333703, 0.3219752754296894559, 0.3333333333333333703, 0.3219752754296894559, 0.3333333333333333703, 0.3219752754296894559, 0.3333333333333333703, 0.3219752754296894559, 0.3333333333333333703, 0.3219752754296894559, 0.3333333333333333703, 0.3219752754296894559, 0.3333333333333333703, 0.3219752754296894559, 0.3333333333333333703, 0.3219752754296894559, 0.3333333333333333703, 0.3219752754296894559, 0.3333333333333333703, 0.3219752754296894559, 0.3333333333333333703, 0.3219752754296894559, 0.3333333333333333703, 0.3219752754296894559, 0.3333333333333333703, 0.3219752754296894559, 0.3333333333333333703, 0.3219752754296894559, 0.3333333333333333703, 0.3219752754296894559, 0.3333333333333333703, 0.3219752754296894559, 0.3333333333333333703, 0.3219752754296894559, 0.3333333333333333703, 0.3219752754296894559, 0.3333333333333333703, 0.3219752754296894559, 0.3333333333333333703, 0.3219752754296894559, 0.3333333333333333703, 0.3219752754296894559, 0.3333333333333333703, 0.3219752754296894559, 0.3333333333333333703, 0.3219752754296894559, 0.3333333333333333703, 0.3219752754296894559, 0.3333333333333333703, 0.3219752754296894559, 0.3333333333333333703, 0.3219752754296894559, 0.3333333333333333703, 0.3219752754296894559, 0.3333333333333333703, 0.3219752754296894559, 0.3333333333333333703, 0.3219752754296894559, 0.3333333333333333703, 0.3219752754296894559, 0.3333333333333333703, 0.3219752754296894559, 0.3333333333333333703, 0.3219752754296894559, 0.3333333333333333703, 0.3219752754296894559, 0.3333333333333333703, 0.3219752754296894559, 0.3333333333333333703, 0.3219752754296894559, 0.3333333333333333703, 0.3219752754296894559, 0.3333333333333333703, 0.3219752754296894559, 0.3333333333333333703, 0.3219752754296894559, 0.3333333333333333703, 0.3219752754296894559, 0.3333333333333333703, 0.3219752754296894559, 0.3333333333333333703, 0.3219752754296894559, 0.3333333333333333703, 0.3219752754296894559, 0.3333333333333333703, 0.3219752754296894559, 0.3333333333333333703, 0.3219752754296894559, 0.3333333333333333703, 0.3219752754296894559, 0.3333333333333333703, 0.3219752754296894559, 0.3333333333333333703, 0.3219752754296894559, 0.3333333333333333703, 0.3219752754296894559, 0.3333333333333333703, 0.3219752754296894559, 0.3333333333333333703, 0.3219752754296894559, 0.3333333333333333703, 0.3219752754296894559, 0.3333333333333333703, 0.3219752754296894559, 0.3333333333333333703, 0.3219752754296894559, 0.3333333333333333703, 0.3219752754296894559, 0.3333333333333333703, 0.3219752754296894559, 0.3333333333333333703, 0.3219752754296894559, 0.3333333333333333703, 0.3219752754296894559, 0.3333333333333333703, 0.3219752754296894559, 0.3333333333333333703, 0.3219752754296894559, 0.3333333333333333703, 0.3219752754296894559, 0.3333333333333333703, 0.3219752754296894559, 0.3333333333333333703),
 ( 1.000000000000000000, 0.9659258262890683122, 1.000000000000000000, 0.9659258262890683122, 1.000000000000000000, 0.9659258262890683122, 1.000000000000000000, 0.9659258262890683122, 1.000000000000000000, 0.9659258262890683122, 1.000000000000000000, 0.9659258262890683122, 1.000000000000000000, 0.9659258262890683122, 1.000000000000000000, 0.9659258262890683122, 1.000000000000000000, 0.9659258262890683122, 1.000000000000000000, 0.9659258262890683122, 1.000000000000000000, 0.9659258262890683122, 1.000000000000000000, 0.9659258262890683122, 1.000000000000000000, 0.9659258262890683122, 1.000000000000000000, 0.9659258262890683122, 1.000000000000000000, 0.9659258262890683122, 1.000000000000000000, 0.9659258262890683122, 1.000000000000000000, 0.9659258262890683122, 1.000000000000000000, 0.9659258262890683122, 1.000000000000000000, 0.9659258262890683122, 1.000000000000000000, 0.9659258262890683122, 1.000000000000000000, 0.9659258262890683122, 1.000000000000000000, 0.9659258262890683122, 1.000000000000000000, 0.9659258262890683122, 1.000000000000000000, 0.9659258262890683122, 1.000000000000000000, 0.9659258262890683122, 1.000000000000000000, 0.9659258262890683122, 1.000000000000000000, 0.9659258262890683122, 1.000000000000000000, 0.9659258262890683122, 1.000000000000000000, 0.9659258262890683122, 1.000000000000000000, 0.9659258262890683122, 1.000000000000000000, 0.9659258262890683122, 1.000000000000000000, 0.9659258262890683122, 1.000000000000000000, 0.9659258262890683122, 1.000000000000000000, 0.9659258262890683122, 1.000000000000000000, 0.9659258262890683122, 1.000000000000000000, 0.9659258262890683122, 1.000000000000000000, 0.9659258262890683122, 1.000000000000000000, 0.9659258262890683122, 1.000000000000000000, 0.9659258262890683122, 1.000000000000000000, 0.9659258262890683122, 1.000000000000000000, 0.9659258262890683122, 1.000000000000000000, 0.9659258262890683122, 1.000000000000000000, 0.9659258262890683122, 1.000000000000000000, 0.9659258262890683122, 1.000000000000000000, 0.9659258262890683122, 1.000000000000000000, 0.9659258262890683122, 1.000000000000000000, 0.9659258262890683122, 1.000000000000000000, 0.9659258262890683122, 1.000000000000000000, 0.9659258262890683122, 1.000000000000000000, 0.9659258262890683122, 1.000000000000000000, 0.9659258262890683122, 1.000000000000000000, 0.9659258262890683122, 1.000000000000000000, 0.9659258262890683122, 1.000000000000000000, 0.9659258262890683122, 1.000000000000000000, 0.9659258262890683122, 1.000000000000000000, 0.9659258262890683122, 1.000000000000000000, 0.9659258262890683122, 1.000000000000000000, 0.9659258262890683122, 1.000000000000000000, 0.9659258262890683122, 1.000000000000000000, 0.9659258262890683122, 1.000000000000000000, 0.9659258262890683122, 1.000000000000000000, 0.9659258262890683122, 1.000000000000000000, 0.9659258262890683122, 1.000000000000000000, 0.9659258262890683122, 1.000000000000000000, 0.9659258262890683122, 1.000000000000000000, 0.9659258262890683122, 1.000000000000000000, 0.9659258262890683122, 1.000000000000000000, 0.9659258262890683122, 1.000000000000000000, 0.9659258262890683122, 1.000000000000000000, 0.9659258262890683122, 1.000000000000000000, 0.9659258262890683122, 1.000000000000000000, 0.9659258262890683122, 1.000000000000000000, 0.9659258262890683122, 1.000000000000000000, 0.9659258262890683122, 1.000000000000000000, 0.9659258262890683122, 1.000000000000000000, 0.9659258262890683122, 1.000000000000000000, 0.9659258262890683122, 1.000000000000000000, 0.9659258262890683122, 1.000000000000000000, 0.9659258262890683122, 1.000000000000000000, 0.9659258262890683122, 1.000000000000000000, 0.9659258262890683122, 1.000000000000000000, 0.9659258262890683122, 1.000000000000000000, 0.9659258262890683122, 1.000000000000000000, 0.9659258262890683122, 1.000000000000000000, 0.9659258262890683122, 1.000000000000000000, 0.9659258262890683122, 1.000000000000000000, 0.9659258262890683122, 1.000000000000000000, 0.9659258262890683122, 1.000000000000000000, 0.9659258262890683122, 1.000000000000000000, 0.9659258262890683122, 1.000000000000000000, 0.9659258262890683122, 1.000000000000000000, 0.9659258262890683122, 1.000000000000000000, 0.9659258262890683122, 1.000000000000000000, 0.9659258262890683122, 1.000000000000000000, 0.9659258262890683122, 1.000000000000000000, 0.9659258262890683122, 1.000000000000000000, 0.9659258262890683122, 1.000000000000000000, 0.9659258262890683122, 1.000000000000000000, 0.9659258262890683122, 1.000000000000000000, 0.9659258262890683122, 1.000000000000000000, 0.9659258262890683122, 1.000000000000000000, 0.9659258262890683122, 1.000000000000000000, 0.9659258262890683122, 1.000000000000000000, 0.9659258262890683122, 1.000000000000000000, 0.9659258262890683122, 1.000000000000000000, 0.9659258262890683122, 1.000000000000000000, 0.9659258262890683122, 1.000000000000000000, 0.9659258262890683122, 1.000000000000000000, 0.9659258262890683122, 1.000000000000000000, 0.9659258262890683122, 1.000000000000000000, 0.9659258262890683122, 1.000000000000000000, 0.9659258262890683122, 1.000000000000000000, 0.9659258262890683122, 1.000000000000000000, 0.9659258262890683122, 1.000000000000000000, 0.9659258262890683122, 1.000000000000000000, 0.9659258262890683122, 1.000000000000000000, 0.9659258262890683122, 1.000000000000000000, 0.9659258262890683122, 1.000000000000000000, 0.9659258262890683122, 1.000000000000000000, 0.9659258262890683122, 1.000000000000000000, 0.9659258262890683122, 1.000000000000000000, 0.9659258262890683122, 1.000000000000000000, 0.9659258262890683122, 1.000000000000000000, 0.9659258262890683122, 1.000000000000000000, 0.9659258262890683122, 1.000000000000000000, 0.9659258262890683122, 1.000000000000000000, 0.9659258262890683122, 1.000000000000000000, 0.9659258262890683122, 1.000000000000000000, 0.9659258262890683122, 1.000000000000000000, 0.9659258262890683122, 1.000000000000000000, 0.9659258262890683122, 1.000000000000000000, 0.9659258262890683122, 1.000000000000000000, 0.9659258262890683122, 1.000000000000000000, 0.9659258262890683122, 1.000000000000000000, 0.9659258262890683122, 1.000000000000000000, 0.9659258262890683122, 1.000000000000000000, 0.9659258262890683122, 1.000000000000000000, 0.9659258262890683122, 1.000000000000000000, 0.9659258262890683122, 1.000000000000000000, 0.9659258262890683122, 1.000000000000000000, 0.9659258262890683122, 1.000000000000000000, 0.9659258262890683122, 1.000000000000000000, 0.9659258262890683122, 1.000000000000000000, 0.9659258262890683122, 1.000000000000000000, 0.9659258262890683122, 1.000000000000000000, 0.9659258262890683122, 1.000000000000000000, 0.9659258262890683122, 1.000000000000000000, 0.9659258262890683122, 1.000000000000000000, 0.9659258262890683122, 1.000000000000000000, 0.9659258262890683122, 1.000000000000000000, 0.9659258262890683122, 1.000000000000000000, 0.9659258262890683122, 1.000000000000000000, 0.9659258262890683122, 1.000000000000000000, 0.9659258262890683122, 1.000000000000000000, 0.9659258262890683122, 1.000000000000000000, 0.9659258262890683122, 1.000000000000000000, 0.9659258262890683122, 1.000000000000000000, 0.9659258262890683122, 1.000000000000000000, 0.9659258262890683122, 1.000000000000000000, 0.9659258262890683122, 1.000000000000000000, 0.9659258262890683122, 1.000000000000000000, 0.9659258262890683122, 1.000000000000000000, 0.9659258262890683122, 1.000000000000000000, 0.9659258262890683122, 1.000000000000000000, 0.9659258262890683122, 1.000000000000000000, 0.9659258262890683122, 1.000000000000000000, 0.9659258262890683122, 1.000000000000000000, 0.9659258262890683122, 1.000000000000000000, 0.9659258262890683122, 1.000000000000000000, 0.9659258262890683122, 1.000000000000000000, 0.9659258262890683122, 1.000000000000000000, 0.9659258262890683122, 1.000000000000000000, 0.9659258262890683122, 1.000000000000000000, 0.9659258262890683122, 1.000000000000000000, 0.9659258262890683122, 1.000000000000000000, 0.9659258262890683122, 1.000000000000000000, 0.9659258262890683122, 1.000000000000000000, 0.9659258262890683122, 1.000000000000000000, 0.9659258262890683122, 1.000000000000000000, 0.9659258262890683122, 1.000000000000000000, 0.9659258262890683122, 1.000000000000000000, 0.9659258262890683122, 1.000000000000000000, 0.9659258262890683122, 1.000000000000000000, 0.9659258262890683122, 1.000000000000000000, 0.9659258262890683122, 1.000000000000000000, 0.9659258262890683122, 1.000000000000000000, 0.9659258262890683122, 1.000000000000000000, 0.9659258262890683122, 1.000000000000000000, 0.9659258262890683122, 1.000000000000000000, 0.9659258262890683122, 1.000000000000000000, 0.9659258262890683122, 1.000000000000000000, 0.9659258262890683122, 1.000000000000000000, 0.9659258262890683122, 1.000000000000000000, 0.9659258262890683122, 1.000000000000000000, 0.9659258262890683122, 1.000000000000000000, 0.9659258262890683122, 1.000000000000000000, 0.9659258262890683122, 1.000000000000000000, 0.9659258262890683122, 1.000000000000000000, 0.9659258262890683122, 1.000000000000000000, 0.9659258262890683122, 1.000000000000000000, 0.9659258262890683122, 1.000000000000000000, 0.9659258262890683122, 1.000000000000000000, 0.9659258262890683122, 1.000000000000000000, 0.9659258262890683122, 1.000000000000000000, 0.9659258262890683122, 1.000000000000000000, 0.9659258262890683122, 1.000000000000000000, 0.9659258262890683122, 1.000000000000000000, 0.9659258262890683122, 1.000000000000000000, 0.9659258262890683122, 1.000000000000000000, 0.9659258262890683122, 1.000000000000000000, 0.9659258262890683122, 1.000000000000000000, 0.9659258262890683122, 1.000000000000000000, 0.9659258262890683122, 1.000000000000000000, 0.9659258262890683122, 1.000000000000000000, 0.9659258262890683122, 1.000000000000000000, 0.9659258262890683122, 1.000000000000000000, 0.9659258262890683122, 1.000000000000000000, 0.9659258262890683122, 1.000000000000000000, 0.9659258262890683122, 1.000000000000000000, 0.9659258262890683122, 1.000000000000000000, 0.9659258262890683122, 1.000000000000000000, 0.9659258262890683122, 1.000000000000000000, 0.9659258262890683122, 1.000000000000000000, 0.9659258262890683122, 1.000000000000000000, 0.9659258262890683122, 1.000000000000000000, 0.9659258262890683122, 1.000000000000000000, 0.9659258262890683122, 1.000000000000000000, 0.9659258262890683122, 1.000000000000000000),
 ( 0.3333333333333333703, 0.3219752754296894559, 0.3333333333333333703, 0.3219752754296894559, 0.3333333333333333703, 0.3219752754296894559, 0.3333333333333333703, 0.3219752754296894559, 0.3333333333333333703, 0.3219752754296894559, 0.3333333333333333703, 0.3219752754296894559, 0.3333333333333333703, 0.3219752754296894559, 0.3333333333333333703, 0.3219752754296894559, 0.3333333333333333703, 0.3219752754296894559, 0.3333333333333333703, 0.3219752754296894559, 0.3333333333333333703, 0.3219752754296894559, 0.3333333333333333703, 0.3219752754296894559, 0.3333333333333333703, 0.3219752754296894559, 0.3333333333333333703, 0.3219752754296894559, 0.3333333333333333703, 0.3219752754296894559, 0.3333333333333333703, 0.3219752754296894559, 0.3333333333333333703, 0.3219752754296894559, 0.3333333333333333703, 0.3219752754296894559, 0.3333333333333333703, 0.3219752754296894559, 0.3333333333333333703, 0.3219752754296894559, 0.3333333333333333703, 0.3219752754296894559, 0.3333333333333333703, 0.3219752754296894559, 0.3333333333333333703, 0.3219752754296894559, 0.3333333333333333703, 0.3219752754296894559, 0.3333333333333333703, 0.3219752754296894559, 0.3333333333333333703, 0.3219752754296894559, 0.3333333333333333703, 0.3219752754296894559, 0.3333333333333333703, 0.3219752754296894559, 0.3333333333333333703, 0.3219752754296894559, 0.3333333333333333703, 0.3219752754296894559, 0.3333333333333333703, 0.3219752754296894559, 0.3333333333333333703, 0.3219752754296894559, 0.3333333333333333703, 0.3219752754296894559, 0.3333333333333333703, 0.3219752754296894559, 0.3333333333333333703, 0.3219752754296894559, 0.3333333333333333703, 0.3219752754296894559, 0.3333333333333333703, 0.3219752754296894559, 0.3333333333333333703, 0.3219752754296894559, 0.3333333333333333703, 0.3219752754296894559, 0.3333333333333333703, 0.3219752754296894559, 0.3333333333333333703, 0.3219752754296894559, 0.3333333333333333703, 0.3219752754296894559, 0.3333333333333333703, 0.3219752754296894559, 0.3333333333333333703, 0.3219752754296894559, 0.3333333333333333703, 0.3219752754296894559, 0.3333333333333333703, 0.3219752754296894559, 0.3333333333333333703, 0.3219752754296894559, 0.3333333333333333703, 0.3219752754296894559, 0.3333333333333333703, 0.3219752754296894559, 0.3333333333333333703, 0.3219752754296894559, 0.3333333333333333703, 0.3219752754296894559, 0.3333333333333333703, 0.3219752754296894559, 0.3333333333333333703, 0.3219752754296894559, 0.3333333333333333703, 0.3219752754296894559, 0.3333333333333333703, 0.3219752754296894559, 0.3333333333333333703, 0.3219752754296894559, 0.3333333333333333703, 0.3219752754296894559, 0.3333333333333333703, 0.3219752754296894559, 0.3333333333333333703, 0.3219752754296894559, 0.3333333333333333703, 0.3219752754296894559, 0.3333333333333333703, 0.3219752754296894559, 0.3333333333333333703, 0.3219752754296894559, 0.3333333333333333703, 0.3219752754296894559, 0.3333333333333333703, 0.3219752754296894559, 0.3333333333333333703, 0.3219752754296894559, 0.3333333333333333703, 0.3219752754296894559, 0.3333333333333333703, 0.3219752754296894559, 0.3333333333333333703, 0.3219752754296894559, 0.3333333333333333703, 0.3219752754296894559, 0.3333333333333333703, 0.3219752754296894559, 0.3333333333333333703, 0.3219752754296894559, 0.3333333333333333703, 0.3219752754296894559, 0.3333333333333333703, 0.3219752754296894559, 0.3333333333333333703, 0.3219752754296894559, 0.3333333333333333703, 0.3219752754296894559, 0.3333333333333333703, 0.3219752754296894559, 0.3333333333333333703, 0.3219752754296894559, 0.3333333333333333703, 0.3219752754296894559, 0.3333333333333333703, 0.3219752754296894559, 0.3333333333333333703, 0.3219752754296894559, 0.3333333333333333703, 0.3219752754296894559, 0.3333333333333333703, 0.3219752754296894559, 0.3333333333333333703, 0.3219752754296894559, 0.3333333333333333703, 0.3219752754296894559, 0.3333333333333333703, 0.3219752754296894559, 0.3333333333333333703, 0.3219752754296894559, 0.3333333333333333703, 0.3219752754296894559, 0.3333333333333333703, 0.3219752754296894559, 0.3333333333333333703, 0.3219752754296894559, 0.3333333333333333703, 0.3219752754296894559, 0.3333333333333333703, 0.3219752754296894559, 0.3333333333333333703, 0.3219752754296894559, 0.3333333333333333703, 0.3219752754296894559, 0.3333333333333333703, 0.3219752754296894559, 0.3333333333333333703, 0.3219752754296894559, 0.3333333333333333703, 0.3219752754296894559, 0.3333333333333333703, 0.3219752754296894559, 0.3333333333333333703, 0.3219752754296894559, 0.3333333333333333703, 0.3219752754296894559, 0.3333333333333333703, 0.3219752754296894559, 0.3333333333333333703, 0.3219752754296894559, 0.3333333333333333703, 0.3219752754296894559, 0.3333333333333333703, 0.3219752754296894559, 0.3333333333333333703, 0.3219752754296894559, 0.3333333333333333703, 0.3219752754296894559, 0.3333333333333333703, 0.3219752754296894559, 0.3333333333333333703, 0.3219752754296894559, 0.3333333333333333703, 0.3219752754296894559, 0.3333333333333333703, 0.3219752754296894559, 0.3333333333333333703, 0.3219752754296894559, 0.3333333333333333703, 0.3219752754296894559, 0.3333333333333333703, 0.3219752754296894559, 0.3333333333333333703, 0.3219752754296894559, 0.3333333333333333703, 0.3219752754296894559, 0.3333333333333333703, 0.3219752754296894559, 0.3333333333333333703, 0.3219752754296894559, 0.3333333333333333703, 0.3219752754296894559, 0.3333333333333333703, 0.3219752754296894559, 0.3333333333333333703, 0.3219752754296894559, 0.3333333333333333703, 0.3219752754296894559, 0.3333333333333333703, 0.3219752754296894559, 0.3333333333333333703, 0.3219752754296894559, 0.3333333333333333703, 0.3219752754296894559, 0.3333333333333333703, 0.3219752754296894559, 0.3333333333333333703, 0.3219752754296894559, 0.3333333333333333703, 0.3219752754296894559, 0.3333333333333333703, 0.3219752754296894559, 0.3333333333333333703, 0.3219752754296894559, 0.3333333333333333703, 0.3219752754296894559, 0.3333333333333333703, 0.3219752754296894559, 0.3333333333333333703, 0.3219752754296894559, 0.3333333333333333703, 0.3219752754296894559, 0.3333333333333333703, 0.3219752754296894559, 0.3333333333333333703, 0.3219752754296894559, 0.3333333333333333703, 0.3219752754296894559, 0.3333333333333333703, 0.3219752754296894559, 0.3333333333333333703, 0.3219752754296894559, 0.3333333333333333703, 0.3219752754296894559, 0.3333333333333333703, 0.3219752754296894559, 0.3333333333333333703, 0.3219752754296894559, 0.3333333333333333703, 0.3219752754296894559, 0.3333333333333333703, 0.3219752754296894559, 0.3333333333333333703, 0.3219752754296894559, 0.3333333333333333703, 0.3219752754296894559, 0.3333333333333333703, 0.3219752754296894559, 0.3333333333333333703, 0.3219752754296894559, 0.3333333333333333703, 0.3219752754296894559, 0.3333333333333333703, 0.3219752754296894559, 0.3333333333333333703, 0.3219752754296894559, 0.3333333333333333703, 0.3219752754296894559, 0.3333333333333333703, 0.3219752754296894559, 0.3333333333333333703, 0.3219752754296894559, 0.3333333333333333703, 0.3219752754296894559, 0.3333333333333333703, 0.3219752754296894559, 0.3333333333333333703, 0.3219752754296894559, 0.3333333333333333703, 0.3219752754296894559, 0.3333333333333333703, 0.3219752754296894559, 0.3333333333333333703, 0.3219752754296894559, 0.3333333333333333703, 0.3219752754296894559, 0.3333333333333333703, 0.3219752754296894559, 0.3333333333333333703, 0.3219752754296894559, 0.3333333333333333703, 0.3219752754296894559, 0.3333333333333333703, 0.3219752754296894559, 0.3333333333333333703, 0.3219752754296894559, 0.3333333333333333703, 0.3219752754296894559, 0.3333333333333333703, 0.3219752754296894559, 0.3333333333333333703, 0.3219752754296894559, 0.3333333333333333703, 0.3219752754296894559, 0.3333333333333333703, 0.3219752754296894559, 0.3333333333333333703, 0.3219752754296894559, 0.3333333333333333703, 0.3219752754296894559, 0.3333333333333333703, 0.3219752754296894559, 0.3333333333333333703, 0.3219752754296894559, 0.3333333333333333703, 0.3219752754296894559, 0.3333333333333333703, 0.3219752754296894559, 0.3333333333333333703, 0.3219752754296894559, 0.3333333333333333703, 0.3219752754296894559, 0.3333333333333333703, 0.3219752754296894559, 0.3333333333333333703, 0.3219752754296894559, 0.3333333333333333703, 0.3219752754296894559, 0.3333333333333333703, 0.3219752754296894559, 0.3333333333333333703, 0.3219752754296894559, 0.3333333333333333703, 0.3219752754296894559, 0.3333333333333333703, 0.3219752754296894559, 0.3333333333333333703, 0.3219752754296894559, 0.3333333333333333703, 0.3219752754296894559, 0.3333333333333333703, 0.3219752754296894559, 0.3333333333333333703, 0.3219752754296894559, 0.3333333333333333703, 0.3219752754296894559, 0.3333333333333333703, 0.3219752754296894559, 0.3333333333333333703, 0.3219752754296894559, 0.3333333333333333703, 0.3219752754296894559, 0.3333333333333333703, 0.3219752754296894559, 0.3333333333333333703, 0.3219752754296894559, 0.3333333333333333703, 0.3219752754296894559, 0.3333333333333333703, 0.3219752754296894559, 0.3333333333333333703, 0.3219752754296894559, 0.3333333333333333703, 0.3219752754296894559, 0.3333333333333333703, 0.3219752754296894559, 0.3333333333333333703, 0.3219752754296894559, 0.3333333333333333703, 0.3219752754296894559, 0.3333333333333333703, 0.3219752754296894559, 0.3333333333333333703, 0.3219752754296894559, 0.3333333333333333703, 0.3219752754296894559, 0.3333333333333333703, 0.3219752754296894559, 0.3333333333333333703, 0.3219752754296894559, 0.3333333333333333703, 0.3219752754296894559, 0.3333333333333333703, 0.3219752754296894559, 0.3333333333333333703, 0.3219752754296894559, 0.3333333333333333703, 0.3219752754296894559, 0.3333333333333333703, 0.3219752754296894559, 0.3333333333333333703, 0.3219752754296894559, 0.3333333333333333703, 0.3219752754296894559, 0.3333333333333333703, 0.3219752754296894559, 0.3333333333333333703, 0.3219752754296894559, 0.3333333333333333703, 0.3219752754296894559, 0.3333333333333333703, 0.3219752754296894559, 0.3333333333333333703, 0.3219752754296894559, 0.3333333333333333703, 0.3219752754296894559, 0.3333333333333333703, 0.3219752754296894559, 0.3333333333333333703, 0.3219752754296894559, 0.3333333333333333703, 0.3219752754296894559, 0.3333333333333333703, 0.3219752754296894559, 0.3333333333333333703, 0.3219752754296894559, 0.3333333333333333703, 0.3219752754296894559, 0.3333333333333333703, 0.3219752754296894559, 0.3333333333333333703, 0.3219752754296894559, 0.3333333333333333703, 0.3219752754296894559, 0.3333333333333333703),
 ( 0.3333333333333333703, 0.3219752754296894559, 0.3333333333333333703, 0.3219752754296894559, 0.3333333333333333703, 0.3219752754296894559, 0.3333333333333333703, 0.3219752754296894559, 0.3333333333333333703, 0.3219752754296894559, 0.3333333333333333703, 0.3219752754296894559, 0.3333333333333333703, 0.3219752754296894559, 0.3333333333333333703, 0.3219752754296894559, 0.3333333333333333703, 0.3219752754296894559, 0.3333333333333333703, 0.3219752754296894559, 0.3333333333333333703, 0.3219752754296894559, 0.3333333333333333703, 0.3219752754296894559, 0.3333333333333333703, 0.3219752754296894559, 0.3333333333333333703, 0.3219752754296894559, 0.3333333333333333703, 0.3219752754296894559, 0.3333333333333333703, 0.3219752754296894559, 0.3333333333333333703, 0.3219752754296894559, 0.3333333333333333703, 0.3219752754296894559, 0.3333333333333333703, 0.3219752754296894559, 0.3333333333333333703, 0.3219752754296894559, 0.3333333333333333703, 0.3219752754296894559, 0.3333333333333333703, 0.3219752754296894559, 0.3333333333333333703, 0.3219752754296894559, 0.3333333333333333703, 0.3219752754296894559, 0.3333333333333333703, 0.3219752754296894559, 0.3333333333333333703, 0.3219752754296894559, 0.3333333333333333703, 0.3219752754296894559, 0.3333333333333333703, 0.3219752754296894559, 0.3333333333333333703, 0.3219752754296894559, 0.3333333333333333703, 0.3219752754296894559, 0.3333333333333333703, 0.3219752754296894559, 0.3333333333333333703, 0.3219752754296894559, 0.3333333333333333703, 0.3219752754296894559, 0.3333333333333333703, 0.3219752754296894559, 0.3333333333333333703, 0.3219752754296894559, 0.3333333333333333703, 0.3219752754296894559, 0.3333333333333333703, 0.3219752754296894559, 0.3333333333333333703, 0.3219752754296894559, 0.3333333333333333703, 0.3219752754296894559, 0.3333333333333333703, 0.3219752754296894559, 0.3333333333333333703, 0.3219752754296894559, 0.3333333333333333703, 0.3219752754296894559, 0.3333333333333333703, 0.3219752754296894559, 0.3333333333333333703, 0.3219752754296894559, 0.3333333333333333703, 0.3219752754296894559, 0.3333333333333333703, 0.3219752754296894559, 0.3333333333333333703, 0.3219752754296894559, 0.3333333333333333703, 0.3219752754296894559, 0.3333333333333333703, 0.3219752754296894559, 0.3333333333333333703, 0.3219752754296894559, 0.3333333333333333703, 0.3219752754296894559, 0.3333333333333333703, 0.3219752754296894559, 0.3333333333333333703, 0.3219752754296894559, 0.3333333333333333703, 0.3219752754296894559, 0.3333333333333333703, 0.3219752754296894559, 0.3333333333333333703, 0.3219752754296894559, 0.3333333333333333703, 0.3219752754296894559, 0.3333333333333333703, 0.3219752754296894559, 0.3333333333333333703, 0.3219752754296894559, 0.3333333333333333703, 0.3219752754296894559, 0.3333333333333333703, 0.3219752754296894559, 0.3333333333333333703, 0.3219752754296894559, 0.3333333333333333703, 0.3219752754296894559, 0.3333333333333333703, 0.3219752754296894559, 0.3333333333333333703, 0.3219752754296894559, 0.3333333333333333703, 0.3219752754296894559, 0.3333333333333333703, 0.3219752754296894559, 0.3333333333333333703, 0.3219752754296894559, 0.3333333333333333703, 0.3219752754296894559, 0.3333333333333333703, 0.3219752754296894559, 0.3333333333333333703, 0.3219752754296894559, 0.3333333333333333703, 0.3219752754296894559, 0.3333333333333333703, 0.3219752754296894559, 0.3333333333333333703, 0.3219752754296894559, 0.3333333333333333703, 0.3219752754296894559, 0.3333333333333333703, 0.3219752754296894559, 0.3333333333333333703, 0.3219752754296894559, 0.3333333333333333703, 0.3219752754296894559, 0.3333333333333333703, 0.3219752754296894559, 0.3333333333333333703, 0.3219752754296894559, 0.3333333333333333703, 0.3219752754296894559, 0.3333333333333333703, 0.3219752754296894559, 0.3333333333333333703, 0.3219752754296894559, 0.3333333333333333703, 0.3219752754296894559, 0.3333333333333333703, 0.3219752754296894559, 0.3333333333333333703, 0.3219752754296894559, 0.3333333333333333703, 0.3219752754296894559, 0.3333333333333333703, 0.3219752754296894559, 0.3333333333333333703, 0.3219752754296894559, 0.3333333333333333703, 0.3219752754296894559, 0.3333333333333333703, 0.3219752754296894559, 0.3333333333333333703, 0.3219752754296894559, 0.3333333333333333703, 0.3219752754296894559, 0.3333333333333333703, 0.3219752754296894559, 0.3333333333333333703, 0.3219752754296894559, 0.3333333333333333703, 0.3219752754296894559, 0.3333333333333333703, 0.3219752754296894559, 0.3333333333333333703, 0.3219752754296894559, 0.3333333333333333703, 0.3219752754296894559, 0.3333333333333333703, 0.3219752754296894559, 0.3333333333333333703, 0.3219752754296894559, 0.3333333333333333703, 0.3219752754296894559, 0.3333333333333333703, 0.3219752754296894559, 0.3333333333333333703, 0.3219752754296894559, 0.3333333333333333703, 0.3219752754296894559, 0.3333333333333333703, 0.3219752754296894559, 0.3333333333333333703, 0.3219752754296894559, 0.3333333333333333703, 0.3219752754296894559, 0.3333333333333333703, 0.3219752754296894559, 0.3333333333333333703, 0.3219752754296894559, 0.3333333333333333703, 0.3219752754296894559, 0.3333333333333333703, 0.3219752754296894559, 0.3333333333333333703, 0.3219752754296894559, 0.3333333333333333703, 0.3219752754296894559, 0.3333333333333333703, 0.3219752754296894559, 0.3333333333333333703, 0.3219752754296894559, 0.3333333333333333703, 0.3219752754296894559, 0.3333333333333333703, 0.3219752754296894559, 0.3333333333333333703, 0.3219752754296894559, 0.3333333333333333703, 0.3219752754296894559, 0.3333333333333333703, 0.3219752754296894559, 0.3333333333333333703, 0.3219752754296894559, 0.3333333333333333703, 0.3219752754296894559, 0.3333333333333333703, 0.3219752754296894559, 0.3333333333333333703, 0.3219752754296894559, 0.3333333333333333703, 0.3219752754296894559, 0.3333333333333333703, 0.3219752754296894559, 0.3333333333333333703, 0.3219752754296894559, 0.3333333333333333703, 0.3219752754296894559, 0.3333333333333333703, 0.3219752754296894559, 0.3333333333333333703, 0.3219752754296894559, 0.3333333333333333703, 0.3219752754296894559, 0.3333333333333333703, 0.3219752754296894559, 0.3333333333333333703, 0.3219752754296894559, 0.3333333333333333703, 0.3219752754296894559, 0.3333333333333333703, 0.3219752754296894559, 0.3333333333333333703, 0.3219752754296894559, 0.3333333333333333703, 0.3219752754296894559, 0.3333333333333333703, 0.3219752754296894559, 0.3333333333333333703, 0.3219752754296894559, 0.3333333333333333703, 0.3219752754296894559, 0.3333333333333333703, 0.3219752754296894559, 0.3333333333333333703, 0.3219752754296894559, 0.3333333333333333703, 0.3219752754296894559, 0.3333333333333333703, 0.3219752754296894559, 0.3333333333333333703, 0.3219752754296894559, 0.3333333333333333703, 0.3219752754296894559, 0.3333333333333333703, 0.3219752754296894559, 0.3333333333333333703, 0.3219752754296894559, 0.3333333333333333703, 0.3219752754296894559, 0.3333333333333333703, 0.3219752754296894559, 0.3333333333333333703, 0.3219752754296894559, 0.3333333333333333703, 0.3219752754296894559, 0.3333333333333333703, 0.3219752754296894559, 0.3333333333333333703, 0.3219752754296894559, 0.3333333333333333703, 0.3219752754296894559, 0.3333333333333333703, 0.3219752754296894559, 0.3333333333333333703, 0.3219752754296894559, 0.3333333333333333703, 0.3219752754296894559, 0.3333333333333333703, 0.3219752754296894559, 0.3333333333333333703, 0.3219752754296894559, 0.3333333333333333703, 0.3219752754296894559, 0.3333333333333333703, 0.3219752754296894559, 0.3333333333333333703, 0.3219752754296894559, 0.3333333333333333703, 0.3219752754296894559, 0.3333333333333333703, 0.3219752754296894559, 0.3333333333333333703, 0.3219752754296894559, 0.3333333333333333703, 0.3219752754296894559, 0.3333333333333333703, 0.3219752754296894559, 0.3333333333333333703, 0.3219752754296894559, 0.3333333333333333703, 0.3219752754296894559, 0.3333333333333333703, 0.3219752754296894559, 0.3333333333333333703, 0.3219752754296894559, 0.3333333333333333703, 0.3219752754296894559, 0.3333333333333333703, 0.3219752754296894559, 0.3333333333333333703, 0.3219752754296894559, 0.3333333333333333703, 0.3219752754296894559, 0.3333333333333333703, 0.3219752754296894559, 0.3333333333333333703, 0.3219752754296894559, 0.3333333333333333703, 0.3219752754296894559, 0.3333333333333333703, 0.3219752754296894559, 0.3333333333333333703, 0.3219752754296894559, 0.3333333333333333703, 0.3219752754296894559, 0.3333333333333333703, 0.3219752754296894559, 0.3333333333333333703, 0.3219752754296894559, 0.3333333333333333703, 0.3219752754296894559, 0.3333333333333333703, 0.3219752754296894559, 0.3333333333333333703, 0.3219752754296894559, 0.3333333333333333703, 0.3219752754296894559, 0.3333333333333333703, 0.3219752754296894559, 0.3333333333333333703, 0.3219752754296894559, 0.3333333333333333703, 0.3219752754296894559, 0.3333333333333333703, 0.3219752754296894559, 0.3333333333333333703, 0.3219752754296894559, 0.3333333333333333703, 0.3219752754296894559, 0.3333333333333333703, 0.3219752754296894559, 0.3333333333333333703, 0.3219752754296894559, 0.3333333333333333703, 0.3219752754296894559, 0.3333333333333333703, 0.3219752754296894559, 0.3333333333333333703, 0.3219752754296894559, 0.3333333333333333703, 0.3219752754296894559, 0.3333333333333333703, 0.3219752754296894559, 0.3333333333333333703, 0.3219752754296894559, 0.3333333333333333703, 0.3219752754296894559, 0.3333333333333333703, 0.3219752754296894559, 0.3333333333333333703, 0.3219752754296894559, 0.3333333333333333703, 0.3219752754296894559, 0.3333333333333333703, 0.3219752754296894559, 0.3333333333333333703, 0.3219752754296894559, 0.3333333333333333703, 0.3219752754296894559, 0.3333333333333333703, 0.3219752754296894559, 0.3333333333333333703, 0.3219752754296894559, 0.3333333333333333703, 0.3219752754296894559, 0.3333333333333333703, 0.3219752754296894559, 0.3333333333333333703, 0.3219752754296894559, 0.3333333333333333703, 0.3219752754296894559, 0.3333333333333333703, 0.3219752754296894559, 0.3333333333333333703, 0.3219752754296894559, 0.3333333333333333703, 0.3219752754296894559, 0.3333333333333333703, 0.3219752754296894559, 0.3333333333333333703, 0.3219752754296894559, 0.3333333333333333703, 0.3219752754296894559, 0.3333333333333333703, 0.3219752754296894559, 0.3333333333333333703, 0.3219752754296894559, 0.3333333333333333703, 0.3219752754296894559, 0.3333333333333333703, 0.3219752754296894559, 0.3333333333333333703, 0.3219752754296894559, 0.3333333333333333703, 0.3219752754296894559, 0.3333333333333333703),
 ( 1.000000000000000000, 0.9659258262890683122, 1.000000000000000000, 0.9659258262890683122, 1.000000000000000000, 0.9659258262890683122, 1.000000000000000000, 0.9659258262890683122, 1.000000000000000000, 0.9659258262890683122, 1.000000000000000000, 0.9659258262890683122, 1.000000000000000000, 0.9659258262890683122, 1.000000000000000000, 0.9659258262890683122, 1.000000000000000000, 0.9659258262890683122, 1.000000000000000000, 0.9659258262890683122, 1.000000000000000000, 0.9659258262890683122, 1.000000000000000000, 0.9659258262890683122, 1.000000000000000000, 0.9659258262890683122, 1.000000000000000000, 0.9659258262890683122, 1.000000000000000000, 0.9659258262890683122, 1.000000000000000000, 0.9659258262890683122, 1.000000000000000000, 0.9659258262890683122, 1.000000000000000000, 0.9659258262890683122, 1.000000000000000000, 0.9659258262890683122, 1.000000000000000000, 0.9659258262890683122, 1.000000000000000000, 0.9659258262890683122, 1.000000000000000000, 0.9659258262890683122, 1.000000000000000000, 0.9659258262890683122, 1.000000000000000000, 0.9659258262890683122, 1.000000000000000000, 0.9659258262890683122, 1.000000000000000000, 0.9659258262890683122, 1.000000000000000000, 0.9659258262890683122, 1.000000000000000000, 0.9659258262890683122, 1.000000000000000000, 0.9659258262890683122, 1.000000000000000000, 0.9659258262890683122, 1.000000000000000000, 0.9659258262890683122, 1.000000000000000000, 0.9659258262890683122, 1.000000000000000000, 0.9659258262890683122, 1.000000000000000000, 0.9659258262890683122, 1.000000000000000000, 0.9659258262890683122, 1.000000000000000000, 0.9659258262890683122, 1.000000000000000000, 0.9659258262890683122, 1.000000000000000000, 0.9659258262890683122, 1.000000000000000000, 0.9659258262890683122, 1.000000000000000000, 0.9659258262890683122, 1.000000000000000000, 0.9659258262890683122, 1.000000000000000000, 0.9659258262890683122, 1.000000000000000000, 0.9659258262890683122, 1.000000000000000000, 0.9659258262890683122, 1.000000000000000000, 0.9659258262890683122, 1.000000000000000000, 0.9659258262890683122, 1.000000000000000000, 0.9659258262890683122, 1.000000000000000000, 0.9659258262890683122, 1.000000000000000000, 0.9659258262890683122, 1.000000000000000000, 0.9659258262890683122, 1.000000000000000000, 0.9659258262890683122, 1.000000000000000000, 0.9659258262890683122, 1.000000000000000000, 0.9659258262890683122, 1.000000000000000000, 0.9659258262890683122, 1.000000000000000000, 0.9659258262890683122, 1.000000000000000000, 0.9659258262890683122, 1.000000000000000000, 0.9659258262890683122, 1.000000000000000000, 0.9659258262890683122, 1.000000000000000000, 0.9659258262890683122, 1.000000000000000000, 0.9659258262890683122, 1.000000000000000000, 0.9659258262890683122, 1.000000000000000000, 0.9659258262890683122, 1.000000000000000000, 0.9659258262890683122, 1.000000000000000000, 0.9659258262890683122, 1.000000000000000000, 0.9659258262890683122, 1.000000000000000000, 0.9659258262890683122, 1.000000000000000000, 0.9659258262890683122, 1.000000000000000000, 0.9659258262890683122, 1.000000000000000000, 0.9659258262890683122, 1.000000000000000000, 0.9659258262890683122, 1.000000000000000000, 0.9659258262890683122, 1.000000000000000000, 0.9659258262890683122, 1.000000000000000000, 0.9659258262890683122, 1.000000000000000000, 0.9659258262890683122, 1.000000000000000000, 0.9659258262890683122, 1.000000000000000000, 0.9659258262890683122, 1.000000000000000000, 0.9659258262890683122, 1.000000000000000000, 0.9659258262890683122, 1.000000000000000000, 0.9659258262890683122, 1.000000000000000000, 0.9659258262890683122, 1.000000000000000000, 0.9659258262890683122, 1.000000000000000000, 0.9659258262890683122, 1.000000000000000000, 0.9659258262890683122, 1.000000000000000000, 0.9659258262890683122, 1.000000000000000000, 0.9659258262890683122, 1.000000000000000000, 0.9659258262890683122, 1.000000000000000000, 0.9659258262890683122, 1.000000000000000000, 0.9659258262890683122, 1.000000000000000000, 0.9659258262890683122, 1.000000000000000000, 0.9659258262890683122, 1.000000000000000000, 0.9659258262890683122, 1.000000000000000000, 0.9659258262890683122, 1.000000000000000000, 0.9659258262890683122, 1.000000000000000000, 0.9659258262890683122, 1.000000000000000000, 0.9659258262890683122, 1.000000000000000000, 0.9659258262890683122, 1.000000000000000000, 0.9659258262890683122, 1.000000000000000000, 0.9659258262890683122, 1.000000000000000000, 0.9659258262890683122, 1.000000000000000000, 0.9659258262890683122, 1.000000000000000000, 0.9659258262890683122, 1.000000000000000000, 0.9659258262890683122, 1.000000000000000000, 0.9659258262890683122, 1.000000000000000000, 0.9659258262890683122, 1.000000000000000000, 0.9659258262890683122, 1.000000000000000000, 0.9659258262890683122, 1.000000000000000000, 0.9659258262890683122, 1.000000000000000000, 0.9659258262890683122, 1.000000000000000000, 0.9659258262890683122, 1.000000000000000000, 0.9659258262890683122, 1.000000000000000000, 0.9659258262890683122, 1.000000000000000000, 0.9659258262890683122, 1.000000000000000000, 0.9659258262890683122, 1.000000000000000000, 0.9659258262890683122, 1.000000000000000000, 0.9659258262890683122, 1.000000000000000000, 0.9659258262890683122, 1.000000000000000000, 0.9659258262890683122, 1.000000000000000000, 0.9659258262890683122, 1.000000000000000000, 0.9659258262890683122, 1.000000000000000000, 0.9659258262890683122, 1.000000000000000000, 0.9659258262890683122, 1.000000000000000000, 0.9659258262890683122, 1.000000000000000000, 0.9659258262890683122, 1.000000000000000000, 0.9659258262890683122, 1.000000000000000000, 0.9659258262890683122, 1.000000000000000000, 0.9659258262890683122, 1.000000000000000000, 0.9659258262890683122, 1.000000000000000000, 0.9659258262890683122, 1.000000000000000000, 0.9659258262890683122, 1.000000000000000000, 0.9659258262890683122, 1.000000000000000000, 0.9659258262890683122, 1.000000000000000000, 0.9659258262890683122, 1.000000000000000000, 0.9659258262890683122, 1.000000000000000000, 0.9659258262890683122, 1.000000000000000000, 0.9659258262890683122, 1.000000000000000000, 0.9659258262890683122, 1.000000000000000000, 0.9659258262890683122, 1.000000000000000000, 0.9659258262890683122, 1.000000000000000000, 0.9659258262890683122, 1.000000000000000000, 0.9659258262890683122, 1.000000000000000000, 0.9659258262890683122, 1.000000000000000000, 0.9659258262890683122, 1.000000000000000000, 0.9659258262890683122, 1.000000000000000000, 0.9659258262890683122, 1.000000000000000000, 0.9659258262890683122, 1.000000000000000000, 0.9659258262890683122, 1.000000000000000000, 0.9659258262890683122, 1.000000000000000000, 0.9659258262890683122, 1.000000000000000000, 0.9659258262890683122, 1.000000000000000000, 0.9659258262890683122, 1.000000000000000000, 0.9659258262890683122, 1.000000000000000000, 0.9659258262890683122, 1.000000000000000000, 0.9659258262890683122, 1.000000000000000000, 0.9659258262890683122, 1.000000000000000000, 0.9659258262890683122, 1.000000000000000000, 0.9659258262890683122, 1.000000000000000000, 0.9659258262890683122, 1.000000000000000000, 0.9659258262890683122, 1.000000000000000000, 0.9659258262890683122, 1.000000000000000000, 0.9659258262890683122, 1.000000000000000000, 0.9659258262890683122, 1.000000000000000000, 0.9659258262890683122, 1.000000000000000000, 0.9659258262890683122, 1.000000000000000000, 0.9659258262890683122, 1.000000000000000000, 0.9659258262890683122, 1.000000000000000000, 0.9659258262890683122, 1.000000000000000000, 0.9659258262890683122, 1.000000000000000000, 0.9659258262890683122, 1.000000000000000000, 0.9659258262890683122, 1.000000000000000000, 0.9659258262890683122, 1.000000000000000000, 0.9659258262890683122, 1.000000000000000000, 0.9659258262890683122, 1.000000000000000000, 0.9659258262890683122, 1.000000000000000000, 0.9659258262890683122, 1.000000000000000000, 0.9659258262890683122, 1.000000000000000000, 0.9659258262890683122, 1.000000000000000000, 0.9659258262890683122, 1.000000000000000000, 0.9659258262890683122, 1.000000000000000000, 0.9659258262890683122, 1.000000000000000000, 0.9659258262890683122, 1.000000000000000000, 0.9659258262890683122, 1.000000000000000000, 0.9659258262890683122, 1.000000000000000000, 0.9659258262890683122, 1.000000000000000000, 0.9659258262890683122, 1.000000000000000000, 0.9659258262890683122, 1.000000000000000000, 0.9659258262890683122, 1.000000000000000000, 0.9659258262890683122, 1.000000000000000000, 0.9659258262890683122, 1.000000000000000000, 0.9659258262890683122, 1.000000000000000000, 0.9659258262890683122, 1.000000000000000000, 0.9659258262890683122, 1.000000000000000000, 0.9659258262890683122, 1.000000000000000000, 0.9659258262890683122, 1.000000000000000000, 0.9659258262890683122, 1.000000000000000000, 0.9659258262890683122, 1.000000000000000000, 0.9659258262890683122, 1.000000000000000000, 0.9659258262890683122, 1.000000000000000000, 0.9659258262890683122, 1.000000000000000000, 0.9659258262890683122, 1.000000000000000000, 0.9659258262890683122, 1.000000000000000000, 0.9659258262890683122, 1.000000000000000000, 0.9659258262890683122, 1.000000000000000000, 0.9659258262890683122, 1.000000000000000000, 0.9659258262890683122, 1.000000000000000000, 0.9659258262890683122, 1.000000000000000000, 0.9659258262890683122, 1.000000000000000000, 0.9659258262890683122, 1.000000000000000000, 0.9659258262890683122, 1.000000000000000000, 0.9659258262890683122, 1.000000000000000000, 0.9659258262890683122, 1.000000000000000000, 0.9659258262890683122, 1.000000000000000000, 0.9659258262890683122, 1.000000000000000000, 0.9659258262890683122, 1.000000000000000000, 0.9659258262890683122, 1.000000000000000000, 0.9659258262890683122, 1.000000000000000000, 0.9659258262890683122, 1.000000000000000000, 0.9659258262890683122, 1.000000000000000000, 0.9659258262890683122, 1.000000000000000000, 0.9659258262890683122, 1.000000000000000000, 0.9659258262890683122, 1.000000000000000000, 0.9659258262890683122, 1.000000000000000000, 0.9659258262890683122, 1.000000000000000000, 0.9659258262890683122, 1.000000000000000000, 0.9659258262890683122, 1.000000000000000000, 0.9659258262890683122, 1.000000000000000000, 0.9659258262890683122, 1.000000000000000000, 0.9659258262890683122, 1.000000000000000000, 0.9659258262890683122, 1.000000000000000000) ) ) 
 REPRESENTATION_ITEM ( '' )  SURFACE ( )  );
#96545 = CARTESIAN_POINT ( 'NONE',  ( -21.52544592524343514, 5.823673210054127303, 66.04057627198103830 ) ) ;
#96547 = CARTESIAN_POINT ( 'NONE',  ( -10.81492255796105439, 18.62759615963255655, 112.9177570613523329 ) ) ;
#96546 = CARTESIAN_POINT ( 'NONE',  ( -16.53943276465976808, 0.05219959533911058130, 71.24890960531435269 ) ) ;
#96548 = LINE ( 'NONE', #14009, #101846 ) ;
#96549 = CARTESIAN_POINT ( 'NONE',  ( 5.823673210054125526, 21.52544592524343514, 29.79057627198102409 ) ) ;
#96550 = CARTESIAN_POINT ( 'NONE',  ( -19.02544592524342804, 5.153800228976336051, 56.04057627198100988 ) ) ;
#96551 = CARTESIAN_POINT ( 'NONE',  ( 19.02544592524343514, -5.153800228976328945, 33.54057627198102409 ) ) ;
#96552 = CARTESIAN_POINT ( 'NONE',  ( -4.379528057220328563, 16.55341960407611168, 105.2072429386477097 ) ) ;
#96553 = CARTESIAN_POINT ( 'NONE',  ( 18.62759615963271287, -10.81492255796078972, 113.3322429386476955 ) ) ;
#96554 = CARTESIAN_POINT ( 'NONE',  ( 25.25560589046783022, -4.310829775027113620, 167.9999999999999716 ) ) ;
#96555 = CARTESIAN_POINT ( 'NONE',  ( -21.53943276465977519, -0.05219959533937600094, 28.75109039468567929 ) ) ;
#96556 = CARTESIAN_POINT ( 'NONE',  ( 13.89961937509977652, -13.97604488694527269, 23.12390960531436335 ) ) ;
#96557 = CARTESIAN_POINT ( 'NONE',  ( 10.72451020669871369, 18.67979575497193778, 82.08442372801901854 ) ) ;
#96558 = CARTESIAN_POINT ( 'NONE',  ( 21.55341960407610458, 5.719274019375980345, 98.95724293864770971 ) ) ;
#96559 = CARTESIAN_POINT ( 'NONE',  ( -19.03943276465977164, -0.05219959533935918106, 33.75109039468566863 ) ) ;
#96560 = CARTESIAN_POINT ( 'NONE',  ( -9.474510206698964154, 16.51473224551069663, 25.41557627198103120 ) ) ;
#96561 = DIRECTION ( 'NONE',  ( 1.000000000000000000, 0.000000000000000000, 0.000000000000000000 ) ) ;
#96562 = CARTESIAN_POINT ( 'NONE',  ( -17.58332526062525858, 7.635886036038558977, 60.92334959558466778 ) ) ;
#96563 = CARTESIAN_POINT ( 'NONE',  ( 14.34966873604972726, -8.224510206698740333, 45.83442372801901854 ) ) ;
#96564 = CARTESIAN_POINT ( 'NONE',  ( -14.29746914071049879, 8.314922557960819915, 105.8322429386476955 ) ) ;
#96565 = CARTESIAN_POINT ( 'NONE',  ( 33.77897430376540200, -2.912663603757497999, 99.66889340242285300 ) ) ;
#96566 = CARTESIAN_POINT ( 'NONE',  ( -19.02544592524342804, 5.153800228976336051, 66.04057627198103830 ) ) ;
#96567 = CARTESIAN_POINT ( 'NONE',  ( -0.05219959533910754901, -16.53943276465976808, 87.49890960531436690 ) ) ;
#96568 = CARTESIAN_POINT ( 'NONE',  ( -10.81492255796078084, -18.62759615963271287, 52.08224293864768839 ) ) ;
#96569 = CARTESIAN_POINT ( 'NONE',  ( -0.05219959533910754901, -16.53943276465976808, 67.49890960531436690 ) ) ;
#96570 = CARTESIAN_POINT ( 'NONE',  ( -12.14591786802326823, 12.06949235617739902, 38.12609039468567573 ) ) ;
#96571 = CARTESIAN_POINT ( 'NONE',  ( 10.81492255796106328, -18.62759615963255655, 90.41775706135236135 ) ) ;
#96572 = CARTESIAN_POINT ( 'NONE',  ( -0.05219959533936034679, 19.03943276465977164, 62.50109039468566863 ) ) ;
#96573 = CARTESIAN_POINT ( 'NONE',  ( -14.34966873604972548, 8.224510206698743886, 98.33442372801901854 ) ) ;
#96574 = CARTESIAN_POINT ( 'NONE',  ( 4.483927247898545687, 16.52544592524342804, 39.79057627198103830 ) ) ;
#96575 = CARTESIAN_POINT ( 'NONE',  ( 19.05341960407611168, 5.049401038298154454, 43.95724293864769550 ) ) ;
#96576 = CARTESIAN_POINT ( 'NONE',  ( -10.72451020669870658, -18.67979575497194134, 94.58442372801901854 ) ) ;
#96577 = CARTESIAN_POINT ( 'NONE',  ( 21.53943276465977519, -0.05219959533907433946, 103.7489096053143669 ) ) ;
#96578 = CARTESIAN_POINT ( 'NONE',  ( -15.72974639402176322, -15.80617190586768395, 64.37609039468568994 ) ) ;
#96579 = CARTESIAN_POINT ( 'NONE',  ( 16.53943276465976808, 0.05219959533934440121, 41.25109039468568284 ) ) ;
#96581 = CARTESIAN_POINT ( 'NONE',  ( 21.52544592524334988, 5.823673210054432836, 81.45942372801900433 ) ) ;
#96580 = CARTESIAN_POINT ( 'NONE',  ( -16.53943276465976808, 0.05219959533911058130, 66.24890960531436690 ) ) ;
#96582 = CARTESIAN_POINT ( 'NONE',  ( 8.314922557960818139, 14.29746914071049879, 24.58224293864768839 ) ) ;
#96583 = CARTESIAN_POINT ( 'NONE',  ( 16.20579543436680936, 7.371946100354974440, 28.06520834171877965 ) ) ;
#96584 = DIRECTION ( 'NONE',  ( -1.000000000000000000, 0.000000000000000000, -3.642919299551293321E-15 ) ) ;
#96585 = CARTESIAN_POINT ( 'NONE',  ( -12.06949235617756955, 12.14591786802309770, 25.62390960531435624 ) ) ;
#96586 = CARTESIAN_POINT ( 'NONE',  ( -8.314922557961024197, 14.29746914071037800, 77.91775706135231871 ) ) ;
#96587 = CARTESIAN_POINT ( 'NONE',  ( -16.51473224551069308, -9.474510206698971260, 86.66557627198102409 ) ) ;
#96588 = CARTESIAN_POINT ( 'NONE',  ( -16.46253265017160317, 9.564922557960807481, 100.8322429386477097 ) ) ;
#96589 = CARTESIAN_POINT ( 'NONE',  ( -10.81492255796105439, 18.62759615963255655, 87.91775706135234714 ) ) ;
#96590 = CARTESIAN_POINT ( 'NONE',  ( 16.53943276465976808, 0.05219959533934440121, 86.25109039468568994 ) ) ;
#96591 = CARTESIAN_POINT ( 'NONE',  ( -4.379528057220328563, 16.55341960407611168, 60.20724293864768839 ) ) ;
#96592 = CARTESIAN_POINT ( 'NONE',  ( -16.51473224551069308, -9.474510206698971260, 71.66557627198102409 ) ) ;
#96593 = ORIENTED_EDGE ( 'NONE', *, *, #61124, .T. ) ;
#96594 = CARTESIAN_POINT ( 'NONE',  ( -8.314922557961024197, 14.29746914071037800, 22.91775706135235069 ) ) ;
#96595 = CARTESIAN_POINT ( 'NONE',  ( 9.474510206698971260, -16.51473224551069308, 22.91557627198102765 ) ) ;
#96596 = CARTESIAN_POINT ( 'NONE',  ( -19.05341960407611168, -5.049401038298163336, 96.45724293864769550 ) ) ;
#96598 = CARTESIAN_POINT ( 'NONE',  ( 36.91746824999999177, 2.880721459617395097E-14, -5.624999997268813168 ) ) ;
#96597 = CARTESIAN_POINT ( 'NONE',  ( -0.05219959533934338120, 16.53943276465976808, 22.50109039468567573 ) ) ;
#96599 = CARTESIAN_POINT ( 'NONE',  ( -16.46253265017146816, -9.564922557961047289, 24.16775706135233648 ) ) ;
#96600 = CARTESIAN_POINT ( 'NONE',  ( 4.483927247898790824, -16.52544592524335698, 95.20942372801903275 ) ) ;
#96601 = CARTESIAN_POINT ( 'NONE',  ( -16.46253265017146816, -9.564922557961047289, 109.1677570613523471 ) ) ;
#96602 = CARTESIAN_POINT ( 'NONE',  ( -13.89961937509977652, 13.97604488694528158, 25.62390960531434558 ) ) ;
#96603 = CARTESIAN_POINT ( 'NONE',  ( -12.14591786802326823, 12.06949235617739902, 73.12609039468567573 ) ) ;
#96604 = CARTESIAN_POINT ( 'NONE',  ( 16.52544592524335698, 4.483927247898782831, 56.45942372801902565 ) ) ;
#96605 = CARTESIAN_POINT ( 'NONE',  ( -16.51473224551069308, -9.474510206698971260, 21.66557627198102765 ) ) ;
#96606 = CARTESIAN_POINT ( 'NONE',  ( -9.564922557961040184, 16.46253265017147172, 67.91775706135233293 ) ) ;
#96607 = CARTESIAN_POINT ( 'NONE',  ( 10.81492255796106328, -18.62759615963255655, 110.4177570613523756 ) ) ;
#96608 = CARTESIAN_POINT ( 'NONE',  ( 19.03943276465977164, -0.05219959533909143690, 43.74890960531435979 ) ) ;
#96609 = CARTESIAN_POINT ( 'NONE',  ( -0.05219959533909027116, -19.03943276465977164, 77.49890960531435269 ) ) ;
#96610 = CARTESIAN_POINT ( 'NONE',  ( 4.379528057220339221, -16.55341960407611168, 72.70724293864769550 ) ) ;
#96611 = EDGE_CURVE ( 'NONE', #27205, #20950, #76783, .T. ) ;
#96612 = CARTESIAN_POINT ( 'NONE',  ( 0.05219959533936267826, -19.03943276465977164, 45.00109039468566863 ) ) ;
#96613 = CARTESIAN_POINT ( 'NONE',  ( -21.53943276465977519, 0.05219959533907696930, 31.24890960531435979 ) ) ;
#96614 = CARTESIAN_POINT ( 'NONE',  ( -5.719274019375665041, -21.55341960407619695, 109.7927570613523613 ) ) ;
#96615 = CARTESIAN_POINT ( 'NONE',  ( -5.049401038298153566, 19.05341960407611168, 90.20724293864766707 ) ) ;
#96616 = CARTESIAN_POINT ( 'NONE',  ( -10.72451020669870658, -18.67979575497194134, 104.5844237280190185 ) ) ;
#96617 = CARTESIAN_POINT ( 'NONE',  ( 0.05219959533907565091, 21.53943276465977519, 69.99890960531435269 ) ) ;
#96618 = CARTESIAN_POINT ( 'NONE',  ( -13.97604488694527625, -13.89961937509977652, 91.87390960531432427 ) ) ;
#96619 = CARTESIAN_POINT ( 'NONE',  ( 16.46253265017146816, 9.564922557961045513, 91.66775706135234714 ) ) ;
#96620 = CARTESIAN_POINT ( 'NONE',  ( -9.474510206698964154, 16.51473224551069663, 105.4155762719810383 ) ) ;
#96621 = CARTESIAN_POINT ( 'NONE',  ( -14.29746914071037622, -8.314922557961029526, 19.16775706135234714 ) ) ;
#96622 = CARTESIAN_POINT ( 'NONE',  ( -9.474510206698964154, 16.51473224551069663, 25.41557627198103120 ) ) ;
#96623 = CARTESIAN_POINT ( 'NONE',  ( -5.049401038298153566, 19.05341960407611168, 90.20724293864766707 ) ) ;
#96624 = CARTESIAN_POINT ( 'NONE',  ( -21.53943276465977519, 0.05219959533907696930, 61.24890960531435979 ) ) ;
#96625 = CIRCLE ( 'NONE', #51327, 214.0437394197456342 ) ;
#96626 = CARTESIAN_POINT ( 'NONE',  ( 16.55341960407618274, -4.379528057220086978, 41.04275706135236135 ) ) ;
#96627 = CARTESIAN_POINT ( 'NONE',  ( 21.53943276465977519, 0.05219959533937863772, 41.25109039468568284 ) ) ;
#96628 = CARTESIAN_POINT ( 'NONE',  ( -21.55341960407619339, 5.719274019375674811, 93.54275706135234714 ) ) ;
#96629 = CARTESIAN_POINT ( 'NONE',  ( -8.224510206698735004, -14.34966873604973081, 99.58442372801900433 ) ) ;
#96630 = CARTESIAN_POINT ( 'NONE',  ( 5.049401038298161559, -19.05341960407611168, 92.70724293864769550 ) ) ;
#96631 = CARTESIAN_POINT ( 'NONE',  ( -16.52544592524342804, 4.483927247898546575, 86.04057627198102409 ) ) ;
#96632 = CARTESIAN_POINT ( 'NONE',  ( 12.06949235617739724, 12.14591786802326823, 111.8760903946856615 ) ) ;
#96633 = CARTESIAN_POINT ( 'NONE',  ( 19.02544592524334988, 5.153800228976608722, 66.45942372801899012 ) ) ;
#96634 = CARTESIAN_POINT ( 'NONE',  ( 0.05219959533937995610, -21.53943276465977519, 40.00109039468567573 ) ) ;
#96635 = CARTESIAN_POINT ( 'NONE',  ( -14.29746914071049879, 8.314922557960819915, 85.83224293864768129 ) ) ;
#96636 = CARTESIAN_POINT ( 'NONE',  ( -5.153800228976328057, -19.02544592524343514, 107.2905762719810383 ) ) ;
#96637 = CARTESIAN_POINT ( 'NONE',  ( -4.379528057220086978, -16.55341960407618274, 109.7927570613523613 ) ) ;
#96638 = CARTESIAN_POINT ( 'NONE',  ( -10.72451020669870658, -18.67979575497194134, 84.58442372801903275 ) ) ;
#96639 = CARTESIAN_POINT ( 'NONE',  ( -8.224510206698735004, -14.34966873604973081, 59.58442372801901854 ) ) ;
#96640 = CARTESIAN_POINT ( 'NONE',  ( 15.80617190586769283, -15.72974639402175789, 40.62609039468567573 ) ) ;
#96641 = EDGE_LOOP ( 'NONE', ( #76708, #123014, #123310, #116344 ) ) ;
#96642 = CARTESIAN_POINT ( 'NONE',  ( 10.72451020669871369, 18.67979575497193778, 32.08442372801901854 ) ) ;
#96643 = CARTESIAN_POINT ( 'NONE',  ( 4.483927247898545687, 16.52544592524342804, 104.7905762719810241 ) ) ;
#96644 = CARTESIAN_POINT ( 'NONE',  ( 9.474510206698971260, -16.51473224551069308, 22.91557627198102765 ) ) ;
#96645 = CARTESIAN_POINT ( 'NONE',  ( -4.379528057220328563, 16.55341960407611168, 70.20724293864769550 ) ) ;
#96646 = CARTESIAN_POINT ( 'NONE',  ( 5.153800228976335163, 19.02544592524342804, 54.79057627198103120 ) ) ;
#96647 = CARTESIAN_POINT ( 'NONE',  ( 4.379528057220092307, 16.55341960407617563, 107.2927570613523471 ) ) ;
#96648 = CARTESIAN_POINT ( 'NONE',  ( -19.02544592524342804, 5.153800228976336051, 36.04057627198100988 ) ) ;
#96649 = CARTESIAN_POINT ( 'NONE',  ( 10.72451020669898902, -18.67979575497178502, 37.91557627198102409 ) ) ;
#96650 = CARTESIAN_POINT ( 'NONE',  ( -0.05219959533910754901, -16.53943276465976808, 82.49890960531436690 ) ) ;
#96651 = CIRCLE ( 'NONE', #161332, 2.500000000000002220 ) ;
#96652 = CARTESIAN_POINT ( 'NONE',  ( -15.80617190586745835, -15.72974639402198527, 91.87390960531436690 ) ) ;
#96653 = CARTESIAN_POINT ( 'NONE',  ( -13.97604488694527625, -13.89961937509977652, 91.87390960531432427 ) ) ;
#96655 = CARTESIAN_POINT ( 'NONE',  ( 19.05341960407617918, -5.049401038297876454, 91.04275706135234714 ) ) ;
#96654 = CARTESIAN_POINT ( 'NONE',  ( -16.51473224551069308, -9.474510206698971260, 51.66557627198102409 ) ) ;
#96656 = CARTESIAN_POINT ( 'NONE',  ( -21.55341960407610458, -5.719274019375992779, 46.45724293864769550 ) ) ;
#96657 = CARTESIAN_POINT ( 'NONE',  ( 15.80617190586769283, -15.72974639402175789, 70.62609039468567573 ) ) ;
#96658 = CARTESIAN_POINT ( 'NONE',  ( 13.89961937509977652, -13.97604488694527269, 53.12390960531434558 ) ) ;
#96659 = CARTESIAN_POINT ( 'NONE',  ( -9.564922557960796823, -16.46253265017161027, 87.08224293864769550 ) ) ;
#96660 = EDGE_LOOP ( 'NONE', ( #75898, #146330, #83467, #106435 ) ) ;
#96661 = CARTESIAN_POINT ( 'NONE',  ( -8.224510206698735004, -14.34966873604973081, 69.58442372801900433 ) ) ;
#96662 = CARTESIAN_POINT ( 'NONE',  ( -15.80617190586768217, 15.72974639402176855, 43.12609039468568284 ) ) ;
#96663 = CARTESIAN_POINT ( 'NONE',  ( -10.72451020669870658, -18.67979575497194134, 79.58442372801903275 ) ) ;
#96664 = CARTESIAN_POINT ( 'NONE',  ( 18.67979575497178502, 10.72451020669898547, 24.16557627198103120 ) ) ;
#96665 = CARTESIAN_POINT ( 'NONE',  ( 21.53943276465977519, -0.05219959533907433946, 93.74890960531436690 ) ) ;
#96667 = CARTESIAN_POINT ( 'NONE',  ( 4.483927247898790824, -16.52544592524335698, 70.20942372801904696 ) ) ;
#96666 = CARTESIAN_POINT ( 'NONE',  ( 21.55341960407619695, -5.719274019375665929, 36.04275706135234714 ) ) ;
#96668 = CARTESIAN_POINT ( 'NONE',  ( -15.80617190586745835, -15.72974639402198527, 61.87390960531436690 ) ) ;
#96669 = CARTESIAN_POINT ( 'NONE',  ( 16.46253265017146816, 9.564922557961045513, 31.66775706135232937 ) ) ;
#96671 = CARTESIAN_POINT ( 'NONE',  ( -8.314922557961024197, 14.29746914071037800, 102.9177570613523756 ) ) ;
#96670 = CARTESIAN_POINT ( 'NONE',  ( 16.46253265017160672, -9.564922557960803928, 68.33224293864770971 ) ) ;
#96672 = CARTESIAN_POINT ( 'NONE',  ( 11.74264578624800315, -36.14014761921581709, -5.400000000000000355 ) ) ;
#96673 = CARTESIAN_POINT ( 'NONE',  ( -0.05219959533909027116, -19.03943276465977164, 102.4989096053143669 ) ) ;
#96674 = CYLINDRICAL_SURFACE ( 'NONE', #12018, 26.79475375365586487 ) ;
#96675 = CARTESIAN_POINT ( 'NONE',  ( 5.049401038297881783, 19.05341960407617563, 77.29275706135231871 ) ) ;
#96676 = CARTESIAN_POINT ( 'NONE',  ( 18.62759615963271287, -10.81492255796078972, 63.33224293864770260 ) ) ;
#96677 = CARTESIAN_POINT ( 'NONE',  ( -16.55341960407611168, -4.379528057220339221, 41.45724293864769550 ) ) ;
#96678 = CARTESIAN_POINT ( 'NONE',  ( 0.05219959533936267826, -19.03943276465977164, 95.00109039468567573 ) ) ;
#96679 = CARTESIAN_POINT ( 'NONE',  ( 13.97604488694527802, 13.89961937509977652, 34.37390960531436690 ) ) ;
#96680 = CARTESIAN_POINT ( 'NONE',  ( -8.224510206698735004, -14.34966873604973081, 19.58442372801901143 ) ) ;
#96682 = CARTESIAN_POINT ( 'NONE',  ( -16.46253265017146816, -9.564922557961047289, 54.16775706135234003 ) ) ;
#96681 = CARTESIAN_POINT ( 'NONE',  ( 5.719274019375991003, -21.55341960407610458, 87.70724293864769550 ) ) ;
#96683 = CARTESIAN_POINT ( 'NONE',  ( -16.53943276465976808, -0.05219959533934237506, 78.75109039468568994 ) ) ;
#96684 = CARTESIAN_POINT ( 'NONE',  ( -13.97604488694527625, -13.89961937509977652, 71.87390960531433848 ) ) ;
#96685 = CARTESIAN_POINT ( 'NONE',  ( -4.483927247898539470, -16.52544592524342804, 67.29057627198103830 ) ) ;
#96686 = CARTESIAN_POINT ( 'NONE',  ( -5.153800228976328057, -19.02544592524343514, 42.29057627198101699 ) ) ;
#96687 = CARTESIAN_POINT ( 'NONE',  ( 12.14591786802309770, 12.06949235617756955, 54.37390960531435979 ) ) ;
#96688 = CARTESIAN_POINT ( 'NONE',  ( -19.02544592524342804, 5.153800228976336051, 26.04057627198103120 ) ) ;
#96689 = CARTESIAN_POINT ( 'NONE',  ( 31.23842136418743820, -7.314639034718686261, 96.67538241540152910 ) ) ;
#96690 = CARTESIAN_POINT ( 'NONE',  ( 16.55341960407611168, 4.379528057220329451, 33.95724293864769550 ) ) ;
#96691 = CARTESIAN_POINT ( 'NONE',  ( -19.02544592524342804, 5.153800228976336051, 76.04057627198102409 ) ) ;
#96692 = CARTESIAN_POINT ( 'NONE',  ( 19.02544592524334988, 5.153800228976608722, 36.45942372801900433 ) ) ;
#96693 = CARTESIAN_POINT ( 'NONE',  ( -4.483927247898782831, 16.52544592524335698, 42.70942372801901854 ) ) ;
#96694 = CARTESIAN_POINT ( 'NONE',  ( -15.80617190586745835, -15.72974639402198527, 46.87390960531435979 ) ) ;
#96695 = CARTESIAN_POINT ( 'NONE',  ( -19.03943276465977164, -0.05219959533935918106, 18.75109039468567218 ) ) ;
#96696 = CARTESIAN_POINT ( 'NONE',  ( 13.97604488694527802, 13.89961937509977652, 79.37390960531435269 ) ) ;
#96697 = CARTESIAN_POINT ( 'NONE',  ( 19.05341960407611168, 5.049401038298154454, 113.9572429386477097 ) ) ;
#96698 = CARTESIAN_POINT ( 'NONE',  ( -5.049401038298153566, 19.05341960407611168, 110.2072429386476671 ) ) ;
#96699 = CARTESIAN_POINT ( 'NONE',  ( -18.67979575497193778, 10.72451020669871902, 43.33442372801901143 ) ) ;
#96700 = CARTESIAN_POINT ( 'NONE',  ( -16.52544592524342804, 4.483927247898546575, 101.0405762719810383 ) ) ;
#96703 = EDGE_LOOP ( 'NONE', ( #129749, #90221, #4018, #97018 ) ) ;
#96702 = CARTESIAN_POINT ( 'NONE',  ( -13.89961937509977652, 13.97604488694528158, 80.62390960531436690 ) ) ;
#96701 = CARTESIAN_POINT ( 'NONE',  ( -18.67979575497178146, -10.72451020669898902, 81.66557627198103830 ) ) ;
#96704 = CARTESIAN_POINT ( 'NONE',  ( 5.719274019375673035, 21.55341960407619339, 22.29275706135235069 ) ) ;
#96705 = ORIENTED_EDGE ( 'NONE', *, *, #183156, .T. ) ;
#96706 = CARTESIAN_POINT ( 'NONE',  ( -5.153800228976328057, -19.02544592524343514, 92.29057627198099567 ) ) ;
#96707 = EDGE_CURVE ( 'NONE', #149451, #23056, #61604, .T. ) ;
#96708 = LINE ( 'NONE', #157413, #30149 ) ;
#96710 = CARTESIAN_POINT ( 'NONE',  ( -0.05219959533909027116, -19.03943276465977164, 37.49890960531436690 ) ) ;
#96709 = CARTESIAN_POINT ( 'NONE',  ( 9.564922557960805705, 16.46253265017160317, 29.58224293864769550 ) ) ;
#96711 = CARTESIAN_POINT ( 'NONE',  ( 19.05341960407617918, -5.049401038297876454, 106.0427570613523471 ) ) ;
#96712 = CARTESIAN_POINT ( 'NONE',  ( -11.40812507854755609, 35.11059874428196537, -7.524999997268813523 ) ) ;
#96713 = CARTESIAN_POINT ( 'NONE',  ( -0.05219959533910754901, -16.53943276465976808, 107.4989096053143669 ) ) ;
#96714 = CARTESIAN_POINT ( 'NONE',  ( -10.72451020669870658, -18.67979575497194134, 89.58442372801901854 ) ) ;
#96716 = CARTESIAN_POINT ( 'NONE',  ( 10.72451020669871369, 18.67979575497193778, 27.08442372801901854 ) ) ;
#96715 = CARTESIAN_POINT ( 'NONE',  ( -9.474510206698964154, 16.51473224551069663, 65.41557627198102409 ) ) ;
#96717 = CARTESIAN_POINT ( 'NONE',  ( -5.823673210054431948, 21.52544592524334988, 27.70942372801901854 ) ) ;
#96718 = CARTESIAN_POINT ( 'NONE',  ( 27.73933785331498925, -9.013057229001033122, 140.2750000027311330 ) ) ;
#96719 = CARTESIAN_POINT ( 'NONE',  ( 16.51473224551069308, 9.474510206698969483, 89.16557627198103830 ) ) ;
#96720 = CARTESIAN_POINT ( 'NONE',  ( 19.57369961329614227, 19.99890699435813701, 140.0000000000000000 ) ) ;
#96722 = CARTESIAN_POINT ( 'NONE',  ( -18.62759615963270932, 10.81492255796079327, 45.83224293864769550 ) ) ;
#96721 = CARTESIAN_POINT ( 'NONE',  ( 14.34966873604972726, -8.224510206698740333, 30.83442372801902209 ) ) ;
#96723 = CARTESIAN_POINT ( 'NONE',  ( 15.80617190586769283, -15.72974639402175789, 80.62609039468567573 ) ) ;
#96724 = CARTESIAN_POINT ( 'NONE',  ( -13.89961937509977652, 13.97604488694528158, 115.6239096053143669 ) ) ;
#96725 = CARTESIAN_POINT ( 'NONE',  ( 5.153800228976615827, -19.02544592524334988, 95.20942372801897591 ) ) ;
#96726 = CARTESIAN_POINT ( 'NONE',  ( -5.153800228976328057, -19.02544592524343514, 57.29057627198103120 ) ) ;
#96727 = CARTESIAN_POINT ( 'NONE',  ( -0.05219959533909027116, -19.03943276465977164, 87.49890960531436690 ) ) ;
#96728 = CARTESIAN_POINT ( 'NONE',  ( -16.53943276465976808, 0.05219959533911058130, 96.24890960531435269 ) ) ;
#96729 = CARTESIAN_POINT ( 'NONE',  ( -8.314922557960811034, -14.29746914071050412, 102.0822429386476955 ) ) ;
#96730 = CARTESIAN_POINT ( 'NONE',  ( -18.67979575497178146, -10.72451020669898902, 21.66557627198102409 ) ) ;
#96732 = CARTESIAN_POINT ( 'NONE',  ( 13.97604488694527802, 13.89961937509977652, 39.37390960531435269 ) ) ;
#96731 = CARTESIAN_POINT ( 'NONE',  ( -8.314922557960811034, -14.29746914071050412, 52.08224293864768839 ) ) ;
#96733 = CARTESIAN_POINT ( 'NONE',  ( 0.05219959533937995610, -21.53943276465977519, 70.00109039468568994 ) ) ;
#96734 = CARTESIAN_POINT ( 'NONE',  ( -13.97604488694547697, 13.89961937509957934, 88.12609039468563310 ) ) ;
#96735 = CARTESIAN_POINT ( 'NONE',  ( -16.55341960407611168, -4.379528057220339221, 66.45724293864768129 ) ) ;
#96736 = CARTESIAN_POINT ( 'NONE',  ( -10.72451020669898014, 18.67979575497178502, 110.4155762719810383 ) ) ;
#96737 = CARTESIAN_POINT ( 'NONE',  ( -15.80617190586745835, -15.72974639402198527, 46.87390960531435979 ) ) ;
#96738 = CARTESIAN_POINT ( 'NONE',  ( 9.564922557960805705, 16.46253265017160317, 109.5822429386476955 ) ) ;
#96739 = CARTESIAN_POINT ( 'NONE',  ( -28.82186960331499037, 2.428612866367529932E-14, 138.2500000054623683 ) ) ;
#96740 = CARTESIAN_POINT ( 'NONE',  ( -13.97604488694527625, -13.89961937509977652, 71.87390960531433848 ) ) ;
#96741 = CARTESIAN_POINT ( 'NONE',  ( -12.06949235617756955, 12.14591786802309770, 40.62390960531435269 ) ) ;
#96742 = CARTESIAN_POINT ( 'NONE',  ( -16.52544592524335698, -4.483927247898792601, 108.9594237280190185 ) ) ;
#96743 = CARTESIAN_POINT ( 'NONE',  ( 12.06949235617739724, 12.14591786802326823, 81.87609039468568994 ) ) ;
#96744 = CARTESIAN_POINT ( 'NONE',  ( 0.05219959533936267826, -19.03943276465977164, 45.00109039468566863 ) ) ;
#96745 = DIRECTION ( 'NONE',  ( 1.000000000000000000, 0.000000000000000000, 0.000000000000000000 ) ) ;
#96746 = CARTESIAN_POINT ( 'NONE',  ( -19.02544592524342804, 5.153800228976336051, 91.04057627198100988 ) ) ;
#96747 = CARTESIAN_POINT ( 'NONE',  ( 19.03943276465977164, -0.05219959533909143690, 53.74890960531436690 ) ) ;
#96748 = CARTESIAN_POINT ( 'NONE',  ( -4.379528057220328563, 16.55341960407611168, 55.20724293864770260 ) ) ;
#96750 = CARTESIAN_POINT ( 'NONE',  ( -10.72451020669898014, 18.67979575497178502, 25.41557627198103120 ) ) ;
#96749 = CARTESIAN_POINT ( 'NONE',  ( 13.89961937509977652, -13.97604488694527269, 23.12390960531436335 ) ) ;
#96751 = CARTESIAN_POINT ( 'NONE',  ( -0.05219959533907301413, -21.53943276465977519, 47.49890960531435979 ) ) ;
#96752 = CARTESIAN_POINT ( 'NONE',  ( -14.34966873604960291, -8.224510206698953496, 86.66557627198102409 ) ) ;
#96753 = CARTESIAN_POINT ( 'NONE',  ( 16.52544592524335698, 4.483927247898782831, 41.45942372801901143 ) ) ;
#96754 = CARTESIAN_POINT ( 'NONE',  ( 14.34966873604960469, 8.224510206698951720, 74.16557627198102409 ) ) ;
#96755 = DIRECTION ( 'NONE',  ( 0.000000000000000000, 0.000000000000000000, 1.000000000000000000 ) ) ;
#96756 = CARTESIAN_POINT ( 'NONE',  ( -19.05341960407617563, 5.049401038297882671, 83.54275706135233293 ) ) ;
#96757 = CARTESIAN_POINT ( 'NONE',  ( 16.51473224551069308, 9.474510206698969483, 114.1655762719810241 ) ) ;
#96758 = CARTESIAN_POINT ( 'NONE',  ( -11.40812507854754720, -35.11059874428192273, -2.724999997268813257 ) ) ;
#96759 = LINE ( 'NONE', #6747, #76925 ) ;
#96760 = AXIS2_PLACEMENT_3D ( 'NONE', #134923, #196600, #58071 ) ;
#96762 = CARTESIAN_POINT ( 'NONE',  ( -16.52544592524335698, -4.483927247898792601, 108.9594237280190185 ) ) ;
#96761 = CARTESIAN_POINT ( 'NONE',  ( 14.34966873604972726, -8.224510206698740333, 25.83442372801901499 ) ) ;
#96763 = CARTESIAN_POINT ( 'NONE',  ( -5.153800228976607833, 19.02544592524334988, 72.70942372801900433 ) ) ;
#96764 = CARTESIAN_POINT ( 'NONE',  ( -21.53943276465977519, 0.05219959533907696930, 51.24890960531436690 ) ) ;
#96765 = CARTESIAN_POINT ( 'NONE',  ( -0.05219959533937732626, 21.53943276465977519, 62.50109039468568284 ) ) ;
#96766 = CARTESIAN_POINT ( 'NONE',  ( 10.74802307403555268, -10.74802307403551715, -64.92279855667830191 ) ) ;
#96767 = CARTESIAN_POINT ( 'NONE',  ( -8.314922557961024197, 14.29746914071037800, 37.91775706135235424 ) ) ;
#96769 = CARTESIAN_POINT ( 'NONE',  ( -0.05219959533909027116, -19.03943276465977164, 82.49890960531436690 ) ) ;
#96768 = CARTESIAN_POINT ( 'NONE',  ( -28.82186960331499037, 2.428612866367529932E-14, 142.2500000054623683 ) ) ;
#96770 = CARTESIAN_POINT ( 'NONE',  ( 1.500000000002908562, 30.39999999999990266, -50.95361246531977173 ) ) ;
#96771 = CARTESIAN_POINT ( 'NONE',  ( -12.14591786802309592, -12.06949235617757132, 101.8739096053143811 ) ) ;
#96772 = APPLICATION_PROTOCOL_DEFINITION ( 'draft international standard', 'automotive_design', 1998, #172025 ) ;
#96773 = CARTESIAN_POINT ( 'NONE',  ( -13.89961937509977652, 13.97604488694528158, 105.6239096053143527 ) ) ;
#96774 = ORIENTED_EDGE ( 'NONE', *, *, #15073, .T. ) ;
#96775 = CARTESIAN_POINT ( 'NONE',  ( -16.53943276465976808, -0.05219959533934237506, 53.75109039468568994 ) ) ;
#96776 = CARTESIAN_POINT ( 'NONE',  ( 19.05341960407617918, -5.049401038297876454, 106.0427570613523471 ) ) ;
#96777 = CARTESIAN_POINT ( 'NONE',  ( 18.67979575497178502, 10.72451020669898547, 74.16557627198102409 ) ) ;
#96778 = CARTESIAN_POINT ( 'NONE',  ( -13.97604488694527625, -13.89961937509977652, 36.87390960531436690 ) ) ;
#96780 = CARTESIAN_POINT ( 'NONE',  ( 18.67979575497178502, 10.72451020669898547, 109.1655762719810383 ) ) ;
#96779 = CARTESIAN_POINT ( 'NONE',  ( -19.03943276465977164, -0.05219959533935918106, 68.75109039468566152 ) ) ;
#96781 = CARTESIAN_POINT ( 'NONE',  ( 5.153800228976335163, 19.02544592524342804, 69.79057627198103830 ) ) ;
#96782 = CARTESIAN_POINT ( 'NONE',  ( 5.153800228976335163, 19.02544592524342804, 99.79057627198102409 ) ) ;
#96783 = ORIENTED_EDGE ( 'NONE', *, *, #44126, .F. ) ;
#96784 = CARTESIAN_POINT ( 'NONE',  ( 4.379528057220092307, 16.55341960407617563, 32.29275706135235424 ) ) ;
#96785 = CARTESIAN_POINT ( 'NONE',  ( 21.53943276465977519, -0.05219959533907433946, 108.7489096053143669 ) ) ;
#96788 = CARTESIAN_POINT ( 'NONE',  ( 13.89961937509957401, 13.97604488694547697, 76.87609039468566152 ) ) ;
#96787 = CARTESIAN_POINT ( 'NONE',  ( 0.05219959533909260263, 19.03943276465977164, 94.99890960531436690 ) ) ;
#96786 = CARTESIAN_POINT ( 'NONE',  ( -14.34966873604960291, -8.224510206698953496, 106.6655762719810383 ) ) ;
#96789 = CARTESIAN_POINT ( 'NONE',  ( -10.72451020669898014, 18.67979575497178502, 90.41557627198103830 ) ) ;
#96790 = CARTESIAN_POINT ( 'NONE',  ( -8.224510206698948167, 14.34966873604960824, 50.41557627198103120 ) ) ;
#96791 = CARTESIAN_POINT ( 'NONE',  ( 5.153800228976615827, -19.02544592524334988, 25.20942372801900433 ) ) ;
#96792 = CARTESIAN_POINT ( 'NONE',  ( 12.06949235617739724, 12.14591786802326823, 61.87609039468568284 ) ) ;
#96794 = EDGE_LOOP ( 'NONE', ( #67086, #149170, #173715, #64192 ) ) ;
#96793 = CARTESIAN_POINT ( 'NONE',  ( 16.46253265017160672, -9.564922557960803928, 98.33224293864769550 ) ) ;
#96795 = CARTESIAN_POINT ( 'NONE',  ( 19.02544592524343514, -5.153800228976328945, 48.54057627198103120 ) ) ;
#96796 = AXIS2_PLACEMENT_3D ( 'NONE', #25181, #135343, #120150 ) ;
#96797 = CARTESIAN_POINT ( 'NONE',  ( 21.53943276465977519, 0.05219959533937863772, 51.25109039468568994 ) ) ;
#96798 = CARTESIAN_POINT ( 'NONE',  ( -10.72451020669870658, -18.67979575497194134, 64.58442372801900433 ) ) ;
#96799 = CARTESIAN_POINT ( 'NONE',  ( -16.46253265017160317, 9.564922557960807481, 65.83224293864769550 ) ) ;
#96800 = CARTESIAN_POINT ( 'NONE',  ( 15.80617190586769283, -15.72974639402175789, 40.62609039468567573 ) ) ;
#96801 = CARTESIAN_POINT ( 'NONE',  ( -13.89961937509957401, -13.97604488694547875, 79.37609039468567573 ) ) ;
#96802 = EDGE_CURVE ( 'NONE', #150285, #103031, #174182, .T. ) ;
#96803 = B_SPLINE_CURVE_WITH_KNOTS ( 'NONE', 3,
 ( #177088, #53724, #9229, #100216, #176079, #143722, #131559, #5202, #38559, #97203, #37548, #20379 ),
 .UNSPECIFIED., .F., .F.,
 ( 4, 2, 2, 2, 2, 4 ),
 ( -0.003994749848159029684, -0.003130422923337863959, -0.002266095998516698233, -0.0005374421488743676492, 0.001191211700767963802, 0.002919865550410294386 ),
 .UNSPECIFIED. ) ;
#96804 = CARTESIAN_POINT ( 'NONE',  ( -9.474510206698964154, 16.51473224551069663, 45.41557627198103120 ) ) ;
#96805 = CARTESIAN_POINT ( 'NONE',  ( 16.53943276465976808, 0.05219959533934440121, 91.25109039468568994 ) ) ;
#96806 = CARTESIAN_POINT ( 'NONE',  ( 19.03943276465977164, -0.05219959533909143690, 53.74890960531436690 ) ) ;
#96807 = CARTESIAN_POINT ( 'NONE',  ( 5.049401038298161559, -19.05341960407611168, 107.7072429386476955 ) ) ;
#96808 = CARTESIAN_POINT ( 'NONE',  ( 5.153800228976335163, 19.02544592524342804, 34.79057627198102409 ) ) ;
#96809 = CARTESIAN_POINT ( 'NONE',  ( -0.05219959533907301413, -21.53943276465977519, 92.49890960531436690 ) ) ;
#96810 = CARTESIAN_POINT ( 'NONE',  ( 16.53943276465976808, 0.05219959533934440121, 76.25109039468568994 ) ) ;
#96811 = CARTESIAN_POINT ( 'NONE',  ( -21.81230582904512261, 5.969922009378191063, 172.1979875755924922 ) ) ;
#96812 = CARTESIAN_POINT ( 'NONE',  ( 5.049401038297881783, 19.05341960407617563, 37.29275706135232582 ) ) ;
#96813 = CARTESIAN_POINT ( 'NONE',  ( 9.474510206698971260, -16.51473224551069308, 72.91557627198102409 ) ) ;
#96814 = CARTESIAN_POINT ( 'NONE',  ( -4.379528057220328563, 16.55341960407611168, 50.20724293864769550 ) ) ;
#96816 = B_SPLINE_CURVE_WITH_KNOTS ( 'NONE', 3,
 ( #163041, #99357, #69028, #52851, #180239, #179234 ),
 .UNSPECIFIED., .F., .F.,
 ( 4, 2, 4 ),
 ( 3.469446951953614189E-18, 0.0003837532665635135821, 0.0007675065331270236949 ),
 .UNSPECIFIED. ) ;
#96815 = CARTESIAN_POINT ( 'NONE',  ( 14.29746914071049879, -8.314922557960816363, 78.33224293864770971 ) ) ;
#96817 = CARTESIAN_POINT ( 'NONE',  ( 5.049401038298161559, -19.05341960407611168, 102.7072429386476955 ) ) ;
#96818 = CARTESIAN_POINT ( 'NONE',  ( 19.05341960407611168, 5.049401038298154454, 88.95724293864769550 ) ) ;
#96819 = CARTESIAN_POINT ( 'NONE',  ( -18.62759615963255300, -10.81492255796106328, 49.16775706135234003 ) ) ;
#96820 = CARTESIAN_POINT ( 'NONE',  ( 13.97604488694527802, 13.89961937509977652, 99.37390960531436690 ) ) ;
#96821 = CARTESIAN_POINT ( 'NONE',  ( 21.55341960407619695, -5.719274019375665929, 96.04275706135236135 ) ) ;
#96822 = CARTESIAN_POINT ( 'NONE',  ( -14.29746914071037622, -8.314922557961029526, 84.16775706135234714 ) ) ;
#96823 = CARTESIAN_POINT ( 'NONE',  ( 21.53943276465977519, 0.05219959533937863772, 26.25109039468567573 ) ) ;
#96824 = CARTESIAN_POINT ( 'NONE',  ( -9.564922557960796823, -16.46253265017161027, 107.0822429386476955 ) ) ;
#96825 = CARTESIAN_POINT ( 'NONE',  ( 21.55341960407610458, 5.719274019375980345, 108.9572429386476955 ) ) ;
#96826 = CARTESIAN_POINT ( 'NONE',  ( -16.52544592524342804, 4.483927247898546575, 61.04057627198103120 ) ) ;
#96827 = CARTESIAN_POINT ( 'NONE',  ( -9.474510206698964154, 16.51473224551069663, 40.41557627198103120 ) ) ;
#96828 = CARTESIAN_POINT ( 'NONE',  ( 8.314922557960818139, 14.29746914071049879, 69.58224293864769550 ) ) ;
#96829 = CARTESIAN_POINT ( 'NONE',  ( -18.62759615963270932, 10.81492255796079327, 35.83224293864768839 ) ) ;
#96830 = CARTESIAN_POINT ( 'NONE',  ( 0.05219959533936267826, -19.03943276465977164, 25.00109039468566152 ) ) ;
#96831 = CARTESIAN_POINT ( 'NONE',  ( 0.05219959533910956823, 16.53943276465976808, 109.9989096053143527 ) ) ;
#96832 = ORIENTED_EDGE ( 'NONE', *, *, #136692, .T. ) ;
#96833 = CARTESIAN_POINT ( 'NONE',  ( 12.14591786802327356, -12.06949235617739191, 60.62609039468567573 ) ) ;
#96834 = CARTESIAN_POINT ( 'NONE',  ( -13.97604488694527625, -13.89961937509977652, 66.87390960531436690 ) ) ;
#96835 = DIRECTION ( 'NONE',  ( -0.000000000000000000, -0.000000000000000000, 1.000000000000000000 ) ) ;
#96836 = CARTESIAN_POINT ( 'NONE',  ( 0.05219959533910956823, 16.53943276465976808, 84.99890960531436690 ) ) ;
#96837 = CARTESIAN_POINT ( 'NONE',  ( 21.55341960407610458, 5.719274019375980345, 38.95724293864768839 ) ) ;
#96838 = CARTESIAN_POINT ( 'NONE',  ( -16.52544592524335698, -4.483927247898792601, 108.9594237280190185 ) ) ;
#96839 = CARTESIAN_POINT ( 'NONE',  ( 19.05341960407617918, -5.049401038297876454, 106.0427570613523471 ) ) ;
#96840 = CARTESIAN_POINT ( 'NONE',  ( -21.55341960407619339, 5.719274019375674811, 78.54275706135236135 ) ) ;
#96841 = CARTESIAN_POINT ( 'NONE',  ( -5.153800228976328057, -19.02544592524343514, 82.29057627198103830 ) ) ;
#96842 = CARTESIAN_POINT ( 'NONE',  ( 21.55341960407610458, 5.719274019375980345, 108.9572429386476955 ) ) ;
#96843 = CARTESIAN_POINT ( 'NONE',  ( -4.379528057220086978, -16.55341960407618274, 49.79275706135234714 ) ) ;
#96844 = CARTESIAN_POINT ( 'NONE',  ( -19.02544592524342804, 5.153800228976336051, 26.04057627198103120 ) ) ;
#96845 = CARTESIAN_POINT ( 'NONE',  ( 8.314922557961029526, -14.29746914071037800, 25.41775706135235779 ) ) ;
#96846 = CARTESIAN_POINT ( 'NONE',  ( -16.51473224551082808, 9.474510206698731452, 93.33442372801900433 ) ) ;
#96847 = CARTESIAN_POINT ( 'NONE',  ( -21.55341960407610458, -5.719274019375992779, 96.45724293864770971 ) ) ;
#96848 = CARTESIAN_POINT ( 'NONE',  ( 16.51473224551083163, -9.474510206698727899, 55.83442372801899722 ) ) ;
#96849 = CARTESIAN_POINT ( 'NONE',  ( 19.35633801406910592, -5.499999999999574563, 86.63373818172766505 ) ) ;
#96850 = CARTESIAN_POINT ( 'NONE',  ( 18.67979575497178502, 10.72451020669898547, 99.16557627198100988 ) ) ;
#96851 = CARTESIAN_POINT ( 'NONE',  ( 18.22780087662126647, 5.499999999999818812, 61.48236817873107185 ) ) ;
#96852 = CARTESIAN_POINT ( 'NONE',  ( 16.46253265017160672, -9.564922557960803928, 83.33224293864768129 ) ) ;
#96853 = DIRECTION ( 'NONE',  ( -0.7071067811865467956, 2.468850131082262977E-15, 0.7071067811865483499 ) ) ;
#96854 = CARTESIAN_POINT ( 'NONE',  ( 8.224510206698742110, 14.34966873604972548, 37.08442372801901143 ) ) ;
#96855 = CARTESIAN_POINT ( 'NONE',  ( 24.66672740160585064, 7.254147403784513060, 167.4978451254145284 ) ) ;
#96857 = CARTESIAN_POINT ( 'NONE',  ( 12.06949235617757843, -12.14591786802309237, 63.12390960531435979 ) ) ;
#96856 = CARTESIAN_POINT ( 'NONE',  ( -21.52544592524343514, 5.823673210054127303, 111.0405762719810525 ) ) ;
#96858 = CARTESIAN_POINT ( 'NONE',  ( 0.05219959533909260263, 19.03943276465977164, 64.99890960531436690 ) ) ;
#96860 = CARTESIAN_POINT ( 'NONE',  ( -16.46253265017146816, -9.564922557961047289, 44.16775706135232582 ) ) ;
#96859 = CARTESIAN_POINT ( 'NONE',  ( 8.224510206698742110, 14.34966873604972548, 37.08442372801901143 ) ) ;
#96861 = CARTESIAN_POINT ( 'NONE',  ( -21.55341960407619339, 5.719274019375674811, 53.54275706135234714 ) ) ;
#96862 = CARTESIAN_POINT ( 'NONE',  ( 13.97604488694548053, -13.89961937509957401, 110.6260903946856615 ) ) ;
#96863 = CARTESIAN_POINT ( 'NONE',  ( 13.97604488694527802, 13.89961937509977652, 54.37390960531435979 ) ) ;
#96864 = CARTESIAN_POINT ( 'NONE',  ( -13.89961937509957401, -13.97604488694547875, 79.37609039468567573 ) ) ;
#96865 = CARTESIAN_POINT ( 'NONE',  ( -15.72974639402176322, -15.80617190586768395, 89.37609039468568994 ) ) ;
#96866 = CARTESIAN_POINT ( 'NONE',  ( -5.153800228976607833, 19.02544592524334988, 72.70942372801900433 ) ) ;
#96867 = CARTESIAN_POINT ( 'NONE',  ( -9.564922557960796823, -16.46253265017161027, 42.08224293864769550 ) ) ;
#96868 = CARTESIAN_POINT ( 'NONE',  ( 18.67979575497178502, 10.72451020669898547, 54.16557627198103120 ) ) ;
#96869 = CARTESIAN_POINT ( 'NONE',  ( 16.53943276465976808, -0.05219959533910856209, 58.74890960531436690 ) ) ;
#96870 = CARTESIAN_POINT ( 'NONE',  ( -18.22780087662122028, -5.500000000000014211, 101.4845989467389273 ) ) ;
#96871 = CARTESIAN_POINT ( 'NONE',  ( -19.03943276465977164, -0.05219959533935918106, 33.75109039468566863 ) ) ;
#96872 = CARTESIAN_POINT ( 'NONE',  ( -14.29746914071037622, -8.314922557961029526, 104.1677570613523471 ) ) ;
#96873 = CARTESIAN_POINT ( 'NONE',  ( -12.14591786802309592, -12.06949235617757132, 51.87390960531437401 ) ) ;
#96875 = CARTESIAN_POINT ( 'NONE',  ( 8.571926809382597767, 26.38167802310806209, 142.2750000027311899 ) ) ;
#96874 = CARTESIAN_POINT ( 'NONE',  ( -18.67979575497193778, 10.72451020669871902, 93.33442372801901854 ) ) ;
#96876 = CARTESIAN_POINT ( 'NONE',  ( 15.72974639402176855, 15.80617190586768217, 91.87609039468568994 ) ) ;
#96877 = CARTESIAN_POINT ( 'NONE',  ( 21.52544592524344225, -5.823673210054117533, 88.54057627198103830 ) ) ;
#96878 = CARTESIAN_POINT ( 'NONE',  ( -13.89961937509977652, 13.97604488694528158, 55.62390960531434558 ) ) ;
#96879 = CARTESIAN_POINT ( 'NONE',  ( -18.62759615963255300, -10.81492255796106328, 74.16775706135231871 ) ) ;
#96880 = CARTESIAN_POINT ( 'NONE',  ( -19.05341960407611168, -5.049401038298163336, 46.45724293864768129 ) ) ;
#96881 = VERTEX_POINT ( 'NONE', #15121 ) ;
#96882 = CARTESIAN_POINT ( 'NONE',  ( -5.153800228976328057, -19.02544592524343514, 62.29057627198100988 ) ) ;
#96883 = CARTESIAN_POINT ( 'NONE',  ( 16.55341960407611168, 4.379528057220329451, 103.9572429386476813 ) ) ;
#96884 = CARTESIAN_POINT ( 'NONE',  ( -15.80617190586745835, -15.72974639402198527, 21.87390960531436690 ) ) ;
#96885 = CARTESIAN_POINT ( 'NONE',  ( 16.55341960407611168, 4.379528057220329451, 58.95724293864770971 ) ) ;
#96886 = CARTESIAN_POINT ( 'NONE',  ( -19.02544592524342804, 5.153800228976336051, 26.04057627198103120 ) ) ;
#96887 = CARTESIAN_POINT ( 'NONE',  ( -0.05219959533910754901, -16.53943276465976808, 77.49890960531433848 ) ) ;
#96888 = CARTESIAN_POINT ( 'NONE',  ( 18.62759615963271287, -10.81492255796078972, 88.33224293864769550 ) ) ;
#96889 = CARTESIAN_POINT ( 'NONE',  ( -15.72974639402176322, -15.80617190586768395, 34.37609039468568284 ) ) ;
#96890 = CARTESIAN_POINT ( 'NONE',  ( 27.94119071623654094, -7.398115196983436448, 160.8979257793636464 ) ) ;
#96891 = CARTESIAN_POINT ( 'NONE',  ( 16.53943276465976808, 0.05219959533934440121, 31.25109039468568639 ) ) ;
#96892 = CARTESIAN_POINT ( 'NONE',  ( 10.81492255796078972, 18.62759615963270932, 84.58224293864769550 ) ) ;
#96893 = CARTESIAN_POINT ( 'NONE',  ( 21.55341960407619695, -5.719274019375665929, 106.0427570613523471 ) ) ;
#96894 = CARTESIAN_POINT ( 'NONE',  ( -16.46253265017160317, 9.564922557960807481, 95.83224293864769550 ) ) ;
#96895 = CARTESIAN_POINT ( 'NONE',  ( 15.72974639402176855, 15.80617190586768217, 41.87609039468568284 ) ) ;
#96896 = CARTESIAN_POINT ( 'NONE',  ( 21.55341960407610458, 5.719274019375980345, 23.95724293864769550 ) ) ;
#96897 = CARTESIAN_POINT ( 'NONE',  ( 16.52544592524335698, 4.483927247898782831, 106.4594237280190328 ) ) ;
#96899 = CARTESIAN_POINT ( 'NONE',  ( 5.719274019375673035, 21.55341960407619339, 87.29275706135236135 ) ) ;
#96898 = CARTESIAN_POINT ( 'NONE',  ( -15.72974639402176322, -15.80617190586768395, 44.37609039468567573 ) ) ;
#96900 = CARTESIAN_POINT ( 'NONE',  ( 19.03943276465977164, 0.05219959533936151252, 21.25109039468565797 ) ) ;
#96901 = CARTESIAN_POINT ( 'NONE',  ( -12.14591786802326823, 12.06949235617739902, 83.12609039468568994 ) ) ;
#96902 = CARTESIAN_POINT ( 'NONE',  ( -15.80617190586768217, 15.72974639402176855, 48.12609039468568284 ) ) ;
#96903 = CARTESIAN_POINT ( 'NONE',  ( 5.153800228976335163, 19.02544592524342804, 34.79057627198102409 ) ) ;
#96904 = CARTESIAN_POINT ( 'NONE',  ( 10.72451020669871369, 18.67979575497193778, 107.0844237280190043 ) ) ;
#96905 = CARTESIAN_POINT ( 'NONE',  ( -9.564922557960796823, -16.46253265017161027, 107.0822429386476955 ) ) ;
#96906 = CARTESIAN_POINT ( 'NONE',  ( -10.81492255796078084, -18.62759615963271287, 97.08224293864770971 ) ) ;
#96907 = CIRCLE ( 'NONE', #35576, 21.30000000000002913 ) ;
#96909 = CARTESIAN_POINT ( 'NONE',  ( -18.67979575497178146, -10.72451020669898902, 66.66557627198102409 ) ) ;
#96908 = CARTESIAN_POINT ( 'NONE',  ( 19.39056639909674118, 5.500000000000051514, 83.28948781074343799 ) ) ;
#96911 = CARTESIAN_POINT ( 'NONE',  ( 16.55341960407611168, 4.379528057220329451, 63.95724293864770260 ) ) ;
#96910 = CARTESIAN_POINT ( 'NONE',  ( -4.483927247898782831, 16.52544592524335698, 57.70942372801901143 ) ) ;
#96912 = CARTESIAN_POINT ( 'NONE',  ( 19.08440550902509258, -5.500000000000005329, 101.3294784629314762 ) ) ;
#96913 = CARTESIAN_POINT ( 'NONE',  ( -16.51473224551082808, 9.474510206698731452, 93.33442372801900433 ) ) ;
#96914 =( BOUNDED_CURVE ( )  B_SPLINE_CURVE ( 3, ( #45179, #64316, #139156, #156324 ),
 .UNSPECIFIED., .F., .T. ) 
 B_SPLINE_CURVE_WITH_KNOTS ( ( 4, 4 ),
 ( 5.150538010968861435, 5.257537365396776963 ),
 .UNSPECIFIED. ) 
 CURVE ( )  GEOMETRIC_REPRESENTATION_ITEM ( )  RATIONAL_B_SPLINE_CURVE ( ( 1.000000000000000000, 0.9990461557208837329, 0.9990461557208837329, 1.000000000000000000 ) ) 
 REPRESENTATION_ITEM ( '' )  );
#96915 = CARTESIAN_POINT ( 'NONE',  ( -23.94081952771225730, 0.9791052130477023718, -54.49391133501602980 ) ) ;
#96916 = CARTESIAN_POINT ( 'NONE',  ( 16.55341960407618274, -4.379528057220086978, 26.04275706135235779 ) ) ;
#96917 = CARTESIAN_POINT ( 'NONE',  ( -15.80617190586745835, -15.72974639402198527, 91.87390960531436690 ) ) ;
#96918 = CARTESIAN_POINT ( 'NONE',  ( 5.719274019375991003, -21.55341960407610458, 72.70724293864769550 ) ) ;
#96919 = CARTESIAN_POINT ( 'NONE',  ( 5.049401038298161559, -19.05341960407611168, 112.7072429386476813 ) ) ;
#96920 = CARTESIAN_POINT ( 'NONE',  ( -16.52544592524335698, -4.483927247898792601, 48.95942372801902565 ) ) ;
#96921 = CARTESIAN_POINT ( 'NONE',  ( -0.05219959533909027116, -19.03943276465977164, 72.49890960531435269 ) ) ;
#96923 = CARTESIAN_POINT ( 'NONE',  ( -16.46253265017146816, -9.564922557961047289, 99.16775706135233293 ) ) ;
#96922 = CARTESIAN_POINT ( 'NONE',  ( -21.52544592524334988, -5.823673210054445271, 33.95942372801901143 ) ) ;
#96924 = CARTESIAN_POINT ( 'NONE',  ( 13.97604488694527802, 13.89961937509977652, 114.3739096053143669 ) ) ;
#96925 = CARTESIAN_POINT ( 'NONE',  ( -19.02544592524342804, 5.153800228976336051, 86.04057627198103830 ) ) ;
#96926 = CARTESIAN_POINT ( 'NONE',  ( 18.62759615963271287, -10.81492255796078972, 83.33224293864769550 ) ) ;
#96927 = CARTESIAN_POINT ( 'NONE',  ( -9.474510206698964154, 16.51473224551069663, 60.41557627198102409 ) ) ;
#96928 = CARTESIAN_POINT ( 'NONE',  ( -30.74264578624800492, 22.33583958711400186, -0.1999999999999999001 ) ) ;
#96929 = CARTESIAN_POINT ( 'NONE',  ( 8.224510206698953496, -14.34966873604960469, 62.91557627198102409 ) ) ;
#96930 = CARTESIAN_POINT ( 'NONE',  ( -18.67979575497178146, -10.72451020669898902, 26.66557627198103475 ) ) ;
#96931 = CARTESIAN_POINT ( 'NONE',  ( -28.79475375365586842, 2.428612866367529932E-14, 139.9999999999999716 ) ) ;
#96932 = CARTESIAN_POINT ( 'NONE',  ( 18.67979575497178502, 10.72451020669898547, 99.16557627198100988 ) ) ;
#96933 = CARTESIAN_POINT ( 'NONE',  ( -19.05341960407617563, 5.049401038297882671, 58.54275706135234003 ) ) ;
#96934 = CARTESIAN_POINT ( 'NONE',  ( -13.97604488694527625, -13.89961937509977652, 111.8739096053143243 ) ) ;
#96935 = CARTESIAN_POINT ( 'NONE',  ( 19.01529144963336648, 5.499999999999972466, 68.73431955728435128 ) ) ;
#96936 = CARTESIAN_POINT ( 'NONE',  ( -18.67979575497178146, -10.72451020669898902, 61.66557627198103120 ) ) ;
#96937 = AXIS2_PLACEMENT_3D ( 'NONE', #112756, #67252, #33943 ) ;
#96938 = CARTESIAN_POINT ( 'NONE',  ( 0.05219959533909260263, 19.03943276465977164, 84.99890960531436690 ) ) ;
#96939 = CARTESIAN_POINT ( 'NONE',  ( 18.67979575497194134, -10.72451020669871369, 80.83442372801901854 ) ) ;
#96940 = CARTESIAN_POINT ( 'NONE',  ( -16.46253265017160317, 9.564922557960807481, 50.83224293864770260 ) ) ;
#96941 = CARTESIAN_POINT ( 'NONE',  ( 8.314922557960818139, 14.29746914071049879, 84.58224293864769550 ) ) ;
#96942 = CARTESIAN_POINT ( 'NONE',  ( -16.55341960407617563, 4.379528057220093196, 33.54275706135234714 ) ) ;
#96943 = CARTESIAN_POINT ( 'NONE',  ( 15.72974639402176855, 15.80617190586768217, 71.87609039468568994 ) ) ;
#96944 = ORIENTED_EDGE ( 'NONE', *, *, #135116, .F. ) ;
#96945 = CARTESIAN_POINT ( 'NONE',  ( 16.51473224551083163, -9.474510206698727899, 20.83442372801899722 ) ) ;
#96947 = ADVANCED_FACE ( 'NONE', ( #153625 ), #49436, .T. ) ;
#96946 = CARTESIAN_POINT ( 'NONE',  ( -19.02544592524334988, -5.153800228976617603, 78.95942372801900433 ) ) ;
#96948 = CARTESIAN_POINT ( 'NONE',  ( 33.40031027765339644, -22.02106105253703561, -24.45416078184958408 ) ) ;
#96949 = CARTESIAN_POINT ( 'NONE',  ( 5.719274019375673035, 21.55341960407619339, 32.29275706135235424 ) ) ;
#96950 = CARTESIAN_POINT ( 'NONE',  ( -4.313351365237978463, -4.313351365237916291, -62.50719930893269805 ) ) ;
#96951 = CARTESIAN_POINT ( 'NONE',  ( -19.05341960407617563, 5.049401038297882671, 33.54275706135231871 ) ) ;
#96952 = CARTESIAN_POINT ( 'NONE',  ( 19.03943276465977164, -0.05219959533909143690, 58.74890960531435979 ) ) ;
#96953 = CARTESIAN_POINT ( 'NONE',  ( -9.474510206698720793, -16.51473224551083518, 24.58442372801900078 ) ) ;
#96954 = CARTESIAN_POINT ( 'NONE',  ( -4.379528057220086978, -16.55341960407618274, 104.7927570613523898 ) ) ;
#96956 = CARTESIAN_POINT ( 'NONE',  ( 5.719274019375673035, 21.55341960407619339, 87.29275706135236135 ) ) ;
#96955 = CARTESIAN_POINT ( 'NONE',  ( 13.89961937509977652, -13.97604488694527269, 98.12390960531433848 ) ) ;
#96957 = CARTESIAN_POINT ( 'NONE',  ( -36.91746825000001309, 11.99521256947798342, -8.724999997268813701 ) ) ;
#96958 = CARTESIAN_POINT ( 'NONE',  ( -17.49999999999999645, 5.499999999999992895, 98.71769037696435589 ) ) ;
#96959 = CARTESIAN_POINT ( 'NONE',  ( -21.53943276465977519, -0.05219959533937600094, 83.75109039468568994 ) ) ;
#96960 = DIRECTION ( 'NONE',  ( -0.000000000000000000, -0.000000000000000000, 1.000000000000000000 ) ) ;
#96961 = CARTESIAN_POINT ( 'NONE',  ( -9.564922557960796823, -16.46253265017161027, 102.0822429386477097 ) ) ;
#96962 = CARTESIAN_POINT ( 'NONE',  ( 21.64789649210667832, -31.17538106138185938, -22.95353217465963880 ) ) ;
#96963 = CARTESIAN_POINT ( 'NONE',  ( -0.05219959533909027116, -19.03943276465977164, 52.49890960531436690 ) ) ;
#96964 = CARTESIAN_POINT ( 'NONE',  ( 5.823673210054125526, 21.52544592524343514, 59.79057627198103120 ) ) ;
#96965 = CARTESIAN_POINT ( 'NONE',  ( 4.379528057220339221, -16.55341960407611168, 32.70724293864770260 ) ) ;
#96967 = CARTESIAN_POINT ( 'NONE',  ( -19.02544592524342804, 5.153800228976336051, 76.04057627198102409 ) ) ;
#96966 = CARTESIAN_POINT ( 'NONE',  ( -12.14591786802309592, -12.06949235617757132, 101.8739096053143811 ) ) ;
#96968 = CARTESIAN_POINT ( 'NONE',  ( 18.62759615963255655, 10.81492255796105972, 111.6677570613523613 ) ) ;
#96969 = CARTESIAN_POINT ( 'NONE',  ( -9.474510206698964154, 16.51473224551069663, 40.41557627198103120 ) ) ;
#96970 = CARTESIAN_POINT ( 'NONE',  ( 8.314922557960818139, 14.29746914071049879, 104.5822429386477097 ) ) ;
#96971 = CARTESIAN_POINT ( 'NONE',  ( 5.719274019375673035, 21.55341960407619339, 57.29275706135234714 ) ) ;
#96972 = CARTESIAN_POINT ( 'NONE',  ( -21.53943276465977519, 0.05219959533907696930, 81.24890960531436690 ) ) ;
#96973 = CARTESIAN_POINT ( 'NONE',  ( 19.05341960407617918, -5.049401038297876454, 66.04275706135233293 ) ) ;
#96974 = CARTESIAN_POINT ( 'NONE',  ( 10.59477242850415024, -90.60836494048558620, 0.000000000000000000 ) ) ;
#96975 = CARTESIAN_POINT ( 'NONE',  ( 9.564922557960805705, 16.46253265017160317, 109.5822429386476955 ) ) ;
#96976 = CARTESIAN_POINT ( 'NONE',  ( -4.483927247898539470, -16.52544592524342804, 77.29057627198102409 ) ) ;
#96977 = CARTESIAN_POINT ( 'NONE',  ( 19.02544592524334988, 5.153800228976608722, 41.45942372801900433 ) ) ;
#96978 = CARTESIAN_POINT ( 'NONE',  ( 16.51473224551069308, 9.474510206698969483, 64.16557627198102409 ) ) ;
#96979 = CARTESIAN_POINT ( 'NONE',  ( -8.224510206698948167, 14.34966873604960824, 60.41557627198102409 ) ) ;
#96980 = CARTESIAN_POINT ( 'NONE',  ( -5.049401038297874678, -19.05341960407617918, 74.79275706135231871 ) ) ;
#96981 = CYLINDRICAL_SURFACE ( 'NONE', #102080, 8.000000000000000000 ) ;
#96982 = CARTESIAN_POINT ( 'NONE',  ( -21.52544592524343514, 5.823673210054127303, 31.04057627198102409 ) ) ;
#96983 = ORIENTED_EDGE ( 'NONE', *, *, #177098, .F. ) ;
#96984 = CARTESIAN_POINT ( 'NONE',  ( 16.55341960407611168, 4.379528057220329451, 98.95724293864770971 ) ) ;
#96985 = CARTESIAN_POINT ( 'NONE',  ( -17.49999999999997158, -3.512728167237161081, 24.77190004818871572 ) ) ;
#96987 = CARTESIAN_POINT ( 'NONE',  ( -18.67979575497178146, -10.72451020669898902, 56.66557627198103830 ) ) ;
#96986 = CARTESIAN_POINT ( 'NONE',  ( 13.89961937509977652, -13.97604488694527269, 53.12390960531434558 ) ) ;
#96988 = CARTESIAN_POINT ( 'NONE',  ( -0.05219959533909027116, -19.03943276465977164, 37.49890960531436690 ) ) ;
#96990 = CARTESIAN_POINT ( 'NONE',  ( 16.51473224551069308, 9.474510206698969483, 79.16557627198103830 ) ) ;
#96989 = CARTESIAN_POINT ( 'NONE',  ( -16.52544592524335698, -4.483927247898792601, 83.95942372801900433 ) ) ;
#96991 = CARTESIAN_POINT ( 'NONE',  ( -13.97604488694547697, 13.89961937509957934, 58.12609039468566863 ) ) ;
#96992 = CARTESIAN_POINT ( 'NONE',  ( 5.719274019375673035, 21.55341960407619339, 67.29275706135234714 ) ) ;
#96993 = CARTESIAN_POINT ( 'NONE',  ( -10.81492255796078084, -18.62759615963271287, 52.08224293864768839 ) ) ;
#96994 = CARTESIAN_POINT ( 'NONE',  ( -16.53943276465976808, 0.05219959533911058130, 116.2489096053143669 ) ) ;
#96995 = CARTESIAN_POINT ( 'NONE',  ( -16.55341960407617563, 4.379528057220093196, 93.54275706135234714 ) ) ;
#96996 = CARTESIAN_POINT ( 'NONE',  ( -19.03943276465977164, -0.05219959533935918106, 103.7510903946856757 ) ) ;
#96997 = CARTESIAN_POINT ( 'NONE',  ( 18.22780087662123805, -5.499999999999976019, 78.51763182126894947 ) ) ;
#96998 = CARTESIAN_POINT ( 'NONE',  ( 18.56399227203342406, 5.500000000000001776, 76.47830131249902763 ) ) ;
#96999 = CARTESIAN_POINT ( 'NONE',  ( 5.823673210054444382, -21.52544592524334988, 95.20942372801903275 ) ) ;
#97000 = ORIENTED_EDGE ( 'NONE', *, *, #185422, .F. ) ;
#97001 = CARTESIAN_POINT ( 'NONE',  ( -16.55341960407611168, -4.379528057220339221, 41.45724293864769550 ) ) ;
#97002 = CARTESIAN_POINT ( 'NONE',  ( -4.379528057220328563, 16.55341960407611168, 75.20724293864769550 ) ) ;
#97003 = CARTESIAN_POINT ( 'NONE',  ( -10.72451020669898014, 18.67979575497178502, 95.41557627198102409 ) ) ;
#97004 = CARTESIAN_POINT ( 'NONE',  ( 10.81492255796078972, 18.62759615963270932, 89.58224293864768129 ) ) ;
#97005 = CARTESIAN_POINT ( 'NONE',  ( -0.5097844185665340033, -31.81624771892549575, -45.77220262091588410 ) ) ;
#97006 = CARTESIAN_POINT ( 'NONE',  ( -21.53943276465977519, 0.05219959533907696930, 31.24890960531435979 ) ) ;
#97007 = CARTESIAN_POINT ( 'NONE',  ( 4.379528057220092307, 16.55341960407617563, 72.29275706135236135 ) ) ;
#97008 = CARTESIAN_POINT ( 'NONE',  ( -16.55341960407611168, -4.379528057220339221, 81.45724293864769550 ) ) ;
#97009 = CARTESIAN_POINT ( 'NONE',  ( 9.564922557960805705, 16.46253265017160317, 44.58224293864769550 ) ) ;
#97010 = FILL_AREA_STYLE ('',( #84832 ) ) ;
#97011 = CARTESIAN_POINT ( 'NONE',  ( 34.40736802160862595, -7.501760008519349654, 45.46231226804130188 ) ) ;
#97012 = CARTESIAN_POINT ( 'NONE',  ( 0.05219959533934541429, -16.53943276465976808, 95.00109039468568994 ) ) ;
#97013 = CARTESIAN_POINT ( 'NONE',  ( 5.719274019375991003, -21.55341960407610458, 112.7072429386476955 ) ) ;
#97014 = CARTESIAN_POINT ( 'NONE',  ( 19.05341960407611168, 5.049401038298154454, 83.95724293864766707 ) ) ;
#97015 = CARTESIAN_POINT ( 'NONE',  ( -0.05219959533937732626, 21.53943276465977519, 57.50109039468568994 ) ) ;
#97016 = CARTESIAN_POINT ( 'NONE',  ( -19.02544592524342804, 5.153800228976336051, 106.0405762719810241 ) ) ;
#97017 = CARTESIAN_POINT ( 'NONE',  ( -13.56018889279570949, -37.30201529093374546, -30.04439950253825131 ) ) ;
#97018 = ORIENTED_EDGE ( 'NONE', *, *, #24747, .T. ) ;
#97019 = CARTESIAN_POINT ( 'NONE',  ( -21.52544592524334988, -5.823673210054445271, 53.95942372801900433 ) ) ;
#97021 = CARTESIAN_POINT ( 'NONE',  ( 9.564922557960805705, 16.46253265017160317, 24.58224293864769194 ) ) ;
#97020 = CARTESIAN_POINT ( 'NONE',  ( -5.153800228976328057, -19.02544592524343514, 37.29057627198102409 ) ) ;
#97022 = CARTESIAN_POINT ( 'NONE',  ( 0.05219959533936267826, -19.03943276465977164, 70.00109039468566152 ) ) ;
#97023 = CARTESIAN_POINT ( 'NONE',  ( -18.62759615963255300, -10.81492255796106328, 24.16775706135235424 ) ) ;
#97024 = CARTESIAN_POINT ( 'NONE',  ( -9.474510206698720793, -16.51473224551083518, 59.58442372801900433 ) ) ;
#97025 = CARTESIAN_POINT ( 'NONE',  ( 19.05341960407611168, 5.049401038298154454, 28.95724293864769550 ) ) ;
#97026 = CARTESIAN_POINT ( 'NONE',  ( -8.314922557961024197, 14.29746914071037800, 87.91775706135234714 ) ) ;
#97027 = CARTESIAN_POINT ( 'NONE',  ( -5.153800228976607833, 19.02544592524334988, 62.70942372801899722 ) ) ;
#97028 = CARTESIAN_POINT ( 'NONE',  ( 8.224510206698742110, 14.34966873604972548, 112.0844237280190185 ) ) ;
#97029 = CARTESIAN_POINT ( 'NONE',  ( 10.91551912637963540, 12.25159394783730882, -61.48002405683646288 ) ) ;
#97030 = CARTESIAN_POINT ( 'NONE',  ( -13.89961937509977652, 13.97604488694528158, 80.62390960531436690 ) ) ;
#97031 = CARTESIAN_POINT ( 'NONE',  ( -21.52544592524334988, -5.823673210054445271, 88.95942372801901854 ) ) ;
#97032 = CARTESIAN_POINT ( 'NONE',  ( 18.62759615963255655, 10.81492255796105972, 106.6677570613523756 ) ) ;
#97033 = CARTESIAN_POINT ( 'NONE',  ( 0.000000000000000000, 0.000000000000000000, -64.92279855667830191 ) ) ;
#97034 = CARTESIAN_POINT ( 'NONE',  ( -15.80617190586768217, 15.72974639402176855, 73.12609039468567573 ) ) ;
#97035 = CARTESIAN_POINT ( 'NONE',  ( 14.29746914071037800, 8.314922557961029526, 31.66775706135234358 ) ) ;
#97036 = EDGE_CURVE ( 'NONE', #128045, #117002, #200029, .T. ) ;
#97037 = CARTESIAN_POINT ( 'NONE',  ( 13.97604488694527802, 13.89961937509977652, 74.37390960531436690 ) ) ;
#97038 = CARTESIAN_POINT ( 'NONE',  ( -21.55341960407610458, -5.719274019375992779, 36.45724293864768839 ) ) ;
#97039 = CARTESIAN_POINT ( 'NONE',  ( -19.02544592524342804, 5.153800228976336051, 81.04057627198103830 ) ) ;
#97040 = CARTESIAN_POINT ( 'NONE',  ( -18.22780087662121673, -5.500000000000063061, 41.48459894673893444 ) ) ;
#97041 = CARTESIAN_POINT ( 'NONE',  ( 19.05341960407617918, -5.049401038297876454, 76.04275706135230450 ) ) ;
#97042 = CARTESIAN_POINT ( 'NONE',  ( -19.05341960407611168, -5.049401038298163336, 106.4572429386476955 ) ) ;
#97043 = CARTESIAN_POINT ( 'NONE',  ( -15.72974639402176322, -15.80617190586768395, 99.37609039468568994 ) ) ;
#97044 = CARTESIAN_POINT ( 'NONE',  ( -16.55341960407611168, -4.379528057220339221, 81.45724293864769550 ) ) ;
#97045 = CARTESIAN_POINT ( 'NONE',  ( -21.52544592524343514, 5.823673210054127303, 51.04057627198103120 ) ) ;
#97046 = CARTESIAN_POINT ( 'NONE',  ( -21.52544592524343514, 5.823673210054127303, 36.04057627198102409 ) ) ;
#97047 = CARTESIAN_POINT ( 'NONE',  ( -8.224510206698948167, 14.34966873604960824, 100.4155762719810241 ) ) ;
#97048 = CARTESIAN_POINT ( 'NONE',  ( -0.1001428631146457915, -9.099999999999999645, -61.89430850415823215 ) ) ;
#97049 = CARTESIAN_POINT ( 'NONE',  ( 5.153800228976615827, -19.02544592524334988, 60.20942372801899012 ) ) ;
#97050 = CARTESIAN_POINT ( 'NONE',  ( -14.34966873604960291, -8.224510206698953496, 31.66557627198102054 ) ) ;
#97051 = CARTESIAN_POINT ( 'NONE',  ( -19.03943276465977164, 0.05219959533909376836, 96.24890960531436690 ) ) ;
#97052 = CARTESIAN_POINT ( 'NONE',  ( -15.80617190586768217, 15.72974639402176855, 73.12609039468567573 ) ) ;
#97053 = CARTESIAN_POINT ( 'NONE',  ( 18.67979575497178502, 10.72451020669898547, 64.16557627198102409 ) ) ;
#97054 = CARTESIAN_POINT ( 'NONE',  ( 21.52544592524334988, 5.823673210054432836, 51.45942372801901854 ) ) ;
#97055 = CARTESIAN_POINT ( 'NONE',  ( -21.55341960407610458, -5.719274019375992779, 96.45724293864770971 ) ) ;
#97056 = CARTESIAN_POINT ( 'NONE',  ( -18.62759615963255300, -10.81492255796106328, 39.16775706135235424 ) ) ;
#97057 = CARTESIAN_POINT ( 'NONE',  ( -4.379528057220328563, 16.55341960407611168, 115.2072429386476955 ) ) ;
#97058 = EDGE_CURVE ( 'NONE', #137566, #41468, #180718, .T. ) ;
#97059 = CARTESIAN_POINT ( 'NONE',  ( -16.46253265017160317, 9.564922557960807481, 85.83224293864769550 ) ) ;
#97060 = CARTESIAN_POINT ( 'NONE',  ( 0.05219959533910956823, 16.53943276465976808, 99.99890960531436690 ) ) ;
#97061 = CARTESIAN_POINT ( 'NONE',  ( -19.05341960407611168, -5.049401038298163336, 111.4572429386476671 ) ) ;
#97062 = CARTESIAN_POINT ( 'NONE',  ( 16.52544592524342804, -4.483927247898539470, 58.54057627198103120 ) ) ;
#97063 = CARTESIAN_POINT ( 'NONE',  ( -4.483927247898782831, 16.52544592524335698, 112.7094237280190328 ) ) ;
#97064 = CARTESIAN_POINT ( 'NONE',  ( -13.97604488694527625, -13.89961937509977652, 46.87390960531435979 ) ) ;
#97065 = CARTESIAN_POINT ( 'NONE',  ( 16.55341960407611168, 4.379528057220329451, 113.9572429386477239 ) ) ;
#97066 = CARTESIAN_POINT ( 'NONE',  ( -18.62759615963270932, 10.81492255796079327, 45.83224293864769550 ) ) ;
#97067 = CARTESIAN_POINT ( 'NONE',  ( -16.51473224551082808, 9.474510206698731452, 23.33442372801900078 ) ) ;
#97069 = CARTESIAN_POINT ( 'NONE',  ( -4.483927247898539470, -16.52544592524342804, 37.29057627198102409 ) ) ;
#97068 = CARTESIAN_POINT ( 'NONE',  ( -18.09918380851993902, -5.499999999999988454, 86.48618307335611632 ) ) ;
#97070 = VECTOR ( 'NONE', #23267, 1000.000000000000000 ) ;
#97071 = CARTESIAN_POINT ( 'NONE',  ( -18.67979575497193778, 10.72451020669871902, 43.33442372801901143 ) ) ;
#97072 = DIRECTION ( 'NONE',  ( -1.000000000000000000, 0.000000000000000000, 0.000000000000000000 ) ) ;
#97073 = CARTESIAN_POINT ( 'NONE',  ( -0.05219959533934338120, 16.53943276465976808, 62.50109039468568284 ) ) ;
#97074 = CARTESIAN_POINT ( 'NONE',  ( -16.51473224551082808, 9.474510206698731452, 68.33442372801900433 ) ) ;
#97075 = CARTESIAN_POINT ( 'NONE',  ( -14.34966873604960291, -8.224510206698953496, 26.66557627198103475 ) ) ;
#97076 = CARTESIAN_POINT ( 'NONE',  ( -16.55341960407617563, 4.379528057220093196, 108.5427570613523756 ) ) ;
#97077 = CARTESIAN_POINT ( 'NONE',  ( 13.97604488694527802, 13.89961937509977652, 34.37390960531436690 ) ) ;
#97078 = CARTESIAN_POINT ( 'NONE',  ( 13.97604488694527802, 13.89961937509977652, 59.37390960531434558 ) ) ;
#97079 = CARTESIAN_POINT ( 'NONE',  ( -16.46253265017160317, 9.564922557960807481, 30.83224293864769550 ) ) ;
#97080 = CARTESIAN_POINT ( 'NONE',  ( -18.62759615963255300, -10.81492255796106328, 39.16775706135235424 ) ) ;
#97081 = CARTESIAN_POINT ( 'NONE',  ( -9.564922557960796823, -16.46253265017161027, 47.08224293864769550 ) ) ;
#97082 = DIRECTION ( 'NONE',  ( 1.000000000000000000, 0.000000000000000000, 0.000000000000000000 ) ) ;
#97083 = CARTESIAN_POINT ( 'NONE',  ( -16.51473224551069308, -9.474510206698971260, 36.66557627198102409 ) ) ;
#97084 = CARTESIAN_POINT ( 'NONE',  ( 0.05219959533907565091, 21.53943276465977519, 24.99890960531435624 ) ) ;
#97086 = CARTESIAN_POINT ( 'NONE',  ( -8.314922557960811034, -14.29746914071050412, 107.0822429386476955 ) ) ;
#97085 = CARTESIAN_POINT ( 'NONE',  ( 21.53943276465977519, 0.05219959533937863772, 56.25109039468568284 ) ) ;
#97087 = CARTESIAN_POINT ( 'NONE',  ( -13.89961937509977652, 13.97604488694528158, 105.6239096053143527 ) ) ;
#97088 = CARTESIAN_POINT ( 'NONE',  ( -4.483927247898782831, 16.52544592524335698, 77.70942372801900433 ) ) ;
#97089 = CARTESIAN_POINT ( 'NONE',  ( -18.67979575497193778, 10.72451020669871902, 88.33442372801901854 ) ) ;
#97090 = CARTESIAN_POINT ( 'NONE',  ( -8.224510206698735004, -14.34966873604973081, 54.58442372801901143 ) ) ;
#97091 = CARTESIAN_POINT ( 'NONE',  ( -19.02544592524342804, 5.153800228976336051, 96.04057627198103830 ) ) ;
#97092 = CARTESIAN_POINT ( 'NONE',  ( 14.29746914071037800, 8.314922557961029526, 46.66775706135234714 ) ) ;
#97093 = CARTESIAN_POINT ( 'NONE',  ( -8.314922557961024197, 14.29746914071037800, 22.91775706135235069 ) ) ;
#97094 = CARTESIAN_POINT ( 'NONE',  ( -12.14591786802326823, 12.06949235617739902, 83.12609039468568994 ) ) ;
#97095 = CARTESIAN_POINT ( 'NONE',  ( 19.03943276465977164, 0.05219959533936151252, 106.2510903946856615 ) ) ;
#97096 = CARTESIAN_POINT ( 'NONE',  ( -21.53943276465977519, 0.05219959533907696930, 101.2489096053143669 ) ) ;
#97098 = CARTESIAN_POINT ( 'NONE',  ( -5.049401038297874678, -19.05341960407617918, 104.7927570613523471 ) ) ;
#97097 = CARTESIAN_POINT ( 'NONE',  ( 8.224510206698953496, -14.34966873604960469, 102.9155762719810383 ) ) ;
#97099 = CARTESIAN_POINT ( 'NONE',  ( 14.29746914071037800, 8.314922557961029526, 66.66775706135234714 ) ) ;
#97100 = CARTESIAN_POINT ( 'NONE',  ( -16.36317988757095421, 7.306389748694863684, 44.09789608363175972 ) ) ;
#97101 = CARTESIAN_POINT ( 'NONE',  ( -13.89961937509957401, -13.97604488694547875, 64.37609039468567573 ) ) ;
#97102 = CARTESIAN_POINT ( 'NONE',  ( -12.14591786802309592, -12.06949235617757132, 51.87390960531437401 ) ) ;
#97103 = CARTESIAN_POINT ( 'NONE',  ( 14.29746914071049879, -8.314922557960816363, 33.33224293864769550 ) ) ;
#97104 = CARTESIAN_POINT ( 'NONE',  ( 8.224510206698953496, -14.34966873604960469, 87.91557627198103830 ) ) ;
#97106 = CARTESIAN_POINT ( 'NONE',  ( -17.31747979337945154, 6.344076630961115626, 88.62055131934820906 ) ) ;
#97105 = CARTESIAN_POINT ( 'NONE',  ( 16.46253265017146816, 9.564922557961045513, 36.66775706135233293 ) ) ;
#97107 = CARTESIAN_POINT ( 'NONE',  ( 10.72451020669871369, 18.67979575497193778, 42.08442372801901854 ) ) ;
#97108 = CARTESIAN_POINT ( 'NONE',  ( 13.97604488694548053, -13.89961937509957401, 100.6260903946856615 ) ) ;
#97109 = CARTESIAN_POINT ( 'NONE',  ( 19.03943276465977164, -0.05219959533909143690, 113.7489096053143669 ) ) ;
#97110 = CARTESIAN_POINT ( 'NONE',  ( -16.51473224551069308, -9.474510206698971260, 86.66557627198102409 ) ) ;
#97111 = CARTESIAN_POINT ( 'NONE',  ( -9.474510206698964154, 16.51473224551069663, 90.41557627198103830 ) ) ;
#97112 = CARTESIAN_POINT ( 'NONE',  ( -21.55341960407610458, -5.719274019375992779, 61.45724293864770260 ) ) ;
#97113 = CARTESIAN_POINT ( 'NONE',  ( 12.06949235617757843, -12.14591786802309237, 98.12390960531436690 ) ) ;
#97114 = CARTESIAN_POINT ( 'NONE',  ( -13.97604488694527625, -13.89961937509977652, 66.87390960531436690 ) ) ;
#97115 = CARTESIAN_POINT ( 'NONE',  ( 16.53943276465976808, -0.05219959533910856209, 108.7489096053143669 ) ) ;
#97116 = CARTESIAN_POINT ( 'NONE',  ( -21.55341960407619339, 5.719274019375674811, 43.54275706135235424 ) ) ;
#97117 = CARTESIAN_POINT ( 'NONE',  ( 18.67979575497194134, -10.72451020669871369, 75.83442372801900433 ) ) ;
#97118 = CARTESIAN_POINT ( 'NONE',  ( -9.474510206698964154, 16.51473224551069663, 60.41557627198102409 ) ) ;
#97119 = CARTESIAN_POINT ( 'NONE',  ( 16.52544592524335698, 4.483927247898782831, 76.45942372801901854 ) ) ;
#97120 = CARTESIAN_POINT ( 'NONE',  ( -10.72451020669870658, -18.67979575497194134, 34.58442372801900433 ) ) ;
#97121 = CARTESIAN_POINT ( 'NONE',  ( -21.52544592524334988, -5.823673210054445271, 28.95942372801902209 ) ) ;
#97123 = CARTESIAN_POINT ( 'NONE',  ( -9.474510206698964154, 16.51473224551069663, 75.41557627198103830 ) ) ;
#97122 = CARTESIAN_POINT ( 'NONE',  ( 19.02544592524334988, 5.153800228976608722, 46.45942372801899012 ) ) ;
#97124 = CARTESIAN_POINT ( 'NONE',  ( -0.05219959533936034679, 19.03943276465977164, 27.50109039468566507 ) ) ;
#97125 = CARTESIAN_POINT ( 'NONE',  ( 0.05219959533937995610, -21.53943276465977519, 80.00109039468568994 ) ) ;
#97126 = CARTESIAN_POINT ( 'NONE',  ( -10.72451020669898014, 18.67979575497178502, 70.41557627198102409 ) ) ;
#97127 = CARTESIAN_POINT ( 'NONE',  ( -14.29746914071049879, 8.314922557960819915, 50.83224293864770971 ) ) ;
#97129 = CARTESIAN_POINT ( 'NONE',  ( -19.05341960407617563, 5.049401038297882671, 33.54275706135231871 ) ) ;
#97128 = CARTESIAN_POINT ( 'NONE',  ( -21.53943276465977519, -0.05219959533937600094, 93.75109039468567573 ) ) ;
#97130 = CARTESIAN_POINT ( 'NONE',  ( 14.34966873604960469, 8.224510206698951720, 64.16557627198102409 ) ) ;
#97131 = CARTESIAN_POINT ( 'NONE',  ( 16.46253265017160672, -9.564922557960803928, 23.33224293864769194 ) ) ;
#97132 = CARTESIAN_POINT ( 'NONE',  ( 16.46253265017146816, 9.564922557961045513, 56.66775706135233293 ) ) ;
#97133 = CARTESIAN_POINT ( 'NONE',  ( 16.52544592524342804, -4.483927247898539470, 33.54057627198102409 ) ) ;
#97135 = EDGE_CURVE ( 'NONE', #178033, #96037, #16009, .T. ) ;
#97134 = CARTESIAN_POINT ( 'NONE',  ( -5.823673210054431948, 21.52544592524334988, 82.70942372801900433 ) ) ;
#97136 = CARTESIAN_POINT ( 'NONE',  ( -16.51473224551069308, -9.474510206698971260, 81.66557627198103830 ) ) ;
#97137 = CARTESIAN_POINT ( 'NONE',  ( 19.05341960407617918, -5.049401038297876454, 46.04275706135233293 ) ) ;
#97138 = CARTESIAN_POINT ( 'NONE',  ( -5.823673210054116645, -21.52544592524344225, 47.29057627198103120 ) ) ;
#97139 = CARTESIAN_POINT ( 'NONE',  ( 21.52544592524334988, 5.823673210054432836, 51.45942372801901854 ) ) ;
#97140 = CARTESIAN_POINT ( 'NONE',  ( -18.67979575497178146, -10.72451020669898902, 101.6655762719810383 ) ) ;
#97141 = CARTESIAN_POINT ( 'NONE',  ( -5.049401038297874678, -19.05341960407617918, 94.79275706135230450 ) ) ;
#97142 = CARTESIAN_POINT ( 'NONE',  ( -14.29746914071037622, -8.314922557961029526, 64.16775706135234714 ) ) ;
#97144 = CARTESIAN_POINT ( 'NONE',  ( -10.81492255796078084, -18.62759615963271287, 107.0822429386476955 ) ) ;
#97143 = CARTESIAN_POINT ( 'NONE',  ( -4.999999999999996447, 5.000000000000003553, -18.00000000000000000 ) ) ;
#97145 = CARTESIAN_POINT ( 'NONE',  ( -12.14591786802309592, -12.06949235617757132, 101.8739096053143811 ) ) ;
#97146 = DIRECTION ( 'NONE',  ( 0.000000000000000000, 0.000000000000000000, 1.000000000000000000 ) ) ;
#97147 = CARTESIAN_POINT ( 'NONE',  ( 12.14591786802327356, -12.06949235617739191, 40.62609039468567573 ) ) ;
#97148 = CARTESIAN_POINT ( 'NONE',  ( 21.52544592524344225, -5.823673210054117533, 68.54057627198103830 ) ) ;
#97149 = CARTESIAN_POINT ( 'NONE',  ( -12.14591786802326823, 12.06949235617739902, 103.1260903946856757 ) ) ;
#97150 = CARTESIAN_POINT ( 'NONE',  ( -9.564922557960796823, -16.46253265017161027, 32.08224293864769550 ) ) ;
#97151 = CARTESIAN_POINT ( 'NONE',  ( -4.483927247898782831, 16.52544592524335698, 62.70942372801902565 ) ) ;
#97152 = CARTESIAN_POINT ( 'NONE',  ( 5.049401038297881783, 19.05341960407617563, 57.29275706135231871 ) ) ;
#97153 = CARTESIAN_POINT ( 'NONE',  ( 18.67979575497194134, -10.72451020669871369, 40.83442372801901854 ) ) ;
#97154 = CARTESIAN_POINT ( 'NONE',  ( 15.72974639402199770, -15.80617190586745480, 53.12390960531436690 ) ) ;
#97155 = CARTESIAN_POINT ( 'NONE',  ( 0.05219959533934541429, -16.53943276465976808, 100.0010903946857042 ) ) ;
#97156 = CARTESIAN_POINT ( 'NONE',  ( -0.05219959533937732626, 21.53943276465977519, 67.50109039468568994 ) ) ;
#97157 = CARTESIAN_POINT ( 'NONE',  ( 21.52544592524344225, -5.823673210054117533, 58.54057627198103120 ) ) ;
#97158 = CARTESIAN_POINT ( 'NONE',  ( 15.72974639402199770, -15.80617190586745480, 28.12390960531435979 ) ) ;
#97159 = CARTESIAN_POINT ( 'NONE',  ( 8.224510206698742110, 14.34966873604972548, 77.08442372801901854 ) ) ;
#97160 = CARTESIAN_POINT ( 'NONE',  ( -15.72974639402197994, 15.80617190586746368, 30.62390960531436335 ) ) ;
#97161 = CARTESIAN_POINT ( 'NONE',  ( -16.51473224551069308, -9.474510206698971260, 96.66557627198102409 ) ) ;
#97162 = CARTESIAN_POINT ( 'NONE',  ( 16.53943276465976808, 0.05219959533934440121, 111.2510903946856899 ) ) ;
#97163 = CYLINDRICAL_SURFACE ( 'NONE', #163138, 4.999999999999999112 ) ;
#97164 = CARTESIAN_POINT ( 'NONE',  ( 16.55341960407611168, 4.379528057220329451, 103.9572429386476813 ) ) ;
#97165 = CARTESIAN_POINT ( 'NONE',  ( 18.62759615963271287, -10.81492255796078972, 63.33224293864770260 ) ) ;
#97166 = CARTESIAN_POINT ( 'NONE',  ( -14.34966873604972548, 8.224510206698743886, 88.33442372801901854 ) ) ;
#97167 = CARTESIAN_POINT ( 'NONE',  ( 18.67979575497194134, -10.72451020669871369, 50.83442372801901143 ) ) ;
#97168 = CARTESIAN_POINT ( 'NONE',  ( 13.97604488694548053, -13.89961937509957401, 100.6260903946856615 ) ) ;
#97169 = CARTESIAN_POINT ( 'NONE',  ( 8.314922557960818139, 14.29746914071049879, 99.58224293864770971 ) ) ;
#97170 = CARTESIAN_POINT ( 'NONE',  ( -5.049401038298153566, 19.05341960407611168, 60.20724293864768129 ) ) ;
#97171 = CARTESIAN_POINT ( 'NONE',  ( 19.03943276465977164, -0.05219959533909143690, 28.74890960531435624 ) ) ;
#97172 = CARTESIAN_POINT ( 'NONE',  ( 13.70000000000001528, -4.867217739956692332E-14, -62.58071313852362039 ) ) ;
#97173 = CARTESIAN_POINT ( 'NONE',  ( -5.153800228976328057, -19.02544592524343514, 92.29057627198099567 ) ) ;
#97174 = CARTESIAN_POINT ( 'NONE',  ( 4.483927247898790824, -16.52544592524335698, 80.20942372801901854 ) ) ;
#97175 = CARTESIAN_POINT ( 'NONE',  ( 18.62759615963255655, 10.81492255796105972, 106.6677570613523756 ) ) ;
#97176 = CARTESIAN_POINT ( 'NONE',  ( -15.80617190586745835, -15.72974639402198527, 56.87390960531436690 ) ) ;
#97177 = CARTESIAN_POINT ( 'NONE',  ( -16.53943276465976808, -0.05219959533934237506, 83.75109039468568994 ) ) ;
#97178 = CARTESIAN_POINT ( 'NONE',  ( -16.46253265017146816, -9.564922557961047289, 79.16775706135234714 ) ) ;
#97179 = CARTESIAN_POINT ( 'NONE',  ( -19.02544592524342804, 5.153800228976336051, 41.04057627198103120 ) ) ;
#97180 = CARTESIAN_POINT ( 'NONE',  ( -0.05219959533909027116, -19.03943276465977164, 82.49890960531436690 ) ) ;
#97181 = CARTESIAN_POINT ( 'NONE',  ( -5.153800228976328057, -19.02544592524343514, 32.29057627198102409 ) ) ;
#97182 = CARTESIAN_POINT ( 'NONE',  ( 9.564922557961047289, -16.46253265017146816, 75.41775706135234714 ) ) ;
#97183 = CARTESIAN_POINT ( 'NONE',  ( 25.41223161463580027, -11.66315983254895627, 166.2610598689585117 ) ) ;
#97184 = CARTESIAN_POINT ( 'NONE',  ( 13.97604488694527802, 13.89961937509977652, 94.37390960531436690 ) ) ;
#97185 = CARTESIAN_POINT ( 'NONE',  ( -4.379528057220328563, 16.55341960407611168, 45.20724293864769550 ) ) ;
#97186 = CARTESIAN_POINT ( 'NONE',  ( -18.62759615963270932, 10.81492255796079327, 65.83224293864769550 ) ) ;
#97187 = CARTESIAN_POINT ( 'NONE',  ( -17.49999999999999645, 3.189878218039158497, 104.8705143742874810 ) ) ;
#97188 = CARTESIAN_POINT ( 'NONE',  ( 9.564922557961047289, -16.46253265017146816, 35.41775706135233293 ) ) ;
#97189 = CYLINDRICAL_SURFACE ( 'NONE', #121819, 9.100000000000001421 ) ;
#97191 = CARTESIAN_POINT ( 'NONE',  ( -16.46253265017160317, 9.564922557960807481, 70.83224293864770971 ) ) ;
#97190 = CARTESIAN_POINT ( 'NONE',  ( -0.05219959533909027116, -19.03943276465977164, 47.49890960531435979 ) ) ;
#97192 = CARTESIAN_POINT ( 'NONE',  ( 4.483927247898790824, -16.52544592524335698, 35.20942372801901854 ) ) ;
#97193 = CARTESIAN_POINT ( 'NONE',  ( -17.49999999999999645, -5.500000000000000888, 120.0000000000000142 ) ) ;
#97194 = CARTESIAN_POINT ( 'NONE',  ( -16.19135201231366850, 7.376712067591920885, 109.8131914594797252 ) ) ;
#97195 = CARTESIAN_POINT ( 'NONE',  ( -8.224510206698735004, -14.34966873604973081, 69.58442372801900433 ) ) ;
#97196 = CARTESIAN_POINT ( 'NONE',  ( 5.823673210054125526, 21.52544592524343514, 89.79057627198103830 ) ) ;
#97197 = CARTESIAN_POINT ( 'NONE',  ( 8.224510206698742110, 14.34966873604972548, 47.08442372801901854 ) ) ;
#97199 = CARTESIAN_POINT ( 'NONE',  ( 17.50000000000000000, 5.499999999999992895, 81.70309617465829888 ) ) ;
#97198 = CARTESIAN_POINT ( 'NONE',  ( -16.46253265017160317, 9.564922557960807481, 40.83224293864769550 ) ) ;
#97200 = CARTESIAN_POINT ( 'NONE',  ( 10.72451020669871369, 18.67979575497193778, 57.08442372801901854 ) ) ;
#97201 = CARTESIAN_POINT ( 'NONE',  ( 19.03943276465977164, 0.05219959533936151252, 61.25109039468566863 ) ) ;
#97202 = CARTESIAN_POINT ( 'NONE',  ( -21.53943276465977519, -0.05219959533937600094, 88.75109039468567573 ) ) ;
#97203 = CARTESIAN_POINT ( 'NONE',  ( -22.15208335914311988, -5.528296758471276107, 173.4118699040215006 ) ) ;
#97204 = CARTESIAN_POINT ( 'NONE',  ( -4.379528057220328563, 16.55341960407611168, 45.20724293864769550 ) ) ;
#97205 = DIRECTION ( 'NONE',  ( 1.000000000000000000, 1.776356839400250465E-15, 0.000000000000000000 ) ) ;
#97206 = CARTESIAN_POINT ( 'NONE',  ( 21.53943276465977519, -0.05219959533907433946, 58.74890960531436690 ) ) ;
#97207 = CARTESIAN_POINT ( 'NONE',  ( -22.44159573604010305, 16.30477369853692338, 140.6750000027311671 ) ) ;
#97208 = CARTESIAN_POINT ( 'NONE',  ( 16.51473224551069308, 9.474510206698969483, 109.1655762719810383 ) ) ;
#97209 = CARTESIAN_POINT ( 'NONE',  ( 0.05219959533910956823, 16.53943276465976808, 99.99890960531436690 ) ) ;
#97210 = CARTESIAN_POINT ( 'NONE',  ( 12.06949235617739724, 12.14591786802326823, 21.87609039468567573 ) ) ;
#97211 = CARTESIAN_POINT ( 'NONE',  ( -16.53943276465976808, -0.05219959533934237506, 113.7510903946856757 ) ) ;
#97212 = ORIENTED_EDGE ( 'NONE', *, *, #91919, .T. ) ;
#97213 = CARTESIAN_POINT ( 'NONE',  ( -21.52544592524343514, 5.823673210054127303, 96.04057627198102409 ) ) ;
#97215 = CARTESIAN_POINT ( 'NONE',  ( -30.74264578624800492, -22.33583958711396278, -9.799999999999998934 ) ) ;
#97214 = CARTESIAN_POINT ( 'NONE',  ( -16.53943276465976808, 0.05219959533911058130, 26.24890960531435624 ) ) ;
#97216 = CARTESIAN_POINT ( 'NONE',  ( -0.05219959533936034679, 19.03943276465977164, 87.50109039468567573 ) ) ;
#97217 = CARTESIAN_POINT ( 'NONE',  ( 15.72974639402176855, 15.80617190586768217, 106.8760903946856899 ) ) ;
#97218 = CARTESIAN_POINT ( 'NONE',  ( 4.483927247898545687, 16.52544592524342804, 29.79057627198102409 ) ) ;
#97219 = CARTESIAN_POINT ( 'NONE',  ( -5.823673210054116645, -21.52544592524344225, 92.29057627198103830 ) ) ;
#97220 = CARTESIAN_POINT ( 'NONE',  ( 15.72974639402199770, -15.80617190586745480, 48.12390960531436690 ) ) ;
#97221 = CARTESIAN_POINT ( 'NONE',  ( -5.049401038298153566, 19.05341960407611168, 60.20724293864768129 ) ) ;
#97222 = CARTESIAN_POINT ( 'NONE',  ( 4.483927247898545687, 16.52544592524342804, 29.79057627198102409 ) ) ;
#97223 = CARTESIAN_POINT ( 'NONE',  ( -5.153800228976328057, -19.02544592524343514, 97.29057627198099567 ) ) ;
#97224 = CARTESIAN_POINT ( 'NONE',  ( 18.22780087662126647, 5.499999999999818812, 56.48236817873107185 ) ) ;
#97225 = CARTESIAN_POINT ( 'NONE',  ( 9.474510206698729675, 16.51473224551082808, 47.08442372801900433 ) ) ;
#97226 = CARTESIAN_POINT ( 'NONE',  ( 15.80617190586746368, 15.72974639402197994, 79.37390960531436690 ) ) ;
#97227 = CARTESIAN_POINT ( 'NONE',  ( 8.224510206698953496, -14.34966873604960469, 102.9155762719810383 ) ) ;
#97228 = CARTESIAN_POINT ( 'NONE',  ( -10.72451020669870658, -18.67979575497194134, 39.58442372801901143 ) ) ;
#97229 = CARTESIAN_POINT ( 'NONE',  ( -8.571926809382608425, 26.38167802310805854, 140.4750000027312069 ) ) ;
#97230 = CARTESIAN_POINT ( 'NONE',  ( -16.55341960407617563, 4.379528057220093196, 103.5427570613523613 ) ) ;
#97231 = CARTESIAN_POINT ( 'NONE',  ( -13.97604488694527625, -13.89961937509977652, 36.87390960531436690 ) ) ;
#97232 = CARTESIAN_POINT ( 'NONE',  ( -19.05341960407611168, -5.049401038298163336, 86.45724293864769550 ) ) ;
#97233 = CARTESIAN_POINT ( 'NONE',  ( -11.45643923738959735, 5.000000000000007105, -18.00000000000000000 ) ) ;
#97234 = CARTESIAN_POINT ( 'NONE',  ( 16.46253265017160672, -9.564922557960803928, 33.33224293864770260 ) ) ;
#97235 = CARTESIAN_POINT ( 'NONE',  ( -12.14591786802309592, -12.06949235617757132, 41.87390960531435979 ) ) ;
#97236 = CARTESIAN_POINT ( 'NONE',  ( -18.67979575497193778, 10.72451020669871902, 78.33442372801901854 ) ) ;
#97238 = CARTESIAN_POINT ( 'NONE',  ( 16.52544592524335698, 4.483927247898782831, 66.45942372801903275 ) ) ;
#97237 = DIRECTION ( 'NONE',  ( 1.000000000000000000, 0.000000000000000000, 0.000000000000000000 ) ) ;
#97239 = CARTESIAN_POINT ( 'NONE',  ( -9.564922557960796823, -16.46253265017161027, 47.08224293864769550 ) ) ;
#97240 = CARTESIAN_POINT ( 'NONE',  ( -19.03943276465977164, 0.05219959533909376836, 46.24890960531435979 ) ) ;
#97241 = ORIENTED_EDGE ( 'NONE', *, *, #169440, .F. ) ;
#97242 = CARTESIAN_POINT ( 'NONE',  ( -15.80617190586768217, 15.72974639402176855, 108.1260903946856757 ) ) ;
#97243 = CARTESIAN_POINT ( 'NONE',  ( -4.379528057220086978, -16.55341960407618274, 59.79275706135234714 ) ) ;
#97244 = CARTESIAN_POINT ( 'NONE',  ( -5.823673210054431948, 21.52544592524334988, 102.7094237280190185 ) ) ;
#97245 = CARTESIAN_POINT ( 'NONE',  ( 15.72974639402199770, -15.80617190586745480, 38.12390960531436690 ) ) ;
#97246 = CARTESIAN_POINT ( 'NONE',  ( 13.89961937509957401, 13.97604488694547697, 111.8760903946856757 ) ) ;
#97247 = CARTESIAN_POINT ( 'NONE',  ( -18.62759615963255300, -10.81492255796106328, 74.16775706135231871 ) ) ;
#97248 = CARTESIAN_POINT ( 'NONE',  ( 12.14591786802327356, -12.06949235617739191, 35.62609039468568994 ) ) ;
#97249 = CARTESIAN_POINT ( 'NONE',  ( -18.67979575497178146, -10.72451020669898902, 101.6655762719810383 ) ) ;
#97250 = CARTESIAN_POINT ( 'NONE',  ( 5.153800228976615827, -19.02544592524334988, 100.2094237280190043 ) ) ;
#97251 = CARTESIAN_POINT ( 'NONE',  ( 19.02544592524343514, -5.153800228976328945, 68.54057627198103830 ) ) ;
#97252 = CARTESIAN_POINT ( 'NONE',  ( 13.89961937509957401, 13.97604488694547697, 111.8760903946856757 ) ) ;
#97253 = CARTESIAN_POINT ( 'NONE',  ( 19.02544592524334988, 5.153800228976608722, 106.4594237280190185 ) ) ;
#97254 = CARTESIAN_POINT ( 'NONE',  ( -8.224510206698948167, 14.34966873604960824, 70.41557627198102409 ) ) ;
#97255 = CARTESIAN_POINT ( 'NONE',  ( -16.53943276465976808, -0.05219959533934237506, 73.75109039468567573 ) ) ;
#97257 = CARTESIAN_POINT ( 'NONE',  ( 5.049401038298161559, -19.05341960407611168, 52.70724293864767418 ) ) ;
#97256 = CARTESIAN_POINT ( 'NONE',  ( 10.72451020669871369, 18.67979575497193778, 22.08442372801901143 ) ) ;
#97258 = CARTESIAN_POINT ( 'NONE',  ( -13.89961937509977652, 13.97604488694528158, 60.62390960531436690 ) ) ;
#97259 = CARTESIAN_POINT ( 'NONE',  ( 8.314922557961029526, -14.29746914071037800, 70.41775706135236135 ) ) ;
#97260 = CARTESIAN_POINT ( 'NONE',  ( -8.571926809382601320, -26.38167802310801591, 147.7750000027311899 ) ) ;
#97261 = DIRECTION ( 'NONE',  ( 0.000000000000000000, 0.000000000000000000, -1.000000000000000000 ) ) ;
#97262 = ORIENTED_EDGE ( 'NONE', *, *, #181788, .F. ) ;
#97263 = CARTESIAN_POINT ( 'NONE',  ( -9.564922557961040184, 16.46253265017147172, 22.91775706135233648 ) ) ;
#97264 = CARTESIAN_POINT ( 'NONE',  ( 19.03943276465977164, -0.05219959533909143690, 23.74890960531435269 ) ) ;
#97265 = ORIENTED_EDGE ( 'NONE', *, *, #134059, .F. ) ;
#97266 = CARTESIAN_POINT ( 'NONE',  ( -5.049401038297874678, -19.05341960407617918, 109.7927570613523187 ) ) ;
#97267 = CARTESIAN_POINT ( 'NONE',  ( -5.719274019375978568, 21.55341960407610458, 50.20724293864769550 ) ) ;
#97269 = CARTESIAN_POINT ( 'NONE',  ( 12.14591786802327356, -12.06949235617739191, 25.62609039468567929 ) ) ;
#97268 = CARTESIAN_POINT ( 'NONE',  ( 0.05219959533936267826, -19.03943276465977164, 50.00109039468566863 ) ) ;
#97270 = CARTESIAN_POINT ( 'NONE',  ( -19.02544592524342804, 5.153800228976336051, 46.04057627198101699 ) ) ;
#97271 = CARTESIAN_POINT ( 'NONE',  ( 0.05219959533909260263, 19.03943276465977164, 54.99890960531435979 ) ) ;
#97272 = CARTESIAN_POINT ( 'NONE',  ( -21.52544592524343514, 5.823673210054127303, 91.04057627198103830 ) ) ;
#97273 = CARTESIAN_POINT ( 'NONE',  ( -28.79475375365586842, 2.428612866367529932E-14, 155.0000000000000000 ) ) ;
#97274 = CARTESIAN_POINT ( 'NONE',  ( -19.05341960407611168, -5.049401038298163336, 56.45724293864768129 ) ) ;
#97275 = DIRECTION ( 'NONE',  ( -1.000000000000000000, -0.000000000000000000, -0.000000000000000000 ) ) ;
#97276 = CARTESIAN_POINT ( 'NONE',  ( 0.05219959533936267826, -19.03943276465977164, 95.00109039468567573 ) ) ;
#97277 = CARTESIAN_POINT ( 'NONE',  ( -8.314922557960811034, -14.29746914071050412, 62.08224293864769550 ) ) ;
#97278 = CARTESIAN_POINT ( 'NONE',  ( -16.46253265017146816, -9.564922557961047289, 24.16775706135233648 ) ) ;
#97279 = CARTESIAN_POINT ( 'NONE',  ( -21.52544592524343514, 5.823673210054127303, 96.04057627198102409 ) ) ;
#97280 = CARTESIAN_POINT ( 'NONE',  ( -18.67979575497193778, 10.72451020669871902, 88.33442372801901854 ) ) ;
#97281 = CARTESIAN_POINT ( 'NONE',  ( -16.51473224551069308, -9.474510206698971260, 26.66557627198103120 ) ) ;
#97282 = CARTESIAN_POINT ( 'NONE',  ( 21.55341960407619695, -5.719274019375665929, 81.04275706135236135 ) ) ;
#97283 = EDGE_CURVE ( 'NONE', #171715, #9508, #117612, .T. ) ;
#97285 = CARTESIAN_POINT ( 'NONE',  ( 10.81492255796106328, -18.62759615963255655, 80.41775706135234714 ) ) ;
#97284 = CARTESIAN_POINT ( 'NONE',  ( -12.06949235617756955, 12.14591786802309770, 30.62390960531436335 ) ) ;
#97286 = CARTESIAN_POINT ( 'NONE',  ( -19.02544592524342804, 5.153800228976336051, 66.04057627198103830 ) ) ;
#97287 = CARTESIAN_POINT ( 'NONE',  ( 0.05219959533937995610, -21.53943276465977519, 45.00109039468568284 ) ) ;
#97288 = CARTESIAN_POINT ( 'NONE',  ( 19.02544592524343514, -5.153800228976328945, 78.54057627198099567 ) ) ;
#97289 = CARTESIAN_POINT ( 'NONE',  ( -8.314922557960811034, -14.29746914071050412, 92.08224293864769550 ) ) ;
#97290 = CARTESIAN_POINT ( 'NONE',  ( -12.06949235617756955, 12.14591786802309770, 55.62390960531436690 ) ) ;
#97291 = CARTESIAN_POINT ( 'NONE',  ( -10.81492255796078084, -18.62759615963271287, 72.08224293864769550 ) ) ;
#97292 = ADVANCED_FACE ( 'NONE', ( #924, #157612 ), #31285, .F. ) ;
#97293 = CARTESIAN_POINT ( 'NONE',  ( -9.474510206698964154, 16.51473224551069663, 55.41557627198103120 ) ) ;
#97294 = CARTESIAN_POINT ( 'NONE',  ( 21.52544592524344225, -5.823673210054117533, 83.54057627198102409 ) ) ;
#97295 = CARTESIAN_POINT ( 'NONE',  ( 9.564922557961047289, -16.46253265017146816, 65.41775706135233293 ) ) ;
#97297 = CARTESIAN_POINT ( 'NONE',  ( -0.05219959533910754901, -16.53943276465976808, 82.49890960531436690 ) ) ;
#97296 = CARTESIAN_POINT ( 'NONE',  ( 16.51473224551083163, -9.474510206698727899, 35.83442372801899722 ) ) ;
#97298 = CARTESIAN_POINT ( 'NONE',  ( -5.823673210054116645, -21.52544592524344225, 47.29057627198103120 ) ) ;
#97299 = CARTESIAN_POINT ( 'NONE',  ( 17.48847506799969409, 5.747544572773783500, 101.6730256215672057 ) ) ;
#97301 = CARTESIAN_POINT ( 'NONE',  ( 27.73933785331498925, -9.013057229001034898, 144.2750000027311899 ) ) ;
#97300 = CARTESIAN_POINT ( 'NONE',  ( 16.55341960407618274, -4.379528057220086978, 96.04275706135236135 ) ) ;
#97302 = CARTESIAN_POINT ( 'NONE',  ( 19.02544592524334988, 5.153800228976608722, 96.45942372801897591 ) ) ;
#97303 = CARTESIAN_POINT ( 'NONE',  ( 0.05219959533910956823, 16.53943276465976808, 64.99890960531435269 ) ) ;
#97304 = CARTESIAN_POINT ( 'NONE',  ( -17.49999999999999289, 5.068104630630395846, 35.72818405340028391 ) ) ;
#97305 = CARTESIAN_POINT ( 'NONE',  ( -9.564922557960796823, -16.46253265017161027, 62.08224293864769550 ) ) ;
#97306 = CARTESIAN_POINT ( 'NONE',  ( 16.52544592524342804, -4.483927247898539470, 53.54057627198103120 ) ) ;
#97307 = CARTESIAN_POINT ( 'NONE',  ( -19.05341960407611168, -5.049401038298163336, 101.4572429386476955 ) ) ;
#97309 = CARTESIAN_POINT ( 'NONE',  ( -13.97604488694527625, -13.89961937509977652, 71.87390960531433848 ) ) ;
#97308 = CARTESIAN_POINT ( 'NONE',  ( -5.049401038297874678, -19.05341960407617918, 74.79275706135231871 ) ) ;
#97310 = CARTESIAN_POINT ( 'NONE',  ( -5.049401038298153566, 19.05341960407611168, 90.20724293864766707 ) ) ;
#97311 = CARTESIAN_POINT ( 'NONE',  ( -13.97604488694527625, -13.89961937509977652, 81.87390960531436690 ) ) ;
#97312 = CARTESIAN_POINT ( 'NONE',  ( 21.52544592524344225, -5.823673210054117533, 68.54057627198103830 ) ) ;
#97313 = CARTESIAN_POINT ( 'NONE',  ( 12.14591786802327356, -12.06949235617739191, 55.62609039468568284 ) ) ;
#97314 = CARTESIAN_POINT ( 'NONE',  ( -9.564922557961040184, 16.46253265017147172, 102.9177570613523329 ) ) ;
#97315 = CARTESIAN_POINT ( 'NONE',  ( -9.564922557960796823, -16.46253265017161027, 47.08224293864769550 ) ) ;
#97316 = CARTESIAN_POINT ( 'NONE',  ( 10.81492255796078972, 18.62759615963270932, 54.58224293864769550 ) ) ;
#97317 = CARTESIAN_POINT ( 'NONE',  ( -9.564922557961040184, 16.46253265017147172, 97.91775706135233293 ) ) ;
#97319 = CARTESIAN_POINT ( 'NONE',  ( 21.53943276465977519, 0.05219959533937863772, 41.25109039468568284 ) ) ;
#97318 = CARTESIAN_POINT ( 'NONE',  ( 4.379528057220339221, -16.55341960407611168, 22.70724293864769194 ) ) ;
#97320 = CARTESIAN_POINT ( 'NONE',  ( -19.03943276465977164, -0.05219959533935918106, 33.75109039468566863 ) ) ;
#97322 = CARTESIAN_POINT ( 'NONE',  ( -16.52544592524335698, -4.483927247898792601, 88.95942372801901854 ) ) ;
#97321 = CARTESIAN_POINT ( 'NONE',  ( -16.55341960407617563, 4.379528057220093196, 53.54275706135234714 ) ) ;
#97323 = CARTESIAN_POINT ( 'NONE',  ( -18.22780087662122028, 5.500000000000031086, 73.51540105326107266 ) ) ;
#97324 = CARTESIAN_POINT ( 'NONE',  ( -8.224510206698735004, -14.34966873604973081, 79.58442372801903275 ) ) ;
#97326 = CARTESIAN_POINT ( 'NONE',  ( -8.314922557961024197, 14.29746914071037800, 32.91775706135234714 ) ) ;
#97325 = CARTESIAN_POINT ( 'NONE',  ( 10.72451020669898902, -18.67979575497178502, 22.91557627198102765 ) ) ;
#97327 = CARTESIAN_POINT ( 'NONE',  ( -19.05341960407611168, -5.049401038298163336, 51.45724293864770260 ) ) ;
#97328 = CARTESIAN_POINT ( 'NONE',  ( -5.049401038298153566, 19.05341960407611168, 55.20724293864769550 ) ) ;
#97329 = CARTESIAN_POINT ( 'NONE',  ( -0.05219959533909027116, -19.03943276465977164, 57.49890960531435979 ) ) ;
#97330 = CARTESIAN_POINT ( 'NONE',  ( 18.62759615963255655, 10.81492255796105972, 41.66775706135235424 ) ) ;
#97331 = CARTESIAN_POINT ( 'NONE',  ( -4.483927247898782831, 16.52544592524335698, 42.70942372801901854 ) ) ;
#97332 = CARTESIAN_POINT ( 'NONE',  ( -12.14591786802326823, 12.06949235617739902, 108.1260903946856757 ) ) ;
#97333 = CARTESIAN_POINT ( 'NONE',  ( 5.153800228976335163, 19.02544592524342804, 29.79057627198102409 ) ) ;
#97334 = CARTESIAN_POINT ( 'NONE',  ( -9.564922557961040184, 16.46253265017147172, 22.91775706135233648 ) ) ;
#97335 = CARTESIAN_POINT ( 'NONE',  ( -5.049401038297874678, -19.05341960407617918, 109.7927570613523187 ) ) ;
#97336 = CARTESIAN_POINT ( 'NONE',  ( 0.05219959533936267826, -19.03943276465977164, 75.00109039468566152 ) ) ;
#97337 = CARTESIAN_POINT ( 'NONE',  ( 4.483927247898545687, 16.52544592524342804, 64.79057627198103830 ) ) ;
#97338 = CARTESIAN_POINT ( 'NONE',  ( 9.564922557960805705, 16.46253265017160317, 39.58224293864768839 ) ) ;
#97340 = CARTESIAN_POINT ( 'NONE',  ( 16.29526858892876362, -7.335722546920113274, 91.70329402199793378 ) ) ;
#97339 = CARTESIAN_POINT ( 'NONE',  ( -13.89961937509957401, -13.97604488694547875, 74.37609039468566152 ) ) ;
#97341 = CARTESIAN_POINT ( 'NONE',  ( -18.67979575497193778, 10.72451020669871902, 73.33442372801901854 ) ) ;
#97342 = CARTESIAN_POINT ( 'NONE',  ( 16.53943276465976808, 0.05219959533934440121, 46.25109039468567573 ) ) ;
#97343 = CARTESIAN_POINT ( 'NONE',  ( 27.19095269391953806, -8.032454009542492557, 149.5864051666458181 ) ) ;
#97344 = CARTESIAN_POINT ( 'NONE',  ( -10.72451020669898014, 18.67979575497178502, 30.41557627198101699 ) ) ;
#97345 = CARTESIAN_POINT ( 'NONE',  ( -12.06949235617739369, -12.14591786802326823, 29.37609039468568284 ) ) ;
#97346 = CARTESIAN_POINT ( 'NONE',  ( -5.153800228976328057, -19.02544592524343514, 22.29057627198102765 ) ) ;
#97347 = CARTESIAN_POINT ( 'NONE',  ( -19.02544592524334988, -5.153800228976617603, 23.95942372801900078 ) ) ;
#97348 = CARTESIAN_POINT ( 'NONE',  ( 9.979736640218535015, 12.05038478428676463, -59.62998087139816050 ) ) ;
#97349 = CARTESIAN_POINT ( 'NONE',  ( -5.049401038298153566, 19.05341960407611168, 40.20724293864768839 ) ) ;
#97350 = CYLINDRICAL_SURFACE ( 'NONE', #175621, 35.99626262588765258 ) ;
#97351 = CARTESIAN_POINT ( 'NONE',  ( 13.97604488694527802, 13.89961937509977652, 64.37390960531436690 ) ) ;
#97352 = CARTESIAN_POINT ( 'NONE',  ( -17.60728821186566506, 5.500000000000031974, 65.86690927743006796 ) ) ;
#97353 = CARTESIAN_POINT ( 'NONE',  ( 5.153800228976615827, -19.02544592524334988, 20.20942372801899722 ) ) ;
#97354 = CARTESIAN_POINT ( 'NONE',  ( -8.224510206698948167, 14.34966873604960824, 25.41557627198103120 ) ) ;
#97355 = CARTESIAN_POINT ( 'NONE',  ( 13.89961937509977652, -13.97604488694527269, 33.12390960531434558 ) ) ;
#97356 = CARTESIAN_POINT ( 'NONE',  ( 16.51473224551069308, 9.474510206698969483, 94.16557627198103830 ) ) ;
#97357 = CARTESIAN_POINT ( 'NONE',  ( -5.719274019375665041, -21.55341960407619695, 64.79275706135234714 ) ) ;
#97358 = CARTESIAN_POINT ( 'NONE',  ( 9.564922557960805705, 16.46253265017160317, 49.58224293864770260 ) ) ;
#97359 = CARTESIAN_POINT ( 'NONE',  ( -5.823673210054431948, 21.52544592524334988, 62.70942372801902565 ) ) ;
#97361 = CARTESIAN_POINT ( 'NONE',  ( 15.72974639402199770, -15.80617190586745480, 28.12390960531435979 ) ) ;
#97360 = CARTESIAN_POINT ( 'NONE',  ( -19.02544592524334988, -5.153800228976617603, 88.95942372801897591 ) ) ;
#97362 = CARTESIAN_POINT ( 'NONE',  ( 9.474510206698971260, -16.51473224551069308, 37.91557627198102409 ) ) ;
#97363 = CARTESIAN_POINT ( 'NONE',  ( 15.72974639402199770, -15.80617190586745480, 113.1239096053143953 ) ) ;
#97364 = CARTESIAN_POINT ( 'NONE',  ( 0.05219959533936267826, -19.03943276465977164, 35.00109039468566863 ) ) ;
#97365 = CARTESIAN_POINT ( 'NONE',  ( 4.483927247898545687, 16.52544592524342804, 104.7905762719810241 ) ) ;
#97366 = CARTESIAN_POINT ( 'NONE',  ( 5.049401038298161559, -19.05341960407611168, 62.70724293864769550 ) ) ;
#97367 = CARTESIAN_POINT ( 'NONE',  ( 16.51473224551083163, -9.474510206698727899, 110.8344237280190043 ) ) ;
#97368 = CARTESIAN_POINT ( 'NONE',  ( -16.53943276465976808, 0.05219959533911058130, 81.24890960531436690 ) ) ;
#97369 = CARTESIAN_POINT ( 'NONE',  ( -19.02544592524342804, 5.153800228976336051, 116.0405762719810383 ) ) ;
#97370 = CARTESIAN_POINT ( 'NONE',  ( -19.02544592524334988, -5.153800228976617603, 83.95942372801901854 ) ) ;
#97371 = CARTESIAN_POINT ( 'NONE',  ( -15.72974639402197994, 15.80617190586746368, 90.62390960531436690 ) ) ;
#97372 = CARTESIAN_POINT ( 'NONE',  ( -18.67979575497193778, 10.72451020669871902, 38.33442372801900433 ) ) ;
#97373 = CARTESIAN_POINT ( 'NONE',  ( -8.224510206698735004, -14.34966873604973081, 54.58442372801901143 ) ) ;
#97375 = CARTESIAN_POINT ( 'NONE',  ( 21.53943276465977519, 0.05219959533937863772, 51.25109039468568994 ) ) ;
#97374 = CARTESIAN_POINT ( 'NONE',  ( 16.52544592524335698, 4.483927247898782831, 51.45942372801901854 ) ) ;
#97376 = CARTESIAN_POINT ( 'NONE',  ( 15.80617190586746368, 15.72974639402197994, 49.37390960531436690 ) ) ;
#97377 = CARTESIAN_POINT ( 'NONE',  ( 19.02544592524343514, -5.153800228976328945, 53.54057627198102409 ) ) ;
#97378 = CARTESIAN_POINT ( 'NONE',  ( -30.74264578624800492, 22.33583958711400186, -3.949999994537626957 ) ) ;
#97379 = CARTESIAN_POINT ( 'NONE',  ( -14.34966873604972548, 8.224510206698743886, 78.33442372801901854 ) ) ;
#97380 = CARTESIAN_POINT ( 'NONE',  ( -21.55341960407610458, -5.719274019375992779, 106.4572429386477097 ) ) ;
#97381 = CARTESIAN_POINT ( 'NONE',  ( 4.379528057220339221, -16.55341960407611168, 47.70724293864770260 ) ) ;
#97382 = CARTESIAN_POINT ( 'NONE',  ( -16.55341960407617563, 4.379528057220093196, 58.54275706135235424 ) ) ;
#97383 = CARTESIAN_POINT ( 'NONE',  ( -9.474510206698720793, -16.51473224551083518, 99.58442372801900433 ) ) ;
#97384 = CARTESIAN_POINT ( 'NONE',  ( -0.05219959533907301413, -21.53943276465977519, 92.49890960531436690 ) ) ;
#97385 = CARTESIAN_POINT ( 'NONE',  ( 8.314922557960818139, 14.29746914071049879, 49.58224293864769550 ) ) ;
#97386 = VERTEX_POINT ( 'NONE', #33276 ) ;
#97387 = CARTESIAN_POINT ( 'NONE',  ( -17.05116617787824396, 6.768360034955816396, 68.65675553259198693 ) ) ;
#97388 = CARTESIAN_POINT ( 'NONE',  ( -18.67979575497178146, -10.72451020669898902, 71.66557627198100988 ) ) ;
#97389 = CARTESIAN_POINT ( 'NONE',  ( -8.314922557960811034, -14.29746914071050412, 27.08224293864769550 ) ) ;
#97390 = ORIENTED_EDGE ( 'NONE', *, *, #87134, .T. ) ;
#97391 = DIRECTION ( 'NONE',  ( 0.000000000000000000, 0.000000000000000000, 1.000000000000000000 ) ) ;
#97392 = CARTESIAN_POINT ( 'NONE',  ( -5.823673210054116645, -21.52544592524344225, 107.2905762719810525 ) ) ;
#97393 = CARTESIAN_POINT ( 'NONE',  ( 18.67979575497178502, 10.72451020669898547, 114.1655762719810383 ) ) ;
#97394 = CARTESIAN_POINT ( 'NONE',  ( -0.05219959533910754901, -16.53943276465976808, 32.49890960531435979 ) ) ;
#97395 = CARTESIAN_POINT ( 'NONE',  ( -12.14591786802326823, 12.06949235617739902, 48.12609039468568284 ) ) ;
#97396 = CARTESIAN_POINT ( 'NONE',  ( 19.05341960407611168, 5.049401038298154454, 43.95724293864769550 ) ) ;
#97397 = CARTESIAN_POINT ( 'NONE',  ( -19.03943276465977164, 0.05219959533909376836, 81.24890960531436690 ) ) ;
#97398 = CARTESIAN_POINT ( 'NONE',  ( -10.72451020669898014, 18.67979575497178502, 35.41557627198102409 ) ) ;
#97399 = CARTESIAN_POINT ( 'NONE',  ( -27.75745401094723874, -25.59313184531950114, -20.67669038791073177 ) ) ;
#97400 = CARTESIAN_POINT ( 'NONE',  ( -14.29746914071037622, -8.314922557961029526, 19.16775706135234714 ) ) ;
#97401 = CARTESIAN_POINT ( 'NONE',  ( 19.05341960407617918, -5.049401038297876454, 46.04275706135233293 ) ) ;
#97402 = CARTESIAN_POINT ( 'NONE',  ( -10.72451020669898014, 18.67979575497178502, 95.41557627198102409 ) ) ;
#97403 = CARTESIAN_POINT ( 'NONE',  ( -16.53943276465976808, 0.05219959533911058130, 36.24890960531435979 ) ) ;
#97404 = VECTOR ( 'NONE', #195315, 1000.000000000000000 ) ;
#97405 = CARTESIAN_POINT ( 'NONE',  ( 16.46253265017160672, -9.564922557960803928, 83.33224293864768129 ) ) ;
#97406 = CARTESIAN_POINT ( 'NONE',  ( 18.62759615963271287, -10.81492255796078972, 48.33224293864770260 ) ) ;
#97408 = CARTESIAN_POINT ( 'NONE',  ( 16.55341960407618274, -4.379528057220086978, 31.04275706135234714 ) ) ;
#97407 = CARTESIAN_POINT ( 'NONE',  ( 10.72451020669898902, -18.67979575497178502, 87.91557627198103830 ) ) ;
#97409 = CARTESIAN_POINT ( 'NONE',  ( 10.72451020669898902, -18.67979575497178502, 27.91557627198103830 ) ) ;
#97410 = CARTESIAN_POINT ( 'NONE',  ( -15.80617190586768217, 15.72974639402176855, 73.12609039468567573 ) ) ;
#97411 = CARTESIAN_POINT ( 'NONE',  ( 9.564922557960805705, 16.46253265017160317, 69.58224293864770971 ) ) ;
#97412 = CARTESIAN_POINT ( 'NONE',  ( 16.51473224551069308, 9.474510206698969483, 24.16557627198102765 ) ) ;
#97413 = CARTESIAN_POINT ( 'NONE',  ( -9.474510206698964154, 16.51473224551069663, 80.41557627198103830 ) ) ;
#97414 = CARTESIAN_POINT ( 'NONE',  ( 12.14591786802309770, 12.06949235617756955, 94.37390960531436690 ) ) ;
#97415 = EDGE_LOOP ( 'NONE', ( #26019, #196735, #7628, #51964, #8703 ) ) ;
#97416 = CARTESIAN_POINT ( 'NONE',  ( 16.51473224551083163, -9.474510206698727899, 105.8344237280190043 ) ) ;
#97417 = CYLINDRICAL_SURFACE ( 'NONE', #21353, 28.82186960331498682 ) ;
#97418 = EDGE_CURVE ( 'NONE', #117777, #70701, #93938, .T. ) ;
#97419 = CARTESIAN_POINT ( 'NONE',  ( 0.05219959533909260263, 19.03943276465977164, 69.99890960531435269 ) ) ;
#97421 = CARTESIAN_POINT ( 'NONE',  ( -18.67979575497178146, -10.72451020669898902, 21.66557627198102409 ) ) ;
#97420 = CARTESIAN_POINT ( 'NONE',  ( -10.81492255796105439, 18.62759615963255655, 87.91775706135234714 ) ) ;
#97422 = CARTESIAN_POINT ( 'NONE',  ( -16.52544592524335698, -4.483927247898792601, 78.95942372801901854 ) ) ;
#97423 = CARTESIAN_POINT ( 'NONE',  ( -17.13100169013300089, -6.664070546373138448, 74.23210164300155611 ) ) ;
#97424 = CARTESIAN_POINT ( 'NONE',  ( 9.564922557961047289, -16.46253265017146816, 55.41775706135234003 ) ) ;
#97425 = CARTESIAN_POINT ( 'NONE',  ( -9.564922557961040184, 16.46253265017147172, 22.91775706135233648 ) ) ;
#97426 = DIRECTION ( 'NONE',  ( 0.000000000000000000, -1.000000000000000000, 1.287488025362403787E-15 ) ) ;
#97427 = CARTESIAN_POINT ( 'NONE',  ( -19.03943276465977164, 0.05219959533909376836, 21.24890960531436335 ) ) ;
#97428 = CARTESIAN_POINT ( 'NONE',  ( 22.81625015709509441, 31.40387420917330275, -1.824999997268813567 ) ) ;
#97429 = CARTESIAN_POINT ( 'NONE',  ( -4.379528057220328563, 16.55341960407611168, 25.20724293864769550 ) ) ;
#97430 = CARTESIAN_POINT ( 'NONE',  ( -4.500000000000001776, -120.3830222215595001, 15.32139380484325741 ) ) ;
#97431 = CARTESIAN_POINT ( 'NONE',  ( -4.379528057220086978, -16.55341960407618274, 99.79275706135234714 ) ) ;
#97432 = CARTESIAN_POINT ( 'NONE',  ( -19.20446147854523744, -5.500000000000000888, 84.38999695167674986 ) ) ;
#97433 = CARTESIAN_POINT ( 'NONE',  ( 0.05219959533934541429, -16.53943276465976808, 85.00109039468568994 ) ) ;
#97434 = CARTESIAN_POINT ( 'NONE',  ( -19.03943276465977164, 0.05219959533909376836, 21.24890960531436335 ) ) ;
#97435 = CARTESIAN_POINT ( 'NONE',  ( 21.55341960407619695, -5.719274019375665929, 91.04275706135236135 ) ) ;
#97436 = CARTESIAN_POINT ( 'NONE',  ( -19.03943276465977164, -0.05219959533935918106, 108.7510903946856615 ) ) ;
#97437 = CARTESIAN_POINT ( 'NONE',  ( 10.72451020669871369, 18.67979575497193778, 62.08442372801901143 ) ) ;
#97438 = CARTESIAN_POINT ( 'NONE',  ( 9.474510206698729675, 16.51473224551082808, 42.08442372801900433 ) ) ;
#97439 = CARTESIAN_POINT ( 'NONE',  ( 5.049401038298161559, -19.05341960407611168, 77.70724293864765286 ) ) ;
#97440 = CARTESIAN_POINT ( 'NONE',  ( -9.474510206698964154, 16.51473224551069663, 75.41557627198103830 ) ) ;
#97441 = CARTESIAN_POINT ( 'NONE',  ( 0.000000000000000000, -165.0000000000000000, 5.497848452431111532 ) ) ;
#97442 = CARTESIAN_POINT ( 'NONE',  ( 15.72974639402199770, -15.80617190586745480, 53.12390960531436690 ) ) ;
#97443 = CARTESIAN_POINT ( 'NONE',  ( -19.05341960407611168, -5.049401038298163336, 51.45724293864770260 ) ) ;
#97444 = CARTESIAN_POINT ( 'NONE',  ( 0.05219959533934541429, -16.53943276465976808, 80.00109039468568994 ) ) ;
#97445 = ORIENTED_EDGE ( 'NONE', *, *, #64444, .T. ) ;
#97447 = CARTESIAN_POINT ( 'NONE',  ( 22.81625015709509441, 31.40387420917330275, -1.324999997268813123 ) ) ;
#97446 = CARTESIAN_POINT ( 'NONE',  ( -16.55341960407611168, -4.379528057220339221, 76.45724293864769550 ) ) ;
#97448 = CARTESIAN_POINT ( 'NONE',  ( -14.34966873604972548, 8.224510206698743886, 33.33442372801900433 ) ) ;
#97449 = CARTESIAN_POINT ( 'NONE',  ( -4.483927247898539470, -16.52544592524342804, 107.2905762719810525 ) ) ;
#97450 = CARTESIAN_POINT ( 'NONE',  ( -9.564922557961040184, 16.46253265017147172, 67.91775706135233293 ) ) ;
#97451 = CARTESIAN_POINT ( 'NONE',  ( -12.14591786802309592, -12.06949235617757132, 76.87390960531439532 ) ) ;
#97452 = CARTESIAN_POINT ( 'NONE',  ( -15.80617190586768217, 15.72974639402176855, 33.12609039468569705 ) ) ;
#97454 = CARTESIAN_POINT ( 'NONE',  ( 15.80617190586746368, 15.72974639402197994, 89.37390960531435269 ) ) ;
#97453 = CARTESIAN_POINT ( 'NONE',  ( -15.49999999999999822, 0.000000000000000000, 118.0000000000000142 ) ) ;
#97455 = CARTESIAN_POINT ( 'NONE',  ( 13.97604488694527802, 13.89961937509977652, 104.3739096053143385 ) ) ;
#97456 = CARTESIAN_POINT ( 'NONE',  ( 8.314922557960818139, 14.29746914071049879, 69.58224293864769550 ) ) ;
#97457 = CARTESIAN_POINT ( 'NONE',  ( 25.95926362436975765, -29.82107321766389063, -18.67624575279086940 ) ) ;
#97458 = CARTESIAN_POINT ( 'NONE',  ( 9.474510206698971260, -16.51473224551069308, 47.91557627198102409 ) ) ;
#97459 = CARTESIAN_POINT ( 'NONE',  ( -22.81625015709509441, -31.40387420917324590, -4.324999997268813345 ) ) ;
#97460 = CARTESIAN_POINT ( 'NONE',  ( 19.03943276465977164, 0.05219959533936151252, 86.25109039468567573 ) ) ;
#97461 = CARTESIAN_POINT ( 'NONE',  ( 21.52544592524334988, 5.823673210054432836, 21.45942372801901499 ) ) ;
#97462 = CARTESIAN_POINT ( 'NONE',  ( 19.05341960407611168, 5.049401038298154454, 73.95724293864768129 ) ) ;
#97463 = CARTESIAN_POINT ( 'NONE',  ( -9.564922557961040184, 16.46253265017147172, 57.91775706135233293 ) ) ;
#97464 = CARTESIAN_POINT ( 'NONE',  ( -16.46253265017160317, 9.564922557960807481, 40.83224293864769550 ) ) ;
#97465 = ADVANCED_FACE ( 'NONE', ( #188962 ), #111097, .F. ) ;
#97466 = CARTESIAN_POINT ( 'NONE',  ( 12.06949235617757843, -12.14591786802309237, 63.12390960531435979 ) ) ;
#97467 = CARTESIAN_POINT ( 'NONE',  ( 4.379528057220339221, -16.55341960407611168, 47.70724293864770260 ) ) ;
#97468 = CARTESIAN_POINT ( 'NONE',  ( 19.05341960407611168, 5.049401038298154454, 73.95724293864768129 ) ) ;
#97469 = CARTESIAN_POINT ( 'NONE',  ( -18.67979575497178146, -10.72451020669898902, 81.66557627198103830 ) ) ;
#97470 = CARTESIAN_POINT ( 'NONE',  ( 0.05219959533909260263, 19.03943276465977164, 69.99890960531435269 ) ) ;
#97471 = CARTESIAN_POINT ( 'NONE',  ( -21.55341960407610458, -5.719274019375992779, 76.45724293864769550 ) ) ;
#97472 = CARTESIAN_POINT ( 'NONE',  ( 18.67979575497194134, -10.72451020669871369, 110.8344237280190043 ) ) ;
#97475 = CARTESIAN_POINT ( 'NONE',  ( -0.05219959533910754901, -16.53943276465976808, 92.49890960531436690 ) ) ;
#97474 = CARTESIAN_POINT ( 'NONE',  ( 12.06949235617739724, 12.14591786802326823, 111.8760903946856615 ) ) ;
#97473 = CARTESIAN_POINT ( 'NONE',  ( 37.99626262588765258, 2.893932880411085066E-14, 2.000000000000000000 ) ) ;
#97476 = CARTESIAN_POINT ( 'NONE',  ( 13.97604488694548053, -13.89961937509957401, 100.6260903946856615 ) ) ;
#97477 = VERTEX_POINT ( 'NONE', #154624 ) ;
#97478 = CARTESIAN_POINT ( 'NONE',  ( 18.62759615963271287, -10.81492255796078972, 113.3322429386476955 ) ) ;
#97479 = CARTESIAN_POINT ( 'NONE',  ( -9.474510206698720793, -16.51473224551083518, 59.58442372801900433 ) ) ;
#97480 = CARTESIAN_POINT ( 'NONE',  ( 16.53943276465976808, -0.05219959533910856209, 28.74890960531435624 ) ) ;
#97481 = CARTESIAN_POINT ( 'NONE',  ( -19.02544592524334988, -5.153800228976617603, 43.95942372801899012 ) ) ;
#97482 = CARTESIAN_POINT ( 'NONE',  ( -16.46253265017160317, 9.564922557960807481, 95.83224293864769550 ) ) ;
#97483 = CARTESIAN_POINT ( 'NONE',  ( -16.52544592524342804, 4.483927247898546575, 56.04057627198102409 ) ) ;
#97484 = FACE_OUTER_BOUND ( 'NONE', #2662, .T. ) ;
#97485 = CARTESIAN_POINT ( 'NONE',  ( 19.05341960407611168, 5.049401038298154454, 33.95724293864769550 ) ) ;
#97486 = CARTESIAN_POINT ( 'NONE',  ( -5.823673210054431948, 21.52544592524334988, 107.7094237280190328 ) ) ;
#97487 = CARTESIAN_POINT ( 'NONE',  ( -0.05219959533934338120, 16.53943276465976808, 87.50109039468568994 ) ) ;
#97488 = CARTESIAN_POINT ( 'NONE',  ( -5.823673210054431948, 21.52544592524334988, 47.70942372801902565 ) ) ;
#97489 = CARTESIAN_POINT ( 'NONE',  ( 4.379528057220092307, 16.55341960407617563, 42.29275706135235424 ) ) ;
#97490 = CARTESIAN_POINT ( 'NONE',  ( 5.153800228976335163, 19.02544592524342804, 114.7905762719810241 ) ) ;
#97491 = CARTESIAN_POINT ( 'NONE',  ( 5.153800228976335163, 19.02544592524342804, 49.79057627198100988 ) ) ;
#97492 = CARTESIAN_POINT ( 'NONE',  ( 9.564922557960805705, 16.46253265017160317, 59.58224293864769550 ) ) ;
#97493 = CARTESIAN_POINT ( 'NONE',  ( -4.483927247898782831, 16.52544592524335698, 47.70942372801902565 ) ) ;
#97494 = CARTESIAN_POINT ( 'NONE',  ( 16.52544592524342804, -4.483927247898539470, 103.5405762719810383 ) ) ;
#97495 = CARTESIAN_POINT ( 'NONE',  ( -14.34966873604972548, 8.224510206698743886, 108.3344237280190185 ) ) ;
#97496 = DIRECTION ( 'NONE',  ( -0.000000000000000000, -0.000000000000000000, 1.000000000000000000 ) ) ;
#97499 = CARTESIAN_POINT ( 'NONE',  ( -5.153800228976328057, -19.02544592524343514, 82.29057627198103830 ) ) ;
#97498 = CARTESIAN_POINT ( 'NONE',  ( 13.97604488694527802, 13.89961937509977652, 89.37390960531436690 ) ) ;
#97497 = CARTESIAN_POINT ( 'NONE',  ( -5.719274019375665041, -21.55341960407619695, 54.79275706135235424 ) ) ;
#97500 = CARTESIAN_POINT ( 'NONE',  ( 16.46253265017160672, -9.564922557960803928, 98.33224293864769550 ) ) ;
#97501 = CARTESIAN_POINT ( 'NONE',  ( -4.379528057220328563, 16.55341960407611168, 40.20724293864769550 ) ) ;
#97502 = CARTESIAN_POINT ( 'NONE',  ( 16.55341960407611168, 4.379528057220329451, 23.95724293864769550 ) ) ;
#97503 = CARTESIAN_POINT ( 'NONE',  ( 8.224510206698953496, -14.34966873604960469, 37.91557627198102409 ) ) ;
#97504 = ORIENTED_EDGE ( 'NONE', *, *, #96536, .T. ) ;
#97505 = CARTESIAN_POINT ( 'NONE',  ( 17.72560187377285601, 5.500000000000050626, 56.57814504131319921 ) ) ;
#97506 = CARTESIAN_POINT ( 'NONE',  ( -9.564922557961040184, 16.46253265017147172, 42.91775706135234003 ) ) ;
#97507 = CARTESIAN_POINT ( 'NONE',  ( 13.89961937509977652, -13.97604488694527269, 58.12390960531436690 ) ) ;
#97508 = CARTESIAN_POINT ( 'NONE',  ( 19.02544592524334988, 5.153800228976608722, 56.45942372801898301 ) ) ;
#97509 = CARTESIAN_POINT ( 'NONE',  ( -29.86685920354755197, -21.69954338932560134, -10.92499999726881299 ) ) ;
#97510 = CARTESIAN_POINT ( 'NONE',  ( 11.74264578624799427, 36.14014761921585972, -2.349999994537626868 ) ) ;
#97512 = CARTESIAN_POINT ( 'NONE',  ( 8.224510206698742110, 14.34966873604972548, 72.08442372801899012 ) ) ;
#97511 = CARTESIAN_POINT ( 'NONE',  ( -19.05341960407617563, 5.049401038297882671, 83.54275706135233293 ) ) ;
#97513 = PLANE ( 'NONE',  #85195 ) ;
#97514 = CARTESIAN_POINT ( 'NONE',  ( 19.05341960407611168, 5.049401038298154454, 108.9572429386477097 ) ) ;
#97515 = CARTESIAN_POINT ( 'NONE',  ( -15.80617190586768217, 15.72974639402176855, 23.12609039468567573 ) ) ;
#97516 = CARTESIAN_POINT ( 'NONE',  ( 5.153800228976615827, -19.02544592524334988, 85.20942372801900433 ) ) ;
#97518 = CARTESIAN_POINT ( 'NONE',  ( 16.46253265017160672, -9.564922557960803928, 43.33224293864769550 ) ) ;
#97517 = CARTESIAN_POINT ( 'NONE',  ( 17.49999999999999645, 5.624438216177603422, 86.68329655085356933 ) ) ;
#97519 = CARTESIAN_POINT ( 'NONE',  ( 13.97604488694527802, 13.89961937509977652, 94.37390960531436690 ) ) ;
#97521 = CARTESIAN_POINT ( 'NONE',  ( -5.153800228976328057, -19.02544592524343514, 47.29057627198102409 ) ) ;
#97520 = CARTESIAN_POINT ( 'NONE',  ( 14.29746914071049879, -8.314922557960816363, 53.33224293864769550 ) ) ;
#97522 = CARTESIAN_POINT ( 'NONE',  ( 13.97604488694548053, -13.89961937509957401, 60.62609039468564731 ) ) ;
#97523 = CARTESIAN_POINT ( 'NONE',  ( 16.46253265017146816, 9.564922557961045513, 31.66775706135232937 ) ) ;
#97524 = CARTESIAN_POINT ( 'NONE',  ( -16.46253265017160317, 9.564922557960807481, 65.83224293864769550 ) ) ;
#97525 = ADVANCED_FACE ( 'NONE', ( #16118 ), #139442, .T. ) ;
#97526 = CARTESIAN_POINT ( 'NONE',  ( 15.72974639402199770, -15.80617190586745480, 58.12390960531435979 ) ) ;
#97528 = CARTESIAN_POINT ( 'NONE',  ( 9.474510206698729675, 16.51473224551082808, 22.08442372801899722 ) ) ;
#97527 = CARTESIAN_POINT ( 'NONE',  ( -14.34966873604960291, -8.224510206698953496, 66.66557627198102409 ) ) ;
#97529 = CARTESIAN_POINT ( 'NONE',  ( -9.564922557960796823, -16.46253265017161027, 102.0822429386477097 ) ) ;
#97530 = CARTESIAN_POINT ( 'NONE',  ( -15.72974639402197994, 15.80617190586746368, 30.62390960531436335 ) ) ;
#97531 = CARTESIAN_POINT ( 'NONE',  ( -5.049401038298153566, 19.05341960407611168, 50.20724293864770260 ) ) ;
#97532 = CARTESIAN_POINT ( 'NONE',  ( 13.89961937509977652, -13.97604488694527269, 33.12390960531434558 ) ) ;
#97533 = CARTESIAN_POINT ( 'NONE',  ( -14.29746914071049879, 8.314922557960819915, 95.83224293864770971 ) ) ;
#97534 = CARTESIAN_POINT ( 'NONE',  ( -15.72974639402197994, 15.80617190586746368, 115.6239096053143669 ) ) ;
#97535 = CARTESIAN_POINT ( 'NONE',  ( 5.049401038298161559, -19.05341960407611168, 112.7072429386476813 ) ) ;
#97536 = CARTESIAN_POINT ( 'NONE',  ( -21.55341960407619339, 5.719274019375674811, 28.54275706135234358 ) ) ;
#97537 = CARTESIAN_POINT ( 'NONE',  ( 19.05341960407611168, 5.049401038298154454, 108.9572429386477097 ) ) ;
#97538 = CARTESIAN_POINT ( 'NONE',  ( -4.379528057220328563, 16.55341960407611168, 115.2072429386476955 ) ) ;
#97539 = CARTESIAN_POINT ( 'NONE',  ( -5.823673210054431948, 21.52544592524334988, 72.70942372801901854 ) ) ;
#97540 = CARTESIAN_POINT ( 'NONE',  ( 15.80617190586746368, 15.72974639402197994, 94.37390960531436690 ) ) ;
#97541 = CARTESIAN_POINT ( 'NONE',  ( -2.973862142520655727, -93.04182470242766101, -13.00000000000000000 ) ) ;
#97542 = DIRECTION ( 'NONE',  ( 1.000000000000000000, 0.000000000000000000, 0.000000000000000000 ) ) ;
#97543 = CARTESIAN_POINT ( 'NONE',  ( -13.89961937509977830, 13.97604488694528158, 60.62390960531436690 ) ) ;
#97544 = CARTESIAN_POINT ( 'NONE',  ( 12.06949235617739724, 12.14591786802326823, 46.87609039468568994 ) ) ;
#97545 = CARTESIAN_POINT ( 'NONE',  ( 16.53943276465976808, -0.05219959533910856209, 103.7489096053143669 ) ) ;
#97546 = DIRECTION ( 'NONE',  ( 0.000000000000000000, -1.000000000000000000, 0.000000000000000000 ) ) ;
#97547 = CARTESIAN_POINT ( 'NONE',  ( -19.05341960407611168, -5.049401038298163336, 61.45724293864769550 ) ) ;
#97548 = CARTESIAN_POINT ( 'NONE',  ( -16.55341960407611168, -4.379528057220339221, 96.45724293864770971 ) ) ;
#97549 = CARTESIAN_POINT ( 'NONE',  ( -0.05219959533907301413, -21.53943276465977519, 52.49890960531435979 ) ) ;
#97550 = CARTESIAN_POINT ( 'NONE',  ( 4.483927247898545687, 16.52544592524342804, 59.79057627198103120 ) ) ;
#97551 = CARTESIAN_POINT ( 'NONE',  ( -0.05219959533936034679, 19.03943276465977164, 112.5010903946856757 ) ) ;
#97552 = CARTESIAN_POINT ( 'NONE',  ( 18.67979575497194134, -10.72451020669871369, 85.83442372801901854 ) ) ;
#97553 = CARTESIAN_POINT ( 'NONE',  ( 17.05116617787825462, -6.768360034955811066, 76.15675553259197272 ) ) ;
#97554 = CARTESIAN_POINT ( 'NONE',  ( -12.14591786802326823, 12.06949235617739902, 93.12609039468568994 ) ) ;
#97555 = CARTESIAN_POINT ( 'NONE',  ( 12.06949235617757843, -12.14591786802309237, 38.12390960531436690 ) ) ;
#97556 = CARTESIAN_POINT ( 'NONE',  ( -0.05219959533909027116, -19.03943276465977164, 32.49890960531435979 ) ) ;
#97557 = CARTESIAN_POINT ( 'NONE',  ( -9.474510206698964154, 16.51473224551069663, 90.41557627198103830 ) ) ;
#97558 = CARTESIAN_POINT ( 'NONE',  ( -15.80617190586745835, -15.72974639402198527, 96.87390960531436690 ) ) ;
#97559 = CARTESIAN_POINT ( 'NONE',  ( -14.34966873604972548, 8.224510206698743886, 33.33442372801900433 ) ) ;
#97561 = CARTESIAN_POINT ( 'NONE',  ( 5.719274019375673035, 21.55341960407619339, 92.29275706135236135 ) ) ;
#97560 = CARTESIAN_POINT ( 'NONE',  ( 0.05219959533910956823, 16.53943276465976808, 69.99890960531435269 ) ) ;
#97562 = CARTESIAN_POINT ( 'NONE',  ( 12.14591786802327356, -12.06949235617739191, 95.62609039468568994 ) ) ;
#97563 = CARTESIAN_POINT ( 'NONE',  ( 17.05116617787848554, -6.768360034955523297, 46.15675553259190877 ) ) ;
#97564 = DIRECTION ( 'NONE',  ( -1.000000000000000000, 0.000000000000000000, 0.000000000000000000 ) ) ;
#97565 = CARTESIAN_POINT ( 'NONE',  ( -4.483927247898539470, -16.52544592524342804, 27.29057627198103120 ) ) ;
#97566 = CARTESIAN_POINT ( 'NONE',  ( -12.06949235617739369, -12.14591786802326823, 74.37609039468568994 ) ) ;
#97567 = CARTESIAN_POINT ( 'NONE',  ( -9.564922557960796823, -16.46253265017161027, 82.08224293864768129 ) ) ;
#97568 = CARTESIAN_POINT ( 'NONE',  ( -9.474510206698964154, 16.51473224551069663, 100.4155762719810241 ) ) ;
#97569 = CARTESIAN_POINT ( 'NONE',  ( 15.80617190586769283, -15.72974639402175789, 90.62609039468567573 ) ) ;
#97570 = CARTESIAN_POINT ( 'NONE',  ( -12.06949235617739369, -12.14591786802326823, 94.37609039468568994 ) ) ;
#97571 = CARTESIAN_POINT ( 'NONE',  ( -8.224510206698948167, 14.34966873604960824, 65.41557627198102409 ) ) ;
#97572 = CARTESIAN_POINT ( 'NONE',  ( 19.03943276465977164, -0.05219959533909143690, 63.74890960531435979 ) ) ;
#97573 = ORIENTED_EDGE ( 'NONE', *, *, #145835, .F. ) ;
#97574 = CARTESIAN_POINT ( 'NONE',  ( -19.05341960407617563, 5.049401038297882671, 113.5427570613523471 ) ) ;
#97575 = CARTESIAN_POINT ( 'NONE',  ( -13.97604488694527625, -13.89961937509977652, 26.87390960531434558 ) ) ;
#97576 = CARTESIAN_POINT ( 'NONE',  ( 19.05341960407611168, 5.049401038298154454, 78.95724293864769550 ) ) ;
#97578 = CARTESIAN_POINT ( 'NONE',  ( 22.81625015709509441, 31.40387420917330275, -9.324999997268813345 ) ) ;
#97577 = CARTESIAN_POINT ( 'NONE',  ( 8.224510206698742110, 14.34966873604972548, 22.08442372801901143 ) ) ;
#97579 = CARTESIAN_POINT ( 'NONE',  ( 19.03943276465977164, 0.05219959533936151252, 26.25109039468566507 ) ) ;
#97580 = CARTESIAN_POINT ( 'NONE',  ( 16.53943276465976808, 0.05219959533934440121, 81.25109039468568994 ) ) ;
#97581 = CARTESIAN_POINT ( 'NONE',  ( -13.89961937509957401, -13.97604488694547875, 109.3760903946856331 ) ) ;
#97582 = CARTESIAN_POINT ( 'NONE',  ( -14.34966873604960291, -8.224510206698953496, 111.6655762719810525 ) ) ;
#97583 = CARTESIAN_POINT ( 'NONE',  ( 8.314922557961029526, -14.29746914071037800, 60.41775706135235424 ) ) ;
#97584 = CARTESIAN_POINT ( 'NONE',  ( 14.34966873604972726, -8.224510206698740333, 50.83442372801901143 ) ) ;
#97585 = CARTESIAN_POINT ( 'NONE',  ( -0.05219959533909027116, -19.03943276465977164, 27.49890960531435624 ) ) ;
#97586 = CARTESIAN_POINT ( 'NONE',  ( 9.474510206698729675, 16.51473224551082808, 67.08442372801900433 ) ) ;
#97587 = CARTESIAN_POINT ( 'NONE',  ( 13.97604488694548053, -13.89961937509957401, 20.62609039468567573 ) ) ;
#97588 = CARTESIAN_POINT ( 'NONE',  ( 16.51473224551069308, 9.474510206698969483, 29.16557627198103475 ) ) ;
#97589 = CARTESIAN_POINT ( 'NONE',  ( 19.05341960407611168, 5.049401038298154454, 73.95724293864768129 ) ) ;
#97590 = CARTESIAN_POINT ( 'NONE',  ( 0.05219959533910956823, 16.53943276465976808, 74.99890960531435269 ) ) ;
#97591 = CARTESIAN_POINT ( 'NONE',  ( 16.51473224551083163, -9.474510206698727899, 35.83442372801899722 ) ) ;
#97592 = CARTESIAN_POINT ( 'NONE',  ( 5.823673210054125526, 21.52544592524343514, 39.79057627198103830 ) ) ;
#97593 = CARTESIAN_POINT ( 'NONE',  ( -21.53943276465977519, -0.05219959533937600094, 113.7510903946856757 ) ) ;
#97594 = CARTESIAN_POINT ( 'NONE',  ( -19.05341960407611168, -5.049401038298163336, 91.45724293864766707 ) ) ;
#97595 = CARTESIAN_POINT ( 'NONE',  ( 5.823673210054444382, -21.52544592524334988, 110.2094237280190185 ) ) ;
#97596 = CARTESIAN_POINT ( 'NONE',  ( 5.823673210054125526, 21.52544592524343514, 59.79057627198103120 ) ) ;
#97597 = CARTESIAN_POINT ( 'NONE',  ( 13.89961937509977652, -13.97604488694527269, 98.12390960531433848 ) ) ;
#97598 = CARTESIAN_POINT ( 'NONE',  ( 0.05219959533936267826, -19.03943276465977164, 80.00109039468567573 ) ) ;
#97599 = CARTESIAN_POINT ( 'NONE',  ( 5.049401038298161559, -19.05341960407611168, 97.70724293864766707 ) ) ;
#97600 = CARTESIAN_POINT ( 'NONE',  ( -19.05341960407617563, 5.049401038297882671, 93.54275706135234714 ) ) ;
#97601 = CARTESIAN_POINT ( 'NONE',  ( -14.34966873604972548, 8.224510206698743886, 53.33442372801901854 ) ) ;
#97602 = CARTESIAN_POINT ( 'NONE',  ( 16.46253265017160672, -9.564922557960803928, 23.33224293864769194 ) ) ;
#97603 = CARTESIAN_POINT ( 'NONE',  ( -19.02544592524342804, 5.153800228976336051, 81.04057627198103830 ) ) ;
#97604 = CARTESIAN_POINT ( 'NONE',  ( 15.72974639402199770, -15.80617190586745480, 58.12390960531435979 ) ) ;
#97605 = CARTESIAN_POINT ( 'NONE',  ( -8.224510206698735004, -14.34966873604973081, 29.58442372801901854 ) ) ;
#97606 = CARTESIAN_POINT ( 'NONE',  ( -18.62759615963255300, -10.81492255796106328, 29.16775706135234003 ) ) ;
#97607 = CARTESIAN_POINT ( 'NONE',  ( 5.823673210054444382, -21.52544592524334988, 100.2094237280190043 ) ) ;
#97608 = CARTESIAN_POINT ( 'NONE',  ( -0.05219959533934338120, 16.53943276465976808, 97.50109039468567573 ) ) ;
#97609 = CARTESIAN_POINT ( 'NONE',  ( -19.03943276465977164, 0.05219959533909376836, 86.24890960531436690 ) ) ;
#97610 = CARTESIAN_POINT ( 'NONE',  ( -16.53943276465976808, 0.05219959533911058130, 96.24890960531435269 ) ) ;
#97611 = CARTESIAN_POINT ( 'NONE',  ( -16.55341960407617563, 4.379528057220093196, 113.5427570613523756 ) ) ;
#97612 = CARTESIAN_POINT ( 'NONE',  ( 0.05219959533936267826, -19.03943276465977164, 75.00109039468566152 ) ) ;
#97613 = CARTESIAN_POINT ( 'NONE',  ( -5.823673210054431948, 21.52544592524334988, 42.70942372801901854 ) ) ;
#97614 = CARTESIAN_POINT ( 'NONE',  ( 8.224510206698953496, -14.34966873604960469, 87.91557627198103830 ) ) ;
#97615 = CARTESIAN_POINT ( 'NONE',  ( -0.05219959533907301413, -21.53943276465977519, 22.49890960531436335 ) ) ;
#97616 = CARTESIAN_POINT ( 'NONE',  ( 14.29746914071037800, 8.314922557961029526, 101.6677570613523613 ) ) ;
#97617 = CARTESIAN_POINT ( 'NONE',  ( 21.53943276465977519, 0.05219959533937863772, 81.25109039468568994 ) ) ;
#97618 = CARTESIAN_POINT ( 'NONE',  ( -16.55341960407617563, 4.379528057220093196, 43.54275706135235424 ) ) ;
#97619 = CARTESIAN_POINT ( 'NONE',  ( 15.80617190586769283, -15.72974639402175789, 35.62609039468568994 ) ) ;
#97620 = ORIENTED_EDGE ( 'NONE', *, *, #53832, .T. ) ;
#97621 = CARTESIAN_POINT ( 'NONE',  ( 21.55341960407610458, 5.719274019375980345, 113.9572429386477239 ) ) ;
#97622 = CARTESIAN_POINT ( 'NONE',  ( -4.379528057220328563, 16.55341960407611168, 90.20724293864770971 ) ) ;
#97623 = CARTESIAN_POINT ( 'NONE',  ( 17.50000000000001776, -3.345213924137293127, 27.08768623094348271 ) ) ;
#97624 = CARTESIAN_POINT ( 'NONE',  ( -16.53943276465976808, 0.05219959533911058130, 71.24890960531435269 ) ) ;
#97625 = CARTESIAN_POINT ( 'NONE',  ( -5.153800228976328057, -19.02544592524343514, 52.29057627198100988 ) ) ;
#97626 = CARTESIAN_POINT ( 'NONE',  ( -4.379528057220086978, -16.55341960407618274, 109.7927570613523613 ) ) ;
#97627 = CARTESIAN_POINT ( 'NONE',  ( 13.97604488694527802, 13.89961937509977652, 39.37390960531435269 ) ) ;
#97628 = CARTESIAN_POINT ( 'NONE',  ( 15.80617190586746368, 15.72974639402197994, 49.37390960531436690 ) ) ;
#97629 = CARTESIAN_POINT ( 'NONE',  ( 12.06949235617757843, -12.14591786802309237, 73.12390960531436690 ) ) ;
#97630 = CARTESIAN_POINT ( 'NONE',  ( -21.55341960407610458, -5.719274019375992779, 86.45724293864770971 ) ) ;
#97631 = CARTESIAN_POINT ( 'NONE',  ( 19.05341960407611168, 5.049401038298154454, 93.95724293864769550 ) ) ;
#97633 = CARTESIAN_POINT ( 'NONE',  ( -5.153800228976607833, 19.02544592524334988, 92.70942372801901854 ) ) ;
#97632 = CARTESIAN_POINT ( 'NONE',  ( -9.564922557960796823, -16.46253265017161027, 32.08224293864769550 ) ) ;
#97634 = CARTESIAN_POINT ( 'NONE',  ( -10.72451020669898014, 18.67979575497178502, 35.41557627198102409 ) ) ;
#97635 = CARTESIAN_POINT ( 'NONE',  ( 21.55341960407619695, -5.719274019375665929, 66.04275706135236135 ) ) ;
#97636 = CARTESIAN_POINT ( 'NONE',  ( -19.05341960407611168, -5.049401038298163336, 56.45724293864768129 ) ) ;
#97637 = CARTESIAN_POINT ( 'NONE',  ( 0.05219959533909260263, 19.03943276465977164, 89.99890960531436690 ) ) ;
#97638 = ORIENTED_EDGE ( 'NONE', *, *, #2501, .T. ) ;
#97639 = CARTESIAN_POINT ( 'NONE',  ( -4.483927247898782831, 16.52544592524335698, 57.70942372801901143 ) ) ;
#97640 = CARTESIAN_POINT ( 'NONE',  ( 10.81492255796106328, -18.62759615963255655, 45.41775706135234003 ) ) ;
#97641 = CARTESIAN_POINT ( 'NONE',  ( -21.55341960407619339, 5.719274019375674811, 73.54275706135234714 ) ) ;
#97642 = CARTESIAN_POINT ( 'NONE',  ( -9.474510206698964154, 16.51473224551069663, 115.4155762719810241 ) ) ;
#97643 = CARTESIAN_POINT ( 'NONE',  ( -10.72451020669898014, 18.67979575497178502, 100.4155762719810241 ) ) ;
#97645 = CARTESIAN_POINT ( 'NONE',  ( -16.55341960407617563, 4.379528057220093196, 68.54275706135234714 ) ) ;
#97644 = CARTESIAN_POINT ( 'NONE',  ( -5.823673210054431948, 21.52544592524334988, 42.70942372801901854 ) ) ;
#97646 = CARTESIAN_POINT ( 'NONE',  ( -10.81492255796078084, -18.62759615963271287, 67.08224293864770971 ) ) ;
#97647 = CARTESIAN_POINT ( 'NONE',  ( 16.51473224551083163, -9.474510206698727899, 35.83442372801899722 ) ) ;
#97649 = CARTESIAN_POINT ( 'NONE',  ( -0.05219959533934338120, 16.53943276465976808, 107.5010903946856899 ) ) ;
#97648 = CARTESIAN_POINT ( 'NONE',  ( 5.153800228976335163, 19.02544592524342804, 69.79057627198103830 ) ) ;
#97650 = CARTESIAN_POINT ( 'NONE',  ( 17.60728821186569704, -5.500000000000036415, 83.36690927743002533 ) ) ;
#97651 = CARTESIAN_POINT ( 'NONE',  ( 5.049401038298161559, -19.05341960407611168, 102.7072429386476955 ) ) ;
#97652 = CARTESIAN_POINT ( 'NONE',  ( -16.53943276465976808, -0.05219959533934237506, 43.75109039468568284 ) ) ;
#97653 = CARTESIAN_POINT ( 'NONE',  ( 20.09153389842217763, 22.04836444019709418, -48.54295043639822183 ) ) ;
#97654 = ADVANCED_FACE ( 'NONE', ( #47456 ), #109112, .T. ) ;
#97655 = CARTESIAN_POINT ( 'NONE',  ( -19.05341960407617563, 5.049401038297882671, 83.54275706135233293 ) ) ;
#97656 = CARTESIAN_POINT ( 'NONE',  ( 15.80617190586746368, 15.72974639402197994, 59.37390960531436690 ) ) ;
#97657 = CARTESIAN_POINT ( 'NONE',  ( -16.52544592524342804, 4.483927247898546575, 31.04057627198102409 ) ) ;
#97658 = CARTESIAN_POINT ( 'NONE',  ( -9.474510206698720793, -16.51473224551083518, 99.58442372801900433 ) ) ;
#97659 = CARTESIAN_POINT ( 'NONE',  ( -37.66961640367473052, 5.000000000000023981, -15.00000000000000000 ) ) ;
#97660 = CARTESIAN_POINT ( 'NONE',  ( 16.51473224551083163, -9.474510206698727899, 95.83442372801900433 ) ) ;
#97662 = CARTESIAN_POINT ( 'NONE',  ( -19.02544592524334988, -5.153800228976617603, 53.95942372801898301 ) ) ;
#97661 = CARTESIAN_POINT ( 'NONE',  ( -21.55341960407610458, -5.719274019375992779, 91.45724293864769550 ) ) ;
#97663 = CARTESIAN_POINT ( 'NONE',  ( 37.99999999999999289, 2.428612866367529932E-14, -25.00000000000000000 ) ) ;
#97664 = CARTESIAN_POINT ( 'NONE',  ( 9.564922557960805705, 16.46253265017160317, 69.58224293864770971 ) ) ;
#97665 = CARTESIAN_POINT ( 'NONE',  ( 12.14591786802309770, 12.06949235617756955, 69.37390960531436690 ) ) ;
#97666 = CARTESIAN_POINT ( 'NONE',  ( -0.05219959533909027116, -19.03943276465977164, 52.49890960531436690 ) ) ;
#97667 = CARTESIAN_POINT ( 'NONE',  ( -8.314922557960811034, -14.29746914071050412, 47.08224293864770260 ) ) ;
#97668 = LINE ( 'NONE', #140215, #77444 ) ;
#97669 = CARTESIAN_POINT ( 'NONE',  ( 31.24427474013727490, -7.030368782406881678, 97.62376346805382354 ) ) ;
#97670 = CARTESIAN_POINT ( 'NONE',  ( -8.224510206698948167, 14.34966873604960824, 30.41557627198101699 ) ) ;
#97671 = CARTESIAN_POINT ( 'NONE',  ( -19.02544592524342804, 5.153800228976336051, 61.04057627198103120 ) ) ;
#97672 = CARTESIAN_POINT ( 'NONE',  ( 15.06137443927350361, 15.06137443927346098, -58.85720012050613548 ) ) ;
#97673 = CARTESIAN_POINT ( 'NONE',  ( -13.97604488694547697, 13.89961937509957934, 38.12609039468566152 ) ) ;
#97674 = CARTESIAN_POINT ( 'NONE',  ( 4.379528057220092307, 16.55341960407617563, 42.29275706135235424 ) ) ;
#97675 = CARTESIAN_POINT ( 'NONE',  ( 18.62759615963271287, -10.81492255796078972, 53.33224293864769550 ) ) ;
#97676 = CARTESIAN_POINT ( 'NONE',  ( 18.67979575497194134, -10.72451020669871369, 100.8344237280190185 ) ) ;
#97677 = CARTESIAN_POINT ( 'NONE',  ( 19.02544592524343514, -5.153800228976328945, 73.54057627198103830 ) ) ;
#97678 = CARTESIAN_POINT ( 'NONE',  ( 22.55670631985092811, 22.55670631985084640, -45.64921306006598201 ) ) ;
#97679 = CARTESIAN_POINT ( 'NONE',  ( 16.51473224551069308, 9.474510206698969483, 109.1655762719810383 ) ) ;
#97680 = CARTESIAN_POINT ( 'NONE',  ( -5.950531402560715689E-15, 38.81732327939063509, -3.124999997268813168 ) ) ;
#97681 = CARTESIAN_POINT ( 'NONE',  ( 15.80617190586769283, -15.72974639402175789, 35.62609039468568994 ) ) ;
#97682 = CARTESIAN_POINT ( 'NONE',  ( -8.314922557960811034, -14.29746914071050412, 97.08224293864770971 ) ) ;
#97685 = VERTEX_POINT ( 'NONE', #68569 ) ;
#97684 = CARTESIAN_POINT ( 'NONE',  ( -5.153800228976328057, -19.02544592524343514, 77.29057627198099567 ) ) ;
#97683 = CARTESIAN_POINT ( 'NONE',  ( 18.67979575497178502, 10.72451020669898547, 89.16557627198102409 ) ) ;
#97686 = CARTESIAN_POINT ( 'NONE',  ( -0.05219959533909027116, -19.03943276465977164, 87.49890960531436690 ) ) ;
#97687 = CARTESIAN_POINT ( 'NONE',  ( 10.81492255796106328, -18.62759615963255655, 20.41775706135234714 ) ) ;
#97688 = EDGE_LOOP ( 'NONE', ( #58029, #110895 ) ) ;
#97689 = CARTESIAN_POINT ( 'NONE',  ( 19.03943276465977164, -0.05219959533909143690, 93.74890960531435269 ) ) ;
#97690 = DIRECTION ( 'NONE',  ( -0.000000000000000000, -0.000000000000000000, 1.000000000000000000 ) ) ;
#97692 = CARTESIAN_POINT ( 'NONE',  ( -19.02544592524342804, 5.153800228976336051, 31.04057627198102409 ) ) ;
#97691 = CARTESIAN_POINT ( 'NONE',  ( -13.89961937509977652, 13.97604488694528158, 30.62390960531435269 ) ) ;
#97693 = CARTESIAN_POINT ( 'NONE',  ( 19.05341960407617918, -5.049401038297876454, 111.0427570613523329 ) ) ;
#97694 = CARTESIAN_POINT ( 'NONE',  ( 36.91746825000000598, -11.99521256947793546, -10.22499999726881548 ) ) ;
#97695 = CARTESIAN_POINT ( 'NONE',  ( -5.153800228976328057, -19.02544592524343514, 22.29057627198102765 ) ) ;
#97696 = CARTESIAN_POINT ( 'NONE',  ( -21.52544592524334988, -5.823673210054445271, 68.95942372801901854 ) ) ;
#97698 = CARTESIAN_POINT ( 'NONE',  ( 15.80617190586769283, -15.72974639402175789, 30.62609039468567929 ) ) ;
#97697 = CARTESIAN_POINT ( 'NONE',  ( 5.049401038298161559, -19.05341960407611168, 67.70724293864769550 ) ) ;
#97699 = CARTESIAN_POINT ( 'NONE',  ( 21.52544592524344225, -5.823673210054117533, 108.5405762719810241 ) ) ;
#97700 = CARTESIAN_POINT ( 'NONE',  ( -28.82186960331499392, 9.364793116373565596, 145.8999999999999773 ) ) ;
#97701 = CARTESIAN_POINT ( 'NONE',  ( -13.89961937509977652, 13.97604488694528158, 85.62390960531433848 ) ) ;
#97702 = CARTESIAN_POINT ( 'NONE',  ( 21.79132363338460721, 17.42213977941835168, 139.9999999999999432 ) ) ;
#97704 = CARTESIAN_POINT ( 'NONE',  ( 21.52544592524344225, -5.823673210054117533, 48.54057627198103120 ) ) ;
#97703 = CARTESIAN_POINT ( 'NONE',  ( -0.05219959533934338120, 16.53943276465976808, 22.50109039468567573 ) ) ;
#97705 = CARTESIAN_POINT ( 'NONE',  ( -18.67979575497193778, 10.72451020669871902, 68.33442372801900433 ) ) ;
#97706 = CARTESIAN_POINT ( 'NONE',  ( -13.89961937509977652, 13.97604488694528158, 110.6239096053143243 ) ) ;
#97707 = CARTESIAN_POINT ( 'NONE',  ( 9.564922557961047289, -16.46253265017146816, 90.41775706135234714 ) ) ;
#97708 = CARTESIAN_POINT ( 'NONE',  ( -19.02544592524342804, 5.153800228976336051, 66.04057627198103830 ) ) ;
#97709 = CARTESIAN_POINT ( 'NONE',  ( -19.03943276465977164, 0.05219959533909376836, 86.24890960531436690 ) ) ;
#97710 = CARTESIAN_POINT ( 'NONE',  ( 8.224510206698953496, -14.34966873604960469, 87.91557627198103830 ) ) ;
#97711 = CARTESIAN_POINT ( 'NONE',  ( -16.55341960407611168, -4.379528057220339221, 86.45724293864770971 ) ) ;
#97712 = CARTESIAN_POINT ( 'NONE',  ( 5.719274019375991003, -21.55341960407610458, 22.70724293864769194 ) ) ;
#97715 = CARTESIAN_POINT ( 'NONE',  ( -5.153800228976328057, -19.02544592524343514, 37.29057627198102409 ) ) ;
#97714 =( BOUNDED_CURVE ( )  B_SPLINE_CURVE ( 2, ( #160196, #142031, #21686, #126854, #99512, #51027, #83339, #161193, #22689, #188560, #50039, #84336, #112688 ),
 .UNSPECIFIED., .F., .F. ) 
 B_SPLINE_CURVE_WITH_KNOTS ( ( 3, 2, 2, 2, 2, 2, 3 ),
 ( 0.6866409627428347040, 0.6885964912280702066, 0.6929824561403509220, 0.6973684210526315264, 0.7017543859649122417, 0.7061403508771929571, 0.7080501995403384319 ),
 .UNSPECIFIED. ) 
 CURVE ( )  GEOMETRIC_REPRESENTATION_ITEM ( )  RATIONAL_B_SPLINE_CURVE ( ( 0.9831626618144007068, 0.9848076720550096308, 1.000000000000000000, 0.9659258262890683122, 1.000000000000000000, 0.9659258262890683122, 1.000000000000000000, 0.9659258262890683122, 1.000000000000000000, 0.9659258262890683122, 1.000000000000000000, 0.9851625545550091179, 0.9832469066685282089 ) ) 
 REPRESENTATION_ITEM ( '' )  );
#97713 = CARTESIAN_POINT ( 'NONE',  ( -16.52544592524342804, 4.483927247898546575, 56.04057627198102409 ) ) ;
#97716 = CARTESIAN_POINT ( 'NONE',  ( -21.52544592524334988, -5.823673210054445271, 63.95942372801901854 ) ) ;
#97717 = CARTESIAN_POINT ( 'NONE',  ( 9.474510206698729675, 16.51473224551082808, 87.08442372801900433 ) ) ;
#97718 = CARTESIAN_POINT ( 'NONE',  ( -16.53943276465976808, 0.05219959533911058130, 61.24890960531435979 ) ) ;
#97719 = CARTESIAN_POINT ( 'NONE',  ( -21.53943276465977519, 0.05219959533907696930, 111.2489096053143669 ) ) ;
#97720 = CARTESIAN_POINT ( 'NONE',  ( 5.823673210054125526, 21.52544592524343514, 44.79057627198103120 ) ) ;
#97721 = CARTESIAN_POINT ( 'NONE',  ( 19.02544592524343514, -5.153800228976328945, 113.5405762719810241 ) ) ;
#97722 = CARTESIAN_POINT ( 'NONE',  ( -28.82186960331499037, 2.428612866367529932E-14, 140.2500000054623683 ) ) ;
#97723 = CARTESIAN_POINT ( 'NONE',  ( -16.46253265017160317, 9.564922557960807481, 60.83224293864769550 ) ) ;
#97724 = CARTESIAN_POINT ( 'NONE',  ( 8.224510206698953496, -14.34966873604960469, 32.91557627198102409 ) ) ;
#97725 = CARTESIAN_POINT ( 'NONE',  ( -12.14591786802326823, 12.06949235617739902, 98.12609039468570415 ) ) ;
#97726 = CARTESIAN_POINT ( 'NONE',  ( -16.53943276465976808, -0.05219959533934237506, 83.75109039468568994 ) ) ;
#97727 = CARTESIAN_POINT ( 'NONE',  ( -5.153800228976607833, 19.02544592524334988, 42.70942372801901143 ) ) ;
#97728 = CARTESIAN_POINT ( 'NONE',  ( -23.42531737588081242, 11.30614151570994430, 165.8025732123264788 ) ) ;
#97729 = CARTESIAN_POINT ( 'NONE',  ( -13.97604488694527625, -13.89961937509977652, 91.87390960531432427 ) ) ;
#97730 = CARTESIAN_POINT ( 'NONE',  ( -19.05341960407611168, -5.049401038298163336, 46.45724293864768129 ) ) ;
#97731 = EDGE_CURVE ( 'NONE', #31087, #25364, #24085, .T. ) ;
#97732 = CARTESIAN_POINT ( 'NONE',  ( -0.05219959533910754901, -16.53943276465976808, 57.49890960531435979 ) ) ;
#97734 = CARTESIAN_POINT ( 'NONE',  ( 19.03943276465977164, -0.05219959533909143690, 113.7489096053143669 ) ) ;
#97733 = CARTESIAN_POINT ( 'NONE',  ( 19.02544592524343514, -5.153800228976328945, 23.54057627198102054 ) ) ;
#97735 = CARTESIAN_POINT ( 'NONE',  ( 18.62759615963271287, -10.81492255796078972, 43.33224293864769550 ) ) ;
#97736 = CARTESIAN_POINT ( 'NONE',  ( 4.483927247898545687, 16.52544592524342804, 84.79057627198102409 ) ) ;
#97737 = CARTESIAN_POINT ( 'NONE',  ( 0.05219959533934541429, -16.53943276465976808, 45.00109039468568284 ) ) ;
#97738 = CIRCLE ( 'NONE', #75267, 8.000000000000000000 ) ;
#97739 = CARTESIAN_POINT ( 'NONE',  ( 16.53943276465976808, -0.05219959533910856209, 78.74890960531436690 ) ) ;
#97740 = CARTESIAN_POINT ( 'NONE',  ( 24.93942350307308686, 7.769968609432599926, 171.2173313942149946 ) ) ;
#97741 = CARTESIAN_POINT ( 'NONE',  ( -19.03943276465977164, -0.05219959533935918106, 78.75109039468567573 ) ) ;
#97742 = CARTESIAN_POINT ( 'NONE',  ( -5.153800228976328057, -19.02544592524343514, 112.2905762719810099 ) ) ;
#97744 = EDGE_CURVE ( 'NONE', #198744, #154699, #148359, .T. ) ;
#97743 = CARTESIAN_POINT ( 'NONE',  ( -11.40812507854755609, 35.11059874428196537, -1.524999997268813301 ) ) ;
#97745 = CARTESIAN_POINT ( 'NONE',  ( 18.52568451169417685, 5.499999999999960920, 101.4787647167951548 ) ) ;
#97747 = CARTESIAN_POINT ( 'NONE',  ( -12.06949235617739369, -12.14591786802326823, 104.3760903946856899 ) ) ;
#97746 = CARTESIAN_POINT ( 'NONE',  ( -16.53943276465976808, -0.05219959533934237506, 23.75109039468567929 ) ) ;
#97748 = CARTESIAN_POINT ( 'NONE',  ( 0.05219959533936267826, -19.03943276465977164, 75.00109039468566152 ) ) ;
#97749 = CARTESIAN_POINT ( 'NONE',  ( -10.72451020669898014, 18.67979575497178502, 50.41557627198103120 ) ) ;
#97750 = CARTESIAN_POINT ( 'NONE',  ( 21.55341960407619695, -5.719274019375665929, 71.04275706135234714 ) ) ;
#97751 = CARTESIAN_POINT ( 'NONE',  ( -21.94381615377314176, -13.26253372808251108, 167.9278110240112767 ) ) ;
#97752 = CARTESIAN_POINT ( 'NONE',  ( -16.52544592524335698, -4.483927247898792601, 28.95942372801902209 ) ) ;
#97754 = CARTESIAN_POINT ( 'NONE',  ( 19.03943276465977164, -0.05219959533909143690, 93.74890960531435269 ) ) ;
#97753 = CARTESIAN_POINT ( 'NONE',  ( -0.05219959533909027116, -19.03943276465977164, 27.49890960531435624 ) ) ;
#97755 = CARTESIAN_POINT ( 'NONE',  ( 13.97604488694527802, 13.89961937509977652, 24.37390960531435624 ) ) ;
#97756 = CARTESIAN_POINT ( 'NONE',  ( -12.14591786802309592, -12.06949235617757132, 91.87390960531436690 ) ) ;
#97757 = SHAPE_DEFINITION_REPRESENTATION ( #185759, #8335 ) ;
#97758 = CARTESIAN_POINT ( 'NONE',  ( -19.03943276465977164, 0.05219959533909376836, 101.2489096053143669 ) ) ;
#97759 = EDGE_LOOP ( 'NONE', ( #191905, #172822, #30664, #187232 ) ) ;
#97760 = CARTESIAN_POINT ( 'NONE',  ( 13.97604488694548053, -13.89961937509957401, 110.6260903946856615 ) ) ;
#97761 = CARTESIAN_POINT ( 'NONE',  ( -10.81492255796078084, -18.62759615963271287, 72.08224293864769550 ) ) ;
#97762 = CARTESIAN_POINT ( 'NONE',  ( -16.51473224551069308, -9.474510206698971260, 46.66557627198102409 ) ) ;
#97764 = CARTESIAN_POINT ( 'NONE',  ( -21.52544592524343514, 5.823673210054127303, 111.0405762719810525 ) ) ;
#97763 = CARTESIAN_POINT ( 'NONE',  ( 9.474510206698729675, 16.51473224551082808, 72.08442372801900433 ) ) ;
#97765 = CARTESIAN_POINT ( 'NONE',  ( -5.049401038298153566, 19.05341960407611168, 75.20724293864769550 ) ) ;
#97766 = CARTESIAN_POINT ( 'NONE',  ( -0.05219959533909027116, -19.03943276465977164, 107.4989096053143527 ) ) ;
#97767 = ORIENTED_EDGE ( 'NONE', *, *, #93397, .T. ) ;
#97768 = CARTESIAN_POINT ( 'NONE',  ( 8.314922557961029526, -14.29746914071037800, 35.41775706135234003 ) ) ;
#97769 = CARTESIAN_POINT ( 'NONE',  ( -15.80617190586745835, -15.72974639402198527, 96.87390960531436690 ) ) ;
#97772 = CARTESIAN_POINT ( 'NONE',  ( 19.03943276465977164, 0.05219959533936151252, 56.25109039468566863 ) ) ;
#97771 = CARTESIAN_POINT ( 'NONE',  ( 0.05219959533909260263, 19.03943276465977164, 99.99890960531436690 ) ) ;
#97770 = CARTESIAN_POINT ( 'NONE',  ( -14.29746914071049879, 8.314922557960819915, 105.8322429386476955 ) ) ;
#97773 = CARTESIAN_POINT ( 'NONE',  ( 15.72974639402199770, -15.80617190586745480, 93.12390960531436690 ) ) ;
#97774 = CARTESIAN_POINT ( 'NONE',  ( -8.314922557960811034, -14.29746914071050412, 42.08224293864769550 ) ) ;
#97775 = CARTESIAN_POINT ( 'NONE',  ( 16.46253265017146816, 9.564922557961045513, 21.66775706135233648 ) ) ;
#97776 = CARTESIAN_POINT ( 'NONE',  ( -14.34966873604972548, 8.224510206698743886, 68.33442372801900433 ) ) ;
#97777 = CARTESIAN_POINT ( 'NONE',  ( 19.02544592524343514, -5.153800228976328945, 88.54057627198102409 ) ) ;
#97778 = CARTESIAN_POINT ( 'NONE',  ( 9.474510206698971260, -16.51473224551069308, 47.91557627198102409 ) ) ;
#97779 = CARTESIAN_POINT ( 'NONE',  ( -21.55341960407619339, 5.719274019375674811, 48.54275706135234714 ) ) ;
#97780 = CARTESIAN_POINT ( 'NONE',  ( 15.72974639402176855, 15.80617190586768217, 66.87609039468568994 ) ) ;
#97781 = CARTESIAN_POINT ( 'NONE',  ( -16.51473224551069308, -9.474510206698971260, 56.66557627198103120 ) ) ;
#97782 = CARTESIAN_POINT ( 'NONE',  ( 18.62759615963255655, 10.81492255796105972, 36.66775706135234714 ) ) ;
#97783 = CARTESIAN_POINT ( 'NONE',  ( -19.05341960407617563, 5.049401038297882671, 68.54275706135230450 ) ) ;
#97784 = CARTESIAN_POINT ( 'NONE',  ( -19.05341960407617563, 5.049401038297882671, 78.54275706135233293 ) ) ;
#97785 = CARTESIAN_POINT ( 'NONE',  ( -16.46253265017160317, 9.564922557960807481, 45.83224293864769550 ) ) ;
#97786 = CARTESIAN_POINT ( 'NONE',  ( -0.05219959533934338120, 16.53943276465976808, 92.50109039468567573 ) ) ;
#97787 = CARTESIAN_POINT ( 'NONE',  ( 13.97604488694527802, 13.89961937509977652, 49.37390960531434558 ) ) ;
#97788 = CARTESIAN_POINT ( 'NONE',  ( 9.474510206698971260, -16.51473224551069308, 22.91557627198102765 ) ) ;
#97789 = CARTESIAN_POINT ( 'NONE',  ( -19.05341960407611168, -5.049401038298163336, 101.4572429386476955 ) ) ;
#97790 = CARTESIAN_POINT ( 'NONE',  ( 9.474510206698971260, -16.51473224551069308, 32.91557627198102409 ) ) ;
#97791 = CARTESIAN_POINT ( 'NONE',  ( -10.72451020669898014, 18.67979575497178502, 90.41557627198103830 ) ) ;
#97792 = CARTESIAN_POINT ( 'NONE',  ( -16.55341960407617563, 4.379528057220093196, 78.54275706135236135 ) ) ;
#97793 = DIRECTION ( 'NONE',  ( 0.000000000000000000, 0.000000000000000000, -1.000000000000000000 ) ) ;
#97794 = CARTESIAN_POINT ( 'NONE',  ( 19.03943276465977164, 0.05219959533936151252, 26.25109039468566507 ) ) ;
#97795 = CARTESIAN_POINT ( 'NONE',  ( -19.03943276465977164, 0.05219959533909376836, 56.24890960531435979 ) ) ;
#97796 = CARTESIAN_POINT ( 'NONE',  ( -14.29746914071049879, 8.314922557960819915, 40.83224293864769550 ) ) ;
#97797 = CARTESIAN_POINT ( 'NONE',  ( 0.05219959533910956823, 16.53943276465976808, 74.99890960531435269 ) ) ;
#97798 = CARTESIAN_POINT ( 'NONE',  ( -16.51473224551069308, -9.474510206698971260, 96.66557627198102409 ) ) ;
#97799 = CARTESIAN_POINT ( 'NONE',  ( 13.97604488694527802, 13.89961937509977652, 79.37390960531435269 ) ) ;
#97800 = CARTESIAN_POINT ( 'NONE',  ( -15.80617190586768217, 15.72974639402176855, 48.12609039468568284 ) ) ;
#97801 = CARTESIAN_POINT ( 'NONE',  ( -13.89961937509977652, 13.97604488694528158, 90.62390960531432427 ) ) ;
#97802 = CARTESIAN_POINT ( 'NONE',  ( 0.05219959533937995610, -21.53943276465977519, 105.0010903946856757 ) ) ;
#97803 = CARTESIAN_POINT ( 'NONE',  ( 16.55341960407618274, -4.379528057220086978, 76.04275706135237556 ) ) ;
#97804 = CARTESIAN_POINT ( 'NONE',  ( -21.52544592524334988, -5.823673210054445271, 23.95942372801901143 ) ) ;
#97805 = CARTESIAN_POINT ( 'NONE',  ( 15.80617190586746368, 15.72974639402197994, 84.37390960531438111 ) ) ;
#97806 = CARTESIAN_POINT ( 'NONE',  ( 8.224510206698953496, -14.34966873604960469, 52.91557627198103830 ) ) ;
#97807 = CARTESIAN_POINT ( 'NONE',  ( -9.564922557960796823, -16.46253265017161027, 42.08224293864769550 ) ) ;
#97808 = CARTESIAN_POINT ( 'NONE',  ( -16.53943276465976808, 0.05219959533911058130, 71.24890960531435269 ) ) ;
#97809 = CARTESIAN_POINT ( 'NONE',  ( -15.72974639402197994, 15.80617190586746368, 30.62390960531436335 ) ) ;
#97810 = CARTESIAN_POINT ( 'NONE',  ( 16.51473224551083163, -9.474510206698727899, 35.83442372801899722 ) ) ;
#97811 = CARTESIAN_POINT ( 'NONE',  ( 16.52544592524342804, -4.483927247898539470, 103.5405762719810383 ) ) ;
#97812 = ORIENTED_EDGE ( 'NONE', *, *, #85603, .T. ) ;
#97813 = CARTESIAN_POINT ( 'NONE',  ( 12.06949235617739724, 12.14591786802326823, 61.87609039468568284 ) ) ;
#97814 = CARTESIAN_POINT ( 'NONE',  ( -19.02544592524342804, 5.153800228976336051, 71.04057627198099567 ) ) ;
#97815 = CARTESIAN_POINT ( 'NONE',  ( -37.99626262588766679, 2.428612866367529932E-14, -6.002157773949822861 ) ) ;
#97816 = CARTESIAN_POINT ( 'NONE',  ( -18.67979575497178146, -10.72451020669898902, 36.66557627198103120 ) ) ;
#97817 = CARTESIAN_POINT ( 'NONE',  ( 12.06949235617739724, 12.14591786802326823, 96.87609039468568994 ) ) ;
#97818 = CARTESIAN_POINT ( 'NONE',  ( 0.05219959533934541429, -16.53943276465976808, 20.00109039468568639 ) ) ;
#97819 = CARTESIAN_POINT ( 'NONE',  ( -21.53943276465977519, -0.05219959533937600094, 78.75109039468568994 ) ) ;
#97820 = CARTESIAN_POINT ( 'NONE',  ( -19.03943276465977164, 0.05219959533909376836, 76.24890960531435269 ) ) ;
#97821 = CARTESIAN_POINT ( 'NONE',  ( 18.62759615963271287, -10.81492255796078972, 108.3322429386477097 ) ) ;
#97822 = CARTESIAN_POINT ( 'NONE',  ( 4.483927247898790824, -16.52544592524335698, 55.20942372801902565 ) ) ;
#97823 = CARTESIAN_POINT ( 'NONE',  ( 4.379528057220339221, -16.55341960407611168, 112.7072429386476955 ) ) ;
#97824 = CARTESIAN_POINT ( 'NONE',  ( 0.05219959533934541429, -16.53943276465976808, 20.00109039468568639 ) ) ;
#97825 = CARTESIAN_POINT ( 'NONE',  ( 5.049401038297881783, 19.05341960407617563, 82.29275706135229029 ) ) ;
#97826 = EDGE_CURVE ( 'NONE', #53699, #123077, #109237, .T. ) ;
#97827 = CARTESIAN_POINT ( 'NONE',  ( 0.05219959533907565091, 21.53943276465977519, 74.99890960531435269 ) ) ;
#97828 = CARTESIAN_POINT ( 'NONE',  ( 19.02544592524334988, 5.153800228976608722, 56.45942372801898301 ) ) ;
#97829 = CARTESIAN_POINT ( 'NONE',  ( 18.96320343559671073, 23.46320343559620270, 8.889087296526001936 ) ) ;
#97830 = CARTESIAN_POINT ( 'NONE',  ( 0.05219959533907565091, 21.53943276465977519, 109.9989096053143527 ) ) ;
#97831 = DIRECTION ( 'NONE',  ( 0.000000000000000000, 0.000000000000000000, 1.000000000000000000 ) ) ;
#97832 = CARTESIAN_POINT ( 'NONE',  ( 19.03943276465977164, -0.05219959533909143690, 78.74890960531436690 ) ) ;
#97833 = CARTESIAN_POINT ( 'NONE',  ( 26.46959431505287341, -27.26463967846483527, -11.00411086000093519 ) ) ;
#97834 = CARTESIAN_POINT ( 'NONE',  ( 12.06949235617739724, 12.14591786802326823, 36.87609039468568994 ) ) ;
#97835 = CARTESIAN_POINT ( 'NONE',  ( 37.06950394710834473, -4.940869137700747871, 42.55762898535583361 ) ) ;
#97837 = CARTESIAN_POINT ( 'NONE',  ( 16.53943276465976808, -0.05219959533910856209, 63.74890960531435979 ) ) ;
#97836 = CARTESIAN_POINT ( 'NONE',  ( 18.67979575497178502, 10.72451020669898547, 104.1655762719810241 ) ) ;
#97838 = CARTESIAN_POINT ( 'NONE',  ( 19.03943276465977164, -0.05219959533909143690, 63.74890960531435979 ) ) ;
#97839 = CARTESIAN_POINT ( 'NONE',  ( -21.55341960407619339, 5.719274019375674811, 93.54275706135234714 ) ) ;
#97841 = CARTESIAN_POINT ( 'NONE',  ( 5.153800228976615827, -19.02544592524334988, 40.20942372801898301 ) ) ;
#97840 = CARTESIAN_POINT ( 'NONE',  ( -4.483927247898782831, 16.52544592524335698, 32.70942372801900433 ) ) ;
#97842 = CARTESIAN_POINT ( 'NONE',  ( 15.72974639402176855, 15.80617190586768217, 46.87609039468568994 ) ) ;
#97843 = CARTESIAN_POINT ( 'NONE',  ( 21.55341960407610458, 5.719274019375980345, 63.95724293864770260 ) ) ;
#97844 = CARTESIAN_POINT ( 'NONE',  ( -19.05341960407617563, 5.049401038297882671, 113.5427570613523471 ) ) ;
#97845 = CARTESIAN_POINT ( 'NONE',  ( -9.564922557960796823, -16.46253265017161027, 62.08224293864769550 ) ) ;
#97846 = CARTESIAN_POINT ( 'NONE',  ( 16.51473224551083163, -9.474510206698727899, 65.83442372801900433 ) ) ;
#97847 = CARTESIAN_POINT ( 'NONE',  ( -0.05219959533937732626, 21.53943276465977519, 82.50109039468568994 ) ) ;
#97848 = CARTESIAN_POINT ( 'NONE',  ( -9.564922557961040184, 16.46253265017147172, 72.91775706135233293 ) ) ;
#97849 = CARTESIAN_POINT ( 'NONE',  ( -9.564922557960796823, -16.46253265017161027, 32.08224293864769550 ) ) ;
#97850 = CARTESIAN_POINT ( 'NONE',  ( 10.81492255796078972, 18.62759615963270932, 54.58224293864769550 ) ) ;
#97851 = CARTESIAN_POINT ( 'NONE',  ( -16.53943276465976808, 0.05219959533911058130, 66.24890960531436690 ) ) ;
#97852 = CYLINDRICAL_SURFACE ( 'NONE', #89340, 1.499999999999996225 ) ;
#97853 = CARTESIAN_POINT ( 'NONE',  ( -19.05341960407617563, 5.049401038297882671, 33.54275706135231871 ) ) ;
#97854 = CARTESIAN_POINT ( 'NONE',  ( -4.379528057220086978, -16.55341960407618274, 84.79275706135234714 ) ) ;
#97855 = CARTESIAN_POINT ( 'NONE',  ( 14.29746914071049879, -8.314922557960816363, 48.33224293864770260 ) ) ;
#97856 = CARTESIAN_POINT ( 'NONE',  ( -18.67979575497193778, 10.72451020669871902, 88.33442372801901854 ) ) ;
#97857 = CARTESIAN_POINT ( 'NONE',  ( -5.823673210054431948, 21.52544592524334988, 82.70942372801900433 ) ) ;
#97858 = CARTESIAN_POINT ( 'NONE',  ( 5.823673210054125526, 21.52544592524343514, 89.79057627198103830 ) ) ;
#97859 = CARTESIAN_POINT ( 'NONE',  ( -5.153800228976328057, -19.02544592524343514, 47.29057627198102409 ) ) ;
#97860 = CARTESIAN_POINT ( 'NONE',  ( 5.719274019375673035, 21.55341960407619339, 52.29275706135236135 ) ) ;
#97861 = CARTESIAN_POINT ( 'NONE',  ( 9.474510206698971260, -16.51473224551069308, 37.91557627198102409 ) ) ;
#97862 = CARTESIAN_POINT ( 'NONE',  ( -9.474510206698964154, 16.51473224551069663, 70.41557627198102409 ) ) ;
#97863 = CARTESIAN_POINT ( 'NONE',  ( 8.314922557960818139, 14.29746914071049879, 109.5822429386476955 ) ) ;
#97864 = CARTESIAN_POINT ( 'NONE',  ( 13.89961937509977652, -13.97604488694527269, 98.12390960531433848 ) ) ;
#97865 = CARTESIAN_POINT ( 'NONE',  ( 16.55341960407611168, 4.379528057220329451, 48.95724293864770971 ) ) ;
#97866 = CARTESIAN_POINT ( 'NONE',  ( 14.34966873604960469, 8.224510206698951720, 109.1655762719810383 ) ) ;
#97867 = CARTESIAN_POINT ( 'NONE',  ( 21.55341960407610458, 5.719274019375980345, 83.95724293864770971 ) ) ;
#97868 = CARTESIAN_POINT ( 'NONE',  ( 15.72974639402176855, 15.80617190586768217, 36.87609039468568994 ) ) ;
#97869 = DIRECTION ( 'NONE',  ( -1.000000000000000000, 0.000000000000000000, 0.000000000000000000 ) ) ;
#97870 = CARTESIAN_POINT ( 'NONE',  ( -4.483927247898782831, 16.52544592524335698, 42.70942372801901854 ) ) ;
#97871 = CARTESIAN_POINT ( 'NONE',  ( 10.81492255796078972, 18.62759615963270932, 79.58224293864769550 ) ) ;
#97872 = CARTESIAN_POINT ( 'NONE',  ( 18.62759615963255655, 10.81492255796105972, 101.6677570613523613 ) ) ;
#97873 = CARTESIAN_POINT ( 'NONE',  ( 9.564922557960805705, 16.46253265017160317, 94.58224293864769550 ) ) ;
#97874 = CARTESIAN_POINT ( 'NONE',  ( 21.53943276465977519, 0.05219959533937863772, 31.25109039468568639 ) ) ;
#97875 = CIRCLE ( 'NONE', #52723, 2.699999999999993960 ) ;
#97876 = CARTESIAN_POINT ( 'NONE',  ( 5.719274019375991003, -21.55341960407610458, 32.70724293864770260 ) ) ;
#97877 = CARTESIAN_POINT ( 'NONE',  ( 14.34966873604972726, -8.224510206698740333, 100.8344237280190185 ) ) ;
#97879 = CARTESIAN_POINT ( 'NONE',  ( -18.62759615963255300, -10.81492255796106328, 79.16775706135234714 ) ) ;
#97878 = CARTESIAN_POINT ( 'NONE',  ( -10.81492255796105439, 18.62759615963255655, 47.91775706135234714 ) ) ;
#97880 = CARTESIAN_POINT ( 'NONE',  ( 15.80617190586769283, -15.72974639402175789, 110.6260903946857042 ) ) ;
#97881 = CARTESIAN_POINT ( 'NONE',  ( -16.52544592524335698, -4.483927247898792601, 78.95942372801901854 ) ) ;
#97882 = CARTESIAN_POINT ( 'NONE',  ( -21.52544592524334988, -5.823673210054445271, 43.95942372801902565 ) ) ;
#97883 = CARTESIAN_POINT ( 'NONE',  ( 16.46253265017160672, -9.564922557960803928, 28.33224293864769550 ) ) ;
#97884 = CARTESIAN_POINT ( 'NONE',  ( -0.05219959533937732626, 21.53943276465977519, 97.50109039468567573 ) ) ;
#97885 = CARTESIAN_POINT ( 'NONE',  ( -9.474510206698964154, 16.51473224551069663, 100.4155762719810241 ) ) ;
#97886 = CARTESIAN_POINT ( 'NONE',  ( 15.72974639402199770, -15.80617190586745480, 103.1239096053143811 ) ) ;
#97888 = CARTESIAN_POINT ( 'NONE',  ( 21.53943276465977519, -0.05219959533907433946, 68.74890960531435269 ) ) ;
#97887 = DIRECTION ( 'NONE',  ( -0.000000000000000000, 1.000000000000000000, -0.000000000000000000 ) ) ;
#97890 = CARTESIAN_POINT ( 'NONE',  ( 16.55341960407611168, 4.379528057220329451, 48.95724293864770971 ) ) ;
#97889 = CARTESIAN_POINT ( 'NONE',  ( 14.29746914071037800, 8.314922557961029526, 56.66775706135235424 ) ) ;
#97891 = LINE ( 'NONE', #51421, #69212 ) ;
#97892 = CARTESIAN_POINT ( 'NONE',  ( 16.51473224551083163, -9.474510206698727899, 90.83442372801900433 ) ) ;
#97893 = CARTESIAN_POINT ( 'NONE',  ( -1.218621689577036982, -14.30340603398754418, -62.33590500446654659 ) ) ;
#97894 = ADVANCED_FACE ( 'NONE', ( #177771 ), #176775, .F. ) ;
#97895 = CARTESIAN_POINT ( 'NONE',  ( -12.14591786802326823, 12.06949235617739902, 28.12609039468568284 ) ) ;
#97896 = CARTESIAN_POINT ( 'NONE',  ( 5.719274019375991003, -21.55341960407610458, 97.70724293864772392 ) ) ;
#97897 = CARTESIAN_POINT ( 'NONE',  ( -18.62759615963270932, 10.81492255796079327, 75.83224293864769550 ) ) ;
#97898 = CARTESIAN_POINT ( 'NONE',  ( 19.05341960407611168, 5.049401038298154454, 113.9572429386477097 ) ) ;
#97899 = CARTESIAN_POINT ( 'NONE',  ( 16.53943276465976808, 0.05219959533934440121, 41.25109039468568284 ) ) ;
#97900 = CARTESIAN_POINT ( 'NONE',  ( -13.89961937509977652, 13.97604488694528158, 60.62390960531436690 ) ) ;
#97902 = CARTESIAN_POINT ( 'NONE',  ( 0.05219959533936267826, -19.03943276465977164, 100.0010903946856757 ) ) ;
#97901 = CARTESIAN_POINT ( 'NONE',  ( 0.05219959533937995610, -21.53943276465977519, 35.00109039468568284 ) ) ;
#97903 = CARTESIAN_POINT ( 'NONE',  ( -9.474510206698964154, 16.51473224551069663, 110.4155762719810383 ) ) ;
#97904 = CARTESIAN_POINT ( 'NONE',  ( -19.03943276465977164, 0.05219959533909376836, 81.24890960531436690 ) ) ;
#97905 = CARTESIAN_POINT ( 'NONE',  ( -10.81492255796078084, -18.62759615963271287, 92.08224293864769550 ) ) ;
#97906 = CARTESIAN_POINT ( 'NONE',  ( -0.05219959533909027116, -19.03943276465977164, 57.49890960531435979 ) ) ;
#97907 = CARTESIAN_POINT ( 'NONE',  ( -6.020228577223754586E-15, 39.95556452105416412, -0.4999999999999998890 ) ) ;
#97908 = CARTESIAN_POINT ( 'NONE',  ( -14.29746914071049879, 8.314922557960819915, 70.83224293864770971 ) ) ;
#97909 = CARTESIAN_POINT ( 'NONE',  ( -19.05341960407611168, -5.049401038298163336, 101.4572429386476955 ) ) ;
#97910 = CARTESIAN_POINT ( 'NONE',  ( -28.90000000000004121, 0.1280799071100958975, -52.65483682830181777 ) ) ;
#97911 = CARTESIAN_POINT ( 'NONE',  ( 5.049401038297881783, 19.05341960407617563, 72.29275706135234714 ) ) ;
#97912 = CARTESIAN_POINT ( 'NONE',  ( 10.72451020669898902, -18.67979575497178502, 87.91557627198103830 ) ) ;
#97913 = CARTESIAN_POINT ( 'NONE',  ( 19.05341960407617918, -5.049401038297876454, 56.04275706135234714 ) ) ;
#97914 = CARTESIAN_POINT ( 'NONE',  ( 16.46253265017160672, -9.564922557960803928, 113.3322429386476955 ) ) ;
#97915 = DIRECTION ( 'NONE',  ( -0.000000000000000000, -0.000000000000000000, 1.000000000000000000 ) ) ;
#97916 = CARTESIAN_POINT ( 'NONE',  ( -21.53943276465977519, 0.05219959533907696930, 51.24890960531436690 ) ) ;
#97917 = CARTESIAN_POINT ( 'NONE',  ( 5.153800228976335163, 19.02544592524342804, 84.79057627198099567 ) ) ;
#97918 = CARTESIAN_POINT ( 'NONE',  ( 0.05219959533937995610, -21.53943276465977519, 80.00109039468568994 ) ) ;
#97919 = CARTESIAN_POINT ( 'NONE',  ( -19.02544592524342804, 5.153800228976336051, 41.04057627198103120 ) ) ;
#97920 = EDGE_CURVE ( 'NONE', #86773, #2480, #7894, .T. ) ;
#97921 = CARTESIAN_POINT ( 'NONE',  ( 16.55341960407611168, 4.379528057220329451, 68.95724293864769550 ) ) ;
#97922 = CARTESIAN_POINT ( 'NONE',  ( -16.52544592524335698, -4.483927247898792601, 28.95942372801902209 ) ) ;
#97923 = CARTESIAN_POINT ( 'NONE',  ( 18.67979575497194134, -10.72451020669871369, 60.83442372801901854 ) ) ;
#97924 = VERTEX_POINT ( 'NONE', #39241 ) ;
#97925 = CARTESIAN_POINT ( 'NONE',  ( -16.46253265017146816, -9.564922557961047289, 24.16775706135233648 ) ) ;
#97926 = CARTESIAN_POINT ( 'NONE',  ( 0.05219959533936267826, -19.03943276465977164, 75.00109039468566152 ) ) ;
#97927 = DIRECTION ( 'NONE',  ( -0.000000000000000000, 1.000000000000000000, 0.000000000000000000 ) ) ;
#97928 = CARTESIAN_POINT ( 'NONE',  ( 18.67979575497194134, -10.72451020669871369, 20.83442372801901143 ) ) ;
#97929 = CARTESIAN_POINT ( 'NONE',  ( -19.34837522270366250, -5.499999999999742428, 45.86337684832577111 ) ) ;
#97930 = CARTESIAN_POINT ( 'NONE',  ( 9.564922557961047289, -16.46253265017146816, 25.41775706135234003 ) ) ;
#97931 = CARTESIAN_POINT ( 'NONE',  ( -9.474510206698964154, 16.51473224551069663, 55.41557627198103120 ) ) ;
#97932 = CARTESIAN_POINT ( 'NONE',  ( -9.474510206698720793, -16.51473224551083518, 29.58442372801900433 ) ) ;
#97933 = CARTESIAN_POINT ( 'NONE',  ( 8.224510206698742110, 14.34966873604972548, 102.0844237280190185 ) ) ;
#97935 = CARTESIAN_POINT ( 'NONE',  ( -15.80617190586768217, 15.72974639402176855, 68.12609039468567573 ) ) ;
#97934 = CARTESIAN_POINT ( 'NONE',  ( 9.474510206698971260, -16.51473224551069308, 97.91557627198102409 ) ) ;
#97936 = CARTESIAN_POINT ( 'NONE',  ( 29.86685920354754842, -21.69954338932559068, -7.824999997268813345 ) ) ;
#97937 = CARTESIAN_POINT ( 'NONE',  ( -33.70206089117255743, 4.379927107397421082, 98.34612363080974262 ) ) ;
#97938 = CARTESIAN_POINT ( 'NONE',  ( -5.823673210054431948, 21.52544592524334988, 87.70942372801901854 ) ) ;
#97939 = CARTESIAN_POINT ( 'NONE',  ( 21.53943276465977519, 0.05219959533937863772, 106.2510903946856757 ) ) ;
#97940 = CIRCLE ( 'NONE', #84974, 216.0437394197456911 ) ;
#97941 = CYLINDRICAL_SURFACE ( 'NONE', #25158, 10.00000000000000000 ) ;
#97942 = CARTESIAN_POINT ( 'NONE',  ( -0.05219959533909027116, -19.03943276465977164, 102.4989096053143669 ) ) ;
#97943 = CARTESIAN_POINT ( 'NONE',  ( 16.51473224551083163, -9.474510206698727899, 20.83442372801899722 ) ) ;
#97944 = SPHERICAL_SURFACE ( 'NONE', #50200, 2.000000000000000000 ) ;
#97945 = CARTESIAN_POINT ( 'NONE',  ( 19.02544592524343514, -5.153800228976328945, 38.54057627198103120 ) ) ;
#97946 = CARTESIAN_POINT ( 'NONE',  ( -18.67979575497178146, -10.72451020669898902, 61.66557627198103120 ) ) ;
#97947 = CARTESIAN_POINT ( 'NONE',  ( 14.29746914071049879, -8.314922557960816363, 23.33224293864769194 ) ) ;
#97949 = CARTESIAN_POINT ( 'NONE',  ( -19.02544592524342804, 5.153800228976336051, 81.04057627198103830 ) ) ;
#97948 = CARTESIAN_POINT ( 'NONE',  ( -12.14591786802309592, -12.06949235617757132, 91.87390960531436690 ) ) ;
#97950 = CARTESIAN_POINT ( 'NONE',  ( 0.05219959533937995610, -21.53943276465977519, 110.0010903946856757 ) ) ;
#97951 = CARTESIAN_POINT ( 'NONE',  ( 16.46253265017160672, -9.564922557960803928, 43.33224293864769550 ) ) ;
#97952 = CARTESIAN_POINT ( 'NONE',  ( -14.29746914071049879, 8.314922557960819915, 105.8322429386476955 ) ) ;
#97953 = CARTESIAN_POINT ( 'NONE',  ( 5.823673210054444382, -21.52544592524334988, 55.20942372801902565 ) ) ;
#97954 = CARTESIAN_POINT ( 'NONE',  ( 5.719274019375991003, -21.55341960407610458, 92.70724293864770971 ) ) ;
#97955 = CARTESIAN_POINT ( 'NONE',  ( 5.049401038297881783, 19.05341960407617563, 57.29275706135231871 ) ) ;
#97956 = CARTESIAN_POINT ( 'NONE',  ( -17.38101740422981933, -36.03988305276040194, -12.45567487529643635 ) ) ;
#97957 = CARTESIAN_POINT ( 'NONE',  ( -19.02544592524342804, 5.153800228976336051, 116.0405762719810383 ) ) ;
#97958 = CARTESIAN_POINT ( 'NONE',  ( 16.52544592524342804, -4.483927247898539470, 78.54057627198103830 ) ) ;
#97959 = CARTESIAN_POINT ( 'NONE',  ( 16.51473224551083163, -9.474510206698727899, 50.83442372801899722 ) ) ;
#97960 = CARTESIAN_POINT ( 'NONE',  ( 13.97604488694527802, 13.89961937509977652, 59.37390960531434558 ) ) ;
#97961 = CARTESIAN_POINT ( 'NONE',  ( -14.29746914071049879, 8.314922557960819915, 50.83224293864770971 ) ) ;
#97962 = CARTESIAN_POINT ( 'NONE',  ( -5.049401038297874678, -19.05341960407617918, 84.79275706135233293 ) ) ;
#97963 = CARTESIAN_POINT ( 'NONE',  ( -18.22780087662122028, 5.500000000000031086, 83.51540105326107266 ) ) ;
#97964 = CARTESIAN_POINT ( 'NONE',  ( -10.81492255796078084, -18.62759615963271287, 32.08224293864769550 ) ) ;
#97965 = CARTESIAN_POINT ( 'NONE',  ( -16.53943276465976808, 0.05219959533911058130, 106.2489096053143811 ) ) ;
#97966 = LINE ( 'NONE', #37318, #58162 ) ;
#97968 = CARTESIAN_POINT ( 'NONE',  ( -0.05219959533907301413, -21.53943276465977519, 62.49890960531436690 ) ) ;
#97967 = CARTESIAN_POINT ( 'NONE',  ( 0.05219959533909260263, 19.03943276465977164, 59.99890960531436690 ) ) ;
#97969 = CARTESIAN_POINT ( 'NONE',  ( -16.46253265017160317, 9.564922557960807481, 25.83224293864769194 ) ) ;
#97971 = CARTESIAN_POINT ( 'NONE',  ( 16.51473224551069308, 9.474510206698969483, 59.16557627198102409 ) ) ;
#97970 = CARTESIAN_POINT ( 'NONE',  ( -16.52544592524335698, -4.483927247898792601, 78.95942372801901854 ) ) ;
#97972 = CARTESIAN_POINT ( 'NONE',  ( 0.05219959533936267826, -19.03943276465977164, 60.00109039468566863 ) ) ;
#97973 = CARTESIAN_POINT ( 'NONE',  ( 18.62759615963255655, 10.81492255796105972, 71.66775706135234714 ) ) ;
#97974 = CARTESIAN_POINT ( 'NONE',  ( 18.62759615963271287, -10.81492255796078972, 43.33224293864769550 ) ) ;
#97975 = CARTESIAN_POINT ( 'NONE',  ( 16.51473224551069308, 9.474510206698969483, 24.16557627198102765 ) ) ;
#97976 = CARTESIAN_POINT ( 'NONE',  ( 16.55341960407618274, -4.379528057220086978, 86.04275706135236135 ) ) ;
#97977 = CARTESIAN_POINT ( 'NONE',  ( 5.153800228976615827, -19.02544592524334988, 100.2094237280190043 ) ) ;
#97978 = CARTESIAN_POINT ( 'NONE',  ( -13.97604488694527625, -13.89961937509977652, 26.87390960531434558 ) ) ;
#97980 = CARTESIAN_POINT ( 'NONE',  ( -0.05219959533907301413, -21.53943276465977519, 57.49890960531435979 ) ) ;
#97979 = DIRECTION ( 'NONE',  ( -0.000000000000000000, -0.000000000000000000, 1.000000000000000000 ) ) ;
#97981 = CARTESIAN_POINT ( 'NONE',  ( 0.05219959533937995610, -21.53943276465977519, 100.0010903946857042 ) ) ;
#97982 = CARTESIAN_POINT ( 'NONE',  ( -8.314922557960811034, -14.29746914071050412, 42.08224293864769550 ) ) ;
#97983 = CARTESIAN_POINT ( 'NONE',  ( -16.53943276465976808, 0.05219959533911058130, 61.24890960531435979 ) ) ;
#97984 = CARTESIAN_POINT ( 'NONE',  ( 21.55341960407610458, 5.719274019375980345, 78.95724293864769550 ) ) ;
#97985 = CARTESIAN_POINT ( 'NONE',  ( 10.81492255796078972, 18.62759615963270932, 84.58224293864769550 ) ) ;
#97986 = DIRECTION ( 'NONE',  ( 0.000000000000000000, 0.000000000000000000, 1.000000000000000000 ) ) ;
#97987 = CARTESIAN_POINT ( 'NONE',  ( -15.72974639402197994, 15.80617190586746368, 30.62390960531436335 ) ) ;
#97988 = CARTESIAN_POINT ( 'NONE',  ( -8.224510206698735004, -14.34966873604973081, 69.58442372801900433 ) ) ;
#97989 = CARTESIAN_POINT ( 'NONE',  ( 8.314922557960818139, 14.29746914071049879, 84.58224293864769550 ) ) ;
#97990 = CARTESIAN_POINT ( 'NONE',  ( 16.51473224551069308, 9.474510206698969483, 34.16557627198102409 ) ) ;
#97991 = DIRECTION ( 'NONE',  ( 0.07151044867601324961, 0.9974398506828144884, 0.000000000000000000 ) ) ;
#97992 = EDGE_LOOP ( 'NONE', ( #6445, #189868, #128321, #34761, #37161 ) ) ;
#97993 = CARTESIAN_POINT ( 'NONE',  ( -16.53943276465976808, -0.05219959533934237506, 98.75109039468568994 ) ) ;
#97994 = CARTESIAN_POINT ( 'NONE',  ( 18.62759615963271287, -10.81492255796078972, 113.3322429386476955 ) ) ;
#97995 = CARTESIAN_POINT ( 'NONE',  ( 16.46253265017160672, -9.564922557960803928, 88.33224293864769550 ) ) ;
#97996 = CARTESIAN_POINT ( 'NONE',  ( 0.05219959533937995610, -21.53943276465977519, 50.00109039468568994 ) ) ;
#97997 = CARTESIAN_POINT ( 'NONE',  ( -13.89961937509977652, 13.97604488694528158, 105.6239096053143527 ) ) ;
#97998 = CARTESIAN_POINT ( 'NONE',  ( -18.22780087662126647, -5.499999999999827693, 48.98236817873107185 ) ) ;
#97999 = ORIENTED_EDGE ( 'NONE', *, *, #125462, .F. ) ;
#98000 = CARTESIAN_POINT ( 'NONE',  ( -10.72451020669870658, -18.67979575497194134, 44.58442372801901854 ) ) ;
#98002 = CARTESIAN_POINT ( 'NONE',  ( -5.153800228976328057, -19.02544592524343514, 102.2905762719810383 ) ) ;
#98001 = CARTESIAN_POINT ( 'NONE',  ( -9.474510206698964154, 16.51473224551069663, 40.41557627198103120 ) ) ;
#98003 = CARTESIAN_POINT ( 'NONE',  ( 5.049401038297881783, 19.05341960407617563, 52.29275706135234003 ) ) ;
#98004 = CARTESIAN_POINT ( 'NONE',  ( 18.62759615963255655, 10.81492255796105972, 31.66775706135234358 ) ) ;
#98005 = CARTESIAN_POINT ( 'NONE',  ( -19.03943276465977164, -0.05219959533935918106, 63.75109039468566863 ) ) ;
#98006 = CARTESIAN_POINT ( 'NONE',  ( -14.34966873604972548, 8.224510206698743886, 93.33442372801901854 ) ) ;
#98007 = CARTESIAN_POINT ( 'NONE',  ( -0.05219959533936034679, 19.03943276465977164, 57.50109039468566863 ) ) ;
#98008 = CARTESIAN_POINT ( 'NONE',  ( 4.483927247898790824, -16.52544592524335698, 110.2094237280190185 ) ) ;
#98009 = CARTESIAN_POINT ( 'NONE',  ( 18.09867054820430710, 5.500000000000000000, 86.48393025253589883 ) ) ;
#98010 = CARTESIAN_POINT ( 'NONE',  ( -9.564922557960796823, -16.46253265017161027, 82.08224293864768129 ) ) ;
#98011 = CARTESIAN_POINT ( 'NONE',  ( 21.52544592524334988, 5.823673210054432836, 86.45942372801901854 ) ) ;
#98012 = CARTESIAN_POINT ( 'NONE',  ( -5.719274019375665041, -21.55341960407619695, 109.7927570613523613 ) ) ;
#98013 = DIRECTION ( 'NONE',  ( 0.7071067811865414665, -0.7071067811865536790, -0.000000000000000000 ) ) ;
#98014 = CARTESIAN_POINT ( 'NONE',  ( 0.05219959533909260263, 19.03943276465977164, 99.99890960531436690 ) ) ;
#98015 = CARTESIAN_POINT ( 'NONE',  ( -5.719274019375665041, -21.55341960407619695, 69.79275706135234714 ) ) ;
#98016 = CARTESIAN_POINT ( 'NONE',  ( 5.049401038297881783, 19.05341960407617563, 112.2927570613523471 ) ) ;
#98017 = CARTESIAN_POINT ( 'NONE',  ( -19.03943276465977164, 0.05219959533909376836, 81.24890960531436690 ) ) ;
#98018 = CARTESIAN_POINT ( 'NONE',  ( 5.823673210054125526, 21.52544592524343514, 34.79057627198103120 ) ) ;
#98019 = VECTOR ( 'NONE', #93558, 1000.000000000000000 ) ;
#98020 = CARTESIAN_POINT ( 'NONE',  ( -19.03943276465977164, 0.05219959533909376836, 96.24890960531436690 ) ) ;
#98021 = CARTESIAN_POINT ( 'NONE',  ( 3.766062262543149401E-15, -39.95556452105413570, -9.249999994537628112 ) ) ;
#98022 = CARTESIAN_POINT ( 'NONE',  ( -9.474510206698964154, 16.51473224551069663, 75.41557627198103830 ) ) ;
#98023 = CARTESIAN_POINT ( 'NONE',  ( -16.46253265017160317, 9.564922557960807481, 65.83224293864769550 ) ) ;
#98024 = CARTESIAN_POINT ( 'NONE',  ( -4.379528057220086978, -16.55341960407618274, 109.7927570613523613 ) ) ;
#98025 = CARTESIAN_POINT ( 'NONE',  ( -19.39720447994796260, -5.499999999999982236, 39.66317477297176453 ) ) ;
#98026 = CARTESIAN_POINT ( 'NONE',  ( -9.564922557961040184, 16.46253265017147172, 72.91775706135233293 ) ) ;
#98027 = CARTESIAN_POINT ( 'NONE',  ( 16.51473224551069308, 9.474510206698969483, 89.16557627198103830 ) ) ;
#98028 = CARTESIAN_POINT ( 'NONE',  ( 4.483927247898545687, 16.52544592524342804, 84.79057627198102409 ) ) ;
#98029 = CARTESIAN_POINT ( 'NONE',  ( -0.05219959533907301413, -21.53943276465977519, 52.49890960531435979 ) ) ;
#98030 = CARTESIAN_POINT ( 'NONE',  ( 18.67979575497178502, 10.72451020669898547, 24.16557627198103120 ) ) ;
#98031 = CARTESIAN_POINT ( 'NONE',  ( -14.29746914071049879, 8.314922557960819915, 105.8322429386476955 ) ) ;
#98032 = DIRECTION ( 'NONE',  ( 0.1736481776669307198, 0.000000000000000000, -0.9848077530122080203 ) ) ;
#98033 = CARTESIAN_POINT ( 'NONE',  ( 0.05219959533936267826, -19.03943276465977164, 50.00109039468566863 ) ) ;
#98034 = CARTESIAN_POINT ( 'NONE',  ( 14.34966873604960469, 8.224510206698951720, 29.16557627198103120 ) ) ;
#98035 = CARTESIAN_POINT ( 'NONE',  ( -19.03943276465977164, 0.05219959533909376836, 101.2489096053143669 ) ) ;
#98036 = CARTESIAN_POINT ( 'NONE',  ( 5.719274019375673035, 21.55341960407619339, 62.29275706135236845 ) ) ;
#98037 = CARTESIAN_POINT ( 'NONE',  ( 15.72974639402199770, -15.80617190586745480, 63.12390960531435979 ) ) ;
#98038 = CARTESIAN_POINT ( 'NONE',  ( -18.67979575497193778, 10.72451020669871902, 43.33442372801901143 ) ) ;
#98039 = CARTESIAN_POINT ( 'NONE',  ( -21.53943276465977519, 0.05219959533907696930, 101.2489096053143669 ) ) ;
#98040 = CARTESIAN_POINT ( 'NONE',  ( 21.55341960407619695, -5.719274019375665929, 36.04275706135234714 ) ) ;
#98041 = CARTESIAN_POINT ( 'NONE',  ( -12.14591786802309592, -12.06949235617757132, 111.8739096053143669 ) ) ;
#98042 = CARTESIAN_POINT ( 'NONE',  ( 9.474510206698729675, 16.51473224551082808, 77.08442372801900433 ) ) ;
#98043 = CARTESIAN_POINT ( 'NONE',  ( 13.97604488694527802, 13.89961937509977652, 39.37390960531435269 ) ) ;
#98044 = CARTESIAN_POINT ( 'NONE',  ( -0.05219959533910754901, -16.53943276465976808, 102.4989096053143811 ) ) ;
#98045 = CARTESIAN_POINT ( 'NONE',  ( -19.02544592524342804, 5.153800228976336051, 111.0405762719810099 ) ) ;
#98046 = CARTESIAN_POINT ( 'NONE',  ( 14.29746914071049879, -8.314922557960816363, 38.33224293864768839 ) ) ;
#98047 = CARTESIAN_POINT ( 'NONE',  ( -14.29746914071037622, -8.314922557961029526, 109.1677570613523613 ) ) ;
#98048 = CARTESIAN_POINT ( 'NONE',  ( -19.05341960407611168, -5.049401038298163336, 51.45724293864770260 ) ) ;
#98049 = CARTESIAN_POINT ( 'NONE',  ( -8.224510206698948167, 14.34966873604960824, 115.4155762719810241 ) ) ;
#98050 = CARTESIAN_POINT ( 'NONE',  ( -19.05341960407617563, 5.049401038297882671, 28.54275706135232937 ) ) ;
#98052 = CARTESIAN_POINT ( 'NONE',  ( 12.14591786802309770, 12.06949235617756955, 39.37390960531436690 ) ) ;
#98051 = DIRECTION ( 'NONE',  ( -0.9930308165857338887, 0.1178549842436489581, 0.000000000000000000 ) ) ;
#98053 = CARTESIAN_POINT ( 'NONE',  ( 5.719274019375673035, 21.55341960407619339, 52.29275706135236135 ) ) ;
#98054 = CARTESIAN_POINT ( 'NONE',  ( 22.32889156691206267, -5.550768075871988394, 173.1969276168243255 ) ) ;
#98055 = CARTESIAN_POINT ( 'NONE',  ( 0.05219959533934541429, -16.53943276465976808, 55.00109039468568284 ) ) ;
#98056 = CARTESIAN_POINT ( 'NONE',  ( -8.314922557960811034, -14.29746914071050412, 32.08224293864769550 ) ) ;
#98057 = CARTESIAN_POINT ( 'NONE',  ( 12.06949235617739724, 12.14591786802326823, 101.8760903946857042 ) ) ;
#98058 = CARTESIAN_POINT ( 'NONE',  ( -0.05219959533934338120, 16.53943276465976808, 32.50109039468568284 ) ) ;
#98059 = EDGE_CURVE ( 'NONE', #120648, #109472, #63406, .T. ) ;
#98060 = CARTESIAN_POINT ( 'NONE',  ( -13.97604488694527625, -13.89961937509977652, 41.87390960531435979 ) ) ;
#98061 = CARTESIAN_POINT ( 'NONE',  ( -5.049401038298153566, 19.05341960407611168, 30.20724293864768839 ) ) ;
#98062 = CARTESIAN_POINT ( 'NONE',  ( 10.81492255796106328, -18.62759615963255655, 20.41775706135234714 ) ) ;
#98063 = CARTESIAN_POINT ( 'NONE',  ( 19.05341960407611168, 5.049401038298154454, 43.95724293864769550 ) ) ;
#98064 = CARTESIAN_POINT ( 'NONE',  ( 19.02544592524343514, -5.153800228976328945, 113.5405762719810241 ) ) ;
#98065 = CARTESIAN_POINT ( 'NONE',  ( -0.05219959533909027116, -19.03943276465977164, 32.49890960531435979 ) ) ;
#98066 = CARTESIAN_POINT ( 'NONE',  ( -21.55341960407610458, -5.719274019375992779, 21.45724293864769550 ) ) ;
#98067 = CARTESIAN_POINT ( 'NONE',  ( -17.44279575226826040, -5.990770900252400999, 34.16442432485683156 ) ) ;
#98069 = CARTESIAN_POINT ( 'NONE',  ( 16.52544592524342804, -4.483927247898539470, 103.5405762719810383 ) ) ;
#98068 = CARTESIAN_POINT ( 'NONE',  ( -18.62759615963255300, -10.81492255796106328, 44.16775706135234714 ) ) ;
#98070 = CARTESIAN_POINT ( 'NONE',  ( 13.97604488694527802, 13.89961937509977652, 104.3739096053143385 ) ) ;
#98071 = AXIS2_PLACEMENT_3D ( 'NONE', #28402, #90041, #9231 ) ;
#98073 =( BOUNDED_CURVE ( )  B_SPLINE_CURVE ( 2, ( #2707, #126052, #49219, #172562, #34048, #50220, #95705, #69356, #84509, #164388, #163379 ),
 .UNSPECIFIED., .F., .F. ) 
 B_SPLINE_CURVE_WITH_KNOTS ( ( 3, 2, 2, 2, 2, 3 ),
 ( 0.4000000000000000222, 0.4199999999999999845, 0.4400000000000000577, 0.4600000000000000755, 0.4800000000000000933, 0.5000000000000001110 ),
 .UNSPECIFIED. ) 
 CURVE ( )  GEOMETRIC_REPRESENTATION_ITEM ( )  RATIONAL_B_SPLINE_CURVE ( ( 1.000000000000000000, 0.9510565162951535312, 1.000000000000000000, 0.9510565162951535312, 1.000000000000000000, 0.9510565162951535312, 1.000000000000000000, 0.9510565162951535312, 1.000000000000000000, 0.9510565162951533091, 1.000000000000000222 ) ) 
 REPRESENTATION_ITEM ( '' )  );
#98072 = CARTESIAN_POINT ( 'NONE',  ( 16.52544592524335698, 4.483927247898782831, 76.45942372801901854 ) ) ;
#98074 = CARTESIAN_POINT ( 'NONE',  ( 21.55341960407619695, -5.719274019375665929, 96.04275706135236135 ) ) ;
#98075 = CARTESIAN_POINT ( 'NONE',  ( -16.53943276465976808, -0.05219959533934237506, 58.75109039468568994 ) ) ;
#98076 = CARTESIAN_POINT ( 'NONE',  ( -16.46253265017160317, 9.564922557960807481, 90.83224293864769550 ) ) ;
#98077 = CARTESIAN_POINT ( 'NONE',  ( 12.06949235617739724, 12.14591786802326823, 41.87609039468568284 ) ) ;
#98078 = CARTESIAN_POINT ( 'NONE',  ( -4.483927247898782831, 16.52544592524335698, 22.70942372801901499 ) ) ;
#98079 = CARTESIAN_POINT ( 'NONE',  ( -16.52544592524335698, -4.483927247898792601, 88.95942372801901854 ) ) ;
#98080 = CARTESIAN_POINT ( 'NONE',  ( -9.564922557961040184, 16.46253265017147172, 102.9177570613523329 ) ) ;
#98081 = CARTESIAN_POINT ( 'NONE',  ( 19.02544592524343514, -5.153800228976328945, 73.54057627198103830 ) ) ;
#98082 = CARTESIAN_POINT ( 'NONE',  ( -10.81492255796078084, -18.62759615963271287, 97.08224293864770971 ) ) ;
#98084 = CARTESIAN_POINT ( 'NONE',  ( 19.02544592524334988, 5.153800228976608722, 101.4594237280189759 ) ) ;
#98083 = CARTESIAN_POINT ( 'NONE',  ( 16.52544592524342804, -4.483927247898539470, 108.5405762719810241 ) ) ;
#98085 = CARTESIAN_POINT ( 'NONE',  ( -16.53943276465976808, -0.05219959533934237506, 68.75109039468568994 ) ) ;
#98086 = CARTESIAN_POINT ( 'NONE',  ( 21.04946095171257525, 10.24435024061200572, 168.3368280404219774 ) ) ;
#98087 = CARTESIAN_POINT ( 'NONE',  ( -19.03943276465977164, -0.05219959533935918106, 68.75109039468566152 ) ) ;
#98088 = CARTESIAN_POINT ( 'NONE',  ( 12.06949235617757843, -12.14591786802309237, 43.12390960531435269 ) ) ;
#98089 = CARTESIAN_POINT ( 'NONE',  ( 0.05219959533910956823, 16.53943276465976808, 99.99890960531436690 ) ) ;
#98091 = CARTESIAN_POINT ( 'NONE',  ( -16.38665767535054840, 7.295008042176050367, 90.26400864214551234 ) ) ;
#98090 = CARTESIAN_POINT ( 'NONE',  ( 16.51473224551083163, -9.474510206698727899, 35.83442372801899722 ) ) ;
#98092 = CARTESIAN_POINT ( 'NONE',  ( 10.72451020669871369, 18.67979575497193778, 37.08442372801901143 ) ) ;
#98093 = CARTESIAN_POINT ( 'NONE',  ( -16.51473224551082808, 9.474510206698731452, 93.33442372801900433 ) ) ;
#98094 = CARTESIAN_POINT ( 'NONE',  ( -9.474510206698964154, 16.51473224551069663, 115.4155762719810241 ) ) ;
#98095 = CARTESIAN_POINT ( 'NONE',  ( 16.51473224551069308, 9.474510206698969483, 89.16557627198103830 ) ) ;
#98096 = CARTESIAN_POINT ( 'NONE',  ( -16.46253265017146816, -9.564922557961047289, 19.16775706135233293 ) ) ;
#98097 = CARTESIAN_POINT ( 'NONE',  ( 19.03943276465977164, -0.05219959533909143690, 93.74890960531435269 ) ) ;
#98098 = CARTESIAN_POINT ( 'NONE',  ( 5.823673210054125526, 21.52544592524343514, 39.79057627198103830 ) ) ;
#98099 = CARTESIAN_POINT ( 'NONE',  ( -16.53943276465976808, 0.05219959533911058130, 96.24890960531435269 ) ) ;
#98100 = CARTESIAN_POINT ( 'NONE',  ( 13.97604488694527802, 13.89961937509977652, 54.37390960531435979 ) ) ;
#98101 = CARTESIAN_POINT ( 'NONE',  ( -4.483927247898539470, -16.52544592524342804, 107.2905762719810525 ) ) ;
#98102 = AXIS2_PLACEMENT_3D ( 'NONE', #52351, #37182, #127191 ) ;
#98103 = CARTESIAN_POINT ( 'NONE',  ( -21.53943276465977519, -0.05219959533937600094, 23.75109039468567929 ) ) ;
#98104 = B_SPLINE_CURVE_WITH_KNOTS ( 'NONE', 3,
 ( #193504, #8478, #163159, #23651, #53985, #25670 ),
 .UNSPECIFIED., .F., .F.,
 ( 4, 2, 4 ),
 ( 0.007228050697041374893, 0.007608510107494848712, 0.007988969517948321664 ),
 .UNSPECIFIED. ) ;
#98105 = CARTESIAN_POINT ( 'NONE',  ( 5.719274019375673035, 21.55341960407619339, 72.29275706135236135 ) ) ;
#98106 = CARTESIAN_POINT ( 'NONE',  ( -13.89961937509977652, 13.97604488694528158, 50.62390960531435979 ) ) ;
#98107 = CARTESIAN_POINT ( 'NONE',  ( 16.52544592524335698, 4.483927247898782831, 71.45942372801901854 ) ) ;
#98108 = CARTESIAN_POINT ( 'NONE',  ( -21.53943276465977519, 0.05219959533907696930, 116.2489096053143669 ) ) ;
#98109 = ORIENTED_EDGE ( 'NONE', *, *, #132407, .F. ) ;
#98110 = CARTESIAN_POINT ( 'NONE',  ( -5.823673210054431948, 21.52544592524334988, 22.70942372801901499 ) ) ;
#98112 = CARTESIAN_POINT ( 'NONE',  ( -16.51473224551069308, -9.474510206698971260, 66.66557627198102409 ) ) ;
#98111 = CARTESIAN_POINT ( 'NONE',  ( 9.564922557961047289, -16.46253265017146816, 50.41775706135233293 ) ) ;
#98113 = CARTESIAN_POINT ( 'NONE',  ( 5.153800228976615827, -19.02544592524334988, 30.20942372801900433 ) ) ;
#98114 = CARTESIAN_POINT ( 'NONE',  ( 15.80617190586769283, -15.72974639402175789, 75.62609039468567573 ) ) ;
#98115 = CARTESIAN_POINT ( 'NONE',  ( -5.823673210054116645, -21.52544592524344225, 67.29057627198103830 ) ) ;
#98116 = CARTESIAN_POINT ( 'NONE',  ( 14.29746914071049879, -8.314922557960816363, 48.33224293864770260 ) ) ;
#98118 = CARTESIAN_POINT ( 'NONE',  ( -0.05219959533936034679, 19.03943276465977164, 22.50109039468566152 ) ) ;
#98117 = CARTESIAN_POINT ( 'NONE',  ( -10.72451020669870658, -18.67979575497194134, 89.58442372801901854 ) ) ;
#98119 = CARTESIAN_POINT ( 'NONE',  ( 0.05219959533910956823, 16.53943276465976808, 69.99890960531435269 ) ) ;
#98120 = CARTESIAN_POINT ( 'NONE',  ( 19.02544592524343514, -5.153800228976328945, 23.54057627198102054 ) ) ;
#98121 = CARTESIAN_POINT ( 'NONE',  ( -13.97604488694547697, 13.89961937509957934, 53.12609039468565442 ) ) ;
#98122 = CARTESIAN_POINT ( 'NONE',  ( 12.14591786802309770, 12.06949235617756955, 24.37390960531435979 ) ) ;
#98123 = CARTESIAN_POINT ( 'NONE',  ( 21.53943276465977519, 0.05219959533937863772, 86.25109039468568994 ) ) ;
#98124 = CARTESIAN_POINT ( 'NONE',  ( 0.05219959533909260263, 19.03943276465977164, 84.99890960531436690 ) ) ;
#98125 = CARTESIAN_POINT ( 'NONE',  ( -19.02544592524334988, -5.153800228976617603, 53.95942372801898301 ) ) ;
#98126 = CARTESIAN_POINT ( 'NONE',  ( -5.719274019375978568, 21.55341960407610458, 45.20724293864769550 ) ) ;
#98127 = CARTESIAN_POINT ( 'NONE',  ( -21.53943276465977519, -0.05219959533937600094, 43.75109039468568284 ) ) ;
#98128 = CARTESIAN_POINT ( 'NONE',  ( 5.823673210054125526, 21.52544592524343514, 104.7905762719810241 ) ) ;
#98129 = CARTESIAN_POINT ( 'NONE',  ( 9.474510206698729675, 16.51473224551082808, 102.0844237280190043 ) ) ;
#98130 = CARTESIAN_POINT ( 'NONE',  ( 16.53943276465976808, 0.05219959533934440121, 66.25109039468567573 ) ) ;
#98132 = CARTESIAN_POINT ( 'NONE',  ( -0.05219959533907301413, -21.53943276465977519, 107.4989096053143669 ) ) ;
#98131 = CARTESIAN_POINT ( 'NONE',  ( -14.71325192251711833, -16.70647688133528064, -58.23439181598958925 ) ) ;
#98133 = CARTESIAN_POINT ( 'NONE',  ( -16.55341960407611168, -4.379528057220339221, 86.45724293864770971 ) ) ;
#98134 = CARTESIAN_POINT ( 'NONE',  ( -17.26172910966779028, -6.454744622555857347, 99.19353091350777163 ) ) ;
#98135 = CARTESIAN_POINT ( 'NONE',  ( -12.06949235617739369, -12.14591786802326823, 29.37609039468568284 ) ) ;
#98136 = CARTESIAN_POINT ( 'NONE',  ( 15.72974639402199770, -15.80617190586745480, 58.12390960531435979 ) ) ;
#98137 = CARTESIAN_POINT ( 'NONE',  ( -12.06949235617739369, -12.14591786802326823, 94.37609039468568994 ) ) ;
#98138 = CARTESIAN_POINT ( 'NONE',  ( -19.05341960407611168, -5.049401038298163336, 26.45724293864769550 ) ) ;
#98139 = CARTESIAN_POINT ( 'NONE',  ( 8.314922557961029526, -14.29746914071037800, 65.41775706135234714 ) ) ;
#98140 = CARTESIAN_POINT ( 'NONE',  ( -10.72451020669870658, -18.67979575497194134, 39.58442372801901143 ) ) ;
#98141 = CARTESIAN_POINT ( 'NONE',  ( 18.67979575497178502, 10.72451020669898547, 59.16557627198103120 ) ) ;
#98142 = CARTESIAN_POINT ( 'NONE',  ( -8.314922557961024197, 14.29746914071037800, 87.91775706135234714 ) ) ;
#98143 = CARTESIAN_POINT ( 'NONE',  ( -15.80617190586768217, 15.72974639402176855, 63.12609039468568994 ) ) ;
#98144 = CARTESIAN_POINT ( 'NONE',  ( 10.81492255796078972, 18.62759615963270932, 59.58224293864770260 ) ) ;
#98145 = CARTESIAN_POINT ( 'NONE',  ( -10.72451020669898014, 18.67979575497178502, 35.41557627198102409 ) ) ;
#98146 = CARTESIAN_POINT ( 'NONE',  ( 14.29746914071037800, 8.314922557961029526, 66.66775706135234714 ) ) ;
#98147 = CARTESIAN_POINT ( 'NONE',  ( 15.80617190586746368, 15.72974639402197994, 29.37390960531435269 ) ) ;
#98148 = ORIENTED_EDGE ( 'NONE', *, *, #62447, .T. ) ;
#98149 = CARTESIAN_POINT ( 'NONE',  ( 16.46253265017160672, -9.564922557960803928, 98.33224293864769550 ) ) ;
#98150 = CARTESIAN_POINT ( 'NONE',  ( 12.06949235617757843, -12.14591786802309237, 23.12390960531436335 ) ) ;
#98151 = FACE_OUTER_BOUND ( 'NONE', #99641, .T. ) ;
#98152 = CARTESIAN_POINT ( 'NONE',  ( 14.34966873604960469, 8.224510206698951720, 104.1655762719810241 ) ) ;
#98153 = CARTESIAN_POINT ( 'NONE',  ( -5.823673210054116645, -21.52544592524344225, 67.29057627198103830 ) ) ;
#98154 = CARTESIAN_POINT ( 'NONE',  ( -13.89961937509977652, 13.97604488694528158, 40.62390960531435979 ) ) ;
#98155 = CARTESIAN_POINT ( 'NONE',  ( -12.14591786802326823, 12.06949235617739902, 93.12609039468568994 ) ) ;
#98156 = CARTESIAN_POINT ( 'NONE',  ( -10.72451020669870658, -18.67979575497194134, 39.58442372801901143 ) ) ;
#98157 = CARTESIAN_POINT ( 'NONE',  ( -19.05341960407617563, 5.049401038297882671, 108.5427570613523187 ) ) ;
#98158 = CARTESIAN_POINT ( 'NONE',  ( 12.14591786802309770, 12.06949235617756955, 109.3739096053143811 ) ) ;
#98159 = CARTESIAN_POINT ( 'NONE',  ( 19.03943276465977164, -0.05219959533909143690, 48.74890960531435979 ) ) ;
#98160 = CARTESIAN_POINT ( 'NONE',  ( -13.97604488694527625, -13.89961937509977652, 21.87390960531435979 ) ) ;
#98161 = DIRECTION ( 'NONE',  ( 0.000000000000000000, 0.000000000000000000, 1.000000000000000000 ) ) ;
#98162 = CARTESIAN_POINT ( 'NONE',  ( 0.05219959533909260263, 19.03943276465977164, 89.99890960531436690 ) ) ;
#98163 = ADVANCED_FACE ( 'NONE', ( #162581 ), #41441, .T. ) ;
#98164 = CARTESIAN_POINT ( 'NONE',  ( 16.52544592524335698, 4.483927247898782831, 76.45942372801901854 ) ) ;
#98165 = CARTESIAN_POINT ( 'NONE',  ( -10.72451020669870658, -18.67979575497194134, 99.58442372801900433 ) ) ;
#98166 = CARTESIAN_POINT ( 'NONE',  ( -15.80617190586745835, -15.72974639402198527, 46.87390960531435979 ) ) ;
#98167 = CARTESIAN_POINT ( 'NONE',  ( -16.53943276465976808, -0.05219959533934237506, 78.75109039468568994 ) ) ;
#98168 = CARTESIAN_POINT ( 'NONE',  ( -5.153800228976607833, 19.02544592524334988, 67.70942372801900433 ) ) ;
#98169 = CARTESIAN_POINT ( 'NONE',  ( 5.823673210054444382, -21.52544592524334988, 60.20942372801902565 ) ) ;
#98170 = CARTESIAN_POINT ( 'NONE',  ( -16.51473224551069308, -9.474510206698971260, 76.66557627198103830 ) ) ;
#98171 = CARTESIAN_POINT ( 'NONE',  ( -5.049401038298153566, 19.05341960407611168, 35.20724293864768839 ) ) ;
#98172 = CARTESIAN_POINT ( 'NONE',  ( 5.153800228976615827, -19.02544592524334988, 60.20942372801899012 ) ) ;
#98173 = DIRECTION ( 'NONE',  ( 0.000000000000000000, 0.000000000000000000, 1.000000000000000000 ) ) ;
#98174 = CARTESIAN_POINT ( 'NONE',  ( -19.03943276465977164, 0.05219959533909376836, 91.24890960531436690 ) ) ;
#98175 = CARTESIAN_POINT ( 'NONE',  ( -16.52544592524342804, 4.483927247898546575, 46.04057627198103830 ) ) ;
#98176 = CARTESIAN_POINT ( 'NONE',  ( -15.72974639402197994, 15.80617190586746368, 50.62390960531435979 ) ) ;
#98177 = FACE_OUTER_BOUND ( 'NONE', #178181, .T. ) ;
#98178 = CARTESIAN_POINT ( 'NONE',  ( -16.46253265017146816, -9.564922557961047289, 24.16775706135233648 ) ) ;
#98179 = CARTESIAN_POINT ( 'NONE',  ( -16.38665767535055906, -7.295008042176049479, 79.73599135785454450 ) ) ;
#98180 = CARTESIAN_POINT ( 'NONE',  ( 13.97604488694527802, 13.89961937509977652, 49.37390960531434558 ) ) ;
#98181 = CARTESIAN_POINT ( 'NONE',  ( 12.06949235617739724, 12.14591786802326823, 41.87609039468568284 ) ) ;
#98182 = CARTESIAN_POINT ( 'NONE',  ( -33.85315667487628133, 2.014031266883448522E-14, 100.5000000000010232 ) ) ;
#98183 = CARTESIAN_POINT ( 'NONE',  ( -17.12812012977027010, 6.668231424565978394, 108.6405124067685790 ) ) ;
#98184 = CARTESIAN_POINT ( 'NONE',  ( 4.483927247898790824, -16.52544592524335698, 80.20942372801901854 ) ) ;
#98185 = CARTESIAN_POINT ( 'NONE',  ( 10.72451020669898902, -18.67979575497178502, 102.9155762719810383 ) ) ;
#98186 = CIRCLE ( 'NONE', #59840, 8.000000000000001776 ) ;
#98188 = CARTESIAN_POINT ( 'NONE',  ( -7.260022482700430047, -2.182060888568185142, 7.889167669754719725 ) ) ;
#98187 = CARTESIAN_POINT ( 'NONE',  ( -0.05219959533909027116, -19.03943276465977164, 37.49890960531436690 ) ) ;
#98189 = CARTESIAN_POINT ( 'NONE',  ( -18.62759615963255300, -10.81492255796106328, 44.16775706135234714 ) ) ;
#98190 = CARTESIAN_POINT ( 'NONE',  ( -19.05341960407617563, 5.049401038297882671, 53.54275706135231871 ) ) ;
#98191 = CARTESIAN_POINT ( 'NONE',  ( 19.03943276465977164, -0.05219959533909143690, 53.74890960531436690 ) ) ;
#98192 = CARTESIAN_POINT ( 'NONE',  ( 21.52544592524334988, 5.823673210054432836, 91.45942372801901854 ) ) ;
#98193 = CARTESIAN_POINT ( 'NONE',  ( 16.81555441253554051, 7.025013491695493606, 96.86314554665749199 ) ) ;
#98194 = CARTESIAN_POINT ( 'NONE',  ( -8.314922557960811034, -14.29746914071050412, 42.08224293864769550 ) ) ;
#98195 = CARTESIAN_POINT ( 'NONE',  ( -14.82524568295233891, 1.464953661134127172, -59.95866808466630715 ) ) ;
#98196 = CARTESIAN_POINT ( 'NONE',  ( 5.719274019375991003, -21.55341960407610458, 57.70724293864770260 ) ) ;
#98197 = DIRECTION ( 'NONE',  ( -1.734723475976805517E-15, -1.000000000000000000, 6.938893903907222067E-15 ) ) ;
#98198 = CARTESIAN_POINT ( 'NONE',  ( 13.89961937509977652, -13.97604488694527269, 103.1239096053143527 ) ) ;
#98199 = CARTESIAN_POINT ( 'NONE',  ( -0.05219959533910754901, -16.53943276465976808, 97.49890960531436690 ) ) ;
#98200 = CARTESIAN_POINT ( 'NONE',  ( -13.97604488694547697, 13.89961937509957934, 113.1260903946856757 ) ) ;
#98201 = CARTESIAN_POINT ( 'NONE',  ( -16.53943276465976808, 0.05219959533911058130, 21.24890960531436690 ) ) ;
#98202 = VERTEX_POINT ( 'NONE', #98402 ) ;
#98204 = CARTESIAN_POINT ( 'NONE',  ( 15.72974639402199770, -15.80617190586745480, 103.1239096053143811 ) ) ;
#98203 = CARTESIAN_POINT ( 'NONE',  ( -19.05341960407611168, -5.049401038298163336, 96.45724293864769550 ) ) ;
#98206 = CARTESIAN_POINT ( 'NONE',  ( 19.05341960407611168, 5.049401038298154454, 98.95724293864766707 ) ) ;
#98205 = CARTESIAN_POINT ( 'NONE',  ( -14.34966873604960291, -8.224510206698953496, 31.66557627198102054 ) ) ;
#98207 = CARTESIAN_POINT ( 'NONE',  ( -19.05341960407617563, 5.049401038297882671, 93.54275706135234714 ) ) ;
#98208 = CARTESIAN_POINT ( 'NONE',  ( -15.72974639402176322, -15.80617190586768395, 109.3760903946857042 ) ) ;
#98209 = CARTESIAN_POINT ( 'NONE',  ( 15.80617190586746368, 15.72974639402197994, 84.37390960531438111 ) ) ;
#98210 = CARTESIAN_POINT ( 'NONE',  ( -15.80617190586745835, -15.72974639402198527, 51.87390960531437401 ) ) ;
#98211 = CIRCLE ( 'NONE', #133772, 2.500000000000000000 ) ;
#98212 = CARTESIAN_POINT ( 'NONE',  ( 5.153800228976335163, 19.02544592524342804, 69.79057627198103830 ) ) ;
#98213 = CARTESIAN_POINT ( 'NONE',  ( 12.14591786802309770, 12.06949235617756955, 29.37390960531435269 ) ) ;
#98214 = CARTESIAN_POINT ( 'NONE',  ( -13.97604488694527625, -13.89961937509977652, 71.87390960531433848 ) ) ;
#98215 = ORIENTED_EDGE ( 'NONE', *, *, #52209, .T. ) ;
#98216 = CARTESIAN_POINT ( 'NONE',  ( 18.56197773271730611, -5.500000000000111910, 61.05066217314453070 ) ) ;
#98217 = CARTESIAN_POINT ( 'NONE',  ( -5.153800228976607833, 19.02544592524334988, 37.70942372801899722 ) ) ;
#98218 = CARTESIAN_POINT ( 'NONE',  ( -15.80617190586745835, -15.72974639402198527, 81.87390960531435269 ) ) ;
#98219 = CARTESIAN_POINT ( 'NONE',  ( -16.55341960407611168, -4.379528057220339221, 91.45724293864769550 ) ) ;
#98220 = CARTESIAN_POINT ( 'NONE',  ( -21.53943276465977519, -0.05219959533937600094, 43.75109039468568284 ) ) ;
#98221 = CARTESIAN_POINT ( 'NONE',  ( -22.44159573604009950, -16.30477369853688430, 147.5750000027312012 ) ) ;
#98222 = CARTESIAN_POINT ( 'NONE',  ( -4.483927247898782831, 16.52544592524335698, 102.7094237280190185 ) ) ;
#98223 = CARTESIAN_POINT ( 'NONE',  ( -9.474510206698964154, 16.51473224551069663, 25.41557627198103120 ) ) ;
#98224 = CARTESIAN_POINT ( 'NONE',  ( 16.51473224551069308, 9.474510206698969483, 84.16557627198102409 ) ) ;
#98225 = CARTESIAN_POINT ( 'NONE',  ( 17.72696623605160582, -5.500000000000045297, 71.09811031808418136 ) ) ;
#98226 = CARTESIAN_POINT ( 'NONE',  ( -30.73962218707677962, -22.33364281372842441, -5.547842220587804185 ) ) ;
#98227 = CARTESIAN_POINT ( 'NONE',  ( 0.05219959533910956823, 16.53943276465976808, 39.99890960531436690 ) ) ;
#98228 = CARTESIAN_POINT ( 'NONE',  ( 21.53943276465977519, 0.05219959533937863772, 66.25109039468567573 ) ) ;
#98229 = CARTESIAN_POINT ( 'NONE',  ( 27.18398240159043411, -26.16474475603006056, -20.45985799059559085 ) ) ;
#98230 = CARTESIAN_POINT ( 'NONE',  ( 5.049401038298161559, -19.05341960407611168, 47.70724293864770260 ) ) ;
#98231 = CARTESIAN_POINT ( 'NONE',  ( 19.03943276465977164, -0.05219959533909143690, 48.74890960531435979 ) ) ;
#98232 = ORIENTED_EDGE ( 'NONE', *, *, #184834, .F. ) ;
#98233 = CARTESIAN_POINT ( 'NONE',  ( -19.03943276465977164, -0.05219959533935918106, 18.75109039468567218 ) ) ;
#98234 = CARTESIAN_POINT ( 'NONE',  ( 14.29746914071037800, 8.314922557961029526, 61.66775706135235424 ) ) ;
#98235 = CARTESIAN_POINT ( 'NONE',  ( 5.719274019375673035, 21.55341960407619339, 92.29275706135236135 ) ) ;
#98236 = CARTESIAN_POINT ( 'NONE',  ( -19.03943276465977164, 0.05219959533909376836, 111.2489096053143669 ) ) ;
#98237 = CARTESIAN_POINT ( 'NONE',  ( 19.03943276465977164, 0.05219959533936151252, 96.25109039468567573 ) ) ;
#98238 = CARTESIAN_POINT ( 'NONE',  ( -15.80617190586768217, 15.72974639402176855, 73.12609039468567573 ) ) ;
#98239 = CARTESIAN_POINT ( 'NONE',  ( 4.483927247898790824, -16.52544592524335698, 30.20942372801902565 ) ) ;
#98240 = CARTESIAN_POINT ( 'NONE',  ( 21.52544592524344225, -5.823673210054117533, 83.54057627198102409 ) ) ;
#98241 = CARTESIAN_POINT ( 'NONE',  ( -19.02544592524334988, -5.153800228976617603, 93.95942372801900433 ) ) ;
#98242 = CARTESIAN_POINT ( 'NONE',  ( -16.46253265017160317, 9.564922557960807481, 60.83224293864769550 ) ) ;
#98243 = CARTESIAN_POINT ( 'NONE',  ( 16.55341960407618274, -4.379528057220086978, 21.04275706135234714 ) ) ;
#98244 = CIRCLE ( 'NONE', #156451, 2.500000000000002220 ) ;
#98245 = CARTESIAN_POINT ( 'NONE',  ( -13.89961937509957401, -13.97604488694547875, 104.3760903946856757 ) ) ;
#98246 = CARTESIAN_POINT ( 'NONE',  ( -14.34966873604960291, -8.224510206698953496, 46.66557627198102409 ) ) ;
#98247 = CARTESIAN_POINT ( 'NONE',  ( 5.049401038297881783, 19.05341960407617563, 77.29275706135231871 ) ) ;
#98248 = CARTESIAN_POINT ( 'NONE',  ( -14.34966873604972548, 8.224510206698743886, 58.33442372801901143 ) ) ;
#98250 = CARTESIAN_POINT ( 'NONE',  ( 16.51473224551069308, 9.474510206698969483, 39.16557627198103120 ) ) ;
#98249 = CARTESIAN_POINT ( 'NONE',  ( 18.62759615963271287, -10.81492255796078972, 113.3322429386476955 ) ) ;
#98251 = CARTESIAN_POINT ( 'NONE',  ( -13.97604488694527625, -13.89961937509977652, 51.87390960531436690 ) ) ;
#98252 = CARTESIAN_POINT ( 'NONE',  ( -16.52544592524335698, -4.483927247898792601, 58.95942372801902565 ) ) ;
#98253 = CARTESIAN_POINT ( 'NONE',  ( -17.97161686094258215, 5.499999999999975131, 45.99637206859247840 ) ) ;
#98254 = CARTESIAN_POINT ( 'NONE',  ( 23.31738231874054890, -16.94106989632523508, 143.0500000054623513 ) ) ;
#98255 = CARTESIAN_POINT ( 'NONE',  ( -9.474510206698964154, 16.51473224551069663, 100.4155762719810241 ) ) ;
#98256 = EDGE_CURVE ( 'NONE', #93673, #199515, #74734, .T. ) ;
#98257 = CARTESIAN_POINT ( 'NONE',  ( -19.03943276465977164, 0.05219959533909376836, 26.24890960531435624 ) ) ;
#98258 = VERTEX_POINT ( 'NONE', #86252 ) ;
#98259 = CARTESIAN_POINT ( 'NONE',  ( 14.34966873604972726, -8.224510206698740333, 20.83442372801901143 ) ) ;
#98260 = CARTESIAN_POINT ( 'NONE',  ( -10.72451020669898014, 18.67979575497178502, 55.41557627198102409 ) ) ;
#98262 = CARTESIAN_POINT ( 'NONE',  ( 0.05219959533934541429, -16.53943276465976808, 35.00109039468568284 ) ) ;
#98261 = CARTESIAN_POINT ( 'NONE',  ( -19.05341960407617563, 5.049401038297882671, 43.54275706135232582 ) ) ;
#98263 = CARTESIAN_POINT ( 'NONE',  ( -19.02544592524342804, 5.153800228976336051, 26.04057627198103120 ) ) ;
#98264 = CARTESIAN_POINT ( 'NONE',  ( -5.049401038298153566, 19.05341960407611168, 50.20724293864770260 ) ) ;
#98265 = CARTESIAN_POINT ( 'NONE',  ( 5.823673210054125526, 21.52544592524343514, 84.79057627198102409 ) ) ;
#98266 = CARTESIAN_POINT ( 'NONE',  ( 0.05219959533909260263, 19.03943276465977164, 114.9989096053143669 ) ) ;
#98267 = CARTESIAN_POINT ( 'NONE',  ( -16.51473224551069308, -9.474510206698971260, 51.66557627198102409 ) ) ;
#98268 = CARTESIAN_POINT ( 'NONE',  ( -27.73933785331498925, 9.013057229001088189, 141.2750000027311899 ) ) ;
#98269 = CARTESIAN_POINT ( 'NONE',  ( -19.05341960407617563, 5.049401038297882671, 78.54275706135233293 ) ) ;
#98270 = CARTESIAN_POINT ( 'NONE',  ( -8.224510206698948167, 14.34966873604960824, 60.41557627198102409 ) ) ;
#98271 = CARTESIAN_POINT ( 'NONE',  ( 21.53943276465977519, 0.05219959533937863772, 101.2510903946856757 ) ) ;
#98272 = EDGE_CURVE ( 'NONE', #4269, #177278, #53736, .T. ) ;
#98273 = CARTESIAN_POINT ( 'NONE',  ( -15.80617190586745835, -15.72974639402198527, 101.8739096053143811 ) ) ;
#98274 = CARTESIAN_POINT ( 'NONE',  ( 5.823673210054444382, -21.52544592524334988, 80.20942372801901854 ) ) ;
#98275 = CARTESIAN_POINT ( 'NONE',  ( 19.05341960407611168, 5.049401038298154454, 28.95724293864769550 ) ) ;
#98276 = CARTESIAN_POINT ( 'NONE',  ( 15.72974639402176855, 15.80617190586768217, 71.87609039468568994 ) ) ;
#98277 = CARTESIAN_POINT ( 'NONE',  ( 9.564922557960805705, 16.46253265017160317, 109.5822429386476955 ) ) ;
#98279 = CARTESIAN_POINT ( 'NONE',  ( -5.719274019375665041, -21.55341960407619695, 79.79275706135236135 ) ) ;
#98278 = CARTESIAN_POINT ( 'NONE',  ( 16.55341960407618274, -4.379528057220086978, 101.0427570613523756 ) ) ;
#98280 = CARTESIAN_POINT ( 'NONE',  ( -9.564922557960796823, -16.46253265017161027, 62.08224293864769550 ) ) ;
#98281 = CARTESIAN_POINT ( 'NONE',  ( -10.81492255796105439, 18.62759615963255655, 42.91775706135235424 ) ) ;
#98282 = CARTESIAN_POINT ( 'NONE',  ( 19.05341960407611168, 5.049401038298154454, 83.95724293864766707 ) ) ;
#98283 = CARTESIAN_POINT ( 'NONE',  ( -8.224510206698948167, 14.34966873604960824, 100.4155762719810241 ) ) ;
#98284 = CARTESIAN_POINT ( 'NONE',  ( 4.379528057220339221, -16.55341960407611168, 57.70724293864770260 ) ) ;
#98285 = CARTESIAN_POINT ( 'NONE',  ( -5.719274019375978568, 21.55341960407610458, 65.20724293864768129 ) ) ;
#98286 = CARTESIAN_POINT ( 'NONE',  ( -16.51473224551069308, -9.474510206698971260, 56.66557627198103120 ) ) ;
#98287 = CARTESIAN_POINT ( 'NONE',  ( -18.67979575497178146, -10.72451020669898902, 71.66557627198100988 ) ) ;
#98288 = CARTESIAN_POINT ( 'NONE',  ( -13.89961937509957401, -13.97604488694547875, 59.37609039468566863 ) ) ;
#98290 = CARTESIAN_POINT ( 'NONE',  ( 14.34966873604960469, 8.224510206698951720, 74.16557627198102409 ) ) ;
#98289 = CARTESIAN_POINT ( 'NONE',  ( -5.153800228976607833, 19.02544592524335343, 27.70942372801900078 ) ) ;
#98291 = CARTESIAN_POINT ( 'NONE',  ( -15.72974639402197994, 15.80617190586746368, 55.62390960531436690 ) ) ;
#98292 = CARTESIAN_POINT ( 'NONE',  ( 17.50000000000000000, 5.499999999999992895, 101.7030961746583131 ) ) ;
#98294 = CARTESIAN_POINT ( 'NONE',  ( -27.73933785331498925, 2.428612866367529932E-14, 143.3750000027311842 ) ) ;
#98293 = CARTESIAN_POINT ( 'NONE',  ( -0.05219959533934338120, 16.53943276465976808, 97.50109039468567573 ) ) ;
#98295 = CARTESIAN_POINT ( 'NONE',  ( -13.89961937509957401, -13.97604488694547875, 104.3760903946856757 ) ) ;
#98296 = CARTESIAN_POINT ( 'NONE',  ( -12.06949235617756955, 12.14591786802309770, 70.62390960531436690 ) ) ;
#98297 = CARTESIAN_POINT ( 'NONE',  ( 28.82186960331498327, 2.781578969918950771E-14, 141.0000000000000000 ) ) ;
#98298 = CARTESIAN_POINT ( 'NONE',  ( -0.05219959533909027116, -19.03943276465977164, 67.49890960531436690 ) ) ;
#98299 = CARTESIAN_POINT ( 'NONE',  ( -16.55341960407611168, -4.379528057220339221, 51.45724293864770260 ) ) ;
#98300 = EDGE_CURVE ( 'NONE', #35769, #40993, #162247, .T. ) ;
#98301 = CARTESIAN_POINT ( 'NONE',  ( 0.05219959533909260263, 19.03943276465977164, 104.9989096053143669 ) ) ;
#98302 = AXIS2_PLACEMENT_3D ( 'NONE', #49576, #169936, #112238 ) ;
#98304 = CARTESIAN_POINT ( 'NONE',  ( -5.153800228976328057, -19.02544592524343514, 62.29057627198100988 ) ) ;
#98303 = CARTESIAN_POINT ( 'NONE',  ( -13.89961937509957401, -13.97604488694547875, 79.37609039468567573 ) ) ;
#98305 = CARTESIAN_POINT ( 'NONE',  ( -16.51473224551069308, -9.474510206698971260, 86.66557627198102409 ) ) ;
#98306 = CARTESIAN_POINT ( 'NONE',  ( 5.153800228976335163, 19.02544592524342804, 74.79057627198103830 ) ) ;
#98307 = CARTESIAN_POINT ( 'NONE',  ( 10.81492255796078972, 18.62759615963270932, 69.58224293864769550 ) ) ;
#98308 = CARTESIAN_POINT ( 'NONE',  ( 4.379528057220092307, 16.55341960407617563, 57.29275706135234714 ) ) ;
#98309 = CARTESIAN_POINT ( 'NONE',  ( 13.89961937509957579, 13.97604488694547520, 101.8760903946856615 ) ) ;
#98310 = CARTESIAN_POINT ( 'NONE',  ( -5.049401038298153566, 19.05341960407611168, 50.20724293864770260 ) ) ;
#98311 = CARTESIAN_POINT ( 'NONE',  ( -0.05219959533907301413, -21.53943276465977519, 52.49890960531435979 ) ) ;
#98312 = CARTESIAN_POINT ( 'NONE',  ( 19.03943276465977164, 0.05219959533936151252, 76.25109039468566152 ) ) ;
#98314 = CARTESIAN_POINT ( 'NONE',  ( 21.55341960407619695, -5.719274019375665929, 31.04275706135234714 ) ) ;
#98313 = CARTESIAN_POINT ( 'NONE',  ( -8.314922557961024197, 14.29746914071037800, 112.9177570613523329 ) ) ;
#98315 = CARTESIAN_POINT ( 'NONE',  ( 19.03943276465977164, 0.05219959533936151252, 36.25109039468567573 ) ) ;
#98317 = CARTESIAN_POINT ( 'NONE',  ( 14.34966873604972726, -8.224510206698740333, 90.83442372801901854 ) ) ;
#98316 = CARTESIAN_POINT ( 'NONE',  ( 8.314922557961029526, -14.29746914071037800, 65.41775706135234714 ) ) ;
#98318 = CARTESIAN_POINT ( 'NONE',  ( 8.898068258721465895, 27.38543819252877398, 147.6656553485623817 ) ) ;
#98319 = CARTESIAN_POINT ( 'NONE',  ( -12.14591786802326823, 12.06949235617739902, 78.12609039468570415 ) ) ;
#98321 = CARTESIAN_POINT ( 'NONE',  ( -8.224510206698735004, -14.34966873604973081, 39.58442372801901143 ) ) ;
#98320 = CARTESIAN_POINT ( 'NONE',  ( -13.89961937509977652, 13.97604488694528158, 115.6239096053143669 ) ) ;
#98322 = CARTESIAN_POINT ( 'NONE',  ( -13.97604488694527625, -13.89961937509977652, 51.87390960531436690 ) ) ;
#98323 = CARTESIAN_POINT ( 'NONE',  ( 13.97604488694527802, 13.89961937509977652, 54.37390960531435979 ) ) ;
#98324 = CARTESIAN_POINT ( 'NONE',  ( 19.03943276465977164, -0.05219959533909143690, 63.74890960531435979 ) ) ;
#98325 = CARTESIAN_POINT ( 'NONE',  ( -15.80617190586768217, 15.72974639402176855, 38.12609039468567573 ) ) ;
#98326 = CARTESIAN_POINT ( 'NONE',  ( 12.14591786802327356, -12.06949235617739191, 50.62609039468568994 ) ) ;
#98327 = CARTESIAN_POINT ( 'NONE',  ( -8.224510206698735004, -14.34966873604973081, 109.5844237280190328 ) ) ;
#98328 = CARTESIAN_POINT ( 'NONE',  ( 19.05341960407611168, 5.049401038298154454, 28.95724293864769550 ) ) ;
#98329 = CARTESIAN_POINT ( 'NONE',  ( -19.03943276465977164, -0.05219959533935918106, 23.75109039468566152 ) ) ;
#98330 = CARTESIAN_POINT ( 'NONE',  ( 14.29746914071037800, 8.314922557961029526, 21.66775706135235069 ) ) ;
#98331 = AXIS2_PLACEMENT_3D ( 'NONE', #173548, #95689, #83496 ) ;
#98332 = CARTESIAN_POINT ( 'NONE',  ( -5.153800228976607833, 19.02544592524334988, 62.70942372801899722 ) ) ;
#98333 = CARTESIAN_POINT ( 'NONE',  ( 16.52544592524342804, -4.483927247898539470, 68.54057627198103830 ) ) ;
#98334 = CARTESIAN_POINT ( 'NONE',  ( -13.97604488694527625, -13.89961937509977652, 41.87390960531435979 ) ) ;
#98336 = CARTESIAN_POINT ( 'NONE',  ( 17.05587630539785238, -6.762274262135687053, 93.24180309037312497 ) ) ;
#98335 = CARTESIAN_POINT ( 'NONE',  ( 0.05219959533936267826, -19.03943276465977164, 80.00109039468567573 ) ) ;
#98337 = CARTESIAN_POINT ( 'NONE',  ( 15.72974639402176855, 15.80617190586768217, 76.87609039468567573 ) ) ;
#98338 = CARTESIAN_POINT ( 'NONE',  ( -4.379528057220086978, -16.55341960407618274, 44.79275706135234714 ) ) ;
#98339 = CARTESIAN_POINT ( 'NONE',  ( 18.87580814761072645, -5.500000000000034639, 58.37172394265762421 ) ) ;
#98340 = CARTESIAN_POINT ( 'NONE',  ( 21.55341960407610458, 5.719274019375980345, 38.95724293864768839 ) ) ;
#98341 = CARTESIAN_POINT ( 'NONE',  ( -4.483927247898782831, 16.52544592524335698, 27.70942372801901854 ) ) ;
#98342 = CARTESIAN_POINT ( 'NONE',  ( 19.05341960407611168, 5.049401038298154454, 28.95724293864769550 ) ) ;
#98343 = CARTESIAN_POINT ( 'NONE',  ( 18.67979575497194134, -10.72451020669871369, 105.8344237280190328 ) ) ;
#98344 = CARTESIAN_POINT ( 'NONE',  ( 17.72696623605164490, -5.499999999999867661, 66.09811031808418136 ) ) ;
#98345 = CARTESIAN_POINT ( 'NONE',  ( -9.564922557960796823, -16.46253265017161027, 32.08224293864769550 ) ) ;
#98346 = CARTESIAN_POINT ( 'NONE',  ( 11.30153831258470731, -188.0000000000000000, -15.00000000000000178 ) ) ;
#98347 = CARTESIAN_POINT ( 'NONE',  ( -5.153800228976328057, -19.02544592524343514, 57.29057627198103120 ) ) ;
#98348 = CARTESIAN_POINT ( 'NONE',  ( 5.823673210054444382, -21.52544592524334988, 70.20942372801904696 ) ) ;
#98349 = CARTESIAN_POINT ( 'NONE',  ( -9.474510206698720793, -16.51473224551083518, 24.58442372801900078 ) ) ;
#98350 = CARTESIAN_POINT ( 'NONE',  ( 12.14591786802327356, -12.06949235617739191, 110.6260903946857042 ) ) ;
#98351 = CARTESIAN_POINT ( 'NONE',  ( -5.049401038298153566, 19.05341960407611168, 35.20724293864768839 ) ) ;
#98352 = AXIS2_PLACEMENT_3D ( 'NONE', #145184, #193718, #191697 ) ;
#98353 = CARTESIAN_POINT ( 'NONE',  ( -19.05341960407611168, -5.049401038298163336, 91.45724293864766707 ) ) ;
#98354 = CARTESIAN_POINT ( 'NONE',  ( 21.55341960407619695, -5.719274019375665929, 76.04275706135237556 ) ) ;
#98355 = CARTESIAN_POINT ( 'NONE',  ( 9.564922557960805705, 16.46253265017160317, 34.58224293864770260 ) ) ;
#98356 = CARTESIAN_POINT ( 'NONE',  ( -5.823673210054431948, 21.52544592524334988, 67.70942372801901854 ) ) ;
#98358 = CARTESIAN_POINT ( 'NONE',  ( -19.05341960407611168, -5.049401038298163336, 101.4572429386476955 ) ) ;
#98357 = CARTESIAN_POINT ( 'NONE',  ( -0.05219959533936034679, 19.03943276465977164, 92.50109039468566152 ) ) ;
#98359 = CARTESIAN_POINT ( 'NONE',  ( 16.46253265017160672, -9.564922557960803928, 38.33224293864768839 ) ) ;
#98360 = CARTESIAN_POINT ( 'NONE',  ( 18.67979575497178502, 10.72451020669898547, 104.1655762719810241 ) ) ;
#98361 = CARTESIAN_POINT ( 'NONE',  ( -19.03943276465977164, -0.05219959533935918106, 38.75109039468566152 ) ) ;
#98362 = CARTESIAN_POINT ( 'NONE',  ( -16.52544592524342804, 4.483927247898546575, 111.0405762719810525 ) ) ;
#98363 = CARTESIAN_POINT ( 'NONE',  ( 19.05341960407611168, 5.049401038298154454, 63.95724293864769550 ) ) ;
#98365 = VECTOR ( 'NONE', #121947, 1000.000000000000000 ) ;
#98364 = CARTESIAN_POINT ( 'NONE',  ( -9.474510206698720793, -16.51473224551083518, 99.58442372801900433 ) ) ;
#98366 = CARTESIAN_POINT ( 'NONE',  ( 4.483927247898545687, 16.52544592524342804, 64.79057627198103830 ) ) ;
#98367 = CARTESIAN_POINT ( 'NONE',  ( 10.72451020669898902, -18.67979575497178502, 22.91557627198102765 ) ) ;
#98368 = CARTESIAN_POINT ( 'NONE',  ( 16.46253265017146816, 9.564922557961045513, 81.66775706135233293 ) ) ;
#98369 = CARTESIAN_POINT ( 'NONE',  ( -21.53943276465977519, 0.05219959533907696930, 86.24890960531436690 ) ) ;
#98370 = CARTESIAN_POINT ( 'NONE',  ( 10.81492255796106328, -18.62759615963255655, 45.41775706135234003 ) ) ;
#98371 = CARTESIAN_POINT ( 'NONE',  ( 0.05219959533934541429, -16.53943276465976808, 45.00109039468568284 ) ) ;
#98373 = CARTESIAN_POINT ( 'NONE',  ( -21.52544592524334988, -5.823673210054445271, 48.95942372801902565 ) ) ;
#98372 = CARTESIAN_POINT ( 'NONE',  ( 8.314922557961029526, -14.29746914071037800, 40.41775706135234714 ) ) ;
#98374 = CARTESIAN_POINT ( 'NONE',  ( 10.72451020669898902, -18.67979575497178502, 57.91557627198103120 ) ) ;
#98375 = MECHANICAL_DESIGN_GEOMETRIC_PRESENTATION_REPRESENTATION (  '', ( #82207 ), #66064 ) ;
#98376 = CARTESIAN_POINT ( 'NONE',  ( 19.05341960407611168, 5.049401038298154454, 38.95724293864767418 ) ) ;
#98377 = FACE_OUTER_BOUND ( 'NONE', #163865, .T. ) ;
#98378 = CARTESIAN_POINT ( 'NONE',  ( 4.379528057220092307, 16.55341960407617563, 72.29275706135236135 ) ) ;
#98379 = CARTESIAN_POINT ( 'NONE',  ( -10.72451020669898014, 18.67979575497178502, 100.4155762719810241 ) ) ;
#98380 = CARTESIAN_POINT ( 'NONE',  ( 16.52544592524342804, -4.483927247898539470, 38.54057627198103120 ) ) ;
#98381 = CARTESIAN_POINT ( 'NONE',  ( 14.29746914071037800, 8.314922557961029526, 56.66775706135235424 ) ) ;
#98382 = CARTESIAN_POINT ( 'NONE',  ( 0.05219959533936267826, -19.03943276465977164, 95.00109039468567573 ) ) ;
#98383 = CARTESIAN_POINT ( 'NONE',  ( -5.719274019375978568, 21.55341960407610458, 95.20724293864769550 ) ) ;
#98384 = CARTESIAN_POINT ( 'NONE',  ( 0.05219959533910956823, 16.53943276465976808, 29.99890960531435979 ) ) ;
#98385 = ORIENTED_EDGE ( 'NONE', *, *, #144467, .F. ) ;
#98386 = CARTESIAN_POINT ( 'NONE',  ( 14.29746914071037800, 8.314922557961029526, 81.66775706135236135 ) ) ;
#98387 = FACE_OUTER_BOUND ( 'NONE', #91729, .T. ) ;
#98388 = CARTESIAN_POINT ( 'NONE',  ( -15.80617190586745835, -15.72974639402198527, 71.87390960531438111 ) ) ;
#98389 = CARTESIAN_POINT ( 'NONE',  ( 16.52544592524335698, 4.483927247898782831, 106.4594237280190328 ) ) ;
#98390 = ORIENTED_EDGE ( 'NONE', *, *, #16822, .F. ) ;
#98391 = CARTESIAN_POINT ( 'NONE',  ( -17.49999999999999645, -5.499999999999992895, 54.20309617465830598 ) ) ;
#98392 = CARTESIAN_POINT ( 'NONE',  ( 21.55341960407610458, 5.719274019375980345, 98.95724293864770971 ) ) ;
#98393 = CARTESIAN_POINT ( 'NONE',  ( -0.05219959533907301413, -21.53943276465977519, 107.4989096053143669 ) ) ;
#98394 = CARTESIAN_POINT ( 'NONE',  ( -12.14591786802309592, -12.06949235617757132, 41.87390960531435979 ) ) ;
#98396 = CARTESIAN_POINT ( 'NONE',  ( -4.483927247898782831, 16.52544592524335698, 42.70942372801901854 ) ) ;
#98395 = AXIS2_PLACEMENT_3D ( 'NONE', #123091, #126084, #110908 ) ;
#98398 = EDGE_CURVE ( 'NONE', #84229, #30776, #198426, .T. ) ;
#98397 = CARTESIAN_POINT ( 'NONE',  ( 19.02544592524343514, -5.153800228976328945, 48.54057627198103120 ) ) ;
#98399 = CARTESIAN_POINT ( 'NONE',  ( 9.474510206698971260, -16.51473224551069308, 72.91557627198102409 ) ) ;
#98400 = ORIENTED_EDGE ( 'NONE', *, *, #103264, .T. ) ;
#98401 = CARTESIAN_POINT ( 'NONE',  ( 9.474510206698971260, -16.51473224551069308, 112.9155762719810383 ) ) ;
#98402 = CARTESIAN_POINT ( 'NONE',  ( -27.73933785331498925, 2.428612866367529932E-14, 149.3750000027311842 ) ) ;
#98403 = CARTESIAN_POINT ( 'NONE',  ( -0.05219959533936034679, 19.03943276465977164, 107.5010903946856615 ) ) ;
#98404 = CARTESIAN_POINT ( 'NONE',  ( 9.474510206698729675, 16.51473224551082808, 57.08442372801900433 ) ) ;
#98405 = CARTESIAN_POINT ( 'NONE',  ( -21.53943276465977519, 0.05219959533907696930, 86.24890960531436690 ) ) ;
#98406 = CARTESIAN_POINT ( 'NONE',  ( -16.53943276465976808, -0.05219959533934237506, 113.7510903946856757 ) ) ;
#98407 = CARTESIAN_POINT ( 'NONE',  ( 19.03943276465977164, -0.05219959533909143690, 73.74890960531435269 ) ) ;
#98408 = CARTESIAN_POINT ( 'NONE',  ( 18.62759615963271287, -10.81492255796078972, 43.33224293864769550 ) ) ;
#98410 = CARTESIAN_POINT ( 'NONE',  ( 4.379528057220092307, 16.55341960407617563, 27.29275706135234358 ) ) ;
#98409 = CARTESIAN_POINT ( 'NONE',  ( -18.67979575497178146, -10.72451020669898902, 76.66557627198103830 ) ) ;
#98411 = CARTESIAN_POINT ( 'NONE',  ( 19.02544592524343514, -5.153800228976328945, 113.5405762719810241 ) ) ;
#98412 = CARTESIAN_POINT ( 'NONE',  ( 15.80617190586769283, -15.72974639402175789, 80.62609039468567573 ) ) ;
#98413 = CARTESIAN_POINT ( 'NONE',  ( 19.03943276465977164, -0.05219959533909143690, 78.74890960531436690 ) ) ;
#98414 = CARTESIAN_POINT ( 'NONE',  ( -13.97604488694527625, -13.89961937509977652, 21.87390960531435979 ) ) ;
#98415 = CARTESIAN_POINT ( 'NONE',  ( 16.46253265017160672, -9.564922557960803928, 68.33224293864770971 ) ) ;
#98416 = CARTESIAN_POINT ( 'NONE',  ( 8.224510206698953496, -14.34966873604960469, 87.91557627198103830 ) ) ;
#98417 = VERTEX_POINT ( 'NONE', #7401 ) ;
#98418 = CARTESIAN_POINT ( 'NONE',  ( -13.97604488694547697, 13.89961937509957934, 98.12609039468566152 ) ) ;
#98419 = CARTESIAN_POINT ( 'NONE',  ( 22.00000000000000000, -1.163414459189985801E-14, 92.50000000000000000 ) ) ;
#98420 = CARTESIAN_POINT ( 'NONE',  ( -13.89961937509977652, 13.97604488694528158, 75.62390960531438111 ) ) ;
#98422 = CARTESIAN_POINT ( 'NONE',  ( 19.02544592524343514, -5.153800228976328945, 98.54057627198100988 ) ) ;
#98421 = CARTESIAN_POINT ( 'NONE',  ( 5.823673210054444382, -21.52544592524334988, 90.20942372801903275 ) ) ;
#98423 = CARTESIAN_POINT ( 'NONE',  ( 16.53943276465976808, 0.05219959533934440121, 81.25109039468568994 ) ) ;
#98424 = CARTESIAN_POINT ( 'NONE',  ( -16.19135201231366494, -7.376712067591931543, 75.18680854052030327 ) ) ;
#98425 = CARTESIAN_POINT ( 'NONE',  ( 19.03943276465977164, 0.05219959533936151252, 61.25109039468566863 ) ) ;
#98426 = CARTESIAN_POINT ( 'NONE',  ( 5.049401038297881783, 19.05341960407617563, 22.29275706135233648 ) ) ;
#98427 = DIRECTION ( 'NONE',  ( 0.5367108174878537641, 0.8437662581494472791, -0.000000000000000000 ) ) ;
#98428 = CARTESIAN_POINT ( 'NONE',  ( -5.000000000000000000, -120.0000000000000142, -15.00000000000000000 ) ) ;
#98429 = FACE_OUTER_BOUND ( 'NONE', #301, .T. ) ;
#98430 = CARTESIAN_POINT ( 'NONE',  ( 4.379528057220339221, -16.55341960407611168, 27.70724293864769905 ) ) ;
#98431 = EDGE_CURVE ( 'NONE', #179471, #137572, #174325, .T. ) ;
#98432 = FACE_OUTER_BOUND ( 'NONE', #186903, .T. ) ;
#98433 = CARTESIAN_POINT ( 'NONE',  ( -16.55341960407617563, 4.379528057220093196, 103.5427570613523613 ) ) ;
#98434 = CARTESIAN_POINT ( 'NONE',  ( 17.26058549869092928, 6.457015423128506626, 68.87745837476070676 ) ) ;
#98435 = CARTESIAN_POINT ( 'NONE',  ( 4.379528057220092307, 16.55341960407617563, 82.29275706135234714 ) ) ;
#98436 = B_SPLINE_CURVE_WITH_KNOTS ( 'NONE', 3,
 ( #184406, #153055, #170223, #136902, #62030, #31716, #93364, #199575, #198589, #28758, #14557, #197599 ),
 .UNSPECIFIED., .F., .F.,
 ( 4, 2, 2, 2, 2, 4 ),
 ( 1.961533960389205320E-07, 0.0007644364765400004508, 0.001146556638111986392, 0.001528676799683972333, 0.002292917122827955491, 0.003057157445971939082 ),
 .UNSPECIFIED. ) ;
#98437 = CARTESIAN_POINT ( 'NONE',  ( -15.80617190586768217, 15.72974639402176855, 83.12609039468568994 ) ) ;
#98438 = CARTESIAN_POINT ( 'NONE',  ( -5.153800228976607833, 19.02544592524334988, 107.7094237280189759 ) ) ;
#98439 = CARTESIAN_POINT ( 'NONE',  ( -18.62759615963255300, -10.81492255796106328, 64.16775706135234714 ) ) ;
#98440 = CARTESIAN_POINT ( 'NONE',  ( -19.03943276465977164, -0.05219959533935918106, 33.75109039468566863 ) ) ;
#98441 = CARTESIAN_POINT ( 'NONE',  ( -13.89961937509977652, 13.97604488694528158, 75.62390960531438111 ) ) ;
#98442 = CARTESIAN_POINT ( 'NONE',  ( 16.46253265017160672, -9.564922557960803928, 53.33224293864768839 ) ) ;
#98443 = EDGE_CURVE ( 'NONE', #24966, #176032, #193685, .T. ) ;
#98444 = CARTESIAN_POINT ( 'NONE',  ( -19.02130022317637170, 5.499999999999601208, 40.78188669246577547 ) ) ;
#98445 = CARTESIAN_POINT ( 'NONE',  ( 0.05219959533907565091, 21.53943276465977519, 99.99890960531436690 ) ) ;
#98446 = CARTESIAN_POINT ( 'NONE',  ( 10.81492255796078972, 18.62759615963270932, 49.58224293864769550 ) ) ;
#98447 = CARTESIAN_POINT ( 'NONE',  ( 19.03943276465977164, -0.05219959533909143690, 48.74890960531435979 ) ) ;
#98448 = CARTESIAN_POINT ( 'NONE',  ( -16.52544592524335698, -4.483927247898792601, 58.95942372801902565 ) ) ;
#98449 = UNCERTAINTY_MEASURE_WITH_UNIT (LENGTH_MEASURE( 1.000000000000000082E-05 ), #130067, 'distance_accuracy_value', 'NONE');
#98450 = ORIENTED_EDGE ( 'NONE', *, *, #176690, .F. ) ;
#98451 = CARTESIAN_POINT ( 'NONE',  ( -21.52544592524334988, -5.823673210054445271, 38.95942372801901854 ) ) ;
#98453 = CARTESIAN_POINT ( 'NONE',  ( 36.91746824999999887, 11.99521256947799053, -1.524999997268813745 ) ) ;
#98452 = CARTESIAN_POINT ( 'NONE',  ( -12.06949235617756955, 12.14591786802309770, 60.62390960531437401 ) ) ;
#98454 = CARTESIAN_POINT ( 'NONE',  ( 16.53943276465976808, 0.05219959533934440121, 41.25109039468568284 ) ) ;
#98455 = CARTESIAN_POINT ( 'NONE',  ( -0.05219959533910754901, -16.53943276465976808, 97.49890960531436690 ) ) ;
#98456 = CARTESIAN_POINT ( 'NONE',  ( 5.049401038297881783, 19.05341960407617563, 47.29275706135231161 ) ) ;
#98457 = CARTESIAN_POINT ( 'NONE',  ( 12.14591786802309770, 12.06949235617756955, 74.37390960531436690 ) ) ;
#98458 = CARTESIAN_POINT ( 'NONE',  ( 21.53943276465977519, 0.05219959533937863772, 26.25109039468567573 ) ) ;
#98460 = CARTESIAN_POINT ( 'NONE',  ( -10.72451020669898014, 18.67979575497178502, 85.41557627198102409 ) ) ;
#98459 = CARTESIAN_POINT ( 'NONE',  ( 19.02544592524343514, -5.153800228976328945, 23.54057627198102054 ) ) ;
#98461 = CARTESIAN_POINT ( 'NONE',  ( 0.05219959533909260263, 19.03943276465977164, 104.9989096053143669 ) ) ;
#98462 = CARTESIAN_POINT ( 'NONE',  ( 12.06949235617757843, -12.14591786802309237, 78.12390960531436690 ) ) ;
#98463 = CARTESIAN_POINT ( 'NONE',  ( 29.81671572245950230, -26.02765724076281373, -18.90727510134258793 ) ) ;
#98464 = CARTESIAN_POINT ( 'NONE',  ( 22.81625015709509441, 31.40387420917330275, -1.324999997268813123 ) ) ;
#98465 = CARTESIAN_POINT ( 'NONE',  ( -0.05219959533936034679, 19.03943276465977164, 87.50109039468567573 ) ) ;
#98466 = CARTESIAN_POINT ( 'NONE',  ( 10.72451020669871369, 18.67979575497193778, 27.08442372801901854 ) ) ;
#98467 = CARTESIAN_POINT ( 'NONE',  ( -13.89961937509977652, 13.97604488694528158, 65.62390960531436690 ) ) ;
#98468 = CARTESIAN_POINT ( 'NONE',  ( -16.46253265017146816, -9.564922557961047289, 54.16775706135234003 ) ) ;
#98469 = CARTESIAN_POINT ( 'NONE',  ( -5.153800228976328057, -19.02544592524343514, 37.29057627198102409 ) ) ;
#98470 =( REPRESENTATION_RELATIONSHIP ('NONE','NONE', #154205, #9542 ) REPRESENTATION_RELATIONSHIP_WITH_TRANSFORMATION ( #118967 )SHAPE_REPRESENTATION_RELATIONSHIP( ) );
#98471 = CARTESIAN_POINT ( 'NONE',  ( -4.483927247898539470, -16.52544592524342804, 57.29057627198103120 ) ) ;
#98472 = CARTESIAN_POINT ( 'NONE',  ( 8.224510206698953496, -14.34966873604960469, 57.91557627198103120 ) ) ;
#98473 = CARTESIAN_POINT ( 'NONE',  ( -19.03943276465977164, 0.05219959533909376836, 61.24890960531436690 ) ) ;
#98474 = CIRCLE ( 'NONE', #176026, 1.610000000000000098 ) ;
#98475 = CARTESIAN_POINT ( 'NONE',  ( -5.823673210054116645, -21.52544592524344225, 87.29057627198103830 ) ) ;
#98476 = CARTESIAN_POINT ( 'NONE',  ( -13.89961937509977652, 13.97604488694528158, 60.62390960531436690 ) ) ;
#98477 = CARTESIAN_POINT ( 'NONE',  ( -15.80617190586745835, -15.72974639402198527, 81.87390960531435269 ) ) ;
#98478 = CARTESIAN_POINT ( 'NONE',  ( -21.55341960407619339, 5.719274019375674811, 98.54275706135234714 ) ) ;
#98481 = CARTESIAN_POINT ( 'NONE',  ( 0.05219959533910956823, 16.53943276465976808, 94.99890960531436690 ) ) ;
#98480 = CARTESIAN_POINT ( 'NONE',  ( -16.55341960407611168, -4.379528057220339221, 21.45724293864769550 ) ) ;
#98479 = CARTESIAN_POINT ( 'NONE',  ( 13.89961937509977652, -13.97604488694527269, 23.12390960531436335 ) ) ;
#98482 = CARTESIAN_POINT ( 'NONE',  ( 19.03943276465977164, 0.05219959533936151252, 86.25109039468567573 ) ) ;
#98483 = ORIENTED_EDGE ( 'NONE', *, *, #40630, .T. ) ;
#98484 = CARTESIAN_POINT ( 'NONE',  ( 18.67979575497194134, -10.72451020669871369, 20.83442372801901143 ) ) ;
#98485 = CARTESIAN_POINT ( 'NONE',  ( -5.153800228976607833, 19.02544592524334988, 52.70942372801900433 ) ) ;
#98486 = CARTESIAN_POINT ( 'NONE',  ( -4.379528057220086978, -16.55341960407618274, 99.79275706135234714 ) ) ;
#98487 = CARTESIAN_POINT ( 'NONE',  ( 19.02544592524334988, 5.153800228976608722, 26.45942372801899722 ) ) ;
#98488 = CARTESIAN_POINT ( 'NONE',  ( -16.51473224551069308, -9.474510206698971260, 106.6655762719810383 ) ) ;
#98489 = CARTESIAN_POINT ( 'NONE',  ( -10.72451020669898014, 18.67979575497178502, 65.41557627198102409 ) ) ;
#98490 = CARTESIAN_POINT ( 'NONE',  ( -26.53518950525900166, 7.921153050709826893, 167.7791411921787699 ) ) ;
#98491 = CARTESIAN_POINT ( 'NONE',  ( 9.474510206698971260, -16.51473224551069308, 37.91557627198102409 ) ) ;
#98492 = CARTESIAN_POINT ( 'NONE',  ( 21.53943276465977519, 0.05219959533937863772, 111.2510903946856899 ) ) ;
#98493 = CARTESIAN_POINT ( 'NONE',  ( -8.314922557961024197, 14.29746914071037800, 77.91775706135231871 ) ) ;
#98494 = CARTESIAN_POINT ( 'NONE',  ( 21.52544592524334988, 5.823673210054432836, 26.45942372801901854 ) ) ;
#98495 = CARTESIAN_POINT ( 'NONE',  ( 16.52544592524335698, 4.483927247898782831, 41.45942372801901143 ) ) ;
#98496 = CARTESIAN_POINT ( 'NONE',  ( 16.46253265017160672, -9.564922557960803928, 108.3322429386476955 ) ) ;
#98497 = CARTESIAN_POINT ( 'NONE',  ( 9.564922557960805705, 16.46253265017160317, 59.58224293864769550 ) ) ;
#98498 = CARTESIAN_POINT ( 'NONE',  ( 19.03943276465977164, -0.05219959533909143690, 68.74890960531436690 ) ) ;
#98499 = CARTESIAN_POINT ( 'NONE',  ( -8.314922557961024197, 14.29746914071037800, 47.91775706135234714 ) ) ;
#98500 = CARTESIAN_POINT ( 'NONE',  ( -16.52544592524342804, 4.483927247898546575, 106.0405762719810525 ) ) ;
#98501 = CARTESIAN_POINT ( 'NONE',  ( -8.314922557961024197, 14.29746914071037800, 107.9177570613523471 ) ) ;
#98504 = CARTESIAN_POINT ( 'NONE',  ( -19.02544592524342804, 5.153800228976336051, 71.04057627198099567 ) ) ;
#98503 = CARTESIAN_POINT ( 'NONE',  ( -9.564922557960796823, -16.46253265017161027, 72.08224293864770971 ) ) ;
#98502 = CARTESIAN_POINT ( 'NONE',  ( -15.72974639402176322, -15.80617190586768395, 59.37609039468568284 ) ) ;
#98505 = CARTESIAN_POINT ( 'NONE',  ( -9.564922557960796823, -16.46253265017161027, 92.08224293864769550 ) ) ;
#98506 = CARTESIAN_POINT ( 'NONE',  ( -4.483927247898539470, -16.52544592524342804, 47.29057627198103120 ) ) ;
#98507 = CARTESIAN_POINT ( 'NONE',  ( 8.224510206698953496, -14.34966873604960469, 22.91557627198102765 ) ) ;
#98508 = CARTESIAN_POINT ( 'NONE',  ( 4.483927247898545687, 16.52544592524342804, 39.79057627198103830 ) ) ;
#98509 = ORIENTED_EDGE ( 'NONE', *, *, #106967, .F. ) ;
#98510 = CARTESIAN_POINT ( 'NONE',  ( -19.03943276465977164, -0.05219959533935918106, 48.75109039468566863 ) ) ;
#98512 = AXIS2_PLACEMENT_3D ( 'NONE', #39169, #100827, #99834 ) ;
#98511 = LINE ( 'NONE', #175377, #77067 ) ;
#98513 = CARTESIAN_POINT ( 'NONE',  ( -0.05219959533909027116, -19.03943276465977164, 67.49890960531436690 ) ) ;
#98514 = CARTESIAN_POINT ( 'NONE',  ( -9.564922557961040184, 16.46253265017147172, 32.91775706135233293 ) ) ;
#98515 = CARTESIAN_POINT ( 'NONE',  ( -36.91746825000001309, -11.99521256947794789, -11.02499999726881263 ) ) ;
#98516 = CARTESIAN_POINT ( 'NONE',  ( -12.49999999999997691, -89.99999999999997158, -25.00000000000000000 ) ) ;
#98517 = CIRCLE ( 'NONE', #37189, 5.000000000000000000 ) ;
#98519 = CARTESIAN_POINT ( 'NONE',  ( 14.34966873604972726, -8.224510206698740333, 65.83442372801900433 ) ) ;
#98518 = CARTESIAN_POINT ( 'NONE',  ( -19.05341960407617563, 5.049401038297882671, 78.54275706135233293 ) ) ;
#98520 = CARTESIAN_POINT ( 'NONE',  ( 17.49999999999999645, 5.624438216177590100, 91.68329655085358354 ) ) ;
#98521 = CARTESIAN_POINT ( 'NONE',  ( -19.02544592524342804, 5.153800228976336051, 91.04057627198100988 ) ) ;
#98522 = CARTESIAN_POINT ( 'NONE',  ( -21.52544592524334988, -5.823673210054445271, 23.95942372801901143 ) ) ;
#98523 = CARTESIAN_POINT ( 'NONE',  ( 5.153800228976615827, -19.02544592524334988, 75.20942372801896170 ) ) ;
#98525 = CARTESIAN_POINT ( 'NONE',  ( 5.049401038298161559, -19.05341960407611168, 52.70724293864767418 ) ) ;
#98524 = CARTESIAN_POINT ( 'NONE',  ( 17.31747979337950127, 6.344076630961020591, 88.87944868065186199 ) ) ;
#98526 = CARTESIAN_POINT ( 'NONE',  ( 16.51473224551069308, 9.474510206698969483, 84.16557627198102409 ) ) ;
#98528 = CARTESIAN_POINT ( 'NONE',  ( 19.02544592524343514, -5.153800228976328945, 48.54057627198103120 ) ) ;
#98527 = CARTESIAN_POINT ( 'NONE',  ( 14.29746914071049879, -8.314922557960816363, 48.33224293864770260 ) ) ;
#98529 = CARTESIAN_POINT ( 'NONE',  ( 9.474510206698729675, 16.51473224551082808, 47.08442372801900433 ) ) ;
#98530 = CARTESIAN_POINT ( 'NONE',  ( 14.29746914071049879, -8.314922557960816363, 88.33224293864769550 ) ) ;
#98531 = CARTESIAN_POINT ( 'NONE',  ( -19.02544592524334988, -5.153800228976617603, 28.95942372801900433 ) ) ;
#98532 = CARTESIAN_POINT ( 'NONE',  ( -19.02544592524342804, 5.153800228976336051, 61.04057627198103120 ) ) ;
#98533 = CARTESIAN_POINT ( 'NONE',  ( -15.80617190586745835, -15.72974639402198527, 56.87390960531436690 ) ) ;
#98535 = CARTESIAN_POINT ( 'NONE',  ( 13.97604488694548053, -13.89961937509957401, 20.62609039468567573 ) ) ;
#98534 = CARTESIAN_POINT ( 'NONE',  ( -4.379528057220328563, 16.55341960407611168, 70.20724293864769550 ) ) ;
#98536 = CARTESIAN_POINT ( 'NONE',  ( -19.05341960407611168, -5.049401038298163336, 111.4572429386476671 ) ) ;
#98537 = CARTESIAN_POINT ( 'NONE',  ( 18.62759615963271287, -10.81492255796078972, 28.33224293864769550 ) ) ;
#98538 = CARTESIAN_POINT ( 'NONE',  ( -5.153800228976328057, -19.02544592524343514, 47.29057627198102409 ) ) ;
#98539 = CARTESIAN_POINT ( 'NONE',  ( 16.51473224551069308, 9.474510206698969483, 44.16557627198103120 ) ) ;
#98540 = CARTESIAN_POINT ( 'NONE',  ( 8.224510206698953496, -14.34966873604960469, 97.91557627198103830 ) ) ;
#98541 = CIRCLE ( 'NONE', #11430, 39.99999999999999289 ) ;
#98542 = CARTESIAN_POINT ( 'NONE',  ( -15.80617190586745835, -15.72974639402198527, 111.8739096053143669 ) ) ;
#98543 = CARTESIAN_POINT ( 'NONE',  ( -19.03943276465977164, 0.05219959533909376836, 106.2489096053143669 ) ) ;
#98544 = CARTESIAN_POINT ( 'NONE',  ( 15.72974639402199770, -15.80617190586745480, 113.1239096053143953 ) ) ;
#98545 = CARTESIAN_POINT ( 'NONE',  ( 19.05341960407611168, 5.049401038298154454, 103.9572429386476671 ) ) ;
#98546 = CARTESIAN_POINT ( 'NONE',  ( 9.474510206698971260, -16.51473224551069308, 27.91557627198103120 ) ) ;
#98547 = CARTESIAN_POINT ( 'NONE',  ( -18.62759615963255300, -10.81492255796106328, 84.16775706135234714 ) ) ;
#98548 = CARTESIAN_POINT ( 'NONE',  ( -21.52544592524343514, 5.823673210054127303, 91.04057627198103830 ) ) ;
#98549 = FACE_OUTER_BOUND ( 'NONE', #189298, .T. ) ;
#98550 = CARTESIAN_POINT ( 'NONE',  ( 19.26498983726237668, -5.499999999999793943, 78.05319577422000066 ) ) ;
#98551 = CARTESIAN_POINT ( 'NONE',  ( 30.74735067906814479, -1.468823602708525300, -50.54421433284817056 ) ) ;
#98552 = CARTESIAN_POINT ( 'NONE',  ( -16.53943276465976808, -0.05219959533934237506, 48.75109039468568284 ) ) ;
#98553 = CARTESIAN_POINT ( 'NONE',  ( 8.314922557960818139, 14.29746914071049879, 114.5822429386477097 ) ) ;
#98554 = CARTESIAN_POINT ( 'NONE',  ( -69.65682714487590488, -71.74905178543390605, -25.00000000000000000 ) ) ;
#98555 = CARTESIAN_POINT ( 'NONE',  ( 9.474510206698971260, -16.51473224551069308, 57.91557627198103120 ) ) ;
#98556 = CARTESIAN_POINT ( 'NONE',  ( -16.53943276465976808, 0.05219959533911058130, 96.24890960531435269 ) ) ;
#98557 = CARTESIAN_POINT ( 'NONE',  ( 15.80617190586746368, 15.72974639402197994, 49.37390960531436690 ) ) ;
#98558 = CARTESIAN_POINT ( 'NONE',  ( -4.379528057220328563, 16.55341960407611168, 65.20724293864768129 ) ) ;
#98559 = CARTESIAN_POINT ( 'NONE',  ( 16.53943276465976808, 0.05219959533934440121, 26.25109039468567573 ) ) ;
#98560 = CARTESIAN_POINT ( 'NONE',  ( 15.72974639402176855, 15.80617190586768217, 76.87609039468567573 ) ) ;
#98561 = CARTESIAN_POINT ( 'NONE',  ( 13.89961937509957579, 13.97604488694547520, 61.87609039468566863 ) ) ;
#98562 = CARTESIAN_POINT ( 'NONE',  ( -16.52544592524335698, -4.483927247898792601, 98.95942372801903275 ) ) ;
#98563 = CARTESIAN_POINT ( 'NONE',  ( 16.52544592524342804, -4.483927247898539470, 43.54057627198103830 ) ) ;
#98564 = CARTESIAN_POINT ( 'NONE',  ( -13.97604488694527625, -13.89961937509977652, 36.87390960531436690 ) ) ;
#98565 = CARTESIAN_POINT ( 'NONE',  ( 5.153800228976335163, 19.02544592524342804, 94.79057627198103830 ) ) ;
#98566 = CARTESIAN_POINT ( 'NONE',  ( 15.72974639402199770, -15.80617190586745480, 88.12390960531436690 ) ) ;
#98567 = CARTESIAN_POINT ( 'NONE',  ( -12.14591786802326823, 12.06949235617739902, 43.12609039468568284 ) ) ;
#98569 = CARTESIAN_POINT ( 'NONE',  ( -15.72974639402176322, -15.80617190586768395, 69.37609039468567573 ) ) ;
#98568 = CARTESIAN_POINT ( 'NONE',  ( -0.05219959533910754901, -16.53943276465976808, 62.49890960531436690 ) ) ;
#98570 = CARTESIAN_POINT ( 'NONE',  ( 8.224510206698742110, 14.34966873604972548, 102.0844237280190185 ) ) ;
#98571 = DIRECTION ( 'NONE',  ( -6.938893903907222067E-15, 0.000000000000000000, -1.000000000000000000 ) ) ;
#98572 = CARTESIAN_POINT ( 'NONE',  ( -21.46320343559653310, -20.96320343559631638, 5.353553390593268624 ) ) ;
#98573 = CARTESIAN_POINT ( 'NONE',  ( 12.14591786802309770, 12.06949235617756955, 24.37390960531435979 ) ) ;
#98574 = CARTESIAN_POINT ( 'NONE',  ( -14.34966873604972548, 8.224510206698743886, 68.33442372801900433 ) ) ;
#98575 = CARTESIAN_POINT ( 'NONE',  ( 9.474510206698971260, -16.51473224551069308, 87.91557627198102409 ) ) ;
#98576 = CARTESIAN_POINT ( 'NONE',  ( -13.89961937509977652, 13.97604488694528158, 100.6239096053143669 ) ) ;
#98577 = CARTESIAN_POINT ( 'NONE',  ( 18.67979575497194134, -10.72451020669871369, 90.83442372801901854 ) ) ;
#98578 = CARTESIAN_POINT ( 'NONE',  ( 12.06949235617739724, 12.14591786802326823, 91.87609039468568994 ) ) ;
#98579 = CARTESIAN_POINT ( 'NONE',  ( 16.55341960407611168, 4.379528057220329451, 53.95724293864770260 ) ) ;
#98580 = CARTESIAN_POINT ( 'NONE',  ( -5.153800228976328057, -19.02544592524343514, 72.29057627198102409 ) ) ;
#98581 = ORIENTED_EDGE ( 'NONE', *, *, #17432, .F. ) ;
#98582 = CARTESIAN_POINT ( 'NONE',  ( 13.97604488694548053, -13.89961937509957401, 105.6260903946856757 ) ) ;
#98583 = CARTESIAN_POINT ( 'NONE',  ( -14.29746914071049879, 8.314922557960819915, 105.8322429386476955 ) ) ;
#98584 = CARTESIAN_POINT ( 'NONE',  ( 9.474510206698971260, -16.51473224551069308, 77.91557627198103830 ) ) ;
#98586 = CARTESIAN_POINT ( 'NONE',  ( -22.81625015709510507, 31.40387420917330275, -8.924999997268814766 ) ) ;
#98585 = CARTESIAN_POINT ( 'NONE',  ( -14.29746914071037622, -8.314922557961029526, 24.16775706135235424 ) ) ;
#98587 = CARTESIAN_POINT ( 'NONE',  ( 15.72974639402176855, 15.80617190586768217, 111.8760903946856615 ) ) ;
#98588 = CARTESIAN_POINT ( 'NONE',  ( 16.53943276465976808, 0.05219959533934440121, 86.25109039468568994 ) ) ;
#98589 = CARTESIAN_POINT ( 'NONE',  ( -9.474510206698720793, -16.51473224551083518, 89.58442372801900433 ) ) ;
#98590 = CARTESIAN_POINT ( 'NONE',  ( -5.153800228976328057, -19.02544592524343514, 22.29057627198102765 ) ) ;
#98591 = CARTESIAN_POINT ( 'NONE',  ( 8.314922557961029526, -14.29746914071037800, 65.41775706135234714 ) ) ;
#98592 = CARTESIAN_POINT ( 'NONE',  ( -8.224510206698735004, -14.34966873604973081, 54.58442372801901143 ) ) ;
#98593 = CARTESIAN_POINT ( 'NONE',  ( 27.04875460227163586, -29.46888106016232811, -5.722453210188423789 ) ) ;
#98594 = CARTESIAN_POINT ( 'NONE',  ( -16.46253265017146816, -9.564922557961047289, 69.16775706135233293 ) ) ;
#98595 = CIRCLE ( 'NONE', #137297, 2.700000000000000622 ) ;
#98596 = CARTESIAN_POINT ( 'NONE',  ( -21.55341960407619339, 5.719274019375674811, 103.5427570613523613 ) ) ;
#98597 = CARTESIAN_POINT ( 'NONE',  ( -13.89961937509977652, 13.97604488694528158, 35.62390960531435269 ) ) ;
#98598 = CARTESIAN_POINT ( 'NONE',  ( -13.89961937509977652, 13.97604488694528158, 80.62390960531436690 ) ) ;
#98599 = CARTESIAN_POINT ( 'NONE',  ( -12.14591786802309592, -12.06949235617757132, 76.87390960531439532 ) ) ;
#98600 = CARTESIAN_POINT ( 'NONE',  ( 5.719274019375673035, 21.55341960407619339, 92.29275706135236135 ) ) ;
#98601 = CARTESIAN_POINT ( 'NONE',  ( 16.51473224551083163, -9.474510206698727899, 45.83442372801900433 ) ) ;
#98602 = CARTESIAN_POINT ( 'NONE',  ( 5.719274019375991003, -21.55341960407610458, 42.70724293864770260 ) ) ;
#98603 = CARTESIAN_POINT ( 'NONE',  ( 13.97604488694548053, -13.89961937509957401, 20.62609039468567573 ) ) ;
#98604 = CARTESIAN_POINT ( 'NONE',  ( -9.564922557960796823, -16.46253265017161027, 77.08224293864769550 ) ) ;
#98605 = CARTESIAN_POINT ( 'NONE',  ( -15.72974639402176322, -15.80617190586768395, 109.3760903946857042 ) ) ;
#98606 = CARTESIAN_POINT ( 'NONE',  ( 21.52544592524344225, -5.823673210054117533, 63.54057627198103830 ) ) ;
#98607 = CARTESIAN_POINT ( 'NONE',  ( -19.05341960407611168, -5.049401038298163336, 96.45724293864769550 ) ) ;
#98608 = CARTESIAN_POINT ( 'NONE',  ( -16.46253265017146816, -9.564922557961047289, 79.16775706135234714 ) ) ;
#98609 = CARTESIAN_POINT ( 'NONE',  ( -16.51473224551069308, -9.474510206698971260, 96.66557627198102409 ) ) ;
#98610 = CARTESIAN_POINT ( 'NONE',  ( 13.89961937509957401, 13.97604488694547697, 91.87609039468567573 ) ) ;
#98611 = CARTESIAN_POINT ( 'NONE',  ( -16.52544592524335698, -4.483927247898792601, 48.95942372801902565 ) ) ;
#98612 = CARTESIAN_POINT ( 'NONE',  ( 16.51473224551069308, 9.474510206698969483, 24.16557627198102765 ) ) ;
#98613 = CARTESIAN_POINT ( 'NONE',  ( -13.97604488694527625, -13.89961937509977652, 81.87390960531436690 ) ) ;
#98614 = CARTESIAN_POINT ( 'NONE',  ( 10.72451020669898902, -18.67979575497178502, 67.91557627198102409 ) ) ;
#98615 = CARTESIAN_POINT ( 'NONE',  ( 4.379528057220092307, 16.55341960407617563, 27.29275706135234358 ) ) ;
#98616 = CARTESIAN_POINT ( 'NONE',  ( -15.80617190586768217, 15.72974639402176855, 28.12609039468568284 ) ) ;
#98617 = CARTESIAN_POINT ( 'NONE',  ( 0.05219959533937995610, -21.53943276465977519, 80.00109039468568994 ) ) ;
#98618 = CARTESIAN_POINT ( 'NONE',  ( -12.06949235617739369, -12.14591786802326823, 84.37609039468570415 ) ) ;
#98619 = CARTESIAN_POINT ( 'NONE',  ( 5.049401038298161559, -19.05341960407611168, 87.70724293864769550 ) ) ;
#98620 = CARTESIAN_POINT ( 'NONE',  ( 8.224510206698953496, -14.34966873604960469, 72.91557627198103830 ) ) ;
#98621 = CARTESIAN_POINT ( 'NONE',  ( -12.06949235617756955, 12.14591786802309770, 25.62390960531435624 ) ) ;
#98622 = CARTESIAN_POINT ( 'NONE',  ( -5.049401038297874678, -19.05341960407617918, 54.79275706135234003 ) ) ;
#98623 = CARTESIAN_POINT ( 'NONE',  ( -21.52544592524334988, -5.823673210054445271, 48.95942372801902565 ) ) ;
#98624 = CARTESIAN_POINT ( 'NONE',  ( 8.224510206698953496, -14.34966873604960469, 92.91557627198103830 ) ) ;
#98625 = CARTESIAN_POINT ( 'NONE',  ( -9.474510206698964154, 16.51473224551069663, 115.4155762719810241 ) ) ;
#98626 = CARTESIAN_POINT ( 'NONE',  ( -16.53943276465976808, -0.05219959533934237506, 98.75109039468568994 ) ) ;
#98627 = CARTESIAN_POINT ( 'NONE',  ( 18.67979575497194134, -10.72451020669871369, 85.83442372801901854 ) ) ;
#98628 = CARTESIAN_POINT ( 'NONE',  ( 14.29746914071037800, 8.314922557961029526, 46.66775706135234714 ) ) ;
#98629 = CARTESIAN_POINT ( 'NONE',  ( -10.81492255796105439, 18.62759615963255655, 42.91775706135235424 ) ) ;
#98630 = ORIENTED_EDGE ( 'NONE', *, *, #170373, .T. ) ;
#98631 = CARTESIAN_POINT ( 'NONE',  ( 18.62759615963271287, -10.81492255796078972, 113.3322429386476955 ) ) ;
#98632 = CARTESIAN_POINT ( 'NONE',  ( 8.224510206698953496, -14.34966873604960469, 87.91557627198103830 ) ) ;
#98633 = CARTESIAN_POINT ( 'NONE',  ( -18.39639308325436673, -5.500000000000040856, 51.48252246182197922 ) ) ;
#98634 = CARTESIAN_POINT ( 'NONE',  ( 14.29746914071049879, -8.314922557960816363, 68.33224293864769550 ) ) ;
#98635 = CARTESIAN_POINT ( 'NONE',  ( 0.05219959533934541429, -16.53943276465976808, 95.00109039468568994 ) ) ;
#98636 = CARTESIAN_POINT ( 'NONE',  ( -19.02544592524342804, 5.153800228976336051, 41.04057627198103120 ) ) ;
#98637 = CARTESIAN_POINT ( 'NONE',  ( -5.719274019375978568, 21.55341960407610458, 45.20724293864769550 ) ) ;
#98638 = CARTESIAN_POINT ( 'NONE',  ( -12.14591786802309592, -12.06949235617757132, 71.87390960531438111 ) ) ;
#98639 = VECTOR ( 'NONE', #12975, 1000.000000000000000 ) ;
#98640 = CARTESIAN_POINT ( 'NONE',  ( 5.823673210054125526, 21.52544592524343514, 74.79057627198105251 ) ) ;
#98642 = ADVANCED_FACE ( 'NONE', ( #39746 ), #138278, .T. ) ;
#98641 = CARTESIAN_POINT ( 'NONE',  ( 9.564922557960805705, 16.46253265017160317, 94.58224293864769550 ) ) ;
#98644 = CARTESIAN_POINT ( 'NONE',  ( 9.564922557961047289, -16.46253265017146816, 90.41775706135234714 ) ) ;
#98643 = CARTESIAN_POINT ( 'NONE',  ( 9.564922557960805705, 16.46253265017160317, 44.58224293864769550 ) ) ;
#98645 = CARTESIAN_POINT ( 'NONE',  ( -10.81492255796078084, -18.62759615963271287, 32.08224293864769550 ) ) ;
#98646 = CARTESIAN_POINT ( 'NONE',  ( 5.823673210054444382, -21.52544592524334988, 60.20942372801902565 ) ) ;
#98647 = CARTESIAN_POINT ( 'NONE',  ( 19.05341960407611168, 5.049401038298154454, 58.95724293864768129 ) ) ;
#98648 = CARTESIAN_POINT ( 'NONE',  ( -16.46253265017160317, 9.564922557960807481, 90.83224293864769550 ) ) ;
#98649 = ORIENTED_EDGE ( 'NONE', *, *, #8154, .T. ) ;
#98650 = CARTESIAN_POINT ( 'NONE',  ( 0.05219959533934541429, -16.53943276465976808, 45.00109039468568284 ) ) ;
#98651 = CARTESIAN_POINT ( 'NONE',  ( 18.62759615963255655, 10.81492255796105972, 41.66775706135235424 ) ) ;
#98652 = CARTESIAN_POINT ( 'NONE',  ( -21.53943276465977519, -0.05219959533937600094, 73.75109039468567573 ) ) ;
#98653 = CARTESIAN_POINT ( 'NONE',  ( 9.474510206698971260, -16.51473224551069308, 112.9155762719810383 ) ) ;
#98654 = CARTESIAN_POINT ( 'NONE',  ( 10.81492255796078972, 18.62759615963270932, 84.58224293864769550 ) ) ;
#98656 = CARTESIAN_POINT ( 'NONE',  ( 16.53943276465976808, 0.05219959533934440121, 66.25109039468567573 ) ) ;
#98655 = CARTESIAN_POINT ( 'NONE',  ( -18.67979575497193778, 10.72451020669871902, 28.33442372801902209 ) ) ;
#98657 = CARTESIAN_POINT ( 'NONE',  ( -18.67979575497178146, -10.72451020669898902, 61.66557627198103120 ) ) ;
#98658 = CARTESIAN_POINT ( 'NONE',  ( 18.62759615963255655, 10.81492255796105972, 111.6677570613523613 ) ) ;
#98660 = CARTESIAN_POINT ( 'NONE',  ( -16.55341960407617563, 4.379528057220093196, 108.5427570613523756 ) ) ;
#98659 = CARTESIAN_POINT ( 'NONE',  ( 16.51473224551069308, 9.474510206698969483, 74.16557627198103830 ) ) ;
#98661 = CARTESIAN_POINT ( 'NONE',  ( -32.00000000000000711, -1.163414459189985801E-14, 95.00000000000000000 ) ) ;
#98662 = CARTESIAN_POINT ( 'NONE',  ( -19.03943276465977164, 0.05219959533909376836, 91.24890960531436690 ) ) ;
#98663 = CARTESIAN_POINT ( 'NONE',  ( -16.51473224551082808, 9.474510206698731452, 53.33442372801900433 ) ) ;
#98664 = CARTESIAN_POINT ( 'NONE',  ( -5.153800228976607833, 19.02544592524334988, 82.70942372801897591 ) ) ;
#98665 = CARTESIAN_POINT ( 'NONE',  ( 21.52544592524344225, -5.823673210054117533, 53.54057627198103120 ) ) ;
#98666 = CARTESIAN_POINT ( 'NONE',  ( -0.05219959533934338120, 16.53943276465976808, 112.5010903946857042 ) ) ;
#98667 = CARTESIAN_POINT ( 'NONE',  ( -13.89961937509957401, -13.97604488694547875, 104.3760903946856757 ) ) ;
#98668 = CARTESIAN_POINT ( 'NONE',  ( 19.03943276465977164, -0.05219959533909143690, 23.74890960531435269 ) ) ;
#98669 = CARTESIAN_POINT ( 'NONE',  ( -5.153800228976607833, 19.02544592524334988, 102.7094237280189759 ) ) ;
#98671 = CARTESIAN_POINT ( 'NONE',  ( 16.51473224551083163, -9.474510206698727899, 55.83442372801899722 ) ) ;
#98670 = CARTESIAN_POINT ( 'NONE',  ( 10.81492255796078972, 18.62759615963270932, 89.58224293864768129 ) ) ;
#98672 = CARTESIAN_POINT ( 'NONE',  ( 17.48847506799970120, 5.747544572773734650, 106.6730256215672341 ) ) ;
#98673 = CARTESIAN_POINT ( 'NONE',  ( 19.03943276465977164, -0.05219959533909143690, 48.74890960531435979 ) ) ;
#98674 = CARTESIAN_POINT ( 'NONE',  ( -4.379528057220328563, 16.55341960407611168, 60.20724293864768839 ) ) ;
#98675 = ADVANCED_FACE ( 'NONE', ( #116506 ), #178194, .F. ) ;
#98676 = CARTESIAN_POINT ( 'NONE',  ( 16.51473224551069308, 9.474510206698969483, 44.16557627198103120 ) ) ;
#98677 = CARTESIAN_POINT ( 'NONE',  ( -8.224510206698948167, 14.34966873604960824, 55.41557627198102409 ) ) ;
#98678 = CARTESIAN_POINT ( 'NONE',  ( -32.12256032297297992, -23.75458735917140629, -22.83990191704113926 ) ) ;
#98679 = CARTESIAN_POINT ( 'NONE',  ( 31.27032343591156049, -7.501918430611449473, 95.46114142609056330 ) ) ;
#98680 = CARTESIAN_POINT ( 'NONE',  ( 8.224510206698953496, -14.34966873604960469, 27.91557627198103830 ) ) ;
#98681 = CARTESIAN_POINT ( 'NONE',  ( -16.46253265017160317, 9.564922557960807481, 65.83224293864769550 ) ) ;
#98682 = DIRECTION ( 'NONE',  ( 3.469446951953612217E-15, 0.000000000000000000, -1.000000000000000000 ) ) ;
#98683 = CARTESIAN_POINT ( 'NONE',  ( -13.89961937509957401, -13.97604488694547875, 34.37609039468566863 ) ) ;
#98684 = CARTESIAN_POINT ( 'NONE',  ( -12.06949235617739369, -12.14591786802326823, 49.37609039468569705 ) ) ;
#98685 = CARTESIAN_POINT ( 'NONE',  ( 10.81492255796078972, 18.62759615963270932, 44.58224293864769550 ) ) ;
#98686 = CARTESIAN_POINT ( 'NONE',  ( 0.05219959533937995610, -21.53943276465977519, 105.0010903946856757 ) ) ;
#98687 = CARTESIAN_POINT ( 'NONE',  ( 5.049401038298161559, -19.05341960407611168, 67.70724293864769550 ) ) ;
#98688 = CARTESIAN_POINT ( 'NONE',  ( 4.500000000000000888, -139.5000000000000000, 21.32407087589996664 ) ) ;
#98689 = CARTESIAN_POINT ( 'NONE',  ( -16.51473224551069308, -9.474510206698971260, 96.66557627198102409 ) ) ;
#98690 = CARTESIAN_POINT ( 'NONE',  ( 22.81625015709509441, 31.40387420917330275, -5.324999997268813345 ) ) ;
#98691 = CARTESIAN_POINT ( 'NONE',  ( 5.719274019375673035, 21.55341960407619339, 22.29275706135235069 ) ) ;
#98693 = CARTESIAN_POINT ( 'NONE',  ( 16.55341960407611168, 4.379528057220329451, 88.95724293864769550 ) ) ;
#98692 = PRODUCT ( 'socket head cap screw_iso_ISO 4762 M5 x 8 - 8N', 'socket head cap screw_iso_ISO 4762 M5 x 8 - 8N', '', ( #128110 ) ) ;
#98695 = CARTESIAN_POINT ( 'NONE',  ( 13.97604488694527802, 13.89961937509977652, 79.37390960531435269 ) ) ;
#98694 = CARTESIAN_POINT ( 'NONE',  ( 5.823673210054125526, 21.52544592524343514, 84.79057627198102409 ) ) ;
#98696 = CARTESIAN_POINT ( 'NONE',  ( 19.05341960407611168, 5.049401038298154454, 88.95724293864769550 ) ) ;
#98697 = CARTESIAN_POINT ( 'NONE',  ( -21.55341960407610458, -5.719274019375992779, 106.4572429386477097 ) ) ;
#98698 = ORIENTED_EDGE ( 'NONE', *, *, #5174, .T. ) ;
#98699 = CARTESIAN_POINT ( 'NONE',  ( 16.46253265017160672, -9.564922557960803928, 78.33224293864769550 ) ) ;
#98700 = CARTESIAN_POINT ( 'NONE',  ( 19.49149378614659867, -5.499999999999673150, 96.93757513605366682 ) ) ;
#98702 = CARTESIAN_POINT ( 'NONE',  ( -9.474510206698964154, 16.51473224551069663, 35.41557627198102409 ) ) ;
#98701 = CARTESIAN_POINT ( 'NONE',  ( -16.52544592524342804, 4.483927247898546575, 106.0405762719810525 ) ) ;
#98703 = CARTESIAN_POINT ( 'NONE',  ( -19.02544592524334988, -5.153800228976617603, 98.95942372801900433 ) ) ;
#98704 = CARTESIAN_POINT ( 'NONE',  ( -4.379528057220328563, 16.55341960407611168, 115.2072429386476955 ) ) ;
#98705 = CARTESIAN_POINT ( 'NONE',  ( -15.80617190586768217, 15.72974639402176855, 73.12609039468567573 ) ) ;
#98707 = CARTESIAN_POINT ( 'NONE',  ( -18.67979575497193778, 10.72451020669871902, 33.33442372801900433 ) ) ;
#98706 = CARTESIAN_POINT ( 'NONE',  ( -13.97604488694527625, -13.89961937509977652, 66.87390960531436690 ) ) ;
#98708 = CARTESIAN_POINT ( 'NONE',  ( -5.719274019375978568, 21.55341960407610458, 115.2072429386476955 ) ) ;
#98709 = CARTESIAN_POINT ( 'NONE',  ( -17.81289503416611097, -24.51734667627696496, 142.2999999999999829 ) ) ;
#98710 = CARTESIAN_POINT ( 'NONE',  ( -19.02544592524342804, 5.153800228976336051, 91.04057627198100988 ) ) ;
#98711 = CARTESIAN_POINT ( 'NONE',  ( 27.95311704540609199, 7.352561457294874536, 160.8984504615112314 ) ) ;
#98713 = CARTESIAN_POINT ( 'NONE',  ( -21.53943276465977519, 0.05219959533907696930, 36.24890960531435979 ) ) ;
#98712 = CARTESIAN_POINT ( 'NONE',  ( 8.314922557961029526, -14.29746914071037800, 30.41775706135234358 ) ) ;
#98714 = CARTESIAN_POINT ( 'NONE',  ( 21.53943276465977519, 0.05219959533937863772, 66.25109039468567573 ) ) ;
#98715 = CARTESIAN_POINT ( 'NONE',  ( -19.03943276465977164, 0.05219959533909376836, 106.2489096053143669 ) ) ;
#98716 = CARTESIAN_POINT ( 'NONE',  ( 0.05219959533936267826, -19.03943276465977164, 100.0010903946856757 ) ) ;
#98717 = CARTESIAN_POINT ( 'NONE',  ( 16.51473224551069308, 9.474510206698969483, 49.16557627198102409 ) ) ;
#98718 = CARTESIAN_POINT ( 'NONE',  ( 5.153800228976335163, 19.02544592524342804, 79.79057627198102409 ) ) ;
#98719 = CARTESIAN_POINT ( 'NONE',  ( 16.52544592524342804, -4.483927247898539470, 98.54057627198105251 ) ) ;
#98720 = CARTESIAN_POINT ( 'NONE',  ( 5.049401038298163336, -19.05341960407611168, 97.70724293864768129 ) ) ;
#98721 = CARTESIAN_POINT ( 'NONE',  ( 16.52544592524342804, -4.483927247898539470, 88.54057627198103830 ) ) ;
#98722 = CARTESIAN_POINT ( 'NONE',  ( -9.474510206698964154, 16.51473224551069663, 115.4155762719810241 ) ) ;
#98724 = CARTESIAN_POINT ( 'NONE',  ( 19.05341960407611168, 5.049401038298154454, 38.95724293864767418 ) ) ;
#98723 = CARTESIAN_POINT ( 'NONE',  ( -12.14591786802309592, -12.06949235617757132, 61.87390960531436690 ) ) ;
#98725 = CARTESIAN_POINT ( 'NONE',  ( -5.719274019375665041, -21.55341960407619695, 59.79275706135234714 ) ) ;
#98726 = CARTESIAN_POINT ( 'NONE',  ( 5.049401038297881783, 19.05341960407617563, 92.29275706135234714 ) ) ;
#98727 = CARTESIAN_POINT ( 'NONE',  ( 4.379528057220339221, -16.55341960407611168, 47.70724293864770260 ) ) ;
#98728 = CARTESIAN_POINT ( 'NONE',  ( -21.53943276465977519, -0.05219959533937600094, 18.75109039468568639 ) ) ;
#98729 = CARTESIAN_POINT ( 'NONE',  ( -21.55341960407610458, -5.719274019375992779, 51.45724293864770260 ) ) ;
#98731 = CARTESIAN_POINT ( 'NONE',  ( -9.564922557960796823, -16.46253265017161027, 112.0822429386476955 ) ) ;
#98730 = AXIS2_PLACEMENT_3D ( 'NONE', #110546, #62050, #141875 ) ;
#98732 = CARTESIAN_POINT ( 'NONE',  ( -28.82186960331499392, -9.364793116373526516, 140.3500000054623627 ) ) ;
#98733 = CARTESIAN_POINT ( 'NONE',  ( -13.89961937509977652, 13.97604488694528158, 50.62390960531435979 ) ) ;
#98734 = CARTESIAN_POINT ( 'NONE',  ( -16.53943276465976808, 0.05219959533911058130, 21.24890960531436690 ) ) ;
#98735 = CARTESIAN_POINT ( 'NONE',  ( 4.483927247898790824, -16.52544592524335698, 105.2094237280190328 ) ) ;
#98736 = CARTESIAN_POINT ( 'NONE',  ( -12.06949235617739369, -12.14591786802326823, 84.37609039468570415 ) ) ;
#98737 = CARTESIAN_POINT ( 'NONE',  ( -19.03943276465977164, -0.05219959533935918106, 38.75109039468566152 ) ) ;
#98738 = CARTESIAN_POINT ( 'NONE',  ( -24.20534277172201598, 9.236732224056884988, 166.4300944521384906 ) ) ;
#98739 = CARTESIAN_POINT ( 'NONE',  ( 9.474510206698971260, -16.51473224551069308, 87.91557627198102409 ) ) ;
#98740 = CARTESIAN_POINT ( 'NONE',  ( 13.97604488694527802, 13.89961937509977652, 54.37390960531435979 ) ) ;
#98741 = CARTESIAN_POINT ( 'NONE',  ( 12.14591786802309770, 12.06949235617756955, 64.37390960531435269 ) ) ;
#98743 = CARTESIAN_POINT ( 'NONE',  ( -19.03943276465977164, 0.05219959533909376836, 101.2489096053143669 ) ) ;
#98742 = CARTESIAN_POINT ( 'NONE',  ( -17.49999999999999645, 5.499999999999992895, 88.71769037696435589 ) ) ;
#98744 = CARTESIAN_POINT ( 'NONE',  ( -0.05219959533907301413, -21.53943276465977519, 37.49890960531436690 ) ) ;
#98745 = CARTESIAN_POINT ( 'NONE',  ( -4.379528057220328563, 16.55341960407611168, 85.20724293864770971 ) ) ;
#98746 = CARTESIAN_POINT ( 'NONE',  ( -8.314922557961024197, 14.29746914071037800, 37.91775706135235424 ) ) ;
#98747 = CARTESIAN_POINT ( 'NONE',  ( -16.52544592524342804, 4.483927247898546575, 81.04057627198102409 ) ) ;
#98748 = DIRECTION ( 'NONE',  ( 1.000000000000000000, 0.000000000000000000, 0.000000000000000000 ) ) ;
#98749 = CARTESIAN_POINT ( 'NONE',  ( 13.89961937509957401, 13.97604488694547697, 81.87609039468564731 ) ) ;
#98750 = CARTESIAN_POINT ( 'NONE',  ( 16.46253265017160672, -9.564922557960803928, 108.3322429386476955 ) ) ;
#98751 = CARTESIAN_POINT ( 'NONE',  ( 19.02544592524334988, 5.153800228976608722, 81.45942372801897591 ) ) ;
#98752 = CARTESIAN_POINT ( 'NONE',  ( -22.02279270211228734, 20.08125529445633006, -51.67964572521218969 ) ) ;
#98754 = CARTESIAN_POINT ( 'NONE',  ( -16.53943276465976808, -0.05219959533934237506, 108.7510903946857042 ) ) ;
#98753 = CARTESIAN_POINT ( 'NONE',  ( -8.224510206698735004, -14.34966873604973081, 34.58442372801900433 ) ) ;
#98755 = CARTESIAN_POINT ( 'NONE',  ( -19.03943276465977164, -0.05219959533935918106, 73.75109039468566152 ) ) ;
#98756 = CARTESIAN_POINT ( 'NONE',  ( 5.823673210054125526, 21.52544592524343514, 39.79057627198103830 ) ) ;
#98757 = CARTESIAN_POINT ( 'NONE',  ( -15.80617190586768217, 15.72974639402176855, 73.12609039468567573 ) ) ;
#98758 = CARTESIAN_POINT ( 'NONE',  ( -23.03120525563285170, -11.22467059994836269, 168.0473679553712714 ) ) ;
#98759 = CARTESIAN_POINT ( 'NONE',  ( -14.29746914071037622, -8.314922557961029526, 34.16775706135234714 ) ) ;
#98761 = CARTESIAN_POINT ( 'NONE',  ( 5.153800228976335163, 19.02544592524342804, 89.79057627198102409 ) ) ;
#98760 = CARTESIAN_POINT ( 'NONE',  ( 19.02544592524343514, -5.153800228976328945, 23.54057627198102054 ) ) ;
#98762 = CARTESIAN_POINT ( 'NONE',  ( 19.05341960407611168, 5.049401038298154454, 28.95724293864769550 ) ) ;
#98763 = CARTESIAN_POINT ( 'NONE',  ( 4.483927247898545687, 16.52544592524342804, 89.79057627198103830 ) ) ;
#98764 = CONTEXT_DEPENDENT_SHAPE_REPRESENTATION ( #139815, #111554 ) ;
#98765 = CARTESIAN_POINT ( 'NONE',  ( -19.02544592524342804, 5.153800228976336051, 91.04057627198100988 ) ) ;
#98766 = CARTESIAN_POINT ( 'NONE',  ( -19.05341960407617563, 5.049401038297882671, 98.54275706135233293 ) ) ;
#98767 = CARTESIAN_POINT ( 'NONE',  ( -5.719274019375978568, 21.55341960407610458, 80.20724293864769550 ) ) ;
#98768 = CARTESIAN_POINT ( 'NONE',  ( -5.153800228976328057, -19.02544592524343514, 42.29057627198101699 ) ) ;
#98770 = CARTESIAN_POINT ( 'NONE',  ( 15.80617190586769283, -15.72974639402175789, 20.62609039468568639 ) ) ;
#98769 = CARTESIAN_POINT ( 'NONE',  ( -9.474510206698720793, -16.51473224551083518, 74.58442372801900433 ) ) ;
#98771 = CARTESIAN_POINT ( 'NONE',  ( -16.46253265017160317, 9.564922557960807481, 70.83224293864770971 ) ) ;
#98772 = CARTESIAN_POINT ( 'NONE',  ( 19.03943276465977164, -0.05219959533909143690, 103.7489096053143669 ) ) ;
#98773 = ORIENTED_EDGE ( 'NONE', *, *, #149591, .F. ) ;
#98774 = CARTESIAN_POINT ( 'NONE',  ( -12.14591786802326823, 12.06949235617739902, 33.12609039468569705 ) ) ;
#98775 = CARTESIAN_POINT ( 'NONE',  ( -18.62759615963270932, 10.81492255796079327, 105.8322429386476955 ) ) ;
#98778 = CARTESIAN_POINT ( 'NONE',  ( -16.51473224551082808, 9.474510206698731452, 63.33442372801900433 ) ) ;
#98777 = CARTESIAN_POINT ( 'NONE',  ( 5.049401038298161559, -19.05341960407611168, 87.70724293864769550 ) ) ;
#98776 = CARTESIAN_POINT ( 'NONE',  ( 16.55341960407611168, 4.379528057220329451, 103.9572429386476813 ) ) ;
#98779 = CARTESIAN_POINT ( 'NONE',  ( 21.55341960407610458, 5.719274019375980345, 83.95724293864770971 ) ) ;
#98780 = CARTESIAN_POINT ( 'NONE',  ( -10.81492255796078084, -18.62759615963271287, 87.08224293864769550 ) ) ;
#98781 = CARTESIAN_POINT ( 'NONE',  ( -4.379528057220328563, 16.55341960407611168, 45.20724293864769550 ) ) ;
#98782 = CARTESIAN_POINT ( 'NONE',  ( -0.05219959533936034679, 19.03943276465977164, 27.50109039468566507 ) ) ;
#98784 = CIRCLE ( 'NONE', #79470, 59.99999999999998579 ) ;
#98783 = CARTESIAN_POINT ( 'NONE',  ( 16.52544592524335698, 4.483927247898782831, 71.45942372801901854 ) ) ;
#98785 = CARTESIAN_POINT ( 'NONE',  ( -13.97604488694527625, -13.89961937509977652, 86.87390960531436690 ) ) ;
#98786 = CARTESIAN_POINT ( 'NONE',  ( 16.51473224551069308, 9.474510206698969483, 44.16557627198103120 ) ) ;
#98787 = CARTESIAN_POINT ( 'NONE',  ( 18.62759615963255655, 10.81492255796105972, 56.66775706135235424 ) ) ;
#98788 = CARTESIAN_POINT ( 'NONE',  ( 10.72451020669871369, 18.67979575497193778, 67.08442372801901854 ) ) ;
#98789 = CARTESIAN_POINT ( 'NONE',  ( 5.049401038298161559, -19.05341960407611168, 62.70724293864769550 ) ) ;
#98790 = CARTESIAN_POINT ( 'NONE',  ( -18.62759615963255300, -10.81492255796106328, 29.16775706135234003 ) ) ;
#98791 = CARTESIAN_POINT ( 'NONE',  ( -13.89961937509957401, -13.97604488694547875, 74.37609039468566152 ) ) ;
#98792 = CARTESIAN_POINT ( 'NONE',  ( -13.89961937509957401, -13.97604488694547875, 74.37609039468566152 ) ) ;
#98793 = CARTESIAN_POINT ( 'NONE',  ( 9.564922557960805705, 16.46253265017160317, 44.58224293864769550 ) ) ;
#98794 = CARTESIAN_POINT ( 'NONE',  ( 0.05219959533934541429, -16.53943276465976808, 85.00109039468568994 ) ) ;
#98795 = CARTESIAN_POINT ( 'NONE',  ( 13.97604488694527802, 13.89961937509977652, 59.37390960531434558 ) ) ;
#98796 = CARTESIAN_POINT ( 'NONE',  ( 22.65770943308940488, -11.99324031494510479, 167.9410816520762921 ) ) ;
#98797 = CARTESIAN_POINT ( 'NONE',  ( -9.474510206698964154, 16.51473224551069663, 95.41557627198102409 ) ) ;
#98798 = CARTESIAN_POINT ( 'NONE',  ( -9.564922557960796823, -16.46253265017161027, 32.08224293864769550 ) ) ;
#98799 = CARTESIAN_POINT ( 'NONE',  ( -21.52544592524343514, 5.823673210054127303, 91.04057627198103830 ) ) ;
#98800 = CARTESIAN_POINT ( 'NONE',  ( 14.34966873604972726, -8.224510206698740333, 60.83442372801901854 ) ) ;
#98801 = CARTESIAN_POINT ( 'NONE',  ( 13.97604488694548053, -13.89961937509957401, 30.62609039468566863 ) ) ;
#98802 = CARTESIAN_POINT ( 'NONE',  ( 9.474510206698971260, -16.51473224551069308, 52.91557627198102409 ) ) ;
#98803 = CARTESIAN_POINT ( 'NONE',  ( -16.53943276465976808, 0.05219959533911058130, 51.24890960531436690 ) ) ;
#98804 = CARTESIAN_POINT ( 'NONE',  ( 14.34966873604960469, 8.224510206698951720, 79.16557627198103830 ) ) ;
#98805 = CARTESIAN_POINT ( 'NONE',  ( 16.51473224551069308, 9.474510206698969483, 74.16557627198103830 ) ) ;
#98806 = CARTESIAN_POINT ( 'NONE',  ( 21.52544592524334988, 5.823673210054432836, 41.45942372801901143 ) ) ;
#98807 = CARTESIAN_POINT ( 'NONE',  ( -16.51473224551069308, -9.474510206698971260, 86.66557627198102409 ) ) ;
#98808 = CARTESIAN_POINT ( 'NONE',  ( -10.81492255796105439, 18.62759615963255655, 97.91775706135236135 ) ) ;
#98809 = CARTESIAN_POINT ( 'NONE',  ( 12.14591786802327356, -12.06949235617739191, 75.62609039468567573 ) ) ;
#98810 = EDGE_CURVE ( 'NONE', #6817, #108968, #29018, .T. ) ;
#98811 = CARTESIAN_POINT ( 'NONE',  ( -21.55341960407619339, 5.719274019375674811, 23.54275706135235424 ) ) ;
#98812 = CARTESIAN_POINT ( 'NONE',  ( 21.53943276465977519, -0.05219959533907433946, 93.74890960531436690 ) ) ;
#98813 = CARTESIAN_POINT ( 'NONE',  ( 4.379528057220339221, -16.55341960407611168, 42.70724293864770260 ) ) ;
#98814 = CARTESIAN_POINT ( 'NONE',  ( -16.46253265017160317, 9.564922557960807481, 45.83224293864769550 ) ) ;
#98815 = CARTESIAN_POINT ( 'NONE',  ( -16.53943276465976808, 0.05219959533911058130, 66.24890960531436690 ) ) ;
#98816 = CARTESIAN_POINT ( 'NONE',  ( -21.52544592524343514, 5.823673210054127303, 36.04057627198102409 ) ) ;
#98817 = CARTESIAN_POINT ( 'NONE',  ( -5.049401038297874678, -19.05341960407617918, 34.79275706135233293 ) ) ;
#98818 = CARTESIAN_POINT ( 'NONE',  ( -16.55341960407611168, -4.379528057220339221, 106.4572429386477097 ) ) ;
#98819 = CARTESIAN_POINT ( 'NONE',  ( 9.474510206698971260, -16.51473224551069308, 107.9155762719810383 ) ) ;
#98820 = EDGE_LOOP ( 'NONE', ( #130332, #168172, #41375, #89844, #180374, #61969, #57530, #71862, #14291, #142787 ) ) ;
#98821 = CARTESIAN_POINT ( 'NONE',  ( -12.14591786802326823, 12.06949235617739902, 48.12609039468568284 ) ) ;
#98822 = CARTESIAN_POINT ( 'NONE',  ( 16.51473224551069308, 9.474510206698969483, 54.16557627198103120 ) ) ;
#98823 = CARTESIAN_POINT ( 'NONE',  ( -17.30380112737341136, -6.006629661696645250, 21.28751624816027288 ) ) ;
#98824 = CARTESIAN_POINT ( 'NONE',  ( -14.34966873604972548, 8.224510206698743886, 88.33442372801901854 ) ) ;
#98825 = CARTESIAN_POINT ( 'NONE',  ( -5.049401038297874678, -19.05341960407617918, 109.7927570613523187 ) ) ;
#98826 = CARTESIAN_POINT ( 'NONE',  ( -5.823673210054431948, 21.52544592524334988, 82.70942372801900433 ) ) ;
#98827 = CARTESIAN_POINT ( 'NONE',  ( -9.564922557960796823, -16.46253265017161027, 77.08224293864769550 ) ) ;
#98828 = CARTESIAN_POINT ( 'NONE',  ( 21.53943276465977519, -0.05219959533907433946, 108.7489096053143669 ) ) ;
#98829 = CARTESIAN_POINT ( 'NONE',  ( 8.224510206698742110, 14.34966873604972548, 52.08442372801901854 ) ) ;
#98830 = CARTESIAN_POINT ( 'NONE',  ( -16.51473224551069308, -9.474510206698971260, 21.66557627198102765 ) ) ;
#98831 = AXIS2_PLACEMENT_3D ( 'NONE', #101428, #163119, #148958 ) ;
#98832 = CARTESIAN_POINT ( 'NONE',  ( -4.379528057220086978, -16.55341960407618274, 19.79275706135235069 ) ) ;
#98833 = CARTESIAN_POINT ( 'NONE',  ( 0.05219959533936267826, -19.03943276465977164, 80.00109039468567573 ) ) ;
#98834 = CARTESIAN_POINT ( 'NONE',  ( 21.52544592524344225, -5.823673210054117533, 83.54057627198102409 ) ) ;
#98835 = CARTESIAN_POINT ( 'NONE',  ( -19.03943276465977164, -0.05219959533935918106, 53.75109039468566863 ) ) ;
#98836 = CARTESIAN_POINT ( 'NONE',  ( 18.22780087662123805, -5.499999999999976019, 88.51763182126893525 ) ) ;
#98837 = CARTESIAN_POINT ( 'NONE',  ( -5.719274019375978568, 21.55341960407610458, 105.2072429386477097 ) ) ;
#98838 = CARTESIAN_POINT ( 'NONE',  ( 18.09867054820433907, 5.499999999999818812, 61.48393025253584909 ) ) ;
#98839 = CARTESIAN_POINT ( 'NONE',  ( 16.46253265017160672, -9.564922557960803928, 68.33224293864770971 ) ) ;
#98840 = CARTESIAN_POINT ( 'NONE',  ( -34.78522506798723413, -4.592425496937305498E-15, 52.50000000000000000 ) ) ;
#98841 = CARTESIAN_POINT ( 'NONE',  ( -8.224510206698735004, -14.34966873604973081, 24.58442372801901499 ) ) ;
#98842 = CARTESIAN_POINT ( 'NONE',  ( 11.92298843706294420, -38.18315321023221287, -12.32826034376742363 ) ) ;
#98843 = CARTESIAN_POINT ( 'NONE',  ( 10.81492255796106328, -18.62759615963255655, 55.41775706135234714 ) ) ;
#98845 = CARTESIAN_POINT ( 'NONE',  ( 0.05219959533910956823, 16.53943276465976808, 59.99890960531436690 ) ) ;
#98844 = CARTESIAN_POINT ( 'NONE',  ( 0.05219959533907565091, 21.53943276465977519, 104.9989096053143669 ) ) ;
#98846 = CARTESIAN_POINT ( 'NONE',  ( 19.02544592524343514, -5.153800228976328945, 68.54057627198103830 ) ) ;
#98847 = CARTESIAN_POINT ( 'NONE',  ( -21.53943276465977519, -0.05219959533937600094, 78.75109039468568994 ) ) ;
#98849 = CARTESIAN_POINT ( 'NONE',  ( 19.02544592524334988, 5.153800228976608722, 31.45942372801900433 ) ) ;
#98848 = CARTESIAN_POINT ( 'NONE',  ( -0.05219959533934338120, 16.53943276465976808, 27.50109039468567929 ) ) ;
#98850 = CARTESIAN_POINT ( 'NONE',  ( -5.823673210054431948, 21.52544592524334988, 52.70942372801902565 ) ) ;
#98851 = CARTESIAN_POINT ( 'NONE',  ( 21.55341960407610458, 5.719274019375980345, 113.9572429386477239 ) ) ;
#98852 = CARTESIAN_POINT ( 'NONE',  ( 0.05219959533907565091, 21.53943276465977519, 59.99890960531436690 ) ) ;
#98853 = CARTESIAN_POINT ( 'NONE',  ( -5.049401038297874678, -19.05341960407617918, 94.79275706135230450 ) ) ;
#98854 = CARTESIAN_POINT ( 'NONE',  ( -13.97604488694547697, 13.89961937509957934, 73.12609039468568994 ) ) ;
#98855 = CARTESIAN_POINT ( 'NONE',  ( -18.62759615963255300, -10.81492255796106328, 79.16775706135234714 ) ) ;
#98856 = CARTESIAN_POINT ( 'NONE',  ( -16.51473224551082808, 9.474510206698731452, 58.33442372801900433 ) ) ;
#98857 = CARTESIAN_POINT ( 'NONE',  ( -13.97604488694527625, -13.89961937509977652, 36.87390960531436690 ) ) ;
#98858 = CARTESIAN_POINT ( 'NONE',  ( -21.53943276465977519, 0.05219959533907696930, 56.24890960531436690 ) ) ;
#98859 = CARTESIAN_POINT ( 'NONE',  ( -16.52544592524342804, 4.483927247898546575, 51.04057627198103120 ) ) ;
#98860 = CARTESIAN_POINT ( 'NONE',  ( -17.44279575226824619, -5.990770900252396558, 24.16442432485681735 ) ) ;
#98861 = CARTESIAN_POINT ( 'NONE',  ( 13.97604488694548053, -13.89961937509957401, 35.62609039468567573 ) ) ;
#98862 = CARTESIAN_POINT ( 'NONE',  ( -14.29746914071037622, -8.314922557961029526, 84.16775706135234714 ) ) ;
#98863 = CARTESIAN_POINT ( 'NONE',  ( -14.34966873604960291, -8.224510206698953496, 56.66557627198103830 ) ) ;
#98864 = CARTESIAN_POINT ( 'NONE',  ( -21.52544592524334988, -5.823673210054445271, 93.95942372801903275 ) ) ;
#98865 = CARTESIAN_POINT ( 'NONE',  ( -18.67979575497193778, 10.72451020669871902, 83.33442372801903275 ) ) ;
#98866 = CARTESIAN_POINT ( 'NONE',  ( -15.72974639402197994, 15.80617190586746368, 85.62390960531436690 ) ) ;
#98867 = CARTESIAN_POINT ( 'NONE',  ( -0.05219959533909027116, -19.03943276465977164, 57.49890960531435979 ) ) ;
#98868 = CARTESIAN_POINT ( 'NONE',  ( 10.81492255796106328, -18.62759615963255655, 55.41775706135234714 ) ) ;
#98869 = CARTESIAN_POINT ( 'NONE',  ( -0.05219959533909027116, -19.03943276465977164, 32.49890960531435979 ) ) ;
#98870 = CARTESIAN_POINT ( 'NONE',  ( -5.153800228976328057, -19.02544592524343514, 52.29057627198100988 ) ) ;
#98871 = CARTESIAN_POINT ( 'NONE',  ( 8.314922557960818139, 14.29746914071049879, 104.5822429386477097 ) ) ;
#98872 = CARTESIAN_POINT ( 'NONE',  ( 19.03943276465977164, -0.05219959533909143690, 98.74890960531436690 ) ) ;
#98873 = CARTESIAN_POINT ( 'NONE',  ( -14.34966873604960291, -8.224510206698953496, 56.66557627198103830 ) ) ;
#98874 = CARTESIAN_POINT ( 'NONE',  ( 8.314922557960818139, 14.29746914071049879, 109.5822429386476955 ) ) ;
#98875 = CARTESIAN_POINT ( 'NONE',  ( -21.53943276465977519, 0.05219959533907696930, 86.24890960531436690 ) ) ;
#98876 = VECTOR ( 'NONE', #87315, 1000.000000000000000 ) ;
#98877 = CARTESIAN_POINT ( 'NONE',  ( 21.55341960407610458, 5.719274019375980345, 113.9572429386477239 ) ) ;
#98878 = CARTESIAN_POINT ( 'NONE',  ( 27.89903062892809871, -7.496893268503402652, 160.9845644947723429 ) ) ;
#98879 = EDGE_CURVE ( 'NONE', #117432, #179471, #167845, .T. ) ;
#98880 = CARTESIAN_POINT ( 'NONE',  ( 16.53943276465976808, 0.05219959533934440121, 41.25109039468568284 ) ) ;
#98881 = ORIENTED_EDGE ( 'NONE', *, *, #34959, .F. ) ;
#98882 = CARTESIAN_POINT ( 'NONE',  ( 10.81492255796078972, 18.62759615963270932, 69.58224293864769550 ) ) ;
#98883 = CARTESIAN_POINT ( 'NONE',  ( -10.81492255796105439, 18.62759615963255655, 107.9177570613523471 ) ) ;
#98884 = CARTESIAN_POINT ( 'NONE',  ( -19.05341960407611168, -5.049401038298163336, 91.45724293864766707 ) ) ;
#98885 = CARTESIAN_POINT ( 'NONE',  ( 5.719274019375673035, 21.55341960407619339, 32.29275706135235424 ) ) ;
#98886 = CARTESIAN_POINT ( 'NONE',  ( 5.719274019375991003, -21.55341960407610458, 27.70724293864769905 ) ) ;
#98887 = CARTESIAN_POINT ( 'NONE',  ( 8.224510206698742110, 14.34966873604972548, 107.0844237280190043 ) ) ;
#98888 = CARTESIAN_POINT ( 'NONE',  ( 5.823673210054444382, -21.52544592524334988, 90.20942372801903275 ) ) ;
#98889 = CARTESIAN_POINT ( 'NONE',  ( 18.62759615963255655, 10.81492255796105972, 106.6677570613523756 ) ) ;
#98890 = CARTESIAN_POINT ( 'NONE',  ( -16.55341960407617563, 4.379528057220093196, 68.54275706135234714 ) ) ;
#98891 = CARTESIAN_POINT ( 'NONE',  ( 21.55341960407619695, -5.719274019375665929, 31.04275706135234714 ) ) ;
#98892 = CARTESIAN_POINT ( 'NONE',  ( 19.03943276465977164, -0.05219959533909143690, 33.74890960531435979 ) ) ;
#98893 = CARTESIAN_POINT ( 'NONE',  ( 5.719274019375673035, 21.55341960407619339, 107.2927570613523471 ) ) ;
#98894 = CARTESIAN_POINT ( 'NONE',  ( -19.05341960407611168, -5.049401038298163336, 111.4572429386476671 ) ) ;
#98895 = CARTESIAN_POINT ( 'NONE',  ( -18.67979575497178146, -10.72451020669898902, 101.6655762719810383 ) ) ;
#98897 = CARTESIAN_POINT ( 'NONE',  ( 21.55341960407610458, 5.719274019375980345, 68.95724293864769550 ) ) ;
#98896 = CARTESIAN_POINT ( 'NONE',  ( -7.840974544915187749, -46.02298249793906137, -22.40017284086422222 ) ) ;
#98899 = CARTESIAN_POINT ( 'NONE',  ( -16.53943276465976808, 0.05219959533911058130, 51.24890960531436690 ) ) ;
#98898 = CARTESIAN_POINT ( 'NONE',  ( 12.14591786802327356, -12.06949235617739191, 55.62609039468568284 ) ) ;
#98900 = CARTESIAN_POINT ( 'NONE',  ( 18.59930490233255540, -5.499999999999989342, 101.0584990050579250 ) ) ;
#98901 = CARTESIAN_POINT ( 'NONE',  ( 19.02544592524334988, 5.153800228976608722, 76.45942372801897591 ) ) ;
#98902 = CARTESIAN_POINT ( 'NONE',  ( -16.21995358207305316, 7.366697692864160985, 104.9355100151216220 ) ) ;
#98903 = CARTESIAN_POINT ( 'NONE',  ( -4.483927247898782831, 16.52544592524335698, 27.70942372801901854 ) ) ;
#98904 = EDGE_CURVE ( 'NONE', #143427, #187814, #120481, .T. ) ;
#98905 = CARTESIAN_POINT ( 'NONE',  ( 18.62759615963271287, -10.81492255796078972, 98.33224293864769550 ) ) ;
#98906 = CARTESIAN_POINT ( 'NONE',  ( -14.29746914071049879, 8.314922557960819915, 60.83224293864769550 ) ) ;
#98907 = CARTESIAN_POINT ( 'NONE',  ( 19.03943276465977164, -0.05219959533909143690, 113.7489096053143669 ) ) ;
#98908 = CARTESIAN_POINT ( 'NONE',  ( 14.29746914071037800, 8.314922557961029526, 41.66775706135235424 ) ) ;
#98909 = CARTESIAN_POINT ( 'NONE',  ( -19.03943276465977164, 0.05219959533909376836, 61.24890960531436690 ) ) ;
#98911 = CARTESIAN_POINT ( 'NONE',  ( -13.97604488694547697, 13.89961937509957934, 98.12609039468566152 ) ) ;
#98910 = CARTESIAN_POINT ( 'NONE',  ( -21.52544592524334988, -5.823673210054445271, 28.95942372801902209 ) ) ;
#98912 = CARTESIAN_POINT ( 'NONE',  ( -5.049401038298153566, 19.05341960407611168, 95.20724293864770971 ) ) ;
#98913 =( BOUNDED_CURVE ( )  B_SPLINE_CURVE ( 2, ( #120361, #150726, #69880, #105203, #131549, #180087, #166890, #151711, #28390, #178069, #101194 ),
 .UNSPECIFIED., .F., .T. ) 
 B_SPLINE_CURVE_WITH_KNOTS ( ( 3, 2, 2, 2, 2, 3 ),
 ( 0.8000000000000000444, 0.8200000000000000622, 0.8399999999999999689, 0.8599999999999999867, 0.8800000000000000044, 0.9000000000000000222 ),
 .UNSPECIFIED. ) 
 CURVE ( )  GEOMETRIC_REPRESENTATION_ITEM ( )  RATIONAL_B_SPLINE_CURVE ( ( 1.000000000000000000, 0.9510565162951535312, 1.000000000000000000, 0.9510565162951535312, 1.000000000000000000, 0.9510565162951535312, 1.000000000000000000, 0.9510565162951535312, 1.000000000000000000, 0.9510565162951535312, 1.000000000000000000 ) ) 
 REPRESENTATION_ITEM ( '' )  );
#98914 = CARTESIAN_POINT ( 'NONE',  ( 19.03943276465977164, -0.05219959533909143690, 88.74890960531436690 ) ) ;
#98915 = CARTESIAN_POINT ( 'NONE',  ( 21.53943276465977519, -0.05219959533907433946, 88.74890960531436690 ) ) ;
#98916 = CARTESIAN_POINT ( 'NONE',  ( 9.474510206698971260, -16.51473224551069308, 42.91557627198103120 ) ) ;
#98917 = CARTESIAN_POINT ( 'NONE',  ( -16.38665767535053774, -7.295008042176054808, 59.73599135785457293 ) ) ;
#98918 = CARTESIAN_POINT ( 'NONE',  ( 16.52544592524342804, -4.483927247898539470, 68.54057627198103830 ) ) ;
#98919 = CARTESIAN_POINT ( 'NONE',  ( 19.05341960407611168, 5.049401038298154454, 103.9572429386476671 ) ) ;
#98920 = FACE_OUTER_BOUND ( 'NONE', #151783, .T. ) ;
#98921 = CARTESIAN_POINT ( 'NONE',  ( 5.153800228976615827, -19.02544592524334988, 85.20942372801900433 ) ) ;
#98922 = CARTESIAN_POINT ( 'NONE',  ( -15.80617190586745835, -15.72974639402198527, 96.87390960531436690 ) ) ;
#98923 = CARTESIAN_POINT ( 'NONE',  ( 13.89961937509957401, 13.97604488694547697, 51.87609039468566863 ) ) ;
#98924 = CARTESIAN_POINT ( 'NONE',  ( -5.049401038298153566, 19.05341960407611168, 110.2072429386476671 ) ) ;
#98925 = FACE_OUTER_BOUND ( 'NONE', #101307, .T. ) ;
#98926 = CARTESIAN_POINT ( 'NONE',  ( -10.72451020669898014, 18.67979575497178502, 50.41557627198103120 ) ) ;
#98927 = CARTESIAN_POINT ( 'NONE',  ( -19.05341960407611168, -5.049401038298163336, 86.45724293864769550 ) ) ;
#98928 = CARTESIAN_POINT ( 'NONE',  ( -15.72974639402176322, -15.80617190586768395, 74.37609039468568994 ) ) ;
#98929 = CARTESIAN_POINT ( 'NONE',  ( -5.153800228976328057, -19.02544592524343514, 42.29057627198101699 ) ) ;
#98930 = CARTESIAN_POINT ( 'NONE',  ( 12.14591786802309770, 12.06949235617756955, 74.37390960531436690 ) ) ;
#98931 = CARTESIAN_POINT ( 'NONE',  ( -4.483927247898782831, 16.52544592524335698, 27.70942372801901854 ) ) ;
#98932 = CARTESIAN_POINT ( 'NONE',  ( -10.72451020669870658, -18.67979575497194134, 64.58442372801900433 ) ) ;
#98933 = EDGE_LOOP ( 'NONE', ( #89320, #123949, #40034 ) ) ;
#98934 = CARTESIAN_POINT ( 'NONE',  ( 19.03943276465977164, -0.05219959533909143690, 113.7489096053143669 ) ) ;
#98935 = CARTESIAN_POINT ( 'NONE',  ( 9.474510206698729675, 16.51473224551082808, 77.08442372801900433 ) ) ;
#98936 = CARTESIAN_POINT ( 'NONE',  ( 0.000000000000000000, 0.000000000000000000, -62.91767397929362460 ) ) ;
#98937 = CARTESIAN_POINT ( 'NONE',  ( -21.53943276465977519, -0.05219959533937600094, 28.75109039468567929 ) ) ;
#98938 = CARTESIAN_POINT ( 'NONE',  ( -23.48529157249600985, 32.32473071737754111, -2.049999994537626158 ) ) ;
#98939 = CARTESIAN_POINT ( 'NONE',  ( -16.46253265017146816, -9.564922557961047289, 19.16775706135233293 ) ) ;
#98940 = CARTESIAN_POINT ( 'NONE',  ( 16.46253265017160672, -9.564922557960803928, 58.33224293864769550 ) ) ;
#98941 = CARTESIAN_POINT ( 'NONE',  ( 21.52544592524334988, 5.823673210054432836, 106.4594237280190328 ) ) ;
#98942 = CARTESIAN_POINT ( 'NONE',  ( 8.224510206698742110, 14.34966873604972548, 107.0844237280190043 ) ) ;
#98944 = CARTESIAN_POINT ( 'NONE',  ( 15.72974639402176855, 15.80617190586768217, 76.87609039468567573 ) ) ;
#98943 = CARTESIAN_POINT ( 'NONE',  ( 9.474510206698971260, -16.51473224551069308, 102.9155762719810241 ) ) ;
#98945 = B_SPLINE_CURVE_WITH_KNOTS ( 'NONE', 3,
 ( #38845, #127837, #190529, #51015, #130837, #54011, #115685, #82319, #144009, #5490, #52003, #36824, #160183, #186076, #46554, #107215, #185066, #45561, #40840, #132844 ),
 .UNSPECIFIED., .F., .F.,
 ( 4, 2, 2, 2, 2, 2, 2, 2, 2, 4 ),
 ( 0.004000878361811842886, 0.004499404418915854513, 0.004997930476019866140, 0.005496456533123877768, 0.005994982590227890262, 0.006244245618779896076, 0.006493508647331901022, 0.006992034704435916986, 0.007490560761539932083, 0.007989086818643948915 ),
 .UNSPECIFIED. ) ;
#98946 = CARTESIAN_POINT ( 'NONE',  ( 29.86685920354754842, -21.69954338932559068, -3.824999997268813345 ) ) ;
#98947 = CARTESIAN_POINT ( 'NONE',  ( 2.500000000000000000, -165.0000000000000000, 7.000000000000003553 ) ) ;
#98948 = CARTESIAN_POINT ( 'NONE',  ( -18.10062525802553424, 5.500000000000031086, 78.51383468041922242 ) ) ;
#98949 = CARTESIAN_POINT ( 'NONE',  ( 5.823673210054444382, -21.52544592524334988, 75.20942372801901854 ) ) ;
#98950 = CARTESIAN_POINT ( 'NONE',  ( -21.53943276465977519, -0.05219959533937600094, 98.75109039468568994 ) ) ;
#98951 = CARTESIAN_POINT ( 'NONE',  ( 4.999999999999996447, 37.66961640367475184, -25.00000000000000000 ) ) ;
#98952 = CARTESIAN_POINT ( 'NONE',  ( 9.474510206698971260, -16.51473224551069308, 92.91557627198103830 ) ) ;
#98953 = CARTESIAN_POINT ( 'NONE',  ( -21.55341960407619339, 5.719274019375674811, 113.5427570613523756 ) ) ;
#98954 = CARTESIAN_POINT ( 'NONE',  ( 29.12359114459363951, -24.18000288461011493, -21.55587802759514204 ) ) ;
#98955 = CARTESIAN_POINT ( 'NONE',  ( -13.89961937509977652, 13.97604488694528158, 35.62390960531435269 ) ) ;
#98956 = CARTESIAN_POINT ( 'NONE',  ( -15.80617190586745835, -15.72974639402198527, 51.87390960531437401 ) ) ;
#98957 = CARTESIAN_POINT ( 'NONE',  ( 16.53943276465976808, 0.05219959533934440121, 101.2510903946856757 ) ) ;
#98959 = CARTESIAN_POINT ( 'NONE',  ( -9.474510206698964154, 16.51473224551069663, 85.41557627198102409 ) ) ;
#98958 = CARTESIAN_POINT ( 'NONE',  ( 16.52544592524342804, -4.483927247898539470, 103.5405762719810383 ) ) ;
#98960 = CARTESIAN_POINT ( 'NONE',  ( -10.81492255796105439, 18.62759615963255655, 97.91775706135236135 ) ) ;
#98961 = CARTESIAN_POINT ( 'NONE',  ( 13.97604488694527802, 13.89961937509977652, 34.37390960531436690 ) ) ;
#98962 = CARTESIAN_POINT ( 'NONE',  ( 14.29746914071049879, -8.314922557960816363, 103.3322429386476955 ) ) ;
#98963 = CARTESIAN_POINT ( 'NONE',  ( -15.72974639402176322, -15.80617190586768395, 54.37609039468568994 ) ) ;
#98964 = CARTESIAN_POINT ( 'NONE',  ( -21.55341960407610458, -5.719274019375992779, 86.45724293864770971 ) ) ;
#98965 = CARTESIAN_POINT ( 'NONE',  ( 16.46253265017146816, 9.564922557961045513, 46.66775706135233293 ) ) ;
#98966 = CARTESIAN_POINT ( 'NONE',  ( 5.049401038298163336, -19.05341960407611168, 47.70724293864769550 ) ) ;
#98967 = CARTESIAN_POINT ( 'NONE',  ( -19.03943276465977164, 0.05219959533909376836, 96.24890960531436690 ) ) ;
#98968 = CARTESIAN_POINT ( 'NONE',  ( 12.06949235617757843, -12.14591786802309237, 73.12390960531436690 ) ) ;
#98969 = CARTESIAN_POINT ( 'NONE',  ( 13.89961937509957401, 13.97604488694547697, 41.87609039468566152 ) ) ;
#98970 = CARTESIAN_POINT ( 'NONE',  ( -0.05219959533909027116, -19.03943276465977164, 57.49890960531435979 ) ) ;
#98971 = CARTESIAN_POINT ( 'NONE',  ( 16.53943276465976808, -0.05219959533910856209, 43.74890960531435979 ) ) ;
#98972 = CARTESIAN_POINT ( 'NONE',  ( 19.02544592524334988, 5.153800228976608722, 81.45942372801897591 ) ) ;
#98973 = LINE ( 'NONE', #193011, #137578 ) ;
#98974 = CARTESIAN_POINT ( 'NONE',  ( 5.719274019375991003, -21.55341960407610458, 32.70724293864770260 ) ) ;
#98975 = CARTESIAN_POINT ( 'NONE',  ( 8.224510206698953496, -14.34966873604960469, 102.9155762719810383 ) ) ;
#98976 = CARTESIAN_POINT ( 'NONE',  ( -17.49999999999996447, -4.640572885337702402, 24.36211835451159402 ) ) ;
#98978 = CARTESIAN_POINT ( 'NONE',  ( -18.67979575497178146, -10.72451020669898902, 61.66557627198103120 ) ) ;
#98977 = CARTESIAN_POINT ( 'NONE',  ( 16.46253265017160672, -9.564922557960803928, 58.33224293864769550 ) ) ;
#98979 = CARTESIAN_POINT ( 'NONE',  ( 9.564922557960805705, 16.46253265017160317, 29.58224293864769550 ) ) ;
#98981 = CARTESIAN_POINT ( 'NONE',  ( -9.474510206698964154, 16.51473224551069663, 65.41557627198102409 ) ) ;
#98980 = CARTESIAN_POINT ( 'NONE',  ( 16.52544592524335698, 4.483927247898782831, 81.45942372801900433 ) ) ;
#98982 = CARTESIAN_POINT ( 'NONE',  ( -5.049401038297874678, -19.05341960407617918, 39.79275706135232582 ) ) ;
#98983 = CARTESIAN_POINT ( 'NONE',  ( 21.55341960407619695, -5.719274019375665929, 71.04275706135234714 ) ) ;
#98984 = VERTEX_POINT ( 'NONE', #155790 ) ;
#98985 = CARTESIAN_POINT ( 'NONE',  ( -0.05219959533907301413, -21.53943276465977519, 47.49890960531435979 ) ) ;
#98986 = CARTESIAN_POINT ( 'NONE',  ( -0.05219959533909027116, -19.03943276465977164, 27.49890960531435624 ) ) ;
#98987 = CARTESIAN_POINT ( 'NONE',  ( 8.224510206698742110, 14.34966873604972548, 92.08442372801901854 ) ) ;
#98988 = CARTESIAN_POINT ( 'NONE',  ( -5.049401038297874678, -19.05341960407617918, 99.79275706135234714 ) ) ;
#98989 = CARTESIAN_POINT ( 'NONE',  ( -19.05341960407611168, -5.049401038298163336, 21.45724293864768839 ) ) ;
#98991 = CARTESIAN_POINT ( 'NONE',  ( 5.719274019375991003, -21.55341960407610458, 47.70724293864770260 ) ) ;
#98990 = CARTESIAN_POINT ( 'NONE',  ( -2.973862142520655727, -93.04182470242766101, -23.00000000000000000 ) ) ;
#98992 = CARTESIAN_POINT ( 'NONE',  ( -21.55341960407619339, 5.719274019375674811, 83.54275706135234714 ) ) ;
#98993 = CARTESIAN_POINT ( 'NONE',  ( 12.14591786802309770, 12.06949235617756955, 49.37390960531436690 ) ) ;
#98994 = CARTESIAN_POINT ( 'NONE',  ( -12.14591786802309592, -12.06949235617757132, 56.87390960531436690 ) ) ;
#98995 = CARTESIAN_POINT ( 'NONE',  ( 18.67979575497178502, 10.72451020669898547, 84.16557627198103830 ) ) ;
#98996 = CARTESIAN_POINT ( 'NONE',  ( 15.80617190586746368, 15.72974639402197994, 74.37390960531436690 ) ) ;
#98997 = DIRECTION ( 'NONE',  ( 0.000000000000000000, 0.000000000000000000, -1.000000000000000000 ) ) ;
#98998 = CARTESIAN_POINT ( 'NONE',  ( -10.81492255796078084, -18.62759615963271287, 32.08224293864769550 ) ) ;
#98999 = CARTESIAN_POINT ( 'NONE',  ( -16.53943276465976808, -0.05219959533934237506, 68.75109039468568994 ) ) ;
#99000 = CARTESIAN_POINT ( 'NONE',  ( 14.34966873604960469, 8.224510206698951720, 74.16557627198102409 ) ) ;
#99001 = CARTESIAN_POINT ( 'NONE',  ( -9.564922557960796823, -16.46253265017161027, 32.08224293864769550 ) ) ;
#99002 = DIRECTION ( 'NONE',  ( 0.000000000000000000, 1.000000000000000000, 0.000000000000000000 ) ) ;
#99003 = ORIENTED_EDGE ( 'NONE', *, *, #146110, .T. ) ;
#99004 = CARTESIAN_POINT ( 'NONE',  ( 16.53943276465976808, 0.05219959533934440121, 86.25109039468568994 ) ) ;
#99005 = CARTESIAN_POINT ( 'NONE',  ( 15.72974639402176855, 15.80617190586768217, 21.87609039468567573 ) ) ;
#99006 = CARTESIAN_POINT ( 'NONE',  ( -0.05219959533909027116, -19.03943276465977164, 82.49890960531436690 ) ) ;
#99007 = CARTESIAN_POINT ( 'NONE',  ( 21.55341960407619695, -5.719274019375665929, 51.04275706135234714 ) ) ;
#99008 = CARTESIAN_POINT ( 'NONE',  ( -5.049401038298153566, 19.05341960407611168, 105.2072429386476671 ) ) ;
#99009 = CARTESIAN_POINT ( 'NONE',  ( -11.23063180225521407, -38.81524874330040831, -25.08899775095413531 ) ) ;
#99010 = ORIENTED_EDGE ( 'NONE', *, *, #128971, .F. ) ;
#99011 = CARTESIAN_POINT ( 'NONE',  ( -0.05219959533937732626, 21.53943276465977519, 42.50109039468567573 ) ) ;
#99013 = CARTESIAN_POINT ( 'NONE',  ( -19.03943276465977164, 0.05219959533909376836, 106.2489096053143669 ) ) ;
#99012 = CARTESIAN_POINT ( 'NONE',  ( -19.02544592524342804, 5.153800228976336051, 36.04057627198100988 ) ) ;
#99014 = CARTESIAN_POINT ( 'NONE',  ( -19.05341960407617563, 5.049401038297882671, 48.54275706135233293 ) ) ;
#99015 = CARTESIAN_POINT ( 'NONE',  ( 10.72451020669871369, 18.67979575497193778, 27.08442372801901854 ) ) ;
#99016 = CARTESIAN_POINT ( 'NONE',  ( 13.89961937509957401, 13.97604488694547697, 46.87609039468565442 ) ) ;
#99017 = CARTESIAN_POINT ( 'NONE',  ( 0.05219959533909260263, 19.03943276465977164, 24.99890960531435269 ) ) ;
#99018 = CARTESIAN_POINT ( 'NONE',  ( -8.224510206698735004, -14.34966873604973081, 94.58442372801901854 ) ) ;
#99019 = CARTESIAN_POINT ( 'NONE',  ( 0.05219959533936267826, -19.03943276465977164, 60.00109039468566863 ) ) ;
#99020 = CARTESIAN_POINT ( 'NONE',  ( 12.14591786802327356, -12.06949235617739191, 105.6260903946856899 ) ) ;
#99021 = DIRECTION ( 'NONE',  ( 0.000000000000000000, 0.000000000000000000, 1.000000000000000000 ) ) ;
#99022 = CARTESIAN_POINT ( 'NONE',  ( -16.51473224551069308, -9.474510206698971260, 86.66557627198102409 ) ) ;
#99023 = VECTOR ( 'NONE', #81845, 1000.000000000000000 ) ;
#99024 = CARTESIAN_POINT ( 'NONE',  ( 10.72451020669871369, 18.67979575497193778, 92.08442372801901854 ) ) ;
#99025 = CARTESIAN_POINT ( 'NONE',  ( -15.72974639402176322, -15.80617190586768395, 109.3760903946857042 ) ) ;
#99026 = CARTESIAN_POINT ( 'NONE',  ( -12.49999999999997691, -89.99999999999997158, 0.000000000000000000 ) ) ;
#99027 = CARTESIAN_POINT ( 'NONE',  ( 19.05341960407611168, 5.049401038298154454, 103.9572429386476671 ) ) ;
#99028 = CARTESIAN_POINT ( 'NONE',  ( 5.823673210054444382, -21.52544592524334988, 70.20942372801904696 ) ) ;
#99029 = CARTESIAN_POINT ( 'NONE',  ( 13.89961937509957401, 13.97604488694547697, 111.8760903946856757 ) ) ;
#99030 = CARTESIAN_POINT ( 'NONE',  ( -5.049401038298153566, 19.05341960407611168, 85.20724293864766707 ) ) ;
#99031 = CARTESIAN_POINT ( 'NONE',  ( 18.67979575497178502, 10.72451020669898547, 34.16557627198102409 ) ) ;
#99032 = CARTESIAN_POINT ( 'NONE',  ( 16.51473224551069308, 9.474510206698969483, 94.16557627198103830 ) ) ;
#99033 = CARTESIAN_POINT ( 'NONE',  ( -16.62475595723696387, -7.163666690055378261, 89.47286648189532343 ) ) ;
#99034 = CARTESIAN_POINT ( 'NONE',  ( -0.05219959533909027116, -19.03943276465977164, 72.49890960531435269 ) ) ;
#99035 = CARTESIAN_POINT ( 'NONE',  ( 19.02544592524343514, -5.153800228976328945, 68.54057627198103830 ) ) ;
#99036 = CARTESIAN_POINT ( 'NONE',  ( 14.29746914071037800, 8.314922557961029526, 101.6677570613523613 ) ) ;
#99037 = CARTESIAN_POINT ( 'NONE',  ( -16.38665767534994444, 7.295008042176405638, 100.2640086421446597 ) ) ;
#99038 = CARTESIAN_POINT ( 'NONE',  ( 0.05219959533936267826, -19.03943276465977164, 70.00109039468566152 ) ) ;
#99039 = CARTESIAN_POINT ( 'NONE',  ( -5.153800228976328057, -19.02544592524343514, 87.29057627198103830 ) ) ;
#99040 = CARTESIAN_POINT ( 'NONE',  ( 8.224510206698953496, -14.34966873604960469, 82.91557627198103830 ) ) ;
#99041 = CARTESIAN_POINT ( 'NONE',  ( -18.62759615963270932, 10.81492255796079327, 35.83224293864768839 ) ) ;
#99042 = CARTESIAN_POINT ( 'NONE',  ( -19.02544592524342804, 5.153800228976336051, 116.0405762719810383 ) ) ;
#99043 = CARTESIAN_POINT ( 'NONE',  ( -0.05219959533910754901, -16.53943276465976808, 107.4989096053143669 ) ) ;
#99044 = DIRECTION ( 'NONE',  ( 0.000000000000000000, 0.000000000000000000, 1.000000000000000000 ) ) ;
#99045 = CARTESIAN_POINT ( 'NONE',  ( 5.049401038297881783, 19.05341960407617563, 47.29275706135231161 ) ) ;
#99046 = CARTESIAN_POINT ( 'NONE',  ( -4.379528057220328563, 16.55341960407611168, 25.20724293864769550 ) ) ;
#99048 = EDGE_CURVE ( 'NONE', #11685, #100170, #158915, .T. ) ;
#99047 = CARTESIAN_POINT ( 'NONE',  ( 5.049401038298161559, -19.05341960407611168, 102.7072429386476955 ) ) ;
#99049 = CARTESIAN_POINT ( 'NONE',  ( -21.53943276465977519, -0.05219959533937600094, 63.75109039468568284 ) ) ;
#99050 = CARTESIAN_POINT ( 'NONE',  ( -21.53943276465977519, 0.05219959533907696930, 56.24890960531436690 ) ) ;
#99051 = CARTESIAN_POINT ( 'NONE',  ( 15.72974639402176855, 15.80617190586768217, 36.87609039468568994 ) ) ;
#99052 = CARTESIAN_POINT ( 'NONE',  ( 21.52544592524344225, -5.823673210054117533, 88.54057627198103830 ) ) ;
#99053 = CARTESIAN_POINT ( 'NONE',  ( 21.52544592524334988, 5.823673210054432836, 36.45942372801901143 ) ) ;
#99054 = EDGE_CURVE ( 'NONE', #111207, #126376, #16150, .T. ) ;
#99055 = CARTESIAN_POINT ( 'NONE',  ( -12.06949235617756955, 12.14591786802309770, 110.6239096053143669 ) ) ;
#99056 = CARTESIAN_POINT ( 'NONE',  ( 19.03943276465977164, 0.05219959533936151252, 66.25109039468567573 ) ) ;
#99057 = CARTESIAN_POINT ( 'NONE',  ( 16.51473224551069308, 9.474510206698969483, 44.16557627198103120 ) ) ;
#99059 = CARTESIAN_POINT ( 'NONE',  ( 0.05219959533909260263, 19.03943276465977164, 94.99890960531436690 ) ) ;
#99058 = CARTESIAN_POINT ( 'NONE',  ( -14.34966873604960291, -8.224510206698953496, 86.66557627198102409 ) ) ;
#99060 = CARTESIAN_POINT ( 'NONE',  ( 16.51473224551069308, 9.474510206698969483, 114.1655762719810241 ) ) ;
#99061 = CARTESIAN_POINT ( 'NONE',  ( 19.03943276465977164, -0.05219959533909143690, 28.74890960531435624 ) ) ;
#99062 = CARTESIAN_POINT ( 'NONE',  ( -14.34966873604960291, -8.224510206698953496, 36.66557627198103120 ) ) ;
#99063 = CARTESIAN_POINT ( 'NONE',  ( 8.314922557961029526, -14.29746914071037800, 100.4177570613523471 ) ) ;
#99064 = CARTESIAN_POINT ( 'NONE',  ( -9.564922557960796823, -16.46253265017161027, 52.08224293864768839 ) ) ;
#99065 = CARTESIAN_POINT ( 'NONE',  ( -19.03943276465977164, 0.05219959533909376836, 26.24890960531435624 ) ) ;
#99066 = CARTESIAN_POINT ( 'NONE',  ( 5.049401038297881783, 19.05341960407617563, 27.29275706135232937 ) ) ;
#99068 = CARTESIAN_POINT ( 'NONE',  ( -4.483927247898782831, 16.52544592524335698, 112.7094237280190328 ) ) ;
#99067 = CARTESIAN_POINT ( 'NONE',  ( 13.97604488694527802, 13.89961937509977652, 114.3739096053143669 ) ) ;
#99069 = CARTESIAN_POINT ( 'NONE',  ( 21.55341960407619695, -5.719274019375665929, 41.04275706135236135 ) ) ;
#99070 = CARTESIAN_POINT ( 'NONE',  ( -38.00000000000000711, 2.428612866367529932E-14, -4.000000000000000000 ) ) ;
#99071 = CARTESIAN_POINT ( 'NONE',  ( -0.05219959533934338120, 16.53943276465976808, 57.50109039468568994 ) ) ;
#99072 = CARTESIAN_POINT ( 'NONE',  ( 14.29746914071049879, -8.314922557960816363, 33.33224293864769550 ) ) ;
#99073 = CARTESIAN_POINT ( 'NONE',  ( -5.153800228976328057, -19.02544592524343514, 42.29057627198101699 ) ) ;
#99074 = CARTESIAN_POINT ( 'NONE',  ( -16.52544592524335698, -4.483927247898792601, 108.9594237280190185 ) ) ;
#99075 = CARTESIAN_POINT ( 'NONE',  ( 16.55341960407618274, -4.379528057220086978, 21.04275706135234714 ) ) ;
#99076 = CARTESIAN_POINT ( 'NONE',  ( 13.97604488694527802, 13.89961937509977652, 54.37390960531435979 ) ) ;
#99077 = CARTESIAN_POINT ( 'NONE',  ( 12.06949235617757843, -12.14591786802309237, 103.1239096053143811 ) ) ;
#99078 = CARTESIAN_POINT ( 'NONE',  ( 5.823673210054444382, -21.52544592524334988, 20.20942372801900788 ) ) ;
#99079 = CARTESIAN_POINT ( 'NONE',  ( 5.049401038298161559, -19.05341960407611168, 47.70724293864770260 ) ) ;
#99080 = DIRECTION ( 'NONE',  ( -0.000000000000000000, -0.000000000000000000, 1.000000000000000000 ) ) ;
#99081 = CARTESIAN_POINT ( 'NONE',  ( -19.05341960407611168, -5.049401038298163336, 26.45724293864769550 ) ) ;
#99082 = CARTESIAN_POINT ( 'NONE',  ( -15.80617190586745835, -15.72974639402198527, 26.87390960531435979 ) ) ;
#99083 = CYLINDRICAL_SURFACE ( 'NONE', #45439, 2.649999999999999467 ) ;
#99084 = CARTESIAN_POINT ( 'NONE',  ( 13.97604488694527802, 13.89961937509977652, 94.37390960531436690 ) ) ;
#99086 = CARTESIAN_POINT ( 'NONE',  ( 8.224510206698953496, -14.34966873604960469, 97.91557627198103830 ) ) ;
#99085 = CARTESIAN_POINT ( 'NONE',  ( 21.55341960407619695, -5.719274019375665929, 46.04275706135234714 ) ) ;
#99087 = CARTESIAN_POINT ( 'NONE',  ( 0.05219959533909260263, 19.03943276465977164, 114.9989096053143669 ) ) ;
#99088 = CARTESIAN_POINT ( 'NONE',  ( -27.94130797166088698, -7.397772140681734498, 160.8977822374860125 ) ) ;
#99089 = CARTESIAN_POINT ( 'NONE',  ( -16.52544592524335698, -4.483927247898792601, 58.95942372801902565 ) ) ;
#99090 = CARTESIAN_POINT ( 'NONE',  ( -21.53943276465977519, -0.05219959533937600094, 88.75109039468567573 ) ) ;
#99091 = CARTESIAN_POINT ( 'NONE',  ( -4.379528057220086978, -16.55341960407618274, 54.79275706135235424 ) ) ;
#99092 = CARTESIAN_POINT ( 'NONE',  ( 5.153800228976335163, 19.02544592524342804, 99.79057627198102409 ) ) ;
#99093 = CARTESIAN_POINT ( 'NONE',  ( 12.14591786802327356, -12.06949235617739191, 45.62609039468567573 ) ) ;
#99094 = CARTESIAN_POINT ( 'NONE',  ( -16.46253265017146816, -9.564922557961047289, 109.1677570613523471 ) ) ;
#99095 = CARTESIAN_POINT ( 'NONE',  ( 16.53943276465976808, 0.05219959533934440121, 81.25109039468568994 ) ) ;
#99096 = CARTESIAN_POINT ( 'NONE',  ( 5.153800228976615827, -19.02544592524334988, 95.20942372801897591 ) ) ;
#99097 = CARTESIAN_POINT ( 'NONE',  ( -9.474510206698964154, 16.51473224551069663, 70.41557627198102409 ) ) ;
#99098 = CARTESIAN_POINT ( 'NONE',  ( 5.719274019375991003, -21.55341960407610458, 102.7072429386476955 ) ) ;
#99100 = CARTESIAN_POINT ( 'NONE',  ( 16.51473224551083163, -9.474510206698727899, 110.8344237280190043 ) ) ;
#99099 = CARTESIAN_POINT ( 'NONE',  ( 8.224510206698953496, -14.34966873604960469, 87.91557627198103830 ) ) ;
#99101 = CARTESIAN_POINT ( 'NONE',  ( 12.06949235617739724, 12.14591786802326823, 76.87609039468567573 ) ) ;
#99102 = CARTESIAN_POINT ( 'NONE',  ( 20.14845677604831664, 11.63499142542225329, 168.0304984204095149 ) ) ;
#99103 = CARTESIAN_POINT ( 'NONE',  ( 9.564922557961047289, -16.46253265017146816, 70.41775706135233293 ) ) ;
#99104 = CARTESIAN_POINT ( 'NONE',  ( 8.224510206698953496, -14.34966873604960469, 37.91557627198102409 ) ) ;
#99105 = CARTESIAN_POINT ( 'NONE',  ( 0.05219959533910956823, 16.53943276465976808, 94.99890960531436690 ) ) ;
#99107 = DIRECTION ( 'NONE',  ( 0.000000000000000000, 0.000000000000000000, 1.000000000000000000 ) ) ;
#99106 = CARTESIAN_POINT ( 'NONE',  ( 19.02544592524334988, 5.153800228976608722, 36.45942372801900433 ) ) ;
#99108 = CARTESIAN_POINT ( 'NONE',  ( 10.81492255796106328, -18.62759615963255655, 25.41775706135235779 ) ) ;
#99109 = CARTESIAN_POINT ( 'NONE',  ( 9.474510206698729675, 16.51473224551082808, 97.08442372801900433 ) ) ;
#99110 = LINE ( 'NONE', #116289, #115061 ) ;
#99111 = CARTESIAN_POINT ( 'NONE',  ( -9.564922557960796823, -16.46253265017161027, 97.08224293864769550 ) ) ;
#99112 = CARTESIAN_POINT ( 'NONE',  ( 10.81492255796106328, -18.62759615963255655, 100.4177570613523471 ) ) ;
#99113 = CARTESIAN_POINT ( 'NONE',  ( 5.049401038298161559, -19.05341960407611168, 72.70724293864768129 ) ) ;
#99114 = CARTESIAN_POINT ( 'NONE',  ( -10.81492255796078084, -18.62759615963271287, 37.08224293864768129 ) ) ;
#99115 = CARTESIAN_POINT ( 'NONE',  ( -8.224510206698948167, 14.34966873604960824, 100.4155762719810241 ) ) ;
#99116 = CARTESIAN_POINT ( 'NONE',  ( -0.05219959533909027116, -19.03943276465977164, 52.49890960531436690 ) ) ;
#99117 = CARTESIAN_POINT ( 'NONE',  ( -4.379528057220328563, 16.55341960407611168, 105.2072429386477097 ) ) ;
#99118 = CIRCLE ( 'NONE', #176665, 0.5000000000000002220 ) ;
#99119 = CARTESIAN_POINT ( 'NONE',  ( 10.72451020669871369, 18.67979575497193778, 22.08442372801901143 ) ) ;
#99120 = CARTESIAN_POINT ( 'NONE',  ( -5.719274019375665041, -21.55341960407619695, 59.79275706135234714 ) ) ;
#99121 = CARTESIAN_POINT ( 'NONE',  ( -5.049401038298153566, 19.05341960407611168, 40.20724293864768839 ) ) ;
#99122 = ADVANCED_FACE ( 'NONE', ( #167007, #74983, #44650, #77946 ), #28509, .T. ) ;
#99123 = CARTESIAN_POINT ( 'NONE',  ( -16.55341960407617563, 4.379528057220093196, 73.54275706135234714 ) ) ;
#99124 = CARTESIAN_POINT ( 'NONE',  ( 21.52544592524334988, 5.823673210054432836, 21.45942372801901499 ) ) ;
#99125 = VERTEX_POINT ( 'NONE', #14299 ) ;
#99126 = CARTESIAN_POINT ( 'NONE',  ( -15.72974639402197994, 15.80617190586746368, 115.6239096053143669 ) ) ;
#99128 = CARTESIAN_POINT ( 'NONE',  ( 5.049401038298161559, -19.05341960407611168, 67.70724293864769550 ) ) ;
#99127 = CARTESIAN_POINT ( 'NONE',  ( 9.564922557961047289, -16.46253265017146816, 55.41775706135234003 ) ) ;
#99129 = CARTESIAN_POINT ( 'NONE',  ( -19.02544592524334988, -5.153800228976617603, 33.95942372801897591 ) ) ;
#99130 = CARTESIAN_POINT ( 'NONE',  ( 21.52544592524334988, 5.823673210054432836, 66.45942372801903275 ) ) ;
#99131 = CARTESIAN_POINT ( 'NONE',  ( 15.72974639402199770, -15.80617190586745480, 73.12390960531436690 ) ) ;
#99132 = CARTESIAN_POINT ( 'NONE',  ( 12.06949235617757843, -12.14591786802309237, 53.12390960531436690 ) ) ;
#99134 = CARTESIAN_POINT ( 'NONE',  ( 9.564922557961047289, -16.46253265017146816, 25.41775706135234003 ) ) ;
#99133 = CARTESIAN_POINT ( 'NONE',  ( 15.80617190586769283, -15.72974639402175789, 85.62609039468568994 ) ) ;
#99135 = CARTESIAN_POINT ( 'NONE',  ( -16.53943276465976808, 0.05219959533911058130, 66.24890960531436690 ) ) ;
#99136 = CARTESIAN_POINT ( 'NONE',  ( 13.89961937509977652, -13.97604488694527269, 23.12390960531436335 ) ) ;
#99137 = CARTESIAN_POINT ( 'NONE',  ( 13.89961937509957401, 13.97604488694547697, 51.87609039468566863 ) ) ;
#99138 = CARTESIAN_POINT ( 'NONE',  ( -4.379528057220086978, -16.55341960407618274, 109.7927570613523613 ) ) ;
#99139 = AXIS2_PLACEMENT_3D ( 'NONE', #69585, #22086, #161593 ) ;
#99140 = CARTESIAN_POINT ( 'NONE',  ( 15.80617190586769283, -15.72974639402175789, 75.62609039468567573 ) ) ;
#99141 = CARTESIAN_POINT ( 'NONE',  ( 19.03943276465977164, 0.05219959533936151252, 51.25109039468567573 ) ) ;
#99142 = CARTESIAN_POINT ( 'NONE',  ( -18.62759615963270932, 10.81492255796079327, 55.83224293864770260 ) ) ;
#99143 = CARTESIAN_POINT ( 'NONE',  ( 15.72974639402176855, 15.80617190586768217, 41.87609039468568284 ) ) ;
#99144 = CARTESIAN_POINT ( 'NONE',  ( -10.72451020669898014, 18.67979575497178502, 95.41557627198102409 ) ) ;
#99145 = CARTESIAN_POINT ( 'NONE',  ( 5.153800228976615827, -19.02544592524334988, 100.2094237280190043 ) ) ;
#99146 = CARTESIAN_POINT ( 'NONE',  ( -8.314922557961024197, 14.29746914071037800, 72.91775706135234714 ) ) ;
#99148 = CARTESIAN_POINT ( 'NONE',  ( -18.67979575497178146, -10.72451020669898902, 106.6655762719810383 ) ) ;
#99147 = CARTESIAN_POINT ( 'NONE',  ( -37.99999999999997158, 12.34694845685052123, -6.100000000000001421 ) ) ;
#99149 = CARTESIAN_POINT ( 'NONE',  ( 12.06949235617757843, -12.14591786802309237, 88.12390960531436690 ) ) ;
#99150 = CARTESIAN_POINT ( 'NONE',  ( -17.13100169013299734, -6.664070546373157100, 99.23210164300155611 ) ) ;
#99151 = CARTESIAN_POINT ( 'NONE',  ( -16.52544592524335698, -4.483927247898792601, 23.95942372801901143 ) ) ;
#99152 = CARTESIAN_POINT ( 'NONE',  ( 0.05219959533907565091, 21.53943276465977519, 54.99890960531435269 ) ) ;
#99153 = CARTESIAN_POINT ( 'NONE',  ( 16.53943276465976808, 0.05219959533934440121, 86.25109039468568994 ) ) ;
#99154 = CARTESIAN_POINT ( 'NONE',  ( -3.573655867282028392E-15, 2.428612866367529932E-14, 139.9999999999999716 ) ) ;
#99155 = CARTESIAN_POINT ( 'NONE',  ( 16.52544592524335698, 4.483927247898782831, 66.45942372801903275 ) ) ;
#99156 = CARTESIAN_POINT ( 'NONE',  ( -15.72974639402176322, -15.80617190586768395, 44.37609039468567573 ) ) ;
#99157 = CARTESIAN_POINT ( 'NONE',  ( 21.55341960407610458, 5.719274019375980345, 63.95724293864770260 ) ) ;
#99158 = CARTESIAN_POINT ( 'NONE',  ( 0.05219959533934541429, -16.53943276465976808, 85.00109039468568994 ) ) ;
#99159 = CARTESIAN_POINT ( 'NONE',  ( 5.823673210054444382, -21.52544592524334988, 65.20942372801901854 ) ) ;
#99160 = CARTESIAN_POINT ( 'NONE',  ( 10.72451020669898902, -18.67979575497178502, 47.91557627198102409 ) ) ;
#99161 = CARTESIAN_POINT ( 'NONE',  ( -10.72451020669898014, 18.67979575497178502, 40.41557627198103120 ) ) ;
#99162 = ORIENTED_EDGE ( 'NONE', *, *, #171952, .T. ) ;
#99163 = CARTESIAN_POINT ( 'NONE',  ( 8.224510206698742110, 14.34966873604972548, 67.08442372801901854 ) ) ;
#99164 = CARTESIAN_POINT ( 'NONE',  ( -5.823673210054116645, -21.52544592524344225, 37.29057627198102409 ) ) ;
#99165 = ORIENTED_EDGE ( 'NONE', *, *, #196211, .T. ) ;
#99166 = CARTESIAN_POINT ( 'NONE',  ( 5.049401038298161559, -19.05341960407611168, 97.70724293864766707 ) ) ;
#99167 = CARTESIAN_POINT ( 'NONE',  ( 16.55341960407618274, -4.379528057220086978, 111.0427570613523613 ) ) ;
#99168 = CARTESIAN_POINT ( 'NONE',  ( 18.22780087662121673, 5.500000000000056843, 73.98459894673894155 ) ) ;
#99169 = CARTESIAN_POINT ( 'NONE',  ( 8.314922557960818139, 14.29746914071049879, 109.5822429386476955 ) ) ;
#99170 = CARTESIAN_POINT ( 'NONE',  ( 10.72451020669898902, -18.67979575497178502, 42.91557627198103120 ) ) ;
#99171 = CARTESIAN_POINT ( 'NONE',  ( -19.05341960407611168, -5.049401038298163336, 46.45724293864768129 ) ) ;
#99172 = CARTESIAN_POINT ( 'NONE',  ( 8.314922557961029526, -14.29746914071037800, 90.41775706135236135 ) ) ;
#99173 = CARTESIAN_POINT ( 'NONE',  ( -15.80617190586768217, 15.72974639402176855, 28.12609039468568284 ) ) ;
#99174 = CARTESIAN_POINT ( 'NONE',  ( 5.153800228976615827, -19.02544592524334988, 90.20942372801900433 ) ) ;
#99175 = CARTESIAN_POINT ( 'NONE',  ( 4.483927247898545687, 16.52544592524342804, 109.7905762719810383 ) ) ;
#99176 = CARTESIAN_POINT ( 'NONE',  ( 19.02544592524343514, -5.153800228976328945, 53.54057627198102409 ) ) ;
#99177 = AXIS2_PLACEMENT_3D ( 'NONE', #90965, #190949, #36254 ) ;
#99178 = CARTESIAN_POINT ( 'NONE',  ( 19.02544592524343514, -5.153800228976328945, 33.54057627198102409 ) ) ;
#99179 = FACE_OUTER_BOUND ( 'NONE', #46528, .T. ) ;
#99180 = CARTESIAN_POINT ( 'NONE',  ( 5.153800228976335163, 19.02544592524342804, 74.79057627198103830 ) ) ;
#99181 = CARTESIAN_POINT ( 'NONE',  ( 4.483927247898790824, -16.52544592524335698, 60.20942372801902565 ) ) ;
#99182 = CARTESIAN_POINT ( 'NONE',  ( 5.719274019375673035, 21.55341960407619339, 102.2927570613523613 ) ) ;
#99183 = CARTESIAN_POINT ( 'NONE',  ( 21.55341960407610458, 5.719274019375980345, 48.95724293864770971 ) ) ;
#99184 = CARTESIAN_POINT ( 'NONE',  ( 14.29746914071037800, 8.314922557961029526, 76.66775706135234714 ) ) ;
#99185 = CARTESIAN_POINT ( 'NONE',  ( -9.564922557961040184, 16.46253265017147172, 52.91775706135233293 ) ) ;
#99186 = CARTESIAN_POINT ( 'NONE',  ( -0.05219959533936034679, 19.03943276465977164, 62.50109039468566863 ) ) ;
#99187 = ORIENTED_EDGE ( 'NONE', *, *, #5609, .F. ) ;
#99188 = CARTESIAN_POINT ( 'NONE',  ( -21.53943276465977519, -0.05219959533937600094, 58.75109039468568994 ) ) ;
#99189 = CARTESIAN_POINT ( 'NONE',  ( -19.05341960407611168, -5.049401038298163336, 61.45724293864769550 ) ) ;
#99190 = CARTESIAN_POINT ( 'NONE',  ( -5.049401038298153566, 19.05341960407611168, 40.20724293864768839 ) ) ;
#99191 = CARTESIAN_POINT ( 'NONE',  ( 13.97604488694548053, -13.89961937509957401, 65.62609039468567573 ) ) ;
#99192 = CARTESIAN_POINT ( 'NONE',  ( 16.46253265017160672, -9.564922557960803928, 108.3322429386476955 ) ) ;
#99193 = CARTESIAN_POINT ( 'NONE',  ( 19.03943276465977164, -0.05219959533909143690, 98.74890960531436690 ) ) ;
#99194 = CARTESIAN_POINT ( 'NONE',  ( -14.34966873604960291, -8.224510206698953496, 56.66557627198103830 ) ) ;
#99195 = CARTESIAN_POINT ( 'NONE',  ( -0.05219959533907301413, -21.53943276465977519, 42.49890960531435979 ) ) ;
#99196 = DIRECTION ( 'NONE',  ( -1.000000000000000000, 0.000000000000000000, 0.000000000000000000 ) ) ;
#99197 = CARTESIAN_POINT ( 'NONE',  ( -9.474510206698720793, -16.51473224551083518, 34.58442372801899722 ) ) ;
#99198 = DIRECTION ( 'NONE',  ( 0.000000000000000000, 0.000000000000000000, -1.000000000000000000 ) ) ;
#99199 = CARTESIAN_POINT ( 'NONE',  ( 16.51473224551069308, 9.474510206698969483, 44.16557627198103120 ) ) ;
#99200 = CARTESIAN_POINT ( 'NONE',  ( -33.80025371042792415, -2.440809870420988403, 99.93203653199840630 ) ) ;
#99201 = CARTESIAN_POINT ( 'NONE',  ( 21.38418241377623019, -7.427326039334300134, 174.4773576836617224 ) ) ;
#99202 = CARTESIAN_POINT ( 'NONE',  ( 8.314922557961029526, -14.29746914071037800, 75.41775706135233293 ) ) ;
#99203 = CARTESIAN_POINT ( 'NONE',  ( 21.52544592524344225, -5.823673210054117533, 98.54057627198105251 ) ) ;
#99204 = CARTESIAN_POINT ( 'NONE',  ( -16.55341960407611168, -4.379528057220339221, 56.45724293864768839 ) ) ;
#99206 = CARTESIAN_POINT ( 'NONE',  ( 2.200000000000000178, 0.000000000000000000, 3.799999999999999378 ) ) ;
#99205 = CARTESIAN_POINT ( 'NONE',  ( 19.03943276465977164, -0.05219959533909143690, 43.74890960531435979 ) ) ;
#99207 = CARTESIAN_POINT ( 'NONE',  ( 5.823673210054444382, -21.52544592524334988, 45.20942372801901854 ) ) ;
#99208 = CARTESIAN_POINT ( 'NONE',  ( 13.97604488694548053, -13.89961937509957401, 50.62609039468566152 ) ) ;
#99209 = CARTESIAN_POINT ( 'NONE',  ( -5.049401038298153566, 19.05341960407611168, 45.20724293864769550 ) ) ;
#99210 = CARTESIAN_POINT ( 'NONE',  ( -21.53943276465977519, -0.05219959533937600094, 93.75109039468567573 ) ) ;
#99211 = CARTESIAN_POINT ( 'NONE',  ( 17.12812012977027365, 6.668231424565989940, 98.85948759323144941 ) ) ;
#99212 = CARTESIAN_POINT ( 'NONE',  ( -0.05219959533910754901, -16.53943276465976808, 42.49890960531435979 ) ) ;
#99213 = CARTESIAN_POINT ( 'NONE',  ( -15.84196527238551333, 1.359015117358495894, -59.51370404797112457 ) ) ;
#99214 = CARTESIAN_POINT ( 'NONE',  ( 5.823673210054125526, 21.52544592524343514, 44.79057627198103120 ) ) ;
#99215 = CARTESIAN_POINT ( 'NONE',  ( 17.14385361876520264, -23.59649016807270883, 143.5750000027311728 ) ) ;
#99216 = CARTESIAN_POINT ( 'NONE',  ( -0.05219959533909027116, -19.03943276465977164, 102.4989096053143669 ) ) ;
#99217 = CARTESIAN_POINT ( 'NONE',  ( -4.483927247898539470, -16.52544592524342804, 87.29057627198103830 ) ) ;
#99218 = CARTESIAN_POINT ( 'NONE',  ( 0.05219959533934541429, -16.53943276465976808, 25.00109039468567218 ) ) ;
#99219 = CARTESIAN_POINT ( 'NONE',  ( -8.314922557961024197, 14.29746914071037800, 102.9177570613523756 ) ) ;
#99220 = EDGE_LOOP ( 'NONE', ( #198408, #179113, #47714, #9721 ) ) ;
#99221 = ADVANCED_FACE ( 'NONE', ( #92114 ), #116156, .T. ) ;
#99223 = CARTESIAN_POINT ( 'NONE',  ( 21.52544592524344225, -5.823673210054117533, 98.54057627198105251 ) ) ;
#99222 = CARTESIAN_POINT ( 'NONE',  ( -5.049401038298153566, 19.05341960407611168, 95.20724293864770971 ) ) ;
#99225 = CARTESIAN_POINT ( 'NONE',  ( 9.564922557960805705, 16.46253265017160317, 94.58224293864769550 ) ) ;
#99224 = CARTESIAN_POINT ( 'NONE',  ( 16.55341960407611168, 4.379528057220329451, 23.95724293864769550 ) ) ;
#99226 = CARTESIAN_POINT ( 'NONE',  ( 19.02544592524334988, 5.153800228976608722, 91.45942372801900433 ) ) ;
#99227 = CARTESIAN_POINT ( 'NONE',  ( 10.72451020669871369, 18.67979575497193778, 107.0844237280190043 ) ) ;
#99228 = CARTESIAN_POINT ( 'NONE',  ( 21.52544592524344225, -5.823673210054117533, 83.54057627198102409 ) ) ;
#99229 = CARTESIAN_POINT ( 'NONE',  ( -10.72451020669898014, 18.67979575497178502, 50.41557627198103120 ) ) ;
#99230 = CARTESIAN_POINT ( 'NONE',  ( -13.89961937509977652, 13.97604488694528158, 60.62390960531436690 ) ) ;
#99231 = CARTESIAN_POINT ( 'NONE',  ( 16.52544592524342804, -4.483927247898539470, 38.54057627198103120 ) ) ;
#99232 = CARTESIAN_POINT ( 'NONE',  ( 13.97604488694527802, 13.89961937509977652, 79.37390960531435269 ) ) ;
#99233 = VERTEX_POINT ( 'NONE', #93113 ) ;
#99234 = CARTESIAN_POINT ( 'NONE',  ( 18.87075004821569379, -5.500000000000108358, 61.17408112101048090 ) ) ;
#99235 = CARTESIAN_POINT ( 'NONE',  ( 13.97604488694548053, -13.89961937509957401, 40.62609039468564731 ) ) ;
#99236 = CARTESIAN_POINT ( 'NONE',  ( -16.53943276465976808, 0.05219959533911058130, 86.24890960531436690 ) ) ;
#99237 = CARTESIAN_POINT ( 'NONE',  ( -0.05219959533937732626, 21.53943276465977519, 22.50109039468567573 ) ) ;
#99238 = CARTESIAN_POINT ( 'NONE',  ( 1.784210473542230573E-15, -29.16686587814331588, 143.8750000027311557 ) ) ;
#99239 = CARTESIAN_POINT ( 'NONE',  ( -12.14591786802326823, 12.06949235617739902, 103.1260903946856757 ) ) ;
#99240 = CARTESIAN_POINT ( 'NONE',  ( 8.224510206698953496, -14.34966873604960469, 112.9155762719810383 ) ) ;
#99241 = CARTESIAN_POINT ( 'NONE',  ( -9.474510206698964154, 16.51473224551069663, 75.41557627198103830 ) ) ;
#99242 = DIRECTION ( 'NONE',  ( 0.000000000000000000, 0.000000000000000000, 1.000000000000000000 ) ) ;
#99243 = CARTESIAN_POINT ( 'NONE',  ( 5.049401038298161559, -19.05341960407611168, 22.70724293864769194 ) ) ;
#99244 = CARTESIAN_POINT ( 'NONE',  ( 14.34966873604960469, 8.224510206698951720, 44.16557627198103120 ) ) ;
#99245 = CARTESIAN_POINT ( 'NONE',  ( -10.72451020669870658, -18.67979575497194134, 54.58442372801901143 ) ) ;
#99246 = CARTESIAN_POINT ( 'NONE',  ( -2.973862142520662832, -93.04182470242767522, -25.00000000000000000 ) ) ;
#99247 = CARTESIAN_POINT ( 'NONE',  ( 5.719274019375673035, 21.55341960407619339, 92.29275706135236135 ) ) ;
#99248 = CARTESIAN_POINT ( 'NONE',  ( 16.51473224551069308, 9.474510206698969483, 44.16557627198103120 ) ) ;
#99249 = CARTESIAN_POINT ( 'NONE',  ( -9.474510206698964154, 16.51473224551069663, 55.41557627198103120 ) ) ;
#99250 = EDGE_LOOP ( 'NONE', ( #41006, #38510, #20823, #124623 ) ) ;
#99251 = CARTESIAN_POINT ( 'NONE',  ( -10.81492255796105439, 18.62759615963255655, 97.91775706135236135 ) ) ;
#99252 = CARTESIAN_POINT ( 'NONE',  ( 14.29746914071037800, 8.314922557961029526, 56.66775706135235424 ) ) ;
#99253 = CARTESIAN_POINT ( 'NONE',  ( 10.72451020669871369, 18.67979575497193778, 82.08442372801901854 ) ) ;
#99254 = CARTESIAN_POINT ( 'NONE',  ( 18.62759615963271287, -10.81492255796078972, 23.33224293864769194 ) ) ;
#99255 = CARTESIAN_POINT ( 'NONE',  ( -19.02544592524334988, -5.153800228976617603, 88.95942372801897591 ) ) ;
#99256 = CARTESIAN_POINT ( 'NONE',  ( 10.72451020669871369, 18.67979575497193778, 72.08442372801899012 ) ) ;
#99257 = CARTESIAN_POINT ( 'NONE',  ( -12.14591786802326823, 12.06949235617739902, 38.12609039468567573 ) ) ;
#99258 = CARTESIAN_POINT ( 'NONE',  ( -21.52544592524343514, 5.823673210054127303, 91.04057627198103830 ) ) ;
#99259 = CARTESIAN_POINT ( 'NONE',  ( -9.474510206698720793, -16.51473224551083518, 84.58442372801900433 ) ) ;
#99260 = CARTESIAN_POINT ( 'NONE',  ( 19.05341960407611168, 5.049401038298154454, 58.95724293864768129 ) ) ;
#99261 = CARTESIAN_POINT ( 'NONE',  ( 0.05219959533936267826, -19.03943276465977164, 100.0010903946856757 ) ) ;
#99262 = CIRCLE ( 'NONE', #121796, 5.500000000001017852 ) ;
#99263 = CARTESIAN_POINT ( 'NONE',  ( 9.474510206698729675, 16.51473224551082808, 97.08442372801900433 ) ) ;
#99264 = CARTESIAN_POINT ( 'NONE',  ( -16.55341960407611168, -4.379528057220339221, 51.45724293864770260 ) ) ;
#99265 = CARTESIAN_POINT ( 'NONE',  ( 16.46253265017146816, 9.564922557961045513, 71.66775706135233293 ) ) ;
#99266 = CARTESIAN_POINT ( 'NONE',  ( 12.14591786802327356, -12.06949235617739191, 60.62609039468567573 ) ) ;
#99267 = CARTESIAN_POINT ( 'NONE',  ( 19.02544592524343514, -5.153800228976328945, 43.54057627198103120 ) ) ;
#99268 = CARTESIAN_POINT ( 'NONE',  ( -19.02544592524342804, 5.153800228976336051, 51.04057627198103120 ) ) ;
#99269 = CARTESIAN_POINT ( 'NONE',  ( -4.483927247898782831, 16.52544592524335698, 62.70942372801902565 ) ) ;
#99270 = CARTESIAN_POINT ( 'NONE',  ( 27.73933785331498569, 2.768321779492822058E-14, 142.3750000027311842 ) ) ;
#99271 = CARTESIAN_POINT ( 'NONE',  ( 28.82186960331499392, -9.364793116373510529, 139.1500000054623456 ) ) ;
#99272 = CARTESIAN_POINT ( 'NONE',  ( -13.89961937509977652, 13.97604488694528158, 110.6239096053143243 ) ) ;
#99273 = CARTESIAN_POINT ( 'NONE',  ( -13.97604488694527625, -13.89961937509977652, 26.87390960531434558 ) ) ;
#99274 = VERTEX_POINT ( 'NONE', #124456 ) ;
#99275 = CARTESIAN_POINT ( 'NONE',  ( 9.564922557961047289, -16.46253265017146816, 110.4177570613523471 ) ) ;
#99276 = CARTESIAN_POINT ( 'NONE',  ( 10.72451020669898902, -18.67979575497178502, 37.91557627198102409 ) ) ;
#99278 = CARTESIAN_POINT ( 'NONE',  ( 14.29746914071037800, 8.314922557961029526, 26.66775706135235424 ) ) ;
#99277 = CARTESIAN_POINT ( 'NONE',  ( -13.97604488694547697, 13.89961937509957934, 33.12609039468566863 ) ) ;
#99279 = CARTESIAN_POINT ( 'NONE',  ( 19.02544592524343514, -5.153800228976328945, 28.54057627198102409 ) ) ;
#99280 = CARTESIAN_POINT ( 'NONE',  ( -5.153800228976328057, -19.02544592524343514, 57.29057627198103120 ) ) ;
#99281 = CARTESIAN_POINT ( 'NONE',  ( 0.05219959533907565091, 21.53943276465977519, 84.99890960531436690 ) ) ;
#99282 = CARTESIAN_POINT ( 'NONE',  ( 0.05219959533909260263, 19.03943276465977164, 104.9989096053143669 ) ) ;
#99283 = CARTESIAN_POINT ( 'NONE',  ( -16.46253265017160317, 9.564922557960807481, 55.83224293864769550 ) ) ;
#99284 = CARTESIAN_POINT ( 'NONE',  ( -22.44159573604009950, -16.30477369853688430, 143.5750000027311728 ) ) ;
#99285 = CARTESIAN_POINT ( 'NONE',  ( 5.153800228976615827, -19.02544592524334988, 90.20942372801900433 ) ) ;
#99287 = VECTOR ( 'NONE', #104443, 1000.000000000000000 ) ;
#99286 = CARTESIAN_POINT ( 'NONE',  ( -8.224510206698948167, 14.34966873604960824, 70.41557627198102409 ) ) ;
#99288 = CARTESIAN_POINT ( 'NONE',  ( 21.53943276465977519, -0.05219959533907433946, 43.74890960531435979 ) ) ;
#99289 = CARTESIAN_POINT ( 'NONE',  ( 21.55341960407619695, -5.719274019375665929, 101.0427570613523756 ) ) ;
#99290 = CARTESIAN_POINT ( 'NONE',  ( -21.53943276465977519, 0.05219959533907696930, 96.24890960531435269 ) ) ;
#99291 = CARTESIAN_POINT ( 'NONE',  ( -18.67979575497193778, 10.72451020669871902, 78.33442372801901854 ) ) ;
#99292 = CARTESIAN_POINT ( 'NONE',  ( 21.52544592524334988, 5.823673210054432836, 71.45942372801901854 ) ) ;
#99293 = CARTESIAN_POINT ( 'NONE',  ( 19.05341960407611168, 5.049401038298154454, 108.9572429386477097 ) ) ;
#99295 = CARTESIAN_POINT ( 'NONE',  ( -15.80617190586768217, 15.72974639402176855, 73.12609039468567573 ) ) ;
#99294 = CARTESIAN_POINT ( 'NONE',  ( -4.483927247898782831, 16.52544592524335698, 107.7094237280190328 ) ) ;
#99296 = CARTESIAN_POINT ( 'NONE',  ( 13.89961937509977652, -13.97604488694527269, 68.12390960531436690 ) ) ;
#99297 = EDGE_CURVE ( 'NONE', #84653, #172658, #103327, .T. ) ;
#99298 = CARTESIAN_POINT ( 'NONE',  ( 21.55341960407619695, -5.719274019375665929, 31.04275706135234714 ) ) ;
#99299 = CARTESIAN_POINT ( 'NONE',  ( 0.05219959533909260263, 19.03943276465977164, 69.99890960531435269 ) ) ;
#99300 = CARTESIAN_POINT ( 'NONE',  ( -16.55341960407611168, -4.379528057220339221, 86.45724293864770971 ) ) ;
#99301 = CARTESIAN_POINT ( 'NONE',  ( -16.55341960407611168, -4.379528057220339221, 51.45724293864770260 ) ) ;
#99302 = CARTESIAN_POINT ( 'NONE',  ( 18.62759615963271287, -10.81492255796078972, 58.33224293864768839 ) ) ;
#99303 = CARTESIAN_POINT ( 'NONE',  ( -5.049401038298153566, 19.05341960407611168, 60.20724293864768129 ) ) ;
#99304 = CARTESIAN_POINT ( 'NONE',  ( -21.52544592524343514, 5.823673210054127303, 76.04057627198102409 ) ) ;
#99305 = CARTESIAN_POINT ( 'NONE',  ( 13.97604488694548053, -13.89961937509957401, 70.62609039468567573 ) ) ;
#99307 = CARTESIAN_POINT ( 'NONE',  ( -12.06949235617756955, 12.14591786802309770, 75.62390960531439532 ) ) ;
#99306 = CARTESIAN_POINT ( 'NONE',  ( 5.049401038297881783, 19.05341960407617918, 22.29275706135233648 ) ) ;
#99308 = VECTOR ( 'NONE', #31306, 1000.000000000000114 ) ;
#99309 = CARTESIAN_POINT ( 'NONE',  ( -10.81492255796078084, -18.62759615963271287, 57.08224293864769550 ) ) ;
#99310 = VERTEX_POINT ( 'NONE', #75967 ) ;
#99311 = CARTESIAN_POINT ( 'NONE',  ( -3.573655867282028392E-15, 2.428612866367529932E-14, 164.9999999999999716 ) ) ;
#99313 = CARTESIAN_POINT ( 'NONE',  ( -27.73933785331498925, 9.013057229001088189, 145.2750000027311899 ) ) ;
#99312 = CARTESIAN_POINT ( 'NONE',  ( -16.55341960407617563, 4.379528057220093196, 93.54275706135234714 ) ) ;
#99314 = CARTESIAN_POINT ( 'NONE',  ( 19.02544592524334988, 5.153800228976608722, 86.45942372801900433 ) ) ;
#99315 = ADVANCED_FACE ( 'NONE', ( #139613 ), #197349, .F. ) ;
#99316 = CARTESIAN_POINT ( 'NONE',  ( 4.379528057220339221, -16.55341960407611168, 62.70724293864769550 ) ) ;
#99317 = CARTESIAN_POINT ( 'NONE',  ( -17.50000000000000000, 5.499999999999992895, 33.71769037696435589 ) ) ;
#99318 = CARTESIAN_POINT ( 'NONE',  ( 16.51473224551069308, 9.474510206698969483, 64.16557627198102409 ) ) ;
#99319 = CARTESIAN_POINT ( 'NONE',  ( -8.314922557960811034, -14.29746914071050412, 57.08224293864769550 ) ) ;
#99320 = CARTESIAN_POINT ( 'NONE',  ( -9.474510206698964154, 16.51473224551069663, 85.41557627198102409 ) ) ;
#99322 = CARTESIAN_POINT ( 'NONE',  ( -5.049401038298153566, 19.05341960407611168, 55.20724293864769550 ) ) ;
#99321 = CARTESIAN_POINT ( 'NONE',  ( 9.474510206698729675, 16.51473224551082808, 77.08442372801900433 ) ) ;
#99323 = CARTESIAN_POINT ( 'NONE',  ( 16.46253265017160672, -9.564922557960803928, 83.33224293864768129 ) ) ;
#99324 = CARTESIAN_POINT ( 'NONE',  ( -5.153800228976328057, -19.02544592524343514, 72.29057627198102409 ) ) ;
#99325 = CARTESIAN_POINT ( 'NONE',  ( -5.719274019375978568, 21.55341960407610458, 60.20724293864768839 ) ) ;
#99326 = CARTESIAN_POINT ( 'NONE',  ( -8.314922557961024197, 14.29746914071037800, 62.91775706135236135 ) ) ;
#99327 = CARTESIAN_POINT ( 'NONE',  ( 17.58332526062525147, 7.635886036038630920, 101.5766504044153322 ) ) ;
#99328 = CARTESIAN_POINT ( 'NONE',  ( -19.05341960407611168, -5.049401038298163336, 51.45724293864770260 ) ) ;
#99329 = CARTESIAN_POINT ( 'NONE',  ( 18.62759615963271287, -10.81492255796078972, 53.33224293864769550 ) ) ;
#99330 = CARTESIAN_POINT ( 'NONE',  ( -19.02544592524334988, -5.153800228976617603, 78.95942372801900433 ) ) ;
#99331 = CARTESIAN_POINT ( 'NONE',  ( -14.34966873604960291, -8.224510206698953496, 21.66557627198102409 ) ) ;
#99332 = CARTESIAN_POINT ( 'NONE',  ( -13.89961937509957401, -13.97604488694547875, 34.37609039468566863 ) ) ;
#99334 = CARTESIAN_POINT ( 'NONE',  ( 4.483927247898790824, -16.52544592524335698, 90.20942372801903275 ) ) ;
#99333 = CARTESIAN_POINT ( 'NONE',  ( -12.14591786802326823, 12.06949235617739902, 58.12609039468568994 ) ) ;
#99335 = CARTESIAN_POINT ( 'NONE',  ( -28.79475375365585066, 2.428612866367529932E-14, 148.2656553485623760 ) ) ;
#99336 = CARTESIAN_POINT ( 'NONE',  ( 8.224510206698742110, 14.34966873604972548, 82.08442372801901854 ) ) ;
#99337 = CARTESIAN_POINT ( 'NONE',  ( -21.53943276465977519, 0.05219959533907696930, 31.24890960531435979 ) ) ;
#99338 = CARTESIAN_POINT ( 'NONE',  ( 9.564922557960805705, 16.46253265017160317, 39.58224293864768839 ) ) ;
#99339 = CARTESIAN_POINT ( 'NONE',  ( -19.05341960407611168, -5.049401038298163336, 51.45724293864770260 ) ) ;
#99340 = CARTESIAN_POINT ( 'NONE',  ( -16.46253265017160317, 9.564922557960807481, 40.83224293864769550 ) ) ;
#99341 = CARTESIAN_POINT ( 'NONE',  ( -21.55341960407619339, 5.719274019375674811, 33.54275706135234714 ) ) ;
#99342 = CARTESIAN_POINT ( 'NONE',  ( 14.29746914071037800, 8.314922557961029526, 46.66775706135234714 ) ) ;
#99343 = CARTESIAN_POINT ( 'NONE',  ( -14.34966873604960291, -8.224510206698953496, 26.66557627198103475 ) ) ;
#99344 = CARTESIAN_POINT ( 'NONE',  ( 19.03943276465977164, -0.05219959533909143690, 23.74890960531435269 ) ) ;
#99345 = CARTESIAN_POINT ( 'NONE',  ( -16.51473224551082808, 9.474510206698731452, 23.33442372801900078 ) ) ;
#99346 = CARTESIAN_POINT ( 'NONE',  ( 0.05219959533934541429, -16.53943276465976808, 20.00109039468568639 ) ) ;
#99347 = CARTESIAN_POINT ( 'NONE',  ( 13.89961937509957401, 13.97604488694547697, 66.87609039468567573 ) ) ;
#99348 = CARTESIAN_POINT ( 'NONE',  ( 16.52544592524342804, -4.483927247898539470, 73.54057627198102409 ) ) ;
#99349 = CARTESIAN_POINT ( 'NONE',  ( 19.05341960407611168, 5.049401038298154454, 43.95724293864769550 ) ) ;
#99351 = FACE_OUTER_BOUND ( 'NONE', #89002, .T. ) ;
#99350 = CARTESIAN_POINT ( 'NONE',  ( -5.049401038297874678, -19.05341960407617918, 69.79275706135233293 ) ) ;
#99352 = CARTESIAN_POINT ( 'NONE',  ( 15.72974639402176855, 15.80617190586768217, 71.87609039468568994 ) ) ;
#99353 = CARTESIAN_POINT ( 'NONE',  ( 12.06949235617739724, 12.14591786802326823, 46.87609039468568994 ) ) ;
#99354 = DIRECTION ( 'NONE',  ( 0.000000000000000000, 1.000000000000000000, -1.224646799147353207E-16 ) ) ;
#99355 = CARTESIAN_POINT ( 'NONE',  ( -21.52544592524343514, 5.823673210054127303, 36.04057627198102409 ) ) ;
#99356 = CARTESIAN_POINT ( 'NONE',  ( -14.29746914071037622, -8.314922557961029526, 24.16775706135235424 ) ) ;
#99357 = CARTESIAN_POINT ( 'NONE',  ( 18.09805431107249518, -5.499999999999974243, 98.51606229291887473 ) ) ;
#99358 = CARTESIAN_POINT ( 'NONE',  ( -21.96844466259092243, 8.667631922777363940, 171.6690673070886533 ) ) ;
#99359 = CARTESIAN_POINT ( 'NONE',  ( 19.05341960407611168, 5.049401038298154454, 38.95724293864767418 ) ) ;
#99360 = CARTESIAN_POINT ( 'NONE',  ( -9.564922557961040184, 16.46253265017147172, 57.91775706135233293 ) ) ;
#99361 = CARTESIAN_POINT ( 'NONE',  ( -19.02544592524342804, 5.153800228976336051, 51.04057627198103120 ) ) ;
#99362 = CARTESIAN_POINT ( 'NONE',  ( 5.823673210054444382, -21.52544592524334988, 65.20942372801901854 ) ) ;
#99363 = CARTESIAN_POINT ( 'NONE',  ( -18.67979575497193778, 10.72451020669871902, 113.3344237280190328 ) ) ;
#99364 = CARTESIAN_POINT ( 'NONE',  ( -16.55341960407611168, -4.379528057220339221, 26.45724293864768839 ) ) ;
#99365 = CARTESIAN_POINT ( 'NONE',  ( -5.153800228976328057, -19.02544592524343514, 32.29057627198102409 ) ) ;
#99366 = CARTESIAN_POINT ( 'NONE',  ( -5.153800228976328057, -19.02544592524343514, 87.29057627198103830 ) ) ;
#99367 = CARTESIAN_POINT ( 'NONE',  ( -21.53943276465977519, -0.05219959533937600094, 53.75109039468568994 ) ) ;
#99368 = CARTESIAN_POINT ( 'NONE',  ( -19.02544592524342804, 5.153800228976336051, 41.04057627198103120 ) ) ;
#99369 = CARTESIAN_POINT ( 'NONE',  ( 21.55341960407619695, -5.719274019375665929, 71.04275706135234714 ) ) ;
#99371 = CARTESIAN_POINT ( 'NONE',  ( 16.51473224551069308, 9.474510206698969483, 104.1655762719810241 ) ) ;
#99370 = CARTESIAN_POINT ( 'NONE',  ( -19.03943276465977164, -0.05219959533935918106, 98.75109039468567573 ) ) ;
#99372 = CARTESIAN_POINT ( 'NONE',  ( -19.05341960407611168, -5.049401038298163336, 26.45724293864769550 ) ) ;
#99373 = CARTESIAN_POINT ( 'NONE',  ( 21.52544592524344225, -5.823673210054117533, 108.5405762719810241 ) ) ;
#99374 = CARTESIAN_POINT ( 'NONE',  ( 19.02544592524334988, 5.153800228976608722, 36.45942372801900433 ) ) ;
#99375 = CARTESIAN_POINT ( 'NONE',  ( 12.06949235617757843, -12.14591786802309237, 108.1239096053143811 ) ) ;
#99376 = CARTESIAN_POINT ( 'NONE',  ( 19.03943276465977164, -0.05219959533909143690, 63.74890960531435979 ) ) ;
#99377 = CARTESIAN_POINT ( 'NONE',  ( -16.46253265017146816, -9.564922557961047289, 104.1677570613523329 ) ) ;
#99378 = CARTESIAN_POINT ( 'NONE',  ( -4.379528057220328563, 16.55341960407611168, 60.20724293864768839 ) ) ;
#99379 = CARTESIAN_POINT ( 'NONE',  ( 5.049401038297881783, 19.05341960407617563, 22.29275706135233648 ) ) ;
#99380 = CARTESIAN_POINT ( 'NONE',  ( -18.67979575497178146, -10.72451020669898902, 26.66557627198103475 ) ) ;
#99381 = CARTESIAN_POINT ( 'NONE',  ( -5.049401038297874678, -19.05341960407617918, 89.79275706135230450 ) ) ;
#99382 = CARTESIAN_POINT ( 'NONE',  ( -21.55341960407610458, -5.719274019375992779, 91.45724293864769550 ) ) ;
#99383 = CARTESIAN_POINT ( 'NONE',  ( -15.80617190586768217, 15.72974639402176855, 48.12609039468568284 ) ) ;
#99384 = CARTESIAN_POINT ( 'NONE',  ( 16.55341960407618274, -4.379528057220086978, 41.04275706135236135 ) ) ;
#99385 = CARTESIAN_POINT ( 'NONE',  ( 12.06949235617739724, 12.14591786802326823, 111.8760903946856615 ) ) ;
#99387 = CARTESIAN_POINT ( 'NONE',  ( 18.62759615963255655, 10.81492255796105972, 51.66775706135234714 ) ) ;
#99386 = CARTESIAN_POINT ( 'NONE',  ( 14.34966873604972726, -8.224510206698740333, 35.83442372801901143 ) ) ;
#99388 = CARTESIAN_POINT ( 'NONE',  ( 15.72974639402199770, -15.80617190586745480, 53.12390960531436690 ) ) ;
#99389 = CARTESIAN_POINT ( 'NONE',  ( 5.049401038298161559, -19.05341960407611168, 32.70724293864768129 ) ) ;
#99390 = CARTESIAN_POINT ( 'NONE',  ( -23.48529157249600985, 32.32473071737754111, -4.049999994537626158 ) ) ;
#99391 = CARTESIAN_POINT ( 'NONE',  ( -4.379528057220086978, -16.55341960407618274, 74.79275706135234714 ) ) ;
#99392 = CARTESIAN_POINT ( 'NONE',  ( 15.72974639402199770, -15.80617190586745480, 93.12390960531436690 ) ) ;
#99393 = CARTESIAN_POINT ( 'NONE',  ( 8.314922557960818139, 14.29746914071049879, 34.58224293864770260 ) ) ;
#99394 = CARTESIAN_POINT ( 'NONE',  ( -0.05219959533934338120, 16.53943276465976808, 62.50109039468568284 ) ) ;
#99395 = CARTESIAN_POINT ( 'NONE',  ( -5.049401038297874678, -19.05341960407617918, 99.79275706135234714 ) ) ;
#99396 = CARTESIAN_POINT ( 'NONE',  ( -10.81492255796078084, -18.62759615963271287, 102.0822429386476955 ) ) ;
#99397 = CARTESIAN_POINT ( 'NONE',  ( -12.06949235617756955, 12.14591786802309770, 25.62390960531435624 ) ) ;
#99398 = ORIENTED_EDGE ( 'NONE', *, *, #132358, .T. ) ;
#99399 = CARTESIAN_POINT ( 'NONE',  ( -16.55341960407617563, 4.379528057220093196, 78.54275706135236135 ) ) ;
#99400 = CARTESIAN_POINT ( 'NONE',  ( 21.75836449082842705, 9.620754668593672676, 170.8405250346329467 ) ) ;
#99401 = CARTESIAN_POINT ( 'NONE',  ( -21.52544592524343514, 5.823673210054127303, 76.04057627198102409 ) ) ;
#99402 = CARTESIAN_POINT ( 'NONE',  ( 12.06949235617739724, 12.14591786802326823, 111.8760903946856615 ) ) ;
#99403 = ORIENTED_EDGE ( 'NONE', *, *, #193896, .F. ) ;
#99404 = CARTESIAN_POINT ( 'NONE',  ( 19.25176906914651198, 5.499999999999741540, 88.49927264242276692 ) ) ;
#99405 = CARTESIAN_POINT ( 'NONE',  ( 15.72974639402199770, -15.80617190586745480, 83.12390960531436690 ) ) ;
#99406 = CARTESIAN_POINT ( 'NONE',  ( 10.81492255796078972, 18.62759615963270932, 104.5822429386477097 ) ) ;
#99407 = CARTESIAN_POINT ( 'NONE',  ( -8.314922557960811034, -14.29746914071050412, 42.08224293864769550 ) ) ;
#99408 = CARTESIAN_POINT ( 'NONE',  ( -16.52544592524335698, -4.483927247898792601, 38.95942372801901854 ) ) ;
#99409 = CIRCLE ( 'NONE', #5734, 2.000000000000000000 ) ;
#99410 = CARTESIAN_POINT ( 'NONE',  ( -13.97604488694527625, -13.89961937509977652, 41.87390960531435979 ) ) ;
#99411 = CARTESIAN_POINT ( 'NONE',  ( -13.89961937509977652, 13.97604488694528158, 60.62390960531436690 ) ) ;
#99412 = ORIENTED_EDGE ( 'NONE', *, *, #141141, .T. ) ;
#99413 = CARTESIAN_POINT ( 'NONE',  ( -0.05219959533907301413, -21.53943276465977519, 27.49890960531435269 ) ) ;
#99414 = CARTESIAN_POINT ( 'NONE',  ( -5.049401038298153566, 19.05341960407611168, 115.2072429386477097 ) ) ;
#99415 = CARTESIAN_POINT ( 'NONE',  ( -19.02544592524334988, -5.153800228976617603, 103.9594237280190043 ) ) ;
#99416 = CARTESIAN_POINT ( 'NONE',  ( -0.05219959533936034679, 19.03943276465977164, 47.50109039468566863 ) ) ;
#99417 = CARTESIAN_POINT ( 'NONE',  ( 18.62759615963271287, -10.81492255796078972, 83.33224293864769550 ) ) ;
#99418 = CARTESIAN_POINT ( 'NONE',  ( -4.483927247898782831, 16.52544592524335698, 107.7094237280190328 ) ) ;
#99419 = CARTESIAN_POINT ( 'NONE',  ( -21.55341960407610458, -5.719274019375992779, 41.45724293864769550 ) ) ;
#99421 = CARTESIAN_POINT ( 'NONE',  ( 13.97604488694548053, -13.89961937509957401, 100.6260903946856615 ) ) ;
#99420 = CARTESIAN_POINT ( 'NONE',  ( -21.53943276465977519, 0.05219959533907696930, 76.24890960531435269 ) ) ;
#99422 = EDGE_CURVE ( 'NONE', #180473, #175994, #154978, .T. ) ;
#99423 = CARTESIAN_POINT ( 'NONE',  ( 0.05219959533909260263, 19.03943276465977164, 99.99890960531436690 ) ) ;
#99424 = CARTESIAN_POINT ( 'NONE',  ( -18.67979575497193778, 10.72451020669871902, 73.33442372801901854 ) ) ;
#99425 = CARTESIAN_POINT ( 'NONE',  ( -13.89961937509977652, 13.97604488694528158, 70.62390960531432427 ) ) ;
#99426 = DIRECTION ( 'NONE',  ( 1.000000000000000000, -0.000000000000000000, -0.000000000000000000 ) ) ;
#99427 = CARTESIAN_POINT ( 'NONE',  ( -9.564922557960796823, -16.46253265017161027, 77.08224293864769550 ) ) ;
#99428 = CARTESIAN_POINT ( 'NONE',  ( -16.52544592524342804, 4.483927247898546575, 86.04057627198102409 ) ) ;
#99429 = ORIENTED_EDGE ( 'NONE', *, *, #26797, .T. ) ;
#99430 = CARTESIAN_POINT ( 'NONE',  ( 19.02544592524334988, 5.153800228976608722, 106.4594237280190185 ) ) ;
#99431 = CARTESIAN_POINT ( 'NONE',  ( 17.05587630539788080, -6.762274262135693270, 83.24180309037316761 ) ) ;
#99432 = CARTESIAN_POINT ( 'NONE',  ( -16.51473224551069308, -9.474510206698971260, 71.66557627198102409 ) ) ;
#99433 = AXIS2_PLACEMENT_3D ( 'NONE', #188898, #63549, #187906 ) ;
#99435 = CARTESIAN_POINT ( 'NONE',  ( -19.05341960407611168, -5.049401038298163336, 101.4572429386476955 ) ) ;
#99434 = CARTESIAN_POINT ( 'NONE',  ( -15.80617190586768217, 15.72974639402176855, 83.12609039468568994 ) ) ;
#99437 = EDGE_CURVE ( 'NONE', #191847, #89709, #182172, .T. ) ;
#99436 = CARTESIAN_POINT ( 'NONE',  ( -8.314922557961024197, 14.29746914071037800, 72.91775706135234714 ) ) ;
#99438 = CARTESIAN_POINT ( 'NONE',  ( -17.44279575226822843, -5.990770900252439191, 74.16442432485679603 ) ) ;
#99439 = CARTESIAN_POINT ( 'NONE',  ( -16.51473224551082808, 9.474510206698731452, 53.33442372801900433 ) ) ;
#99440 = CARTESIAN_POINT ( 'NONE',  ( -15.72974639402176322, -15.80617190586768395, 109.3760903946857042 ) ) ;
#99441 = CARTESIAN_POINT ( 'NONE',  ( 24.99873734152946270, 24.49873734152885874, 5.353553390593270400 ) ) ;
#99442 = CARTESIAN_POINT ( 'NONE',  ( 6.791538853603062975, 3.181980515339470905, 8.889087296526001936 ) ) ;
#99443 = CARTESIAN_POINT ( 'NONE',  ( -5.950531402560715689E-15, 38.81732327939063509, -1.624999997268813612 ) ) ;
#99444 = CARTESIAN_POINT ( 'NONE',  ( -16.53943276465976808, -0.05219959533934237506, 113.7510903946856757 ) ) ;
#99445 = CARTESIAN_POINT ( 'NONE',  ( -34.77754859679605204, -0.9869066695169159686, 52.45091671276826872 ) ) ;
#99446 = CARTESIAN_POINT ( 'NONE',  ( 4.379528057220092307, 16.55341960407617563, 97.29275706135234714 ) ) ;
#99447 = DIRECTION ( 'NONE',  ( 0.000000000000000000, 0.000000000000000000, 1.000000000000000000 ) ) ;
#99448 = CARTESIAN_POINT ( 'NONE',  ( -4.483927247898782831, 16.52544592524335698, 62.70942372801902565 ) ) ;
#99449 = CARTESIAN_POINT ( 'NONE',  ( -0.05219959533937732626, 21.53943276465977519, 77.50109039468567573 ) ) ;
#99450 = CARTESIAN_POINT ( 'NONE',  ( 0.05219959533936267826, -19.03943276465977164, 95.00109039468567573 ) ) ;
#99451 = CARTESIAN_POINT ( 'NONE',  ( -19.05341960407617563, 5.049401038297882671, 38.54275706135233293 ) ) ;
#99452 = CARTESIAN_POINT ( 'NONE',  ( 13.89961937509977652, -13.97604488694527269, 73.12390960531436690 ) ) ;
#99453 = CARTESIAN_POINT ( 'NONE',  ( 19.03943276465977164, -0.05219959533909143690, 53.74890960531436690 ) ) ;
#99454 = CARTESIAN_POINT ( 'NONE',  ( 13.89961937509978007, -13.97604488694527269, 88.12390960531436690 ) ) ;
#99455 = CARTESIAN_POINT ( 'NONE',  ( 21.53943276465977519, -0.05219959533907433946, 93.74890960531436690 ) ) ;
#99456 = CARTESIAN_POINT ( 'NONE',  ( -15.80617190586745835, -15.72974639402198527, 46.87390960531435979 ) ) ;
#99457 = CARTESIAN_POINT ( 'NONE',  ( -16.51473224551069308, -9.474510206698971260, 31.66557627198102054 ) ) ;
#99458 = CARTESIAN_POINT ( 'NONE',  ( -8.224510206698735004, -14.34966873604973081, 64.58442372801900433 ) ) ;
#99459 = VERTEX_POINT ( 'NONE', #185139 ) ;
#99460 = ADVANCED_FACE ( 'NONE', ( #107289 ), #1099, .F. ) ;
#99461 = CARTESIAN_POINT ( 'NONE',  ( -15.72974639402176322, -15.80617190586768395, 44.37609039468567573 ) ) ;
#99463 = CARTESIAN_POINT ( 'NONE',  ( 3.766062262543149401E-15, -39.95556452105413570, -1.499999999999999778 ) ) ;
#99462 = CARTESIAN_POINT ( 'NONE',  ( 16.52544592524342804, -4.483927247898539470, 63.54057627198103830 ) ) ;
#99464 = CARTESIAN_POINT ( 'NONE',  ( -12.06949235617739369, -12.14591786802326823, 44.37609039468567573 ) ) ;
#99465 = CARTESIAN_POINT ( 'NONE',  ( -16.55341960407611168, -4.379528057220339221, 101.4572429386476955 ) ) ;
#99466 = CARTESIAN_POINT ( 'NONE',  ( 16.46253265017146816, 9.564922557961045513, 46.66775706135233293 ) ) ;
#99467 = CARTESIAN_POINT ( 'NONE',  ( 14.29746914071049879, -8.314922557960816363, 63.33224293864770260 ) ) ;
#99468 = CARTESIAN_POINT ( 'NONE',  ( 5.719274019375673035, 21.55341960407619339, 32.29275706135235424 ) ) ;
#99470 = CARTESIAN_POINT ( 'NONE',  ( -10.81492255796078084, -18.62759615963271287, 97.08224293864770971 ) ) ;
#99469 = CARTESIAN_POINT ( 'NONE',  ( -37.66961640367473052, 5.000000000000023981, -18.00000000000000355 ) ) ;
#99471 = CARTESIAN_POINT ( 'NONE',  ( 19.05341960407611168, 5.049401038298154454, 98.95724293864766707 ) ) ;
#99472 = CARTESIAN_POINT ( 'NONE',  ( -16.53943276465976808, 0.05219959533911058130, 76.24890960531435269 ) ) ;
#99473 = CARTESIAN_POINT ( 'NONE',  ( -9.564922557960796823, -16.46253265017161027, 112.0822429386476955 ) ) ;
#99474 = CARTESIAN_POINT ( 'NONE',  ( -29.86685920354755552, 21.69954338932564397, -4.824999997268814234 ) ) ;
#99475 = CARTESIAN_POINT ( 'NONE',  ( -9.564922557961040184, 16.46253265017147172, 87.91775706135233293 ) ) ;
#99476 = CARTESIAN_POINT ( 'NONE',  ( -18.67979575497193778, 10.72451020669871902, 28.33442372801902209 ) ) ;
#99477 = CARTESIAN_POINT ( 'NONE',  ( -0.05219959533909027116, -19.03943276465977164, 67.49890960531436690 ) ) ;
#99478 = CARTESIAN_POINT ( 'NONE',  ( 19.05341960407617918, -5.049401038297876454, 56.04275706135234714 ) ) ;
#99479 = CARTESIAN_POINT ( 'NONE',  ( 13.97604488694527802, 13.89961937509977652, 34.37390960531436690 ) ) ;
#99480 = CARTESIAN_POINT ( 'NONE',  ( -5.719274019375665041, -21.55341960407619695, 59.79275706135234714 ) ) ;
#99481 = CARTESIAN_POINT ( 'NONE',  ( -11.30153831258470731, -180.0000000000000000, 0.000000000000000000 ) ) ;
#99482 = CARTESIAN_POINT ( 'NONE',  ( 14.29746914071049879, -8.314922557960816363, 53.33224293864769550 ) ) ;
#99483 = CARTESIAN_POINT ( 'NONE',  ( -5.153800228976328057, -19.02544592524343514, 67.29057627198102409 ) ) ;
#99484 = CARTESIAN_POINT ( 'NONE',  ( 15.72974639402199770, -15.80617190586745480, 88.12390960531436690 ) ) ;
#99485 = CARTESIAN_POINT ( 'NONE',  ( -5.153800228976328057, -19.02544592524343514, 52.29057627198100988 ) ) ;
#99486 = ORIENTED_EDGE ( 'NONE', *, *, #155971, .T. ) ;
#99487 = CARTESIAN_POINT ( 'NONE',  ( 10.72451020669898902, -18.67979575497178502, 77.91557627198102409 ) ) ;
#99488 = CARTESIAN_POINT ( 'NONE',  ( 5.823673210054444382, -21.52544592524334988, 95.20942372801903275 ) ) ;
#99491 = CARTESIAN_POINT ( 'NONE',  ( 12.14591786802309770, 12.06949235617756955, 99.37390960531436690 ) ) ;
#99490 = CARTESIAN_POINT ( 'NONE',  ( -16.55341960407617563, 4.379528057220093196, 93.54275706135234714 ) ) ;
#99489 = CARTESIAN_POINT ( 'NONE',  ( -5.153800228976328057, -19.02544592524343514, 27.29057627198103120 ) ) ;
#99492 = CARTESIAN_POINT ( 'NONE',  ( -19.02544592524334988, -5.153800228976617603, 88.95942372801897591 ) ) ;
#99493 = ORIENTED_EDGE ( 'NONE', *, *, #118963, .F. ) ;
#99494 = CARTESIAN_POINT ( 'NONE',  ( -21.53943276465977519, -0.05219959533937600094, 23.75109039468567929 ) ) ;
#99495 = CARTESIAN_POINT ( 'NONE',  ( 16.51473224551083163, -9.474510206698727899, 50.83442372801899722 ) ) ;
#99496 = CARTESIAN_POINT ( 'NONE',  ( -0.05219959533934338120, 16.53943276465976808, 97.50109039468567573 ) ) ;
#99497 = CARTESIAN_POINT ( 'NONE',  ( 16.46253265017146816, 9.564922557961045513, 26.66775706135234003 ) ) ;
#99498 = CARTESIAN_POINT ( 'NONE',  ( 13.89961937509977652, -13.97604488694527269, 98.12390960531433848 ) ) ;
#99499 = CARTESIAN_POINT ( 'NONE',  ( -15.72974639402197994, 15.80617190586746368, 65.62390960531436690 ) ) ;
#99500 = CARTESIAN_POINT ( 'NONE',  ( -24.99734946672227665, 12.60193342193095667, 166.0696721667195845 ) ) ;
#99501 = CARTESIAN_POINT ( 'NONE',  ( -19.03943276465977164, 0.05219959533909376836, 26.24890960531435624 ) ) ;
#99502 = CARTESIAN_POINT ( 'NONE',  ( 18.62759615963255655, 10.81492255796105972, 106.6677570613523756 ) ) ;
#99503 = CARTESIAN_POINT ( 'NONE',  ( -4.379528057220086978, -16.55341960407618274, 69.79275706135234714 ) ) ;
#99504 = CARTESIAN_POINT ( 'NONE',  ( -21.55341960407619339, 5.719274019375674811, 23.54275706135235424 ) ) ;
#99505 = CARTESIAN_POINT ( 'NONE',  ( 12.06949235617739724, 12.14591786802326823, 46.87609039468568994 ) ) ;
#99506 = CARTESIAN_POINT ( 'NONE',  ( 16.46253265017160672, -9.564922557960803928, 103.3322429386476955 ) ) ;
#99507 = CARTESIAN_POINT ( 'NONE',  ( -0.05219959533909027116, -19.03943276465977164, 42.49890960531435269 ) ) ;
#99508 = CARTESIAN_POINT ( 'NONE',  ( -19.05341960407611168, -5.049401038298163336, 66.45724293864769550 ) ) ;
#99509 = CARTESIAN_POINT ( 'NONE',  ( -0.05219959533934338120, 16.53943276465976808, 42.50109039468567573 ) ) ;
#99510 = CARTESIAN_POINT ( 'NONE',  ( -16.52544592524342804, 4.483927247898546575, 91.04057627198103830 ) ) ;
#99511 = CARTESIAN_POINT ( 'NONE',  ( -4.379528057220086978, -16.55341960407618274, 104.7927570613523898 ) ) ;
#99512 = CARTESIAN_POINT ( 'NONE',  ( -9.474510206698964154, 16.51473224551069663, 50.41557627198102409 ) ) ;
#99515 = CARTESIAN_POINT ( 'NONE',  ( 16.46253265017160672, -9.564922557960803928, 63.33224293864769550 ) ) ;
#99514 = CARTESIAN_POINT ( 'NONE',  ( 16.46253265017160672, -9.564922557960803928, 83.33224293864768129 ) ) ;
#99513 = CARTESIAN_POINT ( 'NONE',  ( 0.05219959533937995610, -21.53943276465977519, 55.00109039468568284 ) ) ;
#99516 = CARTESIAN_POINT ( 'NONE',  ( 9.564922557960805705, 16.46253265017160317, 89.58224293864769550 ) ) ;
#99517 = CARTESIAN_POINT ( 'NONE',  ( 16.52544592524342804, -4.483927247898539470, 48.54057627198103120 ) ) ;
#99518 = CARTESIAN_POINT ( 'NONE',  ( 12.14591786802327356, -12.06949235617739191, 95.62609039468568994 ) ) ;
#99519 = CARTESIAN_POINT ( 'NONE',  ( 8.314922557960818139, 14.29746914071049879, 24.58224293864768839 ) ) ;
#99520 = ORIENTED_EDGE ( 'NONE', *, *, #189654, .F. ) ;
#99521 = CARTESIAN_POINT ( 'NONE',  ( -5.049401038297874678, -19.05341960407617918, 44.79275706135232582 ) ) ;
#99522 = CARTESIAN_POINT ( 'NONE',  ( 9.474510206698971260, -16.51473224551069308, 112.9155762719810383 ) ) ;
#99523 = CARTESIAN_POINT ( 'NONE',  ( 9.474510206698971260, -16.51473224551069308, 57.91557627198103120 ) ) ;
#99524 = CARTESIAN_POINT ( 'NONE',  ( -16.51473224551082808, 9.474510206698731452, 33.33442372801899722 ) ) ;
#99525 = CARTESIAN_POINT ( 'NONE',  ( -11.40812507854755609, 35.11059874428196537, -7.024999997268813523 ) ) ;
#99526 = LINE ( 'NONE', #95544, #37792 ) ;
#99528 = CARTESIAN_POINT ( 'NONE',  ( 12.14591786802327356, -12.06949235617739191, 70.62609039468567573 ) ) ;
#99527 = CARTESIAN_POINT ( 'NONE',  ( -5.049401038297874678, -19.05341960407617918, 79.79275706135233293 ) ) ;
#99529 = CARTESIAN_POINT ( 'NONE',  ( 16.38665767535053064, 7.295008042176115204, 92.23599135785453029 ) ) ;
#99530 = CARTESIAN_POINT ( 'NONE',  ( -9.474510206698964154, 16.51473224551069663, 85.41557627198102409 ) ) ;
#99531 = CARTESIAN_POINT ( 'NONE',  ( -21.55341960407619339, 5.719274019375674811, 33.54275706135234714 ) ) ;
#99532 = CARTESIAN_POINT ( 'NONE',  ( 16.51473224551083163, -9.474510206698727899, 70.83442372801900433 ) ) ;
#99534 = CARTESIAN_POINT ( 'NONE',  ( -16.46253265017160317, 9.564922557960807481, 30.83224293864769550 ) ) ;
#99533 = CARTESIAN_POINT ( 'NONE',  ( 17.48853670773247870, 5.747243402303060300, 88.83328700250011423 ) ) ;
#99535 = CARTESIAN_POINT ( 'NONE',  ( 19.05341960407611168, 5.049401038298154454, 88.95724293864769550 ) ) ;
#99537 = CARTESIAN_POINT ( 'NONE',  ( 16.51473224551069308, 9.474510206698969483, 39.16557627198103120 ) ) ;
#99536 = CARTESIAN_POINT ( 'NONE',  ( -4.483927247898539470, -16.52544592524342804, 47.29057627198103120 ) ) ;
#99538 = CARTESIAN_POINT ( 'NONE',  ( 19.05341960407617918, -5.049401038297876454, 46.04275706135233293 ) ) ;
#99539 = ORIENTED_EDGE ( 'NONE', *, *, #47298, .F. ) ;
#99540 = CARTESIAN_POINT ( 'NONE',  ( -8.314922557960811034, -14.29746914071050412, 82.08224293864768129 ) ) ;
#99541 = CARTESIAN_POINT ( 'NONE',  ( -9.474510206698720793, -16.51473224551083518, 34.58442372801899722 ) ) ;
#99542 = CARTESIAN_POINT ( 'NONE',  ( -9.564922557960796823, -16.46253265017161027, 62.08224293864769550 ) ) ;
#99543 = CARTESIAN_POINT ( 'NONE',  ( -21.53943276465977519, 0.05219959533907696930, 61.24890960531435979 ) ) ;
#99545 = CARTESIAN_POINT ( 'NONE',  ( -0.05219959533936034679, 19.03943276465977164, 22.50109039468566152 ) ) ;
#99544 = CARTESIAN_POINT ( 'NONE',  ( 12.14591786802309770, 12.06949235617756955, 49.37390960531436690 ) ) ;
#99546 = CARTESIAN_POINT ( 'NONE',  ( -0.05219959533909027116, -19.03943276465977164, 112.4989096053143669 ) ) ;
#99547 = CARTESIAN_POINT ( 'NONE',  ( -0.05219959533907301413, -21.53943276465977519, 22.49890960531436335 ) ) ;
#99548 = CARTESIAN_POINT ( 'NONE',  ( -5.049401038298153566, 19.05341960407611168, 55.20724293864769550 ) ) ;
#99549 = CARTESIAN_POINT ( 'NONE',  ( 9.474510206698971260, -16.51473224551069308, 22.91557627198102765 ) ) ;
#99550 = CARTESIAN_POINT ( 'NONE',  ( -8.224510206698948167, 14.34966873604960824, 85.41557627198102409 ) ) ;
#99551 = CARTESIAN_POINT ( 'NONE',  ( 18.62759615963271287, -10.81492255796078972, 103.3322429386476955 ) ) ;
#99552 = CARTESIAN_POINT ( 'NONE',  ( -9.564922557960796823, -16.46253265017161027, 102.0822429386477097 ) ) ;
#99553 = CARTESIAN_POINT ( 'NONE',  ( 21.52544592524344225, -5.823673210054117533, 108.5405762719810241 ) ) ;
#99554 = CARTESIAN_POINT ( 'NONE',  ( 5.049401038298161559, -19.05341960407611168, 107.7072429386476955 ) ) ;
#99555 = CARTESIAN_POINT ( 'NONE',  ( -0.05219959533909027116, -19.03943276465977164, 22.49890960531436690 ) ) ;
#99556 = CARTESIAN_POINT ( 'NONE',  ( -21.55341960407619339, 5.719274019375674811, 83.54275706135234714 ) ) ;
#99557 = CARTESIAN_POINT ( 'NONE',  ( -0.05219959533907301413, -21.53943276465977519, 97.49890960531436690 ) ) ;
#99558 = CARTESIAN_POINT ( 'NONE',  ( 35.00000000000000000, -3.181980515339468241, 1.110912703473986074 ) ) ;
#99559 = CARTESIAN_POINT ( 'NONE',  ( 18.87580814761076908, -5.500000000000053291, 78.37172394265758157 ) ) ;
#99560 = CARTESIAN_POINT ( 'NONE',  ( -30.74264578624800492, -22.33583958711396278, -1.800000000000000044 ) ) ;
#99561 = CARTESIAN_POINT ( 'NONE',  ( 8.314922557961029526, -14.29746914071037800, 40.41775706135234714 ) ) ;
#99562 = EDGE_CURVE ( 'NONE', #31966, #122086, #62775, .T. ) ;
#99563 = CARTESIAN_POINT ( 'NONE',  ( 4.483927247898545687, 16.52544592524342804, 109.7905762719810383 ) ) ;
#99564 = CYLINDRICAL_SURFACE ( 'NONE', #148332, 6.100000000000006750 ) ;
#99565 = CARTESIAN_POINT ( 'NONE',  ( 19.05341960407611168, 5.049401038298154454, 53.95724293864770260 ) ) ;
#99566 = CARTESIAN_POINT ( 'NONE',  ( -8.224510206698948167, 14.34966873604960824, 90.41557627198103830 ) ) ;
#99567 = CARTESIAN_POINT ( 'NONE',  ( 10.72451020669898902, -18.67979575497178502, 32.91557627198102409 ) ) ;
#99568 = CARTESIAN_POINT ( 'NONE',  ( -12.14591786802309592, -12.06949235617757132, 61.87390960531436690 ) ) ;
#99569 = CARTESIAN_POINT ( 'NONE',  ( 19.03943276465977164, 0.05219959533936151252, 111.2510903946856757 ) ) ;
#99570 = CARTESIAN_POINT ( 'NONE',  ( -0.05219959533937732626, 21.53943276465977519, 77.50109039468567573 ) ) ;
#99571 = CARTESIAN_POINT ( 'NONE',  ( 17.49999999999999645, -5.624438216177592764, 78.31670344914645909 ) ) ;
#99572 = CARTESIAN_POINT ( 'NONE',  ( 8.314922557961029526, -14.29746914071037800, 100.4177570613523471 ) ) ;
#99573 = CARTESIAN_POINT ( 'NONE',  ( 5.153800228976335163, 19.02544592524342804, 39.79057627198100988 ) ) ;
#99574 = CARTESIAN_POINT ( 'NONE',  ( 13.89961937509977652, -13.97604488694527269, 88.12390960531438111 ) ) ;
#99575 = CARTESIAN_POINT ( 'NONE',  ( 21.52544592524344225, -5.823673210054117533, 93.54057627198103830 ) ) ;
#99576 = CARTESIAN_POINT ( 'NONE',  ( 16.55341960407618274, -4.379528057220086978, 26.04275706135235779 ) ) ;
#99578 = CARTESIAN_POINT ( 'NONE',  ( 15.72974639402176855, 15.80617190586768217, 71.87609039468568994 ) ) ;
#99577 = CARTESIAN_POINT ( 'NONE',  ( 12.14591786802309770, 12.06949235617756955, 69.37390960531436690 ) ) ;
#99579 = VECTOR ( 'NONE', #132190, 1000.000000000000000 ) ;
#99580 = CARTESIAN_POINT ( 'NONE',  ( -16.52544592524335698, -4.483927247898792601, 93.95942372801903275 ) ) ;
#99581 = CARTESIAN_POINT ( 'NONE',  ( 17.50000000000000355, -5.624438216177558125, 48.31670344914645199 ) ) ;
#99582 = CARTESIAN_POINT ( 'NONE',  ( -19.39720447994795549, -5.499999999999980460, 64.66317477297177163 ) ) ;
#99583 = CARTESIAN_POINT ( 'NONE',  ( 14.29746914071049879, -8.314922557960816363, 28.33224293864769550 ) ) ;
#99584 = CARTESIAN_POINT ( 'NONE',  ( -0.05219959533934338120, 16.53943276465976808, 77.50109039468567573 ) ) ;
#99585 = CARTESIAN_POINT ( 'NONE',  ( -13.89961937509977652, 13.97604488694528158, 80.62390960531436690 ) ) ;
#99586 = CARTESIAN_POINT ( 'NONE',  ( -19.05341960407611168, -5.049401038298163336, 91.45724293864766707 ) ) ;
#99587 = CARTESIAN_POINT ( 'NONE',  ( 21.52544592524334988, 5.823673210054432836, 91.45942372801901854 ) ) ;
#99588 = EDGE_CURVE ( 'NONE', #147783, #85848, #55873, .T. ) ;
#99589 = CARTESIAN_POINT ( 'NONE',  ( 4.483927247898790824, -16.52544592524335698, 85.20942372801901854 ) ) ;
#99590 = CARTESIAN_POINT ( 'NONE',  ( -14.29746914071049879, 8.314922557960819915, 65.83224293864769550 ) ) ;
#99591 = CARTESIAN_POINT ( 'NONE',  ( -13.89961937509977652, 13.97604488694528158, 70.62390960531432427 ) ) ;
#99592 = ORIENTED_EDGE ( 'NONE', *, *, #2914, .F. ) ;
#99593 = CARTESIAN_POINT ( 'NONE',  ( 0.05219959533934541429, -16.53943276465976808, 20.00109039468568639 ) ) ;
#99594 = CARTESIAN_POINT ( 'NONE',  ( 4.483927247898545687, 16.52544592524342804, 104.7905762719810241 ) ) ;
#99595 = CARTESIAN_POINT ( 'NONE',  ( -5.153800228976328057, -19.02544592524343514, 77.29057627198099567 ) ) ;
#99597 = CARTESIAN_POINT ( 'NONE',  ( 29.86685920354754487, 21.69954338932564752, -7.424999997268813878 ) ) ;
#99596 = CARTESIAN_POINT ( 'NONE',  ( -9.474510206698720793, -16.51473224551083518, 109.5844237280190043 ) ) ;
#99598 = CARTESIAN_POINT ( 'NONE',  ( 13.89961937509957401, 13.97604488694547697, 26.87609039468566507 ) ) ;
#99599 = CARTESIAN_POINT ( 'NONE',  ( -4.379528057220086978, -16.55341960407618274, 84.79275706135234714 ) ) ;
#99600 = CARTESIAN_POINT ( 'NONE',  ( 9.474510206698729675, 16.51473224551082808, 92.08442372801900433 ) ) ;
#99601 = CARTESIAN_POINT ( 'NONE',  ( -16.55341960407611168, -4.379528057220339221, 111.4572429386476813 ) ) ;
#99602 = CARTESIAN_POINT ( 'NONE',  ( -4.483927247898782831, 16.52544592524335698, 62.70942372801902565 ) ) ;
#99603 = CARTESIAN_POINT ( 'NONE',  ( -0.05219959533934338120, 16.53943276465976808, 52.50109039468567573 ) ) ;
#99604 = CARTESIAN_POINT ( 'NONE',  ( -13.97604488694527625, -13.89961937509977652, 21.87390960531435979 ) ) ;
#99605 = CARTESIAN_POINT ( 'NONE',  ( 13.97604488694548053, -13.89961937509957401, 55.62609039468566863 ) ) ;
#99606 = CARTESIAN_POINT ( 'NONE',  ( 21.52544592524334988, 5.823673210054432836, 91.45942372801901854 ) ) ;
#99607 = CARTESIAN_POINT ( 'NONE',  ( -16.46253265017160317, 9.564922557960807481, 40.83224293864769550 ) ) ;
#99608 = CARTESIAN_POINT ( 'NONE',  ( -19.03943276465977164, 0.05219959533909376836, 76.24890960531435269 ) ) ;
#99609 = CARTESIAN_POINT ( 'NONE',  ( 12.14591786802309770, 12.06949235617756955, 74.37390960531436690 ) ) ;
#99610 = CARTESIAN_POINT ( 'NONE',  ( 18.67979575497194134, -10.72451020669871369, 85.83442372801901854 ) ) ;
#99611 = CARTESIAN_POINT ( 'NONE',  ( 9.564922557961047289, -16.46253265017146816, 55.41775706135234003 ) ) ;
#99612 = CARTESIAN_POINT ( 'NONE',  ( -0.05219959533936034679, 19.03943276465977164, 47.50109039468566863 ) ) ;
#99613 = CARTESIAN_POINT ( 'NONE',  ( -21.55341960407610458, -5.719274019375992779, 31.45724293864769550 ) ) ;
#99614 = CARTESIAN_POINT ( 'NONE',  ( 18.62759615963255655, 10.81492255796105972, 96.66775706135234714 ) ) ;
#99615 = CARTESIAN_POINT ( 'NONE',  ( -5.049401038298153566, 19.05341960407611168, 75.20724293864769550 ) ) ;
#99616 = CARTESIAN_POINT ( 'NONE',  ( -5.719274019375665041, -21.55341960407619695, 109.7927570613523613 ) ) ;
#99617 = CARTESIAN_POINT ( 'NONE',  ( 18.62759615963271287, -10.81492255796078972, 48.33224293864770260 ) ) ;
#99618 = CARTESIAN_POINT ( 'NONE',  ( 0.05219959533909260263, 19.03943276465977164, 94.99890960531436690 ) ) ;
#99619 = CARTESIAN_POINT ( 'NONE',  ( -0.05219959533936034679, 19.03943276465977164, 77.50109039468566152 ) ) ;
#99620 = CARTESIAN_POINT ( 'NONE',  ( -16.51473224551069308, -9.474510206698971260, 101.6655762719810241 ) ) ;
#99621 = CARTESIAN_POINT ( 'NONE',  ( -9.474510206698720793, -16.51473224551083518, 99.58442372801900433 ) ) ;
#99622 = CARTESIAN_POINT ( 'NONE',  ( -16.53943276465976808, -0.05219959533934237506, 38.75109039468567573 ) ) ;
#99623 = CARTESIAN_POINT ( 'NONE',  ( 16.55341960407611168, 4.379528057220329451, 103.9572429386476813 ) ) ;
#99624 = CARTESIAN_POINT ( 'NONE',  ( 9.474510206698971260, -16.51473224551069308, 87.91557627198102409 ) ) ;
#99625 = CARTESIAN_POINT ( 'NONE',  ( -18.62759615963270932, 10.81492255796079327, 65.83224293864769550 ) ) ;
#99626 = CARTESIAN_POINT ( 'NONE',  ( -8.314922557961024197, 14.29746914071037800, 37.91775706135235424 ) ) ;
#99627 = CARTESIAN_POINT ( 'NONE',  ( -5.719274019375665041, -21.55341960407619695, 34.79275706135235424 ) ) ;
#99628 = CARTESIAN_POINT ( 'NONE',  ( -21.55341960407619339, 5.719274019375674811, 78.54275706135236135 ) ) ;
#99629 = CARTESIAN_POINT ( 'NONE',  ( 8.224510206698742110, 14.34966873604972548, 77.08442372801901854 ) ) ;
#99630 = CARTESIAN_POINT ( 'NONE',  ( -5.049401038298153566, 19.05341960407611168, 70.20724293864769550 ) ) ;
#99631 = CARTESIAN_POINT ( 'NONE',  ( -12.14591786802309592, -12.06949235617757132, 76.87390960531439532 ) ) ;
#99632 = CARTESIAN_POINT ( 'NONE',  ( -0.05219959533910754901, -16.53943276465976808, 27.49890960531435269 ) ) ;
#99633 = CARTESIAN_POINT ( 'NONE',  ( 19.05341960407617918, -5.049401038297876454, 61.04275706135232582 ) ) ;
#99634 = CARTESIAN_POINT ( 'NONE',  ( 18.62759615963255655, 10.81492255796105972, 26.66775706135235424 ) ) ;
#99635 = CARTESIAN_POINT ( 'NONE',  ( -0.05219959533910754901, -16.53943276465976808, 72.49890960531435269 ) ) ;
#99636 = CARTESIAN_POINT ( 'NONE',  ( 19.02544592524343514, -5.153800228976328945, 113.5405762719810241 ) ) ;
#99637 = CARTESIAN_POINT ( 'NONE',  ( 16.52544592524335698, 4.483927247898782831, 101.4594237280190185 ) ) ;
#99638 = CARTESIAN_POINT ( 'NONE',  ( -5.719274019375665041, -21.55341960407619695, 74.79275706135234714 ) ) ;
#99639 = CARTESIAN_POINT ( 'NONE',  ( 4.483927247898790824, -16.52544592524335698, 50.20942372801901854 ) ) ;
#99640 = CARTESIAN_POINT ( 'NONE',  ( 21.53943276465977519, 0.05219959533937863772, 36.25109039468567573 ) ) ;
#99641 = EDGE_LOOP ( 'NONE', ( #62638, #180612, #163869, #140696 ) ) ;
#99642 = CARTESIAN_POINT ( 'NONE',  ( 10.81492255796078972, 18.62759615963270932, 114.5822429386477097 ) ) ;
#99643 = CARTESIAN_POINT ( 'NONE',  ( 12.14591786802309770, 12.06949235617756955, 89.37390960531435269 ) ) ;
#99644 = DIRECTION ( 'NONE',  ( -1.000000000000000000, 0.000000000000000000, 0.000000000000000000 ) ) ;
#99645 = CARTESIAN_POINT ( 'NONE',  ( -12.14591786802309592, -12.06949235617757132, 46.87390960531435979 ) ) ;
#99646 = CARTESIAN_POINT ( 'NONE',  ( -19.03943276465977164, 0.05219959533909376836, 26.24890960531435624 ) ) ;
#99647 = CARTESIAN_POINT ( 'NONE',  ( 0.05219959533907565091, 21.53943276465977519, 44.99890960531435979 ) ) ;
#99648 = CARTESIAN_POINT ( 'NONE',  ( 0.05219959533910956823, 16.53943276465976808, 74.99890960531435269 ) ) ;
#99649 = CARTESIAN_POINT ( 'NONE',  ( 21.53943276465977519, -0.05219959533907433946, 78.74890960531436690 ) ) ;
#99650 = CARTESIAN_POINT ( 'NONE',  ( 5.049401038298161559, -19.05341960407611168, 92.70724293864769550 ) ) ;
#99652 = CARTESIAN_POINT ( 'NONE',  ( 9.564922557961047289, -16.46253265017146816, 95.41775706135233293 ) ) ;
#99651 = CARTESIAN_POINT ( 'NONE',  ( 5.153800228976335163, 19.02544592524342804, 44.79057627198103830 ) ) ;
#99653 = CARTESIAN_POINT ( 'NONE',  ( 5.823673210054125526, 21.52544592524343514, 29.79057627198102409 ) ) ;
#99655 = CARTESIAN_POINT ( 'NONE',  ( -10.81492255796078084, -18.62759615963271287, 67.08224293864770971 ) ) ;
#99654 = CARTESIAN_POINT ( 'NONE',  ( 21.52544592524334988, 5.823673210054432836, 56.45942372801902565 ) ) ;
#99656 = CARTESIAN_POINT ( 'NONE',  ( -0.05219959533909027116, -19.03943276465977164, 37.49890960531436690 ) ) ;
#99657 = CARTESIAN_POINT ( 'NONE',  ( 5.153800228976335163, 19.02544592524342804, 74.79057627198103830 ) ) ;
#99658 = ORIENTED_EDGE ( 'NONE', *, *, #16394, .T. ) ;
#99659 = CARTESIAN_POINT ( 'NONE',  ( 16.52544592524335698, 4.483927247898782831, 46.45942372801901854 ) ) ;
#99660 = CARTESIAN_POINT ( 'NONE',  ( -21.53943276465977519, -0.05219959533937600094, 28.75109039468567929 ) ) ;
#99661 = CARTESIAN_POINT ( 'NONE',  ( -18.62759615963255300, -10.81492255796106328, 69.16775706135234714 ) ) ;
#99662 = CARTESIAN_POINT ( 'NONE',  ( -5.719274019375978568, 21.55341960407610458, 25.20724293864769550 ) ) ;
#99663 = CARTESIAN_POINT ( 'NONE',  ( -10.81492255796078084, -18.62759615963271287, 87.08224293864769550 ) ) ;
#99665 = CARTESIAN_POINT ( 'NONE',  ( 8.314922557961029526, -14.29746914071037800, 50.41775706135235424 ) ) ;
#99664 = CARTESIAN_POINT ( 'NONE',  ( -10.81492255796105439, 18.62759615963255655, 22.91775706135235069 ) ) ;
#99666 = ADVANCED_FACE ( 'NONE', ( #187157 ), #35429, .F. ) ;
#99667 = CARTESIAN_POINT ( 'NONE',  ( -18.67979575497178146, -10.72451020669898902, 56.66557627198103830 ) ) ;
#99668 = CARTESIAN_POINT ( 'NONE',  ( 13.97604488694548053, -13.89961937509957401, 20.62609039468567573 ) ) ;
#99669 = CARTESIAN_POINT ( 'NONE',  ( 13.97604488694527802, 13.89961937509977652, 49.37390960531434558 ) ) ;
#99670 = CARTESIAN_POINT ( 'NONE',  ( 19.05341960407611168, 5.049401038298154454, 113.9572429386477097 ) ) ;
#99671 = CARTESIAN_POINT ( 'NONE',  ( -19.03943276465977164, 0.05219959533909376836, 96.24890960531436690 ) ) ;
#99672 = CARTESIAN_POINT ( 'NONE',  ( 20.73749492396215288, -155.7167183371838064, 0.000000000000000000 ) ) ;
#99673 = CARTESIAN_POINT ( 'NONE',  ( 19.02544592524334988, 5.153800228976608722, 66.45942372801899012 ) ) ;
#99674 = CARTESIAN_POINT ( 'NONE',  ( 18.62759615963271287, -10.81492255796078972, 48.33224293864770260 ) ) ;
#99675 = CARTESIAN_POINT ( 'NONE',  ( -14.29746914071049879, 8.314922557960819915, 25.83224293864769194 ) ) ;
#99676 = CARTESIAN_POINT ( 'NONE',  ( 9.564922557961047289, -16.46253265017146816, 95.41775706135233293 ) ) ;
#99677 = CARTESIAN_POINT ( 'NONE',  ( -19.05341960407611168, -5.049401038298163336, 21.45724293864768839 ) ) ;
#99678 = CARTESIAN_POINT ( 'NONE',  ( 16.46253265017146816, 9.564922557961045513, 26.66775706135234003 ) ) ;
#99679 = CARTESIAN_POINT ( 'NONE',  ( -16.46253265017146816, -9.564922557961047289, 99.16775706135233293 ) ) ;
#99681 = CARTESIAN_POINT ( 'NONE',  ( 16.46253265017146816, 9.564922557961045513, 61.66775706135234003 ) ) ;
#99680 = CARTESIAN_POINT ( 'NONE',  ( -0.05219959533907301413, -21.53943276465977519, 87.49890960531436690 ) ) ;
#99682 = CARTESIAN_POINT ( 'NONE',  ( 25.28116846732000766, -11.97242897402594686, 166.1912472719372147 ) ) ;
#99683 = CARTESIAN_POINT ( 'NONE',  ( -13.89961937509977652, 13.97604488694528158, 55.62390960531434558 ) ) ;
#99684 = CARTESIAN_POINT ( 'NONE',  ( -12.06949235617756955, 12.14591786802309770, 65.62390960531436690 ) ) ;
#99685 = CARTESIAN_POINT ( 'NONE',  ( 16.51473224551069308, 9.474510206698969483, 49.16557627198102409 ) ) ;
#99686 = CARTESIAN_POINT ( 'NONE',  ( 8.224510206698953496, -14.34966873604960469, 57.91557627198103120 ) ) ;
#99687 = CARTESIAN_POINT ( 'NONE',  ( -30.20036327792369235, -26.22857331006468229, -17.18026671435357500 ) ) ;
#99688 = CARTESIAN_POINT ( 'NONE',  ( -12.06949235617756955, 12.14591786802309770, 25.62390960531435624 ) ) ;
#99689 = CARTESIAN_POINT ( 'NONE',  ( 16.51473224551069308, 9.474510206698969483, 69.16557627198102409 ) ) ;
#99690 = CARTESIAN_POINT ( 'NONE',  ( -13.89961937509957401, -13.97604488694547875, 29.37609039468565797 ) ) ;
#99691 = CARTESIAN_POINT ( 'NONE',  ( 12.06949235617739724, 12.14591786802326823, 31.87609039468567929 ) ) ;
#99692 = CARTESIAN_POINT ( 'NONE',  ( -21.55341960407610458, -5.719274019375992779, 46.45724293864769550 ) ) ;
#99694 = ORIENTED_EDGE ( 'NONE', *, *, #112389, .T. ) ;
#99693 = CARTESIAN_POINT ( 'NONE',  ( -21.53943276465977519, -0.05219959533937600094, 98.75109039468568994 ) ) ;
#99695 = CARTESIAN_POINT ( 'NONE',  ( -5.049401038298153566, 19.05341960407611168, 60.20724293864768129 ) ) ;
#99696 = CARTESIAN_POINT ( 'NONE',  ( 0.000000000000000000, -78.67194367458512261, -25.00000000000000000 ) ) ;
#99697 = CARTESIAN_POINT ( 'NONE',  ( 5.049401038298161559, -19.05341960407611168, 92.70724293864769550 ) ) ;
#99698 = CARTESIAN_POINT ( 'NONE',  ( -22.81625015709510507, 31.40387420917330275, -4.924999997268813878 ) ) ;
#99699 = CARTESIAN_POINT ( 'NONE',  ( -15.72974639402176322, -15.80617190586768395, 29.37609039468568284 ) ) ;
#99700 = CARTESIAN_POINT ( 'NONE',  ( -8.314922557960811034, -14.29746914071050412, 92.08224293864769550 ) ) ;
#99702 = CARTESIAN_POINT ( 'NONE',  ( 19.02544592524343514, -5.153800228976328945, 68.54057627198103830 ) ) ;
#99701 = CARTESIAN_POINT ( 'NONE',  ( 18.67979575497178502, 10.72451020669898547, 94.16557627198103830 ) ) ;
#99703 = CARTESIAN_POINT ( 'NONE',  ( 13.97604488694527802, 13.89961937509977652, 89.37390960531436690 ) ) ;
#99704 = CARTESIAN_POINT ( 'NONE',  ( -18.67979575497178146, -10.72451020669898902, 111.6655762719810525 ) ) ;
#99705 = ORIENTED_EDGE ( 'NONE', *, *, #30838, .F. ) ;
#99706 = CARTESIAN_POINT ( 'NONE',  ( -9.474510206698964154, 16.51473224551069663, 70.41557627198102409 ) ) ;
#99707 = DIRECTION ( 'NONE',  ( -1.000000000000000000, -0.000000000000000000, -0.000000000000000000 ) ) ;
#99709 = DIRECTION ( 'NONE',  ( 0.000000000000000000, 0.000000000000000000, -1.000000000000000000 ) ) ;
#99708 = CARTESIAN_POINT ( 'NONE',  ( -12.06949235617756955, 12.14591786802309770, 110.6239096053143669 ) ) ;
#99710 = CARTESIAN_POINT ( 'NONE',  ( 13.89961937509957401, 13.97604488694547697, 91.87609039468567573 ) ) ;
#99711 = CARTESIAN_POINT ( 'NONE',  ( 16.52544592524342804, -4.483927247898539470, 113.5405762719810383 ) ) ;
#99712 = CARTESIAN_POINT ( 'NONE',  ( 15.72974639402176855, 15.80617190586768217, 76.87609039468567573 ) ) ;
#99714 = CARTESIAN_POINT ( 'NONE',  ( 21.55341960407619695, -5.719274019375665929, 31.04275706135234714 ) ) ;
#99713 = CARTESIAN_POINT ( 'NONE',  ( 5.153800228976335163, 19.02544592524342804, 64.79057627198100988 ) ) ;
#99715 = CARTESIAN_POINT ( 'NONE',  ( -21.55341960407610458, -5.719274019375992779, 111.4572429386476813 ) ) ;
#99716 = CARTESIAN_POINT ( 'NONE',  ( 23.31738231874054534, 16.94106989632529192, 141.1999999999999886 ) ) ;
#99717 = CARTESIAN_POINT ( 'NONE',  ( -5.049401038298153566, 19.05341960407611168, 70.20724293864769550 ) ) ;
#99718 = CARTESIAN_POINT ( 'NONE',  ( 27.93407901761402456, 7.419329114306494333, 160.9060561961931057 ) ) ;
#99720 = CARTESIAN_POINT ( 'NONE',  ( -10.72451020669898014, 18.67979575497178502, 25.41557627198103120 ) ) ;
#99719 = CARTESIAN_POINT ( 'NONE',  ( -4.483927247898782831, 16.52544592524335698, 27.70942372801901854 ) ) ;
#99721 = CARTESIAN_POINT ( 'NONE',  ( -15.80617190586768217, 15.72974639402176855, 58.12609039468568994 ) ) ;
#99722 = CARTESIAN_POINT ( 'NONE',  ( -19.05341960407611168, -5.049401038298163336, 111.4572429386476671 ) ) ;
#99723 = CARTESIAN_POINT ( 'NONE',  ( -5.153800228976607833, 19.02544592524334988, 97.70942372801900433 ) ) ;
#99724 = CARTESIAN_POINT ( 'NONE',  ( -16.46253265017160317, 9.564922557960807481, 50.83224293864770260 ) ) ;
#99725 = CARTESIAN_POINT ( 'NONE',  ( -9.564922557960796823, -16.46253265017161027, 72.08224293864770971 ) ) ;
#99726 = CARTESIAN_POINT ( 'NONE',  ( -14.29746914071049879, 8.314922557960819915, 90.83224293864769550 ) ) ;
#99727 = CARTESIAN_POINT ( 'NONE',  ( -9.564922557960796823, -16.46253265017161027, 107.0822429386476955 ) ) ;
#99728 = CARTESIAN_POINT ( 'NONE',  ( 0.05219959533910956823, 16.53943276465976808, 89.99890960531438111 ) ) ;
#99729 = CARTESIAN_POINT ( 'NONE',  ( 16.46253265017160672, -9.564922557960803928, 98.33224293864769550 ) ) ;
#99731 = CARTESIAN_POINT ( 'NONE',  ( 16.46253265017160672, -9.564922557960803928, 38.33224293864768839 ) ) ;
#99730 = CARTESIAN_POINT ( 'NONE',  ( 16.52544592524342804, -4.483927247898539470, 58.54057627198103120 ) ) ;
#99732 = CARTESIAN_POINT ( 'NONE',  ( -15.80617190586768217, 15.72974639402176855, 63.12609039468568994 ) ) ;
#99733 = CARTESIAN_POINT ( 'NONE',  ( -9.474510206698720793, -16.51473224551083518, 94.58442372801900433 ) ) ;
#99734 = CARTESIAN_POINT ( 'NONE',  ( 8.314922557960818139, 14.29746914071049879, 44.58224293864769550 ) ) ;
#99735 = CARTESIAN_POINT ( 'NONE',  ( 18.62759615963271287, -10.81492255796078972, 98.33224293864769550 ) ) ;
#99736 = CARTESIAN_POINT ( 'NONE',  ( -0.05219959533907301413, -21.53943276465977519, 47.49890960531435979 ) ) ;
#99738 = CARTESIAN_POINT ( 'NONE',  ( 14.34966873604960469, 8.224510206698951720, 84.16557627198103830 ) ) ;
#99737 = CARTESIAN_POINT ( 'NONE',  ( 9.564922557960805705, 16.46253265017160317, 114.5822429386476955 ) ) ;
#99739 = CARTESIAN_POINT ( 'NONE',  ( 22.44159573604009239, 16.30477369853692693, 144.0750000027311728 ) ) ;
#99740 = CARTESIAN_POINT ( 'NONE',  ( -9.474510206698964154, 16.51473224551069663, 55.41557627198103120 ) ) ;
#99741 = CARTESIAN_POINT ( 'NONE',  ( -12.14591786802309592, -12.06949235617757132, 26.87390960531435979 ) ) ;
#99742 = CARTESIAN_POINT ( 'NONE',  ( 12.06949235617739724, 12.14591786802326823, 96.87609039468568994 ) ) ;
#99743 = CARTESIAN_POINT ( 'NONE',  ( -4.483927247898782831, 16.52544592524335698, 77.70942372801900433 ) ) ;
#99744 = CARTESIAN_POINT ( 'NONE',  ( 9.474510206698729675, 16.51473224551082808, 42.08442372801900433 ) ) ;
#99746 = CARTESIAN_POINT ( 'NONE',  ( 9.564922557960805705, 16.46253265017160317, 109.5822429386476955 ) ) ;
#99745 = CARTESIAN_POINT ( 'NONE',  ( -16.38665767535050577, 7.295008042176172047, 70.26400864214545550 ) ) ;
#99747 = CARTESIAN_POINT ( 'NONE',  ( 13.97604488694527802, 13.89961937509977652, 84.37390960531433848 ) ) ;
#99748 = CARTESIAN_POINT ( 'NONE',  ( 16.46253265017160672, -9.564922557960803928, 43.33224293864769550 ) ) ;
#99749 = CARTESIAN_POINT ( 'NONE',  ( 4.483927247898545687, 16.52544592524342804, 44.79057627198103120 ) ) ;
#99751 = CARTESIAN_POINT ( 'NONE',  ( -5.049401038298153566, 19.05341960407611168, 110.2072429386476671 ) ) ;
#99750 = DIRECTION ( 'NONE',  ( -1.000000000000000000, 4.336808689942018352E-17, 0.000000000000000000 ) ) ;
#99752 = CARTESIAN_POINT ( 'NONE',  ( 5.823673210054125526, 21.52544592524343514, 34.79057627198103120 ) ) ;
#99753 = CARTESIAN_POINT ( 'NONE',  ( 14.29746914071049879, -8.314922557960816363, 88.33224293864769550 ) ) ;
#99754 = CARTESIAN_POINT ( 'NONE',  ( 14.34966873604972726, -8.224510206698740333, 40.83442372801901854 ) ) ;
#99755 = CARTESIAN_POINT ( 'NONE',  ( -0.05219959533910754901, -16.53943276465976808, 72.49890960531435269 ) ) ;
#99756 = CARTESIAN_POINT ( 'NONE',  ( 1.022580077288041090E-15, 16.70000000000002061, -59.13370768023891344 ) ) ;
#99757 = CARTESIAN_POINT ( 'NONE',  ( 9.564922557961047289, -16.46253265017146816, 70.41775706135233293 ) ) ;
#99758 = CARTESIAN_POINT ( 'NONE',  ( 19.02544592524343514, -5.153800228976328945, 103.5405762719809957 ) ) ;
#99759 = CARTESIAN_POINT ( 'NONE',  ( 9.474510206698729675, 16.51473224551082808, 82.08442372801899012 ) ) ;
#99760 = CARTESIAN_POINT ( 'NONE',  ( 0.05219959533936267826, -19.03943276465977164, 95.00109039468567573 ) ) ;
#99762 = CARTESIAN_POINT ( 'NONE',  ( -14.29746914071037622, -8.314922557961029526, 109.1677570613523613 ) ) ;
#99761 = CARTESIAN_POINT ( 'NONE',  ( -4.379528057220086978, -16.55341960407618274, 29.79275706135234358 ) ) ;
#99763 = CARTESIAN_POINT ( 'NONE',  ( -0.05219959533936034679, 19.03943276465977164, 77.50109039468566152 ) ) ;
#99764 = CARTESIAN_POINT ( 'NONE',  ( 5.823673210054125526, 21.52544592524343514, 34.79057627198103120 ) ) ;
#99765 = CARTESIAN_POINT ( 'NONE',  ( 5.719274019375673035, 21.55341960407619339, 67.29275706135234714 ) ) ;
#99766 = CARTESIAN_POINT ( 'NONE',  ( -20.69372460268612457, -10.84650605405325940, 168.1714143675833100 ) ) ;
#99767 = CARTESIAN_POINT ( 'NONE',  ( 5.049401038297881783, 19.05341960407617563, 112.2927570613523471 ) ) ;
#99769 = CARTESIAN_POINT ( 'NONE',  ( 13.97604488694527802, 13.89961937509977652, 84.37390960531433848 ) ) ;
#99768 = CARTESIAN_POINT ( 'NONE',  ( 9.474510206698971260, -16.51473224551069308, 22.91557627198102765 ) ) ;
#99770 = CARTESIAN_POINT ( 'NONE',  ( -0.05219959533909027116, -19.03943276465977164, 27.49890960531435624 ) ) ;
#99772 = CARTESIAN_POINT ( 'NONE',  ( 19.05341960407611168, 5.049401038298154454, 78.95724293864769550 ) ) ;
#99771 = CARTESIAN_POINT ( 'NONE',  ( -16.55341960407611168, -4.379528057220339221, 81.45724293864769550 ) ) ;
#99773 = PRODUCT_CONTEXT ( 'NONE', #110017, 'mechanical' ) ;
#99774 = CARTESIAN_POINT ( 'NONE',  ( -13.97604488694527625, -13.89961937509977652, 91.87390960531432427 ) ) ;
#99775 = VERTEX_POINT ( 'NONE', #188140 ) ;
#99776 = CARTESIAN_POINT ( 'NONE',  ( -5.153800228976607833, 19.02544592524334988, 97.70942372801900433 ) ) ;
#99777 = CARTESIAN_POINT ( 'NONE',  ( -15.80617190586745835, -15.72974639402198527, 81.87390960531435269 ) ) ;
#99778 = CARTESIAN_POINT ( 'NONE',  ( 9.564922557960805705, 16.46253265017160317, 29.58224293864769550 ) ) ;
#99780 = CARTESIAN_POINT ( 'NONE',  ( -21.55341960407610458, -5.719274019375992779, 111.4572429386476813 ) ) ;
#99779 = CARTESIAN_POINT ( 'NONE',  ( -16.46253265017146816, -9.564922557961047289, 74.16775706135234714 ) ) ;
#99781 = CARTESIAN_POINT ( 'NONE',  ( -19.03943276465977164, 0.05219959533909376836, 76.24890960531435269 ) ) ;
#99782 = CARTESIAN_POINT ( 'NONE',  ( 13.89961937509977652, -13.97604488694527269, 108.1239096053143669 ) ) ;
#99783 = VERTEX_POINT ( 'NONE', #34443 ) ;
#99784 = CARTESIAN_POINT ( 'NONE',  ( -15.80617190586745835, -15.72974639402198527, 106.8739096053143811 ) ) ;
#99787 = CARTESIAN_POINT ( 'NONE',  ( -13.97604488694547697, 13.89961937509957934, 68.12609039468563310 ) ) ;
#99786 = CARTESIAN_POINT ( 'NONE',  ( -13.97604488694527625, -13.89961937509977652, 81.87390960531436690 ) ) ;
#99785 = CARTESIAN_POINT ( 'NONE',  ( -16.52544592524342804, 4.483927247898546575, 96.04057627198102409 ) ) ;
#99788 = CARTESIAN_POINT ( 'NONE',  ( 5.719274019375991003, -21.55341960407610458, 87.70724293864769550 ) ) ;
#99789 = CARTESIAN_POINT ( 'NONE',  ( -5.823673210054116645, -21.52544592524344225, 72.29057627198102409 ) ) ;
#99790 = CARTESIAN_POINT ( 'NONE',  ( 16.55341960407611168, 4.379528057220329451, 48.95724293864770971 ) ) ;
#99791 = CARTESIAN_POINT ( 'NONE',  ( -19.05341960407617563, 5.049401038297882671, 23.54275706135233648 ) ) ;
#99792 = CARTESIAN_POINT ( 'NONE',  ( -12.06949235617739369, -12.14591786802326823, 64.37609039468568994 ) ) ;
#99793 = CARTESIAN_POINT ( 'NONE',  ( -13.89961937509977652, 13.97604488694528158, 95.62390960531436690 ) ) ;
#99794 = CARTESIAN_POINT ( 'NONE',  ( -5.049401038298153566, 19.05341960407611168, 40.20724293864768839 ) ) ;
#99795 = CARTESIAN_POINT ( 'NONE',  ( 18.62759615963255655, 10.81492255796105972, 46.66775706135234714 ) ) ;
#99796 = EDGE_CURVE ( 'NONE', #89112, #185003, #132327, .T. ) ;
#99797 = CARTESIAN_POINT ( 'NONE',  ( -21.55341960407619339, 5.719274019375674811, 48.54275706135234714 ) ) ;
#99798 = CARTESIAN_POINT ( 'NONE',  ( 13.97604488694527802, 13.89961937509977652, 59.37390960531434558 ) ) ;
#99799 = CARTESIAN_POINT ( 'NONE',  ( 5.719274019375673035, 21.55341960407619339, 37.29275706135235424 ) ) ;
#99800 = CARTESIAN_POINT ( 'NONE',  ( -16.46253265017146816, -9.564922557961047289, 74.16775706135234714 ) ) ;
#99801 = CARTESIAN_POINT ( 'NONE',  ( -13.97604488694547697, 13.89961937509957934, 68.12609039468563310 ) ) ;
#99802 = CARTESIAN_POINT ( 'NONE',  ( 16.46253265017160672, -9.564922557960803928, 38.33224293864768839 ) ) ;
#99803 = CARTESIAN_POINT ( 'NONE',  ( -14.34966873604972548, 8.224510206698743886, 93.33442372801901854 ) ) ;
#99804 = CARTESIAN_POINT ( 'NONE',  ( 19.03943276465977164, -0.05219959533909143690, 48.74890960531435979 ) ) ;
#99805 = CARTESIAN_POINT ( 'NONE',  ( 21.97054992548899222, -7.027819292989583744, 170.5066066589220100 ) ) ;
#99806 = CARTESIAN_POINT ( 'NONE',  ( 16.51473224551069308, 9.474510206698969483, 94.16557627198103830 ) ) ;
#99807 = CARTESIAN_POINT ( 'NONE',  ( 5.153800228976335163, 19.02544592524342804, 39.79057627198100988 ) ) ;
#99808 = CARTESIAN_POINT ( 'NONE',  ( 15.72974639402199770, -15.80617190586745480, 73.12390960531436690 ) ) ;
#99809 = CARTESIAN_POINT ( 'NONE',  ( 4.379528057220092307, 16.55341960407617563, 67.29275706135234714 ) ) ;
#99810 = CARTESIAN_POINT ( 'NONE',  ( 21.53943276465977519, 0.05219959533937863772, 111.2510903946856899 ) ) ;
#99811 = CARTESIAN_POINT ( 'NONE',  ( -16.46253265017160317, 9.564922557960807481, 55.83224293864769550 ) ) ;
#99812 = CARTESIAN_POINT ( 'NONE',  ( 0.05219959533910956823, 16.53943276465976808, 44.99890960531435979 ) ) ;
#99813 = CARTESIAN_POINT ( 'NONE',  ( -8.224510206698948167, 14.34966873604960824, 80.41557627198103830 ) ) ;
#99814 = CIRCLE ( 'NONE', #60988, 7.500000000000000000 ) ;
#99815 = CARTESIAN_POINT ( 'NONE',  ( -5.153800228976328057, -19.02544592524343514, 72.29057627198102409 ) ) ;
#99816 = CARTESIAN_POINT ( 'NONE',  ( 15.72974639402176855, 15.80617190586768217, 31.87609039468567929 ) ) ;
#99817 = CARTESIAN_POINT ( 'NONE',  ( 5.049401038298161559, -19.05341960407611168, 97.70724293864766707 ) ) ;
#99818 = CARTESIAN_POINT ( 'NONE',  ( 21.53943276465977519, 0.05219959533937863772, 101.2510903946856757 ) ) ;
#99819 = CARTESIAN_POINT ( 'NONE',  ( 0.05219959533934541429, -16.53943276465976808, 70.00109039468568994 ) ) ;
#99820 = CARTESIAN_POINT ( 'NONE',  ( 15.80617190586769283, -15.72974639402175789, 25.62609039468567929 ) ) ;
#99821 = CARTESIAN_POINT ( 'NONE',  ( -19.03943276465977164, 0.05219959533909376836, 106.2489096053143669 ) ) ;
#99822 = CARTESIAN_POINT ( 'NONE',  ( -5.719274019375978568, 21.55341960407610458, 90.20724293864770971 ) ) ;
#99823 = CARTESIAN_POINT ( 'NONE',  ( -16.52544592524342804, 4.483927247898546575, 41.04057627198103120 ) ) ;
#99824 = CARTESIAN_POINT ( 'NONE',  ( -19.03943276465977164, 0.05219959533909376836, 41.24890960531435269 ) ) ;
#99825 = CARTESIAN_POINT ( 'NONE',  ( 12.14591786802309770, 12.06949235617756955, 74.37390960531436690 ) ) ;
#99826 = CARTESIAN_POINT ( 'NONE',  ( 10.81492255796078972, 18.62759615963270932, 24.58224293864768839 ) ) ;
#99827 = CARTESIAN_POINT ( 'NONE',  ( -9.474510206698720793, -16.51473224551083518, 29.58442372801900433 ) ) ;
#99828 = ADVANCED_FACE ( 'NONE', ( #4084 ), #20254, .F. ) ;
#99829 = CARTESIAN_POINT ( 'NONE',  ( 16.55341960407611168, 4.379528057220329451, 103.9572429386476813 ) ) ;
#99830 = CARTESIAN_POINT ( 'NONE',  ( -19.05341960407611168, -5.049401038298163336, 111.4572429386476671 ) ) ;
#99831 = VERTEX_POINT ( 'NONE', #66759 ) ;
#99832 = CARTESIAN_POINT ( 'NONE',  ( 8.314922557961029526, -14.29746914071037800, 55.41775706135234714 ) ) ;
#99833 = CARTESIAN_POINT ( 'NONE',  ( -9.474510206698964154, 16.51473224551069663, 50.41557627198102409 ) ) ;
#99834 = DIRECTION ( 'NONE',  ( -1.000000000000000000, 0.000000000000000000, 0.000000000000000000 ) ) ;
#99835 = CARTESIAN_POINT ( 'NONE',  ( -4.379528057220086978, -16.55341960407618274, 99.79275706135234714 ) ) ;
#99836 = CARTESIAN_POINT ( 'NONE',  ( -19.05341960407617563, 5.049401038297882671, 93.54275706135234714 ) ) ;
#99837 = CARTESIAN_POINT ( 'NONE',  ( -5.719274019375665041, -21.55341960407619695, 69.79275706135234714 ) ) ;
#99838 = CARTESIAN_POINT ( 'NONE',  ( -5.153800228976328057, -19.02544592524343514, 77.29057627198099567 ) ) ;
#99839 = CARTESIAN_POINT ( 'NONE',  ( -10.81492255796078084, -18.62759615963271287, 87.08224293864769550 ) ) ;
#99840 = CARTESIAN_POINT ( 'NONE',  ( 16.55341960407618274, -4.379528057220086978, 41.04275706135236135 ) ) ;
#99841 = CARTESIAN_POINT ( 'NONE',  ( -5.153800228976328057, -19.02544592524343514, 22.29057627198102765 ) ) ;
#99842 = CARTESIAN_POINT ( 'NONE',  ( 16.46253265017146816, 9.564922557961045513, 76.66775706135234714 ) ) ;
#99843 = CARTESIAN_POINT ( 'NONE',  ( -21.52544592524343514, 5.823673210054127303, 76.04057627198102409 ) ) ;
#99844 = CARTESIAN_POINT ( 'NONE',  ( 9.564922557961047289, -16.46253265017146816, 55.41775706135234003 ) ) ;
#99845 = CARTESIAN_POINT ( 'NONE',  ( 19.35543954521081034, 5.499999999999523936, 97.08901960356452321 ) ) ;
#99846 = CARTESIAN_POINT ( 'NONE',  ( 18.62759615963271287, -10.81492255796078972, 88.33224293864769550 ) ) ;
#99847 = CARTESIAN_POINT ( 'NONE',  ( 17.50000000000014211, 3.292511757969722730, 27.43479729789468990 ) ) ;
#99848 = CARTESIAN_POINT ( 'NONE',  ( -5.153800228976328057, -19.02544592524343514, 62.29057627198100988 ) ) ;
#99849 = CARTESIAN_POINT ( 'NONE',  ( 17.50000000000000000, 5.499999999999992895, 56.70309617465829888 ) ) ;
#99850 = CARTESIAN_POINT ( 'NONE',  ( -14.29746914071037622, -8.314922557961029526, 19.16775706135234714 ) ) ;
#99851 = CARTESIAN_POINT ( 'NONE',  ( 7.652493125987820832, -39.26116846142902261, -13.00000000000000000 ) ) ;
#99852 = CARTESIAN_POINT ( 'NONE',  ( -19.05341960407611168, -5.049401038298163336, 41.45724293864769550 ) ) ;
#99854 = CARTESIAN_POINT ( 'NONE',  ( 16.55341960407611168, 4.379528057220329451, 48.95724293864770971 ) ) ;
#99853 = CARTESIAN_POINT ( 'NONE',  ( -18.62759615963270932, 10.81492255796079327, 105.8322429386476955 ) ) ;
#99855 = CARTESIAN_POINT ( 'NONE',  ( -9.564922557960796823, -16.46253265017161027, 67.08224293864769550 ) ) ;
#99856 = CARTESIAN_POINT ( 'NONE',  ( -10.72451020669870658, -18.67979575497194134, 74.58442372801901854 ) ) ;
#99858 = CARTESIAN_POINT ( 'NONE',  ( -0.05219959533936034679, 19.03943276465977164, 32.50109039468566863 ) ) ;
#99857 = CARTESIAN_POINT ( 'NONE',  ( -16.53943276465976808, -0.05219959533934237506, 18.75109039468568639 ) ) ;
#99859 = CARTESIAN_POINT ( 'NONE',  ( -18.67979575497193778, 10.72451020669871902, 38.33442372801900433 ) ) ;
#99860 = CARTESIAN_POINT ( 'NONE',  ( 10.72451020669871369, 18.67979575497193778, 22.08442372801901143 ) ) ;
#99861 = CARTESIAN_POINT ( 'NONE',  ( -5.823673210054116645, -21.52544592524344225, 62.29057627198102409 ) ) ;
#99862 = CARTESIAN_POINT ( 'NONE',  ( -0.05219959533936034679, 19.03943276465977164, 92.50109039468566152 ) ) ;
#99863 = CARTESIAN_POINT ( 'NONE',  ( -13.97604488694547697, 13.89961937509957934, 63.12609039468566152 ) ) ;
#99864 = CARTESIAN_POINT ( 'NONE',  ( 5.719274019375673035, 21.55341960407619339, 82.29275706135234714 ) ) ;
#99865 = CARTESIAN_POINT ( 'NONE',  ( 5.049401038297881783, 19.05341960407617563, 52.29275706135234003 ) ) ;
#99866 = CARTESIAN_POINT ( 'NONE',  ( -9.474510206698964154, 16.51473224551069663, 25.41557627198103120 ) ) ;
#99867 = CARTESIAN_POINT ( 'NONE',  ( 21.53943276465977519, -0.05219959533907433946, 53.74890960531437401 ) ) ;
#99868 = CARTESIAN_POINT ( 'NONE',  ( -16.53943276465976808, 0.05219959533911058130, 51.24890960531436690 ) ) ;
#99869 = CARTESIAN_POINT ( 'NONE',  ( -38.00000000000000711, 12.34694845685046438, -1.849999994537626424 ) ) ;
#99870 = CARTESIAN_POINT ( 'NONE',  ( 13.89961937509957401, 13.97604488694547697, 31.87609039468566863 ) ) ;
#99871 = CARTESIAN_POINT ( 'NONE',  ( -4.483927247898782831, 16.52544592524335698, 82.70942372801900433 ) ) ;
#99872 = CARTESIAN_POINT ( 'NONE',  ( -14.34966873604960291, -8.224510206698953496, 46.66557627198102409 ) ) ;
#99873 = CARTESIAN_POINT ( 'NONE',  ( -0.05219959533937732626, 21.53943276465977519, 77.50109039468567573 ) ) ;
#99874 = CARTESIAN_POINT ( 'NONE',  ( 15.72974639402176855, 15.80617190586768217, 86.87609039468568994 ) ) ;
#99875 = CARTESIAN_POINT ( 'NONE',  ( -21.52544592524343514, 5.823673210054127303, 86.04057627198102409 ) ) ;
#99876 = CARTESIAN_POINT ( 'NONE',  ( 5.049401038298161559, -19.05341960407611168, 37.70724293864768839 ) ) ;
#99877 = CARTESIAN_POINT ( 'NONE',  ( -15.72974639402176322, -15.80617190586768395, 59.37609039468568284 ) ) ;
#99878 = CARTESIAN_POINT ( 'NONE',  ( -16.46253265017160317, 9.564922557960807481, 30.83224293864769550 ) ) ;
#99879 = CARTESIAN_POINT ( 'NONE',  ( -5.153800228976328057, -19.02544592524343514, 57.29057627198103120 ) ) ;
#99880 = CARTESIAN_POINT ( 'NONE',  ( 16.52544592524342804, -4.483927247898539470, 98.54057627198105251 ) ) ;
#99881 = CARTESIAN_POINT ( 'NONE',  ( 9.564922557960805705, 16.46253265017160317, 99.58224293864770971 ) ) ;
#99882 = CARTESIAN_POINT ( 'NONE',  ( -14.29746914071049879, 8.314922557960819915, 45.83224293864769550 ) ) ;
#99883 = CARTESIAN_POINT ( 'NONE',  ( -8.314922557960811034, -14.29746914071050412, 107.0822429386476955 ) ) ;
#99884 = CARTESIAN_POINT ( 'NONE',  ( 10.81492255796078972, 18.62759615963270932, 89.58224293864768129 ) ) ;
#99885 = CARTESIAN_POINT ( 'NONE',  ( 18.67979575497194134, -10.72451020669871369, 25.83442372801901499 ) ) ;
#99886 = CARTESIAN_POINT ( 'NONE',  ( 27.86147134968521755, -7.555459793078237674, 161.1037931155416345 ) ) ;
#99887 = CARTESIAN_POINT ( 'NONE',  ( 16.55341960407618274, -4.379528057220086978, 41.04275706135236135 ) ) ;
#99888 = CARTESIAN_POINT ( 'NONE',  ( -15.80617190586745835, -15.72974639402198527, 71.87390960531438111 ) ) ;
#99889 = CARTESIAN_POINT ( 'NONE',  ( -21.52544592524334988, -5.823673210054445271, 98.95942372801903275 ) ) ;
#99890 = CARTESIAN_POINT ( 'NONE',  ( -16.46253265017160317, 9.564922557960807481, 90.83224293864769550 ) ) ;
#99891 = CARTESIAN_POINT ( 'NONE',  ( 21.53943276465977519, 0.05219959533937863772, 26.25109039468567573 ) ) ;
#99892 = CARTESIAN_POINT ( 'NONE',  ( -10.81492255796078084, -18.62759615963271287, 32.08224293864769550 ) ) ;
#99893 = CARTESIAN_POINT ( 'NONE',  ( -4.483927247898782831, 16.52544592524335698, 92.70942372801901854 ) ) ;
#99894 = CARTESIAN_POINT ( 'NONE',  ( 10.81492255796106328, -18.62759615963255655, 65.41775706135234714 ) ) ;
#99895 = CARTESIAN_POINT ( 'NONE',  ( 19.05341960407617918, -5.049401038297876454, 21.04275706135232582 ) ) ;
#99896 = CARTESIAN_POINT ( 'NONE',  ( 14.34966873604972726, -8.224510206698740333, 70.83442372801901854 ) ) ;
#99897 = CARTESIAN_POINT ( 'NONE',  ( 5.719274019375673035, 21.55341960407619339, 27.29275706135234358 ) ) ;
#99898 = CARTESIAN_POINT ( 'NONE',  ( 13.89961937509977652, -13.97604488694527269, 28.12390960531435624 ) ) ;
#99899 = CARTESIAN_POINT ( 'NONE',  ( 21.55341960407619695, -5.719274019375665929, 106.0427570613523471 ) ) ;
#99900 = CARTESIAN_POINT ( 'NONE',  ( -16.46253265017160317, 9.564922557960807481, 110.8322429386476955 ) ) ;
#99901 = CARTESIAN_POINT ( 'NONE',  ( -5.823673210054116645, -21.52544592524344225, 97.29057627198105251 ) ) ;
#99903 = CARTESIAN_POINT ( 'NONE',  ( -21.55341960407610458, -5.719274019375992779, 56.45724293864768839 ) ) ;
#99902 = CARTESIAN_POINT ( 'NONE',  ( -8.377002814026733191, -36.45346134345093247, -31.71922177526237974 ) ) ;
#99905 = CARTESIAN_POINT ( 'NONE',  ( -14.34966873604960291, -8.224510206698953496, 51.66557627198102409 ) ) ;
#99904 = CARTESIAN_POINT ( 'NONE',  ( 8.314922557961029526, -14.29746914071037800, 50.41775706135235424 ) ) ;
#99906 = CARTESIAN_POINT ( 'NONE',  ( 11.61039618804099049, -9.512461411204764516, -62.07742545104463971 ) ) ;
#99907 = CARTESIAN_POINT ( 'NONE',  ( 19.02544592524334988, 5.153800228976608722, 81.45942372801897591 ) ) ;
#99908 = CARTESIAN_POINT ( 'NONE',  ( -17.40861289039001392, 6.110651285853331949, 103.6276752917256943 ) ) ;
#99909 = CARTESIAN_POINT ( 'NONE',  ( 16.51473224551083163, -9.474510206698727899, 105.8344237280190043 ) ) ;
#99910 = CARTESIAN_POINT ( 'NONE',  ( -5.719274019375978568, 21.55341960407610458, 80.20724293864769550 ) ) ;
#99911 = CARTESIAN_POINT ( 'NONE',  ( -0.05219959533910754901, -16.53943276465976808, 67.49890960531436690 ) ) ;
#99912 = CARTESIAN_POINT ( 'NONE',  ( 9.474510206698971260, -16.51473224551069308, 97.91557627198102409 ) ) ;
#99913 = CARTESIAN_POINT ( 'NONE',  ( 16.52544592524335698, 4.483927247898782831, 46.45942372801901854 ) ) ;
#99914 = CARTESIAN_POINT ( 'NONE',  ( -16.51473224551069308, -9.474510206698971260, 61.66557627198103120 ) ) ;
#99916 = CARTESIAN_POINT ( 'NONE',  ( -9.474510206698720793, -16.51473224551083518, 104.5844237280190043 ) ) ;
#99915 = CARTESIAN_POINT ( 'NONE',  ( 5.719274019375673035, 21.55341960407619339, 32.29275706135235424 ) ) ;
#99917 = CARTESIAN_POINT ( 'NONE',  ( -16.46253265017160317, 9.564922557960807481, 95.83224293864769550 ) ) ;
#99918 = CARTESIAN_POINT ( 'NONE',  ( -19.05341960407611168, -5.049401038298163336, 86.45724293864769550 ) ) ;
#99919 = CARTESIAN_POINT ( 'NONE',  ( -10.72451020669898014, 18.67979575497178502, 85.41557627198102409 ) ) ;
#99920 = CARTESIAN_POINT ( 'NONE',  ( -19.02544592524342804, 5.153800228976336051, 41.04057627198103120 ) ) ;
#99921 = CARTESIAN_POINT ( 'NONE',  ( -16.79531203550651242, -7.028104445595497296, 61.25244988220445919 ) ) ;
#99922 = CARTESIAN_POINT ( 'NONE',  ( 4.483927247898545687, 16.52544592524342804, 64.79057627198103830 ) ) ;
#99923 = CARTESIAN_POINT ( 'NONE',  ( 0.05219959533909260263, 19.03943276465977164, 109.9989096053143669 ) ) ;
#99924 = CARTESIAN_POINT ( 'NONE',  ( -29.61737564226528363, 1.282731051913388320, -51.85482277101433368 ) ) ;
#99925 = CARTESIAN_POINT ( 'NONE',  ( 5.049401038297881783, 19.05341960407617563, 62.29275706135234003 ) ) ;
#99926 = CARTESIAN_POINT ( 'NONE',  ( -18.62759615963270932, 10.81492255796079327, 85.83224293864768129 ) ) ;
#99927 = CARTESIAN_POINT ( 'NONE',  ( 19.03943276465977164, 0.05219959533936151252, 56.25109039468566863 ) ) ;
#99928 = CARTESIAN_POINT ( 'NONE',  ( 19.05341960407611168, 5.049401038298154454, 98.95724293864766707 ) ) ;
#99929 = CARTESIAN_POINT ( 'NONE',  ( 19.53091890409951503, 5.500000000000028422, 67.56097431831419442 ) ) ;
#99930 = CARTESIAN_POINT ( 'NONE',  ( -10.81492255796078084, -18.62759615963271287, 37.08224293864768129 ) ) ;
#99931 = CARTESIAN_POINT ( 'NONE',  ( -13.89961937509977652, 13.97604488694528158, 90.62390960531432427 ) ) ;
#99932 = CARTESIAN_POINT ( 'NONE',  ( -10.72451020669870658, -18.67979575497194134, 59.58442372801901854 ) ) ;
#99933 = CARTESIAN_POINT ( 'NONE',  ( -5.153800228976328057, -19.02544592524343514, 32.29057627198102409 ) ) ;
#99934 = CARTESIAN_POINT ( 'NONE',  ( -4.483927247898539470, -16.52544592524342804, 72.29057627198102409 ) ) ;
#99935 = CARTESIAN_POINT ( 'NONE',  ( 14.29746914071037800, 8.314922557961029526, 21.66775706135235069 ) ) ;
#99936 = CARTESIAN_POINT ( 'NONE',  ( 0.05219959533937995610, -21.53943276465977519, 50.00109039468568994 ) ) ;
#99937 = ORIENTED_EDGE ( 'NONE', *, *, #72705, .T. ) ;
#99938 = FACE_OUTER_BOUND ( 'NONE', #90745, .T. ) ;
#99939 = CARTESIAN_POINT ( 'NONE',  ( -0.05219959533936034679, 19.03943276465977164, 62.50109039468566863 ) ) ;
#99940 = CARTESIAN_POINT ( 'NONE',  ( 9.687362902255733488, -9.687362902255692632, -62.58071313852362039 ) ) ;
#99941 = CARTESIAN_POINT ( 'NONE',  ( -0.05219959533937732626, 21.53943276465977519, 22.50109039468567573 ) ) ;
#99942 = CARTESIAN_POINT ( 'NONE',  ( 38.00000000000000711, -12.34694845685040754, -8.849999994537625980 ) ) ;
#99943 = CARTESIAN_POINT ( 'NONE',  ( 19.03943276465977164, 0.05219959533936151252, 21.25109039468565797 ) ) ;
#99944 = CARTESIAN_POINT ( 'NONE',  ( 13.89961937509977652, -13.97604488694527269, 58.12390960531436690 ) ) ;
#99945 = CARTESIAN_POINT ( 'NONE',  ( -21.55341960407619339, 5.719274019375674811, 113.5427570613523756 ) ) ;
#99946 = CARTESIAN_POINT ( 'NONE',  ( -16.52544592524335698, -4.483927247898792601, 108.9594237280190185 ) ) ;
#99948 = CARTESIAN_POINT ( 'NONE',  ( 21.53943276465977519, 0.05219959533937863772, 76.25109039468568994 ) ) ;
#99947 = CARTESIAN_POINT ( 'NONE',  ( 13.89961937509977652, -13.97604488694527269, 103.1239096053143527 ) ) ;
#99949 = VECTOR ( 'NONE', #59797, 1000.000000000000000 ) ;
#99950 = CARTESIAN_POINT ( 'NONE',  ( -193.3062444957834884, -155.7167183371838064, -15.00000000000000178 ) ) ;
#99951 = CARTESIAN_POINT ( 'NONE',  ( -16.12203461105344005, -16.12203461105316649, -64.92279855667830191 ) ) ;
#99953 = CARTESIAN_POINT ( 'NONE',  ( -10.72451020669870658, -18.67979575497194134, 69.58442372801900433 ) ) ;
#99952 = CARTESIAN_POINT ( 'NONE',  ( -14.29746914071037622, -8.314922557961029526, 69.16775706135234714 ) ) ;
#99954 = CARTESIAN_POINT ( 'NONE',  ( -21.53943276465977519, -0.05219959533937600094, 103.7510903946857042 ) ) ;
#99955 = DIRECTION ( 'NONE',  ( 1.000000000000000000, 0.000000000000000000, 0.000000000000000000 ) ) ;
#99956 = CARTESIAN_POINT ( 'NONE',  ( 19.05341960407611168, 5.049401038298154454, 83.95724293864766707 ) ) ;
#99957 = EDGE_CURVE ( 'NONE', #40990, #46712, #154704, .T. ) ;
#99958 = FACE_OUTER_BOUND ( 'NONE', #7954, .T. ) ;
#99959 = EDGE_LOOP ( 'NONE', ( #55692, #12331, #60000, #50511 ) ) ;
#99960 = CARTESIAN_POINT ( 'NONE',  ( -22.00000000000000000, -5.510910596163089556E-15, 45.00000000000000000 ) ) ;
#99961 = CARTESIAN_POINT ( 'NONE',  ( 19.02544592524343514, -5.153800228976328945, 33.54057627198102409 ) ) ;
#99962 = CARTESIAN_POINT ( 'NONE',  ( 21.55341960407610458, 5.719274019375980345, 38.95724293864768839 ) ) ;
#99963 = CARTESIAN_POINT ( 'NONE',  ( 16.52544592524335698, 4.483927247898782831, 106.4594237280190328 ) ) ;
#99965 = CARTESIAN_POINT ( 'NONE',  ( -13.89961937509977652, 13.97604488694528158, 80.62390960531436690 ) ) ;
#99964 = CARTESIAN_POINT ( 'NONE',  ( -8.224510206698948167, 14.34966873604960824, 100.4155762719810241 ) ) ;
#99966 = CARTESIAN_POINT ( 'NONE',  ( 21.52544592524334988, 5.823673210054432836, 106.4594237280190328 ) ) ;
#99967 = CARTESIAN_POINT ( 'NONE',  ( 5.153800228976335163, 19.02544592524342804, 39.79057627198100988 ) ) ;
#99968 = CARTESIAN_POINT ( 'NONE',  ( -8.224510206698948167, 14.34966873604960824, 90.41557627198103830 ) ) ;
#99969 = CARTESIAN_POINT ( 'NONE',  ( -21.55341960407619339, 5.719274019375674811, 53.54275706135234714 ) ) ;
#99970 = CARTESIAN_POINT ( 'NONE',  ( 15.72974639402199770, -15.80617190586745480, 93.12390960531436690 ) ) ;
#99971 = CARTESIAN_POINT ( 'NONE',  ( -5.153800228976607833, 19.02544592524334988, 52.70942372801900433 ) ) ;
#99972 = CARTESIAN_POINT ( 'NONE',  ( -3.181980515339156934, 30.00000000000003553, 8.889087296526001936 ) ) ;
#99973 = CARTESIAN_POINT ( 'NONE',  ( -13.89961937509977652, 13.97604488694528158, 90.62390960531432427 ) ) ;
#99974 = CARTESIAN_POINT ( 'NONE',  ( -12.14591786802309592, -12.06949235617757132, 61.87390960531436690 ) ) ;
#99975 = CARTESIAN_POINT ( 'NONE',  ( -13.89961937509957401, -13.97604488694547875, 49.37609039468567573 ) ) ;
#99976 = CARTESIAN_POINT ( 'NONE',  ( -0.05219959533910754901, -16.53943276465976808, 42.49890960531435979 ) ) ;
#99977 = CARTESIAN_POINT ( 'NONE',  ( -13.97604488694547697, 13.89961937509957934, 83.12609039468564731 ) ) ;
#99978 = CARTESIAN_POINT ( 'NONE',  ( -13.89961937509957401, -13.97604488694547697, 89.37609039468564731 ) ) ;
#99979 = CARTESIAN_POINT ( 'NONE',  ( -18.62759615963270932, 10.81492255796079327, 35.83224293864768839 ) ) ;
#99980 = CARTESIAN_POINT ( 'NONE',  ( 4.379528057220339221, -16.55341960407611168, 107.7072429386476955 ) ) ;
#99981 = CARTESIAN_POINT ( 'NONE',  ( -17.50000000000001421, -5.499999999999956479, 26.28230962303566542 ) ) ;
#99983 = CARTESIAN_POINT ( 'NONE',  ( 15.80617190586746368, 15.72974639402197994, 49.37390960531436690 ) ) ;
#99982 = CARTESIAN_POINT ( 'NONE',  ( -16.51473224551069308, -9.474510206698971260, 51.66557627198102409 ) ) ;
#99984 = CARTESIAN_POINT ( 'NONE',  ( 19.05341960407611168, 5.049401038298154454, 28.95724293864769550 ) ) ;
#99986 = CARTESIAN_POINT ( 'NONE',  ( 0.05219959533909260263, 19.03943276465977164, 64.99890960531436690 ) ) ;
#99985 = CARTESIAN_POINT ( 'NONE',  ( -14.29746914071037622, -8.314922557961029526, 74.16775706135231871 ) ) ;
#99987 = CARTESIAN_POINT ( 'NONE',  ( 19.03943276465977164, 0.05219959533936151252, 36.25109039468567573 ) ) ;
#99988 = CARTESIAN_POINT ( 'NONE',  ( -15.72974639402176322, -15.80617190586768395, 64.37609039468568994 ) ) ;
#99989 = CARTESIAN_POINT ( 'NONE',  ( -21.55341960407610458, -5.719274019375992779, 51.45724293864770260 ) ) ;
#99990 = CARTESIAN_POINT ( 'NONE',  ( 5.049401038298161559, -19.05341960407611168, 22.70724293864769194 ) ) ;
#99991 = CARTESIAN_POINT ( 'NONE',  ( -13.97604488694547697, 13.89961937509957934, 98.12609039468566152 ) ) ;
#99992 = CARTESIAN_POINT ( 'NONE',  ( 27.60098488412425155, 5.861468761071320976, 164.8187539380863313 ) ) ;
#99994 = CARTESIAN_POINT ( 'NONE',  ( -5.823673210054116645, -21.52544592524344225, 47.29057627198103120 ) ) ;
#99993 = CARTESIAN_POINT ( 'NONE',  ( 17.49999999999999289, 3.270424329314900014, 37.45773515054982283 ) ) ;
#99995 = CARTESIAN_POINT ( 'NONE',  ( 19.03943276465977164, -0.05219959533909143690, 28.74890960531435624 ) ) ;
#99996 = CARTESIAN_POINT ( 'NONE',  ( -15.72974639402176322, -15.80617190586768395, 84.37609039468570415 ) ) ;
#99997 = CARTESIAN_POINT ( 'NONE',  ( -16.53943276465976808, 0.05219959533911058130, 46.24890960531435979 ) ) ;
#99998 = CARTESIAN_POINT ( 'NONE',  ( -4.483927247898539470, -16.52544592524342804, 62.29057627198102409 ) ) ;
#99999 = CARTESIAN_POINT ( 'NONE',  ( -5.719274019375978568, 21.55341960407610458, 85.20724293864770971 ) ) ;
#100000 = CARTESIAN_POINT ( 'NONE',  ( -15.80617190586745835, -15.72974639402198527, 81.87390960531435269 ) ) ;
#100001 = DIRECTION ( 'NONE',  ( -0.4999999999999933387, 0.5000000000000055511, -0.7071067811865484609 ) ) ;
#100002 = CARTESIAN_POINT ( 'NONE',  ( 21.53943276465977519, -0.05219959533907433946, 33.74890960531436690 ) ) ;
#100003 = CARTESIAN_POINT ( 'NONE',  ( 16.55341960407618274, -4.379528057220086978, 51.04275706135234714 ) ) ;
#100004 = CARTESIAN_POINT ( 'NONE',  ( -16.52544592524342804, 4.483927247898546575, 81.04057627198102409 ) ) ;
#100005 = CARTESIAN_POINT ( 'NONE',  ( -9.564922557960796823, -16.46253265017161027, 57.08224293864769550 ) ) ;
#100006 = CARTESIAN_POINT ( 'NONE',  ( 13.89961937509977652, -13.97604488694527269, 38.12390960531436690 ) ) ;
#100007 = CARTESIAN_POINT ( 'NONE',  ( 28.79475375365586132, 2.781246896534039337E-14, 142.9843446568999639 ) ) ;
#100008 = ORIENTED_EDGE ( 'NONE', *, *, #130121, .T. ) ;
#100009 = CARTESIAN_POINT ( 'NONE',  ( -0.05219959533934338120, 16.53943276465976808, 77.50109039468567573 ) ) ;
#100010 = CARTESIAN_POINT ( 'NONE',  ( 21.55341960407619695, -5.719274019375665929, 26.04275706135235779 ) ) ;
#100011 = CARTESIAN_POINT ( 'NONE',  ( -9.474510206698964154, 16.51473224551069663, 75.41557627198103830 ) ) ;
#100012 = CARTESIAN_POINT ( 'NONE',  ( 21.55341960407619695, -5.719274019375665929, 61.04275706135234714 ) ) ;
#100013 = CARTESIAN_POINT ( 'NONE',  ( 0.05219959533909260263, 19.03943276465977164, 114.9989096053143669 ) ) ;
#100014 = CARTESIAN_POINT ( 'NONE',  ( -9.824205582590950669, -39.25481172344220937, -25.36904614590413587 ) ) ;
#100015 = VERTEX_POINT ( 'NONE', #157791 ) ;
#100016 = CARTESIAN_POINT ( 'NONE',  ( -18.62759615963255300, -10.81492255796106328, 39.16775706135235424 ) ) ;
#100018 = CARTESIAN_POINT ( 'NONE',  ( 0.05219959533909260263, 19.03943276465977164, 99.99890960531436690 ) ) ;
#100017 = CARTESIAN_POINT ( 'NONE',  ( 9.564922557960805705, 16.46253265017160317, 24.58224293864769194 ) ) ;
#100019 = CARTESIAN_POINT ( 'NONE',  ( -13.97604488694547697, 13.89961937509957934, 48.12609039468566863 ) ) ;
#100020 = CARTESIAN_POINT ( 'NONE',  ( 21.55341960407619695, -5.719274019375665929, 21.04275706135234714 ) ) ;
#100021 = CARTESIAN_POINT ( 'NONE',  ( -5.153800228976607833, 19.02544592524334988, 47.70942372801900433 ) ) ;
#100022 = CARTESIAN_POINT ( 'NONE',  ( 19.03943276465977164, -0.05219959533909143690, 28.74890960531435624 ) ) ;
#100023 = CARTESIAN_POINT ( 'NONE',  ( 8.314922557961029526, -14.29746914071037800, 95.41775706135234714 ) ) ;
#100024 = CARTESIAN_POINT ( 'NONE',  ( 19.03943276465977164, 0.05219959533936151252, 56.25109039468566863 ) ) ;
#100025 = CARTESIAN_POINT ( 'NONE',  ( -16.53943276465976808, -0.05219959533934237506, 98.75109039468568994 ) ) ;
#100027 = ORIENTED_EDGE ( 'NONE', *, *, #83620, .F. ) ;
#100026 = DIRECTION ( 'NONE',  ( -0.000000000000000000, -1.000000000000000000, 0.000000000000000000 ) ) ;
#100028 = CARTESIAN_POINT ( 'NONE',  ( 5.153800228976335163, 19.02544592524342804, 84.79057627198099567 ) ) ;
#100029 = CARTESIAN_POINT ( 'NONE',  ( -15.72974639402176322, -15.80617190586768395, 89.37609039468568994 ) ) ;
#100031 = ADVANCED_FACE ( 'NONE', ( #65762 ), #190116, .T. ) ;
#100030 = CARTESIAN_POINT ( 'NONE',  ( -10.81492255796105439, 18.62759615963255655, 92.91775706135236135 ) ) ;
#100032 = CARTESIAN_POINT ( 'NONE',  ( -16.51473224551069308, -9.474510206698971260, 21.66557627198102765 ) ) ;
#100033 = CARTESIAN_POINT ( 'NONE',  ( -0.05219959533909027116, -19.03943276465977164, 102.4989096053143669 ) ) ;
#100034 = CARTESIAN_POINT ( 'NONE',  ( 15.80617190586769283, -15.72974639402175789, 75.62609039468567573 ) ) ;
#100035 = CARTESIAN_POINT ( 'NONE',  ( -9.474510206698720793, -16.51473224551083518, 109.5844237280190043 ) ) ;
#100036 = CARTESIAN_POINT ( 'NONE',  ( 19.03943276465977164, -0.05219959533909143690, 83.74890960531436690 ) ) ;
#100037 = CARTESIAN_POINT ( 'NONE',  ( 10.81492255796078972, 18.62759615963270932, 34.58224293864770260 ) ) ;
#100038 = CARTESIAN_POINT ( 'NONE',  ( -19.05341960407611168, -5.049401038298163336, 96.45724293864769550 ) ) ;
#100039 = CARTESIAN_POINT ( 'NONE',  ( -16.18388926212238488, -7.379444403734532365, 90.43953151366152099 ) ) ;
#100040 = CARTESIAN_POINT ( 'NONE',  ( -19.05341960407611168, -5.049401038298163336, 81.45724293864769550 ) ) ;
#100041 = CARTESIAN_POINT ( 'NONE',  ( 5.049401038298161559, -19.05341960407611168, 67.70724293864769550 ) ) ;
#100042 = CARTESIAN_POINT ( 'NONE',  ( 8.314922557961029526, -14.29746914071037800, 100.4177570613523471 ) ) ;
#100043 = DIRECTION ( 'NONE',  ( 0.000000000000000000, 0.000000000000000000, 1.000000000000000000 ) ) ;
#100044 = CARTESIAN_POINT ( 'NONE',  ( 5.153800228976615827, -19.02544592524334988, 55.20942372801899722 ) ) ;
#100045 = CARTESIAN_POINT ( 'NONE',  ( 19.03943276465977164, -0.05219959533909143690, 98.74890960531436690 ) ) ;
#100046 = CARTESIAN_POINT ( 'NONE',  ( -16.52544592524342804, 4.483927247898546575, 86.04057627198102409 ) ) ;
#100047 = CARTESIAN_POINT ( 'NONE',  ( -10.72451020669898014, 18.67979575497178502, 35.41557627198102409 ) ) ;
#100048 = CARTESIAN_POINT ( 'NONE',  ( -15.80617190586745835, -15.72974639402198527, 26.87390960531435979 ) ) ;
#100049 = CARTESIAN_POINT ( 'NONE',  ( -14.29746914071049879, 8.314922557960819915, 85.83224293864768129 ) ) ;
#100050 = CARTESIAN_POINT ( 'NONE',  ( -17.05587630539785948, 6.762274262135695047, 55.74180309037311787 ) ) ;
#100051 = CARTESIAN_POINT ( 'NONE',  ( 19.05341960407617918, -5.049401038297876454, 46.04275706135233293 ) ) ;
#100052 = CARTESIAN_POINT ( 'NONE',  ( 4.379528057220092307, 16.55341960407617563, 112.2927570613523471 ) ) ;
#100053 = CARTESIAN_POINT ( 'NONE',  ( 13.97604488694527802, 13.89961937509977652, 104.3739096053143385 ) ) ;
#100054 = CARTESIAN_POINT ( 'NONE',  ( 0.05219959533937995610, -21.53943276465977519, 65.00109039468568994 ) ) ;
#100055 = CARTESIAN_POINT ( 'NONE',  ( -15.80617190586745835, -15.72974639402198527, 51.87390960531437401 ) ) ;
#100057 = ORIENTED_EDGE ( 'NONE', *, *, #124931, .T. ) ;
#100056 = CARTESIAN_POINT ( 'NONE',  ( 18.67979575497194134, -10.72451020669871369, 30.83442372801902209 ) ) ;
#100058 = CARTESIAN_POINT ( 'NONE',  ( -21.52544592524343514, 5.823673210054127303, 81.04057627198102409 ) ) ;
#100059 = CARTESIAN_POINT ( 'NONE',  ( -18.67979575497193778, 10.72451020669871902, 38.33442372801900433 ) ) ;
#100060 = CARTESIAN_POINT ( 'NONE',  ( -16.55341960407611168, -4.379528057220339221, 111.4572429386476813 ) ) ;
#100061 = CARTESIAN_POINT ( 'NONE',  ( 16.46253265017146816, 9.564922557961045513, 76.66775706135234714 ) ) ;
#100062 = CARTESIAN_POINT ( 'NONE',  ( 16.46253265017160672, -9.564922557960803928, 38.33224293864768839 ) ) ;
#100064 = CARTESIAN_POINT ( 'NONE',  ( 19.05341960407611168, 5.049401038298154454, 98.95724293864766707 ) ) ;
#100063 = CARTESIAN_POINT ( 'NONE',  ( -0.05219959533910754901, -16.53943276465976808, 97.49890960531436690 ) ) ;
#100065 = CARTESIAN_POINT ( 'NONE',  ( 5.153800228976335163, 19.02544592524342804, 89.79057627198102409 ) ) ;
#100066 = CARTESIAN_POINT ( 'NONE',  ( 19.03943276465977164, -0.05219959533909143690, 23.74890960531435269 ) ) ;
#100067 = CARTESIAN_POINT ( 'NONE',  ( 0.05219959533910956823, 16.53943276465976808, 34.99890960531435979 ) ) ;
#100068 = CARTESIAN_POINT ( 'NONE',  ( 16.55341960407618274, -4.379528057220086978, 101.0427570613523756 ) ) ;
#100069 = CARTESIAN_POINT ( 'NONE',  ( 16.46253265017160672, -9.564922557960803928, 53.33224293864768839 ) ) ;
#100070 = CARTESIAN_POINT ( 'NONE',  ( -16.46253265017160317, 9.564922557960807481, 25.83224293864769194 ) ) ;
#100071 = CARTESIAN_POINT ( 'NONE',  ( -9.474510206698720793, -16.51473224551083518, 24.58442372801900078 ) ) ;
#100073 = CARTESIAN_POINT ( 'NONE',  ( -14.34966873604972548, 8.224510206698743886, 113.3344237280190328 ) ) ;
#100072 = DIRECTION ( 'NONE',  ( 1.000000000000000000, 0.000000000000000000, 0.000000000000000000 ) ) ;
#100074 = CARTESIAN_POINT ( 'NONE',  ( -10.81492255796105439, 18.62759615963255655, 47.91775706135234714 ) ) ;
#100075 = CARTESIAN_POINT ( 'NONE',  ( 13.97604488694527802, 13.89961937509977652, 99.37390960531436690 ) ) ;
#100076 = CARTESIAN_POINT ( 'NONE',  ( -14.34966873604972548, 8.224510206698743886, 43.33442372801901143 ) ) ;
#100077 = CARTESIAN_POINT ( 'NONE',  ( 12.14591786802327356, -12.06949235617739191, 105.6260903946856899 ) ) ;
#100078 = CARTESIAN_POINT ( 'NONE',  ( 14.29746914071037800, 8.314922557961029526, 91.66775706135234714 ) ) ;
#100079 = CARTESIAN_POINT ( 'NONE',  ( -4.379528057220086978, -16.55341960407618274, 19.79275706135235069 ) ) ;
#100080 = CARTESIAN_POINT ( 'NONE',  ( 0.05219959533909260263, 19.03943276465977164, 49.99890960531435979 ) ) ;
#100081 = CARTESIAN_POINT ( 'NONE',  ( -8.314922557960811034, -14.29746914071050412, 102.0822429386476955 ) ) ;
#100082 = CARTESIAN_POINT ( 'NONE',  ( -5.719274019375665041, -21.55341960407619695, 19.79275706135235069 ) ) ;
#100083 = CARTESIAN_POINT ( 'NONE',  ( -19.02544592524342804, 5.153800228976336051, 31.04057627198102409 ) ) ;
#100084 = CARTESIAN_POINT ( 'NONE',  ( -9.564922557960796823, -16.46253265017161027, 102.0822429386477097 ) ) ;
#100085 = CARTESIAN_POINT ( 'NONE',  ( 19.02544592524343514, -5.153800228976328945, 33.54057627198102409 ) ) ;
#100086 = CARTESIAN_POINT ( 'NONE',  ( -19.05341960407611168, -5.049401038298163336, 106.4572429386476955 ) ) ;
#100087 = CARTESIAN_POINT ( 'NONE',  ( -15.06137443927351249, 15.06137443927345210, -65.00100000000003320 ) ) ;
#100088 = AXIS2_PLACEMENT_3D ( 'NONE', #52188, #9703, #176556 ) ;
#100089 = CARTESIAN_POINT ( 'NONE',  ( -13.97604488694527625, -13.89961937509977652, 91.87390960531432427 ) ) ;
#100091 = CARTESIAN_POINT ( 'NONE',  ( -14.29746914071049879, 8.314922557960819915, 105.8322429386476955 ) ) ;
#100090 = CARTESIAN_POINT ( 'NONE',  ( 0.05219959533937995610, -21.53943276465977519, 45.00109039468568284 ) ) ;
#100092 = CARTESIAN_POINT ( 'NONE',  ( -5.153800228976328057, -19.02544592524343514, 112.2905762719810099 ) ) ;
#100093 = DIRECTION ( 'NONE',  ( 0.000000000000000000, 0.000000000000000000, 1.000000000000000000 ) ) ;
#100094 = CARTESIAN_POINT ( 'NONE',  ( 16.53943276465976808, 0.05219959533934440121, 61.25109039468567573 ) ) ;
#100095 = CARTESIAN_POINT ( 'NONE',  ( -10.81492255796105439, 18.62759615963255655, 92.91775706135236135 ) ) ;
#100096 = CARTESIAN_POINT ( 'NONE',  ( 8.224510206698742110, 14.34966873604972548, 42.08442372801901854 ) ) ;
#100097 = CARTESIAN_POINT ( 'NONE',  ( -13.97604488694527625, -13.89961937509977652, 81.87390960531436690 ) ) ;
#100098 = CARTESIAN_POINT ( 'NONE',  ( -19.05341960407617563, 5.049401038297882671, 113.5427570613523471 ) ) ;
#100099 = CARTESIAN_POINT ( 'NONE',  ( 12.14591786802327356, -12.06949235617739191, 80.62609039468567573 ) ) ;
#100100 = CARTESIAN_POINT ( 'NONE',  ( -5.153800228976607833, 19.02544592524334988, 87.70942372801897591 ) ) ;
#100101 = CARTESIAN_POINT ( 'NONE',  ( 13.89961937509977652, -13.97604488694527269, 83.12390960531436690 ) ) ;
#100102 = CARTESIAN_POINT ( 'NONE',  ( 5.823673210054125526, 21.52544592524343514, 99.79057627198103830 ) ) ;
#100104 = CARTESIAN_POINT ( 'NONE',  ( 5.153800228976615827, -19.02544592524334988, 85.20942372801900433 ) ) ;
#100103 = CARTESIAN_POINT ( 'NONE',  ( -14.29746914071049879, 8.314922557960819915, 90.83224293864769550 ) ) ;
#100105 = CARTESIAN_POINT ( 'NONE',  ( -12.06949235617739369, -12.14591786802326823, 64.37609039468568994 ) ) ;
#100106 = CARTESIAN_POINT ( 'NONE',  ( 21.73861122199407347, 5.803778330637469729, 172.6157762304496828 ) ) ;
#100107 = CARTESIAN_POINT ( 'NONE',  ( -9.474510206698720793, -16.51473224551083518, 69.58442372801901854 ) ) ;
#100108 = CARTESIAN_POINT ( 'NONE',  ( 4.379528057220339221, -16.55341960407611168, 27.70724293864769905 ) ) ;
#100109 = CARTESIAN_POINT ( 'NONE',  ( 4.379528057220339221, -16.55341960407611168, 92.70724293864770971 ) ) ;
#100111 = CARTESIAN_POINT ( 'NONE',  ( 9.564922557961047289, -16.46253265017146816, 45.41775706135232582 ) ) ;
#100110 = CARTESIAN_POINT ( 'NONE',  ( 0.05219959533936267826, -19.03943276465977164, 25.00109039468566152 ) ) ;
#100112 = CARTESIAN_POINT ( 'NONE',  ( -15.72974639402176322, -15.80617190586768395, 24.37609039468567573 ) ) ;
#100113 =( BOUNDED_CURVE ( )  B_SPLINE_CURVE ( 3, ( #23387, #115395, #98188, #177083 ),
 .UNSPECIFIED., .F., .T. ) 
 B_SPLINE_CURVE_WITH_KNOTS ( ( 4, 4 ),
 ( 1.570796326794896558, 2.008945357379067431 ),
 .UNSPECIFIED. ) 
 CURVE ( )  GEOMETRIC_REPRESENTATION_ITEM ( )  RATIONAL_B_SPLINE_CURVE ( ( 1.000000000000000000, 0.9840659996946589105, 0.9840659996946589105, 1.000000000000000000 ) ) 
 REPRESENTATION_ITEM ( '' )  );
#100114 = CARTESIAN_POINT ( 'NONE',  ( -13.89961937509977652, 13.97604488694528158, 115.6239096053143669 ) ) ;
#100115 = CARTESIAN_POINT ( 'NONE',  ( -16.51473224551069308, -9.474510206698971260, 71.66557627198102409 ) ) ;
#100116 = CARTESIAN_POINT ( 'NONE',  ( -5.719274019375665041, -21.55341960407619695, 94.79275706135234714 ) ) ;
#100117 = CARTESIAN_POINT ( 'NONE',  ( -5.049401038298153566, 19.05341960407611168, 70.20724293864769550 ) ) ;
#100118 = CARTESIAN_POINT ( 'NONE',  ( -21.52544592524343514, 5.823673210054127303, 41.04057627198103120 ) ) ;
#100119 = CARTESIAN_POINT ( 'NONE',  ( -16.53943276465976808, 0.05219959533911058130, 81.24890960531436690 ) ) ;
#100120 = CARTESIAN_POINT ( 'NONE',  ( -16.46253265017160317, 9.564922557960807481, 50.83224293864770260 ) ) ;
#100121 = CARTESIAN_POINT ( 'NONE',  ( -16.53943276465976808, 0.05219959533911058130, 116.2489096053143669 ) ) ;
#100122 = CARTESIAN_POINT ( 'NONE',  ( 10.81492255796106328, -18.62759615963255655, 30.41775706135234358 ) ) ;
#100123 = AXIS2_PLACEMENT_3D ( 'NONE', #109286, #169968, #168960 ) ;
#100124 = CARTESIAN_POINT ( 'NONE',  ( -0.05219959533937732626, 21.53943276465977519, 57.50109039468568994 ) ) ;
#100125 = CARTESIAN_POINT ( 'NONE',  ( -16.46253265017160317, 9.564922557960807481, 45.83224293864769550 ) ) ;
#100126 = CARTESIAN_POINT ( 'NONE',  ( -4.483927247898782831, 16.52544592524335698, 77.70942372801900433 ) ) ;
#100127 = CARTESIAN_POINT ( 'NONE',  ( 15.80617190586769283, -15.72974639402175789, 20.62609039468568639 ) ) ;
#100128 = EDGE_LOOP ( 'NONE', ( #22589, #23138, #173416, #144002 ) ) ;
#100129 = CARTESIAN_POINT ( 'NONE',  ( 0.05219959533907565091, 21.53943276465977519, 104.9989096053143669 ) ) ;
#100131 = CARTESIAN_POINT ( 'NONE',  ( 19.05341960407611168, 5.049401038298154454, 68.95724293864769550 ) ) ;
#100130 = CARTESIAN_POINT ( 'NONE',  ( -13.97604488694547697, 13.89961937509957934, 38.12609039468566152 ) ) ;
#100132 = CARTESIAN_POINT ( 'NONE',  ( -16.46253265017146816, -9.564922557961047289, 34.16775706135233293 ) ) ;
#100133 = CARTESIAN_POINT ( 'NONE',  ( -18.67979575497193778, 10.72451020669871902, 73.33442372801901854 ) ) ;
#100134 = CARTESIAN_POINT ( 'NONE',  ( 15.80617190586746368, 15.72974639402197994, 64.37390960531435269 ) ) ;
#100135 = CARTESIAN_POINT ( 'NONE',  ( 16.52544592524342804, -4.483927247898539470, 38.54057627198103120 ) ) ;
#100137 = CARTESIAN_POINT ( 'NONE',  ( -13.97604488694547697, 13.89961937509957934, 33.12609039468566863 ) ) ;
#100136 = CARTESIAN_POINT ( 'NONE',  ( 18.67979575497194134, -10.72451020669871369, 95.83442372801903275 ) ) ;
#100138 = CARTESIAN_POINT ( 'NONE',  ( -16.55341960407611168, -4.379528057220339221, 61.45724293864770260 ) ) ;
#100139 = CARTESIAN_POINT ( 'NONE',  ( 8.224510206698953496, -14.34966873604960469, 107.9155762719810241 ) ) ;
#100140 = CARTESIAN_POINT ( 'NONE',  ( -16.46253265017146816, -9.564922557961047289, 59.16775706135233293 ) ) ;
#100141 = CARTESIAN_POINT ( 'NONE',  ( -8.224510206698948167, 14.34966873604960824, 25.41557627198103120 ) ) ;
#100142 = CARTESIAN_POINT ( 'NONE',  ( -10.72451020669870658, -18.67979575497194134, 64.58442372801900433 ) ) ;
#100143 = CARTESIAN_POINT ( 'NONE',  ( -19.03943276465977164, 0.05219959533909376836, 76.24890960531435269 ) ) ;
#100144 = CARTESIAN_POINT ( 'NONE',  ( 19.02544592524334988, 5.153800228976608722, 46.45942372801899012 ) ) ;
#100145 = CARTESIAN_POINT ( 'NONE',  ( -15.72974639402197994, 15.80617190586746368, 50.62390960531435979 ) ) ;
#100146 = CARTESIAN_POINT ( 'NONE',  ( -5.823673210054431948, 21.52544592524334988, 47.70942372801902565 ) ) ;
#100147 = CARTESIAN_POINT ( 'NONE',  ( 10.72451020669898902, -18.67979575497178502, 107.9155762719810241 ) ) ;
#100148 = CARTESIAN_POINT ( 'NONE',  ( 0.05219959533936267826, -19.03943276465977164, 100.0010903946856757 ) ) ;
#100149 = CARTESIAN_POINT ( 'NONE',  ( 16.55341960407618274, -4.379528057220086978, 71.04275706135234714 ) ) ;
#100151 = CARTESIAN_POINT ( 'NONE',  ( 15.80617190586746368, 15.72974639402197994, 104.3739096053143669 ) ) ;
#100150 = DIRECTION ( 'NONE',  ( -1.000000000000000000, -0.000000000000000000, -0.000000000000000000 ) ) ;
#100152 = CARTESIAN_POINT ( 'NONE',  ( 12.14591786802309770, 12.06949235617756955, 94.37390960531436690 ) ) ;
#100153 = CARTESIAN_POINT ( 'NONE',  ( -16.18388926212238843, -7.379444403734542135, 100.4395315136615494 ) ) ;
#100154 = CARTESIAN_POINT ( 'NONE',  ( -16.52544592524335698, -4.483927247898792601, 28.95942372801902209 ) ) ;
#100155 = CARTESIAN_POINT ( 'NONE',  ( -5.823673210054116645, -21.52544592524344225, 42.29057627198103120 ) ) ;
#100156 = CARTESIAN_POINT ( 'NONE',  ( 14.29746914071037800, 8.314922557961029526, 91.66775706135234714 ) ) ;
#100157 = CARTESIAN_POINT ( 'NONE',  ( 5.049401038298161559, -19.05341960407611168, 22.70724293864769194 ) ) ;
#100158 = CARTESIAN_POINT ( 'NONE',  ( 8.224510206698742110, 14.34966873604972548, 62.08442372801901143 ) ) ;
#100159 = CARTESIAN_POINT ( 'NONE',  ( -21.52544592524334988, -5.823673210054445271, 33.95942372801901143 ) ) ;
#100160 = CARTESIAN_POINT ( 'NONE',  ( 0.05219959533907565091, 21.53943276465977519, 39.99890960531436690 ) ) ;
#100161 = CARTESIAN_POINT ( 'NONE',  ( -14.34966873604972548, 8.224510206698743886, 83.33442372801903275 ) ) ;
#100162 = CARTESIAN_POINT ( 'NONE',  ( -16.51473224551069308, -9.474510206698971260, 91.66557627198103830 ) ) ;
#100163 = CARTESIAN_POINT ( 'NONE',  ( -15.80617190586768217, 15.72974639402176855, 73.12609039468567573 ) ) ;
#100164 = CARTESIAN_POINT ( 'NONE',  ( 10.81492255796078972, 18.62759615963270932, 34.58224293864770260 ) ) ;
#100165 = CARTESIAN_POINT ( 'NONE',  ( 15.72974639402199770, -15.80617190586745480, 33.12390960531435979 ) ) ;
#100166 = ORIENTED_EDGE ( 'NONE', *, *, #143807, .F. ) ;
#100167 = CARTESIAN_POINT ( 'NONE',  ( 9.474510206698729675, 16.51473224551082808, 47.08442372801900433 ) ) ;
#100168 = CARTESIAN_POINT ( 'NONE',  ( 16.52544592524335698, 4.483927247898782831, 66.45942372801903275 ) ) ;
#100169 = CARTESIAN_POINT ( 'NONE',  ( -21.53943276465977519, 0.05219959533907696930, 31.24890960531435979 ) ) ;
#100170 = VERTEX_POINT ( 'NONE', #172965 ) ;
#100171 = CARTESIAN_POINT ( 'NONE',  ( 19.03943276465977164, -0.05219959533909143690, 88.74890960531436690 ) ) ;
#100172 = CARTESIAN_POINT ( 'NONE',  ( -8.314922557960811034, -14.29746914071050412, 27.08224293864769550 ) ) ;
#100173 = CARTESIAN_POINT ( 'NONE',  ( -18.22780087662121673, -5.500000000000063061, 56.48459894673892734 ) ) ;
#100174 = CARTESIAN_POINT ( 'NONE',  ( 14.34966873604960469, 8.224510206698951720, 114.1655762719810383 ) ) ;
#100175 = CARTESIAN_POINT ( 'NONE',  ( -5.823673210054116645, -21.52544592524344225, 47.29057627198103120 ) ) ;
#100176 = CARTESIAN_POINT ( 'NONE',  ( 9.564922557960805705, 16.46253265017160317, 49.58224293864770260 ) ) ;
#100177 = CARTESIAN_POINT ( 'NONE',  ( -14.29746914071037622, -8.314922557961029526, 79.16775706135234714 ) ) ;
#100178 = CARTESIAN_POINT ( 'NONE',  ( -18.62759615963255300, -10.81492255796106328, 39.16775706135235424 ) ) ;
#100179 = CARTESIAN_POINT ( 'NONE',  ( -13.89961937509957401, -13.97604488694547875, 84.37609039468567573 ) ) ;
#100180 = CARTESIAN_POINT ( 'NONE',  ( 8.314922557960818139, 14.29746914071049879, 84.58224293864769550 ) ) ;
#100181 = CARTESIAN_POINT ( 'NONE',  ( 16.46253265017160672, -9.564922557960803928, 58.33224293864769550 ) ) ;
#100182 = CARTESIAN_POINT ( 'NONE',  ( -16.51473224551069308, -9.474510206698971260, 31.66557627198102054 ) ) ;
#100183 = CARTESIAN_POINT ( 'NONE',  ( 10.81492255796106328, -18.62759615963255655, 100.4177570613523471 ) ) ;
#100184 = CARTESIAN_POINT ( 'NONE',  ( -19.02544592524342804, 5.153800228976336051, 76.04057627198102409 ) ) ;
#100185 = CARTESIAN_POINT ( 'NONE',  ( 8.314922557961029526, -14.29746914071037800, 65.41775706135234714 ) ) ;
#100186 = CARTESIAN_POINT ( 'NONE',  ( -15.72974639402176322, -15.80617190586768395, 99.37609039468568994 ) ) ;
#100187 = CARTESIAN_POINT ( 'NONE',  ( 18.67979575497178502, 10.72451020669898547, 54.16557627198103120 ) ) ;
#100188 = CARTESIAN_POINT ( 'NONE',  ( -16.53943276465976808, -0.05219959533934237506, 68.75109039468568994 ) ) ;
#100189 = CARTESIAN_POINT ( 'NONE',  ( 5.153800228976615827, -19.02544592524334988, 50.20942372801897591 ) ) ;
#100190 = CARTESIAN_POINT ( 'NONE',  ( 9.564922557961047289, -16.46253265017146816, 70.41775706135233293 ) ) ;
#100191 = ORIENTED_EDGE ( 'NONE', *, *, #15456, .F. ) ;
#100192 = CARTESIAN_POINT ( 'NONE',  ( 15.72974639402176855, 15.80617190586768217, 56.87609039468568994 ) ) ;
#100193 = CARTESIAN_POINT ( 'NONE',  ( -16.51473224551069308, -9.474510206698971260, 61.66557627198103120 ) ) ;
#100194 = CARTESIAN_POINT ( 'NONE',  ( -16.46253265017160317, 9.564922557960807481, 35.83224293864768839 ) ) ;
#100195 = CARTESIAN_POINT ( 'NONE',  ( 0.05219959533936267826, -19.03943276465977164, 60.00109039468566863 ) ) ;
#100196 = CARTESIAN_POINT ( 'NONE',  ( -0.05219959533909027116, -19.03943276465977164, 107.4989096053143527 ) ) ;
#100197 = CARTESIAN_POINT ( 'NONE',  ( -16.46253265017160317, 9.564922557960807481, 95.83224293864769550 ) ) ;
#100198 = CARTESIAN_POINT ( 'NONE',  ( -14.29746914071049879, 8.314922557960819915, 55.83224293864770260 ) ) ;
#100199 = CARTESIAN_POINT ( 'NONE',  ( 21.52544592524344225, -5.823673210054117533, 48.54057627198103120 ) ) ;
#100200 = LINE ( 'NONE', #67868, #86839 ) ;
#100201 = CARTESIAN_POINT ( 'NONE',  ( 10.81492255796106328, -18.62759615963255655, 110.4177570613523756 ) ) ;
#100202 = CARTESIAN_POINT ( 'NONE',  ( -16.52216118717208104, -7.221426719304496089, 81.07599021046993926 ) ) ;
#100203 = CARTESIAN_POINT ( 'NONE',  ( -19.05341960407611168, -5.049401038298163336, 46.45724293864768129 ) ) ;
#100204 = EDGE_CURVE ( 'NONE', #64219, #89664, #113256, .T. ) ;
#100205 = CARTESIAN_POINT ( 'NONE',  ( 30.20036327792367814, -26.22857331006468584, -17.18026671435356434 ) ) ;
#100206 = CARTESIAN_POINT ( 'NONE',  ( -17.05116617787824396, 6.768360034955808402, 108.6567555325920296 ) ) ;
#100207 = CARTESIAN_POINT ( 'NONE',  ( 4.379528057220092307, 16.55341960407617563, 67.29275706135234714 ) ) ;
#100208 = CARTESIAN_POINT ( 'NONE',  ( -15.80617190586745835, -15.72974639402198527, 91.87390960531436690 ) ) ;
#100209 = CARTESIAN_POINT ( 'NONE',  ( -8.314922557960811034, -14.29746914071050412, 47.08224293864770260 ) ) ;
#100211 = DIRECTION ( 'NONE',  ( -0.4999999999999933387, 0.5000000000000055511, -0.7071067811865484609 ) ) ;
#100210 = CARTESIAN_POINT ( 'NONE',  ( 19.02544592524343514, -5.153800228976328945, 43.54057627198103120 ) ) ;
#100212 = CARTESIAN_POINT ( 'NONE',  ( 18.67979575497194134, -10.72451020669871369, 35.83442372801901143 ) ) ;
#100213 = CARTESIAN_POINT ( 'NONE',  ( 19.03943276465977164, 0.05219959533936151252, 51.25109039468567573 ) ) ;
#100214 = CARTESIAN_POINT ( 'NONE',  ( -19.05341960407611168, -5.049401038298163336, 36.45724293864766707 ) ) ;
#100215 = CARTESIAN_POINT ( 'NONE',  ( 21.52544592524334988, 5.823673210054432836, 101.4594237280190185 ) ) ;
#100216 = CARTESIAN_POINT ( 'NONE',  ( -24.55187747166650425, -5.935858836270472061, 169.5341757581197726 ) ) ;
#100217 = CARTESIAN_POINT ( 'NONE',  ( -14.34966873604960291, -8.224510206698953496, 41.66557627198103120 ) ) ;
#100218 = DIRECTION ( 'NONE',  ( -0.000000000000000000, 1.000000000000000000, 1.224646799147353207E-16 ) ) ;
#100219 = CARTESIAN_POINT ( 'NONE',  ( -21.55341960407610458, -5.719274019375992779, 36.45724293864768839 ) ) ;
#100220 = CARTESIAN_POINT ( 'NONE',  ( 1.784210473542230573E-15, -29.16686587814331588, 141.3750000027311557 ) ) ;
#100221 = CARTESIAN_POINT ( 'NONE',  ( 5.153800228976335163, 19.02544592524342804, 84.79057627198099567 ) ) ;
#100222 = CARTESIAN_POINT ( 'NONE',  ( 16.52544592524342804, -4.483927247898539470, 83.54057627198102409 ) ) ;
#100223 = CARTESIAN_POINT ( 'NONE',  ( 16.52544592524335698, 4.483927247898782831, 26.45942372801901854 ) ) ;
#100224 = CARTESIAN_POINT ( 'NONE',  ( -8.314922557961024197, 14.29746914071037800, 112.9177570613523329 ) ) ;
#100225 = ORIENTED_EDGE ( 'NONE', *, *, #90031, .T. ) ;
#100227 = CARTESIAN_POINT ( 'NONE',  ( -10.81492255796078084, -18.62759615963271287, 87.08224293864769550 ) ) ;
#100226 = CARTESIAN_POINT ( 'NONE',  ( -9.474510206698964154, 16.51473224551069663, 105.4155762719810383 ) ) ;
#100229 = CARTESIAN_POINT ( 'NONE',  ( -16.51473224551069308, -9.474510206698971260, 101.6655762719810241 ) ) ;
#100228 = CARTESIAN_POINT ( 'NONE',  ( -8.314922557960811034, -14.29746914071050412, 22.08224293864769194 ) ) ;
#100230 = CARTESIAN_POINT ( 'NONE',  ( -19.02544592524334988, -5.153800228976617603, 78.95942372801900433 ) ) ;
#100231 = CARTESIAN_POINT ( 'NONE',  ( 21.55341960407619695, -5.719274019375665929, 106.0427570613523471 ) ) ;
#100232 = CARTESIAN_POINT ( 'NONE',  ( 18.67979575497178502, 10.72451020669898547, 84.16557627198103830 ) ) ;
#100233 = CARTESIAN_POINT ( 'NONE',  ( 18.62759615963271287, -10.81492255796078972, 38.33224293864768839 ) ) ;
#100234 = CARTESIAN_POINT ( 'NONE',  ( -13.89961937509977652, 13.97604488694528158, 65.62390960531436690 ) ) ;
#100235 = CARTESIAN_POINT ( 'NONE',  ( -14.29746914071049879, 8.314922557960819915, 30.83224293864770260 ) ) ;
#100236 = CARTESIAN_POINT ( 'NONE',  ( -0.05219959533909027116, -19.03943276465977164, 72.49890960531435269 ) ) ;
#100237 = ORIENTED_EDGE ( 'NONE', *, *, #186207, .F. ) ;
#100238 = CARTESIAN_POINT ( 'NONE',  ( 5.000000000000000000, -116.8122400552013431, 54.87277500418469600 ) ) ;
#100239 = CARTESIAN_POINT ( 'NONE',  ( 5.049401038297881783, 19.05341960407617563, 32.29275706135233293 ) ) ;
#100240 = CARTESIAN_POINT ( 'NONE',  ( -0.05219959533910754901, -16.53943276465976808, 87.49890960531436690 ) ) ;
#100241 = CARTESIAN_POINT ( 'NONE',  ( 21.52544592524334988, 5.823673210054432836, 26.45942372801901854 ) ) ;
#100242 = CARTESIAN_POINT ( 'NONE',  ( -17.14385361876520619, 23.59649016807275856, 141.0750000027311728 ) ) ;
#100243 = CARTESIAN_POINT ( 'NONE',  ( 10.72451020669898902, -18.67979575497178502, 77.91557627198102409 ) ) ;
#100244 = CARTESIAN_POINT ( 'NONE',  ( -14.29746914071037622, -8.314922557961029526, 94.16775706135237556 ) ) ;
#100245 = CARTESIAN_POINT ( 'NONE',  ( 9.474510206698971260, -16.51473224551069308, 27.91557627198103120 ) ) ;
#100246 = CARTESIAN_POINT ( 'NONE',  ( 19.05341960407611168, 5.049401038298154454, 68.95724293864769550 ) ) ;
#100247 =( NAMED_UNIT ( * ) SI_UNIT ( $, .STERADIAN. ) SOLID_ANGLE_UNIT ( ) );
#100248 = CARTESIAN_POINT ( 'NONE',  ( 19.05341960407611168, 5.049401038298154454, 23.95724293864769194 ) ) ;
#100249 = CARTESIAN_POINT ( 'NONE',  ( -12.06949235617756955, 12.14591786802309770, 25.62390960531435624 ) ) ;
#100250 = CARTESIAN_POINT ( 'NONE',  ( -10.72451020669870658, -18.67979575497194134, 59.58442372801901854 ) ) ;
#100251 = CARTESIAN_POINT ( 'NONE',  ( 32.72233185158318491, -19.32382731392758402, -21.08582493607095998 ) ) ;
#100252 = CARTESIAN_POINT ( 'NONE',  ( -0.05219959533937732626, 21.53943276465977519, 97.50109039468567573 ) ) ;
#100253 = CARTESIAN_POINT ( 'NONE',  ( 19.02544592524343514, -5.153800228976328945, 43.54057627198103120 ) ) ;
#100254 = CARTESIAN_POINT ( 'NONE',  ( -16.46253265017160317, 9.564922557960807481, 55.83224293864769550 ) ) ;
#100255 = ORIENTED_EDGE ( 'NONE', *, *, #89811, .T. ) ;
#100256 = CARTESIAN_POINT ( 'NONE',  ( -21.52544592524334988, -5.823673210054445271, 88.95942372801901854 ) ) ;
#100257 = CARTESIAN_POINT ( 'NONE',  ( 16.52544592524335698, 4.483927247898782831, 66.45942372801903275 ) ) ;
#100258 = CARTESIAN_POINT ( 'NONE',  ( -10.81492255796105439, 18.62759615963255655, 82.91775706135234714 ) ) ;
#100259 = CARTESIAN_POINT ( 'NONE',  ( -10.81492255796078084, -18.62759615963271287, 27.08224293864769550 ) ) ;
#100260 = CARTESIAN_POINT ( 'NONE',  ( -19.05341960407617563, 5.049401038297882671, 98.54275706135233293 ) ) ;
#100261 = CARTESIAN_POINT ( 'NONE',  ( -10.81492255796105439, 18.62759615963255655, 67.91775706135234714 ) ) ;
#100262 = CARTESIAN_POINT ( 'NONE',  ( -16.53943276465976808, -0.05219959533934237506, 38.75109039468567573 ) ) ;
#100263 = CARTESIAN_POINT ( 'NONE',  ( 5.719274019375991003, -21.55341960407610458, 82.70724293864770971 ) ) ;
#100264 = CARTESIAN_POINT ( 'NONE',  ( 13.97604488694548053, -13.89961937509957401, 90.62609039468567573 ) ) ;
#100265 = CARTESIAN_POINT ( 'NONE',  ( 0.05219959533909260263, 19.03943276465977164, 64.99890960531436690 ) ) ;
#100266 = CARTESIAN_POINT ( 'NONE',  ( 5.153800228976615827, -19.02544592524334988, 90.20942372801900433 ) ) ;
#100267 = CARTESIAN_POINT ( 'NONE',  ( 19.03943276465977164, 0.05219959533936151252, 101.2510903946856757 ) ) ;
#100268 = CARTESIAN_POINT ( 'NONE',  ( -0.05219959533910754901, -16.53943276465976808, 57.49890960531435979 ) ) ;
#100270 = ORIENTED_EDGE ( 'NONE', *, *, #164449, .T. ) ;
#100269 = CARTESIAN_POINT ( 'NONE',  ( -5.049401038297874678, -19.05341960407617918, 74.79275706135231871 ) ) ;
#100271 = CARTESIAN_POINT ( 'NONE',  ( -0.05219959533934338120, 16.53943276465976808, 62.50109039468568284 ) ) ;
#100272 = ADVANCED_FACE ( 'NONE', ( #127431 ), #109548, .T. ) ;
#100273 = CARTESIAN_POINT ( 'NONE',  ( 5.153800228976335163, 19.02544592524342804, 44.79057627198103830 ) ) ;
#100274 = CARTESIAN_POINT ( 'NONE',  ( 13.97604488694527802, 13.89961937509977652, 59.37390960531434558 ) ) ;
#100275 = CARTESIAN_POINT ( 'NONE',  ( -14.29746914071037622, -8.314922557961029526, 59.16775706135234714 ) ) ;
#100276 = DIRECTION ( 'NONE',  ( -1.000000000000000000, 0.000000000000000000, 0.000000000000000000 ) ) ;
#100277 = CARTESIAN_POINT ( 'NONE',  ( -28.82186960331499392, -9.364793116373526516, 142.3500000054623342 ) ) ;
#100278 = CARTESIAN_POINT ( 'NONE',  ( 0.05219959533909260263, 19.03943276465977164, 104.9989096053143669 ) ) ;
#100279 = CARTESIAN_POINT ( 'NONE',  ( 0.05219959533909260263, 19.03943276465977164, 24.99890960531435269 ) ) ;
#100280 = ORIENTED_EDGE ( 'NONE', *, *, #11460, .F. ) ;
#100281 = CARTESIAN_POINT ( 'NONE',  ( -13.97604488694547697, 13.89961937509957934, 103.1260903946856473 ) ) ;
#100282 = EDGE_CURVE ( 'NONE', #110833, #88111, #73265, .T. ) ;
#100283 = CARTESIAN_POINT ( 'NONE',  ( -21.55341960407610458, -5.719274019375992779, 31.45724293864769550 ) ) ;
#100285 = CARTESIAN_POINT ( 'NONE',  ( 0.05219959533934541429, -16.53943276465976808, 20.00109039468568639 ) ) ;
#100284 = CARTESIAN_POINT ( 'NONE',  ( -5.153800228976607833, 19.02544592524334988, 37.70942372801899722 ) ) ;
#100286 = CARTESIAN_POINT ( 'NONE',  ( -13.89961937509977652, 13.97604488694528158, 30.62390960531435269 ) ) ;
#100287 = CARTESIAN_POINT ( 'NONE',  ( 5.153800228976335163, 19.02544592524342804, 54.79057627198103120 ) ) ;
#100288 = CARTESIAN_POINT ( 'NONE',  ( -5.823673210054116645, -21.52544592524344225, 72.29057627198102409 ) ) ;
#100289 = CARTESIAN_POINT ( 'NONE',  ( 19.05341960407611168, 5.049401038298154454, 98.95724293864766707 ) ) ;
#100290 = CARTESIAN_POINT ( 'NONE',  ( -19.05341960407611168, -5.049401038298163336, 36.45724293864766707 ) ) ;
#100291 = CARTESIAN_POINT ( 'NONE',  ( -8.571926809382601320, -26.38167802310801591, 141.7750000027311899 ) ) ;
#100292 = CARTESIAN_POINT ( 'NONE',  ( -9.564922557961040184, 16.46253265017147172, 77.91775706135234714 ) ) ;
#100293 = CARTESIAN_POINT ( 'NONE',  ( 16.53943276465976808, -0.05219959533910856209, 63.74890960531435979 ) ) ;
#100294 = CARTESIAN_POINT ( 'NONE',  ( -15.80617190586745835, -15.72974639402198527, 51.87390960531437401 ) ) ;
#100295 = CARTESIAN_POINT ( 'NONE',  ( 18.67979575497194134, -10.72451020669871369, 105.8344237280190328 ) ) ;
#100296 = CARTESIAN_POINT ( 'NONE',  ( 10.81492255796078972, 18.62759615963270932, 94.58224293864769550 ) ) ;
#100297 = CARTESIAN_POINT ( 'NONE',  ( -10.81492255796105439, 18.62759615963255655, 67.91775706135234714 ) ) ;
#100298 = CARTESIAN_POINT ( 'NONE',  ( 0.05219959533937995610, -21.53943276465977519, 75.00109039468568994 ) ) ;
#100299 = CARTESIAN_POINT ( 'NONE',  ( -13.89961937509977652, 13.97604488694528158, 110.6239096053143243 ) ) ;
#100301 = CARTESIAN_POINT ( 'NONE',  ( -15.80617190586768217, 15.72974639402176855, 78.12609039468570415 ) ) ;
#100300 = CARTESIAN_POINT ( 'NONE',  ( 12.14591786802327356, -12.06949235617739191, 110.6260903946857042 ) ) ;
#100302 = CARTESIAN_POINT ( 'NONE',  ( -9.474510206698964154, 16.51473224551069663, 70.41557627198102409 ) ) ;
#100303 = CARTESIAN_POINT ( 'NONE',  ( -16.51473224551082808, 9.474510206698731452, 38.33442372801899722 ) ) ;
#100304 = CARTESIAN_POINT ( 'NONE',  ( -10.72451020669870658, -18.67979575497194134, 24.58442372801901499 ) ) ;
#100305 = CARTESIAN_POINT ( 'NONE',  ( -5.153800228976328057, -19.02544592524343514, 62.29057627198100988 ) ) ;
#100306 = CARTESIAN_POINT ( 'NONE',  ( 4.483927247898545687, 16.52544592524342804, 84.79057627198102409 ) ) ;
#100307 = CARTESIAN_POINT ( 'NONE',  ( 16.53943276465976808, -0.05219959533910856209, 48.74890960531435979 ) ) ;
#100308 = CARTESIAN_POINT ( 'NONE',  ( -15.80617190586745835, -15.72974639402198527, 56.87390960531436690 ) ) ;
#100309 = CARTESIAN_POINT ( 'NONE',  ( 19.02544592524343514, -5.153800228976328945, 58.54057627198102409 ) ) ;
#100310 = CARTESIAN_POINT ( 'NONE',  ( 5.823673210054125526, 21.52544592524343514, 69.79057627198102409 ) ) ;
#100311 = CARTESIAN_POINT ( 'NONE',  ( -13.97604488694547697, 13.89961937509957934, 58.12609039468566863 ) ) ;
#100312 = CARTESIAN_POINT ( 'NONE',  ( 0.05219959533910956823, 16.53943276465976808, 64.99890960531435269 ) ) ;
#100313 = CARTESIAN_POINT ( 'NONE',  ( -21.53943276465977519, 0.05219959533907696930, 46.24890960531435979 ) ) ;
#100314 = VERTEX_POINT ( 'NONE', #90385 ) ;
#100315 = DIRECTION ( 'NONE',  ( 0.000000000000000000, 0.000000000000000000, 1.000000000000000000 ) ) ;
#100317 = CARTESIAN_POINT ( 'NONE',  ( 1.197038699967498898, 6.690841975426986998, -64.41838970491137673 ) ) ;
#100316 = CARTESIAN_POINT ( 'NONE',  ( 16.52544592524335698, 4.483927247898782831, 86.45942372801901854 ) ) ;
#100318 = CARTESIAN_POINT ( 'NONE',  ( -13.97604488694547697, 13.89961937509957934, 83.12609039468564731 ) ) ;
#100319 = CARTESIAN_POINT ( 'NONE',  ( -4.483927247898539470, -16.52544592524342804, 57.29057627198103120 ) ) ;
#100320 = CARTESIAN_POINT ( 'NONE',  ( -19.34837522270366250, -5.499999999999742428, 60.86337684832576400 ) ) ;
#100321 = CARTESIAN_POINT ( 'NONE',  ( 13.89961937509977652, -13.97604488694527269, 48.12390960531435979 ) ) ;
#100322 = CARTESIAN_POINT ( 'NONE',  ( -14.34966873604960291, -8.224510206698953496, 36.66557627198103120 ) ) ;
#100323 = CARTESIAN_POINT ( 'NONE',  ( 0.05219959533909260263, 19.03943276465977164, 84.99890960531436690 ) ) ;
#100325 = CARTESIAN_POINT ( 'NONE',  ( -9.564922557960796823, -16.46253265017161027, 57.08224293864769550 ) ) ;
#100324 = CARTESIAN_POINT ( 'NONE',  ( 5.153800228976615827, -19.02544592524334988, 75.20942372801896170 ) ) ;
#100326 = CARTESIAN_POINT ( 'NONE',  ( 0.05219959533937995610, -21.53943276465977519, 65.00109039468568994 ) ) ;
#100327 = CARTESIAN_POINT ( 'NONE',  ( -19.03943276465977164, 0.05219959533909376836, 86.24890960531436690 ) ) ;
#100328 = CARTESIAN_POINT ( 'NONE',  ( 0.05219959533909260263, 19.03943276465977164, 24.99890960531435269 ) ) ;
#100329 = CARTESIAN_POINT ( 'NONE',  ( -19.02544592524342804, 5.153800228976336051, 76.04057627198102409 ) ) ;
#100330 = CARTESIAN_POINT ( 'NONE',  ( 0.05219959533907565091, 21.53943276465977519, 54.99890960531435269 ) ) ;
#100331 = ADVANCED_BREP_SHAPE_REPRESENTATION ( '', ( #9086, #82054 ), #24091 ) ;
#100332 = CARTESIAN_POINT ( 'NONE',  ( 19.03943276465977164, -0.05219959533909143690, 43.74890960531435979 ) ) ;
#100333 = CARTESIAN_POINT ( 'NONE',  ( -21.55341960407610458, -5.719274019375992779, 56.45724293864768839 ) ) ;
#100334 = CARTESIAN_POINT ( 'NONE',  ( -19.03943276465977164, -0.05219959533935918106, 83.75109039468567573 ) ) ;
#100335 = CARTESIAN_POINT ( 'NONE',  ( -0.05219959533934338120, 16.53943276465976808, 102.5010903946856899 ) ) ;
#100336 = CARTESIAN_POINT ( 'NONE',  ( 16.51473224551083163, -9.474510206698727899, 30.83442372801900433 ) ) ;
#100338 = CARTESIAN_POINT ( 'NONE',  ( -16.53943276465976808, -0.05219959533934237506, 78.75109039468568994 ) ) ;
#100337 = CARTESIAN_POINT ( 'NONE',  ( 16.55341960407618274, -4.379528057220086978, 56.04275706135235424 ) ) ;
#100339 = CARTESIAN_POINT ( 'NONE',  ( -17.49999999999999645, 5.499999999999992895, 68.71769037696435589 ) ) ;
#100340 = CARTESIAN_POINT ( 'NONE',  ( -4.379528057220086978, -16.55341960407618274, 69.79275706135234714 ) ) ;
#100341 = CARTESIAN_POINT ( 'NONE',  ( -10.72451020669898014, 18.67979575497178502, 25.41557627198103120 ) ) ;
#100342 = CARTESIAN_POINT ( 'NONE',  ( -9.564922557960796823, -16.46253265017161027, 32.08224293864769550 ) ) ;
#100343 = CARTESIAN_POINT ( 'NONE',  ( 14.29746914071037800, 8.314922557961029526, 31.66775706135234358 ) ) ;
#100344 = CARTESIAN_POINT ( 'NONE',  ( -16.46253265017160317, 9.564922557960807481, 50.83224293864770260 ) ) ;
#100345 = CARTESIAN_POINT ( 'NONE',  ( -21.52544592524334988, -5.823673210054445271, 38.95942372801901854 ) ) ;
#100346 = CARTESIAN_POINT ( 'NONE',  ( 4.483927247898790824, -16.52544592524335698, 30.20942372801902565 ) ) ;
#100347 = CARTESIAN_POINT ( 'NONE',  ( -14.29746914071049879, 8.314922557960819915, 25.83224293864769194 ) ) ;
#100348 = CARTESIAN_POINT ( 'NONE',  ( -17.72662750342728089, -5.500000000000023093, 71.40179492283743912 ) ) ;
#100349 = CARTESIAN_POINT ( 'NONE',  ( -0.05219959533937732626, 21.53943276465977519, 112.5010903946857042 ) ) ;
#100350 = CARTESIAN_POINT ( 'NONE',  ( 9.474510206698729675, 16.51473224551082808, 107.0844237280190043 ) ) ;
#100351 = CARTESIAN_POINT ( 'NONE',  ( 9.474510206698729675, 16.51473224551082808, 67.08442372801900433 ) ) ;
#100352 = CARTESIAN_POINT ( 'NONE',  ( 0.05219959533910956823, 16.53943276465976808, 64.99890960531435269 ) ) ;
#100353 = CARTESIAN_POINT ( 'NONE',  ( 9.564922557960805705, 16.46253265017160317, 44.58224293864769550 ) ) ;
#100355 = CARTESIAN_POINT ( 'NONE',  ( -38.00000000000000711, 2.428612866367529932E-14, -3.749999994537626780 ) ) ;
#100354 = CARTESIAN_POINT ( 'NONE',  ( -0.05219959533936034679, 19.03943276465977164, 72.50109039468566152 ) ) ;
#100356 = CARTESIAN_POINT ( 'NONE',  ( -18.62759615963255300, -10.81492255796106328, 64.16775706135234714 ) ) ;
#100357 = CARTESIAN_POINT ( 'NONE',  ( -14.29746914071037622, -8.314922557961029526, 44.16775706135234714 ) ) ;
#100358 = CARTESIAN_POINT ( 'NONE',  ( 19.25663599770062362, -5.499999999999449329, 56.49419308057201761 ) ) ;
#100359 = CARTESIAN_POINT ( 'NONE',  ( 5.719274019375991003, -21.55341960407610458, 42.70724293864770260 ) ) ;
#100360 = CARTESIAN_POINT ( 'NONE',  ( 16.55341960407618274, -4.379528057220086978, 21.04275706135234714 ) ) ;
#100361 = CARTESIAN_POINT ( 'NONE',  ( 13.89961937509977652, -13.97604488694527269, 113.1239096053143527 ) ) ;
#100362 = CARTESIAN_POINT ( 'NONE',  ( -26.13941622279051913, 9.616497135380347672, 166.9083969906205311 ) ) ;
#100363 = CARTESIAN_POINT ( 'NONE',  ( -13.89961937509977652, 13.97604488694528158, 35.62390960531435269 ) ) ;
#100364 = CARTESIAN_POINT ( 'NONE',  ( -10.81492255796105439, 18.62759615963255655, 112.9177570613523329 ) ) ;
#100365 = CARTESIAN_POINT ( 'NONE',  ( -19.03943276465977164, 0.05219959533909376836, 56.24890960531435979 ) ) ;
#100366 = CARTESIAN_POINT ( 'NONE',  ( -5.823673210054431948, 21.52544592524334988, 67.70942372801901854 ) ) ;
#100367 = CARTESIAN_POINT ( 'NONE',  ( 15.72974639402176855, 15.80617190586768217, 101.8760903946857042 ) ) ;
#100368 = CARTESIAN_POINT ( 'NONE',  ( 16.53943276465976808, -0.05219959533910856209, 23.74890960531435269 ) ) ;
#100369 = CARTESIAN_POINT ( 'NONE',  ( -5.153800228976328057, -19.02544592524343514, 27.29057627198103120 ) ) ;
#100370 = CARTESIAN_POINT ( 'NONE',  ( -5.153800228976328057, -19.02544592524343514, 92.29057627198099567 ) ) ;
#100371 = CARTESIAN_POINT ( 'NONE',  ( 15.72974639402176855, 15.80617190586768217, 56.87609039468568994 ) ) ;
#100372 = CARTESIAN_POINT ( 'NONE',  ( 13.97604488694527802, 13.89961937509977652, 39.37390960531435269 ) ) ;
#100373 = EDGE_CURVE ( 'NONE', #63341, #11857, #174061, .T. ) ;
#100374 = CARTESIAN_POINT ( 'NONE',  ( -15.80617190586768217, 15.72974639402176855, 53.12609039468568284 ) ) ;
#100376 = CARTESIAN_POINT ( 'NONE',  ( 9.564922557960805705, 16.46253265017160317, 99.58224293864770971 ) ) ;
#100375 = CARTESIAN_POINT ( 'NONE',  ( 9.564922557961047289, -16.46253265017146816, 95.41775706135233293 ) ) ;
#100377 = CARTESIAN_POINT ( 'NONE',  ( 4.483927247898545687, 16.52544592524342804, 114.7905762719810383 ) ) ;
#100378 = CARTESIAN_POINT ( 'NONE',  ( 15.80617190586746368, 15.72974639402197994, 114.3739096053143527 ) ) ;
#100379 = CARTESIAN_POINT ( 'NONE',  ( -16.51473224551082808, 9.474510206698731452, 33.33442372801899722 ) ) ;
#100380 = CARTESIAN_POINT ( 'NONE',  ( -19.05341960407611168, -5.049401038298163336, 21.45724293864768839 ) ) ;
#100381 = CARTESIAN_POINT ( 'NONE',  ( -19.02544592524342804, 5.153800228976336051, 51.04057627198103120 ) ) ;
#100382 = CARTESIAN_POINT ( 'NONE',  ( -19.02544592524334988, -5.153800228976617603, 103.9594237280190043 ) ) ;
#100383 = CARTESIAN_POINT ( 'NONE',  ( 12.06949235617757843, -12.14591786802309237, 58.12390960531435979 ) ) ;
#100384 = CARTESIAN_POINT ( 'NONE',  ( 21.52544592524334988, 5.823673210054432836, 106.4594237280190328 ) ) ;
#100385 = CARTESIAN_POINT ( 'NONE',  ( -10.81492255796078084, -18.62759615963271287, 22.08224293864769194 ) ) ;
#100386 = CARTESIAN_POINT ( 'NONE',  ( 16.51473224551083163, -9.474510206698727899, 85.83442372801900433 ) ) ;
#100387 = CARTESIAN_POINT ( 'NONE',  ( 0.05219959533907565091, 21.53943276465977519, 94.99890960531436690 ) ) ;
#100388 = CARTESIAN_POINT ( 'NONE',  ( 0.05219959533937995610, -21.53943276465977519, 50.00109039468568994 ) ) ;
#100389 = CARTESIAN_POINT ( 'NONE',  ( 8.224510206698742110, 14.34966873604972548, 47.08442372801901854 ) ) ;
#100390 = CARTESIAN_POINT ( 'NONE',  ( 12.14591786802327356, -12.06949235617739191, 105.6260903946856899 ) ) ;
#100392 = CARTESIAN_POINT ( 'NONE',  ( 18.67979575497194134, -10.72451020669871369, 55.83442372801901854 ) ) ;
#100391 = CARTESIAN_POINT ( 'NONE',  ( 4.379528057220092307, 16.55341960407617563, 42.29275706135235424 ) ) ;
#100393 = CARTESIAN_POINT ( 'NONE',  ( 18.67979575497178502, 10.72451020669898547, 44.16557627198103120 ) ) ;
#100394 = CARTESIAN_POINT ( 'NONE',  ( -13.89961937509977652, 13.97604488694528158, 35.62390960531435269 ) ) ;
#100395 = CARTESIAN_POINT ( 'NONE',  ( -38.00000000000001421, -12.34694845685042708, -3.649999994537627135 ) ) ;
#100396 = CARTESIAN_POINT ( 'NONE',  ( 8.224510206698742110, 14.34966873604972548, 67.08442372801901854 ) ) ;
#100397 = CARTESIAN_POINT ( 'NONE',  ( 10.81492255796078972, 18.62759615963270932, 94.58224293864769550 ) ) ;
#100398 = CARTESIAN_POINT ( 'NONE',  ( -4.379528057220328563, 16.55341960407611168, 40.20724293864769550 ) ) ;
#100399 = CARTESIAN_POINT ( 'NONE',  ( 16.53943276465976808, 0.05219959533934440121, 56.25109039468568284 ) ) ;
#100400 = CARTESIAN_POINT ( 'NONE',  ( -19.02544592524334988, -5.153800228976617603, 98.95942372801900433 ) ) ;
#100401 = CARTESIAN_POINT ( 'NONE',  ( 10.81492255796078972, 18.62759615963270932, 104.5822429386477097 ) ) ;
#100402 = CARTESIAN_POINT ( 'NONE',  ( -0.05219959533910754901, -16.53943276465976808, 37.49890960531436690 ) ) ;
#100403 = VERTEX_POINT ( 'NONE', #62020 ) ;
#100404 = CARTESIAN_POINT ( 'NONE',  ( -14.29746914071037622, -8.314922557961029526, 74.16775706135231871 ) ) ;
#100405 = CARTESIAN_POINT ( 'NONE',  ( 24.44405923433096461, 13.71792739260091132, 165.9118100595185297 ) ) ;
#100406 = CARTESIAN_POINT ( 'NONE',  ( -21.55341960407610458, -5.719274019375992779, 76.45724293864769550 ) ) ;
#100407 = CARTESIAN_POINT ( 'NONE',  ( 14.29746914071037800, 8.314922557961029526, 101.6677570613523613 ) ) ;
#100408 = EDGE_LOOP ( 'NONE', ( #36491, #166352, #140992, #169808 ) ) ;
#100409 = CARTESIAN_POINT ( 'NONE',  ( 37.99999999999999289, 2.893978650043524126E-14, -3.000000000000000000 ) ) ;
#100410 = CARTESIAN_POINT ( 'NONE',  ( -18.67979575497178146, -10.72451020669898902, 91.66557627198103830 ) ) ;
#100411 = CARTESIAN_POINT ( 'NONE',  ( -21.52544592524343514, 5.823673210054127303, 111.0405762719810525 ) ) ;
#100412 = CARTESIAN_POINT ( 'NONE',  ( 12.14591786802309770, 12.06949235617756955, 34.37390960531435979 ) ) ;
#100413 = CARTESIAN_POINT ( 'NONE',  ( -12.06949235617739369, -12.14591786802326823, 39.37609039468567573 ) ) ;
#100414 = CARTESIAN_POINT ( 'NONE',  ( 19.03943276465977164, -0.05219959533909143690, 33.74890960531435979 ) ) ;
#100415 = CARTESIAN_POINT ( 'NONE',  ( -0.05219959533909027116, -19.03943276465977164, 72.49890960531435269 ) ) ;
#100416 = CARTESIAN_POINT ( 'NONE',  ( -17.81289503416611808, 24.51734667627700404, 147.6999999999999886 ) ) ;
#100417 = CARTESIAN_POINT ( 'NONE',  ( -5.823673210054116645, -21.52544592524344225, 22.29057627198102765 ) ) ;
#100418 = CARTESIAN_POINT ( 'NONE',  ( -16.51473224551069308, -9.474510206698971260, 111.6655762719810383 ) ) ;
#100419 = CARTESIAN_POINT ( 'NONE',  ( 16.46253265017146816, 9.564922557961045513, 101.6677570613523329 ) ) ;
#100420 = CARTESIAN_POINT ( 'NONE',  ( 16.46253265017146816, 9.564922557961045513, 36.66775706135233293 ) ) ;
#100421 = CARTESIAN_POINT ( 'NONE',  ( 10.81492255796078972, 18.62759615963270932, 89.58224293864768129 ) ) ;
#100422 = CARTESIAN_POINT ( 'NONE',  ( 4.483927247898545687, 16.52544592524342804, 24.79057627198103120 ) ) ;
#100423 = CARTESIAN_POINT ( 'NONE',  ( -15.72974639402197994, 15.80617190586746368, 50.62390960531435979 ) ) ;
#100425 = CARTESIAN_POINT ( 'NONE',  ( 13.97604488694548053, -13.89961937509957401, 105.6260903946856757 ) ) ;
#100424 = CARTESIAN_POINT ( 'NONE',  ( -21.53943276465977519, 0.05219959533907696930, 81.24890960531436690 ) ) ;
#100426 = CARTESIAN_POINT ( 'NONE',  ( 19.03943276465977164, -0.05219959533909143690, 103.7489096053143669 ) ) ;
#100427 = CARTESIAN_POINT ( 'NONE',  ( -5.719274019375665041, -21.55341960407619695, 74.79275706135234714 ) ) ;
#100428 = CARTESIAN_POINT ( 'NONE',  ( 5.049401038298161559, -19.05341960407611168, 67.70724293864769550 ) ) ;
#100429 = CARTESIAN_POINT ( 'NONE',  ( 16.52544592524342804, -4.483927247898539470, 98.54057627198105251 ) ) ;
#100430 = CARTESIAN_POINT ( 'NONE',  ( 31.28760401664903412, 6.510460035718195648, 98.73157056914057250 ) ) ;
#100431 = CARTESIAN_POINT ( 'NONE',  ( 5.153800228976335163, 19.02544592524342804, 64.79057627198100988 ) ) ;
#100432 = CARTESIAN_POINT ( 'NONE',  ( -4.379528057220328563, 16.55341960407611168, 85.20724293864770971 ) ) ;
#100433 = ORIENTED_EDGE ( 'NONE', *, *, #186918, .T. ) ;
#100434 = CARTESIAN_POINT ( 'NONE',  ( 13.97604488694548053, -13.89961937509957401, 105.6260903946856757 ) ) ;
#100435 = FACE_OUTER_BOUND ( 'NONE', #34145, .T. ) ;
#100436 = CARTESIAN_POINT ( 'NONE',  ( -5.049401038298153566, 19.05341960407611168, 55.20724293864769550 ) ) ;
#100438 = CARTESIAN_POINT ( 'NONE',  ( 13.97604488694527802, 13.89961937509977652, 104.3739096053143385 ) ) ;
#100437 = CARTESIAN_POINT ( 'NONE',  ( 5.719274019375673035, 21.55341960407619339, 82.29275706135234714 ) ) ;
#100439 = EDGE_CURVE ( 'NONE', #45079, #119772, #145936, .T. ) ;
#100440 = CARTESIAN_POINT ( 'NONE',  ( 12.06949235617739724, 12.14591786802326823, 81.87609039468568994 ) ) ;
#100441 = CARTESIAN_POINT ( 'NONE',  ( -17.49999999999999645, -5.499999999999992895, 74.20309617465828467 ) ) ;
#100442 = CARTESIAN_POINT ( 'NONE',  ( 16.46253265017146816, 9.564922557961045513, 56.66775706135233293 ) ) ;
#100443 = CARTESIAN_POINT ( 'NONE',  ( -21.55341960407619339, 5.719274019375674811, 93.54275706135234714 ) ) ;
#100444 = CARTESIAN_POINT ( 'NONE',  ( 37.32565804592077541, 3.633088190964871789, 40.85532123380855296 ) ) ;
#100445 = DIRECTION ( 'NONE',  ( 0.000000000000000000, 0.000000000000000000, -1.000000000000000000 ) ) ;
#100446 = CARTESIAN_POINT ( 'NONE',  ( -16.53943276465976808, 0.05219959533911058130, 21.24890960531436690 ) ) ;
#100447 = FACE_OUTER_BOUND ( 'NONE', #73995, .T. ) ;
#100448 = CARTESIAN_POINT ( 'NONE',  ( -12.06949235617739369, -12.14591786802326823, 89.37609039468568994 ) ) ;
#100449 = CARTESIAN_POINT ( 'NONE',  ( 30.20036327792367814, -26.22857331006468584, -17.18026671435356434 ) ) ;
#100450 = CARTESIAN_POINT ( 'NONE',  ( -4.379528057220086978, -16.55341960407618274, 64.79275706135234714 ) ) ;
#100451 = CARTESIAN_POINT ( 'NONE',  ( 21.52544592524334988, 5.823673210054432836, 86.45942372801901854 ) ) ;
#100452 = CARTESIAN_POINT ( 'NONE',  ( -9.564922557961040184, 16.46253265017147172, 87.91775706135233293 ) ) ;
#100453 = CARTESIAN_POINT ( 'NONE',  ( 19.05341960407617918, -5.049401038297876454, 46.04275706135233293 ) ) ;
#100454 = CARTESIAN_POINT ( 'NONE',  ( -0.05219959533909027116, -19.03943276465977164, 67.49890960531436690 ) ) ;
#100455 = CARTESIAN_POINT ( 'NONE',  ( -19.03943276465977164, 0.05219959533909376836, 51.24890960531436690 ) ) ;
#100456 = CARTESIAN_POINT ( 'NONE',  ( -17.59860650958991002, -7.585241751807008548, 86.57662985737509587 ) ) ;
#100457 = CARTESIAN_POINT ( 'NONE',  ( 21.52544592524344225, -5.823673210054117533, 78.54057627198103830 ) ) ;
#100458 = CARTESIAN_POINT ( 'NONE',  ( 5.823673210054125526, 21.52544592524343514, 49.79057627198102409 ) ) ;
#100459 = CARTESIAN_POINT ( 'NONE',  ( -5.153800228976328057, -19.02544592524343514, 37.29057627198102409 ) ) ;
#100460 = CARTESIAN_POINT ( 'NONE',  ( 16.55341960407618274, -4.379528057220086978, 61.04275706135234714 ) ) ;
#100461 = ADVANCED_FACE ( 'NONE', ( #145830 ), #161010, .T. ) ;
#100462 = UNCERTAINTY_MEASURE_WITH_UNIT (LENGTH_MEASURE( 1.000000000000000082E-05 ), #126467, 'distance_accuracy_value', 'NONE');
#100463 = VERTEX_POINT ( 'NONE', #21497 ) ;
#100464 = CARTESIAN_POINT ( 'NONE',  ( -21.52544592524334988, -5.823673210054445271, 43.95942372801902565 ) ) ;
#100466 = CARTESIAN_POINT ( 'NONE',  ( -38.00000000000000711, 2.428612866367529932E-14, 1.084202172485504434E-16 ) ) ;
#100465 = CARTESIAN_POINT ( 'NONE',  ( -0.05219959533910754901, -16.53943276465976808, 67.49890960531436690 ) ) ;
#100467 = CARTESIAN_POINT ( 'NONE',  ( -4.483927247898782831, 16.52544592524335698, 27.70942372801901854 ) ) ;
#100468 = CARTESIAN_POINT ( 'NONE',  ( -9.474510206698720793, -16.51473224551083518, 59.58442372801900433 ) ) ;
#100469 = CARTESIAN_POINT ( 'NONE',  ( -16.55341960407611168, -4.379528057220339221, 61.45724293864770260 ) ) ;
#100470 = CARTESIAN_POINT ( 'NONE',  ( -21.53943276465977519, -0.05219959533937600094, 38.75109039468567573 ) ) ;
#100472 = CARTESIAN_POINT ( 'NONE',  ( 15.72974639402199770, -15.80617190586745480, 93.12390960531436690 ) ) ;
#100471 = CARTESIAN_POINT ( 'NONE',  ( 17.59860650958990647, 7.585241751807016541, 99.07662985737508166 ) ) ;
#100473 = CARTESIAN_POINT ( 'NONE',  ( 19.05341960407611168, 5.049401038298154454, 103.9572429386476671 ) ) ;
#100474 = CARTESIAN_POINT ( 'NONE',  ( 4.483927247898545687, 16.52544592524342804, 74.79057627198105251 ) ) ;
#100475 = CARTESIAN_POINT ( 'NONE',  ( -19.03943276465977164, 0.05219959533909376836, 111.2489096053143669 ) ) ;
#100476 = CARTESIAN_POINT ( 'NONE',  ( -37.07039049082557369, 4.937524616431669067, 42.55055737136175509 ) ) ;
#100477 = CARTESIAN_POINT ( 'NONE',  ( -19.05341960407617563, 5.049401038297882671, 68.54275706135230450 ) ) ;
#100478 = CARTESIAN_POINT ( 'NONE',  ( -18.62759615963270932, 10.81492255796079327, 115.8322429386477097 ) ) ;
#100479 = CARTESIAN_POINT ( 'NONE',  ( -13.89961937509977652, 13.97604488694528158, 60.62390960531436690 ) ) ;
#100480 = CARTESIAN_POINT ( 'NONE',  ( 9.474510206698729675, 16.51473224551082808, 42.08442372801900433 ) ) ;
#100481 = CARTESIAN_POINT ( 'NONE',  ( -19.02544592524342804, 5.153800228976336051, 36.04057627198100988 ) ) ;
#100482 = CARTESIAN_POINT ( 'NONE',  ( -15.80617190586768217, 15.72974639402176855, 63.12609039468568994 ) ) ;
#100483 = CARTESIAN_POINT ( 'NONE',  ( -17.44270441346519718, -5.991230190322950122, 71.36335079264232206 ) ) ;
#100484 = CARTESIAN_POINT ( 'NONE',  ( 12.14591786802309770, 12.06949235617756955, 59.37390960531436690 ) ) ;
#100485 = CARTESIAN_POINT ( 'NONE',  ( 13.97604488694527802, 13.89961937509977652, 59.37390960531434558 ) ) ;
#100486 = CARTESIAN_POINT ( 'NONE',  ( -0.05219959533907301413, -21.53943276465977519, 92.49890960531436690 ) ) ;
#100487 = CARTESIAN_POINT ( 'NONE',  ( -16.51473224551069308, -9.474510206698971260, 61.66557627198103120 ) ) ;
#100488 = ORIENTED_EDGE ( 'NONE', *, *, #125347, .F. ) ;
#100489 = CARTESIAN_POINT ( 'NONE',  ( 0.05219959533907565091, 21.53943276465977519, 69.99890960531435269 ) ) ;
#100490 = CARTESIAN_POINT ( 'NONE',  ( -5.823673210054431948, 21.52544592524334988, 102.7094237280190185 ) ) ;
#100493 = CARTESIAN_POINT ( 'NONE',  ( 8.224510206698953496, -14.34966873604960469, 77.91557627198102409 ) ) ;
#100492 = CARTESIAN_POINT ( 'NONE',  ( -14.34966873604972548, 8.224510206698743886, 93.33442372801901854 ) ) ;
#100491 = CARTESIAN_POINT ( 'NONE',  ( 13.97604488694527802, 13.89961937509977652, 24.37390960531435624 ) ) ;
#100494 = CARTESIAN_POINT ( 'NONE',  ( -5.153800228976607833, 19.02544592524334988, 97.70942372801900433 ) ) ;
#100495 = ORIENTED_EDGE ( 'NONE', *, *, #190781, .T. ) ;
#100496 = CARTESIAN_POINT ( 'NONE',  ( -5.719274019375665041, -21.55341960407619695, 19.79275706135235069 ) ) ;
#100497 = CARTESIAN_POINT ( 'NONE',  ( -13.97604488694547697, 13.89961937509957934, 38.12609039468566152 ) ) ;
#100498 = CARTESIAN_POINT ( 'NONE',  ( -16.53943276465976808, -0.05219959533934237506, 98.75109039468568994 ) ) ;
#100499 = CARTESIAN_POINT ( 'NONE',  ( -13.89961937509957401, -13.97604488694547875, 24.37609039468565442 ) ) ;
#100500 = CARTESIAN_POINT ( 'NONE',  ( -16.51473224551069308, -9.474510206698971260, 86.66557627198102409 ) ) ;
#100501 = CARTESIAN_POINT ( 'NONE',  ( 21.55341960407610458, 5.719274019375980345, 63.95724293864770260 ) ) ;
#100502 = CARTESIAN_POINT ( 'NONE',  ( -5.153800228976328057, -19.02544592524343514, 22.29057627198102765 ) ) ;
#100503 = CARTESIAN_POINT ( 'NONE',  ( 16.52544592524342804, -4.483927247898539470, 113.5405762719810383 ) ) ;
#100504 = CARTESIAN_POINT ( 'NONE',  ( -9.474510206698720793, -16.51473224551083518, 19.58442372801899722 ) ) ;
#100505 = CARTESIAN_POINT ( 'NONE',  ( 14.29746914071037800, 8.314922557961029526, 81.66775706135236135 ) ) ;
#100506 = CARTESIAN_POINT ( 'NONE',  ( -21.55341960407619339, 5.719274019375674811, 33.54275706135234714 ) ) ;
#100507 = CARTESIAN_POINT ( 'NONE',  ( -16.53943276465976808, -0.05219959533934237506, 28.75109039468567929 ) ) ;
#100508 = CARTESIAN_POINT ( 'NONE',  ( -5.153800228976328057, -19.02544592524343514, 102.2905762719810383 ) ) ;
#100509 = CARTESIAN_POINT ( 'NONE',  ( -0.05219959533909027116, -19.03943276465977164, 37.49890960531436690 ) ) ;
#100510 = CARTESIAN_POINT ( 'NONE',  ( -9.564922557960796823, -16.46253265017161027, 67.08224293864769550 ) ) ;
#100511 = CARTESIAN_POINT ( 'NONE',  ( 12.14591786802327356, -12.06949235617739191, 50.62609039468568994 ) ) ;
#100512 = CARTESIAN_POINT ( 'NONE',  ( -0.05219959533910754901, -16.53943276465976808, 97.49890960531436690 ) ) ;
#100513 = CARTESIAN_POINT ( 'NONE',  ( 14.29746914071037800, 8.314922557961029526, 96.66775706135234714 ) ) ;
#100516 = CARTESIAN_POINT ( 'NONE',  ( 19.05341960407611168, 5.049401038298154454, 58.95724293864768129 ) ) ;
#100515 = CARTESIAN_POINT ( 'NONE',  ( 19.03943276465977164, -0.05219959533909143690, 73.74890960531435269 ) ) ;
#100514 = CARTESIAN_POINT ( 'NONE',  ( 18.62759615963255655, 10.81492255796105972, 51.66775706135234714 ) ) ;
#100517 = CARTESIAN_POINT ( 'NONE',  ( 5.153800228976335163, 19.02544592524342804, 99.79057627198102409 ) ) ;
#100518 = CARTESIAN_POINT ( 'NONE',  ( -16.52544592524342804, 4.483927247898546575, 46.04057627198103830 ) ) ;
#100519 = CARTESIAN_POINT ( 'NONE',  ( 12.14591786802327356, -12.06949235617739191, 105.6260903946856899 ) ) ;
#100520 = ORIENTED_EDGE ( 'NONE', *, *, #40971, .T. ) ;
#100521 = CARTESIAN_POINT ( 'NONE',  ( -0.05219959533936034679, 19.03943276465977164, 42.50109039468566152 ) ) ;
#100522 = CARTESIAN_POINT ( 'NONE',  ( -19.03943276465977164, 0.05219959533909376836, 111.2489096053143669 ) ) ;
#100523 = CARTESIAN_POINT ( 'NONE',  ( 5.049401038298161559, -19.05341960407611168, 57.70724293864769550 ) ) ;
#100524 = CARTESIAN_POINT ( 'NONE',  ( 16.46253265017146816, 9.564922557961045513, 36.66775706135233293 ) ) ;
#100525 = CARTESIAN_POINT ( 'NONE',  ( 36.91746825000000598, -11.99521256947793546, -3.724999997268812812 ) ) ;
#100526 = CARTESIAN_POINT ( 'NONE',  ( 28.82186960331498327, 2.781578969918950771E-14, 143.0000000000000000 ) ) ;
#100527 = CARTESIAN_POINT ( 'NONE',  ( -16.52544592524335698, -4.483927247898792601, 58.95942372801902565 ) ) ;
#100529 = CARTESIAN_POINT ( 'NONE',  ( -16.52544592524335698, -4.483927247898792601, 68.95942372801901854 ) ) ;
#100528 = CARTESIAN_POINT ( 'NONE',  ( -5.049401038297874678, -19.05341960407617918, 69.79275706135233293 ) ) ;
#100530 = CARTESIAN_POINT ( 'NONE',  ( 6.852337434880861444, -5.080399118595191332, -64.08013955860572253 ) ) ;
#100531 = CARTESIAN_POINT ( 'NONE',  ( -5.153800228976328057, -19.02544592524343514, 92.29057627198099567 ) ) ;
#100532 = CARTESIAN_POINT ( 'NONE',  ( -5.823673210054116645, -21.52544592524344225, 112.2905762719810241 ) ) ;
#100533 = CARTESIAN_POINT ( 'NONE',  ( 0.05219959533936267826, -19.03943276465977164, 80.00109039468567573 ) ) ;
#100535 = CARTESIAN_POINT ( 'NONE',  ( 19.02544592524343514, -5.153800228976328945, 33.54057627198102409 ) ) ;
#100534 = CARTESIAN_POINT ( 'NONE',  ( 13.97604488694527802, 13.89961937509977652, 99.37390960531436690 ) ) ;
#100536 = CARTESIAN_POINT ( 'NONE',  ( 13.89961937509977652, -13.97604488694527269, 93.12390960531436690 ) ) ;
#100538 = CARTESIAN_POINT ( 'NONE',  ( -16.51473224551069308, -9.474510206698971260, 41.66557627198103120 ) ) ;
#100537 = CARTESIAN_POINT ( 'NONE',  ( -14.29746914071049879, 8.314922557960819915, 45.83224293864769550 ) ) ;
#100539 = CARTESIAN_POINT ( 'NONE',  ( -9.474510206698720793, -16.51473224551083518, 54.58442372801899722 ) ) ;
#100540 = CARTESIAN_POINT ( 'NONE',  ( -16.53943276465976808, 0.05219959533911058130, 86.24890960531436690 ) ) ;
#100541 = CARTESIAN_POINT ( 'NONE',  ( -21.55341960407619339, 5.719274019375674811, 108.5427570613523756 ) ) ;
#100542 = CARTESIAN_POINT ( 'NONE',  ( -16.46253265017160317, 9.564922557960807481, 50.83224293864770260 ) ) ;
#100543 = CARTESIAN_POINT ( 'NONE',  ( 5.719274019375991003, -21.55341960407610458, 62.70724293864769550 ) ) ;
#100545 = CARTESIAN_POINT ( 'NONE',  ( 15.80617190586769283, -15.72974639402175789, 110.6260903946857042 ) ) ;
#100544 = CARTESIAN_POINT ( 'NONE',  ( -16.53943276465976808, 0.05219959533911058130, 56.24890960531436690 ) ) ;
#100546 = CARTESIAN_POINT ( 'NONE',  ( 13.97604488694527802, 13.89961937509977652, 109.3739096053143669 ) ) ;
#100547 = CARTESIAN_POINT ( 'NONE',  ( 19.05341960407611168, 5.049401038298154454, 113.9572429386477097 ) ) ;
#100548 = CARTESIAN_POINT ( 'NONE',  ( -16.51473224551069308, -9.474510206698971260, 36.66557627198102409 ) ) ;
#100549 = CARTESIAN_POINT ( 'NONE',  ( -16.52544592524342804, 4.483927247898546575, 116.0405762719810383 ) ) ;
#100550 = CARTESIAN_POINT ( 'NONE',  ( -4.483927247898539470, -16.52544592524342804, 82.29057627198103830 ) ) ;
#100551 = CARTESIAN_POINT ( 'NONE',  ( 5.719274019375991003, -21.55341960407610458, 97.70724293864772392 ) ) ;
#100552 = CARTESIAN_POINT ( 'NONE',  ( -16.51473224551069308, -9.474510206698971260, 101.6655762719810241 ) ) ;
#100553 = CARTESIAN_POINT ( 'NONE',  ( 21.53943276465977519, -0.05219959533907433946, 108.7489096053143669 ) ) ;
#100554 = CARTESIAN_POINT ( 'NONE',  ( 9.474510206698971260, -16.51473224551069308, 102.9155762719810241 ) ) ;
#100555 = CARTESIAN_POINT ( 'NONE',  ( 8.314922557960818139, 14.29746914071049879, 104.5822429386477097 ) ) ;
#100556 = CARTESIAN_POINT ( 'NONE',  ( 0.05219959533937995610, -21.53943276465977519, 85.00109039468568994 ) ) ;
#100557 = CARTESIAN_POINT ( 'NONE',  ( -0.05219959533907301413, -21.53943276465977519, 77.49890960531433848 ) ) ;
#100558 = CARTESIAN_POINT ( 'NONE',  ( 16.88567814943162304, -6.947325034625676743, 106.2099887734741372 ) ) ;
#100559 = CARTESIAN_POINT ( 'NONE',  ( -0.05219959533909027116, -19.03943276465977164, 52.49890960531436690 ) ) ;
#100560 = DIRECTION ( 'NONE',  ( 0.000000000000000000, 0.000000000000000000, 1.000000000000000000 ) ) ;
#100561 = CARTESIAN_POINT ( 'NONE',  ( -8.224510206698735004, -14.34966873604973081, 34.58442372801900433 ) ) ;
#100562 = CARTESIAN_POINT ( 'NONE',  ( 12.14591786802309770, 12.06949235617756955, 114.3739096053143527 ) ) ;
#100563 = DIRECTION ( 'NONE',  ( -1.000000000000000000, 0.000000000000000000, 0.000000000000000000 ) ) ;
#100564 = CARTESIAN_POINT ( 'NONE',  ( 0.05219959533909260263, 19.03943276465977164, 59.99890960531436690 ) ) ;
#100565 = CARTESIAN_POINT ( 'NONE',  ( 16.52544592524342804, -4.483927247898539470, 88.54057627198103830 ) ) ;
#100566 = CARTESIAN_POINT ( 'NONE',  ( 15.72974639402199770, -15.80617190586745480, 28.12390960531435979 ) ) ;
#100567 = CARTESIAN_POINT ( 'NONE',  ( -8.314922557960811034, -14.29746914071050412, 67.08224293864770971 ) ) ;
#100568 = CARTESIAN_POINT ( 'NONE',  ( 9.474510206698729675, 16.51473224551082808, 112.0844237280190043 ) ) ;
#100569 = CARTESIAN_POINT ( 'NONE',  ( 15.80617190586769283, -15.72974639402175789, 75.62609039468567573 ) ) ;
#100570 = CARTESIAN_POINT ( 'NONE',  ( -67.00000000000000000, -1.163414459189985801E-14, 89.49999999999897682 ) ) ;
#100571 = CARTESIAN_POINT ( 'NONE',  ( 9.474510206698971260, -16.51473224551069308, 112.9155762719810383 ) ) ;
#100572 = CARTESIAN_POINT ( 'NONE',  ( 8.224510206698742110, 14.34966873604972548, 82.08442372801901854 ) ) ;
#100573 = CARTESIAN_POINT ( 'NONE',  ( 16.51473224551069308, 9.474510206698969483, 34.16557627198102409 ) ) ;
#100574 = CARTESIAN_POINT ( 'NONE',  ( -19.02544592524342804, 5.153800228976336051, 86.04057627198103830 ) ) ;
#100575 = CARTESIAN_POINT ( 'NONE',  ( -0.05219959533907301413, -21.53943276465977519, 97.49890960531436690 ) ) ;
#100576 = CARTESIAN_POINT ( 'NONE',  ( -16.52544592524335698, -4.483927247898792601, 28.95942372801902209 ) ) ;
#100578 = CARTESIAN_POINT ( 'NONE',  ( 10.72451020669871369, 18.67979575497193778, 67.08442372801901854 ) ) ;
#100577 = CARTESIAN_POINT ( 'NONE',  ( -14.29746914071049879, 8.314922557960819915, 45.83224293864769550 ) ) ;
#100579 = CARTESIAN_POINT ( 'NONE',  ( -16.52544592524335698, -4.483927247898792601, 98.95942372801903275 ) ) ;
#100580 = CARTESIAN_POINT ( 'NONE',  ( 16.31925111598457079, 7.325300261831474202, 27.33575461032749843 ) ) ;
#100581 = DIRECTION ( 'NONE',  ( 1.000000000000000000, 0.000000000000000000, -0.000000000000000000 ) ) ;
#100582 = CARTESIAN_POINT ( 'NONE',  ( -14.29746914071049879, 8.314922557960819915, 30.83224293864770260 ) ) ;
#100583 = CARTESIAN_POINT ( 'NONE',  ( 8.314922557961029526, -14.29746914071037800, 55.41775706135234714 ) ) ;
#100584 = CARTESIAN_POINT ( 'NONE',  ( -5.049401038298153566, 19.05341960407611168, 75.20724293864769550 ) ) ;
#100585 = CARTESIAN_POINT ( 'NONE',  ( -13.97604488694527625, -13.89961937509977652, 91.87390960531432427 ) ) ;
#100586 = CARTESIAN_POINT ( 'NONE',  ( 0.05219959533937995610, -21.53943276465977519, 85.00109039468568994 ) ) ;
#100587 = CARTESIAN_POINT ( 'NONE',  ( -14.34966873604972548, 8.224510206698743886, 93.33442372801901854 ) ) ;
#100588 = CARTESIAN_POINT ( 'NONE',  ( -0.05219959533910754901, -16.53943276465976808, 62.49890960531436690 ) ) ;
#100589 = CARTESIAN_POINT ( 'NONE',  ( 0.05219959533909260263, 19.03943276465977164, 69.99890960531435269 ) ) ;
#100590 = VERTEX_POINT ( 'NONE', #22504 ) ;
#100591 = CARTESIAN_POINT ( 'NONE',  ( -9.474510206698720793, -16.51473224551083518, 109.5844237280190043 ) ) ;
#100592 = CARTESIAN_POINT ( 'NONE',  ( -16.55341960407611168, -4.379528057220339221, 106.4572429386477097 ) ) ;
#100593 = CARTESIAN_POINT ( 'NONE',  ( 16.51473224551069308, 9.474510206698969483, 79.16557627198103830 ) ) ;
#100595 = CARTESIAN_POINT ( 'NONE',  ( -5.950531402560715689E-15, 38.81732327939063509, -9.124999997268815832 ) ) ;
#100594 = CARTESIAN_POINT ( 'NONE',  ( -5.153800228976607833, 19.02544592524334988, 107.7094237280189759 ) ) ;
#100596 = CARTESIAN_POINT ( 'NONE',  ( 18.67979575497194134, -10.72451020669871369, 105.8344237280190328 ) ) ;
#100597 = CARTESIAN_POINT ( 'NONE',  ( -4.483927247898782831, 16.52544592524335698, 82.70942372801900433 ) ) ;
#100598 = CARTESIAN_POINT ( 'NONE',  ( 13.97604488694548053, -13.89961937509957401, 90.62609039468567573 ) ) ;
#100599 = CARTESIAN_POINT ( 'NONE',  ( 13.97604488694527802, 13.89961937509977652, 24.37390960531435624 ) ) ;
#100600 = CARTESIAN_POINT ( 'NONE',  ( -0.05219959533934338120, 16.53943276465976808, 62.50109039468568284 ) ) ;
#100601 = LINE ( 'NONE', #131952, #79657 ) ;
#100602 = CARTESIAN_POINT ( 'NONE',  ( -13.97604488694547697, 13.89961937509957934, 58.12609039468566863 ) ) ;
#100603 = CARTESIAN_POINT ( 'NONE',  ( -21.53943276465977519, -0.05219959533937600094, 98.75109039468568994 ) ) ;
#100604 = CARTESIAN_POINT ( 'NONE',  ( -19.02544592524342804, 5.153800228976336051, 36.04057627198100988 ) ) ;
#100605 = CARTESIAN_POINT ( 'NONE',  ( 13.97604488694527802, 13.89961937509977652, 84.37390960531433848 ) ) ;
#100606 = CARTESIAN_POINT ( 'NONE',  ( -16.55341960407611168, -4.379528057220339221, 71.45724293864769550 ) ) ;
#100607 = CARTESIAN_POINT ( 'NONE',  ( 15.80617190586769283, -15.72974639402175789, 95.62609039468568994 ) ) ;
#100608 = CARTESIAN_POINT ( 'NONE',  ( 19.02544592524334988, 5.153800228976608722, 41.45942372801900433 ) ) ;
#100609 = CARTESIAN_POINT ( 'NONE',  ( -5.153800228976607833, 19.02544592524334988, 37.70942372801899722 ) ) ;
#100610 = CARTESIAN_POINT ( 'NONE',  ( -21.53943276465977519, 0.05219959533907696930, 41.24890960531435269 ) ) ;
#100611 = CARTESIAN_POINT ( 'NONE',  ( 15.80617190586769283, -15.72974639402175789, 95.62609039468568994 ) ) ;
#100612 = CARTESIAN_POINT ( 'NONE',  ( 16.46253265017160672, -9.564922557960803928, 73.33224293864769550 ) ) ;
#100613 = EDGE_CURVE ( 'NONE', #146440, #167327, #157599, .T. ) ;
#100614 = CARTESIAN_POINT ( 'NONE',  ( -5.823673210054431948, 21.52544592524334988, 87.70942372801901854 ) ) ;
#100615 = CARTESIAN_POINT ( 'NONE',  ( -18.67979575497178146, -10.72451020669898902, 56.66557627198103830 ) ) ;
#100616 = CARTESIAN_POINT ( 'NONE',  ( 0.05219959533909260263, 19.03943276465977164, 84.99890960531436690 ) ) ;
#100617 = CARTESIAN_POINT ( 'NONE',  ( -9.474510206698720793, -16.51473224551083518, 74.58442372801900433 ) ) ;
#100618 = CARTESIAN_POINT ( 'NONE',  ( 19.02544592524343514, -5.153800228976328945, 103.5405762719809957 ) ) ;
#100619 = CARTESIAN_POINT ( 'NONE',  ( 5.049401038297881783, 19.05341960407617563, 92.29275706135234714 ) ) ;
#100620 = CARTESIAN_POINT ( 'NONE',  ( -8.314922557961024197, 14.29746914071037800, 42.91775706135235424 ) ) ;
#100621 = CARTESIAN_POINT ( 'NONE',  ( 14.29746914071049879, -8.314922557960816363, 103.3322429386476955 ) ) ;
#100622 = CARTESIAN_POINT ( 'NONE',  ( -9.564922557960796823, -16.46253265017161027, 67.08224293864769550 ) ) ;
#100623 = CARTESIAN_POINT ( 'NONE',  ( 15.72974639402199770, -15.80617190586745480, 63.12390960531435979 ) ) ;
#100624 = CARTESIAN_POINT ( 'NONE',  ( -4.483927247898782831, 16.52544592524335698, 37.70942372801900433 ) ) ;
#100625 = CARTESIAN_POINT ( 'NONE',  ( 21.55341960407619695, -5.719274019375665929, 36.04275706135234714 ) ) ;
#100626 = CARTESIAN_POINT ( 'NONE',  ( -10.81492255796105439, 18.62759615963255655, 82.91775706135234714 ) ) ;
#100628 = CARTESIAN_POINT ( 'NONE',  ( -14.34966873604972548, 8.224510206698743886, 83.33442372801903275 ) ) ;
#100627 = B_SPLINE_CURVE_WITH_KNOTS ( 'NONE', 3,
 ( #65041, #124728, #172227, #171237, #157059, #3366, #123715, #18556, #185412, #189398, #46903, #49879, #34705, #156058, #96362, #108563, #186426, #112533, #174227, #35696, #20522, #47902, #109556, #32726, #94378, #79215, #140884, #160038, #101349, #9371, #70035, #113520 ),
 .UNSPECIFIED., .F., .F.,
 ( 4, 2, 2, 2, 2, 2, 2, 2, 2, 2, 2, 2, 2, 2, 2, 4 ),
 ( 2.195984522899319715E-17, 0.0003712461730036923074, 0.0007424923460073627138, 0.001113738519011033120, 0.001484984692014703310, 0.002227477038022051062, 0.002598723211025731009, 0.002969969384029411390, 0.003341215557033091772, 0.003712461730036772153, 0.004083707903040452100, 0.004454954076044132481, 0.004826200249047811995, 0.005197446422051492376, 0.005568692595055172757, 0.005939938768058853139 ),
 .UNSPECIFIED. ) ;
#100629 = CARTESIAN_POINT ( 'NONE',  ( -0.05219959533909027116, -19.03943276465977164, 77.49890960531435269 ) ) ;
#100630 = CARTESIAN_POINT ( 'NONE',  ( -14.34966873604960291, -8.224510206698953496, 71.66557627198100988 ) ) ;
#100631 = CARTESIAN_POINT ( 'NONE',  ( 4.379528057220092307, 16.55341960407617563, 107.2927570613523471 ) ) ;
#100632 = CARTESIAN_POINT ( 'NONE',  ( 0.05219959533936267826, -19.03943276465977164, 55.00109039468566863 ) ) ;
#100633 = CARTESIAN_POINT ( 'NONE',  ( -15.80617190586768217, 15.72974639402176855, 28.12609039468568284 ) ) ;
#100634 = CARTESIAN_POINT ( 'NONE',  ( 0.05219959533910956823, 16.53943276465976808, 79.99890960531435269 ) ) ;
#100635 = CARTESIAN_POINT ( 'NONE',  ( 16.51473224551069308, 9.474510206698969483, 104.1655762719810241 ) ) ;
#100636 = CARTESIAN_POINT ( 'NONE',  ( -4.483927247898782831, 16.52544592524335698, 97.70942372801904696 ) ) ;
#100637 = CARTESIAN_POINT ( 'NONE',  ( -21.52544592524334988, -5.823673210054445271, 73.95942372801901854 ) ) ;
#100638 = CARTESIAN_POINT ( 'NONE',  ( -4.483927247898782831, 16.52544592524335698, 42.70942372801901854 ) ) ;
#100639 = CARTESIAN_POINT ( 'NONE',  ( 18.62759615963255655, 10.81492255796105972, 36.66775706135234714 ) ) ;
#100640 = CARTESIAN_POINT ( 'NONE',  ( -8.224510206698948167, 14.34966873604960824, 70.41557627198102409 ) ) ;
#100641 = ORIENTED_EDGE ( 'NONE', *, *, #59210, .F. ) ;
#100642 = CARTESIAN_POINT ( 'NONE',  ( 21.53943276465977519, -0.05219959533907433946, 113.7489096053143527 ) ) ;
#100643 = CARTESIAN_POINT ( 'NONE',  ( 17.49999999999999289, -4.640572885337604703, 28.13788164548842374 ) ) ;
#100644 = CARTESIAN_POINT ( 'NONE',  ( 16.53943276465976808, -0.05219959533910856209, 48.74890960531435979 ) ) ;
#100645 = CARTESIAN_POINT ( 'NONE',  ( -19.05341960407611168, -5.049401038298163336, 21.45724293864768839 ) ) ;
#100646 = CARTESIAN_POINT ( 'NONE',  ( -0.05219959533907301413, -21.53943276465977519, 42.49890960531435979 ) ) ;
#100647 = CARTESIAN_POINT ( 'NONE',  ( -4.379528057220328563, 16.55341960407611168, 80.20724293864769550 ) ) ;
#100648 = CARTESIAN_POINT ( 'NONE',  ( 10.81492255796078972, 18.62759615963270932, 79.58224293864769550 ) ) ;
#100649 = CARTESIAN_POINT ( 'NONE',  ( -13.89961937509977652, 13.97604488694528158, 85.62390960531433848 ) ) ;
#100651 = CARTESIAN_POINT ( 'NONE',  ( -13.97604488694547697, 13.89961937509957934, 78.12609039468567573 ) ) ;
#100650 = CARTESIAN_POINT ( 'NONE',  ( -5.153800228976328057, -19.02544592524343514, 37.29057627198102409 ) ) ;
#100653 = CARTESIAN_POINT ( 'NONE',  ( 18.62759615963271287, -10.81492255796078972, 58.33224293864768839 ) ) ;
#100652 = CARTESIAN_POINT ( 'NONE',  ( 15.80617190586769283, -15.72974639402175789, 60.62609039468567573 ) ) ;
#100654 = CARTESIAN_POINT ( 'NONE',  ( 16.51473224551069308, 9.474510206698969483, 34.16557627198102409 ) ) ;
#100655 = CARTESIAN_POINT ( 'NONE',  ( 13.97604488694527802, 13.89961937509977652, 74.37390960531436690 ) ) ;
#100656 = ORIENTED_EDGE ( 'NONE', *, *, #144097, .F. ) ;
#100657 = CARTESIAN_POINT ( 'NONE',  ( 16.53943276465976808, 0.05219959533934440121, 51.25109039468568994 ) ) ;
#100658 = CARTESIAN_POINT ( 'NONE',  ( 21.53943276465977519, 0.05219959533937863772, 31.25109039468568639 ) ) ;
#100659 = CARTESIAN_POINT ( 'NONE',  ( -5.719274019375665041, -21.55341960407619695, 64.79275706135234714 ) ) ;
#100660 = CARTESIAN_POINT ( 'NONE',  ( 13.97604488694527802, 13.89961937509977652, 109.3739096053143669 ) ) ;
#100661 = CARTESIAN_POINT ( 'NONE',  ( 5.719274019375991003, -21.55341960407610458, 87.70724293864769550 ) ) ;
#100663 = CARTESIAN_POINT ( 'NONE',  ( -12.14591786802326823, 12.06949235617739902, 48.12609039468568284 ) ) ;
#100662 = CARTESIAN_POINT ( 'NONE',  ( -10.81492255796105439, 18.62759615963255655, 27.91775706135234358 ) ) ;
#100664 = CARTESIAN_POINT ( 'NONE',  ( -15.72974639402197994, 15.80617190586746368, 55.62390960531436690 ) ) ;
#100665 = CARTESIAN_POINT ( 'NONE',  ( -18.62759615963255300, -10.81492255796106328, 109.1677570613523613 ) ) ;
#100666 = CARTESIAN_POINT ( 'NONE',  ( 16.46253265017160672, -9.564922557960803928, 58.33224293864769550 ) ) ;
#100667 = CARTESIAN_POINT ( 'NONE',  ( -13.89961937509977652, 13.97604488694528158, 105.6239096053143527 ) ) ;
#100668 = CARTESIAN_POINT ( 'NONE',  ( 19.02544592524343514, -5.153800228976328945, 93.54057627198102409 ) ) ;
#100669 = CARTESIAN_POINT ( 'NONE',  ( 17.50000000000001066, 4.601506711240531899, 103.5269151853245262 ) ) ;
#100670 = CARTESIAN_POINT ( 'NONE',  ( 19.02544592524334988, 5.153800228976608722, 71.45942372801900433 ) ) ;
#100671 = CARTESIAN_POINT ( 'NONE',  ( 21.52544592524344225, -5.823673210054117533, 38.54057627198103120 ) ) ;
#100672 = CARTESIAN_POINT ( 'NONE',  ( 16.55341960407611168, 4.379528057220329451, 23.95724293864769550 ) ) ;
#100673 = CARTESIAN_POINT ( 'NONE',  ( -19.02544592524334988, -5.153800228976617603, 103.9594237280190043 ) ) ;
#100674 = CARTESIAN_POINT ( 'NONE',  ( -37.99626262588766679, 2.428612866367529932E-14, 2.000000000000000000 ) ) ;
#100675 = CARTESIAN_POINT ( 'NONE',  ( 13.97604488694548053, -13.89961937509957401, 20.62609039468567573 ) ) ;
#100676 = CARTESIAN_POINT ( 'NONE',  ( 9.474510206698729675, 16.51473224551082808, 102.0844237280190043 ) ) ;
#100677 = CARTESIAN_POINT ( 'NONE',  ( 9.564922557961047289, -16.46253265017146816, 40.41775706135234003 ) ) ;
#100678 = DIRECTION ( 'NONE',  ( 0.000000000000000000, 0.000000000000000000, -1.000000000000000000 ) ) ;
#100679 = CARTESIAN_POINT ( 'NONE',  ( -16.51473224551069308, -9.474510206698971260, 51.66557627198102409 ) ) ;
#100680 = CARTESIAN_POINT ( 'NONE',  ( 0.05219959533910956823, 16.53943276465976808, 64.99890960531435269 ) ) ;
#100681 = CARTESIAN_POINT ( 'NONE',  ( 9.564922557960805705, 16.46253265017160317, 39.58224293864768839 ) ) ;
#100682 = CARTESIAN_POINT ( 'NONE',  ( -12.14591786802309592, -12.06949235617757132, 46.87390960531435979 ) ) ;
#100683 = DIRECTION ( 'NONE',  ( -0.000000000000000000, -0.000000000000000000, 1.000000000000000000 ) ) ;
#100684 = CARTESIAN_POINT ( 'NONE',  ( -8.314922557961024197, 14.29746914071037800, 102.9177570613523756 ) ) ;
#100685 = CARTESIAN_POINT ( 'NONE',  ( -19.02544592524342804, 5.153800228976336051, 66.04057627198103830 ) ) ;
#100686 = CARTESIAN_POINT ( 'NONE',  ( 19.05341960407617918, -5.049401038297876454, 31.04275706135232227 ) ) ;
#100687 = CARTESIAN_POINT ( 'NONE',  ( 4.483927247898790824, -16.52544592524335698, 40.20942372801901854 ) ) ;
#100688 = CARTESIAN_POINT ( 'NONE',  ( 15.80617190586746368, 15.72974639402197994, 54.37390960531435979 ) ) ;
#100690 = ORIENTED_EDGE ( 'NONE', *, *, #79968, .F. ) ;
#100689 = CARTESIAN_POINT ( 'NONE',  ( 10.81492255796106328, -18.62759615963255655, 110.4177570613523756 ) ) ;
#100691 = CARTESIAN_POINT ( 'NONE',  ( -13.89961937509977652, 13.97604488694528158, 60.62390960531436690 ) ) ;
#100692 = CARTESIAN_POINT ( 'NONE',  ( 19.02544592524343514, -5.153800228976328945, 108.5405762719810383 ) ) ;
#100693 = CARTESIAN_POINT ( 'NONE',  ( -5.153800228976328057, -19.02544592524343514, 97.29057627198099567 ) ) ;
#100694 = CARTESIAN_POINT ( 'NONE',  ( -5.950531402560715689E-15, 38.81732327939063509, -1.124999997268813168 ) ) ;
#100695 = CARTESIAN_POINT ( 'NONE',  ( 21.55341960407619695, -5.719274019375665929, 31.04275706135234714 ) ) ;
#100696 = CARTESIAN_POINT ( 'NONE',  ( 14.29746914071049879, -8.314922557960816363, 98.33224293864769550 ) ) ;
#100698 = CARTESIAN_POINT ( 'NONE',  ( 13.97604488694527802, 13.89961937509977652, 64.37390960531436690 ) ) ;
#100697 = CARTESIAN_POINT ( 'NONE',  ( -21.53943276465977519, 0.05219959533907696930, 91.24890960531436690 ) ) ;
#100699 = CARTESIAN_POINT ( 'NONE',  ( 9.474510206698971260, -16.51473224551069308, 77.91557627198103830 ) ) ;
#100700 = CARTESIAN_POINT ( 'NONE',  ( -5.719274019375978568, 21.55341960407610458, 115.2072429386476955 ) ) ;
#100701 = EDGE_CURVE ( 'NONE', #197216, #71610, #49850, .T. ) ;
#100702 = ORIENTED_EDGE ( 'NONE', *, *, #43792, .F. ) ;
#100703 = CARTESIAN_POINT ( 'NONE',  ( 0.05219959533909260263, 19.03943276465977164, 79.99890960531436690 ) ) ;
#100704 = CARTESIAN_POINT ( 'NONE',  ( -31.56198012149236121, -21.16321310694279489, -23.06581160126869179 ) ) ;
#100706 = FACE_OUTER_BOUND ( 'NONE', #111424, .T. ) ;
#100705 = CARTESIAN_POINT ( 'NONE',  ( 4.483927247898545687, 16.52544592524342804, 99.79057627198103830 ) ) ;
#100707 = CARTESIAN_POINT ( 'NONE',  ( 16.46253265017146816, 9.564922557961045513, 91.66775706135234714 ) ) ;
#100708 = CARTESIAN_POINT ( 'NONE',  ( 4.483927247898545687, 16.52544592524342804, 99.79057627198103830 ) ) ;
#100709 = CARTESIAN_POINT ( 'NONE',  ( -18.62759615963255300, -10.81492255796106328, 74.16775706135231871 ) ) ;
#100711 = CARTESIAN_POINT ( 'NONE',  ( -18.67979575497193778, 10.72451020669871902, 28.33442372801902209 ) ) ;
#100710 = CARTESIAN_POINT ( 'NONE',  ( 5.049401038298161559, -19.05341960407611168, 57.70724293864769550 ) ) ;
#100712 = CARTESIAN_POINT ( 'NONE',  ( -21.52544592524334988, -5.823673210054445271, 18.95942372801901143 ) ) ;
#100713 = DIRECTION ( 'NONE',  ( -1.000000000000000000, 0.000000000000000000, 5.204170427930421283E-16 ) ) ;
#100714 = CARTESIAN_POINT ( 'NONE',  ( -16.51473224551069308, -9.474510206698971260, 76.66557627198103830 ) ) ;
#100715 = CARTESIAN_POINT ( 'NONE',  ( -17.49999999999999645, -5.500000000000000888, 120.0000000000000142 ) ) ;
#100717 = CARTESIAN_POINT ( 'NONE',  ( 5.719274019375991003, -21.55341960407610458, 32.70724293864770260 ) ) ;
#100716 = CARTESIAN_POINT ( 'NONE',  ( -19.05341960407617563, 5.049401038297882671, 113.5427570613523471 ) ) ;
#100718 = CARTESIAN_POINT ( 'NONE',  ( 10.72451020669871369, 18.67979575497193778, 57.08442372801901854 ) ) ;
#100719 = CARTESIAN_POINT ( 'NONE',  ( -13.97604488694527625, -13.89961937509977652, 91.87390960531432427 ) ) ;
#100720 = CARTESIAN_POINT ( 'NONE',  ( -19.05341960407617563, 5.049401038297882671, 93.54275706135234714 ) ) ;
#100721 = CARTESIAN_POINT ( 'NONE',  ( 19.03943276465977164, -0.05219959533909143690, 43.74890960531435979 ) ) ;
#100722 = CARTESIAN_POINT ( 'NONE',  ( 9.564922557960805705, 16.46253265017160317, 69.58224293864770971 ) ) ;
#100723 = CARTESIAN_POINT ( 'NONE',  ( 14.29746914071049879, -8.314922557960816363, 93.33224293864769550 ) ) ;
#100724 = CARTESIAN_POINT ( 'NONE',  ( -19.02544592524342804, 5.153800228976336051, 106.0405762719810241 ) ) ;
#100725 = CARTESIAN_POINT ( 'NONE',  ( -8.314922557960811034, -14.29746914071050412, 92.08224293864769550 ) ) ;
#100726 = CARTESIAN_POINT ( 'NONE',  ( 19.02544592524343514, -5.153800228976328945, 103.5405762719809957 ) ) ;
#100728 = CARTESIAN_POINT ( 'NONE',  ( -19.03943276465977164, 0.05219959533909376836, 46.24890960531435979 ) ) ;
#100727 = CARTESIAN_POINT ( 'NONE',  ( -8.224510206698948167, 14.34966873604960824, 40.41557627198103120 ) ) ;
#100729 = ORIENTED_EDGE ( 'NONE', *, *, #1190, .F. ) ;
#100730 = CARTESIAN_POINT ( 'NONE',  ( 18.67979575497194134, -10.72451020669871369, 60.83442372801901854 ) ) ;
#100731 = CARTESIAN_POINT ( 'NONE',  ( -19.05341960407617563, 5.049401038297882671, 83.54275706135233293 ) ) ;
#100732 = CARTESIAN_POINT ( 'NONE',  ( -0.05219959533910754901, -16.53943276465976808, 47.49890960531435979 ) ) ;
#100733 = CARTESIAN_POINT ( 'NONE',  ( 21.55341960407610458, 5.719274019375980345, 98.95724293864770971 ) ) ;
#100734 = CARTESIAN_POINT ( 'NONE',  ( 21.53943276465977519, -0.05219959533907433946, 38.74890960531435979 ) ) ;
#100735 = CARTESIAN_POINT ( 'NONE',  ( 8.224510206698953496, -14.34966873604960469, 77.91557627198102409 ) ) ;
#100736 = CARTESIAN_POINT ( 'NONE',  ( -16.46253265017160317, 9.564922557960807481, 50.83224293864770260 ) ) ;
#100737 = CARTESIAN_POINT ( 'NONE',  ( 16.55341960407611168, 4.379528057220329451, 28.95724293864769905 ) ) ;
#100738 = CARTESIAN_POINT ( 'NONE',  ( 12.06949235617739724, 12.14591786802326823, 101.8760903946857042 ) ) ;
#100739 = CARTESIAN_POINT ( 'NONE',  ( 8.224510206698742110, 14.34966873604972548, 72.08442372801899012 ) ) ;
#100740 = CARTESIAN_POINT ( 'NONE',  ( 5.049401038297881783, 19.05341960407617563, 22.29275706135233648 ) ) ;
#100742 = CARTESIAN_POINT ( 'NONE',  ( -13.97604488694527625, -13.89961937509977652, 106.8739096053143669 ) ) ;
#100741 = CARTESIAN_POINT ( 'NONE',  ( -24.60782808046178616, 7.576750539519846228, 167.2921137806584113 ) ) ;
#100743 = CARTESIAN_POINT ( 'NONE',  ( -5.153800228976328057, -19.02544592524343514, 72.29057627198102409 ) ) ;
#100744 = CARTESIAN_POINT ( 'NONE',  ( -16.51473224551069308, -9.474510206698971260, 31.66557627198102054 ) ) ;
#100745 = CARTESIAN_POINT ( 'NONE',  ( -12.14591786802309592, -12.06949235617757132, 41.87390960531435979 ) ) ;
#100747 = CARTESIAN_POINT ( 'NONE',  ( -5.049401038298153566, 19.05341960407611168, 100.2072429386476955 ) ) ;
#100746 =( NAMED_UNIT ( * ) SI_UNIT ( $, .STERADIAN. ) SOLID_ANGLE_UNIT ( ) );
#100748 = CARTESIAN_POINT ( 'NONE',  ( -5.719274019375978568, 21.55341960407610458, 40.20724293864769550 ) ) ;
#100749 = CARTESIAN_POINT ( 'NONE',  ( -16.53943276465976808, 0.05219959533911058130, 81.24890960531436690 ) ) ;
#100750 = CARTESIAN_POINT ( 'NONE',  ( -14.29746914071037622, -8.314922557961029526, 24.16775706135235424 ) ) ;
#100751 = CARTESIAN_POINT ( 'NONE',  ( 12.14591786802309770, 12.06949235617756955, 64.37390960531435269 ) ) ;
#100752 = CARTESIAN_POINT ( 'NONE',  ( 30.11448378070090470, -1.481880339025618110, -48.12989299794426756 ) ) ;
#100753 = CARTESIAN_POINT ( 'NONE',  ( -0.05219959533936034679, 19.03943276465977164, 67.50109039468566152 ) ) ;
#100754 = CARTESIAN_POINT ( 'NONE',  ( 19.03943276465977164, -0.05219959533909143690, 103.7489096053143669 ) ) ;
#100755 = CARTESIAN_POINT ( 'NONE',  ( -19.05341960407617563, 5.049401038297882671, 78.54275706135233293 ) ) ;
#100756 = CARTESIAN_POINT ( 'NONE',  ( -27.73933785331498925, 2.428612866367529932E-14, 149.3750000027311842 ) ) ;
#100758 = CARTESIAN_POINT ( 'NONE',  ( 16.52544592524335698, 4.483927247898782831, 111.4594237280190328 ) ) ;
#100757 = CARTESIAN_POINT ( 'NONE',  ( -19.03943276465977164, -0.05219959533935918106, 108.7510903946856615 ) ) ;
#100759 = CARTESIAN_POINT ( 'NONE',  ( -5.153800228976607833, 19.02544592524334988, 67.70942372801900433 ) ) ;
#100760 = CARTESIAN_POINT ( 'NONE',  ( -5.823673210054116645, -21.52544592524344225, 37.29057627198102409 ) ) ;
#100761 = CARTESIAN_POINT ( 'NONE',  ( 0.05219959533937995610, -21.53943276465977519, 65.00109039468568994 ) ) ;
#100762 = CARTESIAN_POINT ( 'NONE',  ( -24.10180676228339536, -9.559744493756875627, 166.3058469464611449 ) ) ;
#100763 = CARTESIAN_POINT ( 'NONE',  ( -8.224510206698735004, -14.34966873604973081, 19.58442372801901143 ) ) ;
#100765 = CARTESIAN_POINT ( 'NONE',  ( -19.02544592524342804, 5.153800228976336051, 81.04057627198103830 ) ) ;
#100764 = CARTESIAN_POINT ( 'NONE',  ( 17.50000000000001066, 3.583808971632316265, 22.23472503527400690 ) ) ;
#100766 = CARTESIAN_POINT ( 'NONE',  ( 14.93915603648730261, 17.06172130128247844, -57.95097928225586514 ) ) ;
#100768 = CARTESIAN_POINT ( 'NONE',  ( 5.153800228976335163, 19.02544592524342804, 79.79057627198102409 ) ) ;
#100767 = CARTESIAN_POINT ( 'NONE',  ( 0.05219959533910956823, 16.53943276465976808, 84.99890960531436690 ) ) ;
#100769 = CARTESIAN_POINT ( 'NONE',  ( 5.049401038298161559, -19.05341960407611168, 92.70724293864769550 ) ) ;
#100770 = CARTESIAN_POINT ( 'NONE',  ( -16.46253265017146816, -9.564922557961047289, 89.16775706135234714 ) ) ;
#100771 = CARTESIAN_POINT ( 'NONE',  ( -21.52544592524343514, 5.823673210054127303, 81.04057627198102409 ) ) ;
#100772 = CARTESIAN_POINT ( 'NONE',  ( 5.153800228976335163, 19.02544592524342804, 24.79057627198102765 ) ) ;
#100773 = CARTESIAN_POINT ( 'NONE',  ( -9.564922557961040184, 16.46253265017147172, 62.91775706135233293 ) ) ;
#100774 = CARTESIAN_POINT ( 'NONE',  ( -16.51473224551069308, -9.474510206698971260, 61.66557627198103120 ) ) ;
#100775 = CARTESIAN_POINT ( 'NONE',  ( 13.89961937509977652, -13.97604488694527269, 98.12390960531433848 ) ) ;
#100776 = ORIENTED_EDGE ( 'NONE', *, *, #175843, .T. ) ;
#100777 = CARTESIAN_POINT ( 'NONE',  ( 10.81492255796078972, 18.62759615963270932, 104.5822429386477097 ) ) ;
#100780 = CARTESIAN_POINT ( 'NONE',  ( -9.564922557961040184, 16.46253265017147172, 62.91775706135233293 ) ) ;
#100779 = CARTESIAN_POINT ( 'NONE',  ( -19.02544592524342804, 5.153800228976336051, 81.04057627198103830 ) ) ;
#100778 = CARTESIAN_POINT ( 'NONE',  ( 4.379528057220339221, -16.55341960407611168, 97.70724293864772392 ) ) ;
#100781 = CARTESIAN_POINT ( 'NONE',  ( -18.62759615963270932, 10.81492255796079327, 85.83224293864768129 ) ) ;
#100782 = CARTESIAN_POINT ( 'NONE',  ( -15.80617190586745835, -15.72974639402198527, 66.87390960531436690 ) ) ;
#100783 = CARTESIAN_POINT ( 'NONE',  ( -16.55341960407611168, -4.379528057220339221, 36.45724293864768839 ) ) ;
#100784 = CARTESIAN_POINT ( 'NONE',  ( -21.53943276465977519, -0.05219959533937600094, 108.7510903946857042 ) ) ;
#100785 = CARTESIAN_POINT ( 'NONE',  ( 4.483927247898790824, -16.52544592524335698, 70.20942372801904696 ) ) ;
#100786 = CARTESIAN_POINT ( 'NONE',  ( 0.05219959533909260263, 19.03943276465977164, 94.99890960531436690 ) ) ;
#100787 = CARTESIAN_POINT ( 'NONE',  ( 19.05341960407611168, 5.049401038298154454, 28.95724293864769550 ) ) ;
#100788 = CARTESIAN_POINT ( 'NONE',  ( -21.53943276465977519, -0.05219959533937600094, 38.75109039468567573 ) ) ;
#100789 = CARTESIAN_POINT ( 'NONE',  ( -10.81492255796105439, 18.62759615963255655, 57.91775706135234714 ) ) ;
#100790 = CARTESIAN_POINT ( 'NONE',  ( -19.02544592524342804, 5.153800228976336051, 56.04057627198100988 ) ) ;
#100791 = CARTESIAN_POINT ( 'NONE',  ( -0.05219959533937732626, 21.53943276465977519, 32.50109039468568284 ) ) ;
#100792 = CARTESIAN_POINT ( 'NONE',  ( 13.89961937509957401, 13.97604488694547697, 76.87609039468566152 ) ) ;
#100793 = CARTESIAN_POINT ( 'NONE',  ( -13.89961937509957401, -13.97604488694547875, 69.37609039468564731 ) ) ;
#100794 = CARTESIAN_POINT ( 'NONE',  ( -5.049401038298153566, 19.05341960407611168, 45.20724293864769550 ) ) ;
#100795 = CARTESIAN_POINT ( 'NONE',  ( 0.05219959533934541429, -16.53943276465976808, 70.00109039468568994 ) ) ;
#100796 = CARTESIAN_POINT ( 'NONE',  ( -5.153800228976328057, -19.02544592524343514, 52.29057627198100988 ) ) ;
#100797 = CARTESIAN_POINT ( 'NONE',  ( 24.73536985823981027, -3.645104810711987664, 171.5180696409406096 ) ) ;
#100798 = CARTESIAN_POINT ( 'NONE',  ( -5.049401038298153566, 19.05341960407611168, 100.2072429386476955 ) ) ;
#100799 = CARTESIAN_POINT ( 'NONE',  ( -0.05219959533909027116, -19.03943276465977164, 37.49890960531436690 ) ) ;
#100800 = CARTESIAN_POINT ( 'NONE',  ( 21.52544592524344225, -5.823673210054117533, 73.54057627198102409 ) ) ;
#100801 = CARTESIAN_POINT ( 'NONE',  ( -4.379528057220086978, -16.55341960407618274, 64.79275706135234714 ) ) ;
#100802 = CARTESIAN_POINT ( 'NONE',  ( -0.05219959533937732626, 21.53943276465977519, 112.5010903946857042 ) ) ;
#100803 = EDGE_CURVE ( 'NONE', #70081, #35831, #39415, .T. ) ;
#100804 = CARTESIAN_POINT ( 'NONE',  ( -0.05219959533909027116, -19.03943276465977164, 57.49890960531435979 ) ) ;
#100805 = CARTESIAN_POINT ( 'NONE',  ( 8.224510206698953496, -14.34966873604960469, 42.91557627198103120 ) ) ;
#100806 = CARTESIAN_POINT ( 'NONE',  ( -16.55341960407611168, -4.379528057220339221, 76.45724293864769550 ) ) ;
#100807 = CARTESIAN_POINT ( 'NONE',  ( 19.02544592524343514, -5.153800228976328945, 78.54057627198099567 ) ) ;
#100808 = CARTESIAN_POINT ( 'NONE',  ( 15.80617190586769283, -15.72974639402175789, 35.62609039468568994 ) ) ;
#100809 = CARTESIAN_POINT ( 'NONE',  ( -13.97604488694527625, -13.89961937509977652, 91.87390960531432427 ) ) ;
#100810 = CARTESIAN_POINT ( 'NONE',  ( -5.823673210054431948, 21.52544592524334988, 97.70942372801904696 ) ) ;
#100811 = CARTESIAN_POINT ( 'NONE',  ( 14.34966873604972726, -8.224510206698740333, 60.83442372801901854 ) ) ;
#100812 = CARTESIAN_POINT ( 'NONE',  ( -5.153800228976328057, -19.02544592524343514, 107.2905762719810383 ) ) ;
#100813 = EDGE_CURVE ( 'NONE', #97685, #60651, #83920, .T. ) ;
#100814 = CARTESIAN_POINT ( 'NONE',  ( -10.72451020669898014, 18.67979575497178502, 95.41557627198102409 ) ) ;
#100815 = CARTESIAN_POINT ( 'NONE',  ( -4.483927247898539470, -16.52544592524342804, 42.29057627198103120 ) ) ;
#100816 = CARTESIAN_POINT ( 'NONE',  ( 9.474510206698971260, -16.51473224551069308, 37.91557627198102409 ) ) ;
#100817 = CARTESIAN_POINT ( 'NONE',  ( 12.06949235617739724, 12.14591786802326823, 46.87609039468568994 ) ) ;
#100818 = CARTESIAN_POINT ( 'NONE',  ( -14.34966873604960291, -8.224510206698953496, 61.66557627198103120 ) ) ;
#100819 = CARTESIAN_POINT ( 'NONE',  ( 19.03943276465977164, -0.05219959533909143690, 108.7489096053143527 ) ) ;
#100820 = CARTESIAN_POINT ( 'NONE',  ( -18.62759615963270932, 10.81492255796079327, 25.83224293864769194 ) ) ;
#100821 = CARTESIAN_POINT ( 'NONE',  ( 0.05219959533936267826, -19.03943276465977164, 30.00109039468566863 ) ) ;
#100822 = CARTESIAN_POINT ( 'NONE',  ( -0.05219959533910754901, -16.53943276465976808, 102.4989096053143811 ) ) ;
#100823 = CARTESIAN_POINT ( 'NONE',  ( 9.474510206698971260, -16.51473224551069308, 102.9155762719810241 ) ) ;
#100824 = ORIENTED_EDGE ( 'NONE', *, *, #82301, .F. ) ;
#100825 = CARTESIAN_POINT ( 'NONE',  ( -4.379528057220086978, -16.55341960407618274, 54.79275706135235424 ) ) ;
#100826 = CARTESIAN_POINT ( 'NONE',  ( 9.474510206698971260, -16.51473224551069308, 57.91557627198103120 ) ) ;
#100827 = DIRECTION ( 'NONE',  ( 0.000000000000000000, 0.000000000000000000, -1.000000000000000000 ) ) ;
#100828 = CARTESIAN_POINT ( 'NONE',  ( -13.89961937509957401, -13.97604488694547875, 59.37609039468566863 ) ) ;
#100829 = CARTESIAN_POINT ( 'NONE',  ( 16.53943276465976808, 0.05219959533934440121, 91.25109039468568994 ) ) ;
#100830 = CARTESIAN_POINT ( 'NONE',  ( 13.89961937509957401, 13.97604488694547697, 91.87609039468567573 ) ) ;
#100831 = CARTESIAN_POINT ( 'NONE',  ( 18.67979575497194134, -10.72451020669871369, 65.83442372801900433 ) ) ;
#100832 = CARTESIAN_POINT ( 'NONE',  ( -0.05219959533909027116, -19.03943276465977164, 72.49890960531435269 ) ) ;
#100833 = CARTESIAN_POINT ( 'NONE',  ( -18.62759615963270932, 10.81492255796079327, 95.83224293864770971 ) ) ;
#100834 = CARTESIAN_POINT ( 'NONE',  ( 16.52544592524342804, -4.483927247898539470, 108.5405762719810241 ) ) ;
#100835 = CARTESIAN_POINT ( 'NONE',  ( 9.564922557961047289, -16.46253265017146816, 75.41775706135234714 ) ) ;
#100836 = CARTESIAN_POINT ( 'NONE',  ( 5.719274019375991003, -21.55341960407610458, 82.70724293864770971 ) ) ;
#100837 = CARTESIAN_POINT ( 'NONE',  ( -13.97604488694547697, 13.89961937509957934, 43.12609039468566152 ) ) ;
#100838 = CARTESIAN_POINT ( 'NONE',  ( 18.56399227203342406, 5.499999999999960920, 96.47830131249901342 ) ) ;
#100839 = ADVANCED_FACE ( 'NONE', ( #189370 ), #16196, .T. ) ;
#100840 = CARTESIAN_POINT ( 'NONE',  ( -21.53943276465977519, 0.05219959533907696930, 86.24890960531436690 ) ) ;
#100841 = CARTESIAN_POINT ( 'NONE',  ( -28.82186960331504721, -9.364793116373462567, 148.0999999999999943 ) ) ;
#100842 = CARTESIAN_POINT ( 'NONE',  ( 0.05219959533909260263, 19.03943276465977164, 64.99890960531436690 ) ) ;
#100843 = LINE ( 'NONE', #84671, #178993 ) ;
#100844 = CARTESIAN_POINT ( 'NONE',  ( 16.51473224551083163, -9.474510206698727899, 110.8344237280190043 ) ) ;
#100845 = CARTESIAN_POINT ( 'NONE',  ( 21.98685479826779243, 13.98560643873834231, 165.5209445330007441 ) ) ;
#100846 = CARTESIAN_POINT ( 'NONE',  ( -13.97604488694527625, -13.89961937509977652, 41.87390960531435979 ) ) ;
#100848 = CARTESIAN_POINT ( 'NONE',  ( 16.53943276465976808, -0.05219959533910856209, 48.74890960531435979 ) ) ;
#100847 = CARTESIAN_POINT ( 'NONE',  ( -21.53943276465977519, 0.05219959533907696930, 106.2489096053143811 ) ) ;
#100849 = CARTESIAN_POINT ( 'NONE',  ( 5.823673210054444382, -21.52544592524334988, 75.20942372801901854 ) ) ;
#100851 = CARTESIAN_POINT ( 'NONE',  ( -9.474510206698720793, -16.51473224551083518, 34.58442372801899722 ) ) ;
#100850 = CARTESIAN_POINT ( 'NONE',  ( 16.52544592524335698, 4.483927247898782831, 21.45942372801901499 ) ) ;
#100852 = CARTESIAN_POINT ( 'NONE',  ( 14.34966873604960469, 8.224510206698951720, 24.16557627198103120 ) ) ;
#100853 = CARTESIAN_POINT ( 'NONE',  ( -21.55341960407619339, 5.719274019375674811, 33.54275706135234714 ) ) ;
#100854 = CARTESIAN_POINT ( 'NONE',  ( -21.52544592524334988, -5.823673210054445271, 18.95942372801901143 ) ) ;
#100855 = CARTESIAN_POINT ( 'NONE',  ( 18.67979575497178502, 10.72451020669898547, 64.16557627198102409 ) ) ;
#100856 = CARTESIAN_POINT ( 'NONE',  ( -5.049401038297874678, -19.05341960407617918, 89.79275706135230450 ) ) ;
#100857 = CARTESIAN_POINT ( 'NONE',  ( -13.97604488694547697, 13.89961937509957934, 68.12609039468563310 ) ) ;
#100858 = CARTESIAN_POINT ( 'NONE',  ( -5.823673210054431948, 21.52544592524334988, 77.70942372801900433 ) ) ;
#100859 = CARTESIAN_POINT ( 'NONE',  ( 5.153800228976615827, -19.02544592524334988, 50.20942372801897591 ) ) ;
#100860 = CARTESIAN_POINT ( 'NONE',  ( 4.483927247898545687, 16.52544592524342804, 114.7905762719810383 ) ) ;
#100861 = CARTESIAN_POINT ( 'NONE',  ( 18.62759615963271287, -10.81492255796078972, 43.33224293864769550 ) ) ;
#100862 = CARTESIAN_POINT ( 'NONE',  ( 14.34966873604960469, 8.224510206698951720, 49.16557627198102409 ) ) ;
#100863 = CARTESIAN_POINT ( 'NONE',  ( -18.22780087662123805, 5.499999999999981348, 96.01763182126897789 ) ) ;
#100864 = CARTESIAN_POINT ( 'NONE',  ( -9.474510206698720793, -16.51473224551083518, 19.58442372801899722 ) ) ;
#100865 = CARTESIAN_POINT ( 'NONE',  ( -16.53943276465976808, -0.05219959533934237506, 83.75109039468568994 ) ) ;
#100866 = CARTESIAN_POINT ( 'NONE',  ( 4.379528057220339221, -16.55341960407611168, 37.70724293864769550 ) ) ;
#100867 = CARTESIAN_POINT ( 'NONE',  ( 21.52544592524334988, 5.823673210054432836, 76.45942372801901854 ) ) ;
#100868 = CARTESIAN_POINT ( 'NONE',  ( 15.72974639402176855, 15.80617190586768217, 81.87609039468568994 ) ) ;
#100869 = CARTESIAN_POINT ( 'NONE',  ( -10.72451020669898014, 18.67979575497178502, 85.41557627198102409 ) ) ;
#100870 = CARTESIAN_POINT ( 'NONE',  ( 9.474510206698971260, -16.51473224551069308, 32.91557627198102409 ) ) ;
#100871 = CARTESIAN_POINT ( 'NONE',  ( -18.67979575497193778, 10.72451020669871902, 58.33442372801901143 ) ) ;
#100872 = CARTESIAN_POINT ( 'NONE',  ( 5.049401038298161559, -19.05341960407611168, 37.70724293864768839 ) ) ;
#100873 = CARTESIAN_POINT ( 'NONE',  ( -16.46253265017160317, 9.564922557960807481, 50.83224293864770260 ) ) ;
#100874 = CARTESIAN_POINT ( 'NONE',  ( -12.06949235617756955, 12.14591786802309770, 95.62390960531436690 ) ) ;
#100875 = CARTESIAN_POINT ( 'NONE',  ( -13.97604488694527625, -13.89961937509977652, 96.87390960531433848 ) ) ;
#100876 = CARTESIAN_POINT ( 'NONE',  ( 16.55341960407611168, 4.379528057220329451, 43.95724293864769550 ) ) ;
#100877 = CARTESIAN_POINT ( 'NONE',  ( 8.314922557960818139, 14.29746914071049879, 114.5822429386477097 ) ) ;
#100878 = CARTESIAN_POINT ( 'NONE',  ( -18.62759615963270932, 10.81492255796079327, 80.83224293864769550 ) ) ;
#100879 = CARTESIAN_POINT ( 'NONE',  ( -5.823673210054431948, 21.52544592524334988, 27.70942372801901854 ) ) ;
#100880 = CYLINDRICAL_SURFACE ( 'NONE', #11677, 1.500000000000001332 ) ;
#100881 = CARTESIAN_POINT ( 'NONE',  ( 12.14591786802327356, -12.06949235617739191, 20.62609039468568639 ) ) ;
#100882 = CARTESIAN_POINT ( 'NONE',  ( -10.72451020669898014, 18.67979575497178502, 70.41557627198102409 ) ) ;
#100883 = CARTESIAN_POINT ( 'NONE',  ( -5.719274019375665041, -21.55341960407619695, 99.79275706135234714 ) ) ;
#100884 = CARTESIAN_POINT ( 'NONE',  ( -5.049401038298153566, 19.05341960407611168, 85.20724293864766707 ) ) ;
#100885 = CARTESIAN_POINT ( 'NONE',  ( 15.80617190586769283, -15.72974639402175789, 35.62609039468568994 ) ) ;
#100886 = CARTESIAN_POINT ( 'NONE',  ( 5.153800228976335163, 19.02544592524342804, 109.7905762719810099 ) ) ;
#100887 = CARTESIAN_POINT ( 'NONE',  ( 8.314922557961029526, -14.29746914071037800, 85.41775706135236135 ) ) ;
#100888 = CARTESIAN_POINT ( 'NONE',  ( 0.05219959533937995610, -21.53943276465977519, 75.00109039468568994 ) ) ;
#100889 = CARTESIAN_POINT ( 'NONE',  ( -0.05219959533937732626, 21.53943276465977519, 112.5010903946857042 ) ) ;
#100890 = CARTESIAN_POINT ( 'NONE',  ( 16.55341960407618274, -4.379528057220086978, 81.04275706135236135 ) ) ;
#100891 = CARTESIAN_POINT ( 'NONE',  ( -15.72974639402176322, -15.80617190586768395, 24.37609039468567573 ) ) ;
#100892 = CARTESIAN_POINT ( 'NONE',  ( 19.05341960407611168, 5.049401038298154454, 28.95724293864769550 ) ) ;
#100893 = CARTESIAN_POINT ( 'NONE',  ( 21.53943276465977519, 0.05219959533937863772, 86.25109039468568994 ) ) ;
#100894 = CARTESIAN_POINT ( 'NONE',  ( 0.05219959533909260263, 19.03943276465977164, 89.99890960531436690 ) ) ;
#100895 = CARTESIAN_POINT ( 'NONE',  ( 18.67979575497178502, 10.72451020669898547, 84.16557627198103830 ) ) ;
#100896 = CARTESIAN_POINT ( 'NONE',  ( -16.46253265017146816, -9.564922557961047289, 54.16775706135234003 ) ) ;
#100898 = CARTESIAN_POINT ( 'NONE',  ( 21.53943276465977519, -0.05219959533907433946, 48.74890960531435979 ) ) ;
#100897 = CARTESIAN_POINT ( 'NONE',  ( 17.72517630441461378, -5.499999999999979572, 88.42175719257600974 ) ) ;
#100900 = CARTESIAN_POINT ( 'NONE',  ( -0.05219959533910754901, -16.53943276465976808, 47.49890960531435979 ) ) ;
#100899 = CARTESIAN_POINT ( 'NONE',  ( -13.97604488694527625, -13.89961937509977652, 91.87390960531432427 ) ) ;
#100901 = CARTESIAN_POINT ( 'NONE',  ( 20.61165082012733762, 10.97245752705834221, 168.1443239908791156 ) ) ;
#100902 = CARTESIAN_POINT ( 'NONE',  ( -16.51473224551082808, 9.474510206698731452, 73.33442372801900433 ) ) ;
#100903 = CARTESIAN_POINT ( 'NONE',  ( -17.44279575226824264, 5.990770900252420539, 105.8355756751431755 ) ) ;
#100904 = CARTESIAN_POINT ( 'NONE',  ( -5.153800228976607833, 19.02544592524334988, 107.7094237280189759 ) ) ;
#100905 = CARTESIAN_POINT ( 'NONE',  ( -10.72451020669898014, 18.67979575497178502, 90.41557627198103830 ) ) ;
#100906 = CARTESIAN_POINT ( 'NONE',  ( -4.483927247898539470, -16.52544592524342804, 67.29057627198103830 ) ) ;
#100907 = CARTESIAN_POINT ( 'NONE',  ( -19.05341960407611168, -5.049401038298163336, 96.45724293864769550 ) ) ;
#100908 = CARTESIAN_POINT ( 'NONE',  ( -8.224510206698735004, -14.34966873604973081, 44.58442372801901854 ) ) ;
#100909 = CARTESIAN_POINT ( 'NONE',  ( 9.564922557960805705, 16.46253265017160317, 59.58224293864769550 ) ) ;
#100911 = CARTESIAN_POINT ( 'NONE',  ( -19.02544592524334988, -5.153800228976617603, 93.95942372801900433 ) ) ;
#100910 = CARTESIAN_POINT ( 'NONE',  ( 10.81492255796106328, -18.62759615963255655, 25.41775706135235779 ) ) ;
#100912 = CARTESIAN_POINT ( 'NONE',  ( -16.46253265017160317, 9.564922557960807481, 90.83224293864769550 ) ) ;
#100913 = CARTESIAN_POINT ( 'NONE',  ( -16.46253265017160317, 9.564922557960807481, 75.83224293864769550 ) ) ;
#100914 = CARTESIAN_POINT ( 'NONE',  ( -15.80617190586745835, -15.72974639402198527, 81.87390960531435269 ) ) ;
#100915 = CARTESIAN_POINT ( 'NONE',  ( 19.03943276465977164, -0.05219959533909143690, 43.74890960531435979 ) ) ;
#100916 = CARTESIAN_POINT ( 'NONE',  ( -21.90810111552704242, 30.97181472859550411, -7.999999999999996447 ) ) ;
#100917 = CARTESIAN_POINT ( 'NONE',  ( -16.53943276465976808, 0.05219959533911058130, 51.24890960531436690 ) ) ;
#100918 = CARTESIAN_POINT ( 'NONE',  ( 19.02544592524343514, -5.153800228976328945, 103.5405762719809957 ) ) ;
#100919 = LINE ( 'NONE', #181778, #115366 ) ;
#100920 = CARTESIAN_POINT ( 'NONE',  ( 16.46253265017146816, 9.564922557961045513, 71.66775706135233293 ) ) ;
#100921 = CARTESIAN_POINT ( 'NONE',  ( 21.53943276465977519, -0.05219959533907433946, 93.74890960531436690 ) ) ;
#100922 = CARTESIAN_POINT ( 'NONE',  ( 16.51473224551083163, -9.474510206698727899, 45.83442372801900433 ) ) ;
#100923 = CARTESIAN_POINT ( 'NONE',  ( -16.46253265017160317, 9.564922557960807481, 95.83224293864769550 ) ) ;
#100924 = CARTESIAN_POINT ( 'NONE',  ( 17.97058386085786097, 5.500000000000042633, 76.50390968646217971 ) ) ;
#100925 = CARTESIAN_POINT ( 'NONE',  ( -0.05219959533907301413, -21.53943276465977519, 42.49890960531435979 ) ) ;
#100926 = CARTESIAN_POINT ( 'NONE',  ( -16.51473224551069308, -9.474510206698971260, 91.66557627198103830 ) ) ;
#100927 = EDGE_CURVE ( 'NONE', #167324, #197337, #107101, .T. ) ;
#100928 = CARTESIAN_POINT ( 'NONE',  ( 18.62759615963255655, 10.81492255796105972, 61.66775706135235424 ) ) ;
#100929 = CARTESIAN_POINT ( 'NONE',  ( 5.153800228976335163, 19.02544592524342804, 34.79057627198102409 ) ) ;
#100931 = ORIENTED_EDGE ( 'NONE', *, *, #69397, .F. ) ;
#100930 = CARTESIAN_POINT ( 'NONE',  ( 16.53943276465976808, -0.05219959533910856209, 73.74890960531433848 ) ) ;
#100932 = CARTESIAN_POINT ( 'NONE',  ( -14.34966873604972548, 8.224510206698743886, 28.33442372801902209 ) ) ;
#100933 = CARTESIAN_POINT ( 'NONE',  ( 18.62759615963255655, 10.81492255796105972, 46.66775706135234714 ) ) ;
#100934 = EDGE_LOOP ( 'NONE', ( #66905, #117342, #77811, #45498, #74370, #130546, #69374, #95850 ) ) ;
#100935 = CARTESIAN_POINT ( 'NONE',  ( -16.51473224551069308, -9.474510206698971260, 111.6655762719810383 ) ) ;
#100936 = CARTESIAN_POINT ( 'NONE',  ( 0.05219959533936267826, -19.03943276465977164, 65.00109039468567573 ) ) ;
#100937 = CARTESIAN_POINT ( 'NONE',  ( -20.84945647820398662, 10.59429869652067069, 168.2340845703681680 ) ) ;
#100938 = CARTESIAN_POINT ( 'NONE',  ( 15.72974639402176855, 15.80617190586768217, 21.87609039468567573 ) ) ;
#100939 = CARTESIAN_POINT ( 'NONE',  ( -5.049401038298153566, 19.05341960407611168, 55.20724293864769550 ) ) ;
#100940 = CARTESIAN_POINT ( 'NONE',  ( 3.766062262543149401E-15, -39.95556452105413570, -5.249999994537625447 ) ) ;
#100941 = CARTESIAN_POINT ( 'NONE',  ( 13.89961937509957401, 13.97604488694547697, 21.87609039468566152 ) ) ;
#100942 = CARTESIAN_POINT ( 'NONE',  ( 13.97604488694527802, 13.89961937509977652, 44.37390960531435269 ) ) ;
#100943 = CARTESIAN_POINT ( 'NONE',  ( -9.564922557961040184, 16.46253265017147172, 22.91775706135233648 ) ) ;
#100944 = CARTESIAN_POINT ( 'NONE',  ( 4.483927247898790824, -16.52544592524335698, 95.20942372801903275 ) ) ;
#100946 = CARTESIAN_POINT ( 'NONE',  ( 10.81492255796106328, -18.62759615963255655, 70.41775706135236135 ) ) ;
#100945 = CARTESIAN_POINT ( 'NONE',  ( -13.97604488694527625, -13.89961937509977652, 106.8739096053143669 ) ) ;
#100947 = CARTESIAN_POINT ( 'NONE',  ( -27.73933785331498925, -9.013057229001049109, 147.4750000027311785 ) ) ;
#100948 = CARTESIAN_POINT ( 'NONE',  ( 19.05341960407611168, 5.049401038298154454, 113.9572429386477097 ) ) ;
#100949 = CARTESIAN_POINT ( 'NONE',  ( 22.87077540613818982, -22.10389085601126169, -45.79323219683391244 ) ) ;
#100951 = CARTESIAN_POINT ( 'NONE',  ( 21.52544592524334988, 5.823673210054432836, 71.45942372801901854 ) ) ;
#100950 = CARTESIAN_POINT ( 'NONE',  ( 4.483927247898790824, -16.52544592524335698, 70.20942372801904696 ) ) ;
#100952 = CARTESIAN_POINT ( 'NONE',  ( 15.80617190586769283, -15.72974639402175789, 105.6260903946856899 ) ) ;
#100953 = CYLINDRICAL_SURFACE ( 'NONE', #12309, 38.00000000000000000 ) ;
#100954 = CARTESIAN_POINT ( 'NONE',  ( 16.53943276465976808, 0.05219959533934440121, 41.25109039468568284 ) ) ;
#100955 = CARTESIAN_POINT ( 'NONE',  ( -0.05219959533909027116, -19.03943276465977164, 92.49890960531436690 ) ) ;
#100956 = CARTESIAN_POINT ( 'NONE',  ( 5.153800228976335163, 19.02544592524342804, 104.7905762719809957 ) ) ;
#100957 = ORIENTED_EDGE ( 'NONE', *, *, #17615, .F. ) ;
#100958 = CARTESIAN_POINT ( 'NONE',  ( 16.20579543436682002, 7.371946100354975329, 43.06520834171879386 ) ) ;
#100959 = CARTESIAN_POINT ( 'NONE',  ( 16.46253265017160672, -9.564922557960803928, 43.33224293864769550 ) ) ;
#100961 = EDGE_CURVE ( 'NONE', #165210, #23117, #32359, .T. ) ;
#100960 = CARTESIAN_POINT ( 'NONE',  ( 21.53943276465977519, -0.05219959533907433946, 38.74890960531435979 ) ) ;
#100962 = CARTESIAN_POINT ( 'NONE',  ( 16.53943276465976808, 0.05219959533934440121, 111.2510903946856899 ) ) ;
#100964 = CARTESIAN_POINT ( 'NONE',  ( -9.564922557960796823, -16.46253265017161027, 77.08224293864769550 ) ) ;
#100963 = CARTESIAN_POINT ( 'NONE',  ( -4.483927247898539470, -16.52544592524342804, 77.29057627198102409 ) ) ;
#100965 = CARTESIAN_POINT ( 'NONE',  ( -21.55341960407619339, 5.719274019375674811, 108.5427570613523756 ) ) ;
#100966 = CARTESIAN_POINT ( 'NONE',  ( -19.02544592524342804, 5.153800228976336051, 31.04057627198102409 ) ) ;
#100967 = CARTESIAN_POINT ( 'NONE',  ( 16.52544592524342804, -4.483927247898539470, 83.54057627198102409 ) ) ;
#100968 = CARTESIAN_POINT ( 'NONE',  ( -21.53943276465977519, -0.05219959533937600094, 43.75109039468568284 ) ) ;
#100969 = CARTESIAN_POINT ( 'NONE',  ( 21.53943276465977519, -0.05219959533907433946, 88.74890960531436690 ) ) ;
#100970 = CARTESIAN_POINT ( 'NONE',  ( -0.05219959533936034679, 19.03943276465977164, 57.50109039468566863 ) ) ;
#100971 = CARTESIAN_POINT ( 'NONE',  ( -34.87691056670620071, 6.486286472422003513, 41.22672555304435349 ) ) ;
#100972 = CARTESIAN_POINT ( 'NONE',  ( 13.97604488694527802, 13.89961937509977652, 94.37390960531436690 ) ) ;
#100973 = CARTESIAN_POINT ( 'NONE',  ( 8.314922557960818139, 14.29746914071049879, 59.58224293864770260 ) ) ;
#100974 = EDGE_CURVE ( 'NONE', #60986, #113568, #119498, .T. ) ;
#100975 = CARTESIAN_POINT ( 'NONE',  ( -14.29746914071049879, 8.314922557960819915, 45.83224293864769550 ) ) ;
#100976 = CARTESIAN_POINT ( 'NONE',  ( 16.52544592524342804, -4.483927247898539470, 28.54057627198103120 ) ) ;
#100977 = CARTESIAN_POINT ( 'NONE',  ( 13.97604488694548053, -13.89961937509957401, 85.62609039468568994 ) ) ;
#100978 = CARTESIAN_POINT ( 'NONE',  ( 18.22780087662122384, -5.500000000000022204, 101.0154010532610869 ) ) ;
#100979 = CARTESIAN_POINT ( 'NONE',  ( -21.52544592524343514, 5.823673210054127303, 26.04057627198103475 ) ) ;
#100980 = CARTESIAN_POINT ( 'NONE',  ( -12.06949235617756955, 12.14591786802309770, 90.62390960531436690 ) ) ;
#100981 = PLANE ( 'NONE',  #38801 ) ;
#100983 = CARTESIAN_POINT ( 'NONE',  ( -5.719274019375978568, 21.55341960407610458, 50.20724293864769550 ) ) ;
#100982 = CARTESIAN_POINT ( 'NONE',  ( -13.89961937509977652, 13.97604488694528158, 50.62390960531435979 ) ) ;
#100984 = CARTESIAN_POINT ( 'NONE',  ( -19.03943276465977164, 0.05219959533909376836, 31.24890960531435979 ) ) ;
#100986 = CARTESIAN_POINT ( 'NONE',  ( -16.51473224551069308, -9.474510206698971260, 66.66557627198102409 ) ) ;
#100985 = CARTESIAN_POINT ( 'NONE',  ( -14.34966873604972548, 8.224510206698743886, 78.33442372801901854 ) ) ;
#100987 = CARTESIAN_POINT ( 'NONE',  ( 13.89961937509957401, 13.97604488694547697, 41.87609039468566152 ) ) ;
#100988 = CARTESIAN_POINT ( 'NONE',  ( 18.62759615963255655, 10.81492255796105972, 66.66775706135234714 ) ) ;
#100989 = CARTESIAN_POINT ( 'NONE',  ( 10.81492255796078972, 18.62759615963270932, 34.58224293864770260 ) ) ;
#100990 = CARTESIAN_POINT ( 'NONE',  ( -16.55341960407611168, -4.379528057220339221, 106.4572429386477097 ) ) ;
#100991 = CARTESIAN_POINT ( 'NONE',  ( 9.474510206698729675, 16.51473224551082808, 87.08442372801900433 ) ) ;
#100992 = CARTESIAN_POINT ( 'NONE',  ( 11.40812507854755253, -35.11059874428192273, -4.524999997268813523 ) ) ;
#100994 = CARTESIAN_POINT ( 'NONE',  ( 18.62759615963271287, -10.81492255796078972, 53.33224293864769550 ) ) ;
#100993 = DIRECTION ( 'NONE',  ( 1.000000000000000000, 0.000000000000000000, 0.000000000000000000 ) ) ;
#100995 = CARTESIAN_POINT ( 'NONE',  ( -13.97604488694527625, -13.89961937509977652, 21.87390960531435979 ) ) ;
#100996 = CARTESIAN_POINT ( 'NONE',  ( -18.62759615963255300, -10.81492255796106328, 89.16775706135236135 ) ) ;
#100997 = CARTESIAN_POINT ( 'NONE',  ( -16.55341960407611168, -4.379528057220339221, 46.45724293864769550 ) ) ;
#100999 = CARTESIAN_POINT ( 'NONE',  ( -4.379528057220328563, 16.55341960407611168, 50.20724293864769550 ) ) ;
#100998 = CARTESIAN_POINT ( 'NONE',  ( 4.483927247898790824, -16.52544592524335698, 65.20942372801901854 ) ) ;
#101000 = CARTESIAN_POINT ( 'NONE',  ( -21.52544592524343514, 5.823673210054127303, 76.04057627198102409 ) ) ;
#101001 = CARTESIAN_POINT ( 'NONE',  ( 15.72974639402199770, -15.80617190586745480, 73.12390960531436690 ) ) ;
#101002 = DIRECTION ( 'NONE',  ( 1.000000000000000000, -5.392603844284257652E-33, 0.000000000000000000 ) ) ;
#101003 = CARTESIAN_POINT ( 'NONE',  ( 5.153800228976335163, 19.02544592524342804, 109.7905762719810099 ) ) ;
#101004 = CARTESIAN_POINT ( 'NONE',  ( 12.14591786802309770, 12.06949235617756955, 84.37390960531438111 ) ) ;
#101005 = CARTESIAN_POINT ( 'NONE',  ( 9.564922557960805705, 16.46253265017160317, 59.58224293864769550 ) ) ;
#101006 = CARTESIAN_POINT ( 'NONE',  ( -19.03943276465977164, 0.05219959533909376836, 31.24890960531435979 ) ) ;
#101007 = FILL_AREA_STYLE ('',( #56520 ) ) ;
#101008 = DIRECTION ( 'NONE',  ( 0.000000000000000000, 1.000000000000000000, 0.000000000000000000 ) ) ;
#101009 = VERTEX_POINT ( 'NONE', #2010 ) ;
#101010 = CARTESIAN_POINT ( 'NONE',  ( 16.53943276465976808, 0.05219959533934440121, 76.25109039468568994 ) ) ;
#101011 = CARTESIAN_POINT ( 'NONE',  ( -18.62759615963270932, 10.81492255796079327, 115.8322429386477097 ) ) ;
#101012 = CARTESIAN_POINT ( 'NONE',  ( 5.049401038298161559, -19.05341960407611168, 72.70724293864768129 ) ) ;
#101013 = CARTESIAN_POINT ( 'NONE',  ( -10.81492255796105439, 18.62759615963255655, 52.91775706135235424 ) ) ;
#101014 = CARTESIAN_POINT ( 'NONE',  ( -13.97604488694527625, -13.89961937509977652, 106.8739096053143669 ) ) ;
#101015 = CARTESIAN_POINT ( 'NONE',  ( -11.94140034372569303, -38.57382067147337779, -24.90972908440997102 ) ) ;
#101016 = VERTEX_POINT ( 'NONE', #157689 ) ;
#101017 = CARTESIAN_POINT ( 'NONE',  ( 18.67979575497194134, -10.72451020669871369, 50.83442372801901143 ) ) ;
#101019 = CARTESIAN_POINT ( 'NONE',  ( 16.51473224551069308, 9.474510206698969483, 99.16557627198102409 ) ) ;
#101018 = CARTESIAN_POINT ( 'NONE',  ( -19.02544592524342804, 5.153800228976336051, 116.0405762719810383 ) ) ;
#101020 = CARTESIAN_POINT ( 'NONE',  ( 9.474510206698729675, 16.51473224551082808, 52.08442372801900433 ) ) ;
#101021 = CARTESIAN_POINT ( 'NONE',  ( 15.72974639402199770, -15.80617190586745480, 108.1239096053143811 ) ) ;
#101022 = CARTESIAN_POINT ( 'NONE',  ( -5.049401038297874678, -19.05341960407617918, 39.79275706135232582 ) ) ;
#101023 = CARTESIAN_POINT ( 'NONE',  ( 16.51473224551083163, -9.474510206698727899, 55.83442372801899722 ) ) ;
#101024 = CARTESIAN_POINT ( 'NONE',  ( 4.379528057220092307, 16.55341960407617563, 102.2927570613523613 ) ) ;
#101026 = ORIENTED_EDGE ( 'NONE', *, *, #171652, .F. ) ;
#101025 = CARTESIAN_POINT ( 'NONE',  ( 69.65682714487590488, -71.74905178543389184, -10.00000000000000000 ) ) ;
#101027 = CARTESIAN_POINT ( 'NONE',  ( 16.51473224551069308, 9.474510206698969483, 74.16557627198103830 ) ) ;
#101028 = CARTESIAN_POINT ( 'NONE',  ( -5.719274019375665041, -21.55341960407619695, 84.79275706135234714 ) ) ;
#101029 = CARTESIAN_POINT ( 'NONE',  ( -21.53943276465977519, -0.05219959533937600094, 88.75109039468567573 ) ) ;
#101030 = DIRECTION ( 'NONE',  ( 0.000000000000000000, 1.000000000000000000, -3.469446951953611033E-15 ) ) ;
#101031 = CARTESIAN_POINT ( 'NONE',  ( -5.153800228976328057, -19.02544592524343514, 97.29057627198099567 ) ) ;
#101032 = CARTESIAN_POINT ( 'NONE',  ( 5.719274019375673035, 21.55341960407619339, 77.29275706135234714 ) ) ;
#101033 = CARTESIAN_POINT ( 'NONE',  ( -4.483927247898782831, 16.52544592524335698, 22.70942372801901499 ) ) ;
#101034 = CARTESIAN_POINT ( 'NONE',  ( -19.02544592524342804, 5.153800228976336051, 76.04057627198102409 ) ) ;
#101035 = CARTESIAN_POINT ( 'NONE',  ( 18.67979575497178502, 10.72451020669898547, 24.16557627198103120 ) ) ;
#101036 = CARTESIAN_POINT ( 'NONE',  ( 19.03943276465977164, -0.05219959533909143690, 93.74890960531435269 ) ) ;
#101037 = CARTESIAN_POINT ( 'NONE',  ( 26.46959431505284499, -27.26463967846488146, -15.00000000000000178 ) ) ;
#101038 = CARTESIAN_POINT ( 'NONE',  ( -16.51473224551069308, -9.474510206698971260, 81.66557627198103830 ) ) ;
#101039 = CARTESIAN_POINT ( 'NONE',  ( 19.03943276465977164, -0.05219959533909143690, 63.74890960531435979 ) ) ;
#101040 = CARTESIAN_POINT ( 'NONE',  ( 10.72451020669898902, -18.67979575497178502, 107.9155762719810241 ) ) ;
#101041 = CARTESIAN_POINT ( 'NONE',  ( -8.224510206698735004, -14.34966873604973081, 94.58442372801901854 ) ) ;
#101042 = LINE ( 'NONE', #195078, #176000 ) ;
#101043 = CARTESIAN_POINT ( 'NONE',  ( 19.02544592524334988, 5.153800228976608722, 56.45942372801898301 ) ) ;
#101044 = CARTESIAN_POINT ( 'NONE',  ( 9.474510206698971260, -16.51473224551069308, 87.91557627198102409 ) ) ;
#101045 = CARTESIAN_POINT ( 'NONE',  ( 14.29746914071049879, -8.314922557960816363, 88.33224293864769550 ) ) ;
#101046 = CARTESIAN_POINT ( 'NONE',  ( -10.81492255796078084, -18.62759615963271287, 27.08224293864769550 ) ) ;
#101047 =( BOUNDED_CURVE ( )  B_SPLINE_CURVE ( 2, ( #79218, #3369, #64057, #33715, #157062, #18559, #72031, #134719, #56874, #26544, #146871 ),
 .UNSPECIFIED., .F., .F. ) 
 B_SPLINE_CURVE_WITH_KNOTS ( ( 3, 2, 2, 2, 2, 3 ),
 ( 0.2000000000000001776, 0.2200000000000001954, 0.2400000000000002132, 0.2600000000000002309, 0.2800000000000003042, 0.3000000000000002665 ),
 .UNSPECIFIED. ) 
 CURVE ( )  GEOMETRIC_REPRESENTATION_ITEM ( )  RATIONAL_B_SPLINE_CURVE ( ( 0.9999999999999995559, 0.9510565162951539753, 1.000000000000000000, 0.9510565162951535312, 1.000000000000000000, 0.9510565162951535312, 1.000000000000000000, 0.9510565162951535312, 1.000000000000000000, 0.9510565162951528650, 1.000000000000000666 ) ) 
 REPRESENTATION_ITEM ( '' )  );
#101048 = CARTESIAN_POINT ( 'NONE',  ( -21.52544592524343514, 5.823673210054127303, 26.04057627198103475 ) ) ;
#101049 = CARTESIAN_POINT ( 'NONE',  ( -8.314922557960811034, -14.29746914071050412, 92.08224293864769550 ) ) ;
#101050 = CARTESIAN_POINT ( 'NONE',  ( -17.44279575226822843, 5.990770900252464060, 55.83557567514321107 ) ) ;
#101051 = CARTESIAN_POINT ( 'NONE',  ( 9.564922557961047289, -16.46253265017146816, 45.41775706135232582 ) ) ;
#101052 = CARTESIAN_POINT ( 'NONE',  ( 8.224510206698742110, 14.34966873604972548, 107.0844237280190043 ) ) ;
#101053 = CARTESIAN_POINT ( 'NONE',  ( -9.564922557960796823, -16.46253265017161027, 92.08224293864769550 ) ) ;
#101054 = CARTESIAN_POINT ( 'NONE',  ( 10.72451020669871369, 18.67979575497193778, 67.08442372801901854 ) ) ;
#101055 = CARTESIAN_POINT ( 'NONE',  ( 21.52544592524344225, -5.823673210054117533, 63.54057627198103830 ) ) ;
#101056 = CARTESIAN_POINT ( 'NONE',  ( 10.81492255796106328, -18.62759615963255655, 30.41775706135234358 ) ) ;
#101057 = CARTESIAN_POINT ( 'NONE',  ( -0.05219959533907301413, -21.53943276465977519, 82.49890960531436690 ) ) ;
#101058 = CARTESIAN_POINT ( 'NONE',  ( -0.05219959533910754901, -16.53943276465976808, 112.4989096053143669 ) ) ;
#101059 = CARTESIAN_POINT ( 'NONE',  ( 9.474510206698729675, 16.51473224551082808, 67.08442372801900433 ) ) ;
#101060 = CARTESIAN_POINT ( 'NONE',  ( -5.153800228976328057, -19.02544592524343514, 42.29057627198101699 ) ) ;
#101061 = CARTESIAN_POINT ( 'NONE',  ( -13.89961937509977652, 13.97604488694528158, 95.62390960531436690 ) ) ;
#101062 = CARTESIAN_POINT ( 'NONE',  ( 19.03943276465977164, -0.05219959533909143690, 88.74890960531436690 ) ) ;
#101063 = CARTESIAN_POINT ( 'NONE',  ( 16.53943276465976808, -0.05219959533910856209, 113.7489096053143527 ) ) ;
#101064 = CARTESIAN_POINT ( 'NONE',  ( 0.05219959533910956823, 16.53943276465976808, 44.99890960531435979 ) ) ;
#101065 = CARTESIAN_POINT ( 'NONE',  ( 16.53943276465976808, 0.05219959533934440121, 41.25109039468568284 ) ) ;
#101066 = CARTESIAN_POINT ( 'NONE',  ( 5.719274019375673035, 21.55341960407619339, 112.2927570613523471 ) ) ;
#101068 = CARTESIAN_POINT ( 'NONE',  ( -8.314922557960811034, -14.29746914071050412, 22.08224293864769194 ) ) ;
#101067 = CYLINDRICAL_SURFACE ( 'NONE', #4217, 1.499999999999997780 ) ;
#101069 = CARTESIAN_POINT ( 'NONE',  ( -21.53943276465977519, -0.05219959533937600094, 28.75109039468567929 ) ) ;
#101070 = CARTESIAN_POINT ( 'NONE',  ( -13.89961937509977652, 13.97604488694528158, 105.6239096053143527 ) ) ;
#101071 = CARTESIAN_POINT ( 'NONE',  ( 16.55341960407618274, -4.379528057220086978, 101.0427570613523756 ) ) ;
#101072 = CARTESIAN_POINT ( 'NONE',  ( -0.05219959533934338120, 16.53943276465976808, 97.50109039468567573 ) ) ;
#101073 = CARTESIAN_POINT ( 'NONE',  ( 14.29746914071037800, 8.314922557961029526, 26.66775706135235424 ) ) ;
#101074 = CARTESIAN_POINT ( 'NONE',  ( -9.474510206698964154, 16.51473224551069663, 50.41557627198102409 ) ) ;
#101075 = CARTESIAN_POINT ( 'NONE',  ( 14.34966873604960469, 8.224510206698951720, 109.1655762719810383 ) ) ;
#101076 = CARTESIAN_POINT ( 'NONE',  ( -10.72451020669898014, 18.67979575497178502, 115.4155762719810241 ) ) ;
#101077 = CARTESIAN_POINT ( 'NONE',  ( 19.03943276465977164, -0.05219959533909143690, 28.74890960531435624 ) ) ;
#101078 = CARTESIAN_POINT ( 'NONE',  ( 13.97604488694527802, 13.89961937509977652, 99.37390960531436690 ) ) ;
#101079 = CARTESIAN_POINT ( 'NONE',  ( -9.474510206698964154, 16.51473224551069663, 30.41557627198102054 ) ) ;
#101080 = CARTESIAN_POINT ( 'NONE',  ( -19.03943276465977164, 0.05219959533909376836, 101.2489096053143669 ) ) ;
#101081 = CARTESIAN_POINT ( 'NONE',  ( 18.22780087662123805, -5.499999999999989342, 63.51763182126896368 ) ) ;
#101082 = B_SPLINE_CURVE_WITH_KNOTS ( 'NONE', 3,
 ( #107868, #129987, #20839, #174538, #191687, #51186, #177545, #112847, #97653, #66349, #178537, #148195, #67341, #38016, #85502, #82496, #36005, #147191, #128011, #159343, #144179, #192699, #7657, #69341 ),
 .UNSPECIFIED., .F., .F.,
 ( 4, 2, 2, 2, 2, 2, 2, 2, 2, 2, 2, 4 ),
 ( 2.775519118949223281E-07, 0.0003993838752237327430, 0.0007984901985355705861, 0.001596702845159246814, 0.002394915491782922609, 0.003193128138406599054, 0.003991340785030274632, 0.004789553431653949776, 0.005188659754965791251, 0.005587766078277632727, 0.005986872401589474202, 0.006385978724901315677 ),
 .UNSPECIFIED. ) ;
#101083 = CARTESIAN_POINT ( 'NONE',  ( 9.564922557960805705, 16.46253265017160317, 104.5822429386476955 ) ) ;
#101085 = CARTESIAN_POINT ( 'NONE',  ( 14.34966873604960469, 8.224510206698951720, 89.16557627198102409 ) ) ;
#101084 = CARTESIAN_POINT ( 'NONE',  ( 21.52544592524334988, 5.823673210054432836, 51.45942372801901854 ) ) ;
#101086 = CARTESIAN_POINT ( 'NONE',  ( -16.46253265017160317, 9.564922557960807481, 90.83224293864769550 ) ) ;
#101087 = DIRECTION ( 'NONE',  ( 0.000000000000000000, 0.000000000000000000, -1.000000000000000000 ) ) ;
#101088 = CARTESIAN_POINT ( 'NONE',  ( 0.05219959533934541429, -16.53943276465976808, 70.00109039468568994 ) ) ;
#101089 = CARTESIAN_POINT ( 'NONE',  ( -15.72974639402176322, -15.80617190586768395, 79.37609039468567573 ) ) ;
#101090 = CARTESIAN_POINT ( 'NONE',  ( 4.483927247898790824, -16.52544592524335698, 40.20942372801901854 ) ) ;
#101091 = CARTESIAN_POINT ( 'NONE',  ( -5.049401038298153566, 19.05341960407611168, 80.20724293864769550 ) ) ;
#101092 = CARTESIAN_POINT ( 'NONE',  ( 19.03943276465977164, 0.05219959533936151252, 111.2510903946856757 ) ) ;
#101093 = CARTESIAN_POINT ( 'NONE',  ( -14.29746914071037622, -8.314922557961029526, 84.16775706135234714 ) ) ;
#101094 = CARTESIAN_POINT ( 'NONE',  ( -16.51473224551082808, 9.474510206698731452, 88.33442372801900433 ) ) ;
#101095 = CARTESIAN_POINT ( 'NONE',  ( -9.564922557960796823, -16.46253265017161027, 57.08224293864769550 ) ) ;
#101096 = CARTESIAN_POINT ( 'NONE',  ( 18.67979575497178502, 10.72451020669898547, 104.1655762719810241 ) ) ;
#101098 = CARTESIAN_POINT ( 'NONE',  ( 13.89961937509957401, 13.97604488694547697, 96.87609039468566152 ) ) ;
#101097 = CARTESIAN_POINT ( 'NONE',  ( -14.34966873604960291, -8.224510206698953496, 86.66557627198102409 ) ) ;
#101099 = CARTESIAN_POINT ( 'NONE',  ( -4.379528057220086978, -16.55341960407618274, 54.79275706135235424 ) ) ;
#101100 = CARTESIAN_POINT ( 'NONE',  ( -19.25663599770060941, 5.499999999999452882, 78.99419308057203182 ) ) ;
#101101 = CARTESIAN_POINT ( 'NONE',  ( -19.02544592524334988, -5.153800228976617603, 58.95942372801900433 ) ) ;
#101102 = CARTESIAN_POINT ( 'NONE',  ( 12.06949235617757843, -12.14591786802309237, 33.12390960531435979 ) ) ;
#101103 = CARTESIAN_POINT ( 'NONE',  ( -16.55341960407611168, -4.379528057220339221, 76.45724293864769550 ) ) ;
#101105 = CARTESIAN_POINT ( 'NONE',  ( 17.50000000000000000, -5.500000000000000888, 103.2969038253417153 ) ) ;
#101104 = CARTESIAN_POINT ( 'NONE',  ( 13.89961937509957401, 13.97604488694547697, 21.87609039468566152 ) ) ;
#101106 = CARTESIAN_POINT ( 'NONE',  ( -18.62759615963255300, -10.81492255796106328, 29.16775706135234003 ) ) ;
#101107 = CARTESIAN_POINT ( 'NONE',  ( 13.97604488694527802, 13.89961937509977652, 114.3739096053143669 ) ) ;
#101108 = CARTESIAN_POINT ( 'NONE',  ( 19.02544592524343514, -5.153800228976328945, 73.54057627198103830 ) ) ;
#101109 = CARTESIAN_POINT ( 'NONE',  ( 15.72974639402176855, 15.80617190586768217, 91.87609039468568994 ) ) ;
#101110 = CARTESIAN_POINT ( 'NONE',  ( 16.46253265017160672, -9.564922557960803928, 78.33224293864769550 ) ) ;
#101111 = CARTESIAN_POINT ( 'NONE',  ( 21.55341960407610458, 5.719274019375980345, 43.95724293864769550 ) ) ;
#101112 = CARTESIAN_POINT ( 'NONE',  ( 12.06949235617757843, -12.14591786802309237, 83.12390960531436690 ) ) ;
#101113 = CARTESIAN_POINT ( 'NONE',  ( -9.564922557960796823, -16.46253265017161027, 57.08224293864769550 ) ) ;
#101114 = CARTESIAN_POINT ( 'NONE',  ( 8.224510206698953496, -14.34966873604960469, 107.9155762719810241 ) ) ;
#101115 = CARTESIAN_POINT ( 'NONE',  ( -0.05219959533937732626, 21.53943276465977519, 22.50109039468567573 ) ) ;
#101116 = CARTESIAN_POINT ( 'NONE',  ( -21.53943276465977519, -0.05219959533937600094, 68.75109039468568994 ) ) ;
#101117 = CARTESIAN_POINT ( 'NONE',  ( 9.474510206698971260, -16.51473224551069308, 47.91557627198102409 ) ) ;
#101118 = CARTESIAN_POINT ( 'NONE',  ( 0.05219959533934541429, -16.53943276465976808, 60.00109039468568284 ) ) ;
#101119 = CARTESIAN_POINT ( 'NONE',  ( 15.72974639402199770, -15.80617190586745480, 113.1239096053143953 ) ) ;
#101120 = CARTESIAN_POINT ( 'NONE',  ( 0.05219959533907565091, 21.53943276465977519, 114.9989096053143669 ) ) ;
#101122 = CARTESIAN_POINT ( 'NONE',  ( -19.02544592524342804, 5.153800228976336051, 61.04057627198103120 ) ) ;
#101121 = CARTESIAN_POINT ( 'NONE',  ( -16.51473224551082808, 9.474510206698731452, 43.33442372801900433 ) ) ;
#101123 = DIRECTION ( 'NONE',  ( 0.000000000000000000, 0.000000000000000000, 1.000000000000000000 ) ) ;
#101124 = CARTESIAN_POINT ( 'NONE',  ( -5.823673210054431948, 21.52544592524334988, 67.70942372801901854 ) ) ;
#101125 = CARTESIAN_POINT ( 'NONE',  ( -21.53943276465977519, 0.05219959533907696930, 56.24890960531436690 ) ) ;
#101126 = CARTESIAN_POINT ( 'NONE',  ( 16.52544592524342804, -4.483927247898539470, 43.54057627198103830 ) ) ;
#101128 = CARTESIAN_POINT ( 'NONE',  ( 18.67979575497194134, -10.72451020669871369, 105.8344237280190328 ) ) ;
#101127 = CARTESIAN_POINT ( 'NONE',  ( 10.81492255796106328, -18.62759615963255655, 75.41775706135233293 ) ) ;
#101129 = CARTESIAN_POINT ( 'NONE',  ( -16.53943276465976808, 0.05219959533911058130, 61.24890960531435979 ) ) ;
#101130 = CARTESIAN_POINT ( 'NONE',  ( -16.52544592524342804, 4.483927247898546575, 101.0405762719810383 ) ) ;
#101131 = CARTESIAN_POINT ( 'NONE',  ( 5.049401038297881783, 19.05341960407617563, 62.29275706135234003 ) ) ;
#101132 = CARTESIAN_POINT ( 'NONE',  ( 4.379528057220092307, 16.55341960407617563, 112.2927570613523471 ) ) ;
#101133 = CARTESIAN_POINT ( 'NONE',  ( -21.55341960407619339, 5.719274019375674811, 63.54275706135234003 ) ) ;
#101134 = CARTESIAN_POINT ( 'NONE',  ( -5.049401038298153566, 19.05341960407611168, 70.20724293864769550 ) ) ;
#101135 = CARTESIAN_POINT ( 'NONE',  ( 16.51473224551083163, -9.474510206698727899, 40.83442372801900433 ) ) ;
#101136 = CARTESIAN_POINT ( 'NONE',  ( 21.52544592524344225, -5.823673210054117533, 33.54057627198102409 ) ) ;
#101137 = CARTESIAN_POINT ( 'NONE',  ( 15.80617190586769283, -15.72974639402175789, 50.62609039468568994 ) ) ;
#101138 = CARTESIAN_POINT ( 'NONE',  ( -10.81492255796078084, -18.62759615963271287, 102.0822429386476955 ) ) ;
#101139 = CARTESIAN_POINT ( 'NONE',  ( -19.02544592524334988, -5.153800228976617603, 103.9594237280190043 ) ) ;
#101140 = CARTESIAN_POINT ( 'NONE',  ( -16.52544592524335698, -4.483927247898792601, 58.95942372801902565 ) ) ;
#101142 = CARTESIAN_POINT ( 'NONE',  ( 21.53943276465977519, -0.05219959533907433946, 93.74890960531436690 ) ) ;
#101141 = DIRECTION ( 'NONE',  ( 0.000000000000000000, 0.000000000000000000, 1.000000000000000000 ) ) ;
#101143 = CARTESIAN_POINT ( 'NONE',  ( 16.55341960407611168, 4.379528057220329451, 83.95724293864770971 ) ) ;
#101144 = CARTESIAN_POINT ( 'NONE',  ( 22.96528548301342809, 5.795830589372932273, 190.0000000000000000 ) ) ;
#101145 = CARTESIAN_POINT ( 'NONE',  ( 16.52544592524335698, 4.483927247898782831, 21.45942372801901499 ) ) ;
#101146 = CARTESIAN_POINT ( 'NONE',  ( 15.80617190586746368, 15.72974639402197994, 49.37390960531436690 ) ) ;
#101147 = CARTESIAN_POINT ( 'NONE',  ( 12.14591786802327356, -12.06949235617739191, 95.62609039468568994 ) ) ;
#101148 = CARTESIAN_POINT ( 'NONE',  ( 33.65002604405838582, -15.23243535768875923, -8.000000000000003553 ) ) ;
#101149 = CARTESIAN_POINT ( 'NONE',  ( -14.29746914071037622, -8.314922557961029526, 59.16775706135234714 ) ) ;
#101150 = CARTESIAN_POINT ( 'NONE',  ( -5.823673210054431948, 21.52544592524334988, 22.70942372801901499 ) ) ;
#101151 = CARTESIAN_POINT ( 'NONE',  ( -15.80617190586745835, -15.72974639402198527, 46.87390960531435979 ) ) ;
#101152 = CARTESIAN_POINT ( 'NONE',  ( -16.52544592524335698, -4.483927247898792601, 78.95942372801901854 ) ) ;
#101153 = CARTESIAN_POINT ( 'NONE',  ( 19.02544592524343514, -5.153800228976328945, 103.5405762719809957 ) ) ;
#101154 = CARTESIAN_POINT ( 'NONE',  ( 21.52544592524334988, 5.823673210054432836, 71.45942372801901854 ) ) ;
#101155 = CARTESIAN_POINT ( 'NONE',  ( 18.67979575497178502, 10.72451020669898547, 44.16557627198103120 ) ) ;
#101156 = CARTESIAN_POINT ( 'NONE',  ( 13.97604488694527802, 13.89961937509977652, 114.3739096053143669 ) ) ;
#101157 = EDGE_LOOP ( 'NONE', ( #190250, #115671, #3708 ) ) ;
#101158 = CARTESIAN_POINT ( 'NONE',  ( 19.05341960407617918, -5.049401038297876454, 46.04275706135233293 ) ) ;
#101159 = CARTESIAN_POINT ( 'NONE',  ( -16.52544592524335698, -4.483927247898792601, 68.95942372801901854 ) ) ;
#101160 = CARTESIAN_POINT ( 'NONE',  ( 21.52544592524344225, -5.823673210054117533, 33.54057627198102409 ) ) ;
#101161 = ORIENTED_EDGE ( 'NONE', *, *, #130358, .T. ) ;
#101162 = CARTESIAN_POINT ( 'NONE',  ( -19.02544592524342804, 5.153800228976336051, 81.04057627198103830 ) ) ;
#101163 = CARTESIAN_POINT ( 'NONE',  ( -16.55341960407617563, 4.379528057220093196, 113.5427570613523756 ) ) ;
#101164 = CARTESIAN_POINT ( 'NONE',  ( 4.962140900324421011, -6.180203150055868733, 3.431593142121016626 ) ) ;
#101165 = CARTESIAN_POINT ( 'NONE',  ( 16.55341960407611168, 4.379528057220329451, 108.9572429386476955 ) ) ;
#101166 = CARTESIAN_POINT ( 'NONE',  ( -10.81492255796078084, -18.62759615963271287, 52.08224293864768839 ) ) ;
#101167 = CARTESIAN_POINT ( 'NONE',  ( -19.02544592524342804, 5.153800228976336051, 46.04057627198101699 ) ) ;
#101168 = CARTESIAN_POINT ( 'NONE',  ( 4.379528057220092307, 16.55341960407617563, 72.29275706135236135 ) ) ;
#101169 = CARTESIAN_POINT ( 'NONE',  ( -21.53943276465977519, -0.05219959533937600094, 33.75109039468568284 ) ) ;
#101170 = CARTESIAN_POINT ( 'NONE',  ( -0.05219959533936034679, 19.03943276465977164, 87.50109039468567573 ) ) ;
#101171 = CARTESIAN_POINT ( 'NONE',  ( 0.05219959533910956823, 16.53943276465976808, 84.99890960531436690 ) ) ;
#101172 = CARTESIAN_POINT ( 'NONE',  ( -9.474510206698964154, 16.51473224551069663, 60.41557627198102409 ) ) ;
#101173 = CARTESIAN_POINT ( 'NONE',  ( -13.89961937509977652, 13.97604488694528158, 25.62390960531434558 ) ) ;
#101174 = CARTESIAN_POINT ( 'NONE',  ( 0.05219959533937995610, -21.53943276465977519, 100.0010903946857042 ) ) ;
#101175 = CARTESIAN_POINT ( 'NONE',  ( -5.153800228976328057, -19.02544592524343514, 82.29057627198103830 ) ) ;
#101176 = CARTESIAN_POINT ( 'NONE',  ( -16.53943276465976808, -0.05219959533934237506, 63.75109039468568284 ) ) ;
#101177 = CARTESIAN_POINT ( 'NONE',  ( -10.72451020669870658, -18.67979575497194134, 89.58442372801901854 ) ) ;
#101178 = CARTESIAN_POINT ( 'NONE',  ( 0.05219959533907565091, 21.53943276465977519, 49.99890960531437401 ) ) ;
#101179 = CARTESIAN_POINT ( 'NONE',  ( 12.14591786802327356, -12.06949235617739191, 70.62609039468567573 ) ) ;
#101180 = CARTESIAN_POINT ( 'NONE',  ( 13.89961937509957401, 13.97604488694547697, 56.87609039468564731 ) ) ;
#101181 = CARTESIAN_POINT ( 'NONE',  ( -19.05341960407617563, 5.049401038297882671, 68.54275706135230450 ) ) ;
#101182 = CARTESIAN_POINT ( 'NONE',  ( 21.52544592524334988, 5.823673210054432836, 66.45942372801903275 ) ) ;
#101183 = CARTESIAN_POINT ( 'NONE',  ( -13.89961937509977652, 13.97604488694528158, 70.62390960531432427 ) ) ;
#101184 = CARTESIAN_POINT ( 'NONE',  ( 18.22780087662119897, -5.500000000000096811, 58.51763182126894947 ) ) ;
#101185 = CARTESIAN_POINT ( 'NONE',  ( 13.97604488694548053, -13.89961937509957401, 55.62609039468566863 ) ) ;
#101186 = CARTESIAN_POINT ( 'NONE',  ( -25.57682740168942814, 5.495034664247683054, 164.9437814717017545 ) ) ;
#101187 = CARTESIAN_POINT ( 'NONE',  ( 16.46253265017160672, -9.564922557960803928, 98.33224293864769550 ) ) ;
#101188 = CARTESIAN_POINT ( 'NONE',  ( 16.55341960407611168, 4.379528057220329451, 48.95724293864770971 ) ) ;
#101189 = CARTESIAN_POINT ( 'NONE',  ( 18.67979575497178502, 10.72451020669898547, 44.16557627198103120 ) ) ;
#101190 = CARTESIAN_POINT ( 'NONE',  ( 10.72451020669871369, 18.67979575497193778, 112.0844237280190185 ) ) ;
#101191 = CARTESIAN_POINT ( 'NONE',  ( -19.02544592524342804, 5.153800228976336051, 46.04057627198101699 ) ) ;
#101192 = CARTESIAN_POINT ( 'NONE',  ( -30.00000000000000000, -1.163414459189985801E-14, 97.50000000000000000 ) ) ;
#101193 = CARTESIAN_POINT ( 'NONE',  ( -34.52594549653174028, -0.3594300054053902183, 89.49999999999896261 ) ) ;
#101194 = CARTESIAN_POINT ( 'NONE',  ( 37.99626262588765258, 2.893932880411085066E-14, -1.002157773949823083 ) ) ;
#101195 = CARTESIAN_POINT ( 'NONE',  ( 16.53943276465976808, 0.05219959533934440121, 61.25109039468567573 ) ) ;
#101197 = ADVANCED_FACE ( 'NONE', ( #122365 ), #185043, .T. ) ;
#101196 = CARTESIAN_POINT ( 'NONE',  ( 18.62759615963271287, -10.81492255796078972, 78.33224293864770971 ) ) ;
#101198 = CARTESIAN_POINT ( 'NONE',  ( 12.06949235617757843, -12.14591786802309237, 58.12390960531435979 ) ) ;
#101200 = CARTESIAN_POINT ( 'NONE',  ( -22.00000000000000000, -5.510910596163089556E-15, 47.50000000000000000 ) ) ;
#101199 = CARTESIAN_POINT ( 'NONE',  ( -16.46253265017160317, 9.564922557960807481, 25.83224293864769194 ) ) ;
#101201 = CARTESIAN_POINT ( 'NONE',  ( 5.719274019375673035, 21.55341960407619339, 47.29275706135234003 ) ) ;
#101202 = CARTESIAN_POINT ( 'NONE',  ( 19.05341960407617918, -5.049401038297876454, 46.04275706135233293 ) ) ;
#101203 = CARTESIAN_POINT ( 'NONE',  ( 5.153800228976335163, 19.02544592524342804, 29.79057627198102409 ) ) ;
#101204 = CARTESIAN_POINT ( 'NONE',  ( 18.67979575497194134, -10.72451020669871369, 75.83442372801900433 ) ) ;
#101205 = CARTESIAN_POINT ( 'NONE',  ( 16.62475595723699229, 7.163666690055317865, 96.97286648189530922 ) ) ;
#101206 = ORIENTED_EDGE ( 'NONE', *, *, #181371, .T. ) ;
#101207 = CARTESIAN_POINT ( 'NONE',  ( 8.224510206698953496, -14.34966873604960469, 42.91557627198103120 ) ) ;
#101208 = CARTESIAN_POINT ( 'NONE',  ( 17.50000000000002842, 4.049696124445913981, 113.3196032933405775 ) ) ;
#101209 = CARTESIAN_POINT ( 'NONE',  ( 0.05219959533907565091, 21.53943276465977519, 39.99890960531436690 ) ) ;
#101210 = CARTESIAN_POINT ( 'NONE',  ( -2.500000000000000000, 3.061616997868383141E-16, -62.91767397929362460 ) ) ;
#101211 = CARTESIAN_POINT ( 'NONE',  ( 13.97604488694527802, 13.89961937509977652, 89.37390960531436690 ) ) ;
#101212 = CARTESIAN_POINT ( 'NONE',  ( 16.52544592524342804, -4.483927247898539470, 88.54057627198103830 ) ) ;
#101213 = CARTESIAN_POINT ( 'NONE',  ( 4.483927247898790824, -16.52544592524335698, 25.20942372801901854 ) ) ;
#101214 = CARTESIAN_POINT ( 'NONE',  ( 5.719274019375991003, -21.55341960407610458, 67.70724293864769550 ) ) ;
#101215 = ORIENTED_EDGE ( 'NONE', *, *, #152294, .T. ) ;
#101216 = CARTESIAN_POINT ( 'NONE',  ( 9.474510206698971260, -16.51473224551069308, 27.91557627198103120 ) ) ;
#101218 = CARTESIAN_POINT ( 'NONE',  ( 21.55341960407610458, 5.719274019375980345, 83.95724293864770971 ) ) ;
#101217 = CARTESIAN_POINT ( 'NONE',  ( 16.46253265017160672, -9.564922557960803928, 83.33224293864768129 ) ) ;
#101219 = VECTOR ( 'NONE', #65985, 1000.000000000000000 ) ;
#101221 = CARTESIAN_POINT ( 'NONE',  ( -5.049401038298153566, 19.05341960407611168, 100.2072429386476955 ) ) ;
#101220 = CARTESIAN_POINT ( 'NONE',  ( -16.55341960407611168, -4.379528057220339221, 21.45724293864769550 ) ) ;
#101222 = CARTESIAN_POINT ( 'NONE',  ( 16.51473224551083163, -9.474510206698727899, 75.83442372801900433 ) ) ;
#101223 = CARTESIAN_POINT ( 'NONE',  ( -21.55341960407619339, 5.719274019375674811, 113.5427570613523756 ) ) ;
#101224 = CARTESIAN_POINT ( 'NONE',  ( -21.55341960407610458, -5.719274019375992779, 81.45724293864769550 ) ) ;
#101225 = CARTESIAN_POINT ( 'NONE',  ( 10.81492255796078972, 18.62759615963270932, 39.58224293864769550 ) ) ;
#101226 = CARTESIAN_POINT ( 'NONE',  ( -16.51473224551069308, -9.474510206698971260, 61.66557627198103120 ) ) ;
#101227 = CARTESIAN_POINT ( 'NONE',  ( -16.52544592524335698, -4.483927247898792601, 108.9594237280190185 ) ) ;
#101228 = CARTESIAN_POINT ( 'NONE',  ( -9.564922557960796823, -16.46253265017161027, 77.08224293864769550 ) ) ;
#101229 = VERTEX_POINT ( 'NONE', #172863 ) ;
#101230 = CARTESIAN_POINT ( 'NONE',  ( 4.500000000000000888, -126.1226662136678272, 8.481152457036388981 ) ) ;
#101231 = CARTESIAN_POINT ( 'NONE',  ( -19.02544592524334988, -5.153800228976617603, 23.95942372801900078 ) ) ;
#101232 = CARTESIAN_POINT ( 'NONE',  ( -8.314922557960811034, -14.29746914071050412, 92.08224293864769550 ) ) ;
#101233 = CARTESIAN_POINT ( 'NONE',  ( -15.80617190586768217, 15.72974639402176855, 23.12609039468567573 ) ) ;
#101234 = CARTESIAN_POINT ( 'NONE',  ( 22.44159573604009594, -16.30477369853687364, 146.1750000027311671 ) ) ;
#101235 = CARTESIAN_POINT ( 'NONE',  ( -18.67979575497178146, -10.72451020669898902, 71.66557627198100988 ) ) ;
#101236 = CARTESIAN_POINT ( 'NONE',  ( -16.55341960407617563, 4.379528057220093196, 88.54275706135236135 ) ) ;
#101237 = CARTESIAN_POINT ( 'NONE',  ( 14.34966873604960469, 8.224510206698951720, 114.1655762719810383 ) ) ;
#101238 = CARTESIAN_POINT ( 'NONE',  ( -19.05341960407611168, -5.049401038298163336, 76.45724293864769550 ) ) ;
#101239 =( LENGTH_UNIT ( ) NAMED_UNIT ( * ) SI_UNIT ( .MILLI., .METRE. ) );
#101240 = CARTESIAN_POINT ( 'NONE',  ( -16.51473224551069308, -9.474510206698971260, 21.66557627198102765 ) ) ;
#101241 = CARTESIAN_POINT ( 'NONE',  ( 12.14591786802309770, 12.06949235617756955, 24.37390960531435979 ) ) ;
#101242 = CARTESIAN_POINT ( 'NONE',  ( 10.81492255796106328, -18.62759615963255655, 65.41775706135234714 ) ) ;
#101243 = CARTESIAN_POINT ( 'NONE',  ( -9.564922557960796823, -16.46253265017161027, 112.0822429386476955 ) ) ;
#101244 = CARTESIAN_POINT ( 'NONE',  ( -5.719274019375665041, -21.55341960407619695, 89.79275706135236135 ) ) ;
#101245 = CARTESIAN_POINT ( 'NONE',  ( -19.02544592524342804, 5.153800228976336051, 46.04057627198101699 ) ) ;
#101246 = CARTESIAN_POINT ( 'NONE',  ( 13.89961937509977652, -13.97604488694527269, 58.12390960531436690 ) ) ;
#101247 = EDGE_LOOP ( 'NONE', ( #183333, #180891 ) ) ;
#101248 = CARTESIAN_POINT ( 'NONE',  ( 18.67979575497194134, -10.72451020669871369, 90.83442372801901854 ) ) ;
#101249 = CARTESIAN_POINT ( 'NONE',  ( 16.53943276465976808, 0.05219959533934440121, 56.25109039468568284 ) ) ;
#101250 = CARTESIAN_POINT ( 'NONE',  ( 21.55341960407619695, -5.719274019375665929, 86.04275706135236135 ) ) ;
#101251 = CARTESIAN_POINT ( 'NONE',  ( -18.62759615963270932, 10.81492255796079327, 25.83224293864769194 ) ) ;
#101252 = CARTESIAN_POINT ( 'NONE',  ( 19.05341960407617918, -5.049401038297876454, 96.04275706135231871 ) ) ;
#101253 = CARTESIAN_POINT ( 'NONE',  ( 0.05219959533937995610, -21.53943276465977519, 50.00109039468568994 ) ) ;
#101254 = CARTESIAN_POINT ( 'NONE',  ( 12.14591786802327356, -12.06949235617739191, 40.62609039468567573 ) ) ;
#101255 = CARTESIAN_POINT ( 'NONE',  ( -18.62759615963270932, 10.81492255796079327, 85.83224293864768129 ) ) ;
#101256 = CARTESIAN_POINT ( 'NONE',  ( 19.05341960407617918, -5.049401038297876454, 86.04275706135233293 ) ) ;
#101257 = CARTESIAN_POINT ( 'NONE',  ( 0.05219959533909260263, 19.03943276465977164, 69.99890960531435269 ) ) ;
#101258 = CARTESIAN_POINT ( 'NONE',  ( 13.89961937509957401, 13.97604488694547697, 91.87609039468567573 ) ) ;
#101259 = CARTESIAN_POINT ( 'NONE',  ( -5.153800228976607833, 19.02544592524334988, 102.7094237280189759 ) ) ;
#101260 = CARTESIAN_POINT ( 'NONE',  ( -16.52544592524342804, 4.483927247898546575, 56.04057627198102409 ) ) ;
#101261 = CARTESIAN_POINT ( 'NONE',  ( 16.51473224551083163, -9.474510206698727899, 80.83442372801899012 ) ) ;
#101262 = CARTESIAN_POINT ( 'NONE',  ( 0.05219959533934541429, -16.53943276465976808, 60.00109039468568284 ) ) ;
#101263 = CARTESIAN_POINT ( 'NONE',  ( 16.51473224551083163, -9.474510206698727899, 35.83442372801899722 ) ) ;
#101264 = CARTESIAN_POINT ( 'NONE',  ( -0.05219959533909027116, -19.03943276465977164, 37.49890960531436690 ) ) ;
#101265 = CARTESIAN_POINT ( 'NONE',  ( -0.05219959533909027116, -19.03943276465977164, 47.49890960531435979 ) ) ;
#101266 = CARTESIAN_POINT ( 'NONE',  ( 16.55341960407618274, -4.379528057220086978, 61.04275706135234714 ) ) ;
#101267 = PLANE ( 'NONE',  #75717 ) ;
#101268 = CARTESIAN_POINT ( 'NONE',  ( 28.82186960331499392, -9.364793116373510529, 141.1500000054623740 ) ) ;
#101269 = CARTESIAN_POINT ( 'NONE',  ( 16.46253265017160672, -9.564922557960803928, 103.3322429386476955 ) ) ;
#101270 = PLANE ( 'NONE',  #78081 ) ;
#101271 = ORIENTED_EDGE ( 'NONE', *, *, #122650, .T. ) ;
#101272 = CARTESIAN_POINT ( 'NONE',  ( 9.474510206698729675, 16.51473224551082808, 97.08442372801900433 ) ) ;
#101273 = CARTESIAN_POINT ( 'NONE',  ( 15.80617190586746368, 15.72974639402197994, 39.37390960531436690 ) ) ;
#101275 = CARTESIAN_POINT ( 'NONE',  ( 5.153800228976615827, -19.02544592524334988, 110.2094237280189901 ) ) ;
#101274 = CARTESIAN_POINT ( 'NONE',  ( 13.97604488694548053, -13.89961937509957401, 35.62609039468567573 ) ) ;
#101276 = CARTESIAN_POINT ( 'NONE',  ( -19.03943276465977164, 0.05219959533909376836, 36.24890960531436690 ) ) ;
#101277 = CARTESIAN_POINT ( 'NONE',  ( -16.46253265017160317, 9.564922557960807481, 50.83224293864770260 ) ) ;
#101278 = CARTESIAN_POINT ( 'NONE',  ( -15.80617190586745835, -15.72974639402198527, 66.87390960531436690 ) ) ;
#101279 = CARTESIAN_POINT ( 'NONE',  ( 16.51473224551069308, 9.474510206698969483, 104.1655762719810241 ) ) ;
#101280 = AXIS2_PLACEMENT_3D ( 'NONE', #4962, #21144, #82799 ) ;
#101281 = CARTESIAN_POINT ( 'NONE',  ( -0.05219959533909027116, -19.03943276465977164, 32.49890960531435979 ) ) ;
#101282 = CARTESIAN_POINT ( 'NONE',  ( 1.784210473542230573E-15, -29.16686587814331588, 145.8750000027311557 ) ) ;
#101283 = CARTESIAN_POINT ( 'NONE',  ( -9.474510206698720793, -16.51473224551083518, 89.58442372801900433 ) ) ;
#101284 = CARTESIAN_POINT ( 'NONE',  ( 8.314922557960818139, 14.29746914071049879, 49.58224293864769550 ) ) ;
#101285 = CARTESIAN_POINT ( 'NONE',  ( 10.72451020669898902, -18.67979575497178502, 37.91557627198102409 ) ) ;
#101286 = CARTESIAN_POINT ( 'NONE',  ( -0.05219959533937732626, 21.53943276465977519, 112.5010903946857042 ) ) ;
#101287 = CARTESIAN_POINT ( 'NONE',  ( 15.72974639402199770, -15.80617190586745480, 93.12390960531436690 ) ) ;
#101288 = CARTESIAN_POINT ( 'NONE',  ( 18.62759615963255655, 10.81492255796105972, 66.66775706135234714 ) ) ;
#101289 = CARTESIAN_POINT ( 'NONE',  ( -5.823673210054431948, 21.52544592524334988, 82.70942372801900433 ) ) ;
#101290 = CARTESIAN_POINT ( 'NONE',  ( -13.97604488694527625, -13.89961937509977652, 106.8739096053143669 ) ) ;
#101292 = CARTESIAN_POINT ( 'NONE',  ( -15.72974639402176322, -15.80617190586768395, 64.37609039468568994 ) ) ;
#101291 = CARTESIAN_POINT ( 'NONE',  ( 12.06949235617739724, 12.14591786802326823, 106.8760903946856899 ) ) ;
#101293 = CARTESIAN_POINT ( 'NONE',  ( -9.564922557960796823, -16.46253265017161027, 67.08224293864769550 ) ) ;
#101294 =( BOUNDED_CURVE ( )  B_SPLINE_CURVE ( 3, ( #55065, #88384, #23740, #12569 ),
 .UNSPECIFIED., .F., .T. ) 
 B_SPLINE_CURVE_WITH_KNOTS ( ( 4, 4 ),
 ( 2.008945357379066987, 2.115944711806982070 ),
 .UNSPECIFIED. ) 
 CURVE ( )  GEOMETRIC_REPRESENTATION_ITEM ( )  RATIONAL_B_SPLINE_CURVE ( ( 1.000000000000000000, 0.9990461557208837329, 0.9990461557208837329, 1.000000000000000000 ) ) 
 REPRESENTATION_ITEM ( '' )  );
#101295 = CARTESIAN_POINT ( 'NONE',  ( 16.51473224551083163, -9.474510206698727899, 30.83442372801900433 ) ) ;
#101296 = CARTESIAN_POINT ( 'NONE',  ( 10.81492255796106328, -18.62759615963255655, 35.41775706135234003 ) ) ;
#101297 = CARTESIAN_POINT ( 'NONE',  ( 16.46253265017160672, -9.564922557960803928, 63.33224293864769550 ) ) ;
#101298 = CARTESIAN_POINT ( 'NONE',  ( -8.314922557960811034, -14.29746914071050412, 87.08224293864769550 ) ) ;
#101299 = CARTESIAN_POINT ( 'NONE',  ( -16.53943276465976808, 0.05219959533911058130, 46.24890960531435979 ) ) ;
#101300 = CARTESIAN_POINT ( 'NONE',  ( 5.719274019375991003, -21.55341960407610458, 52.70724293864769550 ) ) ;
#101301 = CARTESIAN_POINT ( 'NONE',  ( -9.474510206698964154, 16.51473224551069663, 65.41557627198102409 ) ) ;
#101302 = CARTESIAN_POINT ( 'NONE',  ( -21.55341960407610458, -5.719274019375992779, 76.45724293864769550 ) ) ;
#101303 = CARTESIAN_POINT ( 'NONE',  ( -13.97604488694547697, 13.89961937509957934, 53.12609039468565442 ) ) ;
#101305 = CARTESIAN_POINT ( 'NONE',  ( -8.314922557960811034, -14.29746914071050412, 57.08224293864769550 ) ) ;
#101304 = CARTESIAN_POINT ( 'NONE',  ( 0.05219959533936267826, -19.03943276465977164, 25.00109039468566152 ) ) ;
#101306 = CARTESIAN_POINT ( 'NONE',  ( 21.55341960407610458, 5.719274019375980345, 38.95724293864768839 ) ) ;
#101307 = EDGE_LOOP ( 'NONE', ( #104320, #181731, #100656, #130443 ) ) ;
#101308 = DIRECTION ( 'NONE',  ( 0.000000000000000000, 0.5000000000000002220, -0.8660254037844384856 ) ) ;
#101310 = CARTESIAN_POINT ( 'NONE',  ( 1.784210473542230573E-15, -29.16686587814331588, 139.8750000027312126 ) ) ;
#101309 = CARTESIAN_POINT ( 'NONE',  ( 16.55341960407618274, -4.379528057220086978, 86.04275706135236135 ) ) ;
#101311 = CARTESIAN_POINT ( 'NONE',  ( -5.049401038297874678, -19.05341960407617918, 94.79275706135230450 ) ) ;
#101312 = CARTESIAN_POINT ( 'NONE',  ( -14.34966873604960291, -8.224510206698953496, 51.66557627198102409 ) ) ;
#101313 = CARTESIAN_POINT ( 'NONE',  ( -69.65682714487590488, -71.74905178543390605, 0.000000000000000000 ) ) ;
#101314 = CARTESIAN_POINT ( 'NONE',  ( 5.049401038298161559, -19.05341960407611168, 47.70724293864770260 ) ) ;
#101315 = CARTESIAN_POINT ( 'NONE',  ( -16.53943276465976808, 0.05219959533911058130, 36.24890960531435979 ) ) ;
#101316 = CARTESIAN_POINT ( 'NONE',  ( 9.564922557960805705, 16.46253265017160317, 94.58224293864769550 ) ) ;
#101317 = CARTESIAN_POINT ( 'NONE',  ( 13.89961937509977652, -13.97604488694527269, 58.12390960531436690 ) ) ;
#101318 = CARTESIAN_POINT ( 'NONE',  ( 15.72974639402176855, 15.80617190586768217, 56.87609039468568994 ) ) ;
#101319 = CARTESIAN_POINT ( 'NONE',  ( 13.89961937509977652, -13.97604488694527269, 73.12390960531436690 ) ) ;
#101320 = CARTESIAN_POINT ( 'NONE',  ( -67.00000000000000000, -5.510910596163089556E-15, 45.00000000000000000 ) ) ;
#101321 = CARTESIAN_POINT ( 'NONE',  ( -0.05219959533909027116, -19.03943276465977164, 77.49890960531435269 ) ) ;
#101322 = CARTESIAN_POINT ( 'NONE',  ( 18.62759615963271287, -10.81492255796078972, 48.33224293864770260 ) ) ;
#101323 = CARTESIAN_POINT ( 'NONE',  ( -16.46253265017160317, 9.564922557960807481, 30.83224293864769550 ) ) ;
#101324 = CARTESIAN_POINT ( 'NONE',  ( -21.52544592524343514, 5.823673210054127303, 56.04057627198102409 ) ) ;
#101325 = CARTESIAN_POINT ( 'NONE',  ( 14.29746914071037800, 8.314922557961029526, 101.6677570613523613 ) ) ;
#101326 = EDGE_CURVE ( 'NONE', #62281, #52144, #104638, .T. ) ;
#101327 = CARTESIAN_POINT ( 'NONE',  ( 0.05219959533936267826, -19.03943276465977164, 25.00109039468566152 ) ) ;
#101329 = CARTESIAN_POINT ( 'NONE',  ( -16.55341960407617563, 4.379528057220093196, 83.54275706135234714 ) ) ;
#101328 = CARTESIAN_POINT ( 'NONE',  ( -12.14591786802326823, 12.06949235617739902, 48.12609039468568284 ) ) ;
#101330 = FACE_OUTER_BOUND ( 'NONE', #106686, .T. ) ;
#101331 = CARTESIAN_POINT ( 'NONE',  ( -16.55341960407617563, 4.379528057220093196, 73.54275706135234714 ) ) ;
#101332 = CARTESIAN_POINT ( 'NONE',  ( -10.81492255796078084, -18.62759615963271287, 27.08224293864769550 ) ) ;
#101333 = CARTESIAN_POINT ( 'NONE',  ( -0.05219959533909027116, -19.03943276465977164, 32.49890960531435979 ) ) ;
#101334 = CARTESIAN_POINT ( 'NONE',  ( -0.05219959533934338120, 16.53943276465976808, 42.50109039468567573 ) ) ;
#101335 = CARTESIAN_POINT ( 'NONE',  ( 13.89961937509977652, -13.97604488694527269, 48.12390960531435979 ) ) ;
#101336 = CARTESIAN_POINT ( 'NONE',  ( -10.81492255796105439, 18.62759615963255655, 37.91775706135235424 ) ) ;
#101337 = CARTESIAN_POINT ( 'NONE',  ( -4.483927247898782831, 16.52544592524335698, 32.70942372801900433 ) ) ;
#101338 = CARTESIAN_POINT ( 'NONE',  ( 16.55341960407618274, -4.379528057220086978, 96.04275706135236135 ) ) ;
#101339 = DIRECTION ( 'NONE',  ( 0.8660254037844410391, 0.000000000000000000, 0.4999999999999958367 ) ) ;
#101340 = CARTESIAN_POINT ( 'NONE',  ( 18.62759615963255655, 10.81492255796105972, 96.66775706135234714 ) ) ;
#101341 = CARTESIAN_POINT ( 'NONE',  ( -5.153800228976607833, 19.02544592524334988, 112.7094237280190043 ) ) ;
#101342 = CARTESIAN_POINT ( 'NONE',  ( -13.89961937509957401, -13.97604488694547875, 64.37609039468567573 ) ) ;
#101343 = CARTESIAN_POINT ( 'NONE',  ( 8.314922557960818139, 14.29746914071049879, 74.58224293864768129 ) ) ;
#101344 = CARTESIAN_POINT ( 'NONE',  ( -19.02544592524342804, 5.153800228976336051, 31.04057627198102409 ) ) ;
#101346 = CARTESIAN_POINT ( 'NONE',  ( 16.52216118717207038, 7.221426719304519182, 78.57599021046991083 ) ) ;
#101345 = CARTESIAN_POINT ( 'NONE',  ( 9.474510206698729675, 16.51473224551082808, 57.08442372801900433 ) ) ;
#101347 = CARTESIAN_POINT ( 'NONE',  ( -15.80617190586768217, 15.72974639402176855, 58.12609039468568994 ) ) ;
#101348 = CARTESIAN_POINT ( 'NONE',  ( 8.224510206698742110, 14.34966873604972548, 27.08442372801901854 ) ) ;
#101349 = CARTESIAN_POINT ( 'NONE',  ( 17.44270441346512968, 5.991230190323101112, 38.86335079264228654 ) ) ;
#101350 = CARTESIAN_POINT ( 'NONE',  ( 18.62759615963271287, -10.81492255796078972, 28.33224293864769550 ) ) ;
#101351 = CARTESIAN_POINT ( 'NONE',  ( -16.51473224551082808, 9.474510206698731452, 108.3344237280190043 ) ) ;
#101352 = CYLINDRICAL_SURFACE ( 'NONE', #144442, 2.000000000000001776 ) ;
#101353 = CARTESIAN_POINT ( 'NONE',  ( -3.889087296525703508, 30.00000000000004263, 8.181980515339454030 ) ) ;
#101354 = CARTESIAN_POINT ( 'NONE',  ( 9.564922557960805705, 16.46253265017160317, 29.58224293864769550 ) ) ;
#101355 = CARTESIAN_POINT ( 'NONE',  ( 15.72974639402176855, 15.80617190586768217, 106.8760903946856899 ) ) ;
#101356 = CARTESIAN_POINT ( 'NONE',  ( -13.89961937509977652, 13.97604488694528158, 60.62390960531436690 ) ) ;
#101357 = CARTESIAN_POINT ( 'NONE',  ( -21.52544592524334988, -5.823673210054445271, 68.95942372801901854 ) ) ;
#101358 = CARTESIAN_POINT ( 'NONE',  ( 21.53943276465977519, 0.05219959533937863772, 101.2510903946856757 ) ) ;
#101359 = CARTESIAN_POINT ( 'NONE',  ( -16.52544592524342804, 4.483927247898546575, 31.04057627198102409 ) ) ;
#101360 = CARTESIAN_POINT ( 'NONE',  ( -13.89961937509977652, 13.97604488694528158, 85.62390960531433848 ) ) ;
#101361 = CARTESIAN_POINT ( 'NONE',  ( -15.80617190586768217, 15.72974639402176855, 63.12609039468568994 ) ) ;
#101362 = VECTOR ( 'NONE', #52075, 1000.000000000000000 ) ;
#101363 = CARTESIAN_POINT ( 'NONE',  ( 0.05219959533937995610, -21.53943276465977519, 50.00109039468568994 ) ) ;
#101365 = CARTESIAN_POINT ( 'NONE',  ( -13.97604488694527625, -13.89961937509977652, 111.8739096053143243 ) ) ;
#101364 = CARTESIAN_POINT ( 'NONE',  ( -0.05219959533936034679, 19.03943276465977164, 77.50109039468566152 ) ) ;
#101366 = CARTESIAN_POINT ( 'NONE',  ( -13.97604488694527625, -13.89961937509977652, 26.87390960531434558 ) ) ;
#101367 = CARTESIAN_POINT ( 'NONE',  ( -5.719274019375978568, 21.55341960407610458, 105.2072429386477097 ) ) ;
#101368 = CARTESIAN_POINT ( 'NONE',  ( 19.05341960407617918, -5.049401038297876454, 36.04275706135234003 ) ) ;
#101369 = CARTESIAN_POINT ( 'NONE',  ( 8.224510206698953496, -14.34966873604960469, 97.91557627198103830 ) ) ;
#101370 = CARTESIAN_POINT ( 'NONE',  ( 16.46253265017160672, -9.564922557960803928, 43.33224293864769550 ) ) ;
#101371 = CARTESIAN_POINT ( 'NONE',  ( -9.474510206698720793, -16.51473224551083518, 94.58442372801900433 ) ) ;
#101372 = CARTESIAN_POINT ( 'NONE',  ( -16.52544592524342804, 4.483927247898546575, 66.04057627198103830 ) ) ;
#101373 = CARTESIAN_POINT ( 'NONE',  ( -18.62759615963255300, -10.81492255796106328, 104.1677570613523471 ) ) ;
#101374 = CARTESIAN_POINT ( 'NONE',  ( -0.05219959533909027116, -19.03943276465977164, 107.4989096053143527 ) ) ;
#101375 = CARTESIAN_POINT ( 'NONE',  ( 19.03943276465977164, 0.05219959533936151252, 81.25109039468567573 ) ) ;
#101376 = CARTESIAN_POINT ( 'NONE',  ( -15.80617190586745835, -15.72974639402198527, 91.87390960531436690 ) ) ;
#101377 = CARTESIAN_POINT ( 'NONE',  ( -10.72451020669870658, -18.67979575497194134, 39.58442372801901143 ) ) ;
#101378 = CARTESIAN_POINT ( 'NONE',  ( 16.52544592524335698, 4.483927247898782831, 46.45942372801901854 ) ) ;
#101379 = CARTESIAN_POINT ( 'NONE',  ( -14.29746914071037622, -8.314922557961029526, 104.1677570613523471 ) ) ;
#101381 = CARTESIAN_POINT ( 'NONE',  ( -21.53943276465977519, -0.05219959533937600094, 33.75109039468568284 ) ) ;
#101380 = CARTESIAN_POINT ( 'NONE',  ( -12.06949235617739369, -12.14591786802326823, 39.37609039468567573 ) ) ;
#101382 = CARTESIAN_POINT ( 'NONE',  ( -5.823673210054116645, -21.52544592524344225, 47.29057627198103120 ) ) ;
#101383 = CARTESIAN_POINT ( 'NONE',  ( 19.03943276465977164, -0.05219959533909143690, 28.74890960531435624 ) ) ;
#101384 = CARTESIAN_POINT ( 'NONE',  ( -30.74264578624800492, 22.33583958711400186, -7.949999994537626513 ) ) ;
#101385 = CARTESIAN_POINT ( 'NONE',  ( -16.53943276465976808, -0.05219959533934237506, 68.75109039468568994 ) ) ;
#101386 = CARTESIAN_POINT ( 'NONE',  ( -15.72974639402197994, 15.80617190586746368, 90.62390960531436690 ) ) ;
#101387 = CARTESIAN_POINT ( 'NONE',  ( 0.05219959533910956823, 16.53943276465976808, 34.99890960531435979 ) ) ;
#101388 = CARTESIAN_POINT ( 'NONE',  ( 14.34966873604972726, -8.224510206698740333, 65.83442372801900433 ) ) ;
#101389 = CARTESIAN_POINT ( 'NONE',  ( 16.51473224551069308, 9.474510206698969483, 54.16557627198103120 ) ) ;
#101390 = CARTESIAN_POINT ( 'NONE',  ( -19.05341960407617563, 5.049401038297882671, 83.54275706135233293 ) ) ;
#101391 = CARTESIAN_POINT ( 'NONE',  ( -21.52544592524343514, 5.823673210054127303, 86.04057627198102409 ) ) ;
#101392 = CARTESIAN_POINT ( 'NONE',  ( 12.14591786802309770, 12.06949235617756955, 34.37390960531435979 ) ) ;
#101393 = ORIENTED_EDGE ( 'NONE', *, *, #70314, .F. ) ;
#101394 = CARTESIAN_POINT ( 'NONE',  ( 21.51693143705272959, 10.15780255052816550, 170.5200780514257133 ) ) ;
#101395 = CARTESIAN_POINT ( 'NONE',  ( -21.52544592524343514, 5.823673210054127303, 61.04057627198103120 ) ) ;
#101396 = ORIENTED_EDGE ( 'NONE', *, *, #120600, .F. ) ;
#101397 = CARTESIAN_POINT ( 'NONE',  ( -8.224510206698735004, -14.34966873604973081, 104.5844237280190185 ) ) ;
#101398 = ORIENTED_EDGE ( 'NONE', *, *, #196572, .T. ) ;
#101399 = DIRECTION ( 'NONE',  ( 1.000000000000000000, 0.000000000000000000, 0.000000000000000000 ) ) ;
#101400 = CARTESIAN_POINT ( 'NONE',  ( 10.72451020669898902, -18.67979575497178502, 87.91557627198103830 ) ) ;
#101401 = CARTESIAN_POINT ( 'NONE',  ( 21.55341960407610458, 5.719274019375980345, 108.9572429386476955 ) ) ;
#101402 = CARTESIAN_POINT ( 'NONE',  ( -0.05219959533910754901, -16.53943276465976808, 22.49890960531436335 ) ) ;
#101403 = CARTESIAN_POINT ( 'NONE',  ( -16.52544592524335698, -4.483927247898792601, 33.95942372801901143 ) ) ;
#101404 = CARTESIAN_POINT ( 'NONE',  ( -13.89961937509977652, 13.97604488694528158, 40.62390960531435979 ) ) ;
#101405 = CARTESIAN_POINT ( 'NONE',  ( 5.153800228976335163, 19.02544592524342804, 69.79057627198103830 ) ) ;
#101406 = ADVANCED_FACE ( 'NONE', ( #158667 ), #38325, .T. ) ;
#101407 = CARTESIAN_POINT ( 'NONE',  ( -23.31738231874055245, -16.94106989632524574, 146.1999999999999886 ) ) ;
#101408 = CARTESIAN_POINT ( 'NONE',  ( -5.153800228976328057, -19.02544592524343514, 112.2905762719810099 ) ) ;
#101409 = CARTESIAN_POINT ( 'NONE',  ( 1.392837473234412426, 29.83693993229687180, -51.60511860951399399 ) ) ;
#101410 = CARTESIAN_POINT ( 'NONE',  ( 16.46253265017146816, 9.564922557961045513, 111.6677570613523329 ) ) ;
#101411 = CARTESIAN_POINT ( 'NONE',  ( 5.153800228976615827, -19.02544592524334988, 35.20942372801899722 ) ) ;
#101412 = CARTESIAN_POINT ( 'NONE',  ( 18.67979575497178502, 10.72451020669898547, 84.16557627198103830 ) ) ;
#101413 = CARTESIAN_POINT ( 'NONE',  ( 4.379528057220339221, -16.55341960407611168, 22.70724293864769194 ) ) ;
#101414 = CARTESIAN_POINT ( 'NONE',  ( 5.823673210054125526, 21.52544592524343514, 49.79057627198102409 ) ) ;
#101416 = CARTESIAN_POINT ( 'NONE',  ( -13.97604488694547697, 13.89961937509957934, 108.1260903946856331 ) ) ;
#101415 = CARTESIAN_POINT ( 'NONE',  ( -5.823673210054116645, -21.52544592524344225, 82.29057627198103830 ) ) ;
#101418 = CLOSED_SHELL ( 'NONE', ( #130486, #394, #176759, #122577, #156437, #18328, #114410, #15156, #25330, #13706, #55464, #81939, #105243, #26668, #185767, #151408, #4808, #81311, #63491, #55311, #144876, #131527, #92730, #84595, #10575, #103874, #186102, #100031, #53174, #187152, #102491, #148891, #61448, #55170, #175946, #155536, #143932, #153225, #8299, #160955, #184287, #126740, #95794, #127349, #151085, #154838, #198527, #162289, #124239, #9199, #81451, #30281, #138196, #108474 ) ) ;
#101417 = CARTESIAN_POINT ( 'NONE',  ( -13.97604488694527625, -13.89961937509977652, 101.8739096053143811 ) ) ;
#101419 = CARTESIAN_POINT ( 'NONE',  ( 10.81492255796106328, -18.62759615963255655, 70.41775706135236135 ) ) ;
#101420 = CARTESIAN_POINT ( 'NONE',  ( 16.51473224551069308, 9.474510206698969483, 64.16557627198102409 ) ) ;
#101421 = CARTESIAN_POINT ( 'NONE',  ( -14.34966873604960291, -8.224510206698953496, 96.66557627198102409 ) ) ;
#101422 = CARTESIAN_POINT ( 'NONE',  ( 31.23718726401124712, 7.254977440570237412, 96.91727682732810933 ) ) ;
#101423 = CARTESIAN_POINT ( 'NONE',  ( 19.03943276465977164, -0.05219959533909143690, 73.74890960531435269 ) ) ;
#101424 = CARTESIAN_POINT ( 'NONE',  ( -0.05219959533910754901, -16.53943276465976808, 97.49890960531436690 ) ) ;
#101425 = VERTEX_POINT ( 'NONE', #82810 ) ;
#101426 = CARTESIAN_POINT ( 'NONE',  ( 0.05219959533936267826, -19.03943276465977164, 95.00109039468567573 ) ) ;
#101427 = MECHANICAL_DESIGN_GEOMETRIC_PRESENTATION_REPRESENTATION (  '', ( #124084 ), #46593 ) ;
#101428 = CARTESIAN_POINT ( 'NONE',  ( 31.99364916730971231, 1.011436372600181938E-12, 95.00000000000021316 ) ) ;
#101429 = CARTESIAN_POINT ( 'NONE',  ( -5.153800228976328057, -19.02544592524343514, 62.29057627198100988 ) ) ;
#101431 = CARTESIAN_POINT ( 'NONE',  ( 13.89961937509977652, -13.97604488694527269, 98.12390960531433848 ) ) ;
#101430 = CARTESIAN_POINT ( 'NONE',  ( -10.81492255796105439, 18.62759615963255655, 77.91775706135231871 ) ) ;
#101432 = CARTESIAN_POINT ( 'NONE',  ( 16.53943276465976808, 0.05219959533934440121, 76.25109039468568994 ) ) ;
#101433 = CARTESIAN_POINT ( 'NONE',  ( -16.19135201231369692, -7.376712067591815192, 50.18680854052031037 ) ) ;
#101434 = CARTESIAN_POINT ( 'NONE',  ( -16.51473224551082808, 9.474510206698731452, 38.33442372801899722 ) ) ;
#101435 = CARTESIAN_POINT ( 'NONE',  ( 18.67979575497194134, -10.72451020669871369, 95.83442372801903275 ) ) ;
#101436 = CARTESIAN_POINT ( 'NONE',  ( 36.86581981986046230, 2.436233122106823412, 49.93429970834161935 ) ) ;
#101437 = CARTESIAN_POINT ( 'NONE',  ( -3.735172737399431091E-16, -6.100000000000006750, -64.92279855667830191 ) ) ;
#101438 = CARTESIAN_POINT ( 'NONE',  ( -16.52544592524335698, -4.483927247898792601, 103.9594237280190185 ) ) ;
#101439 = CARTESIAN_POINT ( 'NONE',  ( -34.51183469268316628, -7.447092774749549449, 43.98515247788456861 ) ) ;
#101440 = CARTESIAN_POINT ( 'NONE',  ( 16.53943276465976808, 0.05219959533934440121, 91.25109039468568994 ) ) ;
#101441 = FACE_OUTER_BOUND ( 'NONE', #90218, .T. ) ;
#101442 = CARTESIAN_POINT ( 'NONE',  ( -8.314922557961024197, 14.29746914071037800, 72.91775706135234714 ) ) ;
#101443 = EDGE_LOOP ( 'NONE', ( #28496, #11510, #71385, #74681 ) ) ;
#101444 = CARTESIAN_POINT ( 'NONE',  ( 21.55341960407619695, -5.719274019375665929, 76.04275706135237556 ) ) ;
#101445 = CARTESIAN_POINT ( 'NONE',  ( -9.564922557961040184, 16.46253265017147172, 92.91775706135233293 ) ) ;
#101446 = CARTESIAN_POINT ( 'NONE',  ( 5.153800228976615827, -19.02544592524334988, 45.20942372801901143 ) ) ;
#101447 = CARTESIAN_POINT ( 'NONE',  ( -19.05341960407611168, -5.049401038298163336, 71.45724293864766707 ) ) ;
#101448 = CARTESIAN_POINT ( 'NONE',  ( -19.05341960407611168, -5.049401038298163336, 61.45724293864769550 ) ) ;
#101449 = CARTESIAN_POINT ( 'NONE',  ( -18.22780087662123094, -5.499999999999984901, 86.48459894673892734 ) ) ;
#101450 = CARTESIAN_POINT ( 'NONE',  ( 5.823673210054125526, 21.52544592524343514, 84.79057627198102409 ) ) ;
#101451 = AXIS2_PLACEMENT_3D ( 'NONE', #37820, #193511, #103496 ) ;
#101452 = CARTESIAN_POINT ( 'NONE',  ( -15.72974639402197994, 15.80617190586746368, 40.62390960531435269 ) ) ;
#101453 = CARTESIAN_POINT ( 'NONE',  ( -5.049401038298153566, 19.05341960407611168, 30.20724293864768839 ) ) ;
#101454 = CARTESIAN_POINT ( 'NONE',  ( -4.379528057220086978, -16.55341960407618274, 59.79275706135234714 ) ) ;
#101455 = ORIENTED_EDGE ( 'NONE', *, *, #196650, .F. ) ;
#101456 = CARTESIAN_POINT ( 'NONE',  ( -21.55341960407619339, 5.719274019375674811, 28.54275706135234358 ) ) ;
#101458 = CARTESIAN_POINT ( 'NONE',  ( -38.00000000000001421, 12.34694845685046438, -2.099999999999999645 ) ) ;
#101457 = CARTESIAN_POINT ( 'NONE',  ( 0.05219959533910956823, 16.53943276465976808, 69.99890960531435269 ) ) ;
#101459 = CARTESIAN_POINT ( 'NONE',  ( 14.29746914071037800, 8.314922557961029526, 21.66775706135235069 ) ) ;
#101460 = CARTESIAN_POINT ( 'NONE',  ( 9.564922557961047289, -16.46253265017146816, 50.41775706135233293 ) ) ;
#101461 = CARTESIAN_POINT ( 'NONE',  ( -0.05219959533910754901, -16.53943276465976808, 57.49890960531435979 ) ) ;
#101462 = CARTESIAN_POINT ( 'NONE',  ( 15.80617190586769283, -15.72974639402175789, 30.62609039468567929 ) ) ;
#101464 = CARTESIAN_POINT ( 'NONE',  ( -10.81492255796078084, -18.62759615963271287, 82.08224293864768129 ) ) ;
#101463 = CARTESIAN_POINT ( 'NONE',  ( 5.000000000000000888, -130.0000000000000000, -13.99999999999999822 ) ) ;
#101465 = CARTESIAN_POINT ( 'NONE',  ( 19.02544592524343514, -5.153800228976328945, 108.5405762719810383 ) ) ;
#101466 = CARTESIAN_POINT ( 'NONE',  ( -4.379528057220328563, 16.55341960407611168, 55.20724293864770260 ) ) ;
#101467 = CARTESIAN_POINT ( 'NONE',  ( -0.05219959533909027116, -19.03943276465977164, 112.4989096053143669 ) ) ;
#101468 = B_SPLINE_CURVE_WITH_KNOTS ( 'NONE', 3,
 ( #191035, #20181, #128347, #174873, #157717, #52509, #188066, #80856, #67682, #65689, #48554, #172891, #34370, #51521, #96030, #19206, #189067, #111199, #64707, #142532, #143514, #97011, #127354, #170890, #4011, #159685, #63712, #110207, #35359, #79873, #2032, #113183, #50539, #125387, #36338, #32382, #18216, #144517, #158692, #3031, #94037, #81827, #155715 ),
 .UNSPECIFIED., .F., .F.,
 ( 4, 2, 2, 2, 2, 2, 2, 2, 2, 2, 2, 2, 2, 1, 2, 2, 2, 2, 2, 2, 2, 4 ),
 ( 0.04122229388621100749, 0.04269295678691726464, 0.04416361968762351486, 0.04489895113797664344, 0.04563428258832977202, 0.04710494548903602224, 0.04857560838974227940, 0.04931093984009540798, 0.05004627129044854350, 0.05151693419115481454, 0.05298759709186107864, 0.05445825999256734967, 0.05519359144292047825, 0.05592892289327359989, 0.05666425434362672153, 0.05739958579397984317, 0.05887024869468611421, 0.06034091159539237831, 0.06181157449609863547, 0.06254690594645176405, 0.06328223739680489957, 0.06475290029751117060 ),
 .UNSPECIFIED. ) ;
#101469 = CARTESIAN_POINT ( 'NONE',  ( -27.19095269391954517, 8.032454009542490780, 149.5864051666458181 ) ) ;
#101470 = CARTESIAN_POINT ( 'NONE',  ( 9.564922557961047289, -16.46253265017146816, 65.41775706135233293 ) ) ;
#101471 = CARTESIAN_POINT ( 'NONE',  ( 21.55341960407610458, 5.719274019375980345, 108.9572429386476955 ) ) ;
#101472 = CARTESIAN_POINT ( 'NONE',  ( -19.05341960407611168, -5.049401038298163336, 51.45724293864770260 ) ) ;
#101473 = CARTESIAN_POINT ( 'NONE',  ( -16.46253265017146816, -9.564922557961047289, 44.16775706135232582 ) ) ;
#101474 = CARTESIAN_POINT ( 'NONE',  ( -9.474510206698964154, 16.51473224551069663, 35.41557627198102409 ) ) ;
#101475 = CARTESIAN_POINT ( 'NONE',  ( 18.62759615963255655, 10.81492255796105972, 61.66775706135235424 ) ) ;
#101476 = CARTESIAN_POINT ( 'NONE',  ( -18.22780087662123805, 5.499999999999981348, 101.0176318212689495 ) ) ;
#101477 = CARTESIAN_POINT ( 'NONE',  ( 16.53943276465976808, -0.05219959533910856209, 38.74890960531435979 ) ) ;
#101479 = CIRCLE ( 'NONE', #136999, 61.99999999999998579 ) ;
#101478 = CARTESIAN_POINT ( 'NONE',  ( 19.05341960407611168, 5.049401038298154454, 63.95724293864769550 ) ) ;
#101480 = CARTESIAN_POINT ( 'NONE',  ( 5.823673210054125526, 21.52544592524343514, 84.79057627198102409 ) ) ;
#101481 = CARTESIAN_POINT ( 'NONE',  ( -19.05341960407611168, -5.049401038298163336, 56.45724293864768129 ) ) ;
#101482 = EDGE_LOOP ( 'NONE', ( #109039, #162961, #97390, #145523 ) ) ;
#101483 = CARTESIAN_POINT ( 'NONE',  ( 18.62759615963271287, -10.81492255796078972, 63.33224293864770260 ) ) ;
#101484 = EDGE_LOOP ( 'NONE', ( #35122, #73624, #99694, #176507 ) ) ;
#101485 = CARTESIAN_POINT ( 'NONE',  ( -21.52544592524334988, -5.823673210054445271, 98.95942372801903275 ) ) ;
#101488 = CARTESIAN_POINT ( 'NONE',  ( -14.34966873604960291, -8.224510206698953496, 86.66557627198102409 ) ) ;
#101487 = CARTESIAN_POINT ( 'NONE',  ( -0.05219959533934338120, 16.53943276465976808, 97.50109039468567573 ) ) ;
#101486 = CARTESIAN_POINT ( 'NONE',  ( 17.72662750342725602, 5.500000000000081712, 53.90179492283745333 ) ) ;
#101489 = CARTESIAN_POINT ( 'NONE',  ( 13.97604488694548053, -13.89961937509957401, 90.62609039468567573 ) ) ;
#101490 = ORIENTED_EDGE ( 'NONE', *, *, #29212, .F. ) ;
#101491 = CARTESIAN_POINT ( 'NONE',  ( -9.474510206698720793, -16.51473224551083518, 39.58442372801899722 ) ) ;
#101492 = CARTESIAN_POINT ( 'NONE',  ( -8.314922557961024197, 14.29746914071037800, 107.9177570613523471 ) ) ;
#101493 = CARTESIAN_POINT ( 'NONE',  ( 16.51473224551083163, -9.474510206698727899, 30.83442372801900433 ) ) ;
#101494 = CARTESIAN_POINT ( 'NONE',  ( 19.02544592524343514, -5.153800228976328945, 93.54057627198102409 ) ) ;
#101495 = CARTESIAN_POINT ( 'NONE',  ( 18.62759615963271287, -10.81492255796078972, 58.33224293864768839 ) ) ;
#101496 = CARTESIAN_POINT ( 'NONE',  ( -26.58496454517000629, 7.626754437231443084, 167.9682100371138915 ) ) ;
#101497 = CARTESIAN_POINT ( 'NONE',  ( 5.153800228976335163, 19.02544592524342804, 24.79057627198102765 ) ) ;
#101498 = CARTESIAN_POINT ( 'NONE',  ( -21.52544592524334988, -5.823673210054445271, 93.95942372801903275 ) ) ;
#101499 = CARTESIAN_POINT ( 'NONE',  ( 4.379528057220092307, 16.55341960407617563, 72.29275706135236135 ) ) ;
#101500 = CARTESIAN_POINT ( 'NONE',  ( 18.67979575497194134, -10.72451020669871369, 25.83442372801901499 ) ) ;
#101501 = CARTESIAN_POINT ( 'NONE',  ( 12.06949235617739724, 12.14591786802326823, 36.87609039468568994 ) ) ;
#101502 = CARTESIAN_POINT ( 'NONE',  ( -16.46253265017160317, 9.564922557960807481, 100.8322429386477097 ) ) ;
#101503 = CARTESIAN_POINT ( 'NONE',  ( -13.97604488694527625, -13.89961937509977652, 36.87390960531436690 ) ) ;
#101504 = CARTESIAN_POINT ( 'NONE',  ( 5.049401038298161559, -19.05341960407611168, 47.70724293864770260 ) ) ;
#101505 = CARTESIAN_POINT ( 'NONE',  ( 12.06949235617739724, 12.14591786802326823, 41.87609039468568284 ) ) ;
#101506 = CARTESIAN_POINT ( 'NONE',  ( -4.379528057220328563, 16.55341960407611168, 95.20724293864769550 ) ) ;
#101507 = CARTESIAN_POINT ( 'NONE',  ( 4.483927247898790824, -16.52544592524335698, 105.2094237280190328 ) ) ;
#101510 = CARTESIAN_POINT ( 'NONE',  ( -19.03943276465977164, 0.05219959533909376836, 66.24890960531436690 ) ) ;
#101509 = CARTESIAN_POINT ( 'NONE',  ( 0.05219959533909260263, 19.03943276465977164, 79.99890960531436690 ) ) ;
#101508 = CARTESIAN_POINT ( 'NONE',  ( -15.72974639402176322, -15.80617190586768395, 39.37609039468567573 ) ) ;
#101511 = CARTESIAN_POINT ( 'NONE',  ( -0.05219959533909027116, -19.03943276465977164, 92.49890960531436690 ) ) ;
#101512 = CARTESIAN_POINT ( 'NONE',  ( 4.483927247898545687, 16.52544592524342804, 29.79057627198102409 ) ) ;
#101513 = CARTESIAN_POINT ( 'NONE',  ( -4.483927247898782831, 16.52544592524335698, 102.7094237280190185 ) ) ;
#101514 = ORIENTED_EDGE ( 'NONE', *, *, #116186, .T. ) ;
#101515 = CARTESIAN_POINT ( 'NONE',  ( 9.564922557961047289, -16.46253265017146816, 50.41775706135233293 ) ) ;
#101516 = CARTESIAN_POINT ( 'NONE',  ( 13.89961937509977652, -13.97604488694527269, 108.1239096053143669 ) ) ;
#101517 = CARTESIAN_POINT ( 'NONE',  ( -5.153800228976328057, -19.02544592524343514, 57.29057627198103120 ) ) ;
#101518 = CARTESIAN_POINT ( 'NONE',  ( 5.153800228976615827, -19.02544592524334988, 35.20942372801899722 ) ) ;
#101519 = CARTESIAN_POINT ( 'NONE',  ( 22.81625015709510151, -31.40387420917324590, -7.924999997268812990 ) ) ;
#101520 = CARTESIAN_POINT ( 'NONE',  ( 19.26498983726236958, -5.499999999999790390, 73.05319577422000066 ) ) ;
#101521 = CARTESIAN_POINT ( 'NONE',  ( -14.34966873604972548, 8.224510206698743886, 48.33442372801902565 ) ) ;
#101523 = CARTESIAN_POINT ( 'NONE',  ( 0.05219959533934541429, -16.53943276465976808, 55.00109039468568284 ) ) ;
#101522 = CARTESIAN_POINT ( 'NONE',  ( -9.564922557961040184, 16.46253265017147172, 77.91775706135234714 ) ) ;
#101524 = SPHERICAL_SURFACE ( 'NONE', #178910, 2.000000000000000000 ) ;
#101525 = CARTESIAN_POINT ( 'NONE',  ( 13.97604488694527802, 13.89961937509977652, 89.37390960531436690 ) ) ;
#101526 = CARTESIAN_POINT ( 'NONE',  ( 0.05219959533907565091, 21.53943276465977519, 114.9989096053143669 ) ) ;
#101527 = CARTESIAN_POINT ( 'NONE',  ( -9.474510206698720793, -16.51473224551083518, 79.58442372801899012 ) ) ;
#101529 = CARTESIAN_POINT ( 'NONE',  ( 5.153800228976335163, 19.02544592524342804, 39.79057627198100988 ) ) ;
#101528 = CARTESIAN_POINT ( 'NONE',  ( 19.03943276465977164, -0.05219959533909143690, 98.74890960531436690 ) ) ;
#101530 = CARTESIAN_POINT ( 'NONE',  ( -13.97604488694527625, -13.89961937509977652, 71.87390960531433848 ) ) ;
#101532 = CARTESIAN_POINT ( 'NONE',  ( -5.153800228976328057, -19.02544592524343514, 42.29057627198101699 ) ) ;
#101531 = CARTESIAN_POINT ( 'NONE',  ( 16.53943276465976808, -0.05219959533910856209, 33.74890960531436690 ) ) ;
#101533 = CARTESIAN_POINT ( 'NONE',  ( -5.049401038297874678, -19.05341960407617918, 54.79275706135234003 ) ) ;
#101534 = CARTESIAN_POINT ( 'NONE',  ( 16.53943276465976808, -0.05219959533910856209, 93.74890960531436690 ) ) ;
#101535 = CARTESIAN_POINT ( 'NONE',  ( -13.89961937509957401, -13.97604488694547875, 19.37609039468566507 ) ) ;
#101536 = CARTESIAN_POINT ( 'NONE',  ( 9.474510206698971260, -16.51473224551069308, 47.91557627198102409 ) ) ;
#101537 = AXIS2_PLACEMENT_3D ( 'NONE', #98661, #160355, #1692 ) ;
#101538 = CARTESIAN_POINT ( 'NONE',  ( -15.72974639402197994, 15.80617190586746368, 50.62390960531435979 ) ) ;
#101540 = CARTESIAN_POINT ( 'NONE',  ( 15.72974639402176855, 15.80617190586768217, 101.8760903946857042 ) ) ;
#101539 = CARTESIAN_POINT ( 'NONE',  ( 8.224510206698953496, -14.34966873604960469, 57.91557627198103120 ) ) ;
#101541 = CARTESIAN_POINT ( 'NONE',  ( -16.51473224551069308, -9.474510206698971260, 111.6655762719810383 ) ) ;
#101542 = CARTESIAN_POINT ( 'NONE',  ( -5.153800228976328057, -19.02544592524343514, 102.2905762719810383 ) ) ;
#101543 = CARTESIAN_POINT ( 'NONE',  ( 19.05341960407611168, 5.049401038298154454, 43.95724293864769550 ) ) ;
#101544 = CARTESIAN_POINT ( 'NONE',  ( -13.97604488694527625, -13.89961937509977652, 26.87390960531434558 ) ) ;
#101545 = CARTESIAN_POINT ( 'NONE',  ( -12.14591786802309592, -12.06949235617757132, 81.87390960531435269 ) ) ;
#101546 = CARTESIAN_POINT ( 'NONE',  ( -10.81492255796078084, -18.62759615963271287, 102.0822429386476955 ) ) ;
#101547 = CARTESIAN_POINT ( 'NONE',  ( -5.153800228976328057, -19.02544592524343514, 97.29057627198099567 ) ) ;
#101548 = CARTESIAN_POINT ( 'NONE',  ( -5.719274019375978568, 21.55341960407610458, 115.2072429386476955 ) ) ;
#101549 = CARTESIAN_POINT ( 'NONE',  ( -19.03943276465977164, 0.05219959533909376836, 101.2489096053143669 ) ) ;
#101551 = CARTESIAN_POINT ( 'NONE',  ( 0.05219959533910956823, 16.53943276465976808, 104.9989096053143669 ) ) ;
#101550 = CARTESIAN_POINT ( 'NONE',  ( 17.59860650958994555, -7.585241751806880650, 65.92337014262493256 ) ) ;
#101552 = CARTESIAN_POINT ( 'NONE',  ( -16.46253265017160317, 9.564922557960807481, 70.83224293864770971 ) ) ;
#101553 = CARTESIAN_POINT ( 'NONE',  ( -18.67979575497178146, -10.72451020669898902, 76.66557627198103830 ) ) ;
#101554 = DIRECTION ( 'NONE',  ( -0.000000000000000000, -0.000000000000000000, 1.000000000000000000 ) ) ;
#101555 = CARTESIAN_POINT ( 'NONE',  ( -20.85011945226398566, -10.59319688750118083, 168.2343749380337954 ) ) ;
#101557 = CARTESIAN_POINT ( 'NONE',  ( 19.02130022317637881, -5.499999999999590550, 68.28188669246574705 ) ) ;
#101556 = CARTESIAN_POINT ( 'NONE',  ( 0.05219959533907565091, 21.53943276465977519, 24.99890960531435624 ) ) ;
#101558 = CARTESIAN_POINT ( 'NONE',  ( -8.224510206698735004, -14.34966873604973081, 39.58442372801901143 ) ) ;
#101560 = STYLED_ITEM ( 'NONE', ( #49638 ), #11768 ) ;
#101559 = CARTESIAN_POINT ( 'NONE',  ( 8.314922557960818139, 14.29746914071049879, 99.58224293864770971 ) ) ;
#101561 = CARTESIAN_POINT ( 'NONE',  ( 19.49149378614662709, -5.499999999999593214, 51.93757513605365261 ) ) ;
#101562 = CARTESIAN_POINT ( 'NONE',  ( 16.46253265017160672, -9.564922557960803928, 93.33224293864769550 ) ) ;
#101563 = CARTESIAN_POINT ( 'NONE',  ( 9.564922557960805705, 16.46253265017160317, 59.58224293864769550 ) ) ;
#101564 = CARTESIAN_POINT ( 'NONE',  ( -12.06949235617756955, 12.14591786802309770, 80.62390960531438111 ) ) ;
#101565 = CARTESIAN_POINT ( 'NONE',  ( -18.62759615963270932, 10.81492255796079327, 35.83224293864768839 ) ) ;
#101566 = CARTESIAN_POINT ( 'NONE',  ( 16.53943276465976808, -0.05219959533910856209, 53.74890960531437401 ) ) ;
#101567 = CARTESIAN_POINT ( 'NONE',  ( 0.05219959533936267826, -19.03943276465977164, 110.0010903946856757 ) ) ;
#101568 = CARTESIAN_POINT ( 'NONE',  ( 10.81492255796106328, -18.62759615963255655, 75.41775706135233293 ) ) ;
#101569 = CIRCLE ( 'NONE', #53065, 2.649999999999999467 ) ;
#101570 = CARTESIAN_POINT ( 'NONE',  ( 17.50000000000000000, -5.499999999999992895, 76.21769037696435589 ) ) ;
#101571 = CARTESIAN_POINT ( 'NONE',  ( 18.67979575497178502, 10.72451020669898547, 24.16557627198103120 ) ) ;
#101572 = CARTESIAN_POINT ( 'NONE',  ( -16.52544592524335698, -4.483927247898792601, 88.95942372801901854 ) ) ;
#101573 = CARTESIAN_POINT ( 'NONE',  ( -5.049401038298153566, 19.05341960407611168, 25.20724293864768484 ) ) ;
#101574 = CARTESIAN_POINT ( 'NONE',  ( 5.049401038298161559, -19.05341960407611168, 87.70724293864769550 ) ) ;
#101575 = CARTESIAN_POINT ( 'NONE',  ( -21.53943276465977519, 0.05219959533907696930, 91.24890960531436690 ) ) ;
#101576 = AXIS2_PLACEMENT_3D ( 'NONE', #185839, #77647, #32150 ) ;
#101577 = CARTESIAN_POINT ( 'NONE',  ( -16.53943276465976808, -0.05219959533934237506, 28.75109039468567929 ) ) ;
#101579 = CARTESIAN_POINT ( 'NONE',  ( -21.55341960407619339, 5.719274019375674811, 73.54275706135234714 ) ) ;
#101578 = CARTESIAN_POINT ( 'NONE',  ( -16.55341960407611168, -4.379528057220339221, 51.45724293864770260 ) ) ;
#101580 = EDGE_CURVE ( 'NONE', #56947, #45770, #97966, .T. ) ;
#101582 = CARTESIAN_POINT ( 'NONE',  ( -18.62759615963270932, 10.81492255796079327, 30.83224293864770260 ) ) ;
#101581 = CARTESIAN_POINT ( 'NONE',  ( -12.14591786802326823, 12.06949235617739902, 98.12609039468570415 ) ) ;
#101583 = CARTESIAN_POINT ( 'NONE',  ( -19.02544592524342804, 5.153800228976336939, 116.0405762719810383 ) ) ;
#101584 = FACE_BOUND ( 'NONE', #42839, .T. ) ;
#101585 = CARTESIAN_POINT ( 'NONE',  ( -0.05219959533934338120, 16.53943276465976808, 107.5010903946856899 ) ) ;
#101586 = CARTESIAN_POINT ( 'NONE',  ( 8.314922557961029526, -14.29746914071037800, 60.41775706135235424 ) ) ;
#101588 = VERTEX_POINT ( 'NONE', #192000 ) ;
#101587 = CARTESIAN_POINT ( 'NONE',  ( 9.564922557960805705, 16.46253265017160317, 74.58224293864769550 ) ) ;
#101589 = CARTESIAN_POINT ( 'NONE',  ( 19.02544592524343514, -5.153800228976328945, 88.54057627198102409 ) ) ;
#101590 = CARTESIAN_POINT ( 'NONE',  ( 18.62759615963255655, 10.81492255796105972, 76.66775706135234714 ) ) ;
#101591 = CARTESIAN_POINT ( 'NONE',  ( 4.483927247898790824, -16.52544592524335698, 75.20942372801901854 ) ) ;
#101592 = CARTESIAN_POINT ( 'NONE',  ( -14.29746914071049879, 8.314922557960819915, 45.83224293864769550 ) ) ;
#101593 = CARTESIAN_POINT ( 'NONE',  ( -13.89961937509977652, 13.97604488694528158, 55.62390960531434558 ) ) ;
#101594 = ORIENTED_EDGE ( 'NONE', *, *, #3260, .F. ) ;
#101595 = CARTESIAN_POINT ( 'NONE',  ( -0.05219959533936034679, 19.03943276465977164, 112.5010903946856757 ) ) ;
#101596 = CARTESIAN_POINT ( 'NONE',  ( 16.53943276465976808, -0.05219959533910856209, 113.7489096053143527 ) ) ;
#101597 = CARTESIAN_POINT ( 'NONE',  ( 19.05341960407611168, 5.049401038298154454, 63.95724293864769550 ) ) ;
#101599 = CARTESIAN_POINT ( 'NONE',  ( -38.00000000000000711, 2.428612866367529932E-14, -6.000000000000000000 ) ) ;
#101598 = CARTESIAN_POINT ( 'NONE',  ( 13.97604488694548053, -13.89961937509957401, 100.6260903946856615 ) ) ;
#101600 = CARTESIAN_POINT ( 'NONE',  ( -5.823673210054431948, 21.52544592524334988, 102.7094237280190185 ) ) ;
#101601 = CARTESIAN_POINT ( 'NONE',  ( -12.14591786802326823, 12.06949235617739902, 83.12609039468568994 ) ) ;
#101602 = CARTESIAN_POINT ( 'NONE',  ( -9.474510206698720793, -16.51473224551083518, 99.58442372801900433 ) ) ;
#101603 = CARTESIAN_POINT ( 'NONE',  ( -5.823673210054116645, -21.52544592524344225, 62.29057627198102409 ) ) ;
#101604 = CARTESIAN_POINT ( 'NONE',  ( -16.55341960407617563, 4.379528057220093196, 53.54275706135234714 ) ) ;
#101605 = CARTESIAN_POINT ( 'NONE',  ( -19.99999999999998224, -190.0000000000000000, 0.000000000000000000 ) ) ;
#101606 = CARTESIAN_POINT ( 'NONE',  ( 13.89961937509957401, 13.97604488694547697, 56.87609039468564731 ) ) ;
#101607 = CARTESIAN_POINT ( 'NONE',  ( 21.53943276465977519, 0.05219959533937863772, 91.25109039468568994 ) ) ;
#101608 = CARTESIAN_POINT ( 'NONE',  ( -19.03943276465977164, 0.05219959533909376836, 31.24890960531435979 ) ) ;
#101609 = CARTESIAN_POINT ( 'NONE',  ( 16.46253265017160672, -9.564922557960803928, 68.33224293864770971 ) ) ;
#101610 = CARTESIAN_POINT ( 'NONE',  ( 16.55341960407611168, 4.379528057220329451, 58.95724293864770971 ) ) ;
#101611 = VECTOR ( 'NONE', #77641, 1000.000000000000000 ) ;
#101612 = CARTESIAN_POINT ( 'NONE',  ( -18.67979575497193778, 10.72451020669871902, 88.33442372801901854 ) ) ;
#101613 = EDGE_CURVE ( 'NONE', #140935, #112813, #171147, .T. ) ;
#101614 = CARTESIAN_POINT ( 'NONE',  ( 5.049401038297881783, 19.05341960407617563, 47.29275706135231161 ) ) ;
#101615 = CARTESIAN_POINT ( 'NONE',  ( 9.474510206698729675, 16.51473224551082808, 22.08442372801899722 ) ) ;
#101616 = CARTESIAN_POINT ( 'NONE',  ( -13.89961937509977652, 13.97604488694528158, 115.6239096053143669 ) ) ;
#101617 = CARTESIAN_POINT ( 'NONE',  ( 21.53943276465977519, 0.05219959533937863772, 91.25109039468568994 ) ) ;
#101618 = CARTESIAN_POINT ( 'NONE',  ( -13.89961937509977652, 13.97604488694528158, 75.62390960531438111 ) ) ;
#101619 = CARTESIAN_POINT ( 'NONE',  ( 5.719274019375673035, 21.55341960407619339, 87.29275706135236135 ) ) ;
#101620 = CARTESIAN_POINT ( 'NONE',  ( 10.81492255796078972, 18.62759615963270932, 54.58224293864769550 ) ) ;
#101621 = CARTESIAN_POINT ( 'NONE',  ( 16.51473224551069308, 9.474510206698969483, 79.16557627198103830 ) ) ;
#101622 = CARTESIAN_POINT ( 'NONE',  ( -19.02544592524334988, -5.153800228976617603, 68.95942372801896170 ) ) ;
#101623 = CARTESIAN_POINT ( 'NONE',  ( -19.02544592524342804, 5.153800228976336051, 46.04057627198101699 ) ) ;
#101624 = CARTESIAN_POINT ( 'NONE',  ( -9.564922557960796823, -16.46253265017161027, 87.08224293864769550 ) ) ;
#101625 = CARTESIAN_POINT ( 'NONE',  ( 19.02544592524334988, 5.153800228976608722, 96.45942372801897591 ) ) ;
#101626 = CARTESIAN_POINT ( 'NONE',  ( 16.53943276465976808, 0.05219959533934440121, 46.25109039468567573 ) ) ;
#101627 = CARTESIAN_POINT ( 'NONE',  ( 14.34966873604960469, 8.224510206698951720, 104.1655762719810241 ) ) ;
#101628 = CARTESIAN_POINT ( 'NONE',  ( 16.46253265017160672, -9.564922557960803928, 68.33224293864770971 ) ) ;
#101629 = CARTESIAN_POINT ( 'NONE',  ( -21.52544592524343514, 5.823673210054127303, 51.04057627198103120 ) ) ;
#101630 = CARTESIAN_POINT ( 'NONE',  ( 4.483927247898790824, -16.52544592524335698, 35.20942372801901854 ) ) ;
#101631 = CARTESIAN_POINT ( 'NONE',  ( 10.81492255796106328, -18.62759615963255655, 30.41775706135234358 ) ) ;
#101632 = CARTESIAN_POINT ( 'NONE',  ( -5.719274019375665041, -21.55341960407619695, 89.79275706135236135 ) ) ;
#101633 = CARTESIAN_POINT ( 'NONE',  ( 16.53943276465976808, 0.05219959533934440121, 86.25109039468568994 ) ) ;
#101634 = CARTESIAN_POINT ( 'NONE',  ( 16.51473224551069308, 9.474510206698969483, 79.16557627198103830 ) ) ;
#101635 = CARTESIAN_POINT ( 'NONE',  ( 14.29746914071037800, 8.314922557961029526, 101.6677570613523613 ) ) ;
#101636 = CARTESIAN_POINT ( 'NONE',  ( 19.03943276465977164, 0.05219959533936151252, 56.25109039468566863 ) ) ;
#101637 = CARTESIAN_POINT ( 'NONE',  ( -5.719274019375665041, -21.55341960407619695, 24.79275706135235779 ) ) ;
#101638 = CARTESIAN_POINT ( 'NONE',  ( 4.379528057220339221, -16.55341960407611168, 77.70724293864770971 ) ) ;
#101639 = CARTESIAN_POINT ( 'NONE',  ( -0.05219959533909027116, -19.03943276465977164, 97.49890960531436690 ) ) ;
#101640 = CARTESIAN_POINT ( 'NONE',  ( -16.53943276465976808, -0.05219959533934237506, 103.7510903946857042 ) ) ;
#101641 = CARTESIAN_POINT ( 'NONE',  ( -0.05219959533937732626, 21.53943276465977519, 67.50109039468568994 ) ) ;
#101642 = CARTESIAN_POINT ( 'NONE',  ( 12.06949235617739724, 12.14591786802326823, 46.87609039468568994 ) ) ;
#101643 = CARTESIAN_POINT ( 'NONE',  ( -5.823673210054431948, 21.52544592524334988, 32.70942372801900433 ) ) ;
#101644 = CARTESIAN_POINT ( 'NONE',  ( 12.06949235617757843, -12.14591786802309237, 73.12390960531436690 ) ) ;
#101645 = VERTEX_POINT ( 'NONE', #53486 ) ;
#101646 = CARTESIAN_POINT ( 'NONE',  ( -10.81492255796105439, 18.62759615963255655, 22.91775706135235069 ) ) ;
#101647 = CARTESIAN_POINT ( 'NONE',  ( 16.52544592524342804, -4.483927247898539470, 58.54057627198103120 ) ) ;
#101648 = DIRECTION ( 'NONE',  ( -0.000000000000000000, -0.000000000000000000, 1.000000000000000000 ) ) ;
#101649 = CARTESIAN_POINT ( 'NONE',  ( -21.52544592524343514, 5.823673210054127303, 31.04057627198102409 ) ) ;
#101650 = CARTESIAN_POINT ( 'NONE',  ( 0.05219959533937995610, -21.53943276465977519, 45.00109039468568284 ) ) ;
#101651 = CARTESIAN_POINT ( 'NONE',  ( 0.05219959533910956823, 16.53943276465976808, 59.99890960531436690 ) ) ;
#101652 = CARTESIAN_POINT ( 'NONE',  ( 21.52544592524344225, -5.823673210054117533, 78.54057627198103830 ) ) ;
#101653 = CARTESIAN_POINT ( 'NONE',  ( -19.05341960407611168, -5.049401038298163336, 71.45724293864766707 ) ) ;
#101655 = CARTESIAN_POINT ( 'NONE',  ( -5.153800228976607833, 19.02544592524334988, 82.70942372801897591 ) ) ;
#101654 = CARTESIAN_POINT ( 'NONE',  ( 16.46253265017160672, -9.564922557960803928, 33.33224293864770260 ) ) ;
#101656 = ADVANCED_FACE ( 'NONE', ( #144492, #162665 ), #100981, .F. ) ;
#101658 = CARTESIAN_POINT ( 'NONE',  ( 21.53943276465977519, -0.05219959533907433946, 58.74890960531436690 ) ) ;
#101657 = CARTESIAN_POINT ( 'NONE',  ( 10.81492255796106328, -18.62759615963255655, 55.41775706135234714 ) ) ;
#101659 = CARTESIAN_POINT ( 'NONE',  ( 13.97604488694527802, 13.89961937509977652, 44.37390960531435269 ) ) ;
#101660 = CARTESIAN_POINT ( 'NONE',  ( -19.02544592524342804, 5.153800228976336051, 76.04057627198102409 ) ) ;
#101661 = ORIENTED_EDGE ( 'NONE', *, *, #60782, .T. ) ;
#101662 = CARTESIAN_POINT ( 'NONE',  ( 4.379528057220092307, 16.55341960407617563, 47.29275706135234003 ) ) ;
#101663 = CARTESIAN_POINT ( 'NONE',  ( 10.72451020669871369, 18.67979575497193778, 37.08442372801901143 ) ) ;
#101664 = VECTOR ( 'NONE', #107256, 1000.000000000000000 ) ;
#101665 = CARTESIAN_POINT ( 'NONE',  ( 0.05219959533937995610, -21.53943276465977519, 65.00109039468568994 ) ) ;
#101666 = CARTESIAN_POINT ( 'NONE',  ( -5.153800228976328057, -19.02544592524343514, 102.2905762719810383 ) ) ;
#101667 = CARTESIAN_POINT ( 'NONE',  ( -18.62759615963270932, 10.81492255796079327, 85.83224293864768129 ) ) ;
#101669 = CARTESIAN_POINT ( 'NONE',  ( -8.314922557961024197, 14.29746914071037800, 57.91775706135234714 ) ) ;
#101668 = CARTESIAN_POINT ( 'NONE',  ( 10.81492255796106328, -18.62759615963255655, 20.41775706135234714 ) ) ;
#101670 = CARTESIAN_POINT ( 'NONE',  ( 18.67979575497178502, 10.72451020669898547, 44.16557627198103120 ) ) ;
#101671 = CARTESIAN_POINT ( 'NONE',  ( -13.89961937509957401, -13.97604488694547875, 19.37609039468566507 ) ) ;
#101672 = CARTESIAN_POINT ( 'NONE',  ( 19.05341960407611168, 5.049401038298154454, 53.95724293864770260 ) ) ;
#101673 = CARTESIAN_POINT ( 'NONE',  ( 13.97604488694527802, 13.89961937509977652, 109.3739096053143669 ) ) ;
#101674 = CARTESIAN_POINT ( 'NONE',  ( 0.05219959533909260263, 19.03943276465977164, 89.99890960531436690 ) ) ;
#101675 = CARTESIAN_POINT ( 'NONE',  ( 5.049401038297881783, 19.05341960407617918, 52.29275706135233293 ) ) ;
#101676 = CARTESIAN_POINT ( 'NONE',  ( -5.153800228976607833, 19.02544592524334988, 67.70942372801900433 ) ) ;
#101677 = CARTESIAN_POINT ( 'NONE',  ( 10.81492255796078972, 18.62759615963270932, 49.58224293864769550 ) ) ;
#101678 = CARTESIAN_POINT ( 'NONE',  ( 16.53943276465976808, -0.05219959533910856209, 28.74890960531435624 ) ) ;
#101679 = CARTESIAN_POINT ( 'NONE',  ( -0.05219959533936034679, 19.03943276465977164, 92.50109039468566152 ) ) ;
#101680 = CYLINDRICAL_SURFACE ( 'NONE', #65965, 38.00000000000000000 ) ;
#101681 = AXIS2_PLACEMENT_3D ( 'NONE', #162018, #148860, #24525 ) ;
#101682 = CARTESIAN_POINT ( 'NONE',  ( 10.81492255796106328, -18.62759615963255655, 110.4177570613523756 ) ) ;
#101683 = CARTESIAN_POINT ( 'NONE',  ( -13.89961937509957401, -13.97604488694547875, 99.37609039468567573 ) ) ;
#101684 = CARTESIAN_POINT ( 'NONE',  ( -9.474510206698720793, -16.51473224551083518, 49.58442372801899722 ) ) ;
#101685 = FACE_OUTER_BOUND ( 'NONE', #130495, .T. ) ;
#101686 = CARTESIAN_POINT ( 'NONE',  ( -16.51473224551069308, -9.474510206698971260, 61.66557627198103120 ) ) ;
#101687 = CARTESIAN_POINT ( 'NONE',  ( 8.224510206698953496, -14.34966873604960469, 47.91557627198102409 ) ) ;
#101688 = CARTESIAN_POINT ( 'NONE',  ( 13.97604488694527802, 13.89961937509977652, 29.37390960531435979 ) ) ;
#101689 = CARTESIAN_POINT ( 'NONE',  ( 16.53943276465976808, -0.05219959533910856209, 33.74890960531436690 ) ) ;
#101690 = DIRECTION ( 'NONE',  ( -5.392603844284257652E-33, -1.000000000000000000, -0.000000000000000000 ) ) ;
#101691 = CARTESIAN_POINT ( 'NONE',  ( 14.29746914071037800, 8.314922557961029526, 101.6677570613523613 ) ) ;
#101692 = CARTESIAN_POINT ( 'NONE',  ( -9.564922557960796823, -16.46253265017161027, 67.08224293864769550 ) ) ;
#101693 = CARTESIAN_POINT ( 'NONE',  ( 19.03943276465977164, 0.05219959533936151252, 31.25109039468566863 ) ) ;
#101694 = CARTESIAN_POINT ( 'NONE',  ( -12.06949235617739369, -12.14591786802326823, 34.37609039468568284 ) ) ;
#101695 = CARTESIAN_POINT ( 'NONE',  ( -5.719274019375978568, 21.55341960407610458, 35.20724293864768839 ) ) ;
#101696 = CARTESIAN_POINT ( 'NONE',  ( 18.62759615963255655, 10.81492255796105972, 101.6677570613523613 ) ) ;
#101697 = CARTESIAN_POINT ( 'NONE',  ( -0.05219959533909027116, -19.03943276465977164, 62.49890960531435979 ) ) ;
#101698 = CARTESIAN_POINT ( 'NONE',  ( -16.51473224551069308, -9.474510206698971260, 101.6655762719810241 ) ) ;
#101699 = CARTESIAN_POINT ( 'NONE',  ( -13.97604488694527625, -13.89961937509977652, 101.8739096053143811 ) ) ;
#101700 = CARTESIAN_POINT ( 'NONE',  ( 36.91746824999999887, -11.99521256947793546, -1.724999997268813479 ) ) ;
#101701 = CARTESIAN_POINT ( 'NONE',  ( 5.823673210054444382, -21.52544592524334988, 30.20942372801902565 ) ) ;
#101702 = CIRCLE ( 'NONE', #182548, 0.5000000000000004441 ) ;
#101703 = CARTESIAN_POINT ( 'NONE',  ( 12.14591786802309770, 12.06949235617756955, 89.37390960531435269 ) ) ;
#101705 = CARTESIAN_POINT ( 'NONE',  ( -13.97604488694527625, -13.89961937509977652, 71.87390960531433848 ) ) ;
#101704 = CARTESIAN_POINT ( 'NONE',  ( 10.72451020669898902, -18.67979575497178502, 77.91557627198102409 ) ) ;
#101706 = CARTESIAN_POINT ( 'NONE',  ( 16.51473224551069308, 9.474510206698969483, 74.16557627198103830 ) ) ;
#101707 = CARTESIAN_POINT ( 'NONE',  ( -15.80617190586745835, -15.72974639402198527, 106.8739096053143811 ) ) ;
#101708 = ORIENTED_EDGE ( 'NONE', *, *, #125853, .T. ) ;
#101709 = CARTESIAN_POINT ( 'NONE',  ( 19.03943276465977164, -0.05219959533909143690, 78.74890960531436690 ) ) ;
#101710 = CARTESIAN_POINT ( 'NONE',  ( 23.29544513554940011, 16.92513159979228021, 147.1843446568999809 ) ) ;
#101712 = DIRECTION ( 'NONE',  ( 0.000000000000000000, 0.000000000000000000, 1.000000000000000000 ) ) ;
#101711 = CARTESIAN_POINT ( 'NONE',  ( -14.29746914071049879, 8.314922557960819915, 110.8322429386476955 ) ) ;
#101713 = CARTESIAN_POINT ( 'NONE',  ( 13.89961937509977652, -13.97604488694527269, 63.12390960531435979 ) ) ;
#101714 = CARTESIAN_POINT ( 'NONE',  ( 9.474510206698729675, 16.51473224551082808, 97.08442372801900433 ) ) ;
#101715 = CIRCLE ( 'NONE', #117898, 0.2500000000000002220 ) ;
#101716 = CARTESIAN_POINT ( 'NONE',  ( 4.379528057220339221, -16.55341960407611168, 97.70724293864772392 ) ) ;
#101717 = CARTESIAN_POINT ( 'NONE',  ( 18.62759615963255655, 10.81492255796105972, 66.66775706135234714 ) ) ;
#101719 = CARTESIAN_POINT ( 'NONE',  ( -21.52544592524334988, -5.823673210054445271, 18.95942372801901143 ) ) ;
#101718 = CARTESIAN_POINT ( 'NONE',  ( 19.02544592524343514, -5.153800228976328945, 53.54057627198102409 ) ) ;
#101720 = CARTESIAN_POINT ( 'NONE',  ( -10.72451020669898014, 18.67979575497178502, 115.4155762719810241 ) ) ;
#101721 = CARTESIAN_POINT ( 'NONE',  ( -17.81289503416611097, -24.51734667627696496, 144.2999999999999829 ) ) ;
#101722 = CARTESIAN_POINT ( 'NONE',  ( -19.05341960407611168, -5.049401038298163336, 76.45724293864769550 ) ) ;
#101723 = CIRCLE ( 'NONE', #195421, 31.90000000000003411 ) ;
#101724 = CARTESIAN_POINT ( 'NONE',  ( 16.38665767535055195, 7.295008042176099217, 112.2359913578545161 ) ) ;
#101726 = CARTESIAN_POINT ( 'NONE',  ( 15.80617190586746368, 15.72974639402197994, 34.37390960531435979 ) ) ;
#101725 = CARTESIAN_POINT ( 'NONE',  ( 5.049401038297881783, 19.05341960407617563, 102.2927570613523045 ) ) ;
#101727 = CARTESIAN_POINT ( 'NONE',  ( -18.67979575497193778, 10.72451020669871902, 58.33442372801901143 ) ) ;
#101728 = CARTESIAN_POINT ( 'NONE',  ( 0.05219959533910956823, 16.53943276465976808, 104.9989096053143669 ) ) ;
#101729 = CARTESIAN_POINT ( 'NONE',  ( 19.03943276465977164, -0.05219959533909143690, 98.74890960531436690 ) ) ;
#101730 = CARTESIAN_POINT ( 'NONE',  ( -5.049401038297874678, -19.05341960407617918, 79.79275706135233293 ) ) ;
#101731 = CARTESIAN_POINT ( 'NONE',  ( 9.474510206698971260, -16.51473224551069308, 52.91557627198102409 ) ) ;
#101732 = CARTESIAN_POINT ( 'NONE',  ( -19.02544592524342804, 5.153800228976336051, 66.04057627198103830 ) ) ;
#101733 = CARTESIAN_POINT ( 'NONE',  ( -16.55341960407611168, -4.379528057220339221, 86.45724293864770971 ) ) ;
#101734 = CARTESIAN_POINT ( 'NONE',  ( 19.05341960407611168, 5.049401038298154454, 103.9572429386476671 ) ) ;
#101735 = CARTESIAN_POINT ( 'NONE',  ( 16.55341960407611168, 4.379528057220329451, 93.95724293864770971 ) ) ;
#101736 = CARTESIAN_POINT ( 'NONE',  ( -9.474510206698964154, 16.51473224551069663, 95.41557627198102409 ) ) ;
#101738 = CARTESIAN_POINT ( 'NONE',  ( 0.05219959533909260263, 19.03943276465977164, 24.99890960531435269 ) ) ;
#101737 = CARTESIAN_POINT ( 'NONE',  ( -16.55341960407611168, -4.379528057220339221, 41.45724293864769550 ) ) ;
#101739 = VERTEX_POINT ( 'NONE', #52484 ) ;
#101740 = CARTESIAN_POINT ( 'NONE',  ( -5.719274019375665041, -21.55341960407619695, 54.79275706135235424 ) ) ;
#101741 = CARTESIAN_POINT ( 'NONE',  ( -19.03943276465977164, -0.05219959533935918106, 73.75109039468566152 ) ) ;
#101742 = CARTESIAN_POINT ( 'NONE',  ( -16.52544592524342804, 4.483927247898546575, 46.04057627198103830 ) ) ;
#101743 = CARTESIAN_POINT ( 'NONE',  ( 5.719274019375991003, -21.55341960407610458, 102.7072429386476955 ) ) ;
#101744 = CARTESIAN_POINT ( 'NONE',  ( -5.823673210054116645, -21.52544592524344225, 27.29057627198103120 ) ) ;
#101745 = CARTESIAN_POINT ( 'NONE',  ( -16.53943276465976808, 0.05219959533911058130, 86.24890960531436690 ) ) ;
#101746 = CARTESIAN_POINT ( 'NONE',  ( 16.46253265017160672, -9.564922557960803928, 53.33224293864768839 ) ) ;
#101747 = CARTESIAN_POINT ( 'NONE',  ( -16.53943276465976808, 0.05219959533911058130, 26.24890960531435624 ) ) ;
#101748 = AXIS2_PLACEMENT_3D ( 'NONE', #97430, #141961, #68111 ) ;
#101749 = CARTESIAN_POINT ( 'NONE',  ( -4.483927247898782831, 16.52544592524335698, 102.7094237280190185 ) ) ;
#101750 = CARTESIAN_POINT ( 'NONE',  ( -16.52544592524335698, -4.483927247898792601, 68.95942372801901854 ) ) ;
#101751 = CARTESIAN_POINT ( 'NONE',  ( -0.05219959533936034679, 19.03943276465977164, 27.50109039468566507 ) ) ;
#101752 = CARTESIAN_POINT ( 'NONE',  ( 13.89961937509977652, -13.97604488694527269, 108.1239096053143669 ) ) ;
#101753 = CARTESIAN_POINT ( 'NONE',  ( -19.03943276465977164, 0.05219959533909376836, 76.24890960531435269 ) ) ;
#101754 = CARTESIAN_POINT ( 'NONE',  ( -16.51473224551069308, -9.474510206698971260, 36.66557627198102409 ) ) ;
#101755 = CARTESIAN_POINT ( 'NONE',  ( 8.224510206698953496, -14.34966873604960469, 42.91557627198103120 ) ) ;
#101757 = CARTESIAN_POINT ( 'NONE',  ( 5.153800228976335163, 19.02544592524342804, 99.79057627198102409 ) ) ;
#101756 = DIRECTION ( 'NONE',  ( 0.000000000000000000, 0.000000000000000000, 1.000000000000000000 ) ) ;
#101758 = CARTESIAN_POINT ( 'NONE',  ( -21.55341960407610458, -5.719274019375992779, 36.45724293864768839 ) ) ;
#101759 = CARTESIAN_POINT ( 'NONE',  ( 12.14591786802309770, 12.06949235617756955, 69.37390960531436690 ) ) ;
#101760 = CARTESIAN_POINT ( 'NONE',  ( 16.55341960407618274, -4.379528057220086978, 26.04275706135235779 ) ) ;
#101761 = EDGE_CURVE ( 'NONE', #78133, #18983, #22596, .T. ) ;
#101762 = CARTESIAN_POINT ( 'NONE',  ( 16.53943276465976808, -0.05219959533910856209, 68.74890960531435269 ) ) ;
#101763 = CARTESIAN_POINT ( 'NONE',  ( 28.98522958361494872, -0.5143648618586993404, -49.56847006845436709 ) ) ;
#101764 = CARTESIAN_POINT ( 'NONE',  ( 13.97604488694548053, -13.89961937509957401, 70.62609039468567573 ) ) ;
#101765 = CARTESIAN_POINT ( 'NONE',  ( -19.05341960407611168, -5.049401038298163336, 101.4572429386476955 ) ) ;
#101766 = CARTESIAN_POINT ( 'NONE',  ( -9.564922557961040184, 16.46253265017147172, 77.91775706135234714 ) ) ;
#101767 = CARTESIAN_POINT ( 'NONE',  ( -27.73933785331498925, 2.428612866367529932E-14, 147.3750000027311842 ) ) ;
#101769 = CARTESIAN_POINT ( 'NONE',  ( -12.14591786802326823, 12.06949235617739902, 93.12609039468568994 ) ) ;
#101768 = CARTESIAN_POINT ( 'NONE',  ( 13.89961937509957401, 13.97604488694547697, 106.8760903946856757 ) ) ;
#101770 = CARTESIAN_POINT ( 'NONE',  ( -13.97604488694527625, -13.89961937509977652, 36.87390960531436690 ) ) ;
#101771 = CARTESIAN_POINT ( 'NONE',  ( 0.05219959533907565091, 21.53943276465977519, 29.99890960531435979 ) ) ;
#101772 = CARTESIAN_POINT ( 'NONE',  ( 18.62759615963255655, 10.81492255796105972, 56.66775706135235424 ) ) ;
#101773 = CARTESIAN_POINT ( 'NONE',  ( -20.14845677604829888, -11.63499142542225329, 168.0304984204095149 ) ) ;
#101774 = CARTESIAN_POINT ( 'NONE',  ( 8.314922557961029526, -14.29746914071037800, 20.41775706135234714 ) ) ;
#101776 = CARTESIAN_POINT ( 'NONE',  ( 19.05341960407611168, 5.049401038298154454, 68.95724293864769550 ) ) ;
#101775 = CARTESIAN_POINT ( 'NONE',  ( 2.500000000000000000, -105.0000000000000000, 12.00000000000000355 ) ) ;
#101777 = CARTESIAN_POINT ( 'NONE',  ( -19.03943276465977164, 0.05219959533909376836, 116.2489096053143669 ) ) ;
#101779 = CARTESIAN_POINT ( 'NONE',  ( -19.05341960407611168, -5.049401038298163336, 76.45724293864769550 ) ) ;
#101778 = CARTESIAN_POINT ( 'NONE',  ( 14.34966873604960469, 8.224510206698951720, 89.16557627198102409 ) ) ;
#101780 = CARTESIAN_POINT ( 'NONE',  ( 13.89961937509977652, -13.97604488694527269, 93.12390960531436690 ) ) ;
#101781 = ORIENTED_EDGE ( 'NONE', *, *, #59844, .T. ) ;
#101782 = CARTESIAN_POINT ( 'NONE',  ( 19.02544592524334988, 5.153800228976608722, 96.45942372801897591 ) ) ;
#101783 = CARTESIAN_POINT ( 'NONE',  ( -21.52544592524343514, 5.823673210054127303, 61.04057627198103120 ) ) ;
#101784 = CARTESIAN_POINT ( 'NONE',  ( 16.46253265017160672, -9.564922557960803928, 28.33224293864769550 ) ) ;
#101785 = CARTESIAN_POINT ( 'NONE',  ( 19.03943276465977164, 0.05219959533936151252, 51.25109039468567573 ) ) ;
#101786 = CARTESIAN_POINT ( 'NONE',  ( -9.564922557960796823, -16.46253265017161027, 57.08224293864769550 ) ) ;
#101787 = CARTESIAN_POINT ( 'NONE',  ( 0.05219959533909260263, 19.03943276465977164, 94.99890960531436690 ) ) ;
#101788 = EDGE_LOOP ( 'NONE', ( #61221, #196968, #129777 ) ) ;
#101789 = CARTESIAN_POINT ( 'NONE',  ( 21.52544592524344225, -5.823673210054117533, 88.54057627198103830 ) ) ;
#101791 = CARTESIAN_POINT ( 'NONE',  ( 9.564922557961047289, -16.46253265017146816, 65.41775706135233293 ) ) ;
#101790 = CARTESIAN_POINT ( 'NONE',  ( 14.29746914071049879, -8.314922557960816363, 98.33224293864769550 ) ) ;
#101792 = CARTESIAN_POINT ( 'NONE',  ( -5.719274019375978568, 21.55341960407610458, 95.20724293864769550 ) ) ;
#101793 = CARTESIAN_POINT ( 'NONE',  ( 18.62759615963271287, -10.81492255796078972, 78.33224293864770971 ) ) ;
#101794 = CIRCLE ( 'NONE', #121128, 6.100000000000006750 ) ;
#101795 = CARTESIAN_POINT ( 'NONE',  ( -4.483927247898539470, -16.52544592524342804, 27.29057627198103120 ) ) ;
#101796 = CARTESIAN_POINT ( 'NONE',  ( 15.72974639402176855, 15.80617190586768217, 106.8760903946856899 ) ) ;
#101797 = CARTESIAN_POINT ( 'NONE',  ( -0.05219959533934338120, 16.53943276465976808, 52.50109039468567573 ) ) ;
#101798 = CARTESIAN_POINT ( 'NONE',  ( 16.46253265017160672, -9.564922557960803928, 83.33224293864768129 ) ) ;
#101799 = CARTESIAN_POINT ( 'NONE',  ( -5.153800228976328057, -19.02544592524343514, 27.29057627198103120 ) ) ;
#101800 = CARTESIAN_POINT ( 'NONE',  ( 5.823673210054444382, -21.52544592524334988, 40.20942372801901854 ) ) ;
#101801 = CARTESIAN_POINT ( 'NONE',  ( 15.80617190586769283, -15.72974639402175789, 50.62609039468568994 ) ) ;
#101802 = CARTESIAN_POINT ( 'NONE',  ( 19.05341960407611168, 5.049401038298154454, 43.95724293864769550 ) ) ;
#101803 = CARTESIAN_POINT ( 'NONE',  ( -21.52544592524334988, -5.823673210054445271, 23.95942372801901143 ) ) ;
#101804 = CARTESIAN_POINT ( 'NONE',  ( -0.05219959533936034679, 19.03943276465977164, 62.50109039468566863 ) ) ;
#101805 = CARTESIAN_POINT ( 'NONE',  ( 9.474510206698729675, 16.51473224551082808, 72.08442372801900433 ) ) ;
#101806 = CARTESIAN_POINT ( 'NONE',  ( 8.224510206698742110, 14.34966873604972548, 32.08442372801901854 ) ) ;
#101807 = CARTESIAN_POINT ( 'NONE',  ( -9.564922557960796823, -16.46253265017161027, 22.08224293864768839 ) ) ;
#101808 = CARTESIAN_POINT ( 'NONE',  ( -8.224510206698735004, -14.34966873604973081, 79.58442372801903275 ) ) ;
#101809 = CARTESIAN_POINT ( 'NONE',  ( 5.049401038298161559, -19.05341960407611168, 42.70724293864767418 ) ) ;
#101810 = CARTESIAN_POINT ( 'NONE',  ( 24.24393946302988212, -5.863316274099129366, 172.4343578713345266 ) ) ;
#101811 = CARTESIAN_POINT ( 'NONE',  ( -13.89961937509977652, 13.97604488694528158, 105.6239096053143527 ) ) ;
#101812 = CARTESIAN_POINT ( 'NONE',  ( -5.153800228976328057, -19.02544592524343514, 27.29057627198103120 ) ) ;
#101813 = CARTESIAN_POINT ( 'NONE',  ( 10.72451020669898902, -18.67979575497178502, 77.91557627198102409 ) ) ;
#101814 = CARTESIAN_POINT ( 'NONE',  ( 16.52544592524335698, 4.483927247898782831, 61.45942372801901854 ) ) ;
#101815 = CARTESIAN_POINT ( 'NONE',  ( 0.05219959533936267826, -19.03943276465977164, 20.00109039468567218 ) ) ;
#101816 = CARTESIAN_POINT ( 'NONE',  ( 5.153800228976335163, 19.02544592524342804, 49.79057627198100988 ) ) ;
#101817 = CARTESIAN_POINT ( 'NONE',  ( 4.379528057220339221, -16.55341960407611168, 37.70724293864769550 ) ) ;
#101818 = CARTESIAN_POINT ( 'NONE',  ( 14.34966873604960469, 8.224510206698951720, 64.16557627198102409 ) ) ;
#101819 = CARTESIAN_POINT ( 'NONE',  ( 5.153800228976335163, 19.02544592524342804, 84.79057627198099567 ) ) ;
#101820 = CARTESIAN_POINT ( 'NONE',  ( -10.81492255796105439, 18.62759615963255655, 42.91775706135235424 ) ) ;
#101821 = CARTESIAN_POINT ( 'NONE',  ( -19.02544592524342804, 5.153800228976336051, 86.04057627198103830 ) ) ;
#101822 = CARTESIAN_POINT ( 'NONE',  ( 5.719274019375673035, 21.55341960407619339, 87.29275706135236135 ) ) ;
#101823 = CARTESIAN_POINT ( 'NONE',  ( 8.314922557961029526, -14.29746914071037800, 70.41775706135236135 ) ) ;
#101824 = CARTESIAN_POINT ( 'NONE',  ( -13.97604488694527625, -13.89961937509977652, 106.8739096053143669 ) ) ;
#101825 = CARTESIAN_POINT ( 'NONE',  ( -18.67979575497178146, -10.72451020669898902, 91.66557627198103830 ) ) ;
#101826 = CARTESIAN_POINT ( 'NONE',  ( -8.224510206698948167, 14.34966873604960824, 45.41557627198103830 ) ) ;
#101827 = CARTESIAN_POINT ( 'NONE',  ( 9.474510206698971260, -16.51473224551069308, 22.91557627198102765 ) ) ;
#101828 = CARTESIAN_POINT ( 'NONE',  ( -16.55341960407617563, 4.379528057220093196, 53.54275706135234714 ) ) ;
#101829 = CARTESIAN_POINT ( 'NONE',  ( 12.14591786802309770, 12.06949235617756955, 54.37390960531435979 ) ) ;
#101830 = CARTESIAN_POINT ( 'NONE',  ( 16.51473224551069308, 9.474510206698969483, 114.1655762719810241 ) ) ;
#101831 = CARTESIAN_POINT ( 'NONE',  ( -0.05219959533907301413, -21.53943276465977519, 37.49890960531436690 ) ) ;
#101832 = CARTESIAN_POINT ( 'NONE',  ( 18.67979575497194134, -10.72451020669871369, 110.8344237280190043 ) ) ;
#101833 = CARTESIAN_POINT ( 'NONE',  ( -4.483927247898539470, -16.52544592524342804, 97.29057627198105251 ) ) ;
#101834 = CARTESIAN_POINT ( 'NONE',  ( -5.153800228976328057, -19.02544592524343514, 92.29057627198099567 ) ) ;
#101835 = ORIENTED_EDGE ( 'NONE', *, *, #63738, .T. ) ;
#101836 = CARTESIAN_POINT ( 'NONE',  ( -14.29746914071037622, -8.314922557961029526, 49.16775706135234003 ) ) ;
#101837 = CARTESIAN_POINT ( 'NONE',  ( -9.474510206698964154, 16.51473224551069663, 60.41557627198102409 ) ) ;
#101838 = CARTESIAN_POINT ( 'NONE',  ( 5.049401038297881783, 19.05341960407617563, 52.29275706135234003 ) ) ;
#101839 = EDGE_CURVE ( 'NONE', #94667, #33072, #193790, .T. ) ;
#101840 = CARTESIAN_POINT ( 'NONE',  ( 16.52544592524335698, 4.483927247898782831, 91.45942372801901854 ) ) ;
#101841 = CARTESIAN_POINT ( 'NONE',  ( 9.564922557961047289, -16.46253265017146816, 95.41775706135233293 ) ) ;
#101842 = CARTESIAN_POINT ( 'NONE',  ( 15.80617190586769283, -15.72974639402175789, 70.62609039468567573 ) ) ;
#101843 = CARTESIAN_POINT ( 'NONE',  ( -5.049401038298153566, 19.05341960407611168, 80.20724293864769550 ) ) ;
#101844 = CARTESIAN_POINT ( 'NONE',  ( -15.72974639402197994, 15.80617190586746368, 95.62390960531436690 ) ) ;
#101846 = VECTOR ( 'NONE', #74703, 1000.000000000000114 ) ;
#101845 = CARTESIAN_POINT ( 'NONE',  ( -12.06949235617756955, 12.14591786802309770, 115.6239096053143669 ) ) ;
#101847 = EDGE_CURVE ( 'NONE', #16723, #94189, #148502, .T. ) ;
#101848 = B_SPLINE_CURVE_WITH_KNOTS ( 'NONE', 3,
 ( #157019, #97304, #2334, #64015, #174188, #158011, #187382, #35656, #48851, #110506, #80164, #65001, #81147, #4308, #50837, #112494, #158990, #67984, #159999, #129638, #177192, #99317 ),
 .UNSPECIFIED., .F., .F.,
 ( 4, 2, 2, 2, 2, 2, 2, 2, 2, 2, 4 ),
 ( 1.127570259384924457E-17, 0.001309639967555342515, 0.001964459951333006292, 0.002291869943221834169, 0.002455574939166242036, 0.002619279935110649469, 0.002782984931055057336, 0.002946689926999464769, 0.003274099918888280069, 0.003928919902665910235, 0.005238559870221172303 ),
 .UNSPECIFIED. ) ;
#101849 = CARTESIAN_POINT ( 'NONE',  ( 5.153800228976615827, -19.02544592524334988, 75.20942372801896170 ) ) ;
#101850 = CARTESIAN_POINT ( 'NONE',  ( -18.62759615963270932, 10.81492255796079327, 75.83224293864769550 ) ) ;
#101851 = CARTESIAN_POINT ( 'NONE',  ( 13.97604488694548053, -13.89961937509957401, 40.62609039468564731 ) ) ;
#101852 = CARTESIAN_POINT ( 'NONE',  ( 19.49190055781011566, 5.500000000000002665, 98.06116087098784817 ) ) ;
#101853 = CARTESIAN_POINT ( 'NONE',  ( 10.81492255796078972, 18.62759615963270932, 94.58224293864769550 ) ) ;
#101854 = CARTESIAN_POINT ( 'NONE',  ( -17.26172910966778318, 6.454744622555849354, 85.80646908649221416 ) ) ;
#101855 = CARTESIAN_POINT ( 'NONE',  ( -0.05219959533909027116, -19.03943276465977164, 62.49890960531435979 ) ) ;
#101856 = CARTESIAN_POINT ( 'NONE',  ( -17.97058386085788939, -5.499999999999976019, 89.00390968646220813 ) ) ;
#101857 = CARTESIAN_POINT ( 'NONE',  ( 16.52544592524335698, 4.483927247898782831, 26.45942372801901854 ) ) ;
#101858 = DIRECTION ( 'NONE',  ( 0.000000000000000000, 0.000000000000000000, 1.000000000000000000 ) ) ;
#101859 = CARTESIAN_POINT ( 'NONE',  ( -16.46253265017160317, 9.564922557960807481, 40.83224293864769550 ) ) ;
#101860 = CARTESIAN_POINT ( 'NONE',  ( -5.049401038298153566, 19.05341960407611168, 115.2072429386477097 ) ) ;
#101862 = CARTESIAN_POINT ( 'NONE',  ( 8.314922557960818139, 14.29746914071049879, 44.58224293864769550 ) ) ;
#101861 = CARTESIAN_POINT ( 'NONE',  ( -18.67979575497178146, -10.72451020669898902, 101.6655762719810383 ) ) ;
#101863 = CIRCLE ( 'NONE', #189054, 2.000000000000001776 ) ;
#101864 = CARTESIAN_POINT ( 'NONE',  ( 21.52544592524334988, 5.823673210054432836, 71.45942372801901854 ) ) ;
#101866 = CARTESIAN_POINT ( 'NONE',  ( -13.89961937509957401, -13.97604488694547875, 34.37609039468566863 ) ) ;
#101865 = CARTESIAN_POINT ( 'NONE',  ( 16.53943276465976808, 0.05219959533934440121, 21.25109039468567218 ) ) ;
#101867 = CARTESIAN_POINT ( 'NONE',  ( 16.55341960407611168, 4.379528057220329451, 33.95724293864769550 ) ) ;
#101868 = CARTESIAN_POINT ( 'NONE',  ( -21.52544592524343514, 5.823673210054127303, 111.0405762719810525 ) ) ;
#101869 = CARTESIAN_POINT ( 'NONE',  ( -14.34966873604960291, -8.224510206698953496, 46.66557627198102409 ) ) ;
#101870 = CARTESIAN_POINT ( 'NONE',  ( 0.05219959533936267826, -19.03943276465977164, 90.00109039468567573 ) ) ;
#101871 = CARTESIAN_POINT ( 'NONE',  ( 19.03943276465977164, 0.05219959533936151252, 66.25109039468567573 ) ) ;
#101872 = VECTOR ( 'NONE', #45759, 1000.000000000000000 ) ;
#101873 = CARTESIAN_POINT ( 'NONE',  ( 5.823673210054444382, -21.52544592524334988, 65.20942372801901854 ) ) ;
#101874 = CARTESIAN_POINT ( 'NONE',  ( -9.564922557961040184, 16.46253265017147172, 47.91775706135233293 ) ) ;
#101875 = CARTESIAN_POINT ( 'NONE',  ( 16.52544592524342804, -4.483927247898539470, 113.5405762719810383 ) ) ;
#101876 = CARTESIAN_POINT ( 'NONE',  ( -21.53943276465977519, 0.05219959533907696930, 46.24890960531435979 ) ) ;
#101877 = CARTESIAN_POINT ( 'NONE',  ( 14.29746914071049879, -8.314922557960816363, 43.33224293864769550 ) ) ;
#101878 = CARTESIAN_POINT ( 'NONE',  ( -17.05116617787823685, -6.768360034955907878, 26.34324446740804859 ) ) ;
#101879 = CARTESIAN_POINT ( 'NONE',  ( -5.823673210054431948, 21.52544592524334988, 112.7094237280190328 ) ) ;
#101880 = CARTESIAN_POINT ( 'NONE',  ( -12.06949235617739369, -12.14591786802326823, 79.37609039468567573 ) ) ;
#101881 = CARTESIAN_POINT ( 'NONE',  ( 0.05219959533910956823, 16.53943276465976808, 39.99890960531436690 ) ) ;
#101882 = CARTESIAN_POINT ( 'NONE',  ( 18.67979575497194134, -10.72451020669871369, 80.83442372801901854 ) ) ;
#101883 = CARTESIAN_POINT ( 'NONE',  ( -0.05219959533937732626, 21.53943276465977519, 72.50109039468568994 ) ) ;
#101884 = CARTESIAN_POINT ( 'NONE',  ( -10.72451020669898014, 18.67979575497178502, 80.41557627198103830 ) ) ;
#101885 = CARTESIAN_POINT ( 'NONE',  ( 19.05341960407611168, 5.049401038298154454, 43.95724293864769550 ) ) ;
#101886 = CARTESIAN_POINT ( 'NONE',  ( 0.05219959533937995610, -21.53943276465977519, 55.00109039468568284 ) ) ;
#101887 = CARTESIAN_POINT ( 'NONE',  ( 19.03943276465977164, -0.05219959533909143690, 38.74890960531436690 ) ) ;
#101888 = CARTESIAN_POINT ( 'NONE',  ( 5.049401038298161559, -19.05341960407611168, 52.70724293864767418 ) ) ;
#101889 = CARTESIAN_POINT ( 'NONE',  ( 16.53943276465976808, -0.05219959533910856209, 98.74890960531438111 ) ) ;
#101890 = CARTESIAN_POINT ( 'NONE',  ( -5.049401038298153566, 19.05341960407611168, 100.2072429386476955 ) ) ;
#101891 = CARTESIAN_POINT ( 'NONE',  ( 4.379528057220339221, -16.55341960407611168, 37.70724293864769550 ) ) ;
#101892 = CARTESIAN_POINT ( 'NONE',  ( -12.14591786802309592, -12.06949235617757132, 101.8739096053143811 ) ) ;
#101893 = CARTESIAN_POINT ( 'NONE',  ( 21.52544592524344225, -5.823673210054117533, 73.54057627198102409 ) ) ;
#101894 = CARTESIAN_POINT ( 'NONE',  ( 18.67979575497194134, -10.72451020669871369, 20.83442372801901143 ) ) ;
#101895 = CARTESIAN_POINT ( 'NONE',  ( -19.03943276465977164, 0.05219959533909376836, 116.2489096053143669 ) ) ;
#101897 = CARTESIAN_POINT ( 'NONE',  ( 12.06949235617739724, 12.14591786802326823, 21.87609039468567573 ) ) ;
#101896 = CARTESIAN_POINT ( 'NONE',  ( -16.46253265017160317, 9.564922557960807481, 80.83224293864769550 ) ) ;
#101898 = CARTESIAN_POINT ( 'NONE',  ( 5.823673210054125526, 21.52544592524343514, 69.79057627198102409 ) ) ;
#101899 = CARTESIAN_POINT ( 'NONE',  ( 18.62759615963255655, 10.81492255796105972, 96.66775706135234714 ) ) ;
#101900 = CARTESIAN_POINT ( 'NONE',  ( -19.03943276465977164, 0.05219959533909376836, 76.24890960531435269 ) ) ;
#101901 = CARTESIAN_POINT ( 'NONE',  ( 21.55341960407619695, -5.719274019375665929, 36.04275706135234714 ) ) ;
#101902 = CARTESIAN_POINT ( 'NONE',  ( -5.823673210054116645, -21.52544592524344225, 22.29057627198102765 ) ) ;
#101903 = CARTESIAN_POINT ( 'NONE',  ( 14.34966873604972726, -8.224510206698740333, 85.83442372801901854 ) ) ;
#101904 = CARTESIAN_POINT ( 'NONE',  ( 5.719274019375673035, 21.55341960407619339, 67.29275706135234714 ) ) ;
#101905 = CARTESIAN_POINT ( 'NONE',  ( -21.53943276465977519, -0.05219959533937600094, 103.7510903946857042 ) ) ;
#101906 = CARTESIAN_POINT ( 'NONE',  ( -12.14591786802326823, 12.06949235617739902, 58.12609039468568994 ) ) ;
#101907 = CARTESIAN_POINT ( 'NONE',  ( 21.55341960407619695, -5.719274019375665929, 26.04275706135235779 ) ) ;
#101908 = CARTESIAN_POINT ( 'NONE',  ( 19.05341960407611168, 5.049401038298154454, 113.9572429386477097 ) ) ;
#101909 = CARTESIAN_POINT ( 'NONE',  ( -5.719274019375665041, -21.55341960407619695, 94.79275706135234714 ) ) ;
#101910 = CARTESIAN_POINT ( 'NONE',  ( 13.89961937509977652, -13.97604488694527269, 88.12390960531438111 ) ) ;
#101911 = CARTESIAN_POINT ( 'NONE',  ( 21.55341960407610458, 5.719274019375980345, 83.95724293864770971 ) ) ;
#101912 = CARTESIAN_POINT ( 'NONE',  ( 5.049401038297881783, 19.05341960407617563, 62.29275706135234003 ) ) ;
#101914 = CARTESIAN_POINT ( 'NONE',  ( -10.81492255796078084, -18.62759615963271287, 47.08224293864770260 ) ) ;
#101913 = CARTESIAN_POINT ( 'NONE',  ( -21.90755247610416490, -31.73190472514682270, -17.16613178567115483 ) ) ;
#101916 = CARTESIAN_POINT ( 'NONE',  ( 0.05219959533910956823, 16.53943276465976808, 29.99890960531435979 ) ) ;
#101915 = CARTESIAN_POINT ( 'NONE',  ( 13.97604488694527802, 13.89961937509977652, 89.37390960531436690 ) ) ;
#101917 = CARTESIAN_POINT ( 'NONE',  ( 21.75500197730212903, 5.836128546636256686, 172.5265712840238734 ) ) ;
#101918 = CARTESIAN_POINT ( 'NONE',  ( -5.153800228976607833, 19.02544592524334988, 72.70942372801900433 ) ) ;
#101919 = DIRECTION ( 'NONE',  ( -1.000000000000000000, 0.000000000000000000, 0.000000000000000000 ) ) ;
#101920 = CARTESIAN_POINT ( 'NONE',  ( -9.564922557961040184, 16.46253265017147172, 107.9177570613523471 ) ) ;
#101921 = CARTESIAN_POINT ( 'NONE',  ( 0.05219959533907565091, 21.53943276465977519, 89.99890960531438111 ) ) ;
#101922 = CARTESIAN_POINT ( 'NONE',  ( -12.06949235617756955, 12.14591786802309770, 60.62390960531437401 ) ) ;
#101923 = CARTESIAN_POINT ( 'NONE',  ( -9.474510206698964154, 16.51473224551069663, 105.4155762719810383 ) ) ;
#101924 = CARTESIAN_POINT ( 'NONE',  ( 0.05219959533934541429, -16.53943276465976808, 25.00109039468567218 ) ) ;
#101925 = CARTESIAN_POINT ( 'NONE',  ( -5.049401038298153566, 19.05341960407611168, 60.20724293864768129 ) ) ;
#101927 = CARTESIAN_POINT ( 'NONE',  ( -13.89961937509957401, -13.97604488694547875, 79.37609039468567573 ) ) ;
#101926 = CARTESIAN_POINT ( 'NONE',  ( 15.80617190586769283, -15.72974639402175789, 20.62609039468568639 ) ) ;
#101928 = CARTESIAN_POINT ( 'NONE',  ( 9.564922557960805705, 16.46253265017160317, 89.58224293864769550 ) ) ;
#101929 = CARTESIAN_POINT ( 'NONE',  ( -16.46253265017160317, 9.564922557960807481, 80.83224293864769550 ) ) ;
#101930 = CARTESIAN_POINT ( 'NONE',  ( -21.52544592524343514, 5.823673210054127303, 71.04057627198103830 ) ) ;
#101931 = CARTESIAN_POINT ( 'NONE',  ( 9.474510206698971260, -16.51473224551069308, 47.91557627198102409 ) ) ;
#101932 = CARTESIAN_POINT ( 'NONE',  ( -28.82186960331499037, 2.781578969918950771E-14, 139.9999999999999716 ) ) ;
#101933 = CARTESIAN_POINT ( 'NONE',  ( -14.29746914071049879, 8.314922557960819915, 50.83224293864770971 ) ) ;
#101934 = CARTESIAN_POINT ( 'NONE',  ( 13.89961937509977652, -13.97604488694527269, 108.1239096053143669 ) ) ;
#101935 = LINE ( 'NONE', #164618, #160660 ) ;
#101936 = CARTESIAN_POINT ( 'NONE',  ( -13.89961937509957401, -13.97604488694547875, 64.37609039468567573 ) ) ;
#101937 = AXIS2_PLACEMENT_3D ( 'NONE', #109314, #78971, #76985 ) ;
#101938 = CARTESIAN_POINT ( 'NONE',  ( 5.823673210054125526, 21.52544592524343514, 94.79057627198105251 ) ) ;
#101939 = CARTESIAN_POINT ( 'NONE',  ( -19.05341960407617563, 5.049401038297882671, 53.54275706135231871 ) ) ;
#101940 = CARTESIAN_POINT ( 'NONE',  ( -0.05219959533909027116, -19.03943276465977164, 107.4989096053143527 ) ) ;
#101941 = LINE ( 'NONE', #166619, #95199 ) ;
#101942 = CARTESIAN_POINT ( 'NONE',  ( 18.67979575497178502, 10.72451020669898547, 39.16557627198102409 ) ) ;
#101943 = CARTESIAN_POINT ( 'NONE',  ( -5.153800228976328057, -19.02544592524343514, 77.29057627198099567 ) ) ;
#101944 = CARTESIAN_POINT ( 'NONE',  ( -10.81492255796105439, 18.62759615963255655, 62.91775706135236135 ) ) ;
#101945 = CARTESIAN_POINT ( 'NONE',  ( 19.02544592524343514, -5.153800228976328945, 33.54057627198102409 ) ) ;
#101947 = EDGE_LOOP ( 'NONE', ( #164860, #111827, #169160, #95420 ) ) ;
#101946 = CARTESIAN_POINT ( 'NONE',  ( 14.34966873604960469, 8.224510206698951720, 74.16557627198102409 ) ) ;
#101948 = CARTESIAN_POINT ( 'NONE',  ( -18.67979575497193778, 10.72451020669871902, 58.33442372801901143 ) ) ;
#101949 = ORIENTED_EDGE ( 'NONE', *, *, #468, .F. ) ;
#101950 = CARTESIAN_POINT ( 'NONE',  ( -5.049401038298153566, 19.05341960407611168, 110.2072429386476671 ) ) ;
#101951 = CARTESIAN_POINT ( 'NONE',  ( 5.049401038297881783, 19.05341960407617563, 67.29275706135234714 ) ) ;
#101952 = CARTESIAN_POINT ( 'NONE',  ( -20.96276500525453912, 10.40013546722647853, 168.2886347277375592 ) ) ;
#101953 = CARTESIAN_POINT ( 'NONE',  ( 18.62759615963255655, 10.81492255796105972, 26.66775706135235424 ) ) ;
#101954 = CARTESIAN_POINT ( 'NONE',  ( 0.05219959533909260263, 19.03943276465977164, 64.99890960531436690 ) ) ;
#101956 = EDGE_CURVE ( 'NONE', #161389, #166994, #74330, .T. ) ;
#101955 = CARTESIAN_POINT ( 'NONE',  ( -8.314922557961024197, 14.29746914071037800, 32.91775706135234714 ) ) ;
#101957 = CARTESIAN_POINT ( 'NONE',  ( -11.74264578624799782, -36.14014761921581709, -7.349999994537626868 ) ) ;
#101958 = CARTESIAN_POINT ( 'NONE',  ( 5.153800228976615827, -19.02544592524334988, 20.20942372801899722 ) ) ;
#101959 = CARTESIAN_POINT ( 'NONE',  ( 9.564922557960805705, 16.46253265017160317, 39.58224293864768839 ) ) ;
#101960 = CARTESIAN_POINT ( 'NONE',  ( -10.72451020669870658, -18.67979575497194134, 109.5844237280190328 ) ) ;
#101961 = CARTESIAN_POINT ( 'NONE',  ( -16.53943276465976808, -0.05219959533934237506, 88.75109039468567573 ) ) ;
#101963 = CARTESIAN_POINT ( 'NONE',  ( -10.81492255796105439, 18.62759615963255655, 72.91775706135234714 ) ) ;
#101962 = CARTESIAN_POINT ( 'NONE',  ( 13.89961937509977652, -13.97604488694527269, 93.12390960531436690 ) ) ;
#101964 = CARTESIAN_POINT ( 'NONE',  ( 6.091322673906378604, -4.048585108065108074, -62.28976796517032000 ) ) ;
#101965 = CARTESIAN_POINT ( 'NONE',  ( -19.03943276465977164, 0.05219959533909376836, 106.2489096053143669 ) ) ;
#101966 = CARTESIAN_POINT ( 'NONE',  ( 30.00000000000000000, 5.499999999999992895, 102.5000000000000142 ) ) ;
#101968 = CARTESIAN_POINT ( 'NONE',  ( 10.72451020669871369, 18.67979575497193778, 77.08442372801901854 ) ) ;
#101967 = CARTESIAN_POINT ( 'NONE',  ( 4.483927247898790824, -16.52544592524335698, 50.20942372801901854 ) ) ;
#101969 = CARTESIAN_POINT ( 'NONE',  ( 21.52544592524334988, 5.823673210054432836, 96.45942372801901854 ) ) ;
#101970 = DIRECTION ( 'NONE',  ( -6.982962677686266711E-15, 0.000000000000000000, 1.000000000000000000 ) ) ;
#101971 = CARTESIAN_POINT ( 'NONE',  ( -16.55341960407617563, 4.379528057220093196, 33.54275706135234714 ) ) ;
#101972 = CARTESIAN_POINT ( 'NONE',  ( -13.89961937509977652, 13.97604488694528158, 90.62390960531432427 ) ) ;
#101973 = CARTESIAN_POINT ( 'NONE',  ( -13.89961937509977652, 13.97604488694528158, 115.6239096053143669 ) ) ;
#101974 = VERTEX_POINT ( 'NONE', #189038 ) ;
#101975 = EDGE_CURVE ( 'NONE', #125536, #110145, #180850, .T. ) ;
#101976 = DIRECTION ( 'NONE',  ( -1.000000000000000000, -0.000000000000000000, -0.000000000000000000 ) ) ;
#101977 = CARTESIAN_POINT ( 'NONE',  ( 13.97604488694527802, 13.89961937509977652, 29.37390960531435979 ) ) ;
#101978 = CARTESIAN_POINT ( 'NONE',  ( -21.55341960407610458, -5.719274019375992779, 41.45724293864769550 ) ) ;
#101979 = CARTESIAN_POINT ( 'NONE',  ( -0.05219959533934338120, 16.53943276465976808, 102.5010903946856899 ) ) ;
#101981 = CARTESIAN_POINT ( 'NONE',  ( 0.05219959533909260263, 19.03943276465977164, 69.99890960531435269 ) ) ;
#101980 = CARTESIAN_POINT ( 'NONE',  ( -16.55341960407611168, -4.379528057220339221, 86.45724293864770971 ) ) ;
#101982 = CARTESIAN_POINT ( 'NONE',  ( -0.05219959533937732626, 21.53943276465977519, 107.5010903946856899 ) ) ;
#101983 = CARTESIAN_POINT ( 'NONE',  ( 12.14591786802327356, -12.06949235617739191, 20.62609039468568639 ) ) ;
#101984 = CARTESIAN_POINT ( 'NONE',  ( 4.379528057220339221, -16.55341960407611168, 82.70724293864770971 ) ) ;
#101985 = CARTESIAN_POINT ( 'NONE',  ( -5.719274019375665041, -21.55341960407619695, 39.79275706135235424 ) ) ;
#101986 = CARTESIAN_POINT ( 'NONE',  ( 5.823673210054125526, 21.52544592524343514, 79.79057627198102409 ) ) ;
#101987 = CARTESIAN_POINT ( 'NONE',  ( -13.89961937509957401, -13.97604488694547875, 54.37609039468565442 ) ) ;
#101988 = CARTESIAN_POINT ( 'NONE',  ( -13.89961937509977830, 13.97604488694528158, 45.62390960531435269 ) ) ;
#101989 = CARTESIAN_POINT ( 'NONE',  ( -9.564922557960796823, -16.46253265017161027, 97.08224293864769550 ) ) ;
#101990 = CARTESIAN_POINT ( 'NONE',  ( 14.29746914071049879, -8.314922557960816363, 68.33224293864769550 ) ) ;
#101991 = CARTESIAN_POINT ( 'NONE',  ( -14.34966873604960291, -8.224510206698953496, 46.66557627198102409 ) ) ;
#101992 = CARTESIAN_POINT ( 'NONE',  ( 14.34966873604960469, 8.224510206698951720, 24.16557627198103120 ) ) ;
#101993 = CARTESIAN_POINT ( 'NONE',  ( -13.97604488694547697, 13.89961937509957934, 68.12609039468563310 ) ) ;
#101994 = CARTESIAN_POINT ( 'NONE',  ( -19.03943276465977164, 0.05219959533909376836, 116.2489096053143669 ) ) ;
#101995 = CARTESIAN_POINT ( 'NONE',  ( 14.34966873604960469, 8.224510206698951720, 84.16557627198103830 ) ) ;
#101996 = CARTESIAN_POINT ( 'NONE',  ( 9.687362902255731711, -9.687362902255694408, -60.44446360152740993 ) ) ;
#101998 = CARTESIAN_POINT ( 'NONE',  ( -10.72451020669898014, 18.67979575497178502, 50.41557627198103120 ) ) ;
#101997 = CARTESIAN_POINT ( 'NONE',  ( -5.153800228976328057, -19.02544592524343514, 42.29057627198101699 ) ) ;
#101999 = CARTESIAN_POINT ( 'NONE',  ( -21.53943276465977519, 0.05219959533907696930, 76.24890960531435269 ) ) ;
#102000 = CARTESIAN_POINT ( 'NONE',  ( 16.51473224551069308, 9.474510206698969483, 34.16557627198102409 ) ) ;
#102002 = CARTESIAN_POINT ( 'NONE',  ( -19.03943276465977164, 0.05219959533909376836, 66.24890960531436690 ) ) ;
#102001 = CARTESIAN_POINT ( 'NONE',  ( 4.483927247898790824, -16.52544592524335698, 60.20942372801902565 ) ) ;
#102004 = ADVANCED_FACE ( 'NONE', ( #190022, #51496 ), #174846, .T. ) ;
#102003 = CARTESIAN_POINT ( 'NONE',  ( 19.02544592524334988, 5.153800228976608722, 36.45942372801900433 ) ) ;
#102005 = CARTESIAN_POINT ( 'NONE',  ( -21.53943276465977519, -0.05219959533937600094, 48.75109039468568284 ) ) ;
#102006 = CARTESIAN_POINT ( 'NONE',  ( -8.314922557960811034, -14.29746914071050412, 107.0822429386476955 ) ) ;
#102007 = CARTESIAN_POINT ( 'NONE',  ( -5.153800228976607833, 19.02544592524334988, 92.70942372801901854 ) ) ;
#102008 = CARTESIAN_POINT ( 'NONE',  ( -36.91746825000000598, 11.99521256947798520, -3.224999997268813257 ) ) ;
#102010 = CARTESIAN_POINT ( 'NONE',  ( 15.80617190586746368, 15.72974639402197994, 44.37390960531435979 ) ) ;
#102009 = CARTESIAN_POINT ( 'NONE',  ( -193.3062444957834884, -155.7167183371838064, -15.00000000000000000 ) ) ;
#102011 = CARTESIAN_POINT ( 'NONE',  ( 16.38665767535053064, -7.295008042176011287, 67.76400864214545550 ) ) ;
#102012 = CARTESIAN_POINT ( 'NONE',  ( 5.719274019375673035, 21.55341960407619339, 87.29275706135236135 ) ) ;
#102013 = CARTESIAN_POINT ( 'NONE',  ( -12.06949235617756955, 12.14591786802309770, 30.62390960531436335 ) ) ;
#102015 = CARTESIAN_POINT ( 'NONE',  ( -16.55341960407611168, -4.379528057220339221, 61.45724293864770260 ) ) ;
#102014 = CARTESIAN_POINT ( 'NONE',  ( 14.29746914071037800, 8.314922557961029526, 56.66775706135235424 ) ) ;
#102016 = CARTESIAN_POINT ( 'NONE',  ( -5.823673210054116645, -21.52544592524344225, 82.29057627198103830 ) ) ;
#102017 = CARTESIAN_POINT ( 'NONE',  ( 10.81492255796078972, 18.62759615963270932, 79.58224293864769550 ) ) ;
#102018 = CARTESIAN_POINT ( 'NONE',  ( -27.16368555717297184, -26.59078835260040208, -15.56371235017458510 ) ) ;
#102020 = CARTESIAN_POINT ( 'NONE',  ( -16.46253265017160317, 9.564922557960807481, 115.8322429386477097 ) ) ;
#102019 = CARTESIAN_POINT ( 'NONE',  ( -9.564922557961040184, 16.46253265017147172, 82.91775706135233293 ) ) ;
#102021 = CARTESIAN_POINT ( 'NONE',  ( 16.51473224551069308, 9.474510206698969483, 64.16557627198102409 ) ) ;
#102022 = CARTESIAN_POINT ( 'NONE',  ( 19.02544592524343514, -5.153800228976328945, 38.54057627198103120 ) ) ;
#102023 = CARTESIAN_POINT ( 'NONE',  ( -17.60728821186568638, 5.500000000000037303, 75.86690927743003954 ) ) ;
#102024 = ORIENTED_EDGE ( 'NONE', *, *, #107130, .F. ) ;
#102025 = CARTESIAN_POINT ( 'NONE',  ( 12.06949235617739724, 12.14591786802326823, 81.87609039468568994 ) ) ;
#102026 = B_SPLINE_CURVE_WITH_KNOTS ( 'NONE', 3,
 ( #166098, #90225, #138710, #42752, #89238, #181275, #31544, #149921, #150932, #105401, #11427, #134768, #104415, #197429, #61860, #183249, #182255, #73097, #29565, #151909 ),
 .UNSPECIFIED., .F., .F.,
 ( 4, 2, 2, 2, 2, 2, 2, 2, 2, 4 ),
 ( 0.004000878361811999878, 0.004499404418916020179, 0.004997930476020039613, 0.005496456533124059046, 0.005994982590228079347, 0.006244245618780067814, 0.006493508647332058015, 0.006992034704436035815, 0.007490560761540013615, 0.007989086818643992283 ),
 .UNSPECIFIED. ) ;
#102027 = CARTESIAN_POINT ( 'NONE',  ( -15.72974639402197994, 15.80617190586746368, 105.6239096053143669 ) ) ;
#102028 = CARTESIAN_POINT ( 'NONE',  ( -19.05341960407611168, -5.049401038298163336, 76.45724293864769550 ) ) ;
#102029 = CARTESIAN_POINT ( 'NONE',  ( -21.53943276465977519, -0.05219959533937600094, 38.75109039468567573 ) ) ;
#102030 = CARTESIAN_POINT ( 'NONE',  ( 5.153800228976335163, 19.02544592524342804, 94.79057627198103830 ) ) ;
#102031 = CARTESIAN_POINT ( 'NONE',  ( -27.75718128995210776, -28.53842127823990182, -16.93139376986094291 ) ) ;
#102032 = ORIENTED_EDGE ( 'NONE', *, *, #187359, .F. ) ;
#102033 = CARTESIAN_POINT ( 'NONE',  ( -0.05219959533937732626, 21.53943276465977519, 27.50109039468567929 ) ) ;
#102035 = CARTESIAN_POINT ( 'NONE',  ( -16.46253265017160317, 9.564922557960807481, 100.8322429386477097 ) ) ;
#102034 = CARTESIAN_POINT ( 'NONE',  ( 19.38985940809749309, -32.68077955211924035, -24.99999999999992895 ) ) ;
#102036 = CARTESIAN_POINT ( 'NONE',  ( 5.049401038297881783, 19.05341960407617563, 57.29275706135231871 ) ) ;
#102037 = CARTESIAN_POINT ( 'NONE',  ( 15.80617190586769283, -15.72974639402175789, 20.62609039468568639 ) ) ;
#102038 = CARTESIAN_POINT ( 'NONE',  ( -13.97604488694547697, 13.89961937509957934, 43.12609039468566152 ) ) ;
#102039 = CARTESIAN_POINT ( 'NONE',  ( 0.05219959533936267826, -19.03943276465977164, 45.00109039468566863 ) ) ;
#102040 = CARTESIAN_POINT ( 'NONE',  ( 14.29746914071037800, 8.314922557961029526, 101.6677570613523613 ) ) ;
#102041 = CARTESIAN_POINT ( 'NONE',  ( 22.77340942535172985, -12.66915129224429926, 165.5704402759698723 ) ) ;
#102042 = CARTESIAN_POINT ( 'NONE',  ( 9.564922557960805705, 16.46253265017160317, 69.58224293864770971 ) ) ;
#102043 = VECTOR ( 'NONE', #161113, 999.9999999999998863 ) ;
#102044 = CARTESIAN_POINT ( 'NONE',  ( -15.80617190586768217, 15.72974639402176855, 78.12609039468570415 ) ) ;
#102045 = CARTESIAN_POINT ( 'NONE',  ( 0.05219959533937995610, -21.53943276465977519, 90.00109039468567573 ) ) ;
#102046 = CARTESIAN_POINT ( 'NONE',  ( 23.51385019162036016, -1.374935097489230484, -54.82293943248596690 ) ) ;
#102047 = CARTESIAN_POINT ( 'NONE',  ( 13.97604488694527802, 13.89961937509977652, 94.37390960531436690 ) ) ;
#102048 = CARTESIAN_POINT ( 'NONE',  ( 5.719274019375673035, 21.55341960407619339, 62.29275706135236845 ) ) ;
#102049 = CARTESIAN_POINT ( 'NONE',  ( 8.314922557961029526, -14.29746914071037800, 20.41775706135234714 ) ) ;
#102050 = CARTESIAN_POINT ( 'NONE',  ( 19.05341960407611168, 5.049401038298154454, 68.95724293864769550 ) ) ;
#102051 = CARTESIAN_POINT ( 'NONE',  ( -15.80617190586745835, -15.72974639402198527, 21.87390960531436690 ) ) ;
#102052 = CARTESIAN_POINT ( 'NONE',  ( -5.153800228976328057, -19.02544592524343514, 87.29057627198103830 ) ) ;
#102053 = CARTESIAN_POINT ( 'NONE',  ( -5.153800228976607833, 19.02544592524335343, 87.70942372801897591 ) ) ;
#102054 = CARTESIAN_POINT ( 'NONE',  ( -5.049401038298153566, 19.05341960407611168, 85.20724293864766707 ) ) ;
#102055 = CARTESIAN_POINT ( 'NONE',  ( -5.153800228976328057, -19.02544592524343514, 57.29057627198103120 ) ) ;
#102056 = CARTESIAN_POINT ( 'NONE',  ( 18.62759615963271287, -10.81492255796078972, 113.3322429386476955 ) ) ;
#102057 = CARTESIAN_POINT ( 'NONE',  ( 16.52544592524335698, 4.483927247898782831, 106.4594237280190328 ) ) ;
#102058 = CARTESIAN_POINT ( 'NONE',  ( -18.09867054820433907, -5.499999999999827693, 48.98393025253585620 ) ) ;
#102059 = CARTESIAN_POINT ( 'NONE',  ( -16.46253265017146816, -9.564922557961047289, 64.16775706135233293 ) ) ;
#102060 = CARTESIAN_POINT ( 'NONE',  ( 5.049401038298161559, -19.05341960407611168, 97.70724293864766707 ) ) ;
#102061 = CARTESIAN_POINT ( 'NONE',  ( 14.34966873604960469, 8.224510206698951720, 69.16557627198102409 ) ) ;
#102062 = CARTESIAN_POINT ( 'NONE',  ( 14.34966873604960469, 8.224510206698951720, 104.1655762719810241 ) ) ;
#102063 = CARTESIAN_POINT ( 'NONE',  ( -21.52544592524343514, 5.823673210054127303, 31.04057627198102409 ) ) ;
#102064 = CARTESIAN_POINT ( 'NONE',  ( -9.474510206698964154, 16.51473224551069663, 115.4155762719810241 ) ) ;
#102065 = CARTESIAN_POINT ( 'NONE',  ( -16.52544592524342804, 4.483927247898546575, 96.04057627198102409 ) ) ;
#102066 = CARTESIAN_POINT ( 'NONE',  ( -0.2002935562469364550, -6.100000000000008527, -62.50719930893266962 ) ) ;
#102067 = CARTESIAN_POINT ( 'NONE',  ( -19.05341960407617563, 5.049401038297882671, 43.54275706135232582 ) ) ;
#102068 = CARTESIAN_POINT ( 'NONE',  ( 16.55341960407618274, -4.379528057220086978, 101.0427570613523756 ) ) ;
#102069 = CARTESIAN_POINT ( 'NONE',  ( -5.049401038298153566, 19.05341960407611168, 90.20724293864766707 ) ) ;
#102070 = CARTESIAN_POINT ( 'NONE',  ( 21.52544592524334988, 5.823673210054432836, 56.45942372801902565 ) ) ;
#102071 = CARTESIAN_POINT ( 'NONE',  ( 5.719274019375991003, -21.55341960407610458, 47.70724293864770260 ) ) ;
#102072 = CARTESIAN_POINT ( 'NONE',  ( -0.05219959533937732626, 21.53943276465977519, 37.50109039468568284 ) ) ;
#102073 = CARTESIAN_POINT ( 'NONE',  ( 0.05219959533907565091, 21.53943276465977519, 89.99890960531438111 ) ) ;
#102074 = CARTESIAN_POINT ( 'NONE',  ( -0.05219959533910754901, -16.53943276465976808, 102.4989096053143811 ) ) ;
#102075 = CARTESIAN_POINT ( 'NONE',  ( -9.564922557961040184, 16.46253265017147172, 72.91775706135233293 ) ) ;
#102076 = CARTESIAN_POINT ( 'NONE',  ( 5.153800228976335163, 19.02544592524342804, 49.79057627198100988 ) ) ;
#102077 = CARTESIAN_POINT ( 'NONE',  ( -19.03943276465977164, 0.05219959533909376836, 101.2489096053143669 ) ) ;
#102078 = CARTESIAN_POINT ( 'NONE',  ( 0.05219959533909260263, 19.03943276465977164, 94.99890960531436690 ) ) ;
#102079 = CARTESIAN_POINT ( 'NONE',  ( -16.53943276465976808, 0.05219959533911058130, 116.2489096053143669 ) ) ;
#102080 = AXIS2_PLACEMENT_3D ( 'NONE', #183308, #14442, #28648 ) ;
#102081 = CARTESIAN_POINT ( 'NONE',  ( 16.52544592524342804, -4.483927247898539470, 38.54057627198103120 ) ) ;
#102082 = CARTESIAN_POINT ( 'NONE',  ( 4.379528057220092307, 16.55341960407617563, 42.29275706135235424 ) ) ;
#102083 = CARTESIAN_POINT ( 'NONE',  ( 5.719274019375673035, 21.55341960407619339, 107.2927570613523471 ) ) ;
#102085 = CARTESIAN_POINT ( 'NONE',  ( 12.14591786802309770, 12.06949235617756955, 29.37390960531435269 ) ) ;
#102084 = DIRECTION ( 'NONE',  ( 0.000000000000000000, 0.000000000000000000, -1.000000000000000000 ) ) ;
#102086 = CARTESIAN_POINT ( 'NONE',  ( -15.80617190586768217, 15.72974639402176855, 28.12609039468568284 ) ) ;
#102087 = CARTESIAN_POINT ( 'NONE',  ( 9.564922557960805705, 16.46253265017160317, 109.5822429386476955 ) ) ;
#102088 = CARTESIAN_POINT ( 'NONE',  ( -12.06949235617739369, -12.14591786802326823, 104.3760903946856899 ) ) ;
#102089 = CARTESIAN_POINT ( 'NONE',  ( -8.224510206698735004, -14.34966873604973081, 94.58442372801901854 ) ) ;
#102090 = CARTESIAN_POINT ( 'NONE',  ( -14.34966873604972548, 8.224510206698743886, 23.33442372801901499 ) ) ;
#102091 = CARTESIAN_POINT ( 'NONE',  ( 5.049401038298161559, -19.05341960407611168, 52.70724293864767418 ) ) ;
#102092 = CARTESIAN_POINT ( 'NONE',  ( 8.224510206698953496, -14.34966873604960469, 107.9155762719810241 ) ) ;
#102093 = CARTESIAN_POINT ( 'NONE',  ( 10.81492255796078972, 18.62759615963270932, 114.5822429386477097 ) ) ;
#102094 = CARTESIAN_POINT ( 'NONE',  ( 9.474510206698971260, -16.51473224551069308, 37.91557627198102409 ) ) ;
#102095 = CARTESIAN_POINT ( 'NONE',  ( 0.05219959533909260263, 19.03943276465977164, 109.9989096053143669 ) ) ;
#102096 = CARTESIAN_POINT ( 'NONE',  ( -0.05219959533937732626, 21.53943276465977519, 32.50109039468568284 ) ) ;
#102097 = DIRECTION ( 'NONE',  ( -1.000000000000000000, 0.000000000000000000, 0.000000000000000000 ) ) ;
#102098 = CARTESIAN_POINT ( 'NONE',  ( 16.51473224551069308, 9.474510206698969483, 109.1655762719810383 ) ) ;
#102099 = CARTESIAN_POINT ( 'NONE',  ( -22.49873734152892624, 26.99873734152936677, 1.110912703473986074 ) ) ;
#102100 = CARTESIAN_POINT ( 'NONE',  ( -9.564922557960796823, -16.46253265017161027, 97.08224293864769550 ) ) ;
#102102 = CARTESIAN_POINT ( 'NONE',  ( -8.314922557960811034, -14.29746914071050412, 97.08224293864770971 ) ) ;
#102101 = CARTESIAN_POINT ( 'NONE',  ( 21.53943276465977519, 0.05219959533937863772, 46.25109039468567573 ) ) ;
#102103 = CARTESIAN_POINT ( 'NONE',  ( 0.05219959533909260263, 19.03943276465977164, 89.99890960531436690 ) ) ;
#102104 = CARTESIAN_POINT ( 'NONE',  ( 18.22780087662122384, -5.500000000000022204, 71.01540105326107266 ) ) ;
#102105 = CARTESIAN_POINT ( 'NONE',  ( -14.29746914071037622, -8.314922557961029526, 64.16775706135234714 ) ) ;
#102106 = CARTESIAN_POINT ( 'NONE',  ( 10.81492255796106328, -18.62759615963255655, 75.41775706135233293 ) ) ;
#102107 = CARTESIAN_POINT ( 'NONE',  ( 16.55341960407618274, -4.379528057220086978, 36.04275706135234714 ) ) ;
#102108 = CARTESIAN_POINT ( 'NONE',  ( 13.89961937509977652, -13.97604488694527269, 78.12390960531433848 ) ) ;
#102109 = CARTESIAN_POINT ( 'NONE',  ( 16.46253265017146816, 9.564922557961045513, 111.6677570613523329 ) ) ;
#102110 = CARTESIAN_POINT ( 'NONE',  ( -16.53943276465976808, -0.05219959533934237506, 68.75109039468568994 ) ) ;
#102111 = CARTESIAN_POINT ( 'NONE',  ( 18.62759615963255655, 10.81492255796105972, 111.6677570613523613 ) ) ;
#102112 = CARTESIAN_POINT ( 'NONE',  ( -16.51473224551082808, 9.474510206698731452, 98.33442372801900433 ) ) ;
#102113 = CARTESIAN_POINT ( 'NONE',  ( 5.049401038298161559, -19.05341960407611168, 62.70724293864769550 ) ) ;
#102114 = CARTESIAN_POINT ( 'NONE',  ( 18.67979575497178502, 10.72451020669898547, 89.16557627198102409 ) ) ;
#102116 = CARTESIAN_POINT ( 'NONE',  ( -13.89961937509957401, -13.97604488694547875, 94.37609039468566152 ) ) ;
#102115 = CARTESIAN_POINT ( 'NONE',  ( -16.53943276465976808, 0.05219959533911058130, 91.24890960531436690 ) ) ;
#102117 = CARTESIAN_POINT ( 'NONE',  ( -8.314922557961024197, 14.29746914071037800, 52.91775706135235424 ) ) ;
#102118 = CARTESIAN_POINT ( 'NONE',  ( 16.81555441253556182, -7.025013491695411005, 63.13685445334259327 ) ) ;
#102120 = EDGE_CURVE ( 'NONE', #35858, #28673, #57504, .T. ) ;
#102119 = CARTESIAN_POINT ( 'NONE',  ( -13.97604488694547697, 13.89961937509957934, 53.12609039468565442 ) ) ;
#102121 = CARTESIAN_POINT ( 'NONE',  ( 14.34966873604960469, 8.224510206698951720, 34.16557627198102409 ) ) ;
#102122 = CARTESIAN_POINT ( 'NONE',  ( -14.34966873604960291, -8.224510206698953496, 86.66557627198102409 ) ) ;
#102124 = CARTESIAN_POINT ( 'NONE',  ( -19.48894818550245134, 5.499999999999918288, 90.10307310435231898 ) ) ;
#102123 = CARTESIAN_POINT ( 'NONE',  ( -16.51473224551082808, 9.474510206698731452, 23.33442372801900078 ) ) ;
#102125 = CARTESIAN_POINT ( 'NONE',  ( 0.05219959533937995610, -21.53943276465977519, 25.00109039468567218 ) ) ;
#102126 = CARTESIAN_POINT ( 'NONE',  ( 0.05219959533909260263, 19.03943276465977164, 99.99890960531436690 ) ) ;
#102127 = CARTESIAN_POINT ( 'NONE',  ( -16.46253265017160317, 9.564922557960807481, 80.83224293864769550 ) ) ;
#102128 = CARTESIAN_POINT ( 'NONE',  ( 21.55341960407619695, -5.719274019375665929, 101.0427570613523756 ) ) ;
#102129 = CARTESIAN_POINT ( 'NONE',  ( 16.51473224551069308, 9.474510206698969483, 79.16557627198103830 ) ) ;
#102130 = CARTESIAN_POINT ( 'NONE',  ( -21.55341960407610458, -5.719274019375992779, 41.45724293864769550 ) ) ;
#102131 = CARTESIAN_POINT ( 'NONE',  ( 0.05219959533910956823, 16.53943276465976808, 74.99890960531435269 ) ) ;
#102132 = CARTESIAN_POINT ( 'NONE',  ( 19.03943276465977164, -0.05219959533909143690, 58.74890960531435979 ) ) ;
#102133 = CARTESIAN_POINT ( 'NONE',  ( -16.55341960407611168, -4.379528057220339221, 101.4572429386476955 ) ) ;
#102134 = CARTESIAN_POINT ( 'NONE',  ( -21.55341960407619339, 5.719274019375674811, 23.54275706135235424 ) ) ;
#102135 = CARTESIAN_POINT ( 'NONE',  ( 5.823673210054444382, -21.52544592524334988, 60.20942372801902565 ) ) ;
#102136 = CARTESIAN_POINT ( 'NONE',  ( 16.46253265017160672, -9.564922557960803928, 48.33224293864769550 ) ) ;
#102137 = CARTESIAN_POINT ( 'NONE',  ( 4.379528057220092307, 16.55341960407617563, 62.29275706135236845 ) ) ;
#102138 = CARTESIAN_POINT ( 'NONE',  ( 18.62759615963271287, -10.81492255796078972, 108.3322429386477097 ) ) ;
#102139 = CARTESIAN_POINT ( 'NONE',  ( 21.53943276465977519, -0.05219959533907433946, 113.7489096053143527 ) ) ;
#102141 = CARTESIAN_POINT ( 'NONE',  ( 5.153800228976335163, 19.02544592524342804, 59.79057627198100988 ) ) ;
#102140 = CARTESIAN_POINT ( 'NONE',  ( -13.89961937509957401, -13.97604488694547875, 44.37609039468566863 ) ) ;
#102142 = DIRECTION ( 'NONE',  ( -1.000000000000000000, -0.000000000000000000, -0.000000000000000000 ) ) ;
#102143 = CARTESIAN_POINT ( 'NONE',  ( -5.719274019375665041, -21.55341960407619695, 69.79275706135234714 ) ) ;
#102144 = CARTESIAN_POINT ( 'NONE',  ( 18.67979575497178502, 10.72451020669898547, 59.16557627198103120 ) ) ;
#102145 = CARTESIAN_POINT ( 'NONE',  ( 8.314922557960818139, 14.29746914071049879, 34.58224293864770260 ) ) ;
#102147 = CARTESIAN_POINT ( 'NONE',  ( -10.81492255796105439, 18.62759615963255655, 112.9177570613523329 ) ) ;
#102146 = CARTESIAN_POINT ( 'NONE',  ( 15.72974639402176855, 15.80617190586768217, 71.87609039468568994 ) ) ;
#102148 = CARTESIAN_POINT ( 'NONE',  ( 16.53943276465976808, -0.05219959533910856209, 58.74890960531436690 ) ) ;
#102149 = CARTESIAN_POINT ( 'NONE',  ( 16.52544592524342804, -4.483927247898539470, 98.54057627198105251 ) ) ;
#102150 = CARTESIAN_POINT ( 'NONE',  ( -13.89961937509957401, -13.97604488694547875, 49.37609039468567573 ) ) ;
#102151 = CARTESIAN_POINT ( 'NONE',  ( 16.55341960407618274, -4.379528057220086978, 111.0427570613523613 ) ) ;
#102152 = CARTESIAN_POINT ( 'NONE',  ( -15.72974639402176322, -15.80617190586768395, 74.37609039468568994 ) ) ;
#102153 = CARTESIAN_POINT ( 'NONE',  ( 19.02544592524343514, -5.153800228976328945, 58.54057627198102409 ) ) ;
#102154 = CARTESIAN_POINT ( 'NONE',  ( -13.89961937509957401, -13.97604488694547875, 29.37609039468565797 ) ) ;
#102155 = CARTESIAN_POINT ( 'NONE',  ( -10.72451020669898014, 18.67979575497178502, 35.41557627198102409 ) ) ;
#102156 = CARTESIAN_POINT ( 'NONE',  ( 18.62759615963255655, 10.81492255796105972, 36.66775706135234714 ) ) ;
#102157 = CARTESIAN_POINT ( 'NONE',  ( -21.55341960407610458, -5.719274019375992779, 91.45724293864769550 ) ) ;
#102158 = CARTESIAN_POINT ( 'NONE',  ( 19.02544592524334988, 5.153800228976608722, 81.45942372801897591 ) ) ;
#102159 = CARTESIAN_POINT ( 'NONE',  ( 8.224510206698742110, 14.34966873604972548, 47.08442372801901854 ) ) ;
#102161 = CARTESIAN_POINT ( 'NONE',  ( -5.719274019375978568, 21.55341960407610458, 90.20724293864770971 ) ) ;
#102160 = CARTESIAN_POINT ( 'NONE',  ( 23.48529157249599564, 32.32473071737754111, -6.700000000000000178 ) ) ;
#102162 = CARTESIAN_POINT ( 'NONE',  ( -16.53943276465976808, 0.05219959533911058130, 86.24890960531436690 ) ) ;
#102163 = CARTESIAN_POINT ( 'NONE',  ( -29.12359114459359688, -24.18000288461016112, -21.55587802759511717 ) ) ;
#102164 = CARTESIAN_POINT ( 'NONE',  ( -4.483927247898782831, 16.52544592524335698, 22.70942372801901499 ) ) ;
#102165 = CARTESIAN_POINT ( 'NONE',  ( 21.52544592524344225, -5.823673210054117533, 53.54057627198103120 ) ) ;
#102166 = CARTESIAN_POINT ( 'NONE',  ( -14.29746914071037622, -8.314922557961029526, 89.16775706135236135 ) ) ;
#102167 = CARTESIAN_POINT ( 'NONE',  ( 17.50000000000000000, -5.499999999999992895, 56.21769037696436300 ) ) ;
#102168 = CARTESIAN_POINT ( 'NONE',  ( -8.224510206698735004, -14.34966873604973081, 59.58442372801901854 ) ) ;
#102169 = CARTESIAN_POINT ( 'NONE',  ( 18.62759615963255655, 10.81492255796105972, 31.66775706135234358 ) ) ;
#102170 = CARTESIAN_POINT ( 'NONE',  ( -10.72451020669898014, 18.67979575497178502, 50.41557627198103120 ) ) ;
#102171 = CARTESIAN_POINT ( 'NONE',  ( 12.06949235617739724, 12.14591786802326823, 81.87609039468568994 ) ) ;
#102172 = CARTESIAN_POINT ( 'NONE',  ( 9.474510206698971260, -16.51473224551069308, 97.91557627198102409 ) ) ;
#102174 = CARTESIAN_POINT ( 'NONE',  ( -13.89961937509977652, 13.97604488694528158, 30.62390960531435269 ) ) ;
#102173 = CARTESIAN_POINT ( 'NONE',  ( -0.05219959533937732626, 21.53943276465977519, 52.50109039468567573 ) ) ;
#102175 = CARTESIAN_POINT ( 'NONE',  ( 10.72451020669898902, -18.67979575497178502, 37.91557627198102409 ) ) ;
#102176 = CARTESIAN_POINT ( 'NONE',  ( -0.05219959533909027116, -19.03943276465977164, 112.4989096053143669 ) ) ;
#102177 = ORIENTED_EDGE ( 'NONE', *, *, #142029, .F. ) ;
#102178 = CARTESIAN_POINT ( 'NONE',  ( -9.564922557961040184, 16.46253265017147172, 42.91775706135234003 ) ) ;
#102179 = CARTESIAN_POINT ( 'NONE',  ( -16.53943276465976808, -0.05219959533934237506, 63.75109039468568284 ) ) ;
#102180 = CARTESIAN_POINT ( 'NONE',  ( -13.89961937509977652, 13.97604488694528158, 115.6239096053143669 ) ) ;
#102181 = VERTEX_POINT ( 'NONE', #197017 ) ;
#102182 = CARTESIAN_POINT ( 'NONE',  ( 16.46253265017160672, -9.564922557960803928, 88.33224293864769550 ) ) ;
#102183 = CARTESIAN_POINT ( 'NONE',  ( 12.14591786802327356, -12.06949235617739191, 95.62609039468568994 ) ) ;
#102184 = CYLINDRICAL_SURFACE ( 'NONE', #195888, 1.500000000000001332 ) ;
#102185 = CARTESIAN_POINT ( 'NONE',  ( -4.379528057220328563, 16.55341960407611168, 100.2072429386476955 ) ) ;
#102186 = CARTESIAN_POINT ( 'NONE',  ( -15.80617190586745835, -15.72974639402198527, 46.87390960531435979 ) ) ;
#102187 = CARTESIAN_POINT ( 'NONE',  ( 19.05341960407611168, 5.049401038298154454, 28.95724293864769550 ) ) ;
#102188 = CARTESIAN_POINT ( 'NONE',  ( -16.53943276465976808, -0.05219959533934237506, 78.75109039468568994 ) ) ;
#102189 = CARTESIAN_POINT ( 'NONE',  ( 15.80617190586769283, -15.72974639402175789, 30.62609039468567929 ) ) ;
#102190 = CARTESIAN_POINT ( 'NONE',  ( 16.46253265017146816, 9.564922557961045513, 96.66775706135233293 ) ) ;
#102191 = CARTESIAN_POINT ( 'NONE',  ( -8.314922557960811034, -14.29746914071050412, 87.08224293864769550 ) ) ;
#102192 = CARTESIAN_POINT ( 'NONE',  ( -19.05341960407611168, -5.049401038298163336, 36.45724293864766707 ) ) ;
#102193 = AXIS2_PLACEMENT_3D ( 'NONE', #15082, #121258, #124237 ) ;
#102194 = CARTESIAN_POINT ( 'NONE',  ( 13.89961937509977652, -13.97604488694527269, 108.1239096053143669 ) ) ;
#102195 = CARTESIAN_POINT ( 'NONE',  ( 5.719274019375673035, 21.55341960407619339, 102.2927570613523613 ) ) ;
#102196 = CARTESIAN_POINT ( 'NONE',  ( 13.89961937509977652, -13.97604488694527269, 73.12390960531436690 ) ) ;
#102197 = CARTESIAN_POINT ( 'NONE',  ( 0.05219959533934541429, -16.53943276465976808, 60.00109039468568284 ) ) ;
#102198 = CARTESIAN_POINT ( 'NONE',  ( 21.52544592524334988, 5.823673210054432836, 96.45942372801901854 ) ) ;
#102199 = CARTESIAN_POINT ( 'NONE',  ( 0.05219959533934541429, -16.53943276465976808, 75.00109039468568994 ) ) ;
#102200 = CARTESIAN_POINT ( 'NONE',  ( -5.153800228976607833, 19.02544592524334988, 52.70942372801900433 ) ) ;
#102201 = CARTESIAN_POINT ( 'NONE',  ( 9.474510206698729675, 16.51473224551082808, 62.08442372801899722 ) ) ;
#102202 = ORIENTED_EDGE ( 'NONE', *, *, #70410, .T. ) ;
#102203 = CARTESIAN_POINT ( 'NONE',  ( 21.55341960407619695, -5.719274019375665929, 66.04275706135236135 ) ) ;
#102204 = CARTESIAN_POINT ( 'NONE',  ( -16.46253265017160317, 9.564922557960807481, 65.83224293864769550 ) ) ;
#102205 = CARTESIAN_POINT ( 'NONE',  ( -17.59860650958989936, -7.585241751807033417, 56.57662985737508166 ) ) ;
#102206 = CARTESIAN_POINT ( 'NONE',  ( 16.46253265017146816, 9.564922557961045513, 61.66775706135234003 ) ) ;
#102207 = CARTESIAN_POINT ( 'NONE',  ( -25.77168321198461598, 6.124454116751229193, 163.0898522765303085 ) ) ;
#102208 = CARTESIAN_POINT ( 'NONE',  ( -9.474510206698964154, 16.51473224551069663, 80.41557627198103830 ) ) ;
#102209 = CARTESIAN_POINT ( 'NONE',  ( 16.53943276465976808, -0.05219959533910856209, 38.74890960531435979 ) ) ;
#102210 = CARTESIAN_POINT ( 'NONE',  ( -10.81492255796078084, -18.62759615963271287, 42.08224293864769550 ) ) ;
#102211 = CARTESIAN_POINT ( 'NONE',  ( 20.08125529445640467, 22.02279270211222340, -51.67964572521218969 ) ) ;
#102212 = CARTESIAN_POINT ( 'NONE',  ( -16.46253265017146816, -9.564922557961047289, 19.16775706135233293 ) ) ;
#102213 = CARTESIAN_POINT ( 'NONE',  ( -27.96892006433829181, 7.184979517970726981, 161.0508495487520406 ) ) ;
#102214 = CARTESIAN_POINT ( 'NONE',  ( -16.51473224551069308, -9.474510206698971260, 41.66557627198103120 ) ) ;
#102215 = CARTESIAN_POINT ( 'NONE',  ( 40.00000000000001421, 2.428612866367529932E-14, 0.000000000000000000 ) ) ;
#102216 = CARTESIAN_POINT ( 'NONE',  ( -17.97161686093727795, 5.499999999999980460, 80.99637206859165417 ) ) ;
#102217 = CARTESIAN_POINT ( 'NONE',  ( 18.67979575497194134, -10.72451020669871369, 70.83442372801901854 ) ) ;
#102218 = CARTESIAN_POINT ( 'NONE',  ( -33.63107349886310971, -17.13970281212090185, -7.999999999999998224 ) ) ;
#102219 = CARTESIAN_POINT ( 'NONE',  ( 16.52544592524335698, 4.483927247898782831, 61.45942372801901854 ) ) ;
#102220 = CARTESIAN_POINT ( 'NONE',  ( -5.823673210054116645, -21.52544592524344225, 87.29057627198103830 ) ) ;
#102221 = CARTESIAN_POINT ( 'NONE',  ( 0.05219959533910956823, 16.53943276465976808, 54.99890960531435269 ) ) ;
#102223 = CARTESIAN_POINT ( 'NONE',  ( 13.89961937509977652, -13.97604488694527269, 103.1239096053143527 ) ) ;
#102222 = CARTESIAN_POINT ( 'NONE',  ( 16.51473224551069308, 9.474510206698969483, 24.16557627198102765 ) ) ;
#102224 = CARTESIAN_POINT ( 'NONE',  ( -21.53943276465977519, -0.05219959533937600094, 43.75109039468568284 ) ) ;
#102225 = CARTESIAN_POINT ( 'NONE',  ( -19.03943276465977164, -0.05219959533935918106, 43.75109039468566863 ) ) ;
#102226 = CARTESIAN_POINT ( 'NONE',  ( -5.153800228976328057, -19.02544592524343514, 32.29057627198102409 ) ) ;
#102227 = CARTESIAN_POINT ( 'NONE',  ( -21.53943276465977519, -0.05219959533937600094, 83.75109039468568994 ) ) ;
#102228 = LINE ( 'NONE', #179090, #37310 ) ;
#102229 = CARTESIAN_POINT ( 'NONE',  ( 14.29746914071049879, -8.314922557960816363, 28.33224293864769550 ) ) ;
#102230 = CARTESIAN_POINT ( 'NONE',  ( 29.86685920354754842, -21.69954338932559068, -2.324999997268813345 ) ) ;
#102231 = CARTESIAN_POINT ( 'NONE',  ( 15.72974639402199770, -15.80617190586745480, 38.12390960531436690 ) ) ;
#102232 = CARTESIAN_POINT ( 'NONE',  ( -4.521033265328978423, -6.642290809010376051, -64.18582806809564545 ) ) ;
#102233 = AXIS2_PLACEMENT_3D ( 'NONE', #131583, #86075, #7224 ) ;
#102234 = CARTESIAN_POINT ( 'NONE',  ( 16.51473224551069308, 9.474510206698969483, 89.16557627198103830 ) ) ;
#102235 = CARTESIAN_POINT ( 'NONE',  ( -12.06949235617756955, 12.14591786802309770, 85.62390960531436690 ) ) ;
#102236 = CARTESIAN_POINT ( 'NONE',  ( 9.474510206698729675, 16.51473224551082808, 102.0844237280190043 ) ) ;
#102237 = CARTESIAN_POINT ( 'NONE',  ( -21.55341960407610458, -5.719274019375992779, 66.45724293864768129 ) ) ;
#102238 = ORIENTED_EDGE ( 'NONE', *, *, #194670, .F. ) ;
#102239 = CARTESIAN_POINT ( 'NONE',  ( -16.51473224551069308, -9.474510206698971260, 36.66557627198102409 ) ) ;
#102241 = CARTESIAN_POINT ( 'NONE',  ( -10.81492255796078084, -18.62759615963271287, 92.08224293864769550 ) ) ;
#102240 = CARTESIAN_POINT ( 'NONE',  ( -13.97604488694527625, -13.89961937509977652, 86.87390960531436690 ) ) ;
#102243 = CARTESIAN_POINT ( 'NONE',  ( -5.049401038298153566, 19.05341960407611168, 105.2072429386476671 ) ) ;
#102242 = CARTESIAN_POINT ( 'NONE',  ( -4.379528057220086978, -16.55341960407618274, 109.7927570613523613 ) ) ;
#102244 = CARTESIAN_POINT ( 'NONE',  ( 0.05219959533936267826, -19.03943276465977164, 80.00109039468567573 ) ) ;
#102245 = CARTESIAN_POINT ( 'NONE',  ( 21.53943276465977519, 0.05219959533937863772, 96.25109039468568994 ) ) ;
#102246 = CARTESIAN_POINT ( 'NONE',  ( 0.05219959533907565091, 21.53943276465977519, 74.99890960531435269 ) ) ;
#102247 = CARTESIAN_POINT ( 'NONE',  ( -18.62759615963270932, 10.81492255796079327, 40.83224293864769550 ) ) ;
#102248 = CARTESIAN_POINT ( 'NONE',  ( -13.89961937509977652, 13.97604488694528158, 45.62390960531433848 ) ) ;
#102249 = CARTESIAN_POINT ( 'NONE',  ( 4.379528057220092307, 16.55341960407617563, 112.2927570613523471 ) ) ;
#102250 = CARTESIAN_POINT ( 'NONE',  ( 13.89961937509977652, -13.97604488694527269, 63.12390960531435979 ) ) ;
#102251 = ORIENTED_EDGE ( 'NONE', *, *, #88509, .F. ) ;
#102252 = CARTESIAN_POINT ( 'NONE',  ( -31.24427474013728201, -7.030368782406874573, 97.62376346805388039 ) ) ;
#102253 = CARTESIAN_POINT ( 'NONE',  ( 13.89961937509957401, 13.97604488694547697, 31.87609039468566863 ) ) ;
#102254 = CARTESIAN_POINT ( 'NONE',  ( -4.379528057220328563, 16.55341960407611168, 85.20724293864770971 ) ) ;
#102255 =( BOUNDED_SURFACE ( )  B_SPLINE_SURFACE ( 3, 2, ( 
 ( #42518, #104181, #165863, #197199, #120328, #182023, #130141, #40147, #193855, #160505, #68486, #179695, #21995, #191838, #55320, #149337, #83648, #56323, #53319, #116991, #26009, #42172, #39156, #70496, #6808, #176692, #192848, #54328, #25010, #114997, #147340, #180696, #177688, #132164, #164516, #195865, #161506, #8827, #41167, #72503, #145325, #38166, #178685, #100812, #115999, #101824, #10833, #163512, #99821, #148338, #69494, #22996, #86654, #133159, #85653, #9834, #71493, #87652, #84644, #146321, #119013, #194851, #102830, #118006, #134177, #57337, #7810, #131159, #162496, #23996, #199939, #61403, #170587, #32077, #92732, #197946, #91726, #138256, #60410, #123074, #184760, #107899, #44267, #46245, #198943, #74604, #93734, #75581, #166625, #47250, #14920, #181790, #169586, #137260, #43270, #155415, #185762, #77572, #104939, #63400, #122083, #31084, #62391, #140231, #16905, #154420, #78556, #28127, #719, #1724, #136271, #15914, #139244, #90744, #124061, #151452, #108907, #13915, #89767, #12939, #59416, #183774, #121090, #182784, #105925, #167610, #29106, #152427, #45260, #106914, #168587, #30085, #153422, #76580, #6689, #66380, #5695, #36035, #67371, #113862, #19880, #81521, #21878, #175558, #94726, #4688, #158391, #125077, #33071, #144210, #186774, #156404, #143207, #37034, #48245, #20870, #17908, #128041, #190731, #109899, #3705, #35048, #171583, #141231, #157408, #18901, #189742, #79564, #111890, #145206, #142221, #96702, #129030, #160389, #126068, #173579, #52204, #98695, #2722, #64399, #51215, #65383, #80547, #112876, #83528, #174569, #187764, #97684, #34063, #49234, #159374, #82528, #50235, #110892, #172577, #95722, #127043, #188750, #26891, #56206, #87540, #148224, #25895, #86540, #117889, #42054, #180580, #88534, #179579, #161386, #9718, #116875, #38046, #101705, #149227, #71382, #130018, #84524, #102714, #39041, #133046, #178566, #146201, #118895, #57222, #163395, #24892, #165398, #103718, #99702, #194736, #41050, #68367, #176572, #10718, #191717, #22877, #164403, #150231, #53201, #72381, #7687, #134056, #195748, #114878, #147221, #40031, #69371, #131041, #100698, #162379, #192731, #54213, #55206, #115884, #85533, #177574, #23881, #8712, #70381, #132049, #193738, #126557, #137759, #92241, #32578, #154919, #108415, #124579, #3222, #155912, #184275, #2226, #123569, #45758, #62899, #187276, #139732, #63908, #140737, #18413, #138749, #107410, #173084, #125578, #33568, #94231, #172081, #17407, #48746, #188257, #49731, #34563, #110399, #169083, #79064, #186275, #30589, #47754, #95230, #156916, #76083, #153927, #80062, #185264, #141732, #109408, #15421, #64896, #111399, #96219, #14419, #199443, #170090, #60911, #122587, #77080, #231, #61899, #46756, #31584, #93234, #16417, #78064, #1221, #171087, #66878, #68879, #127555, #145714, #190236, #176073, #85032, #69884, #51713, #114369, #19398, #189256, #157908, #131553, #39540, #21378, #50732, #177082, #112391, #38553, #116383, #81047, #99205, #100210, #130539, #161890, #174082, #37541, #191231, #142723, #65881, #23386, #4203, #35551, #52705, #146713, #97198, #53717, #158884, #160893, #8209, #20374, #36532, #67878, #82022, #143717, #113376, #175066, #22385, #5196, #144712, #178073, #98187, #129531, #193238, #54711, #128540, #6198, #159890, #83037, #84035, #7195, #192237, #115394, #195243, #11226, #90033, #42553, #70890, #89040, #10222, #132558, #149725, #73892, #26398, #150730, #27395, #105207, #25407, #194246, #59686, #12230, #120365, #181078, #58695, #119395, #135562, #74871, #13208, #121357, #197234, #55713, #104216, #72900, #117385, #134569, #182058, #165897, #162889, #179084, #43541, #71882, #166894, #196256, #40553, #151715, #28394, #136533, #101199, #183050, #56727, #198214, #24398, #86047, #147736, #9223, #102222, #163911, #87049, #148734, #133552, #118397, #180091, #41559, #103222, #164904, #88037, #57725, #62658, #171845, #156679 ),
 ( #126325, #186033, #125344, #155675, #187042, #33333, #139500, #983, #141500, #94993, #138512, #154683, #18173, #47515, #14178, #32341, #153686, #75848, #92997, #17170, #169852, #93994, #170850, #48512, #168845, #137524, #2984, #78824, #63670, #124337, #1991, #109171, #140502, #79830, #64663, #44534, #110166, #199206, #106189, #16178, #60673, #77833, #167873, #29372, #91003, #122348, #152689, #15182, #184037, #45520, #107174, #30350, #91992, #76841, #101728, #61663, #123332, #185025, #46512, #108171, #31346, #98958, #176838, #188022, #6951, #84788, #80809, #67635, #52466, #96966, #160648, #157672, #175826, #20138, #5957, #115145, #99964, #81783, #144473, #49494, #19161, #111156, #161648, #69642, #51476, #142488, #68631, #3966, #130287, #146467, #172845, #129294, #191981, #22140, #53468, #38309, #82791, #190990, #7959, #23144, #65646, #114124, #21136, #34326, #95987, #127308, #189019, #50493, #37299, #112157, #173846, #83790, #35312, #145470, #158646, #143470, #66639, #97948, #4954, #128302, #190002, #113138, #174828, #36292, #159640, #151481, #148491, #41315, #135325, #166656, #132316, #118154, #150493, #43301, #54475, #8982, #149482, #71642, #196997, #11990, #181822, #26155, #12972, #101980, #56476, #147491, #133309, #120131, #24154, #70650, #196011, #40304, #162648, #73653, #86805, #131308, #116145, #85805, #178836, #104969, #164660, #163660, #177836, #10978, #194998, #194008, #72651, #134326, #28157, #89799, #42315, #55471, #102975, #87797, #9982, #57486, #119156, #180838, #117141, #103976, #179844, #25163, #192998, #165655, #39304, #58464, #27153, #100963, #88800, #168615, #136302, #63432, #153450, #1754, #198971, #30115, #91756, #108937, #125108, #14948, #76608, #61432, #59447, #751, #138286, #29137, #45290, #199967, #123104, #184789, #15944, #60438, #186806, #48276, #62422, #109931, #92762, #156439, #154451, #46275, #77603, #107931, #170618, #169617, #124094, #167641, #139274, #171613, #31114, #33101, #106942, #94757, #74636, #197977, #13944, #185793, #47281, #121120, #182814, #90774, #152458, #44297, #32107, #93764, #105956, #155445, #16935, #78589, #75610, #140262, #137289, #122113, #183802, #34093, #53230, #68395, #172606, #159404, #65412, #130047, #143236, #98723, #3735, #21906, #187793, #190758, #79592, #95751, #52233, #188781, #20899, #66408, #157436, #191747, #83556, #113890, #17938, #99730, #111921, #82557, #160417, #176600, #114906, #129057, #6717, #141261, #37064, #38074, #110920, #97713, #144239, #127073, #175588, #49262, #5723, #50264, #36065, #145236, #2751, #173608, #174599, #64427, #18931, #126096, #80576, #142250, #81550, #35078, #96731, #158420, #19908, #4719, #128070, #67402, #189773, #51245, #112905, #150262, #56237, #117918, #58238, #11756, #131069, #41079, #194763, #161414, #69402, #180610, #22906, #192758, #179607, #73423, #84552, #57251, #54241, #102743, #26921, #43069, #40060, #71409, #7717, #177602, #193767, #55235, #25925, #115912, #148252, #181592, #178597, #133073, #165427, #196770, #162408, #9745, #42083, #135094, #146230, #39070, #164431, #101737, #116904, #87568, #119906, #149255, #100727, #10747, #70411, #23910, #72411, #134088, #86568, #195778, #118925, #88564, #85564, #147250, #8741, #103748, #132078, #163425, #24923, #122868, #154215, #78345, #16695, #124865, #92526, #197746, #184556, #153207, #74406, #138049, #123848, #46037, #28907, #60207, #198742, #139033, #31867, #45055, #121877, #91520, #89565, #30879, #183570, #59213, #75380, #106713, #168387, #14712, #107692, #90547, #93521, #140019, #15705, #155206, #169371, #186564, #77365, #29882, #512, #76372, #62184, #199730, #185546, #120882, #47040, #1508, #61196, #63185, #137052, #104736, #166427, #27922, #44064, #108697, #170376, #151251, #12740, #182581, #105724, #136072, #167411, #152229, #13714, #112666, #173367, #34837, #94512, #190519, #5480, #109693, #49023, #64189, #83317, #98480, #2509 ),
 ( #36814, #189533, #17694, #35828, #157194, #79351, #96492, #20655, #158182, #97474, #174358, #51993, #172358, #141022, #6475, #159160, #67163, #127827, #128820, #66165, #82309, #21663, #160173, #68155, #143999, #125856, #51005, #19672, #187556, #81314, #113652, #175346, #171375, #110678, #144994, #18688, #129807, #142997, #33848, #48037, #32862, #156194, #95508, #80335, #142007, #3496, #65172, #126831, #188537, #50015, #111680, #4475, #195532, #115675, #84314, #150009, #179369, #10505, #71171, #149017, #9505, #40831, #165184, #103508, #11515, #102504, #145993, #132835, #39821, #161170, #24680, #72167, #194522, #52982, #7476, #25686, #162171, #55994, #101487, #69160, #41840, #57006, #87331, #191506, #73185, #85317, #117672, #133842, #114661, #26679, #164188, #180371, #176357, #118679, #88319, #130827, #37830, #99490, #100492, #22667, #192518, #54001, #23669, #177363, #38834, #147009, #8494, #148016, #70171, #131839, #193522, #54997, #116666, #178357, #163176, #86329, #166182, #153969, #93276, #16457, #76126, #15466, #45800, #77123, #123610, #29642, #91274, #31626, #185305, #104501, #14464, #168145, #134856, #42836, #138792, #196534, #27683, #152965, #46796, #58004, #30632, #89324, #137804, #273, #119674, #13477, #44811, #181357, #151016, #167171, #28670, #199488, #12507, #121635, #154961, #151991, #106466, #61942, #170132, #135841, #183330, #108455, #74171, #197510, #58978, #60955, #75142, #90305, #122629, #120645, #184319, #182343, #107452, #43821, #105485, #169127, #92285, #59968, #136813, #198497, #1263, #157946, #18451, #109447, #96260, #19437, #69676, #131343, #189295, #94273, #188297, #34601, #156954, #81085, #142763, #4243, #140777, #65923, #95271, #171130, #193031, #172122, #62940, #143758, #111439, #78106, #127596, #33608, #139775, #54508, #80102, #5239, #2266, #141770, #3263, #112432, #116180, #64936, #126595, #49774, #124620, #50772, #173126, #32619, #48787, #174121, #35592, #97238, #158926, #63949, #177871, #39339, #20415, #100998, #82065, #162683, #186315, #47797, #155951, #17448, #79104, #125618, #187316, #110441, #42349, #151515, #180873, #13006, #56511, #59481, #136337, #74670, #163696, #57520, #165689, #121155, #9017, #178872, #117177, #182848, #104011, #73689, #132351, #88834, #149516, #11013, #70685, #166689, #181856, #85839, #25198, #40339, #44331, #198011, #102014, #27187, #71676, #105988, #72686, #105003, #10017, #28192, #194043, #197032, #89834, #43335, #24189, #119189, #147529, #195034, #134361, #86841, #164695, #55507, #148526, #133343, #150527, #118189, #179880, #41348, #103011, #26190, #87830, #196045, #12026, #135361, #58499, #120165, #171642, #2782, #168647, #154482, #186839, #79624, #90807, #45323, #185827, #107963, #61465, #77635, #156469, #108969, #137322, #155475, #76639, #199003, #15976, #140296, #92794, #16967, #93795, #33132, #91789, #60469, #126128, #78620, #48308, #47314, #125140, #170650, #1787, #141292, #64460, #187823, #63465, #122145, #32138, #139304, #183834, #783, #109963, #94789, #29171, #106973, #17970, #138317, #49292, #62454, #30146, #167674, #152490, #13977, #75644, #153483, #123136, #14979, #199999, #184822, #46307, #169650, #31146, #124128, #130080, #7747, #3764, #190788, #175619, #19939, #21936, #80607, #98753, #143265, #129088, #38106, #22937, #4749, #67431, #172635, #142284, #110950, #84583, #192789, #174629, #65441, #191778, #127102, #53261, #69433, #34123, #52262, #114938, #83587, #176631, #99761, #5755, #113920, #131101, #161446, #188810, #37094, #144268, #95782, #18961, #146263, #157468, #50294, #160446, #111951, #173640, #6748, #35109, #145267, #96761, #158450, #189803, #20929, #81580, #66438, #128099, #51275, #68427, #112936, #97746, #36094, #159433, #82587, #23940, #42115, #163455, #85594, #102773, #26953, #179639, #103777, #180640, #58267, #178627, #147281, #12772, #165456, #73452, #134119, #11788, #72443, #88595, #27954, #166457 ),
 ( #57280, #164460, #70440, #104769, #119936, #150292, #54271, #136103, #148283, #118954, #135125, #74436, #89595, #196799, #43101, #115944, #181621, #151282, #8771, #195808, #177634, #24953, #39101, #132106, #100757, #86600, #162439, #193798, #55265, #9777, #10777, #116934, #40090, #101768, #71439, #133104, #117949, #194793, #56266, #41109, #25954, #87597, #149283, #139068, #78379, #108733, #140055, #186600, #92560, #154248, #94550, #48072, #167442, #77398, #30912, #197779, #105756, #16731, #59245, #28939, #15739, #109728, #120914, #93555, #90580, #546, #63221, #79390, #76406, #107725, #44098, #13746, #29915, #91555, #62217, #152261, #184590, #17732, #14745, #169406, #1545, #32898, #198774, #46071, #124901, #171412, #182613, #75414, #123885, #138082, #153242, #185583, #156231, #47073, #155241, #137086, #60240, #121911, #183604, #45088, #106745, #170410, #168420, #199763, #122901, #61230, #31902, #145031, #110717, #113687, #6513, #160211, #191543, #35865, #161209, #111717, #66203, #157233, #81350, #129844, #33889, #80372, #5518, #50055, #172399, #83355, #96528, #22704, #125893, #95545, #188575, #53020, #174395, #173403, #64228, #20692, #143034, #18725, #159197, #82347, #114701, #176394, #52029, #142045, #51041, #97511, #19708, #144036, #67198, #128856, #3532, #190556, #158218, #65209, #37868, #34874, #187593, #68192, #175382, #141060, #36851, #4512, #2546, #99527, #127865, #49062, #126868, #189569, #112703, #98518, #21701, #24715, #101522, #71206, #69197, #10539, #163213, #38872, #55032, #39856, #86364, #132869, #25720, #70208, #11551, #196564, #72203, #73217, #102540, #166213, #164223, #148049, #87366, #194558, #180404, #56028, #133877, #177400, #149051, #134888, #40866, #58035, #116702, #119705, #181388, #42867, #23705, #117706, #195568, #104532, #130865, #100528, #162207, #84351, #57041, #118715, #192555, #41876, #9539, #179402, #54038, #26713, #85353, #103543, #165218, #193560, #88352, #115712, #150045, #178392, #146029, #7512, #147046, #8530, #131875, #89357, #59010, #27714, #139807, #109481, #91307, #197542, #46828, #120677, #108488, #186349, #151047, #169162, #170167, #138827, #31660, #16490, #122663, #184351, #124653, #78139, #182376, #107484, #60989, #12537, #135871, #93310, #74202, #43854, #45833, #1295, #105519, #123641, #167204, #30666, #154994, #28702, #106502, #137840, #90338, #152023, #60002, #121669, #92319, #13509, #14498, #47829, #44846, #199521, #62973, #75174, #136846, #76160, #198531, #183364, #168179, #29675, #154004, #152999, #15500, #77157, #307, #61975, #185338, #158956, #80131, #140808, #19468, #143789, #96289, #20446, #97268, #175137, #95300, #63980, #129603, #82097, #190308, #50802, #128615, #189325, #5272, #144788, #83111, #191299, #66953, #125650, #112460, #81113, #2298, #4273, #51784, #174152, #32651, #187347, #113444, #141801, #35623, #142793, #48817, #21450, #36604, #98261, #171164, #52775, #64966, #159963, #6271, #94305, #67949, #155983, #17480, #79137, #110470, #172152, #157976, #33638, #156984, #18482, #3294, #126625, #188326, #49805, #111470, #173155, #34630, #65954, #127625, #39615, #195320, #100284, #118473, #84106, #87123, #180163, #133628, #164977, #9297, #134643, #85105, #101274, #130614, #54786, #103298, #7267, #53790, #179157, #23458, #145785, #56800, #69962, #196329, #99277, #68951, #161962, #26472, #147811, #146791, #37615, #194319, #116461, #192310, #132631, #55787, #88114, #149798, #25481, #115465, #24470, #70963, #193312, #117458, #40625, #102295, #177154, #163984, #131628, #38627, #11304, #8284, #160964, #41633, #148808, #114444, #10298, #178150, #176145, #72974, #162964, #22458, #86120, #71955, #151787, #92073, #185099, #198285, #74942, #44607, #42626, #184114, #136605, #12300, #28468, #13278, #59763, #106262, #199282, #43614, #46588, #169929, #45596, #108249, #75924, #139574, #137599, #121431, #60749, #167946, #153762, #29444, #107249, #150804 ),
 ( #31421, #181151, #15257, #73966, #91076, #123406, #57797, #183124, #152763, #14253, #122422, #104290, #135635, #90103, #168920, #30426, #197305, #76915, #77907, #138586, #67, #61738, #93073, #58769, #154758, #16256, #119468, #165971, #120437, #27473, #89116, #182130, #105278, #166966, #172925, #109243, #157750, #125419, #170923, #141575, #142566, #18251, #19242, #80889, #112233, #2066, #32414, #143552, #4045, #127390, #111234, #189100, #49571, #65722, #20215, #158725, #5037, #50573, #94069, #34404, #3063, #155748, #126402, #173923, #96062, #62733, #17246, #35392, #187115, #97043, #64740, #78898, #81863, #66723, #1059, #124415, #186109, #156757, #47590, #140576, #63745, #48587, #110239, #171920, #33410, #95069, #79904, #188098, #139566, #157742, #170913, #47582, #17237, #15247, #156749, #109234, #185090, #1050, #186100, #32406, #78889, #171912, #16247, #19231, #142557, #18243, #80880, #48578, #112224, #110231, #94061, #33401, #140568, #126393, #2058, #79896, #123398, #95059, #4035, #187108, #65713, #62723, #127379, #189091, #50564, #169920, #63736, #141566, #30416, #76906, #46579, #108240, #92064, #3055, #64732, #138577, #188090, #153752, #31412, #49561, #124407, #111225, #125411, #93063, #57, #34396, #172917, #61730, #154750, #155740, #96054, #77899, #132385, #9047, #84858, #162717, #173914, #192055, #20205, #35383, #8028, #38378, #82865, #146535, #143540, #161720, #69710, #114194, #52533, #144543, #129365, #175898, #22210, #115214, #159709, #101032, #85873, #23215, #24223, #53537, #55541, #176907, #191061, #100034, #83859, #131377, #145540, #193065, #66712, #54541, #147562, #130356, #70717, #6028, #194078, #97034, #158715, #113209, #7019, #116214, #81851, #5027, #128373, #190069, #51545, #177905, #39373, #174897, #36363, #99028, #160718, #98015, #21208, #67707, #37370, #68701, #133377, #152523, #167709, #71709, #58533, #164729, #29205, #42381, #198046, #103047, #121189, #86874, #89867, #182882, #136369, #90839, #12060, #137356, #87863, #104044, #195067, #57552, #106022, #10049, #56547, #181889, #26223, #148558, #59512, #72722, #199035, #102048, #118224, #149551, #14011, #150561, #11046, #40374, #197065, #119221, #179915, #135395, #120199, #75677, #117213, #28227, #41381, #27220, #73722, #178906, #134395, #163732, #25233, #196081, #180906, #165724, #44365, #88868, #43367, #105039, #166723, #151549, #13039, #74705, #141330, #49328, #155510, #17005, #157505, #110989, #30182, #140332, #93830, #60505, #168682, #79661, #122180, #91825, #78657, #172674, #183872, #156505, #153518, #1822, #126164, #142321, #139339, #170685, #107009, #76676, #92831, #154516, #125178, #15015, #47350, #80644, #77670, #32174, #64497, #95820, #61502, #109006, #2818, #34159, #45357, #138352, #63503, #818, #16013, #186875, #18998, #48345, #200034, #109999, #169685, #123171, #171679, #33169, #185864, #94828, #18007, #187859, #184859, #46342, #107998, #31180, #62492, #124163, #161485, #21974, #53297, #177668, #115979, #23976, #191816, #96800, #83626, #52299, #173679, #37130, #22973, #145303, #65479, #19975, #38145, #174665, #6786, #113956, #81618, #54307, #7788, #99799, #3801, #85631, #97782, #68465, #84621, #162474, #39136, #114976, #192826, #127141, #130119, #50332, #188848, #146300, #176669, #112973, #69471, #35146, #131138, #67467, #158487, #111988, #100791, #36130, #20965, #190824, #143301, #4787, #144304, #82622, #159470, #5794, #129126, #175656, #66477, #189839, #128139, #51312, #98790, #160484, #165488, #28969, #26984, #102807, #88629, #57313, #43131, #118988, #196830, #40125, #150325, #74469, #103808, #136134, #179673, #182645, #59276, #197810, #86633, #180671, #11820, #44129, #132142, #101803, #163490, #105788, #73485, #58298, #55299, #135157, #72479, #134152, #193835, #89626, #104800, #8807, #148316, #24988, #167474, #120946, #9811, #119966, #194828, #147317, #195840, #27987, #133137, #151314, #116971 ),
 ( #181652, #56301, #178662, #12803, #164493, #70476, #71472, #117983, #41144, #25986, #42148, #87629, #149315, #166489, #10809, #121943, #108763, #170440, #79418, #141088, #1576, #106776, #574, #47102, #169439, #31931, #93585, #16760, #153276, #155271, #107756, #183636, #2574, #184619, #75444, #156259, #123914, #90611, #78408, #46101, #152292, #64255, #30943, #17762, #172428, #137119, #29947, #199795, #125922, #92590, #168451, #154279, #187620, #45118, #91585, #140084, #61262, #14777, #32926, #15769, #13776, #198805, #76437, #138114, #49090, #185613, #122932, #60270, #63251, #77429, #139100, #124930, #186628, #110747, #62245, #48099, #109755, #171439, #94581, #112731, #52061, #190585, #160242, #96558, #175414, #51070, #126898, #146058, #127894, #18755, #99557, #67227, #33917, #113717, #189597, #95574, #22733, #174424, #161239, #115742, #80401, #173433, #143062, #84381, #35893, #97540, #20722, #21731, #68222, #159227, #82379, #4540, #144067, #5548, #128885, #36882, #19736, #7542, #69227, #83384, #130895, #98548, #157260, #145061, #6542, #129874, #191572, #53051, #114731, #176425, #188604, #37899, #192585, #54068, #142074, #66234, #3560, #65238, #50085, #34903, #111745, #158245, #81377, #162236, #131906, #70238, #12566, #195599, #26742, #85385, #41907, #102570, #164255, #23736, #119735, #134917, #38900, #178422, #193590, #74232, #27744, #55061, #118746, #24746, #89387, #25750, #58064, #163245, #181418, #147078, #150075, #42896, #196594, #151075, #72233, #197572, #148079, #87396, #135900, #59039, #40898, #8563, #104561, #116733, #166243, #177429, #100557, #180434, #39886, #88381, #101553, #86395, #133908, #57072, #9570, #71236, #132899, #103573, #10569, #194588, #56058, #117737, #179432, #149081, #165248, #11580, #73247, #16520, #13539, #154034, #186380, #2328, #199549, #30697, #167234, #136876, #153029, #14529, #185366, #75205, #107514, #140839, #137870, #92348, #124683, #156013, #121699, #169190, #139836, #32682, #43884, #198562, #138855, #61019, #76190, #15528, #109511, #62003, #90369, #108518, #29706, #152054, #77185, #93339, #45861, #170197, #46858, #47858, #44876, #60032, #79168, #31690, #1325, #335, #78168, #123669, #155024, #94335, #17510, #120706, #63005, #183394, #171193, #182405, #106532, #105549, #28732, #168209, #91337, #122691, #184380, #34660, #66984, #112488, #80158, #114472, #67978, #159993, #64009, #145814, #158004, #128643, #144816, #22487, #99309, #175168, #52805, #125678, #82126, #110499, #187376, #98291, #190337, #173184, #36634, #33666, #21480, #127654, #18511, #172181, #176175, #96318, #20476, #48845, #95328, #157013, #189354, #50831, #141829, #6299, #83141, #3322, #64995, #126653, #160993, #37645, #188356, #5300, #111498, #84135, #174181, #129632, #49834, #191327, #19496, #81141, #142822, #4302, #65984, #158984, #35650, #97298, #143819, #51814, #113473, #196357, #100313, #146821, #71983, #116491, #38657, #149827, #162995, #89144, #192340, #161992, #54816, #119497, #40655, #39645, #130646, #87154, #147842, #23488, #25510, #148837, #57825, #181179, #118503, #85137, #117490, #164014, #86152, #10327, #133658, #195348, #69992, #56828, #24500, #8316, #42656, #101306, #53822, #73003, #102324, #7297, #180193, #9328, #68981, #104318, #70993, #134672, #115497, #177184, #131660, #178180, #166002, #132661, #194349, #55817, #41663, #103326, #179187, #165006, #26500, #88142, #11332, #27502, #193342, #136631, #77934, #62763, #138613, #139601, #168947, #32443, #30454, #106288, #92101, #60778, #46617, #122450, #95, #43642, #153789, #1087, #107276, #124443, #183151, #186139, #47618, #109272, #90129, #184142, #15285, #170951, #135663, #105305, #166993, #150833, #76944, #61765, #58798, #123433, #12329, #29472, #45624, #197335, #28495, #44636, #167973, #185126, #151813, #137627, #73994, #91105, #108278, #154785, #120466, #13304, #199312, #169956, #182158, #74969, #198313, #31448, #152793 ),
 ( #59791, #93101, #14285, #121459, #75953, #16282, #144335, #8838, #130149, #129156, #17274, #176700, #37160, #125447, #115006, #38174, #85663, #147350, #7818, #110267, #6816, #53327, #175685, #99830, #161514, #23006, #156785, #84652, #113987, #187143, #70506, #190853, #78928, #162506, #191846, #94097, #146329, #52330, #155776, #132174, #98819, #24007, #178696, #140604, #33437, #5823, #193865, #160513, #22004, #83656, #69502, #131168, #145334, #68494, #67499, #192858, #54337, #116008, #177698, #79932, #55331, #117001, #39165, #2094, #100823, #63775, #48615, #171948, #95096, #18278, #136170, #150359, #89663, #133170, #58332, #167509, #196866, #29004, #72513, #75478, #152326, #90644, #179704, #73521, #181686, #137151, #25020, #194860, #56333, #198840, #120000, #151349, #165523, #12838, #166524, #44163, #164525, #118015, #60304, #28021, #59311, #43167, #197845, #104834, #74504, #13812, #121979, #40158, #120980, #41176, #182678, #88664, #9843, #135192, #105822, #101834, #163521, #102839, #86663, #10844, #148347, #11856, #26018, #71502, #87662, #149347, #134188, #195875, #57348, #119023, #180706, #42182, #103842, #27019, #172464, #183670, #1610, #29983, #45155, #17796, #48133, #92622, #94616, #153310, #79452, #47138, #138149, #91622, #95609, #15802, #140119, #106811, #14811, #168485, #157294, #65272, #108796, #76472, #2612, #199830, #64289, #142109, #61297, #124966, #125956, #156295, #187654, #33951, #78445, #63286, #80436, #18791, #122967, #186663, #16795, #184654, #46136, #49125, #107789, #169474, #109790, #3594, #30975, #141122, #154313, #171473, #110783, #77463, #62280, #93620, #139133, #610, #123948, #185646, #32962, #170475, #31965, #155306, #144100, #36917, #130927, #162271, #127928, #113751, #146091, #38932, #50119, #4576, #145093, #67260, #20756, #98580, #115774, #68255, #96592, #114763, #35926, #158281, #175447, #99591, #81411, #34940, #100589, #159260, #83416, #188640, #19770, #126932, #23771, #8598, #190619, #143097, #7575, #66269, #69261, #85421, #111779, #129906, #192618, #37930, #54100, #177463, #21765, #6576, #147112, #173467, #189630, #191606, #160274, #51104, #112764, #174457, #97572, #82411, #53085, #5580, #128918, #22765, #52094, #176457, #161271, #84414, #149116, #180470, #116766, #86429, #102606, #164292, #134952, #24782, #57108, #90402, #87431, #41942, #74266, #105580, #71271, #118782, #89421, #182438, #193624, #148115, #88419, #10607, #25785, #103608, #59072, #11614, #39924, #58099, #179469, #101593, #165284, #42931, #195635, #119769, #196630, #135936, #194623, #163281, #28765, #181453, #151110, #150113, #27779, #73282, #104595, #43918, #167266, #152087, #166282, #9606, #12602, #26777, #132936, #197606, #120739, #70272, #131940, #56094, #55096, #40934, #178457, #117775, #72268, #133945, #17544, #109545, #13572, #95364, #107548, #78201, #94368, #172217, #48881, #124717, #2363, #75239, #31724, #60065, #136910, #47892, #139871, #122724, #186415, #183425, #171227, #77219, #32716, #44909, #156047, #138888, #168243, #121733, #125714, #45895, #170231, #198597, #106566, #29739, #187413, #91372, #368, #153063, #79205, #14565, #140874, #33701, #76223, #155059, #64044, #110536, #137902, #199584, #108552, #93372, #61052, #184414, #169224, #16554, #46892, #30733, #92380, #154066, #15561, #62039, #1360, #123703, #185401, #63039, #49868, #190375, #22521, #38692, #35685, #67019, #3356, #173219, #189388, #50865, #21515, #111534, #143856, #177219, #174217, #128678, #161027, #192374, #158039, #5335, #176210, #69014, #80193, #34695, #175204, #97333, #112523, #51850, #145848, #98328, #126687, #144850, #66020, #188391, #113509, #129665, #82160, #6333, #83176, #84168, #81175, #96352, #115531, #68013, #37679, #36669, #114508, #160028, #191361, #130680, #53857, #157049, #52839, #19530, #99344, #7330, #142857, #18546, #141865, #65031, #4336, #127688, #159019, #20512, #103361, #148870, #116525 ) ),
 .UNSPECIFIED., .T., .F., .F. ) 
 B_SPLINE_SURFACE_WITH_KNOTS ( ( 4, 3, 4 ),
 ( 3, 2, 2, 2, 2, 2, 2, 2, 2, 2, 2, 2, 2, 2, 2, 2, 2, 2, 2, 2, 2, 2, 2, 2, 2, 2, 2, 2, 2, 2, 2, 2, 2, 2, 2, 2, 2, 2, 2, 2, 2, 2, 2, 2, 2, 2, 2, 2, 2, 2, 2, 2, 2, 2, 2, 2, 2, 2, 2, 2, 2, 2, 2, 2, 2, 2, 2, 2, 2, 2, 2, 2, 2, 2, 2, 2, 2, 2, 2, 2, 2, 2, 2, 2, 2, 2, 2, 2, 2, 2, 2, 2, 2, 2, 2, 2, 2, 2, 2, 2, 2, 2, 2, 2, 2, 2, 2, 2, 2, 2, 2, 2, 2, 2, 2, 2, 2, 2, 2, 2, 2, 2, 2, 2, 2, 2, 2, 2, 2, 2, 2, 2, 2, 2, 2, 2, 2, 2, 2, 2, 2, 2, 2, 2, 2, 2, 2, 2, 2, 2, 2, 2, 2, 2, 2, 2, 2, 2, 2, 2, 2, 2, 2, 2, 2, 2, 2, 2, 2, 2, 2, 2, 2, 2, 2, 2, 2, 2, 2, 2, 2, 2, 2, 2, 2, 2, 2, 2, 2, 2, 2, 2, 2, 2, 2, 2, 2, 2, 2, 2, 2, 2, 2, 2, 2, 2, 2, 2, 2, 2, 2, 2, 2, 2, 2, 2, 2, 2, 2, 2, 2, 2, 2, 2, 2, 2, 2, 2, 3 ),
 ( 0.000000000000000000, 0.5000000000000000000, 1.000000000000000000 ),
 ( 0.000000000000000000, 0.004385964912280701511, 0.008771929824561403022, 0.01315789473684210453, 0.01754385964912280604, 0.02192982456140350755, 0.02631578947368420907, 0.03070175438596491058, 0.03508771929824561209, 0.03947368421052631360, 0.04385964912280701511, 0.04824561403508771662, 0.05263157894736841813, 0.05701754385964911964, 0.06140350877192982115, 0.06578947368421052266, 0.07017543859649122417, 0.07456140350877192569, 0.07894736842105262720, 0.08333333333333332871, 0.08771929824561403022, 0.09210526315789473173, 0.09649122807017543324, 0.1008771929824561348, 0.1052631578947368363, 0.1096491228070175378, 0.1140350877192982393, 0.1184210526315789408, 0.1228070175438596423, 0.1271929824561403577, 0.1315789473684210453, 0.1359649122807017607, 0.1403508771929824483, 0.1447368421052631637, 0.1491228070175438514, 0.1535087719298245668, 0.1578947368421052544, 0.1622807017543859698, 0.1666666666666666574, 0.1710526315789473728, 0.1754385964912280604, 0.1798245614035087758, 0.1842105263157894635, 0.1885964912280701788, 0.1929824561403508665, 0.1973684210526315819, 0.2017543859649122695, 0.2061403508771929849, 0.2105263157894736725, 0.2149122807017543879, 0.2192982456140350755, 0.2236842105263157909, 0.2280701754385964786, 0.2324561403508771940, 0.2368421052631578816, 0.2412280701754385970, 0.2456140350877192846, 0.2500000000000000000, 0.2543859649122807154, 0.2587719298245614308, 0.2631578947368420907, 0.2675438596491228060, 0.2719298245614035214, 0.2763157894736842368, 0.2807017543859648967, 0.2850877192982456121, 0.2894736842105263275, 0.2938596491228070429, 0.2982456140350877027, 0.3026315789473684181, 0.3070175438596491335, 0.3114035087719298489, 0.3157894736842105088, 0.3201754385964912242, 0.3245614035087719396, 0.3289473684210526550, 0.3333333333333333148, 0.3377192982456140302, 0.3421052631578947456, 0.3464912280701754610, 0.3508771929824561209, 0.3552631578947368363, 0.3596491228070175517, 0.3640350877192982670, 0.3684210526315789269, 0.3728070175438596423, 0.3771929824561403577, 0.3815789473684210731, 0.3859649122807017330, 0.3903508771929824483, 0.3947368421052631637, 0.3991228070175438791, 0.4035087719298245390, 0.4078947368421052544, 0.4122807017543859698, 0.4166666666666666852, 0.4210526315789473450, 0.4254385964912280604, 0.4298245614035087758, 0.4342105263157894912, 0.4385964912280701511, 0.4429824561403508665, 0.4473684210526315819, 0.4517543859649122973, 0.4561403508771929571, 0.4605263157894736725, 0.4649122807017543879, 0.4692982456140351033, 0.4736842105263157632, 0.4780701754385964786, 0.4824561403508771940, 0.4868421052631579093, 0.4912280701754385692, 0.4956140350877192846, 0.5000000000000000000, 0.5043859649122807154, 0.5087719298245614308, 0.5131578947368421462, 0.5175438596491228616, 0.5219298245614034659, 0.5263157894736841813, 0.5307017543859648967, 0.5350877192982456121, 0.5394736842105263275, 0.5438596491228070429, 0.5482456140350877583, 0.5526315789473684736, 0.5570175438596490780, 0.5614035087719297934, 0.5657894736842105088, 0.5701754385964912242, 0.5745614035087719396, 0.5789473684210526550, 0.5833333333333333703, 0.5877192982456140857, 0.5921052631578946901, 0.5964912280701754055, 0.6008771929824561209, 0.6052631578947368363, 0.6096491228070175517, 0.6140350877192982670, 0.6184210526315789824, 0.6228070175438596978, 0.6271929824561403022, 0.6315789473684210176, 0.6359649122807017330, 0.6403508771929824483, 0.6447368421052631637, 0.6491228070175438791, 0.6535087719298245945, 0.6578947368421053099, 0.6622807017543859143, 0.6666666666666666297, 0.6710526315789473450, 0.6754385964912280604, 0.6798245614035087758, 0.6842105263157894912, 0.6885964912280702066, 0.6929824561403509220, 0.6973684210526315264, 0.7017543859649122417, 0.7061403508771929571, 0.7105263157894736725, 0.7149122807017543879, 0.7192982456140351033, 0.7236842105263158187, 0.7280701754385965341, 0.7324561403508771384, 0.7368421052631578538, 0.7412280701754385692, 0.7456140350877192846, 0.7500000000000000000, 0.7543859649122807154, 0.7587719298245614308, 0.7631578947368421462, 0.7675438596491228616, 0.7719298245614034659, 0.7763157894736841813, 0.7807017543859648967, 0.7850877192982456121, 0.7894736842105263275, 0.7938596491228070429, 0.7982456140350877583, 0.8026315789473684736, 0.8070175438596490780, 0.8114035087719297934, 0.8157894736842105088, 0.8201754385964912242, 0.8245614035087719396, 0.8289473684210526550, 0.8333333333333333703, 0.8377192982456140857, 0.8421052631578946901, 0.8464912280701754055, 0.8508771929824561209, 0.8552631578947368363, 0.8596491228070175517, 0.8640350877192982670, 0.8684210526315789824, 0.8728070175438596978, 0.8771929824561403022, 0.8815789473684210176, 0.8859649122807017330, 0.8903508771929824483, 0.8947368421052631637, 0.8991228070175438791, 0.9035087719298245945, 0.9078947368421053099, 0.9122807017543859143, 0.9166666666666666297, 0.9210526315789473450, 0.9254385964912280604, 0.9298245614035087758, 0.9342105263157894912, 0.9385964912280702066, 0.9429824561403509220, 0.9473684210526315264, 0.9517543859649122417, 0.9561403508771929571, 0.9605263157894736725, 0.9649122807017543879, 0.9692982456140351033, 0.9736842105263158187, 0.9780701754385965341, 0.9824561403508771384, 0.9868421052631578538, 0.9912280701754385692, 0.9956140350877192846, 1.000000000000000000 ),
 .UNSPECIFIED. ) 
 GEOMETRIC_REPRESENTATION_ITEM ( )  RATIONAL_B_SPLINE_SURFACE ( (
 ( 1.000000000000000000, 0.9659258262890683122, 1.000000000000000000, 0.9659258262890683122, 1.000000000000000000, 0.9659258262890683122, 1.000000000000000000, 0.9659258262890683122, 1.000000000000000000, 0.9659258262890683122, 1.000000000000000000, 0.9659258262890683122, 1.000000000000000000, 0.9659258262890683122, 1.000000000000000000, 0.9659258262890683122, 1.000000000000000000, 0.9659258262890683122, 1.000000000000000000, 0.9659258262890683122, 1.000000000000000000, 0.9659258262890683122, 1.000000000000000000, 0.9659258262890683122, 1.000000000000000000, 0.9659258262890683122, 1.000000000000000000, 0.9659258262890683122, 1.000000000000000000, 0.9659258262890683122, 1.000000000000000000, 0.9659258262890683122, 1.000000000000000000, 0.9659258262890683122, 1.000000000000000000, 0.9659258262890683122, 1.000000000000000000, 0.9659258262890683122, 1.000000000000000000, 0.9659258262890683122, 1.000000000000000000, 0.9659258262890683122, 1.000000000000000000, 0.9659258262890683122, 1.000000000000000000, 0.9659258262890683122, 1.000000000000000000, 0.9659258262890683122, 1.000000000000000000, 0.9659258262890683122, 1.000000000000000000, 0.9659258262890683122, 1.000000000000000000, 0.9659258262890683122, 1.000000000000000000, 0.9659258262890683122, 1.000000000000000000, 0.9659258262890683122, 1.000000000000000000, 0.9659258262890683122, 1.000000000000000000, 0.9659258262890683122, 1.000000000000000000, 0.9659258262890683122, 1.000000000000000000, 0.9659258262890683122, 1.000000000000000000, 0.9659258262890683122, 1.000000000000000000, 0.9659258262890683122, 1.000000000000000000, 0.9659258262890683122, 1.000000000000000000, 0.9659258262890683122, 1.000000000000000000, 0.9659258262890683122, 1.000000000000000000, 0.9659258262890683122, 1.000000000000000000, 0.9659258262890683122, 1.000000000000000000, 0.9659258262890683122, 1.000000000000000000, 0.9659258262890683122, 1.000000000000000000, 0.9659258262890683122, 1.000000000000000000, 0.9659258262890683122, 1.000000000000000000, 0.9659258262890683122, 1.000000000000000000, 0.9659258262890683122, 1.000000000000000000, 0.9659258262890683122, 1.000000000000000000, 0.9659258262890683122, 1.000000000000000000, 0.9659258262890683122, 1.000000000000000000, 0.9659258262890683122, 1.000000000000000000, 0.9659258262890683122, 1.000000000000000000, 0.9659258262890683122, 1.000000000000000000, 0.9659258262890683122, 1.000000000000000000, 0.9659258262890683122, 1.000000000000000000, 0.9659258262890683122, 1.000000000000000000, 0.9659258262890683122, 1.000000000000000000, 0.9659258262890683122, 1.000000000000000000, 0.9659258262890683122, 1.000000000000000000, 0.9659258262890683122, 1.000000000000000000, 0.9659258262890683122, 1.000000000000000000, 0.9659258262890683122, 1.000000000000000000, 0.9659258262890683122, 1.000000000000000000, 0.9659258262890683122, 1.000000000000000000, 0.9659258262890683122, 1.000000000000000000, 0.9659258262890683122, 1.000000000000000000, 0.9659258262890683122, 1.000000000000000000, 0.9659258262890683122, 1.000000000000000000, 0.9659258262890683122, 1.000000000000000000, 0.9659258262890683122, 1.000000000000000000, 0.9659258262890683122, 1.000000000000000000, 0.9659258262890683122, 1.000000000000000000, 0.9659258262890683122, 1.000000000000000000, 0.9659258262890683122, 1.000000000000000000, 0.9659258262890683122, 1.000000000000000000, 0.9659258262890683122, 1.000000000000000000, 0.9659258262890683122, 1.000000000000000000, 0.9659258262890683122, 1.000000000000000000, 0.9659258262890683122, 1.000000000000000000, 0.9659258262890683122, 1.000000000000000000, 0.9659258262890683122, 1.000000000000000000, 0.9659258262890683122, 1.000000000000000000, 0.9659258262890683122, 1.000000000000000000, 0.9659258262890683122, 1.000000000000000000, 0.9659258262890683122, 1.000000000000000000, 0.9659258262890683122, 1.000000000000000000, 0.9659258262890683122, 1.000000000000000000, 0.9659258262890683122, 1.000000000000000000, 0.9659258262890683122, 1.000000000000000000, 0.9659258262890683122, 1.000000000000000000, 0.9659258262890683122, 1.000000000000000000, 0.9659258262890683122, 1.000000000000000000, 0.9659258262890683122, 1.000000000000000000, 0.9659258262890683122, 1.000000000000000000, 0.9659258262890683122, 1.000000000000000000, 0.9659258262890683122, 1.000000000000000000, 0.9659258262890683122, 1.000000000000000000, 0.9659258262890683122, 1.000000000000000000, 0.9659258262890683122, 1.000000000000000000, 0.9659258262890683122, 1.000000000000000000, 0.9659258262890683122, 1.000000000000000000, 0.9659258262890683122, 1.000000000000000000, 0.9659258262890683122, 1.000000000000000000, 0.9659258262890683122, 1.000000000000000000, 0.9659258262890683122, 1.000000000000000000, 0.9659258262890683122, 1.000000000000000000, 0.9659258262890683122, 1.000000000000000000, 0.9659258262890683122, 1.000000000000000000, 0.9659258262890683122, 1.000000000000000000, 0.9659258262890683122, 1.000000000000000000, 0.9659258262890683122, 1.000000000000000000, 0.9659258262890683122, 1.000000000000000000, 0.9659258262890683122, 1.000000000000000000, 0.9659258262890683122, 1.000000000000000000, 0.9659258262890683122, 1.000000000000000000, 0.9659258262890683122, 1.000000000000000000, 0.9659258262890683122, 1.000000000000000000, 0.9659258262890683122, 1.000000000000000000, 0.9659258262890683122, 1.000000000000000000, 0.9659258262890683122, 1.000000000000000000, 0.9659258262890683122, 1.000000000000000000, 0.9659258262890683122, 1.000000000000000000, 0.9659258262890683122, 1.000000000000000000, 0.9659258262890683122, 1.000000000000000000, 0.9659258262890683122, 1.000000000000000000, 0.9659258262890683122, 1.000000000000000000, 0.9659258262890683122, 1.000000000000000000, 0.9659258262890683122, 1.000000000000000000, 0.9659258262890683122, 1.000000000000000000, 0.9659258262890683122, 1.000000000000000000, 0.9659258262890683122, 1.000000000000000000, 0.9659258262890683122, 1.000000000000000000, 0.9659258262890683122, 1.000000000000000000, 0.9659258262890683122, 1.000000000000000000, 0.9659258262890683122, 1.000000000000000000, 0.9659258262890683122, 1.000000000000000000, 0.9659258262890683122, 1.000000000000000000, 0.9659258262890683122, 1.000000000000000000, 0.9659258262890683122, 1.000000000000000000, 0.9659258262890683122, 1.000000000000000000, 0.9659258262890683122, 1.000000000000000000, 0.9659258262890683122, 1.000000000000000000, 0.9659258262890683122, 1.000000000000000000, 0.9659258262890683122, 1.000000000000000000, 0.9659258262890683122, 1.000000000000000000, 0.9659258262890683122, 1.000000000000000000, 0.9659258262890683122, 1.000000000000000000, 0.9659258262890683122, 1.000000000000000000, 0.9659258262890683122, 1.000000000000000000, 0.9659258262890683122, 1.000000000000000000, 0.9659258262890683122, 1.000000000000000000, 0.9659258262890683122, 1.000000000000000000, 0.9659258262890683122, 1.000000000000000000, 0.9659258262890683122, 1.000000000000000000, 0.9659258262890683122, 1.000000000000000000, 0.9659258262890683122, 1.000000000000000000, 0.9659258262890683122, 1.000000000000000000, 0.9659258262890683122, 1.000000000000000000, 0.9659258262890683122, 1.000000000000000000, 0.9659258262890683122, 1.000000000000000000, 0.9659258262890683122, 1.000000000000000000, 0.9659258262890683122, 1.000000000000000000, 0.9659258262890683122, 1.000000000000000000, 0.9659258262890683122, 1.000000000000000000, 0.9659258262890683122, 1.000000000000000000, 0.9659258262890683122, 1.000000000000000000, 0.9659258262890683122, 1.000000000000000000, 0.9659258262890683122, 1.000000000000000000, 0.9659258262890683122, 1.000000000000000000, 0.9659258262890683122, 1.000000000000000000, 0.9659258262890683122, 1.000000000000000000, 0.9659258262890683122, 1.000000000000000000, 0.9659258262890683122, 1.000000000000000000, 0.9659258262890683122, 1.000000000000000000, 0.9659258262890683122, 1.000000000000000000, 0.9659258262890683122, 1.000000000000000000, 0.9659258262890683122, 1.000000000000000000, 0.9659258262890683122, 1.000000000000000000, 0.9659258262890683122, 1.000000000000000000, 0.9659258262890683122, 1.000000000000000000, 0.9659258262890683122, 1.000000000000000000, 0.9659258262890683122, 1.000000000000000000, 0.9659258262890683122, 1.000000000000000000, 0.9659258262890683122, 1.000000000000000000, 0.9659258262890683122, 1.000000000000000000, 0.9659258262890683122, 1.000000000000000000, 0.9659258262890683122, 1.000000000000000000, 0.9659258262890683122, 1.000000000000000000, 0.9659258262890683122, 1.000000000000000000, 0.9659258262890683122, 1.000000000000000000, 0.9659258262890683122, 1.000000000000000000, 0.9659258262890683122, 1.000000000000000000, 0.9659258262890683122, 1.000000000000000000, 0.9659258262890683122, 1.000000000000000000, 0.9659258262890683122, 1.000000000000000000, 0.9659258262890683122, 1.000000000000000000, 0.9659258262890683122, 1.000000000000000000, 0.9659258262890683122, 1.000000000000000000, 0.9659258262890683122, 1.000000000000000000, 0.9659258262890683122, 1.000000000000000000, 0.9659258262890683122, 1.000000000000000000, 0.9659258262890683122, 1.000000000000000000, 0.9659258262890683122, 1.000000000000000000, 0.9659258262890683122, 1.000000000000000000, 0.9659258262890683122, 1.000000000000000000, 0.9659258262890683122, 1.000000000000000000, 0.9659258262890683122, 1.000000000000000000, 0.9659258262890683122, 1.000000000000000000, 0.9659258262890683122, 1.000000000000000000, 0.9659258262890683122, 1.000000000000000000, 0.9659258262890683122, 1.000000000000000000, 0.9659258262890683122, 1.000000000000000000, 0.9659258262890683122, 1.000000000000000000, 0.9659258262890683122, 1.000000000000000000, 0.9659258262890683122, 1.000000000000000000, 0.9659258262890683122, 1.000000000000000000, 0.9659258262890683122, 1.000000000000000000, 0.9659258262890683122, 1.000000000000000000, 0.9659258262890683122, 1.000000000000000000, 0.9659258262890683122, 1.000000000000000000, 0.9659258262890683122, 1.000000000000000000, 0.9659258262890683122, 1.000000000000000000, 0.9659258262890683122, 1.000000000000000000, 0.9659258262890683122, 1.000000000000000000, 0.9659258262890683122, 1.000000000000000000, 0.9659258262890683122, 1.000000000000000000, 0.9659258262890683122, 1.000000000000000000, 0.9659258262890683122, 1.000000000000000000, 0.9659258262890683122, 1.000000000000000000),
 ( 0.3333333333333333703, 0.3219752754296894559, 0.3333333333333333703, 0.3219752754296894559, 0.3333333333333333703, 0.3219752754296894559, 0.3333333333333333703, 0.3219752754296894559, 0.3333333333333333703, 0.3219752754296894559, 0.3333333333333333703, 0.3219752754296894559, 0.3333333333333333703, 0.3219752754296894559, 0.3333333333333333703, 0.3219752754296894559, 0.3333333333333333703, 0.3219752754296894559, 0.3333333333333333703, 0.3219752754296894559, 0.3333333333333333703, 0.3219752754296894559, 0.3333333333333333703, 0.3219752754296894559, 0.3333333333333333703, 0.3219752754296894559, 0.3333333333333333703, 0.3219752754296894559, 0.3333333333333333703, 0.3219752754296894559, 0.3333333333333333703, 0.3219752754296894559, 0.3333333333333333703, 0.3219752754296894559, 0.3333333333333333703, 0.3219752754296894559, 0.3333333333333333703, 0.3219752754296894559, 0.3333333333333333703, 0.3219752754296894559, 0.3333333333333333703, 0.3219752754296894559, 0.3333333333333333703, 0.3219752754296894559, 0.3333333333333333703, 0.3219752754296894559, 0.3333333333333333703, 0.3219752754296894559, 0.3333333333333333703, 0.3219752754296894559, 0.3333333333333333703, 0.3219752754296894559, 0.3333333333333333703, 0.3219752754296894559, 0.3333333333333333703, 0.3219752754296894559, 0.3333333333333333703, 0.3219752754296894559, 0.3333333333333333703, 0.3219752754296894559, 0.3333333333333333703, 0.3219752754296894559, 0.3333333333333333703, 0.3219752754296894559, 0.3333333333333333703, 0.3219752754296894559, 0.3333333333333333703, 0.3219752754296894559, 0.3333333333333333703, 0.3219752754296894559, 0.3333333333333333703, 0.3219752754296894559, 0.3333333333333333703, 0.3219752754296894559, 0.3333333333333333703, 0.3219752754296894559, 0.3333333333333333703, 0.3219752754296894559, 0.3333333333333333703, 0.3219752754296894559, 0.3333333333333333703, 0.3219752754296894559, 0.3333333333333333703, 0.3219752754296894559, 0.3333333333333333703, 0.3219752754296894559, 0.3333333333333333703, 0.3219752754296894559, 0.3333333333333333703, 0.3219752754296894559, 0.3333333333333333703, 0.3219752754296894559, 0.3333333333333333703, 0.3219752754296894559, 0.3333333333333333703, 0.3219752754296894559, 0.3333333333333333703, 0.3219752754296894559, 0.3333333333333333703, 0.3219752754296894559, 0.3333333333333333703, 0.3219752754296894559, 0.3333333333333333703, 0.3219752754296894559, 0.3333333333333333703, 0.3219752754296894559, 0.3333333333333333703, 0.3219752754296894559, 0.3333333333333333703, 0.3219752754296894559, 0.3333333333333333703, 0.3219752754296894559, 0.3333333333333333703, 0.3219752754296894559, 0.3333333333333333703, 0.3219752754296894559, 0.3333333333333333703, 0.3219752754296894559, 0.3333333333333333703, 0.3219752754296894559, 0.3333333333333333703, 0.3219752754296894559, 0.3333333333333333703, 0.3219752754296894559, 0.3333333333333333703, 0.3219752754296894559, 0.3333333333333333703, 0.3219752754296894559, 0.3333333333333333703, 0.3219752754296894559, 0.3333333333333333703, 0.3219752754296894559, 0.3333333333333333703, 0.3219752754296894559, 0.3333333333333333703, 0.3219752754296894559, 0.3333333333333333703, 0.3219752754296894559, 0.3333333333333333703, 0.3219752754296894559, 0.3333333333333333703, 0.3219752754296894559, 0.3333333333333333703, 0.3219752754296894559, 0.3333333333333333703, 0.3219752754296894559, 0.3333333333333333703, 0.3219752754296894559, 0.3333333333333333703, 0.3219752754296894559, 0.3333333333333333703, 0.3219752754296894559, 0.3333333333333333703, 0.3219752754296894559, 0.3333333333333333703, 0.3219752754296894559, 0.3333333333333333703, 0.3219752754296894559, 0.3333333333333333703, 0.3219752754296894559, 0.3333333333333333703, 0.3219752754296894559, 0.3333333333333333703, 0.3219752754296894559, 0.3333333333333333703, 0.3219752754296894559, 0.3333333333333333703, 0.3219752754296894559, 0.3333333333333333703, 0.3219752754296894559, 0.3333333333333333703, 0.3219752754296894559, 0.3333333333333333703, 0.3219752754296894559, 0.3333333333333333703, 0.3219752754296894559, 0.3333333333333333703, 0.3219752754296894559, 0.3333333333333333703, 0.3219752754296894559, 0.3333333333333333703, 0.3219752754296894559, 0.3333333333333333703, 0.3219752754296894559, 0.3333333333333333703, 0.3219752754296894559, 0.3333333333333333703, 0.3219752754296894559, 0.3333333333333333703, 0.3219752754296894559, 0.3333333333333333703, 0.3219752754296894559, 0.3333333333333333703, 0.3219752754296894559, 0.3333333333333333703, 0.3219752754296894559, 0.3333333333333333703, 0.3219752754296894559, 0.3333333333333333703, 0.3219752754296894559, 0.3333333333333333703, 0.3219752754296894559, 0.3333333333333333703, 0.3219752754296894559, 0.3333333333333333703, 0.3219752754296894559, 0.3333333333333333703, 0.3219752754296894559, 0.3333333333333333703, 0.3219752754296894559, 0.3333333333333333703, 0.3219752754296894559, 0.3333333333333333703, 0.3219752754296894559, 0.3333333333333333703, 0.3219752754296894559, 0.3333333333333333703, 0.3219752754296894559, 0.3333333333333333703, 0.3219752754296894559, 0.3333333333333333703, 0.3219752754296894559, 0.3333333333333333703, 0.3219752754296894559, 0.3333333333333333703, 0.3219752754296894559, 0.3333333333333333703, 0.3219752754296894559, 0.3333333333333333703, 0.3219752754296894559, 0.3333333333333333703, 0.3219752754296894559, 0.3333333333333333703, 0.3219752754296894559, 0.3333333333333333703, 0.3219752754296894559, 0.3333333333333333703, 0.3219752754296894559, 0.3333333333333333703, 0.3219752754296894559, 0.3333333333333333703, 0.3219752754296894559, 0.3333333333333333703, 0.3219752754296894559, 0.3333333333333333703, 0.3219752754296894559, 0.3333333333333333703, 0.3219752754296894559, 0.3333333333333333703, 0.3219752754296894559, 0.3333333333333333703, 0.3219752754296894559, 0.3333333333333333703, 0.3219752754296894559, 0.3333333333333333703, 0.3219752754296894559, 0.3333333333333333703, 0.3219752754296894559, 0.3333333333333333703, 0.3219752754296894559, 0.3333333333333333703, 0.3219752754296894559, 0.3333333333333333703, 0.3219752754296894559, 0.3333333333333333703, 0.3219752754296894559, 0.3333333333333333703, 0.3219752754296894559, 0.3333333333333333703, 0.3219752754296894559, 0.3333333333333333703, 0.3219752754296894559, 0.3333333333333333703, 0.3219752754296894559, 0.3333333333333333703, 0.3219752754296894559, 0.3333333333333333703, 0.3219752754296894559, 0.3333333333333333703, 0.3219752754296894559, 0.3333333333333333703, 0.3219752754296894559, 0.3333333333333333703, 0.3219752754296894559, 0.3333333333333333703, 0.3219752754296894559, 0.3333333333333333703, 0.3219752754296894559, 0.3333333333333333703, 0.3219752754296894559, 0.3333333333333333703, 0.3219752754296894559, 0.3333333333333333703, 0.3219752754296894559, 0.3333333333333333703, 0.3219752754296894559, 0.3333333333333333703, 0.3219752754296894559, 0.3333333333333333703, 0.3219752754296894559, 0.3333333333333333703, 0.3219752754296894559, 0.3333333333333333703, 0.3219752754296894559, 0.3333333333333333703, 0.3219752754296894559, 0.3333333333333333703, 0.3219752754296894559, 0.3333333333333333703, 0.3219752754296894559, 0.3333333333333333703, 0.3219752754296894559, 0.3333333333333333703, 0.3219752754296894559, 0.3333333333333333703, 0.3219752754296894559, 0.3333333333333333703, 0.3219752754296894559, 0.3333333333333333703, 0.3219752754296894559, 0.3333333333333333703, 0.3219752754296894559, 0.3333333333333333703, 0.3219752754296894559, 0.3333333333333333703, 0.3219752754296894559, 0.3333333333333333703, 0.3219752754296894559, 0.3333333333333333703, 0.3219752754296894559, 0.3333333333333333703, 0.3219752754296894559, 0.3333333333333333703, 0.3219752754296894559, 0.3333333333333333703, 0.3219752754296894559, 0.3333333333333333703, 0.3219752754296894559, 0.3333333333333333703, 0.3219752754296894559, 0.3333333333333333703, 0.3219752754296894559, 0.3333333333333333703, 0.3219752754296894559, 0.3333333333333333703, 0.3219752754296894559, 0.3333333333333333703, 0.3219752754296894559, 0.3333333333333333703, 0.3219752754296894559, 0.3333333333333333703, 0.3219752754296894559, 0.3333333333333333703, 0.3219752754296894559, 0.3333333333333333703, 0.3219752754296894559, 0.3333333333333333703, 0.3219752754296894559, 0.3333333333333333703, 0.3219752754296894559, 0.3333333333333333703, 0.3219752754296894559, 0.3333333333333333703, 0.3219752754296894559, 0.3333333333333333703, 0.3219752754296894559, 0.3333333333333333703, 0.3219752754296894559, 0.3333333333333333703, 0.3219752754296894559, 0.3333333333333333703, 0.3219752754296894559, 0.3333333333333333703, 0.3219752754296894559, 0.3333333333333333703, 0.3219752754296894559, 0.3333333333333333703, 0.3219752754296894559, 0.3333333333333333703, 0.3219752754296894559, 0.3333333333333333703, 0.3219752754296894559, 0.3333333333333333703, 0.3219752754296894559, 0.3333333333333333703, 0.3219752754296894559, 0.3333333333333333703, 0.3219752754296894559, 0.3333333333333333703, 0.3219752754296894559, 0.3333333333333333703, 0.3219752754296894559, 0.3333333333333333703, 0.3219752754296894559, 0.3333333333333333703, 0.3219752754296894559, 0.3333333333333333703, 0.3219752754296894559, 0.3333333333333333703, 0.3219752754296894559, 0.3333333333333333703, 0.3219752754296894559, 0.3333333333333333703, 0.3219752754296894559, 0.3333333333333333703, 0.3219752754296894559, 0.3333333333333333703, 0.3219752754296894559, 0.3333333333333333703, 0.3219752754296894559, 0.3333333333333333703, 0.3219752754296894559, 0.3333333333333333703, 0.3219752754296894559, 0.3333333333333333703, 0.3219752754296894559, 0.3333333333333333703, 0.3219752754296894559, 0.3333333333333333703, 0.3219752754296894559, 0.3333333333333333703, 0.3219752754296894559, 0.3333333333333333703, 0.3219752754296894559, 0.3333333333333333703, 0.3219752754296894559, 0.3333333333333333703, 0.3219752754296894559, 0.3333333333333333703, 0.3219752754296894559, 0.3333333333333333703, 0.3219752754296894559, 0.3333333333333333703, 0.3219752754296894559, 0.3333333333333333703, 0.3219752754296894559, 0.3333333333333333703, 0.3219752754296894559, 0.3333333333333333703, 0.3219752754296894559, 0.3333333333333333703, 0.3219752754296894559, 0.3333333333333333703, 0.3219752754296894559, 0.3333333333333333703, 0.3219752754296894559, 0.3333333333333333703, 0.3219752754296894559, 0.3333333333333333703, 0.3219752754296894559, 0.3333333333333333703, 0.3219752754296894559, 0.3333333333333333703, 0.3219752754296894559, 0.3333333333333333703, 0.3219752754296894559, 0.3333333333333333703),
 ( 0.3333333333333333703, 0.3219752754296894559, 0.3333333333333333703, 0.3219752754296894559, 0.3333333333333333703, 0.3219752754296894559, 0.3333333333333333703, 0.3219752754296894559, 0.3333333333333333703, 0.3219752754296894559, 0.3333333333333333703, 0.3219752754296894559, 0.3333333333333333703, 0.3219752754296894559, 0.3333333333333333703, 0.3219752754296894559, 0.3333333333333333703, 0.3219752754296894559, 0.3333333333333333703, 0.3219752754296894559, 0.3333333333333333703, 0.3219752754296894559, 0.3333333333333333703, 0.3219752754296894559, 0.3333333333333333703, 0.3219752754296894559, 0.3333333333333333703, 0.3219752754296894559, 0.3333333333333333703, 0.3219752754296894559, 0.3333333333333333703, 0.3219752754296894559, 0.3333333333333333703, 0.3219752754296894559, 0.3333333333333333703, 0.3219752754296894559, 0.3333333333333333703, 0.3219752754296894559, 0.3333333333333333703, 0.3219752754296894559, 0.3333333333333333703, 0.3219752754296894559, 0.3333333333333333703, 0.3219752754296894559, 0.3333333333333333703, 0.3219752754296894559, 0.3333333333333333703, 0.3219752754296894559, 0.3333333333333333703, 0.3219752754296894559, 0.3333333333333333703, 0.3219752754296894559, 0.3333333333333333703, 0.3219752754296894559, 0.3333333333333333703, 0.3219752754296894559, 0.3333333333333333703, 0.3219752754296894559, 0.3333333333333333703, 0.3219752754296894559, 0.3333333333333333703, 0.3219752754296894559, 0.3333333333333333703, 0.3219752754296894559, 0.3333333333333333703, 0.3219752754296894559, 0.3333333333333333703, 0.3219752754296894559, 0.3333333333333333703, 0.3219752754296894559, 0.3333333333333333703, 0.3219752754296894559, 0.3333333333333333703, 0.3219752754296894559, 0.3333333333333333703, 0.3219752754296894559, 0.3333333333333333703, 0.3219752754296894559, 0.3333333333333333703, 0.3219752754296894559, 0.3333333333333333703, 0.3219752754296894559, 0.3333333333333333703, 0.3219752754296894559, 0.3333333333333333703, 0.3219752754296894559, 0.3333333333333333703, 0.3219752754296894559, 0.3333333333333333703, 0.3219752754296894559, 0.3333333333333333703, 0.3219752754296894559, 0.3333333333333333703, 0.3219752754296894559, 0.3333333333333333703, 0.3219752754296894559, 0.3333333333333333703, 0.3219752754296894559, 0.3333333333333333703, 0.3219752754296894559, 0.3333333333333333703, 0.3219752754296894559, 0.3333333333333333703, 0.3219752754296894559, 0.3333333333333333703, 0.3219752754296894559, 0.3333333333333333703, 0.3219752754296894559, 0.3333333333333333703, 0.3219752754296894559, 0.3333333333333333703, 0.3219752754296894559, 0.3333333333333333703, 0.3219752754296894559, 0.3333333333333333703, 0.3219752754296894559, 0.3333333333333333703, 0.3219752754296894559, 0.3333333333333333703, 0.3219752754296894559, 0.3333333333333333703, 0.3219752754296894559, 0.3333333333333333703, 0.3219752754296894559, 0.3333333333333333703, 0.3219752754296894559, 0.3333333333333333703, 0.3219752754296894559, 0.3333333333333333703, 0.3219752754296894559, 0.3333333333333333703, 0.3219752754296894559, 0.3333333333333333703, 0.3219752754296894559, 0.3333333333333333703, 0.3219752754296894559, 0.3333333333333333703, 0.3219752754296894559, 0.3333333333333333703, 0.3219752754296894559, 0.3333333333333333703, 0.3219752754296894559, 0.3333333333333333703, 0.3219752754296894559, 0.3333333333333333703, 0.3219752754296894559, 0.3333333333333333703, 0.3219752754296894559, 0.3333333333333333703, 0.3219752754296894559, 0.3333333333333333703, 0.3219752754296894559, 0.3333333333333333703, 0.3219752754296894559, 0.3333333333333333703, 0.3219752754296894559, 0.3333333333333333703, 0.3219752754296894559, 0.3333333333333333703, 0.3219752754296894559, 0.3333333333333333703, 0.3219752754296894559, 0.3333333333333333703, 0.3219752754296894559, 0.3333333333333333703, 0.3219752754296894559, 0.3333333333333333703, 0.3219752754296894559, 0.3333333333333333703, 0.3219752754296894559, 0.3333333333333333703, 0.3219752754296894559, 0.3333333333333333703, 0.3219752754296894559, 0.3333333333333333703, 0.3219752754296894559, 0.3333333333333333703, 0.3219752754296894559, 0.3333333333333333703, 0.3219752754296894559, 0.3333333333333333703, 0.3219752754296894559, 0.3333333333333333703, 0.3219752754296894559, 0.3333333333333333703, 0.3219752754296894559, 0.3333333333333333703, 0.3219752754296894559, 0.3333333333333333703, 0.3219752754296894559, 0.3333333333333333703, 0.3219752754296894559, 0.3333333333333333703, 0.3219752754296894559, 0.3333333333333333703, 0.3219752754296894559, 0.3333333333333333703, 0.3219752754296894559, 0.3333333333333333703, 0.3219752754296894559, 0.3333333333333333703, 0.3219752754296894559, 0.3333333333333333703, 0.3219752754296894559, 0.3333333333333333703, 0.3219752754296894559, 0.3333333333333333703, 0.3219752754296894559, 0.3333333333333333703, 0.3219752754296894559, 0.3333333333333333703, 0.3219752754296894559, 0.3333333333333333703, 0.3219752754296894559, 0.3333333333333333703, 0.3219752754296894559, 0.3333333333333333703, 0.3219752754296894559, 0.3333333333333333703, 0.3219752754296894559, 0.3333333333333333703, 0.3219752754296894559, 0.3333333333333333703, 0.3219752754296894559, 0.3333333333333333703, 0.3219752754296894559, 0.3333333333333333703, 0.3219752754296894559, 0.3333333333333333703, 0.3219752754296894559, 0.3333333333333333703, 0.3219752754296894559, 0.3333333333333333703, 0.3219752754296894559, 0.3333333333333333703, 0.3219752754296894559, 0.3333333333333333703, 0.3219752754296894559, 0.3333333333333333703, 0.3219752754296894559, 0.3333333333333333703, 0.3219752754296894559, 0.3333333333333333703, 0.3219752754296894559, 0.3333333333333333703, 0.3219752754296894559, 0.3333333333333333703, 0.3219752754296894559, 0.3333333333333333703, 0.3219752754296894559, 0.3333333333333333703, 0.3219752754296894559, 0.3333333333333333703, 0.3219752754296894559, 0.3333333333333333703, 0.3219752754296894559, 0.3333333333333333703, 0.3219752754296894559, 0.3333333333333333703, 0.3219752754296894559, 0.3333333333333333703, 0.3219752754296894559, 0.3333333333333333703, 0.3219752754296894559, 0.3333333333333333703, 0.3219752754296894559, 0.3333333333333333703, 0.3219752754296894559, 0.3333333333333333703, 0.3219752754296894559, 0.3333333333333333703, 0.3219752754296894559, 0.3333333333333333703, 0.3219752754296894559, 0.3333333333333333703, 0.3219752754296894559, 0.3333333333333333703, 0.3219752754296894559, 0.3333333333333333703, 0.3219752754296894559, 0.3333333333333333703, 0.3219752754296894559, 0.3333333333333333703, 0.3219752754296894559, 0.3333333333333333703, 0.3219752754296894559, 0.3333333333333333703, 0.3219752754296894559, 0.3333333333333333703, 0.3219752754296894559, 0.3333333333333333703, 0.3219752754296894559, 0.3333333333333333703, 0.3219752754296894559, 0.3333333333333333703, 0.3219752754296894559, 0.3333333333333333703, 0.3219752754296894559, 0.3333333333333333703, 0.3219752754296894559, 0.3333333333333333703, 0.3219752754296894559, 0.3333333333333333703, 0.3219752754296894559, 0.3333333333333333703, 0.3219752754296894559, 0.3333333333333333703, 0.3219752754296894559, 0.3333333333333333703, 0.3219752754296894559, 0.3333333333333333703, 0.3219752754296894559, 0.3333333333333333703, 0.3219752754296894559, 0.3333333333333333703, 0.3219752754296894559, 0.3333333333333333703, 0.3219752754296894559, 0.3333333333333333703, 0.3219752754296894559, 0.3333333333333333703, 0.3219752754296894559, 0.3333333333333333703, 0.3219752754296894559, 0.3333333333333333703, 0.3219752754296894559, 0.3333333333333333703, 0.3219752754296894559, 0.3333333333333333703, 0.3219752754296894559, 0.3333333333333333703, 0.3219752754296894559, 0.3333333333333333703, 0.3219752754296894559, 0.3333333333333333703, 0.3219752754296894559, 0.3333333333333333703, 0.3219752754296894559, 0.3333333333333333703, 0.3219752754296894559, 0.3333333333333333703, 0.3219752754296894559, 0.3333333333333333703, 0.3219752754296894559, 0.3333333333333333703, 0.3219752754296894559, 0.3333333333333333703, 0.3219752754296894559, 0.3333333333333333703, 0.3219752754296894559, 0.3333333333333333703, 0.3219752754296894559, 0.3333333333333333703, 0.3219752754296894559, 0.3333333333333333703, 0.3219752754296894559, 0.3333333333333333703, 0.3219752754296894559, 0.3333333333333333703, 0.3219752754296894559, 0.3333333333333333703, 0.3219752754296894559, 0.3333333333333333703, 0.3219752754296894559, 0.3333333333333333703, 0.3219752754296894559, 0.3333333333333333703, 0.3219752754296894559, 0.3333333333333333703, 0.3219752754296894559, 0.3333333333333333703, 0.3219752754296894559, 0.3333333333333333703, 0.3219752754296894559, 0.3333333333333333703, 0.3219752754296894559, 0.3333333333333333703, 0.3219752754296894559, 0.3333333333333333703, 0.3219752754296894559, 0.3333333333333333703, 0.3219752754296894559, 0.3333333333333333703, 0.3219752754296894559, 0.3333333333333333703, 0.3219752754296894559, 0.3333333333333333703, 0.3219752754296894559, 0.3333333333333333703, 0.3219752754296894559, 0.3333333333333333703, 0.3219752754296894559, 0.3333333333333333703, 0.3219752754296894559, 0.3333333333333333703, 0.3219752754296894559, 0.3333333333333333703, 0.3219752754296894559, 0.3333333333333333703, 0.3219752754296894559, 0.3333333333333333703, 0.3219752754296894559, 0.3333333333333333703, 0.3219752754296894559, 0.3333333333333333703, 0.3219752754296894559, 0.3333333333333333703, 0.3219752754296894559, 0.3333333333333333703, 0.3219752754296894559, 0.3333333333333333703, 0.3219752754296894559, 0.3333333333333333703, 0.3219752754296894559, 0.3333333333333333703, 0.3219752754296894559, 0.3333333333333333703, 0.3219752754296894559, 0.3333333333333333703, 0.3219752754296894559, 0.3333333333333333703, 0.3219752754296894559, 0.3333333333333333703, 0.3219752754296894559, 0.3333333333333333703, 0.3219752754296894559, 0.3333333333333333703, 0.3219752754296894559, 0.3333333333333333703, 0.3219752754296894559, 0.3333333333333333703, 0.3219752754296894559, 0.3333333333333333703, 0.3219752754296894559, 0.3333333333333333703, 0.3219752754296894559, 0.3333333333333333703, 0.3219752754296894559, 0.3333333333333333703, 0.3219752754296894559, 0.3333333333333333703, 0.3219752754296894559, 0.3333333333333333703, 0.3219752754296894559, 0.3333333333333333703, 0.3219752754296894559, 0.3333333333333333703, 0.3219752754296894559, 0.3333333333333333703, 0.3219752754296894559, 0.3333333333333333703, 0.3219752754296894559, 0.3333333333333333703, 0.3219752754296894559, 0.3333333333333333703, 0.3219752754296894559, 0.3333333333333333703),
 ( 1.000000000000000000, 0.9659258262890683122, 1.000000000000000000, 0.9659258262890683122, 1.000000000000000000, 0.9659258262890683122, 1.000000000000000000, 0.9659258262890683122, 1.000000000000000000, 0.9659258262890683122, 1.000000000000000000, 0.9659258262890683122, 1.000000000000000000, 0.9659258262890683122, 1.000000000000000000, 0.9659258262890683122, 1.000000000000000000, 0.9659258262890683122, 1.000000000000000000, 0.9659258262890683122, 1.000000000000000000, 0.9659258262890683122, 1.000000000000000000, 0.9659258262890683122, 1.000000000000000000, 0.9659258262890683122, 1.000000000000000000, 0.9659258262890683122, 1.000000000000000000, 0.9659258262890683122, 1.000000000000000000, 0.9659258262890683122, 1.000000000000000000, 0.9659258262890683122, 1.000000000000000000, 0.9659258262890683122, 1.000000000000000000, 0.9659258262890683122, 1.000000000000000000, 0.9659258262890683122, 1.000000000000000000, 0.9659258262890683122, 1.000000000000000000, 0.9659258262890683122, 1.000000000000000000, 0.9659258262890683122, 1.000000000000000000, 0.9659258262890683122, 1.000000000000000000, 0.9659258262890683122, 1.000000000000000000, 0.9659258262890683122, 1.000000000000000000, 0.9659258262890683122, 1.000000000000000000, 0.9659258262890683122, 1.000000000000000000, 0.9659258262890683122, 1.000000000000000000, 0.9659258262890683122, 1.000000000000000000, 0.9659258262890683122, 1.000000000000000000, 0.9659258262890683122, 1.000000000000000000, 0.9659258262890683122, 1.000000000000000000, 0.9659258262890683122, 1.000000000000000000, 0.9659258262890683122, 1.000000000000000000, 0.9659258262890683122, 1.000000000000000000, 0.9659258262890683122, 1.000000000000000000, 0.9659258262890683122, 1.000000000000000000, 0.9659258262890683122, 1.000000000000000000, 0.9659258262890683122, 1.000000000000000000, 0.9659258262890683122, 1.000000000000000000, 0.9659258262890683122, 1.000000000000000000, 0.9659258262890683122, 1.000000000000000000, 0.9659258262890683122, 1.000000000000000000, 0.9659258262890683122, 1.000000000000000000, 0.9659258262890683122, 1.000000000000000000, 0.9659258262890683122, 1.000000000000000000, 0.9659258262890683122, 1.000000000000000000, 0.9659258262890683122, 1.000000000000000000, 0.9659258262890683122, 1.000000000000000000, 0.9659258262890683122, 1.000000000000000000, 0.9659258262890683122, 1.000000000000000000, 0.9659258262890683122, 1.000000000000000000, 0.9659258262890683122, 1.000000000000000000, 0.9659258262890683122, 1.000000000000000000, 0.9659258262890683122, 1.000000000000000000, 0.9659258262890683122, 1.000000000000000000, 0.9659258262890683122, 1.000000000000000000, 0.9659258262890683122, 1.000000000000000000, 0.9659258262890683122, 1.000000000000000000, 0.9659258262890683122, 1.000000000000000000, 0.9659258262890683122, 1.000000000000000000, 0.9659258262890683122, 1.000000000000000000, 0.9659258262890683122, 1.000000000000000000, 0.9659258262890683122, 1.000000000000000000, 0.9659258262890683122, 1.000000000000000000, 0.9659258262890683122, 1.000000000000000000, 0.9659258262890683122, 1.000000000000000000, 0.9659258262890683122, 1.000000000000000000, 0.9659258262890683122, 1.000000000000000000, 0.9659258262890683122, 1.000000000000000000, 0.9659258262890683122, 1.000000000000000000, 0.9659258262890683122, 1.000000000000000000, 0.9659258262890683122, 1.000000000000000000, 0.9659258262890683122, 1.000000000000000000, 0.9659258262890683122, 1.000000000000000000, 0.9659258262890683122, 1.000000000000000000, 0.9659258262890683122, 1.000000000000000000, 0.9659258262890683122, 1.000000000000000000, 0.9659258262890683122, 1.000000000000000000, 0.9659258262890683122, 1.000000000000000000, 0.9659258262890683122, 1.000000000000000000, 0.9659258262890683122, 1.000000000000000000, 0.9659258262890683122, 1.000000000000000000, 0.9659258262890683122, 1.000000000000000000, 0.9659258262890683122, 1.000000000000000000, 0.9659258262890683122, 1.000000000000000000, 0.9659258262890683122, 1.000000000000000000, 0.9659258262890683122, 1.000000000000000000, 0.9659258262890683122, 1.000000000000000000, 0.9659258262890683122, 1.000000000000000000, 0.9659258262890683122, 1.000000000000000000, 0.9659258262890683122, 1.000000000000000000, 0.9659258262890683122, 1.000000000000000000, 0.9659258262890683122, 1.000000000000000000, 0.9659258262890683122, 1.000000000000000000, 0.9659258262890683122, 1.000000000000000000, 0.9659258262890683122, 1.000000000000000000, 0.9659258262890683122, 1.000000000000000000, 0.9659258262890683122, 1.000000000000000000, 0.9659258262890683122, 1.000000000000000000, 0.9659258262890683122, 1.000000000000000000, 0.9659258262890683122, 1.000000000000000000, 0.9659258262890683122, 1.000000000000000000, 0.9659258262890683122, 1.000000000000000000, 0.9659258262890683122, 1.000000000000000000, 0.9659258262890683122, 1.000000000000000000, 0.9659258262890683122, 1.000000000000000000, 0.9659258262890683122, 1.000000000000000000, 0.9659258262890683122, 1.000000000000000000, 0.9659258262890683122, 1.000000000000000000, 0.9659258262890683122, 1.000000000000000000, 0.9659258262890683122, 1.000000000000000000, 0.9659258262890683122, 1.000000000000000000, 0.9659258262890683122, 1.000000000000000000, 0.9659258262890683122, 1.000000000000000000, 0.9659258262890683122, 1.000000000000000000, 0.9659258262890683122, 1.000000000000000000, 0.9659258262890683122, 1.000000000000000000, 0.9659258262890683122, 1.000000000000000000, 0.9659258262890683122, 1.000000000000000000, 0.9659258262890683122, 1.000000000000000000, 0.9659258262890683122, 1.000000000000000000, 0.9659258262890683122, 1.000000000000000000, 0.9659258262890683122, 1.000000000000000000, 0.9659258262890683122, 1.000000000000000000, 0.9659258262890683122, 1.000000000000000000, 0.9659258262890683122, 1.000000000000000000, 0.9659258262890683122, 1.000000000000000000, 0.9659258262890683122, 1.000000000000000000, 0.9659258262890683122, 1.000000000000000000, 0.9659258262890683122, 1.000000000000000000, 0.9659258262890683122, 1.000000000000000000, 0.9659258262890683122, 1.000000000000000000, 0.9659258262890683122, 1.000000000000000000, 0.9659258262890683122, 1.000000000000000000, 0.9659258262890683122, 1.000000000000000000, 0.9659258262890683122, 1.000000000000000000, 0.9659258262890683122, 1.000000000000000000, 0.9659258262890683122, 1.000000000000000000, 0.9659258262890683122, 1.000000000000000000, 0.9659258262890683122, 1.000000000000000000, 0.9659258262890683122, 1.000000000000000000, 0.9659258262890683122, 1.000000000000000000, 0.9659258262890683122, 1.000000000000000000, 0.9659258262890683122, 1.000000000000000000, 0.9659258262890683122, 1.000000000000000000, 0.9659258262890683122, 1.000000000000000000, 0.9659258262890683122, 1.000000000000000000, 0.9659258262890683122, 1.000000000000000000, 0.9659258262890683122, 1.000000000000000000, 0.9659258262890683122, 1.000000000000000000, 0.9659258262890683122, 1.000000000000000000, 0.9659258262890683122, 1.000000000000000000, 0.9659258262890683122, 1.000000000000000000, 0.9659258262890683122, 1.000000000000000000, 0.9659258262890683122, 1.000000000000000000, 0.9659258262890683122, 1.000000000000000000, 0.9659258262890683122, 1.000000000000000000, 0.9659258262890683122, 1.000000000000000000, 0.9659258262890683122, 1.000000000000000000, 0.9659258262890683122, 1.000000000000000000, 0.9659258262890683122, 1.000000000000000000, 0.9659258262890683122, 1.000000000000000000, 0.9659258262890683122, 1.000000000000000000, 0.9659258262890683122, 1.000000000000000000, 0.9659258262890683122, 1.000000000000000000, 0.9659258262890683122, 1.000000000000000000, 0.9659258262890683122, 1.000000000000000000, 0.9659258262890683122, 1.000000000000000000, 0.9659258262890683122, 1.000000000000000000, 0.9659258262890683122, 1.000000000000000000, 0.9659258262890683122, 1.000000000000000000, 0.9659258262890683122, 1.000000000000000000, 0.9659258262890683122, 1.000000000000000000, 0.9659258262890683122, 1.000000000000000000, 0.9659258262890683122, 1.000000000000000000, 0.9659258262890683122, 1.000000000000000000, 0.9659258262890683122, 1.000000000000000000, 0.9659258262890683122, 1.000000000000000000, 0.9659258262890683122, 1.000000000000000000, 0.9659258262890683122, 1.000000000000000000, 0.9659258262890683122, 1.000000000000000000, 0.9659258262890683122, 1.000000000000000000, 0.9659258262890683122, 1.000000000000000000, 0.9659258262890683122, 1.000000000000000000, 0.9659258262890683122, 1.000000000000000000, 0.9659258262890683122, 1.000000000000000000, 0.9659258262890683122, 1.000000000000000000, 0.9659258262890683122, 1.000000000000000000, 0.9659258262890683122, 1.000000000000000000, 0.9659258262890683122, 1.000000000000000000, 0.9659258262890683122, 1.000000000000000000, 0.9659258262890683122, 1.000000000000000000, 0.9659258262890683122, 1.000000000000000000, 0.9659258262890683122, 1.000000000000000000, 0.9659258262890683122, 1.000000000000000000, 0.9659258262890683122, 1.000000000000000000, 0.9659258262890683122, 1.000000000000000000, 0.9659258262890683122, 1.000000000000000000, 0.9659258262890683122, 1.000000000000000000, 0.9659258262890683122, 1.000000000000000000, 0.9659258262890683122, 1.000000000000000000, 0.9659258262890683122, 1.000000000000000000, 0.9659258262890683122, 1.000000000000000000, 0.9659258262890683122, 1.000000000000000000, 0.9659258262890683122, 1.000000000000000000, 0.9659258262890683122, 1.000000000000000000, 0.9659258262890683122, 1.000000000000000000, 0.9659258262890683122, 1.000000000000000000, 0.9659258262890683122, 1.000000000000000000, 0.9659258262890683122, 1.000000000000000000, 0.9659258262890683122, 1.000000000000000000, 0.9659258262890683122, 1.000000000000000000, 0.9659258262890683122, 1.000000000000000000, 0.9659258262890683122, 1.000000000000000000, 0.9659258262890683122, 1.000000000000000000, 0.9659258262890683122, 1.000000000000000000, 0.9659258262890683122, 1.000000000000000000, 0.9659258262890683122, 1.000000000000000000, 0.9659258262890683122, 1.000000000000000000, 0.9659258262890683122, 1.000000000000000000, 0.9659258262890683122, 1.000000000000000000, 0.9659258262890683122, 1.000000000000000000, 0.9659258262890683122, 1.000000000000000000, 0.9659258262890683122, 1.000000000000000000, 0.9659258262890683122, 1.000000000000000000, 0.9659258262890683122, 1.000000000000000000),
 ( 0.3333333333333333703, 0.3219752754296894559, 0.3333333333333333703, 0.3219752754296894559, 0.3333333333333333703, 0.3219752754296894559, 0.3333333333333333703, 0.3219752754296894559, 0.3333333333333333703, 0.3219752754296894559, 0.3333333333333333703, 0.3219752754296894559, 0.3333333333333333703, 0.3219752754296894559, 0.3333333333333333703, 0.3219752754296894559, 0.3333333333333333703, 0.3219752754296894559, 0.3333333333333333703, 0.3219752754296894559, 0.3333333333333333703, 0.3219752754296894559, 0.3333333333333333703, 0.3219752754296894559, 0.3333333333333333703, 0.3219752754296894559, 0.3333333333333333703, 0.3219752754296894559, 0.3333333333333333703, 0.3219752754296894559, 0.3333333333333333703, 0.3219752754296894559, 0.3333333333333333703, 0.3219752754296894559, 0.3333333333333333703, 0.3219752754296894559, 0.3333333333333333703, 0.3219752754296894559, 0.3333333333333333703, 0.3219752754296894559, 0.3333333333333333703, 0.3219752754296894559, 0.3333333333333333703, 0.3219752754296894559, 0.3333333333333333703, 0.3219752754296894559, 0.3333333333333333703, 0.3219752754296894559, 0.3333333333333333703, 0.3219752754296894559, 0.3333333333333333703, 0.3219752754296894559, 0.3333333333333333703, 0.3219752754296894559, 0.3333333333333333703, 0.3219752754296894559, 0.3333333333333333703, 0.3219752754296894559, 0.3333333333333333703, 0.3219752754296894559, 0.3333333333333333703, 0.3219752754296894559, 0.3333333333333333703, 0.3219752754296894559, 0.3333333333333333703, 0.3219752754296894559, 0.3333333333333333703, 0.3219752754296894559, 0.3333333333333333703, 0.3219752754296894559, 0.3333333333333333703, 0.3219752754296894559, 0.3333333333333333703, 0.3219752754296894559, 0.3333333333333333703, 0.3219752754296894559, 0.3333333333333333703, 0.3219752754296894559, 0.3333333333333333703, 0.3219752754296894559, 0.3333333333333333703, 0.3219752754296894559, 0.3333333333333333703, 0.3219752754296894559, 0.3333333333333333703, 0.3219752754296894559, 0.3333333333333333703, 0.3219752754296894559, 0.3333333333333333703, 0.3219752754296894559, 0.3333333333333333703, 0.3219752754296894559, 0.3333333333333333703, 0.3219752754296894559, 0.3333333333333333703, 0.3219752754296894559, 0.3333333333333333703, 0.3219752754296894559, 0.3333333333333333703, 0.3219752754296894559, 0.3333333333333333703, 0.3219752754296894559, 0.3333333333333333703, 0.3219752754296894559, 0.3333333333333333703, 0.3219752754296894559, 0.3333333333333333703, 0.3219752754296894559, 0.3333333333333333703, 0.3219752754296894559, 0.3333333333333333703, 0.3219752754296894559, 0.3333333333333333703, 0.3219752754296894559, 0.3333333333333333703, 0.3219752754296894559, 0.3333333333333333703, 0.3219752754296894559, 0.3333333333333333703, 0.3219752754296894559, 0.3333333333333333703, 0.3219752754296894559, 0.3333333333333333703, 0.3219752754296894559, 0.3333333333333333703, 0.3219752754296894559, 0.3333333333333333703, 0.3219752754296894559, 0.3333333333333333703, 0.3219752754296894559, 0.3333333333333333703, 0.3219752754296894559, 0.3333333333333333703, 0.3219752754296894559, 0.3333333333333333703, 0.3219752754296894559, 0.3333333333333333703, 0.3219752754296894559, 0.3333333333333333703, 0.3219752754296894559, 0.3333333333333333703, 0.3219752754296894559, 0.3333333333333333703, 0.3219752754296894559, 0.3333333333333333703, 0.3219752754296894559, 0.3333333333333333703, 0.3219752754296894559, 0.3333333333333333703, 0.3219752754296894559, 0.3333333333333333703, 0.3219752754296894559, 0.3333333333333333703, 0.3219752754296894559, 0.3333333333333333703, 0.3219752754296894559, 0.3333333333333333703, 0.3219752754296894559, 0.3333333333333333703, 0.3219752754296894559, 0.3333333333333333703, 0.3219752754296894559, 0.3333333333333333703, 0.3219752754296894559, 0.3333333333333333703, 0.3219752754296894559, 0.3333333333333333703, 0.3219752754296894559, 0.3333333333333333703, 0.3219752754296894559, 0.3333333333333333703, 0.3219752754296894559, 0.3333333333333333703, 0.3219752754296894559, 0.3333333333333333703, 0.3219752754296894559, 0.3333333333333333703, 0.3219752754296894559, 0.3333333333333333703, 0.3219752754296894559, 0.3333333333333333703, 0.3219752754296894559, 0.3333333333333333703, 0.3219752754296894559, 0.3333333333333333703, 0.3219752754296894559, 0.3333333333333333703, 0.3219752754296894559, 0.3333333333333333703, 0.3219752754296894559, 0.3333333333333333703, 0.3219752754296894559, 0.3333333333333333703, 0.3219752754296894559, 0.3333333333333333703, 0.3219752754296894559, 0.3333333333333333703, 0.3219752754296894559, 0.3333333333333333703, 0.3219752754296894559, 0.3333333333333333703, 0.3219752754296894559, 0.3333333333333333703, 0.3219752754296894559, 0.3333333333333333703, 0.3219752754296894559, 0.3333333333333333703, 0.3219752754296894559, 0.3333333333333333703, 0.3219752754296894559, 0.3333333333333333703, 0.3219752754296894559, 0.3333333333333333703, 0.3219752754296894559, 0.3333333333333333703, 0.3219752754296894559, 0.3333333333333333703, 0.3219752754296894559, 0.3333333333333333703, 0.3219752754296894559, 0.3333333333333333703, 0.3219752754296894559, 0.3333333333333333703, 0.3219752754296894559, 0.3333333333333333703, 0.3219752754296894559, 0.3333333333333333703, 0.3219752754296894559, 0.3333333333333333703, 0.3219752754296894559, 0.3333333333333333703, 0.3219752754296894559, 0.3333333333333333703, 0.3219752754296894559, 0.3333333333333333703, 0.3219752754296894559, 0.3333333333333333703, 0.3219752754296894559, 0.3333333333333333703, 0.3219752754296894559, 0.3333333333333333703, 0.3219752754296894559, 0.3333333333333333703, 0.3219752754296894559, 0.3333333333333333703, 0.3219752754296894559, 0.3333333333333333703, 0.3219752754296894559, 0.3333333333333333703, 0.3219752754296894559, 0.3333333333333333703, 0.3219752754296894559, 0.3333333333333333703, 0.3219752754296894559, 0.3333333333333333703, 0.3219752754296894559, 0.3333333333333333703, 0.3219752754296894559, 0.3333333333333333703, 0.3219752754296894559, 0.3333333333333333703, 0.3219752754296894559, 0.3333333333333333703, 0.3219752754296894559, 0.3333333333333333703, 0.3219752754296894559, 0.3333333333333333703, 0.3219752754296894559, 0.3333333333333333703, 0.3219752754296894559, 0.3333333333333333703, 0.3219752754296894559, 0.3333333333333333703, 0.3219752754296894559, 0.3333333333333333703, 0.3219752754296894559, 0.3333333333333333703, 0.3219752754296894559, 0.3333333333333333703, 0.3219752754296894559, 0.3333333333333333703, 0.3219752754296894559, 0.3333333333333333703, 0.3219752754296894559, 0.3333333333333333703, 0.3219752754296894559, 0.3333333333333333703, 0.3219752754296894559, 0.3333333333333333703, 0.3219752754296894559, 0.3333333333333333703, 0.3219752754296894559, 0.3333333333333333703, 0.3219752754296894559, 0.3333333333333333703, 0.3219752754296894559, 0.3333333333333333703, 0.3219752754296894559, 0.3333333333333333703, 0.3219752754296894559, 0.3333333333333333703, 0.3219752754296894559, 0.3333333333333333703, 0.3219752754296894559, 0.3333333333333333703, 0.3219752754296894559, 0.3333333333333333703, 0.3219752754296894559, 0.3333333333333333703, 0.3219752754296894559, 0.3333333333333333703, 0.3219752754296894559, 0.3333333333333333703, 0.3219752754296894559, 0.3333333333333333703, 0.3219752754296894559, 0.3333333333333333703, 0.3219752754296894559, 0.3333333333333333703, 0.3219752754296894559, 0.3333333333333333703, 0.3219752754296894559, 0.3333333333333333703, 0.3219752754296894559, 0.3333333333333333703, 0.3219752754296894559, 0.3333333333333333703, 0.3219752754296894559, 0.3333333333333333703, 0.3219752754296894559, 0.3333333333333333703, 0.3219752754296894559, 0.3333333333333333703, 0.3219752754296894559, 0.3333333333333333703, 0.3219752754296894559, 0.3333333333333333703, 0.3219752754296894559, 0.3333333333333333703, 0.3219752754296894559, 0.3333333333333333703, 0.3219752754296894559, 0.3333333333333333703, 0.3219752754296894559, 0.3333333333333333703, 0.3219752754296894559, 0.3333333333333333703, 0.3219752754296894559, 0.3333333333333333703, 0.3219752754296894559, 0.3333333333333333703, 0.3219752754296894559, 0.3333333333333333703, 0.3219752754296894559, 0.3333333333333333703, 0.3219752754296894559, 0.3333333333333333703, 0.3219752754296894559, 0.3333333333333333703, 0.3219752754296894559, 0.3333333333333333703, 0.3219752754296894559, 0.3333333333333333703, 0.3219752754296894559, 0.3333333333333333703, 0.3219752754296894559, 0.3333333333333333703, 0.3219752754296894559, 0.3333333333333333703, 0.3219752754296894559, 0.3333333333333333703, 0.3219752754296894559, 0.3333333333333333703, 0.3219752754296894559, 0.3333333333333333703, 0.3219752754296894559, 0.3333333333333333703, 0.3219752754296894559, 0.3333333333333333703, 0.3219752754296894559, 0.3333333333333333703, 0.3219752754296894559, 0.3333333333333333703, 0.3219752754296894559, 0.3333333333333333703, 0.3219752754296894559, 0.3333333333333333703, 0.3219752754296894559, 0.3333333333333333703, 0.3219752754296894559, 0.3333333333333333703, 0.3219752754296894559, 0.3333333333333333703, 0.3219752754296894559, 0.3333333333333333703, 0.3219752754296894559, 0.3333333333333333703, 0.3219752754296894559, 0.3333333333333333703, 0.3219752754296894559, 0.3333333333333333703, 0.3219752754296894559, 0.3333333333333333703, 0.3219752754296894559, 0.3333333333333333703, 0.3219752754296894559, 0.3333333333333333703, 0.3219752754296894559, 0.3333333333333333703, 0.3219752754296894559, 0.3333333333333333703, 0.3219752754296894559, 0.3333333333333333703, 0.3219752754296894559, 0.3333333333333333703, 0.3219752754296894559, 0.3333333333333333703, 0.3219752754296894559, 0.3333333333333333703, 0.3219752754296894559, 0.3333333333333333703, 0.3219752754296894559, 0.3333333333333333703, 0.3219752754296894559, 0.3333333333333333703, 0.3219752754296894559, 0.3333333333333333703, 0.3219752754296894559, 0.3333333333333333703, 0.3219752754296894559, 0.3333333333333333703, 0.3219752754296894559, 0.3333333333333333703, 0.3219752754296894559, 0.3333333333333333703, 0.3219752754296894559, 0.3333333333333333703, 0.3219752754296894559, 0.3333333333333333703, 0.3219752754296894559, 0.3333333333333333703, 0.3219752754296894559, 0.3333333333333333703, 0.3219752754296894559, 0.3333333333333333703, 0.3219752754296894559, 0.3333333333333333703, 0.3219752754296894559, 0.3333333333333333703, 0.3219752754296894559, 0.3333333333333333703, 0.3219752754296894559, 0.3333333333333333703, 0.3219752754296894559, 0.3333333333333333703, 0.3219752754296894559, 0.3333333333333333703),
 ( 0.3333333333333333703, 0.3219752754296894559, 0.3333333333333333703, 0.3219752754296894559, 0.3333333333333333703, 0.3219752754296894559, 0.3333333333333333703, 0.3219752754296894559, 0.3333333333333333703, 0.3219752754296894559, 0.3333333333333333703, 0.3219752754296894559, 0.3333333333333333703, 0.3219752754296894559, 0.3333333333333333703, 0.3219752754296894559, 0.3333333333333333703, 0.3219752754296894559, 0.3333333333333333703, 0.3219752754296894559, 0.3333333333333333703, 0.3219752754296894559, 0.3333333333333333703, 0.3219752754296894559, 0.3333333333333333703, 0.3219752754296894559, 0.3333333333333333703, 0.3219752754296894559, 0.3333333333333333703, 0.3219752754296894559, 0.3333333333333333703, 0.3219752754296894559, 0.3333333333333333703, 0.3219752754296894559, 0.3333333333333333703, 0.3219752754296894559, 0.3333333333333333703, 0.3219752754296894559, 0.3333333333333333703, 0.3219752754296894559, 0.3333333333333333703, 0.3219752754296894559, 0.3333333333333333703, 0.3219752754296894559, 0.3333333333333333703, 0.3219752754296894559, 0.3333333333333333703, 0.3219752754296894559, 0.3333333333333333703, 0.3219752754296894559, 0.3333333333333333703, 0.3219752754296894559, 0.3333333333333333703, 0.3219752754296894559, 0.3333333333333333703, 0.3219752754296894559, 0.3333333333333333703, 0.3219752754296894559, 0.3333333333333333703, 0.3219752754296894559, 0.3333333333333333703, 0.3219752754296894559, 0.3333333333333333703, 0.3219752754296894559, 0.3333333333333333703, 0.3219752754296894559, 0.3333333333333333703, 0.3219752754296894559, 0.3333333333333333703, 0.3219752754296894559, 0.3333333333333333703, 0.3219752754296894559, 0.3333333333333333703, 0.3219752754296894559, 0.3333333333333333703, 0.3219752754296894559, 0.3333333333333333703, 0.3219752754296894559, 0.3333333333333333703, 0.3219752754296894559, 0.3333333333333333703, 0.3219752754296894559, 0.3333333333333333703, 0.3219752754296894559, 0.3333333333333333703, 0.3219752754296894559, 0.3333333333333333703, 0.3219752754296894559, 0.3333333333333333703, 0.3219752754296894559, 0.3333333333333333703, 0.3219752754296894559, 0.3333333333333333703, 0.3219752754296894559, 0.3333333333333333703, 0.3219752754296894559, 0.3333333333333333703, 0.3219752754296894559, 0.3333333333333333703, 0.3219752754296894559, 0.3333333333333333703, 0.3219752754296894559, 0.3333333333333333703, 0.3219752754296894559, 0.3333333333333333703, 0.3219752754296894559, 0.3333333333333333703, 0.3219752754296894559, 0.3333333333333333703, 0.3219752754296894559, 0.3333333333333333703, 0.3219752754296894559, 0.3333333333333333703, 0.3219752754296894559, 0.3333333333333333703, 0.3219752754296894559, 0.3333333333333333703, 0.3219752754296894559, 0.3333333333333333703, 0.3219752754296894559, 0.3333333333333333703, 0.3219752754296894559, 0.3333333333333333703, 0.3219752754296894559, 0.3333333333333333703, 0.3219752754296894559, 0.3333333333333333703, 0.3219752754296894559, 0.3333333333333333703, 0.3219752754296894559, 0.3333333333333333703, 0.3219752754296894559, 0.3333333333333333703, 0.3219752754296894559, 0.3333333333333333703, 0.3219752754296894559, 0.3333333333333333703, 0.3219752754296894559, 0.3333333333333333703, 0.3219752754296894559, 0.3333333333333333703, 0.3219752754296894559, 0.3333333333333333703, 0.3219752754296894559, 0.3333333333333333703, 0.3219752754296894559, 0.3333333333333333703, 0.3219752754296894559, 0.3333333333333333703, 0.3219752754296894559, 0.3333333333333333703, 0.3219752754296894559, 0.3333333333333333703, 0.3219752754296894559, 0.3333333333333333703, 0.3219752754296894559, 0.3333333333333333703, 0.3219752754296894559, 0.3333333333333333703, 0.3219752754296894559, 0.3333333333333333703, 0.3219752754296894559, 0.3333333333333333703, 0.3219752754296894559, 0.3333333333333333703, 0.3219752754296894559, 0.3333333333333333703, 0.3219752754296894559, 0.3333333333333333703, 0.3219752754296894559, 0.3333333333333333703, 0.3219752754296894559, 0.3333333333333333703, 0.3219752754296894559, 0.3333333333333333703, 0.3219752754296894559, 0.3333333333333333703, 0.3219752754296894559, 0.3333333333333333703, 0.3219752754296894559, 0.3333333333333333703, 0.3219752754296894559, 0.3333333333333333703, 0.3219752754296894559, 0.3333333333333333703, 0.3219752754296894559, 0.3333333333333333703, 0.3219752754296894559, 0.3333333333333333703, 0.3219752754296894559, 0.3333333333333333703, 0.3219752754296894559, 0.3333333333333333703, 0.3219752754296894559, 0.3333333333333333703, 0.3219752754296894559, 0.3333333333333333703, 0.3219752754296894559, 0.3333333333333333703, 0.3219752754296894559, 0.3333333333333333703, 0.3219752754296894559, 0.3333333333333333703, 0.3219752754296894559, 0.3333333333333333703, 0.3219752754296894559, 0.3333333333333333703, 0.3219752754296894559, 0.3333333333333333703, 0.3219752754296894559, 0.3333333333333333703, 0.3219752754296894559, 0.3333333333333333703, 0.3219752754296894559, 0.3333333333333333703, 0.3219752754296894559, 0.3333333333333333703, 0.3219752754296894559, 0.3333333333333333703, 0.3219752754296894559, 0.3333333333333333703, 0.3219752754296894559, 0.3333333333333333703, 0.3219752754296894559, 0.3333333333333333703, 0.3219752754296894559, 0.3333333333333333703, 0.3219752754296894559, 0.3333333333333333703, 0.3219752754296894559, 0.3333333333333333703, 0.3219752754296894559, 0.3333333333333333703, 0.3219752754296894559, 0.3333333333333333703, 0.3219752754296894559, 0.3333333333333333703, 0.3219752754296894559, 0.3333333333333333703, 0.3219752754296894559, 0.3333333333333333703, 0.3219752754296894559, 0.3333333333333333703, 0.3219752754296894559, 0.3333333333333333703, 0.3219752754296894559, 0.3333333333333333703, 0.3219752754296894559, 0.3333333333333333703, 0.3219752754296894559, 0.3333333333333333703, 0.3219752754296894559, 0.3333333333333333703, 0.3219752754296894559, 0.3333333333333333703, 0.3219752754296894559, 0.3333333333333333703, 0.3219752754296894559, 0.3333333333333333703, 0.3219752754296894559, 0.3333333333333333703, 0.3219752754296894559, 0.3333333333333333703, 0.3219752754296894559, 0.3333333333333333703, 0.3219752754296894559, 0.3333333333333333703, 0.3219752754296894559, 0.3333333333333333703, 0.3219752754296894559, 0.3333333333333333703, 0.3219752754296894559, 0.3333333333333333703, 0.3219752754296894559, 0.3333333333333333703, 0.3219752754296894559, 0.3333333333333333703, 0.3219752754296894559, 0.3333333333333333703, 0.3219752754296894559, 0.3333333333333333703, 0.3219752754296894559, 0.3333333333333333703, 0.3219752754296894559, 0.3333333333333333703, 0.3219752754296894559, 0.3333333333333333703, 0.3219752754296894559, 0.3333333333333333703, 0.3219752754296894559, 0.3333333333333333703, 0.3219752754296894559, 0.3333333333333333703, 0.3219752754296894559, 0.3333333333333333703, 0.3219752754296894559, 0.3333333333333333703, 0.3219752754296894559, 0.3333333333333333703, 0.3219752754296894559, 0.3333333333333333703, 0.3219752754296894559, 0.3333333333333333703, 0.3219752754296894559, 0.3333333333333333703, 0.3219752754296894559, 0.3333333333333333703, 0.3219752754296894559, 0.3333333333333333703, 0.3219752754296894559, 0.3333333333333333703, 0.3219752754296894559, 0.3333333333333333703, 0.3219752754296894559, 0.3333333333333333703, 0.3219752754296894559, 0.3333333333333333703, 0.3219752754296894559, 0.3333333333333333703, 0.3219752754296894559, 0.3333333333333333703, 0.3219752754296894559, 0.3333333333333333703, 0.3219752754296894559, 0.3333333333333333703, 0.3219752754296894559, 0.3333333333333333703, 0.3219752754296894559, 0.3333333333333333703, 0.3219752754296894559, 0.3333333333333333703, 0.3219752754296894559, 0.3333333333333333703, 0.3219752754296894559, 0.3333333333333333703, 0.3219752754296894559, 0.3333333333333333703, 0.3219752754296894559, 0.3333333333333333703, 0.3219752754296894559, 0.3333333333333333703, 0.3219752754296894559, 0.3333333333333333703, 0.3219752754296894559, 0.3333333333333333703, 0.3219752754296894559, 0.3333333333333333703, 0.3219752754296894559, 0.3333333333333333703, 0.3219752754296894559, 0.3333333333333333703, 0.3219752754296894559, 0.3333333333333333703, 0.3219752754296894559, 0.3333333333333333703, 0.3219752754296894559, 0.3333333333333333703, 0.3219752754296894559, 0.3333333333333333703, 0.3219752754296894559, 0.3333333333333333703, 0.3219752754296894559, 0.3333333333333333703, 0.3219752754296894559, 0.3333333333333333703, 0.3219752754296894559, 0.3333333333333333703, 0.3219752754296894559, 0.3333333333333333703, 0.3219752754296894559, 0.3333333333333333703, 0.3219752754296894559, 0.3333333333333333703, 0.3219752754296894559, 0.3333333333333333703, 0.3219752754296894559, 0.3333333333333333703, 0.3219752754296894559, 0.3333333333333333703, 0.3219752754296894559, 0.3333333333333333703, 0.3219752754296894559, 0.3333333333333333703, 0.3219752754296894559, 0.3333333333333333703, 0.3219752754296894559, 0.3333333333333333703, 0.3219752754296894559, 0.3333333333333333703, 0.3219752754296894559, 0.3333333333333333703, 0.3219752754296894559, 0.3333333333333333703, 0.3219752754296894559, 0.3333333333333333703, 0.3219752754296894559, 0.3333333333333333703, 0.3219752754296894559, 0.3333333333333333703, 0.3219752754296894559, 0.3333333333333333703, 0.3219752754296894559, 0.3333333333333333703, 0.3219752754296894559, 0.3333333333333333703, 0.3219752754296894559, 0.3333333333333333703, 0.3219752754296894559, 0.3333333333333333703, 0.3219752754296894559, 0.3333333333333333703, 0.3219752754296894559, 0.3333333333333333703, 0.3219752754296894559, 0.3333333333333333703, 0.3219752754296894559, 0.3333333333333333703, 0.3219752754296894559, 0.3333333333333333703, 0.3219752754296894559, 0.3333333333333333703, 0.3219752754296894559, 0.3333333333333333703, 0.3219752754296894559, 0.3333333333333333703, 0.3219752754296894559, 0.3333333333333333703, 0.3219752754296894559, 0.3333333333333333703, 0.3219752754296894559, 0.3333333333333333703, 0.3219752754296894559, 0.3333333333333333703, 0.3219752754296894559, 0.3333333333333333703, 0.3219752754296894559, 0.3333333333333333703, 0.3219752754296894559, 0.3333333333333333703, 0.3219752754296894559, 0.3333333333333333703, 0.3219752754296894559, 0.3333333333333333703, 0.3219752754296894559, 0.3333333333333333703, 0.3219752754296894559, 0.3333333333333333703, 0.3219752754296894559, 0.3333333333333333703, 0.3219752754296894559, 0.3333333333333333703, 0.3219752754296894559, 0.3333333333333333703, 0.3219752754296894559, 0.3333333333333333703, 0.3219752754296894559, 0.3333333333333333703),
 ( 1.000000000000000000, 0.9659258262890683122, 1.000000000000000000, 0.9659258262890683122, 1.000000000000000000, 0.9659258262890683122, 1.000000000000000000, 0.9659258262890683122, 1.000000000000000000, 0.9659258262890683122, 1.000000000000000000, 0.9659258262890683122, 1.000000000000000000, 0.9659258262890683122, 1.000000000000000000, 0.9659258262890683122, 1.000000000000000000, 0.9659258262890683122, 1.000000000000000000, 0.9659258262890683122, 1.000000000000000000, 0.9659258262890683122, 1.000000000000000000, 0.9659258262890683122, 1.000000000000000000, 0.9659258262890683122, 1.000000000000000000, 0.9659258262890683122, 1.000000000000000000, 0.9659258262890683122, 1.000000000000000000, 0.9659258262890683122, 1.000000000000000000, 0.9659258262890683122, 1.000000000000000000, 0.9659258262890683122, 1.000000000000000000, 0.9659258262890683122, 1.000000000000000000, 0.9659258262890683122, 1.000000000000000000, 0.9659258262890683122, 1.000000000000000000, 0.9659258262890683122, 1.000000000000000000, 0.9659258262890683122, 1.000000000000000000, 0.9659258262890683122, 1.000000000000000000, 0.9659258262890683122, 1.000000000000000000, 0.9659258262890683122, 1.000000000000000000, 0.9659258262890683122, 1.000000000000000000, 0.9659258262890683122, 1.000000000000000000, 0.9659258262890683122, 1.000000000000000000, 0.9659258262890683122, 1.000000000000000000, 0.9659258262890683122, 1.000000000000000000, 0.9659258262890683122, 1.000000000000000000, 0.9659258262890683122, 1.000000000000000000, 0.9659258262890683122, 1.000000000000000000, 0.9659258262890683122, 1.000000000000000000, 0.9659258262890683122, 1.000000000000000000, 0.9659258262890683122, 1.000000000000000000, 0.9659258262890683122, 1.000000000000000000, 0.9659258262890683122, 1.000000000000000000, 0.9659258262890683122, 1.000000000000000000, 0.9659258262890683122, 1.000000000000000000, 0.9659258262890683122, 1.000000000000000000, 0.9659258262890683122, 1.000000000000000000, 0.9659258262890683122, 1.000000000000000000, 0.9659258262890683122, 1.000000000000000000, 0.9659258262890683122, 1.000000000000000000, 0.9659258262890683122, 1.000000000000000000, 0.9659258262890683122, 1.000000000000000000, 0.9659258262890683122, 1.000000000000000000, 0.9659258262890683122, 1.000000000000000000, 0.9659258262890683122, 1.000000000000000000, 0.9659258262890683122, 1.000000000000000000, 0.9659258262890683122, 1.000000000000000000, 0.9659258262890683122, 1.000000000000000000, 0.9659258262890683122, 1.000000000000000000, 0.9659258262890683122, 1.000000000000000000, 0.9659258262890683122, 1.000000000000000000, 0.9659258262890683122, 1.000000000000000000, 0.9659258262890683122, 1.000000000000000000, 0.9659258262890683122, 1.000000000000000000, 0.9659258262890683122, 1.000000000000000000, 0.9659258262890683122, 1.000000000000000000, 0.9659258262890683122, 1.000000000000000000, 0.9659258262890683122, 1.000000000000000000, 0.9659258262890683122, 1.000000000000000000, 0.9659258262890683122, 1.000000000000000000, 0.9659258262890683122, 1.000000000000000000, 0.9659258262890683122, 1.000000000000000000, 0.9659258262890683122, 1.000000000000000000, 0.9659258262890683122, 1.000000000000000000, 0.9659258262890683122, 1.000000000000000000, 0.9659258262890683122, 1.000000000000000000, 0.9659258262890683122, 1.000000000000000000, 0.9659258262890683122, 1.000000000000000000, 0.9659258262890683122, 1.000000000000000000, 0.9659258262890683122, 1.000000000000000000, 0.9659258262890683122, 1.000000000000000000, 0.9659258262890683122, 1.000000000000000000, 0.9659258262890683122, 1.000000000000000000, 0.9659258262890683122, 1.000000000000000000, 0.9659258262890683122, 1.000000000000000000, 0.9659258262890683122, 1.000000000000000000, 0.9659258262890683122, 1.000000000000000000, 0.9659258262890683122, 1.000000000000000000, 0.9659258262890683122, 1.000000000000000000, 0.9659258262890683122, 1.000000000000000000, 0.9659258262890683122, 1.000000000000000000, 0.9659258262890683122, 1.000000000000000000, 0.9659258262890683122, 1.000000000000000000, 0.9659258262890683122, 1.000000000000000000, 0.9659258262890683122, 1.000000000000000000, 0.9659258262890683122, 1.000000000000000000, 0.9659258262890683122, 1.000000000000000000, 0.9659258262890683122, 1.000000000000000000, 0.9659258262890683122, 1.000000000000000000, 0.9659258262890683122, 1.000000000000000000, 0.9659258262890683122, 1.000000000000000000, 0.9659258262890683122, 1.000000000000000000, 0.9659258262890683122, 1.000000000000000000, 0.9659258262890683122, 1.000000000000000000, 0.9659258262890683122, 1.000000000000000000, 0.9659258262890683122, 1.000000000000000000, 0.9659258262890683122, 1.000000000000000000, 0.9659258262890683122, 1.000000000000000000, 0.9659258262890683122, 1.000000000000000000, 0.9659258262890683122, 1.000000000000000000, 0.9659258262890683122, 1.000000000000000000, 0.9659258262890683122, 1.000000000000000000, 0.9659258262890683122, 1.000000000000000000, 0.9659258262890683122, 1.000000000000000000, 0.9659258262890683122, 1.000000000000000000, 0.9659258262890683122, 1.000000000000000000, 0.9659258262890683122, 1.000000000000000000, 0.9659258262890683122, 1.000000000000000000, 0.9659258262890683122, 1.000000000000000000, 0.9659258262890683122, 1.000000000000000000, 0.9659258262890683122, 1.000000000000000000, 0.9659258262890683122, 1.000000000000000000, 0.9659258262890683122, 1.000000000000000000, 0.9659258262890683122, 1.000000000000000000, 0.9659258262890683122, 1.000000000000000000, 0.9659258262890683122, 1.000000000000000000, 0.9659258262890683122, 1.000000000000000000, 0.9659258262890683122, 1.000000000000000000, 0.9659258262890683122, 1.000000000000000000, 0.9659258262890683122, 1.000000000000000000, 0.9659258262890683122, 1.000000000000000000, 0.9659258262890683122, 1.000000000000000000, 0.9659258262890683122, 1.000000000000000000, 0.9659258262890683122, 1.000000000000000000, 0.9659258262890683122, 1.000000000000000000, 0.9659258262890683122, 1.000000000000000000, 0.9659258262890683122, 1.000000000000000000, 0.9659258262890683122, 1.000000000000000000, 0.9659258262890683122, 1.000000000000000000, 0.9659258262890683122, 1.000000000000000000, 0.9659258262890683122, 1.000000000000000000, 0.9659258262890683122, 1.000000000000000000, 0.9659258262890683122, 1.000000000000000000, 0.9659258262890683122, 1.000000000000000000, 0.9659258262890683122, 1.000000000000000000, 0.9659258262890683122, 1.000000000000000000, 0.9659258262890683122, 1.000000000000000000, 0.9659258262890683122, 1.000000000000000000, 0.9659258262890683122, 1.000000000000000000, 0.9659258262890683122, 1.000000000000000000, 0.9659258262890683122, 1.000000000000000000, 0.9659258262890683122, 1.000000000000000000, 0.9659258262890683122, 1.000000000000000000, 0.9659258262890683122, 1.000000000000000000, 0.9659258262890683122, 1.000000000000000000, 0.9659258262890683122, 1.000000000000000000, 0.9659258262890683122, 1.000000000000000000, 0.9659258262890683122, 1.000000000000000000, 0.9659258262890683122, 1.000000000000000000, 0.9659258262890683122, 1.000000000000000000, 0.9659258262890683122, 1.000000000000000000, 0.9659258262890683122, 1.000000000000000000, 0.9659258262890683122, 1.000000000000000000, 0.9659258262890683122, 1.000000000000000000, 0.9659258262890683122, 1.000000000000000000, 0.9659258262890683122, 1.000000000000000000, 0.9659258262890683122, 1.000000000000000000, 0.9659258262890683122, 1.000000000000000000, 0.9659258262890683122, 1.000000000000000000, 0.9659258262890683122, 1.000000000000000000, 0.9659258262890683122, 1.000000000000000000, 0.9659258262890683122, 1.000000000000000000, 0.9659258262890683122, 1.000000000000000000, 0.9659258262890683122, 1.000000000000000000, 0.9659258262890683122, 1.000000000000000000, 0.9659258262890683122, 1.000000000000000000, 0.9659258262890683122, 1.000000000000000000, 0.9659258262890683122, 1.000000000000000000, 0.9659258262890683122, 1.000000000000000000, 0.9659258262890683122, 1.000000000000000000, 0.9659258262890683122, 1.000000000000000000, 0.9659258262890683122, 1.000000000000000000, 0.9659258262890683122, 1.000000000000000000, 0.9659258262890683122, 1.000000000000000000, 0.9659258262890683122, 1.000000000000000000, 0.9659258262890683122, 1.000000000000000000, 0.9659258262890683122, 1.000000000000000000, 0.9659258262890683122, 1.000000000000000000, 0.9659258262890683122, 1.000000000000000000, 0.9659258262890683122, 1.000000000000000000, 0.9659258262890683122, 1.000000000000000000, 0.9659258262890683122, 1.000000000000000000, 0.9659258262890683122, 1.000000000000000000, 0.9659258262890683122, 1.000000000000000000, 0.9659258262890683122, 1.000000000000000000, 0.9659258262890683122, 1.000000000000000000, 0.9659258262890683122, 1.000000000000000000, 0.9659258262890683122, 1.000000000000000000, 0.9659258262890683122, 1.000000000000000000, 0.9659258262890683122, 1.000000000000000000, 0.9659258262890683122, 1.000000000000000000, 0.9659258262890683122, 1.000000000000000000, 0.9659258262890683122, 1.000000000000000000, 0.9659258262890683122, 1.000000000000000000, 0.9659258262890683122, 1.000000000000000000, 0.9659258262890683122, 1.000000000000000000, 0.9659258262890683122, 1.000000000000000000, 0.9659258262890683122, 1.000000000000000000, 0.9659258262890683122, 1.000000000000000000, 0.9659258262890683122, 1.000000000000000000, 0.9659258262890683122, 1.000000000000000000, 0.9659258262890683122, 1.000000000000000000, 0.9659258262890683122, 1.000000000000000000, 0.9659258262890683122, 1.000000000000000000, 0.9659258262890683122, 1.000000000000000000, 0.9659258262890683122, 1.000000000000000000, 0.9659258262890683122, 1.000000000000000000, 0.9659258262890683122, 1.000000000000000000, 0.9659258262890683122, 1.000000000000000000, 0.9659258262890683122, 1.000000000000000000, 0.9659258262890683122, 1.000000000000000000, 0.9659258262890683122, 1.000000000000000000, 0.9659258262890683122, 1.000000000000000000, 0.9659258262890683122, 1.000000000000000000, 0.9659258262890683122, 1.000000000000000000, 0.9659258262890683122, 1.000000000000000000, 0.9659258262890683122, 1.000000000000000000, 0.9659258262890683122, 1.000000000000000000, 0.9659258262890683122, 1.000000000000000000, 0.9659258262890683122, 1.000000000000000000, 0.9659258262890683122, 1.000000000000000000, 0.9659258262890683122, 1.000000000000000000) ) ) 
 REPRESENTATION_ITEM ( '' )  SURFACE ( )  );
#102256 = CARTESIAN_POINT ( 'NONE',  ( -21.53943276465977519, -0.05219959533937600094, 18.75109039468568639 ) ) ;
#102257 = CARTESIAN_POINT ( 'NONE',  ( 8.571926809382603096, -26.38167802310801235, 143.9750000027312069 ) ) ;
#102258 = CARTESIAN_POINT ( 'NONE',  ( 21.55341960407610458, 5.719274019375980345, 63.95724293864770260 ) ) ;
#102259 = CARTESIAN_POINT ( 'NONE',  ( -16.55341960407617563, 4.379528057220093196, 98.54275706135234714 ) ) ;
#102260 = CARTESIAN_POINT ( 'NONE',  ( -12.06949235617756955, 12.14591786802309770, 115.6239096053143669 ) ) ;
#102261 = CARTESIAN_POINT ( 'NONE',  ( -16.46253265017160317, 9.564922557960807481, 70.83224293864770971 ) ) ;
#102262 = CARTESIAN_POINT ( 'NONE',  ( 30.00000000000000711, -1.163414459189985801E-14, 87.50000000000000000 ) ) ;
#102263 = CARTESIAN_POINT ( 'NONE',  ( 8.314922557960818139, 14.29746914071049879, 29.58224293864769905 ) ) ;
#102264 = CARTESIAN_POINT ( 'NONE',  ( 18.67979575497194134, -10.72451020669871369, 60.83442372801901854 ) ) ;
#102265 = CARTESIAN_POINT ( 'NONE',  ( 19.03943276465977164, -0.05219959533909143690, 108.7489096053143527 ) ) ;
#102266 = CARTESIAN_POINT ( 'NONE',  ( 15.72974639402176855, 15.80617190586768217, 96.87609039468568994 ) ) ;
#102267 = CARTESIAN_POINT ( 'NONE',  ( -16.51473224551069308, -9.474510206698971260, 36.66557627198102409 ) ) ;
#102268 = CARTESIAN_POINT ( 'NONE',  ( 16.46253265017160672, -9.564922557960803928, 33.33224293864770260 ) ) ;
#102269 = ORIENTED_EDGE ( 'NONE', *, *, #157283, .T. ) ;
#102270 = CARTESIAN_POINT ( 'NONE',  ( -0.05219959533937732626, 21.53943276465977519, 97.50109039468567573 ) ) ;
#102271 = CARTESIAN_POINT ( 'NONE',  ( 0.05219959533934541429, -16.53943276465976808, 55.00109039468568284 ) ) ;
#102272 = CARTESIAN_POINT ( 'NONE',  ( -18.62759615963255300, -10.81492255796106328, 84.16775706135234714 ) ) ;
#102273 = CARTESIAN_POINT ( 'NONE',  ( 16.46253265017160672, -9.564922557960803928, 113.3322429386476955 ) ) ;
#102274 = CARTESIAN_POINT ( 'NONE',  ( -13.89961937509957401, -13.97604488694547875, 89.37609039468563310 ) ) ;
#102275 = CARTESIAN_POINT ( 'NONE',  ( 5.719274019375673035, 21.55341960407619339, 62.29275706135236845 ) ) ;
#102276 = CARTESIAN_POINT ( 'NONE',  ( -13.97604488694547697, 13.89961937509957934, 113.1260903946856757 ) ) ;
#102277 = CARTESIAN_POINT ( 'NONE',  ( 5.049401038297881783, 19.05341960407617563, 87.29275706135234714 ) ) ;
#102278 = CARTESIAN_POINT ( 'NONE',  ( 19.02544592524343514, -5.153800228976328945, 53.54057627198102409 ) ) ;
#102279 = CARTESIAN_POINT ( 'NONE',  ( 19.05341960407617918, -5.049401038297876454, 96.04275706135231871 ) ) ;
#102280 = CARTESIAN_POINT ( 'NONE',  ( 16.51473224551083163, -9.474510206698727899, 85.83442372801900433 ) ) ;
#102281 = CARTESIAN_POINT ( 'NONE',  ( 14.34966873604960469, 8.224510206698951720, 59.16557627198103120 ) ) ;
#102282 = CARTESIAN_POINT ( 'NONE',  ( -13.97604488694547697, 13.89961937509957934, 78.12609039468567573 ) ) ;
#102283 = CARTESIAN_POINT ( 'NONE',  ( 16.52544592524335698, 4.483927247898782831, 61.45942372801901854 ) ) ;
#102284 = CARTESIAN_POINT ( 'NONE',  ( 19.02544592524334988, 5.153800228976608722, 21.45942372801899012 ) ) ;
#102285 = CARTESIAN_POINT ( 'NONE',  ( 5.049401038298161559, -19.05341960407611168, 32.70724293864768129 ) ) ;
#102286 = CARTESIAN_POINT ( 'NONE',  ( 13.89961937509977652, -13.97604488694527269, 43.12390960531434558 ) ) ;
#102287 = CARTESIAN_POINT ( 'NONE',  ( 8.314922557961029526, -14.29746914071037800, 65.41775706135234714 ) ) ;
#102288 = CARTESIAN_POINT ( 'NONE',  ( 22.44159573604009594, -16.30477369853687364, 142.1750000027311671 ) ) ;
#102289 = CARTESIAN_POINT ( 'NONE',  ( -5.429308488886486681E-15, 30.30510711980690175, 139.7500000054623683 ) ) ;
#102290 = CARTESIAN_POINT ( 'NONE',  ( -19.03943276465977164, 0.05219959533909376836, 106.2489096053143669 ) ) ;
#102291 = DIRECTION ( 'NONE',  ( 0.000000000000000000, 0.000000000000000000, -1.000000000000000000 ) ) ;
#102292 = ORIENTED_EDGE ( 'NONE', *, *, #80974, .F. ) ;
#102293 = CARTESIAN_POINT ( 'NONE',  ( 19.02544592524334988, 5.153800228976608722, 91.45942372801900433 ) ) ;
#102294 = CARTESIAN_POINT ( 'NONE',  ( 21.52544592524344225, -5.823673210054117533, 38.54057627198103120 ) ) ;
#102296 = CARTESIAN_POINT ( 'NONE',  ( 13.97604488694548053, -13.89961937509957401, 110.6260903946856615 ) ) ;
#102295 = CARTESIAN_POINT ( 'NONE',  ( -19.03943276465977164, -0.05219959533935918106, 28.75109039468566507 ) ) ;
#102297 = CARTESIAN_POINT ( 'NONE',  ( 19.05341960407611168, 5.049401038298154454, 28.95724293864769550 ) ) ;
#102298 = CARTESIAN_POINT ( 'NONE',  ( -13.89961937509977652, 13.97604488694528158, 35.62390960531435269 ) ) ;
#102299 = CARTESIAN_POINT ( 'NONE',  ( -18.67979575497178146, -10.72451020669898902, 76.66557627198103830 ) ) ;
#102300 = CARTESIAN_POINT ( 'NONE',  ( -19.03943276465977164, 0.05219959533909376836, 31.24890960531435979 ) ) ;
#102301 = CARTESIAN_POINT ( 'NONE',  ( 8.571926809382597767, 26.38167802310806209, 146.7750000027311899 ) ) ;
#102302 = CARTESIAN_POINT ( 'NONE',  ( -9.564922557961040184, 16.46253265017147172, 87.91775706135233293 ) ) ;
#102303 = CARTESIAN_POINT ( 'NONE',  ( 12.14591786802309770, 12.06949235617756955, 59.37390960531436690 ) ) ;
#102304 = CARTESIAN_POINT ( 'NONE',  ( -21.55341960407610458, -5.719274019375992779, 36.45724293864768839 ) ) ;
#102305 = CARTESIAN_POINT ( 'NONE',  ( 10.81492255796106328, -18.62759615963255655, 105.4177570613523613 ) ) ;
#102306 = CARTESIAN_POINT ( 'NONE',  ( 21.55341960407610458, 5.719274019375980345, 78.95724293864769550 ) ) ;
#102307 = CARTESIAN_POINT ( 'NONE',  ( 21.52544592524334988, 5.823673210054432836, 71.45942372801901854 ) ) ;
#102308 = CARTESIAN_POINT ( 'NONE',  ( -18.67979575497193778, 10.72451020669871902, 63.33442372801900433 ) ) ;
#102309 = CARTESIAN_POINT ( 'NONE',  ( -5.153800228976328057, -19.02544592524343514, 112.2905762719810099 ) ) ;
#102311 = CARTESIAN_POINT ( 'NONE',  ( -21.53943276465977519, -0.05219959533937600094, 58.75109039468568994 ) ) ;
#102310 = CARTESIAN_POINT ( 'NONE',  ( -12.06949235617739369, -12.14591786802326823, 104.3760903946856899 ) ) ;
#102312 = CARTESIAN_POINT ( 'NONE',  ( -5.049401038298153566, 19.05341960407611168, 55.20724293864769550 ) ) ;
#102313 = CARTESIAN_POINT ( 'NONE',  ( 5.049401038297881783, 19.05341960407617563, 32.29275706135233293 ) ) ;
#102314 = CARTESIAN_POINT ( 'NONE',  ( 0.05219959533937995610, -21.53943276465977519, 35.00109039468568284 ) ) ;
#102315 = CARTESIAN_POINT ( 'NONE',  ( 19.02544592524343514, -5.153800228976328945, 73.54057627198103830 ) ) ;
#102316 = CARTESIAN_POINT ( 'NONE',  ( -16.55341960407611168, -4.379528057220339221, 76.45724293864769550 ) ) ;
#102317 = CARTESIAN_POINT ( 'NONE',  ( 8.224510206698953496, -14.34966873604960469, 52.91557627198103830 ) ) ;
#102318 = CARTESIAN_POINT ( 'NONE',  ( 5.719274019375991003, -21.55341960407610458, 62.70724293864769550 ) ) ;
#102319 = CARTESIAN_POINT ( 'NONE',  ( -0.05219959533909027116, -19.03943276465977164, 47.49890960531435979 ) ) ;
#102320 = CARTESIAN_POINT ( 'NONE',  ( 15.72974639402199770, -15.80617190586745480, 68.12390960531436690 ) ) ;
#102321 = CARTESIAN_POINT ( 'NONE',  ( -5.153800228976607833, 19.02544592524334988, 57.70942372801899012 ) ) ;
#102323 = CARTESIAN_POINT ( 'NONE',  ( 12.14591786802309770, 12.06949235617756955, 59.37390960531436690 ) ) ;
#102322 = CIRCLE ( 'NONE', #186332, 1.999999999999999556 ) ;
#102324 = CARTESIAN_POINT ( 'NONE',  ( 18.62759615963271287, -10.81492255796078972, 38.33224293864768839 ) ) ;
#102325 = EDGE_LOOP ( 'NONE', ( #90747, #63401, #153233, #60121 ) ) ;
#102326 = CARTESIAN_POINT ( 'NONE',  ( 17.44270441346516520, 5.991230190323025617, 103.8633507926423079 ) ) ;
#102328 = CARTESIAN_POINT ( 'NONE',  ( 1.784210473542230573E-15, -29.16686587814331588, 147.3750000027311842 ) ) ;
#102327 = CARTESIAN_POINT ( 'NONE',  ( 4.483927247898790824, -16.52544592524335698, 90.20942372801903275 ) ) ;
#102329 = CARTESIAN_POINT ( 'NONE',  ( 9.474510206698729675, 16.51473224551082808, 92.08442372801900433 ) ) ;
#102330 = CARTESIAN_POINT ( 'NONE',  ( 12.06949235617757843, -12.14591786802309237, 48.12390960531436690 ) ) ;
#102331 = DIRECTION ( 'NONE',  ( 1.000000000000000000, 0.000000000000000000, -0.000000000000000000 ) ) ;
#102332 = CARTESIAN_POINT ( 'NONE',  ( 9.474510206698971260, -16.51473224551069308, 47.91557627198102409 ) ) ;
#102333 = CARTESIAN_POINT ( 'NONE',  ( -12.06949235617756955, 12.14591786802309770, 35.62390960531437401 ) ) ;
#102334 = CARTESIAN_POINT ( 'NONE',  ( 19.05341960407611168, 5.049401038298154454, 93.95724293864769550 ) ) ;
#102335 = CARTESIAN_POINT ( 'NONE',  ( -16.51473224551069308, -9.474510206698971260, 51.66557627198102409 ) ) ;
#102336 = CARTESIAN_POINT ( 'NONE',  ( 21.55341960407619695, -5.719274019375665929, 56.04275706135235424 ) ) ;
#102337 = CARTESIAN_POINT ( 'NONE',  ( 13.89961937509977652, -13.97604488694527269, 68.12390960531436690 ) ) ;
#102338 = CARTESIAN_POINT ( 'NONE',  ( 9.564922557960805705, 16.46253265017160317, 24.58224293864769194 ) ) ;
#102339 = AXIS2_PLACEMENT_3D ( 'NONE', #158597, #64612, #66587 ) ;
#102340 = CARTESIAN_POINT ( 'NONE',  ( 19.02544592524343514, -5.153800228976328945, 73.54057627198103830 ) ) ;
#102341 = CARTESIAN_POINT ( 'NONE',  ( 10.81492255796078972, 18.62759615963270932, 54.58224293864769550 ) ) ;
#102342 = CARTESIAN_POINT ( 'NONE',  ( 19.03943276465977164, -0.05219959533909143690, 33.74890960531435979 ) ) ;
#102343 = CARTESIAN_POINT ( 'NONE',  ( -21.53943276465977519, 0.05219959533907696930, 41.24890960531435269 ) ) ;
#102344 = CARTESIAN_POINT ( 'NONE',  ( -8.224510206698735004, -14.34966873604973081, 104.5844237280190185 ) ) ;
#102345 = CARTESIAN_POINT ( 'NONE',  ( 9.474510206698729675, 16.51473224551082808, 22.08442372801899722 ) ) ;
#102347 = CARTESIAN_POINT ( 'NONE',  ( 14.29746914071037800, 8.314922557961029526, 86.66775706135234714 ) ) ;
#102346 = CARTESIAN_POINT ( 'NONE',  ( -0.05219959533934338120, 16.53943276465976808, 42.50109039468567573 ) ) ;
#102348 = CYLINDRICAL_SURFACE ( 'NONE', #11359, 6.100000000000006750 ) ;
#102349 = CARTESIAN_POINT ( 'NONE',  ( -4.379528057220086978, -16.55341960407618274, 64.79275706135234714 ) ) ;
#102350 = CARTESIAN_POINT ( 'NONE',  ( -19.02544592524342804, 5.153800228976336051, 106.0405762719810241 ) ) ;
#102351 = CARTESIAN_POINT ( 'NONE',  ( 16.46253265017160672, -9.564922557960803928, 38.33224293864768839 ) ) ;
#102352 = CARTESIAN_POINT ( 'NONE',  ( -16.52544592524335698, -4.483927247898792601, 38.95942372801901854 ) ) ;
#102353 = CARTESIAN_POINT ( 'NONE',  ( -5.153800228976328057, -19.02544592524343514, 42.29057627198101699 ) ) ;
#102354 = CARTESIAN_POINT ( 'NONE',  ( -5.719274019375665041, -21.55341960407619695, 24.79275706135235779 ) ) ;
#102355 = CARTESIAN_POINT ( 'NONE',  ( -4.379528057220086978, -16.55341960407618274, 39.79275706135235424 ) ) ;
#102356 = CARTESIAN_POINT ( 'NONE',  ( 8.224510206698742110, 14.34966873604972548, 97.08442372801904696 ) ) ;
#102357 = CARTESIAN_POINT ( 'NONE',  ( -21.52544592524334988, -5.823673210054445271, 98.95942372801903275 ) ) ;
#102359 = EDGE_CURVE ( 'NONE', #169284, #125859, #86823, .T. ) ;
#102358 = CARTESIAN_POINT ( 'NONE',  ( -13.97604488694547697, 13.89961937509957934, 93.12609039468566152 ) ) ;
#102360 = CARTESIAN_POINT ( 'NONE',  ( 19.05341960407617918, -5.049401038297876454, 56.04275706135234714 ) ) ;
#102361 = CARTESIAN_POINT ( 'NONE',  ( -14.34966873604960291, -8.224510206698953496, 56.66557627198103830 ) ) ;
#102362 = CARTESIAN_POINT ( 'NONE',  ( 16.53943276465976808, -0.05219959533910856209, 113.7489096053143527 ) ) ;
#102364 = CARTESIAN_POINT ( 'NONE',  ( 17.40805194821983903, -6.112264579160781253, 58.33371272510607497 ) ) ;
#102363 = CARTESIAN_POINT ( 'NONE',  ( 19.05341960407617918, -5.049401038297876454, 61.04275706135232582 ) ) ;
#102365 = CARTESIAN_POINT ( 'NONE',  ( -18.67979575497193778, 10.72451020669871902, 68.33442372801900433 ) ) ;
#102366 = CARTESIAN_POINT ( 'NONE',  ( 14.29746914071037800, 8.314922557961029526, 26.66775706135235424 ) ) ;
#102367 = CARTESIAN_POINT ( 'NONE',  ( 19.35633801406907395, -5.499999999999770850, 56.63373818172765795 ) ) ;
#102368 = CARTESIAN_POINT ( 'NONE',  ( -0.05219959533907301413, -21.53943276465977519, 22.49890960531436335 ) ) ;
#102369 = CARTESIAN_POINT ( 'NONE',  ( -16.46253265017146816, -9.564922557961047289, 109.1677570613523471 ) ) ;
#102370 = CARTESIAN_POINT ( 'NONE',  ( 18.22780087662122384, -5.500000000000022204, 96.01540105326108687 ) ) ;
#102371 = CARTESIAN_POINT ( 'NONE',  ( -21.04946095171258236, 10.86023174791543866, 170.2405914574444239 ) ) ;
#102372 = CARTESIAN_POINT ( 'NONE',  ( -19.05341960407611168, -5.049401038298163336, 21.45724293864768839 ) ) ;
#102373 = CARTESIAN_POINT ( 'NONE',  ( 18.62759615963255655, 10.81492255796105972, 111.6677570613523613 ) ) ;
#102374 = CARTESIAN_POINT ( 'NONE',  ( 0.05219959533909260263, 19.03943276465977164, 54.99890960531435979 ) ) ;
#102376 = CARTESIAN_POINT ( 'NONE',  ( 10.81492255796106328, -18.62759615963255655, 65.41775706135234714 ) ) ;
#102375 = AXIS2_PLACEMENT_3D ( 'NONE', #128842, #97496, #19694 ) ;
#102377 = CARTESIAN_POINT ( 'NONE',  ( -21.53943276465977519, -0.05219959533937600094, 98.75109039468568994 ) ) ;
#102378 = CARTESIAN_POINT ( 'NONE',  ( 14.34966873604972726, -8.224510206698740333, 105.8344237280190328 ) ) ;
#102379 = CARTESIAN_POINT ( 'NONE',  ( -13.89961937509977652, 13.97604488694528158, 80.62390960531436690 ) ) ;
#102380 = CARTESIAN_POINT ( 'NONE',  ( 18.67979575497194134, -10.72451020669871369, 50.83442372801901143 ) ) ;
#102381 = CARTESIAN_POINT ( 'NONE',  ( 15.80617190586769283, -15.72974639402175789, 50.62609039468568994 ) ) ;
#102383 = CARTESIAN_POINT ( 'NONE',  ( -19.03943276465977164, 0.05219959533909376836, 106.2489096053143669 ) ) ;
#102382 = CARTESIAN_POINT ( 'NONE',  ( -9.564922557961040184, 16.46253265017147172, 82.91775706135233293 ) ) ;
#102384 = CARTESIAN_POINT ( 'NONE',  ( 19.03943276465977164, -0.05219959533909143690, 28.74890960531435624 ) ) ;
#102385 = CARTESIAN_POINT ( 'NONE',  ( 5.823673210054125526, 21.52544592524343514, 94.79057627198105251 ) ) ;
#102386 = CARTESIAN_POINT ( 'NONE',  ( 9.474510206698729675, 16.51473224551082808, 27.08442372801900433 ) ) ;
#102387 = CARTESIAN_POINT ( 'NONE',  ( 12.14591786802309770, 12.06949235617756955, 94.37390960531436690 ) ) ;
#102388 = CARTESIAN_POINT ( 'NONE',  ( -9.474510206698964154, 16.51473224551069663, 50.41557627198102409 ) ) ;
#102389 = CARTESIAN_POINT ( 'NONE',  ( -16.51473224551082808, 9.474510206698731452, 93.33442372801900433 ) ) ;
#102390 = CARTESIAN_POINT ( 'NONE',  ( -8.314922557960811034, -14.29746914071050412, 67.08224293864770971 ) ) ;
#102391 = CARTESIAN_POINT ( 'NONE',  ( 15.80617190586769283, -15.72974639402175789, 110.6260903946857042 ) ) ;
#102392 = CARTESIAN_POINT ( 'NONE',  ( 16.46253265017160672, -9.564922557960803928, 108.3322429386476955 ) ) ;
#102393 = CARTESIAN_POINT ( 'NONE',  ( 5.153800228976615827, -19.02544592524334988, 75.20942372801896170 ) ) ;
#102394 = CARTESIAN_POINT ( 'NONE',  ( -21.53943276465977519, 0.05219959533907696930, 81.24890960531436690 ) ) ;
#102395 = CARTESIAN_POINT ( 'NONE',  ( 5.719274019375673035, 21.55341960407619339, 37.29275706135235424 ) ) ;
#102397 = CARTESIAN_POINT ( 'NONE',  ( -8.314922557961024197, 14.29746914071037800, 47.91775706135234714 ) ) ;
#102396 = B_SPLINE_CURVE_WITH_KNOTS ( 'NONE', 3,
 ( #109274, #154786, #2096, #90132, #185127, #46618, #14287, #168949 ),
 .UNSPECIFIED., .F., .F.,
 ( 4, 2, 2, 4 ),
 ( 0.002324770996990997447, 0.005594641632894387095, 0.007229576950846082137, 0.008864512268797777178 ),
 .UNSPECIFIED. ) ;
#102398 = CARTESIAN_POINT ( 'NONE',  ( -0.05219959533934338120, 16.53943276465976808, 97.50109039468567573 ) ) ;
#102400 = CARTESIAN_POINT ( 'NONE',  ( -10.72451020669870658, -18.67979575497194134, 39.58442372801901143 ) ) ;
#102399 = CARTESIAN_POINT ( 'NONE',  ( 4.379528057220092307, 16.55341960407617563, 47.29275706135234003 ) ) ;
#102401 = CARTESIAN_POINT ( 'NONE',  ( 21.53943276465977519, -0.05219959533907433946, 43.74890960531435979 ) ) ;
#102402 = CARTESIAN_POINT ( 'NONE',  ( -9.564922557960796823, -16.46253265017161027, 32.08224293864769550 ) ) ;
#102403 = CARTESIAN_POINT ( 'NONE',  ( 23.48529157249599919, 32.32473071737754111, -8.449999994537625625 ) ) ;
#102404 = CARTESIAN_POINT ( 'NONE',  ( 4.379528057220092307, 16.55341960407617563, 62.29275706135236845 ) ) ;
#102405 = CARTESIAN_POINT ( 'NONE',  ( 21.53943276465977519, -0.05219959533907433946, 83.74890960531435269 ) ) ;
#102406 = CARTESIAN_POINT ( 'NONE',  ( -4.483927247898539470, -16.52544592524342804, 37.29057627198102409 ) ) ;
#102407 = CARTESIAN_POINT ( 'NONE',  ( 14.34966873604972726, -8.224510206698740333, 50.83442372801901143 ) ) ;
#102408 = CARTESIAN_POINT ( 'NONE',  ( 13.89961937509977652, -13.97604488694527269, 58.12390960531436690 ) ) ;
#102409 = CARTESIAN_POINT ( 'NONE',  ( 8.314922557961029526, -14.29746914071037800, 90.41775706135236135 ) ) ;
#102410 = CARTESIAN_POINT ( 'NONE',  ( 19.03943276465977164, 0.05219959533936151252, 91.25109039468566152 ) ) ;
#102411 = CARTESIAN_POINT ( 'NONE',  ( -18.67979575497178146, -10.72451020669898902, 86.66557627198102409 ) ) ;
#102412 = CARTESIAN_POINT ( 'NONE',  ( 16.53943276465976808, -0.05219959533910856209, 28.74890960531435624 ) ) ;
#102413 = VERTEX_POINT ( 'NONE', #104987 ) ;
#102414 = CARTESIAN_POINT ( 'NONE',  ( 18.87580814761076553, -5.499999999999953815, 93.37172394265763842 ) ) ;
#102415 = CARTESIAN_POINT ( 'NONE',  ( -10.72451020669898014, 18.67979575497178502, 55.41557627198102409 ) ) ;
#102416 = CARTESIAN_POINT ( 'NONE',  ( 4.379528057220092307, 16.55341960407617563, 102.2927570613523613 ) ) ;
#102417 = ORIENTED_EDGE ( 'NONE', *, *, #78315, .F. ) ;
#102418 = CARTESIAN_POINT ( 'NONE',  ( 17.50000000000005684, -3.647616755424155865, 102.7966979427856273 ) ) ;
#102419 = CARTESIAN_POINT ( 'NONE',  ( 15.72974639402199770, -15.80617190586745480, 93.12390960531436690 ) ) ;
#102420 = CARTESIAN_POINT ( 'NONE',  ( -16.53943276465976808, -0.05219959533934237506, 113.7510903946856757 ) ) ;
#102421 = CARTESIAN_POINT ( 'NONE',  ( 4.483927247898790824, -16.52544592524335698, 40.20942372801901854 ) ) ;
#102422 = CARTESIAN_POINT ( 'NONE',  ( 5.153800228976335163, 19.02544592524342804, 29.79057627198102409 ) ) ;
#102423 = B_SPLINE_CURVE_WITH_KNOTS ( 'NONE', 3,
 ( #65611, #131268, #22102, #35276, #21099, #128267 ),
 .UNSPECIFIED., .F., .F.,
 ( 4, 2, 4 ),
 ( 0.000000000000000000, 0.0003837532665635023064, 0.0007675065331270046129 ),
 .UNSPECIFIED. ) ;
#102424 = CARTESIAN_POINT ( 'NONE',  ( -5.049401038298153566, 19.05341960407611168, 55.20724293864769550 ) ) ;
#102425 = CARTESIAN_POINT ( 'NONE',  ( 28.82186960331499392, -9.364793116373510529, 148.9000000000000057 ) ) ;
#102426 = CARTESIAN_POINT ( 'NONE',  ( 10.72451020669898902, -18.67979575497178502, 27.91557627198103830 ) ) ;
#102427 = CARTESIAN_POINT ( 'NONE',  ( -9.687362902255793884, -9.687362902255632235, -62.58071313852362039 ) ) ;
#102428 = CARTESIAN_POINT ( 'NONE',  ( 8.314922557961029526, -14.29746914071037800, 100.4177570613523471 ) ) ;
#102429 = CARTESIAN_POINT ( 'NONE',  ( -13.97604488694547697, 13.89961937509957934, 108.1260903946856331 ) ) ;
#102430 = CARTESIAN_POINT ( 'NONE',  ( 19.03943276465977164, 0.05219959533936151252, 41.25109039468566152 ) ) ;
#102431 = CARTESIAN_POINT ( 'NONE',  ( -21.53943276465977519, 0.05219959533907696930, 91.24890960531436690 ) ) ;
#102432 = CARTESIAN_POINT ( 'NONE',  ( -12.14591786802309592, -12.06949235617757132, 26.87390960531435979 ) ) ;
#102433 = CARTESIAN_POINT ( 'NONE',  ( 10.81492255796078972, 18.62759615963270932, 29.58224293864769905 ) ) ;
#102434 = CARTESIAN_POINT ( 'NONE',  ( -16.51473224551082808, 9.474510206698731452, 113.3344237280190043 ) ) ;
#102435 = CARTESIAN_POINT ( 'NONE',  ( -16.51473224551069308, -9.474510206698971260, 111.6655762719810383 ) ) ;
#102436 = CARTESIAN_POINT ( 'NONE',  ( -0.05219959533937732626, 21.53943276465977519, 67.50109039468568994 ) ) ;
#102437 = CARTESIAN_POINT ( 'NONE',  ( 16.51473224551069308, 9.474510206698969483, 54.16557627198103120 ) ) ;
#102438 = CARTESIAN_POINT ( 'NONE',  ( -8.224510206698948167, 14.34966873604960824, 100.4155762719810241 ) ) ;
#102439 = CARTESIAN_POINT ( 'NONE',  ( 32.64453336272027428, 0.4913919212617400833, 87.49999999999998579 ) ) ;
#102440 = CARTESIAN_POINT ( 'NONE',  ( -0.05219959533909027116, -19.03943276465977164, 67.49890960531436690 ) ) ;
#102441 = CARTESIAN_POINT ( 'NONE',  ( 4.483927247898545687, 16.52544592524342804, 74.79057627198105251 ) ) ;
#102442 = VERTEX_POINT ( 'NONE', #43320 ) ;
#102443 = CARTESIAN_POINT ( 'NONE',  ( -19.03943276465977164, -0.05219959533935918106, 88.75109039468567573 ) ) ;
#102444 = CARTESIAN_POINT ( 'NONE',  ( 19.49190055781010145, 5.500000000000001776, 93.06116087098783396 ) ) ;
#102445 = CARTESIAN_POINT ( 'NONE',  ( -16.51473224551069308, -9.474510206698971260, 61.66557627198103120 ) ) ;
#102446 = CARTESIAN_POINT ( 'NONE',  ( 31.51098639601625351, -4.378554692192639486, 101.0941514966582986 ) ) ;
#102448 = CARTESIAN_POINT ( 'NONE',  ( 19.02544592524343514, -5.153800228976328945, 103.5405762719809957 ) ) ;
#102447 = CARTESIAN_POINT ( 'NONE',  ( -16.51473224551069308, -9.474510206698971260, 71.66557627198102409 ) ) ;
#102449 = CARTESIAN_POINT ( 'NONE',  ( -4.379528057220086978, -16.55341960407618274, 59.79275706135234714 ) ) ;
#102450 = CARTESIAN_POINT ( 'NONE',  ( -17.05116617787825106, -6.768360034955700044, 51.34324446740803438 ) ) ;
#102451 = CARTESIAN_POINT ( 'NONE',  ( 9.474510206698729675, 16.51473224551082808, 47.08442372801900433 ) ) ;
#102452 = CARTESIAN_POINT ( 'NONE',  ( 21.52544592524334988, 5.823673210054432836, 96.45942372801901854 ) ) ;
#102453 = DIRECTION ( 'NONE',  ( -0.000000000000000000, 0.7071067811865466846, -0.7071067811865484609 ) ) ;
#102454 = CARTESIAN_POINT ( 'NONE',  ( -5.153800228976328057, -19.02544592524343514, 112.2905762719810099 ) ) ;
#102455 = CARTESIAN_POINT ( 'NONE',  ( -14.29746914071037622, -8.314922557961029526, 104.1677570613523471 ) ) ;
#102456 = CARTESIAN_POINT ( 'NONE',  ( -34.37176626784630429, -7.314009959508100955, 46.67821535514400466 ) ) ;
#102457 = CARTESIAN_POINT ( 'NONE',  ( -16.53943276465976808, -0.05219959533934237506, 98.75109039468568994 ) ) ;
#102458 = CARTESIAN_POINT ( 'NONE',  ( -16.61371651742605238, 7.165104196376023360, 28.85415069992995640 ) ) ;
#102459 = CARTESIAN_POINT ( 'NONE',  ( -12.14591786802326823, 12.06949235617739902, 68.12609039468567573 ) ) ;
#102460 = ORIENTED_EDGE ( 'NONE', *, *, #58823, .F. ) ;
#102461 = CARTESIAN_POINT ( 'NONE',  ( 15.72974639402176855, 15.80617190586768217, 76.87609039468567573 ) ) ;
#102462 = CARTESIAN_POINT ( 'NONE',  ( 5.153800228976615827, -19.02544592524334988, 90.20942372801900433 ) ) ;
#102463 = CARTESIAN_POINT ( 'NONE',  ( -9.564922557961040184, 16.46253265017147172, 27.91775706135232582 ) ) ;
#102464 = CARTESIAN_POINT ( 'NONE',  ( 5.153800228976335163, 19.02544592524342804, 69.79057627198103830 ) ) ;
#102465 = CARTESIAN_POINT ( 'NONE',  ( -9.564922557960796823, -16.46253265017161027, 52.08224293864768839 ) ) ;
#102466 = DIRECTION ( 'NONE',  ( -1.000000000000000000, 1.065814103640150121E-14, 0.000000000000000000 ) ) ;
#102467 = CARTESIAN_POINT ( 'NONE',  ( -10.81492255796078084, -18.62759615963271287, 82.08224293864768129 ) ) ;
#102468 = AXIS2_PLACEMENT_3D ( 'NONE', #94558, #553, #167449 ) ;
#102469 = CARTESIAN_POINT ( 'NONE',  ( -5.719274019375978568, 21.55341960407610458, 40.20724293864769550 ) ) ;
#102470 = CARTESIAN_POINT ( 'NONE',  ( 13.97604488694527802, 13.89961937509977652, 39.37390960531435269 ) ) ;
#102471 = CARTESIAN_POINT ( 'NONE',  ( -0.05219959533934338120, 16.53943276465976808, 62.50109039468568284 ) ) ;
#102472 = ORIENTED_EDGE ( 'NONE', *, *, #139157, .T. ) ;
#102473 = CARTESIAN_POINT ( 'NONE',  ( -21.55341960407619339, 5.719274019375674811, 33.54275706135234714 ) ) ;
#102475 = CARTESIAN_POINT ( 'NONE',  ( -29.86685920354755552, 21.69954338932564397, -8.824999997268815122 ) ) ;
#102474 = CARTESIAN_POINT ( 'NONE',  ( -14.34966873604960291, -8.224510206698953496, 66.66557627198102409 ) ) ;
#102476 = CARTESIAN_POINT ( 'NONE',  ( -12.06949235617739369, -12.14591786802326823, 29.37609039468568284 ) ) ;
#102477 = CARTESIAN_POINT ( 'NONE',  ( -16.46253265017146816, -9.564922557961047289, 49.16775706135233293 ) ) ;
#102478 = CARTESIAN_POINT ( 'NONE',  ( -16.55341960407611168, -4.379528057220339221, 51.45724293864770260 ) ) ;
#102479 = CARTESIAN_POINT ( 'NONE',  ( -5.719274019375665041, -21.55341960407619695, 24.79275706135235779 ) ) ;
#102481 = CARTESIAN_POINT ( 'NONE',  ( -15.72974639402197994, 15.80617190586746368, 75.62390960531439532 ) ) ;
#102480 = CARTESIAN_POINT ( 'NONE',  ( -5.049401038298153566, 19.05341960407611168, 100.2072429386476955 ) ) ;
#102482 = CARTESIAN_POINT ( 'NONE',  ( 13.97604488694527802, 13.89961937509977652, 84.37390960531433848 ) ) ;
#102483 = CARTESIAN_POINT ( 'NONE',  ( -16.55341960407611168, -4.379528057220339221, 56.45724293864768839 ) ) ;
#102484 = CARTESIAN_POINT ( 'NONE',  ( 36.54539699253855645, -20.47674586971434962, -19.42837732572175113 ) ) ;
#102485 = CARTESIAN_POINT ( 'NONE',  ( -20.43538597629143538, -20.43538597629106945, -49.67367017693150189 ) ) ;
#102486 = CARTESIAN_POINT ( 'NONE',  ( -16.46253265017146816, -9.564922557961047289, 69.16775706135233293 ) ) ;
#102487 = CARTESIAN_POINT ( 'NONE',  ( -5.823673210054116645, -21.52544592524344225, 102.2905762719810383 ) ) ;
#102488 = CARTESIAN_POINT ( 'NONE',  ( -16.46253265017160317, 9.564922557960807481, 50.83224293864770260 ) ) ;
#102489 = CARTESIAN_POINT ( 'NONE',  ( -19.02544592524334988, -5.153800228976617603, 38.95942372801900433 ) ) ;
#102490 = CARTESIAN_POINT ( 'NONE',  ( 5.153800228976335163, 19.02544592524342804, 29.79057627198102409 ) ) ;
#102491 = ADVANCED_FACE ( 'NONE', ( #70667 ), #12010, .F. ) ;
#102492 = CARTESIAN_POINT ( 'NONE',  ( 15.80617190586769283, -15.72974639402175789, 70.62609039468567573 ) ) ;
#102493 = MECHANICAL_DESIGN_GEOMETRIC_PRESENTATION_REPRESENTATION (  '', ( #112150 ), #176833 ) ;
#102494 = CARTESIAN_POINT ( 'NONE',  ( -18.56453257813365454, 5.499999999999960032, 100.9900042369068842 ) ) ;
#102495 = CARTESIAN_POINT ( 'NONE',  ( -14.29746914071049879, 8.314922557960819915, 40.83224293864769550 ) ) ;
#102496 = CARTESIAN_POINT ( 'NONE',  ( -9.474510206698964154, 16.51473224551069663, 65.41557627198102409 ) ) ;
#102497 = CARTESIAN_POINT ( 'NONE',  ( -5.719274019375978568, 21.55341960407610458, 70.20724293864769550 ) ) ;
#102498 = CARTESIAN_POINT ( 'NONE',  ( 9.564922557960805705, 16.46253265017160317, 54.58224293864769550 ) ) ;
#102499 = EDGE_LOOP ( 'NONE', ( #156107, #123289, #129157, #57917, #119440 ) ) ;
#102500 = CARTESIAN_POINT ( 'NONE',  ( -15.72974639402197994, 15.80617190586746368, 60.62390960531437401 ) ) ;
#102501 = ORIENTED_EDGE ( 'NONE', *, *, #141568, .T. ) ;
#102502 = CARTESIAN_POINT ( 'NONE',  ( 0.05219959533937995610, -21.53943276465977519, 105.0010903946856757 ) ) ;
#102505 = CARTESIAN_POINT ( 'NONE',  ( -16.53943276465976808, 0.05219959533911058130, 81.24890960531436690 ) ) ;
#102504 = CARTESIAN_POINT ( 'NONE',  ( 4.483927247898790824, -16.52544592524335698, 100.2094237280190043 ) ) ;
#102503 = DIRECTION ( 'NONE',  ( 0.4999999999999933942, -0.5000000000000055511, 0.7071067811865484609 ) ) ;
#102506 = CARTESIAN_POINT ( 'NONE',  ( -9.564922557961040184, 16.46253265017147172, 87.91775706135233293 ) ) ;
#102507 = ORIENTED_EDGE ( 'NONE', *, *, #26552, .F. ) ;
#102508 = CARTESIAN_POINT ( 'NONE',  ( 9.474510206698729675, 16.51473224551082808, 42.08442372801900433 ) ) ;
#102509 = CARTESIAN_POINT ( 'NONE',  ( -14.29746914071037622, -8.314922557961029526, 104.1677570613523471 ) ) ;
#102510 = CARTESIAN_POINT ( 'NONE',  ( 19.03943276465977164, 0.05219959533936151252, 26.25109039468566507 ) ) ;
#102511 = CARTESIAN_POINT ( 'NONE',  ( 13.97604488694527802, 13.89961937509977652, 94.37390960531436690 ) ) ;
#102512 = CARTESIAN_POINT ( 'NONE',  ( -21.52544592524343514, 5.823673210054127303, 56.04057627198102409 ) ) ;
#102513 = CARTESIAN_POINT ( 'NONE',  ( -18.70878831527339159, -37.83292004501378614, -19.76830273372895164 ) ) ;
#102514 = CARTESIAN_POINT ( 'NONE',  ( -4.379528057220328563, 16.55341960407611168, 115.2072429386476955 ) ) ;
#102515 = EDGE_CURVE ( 'NONE', #178033, #197949, #122646, .T. ) ;
#102516 = CARTESIAN_POINT ( 'NONE',  ( 21.55341960407619695, -5.719274019375665929, 91.04275706135236135 ) ) ;
#102517 = CARTESIAN_POINT ( 'NONE',  ( -12.14591786802326823, 12.06949235617739902, 78.12609039468570415 ) ) ;
#102518 = CARTESIAN_POINT ( 'NONE',  ( -21.55341960407619339, 5.719274019375674811, 28.54275706135234358 ) ) ;
#102519 = CARTESIAN_POINT ( 'NONE',  ( -14.29746914071037622, -8.314922557961029526, 24.16775706135235424 ) ) ;
#102520 = CARTESIAN_POINT ( 'NONE',  ( -16.51473224551069308, -9.474510206698971260, 91.66557627198103830 ) ) ;
#102521 = CARTESIAN_POINT ( 'NONE',  ( -13.97604488694527625, -13.89961937509977652, 46.87390960531435979 ) ) ;
#102522 = CARTESIAN_POINT ( 'NONE',  ( -19.03943276465977164, 0.05219959533909376836, 56.24890960531435979 ) ) ;
#102523 = AXIS2_PLACEMENT_3D ( 'NONE', #123062, #78544, #77560 ) ;
#102524 = CARTESIAN_POINT ( 'NONE',  ( 4.483927247898790824, -16.52544592524335698, 30.20942372801902565 ) ) ;
#102525 = CARTESIAN_POINT ( 'NONE',  ( -8.224510206698948167, 14.34966873604960824, 90.41557627198103830 ) ) ;
#102526 = CARTESIAN_POINT ( 'NONE',  ( 16.53943276465976808, 0.05219959533934440121, 106.2510903946856757 ) ) ;
#102529 = CARTESIAN_POINT ( 'NONE',  ( -9.474510206698964154, 16.51473224551069663, 60.41557627198102409 ) ) ;
#102528 = CARTESIAN_POINT ( 'NONE',  ( -19.05341960407611168, -5.049401038298163336, 81.45724293864769550 ) ) ;
#102527 = CARTESIAN_POINT ( 'NONE',  ( 10.72451020669871369, 18.67979575497193778, 37.08442372801901143 ) ) ;
#102530 = CARTESIAN_POINT ( 'NONE',  ( -19.05341960407611168, -5.049401038298163336, 81.45724293864769550 ) ) ;
#102531 = CARTESIAN_POINT ( 'NONE',  ( 4.483927247898545687, 16.52544592524342804, 34.79057627198103120 ) ) ;
#102532 = CARTESIAN_POINT ( 'NONE',  ( -12.06949235617739369, -12.14591786802326823, 99.37609039468568994 ) ) ;
#102533 = ORIENTED_EDGE ( 'NONE', *, *, #15702, .F. ) ;
#102534 = CARTESIAN_POINT ( 'NONE',  ( -9.564922557961040184, 16.46253265017147172, 47.91775706135233293 ) ) ;
#102535 = CARTESIAN_POINT ( 'NONE',  ( -3.503282210674335317, -48.86437366581480291, -34.99999999999999289 ) ) ;
#102536 = CARTESIAN_POINT ( 'NONE',  ( -9.564922557960796823, -16.46253265017161027, 52.08224293864768839 ) ) ;
#102537 = CARTESIAN_POINT ( 'NONE',  ( -13.97604488694547697, 13.89961937509957934, 38.12609039468566152 ) ) ;
#102538 = CARTESIAN_POINT ( 'NONE',  ( 22.81625015709510151, -31.40387420917324590, -3.924999997268811658 ) ) ;
#102539 = CARTESIAN_POINT ( 'NONE',  ( 14.29746914071037800, 8.314922557961029526, 46.66775706135234714 ) ) ;
#102541 = CARTESIAN_POINT ( 'NONE',  ( 12.06949235617739724, 12.14591786802326823, 61.87609039468568284 ) ) ;
#102540 = CARTESIAN_POINT ( 'NONE',  ( -9.474510206698720793, -16.51473224551083518, 74.58442372801900433 ) ) ;
#102542 = CARTESIAN_POINT ( 'NONE',  ( 16.46253265017160672, -9.564922557960803928, 113.3322429386476955 ) ) ;
#102543 = CARTESIAN_POINT ( 'NONE',  ( -19.03943276465977164, 0.05219959533909376836, 76.24890960531435269 ) ) ;
#102544 = CARTESIAN_POINT ( 'NONE',  ( -21.53943276465977519, 0.05219959533907696930, 106.2489096053143811 ) ) ;
#102545 = CARTESIAN_POINT ( 'NONE',  ( -13.89961937509957401, -13.97604488694547875, 74.37609039468566152 ) ) ;
#102547 = CARTESIAN_POINT ( 'NONE',  ( -19.03943276465977164, 0.05219959533909376836, 31.24890960531435979 ) ) ;
#102546 = CARTESIAN_POINT ( 'NONE',  ( -13.97604488694527625, -13.89961937509977652, 111.8739096053143243 ) ) ;
#102548 = CARTESIAN_POINT ( 'NONE',  ( 9.564922557960805705, 16.46253265017160317, 79.58224293864769550 ) ) ;
#102550 = CARTESIAN_POINT ( 'NONE',  ( -9.474510206698964154, 16.51473224551069663, 40.41557627198103120 ) ) ;
#102549 = CARTESIAN_POINT ( 'NONE',  ( -14.34966873604960291, -8.224510206698953496, 31.66557627198102054 ) ) ;
#102551 = CARTESIAN_POINT ( 'NONE',  ( -19.05341960407617563, 5.049401038297882671, 48.54275706135233293 ) ) ;
#102552 = CARTESIAN_POINT ( 'NONE',  ( 8.224510206698953496, -14.34966873604960469, 92.91557627198103830 ) ) ;
#102553 = CARTESIAN_POINT ( 'NONE',  ( 5.823673210054444382, -21.52544592524334988, 110.2094237280190185 ) ) ;
#102554 = CARTESIAN_POINT ( 'NONE',  ( -19.03943276465977164, 0.05219959533909376836, 46.24890960531435979 ) ) ;
#102555 = CARTESIAN_POINT ( 'NONE',  ( -18.62759615963270932, 10.81492255796079327, 45.83224293864769550 ) ) ;
#102557 = CARTESIAN_POINT ( 'NONE',  ( -5.719274019375665041, -21.55341960407619695, 104.7927570613523898 ) ) ;
#102556 = CARTESIAN_POINT ( 'NONE',  ( -0.05219959533910754901, -16.53943276465976808, 52.49890960531435979 ) ) ;
#102558 = CARTESIAN_POINT ( 'NONE',  ( 5.153800228976335163, 19.02544592524342804, 94.79057627198103830 ) ) ;
#102559 = CARTESIAN_POINT ( 'NONE',  ( -9.474510206698964154, 16.51473224551069663, 110.4155762719810383 ) ) ;
#102560 = CARTESIAN_POINT ( 'NONE',  ( -13.97604488694527625, -13.89961937509977652, 41.87390960531435979 ) ) ;
#102561 = CARTESIAN_POINT ( 'NONE',  ( -19.03943276465977164, 0.05219959533909376836, 21.24890960531436335 ) ) ;
#102562 = CARTESIAN_POINT ( 'NONE',  ( 4.379528057220339221, -16.55341960407611168, 82.70724293864770971 ) ) ;
#102563 = CARTESIAN_POINT ( 'NONE',  ( 10.81492255796078972, 18.62759615963270932, 99.58224293864770971 ) ) ;
#102564 = CARTESIAN_POINT ( 'NONE',  ( 19.05341960407611168, 5.049401038298154454, 103.9572429386476671 ) ) ;
#102565 = CARTESIAN_POINT ( 'NONE',  ( -10.72451020669898014, 18.67979575497178502, 115.4155762719810241 ) ) ;
#102566 = CARTESIAN_POINT ( 'NONE',  ( -16.51473224551069308, -9.474510206698971260, 91.66557627198103830 ) ) ;
#102568 = CARTESIAN_POINT ( 'NONE',  ( -14.34966873604960291, -8.224510206698953496, 101.6655762719810383 ) ) ;
#102567 = LINE ( 'NONE', #19984, #20250 ) ;
#102569 = CARTESIAN_POINT ( 'NONE',  ( -19.02544592524342804, 5.153800228976336051, 76.04057627198102409 ) ) ;
#102570 = CARTESIAN_POINT ( 'NONE',  ( 5.823673210054125526, 21.52544592524343514, 84.79057627198102409 ) ) ;
#102571 = ADVANCED_FACE ( 'NONE', ( #59466 ), #163678, .T. ) ;
#102572 = CARTESIAN_POINT ( 'NONE',  ( -16.46253265017160317, 9.564922557960807481, 115.8322429386477097 ) ) ;
#102573 = CARTESIAN_POINT ( 'NONE',  ( -27.19095269391954517, -8.032454009542492557, 149.5864051666458181 ) ) ;
#102575 = FILL_AREA_STYLE ('',( #42899 ) ) ;
#102574 = CARTESIAN_POINT ( 'NONE',  ( -5.719274019375978568, 21.55341960407610458, 25.20724293864769550 ) ) ;
#102576 = CARTESIAN_POINT ( 'NONE',  ( -16.52544592524335698, -4.483927247898792601, 38.95942372801901854 ) ) ;
#102577 = CARTESIAN_POINT ( 'NONE',  ( 4.483927247898545687, 16.52544592524342804, 99.79057627198103830 ) ) ;
#102578 = FACE_OUTER_BOUND ( 'NONE', #178273, .T. ) ;
#102579 = CARTESIAN_POINT ( 'NONE',  ( 9.564922557960805705, 16.46253265017160317, 89.58224293864769550 ) ) ;
#102580 = CARTESIAN_POINT ( 'NONE',  ( -16.51473224551069308, -9.474510206698971260, 51.66557627198102409 ) ) ;
#102581 = CARTESIAN_POINT ( 'NONE',  ( 12.06949235617757843, -12.14591786802309237, 78.12390960531436690 ) ) ;
#102582 = CARTESIAN_POINT ( 'NONE',  ( 5.719274019375991003, -21.55341960407610458, 32.70724293864770260 ) ) ;
#102583 = CARTESIAN_POINT ( 'NONE',  ( 4.483927247898545687, 16.52544592524342804, 49.79057627198102409 ) ) ;
#102584 = CARTESIAN_POINT ( 'NONE',  ( 19.05341960407617918, -5.049401038297876454, 106.0427570613523471 ) ) ;
#102585 = CARTESIAN_POINT ( 'NONE',  ( -10.81492255796105439, 18.62759615963255655, 67.91775706135234714 ) ) ;
#102586 = CARTESIAN_POINT ( 'NONE',  ( 27.73933785331498925, -9.013057229001034898, 145.7750000027311899 ) ) ;
#102587 = CARTESIAN_POINT ( 'NONE',  ( -19.02544592524342804, 5.153800228976336051, 111.0405762719810099 ) ) ;
#102588 = CARTESIAN_POINT ( 'NONE',  ( 4.483927247898790824, -16.52544592524335698, 80.20942372801901854 ) ) ;
#102589 = CARTESIAN_POINT ( 'NONE',  ( -13.97604488694527625, -13.89961937509977652, 21.87390960531435979 ) ) ;
#102590 = CARTESIAN_POINT ( 'NONE',  ( -0.05219959533909027116, -19.03943276465977164, 82.49890960531436690 ) ) ;
#102591 = CARTESIAN_POINT ( 'NONE',  ( -21.52544592524343514, 5.823673210054127303, 86.04057627198102409 ) ) ;
#102592 = CARTESIAN_POINT ( 'NONE',  ( 8.224510206698742110, 14.34966873604972548, 27.08442372801901854 ) ) ;
#102594 = CARTESIAN_POINT ( 'NONE',  ( -18.62759615963255300, -10.81492255796106328, 79.16775706135234714 ) ) ;
#102593 = CARTESIAN_POINT ( 'NONE',  ( 14.34966873604960469, 8.224510206698951720, 49.16557627198102409 ) ) ;
#102596 = CARTESIAN_POINT ( 'NONE',  ( 0.05219959533907565091, 21.53943276465977519, 29.99890960531435979 ) ) ;
#102595 = CARTESIAN_POINT ( 'NONE',  ( -12.06949235617739369, -12.14591786802326823, 89.37609039468568994 ) ) ;
#102597 = CARTESIAN_POINT ( 'NONE',  ( -19.02544592524342804, 5.153800228976336939, 111.0405762719810241 ) ) ;
#102598 = DIRECTION ( 'NONE',  ( 1.000000000000000000, 0.000000000000000000, 0.000000000000000000 ) ) ;
#102599 = CARTESIAN_POINT ( 'NONE',  ( 16.53943276465976808, 0.05219959533934440121, 101.2510903946856757 ) ) ;
#102600 = CARTESIAN_POINT ( 'NONE',  ( -0.05219959533934338120, 16.53943276465976808, 62.50109039468568284 ) ) ;
#102601 = CARTESIAN_POINT ( 'NONE',  ( -16.46253265017160317, 9.564922557960807481, 75.83224293864769550 ) ) ;
#102602 = CARTESIAN_POINT ( 'NONE',  ( 5.049401038298161559, -19.05341960407611168, 92.70724293864769550 ) ) ;
#102603 = CARTESIAN_POINT ( 'NONE',  ( 10.81492255796106328, -18.62759615963255655, 70.41775706135236135 ) ) ;
#102604 = CARTESIAN_POINT ( 'NONE',  ( -8.314922557961024197, 14.29746914071037800, 72.91775706135234714 ) ) ;
#102605 = CARTESIAN_POINT ( 'NONE',  ( -12.14591786802309592, -12.06949235617757132, 51.87390960531437401 ) ) ;
#102606 = CARTESIAN_POINT ( 'NONE',  ( -16.46253265017160317, 9.564922557960807481, 60.83224293864769550 ) ) ;
#102607 = CARTESIAN_POINT ( 'NONE',  ( 9.474510206698971260, -16.51473224551069308, 42.91557627198103120 ) ) ;
#102608 = ORIENTED_EDGE ( 'NONE', *, *, #32278, .F. ) ;
#102609 = CARTESIAN_POINT ( 'NONE',  ( 16.51473224551083163, -9.474510206698727899, 95.83442372801900433 ) ) ;
#102610 = CARTESIAN_POINT ( 'NONE',  ( 8.224510206698953496, -14.34966873604960469, 107.9155762719810241 ) ) ;
#102611 = CARTESIAN_POINT ( 'NONE',  ( 5.049401038298161559, -19.05341960407611168, 62.70724293864769550 ) ) ;
#102613 = CARTESIAN_POINT ( 'NONE',  ( -38.00000000000001421, -12.34694845685042708, -3.899999999999999911 ) ) ;
#102612 = CARTESIAN_POINT ( 'NONE',  ( -9.564922557961040184, 16.46253265017147172, 102.9177570613523329 ) ) ;
#102614 = CARTESIAN_POINT ( 'NONE',  ( -5.823673210054431948, 21.52544592524334988, 107.7094237280190328 ) ) ;
#102615 = CARTESIAN_POINT ( 'NONE',  ( 8.224510206698742110, 14.34966873604972548, 62.08442372801901143 ) ) ;
#102616 = CARTESIAN_POINT ( 'NONE',  ( -19.02544592524334988, -5.153800228976617603, 93.95942372801900433 ) ) ;
#102617 = CARTESIAN_POINT ( 'NONE',  ( 18.62759615963271287, -10.81492255796078972, 63.33224293864770260 ) ) ;
#102618 = CARTESIAN_POINT ( 'NONE',  ( -4.483927247898782831, 16.52544592524335698, 47.70942372801902565 ) ) ;
#102619 = DIRECTION ( 'NONE',  ( -0.000000000000000000, -0.000000000000000000, -1.000000000000000000 ) ) ;
#102620 = CARTESIAN_POINT ( 'NONE',  ( 13.97604488694548053, -13.89961937509957401, 60.62609039468564731 ) ) ;
#102621 = CARTESIAN_POINT ( 'NONE',  ( -10.81492255796105439, 18.62759615963255655, 97.91775706135236135 ) ) ;
#102622 = CARTESIAN_POINT ( 'NONE',  ( -13.89961937509977652, 13.97604488694528158, 25.62390960531434558 ) ) ;
#102623 = CARTESIAN_POINT ( 'NONE',  ( 13.97604488694527802, 13.89961937509977652, 69.37390960531436690 ) ) ;
#102624 = CARTESIAN_POINT ( 'NONE',  ( 8.314922557960818139, 14.29746914071049879, 64.58224293864769550 ) ) ;
#102625 = CIRCLE ( 'NONE', #128407, 5.000000000000000000 ) ;
#102626 = CARTESIAN_POINT ( 'NONE',  ( -21.55341960407619339, 5.719274019375674811, 93.54275706135234714 ) ) ;
#102627 = CARTESIAN_POINT ( 'NONE',  ( -19.03943276465977164, -0.05219959533935918106, 43.75109039468566863 ) ) ;
#102628 = CARTESIAN_POINT ( 'NONE',  ( -19.02544592524334988, -5.153800228976617603, 23.95942372801900078 ) ) ;
#102629 = CARTESIAN_POINT ( 'NONE',  ( 13.97604488694527802, 13.89961937509977652, 114.3739096053143669 ) ) ;
#102630 = CARTESIAN_POINT ( 'NONE',  ( 0.05219959533937995610, -21.53943276465977519, 95.00109039468568994 ) ) ;
#102631 = CARTESIAN_POINT ( 'NONE',  ( -5.153800228976328057, -19.02544592524343514, 72.29057627198102409 ) ) ;
#102632 = CARTESIAN_POINT ( 'NONE',  ( 5.823673210054444382, -21.52544592524334988, 95.20942372801903275 ) ) ;
#102633 = CARTESIAN_POINT ( 'NONE',  ( -10.72451020669898014, 18.67979575497178502, 50.41557627198103120 ) ) ;
#102634 = CARTESIAN_POINT ( 'NONE',  ( -9.474510206698964154, 16.51473224551069663, 85.41557627198102409 ) ) ;
#102635 = CARTESIAN_POINT ( 'NONE',  ( -19.03943276465977164, -0.05219959533935918106, 58.75109039468566863 ) ) ;
#102636 = CARTESIAN_POINT ( 'NONE',  ( -16.51473224551069308, -9.474510206698971260, 36.66557627198102409 ) ) ;
#102637 = CARTESIAN_POINT ( 'NONE',  ( -9.474510206698964154, 16.51473224551069663, 90.41557627198103830 ) ) ;
#102638 = CARTESIAN_POINT ( 'NONE',  ( 5.049401038297881783, 19.05341960407617563, 87.29275706135234714 ) ) ;
#102639 = CARTESIAN_POINT ( 'NONE',  ( -4.379528057220086978, -16.55341960407618274, 44.79275706135234714 ) ) ;
#102640 = CARTESIAN_POINT ( 'NONE',  ( 4.379528057220339221, -16.55341960407611168, 107.7072429386476955 ) ) ;
#102641 = CARTESIAN_POINT ( 'NONE',  ( -9.474510206698964154, 16.51473224551069663, 65.41557627198102409 ) ) ;
#102642 = CARTESIAN_POINT ( 'NONE',  ( -18.67979575497178146, -10.72451020669898902, 51.66557627198102409 ) ) ;
#102643 = CARTESIAN_POINT ( 'NONE',  ( 16.53943276465976808, 0.05219959533934440121, 21.25109039468567218 ) ) ;
#102644 = CARTESIAN_POINT ( 'NONE',  ( 5.719274019375673035, 21.55341960407619339, 27.29275706135234358 ) ) ;
#102645 = CARTESIAN_POINT ( 'NONE',  ( 5.719274019375673035, 21.55341960407619339, 82.29275706135234714 ) ) ;
#102646 = CARTESIAN_POINT ( 'NONE',  ( -4.483927247898782831, 16.52544592524335698, 82.70942372801900433 ) ) ;
#102647 = CARTESIAN_POINT ( 'NONE',  ( -0.05219959533909027116, -19.03943276465977164, 72.49890960531435269 ) ) ;
#102648 = CARTESIAN_POINT ( 'NONE',  ( -16.53943276465976808, -0.05219959533934237506, 98.75109039468568994 ) ) ;
#102649 = CARTESIAN_POINT ( 'NONE',  ( 5.049401038297881783, 19.05341960407617563, 62.29275706135234003 ) ) ;
#102650 = CARTESIAN_POINT ( 'NONE',  ( 18.67979575497194134, -10.72451020669871369, 30.83442372801902209 ) ) ;
#102651 = CARTESIAN_POINT ( 'NONE',  ( 14.34966873604960469, 8.224510206698951720, 74.16557627198102409 ) ) ;
#102652 = CARTESIAN_POINT ( 'NONE',  ( 9.474510206698971260, -16.51473224551069308, 92.91557627198103830 ) ) ;
#102653 = CARTESIAN_POINT ( 'NONE',  ( -4.379528057220086978, -16.55341960407618274, 84.79275706135234714 ) ) ;
#102654 = CARTESIAN_POINT ( 'NONE',  ( -5.823673210054431948, 21.52544592524334988, 67.70942372801901854 ) ) ;
#102655 = CARTESIAN_POINT ( 'NONE',  ( 12.14591786802327356, -12.06949235617739191, 35.62609039468568994 ) ) ;
#102656 = CARTESIAN_POINT ( 'NONE',  ( 18.67979575497194134, -10.72451020669871369, 30.83442372801902209 ) ) ;
#102657 = CARTESIAN_POINT ( 'NONE',  ( 16.55341960407611168, 4.379528057220329451, 68.95724293864769550 ) ) ;
#102658 = ORIENTED_EDGE ( 'NONE', *, *, #86027, .F. ) ;
#102659 = CARTESIAN_POINT ( 'NONE',  ( 21.55341960407610458, 5.719274019375980345, 98.95724293864770971 ) ) ;
#102660 = CARTESIAN_POINT ( 'NONE',  ( 16.52544592524342804, -4.483927247898539470, 53.54057627198103120 ) ) ;
#102661 = ORIENTED_EDGE ( 'NONE', *, *, #131087, .T. ) ;
#102662 = CYLINDRICAL_SURFACE ( 'NONE', #17811, 2.500000000000002220 ) ;
#102663 = CARTESIAN_POINT ( 'NONE',  ( 21.53943276465977519, -0.05219959533907433946, 23.74890960531435269 ) ) ;
#102664 = CARTESIAN_POINT ( 'NONE',  ( -21.53943276465977519, -0.05219959533937600094, 43.75109039468568284 ) ) ;
#102665 = CARTESIAN_POINT ( 'NONE',  ( 16.53943276465976808, -0.05219959533910856209, 58.74890960531436690 ) ) ;
#102666 = CARTESIAN_POINT ( 'NONE',  ( -18.67979575497178146, -10.72451020669898902, 66.66557627198102409 ) ) ;
#102667 = CARTESIAN_POINT ( 'NONE',  ( 19.03943276465977164, -0.05219959533909143690, 68.74890960531436690 ) ) ;
#102669 = CARTESIAN_POINT ( 'NONE',  ( 5.153800228976615827, -19.02544592524334988, 80.20942372801901854 ) ) ;
#102668 = FACE_OUTER_BOUND ( 'NONE', #23198, .T. ) ;
#102670 = CARTESIAN_POINT ( 'NONE',  ( 10.72451020669898902, -18.67979575497178502, 67.91557627198102409 ) ) ;
#102671 = CARTESIAN_POINT ( 'NONE',  ( -13.89961937509977652, 13.97604488694528158, 45.62390960531433848 ) ) ;
#102672 = CARTESIAN_POINT ( 'NONE',  ( -19.05341960407611168, -5.049401038298163336, 76.45724293864769550 ) ) ;
#102673 = EDGE_LOOP ( 'NONE', ( #131560, #50745, #152600, #143286 ) ) ;
#102674 = CARTESIAN_POINT ( 'NONE',  ( -16.55341960407617563, 4.379528057220093196, 53.54275706135234714 ) ) ;
#102675 = CARTESIAN_POINT ( 'NONE',  ( -5.823673210054431948, 21.52544592524334988, 32.70942372801900433 ) ) ;
#102676 = CARTESIAN_POINT ( 'NONE',  ( -5.719274019375665041, -21.55341960407619695, 54.79275706135235424 ) ) ;
#102677 = CARTESIAN_POINT ( 'NONE',  ( 5.153800228976335163, 19.02544592524342804, 99.79057627198102409 ) ) ;
#102678 = CARTESIAN_POINT ( 'NONE',  ( 18.67979575497178502, 10.72451020669898547, 89.16557627198102409 ) ) ;
#102680 = CARTESIAN_POINT ( 'NONE',  ( 14.29746914071037800, 8.314922557961029526, 51.66775706135234714 ) ) ;
#102679 = CARTESIAN_POINT ( 'NONE',  ( -0.05219959533907301413, -21.53943276465977519, 112.4989096053143669 ) ) ;
#102681 = CARTESIAN_POINT ( 'NONE',  ( -10.81492255796078084, -18.62759615963271287, 52.08224293864768839 ) ) ;
#102682 = CARTESIAN_POINT ( 'NONE',  ( 18.62759615963255655, 10.81492255796105972, 106.6677570613523756 ) ) ;
#102683 = CARTESIAN_POINT ( 'NONE',  ( 13.97604488694527802, 13.89961937509977652, 54.37390960531435979 ) ) ;
#102684 = CARTESIAN_POINT ( 'NONE',  ( -16.51473224551069308, -9.474510206698971260, 106.6655762719810383 ) ) ;
#102685 = CARTESIAN_POINT ( 'NONE',  ( 19.03943276465977164, -0.05219959533909143690, 93.74890960531435269 ) ) ;
#102686 = CARTESIAN_POINT ( 'NONE',  ( -12.56216403881615307, -41.81473846791989502, -20.79002063418674240 ) ) ;
#102687 = CARTESIAN_POINT ( 'NONE',  ( 9.474510206698729675, 16.51473224551082808, 67.08442372801900433 ) ) ;
#102688 = CARTESIAN_POINT ( 'NONE',  ( 15.80617190586746368, 15.72974639402197994, 49.37390960531436690 ) ) ;
#102689 = CARTESIAN_POINT ( 'NONE',  ( -8.314922557961024197, 14.29746914071037800, 107.9177570613523471 ) ) ;
#102690 = CARTESIAN_POINT ( 'NONE',  ( -16.46253265017146816, -9.564922557961047289, 89.16775706135234714 ) ) ;
#102691 = DIRECTION ( 'NONE',  ( 0.5000000000000004441, 0.4999999999999986122, -0.7071067811865481278 ) ) ;
#102692 = CARTESIAN_POINT ( 'NONE',  ( -9.474510206698720793, -16.51473224551083518, 24.58442372801900078 ) ) ;
#102693 = CARTESIAN_POINT ( 'NONE',  ( 19.02544592524334988, 5.153800228976608722, 81.45942372801897591 ) ) ;
#102694 = CARTESIAN_POINT ( 'NONE',  ( -9.474510206698720793, -16.51473224551083518, 39.58442372801899722 ) ) ;
#102695 = CARTESIAN_POINT ( 'NONE',  ( -38.00000000000000711, 2.893978650043524126E-14, -18.00000000000000000 ) ) ;
#102696 = CARTESIAN_POINT ( 'NONE',  ( -16.46253265017160317, 9.564922557960807481, 55.83224293864769550 ) ) ;
#102697 = CARTESIAN_POINT ( 'NONE',  ( 16.55341960407611168, 4.379528057220329451, 43.95724293864769550 ) ) ;
#102698 = CARTESIAN_POINT ( 'NONE',  ( -0.05219959533909027116, -19.03943276465977164, 32.49890960531435979 ) ) ;
#102699 = CARTESIAN_POINT ( 'NONE',  ( 16.52544592524342804, -4.483927247898539470, 43.54057627198103830 ) ) ;
#102700 = CARTESIAN_POINT ( 'NONE',  ( -37.99626262588766679, 2.428612866367529932E-14, -3.747842220587803475 ) ) ;
#102701 = CARTESIAN_POINT ( 'NONE',  ( -12.14591786802326823, 12.06949235617739902, 108.1260903946856757 ) ) ;
#102702 = CARTESIAN_POINT ( 'NONE',  ( -13.97604488694527625, -13.89961937509977652, 56.87390960531434558 ) ) ;
#102703 = CARTESIAN_POINT ( 'NONE',  ( -13.89961937509957401, -13.97604488694547875, 24.37609039468565442 ) ) ;
#102704 = CARTESIAN_POINT ( 'NONE',  ( 12.06949235617739724, 12.14591786802326823, 36.87609039468568994 ) ) ;
#102705 = CARTESIAN_POINT ( 'NONE',  ( 10.72451020669898902, -18.67979575497178502, 37.91557627198102409 ) ) ;
#102706 = CARTESIAN_POINT ( 'NONE',  ( -21.53943276465977519, -0.05219959533937600094, 88.75109039468567573 ) ) ;
#102707 = CARTESIAN_POINT ( 'NONE',  ( 9.474510206698971260, -16.51473224551069308, 57.91557627198103120 ) ) ;
#102708 = CARTESIAN_POINT ( 'NONE',  ( -19.02544592524342804, 5.153800228976336051, 106.0405762719810241 ) ) ;
#102709 = CARTESIAN_POINT ( 'NONE',  ( -13.97604488694527625, -13.89961937509977652, 96.87390960531433848 ) ) ;
#102710 = CARTESIAN_POINT ( 'NONE',  ( -33.33806273211352078, -22.10771529531805513, -23.55827701141446440 ) ) ;
#102711 = CARTESIAN_POINT ( 'NONE',  ( 0.05219959533937995610, -21.53943276465977519, 20.00109039468568639 ) ) ;
#102712 = CARTESIAN_POINT ( 'NONE',  ( 12.06949235617757843, -12.14591786802309237, 78.12390960531436690 ) ) ;
#102714 = CARTESIAN_POINT ( 'NONE',  ( -16.46253265017160317, 9.564922557960807481, 70.83224293864770971 ) ) ;
#102713 = CARTESIAN_POINT ( 'NONE',  ( -21.53943276465977519, 0.05219959533907696930, 81.24890960531436690 ) ) ;
#102715 = CARTESIAN_POINT ( 'NONE',  ( -9.564922557960796823, -16.46253265017161027, 77.08224293864769550 ) ) ;
#102716 = CARTESIAN_POINT ( 'NONE',  ( 10.72451020669898902, -18.67979575497178502, 112.9155762719810383 ) ) ;
#102717 = ORIENTED_EDGE ( 'NONE', *, *, #47118, .F. ) ;
#102718 = CARTESIAN_POINT ( 'NONE',  ( -19.03943276465977164, 0.05219959533909376836, 56.24890960531435979 ) ) ;
#102720 = CARTESIAN_POINT ( 'NONE',  ( -5.049401038298153566, 19.05341960407611168, 25.20724293864768484 ) ) ;
#102719 = CARTESIAN_POINT ( 'NONE',  ( 12.14591786802309770, 12.06949235617756955, 99.37390960531436690 ) ) ;
#102721 = CARTESIAN_POINT ( 'NONE',  ( -9.474510206698964154, 16.51473224551069663, 70.41557627198102409 ) ) ;
#102722 = CARTESIAN_POINT ( 'NONE',  ( 5.049401038297881783, 19.05341960407617563, 87.29275706135234714 ) ) ;
#102723 = CARTESIAN_POINT ( 'NONE',  ( 8.314922557960818139, 14.29746914071049879, 94.58224293864769550 ) ) ;
#102724 = CARTESIAN_POINT ( 'NONE',  ( -15.72974639402176322, -15.80617190586768395, 54.37609039468568994 ) ) ;
#102726 = CARTESIAN_POINT ( 'NONE',  ( -18.67979575497193778, 10.72451020669871902, 23.33442372801901499 ) ) ;
#102725 = CARTESIAN_POINT ( 'NONE',  ( -13.89961937509977652, 13.97604488694528158, 55.62390960531434558 ) ) ;
#102727 = CARTESIAN_POINT ( 'NONE',  ( 14.34966873604960469, 8.224510206698951720, 104.1655762719810241 ) ) ;
#102728 = CARTESIAN_POINT ( 'NONE',  ( -8.906447517083060816, 27.41122689804195645, 141.5999999999999943 ) ) ;
#102729 = CARTESIAN_POINT ( 'NONE',  ( -16.46253265017160317, 9.564922557960807481, 70.83224293864770971 ) ) ;
#102730 = CARTESIAN_POINT ( 'NONE',  ( -17.49999999999999645, -5.500000000000000888, 120.0000000000000142 ) ) ;
#102732 = CARTESIAN_POINT ( 'NONE',  ( -10.81492255796078084, -18.62759615963271287, 32.08224293864769550 ) ) ;
#102731 = CARTESIAN_POINT ( 'NONE',  ( -13.89961937509957401, -13.97604488694547875, 109.3760903946856331 ) ) ;
#102733 = CARTESIAN_POINT ( 'NONE',  ( -18.67979575497193778, 10.72451020669871902, 48.33442372801902565 ) ) ;
#102734 = CARTESIAN_POINT ( 'NONE',  ( 9.474510206698971260, -16.51473224551069308, 102.9155762719810241 ) ) ;
#102735 = CARTESIAN_POINT ( 'NONE',  ( 5.049401038297881783, 19.05341960407617563, 87.29275706135234714 ) ) ;
#102736 = CARTESIAN_POINT ( 'NONE',  ( -16.46253265017160317, 9.564922557960807481, 75.83224293864769550 ) ) ;
#102737 = ADVANCED_FACE ( 'NONE', ( #102993 ), #134346, .T. ) ;
#102738 = CARTESIAN_POINT ( 'NONE',  ( -16.52544592524342804, 4.483927247898546575, 76.04057627198102409 ) ) ;
#102739 = CARTESIAN_POINT ( 'NONE',  ( -0.05219959533909027116, -19.03943276465977164, 97.49890960531436690 ) ) ;
#102740 = CARTESIAN_POINT ( 'NONE',  ( -4.483927247898539470, -16.52544592524342804, 77.29057627198102409 ) ) ;
#102741 = CARTESIAN_POINT ( 'NONE',  ( 16.46253265017160672, -9.564922557960803928, 93.33224293864769550 ) ) ;
#102744 = CARTESIAN_POINT ( 'NONE',  ( 19.05341960407611168, 5.049401038298154454, 28.95724293864769550 ) ) ;
#102743 = CARTESIAN_POINT ( 'NONE',  ( -16.55341960407611168, -4.379528057220339221, 46.45724293864769550 ) ) ;
#102742 = CARTESIAN_POINT ( 'NONE',  ( 19.03943276465977164, -0.05219959533909143690, 48.74890960531435979 ) ) ;
#102745 = ORIENTED_EDGE ( 'NONE', *, *, #70632, .F. ) ;
#102746 = CARTESIAN_POINT ( 'NONE',  ( 15.72974639402176855, 15.80617190586768217, 41.87609039468568284 ) ) ;
#102747 = CARTESIAN_POINT ( 'NONE',  ( -9.474510206698720793, -16.51473224551083518, 79.58442372801899012 ) ) ;
#102748 = CARTESIAN_POINT ( 'NONE',  ( -4.379528057220328563, 16.55341960407611168, 55.20724293864770260 ) ) ;
#102749 = CARTESIAN_POINT ( 'NONE',  ( 21.53943276465977519, -0.05219959533907433946, 93.74890960531436690 ) ) ;
#102750 = CARTESIAN_POINT ( 'NONE',  ( -5.823673210054116645, -21.52544592524344225, 32.29057627198102409 ) ) ;
#102751 = CARTESIAN_POINT ( 'NONE',  ( -12.06949235617756955, 12.14591786802309770, 80.62390960531438111 ) ) ;
#102752 = CARTESIAN_POINT ( 'NONE',  ( 9.564922557960805705, 16.46253265017160317, 49.58224293864770260 ) ) ;
#102753 = CARTESIAN_POINT ( 'NONE',  ( -14.34966873604960291, -8.224510206698953496, 26.66557627198103475 ) ) ;
#102754 = CIRCLE ( 'NONE', #199602, 59.99999999999998579 ) ;
#102755 = CARTESIAN_POINT ( 'NONE',  ( 4.379528057220092307, 16.55341960407617563, 87.29275706135236135 ) ) ;
#102756 = CARTESIAN_POINT ( 'NONE',  ( -14.29746914071037622, -8.314922557961029526, 74.16775706135231871 ) ) ;
#102757 = CARTESIAN_POINT ( 'NONE',  ( 5.049401038297881783, 19.05341960407617563, 32.29275706135233293 ) ) ;
#102758 = CARTESIAN_POINT ( 'NONE',  ( -13.97604488694527625, -13.89961937509977652, 96.87390960531433848 ) ) ;
#102759 = CARTESIAN_POINT ( 'NONE',  ( 13.97604488694527802, 13.89961937509977652, 79.37390960531435269 ) ) ;
#102760 = CARTESIAN_POINT ( 'NONE',  ( -8.224510206698735004, -14.34966873604973081, 74.58442372801901854 ) ) ;
#102761 = CARTESIAN_POINT ( 'NONE',  ( 5.153800228976335163, 19.02544592524342804, 39.79057627198100988 ) ) ;
#102762 = CARTESIAN_POINT ( 'NONE',  ( -16.55341960407611168, -4.379528057220339221, 51.45724293864770260 ) ) ;
#102764 = CARTESIAN_POINT ( 'NONE',  ( 16.51473224551069308, 9.474510206698969483, 99.16557627198102409 ) ) ;
#102763 = CARTESIAN_POINT ( 'NONE',  ( -9.474510206698964154, 16.51473224551069663, 115.4155762719810241 ) ) ;
#102765 = CARTESIAN_POINT ( 'NONE',  ( -5.823673210054116645, -21.52544592524344225, 32.29057627198102409 ) ) ;
#102766 = CARTESIAN_POINT ( 'NONE',  ( -4.379528057220328563, 16.55341960407611168, 75.20724293864769550 ) ) ;
#102767 = CARTESIAN_POINT ( 'NONE',  ( 4.483927247898545687, 16.52544592524342804, 69.79057627198102409 ) ) ;
#102768 = CARTESIAN_POINT ( 'NONE',  ( 31.05479031690787650, -1.359215367441156008, -46.85916094508149143 ) ) ;
#102769 = CARTESIAN_POINT ( 'NONE',  ( 5.153800228976615827, -19.02544592524334988, 65.20942372801900433 ) ) ;
#102770 = CARTESIAN_POINT ( 'NONE',  ( -9.474510206698964154, 16.51473224551069663, 100.4155762719810241 ) ) ;
#102771 = CARTESIAN_POINT ( 'NONE',  ( 9.564922557961047289, -16.46253265017146816, 80.41775706135234714 ) ) ;
#102772 = CARTESIAN_POINT ( 'NONE',  ( 8.571926809382597767, 26.38167802310806209, 146.7750000027311899 ) ) ;
#102774 = CARTESIAN_POINT ( 'NONE',  ( -16.53943276465976808, -0.05219959533934237506, 93.75109039468567573 ) ) ;
#102773 = CARTESIAN_POINT ( 'NONE',  ( 8.224510206698742110, 14.34966873604972548, 22.08442372801901143 ) ) ;
#102775 = CARTESIAN_POINT ( 'NONE',  ( 19.03943276465977164, -0.05219959533909143690, 33.74890960531435979 ) ) ;
#102776 = CARTESIAN_POINT ( 'NONE',  ( 18.67979575497178502, 10.72451020669898547, 34.16557627198102409 ) ) ;
#102777 = CARTESIAN_POINT ( 'NONE',  ( -15.80617190586768217, 15.72974639402176855, 53.12609039468568284 ) ) ;
#102778 = CARTESIAN_POINT ( 'NONE',  ( -8.314922557961024197, 14.29746914071037800, 22.91775706135235069 ) ) ;
#102780 = CARTESIAN_POINT ( 'NONE',  ( -13.97604488694527625, -13.89961937509977652, 71.87390960531433848 ) ) ;
#102779 = CARTESIAN_POINT ( 'NONE',  ( -3.573655867282028392E-15, 2.428612866367529932E-14, -18.00000000000000000 ) ) ;
#102781 = AXIS2_PLACEMENT_3D ( 'NONE', #190783, #173635, #80601 ) ;
#102782 = CARTESIAN_POINT ( 'NONE',  ( 13.89961937509977652, -13.97604488694527269, 113.1239096053143527 ) ) ;
#102784 = CARTESIAN_POINT ( 'NONE',  ( 9.564922557960805705, 16.46253265017160317, 79.58224293864769550 ) ) ;
#102783 = CARTESIAN_POINT ( 'NONE',  ( 4.483927247898545687, 16.52544592524342804, 69.79057627198102409 ) ) ;
#102785 = CARTESIAN_POINT ( 'NONE',  ( 13.89961937509977652, -13.97604488694527269, 88.12390960531438111 ) ) ;
#102786 = VERTEX_POINT ( 'NONE', #136321 ) ;
#102787 = CARTESIAN_POINT ( 'NONE',  ( 19.05341960407617918, -5.049401038297876454, 86.04275706135233293 ) ) ;
#102788 = CARTESIAN_POINT ( 'NONE',  ( 21.53943276465977519, -0.05219959533907433946, 58.74890960531436690 ) ) ;
#102789 = CARTESIAN_POINT ( 'NONE',  ( 5.153800228976335163, 19.02544592524342804, 29.79057627198102409 ) ) ;
#102790 = CARTESIAN_POINT ( 'NONE',  ( 16.51473224551083163, -9.474510206698727899, 50.83442372801899722 ) ) ;
#102791 = CARTESIAN_POINT ( 'NONE',  ( -5.049401038298153566, 19.05341960407611168, 55.20724293864769550 ) ) ;
#102792 = CARTESIAN_POINT ( 'NONE',  ( 16.46253265017160672, -9.564922557960803928, 98.33224293864769550 ) ) ;
#102793 = EDGE_LOOP ( 'NONE', ( #72135, #87290, #189442 ) ) ;
#102794 = CARTESIAN_POINT ( 'NONE',  ( -21.52544592524343514, 5.823673210054127303, 86.04057627198102409 ) ) ;
#102796 = CARTESIAN_POINT ( 'NONE',  ( -16.46253265017146816, -9.564922557961047289, 54.16775706135234003 ) ) ;
#102795 = CARTESIAN_POINT ( 'NONE',  ( 16.52544592524342804, -4.483927247898539470, 98.54057627198105251 ) ) ;
#102797 = CARTESIAN_POINT ( 'NONE',  ( -10.72451020669898014, 18.67979575497178502, 95.41557627198102409 ) ) ;
#102798 = CARTESIAN_POINT ( 'NONE',  ( 21.52544592524344225, -5.823673210054117533, 78.54057627198103830 ) ) ;
#102799 = CARTESIAN_POINT ( 'NONE',  ( -16.53943276465976808, 0.05219959533911058130, 26.24890960531435624 ) ) ;
#102800 = CARTESIAN_POINT ( 'NONE',  ( -18.62759615963255300, -10.81492255796106328, 109.1677570613523613 ) ) ;
#102801 = CARTESIAN_POINT ( 'NONE',  ( 0.05219959533934541429, -16.53943276465976808, 55.00109039468568284 ) ) ;
#102802 = CARTESIAN_POINT ( 'NONE',  ( 13.97604488694527802, 13.89961937509977652, 74.37390960531436690 ) ) ;
#102803 = CARTESIAN_POINT ( 'NONE',  ( 5.049401038298161559, -19.05341960407611168, 27.70724293864769550 ) ) ;
#102804 = CARTESIAN_POINT ( 'NONE',  ( 21.55341960407619695, -5.719274019375665929, 36.04275706135234714 ) ) ;
#102805 = CARTESIAN_POINT ( 'NONE',  ( -10.72451020669870658, -18.67979575497194134, 54.58442372801901143 ) ) ;
#102806 = CARTESIAN_POINT ( 'NONE',  ( 19.03943276465977164, -0.05219959533909143690, 53.74890960531436690 ) ) ;
#102807 = CARTESIAN_POINT ( 'NONE',  ( -15.80617190586768217, 15.72974639402176855, 28.12609039468568284 ) ) ;
#102808 = EDGE_CURVE ( 'NONE', #33383, #136214, #179642, .T. ) ;
#102809 = CARTESIAN_POINT ( 'NONE',  ( 19.03943276465977164, 0.05219959533936151252, 66.25109039468567573 ) ) ;
#102810 = CARTESIAN_POINT ( 'NONE',  ( 9.564922557960805705, 16.46253265017160317, 39.58224293864768839 ) ) ;
#102811 = CARTESIAN_POINT ( 'NONE',  ( 4.483927247898790824, -16.52544592524335698, 25.20942372801901854 ) ) ;
#102812 = CARTESIAN_POINT ( 'NONE',  ( -0.05219959533909027116, -19.03943276465977164, 32.49890960531435979 ) ) ;
#102813 = CARTESIAN_POINT ( 'NONE',  ( 12.06949235617739724, 12.14591786802326823, 76.87609039468567573 ) ) ;
#102814 = CARTESIAN_POINT ( 'NONE',  ( -13.89961937509977652, 13.97604488694528158, 45.62390960531433848 ) ) ;
#102815 = CARTESIAN_POINT ( 'NONE',  ( 24.40828949532303227, -2.848420800297167599, 173.9378174459542663 ) ) ;
#102816 = CARTESIAN_POINT ( 'NONE',  ( -9.474510206698964154, 16.51473224551069663, 85.41557627198102409 ) ) ;
#102817 = CARTESIAN_POINT ( 'NONE',  ( 19.02544592524343514, -5.153800228976328945, 23.54057627198102054 ) ) ;
#102818 = CARTESIAN_POINT ( 'NONE',  ( 10.81492255796078972, 18.62759615963270932, 69.58224293864769550 ) ) ;
#102819 = CARTESIAN_POINT ( 'NONE',  ( 12.06949235617739724, 12.14591786802326823, 56.87609039468568994 ) ) ;
#102820 = CARTESIAN_POINT ( 'NONE',  ( 5.719274019375673035, 21.55341960407619339, 107.2927570613523471 ) ) ;
#102821 = CARTESIAN_POINT ( 'NONE',  ( -5.153800228976328057, -19.02544592524343514, 37.29057627198102409 ) ) ;
#102822 = CARTESIAN_POINT ( 'NONE',  ( -8.314922557960811034, -14.29746914071050412, 32.08224293864769550 ) ) ;
#102823 = CARTESIAN_POINT ( 'NONE',  ( 16.55341960407611168, 4.379528057220329451, 73.95724293864769550 ) ) ;
#102824 = CARTESIAN_POINT ( 'NONE',  ( -19.02544592524342804, 5.153800228976336051, 66.04057627198103830 ) ) ;
#102825 = CARTESIAN_POINT ( 'NONE',  ( 21.53943276465977519, 0.05219959533937863772, 111.2510903946856899 ) ) ;
#102826 = CARTESIAN_POINT ( 'NONE',  ( -21.52544592524334988, -5.823673210054445271, 18.95942372801901143 ) ) ;
#102827 = CARTESIAN_POINT ( 'NONE',  ( 5.153800228976335163, 19.02544592524342804, 84.79057627198099567 ) ) ;
#102828 = CARTESIAN_POINT ( 'NONE',  ( -10.72451020669870658, -18.67979575497194134, 84.58442372801903275 ) ) ;
#102829 = CARTESIAN_POINT ( 'NONE',  ( 16.53943276465976808, 0.05219959533934440121, 61.25109039468567573 ) ) ;
#102830 = CARTESIAN_POINT ( 'NONE',  ( 16.46253265017160672, -9.564922557960803928, 103.3322429386476955 ) ) ;
#102831 = CARTESIAN_POINT ( 'NONE',  ( 4.483927247898545687, 16.52544592524342804, 29.79057627198102409 ) ) ;
#102832 = CARTESIAN_POINT ( 'NONE',  ( -13.89961937509977652, 13.97604488694528158, 30.62390960531435269 ) ) ;
#102833 = CARTESIAN_POINT ( 'NONE',  ( 16.55341960407618274, -4.379528057220086978, 56.04275706135235424 ) ) ;
#102834 = CARTESIAN_POINT ( 'NONE',  ( -14.29746914071049879, 8.314922557960819915, 55.83224293864770260 ) ) ;
#102835 = CARTESIAN_POINT ( 'NONE',  ( -19.03943276465977164, 0.05219959533909376836, 106.2489096053143669 ) ) ;
#102836 = CARTESIAN_POINT ( 'NONE',  ( -10.81492255796078084, -18.62759615963271287, 37.08224293864768129 ) ) ;
#102837 = CARTESIAN_POINT ( 'NONE',  ( 15.72974639402176855, 15.80617190586768217, 106.8760903946856899 ) ) ;
#102838 = CARTESIAN_POINT ( 'NONE',  ( 12.06949235617757843, -12.14591786802309237, 88.12390960531436690 ) ) ;
#102839 = CARTESIAN_POINT ( 'NONE',  ( -13.97604488694527625, -13.89961937509977652, 91.87390960531432427 ) ) ;
#102840 = EDGE_LOOP ( 'NONE', ( #169664, #116393, #162459, #110941 ) ) ;
#102841 = CARTESIAN_POINT ( 'NONE',  ( -12.06949235617739369, -12.14591786802326823, 54.37609039468568994 ) ) ;
#102842 = CARTESIAN_POINT ( 'NONE',  ( -19.05341960407611168, -5.049401038298163336, 61.45724293864769550 ) ) ;
#102843 = CARTESIAN_POINT ( 'NONE',  ( -17.29957754486504129, -5.500000000000000888, 21.12734848878977445 ) ) ;
#102844 = CARTESIAN_POINT ( 'NONE',  ( -13.97604488694547697, 13.89961937509957934, 53.12609039468565442 ) ) ;
#102845 = CARTESIAN_POINT ( 'NONE',  ( 9.564922557960805705, 16.46253265017160317, 44.58224293864769550 ) ) ;
#102846 = CARTESIAN_POINT ( 'NONE',  ( -16.52544592524335698, -4.483927247898792601, 78.95942372801901854 ) ) ;
#102847 = CARTESIAN_POINT ( 'NONE',  ( -19.02544592524334988, -5.153800228976617603, 93.95942372801900433 ) ) ;
#102848 = CARTESIAN_POINT ( 'NONE',  ( -0.05219959533937732626, 21.53943276465977519, 67.50109039468568994 ) ) ;
#102849 = CARTESIAN_POINT ( 'NONE',  ( 5.153800228976335163, 19.02544592524342804, 59.79057627198100988 ) ) ;
#102850 = CARTESIAN_POINT ( 'NONE',  ( 10.81492255796078972, 18.62759615963270932, 94.58224293864769550 ) ) ;
#102851 = CARTESIAN_POINT ( 'NONE',  ( 14.34966873604960469, 8.224510206698951720, 99.16557627198100988 ) ) ;
#102852 = CARTESIAN_POINT ( 'NONE',  ( -13.97604488694547697, 13.89961937509957934, 68.12609039468563310 ) ) ;
#102853 = CARTESIAN_POINT ( 'NONE',  ( 21.55341960407610458, 5.719274019375980345, 68.95724293864769550 ) ) ;
#102854 = CARTESIAN_POINT ( 'NONE',  ( -0.05219959533936034679, 19.03943276465977164, 42.50109039468566152 ) ) ;
#102855 = CARTESIAN_POINT ( 'NONE',  ( 18.89770734986047884, 5.499999999999944933, 96.60214472496645044 ) ) ;
#102856 = CARTESIAN_POINT ( 'NONE',  ( 5.719274019375991003, -21.55341960407610458, 92.70724293864770971 ) ) ;
#102857 = CARTESIAN_POINT ( 'NONE',  ( -19.01533133064925352, 5.499999999999451994, 53.76586590595741200 ) ) ;
#102858 = CARTESIAN_POINT ( 'NONE',  ( 16.52544592524335698, 4.483927247898782831, 21.45942372801901499 ) ) ;
#102859 = CARTESIAN_POINT ( 'NONE',  ( 37.58407650405590061, -0.3597885541503427764, 39.49999999999997868 ) ) ;
#102860 = CARTESIAN_POINT ( 'NONE',  ( 14.29746914071037800, 8.314922557961029526, 26.66775706135235424 ) ) ;
#102861 = CARTESIAN_POINT ( 'NONE',  ( -13.97604488694527625, -13.89961937509977652, 46.87390960531435979 ) ) ;
#102862 = CARTESIAN_POINT ( 'NONE',  ( 0.05219959533909260263, 19.03943276465977164, 104.9989096053143669 ) ) ;
#102863 = CARTESIAN_POINT ( 'NONE',  ( -21.53943276465977519, 0.05219959533907696930, 91.24890960531436690 ) ) ;
#102864 = CARTESIAN_POINT ( 'NONE',  ( -5.719274019375665041, -21.55341960407619695, 69.79275706135234714 ) ) ;
#102866 = CARTESIAN_POINT ( 'NONE',  ( 16.46253265017146816, 9.564922557961045513, 31.66775706135232937 ) ) ;
#102865 = CARTESIAN_POINT ( 'NONE',  ( -4.379528057220086978, -16.55341960407618274, 19.79275706135235069 ) ) ;
#102867 = CARTESIAN_POINT ( 'NONE',  ( -0.05219959533910754901, -16.53943276465976808, 32.49890960531435979 ) ) ;
#102868 = CARTESIAN_POINT ( 'NONE',  ( 15.80617190586746368, 15.72974639402197994, 114.3739096053143527 ) ) ;
#102869 = CARTESIAN_POINT ( 'NONE',  ( 16.52544592524342804, -4.483927247898539470, 53.54057627198103120 ) ) ;
#102870 = CARTESIAN_POINT ( 'NONE',  ( 9.474510206698729675, 16.51473224551082808, 97.08442372801900433 ) ) ;
#102871 = CARTESIAN_POINT ( 'NONE',  ( 9.564922557961047289, -16.46253265017146816, 55.41775706135234003 ) ) ;
#102872 = CARTESIAN_POINT ( 'NONE',  ( -15.72974639402176322, -15.80617190586768395, 69.37609039468567573 ) ) ;
#102873 = CARTESIAN_POINT ( 'NONE',  ( -5.153800228976607833, 19.02544592524334988, 57.70942372801899012 ) ) ;
#102874 = CARTESIAN_POINT ( 'NONE',  ( -16.46253265017160317, 9.564922557960807481, 25.83224293864769194 ) ) ;
#102875 = CARTESIAN_POINT ( 'NONE',  ( 15.72974639402199770, -15.80617190586745480, 38.12390960531436690 ) ) ;
#102876 = CARTESIAN_POINT ( 'NONE',  ( 16.52544592524342804, -4.483927247898539470, 48.54057627198103120 ) ) ;
#102877 = CARTESIAN_POINT ( 'NONE',  ( -17.60779699588839975, -5.500000000000025757, 51.34981316670105400 ) ) ;
#102878 = CARTESIAN_POINT ( 'NONE',  ( -13.97604488694547697, 13.89961937509957934, 23.12609039468565442 ) ) ;
#102879 = CARTESIAN_POINT ( 'NONE',  ( 4.483927247898790824, -16.52544592524335698, 65.20942372801901854 ) ) ;
#102880 = CARTESIAN_POINT ( 'NONE',  ( -8.314922557960811034, -14.29746914071050412, 42.08224293864769550 ) ) ;
#102881 = CARTESIAN_POINT ( 'NONE',  ( 15.72974639402176855, 15.80617190586768217, 81.87609039468568994 ) ) ;
#102882 = CARTESIAN_POINT ( 'NONE',  ( 10.72451020669871369, 18.67979575497193778, 67.08442372801901854 ) ) ;
#102883 = CARTESIAN_POINT ( 'NONE',  ( 21.52544592524344225, -5.823673210054117533, 83.54057627198102409 ) ) ;
#102884 = CARTESIAN_POINT ( 'NONE',  ( 19.03943276465977164, -0.05219959533909143690, 43.74890960531435979 ) ) ;
#102885 = CARTESIAN_POINT ( 'NONE',  ( 15.72974639402176855, 15.80617190586768217, 41.87609039468568284 ) ) ;
#102886 = CARTESIAN_POINT ( 'NONE',  ( -9.564922557960796823, -16.46253265017161027, 27.08224293864769550 ) ) ;
#102887 = CARTESIAN_POINT ( 'NONE',  ( 0.05219959533909260263, 19.03943276465977164, 34.99890960531435979 ) ) ;
#102888 = CARTESIAN_POINT ( 'NONE',  ( -14.34966873604960291, -8.224510206698953496, 96.66557627198102409 ) ) ;
#102889 = CARTESIAN_POINT ( 'NONE',  ( -19.03943276465977164, 0.05219959533909376836, 81.24890960531436690 ) ) ;
#102890 = CARTESIAN_POINT ( 'NONE',  ( -16.53943276465976808, 0.05219959533911058130, 41.24890960531435269 ) ) ;
#102891 = CARTESIAN_POINT ( 'NONE',  ( -4.483927247898539470, -16.52544592524342804, 97.29057627198105251 ) ) ;
#102892 = CARTESIAN_POINT ( 'NONE',  ( -5.719274019375978568, 21.55341960407610458, 65.20724293864768129 ) ) ;
#102893 = CARTESIAN_POINT ( 'NONE',  ( -5.823673210054431948, 21.52544592524334988, 22.70942372801901499 ) ) ;
#102894 = CARTESIAN_POINT ( 'NONE',  ( 13.97604488694527802, 13.89961937509977652, 114.3739096053143669 ) ) ;
#102896 = CARTESIAN_POINT ( 'NONE',  ( -14.34966873604972548, 8.224510206698743886, 23.33442372801901499 ) ) ;
#102895 = CARTESIAN_POINT ( 'NONE',  ( -13.89961937509977652, 13.97604488694528158, 60.62390960531436690 ) ) ;
#102897 = CARTESIAN_POINT ( 'NONE',  ( -18.62759615963270932, 10.81492255796079327, 75.83224293864769550 ) ) ;
#102898 = CARTESIAN_POINT ( 'NONE',  ( 21.53943276465977519, 0.05219959533937863772, 91.25109039468568994 ) ) ;
#102899 = CARTESIAN_POINT ( 'NONE',  ( 19.05341960407611168, 5.049401038298154454, 78.95724293864769550 ) ) ;
#102900 = CARTESIAN_POINT ( 'NONE',  ( 15.72974639402199770, -15.80617190586745480, 113.1239096053143953 ) ) ;
#102901 = EDGE_CURVE ( 'NONE', #7679, #65322, #73114, .T. ) ;
#102902 = CARTESIAN_POINT ( 'NONE',  ( -16.46253265017160317, 9.564922557960807481, 115.8322429386477097 ) ) ;
#102903 = CARTESIAN_POINT ( 'NONE',  ( 14.29746914071037800, 8.314922557961029526, 96.66775706135234714 ) ) ;
#102904 = CARTESIAN_POINT ( 'NONE',  ( -5.719274019375665041, -21.55341960407619695, 74.79275706135234714 ) ) ;
#102905 = CARTESIAN_POINT ( 'NONE',  ( -15.72974639402176322, -15.80617190586768395, 104.3760903946856899 ) ) ;
#102906 = CARTESIAN_POINT ( 'NONE',  ( 14.34966873604972726, -8.224510206698740333, 55.83442372801901854 ) ) ;
#102907 = CARTESIAN_POINT ( 'NONE',  ( -18.62759615963255300, -10.81492255796106328, 29.16775706135234003 ) ) ;
#102908 = CARTESIAN_POINT ( 'NONE',  ( 19.02544592524343514, -5.153800228976328945, 113.5405762719810241 ) ) ;
#102909 = CARTESIAN_POINT ( 'NONE',  ( -5.823673210054431948, 21.52544592524334988, 87.70942372801901854 ) ) ;
#102910 = CARTESIAN_POINT ( 'NONE',  ( 19.05341960407611168, 5.049401038298154454, 93.95724293864769550 ) ) ;
#102911 = CARTESIAN_POINT ( 'NONE',  ( -15.80617190586745835, -15.72974639402198527, 86.87390960531438111 ) ) ;
#102912 = CARTESIAN_POINT ( 'NONE',  ( 13.97604488694548053, -13.89961937509957401, 55.62609039468566863 ) ) ;
#102913 = CARTESIAN_POINT ( 'NONE',  ( -21.55341960407610458, -5.719274019375992779, 51.45724293864770260 ) ) ;
#102915 = CARTESIAN_POINT ( 'NONE',  ( -16.55341960407611168, -4.379528057220339221, 36.45724293864768839 ) ) ;
#102914 = CARTESIAN_POINT ( 'NONE',  ( 16.46253265017160672, -9.564922557960803928, 93.33224293864769550 ) ) ;
#102916 = CARTESIAN_POINT ( 'NONE',  ( -8.906447517083060816, 27.41122689804195645, 145.5999999999999943 ) ) ;
#102917 = CARTESIAN_POINT ( 'NONE',  ( 19.05341960407617918, -5.049401038297876454, 71.04275706135234714 ) ) ;
#102918 = CARTESIAN_POINT ( 'NONE',  ( 0.000000000000000000, 0.000000000000000000, -49.67367017693150189 ) ) ;
#102919 = CARTESIAN_POINT ( 'NONE',  ( 13.89961937509957401, 13.97604488694547697, 106.8760903946856757 ) ) ;
#102920 = CARTESIAN_POINT ( 'NONE',  ( 5.823673210054125526, 21.52544592524343514, 79.79057627198102409 ) ) ;
#102921 = CARTESIAN_POINT ( 'NONE',  ( 14.34966873604960469, 8.224510206698951720, 59.16557627198103120 ) ) ;
#102922 = CARTESIAN_POINT ( 'NONE',  ( -12.14591786802326823, 12.06949235617739902, 33.12609039468569705 ) ) ;
#102923 = CARTESIAN_POINT ( 'NONE',  ( 9.564922557960805705, 16.46253265017160317, 44.58224293864769550 ) ) ;
#102925 = CARTESIAN_POINT ( 'NONE',  ( 13.97604488694548053, -13.89961937509957401, 90.62609039468567573 ) ) ;
#102924 = CARTESIAN_POINT ( 'NONE',  ( -21.52544592524334988, -5.823673210054445271, 18.95942372801901143 ) ) ;
#102926 = CARTESIAN_POINT ( 'NONE',  ( -16.51473224551069308, -9.474510206698971260, 91.66557627198103830 ) ) ;
#102927 = CARTESIAN_POINT ( 'NONE',  ( 16.46253265017160672, -9.564922557960803928, 73.33224293864769550 ) ) ;
#102928 = CARTESIAN_POINT ( 'NONE',  ( 5.823673210054125526, 21.52544592524343514, 79.79057627198102409 ) ) ;
#102929 = CARTESIAN_POINT ( 'NONE',  ( 16.51473224551069308, 9.474510206698969483, 44.16557627198103120 ) ) ;
#102930 = CARTESIAN_POINT ( 'NONE',  ( 15.17009418914603280, 34.12532338773831242, -7.999999999999996447 ) ) ;
#102931 = CARTESIAN_POINT ( 'NONE',  ( -4.379528057220328563, 16.55341960407611168, 55.20724293864770260 ) ) ;
#102932 = CARTESIAN_POINT ( 'NONE',  ( -16.51473224551069308, -9.474510206698971260, 86.66557627198102409 ) ) ;
#102933 = CARTESIAN_POINT ( 'NONE',  ( -193.3062444957834884, -155.7167183371838064, 0.000000000000000000 ) ) ;
#102934 = CARTESIAN_POINT ( 'NONE',  ( -19.02544592524334988, -5.153800228976617603, 68.95942372801896170 ) ) ;
#102935 = CARTESIAN_POINT ( 'NONE',  ( 5.719274019375991003, -21.55341960407610458, 77.70724293864770971 ) ) ;
#102936 = CARTESIAN_POINT ( 'NONE',  ( -9.474510206698720793, -16.51473224551083518, 34.58442372801899722 ) ) ;
#102937 = CARTESIAN_POINT ( 'NONE',  ( -9.474510206698964154, 16.51473224551069663, 105.4155762719810383 ) ) ;
#102938 = CARTESIAN_POINT ( 'NONE',  ( -17.50000000000146372, 3.202012800152269190, 114.9282241602726202 ) ) ;
#102940 = EDGE_CURVE ( 'NONE', #147808, #138825, #17384, .T. ) ;
#102939 = CARTESIAN_POINT ( 'NONE',  ( 21.55341960407610458, 5.719274019375980345, 43.95724293864769550 ) ) ;
#102941 = CARTESIAN_POINT ( 'NONE',  ( -19.05341960407611168, -5.049401038298163336, 66.45724293864769550 ) ) ;
#102942 = CARTESIAN_POINT ( 'NONE',  ( -18.62759615963255300, -10.81492255796106328, 69.16775706135234714 ) ) ;
#102943 = CARTESIAN_POINT ( 'NONE',  ( -13.97604488694527625, -13.89961937509977652, 26.87390960531434558 ) ) ;
#102945 = ORIENTED_EDGE ( 'NONE', *, *, #157036, .F. ) ;
#102944 = CARTESIAN_POINT ( 'NONE',  ( 18.62759615963271287, -10.81492255796078972, 113.3322429386476955 ) ) ;
#102946 = CARTESIAN_POINT ( 'NONE',  ( -15.80617190586768217, 15.72974639402176855, 48.12609039468568284 ) ) ;
#102947 = ORIENTED_EDGE ( 'NONE', *, *, #142282, .T. ) ;
#102948 = CARTESIAN_POINT ( 'NONE',  ( -5.049401038298153566, 19.05341960407611168, 115.2072429386477097 ) ) ;
#102949 = CARTESIAN_POINT ( 'NONE',  ( 5.049401038297881783, 19.05341960407617563, 72.29275706135234714 ) ) ;
#102950 = CARTESIAN_POINT ( 'NONE',  ( -20.61108013404310668, 10.97331748574079491, 168.1441487092658349 ) ) ;
#102951 = CARTESIAN_POINT ( 'NONE',  ( 15.72974639402199770, -15.80617190586745480, 108.1239096053143811 ) ) ;
#102952 = CARTESIAN_POINT ( 'NONE',  ( 19.05341960407611168, 5.049401038298154454, 58.95724293864768129 ) ) ;
#102953 = CARTESIAN_POINT ( 'NONE',  ( -16.55341960407617563, 4.379528057220093196, 38.54275706135234714 ) ) ;
#102954 = CARTESIAN_POINT ( 'NONE',  ( -38.00000000000001421, -12.34694845685042708, -9.649999994537626691 ) ) ;
#102955 = CARTESIAN_POINT ( 'NONE',  ( -10.72451020669870658, -18.67979575497194134, 104.5844237280190185 ) ) ;
#102956 = CARTESIAN_POINT ( 'NONE',  ( -19.05341960407611168, -5.049401038298163336, 36.45724293864766707 ) ) ;
#102957 = CARTESIAN_POINT ( 'NONE',  ( -18.62759615963255300, -10.81492255796106328, 109.1677570613523613 ) ) ;
#102959 = CARTESIAN_POINT ( 'NONE',  ( -18.62759615963255300, -10.81492255796106328, 64.16775706135234714 ) ) ;
#102958 = CARTESIAN_POINT ( 'NONE',  ( -9.474510206698964154, 16.51473224551069663, 85.41557627198102409 ) ) ;
#102960 = DIRECTION ( 'NONE',  ( -0.000000000000000000, -0.000000000000000000, -1.000000000000000000 ) ) ;
#102961 = CARTESIAN_POINT ( 'NONE',  ( -11.30153831258470731, -180.0000000000000000, -15.00000000000000000 ) ) ;
#102962 = FACE_OUTER_BOUND ( 'NONE', #100128, .T. ) ;
#102964 = CARTESIAN_POINT ( 'NONE',  ( 5.719274019375673035, 21.55341960407619339, 72.29275706135236135 ) ) ;
#102963 = CARTESIAN_POINT ( 'NONE',  ( -4.483927247898782831, 16.52544592524335698, 47.70942372801902565 ) ) ;
#102965 = CARTESIAN_POINT ( 'NONE',  ( 21.53943276465977519, 0.05219959533937863772, 91.25109039468568994 ) ) ;
#102966 = FACE_OUTER_BOUND ( 'NONE', #140921, .T. ) ;
#102967 = CARTESIAN_POINT ( 'NONE',  ( -14.34966873604972548, 8.224510206698743886, 23.33442372801901499 ) ) ;
#102968 = CARTESIAN_POINT ( 'NONE',  ( -16.51473224551069308, -9.474510206698971260, 91.66557627198103830 ) ) ;
#102969 = CARTESIAN_POINT ( 'NONE',  ( -19.03943276465977164, 0.05219959533909376836, 21.24890960531436335 ) ) ;
#102970 = VERTEX_POINT ( 'NONE', #101996 ) ;
#102971 = CARTESIAN_POINT ( 'NONE',  ( -1.232294487434663965, -29.53952216915897466, -51.94279119241696208 ) ) ;
#102972 = CARTESIAN_POINT ( 'NONE',  ( -0.05219959533909027116, -19.03943276465977164, 22.49890960531436690 ) ) ;
#102973 = CARTESIAN_POINT ( 'NONE',  ( -10.81492255796078084, -18.62759615963271287, 47.08224293864770260 ) ) ;
#102974 = CARTESIAN_POINT ( 'NONE',  ( -0.05219959533934338120, 16.53943276465976808, 107.5010903946856899 ) ) ;
#102976 = CARTESIAN_POINT ( 'NONE',  ( -16.51473224551069308, -9.474510206698971260, 66.66557627198102409 ) ) ;
#102975 = CARTESIAN_POINT ( 'NONE',  ( -8.224510206698948167, 14.34966873604960824, 80.41557627198103830 ) ) ;
#102977 = CARTESIAN_POINT ( 'NONE',  ( 15.72974639402176855, 15.80617190586768217, 91.87609039468568994 ) ) ;
#102978 = CARTESIAN_POINT ( 'NONE',  ( 16.53943276465976808, 0.05219959533934440121, 21.25109039468567218 ) ) ;
#102979 = CARTESIAN_POINT ( 'NONE',  ( 14.29746914071049879, -8.314922557960816363, 88.33224293864769550 ) ) ;
#102980 = CARTESIAN_POINT ( 'NONE',  ( 0.05219959533937995610, -21.53943276465977519, 45.00109039468568284 ) ) ;
#102981 = CARTESIAN_POINT ( 'NONE',  ( -5.823673210054116645, -21.52544592524344225, 77.29057627198102409 ) ) ;
#102982 = CARTESIAN_POINT ( 'NONE',  ( -5.153800228976607833, 19.02544592524334988, 42.70942372801901143 ) ) ;
#102983 = CARTESIAN_POINT ( 'NONE',  ( -34.80630918731043977, 6.717782050307405939, 41.65621224074541828 ) ) ;
#102984 = CARTESIAN_POINT ( 'NONE',  ( 13.89961937509977652, -13.97604488694527269, 98.12390960531433848 ) ) ;
#102985 = CARTESIAN_POINT ( 'NONE',  ( -8.224510206698948167, 14.34966873604960824, 60.41557627198102409 ) ) ;
#102986 = CARTESIAN_POINT ( 'NONE',  ( 14.34966873604960469, 8.224510206698951720, 34.16557627198102409 ) ) ;
#102987 = CARTESIAN_POINT ( 'NONE',  ( -16.52544592524335698, -4.483927247898792601, 108.9594237280190185 ) ) ;
#102988 = CARTESIAN_POINT ( 'NONE',  ( 5.049401038297881783, 19.05341960407617563, 72.29275706135234714 ) ) ;
#102989 = DIRECTION ( 'NONE',  ( 0.000000000000000000, 0.000000000000000000, -1.000000000000000000 ) ) ;
#102990 = CARTESIAN_POINT ( 'NONE',  ( -15.80617190586745835, -15.72974639402198527, 26.87390960531435979 ) ) ;
#102991 = EDGE_CURVE ( 'NONE', #22958, #196449, #12944, .T. ) ;
#102992 = CARTESIAN_POINT ( 'NONE',  ( 0.05219959533910956823, 16.53943276465976808, 89.99890960531438111 ) ) ;
#102993 = FACE_OUTER_BOUND ( 'NONE', #160392, .T. ) ;
#102995 = CARTESIAN_POINT ( 'NONE',  ( 15.72974639402199770, -15.80617190586745480, 48.12390960531436690 ) ) ;
#102994 = CARTESIAN_POINT ( 'NONE',  ( 16.51473224551069308, 9.474510206698969483, 49.16557627198102409 ) ) ;
#102996 = CARTESIAN_POINT ( 'NONE',  ( -18.67979575497178146, -10.72451020669898902, 76.66557627198103830 ) ) ;
#102997 = CARTESIAN_POINT ( 'NONE',  ( -12.06949235617756955, 12.14591786802309770, 110.6239096053143669 ) ) ;
#102999 = CARTESIAN_POINT ( 'NONE',  ( -13.97604488694527625, -13.89961937509977652, 41.87390960531435979 ) ) ;
#102998 = CARTESIAN_POINT ( 'NONE',  ( 12.06949235617739724, 12.14591786802326823, 61.87609039468568284 ) ) ;
#103000 = CARTESIAN_POINT ( 'NONE',  ( -10.81492255796105439, 18.62759615963255655, 52.91775706135235424 ) ) ;
#103001 = ORIENTED_EDGE ( 'NONE', *, *, #49944, .F. ) ;
#103002 = CARTESIAN_POINT ( 'NONE',  ( -16.52544592524342804, 4.483927247898546575, 101.0405762719810383 ) ) ;
#103003 = CARTESIAN_POINT ( 'NONE',  ( -5.049401038297874678, -19.05341960407617918, 84.79275706135233293 ) ) ;
#103004 = CARTESIAN_POINT ( 'NONE',  ( 36.91746824999999177, 2.880721459617395097E-14, -4.124999997268813168 ) ) ;
#103006 = CARTESIAN_POINT ( 'NONE',  ( -21.53943276465977519, 0.05219959533907696930, 51.24890960531436690 ) ) ;
#103005 = CARTESIAN_POINT ( 'NONE',  ( 9.687362902255733488, -9.687362902255692632, -64.92279855667830191 ) ) ;
#103007 = CARTESIAN_POINT ( 'NONE',  ( 17.05587630539787014, -6.762274262135690606, 68.24180309037316761 ) ) ;
#103008 = CARTESIAN_POINT ( 'NONE',  ( -5.719274019375665041, -21.55341960407619695, 79.79275706135236135 ) ) ;
#103009 = AXIS2_PLACEMENT_3D ( 'NONE', #108161, #152680, #90023 ) ;
#103010 = CARTESIAN_POINT ( 'NONE',  ( 4.379528057220339221, -16.55341960407611168, 27.70724293864769905 ) ) ;
#103012 = CARTESIAN_POINT ( 'NONE',  ( 8.314922557960818139, 14.29746914071049879, 39.58224293864769550 ) ) ;
#103011 = CARTESIAN_POINT ( 'NONE',  ( 16.53943276465976808, 0.05219959533934440121, 51.25109039468568994 ) ) ;
#103013 = CARTESIAN_POINT ( 'NONE',  ( 21.55341960407610458, 5.719274019375980345, 63.95724293864770260 ) ) ;
#103015 = CARTESIAN_POINT ( 'NONE',  ( -21.55341960407610458, -5.719274019375992779, 71.45724293864769550 ) ) ;
#103014 = PRODUCT_DEFINITION ( 'UNKNOWN', '', #163074, #143394 ) ;
#103016 = CARTESIAN_POINT ( 'NONE',  ( -21.77219501682365532, 9.607313489129737150, 170.8391438706019585 ) ) ;
#103018 = CARTESIAN_POINT ( 'NONE',  ( -21.52544592524343514, 5.823673210054127303, 26.04057627198103475 ) ) ;
#103017 = CARTESIAN_POINT ( 'NONE',  ( -19.03943276465977164, -0.05219959533935918106, 78.75109039468567573 ) ) ;
#103019 = CARTESIAN_POINT ( 'NONE',  ( -13.89961937509977652, 13.97604488694528158, 55.62390960531434558 ) ) ;
#103020 = CARTESIAN_POINT ( 'NONE',  ( -8.314922557960811034, -14.29746914071050412, 112.0822429386477097 ) ) ;
#103021 = DIRECTION ( 'NONE',  ( 1.000000000000000000, 0.000000000000000000, 0.000000000000000000 ) ) ;
#103022 = LINE ( 'NONE', #87839, #193101 ) ;
#103023 = ORIENTED_EDGE ( 'NONE', *, *, #188637, .F. ) ;
#103024 = CARTESIAN_POINT ( 'NONE',  ( -14.34966873604972548, 8.224510206698743886, 83.33442372801903275 ) ) ;
#103025 = ORIENTED_EDGE ( 'NONE', *, *, #133623, .F. ) ;
#103026 = CARTESIAN_POINT ( 'NONE',  ( -21.52544592524343514, 5.823673210054127303, 111.0405762719810525 ) ) ;
#103027 = CARTESIAN_POINT ( 'NONE',  ( 19.02544592524343514, -5.153800228976328945, 68.54057627198103830 ) ) ;
#103028 = CARTESIAN_POINT ( 'NONE',  ( 0.05219959533937995610, -21.53943276465977519, 35.00109039468568284 ) ) ;
#103029 = CARTESIAN_POINT ( 'NONE',  ( 0.05219959533909260263, 19.03943276465977164, 94.99890960531436690 ) ) ;
#103030 = CARTESIAN_POINT ( 'NONE',  ( -22.61240241995035305, -33.77560033877102796, -17.98683046886889514 ) ) ;
#103031 = VERTEX_POINT ( 'NONE', #149500 ) ;
#103032 = CARTESIAN_POINT ( 'NONE',  ( 10.72451020669871369, 18.67979575497193778, 27.08442372801901854 ) ) ;
#103034 = CARTESIAN_POINT ( 'NONE',  ( 19.03943276465977164, 0.05219959533936151252, 91.25109039468566152 ) ) ;
#103033 = CARTESIAN_POINT ( 'NONE',  ( 19.02544592524343514, -5.153800228976328945, 28.54057627198102409 ) ) ;
#103035 = CARTESIAN_POINT ( 'NONE',  ( -19.02544592524334988, -5.153800228976617603, 43.95942372801899012 ) ) ;
#103036 = CARTESIAN_POINT ( 'NONE',  ( 0.05219959533907565091, 21.53943276465977519, 114.9989096053143669 ) ) ;
#103037 = CARTESIAN_POINT ( 'NONE',  ( -16.51473224551082808, 9.474510206698731452, 43.33442372801900433 ) ) ;
#103038 = CARTESIAN_POINT ( 'NONE',  ( 9.564922557961047289, -16.46253265017146816, 50.41775706135233293 ) ) ;
#103039 = CARTESIAN_POINT ( 'NONE',  ( -16.53943276465976808, -0.05219959533934237506, 93.75109039468567573 ) ) ;
#103041 = ORIENTED_EDGE ( 'NONE', *, *, #180229, .T. ) ;
#103040 = CARTESIAN_POINT ( 'NONE',  ( 30.00000000000000000, -1.163414459189985801E-14, 95.00000000000000000 ) ) ;
#103042 = CARTESIAN_POINT ( 'NONE',  ( -9.474510206698964154, 16.51473224551069663, 70.41557627198102409 ) ) ;
#103043 = CARTESIAN_POINT ( 'NONE',  ( -18.62759615963255300, -10.81492255796106328, 79.16775706135234714 ) ) ;
#103044 = CARTESIAN_POINT ( 'NONE',  ( 10.81492255796106328, -18.62759615963255655, 95.41775706135234714 ) ) ;
#103045 = CARTESIAN_POINT ( 'NONE',  ( 24.06132300323557516, -0.8180345313831565157, -54.40060964255543041 ) ) ;
#103046 = CARTESIAN_POINT ( 'NONE',  ( -5.049401038298153566, 19.05341960407611168, 90.20724293864766707 ) ) ;
#103047 = CARTESIAN_POINT ( 'NONE',  ( 15.72974639402176855, 15.80617190586768217, 66.87609039468568994 ) ) ;
#103048 = CARTESIAN_POINT ( 'NONE',  ( 19.02544592524334988, 5.153800228976608722, 106.4594237280190185 ) ) ;
#103049 = CARTESIAN_POINT ( 'NONE',  ( -16.46253265017160317, 9.564922557960807481, 65.83224293864769550 ) ) ;
#103050 = CARTESIAN_POINT ( 'NONE',  ( -13.89961937509977652, 13.97604488694528158, 105.6239096053143527 ) ) ;
#103051 = CARTESIAN_POINT ( 'NONE',  ( -19.02544592524342804, 5.153800228976336051, 81.04057627198103830 ) ) ;
#103052 = CARTESIAN_POINT ( 'NONE',  ( 13.89961937509957579, 13.97604488694547520, 86.87609039468566152 ) ) ;
#103053 = CARTESIAN_POINT ( 'NONE',  ( 19.02544592524343514, -5.153800228976328945, 63.54057627198103830 ) ) ;
#103054 = CARTESIAN_POINT ( 'NONE',  ( 16.51473224551069308, 9.474510206698969483, 49.16557627198102409 ) ) ;
#103055 = CARTESIAN_POINT ( 'NONE',  ( 15.72974639402199770, -15.80617190586745480, 113.1239096053143953 ) ) ;
#103056 = CARTESIAN_POINT ( 'NONE',  ( 4.483927247898790824, -16.52544592524335698, 100.2094237280190043 ) ) ;
#103057 = CARTESIAN_POINT ( 'NONE',  ( 4.273745901508120504, -6.674792076160531273, 4.009310749147818598 ) ) ;
#103058 = CARTESIAN_POINT ( 'NONE',  ( -9.141470119588789092E-16, -69.45486021086043138, -12.99263613531267936 ) ) ;
#103059 = CARTESIAN_POINT ( 'NONE',  ( 16.51473224551083163, -9.474510206698727899, 55.83442372801899722 ) ) ;
#103060 = CARTESIAN_POINT ( 'NONE',  ( 9.474510206698971260, -16.51473224551069308, 82.91557627198103830 ) ) ;
#103061 = CARTESIAN_POINT ( 'NONE',  ( -4.379528057220328563, 16.55341960407611168, 65.20724293864768129 ) ) ;
#103062 = CARTESIAN_POINT ( 'NONE',  ( -8.314922557960811034, -14.29746914071050412, 112.0822429386477097 ) ) ;
#103063 = CARTESIAN_POINT ( 'NONE',  ( 18.62759615963271287, -10.81492255796078972, 38.33224293864768839 ) ) ;
#103064 = CARTESIAN_POINT ( 'NONE',  ( 13.97604488694527802, 13.89961937509977652, 99.37390960531436690 ) ) ;
#103065 = CARTESIAN_POINT ( 'NONE',  ( 14.29746914071049879, -8.314922557960816363, 88.33224293864769550 ) ) ;
#103066 = DIRECTION ( 'NONE',  ( -1.000000000000000000, 0.000000000000000000, 0.000000000000000000 ) ) ;
#103067 = CARTESIAN_POINT ( 'NONE',  ( -0.05219959533936034679, 19.03943276465977164, 32.50109039468566863 ) ) ;
#103068 = CARTESIAN_POINT ( 'NONE',  ( 4.379528057220092307, 16.55341960407617563, 107.2927570613523471 ) ) ;
#103069 = CARTESIAN_POINT ( 'NONE',  ( 0.05219959533909260263, 19.03943276465977164, 94.99890960531436690 ) ) ;
#103070 = CARTESIAN_POINT ( 'NONE',  ( -21.52544592524334988, -5.823673210054445271, 58.95942372801902565 ) ) ;
#103071 = CARTESIAN_POINT ( 'NONE',  ( -15.72974639402197994, 15.80617190586746368, 50.62390960531435979 ) ) ;
#103072 = CARTESIAN_POINT ( 'NONE',  ( 15.80617190586769283, -15.72974639402175789, 30.62609039468567929 ) ) ;
#103073 = CARTESIAN_POINT ( 'NONE',  ( 21.53943276465977519, -0.05219959533907433946, 78.74890960531436690 ) ) ;
#103074 = CARTESIAN_POINT ( 'NONE',  ( -16.53943276465976808, 0.05219959533911058130, 96.24890960531435269 ) ) ;
#103075 = CARTESIAN_POINT ( 'NONE',  ( -13.89961937509957401, -13.97604488694547875, 59.37609039468566863 ) ) ;
#103076 = CARTESIAN_POINT ( 'NONE',  ( 5.153800228976335163, 19.02544592524342804, 34.79057627198102409 ) ) ;
#103077 =( BOUNDED_SURFACE ( )  B_SPLINE_SURFACE ( 1, 2, ( 
 ( #100756, #135124, #195807, #42114, #56265, #192788, #103776, #148282, #87596, #116933, #193796, #146262, #88594, #7746, #131100, #177632, #132105, #86599, #133103, #117948, #101767, #39100, #179638, #163454, #9775, #41108, #102772, #25953, #105754, #184588, #107723, #15737, #138080, #74434, #62215, #92558, #90578, #123883, #198772, #169404, #185581, #91553, #152259, #30910, #77396, #136101, #76404, #119935, #14743, #183602, #167440, #122899, #197777, #199761, #46069, #154246, #60238, #182611, #151281, #43100, #106743, #45086, #139066, #544, #28937, #12770, #181620, #13744, #166456, #59243, #104768, #153240, #61228, #27953, #121909, #168418, #89594, #120912, #44096, #75412, #29913, #137084, #148939, #162097, #195456, #56931, #70093, #134776, #165107, #42759, #25610, #87254, #135765, #41763, #23593, #26600, #197436, #85240, #131762, #71091, #164112 ),
 ( #193444, #58902, #194445, #10429, #118605, #180295, #132758, #182262, #103428, #54920, #55916, #102425, #72087, #146931, #117590, #57928, #181282, #89247, #149928, #178281, #120568, #166105, #179292, #100416, #133761, #104422, #8421, #88243, #40756, #27607, #74095, #39744, #11435, #116592, #73106, #196458, #119599, #150939, #101407, #12433, #163100, #24603, #86250, #147940, #9426, #105410, #77048, #153895, #16388, #124549, #76055, #75069, #78035, #199415, #167094, #198417, #94200, #138719, #200, #139704, #122556, #30558, #154890, #1191, #61869, #2198, #28595, #15391, #92210, #90233, #59894, #62867, #123539, #151916, #91203, #186246, #47724, #125550, #185232, #43747, #13405, #46723, #170063, #137731, #121561, #108386, #31553, #140708, #93205, #109375, #183256, #171057, #63879, #152893, #136735, #32547, #44737, #106393, #79033, #155880, #107380 ) ),
 .UNSPECIFIED., .F., .F., .F. ) 
 B_SPLINE_SURFACE_WITH_KNOTS ( ( 2, 2 ),
 ( 3, 2, 2, 2, 2, 2, 2, 2, 2, 2, 2, 2, 2, 2, 2, 2, 2, 2, 2, 2, 2, 2, 2, 2, 2, 2, 2, 2, 2, 2, 2, 2, 2, 2, 2, 2, 2, 2, 2, 2, 2, 2, 2, 2, 2, 2, 2, 2, 2, 2, 3 ),
 ( 0.000000000000000000, 1.000000000000000000 ),
 ( 0.000000000000000000, 0.02000000000000000042, 0.04000000000000000083, 0.05999999999999999778, 0.08000000000000000167, 0.1000000000000000056, 0.1199999999999999956, 0.1400000000000000133, 0.1600000000000000033, 0.1799999999999999933, 0.2000000000000000111, 0.2200000000000000011, 0.2399999999999999911, 0.2600000000000000089, 0.2800000000000000266, 0.2999999999999999889, 0.3200000000000000067, 0.3400000000000000244, 0.3599999999999999867, 0.3800000000000000044, 0.4000000000000000222, 0.4199999999999999845, 0.4400000000000000022, 0.4600000000000000200, 0.4799999999999999822, 0.5000000000000000000, 0.5200000000000000178, 0.5400000000000000355, 0.5600000000000000533, 0.5799999999999999600, 0.5999999999999999778, 0.6199999999999999956, 0.6400000000000000133, 0.6600000000000000311, 0.6800000000000000488, 0.6999999999999999556, 0.7199999999999999734, 0.7399999999999999911, 0.7600000000000000089, 0.7800000000000000266, 0.8000000000000000444, 0.8199999999999999512, 0.8399999999999999689, 0.8599999999999999867, 0.8800000000000000044, 0.9000000000000000222, 0.9200000000000000400, 0.9399999999999999467, 0.9599999999999999645, 0.9799999999999999822, 1.000000000000000000 ),
 .UNSPECIFIED. ) 
 GEOMETRIC_REPRESENTATION_ITEM ( )  RATIONAL_B_SPLINE_SURFACE ( (
 ( 1.000000000000000000, 0.9510565162951535312, 1.000000000000000000, 0.9510565162951535312, 1.000000000000000000, 0.9510565162951535312, 1.000000000000000000, 0.9510565162951535312, 1.000000000000000000, 0.9510565162951535312, 1.000000000000000000, 0.9510565162951535312, 1.000000000000000000, 0.9510565162951535312, 1.000000000000000000, 0.9510565162951535312, 1.000000000000000000, 0.9510565162951535312, 1.000000000000000000, 0.9510565162951535312, 1.000000000000000000, 0.9510565162951535312, 1.000000000000000000, 0.9510565162951535312, 1.000000000000000000, 0.9510565162951535312, 1.000000000000000000, 0.9510565162951535312, 1.000000000000000000, 0.9510565162951535312, 1.000000000000000000, 0.9510565162951535312, 1.000000000000000000, 0.9510565162951535312, 1.000000000000000000, 0.9510565162951535312, 1.000000000000000000, 0.9510565162951535312, 1.000000000000000000, 0.9510565162951535312, 1.000000000000000000, 0.9510565162951535312, 1.000000000000000000, 0.9510565162951535312, 1.000000000000000000, 0.9510565162951535312, 1.000000000000000000, 0.9510565162951535312, 1.000000000000000000, 0.9510565162951535312, 1.000000000000000000, 0.9510565162951535312, 1.000000000000000000, 0.9510565162951535312, 1.000000000000000000, 0.9510565162951535312, 1.000000000000000000, 0.9510565162951535312, 1.000000000000000000, 0.9510565162951535312, 1.000000000000000000, 0.9510565162951535312, 1.000000000000000000, 0.9510565162951535312, 1.000000000000000000, 0.9510565162951535312, 1.000000000000000000, 0.9510565162951535312, 1.000000000000000000, 0.9510565162951535312, 1.000000000000000000, 0.9510565162951535312, 1.000000000000000000, 0.9510565162951535312, 1.000000000000000000, 0.9510565162951535312, 1.000000000000000000, 0.9510565162951535312, 1.000000000000000000, 0.9510565162951535312, 1.000000000000000000, 0.9510565162951535312, 1.000000000000000000, 0.9510565162951535312, 1.000000000000000000, 0.9510565162951535312, 1.000000000000000000, 0.9510565162951535312, 1.000000000000000000, 0.9510565162951535312, 1.000000000000000000, 0.9510565162951535312, 1.000000000000000000, 0.9510565162951535312, 1.000000000000000000, 0.9510565162951535312, 1.000000000000000000, 0.9510565162951535312, 1.000000000000000000, 0.9510565162951535312, 1.000000000000000000),
 ( 1.000000000000000000, 0.9510565162951535312, 1.000000000000000000, 0.9510565162951535312, 1.000000000000000000, 0.9510565162951535312, 1.000000000000000000, 0.9510565162951535312, 1.000000000000000000, 0.9510565162951535312, 1.000000000000000000, 0.9510565162951535312, 1.000000000000000000, 0.9510565162951535312, 1.000000000000000000, 0.9510565162951535312, 1.000000000000000000, 0.9510565162951535312, 1.000000000000000000, 0.9510565162951535312, 1.000000000000000000, 0.9510565162951535312, 1.000000000000000000, 0.9510565162951535312, 1.000000000000000000, 0.9510565162951535312, 1.000000000000000000, 0.9510565162951535312, 1.000000000000000000, 0.9510565162951535312, 1.000000000000000000, 0.9510565162951535312, 1.000000000000000000, 0.9510565162951535312, 1.000000000000000000, 0.9510565162951535312, 1.000000000000000000, 0.9510565162951535312, 1.000000000000000000, 0.9510565162951535312, 1.000000000000000000, 0.9510565162951535312, 1.000000000000000000, 0.9510565162951535312, 1.000000000000000000, 0.9510565162951535312, 1.000000000000000000, 0.9510565162951535312, 1.000000000000000000, 0.9510565162951535312, 1.000000000000000000, 0.9510565162951535312, 1.000000000000000000, 0.9510565162951535312, 1.000000000000000000, 0.9510565162951535312, 1.000000000000000000, 0.9510565162951535312, 1.000000000000000000, 0.9510565162951535312, 1.000000000000000000, 0.9510565162951535312, 1.000000000000000000, 0.9510565162951535312, 1.000000000000000000, 0.9510565162951535312, 1.000000000000000000, 0.9510565162951535312, 1.000000000000000000, 0.9510565162951535312, 1.000000000000000000, 0.9510565162951535312, 1.000000000000000000, 0.9510565162951535312, 1.000000000000000000, 0.9510565162951535312, 1.000000000000000000, 0.9510565162951535312, 1.000000000000000000, 0.9510565162951535312, 1.000000000000000000, 0.9510565162951535312, 1.000000000000000000, 0.9510565162951535312, 1.000000000000000000, 0.9510565162951535312, 1.000000000000000000, 0.9510565162951535312, 1.000000000000000000, 0.9510565162951535312, 1.000000000000000000, 0.9510565162951535312, 1.000000000000000000, 0.9510565162951535312, 1.000000000000000000, 0.9510565162951535312, 1.000000000000000000, 0.9510565162951535312, 1.000000000000000000, 0.9510565162951535312, 1.000000000000000000) ) ) 
 REPRESENTATION_ITEM ( '' )  SURFACE ( )  );
#103078 = CARTESIAN_POINT ( 'NONE',  ( 16.46253265017160672, -9.564922557960803928, 98.33224293864769550 ) ) ;
#103079 = CARTESIAN_POINT ( 'NONE',  ( -5.153800228976328057, -19.02544592524343514, 92.29057627198099567 ) ) ;
#103080 = CARTESIAN_POINT ( 'NONE',  ( 0.05219959533910956823, 16.53943276465976808, 109.9989096053143527 ) ) ;
#103081 = CARTESIAN_POINT ( 'NONE',  ( -16.55341960407611168, -4.379528057220339221, 21.45724293864769550 ) ) ;
#103082 = CARTESIAN_POINT ( 'NONE',  ( 8.314922557961029526, -14.29746914071037800, 35.41775706135234003 ) ) ;
#103083 = CARTESIAN_POINT ( 'NONE',  ( 21.55341960407619695, -5.719274019375665929, 111.0427570613523613 ) ) ;
#103085 = CARTESIAN_POINT ( 'NONE',  ( 0.05219959533910956823, 16.53943276465976808, 24.99890960531435624 ) ) ;
#103084 = CARTESIAN_POINT ( 'NONE',  ( 19.05341960407611168, 5.049401038298154454, 113.9572429386477097 ) ) ;
#103086 = CARTESIAN_POINT ( 'NONE',  ( 0.05219959533937995610, -21.53943276465977519, 35.00109039468568284 ) ) ;
#103087 = CARTESIAN_POINT ( 'NONE',  ( -19.05341960407611168, -5.049401038298163336, 46.45724293864768129 ) ) ;
#103088 = CARTESIAN_POINT ( 'NONE',  ( -16.53943276465976808, -0.05219959533934237506, 43.75109039468568284 ) ) ;
#103089 = CARTESIAN_POINT ( 'NONE',  ( -0.05219959533934338120, 16.53943276465976808, 107.5010903946856899 ) ) ;
#103090 = CARTESIAN_POINT ( 'NONE',  ( 4.483927247898790824, -16.52544592524335698, 95.20942372801903275 ) ) ;
#103091 = CARTESIAN_POINT ( 'NONE',  ( 16.46253265017146816, 9.564922557961045513, 106.6677570613523471 ) ) ;
#103092 = CARTESIAN_POINT ( 'NONE',  ( 13.97604488694527802, 13.89961937509977652, 29.37390960531435979 ) ) ;
#103093 = CARTESIAN_POINT ( 'NONE',  ( -0.05219959533910754901, -16.53943276465976808, 97.49890960531436690 ) ) ;
#103094 = CARTESIAN_POINT ( 'NONE',  ( 10.72451020669898902, -18.67979575497178502, 97.91557627198103830 ) ) ;
#103095 = CARTESIAN_POINT ( 'NONE',  ( 0.05219959533909260263, 19.03943276465977164, 29.99890960531435979 ) ) ;
#103096 = CARTESIAN_POINT ( 'NONE',  ( 5.153800228976335163, 19.02544592524342804, 109.7905762719810099 ) ) ;
#103097 = CARTESIAN_POINT ( 'NONE',  ( -18.62759615963255300, -10.81492255796106328, 34.16775706135234714 ) ) ;
#103098 = CARTESIAN_POINT ( 'NONE',  ( 13.97604488694527802, 13.89961937509977652, 24.37390960531435624 ) ) ;
#103099 = EDGE_CURVE ( 'NONE', #3755, #102786, #33545, .T. ) ;
#103100 = CARTESIAN_POINT ( 'NONE',  ( -19.05341960407611168, -5.049401038298163336, 111.4572429386476671 ) ) ;
#103101 = CARTESIAN_POINT ( 'NONE',  ( 17.13100169013302221, -6.664070546373126902, 113.2678983569985292 ) ) ;
#103102 = CARTESIAN_POINT ( 'NONE',  ( 19.05341960407611168, 5.049401038298154454, 83.95724293864766707 ) ) ;
#103104 = CARTESIAN_POINT ( 'NONE',  ( -16.55341960407611168, -4.379528057220339221, 91.45724293864769550 ) ) ;
#103103 = CARTESIAN_POINT ( 'NONE',  ( 5.719274019375673035, 21.55341960407619339, 27.29275706135234358 ) ) ;
#103105 = CARTESIAN_POINT ( 'NONE',  ( -0.05219959533909027116, -19.03943276465977164, 92.49890960531436690 ) ) ;
#103106 = CARTESIAN_POINT ( 'NONE',  ( -27.96809023454855492, -7.159247544375828554, 161.0916313341220416 ) ) ;
#103107 = CARTESIAN_POINT ( 'NONE',  ( 14.34966873604972726, -8.224510206698740333, 65.83442372801900433 ) ) ;
#103108 = CARTESIAN_POINT ( 'NONE',  ( 15.80617190586769283, -15.72974639402175789, 75.62609039468567573 ) ) ;
#103109 = CARTESIAN_POINT ( 'NONE',  ( -12.06949235617739369, -12.14591786802326823, 39.37609039468567573 ) ) ;
#103110 = CARTESIAN_POINT ( 'NONE',  ( 19.03943276465977164, -0.05219959533909143690, 88.74890960531436690 ) ) ;
#103111 = CARTESIAN_POINT ( 'NONE',  ( -13.97604488694547697, 13.89961937509957934, 103.1260903946856473 ) ) ;
#103112 = CARTESIAN_POINT ( 'NONE',  ( 0.05219959533934541429, -16.53943276465976808, 65.00109039468568994 ) ) ;
#103113 = CARTESIAN_POINT ( 'NONE',  ( 19.03943276465977164, 0.05219959533936151252, 21.25109039468565797 ) ) ;
#103114 = CARTESIAN_POINT ( 'NONE',  ( 9.564922557961047289, -16.46253265017146816, 90.41775706135234714 ) ) ;
#103115 = CARTESIAN_POINT ( 'NONE',  ( 0.05219959533909260263, 19.03943276465977164, 69.99890960531435269 ) ) ;
#103116 = CARTESIAN_POINT ( 'NONE',  ( 21.55341960407610458, 5.719274019375980345, 88.95724293864769550 ) ) ;
#103118 = CARTESIAN_POINT ( 'NONE',  ( -13.89961937509957401, -13.97604488694547875, 89.37609039468563310 ) ) ;
#103117 = CARTESIAN_POINT ( 'NONE',  ( 0.05219959533910956823, 16.53943276465976808, 89.99890960531438111 ) ) ;
#103119 = CARTESIAN_POINT ( 'NONE',  ( -14.34966873604972548, 8.224510206698743886, 63.33442372801900433 ) ) ;
#103120 = CARTESIAN_POINT ( 'NONE',  ( -19.52217212775661181, 5.499999999999920064, 79.93993709005260939 ) ) ;
#103121 = CARTESIAN_POINT ( 'NONE',  ( 19.02544592524334988, 5.153800228976608722, 51.45942372801900433 ) ) ;
#103122 = CARTESIAN_POINT ( 'NONE',  ( -8.314922557960811034, -14.29746914071050412, 27.08224293864769550 ) ) ;
#103123 = CARTESIAN_POINT ( 'NONE',  ( 4.483927247898545687, 16.52544592524342804, 79.79057627198102409 ) ) ;
#103125 = CARTESIAN_POINT ( 'NONE',  ( -17.13100169013227259, 6.664070546374130544, 40.76789835699826625 ) ) ;
#103124 = CARTESIAN_POINT ( 'NONE',  ( -21.53943276465977519, -0.05219959533937600094, 113.7510903946856757 ) ) ;
#103126 = CARTESIAN_POINT ( 'NONE',  ( -5.719274019375665041, -21.55341960407619695, 29.79275706135234358 ) ) ;
#103127 = CARTESIAN_POINT ( 'NONE',  ( -5.153800228976328057, -19.02544592524343514, 97.29057627198099567 ) ) ;
#103128 = CARTESIAN_POINT ( 'NONE',  ( 13.89961937509977652, -13.97604488694527269, 78.12390960531433848 ) ) ;
#103129 = CARTESIAN_POINT ( 'NONE',  ( 21.55341960407619695, -5.719274019375665929, 91.04275706135236135 ) ) ;
#103130 = CARTESIAN_POINT ( 'NONE',  ( -9.564922557960796823, -16.46253265017161027, 82.08224293864768129 ) ) ;
#103131 = CARTESIAN_POINT ( 'NONE',  ( -10.81492255796078084, -18.62759615963271287, 32.08224293864769550 ) ) ;
#103132 = CARTESIAN_POINT ( 'NONE',  ( -14.34966873604960291, -8.224510206698953496, 86.66557627198102409 ) ) ;
#103133 = CARTESIAN_POINT ( 'NONE',  ( 16.51473224551069308, 9.474510206698969483, 44.16557627198103120 ) ) ;
#103134 = CARTESIAN_POINT ( 'NONE',  ( 0.05219959533910956823, 16.53943276465976808, 99.99890960531436690 ) ) ;
#103135 = CARTESIAN_POINT ( 'NONE',  ( -18.62759615963270932, 10.81492255796079327, 110.8322429386476955 ) ) ;
#103136 = CARTESIAN_POINT ( 'NONE',  ( 18.62759615963255655, 10.81492255796105972, 66.66775706135234714 ) ) ;
#103137 = CARTESIAN_POINT ( 'NONE',  ( -19.03943276465977164, 0.05219959533909376836, 31.24890960531435979 ) ) ;
#103138 = CARTESIAN_POINT ( 'NONE',  ( -16.53943276465976808, -0.05219959533934237506, 68.75109039468568994 ) ) ;
#103139 = CARTESIAN_POINT ( 'NONE',  ( -21.55341960407610458, -5.719274019375992779, 101.4572429386476955 ) ) ;
#103140 = CARTESIAN_POINT ( 'NONE',  ( 15.72974639402199770, -15.80617190586745480, 113.1239096053143953 ) ) ;
#103142 = CARTESIAN_POINT ( 'NONE',  ( -19.02544592524342804, 5.153800228976336051, 51.04057627198103120 ) ) ;
#103141 = CARTESIAN_POINT ( 'NONE',  ( -13.89961937509957401, -13.97604488694547875, 39.37609039468566152 ) ) ;
#103143 = CARTESIAN_POINT ( 'NONE',  ( 19.05341960407611168, 5.049401038298154454, 113.9572429386477097 ) ) ;
#103144 = CARTESIAN_POINT ( 'NONE',  ( -21.53943276465977519, -0.05219959533937600094, 63.75109039468568284 ) ) ;
#103145 = EDGE_CURVE ( 'NONE', #16134, #133123, #88819, .T. ) ;
#103146 = CARTESIAN_POINT ( 'NONE',  ( 10.81492255796078972, 18.62759615963270932, 59.58224293864770260 ) ) ;
#103147 = CARTESIAN_POINT ( 'NONE',  ( -16.52544592524342804, 4.483927247898546575, 41.04057627198103120 ) ) ;
#103149 = CARTESIAN_POINT ( 'NONE',  ( 0.05219959533937995610, -21.53943276465977519, 105.0010903946856757 ) ) ;
#103148 = CARTESIAN_POINT ( 'NONE',  ( 21.52544592524334988, 5.823673210054432836, 71.45942372801901854 ) ) ;
#103150 = CARTESIAN_POINT ( 'NONE',  ( 16.55341960407611168, 4.379528057220329451, 63.95724293864770260 ) ) ;
#103151 = CARTESIAN_POINT ( 'NONE',  ( -14.34966873604960291, -8.224510206698953496, 106.6655762719810383 ) ) ;
#103152 = CARTESIAN_POINT ( 'NONE',  ( 16.46253265017146816, 9.564922557961045513, 41.66775706135234003 ) ) ;
#103153 = CARTESIAN_POINT ( 'NONE',  ( 14.29746914071037800, 8.314922557961029526, 101.6677570613523613 ) ) ;
#103154 = CARTESIAN_POINT ( 'NONE',  ( 10.72451020669871369, 18.67979575497193778, 72.08442372801899012 ) ) ;
#103155 = CARTESIAN_POINT ( 'NONE',  ( 5.049401038298161559, -19.05341960407611168, 57.70724293864769550 ) ) ;
#103156 = CARTESIAN_POINT ( 'NONE',  ( -19.05341960407617563, 5.049401038297882671, 33.54275706135231871 ) ) ;
#103157 = CARTESIAN_POINT ( 'NONE',  ( 18.62759615963271287, -10.81492255796078972, 38.33224293864768839 ) ) ;
#103158 = CARTESIAN_POINT ( 'NONE',  ( -5.823673210054431948, 21.52544592524334988, 27.70942372801901854 ) ) ;
#103159 = AXIS2_PLACEMENT_3D ( 'NONE', #21738, #40905, #100563 ) ;
#103160 = CARTESIAN_POINT ( 'NONE',  ( 15.80617190586746368, 15.72974639402197994, 84.37390960531438111 ) ) ;
#103161 = CARTESIAN_POINT ( 'NONE',  ( 19.05341960407617918, -5.049401038297876454, 91.04275706135234714 ) ) ;
#103162 = CARTESIAN_POINT ( 'NONE',  ( -8.314922557961024197, 14.29746914071037800, 52.91775706135235424 ) ) ;
#103164 = CARTESIAN_POINT ( 'NONE',  ( -21.53943276465977519, 0.05219959533907696930, 91.24890960531436690 ) ) ;
#103163 = CARTESIAN_POINT ( 'NONE',  ( 17.49999999999999289, -3.341627039121392695, 37.07768976001553085 ) ) ;
#103165 = CARTESIAN_POINT ( 'NONE',  ( -4.379528057220328563, 16.55341960407611168, 80.20724293864769550 ) ) ;
#103166 = CARTESIAN_POINT ( 'NONE',  ( -17.31747979337947285, -6.344076630961058783, 101.3794486806517909 ) ) ;
#103167 = CARTESIAN_POINT ( 'NONE',  ( 16.55341960407618274, -4.379528057220086978, 26.04275706135235779 ) ) ;
#103168 = CARTESIAN_POINT ( 'NONE',  ( -10.81492255796078084, -18.62759615963271287, 42.08224293864769550 ) ) ;
#103169 = CARTESIAN_POINT ( 'NONE',  ( -16.55341960407617563, 4.379528057220093196, 73.54275706135234714 ) ) ;
#103170 = CARTESIAN_POINT ( 'NONE',  ( 16.46253265017160672, -9.564922557960803928, 23.33224293864769194 ) ) ;
#103171 = CARTESIAN_POINT ( 'NONE',  ( 4.379528057220092307, 16.55341960407617563, 57.29275706135234714 ) ) ;
#103172 = CARTESIAN_POINT ( 'NONE',  ( 5.823673210054444382, -21.52544592524334988, 25.20942372801901854 ) ) ;
#103173 = CARTESIAN_POINT ( 'NONE',  ( -18.62759615963270932, 10.81492255796079327, 45.83224293864769550 ) ) ;
#103174 = CARTESIAN_POINT ( 'NONE',  ( 8.314922557961029526, -14.29746914071037800, 70.41775706135236135 ) ) ;
#103175 = CARTESIAN_POINT ( 'NONE',  ( 13.97604488694527802, 13.89961937509977652, 84.37390960531433848 ) ) ;
#103177 = CARTESIAN_POINT ( 'NONE',  ( -0.05219959533909027116, -19.03943276465977164, 22.49890960531436690 ) ) ;
#103176 = CARTESIAN_POINT ( 'NONE',  ( 10.72451020669871369, 18.67979575497193778, 62.08442372801901143 ) ) ;
#103178 = CARTESIAN_POINT ( 'NONE',  ( 21.53943276465977519, -0.05219959533907433946, 38.74890960531435979 ) ) ;
#103179 = CARTESIAN_POINT ( 'NONE',  ( 19.03943276465977164, -0.05219959533909143690, 113.7489096053143669 ) ) ;
#103180 = ORIENTED_EDGE ( 'NONE', *, *, #199664, .T. ) ;
#103181 = CARTESIAN_POINT ( 'NONE',  ( 19.05341960407617918, -5.049401038297876454, 36.04275706135234003 ) ) ;
#103182 = CARTESIAN_POINT ( 'NONE',  ( 12.14591786802327356, -12.06949235617739191, 45.62609039468567573 ) ) ;
#103183 = CARTESIAN_POINT ( 'NONE',  ( -0.05219959533907301413, -21.53943276465977519, 22.49890960531436335 ) ) ;
#103184 = ORIENTED_EDGE ( 'NONE', *, *, #40462, .T. ) ;
#103185 = CARTESIAN_POINT ( 'NONE',  ( -16.51473224551069308, -9.474510206698971260, 91.66557627198103830 ) ) ;
#103186 = CARTESIAN_POINT ( 'NONE',  ( -12.14591786802326823, 12.06949235617739902, 98.12609039468570415 ) ) ;
#103187 = CARTESIAN_POINT ( 'NONE',  ( 0.000000000000000000, -78.67194367458512261, -23.00000000000000000 ) ) ;
#103188 = CARTESIAN_POINT ( 'NONE',  ( 12.14591786802309770, 12.06949235617756955, 89.37390960531435269 ) ) ;
#103189 = CARTESIAN_POINT ( 'NONE',  ( 21.55341960407610458, 5.719274019375980345, 48.95724293864770971 ) ) ;
#103190 = CARTESIAN_POINT ( 'NONE',  ( -0.05219959533909027116, -19.03943276465977164, 32.49890960531435979 ) ) ;
#103191 = CARTESIAN_POINT ( 'NONE',  ( -4.483927247898782831, 16.52544592524335698, 72.70942372801901854 ) ) ;
#103192 = CARTESIAN_POINT ( 'NONE',  ( -18.62759615963255300, -10.81492255796106328, 24.16775706135235424 ) ) ;
#103193 = CARTESIAN_POINT ( 'NONE',  ( -9.474510206698720793, -16.51473224551083518, 94.58442372801900433 ) ) ;
#103194 = CARTESIAN_POINT ( 'NONE',  ( -13.89961937509977652, 13.97604488694528158, 35.62390960531435269 ) ) ;
#103195 = VECTOR ( 'NONE', #49671, 1000.000000000000000 ) ;
#103196 = CARTESIAN_POINT ( 'NONE',  ( -19.02544592524342804, 5.153800228976336051, 111.0405762719810099 ) ) ;
#103197 = CARTESIAN_POINT ( 'NONE',  ( -10.72451020669870658, -18.67979575497194134, 99.58442372801900433 ) ) ;
#103198 = CARTESIAN_POINT ( 'NONE',  ( -19.05341960407611168, -5.049401038298163336, 71.45724293864766707 ) ) ;
#103199 = CARTESIAN_POINT ( 'NONE',  ( 12.14591786802327356, -12.06949235617739191, 65.62609039468568994 ) ) ;
#103200 = CARTESIAN_POINT ( 'NONE',  ( -18.62759615963255300, -10.81492255796106328, 89.16775706135236135 ) ) ;
#103201 = CARTESIAN_POINT ( 'NONE',  ( -19.05341960407617563, 5.049401038297882671, 58.54275706135234003 ) ) ;
#103202 = CARTESIAN_POINT ( 'NONE',  ( 16.51473224551083163, -9.474510206698727899, 55.83442372801899722 ) ) ;
#103203 = EDGE_LOOP ( 'NONE', ( #170048, #171287, #191771, #136982, #63719 ) ) ;
#103204 = CARTESIAN_POINT ( 'NONE',  ( 10.72451020669871369, 18.67979575497193778, 52.08442372801901854 ) ) ;
#103205 = CARTESIAN_POINT ( 'NONE',  ( -18.22780087662121673, -5.500000000000062172, 56.48459894673892734 ) ) ;
#103206 = CARTESIAN_POINT ( 'NONE',  ( 16.51473224551083163, -9.474510206698727899, 50.83442372801899722 ) ) ;
#103207 = CARTESIAN_POINT ( 'NONE',  ( 19.03943276465977164, -0.05219959533909143690, 98.74890960531436690 ) ) ;
#103208 = CARTESIAN_POINT ( 'NONE',  ( 16.46253265017160672, -9.564922557960803928, 88.33224293864769550 ) ) ;
#103209 = CARTESIAN_POINT ( 'NONE',  ( -4.379528057220328563, 16.55341960407611168, 35.20724293864768839 ) ) ;
#103210 = CARTESIAN_POINT ( 'NONE',  ( -21.53943276465977519, 0.05219959533907696930, 36.24890960531435979 ) ) ;
#103211 = CARTESIAN_POINT ( 'NONE',  ( -36.91746825000001309, -11.99521256947794789, -3.024999997268812635 ) ) ;
#103212 = CARTESIAN_POINT ( 'NONE',  ( 21.73741105231470527, 22.97983228106259901, -49.48322453030139911 ) ) ;
#103213 = CARTESIAN_POINT ( 'NONE',  ( -5.719274019375665041, -21.55341960407619695, 109.7927570613523613 ) ) ;
#103214 = DIRECTION ( 'NONE',  ( -0.000000000000000000, -0.000000000000000000, 1.000000000000000000 ) ) ;
#103215 = CARTESIAN_POINT ( 'NONE',  ( -13.97604488694527625, -13.89961937509977652, 31.87390960531435979 ) ) ;
#103216 = CARTESIAN_POINT ( 'NONE',  ( 19.03943276465977164, -0.05219959533909143690, 28.74890960531435624 ) ) ;
#103217 = CARTESIAN_POINT ( 'NONE',  ( -33.72427247603956602, -5.492275790717718209, 95.34298344322783691 ) ) ;
#103218 = CARTESIAN_POINT ( 'NONE',  ( 2.500000000000000000, 2.357898499370431722, -2.818925648462311528E-15 ) ) ;
#103219 = CARTESIAN_POINT ( 'NONE',  ( 12.14591786802327356, -12.06949235617739191, 65.62609039468568994 ) ) ;
#103220 = CARTESIAN_POINT ( 'NONE',  ( -18.67979575497178146, -10.72451020669898902, 86.66557627198102409 ) ) ;
#103221 = CARTESIAN_POINT ( 'NONE',  ( -14.29746914071049879, 8.314922557960819915, 55.83224293864770260 ) ) ;
#103223 = CARTESIAN_POINT ( 'NONE',  ( -9.474510206698964154, 16.51473224551069663, 105.4155762719810383 ) ) ;
#103222 = CARTESIAN_POINT ( 'NONE',  ( -0.05219959533909027116, -19.03943276465977164, 22.49890960531436690 ) ) ;
#103224 = CARTESIAN_POINT ( 'NONE',  ( 15.80617190586769283, -15.72974639402175789, 25.62609039468567929 ) ) ;
#103225 = CARTESIAN_POINT ( 'NONE',  ( 13.97604488694548053, -13.89961937509957401, 30.62609039468566863 ) ) ;
#103226 = CARTESIAN_POINT ( 'NONE',  ( 16.46253265017160672, -9.564922557960803928, 28.33224293864769550 ) ) ;
#103227 = CARTESIAN_POINT ( 'NONE',  ( -15.72974639402176322, -15.80617190586768395, 79.37609039468567573 ) ) ;
#103228 = CARTESIAN_POINT ( 'NONE',  ( -17.49999999999999645, 5.499999999999992895, 48.71769037696437010 ) ) ;
#103229 = CARTESIAN_POINT ( 'NONE',  ( 4.379528057220339221, -16.55341960407611168, 27.70724293864769905 ) ) ;
#103230 = CARTESIAN_POINT ( 'NONE',  ( 17.49999999999999645, 3.805241302050201391, 112.1264752721741758 ) ) ;
#103231 = CARTESIAN_POINT ( 'NONE',  ( -21.53943276465977519, 0.05219959533907696930, 46.24890960531435979 ) ) ;
#103232 = CARTESIAN_POINT ( 'NONE',  ( -14.29746914071049879, 8.314922557960819915, 100.8322429386477097 ) ) ;
#103233 = CARTESIAN_POINT ( 'NONE',  ( -4.926632765927992708, -6.813239905315497502, -64.10665255646803473 ) ) ;
#103234 = CARTESIAN_POINT ( 'NONE',  ( 13.89961937509977652, -13.97604488694527269, 93.12390960531436690 ) ) ;
#103235 = CARTESIAN_POINT ( 'NONE',  ( -4.379528057220328563, 16.55341960407611168, 95.20724293864769550 ) ) ;
#103236 = CARTESIAN_POINT ( 'NONE',  ( 5.049401038297881783, 19.05341960407617563, 102.2927570613523045 ) ) ;
#103237 = CARTESIAN_POINT ( 'NONE',  ( -18.67979575497178146, -10.72451020669898902, 61.66557627198103120 ) ) ;
#103238 = EDGE_LOOP ( 'NONE', ( #125765, #54004, #39848, #146693, #120559 ) ) ;
#103239 = EDGE_CURVE ( 'NONE', #94667, #174040, #133572, .T. ) ;
#103240 = CARTESIAN_POINT ( 'NONE',  ( -19.05341960407611168, -5.049401038298163336, 26.45724293864769550 ) ) ;
#103242 = CARTESIAN_POINT ( 'NONE',  ( 5.823673210054125526, 21.52544592524343514, 89.79057627198103830 ) ) ;
#103241 = CARTESIAN_POINT ( 'NONE',  ( 5.049401038298161559, -19.05341960407611168, 87.70724293864769550 ) ) ;
#103244 = CARTESIAN_POINT ( 'NONE',  ( 13.97604488694527802, 13.89961937509977652, 89.37390960531436690 ) ) ;
#103243 = CARTESIAN_POINT ( 'NONE',  ( 0.05219959533934541429, -16.53943276465976808, 105.0010903946856757 ) ) ;
#103245 = CARTESIAN_POINT ( 'NONE',  ( 19.05341960407617918, -5.049401038297876454, 81.04275706135231871 ) ) ;
#103246 = CARTESIAN_POINT ( 'NONE',  ( 18.67979575497194134, -10.72451020669871369, 100.8344237280190185 ) ) ;
#103247 = CARTESIAN_POINT ( 'NONE',  ( -10.81492255796078084, -18.62759615963271287, 72.08224293864769550 ) ) ;
#103248 = CARTESIAN_POINT ( 'NONE',  ( -21.55341960407610458, -5.719274019375992779, 36.45724293864768839 ) ) ;
#103249 = CARTESIAN_POINT ( 'NONE',  ( -13.89961937509977652, 13.97604488694528158, 55.62390960531434558 ) ) ;
#103250 = CARTESIAN_POINT ( 'NONE',  ( -14.34966873604972548, 8.224510206698743886, 108.3344237280190185 ) ) ;
#103251 = CARTESIAN_POINT ( 'NONE',  ( 16.51473224551069308, 9.474510206698969483, 64.16557627198102409 ) ) ;
#103252 = VERTEX_POINT ( 'NONE', #41332 ) ;
#103253 = FACE_OUTER_BOUND ( 'NONE', #57457, .T. ) ;
#103254 = CARTESIAN_POINT ( 'NONE',  ( -16.46253265017146816, -9.564922557961047289, 29.16775706135232937 ) ) ;
#103255 = CARTESIAN_POINT ( 'NONE',  ( 12.06949235617757843, -12.14591786802309237, 68.12390960531436690 ) ) ;
#103256 = CARTESIAN_POINT ( 'NONE',  ( -10.72451020669898014, 18.67979575497178502, 115.4155762719810241 ) ) ;
#103257 = CARTESIAN_POINT ( 'NONE',  ( 17.14385361876520264, 23.59649016807275856, 144.6750000027311671 ) ) ;
#103258 = CARTESIAN_POINT ( 'NONE',  ( -21.52544592524343514, 5.823673210054127303, 66.04057627198103830 ) ) ;
#103259 = CARTESIAN_POINT ( 'NONE',  ( -12.06949235617739369, -12.14591786802326823, 94.37609039468568994 ) ) ;
#103260 = CARTESIAN_POINT ( 'NONE',  ( -14.34966873604960291, -8.224510206698953496, 106.6655762719810383 ) ) ;
#103261 = CARTESIAN_POINT ( 'NONE',  ( -9.564922557960796823, -16.46253265017161027, 72.08224293864770971 ) ) ;
#103262 = SURFACE_STYLE_USAGE ( .BOTH. , #13247 ) ;
#103263 = CARTESIAN_POINT ( 'NONE',  ( 8.314922557960818139, 14.29746914071049879, 24.58224293864768839 ) ) ;
#103264 = EDGE_CURVE ( 'NONE', #75663, #131752, #69112, .T. ) ;
#103265 = CARTESIAN_POINT ( 'NONE',  ( -21.53943276465977519, -0.05219959533937600094, 43.75109039468568284 ) ) ;
#103266 = CARTESIAN_POINT ( 'NONE',  ( -16.46253265017160317, 9.564922557960807481, 110.8322429386476955 ) ) ;
#103267 = CARTESIAN_POINT ( 'NONE',  ( 21.53943276465977519, 0.05219959533937863772, 86.25109039468568994 ) ) ;
#103268 = CARTESIAN_POINT ( 'NONE',  ( -5.153800228976328057, -19.02544592524343514, 32.29057627198102409 ) ) ;
#103269 = CARTESIAN_POINT ( 'NONE',  ( -5.153800228976328057, -19.02544592524343514, 37.29057627198102409 ) ) ;
#103270 = ORIENTED_EDGE ( 'NONE', *, *, #54728, .F. ) ;
#103271 = CARTESIAN_POINT ( 'NONE',  ( 21.55341960407619695, -5.719274019375665929, 101.0427570613523756 ) ) ;
#103272 = CARTESIAN_POINT ( 'NONE',  ( -8.224510206698735004, -14.34966873604973081, 44.58442372801901854 ) ) ;
#103273 = CARTESIAN_POINT ( 'NONE',  ( -5.719274019375665041, -21.55341960407619695, 74.79275706135234714 ) ) ;
#103274 = CARTESIAN_POINT ( 'NONE',  ( 13.89961937509977652, -13.97604488694527269, 98.12390960531433848 ) ) ;
#103275 = CARTESIAN_POINT ( 'NONE',  ( -9.474510206698720793, -16.51473224551083518, 84.58442372801900433 ) ) ;
#103276 = CARTESIAN_POINT ( 'NONE',  ( -18.67979575497193778, 10.72451020669871902, 58.33442372801901143 ) ) ;
#103277 = CARTESIAN_POINT ( 'NONE',  ( 9.474510206698729675, 16.51473224551082808, 112.0844237280190043 ) ) ;
#103278 = CARTESIAN_POINT ( 'NONE',  ( -19.03943276465977164, -0.05219959533935918106, 88.75109039468567573 ) ) ;
#103279 = CARTESIAN_POINT ( 'NONE',  ( -13.89961937509977652, 13.97604488694528158, 45.62390960531433848 ) ) ;
#103280 = CARTESIAN_POINT ( 'NONE',  ( 16.51473224551083163, -9.474510206698727899, 90.83442372801900433 ) ) ;
#103281 = CARTESIAN_POINT ( 'NONE',  ( -12.14591786802309592, -12.06949235617757132, 26.87390960531435979 ) ) ;
#103282 = CARTESIAN_POINT ( 'NONE',  ( 13.89961937509957401, 13.97604488694547697, 86.87609039468567573 ) ) ;
#103283 = CARTESIAN_POINT ( 'NONE',  ( -14.29746914071049879, 8.314922557960819915, 45.83224293864769550 ) ) ;
#103284 = CARTESIAN_POINT ( 'NONE',  ( 13.89961937509957401, 13.97604488694547697, 66.87609039468567573 ) ) ;
#103285 = CARTESIAN_POINT ( 'NONE',  ( 0.05219959533934541429, -16.53943276465976808, 50.00109039468568994 ) ) ;
#103286 = CARTESIAN_POINT ( 'NONE',  ( -19.05341960407617563, 5.049401038297882671, 28.54275706135232937 ) ) ;
#103287 = CARTESIAN_POINT ( 'NONE',  ( -5.153800228976328057, -19.02544592524343514, 27.29057627198103120 ) ) ;
#103288 = CARTESIAN_POINT ( 'NONE',  ( -13.97604488694527625, -13.89961937509977652, 46.87390960531435979 ) ) ;
#103289 = CARTESIAN_POINT ( 'NONE',  ( -14.34966873604972548, 8.224510206698743886, 43.33442372801901143 ) ) ;
#103290 = CARTESIAN_POINT ( 'NONE',  ( 17.81289503416610742, 24.51734667627700404, 139.5500000054623229 ) ) ;
#103291 = CARTESIAN_POINT ( 'NONE',  ( -17.81289503416611808, 24.51734667627700404, 141.9500000054623285 ) ) ;
#103292 = CARTESIAN_POINT ( 'NONE',  ( -13.97604488694527625, -13.89961937509977652, 86.87390960531436690 ) ) ;
#103293 = CARTESIAN_POINT ( 'NONE',  ( -3.573655867282028392E-15, 12.39993551617566681, 175.0000000000000000 ) ) ;
#103294 = ORIENTED_EDGE ( 'NONE', *, *, #69903, .F. ) ;
#103295 = CARTESIAN_POINT ( 'NONE',  ( 13.97604488694548053, -13.89961937509957401, 100.6260903946856615 ) ) ;
#103297 = CARTESIAN_POINT ( 'NONE',  ( 5.719274019375991003, -21.55341960407610458, 27.70724293864769905 ) ) ;
#103296 = VECTOR ( 'NONE', #108279, 1000.000000000000000 ) ;
#103299 = CARTESIAN_POINT ( 'NONE',  ( 19.03943276465977164, 0.05219959533936151252, 106.2510903946856615 ) ) ;
#103298 = CARTESIAN_POINT ( 'NONE',  ( 0.05219959533936267826, -19.03943276465977164, 35.00109039468566863 ) ) ;
#103300 = CARTESIAN_POINT ( 'NONE',  ( -16.52544592524342804, 4.483927247898546575, 111.0405762719810525 ) ) ;
#103301 = CARTESIAN_POINT ( 'NONE',  ( 5.049401038298161559, -19.05341960407611168, 37.70724293864768839 ) ) ;
#103302 = CARTESIAN_POINT ( 'NONE',  ( 5.719274019375991003, -21.55341960407610458, 77.70724293864770971 ) ) ;
#103303 = CARTESIAN_POINT ( 'NONE',  ( 5.049401038298161559, -19.05341960407611168, 42.70724293864767418 ) ) ;
#103304 = DIRECTION ( 'NONE',  ( 0.000000000000000000, 0.000000000000000000, 1.000000000000000000 ) ) ;
#103305 = CARTESIAN_POINT ( 'NONE',  ( -13.97604488694547697, 13.89961937509957934, 68.12609039468563310 ) ) ;
#103306 = CARTESIAN_POINT ( 'NONE',  ( -16.55341960407611168, -4.379528057220339221, 56.45724293864768839 ) ) ;
#103307 = CARTESIAN_POINT ( 'NONE',  ( -18.67979575497178146, -10.72451020669898902, 36.66557627198103120 ) ) ;
#103308 = CARTESIAN_POINT ( 'NONE',  ( 5.719274019375673035, 21.55341960407619339, 97.29275706135234714 ) ) ;
#103309 = CARTESIAN_POINT ( 'NONE',  ( -0.05219959533907301413, -21.53943276465977519, 82.49890960531436690 ) ) ;
#103310 = CARTESIAN_POINT ( 'NONE',  ( -15.72974639402176322, -15.80617190586768395, 69.37609039468567573 ) ) ;
#103311 = CARTESIAN_POINT ( 'NONE',  ( 18.67979575497194134, -10.72451020669871369, 70.83442372801901854 ) ) ;
#103312 = CARTESIAN_POINT ( 'NONE',  ( -13.89961937509977652, 13.97604488694528158, 90.62390960531432427 ) ) ;
#103314 = CARTESIAN_POINT ( 'NONE',  ( -18.62759615963255300, -10.81492255796106328, 69.16775706135234714 ) ) ;
#103313 = CARTESIAN_POINT ( 'NONE',  ( -12.06949235617739369, -12.14591786802326823, 89.37609039468568994 ) ) ;
#103315 = CARTESIAN_POINT ( 'NONE',  ( 5.049401038298161559, -19.05341960407611168, 52.70724293864767418 ) ) ;
#103316 = CARTESIAN_POINT ( 'NONE',  ( 10.72451020669871369, 18.67979575497193778, 27.08442372801901854 ) ) ;
#103317 = CARTESIAN_POINT ( 'NONE',  ( 19.05341960407611168, 5.049401038298154454, 73.95724293864768129 ) ) ;
#103318 = CARTESIAN_POINT ( 'NONE',  ( -14.29746914071049879, 8.314922557960819915, 75.83224293864769550 ) ) ;
#103319 = CARTESIAN_POINT ( 'NONE',  ( 16.53943276465976808, -0.05219959533910856209, 43.74890960531435979 ) ) ;
#103320 = CARTESIAN_POINT ( 'NONE',  ( -0.05219959533907301413, -21.53943276465977519, 57.49890960531435979 ) ) ;
#103321 = CARTESIAN_POINT ( 'NONE',  ( -5.153800228976328057, -19.02544592524343514, 42.29057627198101699 ) ) ;
#103322 = CARTESIAN_POINT ( 'NONE',  ( 15.72974639402199770, -15.80617190586745480, 63.12390960531435979 ) ) ;
#103323 = CARTESIAN_POINT ( 'NONE',  ( 13.89961937509957401, 13.97604488694547697, 46.87609039468565442 ) ) ;
#103325 = CARTESIAN_POINT ( 'NONE',  ( 16.52544592524342804, -4.483927247898539470, 68.54057627198103830 ) ) ;
#103324 = CARTESIAN_POINT ( 'NONE',  ( -19.03943276465977164, -0.05219959533935946555, 18.75109039468567218 ) ) ;
#103327 = CIRCLE ( 'NONE', #197010, 3.000000000000001776 ) ;
#103326 = CARTESIAN_POINT ( 'NONE',  ( 5.823673210054125526, 21.52544592524343514, 34.79057627198103120 ) ) ;
#103328 = ORIENTED_EDGE ( 'NONE', *, *, #27433, .F. ) ;
#103329 = CARTESIAN_POINT ( 'NONE',  ( 17.50000000000000355, 5.499999999999989342, 103.7823096230356867 ) ) ;
#103330 = CARTESIAN_POINT ( 'NONE',  ( 12.14591786802327356, -12.06949235617739191, 85.62609039468568994 ) ) ;
#103331 = CARTESIAN_POINT ( 'NONE',  ( -5.153800228976607833, 19.02544592524334988, 92.70942372801901854 ) ) ;
#103332 = CARTESIAN_POINT ( 'NONE',  ( -12.14591786802309592, -12.06949235617757132, 56.87390960531436690 ) ) ;
#103333 = PLANE ( 'NONE',  #83777 ) ;
#103334 = CARTESIAN_POINT ( 'NONE',  ( 9.474510206698971260, -16.51473224551069308, 52.91557627198102409 ) ) ;
#103335 = CARTESIAN_POINT ( 'NONE',  ( 12.14591786802309770, 12.06949235617756955, 39.37390960531436690 ) ) ;
#103336 = CARTESIAN_POINT ( 'NONE',  ( 19.02544592524343514, -5.153800228976328945, 73.54057627198103830 ) ) ;
#103337 = CARTESIAN_POINT ( 'NONE',  ( -0.05219959533909027116, -19.03943276465977164, 47.49890960531435979 ) ) ;
#103338 = CARTESIAN_POINT ( 'NONE',  ( -10.72451020669870658, -18.67979575497194134, 64.58442372801900433 ) ) ;
#103339 = CARTESIAN_POINT ( 'NONE',  ( 19.02544592524343514, -5.153800228976328945, 68.54057627198103830 ) ) ;
#103340 = CARTESIAN_POINT ( 'NONE',  ( 16.46253265017160672, -9.564922557960803928, 23.33224293864769194 ) ) ;
#103341 = CARTESIAN_POINT ( 'NONE',  ( 5.049401038298161559, -19.05341960407611168, 62.70724293864769550 ) ) ;
#103342 = ADVANCED_FACE ( 'NONE', ( #98429 ), #186113, .T. ) ;
#103343 = CARTESIAN_POINT ( 'NONE',  ( -5.719274019375978568, 21.55341960407610458, 55.20724293864770260 ) ) ;
#103344 = CARTESIAN_POINT ( 'NONE',  ( -0.05219959533909027116, -19.03943276465977164, 32.49890960531435979 ) ) ;
#103345 = CARTESIAN_POINT ( 'NONE',  ( -5.823673210054116645, -21.52544592524344225, 42.29057627198103120 ) ) ;
#103346 = CARTESIAN_POINT ( 'NONE',  ( 14.34966873604972726, -8.224510206698740333, 100.8344237280190185 ) ) ;
#103347 = CARTESIAN_POINT ( 'NONE',  ( -10.81492255796105439, 18.62759615963255655, 112.9177570613523329 ) ) ;
#103349 = CARTESIAN_POINT ( 'NONE',  ( 16.55341960407618274, -4.379528057220086978, 76.04275706135237556 ) ) ;
#103348 = CARTESIAN_POINT ( 'NONE',  ( 14.34966873604972726, -8.224510206698740333, 40.83442372801901854 ) ) ;
#103350 = CARTESIAN_POINT ( 'NONE',  ( 6.674792076160576570, 4.273745901508052114, 4.009310749147818598 ) ) ;
#103351 = EDGE_CURVE ( 'NONE', #150928, #120381, #184107, .T. ) ;
#103352 = CARTESIAN_POINT ( 'NONE',  ( 14.29746914071037800, 8.314922557961029526, 66.66775706135234714 ) ) ;
#103353 = CARTESIAN_POINT ( 'NONE',  ( 4.483927247898790824, -16.52544592524335698, 60.20942372801902565 ) ) ;
#103354 = CARTESIAN_POINT ( 'NONE',  ( 19.05341960407611168, 5.049401038298154454, 113.9572429386477097 ) ) ;
#103355 = CARTESIAN_POINT ( 'NONE',  ( 19.03943276465977164, -0.05219959533909143690, 38.74890960531436690 ) ) ;
#103356 = CARTESIAN_POINT ( 'NONE',  ( -4.483927247898782831, 16.52544592524335698, 42.70942372801901854 ) ) ;
#103357 = CARTESIAN_POINT ( 'NONE',  ( 0.05219959533909260263, 19.03943276465977164, 49.99890960531435979 ) ) ;
#103358 = CARTESIAN_POINT ( 'NONE',  ( 21.55341960407619695, -5.719274019375665929, 21.04275706135234714 ) ) ;
#103359 = CARTESIAN_POINT ( 'NONE',  ( -14.34966873604972548, 8.224510206698743886, 33.33442372801900433 ) ) ;
#103360 = CARTESIAN_POINT ( 'NONE',  ( -4.483927247898782831, 16.52544592524335698, 97.70942372801904696 ) ) ;
#103361 = CARTESIAN_POINT ( 'NONE',  ( -16.51473224551069308, -9.474510206698971260, 21.66557627198102765 ) ) ;
#103362 = CARTESIAN_POINT ( 'NONE',  ( 21.55341960407619695, -5.719274019375665929, 101.0427570613523756 ) ) ;
#103363 = CARTESIAN_POINT ( 'NONE',  ( 19.02544592524334988, 5.153800228976608722, 101.4594237280189759 ) ) ;
#103364 = CARTESIAN_POINT ( 'NONE',  ( -16.55341960407611168, -4.379528057220339221, 51.45724293864770260 ) ) ;
#103365 = CARTESIAN_POINT ( 'NONE',  ( -5.049401038298153566, 19.05341960407611168, 30.20724293864768839 ) ) ;
#103367 = CARTESIAN_POINT ( 'NONE',  ( 21.99873734152911453, -27.49873734152921045, 1.818019484660534424 ) ) ;
#103366 = CARTESIAN_POINT ( 'NONE',  ( 16.51473224551083163, -9.474510206698727899, 65.83442372801900433 ) ) ;
#103368 = CARTESIAN_POINT ( 'NONE',  ( -15.72974639402176322, -15.80617190586768395, 69.37609039468567573 ) ) ;
#103369 = CARTESIAN_POINT ( 'NONE',  ( 16.52544592524335698, 4.483927247898782831, 21.45942372801901499 ) ) ;
#103370 = CARTESIAN_POINT ( 'NONE',  ( 16.52216118717206683, 7.221426719304520070, 83.57599021046989662 ) ) ;
#103371 = CARTESIAN_POINT ( 'NONE',  ( 13.97604488694527802, 13.89961937509977652, 114.3739096053143669 ) ) ;
#103372 = CARTESIAN_POINT ( 'NONE',  ( 0.05219959533936267826, -19.03943276465977164, 110.0010903946856757 ) ) ;
#103373 = DIRECTION ( 'NONE',  ( -0.1039620511844979445, -0.1039620511844979445, -0.9891328443778539814 ) ) ;
#103374 = CARTESIAN_POINT ( 'NONE',  ( -25.47140278216145859, 9.703455644539296543, 170.7619267275324262 ) ) ;
#103375 = CARTESIAN_POINT ( 'NONE',  ( -0.05219959533909027116, -19.03943276465977164, 22.49890960531436690 ) ) ;
#103376 = CARTESIAN_POINT ( 'NONE',  ( -5.823673210054431948, 21.52544592524334988, 112.7094237280190328 ) ) ;
#103377 = CARTESIAN_POINT ( 'NONE',  ( -16.51473224551069308, -9.474510206698971260, 36.66557627198102409 ) ) ;
#103378 = CARTESIAN_POINT ( 'NONE',  ( 21.55341960407619695, -5.719274019375665929, 46.04275706135234714 ) ) ;
#103379 = CARTESIAN_POINT ( 'NONE',  ( -21.55341960407619339, 5.719274019375674811, 98.54275706135234714 ) ) ;
#103380 = CARTESIAN_POINT ( 'NONE',  ( -14.29746914071037622, -8.314922557961029526, 104.1677570613523471 ) ) ;
#103381 = CARTESIAN_POINT ( 'NONE',  ( -5.049401038298153566, 19.05341960407611168, 85.20724293864766707 ) ) ;
#103382 = CARTESIAN_POINT ( 'NONE',  ( 5.823673210054444382, -21.52544592524334988, 60.20942372801902565 ) ) ;
#103383 = CARTESIAN_POINT ( 'NONE',  ( -0.05219959533937732626, 21.53943276465977519, 47.50109039468568994 ) ) ;
#103385 = CARTESIAN_POINT ( 'NONE',  ( -19.05341960407611168, -5.049401038298163336, 91.45724293864766707 ) ) ;
#103384 = CARTESIAN_POINT ( 'NONE',  ( 5.153800228976615827, -19.02544592524334988, 75.20942372801896170 ) ) ;
#103386 = CARTESIAN_POINT ( 'NONE',  ( 16.55341960407611168, 4.379528057220329451, 113.9572429386477239 ) ) ;
#103387 = CARTESIAN_POINT ( 'NONE',  ( 21.52544592524344225, -5.823673210054117533, 98.54057627198105251 ) ) ;
#103388 = CARTESIAN_POINT ( 'NONE',  ( 16.46253265017146816, 9.564922557961045513, 26.66775706135234003 ) ) ;
#103389 = CARTESIAN_POINT ( 'NONE',  ( -12.14591786802309592, -12.06949235617757132, 101.8739096053143811 ) ) ;
#103390 = CARTESIAN_POINT ( 'NONE',  ( 5.153800228976335163, 19.02544592524342804, 54.79057627198103120 ) ) ;
#103391 = CARTESIAN_POINT ( 'NONE',  ( 13.89961937509957401, 13.97604488694547697, 81.87609039468564731 ) ) ;
#103392 = CARTESIAN_POINT ( 'NONE',  ( 12.14591786802309770, 12.06949235617756955, 54.37390960531435979 ) ) ;
#103393 = CARTESIAN_POINT ( 'NONE',  ( 21.55341960407619695, -5.719274019375665929, 106.0427570613523471 ) ) ;
#103394 = CARTESIAN_POINT ( 'NONE',  ( 16.51473224551069308, 9.474510206698969483, 109.1655762719810383 ) ) ;
#103395 = CARTESIAN_POINT ( 'NONE',  ( 5.049401038297881783, 19.05341960407617563, 72.29275706135234714 ) ) ;
#103396 = CARTESIAN_POINT ( 'NONE',  ( 21.53943276465977519, -0.05219959533907433946, 73.74890960531433848 ) ) ;
#103397 = CARTESIAN_POINT ( 'NONE',  ( -5.823673210054431948, 21.52544592524334988, 32.70942372801900433 ) ) ;
#103398 = CARTESIAN_POINT ( 'NONE',  ( -12.14591786802326823, 12.06949235617739902, 28.12609039468568284 ) ) ;
#103399 = CARTESIAN_POINT ( 'NONE',  ( -14.29746914071037622, -8.314922557961029526, 94.16775706135237556 ) ) ;
#103401 = CARTESIAN_POINT ( 'NONE',  ( 18.67979575497194134, -10.72451020669871369, 30.83442372801902209 ) ) ;
#103400 = CARTESIAN_POINT ( 'NONE',  ( 19.05341960407611168, 5.049401038298154454, 28.95724293864769550 ) ) ;
#103402 = CARTESIAN_POINT ( 'NONE',  ( -15.80617190586745835, -15.72974639402198527, 46.87390960531435979 ) ) ;
#103403 = CARTESIAN_POINT ( 'NONE',  ( 19.05341960407611168, 5.049401038298154454, 23.95724293864769194 ) ) ;
#103404 = CARTESIAN_POINT ( 'NONE',  ( 30.74264578624800137, -22.33583958711395212, -10.94999999453762562 ) ) ;
#103405 = CARTESIAN_POINT ( 'NONE',  ( -0.05219959533934338120, 16.53943276465976808, 67.50109039468568994 ) ) ;
#103406 = CARTESIAN_POINT ( 'NONE',  ( -8.314922557960811034, -14.29746914071050412, 92.08224293864769550 ) ) ;
#103407 = CARTESIAN_POINT ( 'NONE',  ( -21.55341960407610458, -5.719274019375992779, 86.45724293864770971 ) ) ;
#103408 = CARTESIAN_POINT ( 'NONE',  ( -8.314922557961024197, 14.29746914071037800, 112.9177570613523329 ) ) ;
#103409 = CARTESIAN_POINT ( 'NONE',  ( 16.53943276465976808, 0.05219959533934440121, 51.25109039468568994 ) ) ;
#103410 = CARTESIAN_POINT ( 'NONE',  ( 19.03943276465977164, -0.05219959533909143690, 63.74890960531435979 ) ) ;
#103411 = CARTESIAN_POINT ( 'NONE',  ( -4.483927247898782831, 16.52544592524335698, 87.70942372801901854 ) ) ;
#103412 = CARTESIAN_POINT ( 'NONE',  ( 5.049401038297881783, 19.05341960407617563, 92.29275706135234714 ) ) ;
#103413 = CARTESIAN_POINT ( 'NONE',  ( 5.823673210054125526, 21.52544592524343514, 84.79057627198102409 ) ) ;
#103414 = CARTESIAN_POINT ( 'NONE',  ( 16.53943276465976808, 0.05219959533934440121, 106.2510903946856757 ) ) ;
#103415 = ORIENTED_EDGE ( 'NONE', *, *, #22613, .F. ) ;
#103416 = DIRECTION ( 'NONE',  ( 1.000000000000000000, 0.000000000000000000, 0.000000000000000000 ) ) ;
#103417 = CARTESIAN_POINT ( 'NONE',  ( 21.52544592524344225, -5.823673210054117533, 63.54057627198103830 ) ) ;
#103418 = CARTESIAN_POINT ( 'NONE',  ( -0.05219959533934338120, 16.53943276465976808, 92.50109039468567573 ) ) ;
#103419 = VERTEX_POINT ( 'NONE', #103962 ) ;
#103420 = CARTESIAN_POINT ( 'NONE',  ( -5.823673210054116645, -21.52544592524344225, 37.29057627198102409 ) ) ;
#103421 = CARTESIAN_POINT ( 'NONE',  ( 18.22780087662121673, 5.500000000000056843, 88.98459894673892734 ) ) ;
#103422 = CARTESIAN_POINT ( 'NONE',  ( -18.62759615963270932, 10.81492255796079327, 90.83224293864769550 ) ) ;
#103423 = CARTESIAN_POINT ( 'NONE',  ( 16.52544592524335698, 4.483927247898782831, 111.4594237280190328 ) ) ;
#103424 = CARTESIAN_POINT ( 'NONE',  ( -0.05219959533934338120, 16.53943276465976808, 32.50109039468568284 ) ) ;
#103425 = CARTESIAN_POINT ( 'NONE',  ( 13.89961937509977652, -13.97604488694527269, 33.12390960531434558 ) ) ;
#103426 = CARTESIAN_POINT ( 'NONE',  ( 16.52544592524335698, 4.483927247898782831, 26.45942372801901854 ) ) ;
#103427 = CARTESIAN_POINT ( 'NONE',  ( -9.474510206698964154, 16.51473224551069663, 50.41557627198102409 ) ) ;
#103428 = CARTESIAN_POINT ( 'NONE',  ( 23.31738231874054534, 16.94106989632529192, 149.1999999999999886 ) ) ;
#103429 = CARTESIAN_POINT ( 'NONE',  ( 0.05219959533909260263, 19.03943276465977164, 104.9989096053143669 ) ) ;
#103430 = CARTESIAN_POINT ( 'NONE',  ( 13.89961937509977652, -13.97604488694527269, 113.1239096053143527 ) ) ;
#103431 = CARTESIAN_POINT ( 'NONE',  ( -16.52544592524335698, -4.483927247898792601, 98.95942372801903275 ) ) ;
#103432 = CARTESIAN_POINT ( 'NONE',  ( 5.153800228976615827, -19.02544592524334988, 95.20942372801897591 ) ) ;
#103433 = CARTESIAN_POINT ( 'NONE',  ( -5.049401038297874678, -19.05341960407617918, 34.79275706135233293 ) ) ;
#103434 = CARTESIAN_POINT ( 'NONE',  ( 10.72451020669898902, -18.67979575497178502, 72.91557627198103830 ) ) ;
#103435 = CARTESIAN_POINT ( 'NONE',  ( 4.483927247898790824, -16.52544592524335698, 100.2094237280190043 ) ) ;
#103436 = CARTESIAN_POINT ( 'NONE',  ( 21.52544592524344225, -5.823673210054117533, 33.54057627198102409 ) ) ;
#103437 = CARTESIAN_POINT ( 'NONE',  ( 19.05341960407617918, -5.049401038297876454, 106.0427570613523471 ) ) ;
#103438 = CARTESIAN_POINT ( 'NONE',  ( 5.153800228976335163, 19.02544592524342804, 104.7905762719809957 ) ) ;
#103439 = CARTESIAN_POINT ( 'NONE',  ( -0.05219959533937732626, 21.53943276465977519, 62.50109039468568284 ) ) ;
#103440 = CARTESIAN_POINT ( 'NONE',  ( -19.02544592524342804, 5.153800228976336051, 66.04057627198103830 ) ) ;
#103441 = CIRCLE ( 'NONE', #16254, 69.99999999999997158 ) ;
#103442 = CARTESIAN_POINT ( 'NONE',  ( -8.314922557960811034, -14.29746914071050412, 97.08224293864770971 ) ) ;
#103443 = CARTESIAN_POINT ( 'NONE',  ( 32.63002904509641411, 0.9908434387721892778, 87.54952558906809656 ) ) ;
#103444 = CARTESIAN_POINT ( 'NONE',  ( -4.483927247898539470, -16.52544592524342804, 77.29057627198102409 ) ) ;
#103445 = CARTESIAN_POINT ( 'NONE',  ( 18.62759615963271287, -10.81492255796078972, 73.33224293864769550 ) ) ;
#103446 = ORIENTED_EDGE ( 'NONE', *, *, #111919, .T. ) ;
#103447 = CARTESIAN_POINT ( 'NONE',  ( 5.153800228976615827, -19.02544592524334988, 85.20942372801900433 ) ) ;
#103448 =( BOUNDED_SURFACE ( )  B_SPLINE_SURFACE ( 3, 2, ( 
 ( #17824, #122991, #169498, #94643, #109818, #170500, #63315, #199854, #62304, #141151, #31990, #140146, #183692, #91644, #95636, #184677, #46160, #14834, #172492, #60328, #138173, #33980, #157324, #155333, #30997, #18819, #122002, #124995, #137173, #32990, #76497, #186690, #111807, #145122, #190647, #173495, #188668, #7604, #82439, #3621, #66296, #36947, #50147, #83444, #68285, #158309, #34968, #114793, #6606, #22796, #146120, #128946, #96620, #53115, #142137, #129936, #115802, #65300, #19797, #51132, #144127, #100618, #69290, #126959, #81438, #191635, #143124, #176486, #37962, #4604, #99620, #52123, #161300, #84442, #130956, #127955, #112792, #192646, #54129, #113779, #177492, #189659, #159287, #38961, #5608, #160303, #174486, #35953, #162300, #97599, #20784, #67288, #80463, #175475, #98609, #21793, #182471, #40965, #148145, #104627, #85450, #103640, #166316, #58132, #8628, #132966, #55125, #88451, #133977, #116794, #131969, #151143, #25815, #42964, #117807, #41973, #26811, #179500, #147140, #178486, #74299, #57139, #118815, #119801, #102637, #10638, #134985, #181486, #180501, #43952, #70300, #195668, #72298, #193653, #39953, #196663, #165318, #150146, #11648, #27813, #101624, #163313, #89454, #73314, #87461, #12634, #135968, #164322, #24811, #197639, #59105, #120770, #105614, #23800, #86460, #9636, #71303, #194655, #56125, #149148, #75273, #138919, #108586, #106600, #136943, #155092, #187446, #45927, #154099, #78234, #1394, #123737, #125746, #152123, #77251, #15593, #28798, #121766, #139905, #400, #185436, #170263, #109580, #90437, #198632, #47926, #62072, #169259, #46926, #93406, #61084, #44945, #31757, #16586, #64076, #63075, #124754, #168276, #186450, #48914, #171263, #13605, #30766, #60098, #32751, #94402, #29773, #183459, #156083, #167302, #137934, #17579, #79240, #140911, #91408, #2397, #153096, #14600, #76256, #184447, #199618, #122757, #107582, #92413, #176243, #190408, #126720, #37714, #82195, #21549, #189423, #127721, #144884, #175237, #66053, #141897, #7363, #4370, #159052, #67053, #128711, #142888, #192407, #51884, #3388, #50898, #112556, #174251, #35719, #161059, #157083, #98363, #99376, #160062, #188424, #69048, #22554, #97366, #130713, #20546, #191395, #110568, #113543, #143888, #5369, #34727, #172249, #84200, #33736, #36702, #83209, #6366, #68046, #49901, #129698, #52872, #114543, #145880, #96385, #65063, #19563, #95397, #18579, #80226, #111568, #173252, #158072, #81207, #9391, #177251, #8383, #104383, #87219, #148901, #88205, #103390, #131726, #149889, #74056, #118566, #38723, #117554, #162059, #25575, #195414, #193408, #23555, #41726, #135727, #24566, #180256, #165068, #11395, #100381, #10391, #40719, #102388, #85203, #71057, #166066, #27567, #164076, #89207, #119561, #133722, #70058, #181244, #72048, #26562, #132723, #194411, #73065, #134737, #55881, #146891, #150900, #147905, #56892, #196419, #57889, #86215, #53889, #42721, #54883, #179253, #12394, #115564, #116557, #178246, #39707, #101370, #163059, #46681, #75031, #155839, #62825, #14350, #17336, #184204, #77995, #78992, #158, #76015, #122514, #121522, #197398, #171017, #58864, #61827, #107337, #29533, #31511, #136697, #123497, #93164, #154849, #60839, #183217, #28557, #106352, #120530, #185190, #137690, #124508, #199375, #15350, #108340, #152855, #182223, #151877, #47685, #30514, #92166, #16346, #45686, #169010, #170021, #139662, #153852, #43707, #105369, #77006, #138678, #167056, #13367, #1150, #186203, #109335, #32508, #94160, #90194, #198378, #59855, #44698, #168036, #91166, #66808, #34494, #18341, #143643, #81951, #37475, #128471, #174998, #4134, #64829, #172010, #49661, #2158, #190167, #80980, #6129, #142655, #158815, #5126, #96152, #63836, #95158, #191166, #174011, #35482, #36463, #19332, #127482, #51643, #98120, #97131, #99136, #125509, #50660, #189187, #187206, #156846, #113307, #112321, #20303, #159817 ),
 ( #52639, #21312, #114304, #82969, #144646, #67812, #129467, #48677, #176006, #110329, #160826, #157841, #22314, #140666, #33499, #79996, #126491, #141664, #3156, #188189, #111325, #173015, #65813, #118326, #148664, #26328, #149656, #132487, #53644, #56653, #145645, #10152, #119322, #7125, #115321, #54638, #147664, #104146, #11154, #68807, #100139, #71812, #130466, #180019, #41486, #177013, #103151, #55640, #133480, #195172, #164832, #69812, #116313, #87968, #72828, #117313, #134497, #146641, #162816, #196184, #9151, #163834, #192164, #38482, #42483, #8134, #131479, #161820, #57656, #23315, #84959, #181009, #165828, #101130, #193166, #83965, #178002, #25336, #39469, #24325, #85974, #70818, #194176, #179009, #40477, #102149, #86977, #156354, #91675, #126017, #2671, #199888, #64348, #1671, #94675, #79511, #110842, #15862, #62337, #187712, #141181, #63349, #17855, #92680, #108854, #172526, #155365, #109847, #76529, #138206, #188698, #154368, #77520, #61352, #157355, #153366, #31030, #80495, #50179, #47194, #139192, #34011, #14868, #171532, #95668, #49184, #123023, #667, #184708, #18850, #140178, #46193, #107846, #142169, #32024, #3653, #185705, #169530, #65331, #170534, #93682, #124007, #16854, #78505, #125026, #33020, #186722, #48193, #126991, #111836, #27325, #159318, #51162, #112822, #34996, #7635, #175504, #191665, #20813, #161331, #69319, #68314, #96650, #177521, #52152, #130985, #190676, #127986, #160333, #158338, #113809, #83475, #146148, #100647, #23829, #53144, #147168, #192676, #54159, #115832, #114823, #19827, #38991, #81468, #131997, #36978, #162328, #37992, #84470, #143154, #82469, #129965, #4635, #176515, #22824, #174515, #66325, #85479, #99648, #8656, #70330, #21823, #189689, #193683, #35982, #55153, #173525, #97629, #144155, #5640, #145152, #67317, #128977, #98638, #6636, #136972, #87489, #42993, #27842, #74329, #163343, #73342, #103668, #165346, #24838, #134005, #167331, #90467, #26839, #28827, #182501, #196692, #132993, #43980, #88479, #89483, #195696, #57167, #151174, #181514, #72329, #148173, #13634, #10666, #150176, #135015, #58161, #149177, #198662, #119829, #9664, #118846, #180529, #42002, #11676, #152151, #86488, #104658, #105642, #166345, #194684, #75301, #116823, #12662, #178514, #135996, #197667, #39980, #59133, #120800, #101651, #40997, #71331, #56153, #117835, #179528, #102665, #164350, #25845, #137965, #186480, #156112, #94431, #123766, #184477, #91438, #169289, #121795, #47957, #429, #125774, #62103, #78262, #63104, #15623, #183489, #14629, #110596, #93435, #155121, #17609, #138949, #46956, #171292, #79269, #16615, #18607, #44973, #170292, #108615, #106631, #76286, #32779, #31786, #139935, #1424, #2427, #168305, #29802, #140940, #124782, #185465, #109608, #64107, #154129, #199648, #187474, #48943, #157111, #172278, #33767, #61114, #95427, #80255, #141925, #153125, #60128, #122787, #77280, #45956, #107611, #30795, #92443, #50927, #176276, #53921, #96414, #189450, #81235, #142916, #65091, #37747, #5398, #21579, #112585, #191426, #99407, #98394, #126750, #7396, #82226, #161090, #20574, #158100, #190437, #188452, #143917, #113572, #22585, #130746, #115595, #83237, #177284, #84233, #145911, #69080, #144913, #49932, #192439, #111597, #162093, #67081, #38755, #68075, #114577, #173282, #174279, #160093, #34755, #6396, #52902, #4398, #19592, #100412, #129729, #23588, #85236, #51913, #66082, #3416, #127749, #35748, #97394, #159080, #128741, #175266, #36732, #167089, #12427, #70089, #163095, #73100, #8417, #42754, #119594, #116588, #181277, #118600, #11429, #196453, #27602, #132754, #179286, #104417, #57923, #180290, #134770, #9422, #25606, #89241, #72082, #26595, #193440, #54916, #105404, #71087, #194441, #178277, #74090, #131758, #147936, #197431, #28590, #164107, #55912, #150934, #39740, #88238, #135760, #166100, #101402, #117586, #24599, #58897, #56925, #86246, #40752 ),
 ( #102420, #120563, #182257, #87250, #43742, #41758, #146926, #148934, #10424, #133756, #195450, #103423, #165102, #149923, #154884, #152888, #169046, #171051, #15385, #170056, #136730, #198412, #48710, #14383, #137725, #59889, #17371, #13400, #91198, #140701, #110363, #107374, #76049, #32541, #151911, #31547, #94194, #124543, #75064, #199409, #121555, #16382, #194, #183251, #44732, #79026, #92204, #109369, #45721, #29567, #186240, #30552, #153888, #106388, #184240, #77042, #168069, #93199, #60873, #122550, #62861, #2191, #138713, #61863, #123532, #185226, #46717, #47718, #108380, #78029, #139698, #1184, #155874, #63873, #125544, #187240, #172045, #90227, #50699, #188223, #20339, #18377, #112358, #143681, #6166, #160862, #84004, #113344, #7164, #67846, #191201, #129501, #175036, #95194, #52676, #156880, #192202, #174049, #114339, #98155, #144681, #80029, #19365, #190203, #141698, #36501, #21348, #111361, #3189, #176042, #159855, #37510, #99172, #81988, #64862, #22352, #126524, #83006, #68847, #49696, #173050, #4169, #97166, #35518, #157876, #145682, #34527, #130506, #53684, #115361, #96187, #142689, #81014, #33532, #5162, #65847, #127517, #189221, #158851, #66845, #128508, #51682, #72868, #117353, #40517, #146679, #70856, #55679, #193204, #180059, #116351, #24363, #149695, #27363, #69850, #162856, #54677, #178040, #38521, #11193, #179049, #195212, #86014, #164872, #134537, #71851, #100177, #181047, #102188, #196225, #194214, #131518, #163876, #161859, #25375, #87017, #57695, #104185, #89009, #56692, #150700, #119363, #42522, #165867, #118366, #23353, #12198, #84998, #135532, #148703, #73863, #41528, #88007, #8174, #147703, #133520, #39508, #103191, #26367, #101168, #9191, #197203, #58666, #177051, #132525, #10191, #28364, #200161, #182027, #15147, #948, #43510, #90002, #106158, #75814, #124301, #31310, #105176, #92963, #62623, #29341, #60639, #168812, #30316, #167840, #185998, #91959, #151684, #90970, #14147, #137492, #199172, #16144, #166862, #76809, #77799, #138480, #74839, #120332, #13176, #107142, #136502, #61631, #198182, #59652, #154649, #153652, #123299, #122313, #121326, #183018, #152657, #184004, #44502, #184991, #108135, #46475, #45487, #139468, #169819, #151342, #59304, #118009, #25014, #181679, #162500, #180699, #43160, #135185, #85657, #9837, #132168, #165516, #10836, #193859, #8832, #28014, #102833, #119993, #56327, #40152, #196859, #41170, #164519, #70500, #194854, #179698, #116995, #103835, #101828, #148341, #73514, #12831, #55324, #86657, #178690, #163515, #24001, #58325, #26012, #119016, #71496, #88656, #104827, #195868, #147344, #166516, #87655, #89656, #149340, #133162, #72506, #134181, #57341, #42175, #74497, #136163, #197838, #27012, #120973, #182671, #100817, #150352, #11849, #105815, #1602, #167502, #2603, #61289, #16787, #108788, #155297, #28997, #29975, #602, #152319, #47130, #31957, #121970, #13805, #78437, #170467, #186655, #109782, #92614, #75471, #140111, #90637, #93612, #79444, #137144, #198832, #14803, #107781, #64281, #63278, #44155, #125948, #76464, #60296, #124958, #48125, #183662, #171465, #15794, #32953, #94608, #156287, #91614, #138141, #17788, #141114, #77454, #45147, #106803, #122959, #168477, #169466, #123940, #153302, #154305, #199821, #184646, #46127, #30967, #139125, #62272, #185638, #130404, #192102, #98058, #129408, #25276, #8076, #69752, #9091, #53584, #161764, #85916, #70759, #131421, #133422, #159758, #84902, #23259, #36404, #191105, #147604, #146582, #193108, #116255, #117256, #21253, #144586, #55582, #54582, #176954, #177946, #101073, #68746, #52579, #39413, #162758, #71753, #24267, #132427, #114239, #194119, #195111, #178949, #82908, #38423, #6072, #40419, #102090, #175945, #67750, #163775, #56594, #145587, #86918, #148601, #10093, #37415, #174942, #99075, #160765, #22255, #115261, #83904, #7065, #100079, #168722, #183911, #198086, #134439, #45396 ),
 ( #90879, #89906, #182924, #167747, #199076, #104086, #150604, #75718, #29245, #151589, #44407, #180947, #197106, #60545, #43411, #59553, #164772, #26267, #76716, #42423, #165768, #87909, #107049, #41425, #119264, #30223, #138392, #135436, #27263, #122220, #179958, #121231, #91866, #152562, #103091, #88912, #149595, #106061, #57595, #12100, #14051, #153558, #11093, #73763, #196124, #58573, #72769, #137395, #120238, #136408, #181929, #15056, #200073, #13080, #105081, #118268, #166767, #28268, #74745, #16054, #48388, #46383, #140378, #171725, #34203, #188895, #112036, #141376, #35193, #95866, #19042, #157549, #2863, #123210, #80689, #184900, #20019, #78700, #142365, #126207, #172721, #108042, #47393, #18053, #169727, #64541, #49372, #139378, #31221, #3845, #187903, #65524, #127184, #110045, #92871, #50376, #154558, #111034, #96846, #77712, #860, #32217, #125220, #81662, #173724, #61541, #143345, #93874, #62534, #158531, #124209, #185907, #109047, #33213, #170725, #155552, #17046, #1865, #63546, #186917, #94872, #156553, #79707, #67513, #83669, #85675, #130162, #84664, #51356, #113017, #163533, #129170, #52344, #174709, #132187, #128183, #5837, #55343, #25033, #22017, #190868, #147362, #66520, #146343, #8851, #39178, #189881, #114000, #36173, #69516, #115020, #97825, #159514, #193878, #6829, #24021, #161526, #175698, #23018, #162518, #68508, #21010, #98833, #145347, #82666, #70518, #37174, #160528, #117013, #116021, #176713, #131181, #191859, #53341, #178708, #38186, #7830, #144350, #99842, #86676, #192871, #54349, #177710, #40170, #100835, #101849, #4833, #106826, #165536, #72525, #29019, #9855, #28035, #90659, #182693, #133182, #57364, #179719, #12853, #58345, #41190, #56345, #75492, #150374, #167523, #104847, #195889, #166537, #105836, #11870, #118028, #42194, #27033, #164538, #151362, #87675, #119037, #120994, #198854, #102852, #134201, #26030, #149360, #71514, #44178, #73534, #89676, #180719, #136183, #152341, #43179, #194872, #13826, #88678, #137165, #135207, #10856, #196879, #103855, #120013, #181698, #60320, #121995, #183685, #74518, #45171, #168501, #29999, #148360, #197858, #59325, #49144, #14827, #50139, #108814, #64308, #156315, #2632, #76489, #77480, #48152, #199847, #94635, #79474, #169490, #61313, #125976, #17816, #33971, #157315, #140138, #122983, #187674, #153325, #141142, #126951, #138166, #184670, #62297, #155325, #111798, #110802, #91637, #173487, #123967, #46153, #172484, #95628, #107808, #18811, #63307, #80455, #142129, #30990, #185664, #93640, #16813, #78463, #3613, #92639, #65292, #188660, #154329, #15819, #139149, #626, #170493, #47155, #1630, #31983, #124986, #186682, #109810, #171493, #32982, #116786, #8620, #193645, #99612, #145113, #67279, #69282, #112784, #161292, #130948, #192638, #98601, #159279, #66288, #144119, #96612, #22787, #175467, #176478, #34960, #158301, #190639, #52115, #19789, #189650, #85442, #68277, #129928, #54121, #113771, #21785, #146112, #115794, #191627, #55117, #81430, #6598, #83436, #143116, #51124, #7596, #53107, #114785, #37954, #177484, #4596, #127947, #38953, #84434, #36939, #100609, #162292, #128938, #174478, #23792, #147132, #131960, #70292, #35945, #97591, #20776, #82431, #5600, #160295, #41964, #86451, #150136, #119790, #117798, #148136, #166305, #198621, #149138, #104616, #89442, #135957, #24802, #134975, #165306, #26800, #9627, #195659, #28786, #152111, #88441, #90425, #43941, #58121, #194645, #105602, #11637, #151132, #57130, #118806, #73304, #181474, #72289, #167289, #75261, #133967, #196652, #42952, #27801, #10628, #60087, #12623, #180492, #56115, #74288, #179491, #25806, #197627, #13594, #71294, #164313, #40956, #102628, #39944, #59093, #103630, #120759, #87452, #182460, #136932, #178477, #101615, #163304, #132957, #156069, #138908, #76245, #108575, #106589, #388, #31746, #94390, #51621, #174977, #1382, #98096, #17567, #79228 ),
 ( #29762, #124742, #109568, #199607, #91396, #140899, #186438, #66786, #190146, #170252, #153085, #5105, #183448, #47914, #159794, #44932, #14589, #92402, #185424, #144624, #128450, #121755, #6107, #154088, #168265, #113286, #36441, #137923, #21289, #93394, #171250, #32738, #82946, #107570, #15582, #61073, #122745, #155081, #184436, #45916, #62061, #169247, #46915, #63063, #30755, #77240, #123726, #16575, #78222, #139893, #195150, #191144, #68784, #118305, #26305, #84938, #192140, #148640, #129445, #147641, #10130, #102128, #52618, #176990, #99112, #132464, #177981, #160804, #175983, #56631, #69789, #86956, #24304, #115297, #85953, #25314, #131457, #37451, #161799, #22292, #23294, #146619, #83943, #70796, #7102, #38460, #40454, #179997, #145623, #53621, #130441, #100116, #114280, #163812, #193144, #9130, #8111, #55619, #71791, #162795, #54616, #133460, #116291, #41464, #39448, #101109, #194155, #117292, #178987, #103129, #164810, #87945, #149633, #67788, #184934, #183945, #168755, #107083, #152598, #72806, #30258, #134476, #169761, #28304, #45430, #75755, #122255, #196161, #197142, #167783, #119301, #14089, #199112, #88950, #180984, #91901, #137432, #153593, #76751, #59592, #42460, #15091, #57635, #60579, #46419, #104124, #165806, #181967, #74782, #31256, #138426, #11131, #92906, #43450, #27303, #200106, #61574, #150641, #123243, #182960, #108077, #12137, #73801, #58609, #105118, #135474, #120275, #44443, #166804, #89944, #151625, #13118, #136444, #90913, #198125, #121266, #106097, #29282, #1900, #62569, #81695, #77746, #155586, #4870, #113051, #171759, #78735, #35226, #16088, #34237, #96879, #188932, #139412, #63580, #185941, #19075, #64576, #47426, #124246, #143378, #156590, #173758, #111068, #125254, #172757, #112070, #18085, #174743, #157582, #33248, #79740, #140411, #36206, #128218, #154592, #80723, #126241, #186953, #50410, #32250, #142401, #158563, #20052, #141409, #48423, #109082, #110079, #895, #3880, #94906, #95899, #170761, #93908, #2897, #187936, #17081, #49405, #66554, #65559, #127219, #189915, #51390, #84699, #8887, #132222, #54385, #56382, #82701, #7867, #146379, #159550, #52379, #70555, #69553, #116058, #39215, #40207, #21047, #67547, #178743, #131217, #99877, #177746, #24058, #191894, #175734, #100871, #162553, #194907, #85713, #147399, #37212, #193915, #118064, #55378, #144385, #161561, #5871, #192908, #117048, #98868, #129205, #101886, #179754, #68543, #163568, #25068, #86711, #190903, #148396, #9890, #71551, #114036, #115056, #133216, #97860, #160564, #22053, #83704, #145382, #6864, #130199, #53378, #176748, #38222, #23054, #12886, #182727, #135240, #106858, #138199, #196912, #89711, #197891, #59360, #73567, #123016, #121029, #134236, #58379, #43214, #10888, #152374, #74549, #105870, #103888, #120046, #122028, #166570, #44211, #87707, #149393, #199881, #165568, #136216, #75526, #181733, #28070, #13859, #137201, #167557, #61345, #26064, #151396, #29051, #102885, #195921, #198887, #90691, #60355, #183718, #45204, #164570, #72561, #168532, #30030, #104882, #91668, #153359, #14861, #119069, #76522, #41224, #57397, #180751, #42227, #27067, #88713, #150408, #11903, #169523, #48185, #92673, #156347, #126009, #124000, #154361, #172518, #4627, #155358, #110834, #95659, #142161, #31023, #141173, #171525, #33013, #15855, #1664, #34988, #158330, #94668, #96642, #50171, #64340, #660, #111828, #17847, #157347, #63342, #125019, #79504, #187704, #78498, #173516, #81460, #140171, #2663, #49176, #34003, #16847, #66317, #18842, #143146, #108847, #186715, #77513, #109840, #19819, #139185, #80487, #184701, #3645, #62330, #46186, #107839, #65323, #185698, #126983, #188690, #47187, #170527, #32017, #93675, #52145, #9659, #101646, #86483, #192670, #37986, #160326, #162323, #5633, #54153, #23824, #85474, #191658, #113802, #159311, #36970, #189681, #115827, #68307, #69313, #127978, #51153, #83468 ),
 ( #177516, #67310, #147163, #148168, #38986, #112814, #53137, #35974, #99642, #130979, #128969, #97621, #100642, #174507, #98631, #8651, #70325, #131992, #20806, #84464, #114816, #176508, #82462, #145145, #178510, #163338, #161325, #39976, #193678, #7629, #144148, #55148, #22818, #116819, #6628, #129958, #146142, #24833, #21816, #190669, #175497, #165340, #119823, #27836, #89477, #103662, #153118, #151168, #29795, #195690, #150170, #117829, #135009, #121789, #179522, #59127, #60122, #120794, #149171, #91431, #136966, #88473, #71326, #58155, #152145, #132988, #74323, #11670, #196686, #57161, #194679, #44967, #56148, #135990, #181508, #26833, #105636, #10660, #197661, #167325, #28821, #42986, #118840, #102659, #180523, #40991, #182494, #73336, #12656, #164344, #25839, #104652, #166338, #87483, #72323, #183483, #43974, #90461, #13628, #75295, #198655, #106625, #168299, #133999, #41996, #199641, #124775, #63096, #76279, #169282, #187467, #186473, #32772, #156104, #157104, #137958, #184470, #95419, #1417, #16608, #171285, #110589, #17602, #61107, #172270, #122780, #173274, #31779, #48936, #79261, #125767, #45949, #422, #94424, #107604, #140933, #2419, #92436, #30788, #33760, #64100, #18600, #80248, #47950, #154122, #141918, #15616, #3409, #49925, #77273, #138942, #185458, #78255, #34748, #65084, #14622, #96407, #46948, #62096, #126743, #188445, #123759, #111589, #109601, #108608, #170285, #93428, #155114, #139928, #127742, #69073, #129723, #22579, #20568, #36726, #38748, #83232, #37740, #4392, #66076, #116582, #82220, #5392, #189444, #85229, #81229, #159074, #8409, #178271, #175260, #143909, #100406, #19586, #99401, #162087, #192432, #142910, #67075, #50921, #84226, #68069, #112579, #174273, #146920, #160086, #177277, #114571, #128735, #176268, #115589, #21573, #35742, #51907, #98388, #97388, #161084, #190431, #113566, #130740, #70083, #144907, #6390, #191420, #52896, #145905, #53914, #7390, #23581, #131751, #193434, #54909, #39734, #158094, #105396, #180283, #135753, #118594, #55907, #88232, #86240, #41752, #11423, #74083, #28584, #151904, #181271, #75057, #197424, #58890, #183243, #119588, #59882, #25601, #103417, #147930, #165096, #13393, #9416, #89233, #90220, #150927, #179281, #121548, #167082, #26589, #101395, #149917, #182250, #163089, #104410, #73093, #134764, #87245, #24592, #136723, #71082, #166093, #196447, #133749, #120556, #40746, #27595, #43734, #198405, #57916, #148928, #132748, #10417, #194436, #12420, #42748, #117581, #102415, #164102, #56918, #72075, #195443, #199401, #95186, #78020, #139689, #79017, #123523, #31537, #155864, #140693, #1175, #3181, #29560, #154875, #93190, #106380, #60865, #17362, #16372, #62852, #186230, #187231, #168062, #14376, #125534, #124534, #46708, #47710, #171042, #138704, #122540, #109360, #32533, #141690, #94185, #2183, #184231, #63863, #64854, #48702, #91191, #108370, #152881, #110354, #172036, #45712, #76042, #33524, #126516, #15376, #156872, #18369, #80021, #137717, #44724, #107364, #169036, #30543, #61854, #92194, #153878, #77032, #185, #185217, #170047, #4159, #53671, #159844, #99161, #66835, #5153, #21337, #129493, #81978, #115349, #84986, #143672, #36489, #144671, #6156, #20329, #177039, #82995, #160851, #128499, #190194, #67836, #191190, #51670, #38509, #146667, #113333, #98145, #52666, #114328, #175026, #69838, #176031, #8162, #112347, #37499, #34519, #22340, #100165, #96178, #83991, #161847, #145670, #65838, #188214, #23341, #7152, #49686, #68835, #130494, #111351, #192190, #173041, #157867, #174038, #19357, #81006, #142680, #127508, #189212, #50690, #35508, #97158, #158841, #30055, #168558, #195200, #55667, #162844, #40505, #193192, #122053, #71839, #72856, #131505, #54665, #87004, #148691, #116339, #86002, #184729, #164859, #26355, #91697, #10179, #118354, #45231, #153390, #87995, #92700, #178028, #41516, #180047, #39496, #147691, #106885 ),
 ( #134526, #196213, #31051, #183745, #14889, #9178, #76550, #154388, #60381, #101156, #56680, #24351, #103179, #138226, #70845, #132513, #199908, #15883, #102176, #61372, #123043, #46213, #194202, #149683, #11181, #107867, #117341, #133508, #169555, #179037, #163864, #25363, #143177, #157378, #93702, #188720, #111859, #34032, #36004, #62359, #187733, #126037, #139213, #32045, #50204, #49204, #95690, #18871, #19849, #688, #47217, #158361, #64368, #79532, #80517, #3674, #171552, #155385, #142190, #65352, #174537, #127013, #173549, #16874, #35018, #97651, #96673, #124029, #141202, #185728, #110862, #81490, #78525, #108875, #4657, #159340, #48213, #66348, #128010, #189712, #170555, #51185, #172547, #112846, #140199, #94696, #77541, #1693, #63369, #125046, #186742, #109867, #33041, #156374, #17878, #2691, #99671, #38015, #192698, #162350, #114845, #86509, #117857, #176539, #69340, #177544, #39013, #53167, #102685, #100668, #179549, #145174, #161355, #67340, #84493, #71352, #129001, #8679, #9687, #70351, #98662, #41019, #148194, #22846, #20837, #7656, #101674, #82494, #23851, #146171, #131006, #6658, #144177, #194706, #5663, #85500, #54181, #115854, #55176, #160356, #147189, #116845, #178535, #132018, #68336, #52174, #129986, #190699, #193706, #40002, #163364, #113831, #175526, #24860, #133016, #37001, #21846, #56175, #83497, #191686, #198681, #43012, #151193, #42023, #90489, #60148, #121816, #27863, #88503, #195717, #73364, #25865, #152171, #104679, #105665, #164371, #87509, #119848, #181533, #149197, #118866, #14649, #197687, #59152, #183512, #166366, #12682, #75321, #44995, #120822, #122808, #10687, #74348, #136014, #72351, #180550, #136992, #182522, #44003, #167351, #106654, #134025, #57190, #168327, #28849, #89504, #13654, #29823, #58181, #103688, #91459, #153147, #61136, #76309, #137987, #165367, #199670, #184498, #45978, #26861, #150199, #11697, #135036, #196712, #123789, #15645, #125796, #111620, #93459, #2449, #187498, #172300, #92465, #94454, #186503, #47979, #154153, #78285, #3437, #126771, #109632, #65113, #18629, #17633, #451, #80276, #171315, #48964, #139958, #1448, #32802, #79293, #155145, #141947, #49956, #16638, #156134, #140962, #64131, #63126, #173305, #110618, #107632, #170315, #124805, #77304, #33789, #188475, #138973, #95449, #169310, #157134, #185488, #30816, #62126, #46978, #108637, #31808, #168955, #108285, #91112, #105315, #13312, #12338, #169963, #61773, #46625, #152802, #198322, #120475, #122458, #11341, #74002, #44645, #196367, #14294, #75961, #166012, #57835, #184151, #137635, #30461, #153797, #136640, #119508, #60787, #149837, #199322, #123441, #73012, #181189, #58807, #151823, #88152, #45632, #134681, #42666, #182167, #104328, #107284, #92109, #27512, #15292, #59799, #76952, #138622, #103, #89153, #150842, #135672, #185134, #121469, #197344, #43652, #167002, #28504, #74978, #167983, #90138, #183161, #106297, #29481, #78936, #139608, #158758, #154793, #32453, #81895, #190111, #48624, #155785, #112265, #93108, #111269, #173957, #65757, #16291, #140612, #62770, #96097, #141611, #124451, #1094, #20247, #33445, #50606, #188135, #2102, #49606, #189134, #95104, #186147, #125455, #110276, #47626, #34438, #170959, #63783, #4079, #143588, #109280, #17282, #94106, #187151, #77941, #127426, #156793, #172960, #171957, #19276, #35424, #126437, #18286, #97077, #79941, #5071, #3098, #64775, #157786, #80923, #142599, #66754, #128415, #51586, #113251, #31455, #169020, #88215, #90204, #44708, #165078, #43718, #149899, #151887, #121532, #119571, #11406, #168046, #137700, #103400, #138688, #197408, #152865, #106362, #150910, #153862, #76025, #91176, #199385, #26572, #136707, #167066, #28567, #73075, #58874, #30525, #15360, #13377, #92177, #45696, #59865, #196429, #107347, #75041, #14360, #120540, #182233, #198388, #183227, #74066, #77016, #169, #135737, #29543, #60849, #122524, #12404 ) ),
 .UNSPECIFIED., .T., .F., .F. ) 
 B_SPLINE_SURFACE_WITH_KNOTS ( ( 4, 3, 4 ),
 ( 3, 2, 2, 2, 2, 2, 2, 2, 2, 2, 2, 2, 2, 2, 2, 2, 2, 2, 2, 2, 2, 2, 2, 2, 2, 2, 2, 2, 2, 2, 2, 2, 2, 2, 2, 2, 2, 2, 2, 2, 2, 2, 2, 2, 2, 2, 2, 2, 2, 2, 2, 2, 2, 2, 2, 2, 2, 2, 2, 2, 2, 2, 2, 2, 2, 2, 2, 2, 2, 2, 2, 2, 2, 2, 2, 2, 2, 2, 2, 2, 2, 2, 2, 2, 2, 2, 2, 2, 2, 2, 2, 2, 2, 2, 2, 2, 2, 2, 2, 2, 2, 2, 2, 2, 2, 2, 2, 2, 2, 2, 2, 2, 2, 2, 2, 2, 2, 2, 2, 2, 2, 2, 2, 2, 2, 2, 2, 2, 2, 2, 2, 2, 2, 2, 2, 2, 2, 2, 2, 2, 2, 2, 2, 2, 2, 2, 2, 2, 2, 2, 2, 2, 2, 2, 2, 2, 2, 2, 2, 2, 2, 2, 2, 2, 2, 2, 2, 2, 2, 2, 2, 2, 2, 2, 2, 2, 2, 2, 2, 2, 2, 2, 2, 2, 2, 2, 2, 2, 2, 2, 2, 2, 2, 2, 2, 2, 2, 2, 2, 2, 2, 2, 2, 2, 2, 2, 2, 2, 2, 2, 2, 2, 2, 2, 2, 2, 2, 2, 2, 2, 2, 2, 2, 2, 2, 2, 2, 2, 3 ),
 ( 0.000000000000000000, 0.5000000000000000000, 1.000000000000000000 ),
 ( 0.000000000000000000, 0.004385964912280701511, 0.008771929824561403022, 0.01315789473684210453, 0.01754385964912280604, 0.02192982456140350755, 0.02631578947368420907, 0.03070175438596491058, 0.03508771929824561209, 0.03947368421052631360, 0.04385964912280701511, 0.04824561403508771662, 0.05263157894736841813, 0.05701754385964911964, 0.06140350877192982115, 0.06578947368421052266, 0.07017543859649122417, 0.07456140350877192569, 0.07894736842105262720, 0.08333333333333332871, 0.08771929824561403022, 0.09210526315789473173, 0.09649122807017543324, 0.1008771929824561348, 0.1052631578947368363, 0.1096491228070175378, 0.1140350877192982393, 0.1184210526315789408, 0.1228070175438596423, 0.1271929824561403577, 0.1315789473684210453, 0.1359649122807017607, 0.1403508771929824483, 0.1447368421052631637, 0.1491228070175438514, 0.1535087719298245668, 0.1578947368421052544, 0.1622807017543859698, 0.1666666666666666574, 0.1710526315789473728, 0.1754385964912280604, 0.1798245614035087758, 0.1842105263157894635, 0.1885964912280701788, 0.1929824561403508665, 0.1973684210526315819, 0.2017543859649122695, 0.2061403508771929849, 0.2105263157894736725, 0.2149122807017543879, 0.2192982456140350755, 0.2236842105263157909, 0.2280701754385964786, 0.2324561403508771940, 0.2368421052631578816, 0.2412280701754385970, 0.2456140350877192846, 0.2500000000000000000, 0.2543859649122807154, 0.2587719298245614308, 0.2631578947368420907, 0.2675438596491228060, 0.2719298245614035214, 0.2763157894736842368, 0.2807017543859648967, 0.2850877192982456121, 0.2894736842105263275, 0.2938596491228070429, 0.2982456140350877027, 0.3026315789473684181, 0.3070175438596491335, 0.3114035087719298489, 0.3157894736842105088, 0.3201754385964912242, 0.3245614035087719396, 0.3289473684210526550, 0.3333333333333333148, 0.3377192982456140302, 0.3421052631578947456, 0.3464912280701754610, 0.3508771929824561209, 0.3552631578947368363, 0.3596491228070175517, 0.3640350877192982670, 0.3684210526315789269, 0.3728070175438596423, 0.3771929824561403577, 0.3815789473684210731, 0.3859649122807017330, 0.3903508771929824483, 0.3947368421052631637, 0.3991228070175438791, 0.4035087719298245390, 0.4078947368421052544, 0.4122807017543859698, 0.4166666666666666852, 0.4210526315789473450, 0.4254385964912280604, 0.4298245614035087758, 0.4342105263157894912, 0.4385964912280701511, 0.4429824561403508665, 0.4473684210526315819, 0.4517543859649122973, 0.4561403508771929571, 0.4605263157894736725, 0.4649122807017543879, 0.4692982456140351033, 0.4736842105263157632, 0.4780701754385964786, 0.4824561403508771940, 0.4868421052631579093, 0.4912280701754385692, 0.4956140350877192846, 0.5000000000000000000, 0.5043859649122807154, 0.5087719298245614308, 0.5131578947368421462, 0.5175438596491228616, 0.5219298245614034659, 0.5263157894736841813, 0.5307017543859648967, 0.5350877192982456121, 0.5394736842105263275, 0.5438596491228070429, 0.5482456140350877583, 0.5526315789473684736, 0.5570175438596490780, 0.5614035087719297934, 0.5657894736842105088, 0.5701754385964912242, 0.5745614035087719396, 0.5789473684210526550, 0.5833333333333333703, 0.5877192982456140857, 0.5921052631578946901, 0.5964912280701754055, 0.6008771929824561209, 0.6052631578947368363, 0.6096491228070175517, 0.6140350877192982670, 0.6184210526315789824, 0.6228070175438596978, 0.6271929824561403022, 0.6315789473684210176, 0.6359649122807017330, 0.6403508771929824483, 0.6447368421052631637, 0.6491228070175438791, 0.6535087719298245945, 0.6578947368421053099, 0.6622807017543859143, 0.6666666666666666297, 0.6710526315789473450, 0.6754385964912280604, 0.6798245614035087758, 0.6842105263157894912, 0.6885964912280702066, 0.6929824561403509220, 0.6973684210526315264, 0.7017543859649122417, 0.7061403508771929571, 0.7105263157894736725, 0.7149122807017543879, 0.7192982456140351033, 0.7236842105263158187, 0.7280701754385965341, 0.7324561403508771384, 0.7368421052631578538, 0.7412280701754385692, 0.7456140350877192846, 0.7500000000000000000, 0.7543859649122807154, 0.7587719298245614308, 0.7631578947368421462, 0.7675438596491228616, 0.7719298245614034659, 0.7763157894736841813, 0.7807017543859648967, 0.7850877192982456121, 0.7894736842105263275, 0.7938596491228070429, 0.7982456140350877583, 0.8026315789473684736, 0.8070175438596490780, 0.8114035087719297934, 0.8157894736842105088, 0.8201754385964912242, 0.8245614035087719396, 0.8289473684210526550, 0.8333333333333333703, 0.8377192982456140857, 0.8421052631578946901, 0.8464912280701754055, 0.8508771929824561209, 0.8552631578947368363, 0.8596491228070175517, 0.8640350877192982670, 0.8684210526315789824, 0.8728070175438596978, 0.8771929824561403022, 0.8815789473684210176, 0.8859649122807017330, 0.8903508771929824483, 0.8947368421052631637, 0.8991228070175438791, 0.9035087719298245945, 0.9078947368421053099, 0.9122807017543859143, 0.9166666666666666297, 0.9210526315789473450, 0.9254385964912280604, 0.9298245614035087758, 0.9342105263157894912, 0.9385964912280702066, 0.9429824561403509220, 0.9473684210526315264, 0.9517543859649122417, 0.9561403508771929571, 0.9605263157894736725, 0.9649122807017543879, 0.9692982456140351033, 0.9736842105263158187, 0.9780701754385965341, 0.9824561403508771384, 0.9868421052631578538, 0.9912280701754385692, 0.9956140350877192846, 1.000000000000000000 ),
 .UNSPECIFIED. ) 
 GEOMETRIC_REPRESENTATION_ITEM ( )  RATIONAL_B_SPLINE_SURFACE ( (
 ( 1.000000000000000000, 0.9659258262890683122, 1.000000000000000000, 0.9659258262890683122, 1.000000000000000000, 0.9659258262890683122, 1.000000000000000000, 0.9659258262890683122, 1.000000000000000000, 0.9659258262890683122, 1.000000000000000000, 0.9659258262890683122, 1.000000000000000000, 0.9659258262890683122, 1.000000000000000000, 0.9659258262890683122, 1.000000000000000000, 0.9659258262890683122, 1.000000000000000000, 0.9659258262890683122, 1.000000000000000000, 0.9659258262890683122, 1.000000000000000000, 0.9659258262890683122, 1.000000000000000000, 0.9659258262890683122, 1.000000000000000000, 0.9659258262890683122, 1.000000000000000000, 0.9659258262890683122, 1.000000000000000000, 0.9659258262890683122, 1.000000000000000000, 0.9659258262890683122, 1.000000000000000000, 0.9659258262890683122, 1.000000000000000000, 0.9659258262890683122, 1.000000000000000000, 0.9659258262890683122, 1.000000000000000000, 0.9659258262890683122, 1.000000000000000000, 0.9659258262890683122, 1.000000000000000000, 0.9659258262890683122, 1.000000000000000000, 0.9659258262890683122, 1.000000000000000000, 0.9659258262890683122, 1.000000000000000000, 0.9659258262890683122, 1.000000000000000000, 0.9659258262890683122, 1.000000000000000000, 0.9659258262890683122, 1.000000000000000000, 0.9659258262890683122, 1.000000000000000000, 0.9659258262890683122, 1.000000000000000000, 0.9659258262890683122, 1.000000000000000000, 0.9659258262890683122, 1.000000000000000000, 0.9659258262890683122, 1.000000000000000000, 0.9659258262890683122, 1.000000000000000000, 0.9659258262890683122, 1.000000000000000000, 0.9659258262890683122, 1.000000000000000000, 0.9659258262890683122, 1.000000000000000000, 0.9659258262890683122, 1.000000000000000000, 0.9659258262890683122, 1.000000000000000000, 0.9659258262890683122, 1.000000000000000000, 0.9659258262890683122, 1.000000000000000000, 0.9659258262890683122, 1.000000000000000000, 0.9659258262890683122, 1.000000000000000000, 0.9659258262890683122, 1.000000000000000000, 0.9659258262890683122, 1.000000000000000000, 0.9659258262890683122, 1.000000000000000000, 0.9659258262890683122, 1.000000000000000000, 0.9659258262890683122, 1.000000000000000000, 0.9659258262890683122, 1.000000000000000000, 0.9659258262890683122, 1.000000000000000000, 0.9659258262890683122, 1.000000000000000000, 0.9659258262890683122, 1.000000000000000000, 0.9659258262890683122, 1.000000000000000000, 0.9659258262890683122, 1.000000000000000000, 0.9659258262890683122, 1.000000000000000000, 0.9659258262890683122, 1.000000000000000000, 0.9659258262890683122, 1.000000000000000000, 0.9659258262890683122, 1.000000000000000000, 0.9659258262890683122, 1.000000000000000000, 0.9659258262890683122, 1.000000000000000000, 0.9659258262890683122, 1.000000000000000000, 0.9659258262890683122, 1.000000000000000000, 0.9659258262890683122, 1.000000000000000000, 0.9659258262890683122, 1.000000000000000000, 0.9659258262890683122, 1.000000000000000000, 0.9659258262890683122, 1.000000000000000000, 0.9659258262890683122, 1.000000000000000000, 0.9659258262890683122, 1.000000000000000000, 0.9659258262890683122, 1.000000000000000000, 0.9659258262890683122, 1.000000000000000000, 0.9659258262890683122, 1.000000000000000000, 0.9659258262890683122, 1.000000000000000000, 0.9659258262890683122, 1.000000000000000000, 0.9659258262890683122, 1.000000000000000000, 0.9659258262890683122, 1.000000000000000000, 0.9659258262890683122, 1.000000000000000000, 0.9659258262890683122, 1.000000000000000000, 0.9659258262890683122, 1.000000000000000000, 0.9659258262890683122, 1.000000000000000000, 0.9659258262890683122, 1.000000000000000000, 0.9659258262890683122, 1.000000000000000000, 0.9659258262890683122, 1.000000000000000000, 0.9659258262890683122, 1.000000000000000000, 0.9659258262890683122, 1.000000000000000000, 0.9659258262890683122, 1.000000000000000000, 0.9659258262890683122, 1.000000000000000000, 0.9659258262890683122, 1.000000000000000000, 0.9659258262890683122, 1.000000000000000000, 0.9659258262890683122, 1.000000000000000000, 0.9659258262890683122, 1.000000000000000000, 0.9659258262890683122, 1.000000000000000000, 0.9659258262890683122, 1.000000000000000000, 0.9659258262890683122, 1.000000000000000000, 0.9659258262890683122, 1.000000000000000000, 0.9659258262890683122, 1.000000000000000000, 0.9659258262890683122, 1.000000000000000000, 0.9659258262890683122, 1.000000000000000000, 0.9659258262890683122, 1.000000000000000000, 0.9659258262890683122, 1.000000000000000000, 0.9659258262890683122, 1.000000000000000000, 0.9659258262890683122, 1.000000000000000000, 0.9659258262890683122, 1.000000000000000000, 0.9659258262890683122, 1.000000000000000000, 0.9659258262890683122, 1.000000000000000000, 0.9659258262890683122, 1.000000000000000000, 0.9659258262890683122, 1.000000000000000000, 0.9659258262890683122, 1.000000000000000000, 0.9659258262890683122, 1.000000000000000000, 0.9659258262890683122, 1.000000000000000000, 0.9659258262890683122, 1.000000000000000000, 0.9659258262890683122, 1.000000000000000000, 0.9659258262890683122, 1.000000000000000000, 0.9659258262890683122, 1.000000000000000000, 0.9659258262890683122, 1.000000000000000000, 0.9659258262890683122, 1.000000000000000000, 0.9659258262890683122, 1.000000000000000000, 0.9659258262890683122, 1.000000000000000000, 0.9659258262890683122, 1.000000000000000000, 0.9659258262890683122, 1.000000000000000000, 0.9659258262890683122, 1.000000000000000000, 0.9659258262890683122, 1.000000000000000000, 0.9659258262890683122, 1.000000000000000000, 0.9659258262890683122, 1.000000000000000000, 0.9659258262890683122, 1.000000000000000000, 0.9659258262890683122, 1.000000000000000000, 0.9659258262890683122, 1.000000000000000000, 0.9659258262890683122, 1.000000000000000000, 0.9659258262890683122, 1.000000000000000000, 0.9659258262890683122, 1.000000000000000000, 0.9659258262890683122, 1.000000000000000000, 0.9659258262890683122, 1.000000000000000000, 0.9659258262890683122, 1.000000000000000000, 0.9659258262890683122, 1.000000000000000000, 0.9659258262890683122, 1.000000000000000000, 0.9659258262890683122, 1.000000000000000000, 0.9659258262890683122, 1.000000000000000000, 0.9659258262890683122, 1.000000000000000000, 0.9659258262890683122, 1.000000000000000000, 0.9659258262890683122, 1.000000000000000000, 0.9659258262890683122, 1.000000000000000000, 0.9659258262890683122, 1.000000000000000000, 0.9659258262890683122, 1.000000000000000000, 0.9659258262890683122, 1.000000000000000000, 0.9659258262890683122, 1.000000000000000000, 0.9659258262890683122, 1.000000000000000000, 0.9659258262890683122, 1.000000000000000000, 0.9659258262890683122, 1.000000000000000000, 0.9659258262890683122, 1.000000000000000000, 0.9659258262890683122, 1.000000000000000000, 0.9659258262890683122, 1.000000000000000000, 0.9659258262890683122, 1.000000000000000000, 0.9659258262890683122, 1.000000000000000000, 0.9659258262890683122, 1.000000000000000000, 0.9659258262890683122, 1.000000000000000000, 0.9659258262890683122, 1.000000000000000000, 0.9659258262890683122, 1.000000000000000000, 0.9659258262890683122, 1.000000000000000000, 0.9659258262890683122, 1.000000000000000000, 0.9659258262890683122, 1.000000000000000000, 0.9659258262890683122, 1.000000000000000000, 0.9659258262890683122, 1.000000000000000000, 0.9659258262890683122, 1.000000000000000000, 0.9659258262890683122, 1.000000000000000000, 0.9659258262890683122, 1.000000000000000000, 0.9659258262890683122, 1.000000000000000000, 0.9659258262890683122, 1.000000000000000000, 0.9659258262890683122, 1.000000000000000000, 0.9659258262890683122, 1.000000000000000000, 0.9659258262890683122, 1.000000000000000000, 0.9659258262890683122, 1.000000000000000000, 0.9659258262890683122, 1.000000000000000000, 0.9659258262890683122, 1.000000000000000000, 0.9659258262890683122, 1.000000000000000000, 0.9659258262890683122, 1.000000000000000000, 0.9659258262890683122, 1.000000000000000000, 0.9659258262890683122, 1.000000000000000000, 0.9659258262890683122, 1.000000000000000000, 0.9659258262890683122, 1.000000000000000000, 0.9659258262890683122, 1.000000000000000000, 0.9659258262890683122, 1.000000000000000000, 0.9659258262890683122, 1.000000000000000000, 0.9659258262890683122, 1.000000000000000000, 0.9659258262890683122, 1.000000000000000000, 0.9659258262890683122, 1.000000000000000000, 0.9659258262890683122, 1.000000000000000000, 0.9659258262890683122, 1.000000000000000000, 0.9659258262890683122, 1.000000000000000000, 0.9659258262890683122, 1.000000000000000000, 0.9659258262890683122, 1.000000000000000000, 0.9659258262890683122, 1.000000000000000000, 0.9659258262890683122, 1.000000000000000000, 0.9659258262890683122, 1.000000000000000000, 0.9659258262890683122, 1.000000000000000000, 0.9659258262890683122, 1.000000000000000000, 0.9659258262890683122, 1.000000000000000000, 0.9659258262890683122, 1.000000000000000000, 0.9659258262890683122, 1.000000000000000000, 0.9659258262890683122, 1.000000000000000000, 0.9659258262890683122, 1.000000000000000000, 0.9659258262890683122, 1.000000000000000000, 0.9659258262890683122, 1.000000000000000000, 0.9659258262890683122, 1.000000000000000000, 0.9659258262890683122, 1.000000000000000000, 0.9659258262890683122, 1.000000000000000000, 0.9659258262890683122, 1.000000000000000000, 0.9659258262890683122, 1.000000000000000000, 0.9659258262890683122, 1.000000000000000000, 0.9659258262890683122, 1.000000000000000000, 0.9659258262890683122, 1.000000000000000000, 0.9659258262890683122, 1.000000000000000000, 0.9659258262890683122, 1.000000000000000000, 0.9659258262890683122, 1.000000000000000000, 0.9659258262890683122, 1.000000000000000000, 0.9659258262890683122, 1.000000000000000000, 0.9659258262890683122, 1.000000000000000000, 0.9659258262890683122, 1.000000000000000000, 0.9659258262890683122, 1.000000000000000000, 0.9659258262890683122, 1.000000000000000000, 0.9659258262890683122, 1.000000000000000000, 0.9659258262890683122, 1.000000000000000000, 0.9659258262890683122, 1.000000000000000000, 0.9659258262890683122, 1.000000000000000000, 0.9659258262890683122, 1.000000000000000000, 0.9659258262890683122, 1.000000000000000000, 0.9659258262890683122, 1.000000000000000000, 0.9659258262890683122, 1.000000000000000000, 0.9659258262890683122, 1.000000000000000000, 0.9659258262890683122, 1.000000000000000000),
 ( 0.3333333333333333703, 0.3219752754296894559, 0.3333333333333333703, 0.3219752754296894559, 0.3333333333333333703, 0.3219752754296894559, 0.3333333333333333703, 0.3219752754296894559, 0.3333333333333333703, 0.3219752754296894559, 0.3333333333333333703, 0.3219752754296894559, 0.3333333333333333703, 0.3219752754296894559, 0.3333333333333333703, 0.3219752754296894559, 0.3333333333333333703, 0.3219752754296894559, 0.3333333333333333703, 0.3219752754296894559, 0.3333333333333333703, 0.3219752754296894559, 0.3333333333333333703, 0.3219752754296894559, 0.3333333333333333703, 0.3219752754296894559, 0.3333333333333333703, 0.3219752754296894559, 0.3333333333333333703, 0.3219752754296894559, 0.3333333333333333703, 0.3219752754296894559, 0.3333333333333333703, 0.3219752754296894559, 0.3333333333333333703, 0.3219752754296894559, 0.3333333333333333703, 0.3219752754296894559, 0.3333333333333333703, 0.3219752754296894559, 0.3333333333333333703, 0.3219752754296894559, 0.3333333333333333703, 0.3219752754296894559, 0.3333333333333333703, 0.3219752754296894559, 0.3333333333333333703, 0.3219752754296894559, 0.3333333333333333703, 0.3219752754296894559, 0.3333333333333333703, 0.3219752754296894559, 0.3333333333333333703, 0.3219752754296894559, 0.3333333333333333703, 0.3219752754296894559, 0.3333333333333333703, 0.3219752754296894559, 0.3333333333333333703, 0.3219752754296894559, 0.3333333333333333703, 0.3219752754296894559, 0.3333333333333333703, 0.3219752754296894559, 0.3333333333333333703, 0.3219752754296894559, 0.3333333333333333703, 0.3219752754296894559, 0.3333333333333333703, 0.3219752754296894559, 0.3333333333333333703, 0.3219752754296894559, 0.3333333333333333703, 0.3219752754296894559, 0.3333333333333333703, 0.3219752754296894559, 0.3333333333333333703, 0.3219752754296894559, 0.3333333333333333703, 0.3219752754296894559, 0.3333333333333333703, 0.3219752754296894559, 0.3333333333333333703, 0.3219752754296894559, 0.3333333333333333703, 0.3219752754296894559, 0.3333333333333333703, 0.3219752754296894559, 0.3333333333333333703, 0.3219752754296894559, 0.3333333333333333703, 0.3219752754296894559, 0.3333333333333333703, 0.3219752754296894559, 0.3333333333333333703, 0.3219752754296894559, 0.3333333333333333703, 0.3219752754296894559, 0.3333333333333333703, 0.3219752754296894559, 0.3333333333333333703, 0.3219752754296894559, 0.3333333333333333703, 0.3219752754296894559, 0.3333333333333333703, 0.3219752754296894559, 0.3333333333333333703, 0.3219752754296894559, 0.3333333333333333703, 0.3219752754296894559, 0.3333333333333333703, 0.3219752754296894559, 0.3333333333333333703, 0.3219752754296894559, 0.3333333333333333703, 0.3219752754296894559, 0.3333333333333333703, 0.3219752754296894559, 0.3333333333333333703, 0.3219752754296894559, 0.3333333333333333703, 0.3219752754296894559, 0.3333333333333333703, 0.3219752754296894559, 0.3333333333333333703, 0.3219752754296894559, 0.3333333333333333703, 0.3219752754296894559, 0.3333333333333333703, 0.3219752754296894559, 0.3333333333333333703, 0.3219752754296894559, 0.3333333333333333703, 0.3219752754296894559, 0.3333333333333333703, 0.3219752754296894559, 0.3333333333333333703, 0.3219752754296894559, 0.3333333333333333703, 0.3219752754296894559, 0.3333333333333333703, 0.3219752754296894559, 0.3333333333333333703, 0.3219752754296894559, 0.3333333333333333703, 0.3219752754296894559, 0.3333333333333333703, 0.3219752754296894559, 0.3333333333333333703, 0.3219752754296894559, 0.3333333333333333703, 0.3219752754296894559, 0.3333333333333333703, 0.3219752754296894559, 0.3333333333333333703, 0.3219752754296894559, 0.3333333333333333703, 0.3219752754296894559, 0.3333333333333333703, 0.3219752754296894559, 0.3333333333333333703, 0.3219752754296894559, 0.3333333333333333703, 0.3219752754296894559, 0.3333333333333333703, 0.3219752754296894559, 0.3333333333333333703, 0.3219752754296894559, 0.3333333333333333703, 0.3219752754296894559, 0.3333333333333333703, 0.3219752754296894559, 0.3333333333333333703, 0.3219752754296894559, 0.3333333333333333703, 0.3219752754296894559, 0.3333333333333333703, 0.3219752754296894559, 0.3333333333333333703, 0.3219752754296894559, 0.3333333333333333703, 0.3219752754296894559, 0.3333333333333333703, 0.3219752754296894559, 0.3333333333333333703, 0.3219752754296894559, 0.3333333333333333703, 0.3219752754296894559, 0.3333333333333333703, 0.3219752754296894559, 0.3333333333333333703, 0.3219752754296894559, 0.3333333333333333703, 0.3219752754296894559, 0.3333333333333333703, 0.3219752754296894559, 0.3333333333333333703, 0.3219752754296894559, 0.3333333333333333703, 0.3219752754296894559, 0.3333333333333333703, 0.3219752754296894559, 0.3333333333333333703, 0.3219752754296894559, 0.3333333333333333703, 0.3219752754296894559, 0.3333333333333333703, 0.3219752754296894559, 0.3333333333333333703, 0.3219752754296894559, 0.3333333333333333703, 0.3219752754296894559, 0.3333333333333333703, 0.3219752754296894559, 0.3333333333333333703, 0.3219752754296894559, 0.3333333333333333703, 0.3219752754296894559, 0.3333333333333333703, 0.3219752754296894559, 0.3333333333333333703, 0.3219752754296894559, 0.3333333333333333703, 0.3219752754296894559, 0.3333333333333333703, 0.3219752754296894559, 0.3333333333333333703, 0.3219752754296894559, 0.3333333333333333703, 0.3219752754296894559, 0.3333333333333333703, 0.3219752754296894559, 0.3333333333333333703, 0.3219752754296894559, 0.3333333333333333703, 0.3219752754296894559, 0.3333333333333333703, 0.3219752754296894559, 0.3333333333333333703, 0.3219752754296894559, 0.3333333333333333703, 0.3219752754296894559, 0.3333333333333333703, 0.3219752754296894559, 0.3333333333333333703, 0.3219752754296894559, 0.3333333333333333703, 0.3219752754296894559, 0.3333333333333333703, 0.3219752754296894559, 0.3333333333333333703, 0.3219752754296894559, 0.3333333333333333703, 0.3219752754296894559, 0.3333333333333333703, 0.3219752754296894559, 0.3333333333333333703, 0.3219752754296894559, 0.3333333333333333703, 0.3219752754296894559, 0.3333333333333333703, 0.3219752754296894559, 0.3333333333333333703, 0.3219752754296894559, 0.3333333333333333703, 0.3219752754296894559, 0.3333333333333333703, 0.3219752754296894559, 0.3333333333333333703, 0.3219752754296894559, 0.3333333333333333703, 0.3219752754296894559, 0.3333333333333333703, 0.3219752754296894559, 0.3333333333333333703, 0.3219752754296894559, 0.3333333333333333703, 0.3219752754296894559, 0.3333333333333333703, 0.3219752754296894559, 0.3333333333333333703, 0.3219752754296894559, 0.3333333333333333703, 0.3219752754296894559, 0.3333333333333333703, 0.3219752754296894559, 0.3333333333333333703, 0.3219752754296894559, 0.3333333333333333703, 0.3219752754296894559, 0.3333333333333333703, 0.3219752754296894559, 0.3333333333333333703, 0.3219752754296894559, 0.3333333333333333703, 0.3219752754296894559, 0.3333333333333333703, 0.3219752754296894559, 0.3333333333333333703, 0.3219752754296894559, 0.3333333333333333703, 0.3219752754296894559, 0.3333333333333333703, 0.3219752754296894559, 0.3333333333333333703, 0.3219752754296894559, 0.3333333333333333703, 0.3219752754296894559, 0.3333333333333333703, 0.3219752754296894559, 0.3333333333333333703, 0.3219752754296894559, 0.3333333333333333703, 0.3219752754296894559, 0.3333333333333333703, 0.3219752754296894559, 0.3333333333333333703, 0.3219752754296894559, 0.3333333333333333703, 0.3219752754296894559, 0.3333333333333333703, 0.3219752754296894559, 0.3333333333333333703, 0.3219752754296894559, 0.3333333333333333703, 0.3219752754296894559, 0.3333333333333333703, 0.3219752754296894559, 0.3333333333333333703, 0.3219752754296894559, 0.3333333333333333703, 0.3219752754296894559, 0.3333333333333333703, 0.3219752754296894559, 0.3333333333333333703, 0.3219752754296894559, 0.3333333333333333703, 0.3219752754296894559, 0.3333333333333333703, 0.3219752754296894559, 0.3333333333333333703, 0.3219752754296894559, 0.3333333333333333703, 0.3219752754296894559, 0.3333333333333333703, 0.3219752754296894559, 0.3333333333333333703, 0.3219752754296894559, 0.3333333333333333703, 0.3219752754296894559, 0.3333333333333333703, 0.3219752754296894559, 0.3333333333333333703, 0.3219752754296894559, 0.3333333333333333703, 0.3219752754296894559, 0.3333333333333333703, 0.3219752754296894559, 0.3333333333333333703, 0.3219752754296894559, 0.3333333333333333703, 0.3219752754296894559, 0.3333333333333333703, 0.3219752754296894559, 0.3333333333333333703, 0.3219752754296894559, 0.3333333333333333703, 0.3219752754296894559, 0.3333333333333333703, 0.3219752754296894559, 0.3333333333333333703, 0.3219752754296894559, 0.3333333333333333703, 0.3219752754296894559, 0.3333333333333333703, 0.3219752754296894559, 0.3333333333333333703, 0.3219752754296894559, 0.3333333333333333703, 0.3219752754296894559, 0.3333333333333333703, 0.3219752754296894559, 0.3333333333333333703, 0.3219752754296894559, 0.3333333333333333703, 0.3219752754296894559, 0.3333333333333333703, 0.3219752754296894559, 0.3333333333333333703, 0.3219752754296894559, 0.3333333333333333703, 0.3219752754296894559, 0.3333333333333333703, 0.3219752754296894559, 0.3333333333333333703, 0.3219752754296894559, 0.3333333333333333703, 0.3219752754296894559, 0.3333333333333333703, 0.3219752754296894559, 0.3333333333333333703, 0.3219752754296894559, 0.3333333333333333703, 0.3219752754296894559, 0.3333333333333333703, 0.3219752754296894559, 0.3333333333333333703, 0.3219752754296894559, 0.3333333333333333703, 0.3219752754296894559, 0.3333333333333333703, 0.3219752754296894559, 0.3333333333333333703, 0.3219752754296894559, 0.3333333333333333703, 0.3219752754296894559, 0.3333333333333333703, 0.3219752754296894559, 0.3333333333333333703, 0.3219752754296894559, 0.3333333333333333703, 0.3219752754296894559, 0.3333333333333333703, 0.3219752754296894559, 0.3333333333333333703, 0.3219752754296894559, 0.3333333333333333703, 0.3219752754296894559, 0.3333333333333333703, 0.3219752754296894559, 0.3333333333333333703, 0.3219752754296894559, 0.3333333333333333703, 0.3219752754296894559, 0.3333333333333333703, 0.3219752754296894559, 0.3333333333333333703, 0.3219752754296894559, 0.3333333333333333703, 0.3219752754296894559, 0.3333333333333333703, 0.3219752754296894559, 0.3333333333333333703, 0.3219752754296894559, 0.3333333333333333703, 0.3219752754296894559, 0.3333333333333333703, 0.3219752754296894559, 0.3333333333333333703, 0.3219752754296894559, 0.3333333333333333703, 0.3219752754296894559, 0.3333333333333333703, 0.3219752754296894559, 0.3333333333333333703, 0.3219752754296894559, 0.3333333333333333703),
 ( 0.3333333333333333703, 0.3219752754296894559, 0.3333333333333333703, 0.3219752754296894559, 0.3333333333333333703, 0.3219752754296894559, 0.3333333333333333703, 0.3219752754296894559, 0.3333333333333333703, 0.3219752754296894559, 0.3333333333333333703, 0.3219752754296894559, 0.3333333333333333703, 0.3219752754296894559, 0.3333333333333333703, 0.3219752754296894559, 0.3333333333333333703, 0.3219752754296894559, 0.3333333333333333703, 0.3219752754296894559, 0.3333333333333333703, 0.3219752754296894559, 0.3333333333333333703, 0.3219752754296894559, 0.3333333333333333703, 0.3219752754296894559, 0.3333333333333333703, 0.3219752754296894559, 0.3333333333333333703, 0.3219752754296894559, 0.3333333333333333703, 0.3219752754296894559, 0.3333333333333333703, 0.3219752754296894559, 0.3333333333333333703, 0.3219752754296894559, 0.3333333333333333703, 0.3219752754296894559, 0.3333333333333333703, 0.3219752754296894559, 0.3333333333333333703, 0.3219752754296894559, 0.3333333333333333703, 0.3219752754296894559, 0.3333333333333333703, 0.3219752754296894559, 0.3333333333333333703, 0.3219752754296894559, 0.3333333333333333703, 0.3219752754296894559, 0.3333333333333333703, 0.3219752754296894559, 0.3333333333333333703, 0.3219752754296894559, 0.3333333333333333703, 0.3219752754296894559, 0.3333333333333333703, 0.3219752754296894559, 0.3333333333333333703, 0.3219752754296894559, 0.3333333333333333703, 0.3219752754296894559, 0.3333333333333333703, 0.3219752754296894559, 0.3333333333333333703, 0.3219752754296894559, 0.3333333333333333703, 0.3219752754296894559, 0.3333333333333333703, 0.3219752754296894559, 0.3333333333333333703, 0.3219752754296894559, 0.3333333333333333703, 0.3219752754296894559, 0.3333333333333333703, 0.3219752754296894559, 0.3333333333333333703, 0.3219752754296894559, 0.3333333333333333703, 0.3219752754296894559, 0.3333333333333333703, 0.3219752754296894559, 0.3333333333333333703, 0.3219752754296894559, 0.3333333333333333703, 0.3219752754296894559, 0.3333333333333333703, 0.3219752754296894559, 0.3333333333333333703, 0.3219752754296894559, 0.3333333333333333703, 0.3219752754296894559, 0.3333333333333333703, 0.3219752754296894559, 0.3333333333333333703, 0.3219752754296894559, 0.3333333333333333703, 0.3219752754296894559, 0.3333333333333333703, 0.3219752754296894559, 0.3333333333333333703, 0.3219752754296894559, 0.3333333333333333703, 0.3219752754296894559, 0.3333333333333333703, 0.3219752754296894559, 0.3333333333333333703, 0.3219752754296894559, 0.3333333333333333703, 0.3219752754296894559, 0.3333333333333333703, 0.3219752754296894559, 0.3333333333333333703, 0.3219752754296894559, 0.3333333333333333703, 0.3219752754296894559, 0.3333333333333333703, 0.3219752754296894559, 0.3333333333333333703, 0.3219752754296894559, 0.3333333333333333703, 0.3219752754296894559, 0.3333333333333333703, 0.3219752754296894559, 0.3333333333333333703, 0.3219752754296894559, 0.3333333333333333703, 0.3219752754296894559, 0.3333333333333333703, 0.3219752754296894559, 0.3333333333333333703, 0.3219752754296894559, 0.3333333333333333703, 0.3219752754296894559, 0.3333333333333333703, 0.3219752754296894559, 0.3333333333333333703, 0.3219752754296894559, 0.3333333333333333703, 0.3219752754296894559, 0.3333333333333333703, 0.3219752754296894559, 0.3333333333333333703, 0.3219752754296894559, 0.3333333333333333703, 0.3219752754296894559, 0.3333333333333333703, 0.3219752754296894559, 0.3333333333333333703, 0.3219752754296894559, 0.3333333333333333703, 0.3219752754296894559, 0.3333333333333333703, 0.3219752754296894559, 0.3333333333333333703, 0.3219752754296894559, 0.3333333333333333703, 0.3219752754296894559, 0.3333333333333333703, 0.3219752754296894559, 0.3333333333333333703, 0.3219752754296894559, 0.3333333333333333703, 0.3219752754296894559, 0.3333333333333333703, 0.3219752754296894559, 0.3333333333333333703, 0.3219752754296894559, 0.3333333333333333703, 0.3219752754296894559, 0.3333333333333333703, 0.3219752754296894559, 0.3333333333333333703, 0.3219752754296894559, 0.3333333333333333703, 0.3219752754296894559, 0.3333333333333333703, 0.3219752754296894559, 0.3333333333333333703, 0.3219752754296894559, 0.3333333333333333703, 0.3219752754296894559, 0.3333333333333333703, 0.3219752754296894559, 0.3333333333333333703, 0.3219752754296894559, 0.3333333333333333703, 0.3219752754296894559, 0.3333333333333333703, 0.3219752754296894559, 0.3333333333333333703, 0.3219752754296894559, 0.3333333333333333703, 0.3219752754296894559, 0.3333333333333333703, 0.3219752754296894559, 0.3333333333333333703, 0.3219752754296894559, 0.3333333333333333703, 0.3219752754296894559, 0.3333333333333333703, 0.3219752754296894559, 0.3333333333333333703, 0.3219752754296894559, 0.3333333333333333703, 0.3219752754296894559, 0.3333333333333333703, 0.3219752754296894559, 0.3333333333333333703, 0.3219752754296894559, 0.3333333333333333703, 0.3219752754296894559, 0.3333333333333333703, 0.3219752754296894559, 0.3333333333333333703, 0.3219752754296894559, 0.3333333333333333703, 0.3219752754296894559, 0.3333333333333333703, 0.3219752754296894559, 0.3333333333333333703, 0.3219752754296894559, 0.3333333333333333703, 0.3219752754296894559, 0.3333333333333333703, 0.3219752754296894559, 0.3333333333333333703, 0.3219752754296894559, 0.3333333333333333703, 0.3219752754296894559, 0.3333333333333333703, 0.3219752754296894559, 0.3333333333333333703, 0.3219752754296894559, 0.3333333333333333703, 0.3219752754296894559, 0.3333333333333333703, 0.3219752754296894559, 0.3333333333333333703, 0.3219752754296894559, 0.3333333333333333703, 0.3219752754296894559, 0.3333333333333333703, 0.3219752754296894559, 0.3333333333333333703, 0.3219752754296894559, 0.3333333333333333703, 0.3219752754296894559, 0.3333333333333333703, 0.3219752754296894559, 0.3333333333333333703, 0.3219752754296894559, 0.3333333333333333703, 0.3219752754296894559, 0.3333333333333333703, 0.3219752754296894559, 0.3333333333333333703, 0.3219752754296894559, 0.3333333333333333703, 0.3219752754296894559, 0.3333333333333333703, 0.3219752754296894559, 0.3333333333333333703, 0.3219752754296894559, 0.3333333333333333703, 0.3219752754296894559, 0.3333333333333333703, 0.3219752754296894559, 0.3333333333333333703, 0.3219752754296894559, 0.3333333333333333703, 0.3219752754296894559, 0.3333333333333333703, 0.3219752754296894559, 0.3333333333333333703, 0.3219752754296894559, 0.3333333333333333703, 0.3219752754296894559, 0.3333333333333333703, 0.3219752754296894559, 0.3333333333333333703, 0.3219752754296894559, 0.3333333333333333703, 0.3219752754296894559, 0.3333333333333333703, 0.3219752754296894559, 0.3333333333333333703, 0.3219752754296894559, 0.3333333333333333703, 0.3219752754296894559, 0.3333333333333333703, 0.3219752754296894559, 0.3333333333333333703, 0.3219752754296894559, 0.3333333333333333703, 0.3219752754296894559, 0.3333333333333333703, 0.3219752754296894559, 0.3333333333333333703, 0.3219752754296894559, 0.3333333333333333703, 0.3219752754296894559, 0.3333333333333333703, 0.3219752754296894559, 0.3333333333333333703, 0.3219752754296894559, 0.3333333333333333703, 0.3219752754296894559, 0.3333333333333333703, 0.3219752754296894559, 0.3333333333333333703, 0.3219752754296894559, 0.3333333333333333703, 0.3219752754296894559, 0.3333333333333333703, 0.3219752754296894559, 0.3333333333333333703, 0.3219752754296894559, 0.3333333333333333703, 0.3219752754296894559, 0.3333333333333333703, 0.3219752754296894559, 0.3333333333333333703, 0.3219752754296894559, 0.3333333333333333703, 0.3219752754296894559, 0.3333333333333333703, 0.3219752754296894559, 0.3333333333333333703, 0.3219752754296894559, 0.3333333333333333703, 0.3219752754296894559, 0.3333333333333333703, 0.3219752754296894559, 0.3333333333333333703, 0.3219752754296894559, 0.3333333333333333703, 0.3219752754296894559, 0.3333333333333333703, 0.3219752754296894559, 0.3333333333333333703, 0.3219752754296894559, 0.3333333333333333703, 0.3219752754296894559, 0.3333333333333333703, 0.3219752754296894559, 0.3333333333333333703, 0.3219752754296894559, 0.3333333333333333703, 0.3219752754296894559, 0.3333333333333333703, 0.3219752754296894559, 0.3333333333333333703, 0.3219752754296894559, 0.3333333333333333703, 0.3219752754296894559, 0.3333333333333333703, 0.3219752754296894559, 0.3333333333333333703, 0.3219752754296894559, 0.3333333333333333703, 0.3219752754296894559, 0.3333333333333333703, 0.3219752754296894559, 0.3333333333333333703, 0.3219752754296894559, 0.3333333333333333703, 0.3219752754296894559, 0.3333333333333333703, 0.3219752754296894559, 0.3333333333333333703, 0.3219752754296894559, 0.3333333333333333703, 0.3219752754296894559, 0.3333333333333333703, 0.3219752754296894559, 0.3333333333333333703, 0.3219752754296894559, 0.3333333333333333703, 0.3219752754296894559, 0.3333333333333333703, 0.3219752754296894559, 0.3333333333333333703, 0.3219752754296894559, 0.3333333333333333703, 0.3219752754296894559, 0.3333333333333333703, 0.3219752754296894559, 0.3333333333333333703, 0.3219752754296894559, 0.3333333333333333703, 0.3219752754296894559, 0.3333333333333333703, 0.3219752754296894559, 0.3333333333333333703, 0.3219752754296894559, 0.3333333333333333703, 0.3219752754296894559, 0.3333333333333333703, 0.3219752754296894559, 0.3333333333333333703, 0.3219752754296894559, 0.3333333333333333703, 0.3219752754296894559, 0.3333333333333333703, 0.3219752754296894559, 0.3333333333333333703, 0.3219752754296894559, 0.3333333333333333703, 0.3219752754296894559, 0.3333333333333333703, 0.3219752754296894559, 0.3333333333333333703, 0.3219752754296894559, 0.3333333333333333703, 0.3219752754296894559, 0.3333333333333333703, 0.3219752754296894559, 0.3333333333333333703, 0.3219752754296894559, 0.3333333333333333703, 0.3219752754296894559, 0.3333333333333333703, 0.3219752754296894559, 0.3333333333333333703, 0.3219752754296894559, 0.3333333333333333703, 0.3219752754296894559, 0.3333333333333333703, 0.3219752754296894559, 0.3333333333333333703, 0.3219752754296894559, 0.3333333333333333703, 0.3219752754296894559, 0.3333333333333333703, 0.3219752754296894559, 0.3333333333333333703, 0.3219752754296894559, 0.3333333333333333703, 0.3219752754296894559, 0.3333333333333333703, 0.3219752754296894559, 0.3333333333333333703, 0.3219752754296894559, 0.3333333333333333703, 0.3219752754296894559, 0.3333333333333333703, 0.3219752754296894559, 0.3333333333333333703, 0.3219752754296894559, 0.3333333333333333703, 0.3219752754296894559, 0.3333333333333333703, 0.3219752754296894559, 0.3333333333333333703, 0.3219752754296894559, 0.3333333333333333703),
 ( 1.000000000000000000, 0.9659258262890683122, 1.000000000000000000, 0.9659258262890683122, 1.000000000000000000, 0.9659258262890683122, 1.000000000000000000, 0.9659258262890683122, 1.000000000000000000, 0.9659258262890683122, 1.000000000000000000, 0.9659258262890683122, 1.000000000000000000, 0.9659258262890683122, 1.000000000000000000, 0.9659258262890683122, 1.000000000000000000, 0.9659258262890683122, 1.000000000000000000, 0.9659258262890683122, 1.000000000000000000, 0.9659258262890683122, 1.000000000000000000, 0.9659258262890683122, 1.000000000000000000, 0.9659258262890683122, 1.000000000000000000, 0.9659258262890683122, 1.000000000000000000, 0.9659258262890683122, 1.000000000000000000, 0.9659258262890683122, 1.000000000000000000, 0.9659258262890683122, 1.000000000000000000, 0.9659258262890683122, 1.000000000000000000, 0.9659258262890683122, 1.000000000000000000, 0.9659258262890683122, 1.000000000000000000, 0.9659258262890683122, 1.000000000000000000, 0.9659258262890683122, 1.000000000000000000, 0.9659258262890683122, 1.000000000000000000, 0.9659258262890683122, 1.000000000000000000, 0.9659258262890683122, 1.000000000000000000, 0.9659258262890683122, 1.000000000000000000, 0.9659258262890683122, 1.000000000000000000, 0.9659258262890683122, 1.000000000000000000, 0.9659258262890683122, 1.000000000000000000, 0.9659258262890683122, 1.000000000000000000, 0.9659258262890683122, 1.000000000000000000, 0.9659258262890683122, 1.000000000000000000, 0.9659258262890683122, 1.000000000000000000, 0.9659258262890683122, 1.000000000000000000, 0.9659258262890683122, 1.000000000000000000, 0.9659258262890683122, 1.000000000000000000, 0.9659258262890683122, 1.000000000000000000, 0.9659258262890683122, 1.000000000000000000, 0.9659258262890683122, 1.000000000000000000, 0.9659258262890683122, 1.000000000000000000, 0.9659258262890683122, 1.000000000000000000, 0.9659258262890683122, 1.000000000000000000, 0.9659258262890683122, 1.000000000000000000, 0.9659258262890683122, 1.000000000000000000, 0.9659258262890683122, 1.000000000000000000, 0.9659258262890683122, 1.000000000000000000, 0.9659258262890683122, 1.000000000000000000, 0.9659258262890683122, 1.000000000000000000, 0.9659258262890683122, 1.000000000000000000, 0.9659258262890683122, 1.000000000000000000, 0.9659258262890683122, 1.000000000000000000, 0.9659258262890683122, 1.000000000000000000, 0.9659258262890683122, 1.000000000000000000, 0.9659258262890683122, 1.000000000000000000, 0.9659258262890683122, 1.000000000000000000, 0.9659258262890683122, 1.000000000000000000, 0.9659258262890683122, 1.000000000000000000, 0.9659258262890683122, 1.000000000000000000, 0.9659258262890683122, 1.000000000000000000, 0.9659258262890683122, 1.000000000000000000, 0.9659258262890683122, 1.000000000000000000, 0.9659258262890683122, 1.000000000000000000, 0.9659258262890683122, 1.000000000000000000, 0.9659258262890683122, 1.000000000000000000, 0.9659258262890683122, 1.000000000000000000, 0.9659258262890683122, 1.000000000000000000, 0.9659258262890683122, 1.000000000000000000, 0.9659258262890683122, 1.000000000000000000, 0.9659258262890683122, 1.000000000000000000, 0.9659258262890683122, 1.000000000000000000, 0.9659258262890683122, 1.000000000000000000, 0.9659258262890683122, 1.000000000000000000, 0.9659258262890683122, 1.000000000000000000, 0.9659258262890683122, 1.000000000000000000, 0.9659258262890683122, 1.000000000000000000, 0.9659258262890683122, 1.000000000000000000, 0.9659258262890683122, 1.000000000000000000, 0.9659258262890683122, 1.000000000000000000, 0.9659258262890683122, 1.000000000000000000, 0.9659258262890683122, 1.000000000000000000, 0.9659258262890683122, 1.000000000000000000, 0.9659258262890683122, 1.000000000000000000, 0.9659258262890683122, 1.000000000000000000, 0.9659258262890683122, 1.000000000000000000, 0.9659258262890683122, 1.000000000000000000, 0.9659258262890683122, 1.000000000000000000, 0.9659258262890683122, 1.000000000000000000, 0.9659258262890683122, 1.000000000000000000, 0.9659258262890683122, 1.000000000000000000, 0.9659258262890683122, 1.000000000000000000, 0.9659258262890683122, 1.000000000000000000, 0.9659258262890683122, 1.000000000000000000, 0.9659258262890683122, 1.000000000000000000, 0.9659258262890683122, 1.000000000000000000, 0.9659258262890683122, 1.000000000000000000, 0.9659258262890683122, 1.000000000000000000, 0.9659258262890683122, 1.000000000000000000, 0.9659258262890683122, 1.000000000000000000, 0.9659258262890683122, 1.000000000000000000, 0.9659258262890683122, 1.000000000000000000, 0.9659258262890683122, 1.000000000000000000, 0.9659258262890683122, 1.000000000000000000, 0.9659258262890683122, 1.000000000000000000, 0.9659258262890683122, 1.000000000000000000, 0.9659258262890683122, 1.000000000000000000, 0.9659258262890683122, 1.000000000000000000, 0.9659258262890683122, 1.000000000000000000, 0.9659258262890683122, 1.000000000000000000, 0.9659258262890683122, 1.000000000000000000, 0.9659258262890683122, 1.000000000000000000, 0.9659258262890683122, 1.000000000000000000, 0.9659258262890683122, 1.000000000000000000, 0.9659258262890683122, 1.000000000000000000, 0.9659258262890683122, 1.000000000000000000, 0.9659258262890683122, 1.000000000000000000, 0.9659258262890683122, 1.000000000000000000, 0.9659258262890683122, 1.000000000000000000, 0.9659258262890683122, 1.000000000000000000, 0.9659258262890683122, 1.000000000000000000, 0.9659258262890683122, 1.000000000000000000, 0.9659258262890683122, 1.000000000000000000, 0.9659258262890683122, 1.000000000000000000, 0.9659258262890683122, 1.000000000000000000, 0.9659258262890683122, 1.000000000000000000, 0.9659258262890683122, 1.000000000000000000, 0.9659258262890683122, 1.000000000000000000, 0.9659258262890683122, 1.000000000000000000, 0.9659258262890683122, 1.000000000000000000, 0.9659258262890683122, 1.000000000000000000, 0.9659258262890683122, 1.000000000000000000, 0.9659258262890683122, 1.000000000000000000, 0.9659258262890683122, 1.000000000000000000, 0.9659258262890683122, 1.000000000000000000, 0.9659258262890683122, 1.000000000000000000, 0.9659258262890683122, 1.000000000000000000, 0.9659258262890683122, 1.000000000000000000, 0.9659258262890683122, 1.000000000000000000, 0.9659258262890683122, 1.000000000000000000, 0.9659258262890683122, 1.000000000000000000, 0.9659258262890683122, 1.000000000000000000, 0.9659258262890683122, 1.000000000000000000, 0.9659258262890683122, 1.000000000000000000, 0.9659258262890683122, 1.000000000000000000, 0.9659258262890683122, 1.000000000000000000, 0.9659258262890683122, 1.000000000000000000, 0.9659258262890683122, 1.000000000000000000, 0.9659258262890683122, 1.000000000000000000, 0.9659258262890683122, 1.000000000000000000, 0.9659258262890683122, 1.000000000000000000, 0.9659258262890683122, 1.000000000000000000, 0.9659258262890683122, 1.000000000000000000, 0.9659258262890683122, 1.000000000000000000, 0.9659258262890683122, 1.000000000000000000, 0.9659258262890683122, 1.000000000000000000, 0.9659258262890683122, 1.000000000000000000, 0.9659258262890683122, 1.000000000000000000, 0.9659258262890683122, 1.000000000000000000, 0.9659258262890683122, 1.000000000000000000, 0.9659258262890683122, 1.000000000000000000, 0.9659258262890683122, 1.000000000000000000, 0.9659258262890683122, 1.000000000000000000, 0.9659258262890683122, 1.000000000000000000, 0.9659258262890683122, 1.000000000000000000, 0.9659258262890683122, 1.000000000000000000, 0.9659258262890683122, 1.000000000000000000, 0.9659258262890683122, 1.000000000000000000, 0.9659258262890683122, 1.000000000000000000, 0.9659258262890683122, 1.000000000000000000, 0.9659258262890683122, 1.000000000000000000, 0.9659258262890683122, 1.000000000000000000, 0.9659258262890683122, 1.000000000000000000, 0.9659258262890683122, 1.000000000000000000, 0.9659258262890683122, 1.000000000000000000, 0.9659258262890683122, 1.000000000000000000, 0.9659258262890683122, 1.000000000000000000, 0.9659258262890683122, 1.000000000000000000, 0.9659258262890683122, 1.000000000000000000, 0.9659258262890683122, 1.000000000000000000, 0.9659258262890683122, 1.000000000000000000, 0.9659258262890683122, 1.000000000000000000, 0.9659258262890683122, 1.000000000000000000, 0.9659258262890683122, 1.000000000000000000, 0.9659258262890683122, 1.000000000000000000, 0.9659258262890683122, 1.000000000000000000, 0.9659258262890683122, 1.000000000000000000, 0.9659258262890683122, 1.000000000000000000, 0.9659258262890683122, 1.000000000000000000, 0.9659258262890683122, 1.000000000000000000, 0.9659258262890683122, 1.000000000000000000, 0.9659258262890683122, 1.000000000000000000, 0.9659258262890683122, 1.000000000000000000, 0.9659258262890683122, 1.000000000000000000, 0.9659258262890683122, 1.000000000000000000, 0.9659258262890683122, 1.000000000000000000, 0.9659258262890683122, 1.000000000000000000, 0.9659258262890683122, 1.000000000000000000, 0.9659258262890683122, 1.000000000000000000, 0.9659258262890683122, 1.000000000000000000, 0.9659258262890683122, 1.000000000000000000, 0.9659258262890683122, 1.000000000000000000, 0.9659258262890683122, 1.000000000000000000, 0.9659258262890683122, 1.000000000000000000, 0.9659258262890683122, 1.000000000000000000, 0.9659258262890683122, 1.000000000000000000, 0.9659258262890683122, 1.000000000000000000, 0.9659258262890683122, 1.000000000000000000, 0.9659258262890683122, 1.000000000000000000, 0.9659258262890683122, 1.000000000000000000, 0.9659258262890683122, 1.000000000000000000, 0.9659258262890683122, 1.000000000000000000, 0.9659258262890683122, 1.000000000000000000, 0.9659258262890683122, 1.000000000000000000, 0.9659258262890683122, 1.000000000000000000, 0.9659258262890683122, 1.000000000000000000, 0.9659258262890683122, 1.000000000000000000, 0.9659258262890683122, 1.000000000000000000, 0.9659258262890683122, 1.000000000000000000, 0.9659258262890683122, 1.000000000000000000, 0.9659258262890683122, 1.000000000000000000, 0.9659258262890683122, 1.000000000000000000, 0.9659258262890683122, 1.000000000000000000, 0.9659258262890683122, 1.000000000000000000, 0.9659258262890683122, 1.000000000000000000, 0.9659258262890683122, 1.000000000000000000, 0.9659258262890683122, 1.000000000000000000, 0.9659258262890683122, 1.000000000000000000, 0.9659258262890683122, 1.000000000000000000, 0.9659258262890683122, 1.000000000000000000),
 ( 0.3333333333333333703, 0.3219752754296894559, 0.3333333333333333703, 0.3219752754296894559, 0.3333333333333333703, 0.3219752754296894559, 0.3333333333333333703, 0.3219752754296894559, 0.3333333333333333703, 0.3219752754296894559, 0.3333333333333333703, 0.3219752754296894559, 0.3333333333333333703, 0.3219752754296894559, 0.3333333333333333703, 0.3219752754296894559, 0.3333333333333333703, 0.3219752754296894559, 0.3333333333333333703, 0.3219752754296894559, 0.3333333333333333703, 0.3219752754296894559, 0.3333333333333333703, 0.3219752754296894559, 0.3333333333333333703, 0.3219752754296894559, 0.3333333333333333703, 0.3219752754296894559, 0.3333333333333333703, 0.3219752754296894559, 0.3333333333333333703, 0.3219752754296894559, 0.3333333333333333703, 0.3219752754296894559, 0.3333333333333333703, 0.3219752754296894559, 0.3333333333333333703, 0.3219752754296894559, 0.3333333333333333703, 0.3219752754296894559, 0.3333333333333333703, 0.3219752754296894559, 0.3333333333333333703, 0.3219752754296894559, 0.3333333333333333703, 0.3219752754296894559, 0.3333333333333333703, 0.3219752754296894559, 0.3333333333333333703, 0.3219752754296894559, 0.3333333333333333703, 0.3219752754296894559, 0.3333333333333333703, 0.3219752754296894559, 0.3333333333333333703, 0.3219752754296894559, 0.3333333333333333703, 0.3219752754296894559, 0.3333333333333333703, 0.3219752754296894559, 0.3333333333333333703, 0.3219752754296894559, 0.3333333333333333703, 0.3219752754296894559, 0.3333333333333333703, 0.3219752754296894559, 0.3333333333333333703, 0.3219752754296894559, 0.3333333333333333703, 0.3219752754296894559, 0.3333333333333333703, 0.3219752754296894559, 0.3333333333333333703, 0.3219752754296894559, 0.3333333333333333703, 0.3219752754296894559, 0.3333333333333333703, 0.3219752754296894559, 0.3333333333333333703, 0.3219752754296894559, 0.3333333333333333703, 0.3219752754296894559, 0.3333333333333333703, 0.3219752754296894559, 0.3333333333333333703, 0.3219752754296894559, 0.3333333333333333703, 0.3219752754296894559, 0.3333333333333333703, 0.3219752754296894559, 0.3333333333333333703, 0.3219752754296894559, 0.3333333333333333703, 0.3219752754296894559, 0.3333333333333333703, 0.3219752754296894559, 0.3333333333333333703, 0.3219752754296894559, 0.3333333333333333703, 0.3219752754296894559, 0.3333333333333333703, 0.3219752754296894559, 0.3333333333333333703, 0.3219752754296894559, 0.3333333333333333703, 0.3219752754296894559, 0.3333333333333333703, 0.3219752754296894559, 0.3333333333333333703, 0.3219752754296894559, 0.3333333333333333703, 0.3219752754296894559, 0.3333333333333333703, 0.3219752754296894559, 0.3333333333333333703, 0.3219752754296894559, 0.3333333333333333703, 0.3219752754296894559, 0.3333333333333333703, 0.3219752754296894559, 0.3333333333333333703, 0.3219752754296894559, 0.3333333333333333703, 0.3219752754296894559, 0.3333333333333333703, 0.3219752754296894559, 0.3333333333333333703, 0.3219752754296894559, 0.3333333333333333703, 0.3219752754296894559, 0.3333333333333333703, 0.3219752754296894559, 0.3333333333333333703, 0.3219752754296894559, 0.3333333333333333703, 0.3219752754296894559, 0.3333333333333333703, 0.3219752754296894559, 0.3333333333333333703, 0.3219752754296894559, 0.3333333333333333703, 0.3219752754296894559, 0.3333333333333333703, 0.3219752754296894559, 0.3333333333333333703, 0.3219752754296894559, 0.3333333333333333703, 0.3219752754296894559, 0.3333333333333333703, 0.3219752754296894559, 0.3333333333333333703, 0.3219752754296894559, 0.3333333333333333703, 0.3219752754296894559, 0.3333333333333333703, 0.3219752754296894559, 0.3333333333333333703, 0.3219752754296894559, 0.3333333333333333703, 0.3219752754296894559, 0.3333333333333333703, 0.3219752754296894559, 0.3333333333333333703, 0.3219752754296894559, 0.3333333333333333703, 0.3219752754296894559, 0.3333333333333333703, 0.3219752754296894559, 0.3333333333333333703, 0.3219752754296894559, 0.3333333333333333703, 0.3219752754296894559, 0.3333333333333333703, 0.3219752754296894559, 0.3333333333333333703, 0.3219752754296894559, 0.3333333333333333703, 0.3219752754296894559, 0.3333333333333333703, 0.3219752754296894559, 0.3333333333333333703, 0.3219752754296894559, 0.3333333333333333703, 0.3219752754296894559, 0.3333333333333333703, 0.3219752754296894559, 0.3333333333333333703, 0.3219752754296894559, 0.3333333333333333703, 0.3219752754296894559, 0.3333333333333333703, 0.3219752754296894559, 0.3333333333333333703, 0.3219752754296894559, 0.3333333333333333703, 0.3219752754296894559, 0.3333333333333333703, 0.3219752754296894559, 0.3333333333333333703, 0.3219752754296894559, 0.3333333333333333703, 0.3219752754296894559, 0.3333333333333333703, 0.3219752754296894559, 0.3333333333333333703, 0.3219752754296894559, 0.3333333333333333703, 0.3219752754296894559, 0.3333333333333333703, 0.3219752754296894559, 0.3333333333333333703, 0.3219752754296894559, 0.3333333333333333703, 0.3219752754296894559, 0.3333333333333333703, 0.3219752754296894559, 0.3333333333333333703, 0.3219752754296894559, 0.3333333333333333703, 0.3219752754296894559, 0.3333333333333333703, 0.3219752754296894559, 0.3333333333333333703, 0.3219752754296894559, 0.3333333333333333703, 0.3219752754296894559, 0.3333333333333333703, 0.3219752754296894559, 0.3333333333333333703, 0.3219752754296894559, 0.3333333333333333703, 0.3219752754296894559, 0.3333333333333333703, 0.3219752754296894559, 0.3333333333333333703, 0.3219752754296894559, 0.3333333333333333703, 0.3219752754296894559, 0.3333333333333333703, 0.3219752754296894559, 0.3333333333333333703, 0.3219752754296894559, 0.3333333333333333703, 0.3219752754296894559, 0.3333333333333333703, 0.3219752754296894559, 0.3333333333333333703, 0.3219752754296894559, 0.3333333333333333703, 0.3219752754296894559, 0.3333333333333333703, 0.3219752754296894559, 0.3333333333333333703, 0.3219752754296894559, 0.3333333333333333703, 0.3219752754296894559, 0.3333333333333333703, 0.3219752754296894559, 0.3333333333333333703, 0.3219752754296894559, 0.3333333333333333703, 0.3219752754296894559, 0.3333333333333333703, 0.3219752754296894559, 0.3333333333333333703, 0.3219752754296894559, 0.3333333333333333703, 0.3219752754296894559, 0.3333333333333333703, 0.3219752754296894559, 0.3333333333333333703, 0.3219752754296894559, 0.3333333333333333703, 0.3219752754296894559, 0.3333333333333333703, 0.3219752754296894559, 0.3333333333333333703, 0.3219752754296894559, 0.3333333333333333703, 0.3219752754296894559, 0.3333333333333333703, 0.3219752754296894559, 0.3333333333333333703, 0.3219752754296894559, 0.3333333333333333703, 0.3219752754296894559, 0.3333333333333333703, 0.3219752754296894559, 0.3333333333333333703, 0.3219752754296894559, 0.3333333333333333703, 0.3219752754296894559, 0.3333333333333333703, 0.3219752754296894559, 0.3333333333333333703, 0.3219752754296894559, 0.3333333333333333703, 0.3219752754296894559, 0.3333333333333333703, 0.3219752754296894559, 0.3333333333333333703, 0.3219752754296894559, 0.3333333333333333703, 0.3219752754296894559, 0.3333333333333333703, 0.3219752754296894559, 0.3333333333333333703, 0.3219752754296894559, 0.3333333333333333703, 0.3219752754296894559, 0.3333333333333333703, 0.3219752754296894559, 0.3333333333333333703, 0.3219752754296894559, 0.3333333333333333703, 0.3219752754296894559, 0.3333333333333333703, 0.3219752754296894559, 0.3333333333333333703, 0.3219752754296894559, 0.3333333333333333703, 0.3219752754296894559, 0.3333333333333333703, 0.3219752754296894559, 0.3333333333333333703, 0.3219752754296894559, 0.3333333333333333703, 0.3219752754296894559, 0.3333333333333333703, 0.3219752754296894559, 0.3333333333333333703, 0.3219752754296894559, 0.3333333333333333703, 0.3219752754296894559, 0.3333333333333333703, 0.3219752754296894559, 0.3333333333333333703, 0.3219752754296894559, 0.3333333333333333703, 0.3219752754296894559, 0.3333333333333333703, 0.3219752754296894559, 0.3333333333333333703, 0.3219752754296894559, 0.3333333333333333703, 0.3219752754296894559, 0.3333333333333333703, 0.3219752754296894559, 0.3333333333333333703, 0.3219752754296894559, 0.3333333333333333703, 0.3219752754296894559, 0.3333333333333333703, 0.3219752754296894559, 0.3333333333333333703, 0.3219752754296894559, 0.3333333333333333703, 0.3219752754296894559, 0.3333333333333333703, 0.3219752754296894559, 0.3333333333333333703, 0.3219752754296894559, 0.3333333333333333703, 0.3219752754296894559, 0.3333333333333333703, 0.3219752754296894559, 0.3333333333333333703, 0.3219752754296894559, 0.3333333333333333703, 0.3219752754296894559, 0.3333333333333333703, 0.3219752754296894559, 0.3333333333333333703, 0.3219752754296894559, 0.3333333333333333703, 0.3219752754296894559, 0.3333333333333333703, 0.3219752754296894559, 0.3333333333333333703, 0.3219752754296894559, 0.3333333333333333703, 0.3219752754296894559, 0.3333333333333333703, 0.3219752754296894559, 0.3333333333333333703, 0.3219752754296894559, 0.3333333333333333703, 0.3219752754296894559, 0.3333333333333333703, 0.3219752754296894559, 0.3333333333333333703, 0.3219752754296894559, 0.3333333333333333703, 0.3219752754296894559, 0.3333333333333333703, 0.3219752754296894559, 0.3333333333333333703, 0.3219752754296894559, 0.3333333333333333703, 0.3219752754296894559, 0.3333333333333333703, 0.3219752754296894559, 0.3333333333333333703, 0.3219752754296894559, 0.3333333333333333703, 0.3219752754296894559, 0.3333333333333333703, 0.3219752754296894559, 0.3333333333333333703, 0.3219752754296894559, 0.3333333333333333703, 0.3219752754296894559, 0.3333333333333333703, 0.3219752754296894559, 0.3333333333333333703, 0.3219752754296894559, 0.3333333333333333703, 0.3219752754296894559, 0.3333333333333333703, 0.3219752754296894559, 0.3333333333333333703, 0.3219752754296894559, 0.3333333333333333703, 0.3219752754296894559, 0.3333333333333333703, 0.3219752754296894559, 0.3333333333333333703, 0.3219752754296894559, 0.3333333333333333703, 0.3219752754296894559, 0.3333333333333333703, 0.3219752754296894559, 0.3333333333333333703, 0.3219752754296894559, 0.3333333333333333703, 0.3219752754296894559, 0.3333333333333333703, 0.3219752754296894559, 0.3333333333333333703, 0.3219752754296894559, 0.3333333333333333703, 0.3219752754296894559, 0.3333333333333333703, 0.3219752754296894559, 0.3333333333333333703, 0.3219752754296894559, 0.3333333333333333703, 0.3219752754296894559, 0.3333333333333333703, 0.3219752754296894559, 0.3333333333333333703, 0.3219752754296894559, 0.3333333333333333703, 0.3219752754296894559, 0.3333333333333333703, 0.3219752754296894559, 0.3333333333333333703),
 ( 0.3333333333333333703, 0.3219752754296894559, 0.3333333333333333703, 0.3219752754296894559, 0.3333333333333333703, 0.3219752754296894559, 0.3333333333333333703, 0.3219752754296894559, 0.3333333333333333703, 0.3219752754296894559, 0.3333333333333333703, 0.3219752754296894559, 0.3333333333333333703, 0.3219752754296894559, 0.3333333333333333703, 0.3219752754296894559, 0.3333333333333333703, 0.3219752754296894559, 0.3333333333333333703, 0.3219752754296894559, 0.3333333333333333703, 0.3219752754296894559, 0.3333333333333333703, 0.3219752754296894559, 0.3333333333333333703, 0.3219752754296894559, 0.3333333333333333703, 0.3219752754296894559, 0.3333333333333333703, 0.3219752754296894559, 0.3333333333333333703, 0.3219752754296894559, 0.3333333333333333703, 0.3219752754296894559, 0.3333333333333333703, 0.3219752754296894559, 0.3333333333333333703, 0.3219752754296894559, 0.3333333333333333703, 0.3219752754296894559, 0.3333333333333333703, 0.3219752754296894559, 0.3333333333333333703, 0.3219752754296894559, 0.3333333333333333703, 0.3219752754296894559, 0.3333333333333333703, 0.3219752754296894559, 0.3333333333333333703, 0.3219752754296894559, 0.3333333333333333703, 0.3219752754296894559, 0.3333333333333333703, 0.3219752754296894559, 0.3333333333333333703, 0.3219752754296894559, 0.3333333333333333703, 0.3219752754296894559, 0.3333333333333333703, 0.3219752754296894559, 0.3333333333333333703, 0.3219752754296894559, 0.3333333333333333703, 0.3219752754296894559, 0.3333333333333333703, 0.3219752754296894559, 0.3333333333333333703, 0.3219752754296894559, 0.3333333333333333703, 0.3219752754296894559, 0.3333333333333333703, 0.3219752754296894559, 0.3333333333333333703, 0.3219752754296894559, 0.3333333333333333703, 0.3219752754296894559, 0.3333333333333333703, 0.3219752754296894559, 0.3333333333333333703, 0.3219752754296894559, 0.3333333333333333703, 0.3219752754296894559, 0.3333333333333333703, 0.3219752754296894559, 0.3333333333333333703, 0.3219752754296894559, 0.3333333333333333703, 0.3219752754296894559, 0.3333333333333333703, 0.3219752754296894559, 0.3333333333333333703, 0.3219752754296894559, 0.3333333333333333703, 0.3219752754296894559, 0.3333333333333333703, 0.3219752754296894559, 0.3333333333333333703, 0.3219752754296894559, 0.3333333333333333703, 0.3219752754296894559, 0.3333333333333333703, 0.3219752754296894559, 0.3333333333333333703, 0.3219752754296894559, 0.3333333333333333703, 0.3219752754296894559, 0.3333333333333333703, 0.3219752754296894559, 0.3333333333333333703, 0.3219752754296894559, 0.3333333333333333703, 0.3219752754296894559, 0.3333333333333333703, 0.3219752754296894559, 0.3333333333333333703, 0.3219752754296894559, 0.3333333333333333703, 0.3219752754296894559, 0.3333333333333333703, 0.3219752754296894559, 0.3333333333333333703, 0.3219752754296894559, 0.3333333333333333703, 0.3219752754296894559, 0.3333333333333333703, 0.3219752754296894559, 0.3333333333333333703, 0.3219752754296894559, 0.3333333333333333703, 0.3219752754296894559, 0.3333333333333333703, 0.3219752754296894559, 0.3333333333333333703, 0.3219752754296894559, 0.3333333333333333703, 0.3219752754296894559, 0.3333333333333333703, 0.3219752754296894559, 0.3333333333333333703, 0.3219752754296894559, 0.3333333333333333703, 0.3219752754296894559, 0.3333333333333333703, 0.3219752754296894559, 0.3333333333333333703, 0.3219752754296894559, 0.3333333333333333703, 0.3219752754296894559, 0.3333333333333333703, 0.3219752754296894559, 0.3333333333333333703, 0.3219752754296894559, 0.3333333333333333703, 0.3219752754296894559, 0.3333333333333333703, 0.3219752754296894559, 0.3333333333333333703, 0.3219752754296894559, 0.3333333333333333703, 0.3219752754296894559, 0.3333333333333333703, 0.3219752754296894559, 0.3333333333333333703, 0.3219752754296894559, 0.3333333333333333703, 0.3219752754296894559, 0.3333333333333333703, 0.3219752754296894559, 0.3333333333333333703, 0.3219752754296894559, 0.3333333333333333703, 0.3219752754296894559, 0.3333333333333333703, 0.3219752754296894559, 0.3333333333333333703, 0.3219752754296894559, 0.3333333333333333703, 0.3219752754296894559, 0.3333333333333333703, 0.3219752754296894559, 0.3333333333333333703, 0.3219752754296894559, 0.3333333333333333703, 0.3219752754296894559, 0.3333333333333333703, 0.3219752754296894559, 0.3333333333333333703, 0.3219752754296894559, 0.3333333333333333703, 0.3219752754296894559, 0.3333333333333333703, 0.3219752754296894559, 0.3333333333333333703, 0.3219752754296894559, 0.3333333333333333703, 0.3219752754296894559, 0.3333333333333333703, 0.3219752754296894559, 0.3333333333333333703, 0.3219752754296894559, 0.3333333333333333703, 0.3219752754296894559, 0.3333333333333333703, 0.3219752754296894559, 0.3333333333333333703, 0.3219752754296894559, 0.3333333333333333703, 0.3219752754296894559, 0.3333333333333333703, 0.3219752754296894559, 0.3333333333333333703, 0.3219752754296894559, 0.3333333333333333703, 0.3219752754296894559, 0.3333333333333333703, 0.3219752754296894559, 0.3333333333333333703, 0.3219752754296894559, 0.3333333333333333703, 0.3219752754296894559, 0.3333333333333333703, 0.3219752754296894559, 0.3333333333333333703, 0.3219752754296894559, 0.3333333333333333703, 0.3219752754296894559, 0.3333333333333333703, 0.3219752754296894559, 0.3333333333333333703, 0.3219752754296894559, 0.3333333333333333703, 0.3219752754296894559, 0.3333333333333333703, 0.3219752754296894559, 0.3333333333333333703, 0.3219752754296894559, 0.3333333333333333703, 0.3219752754296894559, 0.3333333333333333703, 0.3219752754296894559, 0.3333333333333333703, 0.3219752754296894559, 0.3333333333333333703, 0.3219752754296894559, 0.3333333333333333703, 0.3219752754296894559, 0.3333333333333333703, 0.3219752754296894559, 0.3333333333333333703, 0.3219752754296894559, 0.3333333333333333703, 0.3219752754296894559, 0.3333333333333333703, 0.3219752754296894559, 0.3333333333333333703, 0.3219752754296894559, 0.3333333333333333703, 0.3219752754296894559, 0.3333333333333333703, 0.3219752754296894559, 0.3333333333333333703, 0.3219752754296894559, 0.3333333333333333703, 0.3219752754296894559, 0.3333333333333333703, 0.3219752754296894559, 0.3333333333333333703, 0.3219752754296894559, 0.3333333333333333703, 0.3219752754296894559, 0.3333333333333333703, 0.3219752754296894559, 0.3333333333333333703, 0.3219752754296894559, 0.3333333333333333703, 0.3219752754296894559, 0.3333333333333333703, 0.3219752754296894559, 0.3333333333333333703, 0.3219752754296894559, 0.3333333333333333703, 0.3219752754296894559, 0.3333333333333333703, 0.3219752754296894559, 0.3333333333333333703, 0.3219752754296894559, 0.3333333333333333703, 0.3219752754296894559, 0.3333333333333333703, 0.3219752754296894559, 0.3333333333333333703, 0.3219752754296894559, 0.3333333333333333703, 0.3219752754296894559, 0.3333333333333333703, 0.3219752754296894559, 0.3333333333333333703, 0.3219752754296894559, 0.3333333333333333703, 0.3219752754296894559, 0.3333333333333333703, 0.3219752754296894559, 0.3333333333333333703, 0.3219752754296894559, 0.3333333333333333703, 0.3219752754296894559, 0.3333333333333333703, 0.3219752754296894559, 0.3333333333333333703, 0.3219752754296894559, 0.3333333333333333703, 0.3219752754296894559, 0.3333333333333333703, 0.3219752754296894559, 0.3333333333333333703, 0.3219752754296894559, 0.3333333333333333703, 0.3219752754296894559, 0.3333333333333333703, 0.3219752754296894559, 0.3333333333333333703, 0.3219752754296894559, 0.3333333333333333703, 0.3219752754296894559, 0.3333333333333333703, 0.3219752754296894559, 0.3333333333333333703, 0.3219752754296894559, 0.3333333333333333703, 0.3219752754296894559, 0.3333333333333333703, 0.3219752754296894559, 0.3333333333333333703, 0.3219752754296894559, 0.3333333333333333703, 0.3219752754296894559, 0.3333333333333333703, 0.3219752754296894559, 0.3333333333333333703, 0.3219752754296894559, 0.3333333333333333703, 0.3219752754296894559, 0.3333333333333333703, 0.3219752754296894559, 0.3333333333333333703, 0.3219752754296894559, 0.3333333333333333703, 0.3219752754296894559, 0.3333333333333333703, 0.3219752754296894559, 0.3333333333333333703, 0.3219752754296894559, 0.3333333333333333703, 0.3219752754296894559, 0.3333333333333333703, 0.3219752754296894559, 0.3333333333333333703, 0.3219752754296894559, 0.3333333333333333703, 0.3219752754296894559, 0.3333333333333333703, 0.3219752754296894559, 0.3333333333333333703, 0.3219752754296894559, 0.3333333333333333703, 0.3219752754296894559, 0.3333333333333333703, 0.3219752754296894559, 0.3333333333333333703, 0.3219752754296894559, 0.3333333333333333703, 0.3219752754296894559, 0.3333333333333333703, 0.3219752754296894559, 0.3333333333333333703, 0.3219752754296894559, 0.3333333333333333703, 0.3219752754296894559, 0.3333333333333333703, 0.3219752754296894559, 0.3333333333333333703, 0.3219752754296894559, 0.3333333333333333703, 0.3219752754296894559, 0.3333333333333333703, 0.3219752754296894559, 0.3333333333333333703, 0.3219752754296894559, 0.3333333333333333703, 0.3219752754296894559, 0.3333333333333333703, 0.3219752754296894559, 0.3333333333333333703, 0.3219752754296894559, 0.3333333333333333703, 0.3219752754296894559, 0.3333333333333333703, 0.3219752754296894559, 0.3333333333333333703, 0.3219752754296894559, 0.3333333333333333703, 0.3219752754296894559, 0.3333333333333333703, 0.3219752754296894559, 0.3333333333333333703, 0.3219752754296894559, 0.3333333333333333703, 0.3219752754296894559, 0.3333333333333333703, 0.3219752754296894559, 0.3333333333333333703, 0.3219752754296894559, 0.3333333333333333703, 0.3219752754296894559, 0.3333333333333333703, 0.3219752754296894559, 0.3333333333333333703, 0.3219752754296894559, 0.3333333333333333703, 0.3219752754296894559, 0.3333333333333333703, 0.3219752754296894559, 0.3333333333333333703, 0.3219752754296894559, 0.3333333333333333703, 0.3219752754296894559, 0.3333333333333333703, 0.3219752754296894559, 0.3333333333333333703, 0.3219752754296894559, 0.3333333333333333703, 0.3219752754296894559, 0.3333333333333333703, 0.3219752754296894559, 0.3333333333333333703, 0.3219752754296894559, 0.3333333333333333703, 0.3219752754296894559, 0.3333333333333333703, 0.3219752754296894559, 0.3333333333333333703, 0.3219752754296894559, 0.3333333333333333703, 0.3219752754296894559, 0.3333333333333333703, 0.3219752754296894559, 0.3333333333333333703, 0.3219752754296894559, 0.3333333333333333703, 0.3219752754296894559, 0.3333333333333333703, 0.3219752754296894559, 0.3333333333333333703, 0.3219752754296894559, 0.3333333333333333703, 0.3219752754296894559, 0.3333333333333333703),
 ( 1.000000000000000000, 0.9659258262890683122, 1.000000000000000000, 0.9659258262890683122, 1.000000000000000000, 0.9659258262890683122, 1.000000000000000000, 0.9659258262890683122, 1.000000000000000000, 0.9659258262890683122, 1.000000000000000000, 0.9659258262890683122, 1.000000000000000000, 0.9659258262890683122, 1.000000000000000000, 0.9659258262890683122, 1.000000000000000000, 0.9659258262890683122, 1.000000000000000000, 0.9659258262890683122, 1.000000000000000000, 0.9659258262890683122, 1.000000000000000000, 0.9659258262890683122, 1.000000000000000000, 0.9659258262890683122, 1.000000000000000000, 0.9659258262890683122, 1.000000000000000000, 0.9659258262890683122, 1.000000000000000000, 0.9659258262890683122, 1.000000000000000000, 0.9659258262890683122, 1.000000000000000000, 0.9659258262890683122, 1.000000000000000000, 0.9659258262890683122, 1.000000000000000000, 0.9659258262890683122, 1.000000000000000000, 0.9659258262890683122, 1.000000000000000000, 0.9659258262890683122, 1.000000000000000000, 0.9659258262890683122, 1.000000000000000000, 0.9659258262890683122, 1.000000000000000000, 0.9659258262890683122, 1.000000000000000000, 0.9659258262890683122, 1.000000000000000000, 0.9659258262890683122, 1.000000000000000000, 0.9659258262890683122, 1.000000000000000000, 0.9659258262890683122, 1.000000000000000000, 0.9659258262890683122, 1.000000000000000000, 0.9659258262890683122, 1.000000000000000000, 0.9659258262890683122, 1.000000000000000000, 0.9659258262890683122, 1.000000000000000000, 0.9659258262890683122, 1.000000000000000000, 0.9659258262890683122, 1.000000000000000000, 0.9659258262890683122, 1.000000000000000000, 0.9659258262890683122, 1.000000000000000000, 0.9659258262890683122, 1.000000000000000000, 0.9659258262890683122, 1.000000000000000000, 0.9659258262890683122, 1.000000000000000000, 0.9659258262890683122, 1.000000000000000000, 0.9659258262890683122, 1.000000000000000000, 0.9659258262890683122, 1.000000000000000000, 0.9659258262890683122, 1.000000000000000000, 0.9659258262890683122, 1.000000000000000000, 0.9659258262890683122, 1.000000000000000000, 0.9659258262890683122, 1.000000000000000000, 0.9659258262890683122, 1.000000000000000000, 0.9659258262890683122, 1.000000000000000000, 0.9659258262890683122, 1.000000000000000000, 0.9659258262890683122, 1.000000000000000000, 0.9659258262890683122, 1.000000000000000000, 0.9659258262890683122, 1.000000000000000000, 0.9659258262890683122, 1.000000000000000000, 0.9659258262890683122, 1.000000000000000000, 0.9659258262890683122, 1.000000000000000000, 0.9659258262890683122, 1.000000000000000000, 0.9659258262890683122, 1.000000000000000000, 0.9659258262890683122, 1.000000000000000000, 0.9659258262890683122, 1.000000000000000000, 0.9659258262890683122, 1.000000000000000000, 0.9659258262890683122, 1.000000000000000000, 0.9659258262890683122, 1.000000000000000000, 0.9659258262890683122, 1.000000000000000000, 0.9659258262890683122, 1.000000000000000000, 0.9659258262890683122, 1.000000000000000000, 0.9659258262890683122, 1.000000000000000000, 0.9659258262890683122, 1.000000000000000000, 0.9659258262890683122, 1.000000000000000000, 0.9659258262890683122, 1.000000000000000000, 0.9659258262890683122, 1.000000000000000000, 0.9659258262890683122, 1.000000000000000000, 0.9659258262890683122, 1.000000000000000000, 0.9659258262890683122, 1.000000000000000000, 0.9659258262890683122, 1.000000000000000000, 0.9659258262890683122, 1.000000000000000000, 0.9659258262890683122, 1.000000000000000000, 0.9659258262890683122, 1.000000000000000000, 0.9659258262890683122, 1.000000000000000000, 0.9659258262890683122, 1.000000000000000000, 0.9659258262890683122, 1.000000000000000000, 0.9659258262890683122, 1.000000000000000000, 0.9659258262890683122, 1.000000000000000000, 0.9659258262890683122, 1.000000000000000000, 0.9659258262890683122, 1.000000000000000000, 0.9659258262890683122, 1.000000000000000000, 0.9659258262890683122, 1.000000000000000000, 0.9659258262890683122, 1.000000000000000000, 0.9659258262890683122, 1.000000000000000000, 0.9659258262890683122, 1.000000000000000000, 0.9659258262890683122, 1.000000000000000000, 0.9659258262890683122, 1.000000000000000000, 0.9659258262890683122, 1.000000000000000000, 0.9659258262890683122, 1.000000000000000000, 0.9659258262890683122, 1.000000000000000000, 0.9659258262890683122, 1.000000000000000000, 0.9659258262890683122, 1.000000000000000000, 0.9659258262890683122, 1.000000000000000000, 0.9659258262890683122, 1.000000000000000000, 0.9659258262890683122, 1.000000000000000000, 0.9659258262890683122, 1.000000000000000000, 0.9659258262890683122, 1.000000000000000000, 0.9659258262890683122, 1.000000000000000000, 0.9659258262890683122, 1.000000000000000000, 0.9659258262890683122, 1.000000000000000000, 0.9659258262890683122, 1.000000000000000000, 0.9659258262890683122, 1.000000000000000000, 0.9659258262890683122, 1.000000000000000000, 0.9659258262890683122, 1.000000000000000000, 0.9659258262890683122, 1.000000000000000000, 0.9659258262890683122, 1.000000000000000000, 0.9659258262890683122, 1.000000000000000000, 0.9659258262890683122, 1.000000000000000000, 0.9659258262890683122, 1.000000000000000000, 0.9659258262890683122, 1.000000000000000000, 0.9659258262890683122, 1.000000000000000000, 0.9659258262890683122, 1.000000000000000000, 0.9659258262890683122, 1.000000000000000000, 0.9659258262890683122, 1.000000000000000000, 0.9659258262890683122, 1.000000000000000000, 0.9659258262890683122, 1.000000000000000000, 0.9659258262890683122, 1.000000000000000000, 0.9659258262890683122, 1.000000000000000000, 0.9659258262890683122, 1.000000000000000000, 0.9659258262890683122, 1.000000000000000000, 0.9659258262890683122, 1.000000000000000000, 0.9659258262890683122, 1.000000000000000000, 0.9659258262890683122, 1.000000000000000000, 0.9659258262890683122, 1.000000000000000000, 0.9659258262890683122, 1.000000000000000000, 0.9659258262890683122, 1.000000000000000000, 0.9659258262890683122, 1.000000000000000000, 0.9659258262890683122, 1.000000000000000000, 0.9659258262890683122, 1.000000000000000000, 0.9659258262890683122, 1.000000000000000000, 0.9659258262890683122, 1.000000000000000000, 0.9659258262890683122, 1.000000000000000000, 0.9659258262890683122, 1.000000000000000000, 0.9659258262890683122, 1.000000000000000000, 0.9659258262890683122, 1.000000000000000000, 0.9659258262890683122, 1.000000000000000000, 0.9659258262890683122, 1.000000000000000000, 0.9659258262890683122, 1.000000000000000000, 0.9659258262890683122, 1.000000000000000000, 0.9659258262890683122, 1.000000000000000000, 0.9659258262890683122, 1.000000000000000000, 0.9659258262890683122, 1.000000000000000000, 0.9659258262890683122, 1.000000000000000000, 0.9659258262890683122, 1.000000000000000000, 0.9659258262890683122, 1.000000000000000000, 0.9659258262890683122, 1.000000000000000000, 0.9659258262890683122, 1.000000000000000000, 0.9659258262890683122, 1.000000000000000000, 0.9659258262890683122, 1.000000000000000000, 0.9659258262890683122, 1.000000000000000000, 0.9659258262890683122, 1.000000000000000000, 0.9659258262890683122, 1.000000000000000000, 0.9659258262890683122, 1.000000000000000000, 0.9659258262890683122, 1.000000000000000000, 0.9659258262890683122, 1.000000000000000000, 0.9659258262890683122, 1.000000000000000000, 0.9659258262890683122, 1.000000000000000000, 0.9659258262890683122, 1.000000000000000000, 0.9659258262890683122, 1.000000000000000000, 0.9659258262890683122, 1.000000000000000000, 0.9659258262890683122, 1.000000000000000000, 0.9659258262890683122, 1.000000000000000000, 0.9659258262890683122, 1.000000000000000000, 0.9659258262890683122, 1.000000000000000000, 0.9659258262890683122, 1.000000000000000000, 0.9659258262890683122, 1.000000000000000000, 0.9659258262890683122, 1.000000000000000000, 0.9659258262890683122, 1.000000000000000000, 0.9659258262890683122, 1.000000000000000000, 0.9659258262890683122, 1.000000000000000000, 0.9659258262890683122, 1.000000000000000000, 0.9659258262890683122, 1.000000000000000000, 0.9659258262890683122, 1.000000000000000000, 0.9659258262890683122, 1.000000000000000000, 0.9659258262890683122, 1.000000000000000000, 0.9659258262890683122, 1.000000000000000000, 0.9659258262890683122, 1.000000000000000000, 0.9659258262890683122, 1.000000000000000000, 0.9659258262890683122, 1.000000000000000000, 0.9659258262890683122, 1.000000000000000000, 0.9659258262890683122, 1.000000000000000000, 0.9659258262890683122, 1.000000000000000000, 0.9659258262890683122, 1.000000000000000000, 0.9659258262890683122, 1.000000000000000000, 0.9659258262890683122, 1.000000000000000000, 0.9659258262890683122, 1.000000000000000000, 0.9659258262890683122, 1.000000000000000000, 0.9659258262890683122, 1.000000000000000000, 0.9659258262890683122, 1.000000000000000000, 0.9659258262890683122, 1.000000000000000000, 0.9659258262890683122, 1.000000000000000000, 0.9659258262890683122, 1.000000000000000000, 0.9659258262890683122, 1.000000000000000000, 0.9659258262890683122, 1.000000000000000000, 0.9659258262890683122, 1.000000000000000000, 0.9659258262890683122, 1.000000000000000000, 0.9659258262890683122, 1.000000000000000000, 0.9659258262890683122, 1.000000000000000000, 0.9659258262890683122, 1.000000000000000000, 0.9659258262890683122, 1.000000000000000000, 0.9659258262890683122, 1.000000000000000000, 0.9659258262890683122, 1.000000000000000000, 0.9659258262890683122, 1.000000000000000000, 0.9659258262890683122, 1.000000000000000000, 0.9659258262890683122, 1.000000000000000000, 0.9659258262890683122, 1.000000000000000000, 0.9659258262890683122, 1.000000000000000000, 0.9659258262890683122, 1.000000000000000000, 0.9659258262890683122, 1.000000000000000000, 0.9659258262890683122, 1.000000000000000000, 0.9659258262890683122, 1.000000000000000000, 0.9659258262890683122, 1.000000000000000000, 0.9659258262890683122, 1.000000000000000000, 0.9659258262890683122, 1.000000000000000000, 0.9659258262890683122, 1.000000000000000000, 0.9659258262890683122, 1.000000000000000000, 0.9659258262890683122, 1.000000000000000000, 0.9659258262890683122, 1.000000000000000000, 0.9659258262890683122, 1.000000000000000000, 0.9659258262890683122, 1.000000000000000000, 0.9659258262890683122, 1.000000000000000000, 0.9659258262890683122, 1.000000000000000000, 0.9659258262890683122, 1.000000000000000000) ) ) 
 REPRESENTATION_ITEM ( '' )  SURFACE ( )  );
#103449 = CARTESIAN_POINT ( 'NONE',  ( 18.22780087662123805, 5.499999999999960032, 91.48236817873106475 ) ) ;
#103450 = CARTESIAN_POINT ( 'NONE',  ( 5.153800228976335163, 19.02544592524342804, 64.79057627198100988 ) ) ;
#103451 = DIRECTION ( 'NONE',  ( 0.000000000000000000, -0.000000000000000000, -1.000000000000000000 ) ) ;
#103453 = CARTESIAN_POINT ( 'NONE',  ( 19.03943276465977164, -0.05219959533909143690, 83.74890960531436690 ) ) ;
#103452 = CARTESIAN_POINT ( 'NONE',  ( -0.05219959533909027116, -19.03943276465977164, 77.49890960531435269 ) ) ;
#103454 = CARTESIAN_POINT ( 'NONE',  ( 4.483927247898790824, -16.52544592524335698, 65.20942372801901854 ) ) ;
#103455 = DIRECTION ( 'NONE',  ( -1.000000000000000000, 0.000000000000000000, 0.000000000000000000 ) ) ;
#103456 = CARTESIAN_POINT ( 'NONE',  ( -13.89961937509957401, -13.97604488694547875, 44.37609039468566863 ) ) ;
#103457 = CARTESIAN_POINT ( 'NONE',  ( 36.91128768240057667, 0.3596143131121917191, 50.50000000000004263 ) ) ;
#103458 = CARTESIAN_POINT ( 'NONE',  ( 16.51473224551069308, 9.474510206698969483, 109.1655762719810383 ) ) ;
#103459 = CARTESIAN_POINT ( 'NONE',  ( -16.55341960407617563, 4.379528057220093196, 103.5427570613523613 ) ) ;
#103460 = DIRECTION ( 'NONE',  ( 0.000000000000000000, 0.000000000000000000, -1.000000000000000000 ) ) ;
#103461 = CARTESIAN_POINT ( 'NONE',  ( -12.14591786802326823, 12.06949235617739902, 93.12609039468568994 ) ) ;
#103462 = CARTESIAN_POINT ( 'NONE',  ( -16.62475595723696387, 7.163666690055231712, 30.52713351810466591 ) ) ;
#103463 = CARTESIAN_POINT ( 'NONE',  ( -12.06949235617739369, -12.14591786802326823, 69.37609039468567573 ) ) ;
#103464 = CARTESIAN_POINT ( 'NONE',  ( -5.000000000000000000, -120.0000000000000142, 0.0009999999999992653654 ) ) ;
#103465 = CARTESIAN_POINT ( 'NONE',  ( -21.52544592524334988, -5.823673210054445271, 68.95942372801901854 ) ) ;
#103466 = CARTESIAN_POINT ( 'NONE',  ( -0.05219959533936034679, 19.03943276465977164, 82.50109039468567573 ) ) ;
#103467 = CARTESIAN_POINT ( 'NONE',  ( -13.97604488694547697, 13.89961937509957934, 33.12609039468566863 ) ) ;
#103468 = CARTESIAN_POINT ( 'NONE',  ( -16.46253265017160317, 9.564922557960807481, 65.83224293864769550 ) ) ;
#103469 = CARTESIAN_POINT ( 'NONE',  ( -13.97604488694527625, -13.89961937509977652, 41.87390960531435979 ) ) ;
#103470 = CARTESIAN_POINT ( 'NONE',  ( 17.00313601523450302, -6.825168380507106392, 23.22137502641442808 ) ) ;
#103471 = CARTESIAN_POINT ( 'NONE',  ( -10.72451020669898014, 18.67979575497178502, 80.41557627198103830 ) ) ;
#103472 = AXIS2_PLACEMENT_3D ( 'NONE', #113743, #81403, #65264 ) ;
#103473 = CARTESIAN_POINT ( 'NONE',  ( 18.62759615963271287, -10.81492255796078972, 28.33224293864769550 ) ) ;
#103474 = CARTESIAN_POINT ( 'NONE',  ( 5.049401038298161559, -19.05341960407611168, 32.70724293864768129 ) ) ;
#103475 = CARTESIAN_POINT ( 'NONE',  ( -12.06949235617739369, -12.14591786802326823, 54.37609039468568994 ) ) ;
#103476 = ORIENTED_EDGE ( 'NONE', *, *, #15340, .F. ) ;
#103477 = CARTESIAN_POINT ( 'NONE',  ( -10.81492255796105439, 18.62759615963255655, 32.91775706135234714 ) ) ;
#103479 = CARTESIAN_POINT ( 'NONE',  ( -11.74264578624800670, 36.14014761921585972, -0.3999999999999999112 ) ) ;
#103478 = CARTESIAN_POINT ( 'NONE',  ( 12.06949235617757843, -12.14591786802309237, 53.12390960531436690 ) ) ;
#103480 = CARTESIAN_POINT ( 'NONE',  ( -14.29746914071037622, -8.314922557961029526, 24.16775706135235424 ) ) ;
#103481 = CARTESIAN_POINT ( 'NONE',  ( -19.02544592524334988, -5.153800228976617603, 33.95942372801897591 ) ) ;
#103482 = CARTESIAN_POINT ( 'NONE',  ( 4.379528057220339221, -16.55341960407611168, 52.70724293864769550 ) ) ;
#103483 = CARTESIAN_POINT ( 'NONE',  ( 21.55341960407610458, 5.719274019375980345, 113.9572429386477239 ) ) ;
#103485 = CARTESIAN_POINT ( 'NONE',  ( 5.823673210054125526, 21.52544592524343514, 74.79057627198105251 ) ) ;
#103484 = CYLINDRICAL_SURFACE ( 'NONE', #76238, 13.70000000000001528 ) ;
#103486 = CARTESIAN_POINT ( 'NONE',  ( -19.02544592524342804, 5.153800228976336051, 86.04057627198103830 ) ) ;
#103487 = CARTESIAN_POINT ( 'NONE',  ( 0.05219959533910956823, 16.53943276465976808, 54.99890960531435269 ) ) ;
#103488 = CARTESIAN_POINT ( 'NONE',  ( -19.05341960407611168, -5.049401038298163336, 101.4572429386476955 ) ) ;
#103489 = CARTESIAN_POINT ( 'NONE',  ( -37.47229216401453300, 2.437641287457621875, 40.05669362136318767 ) ) ;
#103490 = CARTESIAN_POINT ( 'NONE',  ( -16.51473224551082808, 9.474510206698731452, 68.33442372801900433 ) ) ;
#103491 = CARTESIAN_POINT ( 'NONE',  ( -21.52544592524343514, 5.823673210054127303, 106.0405762719810525 ) ) ;
#103492 = CARTESIAN_POINT ( 'NONE',  ( -0.05219959533909027116, -19.03943276465977164, 52.49890960531436690 ) ) ;
#103493 = CARTESIAN_POINT ( 'NONE',  ( 5.153800228976615827, -19.02544592524334988, 45.20942372801901143 ) ) ;
#103494 = CARTESIAN_POINT ( 'NONE',  ( -4.483927247898539470, -16.52544592524342804, 107.2905762719810525 ) ) ;
#103495 = CARTESIAN_POINT ( 'NONE',  ( 0.05219959533937995610, -21.53943276465977519, 65.00109039468568994 ) ) ;
#103496 = DIRECTION ( 'NONE',  ( 1.000000000000000000, 5.372046893347532792E-15, 0.000000000000000000 ) ) ;
#103497 = CARTESIAN_POINT ( 'NONE',  ( -12.06949235617756955, 12.14591786802309770, 35.62390960531437401 ) ) ;
#103498 = CARTESIAN_POINT ( 'NONE',  ( 9.474510206698971260, -16.51473224551069308, 52.91557627198102409 ) ) ;
#103499 = CARTESIAN_POINT ( 'NONE',  ( 18.56399227203341695, 5.500000000000001776, 71.47830131249902763 ) ) ;
#103500 = CARTESIAN_POINT ( 'NONE',  ( 10.72451020669898902, -18.67979575497178502, 72.91557627198103830 ) ) ;
#103501 = CARTESIAN_POINT ( 'NONE',  ( -27.73933785331498925, 9.013057229001089965, 142.7750000027311899 ) ) ;
#103502 = CARTESIAN_POINT ( 'NONE',  ( 16.51473224551069308, 9.474510206698969483, 39.16557627198103120 ) ) ;
#103503 = ORIENTED_EDGE ( 'NONE', *, *, #67374, .F. ) ;
#103504 = CARTESIAN_POINT ( 'NONE',  ( -5.823673210054116645, -21.52544592524344225, 67.29057627198103830 ) ) ;
#103505 = ADVANCED_FACE ( 'NONE', ( #53455 ), #10904, .F. ) ;
#103506 = CARTESIAN_POINT ( 'NONE',  ( -21.52544592524334988, -5.823673210054445271, 83.95942372801900433 ) ) ;
#103509 = CARTESIAN_POINT ( 'NONE',  ( -16.55341960407611168, -4.379528057220339221, 86.45724293864770971 ) ) ;
#103508 = CARTESIAN_POINT ( 'NONE',  ( 12.14591786802327356, -12.06949235617739191, 100.6260903946857184 ) ) ;
#103507 = CARTESIAN_POINT ( 'NONE',  ( -4.000000000000000888, -165.0000000000000000, 12.00000000000000355 ) ) ;
#103510 = CARTESIAN_POINT ( 'NONE',  ( -5.049401038298153566, 19.05341960407611168, 70.20724293864769550 ) ) ;
#103511 = ORIENTED_EDGE ( 'NONE', *, *, #173803, .F. ) ;
#103512 = CARTESIAN_POINT ( 'NONE',  ( -16.51473224551082808, 9.474510206698731452, 43.33442372801900433 ) ) ;
#103513 = CARTESIAN_POINT ( 'NONE',  ( -0.05219959533934338120, 16.53943276465976808, 82.50109039468568994 ) ) ;
#103514 = CARTESIAN_POINT ( 'NONE',  ( -5.153800228976607833, 19.02544592524334988, 22.70942372801899012 ) ) ;
#103515 = CARTESIAN_POINT ( 'NONE',  ( -5.153800228976328057, -19.02544592524343514, 87.29057627198103830 ) ) ;
#103516 = CARTESIAN_POINT ( 'NONE',  ( 5.823673210054125526, 21.52544592524343514, 49.79057627198102409 ) ) ;
#103517 = CYLINDRICAL_SURFACE ( 'NONE', #60587, 214.0437394197456911 ) ;
#103518 = CARTESIAN_POINT ( 'NONE',  ( 0.05219959533937995610, -21.53943276465977519, 100.0010903946857042 ) ) ;
#103519 = CARTESIAN_POINT ( 'NONE',  ( 14.34966873604972726, -8.224510206698740333, 65.83442372801900433 ) ) ;
#103520 = CARTESIAN_POINT ( 'NONE',  ( -21.53943276465977519, 0.05219959533907696930, 116.2489096053143669 ) ) ;
#103521 = CARTESIAN_POINT ( 'NONE',  ( -16.52544592524335698, -4.483927247898792601, 28.95942372801902209 ) ) ;
#103523 = EDGE_CURVE ( 'NONE', #157973, #100403, #20538, .T. ) ;
#103522 = CARTESIAN_POINT ( 'NONE',  ( 16.46253265017160672, -9.564922557960803928, 98.33224293864769550 ) ) ;
#103524 = CARTESIAN_POINT ( 'NONE',  ( 5.049401038298161559, -19.05341960407611168, 37.70724293864768839 ) ) ;
#103525 = CARTESIAN_POINT ( 'NONE',  ( 19.02544592524343514, -5.153800228976328945, 53.54057627198102409 ) ) ;
#103526 = CARTESIAN_POINT ( 'NONE',  ( -14.29746914071037622, -8.314922557961029526, 29.16775706135234003 ) ) ;
#103527 = CARTESIAN_POINT ( 'NONE',  ( 4.379528057220339221, -16.55341960407611168, 87.70724293864769550 ) ) ;
#103528 = CARTESIAN_POINT ( 'NONE',  ( 12.06949235617739724, 12.14591786802326823, 96.87609039468568994 ) ) ;
#103531 = CARTESIAN_POINT ( 'NONE',  ( -19.03943276465977164, 0.05219959533909376836, 51.24890960531436690 ) ) ;
#103530 = CARTESIAN_POINT ( 'NONE',  ( -9.474510206698964154, 16.51473224551069663, 70.41557627198102409 ) ) ;
#103529 = CARTESIAN_POINT ( 'NONE',  ( 0.05219959533937995610, -21.53943276465977519, 50.00109039468568994 ) ) ;
#103532 = CARTESIAN_POINT ( 'NONE',  ( 19.02544592524343514, -5.153800228976328945, 78.54057627198099567 ) ) ;
#103533 = CARTESIAN_POINT ( 'NONE',  ( 12.14591786802309770, 12.06949235617756955, 34.37390960531435979 ) ) ;
#103534 = CARTESIAN_POINT ( 'NONE',  ( -4.379528057220086978, -16.55341960407618274, 104.7927570613523898 ) ) ;
#103535 = VERTEX_POINT ( 'NONE', #86789 ) ;
#103536 = CARTESIAN_POINT ( 'NONE',  ( 9.474510206698729675, 16.51473224551082808, 37.08442372801899722 ) ) ;
#103537 = CARTESIAN_POINT ( 'NONE',  ( -5.153800228976328057, -19.02544592524343514, 107.2905762719810383 ) ) ;
#103538 = AXIS2_PLACEMENT_3D ( 'NONE', #7423, #115624, #129756 ) ;
#103539 = CARTESIAN_POINT ( 'NONE',  ( -16.46253265017160317, 9.564922557960807481, 50.83224293864770260 ) ) ;
#103540 = CARTESIAN_POINT ( 'NONE',  ( -16.51473224551082808, 9.474510206698731452, 28.33442372801900433 ) ) ;
#103541 = CARTESIAN_POINT ( 'NONE',  ( 22.81625015709510151, -31.40387420917324590, -5.924999997268812990 ) ) ;
#103542 = CARTESIAN_POINT ( 'NONE',  ( 12.06949235617739724, 12.14591786802326823, 46.87609039468568994 ) ) ;
#103544 = CARTESIAN_POINT ( 'NONE',  ( -4.379528057220086978, -16.55341960407618274, 49.79275706135234714 ) ) ;
#103543 = CARTESIAN_POINT ( 'NONE',  ( 5.049401038297881783, 19.05341960407617563, 67.29275706135234714 ) ) ;
#103545 = CARTESIAN_POINT ( 'NONE',  ( 19.49401214000073779, -12.39993551617566503, 167.9999999999999716 ) ) ;
#103546 = CARTESIAN_POINT ( 'NONE',  ( 16.46253265017160672, -9.564922557960803928, 78.33224293864769550 ) ) ;
#103547 = CARTESIAN_POINT ( 'NONE',  ( 21.55341960407610458, 5.719274019375980345, 113.9572429386477239 ) ) ;
#103548 = CARTESIAN_POINT ( 'NONE',  ( 13.97604488694548053, -13.89961937509957401, 65.62609039468567573 ) ) ;
#103550 = CARTESIAN_POINT ( 'NONE',  ( -16.46253265017160317, 9.564922557960807481, 35.83224293864768839 ) ) ;
#103549 = CARTESIAN_POINT ( 'NONE',  ( 16.46253265017160672, -9.564922557960803928, 103.3322429386476955 ) ) ;
#103551 = CARTESIAN_POINT ( 'NONE',  ( 13.89961937509977652, -13.97604488694527269, 73.12390960531436690 ) ) ;
#103553 = CARTESIAN_POINT ( 'NONE',  ( 9.564922557960805705, 16.46253265017160317, 39.58224293864768839 ) ) ;
#103552 = CARTESIAN_POINT ( 'NONE',  ( 4.379528057220339221, -16.55341960407611168, 37.70724293864769550 ) ) ;
#103554 = CARTESIAN_POINT ( 'NONE',  ( 9.564922557961047289, -16.46253265017146816, 35.41775706135233293 ) ) ;
#103555 = CARTESIAN_POINT ( 'NONE',  ( -4.483927247898539470, -16.52544592524342804, 77.29057627198102409 ) ) ;
#103556 = CARTESIAN_POINT ( 'NONE',  ( 10.72451020669871369, 18.67979575497193778, 112.0844237280190185 ) ) ;
#103557 = CARTESIAN_POINT ( 'NONE',  ( -0.05219959533909027116, -19.03943276465977164, 57.49890960531435979 ) ) ;
#103558 = CARTESIAN_POINT ( 'NONE',  ( -18.67979575497178146, -10.72451020669898902, 51.66557627198102409 ) ) ;
#103560 = CARTESIAN_POINT ( 'NONE',  ( -15.72974639402176322, -15.80617190586768395, 99.37609039468568994 ) ) ;
#103559 = CARTESIAN_POINT ( 'NONE',  ( 4.483927247898545687, 16.52544592524342804, 54.79057627198104541 ) ) ;
#103561 = CARTESIAN_POINT ( 'NONE',  ( 5.153800228976335163, 19.02544592524342804, 89.79057627198102409 ) ) ;
#103562 = CARTESIAN_POINT ( 'NONE',  ( 13.97604488694527802, 13.89961937509977652, 104.3739096053143385 ) ) ;
#103563 = CARTESIAN_POINT ( 'NONE',  ( -16.51473224551069308, -9.474510206698971260, 41.66557627198103120 ) ) ;
#103564 = CARTESIAN_POINT ( 'NONE',  ( 19.05341960407611168, 5.049401038298154454, 28.95724293864769550 ) ) ;
#103565 = CARTESIAN_POINT ( 'NONE',  ( 4.379528057220339221, -16.55341960407611168, 87.70724293864769550 ) ) ;
#103566 = CARTESIAN_POINT ( 'NONE',  ( -5.823673210054116645, -21.52544592524344225, 97.29057627198105251 ) ) ;
#103567 = CARTESIAN_POINT ( 'NONE',  ( -13.97604488694527625, -13.89961937509977652, 81.87390960531436690 ) ) ;
#103568 = CARTESIAN_POINT ( 'NONE',  ( -5.719274019375978568, 21.55341960407610458, 105.2072429386477097 ) ) ;
#103569 = CARTESIAN_POINT ( 'NONE',  ( 13.97604488694527802, 13.89961937509977652, 94.37390960531436690 ) ) ;
#103571 = CARTESIAN_POINT ( 'NONE',  ( 14.34966873604960469, 8.224510206698951720, 109.1655762719810383 ) ) ;
#103570 = LINE ( 'NONE', #117734, #165629 ) ;
#103572 = CARTESIAN_POINT ( 'NONE',  ( 9.474510206698971260, -16.51473224551069308, 67.91557627198102409 ) ) ;
#103573 = CARTESIAN_POINT ( 'NONE',  ( -5.719274019375978568, 21.55341960407610458, 75.20724293864769550 ) ) ;
#103574 = CARTESIAN_POINT ( 'NONE',  ( -32.42786921226274899, 3.325810949901248037, 88.27324663263314619 ) ) ;
#103575 = CARTESIAN_POINT ( 'NONE',  ( 28.82186960331498327, 2.781578969918950771E-14, 147.0000000000000000 ) ) ;
#103577 = DIRECTION ( 'NONE',  ( 0.000000000000000000, 0.000000000000000000, -1.000000000000000000 ) ) ;
#103576 = CARTESIAN_POINT ( 'NONE',  ( -5.719274019375978568, 21.55341960407610458, 35.20724293864768839 ) ) ;
#103578 = CARTESIAN_POINT ( 'NONE',  ( 8.314922557961029526, -14.29746914071037800, 30.41775706135234358 ) ) ;
#103579 = CARTESIAN_POINT ( 'NONE',  ( -4.483927247898539470, -16.52544592524342804, 92.29057627198103830 ) ) ;
#103580 = CARTESIAN_POINT ( 'NONE',  ( 18.56453257813367941, -5.499999999999872102, 53.49000423690684158 ) ) ;
#103581 = CARTESIAN_POINT ( 'NONE',  ( -13.97604488694527625, -13.89961937509977652, 91.87390960531432427 ) ) ;
#103582 = CARTESIAN_POINT ( 'NONE',  ( -16.51473224551069308, -9.474510206698971260, 41.66557627198103120 ) ) ;
#103583 = CARTESIAN_POINT ( 'NONE',  ( -16.53943276465976808, 0.05219959533911058130, 81.24890960531436690 ) ) ;
#103584 = CARTESIAN_POINT ( 'NONE',  ( -21.55341960407610458, -5.719274019375992779, 31.45724293864769550 ) ) ;
#103585 = CARTESIAN_POINT ( 'NONE',  ( 14.29746914071049879, -8.314922557960816363, 48.33224293864770260 ) ) ;
#103586 = CARTESIAN_POINT ( 'NONE',  ( -5.153800228976607833, 19.02544592524334988, 97.70942372801900433 ) ) ;
#103587 = CARTESIAN_POINT ( 'NONE',  ( 18.62759615963255655, 10.81492255796105972, 61.66775706135235424 ) ) ;
#103588 = CARTESIAN_POINT ( 'NONE',  ( 27.73933785331498925, -9.013057229001034898, 147.7750000027311899 ) ) ;
#103589 = CARTESIAN_POINT ( 'NONE',  ( -5.049401038298153566, 19.05341960407611168, 100.2072429386476955 ) ) ;
#103590 = CARTESIAN_POINT ( 'NONE',  ( 12.14591786802327356, -12.06949235617739191, 90.62609039468567573 ) ) ;
#103591 = CARTESIAN_POINT ( 'NONE',  ( -19.03943276465977164, 0.05219959533909376836, 21.24890960531436335 ) ) ;
#103592 = CARTESIAN_POINT ( 'NONE',  ( -5.049401038298153566, 19.05341960407611168, 70.20724293864769550 ) ) ;
#103593 = CARTESIAN_POINT ( 'NONE',  ( -5.719274019375978568, 21.55341960407610458, 75.20724293864769550 ) ) ;
#103594 = CARTESIAN_POINT ( 'NONE',  ( -9.564922557961040184, 16.46253265017147172, 107.9177570613523471 ) ) ;
#103596 = CARTESIAN_POINT ( 'NONE',  ( 21.53943276465977519, 0.05219959533937863772, 56.25109039468568284 ) ) ;
#103595 = CARTESIAN_POINT ( 'NONE',  ( -4.379528057220328563, 16.55341960407611168, 50.20724293864769550 ) ) ;
#103598 = CARTESIAN_POINT ( 'NONE',  ( 21.55341960407610458, 5.719274019375980345, 28.95724293864769905 ) ) ;
#103597 = CARTESIAN_POINT ( 'NONE',  ( 16.52544592524335698, 4.483927247898782831, 81.45942372801900433 ) ) ;
#103599 = CARTESIAN_POINT ( 'NONE',  ( 17.49999999999999645, 5.500000000000000888, 28.78230962303566542 ) ) ;
#103600 = CARTESIAN_POINT ( 'NONE',  ( -16.81555441253552274, 7.025013491695482948, 80.63685445334257906 ) ) ;
#103601 = CARTESIAN_POINT ( 'NONE',  ( -8.224510206698735004, -14.34966873604973081, 104.5844237280190185 ) ) ;
#103602 = CARTESIAN_POINT ( 'NONE',  ( 0.05219959533934541429, -16.53943276465976808, 60.00109039468568284 ) ) ;
#103603 = CARTESIAN_POINT ( 'NONE',  ( 13.97604488694527802, 13.89961937509977652, 74.37390960531436690 ) ) ;
#103604 = CARTESIAN_POINT ( 'NONE',  ( 5.153800228976335163, 19.02544592524342804, 89.79057627198102409 ) ) ;
#103605 = CARTESIAN_POINT ( 'NONE',  ( 21.55341960407619695, -5.719274019375665929, 71.04275706135234714 ) ) ;
#103606 = CARTESIAN_POINT ( 'NONE',  ( 0.05219959533934541429, -16.53943276465976808, 75.00109039468568994 ) ) ;
#103607 = CARTESIAN_POINT ( 'NONE',  ( -16.52544592524342804, 4.483927247898546575, 41.04057627198103120 ) ) ;
#103608 = CARTESIAN_POINT ( 'NONE',  ( -13.97604488694527625, -13.89961937509977652, 56.87390960531434558 ) ) ;
#103609 = CARTESIAN_POINT ( 'NONE',  ( -5.153800228976328057, -19.02544592524343514, 52.29057627198100988 ) ) ;
#103611 = ORIENTED_EDGE ( 'NONE', *, *, #158176, .F. ) ;
#103610 = CARTESIAN_POINT ( 'NONE',  ( 16.53943276465976808, 0.05219959533934440121, 36.25109039468567573 ) ) ;
#103612 = CARTESIAN_POINT ( 'NONE',  ( -19.03943276465977164, -0.05219959533935918106, 93.75109039468566152 ) ) ;
#103613 = CARTESIAN_POINT ( 'NONE',  ( -4.483927247898539470, -16.52544592524342804, 92.29057627198103830 ) ) ;
#103614 = CARTESIAN_POINT ( 'NONE',  ( -9.474510206698964154, 16.51473224551069663, 60.41557627198102409 ) ) ;
#103616 = CARTESIAN_POINT ( 'NONE',  ( 38.00000000000000711, -12.34694845685040754, -5.099999999999999645 ) ) ;
#103615 = CARTESIAN_POINT ( 'NONE',  ( 16.51473224551083163, -9.474510206698727899, 100.8344237280190043 ) ) ;
#103617 = CARTESIAN_POINT ( 'NONE',  ( 15.72974639402176855, 15.80617190586768217, 106.8760903946856899 ) ) ;
#103618 = CARTESIAN_POINT ( 'NONE',  ( -16.55341960407617563, 4.379528057220093196, 63.54275706135234003 ) ) ;
#103619 = FACE_OUTER_BOUND ( 'NONE', #78686, .T. ) ;
#103620 = CARTESIAN_POINT ( 'NONE',  ( 18.67979575497178502, 10.72451020669898547, 59.16557627198103120 ) ) ;
#103621 = CARTESIAN_POINT ( 'NONE',  ( -4.379528057220086978, -16.55341960407618274, 59.79275706135234714 ) ) ;
#103622 = CARTESIAN_POINT ( 'NONE',  ( 4.273745901508211986, 6.674792076160473542, 5.990689250852167191 ) ) ;
#103623 = CARTESIAN_POINT ( 'NONE',  ( 19.05341960407617918, -5.049401038297876454, 61.04275706135232582 ) ) ;
#103624 = CARTESIAN_POINT ( 'NONE',  ( 5.049401038298161559, -19.05341960407611168, 87.70724293864769550 ) ) ;
#103625 = CARTESIAN_POINT ( 'NONE',  ( -0.05219959533909027116, -19.03943276465977164, 22.49890960531436690 ) ) ;
#103626 = CARTESIAN_POINT ( 'NONE',  ( 19.03943276465977164, -0.05219959533909143690, 68.74890960531436690 ) ) ;
#103627 = CARTESIAN_POINT ( 'NONE',  ( 16.53943276465976808, -0.05219959533910856209, 63.74890960531435979 ) ) ;
#103628 = CARTESIAN_POINT ( 'NONE',  ( -21.52544592524334988, -5.823673210054445271, 78.95942372801901854 ) ) ;
#103629 = CARTESIAN_POINT ( 'NONE',  ( -19.05341960407617563, 5.049401038297882671, 43.54275706135232582 ) ) ;
#103630 = CARTESIAN_POINT ( 'NONE',  ( -16.51473224551082808, 9.474510206698731452, 23.33442372801900078 ) ) ;
#103631 = CARTESIAN_POINT ( 'NONE',  ( -16.51473224551069308, -9.474510206698971260, 56.66557627198103120 ) ) ;
#103632 = CARTESIAN_POINT ( 'NONE',  ( 15.80617190586746368, 15.72974639402197994, 24.37390960531435979 ) ) ;
#103633 = CARTESIAN_POINT ( 'NONE',  ( 5.719274019375673035, 21.55341960407619339, 102.2927570613523613 ) ) ;
#103634 = CARTESIAN_POINT ( 'NONE',  ( 5.153800228976335163, 19.02544592524342804, 59.79057627198100988 ) ) ;
#103635 = CARTESIAN_POINT ( 'NONE',  ( -15.72974639402176322, -15.80617190586768395, 99.37609039468568994 ) ) ;
#103636 = CARTESIAN_POINT ( 'NONE',  ( -15.80617190586745835, -15.72974639402198527, 56.87390960531436690 ) ) ;
#103637 = CARTESIAN_POINT ( 'NONE',  ( 0.05219959533909260263, 19.03943276465977164, 79.99890960531436690 ) ) ;
#103638 = CARTESIAN_POINT ( 'NONE',  ( 5.049401038297881783, 19.05341960407617563, 57.29275706135231871 ) ) ;
#103639 = CARTESIAN_POINT ( 'NONE',  ( -19.03943276465977164, 0.05219959533909376836, 36.24890960531436690 ) ) ;
#103640 = CARTESIAN_POINT ( 'NONE',  ( -5.049401038298153566, 19.05341960407611168, 95.20724293864770971 ) ) ;
#103641 = CARTESIAN_POINT ( 'NONE',  ( -19.03943276465977164, -0.05219959533935918106, 88.75109039468567573 ) ) ;
#103642 = CARTESIAN_POINT ( 'NONE',  ( 4.379528057220092307, 16.55341960407617563, 32.29275706135235424 ) ) ;
#103643 = CARTESIAN_POINT ( 'NONE',  ( -12.14591786802309592, -12.06949235617757132, 106.8739096053143811 ) ) ;
#103644 = CARTESIAN_POINT ( 'NONE',  ( -13.97604488694527625, -13.89961937509977652, 71.87390960531433848 ) ) ;
#103645 = CARTESIAN_POINT ( 'NONE',  ( 10.81492255796078972, 18.62759615963270932, 44.58224293864769550 ) ) ;
#103646 = CARTESIAN_POINT ( 'NONE',  ( -9.474510206698720793, -16.51473224551083518, 109.5844237280190043 ) ) ;
#103647 = CARTESIAN_POINT ( 'NONE',  ( -21.55341960407619339, 5.719274019375674811, 23.54275706135235424 ) ) ;
#103648 = CARTESIAN_POINT ( 'NONE',  ( 21.55341960407619695, -5.719274019375665929, 66.04275706135236135 ) ) ;
#103649 = CARTESIAN_POINT ( 'NONE',  ( 14.34966873604972726, -8.224510206698740333, 65.83442372801900433 ) ) ;
#103650 = CARTESIAN_POINT ( 'NONE',  ( -19.02544592524342804, 5.153800228976336051, 76.04057627198102409 ) ) ;
#103651 = CARTESIAN_POINT ( 'NONE',  ( -16.55341960407617563, 4.379528057220093196, 98.54275706135234714 ) ) ;
#103652 = CARTESIAN_POINT ( 'NONE',  ( -5.153800228976607833, 19.02544592524334988, 42.70942372801901143 ) ) ;
#103653 = CARTESIAN_POINT ( 'NONE',  ( -10.72451020669870658, -18.67979575497194134, 29.58442372801901854 ) ) ;
#103654 = CARTESIAN_POINT ( 'NONE',  ( 14.34966873604960469, 8.224510206698951720, 84.16557627198103830 ) ) ;
#103655 = CARTESIAN_POINT ( 'NONE',  ( 19.02544592524343514, -5.153800228976328945, 103.5405762719809957 ) ) ;
#103656 = CARTESIAN_POINT ( 'NONE',  ( 12.14591786802327356, -12.06949235617739191, 85.62609039468568994 ) ) ;
#103657 = CARTESIAN_POINT ( 'NONE',  ( 10.72451020669871369, 18.67979575497193778, 67.08442372801901854 ) ) ;
#103658 = CARTESIAN_POINT ( 'NONE',  ( -0.05219959533934338120, 16.53943276465976808, 27.50109039468567929 ) ) ;
#103659 = CARTESIAN_POINT ( 'NONE',  ( -15.72974639402176322, -15.80617190586768395, 24.37609039468567573 ) ) ;
#103660 = CARTESIAN_POINT ( 'NONE',  ( -4.379528057220328563, 16.55341960407611168, 75.20724293864769550 ) ) ;
#103661 = ORIENTED_EDGE ( 'NONE', *, *, #136149, .T. ) ;
#103662 = CARTESIAN_POINT ( 'NONE',  ( -15.80617190586745835, -15.72974639402198527, 106.8739096053143811 ) ) ;
#103663 = CARTESIAN_POINT ( 'NONE',  ( 14.34966873604960469, 8.224510206698951720, 49.16557627198102409 ) ) ;
#103664 = ORIENTED_EDGE ( 'NONE', *, *, #10693, .F. ) ;
#103665 = CARTESIAN_POINT ( 'NONE',  ( 19.05341960407611168, 5.049401038298154454, 23.95724293864769194 ) ) ;
#103666 = CARTESIAN_POINT ( 'NONE',  ( 10.72451020669898902, -18.67979575497178502, 27.91557627198103830 ) ) ;
#103667 = CARTESIAN_POINT ( 'NONE',  ( -21.53943276465977519, -0.05219959533937600094, 33.75109039468568284 ) ) ;
#103668 = CARTESIAN_POINT ( 'NONE',  ( 0.05219959533910956823, 16.53943276465976808, 69.99890960531435269 ) ) ;
#103669 = CARTESIAN_POINT ( 'NONE',  ( -5.719274019375978568, 21.55341960407610458, 65.20724293864768129 ) ) ;
#103670 = CARTESIAN_POINT ( 'NONE',  ( -19.02544592524342804, 5.153800228976336051, 76.04057627198102409 ) ) ;
#103672 = CARTESIAN_POINT ( 'NONE',  ( -16.46253265017146816, -9.564922557961047289, 84.16775706135233293 ) ) ;
#103671 = CARTESIAN_POINT ( 'NONE',  ( 19.02544592524343514, -5.153800228976328945, 28.54057627198102409 ) ) ;
#103673 = CARTESIAN_POINT ( 'NONE',  ( 21.53943276465977519, -0.05219959533907433946, 53.74890960531437401 ) ) ;
#103674 = CARTESIAN_POINT ( 'NONE',  ( -19.05341960407611168, -5.049401038298163336, 46.45724293864768129 ) ) ;
#103675 = CARTESIAN_POINT ( 'NONE',  ( 5.049401038298161559, -19.05341960407611168, 72.70724293864768129 ) ) ;
#103676 = CARTESIAN_POINT ( 'NONE',  ( 16.53943276465976808, 0.05219959533934440121, 31.25109039468568639 ) ) ;
#103677 = CARTESIAN_POINT ( 'NONE',  ( 21.53943276465977519, 0.05219959533937863772, 26.25109039468567573 ) ) ;
#103678 = CARTESIAN_POINT ( 'NONE',  ( -12.14591786802309592, -12.06949235617757132, 46.87390960531435979 ) ) ;
#103679 = CARTESIAN_POINT ( 'NONE',  ( 10.81492255796106328, -18.62759615963255655, 55.41775706135234714 ) ) ;
#103680 = CARTESIAN_POINT ( 'NONE',  ( -16.51473224551069308, -9.474510206698971260, 106.6655762719810383 ) ) ;
#103681 = CARTESIAN_POINT ( 'NONE',  ( 21.55341960407610458, 5.719274019375980345, 68.95724293864769550 ) ) ;
#103683 = CARTESIAN_POINT ( 'NONE',  ( -12.14591786802326823, 12.06949235617739902, 58.12609039468568994 ) ) ;
#103682 = CARTESIAN_POINT ( 'NONE',  ( -5.823673210054116645, -21.52544592524344225, 107.2905762719810525 ) ) ;
#103684 = CARTESIAN_POINT ( 'NONE',  ( 18.67979575497178502, 10.72451020669898547, 54.16557627198103120 ) ) ;
#103685 = CARTESIAN_POINT ( 'NONE',  ( 10.81492255796106328, -18.62759615963255655, 100.4177570613523471 ) ) ;
#103686 = CARTESIAN_POINT ( 'NONE',  ( -16.51473224551069308, -9.474510206698971260, 56.66557627198103120 ) ) ;
#103687 = CARTESIAN_POINT ( 'NONE',  ( -5.153800228976328057, -19.02544592524343514, 107.2905762719810383 ) ) ;
#103688 = CARTESIAN_POINT ( 'NONE',  ( 5.049401038298161559, -19.05341960407611168, 72.70724293864768129 ) ) ;
#103689 = CARTESIAN_POINT ( 'NONE',  ( 17.05116617787848554, -6.768360034955522408, 86.15675553259193009 ) ) ;
#103690 = CARTESIAN_POINT ( 'NONE',  ( 13.97604488694548053, -13.89961937509957401, 70.62609039468567573 ) ) ;
#103692 = CARTESIAN_POINT ( 'NONE',  ( 21.55341960407610458, 5.719274019375980345, 28.95724293864769905 ) ) ;
#103691 = CARTESIAN_POINT ( 'NONE',  ( -16.46253265017146816, -9.564922557961047289, 19.16775706135233293 ) ) ;
#103693 = CARTESIAN_POINT ( 'NONE',  ( -14.34966873604972548, 8.224510206698743886, 103.3344237280190043 ) ) ;
#103694 = CARTESIAN_POINT ( 'NONE',  ( 13.89961937509957401, 13.97604488694547697, 81.87609039468564731 ) ) ;
#103695 = CARTESIAN_POINT ( 'NONE',  ( -15.06137443927361019, -15.06137443927335440, -58.85720012050613548 ) ) ;
#103696 = CARTESIAN_POINT ( 'NONE',  ( 16.46253265017146816, 9.564922557961045513, 21.66775706135233648 ) ) ;
#103697 = CARTESIAN_POINT ( 'NONE',  ( -13.89961937509957401, -13.97604488694547875, 89.37609039468563310 ) ) ;
#103698 = CARTESIAN_POINT ( 'NONE',  ( 19.03943276465977164, 0.05219959533936151252, 51.25109039468567573 ) ) ;
#103699 = CARTESIAN_POINT ( 'NONE',  ( -17.26172910966777962, -6.454744622555871558, 44.19353091350777163 ) ) ;
#103700 = CARTESIAN_POINT ( 'NONE',  ( -5.153800228976328057, -19.02544592524343514, 37.29057627198102409 ) ) ;
#103701 = CARTESIAN_POINT ( 'NONE',  ( -12.06949235617756955, 12.14591786802309770, 45.62390960531436690 ) ) ;
#103702 = CARTESIAN_POINT ( 'NONE',  ( 9.474510206698971260, -16.51473224551069308, 32.91557627198102409 ) ) ;
#103703 = CARTESIAN_POINT ( 'NONE',  ( 12.06949235617757843, -12.14591786802309237, 38.12390960531436690 ) ) ;
#103704 = LINE ( 'NONE', #26877, #90442 ) ;
#103705 = CARTESIAN_POINT ( 'NONE',  ( 12.06949235617739724, 12.14591786802326823, 111.8760903946856615 ) ) ;
#103706 = CARTESIAN_POINT ( 'NONE',  ( -19.02544592524342804, 5.153800228976336051, 56.04057627198100988 ) ) ;
#103707 = CARTESIAN_POINT ( 'NONE',  ( -0.05219959533936034679, 19.03943276465977164, 27.50109039468566507 ) ) ;
#103708 = CARTESIAN_POINT ( 'NONE',  ( -4.379528057220086978, -16.55341960407618274, 29.79275706135234358 ) ) ;
#103709 = CARTESIAN_POINT ( 'NONE',  ( 18.62759615963271287, -10.81492255796078972, 38.33224293864768839 ) ) ;
#103711 = VERTEX_POINT ( 'NONE', #195997 ) ;
#103710 = CARTESIAN_POINT ( 'NONE',  ( 10.81492255796106328, -18.62759615963255655, 90.41775706135236135 ) ) ;
#103712 = CARTESIAN_POINT ( 'NONE',  ( -0.05219959533909027116, -19.03943276465977164, 102.4989096053143669 ) ) ;
#103713 = CARTESIAN_POINT ( 'NONE',  ( -5.049401038298153566, 19.05341960407611168, 90.20724293864766707 ) ) ;
#103714 = CARTESIAN_POINT ( 'NONE',  ( -32.20268589050812125, -23.72850345486251200, -20.40273169984848778 ) ) ;
#103715 = CARTESIAN_POINT ( 'NONE',  ( -10.72451020669898014, 18.67979575497178502, 115.4155762719810241 ) ) ;
#103716 = CARTESIAN_POINT ( 'NONE',  ( -16.52544592524342804, 4.483927247898546575, 76.04057627198102409 ) ) ;
#103718 = CARTESIAN_POINT ( 'NONE',  ( 19.03943276465977164, -0.05219959533909143690, 68.74890960531436690 ) ) ;
#103717 = CARTESIAN_POINT ( 'NONE',  ( -5.719274019375978568, 21.55341960407610458, 75.20724293864769550 ) ) ;
#103719 = CARTESIAN_POINT ( 'NONE',  ( -9.474510206698964154, 16.51473224551069663, 70.41557627198102409 ) ) ;
#103720 = CARTESIAN_POINT ( 'NONE',  ( -21.55341960407610458, -5.719274019375992779, 91.45724293864769550 ) ) ;
#103721 = ORIENTED_EDGE ( 'NONE', *, *, #111598, .T. ) ;
#103722 = CARTESIAN_POINT ( 'NONE',  ( 9.564922557960805705, 16.46253265017160317, 54.58224293864769550 ) ) ;
#103724 = CARTESIAN_POINT ( 'NONE',  ( 31.99999999999934275, 1.011436372600181938E-12, 95.00000000000021316 ) ) ;
#103723 = CARTESIAN_POINT ( 'NONE',  ( 16.55341960407611168, 4.379528057220329451, 98.95724293864770971 ) ) ;
#103725 = CARTESIAN_POINT ( 'NONE',  ( -16.51473224551069308, -9.474510206698971260, 66.66557627198102409 ) ) ;
#103726 = CARTESIAN_POINT ( 'NONE',  ( 16.46253265017146816, 9.564922557961045513, 81.66775706135233293 ) ) ;
#103727 = CARTESIAN_POINT ( 'NONE',  ( 16.53943276465976808, -0.05219959533910856209, 103.7489096053143669 ) ) ;
#103728 = CARTESIAN_POINT ( 'NONE',  ( 21.55341960407619695, -5.719274019375665929, 56.04275706135235424 ) ) ;
#103730 = CARTESIAN_POINT ( 'NONE',  ( 21.55341960407619695, -5.719274019375665929, 26.04275706135235779 ) ) ;
#103729 = CARTESIAN_POINT ( 'NONE',  ( 5.153800228976335163, 19.02544592524342804, 54.79057627198103120 ) ) ;
#103731 = CARTESIAN_POINT ( 'NONE',  ( -4.379528057220328563, 16.55341960407611168, 105.2072429386477097 ) ) ;
#103732 = CARTESIAN_POINT ( 'NONE',  ( 9.128739734650142879, -39.45218800495355538, -25.46847458086233829 ) ) ;
#103733 = CARTESIAN_POINT ( 'NONE',  ( 16.51473224551069308, 9.474510206698969483, 74.16557627198103830 ) ) ;
#103734 = CARTESIAN_POINT ( 'NONE',  ( -17.81289503416611808, 24.51734667627700404, 143.9500000054623854 ) ) ;
#103736 = CARTESIAN_POINT ( 'NONE',  ( 10.72451020669898902, -18.67979575497178502, 22.91557627198102765 ) ) ;
#103735 = CARTESIAN_POINT ( 'NONE',  ( 5.049401038297881783, 19.05341960407617563, 107.2927570613523187 ) ) ;
#103737 = CARTESIAN_POINT ( 'NONE',  ( -18.62759615963255300, -10.81492255796106328, 44.16775706135234714 ) ) ;
#103738 = CARTESIAN_POINT ( 'NONE',  ( 9.564922557960805705, 16.46253265017160317, 99.58224293864770971 ) ) ;
#103739 = CARTESIAN_POINT ( 'NONE',  ( 19.02544592524334988, 5.153800228976608722, 86.45942372801900433 ) ) ;
#103740 = CARTESIAN_POINT ( 'NONE',  ( -19.05341960407611168, -5.049401038298163336, 51.45724293864770260 ) ) ;
#103741 = CARTESIAN_POINT ( 'NONE',  ( -0.05219959533910754901, -16.53943276465976808, 82.49890960531436690 ) ) ;
#103742 = CARTESIAN_POINT ( 'NONE',  ( -19.05341960407611168, -5.049401038298163336, 106.4572429386476955 ) ) ;
#103743 = CARTESIAN_POINT ( 'NONE',  ( 12.14591786802309770, 12.06949235617756955, 74.37390960531436690 ) ) ;
#103744 = CARTESIAN_POINT ( 'NONE',  ( 16.51473224551069308, 9.474510206698969483, 99.16557627198102409 ) ) ;
#103745 = ADVANCED_FACE ( 'NONE', ( #23129 ), #150926, .F. ) ;
#103746 = CARTESIAN_POINT ( 'NONE',  ( 9.564922557961047289, -16.46253265017146816, 50.41775706135233293 ) ) ;
#103749 = CARTESIAN_POINT ( 'NONE',  ( 13.97604488694527802, 13.89961937509977652, 24.37390960531435624 ) ) ;
#103748 = CARTESIAN_POINT ( 'NONE',  ( 4.379528057220339221, -16.55341960407611168, 37.70724293864769550 ) ) ;
#103747 = CARTESIAN_POINT ( 'NONE',  ( -5.049401038298153566, 19.05341960407611168, 55.20724293864769550 ) ) ;
#103750 = ORIENTED_EDGE ( 'NONE', *, *, #72556, .F. ) ;
#103751 = CARTESIAN_POINT ( 'NONE',  ( 21.55341960407619695, -5.719274019375665929, 51.04275706135234714 ) ) ;
#103752 = CARTESIAN_POINT ( 'NONE',  ( -13.97604488694547697, 13.89961937509957934, 78.12609039468567573 ) ) ;
#103753 = CARTESIAN_POINT ( 'NONE',  ( -14.29746914071049879, 8.314922557960819915, 30.83224293864770260 ) ) ;
#103754 = CARTESIAN_POINT ( 'NONE',  ( 15.80617190586746368, 15.72974639402197994, 104.3739096053143669 ) ) ;
#103755 = CARTESIAN_POINT ( 'NONE',  ( 18.67979575497178502, 10.72451020669898547, 34.16557627198102409 ) ) ;
#103756 = CARTESIAN_POINT ( 'NONE',  ( 16.52544592524342804, -4.483927247898539470, 88.54057627198103830 ) ) ;
#103757 = CARTESIAN_POINT ( 'NONE',  ( -19.03943276465977164, 0.05219959533909376836, 41.24890960531435269 ) ) ;
#103758 = CARTESIAN_POINT ( 'NONE',  ( 14.29746914071037800, 8.314922557961029526, 106.6677570613523756 ) ) ;
#103759 = CARTESIAN_POINT ( 'NONE',  ( -4.483927247898782831, 16.52544592524335698, 72.70942372801901854 ) ) ;
#103760 = CARTESIAN_POINT ( 'NONE',  ( -16.46253265017146816, -9.564922557961047289, 24.16775706135233648 ) ) ;
#103761 = CARTESIAN_POINT ( 'NONE',  ( 16.46253265017160672, -9.564922557960803928, 98.33224293864769550 ) ) ;
#103762 = CARTESIAN_POINT ( 'NONE',  ( -13.89961937509977652, 13.97604488694528158, 80.62390960531436690 ) ) ;
#103763 = CARTESIAN_POINT ( 'NONE',  ( 8.314922557961029526, -14.29746914071037800, 70.41775706135236135 ) ) ;
#103764 = CARTESIAN_POINT ( 'NONE',  ( -9.564922557960796823, -16.46253265017161027, 32.08224293864769550 ) ) ;
#103765 = CARTESIAN_POINT ( 'NONE',  ( -8.224510206698948167, 14.34966873604960824, 45.41557627198103830 ) ) ;
#103767 = CARTESIAN_POINT ( 'NONE',  ( 0.05219959533909260263, 19.03943276465977164, 84.99890960531436690 ) ) ;
#103766 = CARTESIAN_POINT ( 'NONE',  ( 13.89961937509977652, -13.97604488694527269, 113.1239096053143527 ) ) ;
#103768 = CARTESIAN_POINT ( 'NONE',  ( 21.53943276465977519, -0.05219959533907433946, 23.74890960531435269 ) ) ;
#103769 = CARTESIAN_POINT ( 'NONE',  ( 16.55341960407611168, 4.379528057220329451, 73.95724293864769550 ) ) ;
#103770 = CARTESIAN_POINT ( 'NONE',  ( 14.29746914071049879, -8.314922557960816363, 68.33224293864769550 ) ) ;
#103772 = CARTESIAN_POINT ( 'NONE',  ( 17.49999999999999645, -3.805241302050391461, 32.87352472782595214 ) ) ;
#103771 = CARTESIAN_POINT ( 'NONE',  ( -12.06949235617739369, -12.14591786802326823, 49.37609039468569705 ) ) ;
#103773 = CARTESIAN_POINT ( 'NONE',  ( -19.02544592524334988, -5.153800228976617603, 63.95942372801899012 ) ) ;
#103774 = CARTESIAN_POINT ( 'NONE',  ( -19.03943276465977164, 0.05219959533909376836, 86.24890960531436690 ) ) ;
#103775 = CARTESIAN_POINT ( 'NONE',  ( 13.97604488694548053, -13.89961937509957401, 65.62609039468567573 ) ) ;
#103776 = CARTESIAN_POINT ( 'NONE',  ( 8.571926809382597767, 26.38167802310806209, 148.7750000027311899 ) ) ;
#103778 = CARTESIAN_POINT ( 'NONE',  ( 12.14591786802327356, -12.06949235617739191, 95.62609039468568994 ) ) ;
#103777 = CARTESIAN_POINT ( 'NONE',  ( 16.52544592524335698, 4.483927247898782831, 21.45942372801901499 ) ) ;
#103779 = CARTESIAN_POINT ( 'NONE',  ( -19.02544592524342804, 5.153800228976336051, 41.04057627198103120 ) ) ;
#103780 = CARTESIAN_POINT ( 'NONE',  ( -18.67979575497178146, -10.72451020669898902, 21.66557627198102409 ) ) ;
#103781 = CARTESIAN_POINT ( 'NONE',  ( -15.72974639402176322, -15.80617190586768395, 59.37609039468568284 ) ) ;
#103782 = CARTESIAN_POINT ( 'NONE',  ( 4.483927247898790824, -16.52544592524335698, 25.20942372801901854 ) ) ;
#103784 = CARTESIAN_POINT ( 'NONE',  ( 16.51473224551069308, 9.474510206698969483, 74.16557627198103830 ) ) ;
#103783 = CARTESIAN_POINT ( 'NONE',  ( -5.049401038297874678, -19.05341960407618274, 54.79275706135234003 ) ) ;
#103785 = CARTESIAN_POINT ( 'NONE',  ( -13.97604488694527625, -13.89961937509977652, 111.8739096053143243 ) ) ;
#103787 = CARTESIAN_POINT ( 'NONE',  ( 5.049401038298161559, -19.05341960407611168, 82.70724293864770971 ) ) ;
#103786 = CARTESIAN_POINT ( 'NONE',  ( 14.34966873604960469, 8.224510206698951720, 79.16557627198103830 ) ) ;
#103788 = CARTESIAN_POINT ( 'NONE',  ( -5.049401038298153566, 19.05341960407611168, 80.20724293864769550 ) ) ;
#103789 = CARTESIAN_POINT ( 'NONE',  ( -9.564922557961040184, 16.46253265017147172, 97.91775706135233293 ) ) ;
#103790 = CARTESIAN_POINT ( 'NONE',  ( 5.719274019375991003, -21.55341960407610458, 67.70724293864769550 ) ) ;
#103791 = CARTESIAN_POINT ( 'NONE',  ( -5.049401038298153566, 19.05341960407611168, 25.20724293864768484 ) ) ;
#103792 = CARTESIAN_POINT ( 'NONE',  ( 9.474510206698729675, 16.51473224551082808, 57.08442372801900433 ) ) ;
#103793 = CARTESIAN_POINT ( 'NONE',  ( -13.89961937509977652, 13.97604488694528158, 55.62390960531434558 ) ) ;
#103794 = CARTESIAN_POINT ( 'NONE',  ( 9.474510206698971260, -16.51473224551069308, 97.91557627198102409 ) ) ;
#103795 = ORIENTED_EDGE ( 'NONE', *, *, #105746, .T. ) ;
#103796 = CARTESIAN_POINT ( 'NONE',  ( 21.55341960407610458, 5.719274019375980345, 83.95724293864770971 ) ) ;
#103798 = CARTESIAN_POINT ( 'NONE',  ( -19.02544592524334988, -5.153800228976617603, 43.95942372801899012 ) ) ;
#103797 = CARTESIAN_POINT ( 'NONE',  ( -16.53943276465976808, 0.05219959533911058130, 91.24890960531436690 ) ) ;
#103799 = CARTESIAN_POINT ( 'NONE',  ( 5.823673210054125526, 21.52544592524343514, 69.79057627198102409 ) ) ;
#103800 = CARTESIAN_POINT ( 'NONE',  ( 18.62759615963271287, -10.81492255796078972, 73.33224293864769550 ) ) ;
#103801 = CARTESIAN_POINT ( 'NONE',  ( -16.53943276465976808, 0.05219959533911058130, 31.24890960531435979 ) ) ;
#103802 = CARTESIAN_POINT ( 'NONE',  ( 5.823673210054444382, -21.52544592524334988, 105.2094237280190328 ) ) ;
#103803 = CARTESIAN_POINT ( 'NONE',  ( -13.89961937509977652, 13.97604488694528158, 85.62390960531433848 ) ) ;
#103804 = CARTESIAN_POINT ( 'NONE',  ( -5.153800228976328057, -19.02544592524343514, 37.29057627198102409 ) ) ;
#103805 = CARTESIAN_POINT ( 'NONE',  ( 21.55341960407619695, -5.719274019375665929, 41.04275706135236135 ) ) ;
#103806 = CARTESIAN_POINT ( 'NONE',  ( 0.05219959533937995610, -21.53943276465977519, 55.00109039468568284 ) ) ;
#103807 = CARTESIAN_POINT ( 'NONE',  ( 13.89961937509977652, -13.97604488694527269, 48.12390960531435979 ) ) ;
#103808 = CARTESIAN_POINT ( 'NONE',  ( 21.53943276465977519, 0.05219959533937863772, 26.25109039468567573 ) ) ;
#103809 = CARTESIAN_POINT ( 'NONE',  ( -5.153800228976607833, 19.02544592524334988, 62.70942372801899722 ) ) ;
#103810 = CARTESIAN_POINT ( 'NONE',  ( 9.474510206698971260, -16.51473224551069308, 32.91557627198102409 ) ) ;
#103811 = CARTESIAN_POINT ( 'NONE',  ( 14.34966873604972726, -8.224510206698740333, 30.83442372801902209 ) ) ;
#103812 = CARTESIAN_POINT ( 'NONE',  ( -19.03943276465977164, 0.05219959533909376836, 21.24890960531436335 ) ) ;
#103813 = CARTESIAN_POINT ( 'NONE',  ( 14.29746914071037800, 8.314922557961029526, 71.66775706135234714 ) ) ;
#103814 = CARTESIAN_POINT ( 'NONE',  ( -9.564922557960796823, -16.46253265017161027, 37.08224293864768839 ) ) ;
#103815 = CARTESIAN_POINT ( 'NONE',  ( 23.14613071126333921, -10.96668486446927204, 168.1016194467971445 ) ) ;
#103816 = CARTESIAN_POINT ( 'NONE',  ( -13.97604488694527625, -13.89961937509977652, 86.87390960531436690 ) ) ;
#103817 = CARTESIAN_POINT ( 'NONE',  ( 16.46253265017160672, -9.564922557960803928, 28.33224293864769550 ) ) ;
#103818 = CARTESIAN_POINT ( 'NONE',  ( 21.53943276465977519, -0.05219959533907433946, 73.74890960531433848 ) ) ;
#103819 = CARTESIAN_POINT ( 'NONE',  ( 14.29746914071037800, 8.314922557961029526, 51.66775706135234714 ) ) ;
#103820 = CARTESIAN_POINT ( 'NONE',  ( -18.67979575497193778, 10.72451020669871902, 103.3344237280190043 ) ) ;
#103821 = CARTESIAN_POINT ( 'NONE',  ( 19.03943276465977164, -0.05219959533909143690, 38.74890960531436690 ) ) ;
#103822 = CARTESIAN_POINT ( 'NONE',  ( -14.29746914071049879, 8.314922557960819915, 30.83224293864770260 ) ) ;
#103823 = CARTESIAN_POINT ( 'NONE',  ( -12.14591786802309592, -12.06949235617757132, 71.87390960531438111 ) ) ;
#103824 = CARTESIAN_POINT ( 'NONE',  ( -19.03943276465977164, 0.05219959533909376836, 66.24890960531436690 ) ) ;
#103825 = CARTESIAN_POINT ( 'NONE',  ( -21.55341960407619339, 5.719274019375674811, 103.5427570613523613 ) ) ;
#103826 = CARTESIAN_POINT ( 'NONE',  ( 21.55341960407619695, -5.719274019375665929, 26.04275706135235779 ) ) ;
#103827 = CARTESIAN_POINT ( 'NONE',  ( 13.89961937509977652, -13.97604488694527269, 73.12390960531436690 ) ) ;
#103828 = CARTESIAN_POINT ( 'NONE',  ( 18.67979575497194134, -10.72451020669871369, 85.83442372801901854 ) ) ;
#103829 = CARTESIAN_POINT ( 'NONE',  ( -14.29746914071037622, -8.314922557961029526, 64.16775706135234714 ) ) ;
#103830 = CARTESIAN_POINT ( 'NONE',  ( -0.05219959533934338120, 16.53943276465976808, 32.50109039468568284 ) ) ;
#103832 = CARTESIAN_POINT ( 'NONE',  ( 10.81492255796106328, -18.62759615963255655, 100.4177570613523471 ) ) ;
#103831 = CARTESIAN_POINT ( 'NONE',  ( 14.29746914071049879, -8.314922557960816363, 93.33224293864769550 ) ) ;
#103833 = CARTESIAN_POINT ( 'NONE',  ( 14.29746914071049879, -8.314922557960816363, 33.33224293864769550 ) ) ;
#103834 = CARTESIAN_POINT ( 'NONE',  ( -5.049401038298153566, 19.05341960407611168, 30.20724293864768839 ) ) ;
#103835 = CARTESIAN_POINT ( 'NONE',  ( -16.53943276465976808, -0.05219959533934237506, 53.75109039468568994 ) ) ;
#103836 = CARTESIAN_POINT ( 'NONE',  ( -14.34966873604960291, -8.224510206698953496, 56.66557627198103830 ) ) ;
#103837 = CARTESIAN_POINT ( 'NONE',  ( 14.34966873604972726, -8.224510206698740333, 95.83442372801903275 ) ) ;
#103838 = CARTESIAN_POINT ( 'NONE',  ( 9.564922557960805705, 16.46253265017160317, 109.5822429386476955 ) ) ;
#103839 = CARTESIAN_POINT ( 'NONE',  ( 15.72974639402199770, -15.80617190586745480, 38.12390960531436690 ) ) ;
#103840 = CARTESIAN_POINT ( 'NONE',  ( -5.049401038297874678, -19.05341960407617918, 19.79275706135233293 ) ) ;
#103841 = CARTESIAN_POINT ( 'NONE',  ( -14.29746914071049879, 8.314922557960819915, 80.83224293864769550 ) ) ;
#103842 = CARTESIAN_POINT ( 'NONE',  ( 19.03943276465977164, -0.05219959533909143690, 88.74890960531436690 ) ) ;
#103843 = ORIENTED_EDGE ( 'NONE', *, *, #52799, .T. ) ;
#103844 = CARTESIAN_POINT ( 'NONE',  ( -16.52544592524335698, -4.483927247898792601, 33.95942372801901143 ) ) ;
#103845 = CARTESIAN_POINT ( 'NONE',  ( 16.46253265017160672, -9.564922557960803928, 38.33224293864768839 ) ) ;
#103847 =( NAMED_UNIT ( * ) PLANE_ANGLE_UNIT ( ) SI_UNIT ( $, .RADIAN. ) );
#103846 = CARTESIAN_POINT ( 'NONE',  ( -12.06949235617739369, -12.14591786802326823, 39.37609039468567573 ) ) ;
#103848 = CARTESIAN_POINT ( 'NONE',  ( 0.05219959533936267826, -19.03943276465977164, 50.00109039468566863 ) ) ;
#103849 = CARTESIAN_POINT ( 'NONE',  ( 0.05219959533909260263, 19.03943276465977164, 39.99890960531436690 ) ) ;
#103850 = CARTESIAN_POINT ( 'NONE',  ( -16.53943276465976808, -0.05219959533934237506, 73.75109039468567573 ) ) ;
#103851 = CARTESIAN_POINT ( 'NONE',  ( -13.97604488694547697, 13.89961937509957934, 98.12609039468566152 ) ) ;
#103852 = CARTESIAN_POINT ( 'NONE',  ( -13.89961937509957401, -13.97604488694547875, 29.37609039468565797 ) ) ;
#103853 = CARTESIAN_POINT ( 'NONE',  ( -9.564922557960796823, -16.46253265017161027, 62.08224293864769550 ) ) ;
#103854 = CARTESIAN_POINT ( 'NONE',  ( 12.14591786802309770, 12.06949235617756955, 94.37390960531436690 ) ) ;
#103855 = CARTESIAN_POINT ( 'NONE',  ( -16.46253265017146816, -9.564922557961047289, 64.16775706135233293 ) ) ;
#103856 = CARTESIAN_POINT ( 'NONE',  ( 10.81492255796078972, 18.62759615963270932, 59.58224293864770260 ) ) ;
#103857 = CARTESIAN_POINT ( 'NONE',  ( -16.46253265017146816, -9.564922557961047289, 39.16775706135234003 ) ) ;
#103858 = CARTESIAN_POINT ( 'NONE',  ( 19.39056639909673763, 5.500000000000001776, 98.28948781074342378 ) ) ;
#103859 = CARTESIAN_POINT ( 'NONE',  ( -5.719274019375978568, 21.55341960407610458, 85.20724293864770971 ) ) ;
#103860 = CARTESIAN_POINT ( 'NONE',  ( -17.50000000000001776, 5.622605283950872668, 83.68792689403892382 ) ) ;
#103861 = CARTESIAN_POINT ( 'NONE',  ( -16.51473224551082808, 9.474510206698731452, 108.3344237280190043 ) ) ;
#103862 = CARTESIAN_POINT ( 'NONE',  ( -18.56197773271731677, 5.499999999999904965, 58.55066217314453780 ) ) ;
#103863 = CARTESIAN_POINT ( 'NONE',  ( 4.483927247898790824, -16.52544592524335698, 30.20942372801902565 ) ) ;
#103864 = CARTESIAN_POINT ( 'NONE',  ( 19.02544592524343514, -5.153800228976328945, 48.54057627198103120 ) ) ;
#103865 = CARTESIAN_POINT ( 'NONE',  ( 0.05219959533909260263, 19.03943276465977164, 114.9989096053143669 ) ) ;
#103866 = CARTESIAN_POINT ( 'NONE',  ( 21.55341960407610458, 5.719274019375980345, 93.95724293864770971 ) ) ;
#103867 = CARTESIAN_POINT ( 'NONE',  ( -18.62759615963255300, -10.81492255796106328, 64.16775706135234714 ) ) ;
#103869 = CARTESIAN_POINT ( 'NONE',  ( 0.05219959533936267826, -19.03943276465977164, 20.00109039468567218 ) ) ;
#103868 = CARTESIAN_POINT ( 'NONE',  ( 9.474510206698729675, 16.51473224551082808, 102.0844237280190043 ) ) ;
#103870 = CARTESIAN_POINT ( 'NONE',  ( 0.05219959533910956823, 16.53943276465976808, 29.99890960531435979 ) ) ;
#103871 = CARTESIAN_POINT ( 'NONE',  ( -5.823673210054116645, -21.52544592524344225, 102.2905762719810383 ) ) ;
#103872 = CARTESIAN_POINT ( 'NONE',  ( -16.53943276465976808, 0.05219959533911058130, 46.24890960531435979 ) ) ;
#103873 = CARTESIAN_POINT ( 'NONE',  ( -5.153800228976607833, 19.02544592524334988, 87.70942372801897591 ) ) ;
#103874 = ADVANCED_FACE ( 'NONE', ( #145221 ), #178582, .T. ) ;
#103875 = CARTESIAN_POINT ( 'NONE',  ( -16.51473224551082808, 9.474510206698731452, 53.33442372801900433 ) ) ;
#103876 = CARTESIAN_POINT ( 'NONE',  ( 21.53943276465977519, 0.05219959533937863772, 76.25109039468568994 ) ) ;
#103877 = CARTESIAN_POINT ( 'NONE',  ( -9.564922557961040184, 16.46253265017147172, 37.91775706135233293 ) ) ;
#103878 = CARTESIAN_POINT ( 'NONE',  ( -5.049401038298153566, 19.05341960407611168, 25.20724293864768484 ) ) ;
#103879 = CARTESIAN_POINT ( 'NONE',  ( -5.823673210054116645, -21.52544592524344225, 47.29057627198103120 ) ) ;
#103880 = CARTESIAN_POINT ( 'NONE',  ( -16.55341960407611168, -4.379528057220339221, 36.45724293864768839 ) ) ;
#103881 = CARTESIAN_POINT ( 'NONE',  ( -13.89961937509957401, -13.97604488694547875, 19.37609039468566507 ) ) ;
#103882 = CARTESIAN_POINT ( 'NONE',  ( -14.29746914071037622, -8.314922557961029526, 69.16775706135234714 ) ) ;
#103883 = CARTESIAN_POINT ( 'NONE',  ( 4.379528057220339221, -16.55341960407611168, 42.70724293864770260 ) ) ;
#103884 = CARTESIAN_POINT ( 'NONE',  ( 10.72451020669871369, 18.67979575497193778, 72.08442372801899012 ) ) ;
#103885 = CARTESIAN_POINT ( 'NONE',  ( 18.67979575497194134, -10.72451020669871369, 70.83442372801901854 ) ) ;
#103886 = CARTESIAN_POINT ( 'NONE',  ( -15.80617190586745835, -15.72974639402198527, 61.87390960531436690 ) ) ;
#103887 = CARTESIAN_POINT ( 'NONE',  ( -5.153800228976328057, -19.02544592524343514, 42.29057627198101699 ) ) ;
#103888 = CARTESIAN_POINT ( 'NONE',  ( 21.55341960407619695, -5.719274019375665929, 46.04275706135234714 ) ) ;
#103889 = CARTESIAN_POINT ( 'NONE',  ( -4.483927247898539470, -16.52544592524342804, 112.2905762719810241 ) ) ;
#103890 = CARTESIAN_POINT ( 'NONE',  ( 13.97604488694527802, 13.89961937509977652, 39.37390960531435269 ) ) ;
#103891 = CARTESIAN_POINT ( 'NONE',  ( 4.379528057220339221, -16.55341960407611168, 87.70724293864769550 ) ) ;
#103892 = CARTESIAN_POINT ( 'NONE',  ( 19.03943276465977164, -0.05219959533909143690, 83.74890960531436690 ) ) ;
#103893 = CARTESIAN_POINT ( 'NONE',  ( 12.14591786802309770, 12.06949235617756955, 44.37390960531435979 ) ) ;
#103894 = CARTESIAN_POINT ( 'NONE',  ( 8.224510206698953496, -14.34966873604960469, 102.9155762719810383 ) ) ;
#103895 = CARTESIAN_POINT ( 'NONE',  ( 15.72974639402199770, -15.80617190586745480, 63.12390960531435979 ) ) ;
#103896 = CARTESIAN_POINT ( 'NONE',  ( 18.62759615963271287, -10.81492255796078972, 108.3322429386477097 ) ) ;
#103897 = CARTESIAN_POINT ( 'NONE',  ( -16.46253265017160317, 9.564922557960807481, 115.8322429386477097 ) ) ;
#103899 = CARTESIAN_POINT ( 'NONE',  ( 0.05219959533934541429, -16.53943276465976808, 30.00109039468568284 ) ) ;
#103898 = CARTESIAN_POINT ( 'NONE',  ( 5.153800228976335163, 19.02544592524342804, 59.79057627198100988 ) ) ;
#103900 = CARTESIAN_POINT ( 'NONE',  ( -15.80617190586745835, -15.72974639402198527, 56.87390960531436690 ) ) ;
#103901 = CARTESIAN_POINT ( 'NONE',  ( -15.72974639402176322, -15.80617190586768395, 89.37609039468568994 ) ) ;
#103902 = CARTESIAN_POINT ( 'NONE',  ( 19.02544592524343514, -5.153800228976328945, 73.54057627198103830 ) ) ;
#103903 = CARTESIAN_POINT ( 'NONE',  ( 5.823673210054125526, 21.52544592524343514, 114.7905762719810383 ) ) ;
#103904 = CARTESIAN_POINT ( 'NONE',  ( -16.51473224551069308, -9.474510206698971260, 106.6655762719810383 ) ) ;
#103905 = CARTESIAN_POINT ( 'NONE',  ( 4.483927247898790824, -16.52544592524335698, 90.20942372801903275 ) ) ;
#103906 = CARTESIAN_POINT ( 'NONE',  ( 0.05219959533937995610, -21.53943276465977519, 70.00109039468568994 ) ) ;
#103907 = CARTESIAN_POINT ( 'NONE',  ( -0.05219959533937732626, 21.53943276465977519, 102.5010903946856899 ) ) ;
#103908 = CARTESIAN_POINT ( 'NONE',  ( 4.483927247898790824, -16.52544592524335698, 55.20942372801902565 ) ) ;
#103909 = CARTESIAN_POINT ( 'NONE',  ( -21.55341960407610458, -5.719274019375992779, 111.4572429386476813 ) ) ;
#103910 = CARTESIAN_POINT ( 'NONE',  ( -13.97604488694527625, -13.89961937509977652, 21.87390960531435979 ) ) ;
#103911 = CARTESIAN_POINT ( 'NONE',  ( 5.823673210054444382, -21.52544592524334988, 95.20942372801903275 ) ) ;
#103912 = ORIENTED_EDGE ( 'NONE', *, *, #39003, .T. ) ;
#103913 = CARTESIAN_POINT ( 'NONE',  ( 18.62759615963271287, -10.81492255796078972, 88.33224293864769550 ) ) ;
#103914 = CARTESIAN_POINT ( 'NONE',  ( -16.51473224551082808, 9.474510206698731452, 48.33442372801900433 ) ) ;
#103915 = CARTESIAN_POINT ( 'NONE',  ( 15.72974639402199770, -15.80617190586745480, 53.12390960531436690 ) ) ;
#103917 = CARTESIAN_POINT ( 'NONE',  ( -4.379528057220328563, 16.55341960407611168, 40.20724293864769550 ) ) ;
#103916 = CARTESIAN_POINT ( 'NONE',  ( -19.05341960407611168, -5.049401038298163336, 101.4572429386476955 ) ) ;
#103918 = CARTESIAN_POINT ( 'NONE',  ( 12.22613352584845359, -10.45440487129810236, -61.62309247082062313 ) ) ;
#103919 = DIRECTION ( 'NONE',  ( -0.000000000000000000, -0.000000000000000000, 1.000000000000000000 ) ) ;
#103920 = CARTESIAN_POINT ( 'NONE',  ( 19.02544592524334988, 5.153800228976608722, 106.4594237280190185 ) ) ;
#103921 = CARTESIAN_POINT ( 'NONE',  ( 5.719274019375991003, -21.55341960407610458, 87.70724293864769550 ) ) ;
#103922 = CARTESIAN_POINT ( 'NONE',  ( -16.53943276465976808, 0.05219959533911058130, 46.24890960531435979 ) ) ;
#103923 = CARTESIAN_POINT ( 'NONE',  ( -16.52544592524335698, -4.483927247898792601, 28.95942372801902209 ) ) ;
#103924 = CARTESIAN_POINT ( 'NONE',  ( 19.05341960407611168, 5.049401038298154454, 38.95724293864767418 ) ) ;
#103926 = CARTESIAN_POINT ( 'NONE',  ( 9.474510206698729675, 16.51473224551082808, 82.08442372801899012 ) ) ;
#103925 = CARTESIAN_POINT ( 'NONE',  ( -10.72451020669870658, -18.67979575497194134, 19.58442372801901143 ) ) ;
#103927 = CARTESIAN_POINT ( 'NONE',  ( 19.03943276465977164, -0.05219959533909143690, 83.74890960531436690 ) ) ;
#103928 = CARTESIAN_POINT ( 'NONE',  ( 9.564922557960805705, 16.46253265017160317, 74.58224293864769550 ) ) ;
#103929 = CARTESIAN_POINT ( 'NONE',  ( 5.719274019375991003, -21.55341960407610458, 77.70724293864770971 ) ) ;
#103930 = CARTESIAN_POINT ( 'NONE',  ( 13.89961937509977652, -13.97604488694527269, 38.12390960531436690 ) ) ;
#103931 = CARTESIAN_POINT ( 'NONE',  ( 22.33498979914476479, 29.77355716069116198, -8.000000000000000000 ) ) ;
#103932 = CARTESIAN_POINT ( 'NONE',  ( -16.53943276465976808, 0.05219959533911058130, 61.24890960531435979 ) ) ;
#103933 = CARTESIAN_POINT ( 'NONE',  ( 0.05219959533909260263, 19.03943276465977164, 84.99890960531436690 ) ) ;
#103934 = CARTESIAN_POINT ( 'NONE',  ( -8.906447517083053711, -27.41122689804191026, 140.6500000054623740 ) ) ;
#103935 = CARTESIAN_POINT ( 'NONE',  ( 13.97604488694548053, -13.89961937509957401, 60.62609039468564731 ) ) ;
#103936 = CARTESIAN_POINT ( 'NONE',  ( -18.67979575497178146, -10.72451020669898902, 81.66557627198103830 ) ) ;
#103937 = CARTESIAN_POINT ( 'NONE',  ( 19.05341960407617918, -5.049401038297876454, 31.04275706135232227 ) ) ;
#103938 = CARTESIAN_POINT ( 'NONE',  ( -13.89961937509977652, 13.97604488694528158, 105.6239096053143527 ) ) ;
#103939 = DIRECTION ( 'NONE',  ( 0.000000000000000000, 0.000000000000000000, -1.000000000000000000 ) ) ;
#103940 = CARTESIAN_POINT ( 'NONE',  ( 0.05219959533907565091, 21.53943276465977519, 39.99890960531436690 ) ) ;
#103941 = CARTESIAN_POINT ( 'NONE',  ( 0.05219959533909260263, 19.03943276465977164, 74.99890960531435269 ) ) ;
#103942 = CARTESIAN_POINT ( 'NONE',  ( -10.72451020669870658, -18.67979575497194134, 54.58442372801901143 ) ) ;
#103943 = CARTESIAN_POINT ( 'NONE',  ( -19.03943276465977164, 0.05219959533909376836, 31.24890960531435979 ) ) ;
#103944 = EDGE_CURVE ( 'NONE', #170159, #187938, #14259, .T. ) ;
#103946 = ORIENTED_EDGE ( 'NONE', *, *, #163400, .F. ) ;
#103945 = CARTESIAN_POINT ( 'NONE',  ( -5.823673210054431948, 21.52544592524334988, 22.70942372801901499 ) ) ;
#103947 = CARTESIAN_POINT ( 'NONE',  ( 18.62759615963255655, 10.81492255796105972, 36.66775706135234714 ) ) ;
#103948 = ORIENTED_EDGE ( 'NONE', *, *, #79148, .T. ) ;
#103949 = CARTESIAN_POINT ( 'NONE',  ( 19.05341960407611168, 5.049401038298154454, 103.9572429386476671 ) ) ;
#103950 = AXIS2_PLACEMENT_3D ( 'NONE', #177150, #21446, #83107 ) ;
#103951 = CARTESIAN_POINT ( 'NONE',  ( 5.153800228976335163, 19.02544592524342804, 89.79057627198102409 ) ) ;
#103952 = CARTESIAN_POINT ( 'NONE',  ( -10.81492255796078084, -18.62759615963271287, 102.0822429386476955 ) ) ;
#103953 = CARTESIAN_POINT ( 'NONE',  ( -16.51473224551069308, -9.474510206698971260, 56.66557627198103120 ) ) ;
#103954 = CARTESIAN_POINT ( 'NONE',  ( 8.224510206698742110, 14.34966873604972548, 22.08442372801901143 ) ) ;
#103955 = CARTESIAN_POINT ( 'NONE',  ( 11.74264578624799427, 36.14014761921585972, -4.349999994537626868 ) ) ;
#103956 = CARTESIAN_POINT ( 'NONE',  ( -15.80617190586768217, 15.72974639402176855, 103.1260903946856757 ) ) ;
#103957 = CARTESIAN_POINT ( 'NONE',  ( 5.049401038298161559, -19.05341960407611168, 47.70724293864770260 ) ) ;
#103958 = CARTESIAN_POINT ( 'NONE',  ( 15.72974639402176855, 15.80617190586768217, 101.8760903946857042 ) ) ;
#103959 = EDGE_CURVE ( 'NONE', #177278, #44838, #183553, .T. ) ;
#103961 = CARTESIAN_POINT ( 'NONE',  ( -18.62759615963255300, -10.81492255796106328, 59.16775706135234714 ) ) ;
#103960 = CARTESIAN_POINT ( 'NONE',  ( 19.02544592524343514, -5.153800228976328945, 93.54057627198102409 ) ) ;
#103962 = CARTESIAN_POINT ( 'NONE',  ( -1.784589286804201480, 7.284589286804282970, 1.818019484660534424 ) ) ;
#103963 = CARTESIAN_POINT ( 'NONE',  ( 16.46253265017160672, -9.564922557960803928, 108.3322429386476955 ) ) ;
#103964 = CARTESIAN_POINT ( 'NONE',  ( 17.50000000000000000, 5.499999999999992895, 46.70309617465829888 ) ) ;
#103966 = CARTESIAN_POINT ( 'NONE',  ( 0.05219959533937995610, -21.53943276465977519, 60.00109039468568284 ) ) ;
#103965 = CARTESIAN_POINT ( 'NONE',  ( 16.53943276465976808, 0.05219959533934440121, 56.25109039468568284 ) ) ;
#103967 = CARTESIAN_POINT ( 'NONE',  ( -10.72451020669870658, -18.67979575497194134, 84.58442372801903275 ) ) ;
#103968 = CARTESIAN_POINT ( 'NONE',  ( -11.43209428340597711, 9.409695640424857288, -59.99679127084682051 ) ) ;
#103969 = CARTESIAN_POINT ( 'NONE',  ( 12.06949235617739724, 12.14591786802326823, 21.87609039468567573 ) ) ;
#103970 = CARTESIAN_POINT ( 'NONE',  ( -9.564922557960796823, -16.46253265017161027, 67.08224293864769550 ) ) ;
#103971 = CARTESIAN_POINT ( 'NONE',  ( -19.05341960407611168, -5.049401038298163336, 21.45724293864768839 ) ) ;
#103972 = DIRECTION ( 'NONE',  ( 0.000000000000000000, 0.000000000000000000, 1.000000000000000000 ) ) ;
#103973 = CARTESIAN_POINT ( 'NONE',  ( 19.03943276465977164, -0.05219959533909143690, 28.74890960531435624 ) ) ;
#103974 = CARTESIAN_POINT ( 'NONE',  ( 15.80617190586746368, 15.72974639402197994, 39.37390960531436690 ) ) ;
#103975 = CARTESIAN_POINT ( 'NONE',  ( -14.34966873604972548, 8.224510206698743886, 98.33442372801901854 ) ) ;
#103977 = CARTESIAN_POINT ( 'NONE',  ( -9.564922557960796823, -16.46253265017161027, 72.08224293864770971 ) ) ;
#103976 = CARTESIAN_POINT ( 'NONE',  ( 16.55341960407611168, 4.379528057220329451, 78.95724293864769550 ) ) ;
#103978 = CARTESIAN_POINT ( 'NONE',  ( -10.72451020669870658, -18.67979575497194134, 84.58442372801903275 ) ) ;
#103979 = DIRECTION ( 'NONE',  ( 0.000000000000000000, 0.000000000000000000, -1.000000000000000000 ) ) ;
#103980 = CARTESIAN_POINT ( 'NONE',  ( 8.224510206698742110, 14.34966873604972548, 27.08442372801901854 ) ) ;
#103981 = CARTESIAN_POINT ( 'NONE',  ( -4.483927247898539470, -16.52544592524342804, 92.29057627198103830 ) ) ;
#103982 = CARTESIAN_POINT ( 'NONE',  ( 15.72974639402176855, 15.80617190586768217, 36.87609039468568994 ) ) ;
#103983 = CARTESIAN_POINT ( 'NONE',  ( 18.62759615963271287, -10.81492255796078972, 73.33224293864769550 ) ) ;
#103984 = CARTESIAN_POINT ( 'NONE',  ( -16.46253265017146816, -9.564922557961047289, 34.16775706135233293 ) ) ;
#103985 = CARTESIAN_POINT ( 'NONE',  ( -34.36946425582528519, 7.112708652184207558, 47.39170078794325747 ) ) ;
#103986 = CARTESIAN_POINT ( 'NONE',  ( 13.97604488694527802, 13.89961937509977652, 84.37390960531433848 ) ) ;
#103987 = CARTESIAN_POINT ( 'NONE',  ( 16.52544592524342804, -4.483927247898539470, 58.54057627198103120 ) ) ;
#103988 = CARTESIAN_POINT ( 'NONE',  ( -8.224510206698948167, 14.34966873604960824, 35.41557627198102409 ) ) ;
#103989 = CARTESIAN_POINT ( 'NONE',  ( -4.379528057220086978, -16.55341960407618274, 104.7927570613523898 ) ) ;
#103990 = CARTESIAN_POINT ( 'NONE',  ( 16.46253265017146816, 9.564922557961045513, 66.66775706135233293 ) ) ;
#103991 = CARTESIAN_POINT ( 'NONE',  ( 19.25918095147782338, 5.499999999999580780, 51.95284276293935477 ) ) ;
#103992 = CARTESIAN_POINT ( 'NONE',  ( 5.823673210054125526, 21.52544592524343514, 24.79057627198103120 ) ) ;
#103993 = CARTESIAN_POINT ( 'NONE',  ( -16.55341960407611168, -4.379528057220339221, 86.45724293864770971 ) ) ;
#103994 = B_SPLINE_CURVE_WITH_KNOTS ( 'NONE', 3,
 ( #27096, #89737, #139212, #182754, #151423, #168557, #29076, #140198, #61371, #59386, #43243, #12910, #154387, #62358, #123042, #47216, #166598, #169552, #44238, #184728, #198912, #14888, #60380, #122052, #78524, #92699, #31050, #138225, #687, #76549, #120073, #74574 ),
 .UNSPECIFIED., .F., .F.,
 ( 4, 2, 2, 2, 2, 2, 2, 2, 2, 2, 2, 2, 2, 2, 2, 4 ),
 ( 2.539163526713095107E-17, 0.0003712461730036932289, 0.0007424923460073610875, 0.001113738519011029000, 0.001484984692014696805, 0.002227477038022051496, 0.002598723211025728407, 0.002969969384029405319, 0.003341215557033082231, 0.003712461730036759576, 0.004083707903040436488, 0.004454954076044113399, 0.004826200249047790311, 0.005197446422051468090, 0.005568692595055144134, 0.005939938768058821913 ),
 .UNSPECIFIED. ) ;
#103995 = DIRECTION ( 'NONE',  ( 1.000000000000000000, 0.000000000000000000, 0.000000000000000000 ) ) ;
#103997 = CARTESIAN_POINT ( 'NONE',  ( -18.67979575497178146, -10.72451020669898902, 46.66557627198102409 ) ) ;
#103996 = CARTESIAN_POINT ( 'NONE',  ( 19.05341960407611168, 5.049401038298154454, 48.95724293864768129 ) ) ;
#103998 = CARTESIAN_POINT ( 'NONE',  ( -5.719274019375978568, 21.55341960407610458, 65.20724293864768129 ) ) ;
#103999 = CARTESIAN_POINT ( 'NONE',  ( -8.314922557960811034, -14.29746914071050412, 107.0822429386476955 ) ) ;
#104001 = CARTESIAN_POINT ( 'NONE',  ( -16.46253265017160317, 9.564922557960807481, 45.83224293864769550 ) ) ;
#104000 = CARTESIAN_POINT ( 'NONE',  ( 14.34966873604972726, -8.224510206698740333, 65.83442372801900433 ) ) ;
#104002 = CARTESIAN_POINT ( 'NONE',  ( 21.52544592524334988, 5.823673210054432836, 56.45942372801902565 ) ) ;
#104003 = ORIENTED_EDGE ( 'NONE', *, *, #186989, .T. ) ;
#104004 = CARTESIAN_POINT ( 'NONE',  ( -16.52544592524342804, 4.483927247898546575, 106.0405762719810525 ) ) ;
#104005 = CARTESIAN_POINT ( 'NONE',  ( 0.05219959533936267826, -19.03943276465977164, 95.00109039468567573 ) ) ;
#104006 = CARTESIAN_POINT ( 'NONE',  ( -22.81625015709510507, 31.40387420917330275, -7.424999997268812102 ) ) ;
#104008 = CARTESIAN_POINT ( 'NONE',  ( 21.53943276465977519, -0.05219959533907433946, 38.74890960531435979 ) ) ;
#104007 = DIRECTION ( 'NONE',  ( 1.000000000000000000, 0.000000000000000000, 0.000000000000000000 ) ) ;
#104009 = CARTESIAN_POINT ( 'NONE',  ( -9.564922557960796823, -16.46253265017161027, 22.08224293864768839 ) ) ;
#104010 = CARTESIAN_POINT ( 'NONE',  ( 21.53943276465977519, 0.05219959533937863772, 66.25109039468567573 ) ) ;
#104012 = CARTESIAN_POINT ( 'NONE',  ( 16.53943276465976808, -0.05219959533910856209, 43.74890960531435979 ) ) ;
#104011 = CARTESIAN_POINT ( 'NONE',  ( -8.224510206698735004, -14.34966873604973081, 59.58442372801901854 ) ) ;
#104013 = CARTESIAN_POINT ( 'NONE',  ( 15.72974639402199770, -15.80617190586745480, 63.12390960531435979 ) ) ;
#104014 = CARTESIAN_POINT ( 'NONE',  ( 5.719274019375991003, -21.55341960407610458, 67.70724293864769550 ) ) ;
#104015 = DIRECTION ( 'NONE',  ( 0.000000000000000000, 0.000000000000000000, -1.000000000000000000 ) ) ;
#104017 = CARTESIAN_POINT ( 'NONE',  ( -16.51473224551069308, -9.474510206698971260, 111.6655762719810383 ) ) ;
#104016 = CARTESIAN_POINT ( 'NONE',  ( -5.153800228976607833, 19.02544592524334988, 87.70942372801897591 ) ) ;
#104018 = CARTESIAN_POINT ( 'NONE',  ( 19.02544592524343514, -5.153800228976328945, 53.54057627198102409 ) ) ;
#104019 = CARTESIAN_POINT ( 'NONE',  ( 13.97604488694527802, 13.89961937509977652, 24.37390960531435624 ) ) ;
#104020 = SURFACE_STYLE_FILL_AREA ( #101007 ) ;
#104021 = CARTESIAN_POINT ( 'NONE',  ( -5.049401038298153566, 19.05341960407611168, 110.2072429386476671 ) ) ;
#104022 = ORIENTED_EDGE ( 'NONE', *, *, #154133, .F. ) ;
#104023 = CARTESIAN_POINT ( 'NONE',  ( -8.224510206698735004, -14.34966873604973081, 64.58442372801900433 ) ) ;
#104024 = CARTESIAN_POINT ( 'NONE',  ( 18.67979575497178502, 10.72451020669898547, 99.16557627198100988 ) ) ;
#104025 = CARTESIAN_POINT ( 'NONE',  ( -16.46253265017160317, 9.564922557960807481, 75.83224293864769550 ) ) ;
#104026 = CARTESIAN_POINT ( 'NONE',  ( 5.719274019375673035, 21.55341960407619339, 42.29275706135235424 ) ) ;
#104027 = CARTESIAN_POINT ( 'NONE',  ( 13.97604488694527802, 13.89961937509977652, 99.37390960531436690 ) ) ;
#104028 = CARTESIAN_POINT ( 'NONE',  ( -27.05031264677035807, -29.22974442244507998, -16.95124367203715110 ) ) ;
#104029 = ORIENTED_EDGE ( 'NONE', *, *, #176156, .T. ) ;
#104030 = CARTESIAN_POINT ( 'NONE',  ( 18.67979575497194134, -10.72451020669871369, 35.83442372801901143 ) ) ;
#104032 = CARTESIAN_POINT ( 'NONE',  ( 5.153800228976615827, -19.02544592524334988, 85.20942372801900433 ) ) ;
#104031 = CARTESIAN_POINT ( 'NONE',  ( -5.153800228976328057, -19.02544592524343514, 27.29057627198103120 ) ) ;
#104033 = CARTESIAN_POINT ( 'NONE',  ( -13.89961937509957401, -13.97604488694547875, 39.37609039468566152 ) ) ;
#104034 = CARTESIAN_POINT ( 'NONE',  ( -15.72974639402197994, 15.80617190586746368, 110.6239096053143669 ) ) ;
#104035 = CARTESIAN_POINT ( 'NONE',  ( -16.46253265017146816, -9.564922557961047289, 34.16775706135233293 ) ) ;
#104036 = CARTESIAN_POINT ( 'NONE',  ( 5.049401038297881783, 19.05341960407617563, 52.29275706135234003 ) ) ;
#104037 = CARTESIAN_POINT ( 'NONE',  ( -12.14591786802326823, 12.06949235617739902, 88.12609039468570415 ) ) ;
#104038 = CARTESIAN_POINT ( 'NONE',  ( 24.79445957992280469, -6.337972767934337170, 168.1743082258862785 ) ) ;
#104039 = CARTESIAN_POINT ( 'NONE',  ( -5.049401038298153566, 19.05341960407611168, 75.20724293864769550 ) ) ;
#104040 = CARTESIAN_POINT ( 'NONE',  ( 5.823673210054444382, -21.52544592524334988, 85.20942372801901854 ) ) ;
#104041 = CARTESIAN_POINT ( 'NONE',  ( -10.72451020669870658, -18.67979575497194134, 99.58442372801900433 ) ) ;
#104042 = CARTESIAN_POINT ( 'NONE',  ( -0.9968436689772768311, -8.725106586199784076, -64.02420483255117745 ) ) ;
#104043 = CARTESIAN_POINT ( 'NONE',  ( -19.03943276465977164, 0.05219959533909376836, 91.24890960531436690 ) ) ;
#104044 = CARTESIAN_POINT ( 'NONE',  ( -5.719274019375665041, -21.55341960407619695, 64.79275706135234714 ) ) ;
#104045 = CARTESIAN_POINT ( 'NONE',  ( -9.474510206698720793, -16.51473224551083518, 94.58442372801900433 ) ) ;
#104046 = CARTESIAN_POINT ( 'NONE',  ( -16.51473224551069308, -9.474510206698971260, 71.66557627198102409 ) ) ;
#104047 = CARTESIAN_POINT ( 'NONE',  ( -9.564922557960796823, -16.46253265017161027, 112.0822429386476955 ) ) ;
#104048 = CARTESIAN_POINT ( 'NONE',  ( 5.049401038298161559, -19.05341960407611168, 77.70724293864765286 ) ) ;
#104049 = CARTESIAN_POINT ( 'NONE',  ( 17.49999999999996803, -4.264887584952425037, 23.02877294406987474 ) ) ;
#104050 = CARTESIAN_POINT ( 'NONE',  ( -16.46253265017160317, 9.564922557960807481, 70.83224293864770971 ) ) ;
#104051 = CARTESIAN_POINT ( 'NONE',  ( -13.97604488694527625, -13.89961937509977652, 51.87390960531436690 ) ) ;
#104052 = CARTESIAN_POINT ( 'NONE',  ( -21.53943276465977519, -0.05219959533937600094, 18.75109039468568639 ) ) ;
#104053 = CARTESIAN_POINT ( 'NONE',  ( -8.224510206698735004, -14.34966873604973081, 89.58442372801901854 ) ) ;
#104054 = CARTESIAN_POINT ( 'NONE',  ( 4.313351365237949153, 4.313351365237946489, -64.92279855667830191 ) ) ;
#104055 = CARTESIAN_POINT ( 'NONE',  ( 0.000000000000000000, 0.000000000000000000, -18.00000000000000000 ) ) ;
#104056 = CARTESIAN_POINT ( 'NONE',  ( -5.153800228976607833, 19.02544592524334988, 57.70942372801899012 ) ) ;
#104057 = CARTESIAN_POINT ( 'NONE',  ( 13.97604488694527802, 13.89961937509977652, 74.37390960531436690 ) ) ;
#104058 = CARTESIAN_POINT ( 'NONE',  ( -16.53943276465976808, 0.05219959533911058130, 66.24890960531436690 ) ) ;
#104059 = CARTESIAN_POINT ( 'NONE',  ( -8.314922557960811034, -14.29746914071050412, 102.0822429386476955 ) ) ;
#104060 = CARTESIAN_POINT ( 'NONE',  ( 19.03943276465977164, -0.05219959533909143690, 108.7489096053143527 ) ) ;
#104061 = CARTESIAN_POINT ( 'NONE',  ( 16.46253265017160672, -9.564922557960803928, 108.3322429386476955 ) ) ;
#104062 = CARTESIAN_POINT ( 'NONE',  ( -16.53943276465976808, 0.05219959533911058130, 96.24890960531435269 ) ) ;
#104063 = CARTESIAN_POINT ( 'NONE',  ( -19.02544592524342804, 5.153800228976336051, 116.0405762719810383 ) ) ;
#104064 = CARTESIAN_POINT ( 'NONE',  ( 16.51473224551083163, -9.474510206698727899, 35.83442372801899722 ) ) ;
#104065 = CARTESIAN_POINT ( 'NONE',  ( 16.52544592524335698, 4.483927247898782831, 106.4594237280190328 ) ) ;
#104066 = CARTESIAN_POINT ( 'NONE',  ( 5.049401038298161559, -19.05341960407611168, 92.70724293864769550 ) ) ;
#104067 = CARTESIAN_POINT ( 'NONE',  ( -10.72451020669870658, -18.67979575497194134, 54.58442372801901143 ) ) ;
#104068 = CARTESIAN_POINT ( 'NONE',  ( 15.72974639402199770, -15.80617190586745480, 48.12390960531436690 ) ) ;
#104069 = CARTESIAN_POINT ( 'NONE',  ( -18.62759615963255300, -10.81492255796106328, 19.16775706135234714 ) ) ;
#104070 = CARTESIAN_POINT ( 'NONE',  ( 15.72974639402199770, -15.80617190586745480, 68.12390960531436690 ) ) ;
#104071 = CARTESIAN_POINT ( 'NONE',  ( 16.55341960407611168, 4.379528057220329451, 88.95724293864769550 ) ) ;
#104072 = CARTESIAN_POINT ( 'NONE',  ( 0.05219959533936267826, -19.03943276465977164, 60.00109039468566863 ) ) ;
#104073 = CARTESIAN_POINT ( 'NONE',  ( -9.564922557960796823, -16.46253265017161027, 27.08224293864769550 ) ) ;
#104074 = CARTESIAN_POINT ( 'NONE',  ( 0.05219959533909260263, 19.03943276465977164, 84.99890960531436690 ) ) ;
#104075 = CARTESIAN_POINT ( 'NONE',  ( 16.46253265017160672, -9.564922557960803928, 83.33224293864768129 ) ) ;
#104076 = CARTESIAN_POINT ( 'NONE',  ( 0.05219959533910956823, 16.53943276465976808, 104.9989096053143669 ) ) ;
#104077 = ORIENTED_EDGE ( 'NONE', *, *, #62849, .T. ) ;
#104078 = CARTESIAN_POINT ( 'NONE',  ( 12.06949235617757843, -12.14591786802309237, 33.12390960531435979 ) ) ;
#104079 = CARTESIAN_POINT ( 'NONE',  ( -4.379528057220086978, -16.55341960407618274, 39.79275706135235424 ) ) ;
#104080 = CARTESIAN_POINT ( 'NONE',  ( -10.72451020669870658, -18.67979575497194134, 109.5844237280190328 ) ) ;
#104081 = CARTESIAN_POINT ( 'NONE',  ( -0.05219959533909027116, -19.03943276465977164, 107.4989096053143527 ) ) ;
#104082 = CARTESIAN_POINT ( 'NONE',  ( 15.72974639402176855, 15.80617190586768217, 36.87609039468568994 ) ) ;
#104083 = CARTESIAN_POINT ( 'NONE',  ( 5.153800228976335163, 19.02544592524342804, 44.79057627198103830 ) ) ;
#104084 = CARTESIAN_POINT ( 'NONE',  ( 0.05219959533934541429, -16.53943276465976808, 45.00109039468568284 ) ) ;
#104085 = CARTESIAN_POINT ( 'NONE',  ( -16.53943276465976808, -0.05219959533934237506, 88.75109039468567573 ) ) ;
#104086 = CARTESIAN_POINT ( 'NONE',  ( -5.153800228976607833, 19.02544592524334988, 112.7094237280190043 ) ) ;
#104087 = CARTESIAN_POINT ( 'NONE',  ( -16.51473224551069308, -9.474510206698971260, 31.66557627198102054 ) ) ;
#104088 = CARTESIAN_POINT ( 'NONE',  ( -4.483927247898539470, -16.52544592524342804, 92.29057627198103830 ) ) ;
#104089 = CARTESIAN_POINT ( 'NONE',  ( -18.67979575497178146, -10.72451020669898902, 106.6655762719810383 ) ) ;
#104090 = CARTESIAN_POINT ( 'NONE',  ( 13.97604488694548053, -13.89961937509957401, 85.62609039468568994 ) ) ;
#104091 = CARTESIAN_POINT ( 'NONE',  ( -5.153800228976328057, -19.02544592524343514, 27.29057627198103120 ) ) ;
#104092 = CARTESIAN_POINT ( 'NONE',  ( -13.89961937509977652, 13.97604488694528158, 90.62390960531432427 ) ) ;
#104093 = CARTESIAN_POINT ( 'NONE',  ( -0.05219959533937732626, 21.53943276465977519, 37.50109039468568284 ) ) ;
#104094 = CARTESIAN_POINT ( 'NONE',  ( -37.99626262588766679, 2.428612866367529932E-14, -3.747842220587803475 ) ) ;
#104095 = CARTESIAN_POINT ( 'NONE',  ( -9.474510206698964154, 16.51473224551069663, 90.41557627198103830 ) ) ;
#104096 = DIRECTION ( 'NONE',  ( 0.000000000000000000, -1.000000000000000000, 1.287488025362403787E-15 ) ) ;
#104097 = CARTESIAN_POINT ( 'NONE',  ( -5.049401038298153566, 19.05341960407611168, 80.20724293864769550 ) ) ;
#104099 = CARTESIAN_POINT ( 'NONE',  ( -0.05219959533910754901, -16.53943276465976808, 87.49890960531436690 ) ) ;
#104098 = CARTESIAN_POINT ( 'NONE',  ( 21.55341960407619695, -5.719274019375665929, 26.04275706135235779 ) ) ;
#104100 = CARTESIAN_POINT ( 'NONE',  ( -19.05341960407611168, -5.049401038298163336, 91.45724293864766707 ) ) ;
#104101 = CARTESIAN_POINT ( 'NONE',  ( -13.89961937509957401, -13.97604488694547875, 19.37609039468566507 ) ) ;
#104102 = CARTESIAN_POINT ( 'NONE',  ( -16.53943276465976808, -0.05219959533934237506, 53.75109039468568994 ) ) ;
#104103 = CARTESIAN_POINT ( 'NONE',  ( -21.53943276465977519, -0.05219959533937600094, 78.75109039468568994 ) ) ;
#104104 = CARTESIAN_POINT ( 'NONE',  ( 8.314922557961029526, -14.29746914071037800, 40.41775706135234714 ) ) ;
#104106 = EDGE_CURVE ( 'NONE', #199519, #144964, #162721, .T. ) ;
#104105 = CARTESIAN_POINT ( 'NONE',  ( 16.46253265017160672, -9.564922557960803928, 83.33224293864768129 ) ) ;
#104107 = CARTESIAN_POINT ( 'NONE',  ( 9.564922557961047289, -16.46253265017146816, 100.4177570613523329 ) ) ;
#104108 = CARTESIAN_POINT ( 'NONE',  ( -4.379528057220086978, -16.55341960407618274, 64.79275706135234714 ) ) ;
#104109 = CARTESIAN_POINT ( 'NONE',  ( 21.52544592524334988, 5.823673210054432836, 111.4594237280190328 ) ) ;
#104110 = CARTESIAN_POINT ( 'NONE',  ( 5.049401038297881783, 19.05341960407617563, 77.29275706135231871 ) ) ;
#104111 = CARTESIAN_POINT ( 'NONE',  ( -13.89961937509977652, 13.97604488694528158, 65.62390960531436690 ) ) ;
#104112 = CARTESIAN_POINT ( 'NONE',  ( 10.72451020669898902, -18.67979575497178502, 77.91557627198102409 ) ) ;
#104114 = CARTESIAN_POINT ( 'NONE',  ( 16.51473224551083163, -9.474510206698727899, 95.83442372801900433 ) ) ;
#104113 = CARTESIAN_POINT ( 'NONE',  ( -0.05219959533910754901, -16.53943276465976808, 77.49890960531433848 ) ) ;
#104115 = CARTESIAN_POINT ( 'NONE',  ( 24.27957997113399102, 6.290849861789209463, 171.5443985711292214 ) ) ;
#104116 = CARTESIAN_POINT ( 'NONE',  ( 0.05219959533936267826, -19.03943276465977164, 60.00109039468566863 ) ) ;
#104117 = CARTESIAN_POINT ( 'NONE',  ( 16.52544592524335698, 4.483927247898782831, 106.4594237280190328 ) ) ;
#104118 = CARTESIAN_POINT ( 'NONE',  ( -14.29746914071049879, 8.314922557960819915, 75.83224293864769550 ) ) ;
#104120 = CARTESIAN_POINT ( 'NONE',  ( -19.53037848336981597, 5.499999999999898748, 89.85532783611444074 ) ) ;
#104119 = CARTESIAN_POINT ( 'NONE',  ( -15.72974639402176322, -15.80617190586768395, 109.3760903946857042 ) ) ;
#104121 = CARTESIAN_POINT ( 'NONE',  ( 21.55341960407610458, 5.719274019375980345, 108.9572429386476955 ) ) ;
#104122 = CARTESIAN_POINT ( 'NONE',  ( -13.97604488694527625, -13.89961937509977652, 106.8739096053143669 ) ) ;
#104123 = CARTESIAN_POINT ( 'NONE',  ( -9.474510206698964154, 16.51473224551069663, 75.41557627198103830 ) ) ;
#104124 = CARTESIAN_POINT ( 'NONE',  ( -21.55341960407619339, 5.719274019375674811, 83.54275706135234714 ) ) ;
#104125 = CARTESIAN_POINT ( 'NONE',  ( 13.97604488694527802, 13.89961937509977652, 69.37390960531436690 ) ) ;
#104126 = CARTESIAN_POINT ( 'NONE',  ( -5.153800228976328057, -19.02544592524343514, 42.29057627198101699 ) ) ;
#104127 = CARTESIAN_POINT ( 'NONE',  ( -21.55341960407610458, -5.719274019375992779, 26.45724293864768839 ) ) ;
#104128 = CARTESIAN_POINT ( 'NONE',  ( -8.314922557960811034, -14.29746914071050412, 82.08224293864768129 ) ) ;
#104129 = CARTESIAN_POINT ( 'NONE',  ( -0.05219959533909027116, -19.03943276465977164, 47.49890960531435979 ) ) ;
#104130 = CARTESIAN_POINT ( 'NONE',  ( -4.379528057220328563, 16.55341960407611168, 100.2072429386476955 ) ) ;
#104131 = CARTESIAN_POINT ( 'NONE',  ( 18.67979575497178502, 10.72451020669898547, 104.1655762719810241 ) ) ;
#104132 = CARTESIAN_POINT ( 'NONE',  ( -15.80617190586768217, 15.72974639402176855, 53.12609039468568284 ) ) ;
#104133 = CARTESIAN_POINT ( 'NONE',  ( -16.46253265017160317, 9.564922557960807481, 25.83224293864769194 ) ) ;
#104134 = CARTESIAN_POINT ( 'NONE',  ( -14.29746914071037622, -8.314922557961029526, 59.16775706135234714 ) ) ;
#104135 = ADVANCED_FACE ( 'NONE', ( #166411 ), #11741, .T. ) ;
#104136 = CARTESIAN_POINT ( 'NONE',  ( 5.719274019375991003, -21.55341960407610458, 97.70724293864772392 ) ) ;
#104137 = CARTESIAN_POINT ( 'NONE',  ( -0.05219959533907301413, -21.53943276465977519, 97.49890960531436690 ) ) ;
#104139 = CARTESIAN_POINT ( 'NONE',  ( 9.564922557960805705, 16.46253265017160317, 54.58224293864769550 ) ) ;
#104138 = CARTESIAN_POINT ( 'NONE',  ( 16.46253265017146816, 9.564922557961045513, 36.66775706135233293 ) ) ;
#104140 = DIRECTION ( 'NONE',  ( -0.000000000000000000, -0.000000000000000000, 1.000000000000000000 ) ) ;
#104141 = CARTESIAN_POINT ( 'NONE',  ( 21.53943276465977519, 0.05219959533937863772, 61.25109039468567573 ) ) ;
#104142 = CARTESIAN_POINT ( 'NONE',  ( -15.72974639402197994, 15.80617190586746368, 55.62390960531436690 ) ) ;
#104143 = CARTESIAN_POINT ( 'NONE',  ( -14.34966873604960291, -8.224510206698953496, 36.66557627198103120 ) ) ;
#104145 = CARTESIAN_POINT ( 'NONE',  ( 5.049401038297881783, 19.05341960407617563, 22.29275706135233648 ) ) ;
#104144 = CARTESIAN_POINT ( 'NONE',  ( 5.719274019375673035, 21.55341960407619339, 82.29275706135234714 ) ) ;
#104146 = CARTESIAN_POINT ( 'NONE',  ( 16.52544592524342804, -4.483927247898539470, 108.5405762719810241 ) ) ;
#104147 = CARTESIAN_POINT ( 'NONE',  ( 19.03943276465977164, 0.05219959533936151252, 41.25109039468566152 ) ) ;
#104148 = CARTESIAN_POINT ( 'NONE',  ( 16.52544592524335698, 4.483927247898782831, 106.4594237280190328 ) ) ;
#104149 = CARTESIAN_POINT ( 'NONE',  ( -18.62759615963255300, -10.81492255796106328, 74.16775706135231871 ) ) ;
#104150 = CARTESIAN_POINT ( 'NONE',  ( 13.89961937509977652, -13.97604488694527269, 58.12390960531436690 ) ) ;
#104151 = CARTESIAN_POINT ( 'NONE',  ( -9.474510206698720793, -16.51473224551083518, 29.58442372801900433 ) ) ;
#104152 = CARTESIAN_POINT ( 'NONE',  ( -21.53943276465977519, 0.05219959533907696930, 41.24890960531435269 ) ) ;
#104153 = B_SPLINE_CURVE_WITH_KNOTS ( 'NONE', 3,
 ( #33476, #79973, #141641, #64806, #189162, #173986, #143616, #5100, #11127, #104120, #85948, #102124, #118301, #194151, #161795, #115293, #149629, #180980, #177977, #178983 ),
 .UNSPECIFIED., .F., .F.,
 ( 4, 2, 2, 2, 2, 2, 2, 2, 2, 4 ),
 ( 0.004000878361811981664, 0.004499404418915974209, 0.004997930476019966754, 0.005496456533123960167, 0.005994982590227952712, 0.006244245618779948985, 0.006493508647331945258, 0.006992034704435934334, 0.007490560761539921675, 0.007989086818643910751 ),
 .UNSPECIFIED. ) ;
#104154 = CARTESIAN_POINT ( 'NONE',  ( 10.81492255796106328, -18.62759615963255655, 35.41775706135234003 ) ) ;
#104155 = CARTESIAN_POINT ( 'NONE',  ( -0.05219959533907301413, -21.53943276465977519, 87.49890960531436690 ) ) ;
#104156 = CARTESIAN_POINT ( 'NONE',  ( 13.97604488694548053, -13.89961937509957401, 85.62609039468568994 ) ) ;
#104157 = CARTESIAN_POINT ( 'NONE',  ( -16.53943276465976808, -0.05219959533934237506, 48.75109039468568284 ) ) ;
#104159 = CARTESIAN_POINT ( 'NONE',  ( 21.55341960407610458, 5.719274019375980345, 88.95724293864769550 ) ) ;
#104158 = CARTESIAN_POINT ( 'NONE',  ( -6.565741541539673598, 4.457937930945857552, -62.16217994089669219 ) ) ;
#104161 = CARTESIAN_POINT ( 'NONE',  ( 4.379528057220339221, -16.55341960407611168, 82.70724293864770971 ) ) ;
#104160 = CARTESIAN_POINT ( 'NONE',  ( 4.483927247898790824, -16.52544592524335698, 85.20942372801901854 ) ) ;
#104162 = CARTESIAN_POINT ( 'NONE',  ( 1.067013306609913448, 31.46962149133000608, -46.27433572153971397 ) ) ;
#104163 = CARTESIAN_POINT ( 'NONE',  ( -19.02544592524334988, -5.153800228976617603, 108.9594237280189759 ) ) ;
#104164 = CARTESIAN_POINT ( 'NONE',  ( -10.81492255796078084, -18.62759615963271287, 32.08224293864769550 ) ) ;
#104165 = DIRECTION ( 'NONE',  ( -1.000000000000000000, -0.000000000000000000, -0.000000000000000000 ) ) ;
#104166 = CARTESIAN_POINT ( 'NONE',  ( 8.314922557961029526, -14.29746914071037800, 50.41775706135235424 ) ) ;
#104167 = CARTESIAN_POINT ( 'NONE',  ( -21.53943276465977519, -0.05219959533937600094, 23.75109039468567929 ) ) ;
#104168 = CARTESIAN_POINT ( 'NONE',  ( -21.52544592524343514, 5.823673210054127303, 41.04057627198103120 ) ) ;
#104169 = CARTESIAN_POINT ( 'NONE',  ( 16.52544592524335698, 4.483927247898782831, 76.45942372801901854 ) ) ;
#104170 = CARTESIAN_POINT ( 'NONE',  ( -9.474510206698964154, 16.51473224551069663, 80.41557627198103830 ) ) ;
#104172 = CARTESIAN_POINT ( 'NONE',  ( -19.03943276465977164, 0.05219959533909376836, 31.24890960531435979 ) ) ;
#104171 = CARTESIAN_POINT ( 'NONE',  ( 10.72451020669871369, 18.67979575497193778, 57.08442372801901854 ) ) ;
#104173 = CARTESIAN_POINT ( 'NONE',  ( -21.55341960407610458, -5.719274019375992779, 41.45724293864769550 ) ) ;
#104174 = ORIENTED_EDGE ( 'NONE', *, *, #171952, .F. ) ;
#104175 = CARTESIAN_POINT ( 'NONE',  ( -19.05341960407617563, 5.049401038297882671, 43.54275706135232582 ) ) ;
#104176 = CARTESIAN_POINT ( 'NONE',  ( 14.29746914071037800, 8.314922557961029526, 51.66775706135234714 ) ) ;
#104177 = CARTESIAN_POINT ( 'NONE',  ( -9.474510206698964154, 16.51473224551069663, 115.4155762719810241 ) ) ;
#104178 = ORIENTED_EDGE ( 'NONE', *, *, #175605, .F. ) ;
#104179 = CARTESIAN_POINT ( 'NONE',  ( -13.97604488694527625, -13.89961937509977652, 91.87390960531432427 ) ) ;
#104180 = CARTESIAN_POINT ( 'NONE',  ( 16.52544592524335698, 4.483927247898782831, 101.4594237280190185 ) ) ;
#104181 = CARTESIAN_POINT ( 'NONE',  ( -19.02544592524342804, 5.153800228976336051, 116.0405762719810383 ) ) ;
#104182 = CARTESIAN_POINT ( 'NONE',  ( 8.314922557960818139, 14.29746914071049879, 94.58224293864769550 ) ) ;
#104183 = CARTESIAN_POINT ( 'NONE',  ( 15.72974639402199770, -15.80617190586745480, 33.12390960531435979 ) ) ;
#104184 = CARTESIAN_POINT ( 'NONE',  ( 16.46253265017160672, -9.564922557960803928, 38.33224293864768839 ) ) ;
#104185 = CARTESIAN_POINT ( 'NONE',  ( 12.06949235617739724, 12.14591786802326823, 76.87609039468567573 ) ) ;
#104186 = CARTESIAN_POINT ( 'NONE',  ( 5.823673210054444382, -21.52544592524334988, 20.20942372801900788 ) ) ;
#104187 = CARTESIAN_POINT ( 'NONE',  ( 19.05341960407617918, -5.049401038297876454, 71.04275706135234714 ) ) ;
#104188 = CARTESIAN_POINT ( 'NONE',  ( -19.03943276465977164, 0.05219959533909376836, 41.24890960531435269 ) ) ;
#104189 = CARTESIAN_POINT ( 'NONE',  ( -19.05341960407611168, -5.049401038298163336, 111.4572429386476671 ) ) ;
#104190 = CARTESIAN_POINT ( 'NONE',  ( 0.05219959533937995610, -21.53943276465977519, 105.0010903946856757 ) ) ;
#104191 = CARTESIAN_POINT ( 'NONE',  ( -5.049401038298153566, 19.05341960407611168, 60.20724293864768129 ) ) ;
#104192 = EDGE_CURVE ( 'NONE', #56021, #102442, #196322, .T. ) ;
#104193 = CARTESIAN_POINT ( 'NONE',  ( 16.55341960407618274, -4.379528057220086978, 51.04275706135234714 ) ) ;
#104194 = CARTESIAN_POINT ( 'NONE',  ( -15.80617190586768217, 15.72974639402176855, 93.12609039468568994 ) ) ;
#104195 = CARTESIAN_POINT ( 'NONE',  ( -19.03943276465977164, -0.05219959533935918106, 38.75109039468566152 ) ) ;
#104196 = CARTESIAN_POINT ( 'NONE',  ( -0.05219959533936034679, 19.03943276465977164, 47.50109039468566863 ) ) ;
#104197 = ORIENTED_EDGE ( 'NONE', *, *, #294, .F. ) ;
#104198 = CARTESIAN_POINT ( 'NONE',  ( 10.81492255796106328, -18.62759615963255655, 45.41775706135234003 ) ) ;
#104199 = CARTESIAN_POINT ( 'NONE',  ( -9.474510206698964154, 16.51473224551069663, 25.41557627198103120 ) ) ;
#104200 = CARTESIAN_POINT ( 'NONE',  ( 9.474510206698729675, 16.51473224551082808, 52.08442372801900433 ) ) ;
#104201 = CARTESIAN_POINT ( 'NONE',  ( 19.05341960407611168, 5.049401038298154454, 93.95724293864769550 ) ) ;
#104202 = CARTESIAN_POINT ( 'NONE',  ( 9.474510206698971260, -16.51473224551069308, 82.91557627198103830 ) ) ;
#104203 = CARTESIAN_POINT ( 'NONE',  ( -8.314922557960811034, -14.29746914071050412, 32.08224293864769550 ) ) ;
#104204 = CARTESIAN_POINT ( 'NONE',  ( 15.72974639402199770, -15.80617190586745480, 33.12390960531435979 ) ) ;
#104205 = CARTESIAN_POINT ( 'NONE',  ( -36.91746825000001309, 11.99521256947798342, -3.224999997268813257 ) ) ;
#104206 = CARTESIAN_POINT ( 'NONE',  ( 22.46606745562067431, 22.64734518408110020, -49.13275782002543934 ) ) ;
#104207 = CARTESIAN_POINT ( 'NONE',  ( 18.62759615963255655, 10.81492255796105972, 106.6677570613523756 ) ) ;
#104208 = CARTESIAN_POINT ( 'NONE',  ( 23.96320343559665389, 18.46320343559613164, 1.818019484660534424 ) ) ;
#104209 = CARTESIAN_POINT ( 'NONE',  ( -5.049401038298153566, 19.05341960407611168, 35.20724293864768839 ) ) ;
#104210 = CARTESIAN_POINT ( 'NONE',  ( -19.05341960407611168, -5.049401038298163336, 111.4572429386476671 ) ) ;
#104211 = CARTESIAN_POINT ( 'NONE',  ( -38.00000000000000711, 2.428612866367529932E-14, -4.000000000000000000 ) ) ;
#104212 = DIRECTION ( 'NONE',  ( -1.000000000000000000, 0.000000000000000000, 0.000000000000000000 ) ) ;
#104213 = CARTESIAN_POINT ( 'NONE',  ( -4.379528057220086978, -16.55341960407618274, 59.79275706135234714 ) ) ;
#104214 = CARTESIAN_POINT ( 'NONE',  ( 21.55341960407610458, 5.719274019375980345, 88.95724293864769550 ) ) ;
#104215 = CARTESIAN_POINT ( 'NONE',  ( 4.483927247898545687, 16.52544592524342804, 39.79057627198103830 ) ) ;
#104217 = CARTESIAN_POINT ( 'NONE',  ( -13.97604488694527625, -13.89961937509977652, 111.8739096053143243 ) ) ;
#104216 = CARTESIAN_POINT ( 'NONE',  ( 16.51473224551069308, 9.474510206698969483, 29.16557627198103475 ) ) ;
#104218 = CARTESIAN_POINT ( 'NONE',  ( 21.53943276465977519, 0.05219959533937863772, 26.25109039468567573 ) ) ;
#104219 = CARTESIAN_POINT ( 'NONE',  ( 0.05219959533936267826, -19.03943276465977164, 30.00109039468566863 ) ) ;
#104220 = CARTESIAN_POINT ( 'NONE',  ( -0.05219959533909027116, -19.03943276465977164, 32.49890960531435979 ) ) ;
#104221 = CARTESIAN_POINT ( 'NONE',  ( 5.719274019375673035, 21.55341960407619339, 77.29275706135234714 ) ) ;
#104222 = CARTESIAN_POINT ( 'NONE',  ( -37.99626262588766679, 2.428612866367529932E-14, 2.000000000000000000 ) ) ;
#104223 = CARTESIAN_POINT ( 'NONE',  ( -12.14591786802309592, -12.06949235617757132, 31.87390960531435979 ) ) ;
#104224 = CARTESIAN_POINT ( 'NONE',  ( 22.81625015709509441, 31.40387420917330275, -1.824999997268813345 ) ) ;
#104225 = CARTESIAN_POINT ( 'NONE',  ( -21.52544592524343514, 5.823673210054127303, 26.04057627198103475 ) ) ;
#104226 = CARTESIAN_POINT ( 'NONE',  ( 12.14591786802309770, 12.06949235617756955, 99.37390960531436690 ) ) ;
#104227 = LINE ( 'NONE', #151726, #65859 ) ;
#104228 = CARTESIAN_POINT ( 'NONE',  ( 16.51473224551069308, 9.474510206698969483, 94.16557627198103830 ) ) ;
#104229 = CARTESIAN_POINT ( 'NONE',  ( 0.05219959533910956823, 16.53943276465976808, 74.99890960531435269 ) ) ;
#104230 = CARTESIAN_POINT ( 'NONE',  ( 0.05219959533936267826, -19.03943276465977164, 100.0010903946856757 ) ) ;
#104231 = CARTESIAN_POINT ( 'NONE',  ( 18.67979575497178502, 10.72451020669898547, 69.16557627198102409 ) ) ;
#104232 = ORIENTED_EDGE ( 'NONE', *, *, #38420, .F. ) ;
#104233 = CARTESIAN_POINT ( 'NONE',  ( -9.564922557960796823, -16.46253265017161027, 32.08224293864769550 ) ) ;
#104235 = CARTESIAN_POINT ( 'NONE',  ( -15.72974639402197994, 15.80617190586746368, 90.62390960531436690 ) ) ;
#104234 = CARTESIAN_POINT ( 'NONE',  ( -9.474510206698964154, 16.51473224551069663, 90.41557627198103830 ) ) ;
#104237 = CARTESIAN_POINT ( 'NONE',  ( 9.474510206698971260, -16.51473224551069308, 82.91557627198103830 ) ) ;
#104236 = CARTESIAN_POINT ( 'NONE',  ( -8.224510206698735004, -14.34966873604973081, 104.5844237280190185 ) ) ;
#104238 = CARTESIAN_POINT ( 'NONE',  ( 16.46253265017146816, 9.564922557961045513, 76.66775706135234714 ) ) ;
#104239 = CARTESIAN_POINT ( 'NONE',  ( 18.62759615963255655, 10.81492255796105972, 91.66775706135234714 ) ) ;
#104240 = CARTESIAN_POINT ( 'NONE',  ( 5.719274019375991003, -21.55341960407610458, 82.70724293864770971 ) ) ;
#104241 = CARTESIAN_POINT ( 'NONE',  ( -10.81492255796078084, -18.62759615963271287, 32.08224293864769550 ) ) ;
#104242 = CARTESIAN_POINT ( 'NONE',  ( -19.02544592524342804, 5.153800228976336051, 51.04057627198103120 ) ) ;
#104243 = CARTESIAN_POINT ( 'NONE',  ( 4.379528057220339221, -16.55341960407611168, 22.70724293864769194 ) ) ;
#104244 = CARTESIAN_POINT ( 'NONE',  ( -13.89961937509977652, 13.97604488694528158, 70.62390960531432427 ) ) ;
#104245 = CARTESIAN_POINT ( 'NONE',  ( -31.54463713289767313, -7.108708273820908197, 92.55936662351709288 ) ) ;
#104246 = CARTESIAN_POINT ( 'NONE',  ( -21.55341960407619339, 5.719274019375674811, 108.5427570613523756 ) ) ;
#104247 = CARTESIAN_POINT ( 'NONE',  ( 8.224510206698953496, -14.34966873604960469, 72.91557627198103830 ) ) ;
#104248 = CARTESIAN_POINT ( 'NONE',  ( 21.52544592524344225, -5.823673210054117533, 108.5405762719810241 ) ) ;
#104249 = CARTESIAN_POINT ( 'NONE',  ( -10.81492255796078084, -18.62759615963271287, 112.0822429386477097 ) ) ;
#104250 = CARTESIAN_POINT ( 'NONE',  ( -6.297097159419607237, 4.175862767829939592, -64.28037419727766633 ) ) ;
#104251 = CARTESIAN_POINT ( 'NONE',  ( 18.67979575497178502, 10.72451020669898547, 59.16557627198103120 ) ) ;
#104252 = CARTESIAN_POINT ( 'NONE',  ( 12.14591786802327356, -12.06949235617739191, 90.62609039468567573 ) ) ;
#104253 = CARTESIAN_POINT ( 'NONE',  ( 16.55341960407611168, 4.379528057220329451, 98.95724293864770971 ) ) ;
#104254 = CARTESIAN_POINT ( 'NONE',  ( -9.474510206698964154, 16.51473224551069663, 60.41557627198102409 ) ) ;
#104255 = SURFACE_STYLE_USAGE ( .BOTH. , #27437 ) ;
#104256 = CARTESIAN_POINT ( 'NONE',  ( 0.05219959533910956823, 16.53943276465976808, 34.99890960531435979 ) ) ;
#104257 = CARTESIAN_POINT ( 'NONE',  ( -10.72451020669870658, -18.67979575497194134, 44.58442372801901854 ) ) ;
#104258 = CARTESIAN_POINT ( 'NONE',  ( -16.46253265017160317, 9.564922557960807481, 105.8322429386476955 ) ) ;
#104259 = CARTESIAN_POINT ( 'NONE',  ( 10.72451020669871369, 18.67979575497193778, 87.08442372801901854 ) ) ;
#104260 = CARTESIAN_POINT ( 'NONE',  ( -13.89961937509977652, 13.97604488694528158, 30.62390960531435269 ) ) ;
#104261 = CARTESIAN_POINT ( 'NONE',  ( -0.05219959533909027116, -19.03943276465977164, 37.49890960531436690 ) ) ;
#104262 =( BOUNDED_CURVE ( )  B_SPLINE_CURVE ( 2, ( #46749, #171080, #63902, #187270, #16410, #48739, #185256, #124572, #93227, #199436, #152916, #30581, #140731 ),
 .UNSPECIFIED., .F., .T. ) 
 B_SPLINE_CURVE_WITH_KNOTS ( ( 3, 2, 2, 2, 2, 2, 3 ),
 ( 0.3445813794070300973, 0.3464912280701754610, 0.3508771929824561209, 0.3552631578947368363, 0.3596491228070175517, 0.3640350877192982670, 0.3659906162045339362 ),
 .UNSPECIFIED. ) 
 CURVE ( )  GEOMETRIC_REPRESENTATION_ITEM ( )  RATIONAL_B_SPLINE_CURVE ( ( 0.9832469066685285419, 0.9851625545550100060, 1.000000000000000000, 0.9659258262890683122, 1.000000000000000000, 0.9659258262890683122, 1.000000000000000000, 0.9659258262890683122, 1.000000000000000000, 0.9659258262890683122, 1.000000000000000000, 0.9848076720550081875, 0.9831626618144004848 ) ) 
 REPRESENTATION_ITEM ( '' )  );
#104263 = ORIENTED_EDGE ( 'NONE', *, *, #141788, .T. ) ;
#104264 = CARTESIAN_POINT ( 'NONE',  ( 5.823673210054444382, -21.52544592524334988, 85.20942372801901854 ) ) ;
#104265 = CARTESIAN_POINT ( 'NONE',  ( -14.29746914071037622, -8.314922557961029526, 44.16775706135234714 ) ) ;
#104266 = CARTESIAN_POINT ( 'NONE',  ( -18.62759615963255300, -10.81492255796106328, 69.16775706135234714 ) ) ;
#104267 = CARTESIAN_POINT ( 'NONE',  ( 5.049401038298161559, -19.05341960407611168, 102.7072429386476955 ) ) ;
#104268 = CARTESIAN_POINT ( 'NONE',  ( 19.03943276465977164, 0.05219959533936151252, 76.25109039468566152 ) ) ;
#104269 = CARTESIAN_POINT ( 'NONE',  ( 21.52544592524334988, 5.823673210054432836, 56.45942372801902565 ) ) ;
#104270 = CARTESIAN_POINT ( 'NONE',  ( -12.06949235617739369, -12.14591786802326823, 29.37609039468568284 ) ) ;
#104271 = CARTESIAN_POINT ( 'NONE',  ( 19.03943276465977164, 0.05219959533936151252, 76.25109039468566152 ) ) ;
#104272 = CARTESIAN_POINT ( 'NONE',  ( -19.03943276465977164, 0.05219959533909376836, 56.24890960531435979 ) ) ;
#104273 = CARTESIAN_POINT ( 'NONE',  ( 9.474510206698729675, 16.51473224551082808, 87.08442372801900433 ) ) ;
#104274 = CARTESIAN_POINT ( 'NONE',  ( -12.14591786802326823, 12.06949235617739902, 113.1260903946856899 ) ) ;
#104275 = CARTESIAN_POINT ( 'NONE',  ( -16.46253265017146816, -9.564922557961047289, 84.16775706135233293 ) ) ;
#104276 = CARTESIAN_POINT ( 'NONE',  ( -8.224510206698948167, 14.34966873604960824, 45.41557627198103830 ) ) ;
#104277 = CARTESIAN_POINT ( 'NONE',  ( -9.474510206698720793, -16.51473224551083518, 64.58442372801900433 ) ) ;
#104278 = CARTESIAN_POINT ( 'NONE',  ( 8.314922557961029526, -14.29746914071037800, 45.41775706135234003 ) ) ;
#104279 = CARTESIAN_POINT ( 'NONE',  ( -5.049401038297874678, -19.05341960407617918, 29.79275706135232227 ) ) ;
#104280 = CARTESIAN_POINT ( 'NONE',  ( -16.51473224551069308, -9.474510206698971260, 41.66557627198103120 ) ) ;
#104281 = CARTESIAN_POINT ( 'NONE',  ( -12.14591786802326823, 12.06949235617739902, 43.12609039468568284 ) ) ;
#104282 = CARTESIAN_POINT ( 'NONE',  ( 28.82186960331521419, 9.364793116373263615, 139.3500000054624195 ) ) ;
#104283 = EDGE_CURVE ( 'NONE', #55000, #60925, #26905, .T. ) ;
#104284 = AXIS2_PLACEMENT_3D ( 'NONE', #153026, #16517, #78165 ) ;
#104285 = CARTESIAN_POINT ( 'NONE',  ( -22.44159573604010305, 16.30477369853692338, 144.6750000027311671 ) ) ;
#104286 = CARTESIAN_POINT ( 'NONE',  ( -9.474510206698964154, 16.51473224551069663, 90.41557627198103830 ) ) ;
#104287 = CYLINDRICAL_SURFACE ( 'NONE', #155605, 7.000000000000006217 ) ;
#104288 = CARTESIAN_POINT ( 'NONE',  ( -9.474510206698720793, -16.51473224551083518, 99.58442372801900433 ) ) ;
#104289 = CARTESIAN_POINT ( 'NONE',  ( 16.46253265017160672, -9.564922557960803928, 113.3322429386476955 ) ) ;
#104291 = CARTESIAN_POINT ( 'NONE',  ( -14.29746914071037622, -8.314922557961029526, 19.16775706135234714 ) ) ;
#104290 = CARTESIAN_POINT ( 'NONE',  ( 21.52544592524334988, 5.823673210054432836, 111.4594237280190328 ) ) ;
#104292 = CARTESIAN_POINT ( 'NONE',  ( 14.29746914071049879, -8.314922557960816363, 113.3322429386476955 ) ) ;
#104293 = CARTESIAN_POINT ( 'NONE',  ( 5.153800228976335163, 19.02544592524342804, 39.79057627198100988 ) ) ;
#104294 = CARTESIAN_POINT ( 'NONE',  ( -21.53943276465977519, 0.05219959533907696930, 71.24890960531435269 ) ) ;
#104295 = CARTESIAN_POINT ( 'NONE',  ( 13.89961937509977652, -13.97604488694527269, 43.12390960531434558 ) ) ;
#104296 = CARTESIAN_POINT ( 'NONE',  ( -0.05219959533936034679, 19.03943276465977164, 47.50109039468566863 ) ) ;
#104297 = CARTESIAN_POINT ( 'NONE',  ( -9.474510206698720793, -16.51473224551083518, 64.58442372801900433 ) ) ;
#104298 = CARTESIAN_POINT ( 'NONE',  ( -16.52544592524342804, 4.483927247898546575, 51.04057627198103120 ) ) ;
#104299 = CARTESIAN_POINT ( 'NONE',  ( -15.72974639402197994, 15.80617190586746368, 30.62390960531436335 ) ) ;
#104300 = CARTESIAN_POINT ( 'NONE',  ( -10.81492255796105439, 18.62759615963255655, 87.91775706135234714 ) ) ;
#104301 = CARTESIAN_POINT ( 'NONE',  ( -21.52544592524343514, 5.823673210054127303, 86.04057627198102409 ) ) ;
#104302 = CARTESIAN_POINT ( 'NONE',  ( -5.719274019375665041, -21.55341960407619695, 59.79275706135234714 ) ) ;
#104303 = CARTESIAN_POINT ( 'NONE',  ( -15.72974639402176322, -15.80617190586768395, 59.37609039468568284 ) ) ;
#104304 = CARTESIAN_POINT ( 'NONE',  ( 19.02544592524343514, -5.153800228976328945, 98.54057627198100988 ) ) ;
#104306 = CARTESIAN_POINT ( 'NONE',  ( 21.53943276465977519, 0.05219959533937863772, 61.25109039468567573 ) ) ;
#104305 = CARTESIAN_POINT ( 'NONE',  ( -4.483927247898782831, 16.52544592524335698, 87.70942372801901854 ) ) ;
#104307 = CARTESIAN_POINT ( 'NONE',  ( -5.153800228976328057, -19.02544592524343514, 57.29057627198103120 ) ) ;
#104308 = CARTESIAN_POINT ( 'NONE',  ( 9.564922557960805705, 16.46253265017160317, 29.58224293864769550 ) ) ;
#104309 = CARTESIAN_POINT ( 'NONE',  ( -9.564922557960796823, -16.46253265017161027, 52.08224293864768839 ) ) ;
#104310 = CARTESIAN_POINT ( 'NONE',  ( 8.314922557960818139, 14.29746914071049879, 64.58224293864769550 ) ) ;
#104311 = CARTESIAN_POINT ( 'NONE',  ( 16.55341960407611168, 4.379528057220329451, 38.95724293864768839 ) ) ;
#104312 = CARTESIAN_POINT ( 'NONE',  ( -21.55341960407610458, -5.719274019375992779, 46.45724293864769550 ) ) ;
#104313 = CARTESIAN_POINT ( 'NONE',  ( -16.46253265017160317, 9.564922557960807481, 50.83224293864770260 ) ) ;
#104314 = CARTESIAN_POINT ( 'NONE',  ( -0.05219959533907301413, -21.53943276465977519, 57.49890960531435979 ) ) ;
#104315 = CARTESIAN_POINT ( 'NONE',  ( -9.564922557961040184, 16.46253265017147172, 57.91775706135233293 ) ) ;
#104317 = CARTESIAN_POINT ( 'NONE',  ( 4.483927247898545687, 16.52544592524342804, 69.79057627198102409 ) ) ;
#104316 = CARTESIAN_POINT ( 'NONE',  ( -17.13100169013299379, -6.664070546373170423, 39.23210164300152059 ) ) ;
#104318 = CARTESIAN_POINT ( 'NONE',  ( -5.823673210054116645, -21.52544592524344225, 37.29057627198102409 ) ) ;
#104319 = ORIENTED_EDGE ( 'NONE', *, *, #143971, .F. ) ;
#104320 = ORIENTED_EDGE ( 'NONE', *, *, #137670, .T. ) ;
#104321 = CARTESIAN_POINT ( 'NONE',  ( 17.40861289039003523, 6.110651285853316850, 103.8723247082743200 ) ) ;
#104322 = CARTESIAN_POINT ( 'NONE',  ( 14.29746914071037800, 8.314922557961029526, 81.66775706135236135 ) ) ;
#104323 = CARTESIAN_POINT ( 'NONE',  ( -19.03943276465977164, -0.05219959533935918106, 78.75109039468567573 ) ) ;
#104324 = CARTESIAN_POINT ( 'NONE',  ( 12.14591786802309770, 12.06949235617756955, 49.37390960531436690 ) ) ;
#104325 = CARTESIAN_POINT ( 'NONE',  ( -11.30153831258470731, -180.0000000000000000, 1.787262988391354872E-28 ) ) ;
#104326 = CARTESIAN_POINT ( 'NONE',  ( -13.97604488694527625, -13.89961937509977652, 51.87390960531436690 ) ) ;
#104327 = CARTESIAN_POINT ( 'NONE',  ( 16.52544592524342804, -4.483927247898539470, 43.54057627198103830 ) ) ;
#104328 = CARTESIAN_POINT ( 'NONE',  ( 0.05219959533909260263, 19.03943276465977164, 49.99890960531435979 ) ) ;
#104329 = CARTESIAN_POINT ( 'NONE',  ( 16.51473224551069308, 9.474510206698969483, 69.16557627198102409 ) ) ;
#104330 = CARTESIAN_POINT ( 'NONE',  ( -19.03943276465977164, 0.05219959533909376836, 36.24890960531436690 ) ) ;
#104331 = CARTESIAN_POINT ( 'NONE',  ( 10.81492255796106328, -18.62759615963255655, 40.41775706135234714 ) ) ;
#104332 = CARTESIAN_POINT ( 'NONE',  ( 19.05341960407611168, 5.049401038298154454, 73.95724293864768129 ) ) ;
#104333 = CARTESIAN_POINT ( 'NONE',  ( -16.46253265017160317, 9.564922557960807481, 30.83224293864769550 ) ) ;
#104334 = CARTESIAN_POINT ( 'NONE',  ( -16.51473224551069308, -9.474510206698971260, 61.66557627198103120 ) ) ;
#104335 = CARTESIAN_POINT ( 'NONE',  ( 21.53943276465977519, -0.05219959533907433946, 53.74890960531437401 ) ) ;
#104336 = CARTESIAN_POINT ( 'NONE',  ( 5.153800228976335163, 19.02544592524342804, 34.79057627198102409 ) ) ;
#104337 = CARTESIAN_POINT ( 'NONE',  ( -15.72974639402197994, 15.80617190586746368, 40.62390960531435269 ) ) ;
#104338 = CARTESIAN_POINT ( 'NONE',  ( -12.14591786802326823, 12.06949235617739902, 98.12609039468570415 ) ) ;
#104339 = CARTESIAN_POINT ( 'NONE',  ( -5.049401038297874678, -19.05341960407617918, 19.79275706135233293 ) ) ;
#104341 = CARTESIAN_POINT ( 'NONE',  ( -4.483927247898782831, 16.52544592524335698, 82.70942372801900433 ) ) ;
#104340 = CARTESIAN_POINT ( 'NONE',  ( -8.314922557961024197, 14.29746914071037800, 42.91775706135235424 ) ) ;
#104342 = CARTESIAN_POINT ( 'NONE',  ( 0.000000000000000000, 0.000000000000000000, -64.92279855667830191 ) ) ;
#104343 = CARTESIAN_POINT ( 'NONE',  ( 4.483927247898790824, -16.52544592524335698, 70.20942372801904696 ) ) ;
#104344 = CARTESIAN_POINT ( 'NONE',  ( 14.29746914071037800, 8.314922557961029526, 36.66775706135234714 ) ) ;
#104345 = CARTESIAN_POINT ( 'NONE',  ( -9.564922557960796823, -16.46253265017161027, 102.0822429386477097 ) ) ;
#104346 = CARTESIAN_POINT ( 'NONE',  ( -14.29746914071037622, -8.314922557961029526, 39.16775706135235424 ) ) ;
#104347 = CARTESIAN_POINT ( 'NONE',  ( 0.05219959533909260263, 19.03943276465977164, 29.99890960531435979 ) ) ;
#104348 = CARTESIAN_POINT ( 'NONE',  ( 21.55341960407619695, -5.719274019375665929, 31.04275706135234714 ) ) ;
#104349 = CARTESIAN_POINT ( 'NONE',  ( -4.483927247898782831, 16.52544592524335698, 37.70942372801900433 ) ) ;
#104350 = CARTESIAN_POINT ( 'NONE',  ( 4.483927247898790824, -16.52544592524335698, 105.2094237280190328 ) ) ;
#104351 = DIRECTION ( 'NONE',  ( 1.000000000000000000, 0.000000000000000000, 0.000000000000000000 ) ) ;
#104352 = CARTESIAN_POINT ( 'NONE',  ( 18.67979575497194134, -10.72451020669871369, 100.8344237280190185 ) ) ;
#104353 = CARTESIAN_POINT ( 'NONE',  ( 19.02544592524334988, 5.153800228976608722, 96.45942372801897591 ) ) ;
#104354 = CARTESIAN_POINT ( 'NONE',  ( 12.06949235617757843, -12.14591786802309237, 58.12390960531435979 ) ) ;
#104355 = CARTESIAN_POINT ( 'NONE',  ( 19.05341960407611168, 5.049401038298154454, 28.95724293864769550 ) ) ;
#104357 = CARTESIAN_POINT ( 'NONE',  ( 17.50000000000000355, 5.500000000000011546, 78.78230962303567253 ) ) ;
#104356 = CARTESIAN_POINT ( 'NONE',  ( 5.049401038297881783, 19.05341960407617563, 57.29275706135231871 ) ) ;
#104358 = CARTESIAN_POINT ( 'NONE',  ( 10.72451020669871369, 18.67979575497193778, 62.08442372801901143 ) ) ;
#104359 = CARTESIAN_POINT ( 'NONE',  ( -4.483927247898782831, 16.52544592524335698, 27.70942372801901854 ) ) ;
#104360 = CARTESIAN_POINT ( 'NONE',  ( 17.49999999999999645, 5.622605283950889543, 83.81207310596114723 ) ) ;
#104361 = CARTESIAN_POINT ( 'NONE',  ( 16.46253265017160672, -9.564922557960803928, 113.3322429386476955 ) ) ;
#104362 = CARTESIAN_POINT ( 'NONE',  ( 18.62759615963271287, -10.81492255796078972, 78.33224293864770971 ) ) ;
#104363 = CARTESIAN_POINT ( 'NONE',  ( 9.564922557961047289, -16.46253265017146816, 110.4177570613523471 ) ) ;
#104364 = CARTESIAN_POINT ( 'NONE',  ( 9.474510206698971260, -16.51473224551069308, 97.91557627198102409 ) ) ;
#104365 = CARTESIAN_POINT ( 'NONE',  ( -1.435302771838241620, -27.95353791037918256, 140.0000000000001421 ) ) ;
#104366 = CARTESIAN_POINT ( 'NONE',  ( 8.314922557960818139, 14.29746914071049879, 114.5822429386477097 ) ) ;
#104367 = CARTESIAN_POINT ( 'NONE',  ( 21.53943276465977519, 0.05219959533937863772, 111.2510903946856899 ) ) ;
#104368 = CARTESIAN_POINT ( 'NONE',  ( 9.564922557960805705, 16.46253265017160317, 49.58224293864770260 ) ) ;
#104369 = CARTESIAN_POINT ( 'NONE',  ( 5.823673210054444382, -21.52544592524334988, 50.20942372801901854 ) ) ;
#104370 = CARTESIAN_POINT ( 'NONE',  ( 18.67979575497194134, -10.72451020669871369, 95.83442372801903275 ) ) ;
#104371 = CARTESIAN_POINT ( 'NONE',  ( -12.14591786802326823, 12.06949235617739902, 108.1260903946856757 ) ) ;
#104372 = ADVANCED_FACE ( 'NONE', ( #14693 ), #171564, .F. ) ;
#104373 = CARTESIAN_POINT ( 'NONE',  ( -16.46253265017160317, 9.564922557960807481, 75.83224293864769550 ) ) ;
#104374 = CARTESIAN_POINT ( 'NONE',  ( -5.823673210054431948, 21.52544592524334988, 42.70942372801901854 ) ) ;
#104375 = CARTESIAN_POINT ( 'NONE',  ( -5.719274019375665041, -21.55341960407619695, 54.79275706135235424 ) ) ;
#104377 = CARTESIAN_POINT ( 'NONE',  ( -13.97604488694527625, -13.89961937509977652, 86.87390960531436690 ) ) ;
#104376 = CARTESIAN_POINT ( 'NONE',  ( -16.51473224551082808, 9.474510206698731452, 83.33442372801899012 ) ) ;
#104378 = CARTESIAN_POINT ( 'NONE',  ( 12.06949235617757843, -12.14591786802309237, 98.12390960531436690 ) ) ;
#104379 = CARTESIAN_POINT ( 'NONE',  ( 10.72451020669898902, -18.67979575497178502, 97.91557627198103830 ) ) ;
#104380 = CARTESIAN_POINT ( 'NONE',  ( -12.06949235617756955, 12.14591786802309770, 75.62390960531439532 ) ) ;
#104381 = CARTESIAN_POINT ( 'NONE',  ( 15.80617190586769283, -15.72974639402175789, 110.6260903946857042 ) ) ;
#104382 = CARTESIAN_POINT ( 'NONE',  ( -8.224510206698948167, 14.34966873604960824, 95.41557627198102409 ) ) ;
#104383 = CARTESIAN_POINT ( 'NONE',  ( -13.89961937509977652, 13.97604488694528158, 55.62390960531434558 ) ) ;
#104384 = CARTESIAN_POINT ( 'NONE',  ( -16.46253265017146816, -9.564922557961047289, 79.16775706135234714 ) ) ;
#104385 = CARTESIAN_POINT ( 'NONE',  ( 12.06949235617757843, -12.14591786802309237, 53.12390960531436690 ) ) ;
#104386 = CARTESIAN_POINT ( 'NONE',  ( 10.72451020669871369, 18.67979575497193778, 112.0844237280190185 ) ) ;
#104387 = CARTESIAN_POINT ( 'NONE',  ( 9.564922557960805705, 16.46253265017160317, 109.5822429386476955 ) ) ;
#104388 = CARTESIAN_POINT ( 'NONE',  ( -9.474510206698720793, -16.51473224551083518, 79.58442372801899012 ) ) ;
#104389 = CARTESIAN_POINT ( 'NONE',  ( 21.55341960407610458, 5.719274019375980345, 78.95724293864769550 ) ) ;
#104390 = CARTESIAN_POINT ( 'NONE',  ( -10.72451020669870658, -18.67979575497194134, 29.58442372801901854 ) ) ;
#104391 = CARTESIAN_POINT ( 'NONE',  ( -16.52544592524335698, -4.483927247898792601, 28.95942372801902209 ) ) ;
#104392 = CARTESIAN_POINT ( 'NONE',  ( 8.224510206698742110, 14.34966873604972548, 97.08442372801904696 ) ) ;
#104394 = CARTESIAN_POINT ( 'NONE',  ( -15.72974639402176322, -15.80617190586768395, 34.37609039468568284 ) ) ;
#104393 = CARTESIAN_POINT ( 'NONE',  ( 17.31728774477272736, 6.344390552232406222, 61.68093348310681279 ) ) ;
#104395 = CARTESIAN_POINT ( 'NONE',  ( 5.719274019375991003, -21.55341960407610458, 47.70724293864770260 ) ) ;
#104396 = CARTESIAN_POINT ( 'NONE',  ( 4.483927247898545687, 16.52544592524342804, 114.7905762719810383 ) ) ;
#104397 = CARTESIAN_POINT ( 'NONE',  ( -38.00000000000001421, -12.34694845685042708, -11.64999999453762669 ) ) ;
#104398 = CARTESIAN_POINT ( 'NONE',  ( 12.14591786802327356, -12.06949235617739191, 65.62609039468568994 ) ) ;
#104399 = CARTESIAN_POINT ( 'NONE',  ( 14.29746914071049879, -8.314922557960816363, 93.33224293864769550 ) ) ;
#104400 = CARTESIAN_POINT ( 'NONE',  ( -15.72974639402197994, 15.80617190586746368, 75.62390960531439532 ) ) ;
#104401 = CARTESIAN_POINT ( 'NONE',  ( 16.55341960407611168, 4.379528057220329451, 28.95724293864769905 ) ) ;
#104402 = CARTESIAN_POINT ( 'NONE',  ( 12.06949235617739724, 12.14591786802326823, 51.87609039468568284 ) ) ;
#104403 = CARTESIAN_POINT ( 'NONE',  ( -5.153800228976328057, -19.02544592524343514, 42.29057627198101699 ) ) ;
#104404 = CARTESIAN_POINT ( 'NONE',  ( 8.224510206698742110, 14.34966873604972548, 97.08442372801904696 ) ) ;
#104405 = CARTESIAN_POINT ( 'NONE',  ( -16.51473224551082808, 9.474510206698731452, 83.33442372801899012 ) ) ;
#104406 = CARTESIAN_POINT ( 'NONE',  ( -5.823673210054116645, -21.52544592524344225, 82.29057627198103830 ) ) ;
#104407 = CARTESIAN_POINT ( 'NONE',  ( -8.224510206698735004, -14.34966873604973081, 104.5844237280190185 ) ) ;
#104408 = VERTEX_POINT ( 'NONE', #178340 ) ;
#104409 = CARTESIAN_POINT ( 'NONE',  ( 19.02544592524343514, -5.153800228976328945, 113.5405762719810241 ) ) ;
#104410 = CARTESIAN_POINT ( 'NONE',  ( -5.719274019375978568, 21.55341960407610458, 60.20724293864768839 ) ) ;
#104411 = ORIENTED_EDGE ( 'NONE', *, *, #176185, .T. ) ;
#104412 = CARTESIAN_POINT ( 'NONE',  ( 8.224510206698742110, 14.34966873604972548, 97.08442372801904696 ) ) ;
#104413 = EDGE_LOOP ( 'NONE', ( #186853, #23912, #140170, #52275, #200108 ) ) ;
#104414 = CARTESIAN_POINT ( 'NONE',  ( 0.05219959533907565091, 21.53943276465977519, 34.99890960531435979 ) ) ;
#104415 = CARTESIAN_POINT ( 'NONE',  ( -19.46398650005391673, 5.499999999999954703, 75.18269651486372140 ) ) ;
#104416 = CARTESIAN_POINT ( 'NONE',  ( -10.72451020669898014, 18.67979575497178502, 80.41557627198103830 ) ) ;
#104417 = CARTESIAN_POINT ( 'NONE',  ( 12.06949235617757843, -12.14591786802309237, 28.12390960531435979 ) ) ;
#104418 = CARTESIAN_POINT ( 'NONE',  ( 14.34966873604972726, -8.224510206698740333, 25.83442372801901499 ) ) ;
#104419 = CARTESIAN_POINT ( 'NONE',  ( -13.97604488694527625, -13.89961937509977652, 31.87390960531435979 ) ) ;
#104420 = CARTESIAN_POINT ( 'NONE',  ( -14.29746914071037622, -8.314922557961029526, 34.16775706135234714 ) ) ;
#104421 = CARTESIAN_POINT ( 'NONE',  ( 13.89961937509977652, -13.97604488694527269, 53.12390960531434558 ) ) ;
#104422 = CARTESIAN_POINT ( 'NONE',  ( -5.429308488886486681E-15, 30.30510711980690175, 147.5000000000000000 ) ) ;
#104423 = CARTESIAN_POINT ( 'NONE',  ( 16.51473224551069308, 9.474510206698969483, 104.1655762719810241 ) ) ;
#104424 = CARTESIAN_POINT ( 'NONE',  ( -5.049401038298153566, 19.05341960407611168, 105.2072429386476671 ) ) ;
#104425 = CARTESIAN_POINT ( 'NONE',  ( 0.05219959533934541429, -16.53943276465976808, 90.00109039468567573 ) ) ;
#104426 = CARTESIAN_POINT ( 'NONE',  ( 19.05341960407617918, -5.049401038297876454, 91.04275706135234714 ) ) ;
#104427 = CARTESIAN_POINT ( 'NONE',  ( -9.564922557961040184, 16.46253265017147172, 32.91775706135233293 ) ) ;
#104428 = CARTESIAN_POINT ( 'NONE',  ( -18.62759615963270932, 10.81492255796079327, 70.83224293864770971 ) ) ;
#104429 = CARTESIAN_POINT ( 'NONE',  ( 16.53943276465976808, 0.05219959533934440121, 96.25109039468568994 ) ) ;
#104430 = CARTESIAN_POINT ( 'NONE',  ( -5.719274019375978568, 21.55341960407610458, 35.20724293864768839 ) ) ;
#104431 = CARTESIAN_POINT ( 'NONE',  ( 13.97604488694548053, -13.89961937509957401, 90.62609039468567573 ) ) ;
#104432 = CARTESIAN_POINT ( 'NONE',  ( -9.564922557960796823, -16.46253265017161027, 47.08224293864769550 ) ) ;
#104433 = CARTESIAN_POINT ( 'NONE',  ( 5.153800228976335163, 19.02544592524342804, 89.79057627198102409 ) ) ;
#104434 = CARTESIAN_POINT ( 'NONE',  ( 21.53943276465977519, 0.05219959533937863772, 56.25109039468568284 ) ) ;
#104435 = CARTESIAN_POINT ( 'NONE',  ( 5.049401038298161559, -19.05341960407611168, 57.70724293864769550 ) ) ;
#104436 = CARTESIAN_POINT ( 'NONE',  ( 4.483927247898545687, 16.52544592524342804, 104.7905762719810241 ) ) ;
#104437 = DIRECTION ( 'NONE',  ( 0.000000000000000000, 1.000000000000000000, 0.000000000000000000 ) ) ;
#104438 = CARTESIAN_POINT ( 'NONE',  ( -16.52544592524342804, 4.483927247898546575, 81.04057627198102409 ) ) ;
#104439 = CARTESIAN_POINT ( 'NONE',  ( 10.72451020669898902, -18.67979575497178502, 67.91557627198102409 ) ) ;
#104440 = CARTESIAN_POINT ( 'NONE',  ( -5.049401038297874678, -19.05341960407617918, 84.79275706135233293 ) ) ;
#104441 = CARTESIAN_POINT ( 'NONE',  ( 18.39639308325437739, 5.500000000000010658, 93.98252246182197212 ) ) ;
#104442 = CARTESIAN_POINT ( 'NONE',  ( -19.02544592524342804, 5.153800228976336051, 56.04057627198100988 ) ) ;
#104443 = DIRECTION ( 'NONE',  ( -0.7071067811865467956, 2.468850131082262977E-15, 0.7071067811865483499 ) ) ;
#104445 = CARTESIAN_POINT ( 'NONE',  ( 9.564922557960805705, 16.46253265017160317, 89.58224293864769550 ) ) ;
#104444 = CARTESIAN_POINT ( 'NONE',  ( 19.05341960407611168, 5.049401038298154454, 83.95724293864766707 ) ) ;
#104446 = B_SPLINE_CURVE_WITH_KNOTS ( 'NONE', 3,
 ( #198927, #108892, #124046, #30070, #48229, #185745, #155400, #60395 ),
 .UNSPECIFIED., .F., .F.,
 ( 4, 2, 2, 4 ),
 ( 0.004065040094758672930, 0.004372354996941527766, 0.004679669899124381735, 0.005294299703490097479 ),
 .UNSPECIFIED. ) ;
#104447 = CARTESIAN_POINT ( 'NONE',  ( -14.34966873604972548, 8.224510206698743886, 63.33442372801900433 ) ) ;
#104448 = CARTESIAN_POINT ( 'NONE',  ( -16.20579543436680225, -7.371946100354968223, 50.56520834171872991 ) ) ;
#104449 = CARTESIAN_POINT ( 'NONE',  ( -0.05219959533936034679, 19.03943276465977164, 42.50109039468566152 ) ) ;
#104450 = CARTESIAN_POINT ( 'NONE',  ( 36.78335851983071336, 5.362873614019889601, 46.23361200806721882 ) ) ;
#104451 = CARTESIAN_POINT ( 'NONE',  ( -19.05341960407611168, -5.049401038298163336, 111.4572429386476671 ) ) ;
#104452 = CARTESIAN_POINT ( 'NONE',  ( -16.53943276465976808, -0.05219959533934237506, 103.7510903946857042 ) ) ;
#104453 = CARTESIAN_POINT ( 'NONE',  ( 13.74275686049843159, -0.4100021152176986372, -60.42614020214174531 ) ) ;
#104454 = CARTESIAN_POINT ( 'NONE',  ( 16.53943276465976808, 0.05219959533934440121, 76.25109039468568994 ) ) ;
#104455 = CARTESIAN_POINT ( 'NONE',  ( -17.40861289039003523, 6.110651285853254677, 28.62767529172569070 ) ) ;
#104456 = CARTESIAN_POINT ( 'NONE',  ( 8.314922557961029526, -14.29746914071037800, 55.41775706135234714 ) ) ;
#104457 = DIRECTION ( 'NONE',  ( 0.000000000000000000, -0.000000000000000000, -1.000000000000000000 ) ) ;
#104458 = CARTESIAN_POINT ( 'NONE',  ( -15.80617190586768217, 15.72974639402176855, 63.12609039468568994 ) ) ;
#104459 = CARTESIAN_POINT ( 'NONE',  ( 0.05219959533936267826, -19.03943276465977164, 75.00109039468566152 ) ) ;
#104460 = CARTESIAN_POINT ( 'NONE',  ( 19.02544592524334988, 5.153800228976608722, 31.45942372801900433 ) ) ;
#104461 = CARTESIAN_POINT ( 'NONE',  ( -16.46253265017160317, 9.564922557960807481, 60.83224293864769550 ) ) ;
#104462 = CARTESIAN_POINT ( 'NONE',  ( -19.05341960407611168, -5.049401038298163336, 46.45724293864768129 ) ) ;
#104463 = CARTESIAN_POINT ( 'NONE',  ( 16.24969088024964492, -7.354500926750625389, 22.52456153141350370 ) ) ;
#104464 = CARTESIAN_POINT ( 'NONE',  ( 10.72451020669898902, -18.67979575497178502, 72.91557627198103830 ) ) ;
#104465 = CARTESIAN_POINT ( 'NONE',  ( -10.72451020669898014, 18.67979575497178502, 40.41557627198103120 ) ) ;
#104466 = CARTESIAN_POINT ( 'NONE',  ( 14.34966873604960469, 8.224510206698951720, 109.1655762719810383 ) ) ;
#104467 = CARTESIAN_POINT ( 'NONE',  ( 16.52544592524335698, 4.483927247898782831, 56.45942372801902565 ) ) ;
#104468 = EDGE_LOOP ( 'NONE', ( #153357, #40656 ) ) ;
#104469 = CARTESIAN_POINT ( 'NONE',  ( -5.719274019375665041, -21.55341960407619695, 29.79275706135234358 ) ) ;
#104471 = CARTESIAN_POINT ( 'NONE',  ( 23.48529157249599919, 32.32473071737754111, -8.700000000000002842 ) ) ;
#104470 = CARTESIAN_POINT ( 'NONE',  ( -4.379528057220328563, 16.55341960407611168, 55.20724293864770260 ) ) ;
#104472 = CARTESIAN_POINT ( 'NONE',  ( 8.224510206698742110, 14.34966873604972548, 27.08442372801901854 ) ) ;
#104473 = CARTESIAN_POINT ( 'NONE',  ( -13.89961937509957401, -13.97604488694547875, 34.37609039468566863 ) ) ;
#104474 = CARTESIAN_POINT ( 'NONE',  ( -16.55341960407611168, -4.379528057220339221, 46.45724293864769550 ) ) ;
#104476 = ADVANCED_FACE ( 'NONE', ( #10487 ), #63271, .T. ) ;
#104475 = CARTESIAN_POINT ( 'NONE',  ( 5.719274019375991003, -21.55341960407610458, 112.7072429386476955 ) ) ;
#104478 = CARTESIAN_POINT ( 'NONE',  ( 5.719274019375991003, -21.55341960407610458, 82.70724293864770971 ) ) ;
#104477 = DIRECTION ( 'NONE',  ( 0.000000000000000000, -0.7071067811865467956, -0.7071067811865483499 ) ) ;
#104479 = CARTESIAN_POINT ( 'NONE',  ( -0.05219959533909027116, -19.03943276465977164, 92.49890960531436690 ) ) ;
#104480 = CARTESIAN_POINT ( 'NONE',  ( 14.29746914071049879, -8.314922557960816363, 63.33224293864770260 ) ) ;
#104481 = CARTESIAN_POINT ( 'NONE',  ( 19.03943276465977164, -0.05219959533909143690, 108.7489096053143527 ) ) ;
#104482 = CARTESIAN_POINT ( 'NONE',  ( -36.80083376053583066, 5.466397602639213815, 45.70522705241149453 ) ) ;
#104483 = CARTESIAN_POINT ( 'NONE',  ( 0.05219959533936267826, -19.03943276465977164, 65.00109039468567573 ) ) ;
#104484 = CARTESIAN_POINT ( 'NONE',  ( -18.62759615963270932, 10.81492255796079327, 105.8322429386476955 ) ) ;
#104485 = CARTESIAN_POINT ( 'NONE',  ( 16.51473224551069308, 9.474510206698969483, 59.16557627198102409 ) ) ;
#104486 = CARTESIAN_POINT ( 'NONE',  ( 9.474510206698971260, -16.51473224551069308, 22.91557627198102765 ) ) ;
#104487 = AXIS2_PLACEMENT_3D ( 'NONE', #29111, #134301, #91731 ) ;
#104488 = CARTESIAN_POINT ( 'NONE',  ( -15.72974639402176322, -15.80617190586768395, 54.37609039468568994 ) ) ;
#104489 = CARTESIAN_POINT ( 'NONE',  ( 8.571926809382597767, 26.38167802310806209, 148.2750000027311899 ) ) ;
#104490 = EDGE_CURVE ( 'NONE', #69189, #83996, #169410, .T. ) ;
#104491 = CARTESIAN_POINT ( 'NONE',  ( -14.34966873604960291, -8.224510206698953496, 46.66557627198102409 ) ) ;
#104492 = CARTESIAN_POINT ( 'NONE',  ( 13.89961937509977652, -13.97604488694527269, 48.12390960531435979 ) ) ;
#104493 = CARTESIAN_POINT ( 'NONE',  ( -16.51473224551069308, -9.474510206698971260, 101.6655762719810241 ) ) ;
#104494 = CARTESIAN_POINT ( 'NONE',  ( -5.823673210054116645, -21.52544592524344225, 77.29057627198102409 ) ) ;
#104495 = CARTESIAN_POINT ( 'NONE',  ( -27.73933785331498925, -9.013057229001049109, 142.9750000027312069 ) ) ;
#104496 = CARTESIAN_POINT ( 'NONE',  ( 19.03943276465977164, -0.05219959533909143690, 38.74890960531436690 ) ) ;
#104497 = ORIENTED_EDGE ( 'NONE', *, *, #175152, .T. ) ;
#104498 = CARTESIAN_POINT ( 'NONE',  ( -5.823673210054116645, -21.52544592524344225, 62.29057627198102409 ) ) ;
#104499 = CARTESIAN_POINT ( 'NONE',  ( 15.80617190586769283, -15.72974639402175789, 80.62609039468567573 ) ) ;
#104502 = CARTESIAN_POINT ( 'NONE',  ( -14.34966873604960291, -8.224510206698953496, 81.66557627198103830 ) ) ;
#104501 = CARTESIAN_POINT ( 'NONE',  ( 12.06949235617739724, 12.14591786802326823, 86.87609039468568994 ) ) ;
#104500 = FACE_OUTER_BOUND ( 'NONE', #170135, .T. ) ;
#104503 = CARTESIAN_POINT ( 'NONE',  ( 9.474510206698971260, -16.51473224551069308, 67.91557627198102409 ) ) ;
#104504 = ORIENTED_EDGE ( 'NONE', *, *, #76779, .T. ) ;
#104505 = CARTESIAN_POINT ( 'NONE',  ( 19.03943276465977164, 0.05219959533936151252, 36.25109039468567573 ) ) ;
#104506 = CARTESIAN_POINT ( 'NONE',  ( -14.29746914071037622, -8.314922557961029526, 94.16775706135237556 ) ) ;
#104507 = CARTESIAN_POINT ( 'NONE',  ( -0.05219959533937732626, 21.53943276465977519, 112.5010903946857042 ) ) ;
#104508 = CARTESIAN_POINT ( 'NONE',  ( 19.05341960407611168, 5.049401038298154454, 93.95724293864769550 ) ) ;
#104509 = CARTESIAN_POINT ( 'NONE',  ( 10.72451020669898902, -18.67979575497178502, 42.91557627198103120 ) ) ;
#104510 = CARTESIAN_POINT ( 'NONE',  ( 15.72974639402176855, 15.80617190586768217, 91.87609039468568994 ) ) ;
#104511 = CARTESIAN_POINT ( 'NONE',  ( -0.05219959533934338120, 16.53943276465976808, 57.50109039468568994 ) ) ;
#104512 = CARTESIAN_POINT ( 'NONE',  ( 5.719274019375991003, -21.55341960407610458, 112.7072429386476955 ) ) ;
#104513 = CARTESIAN_POINT ( 'NONE',  ( 16.55341960407618274, -4.379528057220086978, 36.04275706135234714 ) ) ;
#104514 = CARTESIAN_POINT ( 'NONE',  ( -9.564922557960796823, -16.46253265017161027, 87.08224293864769550 ) ) ;
#104515 = CARTESIAN_POINT ( 'NONE',  ( 8.314922557961029526, -14.29746914071037800, 25.41775706135235779 ) ) ;
#104516 = CARTESIAN_POINT ( 'NONE',  ( -13.97604488694527625, -13.89961937509977652, 51.87390960531436690 ) ) ;
#104517 = CARTESIAN_POINT ( 'NONE',  ( 8.314922557961029526, -14.29746914071037800, 35.41775706135234003 ) ) ;
#104518 = CARTESIAN_POINT ( 'NONE',  ( 14.34966873604960469, 8.224510206698951720, 79.16557627198103830 ) ) ;
#104519 = CARTESIAN_POINT ( 'NONE',  ( 8.224510206698742110, 14.34966873604972548, 87.08442372801901854 ) ) ;
#104521 = CARTESIAN_POINT ( 'NONE',  ( -19.03943276465977164, 0.05219959533909376836, 71.24890960531435269 ) ) ;
#104520 = CARTESIAN_POINT ( 'NONE',  ( -21.52544592524334988, -5.823673210054445271, 38.95942372801901854 ) ) ;
#104522 = CARTESIAN_POINT ( 'NONE',  ( -13.97604488694527625, -13.89961937509977652, 81.87390960531436690 ) ) ;
#104523 = CARTESIAN_POINT ( 'NONE',  ( 8.314922557960818139, 14.29746914071049879, 29.58224293864769905 ) ) ;
#104524 = CARTESIAN_POINT ( 'NONE',  ( 16.52544592524335698, 4.483927247898782831, 91.45942372801901854 ) ) ;
#104525 = ADVANCED_FACE ( 'NONE', ( #30915 ), #125895, .F. ) ;
#104526 = ORIENTED_EDGE ( 'NONE', *, *, #101847, .T. ) ;
#104527 = CARTESIAN_POINT ( 'NONE',  ( -5.049401038297874678, -19.05341960407617918, 24.79275706135233648 ) ) ;
#104528 = CARTESIAN_POINT ( 'NONE',  ( 13.97604488694527802, 13.89961937509977652, 94.37390960531436690 ) ) ;
#104529 = CARTESIAN_POINT ( 'NONE',  ( -19.02544592524342804, 5.153800228976336051, 56.04057627198100988 ) ) ;
#104530 = CARTESIAN_POINT ( 'NONE',  ( 16.46253265017160672, -9.564922557960803928, 113.3322429386476955 ) ) ;
#104531 = CARTESIAN_POINT ( 'NONE',  ( 4.483927247898790824, -16.52544592524335698, 45.20942372801901854 ) ) ;
#104533 = CARTESIAN_POINT ( 'NONE',  ( 14.34966873604972726, -8.224510206698740333, 55.83442372801901854 ) ) ;
#104532 = CARTESIAN_POINT ( 'NONE',  ( 5.153800228976615827, -19.02544592524334988, 70.20942372801899012 ) ) ;
#104534 = CARTESIAN_POINT ( 'NONE',  ( 15.50000000000000178, 5.499999999999998224, 22.00000000000000000 ) ) ;
#104535 = CARTESIAN_POINT ( 'NONE',  ( 16.51473224551069308, 9.474510206698969483, 79.16557627198103830 ) ) ;
#104536 = CARTESIAN_POINT ( 'NONE',  ( 18.62759615963255655, 10.81492255796105972, 21.66775706135235069 ) ) ;
#104537 = CARTESIAN_POINT ( 'NONE',  ( 0.05219959533936267826, -19.03943276465977164, 65.00109039468567573 ) ) ;
#104539 = CARTESIAN_POINT ( 'NONE',  ( 30.00000000000000000, -1.163414459189985801E-14, 95.00000000000000000 ) ) ;
#104538 = CARTESIAN_POINT ( 'NONE',  ( -16.51473224551069308, -9.474510206698971260, 101.6655762719810241 ) ) ;
#104540 = CARTESIAN_POINT ( 'NONE',  ( -16.46253265017160317, 9.564922557960807481, 70.83224293864770971 ) ) ;
#104542 = CARTESIAN_POINT ( 'NONE',  ( 0.05219959533909260263, 19.03943276465977164, 29.99890960531435979 ) ) ;
#104541 = CARTESIAN_POINT ( 'NONE',  ( 8.314922557960818139, 14.29746914071049879, 34.58224293864770260 ) ) ;
#104543 = CARTESIAN_POINT ( 'NONE',  ( 13.89961937509957401, 13.97604488694547697, 31.87609039468566863 ) ) ;
#104544 = CARTESIAN_POINT ( 'NONE',  ( -4.379528057220328563, 16.55341960407611168, 75.20724293864769550 ) ) ;
#104545 = CARTESIAN_POINT ( 'NONE',  ( -0.05219959533937732626, 21.53943276465977519, 107.5010903946856899 ) ) ;
#104546 = CARTESIAN_POINT ( 'NONE',  ( 19.02544592524343514, -5.153800228976328945, 58.54057627198102409 ) ) ;
#104548 = CARTESIAN_POINT ( 'NONE',  ( 21.55341960407619695, -5.719274019375665929, 106.0427570613523471 ) ) ;
#104547 = CARTESIAN_POINT ( 'NONE',  ( -16.53943276465976808, 0.05219959533911058130, 36.24890960531435979 ) ) ;
#104549 = CARTESIAN_POINT ( 'NONE',  ( 13.89961937509977652, -13.97604488694527269, 88.12390960531438111 ) ) ;
#104550 = CARTESIAN_POINT ( 'NONE',  ( -16.51473224551069308, -9.474510206698971260, 106.6655762719810383 ) ) ;
#104551 = CARTESIAN_POINT ( 'NONE',  ( -13.89961937509977652, 13.97604488694528158, 45.62390960531433848 ) ) ;
#104552 = CARTESIAN_POINT ( 'NONE',  ( 4.379528057220339221, -16.55341960407611168, 112.7072429386476955 ) ) ;
#104553 = CARTESIAN_POINT ( 'NONE',  ( 8.224510206698953496, -14.34966873604960469, 72.91557627198103830 ) ) ;
#104554 = CARTESIAN_POINT ( 'NONE',  ( -5.719274019375978568, 21.55341960407610458, 90.20724293864770971 ) ) ;
#104555 = CARTESIAN_POINT ( 'NONE',  ( 5.049401038298161559, -19.05341960407611168, 92.70724293864769550 ) ) ;
#104556 = CARTESIAN_POINT ( 'NONE',  ( 10.81492255796078972, 18.62759615963270932, 99.58224293864770971 ) ) ;
#104557 = CARTESIAN_POINT ( 'NONE',  ( 13.89961937509977652, -13.97604488694527269, 88.12390960531438111 ) ) ;
#104559 = CARTESIAN_POINT ( 'NONE',  ( 8.224510206698953496, -14.34966873604960469, 102.9155762719810383 ) ) ;
#104558 = DIRECTION ( 'NONE',  ( -1.000000000000000000, -6.451865313697283898E-33, -1.908195823574487804E-15 ) ) ;
#104560 = CARTESIAN_POINT ( 'NONE',  ( -19.02544592524342804, 5.153800228976336051, 71.04057627198099567 ) ) ;
#104561 = CARTESIAN_POINT ( 'NONE',  ( 18.62759615963271287, -10.81492255796078972, 78.33224293864770971 ) ) ;
#104562 = CARTESIAN_POINT ( 'NONE',  ( -21.44939319537014200, -9.428468639168981369, 168.6471776813584995 ) ) ;
#104564 = CARTESIAN_POINT ( 'NONE',  ( 19.53037848336980176, -5.499999999999891642, 67.35532783611444074 ) ) ;
#104563 = CARTESIAN_POINT ( 'NONE',  ( 21.55341960407610458, 5.719274019375980345, 33.95724293864769550 ) ) ;
#104565 = CARTESIAN_POINT ( 'NONE',  ( 16.55341960407618274, -4.379528057220086978, 36.04275706135234714 ) ) ;
#104566 = CARTESIAN_POINT ( 'NONE',  ( -4.379528057220328563, 16.55341960407611168, 100.2072429386476955 ) ) ;
#104567 = CARTESIAN_POINT ( 'NONE',  ( -18.22780087662121673, -5.500000000000063061, 46.48459894673893444 ) ) ;
#104568 = CARTESIAN_POINT ( 'NONE',  ( 9.474510206698971260, -16.51473224551069308, 87.91557627198102409 ) ) ;
#104569 = CARTESIAN_POINT ( 'NONE',  ( -9.474510206698964154, 16.51473224551069663, 45.41557627198103120 ) ) ;
#104570 = CARTESIAN_POINT ( 'NONE',  ( -16.55341960407611168, -4.379528057220339221, 81.45724293864769550 ) ) ;
#104571 = CIRCLE ( 'NONE', #107854, 2.055000000000000160 ) ;
#104572 = CARTESIAN_POINT ( 'NONE',  ( 19.03943276465977164, -0.05219959533909143690, 113.7489096053143669 ) ) ;
#104573 = CARTESIAN_POINT ( 'NONE',  ( 4.379528057220339221, -16.55341960407611168, 52.70724293864769550 ) ) ;
#104574 = CARTESIAN_POINT ( 'NONE',  ( -13.97604488694547697, 13.89961937509957934, 103.1260903946856473 ) ) ;
#104575 = CARTESIAN_POINT ( 'NONE',  ( -21.55341960407619339, 5.719274019375674811, 63.54275706135234003 ) ) ;
#104576 = DIRECTION ( 'NONE',  ( -0.000000000000000000, -0.000000000000000000, 1.000000000000000000 ) ) ;
#104577 = CARTESIAN_POINT ( 'NONE',  ( -13.97604488694527625, -13.89961937509977652, 96.87390960531433848 ) ) ;
#104578 = CARTESIAN_POINT ( 'NONE',  ( -12.06949235617739369, -12.14591786802326823, 84.37609039468570415 ) ) ;
#104579 = CARTESIAN_POINT ( 'NONE',  ( -9.474510206698964154, 16.51473224551069663, 25.41557627198103120 ) ) ;
#104580 = CARTESIAN_POINT ( 'NONE',  ( -19.05341960407611168, -5.049401038298163336, 71.45724293864766707 ) ) ;
#104581 = CARTESIAN_POINT ( 'NONE',  ( -0.05219959533907301413, -21.53943276465977519, 87.49890960531436690 ) ) ;
#104582 = CARTESIAN_POINT ( 'NONE',  ( 9.564922557961047289, -16.46253265017146816, 110.4177570613523471 ) ) ;
#104584 = CARTESIAN_POINT ( 'NONE',  ( 10.72451020669871369, 18.67979575497193778, 57.08442372801901854 ) ) ;
#104583 = CARTESIAN_POINT ( 'NONE',  ( -14.34966873604960291, -8.224510206698953496, 46.66557627198102409 ) ) ;
#104586 = CARTESIAN_POINT ( 'NONE',  ( 9.564922557960805705, 16.46253265017160317, 114.5822429386476955 ) ) ;
#104585 = CARTESIAN_POINT ( 'NONE',  ( -0.05219959533934338120, 16.53943276465976808, 87.50109039468568994 ) ) ;
#104587 = CARTESIAN_POINT ( 'NONE',  ( -16.46253265017160317, 9.564922557960807481, 110.8322429386476955 ) ) ;
#104588 = CARTESIAN_POINT ( 'NONE',  ( -16.53943276465976808, -0.05219959533934237506, 108.7510903946857042 ) ) ;
#104589 = CARTESIAN_POINT ( 'NONE',  ( -0.05219959533934338120, 16.53943276465976808, 57.50109039468568994 ) ) ;
#104590 = CARTESIAN_POINT ( 'NONE',  ( -5.153800228976328057, -19.02544592524343514, 72.29057627198102409 ) ) ;
#104591 = CARTESIAN_POINT ( 'NONE',  ( 9.564922557960805705, 16.46253265017160317, 74.58224293864769550 ) ) ;
#104592 = CARTESIAN_POINT ( 'NONE',  ( 21.53943276465977519, 0.05219959533937863772, 71.25109039468568994 ) ) ;
#104593 = CARTESIAN_POINT ( 'NONE',  ( 12.14591786802327356, -12.06949235617739191, 80.62609039468567573 ) ) ;
#104594 = CARTESIAN_POINT ( 'NONE',  ( -0.05219959533910754901, -16.53943276465976808, 47.49890960531435979 ) ) ;
#104595 = CARTESIAN_POINT ( 'NONE',  ( -0.05219959533909027116, -19.03943276465977164, 52.49890960531436690 ) ) ;
#104596 = CARTESIAN_POINT ( 'NONE',  ( 0.05219959533909260263, 19.03943276465977164, 44.99890960531435979 ) ) ;
#104598 = ORIENTED_EDGE ( 'NONE', *, *, #32592, .T. ) ;
#104597 = CARTESIAN_POINT ( 'NONE',  ( -14.29746914071037622, -8.314922557961029526, 44.16775706135234714 ) ) ;
#104599 = CARTESIAN_POINT ( 'NONE',  ( -19.03943276465977164, -0.05219959533935918106, 98.75109039468567573 ) ) ;
#104600 = CARTESIAN_POINT ( 'NONE',  ( -16.52544592524342804, 4.483927247898546575, 91.04057627198103830 ) ) ;
#104601 = CARTESIAN_POINT ( 'NONE',  ( 5.153800228976335163, 19.02544592524342804, 64.79057627198100988 ) ) ;
#104603 = CARTESIAN_POINT ( 'NONE',  ( -11.74264578624799782, -36.14014761921581709, -5.599999999999999645 ) ) ;
#104602 = CARTESIAN_POINT ( 'NONE',  ( -9.564922557961040184, 16.46253265017147172, 97.91775706135233293 ) ) ;
#104604 = CARTESIAN_POINT ( 'NONE',  ( 0.05219959533937995610, -21.53943276465977519, 100.0010903946857042 ) ) ;
#104605 = CARTESIAN_POINT ( 'NONE',  ( -0.05219959533934338120, 16.53943276465976808, 72.50109039468568994 ) ) ;
#104606 = DIRECTION ( 'NONE',  ( 0.000000000000000000, -0.000000000000000000, 1.000000000000000000 ) ) ;
#104607 = CARTESIAN_POINT ( 'NONE',  ( 10.72451020669898902, -18.67979575497178502, 62.91557627198102409 ) ) ;
#104608 = CARTESIAN_POINT ( 'NONE',  ( -14.34966873604972548, 8.224510206698743886, 53.33442372801901854 ) ) ;
#104609 = CARTESIAN_POINT ( 'NONE',  ( 5.199999999999996625, 0.000000000000000000, 0.000000000000000000 ) ) ;
#104610 = CARTESIAN_POINT ( 'NONE',  ( 0.05219959533936267826, -19.03943276465977164, 40.00109039468566152 ) ) ;
#104611 = CARTESIAN_POINT ( 'NONE',  ( -19.05341960407611168, -5.049401038298163336, 96.45724293864769550 ) ) ;
#104612 = CARTESIAN_POINT ( 'NONE',  ( -13.97604488694527625, -13.89961937509977652, 26.87390960531434558 ) ) ;
#104613 = CARTESIAN_POINT ( 'NONE',  ( -5.049401038298153566, 19.05341960407611168, 60.20724293864768129 ) ) ;
#104614 = CARTESIAN_POINT ( 'NONE',  ( 10.81492255796106328, -18.62759615963255655, 70.41775706135236135 ) ) ;
#104615 = CARTESIAN_POINT ( 'NONE',  ( 19.05341960407617918, -5.049401038297876454, 51.04275706135231871 ) ) ;
#104616 = CARTESIAN_POINT ( 'NONE',  ( -9.564922557961040184, 16.46253265017147172, 32.91775706135233293 ) ) ;
#104617 = CARTESIAN_POINT ( 'NONE',  ( 9.564922557960805705, 16.46253265017160317, 54.58224293864769550 ) ) ;
#104618 = CARTESIAN_POINT ( 'NONE',  ( 0.05219959533907565091, 21.53943276465977519, 29.99890960531435979 ) ) ;
#104619 = CARTESIAN_POINT ( 'NONE',  ( -21.53943276465977519, -0.05219959533937600094, 88.75109039468567573 ) ) ;
#104620 = CARTESIAN_POINT ( 'NONE',  ( 19.05341960407611168, 5.049401038298154454, 68.95724293864769550 ) ) ;
#104621 = CARTESIAN_POINT ( 'NONE',  ( -10.81492255796105439, 18.62759615963255655, 97.91775706135236135 ) ) ;
#104622 = CARTESIAN_POINT ( 'NONE',  ( 15.80617190586746368, 15.72974639402197994, 34.37390960531435979 ) ) ;
#104623 = CARTESIAN_POINT ( 'NONE',  ( 5.049401038298161559, -19.05341960407611168, 82.70724293864770971 ) ) ;
#104624 = CARTESIAN_POINT ( 'NONE',  ( 10.72451020669871369, 18.67979575497193778, 42.08442372801901854 ) ) ;
#104625 = CARTESIAN_POINT ( 'NONE',  ( -13.97604488694547697, 13.89961937509957934, 63.12609039468566152 ) ) ;
#104626 = CARTESIAN_POINT ( 'NONE',  ( 5.153800228976335163, 19.02544592524342804, 39.79057627198100988 ) ) ;
#104627 = CARTESIAN_POINT ( 'NONE',  ( -13.89961937509977652, 13.97604488694528158, 95.62390960531436690 ) ) ;
#104628 = CARTESIAN_POINT ( 'NONE',  ( 0.05219959533934541429, -16.53943276465976808, 25.00109039468567218 ) ) ;
#104629 = CARTESIAN_POINT ( 'NONE',  ( 4.483927247898545687, 16.52544592524342804, 84.79057627198102409 ) ) ;
#104630 = CARTESIAN_POINT ( 'NONE',  ( 19.03943276465977164, -0.05219959533909143690, 73.74890960531435269 ) ) ;
#104631 = CARTESIAN_POINT ( 'NONE',  ( 21.53943276465977519, -0.05219959533907433946, 53.74890960531437401 ) ) ;
#104632 = CARTESIAN_POINT ( 'NONE',  ( -9.564922557961040184, 16.46253265017147172, 112.9177570613523329 ) ) ;
#104633 = CARTESIAN_POINT ( 'NONE',  ( -15.72974639402176322, -15.80617190586768395, 24.37609039468567573 ) ) ;
#104634 = CARTESIAN_POINT ( 'NONE',  ( -15.72974639402176322, -15.80617190586768395, 74.37609039468568994 ) ) ;
#104635 = CARTESIAN_POINT ( 'NONE',  ( -4.379528057220086978, -16.55341960407618274, 69.79275706135234714 ) ) ;
#104636 = CARTESIAN_POINT ( 'NONE',  ( -16.52544592524335698, -4.483927247898792601, 63.95942372801901854 ) ) ;
#104637 = AXIS2_PLACEMENT_3D ( 'NONE', #61936, #30626, #47791 ) ;
#104638 =( BOUNDED_CURVE ( )  B_SPLINE_CURVE ( 2, ( #78842, #93015, #154701, #140520, #77851, #33351, #139518, #95010, #1001, #126343, #45537, #34344, #80829 ),
 .UNSPECIFIED., .F., .F. ) 
 B_SPLINE_CURVE_WITH_KNOTS ( ( 3, 2, 2, 2, 2, 2, 3 ),
 ( 0.1340550636175563970, 0.1359649122807017607, 0.1403508771929824483, 0.1447368421052631637, 0.1491228070175438514, 0.1535087719298245668, 0.1554643004150602359 ),
 .UNSPECIFIED. ) 
 CURVE ( )  GEOMETRIC_REPRESENTATION_ITEM ( )  RATIONAL_B_SPLINE_CURVE ( ( 0.9832469066685285419, 0.9851625545550100060, 1.000000000000000000, 0.9659258262890683122, 1.000000000000000000, 0.9659258262890683122, 1.000000000000000000, 0.9659258262890683122, 1.000000000000000000, 0.9659258262890683122, 1.000000000000000000, 0.9848076720550082985, 0.9831626618144004848 ) ) 
 REPRESENTATION_ITEM ( '' )  );
#104639 = CARTESIAN_POINT ( 'NONE',  ( -16.51473224551069308, -9.474510206698971260, 61.66557627198103120 ) ) ;
#104640 = CARTESIAN_POINT ( 'NONE',  ( -12.06949235617739369, -12.14591786802326823, 104.3760903946856899 ) ) ;
#104641 = CARTESIAN_POINT ( 'NONE',  ( 9.474510206698729675, 16.51473224551082808, 47.08442372801900433 ) ) ;
#104642 = CARTESIAN_POINT ( 'NONE',  ( -10.72451020669898014, 18.67979575497178502, 110.4155762719810383 ) ) ;
#104643 = CARTESIAN_POINT ( 'NONE',  ( -12.06949235617756955, 12.14591786802309770, 65.62390960531436690 ) ) ;
#104644 = CARTESIAN_POINT ( 'NONE',  ( 9.564922557960805705, 16.46253265017160317, 94.58224293864769550 ) ) ;
#104645 = CARTESIAN_POINT ( 'NONE',  ( 4.483927247898790824, -16.52544592524335698, 95.20942372801903275 ) ) ;
#104646 = CARTESIAN_POINT ( 'NONE',  ( -10.72451020669870658, -18.67979575497194134, 54.58442372801901143 ) ) ;
#104647 = CARTESIAN_POINT ( 'NONE',  ( 16.55341960407618274, -4.379528057220086978, 26.04275706135235779 ) ) ;
#104648 = CARTESIAN_POINT ( 'NONE',  ( 15.72974639402176855, 15.80617190586768217, 21.87609039468567573 ) ) ;
#104649 = CARTESIAN_POINT ( 'NONE',  ( -16.53943276465976808, 0.05219959533911058130, 56.24890960531436690 ) ) ;
#104650 = ADVANCED_FACE ( 'NONE', ( #3534 ), #190558, .T. ) ;
#104651 = ORIENTED_EDGE ( 'NONE', *, *, #196038, .T. ) ;
#104652 = CARTESIAN_POINT ( 'NONE',  ( -5.823673210054116645, -21.52544592524344225, 97.29057627198105251 ) ) ;
#104653 = CARTESIAN_POINT ( 'NONE',  ( -4.483927247898539470, -16.52544592524342804, 42.29057627198103120 ) ) ;
#104654 = VERTEX_POINT ( 'NONE', #66206 ) ;
#104655 = CARTESIAN_POINT ( 'NONE',  ( 34.67272174748971736, 7.108278434163713300, 42.55803597338272226 ) ) ;
#104656 = CARTESIAN_POINT ( 'NONE',  ( 18.62759615963271287, -10.81492255796078972, 28.33224293864769550 ) ) ;
#104657 = CARTESIAN_POINT ( 'NONE',  ( -5.823673210054431948, 21.52544592524334988, 37.70942372801900433 ) ) ;
#104658 = CARTESIAN_POINT ( 'NONE',  ( 4.379528057220339221, -16.55341960407611168, 62.70724293864769550 ) ) ;
#104659 = ADVANCED_FACE ( 'NONE', ( #52031 ), #96530, .T. ) ;
#104660 = VECTOR ( 'NONE', #37536, 1000.000000000000000 ) ;
#104661 = CARTESIAN_POINT ( 'NONE',  ( 10.81492255796078972, 18.62759615963270932, 69.58224293864769550 ) ) ;
#104662 = CARTESIAN_POINT ( 'NONE',  ( -0.05219959533909027116, -19.03943276465977164, 77.49890960531435269 ) ) ;
#104664 = CARTESIAN_POINT ( 'NONE',  ( 13.89961937509957401, 13.97604488694547697, 66.87609039468567573 ) ) ;
#104663 = CARTESIAN_POINT ( 'NONE',  ( 16.51473224551069308, 9.474510206698969483, 29.16557627198103475 ) ) ;
#104665 = CARTESIAN_POINT ( 'NONE',  ( 5.823673210054125526, 21.52544592524343514, 54.79057627198104541 ) ) ;
#104666 = CARTESIAN_POINT ( 'NONE',  ( 16.46253265017160672, -9.564922557960803928, 58.33224293864769550 ) ) ;
#104667 = ORIENTED_EDGE ( 'NONE', *, *, #87523, .F. ) ;
#104668 = CARTESIAN_POINT ( 'NONE',  ( -14.29746914071037622, -8.314922557961029526, 39.16775706135235424 ) ) ;
#104669 = CARTESIAN_POINT ( 'NONE',  ( 18.62759615963255655, 10.81492255796105972, 21.66775706135235069 ) ) ;
#104670 = CARTESIAN_POINT ( 'NONE',  ( 4.379528057220339221, -16.55341960407611168, 42.70724293864770260 ) ) ;
#104671 = CARTESIAN_POINT ( 'NONE',  ( -13.89961937509977652, 13.97604488694528158, 100.6239096053143669 ) ) ;
#104672 = CARTESIAN_POINT ( 'NONE',  ( -18.62759615963270932, 10.81492255796079327, 70.83224293864770971 ) ) ;
#104674 = CARTESIAN_POINT ( 'NONE',  ( -4.483927247898782831, 16.52544592524335698, 32.70942372801900433 ) ) ;
#104673 = CARTESIAN_POINT ( 'NONE',  ( -5.823673210054116645, -21.52544592524344225, 102.2905762719810383 ) ) ;
#104675 = CARTESIAN_POINT ( 'NONE',  ( 15.72974639402199770, -15.80617190586745480, 53.12390960531436690 ) ) ;
#104676 = CARTESIAN_POINT ( 'NONE',  ( 15.72974639402176855, 15.80617190586768217, 96.87609039468568994 ) ) ;
#104677 = CARTESIAN_POINT ( 'NONE',  ( -13.97604488694527625, -13.89961937509977652, 41.87390960531435979 ) ) ;
#104678 = CARTESIAN_POINT ( 'NONE',  ( -13.89961937509977652, 13.97604488694528158, 100.6239096053143669 ) ) ;
#104679 = CARTESIAN_POINT ( 'NONE',  ( -5.049401038298153566, 19.05341960407611168, 80.20724293864769550 ) ) ;
#104680 = CARTESIAN_POINT ( 'NONE',  ( 16.31925111598412315, -7.325300261831691806, 87.66424538967174840 ) ) ;
#104681 = CARTESIAN_POINT ( 'NONE',  ( -13.97604488694547697, 13.89961937509957934, 58.12609039468566863 ) ) ;
#104683 = CARTESIAN_POINT ( 'NONE',  ( -5.823673210054116645, -21.52544592524344225, 27.29057627198103120 ) ) ;
#104682 = CARTESIAN_POINT ( 'NONE',  ( 10.72451020669871369, 18.67979575497193778, 107.0844237280190043 ) ) ;
#104684 = CARTESIAN_POINT ( 'NONE',  ( -12.14591786802326823, 12.06949235617739902, 98.12609039468570415 ) ) ;
#104685 = CARTESIAN_POINT ( 'NONE',  ( 13.97604488694548053, -13.89961937509957401, 85.62609039468568994 ) ) ;
#104686 = CARTESIAN_POINT ( 'NONE',  ( 23.96320343559640165, -18.46320343559646560, 8.181980515339454030 ) ) ;
#104687 = CARTESIAN_POINT ( 'NONE',  ( 5.049401038297881783, 19.05341960407617563, 87.29275706135234714 ) ) ;
#104688 = CARTESIAN_POINT ( 'NONE',  ( 16.51473224551083163, -9.474510206698727899, 50.83442372801899722 ) ) ;
#104689 = CARTESIAN_POINT ( 'NONE',  ( 17.05116617787822975, 6.768360034955819948, 108.8432444674080415 ) ) ;
#104690 = CARTESIAN_POINT ( 'NONE',  ( -0.05219959533909027116, -19.03943276465977164, 42.49890960531435269 ) ) ;
#104691 = CARTESIAN_POINT ( 'NONE',  ( 12.14591786802309770, 12.06949235617756955, 49.37390960531436690 ) ) ;
#104692 = CARTESIAN_POINT ( 'NONE',  ( -16.46253265017160317, 9.564922557960807481, 40.83224293864769550 ) ) ;
#104693 = CARTESIAN_POINT ( 'NONE',  ( -14.34966873604960291, -8.224510206698953496, 46.66557627198102409 ) ) ;
#104694 = DIRECTION ( 'NONE',  ( -0.000000000000000000, -1.000000000000000000, -0.000000000000000000 ) ) ;
#104695 = CARTESIAN_POINT ( 'NONE',  ( 12.06949235617739724, 12.14591786802326823, 106.8760903946856899 ) ) ;
#104696 = CARTESIAN_POINT ( 'NONE',  ( -9.564922557960796823, -16.46253265017161027, 52.08224293864768839 ) ) ;
#104697 = CARTESIAN_POINT ( 'NONE',  ( -10.72451020669870658, -18.67979575497194134, 104.5844237280190185 ) ) ;
#104698 = CARTESIAN_POINT ( 'NONE',  ( -16.53943276465976808, -0.05219959533934237506, 23.75109039468567929 ) ) ;
#104699 = CARTESIAN_POINT ( 'NONE',  ( -18.67979575497178146, -10.72451020669898902, 36.66557627198103120 ) ) ;
#104700 = CARTESIAN_POINT ( 'NONE',  ( 10.81492255796106328, -18.62759615963255655, 95.41775706135234714 ) ) ;
#104701 = CARTESIAN_POINT ( 'NONE',  ( 9.564922557960805705, 16.46253265017160317, 109.5822429386476955 ) ) ;
#104702 = CARTESIAN_POINT ( 'NONE',  ( 19.05341960407611168, 5.049401038298154454, 78.95724293864769550 ) ) ;
#104703 = CARTESIAN_POINT ( 'NONE',  ( -22.81625015709510507, 31.40387420917330275, -8.924999997268812990 ) ) ;
#104704 = CARTESIAN_POINT ( 'NONE',  ( 5.719274019375991003, -21.55341960407610458, 112.7072429386476955 ) ) ;
#104705 = CARTESIAN_POINT ( 'NONE',  ( -16.55341960407611168, -4.379528057220339221, 86.45724293864770971 ) ) ;
#104706 = CARTESIAN_POINT ( 'NONE',  ( 5.719274019375991003, -21.55341960407610458, 72.70724293864769550 ) ) ;
#104707 = CARTESIAN_POINT ( 'NONE',  ( 19.05341960407611168, 5.049401038298154454, 68.95724293864769550 ) ) ;
#104708 = CARTESIAN_POINT ( 'NONE',  ( -5.823673210054116645, -21.52544592524344225, 102.2905762719810383 ) ) ;
#104709 = ORIENTED_EDGE ( 'NONE', *, *, #99957, .T. ) ;
#104710 = CARTESIAN_POINT ( 'NONE',  ( 13.97604488694527802, 13.89961937509977652, 64.37390960531436690 ) ) ;
#104712 = LINE ( 'NONE', #122844, #84873 ) ;
#104711 = CARTESIAN_POINT ( 'NONE',  ( -4.379528057220328563, 16.55341960407611168, 90.20724293864770971 ) ) ;
#104713 = CARTESIAN_POINT ( 'NONE',  ( -19.05341960407611168, -5.049401038298163336, 61.45724293864769550 ) ) ;
#104714 = CARTESIAN_POINT ( 'NONE',  ( -5.153800228976607833, 19.02544592524334988, 82.70942372801897591 ) ) ;
#104715 = CARTESIAN_POINT ( 'NONE',  ( 4.379528057220339221, -16.55341960407611168, 102.7072429386476955 ) ) ;
#104716 = CARTESIAN_POINT ( 'NONE',  ( -5.719274019375665041, -21.55341960407619695, 54.79275706135235424 ) ) ;
#104718 = CARTESIAN_POINT ( 'NONE',  ( -15.72974639402176322, -15.80617190586768395, 19.37609039468568639 ) ) ;
#104717 = CARTESIAN_POINT ( 'NONE',  ( -16.46253265017160317, 9.564922557960807481, 45.83224293864769550 ) ) ;
#104719 = CARTESIAN_POINT ( 'NONE',  ( -16.52544592524342804, 4.483927247898546575, 101.0405762719810383 ) ) ;
#104720 = CARTESIAN_POINT ( 'NONE',  ( 11.70497261681111034, -44.13276428439503007, -23.15274968896633467 ) ) ;
#104721 = CARTESIAN_POINT ( 'NONE',  ( 0.05219959533909260263, 19.03943276465977164, 59.99890960531436690 ) ) ;
#104722 = FACE_OUTER_BOUND ( 'NONE', #157490, .T. ) ;
#104724 = CARTESIAN_POINT ( 'NONE',  ( 13.89961937509977652, -13.97604488694527269, 108.1239096053143669 ) ) ;
#104723 = CARTESIAN_POINT ( 'NONE',  ( -16.51473224551082808, 9.474510206698731452, 103.3344237280190043 ) ) ;
#104725 = CARTESIAN_POINT ( 'NONE',  ( -18.67979575497193778, 10.72451020669871902, 53.33442372801901854 ) ) ;
#104726 = CARTESIAN_POINT ( 'NONE',  ( 16.51473224551069308, 9.474510206698969483, 99.16557627198102409 ) ) ;
#104727 = CARTESIAN_POINT ( 'NONE',  ( 9.564922557961047289, -16.46253265017146816, 80.41775706135234714 ) ) ;
#104728 = CARTESIAN_POINT ( 'NONE',  ( 13.89961937509977652, -13.97604488694527269, 53.12390960531434558 ) ) ;
#104729 = CARTESIAN_POINT ( 'NONE',  ( 8.314922557960818139, 14.29746914071049879, 79.58224293864769550 ) ) ;
#104730 = CARTESIAN_POINT ( 'NONE',  ( 9.564922557960805705, 16.46253265017160317, 94.58224293864769550 ) ) ;
#104731 = CARTESIAN_POINT ( 'NONE',  ( -12.06949235617756955, 12.14591786802309770, 80.62390960531438111 ) ) ;
#104732 = CARTESIAN_POINT ( 'NONE',  ( 0.05219959533909260263, 19.03943276465977164, 89.99890960531436690 ) ) ;
#104733 = AXIS2_PLACEMENT_3D ( 'NONE', #87916, #60551, #102097 ) ;
#104734 = CARTESIAN_POINT ( 'NONE',  ( 13.89961937509957401, 13.97604488694547697, 26.87609039468566507 ) ) ;
#104737 = CARTESIAN_POINT ( 'NONE',  ( -13.97604488694527625, -13.89961937509977652, 31.87390960531435979 ) ) ;
#104736 = CARTESIAN_POINT ( 'NONE',  ( -16.55341960407611168, -4.379528057220339221, 26.45724293864768839 ) ) ;
#104735 = CARTESIAN_POINT ( 'NONE',  ( -5.153800228976328057, -19.02544592524343514, 47.29057627198102409 ) ) ;
#104738 = ORIENTED_EDGE ( 'NONE', *, *, #108116, .F. ) ;
#104739 = CARTESIAN_POINT ( 'NONE',  ( 0.05219959533937995610, -21.53943276465977519, 40.00109039468567573 ) ) ;
#104740 = CARTESIAN_POINT ( 'NONE',  ( -13.89961937509957401, -13.97604488694547875, 79.37609039468567573 ) ) ;
#104741 = CARTESIAN_POINT ( 'NONE',  ( -16.53943276465976808, 0.05219959533911058130, 41.24890960531435269 ) ) ;
#104742 = CARTESIAN_POINT ( 'NONE',  ( -21.55341960407610458, -5.719274019375992779, 86.45724293864770971 ) ) ;
#104743 = CARTESIAN_POINT ( 'NONE',  ( 15.80617190586746368, 15.72974639402197994, 29.37390960531435269 ) ) ;
#104744 = CARTESIAN_POINT ( 'NONE',  ( 14.34966873604960469, 8.224510206698951720, 64.16557627198102409 ) ) ;
#104745 = CARTESIAN_POINT ( 'NONE',  ( 5.153800228976335163, 19.02544592524342804, 44.79057627198103830 ) ) ;
#104746 = CARTESIAN_POINT ( 'NONE',  ( -16.53943276465976808, -0.05219959533934237506, 103.7510903946857042 ) ) ;
#104747 = CARTESIAN_POINT ( 'NONE',  ( -4.379528057220086978, -16.55341960407618274, 69.79275706135234714 ) ) ;
#104748 = CARTESIAN_POINT ( 'NONE',  ( 18.67979575497178502, 10.72451020669898547, 34.16557627198102409 ) ) ;
#104749 = CARTESIAN_POINT ( 'NONE',  ( -0.05219959533936034679, 19.03943276465977164, 22.50109039468566152 ) ) ;
#104750 = CARTESIAN_POINT ( 'NONE',  ( 19.05341960407611168, 5.049401038298154454, 93.95724293864769550 ) ) ;
#104751 = CARTESIAN_POINT ( 'NONE',  ( -19.02544592524342804, 5.153800228976336051, 61.04057627198103120 ) ) ;
#104752 = CARTESIAN_POINT ( 'NONE',  ( -12.14591786802326823, 12.06949235617739902, 78.12609039468570415 ) ) ;
#104753 = CARTESIAN_POINT ( 'NONE',  ( 19.05341960407611168, 5.049401038298154454, 28.95724293864769550 ) ) ;
#104754 = CARTESIAN_POINT ( 'NONE',  ( -16.52544592524342804, 4.483927247898546575, 36.04057627198102409 ) ) ;
#104756 = CARTESIAN_POINT ( 'NONE',  ( 19.02544592524343514, -5.153800228976328945, 88.54057627198102409 ) ) ;
#104755 = CARTESIAN_POINT ( 'NONE',  ( 0.05219959533909260263, 19.03943276465977164, 104.9989096053143669 ) ) ;
#104757 = CARTESIAN_POINT ( 'NONE',  ( 21.55341960407610458, 5.719274019375980345, 23.95724293864769550 ) ) ;
#104758 = VECTOR ( 'NONE', #57790, 1000.000000000000000 ) ;
#104759 = CARTESIAN_POINT ( 'NONE',  ( -16.53943276465976808, 0.05219959533911058130, 71.24890960531435269 ) ) ;
#104760 = VERTEX_POINT ( 'NONE', #36853 ) ;
#104761 = CARTESIAN_POINT ( 'NONE',  ( -4.379528057220328563, 16.55341960407611168, 70.20724293864769550 ) ) ;
#104764 = CIRCLE ( 'NONE', #140241, 214.0437394197456342 ) ;
#104763 = DIRECTION ( 'NONE',  ( 0.000000000000000000, -0.4999999999999991118, 0.8660254037844390407 ) ) ;
#104762 = CARTESIAN_POINT ( 'NONE',  ( 8.314922557961029526, -14.29746914071037800, 55.41775706135234714 ) ) ;
#104765 = CARTESIAN_POINT ( 'NONE',  ( -0.05219959533936034679, 19.03943276465977164, 57.50109039468566863 ) ) ;
#104766 = CARTESIAN_POINT ( 'NONE',  ( 19.02544592524343514, -5.153800228976328945, 88.54057627198102409 ) ) ;
#104767 = CARTESIAN_POINT ( 'NONE',  ( -16.46253265017146816, -9.564922557961047289, 59.16775706135233293 ) ) ;
#104768 = CARTESIAN_POINT ( 'NONE',  ( 27.73933785331498569, 2.768321779492822058E-14, 142.3750000027311842 ) ) ;
#104770 = CARTESIAN_POINT ( 'NONE',  ( -0.05219959533934338120, 16.53943276465976808, 92.50109039468567573 ) ) ;
#104769 = CARTESIAN_POINT ( 'NONE',  ( -13.97604488694547697, 13.89961937509957934, 113.1260903946856757 ) ) ;
#104771 = CARTESIAN_POINT ( 'NONE',  ( -13.89961937509977652, 13.97604488694528158, 35.62390960531435269 ) ) ;
#104772 = CARTESIAN_POINT ( 'NONE',  ( 10.81492255796078972, 18.62759615963270932, 24.58224293864768839 ) ) ;
#104773 = CARTESIAN_POINT ( 'NONE',  ( -0.05219959533937732626, 21.53943276465977519, 52.50109039468567573 ) ) ;
#104774 = CARTESIAN_POINT ( 'NONE',  ( -13.97604488694547697, 13.89961937509957934, 108.1260903946856331 ) ) ;
#104776 = CARTESIAN_POINT ( 'NONE',  ( -5.153800228976328057, -19.02544592524343514, 72.29057627198102409 ) ) ;
#104775 = CARTESIAN_POINT ( 'NONE',  ( 0.000000000000000000, -1.178949249685214307, 2.042000000000002036 ) ) ;
#104777 = LINE ( 'NONE', #133112, #137080 ) ;
#104779 = CARTESIAN_POINT ( 'NONE',  ( -19.03943276465977164, 0.05219959533909376836, 66.24890960531436690 ) ) ;
#104778 = CARTESIAN_POINT ( 'NONE',  ( -14.29746914071049879, 8.314922557960819915, 70.83224293864770971 ) ) ;
#104780 = CARTESIAN_POINT ( 'NONE',  ( -16.51473224551069308, -9.474510206698971260, 76.66557627198103830 ) ) ;
#104781 = CARTESIAN_POINT ( 'NONE',  ( 5.153800228976615827, -19.02544592524334988, 75.20942372801896170 ) ) ;
#104782 = CARTESIAN_POINT ( 'NONE',  ( -10.72451020669898014, 18.67979575497178502, 60.41557627198102409 ) ) ;
#104783 = CARTESIAN_POINT ( 'NONE',  ( 8.314922557960818139, 14.29746914071049879, 114.5822429386477097 ) ) ;
#104784 = CARTESIAN_POINT ( 'NONE',  ( -13.97604488694547697, 13.89961937509957934, 53.12609039468565442 ) ) ;
#104785 = CARTESIAN_POINT ( 'NONE',  ( -9.474510206698964154, 16.51473224551069663, 55.41557627198103120 ) ) ;
#104786 = CARTESIAN_POINT ( 'NONE',  ( 0.05219959533909260263, 19.03943276465977164, 89.99890960531436690 ) ) ;
#104787 = CARTESIAN_POINT ( 'NONE',  ( -5.719274019375978568, 21.55341960407610458, 85.20724293864770971 ) ) ;
#104789 = CARTESIAN_POINT ( 'NONE',  ( 16.51473224551083163, -9.474510206698727899, 45.83442372801900433 ) ) ;
#104788 = CARTESIAN_POINT ( 'NONE',  ( 16.53943276465976808, -0.05219959533910856209, 78.74890960531436690 ) ) ;
#104790 = CARTESIAN_POINT ( 'NONE',  ( -0.05219959533907301413, -21.53943276465977519, 82.49890960531436690 ) ) ;
#104791 = CARTESIAN_POINT ( 'NONE',  ( 5.719274019375991003, -21.55341960407610458, 62.70724293864769550 ) ) ;
#104792 = CARTESIAN_POINT ( 'NONE',  ( 12.06949235617757843, -12.14591786802309237, 33.12390960531435979 ) ) ;
#104793 = CARTESIAN_POINT ( 'NONE',  ( 18.62759615963255655, 10.81492255796105972, 106.6677570613523756 ) ) ;
#104794 = CARTESIAN_POINT ( 'NONE',  ( 0.05219959533909260263, 19.03943276465977164, 79.99890960531436690 ) ) ;
#104795 = CARTESIAN_POINT ( 'NONE',  ( 9.564922557960805705, 16.46253265017160317, 29.58224293864769550 ) ) ;
#104796 = VECTOR ( 'NONE', #59517, 1000.000000000000000 ) ;
#104797 = CARTESIAN_POINT ( 'NONE',  ( 10.81492255796106328, -18.62759615963255655, 40.41775706135234714 ) ) ;
#104798 = CARTESIAN_POINT ( 'NONE',  ( -18.62759615963255300, -10.81492255796106328, 39.16775706135235424 ) ) ;
#104799 = CARTESIAN_POINT ( 'NONE',  ( -19.02544592524342804, 5.153800228976336051, 46.04057627198101699 ) ) ;
#104800 = CARTESIAN_POINT ( 'NONE',  ( 18.62759615963255655, 10.81492255796105972, 21.66775706135235069 ) ) ;
#104801 = CARTESIAN_POINT ( 'NONE',  ( -9.474510206698720793, -16.51473224551083518, 64.58442372801900433 ) ) ;
#104802 = CARTESIAN_POINT ( 'NONE',  ( -5.049401038298153566, 19.05341960407611168, 30.20724293864768839 ) ) ;
#104803 = CARTESIAN_POINT ( 'NONE',  ( 8.314922557961029526, -14.29746914071037800, 25.41775706135235779 ) ) ;
#104804 = CYLINDRICAL_SURFACE ( 'NONE', #133924, 5.500000000000032863 ) ;
#104805 = CARTESIAN_POINT ( 'NONE',  ( 8.314922557961029526, -14.29746914071037800, 70.41775706135236135 ) ) ;
#104806 = CARTESIAN_POINT ( 'NONE',  ( -16.46253265017160317, 9.564922557960807481, 45.83224293864769550 ) ) ;
#104807 = CARTESIAN_POINT ( 'NONE',  ( -20.69372460268612457, -11.29034304323151616, 170.1224388339879567 ) ) ;
#104808 = CARTESIAN_POINT ( 'NONE',  ( -13.97604488694527625, -13.89961937509977652, 91.87390960531432427 ) ) ;
#104809 = CARTESIAN_POINT ( 'NONE',  ( -16.53943276465976808, 0.05219959533911058130, 116.2489096053143669 ) ) ;
#104810 = CARTESIAN_POINT ( 'NONE',  ( -10.81492255796078084, -18.62759615963271287, 62.08224293864769550 ) ) ;
#104811 = CARTESIAN_POINT ( 'NONE',  ( -16.55341960407617563, 4.379528057220093196, 43.54275706135235424 ) ) ;
#104812 = CARTESIAN_POINT ( 'NONE',  ( 15.80617190586769283, -15.72974639402175789, 95.62609039468568994 ) ) ;
#104813 = CARTESIAN_POINT ( 'NONE',  ( -13.89961937509977652, 13.97604488694528158, 35.62390960531435269 ) ) ;
#104814 = CARTESIAN_POINT ( 'NONE',  ( -4.483927247898539470, -16.52544592524342804, 32.29057627198102409 ) ) ;
#104815 = CARTESIAN_POINT ( 'NONE',  ( 4.379528057220339221, -16.55341960407611168, 72.70724293864769550 ) ) ;
#104816 = CARTESIAN_POINT ( 'NONE',  ( 16.51473224551069308, 9.474510206698969483, 64.16557627198102409 ) ) ;
#104817 = CARTESIAN_POINT ( 'NONE',  ( -10.72451020669870658, -18.67979575497194134, 109.5844237280190328 ) ) ;
#104818 = CARTESIAN_POINT ( 'NONE',  ( 21.55341960407619695, -5.719274019375665929, 21.04275706135234714 ) ) ;
#104819 = CARTESIAN_POINT ( 'NONE',  ( 9.564922557960805705, 16.46253265017160317, 79.58224293864769550 ) ) ;
#104820 = CARTESIAN_POINT ( 'NONE',  ( 21.55341960407619695, -5.719274019375665929, 86.04275706135236135 ) ) ;
#104821 = CARTESIAN_POINT ( 'NONE',  ( 16.52544592524335698, 4.483927247898782831, 56.45942372801902565 ) ) ;
#104822 = CARTESIAN_POINT ( 'NONE',  ( -8.314922557961024197, 14.29746914071037800, 32.91775706135234714 ) ) ;
#104824 = CARTESIAN_POINT ( 'NONE',  ( -0.05219959533937732626, 21.53943276465977519, 102.5010903946856899 ) ) ;
#104823 = CARTESIAN_POINT ( 'NONE',  ( 16.55341960407611168, 4.379528057220329451, 93.95724293864770971 ) ) ;
#104825 = CARTESIAN_POINT ( 'NONE',  ( -12.14591786802309592, -12.06949235617757132, 36.87390960531435979 ) ) ;
#104826 = CARTESIAN_POINT ( 'NONE',  ( 5.153800228976335163, 19.02544592524342804, 34.79057627198102409 ) ) ;
#104827 = CARTESIAN_POINT ( 'NONE',  ( 12.14591786802327356, -12.06949235617739191, 50.62609039468568994 ) ) ;
#104828 = CARTESIAN_POINT ( 'NONE',  ( 16.52544592524342804, -4.483927247898539470, 58.54057627198103120 ) ) ;
#104829 = CARTESIAN_POINT ( 'NONE',  ( 14.29746914071037800, 8.314922557961029526, 101.6677570613523613 ) ) ;
#104830 = CARTESIAN_POINT ( 'NONE',  ( 21.53943276465977519, -0.05219959533907433946, 23.74890960531435269 ) ) ;
#104831 = CARTESIAN_POINT ( 'NONE',  ( -16.46253265017160317, 9.564922557960807481, 110.8322429386476955 ) ) ;
#104832 = CARTESIAN_POINT ( 'NONE',  ( 5.153800228976615827, -19.02544592524334988, 20.20942372801899722 ) ) ;
#104833 = CARTESIAN_POINT ( 'NONE',  ( -16.55341960407611168, -4.379528057220339221, 91.45724293864769550 ) ) ;
#104834 = CARTESIAN_POINT ( 'NONE',  ( 5.153800228976335163, 19.02544592524342804, 94.79057627198103830 ) ) ;
#104835 = EDGE_LOOP ( 'NONE', ( #93430, #77881, #44969, #175881 ) ) ;
#104836 = CARTESIAN_POINT ( 'NONE',  ( -4.483927247898782831, 16.52544592524335698, 37.70942372801900433 ) ) ;
#104837 = CARTESIAN_POINT ( 'NONE',  ( -19.05341960407611168, -5.049401038298163336, 41.45724293864769550 ) ) ;
#104838 = CARTESIAN_POINT ( 'NONE',  ( -0.05219959533934338120, 16.53943276465976808, 47.50109039468568994 ) ) ;
#104839 = CARTESIAN_POINT ( 'NONE',  ( 13.97604488694548053, -13.89961937509957401, 45.62609039468566863 ) ) ;
#104840 = CARTESIAN_POINT ( 'NONE',  ( -5.153800228976328057, -19.02544592524343514, 52.29057627198100988 ) ) ;
#104841 = CARTESIAN_POINT ( 'NONE',  ( 16.53943276465976808, 0.05219959533934440121, 86.25109039468568994 ) ) ;
#104842 = CARTESIAN_POINT ( 'NONE',  ( 13.89961937509957401, 13.97604488694547697, 86.87609039468567573 ) ) ;
#104843 = CARTESIAN_POINT ( 'NONE',  ( -16.51473224551082808, 9.474510206698731452, 33.33442372801899722 ) ) ;
#104844 = CARTESIAN_POINT ( 'NONE',  ( -5.049401038298153566, 19.05341960407611168, 60.20724293864768129 ) ) ;
#104845 = CARTESIAN_POINT ( 'NONE',  ( -16.55341960407611168, -4.379528057220339221, 101.4572429386476955 ) ) ;
#104846 = ADVANCED_FACE ( 'NONE', ( #175384 ), #88392, .T. ) ;
#104847 = CARTESIAN_POINT ( 'NONE',  ( 19.05341960407617918, -5.049401038297876454, 71.04275706135234714 ) ) ;
#104848 = CARTESIAN_POINT ( 'NONE',  ( 5.823673210054125526, 21.52544592524343514, 69.79057627198102409 ) ) ;
#104849 = CARTESIAN_POINT ( 'NONE',  ( -5.153800228976607833, 19.02544592524334988, 47.70942372801900433 ) ) ;
#104850 = CARTESIAN_POINT ( 'NONE',  ( 16.51473224551069308, 9.474510206698969483, 109.1655762719810383 ) ) ;
#104851 = VECTOR ( 'NONE', #198064, 1000.000000000000000 ) ;
#104852 = CARTESIAN_POINT ( 'NONE',  ( 15.72974639402199770, -15.80617190586745480, 73.12390960531436690 ) ) ;
#104853 = CARTESIAN_POINT ( 'NONE',  ( -17.05116617787824396, 6.768360034955813731, 83.65675553259198693 ) ) ;
#104854 = CARTESIAN_POINT ( 'NONE',  ( 16.46253265017146816, 9.564922557961045513, 106.6677570613523471 ) ) ;
#104855 = CARTESIAN_POINT ( 'NONE',  ( -18.22780087662123805, -5.499999999999968026, 98.98236817873106475 ) ) ;
#104856 = CARTESIAN_POINT ( 'NONE',  ( -4.483927247898782831, 16.52544592524335698, 22.70942372801901499 ) ) ;
#104857 = CARTESIAN_POINT ( 'NONE',  ( 13.97604488694527802, 13.89961937509977652, 34.37390960531436690 ) ) ;
#104858 = CARTESIAN_POINT ( 'NONE',  ( 0.05219959533909260263, 19.03943276465977164, 109.9989096053143669 ) ) ;
#104859 = CARTESIAN_POINT ( 'NONE',  ( 18.67979575497178502, 10.72451020669898547, 94.16557627198103830 ) ) ;
#104860 = CARTESIAN_POINT ( 'NONE',  ( 5.823673210054444382, -21.52544592524334988, 55.20942372801902565 ) ) ;
#104862 = CARTESIAN_POINT ( 'NONE',  ( 19.05341960407617918, -5.049401038297876454, 21.04275706135232582 ) ) ;
#104861 = CARTESIAN_POINT ( 'NONE',  ( 19.03943276465977164, 0.05219959533936151252, 101.2510903946856757 ) ) ;
#104863 = CARTESIAN_POINT ( 'NONE',  ( -12.06949235617739369, -12.14591786802326823, 104.3760903946856899 ) ) ;
#104864 = CARTESIAN_POINT ( 'NONE',  ( -21.55341960407610458, -5.719274019375992779, 101.4572429386476955 ) ) ;
#104865 = CARTESIAN_POINT ( 'NONE',  ( 4.483927247898545687, 16.52544592524342804, 44.79057627198103120 ) ) ;
#104866 = CARTESIAN_POINT ( 'NONE',  ( -16.51473224551082808, 9.474510206698731452, 88.33442372801900433 ) ) ;
#104867 = CARTESIAN_POINT ( 'NONE',  ( 19.05341960407617918, -5.049401038297876454, 51.04275706135231871 ) ) ;
#104868 = CARTESIAN_POINT ( 'NONE',  ( 21.53943276465977519, 0.05219959533937863772, 71.25109039468568994 ) ) ;
#104869 = CARTESIAN_POINT ( 'NONE',  ( 19.02544592524334988, 5.153800228976608722, 36.45942372801900433 ) ) ;
#104870 = CARTESIAN_POINT ( 'NONE',  ( -14.34966873604960291, -8.224510206698953496, 111.6655762719810525 ) ) ;
#104871 = CARTESIAN_POINT ( 'NONE',  ( 18.67979575497178502, 10.72451020669898547, 49.16557627198102409 ) ) ;
#104872 = CARTESIAN_POINT ( 'NONE',  ( 0.05219959533910956823, 16.53943276465976808, 29.99890960531435979 ) ) ;
#104873 = CARTESIAN_POINT ( 'NONE',  ( -18.62759615963255300, -10.81492255796106328, 109.1677570613523613 ) ) ;
#104874 = CARTESIAN_POINT ( 'NONE',  ( 8.224510206698742110, 14.34966873604972548, 72.08442372801899012 ) ) ;
#104875 = CARTESIAN_POINT ( 'NONE',  ( 14.34966873604960469, 8.224510206698951720, 29.16557627198103120 ) ) ;
#104876 = CARTESIAN_POINT ( 'NONE',  ( -10.72451020669870658, -18.67979575497194134, 59.58442372801901854 ) ) ;
#104877 = CARTESIAN_POINT ( 'NONE',  ( -21.53943276465977519, -0.05219959533937600094, 63.75109039468568284 ) ) ;
#104878 = CARTESIAN_POINT ( 'NONE',  ( -10.81492255796078084, -18.62759615963271287, 67.08224293864770971 ) ) ;
#104879 = ADVANCED_FACE ( 'NONE', ( #145033 ), #97513, .T. ) ;
#104880 = VECTOR ( 'NONE', #174714, 1000.000000000000000 ) ;
#104881 = CARTESIAN_POINT ( 'NONE',  ( -16.46253265017160317, 9.564922557960807481, 25.83224293864769194 ) ) ;
#104882 = CARTESIAN_POINT ( 'NONE',  ( -10.72451020669870658, -18.67979575497194134, 39.58442372801901143 ) ) ;
#104883 = CARTESIAN_POINT ( 'NONE',  ( 5.049401038298161559, -19.05341960407611168, 22.70724293864769194 ) ) ;
#104884 = CARTESIAN_POINT ( 'NONE',  ( -5.153800228976328057, -19.02544592524343514, 42.29057627198101699 ) ) ;
#104885 = CARTESIAN_POINT ( 'NONE',  ( -4.379528057220328563, 16.55341960407611168, 75.20724293864769550 ) ) ;
#104886 = CARTESIAN_POINT ( 'NONE',  ( -16.46253265017160317, 9.564922557960807481, 90.83224293864769550 ) ) ;
#104887 = CARTESIAN_POINT ( 'NONE',  ( -4.483927247898539470, -16.52544592524342804, 32.29057627198102409 ) ) ;
#104888 = CARTESIAN_POINT ( 'NONE',  ( -14.29746914071049879, 8.314922557960819915, 100.8322429386477097 ) ) ;
#104889 = CARTESIAN_POINT ( 'NONE',  ( 21.52544592524344225, -5.823673210054117533, 68.54057627198103830 ) ) ;
#104890 = CARTESIAN_POINT ( 'NONE',  ( -18.67979575497178146, -10.72451020669898902, 106.6655762719810383 ) ) ;
#104891 = CARTESIAN_POINT ( 'NONE',  ( 16.46253265017160672, -9.564922557960803928, 108.3322429386476955 ) ) ;
#104893 = CARTESIAN_POINT ( 'NONE',  ( -8.224510206698735004, -14.34966873604973081, 19.58442372801901143 ) ) ;
#104892 = CARTESIAN_POINT ( 'NONE',  ( 19.05341960407611168, 5.049401038298154454, 68.95724293864769550 ) ) ;
#104894 = CARTESIAN_POINT ( 'NONE',  ( -18.67979575497178146, -10.72451020669898902, 51.66557627198102409 ) ) ;
#104895 = CARTESIAN_POINT ( 'NONE',  ( -18.67979575497193778, 10.72451020669871902, 78.33442372801901854 ) ) ;
#104896 = CARTESIAN_POINT ( 'NONE',  ( -9.564922557960796823, -16.46253265017161027, 82.08224293864768129 ) ) ;
#104897 = CARTESIAN_POINT ( 'NONE',  ( -16.46253265017160317, 9.564922557960807481, 105.8322429386476955 ) ) ;
#104898 = CARTESIAN_POINT ( 'NONE',  ( 14.34966873604972726, -8.224510206698740333, 80.83442372801901854 ) ) ;
#104899 = CARTESIAN_POINT ( 'NONE',  ( 10.72451020669871369, 18.67979575497193778, 52.08442372801901854 ) ) ;
#104900 = CARTESIAN_POINT ( 'NONE',  ( 10.81492255796106328, -18.62759615963255655, 105.4177570613523613 ) ) ;
#104901 = CARTESIAN_POINT ( 'NONE',  ( 0.05219959533934541429, -16.53943276465976808, 60.00109039468568284 ) ) ;
#104902 = CARTESIAN_POINT ( 'NONE',  ( 15.72974639402199770, -15.80617190586745480, 108.1239096053143811 ) ) ;
#104903 = AXIS2_PLACEMENT_3D ( 'NONE', #199552, #91341, #138858 ) ;
#104904 = CARTESIAN_POINT ( 'NONE',  ( 9.564922557960805705, 16.46253265017160317, 114.5822429386476955 ) ) ;
#104905 = CARTESIAN_POINT ( 'NONE',  ( -10.81492255796078084, -18.62759615963271287, 87.08224293864769550 ) ) ;
#104906 = CARTESIAN_POINT ( 'NONE',  ( 19.02544592524334988, 5.153800228976608722, 46.45942372801899012 ) ) ;
#104907 = CARTESIAN_POINT ( 'NONE',  ( 5.719274019375991003, -21.55341960407610458, 42.70724293864770260 ) ) ;
#104910 = B_SPLINE_CURVE_WITH_KNOTS ( 'NONE', 3,
 ( #189126, #95094, #17272, #35416, #97068, #139599 ),
 .UNSPECIFIED., .F., .F.,
 ( 4, 2, 4 ),
 ( 0.007228050697041489385, 0.007608510107494970143, 0.007988969517948450033 ),
 .UNSPECIFIED. ) ;
#104909 = CARTESIAN_POINT ( 'NONE',  ( -16.52544592524342804, 4.483927247898546575, 41.04057627198103120 ) ) ;
#104908 = CARTESIAN_POINT ( 'NONE',  ( -16.51473224551069308, -9.474510206698971260, 81.66557627198103830 ) ) ;
#104911 = FACE_OUTER_BOUND ( 'NONE', #177110, .T. ) ;
#104912 = DIRECTION ( 'NONE',  ( 0.000000000000000000, -0.5000000000000011102, -0.8660254037844379305 ) ) ;
#104913 = CARTESIAN_POINT ( 'NONE',  ( -0.05219959533936034679, 19.03943276465977164, 97.50109039468567573 ) ) ;
#104914 = CARTESIAN_POINT ( 'NONE',  ( 21.52544592524344225, -5.823673210054117533, 68.54057627198103830 ) ) ;
#104915 = CARTESIAN_POINT ( 'NONE',  ( 8.314922557960818139, 14.29746914071049879, 49.58224293864769550 ) ) ;
#104916 = CARTESIAN_POINT ( 'NONE',  ( -0.05219959533934338120, 16.53943276465976808, 37.50109039468568284 ) ) ;
#104917 = CARTESIAN_POINT ( 'NONE',  ( -13.97604488694527625, -13.89961937509977652, 41.87390960531435979 ) ) ;
#104919 = CARTESIAN_POINT ( 'NONE',  ( -19.02544592524334988, -5.153800228976617603, 78.95942372801900433 ) ) ;
#104918 = CARTESIAN_POINT ( 'NONE',  ( 21.52544592524334988, 5.823673210054432836, 21.45942372801901499 ) ) ;
#104920 = CARTESIAN_POINT ( 'NONE',  ( -9.564922557960796823, -16.46253265017161027, 77.08224293864769550 ) ) ;
#104921 = CARTESIAN_POINT ( 'NONE',  ( 9.474510206698971260, -16.51473224551069308, 77.91557627198103830 ) ) ;
#104922 = CARTESIAN_POINT ( 'NONE',  ( 15.72974639402199770, -15.80617190586745480, 83.12390960531436690 ) ) ;
#104923 = CARTESIAN_POINT ( 'NONE',  ( 9.474510206698971260, -16.51473224551069308, 32.91557627198102409 ) ) ;
#104924 = DIRECTION ( 'NONE',  ( 5.204170427930421283E-16, 0.000000000000000000, -1.000000000000000000 ) ) ;
#104925 = CARTESIAN_POINT ( 'NONE',  ( -0.05219959533910754901, -16.53943276465976808, 57.49890960531435979 ) ) ;
#104926 = CARTESIAN_POINT ( 'NONE',  ( -9.564922557960796823, -16.46253265017161027, 92.08224293864769550 ) ) ;
#104927 = LINE ( 'NONE', #151440, #76671 ) ;
#104928 = CARTESIAN_POINT ( 'NONE',  ( 16.46253265017146816, 9.564922557961045513, 56.66775706135233293 ) ) ;
#104929 = CARTESIAN_POINT ( 'NONE',  ( 15.72974639402199770, -15.80617190586745480, 73.12390960531436690 ) ) ;
#104930 = CARTESIAN_POINT ( 'NONE',  ( 5.153800228976615827, -19.02544592524334988, 30.20942372801900433 ) ) ;
#104931 = CARTESIAN_POINT ( 'NONE',  ( -5.049401038298153566, 19.05341960407611168, 85.20724293864766707 ) ) ;
#104932 = CARTESIAN_POINT ( 'NONE',  ( -18.09867054820431775, -5.499999999999926281, 73.98393025253585620 ) ) ;
#104933 = CARTESIAN_POINT ( 'NONE',  ( 21.55341960407610458, 5.719274019375980345, 23.95724293864769550 ) ) ;
#104934 = CIRCLE ( 'NONE', #133964, 69.99999999999998579 ) ;
#104935 = CARTESIAN_POINT ( 'NONE',  ( -9.564922557960796823, -16.46253265017161027, 77.08224293864769550 ) ) ;
#104936 = CARTESIAN_POINT ( 'NONE',  ( 21.52544592524334988, 5.823673210054432836, 46.45942372801901854 ) ) ;
#104937 = CARTESIAN_POINT ( 'NONE',  ( -5.153800228976328057, -19.02544592524343514, 27.29057627198103120 ) ) ;
#104940 = ORIENTED_EDGE ( 'NONE', *, *, #127970, .F. ) ;
#104939 = CARTESIAN_POINT ( 'NONE',  ( -16.46253265017160317, 9.564922557960807481, 95.83224293864769550 ) ) ;
#104938 = CARTESIAN_POINT ( 'NONE',  ( 10.81492255796078972, 18.62759615963270932, 114.5822429386477097 ) ) ;
#104941 = CARTESIAN_POINT ( 'NONE',  ( -15.72974639402176322, -15.80617190586768395, 34.37609039468568284 ) ) ;
#104942 = EDGE_LOOP ( 'NONE', ( #60868, #168666, #32770, #143732 ) ) ;
#104943 = CARTESIAN_POINT ( 'NONE',  ( -16.51473224551069308, -9.474510206698971260, 101.6655762719810241 ) ) ;
#104944 = FACE_OUTER_BOUND ( 'NONE', #93490, .T. ) ;
#104945 = CARTESIAN_POINT ( 'NONE',  ( 18.62759615963271287, -10.81492255796078972, 103.3322429386476955 ) ) ;
#104946 = CARTESIAN_POINT ( 'NONE',  ( 13.97604488694527802, 13.89961937509977652, 59.37390960531434558 ) ) ;
#104947 = CARTESIAN_POINT ( 'NONE',  ( 0.05219959533934541429, -16.53943276465976808, 25.00109039468567218 ) ) ;
#104948 = CARTESIAN_POINT ( 'NONE',  ( 11.40812507854755253, -35.11059874428192273, -2.524999997268813523 ) ) ;
#104949 = CARTESIAN_POINT ( 'NONE',  ( 10.81492255796106328, -18.62759615963255655, 100.4177570613523471 ) ) ;
#104950 = CARTESIAN_POINT ( 'NONE',  ( 16.46253265017160672, -9.564922557960803928, 38.33224293864768839 ) ) ;
#104951 = CARTESIAN_POINT ( 'NONE',  ( -18.62759615963255300, -10.81492255796106328, 99.16775706135234714 ) ) ;
#104953 = CARTESIAN_POINT ( 'NONE',  ( -15.80617190586768217, 15.72974639402176855, 58.12609039468568994 ) ) ;
#104952 = CARTESIAN_POINT ( 'NONE',  ( -16.51473224551069308, -9.474510206698971260, 91.66557627198103830 ) ) ;
#104954 = CARTESIAN_POINT ( 'NONE',  ( 22.44159573604009594, -16.30477369853687364, 142.1750000027311671 ) ) ;
#104955 = CARTESIAN_POINT ( 'NONE',  ( -19.03943276465977164, 0.05219959533909376836, 101.2489096053143669 ) ) ;
#104956 = CARTESIAN_POINT ( 'NONE',  ( -17.50000000000000000, 4.013004640162651349, 30.44605720994411513 ) ) ;
#104959 = CARTESIAN_POINT ( 'NONE',  ( -5.823673210054431948, 21.52544592524334988, 52.70942372801902565 ) ) ;
#104958 = CARTESIAN_POINT ( 'NONE',  ( 12.06949235617739724, 12.14591786802326823, 66.87609039468568994 ) ) ;
#104957 = CARTESIAN_POINT ( 'NONE',  ( -14.29746914071037622, -8.314922557961029526, 54.16775706135235424 ) ) ;
#104960 = CARTESIAN_POINT ( 'NONE',  ( -15.80617190586768217, 15.72974639402176855, 88.12609039468570415 ) ) ;
#104961 = CARTESIAN_POINT ( 'NONE',  ( -9.760750291312424665, 9.613975513199005007, -60.44446360152740283 ) ) ;
#104962 = CARTESIAN_POINT ( 'NONE',  ( -16.52544592524335698, -4.483927247898792601, 28.95942372801902209 ) ) ;
#104963 = CARTESIAN_POINT ( 'NONE',  ( 13.97604488694527802, 13.89961937509977652, 69.37390960531436690 ) ) ;
#104964 = CARTESIAN_POINT ( 'NONE',  ( -19.02544592524342804, 5.153800228976336051, 101.0405762719810241 ) ) ;
#104965 = DIRECTION ( 'NONE',  ( 3.469446951953612217E-15, 0.000000000000000000, -1.000000000000000000 ) ) ;
#104966 = CARTESIAN_POINT ( 'NONE',  ( 0.05219959533909260263, 19.03943276465977164, 24.99890960531435269 ) ) ;
#104967 = CARTESIAN_POINT ( 'NONE',  ( 21.55341960407610458, 5.719274019375980345, 33.95724293864769550 ) ) ;
#104968 = CARTESIAN_POINT ( 'NONE',  ( 12.14591786802327356, -12.06949235617739191, 90.62609039468567573 ) ) ;
#104970 = CARTESIAN_POINT ( 'NONE',  ( -13.97604488694527625, -13.89961937509977652, 71.87390960531433848 ) ) ;
#104969 = CARTESIAN_POINT ( 'NONE',  ( 12.06949235617757843, -12.14591786802309237, 83.12390960531436690 ) ) ;
#104971 = CARTESIAN_POINT ( 'NONE',  ( -5.719274019375665041, -21.55341960407619695, 94.79275706135234714 ) ) ;
#104972 = CARTESIAN_POINT ( 'NONE',  ( -21.39352396646987486, 0.5319302666795560075, -58.79417398750191381 ) ) ;
#104973 = CARTESIAN_POINT ( 'NONE',  ( 16.53943276465976808, 0.05219959533934440121, 26.25109039468567573 ) ) ;
#104974 = CARTESIAN_POINT ( 'NONE',  ( 12.14591786802309770, 12.06949235617756955, 74.37390960531436690 ) ) ;
#104975 = CARTESIAN_POINT ( 'NONE',  ( 18.67979575497194134, -10.72451020669871369, 40.83442372801901854 ) ) ;
#104976 = CARTESIAN_POINT ( 'NONE',  ( 5.823673210054125526, 21.52544592524343514, 74.79057627198105251 ) ) ;
#104977 = CARTESIAN_POINT ( 'NONE',  ( 16.46253265017146816, 9.564922557961045513, 41.66775706135234003 ) ) ;
#104978 = CARTESIAN_POINT ( 'NONE',  ( 15.50000000000000178, 5.499999999999998224, 120.0000000000000142 ) ) ;
#104979 = CARTESIAN_POINT ( 'NONE',  ( -5.153800228976328057, -19.02544592524343514, 87.29057627198103830 ) ) ;
#104980 = CARTESIAN_POINT ( 'NONE',  ( 4.483927247898545687, 16.52544592524342804, 44.79057627198103120 ) ) ;
#104981 = CARTESIAN_POINT ( 'NONE',  ( 12.14591786802309770, 12.06949235617756955, 34.37390960531435979 ) ) ;
#104982 = CARTESIAN_POINT ( 'NONE',  ( 4.379528057220092307, 16.55341960407617563, 107.2927570613523471 ) ) ;
#104983 = CARTESIAN_POINT ( 'NONE',  ( 19.03943276465977164, 0.05219959533936151252, 61.25109039468566863 ) ) ;
#104984 = CARTESIAN_POINT ( 'NONE',  ( 26.56065628307859683, 7.402157598701552210, 155.5832749335749270 ) ) ;
#104985 = CARTESIAN_POINT ( 'NONE',  ( -15.80617190586745835, -15.72974639402198527, 21.87390960531436690 ) ) ;
#104986 = CARTESIAN_POINT ( 'NONE',  ( -12.14591786802309592, -12.06949235617757132, 91.87390960531436690 ) ) ;
#104987 = CARTESIAN_POINT ( 'NONE',  ( -22.00000000000000000, -5.204748896376250896E-15, 42.49999999999999289 ) ) ;
#104989 = CARTESIAN_POINT ( 'NONE',  ( -10.72451020669898014, 18.67979575497178502, 30.41557627198101699 ) ) ;
#104988 = CARTESIAN_POINT ( 'NONE',  ( 13.89961937509977652, -13.97604488694527269, 33.12390960531434558 ) ) ;
#104990 = CARTESIAN_POINT ( 'NONE',  ( -21.52544592524343514, 5.823673210054127303, 71.04057627198103830 ) ) ;
#104991 = CARTESIAN_POINT ( 'NONE',  ( -12.14591786802309592, -12.06949235617757132, 111.8739096053143669 ) ) ;
#104993 = CARTESIAN_POINT ( 'NONE',  ( -16.51473224551069308, -9.474510206698971260, 46.66557627198102409 ) ) ;
#104992 = CARTESIAN_POINT ( 'NONE',  ( -14.34966873604972548, 8.224510206698743886, 68.33442372801900433 ) ) ;
#104994 = CARTESIAN_POINT ( 'NONE',  ( 5.823673210054444382, -21.52544592524334988, 50.20942372801901854 ) ) ;
#104995 = CARTESIAN_POINT ( 'NONE',  ( -12.06949235617756955, 12.14591786802309770, 110.6239096053143669 ) ) ;
#104997 = CARTESIAN_POINT ( 'NONE',  ( -19.03943276465977164, -0.05219959533935918106, 93.75109039468566152 ) ) ;
#104996 = B_SPLINE_CURVE_WITH_KNOTS ( 'NONE', 3,
 ( #120373, #151723, #59694, #74879, #103230, #198222, #149733, #166902, #133560, #181086, #178081, #39549, #132565, #42561, #71890, #11234, #163919, #164912, #101208, #87057, #86055, #182066 ),
 .UNSPECIFIED., .F., .F.,
 ( 4, 2, 2, 2, 2, 2, 2, 2, 2, 2, 4 ),
 ( 8.673617379884035472E-19, 0.001309639967555473270, 0.001964459951333209688, 0.002291869943222077897, 0.002455574939166497474, 0.002619279935110917917, 0.002782984931055337927, 0.002946689926999758371, 0.003274099918888572370, 0.003928919902666201669, 0.005238559870221456798 ),
 .UNSPECIFIED. ) ;
#104998 = CARTESIAN_POINT ( 'NONE',  ( 22.81625015709509441, 31.40387420917330275, -7.824999997268813345 ) ) ;
#105000 = CARTESIAN_POINT ( 'NONE',  ( -18.67979575497178146, -10.72451020669898902, 31.66557627198102054 ) ) ;
#104999 = DIRECTION ( 'NONE',  ( 0.000000000000000000, 0.000000000000000000, 1.000000000000000000 ) ) ;
#105001 = DIRECTION ( 'NONE',  ( -0.000000000000000000, -0.000000000000000000, 1.000000000000000000 ) ) ;
#105002 = CARTESIAN_POINT ( 'NONE',  ( -18.62759615963255300, -10.81492255796106328, 64.16775706135234714 ) ) ;
#105004 = CARTESIAN_POINT ( 'NONE',  ( -14.29746914071049879, 8.314922557960819915, 40.83224293864769550 ) ) ;
#105003 = CARTESIAN_POINT ( 'NONE',  ( 12.14591786802327356, -12.06949235617739191, 55.62609039468568284 ) ) ;
#105005 = CARTESIAN_POINT ( 'NONE',  ( 10.72451020669898902, -18.67979575497178502, 72.91557627198103830 ) ) ;
#105006 = CARTESIAN_POINT ( 'NONE',  ( 0.05219959533907565091, 21.53943276465977519, 64.99890960531435269 ) ) ;
#105007 = CARTESIAN_POINT ( 'NONE',  ( -20.51359854606067401, -11.49117151696134087, 170.0775129446642779 ) ) ;
#105010 = EDGE_CURVE ( 'NONE', #95658, #135939, #128556, .T. ) ;
#105009 = CARTESIAN_POINT ( 'NONE',  ( -5.049401038298153566, 19.05341960407611168, 110.2072429386476671 ) ) ;
#105008 = CARTESIAN_POINT ( 'NONE',  ( -16.46253265017146816, -9.564922557961047289, 84.16775706135233293 ) ) ;
#105012 = CARTESIAN_POINT ( 'NONE',  ( 19.05341960407611168, 5.049401038298154454, 48.95724293864768129 ) ) ;
#105011 = B_SPLINE_CURVE_WITH_KNOTS ( 'NONE', 3,
 ( #62579, #184944, #112080, #46429, #79751, #141421, #31266, #177755, #35236, #176758, #130208, #96890, #38231, #191903, #98878, #99886, #131228, #158573, #4881, #113060, #67557, #20062, #55387, #161571, #51400, #53388, #160573, #174752 ),
 .UNSPECIFIED., .F., .F.,
 ( 4, 2, 2, 2, 2, 2, 2, 2, 2, 2, 2, 2, 2, 4 ),
 ( 3.084931484532069451E-17, 0.0005512667261461084295, 0.001102533452292185851, 0.001240350133828705152, 0.001378166815365224453, 0.001447075156133462853, 0.001515983496901700820, 0.001653800178438180439, 0.001929433541511138593, 0.002205066904584096748, 0.003307600356875847400, 0.004410133809167598486, 0.006615200713751101524, 0.008820267618334603696 ),
 .UNSPECIFIED. ) ;
#105013 = CARTESIAN_POINT ( 'NONE',  ( 14.34966873604960469, 8.224510206698951720, 114.1655762719810383 ) ) ;
#105014 = SHAPE_REPRESENTATION_RELATIONSHIP ( 'NONE' , 'NONE' ,  #9542, #22986 ) ;
#105015 = CARTESIAN_POINT ( 'NONE',  ( -9.474510206698964154, 16.51473224551069663, 110.4155762719810383 ) ) ;
#105016 = ORIENTED_EDGE ( 'NONE', *, *, #92523, .F. ) ;
#105017 = CARTESIAN_POINT ( 'NONE',  ( 4.379528057220092307, 16.55341960407617563, 67.29275706135234714 ) ) ;
#105018 = CARTESIAN_POINT ( 'NONE',  ( 21.53943276465977519, -0.05219959533907433946, 108.7489096053143669 ) ) ;
#105019 = CARTESIAN_POINT ( 'NONE',  ( 19.03943276465977164, -0.05219959533909143690, 53.74890960531436690 ) ) ;
#105020 = CARTESIAN_POINT ( 'NONE',  ( 10.81492255796106328, -18.62759615963255655, 40.41775706135234714 ) ) ;
#105021 = CARTESIAN_POINT ( 'NONE',  ( 5.049401038298161559, -19.05341960407611168, 97.70724293864766707 ) ) ;
#105022 = CARTESIAN_POINT ( 'NONE',  ( -29.81671572245832280, -26.02765724076686737, -18.90727510135208078 ) ) ;
#105023 = ORIENTED_EDGE ( 'NONE', *, *, #136828, .T. ) ;
#105024 = CARTESIAN_POINT ( 'NONE',  ( -5.719274019375665041, -21.55341960407619695, 34.79275706135235424 ) ) ;
#105026 = CARTESIAN_POINT ( 'NONE',  ( -19.02544592524334988, -5.153800228976617603, 83.95942372801901854 ) ) ;
#105025 = CARTESIAN_POINT ( 'NONE',  ( 5.049401038298161559, -19.05341960407611168, 112.7072429386476813 ) ) ;
#105027 = CARTESIAN_POINT ( 'NONE',  ( 19.02544592524334988, 5.153800228976608722, 36.45942372801900433 ) ) ;
#105028 = CARTESIAN_POINT ( 'NONE',  ( 15.72974639402199770, -15.80617190586745480, 103.1239096053143811 ) ) ;
#105029 = CARTESIAN_POINT ( 'NONE',  ( -19.03943276465977164, -0.05219959533935918106, 28.75109039468566507 ) ) ;
#105030 = CARTESIAN_POINT ( 'NONE',  ( 9.474510206698729675, 16.51473224551082808, 47.08442372801900433 ) ) ;
#105031 = CARTESIAN_POINT ( 'NONE',  ( 14.29746914071037800, 8.314922557961029526, 86.66775706135234714 ) ) ;
#105032 = CARTESIAN_POINT ( 'NONE',  ( 17.79613651744294245, -24.49428055684527195, 146.6843446569000093 ) ) ;
#105033 = CARTESIAN_POINT ( 'NONE',  ( 19.03943276465977164, -0.05219959533909143690, 73.74890960531435269 ) ) ;
#105034 = VECTOR ( 'NONE', #158617, 1000.000000000000000 ) ;
#105035 = CARTESIAN_POINT ( 'NONE',  ( -0.05219959533937732626, 21.53943276465977519, 77.50109039468567573 ) ) ;
#105036 = CARTESIAN_POINT ( 'NONE',  ( -10.81492255796105439, 18.62759615963255655, 82.91775706135234714 ) ) ;
#105037 = DIRECTION ( 'NONE',  ( 1.000000000000000000, 0.000000000000000000, 0.000000000000000000 ) ) ;
#105038 = CARTESIAN_POINT ( 'NONE',  ( -19.02544592524342804, 5.153800228976336051, 91.04057627198100988 ) ) ;
#105039 = CARTESIAN_POINT ( 'NONE',  ( 21.52544592524334988, 5.823673210054432836, 56.45942372801902565 ) ) ;
#105040 = CARTESIAN_POINT ( 'NONE',  ( 13.97604488694548053, -13.89961937509957401, 100.6260903946856615 ) ) ;
#105041 = CARTESIAN_POINT ( 'NONE',  ( -19.02544592524342804, 5.153800228976336051, 66.04057627198103830 ) ) ;
#105042 = CARTESIAN_POINT ( 'NONE',  ( 19.02544592524343514, -5.153800228976328945, 108.5405762719810383 ) ) ;
#105043 = CARTESIAN_POINT ( 'NONE',  ( 19.05341960407611168, 5.049401038298154454, 78.95724293864769550 ) ) ;
#105044 = CARTESIAN_POINT ( 'NONE',  ( -17.40861289039006010, -6.110651285853244907, 91.37232470827437680 ) ) ;
#105045 = CARTESIAN_POINT ( 'NONE',  ( -13.97604488694527625, -13.89961937509977652, 66.87390960531436690 ) ) ;
#105046 = CARTESIAN_POINT ( 'NONE',  ( -19.02544592524342804, 5.153800228976336051, 51.04057627198103120 ) ) ;
#105047 = CARTESIAN_POINT ( 'NONE',  ( 18.67979575497178502, 10.72451020669898547, 114.1655762719810383 ) ) ;
#105048 = CARTESIAN_POINT ( 'NONE',  ( -8.224510206698735004, -14.34966873604973081, 84.58442372801903275 ) ) ;
#105049 = CIRCLE ( 'NONE', #17870, 5.000000000000000000 ) ;
#105050 = CARTESIAN_POINT ( 'NONE',  ( 16.51473224551083163, -9.474510206698727899, 45.83442372801900433 ) ) ;
#105051 = CARTESIAN_POINT ( 'NONE',  ( 16.46253265017160672, -9.564922557960803928, 83.33224293864768129 ) ) ;
#105052 = CARTESIAN_POINT ( 'NONE',  ( -16.52544592524342804, 4.483927247898546575, 76.04057627198102409 ) ) ;
#105053 = CARTESIAN_POINT ( 'NONE',  ( -12.06949235617756955, 12.14591786802309770, 105.6239096053143669 ) ) ;
#105054 = AXIS2_PLACEMENT_3D ( 'NONE', #169077, #62892, #17402 ) ;
#105055 = CARTESIAN_POINT ( 'NONE',  ( 0.05219959533909260263, 19.03943276465977164, 114.9989096053143669 ) ) ;
#105056 = CARTESIAN_POINT ( 'NONE',  ( 9.474510206698971260, -16.51473224551069308, 102.9155762719810241 ) ) ;
#105057 = CARTESIAN_POINT ( 'NONE',  ( 14.29746914071049879, -8.314922557960816363, 83.33224293864769550 ) ) ;
#105058 = CARTESIAN_POINT ( 'NONE',  ( -193.3062444957834884, -155.7167183371838064, -25.00000000000000000 ) ) ;
#105059 = CARTESIAN_POINT ( 'NONE',  ( 16.46253265017146816, 9.564922557961045513, 26.66775706135234003 ) ) ;
#105060 = CARTESIAN_POINT ( 'NONE',  ( 4.379528057220092307, 16.55341960407617563, 87.29275706135236135 ) ) ;
#105061 = CARTESIAN_POINT ( 'NONE',  ( -13.89961937509977652, 13.97604488694528158, 85.62390960531433848 ) ) ;
#105062 = CARTESIAN_POINT ( 'NONE',  ( -0.05219959533937732626, 21.53943276465977519, 52.50109039468567573 ) ) ;
#105063 = CARTESIAN_POINT ( 'NONE',  ( -10.81492255796078084, -18.62759615963271287, 47.08224293864770260 ) ) ;
#105064 = CARTESIAN_POINT ( 'NONE',  ( 0.05219959533937995610, -21.53943276465977519, 25.00109039468567218 ) ) ;
#105065 = CARTESIAN_POINT ( 'NONE',  ( 21.53943276465977519, -0.05219959533907433946, 68.74890960531435269 ) ) ;
#105066 = CARTESIAN_POINT ( 'NONE',  ( -16.52544592524342804, 4.483927247898546575, 96.04057627198102409 ) ) ;
#105067 = CARTESIAN_POINT ( 'NONE',  ( -19.03943276465977164, -0.05219959533935918106, 53.75109039468566863 ) ) ;
#105068 = CARTESIAN_POINT ( 'NONE',  ( -13.97604488694527625, -13.89961937509977652, 36.87390960531436690 ) ) ;
#105069 = CARTESIAN_POINT ( 'NONE',  ( 16.46253265017160672, -9.564922557960803928, 88.33224293864769550 ) ) ;
#105070 = CARTESIAN_POINT ( 'NONE',  ( -9.564922557960796823, -16.46253265017161027, 77.08224293864769550 ) ) ;
#105071 = CARTESIAN_POINT ( 'NONE',  ( -16.53943276465976808, 0.05219959533911058130, 96.24890960531435269 ) ) ;
#105072 = ORIENTED_EDGE ( 'NONE', *, *, #111223, .T. ) ;
#105073 = CARTESIAN_POINT ( 'NONE',  ( -8.314922557960811034, -14.29746914071050412, 27.08224293864769550 ) ) ;
#105074 = CARTESIAN_POINT ( 'NONE',  ( 12.14591786802327356, -12.06949235617739191, 35.62609039468568994 ) ) ;
#105075 = CARTESIAN_POINT ( 'NONE',  ( -18.62759615963255300, -10.81492255796106328, 109.1677570613523613 ) ) ;
#105076 = CARTESIAN_POINT ( 'NONE',  ( 5.153800228976335163, 19.02544592524342804, 94.79057627198103830 ) ) ;
#105077 = CARTESIAN_POINT ( 'NONE',  ( 10.81492255796106328, -18.62759615963255655, 30.41775706135234358 ) ) ;
#105078 = CARTESIAN_POINT ( 'NONE',  ( 13.97604488694527802, 13.89961937509977652, 39.37390960531435269 ) ) ;
#105079 = EDGE_CURVE ( 'NONE', #137808, #56021, #78077, .T. ) ;
#105080 = CARTESIAN_POINT ( 'NONE',  ( 12.06949235617739724, 12.14591786802326823, 46.87609039468568994 ) ) ;
#105081 = CARTESIAN_POINT ( 'NONE',  ( -0.05219959533936034679, 19.03943276465977164, 102.5010903946856757 ) ) ;
#105082 = CARTESIAN_POINT ( 'NONE',  ( 9.474510206698971260, -16.51473224551069308, 32.91557627198102409 ) ) ;
#105083 = CARTESIAN_POINT ( 'NONE',  ( 16.52544592524342804, -4.483927247898539470, 98.54057627198105251 ) ) ;
#105084 = CARTESIAN_POINT ( 'NONE',  ( 21.55341960407610458, 5.719274019375980345, 103.9572429386476813 ) ) ;
#105085 = CARTESIAN_POINT ( 'NONE',  ( -9.564922557961040184, 16.46253265017147172, 82.91775706135233293 ) ) ;
#105086 = CARTESIAN_POINT ( 'NONE',  ( -37.66961640367473052, 5.000000000000023981, -25.00000000000000000 ) ) ;
#105087 = CARTESIAN_POINT ( 'NONE',  ( -19.03943276465977164, 0.05219959533909376836, 86.24890960531436690 ) ) ;
#105088 = CARTESIAN_POINT ( 'NONE',  ( -15.72974639402176322, -15.80617190586768395, 39.37609039468567573 ) ) ;
#105089 = LINE ( 'NONE', #137402, #24056 ) ;
#105090 = CARTESIAN_POINT ( 'NONE',  ( 16.51473224551069308, 9.474510206698969483, 89.16557627198103830 ) ) ;
#105091 = CARTESIAN_POINT ( 'NONE',  ( 17.26172910966780805, -6.454744622555828037, 113.3064690864922568 ) ) ;
#105092 = CARTESIAN_POINT ( 'NONE',  ( -13.89961937509977652, 13.97604488694528158, 90.62390960531432427 ) ) ;
#105094 = CARTESIAN_POINT ( 'NONE',  ( -16.53943276465976808, 0.05219959533911058130, 91.24890960531436690 ) ) ;
#105093 = CARTESIAN_POINT ( 'NONE',  ( 10.72451020669871369, 18.67979575497193778, 37.08442372801901143 ) ) ;
#105095 = CARTESIAN_POINT ( 'NONE',  ( -5.153800228976328057, -19.02544592524343514, 97.29057627198099567 ) ) ;
#105096 = CARTESIAN_POINT ( 'NONE',  ( 16.51473224551083163, -9.474510206698727899, 20.83442372801899722 ) ) ;
#105097 = CARTESIAN_POINT ( 'NONE',  ( 4.379528057220092307, 16.55341960407617563, 47.29275706135234003 ) ) ;
#105098 = CARTESIAN_POINT ( 'NONE',  ( -21.52544592524334988, -5.823673210054445271, 63.95942372801901854 ) ) ;
#105099 = CARTESIAN_POINT ( 'NONE',  ( 16.55341960407618274, -4.379528057220086978, 26.04275706135235779 ) ) ;
#105100 = CARTESIAN_POINT ( 'NONE',  ( -0.05219959533909027116, -19.03943276465977164, 72.49890960531435269 ) ) ;
#105101 = CARTESIAN_POINT ( 'NONE',  ( -19.02544592524334988, -5.153800228976617603, 98.95942372801900433 ) ) ;
#105102 = CARTESIAN_POINT ( 'NONE',  ( 14.34966873604972726, -8.224510206698740333, 70.83442372801901854 ) ) ;
#105103 = CARTESIAN_POINT ( 'NONE',  ( 21.55341960407619695, -5.719274019375665929, 111.0427570613523613 ) ) ;
#105104 = CARTESIAN_POINT ( 'NONE',  ( -16.46253265017146816, -9.564922557961047289, 74.16775706135234714 ) ) ;
#105105 = CARTESIAN_POINT ( 'NONE',  ( 16.51473224551069308, 9.474510206698969483, 59.16557627198102409 ) ) ;
#105106 = CARTESIAN_POINT ( 'NONE',  ( -18.62759615963270932, 10.81492255796079327, 80.83224293864769550 ) ) ;
#105108 = CARTESIAN_POINT ( 'NONE',  ( 13.89961937509957401, 13.97604488694547697, 76.87609039468566152 ) ) ;
#105107 = CARTESIAN_POINT ( 'NONE',  ( -4.379528057220328563, 16.55341960407611168, 80.20724293864769550 ) ) ;
#105109 = CARTESIAN_POINT ( 'NONE',  ( 11.30153831258471797, -180.0000000000000000, -4.999999999999994671 ) ) ;
#105110 = CARTESIAN_POINT ( 'NONE',  ( -5.049401038297874678, -19.05341960407617918, 59.79275706135231871 ) ) ;
#105111 = CARTESIAN_POINT ( 'NONE',  ( 14.34966873604972726, -8.224510206698740333, 105.8344237280190328 ) ) ;
#105112 = CARTESIAN_POINT ( 'NONE',  ( 14.29746914071049879, -8.314922557960816363, 73.33224293864769550 ) ) ;
#105114 = CARTESIAN_POINT ( 'NONE',  ( -8.571926809382608425, 26.38167802310805854, 144.4750000027312069 ) ) ;
#105113 = CARTESIAN_POINT ( 'NONE',  ( 21.55341960407619695, -5.719274019375665929, 106.0427570613523471 ) ) ;
#105115 = CARTESIAN_POINT ( 'NONE',  ( -5.823673210054116645, -21.52544592524344225, 102.2905762719810383 ) ) ;
#105116 = CARTESIAN_POINT ( 'NONE',  ( -0.05219959533909027116, -19.03943276465977164, 97.49890960531436690 ) ) ;
#105117 = CARTESIAN_POINT ( 'NONE',  ( -0.05219959533909027116, -19.03943276465977164, 67.49890960531436690 ) ) ;
#105118 = CARTESIAN_POINT ( 'NONE',  ( -10.72451020669870658, -18.67979575497194134, 79.58442372801903275 ) ) ;
#105119 = CARTESIAN_POINT ( 'NONE',  ( 5.153800228976335163, 19.02544592524342804, 59.79057627198100988 ) ) ;
#105120 = CARTESIAN_POINT ( 'NONE',  ( -19.05341960407611168, -5.049401038298163336, 41.45724293864769550 ) ) ;
#105121 = CARTESIAN_POINT ( 'NONE',  ( 15.80617190586746368, 15.72974639402197994, 24.37390960531435979 ) ) ;
#105122 = AXIS2_PLACEMENT_3D ( 'NONE', #97343, #33712, #80204 ) ;
#105123 = CARTESIAN_POINT ( 'NONE',  ( 8.224510206698953496, -14.34966873604960469, 67.91557627198102409 ) ) ;
#105124 = CARTESIAN_POINT ( 'NONE',  ( 19.02544592524343514, -5.153800228976328945, 43.54057627198103120 ) ) ;
#105125 = CARTESIAN_POINT ( 'NONE',  ( -0.05219959533910754901, -16.53943276465976808, 97.49890960531436690 ) ) ;
#105126 = CARTESIAN_POINT ( 'NONE',  ( -15.72974639402197994, 15.80617190586746368, 110.6239096053143669 ) ) ;
#105127 = CARTESIAN_POINT ( 'NONE',  ( -15.80617190586768217, 15.72974639402176855, 43.12609039468568284 ) ) ;
#105128 = CARTESIAN_POINT ( 'NONE',  ( 19.02544592524343514, -5.153800228976328945, 33.54057627198102409 ) ) ;
#105129 = CARTESIAN_POINT ( 'NONE',  ( 14.29746914071037800, 8.314922557961029526, 61.66775706135235424 ) ) ;
#105130 = CARTESIAN_POINT ( 'NONE',  ( 10.81492255796078972, 18.62759615963270932, 104.5822429386477097 ) ) ;
#105131 = CARTESIAN_POINT ( 'NONE',  ( -15.72974639402197994, 15.80617190586746368, 95.62390960531436690 ) ) ;
#105133 = CARTESIAN_POINT ( 'NONE',  ( -16.46253265017160317, 9.564922557960807481, 55.83224293864769550 ) ) ;
#105132 = CARTESIAN_POINT ( 'NONE',  ( 19.02544592524334988, 5.153800228976608722, 31.45942372801900433 ) ) ;
#105134 = CARTESIAN_POINT ( 'NONE',  ( -17.49999999999999645, 5.499999999999992895, 83.71769037696435589 ) ) ;
#105135 = CARTESIAN_POINT ( 'NONE',  ( -5.823673210054431948, 21.52544592524334988, 62.70942372801902565 ) ) ;
#105136 = CARTESIAN_POINT ( 'NONE',  ( 21.53943276465977519, -0.05219959533907433946, 58.74890960531436690 ) ) ;
#105137 = CARTESIAN_POINT ( 'NONE',  ( -12.14591786802309592, -12.06949235617757132, 26.87390960531435979 ) ) ;
#105139 = CARTESIAN_POINT ( 'NONE',  ( -21.53943276465977519, -0.05219959533937600094, 103.7510903946857042 ) ) ;
#105138 = CARTESIAN_POINT ( 'NONE',  ( 10.81492255796106328, -18.62759615963255655, 80.41775706135234714 ) ) ;
#105140 = CARTESIAN_POINT ( 'NONE',  ( -19.05341960407617563, 5.049401038297882671, 48.54275706135233293 ) ) ;
#105141 = CARTESIAN_POINT ( 'NONE',  ( 4.483927247898790824, -16.52544592524335698, 100.2094237280190043 ) ) ;
#105142 = CARTESIAN_POINT ( 'NONE',  ( 21.55341960407619695, -5.719274019375665929, 61.04275706135234714 ) ) ;
#105143 = CARTESIAN_POINT ( 'NONE',  ( 5.153800228976335163, 19.02544592524342804, 59.79057627198100988 ) ) ;
#105144 = CARTESIAN_POINT ( 'NONE',  ( -19.02544592524334988, -5.153800228976617603, 38.95942372801900433 ) ) ;
#105145 = CARTESIAN_POINT ( 'NONE',  ( 21.53943276465977519, -0.05219959533907433946, 43.74890960531435979 ) ) ;
#105146 = CARTESIAN_POINT ( 'NONE',  ( -15.80617190586768217, 15.72974639402176855, 38.12609039468567573 ) ) ;
#105147 = CARTESIAN_POINT ( 'NONE',  ( 21.53943276465977519, -0.05219959533907433946, 88.74890960531436690 ) ) ;
#105148 = CARTESIAN_POINT ( 'NONE',  ( -13.89961937509957401, -13.97604488694547875, 89.37609039468563310 ) ) ;
#105149 = CARTESIAN_POINT ( 'NONE',  ( -4.483927247898782831, 16.52544592524335698, 57.70942372801901143 ) ) ;
#105151 = CARTESIAN_POINT ( 'NONE',  ( -10.72451020669898014, 18.67979575497178502, 95.41557627198102409 ) ) ;
#105150 = CARTESIAN_POINT ( 'NONE',  ( -6.434671708797603529, 6.434671708797564449, -61.89430850415821794 ) ) ;
#105153 = CARTESIAN_POINT ( 'NONE',  ( 16.55341960407611168, 4.379528057220329451, 78.95724293864769550 ) ) ;
#105152 = CARTESIAN_POINT ( 'NONE',  ( -12.06949235617739369, -12.14591786802326823, 79.37609039468567573 ) ) ;
#105154 = CARTESIAN_POINT ( 'NONE',  ( -26.88621168971704378, -26.45719545518177185, -20.39628335082763044 ) ) ;
#105155 = CARTESIAN_POINT ( 'NONE',  ( 19.03943276465977164, 0.05219959533936151252, 101.2510903946856757 ) ) ;
#105156 = CARTESIAN_POINT ( 'NONE',  ( -10.72451020669898014, 18.67979575497178502, 30.41557627198101699 ) ) ;
#105157 = DIRECTION ( 'NONE',  ( -0.000000000000000000, -0.000000000000000000, 1.000000000000000000 ) ) ;
#105158 = CARTESIAN_POINT ( 'NONE',  ( 8.224510206698742110, 14.34966873604972548, 57.08442372801901854 ) ) ;
#105159 = CARTESIAN_POINT ( 'NONE',  ( 5.823673210054125526, 21.52544592524343514, 109.7905762719810383 ) ) ;
#105160 = CARTESIAN_POINT ( 'NONE',  ( 15.72974639402199770, -15.80617190586745480, 33.12390960531435979 ) ) ;
#105161 = CARTESIAN_POINT ( 'NONE',  ( -0.05219959533934338120, 16.53943276465976808, 67.50109039468568994 ) ) ;
#105162 = CARTESIAN_POINT ( 'NONE',  ( 19.05341960407611168, 5.049401038298154454, 78.95724293864769550 ) ) ;
#105164 = CARTESIAN_POINT ( 'NONE',  ( 0.05219959533909260263, 19.03943276465977164, 24.99890960531435269 ) ) ;
#105163 = CARTESIAN_POINT ( 'NONE',  ( 0.05219959533937995610, -21.53943276465977519, 55.00109039468568284 ) ) ;
#105165 = CARTESIAN_POINT ( 'NONE',  ( 15.80617190586746368, 15.72974639402197994, 24.37390960531435979 ) ) ;
#105166 = EDGE_LOOP ( 'NONE', ( #67500, #41945 ) ) ;
#105167 = CARTESIAN_POINT ( 'NONE',  ( 9.564922557961047289, -16.46253265017146816, 45.41775706135232582 ) ) ;
#105168 = CARTESIAN_POINT ( 'NONE',  ( 12.06949235617739724, 12.14591786802326823, 56.87609039468568994 ) ) ;
#105169 = CARTESIAN_POINT ( 'NONE',  ( 13.89961937509977652, -13.97604488694527269, 113.1239096053143527 ) ) ;
#105170 = CARTESIAN_POINT ( 'NONE',  ( 19.03943276465977164, -0.05219959533909143690, 78.74890960531436690 ) ) ;
#105171 = CARTESIAN_POINT ( 'NONE',  ( -16.52544592524335698, -4.483927247898792601, 103.9594237280190185 ) ) ;
#105172 = CARTESIAN_POINT ( 'NONE',  ( 6.856101608890801443E-16, -78.63162257080495010, -22.99999901186701123 ) ) ;
#105173 = CARTESIAN_POINT ( 'NONE',  ( -14.29746914071049879, 8.314922557960819915, 100.8322429386477097 ) ) ;
#105174 = CARTESIAN_POINT ( 'NONE',  ( -0.05219959533907301413, -21.53943276465977519, 32.49890960531435979 ) ) ;
#105175 = CARTESIAN_POINT ( 'NONE',  ( -19.02544592524342804, 5.153800228976336051, 31.04057627198102409 ) ) ;
#105176 = CARTESIAN_POINT ( 'NONE',  ( -16.55341960407617563, 4.379528057220093196, 68.54275706135234714 ) ) ;
#105177 = CARTESIAN_POINT ( 'NONE',  ( -10.72451020669898014, 18.67979575497178502, 115.4155762719810241 ) ) ;
#105178 = CARTESIAN_POINT ( 'NONE',  ( -0.05219959533936034679, 19.03943276465977164, 72.50109039468566152 ) ) ;
#105179 = CARTESIAN_POINT ( 'NONE',  ( -5.049401038298153566, 19.05341960407611168, 40.20724293864768839 ) ) ;
#105180 = CARTESIAN_POINT ( 'NONE',  ( 10.72451020669898902, -18.67979575497178502, 72.91557627198103830 ) ) ;
#105181 = DIRECTION ( 'NONE',  ( 0.000000000000000000, 0.000000000000000000, -1.000000000000000000 ) ) ;
#105182 = CARTESIAN_POINT ( 'NONE',  ( 10.81492255796106328, -18.62759615963255655, 85.41775706135236135 ) ) ;
#105183 = CARTESIAN_POINT ( 'NONE',  ( -5.153800228976328057, -19.02544592524343514, 67.29057627198102409 ) ) ;
#105184 = CARTESIAN_POINT ( 'NONE',  ( 12.06949235617739724, 12.14591786802326823, 51.87609039468568284 ) ) ;
#105185 = CARTESIAN_POINT ( 'NONE',  ( 5.823673210054444382, -21.52544592524334988, 75.20942372801901854 ) ) ;
#105186 = CARTESIAN_POINT ( 'NONE',  ( 5.049401038297881783, 19.05341960407617563, 42.29275706135234003 ) ) ;
#105187 = CARTESIAN_POINT ( 'NONE',  ( 13.97604488694548053, -13.89961937509957401, 50.62609039468566152 ) ) ;
#105188 = ORIENTED_EDGE ( 'NONE', *, *, #65989, .T. ) ;
#105189 = CARTESIAN_POINT ( 'NONE',  ( 0.05219959533937995610, -21.53943276465977519, 50.00109039468568994 ) ) ;
#105190 = CARTESIAN_POINT ( 'NONE',  ( -16.51473224551069308, -9.474510206698971260, 21.66557627198102765 ) ) ;
#105191 = CARTESIAN_POINT ( 'NONE',  ( -5.153800228976607833, 19.02544592524334988, 47.70942372801900433 ) ) ;
#105192 = CARTESIAN_POINT ( 'NONE',  ( 9.564922557960805705, 16.46253265017160317, 94.58224293864769550 ) ) ;
#105193 = CARTESIAN_POINT ( 'NONE',  ( -5.153800228976328057, -19.02544592524343514, 77.29057627198099567 ) ) ;
#105194 = CARTESIAN_POINT ( 'NONE',  ( 12.14591786802309770, 12.06949235617756955, 39.37390960531436690 ) ) ;
#105195 = CARTESIAN_POINT ( 'NONE',  ( 18.67979575497178502, 10.72451020669898547, 39.16557627198102409 ) ) ;
#105196 = CARTESIAN_POINT ( 'NONE',  ( -36.91746825000000598, 2.428612866367529932E-14, -11.12499999726881228 ) ) ;
#105197 = CARTESIAN_POINT ( 'NONE',  ( 17.26058549869089731, 6.457015423128627418, 58.87745837476068544 ) ) ;
#105198 = CARTESIAN_POINT ( 'NONE',  ( 10.72451020669871369, 18.67979575497193778, 102.0844237280190185 ) ) ;
#105199 = CARTESIAN_POINT ( 'NONE',  ( 19.24578484527059175, -180.9428398739492820, 0.000000000000000000 ) ) ;
#105200 = CARTESIAN_POINT ( 'NONE',  ( -16.51473224551069308, -9.474510206698971260, 36.66557627198102409 ) ) ;
#105201 = CARTESIAN_POINT ( 'NONE',  ( -9.474510206698964154, 16.51473224551069663, 115.4155762719810241 ) ) ;
#105202 = EDGE_CURVE ( 'NONE', #23611, #26894, #192235, .T. ) ;
#105203 = CARTESIAN_POINT ( 'NONE',  ( -23.48298174826589602, -32.32155151706772500, -1.702157773949823039 ) ) ;
#105204 = CARTESIAN_POINT ( 'NONE',  ( -8.314922557961024197, 14.29746914071037800, 47.91775706135234714 ) ) ;
#105205 = CARTESIAN_POINT ( 'NONE',  ( -0.05219959533907301413, -21.53943276465977519, 77.49890960531433848 ) ) ;
#105206 = CARTESIAN_POINT ( 'NONE',  ( 12.14591786802309770, 12.06949235617756955, 34.37390960531435979 ) ) ;
#105208 = CARTESIAN_POINT ( 'NONE',  ( -5.153800228976328057, -19.02544592524343514, 112.2905762719810099 ) ) ;
#105207 = CARTESIAN_POINT ( 'NONE',  ( -5.153800228976328057, -19.02544592524343514, 32.29057627198102409 ) ) ;
#105209 = CARTESIAN_POINT ( 'NONE',  ( 15.72974639402176855, 15.80617190586768217, 31.87609039468567929 ) ) ;
#105210 = CARTESIAN_POINT ( 'NONE',  ( -13.89961937509957401, -13.97604488694547875, 34.37609039468566863 ) ) ;
#105211 = CARTESIAN_POINT ( 'NONE',  ( -13.89961937509977652, 13.97604488694528158, 25.62390960531434558 ) ) ;
#105212 = CARTESIAN_POINT ( 'NONE',  ( 0.05219959533937995610, -21.53943276465977519, 80.00109039468568994 ) ) ;
#105213 = DIRECTION ( 'NONE',  ( -0.000000000000000000, -0.000000000000000000, 1.000000000000000000 ) ) ;
#105214 = CARTESIAN_POINT ( 'NONE',  ( 16.53943276465976808, -0.05219959533910856209, 33.74890960531436690 ) ) ;
#105215 = CARTESIAN_POINT ( 'NONE',  ( -11.30153831258471442, -180.0000000000000000, -15.00000000000000178 ) ) ;
#105216 = CARTESIAN_POINT ( 'NONE',  ( -10.81492255796078084, -18.62759615963271287, 32.08224293864769550 ) ) ;
#105217 = CARTESIAN_POINT ( 'NONE',  ( -4.379528057220328563, 16.55341960407611168, 85.20724293864770971 ) ) ;
#105218 = CARTESIAN_POINT ( 'NONE',  ( 6.017829804060273347, -47.35862344248570821, -22.79591852006818442 ) ) ;
#105219 = CARTESIAN_POINT ( 'NONE',  ( 13.89961937509977652, -13.97604488694527269, 73.12390960531436690 ) ) ;
#105220 = CARTESIAN_POINT ( 'NONE',  ( -4.379528057220328563, 16.55341960407611168, 70.20724293864769550 ) ) ;
#105221 = CARTESIAN_POINT ( 'NONE',  ( 19.05341960407617918, -5.049401038297876454, 111.0427570613523329 ) ) ;
#105222 = CARTESIAN_POINT ( 'NONE',  ( 21.52544592524344225, -5.823673210054117533, 63.54057627198103830 ) ) ;
#105223 = ORIENTED_EDGE ( 'NONE', *, *, #123966, .T. ) ;
#105224 = CARTESIAN_POINT ( 'NONE',  ( 5.153800228976335163, 19.02544592524342804, 29.79057627198102409 ) ) ;
#105226 = CARTESIAN_POINT ( 'NONE',  ( -5.823673210054116645, -21.52544592524344225, 72.29057627198102409 ) ) ;
#105225 = CARTESIAN_POINT ( 'NONE',  ( -0.05219959533909027116, -19.03943276465977164, 82.49890960531436690 ) ) ;
#105228 = CARTESIAN_POINT ( 'NONE',  ( -0.05219959533909027116, -19.03943276465977164, 82.49890960531436690 ) ) ;
#105227 = CARTESIAN_POINT ( 'NONE',  ( -4.483927247898782831, 16.52544592524335698, 102.7094237280190185 ) ) ;
#105229 = CARTESIAN_POINT ( 'NONE',  ( 9.474510206698729675, 16.51473224551082808, 72.08442372801900433 ) ) ;
#105230 = CARTESIAN_POINT ( 'NONE',  ( 0.05219959533937995610, -21.53943276465977519, 100.0010903946857042 ) ) ;
#105231 = CARTESIAN_POINT ( 'NONE',  ( -0.05219959533907301413, -21.53943276465977519, 72.49890960531435269 ) ) ;
#105232 = CARTESIAN_POINT ( 'NONE',  ( 5.153800228976335163, 19.02544592524342804, 114.7905762719810241 ) ) ;
#105233 = CARTESIAN_POINT ( 'NONE',  ( 0.05219959533909260263, 19.03943276465977164, 44.99890960531435979 ) ) ;
#105234 = CARTESIAN_POINT ( 'NONE',  ( -0.05219959533934338120, 16.53943276465976808, 112.5010903946857042 ) ) ;
#105235 = CARTESIAN_POINT ( 'NONE',  ( -5.153800228976328057, -19.02544592524343514, 67.29057627198102409 ) ) ;
#105236 = DIRECTION ( 'NONE',  ( 0.000000000000000000, 0.000000000000000000, 1.000000000000000000 ) ) ;
#105237 = CARTESIAN_POINT ( 'NONE',  ( -15.72974639402176322, -15.80617190586768395, 104.3760903946856899 ) ) ;
#105238 = CARTESIAN_POINT ( 'NONE',  ( -8.224510206698948167, 14.34966873604960824, 70.41557627198102409 ) ) ;
#105239 = CARTESIAN_POINT ( 'NONE',  ( -15.72974639402197994, 15.80617190586746368, 110.6239096053143669 ) ) ;
#105240 = CARTESIAN_POINT ( 'NONE',  ( -5.719274019375978568, 21.55341960407610458, 105.2072429386477097 ) ) ;
#105241 = DIRECTION ( 'NONE',  ( 0.000000000000000000, 0.000000000000000000, 1.000000000000000000 ) ) ;
#105243 = ADVANCED_FACE ( 'NONE', ( #80374 ), #197544, .F. ) ;
#105242 = CARTESIAN_POINT ( 'NONE',  ( 15.72974639402199770, -15.80617190586745480, 58.12390960531435979 ) ) ;
#105244 = CARTESIAN_POINT ( 'NONE',  ( 14.29746914071037800, 8.314922557961029526, 86.66775706135234714 ) ) ;
#105245 = CARTESIAN_POINT ( 'NONE',  ( -4.483927247898539470, -16.52544592524342804, 107.2905762719810525 ) ) ;
#105246 = CARTESIAN_POINT ( 'NONE',  ( 19.05341960407611168, 5.049401038298154454, 63.95724293864769550 ) ) ;
#105247 = SHAPE_REPRESENTATION_RELATIONSHIP ( 'NONE' , 'NONE' ,  #31381, #35157 ) ;
#105248 = CARTESIAN_POINT ( 'NONE',  ( 16.55341960407618274, -4.379528057220086978, 106.0427570613523471 ) ) ;
#105249 = CARTESIAN_POINT ( 'NONE',  ( -21.55341960407619339, 5.719274019375674811, 43.54275706135235424 ) ) ;
#105250 = CARTESIAN_POINT ( 'NONE',  ( -19.03943276465977164, 0.05219959533909376836, 111.2489096053143669 ) ) ;
#105251 = CARTESIAN_POINT ( 'NONE',  ( 5.719274019375673035, 21.55341960407619339, 87.29275706135236135 ) ) ;
#105252 = CARTESIAN_POINT ( 'NONE',  ( 5.153800228976335163, 19.02544592524342804, 34.79057627198102409 ) ) ;
#105253 = CARTESIAN_POINT ( 'NONE',  ( -9.474510206698964154, 16.51473224551069663, 35.41557627198102409 ) ) ;
#105254 = ORIENTED_EDGE ( 'NONE', *, *, #113740, .T. ) ;
#105255 = CARTESIAN_POINT ( 'NONE',  ( -21.52544592524334988, -5.823673210054445271, 68.95942372801901854 ) ) ;
#105256 = CARTESIAN_POINT ( 'NONE',  ( -5.049401038298153566, 19.05341960407611168, 105.2072429386476671 ) ) ;
#105257 = CARTESIAN_POINT ( 'NONE',  ( 19.02544592524334988, 5.153800228976608722, 81.45942372801897591 ) ) ;
#105258 = CARTESIAN_POINT ( 'NONE',  ( -21.52544592524334988, -5.823673210054445271, 43.95942372801902565 ) ) ;
#105259 = CARTESIAN_POINT ( 'NONE',  ( 14.29746914071037800, 8.314922557961029526, 21.66775706135235069 ) ) ;
#105260 = CARTESIAN_POINT ( 'NONE',  ( 19.02544592524334988, 5.153800228976608722, 71.45942372801900433 ) ) ;
#105261 = CARTESIAN_POINT ( 'NONE',  ( -19.05341960407611168, -5.049401038298163336, 51.45724293864770260 ) ) ;
#105262 = CARTESIAN_POINT ( 'NONE',  ( 19.03943276465977164, 0.05219959533936151252, 81.25109039468567573 ) ) ;
#105263 = CARTESIAN_POINT ( 'NONE',  ( -16.53943276465976808, 0.05219959533911058130, 31.24890960531435979 ) ) ;
#105264 = CARTESIAN_POINT ( 'NONE',  ( 19.05341960407617918, -5.049401038297876454, 86.04275706135233293 ) ) ;
#105265 = CARTESIAN_POINT ( 'NONE',  ( 12.06949235617757843, -12.14591786802309237, 33.12390960531435979 ) ) ;
#105266 = CARTESIAN_POINT ( 'NONE',  ( -16.46253265017146816, -9.564922557961047289, 64.16775706135233293 ) ) ;
#105267 = CARTESIAN_POINT ( 'NONE',  ( -12.06949235617739369, -12.14591786802326823, 49.37609039468569705 ) ) ;
#105268 = CARTESIAN_POINT ( 'NONE',  ( 9.474510206698729675, 16.51473224551082808, 22.08442372801899722 ) ) ;
#105269 = CARTESIAN_POINT ( 'NONE',  ( 19.03943276465977164, -0.05219959533909143690, 43.74890960531435979 ) ) ;
#105270 = CARTESIAN_POINT ( 'NONE',  ( -17.44279575226823908, -5.990770900252488040, 64.16442432485685288 ) ) ;
#105271 = CARTESIAN_POINT ( 'NONE',  ( -12.06949235617739369, -12.14591786802326823, 44.37609039468567573 ) ) ;
#105272 = SPHERICAL_SURFACE ( 'NONE', #72434, 8.000000000000000000 ) ;
#105273 = CARTESIAN_POINT ( 'NONE',  ( -27.73933785331498925, -9.013057229001049109, 144.9750000027312069 ) ) ;
#105274 = CARTESIAN_POINT ( 'NONE',  ( -19.02544592524342804, 5.153800228976336051, 91.04057627198100988 ) ) ;
#105275 = CARTESIAN_POINT ( 'NONE',  ( 16.12203461105332636, 16.12203461105328017, -64.92279855667830191 ) ) ;
#105276 = CARTESIAN_POINT ( 'NONE',  ( 13.89961937509957401, 13.97604488694547697, 86.87609039468567573 ) ) ;
#105277 = CARTESIAN_POINT ( 'NONE',  ( 13.89961937509977652, -13.97604488694527269, 113.1239096053143527 ) ) ;
#105279 = CARTESIAN_POINT ( 'NONE',  ( 16.51473224551083163, -9.474510206698727899, 100.8344237280190043 ) ) ;
#105278 = CARTESIAN_POINT ( 'NONE',  ( 10.72451020669871369, 18.67979575497193778, 107.0844237280190043 ) ) ;
#105280 = CARTESIAN_POINT ( 'NONE',  ( -19.03943276465977164, 0.05219959533909376836, 21.24890960531436335 ) ) ;
#105281 = CARTESIAN_POINT ( 'NONE',  ( 9.474510206698971260, -16.51473224551069308, 42.91557627198103120 ) ) ;
#105282 = CARTESIAN_POINT ( 'NONE',  ( 18.67979575497178502, 10.72451020669898547, 64.16557627198102409 ) ) ;
#105283 = CARTESIAN_POINT ( 'NONE',  ( 13.97604488694527802, 13.89961937509977652, 29.37390960531435979 ) ) ;
#105284 = DIRECTION ( 'NONE',  ( 0.000000000000000000, 0.000000000000000000, -1.000000000000000000 ) ) ;
#105285 = CARTESIAN_POINT ( 'NONE',  ( 9.474510206698729675, 16.51473224551082808, 72.08442372801900433 ) ) ;
#105286 = CARTESIAN_POINT ( 'NONE',  ( 12.14591786802309770, 12.06949235617756955, 54.37390960531435979 ) ) ;
#105287 = CARTESIAN_POINT ( 'NONE',  ( 5.823673210054125526, 21.52544592524343514, 39.79057627198103830 ) ) ;
#105288 = CARTESIAN_POINT ( 'NONE',  ( -21.53943276465977519, -0.05219959533937600094, 98.75109039468568994 ) ) ;
#105289 = CARTESIAN_POINT ( 'NONE',  ( -5.823673210054116645, -21.52544592524344225, 87.29057627198103830 ) ) ;
#105290 = CARTESIAN_POINT ( 'NONE',  ( 21.53943276465977519, 0.05219959533937863772, 61.25109039468567573 ) ) ;
#105291 = CARTESIAN_POINT ( 'NONE',  ( -10.81492255796105439, 18.62759615963255655, 62.91775706135236135 ) ) ;
#105292 = CARTESIAN_POINT ( 'NONE',  ( 9.474510206698971260, -16.51473224551069308, 97.91557627198102409 ) ) ;
#105294 = CARTESIAN_POINT ( 'NONE',  ( -21.53943276465977519, -0.05219959533937600094, 68.75109039468568994 ) ) ;
#105293 = CARTESIAN_POINT ( 'NONE',  ( -16.55341960407617563, 4.379528057220093196, 88.54275706135236135 ) ) ;
#105295 = CARTESIAN_POINT ( 'NONE',  ( -19.03943276465977164, 0.05219959533909376836, 21.24890960531436335 ) ) ;
#105296 = CARTESIAN_POINT ( 'NONE',  ( -8.314922557960811034, -14.29746914071050412, 62.08224293864769550 ) ) ;
#105297 = CARTESIAN_POINT ( 'NONE',  ( -12.14591786802309592, -12.06949235617757132, 31.87390960531435979 ) ) ;
#105298 = CARTESIAN_POINT ( 'NONE',  ( -10.72451020669898014, 18.67979575497178502, 45.41557627198103830 ) ) ;
#105299 = AXIS2_PLACEMENT_3D ( 'NONE', #112732, #148080, #9571 ) ;
#105300 = CARTESIAN_POINT ( 'NONE',  ( 16.51473224551069308, 9.474510206698969483, 49.16557627198102409 ) ) ;
#105301 = CARTESIAN_POINT ( 'NONE',  ( 0.05219959533907565091, 21.53943276465977519, 54.99890960531435269 ) ) ;
#105302 = CARTESIAN_POINT ( 'NONE',  ( 13.97604488694548053, -13.89961937509957401, 45.62609039468566863 ) ) ;
#105304 = CARTESIAN_POINT ( 'NONE',  ( 14.34966873604960469, 8.224510206698951720, 44.16557627198103120 ) ) ;
#105303 = CARTESIAN_POINT ( 'NONE',  ( -16.19135201231369336, -7.376712067591814304, 40.18680854052033169 ) ) ;
#105305 = CARTESIAN_POINT ( 'NONE',  ( -5.823673210054116645, -21.52544592524344225, 27.29057627198103120 ) ) ;
#105306 = VERTEX_POINT ( 'NONE', #27716 ) ;
#105307 = ORIENTED_EDGE ( 'NONE', *, *, #20087, .F. ) ;
#105308 = CARTESIAN_POINT ( 'NONE',  ( -36.91746825000000598, 2.428612866367529932E-14, -0.6249999972688132788 ) ) ;
#105309 = CARTESIAN_POINT ( 'NONE',  ( 16.55341960407618274, -4.379528057220086978, 76.04275706135237556 ) ) ;
#105310 = EDGE_CURVE ( 'NONE', #98202, #180473, #86366, .T. ) ;
#105311 = CARTESIAN_POINT ( 'NONE',  ( 5.049401038297881783, 19.05341960407617563, 77.29275706135231871 ) ) ;
#105312 = CARTESIAN_POINT ( 'NONE',  ( -4.483927247898539470, -16.52544592524342804, 37.29057627198102409 ) ) ;
#105313 = CARTESIAN_POINT ( 'NONE',  ( 31.79999999999970939, 4.794320942884876164E-13, 42.30000000000021743 ) ) ;
#105314 = CARTESIAN_POINT ( 'NONE',  ( -16.52544592524342804, 4.483927247898546575, 31.04057627198102409 ) ) ;
#105315 = CARTESIAN_POINT ( 'NONE',  ( 5.049401038298161559, -19.05341960407611168, 57.70724293864769550 ) ) ;
#105316 = CARTESIAN_POINT ( 'NONE',  ( -19.05341960407611168, -5.049401038298163336, 71.45724293864766707 ) ) ;
#105317 = CARTESIAN_POINT ( 'NONE',  ( 16.51473224551069308, 9.474510206698969483, 39.16557627198103120 ) ) ;
#105318 = CARTESIAN_POINT ( 'NONE',  ( -5.823673210054431948, 21.52544592524334988, 52.70942372801902565 ) ) ;
#105319 = CARTESIAN_POINT ( 'NONE',  ( 16.46253265017160672, -9.564922557960803928, 53.33224293864768839 ) ) ;
#105320 = DIRECTION ( 'NONE',  ( 1.000000000000000000, 0.000000000000000000, 0.000000000000000000 ) ) ;
#105321 = CARTESIAN_POINT ( 'NONE',  ( 19.02544592524343514, -5.153800228976328945, 63.54057627198103830 ) ) ;
#105322 = CARTESIAN_POINT ( 'NONE',  ( -10.81492255796078084, -18.62759615963271287, 42.08224293864769550 ) ) ;
#105323 = CARTESIAN_POINT ( 'NONE',  ( -0.05219959533909027116, -19.03943276465977164, 42.49890960531435269 ) ) ;
#105324 = CARTESIAN_POINT ( 'NONE',  ( 21.52544592524344225, -5.823673210054117533, 43.54057627198103830 ) ) ;
#105325 = CARTESIAN_POINT ( 'NONE',  ( 12.14591786802327356, -12.06949235617739191, 90.62609039468567573 ) ) ;
#105326 = CARTESIAN_POINT ( 'NONE',  ( 0.05219959533936267826, -19.03943276465977164, 20.00109039468567218 ) ) ;
#105327 = CARTESIAN_POINT ( 'NONE',  ( 16.52544592524335698, 4.483927247898782831, 71.45942372801901854 ) ) ;
#105328 = CARTESIAN_POINT ( 'NONE',  ( 9.474510206698971260, -16.51473224551069308, 102.9155762719810241 ) ) ;
#105329 = CARTESIAN_POINT ( 'NONE',  ( 4.483927247898790824, -16.52544592524335698, 50.20942372801901854 ) ) ;
#105330 = CARTESIAN_POINT ( 'NONE',  ( 16.52544592524335698, 4.483927247898782831, 46.45942372801901854 ) ) ;
#105331 = CARTESIAN_POINT ( 'NONE',  ( -9.474510206698964154, 16.51473224551069663, 105.4155762719810383 ) ) ;
#105332 = CARTESIAN_POINT ( 'NONE',  ( -12.14591786802326823, 12.06949235617739902, 28.12609039468568284 ) ) ;
#105333 = CARTESIAN_POINT ( 'NONE',  ( -0.05219959533909027116, -19.03943276465977164, 37.49890960531436690 ) ) ;
#105334 = CARTESIAN_POINT ( 'NONE',  ( -5.823673210054431948, 21.52544592524334988, 32.70942372801900433 ) ) ;
#105335 = CARTESIAN_POINT ( 'NONE',  ( 16.46253265017146816, 9.564922557961045513, 111.6677570613523329 ) ) ;
#105336 = CARTESIAN_POINT ( 'NONE',  ( 16.55341960407618274, -4.379528057220086978, 101.0427570613523756 ) ) ;
#105337 = CARTESIAN_POINT ( 'NONE',  ( -6.674792076160553478, -4.273745901508095635, 4.009310749147813269 ) ) ;
#105338 = CARTESIAN_POINT ( 'NONE',  ( -15.80617190586768217, 15.72974639402176855, 103.1260903946856757 ) ) ;
#105339 = CARTESIAN_POINT ( 'NONE',  ( 16.46253265017146816, 9.564922557961045513, 91.66775706135234714 ) ) ;
#105340 = CARTESIAN_POINT ( 'NONE',  ( 16.53943276465976808, -0.05219959533910856209, 58.74890960531436690 ) ) ;
#105341 = CARTESIAN_POINT ( 'NONE',  ( 5.153800228976335163, 19.02544592524342804, 24.79057627198102765 ) ) ;
#105343 = CARTESIAN_POINT ( 'NONE',  ( -22.96528548301343520, 5.795830589372932273, 190.0000000000000000 ) ) ;
#105342 = CARTESIAN_POINT ( 'NONE',  ( -9.564922557961040184, 16.46253265017147172, 57.91775706135233293 ) ) ;
#105344 = CARTESIAN_POINT ( 'NONE',  ( 0.05219959533937995610, -21.53943276465977519, 55.00109039468568284 ) ) ;
#105345 = CARTESIAN_POINT ( 'NONE',  ( -8.314922557961024197, 14.29746914071037800, 22.91775706135235069 ) ) ;
#105346 = CARTESIAN_POINT ( 'NONE',  ( -17.97182807773875624, 5.499999999999873879, 63.53038844047289047 ) ) ;
#105347 = CARTESIAN_POINT ( 'NONE',  ( -9.474510206698964154, 16.51473224551069663, 105.4155762719810383 ) ) ;
#105348 = CARTESIAN_POINT ( 'NONE',  ( 15.72974639402199770, -15.80617190586745480, 68.12390960531436690 ) ) ;
#105349 = CARTESIAN_POINT ( 'NONE',  ( -8.224510206698735004, -14.34966873604973081, 19.58442372801901143 ) ) ;
#105350 = CARTESIAN_POINT ( 'NONE',  ( 13.89961937509977652, -13.97604488694527269, 108.1239096053143669 ) ) ;
#105351 = CARTESIAN_POINT ( 'NONE',  ( -18.50817386519043595, -21.48060456978424781, 139.9999999999999716 ) ) ;
#105352 = CARTESIAN_POINT ( 'NONE',  ( -5.049401038298153566, 19.05341960407611168, 30.20724293864768839 ) ) ;
#105353 = CARTESIAN_POINT ( 'NONE',  ( 21.55341960407619695, -5.719274019375665929, 96.04275706135236135 ) ) ;
#105354 = CARTESIAN_POINT ( 'NONE',  ( 19.03943276465977164, -0.05219959533909143690, 43.74890960531435979 ) ) ;
#105355 = AXIS2_PLACEMENT_3D ( 'NONE', #118362, #83002, #191197 ) ;
#105356 = CARTESIAN_POINT ( 'NONE',  ( 10.81492255796106328, -18.62759615963255655, 45.41775706135234003 ) ) ;
#105357 = CARTESIAN_POINT ( 'NONE',  ( 18.62759615963255655, 10.81492255796105972, 91.66775706135234714 ) ) ;
#105358 = CARTESIAN_POINT ( 'NONE',  ( 16.53943276465976808, 0.05219959533934440121, 106.2510903946856757 ) ) ;
#105359 = CARTESIAN_POINT ( 'NONE',  ( 5.153800228976335163, 19.02544592524342804, 79.79057627198102409 ) ) ;
#105360 = CARTESIAN_POINT ( 'NONE',  ( 5.823673210054444382, -21.52544592524334988, 45.20942372801901854 ) ) ;
#105361 = CARTESIAN_POINT ( 'NONE',  ( 5.823673210054444382, -21.52544592524334988, 45.20942372801901854 ) ) ;
#105363 = CARTESIAN_POINT ( 'NONE',  ( 19.02544592524343514, -5.153800228976328945, 98.54057627198100988 ) ) ;
#105362 = CARTESIAN_POINT ( 'NONE',  ( 19.05341960407617918, -5.049401038297876454, 66.04275706135233293 ) ) ;
#105364 = CARTESIAN_POINT ( 'NONE',  ( -16.52544592524342804, 4.483927247898546575, 106.0405762719810525 ) ) ;
#105365 = CARTESIAN_POINT ( 'NONE',  ( 18.62759615963271287, -10.81492255796078972, 98.33224293864769550 ) ) ;
#105366 = CARTESIAN_POINT ( 'NONE',  ( -14.29746914071049879, 8.314922557960819915, 60.83224293864769550 ) ) ;
#105367 = CARTESIAN_POINT ( 'NONE',  ( 13.89961937509957401, 13.97604488694547697, 26.87609039468566507 ) ) ;
#105368 = CARTESIAN_POINT ( 'NONE',  ( -0.05219959533910754901, -16.53943276465976808, 97.49890960531436690 ) ) ;
#105369 = CARTESIAN_POINT ( 'NONE',  ( 9.474510206698971260, -16.51473224551069308, 32.91557627198102409 ) ) ;
#105370 = CARTESIAN_POINT ( 'NONE',  ( 13.97604488694548053, -13.89961937509957401, 90.62609039468567573 ) ) ;
#105371 = CARTESIAN_POINT ( 'NONE',  ( -0.05219959533910754901, -16.53943276465976808, 42.49890960531435979 ) ) ;
#105372 = CARTESIAN_POINT ( 'NONE',  ( 10.81492255796106328, -18.62759615963255655, 95.41775706135234714 ) ) ;
#105373 = CARTESIAN_POINT ( 'NONE',  ( -16.51473224551069308, -9.474510206698971260, 101.6655762719810241 ) ) ;
#105374 = CARTESIAN_POINT ( 'NONE',  ( -19.03943276465977164, -0.05219959533935918106, 73.75109039468566152 ) ) ;
#105375 = CARTESIAN_POINT ( 'NONE',  ( 10.72451020669898902, -18.67979575497178502, 77.91557627198102409 ) ) ;
#105376 = CARTESIAN_POINT ( 'NONE',  ( -15.72974639402176322, -15.80617190586768395, 29.37609039468568284 ) ) ;
#105377 = CARTESIAN_POINT ( 'NONE',  ( 0.05219959533934541429, -16.53943276465976808, 35.00109039468568284 ) ) ;
#105378 = CARTESIAN_POINT ( 'NONE',  ( 12.06949235617739724, 12.14591786802326823, 96.87609039468568994 ) ) ;
#105380 = CARTESIAN_POINT ( 'NONE',  ( -10.81492255796105439, 18.62759615963255655, 37.91775706135235424 ) ) ;
#105379 = DIRECTION ( 'NONE',  ( -0.000000000000000000, 1.000000000000000000, 0.000000000000000000 ) ) ;
#105381 = CARTESIAN_POINT ( 'NONE',  ( 5.049401038298161559, -19.05341960407611168, 22.70724293864769194 ) ) ;
#105382 = CARTESIAN_POINT ( 'NONE',  ( -36.91746825000001309, 11.99521256947798342, -3.224999997268813257 ) ) ;
#105383 = CARTESIAN_POINT ( 'NONE',  ( -0.05219959533934338120, 16.53943276465976808, 47.50109039468568994 ) ) ;
#105384 = CARTESIAN_POINT ( 'NONE',  ( 16.55341960407611168, 4.379528057220329451, 78.95724293864769550 ) ) ;
#105385 = CARTESIAN_POINT ( 'NONE',  ( 10.72451020669898902, -18.67979575497178502, 72.91557627198103830 ) ) ;
#105386 = CARTESIAN_POINT ( 'NONE',  ( -0.05219959533910754901, -16.53943276465976808, 27.49890960531435269 ) ) ;
#105387 = CARTESIAN_POINT ( 'NONE',  ( 14.29746914071037800, 8.314922557961029526, 51.66775706135234714 ) ) ;
#105388 = CARTESIAN_POINT ( 'NONE',  ( -16.51473224551069308, -9.474510206698971260, 41.66557627198103120 ) ) ;
#105389 = B_SPLINE_CURVE_WITH_KNOTS ( 'NONE', 3,
 ( #122418, #16252, #2063, #186106, #138582, #185096 ),
 .UNSPECIFIED., .F., .F.,
 ( 4, 2, 4 ),
 ( 3.469446951953614189E-18, 0.0003837532665554453833, 0.0007675065331108872971 ),
 .UNSPECIFIED. ) ;
#105390 = CARTESIAN_POINT ( 'NONE',  ( 16.55341960407618274, -4.379528057220086978, 91.04275706135236135 ) ) ;
#105391 = CARTESIAN_POINT ( 'NONE',  ( 16.51473224551083163, -9.474510206698727899, 85.83442372801900433 ) ) ;
#105392 = CARTESIAN_POINT ( 'NONE',  ( -10.72451020669898014, 18.67979575497178502, 70.41557627198102409 ) ) ;
#105393 = CARTESIAN_POINT ( 'NONE',  ( -14.34966873604972548, 8.224510206698743886, 113.3344237280190328 ) ) ;
#105394 = ORIENTED_EDGE ( 'NONE', *, *, #20087, .T. ) ;
#105395 = LINE ( 'NONE', #25600, #40457 ) ;
#105396 = CARTESIAN_POINT ( 'NONE',  ( 5.719274019375991003, -21.55341960407610458, 67.70724293864769550 ) ) ;
#105397 = ORIENTED_EDGE ( 'NONE', *, *, #32795, .F. ) ;
#105398 = CARTESIAN_POINT ( 'NONE',  ( -16.53943276465976808, -0.05219959533934237506, 98.75109039468568994 ) ) ;
#105399 = ORIENTED_EDGE ( 'NONE', *, *, #6145, .F. ) ;
#105400 = CARTESIAN_POINT ( 'NONE',  ( -19.03943276465977164, 0.05219959533909376836, 111.2489096053143669 ) ) ;
#105401 = CARTESIAN_POINT ( 'NONE',  ( -19.53037848336980886, 5.499999999999896971, 74.85532783611441232 ) ) ;
#105402 = CARTESIAN_POINT ( 'NONE',  ( -21.52544592524343514, 5.823673210054127303, 71.04057627198103830 ) ) ;
#105403 = VECTOR ( 'NONE', #159418, 1000.000000000000000 ) ;
#105404 = CARTESIAN_POINT ( 'NONE',  ( -14.29746914071049879, 8.314922557960819915, 25.83224293864769194 ) ) ;
#105405 = CARTESIAN_POINT ( 'NONE',  ( 8.314922557961029526, -14.29746914071037800, 25.41775706135235779 ) ) ;
#105406 = CARTESIAN_POINT ( 'NONE',  ( -19.03943276465977164, 0.05219959533909376836, 21.24890960531436335 ) ) ;
#105407 = CARTESIAN_POINT ( 'NONE',  ( -16.53943276465976808, -0.05219959533934237506, 28.75109039468567929 ) ) ;
#105408 = AXIS2_PLACEMENT_3D ( 'NONE', #100238, #11257, #38582 ) ;
#105409 = CARTESIAN_POINT ( 'NONE',  ( 9.474510206698971260, -16.51473224551069308, 52.91557627198102409 ) ) ;
#105410 = CARTESIAN_POINT ( 'NONE',  ( -5.429308488886486681E-15, 30.30510711980690175, 145.4999999999999432 ) ) ;
#105411 = CARTESIAN_POINT ( 'NONE',  ( -0.05219959533909027116, -19.03943276465977164, 102.4989096053143669 ) ) ;
#105412 = CARTESIAN_POINT ( 'NONE',  ( 4.483927247898790824, -16.52544592524335698, 90.20942372801903275 ) ) ;
#105413 = CARTESIAN_POINT ( 'NONE',  ( 19.03943276465977164, 0.05219959533936151252, 91.25109039468566152 ) ) ;
#105414 = CARTESIAN_POINT ( 'NONE',  ( 5.153800228976615827, -19.02544592524334988, 30.20942372801900433 ) ) ;
#105415 = CARTESIAN_POINT ( 'NONE',  ( -0.05219959533907301413, -21.53943276465977519, 72.49890960531435269 ) ) ;
#105416 = EDGE_CURVE ( 'NONE', #146440, #197049, #111035, .T. ) ;
#105417 = CARTESIAN_POINT ( 'NONE',  ( 12.06949235617739724, 12.14591786802326823, 106.8760903946856899 ) ) ;
#105418 = CARTESIAN_POINT ( 'NONE',  ( 0.05219959533936267826, -19.03943276465977164, 95.00109039468567573 ) ) ;
#105419 = CARTESIAN_POINT ( 'NONE',  ( -5.049401038298153566, 19.05341960407611168, 55.20724293864769550 ) ) ;
#105420 = CARTESIAN_POINT ( 'NONE',  ( -13.97604488694527625, -13.89961937509977652, 86.87390960531436690 ) ) ;
#105421 = CARTESIAN_POINT ( 'NONE',  ( -5.823673210054431948, 21.52544592524334988, 57.70942372801901143 ) ) ;
#105422 = CARTESIAN_POINT ( 'NONE',  ( -13.89961937509977652, 13.97604488694528158, 60.62390960531436690 ) ) ;
#105423 = CARTESIAN_POINT ( 'NONE',  ( -12.06949235617756955, 12.14591786802309770, 80.62390960531438111 ) ) ;
#105424 = CARTESIAN_POINT ( 'NONE',  ( 13.70000000000001528, 0.000000000000000000, -60.44446360152740283 ) ) ;
#105425 = CARTESIAN_POINT ( 'NONE',  ( 16.52544592524342804, -4.483927247898539470, 78.54057627198103830 ) ) ;
#105426 = CARTESIAN_POINT ( 'NONE',  ( -10.81492255796078084, -18.62759615963271287, 77.08224293864769550 ) ) ;
#105427 = CARTESIAN_POINT ( 'NONE',  ( -19.05341960407617563, 5.049401038297882671, 88.54275706135230450 ) ) ;
#105428 = DIRECTION ( 'NONE',  ( -1.000000000000000000, 0.000000000000000000, 0.000000000000000000 ) ) ;
#105429 = CARTESIAN_POINT ( 'NONE',  ( 19.05341960407617918, -5.049401038297876454, 41.04275706135233293 ) ) ;
#105430 = CARTESIAN_POINT ( 'NONE',  ( 31.64627301717022689, -2.653341670344218084, 102.0192792579183418 ) ) ;
#105432 = CARTESIAN_POINT ( 'NONE',  ( 16.51473224551069308, 9.474510206698969483, 89.16557627198103830 ) ) ;
#105431 = CARTESIAN_POINT ( 'NONE',  ( 19.02544592524343514, -5.153800228976328945, 83.54057627198100988 ) ) ;
#105433 = CARTESIAN_POINT ( 'NONE',  ( -8.314922557961024197, 14.29746914071037800, 62.91775706135236135 ) ) ;
#105434 = CARTESIAN_POINT ( 'NONE',  ( -23.14225647005877917, 5.657937718899317403, 172.1775255543086018 ) ) ;
#105435 = CARTESIAN_POINT ( 'NONE',  ( -13.89961937509957401, -13.97604488694547875, 39.37609039468566152 ) ) ;
#105436 = CARTESIAN_POINT ( 'NONE',  ( 15.31758167559927841, -14.84543115662826374, -58.83804107897447011 ) ) ;
#105437 = CARTESIAN_POINT ( 'NONE',  ( 9.564922557960805705, 16.46253265017160317, 114.5822429386476955 ) ) ;
#105438 = CARTESIAN_POINT ( 'NONE',  ( 16.52544592524335698, 4.483927247898782831, 101.4594237280190185 ) ) ;
#105439 = CARTESIAN_POINT ( 'NONE',  ( -17.49999999999999645, -5.499999999999992895, 89.20309617465829888 ) ) ;
#105440 = CARTESIAN_POINT ( 'NONE',  ( 0.05219959533934541429, -16.53943276465976808, 75.00109039468568994 ) ) ;
#105441 = CARTESIAN_POINT ( 'NONE',  ( 17.49999999999999645, 5.500000000000010658, 53.78230962303567964 ) ) ;
#105442 =( BOUNDED_CURVE ( )  B_SPLINE_CURVE ( 2, ( #138979, #32809, #94460, #45985, #125802, #108644, #33796, #169317, #187504, #155152, #18637 ),
 .UNSPECIFIED., .F., .F. ) 
 B_SPLINE_CURVE_WITH_KNOTS ( ( 3, 2, 2, 2, 2, 3 ),
 ( 0.9000000000000000222, 0.9200000000000000400, 0.9399999999999999467, 0.9599999999999999645, 0.9799999999999999822, 1.000000000000000000 ),
 .UNSPECIFIED. ) 
 CURVE ( )  GEOMETRIC_REPRESENTATION_ITEM ( )  RATIONAL_B_SPLINE_CURVE ( ( 1.000000000000000000, 0.9510565162951535312, 1.000000000000000000, 0.9510565162951535312, 1.000000000000000000, 0.9510565162951535312, 1.000000000000000000, 0.9510565162951535312, 1.000000000000000000, 0.9510565162951535312, 1.000000000000000000 ) ) 
 REPRESENTATION_ITEM ( '' )  );
#105443 = CARTESIAN_POINT ( 'NONE',  ( -8.314922557961024197, 14.29746914071037800, 57.91775706135234714 ) ) ;
#105444 = DIRECTION ( 'NONE',  ( -0.000000000000000000, -0.000000000000000000, 1.000000000000000000 ) ) ;
#105445 = CARTESIAN_POINT ( 'NONE',  ( 21.55341960407619695, -5.719274019375665929, 71.04275706135234714 ) ) ;
#105446 = CARTESIAN_POINT ( 'NONE',  ( -9.564922557961040184, 16.46253265017147172, 72.91775706135233293 ) ) ;
#105447 = CARTESIAN_POINT ( 'NONE',  ( -5.153800228976607833, 19.02544592524334988, 27.70942372801899722 ) ) ;
#105448 = CARTESIAN_POINT ( 'NONE',  ( -5.153800228976328057, -19.02544592524343514, 57.29057627198103120 ) ) ;
#105449 = CARTESIAN_POINT ( 'NONE',  ( 19.05341960407611168, 5.049401038298154454, 48.95724293864768129 ) ) ;
#105450 = CARTESIAN_POINT ( 'NONE',  ( 16.18474525874326631, -7.379450460607309026, 22.26924095202841514 ) ) ;
#105451 = CARTESIAN_POINT ( 'NONE',  ( -5.823673210054116645, -21.52544592524344225, 72.29057627198102409 ) ) ;
#105452 = CARTESIAN_POINT ( 'NONE',  ( -0.05219959533907301413, -21.53943276465977519, 37.49890960531436690 ) ) ;
#105453 = CARTESIAN_POINT ( 'NONE',  ( -19.05341960407611168, -5.049401038298163336, 21.45724293864768839 ) ) ;
#105454 = CARTESIAN_POINT ( 'NONE',  ( -12.14591786802326823, 12.06949235617739902, 48.12609039468568284 ) ) ;
#105455 = EDGE_LOOP ( 'NONE', ( #163204, #52043, #68684, #167702 ) ) ;
#105456 = CARTESIAN_POINT ( 'NONE',  ( -5.823673210054431948, 21.52544592524334988, 27.70942372801901854 ) ) ;
#105458 = CARTESIAN_POINT ( 'NONE',  ( 30.74264578624800137, -22.33583958711395212, -7.200000000000001066 ) ) ;
#105457 = CARTESIAN_POINT ( 'NONE',  ( -12.14591786802309592, -12.06949235617757132, 46.87390960531435979 ) ) ;
#105459 = CARTESIAN_POINT ( 'NONE',  ( 13.97604488694548053, -13.89961937509957401, 100.6260903946856615 ) ) ;
#105460 = CARTESIAN_POINT ( 'NONE',  ( -5.153800228976607833, 19.02544592524334988, 37.70942372801899722 ) ) ;
#105461 = CARTESIAN_POINT ( 'NONE',  ( -0.05219959533910754901, -16.53943276465976808, 42.49890960531435979 ) ) ;
#105462 = CARTESIAN_POINT ( 'NONE',  ( -10.72451020669898014, 18.67979575497178502, 115.4155762719810241 ) ) ;
#105464 = CARTESIAN_POINT ( 'NONE',  ( -0.05219959533907301413, -21.53943276465977519, 72.49890960531435269 ) ) ;
#105463 = DIRECTION ( 'NONE',  ( -0.5000000000000004441, -0.4999999999999987232, 0.7071067811865482389 ) ) ;
#105465 = CARTESIAN_POINT ( 'NONE',  ( 16.51473224551069308, 9.474510206698969483, 89.16557627198103830 ) ) ;
#105466 = CARTESIAN_POINT ( 'NONE',  ( 12.14591786802309770, 12.06949235617756955, 64.37390960531435269 ) ) ;
#105467 = CARTESIAN_POINT ( 'NONE',  ( -9.474510206698964154, 16.51473224551069663, 110.4155762719810383 ) ) ;
#105468 = CARTESIAN_POINT ( 'NONE',  ( -17.58332526062529411, 7.635886036038502134, 80.92334959558466778 ) ) ;
#105469 = CARTESIAN_POINT ( 'NONE',  ( -5.049401038297874678, -19.05341960407617918, 49.79275706135231871 ) ) ;
#105470 = CARTESIAN_POINT ( 'NONE',  ( -21.53943276465977519, 0.05219959533907696930, 106.2489096053143811 ) ) ;
#105471 = CARTESIAN_POINT ( 'NONE',  ( -13.97604488694527625, -13.89961937509977652, 46.87390960531435979 ) ) ;
#105472 = CARTESIAN_POINT ( 'NONE',  ( -4.483927247898539470, -16.52544592524342804, 112.2905762719810241 ) ) ;
#105473 = CARTESIAN_POINT ( 'NONE',  ( -21.55341960407619339, 5.719274019375674811, 48.54275706135234714 ) ) ;
#105474 = CARTESIAN_POINT ( 'NONE',  ( 17.14385361876520264, 23.59649016807275856, 146.1750000027311387 ) ) ;
#105475 = CARTESIAN_POINT ( 'NONE',  ( 16.55341960407611168, 4.379528057220329451, 28.95724293864769905 ) ) ;
#105476 = CARTESIAN_POINT ( 'NONE',  ( 5.153800228976335163, 19.02544592524342804, 44.79057627198103830 ) ) ;
#105477 = CARTESIAN_POINT ( 'NONE',  ( 5.153800228976335163, 19.02544592524342804, 94.79057627198103830 ) ) ;
#105478 = CARTESIAN_POINT ( 'NONE',  ( 18.67979575497178502, 10.72451020669898547, 79.16557627198103830 ) ) ;
#105479 = CARTESIAN_POINT ( 'NONE',  ( 22.44159573604009594, -16.30477369853687364, 145.6750000027311671 ) ) ;
#105480 = CARTESIAN_POINT ( 'NONE',  ( -9.564922557960796823, -16.46253265017161027, 47.08224293864769550 ) ) ;
#105481 = ORIENTED_EDGE ( 'NONE', *, *, #105202, .T. ) ;
#105482 = CARTESIAN_POINT ( 'NONE',  ( 15.72974639402199770, -15.80617190586745480, 58.12390960531435979 ) ) ;
#105483 = CARTESIAN_POINT ( 'NONE',  ( -18.62759615963255300, -10.81492255796106328, 84.16775706135234714 ) ) ;
#105486 = CARTESIAN_POINT ( 'NONE',  ( -16.52544592524342804, 4.483927247898546575, 66.04057627198103830 ) ) ;
#105485 = CARTESIAN_POINT ( 'NONE',  ( -0.05219959533934338120, 16.53943276465976808, 77.50109039468567573 ) ) ;
#105484 = DIRECTION ( 'NONE',  ( -0.000000000000000000, -0.000000000000000000, -1.000000000000000000 ) ) ;
#105487 = CARTESIAN_POINT ( 'NONE',  ( 0.05219959533909260263, 19.03943276465977164, 69.99890960531435269 ) ) ;
#105488 = EDGE_LOOP ( 'NONE', ( #11182, #59994, #56685, #20805 ) ) ;
#105489 = CARTESIAN_POINT ( 'NONE',  ( 5.049401038297881783, 19.05341960407617563, 22.29275706135233648 ) ) ;
#105490 = CARTESIAN_POINT ( 'NONE',  ( 16.55341960407618274, -4.379528057220086978, 91.04275706135236135 ) ) ;
#105491 = CARTESIAN_POINT ( 'NONE',  ( 5.823673210054444382, -21.52544592524334988, 110.2094237280190185 ) ) ;
#105492 = CARTESIAN_POINT ( 'NONE',  ( 19.03943276465977164, -0.05219959533909143690, 73.74890960531435269 ) ) ;
#105493 = CARTESIAN_POINT ( 'NONE',  ( 5.719274019375991003, -21.55341960407610458, 47.70724293864770260 ) ) ;
#105494 = CARTESIAN_POINT ( 'NONE',  ( 12.06949235617739724, 12.14591786802326823, 26.87609039468567218 ) ) ;
#105495 = CARTESIAN_POINT ( 'NONE',  ( -5.719274019375665041, -21.55341960407619695, 94.79275706135234714 ) ) ;
#105496 = CARTESIAN_POINT ( 'NONE',  ( -16.53943276465976808, -0.05219959533934237506, 68.75109039468568994 ) ) ;
#105497 = CARTESIAN_POINT ( 'NONE',  ( 5.823673210054125526, 21.52544592524343514, 109.7905762719810383 ) ) ;
#105498 = CARTESIAN_POINT ( 'NONE',  ( 16.53943276465976808, 0.05219959533934440121, 21.25109039468567218 ) ) ;
#105499 = CARTESIAN_POINT ( 'NONE',  ( -13.89961937509977652, 13.97604488694528158, 85.62390960531433848 ) ) ;
#105500 = CARTESIAN_POINT ( 'NONE',  ( -0.05219959533934338120, 16.53943276465976808, 32.50109039468568284 ) ) ;
#105501 = CARTESIAN_POINT ( 'NONE',  ( -5.049401038298153566, 19.05341960407611168, 50.20724293864770260 ) ) ;
#105502 = VECTOR ( 'NONE', #19707, 1000.000000000000000 ) ;
#105503 = CARTESIAN_POINT ( 'NONE',  ( -16.53943276465976808, -0.05219959533934237506, 33.75109039468568284 ) ) ;
#105504 = CARTESIAN_POINT ( 'NONE',  ( 8.224510206698953496, -14.34966873604960469, 72.91557627198103830 ) ) ;
#105505 = CARTESIAN_POINT ( 'NONE',  ( -12.06949235617739369, -12.14591786802326823, 84.37609039468570415 ) ) ;
#105507 = CARTESIAN_POINT ( 'NONE',  ( 9.474510206698971260, -16.51473224551069308, 62.91557627198102409 ) ) ;
#105506 = CARTESIAN_POINT ( 'NONE',  ( -15.80617190586768217, 15.72974639402176855, 38.12609039468567573 ) ) ;
#105509 = ADVANCED_FACE ( 'NONE', ( #58037 ), #101524, .T. ) ;
#105508 = CARTESIAN_POINT ( 'NONE',  ( 5.049401038298161559, -19.05341960407611168, 87.70724293864769550 ) ) ;
#105510 = CARTESIAN_POINT ( 'NONE',  ( -8.224510206698735004, -14.34966873604973081, 84.58442372801903275 ) ) ;
#105512 = VERTEX_POINT ( 'NONE', #87368 ) ;
#105511 = CARTESIAN_POINT ( 'NONE',  ( -24.17640770809926565, -7.553848413216235791, 169.9412368235645943 ) ) ;
#105513 = EDGE_LOOP ( 'NONE', ( #54205, #126304, #46297, #38658, #160920, #120854 ) ) ;
#105514 = CARTESIAN_POINT ( 'NONE',  ( -16.46253265017146816, -9.564922557961047289, 34.16775706135233293 ) ) ;
#105515 = CARTESIAN_POINT ( 'NONE',  ( -5.049401038298153566, 19.05341960407611168, 100.2072429386476955 ) ) ;
#105516 = CARTESIAN_POINT ( 'NONE',  ( -13.89961937509977652, 13.97604488694528158, 50.62390960531435979 ) ) ;
#105517 = CARTESIAN_POINT ( 'NONE',  ( -36.91746825000000598, 2.428612866367529932E-14, -10.62499999726881406 ) ) ;
#105518 = CARTESIAN_POINT ( 'NONE',  ( 12.06949235617739724, 12.14591786802326823, 36.87609039468568994 ) ) ;
#105520 = CARTESIAN_POINT ( 'NONE',  ( 16.53943276465976808, 0.05219959533934440121, 56.25109039468568284 ) ) ;
#105519 = CARTESIAN_POINT ( 'NONE',  ( -16.51473224551082808, 9.474510206698731452, 58.33442372801900433 ) ) ;
#105521 = CARTESIAN_POINT ( 'NONE',  ( -19.03943276465977164, 0.05219959533909376836, 111.2489096053143669 ) ) ;
#105522 = CARTESIAN_POINT ( 'NONE',  ( 13.89961937509977652, -13.97604488694527269, 83.12390960531436690 ) ) ;
#105523 = CARTESIAN_POINT ( 'NONE',  ( -21.55341960407610458, -5.719274019375992779, 101.4572429386476955 ) ) ;
#105524 = CARTESIAN_POINT ( 'NONE',  ( 5.153800228976615827, -19.02544592524334988, 60.20942372801899012 ) ) ;
#105526 = CARTESIAN_POINT ( 'NONE',  ( -11.30153831258471975, -180.0000000000000000, -4.999999999999999112 ) ) ;
#105525 = CARTESIAN_POINT ( 'NONE',  ( 19.03943276465977164, -0.05219959533909143690, 93.74890960531435269 ) ) ;
#105527 = CARTESIAN_POINT ( 'NONE',  ( -9.564922557960796823, -16.46253265017161027, 77.08224293864769550 ) ) ;
#105529 = CARTESIAN_POINT ( 'NONE',  ( 19.02544592524343514, -5.153800228976328945, 23.54057627198102054 ) ) ;
#105528 = CARTESIAN_POINT ( 'NONE',  ( 12.06949235617757843, -12.14591786802309237, 38.12390960531436690 ) ) ;
#105530 = CARTESIAN_POINT ( 'NONE',  ( 19.03943276465977164, 0.05219959533936151252, 41.25109039468566152 ) ) ;
#105531 = CARTESIAN_POINT ( 'NONE',  ( 16.52544592524342804, -4.483927247898539470, 68.54057627198103830 ) ) ;
#105532 = CARTESIAN_POINT ( 'NONE',  ( -18.62759615963255300, -10.81492255796106328, 104.1677570613523471 ) ) ;
#105533 = CARTESIAN_POINT ( 'NONE',  ( -19.05341960407611168, -5.049401038298163336, 41.45724293864769550 ) ) ;
#105535 = CARTESIAN_POINT ( 'NONE',  ( -15.72974639402176322, -15.80617190586768395, 104.3760903946856899 ) ) ;
#105534 = CARTESIAN_POINT ( 'NONE',  ( 16.55341960407611168, 4.379528057220329451, 33.95724293864769550 ) ) ;
#105536 = CARTESIAN_POINT ( 'NONE',  ( -9.474510206698964154, 16.51473224551069663, 90.41557627198103830 ) ) ;
#105537 = CARTESIAN_POINT ( 'NONE',  ( 19.05341960407611168, 5.049401038298154454, 88.95724293864769550 ) ) ;
#105538 = CARTESIAN_POINT ( 'NONE',  ( -9.474510206698964154, 16.51473224551069663, 30.41557627198102054 ) ) ;
#105539 = CARTESIAN_POINT ( 'NONE',  ( 14.34966873604960469, 8.224510206698951720, 109.1655762719810383 ) ) ;
#105540 = CARTESIAN_POINT ( 'NONE',  ( 8.314922557960818139, 14.29746914071049879, 69.58224293864769550 ) ) ;
#105541 = CARTESIAN_POINT ( 'NONE',  ( 5.823673210054125526, 21.52544592524343514, 79.79057627198102409 ) ) ;
#105542 = CARTESIAN_POINT ( 'NONE',  ( -19.03943276465977164, 0.05219959533909376836, 86.24890960531436690 ) ) ;
#105543 = CARTESIAN_POINT ( 'NONE',  ( -5.823673210054116645, -21.52544592524344225, 102.2905762719810383 ) ) ;
#105544 = CARTESIAN_POINT ( 'NONE',  ( -0.05219959533909027116, -19.03943276465977164, 87.49890960531436690 ) ) ;
#105546 = CARTESIAN_POINT ( 'NONE',  ( -4.379528057220328563, 16.55341960407611168, 95.20724293864769550 ) ) ;
#105545 = CARTESIAN_POINT ( 'NONE',  ( 0.05219959533936267826, -19.03943276465977164, 65.00109039468567573 ) ) ;
#105548 = CARTESIAN_POINT ( 'NONE',  ( 9.474510206698971260, -16.51473224551069308, 72.91557627198102409 ) ) ;
#105547 = CIRCLE ( 'NONE', #18382, 2.649999999999999467 ) ;
#105549 = CARTESIAN_POINT ( 'NONE',  ( -21.52544592524343514, 5.823673210054127303, 61.04057627198103120 ) ) ;
#105550 = DIRECTION ( 'NONE',  ( 0.000000000000000000, 1.000000000000000000, -1.471414886128461669E-15 ) ) ;
#105551 = CARTESIAN_POINT ( 'NONE',  ( -8.224510206698735004, -14.34966873604973081, 109.5844237280190328 ) ) ;
#105552 = CARTESIAN_POINT ( 'NONE',  ( -12.06949235617739369, -12.14591786802326823, 24.37609039468567573 ) ) ;
#105553 = CARTESIAN_POINT ( 'NONE',  ( 16.52544592524342804, -4.483927247898539470, 93.54057627198103830 ) ) ;
#105554 = CARTESIAN_POINT ( 'NONE',  ( -17.40861289039001392, -6.110651285853318626, 96.37232470827430575 ) ) ;
#105555 = CARTESIAN_POINT ( 'NONE',  ( -16.51473224551069308, -9.474510206698971260, 86.66557627198102409 ) ) ;
#105556 = CARTESIAN_POINT ( 'NONE',  ( -13.89961937509977652, 13.97604488694528158, 45.62390960531433848 ) ) ;
#105557 = CARTESIAN_POINT ( 'NONE',  ( 4.483927247898545687, 16.52544592524342804, 79.79057627198102409 ) ) ;
#105558 = CARTESIAN_POINT ( 'NONE',  ( -13.97604488694527625, -13.89961937509977652, 111.8739096053143243 ) ) ;
#105559 = CARTESIAN_POINT ( 'NONE',  ( -19.03943276465977164, -0.05219959533935918106, 103.7510903946856757 ) ) ;
#105560 = CARTESIAN_POINT ( 'NONE',  ( -10.72451020669870658, -18.67979575497194134, 64.58442372801900433 ) ) ;
#105561 = CARTESIAN_POINT ( 'NONE',  ( 16.46253265017160672, -9.564922557960803928, 93.33224293864769550 ) ) ;
#105562 = CARTESIAN_POINT ( 'NONE',  ( -0.05219959533907301413, -21.53943276465977519, 82.49890960531436690 ) ) ;
#105563 = CARTESIAN_POINT ( 'NONE',  ( 16.55341960407618274, -4.379528057220086978, 76.04275706135237556 ) ) ;
#105564 = CARTESIAN_POINT ( 'NONE',  ( -19.05341960407611168, -5.049401038298163336, 21.45724293864768839 ) ) ;
#105565 = CARTESIAN_POINT ( 'NONE',  ( -19.05341960407611168, -5.049401038298163336, 76.45724293864769550 ) ) ;
#105566 = CARTESIAN_POINT ( 'NONE',  ( -0.05219959533907301413, -21.53943276465977519, 77.49890960531433848 ) ) ;
#105567 = CARTESIAN_POINT ( 'NONE',  ( 5.153800228976615827, -19.02544592524334988, 110.2094237280189901 ) ) ;
#105569 = CARTESIAN_POINT ( 'NONE',  ( -21.52544592524334988, -5.823673210054445271, 53.95942372801900433 ) ) ;
#105568 = CARTESIAN_POINT ( 'NONE',  ( 0.05219959533910956823, 16.53943276465976808, 44.99890960531435979 ) ) ;
#105571 = CARTESIAN_POINT ( 'NONE',  ( 15.80617190586746368, 15.72974639402197994, 29.37390960531435269 ) ) ;
#105570 = CARTESIAN_POINT ( 'NONE',  ( -4.483927247898782831, 16.52544592524335698, 87.70942372801901854 ) ) ;
#105572 = CARTESIAN_POINT ( 'NONE',  ( -16.51473224551069308, -9.474510206698971260, 101.6655762719810241 ) ) ;
#105573 = CARTESIAN_POINT ( 'NONE',  ( -17.12812012977028431, 6.668231424565929544, 78.64051240676859322 ) ) ;
#105574 = CARTESIAN_POINT ( 'NONE',  ( -14.34966873604972548, 8.224510206698743886, 113.3344237280190328 ) ) ;
#105575 = CARTESIAN_POINT ( 'NONE',  ( -16.52544592524335698, -4.483927247898792601, 48.95942372801902565 ) ) ;
#105576 = CARTESIAN_POINT ( 'NONE',  ( -16.51473224551069308, -9.474510206698971260, 61.66557627198103120 ) ) ;
#105577 = CARTESIAN_POINT ( 'NONE',  ( 13.89961937509977652, -13.97604488694527269, 68.12390960531436690 ) ) ;
#105578 = CARTESIAN_POINT ( 'NONE',  ( 14.34966873604972726, -8.224510206698740333, 70.83442372801901854 ) ) ;
#105579 = CARTESIAN_POINT ( 'NONE',  ( 12.14591786802309770, 12.06949235617756955, 49.37390960531436690 ) ) ;
#105580 = CARTESIAN_POINT ( 'NONE',  ( 19.05341960407611168, 5.049401038298154454, 58.95724293864768129 ) ) ;
#105581 = CARTESIAN_POINT ( 'NONE',  ( -16.46253265017160317, 9.564922557960807481, 45.83224293864769550 ) ) ;
#105582 = CARTESIAN_POINT ( 'NONE',  ( 8.224510206698742110, 14.34966873604972548, 42.08442372801901854 ) ) ;
#105583 = CARTESIAN_POINT ( 'NONE',  ( 0.05219959533936267826, -19.03943276465977164, 90.00109039468567573 ) ) ;
#105584 = CARTESIAN_POINT ( 'NONE',  ( 12.14591786802309770, 12.06949235617756955, 99.37390960531436690 ) ) ;
#105585 = CARTESIAN_POINT ( 'NONE',  ( 16.51473224551069308, 9.474510206698969483, 59.16557627198102409 ) ) ;
#105587 = CARTESIAN_POINT ( 'NONE',  ( 38.00000000000000000, 12.34694845685046616, -6.899999999999999467 ) ) ;
#105586 = CARTESIAN_POINT ( 'NONE',  ( -9.474510206698720793, -16.51473224551083518, 99.58442372801900433 ) ) ;
#105588 = CARTESIAN_POINT ( 'NONE',  ( 21.55341960407619695, -5.719274019375665929, 91.04275706135236135 ) ) ;
#105589 = CARTESIAN_POINT ( 'NONE',  ( -8.224510206698735004, -14.34966873604973081, 64.58442372801900433 ) ) ;
#105590 = DIRECTION ( 'NONE',  ( 0.000000000000000000, 0.000000000000000000, 1.000000000000000000 ) ) ;
#105591 = CARTESIAN_POINT ( 'NONE',  ( -5.719274019375978568, 21.55341960407610458, 60.20724293864768839 ) ) ;
#105592 = CARTESIAN_POINT ( 'NONE',  ( -12.06949235617739369, -12.14591786802326823, 54.37609039468568994 ) ) ;
#105593 = CARTESIAN_POINT ( 'NONE',  ( 0.05219959533909260263, 19.03943276465977164, 34.99890960531435979 ) ) ;
#105594 = CARTESIAN_POINT ( 'NONE',  ( 19.02544592524334988, 5.153800228976608722, 36.45942372801900433 ) ) ;
#105595 = CARTESIAN_POINT ( 'NONE',  ( 16.46253265017160672, -9.564922557960803928, 93.33224293864769550 ) ) ;
#105596 = CARTESIAN_POINT ( 'NONE',  ( 8.224510206698953496, -14.34966873604960469, 112.9155762719810383 ) ) ;
#105597 = CARTESIAN_POINT ( 'NONE',  ( -13.97604488694527625, -13.89961937509977652, 66.87390960531436690 ) ) ;
#105598 = CARTESIAN_POINT ( 'NONE',  ( 12.24802307403557577, -10.74802307403608737, -59.32879157176802920 ) ) ;
#105599 = CARTESIAN_POINT ( 'NONE',  ( -0.05219959533937732626, 21.53943276465977519, 82.50109039468568994 ) ) ;
#105600 = CARTESIAN_POINT ( 'NONE',  ( -9.564922557960796823, -16.46253265017161027, 92.08224293864769550 ) ) ;
#105601 = CARTESIAN_POINT ( 'NONE',  ( 16.51473224551083163, -9.474510206698727899, 30.83442372801900433 ) ) ;
#105602 = CARTESIAN_POINT ( 'NONE',  ( -9.474510206698720793, -16.51473224551083518, 29.58442372801900433 ) ) ;
#105603 = CARTESIAN_POINT ( 'NONE',  ( -14.29746914071049879, 8.314922557960819915, 50.83224293864770971 ) ) ;
#105604 = CARTESIAN_POINT ( 'NONE',  ( -9.474510206698964154, 16.51473224551069663, 55.41557627198103120 ) ) ;
#105605 = CARTESIAN_POINT ( 'NONE',  ( -5.719274019375978568, 21.55341960407610458, 30.20724293864769550 ) ) ;
#105606 = CARTESIAN_POINT ( 'NONE',  ( 15.80617190586769283, -15.72974639402175789, 80.62609039468567573 ) ) ;
#105607 = CARTESIAN_POINT ( 'NONE',  ( -13.89961937509977652, 13.97604488694528158, 70.62390960531432427 ) ) ;
#105608 = CARTESIAN_POINT ( 'NONE',  ( 21.53943276465977519, 0.05219959533937863772, 81.25109039468568994 ) ) ;
#105609 = CARTESIAN_POINT ( 'NONE',  ( -10.81492255796078084, -18.62759615963271287, 32.08224293864769550 ) ) ;
#105610 = CARTESIAN_POINT ( 'NONE',  ( -19.02544592524342804, 5.153800228976336051, 66.04057627198103830 ) ) ;
#105611 = CARTESIAN_POINT ( 'NONE',  ( -21.55341960407619339, 5.719274019375674811, 38.54275706135234714 ) ) ;
#105612 = CARTESIAN_POINT ( 'NONE',  ( 5.153800228976615827, -19.02544592524334988, 65.20942372801900433 ) ) ;
#105613 = CARTESIAN_POINT ( 'NONE',  ( 19.05341960407611168, 5.049401038298154454, 38.95724293864767418 ) ) ;
#105614 = CARTESIAN_POINT ( 'NONE',  ( 9.564922557960805705, 16.46253265017160317, 84.58224293864769550 ) ) ;
#105615 = CARTESIAN_POINT ( 'NONE',  ( -16.55341960407617563, 4.379528057220093196, 23.54275706135235424 ) ) ;
#105616 = CARTESIAN_POINT ( 'NONE',  ( 8.224510206698953496, -14.34966873604960469, 82.91557627198103830 ) ) ;
#105617 = CARTESIAN_POINT ( 'NONE',  ( 19.02544592524343514, -5.153800228976328945, 63.54057627198103830 ) ) ;
#105618 = CARTESIAN_POINT ( 'NONE',  ( -18.62759615963270932, 10.81492255796079327, 55.83224293864770260 ) ) ;
#105619 = CARTESIAN_POINT ( 'NONE',  ( -14.29746914071037622, -8.314922557961029526, 24.16775706135235424 ) ) ;
#105620 = CARTESIAN_POINT ( 'NONE',  ( -21.52544592524334988, -5.823673210054445271, 23.95942372801901143 ) ) ;
#105621 = CARTESIAN_POINT ( 'NONE',  ( 21.55341960407619695, -5.719274019375665929, 71.04275706135234714 ) ) ;
#105622 = CARTESIAN_POINT ( 'NONE',  ( -14.29746914071037622, -8.314922557961029526, 74.16775706135231871 ) ) ;
#105623 = CARTESIAN_POINT ( 'NONE',  ( 4.483927247898790824, -16.52544592524335698, 70.20942372801904696 ) ) ;
#105624 = CARTESIAN_POINT ( 'NONE',  ( -16.51473224551069308, -9.474510206698971260, 56.66557627198103120 ) ) ;
#105625 = CARTESIAN_POINT ( 'NONE',  ( -16.53943276465976808, -0.05219959533934237506, 93.75109039468567573 ) ) ;
#105626 = CARTESIAN_POINT ( 'NONE',  ( -19.02544592524334988, -5.153800228976617603, 43.95942372801899012 ) ) ;
#105627 = CARTESIAN_POINT ( 'NONE',  ( -21.52544592524334988, -5.823673210054445271, 23.95942372801901143 ) ) ;
#105628 = CARTESIAN_POINT ( 'NONE',  ( -16.52544592524342804, 4.483927247898546575, 61.04057627198103120 ) ) ;
#105629 = CARTESIAN_POINT ( 'NONE',  ( -19.02544592524342804, 5.153800228976336051, 91.04057627198100988 ) ) ;
#105630 = CARTESIAN_POINT ( 'NONE',  ( -16.53943276465976808, -0.05219959533934237506, 93.75109039468567573 ) ) ;
#105631 = CARTESIAN_POINT ( 'NONE',  ( 21.55341960407619695, -5.719274019375665929, 56.04275706135235424 ) ) ;
#105632 = CARTESIAN_POINT ( 'NONE',  ( -8.224510206698735004, -14.34966873604973081, 34.58442372801900433 ) ) ;
#105633 = CARTESIAN_POINT ( 'NONE',  ( -21.53943276465977519, -0.05219959533937600094, 23.75109039468567929 ) ) ;
#105634 = CARTESIAN_POINT ( 'NONE',  ( 8.314922557960818139, 14.29746914071049879, 64.58224293864769550 ) ) ;
#105635 = ORIENTED_EDGE ( 'NONE', *, *, #59575, .T. ) ;
#105636 = CARTESIAN_POINT ( 'NONE',  ( -10.72451020669898014, 18.67979575497178502, 100.4155762719810241 ) ) ;
#105637 = CARTESIAN_POINT ( 'NONE',  ( -16.52544592524342804, 4.483927247898546575, 36.04057627198102409 ) ) ;
#105638 = VERTEX_POINT ( 'NONE', #55034 ) ;
#105639 = CARTESIAN_POINT ( 'NONE',  ( 34.77757469352545172, 0.9858555240219483151, 52.45108825929359142 ) ) ;
#105640 = CARTESIAN_POINT ( 'NONE',  ( 15.80617190586746368, 15.72974639402197994, 29.37390960531435269 ) ) ;
#105641 = CARTESIAN_POINT ( 'NONE',  ( 18.62759615963255655, 10.81492255796105972, 31.66775706135234358 ) ) ;
#105642 = CARTESIAN_POINT ( 'NONE',  ( -0.05219959533910754901, -16.53943276465976808, 62.49890960531436690 ) ) ;
#105643 = CARTESIAN_POINT ( 'NONE',  ( -19.05341960407611168, -5.049401038298163336, 76.45724293864769550 ) ) ;
#105645 = CARTESIAN_POINT ( 'NONE',  ( -5.153800228976607833, 19.02544592524334988, 67.70942372801900433 ) ) ;
#105644 = CARTESIAN_POINT ( 'NONE',  ( -19.03943276465977164, 0.05219959533909376836, 31.24890960531435979 ) ) ;
#105646 = CARTESIAN_POINT ( 'NONE',  ( 15.80617190586746368, 15.72974639402197994, 49.37390960531436690 ) ) ;
#105647 = CARTESIAN_POINT ( 'NONE',  ( -24.50241233882722369, -28.74340065771546904, -20.80149134688043588 ) ) ;
#105648 = CARTESIAN_POINT ( 'NONE',  ( 19.02544592524343514, -5.153800228976328945, 58.54057627198102409 ) ) ;
#105649 = CARTESIAN_POINT ( 'NONE',  ( 8.314922557961029526, -14.29746914071037800, 30.41775706135234358 ) ) ;
#105650 = CARTESIAN_POINT ( 'NONE',  ( -18.62759615963270932, 10.81492255796079327, 115.8322429386477097 ) ) ;
#105651 = EDGE_CURVE ( 'NONE', #4246, #9508, #125291, .T. ) ;
#105652 = CARTESIAN_POINT ( 'NONE',  ( 14.34966873604960469, 8.224510206698951720, 54.16557627198103120 ) ) ;
#105653 = EDGE_LOOP ( 'NONE', ( #110649, #141516, #70461, #162338 ) ) ;
#105654 = CARTESIAN_POINT ( 'NONE',  ( 16.51473224551069308, 9.474510206698969483, 94.16557627198103830 ) ) ;
#105655 = CARTESIAN_POINT ( 'NONE',  ( 18.62759615963271287, -10.81492255796078972, 68.33224293864769550 ) ) ;
#105657 = CARTESIAN_POINT ( 'NONE',  ( 0.05219959533934541429, -16.53943276465976808, 40.00109039468567573 ) ) ;
#105656 = CARTESIAN_POINT ( 'NONE',  ( -0.05219959533907301413, -21.53943276465977519, 107.4989096053143669 ) ) ;
#105658 = AXIS2_PLACEMENT_3D ( 'NONE', #63616, #20086, #124282 ) ;
#105659 = CARTESIAN_POINT ( 'NONE',  ( 15.72974639402199770, -15.80617190586745480, 33.12390960531435979 ) ) ;
#105660 = CARTESIAN_POINT ( 'NONE',  ( 10.72451020669871369, 18.67979575497193778, 102.0844237280190185 ) ) ;
#105661 = CARTESIAN_POINT ( 'NONE',  ( 16.51473224551069308, 9.474510206698969483, 94.16557627198103830 ) ) ;
#105662 = CARTESIAN_POINT ( 'NONE',  ( -13.97604488694527625, -13.89961937509977652, 46.87390960531435979 ) ) ;
#105663 = CARTESIAN_POINT ( 'NONE',  ( 19.02544592524343514, -5.153800228976328945, 103.5405762719809957 ) ) ;
#105664 = B_SPLINE_CURVE_WITH_KNOTS ( 'NONE', 3,
 ( #68309, #98633, #37988, #161327, #51156, #22820, #189683, #147164, #128972, #146144, #7631, #21818, #69315, #190671, #52147, #8652, #112816, #174509, #160328, #76233 ),
 .UNSPECIFIED., .F., .F.,
 ( 4, 2, 2, 2, 2, 2, 2, 2, 2, 4 ),
 ( 0.000000000000000000, 0.0004987090165372536207, 0.0009974180330745072414, 0.001246772541343133889, 0.001496127049611760971, 0.001994836066149014483, 0.002493545082686267778, 0.002742899590954906135, 0.002992254099223544492, 0.003989672132298113100 ),
 .UNSPECIFIED. ) ;
#105665 = CARTESIAN_POINT ( 'NONE',  ( 0.05219959533909260263, 19.03943276465977164, 79.99890960531436690 ) ) ;
#105666 = CARTESIAN_POINT ( 'NONE',  ( 17.05587630539710275, -6.762274262136627634, 88.24180309037284076 ) ) ;
#105667 = CARTESIAN_POINT ( 'NONE',  ( -13.89961937509957401, -13.97604488694547875, 59.37609039468566863 ) ) ;
#105669 = CARTESIAN_POINT ( 'NONE',  ( 21.55341960407610458, 5.719274019375980345, 33.95724293864769550 ) ) ;
#105668 = CARTESIAN_POINT ( 'NONE',  ( -5.823673210054431948, 21.52544592524334988, 112.7094237280190328 ) ) ;
#105670 = CARTESIAN_POINT ( 'NONE',  ( 14.29746914071037800, 8.314922557961029526, 106.6677570613523756 ) ) ;
#105671 = CARTESIAN_POINT ( 'NONE',  ( -19.05341960407617563, 5.049401038297882671, 83.54275706135233293 ) ) ;
#105672 = CARTESIAN_POINT ( 'NONE',  ( 3.889087296525994830, -6.412877669190346630, 8.181980515339454030 ) ) ;
#105673 = CARTESIAN_POINT ( 'NONE',  ( -16.46253265017146816, -9.564922557961047289, 79.16775706135234714 ) ) ;
#105674 = CARTESIAN_POINT ( 'NONE',  ( 13.89961937509957401, 13.97604488694547697, 31.87609039468566863 ) ) ;
#105675 = CARTESIAN_POINT ( 'NONE',  ( 18.09867054820430710, 5.500000000000000000, 71.48393025253585620 ) ) ;
#105676 = CARTESIAN_POINT ( 'NONE',  ( -5.049401038298153566, 19.05341960407611168, 45.20724293864769550 ) ) ;
#105677 = CARTESIAN_POINT ( 'NONE',  ( 12.14591786802309770, 12.06949235617756955, 54.37390960531435979 ) ) ;
#105678 = CARTESIAN_POINT ( 'NONE',  ( -17.49999999999999645, -5.624438216177585659, 109.1832965508535551 ) ) ;
#105679 = CARTESIAN_POINT ( 'NONE',  ( -8.224510206698948167, 14.34966873604960824, 30.41557627198101699 ) ) ;
#105680 = LINE ( 'NONE', #88520, #3246 ) ;
#105681 = CARTESIAN_POINT ( 'NONE',  ( 16.52544592524335698, 4.483927247898782831, 96.45942372801901854 ) ) ;
#105682 = CARTESIAN_POINT ( 'NONE',  ( 19.02544592524343514, -5.153800228976328945, 53.54057627198102409 ) ) ;
#105683 = CARTESIAN_POINT ( 'NONE',  ( -5.719274019375665041, -21.55341960407619695, 109.7927570613523613 ) ) ;
#105684 = CARTESIAN_POINT ( 'NONE',  ( 13.97604488694548053, -13.89961937509957401, 110.6260903946856615 ) ) ;
#105686 = ORIENTED_EDGE ( 'NONE', *, *, #131641, .T. ) ;
#105685 = CARTESIAN_POINT ( 'NONE',  ( -18.67979575497193778, 10.72451020669871902, 93.33442372801901854 ) ) ;
#105687 = CARTESIAN_POINT ( 'NONE',  ( 19.05341960407611168, 5.049401038298154454, 88.95724293864769550 ) ) ;
#105688 = CARTESIAN_POINT ( 'NONE',  ( 19.02544592524343514, -5.153800228976328945, 78.54057627198099567 ) ) ;
#105689 = CARTESIAN_POINT ( 'NONE',  ( -36.91746825000000598, 2.428612866367529932E-14, -8.624999997268814056 ) ) ;
#105690 = CARTESIAN_POINT ( 'NONE',  ( -5.719274019375978568, 21.55341960407610458, 110.2072429386477239 ) ) ;
#105691 = TOROIDAL_SURFACE ( 'NONE', #34659, 1.500000000000001776, 0.5000000000000000000 ) ;
#105692 = CARTESIAN_POINT ( 'NONE',  ( 16.55341960407611168, 4.379528057220329451, 78.95724293864769550 ) ) ;
#105693 = CARTESIAN_POINT ( 'NONE',  ( 21.53943276465977519, -0.05219959533907433946, 73.74890960531433848 ) ) ;
#105694 = CARTESIAN_POINT ( 'NONE',  ( -19.02544592524342804, 5.153800228976336051, 56.04057627198100988 ) ) ;
#105696 = CARTESIAN_POINT ( 'NONE',  ( 0.05219959533934541429, -16.53943276465976808, 85.00109039468568994 ) ) ;
#105695 = CARTESIAN_POINT ( 'NONE',  ( 18.67979575497178502, 10.72451020669898547, 99.16557627198100988 ) ) ;
#105697 = ORIENTED_EDGE ( 'NONE', *, *, #48243, .T. ) ;
#105698 = CARTESIAN_POINT ( 'NONE',  ( -16.46253265017160317, 9.564922557960807481, 65.83224293864769550 ) ) ;
#105700 = CARTESIAN_POINT ( 'NONE',  ( 21.38418241377623019, -5.438282248597753110, 174.2683007571264113 ) ) ;
#105699 = CARTESIAN_POINT ( 'NONE',  ( -0.05219959533910754901, -16.53943276465976808, 87.49890960531436690 ) ) ;
#105701 = CARTESIAN_POINT ( 'NONE',  ( -9.564922557960796823, -16.46253265017161027, 67.08224293864769550 ) ) ;
#105702 = CARTESIAN_POINT ( 'NONE',  ( 13.89961937509957401, 13.97604488694547697, 81.87609039468564731 ) ) ;
#105703 = CARTESIAN_POINT ( 'NONE',  ( -12.06949235617756955, 12.14591786802309770, 80.62390960531438111 ) ) ;
#105704 = CARTESIAN_POINT ( 'NONE',  ( 5.719274019375673035, 21.55341960407619339, 62.29275706135236845 ) ) ;
#105706 = CARTESIAN_POINT ( 'NONE',  ( -10.72451020669870658, -18.67979575497194134, 19.58442372801901143 ) ) ;
#105705 = CARTESIAN_POINT ( 'NONE',  ( 9.474510206698971260, -16.51473224551069308, 47.91557627198102409 ) ) ;
#105707 = CARTESIAN_POINT ( 'NONE',  ( 16.55341960407611168, 4.379528057220329451, 98.95724293864770971 ) ) ;
#105708 = CARTESIAN_POINT ( 'NONE',  ( 17.97214573761834799, 5.499999999999959144, 93.96970049038657180 ) ) ;
#105709 = CARTESIAN_POINT ( 'NONE',  ( 16.51473224551069308, 9.474510206698969483, 54.16557627198103120 ) ) ;
#105710 = CARTESIAN_POINT ( 'NONE',  ( -36.91746825000000598, 11.99521256947798520, -0.7249999972688133676 ) ) ;
#105712 = CARTESIAN_POINT ( 'NONE',  ( 13.97604488694527802, 13.89961937509977652, 109.3739096053143669 ) ) ;
#105711 = CARTESIAN_POINT ( 'NONE',  ( -16.51473224551082808, 9.474510206698731452, 93.33442372801900433 ) ) ;
#105713 = CARTESIAN_POINT ( 'NONE',  ( 5.823673210054444382, -21.52544592524334988, 45.20942372801901854 ) ) ;
#105714 = CARTESIAN_POINT ( 'NONE',  ( 19.02544592524343514, -5.153800228976328945, 88.54057627198102409 ) ) ;
#105715 = CARTESIAN_POINT ( 'NONE',  ( 19.05341960407617918, -5.049401038297876454, 76.04275706135230450 ) ) ;
#105716 = CARTESIAN_POINT ( 'NONE',  ( 16.51473224551069308, 9.474510206698969483, 64.16557627198102409 ) ) ;
#105717 = CARTESIAN_POINT ( 'NONE',  ( 12.14591786802309770, 12.06949235617756955, 79.37390960531436690 ) ) ;
#105718 = CARTESIAN_POINT ( 'NONE',  ( 4.483927247898545687, 16.52544592524342804, 74.79057627198105251 ) ) ;
#105719 = CARTESIAN_POINT ( 'NONE',  ( -5.049401038298153566, 19.05341960407611168, 90.20724293864766707 ) ) ;
#105720 = CARTESIAN_POINT ( 'NONE',  ( 16.55341960407611168, 4.379528057220329451, 78.95724293864769550 ) ) ;
#105721 = CARTESIAN_POINT ( 'NONE',  ( 9.564922557960805705, 16.46253265017160317, 89.58224293864769550 ) ) ;
#105722 = CARTESIAN_POINT ( 'NONE',  ( -19.02544592524334988, -5.153800228976617603, 33.95942372801897591 ) ) ;
#105725 = CARTESIAN_POINT ( 'NONE',  ( 4.379528057220339221, -16.55341960407611168, 112.7072429386476955 ) ) ;
#105724 = CARTESIAN_POINT ( 'NONE',  ( 8.314922557960818139, 14.29746914071049879, 24.58224293864768839 ) ) ;
#105723 = CARTESIAN_POINT ( 'NONE',  ( -0.05219959533909027116, -19.03943276465977164, 47.49890960531435979 ) ) ;
#105726 = VERTEX_POINT ( 'NONE', #103545 ) ;
#105727 = CARTESIAN_POINT ( 'NONE',  ( -10.72451020669870658, -18.67979575497194134, 44.58442372801901854 ) ) ;
#105728 = CARTESIAN_POINT ( 'NONE',  ( 5.153800228976615827, -19.02544592524334988, 70.20942372801899012 ) ) ;
#105729 = CARTESIAN_POINT ( 'NONE',  ( -4.483927247898539470, -16.52544592524342804, 42.29057627198103120 ) ) ;
#105730 = CARTESIAN_POINT ( 'NONE',  ( -18.67979575497178146, -10.72451020669898902, 81.66557627198103830 ) ) ;
#105731 = CARTESIAN_POINT ( 'NONE',  ( -16.51473224551069308, -9.474510206698971260, 111.6655762719810383 ) ) ;
#105732 = CARTESIAN_POINT ( 'NONE',  ( -4.483927247898539470, -16.52544592524342804, 67.29057627198103830 ) ) ;
#105733 = CARTESIAN_POINT ( 'NONE',  ( -5.049401038298153566, 19.05341960407611168, 40.20724293864768839 ) ) ;
#105734 = CARTESIAN_POINT ( 'NONE',  ( 16.46253265017146816, 9.564922557961045513, 46.66775706135233293 ) ) ;
#105735 = CARTESIAN_POINT ( 'NONE',  ( 12.06949235617739724, 12.14591786802326823, 106.8760903946856899 ) ) ;
#105736 = CARTESIAN_POINT ( 'NONE',  ( 8.224510206698742110, 14.34966873604972548, 52.08442372801901854 ) ) ;
#105737 = CARTESIAN_POINT ( 'NONE',  ( 10.81492255796078972, 18.62759615963270932, 39.58224293864769550 ) ) ;
#105738 = CARTESIAN_POINT ( 'NONE',  ( -10.72451020669870658, -18.67979575497194134, 109.5844237280190328 ) ) ;
#105739 = CARTESIAN_POINT ( 'NONE',  ( -13.97604488694527625, -13.89961937509977652, 91.87390960531432427 ) ) ;
#105740 = CARTESIAN_POINT ( 'NONE',  ( -16.52544592524335698, -4.483927247898792601, 78.95942372801901854 ) ) ;
#105741 = CARTESIAN_POINT ( 'NONE',  ( 16.52544592524342804, -4.483927247898539470, 113.5405762719810383 ) ) ;
#105742 = CARTESIAN_POINT ( 'NONE',  ( -16.52544592524342804, 4.483927247898546575, 41.04057627198103120 ) ) ;
#105744 = CARTESIAN_POINT ( 'NONE',  ( -16.46253265017160317, 9.564922557960807481, 95.83224293864769550 ) ) ;
#105743 = CARTESIAN_POINT ( 'NONE',  ( -19.02544592524342804, 5.153800228976336051, 101.0405762719810241 ) ) ;
#105746 = EDGE_CURVE ( 'NONE', #197536, #125394, #82720, .T. ) ;
#105745 = CARTESIAN_POINT ( 'NONE',  ( 5.823673210054125526, 21.52544592524343514, 29.79057627198102409 ) ) ;
#105747 = CARTESIAN_POINT ( 'NONE',  ( -16.55341960407611168, -4.379528057220339221, 71.45724293864769550 ) ) ;
#105748 = CARTESIAN_POINT ( 'NONE',  ( -16.53943276465976808, 0.05219959533911058130, 56.24890960531436690 ) ) ;
#105750 = PLANE ( 'NONE',  #160925 ) ;
#105749 = CARTESIAN_POINT ( 'NONE',  ( -14.34966873604972548, 8.224510206698743886, 58.33442372801901143 ) ) ;
#105751 = CARTESIAN_POINT ( 'NONE',  ( 13.89961937509957401, 13.97604488694547697, 56.87609039468564731 ) ) ;
#105752 = CARTESIAN_POINT ( 'NONE',  ( 19.05341960407611168, 5.049401038298154454, 93.95724293864769550 ) ) ;
#105753 = CARTESIAN_POINT ( 'NONE',  ( 0.05219959533936267826, -19.03943276465977164, 70.00109039468566152 ) ) ;
#105754 = CARTESIAN_POINT ( 'NONE',  ( 22.44159573604009239, 16.30477369853692693, 146.5750000027312012 ) ) ;
#105755 = CARTESIAN_POINT ( 'NONE',  ( -0.05219959533936034679, 19.03943276465977164, 52.50109039468566863 ) ) ;
#105757 = CARTESIAN_POINT ( 'NONE',  ( 8.224510206698742110, 14.34966873604972548, 97.08442372801904696 ) ) ;
#105756 = CARTESIAN_POINT ( 'NONE',  ( 9.474510206698729675, 16.51473224551082808, 102.0844237280190043 ) ) ;
#105758 = CARTESIAN_POINT ( 'NONE',  ( -22.44159573604009950, -16.30477369853688430, 143.5750000027311728 ) ) ;
#105759 = CARTESIAN_POINT ( 'NONE',  ( 5.153800228976335163, 19.02544592524342804, 39.79057627198100988 ) ) ;
#105760 = CARTESIAN_POINT ( 'NONE',  ( 0.05219959533909260263, 19.03943276465977164, 114.9989096053143669 ) ) ;
#105761 = CARTESIAN_POINT ( 'NONE',  ( -21.55341960407619339, 5.719274019375674811, 53.54275706135234714 ) ) ;
#105762 = CARTESIAN_POINT ( 'NONE',  ( -9.474510206698720793, -16.51473224551083518, 109.5844237280190043 ) ) ;
#105764 = CARTESIAN_POINT ( 'NONE',  ( 16.46253265017160672, -9.564922557960803928, 58.33224293864769550 ) ) ;
#105763 = CARTESIAN_POINT ( 'NONE',  ( 17.50000000000001421, 3.817821230385223696, 23.21443863932539742 ) ) ;
#105765 = CARTESIAN_POINT ( 'NONE',  ( 18.46320343559638388, -23.96320343559646915, 1.818019484660536200 ) ) ;
#105767 = CARTESIAN_POINT ( 'NONE',  ( 5.153800228976335163, 19.02544592524342804, 64.79057627198100988 ) ) ;
#105766 = CARTESIAN_POINT ( 'NONE',  ( 16.52544592524342804, -4.483927247898539470, 73.54057627198102409 ) ) ;
#105768 = CARTESIAN_POINT ( 'NONE',  ( -5.153800228976328057, -19.02544592524343514, 72.29057627198102409 ) ) ;
#105769 = CARTESIAN_POINT ( 'NONE',  ( -19.02544592524334988, -5.153800228976617603, 78.95942372801900433 ) ) ;
#105770 = CARTESIAN_POINT ( 'NONE',  ( 10.81492255796078972, 18.62759615963270932, 69.58224293864769550 ) ) ;
#105771 = CARTESIAN_POINT ( 'NONE',  ( 4.379528057220339221, -16.55341960407611168, 112.7072429386476955 ) ) ;
#105772 = CARTESIAN_POINT ( 'NONE',  ( 16.51473224551083163, -9.474510206698727899, 40.83442372801900433 ) ) ;
#105774 = ADVANCED_FACE ( 'NONE', ( #147048 ), #88899, .T. ) ;
#105773 = CARTESIAN_POINT ( 'NONE',  ( 19.03943276465977164, -0.05219959533909143690, 73.74890960531435269 ) ) ;
#105775 = CARTESIAN_POINT ( 'NONE',  ( 10.81492255796078972, 18.62759615963270932, 89.58224293864768129 ) ) ;
#105777 = CARTESIAN_POINT ( 'NONE',  ( -13.89961937509957401, -13.97604488694547875, 44.37609039468566863 ) ) ;
#105776 = CARTESIAN_POINT ( 'NONE',  ( -8.224510206698948167, 14.34966873604960824, 75.41557627198102409 ) ) ;
#105778 = CARTESIAN_POINT ( 'NONE',  ( -0.05219959533907301413, -21.53943276465977519, 77.49890960531433848 ) ) ;
#105779 = CARTESIAN_POINT ( 'NONE',  ( -18.67979575497178146, -10.72451020669898902, 61.66557627198103120 ) ) ;
#105780 = CARTESIAN_POINT ( 'NONE',  ( 15.80617190586746368, 15.72974639402197994, 34.37390960531435979 ) ) ;
#105781 = CARTESIAN_POINT ( 'NONE',  ( 15.72974639402176855, 15.80617190586768217, 96.87609039468568994 ) ) ;
#105782 = CARTESIAN_POINT ( 'NONE',  ( -16.51473224551069308, -9.474510206698971260, 81.66557627198103830 ) ) ;
#105783 = CARTESIAN_POINT ( 'NONE',  ( 8.314922557960818139, 14.29746914071049879, 114.5822429386477097 ) ) ;
#105784 = VECTOR ( 'NONE', #56521, 1000.000000000000000 ) ;
#105785 = CARTESIAN_POINT ( 'NONE',  ( -18.62759615963255300, -10.81492255796106328, 29.16775706135234003 ) ) ;
#105786 = CARTESIAN_POINT ( 'NONE',  ( -0.05219959533937732626, 21.53943276465977519, 37.50109039468568284 ) ) ;
#105787 = CARTESIAN_POINT ( 'NONE',  ( 5.049401038298161559, -19.05341960407611168, 32.70724293864768129 ) ) ;
#105788 = CARTESIAN_POINT ( 'NONE',  ( -21.55341960407619339, 5.719274019375674811, 23.54275706135235424 ) ) ;
#105789 = CARTESIAN_POINT ( 'NONE',  ( -19.05341960407617563, 5.049401038297882671, 58.54275706135234003 ) ) ;
#105790 = CARTESIAN_POINT ( 'NONE',  ( 19.02544592524343514, -5.153800228976328945, 38.54057627198103120 ) ) ;
#105791 = CARTESIAN_POINT ( 'NONE',  ( -14.29746914071037622, -8.314922557961029526, 34.16775706135234714 ) ) ;
#105792 = CARTESIAN_POINT ( 'NONE',  ( 5.153800228976335163, 19.02544592524342804, 24.79057627198102765 ) ) ;
#105793 = CARTESIAN_POINT ( 'NONE',  ( 16.52544592524335698, 4.483927247898782831, 66.45942372801903275 ) ) ;
#105794 = CARTESIAN_POINT ( 'NONE',  ( 5.153800228976335163, 19.02544592524342804, 34.79057627198102409 ) ) ;
#105795 = CARTESIAN_POINT ( 'NONE',  ( -26.77293948118418854, -6.014770499717744912, 169.2063755025621674 ) ) ;
#105796 = CARTESIAN_POINT ( 'NONE',  ( 19.05341960407611168, 5.049401038298154454, 88.95724293864769550 ) ) ;
#105797 = CARTESIAN_POINT ( 'NONE',  ( 0.05219959533909260263, 19.03943276465977164, 29.99890960531435979 ) ) ;
#105798 = CARTESIAN_POINT ( 'NONE',  ( -21.53943276465977519, 0.05219959533907696930, 56.24890960531436690 ) ) ;
#105799 = CARTESIAN_POINT ( 'NONE',  ( -14.34966873604972548, 8.224510206698743886, 48.33442372801902565 ) ) ;
#105800 = CARTESIAN_POINT ( 'NONE',  ( -18.67979575497193778, 10.72451020669871902, 93.33442372801901854 ) ) ;
#105801 = CARTESIAN_POINT ( 'NONE',  ( 13.89961937509977652, -13.97604488694527269, 38.12390960531436690 ) ) ;
#105802 = CARTESIAN_POINT ( 'NONE',  ( 12.06949235617757843, -12.14591786802309237, 38.12390960531436690 ) ) ;
#105803 = CARTESIAN_POINT ( 'NONE',  ( 14.34966873604960469, 8.224510206698951720, 74.16557627198102409 ) ) ;
#105804 = CARTESIAN_POINT ( 'NONE',  ( -5.049401038298153566, 19.05341960407611168, 70.20724293864769550 ) ) ;
#105805 = CARTESIAN_POINT ( 'NONE',  ( 19.05341960407617918, -5.049401038297876454, 21.04275706135232582 ) ) ;
#105806 = CARTESIAN_POINT ( 'NONE',  ( 21.52544592524334988, 5.823673210054432836, 26.45942372801901854 ) ) ;
#105807 = CARTESIAN_POINT ( 'NONE',  ( 10.72451020669871369, 18.67979575497193778, 82.08442372801901854 ) ) ;
#105808 = CARTESIAN_POINT ( 'NONE',  ( -16.55341960407617563, 4.379528057220093196, 48.54275706135234714 ) ) ;
#105809 = CARTESIAN_POINT ( 'NONE',  ( -16.52544592524335698, -4.483927247898792601, 33.95942372801901143 ) ) ;
#105811 = CARTESIAN_POINT ( 'NONE',  ( -5.719274019375665041, -21.55341960407619695, 94.79275706135234714 ) ) ;
#105810 = CARTESIAN_POINT ( 'NONE',  ( 12.14591786802309770, 12.06949235617756955, 89.37390960531435269 ) ) ;
#105812 = AXIS2_PLACEMENT_3D ( 'NONE', #160641, #158640, #81776 ) ;
#105813 = CARTESIAN_POINT ( 'NONE',  ( -4.483927247898539470, -16.52544592524342804, 32.29057627198102409 ) ) ;
#105814 = CARTESIAN_POINT ( 'NONE',  ( 9.474510206698971260, -16.51473224551069308, 27.91557627198103120 ) ) ;
#105815 = CARTESIAN_POINT ( 'NONE',  ( 16.53943276465976808, 0.05219959533934440121, 46.25109039468567573 ) ) ;
#105816 = CARTESIAN_POINT ( 'NONE',  ( -8.224510206698948167, 14.34966873604960824, 55.41557627198102409 ) ) ;
#105817 = CARTESIAN_POINT ( 'NONE',  ( 14.29746914071037800, 8.314922557961029526, 81.66775706135236135 ) ) ;
#105818 = CARTESIAN_POINT ( 'NONE',  ( 19.02544592524343514, -5.153800228976328945, 98.54057627198100988 ) ) ;
#105819 = CARTESIAN_POINT ( 'NONE',  ( 15.80617190586746368, 15.72974639402197994, 24.37390960531435979 ) ) ;
#105820 = CARTESIAN_POINT ( 'NONE',  ( -0.05219959533936034679, 19.03943276465977164, 22.50109039468566152 ) ) ;
#105821 = CARTESIAN_POINT ( 'NONE',  ( 12.14591786802309770, 12.06949235617756955, 84.37390960531438111 ) ) ;
#105822 = CARTESIAN_POINT ( 'NONE',  ( -0.05219959533909027116, -19.03943276465977164, 92.49890960531436690 ) ) ;
#105823 = ORIENTED_EDGE ( 'NONE', *, *, #150034, .F. ) ;
#105824 = CARTESIAN_POINT ( 'NONE',  ( 4.379528057220092307, 16.55341960407617563, 37.29275706135235424 ) ) ;
#105825 = CARTESIAN_POINT ( 'NONE',  ( -19.05341960407611168, -5.049401038298163336, 46.45724293864768129 ) ) ;
#105826 = CARTESIAN_POINT ( 'NONE',  ( 16.51473224551069308, 9.474510206698969483, 109.1655762719810383 ) ) ;
#105828 = CARTESIAN_POINT ( 'NONE',  ( -17.49999999999999645, -5.499999999999992895, 79.20309617465829888 ) ) ;
#105827 = CARTESIAN_POINT ( 'NONE',  ( 12.06949235617739724, 12.14591786802326823, 46.87609039468568994 ) ) ;
#105829 = CARTESIAN_POINT ( 'NONE',  ( -19.05341960407617563, 5.049401038297882671, 43.54275706135232582 ) ) ;
#105830 = CARTESIAN_POINT ( 'NONE',  ( 5.153800228976335163, 19.02544592524342804, 49.79057627198100988 ) ) ;
#105831 = CARTESIAN_POINT ( 'NONE',  ( -0.05219959533934338120, 16.53943276465976808, 77.50109039468567573 ) ) ;
#105832 = CARTESIAN_POINT ( 'NONE',  ( -19.05341960407617563, 5.049401038297882671, 83.54275706135233293 ) ) ;
#105833 = CARTESIAN_POINT ( 'NONE',  ( -9.474510206698720793, -16.51473224551083518, 24.58442372801900078 ) ) ;
#105834 = CARTESIAN_POINT ( 'NONE',  ( -16.46253265017160317, 9.564922557960807481, 55.83224293864769550 ) ) ;
#105835 = CARTESIAN_POINT ( 'NONE',  ( 16.55341960407611168, 4.379528057220329451, 98.95724293864770971 ) ) ;
#105836 = CARTESIAN_POINT ( 'NONE',  ( 9.564922557961047289, -16.46253265017146816, 70.41775706135233293 ) ) ;
#105837 = CARTESIAN_POINT ( 'NONE',  ( -5.719274019375978568, 21.55341960407610458, 70.20724293864769550 ) ) ;
#105838 = CARTESIAN_POINT ( 'NONE',  ( -9.564922557961040184, 16.46253265017147172, 27.91775706135232582 ) ) ;
#105839 = CARTESIAN_POINT ( 'NONE',  ( 19.05341960407611168, 5.049401038298154454, 103.9572429386476671 ) ) ;
#105840 = CARTESIAN_POINT ( 'NONE',  ( 10.72451020669898902, -18.67979575497178502, 82.91557627198103830 ) ) ;
#105841 = LINE ( 'NONE', #56351, #114511 ) ;
#105842 = CARTESIAN_POINT ( 'NONE',  ( 9.564922557961047289, -16.46253265017146816, 100.4177570613523329 ) ) ;
#105843 = DIRECTION ( 'NONE',  ( -1.000000000000000000, -0.000000000000000000, -0.000000000000000000 ) ) ;
#105844 = EDGE_CURVE ( 'NONE', #176035, #115704, #154292, .T. ) ;
#105845 = CARTESIAN_POINT ( 'NONE',  ( -14.34966873604972548, 8.224510206698743886, 28.33442372801902209 ) ) ;
#105846 = CARTESIAN_POINT ( 'NONE',  ( -9.564922557960796823, -16.46253265017161027, 37.08224293864768839 ) ) ;
#105847 = CARTESIAN_POINT ( 'NONE',  ( -13.89961937509977652, 13.97604488694528158, 115.6239096053143669 ) ) ;
#105848 = CARTESIAN_POINT ( 'NONE',  ( 5.823673210054125526, 21.52544592524343514, 94.79057627198105251 ) ) ;
#105849 = CARTESIAN_POINT ( 'NONE',  ( 21.52544592524334988, 5.823673210054432836, 66.45942372801903275 ) ) ;
#105851 = CARTESIAN_POINT ( 'NONE',  ( 21.55341960407619695, -5.719274019375665929, 111.0427570613523613 ) ) ;
#105850 = CARTESIAN_POINT ( 'NONE',  ( 19.03943276465977164, 0.05219959533936151252, 111.2510903946856757 ) ) ;
#105852 = CARTESIAN_POINT ( 'NONE',  ( -16.52544592524335698, -4.483927247898792601, 103.9594237280190185 ) ) ;
#105853 = CARTESIAN_POINT ( 'NONE',  ( 10.81492255796078972, 18.62759615963270932, 99.58224293864770971 ) ) ;
#105854 = CARTESIAN_POINT ( 'NONE',  ( -8.224510206698948167, 14.34966873604960824, 55.41557627198102409 ) ) ;
#105855 = CARTESIAN_POINT ( 'NONE',  ( -16.51473224551082808, 9.474510206698731452, 83.33442372801899012 ) ) ;
#105856 = CARTESIAN_POINT ( 'NONE',  ( -5.153800228976607833, 19.02544592524334988, 52.70942372801900433 ) ) ;
#105857 = CARTESIAN_POINT ( 'NONE',  ( 21.52544592524334988, 5.823673210054432836, 61.45942372801901854 ) ) ;
#105858 = CARTESIAN_POINT ( 'NONE',  ( 16.51473224551083163, -9.474510206698727899, 35.83442372801899722 ) ) ;
#105859 = CARTESIAN_POINT ( 'NONE',  ( 8.314922557960818139, 14.29746914071049879, 99.58224293864770971 ) ) ;
#105860 = CARTESIAN_POINT ( 'NONE',  ( -5.719274019375978568, 21.55341960407610458, 35.20724293864768839 ) ) ;
#105861 = CARTESIAN_POINT ( 'NONE',  ( -0.05219959533910754901, -16.53943276465976808, 32.49890960531435979 ) ) ;
#105862 = CARTESIAN_POINT ( 'NONE',  ( -21.53943276465977519, -0.05219959533937600094, 93.75109039468567573 ) ) ;
#105863 = CARTESIAN_POINT ( 'NONE',  ( -4.483927247898782831, 16.52544592524335698, 72.70942372801901854 ) ) ;
#105864 = CARTESIAN_POINT ( 'NONE',  ( 12.06949235617757843, -12.14591786802309237, 33.12390960531435979 ) ) ;
#105865 = CARTESIAN_POINT ( 'NONE',  ( 21.52544592524334988, 5.823673210054432836, 56.45942372801902565 ) ) ;
#105866 = CARTESIAN_POINT ( 'NONE',  ( -5.823673210054431948, 21.52544592524334988, 72.70942372801901854 ) ) ;
#105867 = CARTESIAN_POINT ( 'NONE',  ( 10.81492255796078972, 18.62759615963270932, 64.58224293864769550 ) ) ;
#105868 = ORIENTED_EDGE ( 'NONE', *, *, #156887, .T. ) ;
#105869 = CARTESIAN_POINT ( 'NONE',  ( -13.97604488694527625, -13.89961937509977652, 26.87390960531434558 ) ) ;
#105870 = CARTESIAN_POINT ( 'NONE',  ( 21.53943276465977519, 0.05219959533937863772, 46.25109039468567573 ) ) ;
#105871 = CARTESIAN_POINT ( 'NONE',  ( -9.564922557960796823, -16.46253265017161027, 22.08224293864768839 ) ) ;
#105872 = CARTESIAN_POINT ( 'NONE',  ( -9.474510206698964154, 16.51473224551069663, 35.41557627198102409 ) ) ;
#105873 = CARTESIAN_POINT ( 'NONE',  ( 16.53943276465976808, -0.05219959533910856209, 83.74890960531435269 ) ) ;
#105874 = CARTESIAN_POINT ( 'NONE',  ( 19.02544592524343514, -5.153800228976328945, 83.54057627198100988 ) ) ;
#105875 = CARTESIAN_POINT ( 'NONE',  ( 14.34966873604960469, 8.224510206698951720, 24.16557627198103120 ) ) ;
#105876 = CARTESIAN_POINT ( 'NONE',  ( 14.34966873604960469, 8.224510206698951720, 99.16557627198100988 ) ) ;
#105877 = CARTESIAN_POINT ( 'NONE',  ( -15.72974639402197994, 15.80617190586746368, 65.62390960531436690 ) ) ;
#105878 = CARTESIAN_POINT ( 'NONE',  ( 15.72974639402199770, -15.80617190586745480, 103.1239096053143811 ) ) ;
#105879 = CARTESIAN_POINT ( 'NONE',  ( -16.46253265017160317, 9.564922557960807481, 110.8322429386476955 ) ) ;
#105881 = CARTESIAN_POINT ( 'NONE',  ( 5.049401038297881783, 19.05341960407617563, 107.2927570613523187 ) ) ;
#105880 = CARTESIAN_POINT ( 'NONE',  ( -13.89961937509977652, 13.97604488694528158, 65.62390960531436690 ) ) ;
#105882 = CARTESIAN_POINT ( 'NONE',  ( -10.81492255796078084, -18.62759615963271287, 57.08224293864769550 ) ) ;
#105883 = CARTESIAN_POINT ( 'NONE',  ( 10.81492255796106328, -18.62759615963255655, 85.41775706135236135 ) ) ;
#105884 = CARTESIAN_POINT ( 'NONE',  ( 5.049401038298161559, -19.05341960407611168, 72.70724293864768129 ) ) ;
#105885 = CARTESIAN_POINT ( 'NONE',  ( 13.97604488694527802, 13.89961937509977652, 94.37390960531436690 ) ) ;
#105886 = CARTESIAN_POINT ( 'NONE',  ( -8.314922557961024197, 14.29746914071037800, 72.91775706135234714 ) ) ;
#105887 = CARTESIAN_POINT ( 'NONE',  ( 15.80617190586769283, -15.72974639402175789, 60.62609039468567573 ) ) ;
#105888 = CARTESIAN_POINT ( 'NONE',  ( -5.823673210054431948, 21.52544592524334988, 102.7094237280190185 ) ) ;
#105889 = CARTESIAN_POINT ( 'NONE',  ( 0.05219959533907565091, 21.53943276465977519, 109.9989096053143527 ) ) ;
#105890 = CARTESIAN_POINT ( 'NONE',  ( 5.719274019375991003, -21.55341960407610458, 77.70724293864770971 ) ) ;
#105891 = CARTESIAN_POINT ( 'NONE',  ( 19.03943276465977164, 0.05219959533936151252, 51.25109039468567573 ) ) ;
#105892 = CARTESIAN_POINT ( 'NONE',  ( -5.823673210054116645, -21.52544592524344225, 37.29057627198102409 ) ) ;
#105894 = CARTESIAN_POINT ( 'NONE',  ( 0.05219959533910956823, 16.53943276465976808, 34.99890960531435979 ) ) ;
#105893 = CARTESIAN_POINT ( 'NONE',  ( 16.51473224551069308, 9.474510206698969483, 79.16557627198103830 ) ) ;
#105895 = FACE_OUTER_BOUND ( 'NONE', #122257, .T. ) ;
#105896 = CARTESIAN_POINT ( 'NONE',  ( 2.200000000000000622, 2.694222958124176020E-16, -2.199999999999999289 ) ) ;
#105897 = CARTESIAN_POINT ( 'NONE',  ( 13.89961937509957401, 13.97604488694547697, 91.87609039468567573 ) ) ;
#105898 = CARTESIAN_POINT ( 'NONE',  ( 10.81492255796078972, 18.62759615963270932, 69.58224293864769550 ) ) ;
#105899 = CARTESIAN_POINT ( 'NONE',  ( -4.483927247898539470, -16.52544592524342804, 52.29057627198102409 ) ) ;
#105900 = CARTESIAN_POINT ( 'NONE',  ( 8.314922557961029526, -14.29746914071037800, 35.41775706135234003 ) ) ;
#105901 = CARTESIAN_POINT ( 'NONE',  ( 19.03943276465977164, -0.05219959533909143690, 43.74890960531435979 ) ) ;
#105903 = CARTESIAN_POINT ( 'NONE',  ( -9.474510206698720793, -16.51473224551083518, 79.58442372801899012 ) ) ;
#105902 = CARTESIAN_POINT ( 'NONE',  ( -21.52544592524343514, 5.823673210054127303, 116.0405762719810383 ) ) ;
#105904 = CARTESIAN_POINT ( 'NONE',  ( -16.46253265017160317, 9.564922557960807481, 85.83224293864769550 ) ) ;
#105905 = CARTESIAN_POINT ( 'NONE',  ( -12.06949235617756955, 12.14591786802309770, 85.62390960531436690 ) ) ;
#105906 = CARTESIAN_POINT ( 'NONE',  ( -16.46253265017160317, 9.564922557960807481, 65.83224293864769550 ) ) ;
#105907 = CARTESIAN_POINT ( 'NONE',  ( 14.34966873604960469, 8.224510206698951720, 69.16557627198102409 ) ) ;
#105908 = CARTESIAN_POINT ( 'NONE',  ( 19.03943276465977164, -0.05219959533909143690, 38.74890960531436690 ) ) ;
#105909 = CARTESIAN_POINT ( 'NONE',  ( -36.76911729423384401, -4.939512937650264668, 47.42567687524350362 ) ) ;
#105910 = CARTESIAN_POINT ( 'NONE',  ( 12.06949235617757843, -12.14591786802309237, 43.12390960531435269 ) ) ;
#105911 = CARTESIAN_POINT ( 'NONE',  ( -16.51473224551069308, -9.474510206698971260, 91.66557627198103830 ) ) ;
#105912 = CARTESIAN_POINT ( 'NONE',  ( -0.5040881997803867698, -16.61636759701970689, -59.17093420172795248 ) ) ;
#105913 = CARTESIAN_POINT ( 'NONE',  ( 16.46253265017146816, 9.564922557961045513, 46.66775706135233293 ) ) ;
#105914 = CARTESIAN_POINT ( 'NONE',  ( 8.314922557961029526, -14.29746914071037800, 55.41775706135234714 ) ) ;
#105915 = CARTESIAN_POINT ( 'NONE',  ( 18.62759615963271287, -10.81492255796078972, 73.33224293864769550 ) ) ;
#105916 = CARTESIAN_POINT ( 'NONE',  ( -16.51473224551082808, 9.474510206698731452, 43.33442372801900433 ) ) ;
#105917 = CARTESIAN_POINT ( 'NONE',  ( 13.97604488694527802, 13.89961937509977652, 94.37390960531436690 ) ) ;
#105918 = CARTESIAN_POINT ( 'NONE',  ( -17.50000000000000355, 5.068104630630384300, 115.7281840534003408 ) ) ;
#105919 = CARTESIAN_POINT ( 'NONE',  ( 0.05219959533907565091, 21.53943276465977519, 29.99890960531435979 ) ) ;
#105920 = AXIS2_PLACEMENT_3D ( 'NONE', #107122, #151664, #73842 ) ;
#105921 = CARTESIAN_POINT ( 'NONE',  ( 13.89961937509977652, -13.97604488694527269, 63.12390960531435979 ) ) ;
#105922 = CARTESIAN_POINT ( 'NONE',  ( -18.67979575497193778, 10.72451020669871902, 48.33442372801902565 ) ) ;
#105923 = CARTESIAN_POINT ( 'NONE',  ( 19.02544592524343514, -5.153800228976328945, 23.54057627198102054 ) ) ;
#105926 = ORIENTED_EDGE ( 'NONE', *, *, #29688, .T. ) ;
#105925 = CARTESIAN_POINT ( 'NONE',  ( -9.474510206698964154, 16.51473224551069663, 90.41557627198103830 ) ) ;
#105924 = CARTESIAN_POINT ( 'NONE',  ( -15.72974639402176322, -15.80617190586768395, 19.37609039468568639 ) ) ;
#105927 = CARTESIAN_POINT ( 'NONE',  ( -18.67979575497193778, 10.72451020669871902, 33.33442372801900433 ) ) ;
#105928 = ORIENTED_EDGE ( 'NONE', *, *, #134324, .T. ) ;
#105929 = CARTESIAN_POINT ( 'NONE',  ( -13.89961937509977652, 13.97604488694528158, 105.6239096053143527 ) ) ;
#105930 = CARTESIAN_POINT ( 'NONE',  ( 28.82186960331498327, 2.428612866367529932E-14, 139.9999999999999716 ) ) ;
#105931 = CARTESIAN_POINT ( 'NONE',  ( 5.823673210054125526, 21.52544592524343514, 109.7905762719810383 ) ) ;
#105932 = CARTESIAN_POINT ( 'NONE',  ( -13.97604488694527625, -13.89961937509977652, 51.87390960531436690 ) ) ;
#105933 = CARTESIAN_POINT ( 'NONE',  ( 16.53943276465976808, 0.05219959533934440121, 31.25109039468568639 ) ) ;
#105934 = CARTESIAN_POINT ( 'NONE',  ( 29.86685920354754487, 21.69954338932564752, -5.924999997268813878 ) ) ;
#105935 = CARTESIAN_POINT ( 'NONE',  ( -21.53943276465977519, -0.05219959533937600094, 98.75109039468568994 ) ) ;
#105936 = CARTESIAN_POINT ( 'NONE',  ( -16.46253265017160317, 9.564922557960807481, 35.83224293864768839 ) ) ;
#105937 = CARTESIAN_POINT ( 'NONE',  ( 15.80617190586769283, -15.72974639402175789, 100.6260903946857184 ) ) ;
#105939 = CARTESIAN_POINT ( 'NONE',  ( -5.719274019375665041, -21.55341960407619695, 59.79275706135234714 ) ) ;
#105938 = CARTESIAN_POINT ( 'NONE',  ( 0.05219959533909260263, 19.03943276465977164, 94.99890960531436690 ) ) ;
#105940 = CARTESIAN_POINT ( 'NONE',  ( 22.44159573604009239, 16.30477369853692693, 144.5750000027311728 ) ) ;
#105941 = CARTESIAN_POINT ( 'NONE',  ( 5.153800228976335163, 19.02544592524342804, 104.7905762719809957 ) ) ;
#105942 = CARTESIAN_POINT ( 'NONE',  ( -22.00000000000000000, -1.163414459189985801E-14, 95.00000000000000000 ) ) ;
#105945 = CARTESIAN_POINT ( 'NONE',  ( -21.53943276465977519, -0.05219959533937600094, 53.75109039468568994 ) ) ;
#105944 = CARTESIAN_POINT ( 'NONE',  ( 12.14591786802327356, -12.06949235617739191, 70.62609039468567573 ) ) ;
#105943 = CARTESIAN_POINT ( 'NONE',  ( 14.29746914071037800, 8.314922557961029526, 56.66775706135235424 ) ) ;
#105946 = CARTESIAN_POINT ( 'NONE',  ( -21.53943276465977519, -0.05219959533937600094, 88.75109039468567573 ) ) ;
#105947 = DIRECTION ( 'NONE',  ( -1.734723475976805122E-15, 0.1033298494363120712, 0.9946471445771455366 ) ) ;
#105948 = CARTESIAN_POINT ( 'NONE',  ( 16.53943276465976808, 0.05219959533934440121, 31.25109039468568639 ) ) ;
#105949 = CARTESIAN_POINT ( 'NONE',  ( 5.153800228976335163, 19.02544592524342804, 79.79057627198102409 ) ) ;
#105950 = CARTESIAN_POINT ( 'NONE',  ( 13.89961937509977652, -13.97604488694527269, 103.1239096053143527 ) ) ;
#105951 = AXIS2_PLACEMENT_3D ( 'NONE', #140381, #113020, #142369 ) ;
#105952 = CARTESIAN_POINT ( 'NONE',  ( -13.89961937509977652, 13.97604488694528158, 110.6239096053143243 ) ) ;
#105953 = CARTESIAN_POINT ( 'NONE',  ( 16.51473224551069308, 9.474510206698969483, 24.16557627198102765 ) ) ;
#105954 = CARTESIAN_POINT ( 'NONE',  ( -0.05219959533907301413, -21.53943276465977519, 32.49890960531435979 ) ) ;
#105955 = CARTESIAN_POINT ( 'NONE',  ( 0.05219959533934541429, -16.53943276465976808, 90.00109039468567573 ) ) ;
#105957 = CARTESIAN_POINT ( 'NONE',  ( -13.97604488694527625, -13.89961937509977652, 66.87390960531436690 ) ) ;
#105956 = CARTESIAN_POINT ( 'NONE',  ( -8.224510206698948167, 14.34966873604960824, 65.41557627198102409 ) ) ;
#105958 = CARTESIAN_POINT ( 'NONE',  ( 15.72974639402176855, 15.80617190586768217, 96.87609039468568994 ) ) ;
#105959 = CARTESIAN_POINT ( 'NONE',  ( 17.47980958864297918, 5.499999999999998224, 21.71653220162190934 ) ) ;
#105960 = CARTESIAN_POINT ( 'NONE',  ( 5.153800228976615827, -19.02544592524334988, 105.2094237280190185 ) ) ;
#105961 = CARTESIAN_POINT ( 'NONE',  ( -16.52544592524342804, 4.483927247898546575, 81.04057627198102409 ) ) ;
#105962 = CARTESIAN_POINT ( 'NONE',  ( -0.05219959533937732626, 21.53943276465977519, 32.50109039468568284 ) ) ;
#105963 = CARTESIAN_POINT ( 'NONE',  ( -5.719274019375978568, 21.55341960407610458, 70.20724293864769550 ) ) ;
#105964 = CARTESIAN_POINT ( 'NONE',  ( 16.46253265017146816, 9.564922557961045513, 36.66775706135233293 ) ) ;
#105965 = CARTESIAN_POINT ( 'NONE',  ( 23.31738231874054890, -16.94106989632523508, 147.0500000054623797 ) ) ;
#105966 = CARTESIAN_POINT ( 'NONE',  ( -13.89961937509977652, 13.97604488694528158, 80.62390960531436690 ) ) ;
#105967 = CARTESIAN_POINT ( 'NONE',  ( -8.224510206698948167, 14.34966873604960824, 55.41557627198102409 ) ) ;
#105968 = CARTESIAN_POINT ( 'NONE',  ( -14.29746914071049879, 8.314922557960819915, 40.83224293864769550 ) ) ;
#105969 = CARTESIAN_POINT ( 'NONE',  ( -8.224510206698735004, -14.34966873604973081, 104.5844237280190185 ) ) ;
#105970 = CARTESIAN_POINT ( 'NONE',  ( -19.02544592524334988, -5.153800228976617603, 68.95942372801896170 ) ) ;
#105971 = CARTESIAN_POINT ( 'NONE',  ( -18.22780087662122028, 5.500000000000031086, 78.51540105326107266 ) ) ;
#105972 = CARTESIAN_POINT ( 'NONE',  ( 16.51473224551069308, 9.474510206698969483, 109.1655762719810383 ) ) ;
#105973 = CARTESIAN_POINT ( 'NONE',  ( -12.06949235617756955, 12.14591786802309770, 75.62390960531439532 ) ) ;
#105974 = CARTESIAN_POINT ( 'NONE',  ( -17.49999999999999645, 5.499999999999992895, 58.71769037696435589 ) ) ;
#105976 = CARTESIAN_POINT ( 'NONE',  ( -21.53943276465977519, 0.05219959533907696930, 31.24890960531435979 ) ) ;
#105975 = CARTESIAN_POINT ( 'NONE',  ( -19.02544592524342804, 5.153800228976336051, 26.04057627198103120 ) ) ;
#105977 = CARTESIAN_POINT ( 'NONE',  ( -0.05219959533907301413, -21.53943276465977519, 72.49890960531435269 ) ) ;
#105978 = CARTESIAN_POINT ( 'NONE',  ( 8.314922557960818139, 14.29746914071049879, 109.5822429386476955 ) ) ;
#105980 = CARTESIAN_POINT ( 'NONE',  ( -13.89961937509977652, 13.97604488694528158, 45.62390960531433848 ) ) ;
#105979 = CARTESIAN_POINT ( 'NONE',  ( 14.29746914071037800, 8.314922557961029526, 71.66775706135234714 ) ) ;
#105981 = CARTESIAN_POINT ( 'NONE',  ( 15.72974639402176855, 15.80617190586768217, 56.87609039468568994 ) ) ;
#105982 = CARTESIAN_POINT ( 'NONE',  ( -16.53943276465976808, 0.05219959533911058130, 91.24890960531436690 ) ) ;
#105983 = ADVANCED_FACE ( 'NONE', ( #139113 ), #108776, .T. ) ;
#105984 = CARTESIAN_POINT ( 'NONE',  ( 193.3062444957835453, -155.7167183371837496, -4.999999999999999112 ) ) ;
#105985 = CARTESIAN_POINT ( 'NONE',  ( 36.91746824999999177, 11.99521256947799230, -10.02499999726881086 ) ) ;
#105986 = CARTESIAN_POINT ( 'NONE',  ( -10.81492255796078084, -18.62759615963271287, 32.08224293864769550 ) ) ;
#105987 = CARTESIAN_POINT ( 'NONE',  ( 19.50973618000807619, -5.499999999999992895, 37.50000000000000000 ) ) ;
#105989 = CARTESIAN_POINT ( 'NONE',  ( 16.52544592524342804, -4.483927247898539470, 38.54057627198103120 ) ) ;
#105988 = CARTESIAN_POINT ( 'NONE',  ( 16.55341960407618274, -4.379528057220086978, 56.04275706135235424 ) ) ;
#105990 = CARTESIAN_POINT ( 'NONE',  ( -15.80617190586745835, -15.72974639402198527, 71.87390960531438111 ) ) ;
#105991 = CARTESIAN_POINT ( 'NONE',  ( 10.81492255796078972, 18.62759615963270932, 64.58224293864769550 ) ) ;
#105992 = CARTESIAN_POINT ( 'NONE',  ( -19.76520975163527538, -12.18675982963091897, 170.0000000000000000 ) ) ;
#105994 = CARTESIAN_POINT ( 'NONE',  ( -19.05341960407611168, -5.049401038298163336, 106.4572429386476955 ) ) ;
#105993 = CARTESIAN_POINT ( 'NONE',  ( -13.97604488694547697, 13.89961937509957934, 78.12609039468567573 ) ) ;
#105995 = CARTESIAN_POINT ( 'NONE',  ( -16.46253265017160317, 9.564922557960807481, 45.83224293864769550 ) ) ;
#105996 = CARTESIAN_POINT ( 'NONE',  ( 9.564922557960805705, 16.46253265017160317, 24.58224293864769194 ) ) ;
#105997 = DIRECTION ( 'NONE',  ( 1.000000000000000000, 0.000000000000000000, 0.000000000000000000 ) ) ;
#105998 = CARTESIAN_POINT ( 'NONE',  ( -2.649999999999999911, -165.0000000000000000, -15.00000000000000000 ) ) ;
#105999 = ORIENTED_EDGE ( 'NONE', *, *, #50678, .T. ) ;
#106000 = CARTESIAN_POINT ( 'NONE',  ( 8.314922557961029526, -14.29746914071037800, 75.41775706135233293 ) ) ;
#106001 = CARTESIAN_POINT ( 'NONE',  ( 0.05219959533907565091, 21.53943276465977519, 99.99890960531436690 ) ) ;
#106002 = CARTESIAN_POINT ( 'NONE',  ( -19.03943276465977164, 0.05219959533909376836, 51.24890960531436690 ) ) ;
#106003 = CARTESIAN_POINT ( 'NONE',  ( -0.05219959533937732626, 21.53943276465977519, 42.50109039468567573 ) ) ;
#106004 = CARTESIAN_POINT ( 'NONE',  ( 5.049401038298161559, -19.05341960407611168, 102.7072429386476955 ) ) ;
#106006 = EDGE_CURVE ( 'NONE', #190052, #106384, #152451, .T. ) ;
#106005 = CARTESIAN_POINT ( 'NONE',  ( 9.564922557960805705, 16.46253265017160317, 114.5822429386476955 ) ) ;
#106007 = ORIENTED_EDGE ( 'NONE', *, *, #125179, .T. ) ;
#106008 = CARTESIAN_POINT ( 'NONE',  ( -21.52544592524334988, -5.823673210054445271, 33.95942372801901143 ) ) ;
#106010 = CARTESIAN_POINT ( 'NONE',  ( 19.02544592524334988, 5.153800228976608722, 91.45942372801900433 ) ) ;
#106009 = CARTESIAN_POINT ( 'NONE',  ( 16.46253265017160672, -9.564922557960803928, 113.3322429386476955 ) ) ;
#106011 = CARTESIAN_POINT ( 'NONE',  ( -5.049401038297874678, -19.05341960407617918, 34.79275706135233293 ) ) ;
#106012 = CARTESIAN_POINT ( 'NONE',  ( 21.53943276465977519, -0.05219959533907433946, 103.7489096053143669 ) ) ;
#106013 = CARTESIAN_POINT ( 'NONE',  ( -16.51473224551082808, 9.474510206698731452, 33.33442372801899722 ) ) ;
#106014 = CARTESIAN_POINT ( 'NONE',  ( 9.474510206698729675, 16.51473224551082808, 42.08442372801900433 ) ) ;
#106015 = CARTESIAN_POINT ( 'NONE',  ( 14.34966873604972726, -8.224510206698740333, 85.83442372801901854 ) ) ;
#106016 = DIRECTION ( 'NONE',  ( 0.000000000000000000, -0.000000000000000000, -1.000000000000000000 ) ) ;
#106017 = CARTESIAN_POINT ( 'NONE',  ( 19.02544592524343514, -5.153800228976328945, 58.54057627198102409 ) ) ;
#106018 = CARTESIAN_POINT ( 'NONE',  ( 21.53943276465977519, 0.05219959533937863772, 66.25109039468567573 ) ) ;
#106019 = CARTESIAN_POINT ( 'NONE',  ( -21.55341960407619339, 5.719274019375674811, 83.54275706135234714 ) ) ;
#106020 = CARTESIAN_POINT ( 'NONE',  ( -18.22780087662126647, -5.499999999999827693, 53.98236817873107185 ) ) ;
#106021 = CARTESIAN_POINT ( 'NONE',  ( -9.474510206698964154, 16.51473224551069663, 85.41557627198102409 ) ) ;
#106022 = CARTESIAN_POINT ( 'NONE',  ( -18.62759615963255300, -10.81492255796106328, 64.16775706135234714 ) ) ;
#106023 = CARTESIAN_POINT ( 'NONE',  ( -19.05341960407617563, 5.049401038297882671, 103.5427570613523329 ) ) ;
#106024 = CARTESIAN_POINT ( 'NONE',  ( 5.049401038298161559, -19.05341960407611168, 67.70724293864769550 ) ) ;
#106025 = CARTESIAN_POINT ( 'NONE',  ( -9.474510206698964154, 16.51473224551069663, 95.41557627198102409 ) ) ;
#106026 = CARTESIAN_POINT ( 'NONE',  ( -13.97604488694527625, -13.89961937509977652, 76.87390960531433848 ) ) ;
#106027 = CARTESIAN_POINT ( 'NONE',  ( -11.30153831258471975, -180.0000000000000000, -4.999999999999999112 ) ) ;
#106028 = CARTESIAN_POINT ( 'NONE',  ( 0.05219959533909260263, 19.03943276465977164, 64.99890960531436690 ) ) ;
#106029 = CARTESIAN_POINT ( 'NONE',  ( 5.719274019375991003, -21.55341960407610458, 102.7072429386476955 ) ) ;
#106030 = CARTESIAN_POINT ( 'NONE',  ( -14.34966873604972548, 8.224510206698743886, 93.33442372801901854 ) ) ;
#106031 = CARTESIAN_POINT ( 'NONE',  ( 8.788868155854864028, -0.9199430937698539479, -64.01178436185549003 ) ) ;
#106032 = CARTESIAN_POINT ( 'NONE',  ( -5.153800228976607833, 19.02544592524334988, 47.70942372801900433 ) ) ;
#106033 = CARTESIAN_POINT ( 'NONE',  ( 19.02544592524343514, -5.153800228976328945, 83.54057627198100988 ) ) ;
#106034 = CARTESIAN_POINT ( 'NONE',  ( -14.29746914071049879, 8.314922557960819915, 75.83224293864769550 ) ) ;
#106035 = CARTESIAN_POINT ( 'NONE',  ( 16.52544592524342804, -4.483927247898539470, 113.5405762719810383 ) ) ;
#106036 = CARTESIAN_POINT ( 'NONE',  ( 0.05219959533909260263, 19.03943276465977164, 109.9989096053143669 ) ) ;
#106037 = CARTESIAN_POINT ( 'NONE',  ( 5.153800228976335163, 19.02544592524342804, 104.7905762719809957 ) ) ;
#106038 = CARTESIAN_POINT ( 'NONE',  ( 13.89961937509978007, -13.97604488694527269, 83.12390960531438111 ) ) ;
#106039 = CARTESIAN_POINT ( 'NONE',  ( 19.02544592524334988, 5.153800228976608722, 31.45942372801900433 ) ) ;
#106040 = CARTESIAN_POINT ( 'NONE',  ( -8.314922557961024197, 14.29746914071037800, 92.91775706135236135 ) ) ;
#106041 = CARTESIAN_POINT ( 'NONE',  ( 9.564922557960805705, 16.46253265017160317, 79.58224293864769550 ) ) ;
#106042 = CARTESIAN_POINT ( 'NONE',  ( -10.72451020669870658, -18.67979575497194134, 49.58442372801901143 ) ) ;
#106043 = CARTESIAN_POINT ( 'NONE',  ( 10.81492255796078972, 18.62759615963270932, 44.58224293864769550 ) ) ;
#106044 = CARTESIAN_POINT ( 'NONE',  ( -10.72451020669898014, 18.67979575497178502, 115.4155762719810241 ) ) ;
#106045 = CARTESIAN_POINT ( 'NONE',  ( 18.62759615963271287, -10.81492255796078972, 68.33224293864769550 ) ) ;
#106046 = CARTESIAN_POINT ( 'NONE',  ( 4.379528057220339221, -16.55341960407611168, 92.70724293864770971 ) ) ;
#106047 = CARTESIAN_POINT ( 'NONE',  ( -19.05341960407617563, 5.049401038297882671, 58.54275706135234003 ) ) ;
#106048 = CARTESIAN_POINT ( 'NONE',  ( -19.02544592524342804, 5.153800228976336051, 31.04057627198102409 ) ) ;
#106049 = CARTESIAN_POINT ( 'NONE',  ( 16.51473224551069308, 9.474510206698969483, 79.16557627198103830 ) ) ;
#106050 = CARTESIAN_POINT ( 'NONE',  ( -9.474510206698964154, 16.51473224551069663, 85.41557627198102409 ) ) ;
#106051 = CARTESIAN_POINT ( 'NONE',  ( -27.73933785331498925, -9.013057229001049109, 139.4750000027311785 ) ) ;
#106052 = CARTESIAN_POINT ( 'NONE',  ( 12.14591786802309770, 12.06949235617756955, 99.37390960531436690 ) ) ;
#106053 = ORIENTED_EDGE ( 'NONE', *, *, #156075, .T. ) ;
#106054 = CARTESIAN_POINT ( 'NONE',  ( -0.05219959533910754901, -16.53943276465976808, 32.49890960531435979 ) ) ;
#106055 = CARTESIAN_POINT ( 'NONE',  ( -16.53943276465976808, -0.05219959533934237506, 28.75109039468567929 ) ) ;
#106056 = CARTESIAN_POINT ( 'NONE',  ( -0.05219959533937732626, 21.53943276465977519, 97.50109039468567573 ) ) ;
#106057 = CARTESIAN_POINT ( 'NONE',  ( 19.03943276465977164, -0.05219959533909143690, 98.74890960531436690 ) ) ;
#106058 = CARTESIAN_POINT ( 'NONE',  ( 21.55341960407619695, -5.719274019375665929, 21.04275706135234714 ) ) ;
#106059 = CARTESIAN_POINT ( 'NONE',  ( 5.049401038298161559, -19.05341960407611168, 42.70724293864767418 ) ) ;
#106060 = CARTESIAN_POINT ( 'NONE',  ( 14.34966873604972726, -8.224510206698740333, 45.83442372801901854 ) ) ;
#106061 = CARTESIAN_POINT ( 'NONE',  ( 19.05341960407617918, -5.049401038297876454, 106.0427570613523471 ) ) ;
#106062 = CARTESIAN_POINT ( 'NONE',  ( -0.05219959533909027116, -19.03943276465977164, 32.49890960531435979 ) ) ;
#106063 = CARTESIAN_POINT ( 'NONE',  ( 16.55341960407611168, 4.379528057220329451, 93.95724293864770971 ) ) ;
#106064 = CARTESIAN_POINT ( 'NONE',  ( 10.72451020669898902, -18.67979575497178502, 102.9155762719810383 ) ) ;
#106065 = CARTESIAN_POINT ( 'NONE',  ( -5.153800228976607833, 19.02544592524334988, 62.70942372801899722 ) ) ;
#106066 = CARTESIAN_POINT ( 'NONE',  ( -193.3062444957834884, -155.7167183371838064, 0.000000000000000000 ) ) ;
#106067 = CARTESIAN_POINT ( 'NONE',  ( 10.81492255796106328, -18.62759615963255655, 25.41775706135235779 ) ) ;
#106068 = CARTESIAN_POINT ( 'NONE',  ( -0.05219959533909027116, -19.03943276465977164, 22.49890960531436690 ) ) ;
#106069 = CARTESIAN_POINT ( 'NONE',  ( -19.03943276465977164, 0.05219959533909376836, 91.24890960531436690 ) ) ;
#106070 = CARTESIAN_POINT ( 'NONE',  ( -19.03943276465977164, 0.05219959533909376836, 91.24890960531436690 ) ) ;
#106072 = CARTESIAN_POINT ( 'NONE',  ( 14.29746914071049879, -8.314922557960816363, 78.33224293864770971 ) ) ;
#106071 = CARTESIAN_POINT ( 'NONE',  ( -10.72451020669870658, -18.67979575497194134, 29.58442372801901854 ) ) ;
#106073 = CARTESIAN_POINT ( 'NONE',  ( 16.51473224551069308, 9.474510206698969483, 79.16557627198103830 ) ) ;
#106074 = CARTESIAN_POINT ( 'NONE',  ( -0.05219959533936034679, 19.03943276465977164, 22.50109039468566152 ) ) ;
#106076 = CARTESIAN_POINT ( 'NONE',  ( -9.564922557961040184, 16.46253265017147172, 52.91775706135233293 ) ) ;
#106075 = CARTESIAN_POINT ( 'NONE',  ( 8.314922557961029526, -14.29746914071037800, 55.41775706135234714 ) ) ;
#106077 = CARTESIAN_POINT ( 'NONE',  ( 10.81492255796106328, -18.62759615963255655, 60.41775706135235424 ) ) ;
#106078 = AXIS2_PLACEMENT_3D ( 'NONE', #109962, #78619, #136336 ) ;
#106079 = CARTESIAN_POINT ( 'NONE',  ( -14.34966873604972548, 8.224510206698743886, 23.33442372801901499 ) ) ;
#106080 = CARTESIAN_POINT ( 'NONE',  ( 13.89961937509977652, -13.97604488694527269, 63.12390960531435979 ) ) ;
#106081 = CARTESIAN_POINT ( 'NONE',  ( 13.89961937509957401, 13.97604488694547697, 96.87609039468566152 ) ) ;
#106082 = CARTESIAN_POINT ( 'NONE',  ( 16.53943276465976808, 0.05219959533934440121, 66.25109039468567573 ) ) ;
#106083 = CARTESIAN_POINT ( 'NONE',  ( -21.55341960407619339, 5.719274019375674811, 103.5427570613523613 ) ) ;
#106084 = CARTESIAN_POINT ( 'NONE',  ( 5.049401038297881783, 19.05341960407617563, 82.29275706135229029 ) ) ;
#106085 = CARTESIAN_POINT ( 'NONE',  ( 5.153800228976335163, 19.02544592524342804, 49.79057627198100988 ) ) ;
#106086 = CARTESIAN_POINT ( 'NONE',  ( -15.72974639402197994, 15.80617190586746368, 65.62390960531436690 ) ) ;
#106088 = CARTESIAN_POINT ( 'NONE',  ( 13.89961937509957401, 13.97604488694547697, 71.87609039468567573 ) ) ;
#106087 = CARTESIAN_POINT ( 'NONE',  ( -4.379528057220328563, 16.55341960407611168, 75.20724293864769550 ) ) ;
#106089 = CARTESIAN_POINT ( 'NONE',  ( 17.50000000000000000, -5.500000000000000888, 120.0000000000000142 ) ) ;
#106090 = CARTESIAN_POINT ( 'NONE',  ( -5.153800228976607833, 19.02544592524334988, 42.70942372801901143 ) ) ;
#106091 = CARTESIAN_POINT ( 'NONE',  ( -12.06949235617739369, -12.14591786802326823, 109.3760903946857042 ) ) ;
#106092 = CARTESIAN_POINT ( 'NONE',  ( 4.483927247898545687, 16.52544592524342804, 69.79057627198102409 ) ) ;
#106094 = CARTESIAN_POINT ( 'NONE',  ( -8.571926809382601320, -26.38167802310801591, 145.2750000027311899 ) ) ;
#106093 = CARTESIAN_POINT ( 'NONE',  ( -21.55341960407619339, 5.719274019375674811, 103.5427570613523613 ) ) ;
#106095 = CARTESIAN_POINT ( 'NONE',  ( -18.67979575497178146, -10.72451020669898902, 101.6655762719810383 ) ) ;
#106096 = CARTESIAN_POINT ( 'NONE',  ( 19.03943276465977164, -0.05219959533909143690, 68.74890960531436690 ) ) ;
#106097 = CARTESIAN_POINT ( 'NONE',  ( 10.72451020669871369, 18.67979575497193778, 77.08442372801901854 ) ) ;
#106098 = CARTESIAN_POINT ( 'NONE',  ( 19.03943276465977164, -0.05219959533909143690, 63.74890960531435979 ) ) ;
#106099 = ORIENTED_EDGE ( 'NONE', *, *, #118820, .T. ) ;
#106100 = CARTESIAN_POINT ( 'NONE',  ( 16.53943276465976808, -0.05219959533910856209, 113.7489096053143527 ) ) ;
#106101 = CARTESIAN_POINT ( 'NONE',  ( -0.05219959533907301413, -21.53943276465977519, 27.49890960531435269 ) ) ;
#106102 = CARTESIAN_POINT ( 'NONE',  ( -8.314922557960811034, -14.29746914071050412, 62.08224293864769550 ) ) ;
#106103 = CARTESIAN_POINT ( 'NONE',  ( -19.02544592524342804, 5.153800228976336051, 46.04057627198101699 ) ) ;
#106104 = CARTESIAN_POINT ( 'NONE',  ( -8.224510206698948167, 14.34966873604960824, 95.41557627198102409 ) ) ;
#106105 = CARTESIAN_POINT ( 'NONE',  ( -21.53943276465977519, 0.05219959533907696930, 111.2489096053143669 ) ) ;
#106106 = CARTESIAN_POINT ( 'NONE',  ( 18.62759615963255655, 10.81492255796105972, 46.66775706135234714 ) ) ;
#106107 = CARTESIAN_POINT ( 'NONE',  ( 0.05219959533909260263, 19.03943276465977164, 24.99890960531435269 ) ) ;
#106108 = CARTESIAN_POINT ( 'NONE',  ( -16.55341960407617563, 4.379528057220093196, 53.54275706135234714 ) ) ;
#106109 = B_SPLINE_CURVE_WITH_KNOTS ( 'NONE', 3,
 ( #84730, #56415, #38251, #101917, #193946, #161591, #164600, #72592, #177775, #163599, #86742, #148427, #134266, #146408, #9922, #100901, #57426, #162585, #71581, #88742 ),
 .UNSPECIFIED., .F., .F.,
 ( 4, 2, 2, 2, 2, 2, 2, 2, 2, 4 ),
 ( 0.000000000000000000, 0.001368201656092171790, 0.002736403312184343579, 0.004104604968276515803, 0.005472806624368687159, 0.006841008280460856780, 0.008209209936553026402, 0.008893310764599102539, 0.009577411592645178676, 0.01094561324873732401 ),
 .UNSPECIFIED. ) ;
#106110 = CARTESIAN_POINT ( 'NONE',  ( -5.823673210054116645, -21.52544592524344225, 102.2905762719810383 ) ) ;
#106111 = CARTESIAN_POINT ( 'NONE',  ( -15.80617190586745835, -15.72974639402198527, 96.87390960531436690 ) ) ;
#106113 = CARTESIAN_POINT ( 'NONE',  ( -19.05341960407611168, -5.049401038298163336, 56.45724293864768129 ) ) ;
#106112 = CARTESIAN_POINT ( 'NONE',  ( 0.05219959533936267826, -19.03943276465977164, 20.00109039468567218 ) ) ;
#106114 = CARTESIAN_POINT ( 'NONE',  ( -5.049401038298153566, 19.05341960407611168, 110.2072429386476671 ) ) ;
#106115 = CARTESIAN_POINT ( 'NONE',  ( -21.53943276465977519, -0.05219959533937600094, 53.75109039468568994 ) ) ;
#106116 = CARTESIAN_POINT ( 'NONE',  ( 21.55341960407610458, 5.719274019375980345, 43.95724293864769550 ) ) ;
#106117 = CARTESIAN_POINT ( 'NONE',  ( -8.224510206698948167, 14.34966873604960824, 25.41557627198103120 ) ) ;
#106119 = CARTESIAN_POINT ( 'NONE',  ( -18.62759615963255300, -10.81492255796106328, 99.16775706135234714 ) ) ;
#106118 = CARTESIAN_POINT ( 'NONE',  ( -21.55341960407619339, 5.719274019375674811, 63.54275706135234003 ) ) ;
#106120 = CARTESIAN_POINT ( 'NONE',  ( 19.02544592524334988, 5.153800228976608722, 46.45942372801899012 ) ) ;
#106121 = CARTESIAN_POINT ( 'NONE',  ( 8.224510206698742110, 14.34966873604972548, 102.0844237280190185 ) ) ;
#106122 = CARTESIAN_POINT ( 'NONE',  ( -21.52544592524334988, -5.823673210054445271, 48.95942372801902565 ) ) ;
#106123 = CARTESIAN_POINT ( 'NONE',  ( -5.153800228976328057, -19.02544592524343514, 57.29057627198103120 ) ) ;
#106124 = CARTESIAN_POINT ( 'NONE',  ( -13.89961937509957401, -13.97604488694547875, 24.37609039468565442 ) ) ;
#106125 = CARTESIAN_POINT ( 'NONE',  ( 21.55341960407610458, 5.719274019375980345, 23.95724293864769550 ) ) ;
#106127 = CARTESIAN_POINT ( 'NONE',  ( 21.55341960407619695, -5.719274019375665929, 26.04275706135235779 ) ) ;
#106126 = B_SPLINE_CURVE_WITH_KNOTS ( 'NONE', 3,
 ( #72352, #88504, #167352, #150200, #136015, #10688, #134026, #197688, #182523, #44004, #11698, #135037, #196713, #102686, #164373, #87510, #12683, #195719, #136993, #121817, #117859, #60149, #179550, #28850 ),
 .UNSPECIFIED., .F., .F.,
 ( 4, 2, 2, 2, 2, 2, 2, 2, 2, 2, 2, 4 ),
 ( 0.000000000000000000, 0.002210131452840893417, 0.004420262905681786834, 0.008840525811363580608, 0.01326078871704536657, 0.01768105162272715428, 0.02210131452840894198, 0.02652157743409072621, 0.02873170888693162006, 0.03094184033977251391, 0.03315197179261340776, 0.03536210324545430161 ),
 .UNSPECIFIED. ) ;
#106128 = CARTESIAN_POINT ( 'NONE',  ( 18.62759615963271287, -10.81492255796078972, 83.33224293864769550 ) ) ;
#106129 = CARTESIAN_POINT ( 'NONE',  ( -12.14591786802326823, 12.06949235617739902, 38.12609039468567573 ) ) ;
#106131 = CARTESIAN_POINT ( 'NONE',  ( -5.719274019375978568, 21.55341960407610458, 85.20724293864770971 ) ) ;
#106130 = CARTESIAN_POINT ( 'NONE',  ( 17.49999999999999289, -4.601506711240598513, 36.47308481467552355 ) ) ;
#106133 = CARTESIAN_POINT ( 'NONE',  ( -14.34966873604960291, -8.224510206698953496, 71.66557627198100988 ) ) ;
#106132 = CARTESIAN_POINT ( 'NONE',  ( 14.34966873604972726, -8.224510206698740333, 60.83442372801901854 ) ) ;
#106134 = CARTESIAN_POINT ( 'NONE',  ( -20.63676584477901699, 20.25987216150948811, -49.65115959356506892 ) ) ;
#106135 = CARTESIAN_POINT ( 'NONE',  ( -16.51473224551082808, 9.474510206698731452, 108.3344237280190043 ) ) ;
#106136 = ADVANCED_FACE ( 'NONE', ( #146071 ), #144080, .T. ) ;
#106137 = CARTESIAN_POINT ( 'NONE',  ( 10.81492255796078972, 18.62759615963270932, 34.58224293864770260 ) ) ;
#106138 = FACE_OUTER_BOUND ( 'NONE', #29163, .T. ) ;
#106139 = CARTESIAN_POINT ( 'NONE',  ( 14.34966873604972726, -8.224510206698740333, 45.83442372801901854 ) ) ;
#106140 = CARTESIAN_POINT ( 'NONE',  ( -5.719274019375665041, -21.55341960407619695, 19.79275706135235069 ) ) ;
#106141 = B_SPLINE_CURVE_WITH_KNOTS ( 'NONE', 3,
 ( #103695, #71358, #166374, #74355, #135043, #163370, #27870, #12689 ),
 .UNSPECIFIED., .F., .F.,
 ( 4, 2, 2, 4 ),
 ( 2.784816081883512217E-07, 0.0003049387032676472830, 0.0006095989249271061916, 0.001218919368246023033 ),
 .UNSPECIFIED. ) ;
#106142 = CARTESIAN_POINT ( 'NONE',  ( 0.05219959533907565091, 21.53943276465977519, 29.99890960531435979 ) ) ;
#106143 = CARTESIAN_POINT ( 'NONE',  ( -16.52544592524335698, -4.483927247898792601, 68.95942372801901854 ) ) ;
#106144 = CARTESIAN_POINT ( 'NONE',  ( -19.02544592524342804, 5.153800228976336051, 91.04057627198100988 ) ) ;
#106146 = CARTESIAN_POINT ( 'NONE',  ( 5.049401038298161559, -19.05341960407611168, 27.70724293864769550 ) ) ;
#106145 = CARTESIAN_POINT ( 'NONE',  ( 10.81492255796106328, -18.62759615963255655, 50.41775706135235424 ) ) ;
#106147 = CARTESIAN_POINT ( 'NONE',  ( -9.474510206698964154, 16.51473224551069663, 115.4155762719810241 ) ) ;
#106148 = ORIENTED_EDGE ( 'NONE', *, *, #3703, .F. ) ;
#106149 = CARTESIAN_POINT ( 'NONE',  ( -19.02544592524334988, -5.153800228976617603, 38.95942372801900433 ) ) ;
#106150 = CARTESIAN_POINT ( 'NONE',  ( 14.29746914071037800, 8.314922557961029526, 46.66775706135234714 ) ) ;
#106151 = CARTESIAN_POINT ( 'NONE',  ( -18.67979575497178146, -10.72451020669898902, 21.66557627198102409 ) ) ;
#106152 = CARTESIAN_POINT ( 'NONE',  ( 16.51473224551069308, 9.474510206698969483, 79.16557627198103830 ) ) ;
#106153 = CARTESIAN_POINT ( 'NONE',  ( -14.29746914071037622, -8.314922557961029526, 94.16775706135237556 ) ) ;
#106154 = CARTESIAN_POINT ( 'NONE',  ( 26.03370437638686852, 6.875205692009825675, 160.5968874236875195 ) ) ;
#106155 = CARTESIAN_POINT ( 'NONE',  ( -12.14591786802309592, -12.06949235617757132, 96.87390960531436690 ) ) ;
#106156 = CARTESIAN_POINT ( 'NONE',  ( 21.55341960407610458, 5.719274019375980345, 38.95724293864768839 ) ) ;
#106157 = CARTESIAN_POINT ( 'NONE',  ( -19.03943276465977164, 0.05219959533909376836, 31.24890960531435979 ) ) ;
#106158 = CARTESIAN_POINT ( 'NONE',  ( -12.06949235617739369, -12.14591786802326823, 69.37609039468567573 ) ) ;
#106159 = CARTESIAN_POINT ( 'NONE',  ( 15.80617190586746368, 15.72974639402197994, 114.3739096053143527 ) ) ;
#106160 = CARTESIAN_POINT ( 'NONE',  ( -9.474510206698720793, -16.51473224551083518, 79.58442372801899012 ) ) ;
#106161 = CARTESIAN_POINT ( 'NONE',  ( 9.564922557960805705, 16.46253265017160317, 44.58224293864769550 ) ) ;
#106162 = CARTESIAN_POINT ( 'NONE',  ( -15.80617190586745835, -15.72974639402198527, 66.87390960531436690 ) ) ;
#106163 = CARTESIAN_POINT ( 'NONE',  ( -16.46253265017160317, 9.564922557960807481, 115.8322429386477097 ) ) ;
#106164 = CARTESIAN_POINT ( 'NONE',  ( -5.719274019375665041, -21.55341960407619695, 89.79275706135236135 ) ) ;
#106165 = CARTESIAN_POINT ( 'NONE',  ( -9.564922557960796823, -16.46253265017161027, 62.08224293864769550 ) ) ;
#106166 = CARTESIAN_POINT ( 'NONE',  ( -16.52544592524335698, -4.483927247898792601, 48.95942372801902565 ) ) ;
#106167 = CARTESIAN_POINT ( 'NONE',  ( -9.474510206698964154, 16.51473224551069663, 60.41557627198102409 ) ) ;
#106168 = CARTESIAN_POINT ( 'NONE',  ( -10.81492255796105439, 18.62759615963255655, 77.91775706135231871 ) ) ;
#106169 = CARTESIAN_POINT ( 'NONE',  ( 9.474510206698729675, 16.51473224551082808, 42.08442372801900433 ) ) ;
#106170 = CARTESIAN_POINT ( 'NONE',  ( -5.049401038297874678, -19.05341960407617918, 49.79275706135231871 ) ) ;
#106171 = CARTESIAN_POINT ( 'NONE',  ( -10.72451020669870658, -18.67979575497194134, 54.58442372801901143 ) ) ;
#106172 = CARTESIAN_POINT ( 'NONE',  ( -17.49999999999999645, -5.500000000000000888, 120.0000000000000142 ) ) ;
#106173 = CARTESIAN_POINT ( 'NONE',  ( 9.474510206698729675, 16.51473224551082808, 47.08442372801900433 ) ) ;
#106174 = CARTESIAN_POINT ( 'NONE',  ( -16.51473224551069308, -9.474510206698971260, 101.6655762719810241 ) ) ;
#106175 = CARTESIAN_POINT ( 'NONE',  ( -13.97604488694527625, -13.89961937509977652, 71.87390960531433848 ) ) ;
#106176 = CARTESIAN_POINT ( 'NONE',  ( 14.29746914071049879, -8.314922557960816363, 23.33224293864769194 ) ) ;
#106178 = CARTESIAN_POINT ( 'NONE',  ( 15.72974639402176855, 15.80617190586768217, 96.87609039468568994 ) ) ;
#106177 = CARTESIAN_POINT ( 'NONE',  ( 10.81492255796078972, 18.62759615963270932, 29.58224293864769905 ) ) ;
#106179 = CARTESIAN_POINT ( 'NONE',  ( 29.86685920354754842, -21.69954338932559068, -1.824999997268813345 ) ) ;
#106180 = CARTESIAN_POINT ( 'NONE',  ( -18.22780087662122028, 5.500000000000031086, 38.51540105326107266 ) ) ;
#106181 = CARTESIAN_POINT ( 'NONE',  ( 15.80617190586769283, -15.72974639402175789, 95.62609039468568994 ) ) ;
#106182 = CARTESIAN_POINT ( 'NONE',  ( -26.58496454517000629, 7.626754437231443084, 167.9682100371138915 ) ) ;
#106183 = CARTESIAN_POINT ( 'NONE',  ( -13.89961937509977652, 13.97604488694528158, 40.62390960531435979 ) ) ;
#106184 = DIRECTION ( 'NONE',  ( -0.000000000000000000, 1.000000000000000000, -0.000000000000000000 ) ) ;
#106185 = CARTESIAN_POINT ( 'NONE',  ( 33.74157273865942130, 3.640299887980672722, 99.13851753912355491 ) ) ;
#106186 = CARTESIAN_POINT ( 'NONE',  ( -4.379528057220086978, -16.55341960407618274, 44.79275706135234714 ) ) ;
#106187 = CARTESIAN_POINT ( 'NONE',  ( 5.823673210054125526, 21.52544592524343514, 64.79057627198103830 ) ) ;
#106188 = CARTESIAN_POINT ( 'NONE',  ( 4.483927247898545687, 16.52544592524342804, 44.79057627198103120 ) ) ;
#106190 = CARTESIAN_POINT ( 'NONE',  ( 9.564922557960805705, 16.46253265017160317, 109.5822429386476955 ) ) ;
#106189 = CARTESIAN_POINT ( 'NONE',  ( 14.29746914071049879, -8.314922557960816363, 108.3322429386477097 ) ) ;
#106191 = CARTESIAN_POINT ( 'NONE',  ( 15.80617190586769283, -15.72974639402175789, 30.62609039468567929 ) ) ;
#106192 = CARTESIAN_POINT ( 'NONE',  ( 9.474510206698729675, 16.51473224551082808, 42.08442372801900433 ) ) ;
#106193 = CARTESIAN_POINT ( 'NONE',  ( -16.55341960407611168, -4.379528057220339221, 111.4572429386476813 ) ) ;
#106194 = CARTESIAN_POINT ( 'NONE',  ( -18.62759615963255300, -10.81492255796106328, 69.16775706135234714 ) ) ;
#106195 = CARTESIAN_POINT ( 'NONE',  ( 17.40805194822031865, -6.112264579159335298, 33.33371272510612471 ) ) ;
#106196 = CARTESIAN_POINT ( 'NONE',  ( 12.06949235617757843, -12.14591786802309237, 23.12390960531436335 ) ) ;
#106197 = CARTESIAN_POINT ( 'NONE',  ( 29.86685920354754842, -21.69954338932559068, -4.324999997268814234 ) ) ;
#106198 = CARTESIAN_POINT ( 'NONE',  ( -10.81492255796078084, -18.62759615963271287, 22.08224293864769194 ) ) ;
#106199 = CARTESIAN_POINT ( 'NONE',  ( 14.34966873604960469, 8.224510206698951720, 89.16557627198102409 ) ) ;
#106200 = CARTESIAN_POINT ( 'NONE',  ( -17.60691670004650433, -5.500000000000071054, 39.13333313366439370 ) ) ;
#106201 = CARTESIAN_POINT ( 'NONE',  ( -5.049401038298153566, 19.05341960407611168, 80.20724293864769550 ) ) ;
#106202 = CARTESIAN_POINT ( 'NONE',  ( 8.224510206698953496, -14.34966873604960469, 77.91557627198102409 ) ) ;
#106203 = CARTESIAN_POINT ( 'NONE',  ( 16.46253265017146816, 9.564922557961045513, 106.6677570613523471 ) ) ;
#106204 = CARTESIAN_POINT ( 'NONE',  ( -10.81492255796078084, -18.62759615963271287, 52.08224293864768839 ) ) ;
#106205 = ORIENTED_EDGE ( 'NONE', *, *, #92889, .F. ) ;
#106206 = CARTESIAN_POINT ( 'NONE',  ( -12.06949235617756955, 12.14591786802309770, 115.6239096053143669 ) ) ;
#106208 = CARTESIAN_POINT ( 'NONE',  ( 18.62759615963271287, -10.81492255796078972, 73.33224293864769550 ) ) ;
#106207 = CARTESIAN_POINT ( 'NONE',  ( 19.03943276465977164, -0.05219959533909143690, 78.74890960531436690 ) ) ;
#106210 = CARTESIAN_POINT ( 'NONE',  ( -5.049401038298153566, 19.05341960407611168, 90.20724293864766707 ) ) ;
#106209 = CARTESIAN_POINT ( 'NONE',  ( 14.29746914071037800, 8.314922557961029526, 106.6677570613523756 ) ) ;
#106211 = CARTESIAN_POINT ( 'NONE',  ( -13.97604488694547697, 13.89961937509957934, 73.12609039468568994 ) ) ;
#106212 = CARTESIAN_POINT ( 'NONE',  ( -21.53943276465977519, -0.05219959533937600094, 93.75109039468567573 ) ) ;
#106213 = CARTESIAN_POINT ( 'NONE',  ( 18.62759615963271287, -10.81492255796078972, 68.33224293864769550 ) ) ;
#106214 = CARTESIAN_POINT ( 'NONE',  ( 13.89961937509977652, -13.97604488694527269, 113.1239096053143527 ) ) ;
#106215 = CARTESIAN_POINT ( 'NONE',  ( -19.05341960407611168, -5.049401038298163336, 36.45724293864766707 ) ) ;
#106216 = CARTESIAN_POINT ( 'NONE',  ( 16.53943276465976808, 0.05219959533934440121, 106.2510903946856757 ) ) ;
#106217 = CARTESIAN_POINT ( 'NONE',  ( -19.03943276465977164, 0.05219959533909376836, 61.24890960531436690 ) ) ;
#106218 = CARTESIAN_POINT ( 'NONE',  ( 4.379528057220092307, 16.55341960407617563, 22.29275706135235069 ) ) ;
#106219 = CARTESIAN_POINT ( 'NONE',  ( 16.62475595723695676, 7.163666690055253028, 51.97286648189534475 ) ) ;
#106220 = CARTESIAN_POINT ( 'NONE',  ( 21.52544592524334988, 5.823673210054432836, 111.4594237280190328 ) ) ;
#106221 = CARTESIAN_POINT ( 'NONE',  ( 4.379528057220339221, -16.55341960407611168, 77.70724293864770971 ) ) ;
#106222 = CARTESIAN_POINT ( 'NONE',  ( 10.81492255796078972, 18.62759615963270932, 114.5822429386477097 ) ) ;
#106223 = CARTESIAN_POINT ( 'NONE',  ( -5.823673210054116645, -21.52544592524344225, 97.29057627198105251 ) ) ;
#106224 = DIRECTION ( 'NONE',  ( -1.000000000000000000, 0.000000000000000000, 0.000000000000000000 ) ) ;
#106225 = CARTESIAN_POINT ( 'NONE',  ( 18.62759615963271287, -10.81492255796078972, 58.33224293864768839 ) ) ;
#106226 = CARTESIAN_POINT ( 'NONE',  ( 12.14591786802327356, -12.06949235617739191, 75.62609039468567573 ) ) ;
#106227 = CARTESIAN_POINT ( 'NONE',  ( -14.34966873604960291, -8.224510206698953496, 101.6655762719810383 ) ) ;
#106228 = CARTESIAN_POINT ( 'NONE',  ( 16.46253265017160672, -9.564922557960803928, 58.33224293864769550 ) ) ;
#106229 =( NAMED_UNIT ( * ) PLANE_ANGLE_UNIT ( ) SI_UNIT ( $, .RADIAN. ) );
#106230 = CARTESIAN_POINT ( 'NONE',  ( 4.483927247898790824, -16.52544592524335698, 110.2094237280190185 ) ) ;
#106231 = CARTESIAN_POINT ( 'NONE',  ( -21.52544592524334988, -5.823673210054445271, 48.95942372801902565 ) ) ;
#106232 = CARTESIAN_POINT ( 'NONE',  ( -5.153800228976328057, -19.02544592524343514, 102.2905762719810383 ) ) ;
#106233 = CARTESIAN_POINT ( 'NONE',  ( 0.05219959533937995610, -21.53943276465977519, 85.00109039468568994 ) ) ;
#106234 = CARTESIAN_POINT ( 'NONE',  ( 19.03943276465977164, -0.05219959533909143690, 23.74890960531435269 ) ) ;
#106236 = EDGE_CURVE ( 'NONE', #58436, #50775, #115755, .T. ) ;
#106235 = CARTESIAN_POINT ( 'NONE',  ( -9.564922557960796823, -16.46253265017161027, 42.08224293864769550 ) ) ;
#106237 = ORIENTED_EDGE ( 'NONE', *, *, #10139, .T. ) ;
#106238 = CARTESIAN_POINT ( 'NONE',  ( 18.67979575497194134, -10.72451020669871369, 75.83442372801900433 ) ) ;
#106239 = CARTESIAN_POINT ( 'NONE',  ( -9.564922557960796823, -16.46253265017161027, 102.0822429386477097 ) ) ;
#106240 = CARTESIAN_POINT ( 'NONE',  ( -13.89961937509957401, -13.97604488694547875, 74.37609039468566152 ) ) ;
#106241 = CARTESIAN_POINT ( 'NONE',  ( -18.62759615963255300, -10.81492255796106328, 44.16775706135234714 ) ) ;
#106242 = CARTESIAN_POINT ( 'NONE',  ( 16.55341960407618274, -4.379528057220086978, 21.04275706135234714 ) ) ;
#106243 = CARTESIAN_POINT ( 'NONE',  ( -19.03943276465977164, -0.05219959533935918106, 68.75109039468566152 ) ) ;
#106244 = CARTESIAN_POINT ( 'NONE',  ( -19.02544592524342804, 5.153800228976336051, 56.04057627198100988 ) ) ;
#106245 = CARTESIAN_POINT ( 'NONE',  ( 5.049401038297881783, 19.05341960407617563, 82.29275706135229029 ) ) ;
#106246 = CARTESIAN_POINT ( 'NONE',  ( -14.34966873604960291, -8.224510206698953496, 31.66557627198102054 ) ) ;
#106247 = CARTESIAN_POINT ( 'NONE',  ( -16.51473224551082808, 9.474510206698731452, 73.33442372801900433 ) ) ;
#106248 = CARTESIAN_POINT ( 'NONE',  ( 4.483927247898545687, 16.52544592524342804, 44.79057627198103120 ) ) ;
#106249 = CARTESIAN_POINT ( 'NONE',  ( -16.46253265017146816, -9.564922557961047289, 59.16775706135233293 ) ) ;
#106250 = CARTESIAN_POINT ( 'NONE',  ( 4.379528057220092307, 16.55341960407617563, 52.29275706135236135 ) ) ;
#106251 = CARTESIAN_POINT ( 'NONE',  ( 19.02544592524334988, 5.153800228976608722, 26.45942372801899722 ) ) ;
#106252 = CARTESIAN_POINT ( 'NONE',  ( 16.46253265017160672, -9.564922557960803928, 33.33224293864770260 ) ) ;
#106253 = CARTESIAN_POINT ( 'NONE',  ( -16.61371651742603106, -7.165104196376047341, 66.14584930007005426 ) ) ;
#106254 = CARTESIAN_POINT ( 'NONE',  ( 4.379528057220092307, 16.55341960407617563, 42.29275706135235424 ) ) ;
#106255 = CARTESIAN_POINT ( 'NONE',  ( 15.50000000000000355, 7.499999999999998224, 118.0000000000000142 ) ) ;
#106256 = CARTESIAN_POINT ( 'NONE',  ( -22.44159573604009950, -16.30477369853688430, 141.0750000027311728 ) ) ;
#106257 = CARTESIAN_POINT ( 'NONE',  ( 13.89961937509977652, -13.97604488694527269, 98.12390960531433848 ) ) ;
#106258 = DIRECTION ( 'NONE',  ( -1.000000000000000000, 0.000000000000000000, 0.000000000000000000 ) ) ;
#106259 = ORIENTED_EDGE ( 'NONE', *, *, #137680, .F. ) ;
#106260 = CARTESIAN_POINT ( 'NONE',  ( 19.03943276465977164, 0.05219959533936151252, 91.25109039468566152 ) ) ;
#106261 = CARTESIAN_POINT ( 'NONE',  ( 5.719274019375991003, -21.55341960407610458, 22.70724293864769194 ) ) ;
#106263 = CARTESIAN_POINT ( 'NONE',  ( -9.564922557961040184, 16.46253265017147172, 102.9177570613523329 ) ) ;
#106262 = CARTESIAN_POINT ( 'NONE',  ( 9.474510206698729675, 16.51473224551082808, 22.08442372801899722 ) ) ;
#106264 = CARTESIAN_POINT ( 'NONE',  ( 16.52544592524342804, -4.483927247898539470, 108.5405762719810241 ) ) ;
#106265 = CARTESIAN_POINT ( 'NONE',  ( -9.474510206698964154, 16.51473224551069663, 40.41557627198103120 ) ) ;
#106266 = CARTESIAN_POINT ( 'NONE',  ( -18.67979575497178146, -10.72451020669898902, 56.66557627198103830 ) ) ;
#106267 = CARTESIAN_POINT ( 'NONE',  ( -4.483927247898539470, -16.52544592524342804, 112.2905762719810241 ) ) ;
#106268 = CARTESIAN_POINT ( 'NONE',  ( -19.03943276465977164, -0.05219959533935918106, 73.75109039468566152 ) ) ;
#106269 = CARTESIAN_POINT ( 'NONE',  ( 8.314922557960818139, 14.29746914071049879, 39.58224293864769550 ) ) ;
#106270 = CARTESIAN_POINT ( 'NONE',  ( 16.51473224551069308, 9.474510206698969483, 109.1655762719810383 ) ) ;
#106271 = CARTESIAN_POINT ( 'NONE',  ( -5.719274019375665041, -21.55341960407619695, 89.79275706135236135 ) ) ;
#106272 = CARTESIAN_POINT ( 'NONE',  ( 21.52544592524344225, -5.823673210054117533, 83.54057627198102409 ) ) ;
#106273 = CARTESIAN_POINT ( 'NONE',  ( 18.62759615963255655, 10.81492255796105972, 61.66775706135235424 ) ) ;
#106274 = CARTESIAN_POINT ( 'NONE',  ( -21.53943276465977519, -0.05219959533937600094, 63.75109039468568284 ) ) ;
#106275 = CARTESIAN_POINT ( 'NONE',  ( -19.03943276465977164, 0.05219959533909376836, 96.24890960531436690 ) ) ;
#106277 = CARTESIAN_POINT ( 'NONE',  ( 18.67979575497194134, -10.72451020669871369, 55.83442372801901854 ) ) ;
#106276 = CARTESIAN_POINT ( 'NONE',  ( 4.483927247898790824, -16.52544592524335698, 95.20942372801903275 ) ) ;
#106278 = CARTESIAN_POINT ( 'NONE',  ( 4.379528057220339221, -16.55341960407611168, 112.7072429386476955 ) ) ;
#106279 = CARTESIAN_POINT ( 'NONE',  ( -14.34966873604960291, -8.224510206698953496, 71.66557627198100988 ) ) ;
#106280 = CARTESIAN_POINT ( 'NONE',  ( -16.53943276465976808, 0.05219959533911058130, 31.24890960531435979 ) ) ;
#106281 = CARTESIAN_POINT ( 'NONE',  ( -21.55341960407610458, -5.719274019375992779, 41.45724293864769550 ) ) ;
#106282 = CARTESIAN_POINT ( 'NONE',  ( 16.51473224551069308, 9.474510206698969483, 64.16557627198102409 ) ) ;
#106283 = CARTESIAN_POINT ( 'NONE',  ( -13.97604488694527625, -13.89961937509977652, 51.87390960531436690 ) ) ;
#106284 = CARTESIAN_POINT ( 'NONE',  ( -15.80617190586745835, -15.72974639402198527, 56.87390960531436690 ) ) ;
#106285 = CARTESIAN_POINT ( 'NONE',  ( 13.89961937509957401, 13.97604488694547697, 41.87609039468566152 ) ) ;
#106287 = CARTESIAN_POINT ( 'NONE',  ( -16.55341960407611168, -4.379528057220339221, 51.45724293864770260 ) ) ;
#106286 = CARTESIAN_POINT ( 'NONE',  ( -16.36317988757057051, -7.306389748694945396, 40.90210391636773579 ) ) ;
#106288 = CARTESIAN_POINT ( 'NONE',  ( -21.55341960407610458, -5.719274019375992779, 31.45724293864769550 ) ) ;
#106289 = EDGE_LOOP ( 'NONE', ( #150748, #69993, #119880, #87663 ) ) ;
#106290 = ORIENTED_EDGE ( 'NONE', *, *, #124857, .T. ) ;
#106291 = DIRECTION ( 'NONE',  ( -1.000000000000000000, -0.000000000000000000, -0.000000000000000000 ) ) ;
#106292 = CARTESIAN_POINT ( 'NONE',  ( 16.52544592524335698, 4.483927247898782831, 76.45942372801901854 ) ) ;
#106293 = CARTESIAN_POINT ( 'NONE',  ( -0.05219959533936034679, 19.03943276465977164, 77.50109039468566152 ) ) ;
#106294 = CARTESIAN_POINT ( 'NONE',  ( 12.06949235617757843, -12.14591786802309237, 43.12390960531435269 ) ) ;
#106295 = CARTESIAN_POINT ( 'NONE',  ( -30.00000000000000000, -5.204748896376250896E-15, 42.49999999999999289 ) ) ;
#106296 = CARTESIAN_POINT ( 'NONE',  ( -8.224510206698948167, 14.34966873604960824, 30.41557627198101699 ) ) ;
#106297 = CARTESIAN_POINT ( 'NONE',  ( -9.474510206698964154, 16.51473224551069663, 45.41557627198103120 ) ) ;
#106298 = CARTESIAN_POINT ( 'NONE',  ( -13.97604488694527625, -13.89961937509977652, 76.87390960531433848 ) ) ;
#106299 = CARTESIAN_POINT ( 'NONE',  ( -5.153800228976328057, -19.02544592524343514, 37.29057627198102409 ) ) ;
#106300 = CARTESIAN_POINT ( 'NONE',  ( 5.719274019375673035, 21.55341960407619339, 47.29275706135234003 ) ) ;
#106301 = CARTESIAN_POINT ( 'NONE',  ( 16.51473224551069308, 9.474510206698969483, 59.16557627198102409 ) ) ;
#106302 = CARTESIAN_POINT ( 'NONE',  ( 18.10062525802553424, -5.500000000000022204, 81.01383468041919400 ) ) ;
#106303 = CARTESIAN_POINT ( 'NONE',  ( 19.05341960407611168, 5.049401038298154454, 63.95724293864769550 ) ) ;
#106304 = CARTESIAN_POINT ( 'NONE',  ( -18.62759615963270932, 10.81492255796079327, 30.83224293864770260 ) ) ;
#106305 = AXIS2_PLACEMENT_3D ( 'NONE', #6188, #7186, #99196 ) ;
#106306 = CARTESIAN_POINT ( 'NONE',  ( 14.29746914071049879, -8.314922557960816363, 113.3322429386476955 ) ) ;
#106307 = CARTESIAN_POINT ( 'NONE',  ( 5.823673210054125526, 21.52544592524343514, 24.79057627198103120 ) ) ;
#106308 = CARTESIAN_POINT ( 'NONE',  ( -4.483927247898782831, 16.52544592524335698, 97.70942372801904696 ) ) ;
#106309 = CARTESIAN_POINT ( 'NONE',  ( 5.719274019375673035, 21.55341960407619339, 112.2927570613523471 ) ) ;
#106310 = CARTESIAN_POINT ( 'NONE',  ( -0.05219959533934338120, 16.53943276465976808, 67.50109039468568994 ) ) ;
#106311 = CARTESIAN_POINT ( 'NONE',  ( 13.97604488694527802, 13.89961937509977652, 114.3739096053143669 ) ) ;
#106312 = CARTESIAN_POINT ( 'NONE',  ( -16.53943276465976808, -0.05219959533934237506, 53.75109039468568994 ) ) ;
#106313 = CARTESIAN_POINT ( 'NONE',  ( -16.52544592524335698, -4.483927247898792601, 33.95942372801901143 ) ) ;
#106314 = CARTESIAN_POINT ( 'NONE',  ( -9.474510206698964154, 16.51473224551069663, 110.4155762719810383 ) ) ;
#106315 = CARTESIAN_POINT ( 'NONE',  ( 14.34966873604972726, -8.224510206698740333, 30.83442372801902209 ) ) ;
#106316 = CARTESIAN_POINT ( 'NONE',  ( -9.474510206698964154, 16.51473224551069663, 35.41557627198102409 ) ) ;
#106317 = CARTESIAN_POINT ( 'NONE',  ( 18.67979575497194134, -10.72451020669871369, 20.83442372801901143 ) ) ;
#106318 = CARTESIAN_POINT ( 'NONE',  ( -12.06949235617739369, -12.14591786802326823, 24.37609039468567573 ) ) ;
#106319 = CARTESIAN_POINT ( 'NONE',  ( -8.224510206698735004, -14.34966873604973081, 79.58442372801903275 ) ) ;
#106320 = DIRECTION ( 'NONE',  ( -1.000000000000000000, 0.000000000000000000, 0.000000000000000000 ) ) ;
#106321 = CARTESIAN_POINT ( 'NONE',  ( 21.53943276465977519, 0.05219959533937863772, 91.25109039468568994 ) ) ;
#106322 = CARTESIAN_POINT ( 'NONE',  ( 19.02544592524334988, 5.153800228976608722, 86.45942372801900433 ) ) ;
#106323 = CARTESIAN_POINT ( 'NONE',  ( -14.34966873604960291, -8.224510206698953496, 61.66557627198103120 ) ) ;
#106324 = CARTESIAN_POINT ( 'NONE',  ( 4.483927247898545687, 16.52544592524342804, 109.7905762719810383 ) ) ;
#106326 = CARTESIAN_POINT ( 'NONE',  ( -6.941067294099585006, 1.351053078614677716, -64.37011660792191492 ) ) ;
#106325 = CARTESIAN_POINT ( 'NONE',  ( -16.51473224551082808, 9.474510206698731452, 43.33442372801900433 ) ) ;
#106327 = CARTESIAN_POINT ( 'NONE',  ( 18.67979575497194134, -10.72451020669871369, 55.83442372801901854 ) ) ;
#106328 = CARTESIAN_POINT ( 'NONE',  ( -19.05341960407617563, 5.049401038297882671, 103.5427570613523329 ) ) ;
#106329 = DIRECTION ( 'NONE',  ( 0.000000000000000000, 0.000000000000000000, -1.000000000000000000 ) ) ;
#106330 = CARTESIAN_POINT ( 'NONE',  ( 5.049401038298161559, -19.05341960407611168, 102.7072429386476955 ) ) ;
#106331 = CARTESIAN_POINT ( 'NONE',  ( 5.719274019375991003, -21.55341960407610458, 77.70724293864770971 ) ) ;
#106332 = CARTESIAN_POINT ( 'NONE',  ( 19.05341960407617918, -5.049401038297876454, 91.04275706135234714 ) ) ;
#106333 = CARTESIAN_POINT ( 'NONE',  ( 16.51473224551069308, 9.474510206698969483, 109.1655762719810383 ) ) ;
#106334 = CARTESIAN_POINT ( 'NONE',  ( -4.817327537821083361, -27.72747260876182551, 139.9999999999999432 ) ) ;
#106335 = CARTESIAN_POINT ( 'NONE',  ( -8.314922557960811034, -14.29746914071050412, 102.0822429386476955 ) ) ;
#106336 = CARTESIAN_POINT ( 'NONE',  ( 21.52544592524334988, 5.823673210054432836, 96.45942372801901854 ) ) ;
#106337 = CARTESIAN_POINT ( 'NONE',  ( 13.97604488694527802, 13.89961937509977652, 39.37390960531435269 ) ) ;
#106338 = CARTESIAN_POINT ( 'NONE',  ( 18.62759615963255655, 10.81492255796105972, 51.66775706135234714 ) ) ;
#106339 = VECTOR ( 'NONE', #10163, 1000.000000000000000 ) ;
#106340 = CARTESIAN_POINT ( 'NONE',  ( -10.81492255796105439, 18.62759615963255655, 82.91775706135234714 ) ) ;
#106341 = CARTESIAN_POINT ( 'NONE',  ( -14.34966873604972548, 8.224510206698743886, 103.3344237280190043 ) ) ;
#106342 = CARTESIAN_POINT ( 'NONE',  ( 9.474510206698971260, -16.51473224551069308, 67.91557627198102409 ) ) ;
#106343 = CARTESIAN_POINT ( 'NONE',  ( 5.719274019375673035, 21.55341960407619339, 42.29275706135235424 ) ) ;
#106344 = CARTESIAN_POINT ( 'NONE',  ( -10.72451020669870658, -18.67979575497194134, 34.58442372801900433 ) ) ;
#106346 = CARTESIAN_POINT ( 'NONE',  ( 19.02544592524343514, -5.153800228976328945, 88.54057627198102409 ) ) ;
#106345 = CARTESIAN_POINT ( 'NONE',  ( -16.46253265017146816, -9.564922557961047289, 64.16775706135233293 ) ) ;
#106347 = CARTESIAN_POINT ( 'NONE',  ( 16.53943276465976808, -0.05219959533910856209, 103.7489096053143669 ) ) ;
#106348 = CARTESIAN_POINT ( 'NONE',  ( -10.72451020669898014, 18.67979575497178502, 90.41557627198103830 ) ) ;
#106349 = CARTESIAN_POINT ( 'NONE',  ( 4.379528057220339221, -16.55341960407611168, 67.70724293864769550 ) ) ;
#106350 = CARTESIAN_POINT ( 'NONE',  ( -19.02544592524334988, -5.153800228976617603, 23.95942372801900078 ) ) ;
#106351 = CARTESIAN_POINT ( 'NONE',  ( -16.55341960407611168, -4.379528057220339221, 86.45724293864770971 ) ) ;
#106352 = CARTESIAN_POINT ( 'NONE',  ( -5.153800228976328057, -19.02544592524343514, 37.29057627198102409 ) ) ;
#106353 = CARTESIAN_POINT ( 'NONE',  ( -16.46253265017146816, -9.564922557961047289, 84.16775706135233293 ) ) ;
#106354 = CARTESIAN_POINT ( 'NONE',  ( -8.314922557960811034, -14.29746914071050412, 47.08224293864770260 ) ) ;
#106355 = CARTESIAN_POINT ( 'NONE',  ( -21.55341960407619339, 5.719274019375674811, 93.54275706135234714 ) ) ;
#106356 = CARTESIAN_POINT ( 'NONE',  ( 9.474510206698971260, -16.51473224551069308, 97.91557627198102409 ) ) ;
#106357 = CARTESIAN_POINT ( 'NONE',  ( -16.51473224551082808, 9.474510206698731452, 63.33442372801900433 ) ) ;
#106358 = CARTESIAN_POINT ( 'NONE',  ( 21.52544592524344225, -5.823673210054117533, 78.54057627198103830 ) ) ;
#106359 = CARTESIAN_POINT ( 'NONE',  ( 21.55341960407619695, -5.719274019375665929, 31.04275706135234714 ) ) ;
#106360 = CARTESIAN_POINT ( 'NONE',  ( -14.29746914071037622, -8.314922557961029526, 34.16775706135234714 ) ) ;
#106361 = CARTESIAN_POINT ( 'NONE',  ( -12.14591786802326823, 12.06949235617739902, 88.12609039468570415 ) ) ;
#106363 = CARTESIAN_POINT ( 'NONE',  ( -21.53943276465977519, 0.05219959533907696930, 116.2489096053143669 ) ) ;
#106362 = CARTESIAN_POINT ( 'NONE',  ( 13.89961937509977652, -13.97604488694527269, 28.12390960531435624 ) ) ;
#106364 =( BOUNDED_CURVE ( )  B_SPLINE_CURVE ( 2, ( #128695, #158057, #36686, #189405, #160045, #21532, #111551, #83193, #80211, #187430, #37696 ),
 .UNSPECIFIED., .F., .T. ) 
 B_SPLINE_CURVE_WITH_KNOTS ( ( 3, 2, 2, 2, 2, 3 ),
 ( 0.5000000000000032196, 0.5200000000000032374, 0.5400000000000032552, 0.5600000000000033840, 0.5800000000000032907, 0.6000000000000033085 ),
 .UNSPECIFIED. ) 
 CURVE ( )  GEOMETRIC_REPRESENTATION_ITEM ( )  RATIONAL_B_SPLINE_CURVE ( ( 0.9999999999999921174, 0.9510565162951614138, 1.000000000000000000, 0.9510565162951535312, 1.000000000000000000, 0.9510565162951535312, 1.000000000000000000, 0.9510565162951535312, 1.000000000000000000, 0.9510565162951454266, 1.000000000000008216 ) ) 
 REPRESENTATION_ITEM ( '' )  );
#106365 = CARTESIAN_POINT ( 'NONE',  ( -16.46253265017160317, 9.564922557960807481, 25.83224293864769194 ) ) ;
#106366 = CARTESIAN_POINT ( 'NONE',  ( -29.86685920354755552, 21.69954338932564397, -3.324999997268813345 ) ) ;
#106367 = CARTESIAN_POINT ( 'NONE',  ( 12.14591786802327356, -12.06949235617739191, 55.62609039468568284 ) ) ;
#106368 = EDGE_CURVE ( 'NONE', #19466, #14496, #69040, .T. ) ;
#106369 = CARTESIAN_POINT ( 'NONE',  ( -8.224510206698948167, 14.34966873604960824, 75.41557627198102409 ) ) ;
#106370 = CARTESIAN_POINT ( 'NONE',  ( -21.55341960407610458, -5.719274019375992779, 71.45724293864769550 ) ) ;
#106371 = CARTESIAN_POINT ( 'NONE',  ( -16.52544592524342804, 4.483927247898546575, 26.04057627198103475 ) ) ;
#106372 = CARTESIAN_POINT ( 'NONE',  ( 14.34966873604972726, -8.224510206698740333, 45.83442372801901854 ) ) ;
#106373 = CARTESIAN_POINT ( 'NONE',  ( -0.05219959533909027116, -19.03943276465977164, 47.49890960531435979 ) ) ;
#106374 = CARTESIAN_POINT ( 'NONE',  ( 16.55341960407618274, -4.379528057220086978, 81.04275706135236135 ) ) ;
#106375 = CARTESIAN_POINT ( 'NONE',  ( 5.153800228976615827, -19.02544592524334988, 75.20942372801896170 ) ) ;
#106376 = CARTESIAN_POINT ( 'NONE',  ( -21.52544592524343514, 5.823673210054127303, 71.04057627198103830 ) ) ;
#106377 = CARTESIAN_POINT ( 'NONE',  ( 12.14591786802309770, 12.06949235617756955, 24.37390960531435979 ) ) ;
#106378 = ORIENTED_EDGE ( 'NONE', *, *, #124946, .F. ) ;
#106379 = CARTESIAN_POINT ( 'NONE',  ( 21.92083080610932200, 8.096106818377439396, 172.4353877980870493 ) ) ;
#106380 = CARTESIAN_POINT ( 'NONE',  ( -21.55341960407610458, -5.719274019375992779, 51.45724293864770260 ) ) ;
#106381 = VERTEX_POINT ( 'NONE', #191587 ) ;
#106382 = VERTEX_POINT ( 'NONE', #173448 ) ;
#106383 = CARTESIAN_POINT ( 'NONE',  ( 16.52544592524335698, 4.483927247898782831, 91.45942372801901854 ) ) ;
#106384 = VERTEX_POINT ( 'NONE', #38913 ) ;
#106385 = CARTESIAN_POINT ( 'NONE',  ( 0.05219959533909260263, 19.03943276465977164, 109.9989096053143669 ) ) ;
#106386 = CARTESIAN_POINT ( 'NONE',  ( 18.22780087662121673, 5.500000000000056843, 48.98459894673892734 ) ) ;
#106387 = CARTESIAN_POINT ( 'NONE',  ( 21.52544592524344225, -5.823673210054117533, 68.54057627198103830 ) ) ;
#106388 = CARTESIAN_POINT ( 'NONE',  ( -4.483927247898782831, 16.52544592524335698, 102.7094237280190185 ) ) ;
#106389 = CARTESIAN_POINT ( 'NONE',  ( 16.52544592524335698, 4.483927247898782831, 26.45942372801901854 ) ) ;
#106390 = CARTESIAN_POINT ( 'NONE',  ( -16.53943276465976808, 0.05219959533911058130, 111.2489096053143669 ) ) ;
#106391 = CARTESIAN_POINT ( 'NONE',  ( -12.06949235617739369, -12.14591786802326823, 24.37609039468567573 ) ) ;
#106392 = CARTESIAN_POINT ( 'NONE',  ( 5.153800228976335163, 19.02544592524342804, 59.79057627198100988 ) ) ;
#106393 = CARTESIAN_POINT ( 'NONE',  ( -17.81289503416611097, -24.51734667627696496, 140.2999999999999545 ) ) ;
#106394 = CARTESIAN_POINT ( 'NONE',  ( 9.564922557960805705, 16.46253265017160317, 99.58224293864770971 ) ) ;
#106395 = CARTESIAN_POINT ( 'NONE',  ( 14.29746914071037800, 8.314922557961029526, 86.66775706135234714 ) ) ;
#106396 = CARTESIAN_POINT ( 'NONE',  ( -0.05219959533936034679, 19.03943276465977164, 92.50109039468566152 ) ) ;
#106397 = CARTESIAN_POINT ( 'NONE',  ( 9.474510206698729675, 16.51473224551082808, 22.08442372801899722 ) ) ;
#106398 = CARTESIAN_POINT ( 'NONE',  ( 18.67979575497178502, 10.72451020669898547, 74.16557627198102409 ) ) ;
#106399 = CARTESIAN_POINT ( 'NONE',  ( 16.55341960407618274, -4.379528057220086978, 101.0427570613523756 ) ) ;
#106400 = CARTESIAN_POINT ( 'NONE',  ( -16.46253265017146816, -9.564922557961047289, 94.16775706135233293 ) ) ;
#106401 = CARTESIAN_POINT ( 'NONE',  ( -5.153800228976328057, -19.02544592524343514, 47.29057627198102409 ) ) ;
#106402 = CARTESIAN_POINT ( 'NONE',  ( 13.97604488694527802, 13.89961937509977652, 89.37390960531436690 ) ) ;
#106403 = CARTESIAN_POINT ( 'NONE',  ( -21.55341960407619339, 5.719274019375674811, 63.54275706135234003 ) ) ;
#106404 = CARTESIAN_POINT ( 'NONE',  ( -5.049401038298153566, 19.05341960407611168, 45.20724293864769550 ) ) ;
#106405 = CARTESIAN_POINT ( 'NONE',  ( -11.30153831258470731, -188.0000000000000000, -4.999999999999999112 ) ) ;
#106406 = CARTESIAN_POINT ( 'NONE',  ( 14.34966873604960469, 8.224510206698951720, 79.16557627198103830 ) ) ;
#106407 = CARTESIAN_POINT ( 'NONE',  ( -5.823673210054116645, -21.52544592524344225, 72.29057627198102409 ) ) ;
#106408 = CARTESIAN_POINT ( 'NONE',  ( 19.50973618000807264, -5.499999999999992895, 102.5000000000000142 ) ) ;
#106409 = CARTESIAN_POINT ( 'NONE',  ( 2.577820198429831642E-15, 9.100000000000001421, -65.00100000000003320 ) ) ;
#106410 = CARTESIAN_POINT ( 'NONE',  ( 9.474510206698729675, 16.51473224551082808, 47.08442372801900433 ) ) ;
#106411 = CARTESIAN_POINT ( 'NONE',  ( 17.05587630539709920, -6.762274262136624969, 73.24180309037285497 ) ) ;
#106413 = CARTESIAN_POINT ( 'NONE',  ( 16.51473224551069308, 9.474510206698969483, 84.16557627198102409 ) ) ;
#106412 = CARTESIAN_POINT ( 'NONE',  ( 13.89961937509977652, -13.97604488694527269, 78.12390960531433848 ) ) ;
#106414 = CARTESIAN_POINT ( 'NONE',  ( -12.06949235617739369, -12.14591786802326823, 64.37609039468568994 ) ) ;
#106415 = CARTESIAN_POINT ( 'NONE',  ( 0.000000000000000000, 0.000000000000000000, -52.65483682830183199 ) ) ;
#106416 = CARTESIAN_POINT ( 'NONE',  ( -13.97604488694547697, 13.89961937509957934, 28.12609039468565797 ) ) ;
#106417 = PLANE ( 'NONE',  #56564 ) ;
#106418 = CARTESIAN_POINT ( 'NONE',  ( 4.483927247898790824, -16.52544592524335698, 85.20942372801901854 ) ) ;
#106419 = CARTESIAN_POINT ( 'NONE',  ( 14.30620887846970746, -1.220661533321876879, -60.18359034246770989 ) ) ;
#106420 = CARTESIAN_POINT ( 'NONE',  ( -12.14591786802326823, 12.06949235617739902, 83.12609039468568994 ) ) ;
#106421 = CARTESIAN_POINT ( 'NONE',  ( -17.31728774477273802, 6.344390552232388458, 30.81906651689318721 ) ) ;
#106422 = CARTESIAN_POINT ( 'NONE',  ( 0.05219959533934541429, -16.53943276465976808, 55.00109039468568284 ) ) ;
#106423 = CARTESIAN_POINT ( 'NONE',  ( 18.22780087662121673, 5.500000000000056843, 73.98459894673894155 ) ) ;
#106424 = CARTESIAN_POINT ( 'NONE',  ( -10.81492255796105439, 18.62759615963255655, 67.91775706135234714 ) ) ;
#106425 = CARTESIAN_POINT ( 'NONE',  ( -19.03943276465977164, -0.05219959533935918106, 78.75109039468567573 ) ) ;
#106426 = CARTESIAN_POINT ( 'NONE',  ( -19.05341960407617563, 5.049401038297882671, 23.54275706135233648 ) ) ;
#106427 = CARTESIAN_POINT ( 'NONE',  ( 5.049401038298161559, -19.05341960407611168, 47.70724293864770260 ) ) ;
#106428 = CARTESIAN_POINT ( 'NONE',  ( 13.97604488694527802, 13.89961937509977652, 39.37390960531435269 ) ) ;
#106429 = CARTESIAN_POINT ( 'NONE',  ( -17.49999999999999645, -5.499999999999992895, 64.20309617465829888 ) ) ;
#106430 = CARTESIAN_POINT ( 'NONE',  ( -15.72974639402197994, 15.80617190586746368, 65.62390960531436690 ) ) ;
#106431 = CARTESIAN_POINT ( 'NONE',  ( -5.049401038298153566, 19.05341960407611168, 115.2072429386477097 ) ) ;
#106432 = CARTESIAN_POINT ( 'NONE',  ( 12.14591786802309770, 12.06949235617756955, 109.3739096053143811 ) ) ;
#106433 = CARTESIAN_POINT ( 'NONE',  ( 12.06949235617739724, 12.14591786802326823, 46.87609039468568994 ) ) ;
#106434 = EDGE_CURVE ( 'NONE', #183542, #87358, #4504, .T. ) ;
#106435 = ORIENTED_EDGE ( 'NONE', *, *, #94772, .F. ) ;
#106436 = CARTESIAN_POINT ( 'NONE',  ( 5.823673210054125526, 21.52544592524343514, 114.7905762719810383 ) ) ;
#106438 = CARTESIAN_POINT ( 'NONE',  ( 38.00000000000000711, -12.34694845685040754, -3.100000000000000533 ) ) ;
#106437 = CARTESIAN_POINT ( 'NONE',  ( 4.483927247898545687, 16.52544592524342804, 49.79057627198102409 ) ) ;
#106439 = CARTESIAN_POINT ( 'NONE',  ( 19.05341960407617918, -5.049401038297876454, 106.0427570613523471 ) ) ;
#106440 = CARTESIAN_POINT ( 'NONE',  ( -19.05341960407617563, 5.049401038297882671, 43.54275706135232582 ) ) ;
#106441 = CARTESIAN_POINT ( 'NONE',  ( 16.55341960407611168, 4.379528057220329451, 38.95724293864768839 ) ) ;
#106442 = CARTESIAN_POINT ( 'NONE',  ( 5.823673210054444382, -21.52544592524334988, 20.20942372801900788 ) ) ;
#106444 = CARTESIAN_POINT ( 'NONE',  ( 21.53943276465977519, -0.05219959533907433946, 63.74890960531435979 ) ) ;
#106443 = CARTESIAN_POINT ( 'NONE',  ( 17.26172910966779384, 6.454744622555870670, 31.69353091350778229 ) ) ;
#106445 = CARTESIAN_POINT ( 'NONE',  ( -9.474510206698964154, 16.51473224551069663, 90.41557627198103830 ) ) ;
#106446 = CARTESIAN_POINT ( 'NONE',  ( -16.55341960407611168, -4.379528057220339221, 51.45724293864770260 ) ) ;
#106447 = CARTESIAN_POINT ( 'NONE',  ( 0.05219959533909260263, 19.03943276465977164, 109.9989096053143669 ) ) ;
#106448 = EDGE_CURVE ( 'NONE', #5512, #49306, #123924, .T. ) ;
#106449 = VECTOR ( 'NONE', #157266, 1000.000000000000000 ) ;
#106450 = DIRECTION ( 'NONE',  ( 0.000000000000000000, -1.000000000000000000, 0.000000000000000000 ) ) ;
#106451 = CARTESIAN_POINT ( 'NONE',  ( -5.049401038297874678, -19.05341960407617918, 59.79275706135231871 ) ) ;
#106452 = CARTESIAN_POINT ( 'NONE',  ( -10.72451020669898014, 18.67979575497178502, 95.41557627198102409 ) ) ;
#106453 = CARTESIAN_POINT ( 'NONE',  ( -5.049401038298153566, 19.05341960407611168, 40.20724293864768839 ) ) ;
#106454 = CARTESIAN_POINT ( 'NONE',  ( 19.05341960407611168, 5.049401038298154454, 23.95724293864769194 ) ) ;
#106455 = CARTESIAN_POINT ( 'NONE',  ( -18.62759615963255300, -10.81492255796106328, 44.16775706135234714 ) ) ;
#106456 = CARTESIAN_POINT ( 'NONE',  ( 27.73933785331498214, 9.013057229001095294, 147.9750000027311501 ) ) ;
#106457 = CARTESIAN_POINT ( 'NONE',  ( -0.05219959533910754901, -16.53943276465976808, 22.49890960531436335 ) ) ;
#106458 = CARTESIAN_POINT ( 'NONE',  ( -13.97604488694527625, -13.89961937509977652, 51.87390960531436690 ) ) ;
#106459 = CARTESIAN_POINT ( 'NONE',  ( -9.474510206698964154, 16.51473224551069663, 100.4155762719810241 ) ) ;
#106460 = CARTESIAN_POINT ( 'NONE',  ( 15.72974639402199770, -15.80617190586745480, 68.12390960531436690 ) ) ;
#106461 = CARTESIAN_POINT ( 'NONE',  ( 27.73933785331498569, 2.768321779492822058E-14, 143.8750000027311842 ) ) ;
#106462 = CARTESIAN_POINT ( 'NONE',  ( 13.97604488694527802, 13.89961937509977652, 44.37390960531435269 ) ) ;
#106463 = CARTESIAN_POINT ( 'NONE',  ( 0.05219959533907565091, 21.53943276465977519, 54.99890960531435269 ) ) ;
#106464 = CARTESIAN_POINT ( 'NONE',  ( 21.55341960407619695, -5.719274019375665929, 86.04275706135236135 ) ) ;
#106467 = CARTESIAN_POINT ( 'NONE',  ( -12.14591786802309592, -12.06949235617757132, 71.87390960531438111 ) ) ;
#106466 = CARTESIAN_POINT ( 'NONE',  ( 16.53943276465976808, 0.05219959533934440121, 81.25109039468568994 ) ) ;
#106465 = CARTESIAN_POINT ( 'NONE',  ( 18.60204571913743976, -35.35091242066980755, -18.26754506500548558 ) ) ;
#106468 = CARTESIAN_POINT ( 'NONE',  ( 8.314922557961029526, -14.29746914071037800, 90.41775706135236135 ) ) ;
#106469 = CARTESIAN_POINT ( 'NONE',  ( -13.89961937509977652, 13.97604488694528158, 75.62390960531438111 ) ) ;
#106470 = ORIENTED_EDGE ( 'NONE', *, *, #137592, .F. ) ;
#106471 = CARTESIAN_POINT ( 'NONE',  ( 16.51473224551083163, -9.474510206698727899, 25.83442372801900078 ) ) ;
#106472 = CARTESIAN_POINT ( 'NONE',  ( 8.224510206698742110, 14.34966873604972548, 92.08442372801901854 ) ) ;
#106473 = CARTESIAN_POINT ( 'NONE',  ( -16.51473224551082808, 9.474510206698731452, 23.33442372801900078 ) ) ;
#106474 = CARTESIAN_POINT ( 'NONE',  ( 13.89961937509977652, -13.97604488694527269, 78.12390960531433848 ) ) ;
#106475 = CARTESIAN_POINT ( 'NONE',  ( 21.55341960407610458, 5.719274019375980345, 48.95724293864770971 ) ) ;
#106476 = CARTESIAN_POINT ( 'NONE',  ( 14.34966873604972726, -8.224510206698740333, 30.83442372801902209 ) ) ;
#106477 = CARTESIAN_POINT ( 'NONE',  ( 15.80617190586769283, -15.72974639402175789, 80.62609039468567573 ) ) ;
#106478 = CARTESIAN_POINT ( 'NONE',  ( -12.06949235617739369, -12.14591786802326823, 69.37609039468567573 ) ) ;
#106479 = CARTESIAN_POINT ( 'NONE',  ( -18.62759615963255300, -10.81492255796106328, 19.16775706135234714 ) ) ;
#106480 = CARTESIAN_POINT ( 'NONE',  ( 5.049401038297881783, 19.05341960407617563, 107.2927570613523187 ) ) ;
#106481 = CARTESIAN_POINT ( 'NONE',  ( 5.153800228976335163, 19.02544592524342804, 89.79057627198102409 ) ) ;
#106482 = CARTESIAN_POINT ( 'NONE',  ( -8.224510206698735004, -14.34966873604973081, 24.58442372801901499 ) ) ;
#106483 = CARTESIAN_POINT ( 'NONE',  ( -13.97604488694527625, -13.89961937509977652, 41.87390960531435979 ) ) ;
#106484 = AXIS2_PLACEMENT_3D ( 'NONE', #38760, #114584, #179294 ) ;
#106485 = CARTESIAN_POINT ( 'NONE',  ( 0.05219959533934541429, -16.53943276465976808, 30.00109039468568284 ) ) ;
#106486 = CARTESIAN_POINT ( 'NONE',  ( -0.05219959533910754901, -16.53943276465976808, 77.49890960531433848 ) ) ;
#106487 = CARTESIAN_POINT ( 'NONE',  ( 14.29746914071037800, 8.314922557961029526, 86.66775706135234714 ) ) ;
#106489 = CARTESIAN_POINT ( 'NONE',  ( 5.153800228976335163, 19.02544592524342804, 69.79057627198103830 ) ) ;
#106488 = CARTESIAN_POINT ( 'NONE',  ( 5.823673210054444382, -21.52544592524334988, 35.20942372801901854 ) ) ;
#106490 = CARTESIAN_POINT ( 'NONE',  ( -16.46253265017160317, 9.564922557960807481, 85.83224293864769550 ) ) ;
#106491 = B_SPLINE_CURVE_WITH_KNOTS ( 'NONE', 3,
 ( #137292, #61435, #183805, #28160, #167644, #105959 ),
 .UNSPECIFIED., .F., .F.,
 ( 4, 2, 4 ),
 ( 0.000000000000000000, 0.0006703399052047476865, 0.001340679810409495373 ),
 .UNSPECIFIED. ) ;
#106492 = CARTESIAN_POINT ( 'NONE',  ( 12.14591786802327356, -12.06949235617739191, 85.62609039468568994 ) ) ;
#106494 = VERTEX_POINT ( 'NONE', #119749 ) ;
#106493 = CARTESIAN_POINT ( 'NONE',  ( -24.04614410381461553, -5.408324479809799357, 174.2944578187863840 ) ) ;
#106495 = ORIENTED_EDGE ( 'NONE', *, *, #129926, .F. ) ;
#106496 = CARTESIAN_POINT ( 'NONE',  ( 13.97604488694548053, -13.89961937509957401, 30.62609039468566863 ) ) ;
#106497 = CARTESIAN_POINT ( 'NONE',  ( 5.049401038298161559, -19.05341960407611168, 92.70724293864769550 ) ) ;
#106498 = CARTESIAN_POINT ( 'NONE',  ( -5.049401038298153566, 19.05341960407611168, 45.20724293864769550 ) ) ;
#106500 = ORIENTED_EDGE ( 'NONE', *, *, #158923, .T. ) ;
#106499 = CARTESIAN_POINT ( 'NONE',  ( 13.97604488694527802, 13.89961937509977652, 114.3739096053143669 ) ) ;
#106501 = CARTESIAN_POINT ( 'NONE',  ( 0.05219959533934541429, -16.53943276465976808, 35.00109039468568284 ) ) ;
#106503 = CARTESIAN_POINT ( 'NONE',  ( 16.53943276465976808, 0.05219959533934440121, 36.25109039468567573 ) ) ;
#106502 = CARTESIAN_POINT ( 'NONE',  ( 9.474510206698729675, 16.51473224551082808, 57.08442372801900433 ) ) ;
#106504 = CARTESIAN_POINT ( 'NONE',  ( -16.46253265017160317, 9.564922557960807481, 100.8322429386477097 ) ) ;
#106505 = CARTESIAN_POINT ( 'NONE',  ( -16.46253265017160317, 9.564922557960807481, 70.83224293864770971 ) ) ;
#106506 = CARTESIAN_POINT ( 'NONE',  ( 18.67979575497178502, 10.72451020669898547, 94.16557627198103830 ) ) ;
#106507 = CARTESIAN_POINT ( 'NONE',  ( -9.474510206698720793, -16.51473224551083518, 59.58442372801900433 ) ) ;
#106509 = DIRECTION ( 'NONE',  ( -1.000000000000000000, 0.000000000000000000, -5.421010862427521184E-16 ) ) ;
#106508 = CARTESIAN_POINT ( 'NONE',  ( -16.46253265017160317, 9.564922557960807481, 85.83224293864769550 ) ) ;
#106510 = CARTESIAN_POINT ( 'NONE',  ( -5.049401038298153566, 19.05341960407611168, 60.20724293864768129 ) ) ;
#106512 = CARTESIAN_POINT ( 'NONE',  ( -5.049401038298153566, 19.05341960407611168, 25.20724293864768484 ) ) ;
#106511 = CARTESIAN_POINT ( 'NONE',  ( -8.314922557960811034, -14.29746914071050412, 27.08224293864769550 ) ) ;
#106513 = CARTESIAN_POINT ( 'NONE',  ( 13.89961937509957401, 13.97604488694547697, 41.87609039468566152 ) ) ;
#106514 = CARTESIAN_POINT ( 'NONE',  ( -8.314922557960811034, -14.29746914071050412, 72.08224293864769550 ) ) ;
#106515 = CARTESIAN_POINT ( 'NONE',  ( -21.53943276465977519, -0.05219959533937600094, 93.75109039468567573 ) ) ;
#106516 = CARTESIAN_POINT ( 'NONE',  ( -9.474510206698964154, 16.51473224551069663, 45.41557627198103120 ) ) ;
#106517 = CARTESIAN_POINT ( 'NONE',  ( -16.52544592524335698, -4.483927247898792601, 53.95942372801900433 ) ) ;
#106519 = CARTESIAN_POINT ( 'NONE',  ( -0.05219959533937732626, 21.53943276465977519, 92.50109039468567573 ) ) ;
#106518 = CARTESIAN_POINT ( 'NONE',  ( 4.379528057220339221, -16.55341960407611168, 42.70724293864770260 ) ) ;
#106520 = CARTESIAN_POINT ( 'NONE',  ( -9.564922557960796823, -16.46253265017161027, 87.08224293864769550 ) ) ;
#106521 = ORIENTED_EDGE ( 'NONE', *, *, #116955, .T. ) ;
#106522 = CARTESIAN_POINT ( 'NONE',  ( 19.03943276465977164, -0.05219959533909143690, 98.74890960531436690 ) ) ;
#106523 = CARTESIAN_POINT ( 'NONE',  ( -16.53943276465976808, 0.05219959533911058130, 101.2489096053143669 ) ) ;
#106524 = CARTESIAN_POINT ( 'NONE',  ( 14.34966873604960469, 8.224510206698951720, 79.16557627198103830 ) ) ;
#106525 = CARTESIAN_POINT ( 'NONE',  ( -18.62759615963270932, 10.81492255796079327, 80.83224293864769550 ) ) ;
#106526 = CARTESIAN_POINT ( 'NONE',  ( 16.46253265017160672, -9.564922557960803928, 83.33224293864768129 ) ) ;
#106527 = CARTESIAN_POINT ( 'NONE',  ( 18.67979575497178502, 10.72451020669898547, 104.1655762719810241 ) ) ;
#106528 = CARTESIAN_POINT ( 'NONE',  ( 16.51473224551069308, 9.474510206698969483, 94.16557627198103830 ) ) ;
#106530 = CARTESIAN_POINT ( 'NONE',  ( 4.483927247898545687, 16.52544592524342804, 94.79057627198105251 ) ) ;
#106529 = CARTESIAN_POINT ( 'NONE',  ( -19.49190055781011210, -5.499999999999966249, 90.56116087098783396 ) ) ;
#106531 = CARTESIAN_POINT ( 'NONE',  ( -13.89961937509977652, 13.97604488694528158, 55.62390960531434558 ) ) ;
#106532 = CARTESIAN_POINT ( 'NONE',  ( -21.53943276465977519, 0.05219959533907696930, 61.24890960531435979 ) ) ;
#106533 = CARTESIAN_POINT ( 'NONE',  ( 17.26058549869091152, -6.457015423128605214, 26.12254162523933232 ) ) ;
#106535 = CARTESIAN_POINT ( 'NONE',  ( 0.000000000000000000, 0.000000000000000000, 4.000000000000000000 ) ) ;
#106534 = CARTESIAN_POINT ( 'NONE',  ( 14.29746914071037800, 8.314922557961029526, 111.6677570613523613 ) ) ;
#106536 = CARTESIAN_POINT ( 'NONE',  ( -19.05341960407617563, 5.049401038297882671, 113.5427570613523471 ) ) ;
#106537 = CARTESIAN_POINT ( 'NONE',  ( -8.314922557960811034, -14.29746914071050412, 87.08224293864769550 ) ) ;
#106538 = CARTESIAN_POINT ( 'NONE',  ( 18.39635199886970440, -5.499999999999988454, 53.51967076360000419 ) ) ;
#106539 = CARTESIAN_POINT ( 'NONE',  ( -5.153800228976328057, -19.02544592524343514, 72.29057627198102409 ) ) ;
#106540 = CARTESIAN_POINT ( 'NONE',  ( 9.564922557960805705, 16.46253265017160317, 39.58224293864768839 ) ) ;
#106542 = EDGE_CURVE ( 'NONE', #197949, #64290, #56212, .T. ) ;
#106541 = CARTESIAN_POINT ( 'NONE',  ( 8.224510206698953496, -14.34966873604960469, 72.91557627198103830 ) ) ;
#106543 = CARTESIAN_POINT ( 'NONE',  ( -9.564922557960796823, -16.46253265017161027, 112.0822429386476955 ) ) ;
#106544 = CARTESIAN_POINT ( 'NONE',  ( -13.89961937509957401, -13.97604488694547875, 99.37609039468567573 ) ) ;
#106545 = CARTESIAN_POINT ( 'NONE',  ( -13.89961937509977652, 13.97604488694528158, 105.6239096053143527 ) ) ;
#106546 = CARTESIAN_POINT ( 'NONE',  ( -5.823673210054116645, -21.52544592524344225, 72.29057627198102409 ) ) ;
#106547 = CARTESIAN_POINT ( 'NONE',  ( -4.379528057220086978, -16.55341960407618274, 74.79275706135234714 ) ) ;
#106548 = CARTESIAN_POINT ( 'NONE',  ( -16.18388926212247725, 7.379444403734498614, 94.56046848633769741 ) ) ;
#106549 = CARTESIAN_POINT ( 'NONE',  ( -19.03943276465977164, 0.05219959533909376836, 76.24890960531435269 ) ) ;
#106550 = CARTESIAN_POINT ( 'NONE',  ( 21.53943276465977519, -0.05219959533907433946, 78.74890960531436690 ) ) ;
#106551 = CARTESIAN_POINT ( 'NONE',  ( 13.97604488694548053, -13.89961937509957401, 110.6260903946856615 ) ) ;
#106553 = CARTESIAN_POINT ( 'NONE',  ( 0.05219959533937995610, -21.53943276465977519, 65.00109039468568994 ) ) ;
#106552 = CARTESIAN_POINT ( 'NONE',  ( -4.379528057220328563, 16.55341960407611168, 35.20724293864768839 ) ) ;
#106554 = CARTESIAN_POINT ( 'NONE',  ( 17.58332526062524437, 7.635886036038643354, 71.57665040441537485 ) ) ;
#106556 = CARTESIAN_POINT ( 'NONE',  ( -19.05341960407611168, -5.049401038298163336, 106.4572429386476955 ) ) ;
#106555 = CARTESIAN_POINT ( 'NONE',  ( 16.53943276465976808, 0.05219959533934440121, 91.25109039468568994 ) ) ;
#106557 = CARTESIAN_POINT ( 'NONE',  ( 0.000000000000000000, 0.000000000000000000, 10.00000000000000000 ) ) ;
#106558 = CARTESIAN_POINT ( 'NONE',  ( -17.50000000000000355, 5.622605283950870891, 78.68792689403892382 ) ) ;
#106559 = CARTESIAN_POINT ( 'NONE',  ( 4.483927247898790824, -16.52544592524335698, 100.2094237280190043 ) ) ;
#106560 = CARTESIAN_POINT ( 'NONE',  ( 14.34966873604972726, -8.224510206698740333, 40.83442372801901854 ) ) ;
#106561 = CARTESIAN_POINT ( 'NONE',  ( -13.97604488694527625, -13.89961937509977652, 56.87390960531434558 ) ) ;
#106562 = CARTESIAN_POINT ( 'NONE',  ( -13.89961937509977652, 13.97604488694528158, 75.62390960531438111 ) ) ;
#106563 = CARTESIAN_POINT ( 'NONE',  ( 21.55341960407619695, -5.719274019375665929, 71.04275706135234714 ) ) ;
#106564 = CARTESIAN_POINT ( 'NONE',  ( 8.224510206698742110, 14.34966873604972548, 67.08442372801901854 ) ) ;
#106565 = CARTESIAN_POINT ( 'NONE',  ( 16.53943276465976808, -0.05219959533910856209, 38.74890960531435979 ) ) ;
#106566 = CARTESIAN_POINT ( 'NONE',  ( -16.51473224551069308, -9.474510206698971260, 41.66557627198103120 ) ) ;
#106567 = CARTESIAN_POINT ( 'NONE',  ( 19.03943276465977164, -0.05219959533909143690, 48.74890960531435979 ) ) ;
#106568 = CARTESIAN_POINT ( 'NONE',  ( 8.314922557961029526, -14.29746914071037800, 35.41775706135234003 ) ) ;
#106569 = CARTESIAN_POINT ( 'NONE',  ( 16.46253265017146816, 9.564922557961045513, 101.6677570613523329 ) ) ;
#106570 = CARTESIAN_POINT ( 'NONE',  ( -8.224510206698948167, 14.34966873604960824, 90.41557627198103830 ) ) ;
#106571 = CARTESIAN_POINT ( 'NONE',  ( 19.03943276465977164, -0.05219959533909143690, 53.74890960531436690 ) ) ;
#106573 = CARTESIAN_POINT ( 'NONE',  ( -28.79475375365586842, 2.428612866367529932E-14, 147.9843446568999923 ) ) ;
#106572 = CARTESIAN_POINT ( 'NONE',  ( 5.153800228976615827, -19.02544592524334988, 85.20942372801900433 ) ) ;
#106574 = CARTESIAN_POINT ( 'NONE',  ( 18.62759615963255655, 10.81492255796105972, 86.66775706135234714 ) ) ;
#106575 = CARTESIAN_POINT ( 'NONE',  ( 0.05219959533934541429, -16.53943276465976808, 50.00109039468568994 ) ) ;
#106576 = DIRECTION ( 'NONE',  ( 0.000000000000000000, -0.000000000000000000, 1.000000000000000000 ) ) ;
#106577 = CARTESIAN_POINT ( 'NONE',  ( 18.67979575497178502, 10.72451020669898547, 49.16557627198102409 ) ) ;
#106578 = CARTESIAN_POINT ( 'NONE',  ( -8.224510206698735004, -14.34966873604973081, 34.58442372801900433 ) ) ;
#106579 = CARTESIAN_POINT ( 'NONE',  ( -18.56197773271725993, 5.500000000000080824, 68.55066217314451649 ) ) ;
#106580 = CARTESIAN_POINT ( 'NONE',  ( 5.049401038297881783, 19.05341960407617563, 47.29275706135231161 ) ) ;
#106581 = CARTESIAN_POINT ( 'NONE',  ( -5.049401038298153566, 19.05341960407611168, 85.20724293864766707 ) ) ;
#106582 = CARTESIAN_POINT ( 'NONE',  ( -19.05341960407611168, -5.049401038298163336, 21.45724293864768839 ) ) ;
#106583 = CARTESIAN_POINT ( 'NONE',  ( -9.564922557960796823, -16.46253265017161027, 57.08224293864769550 ) ) ;
#106584 = CARTESIAN_POINT ( 'NONE',  ( -21.44208882751384593, -23.00296878542015477, -49.72123984779791783 ) ) ;
#106585 = CARTESIAN_POINT ( 'NONE',  ( 18.62759615963255655, 10.81492255796105972, 76.66775706135234714 ) ) ;
#106586 = DIRECTION ( 'NONE',  ( 0.000000000000000000, -1.000000000000000000, 0.000000000000000000 ) ) ;
#106587 = PRODUCT_DEFINITION_SHAPE ( 'NONE', 'NONE',  #200194 ) ;
#106588 = CARTESIAN_POINT ( 'NONE',  ( -13.89961937509957401, -13.97604488694547875, 29.37609039468565797 ) ) ;
#106589 = CARTESIAN_POINT ( 'NONE',  ( 13.97604488694548053, -13.89961937509957401, 20.62609039468567573 ) ) ;
#106590 = CARTESIAN_POINT ( 'NONE',  ( 4.379528057220339221, -16.55341960407611168, 47.70724293864770260 ) ) ;
#106591 = CARTESIAN_POINT ( 'NONE',  ( 19.02544592524343514, -5.153800228976328945, 58.54057627198102409 ) ) ;
#106592 = CARTESIAN_POINT ( 'NONE',  ( 5.049401038298161559, -19.05341960407611168, 107.7072429386476955 ) ) ;
#106593 = CARTESIAN_POINT ( 'NONE',  ( -21.52544592524334988, -5.823673210054445271, 83.95942372801900433 ) ) ;
#106594 = CARTESIAN_POINT ( 'NONE',  ( 0.05219959533909260263, 19.03943276465977164, 69.99890960531435269 ) ) ;
#106595 = CARTESIAN_POINT ( 'NONE',  ( 10.81492255796106328, -18.62759615963255655, 80.41775706135234714 ) ) ;
#106596 = CARTESIAN_POINT ( 'NONE',  ( -5.823673210054116645, -21.52544592524344225, 42.29057627198103120 ) ) ;
#106597 = CARTESIAN_POINT ( 'NONE',  ( -5.719274019375665041, -21.55341960407619695, 39.79275706135235424 ) ) ;
#106598 = CARTESIAN_POINT ( 'NONE',  ( 13.97604488694548053, -13.89961937509957401, 60.62609039468564731 ) ) ;
#106599 = CARTESIAN_POINT ( 'NONE',  ( -5.049401038298153566, 19.05341960407611168, 30.20724293864768839 ) ) ;
#106600 = CARTESIAN_POINT ( 'NONE',  ( -5.153800228976328057, -19.02544592524343514, 82.29057627198103830 ) ) ;
#106601 = CARTESIAN_POINT ( 'NONE',  ( 16.55341960407618274, -4.379528057220086978, 26.04275706135235779 ) ) ;
#106602 = CARTESIAN_POINT ( 'NONE',  ( 0.05219959533910956823, 16.53943276465976808, 89.99890960531438111 ) ) ;
#106603 = CARTESIAN_POINT ( 'NONE',  ( -5.153800228976328057, -19.02544592524343514, 57.29057627198103120 ) ) ;
#106604 = CARTESIAN_POINT ( 'NONE',  ( -10.72451020669898014, 18.67979575497178502, 35.41557627198102409 ) ) ;
#106605 = AXIS2_PLACEMENT_3D ( 'NONE', #34795, #172315, #157150 ) ;
#106606 = CARTESIAN_POINT ( 'NONE',  ( -14.34966873604972548, 8.224510206698743886, 23.33442372801901499 ) ) ;
#106607 = CARTESIAN_POINT ( 'NONE',  ( -21.53943276465977519, 0.05219959533907696930, 116.2489096053143669 ) ) ;
#106608 = CARTESIAN_POINT ( 'NONE',  ( -5.823673210054431948, 21.52544592524334988, 67.70942372801901854 ) ) ;
#106609 = CARTESIAN_POINT ( 'NONE',  ( 8.314922557961029526, -14.29746914071037800, 75.41775706135233293 ) ) ;
#106610 = CARTESIAN_POINT ( 'NONE',  ( -4.379528057220086978, -16.55341960407618274, 74.79275706135234714 ) ) ;
#106611 = ORIENTED_EDGE ( 'NONE', *, *, #119374, .F. ) ;
#106612 = CARTESIAN_POINT ( 'NONE',  ( 19.05341960407611168, 5.049401038298154454, 58.95724293864768129 ) ) ;
#106613 = CARTESIAN_POINT ( 'NONE',  ( -8.224510206698735004, -14.34966873604973081, 84.58442372801903275 ) ) ;
#106614 = CARTESIAN_POINT ( 'NONE',  ( -19.05341960407617563, 5.049401038297882671, 43.54275706135232582 ) ) ;
#106615 = ADVANCED_FACE ( 'NONE', ( #58079 ), #134931, .T. ) ;
#106616 = CARTESIAN_POINT ( 'NONE',  ( 10.81492255796106328, -18.62759615963255655, 20.41775706135234714 ) ) ;
#106617 = CARTESIAN_POINT ( 'NONE',  ( 12.14591786802309770, 12.06949235617756955, 64.37390960531435269 ) ) ;
#106618 = CARTESIAN_POINT ( 'NONE',  ( -16.46253265017160317, 9.564922557960807481, 90.83224293864769550 ) ) ;
#106619 = CARTESIAN_POINT ( 'NONE',  ( 14.29746914071037800, 8.314922557961029526, 86.66775706135234714 ) ) ;
#106620 = CARTESIAN_POINT ( 'NONE',  ( -18.67979575497193778, 10.72451020669871902, 58.33442372801901143 ) ) ;
#106621 = CARTESIAN_POINT ( 'NONE',  ( -16.55341960407617563, 4.379528057220093196, 28.54275706135234358 ) ) ;
#106622 = CARTESIAN_POINT ( 'NONE',  ( 15.72974639402199770, -15.80617190586745480, 113.1239096053143953 ) ) ;
#106623 = CARTESIAN_POINT ( 'NONE',  ( 12.14591786802309770, 12.06949235617756955, 64.37390960531435269 ) ) ;
#106624 = EDGE_LOOP ( 'NONE', ( #85232, #43643, #169587, #102460, #60958, #28696, #68256, #99010, #41575, #91623, #24426, #101026, #106470, #143912, #100702, #124647, #25689, #127740, #43352, #120345, #69156, #53734, #11333, #50317, #9183, #169341, #27065, #182103, #193730, #147553, #97812, #171524, #180281, #13224, #53941, #72374, #42085, #154594, #186049, #26307, #67134, #181521 ) ) ;
#106625 = CARTESIAN_POINT ( 'NONE',  ( -5.719274019375978568, 21.55341960407610458, 95.20724293864769550 ) ) ;
#106626 = CARTESIAN_POINT ( 'NONE',  ( -8.314922557960811034, -14.29746914071050412, 37.08224293864768129 ) ) ;
#106627 = ORIENTED_EDGE ( 'NONE', *, *, #191742, .T. ) ;
#106628 = CARTESIAN_POINT ( 'NONE',  ( 35.24576003106573552, 4.949822944371136124, 39.34410620168028316 ) ) ;
#106629 = CARTESIAN_POINT ( 'NONE',  ( -16.46253265017160317, 9.564922557960807481, 110.8322429386476955 ) ) ;
#106630 = CARTESIAN_POINT ( 'NONE',  ( -15.80617190586768217, 15.72974639402176855, 33.12609039468569705 ) ) ;
#106631 = CARTESIAN_POINT ( 'NONE',  ( -14.34966873604960291, -8.224510206698953496, 51.66557627198102409 ) ) ;
#106632 = VECTOR ( 'NONE', #117767, 1000.000000000000000 ) ;
#106633 = CARTESIAN_POINT ( 'NONE',  ( 16.46253265017160672, -9.564922557960803928, 58.33224293864769550 ) ) ;
#106634 = CARTESIAN_POINT ( 'NONE',  ( 9.474510206698729675, 16.51473224551082808, 67.08442372801900433 ) ) ;
#106635 = CARTESIAN_POINT ( 'NONE',  ( 5.049401038298161559, -19.05341960407611168, 97.70724293864766707 ) ) ;
#106636 = EDGE_CURVE ( 'NONE', #131506, #140232, #173115, .T. ) ;
#106637 = CARTESIAN_POINT ( 'NONE',  ( -21.53943276465977519, 0.05219959533907696930, 51.24890960531436690 ) ) ;
#106638 = CARTESIAN_POINT ( 'NONE',  ( -16.00769354339768924, -38.20109431699814451, -19.33483434993910066 ) ) ;
#106639 = CARTESIAN_POINT ( 'NONE',  ( -5.153800228976328057, -19.02544592524343514, 57.29057627198103120 ) ) ;
#106640 = CARTESIAN_POINT ( 'NONE',  ( -4.483927247898782831, 16.52544592524335698, 42.70942372801901854 ) ) ;
#106641 = CARTESIAN_POINT ( 'NONE',  ( -13.89961937509957401, -13.97604488694547875, 64.37609039468567573 ) ) ;
#106642 = CARTESIAN_POINT ( 'NONE',  ( -10.72451020669898014, 18.67979575497178502, 115.4155762719810241 ) ) ;
#106643 = CARTESIAN_POINT ( 'NONE',  ( -8.224510206698948167, 14.34966873604960824, 45.41557627198103830 ) ) ;
#106644 = ORIENTED_EDGE ( 'NONE', *, *, #46491, .T. ) ;
#106645 = CARTESIAN_POINT ( 'NONE',  ( -19.03943276465977164, 0.05219959533909376836, 96.24890960531436690 ) ) ;
#106646 = CARTESIAN_POINT ( 'NONE',  ( 0.05219959533907565091, 21.53943276465977519, 74.99890960531435269 ) ) ;
#106648 = CARTESIAN_POINT ( 'NONE',  ( 16.52544592524335698, 4.483927247898782831, 41.45942372801901143 ) ) ;
#106647 = CARTESIAN_POINT ( 'NONE',  ( -18.67979575497178146, -10.72451020669898902, 106.6655762719810383 ) ) ;
#106649 = CARTESIAN_POINT ( 'NONE',  ( 18.62759615963271287, -10.81492255796078972, 33.33224293864769550 ) ) ;
#106650 = CARTESIAN_POINT ( 'NONE',  ( 15.80617190586769283, -15.72974639402175789, 105.6260903946856899 ) ) ;
#106651 = CARTESIAN_POINT ( 'NONE',  ( -13.97604488694527625, -13.89961937509977652, 106.8739096053143669 ) ) ;
#106652 = CARTESIAN_POINT ( 'NONE',  ( -5.153800228976328057, -19.02544592524343514, 42.29057627198101699 ) ) ;
#106653 = CARTESIAN_POINT ( 'NONE',  ( -19.02544592524342804, 5.153800228976336051, 101.0405762719810241 ) ) ;
#106654 = CARTESIAN_POINT ( 'NONE',  ( 9.564922557960805705, 16.46253265017160317, 74.58224293864769550 ) ) ;
#106655 = CARTESIAN_POINT ( 'NONE',  ( -16.52544592524335698, -4.483927247898792601, 23.95942372801901143 ) ) ;
#106656 = CARTESIAN_POINT ( 'NONE',  ( 16.29526858892907626, -7.335722546920038667, 86.70329402199736535 ) ) ;
#106657 = CARTESIAN_POINT ( 'NONE',  ( -19.03943276465977164, -0.05219959533935918106, 58.75109039468566863 ) ) ;
#106659 = CARTESIAN_POINT ( 'NONE',  ( 5.719274019375991003, -21.55341960407610458, 37.70724293864769550 ) ) ;
#106658 = CARTESIAN_POINT ( 'NONE',  ( -5.823673210054431948, 21.52544592524334988, 107.7094237280190328 ) ) ;
#106660 = CARTESIAN_POINT ( 'NONE',  ( 16.53943276465976808, 0.05219959533934440121, 101.2510903946856757 ) ) ;
#106661 = CARTESIAN_POINT ( 'NONE',  ( 22.36951698133467303, -20.26978297296616560, -48.08211468429932012 ) ) ;
#106662 = CARTESIAN_POINT ( 'NONE',  ( 0.05219959533936267826, -19.03943276465977164, 80.00109039468567573 ) ) ;
#106663 = CARTESIAN_POINT ( 'NONE',  ( 13.89961937509957401, 13.97604488694547697, 26.87609039468566507 ) ) ;
#106664 = DIRECTION ( 'NONE',  ( -1.000000000000000000, -0.000000000000000000, -0.000000000000000000 ) ) ;
#106665 = CARTESIAN_POINT ( 'NONE',  ( -16.51473224551069308, -9.474510206698971260, 46.66557627198102409 ) ) ;
#106666 = CARTESIAN_POINT ( 'NONE',  ( -16.53943276465976808, 0.05219959533911058130, 36.24890960531435979 ) ) ;
#106667 = CARTESIAN_POINT ( 'NONE',  ( -0.05219959533909027116, -19.03943276465977164, 27.49890960531435624 ) ) ;
#106668 = CARTESIAN_POINT ( 'NONE',  ( 16.52544592524342804, -4.483927247898539470, 23.54057627198102765 ) ) ;
#106669 = CARTESIAN_POINT ( 'NONE',  ( 17.50000000000000000, -5.499999999999992895, 46.21769037696434168 ) ) ;
#106670 = CARTESIAN_POINT ( 'NONE',  ( -4.379528057220086978, -16.55341960407618274, 94.79275706135234714 ) ) ;
#106671 = CARTESIAN_POINT ( 'NONE',  ( -13.97604488694527625, -13.89961937509977652, 46.87390960531435979 ) ) ;
#106672 = CARTESIAN_POINT ( 'NONE',  ( 15.72974639402176855, 15.80617190586768217, 101.8760903946857042 ) ) ;
#106673 = CARTESIAN_POINT ( 'NONE',  ( -9.474510206698720793, -16.51473224551083518, 109.5844237280190043 ) ) ;
#106675 = EDGE_LOOP ( 'NONE', ( #77464, #58154, #111412, #73707, #44984, #89476, #94542, #7392, #12942, #192992, #58333 ) ) ;
#106674 = CARTESIAN_POINT ( 'NONE',  ( -0.05219959533937732626, 21.53943276465977519, 87.50109039468568994 ) ) ;
#106676 = CARTESIAN_POINT ( 'NONE',  ( -19.02544592524334988, -5.153800228976617603, 68.95942372801896170 ) ) ;
#106677 = CARTESIAN_POINT ( 'NONE',  ( -0.05219959533909027116, -19.03943276465977164, 97.49890960531436690 ) ) ;
#106678 = CARTESIAN_POINT ( 'NONE',  ( 19.02544592524343514, -5.153800228976328945, 83.54057627198100988 ) ) ;
#106679 = CARTESIAN_POINT ( 'NONE',  ( -22.81625015709509441, -31.40387420917324590, -6.324999997268814234 ) ) ;
#106680 = CARTESIAN_POINT ( 'NONE',  ( -18.62759615963270932, 10.81492255796079327, 110.8322429386476955 ) ) ;
#106681 = CARTESIAN_POINT ( 'NONE',  ( -4.483927247898539470, -16.52544592524342804, 62.29057627198102409 ) ) ;
#106682 = CARTESIAN_POINT ( 'NONE',  ( -10.81492255796078084, -18.62759615963271287, 57.08224293864769550 ) ) ;
#106683 = CARTESIAN_POINT ( 'NONE',  ( 16.51473224551069308, 9.474510206698969483, 54.16557627198103120 ) ) ;
#106685 = CARTESIAN_POINT ( 'NONE',  ( 14.34966873604972726, -8.224510206698740333, 85.83442372801901854 ) ) ;
#106684 = CARTESIAN_POINT ( 'NONE',  ( 21.52544592524344225, -5.823673210054117533, 93.54057627198103830 ) ) ;
#106686 = EDGE_LOOP ( 'NONE', ( #157166, #195820, #7416, #46421 ) ) ;
#106687 = CARTESIAN_POINT ( 'NONE',  ( -19.05341960407611168, -5.049401038298163336, 61.45724293864769550 ) ) ;
#106689 = CARTESIAN_POINT ( 'NONE',  ( 0.000000000000000000, 0.7216878364870328300, 1.249999999999999778 ) ) ;
#106688 = CARTESIAN_POINT ( 'NONE',  ( 8.314922557960818139, 14.29746914071049879, 89.58224293864768129 ) ) ;
#106690 = CARTESIAN_POINT ( 'NONE',  ( 0.05219959533909260263, 19.03943276465977164, 54.99890960531435979 ) ) ;
#106691 = CARTESIAN_POINT ( 'NONE',  ( 9.474510206698729675, 16.51473224551082808, 82.08442372801899012 ) ) ;
#106692 = CARTESIAN_POINT ( 'NONE',  ( -12.14591786802309592, -12.06949235617757132, 81.87390960531435269 ) ) ;
#106693 = CARTESIAN_POINT ( 'NONE',  ( 10.72451020669871369, 18.67979575497193778, 62.08442372801901143 ) ) ;
#106695 = CARTESIAN_POINT ( 'NONE',  ( 10.72451020669898902, -18.67979575497178502, 97.91557627198103830 ) ) ;
#106694 = CARTESIAN_POINT ( 'NONE',  ( -5.049401038298153566, 19.05341960407611168, 35.20724293864768839 ) ) ;
#106696 = CARTESIAN_POINT ( 'NONE',  ( 12.14591786802309770, 12.06949235617756955, 104.3739096053143669 ) ) ;
#106697 = CARTESIAN_POINT ( 'NONE',  ( -17.81289503416611808, 24.51734667627700404, 147.9500000054623854 ) ) ;
#106698 = CARTESIAN_POINT ( 'NONE',  ( -19.02544592524342804, 5.153800228976336051, 56.04057627198100988 ) ) ;
#106699 = CARTESIAN_POINT ( 'NONE',  ( -9.670372969936114060, -11.80125700695215762, -61.97618590420869111 ) ) ;
#106701 = CARTESIAN_POINT ( 'NONE',  ( -19.02544592524342804, 5.153800228976336051, 111.0405762719810099 ) ) ;
#106700 = CARTESIAN_POINT ( 'NONE',  ( 5.049401038297881783, 19.05341960407617563, 97.29275706135233293 ) ) ;
#106702 = CARTESIAN_POINT ( 'NONE',  ( 18.67979575497194134, -10.72451020669871369, 35.83442372801901143 ) ) ;
#106703 = CARTESIAN_POINT ( 'NONE',  ( 13.97604488694527802, 13.89961937509977652, 89.37390960531436690 ) ) ;
#106704 = CARTESIAN_POINT ( 'NONE',  ( 13.89961937509957401, 13.97604488694547697, 66.87609039468567573 ) ) ;
#106705 = CARTESIAN_POINT ( 'NONE',  ( 19.03943276465977164, -0.05219959533909143690, 53.74890960531436690 ) ) ;
#106706 = CARTESIAN_POINT ( 'NONE',  ( -16.52544592524342804, 4.483927247898546575, 81.04057627198102409 ) ) ;
#106707 = CARTESIAN_POINT ( 'NONE',  ( -16.53943276465976808, 0.05219959533911058130, 71.24890960531435269 ) ) ;
#106708 = CARTESIAN_POINT ( 'NONE',  ( -16.46253265017160317, 9.564922557960807481, 90.83224293864769550 ) ) ;
#106709 = CARTESIAN_POINT ( 'NONE',  ( 0.05219959533910956823, 16.53943276465976808, 74.99890960531435269 ) ) ;
#106710 = CARTESIAN_POINT ( 'NONE',  ( 9.564922557960805705, 16.46253265017160317, 79.58224293864769550 ) ) ;
#106711 = CARTESIAN_POINT ( 'NONE',  ( 13.89961937509957401, 13.97604488694547697, 36.87609039468565442 ) ) ;
#106714 = CARTESIAN_POINT ( 'NONE',  ( -14.29746914071049879, 8.314922557960819915, 105.8322429386476955 ) ) ;
#106713 = CARTESIAN_POINT ( 'NONE',  ( -16.55341960407611168, -4.379528057220339221, 31.45724293864769550 ) ) ;
#106712 = CARTESIAN_POINT ( 'NONE',  ( 5.049401038298161559, -19.05341960407611168, 52.70724293864767418 ) ) ;
#106715 = ORIENTED_EDGE ( 'NONE', *, *, #15614, .T. ) ;
#106716 = CARTESIAN_POINT ( 'NONE',  ( 21.55341960407619695, -5.719274019375665929, 46.04275706135234714 ) ) ;
#106717 = CARTESIAN_POINT ( 'NONE',  ( 0.05219959533936267826, -19.03943276465977164, 70.00109039468566152 ) ) ;
#106718 = CARTESIAN_POINT ( 'NONE',  ( -4.379528057220328563, 16.55341960407611168, 35.20724293864768839 ) ) ;
#106719 = CARTESIAN_POINT ( 'NONE',  ( -15.80617190586745835, -15.72974639402198527, 86.87390960531438111 ) ) ;
#106720 = CARTESIAN_POINT ( 'NONE',  ( -9.564922557960796823, -16.46253265017161027, 112.0822429386476955 ) ) ;
#106721 = CARTESIAN_POINT ( 'NONE',  ( -14.34966873604960291, -8.224510206698953496, 71.66557627198100988 ) ) ;
#106722 = CARTESIAN_POINT ( 'NONE',  ( 19.03943276465977164, -0.05219959533909143690, 38.74890960531436690 ) ) ;
#106723 = CARTESIAN_POINT ( 'NONE',  ( -16.51473224551082808, 9.474510206698731452, 33.33442372801899722 ) ) ;
#106724 = CARTESIAN_POINT ( 'NONE',  ( -16.52544592524335698, -4.483927247898792601, 98.95942372801903275 ) ) ;
#106725 = CARTESIAN_POINT ( 'NONE',  ( -4.379528057220086978, -16.55341960407618274, 59.79275706135234714 ) ) ;
#106726 = CARTESIAN_POINT ( 'NONE',  ( -18.62759615963270932, 10.81492255796079327, 30.83224293864770260 ) ) ;
#106727 = CARTESIAN_POINT ( 'NONE',  ( -10.81492255796105439, 18.62759615963255655, 107.9177570613523471 ) ) ;
#106728 = CARTESIAN_POINT ( 'NONE',  ( -16.46253265017160317, 9.564922557960807481, 90.83224293864769550 ) ) ;
#106729 = CARTESIAN_POINT ( 'NONE',  ( -4.379528057220086978, -16.55341960407618274, 69.79275706135234714 ) ) ;
#106730 = CARTESIAN_POINT ( 'NONE',  ( -16.51473224551069308, -9.474510206698971260, 26.66557627198103120 ) ) ;
#106731 = CARTESIAN_POINT ( 'NONE',  ( 16.53943276465976808, -0.05219959533910856209, 28.74890960531435624 ) ) ;
#106733 = CARTESIAN_POINT ( 'NONE',  ( 5.153800228976335163, 19.02544592524342804, 89.79057627198102409 ) ) ;
#106732 = CARTESIAN_POINT ( 'NONE',  ( 9.474510206698971260, -16.51473224551069308, 102.9155762719810241 ) ) ;
#106734 = CARTESIAN_POINT ( 'NONE',  ( 18.62759615963271287, -10.81492255796078972, 23.33224293864769194 ) ) ;
#106735 = CARTESIAN_POINT ( 'NONE',  ( 8.314922557960818139, 14.29746914071049879, 64.58224293864769550 ) ) ;
#106736 = CARTESIAN_POINT ( 'NONE',  ( 14.29746914071049879, -8.314922557960816363, 38.33224293864768839 ) ) ;
#106737 = CARTESIAN_POINT ( 'NONE',  ( 14.34966873604960469, 8.224510206698951720, 54.16557627198103120 ) ) ;
#106739 = FACE_OUTER_BOUND ( 'NONE', #139317, .T. ) ;
#106738 = CARTESIAN_POINT ( 'NONE',  ( -16.52544592524335698, -4.483927247898792601, 48.95942372801902565 ) ) ;
#106740 = CARTESIAN_POINT ( 'NONE',  ( -13.97604488694547697, 13.89961937509957934, 48.12609039468566863 ) ) ;
#106741 = CARTESIAN_POINT ( 'NONE',  ( -16.46253265017160317, 9.564922557960807481, 90.83224293864769550 ) ) ;
#106742 = CARTESIAN_POINT ( 'NONE',  ( -5.049401038297874678, -19.05341960407617918, 64.79275706135233293 ) ) ;
#106743 = CARTESIAN_POINT ( 'NONE',  ( -27.73933785331498925, 2.428612866367529932E-14, 143.3750000027311842 ) ) ;
#106744 = CARTESIAN_POINT ( 'NONE',  ( -16.51473224551082808, 9.474510206698731452, 53.33442372801900433 ) ) ;
#106746 = CARTESIAN_POINT ( 'NONE',  ( 4.379528057220092307, 16.55341960407617563, 77.29275706135234714 ) ) ;
#106745 = CARTESIAN_POINT ( 'NONE',  ( -9.564922557961040184, 16.46253265017147172, 92.91775706135233293 ) ) ;
#106747 = CARTESIAN_POINT ( 'NONE',  ( 27.73933785331498925, -9.013057229001033122, 146.2750000027311899 ) ) ;
#106748 = CARTESIAN_POINT ( 'NONE',  ( -19.02544592524342804, 5.153800228976336051, 26.04057627198103120 ) ) ;
#106749 = CARTESIAN_POINT ( 'NONE',  ( 15.72974639402199770, -15.80617190586745480, 28.12390960531435979 ) ) ;
#106750 = CARTESIAN_POINT ( 'NONE',  ( 5.823673210054444382, -21.52544592524334988, 40.20942372801901854 ) ) ;
#106751 = CARTESIAN_POINT ( 'NONE',  ( 19.02544592524334988, 5.153800228976608722, 101.4594237280189759 ) ) ;
#106753 = CARTESIAN_POINT ( 'NONE',  ( 5.049401038298161559, -19.05341960407611168, 62.70724293864769550 ) ) ;
#106752 = CARTESIAN_POINT ( 'NONE',  ( 23.48529157249599564, 32.32473071737754111, -2.700000000000000178 ) ) ;
#106754 = CARTESIAN_POINT ( 'NONE',  ( 19.02544592524343514, -5.153800228976328945, 108.5405762719810383 ) ) ;
#106756 = CARTESIAN_POINT ( 'NONE',  ( 9.564922557960805705, 16.46253265017160317, 64.58224293864769550 ) ) ;
#106755 = CARTESIAN_POINT ( 'NONE',  ( 12.06949235617757843, -12.14591786802309237, 78.12390960531436690 ) ) ;
#106757 = CARTESIAN_POINT ( 'NONE',  ( 9.564922557960805705, 16.46253265017160317, 69.58224293864770971 ) ) ;
#106758 = CARTESIAN_POINT ( 'NONE',  ( -19.05341960407617563, 5.049401038297882671, 78.54275706135233293 ) ) ;
#106759 = CARTESIAN_POINT ( 'NONE',  ( -21.52544592524343514, 5.823673210054127303, 56.04057627198102409 ) ) ;
#106760 = CARTESIAN_POINT ( 'NONE',  ( 8.224510206698953496, -14.34966873604960469, 107.9155762719810241 ) ) ;
#106761 = CARTESIAN_POINT ( 'NONE',  ( -16.51473224551082808, 9.474510206698731452, 38.33442372801899722 ) ) ;
#106762 = CARTESIAN_POINT ( 'NONE',  ( -13.89961937509977652, 13.97604488694528158, 85.62390960531433848 ) ) ;
#106763 = CARTESIAN_POINT ( 'NONE',  ( -18.67979575497178146, -10.72451020669898902, 76.66557627198103830 ) ) ;
#106765 = CARTESIAN_POINT ( 'NONE',  ( 19.02544592524334988, 5.153800228976608722, 46.45942372801899012 ) ) ;
#106764 = CARTESIAN_POINT ( 'NONE',  ( -12.06949235617756955, 12.14591786802309770, 80.62390960531438111 ) ) ;
#106766 = CARTESIAN_POINT ( 'NONE',  ( -15.72974639402197994, 15.80617190586746368, 80.62390960531438111 ) ) ;
#106767 = CARTESIAN_POINT ( 'NONE',  ( 0.05219959533907565091, 21.53943276465977519, 64.99890960531435269 ) ) ;
#106768 = CARTESIAN_POINT ( 'NONE',  ( 21.52544592524344225, -5.823673210054117533, 33.54057627198102409 ) ) ;
#106769 = CARTESIAN_POINT ( 'NONE',  ( 18.62759615963255655, 10.81492255796105972, 96.66775706135234714 ) ) ;
#106770 = CARTESIAN_POINT ( 'NONE',  ( -0.05219959533909027116, -19.03943276465977164, 72.49890960531435269 ) ) ;
#106771 = CARTESIAN_POINT ( 'NONE',  ( -12.06949235617756955, 12.14591786802309770, 110.6239096053143669 ) ) ;
#106772 = CIRCLE ( 'NONE', #19594, 37.99626262588765968 ) ;
#106773 = CARTESIAN_POINT ( 'NONE',  ( -10.72451020669870658, -18.67979575497194134, 29.58442372801901854 ) ) ;
#106774 = CARTESIAN_POINT ( 'NONE',  ( 5.719274019375673035, 21.55341960407619339, 47.29275706135234003 ) ) ;
#106775 = CARTESIAN_POINT ( 'NONE',  ( 9.564922557960805705, 16.46253265017160317, 34.58224293864770260 ) ) ;
#106776 = CARTESIAN_POINT ( 'NONE',  ( -15.80617190586745835, -15.72974639402198527, 111.8739096053143669 ) ) ;
#106777 = CARTESIAN_POINT ( 'NONE',  ( -19.05341960407617563, 5.049401038297882671, 48.54275706135233293 ) ) ;
#106778 = CARTESIAN_POINT ( 'NONE',  ( -19.03943276465977164, 0.05219959533909376836, 36.24890960531436690 ) ) ;
#106779 = CARTESIAN_POINT ( 'NONE',  ( 19.03943276465977164, -0.05219959533909143690, 23.74890960531435269 ) ) ;
#106780 = CARTESIAN_POINT ( 'NONE',  ( 12.24802307403546386, -10.94100078822751776, -61.47356435416956799 ) ) ;
#106781 = CARTESIAN_POINT ( 'NONE',  ( -8.224510206698735004, -14.34966873604973081, 54.58442372801901143 ) ) ;
#106782 = CARTESIAN_POINT ( 'NONE',  ( 16.46253265017160672, -9.564922557960803928, 23.33224293864769194 ) ) ;
#106783 = CARTESIAN_POINT ( 'NONE',  ( -25.04733094907770763, -10.92720321514065418, 170.1247377027656285 ) ) ;
#106784 = CARTESIAN_POINT ( 'NONE',  ( -19.03943276465977164, 0.05219959533909376836, 81.24890960531436690 ) ) ;
#106786 = EDGE_CURVE ( 'NONE', #194693, #89112, #182078, .T. ) ;
#106785 = CARTESIAN_POINT ( 'NONE',  ( -8.314922557960811034, -14.29746914071050412, 102.0822429386476955 ) ) ;
#106787 = CARTESIAN_POINT ( 'NONE',  ( 18.62759615963271287, -10.81492255796078972, 63.33224293864770260 ) ) ;
#106788 = CARTESIAN_POINT ( 'NONE',  ( -4.483927247898782831, 16.52544592524335698, 42.70942372801901854 ) ) ;
#106789 = CARTESIAN_POINT ( 'NONE',  ( 10.81492255796106328, -18.62759615963255655, 100.4177570613523471 ) ) ;
#106790 = CARTESIAN_POINT ( 'NONE',  ( 5.153800228976335163, 19.02544592524342804, 24.79057627198102765 ) ) ;
#106791 = CARTESIAN_POINT ( 'NONE',  ( -0.05219959533934338120, 16.53943276465976808, 107.5010903946856899 ) ) ;
#106792 = CARTESIAN_POINT ( 'NONE',  ( 14.29746914071049879, -8.314922557960816363, 53.33224293864769550 ) ) ;
#106793 = CARTESIAN_POINT ( 'NONE',  ( -0.05219959533909027116, -19.03943276465977164, 62.49890960531435979 ) ) ;
#106794 = CARTESIAN_POINT ( 'NONE',  ( -21.55341960407619339, 5.719274019375674811, 113.5427570613523756 ) ) ;
#106795 = CARTESIAN_POINT ( 'NONE',  ( -10.72451020669870658, -18.67979575497194134, 19.58442372801901143 ) ) ;
#106796 = CARTESIAN_POINT ( 'NONE',  ( -18.67979575497193778, 10.72451020669871902, 73.33442372801901854 ) ) ;
#106797 = CARTESIAN_POINT ( 'NONE',  ( -12.06949235617739369, -12.14591786802326823, 59.37609039468568284 ) ) ;
#106798 = CARTESIAN_POINT ( 'NONE',  ( -14.29746914071037622, -8.314922557961029526, 34.16775706135234714 ) ) ;
#106800 = CARTESIAN_POINT ( 'NONE',  ( 21.52544592524334988, 5.823673210054432836, 101.4594237280190185 ) ) ;
#106799 = CARTESIAN_POINT ( 'NONE',  ( -16.53943276465976808, 0.05219959533911058130, 81.24890960531436690 ) ) ;
#106801 = CARTESIAN_POINT ( 'NONE',  ( 8.314922557960818139, 14.29746914071049879, 29.58224293864769905 ) ) ;
#106802 = CARTESIAN_POINT ( 'NONE',  ( -16.88567814943160528, 6.947325034625694506, 113.7099887734741799 ) ) ;
#106803 = CARTESIAN_POINT ( 'NONE',  ( 14.34966873604972726, -8.224510206698740333, 35.83442372801901143 ) ) ;
#106804 = CARTESIAN_POINT ( 'NONE',  ( 0.05219959533910956823, 16.53943276465976808, 44.99890960531435979 ) ) ;
#106805 = CARTESIAN_POINT ( 'NONE',  ( 4.379528057220092307, 16.55341960407617563, 82.29275706135234714 ) ) ;
#106806 = CARTESIAN_POINT ( 'NONE',  ( 16.46253265017160672, -9.564922557960803928, 93.33224293864769550 ) ) ;
#106807 = CARTESIAN_POINT ( 'NONE',  ( 19.02544592524343514, -5.153800228976328945, 113.5405762719810241 ) ) ;
#106808 = CARTESIAN_POINT ( 'NONE',  ( 18.62759615963255655, 10.81492255796105972, 101.6677570613523613 ) ) ;
#106809 = CARTESIAN_POINT ( 'NONE',  ( 14.34966873604972726, -8.224510206698740333, 100.8344237280190185 ) ) ;
#106810 = CARTESIAN_POINT ( 'NONE',  ( -12.06949235617756955, 12.14591786802309770, 85.62390960531436690 ) ) ;
#106811 = CARTESIAN_POINT ( 'NONE',  ( 5.153800228976335163, 19.02544592524342804, 84.79057627198099567 ) ) ;
#106812 = EDGE_LOOP ( 'NONE', ( #172273, #12211, #95417, #147012, #86243, #164100 ) ) ;
#106813 = CARTESIAN_POINT ( 'NONE',  ( 8.314922557961029526, -14.29746914071037800, 40.41775706135234714 ) ) ;
#106814 = CARTESIAN_POINT ( 'NONE',  ( -16.51473224551069308, -9.474510206698971260, 46.66557627198102409 ) ) ;
#106815 = CARTESIAN_POINT ( 'NONE',  ( -16.46253265017160317, 9.564922557960807481, 105.8322429386476955 ) ) ;
#106817 = CARTESIAN_POINT ( 'NONE',  ( 22.81625015709510151, -31.40387420917324590, -1.924999997268813434 ) ) ;
#106816 = CARTESIAN_POINT ( 'NONE',  ( 0.05219959533934541429, -16.53943276465976808, 45.00109039468568284 ) ) ;
#106818 = CARTESIAN_POINT ( 'NONE',  ( 13.97604488694548053, -13.89961937509957401, 30.62609039468566863 ) ) ;
#106819 = CARTESIAN_POINT ( 'NONE',  ( -12.14591786802326823, 12.06949235617739902, 103.1260903946856757 ) ) ;
#106820 = CARTESIAN_POINT ( 'NONE',  ( -16.46253265017160317, 9.564922557960807481, 30.83224293864769550 ) ) ;
#106821 = CARTESIAN_POINT ( 'NONE',  ( 16.55341960407618274, -4.379528057220086978, 76.04275706135237556 ) ) ;
#106822 = CARTESIAN_POINT ( 'NONE',  ( -19.03943276465977164, -0.05219959533935918106, 83.75109039468567573 ) ) ;
#106823 = CARTESIAN_POINT ( 'NONE',  ( -19.02544592524334988, -5.153800228976617603, 33.95942372801897591 ) ) ;
#106824 = CARTESIAN_POINT ( 'NONE',  ( 5.153800228976335163, 19.02544592524342804, 64.79057627198100988 ) ) ;
#106825 = CARTESIAN_POINT ( 'NONE',  ( 8.224510206698953496, -14.34966873604960469, 97.91557627198103830 ) ) ;
#106826 = CARTESIAN_POINT ( 'NONE',  ( -5.049401038297874678, -19.05341960407617918, 74.79275706135231871 ) ) ;
#106827 = CARTESIAN_POINT ( 'NONE',  ( -5.823673210054116645, -21.52544592524344225, 62.29057627198102409 ) ) ;
#106828 = CARTESIAN_POINT ( 'NONE',  ( 16.51473224551083163, -9.474510206698727899, 30.83442372801900433 ) ) ;
#106829 = CARTESIAN_POINT ( 'NONE',  ( 13.89961937509977652, -13.97604488694527269, 103.1239096053143527 ) ) ;
#106830 = CARTESIAN_POINT ( 'NONE',  ( -21.52544592524343514, 5.823673210054127303, 76.04057627198102409 ) ) ;
#106831 = CARTESIAN_POINT ( 'NONE',  ( -19.05341960407611168, -5.049401038298163336, 111.4572429386476671 ) ) ;
#106832 = CARTESIAN_POINT ( 'NONE',  ( 16.46253265017146816, 9.564922557961045513, 101.6677570613523329 ) ) ;
#106833 = DIRECTION ( 'NONE',  ( 0.1039620511844979306, 0.1039620511844979306, 0.9891328443778538704 ) ) ;
#106834 = CARTESIAN_POINT ( 'NONE',  ( 16.53943276465976808, 0.05219959533934440121, 21.25109039468567218 ) ) ;
#106835 = CARTESIAN_POINT ( 'NONE',  ( -9.564922557960796823, -16.46253265017161027, 27.08224293864769550 ) ) ;
#106836 = CARTESIAN_POINT ( 'NONE',  ( 19.03943276465977164, -0.05219959533909143690, 93.74890960531435269 ) ) ;
#106837 = CARTESIAN_POINT ( 'NONE',  ( 18.62759615963271287, -10.81492255796078972, 88.33224293864769550 ) ) ;
#106838 = CARTESIAN_POINT ( 'NONE',  ( 16.55341960407618274, -4.379528057220086978, 61.04275706135234714 ) ) ;
#106839 = CARTESIAN_POINT ( 'NONE',  ( -10.81492255796105439, 18.62759615963255655, 57.91775706135234714 ) ) ;
#106841 = CARTESIAN_POINT ( 'NONE',  ( -5.719274019375665041, -21.55341960407619695, 109.7927570613523613 ) ) ;
#106840 = CARTESIAN_POINT ( 'NONE',  ( -5.153800228976607833, 19.02544592524334988, 107.7094237280189759 ) ) ;
#106842 = CARTESIAN_POINT ( 'NONE',  ( -0.05219959533934338120, 16.53943276465976808, 107.5010903946856899 ) ) ;
#106843 = CARTESIAN_POINT ( 'NONE',  ( 15.72974639402199770, -15.80617190586745480, 103.1239096053143811 ) ) ;
#106844 = CARTESIAN_POINT ( 'NONE',  ( 16.52544592524342804, -4.483927247898539470, 38.54057627198103120 ) ) ;
#106845 = CARTESIAN_POINT ( 'NONE',  ( -16.46253265017146816, -9.564922557961047289, 84.16775706135233293 ) ) ;
#106846 = CARTESIAN_POINT ( 'NONE',  ( -10.72451020669870658, -18.67979575497194134, 54.58442372801901143 ) ) ;
#106847 = CARTESIAN_POINT ( 'NONE',  ( -16.46253265017146816, -9.564922557961047289, 34.16775706135233293 ) ) ;
#106848 = CARTESIAN_POINT ( 'NONE',  ( -12.14591786802309592, -12.06949235617757132, 106.8739096053143811 ) ) ;
#106849 = CARTESIAN_POINT ( 'NONE',  ( 21.53943276465977519, -0.05219959533907433946, 28.74890960531435624 ) ) ;
#106850 = CARTESIAN_POINT ( 'NONE',  ( 12.14591786802309770, 12.06949235617756955, 34.37390960531435979 ) ) ;
#106851 = CARTESIAN_POINT ( 'NONE',  ( 21.55341960407619695, -5.719274019375665929, 96.04275706135236135 ) ) ;
#106852 = CARTESIAN_POINT ( 'NONE',  ( 12.06949235617739724, 12.14591786802326823, 66.87609039468568994 ) ) ;
#106853 = CARTESIAN_POINT ( 'NONE',  ( -12.14591786802309592, -12.06949235617757132, 31.87390960531435979 ) ) ;
#106854 = CARTESIAN_POINT ( 'NONE',  ( -15.80617190586768217, 15.72974639402176855, 68.12609039468567573 ) ) ;
#106855 = CARTESIAN_POINT ( 'NONE',  ( -18.62759615963255300, -10.81492255796106328, 54.16775706135235424 ) ) ;
#106856 = VERTEX_POINT ( 'NONE', #145725 ) ;
#106857 = CARTESIAN_POINT ( 'NONE',  ( -9.564922557960796823, -16.46253265017161027, 62.08224293864769550 ) ) ;
#106858 = CARTESIAN_POINT ( 'NONE',  ( -15.72974639402176322, -15.80617190586768395, 49.37609039468569705 ) ) ;
#106859 = CARTESIAN_POINT ( 'NONE',  ( 16.52544592524342804, -4.483927247898539470, 113.5405762719810383 ) ) ;
#106860 = CARTESIAN_POINT ( 'NONE',  ( 9.564922557960805705, 16.46253265017160317, 44.58224293864769550 ) ) ;
#106861 = CARTESIAN_POINT ( 'NONE',  ( -12.06949235617756955, 12.14591786802309770, 80.62390960531438111 ) ) ;
#106862 = CARTESIAN_POINT ( 'NONE',  ( -5.153800228976328057, -19.02544592524343514, 87.29057627198103830 ) ) ;
#106863 = CARTESIAN_POINT ( 'NONE',  ( -14.29746914071049879, 8.314922557960819915, 25.83224293864769194 ) ) ;
#106864 = CARTESIAN_POINT ( 'NONE',  ( 5.719274019375991003, -21.55341960407610458, 62.70724293864769550 ) ) ;
#106865 = CARTESIAN_POINT ( 'NONE',  ( -15.80617190586745835, -15.72974639402198527, 106.8739096053143811 ) ) ;
#106866 = CARTESIAN_POINT ( 'NONE',  ( -13.97604488694527625, -13.89961937509977652, 106.8739096053143669 ) ) ;
#106868 = CARTESIAN_POINT ( 'NONE',  ( 13.97604488694548053, -13.89961937509957401, 105.6260903946856757 ) ) ;
#106867 = CARTESIAN_POINT ( 'NONE',  ( 9.564922557960805705, 16.46253265017160317, 64.58224293864769550 ) ) ;
#106869 = ADVANCED_FACE ( 'NONE', ( #131564 ), #198234, .F. ) ;
#106870 = CARTESIAN_POINT ( 'NONE',  ( 5.719274019375991003, -21.55341960407610458, 52.70724293864769550 ) ) ;
#106871 = CARTESIAN_POINT ( 'NONE',  ( 5.823673210054444382, -21.52544592524334988, 75.20942372801901854 ) ) ;
#106872 = CARTESIAN_POINT ( 'NONE',  ( -16.46253265017160317, 9.564922557960807481, 70.83224293864770971 ) ) ;
#106873 = CARTESIAN_POINT ( 'NONE',  ( 19.02544592524343514, -5.153800228976328945, 103.5405762719809957 ) ) ;
#106874 = CARTESIAN_POINT ( 'NONE',  ( 8.314922557961029526, -14.29746914071037800, 70.41775706135236135 ) ) ;
#106875 = CARTESIAN_POINT ( 'NONE',  ( -0.05219959533937732626, 21.53943276465977519, 57.50109039468568994 ) ) ;
#106876 = CARTESIAN_POINT ( 'NONE',  ( 21.53943276465977519, 0.05219959533937863772, 91.25109039468568994 ) ) ;
#106877 = CARTESIAN_POINT ( 'NONE',  ( -10.72451020669898014, 18.67979575497178502, 110.4155762719810383 ) ) ;
#106878 = CARTESIAN_POINT ( 'NONE',  ( 16.52544592524335698, 4.483927247898782831, 81.45942372801900433 ) ) ;
#106879 = CARTESIAN_POINT ( 'NONE',  ( -18.62759615963270932, 10.81492255796079327, 70.83224293864770971 ) ) ;
#106880 = CARTESIAN_POINT ( 'NONE',  ( -19.05341960407617563, 5.049401038297882671, 53.54275706135231871 ) ) ;
#106881 = CARTESIAN_POINT ( 'NONE',  ( -0.05219959533907301413, -21.53943276465977519, 42.49890960531435979 ) ) ;
#106883 = CARTESIAN_POINT ( 'NONE',  ( 16.53943276465976808, -0.05219959533910856209, 28.74890960531435624 ) ) ;
#106882 = CARTESIAN_POINT ( 'NONE',  ( -19.05341960407611168, -5.049401038298163336, 81.45724293864769550 ) ) ;
#106884 = CARTESIAN_POINT ( 'NONE',  ( 7.992609269207028790E-30, -165.0000000000000000, -15.00000000000000000 ) ) ;
#106885 = CARTESIAN_POINT ( 'NONE',  ( -21.53943276465977519, 0.05219959533907696930, 21.24890960531436690 ) ) ;
#106886 = CARTESIAN_POINT ( 'NONE',  ( 1.500000000000124123, 15.01136863746049954, -59.87766023546532068 ) ) ;
#106887 = CARTESIAN_POINT ( 'NONE',  ( -13.89961937509957401, -13.97604488694547875, 89.37609039468563310 ) ) ;
#106888 = CARTESIAN_POINT ( 'NONE',  ( 21.53943276465977519, -0.05219959533907433946, 68.74890960531435269 ) ) ;
#106889 = CARTESIAN_POINT ( 'NONE',  ( -16.55341960407611168, -4.379528057220339221, 51.45724293864770260 ) ) ;
#106890 = CARTESIAN_POINT ( 'NONE',  ( -19.03943276465977164, -0.05219959533935918106, 108.7510903946856615 ) ) ;
#106891 = CARTESIAN_POINT ( 'NONE',  ( 9.564922557960805705, 16.46253265017160317, 39.58224293864768839 ) ) ;
#106893 = CARTESIAN_POINT ( 'NONE',  ( -5.153800228976607833, 19.02544592524334988, 77.70942372801900433 ) ) ;
#106892 = CARTESIAN_POINT ( 'NONE',  ( 10.81492255796078972, 18.62759615963270932, 99.58224293864770971 ) ) ;
#106894 = CARTESIAN_POINT ( 'NONE',  ( -13.89961937509977652, 13.97604488694528158, 80.62390960531436690 ) ) ;
#106895 = CARTESIAN_POINT ( 'NONE',  ( -4.379528057220328563, 16.55341960407611168, 90.20724293864770971 ) ) ;
#106896 = CARTESIAN_POINT ( 'NONE',  ( 5.049401038298161559, -19.05341960407611168, 57.70724293864769550 ) ) ;
#106897 = CARTESIAN_POINT ( 'NONE',  ( -16.53943276465976808, 0.05219959533911058130, 61.24890960531435979 ) ) ;
#106898 = CARTESIAN_POINT ( 'NONE',  ( 0.05219959533909260263, 19.03943276465977164, 34.99890960531435979 ) ) ;
#106899 = CARTESIAN_POINT ( 'NONE',  ( -16.99472585857189699, -5.499999999999960032, 20.67116795353343051 ) ) ;
#106900 = CARTESIAN_POINT ( 'NONE',  ( -16.53943276465976808, 0.05219959533911058130, 41.24890960531435269 ) ) ;
#106901 = CARTESIAN_POINT ( 'NONE',  ( -16.46253265017160317, 9.564922557960807481, 95.83224293864769550 ) ) ;
#106902 = CARTESIAN_POINT ( 'NONE',  ( 2.082452769671597245E-15, -69.45644693201178654, -14.99410988519313470 ) ) ;
#106903 = CARTESIAN_POINT ( 'NONE',  ( -19.02544592524334988, -5.153800228976617603, 48.95942372801900433 ) ) ;
#106904 = CARTESIAN_POINT ( 'NONE',  ( 14.29746914071037800, 8.314922557961029526, 61.66775706135235424 ) ) ;
#106905 = CARTESIAN_POINT ( 'NONE',  ( 21.52544592524344225, -5.823673210054117533, 68.54057627198103830 ) ) ;
#106906 = CARTESIAN_POINT ( 'NONE',  ( 13.97604488694548053, -13.89961937509957401, 35.62609039468567573 ) ) ;
#106907 = CARTESIAN_POINT ( 'NONE',  ( 16.46253265017160672, -9.564922557960803928, 88.33224293864769550 ) ) ;
#106908 = FACE_OUTER_BOUND ( 'NONE', #105653, .T. ) ;
#106909 = CARTESIAN_POINT ( 'NONE',  ( -21.53943276465977519, 0.05219959533907696930, 26.24890960531435624 ) ) ;
#106910 = CARTESIAN_POINT ( 'NONE',  ( -9.474510206698964154, 16.51473224551069663, 65.41557627198102409 ) ) ;
#106911 = CARTESIAN_POINT ( 'NONE',  ( -10.81492255796105439, 18.62759615963255655, 47.91775706135234714 ) ) ;
#106912 = CARTESIAN_POINT ( 'NONE',  ( -16.53943276465976808, 0.05219959533911058130, 116.2489096053143669 ) ) ;
#106915 = VERTEX_POINT ( 'NONE', #101210 ) ;
#106914 = CARTESIAN_POINT ( 'NONE',  ( 13.97604488694527802, 13.89961937509977652, 89.37390960531436690 ) ) ;
#106913 = CARTESIAN_POINT ( 'NONE',  ( 15.72974639402199770, -15.80617190586745480, 113.1239096053143953 ) ) ;
#106916 = CARTESIAN_POINT ( 'NONE',  ( 10.81492255796106328, -18.62759615963255655, 35.41775706135234003 ) ) ;
#106917 = VERTEX_POINT ( 'NONE', #162899 ) ;
#106918 = CARTESIAN_POINT ( 'NONE',  ( 16.51473224551069308, 9.474510206698969483, 99.16557627198102409 ) ) ;
#106919 = CARTESIAN_POINT ( 'NONE',  ( -21.97154029300585520, 7.270820338085815848, 170.2141396987978794 ) ) ;
#106920 = CARTESIAN_POINT ( 'NONE',  ( -5.823673210054116645, -21.52544592524344225, 112.2905762719810241 ) ) ;
#106921 = CARTESIAN_POINT ( 'NONE',  ( -5.049401038298153566, 19.05341960407611168, 45.20724293864769550 ) ) ;
#106922 = CARTESIAN_POINT ( 'NONE',  ( 14.34966873604972726, -8.224510206698740333, 25.83442372801901499 ) ) ;
#106923 = CARTESIAN_POINT ( 'NONE',  ( -36.91746825000000598, 2.428612866367529932E-14, -3.124999997268813168 ) ) ;
#106924 = CARTESIAN_POINT ( 'NONE',  ( 5.153800228976335163, 19.02544592524342804, 24.79057627198102765 ) ) ;
#106925 = CARTESIAN_POINT ( 'NONE',  ( -15.72974639402176322, -15.80617190586768395, 99.37609039468568994 ) ) ;
#106927 = CARTESIAN_POINT ( 'NONE',  ( 21.55341960407619695, -5.719274019375665929, 46.04275706135234714 ) ) ;
#106926 = CARTESIAN_POINT ( 'NONE',  ( 0.05219959533909260263, 19.03943276465977164, 69.99890960531435269 ) ) ;
#106928 = CARTESIAN_POINT ( 'NONE',  ( -17.14385361876520619, 23.59649016807275856, 147.0750000027311728 ) ) ;
#106929 = CARTESIAN_POINT ( 'NONE',  ( -13.97604488694527625, -13.89961937509977652, 96.87390960531433848 ) ) ;
#106930 = CARTESIAN_POINT ( 'NONE',  ( 193.3062444957835453, -155.7167183371837496, -15.00000000000000178 ) ) ;
#106933 = CARTESIAN_POINT ( 'NONE',  ( -5.823673210054431948, 21.52544592524334988, 57.70942372801901143 ) ) ;
#106932 = CARTESIAN_POINT ( 'NONE',  ( 12.14591786802327356, -12.06949235617739191, 65.62609039468568994 ) ) ;
#106931 = CARTESIAN_POINT ( 'NONE',  ( 4.483927247898790824, -16.52544592524335698, 40.20942372801901854 ) ) ;
#106934 = CARTESIAN_POINT ( 'NONE',  ( 21.53943276465977519, 0.05219959533937863772, 86.25109039468568994 ) ) ;
#106935 = CARTESIAN_POINT ( 'NONE',  ( 3.920341815485308690, 4.991179326919313652, -62.46637012391575183 ) ) ;
#106936 = CARTESIAN_POINT ( 'NONE',  ( 0.05219959533936267826, -19.03943276465977164, 105.0010903946856615 ) ) ;
#106937 = CARTESIAN_POINT ( 'NONE',  ( 13.89961937509977652, -13.97604488694527269, 73.12390960531436690 ) ) ;
#106938 = CARTESIAN_POINT ( 'NONE',  ( -13.89961937509977652, 13.97604488694528158, 100.6239096053143669 ) ) ;
#106939 = CARTESIAN_POINT ( 'NONE',  ( 14.34966873604960469, 8.224510206698951720, 109.1655762719810383 ) ) ;
#106940 = CARTESIAN_POINT ( 'NONE',  ( -21.55341960407610458, -5.719274019375992779, 31.45724293864769550 ) ) ;
#106941 = CARTESIAN_POINT ( 'NONE',  ( -12.14591786802326823, 12.06949235617739902, 93.12609039468568994 ) ) ;
#106943 = CARTESIAN_POINT ( 'NONE',  ( -16.46253265017160317, 9.564922557960807481, 60.83224293864769550 ) ) ;
#106942 = CARTESIAN_POINT ( 'NONE',  ( 14.29746914071049879, -8.314922557960816363, 68.33224293864769550 ) ) ;
#106944 = CARTESIAN_POINT ( 'NONE',  ( 10.72451020669871369, 18.67979575497193778, 87.08442372801901854 ) ) ;
#106945 = CARTESIAN_POINT ( 'NONE',  ( -23.50300173439379492, 1.337618122189927927, -57.33987540012260098 ) ) ;
#106946 = CARTESIAN_POINT ( 'NONE',  ( -5.153800228976607833, 19.02544592524334988, 102.7094237280189759 ) ) ;
#106947 = CARTESIAN_POINT ( 'NONE',  ( -14.34966873604960291, -8.224510206698953496, 76.66557627198103830 ) ) ;
#106948 = CARTESIAN_POINT ( 'NONE',  ( -18.62759615963255300, -10.81492255796106328, 29.16775706135234003 ) ) ;
#106949 = CARTESIAN_POINT ( 'NONE',  ( -18.62759615963270932, 10.81492255796079327, 60.83224293864769550 ) ) ;
#106950 = CARTESIAN_POINT ( 'NONE',  ( 0.05219959533936267826, -19.03943276465977164, 35.00109039468566863 ) ) ;
#106951 = CARTESIAN_POINT ( 'NONE',  ( 28.82186960331498327, 9.364793116373570925, 147.3500000054623627 ) ) ;
#106952 = CARTESIAN_POINT ( 'NONE',  ( 19.05341960407611168, 5.049401038298154454, 78.95724293864769550 ) ) ;
#106953 = CARTESIAN_POINT ( 'NONE',  ( -14.34966873604960291, -8.224510206698953496, 51.66557627198102409 ) ) ;
#106954 = CARTESIAN_POINT ( 'NONE',  ( -0.05219959533910754901, -16.53943276465976808, 37.49890960531436690 ) ) ;
#106955 = CARTESIAN_POINT ( 'NONE',  ( -12.06949235617739369, -12.14591786802326823, 99.37609039468568994 ) ) ;
#106956 = CARTESIAN_POINT ( 'NONE',  ( -9.564922557961040184, 16.46253265017147172, 47.91775706135233293 ) ) ;
#106957 = CARTESIAN_POINT ( 'NONE',  ( 9.564922557960805705, 16.46253265017160317, 99.58224293864770971 ) ) ;
#106958 = CARTESIAN_POINT ( 'NONE',  ( -8.314922557960811034, -14.29746914071050412, 72.08224293864769550 ) ) ;
#106959 = CARTESIAN_POINT ( 'NONE',  ( 13.97604488694548053, -13.89961937509957401, 45.62609039468566863 ) ) ;
#106961 = CARTESIAN_POINT ( 'NONE',  ( 15.72974639402199770, -15.80617190586745480, 38.12390960531436690 ) ) ;
#106960 = CARTESIAN_POINT ( 'NONE',  ( 19.02544592524343514, -5.153800228976328945, 38.54057627198103120 ) ) ;
#106962 = CARTESIAN_POINT ( 'NONE',  ( 21.55341960407610458, 5.719274019375980345, 63.95724293864770260 ) ) ;
#106963 = CARTESIAN_POINT ( 'NONE',  ( 0.05219959533910956823, 16.53943276465976808, 99.99890960531436690 ) ) ;
#106964 = CARTESIAN_POINT ( 'NONE',  ( 14.29746914071037800, 8.314922557961029526, 56.66775706135235424 ) ) ;
#106965 = CARTESIAN_POINT ( 'NONE',  ( 0.05219959533937995610, -21.53943276465977519, 45.00109039468568284 ) ) ;
#106966 = CARTESIAN_POINT ( 'NONE',  ( 14.34966873604960469, 8.224510206698951720, 94.16557627198103830 ) ) ;
#106967 = EDGE_CURVE ( 'NONE', #87616, #66950, #175563, .T. ) ;
#106968 = CARTESIAN_POINT ( 'NONE',  ( -4.500000000000001776, -139.5000000000000000, 22.27940468532398910 ) ) ;
#106969 = CARTESIAN_POINT ( 'NONE',  ( -16.38665767535054130, 7.295008042176025498, 50.26400864214546260 ) ) ;
#106970 = CARTESIAN_POINT ( 'NONE',  ( -15.72974639402197994, 15.80617190586746368, 40.62390960531435269 ) ) ;
#106971 = FACE_OUTER_BOUND ( 'NONE', #68948, .T. ) ;
#106972 = CARTESIAN_POINT ( 'NONE',  ( 37.99626262588765258, 2.893932880411085066E-14, -6.747842220587804363 ) ) ;
#106974 = CARTESIAN_POINT ( 'NONE',  ( -16.55341960407611168, -4.379528057220339221, 46.45724293864769550 ) ) ;
#106973 = CARTESIAN_POINT ( 'NONE',  ( 4.483927247898790824, -16.52544592524335698, 40.20942372801901854 ) ) ;
#106975 = CARTESIAN_POINT ( 'NONE',  ( -21.52544592524343514, 5.823673210054127303, 66.04057627198103830 ) ) ;
#106976 = CARTESIAN_POINT ( 'NONE',  ( 19.02544592524334988, 5.153800228976608722, 91.45942372801900433 ) ) ;
#106977 = CARTESIAN_POINT ( 'NONE',  ( -5.823673210054116645, -21.52544592524344225, 62.29057627198102409 ) ) ;
#106978 = CARTESIAN_POINT ( 'NONE',  ( 31.67388030095421314, -20.99825235784043187, -23.44681632512342873 ) ) ;
#106980 = CARTESIAN_POINT ( 'NONE',  ( 19.02544592524343514, -5.153800228976328945, 98.54057627198100988 ) ) ;
#106979 = CARTESIAN_POINT ( 'NONE',  ( -13.97604488694527625, -13.89961937509977652, 36.87390960531436690 ) ) ;
#106981 = CARTESIAN_POINT ( 'NONE',  ( 0.05219959533909260263, 19.03943276465977164, 34.99890960531435979 ) ) ;
#106983 = EDGE_CURVE ( 'NONE', #3247, #149477, #130550, .T. ) ;
#106982 = CARTESIAN_POINT ( 'NONE',  ( 14.29746914071049879, -8.314922557960816363, 108.3322429386477097 ) ) ;
#106984 = DIRECTION ( 'NONE',  ( 6.982962677686266711E-15, 0.000000000000000000, -1.000000000000000000 ) ) ;
#106985 = CARTESIAN_POINT ( 'NONE',  ( -5.153800228976328057, -19.02544592524343514, 112.2905762719810099 ) ) ;
#106986 = ORIENTED_EDGE ( 'NONE', *, *, #188131, .T. ) ;
#106987 = CARTESIAN_POINT ( 'NONE',  ( -8.224510206698735004, -14.34966873604973081, 74.58442372801901854 ) ) ;
#106988 = CARTESIAN_POINT ( 'NONE',  ( 18.62759615963271287, -10.81492255796078972, 88.33224293864769550 ) ) ;
#106989 = CARTESIAN_POINT ( 'NONE',  ( 19.02544592524343514, -5.153800228976328945, 58.54057627198102409 ) ) ;
#106990 = CARTESIAN_POINT ( 'NONE',  ( 10.72451020669871369, 18.67979575497193778, 32.08442372801901854 ) ) ;
#106991 = CARTESIAN_POINT ( 'NONE',  ( 19.03943276465977164, -0.05219959533909143690, 78.74890960531436690 ) ) ;
#106992 = DIRECTION ( 'NONE',  ( 0.000000000000000000, 0.000000000000000000, -1.000000000000000000 ) ) ;
#106993 = ORIENTED_EDGE ( 'NONE', *, *, #169362, .T. ) ;
#106994 = CARTESIAN_POINT ( 'NONE',  ( 15.72974639402199770, -15.80617190586745480, 113.1239096053143953 ) ) ;
#106997 = CARTESIAN_POINT ( 'NONE',  ( 13.89961937509957401, 13.97604488694547697, 81.87609039468564731 ) ) ;
#106996 = CARTESIAN_POINT ( 'NONE',  ( -19.02544592524342804, 5.153800228976336051, 106.0405762719810241 ) ) ;
#106995 = CARTESIAN_POINT ( 'NONE',  ( 13.97604488694527802, 13.89961937509977652, 24.37390960531435624 ) ) ;
#106998 = CARTESIAN_POINT ( 'NONE',  ( 0.05219959533936267826, -19.03943276465977164, 30.00109039468566863 ) ) ;
#106999 = CARTESIAN_POINT ( 'NONE',  ( -21.53943276465977519, 0.05219959533907696930, 96.24890960531435269 ) ) ;
#107000 = CARTESIAN_POINT ( 'NONE',  ( -0.05219959533936034679, 19.03943276465977164, 32.50109039468566863 ) ) ;
#107001 = CARTESIAN_POINT ( 'NONE',  ( 16.46253265017146816, 9.564922557961045513, 36.66775706135233293 ) ) ;
#107002 = CARTESIAN_POINT ( 'NONE',  ( 16.55341960407618274, -4.379528057220086978, 86.04275706135236135 ) ) ;
#107003 = CARTESIAN_POINT ( 'NONE',  ( 19.03943276465977164, -0.05219959533909143690, 103.7489096053143669 ) ) ;
#107004 = CARTESIAN_POINT ( 'NONE',  ( 19.03943276465977164, -0.05219959533909143690, 53.74890960531436690 ) ) ;
#107005 = CARTESIAN_POINT ( 'NONE',  ( 21.53943276465977519, 0.05219959533937863772, 71.25109039468568994 ) ) ;
#107006 = CARTESIAN_POINT ( 'NONE',  ( 0.05219959533937995610, -21.53943276465977519, 80.00109039468568994 ) ) ;
#107007 = CARTESIAN_POINT ( 'NONE',  ( 13.97604488694527802, 13.89961937509977652, 114.3739096053143669 ) ) ;
#107008 = CARTESIAN_POINT ( 'NONE',  ( -13.89961937509977652, 13.97604488694528158, 75.62390960531438111 ) ) ;
#107009 = CARTESIAN_POINT ( 'NONE',  ( 10.81492255796106328, -18.62759615963255655, 50.41775706135235424 ) ) ;
#107010 = CARTESIAN_POINT ( 'NONE',  ( 5.049401038297881783, 19.05341960407617563, 97.29275706135233293 ) ) ;
#107011 = CARTESIAN_POINT ( 'NONE',  ( 13.89961937509977652, -13.97604488694527269, 48.12390960531435979 ) ) ;
#107012 = CARTESIAN_POINT ( 'NONE',  ( 13.97604488694527802, 13.89961937509977652, 94.37390960531436690 ) ) ;
#107013 = CARTESIAN_POINT ( 'NONE',  ( -19.02544592524342804, 5.153800228976336051, 86.04057627198103830 ) ) ;
#107014 = SPHERICAL_SURFACE ( 'NONE', #124254, 10.00000000000000000 ) ;
#107016 = EDGE_CURVE ( 'NONE', #28823, #40299, #8580, .T. ) ;
#107015 = CARTESIAN_POINT ( 'NONE',  ( 13.97604488694527802, 13.89961937509977652, 54.37390960531435979 ) ) ;
#107017 = CARTESIAN_POINT ( 'NONE',  ( 21.52544592524344225, -5.823673210054117533, 93.54057627198103830 ) ) ;
#107018 = CARTESIAN_POINT ( 'NONE',  ( -4.483927247898782831, 16.52544592524335698, 82.70942372801900433 ) ) ;
#107019 = CYLINDRICAL_SURFACE ( 'NONE', #195071, 5.000000000000000888 ) ;
#107020 = CARTESIAN_POINT ( 'NONE',  ( -0.05219959533936034679, 19.03943276465977164, 47.50109039468566863 ) ) ;
#107021 = CARTESIAN_POINT ( 'NONE',  ( -9.564922557960796823, -16.46253265017161027, 82.08224293864768129 ) ) ;
#107022 = CARTESIAN_POINT ( 'NONE',  ( -14.29746914071049879, 8.314922557960819915, 55.83224293864770260 ) ) ;
#107023 = CARTESIAN_POINT ( 'NONE',  ( 4.379528057220339221, -16.55341960407611168, 97.70724293864772392 ) ) ;
#107024 = CARTESIAN_POINT ( 'NONE',  ( -10.72451020669898014, 18.67979575497178502, 25.41557627198103120 ) ) ;
#107025 = CARTESIAN_POINT ( 'NONE',  ( -5.153800228976328057, -19.02544592524343514, 107.2905762719810383 ) ) ;
#107026 = CARTESIAN_POINT ( 'NONE',  ( 9.564922557960805705, 16.46253265017160317, 114.5822429386476955 ) ) ;
#107027 = CARTESIAN_POINT ( 'NONE',  ( -16.51473224551082808, 9.474510206698731452, 28.33442372801900433 ) ) ;
#107028 = CARTESIAN_POINT ( 'NONE',  ( -16.52544592524335698, -4.483927247898792601, 93.95942372801903275 ) ) ;
#107029 = CARTESIAN_POINT ( 'NONE',  ( -19.05341960407611168, -5.049401038298163336, 76.45724293864769550 ) ) ;
#107030 = CARTESIAN_POINT ( 'NONE',  ( -15.72974639402176322, -15.80617190586768395, 34.37609039468568284 ) ) ;
#107031 = CARTESIAN_POINT ( 'NONE',  ( -5.823673210054116645, -21.52544592524344225, 32.29057627198102409 ) ) ;
#107032 = CARTESIAN_POINT ( 'NONE',  ( 15.80617190586769283, -15.72974639402175789, 20.62609039468568639 ) ) ;
#107033 = CARTESIAN_POINT ( 'NONE',  ( -21.53943276465977519, 0.05219959533907696930, 66.24890960531436690 ) ) ;
#107034 = CARTESIAN_POINT ( 'NONE',  ( 14.34966873604960469, 8.224510206698951720, 94.16557627198103830 ) ) ;
#107035 = CARTESIAN_POINT ( 'NONE',  ( -19.03943276465977164, -0.05219959533935918106, 43.75109039468566863 ) ) ;
#107036 = CARTESIAN_POINT ( 'NONE',  ( -5.049401038298153566, 19.05341960407611168, 30.20724293864768839 ) ) ;
#107037 = CARTESIAN_POINT ( 'NONE',  ( -5.153800228976328057, -19.02544592524343514, 87.29057627198103830 ) ) ;
#107038 = CARTESIAN_POINT ( 'NONE',  ( 9.564922557960805705, 16.46253265017160317, 84.58224293864769550 ) ) ;
#107039 = CARTESIAN_POINT ( 'NONE',  ( -27.73933785331498925, 9.013057229001088189, 148.7750000027311899 ) ) ;
#107040 = CARTESIAN_POINT ( 'NONE',  ( 16.52544592524342804, -4.483927247898539470, 103.5405762719810383 ) ) ;
#107041 = ORIENTED_EDGE ( 'NONE', *, *, #140339, .T. ) ;
#107042 = CARTESIAN_POINT ( 'NONE',  ( -12.06949235617756955, 12.14591786802309770, 30.62390960531436335 ) ) ;
#107043 = CARTESIAN_POINT ( 'NONE',  ( -14.34966873604972548, 8.224510206698743886, 33.33442372801900433 ) ) ;
#107044 = CARTESIAN_POINT ( 'NONE',  ( -10.81492255796105439, 18.62759615963255655, 87.91775706135234714 ) ) ;
#107045 = CARTESIAN_POINT ( 'NONE',  ( 9.474510206698971260, -16.51473224551069308, 97.91557627198102409 ) ) ;
#107046 = CARTESIAN_POINT ( 'NONE',  ( -21.55341960407610458, -5.719274019375992779, 111.4572429386476813 ) ) ;
#107047 = CARTESIAN_POINT ( 'NONE',  ( -0.05219959533909027116, -19.03943276465977164, 42.49890960531435269 ) ) ;
#107048 = CARTESIAN_POINT ( 'NONE',  ( 8.224510206698742110, 14.34966873604972548, 47.08442372801901854 ) ) ;
#107049 = CARTESIAN_POINT ( 'NONE',  ( -16.46253265017146816, -9.564922557961047289, 109.1677570613523471 ) ) ;
#107050 = CARTESIAN_POINT ( 'NONE',  ( 0.05219959533910956823, 16.53943276465976808, 94.99890960531436690 ) ) ;
#107051 = CARTESIAN_POINT ( 'NONE',  ( 5.719274019375991003, -21.55341960407610458, 102.7072429386476955 ) ) ;
#107052 = CARTESIAN_POINT ( 'NONE',  ( -16.46253265017146816, -9.564922557961047289, 69.16775706135233293 ) ) ;
#107053 = LINE ( 'NONE', #105086, #96110 ) ;
#107054 = CARTESIAN_POINT ( 'NONE',  ( -18.62759615963270932, 10.81492255796079327, 115.8322429386477097 ) ) ;
#107055 = CARTESIAN_POINT ( 'NONE',  ( -11.30153831258471442, -180.0000000000000000, -23.00000000000000000 ) ) ;
#107056 = CARTESIAN_POINT ( 'NONE',  ( 0.05219959533909260263, 19.03943276465977164, 89.99890960531436690 ) ) ;
#107057 = CARTESIAN_POINT ( 'NONE',  ( 19.78966525663867060, -34.76164524278549095, -6.188629846543125979 ) ) ;
#107058 = CARTESIAN_POINT ( 'NONE',  ( -9.474510206698964154, 16.51473224551069663, 90.41557627198103830 ) ) ;
#107060 = CARTESIAN_POINT ( 'NONE',  ( -14.29746914071049879, 8.314922557960819915, 75.83224293864769550 ) ) ;
#107059 = CARTESIAN_POINT ( 'NONE',  ( -21.53943276465977519, -0.05219959533937600094, 38.75109039468567573 ) ) ;
#107061 = CARTESIAN_POINT ( 'NONE',  ( -9.564922557960796823, -16.46253265017161027, 87.08224293864769550 ) ) ;
#107063 = CARTESIAN_POINT ( 'NONE',  ( 16.51473224551083163, -9.474510206698727899, 55.83442372801899722 ) ) ;
#107062 = CARTESIAN_POINT ( 'NONE',  ( -12.14591786802326823, 12.06949235617739902, 48.12609039468568284 ) ) ;
#107064 = CARTESIAN_POINT ( 'NONE',  ( -18.62759615963255300, -10.81492255796106328, 59.16775706135234714 ) ) ;
#107065 = CARTESIAN_POINT ( 'NONE',  ( 8.314922557961029526, -14.29746914071037800, 25.41775706135235779 ) ) ;
#107066 = CARTESIAN_POINT ( 'NONE',  ( 0.05219959533909260263, 19.03943276465977164, 69.99890960531435269 ) ) ;
#107067 = CARTESIAN_POINT ( 'NONE',  ( -13.89961937509957401, -13.97604488694547875, 94.37609039468566152 ) ) ;
#107068 = CARTESIAN_POINT ( 'NONE',  ( -4.483927247898782831, 16.52544592524335698, 52.70942372801902565 ) ) ;
#107069 = CARTESIAN_POINT ( 'NONE',  ( -5.823673210054431948, 21.52544592524334988, 102.7094237280190185 ) ) ;
#107070 = CARTESIAN_POINT ( 'NONE',  ( -19.02544592524334988, -5.153800228976617603, 78.95942372801900433 ) ) ;
#107071 = CARTESIAN_POINT ( 'NONE',  ( -16.51473224551069308, -9.474510206698971260, 46.66557627198102409 ) ) ;
#107072 = CARTESIAN_POINT ( 'NONE',  ( -15.80617190586745835, -15.72974639402198527, 76.87390960531439532 ) ) ;
#107074 = CARTESIAN_POINT ( 'NONE',  ( 19.02544592524334988, 5.153800228976608722, 81.45942372801897591 ) ) ;
#107073 = CARTESIAN_POINT ( 'NONE',  ( 14.34966873604960469, 8.224510206698951720, 79.16557627198103830 ) ) ;
#107075 = CARTESIAN_POINT ( 'NONE',  ( -19.53091890409952924, -5.499999999999944933, 70.06097431831416600 ) ) ;
#107076 = CARTESIAN_POINT ( 'NONE',  ( 16.51473224551083163, -9.474510206698727899, 45.83442372801900433 ) ) ;
#107077 = CARTESIAN_POINT ( 'NONE',  ( 16.55341960407618274, -4.379528057220086978, 111.0427570613523613 ) ) ;
#107078 = CARTESIAN_POINT ( 'NONE',  ( -0.05219959533910754901, -16.53943276465976808, 67.49890960531436690 ) ) ;
#107080 = CARTESIAN_POINT ( 'NONE',  ( -8.571926809382601320, -26.38167802310801591, 143.2750000027311899 ) ) ;
#107079 = CARTESIAN_POINT ( 'NONE',  ( 10.81492255796106328, -18.62759615963255655, 105.4177570613523613 ) ) ;
#107081 = CARTESIAN_POINT ( 'NONE',  ( -21.55341960407610458, -5.719274019375992779, 106.4572429386477097 ) ) ;
#107082 = CARTESIAN_POINT ( 'NONE',  ( 9.474510206698971260, -16.51473224551069308, 67.91557627198102409 ) ) ;
#107083 = CARTESIAN_POINT ( 'NONE',  ( -15.72974639402176322, -15.80617190586768395, 89.37609039468568994 ) ) ;
#107084 = CARTESIAN_POINT ( 'NONE',  ( 16.51473224551069308, 9.474510206698969483, 64.16557627198102409 ) ) ;
#107085 = VERTEX_POINT ( 'NONE', #59697 ) ;
#107086 = CARTESIAN_POINT ( 'NONE',  ( 16.51473224551069308, 9.474510206698969483, 29.16557627198103475 ) ) ;
#107087 = CARTESIAN_POINT ( 'NONE',  ( -15.72974639402197994, 15.80617190586746368, 30.62390960531436335 ) ) ;
#107088 = CARTESIAN_POINT ( 'NONE',  ( -4.483927247898539470, -16.52544592524342804, 72.29057627198102409 ) ) ;
#107089 = CARTESIAN_POINT ( 'NONE',  ( 5.049401038298161559, -19.05341960407611168, 47.70724293864770260 ) ) ;
#107090 = CARTESIAN_POINT ( 'NONE',  ( -16.55341960407611168, -4.379528057220339221, 81.45724293864769550 ) ) ;
#107091 = CARTESIAN_POINT ( 'NONE',  ( -21.52544592524343514, 5.823673210054127303, 111.0405762719810525 ) ) ;
#107092 = EDGE_CURVE ( 'NONE', #6179, #24124, #42256, .T. ) ;
#107093 = CARTESIAN_POINT ( 'NONE',  ( -5.823673210054431948, 21.52544592524334988, 52.70942372801902565 ) ) ;
#107094 = CARTESIAN_POINT ( 'NONE',  ( -19.05341960407611168, -5.049401038298163336, 36.45724293864766707 ) ) ;
#107095 = CARTESIAN_POINT ( 'NONE',  ( -8.314922557961024197, 14.29746914071037800, 47.91775706135234714 ) ) ;
#107096 = CARTESIAN_POINT ( 'NONE',  ( 5.823673210054125526, 21.52544592524343514, 99.79057627198103830 ) ) ;
#107098 = CARTESIAN_POINT ( 'NONE',  ( 0.05219959533909260263, 19.03943276465977164, 54.99890960531435979 ) ) ;
#107097 = CARTESIAN_POINT ( 'NONE',  ( -5.049401038297874678, -19.05341960407617918, 24.79275706135233648 ) ) ;
#107099 = CARTESIAN_POINT ( 'NONE',  ( 13.89961937509977652, -13.97604488694527269, 108.1239096053143669 ) ) ;
#107100 = CARTESIAN_POINT ( 'NONE',  ( -21.55341960407619339, 5.719274019375674811, 53.54275706135234714 ) ) ;
#107101 = B_SPLINE_CURVE_WITH_KNOTS ( 'NONE', 3,
 ( #96005, #155693, #62675, #187060, #107191, #123350, #169872, #142506, #18192, #47535, #30367, #79849, #184054, #17188, #156698, #7, #48530, #141518, #3005, #109189, #46530, #153704, #92011, #49510, #124356, #64681, #63689, #15200, #125364, #111173, #170868, #76858 ),
 .UNSPECIFIED., .F., .F.,
 ( 4, 2, 2, 2, 2, 2, 2, 2, 2, 2, 2, 2, 2, 2, 2, 4 ),
 ( 2.195984522899319407E-17, 0.0003712461730036906811, 0.0007424923460073594612, 0.001113738519011028133, 0.001484984692014696805, 0.002227477038022034582, 0.002598723211025703254, 0.002969969384029371925, 0.003341215557033051006, 0.003712461730036730519, 0.004083707903040409599, 0.004454954076044089113, 0.004826200249047772096, 0.005197446422051455080, 0.005568692595055138063, 0.005939938768058821913 ),
 .UNSPECIFIED. ) ;
#107102 = CARTESIAN_POINT ( 'NONE',  ( -18.67979575497178146, -10.72451020669898902, 46.66557627198102409 ) ) ;
#107103 = CARTESIAN_POINT ( 'NONE',  ( -12.06949235617756955, 12.14591786802309770, 25.62390960531435624 ) ) ;
#107105 = CARTESIAN_POINT ( 'NONE',  ( -18.67979575497193778, 10.72451020669871902, 93.33442372801901854 ) ) ;
#107104 = CARTESIAN_POINT ( 'NONE',  ( 5.719274019375673035, 21.55341960407619339, 57.29275706135234714 ) ) ;
#107106 = CARTESIAN_POINT ( 'NONE',  ( -9.474510206698720793, -16.51473224551083518, 29.58442372801900433 ) ) ;
#107107 = CARTESIAN_POINT ( 'NONE',  ( -16.55341960407617563, 4.379528057220093196, 103.5427570613523613 ) ) ;
#107108 = CARTESIAN_POINT ( 'NONE',  ( -5.823673210054431948, 21.52544592524334988, 57.70942372801901143 ) ) ;
#107109 = CARTESIAN_POINT ( 'NONE',  ( -19.03943276465977164, 0.05219959533909376836, 51.24890960531436690 ) ) ;
#107110 = CARTESIAN_POINT ( 'NONE',  ( -9.474510206698720793, -16.51473224551083518, 24.58442372801900078 ) ) ;
#107111 = CARTESIAN_POINT ( 'NONE',  ( 9.564922557960805705, 16.46253265017160317, 114.5822429386476955 ) ) ;
#107112 = CARTESIAN_POINT ( 'NONE',  ( -18.62759615963255300, -10.81492255796106328, 19.16775706135234714 ) ) ;
#107113 = CARTESIAN_POINT ( 'NONE',  ( -21.55341960407610458, -5.719274019375992779, 81.45724293864769550 ) ) ;
#107114 = CARTESIAN_POINT ( 'NONE',  ( -14.34966873604972548, 8.224510206698743886, 43.33442372801901143 ) ) ;
#107116 = CARTESIAN_POINT ( 'NONE',  ( 21.52544592524344225, -5.823673210054117533, 83.54057627198102409 ) ) ;
#107115 = FACE_OUTER_BOUND ( 'NONE', #4394, .T. ) ;
#107118 = CARTESIAN_POINT ( 'NONE',  ( -14.29746914071049879, 8.314922557960819915, 70.83224293864770971 ) ) ;
#107117 = CARTESIAN_POINT ( 'NONE',  ( 0.05219959533934541429, -16.53943276465976808, 60.00109039468568284 ) ) ;
#107119 = CARTESIAN_POINT ( 'NONE',  ( -27.74069374691385192, -6.311165852667877552, 163.4895129000211114 ) ) ;
#107120 = CARTESIAN_POINT ( 'NONE',  ( 5.049401038297881783, 19.05341960407617563, 102.2927570613523045 ) ) ;
#107121 = CARTESIAN_POINT ( 'NONE',  ( 18.67979575497178502, 10.72451020669898547, 29.16557627198103120 ) ) ;
#107122 = CARTESIAN_POINT ( 'NONE',  ( -4.500000000000000888, -139.5000000000000000, 21.32407087589996308 ) ) ;
#107123 = CARTESIAN_POINT ( 'NONE',  ( -4.379528057220086978, -16.55341960407618274, 44.79275706135234714 ) ) ;
#107124 = CARTESIAN_POINT ( 'NONE',  ( 10.72451020669898902, -18.67979575497178502, 107.9155762719810241 ) ) ;
#107125 = CARTESIAN_POINT ( 'NONE',  ( 10.72451020669898902, -18.67979575497178502, 27.91557627198103830 ) ) ;
#107126 = CARTESIAN_POINT ( 'NONE',  ( 4.483927247898790824, -16.52544592524335698, 75.20942372801901854 ) ) ;
#107127 = CARTESIAN_POINT ( 'NONE',  ( -13.89961937509977652, 13.97604488694528158, 85.62390960531433848 ) ) ;
#107129 = CARTESIAN_POINT ( 'NONE',  ( 4.483927247898790824, -16.52544592524335698, 20.20942372801900788 ) ) ;
#107128 = CARTESIAN_POINT ( 'NONE',  ( -18.62759615963255300, -10.81492255796106328, 39.16775706135235424 ) ) ;
#107130 = EDGE_CURVE ( 'NONE', #16989, #63341, #104227, .T. ) ;
#107131 = CARTESIAN_POINT ( 'NONE',  ( -15.80617190586745835, -15.72974639402198527, 31.87390960531435979 ) ) ;
#107132 = ORIENTED_EDGE ( 'NONE', *, *, #112783, .T. ) ;
#107133 = CARTESIAN_POINT ( 'NONE',  ( -9.474510206698720793, -16.51473224551083518, 29.58442372801900433 ) ) ;
#107134 = CARTESIAN_POINT ( 'NONE',  ( -16.52544592524335698, -4.483927247898792601, 48.95942372801902565 ) ) ;
#107135 = CARTESIAN_POINT ( 'NONE',  ( -19.05341960407611168, -5.049401038298163336, 96.45724293864769550 ) ) ;
#107136 = CARTESIAN_POINT ( 'NONE',  ( -5.719274019375978568, 21.55341960407610458, 100.2072429386476955 ) ) ;
#107137 = CARTESIAN_POINT ( 'NONE',  ( -19.03943276465977164, 0.05219959533909376836, 71.24890960531435269 ) ) ;
#107138 = CARTESIAN_POINT ( 'NONE',  ( -17.31728774477272736, 6.344390552232388458, 25.81906651689319432 ) ) ;
#107139 = CARTESIAN_POINT ( 'NONE',  ( -4.379528057220328563, 16.55341960407611168, 85.20724293864770971 ) ) ;
#107140 = CARTESIAN_POINT ( 'NONE',  ( -18.62759615963270932, 10.81492255796079327, 35.83224293864768839 ) ) ;
#107141 = CARTESIAN_POINT ( 'NONE',  ( -17.26172910966779739, 6.454744622555853795, 35.80646908649224969 ) ) ;
#107142 = CARTESIAN_POINT ( 'NONE',  ( -16.53943276465976808, -0.05219959533934237506, 63.75109039468568284 ) ) ;
#107143 = CARTESIAN_POINT ( 'NONE',  ( -5.823673210054116645, -21.52544592524344225, 112.2905762719810241 ) ) ;
#107144 = CARTESIAN_POINT ( 'NONE',  ( 9.474510206698729675, 16.51473224551082808, 82.08442372801899012 ) ) ;
#107145 = CARTESIAN_POINT ( 'NONE',  ( 13.89961937509977652, -13.97604488694527269, 28.12390960531435624 ) ) ;
#107146 = CARTESIAN_POINT ( 'NONE',  ( -0.05219959533907301413, -21.53943276465977519, 62.49890960531436690 ) ) ;
#107147 = CARTESIAN_POINT ( 'NONE',  ( -16.51473224551069308, -9.474510206698971260, 96.66557627198102409 ) ) ;
#107148 = CARTESIAN_POINT ( 'NONE',  ( -0.05219959533937732626, 21.53943276465977519, 87.50109039468568994 ) ) ;
#107149 = CARTESIAN_POINT ( 'NONE',  ( 9.474510206698971260, -16.51473224551069308, 67.91557627198102409 ) ) ;
#107150 = CARTESIAN_POINT ( 'NONE',  ( 0.05219959533934541429, -16.53943276465976808, 45.00109039468568284 ) ) ;
#107151 = CARTESIAN_POINT ( 'NONE',  ( -19.03943276465977164, 0.05219959533909376836, 61.24890960531436690 ) ) ;
#107152 = CARTESIAN_POINT ( 'NONE',  ( 5.823673210054444382, -21.52544592524334988, 85.20942372801901854 ) ) ;
#107153 = EDGE_LOOP ( 'NONE', ( #77034, #31839, #132041 ) ) ;
#107154 = CARTESIAN_POINT ( 'NONE',  ( -16.51473224551082808, 9.474510206698731452, 38.33442372801899722 ) ) ;
#107155 = CARTESIAN_POINT ( 'NONE',  ( 5.049401038297881783, 19.05341960407617563, 52.29275706135234003 ) ) ;
#107156 = CARTESIAN_POINT ( 'NONE',  ( -18.62759615963255300, -10.81492255796106328, 49.16775706135234003 ) ) ;
#107157 = CARTESIAN_POINT ( 'NONE',  ( -6.100000000000010303, 0.2002935562470000430, -62.50719930893271226 ) ) ;
#107158 = CARTESIAN_POINT ( 'NONE',  ( 9.564922557961047289, -16.46253265017146816, 40.41775706135234003 ) ) ;
#107159 = CARTESIAN_POINT ( 'NONE',  ( -5.153800228976328057, -19.02544592524343514, 97.29057627198099567 ) ) ;
#107160 = CARTESIAN_POINT ( 'NONE',  ( -9.474510206698964154, 16.51473224551069663, 70.41557627198102409 ) ) ;
#107161 = CARTESIAN_POINT ( 'NONE',  ( 8.224510206698742110, 14.34966873604972548, 112.0844237280190185 ) ) ;
#107163 = CARTESIAN_POINT ( 'NONE',  ( 15.80617190586769283, -15.72974639402175789, 100.6260903946857184 ) ) ;
#107162 = CARTESIAN_POINT ( 'NONE',  ( 15.80617190586746368, 15.72974639402197994, 34.37390960531435979 ) ) ;
#107164 = CARTESIAN_POINT ( 'NONE',  ( 36.91746824999999177, 2.880721459617395097E-14, -10.12499999726881583 ) ) ;
#107165 = CARTESIAN_POINT ( 'NONE',  ( 16.79531203550650886, 7.028104445595491079, 58.75244988220443787 ) ) ;
#107166 = CARTESIAN_POINT ( 'NONE',  ( 21.52544592524334988, 5.823673210054432836, 101.4594237280190185 ) ) ;
#107167 = CARTESIAN_POINT ( 'NONE',  ( 16.18388926212234935, -7.379444403734657598, 42.06046848633847191 ) ) ;
#107168 = CARTESIAN_POINT ( 'NONE',  ( -13.97604488694527625, -13.89961937509977652, 21.87390960531435979 ) ) ;
#107169 = CARTESIAN_POINT ( 'NONE',  ( -9.564922557960796823, -16.46253265017161027, 107.0822429386476955 ) ) ;
#107170 = LINE ( 'NONE', #152685, #27575 ) ;
#107171 = CARTESIAN_POINT ( 'NONE',  ( 14.34966873604972726, -8.224510206698740333, 55.83442372801901854 ) ) ;
#107172 = CARTESIAN_POINT ( 'NONE',  ( -10.72451020669898014, 18.67979575497178502, 65.41557627198102409 ) ) ;
#107173 = CARTESIAN_POINT ( 'NONE',  ( -14.29746914071049879, 8.314922557960819915, 45.83224293864769550 ) ) ;
#107175 = CARTESIAN_POINT ( 'NONE',  ( -19.02544592524342804, 5.153800228976336051, 101.0405762719810241 ) ) ;
#107174 = CARTESIAN_POINT ( 'NONE',  ( -14.29746914071049879, 8.314922557960819915, 105.8322429386476955 ) ) ;
#107176 = CARTESIAN_POINT ( 'NONE',  ( -16.46253265017146816, -9.564922557961047289, 34.16775706135233293 ) ) ;
#107177 = CARTESIAN_POINT ( 'NONE',  ( -19.05341960407611168, -5.049401038298163336, 21.45724293864768839 ) ) ;
#107178 = CARTESIAN_POINT ( 'NONE',  ( -21.53943276465977519, -0.05219959533937600094, 73.75109039468567573 ) ) ;
#107179 = DIRECTION ( 'NONE',  ( -0.000000000000000000, -0.000000000000000000, 1.000000000000000000 ) ) ;
#107180 = CARTESIAN_POINT ( 'NONE',  ( -4.483927247898782831, 16.52544592524335698, 107.7094237280190328 ) ) ;
#107181 = CARTESIAN_POINT ( 'NONE',  ( -3.573655867282028392E-15, 2.428612866367529932E-14, 1.984260520772446048E-44 ) ) ;
#107182 = CARTESIAN_POINT ( 'NONE',  ( 18.62759615963271287, -10.81492255796078972, 23.33224293864769194 ) ) ;
#107183 = CARTESIAN_POINT ( 'NONE',  ( 16.53943276465976808, -0.05219959533910856209, 88.74890960531436690 ) ) ;
#107184 = CARTESIAN_POINT ( 'NONE',  ( -16.51473224551082808, 9.474510206698731452, 63.33442372801900433 ) ) ;
#107185 = CARTESIAN_POINT ( 'NONE',  ( -16.51473224551069308, -9.474510206698971260, 71.66557627198102409 ) ) ;
#107186 = CARTESIAN_POINT ( 'NONE',  ( 16.52544592524342804, -4.483927247898539470, 78.54057627198103830 ) ) ;
#107187 = CARTESIAN_POINT ( 'NONE',  ( -19.03943276465977164, -0.05219959533935918106, 98.75109039468567573 ) ) ;
#107188 = CARTESIAN_POINT ( 'NONE',  ( 18.67979575497178502, 10.72451020669898547, 54.16557627198103120 ) ) ;
#107189 = ORIENTED_EDGE ( 'NONE', *, *, #190681, .F. ) ;
#107190 = CARTESIAN_POINT ( 'NONE',  ( 19.02544592524343514, -5.153800228976328945, 23.54057627198102054 ) ) ;
#107191 = CARTESIAN_POINT ( 'NONE',  ( -17.40805194822029378, -6.112264579159358391, 29.16628727489389661 ) ) ;
#107193 = CARTESIAN_POINT ( 'NONE',  ( -18.62759615963270932, 10.81492255796079327, 75.83224293864769550 ) ) ;
#107192 = CARTESIAN_POINT ( 'NONE',  ( 13.89961937509977652, -13.97604488694527269, 78.12390960531433848 ) ) ;
#107195 = CARTESIAN_POINT ( 'NONE',  ( -9.474510206698964154, 16.51473224551069663, 85.41557627198102409 ) ) ;
#107194 = CARTESIAN_POINT ( 'NONE',  ( 12.14591786802327356, -12.06949235617739191, 85.62609039468568994 ) ) ;
#107196 = CARTESIAN_POINT ( 'NONE',  ( 16.46253265017146816, 9.564922557961045513, 66.66775706135233293 ) ) ;
#107197 = CARTESIAN_POINT ( 'NONE',  ( -15.72974639402176322, -15.80617190586768395, 79.37609039468567573 ) ) ;
#107198 = ORIENTED_EDGE ( 'NONE', *, *, #154789, .T. ) ;
#107199 = CARTESIAN_POINT ( 'NONE',  ( 10.81492255796078972, 18.62759615963270932, 59.58224293864770260 ) ) ;
#107200 = CARTESIAN_POINT ( 'NONE',  ( -21.53943276465977519, 0.05219959533907696930, 21.24890960531436690 ) ) ;
#107201 = CARTESIAN_POINT ( 'NONE',  ( 9.564922557960805705, 16.46253265017160317, 39.58224293864768839 ) ) ;
#107202 = CARTESIAN_POINT ( 'NONE',  ( 4.483927247898790824, -16.52544592524335698, 105.2094237280190328 ) ) ;
#107203 = CARTESIAN_POINT ( 'NONE',  ( 19.02544592524343514, -5.153800228976328945, 48.54057627198103120 ) ) ;
#107204 = CARTESIAN_POINT ( 'NONE',  ( 13.89961937509957401, 13.97604488694547697, 111.8760903946856757 ) ) ;
#107205 = CARTESIAN_POINT ( 'NONE',  ( 17.44279575226822487, 5.990770900252483600, 51.66442432485681735 ) ) ;
#107206 = CARTESIAN_POINT ( 'NONE',  ( -0.05219959533937732626, 21.53943276465977519, 107.5010903946856899 ) ) ;
#107207 = CARTESIAN_POINT ( 'NONE',  ( -4.379528057220328563, 16.55341960407611168, 60.20724293864768839 ) ) ;
#107208 = CARTESIAN_POINT ( 'NONE',  ( 21.55341960407610458, 5.719274019375980345, 103.9572429386476813 ) ) ;
#107209 = CARTESIAN_POINT ( 'NONE',  ( -21.52544592524343514, 5.823673210054127303, 106.0405762719810525 ) ) ;
#107210 = CARTESIAN_POINT ( 'NONE',  ( -5.576804854476224094, 3.874965782148136029, -64.41982836185007955 ) ) ;
#107211 = CARTESIAN_POINT ( 'NONE',  ( -10.81492255796078084, -18.62759615963271287, 47.08224293864770260 ) ) ;
#107212 = CARTESIAN_POINT ( 'NONE',  ( -8.224510206698735004, -14.34966873604973081, 79.58442372801903275 ) ) ;
#107213 = CARTESIAN_POINT ( 'NONE',  ( -16.55341960407611168, -4.379528057220339221, 106.4572429386477097 ) ) ;
#107214 = CARTESIAN_POINT ( 'NONE',  ( 13.97604488694527802, 13.89961937509977652, 54.37390960531435979 ) ) ;
#107215 = CARTESIAN_POINT ( 'NONE',  ( -19.02130022317638947, 5.499999999999605649, 50.78188669246576126 ) ) ;
#107216 = CARTESIAN_POINT ( 'NONE',  ( 8.314922557961029526, -14.29746914071037800, 110.4177570613523756 ) ) ;
#107217 = CARTESIAN_POINT ( 'NONE',  ( 15.72974639402176855, 15.80617190586768217, 51.87609039468568284 ) ) ;
#107218 = CARTESIAN_POINT ( 'NONE',  ( 9.474510206698971260, -16.51473224551069308, 102.9155762719810241 ) ) ;
#107219 = CARTESIAN_POINT ( 'NONE',  ( -21.52544592524334988, -5.823673210054445271, 83.95942372801900433 ) ) ;
#107220 = DIRECTION ( 'NONE',  ( -1.000000000000000000, -0.000000000000000000, -0.000000000000000000 ) ) ;
#107221 = LINE ( 'NONE', #31395, #131463 ) ;
#107222 = ORIENTED_EDGE ( 'NONE', *, *, #124857, .F. ) ;
#107223 = CARTESIAN_POINT ( 'NONE',  ( -21.52544592524334988, -5.823673210054445271, 73.95942372801901854 ) ) ;
#107224 = CARTESIAN_POINT ( 'NONE',  ( -13.97604488694527625, -13.89961937509977652, 46.87390960531435979 ) ) ;
#107225 = CARTESIAN_POINT ( 'NONE',  ( 9.564922557960805705, 16.46253265017160317, 99.58224293864770971 ) ) ;
#107226 = CARTESIAN_POINT ( 'NONE',  ( -9.474510206698720793, -16.51473224551083518, 79.58442372801899012 ) ) ;
#107227 = CARTESIAN_POINT ( 'NONE',  ( 18.62759615963255655, 10.81492255796105972, 36.66775706135234714 ) ) ;
#107228 = CARTESIAN_POINT ( 'NONE',  ( 9.474510206698729675, 16.51473224551082808, 107.0844237280190043 ) ) ;
#107229 = CARTESIAN_POINT ( 'NONE',  ( 5.153800228976615827, -19.02544592524334988, 75.20942372801896170 ) ) ;
#107230 = CARTESIAN_POINT ( 'NONE',  ( 5.049401038298161559, -19.05341960407611168, 42.70724293864767418 ) ) ;
#107231 = CARTESIAN_POINT ( 'NONE',  ( 9.564922557961047289, -16.46253265017146816, 85.41775706135233293 ) ) ;
#107232 = CARTESIAN_POINT ( 'NONE',  ( 12.14591786802327356, -12.06949235617739191, 105.6260903946856899 ) ) ;
#107233 = CARTESIAN_POINT ( 'NONE',  ( -13.97604488694547697, 13.89961937509957934, 73.12609039468568994 ) ) ;
#107234 = CARTESIAN_POINT ( 'NONE',  ( -14.34966873604960291, -8.224510206698953496, 41.66557627198103120 ) ) ;
#107235 = CARTESIAN_POINT ( 'NONE',  ( 16.51473224551083163, -9.474510206698727899, 60.83442372801900433 ) ) ;
#107236 = CARTESIAN_POINT ( 'NONE',  ( -21.53943276465977519, -0.05219959533937600094, 103.7510903946857042 ) ) ;
#107237 = CARTESIAN_POINT ( 'NONE',  ( 16.46253265017146816, 9.564922557961045513, 26.66775706135234003 ) ) ;
#107238 = CARTESIAN_POINT ( 'NONE',  ( -19.05341960407611168, -5.049401038298163336, 26.45724293864769550 ) ) ;
#107239 = LINE ( 'NONE', #168910, #76488 ) ;
#107240 = CARTESIAN_POINT ( 'NONE',  ( -4.483927247898782831, 16.52544592524335698, 42.70942372801901854 ) ) ;
#107241 = B_SPLINE_CURVE_WITH_KNOTS ( 'NONE', 3,
 ( #152186, #45009, #167366, #168342, #13670, #121832, #14664, #95464, #96450, #33804, #77319, #31823, #49971, #186519, #174315, #141963, #142953, #173320, #48979, #110634, #111635, #63140 ),
 .UNSPECIFIED., .F., .F.,
 ( 4, 2, 2, 2, 2, 2, 2, 2, 2, 2, 4 ),
 ( 2.778238173728123515E-07, 0.0002956205979242803109, 0.0005909633720311878793, 0.0008863061461380952310, 0.001181648920245002799, 0.001772334468458817069, 0.002363020016672631556, 0.002953705564886446259, 0.003544391113100260095, 0.004135076661314075232, 0.004725762209527889501 ),
 .UNSPECIFIED. ) ;
#107242 = CARTESIAN_POINT ( 'NONE',  ( -5.049401038298153566, 19.05341960407611168, 95.20724293864770971 ) ) ;
#107243 = CARTESIAN_POINT ( 'NONE',  ( 22.44159573604009239, 16.30477369853692693, 142.0750000027311728 ) ) ;
#107244 = CARTESIAN_POINT ( 'NONE',  ( -13.97604488694527625, -13.89961937509977652, 91.87390960531432427 ) ) ;
#107245 = CARTESIAN_POINT ( 'NONE',  ( -17.40805194821983193, 6.112264579160852307, 100.8337127251061247 ) ) ;
#107246 = ORIENTED_EDGE ( 'NONE', *, *, #197919, .T. ) ;
#107247 = CARTESIAN_POINT ( 'NONE',  ( -9.564922557961040184, 16.46253265017147172, 82.91775706135233293 ) ) ;
#107248 = CARTESIAN_POINT ( 'NONE',  ( -21.53943276465977519, 0.05219959533907696930, 26.24890960531435624 ) ) ;
#107250 = CARTESIAN_POINT ( 'NONE',  ( -19.03943276465977164, -0.05219959533935918106, 103.7510903946856757 ) ) ;
#107249 = CARTESIAN_POINT ( 'NONE',  ( -19.02544592524334988, -5.153800228976617603, 18.95942372801899722 ) ) ;
#107251 = CARTESIAN_POINT ( 'NONE',  ( -0.05219959533910754901, -16.53943276465976808, 112.4989096053143669 ) ) ;
#107252 = CARTESIAN_POINT ( 'NONE',  ( -13.89961937509977652, 13.97604488694528158, 25.62390960531434558 ) ) ;
#107253 = CARTESIAN_POINT ( 'NONE',  ( -18.67979575497178146, -10.72451020669898902, 61.66557627198103120 ) ) ;
#107254 = CARTESIAN_POINT ( 'NONE',  ( 18.67979575497178502, 10.72451020669898547, 44.16557627198103120 ) ) ;
#107255 = CARTESIAN_POINT ( 'NONE',  ( 9.564922557960805705, 16.46253265017160317, 24.58224293864769194 ) ) ;
#107256 = DIRECTION ( 'NONE',  ( 0.000000000000000000, 1.000000000000000000, -1.471414886128461669E-15 ) ) ;
#107257 = CARTESIAN_POINT ( 'NONE',  ( 13.89961937509957401, 13.97604488694547697, 71.87609039468567573 ) ) ;
#107258 = CARTESIAN_POINT ( 'NONE',  ( -12.06949235617756955, 12.14591786802309770, 40.62390960531435269 ) ) ;
#107259 = CARTESIAN_POINT ( 'NONE',  ( -21.52544592524343514, 5.823673210054127303, 26.04057627198103475 ) ) ;
#107260 = CARTESIAN_POINT ( 'NONE',  ( 21.55341960407619695, -5.719274019375665929, 96.04275706135236135 ) ) ;
#107261 = CARTESIAN_POINT ( 'NONE',  ( -15.72974639402197994, 15.80617190586746368, 65.62390960531436690 ) ) ;
#107262 = CARTESIAN_POINT ( 'NONE',  ( -0.05219959533937732626, 21.53943276465977519, 62.50109039468568284 ) ) ;
#107263 = CARTESIAN_POINT ( 'NONE',  ( 15.72974639402176855, 15.80617190586768217, 46.87609039468568994 ) ) ;
#107264 = CARTESIAN_POINT ( 'NONE',  ( -16.51473224551069308, -9.474510206698971260, 91.66557627198103830 ) ) ;
#107265 = CARTESIAN_POINT ( 'NONE',  ( 8.224510206698742110, 14.34966873604972548, 92.08442372801901854 ) ) ;
#107266 = CARTESIAN_POINT ( 'NONE',  ( 9.474510206698971260, -16.51473224551069308, 22.91557627198102765 ) ) ;
#107267 = CARTESIAN_POINT ( 'NONE',  ( -31.65987002919144899, 2.420393710425506661, 102.1029948765363997 ) ) ;
#107268 = CARTESIAN_POINT ( 'NONE',  ( -4.483927247898539470, -16.52544592524342804, 67.29057627198103830 ) ) ;
#107269 = CARTESIAN_POINT ( 'NONE',  ( 8.314922557960818139, 14.29746914071049879, 39.58224293864769550 ) ) ;
#107270 = CARTESIAN_POINT ( 'NONE',  ( 19.03943276465977164, -0.05219959533909143690, 68.74890960531436690 ) ) ;
#107271 = CARTESIAN_POINT ( 'NONE',  ( 13.89961937509977652, -13.97604488694527269, 28.12390960531435624 ) ) ;
#107272 = CARTESIAN_POINT ( 'NONE',  ( -18.67979575497178146, -10.72451020669898902, 56.66557627198103830 ) ) ;
#107273 = CARTESIAN_POINT ( 'NONE',  ( -0.05219959533936034679, 19.03943276465977164, 37.50109039468567573 ) ) ;
#107275 = CARTESIAN_POINT ( 'NONE',  ( 12.06949235617757843, -12.14591786802309237, 53.12390960531436690 ) ) ;
#107274 = DIRECTION ( 'NONE',  ( 1.000000000000000000, 0.000000000000000000, 0.000000000000000000 ) ) ;
#107276 = CARTESIAN_POINT ( 'NONE',  ( 10.81492255796078972, 18.62759615963270932, 29.58224293864769905 ) ) ;
#107277 = ORIENTED_EDGE ( 'NONE', *, *, #197214, .F. ) ;
#107278 = DIRECTION ( 'NONE',  ( 0.000000000000000000, 0.000000000000000000, -1.000000000000000000 ) ) ;
#107279 = CARTESIAN_POINT ( 'NONE',  ( -16.53943276465976808, -0.05219959533934237506, 73.75109039468567573 ) ) ;
#107280 = CARTESIAN_POINT ( 'NONE',  ( 13.89961937509957401, 13.97604488694547697, 71.87609039468567573 ) ) ;
#107281 = CARTESIAN_POINT ( 'NONE',  ( 16.53943276465976808, -0.05219959533910856209, 38.74890960531435979 ) ) ;
#107282 = CARTESIAN_POINT ( 'NONE',  ( -4.622231866529366047E-30, -105.0000000000000000, -15.00000000000000000 ) ) ;
#107283 = CARTESIAN_POINT ( 'NONE',  ( 12.06949235617757843, -12.14591786802309237, 33.12390960531435979 ) ) ;
#107284 = CARTESIAN_POINT ( 'NONE',  ( 5.153800228976335163, 19.02544592524342804, 49.79057627198100988 ) ) ;
#107285 = CARTESIAN_POINT ( 'NONE',  ( 16.46253265017160672, -9.564922557960803928, 73.33224293864769550 ) ) ;
#107286 = CARTESIAN_POINT ( 'NONE',  ( 9.474510206698971260, -16.51473224551069308, 37.91557627198102409 ) ) ;
#107287 = CARTESIAN_POINT ( 'NONE',  ( 5.719274019375673035, 21.55341960407619339, 42.29275706135235424 ) ) ;
#107288 = CARTESIAN_POINT ( 'NONE',  ( -5.049401038298153566, 19.05341960407611168, 65.20724293864765286 ) ) ;
#107289 = FACE_OUTER_BOUND ( 'NONE', #193819, .T. ) ;
#107290 = CARTESIAN_POINT ( 'NONE',  ( -9.564922557960796823, -16.46253265017161027, 62.08224293864769550 ) ) ;
#107291 = CARTESIAN_POINT ( 'NONE',  ( -5.719274019375978568, 21.55341960407610458, 30.20724293864769550 ) ) ;
#107292 = CARTESIAN_POINT ( 'NONE',  ( -12.06949235617756955, 12.14591786802309770, 115.6239096053143669 ) ) ;
#107293 = CARTESIAN_POINT ( 'NONE',  ( 21.52544592524344225, -5.823673210054117533, 23.54057627198102765 ) ) ;
#107294 = CARTESIAN_POINT ( 'NONE',  ( -4.379528057220086978, -16.55341960407618274, 89.79275706135236135 ) ) ;
#107295 = CARTESIAN_POINT ( 'NONE',  ( 21.55341960407619695, -5.719274019375665929, 111.0427570613523613 ) ) ;
#107296 = CARTESIAN_POINT ( 'NONE',  ( -0.05219959533934338120, 16.53943276465976808, 62.50109039468568284 ) ) ;
#107297 = CARTESIAN_POINT ( 'NONE',  ( 16.51473224551069308, 9.474510206698969483, 114.1655762719810241 ) ) ;
#107298 = CARTESIAN_POINT ( 'NONE',  ( 8.314922557961029526, -14.29746914071037800, 50.41775706135235424 ) ) ;
#107299 = CARTESIAN_POINT ( 'NONE',  ( -0.05219959533934338120, 16.53943276465976808, 37.50109039468568284 ) ) ;
#107300 = CARTESIAN_POINT ( 'NONE',  ( -4.483927247898782831, 16.52544592524335698, 92.70942372801901854 ) ) ;
#107301 = CARTESIAN_POINT ( 'NONE',  ( 12.14591786802327356, -12.06949235617739191, 30.62609039468567929 ) ) ;
#107302 = CARTESIAN_POINT ( 'NONE',  ( 16.51473224551069308, 9.474510206698969483, 34.16557627198102409 ) ) ;
#107303 = CARTESIAN_POINT ( 'NONE',  ( 15.72974639402199770, -15.80617190586745480, 113.1239096053143953 ) ) ;
#107304 = CARTESIAN_POINT ( 'NONE',  ( 13.89961937509957401, 13.97604488694547697, 111.8760903946856757 ) ) ;
#107305 = CARTESIAN_POINT ( 'NONE',  ( 16.55341960407618274, -4.379528057220086978, 86.04275706135236135 ) ) ;
#107306 = DIRECTION ( 'NONE',  ( 0.000000000000000000, 0.000000000000000000, -1.000000000000000000 ) ) ;
#107307 = CARTESIAN_POINT ( 'NONE',  ( -18.62759615963255300, -10.81492255796106328, 89.16775706135236135 ) ) ;
#107308 = CARTESIAN_POINT ( 'NONE',  ( -19.02544592524334988, -5.153800228976617603, 88.95942372801897591 ) ) ;
#107309 = CARTESIAN_POINT ( 'NONE',  ( -8.314922557960811034, -14.29746914071050412, 57.08224293864769550 ) ) ;
#107310 = CARTESIAN_POINT ( 'NONE',  ( 8.224510206698953496, -14.34966873604960469, 42.91557627198103120 ) ) ;
#107311 = CARTESIAN_POINT ( 'NONE',  ( -14.29746914071049879, 8.314922557960819915, 110.8322429386476955 ) ) ;
#107313 = CARTESIAN_POINT ( 'NONE',  ( -9.100000000000003197, 0.1000365528947574634, -63.95112321872120731 ) ) ;
#107312 = CARTESIAN_POINT ( 'NONE',  ( 19.03943276465977164, 0.05219959533936151252, 41.25109039468566152 ) ) ;
#107314 = CARTESIAN_POINT ( 'NONE',  ( -15.80617190586768217, 15.72974639402176855, 48.12609039468568284 ) ) ;
#107315 = CARTESIAN_POINT ( 'NONE',  ( -5.153800228976607833, 19.02544592524334988, 102.7094237280189759 ) ) ;
#107316 = DIRECTION ( 'NONE',  ( 0.000000000000000000, 0.000000000000000000, -1.000000000000000000 ) ) ;
#107317 = CARTESIAN_POINT ( 'NONE',  ( 13.97604488694527802, 13.89961937509977652, 109.3739096053143669 ) ) ;
#107318 = CARTESIAN_POINT ( 'NONE',  ( -10.72451020669898014, 18.67979575497178502, 70.41557627198102409 ) ) ;
#107319 = CARTESIAN_POINT ( 'NONE',  ( 13.97604488694548053, -13.89961937509957401, 95.62609039468563310 ) ) ;
#107320 = CARTESIAN_POINT ( 'NONE',  ( 5.153800228976335163, 19.02544592524342804, 104.7905762719809957 ) ) ;
#107321 = CARTESIAN_POINT ( 'NONE',  ( 17.59860650958997397, -7.585241751806833577, 50.92337014262493256 ) ) ;
#107322 = CARTESIAN_POINT ( 'NONE',  ( 14.29746914071049879, -8.314922557960816363, 108.3322429386477097 ) ) ;
#107323 = CARTESIAN_POINT ( 'NONE',  ( -5.719274019375665041, -21.55341960407619695, 99.79275706135234714 ) ) ;
#107324 = CARTESIAN_POINT ( 'NONE',  ( 16.51473224551069308, 9.474510206698969483, 49.16557627198102409 ) ) ;
#107325 = CARTESIAN_POINT ( 'NONE',  ( 21.53943276465977519, 0.05219959533937863772, 56.25109039468568284 ) ) ;
#107326 = CARTESIAN_POINT ( 'NONE',  ( -18.67979575497193778, 10.72451020669871902, 93.33442372801901854 ) ) ;
#107327 = CARTESIAN_POINT ( 'NONE',  ( -4.379528057220086978, -16.55341960407618274, 89.79275706135236135 ) ) ;
#107328 = CARTESIAN_POINT ( 'NONE',  ( 10.81492255796106328, -18.62759615963255655, 40.41775706135234714 ) ) ;
#107329 = CARTESIAN_POINT ( 'NONE',  ( -10.72451020669870658, -18.67979575497194134, 39.58442372801901143 ) ) ;
#107331 = CARTESIAN_POINT ( 'NONE',  ( 13.89961937509977652, -13.97604488694527269, 98.12390960531433848 ) ) ;
#107330 = CARTESIAN_POINT ( 'NONE',  ( 9.564922557961047289, -16.46253265017146816, 65.41775706135233293 ) ) ;
#107332 = CARTESIAN_POINT ( 'NONE',  ( -4.379528057220328563, 16.55341960407611168, 100.2072429386476955 ) ) ;
#107333 = CARTESIAN_POINT ( 'NONE',  ( 18.62759615963271287, -10.81492255796078972, 88.33224293864769550 ) ) ;
#107334 = CARTESIAN_POINT ( 'NONE',  ( -16.53943276465976808, 0.05219959533911058130, 66.24890960531436690 ) ) ;
#107335 = CARTESIAN_POINT ( 'NONE',  ( 10.81492255796106328, -18.62759615963255655, 100.4177570613523471 ) ) ;
#107336 = CARTESIAN_POINT ( 'NONE',  ( 12.06949235617757843, -12.14591786802309237, 78.12390960531436690 ) ) ;
#107337 = CARTESIAN_POINT ( 'NONE',  ( 13.97604488694527802, 13.89961937509977652, 39.37390960531435269 ) ) ;
#107338 = CARTESIAN_POINT ( 'NONE',  ( -9.474510206698720793, -16.51473224551083518, 79.58442372801899012 ) ) ;
#107339 = CARTESIAN_POINT ( 'NONE',  ( 4.483927247898545687, 16.52544592524342804, 49.79057627198102409 ) ) ;
#107340 = CARTESIAN_POINT ( 'NONE',  ( -21.52544592524334988, -5.823673210054445271, 88.95942372801901854 ) ) ;
#107341 = CARTESIAN_POINT ( 'NONE',  ( -19.02544592524342804, 5.153800228976336051, 96.04057627198103830 ) ) ;
#107342 = CARTESIAN_POINT ( 'NONE',  ( 13.89961937509957401, 13.97604488694547697, 56.87609039468564731 ) ) ;
#107343 = CARTESIAN_POINT ( 'NONE',  ( 5.719274019375991003, -21.55341960407610458, 67.70724293864769550 ) ) ;
#107344 = CARTESIAN_POINT ( 'NONE',  ( -21.52544592524343514, 5.823673210054127303, 116.0405762719810383 ) ) ;
#107345 = CARTESIAN_POINT ( 'NONE',  ( -0.05219959533934338120, 16.53943276465976808, 32.50109039468568284 ) ) ;
#107346 = CARTESIAN_POINT ( 'NONE',  ( -4.379528057220086978, -16.55341960407618274, 79.79275706135236135 ) ) ;
#107348 = CARTESIAN_POINT ( 'NONE',  ( 10.81492255796106328, -18.62759615963255655, 25.41775706135235779 ) ) ;
#107347 = CARTESIAN_POINT ( 'NONE',  ( 16.51473224551069308, 9.474510206698969483, 24.16557627198102765 ) ) ;
#107349 = CARTESIAN_POINT ( 'NONE',  ( -0.05219959533909027116, -19.03943276465977164, 27.49890960531435624 ) ) ;
#107350 = CARTESIAN_POINT ( 'NONE',  ( -29.86685920354755197, -21.69954338932560134, -4.924999997268813878 ) ) ;
#107351 = CARTESIAN_POINT ( 'NONE',  ( -4.483927247898782831, 16.52544592524335698, 52.70942372801902565 ) ) ;
#107352 = CARTESIAN_POINT ( 'NONE',  ( 14.34966873604960469, 8.224510206698951720, 79.16557627198103830 ) ) ;
#107353 = CARTESIAN_POINT ( 'NONE',  ( -10.72451020669898014, 18.67979575497178502, 75.41557627198102409 ) ) ;
#107354 = CARTESIAN_POINT ( 'NONE',  ( -4.379528057220328563, 16.55341960407611168, 30.20724293864769550 ) ) ;
#107355 = CARTESIAN_POINT ( 'NONE',  ( 16.53943276465976808, 0.05219959533934440121, 41.25109039468568284 ) ) ;
#107356 = CARTESIAN_POINT ( 'NONE',  ( 0.05219959533909260263, 19.03943276465977164, 39.99890960531436690 ) ) ;
#107357 = CARTESIAN_POINT ( 'NONE',  ( 0.05219959533934541429, -16.53943276465976808, 75.00109039468568994 ) ) ;
#107358 = CARTESIAN_POINT ( 'NONE',  ( -5.049401038297874678, -19.05341960407617918, 74.79275706135231871 ) ) ;
#107359 = CARTESIAN_POINT ( 'NONE',  ( -21.55341960407610458, -5.719274019375992779, 71.45724293864769550 ) ) ;
#107360 = CARTESIAN_POINT ( 'NONE',  ( -4.483927247898782831, 16.52544592524335698, 107.7094237280190328 ) ) ;
#107361 = EDGE_LOOP ( 'NONE', ( #89491, #93279, #199405, #19440 ) ) ;
#107362 = CARTESIAN_POINT ( 'NONE',  ( -21.53943276465977519, -0.05219959533937600094, 78.75109039468568994 ) ) ;
#107363 = EDGE_CURVE ( 'NONE', #60866, #78316, #126727, .T. ) ;
#107364 = CARTESIAN_POINT ( 'NONE',  ( 15.72974639402199770, -15.80617190586745480, 43.12390960531435269 ) ) ;
#107365 = ORIENTED_EDGE ( 'NONE', *, *, #29998, .F. ) ;
#107366 = ORIENTED_EDGE ( 'NONE', *, *, #196169, .T. ) ;
#107367 = CARTESIAN_POINT ( 'NONE',  ( -4.483927247898782831, 16.52544592524335698, 87.70942372801901854 ) ) ;
#107368 = CARTESIAN_POINT ( 'NONE',  ( -5.823673210054116645, -21.52544592524344225, 47.29057627198103120 ) ) ;
#107369 = EDGE_LOOP ( 'NONE', ( #12478, #117942, #98630, #70139 ) ) ;
#107370 = CARTESIAN_POINT ( 'NONE',  ( -13.89961937509977652, 13.97604488694528158, 110.6239096053143243 ) ) ;
#107371 = CARTESIAN_POINT ( 'NONE',  ( 23.48529157249599564, 32.32473071737754111, -8.449999994537627401 ) ) ;
#107372 = CARTESIAN_POINT ( 'NONE',  ( -19.02544592524342804, 5.153800228976336051, 26.04057627198103120 ) ) ;
#107373 = CARTESIAN_POINT ( 'NONE',  ( -18.67979575497178146, -10.72451020669898902, 71.66557627198100988 ) ) ;
#107374 = CARTESIAN_POINT ( 'NONE',  ( 4.379528057220092307, 16.55341960407617563, 107.2927570613523471 ) ) ;
#107375 = CARTESIAN_POINT ( 'NONE',  ( -18.62759615963255300, -10.81492255796106328, 64.16775706135234714 ) ) ;
#107376 = CARTESIAN_POINT ( 'NONE',  ( 16.53943276465976808, 0.05219959533934440121, 26.25109039468567573 ) ) ;
#107377 = CARTESIAN_POINT ( 'NONE',  ( 14.34966873604960469, 8.224510206698951720, 114.1655762719810383 ) ) ;
#107378 = CARTESIAN_POINT ( 'NONE',  ( -8.224510206698735004, -14.34966873604973081, 34.58442372801900433 ) ) ;
#107379 = CARTESIAN_POINT ( 'NONE',  ( -16.46253265017160317, 9.564922557960807481, 45.83224293864769550 ) ) ;
#107380 = CARTESIAN_POINT ( 'NONE',  ( -28.82186960331499037, 2.428612866367529932E-14, 139.9999999999999716 ) ) ;
#107381 = CARTESIAN_POINT ( 'NONE',  ( 19.02544592524343514, -5.153800228976328945, 108.5405762719810383 ) ) ;
#107382 = CARTESIAN_POINT ( 'NONE',  ( -8.224510206698735004, -14.34966873604973081, 89.58442372801901854 ) ) ;
#107383 = CARTESIAN_POINT ( 'NONE',  ( 16.51473224551083163, -9.474510206698727899, 90.83442372801900433 ) ) ;
#107384 = CARTESIAN_POINT ( 'NONE',  ( -10.81492255796105439, 18.62759615963255655, 112.9177570613523329 ) ) ;
#107385 = CARTESIAN_POINT ( 'NONE',  ( 10.72451020669898902, -18.67979575497178502, 77.91557627198102409 ) ) ;
#107386 = CARTESIAN_POINT ( 'NONE',  ( 16.55341960407618274, -4.379528057220086978, 96.04275706135236135 ) ) ;
#107387 = CARTESIAN_POINT ( 'NONE',  ( 0.05219959533936267826, -19.03943276465977164, 90.00109039468567573 ) ) ;
#107388 = CARTESIAN_POINT ( 'NONE',  ( -0.05219959533909027116, -19.03943276465977164, 47.49890960531435979 ) ) ;
#107389 = CARTESIAN_POINT ( 'NONE',  ( 9.564922557960805705, 16.46253265017160317, 89.58224293864769550 ) ) ;
#107390 = CARTESIAN_POINT ( 'NONE',  ( 15.72974639402176855, 15.80617190586768217, 51.87609039468568284 ) ) ;
#107391 = CARTESIAN_POINT ( 'NONE',  ( 9.474510206698971260, -16.51473224551069308, 42.91557627198103120 ) ) ;
#107392 = DIRECTION ( 'NONE',  ( 0.8164965809277261455, 0.000000000000000000, 0.5773502691896257311 ) ) ;
#107393 = CARTESIAN_POINT ( 'NONE',  ( 13.89961937509977652, -13.97604488694527269, 113.1239096053143527 ) ) ;
#107394 = CARTESIAN_POINT ( 'NONE',  ( 12.14591786802309770, 12.06949235617756955, 64.37390960531435269 ) ) ;
#107395 = CARTESIAN_POINT ( 'NONE',  ( 21.53943276465977519, -0.05219959533907433946, 68.74890960531435269 ) ) ;
#107396 = FACE_OUTER_BOUND ( 'NONE', #198040, .T. ) ;
#107397 = CARTESIAN_POINT ( 'NONE',  ( 19.03943276465977164, 0.05219959533936151252, 46.25109039468566863 ) ) ;
#107398 = DIRECTION ( 'NONE',  ( -7.774220206137126725E-15, -0.8283630648959139364, 0.5601916035752839695 ) ) ;
#107400 = CARTESIAN_POINT ( 'NONE',  ( -13.97604488694527625, -13.89961937509977652, 86.87390960531436690 ) ) ;
#107399 = CARTESIAN_POINT ( 'NONE',  ( 13.97604488694527802, 13.89961937509977652, 69.37390960531436690 ) ) ;
#107401 = CARTESIAN_POINT ( 'NONE',  ( -16.52544592524335698, -4.483927247898792601, 48.95942372801902565 ) ) ;
#107402 = CARTESIAN_POINT ( 'NONE',  ( 25.83521962401025007, -30.44105770729786542, -17.07601944841966812 ) ) ;
#107403 = CARTESIAN_POINT ( 'NONE',  ( 13.97604488694548053, -13.89961937509957401, 35.62609039468567573 ) ) ;
#107404 = CARTESIAN_POINT ( 'NONE',  ( -17.81289503416611808, 24.51734667627700404, 145.9500000054623854 ) ) ;
#107405 = CARTESIAN_POINT ( 'NONE',  ( -16.52544592524335698, -4.483927247898792601, 93.95942372801903275 ) ) ;
#107406 = DIRECTION ( 'NONE',  ( 5.392603844284257652E-33, -1.000000000000000000, 0.000000000000000000 ) ) ;
#107407 = CARTESIAN_POINT ( 'NONE',  ( -4.483927247898782831, 16.52544592524335698, 82.70942372801900433 ) ) ;
#107408 = CARTESIAN_POINT ( 'NONE',  ( 14.34966873604972726, -8.224510206698740333, 55.83442372801901854 ) ) ;
#107409 = CARTESIAN_POINT ( 'NONE',  ( 19.03943276465977164, 0.05219959533936151252, 26.25109039468566507 ) ) ;
#107411 = CARTESIAN_POINT ( 'NONE',  ( 30.00000000000000355, -3.181980515339468241, 1.110912703473986074 ) ) ;
#107410 = CARTESIAN_POINT ( 'NONE',  ( -0.05219959533909027116, -19.03943276465977164, 57.49890960531435979 ) ) ;
#107412 = CARTESIAN_POINT ( 'NONE',  ( 10.72451020669871369, 18.67979575497193778, 67.08442372801901854 ) ) ;
#107413 = CARTESIAN_POINT ( 'NONE',  ( 13.89961937509957401, 13.97604488694547697, 81.87609039468564731 ) ) ;
#107414 = CARTESIAN_POINT ( 'NONE',  ( -19.03943276465977164, -0.05219959533935918106, 18.75109039468567218 ) ) ;
#107415 = CARTESIAN_POINT ( 'NONE',  ( -19.02544592524342804, 5.153800228976336051, 46.04057627198101699 ) ) ;
#107416 = CARTESIAN_POINT ( 'NONE',  ( -23.48298174826589602, -32.32155151706772500, -7.702157773949822150 ) ) ;
#107417 = CARTESIAN_POINT ( 'NONE',  ( 15.80617190586746368, 15.72974639402197994, 69.37390960531436690 ) ) ;
#107418 = CARTESIAN_POINT ( 'NONE',  ( -19.02544592524342804, 5.153800228976336051, 116.0405762719810383 ) ) ;
#107419 = CARTESIAN_POINT ( 'NONE',  ( -0.05219959533910754901, -16.53943276465976808, 112.4989096053143669 ) ) ;
#107420 = CARTESIAN_POINT ( 'NONE',  ( -14.29746914071037622, -8.314922557961029526, 44.16775706135234714 ) ) ;
#107421 = CARTESIAN_POINT ( 'NONE',  ( -0.05219959533910754901, -16.53943276465976808, 27.49890960531435269 ) ) ;
#107422 = ORIENTED_EDGE ( 'NONE', *, *, #155322, .F. ) ;
#107423 = CARTESIAN_POINT ( 'NONE',  ( -10.72451020669898014, 18.67979575497178502, 115.4155762719810241 ) ) ;
#107424 = CIRCLE ( 'NONE', #55779, 21.30000000000002913 ) ;
#107426 = CARTESIAN_POINT ( 'NONE',  ( -23.48529157249599919, -32.32473071737750558, -3.699999999999999734 ) ) ;
#107425 = CARTESIAN_POINT ( 'NONE',  ( -16.53943276465976808, 0.05219959533911058130, 46.24890960531435979 ) ) ;
#107427 = CARTESIAN_POINT ( 'NONE',  ( 16.46253265017146816, 9.564922557961045513, 111.6677570613523329 ) ) ;
#107428 = CARTESIAN_POINT ( 'NONE',  ( -16.46253265017146816, -9.564922557961047289, 29.16775706135232937 ) ) ;
#107429 = CARTESIAN_POINT ( 'NONE',  ( 4.483927247898545687, 16.52544592524342804, 49.79057627198102409 ) ) ;
#107430 = CARTESIAN_POINT ( 'NONE',  ( -10.72451020669898014, 18.67979575497178502, 100.4155762719810241 ) ) ;
#107432 = CARTESIAN_POINT ( 'NONE',  ( 15.72974639402199770, -15.80617190586745480, 63.12390960531435979 ) ) ;
#107431 = CARTESIAN_POINT ( 'NONE',  ( 17.50000000000000000, 5.500000000000001776, 33.78230962303567253 ) ) ;
#107433 = CARTESIAN_POINT ( 'NONE',  ( -5.153800228976328057, -19.02544592524343514, 77.29057627198099567 ) ) ;
#107434 = CARTESIAN_POINT ( 'NONE',  ( -12.06949235617756955, 12.14591786802309770, 50.62390960531435979 ) ) ;
#107435 = CARTESIAN_POINT ( 'NONE',  ( 19.05341960407611168, 5.049401038298154454, 98.95724293864766707 ) ) ;
#107436 = CARTESIAN_POINT ( 'NONE',  ( -36.89613260305527831, 1.429147721188399389, 50.32345767270690118 ) ) ;
#107437 = CARTESIAN_POINT ( 'NONE',  ( -13.97604488694547697, 13.89961937509957934, 58.12609039468566863 ) ) ;
#107438 = CARTESIAN_POINT ( 'NONE',  ( -15.80617190586745835, -15.72974639402198527, 96.87390960531436690 ) ) ;
#107439 = CARTESIAN_POINT ( 'NONE',  ( 9.474510206698971260, -16.51473224551069308, 42.91557627198103120 ) ) ;
#107440 = CARTESIAN_POINT ( 'NONE',  ( 16.51473224551069308, 9.474510206698969483, 24.16557627198102765 ) ) ;
#107441 = CARTESIAN_POINT ( 'NONE',  ( -15.72974639402176322, -15.80617190586768395, 49.37609039468569705 ) ) ;
#107442 = CARTESIAN_POINT ( 'NONE',  ( -8.571926809382608425, 26.38167802310805854, 144.4750000027312069 ) ) ;
#107443 = CARTESIAN_POINT ( 'NONE',  ( 16.55341960407611168, 4.379528057220329451, 33.95724293864769550 ) ) ;
#107444 = CARTESIAN_POINT ( 'NONE',  ( -19.02544592524342804, 5.153800228976336051, 56.04057627198100988 ) ) ;
#107445 = CARTESIAN_POINT ( 'NONE',  ( -16.51473224551069308, -9.474510206698971260, 96.66557627198102409 ) ) ;
#107446 = CARTESIAN_POINT ( 'NONE',  ( 21.55341960407610458, 5.719274019375980345, 58.95724293864770971 ) ) ;
#107447 = CARTESIAN_POINT ( 'NONE',  ( -19.52837319214027900, 5.499999999999900524, 44.60471352585542348 ) ) ;
#107448 = CARTESIAN_POINT ( 'NONE',  ( -19.03943276465977164, 0.05219959533909376836, 41.24890960531435269 ) ) ;
#107449 = CARTESIAN_POINT ( 'NONE',  ( -21.55341960407610458, -5.719274019375992779, 56.45724293864768839 ) ) ;
#107450 = CARTESIAN_POINT ( 'NONE',  ( 21.52544592524334988, 5.823673210054432836, 86.45942372801901854 ) ) ;
#107452 = CARTESIAN_POINT ( 'NONE',  ( -8.314922557961024197, 14.29746914071037800, 77.91775706135231871 ) ) ;
#107451 = CARTESIAN_POINT ( 'NONE',  ( 22.01160362600695564, -30.88790364210955275, -22.63296439182117581 ) ) ;
#107453 = CARTESIAN_POINT ( 'NONE',  ( -0.05219959533934338120, 16.53943276465976808, 87.50109039468568994 ) ) ;
#107454 = CARTESIAN_POINT ( 'NONE',  ( -19.03943276465977164, 0.05219959533909376836, 66.24890960531436690 ) ) ;
#107455 = EDGE_LOOP ( 'NONE', ( #106378, #157458, #190914, #113337, #87272, #78132, #198230, #180194, #81602, #114329, #147252, #80826 ) ) ;
#107456 = CARTESIAN_POINT ( 'NONE',  ( -13.97604488694547697, 13.89961937509957934, 28.12609039468565797 ) ) ;
#107457 = CARTESIAN_POINT ( 'NONE',  ( 16.52544592524335698, 4.483927247898782831, 86.45942372801901854 ) ) ;
#107458 = CARTESIAN_POINT ( 'NONE',  ( 15.72974639402176855, 15.80617190586768217, 111.8760903946856615 ) ) ;
#107459 = CARTESIAN_POINT ( 'NONE',  ( 0.05219959533909260263, 19.03943276465977164, 74.99890960531435269 ) ) ;
#107460 = CARTESIAN_POINT ( 'NONE',  ( 21.55341960407610458, 5.719274019375980345, 53.95724293864770260 ) ) ;
#107461 = CARTESIAN_POINT ( 'NONE',  ( 16.52544592524335698, 4.483927247898782831, 21.45942372801901499 ) ) ;
#107462 = CARTESIAN_POINT ( 'NONE',  ( 21.55341960407619695, -5.719274019375665929, 76.04275706135237556 ) ) ;
#107463 = CARTESIAN_POINT ( 'NONE',  ( -8.314922557961024197, 14.29746914071037800, 67.91775706135234714 ) ) ;
#107464 = CARTESIAN_POINT ( 'NONE',  ( -10.81492255796078084, -18.62759615963271287, 112.0822429386477097 ) ) ;
#107465 = CARTESIAN_POINT ( 'NONE',  ( -19.03943276465977164, -0.05219959533935918106, 108.7510903946856615 ) ) ;
#107466 = CARTESIAN_POINT ( 'NONE',  ( 19.03943276465977164, -0.05219959533909143690, 73.74890960531435269 ) ) ;
#107467 = CARTESIAN_POINT ( 'NONE',  ( -14.29746914071037622, -8.314922557961029526, 24.16775706135235424 ) ) ;
#107468 = CARTESIAN_POINT ( 'NONE',  ( 5.049401038298161559, -19.05341960407611168, 37.70724293864768839 ) ) ;
#107469 = CARTESIAN_POINT ( 'NONE',  ( 5.049401038297881783, 19.05341960407617563, 112.2927570613523471 ) ) ;
#107470 = CARTESIAN_POINT ( 'NONE',  ( 8.224510206698953496, -14.34966873604960469, 82.91557627198103830 ) ) ;
#107471 = CARTESIAN_POINT ( 'NONE',  ( -16.55341960407617563, 4.379528057220093196, 93.54275706135234714 ) ) ;
#107473 = CARTESIAN_POINT ( 'NONE',  ( 9.564922557960805705, 16.46253265017160317, 69.58224293864770971 ) ) ;
#107472 = CARTESIAN_POINT ( 'NONE',  ( 21.55341960407619695, -5.719274019375665929, 36.04275706135234714 ) ) ;
#107474 = CARTESIAN_POINT ( 'NONE',  ( 5.049401038298161559, -19.05341960407611168, 62.70724293864769550 ) ) ;
#107475 = CARTESIAN_POINT ( 'NONE',  ( -8.224510206698735004, -14.34966873604973081, 89.58442372801901854 ) ) ;
#107477 = ORIENTED_EDGE ( 'NONE', *, *, #111650, .F. ) ;
#107476 = CARTESIAN_POINT ( 'NONE',  ( -21.56952297831670151, -5.557039098534934496, 173.4609804364286276 ) ) ;
#107478 = EDGE_LOOP ( 'NONE', ( #109473, #136816, #64481, #175049 ) ) ;
#107479 = CARTESIAN_POINT ( 'NONE',  ( 19.05341960407617918, -5.049401038297876454, 26.04275706135233293 ) ) ;
#107480 = CARTESIAN_POINT ( 'NONE',  ( 9.474510206698971260, -16.51473224551069308, 32.91557627198102409 ) ) ;
#107481 = ADVANCED_BREP_SHAPE_REPRESENTATION ( '', ( #5735, #82054 ), #188624 ) ;
#107482 = VERTEX_POINT ( 'NONE', #89052 ) ;
#107483 = CARTESIAN_POINT ( 'NONE',  ( 4.379528057220092307, 16.55341960407617563, 27.29275706135234358 ) ) ;
#107485 = CARTESIAN_POINT ( 'NONE',  ( -4.483927247898782831, 16.52544592524335698, 47.70942372801902565 ) ) ;
#107484 = CARTESIAN_POINT ( 'NONE',  ( 5.153800228976615827, -19.02544592524334988, 60.20942372801899012 ) ) ;
#107486 = CARTESIAN_POINT ( 'NONE',  ( -19.05341960407611168, -5.049401038298163336, 111.4572429386476671 ) ) ;
#107487 = CARTESIAN_POINT ( 'NONE',  ( 16.51473224551069308, 9.474510206698969483, 69.16557627198102409 ) ) ;
#107488 = CARTESIAN_POINT ( 'NONE',  ( -15.80617190586745835, -15.72974639402198527, 96.87390960531436690 ) ) ;
#107490 = CARTESIAN_POINT ( 'NONE',  ( -5.153800228976328057, -19.02544592524343514, 27.29057627198103120 ) ) ;
#107489 = CARTESIAN_POINT ( 'NONE',  ( 0.05219959533909260263, 19.03943276465977164, 94.99890960531436690 ) ) ;
#107491 = ADVANCED_FACE ( 'NONE', ( #12241 ), #25417, .T. ) ;
#107492 = CARTESIAN_POINT ( 'NONE',  ( -19.03943276465977164, 0.05219959533909376836, 66.24890960531436690 ) ) ;
#107494 = CARTESIAN_POINT ( 'NONE',  ( 9.474510206698971260, -16.51473224551069308, 22.91557627198102765 ) ) ;
#107493 = CARTESIAN_POINT ( 'NONE',  ( 16.55341960407611168, 4.379528057220329451, 23.95724293864769550 ) ) ;
#107495 = CARTESIAN_POINT ( 'NONE',  ( -19.03943276465977164, -0.05219959533935918106, 43.75109039468566863 ) ) ;
#107496 = EDGE_CURVE ( 'NONE', #156506, #147808, #6041, .T. ) ;
#107497 = CARTESIAN_POINT ( 'NONE',  ( 16.52544592524342804, -4.483927247898539470, 73.54057627198102409 ) ) ;
#107498 = CARTESIAN_POINT ( 'NONE',  ( 5.719274019375673035, 21.55341960407619339, 92.29275706135236135 ) ) ;
#107499 = CARTESIAN_POINT ( 'NONE',  ( -13.97604488694527625, -13.89961937509977652, 36.87390960531436690 ) ) ;
#107500 = CARTESIAN_POINT ( 'NONE',  ( -12.14591786802326823, 12.06949235617739902, 48.12609039468568284 ) ) ;
#107502 = CARTESIAN_POINT ( 'NONE',  ( -5.719274019375665041, -21.55341960407619695, 94.79275706135234714 ) ) ;
#107501 = CARTESIAN_POINT ( 'NONE',  ( -16.52544592524342804, 4.483927247898546575, 46.04057627198103830 ) ) ;
#107503 = CARTESIAN_POINT ( 'NONE',  ( -9.474510206698964154, 16.51473224551069663, 85.41557627198102409 ) ) ;
#107504 = CARTESIAN_POINT ( 'NONE',  ( -19.03943276465977164, 0.05219959533909376836, 91.24890960531436690 ) ) ;
#107505 = CARTESIAN_POINT ( 'NONE',  ( 16.52544592524342804, -4.483927247898539470, 108.5405762719810241 ) ) ;
#107506 = CARTESIAN_POINT ( 'NONE',  ( -16.55341960407611168, -4.379528057220339221, 76.45724293864769550 ) ) ;
#107507 = CARTESIAN_POINT ( 'NONE',  ( -15.80617190586745835, -15.72974639402198527, 86.87390960531438111 ) ) ;
#107508 = CARTESIAN_POINT ( 'NONE',  ( -13.97604488694527625, -13.89961937509977652, 91.87390960531432427 ) ) ;
#107509 = CARTESIAN_POINT ( 'NONE',  ( 0.05219959533907565091, 21.53943276465977519, 94.99890960531436690 ) ) ;
#107510 = CARTESIAN_POINT ( 'NONE',  ( 9.474510206698729675, 16.51473224551082808, 72.08442372801900433 ) ) ;
#107512 = CARTESIAN_POINT ( 'NONE',  ( -14.29746914071049879, 8.314922557960819915, 95.83224293864770971 ) ) ;
#107511 = DIRECTION ( 'NONE',  ( 0.7071067811865466846, -7.406550393246786959E-15, 0.7071067811865484609 ) ) ;
#107513 = CARTESIAN_POINT ( 'NONE',  ( -13.97604488694527625, -13.89961937509977652, 51.87390960531436690 ) ) ;
#107514 = CARTESIAN_POINT ( 'NONE',  ( -10.72451020669898014, 18.67979575497178502, 70.41557627198102409 ) ) ;
#107515 = CARTESIAN_POINT ( 'NONE',  ( 17.44270441346514033, -5.991230190323081573, 26.13664920735773478 ) ) ;
#107517 = CARTESIAN_POINT ( 'NONE',  ( 22.44159573604009239, 16.30477369853692693, 148.5750000027312012 ) ) ;
#107516 = CARTESIAN_POINT ( 'NONE',  ( 14.34966873604972726, -8.224510206698740333, 105.8344237280190328 ) ) ;
#107518 = CARTESIAN_POINT ( 'NONE',  ( 16.51473224551083163, -9.474510206698727899, 110.8344237280190043 ) ) ;
#107519 = CARTESIAN_POINT ( 'NONE',  ( 8.314922557960818139, 14.29746914071049879, 79.58224293864769550 ) ) ;
#107520 = CARTESIAN_POINT ( 'NONE',  ( 0.000000000000000000, 0.000000000000000000, -20.00000000000000000 ) ) ;
#107521 = CARTESIAN_POINT ( 'NONE',  ( 19.03943276465977164, -0.05219959533909143690, 68.74890960531436690 ) ) ;
#107522 = CARTESIAN_POINT ( 'NONE',  ( 9.474510206698971260, -16.51473224551069308, 37.91557627198102409 ) ) ;
#107523 = CARTESIAN_POINT ( 'NONE',  ( -12.14591786802309592, -12.06949235617757132, 71.87390960531438111 ) ) ;
#107524 = CARTESIAN_POINT ( 'NONE',  ( -21.53943276465977519, 0.05219959533907696930, 26.24890960531435624 ) ) ;
#107525 = CARTESIAN_POINT ( 'NONE',  ( 16.51473224551083163, -9.474510206698727899, 90.83442372801900433 ) ) ;
#107526 = CARTESIAN_POINT ( 'NONE',  ( -16.46253265017160317, 9.564922557960807481, 100.8322429386477097 ) ) ;
#107527 = CARTESIAN_POINT ( 'NONE',  ( -15.80617190586745835, -15.72974639402198527, 81.87390960531435269 ) ) ;
#107528 = CARTESIAN_POINT ( 'NONE',  ( 8.314922557961029526, -14.29746914071037800, 70.41775706135236135 ) ) ;
#107529 = CARTESIAN_POINT ( 'NONE',  ( -16.62475595723611832, 7.163666690055876529, 95.52713351810403708 ) ) ;
#107530 = CARTESIAN_POINT ( 'NONE',  ( 13.97604488694527802, 13.89961937509977652, 64.37390960531436690 ) ) ;
#107531 = CARTESIAN_POINT ( 'NONE',  ( 5.719274019375991003, -21.55341960407610458, 62.70724293864769550 ) ) ;
#107532 =( BOUNDED_CURVE ( )  B_SPLINE_CURVE ( 3, ( #689, #19850, #2692, #34033 ),
 .UNSPECIFIED., .F., .F. ) 
 B_SPLINE_CURVE_WITH_KNOTS ( ( 4, 4 ),
 ( 5.150538010968860547, 5.257537365396775186 ),
 .UNSPECIFIED. ) 
 CURVE ( )  GEOMETRIC_REPRESENTATION_ITEM ( )  RATIONAL_B_SPLINE_CURVE ( ( 1.000000000000000000, 0.9990461557208837329, 0.9990461557208837329, 1.000000000000000000 ) ) 
 REPRESENTATION_ITEM ( '' )  );
#107533 = CARTESIAN_POINT ( 'NONE',  ( 13.89961937509957401, 13.97604488694547697, 101.8760903946856331 ) ) ;
#107535 = CARTESIAN_POINT ( 'NONE',  ( -15.80617190586768217, 15.72974639402176855, 58.12609039468568994 ) ) ;
#107534 = CARTESIAN_POINT ( 'NONE',  ( 12.06949235617757843, -12.14591786802309237, 33.12390960531435979 ) ) ;
#107536 = CARTESIAN_POINT ( 'NONE',  ( 17.72662750342724536, 5.500000000000079048, 83.90179492283742491 ) ) ;
#107538 = CARTESIAN_POINT ( 'NONE',  ( 16.51473224551069308, 9.474510206698969483, 109.1655762719810383 ) ) ;
#107537 = CARTESIAN_POINT ( 'NONE',  ( -8.224510206698735004, -14.34966873604973081, 69.58442372801900433 ) ) ;
#107539 = CARTESIAN_POINT ( 'NONE',  ( 5.153800228976335163, 19.02544592524342804, 104.7905762719810241 ) ) ;
#107540 = CYLINDRICAL_SURFACE ( 'NONE', #35607, 7.500000000000007105 ) ;
#107541 = CARTESIAN_POINT ( 'NONE',  ( -14.29746914071037622, -8.314922557961029526, 99.16775706135234714 ) ) ;
#107542 = CARTESIAN_POINT ( 'NONE',  ( -8.224510206698735004, -14.34966873604973081, 49.58442372801901143 ) ) ;
#107543 = CARTESIAN_POINT ( 'NONE',  ( -19.02544592524342804, 5.153800228976336051, 56.04057627198100988 ) ) ;
#107544 = CARTESIAN_POINT ( 'NONE',  ( -5.049401038298153566, 19.05341960407611168, 70.20724293864769550 ) ) ;
#107545 = CARTESIAN_POINT ( 'NONE',  ( -10.81492255796105439, 18.62759615963255655, 52.91775706135235424 ) ) ;
#107546 = CARTESIAN_POINT ( 'NONE',  ( 16.52544592524335698, 4.483927247898782831, 56.45942372801902565 ) ) ;
#107547 = CARTESIAN_POINT ( 'NONE',  ( 8.314922557960818139, 14.29746914071049879, 34.58224293864770260 ) ) ;
#107548 = CARTESIAN_POINT ( 'NONE',  ( -0.05219959533909027116, -19.03943276465977164, 47.49890960531435979 ) ) ;
#107549 = CARTESIAN_POINT ( 'NONE',  ( 16.46253265017160672, -9.564922557960803928, 33.33224293864770260 ) ) ;
#107550 = CARTESIAN_POINT ( 'NONE',  ( -4.483927247898782831, 16.52544592524335698, 27.70942372801901854 ) ) ;
#107551 = CARTESIAN_POINT ( 'NONE',  ( 16.46253265017146816, 9.564922557961045513, 76.66775706135234714 ) ) ;
#107552 = CARTESIAN_POINT ( 'NONE',  ( 8.314922557960818139, 14.29746914071049879, 89.58224293864768129 ) ) ;
#107553 = CARTESIAN_POINT ( 'NONE',  ( 19.02544592524343514, -5.153800228976328945, 48.54057627198103120 ) ) ;
#107555 = CARTESIAN_POINT ( 'NONE',  ( 37.99999999999999289, 2.893978650043524126E-14, -9.000000000000001776 ) ) ;
#107554 = CARTESIAN_POINT ( 'NONE',  ( 16.46253265017146816, 9.564922557961045513, 81.66775706135233293 ) ) ;
#107556 = CARTESIAN_POINT ( 'NONE',  ( -5.719274019375665041, -21.55341960407619695, 84.79275706135234714 ) ) ;
#107557 = CARTESIAN_POINT ( 'NONE',  ( -8.224510206698735004, -14.34966873604973081, 49.58442372801901143 ) ) ;
#107558 = DIRECTION ( 'NONE',  ( -0.000000000000000000, 0.000000000000000000, 1.000000000000000000 ) ) ;
#107559 = CARTESIAN_POINT ( 'NONE',  ( -18.62759615963270932, 10.81492255796079327, 50.83224293864770971 ) ) ;
#107560 = CARTESIAN_POINT ( 'NONE',  ( -16.52544592524335698, -4.483927247898792601, 38.95942372801901854 ) ) ;
#107561 = CARTESIAN_POINT ( 'NONE',  ( -19.36337904590693171, 5.499999999999952927, 70.41494137495622851 ) ) ;
#107562 = CARTESIAN_POINT ( 'NONE',  ( 13.89961937509957401, 13.97604488694547697, 46.87609039468565442 ) ) ;
#107563 = CARTESIAN_POINT ( 'NONE',  ( 19.03943276465977164, -0.05219959533909143690, 93.74890960531435269 ) ) ;
#107564 = CARTESIAN_POINT ( 'NONE',  ( -16.51473224551069308, -9.474510206698971260, 56.66557627198103120 ) ) ;
#107565 = CARTESIAN_POINT ( 'NONE',  ( 17.50000000000000000, 5.499999999999992895, 86.70309617465828467 ) ) ;
#107566 = CARTESIAN_POINT ( 'NONE',  ( 5.719274019375673035, 21.55341960407619339, 72.29275706135236135 ) ) ;
#107567 = CARTESIAN_POINT ( 'NONE',  ( -38.00000000000000711, 2.428612866367529932E-14, -9.749999994537626336 ) ) ;
#107568 = EDGE_CURVE ( 'NONE', #150536, #141411, #109916, .T. ) ;
#107569 = CARTESIAN_POINT ( 'NONE',  ( -13.89961937509957401, -13.97604488694547875, 34.37609039468566863 ) ) ;
#107570 = CARTESIAN_POINT ( 'NONE',  ( 15.72974639402176855, 15.80617190586768217, 106.8760903946856899 ) ) ;
#107571 = CARTESIAN_POINT ( 'NONE',  ( -16.53943276465976808, 0.05219959533911058130, 31.24890960531435979 ) ) ;
#107572 = CARTESIAN_POINT ( 'NONE',  ( 13.89961937509977652, -13.97604488694527269, 58.12390960531436690 ) ) ;
#107573 = CARTESIAN_POINT ( 'NONE',  ( 13.97604488694527802, 13.89961937509977652, 104.3739096053143385 ) ) ;
#107574 = CARTESIAN_POINT ( 'NONE',  ( 21.55341960407619695, -5.719274019375665929, 86.04275706135236135 ) ) ;
#107575 = CARTESIAN_POINT ( 'NONE',  ( 13.97604488694527802, 13.89961937509977652, 64.37390960531436690 ) ) ;
#107576 = CARTESIAN_POINT ( 'NONE',  ( -0.05219959533937732626, 21.53943276465977519, 82.50109039468568994 ) ) ;
#107577 = CARTESIAN_POINT ( 'NONE',  ( 18.62759615963271287, -10.81492255796078972, 38.33224293864768839 ) ) ;
#107578 = B_SPLINE_CURVE_WITH_KNOTS ( 'NONE', 3,
 ( #28196, #153488, #72690, #138322, #122150, #200004, #179884, #41352, #103016, #164699, #26195, #155481, #109969, #17976, #140302, #61470, #33138, #16973 ),
 .UNSPECIFIED., .F., .F.,
 ( 4, 2, 2, 2, 2, 2, 2, 2, 4 ),
 ( 3.878959614448864246E-18, 0.001023866006848668780, 0.002047732013697333656, 0.003071598020545998533, 0.004095464027394662976, 0.005119330034243327852, 0.006143196041091992729, 0.007167062047940657606, 0.008190928054789322482 ),
 .UNSPECIFIED. ) ;
#107579 = CARTESIAN_POINT ( 'NONE',  ( 18.67979575497194134, -10.72451020669871369, 30.83442372801902209 ) ) ;
#107580 = CARTESIAN_POINT ( 'NONE',  ( -5.049401038297874678, -19.05341960407617918, 54.79275706135234003 ) ) ;
#107581 = CARTESIAN_POINT ( 'NONE',  ( 19.05341960407611168, 5.049401038298154454, 23.95724293864769194 ) ) ;
#107582 = CARTESIAN_POINT ( 'NONE',  ( 0.05219959533909260263, 19.03943276465977164, 69.99890960531435269 ) ) ;
#107583 = CARTESIAN_POINT ( 'NONE',  ( -14.34966873604972548, 8.224510206698743886, 23.33442372801901499 ) ) ;
#107584 = CARTESIAN_POINT ( 'NONE',  ( 4.483927247898545687, 16.52544592524342804, 89.79057627198103830 ) ) ;
#107585 = CARTESIAN_POINT ( 'NONE',  ( -5.049401038298153566, 19.05341960407611168, 55.20724293864769550 ) ) ;
#107586 = CARTESIAN_POINT ( 'NONE',  ( -10.81492255796078084, -18.62759615963271287, 42.08224293864769550 ) ) ;
#107587 = CARTESIAN_POINT ( 'NONE',  ( 9.564922557961047289, -16.46253265017146816, 105.4177570613523471 ) ) ;
#107588 = CARTESIAN_POINT ( 'NONE',  ( 0.05219959533907565091, 21.53943276465977519, 104.9989096053143669 ) ) ;
#107589 = CARTESIAN_POINT ( 'NONE',  ( -5.719274019375665041, -21.55341960407619695, 69.79275706135234714 ) ) ;
#107590 = CARTESIAN_POINT ( 'NONE',  ( 8.224510206698742110, 14.34966873604972548, 72.08442372801899012 ) ) ;
#107591 = CARTESIAN_POINT ( 'NONE',  ( -14.34966873604972548, 8.224510206698743886, 63.33442372801900433 ) ) ;
#107592 = CARTESIAN_POINT ( 'NONE',  ( -5.153800228976328057, -19.02544592524343514, 67.29057627198102409 ) ) ;
#107593 = CARTESIAN_POINT ( 'NONE',  ( 14.29746914071037800, 8.314922557961029526, 91.66775706135234714 ) ) ;
#107594 = CARTESIAN_POINT ( 'NONE',  ( -19.02544592524334988, -5.153800228976617603, 38.95942372801900433 ) ) ;
#107595 = CARTESIAN_POINT ( 'NONE',  ( -0.05219959533937732626, 21.53943276465977519, 22.50109039468567573 ) ) ;
#107596 = CARTESIAN_POINT ( 'NONE',  ( 4.379528057220339221, -16.55341960407611168, 62.70724293864769550 ) ) ;
#107597 = CARTESIAN_POINT ( 'NONE',  ( 5.153800228976335163, 19.02544592524342804, 79.79057627198102409 ) ) ;
#107598 = CARTESIAN_POINT ( 'NONE',  ( 4.379528057220092307, 16.55341960407617563, 82.29275706135234714 ) ) ;
#107599 = CARTESIAN_POINT ( 'NONE',  ( -18.67979575497193778, 10.72451020669871902, 63.33442372801900433 ) ) ;
#107600 = CARTESIAN_POINT ( 'NONE',  ( -16.52544592524335698, -4.483927247898792601, 23.95942372801901143 ) ) ;
#107601 = CARTESIAN_POINT ( 'NONE',  ( -18.62759615963270932, 10.81492255796079327, 110.8322429386476955 ) ) ;
#107602 = CARTESIAN_POINT ( 'NONE',  ( 16.53943276465976808, -0.05219959533910856209, 53.74890960531437401 ) ) ;
#107603 = VERTEX_POINT ( 'NONE', #15024 ) ;
#107604 = CARTESIAN_POINT ( 'NONE',  ( 18.62759615963271287, -10.81492255796078972, 88.33224293864769550 ) ) ;
#107605 = CARTESIAN_POINT ( 'NONE',  ( 8.314922557960818139, 14.29746914071049879, 39.58224293864769550 ) ) ;
#107606 = VERTEX_POINT ( 'NONE', #14020 ) ;
#107607 = CARTESIAN_POINT ( 'NONE',  ( 35.41256452865196991, 3.967314244253455691, 38.63057146076393877 ) ) ;
#107608 = CARTESIAN_POINT ( 'NONE',  ( 0.05219959533907565091, 21.53943276465977519, 114.9989096053143669 ) ) ;
#107609 = CARTESIAN_POINT ( 'NONE',  ( 13.97604488694527802, 13.89961937509977652, 109.3739096053143669 ) ) ;
#107610 = CARTESIAN_POINT ( 'NONE',  ( 10.72451020669871369, 18.67979575497193778, 42.08442372801901854 ) ) ;
#107611 = CARTESIAN_POINT ( 'NONE',  ( -8.224510206698948167, 14.34966873604960824, 45.41557627198103830 ) ) ;
#107612 = CARTESIAN_POINT ( 'NONE',  ( -5.153800228976328057, -19.02544592524343514, 62.29057627198100988 ) ) ;
#107613 = CARTESIAN_POINT ( 'NONE',  ( 13.97604488694548053, -13.89961937509957401, 60.62609039468564731 ) ) ;
#107614 = CARTESIAN_POINT ( 'NONE',  ( -5.049401038298153566, 19.05341960407611168, 95.20724293864770971 ) ) ;
#107615 = CARTESIAN_POINT ( 'NONE',  ( 21.55341960407610458, 5.719274019375980345, 53.95724293864770260 ) ) ;
#107616 = CARTESIAN_POINT ( 'NONE',  ( -14.20416113189184593, -35.58439206127017229, -22.81347619872354215 ) ) ;
#107617 = CARTESIAN_POINT ( 'NONE',  ( 16.51473224551069308, 9.474510206698969483, 54.16557627198103120 ) ) ;
#107618 = CARTESIAN_POINT ( 'NONE',  ( -14.29746914071037622, -8.314922557961029526, 34.16775706135234714 ) ) ;
#107619 = CARTESIAN_POINT ( 'NONE',  ( -9.564922557961040184, 16.46253265017147172, 62.91775706135233293 ) ) ;
#107620 = CARTESIAN_POINT ( 'NONE',  ( -10.72451020669870658, -18.67979575497194134, 19.58442372801901143 ) ) ;
#107621 = CARTESIAN_POINT ( 'NONE',  ( -16.53943276465976808, 0.05219959533911058130, 46.24890960531435979 ) ) ;
#107622 = CARTESIAN_POINT ( 'NONE',  ( -16.51473224551069308, -9.474510206698971260, 91.66557627198103830 ) ) ;
#107623 = CARTESIAN_POINT ( 'NONE',  ( -5.719274019375978568, 21.55341960407610458, 75.20724293864769550 ) ) ;
#107625 = CARTESIAN_POINT ( 'NONE',  ( 4.379528057220092307, 16.55341960407617563, 37.29275706135235424 ) ) ;
#107624 = CARTESIAN_POINT ( 'NONE',  ( -0.05219959533907301413, -21.53943276465977519, 97.49890960531436690 ) ) ;
#107626 = CARTESIAN_POINT ( 'NONE',  ( 21.55341960407610458, 5.719274019375980345, 38.95724293864768839 ) ) ;
#107627 = CARTESIAN_POINT ( 'NONE',  ( -10.81492255796105439, 18.62759615963255655, 82.91775706135234714 ) ) ;
#107628 = CARTESIAN_POINT ( 'NONE',  ( -5.153800228976328057, -19.02544592524343514, 87.29057627198103830 ) ) ;
#107629 = CARTESIAN_POINT ( 'NONE',  ( 9.564922557960805705, 16.46253265017160317, 44.58224293864769550 ) ) ;
#107630 = CARTESIAN_POINT ( 'NONE',  ( 0.05219959533909260263, 19.03943276465977164, 99.99890960531436690 ) ) ;
#107631 = CARTESIAN_POINT ( 'NONE',  ( 14.29746914071049879, -8.314922557960816363, 98.33224293864769550 ) ) ;
#107632 = CARTESIAN_POINT ( 'NONE',  ( -16.51473224551069308, -9.474510206698971260, 61.66557627198103120 ) ) ;
#107633 = CARTESIAN_POINT ( 'NONE',  ( 8.224510206698742110, 14.34966873604972548, 27.08442372801901854 ) ) ;
#107634 = VECTOR ( 'NONE', #87769, 1000.000000000000000 ) ;
#107635 = CARTESIAN_POINT ( 'NONE',  ( 17.49999999999999645, 4.640572885337623354, 31.86211835451160113 ) ) ;
#107636 = CARTESIAN_POINT ( 'NONE',  ( 16.46253265017146816, 9.564922557961045513, 51.66775706135233293 ) ) ;
#107638 = CARTESIAN_POINT ( 'NONE',  ( -21.52544592524343514, 5.823673210054127303, 36.04057627198102409 ) ) ;
#107637 = CARTESIAN_POINT ( 'NONE',  ( 9.564922557961047289, -16.46253265017146816, 20.41775706135233293 ) ) ;
#107639 = CARTESIAN_POINT ( 'NONE',  ( 4.483927247898790824, -16.52544592524335698, 95.20942372801903275 ) ) ;
#107640 = CARTESIAN_POINT ( 'NONE',  ( 22.97440419758976304, -21.21004173184712727, -46.59523340014560233 ) ) ;
#107641 = CARTESIAN_POINT ( 'NONE',  ( -16.51473224551082808, 9.474510206698731452, 73.33442372801900433 ) ) ;
#107642 = CARTESIAN_POINT ( 'NONE',  ( -5.153800228976607833, 19.02544592524334988, 37.70942372801899722 ) ) ;
#107643 = CARTESIAN_POINT ( 'NONE',  ( -17.31747979337948351, -6.344076630961018815, 46.37944868065184068 ) ) ;
#107644 = CARTESIAN_POINT ( 'NONE',  ( -13.97604488694527625, -13.89961937509977652, 46.87390960531435979 ) ) ;
#107645 = CARTESIAN_POINT ( 'NONE',  ( 12.06949235617757843, -12.14591786802309237, 43.12390960531435269 ) ) ;
#107646 = CARTESIAN_POINT ( 'NONE',  ( 19.02544592524343514, -5.153800228976328945, 23.54057627198102054 ) ) ;
#107647 = CARTESIAN_POINT ( 'NONE',  ( -8.314922557960811034, -14.29746914071050412, 27.08224293864769550 ) ) ;
#107648 = DIRECTION ( 'NONE',  ( 1.000000000000000000, 0.000000000000000000, 0.000000000000000000 ) ) ;
#107649 = CARTESIAN_POINT ( 'NONE',  ( -16.55341960407617563, 4.379528057220093196, 93.54275706135234714 ) ) ;
#107650 = CARTESIAN_POINT ( 'NONE',  ( 16.51473224551069308, 9.474510206698969483, 34.16557627198102409 ) ) ;
#107651 = CARTESIAN_POINT ( 'NONE',  ( 18.62759615963255655, 10.81492255796105972, 101.6677570613523613 ) ) ;
#107652 = CARTESIAN_POINT ( 'NONE',  ( -16.55341960407617563, 4.379528057220093196, 23.54275706135235424 ) ) ;
#107653 = CARTESIAN_POINT ( 'NONE',  ( 10.81492255796106328, -18.62759615963255655, 80.41775706135234714 ) ) ;
#107654 = CARTESIAN_POINT ( 'NONE',  ( 16.51473224551083163, -9.474510206698727899, 50.83442372801899722 ) ) ;
#107655 = CARTESIAN_POINT ( 'NONE',  ( 13.89961937509977652, -13.97604488694527269, 93.12390960531436690 ) ) ;
#107656 = CARTESIAN_POINT ( 'NONE',  ( 9.564922557960805705, 16.46253265017160317, 84.58224293864769550 ) ) ;
#107657 = CARTESIAN_POINT ( 'NONE',  ( -19.01533133064924996, 5.499999999999452882, 38.76586590595740489 ) ) ;
#107658 = CARTESIAN_POINT ( 'NONE',  ( 18.62759615963271287, -10.81492255796078972, 103.3322429386476955 ) ) ;
#107659 = CARTESIAN_POINT ( 'NONE',  ( 8.224510206698953496, -14.34966873604960469, 62.91557627198102409 ) ) ;
#107660 = CARTESIAN_POINT ( 'NONE',  ( -10.72451020669898014, 18.67979575497178502, 55.41557627198102409 ) ) ;
#107661 = CARTESIAN_POINT ( 'NONE',  ( -13.97604488694527625, -13.89961937509977652, 56.87390960531434558 ) ) ;
#107663 = CARTESIAN_POINT ( 'NONE',  ( -8.224510206698735004, -14.34966873604973081, 89.58442372801901854 ) ) ;
#107662 = CARTESIAN_POINT ( 'NONE',  ( -21.53943276465977519, 0.05219959533907696930, 91.24890960531436690 ) ) ;
#107664 = VERTEX_POINT ( 'NONE', #59522 ) ;
#107665 = CARTESIAN_POINT ( 'NONE',  ( -13.97604488694527625, -13.89961937509977652, 41.87390960531435979 ) ) ;
#107667 = CARTESIAN_POINT ( 'NONE',  ( 19.49401214000073779, -12.39993551617566503, 167.9999999999999716 ) ) ;
#107666 = CARTESIAN_POINT ( 'NONE',  ( -16.52544592524342804, 4.483927247898546575, 96.04057627198102409 ) ) ;
#107668 = CARTESIAN_POINT ( 'NONE',  ( -5.049401038298153566, 19.05341960407611168, 50.20724293864770260 ) ) ;
#107669 = CARTESIAN_POINT ( 'NONE',  ( -9.564922557960796823, -16.46253265017161027, 22.08224293864768839 ) ) ;
#107670 = CARTESIAN_POINT ( 'NONE',  ( 13.97604488694548053, -13.89961937509957401, 75.62609039468564731 ) ) ;
#107671 = CARTESIAN_POINT ( 'NONE',  ( 16.52544592524342804, -4.483927247898539470, 88.54057627198103830 ) ) ;
#107672 = CARTESIAN_POINT ( 'NONE',  ( 21.55341960407619695, -5.719274019375665929, 51.04275706135234714 ) ) ;
#107674 = CARTESIAN_POINT ( 'NONE',  ( -18.62759615963270932, 10.81492255796079327, 100.8322429386477097 ) ) ;
#107673 = CARTESIAN_POINT ( 'NONE',  ( 19.03943276465977164, -0.05219959533909143690, 33.74890960531435979 ) ) ;
#107675 = CARTESIAN_POINT ( 'NONE',  ( 16.52544592524342804, -4.483927247898539470, 93.54057627198103830 ) ) ;
#107676 = CARTESIAN_POINT ( 'NONE',  ( 17.60779699588841041, 5.499999999999981348, 93.84981316670106821 ) ) ;
#107677 = CARTESIAN_POINT ( 'NONE',  ( 19.02544592524343514, -5.153800228976328945, 53.54057627198102409 ) ) ;
#107678 = CARTESIAN_POINT ( 'NONE',  ( 18.56399227203345603, 5.499999999999817923, 46.47830131249904895 ) ) ;
#107680 = CARTESIAN_POINT ( 'NONE',  ( 21.53943276465977519, -0.05219959533907433946, 23.74890960531435269 ) ) ;
#107679 = CARTESIAN_POINT ( 'NONE',  ( 5.049401038297881783, 19.05341960407617563, 92.29275706135234714 ) ) ;
#107681 = CARTESIAN_POINT ( 'NONE',  ( 21.55341960407619695, -5.719274019375665929, 31.04275706135234714 ) ) ;
#107682 = CARTESIAN_POINT ( 'NONE',  ( -19.02544592524342804, 5.153800228976336051, 86.04057627198103830 ) ) ;
#107683 = CARTESIAN_POINT ( 'NONE',  ( -19.03943276465977164, -0.05219959533935918106, 63.75109039468566863 ) ) ;
#107684 = CARTESIAN_POINT ( 'NONE',  ( -5.049401038298153566, 19.05341960407611168, 55.20724293864769550 ) ) ;
#107685 = CARTESIAN_POINT ( 'NONE',  ( 12.06949235617757843, -12.14591786802309237, 73.12390960531436690 ) ) ;
#107686 = CARTESIAN_POINT ( 'NONE',  ( 4.379528057220339221, -16.55341960407611168, 72.70724293864769550 ) ) ;
#107687 = CARTESIAN_POINT ( 'NONE',  ( 13.89961937509977652, -13.97604488694527269, 88.12390960531438111 ) ) ;
#107688 = CARTESIAN_POINT ( 'NONE',  ( -18.62759615963270932, 10.81492255796079327, 95.83224293864770971 ) ) ;
#107689 = CARTESIAN_POINT ( 'NONE',  ( -19.03943276465977164, 0.05219959533909376836, 91.24890960531436690 ) ) ;
#107690 = CARTESIAN_POINT ( 'NONE',  ( -16.46253265017146816, -9.564922557961047289, 29.16775706135232937 ) ) ;
#107693 = CARTESIAN_POINT ( 'NONE',  ( 12.14591786802309770, 12.06949235617756955, 109.3739096053143811 ) ) ;
#107692 = CARTESIAN_POINT ( 'NONE',  ( -14.29746914071049879, 8.314922557960819915, 30.83224293864770260 ) ) ;
#107691 = CARTESIAN_POINT ( 'NONE',  ( -13.89961937509977652, 13.97604488694528158, 40.62390960531435979 ) ) ;
#107694 = ORIENTED_EDGE ( 'NONE', *, *, #83071, .T. ) ;
#107695 = CARTESIAN_POINT ( 'NONE',  ( -10.81492255796105439, 18.62759615963255655, 32.91775706135234714 ) ) ;
#107696 = CARTESIAN_POINT ( 'NONE',  ( 16.51473224551083163, -9.474510206698727899, 65.83442372801900433 ) ) ;
#107697 = CARTESIAN_POINT ( 'NONE',  ( -14.34966873604960291, -8.224510206698953496, 31.66557627198102054 ) ) ;
#107698 = CARTESIAN_POINT ( 'NONE',  ( 15.80617190586746368, 15.72974639402197994, 89.37390960531435269 ) ) ;
#107699 = CARTESIAN_POINT ( 'NONE',  ( -21.55341960407610458, -5.719274019375992779, 21.45724293864769550 ) ) ;
#107700 = CARTESIAN_POINT ( 'NONE',  ( 16.52544592524342804, -4.483927247898539470, 73.54057627198102409 ) ) ;
#107701 = CARTESIAN_POINT ( 'NONE',  ( -13.97604488694527625, -13.89961937509977652, 26.87390960531434558 ) ) ;
#107702 = CARTESIAN_POINT ( 'NONE',  ( -5.153800228976607833, 19.02544592524334988, 22.70942372801899012 ) ) ;
#107703 = CARTESIAN_POINT ( 'NONE',  ( 4.483927247898790824, -16.52544592524335698, 105.2094237280190328 ) ) ;
#107704 = CARTESIAN_POINT ( 'NONE',  ( 16.52544592524335698, 4.483927247898782831, 56.45942372801902565 ) ) ;
#107705 = CARTESIAN_POINT ( 'NONE',  ( -10.81492255796078084, -18.62759615963271287, 37.08224293864768129 ) ) ;
#107706 = CARTESIAN_POINT ( 'NONE',  ( 5.823673210054444382, -21.52544592524334988, 105.2094237280190328 ) ) ;
#107707 = CARTESIAN_POINT ( 'NONE',  ( -16.46253265017160317, 9.564922557960807481, 85.83224293864769550 ) ) ;
#107708 = CARTESIAN_POINT ( 'NONE',  ( 4.483927247898790824, -16.52544592524335698, 55.20942372801902565 ) ) ;
#107709 = CARTESIAN_POINT ( 'NONE',  ( -19.05341960407611168, -5.049401038298163336, 26.45724293864769550 ) ) ;
#107710 = CARTESIAN_POINT ( 'NONE',  ( -16.52544592524342804, 4.483927247898546575, 31.04057627198102409 ) ) ;
#107712 = CARTESIAN_POINT ( 'NONE',  ( 19.03943276465977164, -0.05219959533909143690, 93.74890960531435269 ) ) ;
#107711 = CARTESIAN_POINT ( 'NONE',  ( -9.474510206698964154, 16.51473224551069663, 110.4155762719810383 ) ) ;
#107713 = CARTESIAN_POINT ( 'NONE',  ( -0.05219959533909027116, -19.03943276465977164, 112.4989096053143669 ) ) ;
#107714 = CARTESIAN_POINT ( 'NONE',  ( 8.224510206698953496, -14.34966873604960469, 52.91557627198103830 ) ) ;
#107715 = CARTESIAN_POINT ( 'NONE',  ( 14.29746914071049879, -8.314922557960816363, 28.33224293864769550 ) ) ;
#107716 = AXIS2_PLACEMENT_3D ( 'NONE', #92563, #187595, #49064 ) ;
#107717 = CARTESIAN_POINT ( 'NONE',  ( 8.314922557960818139, 14.29746914071049879, 49.58224293864769550 ) ) ;
#107719 = CARTESIAN_POINT ( 'NONE',  ( 17.49999999999998579, -3.471454075611618784, 31.98332581144368447 ) ) ;
#107718 = CARTESIAN_POINT ( 'NONE',  ( -16.53943276465976808, -0.05219959533934237506, 38.75109039468567573 ) ) ;
#107720 = CARTESIAN_POINT ( 'NONE',  ( 19.05341960407617918, -5.049401038297876454, 46.04275706135233293 ) ) ;
#107721 = CARTESIAN_POINT ( 'NONE',  ( 0.05219959533909260263, 19.03943276465977164, 84.99890960531436690 ) ) ;
#107722 = CARTESIAN_POINT ( 'NONE',  ( 13.97604488694548053, -13.89961937509957401, 70.62609039468567573 ) ) ;
#107723 = CARTESIAN_POINT ( 'NONE',  ( 27.73933785331498569, 2.768321779492822058E-14, 146.3750000027311842 ) ) ;
#107724 = CARTESIAN_POINT ( 'NONE',  ( 9.564922557961047289, -16.46253265017146816, 50.41775706135233293 ) ) ;
#107726 = CARTESIAN_POINT ( 'NONE',  ( -4.483927247898782831, 16.52544592524335698, 82.70942372801900433 ) ) ;
#107725 = CARTESIAN_POINT ( 'NONE',  ( -13.89961937509957401, -13.97604488694547875, 99.37609039468567573 ) ) ;
#107727 = CARTESIAN_POINT ( 'NONE',  ( -27.73933785331498925, 2.428612866367529932E-14, 145.3750000027311842 ) ) ;
#107728 = CARTESIAN_POINT ( 'NONE',  ( -19.03943276465977164, 0.05219959533909376836, 21.24890960531436335 ) ) ;
#107729 = CARTESIAN_POINT ( 'NONE',  ( 5.823673210054125526, 21.52544592524343514, 24.79057627198103120 ) ) ;
#107730 = CARTESIAN_POINT ( 'NONE',  ( -15.80617190586768217, 15.72974639402176855, 43.12609039468568284 ) ) ;
#107731 = CARTESIAN_POINT ( 'NONE',  ( -16.51473224551082808, 9.474510206698731452, 108.3344237280190043 ) ) ;
#107733 = CARTESIAN_POINT ( 'NONE',  ( 9.564922557960805705, 16.46253265017160317, 64.58224293864769550 ) ) ;
#107732 = CARTESIAN_POINT ( 'NONE',  ( 9.656827144875922642, -71.74905178543389184, -4.999999999999999112 ) ) ;
#107734 = ADVANCED_FACE ( 'NONE', ( #122189 ), #27230, .T. ) ;
#107735 = CARTESIAN_POINT ( 'NONE',  ( -9.564922557960796823, -16.46253265017161027, 107.0822429386476955 ) ) ;
#107737 = CARTESIAN_POINT ( 'NONE',  ( -5.049401038298153566, 19.05341960407611168, 60.20724293864768129 ) ) ;
#107736 = CARTESIAN_POINT ( 'NONE',  ( -14.34966873604960291, -8.224510206698953496, 61.66557627198103120 ) ) ;
#107738 = CARTESIAN_POINT ( 'NONE',  ( -16.46253265017160317, 9.564922557960807481, 70.83224293864770971 ) ) ;
#107739 = CARTESIAN_POINT ( 'NONE',  ( 19.03943276465977164, 0.05219959533936151252, 81.25109039468567573 ) ) ;
#107740 = CARTESIAN_POINT ( 'NONE',  ( -18.62759615963270932, 10.81492255796079327, 50.83224293864770971 ) ) ;
#107741 = CARTESIAN_POINT ( 'NONE',  ( -4.483927247898539470, -16.52544592524342804, 112.2905762719810241 ) ) ;
#107742 = CARTESIAN_POINT ( 'NONE',  ( 13.97604488694548053, -13.89961937509957401, 45.62609039468566863 ) ) ;
#107743 = CARTESIAN_POINT ( 'NONE',  ( -19.02544592524342804, 5.153800228976336051, 81.04057627198103830 ) ) ;
#107744 = CARTESIAN_POINT ( 'NONE',  ( -15.80617190586745835, -15.72974639402198527, 71.87390960531438111 ) ) ;
#107746 = CARTESIAN_POINT ( 'NONE',  ( -19.02544592524334988, -5.153800228976617603, 28.95942372801900433 ) ) ;
#107745 = CARTESIAN_POINT ( 'NONE',  ( -12.06949235617756955, 12.14591786802309770, 75.62390960531439532 ) ) ;
#107747 = CARTESIAN_POINT ( 'NONE',  ( -15.80617190586745835, -15.72974639402198527, 56.87390960531436690 ) ) ;
#107748 = CARTESIAN_POINT ( 'NONE',  ( 10.81492255796078972, 18.62759615963270932, 44.58224293864769550 ) ) ;
#107749 = CARTESIAN_POINT ( 'NONE',  ( 15.80617190586769283, -15.72974639402175789, 90.62609039468567573 ) ) ;
#107750 = CARTESIAN_POINT ( 'NONE',  ( -13.89961937509977652, 13.97604488694528158, 60.62390960531436690 ) ) ;
#107751 = CARTESIAN_POINT ( 'NONE',  ( 8.314922557960818139, 14.29746914071049879, 109.5822429386476955 ) ) ;
#107752 = CARTESIAN_POINT ( 'NONE',  ( 5.719274019375673035, 21.55341960407619339, 27.29275706135234358 ) ) ;
#107753 = CARTESIAN_POINT ( 'NONE',  ( 0.2046014141641599449, 16.68944534439192040, -61.35149151744828089 ) ) ;
#107754 = CARTESIAN_POINT ( 'NONE',  ( 5.719274019375673035, 21.55341960407619339, 42.29275706135235424 ) ) ;
#107755 = CARTESIAN_POINT ( 'NONE',  ( -19.02544592524342804, 5.153800228976336051, 41.04057627198103120 ) ) ;
#107756 = CARTESIAN_POINT ( 'NONE',  ( 0.05219959533907565091, 21.53943276465977519, 109.9989096053143527 ) ) ;
#107757 = CARTESIAN_POINT ( 'NONE',  ( -5.153800228976607833, 19.02544592524334988, 47.70942372801900433 ) ) ;
#107758 = CARTESIAN_POINT ( 'NONE',  ( -16.51473224551069308, -9.474510206698971260, 26.66557627198103120 ) ) ;
#107759 = CARTESIAN_POINT ( 'NONE',  ( 13.89961937509977652, -13.97604488694527269, 28.12390960531435624 ) ) ;
#107760 = CARTESIAN_POINT ( 'NONE',  ( -4.379528057220086978, -16.55341960407618274, 54.79275706135235424 ) ) ;
#107761 = CARTESIAN_POINT ( 'NONE',  ( -19.03943276465977164, 0.05219959533909376836, 26.24890960531435624 ) ) ;
#107762 = CARTESIAN_POINT ( 'NONE',  ( -26.79623349963142331, -5.044589688426236229, 170.2051123914322375 ) ) ;
#107763 = CARTESIAN_POINT ( 'NONE',  ( 19.02544592524343514, -5.153800228976328945, 68.54057627198103830 ) ) ;
#107764 = CARTESIAN_POINT ( 'NONE',  ( -14.29746914071049879, 8.314922557960819915, 100.8322429386477097 ) ) ;
#107765 = CARTESIAN_POINT ( 'NONE',  ( 15.80617190586746368, 15.72974639402197994, 64.37390960531435269 ) ) ;
#107766 = CARTESIAN_POINT ( 'NONE',  ( -16.55341960407617563, 4.379528057220093196, 38.54275706135234714 ) ) ;
#107767 = CARTESIAN_POINT ( 'NONE',  ( 18.67979575497194134, -10.72451020669871369, 100.8344237280190185 ) ) ;
#107768 = CARTESIAN_POINT ( 'NONE',  ( 9.474510206698971260, -16.51473224551069308, 22.91557627198102765 ) ) ;
#107769 = CARTESIAN_POINT ( 'NONE',  ( 8.314922557961029526, -14.29746914071037800, 110.4177570613523756 ) ) ;
#107770 = CARTESIAN_POINT ( 'NONE',  ( 0.05219959533910956823, 16.53943276465976808, 49.99890960531437401 ) ) ;
#107771 = CARTESIAN_POINT ( 'NONE',  ( -13.89961937509977652, 13.97604488694528158, 55.62390960531434558 ) ) ;
#107772 = CARTESIAN_POINT ( 'NONE',  ( -5.823673210054431948, 21.52544592524334988, 92.70942372801901854 ) ) ;
#107773 = CARTESIAN_POINT ( 'NONE',  ( -18.67979575497178146, -10.72451020669898902, 111.6655762719810525 ) ) ;
#107774 = CIRCLE ( 'NONE', #110953, 0.2500000000000002220 ) ;
#107775 = CARTESIAN_POINT ( 'NONE',  ( -10.81492255796105439, 18.62759615963255655, 67.91775706135234714 ) ) ;
#107776 = CARTESIAN_POINT ( 'NONE',  ( -14.29746914071037622, -8.314922557961029526, 54.16775706135235424 ) ) ;
#107778 = CARTESIAN_POINT ( 'NONE',  ( 0.05219959533937995610, -21.53943276465977519, 100.0010903946857042 ) ) ;
#107777 = CARTESIAN_POINT ( 'NONE',  ( -8.314922557960811034, -14.29746914071050412, 82.08224293864768129 ) ) ;
#107779 = CARTESIAN_POINT ( 'NONE',  ( -8.314922557960811034, -14.29746914071050412, 27.08224293864769550 ) ) ;
#107780 = CARTESIAN_POINT ( 'NONE',  ( -16.36317988757057051, 7.306389748694942732, 114.0978960836323068 ) ) ;
#107781 = CARTESIAN_POINT ( 'NONE',  ( 4.483927247898790824, -16.52544592524335698, 40.20942372801901854 ) ) ;
#107782 = CARTESIAN_POINT ( 'NONE',  ( -14.29746914071049879, 8.314922557960819915, 40.83224293864769550 ) ) ;
#107783 = CARTESIAN_POINT ( 'NONE',  ( 8.224510206698742110, 14.34966873604972548, 82.08442372801901854 ) ) ;
#107784 = CARTESIAN_POINT ( 'NONE',  ( -9.474510206698964154, 16.51473224551069663, 105.4155762719810383 ) ) ;
#107785 = CARTESIAN_POINT ( 'NONE',  ( 19.05341960407611168, 5.049401038298154454, 113.9572429386477097 ) ) ;
#107786 = CARTESIAN_POINT ( 'NONE',  ( -18.62759615963255300, -10.81492255796106328, 104.1677570613523471 ) ) ;
#107787 = CARTESIAN_POINT ( 'NONE',  ( 8.224510206698742110, 14.34966873604972548, 97.08442372801904696 ) ) ;
#107788 = CARTESIAN_POINT ( 'NONE',  ( 16.55341960407611168, 4.379528057220329451, 78.95724293864769550 ) ) ;
#107789 = CARTESIAN_POINT ( 'NONE',  ( 16.51473224551069308, 9.474510206698969483, 79.16557627198103830 ) ) ;
#107790 = VERTEX_POINT ( 'NONE', #45366 ) ;
#107792 =( BOUNDED_CURVE ( )  B_SPLINE_CURVE ( 3, ( #159891, #55714, #67879, #146714 ),
 .UNSPECIFIED., .F., .T. ) 
 B_SPLINE_CURVE_WITH_KNOTS ( ( 4, 4 ),
 ( 1.025647941782810824, 1.570796326794896780 ),
 .UNSPECIFIED. ) 
 CURVE ( )  GEOMETRIC_REPRESENTATION_ITEM ( )  RATIONAL_B_SPLINE_CURVE ( ( 1.000000000000000000, 0.9753873905749756990, 0.9753873905749756990, 1.000000000000000000 ) ) 
 REPRESENTATION_ITEM ( '' )  );
#107791 = CARTESIAN_POINT ( 'NONE',  ( 12.14591786802327356, -12.06949235617739191, 45.62609039468567573 ) ) ;
#107793 = CARTESIAN_POINT ( 'NONE',  ( -16.51473224551069308, -9.474510206698971260, 36.66557627198102409 ) ) ;
#107794 = CARTESIAN_POINT ( 'NONE',  ( -9.564922557960796823, -16.46253265017161027, 97.08224293864769550 ) ) ;
#107796 = CARTESIAN_POINT ( 'NONE',  ( -22.81625015709510507, 31.40387420917330275, -0.9249999972688132122 ) ) ;
#107795 = CARTESIAN_POINT ( 'NONE',  ( 16.52544592524335698, 4.483927247898782831, 31.45942372801901854 ) ) ;
#107797 = CARTESIAN_POINT ( 'NONE',  ( -13.89961937509957401, -13.97604488694547875, 34.37609039468566863 ) ) ;
#107798 = CARTESIAN_POINT ( 'NONE',  ( 16.53943276465976808, 0.05219959533934440121, 96.25109039468568994 ) ) ;
#107799 = CARTESIAN_POINT ( 'NONE',  ( 19.02544592524343514, -5.153800228976328945, 33.54057627198102409 ) ) ;
#107800 = CARTESIAN_POINT ( 'NONE',  ( -0.05219959533934338120, 16.53943276465976808, 77.50109039468567573 ) ) ;
#107801 = CARTESIAN_POINT ( 'NONE',  ( -8.314922557961024197, 14.29746914071037800, 62.91775706135236135 ) ) ;
#107802 = CARTESIAN_POINT ( 'NONE',  ( 9.564922557961047289, -16.46253265017146816, 80.41775706135234714 ) ) ;
#107803 = CARTESIAN_POINT ( 'NONE',  ( -5.153800228976607833, 19.02544592524334988, 27.70942372801899722 ) ) ;
#107804 = CARTESIAN_POINT ( 'NONE',  ( 5.153800228976335163, 19.02544592524342804, 49.79057627198100988 ) ) ;
#107805 = CARTESIAN_POINT ( 'NONE',  ( -12.06949235617756955, 12.14591786802309770, 85.62390960531436690 ) ) ;
#107806 = AXIS2_PLACEMENT_3D ( 'NONE', #121394, #44569, #106224 ) ;
#107807 = ADVANCED_FACE ( 'NONE', ( #13049 ), #164740, .F. ) ;
#107808 = CARTESIAN_POINT ( 'NONE',  ( -19.03943276465977164, -0.05219959533935918106, 53.75109039468566863 ) ) ;
#107809 = CARTESIAN_POINT ( 'NONE',  ( -21.53943276465977519, 0.05219959533907696930, 56.24890960531436690 ) ) ;
#107810 = CARTESIAN_POINT ( 'NONE',  ( 13.97604488694548053, -13.89961937509957401, 30.62609039468566863 ) ) ;
#107811 = CARTESIAN_POINT ( 'NONE',  ( -19.02544592524342804, 5.153800228976336051, 101.0405762719810241 ) ) ;
#107812 = CARTESIAN_POINT ( 'NONE',  ( 10.81492255796078972, 18.62759615963270932, 79.58224293864769550 ) ) ;
#107813 = CARTESIAN_POINT ( 'NONE',  ( 19.02544592524343514, -5.153800228976328945, 113.5405762719810241 ) ) ;
#107814 = CARTESIAN_POINT ( 'NONE',  ( 16.51473224551083163, -9.474510206698727899, 100.8344237280190043 ) ) ;
#107815 = CARTESIAN_POINT ( 'NONE',  ( -19.05341960407617563, 5.049401038297882671, 113.5427570613523471 ) ) ;
#107816 = CARTESIAN_POINT ( 'NONE',  ( 19.05341960407611168, 5.049401038298154454, 33.95724293864769550 ) ) ;
#107817 = CARTESIAN_POINT ( 'NONE',  ( 19.05341960407611168, 5.049401038298154454, 93.95724293864769550 ) ) ;
#107818 = CARTESIAN_POINT ( 'NONE',  ( 15.72974639402199770, -15.80617190586745480, 78.12390960531436690 ) ) ;
#107819 = CARTESIAN_POINT ( 'NONE',  ( 16.52544592524335698, 4.483927247898782831, 41.45942372801901143 ) ) ;
#107820 = CARTESIAN_POINT ( 'NONE',  ( 21.55341960407619695, -5.719274019375665929, 61.04275706135234714 ) ) ;
#107822 = CARTESIAN_POINT ( 'NONE',  ( -18.67979575497193778, 10.72451020669871902, 108.3344237280190185 ) ) ;
#107821 = CARTESIAN_POINT ( 'NONE',  ( 13.97604488694548053, -13.89961937509957401, 100.6260903946856615 ) ) ;
#107823 = CARTESIAN_POINT ( 'NONE',  ( -16.53943276465976808, -0.05219959533934237506, 108.7510903946857042 ) ) ;
#107824 = CARTESIAN_POINT ( 'NONE',  ( -15.80617190586745835, -15.72974639402198527, 96.87390960531436690 ) ) ;
#107825 = CARTESIAN_POINT ( 'NONE',  ( -14.29746914071049879, 8.314922557960819915, 35.83224293864768839 ) ) ;
#107826 = CARTESIAN_POINT ( 'NONE',  ( -13.89961937509957401, -13.97604488694547875, 79.37609039468567573 ) ) ;
#107827 = CARTESIAN_POINT ( 'NONE',  ( -15.72974639402176322, -15.80617190586768395, 54.37609039468568994 ) ) ;
#107828 = CARTESIAN_POINT ( 'NONE',  ( -19.05341960407617563, 5.049401038297882671, 33.54275706135231871 ) ) ;
#107829 = CARTESIAN_POINT ( 'NONE',  ( 12.14591786802309770, 12.06949235617756955, 99.37390960531436690 ) ) ;
#107830 = CARTESIAN_POINT ( 'NONE',  ( -18.62759615963270932, 10.81492255796079327, 30.83224293864770260 ) ) ;
#107831 = CARTESIAN_POINT ( 'NONE',  ( -8.224510206698948167, 14.34966873604960824, 40.41557627198103120 ) ) ;
#107832 = CARTESIAN_POINT ( 'NONE',  ( 15.80617190586769283, -15.72974639402175789, 100.6260903946857184 ) ) ;
#107833 = CARTESIAN_POINT ( 'NONE',  ( 16.52544592524335698, 4.483927247898782831, 56.45942372801902565 ) ) ;
#107834 = CARTESIAN_POINT ( 'NONE',  ( -8.314922557960811034, -14.29746914071050412, 27.08224293864769550 ) ) ;
#107835 = CARTESIAN_POINT ( 'NONE',  ( -10.81492255796105439, 18.62759615963255655, 57.91775706135234714 ) ) ;
#107836 = CARTESIAN_POINT ( 'NONE',  ( 21.55341960407619695, -5.719274019375665929, 51.04275706135234714 ) ) ;
#107837 = ORIENTED_EDGE ( 'NONE', *, *, #221, .T. ) ;
#107838 = CARTESIAN_POINT ( 'NONE',  ( 9.474510206698971260, -16.51473224551069308, 62.91557627198102409 ) ) ;
#107839 = CARTESIAN_POINT ( 'NONE',  ( 5.823673210054444382, -21.52544592524334988, 25.20942372801901854 ) ) ;
#107840 = CARTESIAN_POINT ( 'NONE',  ( 16.53943276465976808, -0.05219959533910856209, 108.7489096053143669 ) ) ;
#107841 = CARTESIAN_POINT ( 'NONE',  ( 16.46253265017160672, -9.564922557960803928, 28.33224293864769550 ) ) ;
#107842 = CARTESIAN_POINT ( 'NONE',  ( -16.55341960407611168, -4.379528057220339221, 76.45724293864769550 ) ) ;
#107843 = CARTESIAN_POINT ( 'NONE',  ( -19.03943276465977164, 0.05219959533909376836, 71.24890960531435269 ) ) ;
#107844 = CARTESIAN_POINT ( 'NONE',  ( 16.52544592524342804, -4.483927247898539470, 33.54057627198102409 ) ) ;
#107845 = CARTESIAN_POINT ( 'NONE',  ( 15.72974639402199770, -15.80617190586745480, 53.12390960531436690 ) ) ;
#107846 = CARTESIAN_POINT ( 'NONE',  ( 16.53943276465976808, -0.05219959533910856209, 88.74890960531436690 ) ) ;
#107847 = CARTESIAN_POINT ( 'NONE',  ( 5.823673210054125526, 21.52544592524343514, 109.7905762719810383 ) ) ;
#107848 = CARTESIAN_POINT ( 'NONE',  ( -19.05341960407611168, -5.049401038298163336, 106.4572429386476955 ) ) ;
#107850 = CARTESIAN_POINT ( 'NONE',  ( -9.474510206698720793, -16.51473224551083518, 109.5844237280190043 ) ) ;
#107849 = CARTESIAN_POINT ( 'NONE',  ( 9.474510206698971260, -16.51473224551069308, 47.91557627198102409 ) ) ;
#107851 = CARTESIAN_POINT ( 'NONE',  ( -15.72974639402197994, 15.80617190586746368, 60.62390960531437401 ) ) ;
#107852 = CARTESIAN_POINT ( 'NONE',  ( -10.81492255796105439, 18.62759615963255655, 82.91775706135234714 ) ) ;
#107853 = CARTESIAN_POINT ( 'NONE',  ( -13.97604488694527625, -13.89961937509977652, 71.87390960531433848 ) ) ;
#107854 = AXIS2_PLACEMENT_3D ( 'NONE', #29215, #90848, #88879 ) ;
#107855 = CARTESIAN_POINT ( 'NONE',  ( -0.05219959533909027116, -19.03943276465977164, 102.4989096053143669 ) ) ;
#107856 = CARTESIAN_POINT ( 'NONE',  ( 4.379528057220092307, 16.55341960407617563, 82.29275706135234714 ) ) ;
#107857 = CARTESIAN_POINT ( 'NONE',  ( 21.55341960407619695, -5.719274019375665929, 61.04275706135234714 ) ) ;
#107858 = CARTESIAN_POINT ( 'NONE',  ( -15.80617190586768217, 15.72974639402176855, 83.12609039468568994 ) ) ;
#107859 = CARTESIAN_POINT ( 'NONE',  ( 0.05219959533907565091, 21.53943276465977519, 114.9989096053143669 ) ) ;
#107860 = CARTESIAN_POINT ( 'NONE',  ( -12.14591786802326823, 12.06949235617739902, 73.12609039468567573 ) ) ;
#107861 = CARTESIAN_POINT ( 'NONE',  ( -5.719274019375978568, 21.55341960407610458, 80.20724293864769550 ) ) ;
#107862 = CARTESIAN_POINT ( 'NONE',  ( 5.153800228976615827, -19.02544592524334988, 50.20942372801897591 ) ) ;
#107863 = CARTESIAN_POINT ( 'NONE',  ( -5.719274019375978568, 21.55341960407610458, 45.20724293864769550 ) ) ;
#107865 = CARTESIAN_POINT ( 'NONE',  ( -16.55341960407617563, 4.379528057220093196, 113.5427570613523756 ) ) ;
#107864 = CARTESIAN_POINT ( 'NONE',  ( 19.02544592524343514, -5.153800228976328945, 78.54057627198099567 ) ) ;
#107866 = CARTESIAN_POINT ( 'NONE',  ( -4.000000000000000888, -165.0000000000000000, 12.00000000000000355 ) ) ;
#107867 = CARTESIAN_POINT ( 'NONE',  ( -19.02544592524342804, 5.153800228976336051, 111.0405762719810099 ) ) ;
#107868 = CARTESIAN_POINT ( 'NONE',  ( 20.43538597629129328, 20.43538597629121156, -49.67367017693150189 ) ) ;
#107869 = CARTESIAN_POINT ( 'NONE',  ( 19.03943276465977164, 0.05219959533936151252, 96.25109039468567573 ) ) ;
#107870 = CARTESIAN_POINT ( 'NONE',  ( 21.55341960407610458, 5.719274019375980345, 68.95724293864769550 ) ) ;
#107871 = CARTESIAN_POINT ( 'NONE',  ( -4.483927247898539470, -16.52544592524342804, 47.29057627198103120 ) ) ;
#107872 = CARTESIAN_POINT ( 'NONE',  ( -13.89961937509957401, -13.97604488694547875, 109.3760903946856331 ) ) ;
#107873 = CARTESIAN_POINT ( 'NONE',  ( -16.46253265017160317, 9.564922557960807481, 25.83224293864769194 ) ) ;
#107874 = CARTESIAN_POINT ( 'NONE',  ( 0.05219959533936267826, -19.03943276465977164, 105.0010903946856615 ) ) ;
#107876 = CARTESIAN_POINT ( 'NONE',  ( 5.049401038297881783, 19.05341960407617563, 72.29275706135234714 ) ) ;
#107875 = CARTESIAN_POINT ( 'NONE',  ( 18.67979575497178502, 10.72451020669898547, 94.16557627198103830 ) ) ;
#107877 = CARTESIAN_POINT ( 'NONE',  ( 12.14591786802327356, -12.06949235617739191, 85.62609039468568994 ) ) ;
#107878 = CARTESIAN_POINT ( 'NONE',  ( -0.05219959533909027116, -19.03943276465977164, 77.49890960531435269 ) ) ;
#107879 = CARTESIAN_POINT ( 'NONE',  ( -0.05219959533910754901, -16.53943276465976808, 82.49890960531436690 ) ) ;
#107880 = CONICAL_SURFACE ( 'NONE', #14676, 40.00000000000002132, 0.06108652381980166773 ) ;
#107881 = CARTESIAN_POINT ( 'NONE',  ( 13.89961937509977652, -13.97604488694527269, 63.12390960531435979 ) ) ;
#107882 = CARTESIAN_POINT ( 'NONE',  ( -8.224510206698948167, 14.34966873604960824, 60.41557627198102409 ) ) ;
#107883 = CARTESIAN_POINT ( 'NONE',  ( 5.049401038298161559, -19.05341960407611168, 32.70724293864768129 ) ) ;
#107884 = CARTESIAN_POINT ( 'NONE',  ( -37.48574882824303955, -2.272739345372926767, 39.98829423970373398 ) ) ;
#107885 = CARTESIAN_POINT ( 'NONE',  ( -12.14591786802309592, -12.06949235617757132, 46.87390960531435979 ) ) ;
#107886 = CARTESIAN_POINT ( 'NONE',  ( -9.474510206698964154, 16.51473224551069663, 75.41557627198103830 ) ) ;
#107887 = CARTESIAN_POINT ( 'NONE',  ( -1.491100297015943488, -15.38830714838547919, -59.71292413584865244 ) ) ;
#107888 = CARTESIAN_POINT ( 'NONE',  ( 19.05341960407617918, -5.049401038297876454, 56.04275706135234714 ) ) ;
#107889 = CARTESIAN_POINT ( 'NONE',  ( 12.14591786802327356, -12.06949235617739191, 60.62609039468567573 ) ) ;
#107890 = CARTESIAN_POINT ( 'NONE',  ( -18.62759615963270932, 10.81492255796079327, 65.83224293864769550 ) ) ;
#107891 = CARTESIAN_POINT ( 'NONE',  ( -19.02544592524334988, -5.153800228976617603, 23.95942372801900078 ) ) ;
#107892 = CARTESIAN_POINT ( 'NONE',  ( -13.97604488694527625, -13.89961937509977652, 91.87390960531432427 ) ) ;
#107893 = CARTESIAN_POINT ( 'NONE',  ( -21.41434933286226538, -23.00156705360894804, -46.36348427009351525 ) ) ;
#107894 = CARTESIAN_POINT ( 'NONE',  ( 21.53943276465977519, -0.05219959533907433946, 28.74890960531435624 ) ) ;
#107895 = CARTESIAN_POINT ( 'NONE',  ( 19.03943276465977164, -0.05219959533909143690, 58.74890960531435979 ) ) ;
#107896 = CARTESIAN_POINT ( 'NONE',  ( 5.823673210054444382, -21.52544592524334988, 55.20942372801902565 ) ) ;
#107897 = CARTESIAN_POINT ( 'NONE',  ( -8.224510206698948167, 14.34966873604960824, 105.4155762719810383 ) ) ;
#107900 = EDGE_LOOP ( 'NONE', ( #17150, #140022, #180284 ) ) ;
#107899 = CARTESIAN_POINT ( 'NONE',  ( 13.97604488694527802, 13.89961937509977652, 99.37390960531436690 ) ) ;
#107898 = CARTESIAN_POINT ( 'NONE',  ( -5.719274019375978568, 21.55341960407610458, 100.2072429386476955 ) ) ;
#107901 = CARTESIAN_POINT ( 'NONE',  ( 18.67979575497194134, -10.72451020669871369, 40.83442372801901854 ) ) ;
#107902 = ORIENTED_EDGE ( 'NONE', *, *, #21762, .F. ) ;
#107903 = CARTESIAN_POINT ( 'NONE',  ( -9.564922557960796823, -16.46253265017161027, 97.08224293864769550 ) ) ;
#107904 = ADVANCED_FACE ( 'NONE', ( #74716 ), #26235, .T. ) ;
#107905 = CARTESIAN_POINT ( 'NONE',  ( -18.22780087662123805, 5.499999999999981348, 91.01763182126894947 ) ) ;
#107906 = CARTESIAN_POINT ( 'NONE',  ( -15.72974639402197994, 15.80617190586746368, 90.62390960531436690 ) ) ;
#107907 = CARTESIAN_POINT ( 'NONE',  ( -19.05341960407611168, -5.049401038298163336, 41.45724293864769550 ) ) ;
#107908 = CARTESIAN_POINT ( 'NONE',  ( 16.55341960407618274, -4.379528057220086978, 31.04275706135234714 ) ) ;
#107909 = CARTESIAN_POINT ( 'NONE',  ( 11.40812507854754365, 35.11059874428196537, -3.724999997268813701 ) ) ;
#107910 = VECTOR ( 'NONE', #10463, 1000.000000000000000 ) ;
#107911 = CARTESIAN_POINT ( 'NONE',  ( -19.03943276465977164, 0.05219959533909376836, 26.24890960531435624 ) ) ;
#107912 = CARTESIAN_POINT ( 'NONE',  ( -15.80617190586768217, 15.72974639402176855, 98.12609039468570415 ) ) ;
#107914 = CARTESIAN_POINT ( 'NONE',  ( -10.72451020669870658, -18.67979575497194134, 49.58442372801901143 ) ) ;
#107913 = CARTESIAN_POINT ( 'NONE',  ( 19.05341960407611168, 5.049401038298154454, 73.95724293864768129 ) ) ;
#107915 = CARTESIAN_POINT ( 'NONE',  ( -15.80617190586768217, 15.72974639402176855, 28.12609039468568284 ) ) ;
#107916 = CARTESIAN_POINT ( 'NONE',  ( 22.44159573604009239, 16.30477369853692693, 146.5750000027312012 ) ) ;
#107917 = CARTESIAN_POINT ( 'NONE',  ( 0.05219959533909260263, 19.03943276465977164, 104.9989096053143669 ) ) ;
#107918 = CARTESIAN_POINT ( 'NONE',  ( 19.39056639909673763, 5.500000000000046185, 63.28948781074346641 ) ) ;
#107921 = CARTESIAN_POINT ( 'NONE',  ( -15.80617190586768217, 15.72974639402176855, 63.12609039468568994 ) ) ;
#107920 = CARTESIAN_POINT ( 'NONE',  ( -14.29746914071037622, -8.314922557961029526, 69.16775706135234714 ) ) ;
#107919 = CARTESIAN_POINT ( 'NONE',  ( 0.05219959533934541429, -16.53943276465976808, 35.00109039468568284 ) ) ;
#107922 = CARTESIAN_POINT ( 'NONE',  ( 10.72451020669871369, 18.67979575497193778, 77.08442372801901854 ) ) ;
#107923 = CARTESIAN_POINT ( 'NONE',  ( 4.065169771515699360, 6.132035242901161531, -62.28151743970308729 ) ) ;
#107924 = CARTESIAN_POINT ( 'NONE',  ( -16.51473224551082808, 9.474510206698731452, 103.3344237280190043 ) ) ;
#107925 = CARTESIAN_POINT ( 'NONE',  ( -19.05341960407611168, -5.049401038298163336, 71.45724293864766707 ) ) ;
#107926 = CARTESIAN_POINT ( 'NONE',  ( -0.05219959533909027116, -19.03943276465977164, 102.4989096053143669 ) ) ;
#107927 = CARTESIAN_POINT ( 'NONE',  ( -14.29746914071049879, 8.314922557960819915, 105.8322429386476955 ) ) ;
#107928 = CARTESIAN_POINT ( 'NONE',  ( -16.53943276465976808, 0.05219959533911058130, 101.2489096053143669 ) ) ;
#107929 = CARTESIAN_POINT ( 'NONE',  ( -15.72974639402197994, 15.80617190586746368, 25.62390960531435624 ) ) ;
#107930 = CARTESIAN_POINT ( 'NONE',  ( -12.06949235617739369, -12.14591786802326823, 94.37609039468568994 ) ) ;
#107932 = CARTESIAN_POINT ( 'NONE',  ( 9.564922557960805705, 16.46253265017160317, 54.58224293864769550 ) ) ;
#107931 = CARTESIAN_POINT ( 'NONE',  ( -4.379528057220328563, 16.55341960407611168, 70.20724293864769550 ) ) ;
#107933 = CARTESIAN_POINT ( 'NONE',  ( -21.55341960407619339, 5.719274019375674811, 73.54275706135234714 ) ) ;
#107934 = CARTESIAN_POINT ( 'NONE',  ( -28.79475375365676726, -9.355982642737950883, 144.3656553485623704 ) ) ;
#107935 = CARTESIAN_POINT ( 'NONE',  ( 0.05219959533936267826, -19.03943276465977164, 100.0010903946856757 ) ) ;
#107936 = CARTESIAN_POINT ( 'NONE',  ( 16.52544592524342804, -4.483927247898539470, 73.54057627198102409 ) ) ;
#107937 = CARTESIAN_POINT ( 'NONE',  ( -10.72451020669870658, -18.67979575497194134, 34.58442372801900433 ) ) ;
#107938 = CARTESIAN_POINT ( 'NONE',  ( 0.05219959533907565091, 21.53943276465977519, 59.99890960531436690 ) ) ;
#107939 = CARTESIAN_POINT ( 'NONE',  ( -17.40805194822030799, -6.112264579159321087, 104.1662872748939179 ) ) ;
#107940 = CARTESIAN_POINT ( 'NONE',  ( -5.429308488886486681E-15, 30.30510711980690175, 147.7500000054623683 ) ) ;
#107941 = CARTESIAN_POINT ( 'NONE',  ( -16.51473224551069308, -9.474510206698971260, 71.66557627198102409 ) ) ;
#107942 = CARTESIAN_POINT ( 'NONE',  ( 12.06949235617757843, -12.14591786802309237, 48.12390960531436690 ) ) ;
#107943 = VECTOR ( 'NONE', #54512, 1000.000000000000000 ) ;
#107944 = CARTESIAN_POINT ( 'NONE',  ( 12.06949235617757843, -12.14591786802309237, 28.12390960531435979 ) ) ;
#107945 = CARTESIAN_POINT ( 'NONE',  ( 8.224510206698742110, 14.34966873604972548, 92.08442372801901854 ) ) ;
#107946 = CARTESIAN_POINT ( 'NONE',  ( 19.03943276465977164, 0.05219959533936151252, 46.25109039468566863 ) ) ;
#107947 = CARTESIAN_POINT ( 'NONE',  ( 16.29526858892879204, 7.335722546919999587, 48.29670597800208043 ) ) ;
#107948 = CARTESIAN_POINT ( 'NONE',  ( 19.03943276465977164, -0.05219959533909143690, 103.7489096053143669 ) ) ;
#107949 = CARTESIAN_POINT ( 'NONE',  ( 12.06949235617757843, -12.14591786802309237, 73.12390960531436690 ) ) ;
#107950 = CARTESIAN_POINT ( 'NONE',  ( 19.05341960407617918, -5.049401038297876454, 46.04275706135233293 ) ) ;
#107952 = CARTESIAN_POINT ( 'NONE',  ( 5.719274019375991003, -21.55341960407610458, 37.70724293864769550 ) ) ;
#107951 = CARTESIAN_POINT ( 'NONE',  ( 5.049401038298161559, -19.05341960407611168, 32.70724293864768129 ) ) ;
#107954 = ORIENTED_EDGE ( 'NONE', *, *, #13961, .F. ) ;
#107953 = CARTESIAN_POINT ( 'NONE',  ( -15.72974639402197994, 15.80617190586746368, 70.62390960531436690 ) ) ;
#107955 = CARTESIAN_POINT ( 'NONE',  ( 16.53943276465976808, -0.05219959533910856209, 93.74890960531436690 ) ) ;
#107956 = CARTESIAN_POINT ( 'NONE',  ( 8.224510206698742110, 14.34966873604972548, 47.08442372801901854 ) ) ;
#107957 = CARTESIAN_POINT ( 'NONE',  ( -14.34966873604960291, -8.224510206698953496, 96.66557627198102409 ) ) ;
#107958 = CARTESIAN_POINT ( 'NONE',  ( 17.48853670773243252, -5.747243402303151782, 36.16671299749992130 ) ) ;
#107959 = CARTESIAN_POINT ( 'NONE',  ( -16.61371651742604882, 7.165104196376025136, 48.85415069992998127 ) ) ;
#107960 = CARTESIAN_POINT ( 'NONE',  ( 0.05219959533907565091, 21.53943276465977519, 34.99890960531435979 ) ) ;
#107961 = CARTESIAN_POINT ( 'NONE',  ( 0.000000000000000000, -165.0000000000000000, 12.00000000000000355 ) ) ;
#107962 = CARTESIAN_POINT ( 'NONE',  ( 0.9971028448357464047, 8.724879486844042020, -64.02424906291095397 ) ) ;
#107964 = CARTESIAN_POINT ( 'NONE',  ( 16.55341960407611168, 4.379528057220329451, 33.95724293864769550 ) ) ;
#107963 = CARTESIAN_POINT ( 'NONE',  ( -4.483927247898782831, 16.52544592524335698, 47.70942372801902565 ) ) ;
#107965 = CARTESIAN_POINT ( 'NONE',  ( 18.62759615963271287, -10.81492255796078972, 53.33224293864769550 ) ) ;
#107966 = CARTESIAN_POINT ( 'NONE',  ( -5.049401038297874678, -19.05341960407617918, 79.79275706135233293 ) ) ;
#107967 = CARTESIAN_POINT ( 'NONE',  ( 0.05219959533907565091, 21.53943276465977519, 59.99890960531436690 ) ) ;
#107968 = CARTESIAN_POINT ( 'NONE',  ( 18.62759615963255655, 10.81492255796105972, 76.66775706135234714 ) ) ;
#107969 = CARTESIAN_POINT ( 'NONE',  ( -12.21717160642880451, 11.11254985580163357, -61.43205129781978258 ) ) ;
#107970 = CARTESIAN_POINT ( 'NONE',  ( -14.34966873604972548, 8.224510206698743886, 43.33442372801901143 ) ) ;
#107972 = CARTESIAN_POINT ( 'NONE',  ( -9.564922557960796823, -16.46253265017161027, 97.08224293864769550 ) ) ;
#107971 = CARTESIAN_POINT ( 'NONE',  ( -5.153800228976328057, -19.02544592524343514, 32.29057627198102409 ) ) ;
#107973 = CARTESIAN_POINT ( 'NONE',  ( 19.02544592524343514, -5.153800228976328945, 33.54057627198102409 ) ) ;
#107974 = CARTESIAN_POINT ( 'NONE',  ( 4.379528057220339221, -16.55341960407611168, 97.70724293864772392 ) ) ;
#107975 = DIRECTION ( 'NONE',  ( 0.000000000000000000, 0.000000000000000000, 1.000000000000000000 ) ) ;
#107976 = FACE_BOUND ( 'NONE', #73425, .T. ) ;
#107977 = CARTESIAN_POINT ( 'NONE',  ( -14.29746914071037622, -8.314922557961029526, 74.16775706135231871 ) ) ;
#107978 = CARTESIAN_POINT ( 'NONE',  ( -18.67979575497178146, -10.72451020669898902, 86.66557627198102409 ) ) ;
#107979 = CARTESIAN_POINT ( 'NONE',  ( -5.153800228976328057, -19.02544592524343514, 62.29057627198100988 ) ) ;
#107980 = CARTESIAN_POINT ( 'NONE',  ( -21.52544592524334988, -5.823673210054445271, 28.95942372801902209 ) ) ;
#107981 = CARTESIAN_POINT ( 'NONE',  ( -19.03943276465977164, 0.05219959533909376836, 86.24890960531436690 ) ) ;
#107982 = CARTESIAN_POINT ( 'NONE',  ( -37.24154831888154860, -19.83237144080716519, -19.76300508100580444 ) ) ;
#107983 = EDGE_LOOP ( 'NONE', ( #94276, #106099, #99165, #154359 ) ) ;
#107984 = CARTESIAN_POINT ( 'NONE',  ( 5.823673210054125526, 21.52544592524343514, 114.7905762719810383 ) ) ;
#107987 = CARTESIAN_POINT ( 'NONE',  ( -19.05341960407617563, 5.049401038297882671, 73.54275706135233293 ) ) ;
#107986 = CARTESIAN_POINT ( 'NONE',  ( -5.049401038298153566, 19.05341960407611168, 105.2072429386476671 ) ) ;
#107985 = CARTESIAN_POINT ( 'NONE',  ( -19.05341960407611168, -5.049401038298163336, 31.45724293864769550 ) ) ;
#107988 = EDGE_CURVE ( 'NONE', #92733, #168893, #104571, .T. ) ;
#107989 = CARTESIAN_POINT ( 'NONE',  ( 9.564922557961047289, -16.46253265017146816, 25.41775706135234003 ) ) ;
#107990 = CARTESIAN_POINT ( 'NONE',  ( 0.05219959533907565091, 21.53943276465977519, 94.99890960531436690 ) ) ;
#107991 = CARTESIAN_POINT ( 'NONE',  ( 16.51473224551083163, -9.474510206698727899, 35.83442372801899722 ) ) ;
#107992 = CARTESIAN_POINT ( 'NONE',  ( -8.314922557961024197, 14.29746914071037800, 82.91775706135234714 ) ) ;
#107993 = CARTESIAN_POINT ( 'NONE',  ( 0.05219959533909260263, 19.03943276465977164, 109.9989096053143669 ) ) ;
#107994 = CARTESIAN_POINT ( 'NONE',  ( 0.05219959533909260263, 19.03943276465977164, 59.99890960531436690 ) ) ;
#107995 = CARTESIAN_POINT ( 'NONE',  ( 15.80617190586769283, -15.72974639402175789, 60.62609039468567573 ) ) ;
#107996 = CARTESIAN_POINT ( 'NONE',  ( -15.72974639402176322, -15.80617190586768395, 79.37609039468567573 ) ) ;
#107997 = CARTESIAN_POINT ( 'NONE',  ( -0.05219959533909027116, -19.03943276465977164, 77.49890960531435269 ) ) ;
#107998 = CARTESIAN_POINT ( 'NONE',  ( -10.81492255796105439, 18.62759615963255655, 42.91775706135235424 ) ) ;
#107999 = CARTESIAN_POINT ( 'NONE',  ( -19.02544592524334988, -5.153800228976617603, 83.95942372801901854 ) ) ;
#108000 = ADVANCED_FACE ( 'NONE', ( #43377 ), #107019, .T. ) ;
#108001 = CARTESIAN_POINT ( 'NONE',  ( 19.05341960407611168, 5.049401038298154454, 58.95724293864768129 ) ) ;
#108002 = CARTESIAN_POINT ( 'NONE',  ( -0.05219959533909027116, -19.03943276465977164, 92.49890960531436690 ) ) ;
#108003 = CARTESIAN_POINT ( 'NONE',  ( 19.05341960407611168, 5.049401038298154454, 63.95724293864769550 ) ) ;
#108004 = CARTESIAN_POINT ( 'NONE',  ( -5.153800228976328057, -19.02544592524343514, 77.29057627198100988 ) ) ;
#108005 = CARTESIAN_POINT ( 'NONE',  ( 9.474510206698971260, -16.51473224551069308, 57.91557627198103120 ) ) ;
#108006 = AXIS2_PLACEMENT_3D ( 'NONE', #139580, #17252, #127396 ) ;
#108007 = CARTESIAN_POINT ( 'NONE',  ( 18.62759615963271287, -10.81492255796078972, 98.33224293864769550 ) ) ;
#108008 = CARTESIAN_POINT ( 'NONE',  ( -16.52544592524335698, -4.483927247898792601, 83.95942372801900433 ) ) ;
#108009 = CARTESIAN_POINT ( 'NONE',  ( -21.94905633995364269, 7.481063542984161430, 170.0146117665088923 ) ) ;
#108010 = CARTESIAN_POINT ( 'NONE',  ( 16.46253265017146816, 9.564922557961045513, 41.66775706135234003 ) ) ;
#108011 = CARTESIAN_POINT ( 'NONE',  ( 0.05219959533909260263, 19.03943276465977164, 69.99890960531435269 ) ) ;
#108012 = CARTESIAN_POINT ( 'NONE',  ( -16.52544592524342804, 4.483927247898546575, 56.04057627198102409 ) ) ;
#108013 = CARTESIAN_POINT ( 'NONE',  ( 16.55341960407611168, 4.379528057220329451, 98.95724293864770971 ) ) ;
#108014 = CARTESIAN_POINT ( 'NONE',  ( -5.153800228976328057, -19.02544592524343514, 112.2905762719810099 ) ) ;
#108015 = CARTESIAN_POINT ( 'NONE',  ( -13.97604488694527625, -13.89961937509977652, 96.87390960531433848 ) ) ;
#108016 = CARTESIAN_POINT ( 'NONE',  ( -16.46253265017160317, 9.564922557960807481, 110.8322429386476955 ) ) ;
#108017 = CARTESIAN_POINT ( 'NONE',  ( -5.153800228976607833, 19.02544592524334988, 22.70942372801899012 ) ) ;
#108018 = CARTESIAN_POINT ( 'NONE',  ( -16.55341960407617563, 4.379528057220093196, 93.54275706135234714 ) ) ;
#108019 = CARTESIAN_POINT ( 'NONE',  ( -19.05341960407611168, -5.049401038298163336, 71.45724293864766707 ) ) ;
#108020 = CARTESIAN_POINT ( 'NONE',  ( -21.52544592524334988, -5.823673210054445271, 33.95942372801901143 ) ) ;
#108021 = CARTESIAN_POINT ( 'NONE',  ( -5.719274019375978568, 21.55341960407610458, 30.20724293864769550 ) ) ;
#108022 = CARTESIAN_POINT ( 'NONE',  ( -18.62759615963255300, -10.81492255796106328, 24.16775706135235424 ) ) ;
#108023 = CARTESIAN_POINT ( 'NONE',  ( -14.29746914071049879, 8.314922557960819915, 65.83224293864769550 ) ) ;
#108024 = CARTESIAN_POINT ( 'NONE',  ( -16.46253265017160317, 9.564922557960807481, 60.83224293864769550 ) ) ;
#108025 = CARTESIAN_POINT ( 'NONE',  ( 4.379528057220339221, -16.55341960407611168, 77.70724293864770971 ) ) ;
#108026 = CARTESIAN_POINT ( 'NONE',  ( -19.03943276465977164, -0.05219959533935918106, 48.75109039468566863 ) ) ;
#108027 = VECTOR ( 'NONE', #70586, 1000.000000000000000 ) ;
#108028 = CARTESIAN_POINT ( 'NONE',  ( 13.89961937509977652, -13.97604488694527269, 23.12390960531436335 ) ) ;
#108029 = CARTESIAN_POINT ( 'NONE',  ( -19.05341960407611168, -5.049401038298163336, 81.45724293864769550 ) ) ;
#108030 = CARTESIAN_POINT ( 'NONE',  ( 5.153800228976335163, 19.02544592524342804, 79.79057627198102409 ) ) ;
#108031 = CARTESIAN_POINT ( 'NONE',  ( -8.571926809382601320, -26.38167802310801591, 143.2750000027311899 ) ) ;
#108032 = CARTESIAN_POINT ( 'NONE',  ( -16.53943276465976808, 0.05219959533911058130, 106.2489096053143811 ) ) ;
#108033 = ORIENTED_EDGE ( 'NONE', *, *, #60120, .T. ) ;
#108034 = CARTESIAN_POINT ( 'NONE',  ( 8.224510206698742110, 14.34966873604972548, 102.0844237280190185 ) ) ;
#108035 = CARTESIAN_POINT ( 'NONE',  ( 8.314922557961029526, -14.29746914071037800, 25.41775706135235779 ) ) ;
#108036 = CARTESIAN_POINT ( 'NONE',  ( -18.67979575497193778, 10.72451020669871902, 98.33442372801901854 ) ) ;
#108037 = CARTESIAN_POINT ( 'NONE',  ( 0.05219959533909260263, 19.03943276465977164, 99.99890960531436690 ) ) ;
#108038 = CARTESIAN_POINT ( 'NONE',  ( 10.81492255796106328, -18.62759615963255655, 25.41775706135235779 ) ) ;
#108039 = CARTESIAN_POINT ( 'NONE',  ( -13.97604488694527625, -13.89961937509977652, 26.87390960531434558 ) ) ;
#108040 = CARTESIAN_POINT ( 'NONE',  ( -0.05219959533934338120, 16.53943276465976808, 32.50109039468568284 ) ) ;
#108041 = AXIS2_PLACEMENT_3D ( 'NONE', #36597, #131620, #68944 ) ;
#108042 = CARTESIAN_POINT ( 'NONE',  ( 13.89961937509957401, 13.97604488694547697, 96.87609039468566152 ) ) ;
#108043 = CARTESIAN_POINT ( 'NONE',  ( -18.62759615963270932, 10.81492255796079327, 90.83224293864769550 ) ) ;
#108044 = CARTESIAN_POINT ( 'NONE',  ( -13.97604488694547697, 13.89961937509957934, 63.12609039468566152 ) ) ;
#108045 = CARTESIAN_POINT ( 'NONE',  ( -17.49999999999999645, -5.499999999999992895, 64.20309617465829888 ) ) ;
#108046 = CARTESIAN_POINT ( 'NONE',  ( 21.55341960407619695, -5.719274019375665929, 21.04275706135234714 ) ) ;
#108047 = CARTESIAN_POINT ( 'NONE',  ( 11.74149087413294268, 36.13659316521247433, -4.347842220587804007 ) ) ;
#108048 = CARTESIAN_POINT ( 'NONE',  ( -16.46253265017160317, 9.564922557960807481, 95.83224293864769550 ) ) ;
#108049 = CARTESIAN_POINT ( 'NONE',  ( 14.29746914071037800, 8.314922557961029526, 46.66775706135234714 ) ) ;
#108050 = DIRECTION ( 'NONE',  ( -1.000000000000000000, 0.000000000000000000, 0.000000000000000000 ) ) ;
#108051 = CARTESIAN_POINT ( 'NONE',  ( 19.03943276465977164, 0.05219959533936151252, 56.25109039468566863 ) ) ;
#108053 = CARTESIAN_POINT ( 'NONE',  ( 4.483927247898545687, 16.52544592524342804, 79.79057627198102409 ) ) ;
#108052 = CARTESIAN_POINT ( 'NONE',  ( -18.62759615963270932, 10.81492255796079327, 110.8322429386476955 ) ) ;
#108054 = CARTESIAN_POINT ( 'NONE',  ( -19.05341960407611168, -5.049401038298163336, 86.45724293864769550 ) ) ;
#108055 = PRESENTATION_LAYER_ASSIGNMENT (  '', '', ( #79052 ) ) ;
#108057 = CARTESIAN_POINT ( 'NONE',  ( 19.02544592524334988, 5.153800228976608722, 61.45942372801900433 ) ) ;
#108056 = CARTESIAN_POINT ( 'NONE',  ( -16.53943276465976808, -0.05219959533934237506, 48.75109039468568284 ) ) ;
#108058 = CARTESIAN_POINT ( 'NONE',  ( -5.823673210054431948, 21.52544592524334988, 62.70942372801902565 ) ) ;
#108059 = CARTESIAN_POINT ( 'NONE',  ( 4.379528057220092307, 16.55341960407617563, 27.29275706135234358 ) ) ;
#108060 = CARTESIAN_POINT ( 'NONE',  ( 19.05341960407611168, 5.049401038298154454, 68.95724293864769550 ) ) ;
#108061 = CARTESIAN_POINT ( 'NONE',  ( -16.46253265017146816, -9.564922557961047289, 99.16775706135233293 ) ) ;
#108062 = CARTESIAN_POINT ( 'NONE',  ( -16.55341960407617563, 4.379528057220093196, 58.54275706135235424 ) ) ;
#108063 = CARTESIAN_POINT ( 'NONE',  ( -10.81492255796105439, 18.62759615963255655, 97.91775706135236135 ) ) ;
#108064 = CARTESIAN_POINT ( 'NONE',  ( 13.89961937509957401, 13.97604488694547697, 76.87609039468566152 ) ) ;
#108065 = CARTESIAN_POINT ( 'NONE',  ( -5.049401038298153566, 19.05341960407611168, 55.20724293864769550 ) ) ;
#108066 = CARTESIAN_POINT ( 'NONE',  ( -10.81492255796078084, -18.62759615963271287, 67.08224293864770971 ) ) ;
#108068 = CARTESIAN_POINT ( 'NONE',  ( 19.05341960407617918, -5.049401038297876454, 76.04275706135230450 ) ) ;
#108067 = CARTESIAN_POINT ( 'NONE',  ( 12.14591786802309770, 12.06949235617756955, 79.37390960531436690 ) ) ;
#108069 = CARTESIAN_POINT ( 'NONE',  ( 17.40861289038999971, -6.110651285853406556, 61.12767529172568715 ) ) ;
#108070 = CARTESIAN_POINT ( 'NONE',  ( 9.564922557961047289, -16.46253265017146816, 40.41775706135234003 ) ) ;
#108071 = CARTESIAN_POINT ( 'NONE',  ( 4.379528057220092307, 16.55341960407617563, 107.2927570613523471 ) ) ;
#108072 = CARTESIAN_POINT ( 'NONE',  ( 8.224510206698953496, -14.34966873604960469, 72.91557627198103830 ) ) ;
#108074 = CARTESIAN_POINT ( 'NONE',  ( -22.44159573604010305, 16.30477369853692338, 144.6750000027311671 ) ) ;
#108073 = CARTESIAN_POINT ( 'NONE',  ( -15.72974639402176322, -15.80617190586768395, 99.37609039468568994 ) ) ;
#108075 = CARTESIAN_POINT ( 'NONE',  ( 5.823673210054125526, 21.52544592524343514, 104.7905762719810241 ) ) ;
#108076 = CARTESIAN_POINT ( 'NONE',  ( 9.564922557960805705, 16.46253265017160317, 59.58224293864769550 ) ) ;
#108077 = CARTESIAN_POINT ( 'NONE',  ( 10.81492255796106328, -18.62759615963255655, 80.41775706135234714 ) ) ;
#108078 = CARTESIAN_POINT ( 'NONE',  ( 13.97604488694527802, 13.89961937509977652, 64.37390960531436690 ) ) ;
#108079 = ORIENTED_EDGE ( 'NONE', *, *, #73257, .F. ) ;
#108080 = CARTESIAN_POINT ( 'NONE',  ( 13.89961937509977652, -13.97604488694527269, 28.12390960531435624 ) ) ;
#108081 = CARTESIAN_POINT ( 'NONE',  ( 19.05341960407611168, 5.049401038298154454, 113.9572429386477097 ) ) ;
#108082 = CARTESIAN_POINT ( 'NONE',  ( -14.34966873604960291, -8.224510206698953496, 66.66557627198102409 ) ) ;
#108083 = CARTESIAN_POINT ( 'NONE',  ( -16.51473224551069308, -9.474510206698971260, 31.66557627198102054 ) ) ;
#108084 = CARTESIAN_POINT ( 'NONE',  ( 8.314922557960818139, 14.29746914071049879, 89.58224293864768129 ) ) ;
#108085 = AXIS2_PLACEMENT_3D ( 'NONE', #20611, #50962, #18643 ) ;
#108086 = CARTESIAN_POINT ( 'NONE',  ( -5.823673210054116645, -21.52544592524344225, 92.29057627198103830 ) ) ;
#108087 = CARTESIAN_POINT ( 'NONE',  ( -21.55341960407619339, 5.719274019375674811, 43.54275706135235424 ) ) ;
#108088 = CARTESIAN_POINT ( 'NONE',  ( -25.63014143074632400, -6.600872056147844447, 163.2069976173303871 ) ) ;
#108089 = CARTESIAN_POINT ( 'NONE',  ( 4.379528057220092307, 16.55341960407617563, 52.29275706135236135 ) ) ;
#108090 = CARTESIAN_POINT ( 'NONE',  ( -21.53943276465977519, 0.05219959533907696930, 96.24890960531435269 ) ) ;
#108091 = CARTESIAN_POINT ( 'NONE',  ( -13.97604488694547697, 13.89961937509957934, 23.12609039468565442 ) ) ;
#108092 = CARTESIAN_POINT ( 'NONE',  ( 5.049401038298161559, -19.05341960407611168, 107.7072429386476955 ) ) ;
#108093 = CARTESIAN_POINT ( 'NONE',  ( 10.72451020669871369, 18.67979575497193778, 42.08442372801901854 ) ) ;
#108094 = CARTESIAN_POINT ( 'NONE',  ( 18.62759615963271287, -10.81492255796078972, 48.33224293864770260 ) ) ;
#108095 = CARTESIAN_POINT ( 'NONE',  ( -14.29746914071049879, 8.314922557960819915, 30.83224293864770260 ) ) ;
#108097 = CARTESIAN_POINT ( 'NONE',  ( -0.05219959533937732626, 21.53943276465977519, 102.5010903946856899 ) ) ;
#108096 = CARTESIAN_POINT ( 'NONE',  ( -5.719274019375665041, -21.55341960407619695, 64.79275706135234714 ) ) ;
#108098 = CARTESIAN_POINT ( 'NONE',  ( -5.049401038297874678, -19.05341960407617918, 29.79275706135232227 ) ) ;
#108099 = CARTESIAN_POINT ( 'NONE',  ( -8.314922557961024197, 14.29746914071037800, 82.91775706135234714 ) ) ;
#108101 = EDGE_CURVE ( 'NONE', #67444, #38560, #72386, .T. ) ;
#108100 = CARTESIAN_POINT ( 'NONE',  ( 21.53943276465977519, 0.05219959533937863772, 56.25109039468568284 ) ) ;
#108102 = CARTESIAN_POINT ( 'NONE',  ( -16.51473224551069308, -9.474510206698971260, 41.66557627198103120 ) ) ;
#108103 = CARTESIAN_POINT ( 'NONE',  ( 19.05341960407617918, -5.049401038297876454, 21.04275706135232582 ) ) ;
#108104 = CARTESIAN_POINT ( 'NONE',  ( 18.67979575497178502, 10.72451020669898547, 29.16557627198103120 ) ) ;
#108105 = CARTESIAN_POINT ( 'NONE',  ( 15.80617190586746368, 15.72974639402197994, 114.3739096053143527 ) ) ;
#108106 = CARTESIAN_POINT ( 'NONE',  ( 5.719274019375991003, -21.55341960407610458, 77.70724293864770971 ) ) ;
#108107 = CARTESIAN_POINT ( 'NONE',  ( -14.29746914071037622, -8.314922557961029526, 39.16775706135235424 ) ) ;
#108109 = CARTESIAN_POINT ( 'NONE',  ( 15.80617190586746368, 15.72974639402197994, 74.37390960531436690 ) ) ;
#108108 = DIRECTION ( 'NONE',  ( 0.4999999999999932276, -0.5000000000000055511, 0.7071067811865484609 ) ) ;
#108111 = CARTESIAN_POINT ( 'NONE',  ( 8.314922557960818139, 14.29746914071049879, 64.58224293864769550 ) ) ;
#108110 = CARTESIAN_POINT ( 'NONE',  ( 16.53943276465976808, 0.05219959533934440121, 71.25109039468568994 ) ) ;
#108112 = CARTESIAN_POINT ( 'NONE',  ( 0.6176563088794523315, 29.02844413588608319, -49.51499673148455827 ) ) ;
#108113 = CARTESIAN_POINT ( 'NONE',  ( -19.05341960407617563, 5.049401038297882671, 103.5427570613523329 ) ) ;
#108114 = CARTESIAN_POINT ( 'NONE',  ( -0.05219959533909027116, -19.03943276465977164, 112.4989096053143669 ) ) ;
#108115 = CARTESIAN_POINT ( 'NONE',  ( 18.22780087662122384, 5.500000000000018652, 93.98459894673892734 ) ) ;
#108116 = EDGE_CURVE ( 'NONE', #143210, #190550, #149562, .T. ) ;
#108117 = CARTESIAN_POINT ( 'NONE',  ( -8.314922557961024197, 14.29746914071037800, 42.91775706135235424 ) ) ;
#108118 = CARTESIAN_POINT ( 'NONE',  ( -5.719274019375978568, 21.55341960407610458, 110.2072429386477239 ) ) ;
#108119 = CARTESIAN_POINT ( 'NONE',  ( -21.53943276465977519, 0.05219959533907696930, 26.24890960531435624 ) ) ;
#108120 = CARTESIAN_POINT ( 'NONE',  ( -14.34966873604972548, 8.224510206698743886, 58.33442372801901143 ) ) ;
#108121 = CARTESIAN_POINT ( 'NONE',  ( 9.474510206698971260, -16.51473224551069308, 67.91557627198102409 ) ) ;
#108123 = CARTESIAN_POINT ( 'NONE',  ( 4.379528057220092307, 16.55341960407617563, 22.29275706135235069 ) ) ;
#108122 = CARTESIAN_POINT ( 'NONE',  ( -0.05219959533937732626, 21.53943276465977519, 47.50109039468568994 ) ) ;
#108124 = CARTESIAN_POINT ( 'NONE',  ( 10.81492255796078972, 18.62759615963270932, 24.58224293864768839 ) ) ;
#108125 = ORIENTED_EDGE ( 'NONE', *, *, #53169, .T. ) ;
#108126 = CARTESIAN_POINT ( 'NONE',  ( 16.46253265017146816, 9.564922557961045513, 21.66775706135233648 ) ) ;
#108127 = CARTESIAN_POINT ( 'NONE',  ( 14.29746914071037800, 8.314922557961029526, 36.66775706135234714 ) ) ;
#108128 = CARTESIAN_POINT ( 'NONE',  ( -5.153800228976328057, -19.02544592524343514, 107.2905762719810383 ) ) ;
#108129 = CARTESIAN_POINT ( 'NONE',  ( -0.05219959533907301413, -21.53943276465977519, 97.49890960531436690 ) ) ;
#108130 = CARTESIAN_POINT ( 'NONE',  ( 19.03943276465977164, -0.05219959533909143690, 68.74890960531436690 ) ) ;
#108131 = CARTESIAN_POINT ( 'NONE',  ( 2.021687836487040535, 2.655529440325959183E-32, -2.168404344971008868E-16 ) ) ;
#108132 = CARTESIAN_POINT ( 'NONE',  ( 14.29746914071049879, -8.314922557960816363, 88.33224293864769550 ) ) ;
#108133 = CARTESIAN_POINT ( 'NONE',  ( -21.52544592524343514, 5.823673210054127303, 41.04057627198103120 ) ) ;
#108134 = CARTESIAN_POINT ( 'NONE',  ( 5.049401038298161559, -19.05341960407611168, 22.70724293864769194 ) ) ;
#108135 = CARTESIAN_POINT ( 'NONE',  ( 12.14591786802327356, -12.06949235617739191, 60.62609039468567573 ) ) ;
#108136 = CARTESIAN_POINT ( 'NONE',  ( -5.719274019375978568, 21.55341960407610458, 105.2072429386477097 ) ) ;
#108137 = CARTESIAN_POINT ( 'NONE',  ( 19.03943276465977164, 0.05219959533936151252, 66.25109039468567573 ) ) ;
#108138 = CARTESIAN_POINT ( 'NONE',  ( -15.80617190586745835, -15.72974639402198527, 31.87390960531435979 ) ) ;
#108139 = CARTESIAN_POINT ( 'NONE',  ( -9.474510206698964154, 16.51473224551069663, 25.41557627198103120 ) ) ;
#108140 = CARTESIAN_POINT ( 'NONE',  ( -18.62759615963270932, 10.81492255796079327, 70.83224293864770971 ) ) ;
#108141 = CARTESIAN_POINT ( 'NONE',  ( 13.97604488694527802, 13.89961937509977652, 94.37390960531436690 ) ) ;
#108142 = CARTESIAN_POINT ( 'NONE',  ( 10.72451020669871369, 18.67979575497193778, 97.08442372801904696 ) ) ;
#108143 = CARTESIAN_POINT ( 'NONE',  ( -13.97604488694527625, -13.89961937509977652, 56.87390960531434558 ) ) ;
#108144 = CARTESIAN_POINT ( 'NONE',  ( 8.314922557961029526, -14.29746914071037800, 35.41775706135234003 ) ) ;
#108145 = CARTESIAN_POINT ( 'NONE',  ( -9.564922557960796823, -16.46253265017161027, 62.08224293864769550 ) ) ;
#108146 = CARTESIAN_POINT ( 'NONE',  ( -21.53943276465977519, -0.05219959533937600094, 83.75109039468568994 ) ) ;
#108147 = ORIENTED_EDGE ( 'NONE', *, *, #139759, .F. ) ;
#108148 = CARTESIAN_POINT ( 'NONE',  ( -16.51473224551082808, 9.474510206698731452, 33.33442372801899722 ) ) ;
#108149 = ADVANCED_FACE ( 'NONE', ( #135405 ), #111103, .F. ) ;
#108150 = VECTOR ( 'NONE', #80894, 1000.000000000000000 ) ;
#108151 = CARTESIAN_POINT ( 'NONE',  ( -0.05219959533936034679, 19.03943276465977164, 37.50109039468567573 ) ) ;
#108152 = CARTESIAN_POINT ( 'NONE',  ( -10.81492255796105439, 18.62759615963255655, 32.91775706135234714 ) ) ;
#108153 = CARTESIAN_POINT ( 'NONE',  ( -6.139906835403841967, 0.3968392070110091097, -62.49911542708240120 ) ) ;
#108154 = CARTESIAN_POINT ( 'NONE',  ( 16.46253265017146816, 9.564922557961045513, 26.66775706135234003 ) ) ;
#108155 = CARTESIAN_POINT ( 'NONE',  ( -9.564922557960796823, -16.46253265017161027, 92.08224293864769550 ) ) ;
#108156 = CARTESIAN_POINT ( 'NONE',  ( 0.05219959533909260263, 19.03943276465977164, 64.99890960531436690 ) ) ;
#108157 = CARTESIAN_POINT ( 'NONE',  ( 16.52544592524335698, 4.483927247898782831, 111.4594237280190328 ) ) ;
#108159 = CARTESIAN_POINT ( 'NONE',  ( 18.62759615963255655, 10.81492255796105972, 86.66775706135234714 ) ) ;
#108158 = CARTESIAN_POINT ( 'NONE',  ( -18.67979575497178146, -10.72451020669898902, 21.66557627198102409 ) ) ;
#108160 = CARTESIAN_POINT ( 'NONE',  ( -36.91746825000000598, 2.428612866367529932E-14, -0.6249999972688132788 ) ) ;
#108161 = CARTESIAN_POINT ( 'NONE',  ( 0.000000000000000000, 0.000000000000000000, -64.53213882399991519 ) ) ;
#108162 = CARTESIAN_POINT ( 'NONE',  ( -15.80617190586768217, 15.72974639402176855, 103.1260903946856757 ) ) ;
#108163 = CARTESIAN_POINT ( 'NONE',  ( 24.24152472029838634, -0.4285070731208356909, -56.81472536503797954 ) ) ;
#108164 = CARTESIAN_POINT ( 'NONE',  ( 14.29746914071049879, -8.314922557960816363, 113.3322429386476955 ) ) ;
#108165 = CARTESIAN_POINT ( 'NONE',  ( 9.564922557960805705, 16.46253265017160317, 114.5822429386476955 ) ) ;
#108166 = CARTESIAN_POINT ( 'NONE',  ( 34.51819068884489639, 0.7175229865516599137, 89.53493623002428592 ) ) ;
#108167 = VECTOR ( 'NONE', #5880, 1000.000000000000000 ) ;
#108168 = CARTESIAN_POINT ( 'NONE',  ( -4.379528057220086978, -16.55341960407618274, 49.79275706135234714 ) ) ;
#108169 = CARTESIAN_POINT ( 'NONE',  ( -10.81492255796078084, -18.62759615963271287, 67.08224293864770971 ) ) ;
#108170 = CARTESIAN_POINT ( 'NONE',  ( -14.34966873604960291, -8.224510206698953496, 36.66557627198103120 ) ) ;
#108172 = CARTESIAN_POINT ( 'NONE',  ( -19.02544592524342804, 5.153800228976336051, 91.04057627198100988 ) ) ;
#108171 = CARTESIAN_POINT ( 'NONE',  ( 16.55341960407611168, 4.379528057220329451, 103.9572429386476813 ) ) ;
#108173 = CARTESIAN_POINT ( 'NONE',  ( -5.049401038297874678, -19.05341960407617918, 24.79275706135233648 ) ) ;
#108174 = CARTESIAN_POINT ( 'NONE',  ( -4.379528057220328563, 16.55341960407611168, 115.2072429386476955 ) ) ;
#108175 = CARTESIAN_POINT ( 'NONE',  ( -5.719274019375665041, -21.55341960407619695, 74.79275706135234714 ) ) ;
#108176 = CARTESIAN_POINT ( 'NONE',  ( -19.05341960407611168, -5.049401038298163336, 111.4572429386476671 ) ) ;
#108177 = CARTESIAN_POINT ( 'NONE',  ( 16.55341960407618274, -4.379528057220086978, 101.0427570613523756 ) ) ;
#108178 = CARTESIAN_POINT ( 'NONE',  ( -13.97604488694547697, 13.89961937509957934, 68.12609039468563310 ) ) ;
#108179 = CARTESIAN_POINT ( 'NONE',  ( 22.81625015709509441, 31.40387420917330275, -5.824999997268813345 ) ) ;
#108180 = CARTESIAN_POINT ( 'NONE',  ( -21.53943276465977519, 0.05219959533907696930, 21.24890960531436690 ) ) ;
#108181 = CARTESIAN_POINT ( 'NONE',  ( -8.314922557960811034, -14.29746914071050412, 92.08224293864769550 ) ) ;
#108182 =( GEOMETRIC_REPRESENTATION_CONTEXT ( 3 ) GLOBAL_UNCERTAINTY_ASSIGNED_CONTEXT ( ( #21632 ) ) GLOBAL_UNIT_ASSIGNED_CONTEXT ( ( #176802, #130253, #112123 ) ) REPRESENTATION_CONTEXT ( 'NONE', 'WORKASPACE' ) );
#108183 = CARTESIAN_POINT ( 'NONE',  ( -19.05341960407617563, 5.049401038297882671, 63.54275706135234003 ) ) ;
#108184 = CARTESIAN_POINT ( 'NONE',  ( -19.02544592524342804, 5.153800228976336051, 71.04057627198099567 ) ) ;
#108185 = CARTESIAN_POINT ( 'NONE',  ( -14.34966873604960291, -8.224510206698953496, 81.66557627198103830 ) ) ;
#108186 = CARTESIAN_POINT ( 'NONE',  ( 5.049401038297881783, 19.05341960407617563, 92.29275706135234714 ) ) ;
#108187 = CARTESIAN_POINT ( 'NONE',  ( 0.05219959533907565091, 21.53943276465977519, 49.99890960531437401 ) ) ;
#108188 = ORIENTED_EDGE ( 'NONE', *, *, #67646, .F. ) ;
#108189 = CARTESIAN_POINT ( 'NONE',  ( 4.379528057220339221, -16.55341960407611168, 112.7072429386476955 ) ) ;
#108190 = CARTESIAN_POINT ( 'NONE',  ( -3.181980515339590365, -34.99999999999999289, 1.110912703473986074 ) ) ;
#108192 = CARTESIAN_POINT ( 'NONE',  ( 18.67979575497178502, 10.72451020669898547, 74.16557627198102409 ) ) ;
#108191 = CARTESIAN_POINT ( 'NONE',  ( -13.89961937509977652, 13.97604488694528158, 75.62390960531438111 ) ) ;
#108194 = CARTESIAN_POINT ( 'NONE',  ( 13.97604488694527802, 13.89961937509977652, 69.37390960531436690 ) ) ;
#108193 = CARTESIAN_POINT ( 'NONE',  ( -8.224510206698735004, -14.34966873604973081, 89.58442372801901854 ) ) ;
#108195 = CARTESIAN_POINT ( 'NONE',  ( 0.05219959533936267826, -19.03943276465977164, 65.00109039468567573 ) ) ;
#108196 = CARTESIAN_POINT ( 'NONE',  ( -10.81492255796105439, 18.62759615963255655, 77.91775706135231871 ) ) ;
#108197 = CARTESIAN_POINT ( 'NONE',  ( -10.81492255796078084, -18.62759615963271287, 67.08224293864770971 ) ) ;
#108198 = CARTESIAN_POINT ( 'NONE',  ( 10.81492255796078972, 18.62759615963270932, 29.58224293864769905 ) ) ;
#108199 = TOROIDAL_SURFACE ( 'NONE', #98512, 206.0437394197456342, 8.000000000000000000 ) ;
#108200 = CARTESIAN_POINT ( 'NONE',  ( -13.97604488694527625, -13.89961937509977652, 36.87390960531436690 ) ) ;
#108201 = CARTESIAN_POINT ( 'NONE',  ( -12.14591786802326823, 12.06949235617739902, 103.1260903946856757 ) ) ;
#108202 = CARTESIAN_POINT ( 'NONE',  ( -5.049401038298153566, 19.05341960407611168, 55.20724293864769550 ) ) ;
#108203 = CARTESIAN_POINT ( 'NONE',  ( -0.05219959533934338120, 16.53943276465976808, 22.50109039468567573 ) ) ;
#108204 = CARTESIAN_POINT ( 'NONE',  ( 16.18388926212240975, 7.379444403734405356, 52.93953151366151388 ) ) ;
#108205 = CARTESIAN_POINT ( 'NONE',  ( 15.80617190586769283, -15.72974639402175789, 105.6260903946856899 ) ) ;
#108206 = AXIS2_PLACEMENT_3D ( 'NONE', #47748, #80057, #185258 ) ;
#108207 = CARTESIAN_POINT ( 'NONE',  ( 4.483927247898545687, 16.52544592524342804, 64.79057627198103830 ) ) ;
#108208 = PRODUCT_DEFINITION_FORMATION_WITH_SPECIFIED_SOURCE ( 'ANY', '', #113205, .NOT_KNOWN. ) ;
#108209 = CARTESIAN_POINT ( 'NONE',  ( -0.05219959533907301413, -21.53943276465977519, 112.4989096053143669 ) ) ;
#108210 = CARTESIAN_POINT ( 'NONE',  ( -10.72451020669898014, 18.67979575497178502, 105.4155762719810383 ) ) ;
#108211 = CARTESIAN_POINT ( 'NONE',  ( -5.283393095647520354, 3.873560230149188488, -64.45999282322711110 ) ) ;
#108212 = CARTESIAN_POINT ( 'NONE',  ( 5.719274019375991003, -21.55341960407610458, 42.70724293864770260 ) ) ;
#108213 = CARTESIAN_POINT ( 'NONE',  ( 12.14591786802327356, -12.06949235617739191, 80.62609039468567573 ) ) ;
#108214 = CARTESIAN_POINT ( 'NONE',  ( -16.55341960407611168, -4.379528057220339221, 86.45724293864770971 ) ) ;
#108215 = CARTESIAN_POINT ( 'NONE',  ( -5.049401038298153566, 19.05341960407611168, 55.20724293864769550 ) ) ;
#108216 = CARTESIAN_POINT ( 'NONE',  ( -24.26175155739904099, -32.05389003868044284, -17.42962289376371743 ) ) ;
#108217 = CARTESIAN_POINT ( 'NONE',  ( -8.224510206698735004, -14.34966873604973081, 104.5844237280190185 ) ) ;
#108218 = CARTESIAN_POINT ( 'NONE',  ( -21.52544592524334988, -5.823673210054445271, 28.95942372801902209 ) ) ;
#108219 = CARTESIAN_POINT ( 'NONE',  ( 13.97604488694527802, 13.89961937509977652, 94.37390960531436690 ) ) ;
#108220 = CARTESIAN_POINT ( 'NONE',  ( -21.55341960407619339, 5.719274019375674811, 63.54275706135234003 ) ) ;
#108221 = CYLINDRICAL_SURFACE ( 'NONE', #143393, 1.999999999999999112 ) ;
#108222 = CARTESIAN_POINT ( 'NONE',  ( -19.05341960407611168, -5.049401038298163336, 26.45724293864769550 ) ) ;
#108223 = EDGE_LOOP ( 'NONE', ( #115914, #137718, #99539, #41808 ) ) ;
#108224 = CARTESIAN_POINT ( 'NONE',  ( 0.05219959533937995610, -21.53943276465977519, 65.00109039468568994 ) ) ;
#108225 = CARTESIAN_POINT ( 'NONE',  ( -16.51473224551069308, -9.474510206698971260, 46.66557627198102409 ) ) ;
#108226 = CARTESIAN_POINT ( 'NONE',  ( 19.05341960407611168, 5.049401038298154454, 83.95724293864766707 ) ) ;
#108227 = CARTESIAN_POINT ( 'NONE',  ( -16.51473224551082808, 9.474510206698731452, 68.33442372801900433 ) ) ;
#108228 = CARTESIAN_POINT ( 'NONE',  ( 15.72974639402176855, 15.80617190586768217, 46.87609039468568994 ) ) ;
#108229 = CARTESIAN_POINT ( 'NONE',  ( -13.89961937509957401, -13.97604488694547875, 99.37609039468567573 ) ) ;
#108230 = CARTESIAN_POINT ( 'NONE',  ( 5.049401038297881783, 19.05341960407617563, 67.29275706135234714 ) ) ;
#108231 = CARTESIAN_POINT ( 'NONE',  ( -9.474510206698964154, 16.51473224551069663, 35.41557627198102409 ) ) ;
#108232 = VECTOR ( 'NONE', #81538, 1000.000000000000000 ) ;
#108233 = CARTESIAN_POINT ( 'NONE',  ( 12.14591786802327356, -12.06949235617739191, 110.6260903946857042 ) ) ;
#108234 = CARTESIAN_POINT ( 'NONE',  ( 19.03943276465977164, 0.05219959533936151252, 71.25109039468566152 ) ) ;
#108235 = CARTESIAN_POINT ( 'NONE',  ( 12.14591786802309770, 12.06949235617756955, 24.37390960531435979 ) ) ;
#108236 = CARTESIAN_POINT ( 'NONE',  ( 16.51473224551083163, -9.474510206698727899, 55.83442372801899722 ) ) ;
#108237 = CARTESIAN_POINT ( 'NONE',  ( 5.823673210054444382, -21.52544592524334988, 105.2094237280190328 ) ) ;
#108238 = CARTESIAN_POINT ( 'NONE',  ( 9.474510206698729675, 16.51473224551082808, 27.08442372801900433 ) ) ;
#108239 = CARTESIAN_POINT ( 'NONE',  ( 19.02544592524343514, -5.153800228976328945, 23.54057627198102054 ) ) ;
#108240 = CARTESIAN_POINT ( 'NONE',  ( 21.52544592524334988, 5.823673210054432836, 86.45942372801901854 ) ) ;
#108241 = CARTESIAN_POINT ( 'NONE',  ( -14.34966873604972548, 8.224510206698743886, 38.33442372801900433 ) ) ;
#108242 = ADVANCED_FACE ( 'NONE', ( #131903 ), #124015, .T. ) ;
#108243 = CARTESIAN_POINT ( 'NONE',  ( -9.564922557960796823, -16.46253265017161027, 87.08224293864769550 ) ) ;
#108244 = CARTESIAN_POINT ( 'NONE',  ( -8.571926809382601320, -26.38167802310801591, 143.2750000027311899 ) ) ;
#108245 = CARTESIAN_POINT ( 'NONE',  ( -16.51473224551069308, -9.474510206698971260, 81.66557627198103830 ) ) ;
#108246 = DIRECTION ( 'NONE',  ( 0.000000000000000000, 0.000000000000000000, 1.000000000000000000 ) ) ;
#108247 = CARTESIAN_POINT ( 'NONE',  ( -19.05341960407617563, 5.049401038297882671, 88.54275706135230450 ) ) ;
#108248 = CARTESIAN_POINT ( 'NONE',  ( 0.05219959533909260263, 19.03943276465977164, 109.9989096053143669 ) ) ;
#108250 = CARTESIAN_POINT ( 'NONE',  ( -5.153800228976607833, 19.02544592524334988, 97.70942372801900433 ) ) ;
#108249 = CARTESIAN_POINT ( 'NONE',  ( 16.51473224551083163, -9.474510206698727899, 20.83442372801899722 ) ) ;
#108251 = CARTESIAN_POINT ( 'NONE',  ( 12.06949235617757843, -12.14591786802309237, 93.12390960531436690 ) ) ;
#108252 = CARTESIAN_POINT ( 'NONE',  ( 21.94381615377040973, -13.26253372808111308, 167.9278110240102251 ) ) ;
#108253 = CARTESIAN_POINT ( 'NONE',  ( 10.81492255796078972, 18.62759615963270932, 54.58224293864769550 ) ) ;
#108254 = CARTESIAN_POINT ( 'NONE',  ( -5.719274019375978568, 21.55341960407610458, 35.20724293864768839 ) ) ;
#108255 = CARTESIAN_POINT ( 'NONE',  ( 0.05219959533909260263, 19.03943276465977164, 29.99890960531435979 ) ) ;
#108256 = CARTESIAN_POINT ( 'NONE',  ( -16.68945015508926843, 0.2045547421927693954, -61.35148950497488585 ) ) ;
#108257 = CARTESIAN_POINT ( 'NONE',  ( 16.46253265017146816, 9.564922557961045513, 51.66775706135233293 ) ) ;
#108258 = CARTESIAN_POINT ( 'NONE',  ( -16.55341960407611168, -4.379528057220339221, 36.45724293864768839 ) ) ;
#108259 = CARTESIAN_POINT ( 'NONE',  ( -18.67979575497178146, -10.72451020669898902, 21.66557627198102409 ) ) ;
#108260 = CARTESIAN_POINT ( 'NONE',  ( 5.823673210054444382, -21.52544592524334988, 75.20942372801901854 ) ) ;
#108261 = CARTESIAN_POINT ( 'NONE',  ( 15.80617190586746368, 15.72974639402197994, 64.37390960531435269 ) ) ;
#108262 = CARTESIAN_POINT ( 'NONE',  ( 0.05219959533937995610, -21.53943276465977519, 60.00109039468568284 ) ) ;
#108263 = CARTESIAN_POINT ( 'NONE',  ( 21.52544592524334988, 5.823673210054432836, 56.45942372801902565 ) ) ;
#108264 = ADVANCED_FACE ( 'NONE', ( #180431, #116730 ), #40894, .F. ) ;
#108265 = CARTESIAN_POINT ( 'NONE',  ( -16.51473224551069308, -9.474510206698971260, 81.66557627198103830 ) ) ;
#108266 = CARTESIAN_POINT ( 'NONE',  ( 12.06949235617739724, 12.14591786802326823, 81.87609039468568994 ) ) ;
#108267 = CARTESIAN_POINT ( 'NONE',  ( -19.05341960407611168, -5.049401038298163336, 21.45724293864768839 ) ) ;
#108268 = CARTESIAN_POINT ( 'NONE',  ( -32.63002904509643542, 0.9908434387722265813, 87.54952558906812499 ) ) ;
#108269 = AXIS2_PLACEMENT_3D ( 'NONE', #199644, #45952, #182497 ) ;
#108270 = CARTESIAN_POINT ( 'NONE',  ( -16.53943276465976808, 0.05219959533911058130, 51.24890960531436690 ) ) ;
#108271 = CARTESIAN_POINT ( 'NONE',  ( 16.55341960407611168, 4.379528057220329451, 28.95724293864769905 ) ) ;
#108272 = CARTESIAN_POINT ( 'NONE',  ( -13.97604488694527625, -13.89961937509977652, 66.87390960531436690 ) ) ;
#108273 = CARTESIAN_POINT ( 'NONE',  ( 16.51473224551069308, 9.474510206698969483, 39.16557627198103120 ) ) ;
#108274 = CARTESIAN_POINT ( 'NONE',  ( 5.823673210054125526, 21.52544592524343514, 39.79057627198103830 ) ) ;
#108275 = CARTESIAN_POINT ( 'NONE',  ( 13.89961937509957401, 13.97604488694547697, 31.87609039468566863 ) ) ;
#108277 = CARTESIAN_POINT ( 'NONE',  ( -12.06949235617756955, 12.14591786802309770, 55.62390960531436690 ) ) ;
#108276 = DIRECTION ( 'NONE',  ( 1.000000000000000000, 0.000000000000000000, 0.000000000000000000 ) ) ;
#108278 = CARTESIAN_POINT ( 'NONE',  ( 18.62759615963271287, -10.81492255796078972, 23.33224293864769194 ) ) ;
#108279 = DIRECTION ( 'NONE',  ( 0.000000000000000000, 0.000000000000000000, -1.000000000000000000 ) ) ;
#108280 = CARTESIAN_POINT ( 'NONE',  ( 12.14591786802327356, -12.06949235617739191, 70.62609039468567573 ) ) ;
#108281 = CARTESIAN_POINT ( 'NONE',  ( -9.564922557961040184, 16.46253265017147172, 72.91775706135233293 ) ) ;
#108282 = CARTESIAN_POINT ( 'NONE',  ( 8.224510206698953496, -14.34966873604960469, 42.91557627198103120 ) ) ;
#108283 = CARTESIAN_POINT ( 'NONE',  ( 17.26058549869091507, -6.457015423128522613, 51.12254162523935008 ) ) ;
#108284 = CARTESIAN_POINT ( 'NONE',  ( -16.55341960407611168, -4.379528057220339221, 26.45724293864768839 ) ) ;
#108285 = CARTESIAN_POINT ( 'NONE',  ( 13.89961937509977652, -13.97604488694527269, 58.12390960531436690 ) ) ;
#108286 = CARTESIAN_POINT ( 'NONE',  ( -9.564922557960796823, -16.46253265017161027, 57.08224293864769550 ) ) ;
#108287 = CARTESIAN_POINT ( 'NONE',  ( 9.564922557960805705, 16.46253265017160317, 39.58224293864768839 ) ) ;
#108288 = CARTESIAN_POINT ( 'NONE',  ( 21.55341960407619695, -5.719274019375665929, 46.04275706135234714 ) ) ;
#108289 = CARTESIAN_POINT ( 'NONE',  ( -0.05219959533909027116, -19.03943276465977164, 57.49890960531435979 ) ) ;
#108290 = CARTESIAN_POINT ( 'NONE',  ( 0.000000000000000000, 0.000000000000000000, 10.00000000000000000 ) ) ;
#108291 = CARTESIAN_POINT ( 'NONE',  ( -19.02544592524342804, 5.153800228976336051, 51.04057627198103120 ) ) ;
#108292 = CARTESIAN_POINT ( 'NONE',  ( 18.67979575497178502, 10.72451020669898547, 39.16557627198102409 ) ) ;
#108294 = CARTESIAN_POINT ( 'NONE',  ( 5.153800228976335163, 19.02544592524342804, 24.79057627198102765 ) ) ;
#108293 = CARTESIAN_POINT ( 'NONE',  ( -15.72974639402176322, -15.80617190586768395, 74.37609039468568994 ) ) ;
#108295 = CARTESIAN_POINT ( 'NONE',  ( 5.719274019375991003, -21.55341960407610458, 22.70724293864769194 ) ) ;
#108296 = CARTESIAN_POINT ( 'NONE',  ( 0.05219959533934541429, -16.53943276465976808, 90.00109039468567573 ) ) ;
#108297 = CARTESIAN_POINT ( 'NONE',  ( 15.72974639402176855, 15.80617190586768217, 111.8760903946856615 ) ) ;
#108298 = CARTESIAN_POINT ( 'NONE',  ( -4.379528057220086978, -16.55341960407618274, 69.79275706135234714 ) ) ;
#108299 = CARTESIAN_POINT ( 'NONE',  ( 19.03943276465977164, -0.05219959533909143690, 113.7489096053143669 ) ) ;
#108300 = CARTESIAN_POINT ( 'NONE',  ( -8.314922557961024197, 14.29746914071037800, 57.91775706135234714 ) ) ;
#108301 = CARTESIAN_POINT ( 'NONE',  ( 12.06949235617739724, 12.14591786802326823, 36.87609039468568994 ) ) ;
#108302 = CARTESIAN_POINT ( 'NONE',  ( 8.224510206698742110, 14.34966873604972548, 97.08442372801904696 ) ) ;
#108303 = CARTESIAN_POINT ( 'NONE',  ( -18.62759615963255300, -10.81492255796106328, 59.16775706135234714 ) ) ;
#108304 = CARTESIAN_POINT ( 'NONE',  ( -16.53943276465976808, -0.05219959533934237506, 18.75109039468568639 ) ) ;
#108305 = CARTESIAN_POINT ( 'NONE',  ( 15.80617190586746368, 15.72974639402197994, 109.3739096053143811 ) ) ;
#108306 = CARTESIAN_POINT ( 'NONE',  ( -16.53943276465976808, -0.05219959533934237506, 28.75109039468567929 ) ) ;
#108307 = CARTESIAN_POINT ( 'NONE',  ( 4.379528057220092307, 16.55341960407617563, 92.29275706135236135 ) ) ;
#108308 = CARTESIAN_POINT ( 'NONE',  ( -30.74264578624800492, 22.33583958711400186, -3.949999994537626957 ) ) ;
#108309 = CARTESIAN_POINT ( 'NONE',  ( -21.53943276465977519, -0.05219959533937600094, 88.75109039468567573 ) ) ;
#108310 = CARTESIAN_POINT ( 'NONE',  ( 5.153800228976615827, -19.02544592524334988, 85.20942372801900433 ) ) ;
#108311 = CARTESIAN_POINT ( 'NONE',  ( 0.05219959533910956823, 16.53943276465976808, 54.99890960531435269 ) ) ;
#108312 = CARTESIAN_POINT ( 'NONE',  ( -4.379528057220328563, 16.55341960407611168, 50.20724293864769550 ) ) ;
#108313 = CARTESIAN_POINT ( 'NONE',  ( 14.29746914071049879, -8.314922557960816363, 108.3322429386477097 ) ) ;
#108315 = CARTESIAN_POINT ( 'NONE',  ( 16.88567814943194634, -6.947325034625403184, 56.20998877347405909 ) ) ;
#108314 = CARTESIAN_POINT ( 'NONE',  ( -13.97604488694547697, 13.89961937509957934, 48.12609039468566863 ) ) ;
#108316 = CARTESIAN_POINT ( 'NONE',  ( -15.72974639402176322, -15.80617190586768395, 44.37609039468567573 ) ) ;
#108317 = CARTESIAN_POINT ( 'NONE',  ( -13.89961937509957401, -13.97604488694547875, 109.3760903946856331 ) ) ;
#108318 = CARTESIAN_POINT ( 'NONE',  ( 19.24578484527059175, -180.9428398739492820, -15.00000000000000178 ) ) ;
#108319 = CARTESIAN_POINT ( 'NONE',  ( 5.153800228976335163, 19.02544592524342804, 109.7905762719810099 ) ) ;
#108320 = CARTESIAN_POINT ( 'NONE',  ( -21.52544592524343514, 5.823673210054127303, 71.04057627198103830 ) ) ;
#108321 = CARTESIAN_POINT ( 'NONE',  ( 16.51473224551083163, -9.474510206698727899, 95.83442372801900433 ) ) ;
#108322 = CARTESIAN_POINT ( 'NONE',  ( 5.153800228976335163, 19.02544592524342804, 99.79057627198102409 ) ) ;
#108323 = CARTESIAN_POINT ( 'NONE',  ( -26.61723430050333050, 3.645106422946821301, 172.4622069319858895 ) ) ;
#108324 = CARTESIAN_POINT ( 'NONE',  ( -12.14591786802309592, -12.06949235617757132, 101.8739096053143811 ) ) ;
#108325 = CARTESIAN_POINT ( 'NONE',  ( 21.53943276465977519, 0.05219959533937863772, 91.25109039468568994 ) ) ;
#108326 = CARTESIAN_POINT ( 'NONE',  ( 19.03943276465977164, -0.05219959533909143690, 28.74890960531435624 ) ) ;
#108327 = TOROIDAL_SURFACE ( 'NONE', #195096, 2.700000000000000622, 0.2000000000000000111 ) ;
#108328 = CARTESIAN_POINT ( 'NONE',  ( -21.53943276465977519, -0.05219959533937600094, 38.75109039468567573 ) ) ;
#108329 = CARTESIAN_POINT ( 'NONE',  ( 21.53943276465977519, 0.05219959533937863772, 86.25109039468568994 ) ) ;
#108330 = CARTESIAN_POINT ( 'NONE',  ( -8.224510206698735004, -14.34966873604973081, 84.58442372801903275 ) ) ;
#108331 = CARTESIAN_POINT ( 'NONE',  ( -21.55341960407619339, 5.719274019375674811, 48.54275706135234714 ) ) ;
#108332 = CARTESIAN_POINT ( 'NONE',  ( 5.719274019375673035, 21.55341960407619339, 42.29275706135235424 ) ) ;
#108334 = CARTESIAN_POINT ( 'NONE',  ( -16.46253265017160317, 9.564922557960807481, 75.83224293864769550 ) ) ;
#108333 = CARTESIAN_POINT ( 'NONE',  ( -5.153800228976607833, 19.02544592524334988, 62.70942372801899722 ) ) ;
#108335 = CARTESIAN_POINT ( 'NONE',  ( -4.379528057220328563, 16.55341960407611168, 110.2072429386477239 ) ) ;
#108336 = CARTESIAN_POINT ( 'NONE',  ( -5.823673210054116645, -21.52544592524344225, 77.29057627198102409 ) ) ;
#108337 = CARTESIAN_POINT ( 'NONE',  ( -4.483927247898539470, -16.52544592524342804, 67.29057627198103830 ) ) ;
#108338 = CARTESIAN_POINT ( 'NONE',  ( -10.81492255796105439, 18.62759615963255655, 107.9177570613523471 ) ) ;
#108339 = CARTESIAN_POINT ( 'NONE',  ( -8.314922557960811034, -14.29746914071050412, 82.08224293864768129 ) ) ;
#108340 = CARTESIAN_POINT ( 'NONE',  ( -16.46253265017160317, 9.564922557960807481, 35.83224293864768839 ) ) ;
#108341 = CARTESIAN_POINT ( 'NONE',  ( 5.153800228976615827, -19.02544592524334988, 65.20942372801900433 ) ) ;
#108342 = CARTESIAN_POINT ( 'NONE',  ( 14.34966873604960469, 8.224510206698951720, 29.16557627198103120 ) ) ;
#108344 = EDGE_CURVE ( 'NONE', #122302, #44638, #195596, .T. ) ;
#108343 = CARTESIAN_POINT ( 'NONE',  ( 21.55341960407619695, -5.719274019375665929, 96.04275706135236135 ) ) ;
#108345 = CARTESIAN_POINT ( 'NONE',  ( 16.46253265017160672, -9.564922557960803928, 98.33224293864769550 ) ) ;
#108346 = CARTESIAN_POINT ( 'NONE',  ( -5.049401038297874678, -19.05341960407617918, 54.79275706135234003 ) ) ;
#108347 = CARTESIAN_POINT ( 'NONE',  ( 5.823673210054125526, 21.52544592524343514, 59.79057627198103120 ) ) ;
#108348 = AXIS2_PLACEMENT_3D ( 'NONE', #156729, #17217, #3036 ) ;
#108349 = CARTESIAN_POINT ( 'NONE',  ( 5.719274019375673035, 21.55341960407619339, 22.29275706135235069 ) ) ;
#108350 = CARTESIAN_POINT ( 'NONE',  ( -16.51473224551082808, 9.474510206698731452, 113.3344237280190043 ) ) ;
#108351 = CARTESIAN_POINT ( 'NONE',  ( -12.06949235617739369, -12.14591786802326823, 74.37609039468568994 ) ) ;
#108353 = CARTESIAN_POINT ( 'NONE',  ( -21.53943276465977519, -0.05219959533937600094, 28.75109039468567929 ) ) ;
#108352 = DIRECTION ( 'NONE',  ( 1.000000000000000000, 0.000000000000000000, 0.000000000000000000 ) ) ;
#108354 = CARTESIAN_POINT ( 'NONE',  ( -14.34966873604960291, -8.224510206698953496, 101.6655762719810383 ) ) ;
#108355 = CARTESIAN_POINT ( 'NONE',  ( -11.40812507854755609, 35.11059874428196537, -9.524999997268816188 ) ) ;
#108356 = CARTESIAN_POINT ( 'NONE',  ( 4.483927247898790824, -16.52544592524335698, 45.20942372801901854 ) ) ;
#108357 = CARTESIAN_POINT ( 'NONE',  ( -4.379528057220328563, 16.55341960407611168, 75.20724293864769550 ) ) ;
#108358 = CARTESIAN_POINT ( 'NONE',  ( -5.823673210054116645, -21.52544592524344225, 72.29057627198102409 ) ) ;
#108359 = VECTOR ( 'NONE', #90265, 1000.000000000000000 ) ;
#108360 = CARTESIAN_POINT ( 'NONE',  ( -8.224510206698735004, -14.34966873604973081, 99.58442372801900433 ) ) ;
#108361 = CARTESIAN_POINT ( 'NONE',  ( 4.379528057220092307, 16.55341960407617563, 32.29275706135235424 ) ) ;
#108362 = CARTESIAN_POINT ( 'NONE',  ( -13.89961937509977652, 13.97604488694528158, 50.62390960531435979 ) ) ;
#108363 = CARTESIAN_POINT ( 'NONE',  ( 4.483927247898790824, -16.52544592524335698, 85.20942372801901854 ) ) ;
#108364 = CARTESIAN_POINT ( 'NONE',  ( -9.564922557961040184, 16.46253265017147172, 67.91775706135233293 ) ) ;
#108365 = CARTESIAN_POINT ( 'NONE',  ( 10.72451020669898902, -18.67979575497178502, 77.91557627198102409 ) ) ;
#108366 = CARTESIAN_POINT ( 'NONE',  ( -12.06949235617739369, -12.14591786802326823, 99.37609039468568994 ) ) ;
#108367 = ADVANCED_FACE ( 'NONE', ( #149078 ), #57068, .T. ) ;
#108368 = CARTESIAN_POINT ( 'NONE',  ( -21.53943276465977519, -0.05219959533937600094, 83.75109039468568994 ) ) ;
#108369 = CARTESIAN_POINT ( 'NONE',  ( -18.62759615963270932, 10.81492255796079327, 70.83224293864770971 ) ) ;
#108370 = CARTESIAN_POINT ( 'NONE',  ( -21.52544592524343514, 5.823673210054127303, 46.04057627198103830 ) ) ;
#108371 = ORIENTED_EDGE ( 'NONE', *, *, #10693, .T. ) ;
#108372 = ORIENTED_EDGE ( 'NONE', *, *, #5508, .T. ) ;
#108373 = CARTESIAN_POINT ( 'NONE',  ( -12.06949235617739369, -12.14591786802326823, 79.37609039468567573 ) ) ;
#108374 = CARTESIAN_POINT ( 'NONE',  ( -0.05219959533907301413, -21.53943276465977519, 52.49890960531435979 ) ) ;
#108375 = VERTEX_POINT ( 'NONE', #178419 ) ;
#108376 = CARTESIAN_POINT ( 'NONE',  ( -21.53943276465977519, 0.05219959533907696930, 21.24890960531436690 ) ) ;
#108377 = CARTESIAN_POINT ( 'NONE',  ( 38.00000000000008527, 12.34694845685035069, -8.649999994537628467 ) ) ;
#108378 = CARTESIAN_POINT ( 'NONE',  ( -13.89961937509977652, 13.97604488694528158, 30.62390960531435269 ) ) ;
#108379 = CARTESIAN_POINT ( 'NONE',  ( -18.67979575497178146, -10.72451020669898902, 81.66557627198103830 ) ) ;
#108380 = CARTESIAN_POINT ( 'NONE',  ( -8.224510206698735004, -14.34966873604973081, 99.58442372801900433 ) ) ;
#108381 = CARTESIAN_POINT ( 'NONE',  ( 21.52544592524334988, 5.823673210054432836, 46.45942372801901854 ) ) ;
#108382 = CARTESIAN_POINT ( 'NONE',  ( -16.51473224551082808, 9.474510206698731452, 113.3344237280190043 ) ) ;
#108383 = CARTESIAN_POINT ( 'NONE',  ( -4.483927247898539470, -16.52544592524342804, 112.2905762719810241 ) ) ;
#108384 = CARTESIAN_POINT ( 'NONE',  ( -19.05341960407617563, 5.049401038297882671, 108.5427570613523187 ) ) ;
#108385 = CARTESIAN_POINT ( 'NONE',  ( 16.51473224551069308, 9.474510206698969483, 34.16557627198102409 ) ) ;
#108386 = CARTESIAN_POINT ( 'NONE',  ( -5.429308488886486681E-15, 30.30510711980690175, 141.5000000000000000 ) ) ;
#108387 = CARTESIAN_POINT ( 'NONE',  ( 13.97604488694527802, 13.89961937509977652, 104.3739096053143385 ) ) ;
#108388 = CARTESIAN_POINT ( 'NONE',  ( -4.483927247898782831, 16.52544592524335698, 82.70942372801900433 ) ) ;
#108389 = CARTESIAN_POINT ( 'NONE',  ( 5.049401038297881783, 19.05341960407617563, 77.29275706135231871 ) ) ;
#108390 = CARTESIAN_POINT ( 'NONE',  ( -5.153800228976607833, 19.02544592524334988, 22.70942372801899012 ) ) ;
#108391 = CARTESIAN_POINT ( 'NONE',  ( -21.55341960407610458, -5.719274019375992779, 56.45724293864768839 ) ) ;
#108392 = CARTESIAN_POINT ( 'NONE',  ( -12.14591786802326823, 12.06949235617739902, 83.12609039468568994 ) ) ;
#108393 = CARTESIAN_POINT ( 'NONE',  ( -19.03943276465977164, -0.05219959533935918106, 88.75109039468567573 ) ) ;
#108394 = CARTESIAN_POINT ( 'NONE',  ( 5.049401038298161559, -19.05341960407611168, 52.70724293864767418 ) ) ;
#108395 = CARTESIAN_POINT ( 'NONE',  ( 13.89961937509977652, -13.97604488694527269, 98.12390960531433848 ) ) ;
#108396 = CARTESIAN_POINT ( 'NONE',  ( 21.55341960407619695, -5.719274019375665929, 46.04275706135234714 ) ) ;
#108397 = CARTESIAN_POINT ( 'NONE',  ( 9.474510206698971260, -16.51473224551069308, 52.91557627198102409 ) ) ;
#108398 = CARTESIAN_POINT ( 'NONE',  ( 26.57611637973592877, -7.696099174150921485, 167.9177021574032267 ) ) ;
#108399 = CARTESIAN_POINT ( 'NONE',  ( -5.049401038298153566, 19.05341960407611168, 110.2072429386476671 ) ) ;
#108400 = CARTESIAN_POINT ( 'NONE',  ( 14.34966873604960469, 8.224510206698951720, 69.16557627198102409 ) ) ;
#108401 = CARTESIAN_POINT ( 'NONE',  ( 0.05219959533907565091, 21.53943276465977519, 54.99890960531435269 ) ) ;
#108402 = CARTESIAN_POINT ( 'NONE',  ( 19.76836671444428006, -4.606730274327726526, 102.5000000000000284 ) ) ;
#108403 = CARTESIAN_POINT ( 'NONE',  ( 19.02544592524334988, 5.153800228976608722, 46.45942372801899012 ) ) ;
#108404 = FILL_AREA_STYLE ('',( #35542 ) ) ;
#108406 = CARTESIAN_POINT ( 'NONE',  ( 19.03943276465977164, -0.05219959533909143690, 78.74890960531436690 ) ) ;
#108405 = CARTESIAN_POINT ( 'NONE',  ( 13.89961937509977652, -13.97604488694527269, 63.12390960531435979 ) ) ;
#108407 = CARTESIAN_POINT ( 'NONE',  ( -16.52544592524335698, -4.483927247898792601, 53.95942372801900433 ) ) ;
#108408 = CARTESIAN_POINT ( 'NONE',  ( -18.22780087662121673, -5.500000000000063061, 66.48459894673892734 ) ) ;
#108409 = CARTESIAN_POINT ( 'NONE',  ( 17.97161686093727795, -5.499999999999969802, 93.49637206859166838 ) ) ;
#108410 = CARTESIAN_POINT ( 'NONE',  ( -14.29746914071037622, -8.314922557961029526, 84.16775706135234714 ) ) ;
#108411 = CARTESIAN_POINT ( 'NONE',  ( 15.84196527238554353, -1.359015117358377323, -59.51370404797111036 ) ) ;
#108412 = CARTESIAN_POINT ( 'NONE',  ( -16.55341960407617563, 4.379528057220093196, 78.54275706135236135 ) ) ;
#108413 = CARTESIAN_POINT ( 'NONE',  ( 8.314922557961029526, -14.29746914071037800, 50.41775706135235424 ) ) ;
#108414 = CARTESIAN_POINT ( 'NONE',  ( 19.05341960407617918, -5.049401038297876454, 21.04275706135232582 ) ) ;
#108415 = CARTESIAN_POINT ( 'NONE',  ( -13.89961937509977652, 13.97604488694528158, 60.62390960531436690 ) ) ;
#108416 = CARTESIAN_POINT ( 'NONE',  ( -21.55341960407619339, 5.719274019375674811, 48.54275706135234714 ) ) ;
#108417 = CARTESIAN_POINT ( 'NONE',  ( -9.564922557961040184, 16.46253265017147172, 77.91775706135234714 ) ) ;
#108418 = CARTESIAN_POINT ( 'NONE',  ( -9.474510206698720793, -16.51473224551083518, 19.58442372801899722 ) ) ;
#108419 = CIRCLE ( 'NONE', #114913, 2.649999999999999467 ) ;
#108420 = CARTESIAN_POINT ( 'NONE',  ( -16.46253265017160317, 9.564922557960807481, 30.83224293864769550 ) ) ;
#108421 = CARTESIAN_POINT ( 'NONE',  ( -17.44568526726164848, 16.83584321579681742, -56.81531555676559009 ) ) ;
#108422 = CARTESIAN_POINT ( 'NONE',  ( 10.72451020669898902, -18.67979575497178502, 67.91557627198102409 ) ) ;
#108423 = CARTESIAN_POINT ( 'NONE',  ( 5.823673210054125526, 21.52544592524343514, 24.79057627198103120 ) ) ;
#108424 = CARTESIAN_POINT ( 'NONE',  ( -0.05219959533909027116, -19.03943276465977164, 22.49890960531436690 ) ) ;
#108425 = CARTESIAN_POINT ( 'NONE',  ( 12.06949235617739724, 12.14591786802326823, 31.87609039468567929 ) ) ;
#108426 = CARTESIAN_POINT ( 'NONE',  ( 16.53943276465976808, -0.05219959533910856209, 23.74890960531435269 ) ) ;
#108427 = EDGE_LOOP ( 'NONE', ( #16488, #148216, #19213, #68079 ) ) ;
#108428 = CARTESIAN_POINT ( 'NONE',  ( -18.67979575497178146, -10.72451020669898902, 111.6655762719810525 ) ) ;
#108430 = CARTESIAN_POINT ( 'NONE',  ( -38.00000000000001421, -12.34694845685042708, -7.900000000000001243 ) ) ;
#108429 = CARTESIAN_POINT ( 'NONE',  ( 12.14591786802309770, 12.06949235617756955, 39.37390960531436690 ) ) ;
#108431 = CARTESIAN_POINT ( 'NONE',  ( 19.03943276465977164, 0.05219959533936151252, 111.2510903946856757 ) ) ;
#108432 = CARTESIAN_POINT ( 'NONE',  ( 13.97604488694548053, -13.89961937509957401, 20.62609039468567573 ) ) ;
#108433 = CARTESIAN_POINT ( 'NONE',  ( -16.53943276465976808, 0.05219959533911058130, 41.24890960531435269 ) ) ;
#108434 = CARTESIAN_POINT ( 'NONE',  ( 5.719274019375991003, -21.55341960407610458, 102.7072429386476955 ) ) ;
#108436 = CARTESIAN_POINT ( 'NONE',  ( -10.72451020669898014, 18.67979575497178502, 65.41557627198102409 ) ) ;
#108435 = CARTESIAN_POINT ( 'NONE',  ( 17.50000000000000000, 5.499999999999997335, 31.70309617465830243 ) ) ;
#108437 = CARTESIAN_POINT ( 'NONE',  ( 19.02544592524343514, -5.153800228976328945, 78.54057627198099567 ) ) ;
#108438 = CARTESIAN_POINT ( 'NONE',  ( 8.224510206698953496, -14.34966873604960469, 42.91557627198103120 ) ) ;
#108439 = CARTESIAN_POINT ( 'NONE',  ( -9.564922557960796823, -16.46253265017161027, 87.08224293864769550 ) ) ;
#108440 = CARTESIAN_POINT ( 'NONE',  ( -18.22780087662123094, -5.499999999999984901, 86.48459894673892734 ) ) ;
#108441 = CARTESIAN_POINT ( 'NONE',  ( -9.474510206698720793, -16.51473224551083518, 54.58442372801899722 ) ) ;
#108442 = CARTESIAN_POINT ( 'NONE',  ( 10.72451020669898902, -18.67979575497178502, 87.91557627198103830 ) ) ;
#108443 = CARTESIAN_POINT ( 'NONE',  ( 16.55341960407611168, 4.379528057220329451, 98.95724293864770971 ) ) ;
#108444 = CARTESIAN_POINT ( 'NONE',  ( -18.67979575497193778, 10.72451020669871902, 53.33442372801901854 ) ) ;
#108445 = CARTESIAN_POINT ( 'NONE',  ( -27.73933785331498925, 9.013057229001089965, 144.7750000027311614 ) ) ;
#108446 = CARTESIAN_POINT ( 'NONE',  ( 14.29746914071049879, -8.314922557960816363, 28.33224293864769550 ) ) ;
#108447 = CARTESIAN_POINT ( 'NONE',  ( 19.05341960407611168, 5.049401038298154454, 38.95724293864767418 ) ) ;
#108448 = CARTESIAN_POINT ( 'NONE',  ( -16.46253265017160317, 9.564922557960807481, 95.83224293864769550 ) ) ;
#108449 = CARTESIAN_POINT ( 'NONE',  ( -18.62759615963270932, 10.81492255796079327, 65.83224293864769550 ) ) ;
#108450 = CARTESIAN_POINT ( 'NONE',  ( 9.474510206698729675, 16.51473224551082808, 92.08442372801900433 ) ) ;
#108451 = CARTESIAN_POINT ( 'NONE',  ( -13.97604488694527625, -13.89961937509977652, 31.87390960531435979 ) ) ;
#108452 = CARTESIAN_POINT ( 'NONE',  ( 21.52544592524344225, -5.823673210054117533, 53.54057627198103120 ) ) ;
#108453 = CARTESIAN_POINT ( 'NONE',  ( -21.52544592524334988, -5.823673210054445271, 78.95942372801901854 ) ) ;
#108455 = CARTESIAN_POINT ( 'NONE',  ( 4.483927247898790824, -16.52544592524335698, 80.20942372801901854 ) ) ;
#108454 = CARTESIAN_POINT ( 'NONE',  ( 20.92307141426025296, -31.70153649905323334, -23.60833562325456825 ) ) ;
#108456 = CARTESIAN_POINT ( 'NONE',  ( -13.97604488694527625, -13.89961937509977652, 51.87390960531436690 ) ) ;
#108457 = CARTESIAN_POINT ( 'NONE',  ( 9.564922557960805705, 16.46253265017160317, 59.58224293864769550 ) ) ;
#108458 = ORIENTED_EDGE ( 'NONE', *, *, #184866, .T. ) ;
#108459 = CARTESIAN_POINT ( 'NONE',  ( 9.474510206698729675, 16.51473224551082808, 32.08442372801900433 ) ) ;
#108460 = CARTESIAN_POINT ( 'NONE',  ( 4.379528057220092307, 16.55341960407617563, 77.29275706135234714 ) ) ;
#108461 = CARTESIAN_POINT ( 'NONE',  ( -10.72451020669870658, -18.67979575497194134, 94.58442372801901854 ) ) ;
#108462 = CARTESIAN_POINT ( 'NONE',  ( 9.564922557960805705, 16.46253265017160317, 74.58224293864769550 ) ) ;
#108463 = CARTESIAN_POINT ( 'NONE',  ( -10.81492255796078084, -18.62759615963271287, 37.08224293864768129 ) ) ;
#108464 = CARTESIAN_POINT ( 'NONE',  ( 9.564922557961047289, -16.46253265017146816, 110.4177570613523471 ) ) ;
#108465 = CARTESIAN_POINT ( 'NONE',  ( -18.62759615963255300, -10.81492255796106328, 79.16775706135234714 ) ) ;
#108466 = CARTESIAN_POINT ( 'NONE',  ( 12.14591786802327356, -12.06949235617739191, 45.62609039468567573 ) ) ;
#108467 = CARTESIAN_POINT ( 'NONE',  ( 15.72974639402199770, -15.80617190586745480, 103.1239096053143811 ) ) ;
#108468 = CARTESIAN_POINT ( 'NONE',  ( 19.03943276465977164, 0.05219959533936151252, 106.2510903946856615 ) ) ;
#108469 = CARTESIAN_POINT ( 'NONE',  ( 19.02544592524343514, -5.153800228976328945, 78.54057627198099567 ) ) ;
#108470 = CARTESIAN_POINT ( 'NONE',  ( 8.224510206698742110, 14.34966873604972548, 32.08442372801901854 ) ) ;
#108471 = CARTESIAN_POINT ( 'NONE',  ( -5.153800228976328057, -19.02544592524343514, 37.29057627198102409 ) ) ;
#108472 = CARTESIAN_POINT ( 'NONE',  ( 12.14591786802327356, -12.06949235617739191, 20.62609039468568639 ) ) ;
#108473 = CARTESIAN_POINT ( 'NONE',  ( -16.52544592524342804, 4.483927247898546575, 71.04057627198103830 ) ) ;
#108474 = ADVANCED_FACE ( 'NONE', ( #133905 ), #42893, .F. ) ;
#108475 = CARTESIAN_POINT ( 'NONE',  ( -14.34966873604972548, 8.224510206698743886, 83.33442372801903275 ) ) ;
#108477 = CARTESIAN_POINT ( 'NONE',  ( 0.05219959533909260263, 19.03943276465977164, 49.99890960531435979 ) ) ;
#108476 = CARTESIAN_POINT ( 'NONE',  ( -21.55341960407619339, 5.719274019375674811, 33.54275706135234714 ) ) ;
#108478 = CARTESIAN_POINT ( 'NONE',  ( -9.474510206698964154, 16.51473224551069663, 75.41557627198103830 ) ) ;
#108479 = CARTESIAN_POINT ( 'NONE',  ( 12.14591786802327356, -12.06949235617739191, 90.62609039468567573 ) ) ;
#108481 = VERTEX_POINT ( 'NONE', #147075 ) ;
#108480 = CARTESIAN_POINT ( 'NONE',  ( -17.97214573761834089, -5.500000000000018652, 81.46970049038658601 ) ) ;
#108482 = ORIENTED_EDGE ( 'NONE', *, *, #125633, .T. ) ;
#108483 = CARTESIAN_POINT ( 'NONE',  ( 21.52544592524334988, 5.823673210054432836, 111.4594237280190328 ) ) ;
#108484 = CARTESIAN_POINT ( 'NONE',  ( 5.153800228976335163, 19.02544592524342804, 29.79057627198102409 ) ) ;
#108486 = ORIENTED_EDGE ( 'NONE', *, *, #78126, .T. ) ;
#108485 = CARTESIAN_POINT ( 'NONE',  ( 1.500000000000005329, 15.20000000000001883, -61.96904110198155280 ) ) ;
#108487 = CARTESIAN_POINT ( 'NONE',  ( -4.379528057220086978, -16.55341960407618274, 34.79275706135235424 ) ) ;
#108489 = CARTESIAN_POINT ( 'NONE',  ( -0.05219959533934338120, 16.53943276465976808, 42.50109039468567573 ) ) ;
#108488 = CARTESIAN_POINT ( 'NONE',  ( -9.564922557961040184, 16.46253265017147172, 62.91775706135233293 ) ) ;
#108490 = CARTESIAN_POINT ( 'NONE',  ( -0.05219959533909027116, -19.03943276465977164, 47.49890960531435979 ) ) ;
#108491 = CARTESIAN_POINT ( 'NONE',  ( 9.564922557960805705, 16.46253265017160317, 109.5822429386476955 ) ) ;
#108492 = CARTESIAN_POINT ( 'NONE',  ( -19.05341960407611168, -5.049401038298163336, 66.45724293864769550 ) ) ;
#108493 = CARTESIAN_POINT ( 'NONE',  ( 21.52544592524344225, -5.823673210054117533, 93.54057627198103830 ) ) ;
#108495 = CARTESIAN_POINT ( 'NONE',  ( 5.049401038298161559, -19.05341960407611168, 27.70724293864769550 ) ) ;
#108494 = CARTESIAN_POINT ( 'NONE',  ( 13.89961937509977652, -13.97604488694527269, 88.12390960531438111 ) ) ;
#108496 = CARTESIAN_POINT ( 'NONE',  ( 5.153800228976335163, 19.02544592524342804, 64.79057627198100988 ) ) ;
#108498 = CARTESIAN_POINT ( 'NONE',  ( -16.51473224551069308, -9.474510206698971260, 26.66557627198103120 ) ) ;
#108497 = CARTESIAN_POINT ( 'NONE',  ( -4.483927247898782831, 16.52544592524335698, 107.7094237280190328 ) ) ;
#108499 = CARTESIAN_POINT ( 'NONE',  ( -19.03943276465977164, -0.05219959533935918106, 18.75109039468567218 ) ) ;
#108500 = CARTESIAN_POINT ( 'NONE',  ( -16.55341960407611168, -4.379528057220339221, 61.45724293864770260 ) ) ;
#108501 = CARTESIAN_POINT ( 'NONE',  ( -10.72451020669870658, -18.67979575497194134, 99.58442372801900433 ) ) ;
#108502 = CARTESIAN_POINT ( 'NONE',  ( 5.153800228976335163, 19.02544592524342804, 34.79057627198102409 ) ) ;
#108503 = EDGE_CURVE ( 'NONE', #150593, #60986, #102567, .T. ) ;
#108505 = CARTESIAN_POINT ( 'NONE',  ( 10.81492255796106328, -18.62759615963255655, 85.41775706135236135 ) ) ;
#108504 = CARTESIAN_POINT ( 'NONE',  ( -14.29746914071049879, 8.314922557960819915, 35.83224293864768839 ) ) ;
#108506 = CARTESIAN_POINT ( 'NONE',  ( -0.05219959533909027116, -19.03943276465977164, 82.49890960531436690 ) ) ;
#108507 = CARTESIAN_POINT ( 'NONE',  ( 16.46253265017160672, -9.564922557960803928, 98.33224293864769550 ) ) ;
#108508 = CARTESIAN_POINT ( 'NONE',  ( -8.224510206698948167, 14.34966873604960824, 110.4155762719810383 ) ) ;
#108509 = CARTESIAN_POINT ( 'NONE',  ( 8.224510206698953496, -14.34966873604960469, 77.91557627198102409 ) ) ;
#108510 = CARTESIAN_POINT ( 'NONE',  ( 15.72974639402199770, -15.80617190586745480, 83.12390960531436690 ) ) ;
#108511 = CARTESIAN_POINT ( 'NONE',  ( 16.51473224551069308, 9.474510206698969483, 69.16557627198102409 ) ) ;
#108512 = CARTESIAN_POINT ( 'NONE',  ( -21.55341960407610458, -5.719274019375992779, 91.45724293864769550 ) ) ;
#108513 = CARTESIAN_POINT ( 'NONE',  ( -16.51473224551082808, 9.474510206698731452, 78.33442372801900433 ) ) ;
#108516 = CARTESIAN_POINT ( 'NONE',  ( -12.06949235617756955, 12.14591786802309770, 95.62390960531436690 ) ) ;
#108515 = CARTESIAN_POINT ( 'NONE',  ( 18.22780087662119897, -5.500000000000096811, 48.51763182126894236 ) ) ;
#108514 = AXIS2_PLACEMENT_3D ( 'NONE', #114600, #51936, #176297 ) ;
#108517 = CARTESIAN_POINT ( 'NONE',  ( -19.05341960407611168, -5.049401038298163336, 61.45724293864769550 ) ) ;
#108518 = CARTESIAN_POINT ( 'NONE',  ( -21.55341960407610458, -5.719274019375992779, 66.45724293864768129 ) ) ;
#108519 = CARTESIAN_POINT ( 'NONE',  ( -26.58496454516998853, -7.626754437231455519, 167.9682100371138915 ) ) ;
#108521 =( NAMED_UNIT ( * ) PLANE_ANGLE_UNIT ( ) SI_UNIT ( $, .RADIAN. ) );
#108520 = CARTESIAN_POINT ( 'NONE',  ( -14.34966873604972548, 8.224510206698743886, 108.3344237280190185 ) ) ;
#108522 = CARTESIAN_POINT ( 'NONE',  ( -16.52544592524335698, -4.483927247898792601, 23.95942372801901143 ) ) ;
#108523 = CARTESIAN_POINT ( 'NONE',  ( 4.483927247898545687, 16.52544592524342804, 74.79057627198105251 ) ) ;
#108524 = CARTESIAN_POINT ( 'NONE',  ( 9.100000000000003197, -0.1001428631146442511, -61.89430850415823215 ) ) ;
#108525 = CARTESIAN_POINT ( 'NONE',  ( -9.564922557960796823, -16.46253265017161027, 77.08224293864769550 ) ) ;
#108526 = CARTESIAN_POINT ( 'NONE',  ( 9.474510206698971260, -16.51473224551069308, 32.91557627198102409 ) ) ;
#108527 = CARTESIAN_POINT ( 'NONE',  ( -12.06949235617756955, 12.14591786802309770, 70.62390960531436690 ) ) ;
#108528 = CARTESIAN_POINT ( 'NONE',  ( 19.05341960407611168, 5.049401038298154454, 108.9572429386477097 ) ) ;
#108530 = CARTESIAN_POINT ( 'NONE',  ( -19.05341960407611168, -5.049401038298163336, 76.45724293864769550 ) ) ;
#108529 = CARTESIAN_POINT ( 'NONE',  ( -19.05341960407617563, 5.049401038297882671, 93.54275706135234714 ) ) ;
#108531 = CARTESIAN_POINT ( 'NONE',  ( 19.05341960407611168, 5.049401038298154454, 83.95724293864766707 ) ) ;
#108532 = CARTESIAN_POINT ( 'NONE',  ( 15.80617190586746368, 15.72974639402197994, 79.37390960531436690 ) ) ;
#108533 = CARTESIAN_POINT ( 'NONE',  ( -14.29746914071037622, -8.314922557961029526, 69.16775706135234714 ) ) ;
#108534 = CARTESIAN_POINT ( 'NONE',  ( -16.21995358207276894, 7.366697692864291547, 94.93551001512068410 ) ) ;
#108535 = CARTESIAN_POINT ( 'NONE',  ( -9.564922557960796823, -16.46253265017161027, 62.08224293864769550 ) ) ;
#108536 = CARTESIAN_POINT ( 'NONE',  ( 21.52544592524344225, -5.823673210054117533, 73.54057627198102409 ) ) ;
#108537 = CARTESIAN_POINT ( 'NONE',  ( 16.51473224551083163, -9.474510206698727899, 100.8344237280190043 ) ) ;
#108539 = CARTESIAN_POINT ( 'NONE',  ( -0.05219959533937732626, 21.53943276465977519, 52.50109039468567573 ) ) ;
#108538 = CARTESIAN_POINT ( 'NONE',  ( -14.34966873604960291, -8.224510206698953496, 36.66557627198103120 ) ) ;
#108540 = CARTESIAN_POINT ( 'NONE',  ( 17.60779699588839620, 5.500000000000007105, 83.84981316670105400 ) ) ;
#108542 = CARTESIAN_POINT ( 'NONE',  ( -9.474510206698964154, 16.51473224551069663, 105.4155762719810383 ) ) ;
#108541 = CARTESIAN_POINT ( 'NONE',  ( 16.55341960407618274, -4.379528057220086978, 76.04275706135237556 ) ) ;
#108543 = FACE_BOUND ( 'NONE', #194261, .T. ) ;
#108544 = CARTESIAN_POINT ( 'NONE',  ( -16.79531203550647689, 7.028104445595609207, 78.74755011779562608 ) ) ;
#108545 = CARTESIAN_POINT ( 'NONE',  ( -12.06949235617739369, -12.14591786802326823, 89.37609039468568994 ) ) ;
#108546 = CARTESIAN_POINT ( 'NONE',  ( -8.314922557961024197, 14.29746914071037800, 47.91775706135234714 ) ) ;
#108547 = CARTESIAN_POINT ( 'NONE',  ( 16.46253265017160672, -9.564922557960803928, 58.33224293864769550 ) ) ;
#108548 = CARTESIAN_POINT ( 'NONE',  ( -19.03943276465977164, 0.05219959533909376836, 71.24890960531435269 ) ) ;
#108549 = CARTESIAN_POINT ( 'NONE',  ( -0.05219959533937732626, 21.53943276465977519, 52.50109039468567573 ) ) ;
#108550 = CARTESIAN_POINT ( 'NONE',  ( 16.53943276465976808, 0.05219959533934440121, 66.25109039468567573 ) ) ;
#108551 = CARTESIAN_POINT ( 'NONE',  ( 8.224510206698953496, -14.34966873604960469, 32.91557627198102409 ) ) ;
#108552 = CARTESIAN_POINT ( 'NONE',  ( 16.46253265017160672, -9.564922557960803928, 38.33224293864768839 ) ) ;
#108553 = CARTESIAN_POINT ( 'NONE',  ( 9.564922557960805705, 16.46253265017160317, 29.58224293864769550 ) ) ;
#108555 = ORIENTED_EDGE ( 'NONE', *, *, #44393, .F. ) ;
#108554 = CARTESIAN_POINT ( 'NONE',  ( 12.14591786802327356, -12.06949235617739191, 30.62609039468567929 ) ) ;
#108556 = CARTESIAN_POINT ( 'NONE',  ( 9.564922557961047289, -16.46253265017146816, 80.41775706135234714 ) ) ;
#108557 = CARTESIAN_POINT ( 'NONE',  ( -0.05219959533910754901, -16.53943276465976808, 77.49890960531433848 ) ) ;
#108558 = CARTESIAN_POINT ( 'NONE',  ( 16.51473224551069308, 9.474510206698969483, 54.16557627198103120 ) ) ;
#108560 = CARTESIAN_POINT ( 'NONE',  ( 17.79613651744294245, -24.49428055684527195, 148.6843446568999809 ) ) ;
#108559 = CARTESIAN_POINT ( 'NONE',  ( -5.153800228976607833, 19.02544592524334988, 92.70942372801901854 ) ) ;
#108561 = CARTESIAN_POINT ( 'NONE',  ( -0.05219959533937732626, 21.53943276465977519, 92.50109039468567573 ) ) ;
#108562 = CARTESIAN_POINT ( 'NONE',  ( 4.379528057220092307, 16.55341960407617563, 52.29275706135236135 ) ) ;
#108563 = CARTESIAN_POINT ( 'NONE',  ( 16.18388926212240619, 7.379444403734400915, 37.93953151366152809 ) ) ;
#108564 = CARTESIAN_POINT ( 'NONE',  ( 5.823673210054125526, 21.52544592524343514, 49.79057627198102409 ) ) ;
#108565 = CARTESIAN_POINT ( 'NONE',  ( -16.53943276465976808, -0.05219959533934237506, 38.75109039468567573 ) ) ;
#108566 = CARTESIAN_POINT ( 'NONE',  ( 13.89961937509978007, -13.97604488694527269, 38.12390960531436690 ) ) ;
#108567 = CARTESIAN_POINT ( 'NONE',  ( 9.474510206698729675, 16.51473224551082808, 42.08442372801900433 ) ) ;
#108568 = CIRCLE ( 'NONE', #140889, 40.00000000000000711 ) ;
#108569 = CARTESIAN_POINT ( 'NONE',  ( -9.564922557960796823, -16.46253265017161027, 77.08224293864769550 ) ) ;
#108570 = CARTESIAN_POINT ( 'NONE',  ( 5.049401038298161559, -19.05341960407611168, 57.70724293864769550 ) ) ;
#108571 = LINE ( 'NONE', #63057, #65639 ) ;
#108572 = CARTESIAN_POINT ( 'NONE',  ( 19.03943276465977164, -0.05219959533909143690, 63.74890960531435979 ) ) ;
#108573 = CARTESIAN_POINT ( 'NONE',  ( -20.13687146691627561, -33.41269836094262047, -11.42148495485635529 ) ) ;
#108574 = CARTESIAN_POINT ( 'NONE',  ( -9.474510206698720793, -16.51473224551083518, 34.58442372801899722 ) ) ;
#108575 = CARTESIAN_POINT ( 'NONE',  ( 16.51473224551083163, -9.474510206698727899, 20.83442372801899722 ) ) ;
#108576 = CARTESIAN_POINT ( 'NONE',  ( -16.55341960407611168, -4.379528057220339221, 41.45724293864769550 ) ) ;
#108577 = CARTESIAN_POINT ( 'NONE',  ( 5.049401038298161559, -19.05341960407611168, 37.70724293864768839 ) ) ;
#108578 = CARTESIAN_POINT ( 'NONE',  ( 16.51473224551069308, 9.474510206698969483, 104.1655762719810241 ) ) ;
#108579 = CARTESIAN_POINT ( 'NONE',  ( -18.62759615963255300, -10.81492255796106328, 79.16775706135234714 ) ) ;
#108580 = CARTESIAN_POINT ( 'NONE',  ( 16.46253265017160672, -9.564922557960803928, 53.33224293864768839 ) ) ;
#108581 = CARTESIAN_POINT ( 'NONE',  ( 21.52544592524334988, 5.823673210054432836, 81.45942372801900433 ) ) ;
#108582 = CARTESIAN_POINT ( 'NONE',  ( 21.55341960407610458, 5.719274019375980345, 38.95724293864768839 ) ) ;
#108583 = CARTESIAN_POINT ( 'NONE',  ( 10.81492255796106328, -18.62759615963255655, 20.41775706135234714 ) ) ;
#108584 = CARTESIAN_POINT ( 'NONE',  ( 19.03943276465977164, 0.05219959533936151252, 46.25109039468566863 ) ) ;
#108585 = CARTESIAN_POINT ( 'NONE',  ( 19.03943276465977164, -0.05219959533909143690, 33.74890960531435979 ) ) ;
#108586 = CARTESIAN_POINT ( 'NONE',  ( -0.05219959533909027116, -19.03943276465977164, 82.49890960531436690 ) ) ;
#108587 = CARTESIAN_POINT ( 'NONE',  ( -0.05219959533934338120, 16.53943276465976808, 22.50109039468567573 ) ) ;
#108588 = CARTESIAN_POINT ( 'NONE',  ( -14.34966873604960291, -8.224510206698953496, 86.66557627198102409 ) ) ;
#108589 = CARTESIAN_POINT ( 'NONE',  ( -5.719274019375978568, 21.55341960407610458, 30.20724293864769550 ) ) ;
#108590 = CARTESIAN_POINT ( 'NONE',  ( 16.51473224551083163, -9.474510206698727899, 95.83442372801900433 ) ) ;
#108591 = CARTESIAN_POINT ( 'NONE',  ( 21.55341960407610458, 5.719274019375980345, 103.9572429386476813 ) ) ;
#108592 = CARTESIAN_POINT ( 'NONE',  ( 15.72974639402176855, 15.80617190586768217, 51.87609039468568284 ) ) ;
#108593 = CARTESIAN_POINT ( 'NONE',  ( 4.379528057220092307, 16.55341960407617563, 52.29275706135236135 ) ) ;
#108594 = CARTESIAN_POINT ( 'NONE',  ( -4.483927247898782831, 16.52544592524335698, 67.70942372801901854 ) ) ;
#108595 = ORIENTED_EDGE ( 'NONE', *, *, #13466, .F. ) ;
#108596 = CARTESIAN_POINT ( 'NONE',  ( -13.97604488694527625, -13.89961937509977652, 56.87390960531434558 ) ) ;
#108597 = CARTESIAN_POINT ( 'NONE',  ( 8.314922557961029526, -14.29746914071037800, 90.41775706135236135 ) ) ;
#108598 = CARTESIAN_POINT ( 'NONE',  ( 10.72451020669871369, 18.67979575497193778, 22.08442372801901143 ) ) ;
#108599 = CARTESIAN_POINT ( 'NONE',  ( -8.224510206698948167, 14.34966873604960824, 65.41557627198102409 ) ) ;
#108600 = CARTESIAN_POINT ( 'NONE',  ( 5.049401038298161559, -19.05341960407611168, 82.70724293864770971 ) ) ;
#108601 = CARTESIAN_POINT ( 'NONE',  ( 8.314922557961029526, -14.29746914071037800, 70.41775706135236135 ) ) ;
#108602 = CARTESIAN_POINT ( 'NONE',  ( 0.05219959533937995610, -21.53943276465977519, 60.00109039468568284 ) ) ;
#108603 = CARTESIAN_POINT ( 'NONE',  ( 12.14591786802327356, -12.06949235617739191, 20.62609039468568639 ) ) ;
#108604 = CARTESIAN_POINT ( 'NONE',  ( 5.823673210054125526, 21.52544592524343514, 114.7905762719810383 ) ) ;
#108605 = CARTESIAN_POINT ( 'NONE',  ( 14.29746914071049879, -8.314922557960816363, 53.33224293864769550 ) ) ;
#108606 = ORIENTED_EDGE ( 'NONE', *, *, #158775, .T. ) ;
#108607 = CARTESIAN_POINT ( 'NONE',  ( -16.20579543436678094, 7.371946100355086351, 74.43479165828127009 ) ) ;
#108608 = CARTESIAN_POINT ( 'NONE',  ( -10.81492255796078084, -18.62759615963271287, 82.08224293864768129 ) ) ;
#108609 = CARTESIAN_POINT ( 'NONE',  ( 16.55341960407611168, 4.379528057220329451, 43.95724293864769550 ) ) ;
#108610 = ORIENTED_EDGE ( 'NONE', *, *, #151508, .T. ) ;
#108611 = CARTESIAN_POINT ( 'NONE',  ( 6.434671708797586653, 6.434671708797580436, -64.92279855667830191 ) ) ;
#108612 = CARTESIAN_POINT ( 'NONE',  ( 5.823673210054125526, 21.52544592524343514, 109.7905762719810383 ) ) ;
#108613 = CARTESIAN_POINT ( 'NONE',  ( -19.05341960407611168, -5.049401038298163336, 111.4572429386476671 ) ) ;
#108614 = CARTESIAN_POINT ( 'NONE',  ( 5.719274019375673035, 21.55341960407619339, 22.29275706135235069 ) ) ;
#108615 = CARTESIAN_POINT ( 'NONE',  ( -12.14591786802309592, -12.06949235617757132, 51.87390960531437401 ) ) ;
#108616 = CARTESIAN_POINT ( 'NONE',  ( -14.34966873604972548, 8.224510206698743886, 58.33442372801901143 ) ) ;
#108617 = CARTESIAN_POINT ( 'NONE',  ( 16.51473224551069308, 9.474510206698969483, 64.16557627198102409 ) ) ;
#108618 = CARTESIAN_POINT ( 'NONE',  ( -19.05341960407617563, 5.049401038297882671, 68.54275706135230450 ) ) ;
#108619 = CARTESIAN_POINT ( 'NONE',  ( -19.05341960407611168, -5.049401038298163336, 86.45724293864769550 ) ) ;
#108620 = CARTESIAN_POINT ( 'NONE',  ( 21.52544592524344225, -5.823673210054117533, 38.54057627198103120 ) ) ;
#108621 = CARTESIAN_POINT ( 'NONE',  ( -20.12333042654506343, -32.04799867105109712, -20.24659421909778700 ) ) ;
#108622 = CARTESIAN_POINT ( 'NONE',  ( 9.474510206698971260, -16.51473224551069308, 57.91557627198103120 ) ) ;
#108623 = CARTESIAN_POINT ( 'NONE',  ( 16.53943276465976808, 0.05219959533934440121, 26.25109039468567573 ) ) ;
#108624 = CARTESIAN_POINT ( 'NONE',  ( 13.97604488694548053, -13.89961937509957401, 70.62609039468567573 ) ) ;
#108625 = CARTESIAN_POINT ( 'NONE',  ( -21.52544592524343514, 5.823673210054127303, 101.0405762719810383 ) ) ;
#108626 = CARTESIAN_POINT ( 'NONE',  ( 4.483927247898545687, 16.52544592524342804, 29.79057627198102409 ) ) ;
#108627 = CARTESIAN_POINT ( 'NONE',  ( -5.049401038298153566, 19.05341960407611168, 90.20724293864766707 ) ) ;
#108628 = CARTESIAN_POINT ( 'NONE',  ( -21.53943276465977519, 0.05219959533907696930, 56.24890960531436690 ) ) ;
#108630 = CARTESIAN_POINT ( 'NONE',  ( -16.53943276465976808, -0.05219959533934237506, 33.75109039468568284 ) ) ;
#108629 = CARTESIAN_POINT ( 'NONE',  ( 5.719274019375991003, -21.55341960407610458, 92.70724293864770971 ) ) ;
#108631 = CARTESIAN_POINT ( 'NONE',  ( -15.72974639402197994, 15.80617190586746368, 35.62390960531437401 ) ) ;
#108632 = CARTESIAN_POINT ( 'NONE',  ( 21.53943276465977519, 0.05219959533937863772, 86.25109039468568994 ) ) ;
#108633 = CARTESIAN_POINT ( 'NONE',  ( 9.474510206698971260, -16.51473224551069308, 92.91557627198103830 ) ) ;
#108634 = CARTESIAN_POINT ( 'NONE',  ( 5.049401038298161559, -19.05341960407611168, 42.70724293864767418 ) ) ;
#108635 = CARTESIAN_POINT ( 'NONE',  ( -16.51473224551069308, -9.474510206698971260, 96.66557627198102409 ) ) ;
#108636 = CARTESIAN_POINT ( 'NONE',  ( 14.34966873604960469, 8.224510206698951720, 99.16557627198100988 ) ) ;
#108637 = CARTESIAN_POINT ( 'NONE',  ( 19.03943276465977164, -0.05219959533909143690, 58.74890960531435979 ) ) ;
#108638 = CARTESIAN_POINT ( 'NONE',  ( 13.89961937509957401, 13.97604488694547697, 111.8760903946856757 ) ) ;
#108639 = CARTESIAN_POINT ( 'NONE',  ( -69.65682714487590488, -71.74905178543390605, -4.999999999999999112 ) ) ;
#108640 = EDGE_CURVE ( 'NONE', #53672, #71844, #103570, .T. ) ;
#108642 = CARTESIAN_POINT ( 'NONE',  ( 13.97604488694527802, 13.89961937509977652, 109.3739096053143669 ) ) ;
#108641 = CARTESIAN_POINT ( 'NONE',  ( -21.55341960407619339, 5.719274019375674811, 103.5427570613523613 ) ) ;
#108643 = CARTESIAN_POINT ( 'NONE',  ( 16.53943276465976808, 0.05219959533934440121, 86.25109039468568994 ) ) ;
#108644 = CARTESIAN_POINT ( 'NONE',  ( 3.766062262543149401E-15, -39.95556452105413570, -9.500000000000000000 ) ) ;
#108645 = CARTESIAN_POINT ( 'NONE',  ( 0.05219959533936267826, -19.03943276465977164, 70.00109039468566152 ) ) ;
#108646 = CARTESIAN_POINT ( 'NONE',  ( -13.97604488694547697, 13.89961937509957934, 33.12609039468566863 ) ) ;
#108647 = CARTESIAN_POINT ( 'NONE',  ( 10.65970682939788716, -25.60940286011448919, 139.9999999999999716 ) ) ;
#108648 = CARTESIAN_POINT ( 'NONE',  ( -5.153800228976328057, -19.02544592524343514, 32.29057627198102409 ) ) ;
#108649 = CARTESIAN_POINT ( 'NONE',  ( -8.314922557960811034, -14.29746914071050412, 32.08224293864769550 ) ) ;
#108650 = CARTESIAN_POINT ( 'NONE',  ( -16.46253265017160317, 9.564922557960807481, 25.83224293864769194 ) ) ;
#108651 = CARTESIAN_POINT ( 'NONE',  ( -4.483927247898539470, -16.52544592524342804, 22.29057627198102765 ) ) ;
#108652 = CARTESIAN_POINT ( 'NONE',  ( 17.31728774477273092, 6.344390552232405334, 66.68093348310682700 ) ) ;
#108653 = CARTESIAN_POINT ( 'NONE',  ( 14.34966873604972726, -8.224510206698740333, 90.83442372801901854 ) ) ;
#108654 = CARTESIAN_POINT ( 'NONE',  ( -19.03943276465977164, 0.05219959533909376836, 31.24890960531435979 ) ) ;
#108655 = CARTESIAN_POINT ( 'NONE',  ( -0.05219959533937732626, 21.53943276465977519, 112.5010903946857042 ) ) ;
#108656 = CARTESIAN_POINT ( 'NONE',  ( -12.06949235617739369, -12.14591786802326823, 19.37609039468568639 ) ) ;
#108657 = CARTESIAN_POINT ( 'NONE',  ( -21.52544592524334988, -5.823673210054445271, 83.95942372801900433 ) ) ;
#108658 = CARTESIAN_POINT ( 'NONE',  ( -19.02544592524334988, -5.153800228976617603, 48.95942372801900433 ) ) ;
#108659 = CARTESIAN_POINT ( 'NONE',  ( 16.51473224551069308, 9.474510206698969483, 89.16557627198103830 ) ) ;
#108660 = CARTESIAN_POINT ( 'NONE',  ( -16.46253265017160317, 9.564922557960807481, 75.83224293864769550 ) ) ;
#108661 = CARTESIAN_POINT ( 'NONE',  ( -19.52217212775656563, 5.500000000000114575, 39.93993709005260939 ) ) ;
#108662 = CARTESIAN_POINT ( 'NONE',  ( -5.823673210054116645, -21.52544592524344225, 92.29057627198103830 ) ) ;
#108663 = VECTOR ( 'NONE', #44667, 1000.000000000000000 ) ;
#108664 = CARTESIAN_POINT ( 'NONE',  ( 12.14591786802309770, 12.06949235617756955, 69.37390960531436690 ) ) ;
#108665 = CARTESIAN_POINT ( 'NONE',  ( -15.72974639402197994, 15.80617190586746368, 65.62390960531436690 ) ) ;
#108666 = CARTESIAN_POINT ( 'NONE',  ( 19.05341960407611168, 5.049401038298154454, 53.95724293864770260 ) ) ;
#108668 = CARTESIAN_POINT ( 'NONE',  ( -8.314922557961024197, 14.29746914071037800, 72.91775706135234714 ) ) ;
#108667 = CARTESIAN_POINT ( 'NONE',  ( -18.62759615963270932, 10.81492255796079327, 85.83224293864768129 ) ) ;
#108669 = ORIENTED_EDGE ( 'NONE', *, *, #53035, .F. ) ;
#108670 = CARTESIAN_POINT ( 'NONE',  ( 0.05219959533909260263, 19.03943276465977164, 49.99890960531435979 ) ) ;
#108672 = CARTESIAN_POINT ( 'NONE',  ( 21.75476783670601222, -5.835674035550355576, 172.5278397751181387 ) ) ;
#108671 = CARTESIAN_POINT ( 'NONE',  ( 16.52544592524342804, -4.483927247898539470, 83.54057627198102409 ) ) ;
#108673 = CARTESIAN_POINT ( 'NONE',  ( -19.03943276465977164, 0.05219959533909376836, 51.24890960531436690 ) ) ;
#108674 = CARTESIAN_POINT ( 'NONE',  ( 12.06949235617757843, -12.14591786802309237, 113.1239096053143953 ) ) ;
#108675 = CARTESIAN_POINT ( 'NONE',  ( 16.51473224551083163, -9.474510206698727899, 60.83442372801900433 ) ) ;
#108676 = CARTESIAN_POINT ( 'NONE',  ( 0.05219959533910956823, 16.53943276465976808, 79.99890960531435269 ) ) ;
#108677 = CARTESIAN_POINT ( 'NONE',  ( -18.67979575497193778, 10.72451020669871902, 43.33442372801901143 ) ) ;
#108679 = CARTESIAN_POINT ( 'NONE',  ( -5.719274019375978568, 21.55341960407610458, 100.2072429386476955 ) ) ;
#108678 = CARTESIAN_POINT ( 'NONE',  ( 13.89961937509977652, -13.97604488694527269, 38.12390960531436690 ) ) ;
#108680 = CARTESIAN_POINT ( 'NONE',  ( -0.05219959533910754901, -16.53943276465976808, 92.49890960531436690 ) ) ;
#108681 = CARTESIAN_POINT ( 'NONE',  ( 25.49187754477041779, -30.53313611124049487, -20.74730905734758224 ) ) ;
#108682 = CARTESIAN_POINT ( 'NONE',  ( 9.564922557960805705, 16.46253265017160317, 49.58224293864770260 ) ) ;
#108683 = PLANE ( 'NONE',  #134581 ) ;
#108685 = CARTESIAN_POINT ( 'NONE',  ( 9.564922557960805705, 16.46253265017160317, 94.58224293864769550 ) ) ;
#108684 = CARTESIAN_POINT ( 'NONE',  ( 19.05341960407617918, -5.049401038297876454, 101.0427570613523045 ) ) ;
#108686 = CARTESIAN_POINT ( 'NONE',  ( 18.62759615963255655, 10.81492255796105972, 36.66775706135234714 ) ) ;
#108687 = CARTESIAN_POINT ( 'NONE',  ( -0.05219959533909027116, -19.03943276465977164, 87.49890960531436690 ) ) ;
#108688 = CARTESIAN_POINT ( 'NONE',  ( -9.564922557961040184, 16.46253265017147172, 67.91775706135233293 ) ) ;
#108689 = CARTESIAN_POINT ( 'NONE',  ( 0.05219959533909260263, 19.03943276465977164, 44.99890960531435979 ) ) ;
#108690 = CARTESIAN_POINT ( 'NONE',  ( -4.483927247898539470, -16.52544592524342804, 72.29057627198102409 ) ) ;
#108691 = CARTESIAN_POINT ( 'NONE',  ( 14.29746914071049879, -8.314922557960816363, 73.33224293864769550 ) ) ;
#108692 = CARTESIAN_POINT ( 'NONE',  ( 5.153800228976335163, 19.02544592524342804, 89.79057627198102409 ) ) ;
#108693 = CARTESIAN_POINT ( 'NONE',  ( 15.72974639402199770, -15.80617190586745480, 98.12390960531436690 ) ) ;
#108694 = CARTESIAN_POINT ( 'NONE',  ( 19.03943276465977164, -0.05219959533909143690, 78.74890960531436690 ) ) ;
#108695 = CARTESIAN_POINT ( 'NONE',  ( 9.564922557961047289, -16.46253265017146816, 30.41775706135232937 ) ) ;
#108698 = CARTESIAN_POINT ( 'NONE',  ( 16.53943276465976808, -0.05219959533910856209, 113.7489096053143527 ) ) ;
#108697 = CARTESIAN_POINT ( 'NONE',  ( -12.06949235617756955, 12.14591786802309770, 25.62390960531435624 ) ) ;
#108696 = CARTESIAN_POINT ( 'NONE',  ( 5.153800228976335163, 19.02544592524342804, 39.79057627198100988 ) ) ;
#108699 = CARTESIAN_POINT ( 'NONE',  ( 13.97604488694548053, -13.89961937509957401, 105.6260903946856757 ) ) ;
#108700 = ORIENTED_EDGE ( 'NONE', *, *, #114298, .T. ) ;
#108701 = CARTESIAN_POINT ( 'NONE',  ( -5.719274019375665041, -21.55341960407619695, 29.79275706135234358 ) ) ;
#108702 = CARTESIAN_POINT ( 'NONE',  ( -13.89961937509957401, -13.97604488694547875, 69.37609039468564731 ) ) ;
#108703 = CARTESIAN_POINT ( 'NONE',  ( 8.224510206698953496, -14.34966873604960469, 22.91557627198102765 ) ) ;
#108704 = CARTESIAN_POINT ( 'NONE',  ( 18.62759615963271287, -10.81492255796078972, 88.33224293864769550 ) ) ;
#108705 = CARTESIAN_POINT ( 'NONE',  ( 16.46253265017160672, -9.564922557960803928, 113.3322429386476955 ) ) ;
#108706 = CARTESIAN_POINT ( 'NONE',  ( 16.53943276465976808, -0.05219959533910856209, 63.74890960531435979 ) ) ;
#108707 = CARTESIAN_POINT ( 'NONE',  ( 9.474510206698971260, -16.51473224551069308, 32.91557627198102409 ) ) ;
#108708 = CARTESIAN_POINT ( 'NONE',  ( 5.049401038297881783, 19.05341960407617563, 27.29275706135232937 ) ) ;
#108709 = CARTESIAN_POINT ( 'NONE',  ( 0.05219959533934541429, -16.53943276465976808, 85.00109039468568994 ) ) ;
#108710 = CARTESIAN_POINT ( 'NONE',  ( -12.06949235617739369, -12.14591786802326823, 59.37609039468568284 ) ) ;
#108711 = CARTESIAN_POINT ( 'NONE',  ( 19.02544592524343514, -5.153800228976328945, 113.5405762719810241 ) ) ;
#108712 = CARTESIAN_POINT ( 'NONE',  ( 5.823673210054444382, -21.52544592524334988, 110.2094237280190185 ) ) ;
#108713 = CARTESIAN_POINT ( 'NONE',  ( -9.564922557960796823, -16.46253265017161027, 82.08224293864768129 ) ) ;
#108714 = AXIS2_PLACEMENT_3D ( 'NONE', #20169, #78854, #127340 ) ;
#108715 = CARTESIAN_POINT ( 'NONE',  ( 8.224510206698742110, 14.34966873604972548, 62.08442372801901143 ) ) ;
#108716 = CARTESIAN_POINT ( 'NONE',  ( 13.89961937509977652, -13.97604488694527269, 28.12390960531435624 ) ) ;
#108717 = EDGE_CURVE ( 'NONE', #85078, #187938, #88378, .T. ) ;
#108718 = CARTESIAN_POINT ( 'NONE',  ( 4.483927247898545687, 16.52544592524342804, 34.79057627198103120 ) ) ;
#108719 = CYLINDRICAL_SURFACE ( 'NONE', #147557, 5.000000000000000888 ) ;
#108722 = CARTESIAN_POINT ( 'NONE',  ( 19.03943276465977164, -0.05219959533909143690, 73.74890960531435269 ) ) ;
#108721 = CARTESIAN_POINT ( 'NONE',  ( 9.564922557960805705, 16.46253265017160317, 109.5822429386476955 ) ) ;
#108720 = CARTESIAN_POINT ( 'NONE',  ( -21.53943276465977519, -0.05219959533937600094, 63.75109039468568284 ) ) ;
#108723 = CARTESIAN_POINT ( 'NONE',  ( -9.474510206698964154, 16.51473224551069663, 110.4155762719810383 ) ) ;
#108724 = CARTESIAN_POINT ( 'NONE',  ( 0.05219959533910956823, 16.53943276465976808, 54.99890960531435269 ) ) ;
#108725 = CARTESIAN_POINT ( 'NONE',  ( 4.379528057220339221, -16.55341960407611168, 32.70724293864770260 ) ) ;
#108726 = CARTESIAN_POINT ( 'NONE',  ( -12.14591786802309592, -12.06949235617757132, 56.87390960531436690 ) ) ;
#108728 = CARTESIAN_POINT ( 'NONE',  ( -193.3062444957834884, -155.7167183371838064, 0.000000000000000000 ) ) ;
#108727 = CARTESIAN_POINT ( 'NONE',  ( -0.05219959533934338120, 16.53943276465976808, 42.50109039468567573 ) ) ;
#108729 = CARTESIAN_POINT ( 'NONE',  ( 19.02544592524334988, 5.153800228976608722, 51.45942372801900433 ) ) ;
#108730 = CARTESIAN_POINT ( 'NONE',  ( -13.89961937509977652, 13.97604488694528158, 70.62390960531432427 ) ) ;
#108731 = CARTESIAN_POINT ( 'NONE',  ( -9.564922557961040184, 16.46253265017147172, 47.91775706135233293 ) ) ;
#108732 = CARTESIAN_POINT ( 'NONE',  ( -0.05219959533936034679, 19.03943276465977164, 62.50109039468566863 ) ) ;
#108734 = CARTESIAN_POINT ( 'NONE',  ( 8.224510206698742110, 14.34966873604972548, 87.08442372801901854 ) ) ;
#108733 = CARTESIAN_POINT ( 'NONE',  ( -13.89961937509957401, -13.97604488694547875, 104.3760903946856757 ) ) ;
#108735 = CARTESIAN_POINT ( 'NONE',  ( -17.14385361876520619, 23.59649016807275856, 147.0750000027311728 ) ) ;
#108736 = CARTESIAN_POINT ( 'NONE',  ( -13.89961937509977652, 13.97604488694528158, 30.62390960531435269 ) ) ;
#108737 =( BOUNDED_CURVE ( )  B_SPLINE_CURVE ( 2, ( #187024, #44753, #48495, #91219, #157652, #142470, #110149, #113116, #65627, #168090, #112135 ),
 .UNSPECIFIED., .F., .T. ) 
 B_SPLINE_CURVE_WITH_KNOTS ( ( 3, 2, 2, 2, 2, 3 ),
 ( 0.4000000000000000222, 0.4199999999999999845, 0.4400000000000000577, 0.4600000000000000755, 0.4800000000000000933, 0.5000000000000001110 ),
 .UNSPECIFIED. ) 
 CURVE ( )  GEOMETRIC_REPRESENTATION_ITEM ( )  RATIONAL_B_SPLINE_CURVE ( ( 1.000000000000000000, 0.9510565162951535312, 1.000000000000000000, 0.9510565162951535312, 1.000000000000000000, 0.9510565162951535312, 1.000000000000000000, 0.9510565162951535312, 1.000000000000000000, 0.9510565162951533091, 1.000000000000000222 ) ) 
 REPRESENTATION_ITEM ( '' )  );
#108738 = CARTESIAN_POINT ( 'NONE',  ( -13.97604488694527625, -13.89961937509977652, 106.8739096053143669 ) ) ;
#108739 = CARTESIAN_POINT ( 'NONE',  ( 10.72451020669871369, 18.67979575497193778, 42.08442372801901854 ) ) ;
#108740 = CARTESIAN_POINT ( 'NONE',  ( -9.474510206698720793, -16.51473224551083518, 104.5844237280190043 ) ) ;
#108742 = CARTESIAN_POINT ( 'NONE',  ( -19.05341960407611168, -5.049401038298163336, 66.45724293864769550 ) ) ;
#108741 = CARTESIAN_POINT ( 'NONE',  ( 17.50000000000000000, -5.068104630630386964, 108.2281840534002697 ) ) ;
#108743 = CARTESIAN_POINT ( 'NONE',  ( 9.564922557960805705, 16.46253265017160317, 109.5822429386476955 ) ) ;
#108745 = CARTESIAN_POINT ( 'NONE',  ( 19.05341960407611168, 5.049401038298154454, 58.95724293864768129 ) ) ;
#108744 = CARTESIAN_POINT ( 'NONE',  ( 16.52544592524342804, -4.483927247898539470, 58.54057627198103120 ) ) ;
#108746 = CARTESIAN_POINT ( 'NONE',  ( -0.05219959533909027116, -19.03943276465977164, 57.49890960531435979 ) ) ;
#108747 = CARTESIAN_POINT ( 'NONE',  ( -5.153800228976607833, 19.02544592524334988, 77.70942372801900433 ) ) ;
#108748 = CARTESIAN_POINT ( 'NONE',  ( 21.55341960407610458, 5.719274019375980345, 48.95724293864770971 ) ) ;
#108749 = CARTESIAN_POINT ( 'NONE',  ( -16.46253265017146816, -9.564922557961047289, 44.16775706135232582 ) ) ;
#108750 = CARTESIAN_POINT ( 'NONE',  ( 16.46253265017160672, -9.564922557960803928, 83.33224293864768129 ) ) ;
#108751 = CARTESIAN_POINT ( 'NONE',  ( -10.81492255796078084, -18.62759615963271287, 77.08224293864769550 ) ) ;
#108753 = CARTESIAN_POINT ( 'NONE',  ( 0.05219959533936267826, -19.03943276465977164, 40.00109039468566152 ) ) ;
#108752 = CARTESIAN_POINT ( 'NONE',  ( -16.52544592524342804, 4.483927247898546575, 86.04057627198102409 ) ) ;
#108754 = CARTESIAN_POINT ( 'NONE',  ( -5.823673210054116645, -21.52544592524344225, 47.29057627198103120 ) ) ;
#108755 = CARTESIAN_POINT ( 'NONE',  ( 21.55341960407610458, 5.719274019375980345, 38.95724293864768839 ) ) ;
#108756 = CARTESIAN_POINT ( 'NONE',  ( 5.049401038298161559, -19.05341960407611168, 62.70724293864769550 ) ) ;
#108757 = CARTESIAN_POINT ( 'NONE',  ( 13.89961937509977652, -13.97604488694527269, 48.12390960531435979 ) ) ;
#108758 = CARTESIAN_POINT ( 'NONE',  ( -16.51473224551069308, -9.474510206698971260, 21.66557627198102765 ) ) ;
#108759 = CARTESIAN_POINT ( 'NONE',  ( -18.67979575497193778, 10.72451020669871902, 28.33442372801902209 ) ) ;
#108760 = CARTESIAN_POINT ( 'NONE',  ( -19.02544592524342804, 5.153800228976336051, 111.0405762719810099 ) ) ;
#108761 = CARTESIAN_POINT ( 'NONE',  ( -15.80617190586768217, 15.72974639402176855, 38.12609039468567573 ) ) ;
#108762 = CARTESIAN_POINT ( 'NONE',  ( -19.03943276465977164, 0.05219959533909376836, 36.24890960531436690 ) ) ;
#108763 = CARTESIAN_POINT ( 'NONE',  ( 10.72451020669898902, -18.67979575497178502, 112.9155762719810383 ) ) ;
#108764 = CARTESIAN_POINT ( 'NONE',  ( 19.02544592524334988, 5.153800228976608722, 41.45942372801900433 ) ) ;
#108765 = PLANE ( 'NONE',  #192481 ) ;
#108766 = CARTESIAN_POINT ( 'NONE',  ( 13.89961937509977652, -13.97604488694527269, 23.12390960531436335 ) ) ;
#108767 = CARTESIAN_POINT ( 'NONE',  ( 4.483927247898790824, -16.52544592524335698, 55.20942372801902565 ) ) ;
#108768 = CARTESIAN_POINT ( 'NONE',  ( 19.05341960407611168, 5.049401038298154454, 28.95724293864769550 ) ) ;
#108769 = CARTESIAN_POINT ( 'NONE',  ( -31.80000000000000782, -5.510910596163089556E-15, 42.29999999999999716 ) ) ;
#108770 = CARTESIAN_POINT ( 'NONE',  ( 5.049401038298161559, -19.05341960407611168, 77.70724293864765286 ) ) ;
#108771 = CARTESIAN_POINT ( 'NONE',  ( 16.52544592524342804, -4.483927247898539470, 113.5405762719810383 ) ) ;
#108772 = CARTESIAN_POINT ( 'NONE',  ( -21.52544592524343514, 5.823673210054127303, 61.04057627198103120 ) ) ;
#108773 = CARTESIAN_POINT ( 'NONE',  ( -12.14591786802309592, -12.06949235617757132, 76.87390960531439532 ) ) ;
#108774 = CARTESIAN_POINT ( 'NONE',  ( 16.52544592524335698, 4.483927247898782831, 36.45942372801901143 ) ) ;
#108775 = CARTESIAN_POINT ( 'NONE',  ( -5.823673210054431948, 21.52544592524334988, 92.70942372801901854 ) ) ;
#108776 = CYLINDRICAL_SURFACE ( 'NONE', #1198, 5.000000000000000888 ) ;
#108777 = CARTESIAN_POINT ( 'NONE',  ( 12.14591786802327356, -12.06949235617739191, 105.6260903946856899 ) ) ;
#108778 = CARTESIAN_POINT ( 'NONE',  ( 12.06949235617757843, -12.14591786802309237, 48.12390960531436690 ) ) ;
#108779 = CARTESIAN_POINT ( 'NONE',  ( -13.89961937509977652, 13.97604488694528158, 50.62390960531435979 ) ) ;
#108780 = CARTESIAN_POINT ( 'NONE',  ( -5.719274019375665041, -21.55341960407619695, 89.79275706135236135 ) ) ;
#108781 = CARTESIAN_POINT ( 'NONE',  ( 10.81492255796078972, 18.62759615963270932, 104.5822429386477097 ) ) ;
#108782 = CARTESIAN_POINT ( 'NONE',  ( 18.67979575497194134, -10.72451020669871369, 75.83442372801900433 ) ) ;
#108783 = CARTESIAN_POINT ( 'NONE',  ( -14.34966873604972548, 8.224510206698743886, 58.33442372801901143 ) ) ;
#108785 = CARTESIAN_POINT ( 'NONE',  ( 18.67979575497194134, -10.72451020669871369, 90.83442372801901854 ) ) ;
#108784 = CARTESIAN_POINT ( 'NONE',  ( 8.224510206698953496, -14.34966873604960469, 82.91557627198103830 ) ) ;
#108786 = CARTESIAN_POINT ( 'NONE',  ( -8.314922557961024197, 14.29746914071037800, 107.9177570613523471 ) ) ;
#108787 = CARTESIAN_POINT ( 'NONE',  ( -16.38665767535054840, 7.295008042176092111, 115.2640086421455408 ) ) ;
#108788 = CARTESIAN_POINT ( 'NONE',  ( 0.05219959533934541429, -16.53943276465976808, 45.00109039468568284 ) ) ;
#108789 = CARTESIAN_POINT ( 'NONE',  ( -14.34966873604960291, -8.224510206698953496, 36.66557627198103120 ) ) ;
#108790 = CARTESIAN_POINT ( 'NONE',  ( 8.314922557961029526, -14.29746914071037800, 80.41775706135234714 ) ) ;
#108791 = CARTESIAN_POINT ( 'NONE',  ( -19.02544592524342804, 5.153800228976336051, 101.0405762719810241 ) ) ;
#108792 = CARTESIAN_POINT ( 'NONE',  ( -5.719274019375978568, 21.55341960407610458, 25.20724293864769550 ) ) ;
#108793 = CARTESIAN_POINT ( 'NONE',  ( 0.05219959533937995610, -21.53943276465977519, 95.00109039468568994 ) ) ;
#108794 = CARTESIAN_POINT ( 'NONE',  ( 16.55341960407618274, -4.379528057220086978, 96.04275706135236135 ) ) ;
#108795 = CARTESIAN_POINT ( 'NONE',  ( 12.14591786802309770, 12.06949235617756955, 69.37390960531436690 ) ) ;
#108796 = CARTESIAN_POINT ( 'NONE',  ( 19.03943276465977164, -0.05219959533909143690, 83.74890960531436690 ) ) ;
#108797 = EDGE_LOOP ( 'NONE', ( #101708, #70995, #154186, #62470 ) ) ;
#108798 = CARTESIAN_POINT ( 'NONE',  ( -16.53943276465976808, -0.05219959533934237506, 23.75109039468567929 ) ) ;
#108799 = CARTESIAN_POINT ( 'NONE',  ( 19.05341960407611168, 5.049401038298154454, 28.95724293864769550 ) ) ;
#108800 = CARTESIAN_POINT ( 'NONE',  ( -16.46253265017160317, 9.564922557960807481, 85.83224293864769550 ) ) ;
#108802 = CARTESIAN_POINT ( 'NONE',  ( -5.950531402560715689E-15, 38.81732327939063509, -5.124999997268813168 ) ) ;
#108801 = CARTESIAN_POINT ( 'NONE',  ( -14.34966873604972548, 8.224510206698743886, 28.33442372801902209 ) ) ;
#108803 = CARTESIAN_POINT ( 'NONE',  ( -19.03943276465977164, -0.05219959533935918106, 33.75109039468566863 ) ) ;
#108804 = CARTESIAN_POINT ( 'NONE',  ( -16.52544592524335698, -4.483927247898792601, 98.95942372801903275 ) ) ;
#108805 = CARTESIAN_POINT ( 'NONE',  ( 5.153800228976335163, 19.02544592524342804, 29.79057627198102409 ) ) ;
#108806 = CARTESIAN_POINT ( 'NONE',  ( -14.34966873604972548, 8.224510206698743886, 73.33442372801901854 ) ) ;
#108807 = CARTESIAN_POINT ( 'NONE',  ( 14.34966873604972726, -8.224510206698740333, 70.83442372801901854 ) ) ;
#108808 = CARTESIAN_POINT ( 'NONE',  ( -16.51473224551082808, 9.474510206698731452, 78.33442372801900433 ) ) ;
#108809 = CARTESIAN_POINT ( 'NONE',  ( -18.67979575497193778, 10.72451020669871902, 108.3344237280190185 ) ) ;
#108810 = CARTESIAN_POINT ( 'NONE',  ( -0.05219959533909027116, -19.03943276465977164, 47.49890960531435979 ) ) ;
#108811 = CARTESIAN_POINT ( 'NONE',  ( -19.02544592524342804, 5.153800228976336051, 86.04057627198103830 ) ) ;
#108812 = CARTESIAN_POINT ( 'NONE',  ( -16.52544592524342804, 4.483927247898546575, 91.04057627198103830 ) ) ;
#108813 = AXIS2_PLACEMENT_3D ( 'NONE', #50132, #110796, #21778 ) ;
#108814 = CARTESIAN_POINT ( 'NONE',  ( 16.51473224551083163, -9.474510206698727899, 60.83442372801900433 ) ) ;
#108815 = CARTESIAN_POINT ( 'NONE',  ( 5.823673210054125526, 21.52544592524343514, 44.79057627198103120 ) ) ;
#108816 = CARTESIAN_POINT ( 'NONE',  ( -19.02544592524334988, -5.153800228976617603, 28.95942372801900433 ) ) ;
#108817 = CARTESIAN_POINT ( 'NONE',  ( -13.89961937509977652, 13.97604488694528158, 85.62390960531433848 ) ) ;
#108818 = CARTESIAN_POINT ( 'NONE',  ( 18.67979575497178502, 10.72451020669898547, 79.16557627198103830 ) ) ;
#108819 = CARTESIAN_POINT ( 'NONE',  ( -5.049401038298153566, 19.05341960407611168, 115.2072429386477097 ) ) ;
#108820 = CARTESIAN_POINT ( 'NONE',  ( -0.05219959533936034679, 19.03943276465977164, 92.50109039468566152 ) ) ;
#108821 = CARTESIAN_POINT ( 'NONE',  ( -17.49999999999999645, 3.305555262949665618, 109.6251715215659317 ) ) ;
#108822 = CARTESIAN_POINT ( 'NONE',  ( -5.153800228976607833, 19.02544592524334988, 107.7094237280189759 ) ) ;
#108823 = CARTESIAN_POINT ( 'NONE',  ( 9.564922557960805705, 16.46253265017160317, 29.58224293864769550 ) ) ;
#108824 = CARTESIAN_POINT ( 'NONE',  ( 19.05341960407611168, 5.049401038298154454, 103.9572429386476671 ) ) ;
#108825 = CARTESIAN_POINT ( 'NONE',  ( -15.72974639402197994, 15.80617190586746368, 70.62390960531436690 ) ) ;
#108826 = CARTESIAN_POINT ( 'NONE',  ( 14.34966873604972726, -8.224510206698740333, 45.83442372801901854 ) ) ;
#108827 = CARTESIAN_POINT ( 'NONE',  ( -21.53943276465977519, -0.05219959533937600094, 48.75109039468568284 ) ) ;
#108829 = CARTESIAN_POINT ( 'NONE',  ( 21.55341960407619695, -5.719274019375665929, 101.0427570613523756 ) ) ;
#108828 = CARTESIAN_POINT ( 'NONE',  ( 5.049401038297881783, 19.05341960407617563, 87.29275706135234714 ) ) ;
#108830 = CARTESIAN_POINT ( 'NONE',  ( 8.314922557961029526, -14.29746914071037800, 110.4177570613523756 ) ) ;
#108831 = CARTESIAN_POINT ( 'NONE',  ( -5.153800228976328057, -19.02544592524343514, 107.2905762719810383 ) ) ;
#108832 = CARTESIAN_POINT ( 'NONE',  ( -8.224510206698948167, 14.34966873604960824, 90.41557627198103830 ) ) ;
#108833 = CARTESIAN_POINT ( 'NONE',  ( 12.14591786802309770, 12.06949235617756955, 34.37390960531435979 ) ) ;
#108834 = CARTESIAN_POINT ( 'NONE',  ( -13.89961937509957401, -13.97604488694547875, 69.37609039468564731 ) ) ;
#108835 = CARTESIAN_POINT ( 'NONE',  ( -21.55341960407619339, 5.719274019375674811, 58.54275706135235424 ) ) ;
#108836 = CARTESIAN_POINT ( 'NONE',  ( -13.89961937509957401, -13.97604488694547875, 29.37609039468565797 ) ) ;
#108837 = CARTESIAN_POINT ( 'NONE',  ( -16.52544592524342804, 4.483927247898546575, 106.0405762719810525 ) ) ;
#108838 = CARTESIAN_POINT ( 'NONE',  ( 21.55341960407610458, 5.719274019375980345, 33.95724293864769550 ) ) ;
#108839 = CARTESIAN_POINT ( 'NONE',  ( 8.224510206698953496, -14.34966873604960469, 27.91557627198103830 ) ) ;
#108840 = CARTESIAN_POINT ( 'NONE',  ( 18.62759615963255655, 10.81492255796105972, 101.6677570613523613 ) ) ;
#108841 = CARTESIAN_POINT ( 'NONE',  ( 8.224510206698742110, 14.34966873604972548, 57.08442372801901854 ) ) ;
#108842 = CARTESIAN_POINT ( 'NONE',  ( -14.34966873604960291, -8.224510206698953496, 31.66557627198102054 ) ) ;
#108843 = CARTESIAN_POINT ( 'NONE',  ( -21.53943276465977519, -0.05219959533937600094, 63.75109039468568284 ) ) ;
#108844 = CARTESIAN_POINT ( 'NONE',  ( -21.52544592524334988, -5.823673210054445271, 58.95942372801902565 ) ) ;
#108845 = ORIENTED_EDGE ( 'NONE', *, *, #149178, .T. ) ;
#108846 = CARTESIAN_POINT ( 'NONE',  ( -23.48529157249600985, 32.32473071737754111, -6.049999994537625270 ) ) ;
#108847 = CARTESIAN_POINT ( 'NONE',  ( -0.05219959533937732626, 21.53943276465977519, 27.50109039468567929 ) ) ;
#108848 = CARTESIAN_POINT ( 'NONE',  ( 0.05219959533910956823, 16.53943276465976808, 109.9989096053143527 ) ) ;
#108849 = CARTESIAN_POINT ( 'NONE',  ( -13.89961937509977652, 13.97604488694528158, 25.62390960531434558 ) ) ;
#108850 = CARTESIAN_POINT ( 'NONE',  ( -14.29746914071049879, 8.314922557960819915, 80.83224293864769550 ) ) ;
#108851 = CARTESIAN_POINT ( 'NONE',  ( -9.564922557960796823, -16.46253265017161027, 67.08224293864769550 ) ) ;
#108852 = CARTESIAN_POINT ( 'NONE',  ( 4.379528057220339221, -16.55341960407611168, 22.70724293864769194 ) ) ;
#108853 = CARTESIAN_POINT ( 'NONE',  ( 5.823673210054125526, 21.52544592524343514, 49.79057627198102409 ) ) ;
#108854 = CARTESIAN_POINT ( 'NONE',  ( 8.314922557960818139, 14.29746914071049879, 94.58224293864769550 ) ) ;
#108855 = VECTOR ( 'NONE', #77384, 1000.000000000000000 ) ;
#108856 = CARTESIAN_POINT ( 'NONE',  ( 15.80617190586746368, 15.72974639402197994, 99.37390960531436690 ) ) ;
#108857 = CARTESIAN_POINT ( 'NONE',  ( -9.564922557960796823, -16.46253265017161027, 107.0822429386476955 ) ) ;
#108859 = CARTESIAN_POINT ( 'NONE',  ( -5.153800228976607833, 19.02544592524334988, 107.7094237280189759 ) ) ;
#108858 = CARTESIAN_POINT ( 'NONE',  ( 9.474510206698971260, -16.51473224551069308, 52.91557627198102409 ) ) ;
#108860 = CARTESIAN_POINT ( 'NONE',  ( -10.72451020669898014, 18.67979575497178502, 50.41557627198103120 ) ) ;
#108861 = CARTESIAN_POINT ( 'NONE',  ( 10.72451020669871369, 18.67979575497193778, 67.08442372801901854 ) ) ;
#108862 = CARTESIAN_POINT ( 'NONE',  ( 13.89961937509977652, -13.97604488694527269, 63.12390960531435979 ) ) ;
#108863 = CARTESIAN_POINT ( 'NONE',  ( -13.89961937509977652, 13.97604488694528158, 95.62390960531436690 ) ) ;
#108864 = CARTESIAN_POINT ( 'NONE',  ( 16.53943276465976808, 0.05219959533934440121, 61.25109039468567573 ) ) ;
#108865 = CARTESIAN_POINT ( 'NONE',  ( 15.72974639402176855, 15.80617190586768217, 56.87609039468568994 ) ) ;
#108866 = CARTESIAN_POINT ( 'NONE',  ( -21.53943276465977519, -0.05219959533937600094, 88.75109039468567573 ) ) ;
#108867 = CARTESIAN_POINT ( 'NONE',  ( -15.80617190586745835, -15.72974639402198527, 96.87390960531436690 ) ) ;
#108869 = CARTESIAN_POINT ( 'NONE',  ( -12.06949235617739369, -12.14591786802326823, 74.37609039468568994 ) ) ;
#108868 = CARTESIAN_POINT ( 'NONE',  ( -18.67979575497193778, 10.72451020669871902, 38.33442372801900433 ) ) ;
#108870 = CARTESIAN_POINT ( 'NONE',  ( 5.719274019375991003, -21.55341960407610458, 82.70724293864770971 ) ) ;
#108871 = CARTESIAN_POINT ( 'NONE',  ( 19.03943276465977164, 0.05219959533936151252, 31.25109039468566863 ) ) ;
#108873 = CARTESIAN_POINT ( 'NONE',  ( -4.483927247898539470, -16.52544592524342804, 27.29057627198103120 ) ) ;
#108872 = CARTESIAN_POINT ( 'NONE',  ( 19.03943276465977164, -0.05219959533909143690, 83.74890960531436690 ) ) ;
#108874 = SPHERICAL_SURFACE ( 'NONE', #133892, 0.5000000000000000000 ) ;
#108875 = CARTESIAN_POINT ( 'NONE',  ( -19.02544592524342804, 5.153800228976336051, 101.0405762719810241 ) ) ;
#108876 = DIRECTION ( 'NONE',  ( -1.000000000000000000, 0.000000000000000000, 0.000000000000000000 ) ) ;
#108877 = ADVANCED_FACE ( 'NONE', ( #81627 ), #11577, .F. ) ;
#108878 = CARTESIAN_POINT ( 'NONE',  ( -19.03943276465977164, -0.05219959533935918106, 93.75109039468566152 ) ) ;
#108879 = CARTESIAN_POINT ( 'NONE',  ( 10.72451020669898902, -18.67979575497178502, 72.91557627198103830 ) ) ;
#108880 = CARTESIAN_POINT ( 'NONE',  ( -16.53943276465976808, 0.05219959533911058130, 41.24890960531435269 ) ) ;
#108881 = CARTESIAN_POINT ( 'NONE',  ( -5.153800228976607833, 19.02544592524334988, 107.7094237280189759 ) ) ;
#108882 = CARTESIAN_POINT ( 'NONE',  ( 16.46253265017160672, -9.564922557960803928, 33.33224293864770260 ) ) ;
#108883 = CARTESIAN_POINT ( 'NONE',  ( -9.474510206698720793, -16.51473224551083518, 104.5844237280190043 ) ) ;
#108885 = CARTESIAN_POINT ( 'NONE',  ( 16.51473224551083163, -9.474510206698727899, 70.83442372801900433 ) ) ;
#108884 = CARTESIAN_POINT ( 'NONE',  ( -21.55341960407610458, -5.719274019375992779, 101.4572429386476955 ) ) ;
#108886 = CARTESIAN_POINT ( 'NONE',  ( 16.53943276465976808, 0.05219959533934440121, 81.25109039468568994 ) ) ;
#108887 = CARTESIAN_POINT ( 'NONE',  ( -5.153800228976328057, -19.02544592524343514, 67.29057627198102409 ) ) ;
#108888 = CARTESIAN_POINT ( 'NONE',  ( 12.06949235617757843, -12.14591786802309237, 83.12390960531436690 ) ) ;
#108889 = CARTESIAN_POINT ( 'NONE',  ( 9.474510206698971260, -16.51473224551069308, 62.91557627198102409 ) ) ;
#108890 = CARTESIAN_POINT ( 'NONE',  ( 4.379528057220339221, -16.55341960407611168, 62.70724293864769550 ) ) ;
#108891 = CARTESIAN_POINT ( 'NONE',  ( -15.49999999999999822, -7.500000000000000888, 118.0000000000000142 ) ) ;
#108892 = CARTESIAN_POINT ( 'NONE',  ( 17.62203461105333346, -16.21325560958408474, -54.50601694470664427 ) ) ;
#108893 = CARTESIAN_POINT ( 'NONE',  ( 0.05219959533910956823, 16.53943276465976808, 39.99890960531436690 ) ) ;
#108894 = CARTESIAN_POINT ( 'NONE',  ( -9.564922557960796823, -16.46253265017161027, 72.08224293864770971 ) ) ;
#108895 = LINE ( 'NONE', #184748, #189690 ) ;
#108896 = CARTESIAN_POINT ( 'NONE',  ( -19.05341960407617563, 5.049401038297882671, 58.54275706135234003 ) ) ;
#108897 = CARTESIAN_POINT ( 'NONE',  ( 8.314922557961029526, -14.29746914071037800, 60.41775706135235424 ) ) ;
#108898 = CARTESIAN_POINT ( 'NONE',  ( 5.823673210054125526, 21.52544592524343514, 64.79057627198103830 ) ) ;
#108899 = CARTESIAN_POINT ( 'NONE',  ( -13.97604488694547697, 13.89961937509957934, 28.12609039468565797 ) ) ;
#108900 = CARTESIAN_POINT ( 'NONE',  ( -9.564922557960796823, -16.46253265017161027, 82.08224293864768129 ) ) ;
#108901 = CARTESIAN_POINT ( 'NONE',  ( 0.8180779778021126658, 21.52520729097319574, -58.70525297292005718 ) ) ;
#108902 = CARTESIAN_POINT ( 'NONE',  ( -5.153800228976328057, -19.02544592524343514, 107.2905762719810383 ) ) ;
#108903 = CARTESIAN_POINT ( 'NONE',  ( 9.474510206698971260, -16.51473224551069308, 57.91557627198103120 ) ) ;
#108904 = CARTESIAN_POINT ( 'NONE',  ( 21.55341960407619695, -5.719274019375665929, 41.04275706135236135 ) ) ;
#108905 = CARTESIAN_POINT ( 'NONE',  ( -8.224510206698948167, 14.34966873604960824, 100.4155762719810241 ) ) ;
#108908 = ORIENTED_EDGE ( 'NONE', *, *, #118105, .F. ) ;
#108907 = CARTESIAN_POINT ( 'NONE',  ( -9.564922557960796823, -16.46253265017161027, 92.08224293864769550 ) ) ;
#108906 = CARTESIAN_POINT ( 'NONE',  ( -21.55341960407610458, -5.719274019375992779, 101.4572429386476955 ) ) ;
#108909 = CARTESIAN_POINT ( 'NONE',  ( -5.719274019375665041, -21.55341960407619695, 29.79275706135234358 ) ) ;
#108910 = ORIENTED_EDGE ( 'NONE', *, *, #96536, .F. ) ;
#108911 = CARTESIAN_POINT ( 'NONE',  ( 13.97604488694527802, 13.89961937509977652, 84.37390960531433848 ) ) ;
#108912 = CARTESIAN_POINT ( 'NONE',  ( 0.000000000000000000, 0.000000000000000000, -64.92279855667830191 ) ) ;
#108913 = CARTESIAN_POINT ( 'NONE',  ( 21.55341960407610458, 5.719274019375980345, 98.95724293864770971 ) ) ;
#108914 = CARTESIAN_POINT ( 'NONE',  ( -0.05219959533909027116, -19.03943276465977164, 52.49890960531436690 ) ) ;
#108915 = CARTESIAN_POINT ( 'NONE',  ( 13.89961937509957401, 13.97604488694547697, 106.8760903946856757 ) ) ;
#108916 = CARTESIAN_POINT ( 'NONE',  ( -29.86685920354755552, 21.69954338932564397, -3.324999997268813345 ) ) ;
#108917 = CARTESIAN_POINT ( 'NONE',  ( 5.153800228976335163, 19.02544592524342804, 29.79057627198102409 ) ) ;
#108918 = CARTESIAN_POINT ( 'NONE',  ( -21.55341960407619339, 5.719274019375674811, 83.54275706135234714 ) ) ;
#108920 = CARTESIAN_POINT ( 'NONE',  ( 0.05219959533937995610, -21.53943276465977519, 45.00109039468568284 ) ) ;
#108919 = CARTESIAN_POINT ( 'NONE',  ( 19.05341960407611168, 5.049401038298154454, 78.95724293864769550 ) ) ;
#108921 = CARTESIAN_POINT ( 'NONE',  ( 5.823673210054444382, -21.52544592524334988, 25.20942372801901854 ) ) ;
#108922 = CARTESIAN_POINT ( 'NONE',  ( 22.44159573604009594, -16.30477369853687364, 144.1750000027311671 ) ) ;
#108923 = CARTESIAN_POINT ( 'NONE',  ( 16.46253265017160672, -9.564922557960803928, 98.33224293864769550 ) ) ;
#108924 = CARTESIAN_POINT ( 'NONE',  ( 19.01529144963331674, 5.500000000000158096, 63.73431955728439391 ) ) ;
#108927 = CARTESIAN_POINT ( 'NONE',  ( -18.62759615963255300, -10.81492255796106328, 49.16775706135234003 ) ) ;
#108926 = CARTESIAN_POINT ( 'NONE',  ( 21.52544592524344225, -5.823673210054117533, 43.54057627198103830 ) ) ;
#108925 = CARTESIAN_POINT ( 'NONE',  ( -16.53943276465976808, -0.05219959533934237506, 43.75109039468568284 ) ) ;
#108928 = CARTESIAN_POINT ( 'NONE',  ( 5.823673210054444382, -21.52544592524334988, 75.20942372801901854 ) ) ;
#108929 = DIRECTION ( 'NONE',  ( 0.000000000000000000, 0.000000000000000000, 1.000000000000000000 ) ) ;
#108930 = CARTESIAN_POINT ( 'NONE',  ( -16.51473224551082808, 9.474510206698731452, 113.3344237280190043 ) ) ;
#108931 = CARTESIAN_POINT ( 'NONE',  ( 19.05341960407611168, 5.049401038298154454, 63.95724293864769550 ) ) ;
#108932 = CARTESIAN_POINT ( 'NONE',  ( 16.46253265017160672, -9.564922557960803928, 103.3322429386476955 ) ) ;
#108933 = CARTESIAN_POINT ( 'NONE',  ( 14.29746914071049879, -8.314922557960816363, 113.3322429386476955 ) ) ;
#108934 = CARTESIAN_POINT ( 'NONE',  ( -8.314922557960811034, -14.29746914071050412, 107.0822429386476955 ) ) ;
#108935 = CARTESIAN_POINT ( 'NONE',  ( -15.80617190586745835, -15.72974639402198527, 31.87390960531435979 ) ) ;
#108936 = CARTESIAN_POINT ( 'NONE',  ( 8.314922557961029526, -14.29746914071037800, 80.41775706135234714 ) ) ;
#108938 = CARTESIAN_POINT ( 'NONE',  ( 16.51473224551069308, 9.474510206698969483, 54.16557627198103120 ) ) ;
#108937 = CARTESIAN_POINT ( 'NONE',  ( -4.379528057220328563, 16.55341960407611168, 75.20724293864769550 ) ) ;
#108939 = CARTESIAN_POINT ( 'NONE',  ( 18.62759615963255655, 10.81492255796105972, 76.66775706135234714 ) ) ;
#108940 = CARTESIAN_POINT ( 'NONE',  ( -0.05219959533937732626, 21.53943276465977519, 77.50109039468567573 ) ) ;
#108941 = CARTESIAN_POINT ( 'NONE',  ( -13.97604488694547697, 13.89961937509957934, 103.1260903946856473 ) ) ;
#108942 = CARTESIAN_POINT ( 'NONE',  ( 4.483927247898545687, 16.52544592524342804, 59.79057627198103120 ) ) ;
#108943 = CARTESIAN_POINT ( 'NONE',  ( -21.55341960407619339, 5.719274019375674811, 28.54275706135234358 ) ) ;
#108944 = CARTESIAN_POINT ( 'NONE',  ( 21.55341960407610458, 5.719274019375980345, 58.95724293864770971 ) ) ;
#108945 = CARTESIAN_POINT ( 'NONE',  ( -21.30000000000002913, 2.244099063931684814E-13, -56.46919128290398504 ) ) ;
#108946 = CARTESIAN_POINT ( 'NONE',  ( -35.44323460151743888, 3.757829821678503546, 38.50466947567799991 ) ) ;
#108947 = CARTESIAN_POINT ( 'NONE',  ( -5.153800228976328057, -19.02544592524343514, 67.29057627198102409 ) ) ;
#108948 = CARTESIAN_POINT ( 'NONE',  ( -14.34966873604960291, -8.224510206698953496, 56.66557627198103830 ) ) ;
#108949 = VECTOR ( 'NONE', #179646, 1000.000000000000000 ) ;
#108950 = CARTESIAN_POINT ( 'NONE',  ( 16.53943276465976808, 0.05219959533934440121, 111.2510903946856899 ) ) ;
#108951 = CARTESIAN_POINT ( 'NONE',  ( -16.53943276465976808, -0.05219959533934237506, 98.75109039468568994 ) ) ;
#108952 = CARTESIAN_POINT ( 'NONE',  ( 9.474510206698729675, 16.51473224551082808, 52.08442372801900433 ) ) ;
#108953 = CARTESIAN_POINT ( 'NONE',  ( 17.44270441346512968, 5.991230190323099336, 48.86335079264230075 ) ) ;
#108954 = CARTESIAN_POINT ( 'NONE',  ( -16.51473224551069308, -9.474510206698971260, 101.6655762719810241 ) ) ;
#108955 = EDGE_CURVE ( 'NONE', #142920, #96037, #113913, .T. ) ;
#108956 = CARTESIAN_POINT ( 'NONE',  ( 12.06949235617757843, -12.14591786802309237, 78.12390960531436690 ) ) ;
#108957 = CARTESIAN_POINT ( 'NONE',  ( 0.05219959533936267826, -19.03943276465977164, 45.00109039468566863 ) ) ;
#108959 = CARTESIAN_POINT ( 'NONE',  ( -0.05219959533907301413, -21.53943276465977519, 32.49890960531435979 ) ) ;
#108958 = CARTESIAN_POINT ( 'NONE',  ( 9.474510206698971260, -16.51473224551069308, 37.91557627198102409 ) ) ;
#108960 = CARTESIAN_POINT ( 'NONE',  ( 18.62759615963271287, -10.81492255796078972, 58.33224293864768839 ) ) ;
#108961 = CARTESIAN_POINT ( 'NONE',  ( -4.483927247898539470, -16.52544592524342804, 102.2905762719810383 ) ) ;
#108962 = CARTESIAN_POINT ( 'NONE',  ( -14.29746914071037622, -8.314922557961029526, 54.16775706135235424 ) ) ;
#108963 = CARTESIAN_POINT ( 'NONE',  ( 8.314922557960818139, 14.29746914071049879, 94.58224293864769550 ) ) ;
#108964 = CARTESIAN_POINT ( 'NONE',  ( 22.81625015709510151, -31.40387420917324590, -8.424999997268812990 ) ) ;
#108965 = CARTESIAN_POINT ( 'NONE',  ( -13.89961937509977652, 13.97604488694528158, 110.6239096053143243 ) ) ;
#108966 = FACE_OUTER_BOUND ( 'NONE', #147751, .T. ) ;
#108967 = CARTESIAN_POINT ( 'NONE',  ( 30.73962218707677607, -22.33364281372841376, -6.947842220587805429 ) ) ;
#108968 = VERTEX_POINT ( 'NONE', #143310 ) ;
#108970 = CARTESIAN_POINT ( 'NONE',  ( -14.29746914071049879, 8.314922557960819915, 30.83224293864770260 ) ) ;
#108969 = CARTESIAN_POINT ( 'NONE',  ( 12.06949235617739724, 12.14591786802326823, 46.87609039468568994 ) ) ;
#108971 = CARTESIAN_POINT ( 'NONE',  ( 18.67979575497178502, 10.72451020669898547, 59.16557627198103120 ) ) ;
#108972 = CARTESIAN_POINT ( 'NONE',  ( -19.02544592524334988, -5.153800228976617603, 83.95942372801901854 ) ) ;
#108973 = CARTESIAN_POINT ( 'NONE',  ( 5.719274019375991003, -21.55341960407610458, 42.70724293864770260 ) ) ;
#108974 = CARTESIAN_POINT ( 'NONE',  ( 10.81492255796106328, -18.62759615963255655, 75.41775706135233293 ) ) ;
#108975 = DIRECTION ( 'NONE',  ( -1.000000000000000000, 0.000000000000000000, 0.000000000000000000 ) ) ;
#108976 = CARTESIAN_POINT ( 'NONE',  ( 16.52544592524335698, 4.483927247898782831, 51.45942372801901854 ) ) ;
#108978 = CARTESIAN_POINT ( 'NONE',  ( -19.03943276465977164, 0.05219959533909376836, 106.2489096053143669 ) ) ;
#108977 = CARTESIAN_POINT ( 'NONE',  ( -9.474510206698964154, 16.51473224551069663, 40.41557627198103120 ) ) ;
#108979 = VECTOR ( 'NONE', #57717, 1000.000000000000114 ) ;
#108980 = CARTESIAN_POINT ( 'NONE',  ( 5.153800228976335163, 19.02544592524342804, 29.79057627198102409 ) ) ;
#108981 = CARTESIAN_POINT ( 'NONE',  ( 12.14591786802309770, 12.06949235617756955, 99.37390960531436690 ) ) ;
#108982 = DIRECTION ( 'NONE',  ( 0.000000000000000000, 0.000000000000000000, 1.000000000000000000 ) ) ;
#108983 = CARTESIAN_POINT ( 'NONE',  ( -16.51473224551069308, -9.474510206698971260, 101.6655762719810241 ) ) ;
#108984 = CARTESIAN_POINT ( 'NONE',  ( 4.379528057220092307, 16.55341960407617563, 57.29275706135234714 ) ) ;
#108985 = CARTESIAN_POINT ( 'NONE',  ( -21.52544592524343514, 5.823673210054127303, 96.04057627198102409 ) ) ;
#108986 = CARTESIAN_POINT ( 'NONE',  ( 5.049401038298161559, -19.05341960407611168, 62.70724293864769550 ) ) ;
#108987 = CARTESIAN_POINT ( 'NONE',  ( 10.81492255796106328, -18.62759615963255655, 30.41775706135234358 ) ) ;
#108988 = CARTESIAN_POINT ( 'NONE',  ( 19.05341960407611168, 5.049401038298154454, 83.95724293864766707 ) ) ;
#108989 = FACE_OUTER_BOUND ( 'NONE', #179609, .T. ) ;
#108990 = ORIENTED_EDGE ( 'NONE', *, *, #78055, .F. ) ;
#108991 = CARTESIAN_POINT ( 'NONE',  ( -15.80617190586768217, 15.72974639402176855, 23.12609039468567573 ) ) ;
#108994 = CARTESIAN_POINT ( 'NONE',  ( 19.05341960407617918, -5.049401038297876454, 76.04275706135230450 ) ) ;
#108993 = CARTESIAN_POINT ( 'NONE',  ( -9.564922557960796823, -16.46253265017161027, 107.0822429386476955 ) ) ;
#108992 = CARTESIAN_POINT ( 'NONE',  ( -0.05219959533909027116, -19.03943276465977164, 22.49890960531436690 ) ) ;
#108995 = CARTESIAN_POINT ( 'NONE',  ( -19.03943276465977164, -0.05219959533935918106, 23.75109039468566152 ) ) ;
#108996 = CARTESIAN_POINT ( 'NONE',  ( -10.72451020669898014, 18.67979575497178502, 95.41557627198102409 ) ) ;
#108997 = CARTESIAN_POINT ( 'NONE',  ( 16.51473224551083163, -9.474510206698727899, 40.83442372801900433 ) ) ;
#108998 = CARTESIAN_POINT ( 'NONE',  ( -0.05219959533934338120, 16.53943276465976808, 72.50109039468568994 ) ) ;
#109000 = ORIENTED_EDGE ( 'NONE', *, *, #49532, .T. ) ;
#108999 = CARTESIAN_POINT ( 'NONE',  ( 5.049401038298161559, -19.05341960407611168, 102.7072429386476955 ) ) ;
#109001 = CARTESIAN_POINT ( 'NONE',  ( 19.05341960407611168, 5.049401038298154454, 58.95724293864768129 ) ) ;
#109002 = AXIS2_PLACEMENT_3D ( 'NONE', #17532, #62026, #123691 ) ;
#109003 = CARTESIAN_POINT ( 'NONE',  ( -21.52544592524334988, -5.823673210054445271, 68.95942372801901854 ) ) ;
#109004 = CARTESIAN_POINT ( 'NONE',  ( 15.72974639402176855, 15.80617190586768217, 81.87609039468568994 ) ) ;
#109005 = CARTESIAN_POINT ( 'NONE',  ( -13.97604488694527625, -13.89961937509977652, 76.87390960531433848 ) ) ;
#109006 = CARTESIAN_POINT ( 'NONE',  ( -5.823673210054431948, 21.52544592524334988, 47.70942372801902565 ) ) ;
#109007 = CARTESIAN_POINT ( 'NONE',  ( 19.03943276465977164, 0.05219959533936151252, 91.25109039468566152 ) ) ;
#109008 = CARTESIAN_POINT ( 'NONE',  ( 5.049401038298161559, -19.05341960407611168, 52.70724293864767418 ) ) ;
#109009 = CARTESIAN_POINT ( 'NONE',  ( 0.05219959533909260263, 19.03943276465977164, 104.9989096053143669 ) ) ;
#109010 = CARTESIAN_POINT ( 'NONE',  ( 5.153800228976335163, 19.02544592524342804, 64.79057627198100988 ) ) ;
#109011 = CARTESIAN_POINT ( 'NONE',  ( -16.46253265017160317, 9.564922557960807481, 105.8322429386476955 ) ) ;
#109012 = CARTESIAN_POINT ( 'NONE',  ( -9.564922557960796823, -16.46253265017161027, 57.08224293864769550 ) ) ;
#109013 = CARTESIAN_POINT ( 'NONE',  ( 18.62759615963271287, -10.81492255796078972, 103.3322429386476955 ) ) ;
#109014 = CARTESIAN_POINT ( 'NONE',  ( -12.14591786802326823, 12.06949235617739902, 78.12609039468570415 ) ) ;
#109015 = CARTESIAN_POINT ( 'NONE',  ( -24.66578506923906033, 3.377805382905409104, 172.1149105766468494 ) ) ;
#109016 = CARTESIAN_POINT ( 'NONE',  ( -16.46253265017146816, -9.564922557961047289, 44.16775706135232582 ) ) ;
#109017 = CARTESIAN_POINT ( 'NONE',  ( -13.97604488694527625, -13.89961937509977652, 71.87390960531433848 ) ) ;
#109018 = CARTESIAN_POINT ( 'NONE',  ( 14.34966873604960469, 8.224510206698951720, 64.16557627198102409 ) ) ;
#109019 = CARTESIAN_POINT ( 'NONE',  ( 16.53943276465976808, -0.05219959533910856209, 88.74890960531436690 ) ) ;
#109020 = CARTESIAN_POINT ( 'NONE',  ( -0.05219959533909027116, -19.03943276465977164, 102.4989096053143669 ) ) ;
#109021 = CARTESIAN_POINT ( 'NONE',  ( -19.05341960407611168, -5.049401038298163336, 96.45724293864769550 ) ) ;
#109022 = CARTESIAN_POINT ( 'NONE',  ( 16.51473224551069308, 9.474510206698969483, 104.1655762719810241 ) ) ;
#109023 = CARTESIAN_POINT ( 'NONE',  ( 21.53943276465977519, 0.05219959533937863772, 106.2510903946856757 ) ) ;
#109024 = CARTESIAN_POINT ( 'NONE',  ( -8.224510206698735004, -14.34966873604973081, 89.58442372801901854 ) ) ;
#109025 = CARTESIAN_POINT ( 'NONE',  ( 13.89961937509977652, -13.97604488694527269, 73.12390960531436690 ) ) ;
#109026 = CARTESIAN_POINT ( 'NONE',  ( 10.81492255796106328, -18.62759615963255655, 45.41775706135234003 ) ) ;
#109027 = CARTESIAN_POINT ( 'NONE',  ( -0.05219959533907301413, -21.53943276465977519, 27.49890960531435269 ) ) ;
#109028 = CARTESIAN_POINT ( 'NONE',  ( 21.55341960407610458, 5.719274019375980345, 98.95724293864770971 ) ) ;
#109029 = CARTESIAN_POINT ( 'NONE',  ( -4.379528057220328563, 16.55341960407611168, 65.20724293864768129 ) ) ;
#109030 = CARTESIAN_POINT ( 'NONE',  ( -19.05341960407611168, -5.049401038298163336, 56.45724293864768129 ) ) ;
#109031 = CARTESIAN_POINT ( 'NONE',  ( -8.224510206698948167, 14.34966873604960824, 75.41557627198102409 ) ) ;
#109032 = CARTESIAN_POINT ( 'NONE',  ( -5.153800228976607833, 19.02544592524334988, 47.70942372801900433 ) ) ;
#109033 = CARTESIAN_POINT ( 'NONE',  ( -8.314922557960811034, -14.29746914071050412, 107.0822429386476955 ) ) ;
#109034 = CARTESIAN_POINT ( 'NONE',  ( -16.52544592524335698, -4.483927247898792601, 63.95942372801901854 ) ) ;
#109035 = CARTESIAN_POINT ( 'NONE',  ( 5.049401038298161559, -19.05341960407611168, 67.70724293864769550 ) ) ;
#109036 = CARTESIAN_POINT ( 'NONE',  ( -8.571926809382608425, 26.38167802310805854, 144.4750000027312069 ) ) ;
#109037 = CARTESIAN_POINT ( 'NONE',  ( -8.314922557960811034, -14.29746914071050412, 92.08224293864769550 ) ) ;
#109038 = CARTESIAN_POINT ( 'NONE',  ( -15.80617190586745835, -15.72974639402198527, 36.87390960531435979 ) ) ;
#109039 = ORIENTED_EDGE ( 'NONE', *, *, #132232, .F. ) ;
#109040 = CARTESIAN_POINT ( 'NONE',  ( -16.52544592524335698, -4.483927247898792601, 103.9594237280190185 ) ) ;
#109041 = CARTESIAN_POINT ( 'NONE',  ( 14.29746914071037800, 8.314922557961029526, 26.66775706135235424 ) ) ;
#109042 = CARTESIAN_POINT ( 'NONE',  ( -5.823673210054431948, 21.52544592524334988, 97.70942372801904696 ) ) ;
#109043 = CARTESIAN_POINT ( 'NONE',  ( -16.51473224551069308, -9.474510206698971260, 81.66557627198103830 ) ) ;
#109044 = CARTESIAN_POINT ( 'NONE',  ( -10.72451020669898014, 18.67979575497178502, 115.4155762719810241 ) ) ;
#109045 = CARTESIAN_POINT ( 'NONE',  ( 16.51473224551069308, 9.474510206698969483, 24.16557627198102765 ) ) ;
#109046 = CARTESIAN_POINT ( 'NONE',  ( 12.06949235617739724, 12.14591786802326823, 26.87609039468567218 ) ) ;
#109047 = CARTESIAN_POINT ( 'NONE',  ( 9.564922557961047289, -16.46253265017146816, 90.41775706135234714 ) ) ;
#109048 = ADVANCED_FACE ( 'NONE', ( #4797 ), #66486, .F. ) ;
#109049 = CARTESIAN_POINT ( 'NONE',  ( 10.81492255796078972, 18.62759615963270932, 84.58224293864769550 ) ) ;
#109050 = CARTESIAN_POINT ( 'NONE',  ( 13.97604488694548053, -13.89961937509957401, 70.62609039468567573 ) ) ;
#109051 = CARTESIAN_POINT ( 'NONE',  ( 16.46253265017160672, -9.564922557960803928, 23.33224293864769194 ) ) ;
#109052 = CARTESIAN_POINT ( 'NONE',  ( 10.81492255796106328, -18.62759615963255655, 20.41775706135234714 ) ) ;
#109053 = CARTESIAN_POINT ( 'NONE',  ( -8.906447517083060816, 27.41122689804195645, 141.8500000054623911 ) ) ;
#109054 = CARTESIAN_POINT ( 'NONE',  ( 5.153800228976335163, 19.02544592524342804, 84.79057627198099567 ) ) ;
#109055 = CARTESIAN_POINT ( 'NONE',  ( -12.14591786802326823, 12.06949235617739902, 33.12609039468569705 ) ) ;
#109056 = LINE ( 'NONE', #111043, #145153 ) ;
#109057 = CARTESIAN_POINT ( 'NONE',  ( -0.05219959533936034679, 19.03943276465977164, 62.50109039468566863 ) ) ;
#109059 = CARTESIAN_POINT ( 'NONE',  ( -14.34966873604960291, -8.224510206698953496, 81.66557627198103830 ) ) ;
#109058 = CARTESIAN_POINT ( 'NONE',  ( 15.80617190586769283, -15.72974639402175789, 25.62609039468567929 ) ) ;
#109060 = CARTESIAN_POINT ( 'NONE',  ( 16.46253265017160672, -9.564922557960803928, 83.33224293864768129 ) ) ;
#109062 = CARTESIAN_POINT ( 'NONE',  ( 16.51473224551083163, -9.474510206698727899, 50.83442372801899722 ) ) ;
#109061 = CARTESIAN_POINT ( 'NONE',  ( 14.34966873604972726, -8.224510206698740333, 40.83442372801901854 ) ) ;
#109063 = CARTESIAN_POINT ( 'NONE',  ( 5.823673210054444382, -21.52544592524334988, 65.20942372801901854 ) ) ;
#109064 = CARTESIAN_POINT ( 'NONE',  ( 4.379528057220092307, 16.55341960407617563, 22.29275706135235069 ) ) ;
#109065 = CARTESIAN_POINT ( 'NONE',  ( -13.97604488694527625, -13.89961937509977652, 51.87390960531436690 ) ) ;
#109066 = CARTESIAN_POINT ( 'NONE',  ( 9.564922557961047289, -16.46253265017146816, 80.41775706135234714 ) ) ;
#109067 = CARTESIAN_POINT ( 'NONE',  ( 16.52544592524335698, 4.483927247898782831, 56.45942372801902565 ) ) ;
#109068 = CARTESIAN_POINT ( 'NONE',  ( -21.55341960407619339, 5.719274019375674811, 98.54275706135234714 ) ) ;
#109069 = CARTESIAN_POINT ( 'NONE',  ( -16.46253265017146816, -9.564922557961047289, 64.16775706135233293 ) ) ;
#109070 = CARTESIAN_POINT ( 'NONE',  ( -19.03943276465977164, 0.05219959533909376836, 51.24890960531436690 ) ) ;
#109071 = CARTESIAN_POINT ( 'NONE',  ( -15.80617190586745835, -15.72974639402198527, 66.87390960531436690 ) ) ;
#109073 = CARTESIAN_POINT ( 'NONE',  ( 19.05341960407617918, -5.049401038297876454, 81.04275706135231871 ) ) ;
#109072 = CARTESIAN_POINT ( 'NONE',  ( 14.34966873604960469, 8.224510206698951720, 64.16557627198102409 ) ) ;
#109074 = CARTESIAN_POINT ( 'NONE',  ( 16.19135201231364718, -7.376712067592015920, 62.31319145947974647 ) ) ;
#109075 = CARTESIAN_POINT ( 'NONE',  ( -19.03943276465977164, -0.05219959533935918106, 48.75109039468566863 ) ) ;
#109076 = CARTESIAN_POINT ( 'NONE',  ( -16.53943276465976808, -0.05219959533934237506, 98.75109039468568994 ) ) ;
#109077 = CARTESIAN_POINT ( 'NONE',  ( 8.314922557960818139, 14.29746914071049879, 69.58224293864769550 ) ) ;
#109079 = CARTESIAN_POINT ( 'NONE',  ( -17.14385361876520264, -23.59649016807271593, 147.1750000027311671 ) ) ;
#109078 = CARTESIAN_POINT ( 'NONE',  ( -21.55341960407619339, 5.719274019375674811, 98.54275706135234714 ) ) ;
#109080 = CARTESIAN_POINT ( 'NONE',  ( -15.80617190586745835, -15.72974639402198527, 91.87390960531436690 ) ) ;
#109081 = CARTESIAN_POINT ( 'NONE',  ( 19.03943276465977164, -0.05219959533909143690, 58.74890960531435979 ) ) ;
#109082 = CARTESIAN_POINT ( 'NONE',  ( 15.72974639402176855, 15.80617190586768217, 66.87609039468568994 ) ) ;
#109083 = CARTESIAN_POINT ( 'NONE',  ( -5.049401038298153566, 19.05341960407611168, 50.20724293864770260 ) ) ;
#109084 = EDGE_LOOP ( 'NONE', ( #40622, #141025, #96405, #100488, #178900 ) ) ;
#109085 = CARTESIAN_POINT ( 'NONE',  ( -19.03943276465977164, 0.05219959533909376836, 21.24890960531436335 ) ) ;
#109086 = CARTESIAN_POINT ( 'NONE',  ( 9.474510206698971260, -16.51473224551069308, 107.9155762719810383 ) ) ;
#109087 = CARTESIAN_POINT ( 'NONE',  ( -16.53943276465976808, 0.05219959533911058130, 71.24890960531435269 ) ) ;
#109088 = CARTESIAN_POINT ( 'NONE',  ( 5.049401038298161559, -19.05341960407611168, 32.70724293864768129 ) ) ;
#109089 = CARTESIAN_POINT ( 'NONE',  ( 16.55341960407611168, 4.379528057220329451, 78.95724293864769550 ) ) ;
#109090 = CIRCLE ( 'NONE', #34757, 10.00000000000000000 ) ;
#109091 = CARTESIAN_POINT ( 'NONE',  ( -21.53943276465977519, 0.05219959533907696930, 101.2489096053143669 ) ) ;
#109092 = CARTESIAN_POINT ( 'NONE',  ( -18.62759615963255300, -10.81492255796106328, 34.16775706135234714 ) ) ;
#109093 = CARTESIAN_POINT ( 'NONE',  ( 19.05341960407611168, 5.049401038298154454, 23.95724293864769194 ) ) ;
#109094 = CARTESIAN_POINT ( 'NONE',  ( 8.314922557961029526, -14.29746914071037800, 55.41775706135234714 ) ) ;
#109095 = CARTESIAN_POINT ( 'NONE',  ( -10.72451020669898014, 18.67979575497178502, 80.41557627198103830 ) ) ;
#109096 = CARTESIAN_POINT ( 'NONE',  ( 19.03943276465977164, 0.05219959533936151252, 21.25109039468565797 ) ) ;
#109097 = CARTESIAN_POINT ( 'NONE',  ( -19.03943276465977164, 0.05219959533909376836, 111.2489096053143669 ) ) ;
#109098 = CARTESIAN_POINT ( 'NONE',  ( -21.53943276465977519, -0.05219959533937600094, 38.75109039468567573 ) ) ;
#109099 = CARTESIAN_POINT ( 'NONE',  ( 15.72974639402199770, -15.80617190586745480, 38.12390960531436690 ) ) ;
#109100 = CARTESIAN_POINT ( 'NONE',  ( -16.53943276465976808, 0.05219959533911058130, 26.24890960531435624 ) ) ;
#109102 = CARTESIAN_POINT ( 'NONE',  ( -18.62759615963255300, -10.81492255796106328, 94.16775706135237556 ) ) ;
#109101 = CARTESIAN_POINT ( 'NONE',  ( 18.62759615963255655, 10.81492255796105972, 61.66775706135235424 ) ) ;
#109103 = CARTESIAN_POINT ( 'NONE',  ( -9.564922557961040184, 16.46253265017147172, 32.91775706135233293 ) ) ;
#109104 = CARTESIAN_POINT ( 'NONE',  ( 12.06949235617739724, 12.14591786802326823, 81.87609039468568994 ) ) ;
#109105 = CARTESIAN_POINT ( 'NONE',  ( -21.53943276465977519, -0.05219959533937600094, 53.75109039468568994 ) ) ;
#109106 = CARTESIAN_POINT ( 'NONE',  ( 5.153800228976335163, 19.02544592524342804, 39.79057627198100988 ) ) ;
#109107 = CARTESIAN_POINT ( 'NONE',  ( -16.46253265017146816, -9.564922557961047289, 24.16775706135233648 ) ) ;
#109108 = CARTESIAN_POINT ( 'NONE',  ( -10.72451020669898014, 18.67979575497178502, 30.41557627198101699 ) ) ;
#109109 = CARTESIAN_POINT ( 'NONE',  ( -10.72451020669898014, 18.67979575497178502, 115.4155762719810241 ) ) ;
#109110 = CARTESIAN_POINT ( 'NONE',  ( -21.52544592524343514, 5.823673210054127303, 71.04057627198103830 ) ) ;
#109111 = CARTESIAN_POINT ( 'NONE',  ( -16.52544592524335698, -4.483927247898792601, 43.95942372801902565 ) ) ;
#109113 = CARTESIAN_POINT ( 'NONE',  ( 15.72974639402199770, -15.80617190586745480, 78.12390960531436690 ) ) ;
#109112 = CYLINDRICAL_SURFACE ( 'NONE', #61163, 216.0437394197456911 ) ;
#109115 = CARTESIAN_POINT ( 'NONE',  ( 16.55341960407611168, 4.379528057220329451, 68.95724293864769550 ) ) ;
#109114 = CARTESIAN_POINT ( 'NONE',  ( -4.483927247898782831, 16.52544592524335698, 67.70942372801901854 ) ) ;
#109116 = CARTESIAN_POINT ( 'NONE',  ( -22.96531869715557761, 21.81714873624716233, -45.99103957044147961 ) ) ;
#109117 = CARTESIAN_POINT ( 'NONE',  ( -19.02544592524334988, -5.153800228976617603, 93.95942372801900433 ) ) ;
#109118 = VECTOR ( 'NONE', #37177, 1000.000000000000000 ) ;
#109119 = CARTESIAN_POINT ( 'NONE',  ( 6.874011537017776341, -5.570592230301131487, -61.95613518020381605 ) ) ;
#109120 = CARTESIAN_POINT ( 'NONE',  ( 0.05219959533934541429, -16.53943276465976808, 35.00109039468568284 ) ) ;
#109121 = CARTESIAN_POINT ( 'NONE',  ( -18.62759615963270932, 10.81492255796079327, 115.8322429386477097 ) ) ;
#109122 = CARTESIAN_POINT ( 'NONE',  ( -21.52544592524343514, 5.823673210054127303, 81.04057627198102409 ) ) ;
#109123 = CARTESIAN_POINT ( 'NONE',  ( -10.81492255796078084, -18.62759615963271287, 37.08224293864768129 ) ) ;
#109124 = CARTESIAN_POINT ( 'NONE',  ( 16.55341960407618274, -4.379528057220086978, 61.04275706135234714 ) ) ;
#109125 = CARTESIAN_POINT ( 'NONE',  ( -19.03943276465977164, 0.05219959533909376836, 76.24890960531435269 ) ) ;
#109127 = CARTESIAN_POINT ( 'NONE',  ( 19.05341960407617918, -5.049401038297876454, 106.0427570613523471 ) ) ;
#109126 = CARTESIAN_POINT ( 'NONE',  ( 10.81492255796106328, -18.62759615963255655, 40.41775706135234714 ) ) ;
#109128 = CARTESIAN_POINT ( 'NONE',  ( -21.52544592524343514, 5.823673210054127303, 26.04057627198103475 ) ) ;
#109129 = CARTESIAN_POINT ( 'NONE',  ( -19.03943276465977164, -0.05219959533935918106, 28.75109039468566507 ) ) ;
#109130 = CARTESIAN_POINT ( 'NONE',  ( 16.53943276465976808, 0.05219959533934440121, 41.25109039468568284 ) ) ;
#109131 = CARTESIAN_POINT ( 'NONE',  ( -16.46253265017160317, 9.564922557960807481, 100.8322429386477097 ) ) ;
#109132 = CARTESIAN_POINT ( 'NONE',  ( 10.81492255796078972, 18.62759615963270932, 104.5822429386477097 ) ) ;
#109133 = CARTESIAN_POINT ( 'NONE',  ( -9.474510206698964154, 16.51473224551069663, 75.41557627198103830 ) ) ;
#109134 = CARTESIAN_POINT ( 'NONE',  ( -3.573655867282028392E-15, 2.428612866367529932E-14, 139.9999999999999716 ) ) ;
#109135 = CARTESIAN_POINT ( 'NONE',  ( 12.14591786802309770, 12.06949235617756955, 84.37390960531438111 ) ) ;
#109136 = CARTESIAN_POINT ( 'NONE',  ( 5.719274019375991003, -21.55341960407610458, 27.70724293864769905 ) ) ;
#109137 = CARTESIAN_POINT ( 'NONE',  ( -17.49999999999999645, 5.624438216177594541, 35.81670344914645199 ) ) ;
#109138 = CARTESIAN_POINT ( 'NONE',  ( 5.823673210054125526, 21.52544592524343514, 109.7905762719810383 ) ) ;
#109139 = CARTESIAN_POINT ( 'NONE',  ( 13.89961937509957401, 13.97604488694547697, 61.87609039468566863 ) ) ;
#109140 = CARTESIAN_POINT ( 'NONE',  ( 15.80617190586746368, 15.72974639402197994, 29.37390960531435269 ) ) ;
#109141 = CARTESIAN_POINT ( 'NONE',  ( 13.97604488694527802, 13.89961937509977652, 24.37390960531435624 ) ) ;
#109142 = CARTESIAN_POINT ( 'NONE',  ( 5.823673210054125526, 21.52544592524343514, 69.79057627198102409 ) ) ;
#109143 = CARTESIAN_POINT ( 'NONE',  ( 0.05219959533909260263, 19.03943276465977164, 104.9989096053143669 ) ) ;
#109144 = CARTESIAN_POINT ( 'NONE',  ( -21.55341960407619339, 5.719274019375674811, 88.54275706135236135 ) ) ;
#109145 = CARTESIAN_POINT ( 'NONE',  ( 19.03943276465977164, -0.05219959533909143690, 53.74890960531436690 ) ) ;
#109146 = ADVANCED_FACE ( 'NONE', ( #70235 ), #59098, .T. ) ;
#109147 = CARTESIAN_POINT ( 'NONE',  ( -8.314922557960811034, -14.29746914071050412, 82.08224293864768129 ) ) ;
#109148 = CARTESIAN_POINT ( 'NONE',  ( 16.55341960407618274, -4.379528057220086978, 36.04275706135234714 ) ) ;
#109149 = CARTESIAN_POINT ( 'NONE',  ( -13.97604488694527625, -13.89961937509977652, 56.87390960531434558 ) ) ;
#109150 = CARTESIAN_POINT ( 'NONE',  ( -21.52544592524334988, -5.823673210054445271, 73.95942372801901854 ) ) ;
#109151 = ORIENTED_EDGE ( 'NONE', *, *, #108344, .F. ) ;
#109152 = CARTESIAN_POINT ( 'NONE',  ( 9.564922557961047289, -16.46253265017146816, 25.41775706135234003 ) ) ;
#109153 = CARTESIAN_POINT ( 'NONE',  ( 0.05219959533936267826, -19.03943276465977164, 45.00109039468566863 ) ) ;
#109154 = CARTESIAN_POINT ( 'NONE',  ( 15.80617190586769283, -15.72974639402175789, 30.62609039468567929 ) ) ;
#109155 = DIRECTION ( 'NONE',  ( -0.000000000000000000, 0.000000000000000000, 1.000000000000000000 ) ) ;
#109156 = CARTESIAN_POINT ( 'NONE',  ( 9.564922557961047289, -16.46253265017146816, 30.41775706135232937 ) ) ;
#109157 = CARTESIAN_POINT ( 'NONE',  ( -9.564922557960796823, -16.46253265017161027, 82.08224293864768129 ) ) ;
#109158 = CARTESIAN_POINT ( 'NONE',  ( -5.049401038298153566, 19.05341960407611168, 70.20724293864769550 ) ) ;
#109159 = CARTESIAN_POINT ( 'NONE',  ( 16.52544592524342804, -4.483927247898539470, 28.54057627198103120 ) ) ;
#109161 = CARTESIAN_POINT ( 'NONE',  ( 5.823673210054444382, -21.52544592524334988, 85.20942372801901854 ) ) ;
#109160 = CARTESIAN_POINT ( 'NONE',  ( -16.51473224551069308, -9.474510206698971260, 111.6655762719810383 ) ) ;
#109162 = CARTESIAN_POINT ( 'NONE',  ( -22.81625015709509441, -31.40387420917324590, -8.824999997268811569 ) ) ;
#109163 = CARTESIAN_POINT ( 'NONE',  ( -3.573655867282028392E-15, 2.428612866367529932E-14, -25.00000000000000000 ) ) ;
#109164 = CARTESIAN_POINT ( 'NONE',  ( -21.53943276465977519, -0.05219959533937600094, 88.75109039468567573 ) ) ;
#109165 = CARTESIAN_POINT ( 'NONE',  ( 16.31925111598458500, -7.325300261831445781, 42.66424538967253000 ) ) ;
#109166 = CARTESIAN_POINT ( 'NONE',  ( -5.153800228976328057, -19.02544592524343514, 97.29057627198099567 ) ) ;
#109167 = CARTESIAN_POINT ( 'NONE',  ( 33.71430530369729439, 4.147805181855619416, 98.62971388258593208 ) ) ;
#109168 = CARTESIAN_POINT ( 'NONE',  ( -14.29746914071037622, -8.314922557961029526, 49.16775706135234003 ) ) ;
#109169 = CARTESIAN_POINT ( 'NONE',  ( 18.62759615963271287, -10.81492255796078972, 73.33224293864769550 ) ) ;
#109170 = CARTESIAN_POINT ( 'NONE',  ( -4.483927247898539470, -16.52544592524342804, 32.29057627198102409 ) ) ;
#109172 = CARTESIAN_POINT ( 'NONE',  ( 19.05341960407611168, 5.049401038298154454, 98.95724293864766707 ) ) ;
#109171 = CARTESIAN_POINT ( 'NONE',  ( 4.483927247898545687, 16.52544592524342804, 109.7905762719810383 ) ) ;
#109173 = CARTESIAN_POINT ( 'NONE',  ( -10.81492255796105439, 18.62759615963255655, 112.9177570613523329 ) ) ;
#109174 = CARTESIAN_POINT ( 'NONE',  ( 4.483927247898545687, 16.52544592524342804, 109.7905762719810383 ) ) ;
#109175 = CARTESIAN_POINT ( 'NONE',  ( 18.62759615963255655, 10.81492255796105972, 66.66775706135234714 ) ) ;
#109176 = CARTESIAN_POINT ( 'NONE',  ( 0.05219959533909260263, 19.03943276465977164, 109.9989096053143669 ) ) ;
#109177 = CARTESIAN_POINT ( 'NONE',  ( 12.06949235617739724, 12.14591786802326823, 106.8760903946856899 ) ) ;
#109178 = CARTESIAN_POINT ( 'NONE',  ( -16.51473224551082808, 9.474510206698731452, 58.33442372801900433 ) ) ;
#109179 = CARTESIAN_POINT ( 'NONE',  ( 5.049401038297881783, 19.05341960407617918, 67.29275706135233293 ) ) ;
#109180 = CARTESIAN_POINT ( 'NONE',  ( -5.049401038298153566, 19.05341960407611168, 105.2072429386476671 ) ) ;
#109181 = CARTESIAN_POINT ( 'NONE',  ( 4.379528057220339221, -16.55341960407611168, 87.70724293864769550 ) ) ;
#109182 = CARTESIAN_POINT ( 'NONE',  ( -16.46253265017146816, -9.564922557961047289, 64.16775706135233293 ) ) ;
#109183 = CARTESIAN_POINT ( 'NONE',  ( -9.564922557960796823, -16.46253265017161027, 82.08224293864768129 ) ) ;
#109184 = CARTESIAN_POINT ( 'NONE',  ( -8.314922557960811034, -14.29746914071050412, 67.08224293864770971 ) ) ;
#109185 = CARTESIAN_POINT ( 'NONE',  ( 9.564922557961047289, -16.46253265017146816, 90.41775706135234714 ) ) ;
#109186 = CARTESIAN_POINT ( 'NONE',  ( 21.55341960407610458, 5.719274019375980345, 48.95724293864770971 ) ) ;
#109187 = ORIENTED_EDGE ( 'NONE', *, *, #93066, .F. ) ;
#109188 = CARTESIAN_POINT ( 'NONE',  ( 9.564922557960805705, 16.46253265017160317, 24.58224293864769194 ) ) ;
#109189 = CARTESIAN_POINT ( 'NONE',  ( -16.52216118717207394, -7.221426719304521846, 31.07599021046992505 ) ) ;
#109191 = CARTESIAN_POINT ( 'NONE',  ( 21.53943276465977519, -0.05219959533907433946, 78.74890960531436690 ) ) ;
#109190 = CARTESIAN_POINT ( 'NONE',  ( 19.02544592524343514, -5.153800228976328945, 78.54057627198099567 ) ) ;
#109193 = CARTESIAN_POINT ( 'NONE',  ( 5.153800228976335163, 19.02544592524342804, 69.79057627198103830 ) ) ;
#109192 = CARTESIAN_POINT ( 'NONE',  ( -4.379528057220086978, -16.55341960407618274, 89.79275706135236135 ) ) ;
#109194 = CARTESIAN_POINT ( 'NONE',  ( -0.05219959533936034679, 19.03943276465977164, 62.50109039468566863 ) ) ;
#109195 = CARTESIAN_POINT ( 'NONE',  ( 10.81492255796106328, -18.62759615963255655, 80.41775706135234714 ) ) ;
#109196 = CARTESIAN_POINT ( 'NONE',  ( 18.62759615963271287, -10.81492255796078972, 63.33224293864770260 ) ) ;
#109197 = CARTESIAN_POINT ( 'NONE',  ( -5.823673210054116645, -21.52544592524344225, 22.29057627198102765 ) ) ;
#109198 = CARTESIAN_POINT ( 'NONE',  ( -9.474510206698964154, 16.51473224551069663, 35.41557627198102409 ) ) ;
#109199 = CARTESIAN_POINT ( 'NONE',  ( 0.05219959533934541429, -16.53943276465976808, 100.0010903946857042 ) ) ;
#109200 = CARTESIAN_POINT ( 'NONE',  ( -8.224510206698735004, -14.34966873604973081, 19.58442372801901143 ) ) ;
#109201 = CARTESIAN_POINT ( 'NONE',  ( 16.36317988757059183, 7.306389748694952502, 53.40210391636777842 ) ) ;
#109202 = CARTESIAN_POINT ( 'NONE',  ( 21.53943276465977519, 0.05219959533937863772, 91.25109039468568994 ) ) ;
#109203 = CARTESIAN_POINT ( 'NONE',  ( 16.53943276465976808, -0.05219959533910856209, 53.74890960531437401 ) ) ;
#109204 = CARTESIAN_POINT ( 'NONE',  ( -10.81492255796078084, -18.62759615963271287, 92.08224293864769550 ) ) ;
#109205 = CARTESIAN_POINT ( 'NONE',  ( -5.823673210054116645, -21.52544592524344225, 102.2905762719810383 ) ) ;
#109206 = CARTESIAN_POINT ( 'NONE',  ( 16.61371651742602396, -7.165104196376141488, 96.35415069992994574 ) ) ;
#109207 = CARTESIAN_POINT ( 'NONE',  ( -10.81492255796078084, -18.62759615963271287, 42.08224293864769550 ) ) ;
#109208 = CARTESIAN_POINT ( 'NONE',  ( -14.29746914071037622, -8.314922557961029526, 74.16775706135231871 ) ) ;
#109209 = CARTESIAN_POINT ( 'NONE',  ( -4.379528057220328563, 16.55341960407611168, 90.20724293864770971 ) ) ;
#109210 = CARTESIAN_POINT ( 'NONE',  ( -19.03943276465977164, 0.05219959533909376836, 41.24890960531435269 ) ) ;
#109211 = CARTESIAN_POINT ( 'NONE',  ( -27.99526582847389022, -28.30548820594175297, -16.92425894792109275 ) ) ;
#109212 = CARTESIAN_POINT ( 'NONE',  ( -16.52544592524335698, -4.483927247898792601, 108.9594237280190185 ) ) ;
#109213 = CARTESIAN_POINT ( 'NONE',  ( 5.719274019375673035, 21.55341960407619339, 27.29275706135234358 ) ) ;
#109214 = CARTESIAN_POINT ( 'NONE',  ( -16.46253265017160317, 9.564922557960807481, 90.83224293864769550 ) ) ;
#109215 = CARTESIAN_POINT ( 'NONE',  ( 0.05219959533937995610, -21.53943276465977519, 70.00109039468568994 ) ) ;
#109216 = CARTESIAN_POINT ( 'NONE',  ( 193.3062444957835453, -155.7167183371837496, -25.00000000000000000 ) ) ;
#109217 = CARTESIAN_POINT ( 'NONE',  ( -19.03943276465977164, 0.05219959533909376836, 31.24890960531435979 ) ) ;
#109218 = ORIENTED_EDGE ( 'NONE', *, *, #127529, .F. ) ;
#109219 = CARTESIAN_POINT ( 'NONE',  ( -5.823673210054431948, 21.52544592524334988, 62.70942372801902565 ) ) ;
#109221 = CARTESIAN_POINT ( 'NONE',  ( 13.97604488694527802, 13.89961937509977652, 114.3739096053143669 ) ) ;
#109220 = CARTESIAN_POINT ( 'NONE',  ( -13.89961937509977652, 13.97604488694528158, 50.62390960531435979 ) ) ;
#109222 = CARTESIAN_POINT ( 'NONE',  ( -5.049401038298153566, 19.05341960407611168, 85.20724293864766707 ) ) ;
#109223 = CARTESIAN_POINT ( 'NONE',  ( 9.564922557961047289, -16.46253265017146816, 65.41775706135233293 ) ) ;
#109224 = CARTESIAN_POINT ( 'NONE',  ( 10.81492255796106328, -18.62759615963255655, 45.41775706135234003 ) ) ;
#109225 = CARTESIAN_POINT ( 'NONE',  ( -13.89961937509957401, -13.97604488694547875, 64.37609039468567573 ) ) ;
#109226 = CARTESIAN_POINT ( 'NONE',  ( -5.153800228976328057, -19.02544592524343514, 37.29057627198102409 ) ) ;
#109227 = CARTESIAN_POINT ( 'NONE',  ( 14.29746914071037800, 8.314922557961029526, 101.6677570613523613 ) ) ;
#109228 = CARTESIAN_POINT ( 'NONE',  ( 19.02544592524334988, 5.153800228976608722, 81.45942372801897591 ) ) ;
#109229 = CARTESIAN_POINT ( 'NONE',  ( -16.53943276465976808, 0.05219959533911058130, 26.24890960531435624 ) ) ;
#109230 = CARTESIAN_POINT ( 'NONE',  ( -16.46253265017146816, -9.564922557961047289, 44.16775706135232582 ) ) ;
#109231 = CARTESIAN_POINT ( 'NONE',  ( 21.55341960407619695, -5.719274019375665929, 106.0427570613523471 ) ) ;
#109232 = CARTESIAN_POINT ( 'NONE',  ( -13.89961937509957401, -13.97604488694547875, 29.37609039468565797 ) ) ;
#109233 = CARTESIAN_POINT ( 'NONE',  ( -16.51473224551069308, -9.474510206698971260, 31.66557627198102054 ) ) ;
#109234 = CARTESIAN_POINT ( 'NONE',  ( -21.52544592524334988, -5.823673210054445271, 93.95942372801903275 ) ) ;
#109235 = CARTESIAN_POINT ( 'NONE',  ( 12.06949235617739724, 12.14591786802326823, 36.87609039468568994 ) ) ;
#109236 = CARTESIAN_POINT ( 'NONE',  ( -16.51473224551069308, -9.474510206698971260, 86.66557627198102409 ) ) ;
#109237 = B_SPLINE_CURVE_WITH_KNOTS ( 'NONE', 3,
 ( #23081, #132251, #158591, #66580, #67576, #160590, #117075, #131245, #96908, #178771, #129234, #20080, #192934, #54411, #128245, #116083, #130226, #161587, #146404, #84726 ),
 .UNSPECIFIED., .F., .F.,
 ( 4, 2, 2, 2, 2, 2, 2, 2, 2, 4 ),
 ( 0.000000000000000000, 0.0004987090165372625112, 0.0009974180330745250223, 0.001246772541343159910, 0.001496127049611795014, 0.001994836066149060453, 0.002493545082686326325, 0.002742899590954956876, 0.002992254099223587861, 0.003989672132298188560 ),
 .UNSPECIFIED. ) ;
#109238 = CARTESIAN_POINT ( 'NONE',  ( 17.14385361876520264, 23.59649016807275856, 140.1750000027311955 ) ) ;
#109239 = CARTESIAN_POINT ( 'NONE',  ( -9.474510206698964154, 16.51473224551069663, 85.41557627198102409 ) ) ;
#109240 = DIRECTION ( 'NONE',  ( 0.000000000000000000, 0.000000000000000000, -1.000000000000000000 ) ) ;
#109241 = CARTESIAN_POINT ( 'NONE',  ( 19.02544592524334988, 5.153800228976608722, 81.45942372801897591 ) ) ;
#109242 = CARTESIAN_POINT ( 'NONE',  ( 9.474510206698971260, -16.51473224551069308, 112.9155762719810383 ) ) ;
#109243 = CARTESIAN_POINT ( 'NONE',  ( 21.52544592524334988, 5.823673210054432836, 106.4594237280190328 ) ) ;
#109244 = CARTESIAN_POINT ( 'NONE',  ( 0.05219959533910956823, 16.53943276465976808, 104.9989096053143669 ) ) ;
#109245 = CARTESIAN_POINT ( 'NONE',  ( 20.56371838171487454, -11.04494471775322495, 168.1294998094270170 ) ) ;
#109246 = CARTESIAN_POINT ( 'NONE',  ( -15.72974639402197994, 15.80617190586746368, 55.62390960531436690 ) ) ;
#109247 = CARTESIAN_POINT ( 'NONE',  ( 21.55341960407610458, 5.719274019375980345, 33.95724293864769550 ) ) ;
#109248 = CARTESIAN_POINT ( 'NONE',  ( 19.03943276465977164, -0.05219959533909143690, 23.74890960531435269 ) ) ;
#109249 = CARTESIAN_POINT ( 'NONE',  ( -16.61713888009425588, 0.5018587474794012904, -61.38171595447353468 ) ) ;
#109250 = CARTESIAN_POINT ( 'NONE',  ( 5.153800228976615827, -19.02544592524334988, 55.20942372801899722 ) ) ;
#109252 = VECTOR ( 'NONE', #198768, 1000.000000000000000 ) ;
#109251 = CARTESIAN_POINT ( 'NONE',  ( 16.53943276465976808, -0.05219959533910856209, 43.74890960531435979 ) ) ;
#109253 = CARTESIAN_POINT ( 'NONE',  ( -10.81492255796078084, -18.62759615963271287, 22.08224293864769194 ) ) ;
#109254 = CARTESIAN_POINT ( 'NONE',  ( -10.72451020669870658, -18.67979575497194134, 74.58442372801901854 ) ) ;
#109255 = CARTESIAN_POINT ( 'NONE',  ( -21.53943276465977519, 0.05219959533907696930, 71.24890960531435269 ) ) ;
#109256 = CARTESIAN_POINT ( 'NONE',  ( 18.67979575497194134, -10.72451020669871369, 45.83442372801901854 ) ) ;
#109257 = CARTESIAN_POINT ( 'NONE',  ( 15.72974639402199770, -15.80617190586745480, 103.1239096053143811 ) ) ;
#109258 = CARTESIAN_POINT ( 'NONE',  ( 5.823673210054444382, -21.52544592524334988, 45.20942372801901854 ) ) ;
#109259 = CARTESIAN_POINT ( 'NONE',  ( 16.51473224551069308, 9.474510206698969483, 29.16557627198103475 ) ) ;
#109260 = CARTESIAN_POINT ( 'NONE',  ( -19.05341960407611168, -5.049401038298163336, 76.45724293864769550 ) ) ;
#109261 = CARTESIAN_POINT ( 'NONE',  ( 4.379528057220092307, 16.55341960407617563, 77.29275706135234714 ) ) ;
#109262 = CARTESIAN_POINT ( 'NONE',  ( -12.14591786802309592, -12.06949235617757132, 106.8739096053143811 ) ) ;
#109263 = CARTESIAN_POINT ( 'NONE',  ( -31.64990063023044442, 6.823060802858329943, 91.87658598273998223 ) ) ;
#109264 = CARTESIAN_POINT ( 'NONE',  ( -12.14591786802309592, -12.06949235617757132, 56.87390960531436690 ) ) ;
#109265 = CARTESIAN_POINT ( 'NONE',  ( 4.483927247898545687, 16.52544592524342804, 24.79057627198103120 ) ) ;
#109266 = CARTESIAN_POINT ( 'NONE',  ( 5.049401038298161559, -19.05341960407611168, 62.70724293864769550 ) ) ;
#109267 = CARTESIAN_POINT ( 'NONE',  ( -9.474510206698964154, 16.51473224551069663, 30.41557627198102054 ) ) ;
#109268 = CARTESIAN_POINT ( 'NONE',  ( -0.05219959533907301413, -21.53943276465977519, 47.49890960531435979 ) ) ;
#109269 = CARTESIAN_POINT ( 'NONE',  ( 16.51473224551083163, -9.474510206698727899, 35.83442372801899722 ) ) ;
#109271 = CARTESIAN_POINT ( 'NONE',  ( 16.52544592524342804, -4.483927247898539470, 38.54057627198103120 ) ) ;
#109270 = CARTESIAN_POINT ( 'NONE',  ( -17.31747979337948351, -6.344076630961017926, 41.37944868065184778 ) ) ;
#109272 = CARTESIAN_POINT ( 'NONE',  ( 21.52544592524344225, -5.823673210054117533, 28.54057627198103120 ) ) ;
#109273 = CARTESIAN_POINT ( 'NONE',  ( -15.80617190586768217, 15.72974639402176855, 63.12609039468568994 ) ) ;
#109274 = CARTESIAN_POINT ( 'NONE',  ( 17.50000000000001776, -3.242565516147306592, 37.50000000000000000 ) ) ;
#109275 = CARTESIAN_POINT ( 'NONE',  ( 16.53943276465976808, 0.05219959533934440121, 66.25109039468567573 ) ) ;
#109276 = CARTESIAN_POINT ( 'NONE',  ( 16.46253265017146816, 9.564922557961045513, 56.66775706135233293 ) ) ;
#109277 = CARTESIAN_POINT ( 'NONE',  ( -0.05219959533910754901, -16.53943276465976808, 42.49890960531435979 ) ) ;
#109278 = CARTESIAN_POINT ( 'NONE',  ( 17.12812012977027720, -6.668231424565973953, 51.14051240676860743 ) ) ;
#109279 = CARTESIAN_POINT ( 'NONE',  ( -14.29746914071049879, 8.314922557960819915, 25.83224293864769194 ) ) ;
#109280 = CARTESIAN_POINT ( 'NONE',  ( -9.564922557960796823, -16.46253265017161027, 37.08224293864768839 ) ) ;
#109281 = EDGE_CURVE ( 'NONE', #122538, #128850, #26922, .T. ) ;
#109282 = CARTESIAN_POINT ( 'NONE',  ( -19.03943276465977164, 0.05219959533909376836, 56.24890960531435979 ) ) ;
#109283 = CARTESIAN_POINT ( 'NONE',  ( -4.379528057220328563, 16.55341960407611168, 115.2072429386476955 ) ) ;
#109284 = CARTESIAN_POINT ( 'NONE',  ( 5.719274019375673035, 21.55341960407619339, 32.29275706135235424 ) ) ;
#109285 = CARTESIAN_POINT ( 'NONE',  ( -13.89961937509977652, 13.97604488694528158, 55.62390960531434558 ) ) ;
#109286 = CARTESIAN_POINT ( 'NONE',  ( -69.65682714487590488, -71.74905178543390605, 0.000000000000000000 ) ) ;
#109287 = CARTESIAN_POINT ( 'NONE',  ( 19.05341960407611168, 5.049401038298154454, 43.95724293864769550 ) ) ;
#109288 = CARTESIAN_POINT ( 'NONE',  ( 18.62759615963271287, -10.81492255796078972, 38.33224293864768839 ) ) ;
#109290 = CARTESIAN_POINT ( 'NONE',  ( -12.14591786802309592, -12.06949235617757132, 111.8739096053143669 ) ) ;
#109289 = CARTESIAN_POINT ( 'NONE',  ( 0.05219959533937995610, -21.53943276465977519, 55.00109039468568284 ) ) ;
#109291 = CARTESIAN_POINT ( 'NONE',  ( -21.55341960407610458, -5.719274019375992779, 21.45724293864769550 ) ) ;
#109292 = CARTESIAN_POINT ( 'NONE',  ( 4.483927247898790824, -16.52544592524335698, 95.20942372801903275 ) ) ;
#109293 = CARTESIAN_POINT ( 'NONE',  ( 15.80617190586769283, -15.72974639402175789, 110.6260903946857042 ) ) ;
#109294 = CARTESIAN_POINT ( 'NONE',  ( 14.34966873604972726, -8.224510206698740333, 60.83442372801901854 ) ) ;
#109295 = CARTESIAN_POINT ( 'NONE',  ( 9.564922557960805705, 16.46253265017160317, 114.5822429386476955 ) ) ;
#109296 = CARTESIAN_POINT ( 'NONE',  ( -16.52544592524335698, -4.483927247898792601, 48.95942372801902565 ) ) ;
#109297 = CARTESIAN_POINT ( 'NONE',  ( 0.05219959533934541429, -16.53943276465976808, 25.00109039468567218 ) ) ;
#109298 = CARTESIAN_POINT ( 'NONE',  ( 4.379528057220092307, 16.55341960407617563, 92.29275706135236135 ) ) ;
#109299 = CARTESIAN_POINT ( 'NONE',  ( -10.81492255796105439, 18.62759615963255655, 47.91775706135234714 ) ) ;
#109300 = CARTESIAN_POINT ( 'NONE',  ( 0.05219959533936267826, -19.03943276465977164, 110.0010903946856757 ) ) ;
#109301 = CARTESIAN_POINT ( 'NONE',  ( -21.52544592524334988, -5.823673210054445271, 18.95942372801901143 ) ) ;
#109302 = CARTESIAN_POINT ( 'NONE',  ( -14.29746914071037622, -8.314922557961029526, 29.16775706135234003 ) ) ;
#109303 = CARTESIAN_POINT ( 'NONE',  ( 0.05219959533934541429, -16.53943276465976808, 85.00109039468568994 ) ) ;
#109304 = CARTESIAN_POINT ( 'NONE',  ( 5.000000000000000000, -126.1226662136678556, 8.481152457036387204 ) ) ;
#109305 = CARTESIAN_POINT ( 'NONE',  ( 5.719274019375673035, 21.55341960407619339, 92.29275706135236135 ) ) ;
#109306 = CARTESIAN_POINT ( 'NONE',  ( -13.89961937509957401, -13.97604488694547875, 84.37609039468567573 ) ) ;
#109307 = CARTESIAN_POINT ( 'NONE',  ( 0.05219959533910956823, 16.53943276465976808, 44.99890960531435979 ) ) ;
#109308 = CARTESIAN_POINT ( 'NONE',  ( -16.55341960407611168, -4.379528057220339221, 41.45724293864769550 ) ) ;
#109309 = CARTESIAN_POINT ( 'NONE',  ( -12.06949235617756955, 12.14591786802309770, 105.6239096053143669 ) ) ;
#109311 = CARTESIAN_POINT ( 'NONE',  ( 17.50000000000002487, -5.499999999999880984, 53.29690382534172244 ) ) ;
#109310 = CARTESIAN_POINT ( 'NONE',  ( -13.97604488694547697, 13.89961937509957934, 53.12609039468565442 ) ) ;
#109312 = CARTESIAN_POINT ( 'NONE',  ( 21.55341960407619695, -5.719274019375665929, 46.04275706135234714 ) ) ;
#109313 = CARTESIAN_POINT ( 'NONE',  ( 19.05341960407617918, -5.049401038297876454, 111.0427570613523329 ) ) ;
#109314 = CARTESIAN_POINT ( 'NONE',  ( 2.500000000000000000, 0.000000000000000000, 0.000000000000000000 ) ) ;
#109315 = CARTESIAN_POINT ( 'NONE',  ( 9.564922557960805705, 16.46253265017160317, 99.58224293864770971 ) ) ;
#109316 = CARTESIAN_POINT ( 'NONE',  ( -21.52544592524343514, 5.823673210054127303, 56.04057627198102409 ) ) ;
#109317 = CARTESIAN_POINT ( 'NONE',  ( 5.049401038297881783, 19.05341960407617563, 97.29275706135233293 ) ) ;
#109318 = CARTESIAN_POINT ( 'NONE',  ( 16.51473224551069308, 9.474510206698969483, 89.16557627198103830 ) ) ;
#109319 = CARTESIAN_POINT ( 'NONE',  ( -21.53943276465977519, 0.05219959533907696930, 56.24890960531436690 ) ) ;
#109320 = CARTESIAN_POINT ( 'NONE',  ( -16.52544592524342804, 4.483927247898546575, 106.0405762719810525 ) ) ;
#109321 = CARTESIAN_POINT ( 'NONE',  ( 13.97604488694527802, 13.89961937509977652, 64.37390960531436690 ) ) ;
#109322 = CARTESIAN_POINT ( 'NONE',  ( 13.97604488694527802, 13.89961937509977652, 29.37390960531435979 ) ) ;
#109323 = CARTESIAN_POINT ( 'NONE',  ( -18.67979575497193778, 10.72451020669871902, 43.33442372801901143 ) ) ;
#109324 = CARTESIAN_POINT ( 'NONE',  ( -15.72974639402176322, -15.80617190586768395, 74.37609039468568994 ) ) ;
#109325 = CARTESIAN_POINT ( 'NONE',  ( 16.53943276465976808, 0.05219959533934440121, 91.25109039468568994 ) ) ;
#109326 = CARTESIAN_POINT ( 'NONE',  ( -10.81492255796105439, 18.62759615963255655, 27.91775706135234358 ) ) ;
#109327 = CARTESIAN_POINT ( 'NONE',  ( 18.67979575497194134, -10.72451020669871369, 35.83442372801901143 ) ) ;
#109329 = CARTESIAN_POINT ( 'NONE',  ( 9.564922557960805705, 16.46253265017160317, 74.58224293864769550 ) ) ;
#109328 = CARTESIAN_POINT ( 'NONE',  ( -5.049401038297874678, -19.05341960407617918, 69.79275706135233293 ) ) ;
#109330 = CARTESIAN_POINT ( 'NONE',  ( 21.55341960407619695, -5.719274019375665929, 81.04275706135236135 ) ) ;
#109331 = CARTESIAN_POINT ( 'NONE',  ( 21.53943276465977519, -0.05219959533907433946, 83.74890960531435269 ) ) ;
#109332 = CARTESIAN_POINT ( 'NONE',  ( 16.52544592524342804, -4.483927247898539470, 68.54057627198103830 ) ) ;
#109333 = CARTESIAN_POINT ( 'NONE',  ( 18.67979575497194134, -10.72451020669871369, 105.8344237280190328 ) ) ;
#109334 = CARTESIAN_POINT ( 'NONE',  ( -12.06949235617756955, 12.14591786802309770, 80.62390960531438111 ) ) ;
#109335 = CARTESIAN_POINT ( 'NONE',  ( -19.05341960407611168, -5.049401038298163336, 31.45724293864769550 ) ) ;
#109336 = CARTESIAN_POINT ( 'NONE',  ( -9.474510206698720793, -16.51473224551083518, 69.58442372801901854 ) ) ;
#109337 = CARTESIAN_POINT ( 'NONE',  ( 16.53943276465976808, -0.05219959533910856209, 38.74890960531435979 ) ) ;
#109338 = CARTESIAN_POINT ( 'NONE',  ( -10.81492255796105439, 18.62759615963255655, 97.91775706135236135 ) ) ;
#109339 = CARTESIAN_POINT ( 'NONE',  ( 19.02544592524343514, -5.153800228976328945, 98.54057627198100988 ) ) ;
#109340 = CARTESIAN_POINT ( 'NONE',  ( 5.049401038297881783, 19.05341960407617563, 62.29275706135234003 ) ) ;
#109341 = CARTESIAN_POINT ( 'NONE',  ( -15.80617190586745835, -15.72974639402198527, 66.87390960531436690 ) ) ;
#109342 = CARTESIAN_POINT ( 'NONE',  ( -21.53943276465977519, -0.05219959533937600094, 23.75109039468567929 ) ) ;
#109343 = CARTESIAN_POINT ( 'NONE',  ( -5.153800228976607833, 19.02544592524334988, 112.7094237280190043 ) ) ;
#109344 = CARTESIAN_POINT ( 'NONE',  ( 16.52544592524335698, 4.483927247898782831, 81.45942372801900433 ) ) ;
#109346 = CARTESIAN_POINT ( 'NONE',  ( -15.80617190586768217, 15.72974639402176855, 28.12609039468568284 ) ) ;
#109345 = CARTESIAN_POINT ( 'NONE',  ( -6.856101608890825108E-16, -71.74905178543389184, -12.99263613531267936 ) ) ;
#109347 = CARTESIAN_POINT ( 'NONE',  ( 16.55341960407611168, 4.379528057220329451, 108.9572429386476955 ) ) ;
#109348 = CARTESIAN_POINT ( 'NONE',  ( -5.950531402560715689E-15, 38.81732327939063509, -3.624999997268813168 ) ) ;
#109349 = CARTESIAN_POINT ( 'NONE',  ( 8.224510206698742110, 14.34966873604972548, 52.08442372801901854 ) ) ;
#109350 = CARTESIAN_POINT ( 'NONE',  ( -10.81492255796078084, -18.62759615963271287, 67.08224293864770971 ) ) ;
#109351 = CARTESIAN_POINT ( 'NONE',  ( 4.483927247898790824, -16.52544592524335698, 100.2094237280190043 ) ) ;
#109352 = CARTESIAN_POINT ( 'NONE',  ( 12.06949235617739724, 12.14591786802326823, 31.87609039468567929 ) ) ;
#109353 = CARTESIAN_POINT ( 'NONE',  ( -9.564922557960796823, -16.46253265017161027, 27.08224293864769550 ) ) ;
#109354 = CARTESIAN_POINT ( 'NONE',  ( -16.53943276465976808, -0.05219959533934237506, 78.75109039468568994 ) ) ;
#109355 = CARTESIAN_POINT ( 'NONE',  ( -9.564922557961040184, 16.46253265017147172, 77.91775706135234714 ) ) ;
#109356 = CARTESIAN_POINT ( 'NONE',  ( -5.719274019375978568, 21.55341960407610458, 70.20724293864769550 ) ) ;
#109357 = CARTESIAN_POINT ( 'NONE',  ( -8.224510206698735004, -14.34966873604973081, 94.58442372801901854 ) ) ;
#109358 = CARTESIAN_POINT ( 'NONE',  ( -15.72974639402176322, -15.80617190586768395, 84.37609039468570415 ) ) ;
#109359 = CARTESIAN_POINT ( 'NONE',  ( -0.05219959533907301413, -21.53943276465977519, 67.49890960531436690 ) ) ;
#109360 = CARTESIAN_POINT ( 'NONE',  ( 15.72974639402199770, -15.80617190586745480, 48.12390960531436690 ) ) ;
#109361 = ORIENTED_EDGE ( 'NONE', *, *, #43460, .T. ) ;
#109362 = CARTESIAN_POINT ( 'NONE',  ( 0.05219959533934541429, -16.53943276465976808, 85.00109039468568994 ) ) ;
#109363 = CARTESIAN_POINT ( 'NONE',  ( -0.05219959533907301413, -21.53943276465977519, 47.49890960531435979 ) ) ;
#109364 = ORIENTED_EDGE ( 'NONE', *, *, #119692, .F. ) ;
#109365 = CARTESIAN_POINT ( 'NONE',  ( -13.97604488694527625, -13.89961937509977652, 111.8739096053143243 ) ) ;
#109366 = DIRECTION ( 'NONE',  ( -1.000000000000000000, -0.000000000000000000, -0.000000000000000000 ) ) ;
#109367 = CARTESIAN_POINT ( 'NONE',  ( 19.02544592524343514, -5.153800228976328945, 28.54057627198102409 ) ) ;
#109368 = CARTESIAN_POINT ( 'NONE',  ( -5.823673210054116645, -21.52544592524344225, 57.29057627198103120 ) ) ;
#109369 = CARTESIAN_POINT ( 'NONE',  ( -16.52544592524335698, -4.483927247898792601, 103.9594237280190185 ) ) ;
#109370 = CARTESIAN_POINT ( 'NONE',  ( 21.53943276465977519, 0.05219959533937863772, 41.25109039468568284 ) ) ;
#109371 = CARTESIAN_POINT ( 'NONE',  ( 0.05219959533936267826, -19.03943276465977164, 100.0010903946856757 ) ) ;
#109372 = CARTESIAN_POINT ( 'NONE',  ( -19.05341960407611168, -5.049401038298163336, 26.45724293864769550 ) ) ;
#109373 = CARTESIAN_POINT ( 'NONE',  ( -9.474510206698720793, -16.51473224551083518, 109.5844237280190043 ) ) ;
#109374 = CARTESIAN_POINT ( 'NONE',  ( 9.474510206698971260, -16.51473224551069308, 42.91557627198103120 ) ) ;
#109375 = CARTESIAN_POINT ( 'NONE',  ( 28.82186960331498327, 9.364793116373570925, 141.0999999999999943 ) ) ;
#109376 = CARTESIAN_POINT ( 'NONE',  ( 9.474510206698971260, -16.51473224551069308, 97.91557627198102409 ) ) ;
#109377 = ADVANCED_FACE ( 'NONE', ( #1322 ), #47855, .T. ) ;
#109379 = B_SPLINE_CURVE_WITH_KNOTS ( 'NONE', 3,
 ( #96958, #175816, #6940, #20129, #68619, #33324 ),
 .UNSPECIFIED., .F., .F.,
 ( 4, 2, 4 ),
 ( 0.003239945802372283350, 0.003620412082092137277, 0.004000878361811991205 ),
 .UNSPECIFIED. ) ;
#109378 = CARTESIAN_POINT ( 'NONE',  ( 16.53943276465976808, 0.05219959533934440121, 76.25109039468568994 ) ) ;
#109380 = CARTESIAN_POINT ( 'NONE',  ( 0.05219959533936267826, -19.03943276465977164, 85.00109039468567573 ) ) ;
#109381 = CARTESIAN_POINT ( 'NONE',  ( -19.02544592524334988, -5.153800228976617603, 18.95942372801899722 ) ) ;
#109382 = CARTESIAN_POINT ( 'NONE',  ( -18.67979575497178146, -10.72451020669898902, 66.66557627198102409 ) ) ;
#109383 = CARTESIAN_POINT ( 'NONE',  ( 14.34966873604972726, -8.224510206698740333, 90.83442372801901854 ) ) ;
#109384 = CARTESIAN_POINT ( 'NONE',  ( -19.02544592524334988, -5.153800228976617603, 83.95942372801901854 ) ) ;
#109385 = CARTESIAN_POINT ( 'NONE',  ( -9.564922557960796823, -16.46253265017161027, 42.08224293864769550 ) ) ;
#109386 = CARTESIAN_POINT ( 'NONE',  ( -9.474510206698964154, 16.51473224551069663, 75.41557627198103830 ) ) ;
#109387 = CARTESIAN_POINT ( 'NONE',  ( -10.81492255796105439, 18.62759615963255655, 52.91775706135235424 ) ) ;
#109388 = CARTESIAN_POINT ( 'NONE',  ( 9.564922557960805705, 16.46253265017160317, 44.58224293864769550 ) ) ;
#109389 = CARTESIAN_POINT ( 'NONE',  ( 0.05219959533936267826, -19.03943276465977164, 75.00109039468566152 ) ) ;
#109390 = CARTESIAN_POINT ( 'NONE',  ( 26.73207562759457190, -6.543912086049391341, 168.7462576975893285 ) ) ;
#109391 = CARTESIAN_POINT ( 'NONE',  ( 5.049401038298161559, -19.05341960407611168, 107.7072429386476955 ) ) ;
#109392 = CARTESIAN_POINT ( 'NONE',  ( 8.224510206698953496, -14.34966873604960469, 62.91557627198102409 ) ) ;
#109393 = CARTESIAN_POINT ( 'NONE',  ( 10.81492255796078972, 18.62759615963270932, 59.58224293864770260 ) ) ;
#109394 = CARTESIAN_POINT ( 'NONE',  ( 4.500000000000000888, -120.6140767358124180, 14.26817184396703198 ) ) ;
#109395 = CARTESIAN_POINT ( 'NONE',  ( -19.03943276465977164, -0.05219959533935918106, 38.75109039468566152 ) ) ;
#109396 = CARTESIAN_POINT ( 'NONE',  ( -17.72696623605160582, 5.500000000000055955, 88.59811031808420978 ) ) ;
#109398 = CARTESIAN_POINT ( 'NONE',  ( -16.51473224551069308, -9.474510206698971260, 71.66557627198102409 ) ) ;
#109397 = CARTESIAN_POINT ( 'NONE',  ( -19.02544592524342804, 5.153800228976336051, 61.04057627198103120 ) ) ;
#109399 = CARTESIAN_POINT ( 'NONE',  ( 0.05219959533934541429, -16.53943276465976808, 45.00109039468568284 ) ) ;
#109400 = CARTESIAN_POINT ( 'NONE',  ( -24.27707668318815237, 5.858708095980201591, 170.2635530474734651 ) ) ;
#109401 = CARTESIAN_POINT ( 'NONE',  ( 2.500000000000000000, 2.357898499370431722, -2.818925648462311528E-15 ) ) ;
#109402 = CARTESIAN_POINT ( 'NONE',  ( -16.55341960407617563, 4.379528057220093196, 93.54275706135234714 ) ) ;
#109403 = EDGE_CURVE ( 'NONE', #184582, #154217, #143554, .T. ) ;
#109404 = CARTESIAN_POINT ( 'NONE',  ( 17.97058386085787163, 5.500000000000006217, 96.50390968646217971 ) ) ;
#109405 = CARTESIAN_POINT ( 'NONE',  ( 4.483927247898790824, -16.52544592524335698, 65.20942372801901854 ) ) ;
#109406 = CARTESIAN_POINT ( 'NONE',  ( 16.52544592524335698, 4.483927247898782831, 46.45942372801901854 ) ) ;
#109407 = CARTESIAN_POINT ( 'NONE',  ( -13.89961937509957401, -13.97604488694547875, 24.37609039468565442 ) ) ;
#109409 = CARTESIAN_POINT ( 'NONE',  ( -3.573655867282028392E-15, 2.428612866367529932E-14, 2.000000000000000000 ) ) ;
#109408 = CARTESIAN_POINT ( 'NONE',  ( -0.05219959533909027116, -19.03943276465977164, 52.49890960531436690 ) ) ;
#109410 = CARTESIAN_POINT ( 'NONE',  ( -10.72451020669870658, -18.67979575497194134, 54.58442372801901143 ) ) ;
#109411 = CARTESIAN_POINT ( 'NONE',  ( -16.51473224551082808, 9.474510206698731452, 63.33442372801900433 ) ) ;
#109412 = CARTESIAN_POINT ( 'NONE',  ( 21.53943276465977519, 0.05219959533937863772, 106.2510903946856757 ) ) ;
#109413 = CARTESIAN_POINT ( 'NONE',  ( -16.46253265017160317, 9.564922557960807481, 35.83224293864768839 ) ) ;
#109414 = CARTESIAN_POINT ( 'NONE',  ( 4.500000000000000888, -139.5000000000000000, 21.82407087589996664 ) ) ;
#109415 = CARTESIAN_POINT ( 'NONE',  ( 21.55341960407610458, 5.719274019375980345, 53.95724293864770260 ) ) ;
#109416 = CARTESIAN_POINT ( 'NONE',  ( 10.72451020669898902, -18.67979575497178502, 27.91557627198103830 ) ) ;
#109417 = CARTESIAN_POINT ( 'NONE',  ( -4.483927247898539470, -16.52544592524342804, 97.29057627198105251 ) ) ;
#109418 = CARTESIAN_POINT ( 'NONE',  ( 14.34966873604972726, -8.224510206698740333, 30.83442372801902209 ) ) ;
#109419 = CARTESIAN_POINT ( 'NONE',  ( 14.29746914071049879, -8.314922557960816363, 28.33224293864769550 ) ) ;
#109420 = ORIENTED_EDGE ( 'NONE', *, *, #18488, .T. ) ;
#109421 = CARTESIAN_POINT ( 'NONE',  ( -15.72974639402197994, 15.80617190586746368, 110.6239096053143669 ) ) ;
#109423 = CARTESIAN_POINT ( 'NONE',  ( 9.564922557960805705, 16.46253265017160317, 114.5822429386476955 ) ) ;
#109422 = CARTESIAN_POINT ( 'NONE',  ( -8.224510206698948167, 14.34966873604960824, 35.41557627198102409 ) ) ;
#109424 = CARTESIAN_POINT ( 'NONE',  ( 16.46253265017146816, 9.564922557961045513, 106.6677570613523471 ) ) ;
#109425 = CARTESIAN_POINT ( 'NONE',  ( -16.46253265017146816, -9.564922557961047289, 24.16775706135233648 ) ) ;
#109426 = CARTESIAN_POINT ( 'NONE',  ( -16.55341960407611168, -4.379528057220339221, 31.45724293864769550 ) ) ;
#109427 = CARTESIAN_POINT ( 'NONE',  ( 10.81492255796078972, 18.62759615963270932, 109.5822429386476955 ) ) ;
#109429 = CARTESIAN_POINT ( 'NONE',  ( 0.05219959533907565091, 21.53943276465977519, 64.99890960531435269 ) ) ;
#109428 = CARTESIAN_POINT ( 'NONE',  ( 16.20579543436681647, 7.371946100354974440, 33.06520834171879386 ) ) ;
#109430 = CARTESIAN_POINT ( 'NONE',  ( -19.02544592524342804, 5.153800228976336051, 76.04057627198102409 ) ) ;
#109431 = CARTESIAN_POINT ( 'NONE',  ( 14.34966873604960469, 8.224510206698951720, 54.16557627198103120 ) ) ;
#109432 = CARTESIAN_POINT ( 'NONE',  ( -16.46253265017160317, 9.564922557960807481, 95.83224293864769550 ) ) ;
#109433 = CARTESIAN_POINT ( 'NONE',  ( 16.46253265017146816, 9.564922557961045513, 56.66775706135233293 ) ) ;
#109434 = CARTESIAN_POINT ( 'NONE',  ( 18.62759615963271287, -10.81492255796078972, 98.33224293864769550 ) ) ;
#109435 = CARTESIAN_POINT ( 'NONE',  ( 14.34966873604960469, 8.224510206698951720, 94.16557627198103830 ) ) ;
#109436 = CARTESIAN_POINT ( 'NONE',  ( 5.719274019375673035, 21.55341960407619339, 42.29275706135235424 ) ) ;
#109437 = CARTESIAN_POINT ( 'NONE',  ( 27.73933785331498569, 2.768321779492822058E-14, 141.8750000027311842 ) ) ;
#109438 = CARTESIAN_POINT ( 'NONE',  ( -14.34966873604960291, -8.224510206698953496, 26.66557627198103475 ) ) ;
#109439 = CARTESIAN_POINT ( 'NONE',  ( -0.05219959533909027116, -19.03943276465977164, 32.49890960531435979 ) ) ;
#109440 = CARTESIAN_POINT ( 'NONE',  ( 0.05219959533909260263, 19.03943276465977164, 79.99890960531436690 ) ) ;
#109441 = CARTESIAN_POINT ( 'NONE',  ( 21.53943276465977519, -0.05219959533907433946, 63.74890960531435979 ) ) ;
#109442 = CARTESIAN_POINT ( 'NONE',  ( -19.01533133064926062, 5.499999999999455547, 43.76586590595741200 ) ) ;
#109443 = CARTESIAN_POINT ( 'NONE',  ( -9.564922557960796823, -16.46253265017161027, 32.08224293864769550 ) ) ;
#109444 = CARTESIAN_POINT ( 'NONE',  ( 18.62759615963271287, -10.81492255796078972, 48.33224293864770260 ) ) ;
#109445 = CARTESIAN_POINT ( 'NONE',  ( -15.72974639402176322, -15.80617190586768395, 74.37609039468568994 ) ) ;
#109447 = CARTESIAN_POINT ( 'NONE',  ( 12.14591786802327356, -12.06949235617739191, 75.62609039468567573 ) ) ;
#109446 = CARTESIAN_POINT ( 'NONE',  ( 20.00963169948072462, -33.79917020546515971, -17.75419178524472130 ) ) ;
#109448 = CARTESIAN_POINT ( 'NONE',  ( -9.564922557960796823, -16.46253265017161027, 62.08224293864769550 ) ) ;
#109449 = CARTESIAN_POINT ( 'NONE',  ( 9.564922557960805705, 16.46253265017160317, 69.58224293864770971 ) ) ;
#109450 = ORIENTED_EDGE ( 'NONE', *, *, #51790, .F. ) ;
#109451 = CARTESIAN_POINT ( 'NONE',  ( -18.62759615963255300, -10.81492255796106328, 109.1677570613523613 ) ) ;
#109452 = CARTESIAN_POINT ( 'NONE',  ( -8.314922557961024197, 14.29746914071037800, 77.91775706135231871 ) ) ;
#109453 = CARTESIAN_POINT ( 'NONE',  ( -15.72974639402176322, -15.80617190586768395, 94.37609039468568994 ) ) ;
#109454 = CARTESIAN_POINT ( 'NONE',  ( -19.03943276465977164, 0.05219959533909376836, 71.24890960531435269 ) ) ;
#109455 = CARTESIAN_POINT ( 'NONE',  ( 5.719274019375991003, -21.55341960407610458, 37.70724293864769550 ) ) ;
#109456 = CARTESIAN_POINT ( 'NONE',  ( -19.02544592524334988, -5.153800228976617603, 108.9594237280189759 ) ) ;
#109457 = CARTESIAN_POINT ( 'NONE',  ( 5.823673210054444382, -21.52544592524334988, 80.20942372801901854 ) ) ;
#109458 = CARTESIAN_POINT ( 'NONE',  ( -8.224510206698735004, -14.34966873604973081, 44.58442372801901854 ) ) ;
#109459 = CARTESIAN_POINT ( 'NONE',  ( 21.53943276465977519, -0.05219959533907433946, 93.74890960531436690 ) ) ;
#109460 = CARTESIAN_POINT ( 'NONE',  ( -12.14591786802326823, 12.06949235617739902, 23.12609039468567573 ) ) ;
#109461 = CARTESIAN_POINT ( 'NONE',  ( -9.564922557960796823, -16.46253265017161027, 77.08224293864769550 ) ) ;
#109462 = CARTESIAN_POINT ( 'NONE',  ( 16.46253265017146816, 9.564922557961045513, 111.6677570613523329 ) ) ;
#109463 = CARTESIAN_POINT ( 'NONE',  ( -13.89961937509977652, 13.97604488694528158, 40.62390960531435979 ) ) ;
#109464 = CARTESIAN_POINT ( 'NONE',  ( -0.05219959533936034679, 19.03943276465977164, 112.5010903946856757 ) ) ;
#109465 = CARTESIAN_POINT ( 'NONE',  ( -14.29746914071049879, 8.314922557960819915, 65.83224293864769550 ) ) ;
#109466 = CARTESIAN_POINT ( 'NONE',  ( 12.06949235617739724, 12.14591786802326823, 71.87609039468568994 ) ) ;
#109468 = CARTESIAN_POINT ( 'NONE',  ( -16.46253265017160317, 9.564922557960807481, 45.83224293864769550 ) ) ;
#109467 = CARTESIAN_POINT ( 'NONE',  ( 21.52544592524334988, 5.823673210054432836, 26.45942372801901854 ) ) ;
#109469 = CARTESIAN_POINT ( 'NONE',  ( 5.153800228976335163, 19.02544592524342804, 64.79057627198100988 ) ) ;
#109470 = CARTESIAN_POINT ( 'NONE',  ( 16.52544592524335698, 4.483927247898782831, 76.45942372801901854 ) ) ;
#109472 = VERTEX_POINT ( 'NONE', #135897 ) ;
#109471 = CARTESIAN_POINT ( 'NONE',  ( -24.73536985823983869, -3.645104810711615961, 171.5180696409408085 ) ) ;
#109473 = ORIENTED_EDGE ( 'NONE', *, *, #171282, .F. ) ;
#109474 = CARTESIAN_POINT ( 'NONE',  ( 5.823673210054444382, -21.52544592524334988, 110.2094237280190185 ) ) ;
#109475 = EDGE_CURVE ( 'NONE', #104654, #111651, #59036, .T. ) ;
#109476 = CARTESIAN_POINT ( 'NONE',  ( 13.89961937509977652, -13.97604488694527269, 33.12390960531434558 ) ) ;
#109478 = ORIENTED_EDGE ( 'NONE', *, *, #61610, .F. ) ;
#109477 = CARTESIAN_POINT ( 'NONE',  ( -19.05341960407611168, -5.049401038298163336, 101.4572429386476955 ) ) ;
#109479 = CARTESIAN_POINT ( 'NONE',  ( 14.29746914071037800, 8.314922557961029526, 31.66775706135234358 ) ) ;
#109480 = CIRCLE ( 'NONE', #22321, 61.99999999999998579 ) ;
#109482 = CARTESIAN_POINT ( 'NONE',  ( 8.224510206698742110, 14.34966873604972548, 37.08442372801901143 ) ) ;
#109481 = CARTESIAN_POINT ( 'NONE',  ( -19.02544592524334988, -5.153800228976617603, 63.95942372801899012 ) ) ;
#109483 = CARTESIAN_POINT ( 'NONE',  ( -19.02544592524342804, 5.153800228976336051, 41.04057627198103120 ) ) ;
#109484 = CARTESIAN_POINT ( 'NONE',  ( 9.474510206698971260, -16.51473224551069308, 107.9155762719810383 ) ) ;
#109485 = CARTESIAN_POINT ( 'NONE',  ( -19.02544592524342804, 5.153800228976336051, 66.04057627198103830 ) ) ;
#109486 = CARTESIAN_POINT ( 'NONE',  ( -15.72974639402197994, 15.80617190586746368, 105.6239096053143669 ) ) ;
#109488 = FACE_OUTER_BOUND ( 'NONE', #133513, .T. ) ;
#109487 = CARTESIAN_POINT ( 'NONE',  ( 9.564922557960805705, 16.46253265017160317, 94.58224293864769550 ) ) ;
#109489 = CARTESIAN_POINT ( 'NONE',  ( 13.97604488694527802, 13.89961937509977652, 69.37390960531436690 ) ) ;
#109491 = CARTESIAN_POINT ( 'NONE',  ( 32.00000000000000000, -1.130961319012580892E-14, 97.65000000000000568 ) ) ;
#109490 = CARTESIAN_POINT ( 'NONE',  ( 14.34966873604960469, 8.224510206698951720, 24.16557627198103120 ) ) ;
#109492 = CARTESIAN_POINT ( 'NONE',  ( -19.03943276465977164, -0.05219959533935918106, 98.75109039468567573 ) ) ;
#109493 = CARTESIAN_POINT ( 'NONE',  ( -5.049401038297874678, -19.05341960407617918, 29.79275706135232227 ) ) ;
#109494 = EDGE_CURVE ( 'NONE', #175496, #27947, #94591, .T. ) ;
#109495 = CARTESIAN_POINT ( 'NONE',  ( 8.314922557960818139, 14.29746914071049879, 54.58224293864769550 ) ) ;
#109496 = CARTESIAN_POINT ( 'NONE',  ( -5.823673210054431948, 21.52544592524334988, 92.70942372801901854 ) ) ;
#109497 = CARTESIAN_POINT ( 'NONE',  ( -19.05341960407611168, -5.049401038298163336, 31.45724293864769550 ) ) ;
#109499 = CARTESIAN_POINT ( 'NONE',  ( -21.52544592524334988, -5.823673210054445271, 83.95942372801900433 ) ) ;
#109498 = CARTESIAN_POINT ( 'NONE',  ( -4.483927247898539470, -16.52544592524342804, 27.29057627198103120 ) ) ;
#109500 = CARTESIAN_POINT ( 'NONE',  ( -0.05219959533909027116, -19.03943276465977164, 77.49890960531435269 ) ) ;
#109501 = CARTESIAN_POINT ( 'NONE',  ( 19.05341960407611168, 5.049401038298154454, 98.95724293864766707 ) ) ;
#109502 = CARTESIAN_POINT ( 'NONE',  ( -4.379528057220328563, 16.55341960407611168, 100.2072429386476955 ) ) ;
#109503 = CARTESIAN_POINT ( 'NONE',  ( 4.483927247898545687, 16.52544592524342804, 64.79057627198103830 ) ) ;
#109504 = CARTESIAN_POINT ( 'NONE',  ( -18.67979575497178146, -10.72451020669898902, 76.66557627198103830 ) ) ;
#109505 = CARTESIAN_POINT ( 'NONE',  ( 13.89961937509977652, -13.97604488694527269, 73.12390960531436690 ) ) ;
#109506 = CARTESIAN_POINT ( 'NONE',  ( -15.80617190586745835, -15.72974639402198527, 86.87390960531438111 ) ) ;
#109507 = CARTESIAN_POINT ( 'NONE',  ( 9.474510206698729675, 16.51473224551082808, 82.08442372801899012 ) ) ;
#109509 = CARTESIAN_POINT ( 'NONE',  ( -16.55341960407611168, -4.379528057220339221, 86.45724293864770971 ) ) ;
#109508 = CARTESIAN_POINT ( 'NONE',  ( -0.05219959533936034679, 19.03943276465977164, 32.50109039468566863 ) ) ;
#109510 = CARTESIAN_POINT ( 'NONE',  ( -19.02544592524342804, 5.153800228976336051, 61.04057627198103120 ) ) ;
#109511 = CARTESIAN_POINT ( 'NONE',  ( -10.81492255796078084, -18.62759615963271287, 67.08224293864770971 ) ) ;
#109512 = CARTESIAN_POINT ( 'NONE',  ( 16.20579543436675252, -7.371946100355229348, 26.93479165828123811 ) ) ;
#109514 = FACE_OUTER_BOUND ( 'NONE', #68066, .T. ) ;
#109513 = CARTESIAN_POINT ( 'NONE',  ( 8.224510206698953496, -14.34966873604960469, 22.91557627198102765 ) ) ;
#109515 = CARTESIAN_POINT ( 'NONE',  ( 19.02544592524334988, 5.153800228976608722, 101.4594237280189759 ) ) ;
#109516 = CARTESIAN_POINT ( 'NONE',  ( 16.52544592524342804, -4.483927247898539470, 78.54057627198103830 ) ) ;
#109517 = CARTESIAN_POINT ( 'NONE',  ( 7.215019197202733992, -1.452998035947227873, -62.28058590214430978 ) ) ;
#109518 = CARTESIAN_POINT ( 'NONE',  ( 13.89961937509977652, -13.97604488694527269, 78.12390960531433848 ) ) ;
#109519 = CARTESIAN_POINT ( 'NONE',  ( -16.51473224551069308, -9.474510206698971260, 31.66557627198102054 ) ) ;
#109520 = CARTESIAN_POINT ( 'NONE',  ( -8.314922557960811034, -14.29746914071050412, 67.08224293864770971 ) ) ;
#109521 = CARTESIAN_POINT ( 'NONE',  ( 5.049401038298161559, -19.05341960407611168, 107.7072429386476955 ) ) ;
#109523 = CARTESIAN_POINT ( 'NONE',  ( 13.89961937509977652, -13.97604488694527269, 68.12390960531436690 ) ) ;
#109522 = CARTESIAN_POINT ( 'NONE',  ( 13.97604488694548053, -13.89961937509957401, 95.62609039468563310 ) ) ;
#109524 = CARTESIAN_POINT ( 'NONE',  ( 19.03943276465977164, -0.05219959533909143690, 88.74890960531436690 ) ) ;
#109525 = CARTESIAN_POINT ( 'NONE',  ( 5.823673210054125526, 21.52544592524343514, 74.79057627198105251 ) ) ;
#109526 = CARTESIAN_POINT ( 'NONE',  ( -14.29746914071037622, -8.314922557961029526, 74.16775706135231871 ) ) ;
#109527 = CARTESIAN_POINT ( 'NONE',  ( -17.49999999999999645, 5.499999999999992895, 93.71769037696437010 ) ) ;
#109528 = CARTESIAN_POINT ( 'NONE',  ( 16.51473224551069308, 9.474510206698969483, 64.16557627198102409 ) ) ;
#109529 = CARTESIAN_POINT ( 'NONE',  ( 21.52544592524344225, -5.823673210054117533, 68.54057627198103830 ) ) ;
#109530 = CARTESIAN_POINT ( 'NONE',  ( 0.05219959533936267826, -19.03943276465977164, 90.00109039468567573 ) ) ;
#109532 = CARTESIAN_POINT ( 'NONE',  ( 21.52544592524334988, 5.823673210054432836, 41.45942372801901143 ) ) ;
#109531 = CARTESIAN_POINT ( 'NONE',  ( 16.52544592524342804, -4.483927247898539470, 38.54057627198103120 ) ) ;
#109533 = CARTESIAN_POINT ( 'NONE',  ( 28.82186960331491221, -9.364793116373624215, 145.1500000054623740 ) ) ;
#109535 = CARTESIAN_POINT ( 'NONE',  ( -5.153800228976328057, -19.02544592524343514, 102.2905762719810383 ) ) ;
#109534 = CARTESIAN_POINT ( 'NONE',  ( 12.14591786802327356, -12.06949235617739191, 75.62609039468567573 ) ) ;
#109536 = CARTESIAN_POINT ( 'NONE',  ( 9.474510206698971260, -16.51473224551069308, 102.9155762719810241 ) ) ;
#109537 = DIRECTION ( 'NONE',  ( 0.000000000000000000, 0.000000000000000000, -1.000000000000000000 ) ) ;
#109538 = CARTESIAN_POINT ( 'NONE',  ( -4.483927247898782831, 16.52544592524335698, 87.70942372801901854 ) ) ;
#109539 = CARTESIAN_POINT ( 'NONE',  ( 16.55341960407618274, -4.379528057220086978, 46.04275706135234714 ) ) ;
#109540 = CARTESIAN_POINT ( 'NONE',  ( -16.46253265017160317, 9.564922557960807481, 60.83224293864769550 ) ) ;
#109541 = CARTESIAN_POINT ( 'NONE',  ( -16.46253265017160317, 9.564922557960807481, 55.83224293864769550 ) ) ;
#109542 = CARTESIAN_POINT ( 'NONE',  ( 5.823673210054444382, -21.52544592524334988, 50.20942372801901854 ) ) ;
#109543 = CARTESIAN_POINT ( 'NONE',  ( 12.06949235617739724, 12.14591786802326823, 61.87609039468568284 ) ) ;
#109544 = CARTESIAN_POINT ( 'NONE',  ( -14.29746914071049879, 8.314922557960819915, 30.83224293864770260 ) ) ;
#109545 = CARTESIAN_POINT ( 'NONE',  ( 13.89961937509977652, -13.97604488694527269, 48.12390960531435979 ) ) ;
#109546 = CARTESIAN_POINT ( 'NONE',  ( 19.05341960407611168, 5.049401038298154454, 28.95724293864769550 ) ) ;
#109547 = CARTESIAN_POINT ( 'NONE',  ( 4.379528057220092307, 16.55341960407617563, 32.29275706135235424 ) ) ;
#109549 = CARTESIAN_POINT ( 'NONE',  ( -19.05341960407617563, 5.049401038297882671, 83.54275706135233293 ) ) ;
#109548 =( BOUNDED_SURFACE ( )  B_SPLINE_SURFACE ( 3, 2, ( 
 ( #95109, #126442, #140617, #174948, #50611, #37420, #129413, #156798, #112270, #173962, #2107, #18291, #17287, #98064, #159763, #21258, #82913, #63788, #79946, #3103, #64781, #119269, #145592, #70764, #9097, #23264, #25281, #177951, #26272, #178954, #102095, #103096, #195116, #117262, #180952, #7071, #132432, #194124, #84908, #86924, #39419, #87914, #40424, #163780, #164778, #22260, #130409, #41430, #147609, #162763, #148606, #10098, #54587, #38428, #71758, #133428, #57600, #56599, #149601, #24272, #85921, #83909, #118273, #68752, #55587, #192107, #179964, #11098, #100084, #53590, #72774, #131427, #134444, #196129, #42430, #160770, #115266, #176959, #161769, #146587, #8081, #101078, #69757, #193113, #116260, #157311, #172481, #186680, #120244, #33969, #78461, #17814, #185661, #123963, #140135, #48150, #198094, #95626, #3611, #59559, #155323, #63304, #124983, #136414, #188657, #109807, #93637, #142126, #150610, #12106, #170490, #18808, #73769, #94633, #65290, #171490, #181935, #32979, #79471, #80453, #126949, #1627, #187672, #104092, #156312, #47153, #31981, #28274, #165775, #27269, #135442, #64306, #88918, #141139, #2629, #43417, #125973, #49142, #110800, #16811, #89913, #197111, #13086, #58578, #105087, #108811, #166773, #151595, #74751, #144117, #5597, #173484, #4593, #100605, #83433, #145110, #84430, #128935, #36935, #161288, #66286, #191623, #158298, #53102, #37948, #127945, #19787, #146107, #114781, #192634, #115790, #98598, #81428, #22782, #111796, #176474, #85437, #34957, #143114, #20773, #113768, #70288, #7591, #50137, #131956, #82429, #96609, #69277, #130944, #189647, #54116, #21782, #99608, #177479, #51122, #23787, #112781, #174474, #38948, #6593, #162287, #35943, #147128, #97589, #8615, #68272, #159277, #67277, #160291, #190636, #52111, #175464, #129923, #116782, #194641, #43936, #152105, #10624, #42949, #39940, #182455, #13589, #74284, #27798, #178473, #102623, #24798, #58117, #103626, #86446, #101609, #120756, #195654, #12620, #134970, #163299, #196647, #105597, #57126, #148132, #87448, #72285, #9623, #119787, #132953, #40951, #166301, #167283, #71288, #179487, #56111, #117792, #55112, #89439, #41960, #28781, #164309, #90420, #151127, #75256, #133962, #25802, #135954, #180488, #118800, #150131, #181471, #149133, #165302, #104613, #197624, #193640, #59089, #26795, #88437, #11633, #73300, #1377, #121750, #384, #44927, #108570, #78217, #76240, #106583, #185418, #107564, #110552, #32733, #109563, #168260, #171244, #170247, #63056, #186433, #29756, #172233, #91391, #18562, #47909, #31741, #124736, #199601, #94385, #183442, #79222, #93389, #61068, #153080, #46909, #169242, #184431, #14582, #64060, #60082, #137918, #187429, #95380, #154083, #156064, #122740, #125730, #157066, #17562, #140892, #45911, #30748, #92397, #2381, #155075, #15577, #77235, #48897, #138904, #33718, #139888, #62056, #136927, #198614, #123721, #16570, #174233, #159035, #96368, #83192, #19546, #127704, #52854, #130695, #173235, #66037, #158056, #81191, #141881, #114525, #128694, #69030, #3372, #115546, #191378, #177234, #37695, #190391, #20528, #176226, #97349, #34711, #67035, #65047, #82176, #51866, #99359, #7345, #192389, #160044, #53872, #68029, #142872, #143872, #21531, #126703, #161042, #188407, #38706, #5351, #22536, #144866, #100363, #162042, #4352, #6349, #49885, #129680, #84183, #189404, #111550, #145863, #80210, #50881, #112539, #113526, #35702, #175220, #36685, #98345, #58847, #85184, #193390, #194396, #87204, #43690, #196404, #23538, #105352, #55864, #146873, #101354, #26546, #165053, #120514, #11379, #27550, #25560, #148885, #8365, #88190, #70040, #10376, #131709, #195398, #149874, #163043, #54866, #72033, #117538, #197382, #119546, #134721, #181229, #116540, #180241, #133706, #56876, #178228, #40702, #74040, #182206, #118550, #135711, #89190, #103375, #39692, #150883, #41710, #57874, #102372, #164061 ),
 ( #24550, #86200, #147890, #73049, #9376, #71041, #42705, #132708, #104366, #179236, #166050, #12378, #140651, #2141, #143, #47668, #187190, #170004, #184189, #92150, #91151, #48661, #63820, #75015, #124491, #28541, #61812, #1135, #44682, #93148, #62809, #186187, #30499, #152840, #198362, #75999, #90177, #154832, #107322, #125493, #17321, #183200, #60824, #122498, #151860, #121506, #78976, #123482, #185174, #109320, #45671, #153836, #77980, #171000, #46665, #167039, #13351, #76991, #15333, #29517, #31495, #168995, #32492, #94145, #155824, #136680, #138662, #59837, #106335, #108324, #16330, #139647, #168021, #14334, #137673, #199359, #99115, #33483, #145626, #21292, #7106, #67792, #158796, #189169, #144627, #127463, #64813, #97113, #95141, #50641, #20285, #82949, #37454, #160807, #190149, #22295, #98099, #3138, #173993, #51624, #171995, #129448, #156830, #68787, #112303, #6110, #174980, #130445, #192144, #126474, #113289, #18323, #36444, #159797, #188172, #79980, #191147, #52621, #114283, #175986, #81931, #141648, #83946, #49645, #110313, #111308, #172997, #34475, #80961, #35462, #96134, #157823, #19313, #142637, #4115, #65794, #143623, #5108, #66789, #128453, #25317, #118308, #103132, #146622, #27307, #23297, #135478, #164813, #86959, #180000, #116294, #26309, #38463, #196164, #10133, #177984, #8115, #163815, #24307, #101112, #161802, #180988, #176993, #54619, #104128, #12142, #70799, #87949, #100119, #42465, #73806, #134479, #149637, #84941, #162798, #69792, #41467, #148644, #131460, #193147, #165810, #55622, #72810, #195153, #39451, #56635, #88955, #117295, #85956, #147644, #132467, #9133, #11135, #194158, #178990, #57638, #150645, #40458, #102131, #71794, #133463, #115300, #119304, #53624, #75760, #31260, #14093, #151629, #183949, #181972, #137438, #107088, #169767, #124251, #47431, #76755, #109087, #184939, #89949, #60584, #138430, #58613, #154597, #120280, #155592, #199117, #92911, #61579, #17087, #78740, #13123, #200111, #105123, #123248, #46424, #74786, #166809, #16093, #108082, #139417, #62573, #45435, #28309, #77751, #43454, #899, #32256, #136448, #198129, #167787, #122260, #197147, #185947, #59597, #121271, #29286, #182965, #170767, #93914, #44448, #106102, #168759, #90917, #152603, #30262, #91906, #153599, #15096, #51396, #112075, #4876, #2903, #113056, #125260, #82708, #96885, #64581, #33253, #50416, #111074, #187942, #48429, #67553, #63586, #141415, #190908, #98873, #157588, #189921, #186958, #129210, #160569, #21052, #174748, #110085, #49411, #171764, #66559, #173764, #94911, #156596, #52385, #142407, #159555, #81701, #18091, #143384, #114042, #3885, #79746, #34244, #19080, #126246, #128224, #172763, #95904, #36212, #175740, #80728, #65564, #127224, #188938, #1907, #97865, #35231, #37217, #158568, #22058, #144391, #140416, #20057, #5876, #147404, #134241, #130204, #71556, #119074, #25073, #99882, #86716, #194912, #57402, #180756, #117053, #164575, #103893, #148401, #100876, #8892, #7872, #165573, #42232, #191899, #41229, #145387, #178748, #118069, #161567, #9895, #179759, #102890, #70560, #69558, #115062, #192913, #6869, #133221, #24063, #83709, #195926, #23060, #177751, #39220, #68548, #38227, #53384, #40212, #101891, #26069, #162558, #132227, #56387, #87712, #163573, #176754, #84705, #193920, #55383, #146384, #149398, #85718, #10893, #72566, #131223, #54390, #116063, #196917, #107844, #13864, #29056, #183723, #153364, #121034, #104887, #30035, #168537, #124005, #14866, #31028, #90696, #152379, #150413, #91673, #11908, #75531, #135245, #198892, #76527, #166575, #58384, #137206, #197896, #665, #123021, #138204, #184706, #73572, #45209, #60360, #122033, #120051, #44216, #77518, #62335, #106863, #139190, #92678, #199886, #43219, #154366, #61350, #46191, #105875, #167562, #169528, #15860, #182732, #185703, #47192, #108852, #27072, #88718, #181738, #59365, #28075, #89716, #151401 ),
 ( #12891, #74554, #136221, #20810, #128974, #187709, #19824, #16852, #159315, #190673, #51159, #4632, #155363, #79509, #1669, #34993, #80492, #63347, #78503, #97626, #172523, #189686, #111833, #140176, #173522, #82466, #34008, #125024, #64345, #49181, #186720, #96647, #109845, #17853, #143151, #144152, #48190, #156352, #171530, #33018, #32022, #66322, #18847, #5637, #93680, #67314, #81465, #52149, #127983, #142166, #110839, #112819, #95665, #94673, #157352, #141178, #3650, #65328, #174512, #170532, #2668, #50176, #126014, #158335, #126988, #188695, #35979, #175501, #74076, #36974, #75051, #133742, #89227, #181265, #136717, #198398, #68311, #57910, #21820, #119582, #104404, #191662, #83472, #150921, #42742, #58884, #182243, #165089, #145149, #12414, #98635, #166086, #151897, #160330, #6633, #87239, #180277, #113806, #135747, #129962, #53141, #148922, #114820, #197418, #120550, #176512, #43728, #88226, #27589, #105390, #40739, #90214, #102409, #164096, #167076, #149910, #10411, #195437, #25595, #28578, #72069, #56912, #13387, #118587, #41747, #103411, #26583, #11417, #73087, #134758, #196440, #48696, #183237, #95178, #171036, #156865, #17356, #108363, #138698, #94179, #77026, #14370, #46701, #44718, #180, #170041, #32527, #187225, #110348, #139682, #172030, #47704, #152875, #123517, #1169, #121542, #79011, #106374, #18361, #61848, #155858, #124528, #80014, #141683, #76036, #62844, #168056, #186223, #109354, #137711, #29553, #140685, #2177, #63857, #125528, #31531, #91186, #33518, #199395, #59876, #60859, #122534, #184225, #30536, #185210, #45706, #107357, #169030, #92188, #153872, #15370, #93184, #154869, #16366, #78014, #175019, #67830, #52660, #96170, #177032, #173034, #84978, #114322, #36483, #129486, #65831, #176024, #188207, #145663, #159837, #127500, #157860, #113326, #174030, #50682, #111343, #130487, #126509, #4152, #53664, #161840, #20322, #37493, #49679, #192183, #23334, #83984, #99155, #34512, #112340, #19350, #191184, #98139, #80999, #142673, #115342, #5146, #22333, #144665, #189205, #6150, #38502, #66828, #35501, #160844, #97151, #7144, #68828, #100158, #128492, #158834, #81971, #143664, #64847, #3174, #190187, #51662, #21331, #82989, #40496, #102168, #69831, #101149, #197185, #180039, #41508, #181028, #25355, #133500, #57676, #42502, #103171, #105158, #131498, #56672, #195192, #9171, #11173, #163856, #12179, #165848, #88990, #28346, #86996, #116332, #27344, #118345, #148683, #164851, #72848, #10171, #24344, #149675, #87987, #43491, #134518, #150681, #71831, #26347, #193185, #196204, #54658, #119344, #178021, #104166, #73843, #85995, #39489, #135514, #117334, #120315, #58649, #182009, #166844, #162835, #146660, #8155, #147684, #70838, #132506, #194195, #55660, #179028, #140448, #155624, #169800, #106139, #17120, #61613, #931, #168794, #107123, #123281, #31293, #183984, #78772, #186990, #45469, #138462, #46457, #108117, #122294, #171795, #92945, #76791, #125294, #136484, #198164, #153634, #1938, #59634, #77781, #48460, #154631, #167822, #16126, #62605, #63618, #110117, #184972, #170798, #89984, #139450, #121308, #90951, #151665, #13159, #30298, #124283, #183000, #74823, #44484, #29321, #152638, #14128, #47463, #75795, #185980, #109120, #137473, #32290, #93945, #199153, #15129, #60620, #91941, #200143, #94943, #21083, #173795, #6898, #83737, #49442, #127256, #188969, #156627, #187973, #145416, #66588, #128252, #67583, #112104, #20088, #144420, #129241, #189950, #191929, #18122, #143418, #81732, #95934, #97895, #50445, #98903, #52414, #175773, #115090, #35261, #2934, #114072, #4905, #96916, #51424, #159586, #158598, #111105, #36242, #174776, #130233, #82740, #37247, #113084, #5906, #79777, #190937, #141449, #160597, #64614, #22087, #68577, #172794, #126276, #53413, #3916, #33283, #34275, #157620, #19110, #80760, #142438, #65596, #163602, #84733, #193949, #27099, #150438, #25103 ),
 ( #73597, #70590, #86747, #133250, #194942, #8922, #58409, #56418, #148430, #11934, #23088, #146411, #40246, #88745, #7902, #164604, #135269, #118098, #192941, #179788, #87741, #196941, #176782, #9925, #117083, #41257, #161594, #177778, #101920, #100904, #71584, #69586, #55412, #102919, #149426, #103920, #38255, #26098, #99909, #10922, #131253, #72595, #134269, #54420, #195956, #116090, #39248, #178778, #57429, #119102, #162588, #24093, #85747, #180783, #147434, #42260, #165600, #132258, #89739, #154390, #184731, #62362, #185730, #168560, #151425, #92702, #181764, #46216, #155386, #43245, #12912, #90717, #183747, #140201, #15885, #120076, #1695, #152400, #104913, #77543, #139215, #74576, #690, #91699, #107869, #169557, #136244, #93704, #197920, #166600, #31054, #153393, #124031, #182756, #47219, #28100, #108878, #76552, #44240, #59388, #30058, #13887, #14891, #121062, #170557, #105897, #167583, #32047, #78527, #137230, #16876, #29078, #75554, #198914, #60383, #122055, #45233, #106887, #138228, #199910, #61374, #123045, #171553, #190702, #65354, #82497, #4659, #33043, #66350, #52175, #127015, #94698, #157380, #142193, #79534, #128012, #2694, #110864, #36006, #113833, #156375, #49206, #141204, #64371, #125048, #97655, #111861, #175529, #186745, #98664, #174539, #160358, #20840, #173551, #3676, #159344, #80519, #17880, #126039, #189714, #144180, #5666, #188722, #187735, #172549, #34034, #48215, #51187, #50206, #37003, #21848, #95692, #18873, #35020, #109869, #96675, #83499, #158363, #19852, #67342, #81492, #143179, #129003, #145176, #112848, #63371, #191688, #116847, #55178, #69342, #71354, #23853, #72353, #25868, #149199, #88505, #147192, #176541, #87511, #193709, #8682, #163366, #133018, #100670, #84495, #9689, #148196, #103690, #194708, #10689, #70353, #132020, #129988, #56177, #53170, #178538, #114847, #40004, #117860, #146173, #38017, #101676, #177546, #180552, #102687, #179551, #164375, #99673, #24862, #86512, #41021, #161357, #85503, #57193, #42026, #134027, #118868, #195720, #165369, #22848, #26863, #6660, #68338, #7658, #131009, #192700, #54183, #162352, #115856, #39015, #59155, #90491, #198683, #60150, #197690, #15648, #121818, #28851, #30820, #135038, #196714, #105667, #45981, #58183, #106657, #169313, #183514, #104681, #44997, #29826, #92468, #154156, #75324, #44005, #168330, #119851, #27865, #152173, #151196, #150201, #11699, #181535, #137989, #43014, #91463, #14652, #153150, #136994, #76312, #12684, #199673, #166368, #122811, #61139, #74350, #89506, #184501, #120824, #107636, #136016, #73366, #13656, #182524, #167353, #77622, #60457, #109950, #13963, #47300, #186825, #30133, #78607, #48294, #174365, #15962, #76626, #183819, #61452, #75630, #140281, #92781, #128827, #5487, #168633, #46293, #107950, #137308, #106959, #67170, #185813, #108957, #35835, #31133, #139292, #63451, #97481, #170636, #113659, #198989, #62439, #769, #14966, #16953, #169637, #20662, #159167, #82316, #36821, #154470, #122132, #144006, #124113, #32125, #93782, #1773, #155463, #91776, #125128, #190526, #52000, #175353, #152476, #45309, #153470, #138304, #199985, #123122, #184807, #6482, #70178, #39827, #37837, #68162, #147016, #69167, #72174, #194529, #9511, #56000, #145001, #55003, #85324, #8501, #129814, #115682, #149023, #133848, #131846, #10511, #164194, #178363, #114668, #25692, #193529, #71177, #177370, #38842, #116673, #101493, #192525, #87337, #195538, #54008, #163182, #24686, #86335, #130834, #180377, #148022, #132841, #57012, #191513, #52990, #117678, #179375, #40837, #176364, #118685, #99497, #98487, #102510, #160180, #21670, #161178, #83324, #22674, #84321, #146000, #7483, #100499, #162178, #23676, #75148, #73191, #106473, #134862, #28676, #103514, #11521, #41847, #91281, #88325, #30639, #61949, #122635, #76133, #26685, #151022, #196540, #168152, #151997, #58010, #150016, #169134, #43827, #60961, #183336 ),
 ( #137811, #198503, #280, #119680, #13483, #90311, #104507, #29649, #58984, #107458, #184325, #45807, #123616, #182349, #181363, #92292, #136819, #105491, #59974, #152972, #135847, #42842, #44818, #14471, #138799, #199495, #153976, #167177, #121641, #165190, #15473, #166188, #77130, #27689, #89330, #12513, #74177, #197516, #120651, #155957, #158932, #81091, #96266, #142769, #31633, #141776, #172128, #33614, #93282, #2272, #35598, #20421, #95277, #97244, #50778, #64942, #1269, #112438, #156960, #157952, #63955, #125624, #18457, #126601, #79110, #174127, #82071, #140783, #80108, #3270, #188303, #17454, #187322, #46802, #4250, #19443, #154967, #65929, #49780, #111445, #34607, #78112, #143764, #16463, #66926, #127602, #173132, #189301, #47803, #5245, #170138, #185311, #108461, #109453, #139781, #62946, #48793, #124626, #186321, #171136, #32625, #94279, #110447, #98235, #128589, #178123, #175112, #117435, #148783, #9272, #162939, #113420, #37591, #159938, #193287, #38602, #21425, #36580, #55761, #130590, #147786, #69938, #83085, #131602, #179133, #192286, #144761, #22432, #7243, #6246, #54761, #67925, #176120, #101250, #40601, #129578, #114419, #191275, #52750, #190283, #24446, #177131, #102272, #51759, #163960, #39591, #25458, #86095, #100258, #68928, #70938, #145761, #99253, #115440, #160940, #53766, #161939, #132606, #87098, #10272, #8258, #84082, #116435, #23434, #85081, #194295, #146765, #29420, #195293, #30400, #89089, #44581, #136581, #92046, #153735, #26446, #13255, #180139, #74918, #59737, #149774, #41608, #106238, #198261, #14228, #137573, #120413, #103273, #167920, #133601, #121406, #107223, #56774, #164953, #42602, #135610, #71931, #91051, #118447, #88088, #45570, #11276, #72949, #183100, #43589, #152738, #134619, #75899, #196303, #199256, #28444, #57773, #119443, #182104, #104266, #105255, #181128, #60723, #165948, #58744, #27448, #150781, #12276, #122397, #73941, #184087, #197281, #168894, #166941, #90080, #151762, #46563, #79881, #125395, #108224, #123382, #142540, #17221, #34378, #156732, #185074, #18225, #4019, #78873, #169904, #109219, #94045, #31397, #141550, #154734, #62707, #188074, #65697, #93047, #1034, #16230, #77882, #76890, #49545, #63720, #127363, #138561, #50548, #126377, #112208, #172900, #187092, #155723, #111208, #32390, #139550, #2040, #39, #140552, #48562, #96038, #189075, #173898, #95043, #35367, #3039, #124389, #110215, #64715, #61714, #157725, #186084, #97019, #171896, #19214, #80864, #15231, #47567, #170898, #33384, #66693, #161703, #146521, #36347, #128357, #193050, #23199, #101017, #24207, #7003, #190053, #131361, #20189, #84842, #194063, #81835, #51529, #129349, #22193, #178890, #54527, #158700, #40358, #191044, #143523, #116200, #177889, #113192, #39359, #130340, #8011, #69694, #174881, #162702, #5011, #53520, #85856, #98000, #147545, #9033, #70702, #83842, #82847, #159694, #67691, #21191, #132370, #99011, #55524, #117198, #144526, #52517, #114178, #6012, #175882, #37353, #192039, #115198, #160702, #145524, #68685, #176890, #38361, #100016, #60490, #86860, #12044, #150545, #164714, #166708, #119207, #167694, #121174, #44349, #183855, #42367, #71695, #182868, #88852, #104030, #58518, #28212, #196065, #179900, #105024, #43353, #199021, #89852, #106008, #165709, #27206, #25218, #151535, #148544, #73708, #10035, #135380, #13024, #41366, #133362, #197050, #72707, #75664, #198031, #74689, #59499, #195053, #120184, #181874, #136355, #56531, #180892, #152508, #137341, #29191, #13997, #90825, #122165, #118209, #102033, #163716, #103032, #26209, #87848, #149536, #11031, #57538, #134379, #142308, #139326, #93817, #1809, #63487, #77657, #127128, #125163, #32160, #80631, #91811, #153503, #108991, #95806, #15000, #33155, #3788, #186862, #61487, #48331, #156492, #18985, #65465, #78644, #185849, #109986, #30167, #46329, #92817, #45342, #141316, #170672, #76660, #138339 ),
 ( #184845, #154503, #17994, #157492, #200019, #31167, #123157, #107984, #47336, #169671, #171666, #62478, #110975, #64483, #187846, #106994, #155497, #15999, #126150, #16990, #140319, #94814, #79647, #805, #124150, #2805, #49315, #168667, #172660, #34147, #190811, #52286, #111974, #53282, #173666, #113943, #96785, #160469, #130105, #128124, #158474, #37116, #159456, #162460, #84607, #99784, #146286, #35133, #145289, #175642, #98775, #19962, #5780, #39122, #23961, #21960, #100777, #54293, #68451, #4774, #115965, #83611, #161470, #67454, #129112, #6772, #191801, #82609, #177653, #85616, #144290, #114961, #176654, #38131, #20952, #70462, #22959, #7773, #147303, #81604, #143288, #69456, #8792, #66462, #131123, #188834, #192811, #189826, #50319, #51298, #112959, #174652, #36117, #97769, #196818, #116957, #133124, #179660, #152280, #27974, #57299, #40111, #89613, #193820, #26972, #166475, #9797, #58285, #151302, #12791, #195828, #56287, #163477, #74456, #55285, #88615, #136122, #71459, #119954, #197798, #59264, #118976, #117969, #24974, #41130, #178648, #181640, #72466, #105775, #182632, #148303, #25974, #87617, #101789, #86620, #44116, #165476, #150312, #120933, #10797, #180659, #43119, #167462, #11808, #194814, #102794, #132127, #134139, #164480, #104787, #149303, #28957, #90598, #13764, #42135, #103796, #73472, #135145, #62234, #77416, #31919, #1563, #169425, #153262, #78396, #16748, #172415, #63238, #79405, #139088, #563, #198792, #140072, #60258, #123902, #183624, #47090, #124918, #14763, #45106, #185601, #46089, #49077, #171427, #186615, #32914, #121929, #93573, #108751, #170427, #106763, #92578, #125910, #110734, #155258, #187608, #141076, #48087, #91573, #2561, #109743, #94569, #154266, #15757, #156247, #17749, #30930, #64243, #33903, #95560, #157247, #75432, #137106, #107744, #168438, #29934, #76424, #138100, #199781, #61249, #122920, #184608, #65224, #6528, #54054, #160226, #34889, #21717, #129860, #192570, #115728, #52047, #159213, #83370, #3546, #19723, #66219, #38886, #114717, #144052, #126884, #96545, #188590, #53037, #145047, #161225, #84367, #67213, #50071, #191558, #80388, #68208, #177415, #142060, #111732, #189583, #82364, #100543, #176409, #18741, #173419, #51055, #158232, #37885, #99543, #81364, #22719, #190571, #146044, #7528, #143048, #4527, #127879, #112717, #69213, #113703, #130881, #174410, #35879, #97526, #20708, #175400, #5534, #128871, #36868, #98533, #195584, #193575, #29449, #55047, #149066, #23721, #131891, #162222, #14260, #8546, #153767, #185104, #45601, #199287, #147063, #71221, #116718, #91081, #72218, #178407, #70223, #92078, #164240, #184119, #103558, #39871, #165233, #15262, #25735, #101538, #56043, #40882, #163230, #152768, #24730, #9555, #137604, #76920, #86380, #148064, #138591, #41892, #73, #10554, #133893, #61743, #85370, #123411, #75929, #46594, #122427, #57056, #102555, #60754, #179417, #132884, #118731, #194573, #87381, #180419, #107254, #117722, #168925, #30431, #158728, #96065, #1063, #171924, #49574, #169934, #65725, #31425, #66726, #125423, #80892, #172928, #128386, #190082, #62738, #111237, #16260, #34407, #157754, #77911, #2070, #187119, #124418, #19245, #47594, #155752, #142569, #20218, #186114, #94073, #81866, #188101, #143557, #156760, #18254, #97046, #93078, #5040, #4048, #108254, #127394, #79907, #48591, #189103, #110242, #109247, #95072, #154762, #33413, #141578, #50576, #35395, #139578, #112236, #170927, #173926, #32418, #3066, #17250, #78903, #140580, #63749, #64743, #126405, #24241, #116229, #71725, #133394, #6043, #193081, #159727, #54556, #39388, #129379, #21223, #85890, #177920, #194094, #117229, #100048, #82879, #147578, #113222, #101048, #86891, #174912, #144557, #22224, #115230, #51558, #9064, #36376, #98030, #83873, #67721, #70734, #132401, #191075, #55556, #23229, #162733, #178923, #52548, #25249, #114209, #175914, #40393 ),
 ( #37385, #99042, #160732, #145555, #102064, #176921, #7033, #163749, #68715, #146550, #148575, #130372, #10065, #192070, #53551, #38392, #161734, #84872, #8046, #69725, #131393, #135411, #168697, #45372, #11064, #88885, #150577, #118241, #56567, #89883, #29221, #72742, #121206, #90854, #152539, #58549, #119239, #26241, #104061, #179932, #182897, #197082, #30199, #107025, #134413, #12076, #73739, #41399, #149568, #91840, #28243, #151566, #14027, #120215, #181905, #106037, #75692, #13055, #87880, #164746, #195085, #43384, #57569, #59528, #105056, #60521, #137372, #199050, #76691, #166740, #196099, #122195, #74722, #136385, #198062, #44382, #167723, #180923, #183887, #153534, #15031, #103064, #42398, #165741, #27236, #61517, #2834, #123186, #1837, #46357, #110014, #79676, #77686, #108015, #186890, #109021, #112006, #34175, #49342, #95836, #184875, #94843, #125194, #48360, #169701, #155525, #188864, #173695, #171695, #50347, #3816, #18023, #154531, #65494, #33184, #111004, #17020, #78673, #156524, #141347, #32189, #127156, #35163, #93847, #64512, #126179, #187874, #170700, #19990, #172690, #157520, #96818, #31195, #92846, #63519, #158503, #16028, #19014, #138367, #80660, #139354, #142336, #200048, #835, #62508, #124179, #140349, #185881, #47366, #82638, #129143, #101819, #177683, #6802, #189855, #39151, #146315, #163507, #81633, #36147, #22990, #51329, #84638, #69488, #159488, #112989, #115994, #7804, #23991, #147335, #130135, #174682, #54322, #143316, #131153, #116986, #4803, #97799, #52316, #145319, #66492, #100807, #128155, #20981, #113974, #144321, #162490, #85648, #5810, #8822, #53313, #192842, #70491, #67485, #55315, #190840, #175672, #132158, #114991, #193850, #37146, #178679, #98805, #40142, #38160, #160499, #21989, #191832, #83642, #176685, #68480, #99815, #161500, #11837, #86649, #194845, #25005, #74486, #71488, #13795, #45136, #105804, #59293, #9828, #134169, #56318, #89643, #135174, #118000, #133154, #152309, #27000, #44145, #166505, #179689, #28003, #75460, #88645, #41161, #119005, #103824, #102824, #151331, #164510, #72495, #197827, #137134, #26003, #10825, #198821, #104816, #60286, #73502, #196848, #121959, #148333, #183652, #136152, #106793, #182661, #58314, #165504, #120962, #42164, #87645, #119982, #149331, #150341, #181668, #167491, #195857, #57329, #12820, #180688, #28987, #43147, #90627, #109773, #29965, #125939, #91603, #126915, #185629, #141105, #153292, #32944, #14793, #31948, #76453, #140102, #171456, #107771, #138130, #16778, #139116, #142092, #64272, #79434, #187637, #199811, #124949, #155288, #78427, #61279, #47121, #18772, #3577, #1593, #80419, #33934, #48116, #184637, #95592, #63268, #2593, #108779, #170457, #186645, #94599, #62263, #157276, #65255, #123931, #156278, #17779, #49107, #592, #50102, #110765, #172446, #188621, #122949, #46118, #93603, #168467, #169457, #30958, #92605, #154295, #15785, #77445, #22749, #85404, #147096, #145077, #52078, #176441, #96575, #112747, #159244, #131923, #7559, #36900, #19753, #69245, #173451, #6559, #146074, #189613, #37914, #130911, #192601, #175431, #35910, #143080, #20739, #34919, #99573, #113734, #8581, #162255, #127911, #5564, #67243, #158264, #66251, #23754, #68237, #129890, #54084, #190602, #98564, #84398, #115758, #191590, #4559, #81394, #111762, #160258, #174441, #161255, #128902, #177446, #38916, #100573, #193607, #21748, #51087, #70255, #83399, #53069, #114747, #97556, #82395, #144083, #58082, #196612, #152070, #42913, #59056, #57090, #118764, #148097, #28749, #24765, #136893, #166263, #26760, #119752, #117758, #27762, #39907, #197590, #11597, #179450, #9589, #165266, #25768, #88400, #86412, #181435, #71254, #41925, #116749, #132918, #55079, #104579, #101573, #43901, #75221, #135919, #89405, #163263, #164273, #194605, #151094, #150094, #56077, #40916, #182423, #180453, #74250, #12585, #102589, #120723, #105564, #103591 ) ),
 .UNSPECIFIED., .T., .F., .F. ) 
 B_SPLINE_SURFACE_WITH_KNOTS ( ( 4, 3, 4 ),
 ( 3, 2, 2, 2, 2, 2, 2, 2, 2, 2, 2, 2, 2, 2, 2, 2, 2, 2, 2, 2, 2, 2, 2, 2, 2, 2, 2, 2, 2, 2, 2, 2, 2, 2, 2, 2, 2, 2, 2, 2, 2, 2, 2, 2, 2, 2, 2, 2, 2, 2, 2, 2, 2, 2, 2, 2, 2, 2, 2, 2, 2, 2, 2, 2, 2, 2, 2, 2, 2, 2, 2, 2, 2, 2, 2, 2, 2, 2, 2, 2, 2, 2, 2, 2, 2, 2, 2, 2, 2, 2, 2, 2, 2, 2, 2, 2, 2, 2, 2, 2, 2, 2, 2, 2, 2, 2, 2, 2, 2, 2, 2, 2, 2, 2, 2, 2, 2, 2, 2, 2, 2, 2, 2, 2, 2, 2, 2, 2, 2, 2, 2, 2, 2, 2, 2, 2, 2, 2, 2, 2, 2, 2, 2, 2, 2, 2, 2, 2, 2, 2, 2, 2, 2, 2, 2, 2, 2, 2, 2, 2, 2, 2, 2, 2, 2, 2, 2, 2, 2, 2, 2, 2, 2, 2, 2, 2, 2, 2, 2, 2, 2, 2, 2, 2, 2, 2, 2, 2, 2, 2, 2, 2, 2, 2, 2, 2, 2, 2, 2, 2, 2, 2, 2, 2, 2, 2, 2, 2, 2, 2, 2, 2, 2, 2, 2, 2, 2, 2, 2, 2, 2, 2, 2, 2, 2, 2, 2, 2, 3 ),
 ( 0.000000000000000000, 0.5000000000000000000, 1.000000000000000000 ),
 ( 0.000000000000000000, 0.004385964912280701511, 0.008771929824561403022, 0.01315789473684210453, 0.01754385964912280604, 0.02192982456140350755, 0.02631578947368420907, 0.03070175438596491058, 0.03508771929824561209, 0.03947368421052631360, 0.04385964912280701511, 0.04824561403508771662, 0.05263157894736841813, 0.05701754385964911964, 0.06140350877192982115, 0.06578947368421052266, 0.07017543859649122417, 0.07456140350877192569, 0.07894736842105262720, 0.08333333333333332871, 0.08771929824561403022, 0.09210526315789473173, 0.09649122807017543324, 0.1008771929824561348, 0.1052631578947368363, 0.1096491228070175378, 0.1140350877192982393, 0.1184210526315789408, 0.1228070175438596423, 0.1271929824561403577, 0.1315789473684210453, 0.1359649122807017607, 0.1403508771929824483, 0.1447368421052631637, 0.1491228070175438514, 0.1535087719298245668, 0.1578947368421052544, 0.1622807017543859698, 0.1666666666666666574, 0.1710526315789473728, 0.1754385964912280604, 0.1798245614035087758, 0.1842105263157894635, 0.1885964912280701788, 0.1929824561403508665, 0.1973684210526315819, 0.2017543859649122695, 0.2061403508771929849, 0.2105263157894736725, 0.2149122807017543879, 0.2192982456140350755, 0.2236842105263157909, 0.2280701754385964786, 0.2324561403508771940, 0.2368421052631578816, 0.2412280701754385970, 0.2456140350877192846, 0.2500000000000000000, 0.2543859649122807154, 0.2587719298245614308, 0.2631578947368420907, 0.2675438596491228060, 0.2719298245614035214, 0.2763157894736842368, 0.2807017543859648967, 0.2850877192982456121, 0.2894736842105263275, 0.2938596491228070429, 0.2982456140350877027, 0.3026315789473684181, 0.3070175438596491335, 0.3114035087719298489, 0.3157894736842105088, 0.3201754385964912242, 0.3245614035087719396, 0.3289473684210526550, 0.3333333333333333148, 0.3377192982456140302, 0.3421052631578947456, 0.3464912280701754610, 0.3508771929824561209, 0.3552631578947368363, 0.3596491228070175517, 0.3640350877192982670, 0.3684210526315789269, 0.3728070175438596423, 0.3771929824561403577, 0.3815789473684210731, 0.3859649122807017330, 0.3903508771929824483, 0.3947368421052631637, 0.3991228070175438791, 0.4035087719298245390, 0.4078947368421052544, 0.4122807017543859698, 0.4166666666666666852, 0.4210526315789473450, 0.4254385964912280604, 0.4298245614035087758, 0.4342105263157894912, 0.4385964912280701511, 0.4429824561403508665, 0.4473684210526315819, 0.4517543859649122973, 0.4561403508771929571, 0.4605263157894736725, 0.4649122807017543879, 0.4692982456140351033, 0.4736842105263157632, 0.4780701754385964786, 0.4824561403508771940, 0.4868421052631579093, 0.4912280701754385692, 0.4956140350877192846, 0.5000000000000000000, 0.5043859649122807154, 0.5087719298245614308, 0.5131578947368421462, 0.5175438596491228616, 0.5219298245614034659, 0.5263157894736841813, 0.5307017543859648967, 0.5350877192982456121, 0.5394736842105263275, 0.5438596491228070429, 0.5482456140350877583, 0.5526315789473684736, 0.5570175438596490780, 0.5614035087719297934, 0.5657894736842105088, 0.5701754385964912242, 0.5745614035087719396, 0.5789473684210526550, 0.5833333333333333703, 0.5877192982456140857, 0.5921052631578946901, 0.5964912280701754055, 0.6008771929824561209, 0.6052631578947368363, 0.6096491228070175517, 0.6140350877192982670, 0.6184210526315789824, 0.6228070175438596978, 0.6271929824561403022, 0.6315789473684210176, 0.6359649122807017330, 0.6403508771929824483, 0.6447368421052631637, 0.6491228070175438791, 0.6535087719298245945, 0.6578947368421053099, 0.6622807017543859143, 0.6666666666666666297, 0.6710526315789473450, 0.6754385964912280604, 0.6798245614035087758, 0.6842105263157894912, 0.6885964912280702066, 0.6929824561403509220, 0.6973684210526315264, 0.7017543859649122417, 0.7061403508771929571, 0.7105263157894736725, 0.7149122807017543879, 0.7192982456140351033, 0.7236842105263158187, 0.7280701754385965341, 0.7324561403508771384, 0.7368421052631578538, 0.7412280701754385692, 0.7456140350877192846, 0.7500000000000000000, 0.7543859649122807154, 0.7587719298245614308, 0.7631578947368421462, 0.7675438596491228616, 0.7719298245614034659, 0.7763157894736841813, 0.7807017543859648967, 0.7850877192982456121, 0.7894736842105263275, 0.7938596491228070429, 0.7982456140350877583, 0.8026315789473684736, 0.8070175438596490780, 0.8114035087719297934, 0.8157894736842105088, 0.8201754385964912242, 0.8245614035087719396, 0.8289473684210526550, 0.8333333333333333703, 0.8377192982456140857, 0.8421052631578946901, 0.8464912280701754055, 0.8508771929824561209, 0.8552631578947368363, 0.8596491228070175517, 0.8640350877192982670, 0.8684210526315789824, 0.8728070175438596978, 0.8771929824561403022, 0.8815789473684210176, 0.8859649122807017330, 0.8903508771929824483, 0.8947368421052631637, 0.8991228070175438791, 0.9035087719298245945, 0.9078947368421053099, 0.9122807017543859143, 0.9166666666666666297, 0.9210526315789473450, 0.9254385964912280604, 0.9298245614035087758, 0.9342105263157894912, 0.9385964912280702066, 0.9429824561403509220, 0.9473684210526315264, 0.9517543859649122417, 0.9561403508771929571, 0.9605263157894736725, 0.9649122807017543879, 0.9692982456140351033, 0.9736842105263158187, 0.9780701754385965341, 0.9824561403508771384, 0.9868421052631578538, 0.9912280701754385692, 0.9956140350877192846, 1.000000000000000000 ),
 .UNSPECIFIED. ) 
 GEOMETRIC_REPRESENTATION_ITEM ( )  RATIONAL_B_SPLINE_SURFACE ( (
 ( 1.000000000000000000, 0.9659258262890683122, 1.000000000000000000, 0.9659258262890683122, 1.000000000000000000, 0.9659258262890683122, 1.000000000000000000, 0.9659258262890683122, 1.000000000000000000, 0.9659258262890683122, 1.000000000000000000, 0.9659258262890683122, 1.000000000000000000, 0.9659258262890683122, 1.000000000000000000, 0.9659258262890683122, 1.000000000000000000, 0.9659258262890683122, 1.000000000000000000, 0.9659258262890683122, 1.000000000000000000, 0.9659258262890683122, 1.000000000000000000, 0.9659258262890683122, 1.000000000000000000, 0.9659258262890683122, 1.000000000000000000, 0.9659258262890683122, 1.000000000000000000, 0.9659258262890683122, 1.000000000000000000, 0.9659258262890683122, 1.000000000000000000, 0.9659258262890683122, 1.000000000000000000, 0.9659258262890683122, 1.000000000000000000, 0.9659258262890683122, 1.000000000000000000, 0.9659258262890683122, 1.000000000000000000, 0.9659258262890683122, 1.000000000000000000, 0.9659258262890683122, 1.000000000000000000, 0.9659258262890683122, 1.000000000000000000, 0.9659258262890683122, 1.000000000000000000, 0.9659258262890683122, 1.000000000000000000, 0.9659258262890683122, 1.000000000000000000, 0.9659258262890683122, 1.000000000000000000, 0.9659258262890683122, 1.000000000000000000, 0.9659258262890683122, 1.000000000000000000, 0.9659258262890683122, 1.000000000000000000, 0.9659258262890683122, 1.000000000000000000, 0.9659258262890683122, 1.000000000000000000, 0.9659258262890683122, 1.000000000000000000, 0.9659258262890683122, 1.000000000000000000, 0.9659258262890683122, 1.000000000000000000, 0.9659258262890683122, 1.000000000000000000, 0.9659258262890683122, 1.000000000000000000, 0.9659258262890683122, 1.000000000000000000, 0.9659258262890683122, 1.000000000000000000, 0.9659258262890683122, 1.000000000000000000, 0.9659258262890683122, 1.000000000000000000, 0.9659258262890683122, 1.000000000000000000, 0.9659258262890683122, 1.000000000000000000, 0.9659258262890683122, 1.000000000000000000, 0.9659258262890683122, 1.000000000000000000, 0.9659258262890683122, 1.000000000000000000, 0.9659258262890683122, 1.000000000000000000, 0.9659258262890683122, 1.000000000000000000, 0.9659258262890683122, 1.000000000000000000, 0.9659258262890683122, 1.000000000000000000, 0.9659258262890683122, 1.000000000000000000, 0.9659258262890683122, 1.000000000000000000, 0.9659258262890683122, 1.000000000000000000, 0.9659258262890683122, 1.000000000000000000, 0.9659258262890683122, 1.000000000000000000, 0.9659258262890683122, 1.000000000000000000, 0.9659258262890683122, 1.000000000000000000, 0.9659258262890683122, 1.000000000000000000, 0.9659258262890683122, 1.000000000000000000, 0.9659258262890683122, 1.000000000000000000, 0.9659258262890683122, 1.000000000000000000, 0.9659258262890683122, 1.000000000000000000, 0.9659258262890683122, 1.000000000000000000, 0.9659258262890683122, 1.000000000000000000, 0.9659258262890683122, 1.000000000000000000, 0.9659258262890683122, 1.000000000000000000, 0.9659258262890683122, 1.000000000000000000, 0.9659258262890683122, 1.000000000000000000, 0.9659258262890683122, 1.000000000000000000, 0.9659258262890683122, 1.000000000000000000, 0.9659258262890683122, 1.000000000000000000, 0.9659258262890683122, 1.000000000000000000, 0.9659258262890683122, 1.000000000000000000, 0.9659258262890683122, 1.000000000000000000, 0.9659258262890683122, 1.000000000000000000, 0.9659258262890683122, 1.000000000000000000, 0.9659258262890683122, 1.000000000000000000, 0.9659258262890683122, 1.000000000000000000, 0.9659258262890683122, 1.000000000000000000, 0.9659258262890683122, 1.000000000000000000, 0.9659258262890683122, 1.000000000000000000, 0.9659258262890683122, 1.000000000000000000, 0.9659258262890683122, 1.000000000000000000, 0.9659258262890683122, 1.000000000000000000, 0.9659258262890683122, 1.000000000000000000, 0.9659258262890683122, 1.000000000000000000, 0.9659258262890683122, 1.000000000000000000, 0.9659258262890683122, 1.000000000000000000, 0.9659258262890683122, 1.000000000000000000, 0.9659258262890683122, 1.000000000000000000, 0.9659258262890683122, 1.000000000000000000, 0.9659258262890683122, 1.000000000000000000, 0.9659258262890683122, 1.000000000000000000, 0.9659258262890683122, 1.000000000000000000, 0.9659258262890683122, 1.000000000000000000, 0.9659258262890683122, 1.000000000000000000, 0.9659258262890683122, 1.000000000000000000, 0.9659258262890683122, 1.000000000000000000, 0.9659258262890683122, 1.000000000000000000, 0.9659258262890683122, 1.000000000000000000, 0.9659258262890683122, 1.000000000000000000, 0.9659258262890683122, 1.000000000000000000, 0.9659258262890683122, 1.000000000000000000, 0.9659258262890683122, 1.000000000000000000, 0.9659258262890683122, 1.000000000000000000, 0.9659258262890683122, 1.000000000000000000, 0.9659258262890683122, 1.000000000000000000, 0.9659258262890683122, 1.000000000000000000, 0.9659258262890683122, 1.000000000000000000, 0.9659258262890683122, 1.000000000000000000, 0.9659258262890683122, 1.000000000000000000, 0.9659258262890683122, 1.000000000000000000, 0.9659258262890683122, 1.000000000000000000, 0.9659258262890683122, 1.000000000000000000, 0.9659258262890683122, 1.000000000000000000, 0.9659258262890683122, 1.000000000000000000, 0.9659258262890683122, 1.000000000000000000, 0.9659258262890683122, 1.000000000000000000, 0.9659258262890683122, 1.000000000000000000, 0.9659258262890683122, 1.000000000000000000, 0.9659258262890683122, 1.000000000000000000, 0.9659258262890683122, 1.000000000000000000, 0.9659258262890683122, 1.000000000000000000, 0.9659258262890683122, 1.000000000000000000, 0.9659258262890683122, 1.000000000000000000, 0.9659258262890683122, 1.000000000000000000, 0.9659258262890683122, 1.000000000000000000, 0.9659258262890683122, 1.000000000000000000, 0.9659258262890683122, 1.000000000000000000, 0.9659258262890683122, 1.000000000000000000, 0.9659258262890683122, 1.000000000000000000, 0.9659258262890683122, 1.000000000000000000, 0.9659258262890683122, 1.000000000000000000, 0.9659258262890683122, 1.000000000000000000, 0.9659258262890683122, 1.000000000000000000, 0.9659258262890683122, 1.000000000000000000, 0.9659258262890683122, 1.000000000000000000, 0.9659258262890683122, 1.000000000000000000, 0.9659258262890683122, 1.000000000000000000, 0.9659258262890683122, 1.000000000000000000, 0.9659258262890683122, 1.000000000000000000, 0.9659258262890683122, 1.000000000000000000, 0.9659258262890683122, 1.000000000000000000, 0.9659258262890683122, 1.000000000000000000, 0.9659258262890683122, 1.000000000000000000, 0.9659258262890683122, 1.000000000000000000, 0.9659258262890683122, 1.000000000000000000, 0.9659258262890683122, 1.000000000000000000, 0.9659258262890683122, 1.000000000000000000, 0.9659258262890683122, 1.000000000000000000, 0.9659258262890683122, 1.000000000000000000, 0.9659258262890683122, 1.000000000000000000, 0.9659258262890683122, 1.000000000000000000, 0.9659258262890683122, 1.000000000000000000, 0.9659258262890683122, 1.000000000000000000, 0.9659258262890683122, 1.000000000000000000, 0.9659258262890683122, 1.000000000000000000, 0.9659258262890683122, 1.000000000000000000, 0.9659258262890683122, 1.000000000000000000, 0.9659258262890683122, 1.000000000000000000, 0.9659258262890683122, 1.000000000000000000, 0.9659258262890683122, 1.000000000000000000, 0.9659258262890683122, 1.000000000000000000, 0.9659258262890683122, 1.000000000000000000, 0.9659258262890683122, 1.000000000000000000, 0.9659258262890683122, 1.000000000000000000, 0.9659258262890683122, 1.000000000000000000, 0.9659258262890683122, 1.000000000000000000, 0.9659258262890683122, 1.000000000000000000, 0.9659258262890683122, 1.000000000000000000, 0.9659258262890683122, 1.000000000000000000, 0.9659258262890683122, 1.000000000000000000, 0.9659258262890683122, 1.000000000000000000, 0.9659258262890683122, 1.000000000000000000, 0.9659258262890683122, 1.000000000000000000, 0.9659258262890683122, 1.000000000000000000, 0.9659258262890683122, 1.000000000000000000, 0.9659258262890683122, 1.000000000000000000, 0.9659258262890683122, 1.000000000000000000, 0.9659258262890683122, 1.000000000000000000, 0.9659258262890683122, 1.000000000000000000, 0.9659258262890683122, 1.000000000000000000, 0.9659258262890683122, 1.000000000000000000, 0.9659258262890683122, 1.000000000000000000, 0.9659258262890683122, 1.000000000000000000, 0.9659258262890683122, 1.000000000000000000, 0.9659258262890683122, 1.000000000000000000, 0.9659258262890683122, 1.000000000000000000, 0.9659258262890683122, 1.000000000000000000, 0.9659258262890683122, 1.000000000000000000, 0.9659258262890683122, 1.000000000000000000, 0.9659258262890683122, 1.000000000000000000, 0.9659258262890683122, 1.000000000000000000, 0.9659258262890683122, 1.000000000000000000, 0.9659258262890683122, 1.000000000000000000, 0.9659258262890683122, 1.000000000000000000, 0.9659258262890683122, 1.000000000000000000, 0.9659258262890683122, 1.000000000000000000, 0.9659258262890683122, 1.000000000000000000, 0.9659258262890683122, 1.000000000000000000, 0.9659258262890683122, 1.000000000000000000, 0.9659258262890683122, 1.000000000000000000, 0.9659258262890683122, 1.000000000000000000, 0.9659258262890683122, 1.000000000000000000, 0.9659258262890683122, 1.000000000000000000, 0.9659258262890683122, 1.000000000000000000, 0.9659258262890683122, 1.000000000000000000, 0.9659258262890683122, 1.000000000000000000, 0.9659258262890683122, 1.000000000000000000, 0.9659258262890683122, 1.000000000000000000, 0.9659258262890683122, 1.000000000000000000, 0.9659258262890683122, 1.000000000000000000, 0.9659258262890683122, 1.000000000000000000, 0.9659258262890683122, 1.000000000000000000, 0.9659258262890683122, 1.000000000000000000, 0.9659258262890683122, 1.000000000000000000, 0.9659258262890683122, 1.000000000000000000, 0.9659258262890683122, 1.000000000000000000, 0.9659258262890683122, 1.000000000000000000, 0.9659258262890683122, 1.000000000000000000, 0.9659258262890683122, 1.000000000000000000, 0.9659258262890683122, 1.000000000000000000, 0.9659258262890683122, 1.000000000000000000, 0.9659258262890683122, 1.000000000000000000, 0.9659258262890683122, 1.000000000000000000, 0.9659258262890683122, 1.000000000000000000, 0.9659258262890683122, 1.000000000000000000, 0.9659258262890683122, 1.000000000000000000),
 ( 0.3333333333333333703, 0.3219752754296894559, 0.3333333333333333703, 0.3219752754296894559, 0.3333333333333333703, 0.3219752754296894559, 0.3333333333333333703, 0.3219752754296894559, 0.3333333333333333703, 0.3219752754296894559, 0.3333333333333333703, 0.3219752754296894559, 0.3333333333333333703, 0.3219752754296894559, 0.3333333333333333703, 0.3219752754296894559, 0.3333333333333333703, 0.3219752754296894559, 0.3333333333333333703, 0.3219752754296894559, 0.3333333333333333703, 0.3219752754296894559, 0.3333333333333333703, 0.3219752754296894559, 0.3333333333333333703, 0.3219752754296894559, 0.3333333333333333703, 0.3219752754296894559, 0.3333333333333333703, 0.3219752754296894559, 0.3333333333333333703, 0.3219752754296894559, 0.3333333333333333703, 0.3219752754296894559, 0.3333333333333333703, 0.3219752754296894559, 0.3333333333333333703, 0.3219752754296894559, 0.3333333333333333703, 0.3219752754296894559, 0.3333333333333333703, 0.3219752754296894559, 0.3333333333333333703, 0.3219752754296894559, 0.3333333333333333703, 0.3219752754296894559, 0.3333333333333333703, 0.3219752754296894559, 0.3333333333333333703, 0.3219752754296894559, 0.3333333333333333703, 0.3219752754296894559, 0.3333333333333333703, 0.3219752754296894559, 0.3333333333333333703, 0.3219752754296894559, 0.3333333333333333703, 0.3219752754296894559, 0.3333333333333333703, 0.3219752754296894559, 0.3333333333333333703, 0.3219752754296894559, 0.3333333333333333703, 0.3219752754296894559, 0.3333333333333333703, 0.3219752754296894559, 0.3333333333333333703, 0.3219752754296894559, 0.3333333333333333703, 0.3219752754296894559, 0.3333333333333333703, 0.3219752754296894559, 0.3333333333333333703, 0.3219752754296894559, 0.3333333333333333703, 0.3219752754296894559, 0.3333333333333333703, 0.3219752754296894559, 0.3333333333333333703, 0.3219752754296894559, 0.3333333333333333703, 0.3219752754296894559, 0.3333333333333333703, 0.3219752754296894559, 0.3333333333333333703, 0.3219752754296894559, 0.3333333333333333703, 0.3219752754296894559, 0.3333333333333333703, 0.3219752754296894559, 0.3333333333333333703, 0.3219752754296894559, 0.3333333333333333703, 0.3219752754296894559, 0.3333333333333333703, 0.3219752754296894559, 0.3333333333333333703, 0.3219752754296894559, 0.3333333333333333703, 0.3219752754296894559, 0.3333333333333333703, 0.3219752754296894559, 0.3333333333333333703, 0.3219752754296894559, 0.3333333333333333703, 0.3219752754296894559, 0.3333333333333333703, 0.3219752754296894559, 0.3333333333333333703, 0.3219752754296894559, 0.3333333333333333703, 0.3219752754296894559, 0.3333333333333333703, 0.3219752754296894559, 0.3333333333333333703, 0.3219752754296894559, 0.3333333333333333703, 0.3219752754296894559, 0.3333333333333333703, 0.3219752754296894559, 0.3333333333333333703, 0.3219752754296894559, 0.3333333333333333703, 0.3219752754296894559, 0.3333333333333333703, 0.3219752754296894559, 0.3333333333333333703, 0.3219752754296894559, 0.3333333333333333703, 0.3219752754296894559, 0.3333333333333333703, 0.3219752754296894559, 0.3333333333333333703, 0.3219752754296894559, 0.3333333333333333703, 0.3219752754296894559, 0.3333333333333333703, 0.3219752754296894559, 0.3333333333333333703, 0.3219752754296894559, 0.3333333333333333703, 0.3219752754296894559, 0.3333333333333333703, 0.3219752754296894559, 0.3333333333333333703, 0.3219752754296894559, 0.3333333333333333703, 0.3219752754296894559, 0.3333333333333333703, 0.3219752754296894559, 0.3333333333333333703, 0.3219752754296894559, 0.3333333333333333703, 0.3219752754296894559, 0.3333333333333333703, 0.3219752754296894559, 0.3333333333333333703, 0.3219752754296894559, 0.3333333333333333703, 0.3219752754296894559, 0.3333333333333333703, 0.3219752754296894559, 0.3333333333333333703, 0.3219752754296894559, 0.3333333333333333703, 0.3219752754296894559, 0.3333333333333333703, 0.3219752754296894559, 0.3333333333333333703, 0.3219752754296894559, 0.3333333333333333703, 0.3219752754296894559, 0.3333333333333333703, 0.3219752754296894559, 0.3333333333333333703, 0.3219752754296894559, 0.3333333333333333703, 0.3219752754296894559, 0.3333333333333333703, 0.3219752754296894559, 0.3333333333333333703, 0.3219752754296894559, 0.3333333333333333703, 0.3219752754296894559, 0.3333333333333333703, 0.3219752754296894559, 0.3333333333333333703, 0.3219752754296894559, 0.3333333333333333703, 0.3219752754296894559, 0.3333333333333333703, 0.3219752754296894559, 0.3333333333333333703, 0.3219752754296894559, 0.3333333333333333703, 0.3219752754296894559, 0.3333333333333333703, 0.3219752754296894559, 0.3333333333333333703, 0.3219752754296894559, 0.3333333333333333703, 0.3219752754296894559, 0.3333333333333333703, 0.3219752754296894559, 0.3333333333333333703, 0.3219752754296894559, 0.3333333333333333703, 0.3219752754296894559, 0.3333333333333333703, 0.3219752754296894559, 0.3333333333333333703, 0.3219752754296894559, 0.3333333333333333703, 0.3219752754296894559, 0.3333333333333333703, 0.3219752754296894559, 0.3333333333333333703, 0.3219752754296894559, 0.3333333333333333703, 0.3219752754296894559, 0.3333333333333333703, 0.3219752754296894559, 0.3333333333333333703, 0.3219752754296894559, 0.3333333333333333703, 0.3219752754296894559, 0.3333333333333333703, 0.3219752754296894559, 0.3333333333333333703, 0.3219752754296894559, 0.3333333333333333703, 0.3219752754296894559, 0.3333333333333333703, 0.3219752754296894559, 0.3333333333333333703, 0.3219752754296894559, 0.3333333333333333703, 0.3219752754296894559, 0.3333333333333333703, 0.3219752754296894559, 0.3333333333333333703, 0.3219752754296894559, 0.3333333333333333703, 0.3219752754296894559, 0.3333333333333333703, 0.3219752754296894559, 0.3333333333333333703, 0.3219752754296894559, 0.3333333333333333703, 0.3219752754296894559, 0.3333333333333333703, 0.3219752754296894559, 0.3333333333333333703, 0.3219752754296894559, 0.3333333333333333703, 0.3219752754296894559, 0.3333333333333333703, 0.3219752754296894559, 0.3333333333333333703, 0.3219752754296894559, 0.3333333333333333703, 0.3219752754296894559, 0.3333333333333333703, 0.3219752754296894559, 0.3333333333333333703, 0.3219752754296894559, 0.3333333333333333703, 0.3219752754296894559, 0.3333333333333333703, 0.3219752754296894559, 0.3333333333333333703, 0.3219752754296894559, 0.3333333333333333703, 0.3219752754296894559, 0.3333333333333333703, 0.3219752754296894559, 0.3333333333333333703, 0.3219752754296894559, 0.3333333333333333703, 0.3219752754296894559, 0.3333333333333333703, 0.3219752754296894559, 0.3333333333333333703, 0.3219752754296894559, 0.3333333333333333703, 0.3219752754296894559, 0.3333333333333333703, 0.3219752754296894559, 0.3333333333333333703, 0.3219752754296894559, 0.3333333333333333703, 0.3219752754296894559, 0.3333333333333333703, 0.3219752754296894559, 0.3333333333333333703, 0.3219752754296894559, 0.3333333333333333703, 0.3219752754296894559, 0.3333333333333333703, 0.3219752754296894559, 0.3333333333333333703, 0.3219752754296894559, 0.3333333333333333703, 0.3219752754296894559, 0.3333333333333333703, 0.3219752754296894559, 0.3333333333333333703, 0.3219752754296894559, 0.3333333333333333703, 0.3219752754296894559, 0.3333333333333333703, 0.3219752754296894559, 0.3333333333333333703, 0.3219752754296894559, 0.3333333333333333703, 0.3219752754296894559, 0.3333333333333333703, 0.3219752754296894559, 0.3333333333333333703, 0.3219752754296894559, 0.3333333333333333703, 0.3219752754296894559, 0.3333333333333333703, 0.3219752754296894559, 0.3333333333333333703, 0.3219752754296894559, 0.3333333333333333703, 0.3219752754296894559, 0.3333333333333333703, 0.3219752754296894559, 0.3333333333333333703, 0.3219752754296894559, 0.3333333333333333703, 0.3219752754296894559, 0.3333333333333333703, 0.3219752754296894559, 0.3333333333333333703, 0.3219752754296894559, 0.3333333333333333703, 0.3219752754296894559, 0.3333333333333333703, 0.3219752754296894559, 0.3333333333333333703, 0.3219752754296894559, 0.3333333333333333703, 0.3219752754296894559, 0.3333333333333333703, 0.3219752754296894559, 0.3333333333333333703, 0.3219752754296894559, 0.3333333333333333703, 0.3219752754296894559, 0.3333333333333333703, 0.3219752754296894559, 0.3333333333333333703, 0.3219752754296894559, 0.3333333333333333703, 0.3219752754296894559, 0.3333333333333333703, 0.3219752754296894559, 0.3333333333333333703, 0.3219752754296894559, 0.3333333333333333703, 0.3219752754296894559, 0.3333333333333333703, 0.3219752754296894559, 0.3333333333333333703, 0.3219752754296894559, 0.3333333333333333703, 0.3219752754296894559, 0.3333333333333333703, 0.3219752754296894559, 0.3333333333333333703, 0.3219752754296894559, 0.3333333333333333703, 0.3219752754296894559, 0.3333333333333333703, 0.3219752754296894559, 0.3333333333333333703, 0.3219752754296894559, 0.3333333333333333703, 0.3219752754296894559, 0.3333333333333333703, 0.3219752754296894559, 0.3333333333333333703, 0.3219752754296894559, 0.3333333333333333703, 0.3219752754296894559, 0.3333333333333333703, 0.3219752754296894559, 0.3333333333333333703, 0.3219752754296894559, 0.3333333333333333703, 0.3219752754296894559, 0.3333333333333333703, 0.3219752754296894559, 0.3333333333333333703, 0.3219752754296894559, 0.3333333333333333703, 0.3219752754296894559, 0.3333333333333333703, 0.3219752754296894559, 0.3333333333333333703, 0.3219752754296894559, 0.3333333333333333703, 0.3219752754296894559, 0.3333333333333333703, 0.3219752754296894559, 0.3333333333333333703, 0.3219752754296894559, 0.3333333333333333703, 0.3219752754296894559, 0.3333333333333333703, 0.3219752754296894559, 0.3333333333333333703, 0.3219752754296894559, 0.3333333333333333703, 0.3219752754296894559, 0.3333333333333333703, 0.3219752754296894559, 0.3333333333333333703, 0.3219752754296894559, 0.3333333333333333703, 0.3219752754296894559, 0.3333333333333333703, 0.3219752754296894559, 0.3333333333333333703, 0.3219752754296894559, 0.3333333333333333703, 0.3219752754296894559, 0.3333333333333333703, 0.3219752754296894559, 0.3333333333333333703, 0.3219752754296894559, 0.3333333333333333703, 0.3219752754296894559, 0.3333333333333333703, 0.3219752754296894559, 0.3333333333333333703, 0.3219752754296894559, 0.3333333333333333703, 0.3219752754296894559, 0.3333333333333333703, 0.3219752754296894559, 0.3333333333333333703, 0.3219752754296894559, 0.3333333333333333703, 0.3219752754296894559, 0.3333333333333333703, 0.3219752754296894559, 0.3333333333333333703, 0.3219752754296894559, 0.3333333333333333703, 0.3219752754296894559, 0.3333333333333333703, 0.3219752754296894559, 0.3333333333333333703),
 ( 0.3333333333333333703, 0.3219752754296894559, 0.3333333333333333703, 0.3219752754296894559, 0.3333333333333333703, 0.3219752754296894559, 0.3333333333333333703, 0.3219752754296894559, 0.3333333333333333703, 0.3219752754296894559, 0.3333333333333333703, 0.3219752754296894559, 0.3333333333333333703, 0.3219752754296894559, 0.3333333333333333703, 0.3219752754296894559, 0.3333333333333333703, 0.3219752754296894559, 0.3333333333333333703, 0.3219752754296894559, 0.3333333333333333703, 0.3219752754296894559, 0.3333333333333333703, 0.3219752754296894559, 0.3333333333333333703, 0.3219752754296894559, 0.3333333333333333703, 0.3219752754296894559, 0.3333333333333333703, 0.3219752754296894559, 0.3333333333333333703, 0.3219752754296894559, 0.3333333333333333703, 0.3219752754296894559, 0.3333333333333333703, 0.3219752754296894559, 0.3333333333333333703, 0.3219752754296894559, 0.3333333333333333703, 0.3219752754296894559, 0.3333333333333333703, 0.3219752754296894559, 0.3333333333333333703, 0.3219752754296894559, 0.3333333333333333703, 0.3219752754296894559, 0.3333333333333333703, 0.3219752754296894559, 0.3333333333333333703, 0.3219752754296894559, 0.3333333333333333703, 0.3219752754296894559, 0.3333333333333333703, 0.3219752754296894559, 0.3333333333333333703, 0.3219752754296894559, 0.3333333333333333703, 0.3219752754296894559, 0.3333333333333333703, 0.3219752754296894559, 0.3333333333333333703, 0.3219752754296894559, 0.3333333333333333703, 0.3219752754296894559, 0.3333333333333333703, 0.3219752754296894559, 0.3333333333333333703, 0.3219752754296894559, 0.3333333333333333703, 0.3219752754296894559, 0.3333333333333333703, 0.3219752754296894559, 0.3333333333333333703, 0.3219752754296894559, 0.3333333333333333703, 0.3219752754296894559, 0.3333333333333333703, 0.3219752754296894559, 0.3333333333333333703, 0.3219752754296894559, 0.3333333333333333703, 0.3219752754296894559, 0.3333333333333333703, 0.3219752754296894559, 0.3333333333333333703, 0.3219752754296894559, 0.3333333333333333703, 0.3219752754296894559, 0.3333333333333333703, 0.3219752754296894559, 0.3333333333333333703, 0.3219752754296894559, 0.3333333333333333703, 0.3219752754296894559, 0.3333333333333333703, 0.3219752754296894559, 0.3333333333333333703, 0.3219752754296894559, 0.3333333333333333703, 0.3219752754296894559, 0.3333333333333333703, 0.3219752754296894559, 0.3333333333333333703, 0.3219752754296894559, 0.3333333333333333703, 0.3219752754296894559, 0.3333333333333333703, 0.3219752754296894559, 0.3333333333333333703, 0.3219752754296894559, 0.3333333333333333703, 0.3219752754296894559, 0.3333333333333333703, 0.3219752754296894559, 0.3333333333333333703, 0.3219752754296894559, 0.3333333333333333703, 0.3219752754296894559, 0.3333333333333333703, 0.3219752754296894559, 0.3333333333333333703, 0.3219752754296894559, 0.3333333333333333703, 0.3219752754296894559, 0.3333333333333333703, 0.3219752754296894559, 0.3333333333333333703, 0.3219752754296894559, 0.3333333333333333703, 0.3219752754296894559, 0.3333333333333333703, 0.3219752754296894559, 0.3333333333333333703, 0.3219752754296894559, 0.3333333333333333703, 0.3219752754296894559, 0.3333333333333333703, 0.3219752754296894559, 0.3333333333333333703, 0.3219752754296894559, 0.3333333333333333703, 0.3219752754296894559, 0.3333333333333333703, 0.3219752754296894559, 0.3333333333333333703, 0.3219752754296894559, 0.3333333333333333703, 0.3219752754296894559, 0.3333333333333333703, 0.3219752754296894559, 0.3333333333333333703, 0.3219752754296894559, 0.3333333333333333703, 0.3219752754296894559, 0.3333333333333333703, 0.3219752754296894559, 0.3333333333333333703, 0.3219752754296894559, 0.3333333333333333703, 0.3219752754296894559, 0.3333333333333333703, 0.3219752754296894559, 0.3333333333333333703, 0.3219752754296894559, 0.3333333333333333703, 0.3219752754296894559, 0.3333333333333333703, 0.3219752754296894559, 0.3333333333333333703, 0.3219752754296894559, 0.3333333333333333703, 0.3219752754296894559, 0.3333333333333333703, 0.3219752754296894559, 0.3333333333333333703, 0.3219752754296894559, 0.3333333333333333703, 0.3219752754296894559, 0.3333333333333333703, 0.3219752754296894559, 0.3333333333333333703, 0.3219752754296894559, 0.3333333333333333703, 0.3219752754296894559, 0.3333333333333333703, 0.3219752754296894559, 0.3333333333333333703, 0.3219752754296894559, 0.3333333333333333703, 0.3219752754296894559, 0.3333333333333333703, 0.3219752754296894559, 0.3333333333333333703, 0.3219752754296894559, 0.3333333333333333703, 0.3219752754296894559, 0.3333333333333333703, 0.3219752754296894559, 0.3333333333333333703, 0.3219752754296894559, 0.3333333333333333703, 0.3219752754296894559, 0.3333333333333333703, 0.3219752754296894559, 0.3333333333333333703, 0.3219752754296894559, 0.3333333333333333703, 0.3219752754296894559, 0.3333333333333333703, 0.3219752754296894559, 0.3333333333333333703, 0.3219752754296894559, 0.3333333333333333703, 0.3219752754296894559, 0.3333333333333333703, 0.3219752754296894559, 0.3333333333333333703, 0.3219752754296894559, 0.3333333333333333703, 0.3219752754296894559, 0.3333333333333333703, 0.3219752754296894559, 0.3333333333333333703, 0.3219752754296894559, 0.3333333333333333703, 0.3219752754296894559, 0.3333333333333333703, 0.3219752754296894559, 0.3333333333333333703, 0.3219752754296894559, 0.3333333333333333703, 0.3219752754296894559, 0.3333333333333333703, 0.3219752754296894559, 0.3333333333333333703, 0.3219752754296894559, 0.3333333333333333703, 0.3219752754296894559, 0.3333333333333333703, 0.3219752754296894559, 0.3333333333333333703, 0.3219752754296894559, 0.3333333333333333703, 0.3219752754296894559, 0.3333333333333333703, 0.3219752754296894559, 0.3333333333333333703, 0.3219752754296894559, 0.3333333333333333703, 0.3219752754296894559, 0.3333333333333333703, 0.3219752754296894559, 0.3333333333333333703, 0.3219752754296894559, 0.3333333333333333703, 0.3219752754296894559, 0.3333333333333333703, 0.3219752754296894559, 0.3333333333333333703, 0.3219752754296894559, 0.3333333333333333703, 0.3219752754296894559, 0.3333333333333333703, 0.3219752754296894559, 0.3333333333333333703, 0.3219752754296894559, 0.3333333333333333703, 0.3219752754296894559, 0.3333333333333333703, 0.3219752754296894559, 0.3333333333333333703, 0.3219752754296894559, 0.3333333333333333703, 0.3219752754296894559, 0.3333333333333333703, 0.3219752754296894559, 0.3333333333333333703, 0.3219752754296894559, 0.3333333333333333703, 0.3219752754296894559, 0.3333333333333333703, 0.3219752754296894559, 0.3333333333333333703, 0.3219752754296894559, 0.3333333333333333703, 0.3219752754296894559, 0.3333333333333333703, 0.3219752754296894559, 0.3333333333333333703, 0.3219752754296894559, 0.3333333333333333703, 0.3219752754296894559, 0.3333333333333333703, 0.3219752754296894559, 0.3333333333333333703, 0.3219752754296894559, 0.3333333333333333703, 0.3219752754296894559, 0.3333333333333333703, 0.3219752754296894559, 0.3333333333333333703, 0.3219752754296894559, 0.3333333333333333703, 0.3219752754296894559, 0.3333333333333333703, 0.3219752754296894559, 0.3333333333333333703, 0.3219752754296894559, 0.3333333333333333703, 0.3219752754296894559, 0.3333333333333333703, 0.3219752754296894559, 0.3333333333333333703, 0.3219752754296894559, 0.3333333333333333703, 0.3219752754296894559, 0.3333333333333333703, 0.3219752754296894559, 0.3333333333333333703, 0.3219752754296894559, 0.3333333333333333703, 0.3219752754296894559, 0.3333333333333333703, 0.3219752754296894559, 0.3333333333333333703, 0.3219752754296894559, 0.3333333333333333703, 0.3219752754296894559, 0.3333333333333333703, 0.3219752754296894559, 0.3333333333333333703, 0.3219752754296894559, 0.3333333333333333703, 0.3219752754296894559, 0.3333333333333333703, 0.3219752754296894559, 0.3333333333333333703, 0.3219752754296894559, 0.3333333333333333703, 0.3219752754296894559, 0.3333333333333333703, 0.3219752754296894559, 0.3333333333333333703, 0.3219752754296894559, 0.3333333333333333703, 0.3219752754296894559, 0.3333333333333333703, 0.3219752754296894559, 0.3333333333333333703, 0.3219752754296894559, 0.3333333333333333703, 0.3219752754296894559, 0.3333333333333333703, 0.3219752754296894559, 0.3333333333333333703, 0.3219752754296894559, 0.3333333333333333703, 0.3219752754296894559, 0.3333333333333333703, 0.3219752754296894559, 0.3333333333333333703, 0.3219752754296894559, 0.3333333333333333703, 0.3219752754296894559, 0.3333333333333333703, 0.3219752754296894559, 0.3333333333333333703, 0.3219752754296894559, 0.3333333333333333703, 0.3219752754296894559, 0.3333333333333333703, 0.3219752754296894559, 0.3333333333333333703, 0.3219752754296894559, 0.3333333333333333703, 0.3219752754296894559, 0.3333333333333333703, 0.3219752754296894559, 0.3333333333333333703, 0.3219752754296894559, 0.3333333333333333703, 0.3219752754296894559, 0.3333333333333333703, 0.3219752754296894559, 0.3333333333333333703, 0.3219752754296894559, 0.3333333333333333703, 0.3219752754296894559, 0.3333333333333333703, 0.3219752754296894559, 0.3333333333333333703, 0.3219752754296894559, 0.3333333333333333703, 0.3219752754296894559, 0.3333333333333333703, 0.3219752754296894559, 0.3333333333333333703, 0.3219752754296894559, 0.3333333333333333703, 0.3219752754296894559, 0.3333333333333333703, 0.3219752754296894559, 0.3333333333333333703, 0.3219752754296894559, 0.3333333333333333703, 0.3219752754296894559, 0.3333333333333333703, 0.3219752754296894559, 0.3333333333333333703, 0.3219752754296894559, 0.3333333333333333703, 0.3219752754296894559, 0.3333333333333333703, 0.3219752754296894559, 0.3333333333333333703, 0.3219752754296894559, 0.3333333333333333703, 0.3219752754296894559, 0.3333333333333333703, 0.3219752754296894559, 0.3333333333333333703, 0.3219752754296894559, 0.3333333333333333703, 0.3219752754296894559, 0.3333333333333333703, 0.3219752754296894559, 0.3333333333333333703, 0.3219752754296894559, 0.3333333333333333703, 0.3219752754296894559, 0.3333333333333333703, 0.3219752754296894559, 0.3333333333333333703, 0.3219752754296894559, 0.3333333333333333703, 0.3219752754296894559, 0.3333333333333333703, 0.3219752754296894559, 0.3333333333333333703, 0.3219752754296894559, 0.3333333333333333703, 0.3219752754296894559, 0.3333333333333333703, 0.3219752754296894559, 0.3333333333333333703, 0.3219752754296894559, 0.3333333333333333703, 0.3219752754296894559, 0.3333333333333333703, 0.3219752754296894559, 0.3333333333333333703, 0.3219752754296894559, 0.3333333333333333703, 0.3219752754296894559, 0.3333333333333333703, 0.3219752754296894559, 0.3333333333333333703),
 ( 1.000000000000000000, 0.9659258262890683122, 1.000000000000000000, 0.9659258262890683122, 1.000000000000000000, 0.9659258262890683122, 1.000000000000000000, 0.9659258262890683122, 1.000000000000000000, 0.9659258262890683122, 1.000000000000000000, 0.9659258262890683122, 1.000000000000000000, 0.9659258262890683122, 1.000000000000000000, 0.9659258262890683122, 1.000000000000000000, 0.9659258262890683122, 1.000000000000000000, 0.9659258262890683122, 1.000000000000000000, 0.9659258262890683122, 1.000000000000000000, 0.9659258262890683122, 1.000000000000000000, 0.9659258262890683122, 1.000000000000000000, 0.9659258262890683122, 1.000000000000000000, 0.9659258262890683122, 1.000000000000000000, 0.9659258262890683122, 1.000000000000000000, 0.9659258262890683122, 1.000000000000000000, 0.9659258262890683122, 1.000000000000000000, 0.9659258262890683122, 1.000000000000000000, 0.9659258262890683122, 1.000000000000000000, 0.9659258262890683122, 1.000000000000000000, 0.9659258262890683122, 1.000000000000000000, 0.9659258262890683122, 1.000000000000000000, 0.9659258262890683122, 1.000000000000000000, 0.9659258262890683122, 1.000000000000000000, 0.9659258262890683122, 1.000000000000000000, 0.9659258262890683122, 1.000000000000000000, 0.9659258262890683122, 1.000000000000000000, 0.9659258262890683122, 1.000000000000000000, 0.9659258262890683122, 1.000000000000000000, 0.9659258262890683122, 1.000000000000000000, 0.9659258262890683122, 1.000000000000000000, 0.9659258262890683122, 1.000000000000000000, 0.9659258262890683122, 1.000000000000000000, 0.9659258262890683122, 1.000000000000000000, 0.9659258262890683122, 1.000000000000000000, 0.9659258262890683122, 1.000000000000000000, 0.9659258262890683122, 1.000000000000000000, 0.9659258262890683122, 1.000000000000000000, 0.9659258262890683122, 1.000000000000000000, 0.9659258262890683122, 1.000000000000000000, 0.9659258262890683122, 1.000000000000000000, 0.9659258262890683122, 1.000000000000000000, 0.9659258262890683122, 1.000000000000000000, 0.9659258262890683122, 1.000000000000000000, 0.9659258262890683122, 1.000000000000000000, 0.9659258262890683122, 1.000000000000000000, 0.9659258262890683122, 1.000000000000000000, 0.9659258262890683122, 1.000000000000000000, 0.9659258262890683122, 1.000000000000000000, 0.9659258262890683122, 1.000000000000000000, 0.9659258262890683122, 1.000000000000000000, 0.9659258262890683122, 1.000000000000000000, 0.9659258262890683122, 1.000000000000000000, 0.9659258262890683122, 1.000000000000000000, 0.9659258262890683122, 1.000000000000000000, 0.9659258262890683122, 1.000000000000000000, 0.9659258262890683122, 1.000000000000000000, 0.9659258262890683122, 1.000000000000000000, 0.9659258262890683122, 1.000000000000000000, 0.9659258262890683122, 1.000000000000000000, 0.9659258262890683122, 1.000000000000000000, 0.9659258262890683122, 1.000000000000000000, 0.9659258262890683122, 1.000000000000000000, 0.9659258262890683122, 1.000000000000000000, 0.9659258262890683122, 1.000000000000000000, 0.9659258262890683122, 1.000000000000000000, 0.9659258262890683122, 1.000000000000000000, 0.9659258262890683122, 1.000000000000000000, 0.9659258262890683122, 1.000000000000000000, 0.9659258262890683122, 1.000000000000000000, 0.9659258262890683122, 1.000000000000000000, 0.9659258262890683122, 1.000000000000000000, 0.9659258262890683122, 1.000000000000000000, 0.9659258262890683122, 1.000000000000000000, 0.9659258262890683122, 1.000000000000000000, 0.9659258262890683122, 1.000000000000000000, 0.9659258262890683122, 1.000000000000000000, 0.9659258262890683122, 1.000000000000000000, 0.9659258262890683122, 1.000000000000000000, 0.9659258262890683122, 1.000000000000000000, 0.9659258262890683122, 1.000000000000000000, 0.9659258262890683122, 1.000000000000000000, 0.9659258262890683122, 1.000000000000000000, 0.9659258262890683122, 1.000000000000000000, 0.9659258262890683122, 1.000000000000000000, 0.9659258262890683122, 1.000000000000000000, 0.9659258262890683122, 1.000000000000000000, 0.9659258262890683122, 1.000000000000000000, 0.9659258262890683122, 1.000000000000000000, 0.9659258262890683122, 1.000000000000000000, 0.9659258262890683122, 1.000000000000000000, 0.9659258262890683122, 1.000000000000000000, 0.9659258262890683122, 1.000000000000000000, 0.9659258262890683122, 1.000000000000000000, 0.9659258262890683122, 1.000000000000000000, 0.9659258262890683122, 1.000000000000000000, 0.9659258262890683122, 1.000000000000000000, 0.9659258262890683122, 1.000000000000000000, 0.9659258262890683122, 1.000000000000000000, 0.9659258262890683122, 1.000000000000000000, 0.9659258262890683122, 1.000000000000000000, 0.9659258262890683122, 1.000000000000000000, 0.9659258262890683122, 1.000000000000000000, 0.9659258262890683122, 1.000000000000000000, 0.9659258262890683122, 1.000000000000000000, 0.9659258262890683122, 1.000000000000000000, 0.9659258262890683122, 1.000000000000000000, 0.9659258262890683122, 1.000000000000000000, 0.9659258262890683122, 1.000000000000000000, 0.9659258262890683122, 1.000000000000000000, 0.9659258262890683122, 1.000000000000000000, 0.9659258262890683122, 1.000000000000000000, 0.9659258262890683122, 1.000000000000000000, 0.9659258262890683122, 1.000000000000000000, 0.9659258262890683122, 1.000000000000000000, 0.9659258262890683122, 1.000000000000000000, 0.9659258262890683122, 1.000000000000000000, 0.9659258262890683122, 1.000000000000000000, 0.9659258262890683122, 1.000000000000000000, 0.9659258262890683122, 1.000000000000000000, 0.9659258262890683122, 1.000000000000000000, 0.9659258262890683122, 1.000000000000000000, 0.9659258262890683122, 1.000000000000000000, 0.9659258262890683122, 1.000000000000000000, 0.9659258262890683122, 1.000000000000000000, 0.9659258262890683122, 1.000000000000000000, 0.9659258262890683122, 1.000000000000000000, 0.9659258262890683122, 1.000000000000000000, 0.9659258262890683122, 1.000000000000000000, 0.9659258262890683122, 1.000000000000000000, 0.9659258262890683122, 1.000000000000000000, 0.9659258262890683122, 1.000000000000000000, 0.9659258262890683122, 1.000000000000000000, 0.9659258262890683122, 1.000000000000000000, 0.9659258262890683122, 1.000000000000000000, 0.9659258262890683122, 1.000000000000000000, 0.9659258262890683122, 1.000000000000000000, 0.9659258262890683122, 1.000000000000000000, 0.9659258262890683122, 1.000000000000000000, 0.9659258262890683122, 1.000000000000000000, 0.9659258262890683122, 1.000000000000000000, 0.9659258262890683122, 1.000000000000000000, 0.9659258262890683122, 1.000000000000000000, 0.9659258262890683122, 1.000000000000000000, 0.9659258262890683122, 1.000000000000000000, 0.9659258262890683122, 1.000000000000000000, 0.9659258262890683122, 1.000000000000000000, 0.9659258262890683122, 1.000000000000000000, 0.9659258262890683122, 1.000000000000000000, 0.9659258262890683122, 1.000000000000000000, 0.9659258262890683122, 1.000000000000000000, 0.9659258262890683122, 1.000000000000000000, 0.9659258262890683122, 1.000000000000000000, 0.9659258262890683122, 1.000000000000000000, 0.9659258262890683122, 1.000000000000000000, 0.9659258262890683122, 1.000000000000000000, 0.9659258262890683122, 1.000000000000000000, 0.9659258262890683122, 1.000000000000000000, 0.9659258262890683122, 1.000000000000000000, 0.9659258262890683122, 1.000000000000000000, 0.9659258262890683122, 1.000000000000000000, 0.9659258262890683122, 1.000000000000000000, 0.9659258262890683122, 1.000000000000000000, 0.9659258262890683122, 1.000000000000000000, 0.9659258262890683122, 1.000000000000000000, 0.9659258262890683122, 1.000000000000000000, 0.9659258262890683122, 1.000000000000000000, 0.9659258262890683122, 1.000000000000000000, 0.9659258262890683122, 1.000000000000000000, 0.9659258262890683122, 1.000000000000000000, 0.9659258262890683122, 1.000000000000000000, 0.9659258262890683122, 1.000000000000000000, 0.9659258262890683122, 1.000000000000000000, 0.9659258262890683122, 1.000000000000000000, 0.9659258262890683122, 1.000000000000000000, 0.9659258262890683122, 1.000000000000000000, 0.9659258262890683122, 1.000000000000000000, 0.9659258262890683122, 1.000000000000000000, 0.9659258262890683122, 1.000000000000000000, 0.9659258262890683122, 1.000000000000000000, 0.9659258262890683122, 1.000000000000000000, 0.9659258262890683122, 1.000000000000000000, 0.9659258262890683122, 1.000000000000000000, 0.9659258262890683122, 1.000000000000000000, 0.9659258262890683122, 1.000000000000000000, 0.9659258262890683122, 1.000000000000000000, 0.9659258262890683122, 1.000000000000000000, 0.9659258262890683122, 1.000000000000000000, 0.9659258262890683122, 1.000000000000000000, 0.9659258262890683122, 1.000000000000000000, 0.9659258262890683122, 1.000000000000000000, 0.9659258262890683122, 1.000000000000000000, 0.9659258262890683122, 1.000000000000000000, 0.9659258262890683122, 1.000000000000000000, 0.9659258262890683122, 1.000000000000000000, 0.9659258262890683122, 1.000000000000000000, 0.9659258262890683122, 1.000000000000000000, 0.9659258262890683122, 1.000000000000000000, 0.9659258262890683122, 1.000000000000000000, 0.9659258262890683122, 1.000000000000000000, 0.9659258262890683122, 1.000000000000000000, 0.9659258262890683122, 1.000000000000000000, 0.9659258262890683122, 1.000000000000000000, 0.9659258262890683122, 1.000000000000000000, 0.9659258262890683122, 1.000000000000000000, 0.9659258262890683122, 1.000000000000000000, 0.9659258262890683122, 1.000000000000000000, 0.9659258262890683122, 1.000000000000000000, 0.9659258262890683122, 1.000000000000000000, 0.9659258262890683122, 1.000000000000000000, 0.9659258262890683122, 1.000000000000000000, 0.9659258262890683122, 1.000000000000000000, 0.9659258262890683122, 1.000000000000000000, 0.9659258262890683122, 1.000000000000000000, 0.9659258262890683122, 1.000000000000000000, 0.9659258262890683122, 1.000000000000000000, 0.9659258262890683122, 1.000000000000000000, 0.9659258262890683122, 1.000000000000000000, 0.9659258262890683122, 1.000000000000000000, 0.9659258262890683122, 1.000000000000000000, 0.9659258262890683122, 1.000000000000000000, 0.9659258262890683122, 1.000000000000000000, 0.9659258262890683122, 1.000000000000000000, 0.9659258262890683122, 1.000000000000000000, 0.9659258262890683122, 1.000000000000000000, 0.9659258262890683122, 1.000000000000000000, 0.9659258262890683122, 1.000000000000000000),
 ( 0.3333333333333333703, 0.3219752754296894559, 0.3333333333333333703, 0.3219752754296894559, 0.3333333333333333703, 0.3219752754296894559, 0.3333333333333333703, 0.3219752754296894559, 0.3333333333333333703, 0.3219752754296894559, 0.3333333333333333703, 0.3219752754296894559, 0.3333333333333333703, 0.3219752754296894559, 0.3333333333333333703, 0.3219752754296894559, 0.3333333333333333703, 0.3219752754296894559, 0.3333333333333333703, 0.3219752754296894559, 0.3333333333333333703, 0.3219752754296894559, 0.3333333333333333703, 0.3219752754296894559, 0.3333333333333333703, 0.3219752754296894559, 0.3333333333333333703, 0.3219752754296894559, 0.3333333333333333703, 0.3219752754296894559, 0.3333333333333333703, 0.3219752754296894559, 0.3333333333333333703, 0.3219752754296894559, 0.3333333333333333703, 0.3219752754296894559, 0.3333333333333333703, 0.3219752754296894559, 0.3333333333333333703, 0.3219752754296894559, 0.3333333333333333703, 0.3219752754296894559, 0.3333333333333333703, 0.3219752754296894559, 0.3333333333333333703, 0.3219752754296894559, 0.3333333333333333703, 0.3219752754296894559, 0.3333333333333333703, 0.3219752754296894559, 0.3333333333333333703, 0.3219752754296894559, 0.3333333333333333703, 0.3219752754296894559, 0.3333333333333333703, 0.3219752754296894559, 0.3333333333333333703, 0.3219752754296894559, 0.3333333333333333703, 0.3219752754296894559, 0.3333333333333333703, 0.3219752754296894559, 0.3333333333333333703, 0.3219752754296894559, 0.3333333333333333703, 0.3219752754296894559, 0.3333333333333333703, 0.3219752754296894559, 0.3333333333333333703, 0.3219752754296894559, 0.3333333333333333703, 0.3219752754296894559, 0.3333333333333333703, 0.3219752754296894559, 0.3333333333333333703, 0.3219752754296894559, 0.3333333333333333703, 0.3219752754296894559, 0.3333333333333333703, 0.3219752754296894559, 0.3333333333333333703, 0.3219752754296894559, 0.3333333333333333703, 0.3219752754296894559, 0.3333333333333333703, 0.3219752754296894559, 0.3333333333333333703, 0.3219752754296894559, 0.3333333333333333703, 0.3219752754296894559, 0.3333333333333333703, 0.3219752754296894559, 0.3333333333333333703, 0.3219752754296894559, 0.3333333333333333703, 0.3219752754296894559, 0.3333333333333333703, 0.3219752754296894559, 0.3333333333333333703, 0.3219752754296894559, 0.3333333333333333703, 0.3219752754296894559, 0.3333333333333333703, 0.3219752754296894559, 0.3333333333333333703, 0.3219752754296894559, 0.3333333333333333703, 0.3219752754296894559, 0.3333333333333333703, 0.3219752754296894559, 0.3333333333333333703, 0.3219752754296894559, 0.3333333333333333703, 0.3219752754296894559, 0.3333333333333333703, 0.3219752754296894559, 0.3333333333333333703, 0.3219752754296894559, 0.3333333333333333703, 0.3219752754296894559, 0.3333333333333333703, 0.3219752754296894559, 0.3333333333333333703, 0.3219752754296894559, 0.3333333333333333703, 0.3219752754296894559, 0.3333333333333333703, 0.3219752754296894559, 0.3333333333333333703, 0.3219752754296894559, 0.3333333333333333703, 0.3219752754296894559, 0.3333333333333333703, 0.3219752754296894559, 0.3333333333333333703, 0.3219752754296894559, 0.3333333333333333703, 0.3219752754296894559, 0.3333333333333333703, 0.3219752754296894559, 0.3333333333333333703, 0.3219752754296894559, 0.3333333333333333703, 0.3219752754296894559, 0.3333333333333333703, 0.3219752754296894559, 0.3333333333333333703, 0.3219752754296894559, 0.3333333333333333703, 0.3219752754296894559, 0.3333333333333333703, 0.3219752754296894559, 0.3333333333333333703, 0.3219752754296894559, 0.3333333333333333703, 0.3219752754296894559, 0.3333333333333333703, 0.3219752754296894559, 0.3333333333333333703, 0.3219752754296894559, 0.3333333333333333703, 0.3219752754296894559, 0.3333333333333333703, 0.3219752754296894559, 0.3333333333333333703, 0.3219752754296894559, 0.3333333333333333703, 0.3219752754296894559, 0.3333333333333333703, 0.3219752754296894559, 0.3333333333333333703, 0.3219752754296894559, 0.3333333333333333703, 0.3219752754296894559, 0.3333333333333333703, 0.3219752754296894559, 0.3333333333333333703, 0.3219752754296894559, 0.3333333333333333703, 0.3219752754296894559, 0.3333333333333333703, 0.3219752754296894559, 0.3333333333333333703, 0.3219752754296894559, 0.3333333333333333703, 0.3219752754296894559, 0.3333333333333333703, 0.3219752754296894559, 0.3333333333333333703, 0.3219752754296894559, 0.3333333333333333703, 0.3219752754296894559, 0.3333333333333333703, 0.3219752754296894559, 0.3333333333333333703, 0.3219752754296894559, 0.3333333333333333703, 0.3219752754296894559, 0.3333333333333333703, 0.3219752754296894559, 0.3333333333333333703, 0.3219752754296894559, 0.3333333333333333703, 0.3219752754296894559, 0.3333333333333333703, 0.3219752754296894559, 0.3333333333333333703, 0.3219752754296894559, 0.3333333333333333703, 0.3219752754296894559, 0.3333333333333333703, 0.3219752754296894559, 0.3333333333333333703, 0.3219752754296894559, 0.3333333333333333703, 0.3219752754296894559, 0.3333333333333333703, 0.3219752754296894559, 0.3333333333333333703, 0.3219752754296894559, 0.3333333333333333703, 0.3219752754296894559, 0.3333333333333333703, 0.3219752754296894559, 0.3333333333333333703, 0.3219752754296894559, 0.3333333333333333703, 0.3219752754296894559, 0.3333333333333333703, 0.3219752754296894559, 0.3333333333333333703, 0.3219752754296894559, 0.3333333333333333703, 0.3219752754296894559, 0.3333333333333333703, 0.3219752754296894559, 0.3333333333333333703, 0.3219752754296894559, 0.3333333333333333703, 0.3219752754296894559, 0.3333333333333333703, 0.3219752754296894559, 0.3333333333333333703, 0.3219752754296894559, 0.3333333333333333703, 0.3219752754296894559, 0.3333333333333333703, 0.3219752754296894559, 0.3333333333333333703, 0.3219752754296894559, 0.3333333333333333703, 0.3219752754296894559, 0.3333333333333333703, 0.3219752754296894559, 0.3333333333333333703, 0.3219752754296894559, 0.3333333333333333703, 0.3219752754296894559, 0.3333333333333333703, 0.3219752754296894559, 0.3333333333333333703, 0.3219752754296894559, 0.3333333333333333703, 0.3219752754296894559, 0.3333333333333333703, 0.3219752754296894559, 0.3333333333333333703, 0.3219752754296894559, 0.3333333333333333703, 0.3219752754296894559, 0.3333333333333333703, 0.3219752754296894559, 0.3333333333333333703, 0.3219752754296894559, 0.3333333333333333703, 0.3219752754296894559, 0.3333333333333333703, 0.3219752754296894559, 0.3333333333333333703, 0.3219752754296894559, 0.3333333333333333703, 0.3219752754296894559, 0.3333333333333333703, 0.3219752754296894559, 0.3333333333333333703, 0.3219752754296894559, 0.3333333333333333703, 0.3219752754296894559, 0.3333333333333333703, 0.3219752754296894559, 0.3333333333333333703, 0.3219752754296894559, 0.3333333333333333703, 0.3219752754296894559, 0.3333333333333333703, 0.3219752754296894559, 0.3333333333333333703, 0.3219752754296894559, 0.3333333333333333703, 0.3219752754296894559, 0.3333333333333333703, 0.3219752754296894559, 0.3333333333333333703, 0.3219752754296894559, 0.3333333333333333703, 0.3219752754296894559, 0.3333333333333333703, 0.3219752754296894559, 0.3333333333333333703, 0.3219752754296894559, 0.3333333333333333703, 0.3219752754296894559, 0.3333333333333333703, 0.3219752754296894559, 0.3333333333333333703, 0.3219752754296894559, 0.3333333333333333703, 0.3219752754296894559, 0.3333333333333333703, 0.3219752754296894559, 0.3333333333333333703, 0.3219752754296894559, 0.3333333333333333703, 0.3219752754296894559, 0.3333333333333333703, 0.3219752754296894559, 0.3333333333333333703, 0.3219752754296894559, 0.3333333333333333703, 0.3219752754296894559, 0.3333333333333333703, 0.3219752754296894559, 0.3333333333333333703, 0.3219752754296894559, 0.3333333333333333703, 0.3219752754296894559, 0.3333333333333333703, 0.3219752754296894559, 0.3333333333333333703, 0.3219752754296894559, 0.3333333333333333703, 0.3219752754296894559, 0.3333333333333333703, 0.3219752754296894559, 0.3333333333333333703, 0.3219752754296894559, 0.3333333333333333703, 0.3219752754296894559, 0.3333333333333333703, 0.3219752754296894559, 0.3333333333333333703, 0.3219752754296894559, 0.3333333333333333703, 0.3219752754296894559, 0.3333333333333333703, 0.3219752754296894559, 0.3333333333333333703, 0.3219752754296894559, 0.3333333333333333703, 0.3219752754296894559, 0.3333333333333333703, 0.3219752754296894559, 0.3333333333333333703, 0.3219752754296894559, 0.3333333333333333703, 0.3219752754296894559, 0.3333333333333333703, 0.3219752754296894559, 0.3333333333333333703, 0.3219752754296894559, 0.3333333333333333703, 0.3219752754296894559, 0.3333333333333333703, 0.3219752754296894559, 0.3333333333333333703, 0.3219752754296894559, 0.3333333333333333703, 0.3219752754296894559, 0.3333333333333333703, 0.3219752754296894559, 0.3333333333333333703, 0.3219752754296894559, 0.3333333333333333703, 0.3219752754296894559, 0.3333333333333333703, 0.3219752754296894559, 0.3333333333333333703, 0.3219752754296894559, 0.3333333333333333703, 0.3219752754296894559, 0.3333333333333333703, 0.3219752754296894559, 0.3333333333333333703, 0.3219752754296894559, 0.3333333333333333703, 0.3219752754296894559, 0.3333333333333333703, 0.3219752754296894559, 0.3333333333333333703, 0.3219752754296894559, 0.3333333333333333703, 0.3219752754296894559, 0.3333333333333333703, 0.3219752754296894559, 0.3333333333333333703, 0.3219752754296894559, 0.3333333333333333703, 0.3219752754296894559, 0.3333333333333333703, 0.3219752754296894559, 0.3333333333333333703, 0.3219752754296894559, 0.3333333333333333703, 0.3219752754296894559, 0.3333333333333333703, 0.3219752754296894559, 0.3333333333333333703, 0.3219752754296894559, 0.3333333333333333703, 0.3219752754296894559, 0.3333333333333333703, 0.3219752754296894559, 0.3333333333333333703, 0.3219752754296894559, 0.3333333333333333703, 0.3219752754296894559, 0.3333333333333333703, 0.3219752754296894559, 0.3333333333333333703, 0.3219752754296894559, 0.3333333333333333703, 0.3219752754296894559, 0.3333333333333333703, 0.3219752754296894559, 0.3333333333333333703, 0.3219752754296894559, 0.3333333333333333703, 0.3219752754296894559, 0.3333333333333333703, 0.3219752754296894559, 0.3333333333333333703, 0.3219752754296894559, 0.3333333333333333703, 0.3219752754296894559, 0.3333333333333333703, 0.3219752754296894559, 0.3333333333333333703, 0.3219752754296894559, 0.3333333333333333703, 0.3219752754296894559, 0.3333333333333333703, 0.3219752754296894559, 0.3333333333333333703, 0.3219752754296894559, 0.3333333333333333703, 0.3219752754296894559, 0.3333333333333333703),
 ( 0.3333333333333333703, 0.3219752754296894559, 0.3333333333333333703, 0.3219752754296894559, 0.3333333333333333703, 0.3219752754296894559, 0.3333333333333333703, 0.3219752754296894559, 0.3333333333333333703, 0.3219752754296894559, 0.3333333333333333703, 0.3219752754296894559, 0.3333333333333333703, 0.3219752754296894559, 0.3333333333333333703, 0.3219752754296894559, 0.3333333333333333703, 0.3219752754296894559, 0.3333333333333333703, 0.3219752754296894559, 0.3333333333333333703, 0.3219752754296894559, 0.3333333333333333703, 0.3219752754296894559, 0.3333333333333333703, 0.3219752754296894559, 0.3333333333333333703, 0.3219752754296894559, 0.3333333333333333703, 0.3219752754296894559, 0.3333333333333333703, 0.3219752754296894559, 0.3333333333333333703, 0.3219752754296894559, 0.3333333333333333703, 0.3219752754296894559, 0.3333333333333333703, 0.3219752754296894559, 0.3333333333333333703, 0.3219752754296894559, 0.3333333333333333703, 0.3219752754296894559, 0.3333333333333333703, 0.3219752754296894559, 0.3333333333333333703, 0.3219752754296894559, 0.3333333333333333703, 0.3219752754296894559, 0.3333333333333333703, 0.3219752754296894559, 0.3333333333333333703, 0.3219752754296894559, 0.3333333333333333703, 0.3219752754296894559, 0.3333333333333333703, 0.3219752754296894559, 0.3333333333333333703, 0.3219752754296894559, 0.3333333333333333703, 0.3219752754296894559, 0.3333333333333333703, 0.3219752754296894559, 0.3333333333333333703, 0.3219752754296894559, 0.3333333333333333703, 0.3219752754296894559, 0.3333333333333333703, 0.3219752754296894559, 0.3333333333333333703, 0.3219752754296894559, 0.3333333333333333703, 0.3219752754296894559, 0.3333333333333333703, 0.3219752754296894559, 0.3333333333333333703, 0.3219752754296894559, 0.3333333333333333703, 0.3219752754296894559, 0.3333333333333333703, 0.3219752754296894559, 0.3333333333333333703, 0.3219752754296894559, 0.3333333333333333703, 0.3219752754296894559, 0.3333333333333333703, 0.3219752754296894559, 0.3333333333333333703, 0.3219752754296894559, 0.3333333333333333703, 0.3219752754296894559, 0.3333333333333333703, 0.3219752754296894559, 0.3333333333333333703, 0.3219752754296894559, 0.3333333333333333703, 0.3219752754296894559, 0.3333333333333333703, 0.3219752754296894559, 0.3333333333333333703, 0.3219752754296894559, 0.3333333333333333703, 0.3219752754296894559, 0.3333333333333333703, 0.3219752754296894559, 0.3333333333333333703, 0.3219752754296894559, 0.3333333333333333703, 0.3219752754296894559, 0.3333333333333333703, 0.3219752754296894559, 0.3333333333333333703, 0.3219752754296894559, 0.3333333333333333703, 0.3219752754296894559, 0.3333333333333333703, 0.3219752754296894559, 0.3333333333333333703, 0.3219752754296894559, 0.3333333333333333703, 0.3219752754296894559, 0.3333333333333333703, 0.3219752754296894559, 0.3333333333333333703, 0.3219752754296894559, 0.3333333333333333703, 0.3219752754296894559, 0.3333333333333333703, 0.3219752754296894559, 0.3333333333333333703, 0.3219752754296894559, 0.3333333333333333703, 0.3219752754296894559, 0.3333333333333333703, 0.3219752754296894559, 0.3333333333333333703, 0.3219752754296894559, 0.3333333333333333703, 0.3219752754296894559, 0.3333333333333333703, 0.3219752754296894559, 0.3333333333333333703, 0.3219752754296894559, 0.3333333333333333703, 0.3219752754296894559, 0.3333333333333333703, 0.3219752754296894559, 0.3333333333333333703, 0.3219752754296894559, 0.3333333333333333703, 0.3219752754296894559, 0.3333333333333333703, 0.3219752754296894559, 0.3333333333333333703, 0.3219752754296894559, 0.3333333333333333703, 0.3219752754296894559, 0.3333333333333333703, 0.3219752754296894559, 0.3333333333333333703, 0.3219752754296894559, 0.3333333333333333703, 0.3219752754296894559, 0.3333333333333333703, 0.3219752754296894559, 0.3333333333333333703, 0.3219752754296894559, 0.3333333333333333703, 0.3219752754296894559, 0.3333333333333333703, 0.3219752754296894559, 0.3333333333333333703, 0.3219752754296894559, 0.3333333333333333703, 0.3219752754296894559, 0.3333333333333333703, 0.3219752754296894559, 0.3333333333333333703, 0.3219752754296894559, 0.3333333333333333703, 0.3219752754296894559, 0.3333333333333333703, 0.3219752754296894559, 0.3333333333333333703, 0.3219752754296894559, 0.3333333333333333703, 0.3219752754296894559, 0.3333333333333333703, 0.3219752754296894559, 0.3333333333333333703, 0.3219752754296894559, 0.3333333333333333703, 0.3219752754296894559, 0.3333333333333333703, 0.3219752754296894559, 0.3333333333333333703, 0.3219752754296894559, 0.3333333333333333703, 0.3219752754296894559, 0.3333333333333333703, 0.3219752754296894559, 0.3333333333333333703, 0.3219752754296894559, 0.3333333333333333703, 0.3219752754296894559, 0.3333333333333333703, 0.3219752754296894559, 0.3333333333333333703, 0.3219752754296894559, 0.3333333333333333703, 0.3219752754296894559, 0.3333333333333333703, 0.3219752754296894559, 0.3333333333333333703, 0.3219752754296894559, 0.3333333333333333703, 0.3219752754296894559, 0.3333333333333333703, 0.3219752754296894559, 0.3333333333333333703, 0.3219752754296894559, 0.3333333333333333703, 0.3219752754296894559, 0.3333333333333333703, 0.3219752754296894559, 0.3333333333333333703, 0.3219752754296894559, 0.3333333333333333703, 0.3219752754296894559, 0.3333333333333333703, 0.3219752754296894559, 0.3333333333333333703, 0.3219752754296894559, 0.3333333333333333703, 0.3219752754296894559, 0.3333333333333333703, 0.3219752754296894559, 0.3333333333333333703, 0.3219752754296894559, 0.3333333333333333703, 0.3219752754296894559, 0.3333333333333333703, 0.3219752754296894559, 0.3333333333333333703, 0.3219752754296894559, 0.3333333333333333703, 0.3219752754296894559, 0.3333333333333333703, 0.3219752754296894559, 0.3333333333333333703, 0.3219752754296894559, 0.3333333333333333703, 0.3219752754296894559, 0.3333333333333333703, 0.3219752754296894559, 0.3333333333333333703, 0.3219752754296894559, 0.3333333333333333703, 0.3219752754296894559, 0.3333333333333333703, 0.3219752754296894559, 0.3333333333333333703, 0.3219752754296894559, 0.3333333333333333703, 0.3219752754296894559, 0.3333333333333333703, 0.3219752754296894559, 0.3333333333333333703, 0.3219752754296894559, 0.3333333333333333703, 0.3219752754296894559, 0.3333333333333333703, 0.3219752754296894559, 0.3333333333333333703, 0.3219752754296894559, 0.3333333333333333703, 0.3219752754296894559, 0.3333333333333333703, 0.3219752754296894559, 0.3333333333333333703, 0.3219752754296894559, 0.3333333333333333703, 0.3219752754296894559, 0.3333333333333333703, 0.3219752754296894559, 0.3333333333333333703, 0.3219752754296894559, 0.3333333333333333703, 0.3219752754296894559, 0.3333333333333333703, 0.3219752754296894559, 0.3333333333333333703, 0.3219752754296894559, 0.3333333333333333703, 0.3219752754296894559, 0.3333333333333333703, 0.3219752754296894559, 0.3333333333333333703, 0.3219752754296894559, 0.3333333333333333703, 0.3219752754296894559, 0.3333333333333333703, 0.3219752754296894559, 0.3333333333333333703, 0.3219752754296894559, 0.3333333333333333703, 0.3219752754296894559, 0.3333333333333333703, 0.3219752754296894559, 0.3333333333333333703, 0.3219752754296894559, 0.3333333333333333703, 0.3219752754296894559, 0.3333333333333333703, 0.3219752754296894559, 0.3333333333333333703, 0.3219752754296894559, 0.3333333333333333703, 0.3219752754296894559, 0.3333333333333333703, 0.3219752754296894559, 0.3333333333333333703, 0.3219752754296894559, 0.3333333333333333703, 0.3219752754296894559, 0.3333333333333333703, 0.3219752754296894559, 0.3333333333333333703, 0.3219752754296894559, 0.3333333333333333703, 0.3219752754296894559, 0.3333333333333333703, 0.3219752754296894559, 0.3333333333333333703, 0.3219752754296894559, 0.3333333333333333703, 0.3219752754296894559, 0.3333333333333333703, 0.3219752754296894559, 0.3333333333333333703, 0.3219752754296894559, 0.3333333333333333703, 0.3219752754296894559, 0.3333333333333333703, 0.3219752754296894559, 0.3333333333333333703, 0.3219752754296894559, 0.3333333333333333703, 0.3219752754296894559, 0.3333333333333333703, 0.3219752754296894559, 0.3333333333333333703, 0.3219752754296894559, 0.3333333333333333703, 0.3219752754296894559, 0.3333333333333333703, 0.3219752754296894559, 0.3333333333333333703, 0.3219752754296894559, 0.3333333333333333703, 0.3219752754296894559, 0.3333333333333333703, 0.3219752754296894559, 0.3333333333333333703, 0.3219752754296894559, 0.3333333333333333703, 0.3219752754296894559, 0.3333333333333333703, 0.3219752754296894559, 0.3333333333333333703, 0.3219752754296894559, 0.3333333333333333703, 0.3219752754296894559, 0.3333333333333333703, 0.3219752754296894559, 0.3333333333333333703, 0.3219752754296894559, 0.3333333333333333703, 0.3219752754296894559, 0.3333333333333333703, 0.3219752754296894559, 0.3333333333333333703, 0.3219752754296894559, 0.3333333333333333703, 0.3219752754296894559, 0.3333333333333333703, 0.3219752754296894559, 0.3333333333333333703, 0.3219752754296894559, 0.3333333333333333703, 0.3219752754296894559, 0.3333333333333333703, 0.3219752754296894559, 0.3333333333333333703, 0.3219752754296894559, 0.3333333333333333703, 0.3219752754296894559, 0.3333333333333333703, 0.3219752754296894559, 0.3333333333333333703, 0.3219752754296894559, 0.3333333333333333703, 0.3219752754296894559, 0.3333333333333333703, 0.3219752754296894559, 0.3333333333333333703, 0.3219752754296894559, 0.3333333333333333703, 0.3219752754296894559, 0.3333333333333333703, 0.3219752754296894559, 0.3333333333333333703, 0.3219752754296894559, 0.3333333333333333703, 0.3219752754296894559, 0.3333333333333333703, 0.3219752754296894559, 0.3333333333333333703, 0.3219752754296894559, 0.3333333333333333703, 0.3219752754296894559, 0.3333333333333333703, 0.3219752754296894559, 0.3333333333333333703, 0.3219752754296894559, 0.3333333333333333703, 0.3219752754296894559, 0.3333333333333333703, 0.3219752754296894559, 0.3333333333333333703, 0.3219752754296894559, 0.3333333333333333703, 0.3219752754296894559, 0.3333333333333333703, 0.3219752754296894559, 0.3333333333333333703, 0.3219752754296894559, 0.3333333333333333703, 0.3219752754296894559, 0.3333333333333333703, 0.3219752754296894559, 0.3333333333333333703, 0.3219752754296894559, 0.3333333333333333703, 0.3219752754296894559, 0.3333333333333333703, 0.3219752754296894559, 0.3333333333333333703, 0.3219752754296894559, 0.3333333333333333703, 0.3219752754296894559, 0.3333333333333333703, 0.3219752754296894559, 0.3333333333333333703, 0.3219752754296894559, 0.3333333333333333703, 0.3219752754296894559, 0.3333333333333333703),
 ( 1.000000000000000000, 0.9659258262890683122, 1.000000000000000000, 0.9659258262890683122, 1.000000000000000000, 0.9659258262890683122, 1.000000000000000000, 0.9659258262890683122, 1.000000000000000000, 0.9659258262890683122, 1.000000000000000000, 0.9659258262890683122, 1.000000000000000000, 0.9659258262890683122, 1.000000000000000000, 0.9659258262890683122, 1.000000000000000000, 0.9659258262890683122, 1.000000000000000000, 0.9659258262890683122, 1.000000000000000000, 0.9659258262890683122, 1.000000000000000000, 0.9659258262890683122, 1.000000000000000000, 0.9659258262890683122, 1.000000000000000000, 0.9659258262890683122, 1.000000000000000000, 0.9659258262890683122, 1.000000000000000000, 0.9659258262890683122, 1.000000000000000000, 0.9659258262890683122, 1.000000000000000000, 0.9659258262890683122, 1.000000000000000000, 0.9659258262890683122, 1.000000000000000000, 0.9659258262890683122, 1.000000000000000000, 0.9659258262890683122, 1.000000000000000000, 0.9659258262890683122, 1.000000000000000000, 0.9659258262890683122, 1.000000000000000000, 0.9659258262890683122, 1.000000000000000000, 0.9659258262890683122, 1.000000000000000000, 0.9659258262890683122, 1.000000000000000000, 0.9659258262890683122, 1.000000000000000000, 0.9659258262890683122, 1.000000000000000000, 0.9659258262890683122, 1.000000000000000000, 0.9659258262890683122, 1.000000000000000000, 0.9659258262890683122, 1.000000000000000000, 0.9659258262890683122, 1.000000000000000000, 0.9659258262890683122, 1.000000000000000000, 0.9659258262890683122, 1.000000000000000000, 0.9659258262890683122, 1.000000000000000000, 0.9659258262890683122, 1.000000000000000000, 0.9659258262890683122, 1.000000000000000000, 0.9659258262890683122, 1.000000000000000000, 0.9659258262890683122, 1.000000000000000000, 0.9659258262890683122, 1.000000000000000000, 0.9659258262890683122, 1.000000000000000000, 0.9659258262890683122, 1.000000000000000000, 0.9659258262890683122, 1.000000000000000000, 0.9659258262890683122, 1.000000000000000000, 0.9659258262890683122, 1.000000000000000000, 0.9659258262890683122, 1.000000000000000000, 0.9659258262890683122, 1.000000000000000000, 0.9659258262890683122, 1.000000000000000000, 0.9659258262890683122, 1.000000000000000000, 0.9659258262890683122, 1.000000000000000000, 0.9659258262890683122, 1.000000000000000000, 0.9659258262890683122, 1.000000000000000000, 0.9659258262890683122, 1.000000000000000000, 0.9659258262890683122, 1.000000000000000000, 0.9659258262890683122, 1.000000000000000000, 0.9659258262890683122, 1.000000000000000000, 0.9659258262890683122, 1.000000000000000000, 0.9659258262890683122, 1.000000000000000000, 0.9659258262890683122, 1.000000000000000000, 0.9659258262890683122, 1.000000000000000000, 0.9659258262890683122, 1.000000000000000000, 0.9659258262890683122, 1.000000000000000000, 0.9659258262890683122, 1.000000000000000000, 0.9659258262890683122, 1.000000000000000000, 0.9659258262890683122, 1.000000000000000000, 0.9659258262890683122, 1.000000000000000000, 0.9659258262890683122, 1.000000000000000000, 0.9659258262890683122, 1.000000000000000000, 0.9659258262890683122, 1.000000000000000000, 0.9659258262890683122, 1.000000000000000000, 0.9659258262890683122, 1.000000000000000000, 0.9659258262890683122, 1.000000000000000000, 0.9659258262890683122, 1.000000000000000000, 0.9659258262890683122, 1.000000000000000000, 0.9659258262890683122, 1.000000000000000000, 0.9659258262890683122, 1.000000000000000000, 0.9659258262890683122, 1.000000000000000000, 0.9659258262890683122, 1.000000000000000000, 0.9659258262890683122, 1.000000000000000000, 0.9659258262890683122, 1.000000000000000000, 0.9659258262890683122, 1.000000000000000000, 0.9659258262890683122, 1.000000000000000000, 0.9659258262890683122, 1.000000000000000000, 0.9659258262890683122, 1.000000000000000000, 0.9659258262890683122, 1.000000000000000000, 0.9659258262890683122, 1.000000000000000000, 0.9659258262890683122, 1.000000000000000000, 0.9659258262890683122, 1.000000000000000000, 0.9659258262890683122, 1.000000000000000000, 0.9659258262890683122, 1.000000000000000000, 0.9659258262890683122, 1.000000000000000000, 0.9659258262890683122, 1.000000000000000000, 0.9659258262890683122, 1.000000000000000000, 0.9659258262890683122, 1.000000000000000000, 0.9659258262890683122, 1.000000000000000000, 0.9659258262890683122, 1.000000000000000000, 0.9659258262890683122, 1.000000000000000000, 0.9659258262890683122, 1.000000000000000000, 0.9659258262890683122, 1.000000000000000000, 0.9659258262890683122, 1.000000000000000000, 0.9659258262890683122, 1.000000000000000000, 0.9659258262890683122, 1.000000000000000000, 0.9659258262890683122, 1.000000000000000000, 0.9659258262890683122, 1.000000000000000000, 0.9659258262890683122, 1.000000000000000000, 0.9659258262890683122, 1.000000000000000000, 0.9659258262890683122, 1.000000000000000000, 0.9659258262890683122, 1.000000000000000000, 0.9659258262890683122, 1.000000000000000000, 0.9659258262890683122, 1.000000000000000000, 0.9659258262890683122, 1.000000000000000000, 0.9659258262890683122, 1.000000000000000000, 0.9659258262890683122, 1.000000000000000000, 0.9659258262890683122, 1.000000000000000000, 0.9659258262890683122, 1.000000000000000000, 0.9659258262890683122, 1.000000000000000000, 0.9659258262890683122, 1.000000000000000000, 0.9659258262890683122, 1.000000000000000000, 0.9659258262890683122, 1.000000000000000000, 0.9659258262890683122, 1.000000000000000000, 0.9659258262890683122, 1.000000000000000000, 0.9659258262890683122, 1.000000000000000000, 0.9659258262890683122, 1.000000000000000000, 0.9659258262890683122, 1.000000000000000000, 0.9659258262890683122, 1.000000000000000000, 0.9659258262890683122, 1.000000000000000000, 0.9659258262890683122, 1.000000000000000000, 0.9659258262890683122, 1.000000000000000000, 0.9659258262890683122, 1.000000000000000000, 0.9659258262890683122, 1.000000000000000000, 0.9659258262890683122, 1.000000000000000000, 0.9659258262890683122, 1.000000000000000000, 0.9659258262890683122, 1.000000000000000000, 0.9659258262890683122, 1.000000000000000000, 0.9659258262890683122, 1.000000000000000000, 0.9659258262890683122, 1.000000000000000000, 0.9659258262890683122, 1.000000000000000000, 0.9659258262890683122, 1.000000000000000000, 0.9659258262890683122, 1.000000000000000000, 0.9659258262890683122, 1.000000000000000000, 0.9659258262890683122, 1.000000000000000000, 0.9659258262890683122, 1.000000000000000000, 0.9659258262890683122, 1.000000000000000000, 0.9659258262890683122, 1.000000000000000000, 0.9659258262890683122, 1.000000000000000000, 0.9659258262890683122, 1.000000000000000000, 0.9659258262890683122, 1.000000000000000000, 0.9659258262890683122, 1.000000000000000000, 0.9659258262890683122, 1.000000000000000000, 0.9659258262890683122, 1.000000000000000000, 0.9659258262890683122, 1.000000000000000000, 0.9659258262890683122, 1.000000000000000000, 0.9659258262890683122, 1.000000000000000000, 0.9659258262890683122, 1.000000000000000000, 0.9659258262890683122, 1.000000000000000000, 0.9659258262890683122, 1.000000000000000000, 0.9659258262890683122, 1.000000000000000000, 0.9659258262890683122, 1.000000000000000000, 0.9659258262890683122, 1.000000000000000000, 0.9659258262890683122, 1.000000000000000000, 0.9659258262890683122, 1.000000000000000000, 0.9659258262890683122, 1.000000000000000000, 0.9659258262890683122, 1.000000000000000000, 0.9659258262890683122, 1.000000000000000000, 0.9659258262890683122, 1.000000000000000000, 0.9659258262890683122, 1.000000000000000000, 0.9659258262890683122, 1.000000000000000000, 0.9659258262890683122, 1.000000000000000000, 0.9659258262890683122, 1.000000000000000000, 0.9659258262890683122, 1.000000000000000000, 0.9659258262890683122, 1.000000000000000000, 0.9659258262890683122, 1.000000000000000000, 0.9659258262890683122, 1.000000000000000000, 0.9659258262890683122, 1.000000000000000000, 0.9659258262890683122, 1.000000000000000000, 0.9659258262890683122, 1.000000000000000000, 0.9659258262890683122, 1.000000000000000000, 0.9659258262890683122, 1.000000000000000000, 0.9659258262890683122, 1.000000000000000000, 0.9659258262890683122, 1.000000000000000000, 0.9659258262890683122, 1.000000000000000000, 0.9659258262890683122, 1.000000000000000000, 0.9659258262890683122, 1.000000000000000000, 0.9659258262890683122, 1.000000000000000000, 0.9659258262890683122, 1.000000000000000000, 0.9659258262890683122, 1.000000000000000000, 0.9659258262890683122, 1.000000000000000000, 0.9659258262890683122, 1.000000000000000000, 0.9659258262890683122, 1.000000000000000000, 0.9659258262890683122, 1.000000000000000000, 0.9659258262890683122, 1.000000000000000000, 0.9659258262890683122, 1.000000000000000000, 0.9659258262890683122, 1.000000000000000000, 0.9659258262890683122, 1.000000000000000000, 0.9659258262890683122, 1.000000000000000000, 0.9659258262890683122, 1.000000000000000000, 0.9659258262890683122, 1.000000000000000000, 0.9659258262890683122, 1.000000000000000000, 0.9659258262890683122, 1.000000000000000000, 0.9659258262890683122, 1.000000000000000000, 0.9659258262890683122, 1.000000000000000000, 0.9659258262890683122, 1.000000000000000000, 0.9659258262890683122, 1.000000000000000000, 0.9659258262890683122, 1.000000000000000000, 0.9659258262890683122, 1.000000000000000000, 0.9659258262890683122, 1.000000000000000000, 0.9659258262890683122, 1.000000000000000000, 0.9659258262890683122, 1.000000000000000000, 0.9659258262890683122, 1.000000000000000000, 0.9659258262890683122, 1.000000000000000000, 0.9659258262890683122, 1.000000000000000000, 0.9659258262890683122, 1.000000000000000000, 0.9659258262890683122, 1.000000000000000000, 0.9659258262890683122, 1.000000000000000000, 0.9659258262890683122, 1.000000000000000000, 0.9659258262890683122, 1.000000000000000000, 0.9659258262890683122, 1.000000000000000000, 0.9659258262890683122, 1.000000000000000000, 0.9659258262890683122, 1.000000000000000000, 0.9659258262890683122, 1.000000000000000000, 0.9659258262890683122, 1.000000000000000000, 0.9659258262890683122, 1.000000000000000000, 0.9659258262890683122, 1.000000000000000000, 0.9659258262890683122, 1.000000000000000000, 0.9659258262890683122, 1.000000000000000000, 0.9659258262890683122, 1.000000000000000000, 0.9659258262890683122, 1.000000000000000000, 0.9659258262890683122, 1.000000000000000000) ) ) 
 REPRESENTATION_ITEM ( '' )  SURFACE ( )  );
#109550 = CARTESIAN_POINT ( 'NONE',  ( 8.224510206698953496, -14.34966873604960469, 87.91557627198103830 ) ) ;
#109551 = CARTESIAN_POINT ( 'NONE',  ( 19.05341960407611168, 5.049401038298154454, 48.95724293864768129 ) ) ;
#109553 = CARTESIAN_POINT ( 'NONE',  ( 17.49999999999999645, -5.500000000000031974, 93.29690382534172954 ) ) ;
#109552 = CARTESIAN_POINT ( 'NONE',  ( -16.51473224551082808, 9.474510206698731452, 93.33442372801900433 ) ) ;
#109554 = CARTESIAN_POINT ( 'NONE',  ( 5.823673210054444382, -21.52544592524334988, 85.20942372801901854 ) ) ;
#109555 = CARTESIAN_POINT ( 'NONE',  ( -8.314922557961024197, 14.29746914071037800, 57.91775706135234714 ) ) ;
#109556 = CARTESIAN_POINT ( 'NONE',  ( 16.88567814943165857, 6.947325034625600360, 38.79001122652587696 ) ) ;
#109557 = CARTESIAN_POINT ( 'NONE',  ( 5.823673210054125526, 21.52544592524343514, 44.79057627198103120 ) ) ;
#109558 = CARTESIAN_POINT ( 'NONE',  ( 8.314922557961029526, -14.29746914071037800, 40.41775706135234714 ) ) ;
#109559 = CARTESIAN_POINT ( 'NONE',  ( -19.02544592524342804, 5.153800228976336939, 26.04057627198103120 ) ) ;
#109560 = CARTESIAN_POINT ( 'NONE',  ( 9.474510206698729675, 16.51473224551082808, 32.08442372801900433 ) ) ;
#109561 = CARTESIAN_POINT ( 'NONE',  ( -19.02544592524342804, 5.153800228976336051, 71.04057627198099567 ) ) ;
#109562 = CARTESIAN_POINT ( 'NONE',  ( 11.74264578624800315, -36.14014761921581709, -7.400000000000000355 ) ) ;
#109563 = CARTESIAN_POINT ( 'NONE',  ( -19.02544592524342804, 5.153800228976336051, 56.04057627198100988 ) ) ;
#109564 = CARTESIAN_POINT ( 'NONE',  ( 16.43460366218431901, 17.60430054815008205, -54.39459263522238786 ) ) ;
#109565 = CARTESIAN_POINT ( 'NONE',  ( -9.474510206698964154, 16.51473224551069663, 65.41557627198102409 ) ) ;
#109566 = CARTESIAN_POINT ( 'NONE',  ( -18.22780087662126647, -5.499999999999827693, 53.98236817873107185 ) ) ;
#109567 = CARTESIAN_POINT ( 'NONE',  ( -13.97604488694547697, 13.89961937509957934, 28.12609039468565797 ) ) ;
#109568 = CARTESIAN_POINT ( 'NONE',  ( -18.67979575497193778, 10.72451020669871902, 113.3344237280190328 ) ) ;
#109569 = CARTESIAN_POINT ( 'NONE',  ( 8.224510206698953496, -14.34966873604960469, 32.91557627198102409 ) ) ;
#109570 = CARTESIAN_POINT ( 'NONE',  ( -13.97604488694527625, -13.89961937509977652, 41.87390960531435979 ) ) ;
#109571 = CARTESIAN_POINT ( 'NONE',  ( -5.153800228976328057, -19.02544592524343514, 102.2905762719810383 ) ) ;
#109572 = CARTESIAN_POINT ( 'NONE',  ( 21.53943276465977519, 0.05219959533937863772, 76.25109039468568994 ) ) ;
#109573 = CARTESIAN_POINT ( 'NONE',  ( -13.97604488694527625, -13.89961937509977652, 51.87390960531436690 ) ) ;
#109574 = CARTESIAN_POINT ( 'NONE',  ( 0.05219959533937995610, -21.53943276465977519, 80.00109039468568994 ) ) ;
#109575 = CARTESIAN_POINT ( 'NONE',  ( -19.02544592524342804, 5.153800228976336051, 116.0405762719810383 ) ) ;
#109576 = CARTESIAN_POINT ( 'NONE',  ( 5.049401038298161559, -19.05341960407611168, 32.70724293864768129 ) ) ;
#109577 = CARTESIAN_POINT ( 'NONE',  ( 18.62759615963255655, 10.81492255796105972, 31.66775706135234358 ) ) ;
#109578 = CARTESIAN_POINT ( 'NONE',  ( 13.89961937509957401, 13.97604488694547697, 46.87609039468565442 ) ) ;
#109579 = CARTESIAN_POINT ( 'NONE',  ( -9.474510206698964154, 16.51473224551069663, 30.41557627198102054 ) ) ;
#109580 = CARTESIAN_POINT ( 'NONE',  ( 16.46253265017160672, -9.564922557960803928, 78.33224293864769550 ) ) ;
#109581 = CARTESIAN_POINT ( 'NONE',  ( -13.97604488694547697, 13.89961937509957934, 108.1260903946856331 ) ) ;
#109582 = CARTESIAN_POINT ( 'NONE',  ( -16.53943276465976808, 0.05219959533911058130, 76.24890960531435269 ) ) ;
#109583 = CARTESIAN_POINT ( 'NONE',  ( 21.53943276465977519, -0.05219959533907433946, 33.74890960531436690 ) ) ;
#109584 = CARTESIAN_POINT ( 'NONE',  ( 16.46253265017146816, 9.564922557961045513, 101.6677570613523329 ) ) ;
#109585 = CARTESIAN_POINT ( 'NONE',  ( 15.72974639402199770, -15.80617190586745480, 108.1239096053143811 ) ) ;
#109586 = CARTESIAN_POINT ( 'NONE',  ( -21.52544592524334988, -5.823673210054445271, 58.95942372801902565 ) ) ;
#109587 = CARTESIAN_POINT ( 'NONE',  ( 16.53943276465976808, 0.05219959533934440121, 51.25109039468568994 ) ) ;
#109588 = CARTESIAN_POINT ( 'NONE',  ( 16.55341960407618274, -4.379528057220086978, 56.04275706135235424 ) ) ;
#109589 = CARTESIAN_POINT ( 'NONE',  ( -15.72974639402197994, 15.80617190586746368, 65.62390960531436690 ) ) ;
#109590 = CARTESIAN_POINT ( 'NONE',  ( -16.51473224551069308, -9.474510206698971260, 46.66557627198102409 ) ) ;
#109591 = CARTESIAN_POINT ( 'NONE',  ( -12.14591786802326823, 12.06949235617739902, 83.12609039468568994 ) ) ;
#109592 = CARTESIAN_POINT ( 'NONE',  ( -0.05219959533907301413, -21.53943276465977519, 97.49890960531436690 ) ) ;
#109593 = CARTESIAN_POINT ( 'NONE',  ( -14.34966873604960291, -8.224510206698953496, 46.66557627198102409 ) ) ;
#109594 = CARTESIAN_POINT ( 'NONE',  ( -19.05341960407611168, -5.049401038298163336, 71.45724293864766707 ) ) ;
#109595 = CARTESIAN_POINT ( 'NONE',  ( -16.55341960407617563, 4.379528057220093196, 78.54275706135236135 ) ) ;
#109596 = CARTESIAN_POINT ( 'NONE',  ( 16.53943276465976808, 0.05219959533934440121, 21.25109039468567218 ) ) ;
#109597 = CARTESIAN_POINT ( 'NONE',  ( 21.53943276465977519, -0.05219959533907433946, 113.7489096053143527 ) ) ;
#109598 = CARTESIAN_POINT ( 'NONE',  ( 12.06949235617757843, -12.14591786802309237, 43.12390960531435269 ) ) ;
#109599 = VERTEX_POINT ( 'NONE', #15525 ) ;
#109600 = CARTESIAN_POINT ( 'NONE',  ( -17.31728774477273447, 6.344390552232393787, 75.81906651689320142 ) ) ;
#109601 = CARTESIAN_POINT ( 'NONE',  ( -5.823673210054116645, -21.52544592524344225, 82.29057627198103830 ) ) ;
#109602 = CARTESIAN_POINT ( 'NONE',  ( 16.52544592524342804, -4.483927247898539470, 28.54057627198103120 ) ) ;
#109603 = ORIENTED_EDGE ( 'NONE', *, *, #137192, .F. ) ;
#109604 = CARTESIAN_POINT ( 'NONE',  ( -16.29526858892878849, -7.335722546920003140, 55.79670597800208753 ) ) ;
#109605 = CARTESIAN_POINT ( 'NONE',  ( -21.53943276465977519, 0.05219959533907696930, 111.2489096053143669 ) ) ;
#109606 = CARTESIAN_POINT ( 'NONE',  ( 13.89961937509977652, -13.97604488694527269, 108.1239096053143669 ) ) ;
#109607 = CARTESIAN_POINT ( 'NONE',  ( -21.53943276465977519, -0.05219959533937600094, 23.75109039468567929 ) ) ;
#109608 = CARTESIAN_POINT ( 'NONE',  ( 14.34966873604960469, 8.224510206698951720, 49.16557627198102409 ) ) ;
#109609 = CARTESIAN_POINT ( 'NONE',  ( -16.55341960407617563, 4.379528057220093196, 48.54275706135234714 ) ) ;
#109611 = ADVANCED_FACE ( 'NONE', ( #183391 ), #93336, .F. ) ;
#109610 = CARTESIAN_POINT ( 'NONE',  ( 19.02544592524343514, -5.153800228976328945, 58.54057627198102409 ) ) ;
#109612 = CARTESIAN_POINT ( 'NONE',  ( 13.97604488694548053, -13.89961937509957401, 50.62609039468566152 ) ) ;
#109613 = CARTESIAN_POINT ( 'NONE',  ( -5.153800228976328057, -19.02544592524343514, 82.29057627198103830 ) ) ;
#109614 = CARTESIAN_POINT ( 'NONE',  ( 21.55341960407610458, 5.719274019375980345, 33.95724293864769550 ) ) ;
#109615 = CARTESIAN_POINT ( 'NONE',  ( -25.90290776672046746, -27.60635150542758254, -16.55190051048584010 ) ) ;
#109616 = CARTESIAN_POINT ( 'NONE',  ( -5.153800228976328057, -19.02544592524343514, 42.29057627198101699 ) ) ;
#109617 = CARTESIAN_POINT ( 'NONE',  ( -4.379528057220086978, -16.55341960407618274, 24.79275706135235779 ) ) ;
#109618 = CARTESIAN_POINT ( 'NONE',  ( -16.46253265017146816, -9.564922557961047289, 64.16775706135233293 ) ) ;
#109619 = CARTESIAN_POINT ( 'NONE',  ( 10.72451020669898902, -18.67979575497178502, 97.91557627198103830 ) ) ;
#109620 = CARTESIAN_POINT ( 'NONE',  ( -14.29746914071049879, 8.314922557960819915, 30.83224293864770260 ) ) ;
#109621 = CARTESIAN_POINT ( 'NONE',  ( -19.05341960407611168, -5.049401038298163336, 91.45724293864766707 ) ) ;
#109622 = CARTESIAN_POINT ( 'NONE',  ( 15.72974639402199770, -15.80617190586745480, 53.12390960531436690 ) ) ;
#109624 = CARTESIAN_POINT ( 'NONE',  ( -12.06949235617739369, -12.14591786802326823, 24.37609039468567573 ) ) ;
#109623 = CARTESIAN_POINT ( 'NONE',  ( 18.62759615963271287, -10.81492255796078972, 98.33224293864769550 ) ) ;
#109625 = CARTESIAN_POINT ( 'NONE',  ( 15.80617190586746368, 15.72974639402197994, 39.37390960531436690 ) ) ;
#109626 = CARTESIAN_POINT ( 'NONE',  ( -21.53943276465977519, -0.05219959533937600094, 83.75109039468568994 ) ) ;
#109627 = CARTESIAN_POINT ( 'NONE',  ( -13.89961937509977652, 13.97604488694528158, 85.62390960531433848 ) ) ;
#109628 = VECTOR ( 'NONE', #199556, 1000.000000000000000 ) ;
#109629 = CARTESIAN_POINT ( 'NONE',  ( 16.46253265017160672, -9.564922557960803928, 33.33224293864770260 ) ) ;
#109630 = CARTESIAN_POINT ( 'NONE',  ( -9.474510206698964154, 16.51473224551069663, 90.41557627198103830 ) ) ;
#109631 = CARTESIAN_POINT ( 'NONE',  ( 12.06949235617757843, -12.14591786802309237, 98.12390960531436690 ) ) ;
#109632 = CARTESIAN_POINT ( 'NONE',  ( -19.03943276465977164, 0.05219959533909376836, 66.24890960531436690 ) ) ;
#109633 = CARTESIAN_POINT ( 'NONE',  ( 14.29746914071037800, 8.314922557961029526, 21.66775706135235069 ) ) ;
#109634 = CARTESIAN_POINT ( 'NONE',  ( -18.22780087662122028, 5.500000000000031086, 43.51540105326107977 ) ) ;
#109636 = CARTESIAN_POINT ( 'NONE',  ( 10.72451020669898902, -18.67979575497178502, 22.91557627198102765 ) ) ;
#109635 = CARTESIAN_POINT ( 'NONE',  ( -15.72974639402176322, -15.80617190586768395, 99.37609039468568994 ) ) ;
#109637 = CARTESIAN_POINT ( 'NONE',  ( 16.53943276465976808, 0.05219959533934440121, 91.25109039468568994 ) ) ;
#109638 = DIRECTION ( 'NONE',  ( 0.000000000000000000, 0.000000000000000000, -1.000000000000000000 ) ) ;
#109639 = CARTESIAN_POINT ( 'NONE',  ( -9.564922557961040184, 16.46253265017147172, 72.91775706135233293 ) ) ;
#109640 = CARTESIAN_POINT ( 'NONE',  ( -9.564922557961040184, 16.46253265017147172, 32.91775706135233293 ) ) ;
#109641 = CARTESIAN_POINT ( 'NONE',  ( 27.51614237185798117, -3.626410569495110980, 140.0000000000000000 ) ) ;
#109642 = CARTESIAN_POINT ( 'NONE',  ( 16.46253265017160672, -9.564922557960803928, 23.33224293864769194 ) ) ;
#109643 = CARTESIAN_POINT ( 'NONE',  ( -12.06949235617756955, 12.14591786802309770, 35.62390960531437401 ) ) ;
#109644 = EDGE_CURVE ( 'NONE', #65926, #66950, #120703, .T. ) ;
#109645 = CARTESIAN_POINT ( 'NONE',  ( 5.049401038298161559, -19.05341960407611168, 27.70724293864769550 ) ) ;
#109646 = CARTESIAN_POINT ( 'NONE',  ( -0.05219959533910754901, -16.53943276465976808, 27.49890960531435269 ) ) ;
#109647 = CARTESIAN_POINT ( 'NONE',  ( -18.56399227203343472, -5.499999999999928946, 83.97830131249904184 ) ) ;
#109648 = CARTESIAN_POINT ( 'NONE',  ( 12.14591786802327356, -12.06949235617739191, 95.62609039468568994 ) ) ;
#109649 = CARTESIAN_POINT ( 'NONE',  ( 9.564922557960805705, 16.46253265017160317, 34.58224293864770260 ) ) ;
#109650 = CARTESIAN_POINT ( 'NONE',  ( -21.53943276465977519, -0.05219959533937600094, 88.75109039468567573 ) ) ;
#109651 = CARTESIAN_POINT ( 'NONE',  ( -19.02544592524334988, -5.153800228976617603, 103.9594237280190043 ) ) ;
#109652 = CARTESIAN_POINT ( 'NONE',  ( 10.72451020669871369, 18.67979575497193778, 82.08442372801901854 ) ) ;
#109653 = CARTESIAN_POINT ( 'NONE',  ( 19.05341960407617918, -5.049401038297876454, 56.04275706135234714 ) ) ;
#109654 = CARTESIAN_POINT ( 'NONE',  ( 19.02544592524343514, -5.153800228976328945, 93.54057627198102409 ) ) ;
#109655 = CARTESIAN_POINT ( 'NONE',  ( -16.46253265017160317, 9.564922557960807481, 70.83224293864770971 ) ) ;
#109656 = EDGE_CURVE ( 'NONE', #63455, #132514, #131391, .T. ) ;
#109657 = CARTESIAN_POINT ( 'NONE',  ( 16.79531203550646623, 7.028104445595625194, 73.75244988220441655 ) ) ;
#109658 = CIRCLE ( 'NONE', #132186, 1.249999999999999778 ) ;
#109659 = CARTESIAN_POINT ( 'NONE',  ( 14.29746914071049879, -8.314922557960816363, 68.33224293864769550 ) ) ;
#109660 = CARTESIAN_POINT ( 'NONE',  ( -21.52544592524343514, 5.823673210054127303, 61.04057627198103120 ) ) ;
#109661 = CARTESIAN_POINT ( 'NONE',  ( -5.153800228976328057, -19.02544592524343514, 57.29057627198103120 ) ) ;
#109663 = CARTESIAN_POINT ( 'NONE',  ( 14.34966873604972726, -8.224510206698740333, 80.83442372801901854 ) ) ;
#109662 = CARTESIAN_POINT ( 'NONE',  ( -15.72974639402197994, 15.80617190586746368, 85.62390960531436690 ) ) ;
#109664 = VERTEX_POINT ( 'NONE', #5298 ) ;
#109665 = CARTESIAN_POINT ( 'NONE',  ( -13.97604488694527625, -13.89961937509977652, 46.87390960531435979 ) ) ;
#109667 = CARTESIAN_POINT ( 'NONE',  ( 11.40812507854754365, 35.11059874428196537, -3.224999997268813701 ) ) ;
#109666 = CARTESIAN_POINT ( 'NONE',  ( 14.34966873604960469, 8.224510206698951720, 74.16557627198102409 ) ) ;
#109668 = CARTESIAN_POINT ( 'NONE',  ( -19.05341960407611168, -5.049401038298163336, 46.45724293864768129 ) ) ;
#109669 = CARTESIAN_POINT ( 'NONE',  ( -4.379528057220328563, 16.55341960407611168, 110.2072429386477239 ) ) ;
#109670 = CARTESIAN_POINT ( 'NONE',  ( -13.97604488694547697, 13.89961937509957934, 68.12609039468563310 ) ) ;
#109671 = CARTESIAN_POINT ( 'NONE',  ( -16.52544592524342804, 4.483927247898546575, 66.04057627198103830 ) ) ;
#109672 = CARTESIAN_POINT ( 'NONE',  ( -18.62759615963255300, -10.81492255796106328, 39.16775706135235424 ) ) ;
#109674 = CARTESIAN_POINT ( 'NONE',  ( -15.80617190586745835, -15.72974639402198527, 101.8739096053143811 ) ) ;
#109673 = CARTESIAN_POINT ( 'NONE',  ( -19.02544592524342804, 5.153800228976336051, 31.04057627198102409 ) ) ;
#109675 = CARTESIAN_POINT ( 'NONE',  ( -31.74999999999995737, 0.000000000000000000, 0.000000000000000000 ) ) ;
#109676 = CARTESIAN_POINT ( 'NONE',  ( 14.34966873604960469, 8.224510206698951720, 84.16557627198103830 ) ) ;
#109677 = CARTESIAN_POINT ( 'NONE',  ( 26.94323156051284229, -28.89364864972473868, -18.52709669219397526 ) ) ;
#109678 = CARTESIAN_POINT ( 'NONE',  ( -13.89961937509977652, 13.97604488694528158, 45.62390960531433848 ) ) ;
#109679 = CARTESIAN_POINT ( 'NONE',  ( 17.50000000000000000, 5.499999999999995559, 113.7823096230356583 ) ) ;
#109681 = CARTESIAN_POINT ( 'NONE',  ( 5.049401038298161559, -19.05341960407611168, 97.70724293864766707 ) ) ;
#109680 = CARTESIAN_POINT ( 'NONE',  ( -19.02544592524334988, -5.153800228976617603, 88.95942372801897591 ) ) ;
#109682 = CARTESIAN_POINT ( 'NONE',  ( 15.80617190586769283, -15.72974639402175789, 40.62609039468567573 ) ) ;
#109683 = CARTESIAN_POINT ( 'NONE',  ( -16.46253265017160317, 9.564922557960807481, 80.83224293864769550 ) ) ;
#109684 = CARTESIAN_POINT ( 'NONE',  ( 0.05219959533936267826, -19.03943276465977164, 70.00109039468566152 ) ) ;
#109685 = CARTESIAN_POINT ( 'NONE',  ( -5.153800228976328057, -19.02544592524343514, 47.29057627198102409 ) ) ;
#109686 = CARTESIAN_POINT ( 'NONE',  ( 0.05219959533910956823, 16.53943276465976808, 69.99890960531435269 ) ) ;
#109687 = CARTESIAN_POINT ( 'NONE',  ( -14.29746914071049879, 8.314922557960819915, 65.83224293864769550 ) ) ;
#109688 = CARTESIAN_POINT ( 'NONE',  ( -19.02544592524342804, 5.153800228976336051, 76.04057627198102409 ) ) ;
#109689 = CARTESIAN_POINT ( 'NONE',  ( 5.719274019375991003, -21.55341960407610458, 102.7072429386476955 ) ) ;
#109690 = CARTESIAN_POINT ( 'NONE',  ( 9.474510206698971260, -16.51473224551069308, 67.91557627198102409 ) ) ;
#109691 = CARTESIAN_POINT ( 'NONE',  ( 13.97604488694548053, -13.89961937509957401, 20.62609039468567573 ) ) ;
#109694 = CARTESIAN_POINT ( 'NONE',  ( 16.55341960407611168, 4.379528057220329451, 113.9572429386477239 ) ) ;
#109693 = CARTESIAN_POINT ( 'NONE',  ( -4.483927247898539470, -16.52544592524342804, 22.29057627198102765 ) ) ;
#109692 = CARTESIAN_POINT ( 'NONE',  ( -5.049401038298153566, 19.05341960407611168, 35.20724293864768839 ) ) ;
#109695 = CARTESIAN_POINT ( 'NONE',  ( 5.153800228976615827, -19.02544592524334988, 110.2094237280189901 ) ) ;
#109696 = ORIENTED_EDGE ( 'NONE', *, *, #144706, .T. ) ;
#109697 = CARTESIAN_POINT ( 'NONE',  ( -21.53943276465977519, -0.05219959533937600094, 28.75109039468567929 ) ) ;
#109698 = CARTESIAN_POINT ( 'NONE',  ( 5.049401038297881783, 19.05341960407617563, 72.29275706135234714 ) ) ;
#109699 = CARTESIAN_POINT ( 'NONE',  ( 12.14591786802327356, -12.06949235617739191, 110.6260903946857042 ) ) ;
#109700 = CARTESIAN_POINT ( 'NONE',  ( -0.05219959533907301413, -21.53943276465977519, 77.49890960531433848 ) ) ;
#109701 = CARTESIAN_POINT ( 'NONE',  ( -5.719274019375978568, 21.55341960407610458, 25.20724293864769550 ) ) ;
#109702 = CARTESIAN_POINT ( 'NONE',  ( -16.55341960407611168, -4.379528057220339221, 51.45724293864770260 ) ) ;
#109703 = CARTESIAN_POINT ( 'NONE',  ( 5.153800228976335163, 19.02544592524342804, 24.79057627198102765 ) ) ;
#109704 = CARTESIAN_POINT ( 'NONE',  ( 19.02544592524343514, -5.153800228976328945, 43.54057627198103120 ) ) ;
#109705 = CARTESIAN_POINT ( 'NONE',  ( 13.97604488694548053, -13.89961937509957401, 30.62609039468566863 ) ) ;
#109706 = CARTESIAN_POINT ( 'NONE',  ( -12.14591786802326823, 12.06949235617739902, 83.12609039468568994 ) ) ;
#109707 = CARTESIAN_POINT ( 'NONE',  ( -14.29746914071037622, -8.314922557961029526, 59.16775706135234714 ) ) ;
#109708 = CARTESIAN_POINT ( 'NONE',  ( 15.72974639402199770, -15.80617190586745480, 23.12390960531436335 ) ) ;
#109709 = CARTESIAN_POINT ( 'NONE',  ( 10.72451020669871369, 18.67979575497193778, 112.0844237280190185 ) ) ;
#109710 = CARTESIAN_POINT ( 'NONE',  ( -19.02544592524342804, 5.153800228976336051, 81.04057627198103830 ) ) ;
#109711 = CARTESIAN_POINT ( 'NONE',  ( 14.34966873604972726, -8.224510206698740333, 60.83442372801901854 ) ) ;
#109712 = CARTESIAN_POINT ( 'NONE',  ( -8.314922557960811034, -14.29746914071050412, 107.0822429386476955 ) ) ;
#109713 = CARTESIAN_POINT ( 'NONE',  ( 16.52544592524342804, -4.483927247898539470, 23.54057627198102765 ) ) ;
#109714 = CARTESIAN_POINT ( 'NONE',  ( -0.5319302666793322976, -21.39352396646987842, -58.79417398750189960 ) ) ;
#109717 = CARTESIAN_POINT ( 'NONE',  ( -5.049401038298153566, 19.05341960407611168, 80.20724293864769550 ) ) ;
#109716 = CARTESIAN_POINT ( 'NONE',  ( 19.03943276465977164, -0.05219959533909143690, 93.74890960531435269 ) ) ;
#109715 = CARTESIAN_POINT ( 'NONE',  ( 18.67979575497194134, -10.72451020669871369, 65.83442372801900433 ) ) ;
#109718 = CARTESIAN_POINT ( 'NONE',  ( 5.153800228976335163, 19.02544592524342804, 114.7905762719810241 ) ) ;
#109719 = CARTESIAN_POINT ( 'NONE',  ( 4.379528057220339221, -16.55341960407611168, 52.70724293864769550 ) ) ;
#109720 = CARTESIAN_POINT ( 'NONE',  ( 16.55341960407618274, -4.379528057220086978, 106.0427570613523471 ) ) ;
#109721 = CARTESIAN_POINT ( 'NONE',  ( -8.224510206698948167, 14.34966873604960824, 35.41557627198102409 ) ) ;
#109723 = CARTESIAN_POINT ( 'NONE',  ( -15.59328001550075271, -17.53262387181210968, -54.89123680731869115 ) ) ;
#109722 = CARTESIAN_POINT ( 'NONE',  ( 12.14591786802327356, -12.06949235617739191, 45.62609039468567573 ) ) ;
#109724 = CARTESIAN_POINT ( 'NONE',  ( 5.153800228976615827, -19.02544592524334988, 40.20942372801898301 ) ) ;
#109725 = CARTESIAN_POINT ( 'NONE',  ( -13.97604488694527625, -13.89961937509977652, 71.87390960531433848 ) ) ;
#109726 = CARTESIAN_POINT ( 'NONE',  ( -16.51473224551082808, 9.474510206698731452, 48.33442372801900433 ) ) ;
#109727 = CARTESIAN_POINT ( 'NONE',  ( -13.89961937509957401, -13.97604488694547875, 54.37609039468565442 ) ) ;
#109729 = CARTESIAN_POINT ( 'NONE',  ( 4.379528057220092307, 16.55341960407617563, 82.29275706135234714 ) ) ;
#109728 = CARTESIAN_POINT ( 'NONE',  ( 19.05341960407617918, -5.049401038297876454, 101.0427570613523045 ) ) ;
#109730 = CARTESIAN_POINT ( 'NONE',  ( 5.049401038298161559, -19.05341960407611168, 32.70724293864768129 ) ) ;
#109731 = CARTESIAN_POINT ( 'NONE',  ( 5.049401038298161559, -19.05341960407611168, 102.7072429386476955 ) ) ;
#109732 = CARTESIAN_POINT ( 'NONE',  ( 21.52544592524334988, 5.823673210054432836, 46.45942372801901854 ) ) ;
#109733 = CARTESIAN_POINT ( 'NONE',  ( 19.03943276465977164, 0.05219959533936151252, 86.25109039468567573 ) ) ;
#109735 = CARTESIAN_POINT ( 'NONE',  ( -9.474510206698964154, 16.51473224551069663, 55.41557627198103120 ) ) ;
#109734 = CARTESIAN_POINT ( 'NONE',  ( 17.50000000000013500, -3.292511757969739605, 107.5652027021053527 ) ) ;
#109736 = CARTESIAN_POINT ( 'NONE',  ( -5.153800228976328057, -19.02544592524343514, 97.29057627198099567 ) ) ;
#109738 = CARTESIAN_POINT ( 'NONE',  ( 9.564922557960805705, 16.46253265017160317, 54.58224293864769550 ) ) ;
#109737 = CARTESIAN_POINT ( 'NONE',  ( 8.314922557960818139, 14.29746914071049879, 59.58224293864770260 ) ) ;
#109739 = CARTESIAN_POINT ( 'NONE',  ( 5.049401038298161559, -19.05341960407611168, 67.70724293864769550 ) ) ;
#109740 = CARTESIAN_POINT ( 'NONE',  ( 5.049401038297881783, 19.05341960407617563, 67.29275706135234714 ) ) ;
#109741 = CARTESIAN_POINT ( 'NONE',  ( -0.05219959533936034679, 19.03943276465977164, 47.50109039468566863 ) ) ;
#109742 = CARTESIAN_POINT ( 'NONE',  ( -19.05341960407611168, -5.049401038298163336, 81.45724293864769550 ) ) ;
#109743 = CARTESIAN_POINT ( 'NONE',  ( 10.81492255796078972, 18.62759615963270932, 74.58224293864768129 ) ) ;
#109745 = CARTESIAN_POINT ( 'NONE',  ( -0.05219959533936034679, 19.03943276465977164, 37.50109039468567573 ) ) ;
#109744 = CARTESIAN_POINT ( 'NONE',  ( 16.52544592524342804, -4.483927247898539470, 73.54057627198102409 ) ) ;
#109746 = CARTESIAN_POINT ( 'NONE',  ( -15.80617190586745835, -15.72974639402198527, 41.87390960531435979 ) ) ;
#109747 = CARTESIAN_POINT ( 'NONE',  ( 21.55341960407610458, 5.719274019375980345, 43.95724293864769550 ) ) ;
#109748 = CARTESIAN_POINT ( 'NONE',  ( -13.97604488694527625, -13.89961937509977652, 61.87390960531435979 ) ) ;
#109749 = CARTESIAN_POINT ( 'NONE',  ( -16.51473224551069308, -9.474510206698971260, 41.66557627198103120 ) ) ;
#109750 = CARTESIAN_POINT ( 'NONE',  ( 4.379528057220339221, -16.55341960407611168, 107.7072429386476955 ) ) ;
#109751 = CARTESIAN_POINT ( 'NONE',  ( 10.72451020669871369, 18.67979575497193778, 27.08442372801901854 ) ) ;
#109752 = CARTESIAN_POINT ( 'NONE',  ( 5.153800228976335163, 19.02544592524342804, 109.7905762719810099 ) ) ;
#109753 = CARTESIAN_POINT ( 'NONE',  ( 10.72451020669871369, 18.67979575497193778, 22.08442372801901143 ) ) ;
#109754 = CARTESIAN_POINT ( 'NONE',  ( 0.05219959533909260263, 19.03943276465977164, 29.99890960531435979 ) ) ;
#109755 = CARTESIAN_POINT ( 'NONE',  ( -10.72451020669898014, 18.67979575497178502, 100.4155762719810241 ) ) ;
#109756 = CARTESIAN_POINT ( 'NONE',  ( 19.03943276465977164, 0.05219959533936151252, 51.25109039468567573 ) ) ;
#109757 = CARTESIAN_POINT ( 'NONE',  ( -9.564922557960796823, -16.46253265017161027, 22.08224293864768839 ) ) ;
#109758 = CARTESIAN_POINT ( 'NONE',  ( -19.02544592524342804, 5.153800228976336051, 26.04057627198103120 ) ) ;
#109759 = DIRECTION ( 'NONE',  ( 0.000000000000000000, -1.000000000000000000, 0.000000000000000000 ) ) ;
#109760 = CARTESIAN_POINT ( 'NONE',  ( 0.05219959533934541429, -16.53943276465976808, 65.00109039468568994 ) ) ;
#109761 = CARTESIAN_POINT ( 'NONE',  ( 13.89961937509977652, -13.97604488694527269, 28.12390960531435624 ) ) ;
#109762 = CARTESIAN_POINT ( 'NONE',  ( 33.84943726220063098, -0.7253354391803923384, 100.4638154892406021 ) ) ;
#109763 = CARTESIAN_POINT ( 'NONE',  ( -13.89961937509977652, 13.97604488694528158, 75.62390960531438111 ) ) ;
#109764 = CARTESIAN_POINT ( 'NONE',  ( -4.483927247898539470, -16.52544592524342804, 107.2905762719810525 ) ) ;
#109765 = CARTESIAN_POINT ( 'NONE',  ( -10.81492255796078084, -18.62759615963271287, 42.08224293864769550 ) ) ;
#109766 = CARTESIAN_POINT ( 'NONE',  ( 4.379528057220339221, -16.55341960407611168, 72.70724293864769550 ) ) ;
#109767 = CARTESIAN_POINT ( 'NONE',  ( -0.05219959533934338120, 16.53943276465976808, 27.50109039468567929 ) ) ;
#109768 = CARTESIAN_POINT ( 'NONE',  ( 5.719274019375673035, 21.55341960407619339, 82.29275706135234714 ) ) ;
#109769 = CARTESIAN_POINT ( 'NONE',  ( -13.97604488694527625, -13.89961937509977652, 26.87390960531434558 ) ) ;
#109770 = CARTESIAN_POINT ( 'NONE',  ( 12.14591786802327356, -12.06949235617739191, 110.6260903946857042 ) ) ;
#109771 = CARTESIAN_POINT ( 'NONE',  ( -4.379528057220328563, 16.55341960407611168, 55.20724293864770260 ) ) ;
#109772 = AXIS2_PLACEMENT_3D ( 'NONE', #139602, #182161, #15286 ) ;
#109773 = CARTESIAN_POINT ( 'NONE',  ( 19.02544592524343514, -5.153800228976328945, 58.54057627198102409 ) ) ;
#109774 = CARTESIAN_POINT ( 'NONE',  ( 10.72451020669871369, 18.67979575497193778, 92.08442372801901854 ) ) ;
#109775 = CARTESIAN_POINT ( 'NONE',  ( 10.81492255796078972, 18.62759615963270932, 109.5822429386476955 ) ) ;
#109776 = CARTESIAN_POINT ( 'NONE',  ( -18.67979575497193778, 10.72451020669871902, 78.33442372801901854 ) ) ;
#109777 = CARTESIAN_POINT ( 'NONE',  ( -16.53943276465976808, -0.05219959533934237506, 43.75109039468568284 ) ) ;
#109779 = CARTESIAN_POINT ( 'NONE',  ( 18.62759615963255655, 10.81492255796105972, 81.66775706135236135 ) ) ;
#109778 = CARTESIAN_POINT ( 'NONE',  ( 14.29746914071049879, -8.314922557960816363, 83.33224293864769550 ) ) ;
#109780 = CARTESIAN_POINT ( 'NONE',  ( -12.06949235617739369, -12.14591786802326823, 109.3760903946857042 ) ) ;
#109781 = CARTESIAN_POINT ( 'NONE',  ( -17.26172910966779739, 6.454744622555818268, 115.8064690864922710 ) ) ;
#109782 = CARTESIAN_POINT ( 'NONE',  ( 4.379528057220092307, 16.55341960407617563, 42.29275706135235424 ) ) ;
#109783 = CARTESIAN_POINT ( 'NONE',  ( -14.34966873604960291, -8.224510206698953496, 46.66557627198102409 ) ) ;
#109784 = CARTESIAN_POINT ( 'NONE',  ( 8.224510206698742110, 14.34966873604972548, 87.08442372801901854 ) ) ;
#109785 = CARTESIAN_POINT ( 'NONE',  ( 19.03943276465977164, -0.05219959533909143690, 103.7489096053143669 ) ) ;
#109786 = CARTESIAN_POINT ( 'NONE',  ( 5.153800228976335163, 19.02544592524342804, 99.79057627198102409 ) ) ;
#109787 = CARTESIAN_POINT ( 'NONE',  ( -5.719274019375665041, -21.55341960407619695, 94.79275706135234714 ) ) ;
#109788 = CARTESIAN_POINT ( 'NONE',  ( -14.34966873604972548, 8.224510206698743886, 103.3344237280190043 ) ) ;
#109789 = CARTESIAN_POINT ( 'NONE',  ( -16.53943276465976808, 0.05219959533911058130, 76.24890960531435269 ) ) ;
#109790 = CARTESIAN_POINT ( 'NONE',  ( 19.03943276465977164, -0.05219959533909143690, 78.74890960531436690 ) ) ;
#109791 = ORIENTED_EDGE ( 'NONE', *, *, #78302, .F. ) ;
#109792 = CARTESIAN_POINT ( 'NONE',  ( 14.34966873604972726, -8.224510206698740333, 20.83442372801901143 ) ) ;
#109793 = CARTESIAN_POINT ( 'NONE',  ( -5.049401038298153566, 19.05341960407611168, 30.20724293864768839 ) ) ;
#109794 = CARTESIAN_POINT ( 'NONE',  ( 9.474510206698971260, -16.51473224551069308, 97.91557627198102409 ) ) ;
#109796 = CARTESIAN_POINT ( 'NONE',  ( 17.50000000000000000, 5.499999999999997335, 106.7030961746582847 ) ) ;
#109795 = CARTESIAN_POINT ( 'NONE',  ( 14.34966873604972726, -8.224510206698740333, 35.83442372801901143 ) ) ;
#109797 = CARTESIAN_POINT ( 'NONE',  ( 19.05341960407617918, -5.049401038297876454, 36.04275706135234003 ) ) ;
#109798 = CARTESIAN_POINT ( 'NONE',  ( -16.53943276465976808, -0.05219959533934237506, 93.75109039468567573 ) ) ;
#109799 = CARTESIAN_POINT ( 'NONE',  ( 5.049401038297881783, 19.05341960407617563, 107.2927570613523187 ) ) ;
#109800 = CARTESIAN_POINT ( 'NONE',  ( -19.02544592524342804, 5.153800228976336051, 36.04057627198100988 ) ) ;
#109801 = CARTESIAN_POINT ( 'NONE',  ( 0.05219959533934541429, -16.53943276465976808, 80.00109039468568994 ) ) ;
#109802 = CARTESIAN_POINT ( 'NONE',  ( -14.34966873604972548, 8.224510206698743886, 68.33442372801900433 ) ) ;
#109803 = CARTESIAN_POINT ( 'NONE',  ( -19.05341960407611168, -5.049401038298163336, 36.45724293864766707 ) ) ;
#109804 = CARTESIAN_POINT ( 'NONE',  ( 13.89961937509957401, 13.97604488694547697, 71.87609039468567573 ) ) ;
#109805 = CARTESIAN_POINT ( 'NONE',  ( 19.05341960407617918, -5.049401038297876454, 21.04275706135232582 ) ) ;
#109806 = CARTESIAN_POINT ( 'NONE',  ( -16.46253265017160317, 9.564922557960807481, 50.83224293864770260 ) ) ;
#109807 = CARTESIAN_POINT ( 'NONE',  ( 13.97604488694527802, 13.89961937509977652, 94.37390960531436690 ) ) ;
#109808 = CARTESIAN_POINT ( 'NONE',  ( 12.06949235617757843, -12.14591786802309237, 83.12390960531436690 ) ) ;
#109809 = AXIS2_PLACEMENT_3D ( 'NONE', #49611, #99080, #97082 ) ;
#109810 = CARTESIAN_POINT ( 'NONE',  ( -19.03943276465977164, -0.05219959533935918106, 48.75109039468566863 ) ) ;
#109811 = CARTESIAN_POINT ( 'NONE',  ( -21.52544592524343514, 5.823673210054127303, 51.04057627198103120 ) ) ;
#109812 = CARTESIAN_POINT ( 'NONE',  ( -18.62759615963255300, -10.81492255796106328, 104.1677570613523471 ) ) ;
#109813 = CARTESIAN_POINT ( 'NONE',  ( 5.153800228976335163, 19.02544592524342804, 84.79057627198099567 ) ) ;
#109814 = CARTESIAN_POINT ( 'NONE',  ( -16.46253265017146816, -9.564922557961047289, 19.16775706135233293 ) ) ;
#109815 = CARTESIAN_POINT ( 'NONE',  ( 21.52544592524344225, -5.823673210054117533, 68.54057627198103830 ) ) ;
#109816 = CARTESIAN_POINT ( 'NONE',  ( -16.51473224551069308, -9.474510206698971260, 111.6655762719810383 ) ) ;
#109817 = CARTESIAN_POINT ( 'NONE',  ( 13.89961937509957401, 13.97604488694547697, 86.87609039468567573 ) ) ;
#109818 = CARTESIAN_POINT ( 'NONE',  ( -9.474510206698964154, 16.51473224551069663, 115.4155762719810241 ) ) ;
#109819 = CARTESIAN_POINT ( 'NONE',  ( -13.89961937509957401, -13.97604488694547875, 109.3760903946856331 ) ) ;
#109820 = CARTESIAN_POINT ( 'NONE',  ( -5.153800228976328057, -19.02544592524343514, 22.29057627198102765 ) ) ;
#109821 = CARTESIAN_POINT ( 'NONE',  ( 5.049401038298161559, -19.05341960407611168, 102.7072429386476955 ) ) ;
#109822 = CARTESIAN_POINT ( 'NONE',  ( 10.81492255796078972, 18.62759615963270932, 79.58224293864769550 ) ) ;
#109823 = CARTESIAN_POINT ( 'NONE',  ( 8.224510206698742110, 14.34966873604972548, 42.08442372801901854 ) ) ;
#109824 = CARTESIAN_POINT ( 'NONE',  ( 15.80617190586769283, -15.72974639402175789, 45.62609039468567573 ) ) ;
#109825 = CARTESIAN_POINT ( 'NONE',  ( -18.67979575497193778, 10.72451020669871902, 98.33442372801901854 ) ) ;
#109826 = CARTESIAN_POINT ( 'NONE',  ( -0.05219959533934338120, 16.53943276465976808, 92.50109039468567573 ) ) ;
#109827 = CARTESIAN_POINT ( 'NONE',  ( 19.02544592524343514, -5.153800228976328945, 88.54057627198102409 ) ) ;
#109828 = CARTESIAN_POINT ( 'NONE',  ( 4.379528057220339221, -16.55341960407611168, 87.70724293864769550 ) ) ;
#109829 = CARTESIAN_POINT ( 'NONE',  ( 4.483927247898545687, 16.52544592524342804, 39.79057627198103830 ) ) ;
#109830 = CARTESIAN_POINT ( 'NONE',  ( 5.153800228976615827, -19.02544592524334988, 65.20942372801900433 ) ) ;
#109831 = CARTESIAN_POINT ( 'NONE',  ( 21.52544592524334988, 5.823673210054432836, 51.45942372801901854 ) ) ;
#109832 = CARTESIAN_POINT ( 'NONE',  ( 16.51473224551083163, -9.474510206698727899, 20.83442372801899722 ) ) ;
#109833 = CARTESIAN_POINT ( 'NONE',  ( 4.483927247898545687, 16.52544592524342804, 89.79057627198103830 ) ) ;
#109834 = CARTESIAN_POINT ( 'NONE',  ( -5.823673210054116645, -21.52544592524344225, 32.29057627198102409 ) ) ;
#109835 = CARTESIAN_POINT ( 'NONE',  ( 14.34966873604972726, -8.224510206698740333, 110.8344237280190043 ) ) ;
#109836 = CARTESIAN_POINT ( 'NONE',  ( 10.81492255796106328, -18.62759615963255655, 85.41775706135236135 ) ) ;
#109837 = CARTESIAN_POINT ( 'NONE',  ( 16.55341960407618274, -4.379528057220086978, 61.04275706135234714 ) ) ;
#109838 = CARTESIAN_POINT ( 'NONE',  ( -4.483927247898782831, 16.52544592524335698, 107.7094237280190328 ) ) ;
#109839 = CARTESIAN_POINT ( 'NONE',  ( 5.823673210054444382, -21.52544592524334988, 55.20942372801902565 ) ) ;
#109840 = CARTESIAN_POINT ( 'NONE',  ( 15.72974639402176855, 15.80617190586768217, 26.87609039468567218 ) ) ;
#109841 = CARTESIAN_POINT ( 'NONE',  ( 0.05219959533910956823, 16.53943276465976808, 99.99890960531436690 ) ) ;
#109842 = CARTESIAN_POINT ( 'NONE',  ( -0.05219959533909027116, -19.03943276465977164, 27.49890960531435624 ) ) ;
#109843 = CARTESIAN_POINT ( 'NONE',  ( -16.52544592524342804, 4.483927247898546575, 71.04057627198103830 ) ) ;
#109844 = CARTESIAN_POINT ( 'NONE',  ( -0.05219959533909027116, -19.03943276465977164, 67.49890960531436690 ) ) ;
#109845 = CARTESIAN_POINT ( 'NONE',  ( 8.224510206698742110, 14.34966873604972548, 107.0844237280190043 ) ) ;
#109846 = CARTESIAN_POINT ( 'NONE',  ( -10.81492255796078084, -18.62759615963271287, 62.08224293864769550 ) ) ;
#109847 = CARTESIAN_POINT ( 'NONE',  ( 16.55341960407611168, 4.379528057220329451, 93.95724293864770971 ) ) ;
#109848 = CARTESIAN_POINT ( 'NONE',  ( -15.80617190586745835, -15.72974639402198527, 96.87390960531436690 ) ) ;
#109849 = CARTESIAN_POINT ( 'NONE',  ( -19.05341960407611168, -5.049401038298163336, 96.45724293864769550 ) ) ;
#109851 = CARTESIAN_POINT ( 'NONE',  ( -5.049401038297874678, -19.05341960407617918, 104.7927570613523471 ) ) ;
#109850 = CARTESIAN_POINT ( 'NONE',  ( -9.474510206698964154, 16.51473224551069663, 50.41557627198102409 ) ) ;
#109852 = CARTESIAN_POINT ( 'NONE',  ( 15.72974639402199770, -15.80617190586745480, 38.12390960531436690 ) ) ;
#109853 = CARTESIAN_POINT ( 'NONE',  ( 18.62759615963255655, 10.81492255796105972, 66.66775706135234714 ) ) ;
#109854 = CARTESIAN_POINT ( 'NONE',  ( -13.97604488694527625, -13.89961937509977652, 61.87390960531435979 ) ) ;
#109855 = CARTESIAN_POINT ( 'NONE',  ( -5.049401038298153566, 19.05341960407611168, 95.20724293864770971 ) ) ;
#109856 = CARTESIAN_POINT ( 'NONE',  ( -0.05219959533934338120, 16.53943276465976808, 57.50109039468568994 ) ) ;
#109857 = CARTESIAN_POINT ( 'NONE',  ( -5.719274019375665041, -21.55341960407619695, 49.79275706135234714 ) ) ;
#109858 = CARTESIAN_POINT ( 'NONE',  ( -10.81492255796105439, 18.62759615963255655, 92.91775706135236135 ) ) ;
#109859 = CARTESIAN_POINT ( 'NONE',  ( -15.72974639402197994, 15.80617190586746368, 105.6239096053143669 ) ) ;
#109861 = CARTESIAN_POINT ( 'NONE',  ( 16.55341960407618274, -4.379528057220086978, 81.04275706135236135 ) ) ;
#109860 = CARTESIAN_POINT ( 'NONE',  ( -18.62759615963255300, -10.81492255796106328, 34.16775706135234714 ) ) ;
#109862 = CARTESIAN_POINT ( 'NONE',  ( 15.80617190586746368, 15.72974639402197994, 74.37390960531436690 ) ) ;
#109863 = CARTESIAN_POINT ( 'NONE',  ( -16.51473224551082808, 9.474510206698731452, 28.33442372801900433 ) ) ;
#109865 = CARTESIAN_POINT ( 'NONE',  ( 16.52544592524342804, -4.483927247898539470, 28.54057627198103120 ) ) ;
#109864 = CARTESIAN_POINT ( 'NONE',  ( 9.474510206698971260, -16.51473224551069308, 72.91557627198102409 ) ) ;
#109866 = CARTESIAN_POINT ( 'NONE',  ( 2.973862142520690366, -93.04182470242774627, -23.00000000000000000 ) ) ;
#109867 = CARTESIAN_POINT ( 'NONE',  ( -5.153800228976328057, -19.02544592524343514, 97.29057627198099567 ) ) ;
#109868 = FACE_OUTER_BOUND ( 'NONE', #135068, .T. ) ;
#109869 = CARTESIAN_POINT ( 'NONE',  ( -0.05219959533936034679, 19.03943276465977164, 77.50109039468566152 ) ) ;
#109870 = CARTESIAN_POINT ( 'NONE',  ( 18.67979575497178502, 10.72451020669898547, 64.16557627198102409 ) ) ;
#109871 = CARTESIAN_POINT ( 'NONE',  ( 14.29746914071049879, -8.314922557960816363, 38.33224293864768839 ) ) ;
#109872 = CARTESIAN_POINT ( 'NONE',  ( 9.474510206698729675, 16.51473224551082808, 112.0844237280190043 ) ) ;
#109873 = CARTESIAN_POINT ( 'NONE',  ( -16.51473224551069308, -9.474510206698971260, 36.66557627198102409 ) ) ;
#109874 = CARTESIAN_POINT ( 'NONE',  ( -19.02544592524334988, -5.153800228976617603, 103.9594237280190043 ) ) ;
#109876 = CARTESIAN_POINT ( 'NONE',  ( -13.89961937509957401, -13.97604488694547875, 74.37609039468566152 ) ) ;
#109875 = CARTESIAN_POINT ( 'NONE',  ( 21.53943276465977519, -0.05219959533907433946, 103.7489096053143669 ) ) ;
#109877 = CARTESIAN_POINT ( 'NONE',  ( 14.29746914071037800, 8.314922557961029526, 86.66775706135234714 ) ) ;
#109878 = CARTESIAN_POINT ( 'NONE',  ( -9.564922557960796823, -16.46253265017161027, 62.08224293864769550 ) ) ;
#109879 = CARTESIAN_POINT ( 'NONE',  ( -8.224510206698948167, 14.34966873604960824, 70.41557627198102409 ) ) ;
#109880 = EDGE_CURVE ( 'NONE', #125647, #96182, #139448, .T. ) ;
#109881 = CARTESIAN_POINT ( 'NONE',  ( -19.03943276465977164, 0.05219959533909376836, 56.24890960531435979 ) ) ;
#109882 = CARTESIAN_POINT ( 'NONE',  ( -4.483927247898539470, -16.52544592524342804, 62.29057627198102409 ) ) ;
#109883 = CARTESIAN_POINT ( 'NONE',  ( -16.46253265017160317, 9.564922557960807481, 25.83224293864769194 ) ) ;
#109884 = CARTESIAN_POINT ( 'NONE',  ( -37.32596994906253229, -3.631267627803094644, 40.85341334860915907 ) ) ;
#109885 = CARTESIAN_POINT ( 'NONE',  ( 16.55341960407611168, 4.379528057220329451, 38.95724293864768839 ) ) ;
#109886 = CARTESIAN_POINT ( 'NONE',  ( -13.97604488694527625, -13.89961937509977652, 71.87390960531433848 ) ) ;
#109887 = CARTESIAN_POINT ( 'NONE',  ( -1.464953661133971963, -14.82524568295235134, -59.95866808466630005 ) ) ;
#109888 = CARTESIAN_POINT ( 'NONE',  ( -16.46253265017146816, -9.564922557961047289, 34.16775706135233293 ) ) ;
#109889 = CARTESIAN_POINT ( 'NONE',  ( 4.483927247898790824, -16.52544592524335698, 45.20942372801901854 ) ) ;
#109890 = CARTESIAN_POINT ( 'NONE',  ( -10.81492255796078084, -18.62759615963271287, 62.08224293864769550 ) ) ;
#109891 = CARTESIAN_POINT ( 'NONE',  ( -13.89961937509957401, -13.97604488694547875, 24.37609039468565442 ) ) ;
#109892 = CARTESIAN_POINT ( 'NONE',  ( 9.564922557960805705, 16.46253265017160317, 74.58224293864769550 ) ) ;
#109893 = DIRECTION ( 'NONE',  ( 0.000000000000000000, 0.000000000000000000, -1.000000000000000000 ) ) ;
#109894 = CARTESIAN_POINT ( 'NONE',  ( -19.05341960407611168, -5.049401038298163336, 106.4572429386476955 ) ) ;
#109895 = CARTESIAN_POINT ( 'NONE',  ( -19.03943276465977164, 0.05219959533909376836, 61.24890960531436690 ) ) ;
#109896 = CARTESIAN_POINT ( 'NONE',  ( 5.719274019375673035, 21.55341960407619339, 32.29275706135235424 ) ) ;
#109897 = CARTESIAN_POINT ( 'NONE',  ( -16.55341960407611168, -4.379528057220339221, 111.4572429386476813 ) ) ;
#109900 = ORIENTED_EDGE ( 'NONE', *, *, #157130, .T. ) ;
#109899 = CARTESIAN_POINT ( 'NONE',  ( 13.89961937509977652, -13.97604488694527269, 83.12390960531436690 ) ) ;
#109898 = CARTESIAN_POINT ( 'NONE',  ( -21.53943276465977519, 0.05219959533907696930, 96.24890960531435269 ) ) ;
#109901 = CARTESIAN_POINT ( 'NONE',  ( -10.72451020669870658, -18.67979575497194134, 29.58442372801901854 ) ) ;
#109902 = ORIENTED_EDGE ( 'NONE', *, *, #135559, .F. ) ;
#109903 = CARTESIAN_POINT ( 'NONE',  ( 16.46253265017160672, -9.564922557960803928, 93.33224293864769550 ) ) ;
#109904 = CARTESIAN_POINT ( 'NONE',  ( 19.49149378614661643, -5.499999999999573674, 81.93757513605360998 ) ) ;
#109905 = CARTESIAN_POINT ( 'NONE',  ( -18.62759615963270932, 10.81492255796079327, 100.8322429386477097 ) ) ;
#109906 = CARTESIAN_POINT ( 'NONE',  ( -19.05341960407611168, -5.049401038298163336, 36.45724293864766707 ) ) ;
#109907 = CARTESIAN_POINT ( 'NONE',  ( 16.51473224551083163, -9.474510206698727899, 100.8344237280190043 ) ) ;
#109908 = CARTESIAN_POINT ( 'NONE',  ( -22.81625015709509441, -31.40387420917324590, -6.824999997268814234 ) ) ;
#109909 = CARTESIAN_POINT ( 'NONE',  ( 13.97604488694527802, 13.89961937509977652, 24.37390960531435624 ) ) ;
#109910 = CARTESIAN_POINT ( 'NONE',  ( -18.62759615963255300, -10.81492255796106328, 84.16775706135234714 ) ) ;
#109912 = CARTESIAN_POINT ( 'NONE',  ( 5.719274019375673035, 21.55341960407619339, 47.29275706135234003 ) ) ;
#109911 = CARTESIAN_POINT ( 'NONE',  ( -19.03943276465977164, 0.05219959533909376836, 81.24890960531436690 ) ) ;
#109913 = CARTESIAN_POINT ( 'NONE',  ( -5.823673210054431948, 21.52544592524334988, 22.70942372801901499 ) ) ;
#109914 = CARTESIAN_POINT ( 'NONE',  ( 28.82186960331499392, -9.364793116373510529, 146.8999999999999773 ) ) ;
#109915 = CARTESIAN_POINT ( 'NONE',  ( -0.05219959533909027116, -19.03943276465977164, 87.49890960531436690 ) ) ;
#109916 = B_SPLINE_CURVE_WITH_KNOTS ( 'NONE', 3,
 ( #168691, #179926, #41393, #197076, #183881, #103058, #121199 ),
 .UNSPECIFIED., .F., .F.,
 ( 4, 3, 4 ),
 ( -4.032110379226884939E-05, 0.000000000000000000, 0.006882574723720362095 ),
 .UNSPECIFIED. ) ;
#109917 = CARTESIAN_POINT ( 'NONE',  ( 19.52851543214742591, 5.500000000000027534, 62.89357721762582543 ) ) ;
#109920 = CARTESIAN_POINT ( 'NONE',  ( 21.52544592524334988, 5.823673210054432836, 46.45942372801901854 ) ) ;
#109919 = CARTESIAN_POINT ( 'NONE',  ( 5.823673210054125526, 21.52544592524343514, 49.79057627198102409 ) ) ;
#109918 = CARTESIAN_POINT ( 'NONE',  ( 12.14591786802327356, -12.06949235617739191, 40.62609039468567573 ) ) ;
#109921 = CARTESIAN_POINT ( 'NONE',  ( 0.05219959533937995610, -21.53943276465977519, 80.00109039468568994 ) ) ;
#109922 = CARTESIAN_POINT ( 'NONE',  ( 4.978841623633263325, 6.824288631998587817, -62.04929096494494445 ) ) ;
#109923 =( BOUNDED_CURVE ( )  B_SPLINE_CURVE ( 3, ( #46389, #144355, #159519, #35198 ),
 .UNSPECIFIED., .F., .T. ) 
 B_SPLINE_CURVE_WITH_KNOTS ( ( 4, 4 ),
 ( 1.132647296210726351, 1.570796326794896780 ),
 .UNSPECIFIED. ) 
 CURVE ( )  GEOMETRIC_REPRESENTATION_ITEM ( )  RATIONAL_B_SPLINE_CURVE ( ( 1.000000000000000000, 0.9840659996946589105, 0.9840659996946589105, 1.000000000000000000 ) ) 
 REPRESENTATION_ITEM ( '' )  );
#109924 = CARTESIAN_POINT ( 'NONE',  ( -5.049401038297874678, -19.05341960407617918, 109.7927570613523187 ) ) ;
#109925 = CARTESIAN_POINT ( 'NONE',  ( 5.049401038298161559, -19.05341960407611168, 57.70724293864769550 ) ) ;
#109926 = CARTESIAN_POINT ( 'NONE',  ( 19.05341960407611168, 5.049401038298154454, 83.95724293864766707 ) ) ;
#109927 = CARTESIAN_POINT ( 'NONE',  ( -0.05219959533910754901, -16.53943276465976808, 102.4989096053143811 ) ) ;
#109928 = CARTESIAN_POINT ( 'NONE',  ( -14.29746914071049879, 8.314922557960819915, 105.8322429386476955 ) ) ;
#109929 = CARTESIAN_POINT ( 'NONE',  ( 19.02544592524343514, -5.153800228976328945, 113.5405762719810241 ) ) ;
#109930 = CARTESIAN_POINT ( 'NONE',  ( -0.05219959533934338120, 16.53943276465976808, 77.50109039468567573 ) ) ;
#109932 = CARTESIAN_POINT ( 'NONE',  ( -13.97604488694527625, -13.89961937509977652, 51.87390960531436690 ) ) ;
#109931 = CARTESIAN_POINT ( 'NONE',  ( -16.55341960407611168, -4.379528057220339221, 71.45724293864769550 ) ) ;
#109933 = CARTESIAN_POINT ( 'NONE',  ( 5.823673210054444382, -21.52544592524334988, 80.20942372801901854 ) ) ;
#109934 = CARTESIAN_POINT ( 'NONE',  ( -5.719274019375665041, -21.55341960407619695, 74.79275706135234714 ) ) ;
#109935 = CARTESIAN_POINT ( 'NONE',  ( 5.049401038297881783, 19.05341960407617563, 112.2927570613523471 ) ) ;
#109936 = CARTESIAN_POINT ( 'NONE',  ( -14.34966873604960291, -8.224510206698953496, 66.66557627198102409 ) ) ;
#109937 = CARTESIAN_POINT ( 'NONE',  ( -5.719274019375665041, -21.55341960407619695, 34.79275706135235424 ) ) ;
#109938 = CARTESIAN_POINT ( 'NONE',  ( -15.72974639402197994, 15.80617190586746368, 60.62390960531437401 ) ) ;
#109939 = CARTESIAN_POINT ( 'NONE',  ( -3.573655867282028392E-15, 2.428612866367529932E-14, -15.00000000000000000 ) ) ;
#109940 = CARTESIAN_POINT ( 'NONE',  ( 23.31738231874054534, 16.94106989632529192, 147.4500000054623854 ) ) ;
#109941 = CARTESIAN_POINT ( 'NONE',  ( -19.03943276465977164, 0.05219959533909376836, 66.24890960531436690 ) ) ;
#109942 = CARTESIAN_POINT ( 'NONE',  ( 4.483927247898545687, 16.52544592524342804, 39.79057627198103830 ) ) ;
#109943 = AXIS2_PLACEMENT_3D ( 'NONE', #102535, #26708, #54032 ) ;
#109944 = CARTESIAN_POINT ( 'NONE',  ( -8.314922557960811034, -14.29746914071050412, 22.08224293864769194 ) ) ;
#109945 = CARTESIAN_POINT ( 'NONE',  ( -0.05219959533934338120, 16.53943276465976808, 92.50109039468567573 ) ) ;
#109946 = CARTESIAN_POINT ( 'NONE',  ( -19.02544592524334988, -5.153800228976617603, 53.95942372801898301 ) ) ;
#109947 = CARTESIAN_POINT ( 'NONE',  ( 16.18388926212241685, 7.379444403734403579, 47.93953151366155652 ) ) ;
#109948 = CARTESIAN_POINT ( 'NONE',  ( 19.05341960407611168, 5.049401038298154454, 108.9572429386477097 ) ) ;
#109949 = CARTESIAN_POINT ( 'NONE',  ( 4.483927247898545687, 16.52544592524342804, 79.79057627198102409 ) ) ;
#109950 = CARTESIAN_POINT ( 'NONE',  ( 0.05219959533936267826, -19.03943276465977164, 50.00109039468566863 ) ) ;
#109952 = CARTESIAN_POINT ( 'NONE',  ( -13.89961937509977652, 13.97604488694528158, 115.6239096053143669 ) ) ;
#109951 = CARTESIAN_POINT ( 'NONE',  ( 17.48847506799970475, -5.747544572773726657, 103.3269743784328085 ) ) ;
#109954 = ORIENTED_EDGE ( 'NONE', *, *, #70616, .T. ) ;
#109953 = CARTESIAN_POINT ( 'NONE',  ( -5.823673210054116645, -21.52544592524344225, 52.29057627198102409 ) ) ;
#109955 = CARTESIAN_POINT ( 'NONE',  ( 4.483927247898545687, 16.52544592524342804, 99.79057627198103830 ) ) ;
#109956 = CARTESIAN_POINT ( 'NONE',  ( -16.55341960407617563, 4.379528057220093196, 53.54275706135234714 ) ) ;
#109957 = CARTESIAN_POINT ( 'NONE',  ( 0.05219959533910956823, 16.53943276465976808, 89.99890960531438111 ) ) ;
#109958 = CARTESIAN_POINT ( 'NONE',  ( 16.79531203550644847, -7.028104445595739769, 36.24755011779556924 ) ) ;
#109959 = CARTESIAN_POINT ( 'NONE',  ( -17.26058549869090797, 6.457015423128607878, 48.62254162523932166 ) ) ;
#109960 = CARTESIAN_POINT ( 'NONE',  ( 15.80617190586746368, 15.72974639402197994, 24.37390960531435979 ) ) ;
#109961 = CARTESIAN_POINT ( 'NONE',  ( -29.86685920354755552, 21.69954338932564397, -7.324999997268814234 ) ) ;
#109962 = CARTESIAN_POINT ( 'NONE',  ( -15.49999999999999822, -5.500000000000000888, 118.0000000000000142 ) ) ;
#109964 = CARTESIAN_POINT ( 'NONE',  ( 14.29746914071049879, -8.314922557960816363, 23.33224293864769194 ) ) ;
#109963 = CARTESIAN_POINT ( 'NONE',  ( 14.34966873604972726, -8.224510206698740333, 40.83442372801901854 ) ) ;
#109965 = CARTESIAN_POINT ( 'NONE',  ( 21.52544592524344225, -5.823673210054117533, 58.54057627198103120 ) ) ;
#109966 = CARTESIAN_POINT ( 'NONE',  ( -0.05219959533936034679, 19.03943276465977164, 82.50109039468567573 ) ) ;
#109967 = CARTESIAN_POINT ( 'NONE',  ( 21.55341960407610458, 5.719274019375980345, 48.95724293864770971 ) ) ;
#109968 = CARTESIAN_POINT ( 'NONE',  ( -21.52544592524334988, -5.823673210054445271, 83.95942372801900433 ) ) ;
#109969 = CARTESIAN_POINT ( 'NONE',  ( -21.94207162742807071, 8.184381772639664376, 172.2902002187020116 ) ) ;
#109970 = CARTESIAN_POINT ( 'NONE',  ( -16.52544592524335698, -4.483927247898792601, 38.95942372801901854 ) ) ;
#109972 = CARTESIAN_POINT ( 'NONE',  ( 19.03943276465977164, -0.05219959533909143690, 103.7489096053143669 ) ) ;
#109971 = CARTESIAN_POINT ( 'NONE',  ( -5.049401038298153566, 19.05341960407611168, 35.20724293864768839 ) ) ;
#109973 = CARTESIAN_POINT ( 'NONE',  ( -5.049401038298153566, 19.05341960407611168, 30.20724293864768839 ) ) ;
#109974 = CARTESIAN_POINT ( 'NONE',  ( -8.314922557960811034, -14.29746914071050412, 97.08224293864770971 ) ) ;
#109975 = DIRECTION ( 'NONE',  ( 0.000000000000000000, 0.000000000000000000, 1.000000000000000000 ) ) ;
#109976 = CARTESIAN_POINT ( 'NONE',  ( -5.049401038298153566, 19.05341960407611168, 105.2072429386476671 ) ) ;
#109977 = ORIENTED_EDGE ( 'NONE', *, *, #93425, .T. ) ;
#109978 = CARTESIAN_POINT ( 'NONE',  ( 16.52544592524335698, 4.483927247898782831, 56.45942372801902565 ) ) ;
#109979 = CARTESIAN_POINT ( 'NONE',  ( -10.81492255796078084, -18.62759615963271287, 87.08224293864769550 ) ) ;
#109980 = CARTESIAN_POINT ( 'NONE',  ( -13.89961937509977652, 13.97604488694528158, 45.62390960531433848 ) ) ;
#109981 = CARTESIAN_POINT ( 'NONE',  ( 10.72451020669871369, 18.67979575497193778, 27.08442372801901854 ) ) ;
#109982 = CARTESIAN_POINT ( 'NONE',  ( -9.474510206698964154, 16.51473224551069663, 80.41557627198103830 ) ) ;
#109983 = CARTESIAN_POINT ( 'NONE',  ( -5.049401038298153566, 19.05341960407611168, 115.2072429386477097 ) ) ;
#109984 = ORIENTED_EDGE ( 'NONE', *, *, #188361, .F. ) ;
#109985 = CARTESIAN_POINT ( 'NONE',  ( 8.224510206698742110, 14.34966873604972548, 47.08442372801901854 ) ) ;
#109986 = CARTESIAN_POINT ( 'NONE',  ( 10.81492255796106328, -18.62759615963255655, 20.41775706135234714 ) ) ;
#109989 = CARTESIAN_POINT ( 'NONE',  ( -9.474510206698720793, -16.51473224551083518, 69.58442372801901854 ) ) ;
#109988 = CARTESIAN_POINT ( 'NONE',  ( -9.564922557960796823, -16.46253265017161027, 97.08224293864769550 ) ) ;
#109987 = CARTESIAN_POINT ( 'NONE',  ( -14.29746914071049879, 8.314922557960819915, 115.8322429386477097 ) ) ;
#109990 = CARTESIAN_POINT ( 'NONE',  ( -9.564922557961040184, 16.46253265017147172, 32.91775706135233293 ) ) ;
#109991 = CARTESIAN_POINT ( 'NONE',  ( 21.53943276465977519, -0.05219959533907433946, 83.74890960531435269 ) ) ;
#109992 = CARTESIAN_POINT ( 'NONE',  ( 13.89961937509957401, 13.97604488694547697, 31.87609039468566863 ) ) ;
#109993 = CARTESIAN_POINT ( 'NONE',  ( -4.379528057220086978, -16.55341960407618274, 84.79275706135234714 ) ) ;
#109994 = CARTESIAN_POINT ( 'NONE',  ( 9.564922557960805705, 16.46253265017160317, 109.5822429386476955 ) ) ;
#109995 = CARTESIAN_POINT ( 'NONE',  ( 19.02544592524343514, -5.153800228976328945, 63.54057627198103830 ) ) ;
#109996 = CARTESIAN_POINT ( 'NONE',  ( -5.719274019375665041, -21.55341960407619695, 64.79275706135234714 ) ) ;
#109997 = CARTESIAN_POINT ( 'NONE',  ( -21.52544592524334988, -5.823673210054445271, 73.95942372801901854 ) ) ;
#109998 = CARTESIAN_POINT ( 'NONE',  ( -16.46253265017160317, 9.564922557960807481, 80.83224293864769550 ) ) ;
#109999 = CARTESIAN_POINT ( 'NONE',  ( 5.823673210054444382, -21.52544592524334988, 45.20942372801901854 ) ) ;
#110000 = CARTESIAN_POINT ( 'NONE',  ( 13.97604488694548053, -13.89961937509957401, 90.62609039468567573 ) ) ;
#110001 = CARTESIAN_POINT ( 'NONE',  ( 13.97604488694527802, 13.89961937509977652, 59.37390960531434558 ) ) ;
#110002 = CARTESIAN_POINT ( 'NONE',  ( -9.564922557960796823, -16.46253265017161027, 97.08224293864769550 ) ) ;
#110003 = CARTESIAN_POINT ( 'NONE',  ( 0.05219959533909260263, 19.03943276465977164, 69.99890960531435269 ) ) ;
#110004 = CARTESIAN_POINT ( 'NONE',  ( 5.153800228976335163, 19.02544592524342804, 114.7905762719810241 ) ) ;
#110005 = CARTESIAN_POINT ( 'NONE',  ( -9.474510206698964154, 16.51473224551069663, 50.41557627198102409 ) ) ;
#110006 = CARTESIAN_POINT ( 'NONE',  ( 15.80617190586746368, 15.72974639402197994, 99.37390960531436690 ) ) ;
#110007 = CARTESIAN_POINT ( 'NONE',  ( 8.224510206698742110, 14.34966873604972548, 72.08442372801899012 ) ) ;
#110008 = CARTESIAN_POINT ( 'NONE',  ( -24.27995301597377775, 6.552671593954475071, 171.1165850637241874 ) ) ;
#110009 = CARTESIAN_POINT ( 'NONE',  ( -16.51473224551082808, 9.474510206698731452, 28.33442372801900433 ) ) ;
#110010 = CARTESIAN_POINT ( 'NONE',  ( -5.153800228976328057, -19.02544592524343514, 67.29057627198102409 ) ) ;
#110011 = CARTESIAN_POINT ( 'NONE',  ( 16.55341960407611168, 4.379528057220329451, 63.95724293864770260 ) ) ;
#110012 = CARTESIAN_POINT ( 'NONE',  ( -12.06949235617756955, 12.14591786802309770, 100.6239096053143811 ) ) ;
#110013 = CARTESIAN_POINT ( 'NONE',  ( -0.05219959533909027116, -19.03943276465977164, 97.49890960531436690 ) ) ;
#110014 = CARTESIAN_POINT ( 'NONE',  ( -0.05219959533909027116, -19.03943276465977164, 97.49890960531436690 ) ) ;
#110015 = CARTESIAN_POINT ( 'NONE',  ( 15.72974639402176855, 15.80617190586768217, 56.87609039468568994 ) ) ;
#110016 = CARTESIAN_POINT ( 'NONE',  ( -5.153800228976328057, -19.02544592524343514, 102.2905762719810383 ) ) ;
#110017 = APPLICATION_CONTEXT ( 'automotive_design' ) ;
#110018 = CARTESIAN_POINT ( 'NONE',  ( 15.72974639402176855, 15.80617190586768217, 111.8760903946856615 ) ) ;
#110019 = CARTESIAN_POINT ( 'NONE',  ( -12.14591786802326823, 12.06949235617739902, 83.12609039468568994 ) ) ;
#110020 = EDGE_CURVE ( 'NONE', #85800, #56096, #90448, .T. ) ;
#110021 = CARTESIAN_POINT ( 'NONE',  ( -18.67979575497193778, 10.72451020669871902, 43.33442372801901143 ) ) ;
#110022 = CARTESIAN_POINT ( 'NONE',  ( 18.67979575497178502, 10.72451020669898547, 29.16557627198103120 ) ) ;
#110023 = CARTESIAN_POINT ( 'NONE',  ( 0.05219959533907565091, 21.53943276465977519, 104.9989096053143669 ) ) ;
#110024 = ADVANCED_FACE ( 'NONE', ( #192338 ), #38655, .F. ) ;
#110025 = CARTESIAN_POINT ( 'NONE',  ( -14.34966873604960291, -8.224510206698953496, 61.66557627198103120 ) ) ;
#110026 = CARTESIAN_POINT ( 'NONE',  ( 19.02544592524343514, -5.153800228976328945, 53.54057627198102409 ) ) ;
#110027 = CARTESIAN_POINT ( 'NONE',  ( -16.55341960407611168, -4.379528057220339221, 86.45724293864770971 ) ) ;
#110028 = CARTESIAN_POINT ( 'NONE',  ( 18.62759615963271287, -10.81492255796078972, 43.33224293864769550 ) ) ;
#110029 = CARTESIAN_POINT ( 'NONE',  ( 19.03943276465977164, 0.05219959533936151252, 41.25109039468566152 ) ) ;
#110030 = CARTESIAN_POINT ( 'NONE',  ( -0.05219959533909027116, -19.03943276465977164, 22.49890960531436690 ) ) ;
#110031 = ORIENTED_EDGE ( 'NONE', *, *, #109494, .T. ) ;
#110032 = CARTESIAN_POINT ( 'NONE',  ( 14.29746914071037800, 8.314922557961029526, 71.66775706135234714 ) ) ;
#110033 = CARTESIAN_POINT ( 'NONE',  ( 9.474510206698971260, -16.51473224551069308, 67.91557627198102409 ) ) ;
#110034 = CARTESIAN_POINT ( 'NONE',  ( -27.73933785331498925, 2.428612866367529932E-14, 142.8750000027311842 ) ) ;
#110035 = CARTESIAN_POINT ( 'NONE',  ( -0.05219959533910754901, -16.53943276465976808, 87.49890960531436690 ) ) ;
#110036 = CARTESIAN_POINT ( 'NONE',  ( 18.62759615963271287, -10.81492255796078972, 33.33224293864769550 ) ) ;
#110037 = CARTESIAN_POINT ( 'NONE',  ( 14.29746914071037800, 8.314922557961029526, 111.6677570613523613 ) ) ;
#110038 = CARTESIAN_POINT ( 'NONE',  ( -16.52544592524335698, -4.483927247898792601, 23.95942372801901143 ) ) ;
#110039 = CARTESIAN_POINT ( 'NONE',  ( -10.72451020669870658, -18.67979575497194134, 94.58442372801901854 ) ) ;
#110040 = CARTESIAN_POINT ( 'NONE',  ( 19.03943276465977164, -0.05219959533909143690, 88.74890960531436690 ) ) ;
#110041 = CARTESIAN_POINT ( 'NONE',  ( -10.72451020669898014, 18.67979575497178502, 110.4155762719810383 ) ) ;
#110042 = CARTESIAN_POINT ( 'NONE',  ( 16.55341960407618274, -4.379528057220086978, 51.04275706135234714 ) ) ;
#110043 = CARTESIAN_POINT ( 'NONE',  ( 16.51473224551069308, 9.474510206698969483, 29.16557627198103475 ) ) ;
#110044 = CARTESIAN_POINT ( 'NONE',  ( 4.379528057220092307, 16.55341960407617563, 32.29275706135235424 ) ) ;
#110045 = CARTESIAN_POINT ( 'NONE',  ( -13.89961937509957401, -13.97604488694547875, 94.37609039468566152 ) ) ;
#110046 = CARTESIAN_POINT ( 'NONE',  ( -10.72451020669898014, 18.67979575497178502, 90.41557627198103830 ) ) ;
#110047 = CARTESIAN_POINT ( 'NONE',  ( -16.46253265017146816, -9.564922557961047289, 74.16775706135234714 ) ) ;
#110048 = CARTESIAN_POINT ( 'NONE',  ( -9.248023074035629065, -10.74802307403544077, -64.92279855667830191 ) ) ;
#110049 = CARTESIAN_POINT ( 'NONE',  ( 15.72974639402199770, -15.80617190586745480, 108.1239096053143811 ) ) ;
#110050 = CARTESIAN_POINT ( 'NONE',  ( 23.31738231874054534, 16.94106989632529192, 141.4500000054623854 ) ) ;
#110051 = CARTESIAN_POINT ( 'NONE',  ( -16.51473224551069308, -9.474510206698971260, 81.66557627198103830 ) ) ;
#110052 = CARTESIAN_POINT ( 'NONE',  ( 14.29746914071037800, 8.314922557961029526, 36.66775706135234714 ) ) ;
#110053 = LINE ( 'NONE', #153566, #128978 ) ;
#110054 = CARTESIAN_POINT ( 'NONE',  ( -16.51473224551082808, 9.474510206698731452, 58.33442372801900433 ) ) ;
#110056 = CARTESIAN_POINT ( 'NONE',  ( 12.06949235617757843, -12.14591786802309237, 73.12390960531436690 ) ) ;
#110055 = CARTESIAN_POINT ( 'NONE',  ( 21.53943276465977519, 0.05219959533937863772, 21.25109039468567218 ) ) ;
#110057 = CARTESIAN_POINT ( 'NONE',  ( 5.153800228976335163, 19.02544592524342804, 84.79057627198099567 ) ) ;
#110059 = CARTESIAN_POINT ( 'NONE',  ( 13.97604488694548053, -13.89961937509957401, 35.62609039468567573 ) ) ;
#110058 = CARTESIAN_POINT ( 'NONE',  ( -12.14591786802326823, 12.06949235617739902, 33.12609039468569705 ) ) ;
#110060 = CARTESIAN_POINT ( 'NONE',  ( 10.72451020669871369, 18.67979575497193778, 57.08442372801901854 ) ) ;
#110061 = CARTESIAN_POINT ( 'NONE',  ( -19.05341960407617563, 5.049401038297882671, 108.5427570613523187 ) ) ;
#110062 = CARTESIAN_POINT ( 'NONE',  ( -5.049401038298153566, 19.05341960407611168, 55.20724293864769550 ) ) ;
#110063 = CARTESIAN_POINT ( 'NONE',  ( 0.05219959533936267826, -19.03943276465977164, 80.00109039468567573 ) ) ;
#110064 = CARTESIAN_POINT ( 'NONE',  ( 4.379528057220092307, 16.55341960407617563, 57.29275706135234714 ) ) ;
#110065 = CARTESIAN_POINT ( 'NONE',  ( 10.81492255796106328, -18.62759615963255655, 95.41775706135234714 ) ) ;
#110066 = CARTESIAN_POINT ( 'NONE',  ( 19.03943276465977164, 0.05219959533936151252, 66.25109039468567573 ) ) ;
#110067 = CARTESIAN_POINT ( 'NONE',  ( 9.564922557960805705, 16.46253265017160317, 34.58224293864770260 ) ) ;
#110068 = CARTESIAN_POINT ( 'NONE',  ( -21.52544592524343514, 5.823673210054127303, 71.04057627198103830 ) ) ;
#110070 = CARTESIAN_POINT ( 'NONE',  ( 0.05219959533936267826, -19.03943276465977164, 65.00109039468567573 ) ) ;
#110069 = CARTESIAN_POINT ( 'NONE',  ( 16.53943276465976808, -0.05219959533910856209, 68.74890960531435269 ) ) ;
#110071 = CARTESIAN_POINT ( 'NONE',  ( 19.76520975163528249, 12.18675982963092075, 169.9999999999999716 ) ) ;
#110072 = CARTESIAN_POINT ( 'NONE',  ( -16.51473224551082808, 9.474510206698731452, 38.33442372801899722 ) ) ;
#110073 = CARTESIAN_POINT ( 'NONE',  ( -14.34966873604972548, 8.224510206698743886, 93.33442372801901854 ) ) ;
#110074 = CARTESIAN_POINT ( 'NONE',  ( -0.05219959533910754901, -16.53943276465976808, 52.49890960531435979 ) ) ;
#110076 = CARTESIAN_POINT ( 'NONE',  ( -27.73933785331498925, -9.013057229001049109, 140.9750000027311501 ) ) ;
#110075 = CARTESIAN_POINT ( 'NONE',  ( -5.719274019375665041, -21.55341960407619695, 89.79275706135236135 ) ) ;
#110077 = CARTESIAN_POINT ( 'NONE',  ( -21.52544592524343514, 5.823673210054127303, 101.0405762719810383 ) ) ;
#110078 = CARTESIAN_POINT ( 'NONE',  ( 19.05341960407611168, 5.049401038298154454, 53.95724293864770260 ) ) ;
#110079 = CARTESIAN_POINT ( 'NONE',  ( 18.62759615963255655, 10.81492255796105972, 66.66775706135234714 ) ) ;
#110080 = CARTESIAN_POINT ( 'NONE',  ( 5.153800228976335163, 19.02544592524342804, 49.79057627198100988 ) ) ;
#110081 = VERTEX_POINT ( 'NONE', #194347 ) ;
#110082 = CARTESIAN_POINT ( 'NONE',  ( 5.153800228976335163, 19.02544592524342804, 59.79057627198100988 ) ) ;
#110083 = CARTESIAN_POINT ( 'NONE',  ( -16.53943276465976808, 0.05219959533911058130, 116.2489096053143669 ) ) ;
#110084 = CARTESIAN_POINT ( 'NONE',  ( -10.81492255796078084, -18.62759615963271287, 22.08224293864769194 ) ) ;
#110085 = CARTESIAN_POINT ( 'NONE',  ( 0.05219959533910956823, 16.53943276465976808, 54.99890960531435269 ) ) ;
#110086 = CARTESIAN_POINT ( 'NONE',  ( 5.153800228976335163, 19.02544592524342804, 34.79057627198102409 ) ) ;
#110087 = CARTESIAN_POINT ( 'NONE',  ( 0.05219959533910956823, 16.53943276465976808, 79.99890960531435269 ) ) ;
#110088 = CARTESIAN_POINT ( 'NONE',  ( 15.80617190586746368, 15.72974639402197994, 99.37390960531436690 ) ) ;
#110089 = CARTESIAN_POINT ( 'NONE',  ( 10.81492255796106328, -18.62759615963255655, 30.41775706135234358 ) ) ;
#110090 = CARTESIAN_POINT ( 'NONE',  ( -25.22510128165246712, -6.326562104755758753, 165.8168824682947502 ) ) ;
#110091 = EDGE_CURVE ( 'NONE', #16610, #167085, #142927, .T. ) ;
#110092 = CARTESIAN_POINT ( 'NONE',  ( 8.224510206698742110, 14.34966873604972548, 57.08442372801901854 ) ) ;
#110093 = CARTESIAN_POINT ( 'NONE',  ( -15.72974639402197994, 15.80617190586746368, 90.62390960531436690 ) ) ;
#110094 = CARTESIAN_POINT ( 'NONE',  ( 18.67979575497194134, -10.72451020669871369, 110.8344237280190043 ) ) ;
#110095 = CARTESIAN_POINT ( 'NONE',  ( 16.46253265017160672, -9.564922557960803928, 113.3322429386476955 ) ) ;
#110096 = CARTESIAN_POINT ( 'NONE',  ( 18.62759615963255655, 10.81492255796105972, 46.66775706135234714 ) ) ;
#110097 = CARTESIAN_POINT ( 'NONE',  ( -0.05219959533907301413, -21.53943276465977519, 42.49890960531435979 ) ) ;
#110098 = CARTESIAN_POINT ( 'NONE',  ( -8.314922557961024197, 14.29746914071037800, 107.9177570613523471 ) ) ;
#110100 = CARTESIAN_POINT ( 'NONE',  ( 10.72451020669871369, 18.67979575497193778, 82.08442372801901854 ) ) ;
#110099 = CARTESIAN_POINT ( 'NONE',  ( -15.72974639402176322, -15.80617190586768395, 59.37609039468568284 ) ) ;
#110101 = CARTESIAN_POINT ( 'NONE',  ( 0.05219959533936267826, -19.03943276465977164, 35.00109039468566863 ) ) ;
#110102 = CARTESIAN_POINT ( 'NONE',  ( -16.55341960407617563, 4.379528057220093196, 83.54275706135234714 ) ) ;
#110103 = CARTESIAN_POINT ( 'NONE',  ( 21.52544592524334988, 5.823673210054432836, 36.45942372801901143 ) ) ;
#110104 = CARTESIAN_POINT ( 'NONE',  ( 0.05219959533909260263, 19.03943276465977164, 49.99890960531435979 ) ) ;
#110105 = CARTESIAN_POINT ( 'NONE',  ( 13.89961937509957401, 13.97604488694547697, 21.87609039468566152 ) ) ;
#110106 = CARTESIAN_POINT ( 'NONE',  ( -21.53943276465977519, 0.05219959533907696930, 31.24890960531435979 ) ) ;
#110107 = ADVANCED_FACE ( 'NONE', ( #55815 ), #117488, .T. ) ;
#110108 = CARTESIAN_POINT ( 'NONE',  ( 0.05219959533937995610, -21.53943276465977519, 20.00109039468568639 ) ) ;
#110109 = CARTESIAN_POINT ( 'NONE',  ( -5.719274019375978568, 21.55341960407610458, 70.20724293864769550 ) ) ;
#110111 = CARTESIAN_POINT ( 'NONE',  ( -21.55341960407610458, -5.719274019375992779, 86.45724293864770971 ) ) ;
#110110 = CARTESIAN_POINT ( 'NONE',  ( -17.72662750342724891, -5.500000000000087930, 61.40179492283743201 ) ) ;
#110113 = CARTESIAN_POINT ( 'NONE',  ( -12.14591786802309592, -12.06949235617757132, 66.87390960531436690 ) ) ;
#110112 = CARTESIAN_POINT ( 'NONE',  ( -4.379528057220086978, -16.55341960407618274, 59.79275706135234714 ) ) ;
#110114 = CARTESIAN_POINT ( 'NONE',  ( 0.2641003901806721066, 28.91815444374861599, -49.65132406768935880 ) ) ;
#110115 = CARTESIAN_POINT ( 'NONE',  ( 16.51473224551083163, -9.474510206698727899, 95.83442372801900433 ) ) ;
#110116 = CARTESIAN_POINT ( 'NONE',  ( -9.553307302758575759, -9.835630382207714462, -60.44015478763000715 ) ) ;
#110117 = CARTESIAN_POINT ( 'NONE',  ( -14.29746914071037622, -8.314922557961029526, 39.16775706135235424 ) ) ;
#110118 = CARTESIAN_POINT ( 'NONE',  ( 5.719274019375991003, -21.55341960407610458, 92.70724293864770971 ) ) ;
#110119 = CARTESIAN_POINT ( 'NONE',  ( -21.53943276465977519, 0.05219959533907696930, 81.24890960531436690 ) ) ;
#110120 = CARTESIAN_POINT ( 'NONE',  ( -21.53943276465977519, 0.05219959533907696930, 21.24890960531436690 ) ) ;
#110121 = CARTESIAN_POINT ( 'NONE',  ( 16.53943276465976808, 0.05219959533934440121, 61.25109039468567573 ) ) ;
#110122 = CARTESIAN_POINT ( 'NONE',  ( -16.46253265017160317, 9.564922557960807481, 65.83224293864769550 ) ) ;
#110124 = CARTESIAN_POINT ( 'NONE',  ( 19.03943276465977164, 0.05219959533936151252, 111.2510903946856757 ) ) ;
#110123 = CARTESIAN_POINT ( 'NONE',  ( -21.52544592524334988, -5.823673210054445271, 38.95942372801901854 ) ) ;
#110125 = CARTESIAN_POINT ( 'NONE',  ( 13.89961937509977652, -13.97604488694527269, 108.1239096053143669 ) ) ;
#110126 = CARTESIAN_POINT ( 'NONE',  ( -0.05219959533936034679, 19.03943276465977164, 27.50109039468566507 ) ) ;
#110127 = CARTESIAN_POINT ( 'NONE',  ( -12.14591786802326823, 12.06949235617739902, 38.12609039468567573 ) ) ;
#110128 = CARTESIAN_POINT ( 'NONE',  ( -13.97604488694527625, -13.89961937509977652, 96.87390960531433848 ) ) ;
#110129 = CARTESIAN_POINT ( 'NONE',  ( 21.53943276465977519, -0.05219959533907433946, 108.7489096053143669 ) ) ;
#110130 = CARTESIAN_POINT ( 'NONE',  ( -5.049401038298153566, 19.05341960407611168, 55.20724293864769550 ) ) ;
#110131 = CARTESIAN_POINT ( 'NONE',  ( -12.06949235617756955, 12.14591786802309770, 85.62390960531436690 ) ) ;
#110132 = CARTESIAN_POINT ( 'NONE',  ( 10.72451020669898902, -18.67979575497178502, 27.91557627198103830 ) ) ;
#110133 = CARTESIAN_POINT ( 'NONE',  ( -16.52216118717208104, 7.221426719304501418, 33.92400978953008206 ) ) ;
#110134 = CARTESIAN_POINT ( 'NONE',  ( 10.81492255796078972, 18.62759615963270932, 109.5822429386476955 ) ) ;
#110135 = CARTESIAN_POINT ( 'NONE',  ( -9.564922557961040184, 16.46253265017147172, 62.91775706135233293 ) ) ;
#110136 = CARTESIAN_POINT ( 'NONE',  ( -16.51473224551069308, -9.474510206698971260, 111.6655762719810383 ) ) ;
#110137 = CARTESIAN_POINT ( 'NONE',  ( 19.02544592524343514, -5.153800228976328945, 23.54057627198102054 ) ) ;
#110138 = CARTESIAN_POINT ( 'NONE',  ( 10.72451020669898902, -18.67979575497178502, 57.91557627198103120 ) ) ;
#110139 = CARTESIAN_POINT ( 'NONE',  ( 13.97604488694527802, 13.89961937509977652, 99.37390960531436690 ) ) ;
#110140 = CARTESIAN_POINT ( 'NONE',  ( 5.719274019375673035, 21.55341960407619339, 77.29275706135234714 ) ) ;
#110141 = CARTESIAN_POINT ( 'NONE',  ( 13.89961937509977652, -13.97604488694527269, 58.12390960531436690 ) ) ;
#110142 = CARTESIAN_POINT ( 'NONE',  ( 8.224510206698953496, -14.34966873604960469, 87.91557627198103830 ) ) ;
#110143 = CARTESIAN_POINT ( 'NONE',  ( 8.314922557961029526, -14.29746914071037800, 40.41775706135234714 ) ) ;
#110144 = CARTESIAN_POINT ( 'NONE',  ( -18.67979575497193778, 10.72451020669871902, 68.33442372801900433 ) ) ;
#110145 = VERTEX_POINT ( 'NONE', #73001 ) ;
#110146 = CARTESIAN_POINT ( 'NONE',  ( 19.03943276465977164, 0.05219959533936151252, 21.25109039468565797 ) ) ;
#110147 = CARTESIAN_POINT ( 'NONE',  ( -0.05219959533936034679, 19.03943276465977164, 82.50109039468567573 ) ) ;
#110148 = CARTESIAN_POINT ( 'NONE',  ( 5.153800228976615827, -19.02544592524334988, 40.20942372801898301 ) ) ;
#110149 = CARTESIAN_POINT ( 'NONE',  ( 11.74264578624799427, 36.14014761921585972, -6.349999994537625980 ) ) ;
#110150 = CARTESIAN_POINT ( 'NONE',  ( 5.719274019375673035, 21.55341960407619339, 37.29275706135235424 ) ) ;
#110151 = CARTESIAN_POINT ( 'NONE',  ( -3.573655867282028392E-15, 2.428612866367529932E-14, -0.1220970790697140096 ) ) ;
#110152 = CARTESIAN_POINT ( 'NONE',  ( 13.97604488694548053, -13.89961937509957401, 30.62609039468566863 ) ) ;
#110153 = CARTESIAN_POINT ( 'NONE',  ( -19.03943276465977164, 0.05219959533909376836, 71.24890960531435269 ) ) ;
#110154 = CARTESIAN_POINT ( 'NONE',  ( 4.379528057220339221, -16.55341960407611168, 22.70724293864769194 ) ) ;
#110156 = CARTESIAN_POINT ( 'NONE',  ( -18.67979575497193778, 10.72451020669871902, 88.33442372801901854 ) ) ;
#110155 = CARTESIAN_POINT ( 'NONE',  ( -18.67979575497178146, -10.72451020669898902, 26.66557627198103475 ) ) ;
#110157 = CARTESIAN_POINT ( 'NONE',  ( -22.81625015709509441, -31.40387420917324590, -4.324999997268812457 ) ) ;
#110158 = CARTESIAN_POINT ( 'NONE',  ( 37.99999999999999289, 2.893978650043524126E-14, -7.000000000000000000 ) ) ;
#110159 = CARTESIAN_POINT ( 'NONE',  ( -18.62759615963255300, -10.81492255796106328, 79.16775706135234714 ) ) ;
#110160 = CARTESIAN_POINT ( 'NONE',  ( 21.94104750614016552, -1.245073757423053484, -58.42286556281732857 ) ) ;
#110161 = CARTESIAN_POINT ( 'NONE',  ( -19.02544592524342804, 5.153800228976336051, 106.0405762719810241 ) ) ;
#110162 = CARTESIAN_POINT ( 'NONE',  ( -24.37439536253436501, -13.84063584238319500, 165.9041067986157998 ) ) ;
#110163 = CARTESIAN_POINT ( 'NONE',  ( 5.153800228976335163, 19.02544592524342804, 54.79057627198103120 ) ) ;
#110164 = CARTESIAN_POINT ( 'NONE',  ( -21.52544592524343514, 5.823673210054127303, 51.04057627198103120 ) ) ;
#110165 = CARTESIAN_POINT ( 'NONE',  ( 16.53943276465976808, -0.05219959533910856209, 28.74890960531435624 ) ) ;
#110167 = CARTESIAN_POINT ( 'NONE',  ( -9.564922557960796823, -16.46253265017161027, 97.08224293864769550 ) ) ;
#110166 = CARTESIAN_POINT ( 'NONE',  ( 16.53943276465976808, -0.05219959533910856209, 108.7489096053143669 ) ) ;
#110168 = CARTESIAN_POINT ( 'NONE',  ( 18.67979575497194134, -10.72451020669871369, 110.8344237280190043 ) ) ;
#110169 = CARTESIAN_POINT ( 'NONE',  ( 16.55341960407611168, 4.379528057220329451, 108.9572429386476955 ) ) ;
#110170 = CARTESIAN_POINT ( 'NONE',  ( 10.81492255796106328, -18.62759615963255655, 65.41775706135234714 ) ) ;
#110171 = DIRECTION ( 'NONE',  ( -1.000000000000000000, -1.070572202317115416E-14, 0.000000000000000000 ) ) ;
#110172 = CARTESIAN_POINT ( 'NONE',  ( -16.52544592524335698, -4.483927247898792601, 108.9594237280190185 ) ) ;
#110173 = CARTESIAN_POINT ( 'NONE',  ( 9.564922557961047289, -16.46253265017146816, 60.41775706135233293 ) ) ;
#110174 = CARTESIAN_POINT ( 'NONE',  ( 11.40812507854755253, -35.11059874428192273, -4.524999997268813523 ) ) ;
#110175 = CARTESIAN_POINT ( 'NONE',  ( -13.89961937509977652, 13.97604488694528158, 105.6239096053143527 ) ) ;
#110176 = CARTESIAN_POINT ( 'NONE',  ( -14.29746914071049879, 8.314922557960819915, 70.83224293864770971 ) ) ;
#110177 = CARTESIAN_POINT ( 'NONE',  ( 19.03943276465977164, 0.05219959533936151252, 56.25109039468566863 ) ) ;
#110178 = CARTESIAN_POINT ( 'NONE',  ( 19.05341960407611168, 5.049401038298154454, 68.95724293864769550 ) ) ;
#110179 = CARTESIAN_POINT ( 'NONE',  ( 16.53943276465976808, -0.05219959533910856209, 63.74890960531435979 ) ) ;
#110180 = CARTESIAN_POINT ( 'NONE',  ( -5.153800228976607833, 19.02544592524334988, 87.70942372801897591 ) ) ;
#110181 = CARTESIAN_POINT ( 'NONE',  ( -21.55341960407610458, -5.719274019375992779, 56.45724293864768839 ) ) ;
#110182 = ORIENTED_EDGE ( 'NONE', *, *, #154932, .T. ) ;
#110183 = CARTESIAN_POINT ( 'NONE',  ( -16.55341960407611168, -4.379528057220339221, 111.4572429386476813 ) ) ;
#110184 = DIRECTION ( 'NONE',  ( -1.000000000000000000, 5.392603844284257652E-33, 0.000000000000000000 ) ) ;
#110186 = CARTESIAN_POINT ( 'NONE',  ( -21.52544592524343514, 5.823673210054127303, 61.04057627198103120 ) ) ;
#110185 = CARTESIAN_POINT ( 'NONE',  ( -5.049401038298153566, 19.05341960407611168, 75.20724293864769550 ) ) ;
#110188 = CARTESIAN_POINT ( 'NONE',  ( 5.049401038298161559, -19.05341960407611168, 72.70724293864768129 ) ) ;
#110187 = CARTESIAN_POINT ( 'NONE',  ( 4.379528057220092307, 16.55341960407617563, 87.29275706135236135 ) ) ;
#110189 = CARTESIAN_POINT ( 'NONE',  ( -19.02544592524334988, -5.153800228976617603, 53.95942372801898301 ) ) ;
#110190 = CARTESIAN_POINT ( 'NONE',  ( -10.81492255796105439, 18.62759615963255655, 82.91775706135234714 ) ) ;
#110191 = CARTESIAN_POINT ( 'NONE',  ( -21.52544592524343514, 5.823673210054127303, 61.04057627198103120 ) ) ;
#110192 = CARTESIAN_POINT ( 'NONE',  ( 9.474510206698971260, -16.51473224551069308, 102.9155762719810241 ) ) ;
#110193 = CARTESIAN_POINT ( 'NONE',  ( -0.05219959533909027116, -19.03943276465977164, 32.49890960531435979 ) ) ;
#110194 = CARTESIAN_POINT ( 'NONE',  ( 16.52544592524335698, 4.483927247898782831, 96.45942372801901854 ) ) ;
#110195 = CARTESIAN_POINT ( 'NONE',  ( 0.05219959533934541429, -16.53943276465976808, 25.00109039468567218 ) ) ;
#110196 = CARTESIAN_POINT ( 'NONE',  ( -0.3431728551240714742, -71.74905178543389184, -15.00000000000000178 ) ) ;
#110197 = CARTESIAN_POINT ( 'NONE',  ( 10.81492255796106328, -18.62759615963255655, 90.41775706135236135 ) ) ;
#110198 = CARTESIAN_POINT ( 'NONE',  ( -16.55341960407611168, -4.379528057220339221, 66.45724293864768129 ) ) ;
#110199 = CARTESIAN_POINT ( 'NONE',  ( -8.224510206698948167, 14.34966873604960824, 75.41557627198102409 ) ) ;
#110200 = CARTESIAN_POINT ( 'NONE',  ( 18.67979575497178502, 10.72451020669898547, 89.16557627198102409 ) ) ;
#110201 = CARTESIAN_POINT ( 'NONE',  ( -10.72451020669898014, 18.67979575497178502, 85.41557627198102409 ) ) ;
#110202 = CARTESIAN_POINT ( 'NONE',  ( 17.13100169013301155, -6.664070546373149995, 98.26789835699852915 ) ) ;
#110203 = CARTESIAN_POINT ( 'NONE',  ( -21.52544592524343514, 5.823673210054127303, 51.04057627198103120 ) ) ;
#110204 = CARTESIAN_POINT ( 'NONE',  ( 14.29746914071037800, 8.314922557961029526, 66.66775706135234714 ) ) ;
#110205 = CARTESIAN_POINT ( 'NONE',  ( -14.29746914071049879, 8.314922557960819915, 95.83224293864770971 ) ) ;
#110206 = CARTESIAN_POINT ( 'NONE',  ( -19.02544592524342804, 5.153800228976336051, 41.04057627198103120 ) ) ;
#110207 = CARTESIAN_POINT ( 'NONE',  ( 34.38809498607732706, -6.739667044264573192, 48.29962152465627412 ) ) ;
#110208 = CARTESIAN_POINT ( 'NONE',  ( -0.05219959533934338120, 16.53943276465976808, 97.50109039468567573 ) ) ;
#110209 = CARTESIAN_POINT ( 'NONE',  ( -21.55341960407619339, 5.719274019375674811, 38.54275706135234714 ) ) ;
#110210 = CARTESIAN_POINT ( 'NONE',  ( 16.46253265017160672, -9.564922557960803928, 93.33224293864769550 ) ) ;
#110211 = CARTESIAN_POINT ( 'NONE',  ( -18.67979575497193778, 10.72451020669871902, 63.33442372801900433 ) ) ;
#110212 = CARTESIAN_POINT ( 'NONE',  ( 34.12434206616184440, 14.08647367304311260, -8.000000000000001776 ) ) ;
#110213 = CARTESIAN_POINT ( 'NONE',  ( 16.51473224551069308, 9.474510206698969483, 24.16557627198102765 ) ) ;
#110214 = ORIENTED_EDGE ( 'NONE', *, *, #150915, .F. ) ;
#110215 = CARTESIAN_POINT ( 'NONE',  ( 0.05219959533937995610, -21.53943276465977519, 55.00109039468568284 ) ) ;
#110217 = CARTESIAN_POINT ( 'NONE',  ( 16.51473224551069308, 9.474510206698969483, 24.16557627198102765 ) ) ;
#110216 = CARTESIAN_POINT ( 'NONE',  ( 0.05219959533909260263, 19.03943276465977164, 44.99890960531435979 ) ) ;
#110218 = CARTESIAN_POINT ( 'NONE',  ( -16.46253265017160317, 9.564922557960807481, 90.83224293864769550 ) ) ;
#110219 = CARTESIAN_POINT ( 'NONE',  ( -13.97604488694547697, 13.89961937509957934, 73.12609039468568994 ) ) ;
#110220 = CARTESIAN_POINT ( 'NONE',  ( -0.05219959533937732626, 21.53943276465977519, 32.50109039468568284 ) ) ;
#110221 = CARTESIAN_POINT ( 'NONE',  ( 19.05341960407617918, -5.049401038297876454, 56.04275706135234714 ) ) ;
#110222 = CARTESIAN_POINT ( 'NONE',  ( 19.05341960407611168, 5.049401038298154454, 33.95724293864769550 ) ) ;
#110223 = CARTESIAN_POINT ( 'NONE',  ( 8.224510206698742110, 14.34966873604972548, 107.0844237280190043 ) ) ;
#110224 = CARTESIAN_POINT ( 'NONE',  ( -19.02544592524334988, -5.153800228976617603, 78.95942372801900433 ) ) ;
#110225 = CARTESIAN_POINT ( 'NONE',  ( 12.06949235617757843, -12.14591786802309237, 28.12390960531435979 ) ) ;
#110226 = CARTESIAN_POINT ( 'NONE',  ( -9.474510206698720793, -16.51473224551083518, 44.58442372801900433 ) ) ;
#110227 = CARTESIAN_POINT ( 'NONE',  ( -0.05219959533909027116, -19.03943276465977164, 102.4989096053143669 ) ) ;
#110228 = CARTESIAN_POINT ( 'NONE',  ( -5.823673210054431948, 21.52544592524334988, 102.7094237280190185 ) ) ;
#110229 = CARTESIAN_POINT ( 'NONE',  ( 19.03943276465977164, 0.05219959533936151252, 21.25109039468565797 ) ) ;
#110230 = CARTESIAN_POINT ( 'NONE',  ( -9.564922557960796823, -16.46253265017161027, 32.08224293864769550 ) ) ;
#110231 = CARTESIAN_POINT ( 'NONE',  ( 21.55341960407619695, -5.719274019375665929, 91.04275706135236135 ) ) ;
#110232 = CARTESIAN_POINT ( 'NONE',  ( 14.34966873604972726, -8.224510206698740333, 35.83442372801901143 ) ) ;
#110233 = CARTESIAN_POINT ( 'NONE',  ( -13.89961937509977652, 13.97604488694528158, 90.62390960531432427 ) ) ;
#110234 = PLANE ( 'NONE',  #172618 ) ;
#110235 = CARTESIAN_POINT ( 'NONE',  ( 13.89961937509977652, -13.97604488694527269, 83.12390960531436690 ) ) ;
#110236 = CARTESIAN_POINT ( 'NONE',  ( -17.50000000000000000, 5.499999999999992895, 37.50000000000000000 ) ) ;
#110237 = CARTESIAN_POINT ( 'NONE',  ( 9.474510206698729675, 16.51473224551082808, 67.08442372801900433 ) ) ;
#110238 = CARTESIAN_POINT ( 'NONE',  ( 0.05219959533909260263, 19.03943276465977164, 99.99890960531436690 ) ) ;
#110239 = CARTESIAN_POINT ( 'NONE',  ( 18.62759615963255655, 10.81492255796105972, 96.66775706135234714 ) ) ;
#110240 = CARTESIAN_POINT ( 'NONE',  ( -14.34966873604960291, -8.224510206698953496, 96.66557627198102409 ) ) ;
#110241 = CARTESIAN_POINT ( 'NONE',  ( 21.52544592524344225, -5.823673210054117533, 43.54057627198103830 ) ) ;
#110242 = CARTESIAN_POINT ( 'NONE',  ( 18.67979575497178502, 10.72451020669898547, 34.16557627198102409 ) ) ;
#110243 = CARTESIAN_POINT ( 'NONE',  ( -0.05219959533910754901, -16.53943276465976808, 102.4989096053143811 ) ) ;
#110244 = LINE ( 'NONE', #47596, #108150 ) ;
#110245 = CARTESIAN_POINT ( 'NONE',  ( -19.03943276465977164, -0.05219959533935918106, 63.75109039468566863 ) ) ;
#110246 = CARTESIAN_POINT ( 'NONE',  ( 4.483927247898545687, 16.52544592524342804, 39.79057627198103830 ) ) ;
#110248 = ADVANCED_FACE ( 'NONE', ( #134670 ), #60776, .T. ) ;
#110247 = CARTESIAN_POINT ( 'NONE',  ( 15.80617190586746368, 15.72974639402197994, 24.37390960531435979 ) ) ;
#110249 = CARTESIAN_POINT ( 'NONE',  ( -5.823673210054431948, 21.52544592524334988, 77.70942372801900433 ) ) ;
#110250 = CARTESIAN_POINT ( 'NONE',  ( 21.52544592524344225, -5.823673210054117533, 73.54057627198102409 ) ) ;
#110251 = CARTESIAN_POINT ( 'NONE',  ( 10.72451020669871369, 18.67979575497193778, 42.08442372801901854 ) ) ;
#110252 = CARTESIAN_POINT ( 'NONE',  ( 21.53943276465977519, -0.05219959533907433946, 93.74890960531436690 ) ) ;
#110253 = CARTESIAN_POINT ( 'NONE',  ( 5.719274019375673035, 21.55341960407619339, 57.29275706135234714 ) ) ;
#110254 = CARTESIAN_POINT ( 'NONE',  ( 5.049401038298161559, -19.05341960407611168, 27.70724293864769550 ) ) ;
#110255 = CARTESIAN_POINT ( 'NONE',  ( 9.474510206698971260, -16.51473224551069308, 82.91557627198103830 ) ) ;
#110256 = CARTESIAN_POINT ( 'NONE',  ( -16.52544592524335698, -4.483927247898792601, 83.95942372801900433 ) ) ;
#110257 = CARTESIAN_POINT ( 'NONE',  ( 12.14591786802309770, 12.06949235617756955, 109.3739096053143811 ) ) ;
#110258 = CARTESIAN_POINT ( 'NONE',  ( -9.564922557960796823, -16.46253265017161027, 112.0822429386476955 ) ) ;
#110259 = CARTESIAN_POINT ( 'NONE',  ( -8.314922557960811034, -14.29746914071050412, 52.08224293864768839 ) ) ;
#110260 = CARTESIAN_POINT ( 'NONE',  ( -14.34966873604972548, 8.224510206698743886, 113.3344237280190328 ) ) ;
#110261 = CARTESIAN_POINT ( 'NONE',  ( -19.05341960407611168, -5.049401038298163336, 71.45724293864766707 ) ) ;
#110262 = CARTESIAN_POINT ( 'NONE',  ( -16.46253265017160317, 9.564922557960807481, 35.83224293864768839 ) ) ;
#110263 = CARTESIAN_POINT ( 'NONE',  ( -10.72451020669898014, 18.67979575497178502, 45.41557627198103830 ) ) ;
#110264 = CARTESIAN_POINT ( 'NONE',  ( -13.97604488694547697, 13.89961937509957934, 43.12609039468566152 ) ) ;
#110266 = CARTESIAN_POINT ( 'NONE',  ( 16.55341960407611168, 4.379528057220329451, 33.95724293864769550 ) ) ;
#110265 = CARTESIAN_POINT ( 'NONE',  ( -3.573655867282028392E-15, 2.428612866367529932E-14, 0.000000000000000000 ) ) ;
#110267 = CARTESIAN_POINT ( 'NONE',  ( -5.153800228976328057, -19.02544592524343514, 112.2905762719810099 ) ) ;
#110268 = CARTESIAN_POINT ( 'NONE',  ( -21.53943276465977519, -0.05219959533937600094, 53.75109039468568994 ) ) ;
#110269 = CARTESIAN_POINT ( 'NONE',  ( -16.46253265017160317, 9.564922557960807481, 115.8322429386477097 ) ) ;
#110270 = CARTESIAN_POINT ( 'NONE',  ( -16.55341960407617563, 4.379528057220093196, 58.54275706135235424 ) ) ;
#110271 = CARTESIAN_POINT ( 'NONE',  ( 13.89961937509957401, 13.97604488694547697, 61.87609039468566863 ) ) ;
#110272 = EDGE_CURVE ( 'NONE', #139247, #107606, #117079, .T. ) ;
#110273 = CARTESIAN_POINT ( 'NONE',  ( -4.379528057220328563, 16.55341960407611168, 25.20724293864769550 ) ) ;
#110274 = CARTESIAN_POINT ( 'NONE',  ( 16.19135201231364363, -7.376712067592015920, 52.31319145947973226 ) ) ;
#110275 = CARTESIAN_POINT ( 'NONE',  ( 4.483927247898790824, -16.52544592524335698, 110.2094237280190185 ) ) ;
#110276 = CARTESIAN_POINT ( 'NONE',  ( 19.02544592524343514, -5.153800228976328945, 38.54057627198103120 ) ) ;
#110277 = CARTESIAN_POINT ( 'NONE',  ( 16.51473224551069308, 9.474510206698969483, 64.16557627198102409 ) ) ;
#110278 = CARTESIAN_POINT ( 'NONE',  ( -9.564922557960796823, -16.46253265017161027, 32.08224293864769550 ) ) ;
#110279 = CARTESIAN_POINT ( 'NONE',  ( 15.72974639402176855, 15.80617190586768217, 31.87609039468567929 ) ) ;
#110280 = CARTESIAN_POINT ( 'NONE',  ( 13.89961937509977652, -13.97604488694527269, 48.12390960531435979 ) ) ;
#110281 = CARTESIAN_POINT ( 'NONE',  ( -4.925740194183259923, -6.812954659138648061, -62.05864287809313851 ) ) ;
#110282 = CARTESIAN_POINT ( 'NONE',  ( -19.05341960407611168, -5.049401038298163336, 51.45724293864770260 ) ) ;
#110283 = CARTESIAN_POINT ( 'NONE',  ( -18.62759615963270932, 10.81492255796079327, 25.83224293864769194 ) ) ;
#110285 = CARTESIAN_POINT ( 'NONE',  ( -19.05341960407611168, -5.049401038298163336, 26.45724293864769550 ) ) ;
#110284 = CARTESIAN_POINT ( 'NONE',  ( 18.67979575497194134, -10.72451020669871369, 60.83442372801901854 ) ) ;
#110286 = CARTESIAN_POINT ( 'NONE',  ( -10.81492255796078084, -18.62759615963271287, 27.08224293864769550 ) ) ;
#110287 = CARTESIAN_POINT ( 'NONE',  ( -14.34966873604972548, 8.224510206698743886, 73.33442372801901854 ) ) ;
#110288 = CARTESIAN_POINT ( 'NONE',  ( -18.67979575497193778, 10.72451020669871902, 108.3344237280190185 ) ) ;
#110289 = CARTESIAN_POINT ( 'NONE',  ( -14.34966873604972548, 8.224510206698743886, 53.33442372801901854 ) ) ;
#110290 = CARTESIAN_POINT ( 'NONE',  ( 0.05219959533909260263, 19.03943276465977164, 94.99890960531436690 ) ) ;
#110291 = CARTESIAN_POINT ( 'NONE',  ( 12.06949235617739724, 12.14591786802326823, 36.87609039468568994 ) ) ;
#110292 = CARTESIAN_POINT ( 'NONE',  ( 8.314922557961029526, -14.29746914071037800, 20.41775706135234714 ) ) ;
#110293 = CARTESIAN_POINT ( 'NONE',  ( 16.52544592524335698, 4.483927247898782831, 91.45942372801901854 ) ) ;
#110294 = CARTESIAN_POINT ( 'NONE',  ( -5.719274019375665041, -21.55341960407619695, 59.79275706135234714 ) ) ;
#110295 = CARTESIAN_POINT ( 'NONE',  ( 9.474510206698729675, 16.51473224551082808, 112.0844237280190043 ) ) ;
#110296 = CARTESIAN_POINT ( 'NONE',  ( -10.81492255796078084, -18.62759615963271287, 107.0822429386476955 ) ) ;
#110298 = CARTESIAN_POINT ( 'NONE',  ( 13.97604488694548053, -13.89961937509957401, 105.6260903946856757 ) ) ;
#110297 = CARTESIAN_POINT ( 'NONE',  ( 12.14591786802309770, 12.06949235617756955, 104.3739096053143669 ) ) ;
#110299 = CARTESIAN_POINT ( 'NONE',  ( 14.34966873604972726, -8.224510206698740333, 85.83442372801901854 ) ) ;
#110300 = CARTESIAN_POINT ( 'NONE',  ( 22.24685556490157978, 12.75834802357609377, 167.9013491530738520 ) ) ;
#110301 = CARTESIAN_POINT ( 'NONE',  ( -9.564922557961040184, 16.46253265017147172, 77.91775706135234714 ) ) ;
#110302 = CARTESIAN_POINT ( 'NONE',  ( -12.06949235617756955, 12.14591786802309770, 40.62390960531435269 ) ) ;
#110303 = CARTESIAN_POINT ( 'NONE',  ( -14.34966873604960291, -8.224510206698953496, 46.66557627198102409 ) ) ;
#110304 = CARTESIAN_POINT ( 'NONE',  ( 8.314922557960818139, 14.29746914071049879, 109.5822429386476955 ) ) ;
#110306 = CARTESIAN_POINT ( 'NONE',  ( -17.05587630539787369, 6.762274262135701264, 90.74180309037315340 ) ) ;
#110305 = CARTESIAN_POINT ( 'NONE',  ( 9.564922557961047289, -16.46253265017146816, 50.41775706135233293 ) ) ;
#110307 = CARTESIAN_POINT ( 'NONE',  ( -0.05219959533937732626, 21.53943276465977519, 42.50109039468567573 ) ) ;
#110308 = CARTESIAN_POINT ( 'NONE',  ( 5.153800228976615827, -19.02544592524334988, 110.2094237280189901 ) ) ;
#110309 = CARTESIAN_POINT ( 'NONE',  ( -3.181980515339590365, -34.99999999999999289, 1.110912703473986074 ) ) ;
#110310 = CARTESIAN_POINT ( 'NONE',  ( -13.97604488694527625, -13.89961937509977652, 91.87390960531432427 ) ) ;
#110311 = CARTESIAN_POINT ( 'NONE',  ( -9.474510206698964154, 16.51473224551069663, 95.41557627198102409 ) ) ;
#110312 = CARTESIAN_POINT ( 'NONE',  ( -15.80617190586745835, -15.72974639402198527, 61.87390960531436690 ) ) ;
#110313 = CARTESIAN_POINT ( 'NONE',  ( -8.224510206698948167, 14.34966873604960824, 90.41557627198103830 ) ) ;
#110314 = CARTESIAN_POINT ( 'NONE',  ( 13.89961937509977652, -13.97604488694527269, 68.12390960531436690 ) ) ;
#110315 = CARTESIAN_POINT ( 'NONE',  ( 19.03943276465977164, -0.05219959533909143690, 33.74890960531435979 ) ) ;
#110316 = CARTESIAN_POINT ( 'NONE',  ( -10.81492255796105439, 18.62759615963255655, 42.91775706135235424 ) ) ;
#110317 = CARTESIAN_POINT ( 'NONE',  ( -10.81492255796105439, 18.62759615963255655, 72.91775706135234714 ) ) ;
#110318 = EDGE_CURVE ( 'NONE', #123524, #80629, #152756, .T. ) ;
#110319 = CARTESIAN_POINT ( 'NONE',  ( -14.29746914071037622, -8.314922557961029526, 89.16775706135236135 ) ) ;
#110320 = CARTESIAN_POINT ( 'NONE',  ( 5.719274019375673035, 21.55341960407619339, 27.29275706135234358 ) ) ;
#110321 = CARTESIAN_POINT ( 'NONE',  ( 5.823673210054444382, -21.52544592524334988, 25.20942372801901854 ) ) ;
#110323 = CARTESIAN_POINT ( 'NONE',  ( 13.97604488694527802, 13.89961937509977652, 84.37390960531433848 ) ) ;
#110322 = CARTESIAN_POINT ( 'NONE',  ( -9.474510206698720793, -16.51473224551083518, 54.58442372801899722 ) ) ;
#110324 = CARTESIAN_POINT ( 'NONE',  ( 0.05219959533937995610, -21.53943276465977519, 85.00109039468568994 ) ) ;
#110325 = CARTESIAN_POINT ( 'NONE',  ( -5.823673210054116645, -21.52544592524344225, 82.29057627198103830 ) ) ;
#110326 = CARTESIAN_POINT ( 'NONE',  ( -4.483927247898539470, -16.52544592524342804, 47.29057627198103120 ) ) ;
#110327 = CARTESIAN_POINT ( 'NONE',  ( -15.80617190586768217, 15.72974639402176855, 103.1260903946856757 ) ) ;
#110328 = CARTESIAN_POINT ( 'NONE',  ( 14.34966873604960469, 8.224510206698951720, 79.16557627198103830 ) ) ;
#110329 = CARTESIAN_POINT ( 'NONE',  ( 12.14591786802309770, 12.06949235617756955, 114.3739096053143527 ) ) ;
#110330 = CARTESIAN_POINT ( 'NONE',  ( 16.46253265017146816, 9.564922557961045513, 76.66775706135234714 ) ) ;
#110331 = CARTESIAN_POINT ( 'NONE',  ( -16.55341960407611168, -4.379528057220339221, 36.45724293864768839 ) ) ;
#110332 = CARTESIAN_POINT ( 'NONE',  ( -5.823673210054431948, 21.52544592524334988, 87.70942372801901854 ) ) ;
#110333 = CARTESIAN_POINT ( 'NONE',  ( -19.03943276465977164, 0.05219959533909376836, 91.24890960531436690 ) ) ;
#110334 = CARTESIAN_POINT ( 'NONE',  ( 0.05219959533936267826, -19.03943276465977164, 60.00109039468566863 ) ) ;
#110335 = CARTESIAN_POINT ( 'NONE',  ( 15.72974639402199770, -15.80617190586745480, 68.12390960531436690 ) ) ;
#110336 = CARTESIAN_POINT ( 'NONE',  ( -10.72451020669870658, -18.67979575497194134, 19.58442372801901143 ) ) ;
#110337 = CARTESIAN_POINT ( 'NONE',  ( -8.224510206698735004, -14.34966873604973081, 19.58442372801901143 ) ) ;
#110338 = CARTESIAN_POINT ( 'NONE',  ( -14.34966873604972548, 8.224510206698743886, 73.33442372801901854 ) ) ;
#110340 = CARTESIAN_POINT ( 'NONE',  ( -21.55341960407619339, 5.719274019375674811, 28.54275706135234358 ) ) ;
#110339 = CARTESIAN_POINT ( 'NONE',  ( -37.99626262588766679, 2.428612866367529932E-14, -6.002157773949822861 ) ) ;
#110341 = CARTESIAN_POINT ( 'NONE',  ( 12.14591786802309770, 12.06949235617756955, 99.37390960531436690 ) ) ;
#110342 = CARTESIAN_POINT ( 'NONE',  ( 22.81625015709510151, -31.40387420917324590, -8.424999997268812990 ) ) ;
#110343 = CARTESIAN_POINT ( 'NONE',  ( -14.29746914071037622, -8.314922557961029526, 29.16775706135234003 ) ) ;
#110344 = CARTESIAN_POINT ( 'NONE',  ( -21.55341960407610458, -5.719274019375992779, 56.45724293864768839 ) ) ;
#110345 = CARTESIAN_POINT ( 'NONE',  ( -16.55341960407617563, 4.379528057220093196, 98.54275706135234714 ) ) ;
#110346 = CARTESIAN_POINT ( 'NONE',  ( -4.379528057220086978, -16.55341960407618274, 39.79275706135235424 ) ) ;
#110347 = CARTESIAN_POINT ( 'NONE',  ( 5.049401038298161559, -19.05341960407611168, 27.70724293864769550 ) ) ;
#110348 = CARTESIAN_POINT ( 'NONE',  ( -8.314922557961024197, 14.29746914071037800, 82.91775706135234714 ) ) ;
#110349 = CARTESIAN_POINT ( 'NONE',  ( -13.89961937509957401, -13.97604488694547875, 79.37609039468567573 ) ) ;
#110350 = CARTESIAN_POINT ( 'NONE',  ( 15.72974639402199770, -15.80617190586745480, 58.12390960531435979 ) ) ;
#110351 = CARTESIAN_POINT ( 'NONE',  ( -12.14591786802326823, 12.06949235617739902, 98.12609039468570415 ) ) ;
#110352 = CARTESIAN_POINT ( 'NONE',  ( 15.72974639402176855, 15.80617190586768217, 76.87609039468567573 ) ) ;
#110353 = CARTESIAN_POINT ( 'NONE',  ( 0.05219959533907565091, 21.53943276465977519, 54.99890960531435269 ) ) ;
#110354 = CARTESIAN_POINT ( 'NONE',  ( -15.72974639402197994, 15.80617190586746368, 45.62390960531436690 ) ) ;
#110355 = ORIENTED_EDGE ( 'NONE', *, *, #184866, .F. ) ;
#110356 = CARTESIAN_POINT ( 'NONE',  ( -16.55341960407617563, 4.379528057220093196, 78.54275706135236135 ) ) ;
#110357 = CARTESIAN_POINT ( 'NONE',  ( -5.823673210054116645, -21.52544592524344225, 52.29057627198102409 ) ) ;
#110358 = EDGE_LOOP ( 'NONE', ( #166285, #30540, #182860, #63478 ) ) ;
#110359 = CARTESIAN_POINT ( 'NONE',  ( 19.05341960407611168, 5.049401038298154454, 98.95724293864766707 ) ) ;
#110360 = CARTESIAN_POINT ( 'NONE',  ( 1.734723475976807094E-15, -15.20000000000001883, -64.92279855667830191 ) ) ;
#110361 = CARTESIAN_POINT ( 'NONE',  ( -13.97604488694527625, -13.89961937509977652, 21.87390960531435979 ) ) ;
#110362 = CARTESIAN_POINT ( 'NONE',  ( -10.72451020669898014, 18.67979575497178502, 65.41557627198102409 ) ) ;
#110363 = CARTESIAN_POINT ( 'NONE',  ( -0.05219959533934338120, 16.53943276465976808, 107.5010903946856899 ) ) ;
#110364 = CARTESIAN_POINT ( 'NONE',  ( 18.67979575497194134, -10.72451020669871369, 45.83442372801901854 ) ) ;
#110365 = CARTESIAN_POINT ( 'NONE',  ( -9.474510206698720793, -16.51473224551083518, 109.5844237280190043 ) ) ;
#110366 = CARTESIAN_POINT ( 'NONE',  ( -14.29746914071049879, 8.314922557960819915, 105.8322429386476955 ) ) ;
#110367 = CARTESIAN_POINT ( 'NONE',  ( 9.564922557961047289, -16.46253265017146816, 110.4177570613523471 ) ) ;
#110368 = CARTESIAN_POINT ( 'NONE',  ( 9.564922557960805705, 16.46253265017160317, 39.58224293864768839 ) ) ;
#110369 = DIRECTION ( 'NONE',  ( 0.000000000000000000, 0.000000000000000000, -1.000000000000000000 ) ) ;
#110370 = CARTESIAN_POINT ( 'NONE',  ( -19.03943276465977164, 0.05219959533909376836, 91.24890960531436690 ) ) ;
#110371 = CARTESIAN_POINT ( 'NONE',  ( -14.34966873604972548, 8.224510206698743886, 78.33442372801901854 ) ) ;
#110372 = CARTESIAN_POINT ( 'NONE',  ( 9.474510206698729675, 16.51473224551082808, 82.08442372801899012 ) ) ;
#110373 = CARTESIAN_POINT ( 'NONE',  ( -18.67979575497193778, 10.72451020669871902, 103.3344237280190043 ) ) ;
#110374 = CARTESIAN_POINT ( 'NONE',  ( -10.72451020669898014, 18.67979575497178502, 60.41557627198102409 ) ) ;
#110375 = CARTESIAN_POINT ( 'NONE',  ( -0.05219959533934338120, 16.53943276465976808, 92.50109039468567573 ) ) ;
#110376 = CARTESIAN_POINT ( 'NONE',  ( -5.049401038297874678, -19.05341960407617918, 74.79275706135231871 ) ) ;
#110377 = CARTESIAN_POINT ( 'NONE',  ( 19.02544592524343514, -5.153800228976328945, 33.54057627198102409 ) ) ;
#110378 = CARTESIAN_POINT ( 'NONE',  ( -9.564922557960796823, -16.46253265017161027, 72.08224293864770971 ) ) ;
#110379 = CARTESIAN_POINT ( 'NONE',  ( 5.719274019375673035, 21.55341960407619339, 47.29275706135234003 ) ) ;
#110380 = CARTESIAN_POINT ( 'NONE',  ( -0.05219959533909027116, -19.03943276465977164, 52.49890960531436690 ) ) ;
#110381 = CARTESIAN_POINT ( 'NONE',  ( -9.564922557961040184, 16.46253265017147172, 67.91775706135233293 ) ) ;
#110382 = B_SPLINE_CURVE_WITH_KNOTS ( 'NONE', 3,
 ( #1376, #20527, #98344, #21530, #35701, #17561 ),
 .UNSPECIFIED., .F., .F.,
 ( 4, 2, 4 ),
 ( 0.003239945802372225670, 0.003620412082092076995, 0.004000878361811928755 ),
 .UNSPECIFIED. ) ;
#110383 = CARTESIAN_POINT ( 'NONE',  ( 26.13941622279003951, -9.616497135381504080, 166.9083969906208722 ) ) ;
#110384 = CARTESIAN_POINT ( 'NONE',  ( -9.474510206698964154, 16.51473224551069663, 105.4155762719810383 ) ) ;
#110385 = CARTESIAN_POINT ( 'NONE',  ( 4.483927247898545687, 16.52544592524342804, 64.79057627198103830 ) ) ;
#110386 = CARTESIAN_POINT ( 'NONE',  ( -15.80617190586745835, -15.72974639402198527, 61.87390960531436690 ) ) ;
#110387 = CARTESIAN_POINT ( 'NONE',  ( 0.000000000000000000, -2.357898499370432610, 3.252606517456513302E-15 ) ) ;
#110388 = CARTESIAN_POINT ( 'NONE',  ( -19.03943276465977164, -0.05219959533935918106, 23.75109039468566152 ) ) ;
#110389 = CARTESIAN_POINT ( 'NONE',  ( 20.02432819973540035, -11.96332215053014991, 170.0134113894037000 ) ) ;
#110391 = CARTESIAN_POINT ( 'NONE',  ( 16.51473224551069308, 9.474510206698969483, 74.16557627198103830 ) ) ;
#110390 = CARTESIAN_POINT ( 'NONE',  ( -13.97604488694527625, -13.89961937509977652, 66.87390960531436690 ) ) ;
#110392 = CARTESIAN_POINT ( 'NONE',  ( 16.52544592524335698, 4.483927247898782831, 51.45942372801901854 ) ) ;
#110393 = CARTESIAN_POINT ( 'NONE',  ( 19.50973618000806198, 5.499999999999992895, 37.50000000000000000 ) ) ;
#110394 = CARTESIAN_POINT ( 'NONE',  ( 28.82186960331507208, 9.364793116373459014, 145.3500000054623911 ) ) ;
#110395 = CARTESIAN_POINT ( 'NONE',  ( -14.29746914071037622, -8.314922557961029526, 94.16775706135237556 ) ) ;
#110396 = DIRECTION ( 'NONE',  ( 1.000000000000000000, 0.000000000000000000, 0.000000000000000000 ) ) ;
#110397 = CARTESIAN_POINT ( 'NONE',  ( -4.483927247898782831, 16.52544592524335698, 62.70942372801902565 ) ) ;
#110398 = CARTESIAN_POINT ( 'NONE',  ( -14.34966873604972548, 8.224510206698743886, 43.33442372801901143 ) ) ;
#110400 = DIRECTION ( 'NONE',  ( -0.000000000000000000, -0.000000000000000000, 1.000000000000000000 ) ) ;
#110399 = CARTESIAN_POINT ( 'NONE',  ( -5.049401038298153566, 19.05341960407611168, 55.20724293864769550 ) ) ;
#110401 = CARTESIAN_POINT ( 'NONE',  ( 15.80617190586769283, -15.72974639402175789, 55.62609039468568284 ) ) ;
#110402 = CARTESIAN_POINT ( 'NONE',  ( 16.46253265017146816, 9.564922557961045513, 66.66775706135233293 ) ) ;
#110403 = CARTESIAN_POINT ( 'NONE',  ( -21.52544592524334988, -5.823673210054445271, 108.9594237280190185 ) ) ;
#110404 = CARTESIAN_POINT ( 'NONE',  ( 16.46253265017160672, -9.564922557960803928, 33.33224293864770260 ) ) ;
#110405 = CARTESIAN_POINT ( 'NONE',  ( 16.19062691409071064, 7.376977991747391883, 22.65583381035920141 ) ) ;
#110406 = CARTESIAN_POINT ( 'NONE',  ( 0.05219959533907565091, 21.53943276465977519, 54.99890960531435269 ) ) ;
#110407 = CARTESIAN_POINT ( 'NONE',  ( -9.564922557960796823, -16.46253265017161027, 112.0822429386476955 ) ) ;
#110408 = CARTESIAN_POINT ( 'NONE',  ( -14.29746914071049879, 8.314922557960819915, 95.83224293864770971 ) ) ;
#110409 = CARTESIAN_POINT ( 'NONE',  ( -16.52544592524335698, -4.483927247898792601, 43.95942372801902565 ) ) ;
#110410 = CARTESIAN_POINT ( 'NONE',  ( 8.314922557960818139, 14.29746914071049879, 29.58224293864769905 ) ) ;
#110411 = ORIENTED_EDGE ( 'NONE', *, *, #130059, .T. ) ;
#110412 = EDGE_CURVE ( 'NONE', #101425, #125361, #31446, .T. ) ;
#110413 = CARTESIAN_POINT ( 'NONE',  ( -21.53943276465977519, -0.05219959533937600094, 18.75109039468568639 ) ) ;
#110415 = CARTESIAN_POINT ( 'NONE',  ( -16.46253265017160317, 9.564922557960807481, 110.8322429386476955 ) ) ;
#110414 = CARTESIAN_POINT ( 'NONE',  ( -4.379528057220328563, 16.55341960407611168, 35.20724293864768839 ) ) ;
#110416 = AXIS2_PLACEMENT_3D ( 'NONE', #53546, #176916, #38387 ) ;
#110417 = CARTESIAN_POINT ( 'NONE',  ( -13.97604488694547697, 13.89961937509957934, 93.12609039468566152 ) ) ;
#110418 = CARTESIAN_POINT ( 'NONE',  ( 9.564922557961047289, -16.46253265017146816, 30.41775706135232937 ) ) ;
#110419 = CARTESIAN_POINT ( 'NONE',  ( -8.224510206698948167, 14.34966873604960824, 30.41557627198101699 ) ) ;
#110420 = CARTESIAN_POINT ( 'NONE',  ( 15.72974639402199770, -15.80617190586745480, 98.12390960531436690 ) ) ;
#110421 = CARTESIAN_POINT ( 'NONE',  ( 21.53943276465977519, -0.05219959533907433946, 53.74890960531437401 ) ) ;
#110422 = CARTESIAN_POINT ( 'NONE',  ( 9.474510206698971260, -16.51473224551069308, 77.91557627198103830 ) ) ;
#110423 = CARTESIAN_POINT ( 'NONE',  ( 4.379528057220339221, -16.55341960407611168, 47.70724293864770260 ) ) ;
#110424 = CARTESIAN_POINT ( 'NONE',  ( -13.89961937509977652, 13.97604488694528158, 90.62390960531432427 ) ) ;
#110425 = ORIENTED_EDGE ( 'NONE', *, *, #97036, .F. ) ;
#110426 = CARTESIAN_POINT ( 'NONE',  ( 19.35543954521081744, 5.499999999999578115, 57.08901960356452321 ) ) ;
#110427 = CARTESIAN_POINT ( 'NONE',  ( 16.51473224551083163, -9.474510206698727899, 45.83442372801900433 ) ) ;
#110428 = CARTESIAN_POINT ( 'NONE',  ( 18.62759615963271287, -10.81492255796078972, 88.33224293864769550 ) ) ;
#110429 = CARTESIAN_POINT ( 'NONE',  ( -12.14591786802309592, -12.06949235617757132, 96.87390960531436690 ) ) ;
#110430 = CARTESIAN_POINT ( 'NONE',  ( 5.719274019375673035, 21.55341960407619339, 32.29275706135235424 ) ) ;
#110431 = CARTESIAN_POINT ( 'NONE',  ( -5.359611314223446995E-15, 29.16686587814335496, 148.8750000027311842 ) ) ;
#110432 = CARTESIAN_POINT ( 'NONE',  ( 4.483927247898790824, -16.52544592524335698, 105.2094237280190328 ) ) ;
#110433 = CARTESIAN_POINT ( 'NONE',  ( -13.97604488694527625, -13.89961937509977652, 31.87390960531435979 ) ) ;
#110434 = CARTESIAN_POINT ( 'NONE',  ( -0.05219959533909027116, -19.03943276465977164, 87.49890960531436690 ) ) ;
#110435 = CARTESIAN_POINT ( 'NONE',  ( 5.719274019375991003, -21.55341960407610458, 62.70724293864769550 ) ) ;
#110436 = CARTESIAN_POINT ( 'NONE',  ( -27.73933785331498925, 2.428612866367529932E-14, 140.8750000027311842 ) ) ;
#110437 = CARTESIAN_POINT ( 'NONE',  ( -0.05219959533909027116, -19.03943276465977164, 37.49890960531436690 ) ) ;
#110438 = CARTESIAN_POINT ( 'NONE',  ( -16.53943276465976808, 0.05219959533911058130, 41.24890960531435269 ) ) ;
#110439 = CARTESIAN_POINT ( 'NONE',  ( -15.80617190586768217, 15.72974639402176855, 78.12609039468570415 ) ) ;
#110441 = CARTESIAN_POINT ( 'NONE',  ( -12.14591786802326823, 12.06949235617739902, 63.12609039468568994 ) ) ;
#110440 = CARTESIAN_POINT ( 'NONE',  ( 23.76806875052803747, -29.07479876791797579, -18.77372378130564456 ) ) ;
#110442 = CARTESIAN_POINT ( 'NONE',  ( -16.46253265017160317, 9.564922557960807481, 50.83224293864770260 ) ) ;
#110443 = CARTESIAN_POINT ( 'NONE',  ( -13.89961937509977652, 13.97604488694528158, 65.62390960531436690 ) ) ;
#110444 = ORIENTED_EDGE ( 'NONE', *, *, #179839, .T. ) ;
#110445 = CARTESIAN_POINT ( 'NONE',  ( 15.80617190586769283, -15.72974639402175789, 105.6260903946856899 ) ) ;
#110446 = CARTESIAN_POINT ( 'NONE',  ( 16.52544592524335698, 4.483927247898782831, 81.45942372801900433 ) ) ;
#110447 = CARTESIAN_POINT ( 'NONE',  ( -0.05219959533937732626, 21.53943276465977519, 92.50109039468567573 ) ) ;
#110448 = CARTESIAN_POINT ( 'NONE',  ( -19.02544592524342804, 5.153800228976336051, 61.04057627198103120 ) ) ;
#110449 = CARTESIAN_POINT ( 'NONE',  ( -18.62759615963270932, 10.81492255796079327, 35.83224293864768839 ) ) ;
#110450 = CARTESIAN_POINT ( 'NONE',  ( 5.049401038297881783, 19.05341960407617563, 107.2927570613523187 ) ) ;
#110451 = CARTESIAN_POINT ( 'NONE',  ( -21.53943276465977519, -0.05219959533937600094, 78.75109039468568994 ) ) ;
#110452 = CARTESIAN_POINT ( 'NONE',  ( 14.34966873604972726, -8.224510206698740333, 50.83442372801901143 ) ) ;
#110453 = CARTESIAN_POINT ( 'NONE',  ( 5.719274019375991003, -21.55341960407610458, 97.70724293864772392 ) ) ;
#110454 = CARTESIAN_POINT ( 'NONE',  ( 0.05219959533936267826, -19.03943276465977164, 105.0010903946856615 ) ) ;
#110455 = CARTESIAN_POINT ( 'NONE',  ( 5.049401038298161559, -19.05341960407611168, 82.70724293864770971 ) ) ;
#110456 = CARTESIAN_POINT ( 'NONE',  ( 9.564922557961047289, -16.46253265017146816, 105.4177570613523471 ) ) ;
#110457 = CARTESIAN_POINT ( 'NONE',  ( -16.53943276465976808, -0.05219959533934237506, 18.75109039468568639 ) ) ;
#110458 = CARTESIAN_POINT ( 'NONE',  ( 8.224510206698953496, -14.34966873604960469, 67.91557627198102409 ) ) ;
#110459 = CARTESIAN_POINT ( 'NONE',  ( -4.379528057220086978, -16.55341960407618274, 69.79275706135234714 ) ) ;
#110461 = CARTESIAN_POINT ( 'NONE',  ( 13.89961937509977652, -13.97604488694527269, 58.12390960531436690 ) ) ;
#110460 = CARTESIAN_POINT ( 'NONE',  ( 21.55341960407610458, 5.719274019375980345, 113.9572429386477239 ) ) ;
#110462 = CARTESIAN_POINT ( 'NONE',  ( 13.97604488694527802, 13.89961937509977652, 64.37390960531436690 ) ) ;
#110463 = CARTESIAN_POINT ( 'NONE',  ( 12.06949235617739724, 12.14591786802326823, 66.87609039468568994 ) ) ;
#110464 = CARTESIAN_POINT ( 'NONE',  ( 28.82186960331499392, -9.364793116373510529, 145.1500000054623456 ) ) ;
#110465 = ORIENTED_EDGE ( 'NONE', *, *, #129852, .T. ) ;
#110466 = CARTESIAN_POINT ( 'NONE',  ( 15.72974639402176855, 15.80617190586768217, 106.8760903946856899 ) ) ;
#110467 = CARTESIAN_POINT ( 'NONE',  ( 5.153800228976335163, 19.02544592524342804, 39.79057627198100988 ) ) ;
#110468 = ORIENTED_EDGE ( 'NONE', *, *, #131008, .T. ) ;
#110469 = CARTESIAN_POINT ( 'NONE',  ( -8.314922557961024197, 14.29746914071037800, 32.91775706135234714 ) ) ;
#110471 = CARTESIAN_POINT ( 'NONE',  ( -16.55341960407617563, 4.379528057220093196, 43.54275706135235424 ) ) ;
#110470 = CARTESIAN_POINT ( 'NONE',  ( 19.03943276465977164, 0.05219959533936151252, 41.25109039468566152 ) ) ;
#110472 = CARTESIAN_POINT ( 'NONE',  ( 16.51473224551069308, 9.474510206698969483, 44.16557627198103120 ) ) ;
#110473 = CARTESIAN_POINT ( 'NONE',  ( 19.03943276465977164, -0.05219959533909143690, 63.74890960531435979 ) ) ;
#110474 = CARTESIAN_POINT ( 'NONE',  ( 15.72974639402199770, -15.80617190586745480, 83.12390960531436690 ) ) ;
#110476 = CARTESIAN_POINT ( 'NONE',  ( -9.564922557960796823, -16.46253265017161027, 107.0822429386476955 ) ) ;
#110475 = CARTESIAN_POINT ( 'NONE',  ( 19.05341960407611168, 5.049401038298154454, 78.95724293864769550 ) ) ;
#110477 = CARTESIAN_POINT ( 'NONE',  ( -9.564922557960796823, -16.46253265017161027, 52.08224293864768839 ) ) ;
#110478 = CARTESIAN_POINT ( 'NONE',  ( -8.571926809382608425, 26.38167802310805854, 148.9750000027311785 ) ) ;
#110479 = CARTESIAN_POINT ( 'NONE',  ( 9.564922557961047289, -16.46253265017146816, 100.4177570613523329 ) ) ;
#110480 = CARTESIAN_POINT ( 'NONE',  ( 10.72451020669898902, -18.67979575497178502, 77.91557627198102409 ) ) ;
#110481 = CARTESIAN_POINT ( 'NONE',  ( -5.153800228976607833, 19.02544592524334988, 22.70942372801899012 ) ) ;
#110482 = CARTESIAN_POINT ( 'NONE',  ( -0.05219959533910754901, -16.53943276465976808, 62.49890960531436690 ) ) ;
#110483 = CARTESIAN_POINT ( 'NONE',  ( -5.823673210054431948, 21.52544592524334988, 87.70942372801901854 ) ) ;
#110484 = CARTESIAN_POINT ( 'NONE',  ( -4.379528057220328563, 16.55341960407611168, 115.2072429386476955 ) ) ;
#110486 = CARTESIAN_POINT ( 'NONE',  ( 5.823673210054444382, -21.52544592524334988, 95.20942372801903275 ) ) ;
#110485 = CARTESIAN_POINT ( 'NONE',  ( 12.06949235617757843, -12.14591786802309237, 33.12390960531435979 ) ) ;
#110487 = CARTESIAN_POINT ( 'NONE',  ( -5.153800228976328057, -19.02544592524343514, 82.29057627198103830 ) ) ;
#110488 = EDGE_CURVE ( 'NONE', #173655, #173153, #166000, .T. ) ;
#110489 = CARTESIAN_POINT ( 'NONE',  ( 10.72451020669871369, 18.67979575497193778, 47.08442372801901854 ) ) ;
#110490 = CARTESIAN_POINT ( 'NONE',  ( -16.51473224551069308, -9.474510206698971260, 76.66557627198103830 ) ) ;
#110491 = CARTESIAN_POINT ( 'NONE',  ( -16.53943276465976808, 0.05219959533911058130, 91.24890960531436690 ) ) ;
#110492 = CARTESIAN_POINT ( 'NONE',  ( -12.06949235617756955, 12.14591786802309770, 65.62390960531436690 ) ) ;
#110493 = CARTESIAN_POINT ( 'NONE',  ( -21.55341960407610458, -5.719274019375992779, 71.45724293864769550 ) ) ;
#110494 = CARTESIAN_POINT ( 'NONE',  ( 5.153800228976335163, 19.02544592524342804, 69.79057627198103830 ) ) ;
#110495 = CARTESIAN_POINT ( 'NONE',  ( 18.62759615963271287, -10.81492255796078972, 83.33224293864769550 ) ) ;
#110496 = CARTESIAN_POINT ( 'NONE',  ( 19.02544592524334988, 5.153800228976608722, 81.45942372801897591 ) ) ;
#110498 = CARTESIAN_POINT ( 'NONE',  ( -12.06949235617756955, 12.14591786802309770, 70.62390960531436690 ) ) ;
#110497 = CARTESIAN_POINT ( 'NONE',  ( -16.51473224551082808, 9.474510206698731452, 33.33442372801899722 ) ) ;
#110499 = CARTESIAN_POINT ( 'NONE',  ( -21.52544592524343514, 5.823673210054127303, 56.04057627198102409 ) ) ;
#110500 = DIRECTION ( 'NONE',  ( 1.000000000000000000, 0.000000000000000000, 0.000000000000000000 ) ) ;
#110502 = CARTESIAN_POINT ( 'NONE',  ( 22.44159573604009239, 16.30477369853692693, 142.5750000027311728 ) ) ;
#110501 = CARTESIAN_POINT ( 'NONE',  ( 8.314922557961029526, -14.29746914071037800, 105.4177570613523613 ) ) ;
#110503 = CARTESIAN_POINT ( 'NONE',  ( -19.05341960407617563, 5.049401038297882671, 103.5427570613523329 ) ) ;
#110504 = EDGE_CURVE ( 'NONE', #148642, #145210, #196611, .T. ) ;
#110505 = CARTESIAN_POINT ( 'NONE',  ( 16.53943276465976808, -0.05219959533910856209, 78.74890960531436690 ) ) ;
#110506 = CARTESIAN_POINT ( 'NONE',  ( -17.50000000000147793, 3.202012800152213678, 34.92822416027257759 ) ) ;
#110507 = CARTESIAN_POINT ( 'NONE',  ( -19.02544592524342804, 5.153800228976336051, 71.04057627198099567 ) ) ;
#110508 = CARTESIAN_POINT ( 'NONE',  ( 19.02544592524343514, -5.153800228976328945, 28.54057627198102409 ) ) ;
#110509 = CARTESIAN_POINT ( 'NONE',  ( -0.05219959533910754901, -16.53943276465976808, 57.49890960531435979 ) ) ;
#110510 = CARTESIAN_POINT ( 'NONE',  ( -19.02544592524342804, 5.153800228976336051, 106.0405762719810241 ) ) ;
#110512 = CARTESIAN_POINT ( 'NONE',  ( -5.049401038298153566, 19.05341960407611168, 60.20724293864768129 ) ) ;
#110511 = CARTESIAN_POINT ( 'NONE',  ( 0.05219959533936267826, -19.03943276465977164, 90.00109039468567573 ) ) ;
#110513 = CARTESIAN_POINT ( 'NONE',  ( -16.53943276465976808, -0.05219959533934237506, 23.75109039468567929 ) ) ;
#110514 = CARTESIAN_POINT ( 'NONE',  ( 9.474510206698971260, -16.51473224551069308, 82.91557627198103830 ) ) ;
#110515 = CARTESIAN_POINT ( 'NONE',  ( 10.72451020669898902, -18.67979575497178502, 62.91557627198102409 ) ) ;
#110516 = CARTESIAN_POINT ( 'NONE',  ( -16.55341960407617563, 4.379528057220093196, 58.54275706135235424 ) ) ;
#110517 = CARTESIAN_POINT ( 'NONE',  ( 19.02544592524335343, 5.153800228976608722, 111.4594237280190043 ) ) ;
#110518 = CARTESIAN_POINT ( 'NONE',  ( 13.89961937509977652, -13.97604488694527269, 68.12390960531436690 ) ) ;
#110519 = CARTESIAN_POINT ( 'NONE',  ( 21.55341960407610458, 5.719274019375980345, 63.95724293864770260 ) ) ;
#110520 = CARTESIAN_POINT ( 'NONE',  ( 16.51473224551083163, -9.474510206698727899, 90.83442372801900433 ) ) ;
#110522 = CARTESIAN_POINT ( 'NONE',  ( -15.80617190586768217, 15.72974639402176855, 48.12609039468568284 ) ) ;
#110521 = CARTESIAN_POINT ( 'NONE',  ( -12.06949235617756955, 12.14591786802309770, 25.62390960531435624 ) ) ;
#110523 = CARTESIAN_POINT ( 'NONE',  ( 67.00000000000000000, -5.510910596163089556E-15, 39.49999999999996447 ) ) ;
#110525 = CARTESIAN_POINT ( 'NONE',  ( 9.474510206698971260, -16.51473224551069308, 102.9155762719810241 ) ) ;
#110524 = CARTESIAN_POINT ( 'NONE',  ( 16.55341960407618274, -4.379528057220086978, 71.04275706135234714 ) ) ;
#110526 = CARTESIAN_POINT ( 'NONE',  ( 19.25663599770059164, -5.499999999999425349, 41.49419308057198208 ) ) ;
#110527 = CARTESIAN_POINT ( 'NONE',  ( -16.88567814943160883, -6.947325034625784212, 36.29001122652586986 ) ) ;
#110528 = CARTESIAN_POINT ( 'NONE',  ( 0.05219959533934541429, -16.53943276465976808, 100.0010903946857042 ) ) ;
#110529 = CARTESIAN_POINT ( 'NONE',  ( -4.379528057220086978, -16.55341960407618274, 34.79275706135235424 ) ) ;
#110530 = CARTESIAN_POINT ( 'NONE',  ( 5.153800228976335163, 19.02544592524342804, 49.79057627198100988 ) ) ;
#110531 = CARTESIAN_POINT ( 'NONE',  ( 16.46253265017160672, -9.564922557960803928, 53.33224293864768839 ) ) ;
#110532 = CARTESIAN_POINT ( 'NONE',  ( 5.049401038298161559, -19.05341960407611168, 62.70724293864769550 ) ) ;
#110533 = CARTESIAN_POINT ( 'NONE',  ( 21.52544592524334988, 5.823673210054432836, 56.45942372801902565 ) ) ;
#110534 = CARTESIAN_POINT ( 'NONE',  ( 8.224510206698742110, 14.34966873604972548, 57.08442372801901854 ) ) ;
#110535 = CARTESIAN_POINT ( 'NONE',  ( -8.224510206698948167, 14.34966873604960824, 35.41557627198102409 ) ) ;
#110536 = CARTESIAN_POINT ( 'NONE',  ( 19.05341960407611168, 5.049401038298154454, 38.95724293864767418 ) ) ;
#110537 = CARTESIAN_POINT ( 'NONE',  ( 13.97604488694527802, 13.89961937509977652, 39.37390960531435269 ) ) ;
#110538 = CARTESIAN_POINT ( 'NONE',  ( 12.06949235617739724, 12.14591786802326823, 26.87609039468567218 ) ) ;
#110539 = CARTESIAN_POINT ( 'NONE',  ( -5.153800228976607833, 19.02544592524334988, 87.70942372801897591 ) ) ;
#110540 = CARTESIAN_POINT ( 'NONE',  ( 16.52544592524342804, -4.483927247898539470, 88.54057627198103830 ) ) ;
#110541 = CARTESIAN_POINT ( 'NONE',  ( -19.05341960407611168, -5.049401038298163336, 46.45724293864768129 ) ) ;
#110543 = CARTESIAN_POINT ( 'NONE',  ( 17.40805194822031154, -6.112264579159333522, 93.33371272510611050 ) ) ;
#110542 = CARTESIAN_POINT ( 'NONE',  ( -13.97604488694547697, 13.89961937509957934, 88.12609039468563310 ) ) ;
#110544 = CARTESIAN_POINT ( 'NONE',  ( 21.53943276465977519, 0.05219959533937863772, 71.25109039468568994 ) ) ;
#110545 = CARTESIAN_POINT ( 'NONE',  ( 8.224510206698742110, 14.34966873604972548, 57.08442372801901854 ) ) ;
#110546 = CARTESIAN_POINT ( 'NONE',  ( 4.500000000000000888, -126.1226662136678272, 8.481152457036385428 ) ) ;
#110547 = CARTESIAN_POINT ( 'NONE',  ( 15.80617190586746368, 15.72974639402197994, 54.37390960531435979 ) ) ;
#110548 = CARTESIAN_POINT ( 'NONE',  ( 0.05219959533934541429, -16.53943276465976808, 40.00109039468567573 ) ) ;
#110549 = CARTESIAN_POINT ( 'NONE',  ( -13.97604488694527625, -13.89961937509977830, 21.87390960531435979 ) ) ;
#110550 = CARTESIAN_POINT ( 'NONE',  ( -16.51473224551082808, 9.474510206698731452, 33.33442372801899722 ) ) ;
#110551 = FACE_BOUND ( 'NONE', #195349, .T. ) ;
#110552 = CARTESIAN_POINT ( 'NONE',  ( -19.05341960407611168, -5.049401038298163336, 56.45724293864768129 ) ) ;
#110553 = FACE_OUTER_BOUND ( 'NONE', #90824, .T. ) ;
#110554 = CARTESIAN_POINT ( 'NONE',  ( -19.03943276465977164, 0.05219959533909376836, 66.24890960531436690 ) ) ;
#110555 = CARTESIAN_POINT ( 'NONE',  ( 17.18269478283316332, -17.18269478283309226, -56.77278709839600879 ) ) ;
#110556 = CARTESIAN_POINT ( 'NONE',  ( 10.72451020669871369, 18.67979575497193778, 112.0844237280190185 ) ) ;
#110557 = CARTESIAN_POINT ( 'NONE',  ( 4.379528057220339221, -16.55341960407611168, 37.70724293864769550 ) ) ;
#110558 = CARTESIAN_POINT ( 'NONE',  ( 13.97604488694527802, 13.89961937509977652, 39.37390960531435269 ) ) ;
#110559 = CARTESIAN_POINT ( 'NONE',  ( 5.153800228976335163, 19.02544592524342804, 99.79057627198102409 ) ) ;
#110560 = CARTESIAN_POINT ( 'NONE',  ( 10.72451020669871369, 18.67979575497193778, 67.08442372801901854 ) ) ;
#110561 = CARTESIAN_POINT ( 'NONE',  ( -19.03943276465977164, 0.05219959533909376836, 46.24890960531435979 ) ) ;
#110562 = CARTESIAN_POINT ( 'NONE',  ( -18.62759615963255300, -10.81492255796106328, 64.16775706135234714 ) ) ;
#110563 = CARTESIAN_POINT ( 'NONE',  ( 5.719274019375991003, -21.55341960407610458, 22.70724293864769194 ) ) ;
#110564 = CARTESIAN_POINT ( 'NONE',  ( -19.02544592524342804, 5.153800228976336051, 31.04057627198102409 ) ) ;
#110565 = CARTESIAN_POINT ( 'NONE',  ( 21.55341960407619695, -5.719274019375665929, 31.04275706135234714 ) ) ;
#110566 = CARTESIAN_POINT ( 'NONE',  ( 9.564922557961047289, -16.46253265017146816, 50.41775706135233293 ) ) ;
#110567 = CARTESIAN_POINT ( 'NONE',  ( 9.564922557960805705, 16.46253265017160317, 24.58224293864769194 ) ) ;
#110568 = CARTESIAN_POINT ( 'NONE',  ( -13.97604488694527625, -13.89961937509977652, 61.87390960531435979 ) ) ;
#110569 = CARTESIAN_POINT ( 'NONE',  ( -5.049401038297874678, -19.05341960407617918, 104.7927570613523471 ) ) ;
#110570 = CARTESIAN_POINT ( 'NONE',  ( 4.483927247898545687, 16.52544592524342804, 69.79057627198102409 ) ) ;
#110571 = CARTESIAN_POINT ( 'NONE',  ( -5.823673210054116645, -21.52544592524344225, 37.29057627198102409 ) ) ;
#110572 = CARTESIAN_POINT ( 'NONE',  ( -13.89961937509957401, -13.97604488694547875, 104.3760903946856757 ) ) ;
#110573 = CARTESIAN_POINT ( 'NONE',  ( -18.67979575497178146, -10.72451020669898902, 101.6655762719810383 ) ) ;
#110574 = CARTESIAN_POINT ( 'NONE',  ( -21.52544592524334988, -5.823673210054445271, 53.95942372801900433 ) ) ;
#110575 = CARTESIAN_POINT ( 'NONE',  ( -4.483927247898782831, 16.52544592524335698, 52.70942372801902565 ) ) ;
#110576 = CARTESIAN_POINT ( 'NONE',  ( -8.224510206698735004, -14.34966873604973081, 59.58442372801901854 ) ) ;
#110577 = CARTESIAN_POINT ( 'NONE',  ( 5.719274019375991003, -21.55341960407610458, 62.70724293864769550 ) ) ;
#110578 = CARTESIAN_POINT ( 'NONE',  ( -9.564922557960796823, -16.46253265017161027, 42.08224293864769550 ) ) ;
#110579 = CARTESIAN_POINT ( 'NONE',  ( -14.29746914071037622, -8.314922557961029526, 74.16775706135231871 ) ) ;
#110580 = CARTESIAN_POINT ( 'NONE',  ( -15.80617190586745835, -15.72974639402198527, 101.8739096053143811 ) ) ;
#110581 = CARTESIAN_POINT ( 'NONE',  ( -16.52544592524342804, 4.483927247898546575, 51.04057627198103120 ) ) ;
#110582 = CARTESIAN_POINT ( 'NONE',  ( 19.05341960407611168, 5.049401038298154454, 78.95724293864769550 ) ) ;
#110583 = CARTESIAN_POINT ( 'NONE',  ( 12.14591786802327356, -12.06949235617739191, 75.62609039468567573 ) ) ;
#110584 = CARTESIAN_POINT ( 'NONE',  ( 9.474510206698729675, 16.51473224551082808, 112.0844237280190043 ) ) ;
#110585 = CARTESIAN_POINT ( 'NONE',  ( -18.62759615963270932, 10.81492255796079327, 105.8322429386476955 ) ) ;
#110586 = CARTESIAN_POINT ( 'NONE',  ( 16.52544592524342804, -4.483927247898539470, 38.54057627198103120 ) ) ;
#110587 = ORIENTED_EDGE ( 'NONE', *, *, #18566, .F. ) ;
#110588 = CARTESIAN_POINT ( 'NONE',  ( 19.49149378614659511, -5.499999999999668709, 91.93757513605362419 ) ) ;
#110589 = CARTESIAN_POINT ( 'NONE',  ( -21.52544592524343514, 5.823673210054127303, 91.04057627198103830 ) ) ;
#110590 = CARTESIAN_POINT ( 'NONE',  ( -0.05219959533910754901, -16.53943276465976808, 22.49890960531436335 ) ) ;
#110591 = ORIENTED_EDGE ( 'NONE', *, *, #155903, .T. ) ;
#110592 = CARTESIAN_POINT ( 'NONE',  ( -17.31747979337947996, -6.344076630961018815, 56.37944868065183357 ) ) ;
#110593 = CARTESIAN_POINT ( 'NONE',  ( 21.52544592524344225, -5.823673210054117533, 98.54057627198105251 ) ) ;
#110594 = CARTESIAN_POINT ( 'NONE',  ( 16.46253265017160672, -9.564922557960803928, 113.3322429386476955 ) ) ;
#110595 = CARTESIAN_POINT ( 'NONE',  ( -10.72451020669870658, -18.67979575497194134, 24.58442372801901499 ) ) ;
#110596 = CARTESIAN_POINT ( 'NONE',  ( 12.14591786802309770, 12.06949235617756955, 54.37390960531435979 ) ) ;
#110597 = CARTESIAN_POINT ( 'NONE',  ( 8.314922557961029526, -14.29746914071037800, 45.41775706135234003 ) ) ;
#110598 = CARTESIAN_POINT ( 'NONE',  ( 16.51473224551069308, 9.474510206698969483, 59.16557627198102409 ) ) ;
#110599 = CARTESIAN_POINT ( 'NONE',  ( 5.049401038297881783, 19.05341960407617563, 52.29275706135234003 ) ) ;
#110600 = CARTESIAN_POINT ( 'NONE',  ( -19.02544592524342804, 5.153800228976336051, 81.04057627198103830 ) ) ;
#110601 = CARTESIAN_POINT ( 'NONE',  ( -10.81492255796078084, -18.62759615963271287, 32.08224293864769550 ) ) ;
#110602 = CARTESIAN_POINT ( 'NONE',  ( -27.18398240159013568, -26.16474475602790406, -20.45985799058115262 ) ) ;
#110603 = CARTESIAN_POINT ( 'NONE',  ( 0.05219959533934541429, -16.53943276465976808, 25.00109039468567218 ) ) ;
#110604 = CARTESIAN_POINT ( 'NONE',  ( -19.05341960407617563, 5.049401038297882671, 68.54275706135230450 ) ) ;
#110605 = CARTESIAN_POINT ( 'NONE',  ( -18.62759615963270932, 10.81492255796079327, 100.8322429386477097 ) ) ;
#110606 = CARTESIAN_POINT ( 'NONE',  ( 8.314922557960818139, 14.29746914071049879, 39.58224293864769550 ) ) ;
#110607 = CARTESIAN_POINT ( 'NONE',  ( 19.05341960407611168, 5.049401038298154454, 78.95724293864769550 ) ) ;
#110608 = CARTESIAN_POINT ( 'NONE',  ( 10.72451020669898902, -18.67979575497178502, 62.91557627198102409 ) ) ;
#110610 = CARTESIAN_POINT ( 'NONE',  ( 16.52544592524335698, 4.483927247898782831, 21.45942372801901499 ) ) ;
#110609 = CARTESIAN_POINT ( 'NONE',  ( -21.52544592524343514, 5.823673210054127303, 101.0405762719810383 ) ) ;
#110611 = EDGE_CURVE ( 'NONE', #116458, #91244, #107424, .T. ) ;
#110612 = CARTESIAN_POINT ( 'NONE',  ( 10.81492255796078972, 18.62759615963270932, 24.58224293864768839 ) ) ;
#110613 = CARTESIAN_POINT ( 'NONE',  ( 10.72451020669871369, 18.67979575497193778, 87.08442372801901854 ) ) ;
#110614 = CARTESIAN_POINT ( 'NONE',  ( 19.03943276465977164, -0.05219959533909143690, 93.74890960531435269 ) ) ;
#110615 = CARTESIAN_POINT ( 'NONE',  ( -19.05341960407611168, -5.049401038298163336, 31.45724293864769550 ) ) ;
#110616 = CARTESIAN_POINT ( 'NONE',  ( 19.03943276465977164, -0.05219959533909143690, 78.74890960531436690 ) ) ;
#110617 = CARTESIAN_POINT ( 'NONE',  ( -0.05219959533910754901, -16.53943276465976808, 107.4989096053143669 ) ) ;
#110618 = CARTESIAN_POINT ( 'NONE',  ( -13.97604488694527625, -13.89961937509977652, 61.87390960531435979 ) ) ;
#110619 = CARTESIAN_POINT ( 'NONE',  ( 5.049401038297881783, 19.05341960407617563, 112.2927570613523471 ) ) ;
#110620 = CARTESIAN_POINT ( 'NONE',  ( -17.59860650958993844, 7.585241751806885979, 43.42337014262493256 ) ) ;
#110621 = CARTESIAN_POINT ( 'NONE',  ( 19.02544592524343514, -5.153800228976328945, 68.54057627198103830 ) ) ;
#110623 = CARTESIAN_POINT ( 'NONE',  ( 0.05219959533909260263, 19.03943276465977164, 109.9989096053143669 ) ) ;
#110622 = CARTESIAN_POINT ( 'NONE',  ( 5.719274019375673035, 21.55341960407619339, 102.2927570613523613 ) ) ;
#110625 = ADVANCED_FACE ( 'NONE', ( #44634 ), #28493, .F. ) ;
#110624 = CARTESIAN_POINT ( 'NONE',  ( -4.483927247898782831, 16.52544592524335698, 97.70942372801904696 ) ) ;
#110626 = DIRECTION ( 'NONE',  ( 0.000000000000000000, 0.000000000000000000, -1.000000000000000000 ) ) ;
#110627 = CARTESIAN_POINT ( 'NONE',  ( -5.153800228976607833, 19.02544592524334988, 72.70942372801900433 ) ) ;
#110628 = CARTESIAN_POINT ( 'NONE',  ( -19.03943276465977164, -0.05219959533935918106, 23.75109039468566152 ) ) ;
#110629 = CARTESIAN_POINT ( 'NONE',  ( 4.023676584314517690, 4.713425861958483232, -64.51712888360830789 ) ) ;
#110630 = CARTESIAN_POINT ( 'NONE',  ( 9.564922557960805705, 16.46253265017160317, 24.58224293864769194 ) ) ;
#110631 = CARTESIAN_POINT ( 'NONE',  ( 16.55341960407611168, 4.379528057220329451, 33.95724293864769550 ) ) ;
#110632 = CARTESIAN_POINT ( 'NONE',  ( -31.90000000000003411, 3.219216299777112361E-13, -64.92279855667830191 ) ) ;
#110633 = CARTESIAN_POINT ( 'NONE',  ( -14.34966873604972548, 8.224510206698743886, 108.3344237280190185 ) ) ;
#110634 = CARTESIAN_POINT ( 'NONE',  ( 22.97392636501382768, -21.20633172485417006, -49.95052365407170925 ) ) ;
#110635 = CARTESIAN_POINT ( 'NONE',  ( -12.06949235617739369, -12.14591786802326823, 84.37609039468570415 ) ) ;
#110636 = CARTESIAN_POINT ( 'NONE',  ( 19.02544592524343514, -5.153800228976328945, 33.54057627198102409 ) ) ;
#110637 = CARTESIAN_POINT ( 'NONE',  ( -15.80617190586768217, 15.72974639402176855, 98.12609039468570415 ) ) ;
#110638 = CARTESIAN_POINT ( 'NONE',  ( -13.89961937509957401, -13.97604488694547875, 99.37609039468567573 ) ) ;
#110639 = CARTESIAN_POINT ( 'NONE',  ( 21.52544592524334988, 5.823673210054432836, 81.45942372801900433 ) ) ;
#110640 = CARTESIAN_POINT ( 'NONE',  ( -13.97604488694547697, 13.89961937509957934, 53.12609039468565442 ) ) ;
#110641 = CARTESIAN_POINT ( 'NONE',  ( 5.153800228976335163, 19.02544592524342804, 74.79057627198103830 ) ) ;
#110642 = CARTESIAN_POINT ( 'NONE',  ( 5.153800228976335163, 19.02544592524342804, 64.79057627198100988 ) ) ;
#110643 = CARTESIAN_POINT ( 'NONE',  ( 17.12812012977027010, 6.668231424565943755, 73.85948759323143520 ) ) ;
#110644 = CARTESIAN_POINT ( 'NONE',  ( 12.14591786802309770, 12.06949235617756955, 64.37390960531435269 ) ) ;
#110645 = CARTESIAN_POINT ( 'NONE',  ( -10.81492255796078084, -18.62759615963271287, 62.08224293864769550 ) ) ;
#110646 = CARTESIAN_POINT ( 'NONE',  ( -5.049401038298153566, 19.05341960407611168, 50.20724293864770260 ) ) ;
#110648 = CARTESIAN_POINT ( 'NONE',  ( 8.314922557961029526, -14.29746914071037800, 80.41775706135234714 ) ) ;
#110647 = CARTESIAN_POINT ( 'NONE',  ( 15.72974639402199770, -15.80617190586745480, 83.12390960531436690 ) ) ;
#110649 = ORIENTED_EDGE ( 'NONE', *, *, #11729, .T. ) ;
#110650 = CARTESIAN_POINT ( 'NONE',  ( -9.564922557960796823, -16.46253265017161027, 52.08224293864768839 ) ) ;
#110651 = ADVANCED_FACE ( 'NONE', ( #93099 ), #45622, .F. ) ;
#110653 = CARTESIAN_POINT ( 'NONE',  ( -36.91746825000001309, 11.99521256947798342, -2.724999997268813701 ) ) ;
#110652 = CARTESIAN_POINT ( 'NONE',  ( -14.34966873604960291, -8.224510206698953496, 76.66557627198103830 ) ) ;
#110654 = CARTESIAN_POINT ( 'NONE',  ( 5.049401038298161559, -19.05341960407611168, 52.70724293864767418 ) ) ;
#110655 = CARTESIAN_POINT ( 'NONE',  ( -12.06949235617756955, 12.14591786802309770, 115.6239096053143669 ) ) ;
#110656 = CARTESIAN_POINT ( 'NONE',  ( 5.049401038297881783, 19.05341960407617563, 72.29275706135234714 ) ) ;
#110657 = CARTESIAN_POINT ( 'NONE',  ( 4.483927247898545687, 16.52544592524342804, 74.79057627198105251 ) ) ;
#110658 = CARTESIAN_POINT ( 'NONE',  ( 5.719274019375673035, 21.55341960407619339, 42.29275706135235424 ) ) ;
#110660 = CARTESIAN_POINT ( 'NONE',  ( -15.72974639402197994, 15.80617190586746368, 105.6239096053143669 ) ) ;
#110659 = CARTESIAN_POINT ( 'NONE',  ( 16.46253265017160672, -9.564922557960803928, 33.33224293864770260 ) ) ;
#110661 = CARTESIAN_POINT ( 'NONE',  ( 0.05219959533909260263, 19.03943276465977164, 114.9989096053143669 ) ) ;
#110662 = CARTESIAN_POINT ( 'NONE',  ( -4.483927247898539470, -16.52544592524342804, 82.29057627198103830 ) ) ;
#110663 = CARTESIAN_POINT ( 'NONE',  ( 18.37518290866868398, -35.61898371402006802, -22.28534798803313777 ) ) ;
#110664 = CARTESIAN_POINT ( 'NONE',  ( -9.474510206698964154, 16.51473224551069663, 50.41557627198102409 ) ) ;
#110665 = CARTESIAN_POINT ( 'NONE',  ( -11.40812507854755609, 35.11059874428196537, -1.024999997268813301 ) ) ;
#110666 = CARTESIAN_POINT ( 'NONE',  ( -19.03943276465977164, -0.05219959533935918106, 83.75109039468567573 ) ) ;
#110667 = CARTESIAN_POINT ( 'NONE',  ( 0.05219959533937995610, -21.53943276465977519, 30.00109039468568284 ) ) ;
#110668 = CARTESIAN_POINT ( 'NONE',  ( 5.153800228976335163, 19.02544592524342804, 74.79057627198103830 ) ) ;
#110669 = CARTESIAN_POINT ( 'NONE',  ( 19.02544592524334988, 5.153800228976608722, 51.45942372801900433 ) ) ;
#110670 = CARTESIAN_POINT ( 'NONE',  ( 19.03943276465977164, -0.05219959533909143690, 43.74890960531435979 ) ) ;
#110671 = CARTESIAN_POINT ( 'NONE',  ( 8.314922557960818139, 14.29746914071049879, 64.58224293864769550 ) ) ;
#110672 = CARTESIAN_POINT ( 'NONE',  ( -12.14591786802309592, -12.06949235617757132, 71.87390960531438111 ) ) ;
#110673 = CARTESIAN_POINT ( 'NONE',  ( -13.97604488694527625, -13.89961937509977652, 71.87390960531433848 ) ) ;
#110674 = CARTESIAN_POINT ( 'NONE',  ( -21.52544592524343514, 5.823673210054127303, 101.0405762719810383 ) ) ;
#110675 = CARTESIAN_POINT ( 'NONE',  ( 5.153800228976335163, 19.02544592524342804, 69.79057627198103830 ) ) ;
#110676 = CARTESIAN_POINT ( 'NONE',  ( -0.05219959533937732626, 21.53943276465977519, 107.5010903946856899 ) ) ;
#110679 = CARTESIAN_POINT ( 'NONE',  ( -4.483927247898539470, -16.52544592524342804, 92.29057627198103830 ) ) ;
#110678 = CARTESIAN_POINT ( 'NONE',  ( 12.06949235617739724, 12.14591786802326823, 106.8760903946856899 ) ) ;
#110677 = CARTESIAN_POINT ( 'NONE',  ( 16.51473224551069308, 9.474510206698969483, 39.16557627198103120 ) ) ;
#110680 = CARTESIAN_POINT ( 'NONE',  ( 9.474510206698729675, 16.51473224551082808, 102.0844237280190043 ) ) ;
#110681 = EDGE_LOOP ( 'NONE', ( #183357, #52720, #105188, #169041 ) ) ;
#110682 = CARTESIAN_POINT ( 'NONE',  ( 15.72974639402176855, 15.80617190586768217, 36.87609039468568994 ) ) ;
#110683 = CARTESIAN_POINT ( 'NONE',  ( -13.97604488694547697, 13.89961937509957934, 53.12609039468565442 ) ) ;
#110684 = CARTESIAN_POINT ( 'NONE',  ( -16.52544592524335698, -4.483927247898792601, 108.9594237280190185 ) ) ;
#110685 = CARTESIAN_POINT ( 'NONE',  ( -5.823673210054116645, -21.52544592524344225, 67.29057627198103830 ) ) ;
#110686 = CARTESIAN_POINT ( 'NONE',  ( 13.89961937509977652, -13.97604488694527269, 108.1239096053143669 ) ) ;
#110687 = CARTESIAN_POINT ( 'NONE',  ( -4.483927247898539470, -16.52544592524342804, 52.29057627198102409 ) ) ;
#110688 = CARTESIAN_POINT ( 'NONE',  ( -19.03943276465977164, 0.05219959533909376836, 26.24890960531435624 ) ) ;
#110689 = CARTESIAN_POINT ( 'NONE',  ( -5.049401038298153566, 19.05341960407611168, 40.20724293864768839 ) ) ;
#110690 = CARTESIAN_POINT ( 'NONE',  ( 19.02544592524334988, 5.153800228976608722, 26.45942372801899722 ) ) ;
#110691 = CARTESIAN_POINT ( 'NONE',  ( 14.34966873604972726, -8.224510206698740333, 95.83442372801903275 ) ) ;
#110692 = CARTESIAN_POINT ( 'NONE',  ( 21.55341960407619695, -5.719274019375665929, 41.04275706135236135 ) ) ;
#110693 = CARTESIAN_POINT ( 'NONE',  ( 14.29746914071037800, 8.314922557961029526, 41.66775706135235424 ) ) ;
#110694 = CARTESIAN_POINT ( 'NONE',  ( -5.049401038298153566, 19.05341960407611168, 115.2072429386477097 ) ) ;
#110696 = CARTESIAN_POINT ( 'NONE',  ( -18.67979575497193778, 10.72451020669871902, 98.33442372801901854 ) ) ;
#110695 = CARTESIAN_POINT ( 'NONE',  ( -13.97604488694527625, -13.89961937509977652, 56.87390960531434558 ) ) ;
#110697 = CARTESIAN_POINT ( 'NONE',  ( -19.05341960407611168, -5.049401038298163336, 76.45724293864769550 ) ) ;
#110698 = CARTESIAN_POINT ( 'NONE',  ( 4.379528057220092307, 16.55341960407617563, 67.29275706135234714 ) ) ;
#110699 = CARTESIAN_POINT ( 'NONE',  ( -4.483927247898539470, -16.52544592524342804, 102.2905762719810383 ) ) ;
#110700 = CARTESIAN_POINT ( 'NONE',  ( -16.55341960407617563, 4.379528057220093196, 113.5427570613523756 ) ) ;
#110701 = CARTESIAN_POINT ( 'NONE',  ( -0.3535533905933752052, -30.00000000000000355, 5.353553390593268624 ) ) ;
#110704 = CARTESIAN_POINT ( 'NONE',  ( 9.564922557960805705, 16.46253265017160317, 79.58224293864769550 ) ) ;
#110703 = CARTESIAN_POINT ( 'NONE',  ( -5.049401038298153566, 19.05341960407611168, 85.20724293864766707 ) ) ;
#110702 = CARTESIAN_POINT ( 'NONE',  ( 10.81492255796106328, -18.62759615963255655, 70.41775706135236135 ) ) ;
#110705 = CARTESIAN_POINT ( 'NONE',  ( -5.153800228976328057, -19.02544592524343514, 112.2905762719810099 ) ) ;
#110706 = CARTESIAN_POINT ( 'NONE',  ( 12.14591786802309770, 12.06949235617756955, 64.37390960531435269 ) ) ;
#110707 = CARTESIAN_POINT ( 'NONE',  ( -16.53943276465976808, -0.05219959533934237506, 108.7510903946857042 ) ) ;
#110708 = EDGE_LOOP ( 'NONE', ( #47010, #135059, #44844, #127580 ) ) ;
#110709 = CARTESIAN_POINT ( 'NONE',  ( 14.29746914071049879, -8.314922557960816363, 33.33224293864769550 ) ) ;
#110711 = CARTESIAN_POINT ( 'NONE',  ( -15.02701145101215907, -17.15609852811352809, -55.39549205246427022 ) ) ;
#110710 = CARTESIAN_POINT ( 'NONE',  ( 12.06949235617739724, 12.14591786802326823, 36.87609039468568994 ) ) ;
#110712 = CARTESIAN_POINT ( 'NONE',  ( -19.05341960407617563, 5.049401038297882671, 33.54275706135231871 ) ) ;
#110713 = CARTESIAN_POINT ( 'NONE',  ( 13.97604488694527802, 13.89961937509977652, 74.37390960531436690 ) ) ;
#110714 = CARTESIAN_POINT ( 'NONE',  ( 16.51473224551083163, -9.474510206698727899, 50.83442372801899722 ) ) ;
#110715 = CARTESIAN_POINT ( 'NONE',  ( -22.81625015709510507, 31.40387420917330275, -2.924999997268813434 ) ) ;
#110716 = DIRECTION ( 'NONE',  ( -1.000000000000000000, 0.000000000000000000, 0.000000000000000000 ) ) ;
#110718 = CARTESIAN_POINT ( 'NONE',  ( -8.314922557961024197, 14.29746914071037800, 77.91775706135231871 ) ) ;
#110717 = CARTESIAN_POINT ( 'NONE',  ( 19.03943276465977164, 0.05219959533936151252, 91.25109039468566152 ) ) ;
#110719 = CARTESIAN_POINT ( 'NONE',  ( 16.51473224551069308, 9.474510206698969483, 29.16557627198103475 ) ) ;
#110720 = CARTESIAN_POINT ( 'NONE',  ( 0.05219959533909260263, 19.03943276465977164, 104.9989096053143669 ) ) ;
#110721 = CARTESIAN_POINT ( 'NONE',  ( -21.53943276465977519, -0.05219959533937600094, 43.75109039468568284 ) ) ;
#110722 = VECTOR ( 'NONE', #99709, 1000.000000000000000 ) ;
#110723 = CARTESIAN_POINT ( 'NONE',  ( -9.564922557961040184, 16.46253265017147172, 92.91775706135233293 ) ) ;
#110725 = CARTESIAN_POINT ( 'NONE',  ( -13.97604488694527625, -13.89961937509977652, 51.87390960531436690 ) ) ;
#110724 = CARTESIAN_POINT ( 'NONE',  ( 17.44270441346519362, 5.991230190322986537, 88.86335079264232206 ) ) ;
#110726 = CARTESIAN_POINT ( 'NONE',  ( 9.474510206698971260, -16.51473224551069308, 102.9155762719810241 ) ) ;
#110728 = CARTESIAN_POINT ( 'NONE',  ( 16.51473224551069308, 9.474510206698969483, 54.16557627198103120 ) ) ;
#110727 = CARTESIAN_POINT ( 'NONE',  ( -8.314922557960811034, -14.29746914071050412, 57.08224293864769550 ) ) ;
#110729 = CARTESIAN_POINT ( 'NONE',  ( -9.474510206698964154, 16.51473224551069663, 60.41557627198102409 ) ) ;
#110730 = CARTESIAN_POINT ( 'NONE',  ( 9.564922557961047289, -16.46253265017146816, 65.41775706135233293 ) ) ;
#110731 = CARTESIAN_POINT ( 'NONE',  ( -13.89961937509957401, -13.97604488694547875, 34.37609039468566863 ) ) ;
#110732 = CARTESIAN_POINT ( 'NONE',  ( -5.049401038298153566, 19.05341960407611168, 70.20724293864769550 ) ) ;
#110733 =( BOUNDED_CURVE ( )  B_SPLINE_CURVE ( 2, ( #72258, #101583, #178448, #133936, #42922, #117766, #163271, #147103, #179459, #88408, #150104, #162262, #40924, #70262, #134943, #73273, #193614, #116757, #197598, #196620, #195626, #58090, #181444, #164283, #166272, #102597, #104587, #89413, #74258, #39915, #151102, #25776, #87422, #12594, #135928, #59064, #64034, #63031, #171218, #185392, #121724, #167258, #139862, #90394, #76214, #91363, #136901, #15552, #47883, #28757, #140864, #137893, #60056, #2353, #32707, #107539, #359, #125704, #75230, #30724, #199574, #94359, #92371, #14556, #109536, #156038, #187403, #77210, #152078, #13563, #105572, #170222, #183416 ),
 .UNSPECIFIED., .F., .T. ) 
 B_SPLINE_CURVE_WITH_KNOTS ( ( 3, 2, 2, 2, 2, 2, 2, 2, 2, 2, 2, 2, 2, 2, 2, 2, 2, 2, 2, 2, 2, 2, 2, 2, 2, 2, 2, 2, 2, 2, 2, 2, 2, 2, 2, 2, 3 ),
 ( 0.000000000000000000, 0.004385964912280701511, 0.008771929824561403022, 0.01315789473684210280, 0.01754385964912280604, 0.02192982456140350755, 0.02631578947368420560, 0.03070175438596491405, 0.03508771929824561209, 0.03947368421052631360, 0.04385964912280701511, 0.04824561403508771662, 0.05263157894736841119, 0.05701754385964912658, 0.06140350877192982809, 0.06578947368421052266, 0.07017543859649122417, 0.07456140350877192569, 0.07894736842105262720, 0.08333333333333332871, 0.08771929824561403022, 0.09210526315789473173, 0.09649122807017543324, 0.1008771929824561209, 0.1052631578947368224, 0.1096491228070175239, 0.1140350877192982532, 0.1184210526315789547, 0.1228070175438596562, 0.1271929824561403577, 0.1315789473684210453, 0.1359649122807017607, 0.1403508771929824483, 0.1447368421052631637, 0.1491228070175438514, 0.1535087719298245668, 0.1554186205929700415 ),
 .UNSPECIFIED. ) 
 CURVE ( )  GEOMETRIC_REPRESENTATION_ITEM ( )  RATIONAL_B_SPLINE_CURVE ( ( 1.000000000000000000, 0.9659258262890683122, 1.000000000000000000, 0.9659258262890683122, 1.000000000000000000, 0.9659258262890683122, 1.000000000000000000, 0.9659258262890683122, 1.000000000000000000, 0.9659258262890683122, 1.000000000000000000, 0.9659258262890683122, 1.000000000000000000, 0.9659258262890683122, 1.000000000000000000, 0.9659258262890683122, 1.000000000000000000, 0.9659258262890683122, 1.000000000000000000, 0.9659258262890683122, 1.000000000000000000, 0.9659258262890683122, 1.000000000000000000, 0.9659258262890683122, 1.000000000000000000, 0.9659258262890683122, 1.000000000000000000, 0.9659258262890683122, 1.000000000000000000, 0.9659258262890683122, 1.000000000000000000, 0.9659258262890683122, 1.000000000000000000, 0.9659258262890683122, 1.000000000000000000, 0.9659258262890683122, 1.000000000000000000, 0.9659258262890683122, 1.000000000000000000, 0.9659258262890683122, 1.000000000000000000, 0.9659258262890683122, 1.000000000000000000, 0.9659258262890683122, 1.000000000000000000, 0.9659258262890683122, 1.000000000000000000, 0.9659258262890683122, 1.000000000000000000, 0.9659258262890683122, 1.000000000000000000, 0.9659258262890683122, 1.000000000000000000, 0.9659258262890683122, 1.000000000000000000, 0.9659258262890683122, 1.000000000000000000, 0.9659258262890683122, 1.000000000000000000, 0.9659258262890683122, 1.000000000000000000, 0.9659258262890683122, 1.000000000000000000, 0.9659258262890683122, 1.000000000000000000, 0.9659258262890683122, 1.000000000000000000, 0.9659258262890683122, 1.000000000000000000, 0.9659258262890683122, 1.000000000000000000, 0.9851625545550090068, 0.9832469066685280978 ) ) 
 REPRESENTATION_ITEM ( '' )  );
#110734 = CARTESIAN_POINT ( 'NONE',  ( -21.52544592524343514, 5.823673210054127303, 76.04057627198102409 ) ) ;
#110736 = CARTESIAN_POINT ( 'NONE',  ( 5.049401038297881783, 19.05341960407617563, 32.29275706135233293 ) ) ;
#110735 = CARTESIAN_POINT ( 'NONE',  ( -12.06949235617756955, 12.14591786802309770, 70.62390960531436690 ) ) ;
#110737 = CARTESIAN_POINT ( 'NONE',  ( 30.74264578624800137, -22.33583958711395212, -10.94999999453762562 ) ) ;
#110738 = CARTESIAN_POINT ( 'NONE',  ( 18.62759615963271287, -10.81492255796078972, 43.33224293864769550 ) ) ;
#110739 = CARTESIAN_POINT ( 'NONE',  ( -10.81492255796078084, -18.62759615963271287, 32.08224293864769550 ) ) ;
#110740 = CARTESIAN_POINT ( 'NONE',  ( -19.05341960407611168, -5.049401038298163336, 66.45724293864769550 ) ) ;
#110741 = CARTESIAN_POINT ( 'NONE',  ( 19.03943276465977164, -0.05219959533909143690, 38.74890960531436690 ) ) ;
#110742 = CARTESIAN_POINT ( 'NONE',  ( 16.53943276465976808, -0.05219959533910856209, 103.7489096053143669 ) ) ;
#110743 = CARTESIAN_POINT ( 'NONE',  ( -18.62759615963270932, 10.81492255796079327, 115.8322429386477097 ) ) ;
#110744 = CARTESIAN_POINT ( 'NONE',  ( 16.51473224551069308, 9.474510206698969483, 114.1655762719810241 ) ) ;
#110745 = CARTESIAN_POINT ( 'NONE',  ( 21.52544592524334988, 5.823673210054432836, 26.45942372801901854 ) ) ;
#110746 = CARTESIAN_POINT ( 'NONE',  ( -5.153800228976328057, -19.02544592524343514, 27.29057627198103120 ) ) ;
#110747 = CARTESIAN_POINT ( 'NONE',  ( -21.52544592524343514, 5.823673210054127303, 101.0405762719810383 ) ) ;
#110748 = CARTESIAN_POINT ( 'NONE',  ( 5.153800228976615827, -19.02544592524334988, 45.20942372801901143 ) ) ;
#110749 = CARTESIAN_POINT ( 'NONE',  ( 9.564922557960805705, 16.46253265017160317, 29.58224293864769550 ) ) ;
#110750 = CARTESIAN_POINT ( 'NONE',  ( 18.22780087662122384, -5.500000000000022204, 76.01540105326107266 ) ) ;
#110751 = CYLINDRICAL_SURFACE ( 'NONE', #95066, 4.000000000000000888 ) ;
#110752 = CARTESIAN_POINT ( 'NONE',  ( -16.53943276465976808, -0.05219959533934237506, 43.75109039468568284 ) ) ;
#110753 = CARTESIAN_POINT ( 'NONE',  ( -16.51473224551069308, -9.474510206698971260, 21.66557627198102765 ) ) ;
#110754 = CARTESIAN_POINT ( 'NONE',  ( 34.52594549653173317, 2.428612888752089207E-14, 89.49999999999897682 ) ) ;
#110755 = CARTESIAN_POINT ( 'NONE',  ( -16.51473224551069308, -9.474510206698971260, 71.66557627198102409 ) ) ;
#110756 = CARTESIAN_POINT ( 'NONE',  ( 16.52544592524342804, -4.483927247898539470, 108.5405762719810241 ) ) ;
#110757 = AXIS2_PLACEMENT_3D ( 'NONE', #58796, #168945, #181177 ) ;
#110758 = CARTESIAN_POINT ( 'NONE',  ( -10.72451020669898014, 18.67979575497178502, 40.41557627198103120 ) ) ;
#110759 = CARTESIAN_POINT ( 'NONE',  ( -4.483927247898539470, -16.52544592524342804, 72.29057627198102409 ) ) ;
#110760 = CARTESIAN_POINT ( 'NONE',  ( -12.06949235617739369, -12.14591786802326823, 34.37609039468568284 ) ) ;
#110761 = CARTESIAN_POINT ( 'NONE',  ( 0.05219959533937995610, -21.53943276465977519, 80.00109039468568994 ) ) ;
#110762 = CARTESIAN_POINT ( 'NONE',  ( -13.97604488694527625, -13.89961937509977652, 31.87390960531435979 ) ) ;
#110763 = CARTESIAN_POINT ( 'NONE',  ( -14.34966873604960291, -8.224510206698953496, 21.66557627198102409 ) ) ;
#110764 = CARTESIAN_POINT ( 'NONE',  ( -16.53943276465976808, 0.05219959533911058130, 56.24890960531436690 ) ) ;
#110765 = CARTESIAN_POINT ( 'NONE',  ( 9.474510206698971260, -16.51473224551069308, 47.91557627198102409 ) ) ;
#110766 = CARTESIAN_POINT ( 'NONE',  ( 5.719274019375673035, 21.55341960407619339, 102.2927570613523613 ) ) ;
#110767 = CARTESIAN_POINT ( 'NONE',  ( 10.72451020669898902, -18.67979575497178502, 107.9155762719810241 ) ) ;
#110768 = CARTESIAN_POINT ( 'NONE',  ( -18.62759615963255300, -10.81492255796106328, 69.16775706135234714 ) ) ;
#110769 = CARTESIAN_POINT ( 'NONE',  ( -4.379528057220086978, -16.55341960407618274, 34.79275706135235424 ) ) ;
#110771 = CARTESIAN_POINT ( 'NONE',  ( -18.62759615963255300, -10.81492255796106328, 84.16775706135234714 ) ) ;
#110770 = CARTESIAN_POINT ( 'NONE',  ( 8.224510206698953496, -14.34966873604960469, 77.91557627198102409 ) ) ;
#110772 = CARTESIAN_POINT ( 'NONE',  ( -0.05219959533934338120, 16.53943276465976808, 112.5010903946857042 ) ) ;
#110773 = CARTESIAN_POINT ( 'NONE',  ( -22.49873734152892624, 26.99873734152936677, 1.110912703473986074 ) ) ;
#110774 = CARTESIAN_POINT ( 'NONE',  ( -18.39639308325436673, -5.500000000000039080, 66.48252246182197212 ) ) ;
#110775 = CARTESIAN_POINT ( 'NONE',  ( 16.53943276465976808, -0.05219959533910856209, 38.74890960531435979 ) ) ;
#110776 = CARTESIAN_POINT ( 'NONE',  ( 16.52544592524335698, 4.483927247898782831, 76.45942372801901854 ) ) ;
#110777 = CARTESIAN_POINT ( 'NONE',  ( -19.05341960407611168, -5.049401038298163336, 91.45724293864766707 ) ) ;
#110778 = CARTESIAN_POINT ( 'NONE',  ( -19.05341960407611168, -5.049401038298163336, 96.45724293864769550 ) ) ;
#110779 = CARTESIAN_POINT ( 'NONE',  ( -10.72451020669870658, -18.67979575497194134, 99.58442372801900433 ) ) ;
#110780 = EDGE_CURVE ( 'NONE', #16981, #11758, #46111, .T. ) ;
#110781 = CARTESIAN_POINT ( 'NONE',  ( -8.314922557961024197, 14.29746914071037800, 107.9177570613523471 ) ) ;
#110782 = CARTESIAN_POINT ( 'NONE',  ( -14.29746914071049879, 8.314922557960819915, 70.83224293864770971 ) ) ;
#110783 = CARTESIAN_POINT ( 'NONE',  ( -0.05219959533909027116, -19.03943276465977164, 77.49890960531435269 ) ) ;
#110784 = VERTEX_POINT ( 'NONE', #76942 ) ;
#110785 = CARTESIAN_POINT ( 'NONE',  ( -14.29746914071037622, -8.314922557961029526, 29.16775706135234003 ) ) ;
#110786 = CARTESIAN_POINT ( 'NONE',  ( 5.049401038298161559, -19.05341960407611168, 27.70724293864769550 ) ) ;
#110787 = CARTESIAN_POINT ( 'NONE',  ( -5.153800228976328057, -19.02544592524343514, 97.29057627198099567 ) ) ;
#110789 = CARTESIAN_POINT ( 'NONE',  ( 3.556970738554033499E-15, -38.81732327939057825, -4.124999997268814056 ) ) ;
#110788 = CARTESIAN_POINT ( 'NONE',  ( -4.483927247898782831, 16.52544592524335698, 27.70942372801901854 ) ) ;
#110790 = CARTESIAN_POINT ( 'NONE',  ( -19.02544592524334988, -5.153800228976617603, 38.95942372801900433 ) ) ;
#110791 = CARTESIAN_POINT ( 'NONE',  ( -8.224510206698735004, -14.34966873604973081, 99.58442372801900433 ) ) ;
#110792 = CARTESIAN_POINT ( 'NONE',  ( 13.97604488694548053, -13.89961937509957401, 105.6260903946856757 ) ) ;
#110793 = CARTESIAN_POINT ( 'NONE',  ( -9.564922557960796823, -16.46253265017161027, 27.08224293864769550 ) ) ;
#110794 = CARTESIAN_POINT ( 'NONE',  ( 4.483927247898790824, -16.52544592524335698, 80.20942372801901854 ) ) ;
#110795 = CARTESIAN_POINT ( 'NONE',  ( 16.53943276465976808, 0.05219959533934440121, 61.25109039468567573 ) ) ;
#110796 = DIRECTION ( 'NONE',  ( 0.000000000000000000, 0.000000000000000000, 1.000000000000000000 ) ) ;
#110797 = CARTESIAN_POINT ( 'NONE',  ( -9.564922557961040184, 16.46253265017147172, 62.91775706135233293 ) ) ;
#110798 = CARTESIAN_POINT ( 'NONE',  ( 15.72974639402176855, 15.80617190586768217, 111.8760903946856615 ) ) ;
#110799 = CARTESIAN_POINT ( 'NONE',  ( 16.51473224551069308, 9.474510206698969483, 44.16557627198103120 ) ) ;
#110800 = CARTESIAN_POINT ( 'NONE',  ( -0.05219959533909027116, -19.03943276465977164, 87.49890960531436690 ) ) ;
#110801 = CARTESIAN_POINT ( 'NONE',  ( 8.314922557960818139, 14.29746914071049879, 89.58224293864768129 ) ) ;
#110802 = CARTESIAN_POINT ( 'NONE',  ( 5.153800228976615827, -19.02544592524334988, 55.20942372801899722 ) ) ;
#110803 = CARTESIAN_POINT ( 'NONE',  ( 15.72974639402199770, -15.80617190586745480, 53.12390960531436690 ) ) ;
#110804 = CARTESIAN_POINT ( 'NONE',  ( -10.81492255796105439, 18.62759615963255655, 107.9177570613523471 ) ) ;
#110805 = CARTESIAN_POINT ( 'NONE',  ( 9.564922557960805705, 16.46253265017160317, 89.58224293864769550 ) ) ;
#110806 = CARTESIAN_POINT ( 'NONE',  ( -16.51473224551082808, 9.474510206698731452, 23.33442372801900078 ) ) ;
#110807 = CARTESIAN_POINT ( 'NONE',  ( 18.67979575497178502, 10.72451020669898547, 59.16557627198103120 ) ) ;
#110808 = CARTESIAN_POINT ( 'NONE',  ( 5.153800228976335163, 19.02544592524342804, 109.7905762719810099 ) ) ;
#110809 = CARTESIAN_POINT ( 'NONE',  ( 9.474510206698729675, 16.51473224551082808, 92.08442372801900433 ) ) ;
#110810 = CARTESIAN_POINT ( 'NONE',  ( -17.50000000000014566, 3.417042746626926863, 110.1738039623247545 ) ) ;
#110811 = CARTESIAN_POINT ( 'NONE',  ( 9.564922557961047289, -16.46253265017146816, 110.4177570613523471 ) ) ;
#110812 = CARTESIAN_POINT ( 'NONE',  ( 19.03943276465977164, -0.05219959533909143690, 23.74890960531435269 ) ) ;
#110813 = CARTESIAN_POINT ( 'NONE',  ( -9.474510206698964154, 16.51473224551069663, 85.41557627198102409 ) ) ;
#110814 = CARTESIAN_POINT ( 'NONE',  ( 5.823673210054125526, 21.52544592524343514, 79.79057627198102409 ) ) ;
#110815 = CARTESIAN_POINT ( 'NONE',  ( -14.34966873604972548, 8.224510206698743886, 43.33442372801901143 ) ) ;
#110816 = CARTESIAN_POINT ( 'NONE',  ( 10.72451020669871369, 18.67979575497193778, 47.08442372801901854 ) ) ;
#110817 = CARTESIAN_POINT ( 'NONE',  ( 18.67979575497194134, -10.72451020669871369, 95.83442372801903275 ) ) ;
#110818 = CARTESIAN_POINT ( 'NONE',  ( 4.483927247898790824, -16.52544592524335698, 90.20942372801903275 ) ) ;
#110819 = AXIS2_PLACEMENT_3D ( 'NONE', #140487, #136517, #169835 ) ;
#110820 = CARTESIAN_POINT ( 'NONE',  ( -0.05219959533909027116, -19.03943276465977164, 82.49890960531436690 ) ) ;
#110821 = CARTESIAN_POINT ( 'NONE',  ( 4.483927247898545687, 16.52544592524342804, 89.79057627198103830 ) ) ;
#110822 = CARTESIAN_POINT ( 'NONE',  ( 8.224510206698953496, -14.34966873604960469, 42.91557627198103120 ) ) ;
#110823 = CARTESIAN_POINT ( 'NONE',  ( -5.049401038297874678, -19.05341960407617918, 74.79275706135231871 ) ) ;
#110824 = CARTESIAN_POINT ( 'NONE',  ( -18.67979575497193778, 10.72451020669871902, 48.33442372801902565 ) ) ;
#110825 = CARTESIAN_POINT ( 'NONE',  ( -5.153800228976607833, 19.02544592524334988, 27.70942372801899722 ) ) ;
#110826 = CARTESIAN_POINT ( 'NONE',  ( -8.314922557960811034, -14.29746914071050412, 87.08224293864769550 ) ) ;
#110827 = CARTESIAN_POINT ( 'NONE',  ( 19.02544592524343514, -5.153800228976328945, 108.5405762719810383 ) ) ;
#110828 = CARTESIAN_POINT ( 'NONE',  ( 16.55341960407611168, 4.379528057220329451, 28.95724293864769905 ) ) ;
#110829 = CARTESIAN_POINT ( 'NONE',  ( -18.62759615963255300, -10.81492255796106328, 84.16775706135234714 ) ) ;
#110830 = CARTESIAN_POINT ( 'NONE',  ( -14.29746914071037622, -8.314922557961029526, 54.16775706135235424 ) ) ;
#110831 = CARTESIAN_POINT ( 'NONE',  ( 16.53943276465976808, 0.05219959533934440121, 111.2510903946856899 ) ) ;
#110832 = CARTESIAN_POINT ( 'NONE',  ( 5.823673210054444382, -21.52544592524334988, 50.20942372801901854 ) ) ;
#110833 = VERTEX_POINT ( 'NONE', #61763 ) ;
#110834 = CARTESIAN_POINT ( 'NONE',  ( -10.72451020669870658, -18.67979575497194134, 34.58442372801900433 ) ) ;
#110835 = CARTESIAN_POINT ( 'NONE',  ( 4.483927247898545687, 16.52544592524342804, 109.7905762719810383 ) ) ;
#110836 = CARTESIAN_POINT ( 'NONE',  ( -21.38418241377623374, -7.427326039334300134, 174.4773576836617224 ) ) ;
#110837 = CARTESIAN_POINT ( 'NONE',  ( -12.14591786802309592, -12.06949235617757132, 71.87390960531438111 ) ) ;
#110838 = CARTESIAN_POINT ( 'NONE',  ( 16.46253265017160672, -9.564922557960803928, 78.33224293864769550 ) ) ;
#110839 = CARTESIAN_POINT ( 'NONE',  ( -14.34966873604972548, 8.224510206698743886, 103.3344237280190043 ) ) ;
#110840 = CARTESIAN_POINT ( 'NONE',  ( -5.049401038298153566, 19.05341960407611168, 35.20724293864768839 ) ) ;
#110841 = CARTESIAN_POINT ( 'NONE',  ( 21.52544592524344225, -5.823673210054117533, 58.54057627198103120 ) ) ;
#110842 = CARTESIAN_POINT ( 'NONE',  ( -16.53943276465976808, 0.05219959533911058130, 96.24890960531435269 ) ) ;
#110843 = CARTESIAN_POINT ( 'NONE',  ( -18.67979575497178146, -10.72451020669898902, 96.66557627198102409 ) ) ;
#110844 = CARTESIAN_POINT ( 'NONE',  ( -5.049401038298153566, 19.05341960407611168, 105.2072429386476671 ) ) ;
#110846 = CARTESIAN_POINT ( 'NONE',  ( -9.564922557961040184, 16.46253265017147172, 92.91775706135233293 ) ) ;
#110845 = CARTESIAN_POINT ( 'NONE',  ( -9.564922557960796823, -16.46253265017161027, 52.08224293864768839 ) ) ;
#110847 = CARTESIAN_POINT ( 'NONE',  ( -18.62759615963270932, 10.81492255796079327, 40.83224293864769550 ) ) ;
#110848 = CARTESIAN_POINT ( 'NONE',  ( 21.52544592524334988, 5.823673210054432836, 66.45942372801903275 ) ) ;
#110849 = CARTESIAN_POINT ( 'NONE',  ( 16.46253265017160672, -9.564922557960803928, 53.33224293864768839 ) ) ;
#110850 = CARTESIAN_POINT ( 'NONE',  ( -5.049401038298153566, 19.05341960407611168, 90.20724293864766707 ) ) ;
#110851 = CARTESIAN_POINT ( 'NONE',  ( -16.52544592524335698, -4.483927247898792601, 63.95942372801901854 ) ) ;
#110852 = CARTESIAN_POINT ( 'NONE',  ( 15.72974639402176855, 15.80617190586768217, 41.87609039468568284 ) ) ;
#110853 = CARTESIAN_POINT ( 'NONE',  ( 21.55341960407619695, -5.719274019375665929, 91.04275706135236135 ) ) ;
#110854 = CARTESIAN_POINT ( 'NONE',  ( -5.719274019375978568, 21.55341960407610458, 105.2072429386477097 ) ) ;
#110856 = CARTESIAN_POINT ( 'NONE',  ( 12.14591786802327356, -12.06949235617739191, 60.62609039468567573 ) ) ;
#110855 = CARTESIAN_POINT ( 'NONE',  ( -21.52544592524334988, -5.823673210054445271, 43.95942372801902565 ) ) ;
#110857 = CARTESIAN_POINT ( 'NONE',  ( 10.81492255796078972, 18.62759615963270932, 69.58224293864769550 ) ) ;
#110858 = CARTESIAN_POINT ( 'NONE',  ( -5.049401038297874678, -19.05341960407617918, 29.79275706135232227 ) ) ;
#110860 = CARTESIAN_POINT ( 'NONE',  ( 12.14591786802327356, -12.06949235617739191, 110.6260903946857042 ) ) ;
#110859 = CARTESIAN_POINT ( 'NONE',  ( 19.02544592524343514, -5.153800228976328945, 73.54057627198103830 ) ) ;
#110861 = CARTESIAN_POINT ( 'NONE',  ( 32.00000000000000000, -1.163414459189985801E-14, 95.00000000000000000 ) ) ;
#110862 = CARTESIAN_POINT ( 'NONE',  ( -16.51473224551069308, -9.474510206698971260, 101.6655762719810241 ) ) ;
#110863 = DIRECTION ( 'NONE',  ( 0.000000000000000000, 0.000000000000000000, -1.000000000000000000 ) ) ;
#110864 = CARTESIAN_POINT ( 'NONE',  ( 5.153800228976615827, -19.02544592524334988, 85.20942372801900433 ) ) ;
#110865 = CARTESIAN_POINT ( 'NONE',  ( -15.80617190586745835, -15.72974639402198527, 61.87390960531436690 ) ) ;
#110866 = CARTESIAN_POINT ( 'NONE',  ( 16.52544592524342804, -4.483927247898539470, 33.54057627198102409 ) ) ;
#110867 = CARTESIAN_POINT ( 'NONE',  ( 4.379528057220092307, 16.55341960407617563, 22.29275706135235069 ) ) ;
#110868 = CARTESIAN_POINT ( 'NONE',  ( 0.05219959533909260263, 19.03943276465977164, 34.99890960531435979 ) ) ;
#110869 = CARTESIAN_POINT ( 'NONE',  ( 16.53943276465976808, 0.05219959533934440121, 21.25109039468567218 ) ) ;
#110871 = CARTESIAN_POINT ( 'NONE',  ( 16.51473224551083163, -9.474510206698727899, 65.83442372801900433 ) ) ;
#110870 = CARTESIAN_POINT ( 'NONE',  ( 5.823673210054125526, 21.52544592524343514, 89.79057627198103830 ) ) ;
#110872 = CARTESIAN_POINT ( 'NONE',  ( -16.53943276465976808, -0.05219959533934237506, 83.75109039468568994 ) ) ;
#110873 = CARTESIAN_POINT ( 'NONE',  ( 5.153800228976335163, 19.02544592524342804, 74.79057627198103830 ) ) ;
#110874 = CARTESIAN_POINT ( 'NONE',  ( 8.224510206698953496, -14.34966873604960469, 72.91557627198103830 ) ) ;
#110875 = CARTESIAN_POINT ( 'NONE',  ( 9.564922557960805705, 16.46253265017160317, 44.58224293864769550 ) ) ;
#110876 = CARTESIAN_POINT ( 'NONE',  ( 16.52544592524342804, -4.483927247898539470, 53.54057627198103120 ) ) ;
#110877 = CARTESIAN_POINT ( 'NONE',  ( -27.86473085795038429, -129.0000000000000000, -13.99999999999999822 ) ) ;
#110878 = CARTESIAN_POINT ( 'NONE',  ( 32.63052366545710470, -0.9798963808689128419, 87.54781425814060469 ) ) ;
#110879 = CARTESIAN_POINT ( 'NONE',  ( 16.55341960407611168, 4.379528057220329451, 23.95724293864769550 ) ) ;
#110880 = CARTESIAN_POINT ( 'NONE',  ( -0.05219959533909027116, -19.03943276465977164, 82.49890960531436690 ) ) ;
#110881 = FACE_OUTER_BOUND ( 'NONE', #12531, .T. ) ;
#110882 = CARTESIAN_POINT ( 'NONE',  ( 9.474510206698729675, 16.51473224551082808, 37.08442372801899722 ) ) ;
#110883 = CARTESIAN_POINT ( 'NONE',  ( -4.483927247898782831, 16.52544592524335698, 47.70942372801902565 ) ) ;
#110884 = CARTESIAN_POINT ( 'NONE',  ( 18.67979575497178502, 10.72451020669898547, 59.16557627198103120 ) ) ;
#110885 = CARTESIAN_POINT ( 'NONE',  ( 16.51473224551083163, -9.474510206698727899, 20.83442372801899722 ) ) ;
#110886 = CARTESIAN_POINT ( 'NONE',  ( 19.03943276465977164, -0.05219959533909143690, 68.74890960531436690 ) ) ;
#110887 = CARTESIAN_POINT ( 'NONE',  ( -22.55670631985108443, -22.55670631985069008, -45.64921306006598201 ) ) ;
#110888 = CARTESIAN_POINT ( 'NONE',  ( -19.02544592524342804, 5.153800228976336051, 111.0405762719810099 ) ) ;
#110889 = CARTESIAN_POINT ( 'NONE',  ( 18.62759615963255655, 10.81492255796105972, 41.66775706135235424 ) ) ;
#110890 = CARTESIAN_POINT ( 'NONE',  ( -12.14591786802309592, -12.06949235617757132, 106.8739096053143811 ) ) ;
#110893 = EDGE_LOOP ( 'NONE', ( #153664, #114582, #83259, #175632 ) ) ;
#110892 = CARTESIAN_POINT ( 'NONE',  ( -19.02544592524342804, 5.153800228976336051, 76.04057627198102409 ) ) ;
#110891 = CARTESIAN_POINT ( 'NONE',  ( 5.823673210054125526, 21.52544592524343514, 94.79057627198105251 ) ) ;
#110894 = CARTESIAN_POINT ( 'NONE',  ( 10.72451020669871369, 18.67979575497193778, 27.08442372801901854 ) ) ;
#110895 = ORIENTED_EDGE ( 'NONE', *, *, #54327, .T. ) ;
#110896 = CARTESIAN_POINT ( 'NONE',  ( -5.153800228976328057, -19.02544592524343514, 87.29057627198103830 ) ) ;
#110897 = CYLINDRICAL_SURFACE ( 'NONE', #20452, 2.000000000000001776 ) ;
#110898 = CARTESIAN_POINT ( 'NONE',  ( 19.02544592524343514, -5.153800228976328945, 33.54057627198102409 ) ) ;
#110899 = CARTESIAN_POINT ( 'NONE',  ( 13.97604488694548053, -13.89961937509957401, 105.6260903946856757 ) ) ;
#110900 = CARTESIAN_POINT ( 'NONE',  ( 36.91746824999999177, 2.880721459617395097E-14, -8.124999997268814056 ) ) ;
#110901 = CARTESIAN_POINT ( 'NONE',  ( 4.483927247898545687, 16.52544592524342804, 109.7905762719810383 ) ) ;
#110902 = CARTESIAN_POINT ( 'NONE',  ( -15.72974639402176322, -15.80617190586768395, 89.37609039468568994 ) ) ;
#110904 = CARTESIAN_POINT ( 'NONE',  ( -10.81492255796105439, 18.62759615963255655, 47.91775706135234714 ) ) ;
#110903 = CARTESIAN_POINT ( 'NONE',  ( 13.97604488694527802, 13.89961937509977652, 79.37390960531435269 ) ) ;
#110905 = CARTESIAN_POINT ( 'NONE',  ( -10.81492255796105439, 18.62759615963255655, 22.91775706135235069 ) ) ;
#110906 = CARTESIAN_POINT ( 'NONE',  ( 8.906447517083050158, 27.41122689804195645, 149.4000000000000057 ) ) ;
#110907 = CARTESIAN_POINT ( 'NONE',  ( 19.02544592524343514, -5.153800228976328945, 83.54057627198100988 ) ) ;
#110908 = DIRECTION ( 'NONE',  ( 1.000000000000000000, 0.000000000000000000, 0.000000000000000000 ) ) ;
#110910 = CARTESIAN_POINT ( 'NONE',  ( -10.72451020669898014, 18.67979575497178502, 50.41557627198103120 ) ) ;
#110909 = CARTESIAN_POINT ( 'NONE',  ( -14.29746914071037622, -8.314922557961029526, 44.16775706135234714 ) ) ;
#110911 = CARTESIAN_POINT ( 'NONE',  ( 5.719274019375673035, 21.55341960407619339, 82.29275706135234714 ) ) ;
#110912 = CARTESIAN_POINT ( 'NONE',  ( 3.882744257519136433, 5.184702103851150490, -62.44399821614913293 ) ) ;
#110913 = CARTESIAN_POINT ( 'NONE',  ( 16.51473224551083163, -9.474510206698727899, 110.8344237280190043 ) ) ;
#110914 = CARTESIAN_POINT ( 'NONE',  ( 13.97604488694527802, 13.89961937509977652, 54.37390960531435979 ) ) ;
#110915 = CARTESIAN_POINT ( 'NONE',  ( -9.474510206698964154, 16.51473224551069663, 80.41557627198103830 ) ) ;
#110916 = CARTESIAN_POINT ( 'NONE',  ( 8.224510206698953496, -14.34966873604960469, 102.9155762719810383 ) ) ;
#110917 = CARTESIAN_POINT ( 'NONE',  ( -12.06949235617756955, 12.14591786802309770, 110.6239096053143669 ) ) ;
#110918 = CARTESIAN_POINT ( 'NONE',  ( -16.46253265017160317, 9.564922557960807481, 110.8322429386476955 ) ) ;
#110919 = CARTESIAN_POINT ( 'NONE',  ( 16.52544592524335698, 4.483927247898782831, 81.45942372801900433 ) ) ;
#110921 = CARTESIAN_POINT ( 'NONE',  ( 9.474510206698971260, -16.51473224551069308, 57.91557627198103120 ) ) ;
#110920 = CARTESIAN_POINT ( 'NONE',  ( -16.53943276465976808, 0.05219959533911058130, 56.24890960531436690 ) ) ;
#110922 = CARTESIAN_POINT ( 'NONE',  ( -18.67979575497193778, 10.72451020669871902, 83.33442372801903275 ) ) ;
#110923 = CARTESIAN_POINT ( 'NONE',  ( 10.81492255796106328, -18.62759615963255655, 75.41775706135233293 ) ) ;
#110924 = CARTESIAN_POINT ( 'NONE',  ( -9.474510206698720793, -16.51473224551083518, 89.58442372801900433 ) ) ;
#110925 = CARTESIAN_POINT ( 'NONE',  ( 0.05219959533910956823, 16.53943276465976808, 64.99890960531435269 ) ) ;
#110926 = CARTESIAN_POINT ( 'NONE',  ( 5.823673210054125526, 21.52544592524343514, 114.7905762719810383 ) ) ;
#110927 = CARTESIAN_POINT ( 'NONE',  ( -21.52544592524343514, 5.823673210054127303, 66.04057627198103830 ) ) ;
#110928 = CARTESIAN_POINT ( 'NONE',  ( -28.82186960331499037, 2.428612866367529932E-14, 139.9999999999999716 ) ) ;
#110929 = CARTESIAN_POINT ( 'NONE',  ( 17.81289503416610742, 24.51734667627700404, 141.5500000054623797 ) ) ;
#110930 = CARTESIAN_POINT ( 'NONE',  ( 16.51473224551069308, 9.474510206698969483, 74.16557627198103830 ) ) ;
#110931 = CARTESIAN_POINT ( 'NONE',  ( -14.34966873604960291, -8.224510206698953496, 36.66557627198103120 ) ) ;
#110932 = CARTESIAN_POINT ( 'NONE',  ( -0.05219959533934338120, 16.53943276465976808, 112.5010903946857042 ) ) ;
#110933 = CARTESIAN_POINT ( 'NONE',  ( 16.53943276465976808, 0.05219959533934440121, 101.2510903946856757 ) ) ;
#110934 = CARTESIAN_POINT ( 'NONE',  ( -13.89961937509957401, -13.97604488694547875, 49.37609039468567573 ) ) ;
#110935 = CARTESIAN_POINT ( 'NONE',  ( -38.00000000000000711, 12.34694845685046438, -8.099999999999997868 ) ) ;
#110936 = CARTESIAN_POINT ( 'NONE',  ( -16.46253265017160317, 9.564922557960807481, 85.83224293864769550 ) ) ;
#110937 = CARTESIAN_POINT ( 'NONE',  ( 4.379528057220339221, -16.55341960407611168, 57.70724293864770260 ) ) ;
#110939 = CARTESIAN_POINT ( 'NONE',  ( -9.474510206698964154, 16.51473224551069663, 115.4155762719810241 ) ) ;
#110938 = CARTESIAN_POINT ( 'NONE',  ( 16.38665767535053419, -7.295008042176110763, 102.7640086421455123 ) ) ;
#110941 = ORIENTED_EDGE ( 'NONE', *, *, #197763, .T. ) ;
#110940 = CARTESIAN_POINT ( 'NONE',  ( -18.62759615963270932, 10.81492255796079327, 55.83224293864770260 ) ) ;
#110942 = CARTESIAN_POINT ( 'NONE',  ( -4.483927247898539470, -16.52544592524342804, 92.29057627198103830 ) ) ;
#110943 = CARTESIAN_POINT ( 'NONE',  ( 12.14591786802327356, -12.06949235617739191, 50.62609039468568994 ) ) ;
#110944 = CARTESIAN_POINT ( 'NONE',  ( -8.224510206698948167, 14.34966873604960824, 85.41557627198102409 ) ) ;
#110945 = CARTESIAN_POINT ( 'NONE',  ( 5.000000000000000888, -130.0000000000000000, -13.99999999999999822 ) ) ;
#110946 = CARTESIAN_POINT ( 'NONE',  ( 13.97604488694548053, -13.89961937509957401, 75.62609039468564731 ) ) ;
#110947 = CARTESIAN_POINT ( 'NONE',  ( -5.823673210054116645, -21.52544592524344225, 27.29057627198103120 ) ) ;
#110948 = CARTESIAN_POINT ( 'NONE',  ( 36.91746824999999177, 2.880721459617395097E-14, -6.124999997268813168 ) ) ;
#110949 = CARTESIAN_POINT ( 'NONE',  ( -16.51473224551069308, -9.474510206698971260, 41.66557627198103120 ) ) ;
#110951 = CARTESIAN_POINT ( 'NONE',  ( -16.53943276465976808, 0.05219959533911058130, 36.24890960531435979 ) ) ;
#110950 = CARTESIAN_POINT ( 'NONE',  ( -4.483927247898782831, 16.52544592524335698, 32.70942372801900433 ) ) ;
#110952 = CARTESIAN_POINT ( 'NONE',  ( -21.55341960407610458, -5.719274019375992779, 61.45724293864770260 ) ) ;
#110954 = CARTESIAN_POINT ( 'NONE',  ( 16.51473224551083163, -9.474510206698727899, 90.83442372801900433 ) ) ;
#110953 = AXIS2_PLACEMENT_3D ( 'NONE', #192245, #100218, #8218 ) ;
#110955 = CARTESIAN_POINT ( 'NONE',  ( -15.72974639402197994, 15.80617190586746368, 45.62390960531436690 ) ) ;
#110956 = CARTESIAN_POINT ( 'NONE',  ( -10.81492255796105439, 18.62759615963255655, 77.91775706135231871 ) ) ;
#110957 = CARTESIAN_POINT ( 'NONE',  ( 18.27284445343954289, -33.31360383038287409, -25.98075878691503959 ) ) ;
#110958 = CARTESIAN_POINT ( 'NONE',  ( -4.379528057220086978, -16.55341960407618274, 29.79275706135234358 ) ) ;
#110960 = CARTESIAN_POINT ( 'NONE',  ( 19.05341960407611168, 5.049401038298154454, 83.95724293864766707 ) ) ;
#110959 = CARTESIAN_POINT ( 'NONE',  ( -16.46253265017160317, 9.564922557960807481, 40.83224293864769550 ) ) ;
#110961 = CARTESIAN_POINT ( 'NONE',  ( -5.153800228976328057, -19.02544592524343514, 37.29057627198102409 ) ) ;
#110962 = CARTESIAN_POINT ( 'NONE',  ( -12.06949235617756955, 12.14591786802309770, 105.6239096053143669 ) ) ;
#110963 = APPLICATION_PROTOCOL_DEFINITION ( 'draft international standard', 'automotive_design', 1998, #88162 ) ;
#110964 = CARTESIAN_POINT ( 'NONE',  ( -19.03943276465977164, 0.05219959533909376836, 106.2489096053143669 ) ) ;
#110965 = ORIENTED_EDGE ( 'NONE', *, *, #76057, .F. ) ;
#110966 = CARTESIAN_POINT ( 'NONE',  ( 12.06949235617739724, 12.14591786802326823, 61.87609039468568284 ) ) ;
#110967 = CARTESIAN_POINT ( 'NONE',  ( -18.62759615963270932, 10.81492255796079327, 85.83224293864768129 ) ) ;
#110968 = CARTESIAN_POINT ( 'NONE',  ( 9.564922557960805705, 16.46253265017160317, 49.58224293864770260 ) ) ;
#110970 = CARTESIAN_POINT ( 'NONE',  ( -21.52544592524334988, -5.823673210054445271, 23.95942372801901143 ) ) ;
#110969 = CARTESIAN_POINT ( 'NONE',  ( -19.03943276465977164, -0.05219959533935918106, 78.75109039468567573 ) ) ;
#110971 = CARTESIAN_POINT ( 'NONE',  ( 9.474510206698971260, -16.51473224551069308, 77.91557627198103830 ) ) ;
#110972 = CARTESIAN_POINT ( 'NONE',  ( -13.97604488694527625, -13.89961937509977652, 106.8739096053143669 ) ) ;
#110973 = ORIENTED_EDGE ( 'NONE', *, *, #177696, .T. ) ;
#110974 = CARTESIAN_POINT ( 'NONE',  ( -16.52544592524335698, -4.483927247898792601, 33.95942372801901143 ) ) ;
#110975 = CARTESIAN_POINT ( 'NONE',  ( 21.53943276465977519, -0.05219959533907433946, 113.7489096053143527 ) ) ;
#110978 = CARTESIAN_POINT ( 'NONE',  ( 16.46253265017146816, 9.564922557961045513, 76.66775706135234714 ) ) ;
#110977 = CARTESIAN_POINT ( 'NONE',  ( 13.89961937509977652, -13.97604488694527269, 93.12390960531436690 ) ) ;
#110976 = CARTESIAN_POINT ( 'NONE',  ( -8.314922557960811034, -14.29746914071050412, 107.0822429386476955 ) ) ;
#110979 = CARTESIAN_POINT ( 'NONE',  ( 19.02544592524334988, 5.153800228976608722, 31.45942372801900433 ) ) ;
#110980 = CARTESIAN_POINT ( 'NONE',  ( 10.81492255796078972, 18.62759615963270932, 89.58224293864768129 ) ) ;
#110981 = CARTESIAN_POINT ( 'NONE',  ( 0.05219959533936267826, -19.03943276465977164, 25.00109039468566152 ) ) ;
#110982 = CARTESIAN_POINT ( 'NONE',  ( 16.52544592524335698, 4.483927247898782831, 81.45942372801900433 ) ) ;
#110983 = CARTESIAN_POINT ( 'NONE',  ( 16.46253265017160672, -9.564922557960803928, 103.3322429386476955 ) ) ;
#110984 = CARTESIAN_POINT ( 'NONE',  ( 19.03943276465977164, -0.05219959533909143690, 48.74890960531435979 ) ) ;
#110985 = CARTESIAN_POINT ( 'NONE',  ( -21.53943276465977519, -0.05219959533937600094, 53.75109039468568994 ) ) ;
#110986 = EDGE_CURVE ( 'NONE', #179364, #16960, #130072, .T. ) ;
#110987 = CARTESIAN_POINT ( 'NONE',  ( -10.81492255796105439, 18.62759615963255655, 62.91775706135236135 ) ) ;
#110988 = CARTESIAN_POINT ( 'NONE',  ( 13.97604488694527802, 13.89961937509977652, 74.37390960531436690 ) ) ;
#110989 = CARTESIAN_POINT ( 'NONE',  ( -15.72974639402176322, -15.80617190586768395, 54.37609039468568994 ) ) ;
#110990 = CARTESIAN_POINT ( 'NONE',  ( -9.564922557961040184, 16.46253265017147172, 92.91775706135233293 ) ) ;
#110991 = CARTESIAN_POINT ( 'NONE',  ( -9.474510206698964154, 16.51473224551069663, 50.41557627198102409 ) ) ;
#110992 = CARTESIAN_POINT ( 'NONE',  ( 4.379528057220092307, 16.55341960407617563, 92.29275706135236135 ) ) ;
#110993 = CARTESIAN_POINT ( 'NONE',  ( 16.51473224551069308, 9.474510206698969483, 69.16557627198102409 ) ) ;
#110994 = FACE_OUTER_BOUND ( 'NONE', #128745, .T. ) ;
#110995 = CARTESIAN_POINT ( 'NONE',  ( -16.51473224551069308, -9.474510206698971260, 51.66557627198102409 ) ) ;
#110996 = CARTESIAN_POINT ( 'NONE',  ( 21.52544592524344225, -5.823673210054117533, 88.54057627198103830 ) ) ;
#110997 = CARTESIAN_POINT ( 'NONE',  ( 4.379528057220092307, 16.55341960407617563, 72.29275706135236135 ) ) ;
#110998 = CARTESIAN_POINT ( 'NONE',  ( -19.49401214000077687, 12.39993551617566681, 167.9999999999999716 ) ) ;
#110999 = CARTESIAN_POINT ( 'NONE',  ( 5.153800228976615827, -19.02544592524334988, 25.20942372801900433 ) ) ;
#111000 = CARTESIAN_POINT ( 'NONE',  ( -19.05341960407611168, -5.049401038298163336, 71.45724293864766707 ) ) ;
#111001 = CARTESIAN_POINT ( 'NONE',  ( -14.34966873604960291, -8.224510206698953496, 61.66557627198103120 ) ) ;
#111002 = CARTESIAN_POINT ( 'NONE',  ( -0.05219959533910754901, -16.53943276465976808, 97.49890960531436690 ) ) ;
#111003 = CARTESIAN_POINT ( 'NONE',  ( -9.474510206698964154, 16.51473224551069663, 95.41557627198102409 ) ) ;
#111004 = CARTESIAN_POINT ( 'NONE',  ( -5.153800228976328057, -19.02544592524343514, 92.29057627198099567 ) ) ;
#111005 = CARTESIAN_POINT ( 'NONE',  ( 21.52544592524334988, 5.823673210054432836, 46.45942372801901854 ) ) ;
#111006 = CARTESIAN_POINT ( 'NONE',  ( 19.03943276465977164, -0.05219959533909143690, 103.7489096053143669 ) ) ;
#111007 = CARTESIAN_POINT ( 'NONE',  ( 21.53943276465977519, 0.05219959533937863772, 111.2510903946856899 ) ) ;
#111008 = CARTESIAN_POINT ( 'NONE',  ( 0.05219959533934541429, -16.53943276465976808, 75.00109039468568994 ) ) ;
#111009 = CARTESIAN_POINT ( 'NONE',  ( 15.80617190586769283, -15.72974639402175789, 40.62609039468567573 ) ) ;
#111010 = CARTESIAN_POINT ( 'NONE',  ( -5.719274019375978568, 21.55341960407610458, 35.20724293864768839 ) ) ;
#111011 = CARTESIAN_POINT ( 'NONE',  ( -18.67979575497178146, -10.72451020669898902, 96.66557627198102409 ) ) ;
#111012 = CARTESIAN_POINT ( 'NONE',  ( -16.55341960407611168, -4.379528057220339221, 66.45724293864768129 ) ) ;
#111013 = CARTESIAN_POINT ( 'NONE',  ( 13.89961937509977652, -13.97604488694527269, 58.12390960531436690 ) ) ;
#111014 = CARTESIAN_POINT ( 'NONE',  ( 16.53943276465976808, -0.05219959533910856209, 78.74890960531436690 ) ) ;
#111015 = CARTESIAN_POINT ( 'NONE',  ( 18.62759615963271287, -10.81492255796078972, 38.33224293864768839 ) ) ;
#111016 = CARTESIAN_POINT ( 'NONE',  ( 0.05219959533936267826, -19.03943276465977164, 40.00109039468566152 ) ) ;
#111017 = EDGE_CURVE ( 'NONE', #78316, #658, #64083, .T. ) ;
#111018 = CARTESIAN_POINT ( 'NONE',  ( -12.06949235617756955, 12.14591786802309770, 110.6239096053143669 ) ) ;
#111019 = ORIENTED_EDGE ( 'NONE', *, *, #176927, .F. ) ;
#111020 = CARTESIAN_POINT ( 'NONE',  ( -8.314922557961024197, 14.29746914071037800, 72.91775706135234714 ) ) ;
#111021 = CARTESIAN_POINT ( 'NONE',  ( 13.97604488694527802, 13.89961937509977652, 64.37390960531436690 ) ) ;
#111022 = CARTESIAN_POINT ( 'NONE',  ( 8.571926809382603096, -26.38167802310801235, 141.4750000027312069 ) ) ;
#111023 = CARTESIAN_POINT ( 'NONE',  ( -14.29746914071049879, 8.314922557960819915, 85.83224293864768129 ) ) ;
#111024 = CARTESIAN_POINT ( 'NONE',  ( -21.55341960407610458, -5.719274019375992779, 36.45724293864768839 ) ) ;
#111025 = VERTEX_POINT ( 'NONE', #141602 ) ;
#111026 = CARTESIAN_POINT ( 'NONE',  ( -8.224510206698735004, -14.34966873604973081, 109.5844237280190328 ) ) ;
#111027 = CARTESIAN_POINT ( 'NONE',  ( 5.049401038297881783, 19.05341960407617563, 107.2927570613523187 ) ) ;
#111028 = CARTESIAN_POINT ( 'NONE',  ( 21.52544592524334988, 5.823673210054432836, 81.45942372801900433 ) ) ;
#111029 = CARTESIAN_POINT ( 'NONE',  ( -19.02544592524342804, 5.153800228976336051, 91.04057627198100988 ) ) ;
#111030 = CARTESIAN_POINT ( 'NONE',  ( 5.823673210054125526, 21.52544592524343514, 99.79057627198103830 ) ) ;
#111031 = CARTESIAN_POINT ( 'NONE',  ( 4.483927247898790824, -16.52544592524335698, 50.20942372801901854 ) ) ;
#111032 = CARTESIAN_POINT ( 'NONE',  ( -19.03943276465977164, 0.05219959533909376836, 26.24890960531435624 ) ) ;
#111033 = CARTESIAN_POINT ( 'NONE',  ( -16.53943276465976808, -0.05219959533934237506, 33.75109039468568284 ) ) ;
#111034 = CARTESIAN_POINT ( 'NONE',  ( -19.05341960407617563, 5.049401038297882671, 93.54275706135234714 ) ) ;
#111035 = CIRCLE ( 'NONE', #62535, 69.99999999999997158 ) ;
#111036 = CARTESIAN_POINT ( 'NONE',  ( -0.05219959533907301413, -21.53943276465977519, 87.49890960531436690 ) ) ;
#111037 = CARTESIAN_POINT ( 'NONE',  ( -13.89961937509957401, -13.97604488694547875, 54.37609039468565442 ) ) ;
#111038 = LINE ( 'NONE', #64545, #67107 ) ;
#111039 = CARTESIAN_POINT ( 'NONE',  ( 21.52544592524344225, -5.823673210054117533, 103.5405762719810383 ) ) ;
#111040 = LINE ( 'NONE', #61546, #49871 ) ;
#111041 = CARTESIAN_POINT ( 'NONE',  ( 19.05341960407611168, 5.049401038298154454, 73.95724293864768129 ) ) ;
#111042 = CARTESIAN_POINT ( 'NONE',  ( -4.483927247898782831, 16.52544592524335698, 37.70942372801900433 ) ) ;
#111043 = CARTESIAN_POINT ( 'NONE',  ( 5.000000000000000000, -130.0000000000000000, 12.99999999999999822 ) ) ;
#111044 = CARTESIAN_POINT ( 'NONE',  ( -5.049401038297874678, -19.05341960407617918, 64.79275706135233293 ) ) ;
#111046 = CARTESIAN_POINT ( 'NONE',  ( 4.483927247898545687, 16.52544592524342804, 64.79057627198103830 ) ) ;
#111045 = CARTESIAN_POINT ( 'NONE',  ( 18.62759615963255655, 10.81492255796105972, 21.66775706135235069 ) ) ;
#111047 = CARTESIAN_POINT ( 'NONE',  ( 9.474510206698971260, -16.51473224551069308, 72.91557627198102409 ) ) ;
#111049 = CARTESIAN_POINT ( 'NONE',  ( -13.89961937509957401, -13.97604488694547875, 39.37609039468566152 ) ) ;
#111048 = CARTESIAN_POINT ( 'NONE',  ( -14.34966873604972548, 8.224510206698743886, 38.33442372801900433 ) ) ;
#111050 = CARTESIAN_POINT ( 'NONE',  ( 15.72974639402176855, 15.80617190586768217, 56.87609039468568994 ) ) ;
#111051 = CARTESIAN_POINT ( 'NONE',  ( 0.05219959533934541429, -16.53943276465976808, 20.00109039468568639 ) ) ;
#111052 = CARTESIAN_POINT ( 'NONE',  ( 13.97604488694527802, 13.89961937509977652, 49.37390960531434558 ) ) ;
#111053 = CARTESIAN_POINT ( 'NONE',  ( -9.474510206698720793, -16.51473224551083518, 84.58442372801900433 ) ) ;
#111054 = CARTESIAN_POINT ( 'NONE',  ( -21.53943276465977519, -0.05219959533937600094, 88.75109039468567573 ) ) ;
#111055 = CARTESIAN_POINT ( 'NONE',  ( -19.03943276465977164, -0.05219959533935918106, 68.75109039468566152 ) ) ;
#111056 = CARTESIAN_POINT ( 'NONE',  ( -0.05219959533909027116, -19.03943276465977164, 37.49890960531436690 ) ) ;
#111057 = CARTESIAN_POINT ( 'NONE',  ( -21.55341960407610458, -5.719274019375992779, 51.45724293864770260 ) ) ;
#111059 = CARTESIAN_POINT ( 'NONE',  ( 16.51473224551083163, -9.474510206698727899, 70.83442372801900433 ) ) ;
#111058 = CARTESIAN_POINT ( 'NONE',  ( -12.14591786802309592, -12.06949235617757132, 66.87390960531436690 ) ) ;
#111060 = CARTESIAN_POINT ( 'NONE',  ( -16.31925111598458500, -7.325300261831428905, 24.83575461032751264 ) ) ;
#111061 = CARTESIAN_POINT ( 'NONE',  ( 19.03943276465977164, 0.05219959533936151252, 31.25109039468566863 ) ) ;
#111062 = CARTESIAN_POINT ( 'NONE',  ( 16.55341960407618274, -4.379528057220086978, 101.0427570613523756 ) ) ;
#111063 = CARTESIAN_POINT ( 'NONE',  ( 16.53943276465976808, -0.05219959533910856209, 53.74890960531437401 ) ) ;
#111065 = CARTESIAN_POINT ( 'NONE',  ( -8.571926809382601320, -26.38167802310801591, 141.2750000027311899 ) ) ;
#111064 = CARTESIAN_POINT ( 'NONE',  ( 21.55341960407619695, -5.719274019375665929, 91.04275706135236135 ) ) ;
#111066 = CARTESIAN_POINT ( 'NONE',  ( -21.55341960407610458, -5.719274019375992779, 101.4572429386476955 ) ) ;
#111067 = CARTESIAN_POINT ( 'NONE',  ( -5.153800228976328057, -19.02544592524343514, 57.29057627198103120 ) ) ;
#111068 = CARTESIAN_POINT ( 'NONE',  ( 18.62759615963255655, 10.81492255796105972, 71.66775706135234714 ) ) ;
#111069 = CARTESIAN_POINT ( 'NONE',  ( -5.049401038298153566, 19.05341960407611168, 45.20724293864769550 ) ) ;
#111070 = ORIENTED_EDGE ( 'NONE', *, *, #17592, .T. ) ;
#111071 = CARTESIAN_POINT ( 'NONE',  ( 0.05219959533909260263, 19.03943276465977164, 59.99890960531436690 ) ) ;
#111072 = CARTESIAN_POINT ( 'NONE',  ( 4.483927247898545687, 16.52544592524342804, 109.7905762719810383 ) ) ;
#111073 = CARTESIAN_POINT ( 'NONE',  ( -16.46253265017160317, 9.564922557960807481, 115.8322429386477097 ) ) ;
#111074 = CARTESIAN_POINT ( 'NONE',  ( 12.06949235617757843, -12.14591786802309237, 58.12390960531435979 ) ) ;
#111075 = CARTESIAN_POINT ( 'NONE',  ( 9.564922557960805705, 16.46253265017160317, 29.58224293864769550 ) ) ;
#111076 = CARTESIAN_POINT ( 'NONE',  ( 8.224510206698953496, -14.34966873604960469, 87.91557627198103830 ) ) ;
#111077 = CARTESIAN_POINT ( 'NONE',  ( -5.719274019375978568, 21.55341960407610458, 95.20724293864769550 ) ) ;
#111078 = CARTESIAN_POINT ( 'NONE',  ( 10.81492255796106328, -18.62759615963255655, 35.41775706135234003 ) ) ;
#111079 = CARTESIAN_POINT ( 'NONE',  ( 16.51473224551069308, 9.474510206698969483, 24.16557627198102765 ) ) ;
#111080 = CARTESIAN_POINT ( 'NONE',  ( -14.29746914071037622, -8.314922557961029526, 34.16775706135234714 ) ) ;
#111081 = CARTESIAN_POINT ( 'NONE',  ( 21.52544592524344225, -5.823673210054117533, 88.54057627198103830 ) ) ;
#111082 = CARTESIAN_POINT ( 'NONE',  ( -21.52544592524334988, -5.823673210054445271, 108.9594237280190185 ) ) ;
#111083 = CARTESIAN_POINT ( 'NONE',  ( 19.03943276465977164, -0.05219959533909143690, 88.74890960531436690 ) ) ;
#111084 = CARTESIAN_POINT ( 'NONE',  ( -18.67979575497193778, 10.72451020669871902, 43.33442372801901143 ) ) ;
#111085 = CARTESIAN_POINT ( 'NONE',  ( 18.67979575497178502, 10.72451020669898547, 29.16557627198103120 ) ) ;
#111086 = CARTESIAN_POINT ( 'NONE',  ( 4.379528057220092307, 16.55341960407617563, 102.2927570613523613 ) ) ;
#111088 = CARTESIAN_POINT ( 'NONE',  ( 15.72974639402176855, 15.80617190586768217, 86.87609039468568994 ) ) ;
#111087 = CARTESIAN_POINT ( 'NONE',  ( 18.67979575497194134, -10.72451020669871369, 55.83442372801901854 ) ) ;
#111089 = CARTESIAN_POINT ( 'NONE',  ( 9.474510206698729675, 16.51473224551082808, 27.08442372801900433 ) ) ;
#111090 = CARTESIAN_POINT ( 'NONE',  ( 12.06949235617739724, 12.14591786802326823, 86.87609039468568994 ) ) ;
#111091 = CARTESIAN_POINT ( 'NONE',  ( -21.55341960407619339, 5.719274019375674811, 38.54275706135234714 ) ) ;
#111092 = CARTESIAN_POINT ( 'NONE',  ( -19.02544592524342804, 5.153800228976336051, 41.04057627198103120 ) ) ;
#111093 = CARTESIAN_POINT ( 'NONE',  ( -10.72451020669870658, -18.67979575497194134, 99.58442372801900433 ) ) ;
#111094 = CARTESIAN_POINT ( 'NONE',  ( -19.03943276465977164, 0.05219959533909376836, 101.2489096053143669 ) ) ;
#111095 = CARTESIAN_POINT ( 'NONE',  ( -0.05219959533937732626, 21.53943276465977519, 22.50109039468567573 ) ) ;
#111096 = CARTESIAN_POINT ( 'NONE',  ( 10.81492255796078972, 18.62759615963270932, 79.58224293864769550 ) ) ;
#111098 = CARTESIAN_POINT ( 'NONE',  ( 18.67979575497178502, 10.72451020669898547, 64.16557627198102409 ) ) ;
#111097 = PLANE ( 'NONE',  #12851 ) ;
#111100 = CARTESIAN_POINT ( 'NONE',  ( 8.224510206698953496, -14.34966873604960469, 62.91557627198102409 ) ) ;
#111099 = CARTESIAN_POINT ( 'NONE',  ( -16.52544592524335698, -4.483927247898792601, 48.95942372801902565 ) ) ;
#111101 = CARTESIAN_POINT ( 'NONE',  ( -8.898068258721469448, -27.38543819252872069, 146.6656553485624102 ) ) ;
#111102 = CARTESIAN_POINT ( 'NONE',  ( -16.46253265017146816, -9.564922557961047289, 94.16775706135233293 ) ) ;
#111103 =( BOUNDED_SURFACE ( )  B_SPLINE_SURFACE ( 3, 2, ( 
 ( #166733, #28237, #110998 ),
 ( #170694, #76685, #169694 ),
 ( #123180, #32183, #126173 ),
 ( #139348, #141341, #93840 ),
 ( #33178, #154525, #111999 ),
 ( #157514, #16022, #77680 ),
 ( #94837, #2828, #155519 ),
 ( #79670, #18017, #173689 ),
 ( #80654, #78666, #140343 ),
 ( #64506, #61511, #1831 ),
 ( #49336, #827, #17014 ),
 ( #125188, #156516, #142330 ),
 ( #34168, #172684, #48354 ),
 ( #46351, #184869, #35155 ),
 ( #50341, #63513, #108009 ),
 ( #187868, #95830, #31188 ),
 ( #92840, #47360, #186884 ),
 ( #62502, #110008, #171689 ),
 ( #19008, #124173, #3810 ),
 ( #185874, #65488, #96811 ),
 ( #109015, #158497, #127150 ),
 ( #188858, #138361, #200042 ),
 ( #164252, #36141, #25747 ),
 ( #196591, #58061, #56055 ) ),
 .UNSPECIFIED., .F., .F., .T. ) 
 B_SPLINE_SURFACE_WITH_KNOTS ( ( 4, 2, 2, 2, 2, 2, 2, 2, 2, 2, 2, 4 ),
 ( 3, 3 ),
 ( -4.336808689942017736E-18, 0.001899702839891686873, 0.002849554259837532369, 0.003799405679783378082, 0.005699108519675069075, 0.006648959939620915222, 0.007598811359566760501, 0.008548662779512605780, 0.009498514199458452795, 0.01139821703935014335, 0.01329791987924183391, 0.01519762271913352447 ),
 ( 0.000000000000000000, 1.000000000000000000 ),
 .UNSPECIFIED. ) 
 GEOMETRIC_REPRESENTATION_ITEM ( )  RATIONAL_B_SPLINE_SURFACE ( (
 ( 1.000000000000000000, 0.7660444431189795678, 1.000000000000000000),
 ( 1.000000000000000000, 0.7753720600382404404, 1.000000000000000000),
 ( 1.000000000000000000, 0.7832595754285938128, 1.000000000000000000),
 ( 1.000000000000000000, 0.7928595458705487431, 1.000000000000000000),
 ( 1.000000000000000000, 0.7956872332516108370, 1.000000000000000000),
 ( 1.000000000000000000, 0.8005750596157604759, 1.000000000000000000),
 ( 1.000000000000000000, 0.8026302056541175789, 1.000000000000000000),
 ( 1.000000000000000000, 0.8075080643849508188, 1.000000000000000000),
 ( 1.000000000000000000, 0.8091143015810811079, 1.000000000000000000),
 ( 1.000000000000000000, 0.8093067629632566540, 1.000000000000000000),
 ( 1.000000000000000000, 0.8089952915731981609, 1.000000000000000000),
 ( 1.000000000000000000, 0.8076919994862008512, 1.000000000000000000),
 ( 1.000000000000000000, 0.8067078407648894389, 1.000000000000000000),
 ( 1.000000000000000000, 0.8041786842467456564, 1.000000000000000000),
 ( 1.000000000000000000, 0.8026334674876740571, 1.000000000000000000),
 ( 1.000000000000000000, 0.7990747329469689575, 1.000000000000000000),
 ( 1.000000000000000000, 0.7970509760941789645, 1.000000000000000000),
 ( 1.000000000000000000, 0.7904793850863397475, 1.000000000000000000),
 ( 1.000000000000000000, 0.7855040224313790675, 1.000000000000000000),
 ( 1.000000000000000000, 0.7751942650507511745, 1.000000000000000000),
 ( 1.000000000000000000, 0.7698260778212776545, 1.000000000000000000),
 ( 1.000000000000000000, 0.7598259884959711608, 1.000000000000000000),
 ( 1.000000000000000000, 0.7551428682221226207, 1.000000000000000000),
 ( 1.000000000000000000, 0.7510191126010858920, 1.000000000000000000) ) ) 
 REPRESENTATION_ITEM ( '' )  SURFACE ( )  );
#111104 = DIRECTION ( 'NONE',  ( 0.7071067811865467956, 0.000000000000000000, -0.7071067811865483499 ) ) ;
#111105 = CARTESIAN_POINT ( 'NONE',  ( 4.483927247898790824, -16.52544592524335698, 25.20942372801901854 ) ) ;
#111106 = CARTESIAN_POINT ( 'NONE',  ( 15.80617190586746368, 15.72974639402197994, 99.37390960531436690 ) ) ;
#111107 = CARTESIAN_POINT ( 'NONE',  ( 10.81492255796078972, 18.62759615963270932, 79.58224293864769550 ) ) ;
#111108 = CARTESIAN_POINT ( 'NONE',  ( -16.46253265017160317, 9.564922557960807481, 110.8322429386476955 ) ) ;
#111109 = CARTESIAN_POINT ( 'NONE',  ( 12.06949235617739724, 12.14591786802326823, 61.87609039468568284 ) ) ;
#111110 = CARTESIAN_POINT ( 'NONE',  ( 19.05341960407611168, 5.049401038298154454, 68.95724293864769550 ) ) ;
#111112 = CARTESIAN_POINT ( 'NONE',  ( -19.05341960407617563, 5.049401038297882671, 108.5427570613523187 ) ) ;
#111111 = CARTESIAN_POINT ( 'NONE',  ( 18.62759615963255655, 10.81492255796105972, 46.66775706135234714 ) ) ;
#111113 = CARTESIAN_POINT ( 'NONE',  ( -5.153800228976328057, -19.02544592524343514, 102.2905762719810383 ) ) ;
#111114 = CARTESIAN_POINT ( 'NONE',  ( -5.049401038298153566, 19.05341960407611168, 100.2072429386476955 ) ) ;
#111115 = CARTESIAN_POINT ( 'NONE',  ( 10.72451020669898902, -18.67979575497178502, 97.91557627198103830 ) ) ;
#111116 = CARTESIAN_POINT ( 'NONE',  ( 19.02544592524343514, -5.153800228976328945, 53.54057627198102409 ) ) ;
#111117 = SPHERICAL_SURFACE ( 'NONE', #99177, 2.000000000000000000 ) ;
#111118 = CARTESIAN_POINT ( 'NONE',  ( -14.29746914071049879, 8.314922557960819915, 75.83224293864769550 ) ) ;
#111119 = CARTESIAN_POINT ( 'NONE',  ( -0.05219959533907301413, -21.53943276465977519, 27.49890960531435269 ) ) ;
#111120 = CARTESIAN_POINT ( 'NONE',  ( 13.89961937509977652, -13.97604488694527269, 23.12390960531436335 ) ) ;
#111121 = CARTESIAN_POINT ( 'NONE',  ( -5.719274019375978568, 21.55341960407610458, 100.2072429386476955 ) ) ;
#111122 = CARTESIAN_POINT ( 'NONE',  ( -16.51473224551082808, 9.474510206698731452, 63.33442372801900433 ) ) ;
#111123 = CARTESIAN_POINT ( 'NONE',  ( 15.72974639402199770, -15.80617190586745480, 23.12390960531436335 ) ) ;
#111124 = CARTESIAN_POINT ( 'NONE',  ( 9.474510206698971260, -16.51473224551069308, 32.91557627198102409 ) ) ;
#111125 = CARTESIAN_POINT ( 'NONE',  ( 15.80617190586746368, 15.72974639402197994, 49.37390960531436690 ) ) ;
#111126 = AXIS2_PLACEMENT_3D ( 'NONE', #163540, #183446, #194879 ) ;
#111127 = CARTESIAN_POINT ( 'NONE',  ( 9.564922557960805705, 16.46253265017160317, 104.5822429386476955 ) ) ;
#111128 = CARTESIAN_POINT ( 'NONE',  ( -21.53943276465977519, -0.05219959533937600094, 73.75109039468567573 ) ) ;
#111129 = CARTESIAN_POINT ( 'NONE',  ( -13.89961937509977652, 13.97604488694528158, 55.62390960531434558 ) ) ;
#111130 = CARTESIAN_POINT ( 'NONE',  ( 14.34966873604960469, 8.224510206698951720, 84.16557627198103830 ) ) ;
#111131 = CARTESIAN_POINT ( 'NONE',  ( 12.14591786802327356, -12.06949235617739191, 35.62609039468568994 ) ) ;
#111132 = CARTESIAN_POINT ( 'NONE',  ( 10.81492255796106328, -18.62759615963255655, 60.41775706135235424 ) ) ;
#111133 = ORIENTED_EDGE ( 'NONE', *, *, #88147, .T. ) ;
#111134 = CARTESIAN_POINT ( 'NONE',  ( -5.049401038297874678, -19.05341960407617918, 24.79275706135233648 ) ) ;
#111135 = CARTESIAN_POINT ( 'NONE',  ( -16.46253265017146816, -9.564922557961047289, 84.16775706135233293 ) ) ;
#111136 = CARTESIAN_POINT ( 'NONE',  ( 0.05219959533936267826, -19.03943276465977164, 40.00109039468566152 ) ) ;
#111137 = LINE ( 'NONE', #106409, #160192 ) ;
#111138 = CARTESIAN_POINT ( 'NONE',  ( 10.72451020669871369, 18.67979575497193778, 42.08442372801901854 ) ) ;
#111139 = DIRECTION ( 'NONE',  ( 0.000000000000000000, 0.000000000000000000, -1.000000000000000000 ) ) ;
#111140 = CARTESIAN_POINT ( 'NONE',  ( 9.474510206698729675, 16.51473224551082808, 32.08442372801900433 ) ) ;
#111141 = CARTESIAN_POINT ( 'NONE',  ( -13.89961937509977652, 13.97604488694528158, 55.62390960531434558 ) ) ;
#111142 = CARTESIAN_POINT ( 'NONE',  ( -19.05341960407617563, 5.049401038297882671, 33.54275706135231871 ) ) ;
#111143 = CARTESIAN_POINT ( 'NONE',  ( -14.34966873604972548, 8.224510206698743886, 108.3344237280190185 ) ) ;
#111145 = CARTESIAN_POINT ( 'NONE',  ( 10.81492255796106328, -18.62759615963255655, 80.41775706135234714 ) ) ;
#111144 = CARTESIAN_POINT ( 'NONE',  ( -0.05219959533907301413, -21.53943276465977519, 22.49890960531436335 ) ) ;
#111146 = CARTESIAN_POINT ( 'NONE',  ( -11.40812507854755609, 35.11059874428196537, -9.024999997268814411 ) ) ;
#111147 = CARTESIAN_POINT ( 'NONE',  ( -33.85315667487628133, 2.014031266883448522E-14, 100.5000000000010232 ) ) ;
#111148 = CARTESIAN_POINT ( 'NONE',  ( 21.52544592524334988, 5.823673210054432836, 86.45942372801901854 ) ) ;
#111149 = CARTESIAN_POINT ( 'NONE',  ( 23.66491666289346085, -1.240847218223132487, -57.22545927231449525 ) ) ;
#111150 = CARTESIAN_POINT ( 'NONE',  ( -16.51473224551069308, -9.474510206698971260, 101.6655762719810241 ) ) ;
#111151 = EDGE_CURVE ( 'NONE', #14621, #50977, #114552, .T. ) ;
#111152 = CARTESIAN_POINT ( 'NONE',  ( 0.000000000000000000, 3.784814030245899019, 190.0000000000000000 ) ) ;
#111153 = CARTESIAN_POINT ( 'NONE',  ( 13.97604488694527802, 13.89961937509977652, 54.37390960531435979 ) ) ;
#111154 = CARTESIAN_POINT ( 'NONE',  ( -10.72451020669898014, 18.67979575497178502, 50.41557627198103120 ) ) ;
#111155 = CARTESIAN_POINT ( 'NONE',  ( 0.05219959533910956823, 16.53943276465976808, 24.99890960531435624 ) ) ;
#111157 = CARTESIAN_POINT ( 'NONE',  ( 13.89961937509977652, -13.97604488694527269, 98.12390960531433848 ) ) ;
#111156 = CARTESIAN_POINT ( 'NONE',  ( 12.14591786802309770, 12.06949235617756955, 99.37390960531436690 ) ) ;
#111158 = CARTESIAN_POINT ( 'NONE',  ( -9.474510206698720793, -16.51473224551083518, 24.58442372801900078 ) ) ;
#111159 = CARTESIAN_POINT ( 'NONE',  ( -12.14591786802309592, -12.06949235617757132, 101.8739096053143811 ) ) ;
#111160 = CARTESIAN_POINT ( 'NONE',  ( 18.67979575497194134, -10.72451020669871369, 55.83442372801901854 ) ) ;
#111161 = CARTESIAN_POINT ( 'NONE',  ( -8.314922557961024197, 14.29746914071037800, 102.9177570613523756 ) ) ;
#111162 = CARTESIAN_POINT ( 'NONE',  ( -5.153800228976607833, 19.02544592524334988, 67.70942372801900433 ) ) ;
#111163 = CARTESIAN_POINT ( 'NONE',  ( -27.53954565730104065, -29.01074954818684404, -5.289573041754675131 ) ) ;
#111164 = CARTESIAN_POINT ( 'NONE',  ( -16.51473224551069308, -9.474510206698971260, 111.6655762719810383 ) ) ;
#111165 = CARTESIAN_POINT ( 'NONE',  ( -8.224510206698948167, 14.34966873604960824, 70.41557627198102409 ) ) ;
#111166 = CARTESIAN_POINT ( 'NONE',  ( 13.97604488694548053, -13.89961937509957401, 60.62609039468564731 ) ) ;
#111167 = CARTESIAN_POINT ( 'NONE',  ( -13.97604488694527625, -13.89961937509977652, 56.87390960531434558 ) ) ;
#111168 = CARTESIAN_POINT ( 'NONE',  ( 4.379528057220339221, -16.55341960407611168, 67.70724293864769550 ) ) ;
#111169 = CARTESIAN_POINT ( 'NONE',  ( -13.97604488694547697, 13.89961937509957934, 93.12609039468566152 ) ) ;
#111170 = CARTESIAN_POINT ( 'NONE',  ( 15.72974639402199770, -15.80617190586745480, 33.12390960531435979 ) ) ;
#111171 = ORIENTED_EDGE ( 'NONE', *, *, #169970, .T. ) ;
#111172 = CARTESIAN_POINT ( 'NONE',  ( 16.53943276465976808, -0.05219959533910856209, 98.74890960531438111 ) ) ;
#111173 = CARTESIAN_POINT ( 'NONE',  ( -17.48853670773242897, -5.747243402303181981, 31.33328700250011778 ) ) ;
#111175 = CARTESIAN_POINT ( 'NONE',  ( 15.72974639402199770, -15.80617190586745480, 68.12390960531436690 ) ) ;
#111174 = CARTESIAN_POINT ( 'NONE',  ( -16.51473224551069308, -9.474510206698971260, 61.66557627198103120 ) ) ;
#111176 = CARTESIAN_POINT ( 'NONE',  ( 13.89961937509977652, -13.97604488694527269, 48.12390960531435979 ) ) ;
#111178 = CARTESIAN_POINT ( 'NONE',  ( 19.05341960407611168, 5.049401038298154454, 68.95724293864769550 ) ) ;
#111177 = CARTESIAN_POINT ( 'NONE',  ( 16.52544592524335698, 4.483927247898782831, 86.45942372801901854 ) ) ;
#111179 = CARTESIAN_POINT ( 'NONE',  ( -5.049401038297874678, -19.05341960407617918, 54.79275706135234003 ) ) ;
#111180 = CARTESIAN_POINT ( 'NONE',  ( -10.81492255796105439, 18.62759615963255655, 87.91775706135234714 ) ) ;
#111181 = CARTESIAN_POINT ( 'NONE',  ( -10.72451020669898014, 18.67979575497178502, 50.41557627198103120 ) ) ;
#111182 = CARTESIAN_POINT ( 'NONE',  ( -13.89961937509977652, 13.97604488694528158, 110.6239096053143243 ) ) ;
#111183 = CARTESIAN_POINT ( 'NONE',  ( -16.52544592524342804, 4.483927247898546575, 116.0405762719810383 ) ) ;
#111184 = CARTESIAN_POINT ( 'NONE',  ( -16.53943276465976808, -0.05219959533934237506, 88.75109039468567573 ) ) ;
#111185 = CARTESIAN_POINT ( 'NONE',  ( -13.89961937509957401, -13.97604488694547875, 109.3760903946856331 ) ) ;
#111186 = CARTESIAN_POINT ( 'NONE',  ( -16.46253265017160317, 9.564922557960807481, 25.83224293864769194 ) ) ;
#111187 = DIRECTION ( 'NONE',  ( 0.000000000000000000, 0.000000000000000000, -1.000000000000000000 ) ) ;
#111188 = CARTESIAN_POINT ( 'NONE',  ( 10.72451020669871369, 18.67979575497193778, 102.0844237280190185 ) ) ;
#111189 = CARTESIAN_POINT ( 'NONE',  ( -16.52544592524342804, 4.483927247898546575, 66.04057627198103830 ) ) ;
#111190 = CARTESIAN_POINT ( 'NONE',  ( 0.05219959533910956823, 16.53943276465976808, 64.99890960531435269 ) ) ;
#111191 = CARTESIAN_POINT ( 'NONE',  ( -18.62759615963270932, 10.81492255796079327, 100.8322429386477097 ) ) ;
#111192 = CARTESIAN_POINT ( 'NONE',  ( 18.62759615963271287, -10.81492255796078972, 83.33224293864769550 ) ) ;
#111193 = CARTESIAN_POINT ( 'NONE',  ( 16.62475595723697097, -7.163666690055294772, 98.02713351810470499 ) ) ;
#111194 = CARTESIAN_POINT ( 'NONE',  ( -5.719274019375978568, 21.55341960407610458, 50.20724293864769550 ) ) ;
#111195 = CARTESIAN_POINT ( 'NONE',  ( -8.314922557961024197, 14.29746914071037800, 67.91775706135234714 ) ) ;
#111196 = CARTESIAN_POINT ( 'NONE',  ( 8.224510206698953496, -14.34966873604960469, 97.91557627198103830 ) ) ;
#111197 = CARTESIAN_POINT ( 'NONE',  ( 19.03943276465977164, -0.05219959533909143690, 43.74890960531435979 ) ) ;
#111198 =( NAMED_UNIT ( * ) SI_UNIT ( $, .STERADIAN. ) SOLID_ANGLE_UNIT ( ) );
#111199 = CARTESIAN_POINT ( 'NONE',  ( 34.67225235875022804, -7.109416101192572945, 42.56171885070867944 ) ) ;
#111200 = CARTESIAN_POINT ( 'NONE',  ( 14.29746914071037800, 8.314922557961029526, 101.6677570613523613 ) ) ;
#111201 = CARTESIAN_POINT ( 'NONE',  ( -18.67979575497193778, 10.72451020669871902, 33.33442372801900433 ) ) ;
#111202 = CARTESIAN_POINT ( 'NONE',  ( 5.049401038298161559, -19.05341960407611168, 87.70724293864769550 ) ) ;
#111203 = CARTESIAN_POINT ( 'NONE',  ( -0.05219959533937732626, 21.53943276465977519, 67.50109039468568994 ) ) ;
#111204 = DIRECTION ( 'NONE',  ( -1.000000000000000000, 0.000000000000000000, 0.000000000000000000 ) ) ;
#111205 = CARTESIAN_POINT ( 'NONE',  ( -16.46253265017160317, 9.564922557960807481, 30.83224293864769550 ) ) ;
#111206 = AXIS2_PLACEMENT_3D ( 'NONE', #41432, #136416, #44414 ) ;
#111207 = VERTEX_POINT ( 'NONE', #5062 ) ;
#111208 = CARTESIAN_POINT ( 'NONE',  ( -10.81492255796105439, 18.62759615963255655, 57.91775706135234714 ) ) ;
#111210 = CARTESIAN_POINT ( 'NONE',  ( -16.51473224551069308, -9.474510206698971260, 21.66557627198102765 ) ) ;
#111209 = CARTESIAN_POINT ( 'NONE',  ( -13.97604488694527625, -13.89961937509977652, 31.87390960531435979 ) ) ;
#111211 = CARTESIAN_POINT ( 'NONE',  ( -9.474510206698964154, 16.51473224551069663, 90.41557627198103830 ) ) ;
#111212 = CARTESIAN_POINT ( 'NONE',  ( -5.153800228976607833, 19.02544592524334988, 62.70942372801899722 ) ) ;
#111213 = CARTESIAN_POINT ( 'NONE',  ( -21.55341960407619339, 5.719274019375674811, 23.54275706135235424 ) ) ;
#111214 = CARTESIAN_POINT ( 'NONE',  ( 5.153800228976615827, -19.02544592524334988, 55.20942372801899722 ) ) ;
#111215 = CARTESIAN_POINT ( 'NONE',  ( 0.05219959533909260263, 19.03943276465977164, 44.99890960531435979 ) ) ;
#111216 = CARTESIAN_POINT ( 'NONE',  ( -16.53943276465976808, -0.05219959533934237506, 103.7510903946857042 ) ) ;
#111217 = CARTESIAN_POINT ( 'NONE',  ( -16.46253265017146816, -9.564922557961047289, 59.16775706135233293 ) ) ;
#111218 = CARTESIAN_POINT ( 'NONE',  ( -4.483927247898539470, -16.52544592524342804, 27.29057627198103120 ) ) ;
#111219 = CARTESIAN_POINT ( 'NONE',  ( -19.05341960407617563, 5.049401038297882671, 53.54275706135231871 ) ) ;
#111220 = CARTESIAN_POINT ( 'NONE',  ( -19.03943276465977164, 0.05219959533909376836, 101.2489096053143669 ) ) ;
#111221 = CARTESIAN_POINT ( 'NONE',  ( -15.72974639402176322, -15.80617190586768395, 109.3760903946857042 ) ) ;
#111223 = EDGE_CURVE ( 'NONE', #171283, #181594, #7406, .T. ) ;
#111222 = CARTESIAN_POINT ( 'NONE',  ( -21.55341960407619339, 5.719274019375674811, 108.5427570613523756 ) ) ;
#111224 = CARTESIAN_POINT ( 'NONE',  ( 37.99626262588765258, 2.893932880411085066E-14, -5.002157773949823749 ) ) ;
#111225 = CARTESIAN_POINT ( 'NONE',  ( -15.72974639402176322, -15.80617190586768395, 84.37609039468570415 ) ) ;
#111226 = CARTESIAN_POINT ( 'NONE',  ( -12.14591786802326823, 12.06949235617739902, 33.12609039468569705 ) ) ;
#111227 = CARTESIAN_POINT ( 'NONE',  ( 16.46253265017160672, -9.564922557960803928, 98.33224293864769550 ) ) ;
#111228 = CARTESIAN_POINT ( 'NONE',  ( 8.571926809382603096, -26.38167802310801235, 139.4750000027311785 ) ) ;
#111229 = CARTESIAN_POINT ( 'NONE',  ( 0.05219959533909260263, 19.03943276465977164, 74.99890960531435269 ) ) ;
#111230 = CARTESIAN_POINT ( 'NONE',  ( 8.906447517083050158, 27.41122689804195645, 141.4000000000000057 ) ) ;
#111231 = VECTOR ( 'NONE', #100560, 1000.000000000000000 ) ;
#111232 = CARTESIAN_POINT ( 'NONE',  ( -19.02544592524334988, -5.153800228976617603, 68.95942372801896170 ) ) ;
#111233 = CARTESIAN_POINT ( 'NONE',  ( -13.89961937509977652, 13.97604488694528158, 110.6239096053143243 ) ) ;
#111234 = CARTESIAN_POINT ( 'NONE',  ( -18.67979575497193778, 10.72451020669871902, 103.3344237280190043 ) ) ;
#111235 = CARTESIAN_POINT ( 'NONE',  ( 16.55341960407611168, 4.379528057220329451, 93.95724293864770971 ) ) ;
#111236 = CARTESIAN_POINT ( 'NONE',  ( -21.52544592524343514, 5.823673210054127303, 41.04057627198103120 ) ) ;
#111237 = CARTESIAN_POINT ( 'NONE',  ( -5.719274019375978568, 21.55341960407610458, 40.20724293864769550 ) ) ;
#111238 = CARTESIAN_POINT ( 'NONE',  ( -16.55341960407611168, -4.379528057220339221, 101.4572429386476955 ) ) ;
#111239 = CARTESIAN_POINT ( 'NONE',  ( -1.490485923554860426, -7.405410116723224689, -62.24175268741321787 ) ) ;
#111240 = CARTESIAN_POINT ( 'NONE',  ( 16.51473224551083163, -9.474510206698727899, 60.83442372801900433 ) ) ;
#111241 = CARTESIAN_POINT ( 'NONE',  ( 8.314922557960818139, 14.29746914071049879, 24.58224293864768839 ) ) ;
#111242 = CARTESIAN_POINT ( 'NONE',  ( -16.46253265017160317, 9.564922557960807481, 105.8322429386476955 ) ) ;
#111243 = CARTESIAN_POINT ( 'NONE',  ( 0.05219959533937995610, -21.53943276465977519, 80.00109039468568994 ) ) ;
#111244 = CARTESIAN_POINT ( 'NONE',  ( 21.52544592524344225, -5.823673210054117533, 68.54057627198103830 ) ) ;
#111245 = CARTESIAN_POINT ( 'NONE',  ( -15.72974639402176322, -15.80617190586768395, 39.37609039468567573 ) ) ;
#111246 = CARTESIAN_POINT ( 'NONE',  ( -21.52544592524343514, 5.823673210054127303, 91.04057627198103830 ) ) ;
#111247 = CARTESIAN_POINT ( 'NONE',  ( -0.05219959533937732626, 21.53943276465977519, 47.50109039468568994 ) ) ;
#111248 = CARTESIAN_POINT ( 'NONE',  ( -19.05341960407611168, -5.049401038298163336, 31.45724293864769550 ) ) ;
#111249 = CARTESIAN_POINT ( 'NONE',  ( -19.03943276465977164, 0.05219959533909376836, 81.24890960531436690 ) ) ;
#111250 = CARTESIAN_POINT ( 'NONE',  ( 14.34966873604972726, -8.224510206698740333, 80.83442372801901854 ) ) ;
#111251 = CARTESIAN_POINT ( 'NONE',  ( 12.14591786802309770, 12.06949235617756955, 99.37390960531436690 ) ) ;
#111252 = CARTESIAN_POINT ( 'NONE',  ( 13.89961937509977652, -13.97604488694527269, 103.1239096053143527 ) ) ;
#111253 = CARTESIAN_POINT ( 'NONE',  ( -16.55341960407611168, -4.379528057220339221, 51.45724293864770260 ) ) ;
#111254 = CARTESIAN_POINT ( 'NONE',  ( -0.05219959533910754901, -16.53943276465976808, 22.49890960531436335 ) ) ;
#111255 = CARTESIAN_POINT ( 'NONE',  ( 16.46253265017160672, -9.564922557960803928, 48.33224293864769550 ) ) ;
#111256 = CARTESIAN_POINT ( 'NONE',  ( -13.97604488694527625, -13.89961937509977652, 31.87390960531435979 ) ) ;
#111257 = CARTESIAN_POINT ( 'NONE',  ( -21.53943276465977519, 0.05219959533907696930, 41.24890960531435269 ) ) ;
#111259 = VECTOR ( 'NONE', #156752, 1000.000000000000000 ) ;
#111258 = CARTESIAN_POINT ( 'NONE',  ( 9.564922557961047289, -16.46253265017146816, 25.41775706135234003 ) ) ;
#111261 = CARTESIAN_POINT ( 'NONE',  ( 4.483927247898545687, 16.52544592524342804, 34.79057627198103120 ) ) ;
#111260 = CARTESIAN_POINT ( 'NONE',  ( -17.48853670773242541, -5.747243402303178428, 41.33328700250010712 ) ) ;
#111262 = CARTESIAN_POINT ( 'NONE',  ( 15.80617190586769283, -15.72974639402175789, 40.62609039468567573 ) ) ;
#111263 = CARTESIAN_POINT ( 'NONE',  ( 24.81835880841864039, -6.052260367207979996, 168.4265213779230521 ) ) ;
#111264 = CARTESIAN_POINT ( 'NONE',  ( 14.34966873604972726, -8.224510206698740333, 60.83442372801901854 ) ) ;
#111265 = CARTESIAN_POINT ( 'NONE',  ( 19.03943276465977164, 0.05219959533936151252, 61.25109039468566863 ) ) ;
#111266 = CARTESIAN_POINT ( 'NONE',  ( -8.314922557960811034, -14.29746914071050412, 27.08224293864769550 ) ) ;
#111267 = CARTESIAN_POINT ( 'NONE',  ( 17.31747979337945154, -6.344076630961154706, 51.12055131934818775 ) ) ;
#111268 = CARTESIAN_POINT ( 'NONE',  ( 12.14591786802327356, -12.06949235617739191, 105.6260903946856899 ) ) ;
#111269 = CARTESIAN_POINT ( 'NONE',  ( 5.049401038298161559, -19.05341960407611168, 42.70724293864767418 ) ) ;
#111270 = CARTESIAN_POINT ( 'NONE',  ( 16.46253265017160672, -9.564922557960803928, 63.33224293864769550 ) ) ;
#111271 = CARTESIAN_POINT ( 'NONE',  ( 13.89961937509977652, -13.97604488694527269, 23.12390960531436335 ) ) ;
#111272 = CARTESIAN_POINT ( 'NONE',  ( -0.05219959533937732626, 21.53943276465977519, 32.50109039468568284 ) ) ;
#111273 = CARTESIAN_POINT ( 'NONE',  ( -16.46253265017160317, 9.564922557960807481, 50.83224293864770260 ) ) ;
#111274 = CARTESIAN_POINT ( 'NONE',  ( -5.944577070221434667, -6.769145669310464797, -61.91697028796055235 ) ) ;
#111275 = CARTESIAN_POINT ( 'NONE',  ( 0.05219959533909260263, 19.03943276465977164, 49.99890960531435979 ) ) ;
#111276 = CARTESIAN_POINT ( 'NONE',  ( 18.67979575497178502, 10.72451020669898547, 24.16557627198103120 ) ) ;
#111277 = B_SPLINE_CURVE_WITH_KNOTS ( 'NONE', 3,
 ( #128685, #111541, #175211, #3363, #190382, #49876, #96359, #158047, #159026, #6340, #20519, #82167, #40694, #74031, #165045, #71033, #57865, #42696, #117530, #101346, #10368, #27541, #26538, #88182, #12368, #163035, #8357, #87196, #24542, #86192, #134713, #104357 ),
 .UNSPECIFIED., .F., .F.,
 ( 4, 2, 2, 2, 2, 2, 2, 2, 2, 2, 2, 2, 2, 2, 2, 4 ),
 ( 2.625112965618923374E-17, 0.0003712461730036961563, 0.0007424923460073660749, 0.001113738519011035939, 0.001484984692014705912, 0.002227477038022045858, 0.002598723211025716698, 0.002969969384029387104, 0.003341215557033057511, 0.003712461730036728785, 0.004083707903040398324, 0.004454954076044069164, 0.004826200249047740004, 0.005197446422051409977, 0.005568692595055081684, 0.005939938768058751657 ),
 .UNSPECIFIED. ) ;
#111279 = CARTESIAN_POINT ( 'NONE',  ( 14.29746914071049879, -8.314922557960816363, 98.33224293864769550 ) ) ;
#111278 = CARTESIAN_POINT ( 'NONE',  ( -15.80617190586768217, 15.72974639402176855, 58.12609039468568994 ) ) ;
#111280 = CARTESIAN_POINT ( 'NONE',  ( 9.564922557960805705, 16.46253265017160317, 109.5822429386476955 ) ) ;
#111281 = CARTESIAN_POINT ( 'NONE',  ( -0.05219959533934338120, 16.53943276465976808, 77.50109039468567573 ) ) ;
#111282 = CARTESIAN_POINT ( 'NONE',  ( 18.62759615963255655, 10.81492255796105972, 96.66775706135234714 ) ) ;
#111283 = CARTESIAN_POINT ( 'NONE',  ( 16.55341960407618274, -4.379528057220086978, 56.04275706135235424 ) ) ;
#111284 = CARTESIAN_POINT ( 'NONE',  ( -5.049401038298153566, 19.05341960407611168, 95.20724293864770971 ) ) ;
#111285 = CARTESIAN_POINT ( 'NONE',  ( 16.55341960407618274, -4.379528057220086978, 41.04275706135236135 ) ) ;
#111286 = CARTESIAN_POINT ( 'NONE',  ( -12.14591786802326823, 12.06949235617739902, 28.12609039468568284 ) ) ;
#111287 = CARTESIAN_POINT ( 'NONE',  ( -12.14591786802326823, 12.06949235617739902, 98.12609039468570415 ) ) ;
#111288 = CARTESIAN_POINT ( 'NONE',  ( -21.52544592524334988, -5.823673210054445271, 48.95942372801902565 ) ) ;
#111289 = CARTESIAN_POINT ( 'NONE',  ( 5.153800228976615827, -19.02544592524334988, 100.2094237280190043 ) ) ;
#111290 = B_SPLINE_CURVE_WITH_KNOTS ( 'NONE', 3,
 ( #134467, #85943, #12128, #176981, #161790, #101100, #27294, #25305, #162786, #38451, #103120, #132455, #146609, #164801, #26296, #180975, #150632, #87937, #8102, #40445 ),
 .UNSPECIFIED., .F., .F.,
 ( 4, 2, 2, 2, 2, 2, 2, 2, 2, 4 ),
 ( 0.004000878361812008552, 0.004499404418916014975, 0.004997930476020021398, 0.005496456533124028689, 0.005994982590228035112, 0.006244245618780038323, 0.006493508647332041535, 0.006992034704436048825, 0.007490560761540055248, 0.007989086818644061672 ),
 .UNSPECIFIED. ) ;
#111291 = CARTESIAN_POINT ( 'NONE',  ( 5.823673210054125526, 21.52544592524343514, 114.7905762719810383 ) ) ;
#111293 = CARTESIAN_POINT ( 'NONE',  ( 16.46253265017146816, 9.564922557961045513, 101.6677570613523329 ) ) ;
#111292 = CARTESIAN_POINT ( 'NONE',  ( 12.14591786802309770, 12.06949235617756955, 109.3739096053143811 ) ) ;
#111294 = CARTESIAN_POINT ( 'NONE',  ( 8.224510206698742110, 14.34966873604972548, 72.08442372801899012 ) ) ;
#111295 = CARTESIAN_POINT ( 'NONE',  ( 21.35462415990330243, 9.648971641161622870, 168.5494316893080793 ) ) ;
#111296 = CARTESIAN_POINT ( 'NONE',  ( -9.474510206698720793, -16.51473224551083518, 74.58442372801900433 ) ) ;
#111297 = CARTESIAN_POINT ( 'NONE',  ( 4.483927247898545687, 16.52544592524342804, 39.79057627198103830 ) ) ;
#111298 = CARTESIAN_POINT ( 'NONE',  ( 14.34966873604960469, 8.224510206698951720, 39.16557627198102409 ) ) ;
#111299 = CARTESIAN_POINT ( 'NONE',  ( 12.14591786802309770, 12.06949235617756955, 99.37390960531436690 ) ) ;
#111301 = CARTESIAN_POINT ( 'NONE',  ( -17.48853670773247160, 5.747243402303041648, 88.66671299749997104 ) ) ;
#111300 = CARTESIAN_POINT ( 'NONE',  ( -9.474510206698720793, -16.51473224551083518, 34.58442372801899722 ) ) ;
#111302 = CARTESIAN_POINT ( 'NONE',  ( 5.719274019375673035, 21.55341960407619339, 37.29275706135235424 ) ) ;
#111303 = CARTESIAN_POINT ( 'NONE',  ( -0.05219959533936034679, 19.03943276465977164, 97.50109039468567573 ) ) ;
#111304 = LINE ( 'NONE', #4111, #166480 ) ;
#111305 = CARTESIAN_POINT ( 'NONE',  ( 5.049401038298161559, -19.05341960407611168, 92.70724293864769550 ) ) ;
#111306 = CARTESIAN_POINT ( 'NONE',  ( -13.97604488694527625, -13.89961937509977652, 91.87390960531432427 ) ) ;
#111307 = CARTESIAN_POINT ( 'NONE',  ( 21.55341960407610458, 5.719274019375980345, 53.95724293864770260 ) ) ;
#111308 = CARTESIAN_POINT ( 'NONE',  ( -4.379528057220328563, 16.55341960407611168, 90.20724293864770971 ) ) ;
#111309 = CARTESIAN_POINT ( 'NONE',  ( -5.049401038298153566, 19.05341960407611168, 70.20724293864769550 ) ) ;
#111310 = CARTESIAN_POINT ( 'NONE',  ( 9.474510206698971260, -16.51473224551069308, 27.91557627198103120 ) ) ;
#111311 = CARTESIAN_POINT ( 'NONE',  ( -5.719274019375665041, -21.55341960407619695, 44.79275706135234714 ) ) ;
#111312 = CARTESIAN_POINT ( 'NONE',  ( -0.05219959533937732626, 21.53943276465977519, 77.50109039468567573 ) ) ;
#111313 = CARTESIAN_POINT ( 'NONE',  ( -16.51473224551069308, -9.474510206698971260, 51.66557627198102409 ) ) ;
#111314 = CARTESIAN_POINT ( 'NONE',  ( 14.34966873604972726, -8.224510206698740333, 85.83442372801901854 ) ) ;
#111315 = CARTESIAN_POINT ( 'NONE',  ( -21.52544592524334988, -5.823673210054445271, 28.95942372801902209 ) ) ;
#111316 = CARTESIAN_POINT ( 'NONE',  ( 15.72974639402176855, 15.80617190586768217, 21.87609039468567573 ) ) ;
#111318 = CARTESIAN_POINT ( 'NONE',  ( -19.03943276465977164, 0.05219959533909376836, 76.24890960531435269 ) ) ;
#111317 = CARTESIAN_POINT ( 'NONE',  ( 16.51473224551083163, -9.474510206698727899, 50.83442372801899722 ) ) ;
#111319 = CARTESIAN_POINT ( 'NONE',  ( -15.72974639402176322, -15.80617190586768395, 79.37609039468567573 ) ) ;
#111320 = CARTESIAN_POINT ( 'NONE',  ( 10.81492255796078972, 18.62759615963270932, 74.58224293864768129 ) ) ;
#111321 = CARTESIAN_POINT ( 'NONE',  ( -12.06949235617756955, 12.14591786802309770, 45.62390960531436690 ) ) ;
#111323 = CARTESIAN_POINT ( 'NONE',  ( -9.564922557961040184, 16.46253265017147172, 27.91775706135232582 ) ) ;
#111322 = CARTESIAN_POINT ( 'NONE',  ( -15.80617190586768217, 15.72974639402176855, 108.1260903946856757 ) ) ;
#111324 = CARTESIAN_POINT ( 'NONE',  ( -8.224510206698948167, 14.34966873604960824, 70.41557627198102409 ) ) ;
#111325 = CARTESIAN_POINT ( 'NONE',  ( -8.314922557960811034, -14.29746914071050412, 112.0822429386477097 ) ) ;
#111326 = CARTESIAN_POINT ( 'NONE',  ( -9.564922557961040184, 16.46253265017147172, 77.91775706135234714 ) ) ;
#111327 = CARTESIAN_POINT ( 'NONE',  ( -8.224510206698948167, 14.34966873604960824, 35.41557627198102409 ) ) ;
#111328 = CARTESIAN_POINT ( 'NONE',  ( 18.67979575497194134, -10.72451020669871369, 75.83442372801900433 ) ) ;
#111329 = CARTESIAN_POINT ( 'NONE',  ( 0.05219959533909260263, 19.03943276465977164, 74.99890960531435269 ) ) ;
#111330 = CARTESIAN_POINT ( 'NONE',  ( 16.46253265017146816, 9.564922557961045513, 41.66775706135234003 ) ) ;
#111331 = CARTESIAN_POINT ( 'NONE',  ( -10.72451020669898014, 18.67979575497178502, 70.41557627198102409 ) ) ;
#111332 = CARTESIAN_POINT ( 'NONE',  ( -21.52544592524343514, 5.823673210054127303, 111.0405762719810525 ) ) ;
#111333 = CARTESIAN_POINT ( 'NONE',  ( 12.06949235617739724, 12.14591786802326823, 21.87609039468567573 ) ) ;
#111334 = CARTESIAN_POINT ( 'NONE',  ( 16.52544592524335698, 4.483927247898782831, 71.45942372801901854 ) ) ;
#111336 = CARTESIAN_POINT ( 'NONE',  ( 21.53943276465977519, -0.05219959533907433946, 108.7489096053143669 ) ) ;
#111335 = CARTESIAN_POINT ( 'NONE',  ( 16.38665767535053064, 7.295008042176049479, 62.23599135785456582 ) ) ;
#111337 = CARTESIAN_POINT ( 'NONE',  ( 8.224510206698953496, -14.34966873604960469, 107.9155762719810241 ) ) ;
#111338 = CARTESIAN_POINT ( 'NONE',  ( 17.50000000000000000, -3.456093896842488800, 22.00000000000000711 ) ) ;
#111339 = CARTESIAN_POINT ( 'NONE',  ( -16.53943276465976808, -0.05219959533934237506, 38.75109039468567573 ) ) ;
#111340 = CARTESIAN_POINT ( 'NONE',  ( 15.80617190586746368, 15.72974639402197994, 59.37390960531436690 ) ) ;
#111341 = CARTESIAN_POINT ( 'NONE',  ( 4.379528057220092307, 16.55341960407617563, 107.2927570613523471 ) ) ;
#111342 = CARTESIAN_POINT ( 'NONE',  ( -19.02544592524342804, 5.153800228976336051, 36.04057627198100988 ) ) ;
#111343 = CARTESIAN_POINT ( 'NONE',  ( -16.52544592524335698, -4.483927247898792601, 68.95942372801901854 ) ) ;
#111344 = CARTESIAN_POINT ( 'NONE',  ( 5.153800228976615827, -19.02544592524334988, 65.20942372801900433 ) ) ;
#111345 = CARTESIAN_POINT ( 'NONE',  ( -18.62759615963255300, -10.81492255796106328, 44.16775706135234714 ) ) ;
#111346 = AXIS2_PLACEMENT_3D ( 'NONE', #106557, #154057, #168234 ) ;
#111347 = CARTESIAN_POINT ( 'NONE',  ( -10.72451020669898014, 18.67979575497178502, 55.41557627198102409 ) ) ;
#111348 = CARTESIAN_POINT ( 'NONE',  ( 4.483927247898790824, -16.52544592524335698, 95.20942372801903275 ) ) ;
#111349 = CARTESIAN_POINT ( 'NONE',  ( -21.52544592524334988, -5.823673210054445271, 88.95942372801901854 ) ) ;
#111350 = CARTESIAN_POINT ( 'NONE',  ( -15.80617190586745835, -15.72974639402198527, 46.87390960531435979 ) ) ;
#111351 = CARTESIAN_POINT ( 'NONE',  ( -15.72974639402197994, 15.80617190586746368, 30.62390960531436335 ) ) ;
#111352 = VERTEX_POINT ( 'NONE', #48613 ) ;
#111353 = ORIENTED_EDGE ( 'NONE', *, *, #195701, .T. ) ;
#111354 = CARTESIAN_POINT ( 'NONE',  ( -8.224510206698735004, -14.34966873604973081, 74.58442372801901854 ) ) ;
#111355 = CARTESIAN_POINT ( 'NONE',  ( -21.55341960407610458, -5.719274019375992779, 41.45724293864769550 ) ) ;
#111356 = ORIENTED_EDGE ( 'NONE', *, *, #38347, .F. ) ;
#111357 = CARTESIAN_POINT ( 'NONE',  ( 19.02544592524343514, -5.153800228976328945, 93.54057627198102409 ) ) ;
#111358 = CARTESIAN_POINT ( 'NONE',  ( -20.96320343559624177, 21.46320343559661126, 5.353553390593268624 ) ) ;
#111359 = CARTESIAN_POINT ( 'NONE',  ( 9.474510206698971260, -16.51473224551069308, 27.91557627198103120 ) ) ;
#111360 = CARTESIAN_POINT ( 'NONE',  ( -18.62759615963270932, 10.81492255796079327, 65.83224293864769550 ) ) ;
#111361 = CARTESIAN_POINT ( 'NONE',  ( 16.52544592524335698, 4.483927247898782831, 91.45942372801901854 ) ) ;
#111362 = CARTESIAN_POINT ( 'NONE',  ( -5.823673210054431948, 21.52544592524334988, 42.70942372801901854 ) ) ;
#111363 = CARTESIAN_POINT ( 'NONE',  ( 5.153800228976615827, -19.02544592524334988, 100.2094237280190043 ) ) ;
#111364 = CARTESIAN_POINT ( 'NONE',  ( -4.483927247898539470, -16.52544592524342804, 97.29057627198105251 ) ) ;
#111365 = CARTESIAN_POINT ( 'NONE',  ( 8.224510206698742110, 14.34966873604972548, 22.08442372801901143 ) ) ;
#111366 = VECTOR ( 'NONE', #117938, 1000.000000000000000 ) ;
#111367 = CARTESIAN_POINT ( 'NONE',  ( -9.564922557960796823, -16.46253265017161027, 37.08224293864768839 ) ) ;
#111368 = CARTESIAN_POINT ( 'NONE',  ( -5.000000000000000888, -130.0000000000000000, -13.99999999999999822 ) ) ;
#111369 = CARTESIAN_POINT ( 'NONE',  ( 13.97604488694527802, 13.89961937509977652, 89.37390960531436690 ) ) ;
#111370 = CARTESIAN_POINT ( 'NONE',  ( 4.379528057220092307, 16.55341960407617563, 77.29275706135234714 ) ) ;
#111371 = CARTESIAN_POINT ( 'NONE',  ( -0.05219959533937732626, 21.53943276465977519, 107.5010903946856899 ) ) ;
#111372 = CARTESIAN_POINT ( 'NONE',  ( -10.81492255796078084, -18.62759615963271287, 67.08224293864770971 ) ) ;
#111373 = CARTESIAN_POINT ( 'NONE',  ( 8.224510206698742110, 14.34966873604972548, 87.08442372801901854 ) ) ;
#111374 = CARTESIAN_POINT ( 'NONE',  ( 16.51473224551083163, -9.474510206698727899, 75.83442372801900433 ) ) ;
#111375 = CARTESIAN_POINT ( 'NONE',  ( -19.03943276465977164, 0.05219959533909376836, 36.24890960531436690 ) ) ;
#111377 = CIRCLE ( 'NONE', #130715, 16.70000000000002061 ) ;
#111376 = CARTESIAN_POINT ( 'NONE',  ( 16.51473224551069308, 9.474510206698969483, 74.16557627198103830 ) ) ;
#111378 = CARTESIAN_POINT ( 'NONE',  ( -9.474510206698964154, 16.51473224551069663, 35.41557627198102409 ) ) ;
#111379 = CARTESIAN_POINT ( 'NONE',  ( 5.049401038297881783, 19.05341960407617563, 77.29275706135231871 ) ) ;
#111380 = CARTESIAN_POINT ( 'NONE',  ( 26.45763050569066266, -3.219288925403527735, 173.6696415116520598 ) ) ;
#111381 = CARTESIAN_POINT ( 'NONE',  ( -9.564922557960796823, -16.46253265017161027, 107.0822429386476955 ) ) ;
#111382 = CARTESIAN_POINT ( 'NONE',  ( -16.53943276465976808, 0.05219959533911058130, 66.24890960531436690 ) ) ;
#111383 = CARTESIAN_POINT ( 'NONE',  ( -15.80617190586745835, -15.72974639402198527, 66.87390960531436690 ) ) ;
#111384 = AXIS2_PLACEMENT_3D ( 'NONE', #68875, #161886, #158880 ) ;
#111385 = FACE_OUTER_BOUND ( 'NONE', #173580, .T. ) ;
#111386 =( GEOMETRIC_REPRESENTATION_CONTEXT ( 3 ) GLOBAL_UNCERTAINTY_ASSIGNED_CONTEXT ( ( #5450 ) ) GLOBAL_UNIT_ASSIGNED_CONTEXT ( ( #162691, #120174, #196055 ) ) REPRESENTATION_CONTEXT ( 'NONE', 'WORKASPACE' ) );
#111387 = CARTESIAN_POINT ( 'NONE',  ( 9.564922557961047289, -16.46253265017146816, 25.41775706135234003 ) ) ;
#111388 = CARTESIAN_POINT ( 'NONE',  ( 21.77219501682363401, -9.607313489129742479, 170.8391438706019585 ) ) ;
#111390 = CARTESIAN_POINT ( 'NONE',  ( 0.05219959533909260263, 19.03943276465977164, 69.99890960531435269 ) ) ;
#111389 = CARTESIAN_POINT ( 'NONE',  ( 19.02544592524343514, -5.153800228976328945, 58.54057627198102409 ) ) ;
#111391 = EDGE_CURVE ( 'NONE', #165125, #82999, #3089, .T. ) ;
#111392 = CARTESIAN_POINT ( 'NONE',  ( -8.314922557961024197, 14.29746914071037800, 47.91775706135234714 ) ) ;
#111393 = CARTESIAN_POINT ( 'NONE',  ( -19.34837522270366250, -5.499999999999802824, 100.8633768483257711 ) ) ;
#111394 = CARTESIAN_POINT ( 'NONE',  ( 22.68041372103478182, -7.529096845820644646, 173.5090731399503454 ) ) ;
#111395 = CARTESIAN_POINT ( 'NONE',  ( 14.29746914071037800, 8.314922557961029526, 71.66775706135234714 ) ) ;
#111396 = CARTESIAN_POINT ( 'NONE',  ( 32.09281931051394565, -20.34824190692416934, -24.99999999999997868 ) ) ;
#111397 = CARTESIAN_POINT ( 'NONE',  ( 16.52544592524335698, 4.483927247898782831, 66.45942372801903275 ) ) ;
#111398 = CARTESIAN_POINT ( 'NONE',  ( -14.29746914071037622, -8.314922557961029526, 44.16775706135234714 ) ) ;
#111400 = CARTESIAN_POINT ( 'NONE',  ( -32.00000000000000000, -1.096058885236868847E-14, 100.5000000000010232 ) ) ;
#111399 = CARTESIAN_POINT ( 'NONE',  ( -13.97604488694527625, -13.89961937509977652, 51.87390960531436690 ) ) ;
#111401 = CARTESIAN_POINT ( 'NONE',  ( -5.823673210054431948, 21.52544592524334988, 57.70942372801901143 ) ) ;
#111402 = CARTESIAN_POINT ( 'NONE',  ( 5.153800228976615827, -19.02544592524334988, 60.20942372801899012 ) ) ;
#111403 = CARTESIAN_POINT ( 'NONE',  ( -15.72974639402176322, -15.80617190586768395, 89.37609039468568994 ) ) ;
#111404 = CARTESIAN_POINT ( 'NONE',  ( 13.97604488694527802, 13.89961937509977652, 29.37390960531435979 ) ) ;
#111405 = CARTESIAN_POINT ( 'NONE',  ( 3.765340386950246872E-15, -39.95163481335715971, -7.502157773949823749 ) ) ;
#111406 = CARTESIAN_POINT ( 'NONE',  ( -15.80617190586745835, -15.72974639402198527, 51.87390960531437401 ) ) ;
#111407 = AXIS2_PLACEMENT_3D ( 'NONE', #63905, #54463, #155908 ) ;
#111408 = CARTESIAN_POINT ( 'NONE',  ( -5.049401038298153566, 19.05341960407611168, 105.2072429386476671 ) ) ;
#111409 = CARTESIAN_POINT ( 'NONE',  ( -14.29746914071049879, 8.314922557960819915, 100.8322429386477097 ) ) ;
#111410 = CARTESIAN_POINT ( 'NONE',  ( 14.29746914071037800, 8.314922557961029526, 36.66775706135234714 ) ) ;
#111411 = CARTESIAN_POINT ( 'NONE',  ( 16.55341960407611168, 4.379528057220329451, 23.95724293864769550 ) ) ;
#111412 = ORIENTED_EDGE ( 'NONE', *, *, #121041, .T. ) ;
#111413 = CARTESIAN_POINT ( 'NONE',  ( -15.80617190586745835, -15.72974639402198527, 106.8739096053143811 ) ) ;
#111415 = CARTESIAN_POINT ( 'NONE',  ( -18.22780087662123805, 5.499999999999981348, 86.01763182126894947 ) ) ;
#111414 = CARTESIAN_POINT ( 'NONE',  ( -12.06949235617756955, 12.14591786802309770, 35.62390960531437401 ) ) ;
#111416 = CARTESIAN_POINT ( 'NONE',  ( -16.46253265017146816, -9.564922557961047289, 89.16775706135234714 ) ) ;
#111417 = CARTESIAN_POINT ( 'NONE',  ( 19.03943276465977164, 0.05219959533936151252, 26.25109039468566507 ) ) ;
#111418 = CARTESIAN_POINT ( 'NONE',  ( -4.379528057220328563, 16.55341960407611168, 25.20724293864769550 ) ) ;
#111419 = CARTESIAN_POINT ( 'NONE',  ( -21.55341960407610458, -5.719274019375992779, 101.4572429386476955 ) ) ;
#111420 = CARTESIAN_POINT ( 'NONE',  ( -10.81492255796078084, -18.62759615963271287, 47.08224293864770260 ) ) ;
#111421 = CARTESIAN_POINT ( 'NONE',  ( 5.049401038298161559, -19.05341960407611168, 77.70724293864765286 ) ) ;
#111422 = CARTESIAN_POINT ( 'NONE',  ( -14.29746914071049879, 8.314922557960819915, 35.83224293864768839 ) ) ;
#111423 = CARTESIAN_POINT ( 'NONE',  ( 19.03943276465977164, -0.05219959533909143690, 88.74890960531436690 ) ) ;
#111424 = EDGE_LOOP ( 'NONE', ( #139914, #172899 ) ) ;
#111425 = CARTESIAN_POINT ( 'NONE',  ( 19.53091890409951858, 5.500000000000024869, 57.56097431831420153 ) ) ;
#111426 = CARTESIAN_POINT ( 'NONE',  ( -19.02544592524334988, -5.153800228976617603, 43.95942372801899012 ) ) ;
#111427 = CARTESIAN_POINT ( 'NONE',  ( 18.67979575497178502, 10.72451020669898547, 79.16557627198103830 ) ) ;
#111428 = CARTESIAN_POINT ( 'NONE',  ( 12.14591786802309770, 12.06949235617756955, 94.37390960531436690 ) ) ;
#111429 = CARTESIAN_POINT ( 'NONE',  ( -21.53943276465977519, -0.05219959533937600094, 38.75109039468567573 ) ) ;
#111430 = CARTESIAN_POINT ( 'NONE',  ( -27.73933785331498925, -9.013057229001049109, 142.9750000027312069 ) ) ;
#111431 = CARTESIAN_POINT ( 'NONE',  ( 16.55341960407618274, -4.379528057220086978, 106.0427570613523471 ) ) ;
#111432 = CARTESIAN_POINT ( 'NONE',  ( 13.89961937509977652, -13.97604488694527269, 38.12390960531436690 ) ) ;
#111433 = CARTESIAN_POINT ( 'NONE',  ( -19.03943276465977164, 0.05219959533909376836, 81.24890960531436690 ) ) ;
#111434 = CARTESIAN_POINT ( 'NONE',  ( 22.44159573604009239, 16.30477369853692693, 140.0750000027311728 ) ) ;
#111435 = CARTESIAN_POINT ( 'NONE',  ( -13.97604488694527625, -13.89961937509977652, 26.87390960531434558 ) ) ;
#111436 = CARTESIAN_POINT ( 'NONE',  ( 16.52544592524342804, -4.483927247898539470, 38.54057627198103120 ) ) ;
#111437 = CARTESIAN_POINT ( 'NONE',  ( 5.823673210054444382, -21.52544592524334988, 70.20942372801904696 ) ) ;
#111439 = CARTESIAN_POINT ( 'NONE',  ( 16.53943276465976808, 0.05219959533934440121, 71.25109039468568994 ) ) ;
#111438 = CARTESIAN_POINT ( 'NONE',  ( 33.60028042027824569, -17.96933036163179764, -21.71044752825890711 ) ) ;
#111440 = CARTESIAN_POINT ( 'NONE',  ( -9.474510206698964154, 16.51473224551069663, 50.41557627198102409 ) ) ;
#111441 = CARTESIAN_POINT ( 'NONE',  ( 13.89961937509977652, -13.97604488694527269, 63.12390960531435979 ) ) ;
#111442 = ORIENTED_EDGE ( 'NONE', *, *, #197557, .F. ) ;
#111443 = CARTESIAN_POINT ( 'NONE',  ( 10.72451020669871369, 18.67979575497193778, 102.0844237280190185 ) ) ;
#111444 = CARTESIAN_POINT ( 'NONE',  ( 16.52544592524335698, 4.483927247898782831, 76.45942372801901854 ) ) ;
#111445 = CARTESIAN_POINT ( 'NONE',  ( 5.719274019375673035, 21.55341960407619339, 97.29275706135234714 ) ) ;
#111446 = CARTESIAN_POINT ( 'NONE',  ( -9.474510206698964154, 16.51473224551069663, 60.41557627198102409 ) ) ;
#111447 = CARTESIAN_POINT ( 'NONE',  ( -15.72974639402197994, 15.80617190586746368, 35.62390960531437401 ) ) ;
#111448 = CARTESIAN_POINT ( 'NONE',  ( 0.05219959533936267826, -19.03943276465977164, 105.0010903946856615 ) ) ;
#111449 = CARTESIAN_POINT ( 'NONE',  ( 10.81492255796106328, -18.62759615963255655, 70.41775706135236135 ) ) ;
#111450 = CARTESIAN_POINT ( 'NONE',  ( 16.55341960407618274, -4.379528057220086978, 56.04275706135235424 ) ) ;
#111452 = CARTESIAN_POINT ( 'NONE',  ( -5.719274019375978568, 21.55341960407610458, 100.2072429386476955 ) ) ;
#111451 = AXIS2_PLACEMENT_3D ( 'NONE', #41756, #23585, #193437 ) ;
#111453 = CARTESIAN_POINT ( 'NONE',  ( -13.89961937509957401, -13.97604488694547875, 94.37609039468566152 ) ) ;
#111454 = CARTESIAN_POINT ( 'NONE',  ( -0.05219959533909027116, -19.03943276465977164, 77.49890960531435269 ) ) ;
#111455 = CARTESIAN_POINT ( 'NONE',  ( 16.52544592524335698, 4.483927247898782831, 21.45942372801901499 ) ) ;
#111456 = CARTESIAN_POINT ( 'NONE',  ( -14.29746914071037622, -8.314922557961029526, 19.16775706135234714 ) ) ;
#111457 = CARTESIAN_POINT ( 'NONE',  ( -8.314922557960811034, -14.29746914071050412, 67.08224293864770971 ) ) ;
#111458 = CARTESIAN_POINT ( 'NONE',  ( -16.52544592524335698, -4.483927247898792601, 78.95942372801901854 ) ) ;
#111459 = EDGE_CURVE ( 'NONE', #94189, #16723, #162432, .T. ) ;
#111461 = CARTESIAN_POINT ( 'NONE',  ( -16.46253265017160317, 9.564922557960807481, 50.83224293864770260 ) ) ;
#111460 = CARTESIAN_POINT ( 'NONE',  ( -21.55341960407610458, -5.719274019375992779, 111.4572429386476813 ) ) ;
#111462 = CARTESIAN_POINT ( 'NONE',  ( 9.564922557960805705, 16.46253265017160317, 64.58224293864769550 ) ) ;
#111463 = CARTESIAN_POINT ( 'NONE',  ( -16.55341960407617563, 4.379528057220093196, 78.54275706135236135 ) ) ;
#111464 = CARTESIAN_POINT ( 'NONE',  ( 28.82186960331498327, 9.364793116373570925, 147.3500000054623627 ) ) ;
#111465 = VERTEX_POINT ( 'NONE', #128408 ) ;
#111466 = CARTESIAN_POINT ( 'NONE',  ( -10.81492255796105439, 18.62759615963255655, 107.9177570613523471 ) ) ;
#111467 = CARTESIAN_POINT ( 'NONE',  ( -13.89961937509977652, 13.97604488694528158, 35.62390960531435269 ) ) ;
#111468 = ORIENTED_EDGE ( 'NONE', *, *, #66112, .F. ) ;
#111469 = CARTESIAN_POINT ( 'NONE',  ( 5.153800228976615827, -19.02544592524334988, 105.2094237280190185 ) ) ;
#111471 = CARTESIAN_POINT ( 'NONE',  ( 16.52544592524335698, 4.483927247898782831, 31.45942372801901854 ) ) ;
#111470 = CARTESIAN_POINT ( 'NONE',  ( -16.46253265017146816, -9.564922557961047289, 39.16775706135234003 ) ) ;
#111472 = CARTESIAN_POINT ( 'NONE',  ( 19.02544592524343514, -5.153800228976328945, 43.54057627198103120 ) ) ;
#111473 = CARTESIAN_POINT ( 'NONE',  ( -19.05341960407611168, -5.049401038298163336, 61.45724293864769550 ) ) ;
#111474 = CARTESIAN_POINT ( 'NONE',  ( 5.823673210054125526, 21.52544592524343514, 79.79057627198102409 ) ) ;
#111475 = CARTESIAN_POINT ( 'NONE',  ( -3.573655867282028392E-15, 2.428612866367529932E-14, 1.984260520772446048E-44 ) ) ;
#111476 = CARTESIAN_POINT ( 'NONE',  ( -19.02544592524342804, 5.153800228976336051, 56.04057627198100988 ) ) ;
#111477 = CARTESIAN_POINT ( 'NONE',  ( 17.50000000000000000, -5.500000000000000888, 120.0000000000000142 ) ) ;
#111478 = CARTESIAN_POINT ( 'NONE',  ( -0.05219959533936034679, 19.03943276465977164, 92.50109039468566152 ) ) ;
#111479 = CARTESIAN_POINT ( 'NONE',  ( 4.483927247898545687, 16.52544592524342804, 69.79057627198102409 ) ) ;
#111480 = CARTESIAN_POINT ( 'NONE',  ( -0.05219959533936034679, 19.03943276465977164, 27.50109039468566507 ) ) ;
#111481 = CARTESIAN_POINT ( 'NONE',  ( 8.314922557960818139, 14.29746914071049879, 59.58224293864770260 ) ) ;
#111482 = CARTESIAN_POINT ( 'NONE',  ( -15.80617190586768217, 15.72974639402176855, 83.12609039468568994 ) ) ;
#111483 = CARTESIAN_POINT ( 'NONE',  ( -5.153800228976328057, -19.02544592524343514, 27.29057627198103120 ) ) ;
#111484 = CARTESIAN_POINT ( 'NONE',  ( 5.823673210054444382, -21.52544592524334988, 95.20942372801903275 ) ) ;
#111486 = CARTESIAN_POINT ( 'NONE',  ( 15.80617190586769283, -15.72974639402175789, 75.62609039468567573 ) ) ;
#111485 = CARTESIAN_POINT ( 'NONE',  ( 8.314922557960818139, 14.29746914071049879, 24.58224293864768839 ) ) ;
#111487 = CARTESIAN_POINT ( 'NONE',  ( 13.97604488694527802, 13.89961937509977652, 84.37390960531433848 ) ) ;
#111488 = CARTESIAN_POINT ( 'NONE',  ( 10.72451020669871369, 18.67979575497193778, 37.08442372801901143 ) ) ;
#111489 = CARTESIAN_POINT ( 'NONE',  ( 5.049401038298161559, -19.05341960407611168, 77.70724293864765286 ) ) ;
#111490 = CARTESIAN_POINT ( 'NONE',  ( -16.52544592524342804, 4.483927247898546575, 91.04057627198103830 ) ) ;
#111491 = CARTESIAN_POINT ( 'NONE',  ( -14.34966873604960291, -8.224510206698953496, 66.66557627198102409 ) ) ;
#111492 = CARTESIAN_POINT ( 'NONE',  ( 21.53943276465977519, -0.05219959533907433946, 68.74890960531435269 ) ) ;
#111493 = CARTESIAN_POINT ( 'NONE',  ( -5.049401038298153566, 19.05341960407611168, 80.20724293864769550 ) ) ;
#111494 = CARTESIAN_POINT ( 'NONE',  ( -10.72451020669898014, 18.67979575497178502, 85.41557627198102409 ) ) ;
#111495 = CARTESIAN_POINT ( 'NONE',  ( 9.564922557961047289, -16.46253265017146816, 75.41775706135234714 ) ) ;
#111497 = CARTESIAN_POINT ( 'NONE',  ( -16.52544592524342804, 4.483927247898546575, 81.04057627198102409 ) ) ;
#111496 = CARTESIAN_POINT ( 'NONE',  ( 13.89961937509957579, 13.97604488694547520, 31.87609039468566863 ) ) ;
#111498 = CARTESIAN_POINT ( 'NONE',  ( 0.05219959533907565091, 21.53943276465977519, 49.99890960531437401 ) ) ;
#111499 = CARTESIAN_POINT ( 'NONE',  ( -18.09918380851992126, -5.500000000000039968, 41.48618307335612343 ) ) ;
#111501 = CARTESIAN_POINT ( 'NONE',  ( 8.571926809382597767, 26.38167802310806209, 146.7750000027311899 ) ) ;
#111500 = CARTESIAN_POINT ( 'NONE',  ( -4.379528057220086978, -16.55341960407618274, 94.79275706135234714 ) ) ;
#111502 = CARTESIAN_POINT ( 'NONE',  ( 13.97604488694548053, -13.89961937509957401, 105.6260903946856757 ) ) ;
#111503 = CARTESIAN_POINT ( 'NONE',  ( -8.224510206698948167, 14.34966873604960824, 65.41557627198102409 ) ) ;
#111504 = CARTESIAN_POINT ( 'NONE',  ( -19.01529144963335582, -5.500000000000032863, 96.23431955728437970 ) ) ;
#111505 = CARTESIAN_POINT ( 'NONE',  ( 13.89961937509977652, -13.97604488694527269, 58.12390960531436690 ) ) ;
#111506 = CARTESIAN_POINT ( 'NONE',  ( -4.379528057220328563, 16.55341960407611168, 50.20724293864769550 ) ) ;
#111507 = CARTESIAN_POINT ( 'NONE',  ( 5.153800228976335163, 19.02544592524342804, 104.7905762719809957 ) ) ;
#111509 = CARTESIAN_POINT ( 'NONE',  ( 9.564922557960805705, 16.46253265017160317, 69.58224293864770971 ) ) ;
#111508 = CARTESIAN_POINT ( 'NONE',  ( -0.05219959533936034679, 19.03943276465977164, 87.50109039468567573 ) ) ;
#111510 = CARTESIAN_POINT ( 'NONE',  ( 0.05219959533909260263, 19.03943276465977164, 89.99890960531436690 ) ) ;
#111511 = CARTESIAN_POINT ( 'NONE',  ( -9.474510206698964154, 16.51473224551069663, 85.41557627198102409 ) ) ;
#111512 = CARTESIAN_POINT ( 'NONE',  ( 21.52544592524344225, -5.823673210054117533, 58.54057627198103120 ) ) ;
#111513 = CARTESIAN_POINT ( 'NONE',  ( -16.53943276465976808, -0.05219959533934237506, 58.75109039468568994 ) ) ;
#111514 = VECTOR ( 'NONE', #192994, 1000.000000000000000 ) ;
#111515 = CARTESIAN_POINT ( 'NONE',  ( 13.97604488694548053, -13.89961937509957401, 105.6260903946856757 ) ) ;
#111516 = CARTESIAN_POINT ( 'NONE',  ( -13.89961937509977652, 13.97604488694528158, 60.62390960531436690 ) ) ;
#111517 = CARTESIAN_POINT ( 'NONE',  ( 18.62759615963271287, -10.81492255796078972, 73.33224293864769550 ) ) ;
#111518 = CARTESIAN_POINT ( 'NONE',  ( -19.02544592524334988, -5.153800228976617603, 98.95942372801900433 ) ) ;
#111520 = CARTESIAN_POINT ( 'NONE',  ( 18.67979575497194134, -10.72451020669871369, 45.83442372801901854 ) ) ;
#111519 = CARTESIAN_POINT ( 'NONE',  ( -16.53943276465976808, 0.05219959533911058130, 26.24890960531435624 ) ) ;
#111521 = CARTESIAN_POINT ( 'NONE',  ( -19.05341960407617563, 5.049401038297882671, 43.54275706135232582 ) ) ;
#111522 = CLOSED_SHELL ( 'NONE', ( #2768, #124493, #4122, #67283, #190608, #41538, #183853, #20622, #102004, #107734, #108242, #14106, #168748, #74082, #71988, #56314, #22134, #86106, #147858, #78434, #49489, #167639, #17771, #25683, #18733, #109048, #150283 ) ) ;
#111524 = CARTESIAN_POINT ( 'NONE',  ( -16.52544592524335698, -4.483927247898792601, 93.95942372801903275 ) ) ;
#111523 = CARTESIAN_POINT ( 'NONE',  ( -12.06949235617739369, -12.14591786802326823, 59.37609039468568284 ) ) ;
#111525 = DIRECTION ( 'NONE',  ( 1.000000000000000000, 0.000000000000000000, 0.000000000000000000 ) ) ;
#111526 = CARTESIAN_POINT ( 'NONE',  ( 0.05219959533934541429, -16.53943276465976808, 80.00109039468568994 ) ) ;
#111527 = CARTESIAN_POINT ( 'NONE',  ( -4.483927247898782831, 16.52544592524335698, 37.70942372801900433 ) ) ;
#111528 = CARTESIAN_POINT ( 'NONE',  ( 19.03943276465977164, -0.05219959533909143690, 48.74890960531435979 ) ) ;
#111529 = CARTESIAN_POINT ( 'NONE',  ( 19.02544592524343514, -5.153800228976328945, 53.54057627198102409 ) ) ;
#111530 = CARTESIAN_POINT ( 'NONE',  ( 16.51473224551069308, 9.474510206698969483, 54.16557627198103120 ) ) ;
#111531 = CARTESIAN_POINT ( 'NONE',  ( -10.72451020669870658, -18.67979575497194134, 59.58442372801901854 ) ) ;
#111532 = CARTESIAN_POINT ( 'NONE',  ( -14.29746914071037622, -8.314922557961029526, 54.16775706135235424 ) ) ;
#111533 = CARTESIAN_POINT ( 'NONE',  ( 12.06949235617757843, -12.14591786802309237, 23.12390960531436335 ) ) ;
#111534 = CARTESIAN_POINT ( 'NONE',  ( 5.049401038298161559, -19.05341960407611168, 32.70724293864768129 ) ) ;
#111535 = CARTESIAN_POINT ( 'NONE',  ( -9.474510206698964154, 16.51473224551069663, 40.41557627198103120 ) ) ;
#111536 = CARTESIAN_POINT ( 'NONE',  ( -14.29746914071037622, -8.314922557961029526, 29.16775706135234003 ) ) ;
#111537 = CARTESIAN_POINT ( 'NONE',  ( -5.049401038297874678, -19.05341960407617918, 84.79275706135233293 ) ) ;
#111538 = CARTESIAN_POINT ( 'NONE',  ( 4.379528057220339221, -16.55341960407611168, 87.70724293864769550 ) ) ;
#111539 = CARTESIAN_POINT ( 'NONE',  ( 19.03943276465977164, -0.05219959533909143690, 33.74890960531435979 ) ) ;
#111541 = CARTESIAN_POINT ( 'NONE',  ( 17.49999999999999645, 5.624438216177603422, 76.68329655085356933 ) ) ;
#111540 = CARTESIAN_POINT ( 'NONE',  ( -9.474510206698720793, -16.51473224551083518, 74.58442372801900433 ) ) ;
#111542 = CARTESIAN_POINT ( 'NONE',  ( -15.80617190586768217, 15.72974639402176855, 78.12609039468570415 ) ) ;
#111543 = CARTESIAN_POINT ( 'NONE',  ( 14.29746914071037800, 8.314922557961029526, 36.66775706135234714 ) ) ;
#111544 = CARTESIAN_POINT ( 'NONE',  ( -17.49999999999998934, 3.471454075611624113, 24.48332581144370934 ) ) ;
#111545 = CARTESIAN_POINT ( 'NONE',  ( 18.62759615963271287, -10.81492255796078972, 38.33224293864768839 ) ) ;
#111546 = CARTESIAN_POINT ( 'NONE',  ( 12.14591786802327356, -12.06949235617739191, 20.62609039468568639 ) ) ;
#111547 = CARTESIAN_POINT ( 'NONE',  ( 19.02544592524343514, -5.153800228976328945, 28.54057627198103120 ) ) ;
#111548 = CARTESIAN_POINT ( 'NONE',  ( -13.97604488694547697, 13.89961937509957934, 33.12609039468566863 ) ) ;
#111549 = CARTESIAN_POINT ( 'NONE',  ( 11.66180171105669672, 11.95556478057400795, -59.13370768023890633 ) ) ;
#111550 = CARTESIAN_POINT ( 'NONE',  ( 19.05341960407611168, 5.049401038298154454, 33.95724293864769550 ) ) ;
#111551 = CARTESIAN_POINT ( 'NONE',  ( -8.898068258721469448, -27.38543819252872069, 142.6656553485623817 ) ) ;
#111552 = CARTESIAN_POINT ( 'NONE',  ( -19.05341960407611168, -5.049401038298163336, 66.45724293864769550 ) ) ;
#111553 = CARTESIAN_POINT ( 'NONE',  ( 17.50000000000000000, -5.500000000000000000, 111.2176903769643559 ) ) ;
#111554 = PRODUCT_DEFINITION_SHAPE ( 'NONE', 'NONE',  #200195 ) ;
#111555 = CARTESIAN_POINT ( 'NONE',  ( -10.72451020669870658, -18.67979575497194134, 109.5844237280190328 ) ) ;
#111556 = CARTESIAN_POINT ( 'NONE',  ( -12.14591786802309592, -12.06949235617757132, 31.87390960531435979 ) ) ;
#111557 = CARTESIAN_POINT ( 'NONE',  ( 9.564922557960805705, 16.46253265017160317, 44.58224293864769550 ) ) ;
#111558 = CARTESIAN_POINT ( 'NONE',  ( -13.97604488694527625, -13.89961937509977652, 86.87390960531436690 ) ) ;
#111559 = CARTESIAN_POINT ( 'NONE',  ( -18.62759615963255300, -10.81492255796106328, 69.16775706135234714 ) ) ;
#111560 = CARTESIAN_POINT ( 'NONE',  ( -16.46253265017160317, 9.564922557960807481, 45.83224293864769550 ) ) ;
#111561 = ADVANCED_FACE ( 'NONE', ( #64765, #125445 ), #159751, .F. ) ;
#111562 = CARTESIAN_POINT ( 'NONE',  ( 21.53943276465977519, 0.05219959533937863772, 61.25109039468567573 ) ) ;
#111563 = CARTESIAN_POINT ( 'NONE',  ( 21.53943276465977519, -0.05219959533907433946, 23.74890960531435269 ) ) ;
#111564 = CARTESIAN_POINT ( 'NONE',  ( -13.97604488694527625, -13.89961937509977652, 31.87390960531435979 ) ) ;
#111565 = CARTESIAN_POINT ( 'NONE',  ( -18.67979575497193778, 10.72451020669871902, 23.33442372801901499 ) ) ;
#111566 = CARTESIAN_POINT ( 'NONE',  ( -16.51473224551082808, 9.474510206698731452, 48.33442372801900433 ) ) ;
#111567 = CARTESIAN_POINT ( 'NONE',  ( -19.03943276465977164, 0.05219959533909376836, 21.24890960531436335 ) ) ;
#111568 = CARTESIAN_POINT ( 'NONE',  ( -9.564922557960796823, -16.46253265017161027, 57.08224293864769550 ) ) ;
#111569 = CARTESIAN_POINT ( 'NONE',  ( -19.03943276465977164, -0.05219959533935918106, 113.7510903946856757 ) ) ;
#111570 = CARTESIAN_POINT ( 'NONE',  ( -8.314922557960811034, -14.29746914071050412, 82.08224293864768129 ) ) ;
#111571 = CARTESIAN_POINT ( 'NONE',  ( 10.72451020669898902, -18.67979575497178502, 27.91557627198103830 ) ) ;
#111572 = CARTESIAN_POINT ( 'NONE',  ( -16.46253265017146816, -9.564922557961047289, 99.16775706135233293 ) ) ;
#111573 = CARTESIAN_POINT ( 'NONE',  ( 18.67979575497178502, 10.72451020669898547, 109.1655762719810383 ) ) ;
#111574 = CARTESIAN_POINT ( 'NONE',  ( 18.62759615963255655, 10.81492255796105972, 51.66775706135234714 ) ) ;
#111575 = CARTESIAN_POINT ( 'NONE',  ( 14.29746914071037800, 8.314922557961029526, 56.66775706135235424 ) ) ;
#111576 = CARTESIAN_POINT ( 'NONE',  ( 8.314922557961029526, -14.29746914071037800, 55.41775706135234714 ) ) ;
#111577 = CARTESIAN_POINT ( 'NONE',  ( -18.62759615963270932, 10.81492255796079327, 50.83224293864770971 ) ) ;
#111578 = CARTESIAN_POINT ( 'NONE',  ( -16.51473224551069308, -9.474510206698971260, 51.66557627198102409 ) ) ;
#111579 = CARTESIAN_POINT ( 'NONE',  ( 16.53943276465976808, 0.05219959533934440121, 81.25109039468568994 ) ) ;
#111580 = CARTESIAN_POINT ( 'NONE',  ( 18.67979575497178502, 10.72451020669898547, 104.1655762719810241 ) ) ;
#111581 = CARTESIAN_POINT ( 'NONE',  ( -16.52544592524342804, 4.483927247898546575, 46.04057627198103830 ) ) ;
#111582 = CARTESIAN_POINT ( 'NONE',  ( 19.02544592524343514, -5.153800228976328945, 68.54057627198103830 ) ) ;
#111583 = CARTESIAN_POINT ( 'NONE',  ( -14.29746914071037622, -8.314922557961029526, 79.16775706135234714 ) ) ;
#111584 = CARTESIAN_POINT ( 'NONE',  ( -16.55341960407617563, 4.379528057220093196, 23.54275706135235424 ) ) ;
#111585 = CARTESIAN_POINT ( 'NONE',  ( 21.52544592524344225, -5.823673210054117533, 98.54057627198105251 ) ) ;
#111586 = CARTESIAN_POINT ( 'NONE',  ( 8.314922557960818139, 14.29746914071049879, 44.58224293864769550 ) ) ;
#111587 = ORIENTED_EDGE ( 'NONE', *, *, #10842, .F. ) ;
#111588 = CARTESIAN_POINT ( 'NONE',  ( -16.61371651742600974, 7.165104196376139711, 73.85415069993000259 ) ) ;
#111589 = CARTESIAN_POINT ( 'NONE',  ( -0.05219959533907301413, -21.53943276465977519, 82.49890960531436690 ) ) ;
#111590 = CARTESIAN_POINT ( 'NONE',  ( -0.05219959533910754901, -16.53943276465976808, 32.49890960531435979 ) ) ;
#111591 = ORIENTED_EDGE ( 'NONE', *, *, #84711, .F. ) ;
#111592 = LINE ( 'NONE', #94427, #88808 ) ;
#111593 = CARTESIAN_POINT ( 'NONE',  ( 10.72451020669898902, -18.67979575497178502, 102.9155762719810383 ) ) ;
#111594 = VECTOR ( 'NONE', #92144, 1000.000000000000000 ) ;
#111595 = CARTESIAN_POINT ( 'NONE',  ( -13.97604488694527625, -13.89961937509977652, 96.87390960531433848 ) ) ;
#111596 = CARTESIAN_POINT ( 'NONE',  ( 5.823673210054125526, 21.52544592524343514, 114.7905762719810383 ) ) ;
#111597 = CARTESIAN_POINT ( 'NONE',  ( -4.483927247898539470, -16.52544592524342804, 37.29057627198102409 ) ) ;
#111598 = EDGE_CURVE ( 'NONE', #93910, #150285, #97738, .T. ) ;
#111599 = CARTESIAN_POINT ( 'NONE',  ( -16.53943276465976808, -0.05219959533934237506, 43.75109039468568284 ) ) ;
#111600 = CARTESIAN_POINT ( 'NONE',  ( -13.89961937509977652, 13.97604488694528158, 50.62390960531435979 ) ) ;
#111601 = CARTESIAN_POINT ( 'NONE',  ( -5.049401038297874678, -19.05341960407617918, 49.79275706135231871 ) ) ;
#111602 = CARTESIAN_POINT ( 'NONE',  ( 9.474510206698971260, -16.51473224551069308, 77.91557627198103830 ) ) ;
#111603 = ORIENTED_EDGE ( 'NONE', *, *, #55067, .F. ) ;
#111604 = CARTESIAN_POINT ( 'NONE',  ( 5.823673210054125526, 21.52544592524343514, 29.79057627198102409 ) ) ;
#111605 = CARTESIAN_POINT ( 'NONE',  ( -32.19332086309597685, -20.18834286810128376, -25.14458231473970073 ) ) ;
#111606 = CARTESIAN_POINT ( 'NONE',  ( 4.483927247898790824, -16.52544592524335698, 30.20942372801902565 ) ) ;
#111607 = CARTESIAN_POINT ( 'NONE',  ( 5.049401038297881783, 19.05341960407617563, 47.29275706135231161 ) ) ;
#111608 = CARTESIAN_POINT ( 'NONE',  ( 10.81492255796078972, 18.62759615963270932, 104.5822429386477097 ) ) ;
#111609 = CARTESIAN_POINT ( 'NONE',  ( -12.06949235617756955, 12.14591786802309770, 30.62390960531436335 ) ) ;
#111610 = CARTESIAN_POINT ( 'NONE',  ( 5.153800228976335163, 19.02544592524342804, 74.79057627198103830 ) ) ;
#111611 = CARTESIAN_POINT ( 'NONE',  ( -5.719274019375978568, 21.55341960407610458, 55.20724293864770260 ) ) ;
#111613 = CARTESIAN_POINT ( 'NONE',  ( -16.53943276465976808, -0.05219959533934237506, 18.75109039468568639 ) ) ;
#111612 = CARTESIAN_POINT ( 'NONE',  ( 5.823673210054125526, 21.52544592524343514, 89.79057627198103830 ) ) ;
#111614 = CARTESIAN_POINT ( 'NONE',  ( -21.53943276465977519, 0.05219959533907696930, 26.24890960531435624 ) ) ;
#111615 = CARTESIAN_POINT ( 'NONE',  ( 15.72974639402176855, 15.80617190586768217, 91.87609039468568994 ) ) ;
#111616 = CARTESIAN_POINT ( 'NONE',  ( -19.03943276465977164, 0.05219959533909376836, 76.24890960531435269 ) ) ;
#111617 = CARTESIAN_POINT ( 'NONE',  ( -16.51473224551069308, -9.474510206698971260, 31.66557627198102054 ) ) ;
#111618 = CARTESIAN_POINT ( 'NONE',  ( 0.05219959533909260263, 19.03943276465977164, 89.99890960531436690 ) ) ;
#111619 = CARTESIAN_POINT ( 'NONE',  ( 14.34966873604960469, 8.224510206698951720, 109.1655762719810383 ) ) ;
#111620 = CARTESIAN_POINT ( 'NONE',  ( 19.05341960407611168, 5.049401038298154454, 68.95724293864769550 ) ) ;
#111621 = CARTESIAN_POINT ( 'NONE',  ( 9.564922557961047289, -16.46253265017146816, 100.4177570613523329 ) ) ;
#111622 = CARTESIAN_POINT ( 'NONE',  ( 17.50000000000001421, 3.565345528327899416, 33.07505513193528657 ) ) ;
#111623 = CARTESIAN_POINT ( 'NONE',  ( -5.049401038298153566, 19.05341960407611168, 70.20724293864769550 ) ) ;
#111625 = CARTESIAN_POINT ( 'NONE',  ( 15.80617190586746368, 15.72974639402197994, 24.37390960531435979 ) ) ;
#111624 = CARTESIAN_POINT ( 'NONE',  ( 10.72451020669871369, 18.67979575497193778, 102.0844237280190185 ) ) ;
#111626 = CARTESIAN_POINT ( 'NONE',  ( -0.05219959533934338120, 16.53943276465976808, 97.50109039468567573 ) ) ;
#111627 = CARTESIAN_POINT ( 'NONE',  ( -5.000000000000000000, -126.1226662136678272, 8.481152457036387204 ) ) ;
#111628 = CARTESIAN_POINT ( 'NONE',  ( 19.02544592524334988, 5.153800228976608722, 71.45942372801900433 ) ) ;
#111629 = CARTESIAN_POINT ( 'NONE',  ( -18.67979575497193778, 10.72451020669871902, 108.3344237280190185 ) ) ;
#111630 = DIRECTION ( 'NONE',  ( 0.5150380749100522682, 0.000000000000000000, -0.8571673007021134438 ) ) ;
#111631 = CARTESIAN_POINT ( 'NONE',  ( 19.02544592524343514, -5.153800228976328945, 23.54057627198102054 ) ) ;
#111632 = CARTESIAN_POINT ( 'NONE',  ( 12.06949235617757843, -12.14591786802309237, 23.12390960531436335 ) ) ;
#111633 = CARTESIAN_POINT ( 'NONE',  ( -35.44379935611748067, -3.753814927773975185, 38.50236686201313319 ) ) ;
#111634 = CARTESIAN_POINT ( 'NONE',  ( 12.06949235617739724, 12.14591786802326823, 106.8760903946856899 ) ) ;
#111635 = CARTESIAN_POINT ( 'NONE',  ( 22.99604614807110536, -21.34730593735726245, -49.80954046291019921 ) ) ;
#111636 = CARTESIAN_POINT ( 'NONE',  ( 8.314922557961029526, -14.29746914071037800, 75.41775706135233293 ) ) ;
#111637 = CARTESIAN_POINT ( 'NONE',  ( -5.049401038298153566, 19.05341960407611168, 40.20724293864768839 ) ) ;
#111638 = CARTESIAN_POINT ( 'NONE',  ( 18.62759615963255655, 10.81492255796105972, 91.66775706135234714 ) ) ;
#111639 = CARTESIAN_POINT ( 'NONE',  ( -5.049401038297874678, -19.05341960407617918, 99.79275706135234714 ) ) ;
#111640 = CARTESIAN_POINT ( 'NONE',  ( 21.55341960407619695, -5.719274019375665929, 66.04275706135236135 ) ) ;
#111641 = CARTESIAN_POINT ( 'NONE',  ( -9.564922557961040184, 16.46253265017147172, 47.91775706135233293 ) ) ;
#111642 = CARTESIAN_POINT ( 'NONE',  ( 5.049401038298161559, -19.05341960407611168, 72.70724293864768129 ) ) ;
#111643 = CARTESIAN_POINT ( 'NONE',  ( -9.474510206698964154, 16.51473224551069663, 65.41557627198102409 ) ) ;
#111644 = CARTESIAN_POINT ( 'NONE',  ( 17.49999999999999645, 5.624438216177600758, 71.68329655085361196 ) ) ;
#111645 = CARTESIAN_POINT ( 'NONE',  ( -4.483927247898539470, -16.52544592524342804, 52.29057627198102409 ) ) ;
#111646 = CARTESIAN_POINT ( 'NONE',  ( 10.72451020669898902, -18.67979575497178502, 42.91557627198103120 ) ) ;
#111647 = CARTESIAN_POINT ( 'NONE',  ( -16.46253265017160317, 9.564922557960807481, 50.83224293864770260 ) ) ;
#111649 = CARTESIAN_POINT ( 'NONE',  ( 14.34966873604972726, -8.224510206698740333, 70.83442372801901854 ) ) ;
#111648 = CARTESIAN_POINT ( 'NONE',  ( -10.81492255796078084, -18.62759615963271287, 82.08224293864768129 ) ) ;
#111650 = EDGE_CURVE ( 'NONE', #120101, #167889, #65748, .T. ) ;
#111651 = VERTEX_POINT ( 'NONE', #63773 ) ;
#111653 = FACE_OUTER_BOUND ( 'NONE', #173098, .T. ) ;
#111652 = CARTESIAN_POINT ( 'NONE',  ( -16.52544592524342804, 4.483927247898546575, 76.04057627198102409 ) ) ;
#111654 = CARTESIAN_POINT ( 'NONE',  ( 4.483927247898790824, -16.52544592524335698, 35.20942372801901854 ) ) ;
#111655 = CARTESIAN_POINT ( 'NONE',  ( 13.89961937509977652, -13.97604488694527269, 28.12390960531435624 ) ) ;
#111656 = CARTESIAN_POINT ( 'NONE',  ( -16.51473224551082808, 9.474510206698731452, 63.33442372801900433 ) ) ;
#111657 = CARTESIAN_POINT ( 'NONE',  ( 16.55341960407611168, 4.379528057220329451, 68.95724293864769550 ) ) ;
#111658 = CARTESIAN_POINT ( 'NONE',  ( -5.719274019375665041, -21.55341960407619695, 49.79275706135234714 ) ) ;
#111660 = CARTESIAN_POINT ( 'NONE',  ( -5.719274019375978568, 21.55341960407610458, 90.20724293864770971 ) ) ;
#111659 = CARTESIAN_POINT ( 'NONE',  ( 5.153800228976335163, 19.02544592524342804, 24.79057627198102765 ) ) ;
#111661 = CARTESIAN_POINT ( 'NONE',  ( -19.02544592524342804, 5.153800228976336051, 111.0405762719810099 ) ) ;
#111662 = CARTESIAN_POINT ( 'NONE',  ( 8.224510206698953496, -14.34966873604960469, 92.91557627198103830 ) ) ;
#111663 = CARTESIAN_POINT ( 'NONE',  ( 19.77856019329516002, -34.75272400652957572, -21.53639161265285651 ) ) ;
#111664 = CARTESIAN_POINT ( 'NONE',  ( -5.153800228976328057, -19.02544592524343514, 47.29057627198102409 ) ) ;
#111665 = CARTESIAN_POINT ( 'NONE',  ( -36.91746825000000598, -11.99521256947794789, -4.524999997268813523 ) ) ;
#111666 = CARTESIAN_POINT ( 'NONE',  ( 16.51473224551083163, -9.474510206698727899, 85.83442372801900433 ) ) ;
#111667 = CARTESIAN_POINT ( 'NONE',  ( -21.53943276465977519, -0.05219959533937600094, 23.75109039468567929 ) ) ;
#111668 = CARTESIAN_POINT ( 'NONE',  ( 5.049401038298161559, -19.05341960407611168, 67.70724293864769550 ) ) ;
#111669 = CARTESIAN_POINT ( 'NONE',  ( 19.05341960407617918, -5.049401038297876454, 51.04275706135231871 ) ) ;
#111670 = CARTESIAN_POINT ( 'NONE',  ( 19.05341960407611168, 5.049401038298154454, 48.95724293864768129 ) ) ;
#111671 = PRODUCT_RELATED_PRODUCT_CATEGORY ( 'part', '', ( #95384 ) ) ;
#111672 = CARTESIAN_POINT ( 'NONE',  ( -14.34966873604960291, -8.224510206698953496, 56.66557627198103830 ) ) ;
#111673 = CARTESIAN_POINT ( 'NONE',  ( 0.05219959533910956823, 16.53943276465976808, 59.99890960531436690 ) ) ;
#111674 = CARTESIAN_POINT ( 'NONE',  ( -13.97604488694527625, -13.89961937509977652, 76.87390960531433848 ) ) ;
#111675 = CARTESIAN_POINT ( 'NONE',  ( -0.05219959533907301413, -21.53943276465977519, 107.4989096053143669 ) ) ;
#111676 = CARTESIAN_POINT ( 'NONE',  ( 19.02544592524343514, -5.153800228976328945, 73.54057627198103830 ) ) ;
#111677 = CARTESIAN_POINT ( 'NONE',  ( -18.67979575497178146, -10.72451020669898902, 81.66557627198103830 ) ) ;
#111678 = CARTESIAN_POINT ( 'NONE',  ( 15.72974639402176855, 15.80617190586768217, 106.8760903946856899 ) ) ;
#111681 = CARTESIAN_POINT ( 'NONE',  ( -8.314922557960811034, -14.29746914071050412, 102.0822429386476955 ) ) ;
#111680 = CARTESIAN_POINT ( 'NONE',  ( -14.34966873604972548, 8.224510206698743886, 103.3344237280190043 ) ) ;
#111679 = CARTESIAN_POINT ( 'NONE',  ( 9.564922557960805705, 16.46253265017160317, 39.58224293864768839 ) ) ;
#111682 = CARTESIAN_POINT ( 'NONE',  ( -19.03943276465977164, -0.05219959533935918106, 103.7510903946856757 ) ) ;
#111683 = ORIENTED_EDGE ( 'NONE', *, *, #79441, .F. ) ;
#111684 = CARTESIAN_POINT ( 'NONE',  ( 18.62759615963255655, 10.81492255796105972, 36.66775706135234714 ) ) ;
#111685 = CARTESIAN_POINT ( 'NONE',  ( -13.97604488694547697, 13.89961937509957934, 48.12609039468566863 ) ) ;
#111686 = CARTESIAN_POINT ( 'NONE',  ( -16.53943276465976808, -0.05219959533934237506, 108.7510903946857042 ) ) ;
#111687 = CARTESIAN_POINT ( 'NONE',  ( 21.52544592524344225, -5.823673210054117533, 73.54057627198102409 ) ) ;
#111688 = CARTESIAN_POINT ( 'NONE',  ( -5.153800228976328057, -19.02544592524343514, 107.2905762719810383 ) ) ;
#111689 = CARTESIAN_POINT ( 'NONE',  ( 8.314922557960818139, 14.29746914071049879, 59.58224293864770260 ) ) ;
#111690 = CARTESIAN_POINT ( 'NONE',  ( 9.564922557960805705, 16.46253265017160317, 24.58224293864769194 ) ) ;
#111691 = CARTESIAN_POINT ( 'NONE',  ( 13.89961937509977652, -13.97604488694527269, 28.12390960531435624 ) ) ;
#111692 = CARTESIAN_POINT ( 'NONE',  ( -5.719274019375665041, -21.55341960407619695, 109.7927570613523613 ) ) ;
#111693 = CARTESIAN_POINT ( 'NONE',  ( -12.14591786802326823, 12.06949235617739902, 88.12609039468570415 ) ) ;
#111694 = CARTESIAN_POINT ( 'NONE',  ( -18.67979575497193778, 10.72451020669871902, 38.33442372801900433 ) ) ;
#111695 = CARTESIAN_POINT ( 'NONE',  ( 8.314922557961029526, -14.29746914071037800, 40.41775706135234714 ) ) ;
#111696 = CARTESIAN_POINT ( 'NONE',  ( 9.474510206698971260, -16.51473224551069308, 112.9155762719810383 ) ) ;
#111697 = CARTESIAN_POINT ( 'NONE',  ( 13.89961937509977652, -13.97604488694527269, 53.12390960531434558 ) ) ;
#111698 = CARTESIAN_POINT ( 'NONE',  ( 19.02544592524343514, -5.153800228976328945, 73.54057627198103830 ) ) ;
#111699 = AXIS2_PLACEMENT_3D ( 'NONE', #129274, #38286, #37279 ) ;
#111700 = CARTESIAN_POINT ( 'NONE',  ( 4.379528057220092307, 16.55341960407617563, 62.29275706135236845 ) ) ;
#111701 = CARTESIAN_POINT ( 'NONE',  ( -12.06949235617756955, 12.14591786802309770, 100.6239096053143811 ) ) ;
#111702 = CARTESIAN_POINT ( 'NONE',  ( -14.29746914071049879, 8.314922557960819915, 25.83224293864769194 ) ) ;
#111703 = DIRECTION ( 'NONE',  ( 0.000000000000000000, 0.000000000000000000, 1.000000000000000000 ) ) ;
#111706 = CARTESIAN_POINT ( 'NONE',  ( 13.89961937509977652, -13.97604488694527269, 83.12390960531436690 ) ) ;
#111705 = CARTESIAN_POINT ( 'NONE',  ( 9.564922557960805705, 16.46253265017160317, 94.58224293864769550 ) ) ;
#111704 = CARTESIAN_POINT ( 'NONE',  ( 21.52544592524334988, 5.823673210054432836, 61.45942372801901854 ) ) ;
#111707 = CARTESIAN_POINT ( 'NONE',  ( 16.46253265017160672, -9.564922557960803928, 108.3322429386476955 ) ) ;
#111708 = CARTESIAN_POINT ( 'NONE',  ( -4.379528057220328563, 16.55341960407611168, 50.20724293864769550 ) ) ;
#111709 = CARTESIAN_POINT ( 'NONE',  ( 4.379528057220092307, 16.55341960407617563, 112.2927570613523471 ) ) ;
#111710 = CARTESIAN_POINT ( 'NONE',  ( -4.379528057220328563, 16.55341960407611168, 45.20724293864769550 ) ) ;
#111711 = CARTESIAN_POINT ( 'NONE',  ( -16.91829712735633606, -17.40385595850962730, -54.23877452087121753 ) ) ;
#111712 = CARTESIAN_POINT ( 'NONE',  ( 16.46253265017146816, 9.564922557961045513, 31.66775706135232937 ) ) ;
#111713 = CARTESIAN_POINT ( 'NONE',  ( -5.049401038298153566, 19.05341960407611168, 75.20724293864769550 ) ) ;
#111714 = CARTESIAN_POINT ( 'NONE',  ( -13.97604488694547697, 13.89961937509957934, 58.12609039468566863 ) ) ;
#111715 = CARTESIAN_POINT ( 'NONE',  ( 29.86685920354754487, 21.69954338932564752, -3.424999997268813434 ) ) ;
#111716 = DIRECTION ( 'NONE',  ( -0.4999999999999966693, 0.5000000000000019984, 0.7071067811865484609 ) ) ;
#111718 = CARTESIAN_POINT ( 'NONE',  ( 14.29746914071037800, 8.314922557961029526, 71.66775706135234714 ) ) ;
#111717 = CARTESIAN_POINT ( 'NONE',  ( -5.049401038297874678, -19.05341960407617918, 89.79275706135230450 ) ) ;
#111719 = CARTESIAN_POINT ( 'NONE',  ( 17.05587630539788435, 6.762274262135705705, 91.75819690962693187 ) ) ;
#111720 = CARTESIAN_POINT ( 'NONE',  ( -13.97604488694527625, -13.89961937509977652, 101.8739096053143811 ) ) ;
#111721 = CARTESIAN_POINT ( 'NONE',  ( 0.05219959533937995610, -21.53943276465977519, 30.00109039468568284 ) ) ;
#111722 = CARTESIAN_POINT ( 'NONE',  ( 13.89961937509957401, 13.97604488694547697, 91.87609039468567573 ) ) ;
#111724 = CARTESIAN_POINT ( 'NONE',  ( -19.03943276465977164, 0.05219959533909376836, 51.24890960531436690 ) ) ;
#111723 = CARTESIAN_POINT ( 'NONE',  ( 16.51473224551069308, 9.474510206698969483, 114.1655762719810241 ) ) ;
#111725 = CARTESIAN_POINT ( 'NONE',  ( 19.02544592524343514, -5.153800228976328945, 93.54057627198102409 ) ) ;
#111727 = CARTESIAN_POINT ( 'NONE',  ( 5.153800228976335163, 19.02544592524342804, 54.79057627198103120 ) ) ;
#111726 = CARTESIAN_POINT ( 'NONE',  ( 16.53943276465976808, -0.05219959533910856209, 63.74890960531435979 ) ) ;
#111728 = CARTESIAN_POINT ( 'NONE',  ( -13.97604488694527625, -13.89961937509977652, 66.87390960531436690 ) ) ;
#111729 = CARTESIAN_POINT ( 'NONE',  ( 19.02544592524334988, 5.153800228976608722, 66.45942372801899012 ) ) ;
#111730 = CARTESIAN_POINT ( 'NONE',  ( 0.05219959533936267826, -19.03943276465977164, 25.00109039468566152 ) ) ;
#111731 = CARTESIAN_POINT ( 'NONE',  ( 16.46253265017160672, -9.564922557960803928, 68.33224293864770971 ) ) ;
#111732 = CARTESIAN_POINT ( 'NONE',  ( 18.62759615963271287, -10.81492255796078972, 63.33224293864770260 ) ) ;
#111734 = CARTESIAN_POINT ( 'NONE',  ( 5.153800228976615827, -19.02544592524334988, 35.20942372801899722 ) ) ;
#111733 = CARTESIAN_POINT ( 'NONE',  ( 14.34966873604960469, 8.224510206698951720, 64.16557627198102409 ) ) ;
#111735 = FACE_OUTER_BOUND ( 'NONE', #52161, .T. ) ;
#111736 = CARTESIAN_POINT ( 'NONE',  ( -15.72974639402197994, 15.80617190586746368, 50.62390960531435979 ) ) ;
#111737 = CARTESIAN_POINT ( 'NONE',  ( -18.62759615963270932, 10.81492255796079327, 25.83224293864769194 ) ) ;
#111738 = CARTESIAN_POINT ( 'NONE',  ( -19.02544592524342804, 5.153800228976336051, 51.04057627198103120 ) ) ;
#111739 = CARTESIAN_POINT ( 'NONE',  ( 19.05341960407611168, 5.049401038298154454, 33.95724293864769550 ) ) ;
#111740 = CARTESIAN_POINT ( 'NONE',  ( -8.224510206698948167, 14.34966873604960824, 105.4155762719810383 ) ) ;
#111741 = CARTESIAN_POINT ( 'NONE',  ( -5.823673210054116645, -21.52544592524344225, 107.2905762719810525 ) ) ;
#111742 = CARTESIAN_POINT ( 'NONE',  ( -18.62759615963255300, -10.81492255796106328, 29.16775706135234003 ) ) ;
#111743 = CARTESIAN_POINT ( 'NONE',  ( -4.379528057220328563, 16.55341960407611168, 110.2072429386477239 ) ) ;
#111744 = CARTESIAN_POINT ( 'NONE',  ( 18.67979575497194134, -10.72451020669871369, 75.83442372801900433 ) ) ;
#111745 = CARTESIAN_POINT ( 'NONE',  ( -10.81492255796078084, -18.62759615963271287, 87.08224293864769550 ) ) ;
#111746 = CARTESIAN_POINT ( 'NONE',  ( 19.05341960407617918, -5.049401038297876454, 36.04275706135234003 ) ) ;
#111747 = CARTESIAN_POINT ( 'NONE',  ( 17.72696623605159516, -5.500000000000042633, 76.09811031808418136 ) ) ;
#111748 = CARTESIAN_POINT ( 'NONE',  ( 0.000000000000000000, 0.000000000000000000, -20.00000000000000000 ) ) ;
#111749 = CARTESIAN_POINT ( 'NONE',  ( -3.874011537017815421, -5.374011537017721274, -64.44758591613756948 ) ) ;
#111750 = CARTESIAN_POINT ( 'NONE',  ( -8.224510206698735004, -14.34966873604973081, 49.58442372801901143 ) ) ;
#111751 = CARTESIAN_POINT ( 'NONE',  ( -8.224510206698948167, 14.34966873604960824, 110.4155762719810383 ) ) ;
#111752 = CARTESIAN_POINT ( 'NONE',  ( 34.25242159400494302, -3.629837513186700448, 90.85215659754990725 ) ) ;
#111753 = CARTESIAN_POINT ( 'NONE',  ( -19.05341960407611168, -5.049401038298163336, 71.45724293864766707 ) ) ;
#111754 = CARTESIAN_POINT ( 'NONE',  ( 12.06949235617757843, -12.14591786802309237, 98.12390960531436690 ) ) ;
#111755 = CARTESIAN_POINT ( 'NONE',  ( -21.53943276465977519, 0.05219959533907696930, 46.24890960531435979 ) ) ;
#111756 = CARTESIAN_POINT ( 'NONE',  ( -12.06949235617756955, 12.14591786802309770, 80.62390960531438111 ) ) ;
#111757 = CARTESIAN_POINT ( 'NONE',  ( -14.34966873604972548, 8.224510206698743886, 28.33442372801902209 ) ) ;
#111758 = CARTESIAN_POINT ( 'NONE',  ( 15.80617190586769283, -15.72974639402175789, 90.62609039468567573 ) ) ;
#111759 = CARTESIAN_POINT ( 'NONE',  ( 4.500000000000000888, -139.5000000000000000, 13.35010376910484275 ) ) ;
#111760 = CARTESIAN_POINT ( 'NONE',  ( 12.14591786802327356, -12.06949235617739191, 100.6260903946857184 ) ) ;
#111761 = CARTESIAN_POINT ( 'NONE',  ( 8.314922557960818139, 14.29746914071049879, 44.58224293864769550 ) ) ;
#111762 = CARTESIAN_POINT ( 'NONE',  ( -13.89961937509977652, 13.97604488694528158, 35.62390960531435269 ) ) ;
#111763 = CARTESIAN_POINT ( 'NONE',  ( 18.62759615963255655, 10.81492255796105972, 96.66775706135234714 ) ) ;
#111764 = CARTESIAN_POINT ( 'NONE',  ( 15.80617190586746368, 15.72974639402197994, 104.3739096053143669 ) ) ;
#111765 = CARTESIAN_POINT ( 'NONE',  ( 21.53943276465977519, 0.05219959533937863772, 61.25109039468567573 ) ) ;
#111766 = CARTESIAN_POINT ( 'NONE',  ( -8.224510206698735004, -14.34966873604973081, 44.58442372801901854 ) ) ;
#111768 = CARTESIAN_POINT ( 'NONE',  ( -0.05219959533937732626, 21.53943276465977519, 87.50109039468568994 ) ) ;
#111767 = CARTESIAN_POINT ( 'NONE',  ( -8.224510206698948167, 14.34966873604960824, 70.41557627198102409 ) ) ;
#111769 = CARTESIAN_POINT ( 'NONE',  ( 8.224510206698742110, 14.34966873604972548, 107.0844237280190043 ) ) ;
#111770 = CARTESIAN_POINT ( 'NONE',  ( -28.79475375365689160, -9.355982642737773247, 140.3656553485623135 ) ) ;
#111771 = DIRECTION ( 'NONE',  ( 3.613946018757868503E-15, 0.000000000000000000, -1.000000000000000000 ) ) ;
#111772 = CARTESIAN_POINT ( 'NONE',  ( 8.314922557960818139, 14.29746914071049879, 29.58224293864769905 ) ) ;
#111773 = CARTESIAN_POINT ( 'NONE',  ( 14.29746914071037800, 8.314922557961029526, 76.66775706135234714 ) ) ;
#111774 = CARTESIAN_POINT ( 'NONE',  ( -9.564922557960796823, -16.46253265017161027, 87.08224293864769550 ) ) ;
#111775 = CARTESIAN_POINT ( 'NONE',  ( -9.474510206698964154, 16.51473224551069663, 95.41557627198102409 ) ) ;
#111776 = CARTESIAN_POINT ( 'NONE',  ( 0.05219959533937995610, -21.53943276465977519, 90.00109039468567573 ) ) ;
#111777 = CARTESIAN_POINT ( 'NONE',  ( -14.34966873604972548, 8.224510206698743886, 83.33442372801903275 ) ) ;
#111778 = CARTESIAN_POINT ( 'NONE',  ( 14.34966873604960469, 8.224510206698951720, 74.16557627198102409 ) ) ;
#111779 = CARTESIAN_POINT ( 'NONE',  ( -9.564922557960796823, -16.46253265017161027, 67.08224293864769550 ) ) ;
#111780 = VERTEX_POINT ( 'NONE', #112257 ) ;
#111781 = CARTESIAN_POINT ( 'NONE',  ( -4.379528057220086978, -16.55341960407618274, 24.79275706135235779 ) ) ;
#111782 = CARTESIAN_POINT ( 'NONE',  ( -9.564922557960796823, -16.46253265017161027, 22.08224293864768839 ) ) ;
#111783 = CARTESIAN_POINT ( 'NONE',  ( 9.564922557960805705, 16.46253265017160317, 94.58224293864769550 ) ) ;
#111785 = CARTESIAN_POINT ( 'NONE',  ( -36.91746825000001309, -11.99521256947794789, -10.52499999726881441 ) ) ;
#111784 = CARTESIAN_POINT ( 'NONE',  ( -16.51473224551082808, 9.474510206698731452, 113.3344237280190043 ) ) ;
#111786 = CARTESIAN_POINT ( 'NONE',  ( 13.97604488694548053, -13.89961937509957401, 25.62609039468566507 ) ) ;
#111787 = CARTESIAN_POINT ( 'NONE',  ( -12.14591786802326823, 12.06949235617739902, 98.12609039468570415 ) ) ;
#111788 = CARTESIAN_POINT ( 'NONE',  ( 19.03943276465977164, 0.05219959533936151252, 106.2510903946856615 ) ) ;
#111789 = CARTESIAN_POINT ( 'NONE',  ( 12.06949235617757843, -12.14591786802309237, 108.1239096053143811 ) ) ;
#111790 = CARTESIAN_POINT ( 'NONE',  ( -16.53943276465976808, -0.05219959533934237506, 83.75109039468568994 ) ) ;
#111791 = CARTESIAN_POINT ( 'NONE',  ( 16.52544592524335698, 4.483927247898782831, 51.45942372801901854 ) ) ;
#111792 = CARTESIAN_POINT ( 'NONE',  ( 18.25458402832055071, -35.60444695113565672, -12.00144453093060903 ) ) ;
#111793 = CARTESIAN_POINT ( 'NONE',  ( -19.05341960407617563, 5.049401038297882671, 68.54275706135230450 ) ) ;
#111794 = CARTESIAN_POINT ( 'NONE',  ( -19.02544592524334988, -5.153800228976617603, 18.95942372801899722 ) ) ;
#111795 = CARTESIAN_POINT ( 'NONE',  ( -9.474510206698964154, 16.51473224551069663, 45.41557627198103120 ) ) ;
#111796 = CARTESIAN_POINT ( 'NONE',  ( 0.05219959533909260263, 19.03943276465977164, 79.99890960531436690 ) ) ;
#111797 = CARTESIAN_POINT ( 'NONE',  ( 16.52544592524342804, -4.483927247898539470, 88.54057627198103830 ) ) ;
#111798 = CARTESIAN_POINT ( 'NONE',  ( 9.564922557961047289, -16.46253265017146816, 55.41775706135234003 ) ) ;
#111799 = CARTESIAN_POINT ( 'NONE',  ( -10.81492255796078084, -18.62759615963271287, 52.08224293864768839 ) ) ;
#111800 = CARTESIAN_POINT ( 'NONE',  ( -21.55341960407619339, 5.719274019375674811, 103.5427570613523613 ) ) ;
#111801 = CARTESIAN_POINT ( 'NONE',  ( 16.46253265017160672, -9.564922557960803928, 88.33224293864769550 ) ) ;
#111802 = EDGE_CURVE ( 'NONE', #129803, #60482, #104910, .T. ) ;
#111803 = CARTESIAN_POINT ( 'NONE',  ( -15.72974639402176322, -15.80617190586768395, 104.3760903946856899 ) ) ;
#111804 = CARTESIAN_POINT ( 'NONE',  ( 15.72974639402199770, -15.80617190586745480, 58.12390960531435979 ) ) ;
#111805 = CARTESIAN_POINT ( 'NONE',  ( 19.03943276465977164, -0.05219959533909143690, 98.74890960531436690 ) ) ;
#111806 = CARTESIAN_POINT ( 'NONE',  ( -13.97604488694547697, 13.89961937509957934, 93.12609039468566152 ) ) ;
#111807 = CARTESIAN_POINT ( 'NONE',  ( 9.564922557960805705, 16.46253265017160317, 109.5822429386476955 ) ) ;
#111808 = CARTESIAN_POINT ( 'NONE',  ( -19.05341960407617563, 5.049401038297882671, 103.5427570613523329 ) ) ;
#111809 = CARTESIAN_POINT ( 'NONE',  ( -19.02544592524342804, 5.153800228976336051, 26.04057627198103120 ) ) ;
#111810 = CARTESIAN_POINT ( 'NONE',  ( -16.51473224551069308, -9.474510206698971260, 81.66557627198103830 ) ) ;
#111811 = CARTESIAN_POINT ( 'NONE',  ( 18.62759615963271287, -10.81492255796078972, 83.33224293864769550 ) ) ;
#111812 = CARTESIAN_POINT ( 'NONE',  ( -8.314922557961024197, 14.29746914071037800, 47.91775706135234714 ) ) ;
#111813 = CARTESIAN_POINT ( 'NONE',  ( 5.719274019375673035, 21.55341960407619339, 42.29275706135235424 ) ) ;
#111814 = CARTESIAN_POINT ( 'NONE',  ( 15.72974639402176855, 15.80617190586768217, 101.8760903946857042 ) ) ;
#111815 = CARTESIAN_POINT ( 'NONE',  ( -4.483927247898782831, 16.52544592524335698, 102.7094237280190185 ) ) ;
#111816 = CARTESIAN_POINT ( 'NONE',  ( 13.97604488694527802, 13.89961937509977652, 89.37390960531436690 ) ) ;
#111817 = CARTESIAN_POINT ( 'NONE',  ( -16.53943276465976808, 0.05219959533911058130, 91.24890960531436690 ) ) ;
#111818 = CARTESIAN_POINT ( 'NONE',  ( -14.34966873604960291, -8.224510206698953496, 26.66557627198103475 ) ) ;
#111819 = CARTESIAN_POINT ( 'NONE',  ( -19.02544592524334988, -5.153800228976617603, 68.95942372801896170 ) ) ;
#111820 = CARTESIAN_POINT ( 'NONE',  ( 21.55341960407619695, -5.719274019375665929, 41.04275706135236135 ) ) ;
#111821 = CARTESIAN_POINT ( 'NONE',  ( -16.52544592524342804, 4.483927247898546575, 91.04057627198103830 ) ) ;
#111822 = CARTESIAN_POINT ( 'NONE',  ( 19.03943276465977164, -0.05219959533909143690, 108.7489096053143527 ) ) ;
#111823 = CARTESIAN_POINT ( 'NONE',  ( 16.53943276465976808, -0.05219959533910856209, 28.74890960531435624 ) ) ;
#111824 = CARTESIAN_POINT ( 'NONE',  ( -21.52544592524334988, -5.823673210054445271, 88.95942372801901854 ) ) ;
#111825 = CARTESIAN_POINT ( 'NONE',  ( 4.379528057220092307, 16.55341960407617563, 52.29275706135236135 ) ) ;
#111826 = CARTESIAN_POINT ( 'NONE',  ( -0.05219959533937732626, 21.53943276465977519, 37.50109039468568284 ) ) ;
#111827 = ORIENTED_EDGE ( 'NONE', *, *, #139759, .T. ) ;
#111828 = CARTESIAN_POINT ( 'NONE',  ( 21.53943276465977519, 0.05219959533937863772, 31.25109039468568639 ) ) ;
#111829 = CARTESIAN_POINT ( 'NONE',  ( 16.52544592524342804, -4.483927247898539470, 108.5405762719810241 ) ) ;
#111830 = CARTESIAN_POINT ( 'NONE',  ( 19.02544592524343514, -5.153800228976328945, 28.54057627198102409 ) ) ;
#111831 = CARTESIAN_POINT ( 'NONE',  ( -14.34966873604960291, -8.224510206698953496, 71.66557627198100988 ) ) ;
#111832 = CARTESIAN_POINT ( 'NONE',  ( 13.89961937509977652, -13.97604488694527269, 73.12390960531436690 ) ) ;
#111833 = CARTESIAN_POINT ( 'NONE',  ( -14.29746914071037622, -8.314922557961029526, 109.1677570613523613 ) ) ;
#111834 = CARTESIAN_POINT ( 'NONE',  ( -13.89961937509977652, 13.97604488694528158, 40.62390960531435979 ) ) ;
#111835 = CARTESIAN_POINT ( 'NONE',  ( -15.72974639402197994, 15.80617190586746368, 45.62390960531436690 ) ) ;
#111836 = CARTESIAN_POINT ( 'NONE',  ( -4.379528057220328563, 16.55341960407611168, 85.20724293864770971 ) ) ;
#111837 = AXIS2_PLACEMENT_3D ( 'NONE', #158554, #112061, #1891 ) ;
#111838 = CARTESIAN_POINT ( 'NONE',  ( 5.719274019375991003, -21.55341960407610458, 87.70724293864769550 ) ) ;
#111839 = CARTESIAN_POINT ( 'NONE',  ( 19.03943276465977164, -0.05219959533909143690, 88.74890960531436690 ) ) ;
#111841 = CARTESIAN_POINT ( 'NONE',  ( -19.02544592524334988, -5.153800228976617603, 98.95942372801900433 ) ) ;
#111840 = CARTESIAN_POINT ( 'NONE',  ( -19.03943276465977164, 0.05219959533909376836, 56.24890960531435979 ) ) ;
#111842 = CARTESIAN_POINT ( 'NONE',  ( -0.05219959533907301413, -21.53943276465977519, 47.49890960531435979 ) ) ;
#111843 = CARTESIAN_POINT ( 'NONE',  ( -18.67979575497193778, 10.72451020669871902, 73.33442372801901854 ) ) ;
#111844 = CARTESIAN_POINT ( 'NONE',  ( -19.05341960407611168, -5.049401038298163336, 51.45724293864770260 ) ) ;
#111845 = CARTESIAN_POINT ( 'NONE',  ( 16.46253265017160672, -9.564922557960803928, 83.33224293864768129 ) ) ;
#111846 = ORIENTED_EDGE ( 'NONE', *, *, #32592, .F. ) ;
#111847 = CARTESIAN_POINT ( 'NONE',  ( -4.483927247898782831, 16.52544592524335698, 67.70942372801901854 ) ) ;
#111848 = CARTESIAN_POINT ( 'NONE',  ( 21.52544592524334988, 5.823673210054432836, 46.45942372801901854 ) ) ;
#111849 = CARTESIAN_POINT ( 'NONE',  ( -21.55341960407619339, 5.719274019375674811, 68.54275706135234714 ) ) ;
#111850 = CARTESIAN_POINT ( 'NONE',  ( -21.53943276465977519, 0.05219959533907696930, 21.24890960531436690 ) ) ;
#111851 = CARTESIAN_POINT ( 'NONE',  ( 18.67979575497178502, 10.72451020669898547, 94.16557627198103830 ) ) ;
#111853 = CARTESIAN_POINT ( 'NONE',  ( -8.224510206698735004, -14.34966873604973081, 64.58442372801900433 ) ) ;
#111852 = CARTESIAN_POINT ( 'NONE',  ( 21.52544592524334988, 5.823673210054432836, 36.45942372801901143 ) ) ;
#111854 = CARTESIAN_POINT ( 'NONE',  ( 15.80617190586746368, 15.72974639402197994, 59.37390960531436690 ) ) ;
#111855 = CARTESIAN_POINT ( 'NONE',  ( -16.46253265017146816, -9.564922557961047289, 34.16775706135233293 ) ) ;
#111857 = CARTESIAN_POINT ( 'NONE',  ( 12.06949235617739724, 12.14591786802326823, 96.87609039468568994 ) ) ;
#111856 = CARTESIAN_POINT ( 'NONE',  ( 16.51473224551069308, 9.474510206698969483, 69.16557627198102409 ) ) ;
#111858 = CARTESIAN_POINT ( 'NONE',  ( -11.74264578624799782, -36.14014761921581709, -5.599999999999999645 ) ) ;
#111859 = CARTESIAN_POINT ( 'NONE',  ( 19.03943276465977164, -0.05219959533909143690, 108.7489096053143527 ) ) ;
#111860 = DIRECTION ( 'NONE',  ( -1.000000000000000000, 0.000000000000000000, -0.000000000000000000 ) ) ;
#111861 = CARTESIAN_POINT ( 'NONE',  ( -16.51473224551082808, 9.474510206698731452, 83.33442372801899012 ) ) ;
#111862 = CARTESIAN_POINT ( 'NONE',  ( 5.719274019375991003, -21.55341960407610458, 52.70724293864769550 ) ) ;
#111863 = CARTESIAN_POINT ( 'NONE',  ( 16.55341960407611168, 4.379528057220329451, 38.95724293864768839 ) ) ;
#111864 = CARTESIAN_POINT ( 'NONE',  ( -19.02544592524334988, -5.153800228976617603, 93.95942372801900433 ) ) ;
#111865 = CARTESIAN_POINT ( 'NONE',  ( -5.153800228976328057, -19.02544592524343514, 27.29057627198103120 ) ) ;
#111866 = CARTESIAN_POINT ( 'NONE',  ( 13.97604488694548053, -13.89961937509957401, 105.6260903946856757 ) ) ;
#111868 = CARTESIAN_POINT ( 'NONE',  ( 0.05219959533936267826, -19.03943276465977164, 55.00109039468566863 ) ) ;
#111867 = CARTESIAN_POINT ( 'NONE',  ( -10.72451020669898014, 18.67979575497178502, 90.41557627198103830 ) ) ;
#111869 = CARTESIAN_POINT ( 'NONE',  ( -12.06949235617739369, -12.14591786802326823, 74.37609039468568994 ) ) ;
#111870 = CARTESIAN_POINT ( 'NONE',  ( 9.474510206698971260, -16.51473224551069308, 67.91557627198102409 ) ) ;
#111871 = CARTESIAN_POINT ( 'NONE',  ( 12.06949235617757843, -12.14591786802309237, 73.12390960531436690 ) ) ;
#111872 = CARTESIAN_POINT ( 'NONE',  ( 0.05219959533909260263, 19.03943276465977164, 44.99890960531435979 ) ) ;
#111873 = CARTESIAN_POINT ( 'NONE',  ( 16.55341960407611168, 4.379528057220329451, 48.95724293864770971 ) ) ;
#111874 = CARTESIAN_POINT ( 'NONE',  ( -0.05219959533909027116, -19.03943276465977164, 22.49890960531436690 ) ) ;
#111875 = CARTESIAN_POINT ( 'NONE',  ( 31.64921935833421429, -6.825000981063964467, 91.88079052344200193 ) ) ;
#111876 = CARTESIAN_POINT ( 'NONE',  ( 8.224510206698953496, -14.34966873604960469, 32.91557627198102409 ) ) ;
#111877 = CARTESIAN_POINT ( 'NONE',  ( -19.03943276465977164, 0.05219959533909376836, 71.24890960531435269 ) ) ;
#111878 = CARTESIAN_POINT ( 'NONE',  ( 17.50000000000000000, 5.500000000000011546, 68.78230962303564411 ) ) ;
#111879 = CARTESIAN_POINT ( 'NONE',  ( -9.474510206698720793, -16.51473224551083518, 39.58442372801899722 ) ) ;
#111880 = CARTESIAN_POINT ( 'NONE',  ( -12.14591786802326823, 12.06949235617739902, 48.12609039468568284 ) ) ;
#111881 = CARTESIAN_POINT ( 'NONE',  ( 18.62759615963271287, -10.81492255796078972, 48.33224293864770260 ) ) ;
#111882 = CARTESIAN_POINT ( 'NONE',  ( -5.823673210054431948, 21.52544592524334988, 112.7094237280190328 ) ) ;
#111883 = CARTESIAN_POINT ( 'NONE',  ( 13.89961937509977652, -13.97604488694527269, 78.12390960531433848 ) ) ;
#111884 = CARTESIAN_POINT ( 'NONE',  ( 0.05219959533909260263, 19.03943276465977164, 114.9989096053143669 ) ) ;
#111885 = CARTESIAN_POINT ( 'NONE',  ( 13.89961937509977652, -13.97604488694527269, 113.1239096053143527 ) ) ;
#111886 = CARTESIAN_POINT ( 'NONE',  ( 10.81492255796106328, -18.62759615963255655, 35.41775706135234003 ) ) ;
#111887 = AXIS2_PLACEMENT_3D ( 'NONE', #134599, #57754, #196285 ) ;
#111888 = CARTESIAN_POINT ( 'NONE',  ( -12.06949235617756955, 12.14591786802309770, 100.6239096053143811 ) ) ;
#111891 = EDGE_LOOP ( 'NONE', ( #55534, #7211, #47251, #181873, #61855, #84841, #146022, #90463, #131370, #6577, #173272, #147351, #137977, #67261 ) ) ;
#111890 = CARTESIAN_POINT ( 'NONE',  ( -19.03943276465977164, 0.05219959533909376836, 81.24890960531436690 ) ) ;
#111889 = CARTESIAN_POINT ( 'NONE',  ( 18.67979575497178502, 10.72451020669898547, 99.16557627198100988 ) ) ;
#111892 = CARTESIAN_POINT ( 'NONE',  ( 21.52544592524334988, 5.823673210054432836, 26.45942372801901854 ) ) ;
#111893 = EDGE_CURVE ( 'NONE', #123757, #179471, #120431, .T. ) ;
#111894 = EDGE_LOOP ( 'NONE', ( #48938, #20757, #132831, #94422, #130555, #71694, #57919, #173468, #178269, #162904, #152760, #141314, #96232, #185848, #102251 ) ) ;
#111895 = CARTESIAN_POINT ( 'NONE',  ( 9.564922557960805705, 16.46253265017160317, 89.58224293864769550 ) ) ;
#111896 = CARTESIAN_POINT ( 'NONE',  ( 19.26498983726237313, -5.499999999999792166, 83.05319577421998645 ) ) ;
#111898 = CARTESIAN_POINT ( 'NONE',  ( 16.51473224551069308, 9.474510206698969483, 34.16557627198102409 ) ) ;
#111897 = CARTESIAN_POINT ( 'NONE',  ( -19.05341960407611168, -5.049401038298163336, 21.45724293864768839 ) ) ;
#111899 = CARTESIAN_POINT ( 'NONE',  ( -19.05341960407617563, 5.049401038297882671, 108.5427570613523187 ) ) ;
#111900 = CARTESIAN_POINT ( 'NONE',  ( 11.40812507854754365, 35.11059874428196537, -9.724999997268813701 ) ) ;
#111901 = CARTESIAN_POINT ( 'NONE',  ( 8.224510206698953496, -14.34966873604960469, 107.9155762719810241 ) ) ;
#111902 = CARTESIAN_POINT ( 'NONE',  ( 15.72974639402176855, 15.80617190586768217, 91.87609039468568994 ) ) ;
#111904 = CARTESIAN_POINT ( 'NONE',  ( 0.05219959533937995610, -21.53943276465977519, 35.00109039468568284 ) ) ;
#111903 = CARTESIAN_POINT ( 'NONE',  ( 13.97604488694527802, 13.89961937509977652, 64.37390960531436690 ) ) ;
#111905 = CARTESIAN_POINT ( 'NONE',  ( 18.67979575497194134, -10.72451020669871369, 20.83442372801901143 ) ) ;
#111906 = CARTESIAN_POINT ( 'NONE',  ( -17.14385361876520264, -23.59649016807271593, 139.6750000027311955 ) ) ;
#111907 = CARTESIAN_POINT ( 'NONE',  ( -9.474510206698964154, 16.51473224551069663, 90.41557627198103830 ) ) ;
#111908 = CARTESIAN_POINT ( 'NONE',  ( 23.74938543818037218, 14.67923089136166936, 139.9999999999999716 ) ) ;
#111910 = CARTESIAN_POINT ( 'NONE',  ( 0.05219959533907565091, 21.53943276465977519, 49.99890960531437401 ) ) ;
#111909 = CARTESIAN_POINT ( 'NONE',  ( -4.379528057220086978, -16.55341960407618274, 29.79275706135234358 ) ) ;
#111911 = CARTESIAN_POINT ( 'NONE',  ( -21.52544592524334988, -5.823673210054445271, 78.95942372801901854 ) ) ;
#111912 = CARTESIAN_POINT ( 'NONE',  ( -19.02544592524342804, 5.153800228976336051, 106.0405762719810241 ) ) ;
#111913 = CARTESIAN_POINT ( 'NONE',  ( 9.474510206698729675, 16.51473224551082808, 102.0844237280190043 ) ) ;
#111914 = CARTESIAN_POINT ( 'NONE',  ( 19.05341960407611168, 5.049401038298154454, 58.95724293864768129 ) ) ;
#111915 = CARTESIAN_POINT ( 'NONE',  ( 0.05219959533909260263, 19.03943276465977164, 84.99890960531436690 ) ) ;
#111916 = CARTESIAN_POINT ( 'NONE',  ( 14.29746914071049879, -8.314922557960816363, 88.33224293864769550 ) ) ;
#111917 = CARTESIAN_POINT ( 'NONE',  ( -16.55341960407611168, -4.379528057220339221, 101.4572429386476955 ) ) ;
#111919 = EDGE_CURVE ( 'NONE', #74166, #59417, #62256, .T. ) ;
#111918 = CARTESIAN_POINT ( 'NONE',  ( 16.46253265017160672, -9.564922557960803928, 108.3322429386476955 ) ) ;
#111920 = CARTESIAN_POINT ( 'NONE',  ( 12.14591786802327356, -12.06949235617739191, 75.62609039468567573 ) ) ;
#111923 = CARTESIAN_POINT ( 'NONE',  ( -9.474510206698964154, 16.51473224551069663, 40.41557627198103120 ) ) ;
#111922 =( BOUNDED_CURVE ( )  B_SPLINE_CURVE ( 3, ( #5918, #35273, #50457, #21095 ),
 .UNSPECIFIED., .F., .F. ) 
 B_SPLINE_CURVE_WITH_KNOTS ( ( 4, 4 ),
 ( 1.132647296210726129, 1.570796326794896558 ),
 .UNSPECIFIED. ) 
 CURVE ( )  GEOMETRIC_REPRESENTATION_ITEM ( )  RATIONAL_B_SPLINE_CURVE ( ( 1.000000000000000000, 0.9840659996946589105, 0.9840659996946589105, 1.000000000000000000 ) ) 
 REPRESENTATION_ITEM ( '' )  );
#111921 = CARTESIAN_POINT ( 'NONE',  ( 14.29746914071049879, -8.314922557960816363, 58.33224293864768839 ) ) ;
#111924 = CARTESIAN_POINT ( 'NONE',  ( 21.52544592524334988, 5.823673210054432836, 66.45942372801903275 ) ) ;
#111925 = CARTESIAN_POINT ( 'NONE',  ( 9.474510206698729675, 16.51473224551082808, 97.08442372801900433 ) ) ;
#111926 = CARTESIAN_POINT ( 'NONE',  ( 14.29746914071049879, -8.314922557960816363, 63.33224293864770260 ) ) ;
#111927 = CARTESIAN_POINT ( 'NONE',  ( -18.67979575497178146, -10.72451020669898902, 106.6655762719810383 ) ) ;
#111928 = CARTESIAN_POINT ( 'NONE',  ( 21.52544592524344225, -5.823673210054117533, 48.54057627198103120 ) ) ;
#111929 = CARTESIAN_POINT ( 'NONE',  ( -17.13100169013300444, -6.664070546373138448, 104.2321016430015135 ) ) ;
#111930 = CARTESIAN_POINT ( 'NONE',  ( -28.82186960331499392, 9.364793116373565596, 142.1500000054623740 ) ) ;
#111931 = CARTESIAN_POINT ( 'NONE',  ( -19.05341960407611168, -5.049401038298163336, 66.45724293864769550 ) ) ;
#111932 = CARTESIAN_POINT ( 'NONE',  ( 14.29746914071049879, -8.314922557960816363, 38.33224293864768839 ) ) ;
#111933 = CARTESIAN_POINT ( 'NONE',  ( 16.55341960407618274, -4.379528057220086978, 111.0427570613523613 ) ) ;
#111934 = CARTESIAN_POINT ( 'NONE',  ( 12.06949235617739724, 12.14591786802326823, 86.87609039468568994 ) ) ;
#111935 = CARTESIAN_POINT ( 'NONE',  ( -13.89961937509957401, -13.97604488694547875, 39.37609039468566152 ) ) ;
#111936 = CARTESIAN_POINT ( 'NONE',  ( -9.656827144875922642, -71.74905178543390605, 8.936314941956774358E-29 ) ) ;
#111937 = CARTESIAN_POINT ( 'NONE',  ( 19.05341960407611168, 5.049401038298154454, 93.95724293864769550 ) ) ;
#111938 = CARTESIAN_POINT ( 'NONE',  ( 19.05341960407611168, 5.049401038298154454, 48.95724293864768129 ) ) ;
#111939 = CARTESIAN_POINT ( 'NONE',  ( -14.34966873604960291, -8.224510206698953496, 56.66557627198103830 ) ) ;
#111941 = CARTESIAN_POINT ( 'NONE',  ( 5.153800228976335163, 19.02544592524342804, 114.7905762719810241 ) ) ;
#111940 = CARTESIAN_POINT ( 'NONE',  ( -19.03943276465977164, 0.05219959533909376836, 21.24890960531436335 ) ) ;
#111942 = CARTESIAN_POINT ( 'NONE',  ( 5.719274019375991003, -21.55341960407610458, 47.70724293864770260 ) ) ;
#111943 = CARTESIAN_POINT ( 'NONE',  ( -14.34966873604960291, -8.224510206698953496, 91.66557627198103830 ) ) ;
#111944 = CARTESIAN_POINT ( 'NONE',  ( -16.53943276465976808, -0.05219959533934237506, 33.75109039468568284 ) ) ;
#111945 = CARTESIAN_POINT ( 'NONE',  ( 16.52544592524342804, -4.483927247898539470, 78.54057627198103830 ) ) ;
#111946 = CARTESIAN_POINT ( 'NONE',  ( 6.791538853603070081, -3.181980515339468241, 1.110912703473986074 ) ) ;
#111947 = CARTESIAN_POINT ( 'NONE',  ( 16.51473224551083163, -9.474510206698727899, 75.83442372801900433 ) ) ;
#111948 = CARTESIAN_POINT ( 'NONE',  ( 15.72974639402199770, -15.80617190586745480, 23.12390960531436335 ) ) ;
#111949 = CARTESIAN_POINT ( 'NONE',  ( -36.91746825000001309, -11.99521256947794789, -7.024999997268812635 ) ) ;
#111950 = CARTESIAN_POINT ( 'NONE',  ( 17.58332526062526568, -7.635886036038552760, 43.42334959558467489 ) ) ;
#111952 = CARTESIAN_POINT ( 'NONE',  ( -14.34966873604972548, 8.224510206698743886, 108.3344237280190185 ) ) ;
#111951 = CARTESIAN_POINT ( 'NONE',  ( 12.06949235617739724, 12.14591786802326823, 26.87609039468567218 ) ) ;
#111953 = CARTESIAN_POINT ( 'NONE',  ( 19.03943276465977164, 0.05219959533936151252, 66.25109039468567573 ) ) ;
#111954 = CARTESIAN_POINT ( 'NONE',  ( -0.05219959533907301413, -21.53943276465977519, 47.49890960531435979 ) ) ;
#111955 = CARTESIAN_POINT ( 'NONE',  ( 10.81492255796106328, -18.62759615963255655, 65.41775706135234714 ) ) ;
#111956 = CARTESIAN_POINT ( 'NONE',  ( 14.61778469963306470, -34.91027835867544837, -28.77367925216604050 ) ) ;
#111957 = CARTESIAN_POINT ( 'NONE',  ( -16.55341960407617563, 4.379528057220093196, 38.54275706135234714 ) ) ;
#111959 = CARTESIAN_POINT ( 'NONE',  ( 13.89961937509977652, -13.97604488694527269, 83.12390960531436690 ) ) ;
#111958 = CARTESIAN_POINT ( 'NONE',  ( 16.51473224551069308, 9.474510206698969483, 24.16557627198102765 ) ) ;
#111960 = CARTESIAN_POINT ( 'NONE',  ( 9.474510206698971260, -16.51473224551069308, 27.91557627198103120 ) ) ;
#111961 = CARTESIAN_POINT ( 'NONE',  ( -8.224510206698948167, 14.34966873604960824, 105.4155762719810383 ) ) ;
#111962 = CARTESIAN_POINT ( 'NONE',  ( -5.153800228976328057, -19.02544592524343514, 97.29057627198099567 ) ) ;
#111963 = ORIENTED_EDGE ( 'NONE', *, *, #114488, .F. ) ;
#111964 = CARTESIAN_POINT ( 'NONE',  ( -12.06949235617739369, -12.14591786802326823, 54.37609039468568994 ) ) ;
#111965 = CARTESIAN_POINT ( 'NONE',  ( 16.51473224551083163, -9.474510206698727899, 105.8344237280190043 ) ) ;
#111966 = CARTESIAN_POINT ( 'NONE',  ( 10.81492255796078972, 18.62759615963270932, 79.58224293864769550 ) ) ;
#111967 = CARTESIAN_POINT ( 'NONE',  ( 9.474510206698971260, -16.51473224551069308, 47.91557627198102409 ) ) ;
#111969 = CARTESIAN_POINT ( 'NONE',  ( 5.719274019375991003, -21.55341960407610458, 107.7072429386476955 ) ) ;
#111968 = CARTESIAN_POINT ( 'NONE',  ( 5.153800228976615827, -19.02544592524334988, 75.20942372801896170 ) ) ;
#111970 = CARTESIAN_POINT ( 'NONE',  ( 0.05219959533909260263, 19.03943276465977164, 64.99890960531436690 ) ) ;
#111971 = CARTESIAN_POINT ( 'NONE',  ( -5.049401038298153566, 19.05341960407611168, 100.2072429386476955 ) ) ;
#111972 = ORIENTED_EDGE ( 'NONE', *, *, #100961, .T. ) ;
#111973 = CARTESIAN_POINT ( 'NONE',  ( -16.55341960407617563, 4.379528057220093196, 33.54275706135234714 ) ) ;
#111974 = CARTESIAN_POINT ( 'NONE',  ( 10.81492255796078972, 18.62759615963270932, 109.5822429386476955 ) ) ;
#111977 = CARTESIAN_POINT ( 'NONE',  ( 13.97604488694548053, -13.89961937509957401, 80.62609039468567573 ) ) ;
#111976 = CARTESIAN_POINT ( 'NONE',  ( -19.03943276465977164, 0.05219959533909376836, 91.24890960531436690 ) ) ;
#111975 = CARTESIAN_POINT ( 'NONE',  ( -16.55341960407611168, -4.379528057220339221, 106.4572429386477097 ) ) ;
#111978 = CARTESIAN_POINT ( 'NONE',  ( -18.62759615963270932, 10.81492255796079327, 90.83224293864769550 ) ) ;
#111979 = CARTESIAN_POINT ( 'NONE',  ( -8.314922557960811034, -14.29746914071050412, 47.08224293864770260 ) ) ;
#111980 = CARTESIAN_POINT ( 'NONE',  ( -18.67979575497193778, 10.72451020669871902, 113.3344237280190328 ) ) ;
#111981 = CARTESIAN_POINT ( 'NONE',  ( 14.34966873604972726, -8.224510206698740333, 70.83442372801901854 ) ) ;
#111982 = CARTESIAN_POINT ( 'NONE',  ( 19.03943276465977164, -0.05219959533909143690, 88.74890960531436690 ) ) ;
#111983 = CARTESIAN_POINT ( 'NONE',  ( -9.474510206698964154, 16.51473224551069663, 50.41557627198102409 ) ) ;
#111984 = AXIS2_PLACEMENT_3D ( 'NONE', #55108, #179482, #84426 ) ;
#111985 = CARTESIAN_POINT ( 'NONE',  ( -15.72974639402176322, -15.80617190586768395, 59.37609039468568284 ) ) ;
#111986 = CARTESIAN_POINT ( 'NONE',  ( 21.52544592524334988, 5.823673210054432836, 71.45942372801901854 ) ) ;
#111987 = CARTESIAN_POINT ( 'NONE',  ( -5.049401038298153566, 19.05341960407611168, 60.20724293864768129 ) ) ;
#111988 = CARTESIAN_POINT ( 'NONE',  ( -5.823673210054431948, 21.52544592524334988, 32.70942372801900433 ) ) ;
#111989 = ORIENTED_EDGE ( 'NONE', *, *, #2914, .T. ) ;
#111990 = CARTESIAN_POINT ( 'NONE',  ( 9.474510206698729675, 16.51473224551082808, 82.08442372801899012 ) ) ;
#111991 = CARTESIAN_POINT ( 'NONE',  ( -19.02544592524342804, 5.153800228976336051, 46.04057627198101699 ) ) ;
#111992 = CARTESIAN_POINT ( 'NONE',  ( -16.52544592524335698, -4.483927247898792601, 83.95942372801900433 ) ) ;
#111993 = CARTESIAN_POINT ( 'NONE',  ( -13.89961937509977652, 13.97604488694528158, 60.62390960531436690 ) ) ;
#111994 = CARTESIAN_POINT ( 'NONE',  ( -0.05219959533909027116, -19.03943276465977164, 107.4989096053143527 ) ) ;
#111995 = CARTESIAN_POINT ( 'NONE',  ( 9.474510206698971260, -16.51473224551069308, 42.91557627198103120 ) ) ;
#111996 = CARTESIAN_POINT ( 'NONE',  ( -5.719274019375978568, 21.55341960407610458, 80.20724293864769550 ) ) ;
#111997 = CARTESIAN_POINT ( 'NONE',  ( 12.06949235617739724, 12.14591786802326823, 71.87609039468568994 ) ) ;
#111999 = CARTESIAN_POINT ( 'NONE',  ( -20.69372460268614589, 10.84650605405326296, 168.1714143675833100 ) ) ;
#111998 = CIRCLE ( 'NONE', #47498, 0.5000000000000004441 ) ;
#112000 = CARTESIAN_POINT ( 'NONE',  ( 19.03943276465977164, 0.05219959533936151252, 31.25109039468566863 ) ) ;
#112001 = ADVANCED_FACE ( 'NONE', ( #47616 ), #170949, .F. ) ;
#112002 = CARTESIAN_POINT ( 'NONE',  ( 19.03943276465977164, -0.05219959533909143690, 63.74890960531435979 ) ) ;
#112003 = CARTESIAN_POINT ( 'NONE',  ( 16.53943276465976808, -0.05219959533910856209, 38.74890960531435979 ) ) ;
#112004 = CARTESIAN_POINT ( 'NONE',  ( 12.06949235617757843, -12.14591786802309237, 83.12390960531436690 ) ) ;
#112005 = CARTESIAN_POINT ( 'NONE',  ( 0.05219959533909260263, 19.03943276465977164, 99.99890960531436690 ) ) ;
#112006 = CARTESIAN_POINT ( 'NONE',  ( -19.03943276465977164, 0.05219959533909376836, 96.24890960531436690 ) ) ;
#112007 = CARTESIAN_POINT ( 'NONE',  ( 10.81492255796106328, -18.62759615963255655, 50.41775706135235424 ) ) ;
#112008 = CARTESIAN_POINT ( 'NONE',  ( -9.564922557960796823, -16.46253265017161027, 112.0822429386476955 ) ) ;
#112009 = CARTESIAN_POINT ( 'NONE',  ( -0.05219959533936034679, 19.03943276465977164, 22.50109039468566152 ) ) ;
#112010 = CARTESIAN_POINT ( 'NONE',  ( -8.224510206698735004, -14.34966873604973081, 74.58442372801901854 ) ) ;
#112011 = CARTESIAN_POINT ( 'NONE',  ( 18.62759615963255655, 10.81492255796105972, 26.66775706135235424 ) ) ;
#112012 = CARTESIAN_POINT ( 'NONE',  ( 5.049401038298161559, -19.05341960407611168, 107.7072429386476955 ) ) ;
#112013 = CARTESIAN_POINT ( 'NONE',  ( -0.05219959533907301413, -21.53943276465977519, 107.4989096053143669 ) ) ;
#112014 = CARTESIAN_POINT ( 'NONE',  ( 16.55341960407611168, 4.379528057220329451, 63.95724293864770260 ) ) ;
#112015 = CARTESIAN_POINT ( 'NONE',  ( -9.564922557960796823, -16.46253265017161027, 47.08224293864769550 ) ) ;
#112016 = CARTESIAN_POINT ( 'NONE',  ( 16.52544592524342804, -4.483927247898539470, 78.54057627198103830 ) ) ;
#112017 = CARTESIAN_POINT ( 'NONE',  ( 10.72451020669898902, -18.67979575497178502, 27.91557627198103830 ) ) ;
#112018 = CARTESIAN_POINT ( 'NONE',  ( 16.51473224551083163, -9.474510206698727899, 25.83442372801900078 ) ) ;
#112019 = CARTESIAN_POINT ( 'NONE',  ( 8.314922557960818139, 14.29746914071049879, 109.5822429386476955 ) ) ;
#112020 = ORIENTED_EDGE ( 'NONE', *, *, #13338, .F. ) ;
#112021 = CARTESIAN_POINT ( 'NONE',  ( -4.379528057220086978, -16.55341960407618274, 64.79275706135234714 ) ) ;
#112022 = CARTESIAN_POINT ( 'NONE',  ( 16.46253265017160672, -9.564922557960803928, 63.33224293864769550 ) ) ;
#112023 = CARTESIAN_POINT ( 'NONE',  ( 17.14385361876520264, -23.59649016807270883, 143.5750000027311728 ) ) ;
#112024 = CARTESIAN_POINT ( 'NONE',  ( -8.224510206698948167, 14.34966873604960824, 90.41557627198103830 ) ) ;
#112025 = CARTESIAN_POINT ( 'NONE',  ( 0.05219959533907565091, 21.53943276465977519, 39.99890960531436690 ) ) ;
#112026 = ORIENTED_EDGE ( 'NONE', *, *, #28043, .F. ) ;
#112027 = CARTESIAN_POINT ( 'NONE',  ( -14.34966873604972548, 8.224510206698743886, 113.3344237280190328 ) ) ;
#112028 = CARTESIAN_POINT ( 'NONE',  ( 5.049401038297881783, 19.05341960407617563, 112.2927570613523471 ) ) ;
#112029 = CARTESIAN_POINT ( 'NONE',  ( -10.72451020669870658, -18.67979575497194134, 74.58442372801901854 ) ) ;
#112030 = CARTESIAN_POINT ( 'NONE',  ( -9.564922557960796823, -16.46253265017161027, 87.08224293864769550 ) ) ;
#112031 = CARTESIAN_POINT ( 'NONE',  ( 15.72974639402199770, -15.80617190586745480, 98.12390960531436690 ) ) ;
#112032 = CARTESIAN_POINT ( 'NONE',  ( -16.53943276465976808, -0.05219959533934237506, 48.75109039468568284 ) ) ;
#112033 = CARTESIAN_POINT ( 'NONE',  ( 19.02544592524343514, -5.153800228976328945, 33.54057627198102409 ) ) ;
#112034 = CIRCLE ( 'NONE', #44219, 2.649999999999999467 ) ;
#112035 = CARTESIAN_POINT ( 'NONE',  ( 16.53943276465976808, 0.05219959533934440121, 26.25109039468567573 ) ) ;
#112036 = CARTESIAN_POINT ( 'NONE',  ( 0.05219959533936267826, -19.03943276465977164, 100.0010903946856757 ) ) ;
#112037 = CARTESIAN_POINT ( 'NONE',  ( 15.72974639402199770, -15.80617190586745480, 93.12390960531436690 ) ) ;
#112038 = CARTESIAN_POINT ( 'NONE',  ( 5.153800228976615827, -19.02544592524334988, 50.20942372801897591 ) ) ;
#112039 = CARTESIAN_POINT ( 'NONE',  ( 19.26498983726236958, -5.499999999999793943, 88.05319577422001487 ) ) ;
#112040 = CARTESIAN_POINT ( 'NONE',  ( 0.05219959533907565091, 21.53943276465977519, 99.99890960531436690 ) ) ;
#112041 = DIRECTION ( 'NONE',  ( 0.5367108174878537641, -0.8437662581494472791, 0.000000000000000000 ) ) ;
#112042 = CARTESIAN_POINT ( 'NONE',  ( 19.02544592524343514, -5.153800228976328945, 83.54057627198100988 ) ) ;
#112043 = CYLINDRICAL_SURFACE ( 'NONE', #98102, 2.649999999999992806 ) ;
#112044 = CARTESIAN_POINT ( 'NONE',  ( 8.224510206698742110, 14.34966873604972548, 32.08442372801901854 ) ) ;
#112045 = CARTESIAN_POINT ( 'NONE',  ( 24.81835718235489807, 6.052279806424484931, 168.4265042179603142 ) ) ;
#112047 = CARTESIAN_POINT ( 'NONE',  ( -14.29746914071049879, 8.314922557960819915, 60.83224293864769550 ) ) ;
#112046 = CARTESIAN_POINT ( 'NONE',  ( -21.52544592524334988, -5.823673210054445271, 23.95942372801901143 ) ) ;
#112048 = CARTESIAN_POINT ( 'NONE',  ( 16.51473224551069308, 9.474510206698969483, 74.16557627198103830 ) ) ;
#112050 = CARTESIAN_POINT ( 'NONE',  ( 9.474510206698729675, 16.51473224551082808, 47.08442372801900433 ) ) ;
#112049 = CARTESIAN_POINT ( 'NONE',  ( 8.314922557961029526, -14.29746914071037800, 35.41775706135234003 ) ) ;
#112051 = CARTESIAN_POINT ( 'NONE',  ( -10.81492255796105439, 18.62759615963255655, 47.91775706135234714 ) ) ;
#112052 = CARTESIAN_POINT ( 'NONE',  ( 9.564922557961047289, -16.46253265017146816, 110.4177570613523471 ) ) ;
#112053 = CARTESIAN_POINT ( 'NONE',  ( -9.564922557960796823, -16.46253265017161027, 57.08224293864769550 ) ) ;
#112054 = CARTESIAN_POINT ( 'NONE',  ( 19.02544592524334988, 5.153800228976608722, 86.45942372801900433 ) ) ;
#112055 = CARTESIAN_POINT ( 'NONE',  ( -10.81492255796105439, 18.62759615963255655, 82.91775706135234714 ) ) ;
#112056 = CARTESIAN_POINT ( 'NONE',  ( 19.05341960407617918, -5.049401038297876454, 61.04275706135232582 ) ) ;
#112057 = CARTESIAN_POINT ( 'NONE',  ( 19.02544592524343514, -5.153800228976328945, 43.54057627198103120 ) ) ;
#112058 = CARTESIAN_POINT ( 'NONE',  ( 18.62759615963271287, -10.81492255796078972, 63.33224293864770260 ) ) ;
#112060 = CARTESIAN_POINT ( 'NONE',  ( -19.02544592524334988, -5.153800228976617603, 68.95942372801896170 ) ) ;
#112059 = CARTESIAN_POINT ( 'NONE',  ( 14.29746914071049879, -8.314922557960816363, 58.33224293864768839 ) ) ;
#112061 = DIRECTION ( 'NONE',  ( 0.000000000000000000, 0.000000000000000000, 1.000000000000000000 ) ) ;
#112062 = CARTESIAN_POINT ( 'NONE',  ( -16.46253265017146816, -9.564922557961047289, 34.16775706135233293 ) ) ;
#112063 = CARTESIAN_POINT ( 'NONE',  ( -16.55341960407617563, 4.379528057220093196, 98.54275706135234714 ) ) ;
#112064 = CARTESIAN_POINT ( 'NONE',  ( -12.14591786802309592, -12.06949235617757132, 56.87390960531436690 ) ) ;
#112066 = CARTESIAN_POINT ( 'NONE',  ( 22.44159573604009594, -16.30477369853687364, 141.6750000027311671 ) ) ;
#112065 = CARTESIAN_POINT ( 'NONE',  ( 5.823673210054444382, -21.52544592524334988, 95.20942372801903275 ) ) ;
#112067 = CARTESIAN_POINT ( 'NONE',  ( -5.823673210054431948, 21.52544592524334988, 97.70942372801904696 ) ) ;
#112068 = CARTESIAN_POINT ( 'NONE',  ( -5.823673210054116645, -21.52544592524344225, 92.29057627198103830 ) ) ;
#112069 = CARTESIAN_POINT ( 'NONE',  ( -19.03943276465977164, 0.05219959533909376836, 51.24890960531436690 ) ) ;
#112070 = CARTESIAN_POINT ( 'NONE',  ( 21.55341960407619695, -5.719274019375665929, 71.04275706135234714 ) ) ;
#112071 = CARTESIAN_POINT ( 'NONE',  ( 5.049401038298161559, -19.05341960407611168, 47.70724293864770260 ) ) ;
#112072 = CARTESIAN_POINT ( 'NONE',  ( 19.02544592524343514, -5.153800228976328945, 68.54057627198103830 ) ) ;
#112073 = CARTESIAN_POINT ( 'NONE',  ( -8.314922557960811034, -14.29746914071050412, 102.0822429386476955 ) ) ;
#112074 = CARTESIAN_POINT ( 'NONE',  ( 0.05219959533909260263, 19.03943276465977164, 114.9989096053143669 ) ) ;
#112075 = CARTESIAN_POINT ( 'NONE',  ( -4.379528057220328563, 16.55341960407611168, 60.20724293864768839 ) ) ;
#112076 = CARTESIAN_POINT ( 'NONE',  ( -13.97604488694527625, -13.89961937509977652, 31.87390960531435979 ) ) ;
#112077 = CARTESIAN_POINT ( 'NONE',  ( -8.224510206698948167, 14.34966873604960824, 65.41557627198102409 ) ) ;
#112078 = CARTESIAN_POINT ( 'NONE',  ( 5.719274019375991003, -21.55341960407610458, 102.7072429386476955 ) ) ;
#112079 = CARTESIAN_POINT ( 'NONE',  ( 10.81492255796106328, -18.62759615963255655, 40.41775706135234714 ) ) ;
#112080 = CARTESIAN_POINT ( 'NONE',  ( 27.91697786073761023, -6.847065636290183832, 161.8035115693297143 ) ) ;
#112081 = CARTESIAN_POINT ( 'NONE',  ( -12.14591786802326823, 12.06949235617739902, 38.12609039468567573 ) ) ;
#112082 = CARTESIAN_POINT ( 'NONE',  ( -21.52544592524343514, 5.823673210054127303, 86.04057627198102409 ) ) ;
#112083 = CARTESIAN_POINT ( 'NONE',  ( -18.62759615963255300, -10.81492255796106328, 109.1677570613523613 ) ) ;
#112084 = CARTESIAN_POINT ( 'NONE',  ( -13.97604488694527625, -13.89961937509977652, 86.87390960531436690 ) ) ;
#112085 = CARTESIAN_POINT ( 'NONE',  ( 5.823673210054444382, -21.52544592524334988, 50.20942372801901854 ) ) ;
#112086 = CARTESIAN_POINT ( 'NONE',  ( 15.80617190586746368, 15.72974639402197994, 24.37390960531435979 ) ) ;
#112087 = CARTESIAN_POINT ( 'NONE',  ( -4.483927247898782831, 16.52544592524335698, 102.7094237280190185 ) ) ;
#112089 = CARTESIAN_POINT ( 'NONE',  ( 0.05219959533937995610, -21.53943276465977519, 90.00109039468567573 ) ) ;
#112088 = CARTESIAN_POINT ( 'NONE',  ( 18.67979575497194134, -10.72451020669871369, 45.83442372801901854 ) ) ;
#112090 = CARTESIAN_POINT ( 'NONE',  ( -18.62759615963255300, -10.81492255796106328, 109.1677570613523613 ) ) ;
#112091 = CARTESIAN_POINT ( 'NONE',  ( 16.52544592524335698, 4.483927247898782831, 91.45942372801901854 ) ) ;
#112092 = CARTESIAN_POINT ( 'NONE',  ( -18.62759615963255300, -10.81492255796106328, 39.16775706135235424 ) ) ;
#112093 = CARTESIAN_POINT ( 'NONE',  ( -19.03943276465977164, 0.05219959533909376836, 26.24890960531435624 ) ) ;
#112094 = CARTESIAN_POINT ( 'NONE',  ( -5.719274019375665041, -21.55341960407619695, 104.7927570613523898 ) ) ;
#112095 = CARTESIAN_POINT ( 'NONE',  ( -9.564922557960796823, -16.46253265017161027, 112.0822429386476955 ) ) ;
#112096 = CARTESIAN_POINT ( 'NONE',  ( 21.53943276465977519, -0.05219959533907433946, 103.7489096053143669 ) ) ;
#112098 = CARTESIAN_POINT ( 'NONE',  ( -18.67979575497178146, -10.72451020669898902, 71.66557627198100988 ) ) ;
#112097 = CARTESIAN_POINT ( 'NONE',  ( -17.97214573761830536, -5.500000000000087930, 61.46970049038655759 ) ) ;
#112100 = CARTESIAN_POINT ( 'NONE',  ( -4.379528057220328563, 16.55341960407611168, 65.20724293864768129 ) ) ;
#112099 = CARTESIAN_POINT ( 'NONE',  ( 16.55341960407618274, -4.379528057220086978, 56.04275706135235424 ) ) ;
#112101 = DIRECTION ( 'NONE',  ( -0.000000000000000000, 0.000000000000000000, 1.000000000000000000 ) ) ;
#112102 = CARTESIAN_POINT ( 'NONE',  ( 9.474510206698729675, 16.51473224551082808, 92.08442372801900433 ) ) ;
#112103 = DIRECTION ( 'NONE',  ( -0.5000000000000004441, -0.4999999999999987232, 0.7071067811865481278 ) ) ;
#112104 = CARTESIAN_POINT ( 'NONE',  ( 4.483927247898790824, -16.52544592524335698, 30.20942372801902565 ) ) ;
#112105 = CARTESIAN_POINT ( 'NONE',  ( -21.55341960407610458, -5.719274019375992779, 101.4572429386476955 ) ) ;
#112106 = CARTESIAN_POINT ( 'NONE',  ( 21.55341960407610458, 5.719274019375980345, 73.95724293864769550 ) ) ;
#112107 = CARTESIAN_POINT ( 'NONE',  ( 0.05219959533907565091, 21.53943276465977519, 24.99890960531435624 ) ) ;
#112108 = CARTESIAN_POINT ( 'NONE',  ( 8.314922557961029526, -14.29746914071037800, 55.41775706135234714 ) ) ;
#112109 = CARTESIAN_POINT ( 'NONE',  ( 19.02544592524343514, -5.153800228976328945, 73.54057627198103830 ) ) ;
#112111 = CARTESIAN_POINT ( 'NONE',  ( 13.97604488694548053, -13.89961937509957401, 100.6260903946856615 ) ) ;
#112110 = CARTESIAN_POINT ( 'NONE',  ( -5.719274019375665041, -21.55341960407619695, 34.79275706135235424 ) ) ;
#112112 = CARTESIAN_POINT ( 'NONE',  ( 19.05341960407611168, 5.049401038298154454, 103.9572429386476671 ) ) ;
#112113 = CARTESIAN_POINT ( 'NONE',  ( -16.51473224551069308, -9.474510206698971260, 81.66557627198103830 ) ) ;
#112114 = CARTESIAN_POINT ( 'NONE',  ( 18.67979575497178502, 10.72451020669898547, 84.16557627198103830 ) ) ;
#112115 = CARTESIAN_POINT ( 'NONE',  ( -19.05341960407611168, -5.049401038298163336, 56.45724293864768129 ) ) ;
#112116 = CARTESIAN_POINT ( 'NONE',  ( -38.00000000000000711, 12.34694845685046438, -0.09999999999999989453 ) ) ;
#112117 = CARTESIAN_POINT ( 'NONE',  ( 14.29746914071049879, -8.314922557960816363, 63.33224293864770260 ) ) ;
#112118 = CARTESIAN_POINT ( 'NONE',  ( -10.81492255796078084, -18.62759615963271287, 27.08224293864769550 ) ) ;
#112119 = CARTESIAN_POINT ( 'NONE',  ( -30.09553654342099449, 1.478515647795847654, -51.30846887466858419 ) ) ;
#112120 = CARTESIAN_POINT ( 'NONE',  ( -15.72974639402197994, 15.80617190586746368, 110.6239096053143669 ) ) ;
#112121 = CARTESIAN_POINT ( 'NONE',  ( 13.97604488694548053, -13.89961937509957401, 65.62609039468567573 ) ) ;
#112122 = CARTESIAN_POINT ( 'NONE',  ( 18.67979575497178502, 10.72451020669898547, 24.16557627198103120 ) ) ;
#112123 =( NAMED_UNIT ( * ) SI_UNIT ( $, .STERADIAN. ) SOLID_ANGLE_UNIT ( ) );
#112124 = CARTESIAN_POINT ( 'NONE',  ( 5.823673210054125526, 21.52544592524343514, 59.79057627198103120 ) ) ;
#112125 = AXIS2_PLACEMENT_3D ( 'NONE', #169414, #30919, #92567 ) ;
#112126 = CARTESIAN_POINT ( 'NONE',  ( -16.46253265017160317, 9.564922557960807481, 90.83224293864769550 ) ) ;
#112127 = CARTESIAN_POINT ( 'NONE',  ( 10.72451020669871369, 18.67979575497193778, 77.08442372801901854 ) ) ;
#112128 = CARTESIAN_POINT ( 'NONE',  ( -9.564922557960796823, -16.46253265017161027, 47.08224293864769550 ) ) ;
#112129 = CARTESIAN_POINT ( 'NONE',  ( 8.314922557960818139, 14.29746914071049879, 89.58224293864768129 ) ) ;
#112130 = CARTESIAN_POINT ( 'NONE',  ( -16.52544592524335698, -4.483927247898792601, 33.95942372801901143 ) ) ;
#112131 = CARTESIAN_POINT ( 'NONE',  ( -15.80617190586768217, 15.72974639402176855, 68.12609039468567573 ) ) ;
#112132 = VERTEX_POINT ( 'NONE', #172951 ) ;
#112133 = CARTESIAN_POINT ( 'NONE',  ( -9.564922557961040184, 16.46253265017147172, 27.91775706135232582 ) ) ;
#112134 = CARTESIAN_POINT ( 'NONE',  ( -9.474510206698720793, -16.51473224551083518, 79.58442372801899012 ) ) ;
#112135 = CARTESIAN_POINT ( 'NONE',  ( 37.99999999999999289, 2.893978650043524126E-14, -6.749999994537627224 ) ) ;
#112136 = CARTESIAN_POINT ( 'NONE',  ( -21.53943276465977519, -0.05219959533937600094, 33.75109039468568284 ) ) ;
#112137 = DIRECTION ( 'NONE',  ( -1.000000000000000000, -4.336808689942017736E-16, 0.000000000000000000 ) ) ;
#112138 = CARTESIAN_POINT ( 'NONE',  ( -13.97604488694547697, 13.89961937509957934, 33.12609039468566863 ) ) ;
#112139 = CARTESIAN_POINT ( 'NONE',  ( 13.97604488694527802, 13.89961937509977652, 59.37390960531434558 ) ) ;
#112140 = CARTESIAN_POINT ( 'NONE',  ( 19.03943276465977164, 0.05219959533936151252, 26.25109039468566507 ) ) ;
#112141 = CARTESIAN_POINT ( 'NONE',  ( 14.34966873604972726, -8.224510206698740333, 100.8344237280190185 ) ) ;
#112143 = CARTESIAN_POINT ( 'NONE',  ( 5.823673210054444382, -21.52544592524334988, 80.20942372801901854 ) ) ;
#112142 = CARTESIAN_POINT ( 'NONE',  ( 9.564922557960805705, 16.46253265017160317, 114.5822429386476955 ) ) ;
#112144 = CARTESIAN_POINT ( 'NONE',  ( 29.86685920354754842, -21.69954338932559068, -5.824999997268813345 ) ) ;
#112145 = CARTESIAN_POINT ( 'NONE',  ( -17.49999999999995381, -3.850315288879052389, 35.73370869396556770 ) ) ;
#112146 = CARTESIAN_POINT ( 'NONE',  ( -10.72451020669870658, -18.67979575497194134, 89.58442372801901854 ) ) ;
#112147 = CARTESIAN_POINT ( 'NONE',  ( 17.05116617787827593, -6.768360034955678728, 41.15675553259200825 ) ) ;
#112148 = CARTESIAN_POINT ( 'NONE',  ( -0.05219959533909027116, -19.03943276465977164, 97.49890960531436690 ) ) ;
#112149 = ORIENTED_EDGE ( 'NONE', *, *, #102940, .F. ) ;
#112150 = STYLED_ITEM ( 'NONE', ( #34551 ), #73950 ) ;
#112151 = B_SPLINE_CURVE_WITH_KNOTS ( 'NONE', 3,
 ( #95909, #19085, #170772, #91912, #1912, #185952, #77756, #63591, #93919, #33258, #169772, #188944, #153605, #78745 ),
 .UNSPECIFIED., .F., .F.,
 ( 4, 2, 2, 2, 2, 2, 4 ),
 ( 0.002370014825004548333, 0.002666056695728372464, 0.002962098566452196595, 0.003258140437176020726, 0.003554182307899844857, 0.004146266049347488783, 0.004738349790795131841 ),
 .UNSPECIFIED. ) ;
#112152 = DIRECTION ( 'NONE',  ( -0.000000000000000000, 1.000000000000000000, 0.000000000000000000 ) ) ;
#112153 = CARTESIAN_POINT ( 'NONE',  ( -19.02544592524342804, 5.153800228976336051, 46.04057627198101699 ) ) ;
#112155 = EDGE_CURVE ( 'NONE', #33153, #28306, #71744, .T. ) ;
#112154 = CARTESIAN_POINT ( 'NONE',  ( -5.823673210054116645, -21.52544592524344225, 62.29057627198102409 ) ) ;
#112156 = CARTESIAN_POINT ( 'NONE',  ( -14.29746914071049879, 8.314922557960819915, 30.83224293864770260 ) ) ;
#112158 = CARTESIAN_POINT ( 'NONE',  ( -16.46253265017160317, 9.564922557960807481, 85.83224293864769550 ) ) ;
#112157 = CARTESIAN_POINT ( 'NONE',  ( 16.52544592524342804, -4.483927247898539470, 93.54057627198103830 ) ) ;
#112159 = CARTESIAN_POINT ( 'NONE',  ( 9.474510206698729675, 16.51473224551082808, 22.08442372801899722 ) ) ;
#112160 = CARTESIAN_POINT ( 'NONE',  ( 5.049401038298161559, -19.05341960407611168, 42.70724293864767418 ) ) ;
#112161 = CARTESIAN_POINT ( 'NONE',  ( -16.52544592524342804, 4.483927247898546575, 101.0405762719810383 ) ) ;
#112162 = CARTESIAN_POINT ( 'NONE',  ( 21.55341960407619695, -5.719274019375665929, 56.04275706135235424 ) ) ;
#112163 = CARTESIAN_POINT ( 'NONE',  ( -10.72451020669898014, 18.67979575497178502, 85.41557627198102409 ) ) ;
#112164 = CARTESIAN_POINT ( 'NONE',  ( 16.51473224551083163, -9.474510206698727899, 60.83442372801900433 ) ) ;
#112165 = CARTESIAN_POINT ( 'NONE',  ( -25.19092422046364987, -31.08406191321079959, -7.296300659524873389 ) ) ;
#112166 = CARTESIAN_POINT ( 'NONE',  ( -19.05341960407611168, -5.049401038298163336, 111.4572429386476671 ) ) ;
#112167 = CARTESIAN_POINT ( 'NONE',  ( -4.483927247898539470, -16.52544592524342804, 72.29057627198102409 ) ) ;
#112168 = CARTESIAN_POINT ( 'NONE',  ( -16.51473224551082808, 9.474510206698731452, 48.33442372801900433 ) ) ;
#112169 = AXIS2_PLACEMENT_3D ( 'NONE', #57443, #119116, #180797 ) ;
#112170 = CARTESIAN_POINT ( 'NONE',  ( -9.474510206698964154, 16.51473224551069663, 65.41557627198102409 ) ) ;
#112171 = CARTESIAN_POINT ( 'NONE',  ( 0.05219959533910956823, 16.53943276465976808, 64.99890960531435269 ) ) ;
#112172 = CARTESIAN_POINT ( 'NONE',  ( -16.46253265017146816, -9.564922557961047289, 79.16775706135234714 ) ) ;
#112173 = CARTESIAN_POINT ( 'NONE',  ( 10.72451020669898902, -18.67979575497178502, 32.91557627198102409 ) ) ;
#112174 = ORIENTED_EDGE ( 'NONE', *, *, #25449, .F. ) ;
#112175 = CARTESIAN_POINT ( 'NONE',  ( 4.379528057220339221, -16.55341960407611168, 102.7072429386476955 ) ) ;
#112176 = CARTESIAN_POINT ( 'NONE',  ( -17.50000000000001421, -3.237210098469450070, 25.28763012620440520 ) ) ;
#112178 = CARTESIAN_POINT ( 'NONE',  ( 18.67979575497178502, 10.72451020669898547, 69.16557627198102409 ) ) ;
#112177 = CARTESIAN_POINT ( 'NONE',  ( 5.153800228976335163, 19.02544592524342804, 59.79057627198100988 ) ) ;
#112179 = CARTESIAN_POINT ( 'NONE',  ( 16.46253265017160672, -9.564922557960803928, 38.33224293864768839 ) ) ;
#112181 = CARTESIAN_POINT ( 'NONE',  ( -13.97604488694527625, -13.89961937509977652, 71.87390960531433848 ) ) ;
#112180 = CARTESIAN_POINT ( 'NONE',  ( 16.55341960407618274, -4.379528057220086978, 76.04275706135237556 ) ) ;
#112182 = CARTESIAN_POINT ( 'NONE',  ( 13.97604488694548053, -13.89961937509957401, 55.62609039468566863 ) ) ;
#112183 = CARTESIAN_POINT ( 'NONE',  ( -18.67979575497193778, 10.72451020669871902, 68.33442372801900433 ) ) ;
#112184 = CARTESIAN_POINT ( 'NONE',  ( 21.52544592524344225, -5.823673210054117533, 48.54057627198103120 ) ) ;
#112185 = CARTESIAN_POINT ( 'NONE',  ( 4.379528057220339221, -16.55341960407611168, 112.7072429386476955 ) ) ;
#112186 = CARTESIAN_POINT ( 'NONE',  ( 16.55341960407618274, -4.379528057220086978, 81.04275706135236135 ) ) ;
#112187 = CARTESIAN_POINT ( 'NONE',  ( 9.474510206698729675, 16.51473224551082808, 107.0844237280190043 ) ) ;
#112188 = CARTESIAN_POINT ( 'NONE',  ( 13.89961937509977652, -13.97604488694527269, 23.12390960531436335 ) ) ;
#112189 = CARTESIAN_POINT ( 'NONE',  ( 18.09805431107247387, -5.500000000000095923, 43.51606229291886052 ) ) ;
#112190 = CARTESIAN_POINT ( 'NONE',  ( 18.67979575497194134, -10.72451020669871369, 100.8344237280190185 ) ) ;
#112191 = CARTESIAN_POINT ( 'NONE',  ( -8.224510206698948167, 14.34966873604960824, 50.41557627198103120 ) ) ;
#112192 = CARTESIAN_POINT ( 'NONE',  ( -16.52544592524342804, 4.483927247898546575, 76.04057627198102409 ) ) ;
#112193 = CARTESIAN_POINT ( 'NONE',  ( -21.53943276465977519, 0.05219959533907696930, 96.24890960531435269 ) ) ;
#112194 = CARTESIAN_POINT ( 'NONE',  ( 10.81492255796078972, 18.62759615963270932, 94.58224293864769550 ) ) ;
#112195 = CARTESIAN_POINT ( 'NONE',  ( 17.05587630539786304, -6.762274262135686165, 98.24180309037313918 ) ) ;
#112196 = CARTESIAN_POINT ( 'NONE',  ( 5.719274019375991003, -21.55341960407610458, 32.70724293864770260 ) ) ;
#112197 = CARTESIAN_POINT ( 'NONE',  ( 8.314922557961029526, -14.29746914071037800, 70.41775706135236135 ) ) ;
#112198 = CARTESIAN_POINT ( 'NONE',  ( -0.05219959533910754901, -16.53943276465976808, 87.49890960531436690 ) ) ;
#112199 = CARTESIAN_POINT ( 'NONE',  ( 9.474510206698971260, -16.51473224551069308, 42.91557627198103120 ) ) ;
#112200 = DIRECTION ( 'NONE',  ( 1.000000000000000000, -0.000000000000000000, 6.982962677686266711E-15 ) ) ;
#112201 = CARTESIAN_POINT ( 'NONE',  ( 16.55341960407618274, -4.379528057220086978, 96.04275706135236135 ) ) ;
#112202 = CARTESIAN_POINT ( 'NONE',  ( -10.72451020669870658, -18.67979575497194134, 34.58442372801900433 ) ) ;
#112203 = CARTESIAN_POINT ( 'NONE',  ( 19.02544592524343514, -5.153800228976328945, 88.54057627198102409 ) ) ;
#112204 = CARTESIAN_POINT ( 'NONE',  ( 21.52544592524334988, 5.823673210054432836, 66.45942372801903275 ) ) ;
#112205 = CARTESIAN_POINT ( 'NONE',  ( 9.474510206698971260, -16.51473224551069308, 107.9155762719810383 ) ) ;
#112206 = DIRECTION ( 'NONE',  ( 0.000000000000000000, 0.000000000000000000, 1.000000000000000000 ) ) ;
#112207 = VERTEX_POINT ( 'NONE', #176946 ) ;
#112208 = CARTESIAN_POINT ( 'NONE',  ( -21.53943276465977519, -0.05219959533937600094, 58.75109039468568994 ) ) ;
#112210 = CARTESIAN_POINT ( 'NONE',  ( -9.474510206698964154, 16.51473224551069663, 115.4155762719810241 ) ) ;
#112209 = CARTESIAN_POINT ( 'NONE',  ( 16.46253265017160672, -9.564922557960803928, 33.33224293864770260 ) ) ;
#112211 = CARTESIAN_POINT ( 'NONE',  ( 13.89961937509957401, 13.97604488694547697, 71.87609039468567573 ) ) ;
#112212 = CARTESIAN_POINT ( 'NONE',  ( 21.55341960407619695, -5.719274019375665929, 26.04275706135235779 ) ) ;
#112213 = CARTESIAN_POINT ( 'NONE',  ( -16.51473224551082808, 9.474510206698731452, 63.33442372801900433 ) ) ;
#112214 = CARTESIAN_POINT ( 'NONE',  ( -13.89961937509977652, 13.97604488694528158, 30.62390960531435269 ) ) ;
#112215 = CARTESIAN_POINT ( 'NONE',  ( -4.379528057220086978, -16.55341960407618274, 89.79275706135236135 ) ) ;
#112216 = CARTESIAN_POINT ( 'NONE',  ( 16.46253265017146816, 9.564922557961045513, 66.66775706135233293 ) ) ;
#112217 = CARTESIAN_POINT ( 'NONE',  ( 16.55341960407611168, 4.379528057220329451, 28.95724293864769905 ) ) ;
#112219 = ORIENTED_EDGE ( 'NONE', *, *, #955, .T. ) ;
#112218 = CARTESIAN_POINT ( 'NONE',  ( -5.153800228976607833, 19.02544592524334988, 47.70942372801900433 ) ) ;
#112220 = CARTESIAN_POINT ( 'NONE',  ( 9.474510206698971260, -16.51473224551069308, 82.91557627198103830 ) ) ;
#112221 = CARTESIAN_POINT ( 'NONE',  ( 5.719274019375673035, 21.55341960407619339, 92.29275706135236135 ) ) ;
#112222 = CARTESIAN_POINT ( 'NONE',  ( 15.80617190586769283, -15.72974639402175789, 105.6260903946856899 ) ) ;
#112223 = CARTESIAN_POINT ( 'NONE',  ( -0.3535533905929594267, 30.00000000000000711, 4.646446609406718942 ) ) ;
#112224 = CARTESIAN_POINT ( 'NONE',  ( 21.53943276465977519, 0.05219959533937863772, 91.25109039468568994 ) ) ;
#112225 = CARTESIAN_POINT ( 'NONE',  ( 16.53943276465976808, 0.05219959533934440121, 36.25109039468567573 ) ) ;
#112226 = CARTESIAN_POINT ( 'NONE',  ( 16.51473224551069308, 9.474510206698969483, 84.16557627198102409 ) ) ;
#112227 = CARTESIAN_POINT ( 'NONE',  ( 18.67979575497178502, 10.72451020669898547, 29.16557627198103120 ) ) ;
#112228 = FACE_OUTER_BOUND ( 'NONE', #8167, .T. ) ;
#112229 = CARTESIAN_POINT ( 'NONE',  ( -5.153800228976328057, -19.02544592524343514, 77.29057627198099567 ) ) ;
#112230 = CARTESIAN_POINT ( 'NONE',  ( -19.49190055781009789, -5.500000000000055067, 40.56116087098780554 ) ) ;
#112231 = CARTESIAN_POINT ( 'NONE',  ( 5.049401038297881783, 19.05341960407617563, 72.29275706135234714 ) ) ;
#112232 = CARTESIAN_POINT ( 'NONE',  ( 5.153800228976335163, 19.02544592524342804, 104.7905762719809957 ) ) ;
#112233 = CARTESIAN_POINT ( 'NONE',  ( -10.72451020669870658, -18.67979575497194134, 104.5844237280190185 ) ) ;
#112234 = CARTESIAN_POINT ( 'NONE',  ( -14.29746914071049879, 8.314922557960819915, 95.83224293864770971 ) ) ;
#112235 = CARTESIAN_POINT ( 'NONE',  ( 18.62759615963271287, -10.81492255796078972, 43.33224293864769550 ) ) ;
#112236 = CARTESIAN_POINT ( 'NONE',  ( -5.823673210054116645, -21.52544592524344225, 32.29057627198102409 ) ) ;
#112237 = CARTESIAN_POINT ( 'NONE',  ( 12.06949235617757843, -12.14591786802309237, 103.1239096053143811 ) ) ;
#112238 = DIRECTION ( 'NONE',  ( 1.000000000000000000, 0.000000000000000000, 0.000000000000000000 ) ) ;
#112239 = CARTESIAN_POINT ( 'NONE',  ( 5.049401038297881783, 19.05341960407617563, 52.29275706135234003 ) ) ;
#112240 = CARTESIAN_POINT ( 'NONE',  ( -14.29746914071049879, 8.314922557960819915, 30.83224293864770260 ) ) ;
#112241 = CARTESIAN_POINT ( 'NONE',  ( 16.46253265017160672, -9.564922557960803928, 108.3322429386476955 ) ) ;
#112242 = CARTESIAN_POINT ( 'NONE',  ( 21.53943276465977519, 0.05219959533937863772, 76.25109039468568994 ) ) ;
#112243 = CARTESIAN_POINT ( 'NONE',  ( 21.55341960407610458, 5.719274019375980345, 63.95724293864770260 ) ) ;
#112244 = CARTESIAN_POINT ( 'NONE',  ( -5.719274019375665041, -21.55341960407619695, 49.79275706135234714 ) ) ;
#112245 = CARTESIAN_POINT ( 'NONE',  ( -5.719274019375978568, 21.55341960407610458, 90.20724293864770971 ) ) ;
#112246 = CARTESIAN_POINT ( 'NONE',  ( -15.72974639402176322, -15.80617190586768395, 44.37609039468567573 ) ) ;
#112247 = CARTESIAN_POINT ( 'NONE',  ( 13.97604488694527802, 13.89961937509977652, 24.37390960531435624 ) ) ;
#112248 = CARTESIAN_POINT ( 'NONE',  ( 16.51473224551069308, 9.474510206698969483, 89.16557627198103830 ) ) ;
#112249 = CARTESIAN_POINT ( 'NONE',  ( -8.224510206698948167, 14.34966873604960824, 100.4155762719810241 ) ) ;
#112250 = CARTESIAN_POINT ( 'NONE',  ( -13.97604488694527625, -13.89961937509977652, 111.8739096053143243 ) ) ;
#112251 = CARTESIAN_POINT ( 'NONE',  ( -8.224510206698948167, 14.34966873604960824, 50.41557627198103120 ) ) ;
#112252 = CARTESIAN_POINT ( 'NONE',  ( 16.53943276465976808, -0.05219959533910856209, 23.74890960531435269 ) ) ;
#112253 = CARTESIAN_POINT ( 'NONE',  ( -0.05219959533909027116, -19.03943276465977164, 47.49890960531435979 ) ) ;
#112254 = CARTESIAN_POINT ( 'NONE',  ( -0.05219959533909027116, -19.03943276465977164, 22.49890960531436690 ) ) ;
#112255 = CARTESIAN_POINT ( 'NONE',  ( 15.80617190586746368, 15.72974639402197994, 49.37390960531436690 ) ) ;
#112256 = CARTESIAN_POINT ( 'NONE',  ( 19.05341960407617918, -5.049401038297876454, 21.04275706135232582 ) ) ;
#112258 = CARTESIAN_POINT ( 'NONE',  ( -12.06949235617756955, 12.14591786802309770, 40.62390960531435269 ) ) ;
#112257 = CARTESIAN_POINT ( 'NONE',  ( 3.735172737399431091E-16, 6.100000000000006750, -64.53213882399991519 ) ) ;
#112259 = CARTESIAN_POINT ( 'NONE',  ( 15.72974639402176855, 15.80617190586768217, 46.87609039468568994 ) ) ;
#112260 = CARTESIAN_POINT ( 'NONE',  ( -5.049401038298153566, 19.05341960407611168, 115.2072429386477097 ) ) ;
#112261 = CARTESIAN_POINT ( 'NONE',  ( 16.52544592524335698, 4.483927247898782831, 61.45942372801901854 ) ) ;
#112262 = CARTESIAN_POINT ( 'NONE',  ( -9.564922557961040184, 16.46253265017147172, 62.91775706135233293 ) ) ;
#112263 = CARTESIAN_POINT ( 'NONE',  ( -16.55341960407611168, -4.379528057220339221, 21.45724293864769550 ) ) ;
#112264 = CARTESIAN_POINT ( 'NONE',  ( 16.52544592524335698, 4.483927247898782831, 106.4594237280190328 ) ) ;
#112265 = CARTESIAN_POINT ( 'NONE',  ( 13.89961937509977652, -13.97604488694527269, 43.12390960531434558 ) ) ;
#112266 = CARTESIAN_POINT ( 'NONE',  ( 19.02544592524343514, -5.153800228976328945, 58.54057627198102409 ) ) ;
#112267 = CARTESIAN_POINT ( 'NONE',  ( -16.51473224551069308, -9.474510206698971260, 31.66557627198102054 ) ) ;
#112268 = CARTESIAN_POINT ( 'NONE',  ( -21.52544592524334988, -5.823673210054445271, 38.95942372801901854 ) ) ;
#112269 = CARTESIAN_POINT ( 'NONE',  ( -9.474510206698964154, 16.51473224551069663, 45.41557627198103120 ) ) ;
#112270 = CARTESIAN_POINT ( 'NONE',  ( 9.564922557960805705, 16.46253265017160317, 114.5822429386476955 ) ) ;
#112271 = CARTESIAN_POINT ( 'NONE',  ( -0.05219959533909027116, -19.03943276465977164, 52.49890960531436690 ) ) ;
#112272 = CARTESIAN_POINT ( 'NONE',  ( 0.05219959533909260263, 19.03943276465977164, 114.9989096053143669 ) ) ;
#112274 = CARTESIAN_POINT ( 'NONE',  ( 16.55341960407611168, 4.379528057220329451, 98.95724293864770971 ) ) ;
#112273 = CARTESIAN_POINT ( 'NONE',  ( -21.53943276465977519, -0.05219959533937600094, 58.75109039468568994 ) ) ;
#112275 = CARTESIAN_POINT ( 'NONE',  ( -5.049401038298153566, 19.05341960407611168, 110.2072429386476671 ) ) ;
#112276 = CARTESIAN_POINT ( 'NONE',  ( -16.52544592524335698, -4.483927247898792601, 78.95942372801901854 ) ) ;
#112277 = ADVANCED_FACE ( 'NONE', ( #147598 ), #101067, .F. ) ;
#112278 = CARTESIAN_POINT ( 'NONE',  ( -0.05219959533937732626, 21.53943276465977519, 87.50109039468568994 ) ) ;
#112279 = AXIS2_PLACEMENT_3D ( 'NONE', #122224, #30227, #35196 ) ;
#112280 = CARTESIAN_POINT ( 'NONE',  ( 4.483927247898790824, -16.52544592524335698, 50.20942372801901854 ) ) ;
#112281 = CARTESIAN_POINT ( 'NONE',  ( -13.89961937509977652, 13.97604488694528158, 95.62390960531436690 ) ) ;
#112282 = CARTESIAN_POINT ( 'NONE',  ( -16.52544592524335698, -4.483927247898792601, 38.95942372801901854 ) ) ;
#112283 = CARTESIAN_POINT ( 'NONE',  ( -16.55341960407617563, 4.379528057220093196, 33.54275706135234714 ) ) ;
#112284 = CARTESIAN_POINT ( 'NONE',  ( -12.14591786802326823, 12.06949235617739902, 88.12609039468570415 ) ) ;
#112285 = CARTESIAN_POINT ( 'NONE',  ( -19.05341960407617563, 5.049401038297882671, 108.5427570613523187 ) ) ;
#112286 = CARTESIAN_POINT ( 'NONE',  ( -10.81492255796078084, -18.62759615963271287, 102.0822429386476955 ) ) ;
#112288 = CARTESIAN_POINT ( 'NONE',  ( -19.05341960407617563, 5.049401038297882671, 98.54275706135233293 ) ) ;
#112287 = CARTESIAN_POINT ( 'NONE',  ( -14.29746914071049879, 8.314922557960819915, 100.8322429386477097 ) ) ;
#112289 = CARTESIAN_POINT ( 'NONE',  ( 12.06949235617739724, 12.14591786802326823, 66.87609039468568994 ) ) ;
#112290 = CARTESIAN_POINT ( 'NONE',  ( -17.12812012977051523, 6.668231424565586707, 43.64051240676855770 ) ) ;
#112291 = CARTESIAN_POINT ( 'NONE',  ( 19.03943276465977164, 0.05219959533936151252, 76.25109039468566152 ) ) ;
#112292 = CARTESIAN_POINT ( 'NONE',  ( -12.06949235617756955, 12.14591786802309770, 45.62390960531436690 ) ) ;
#112293 = CARTESIAN_POINT ( 'NONE',  ( 8.224510206698953496, -14.34966873604960469, 27.91557627198103830 ) ) ;
#112294 = CARTESIAN_POINT ( 'NONE',  ( 14.29746914071049879, -8.314922557960816363, 88.33224293864769550 ) ) ;
#112296 = CARTESIAN_POINT ( 'NONE',  ( -17.40861289039000681, 6.110651285853376358, 88.62767529172568004 ) ) ;
#112295 = CARTESIAN_POINT ( 'NONE',  ( -19.03943276465977164, -0.05219959533935918106, 38.75109039468566152 ) ) ;
#112297 = CARTESIAN_POINT ( 'NONE',  ( 18.62759615963255655, 10.81492255796105972, 36.66775706135234714 ) ) ;
#112298 = CARTESIAN_POINT ( 'NONE',  ( -19.02544592524334988, -5.153800228976617603, 98.95942372801900433 ) ) ;
#112299 = CARTESIAN_POINT ( 'NONE',  ( -18.00321789565186847, -35.67122027912861171, -27.04300662093954344 ) ) ;
#112300 = CARTESIAN_POINT ( 'NONE',  ( -19.03943276465977164, 0.05219959533909376836, 91.24890960531436690 ) ) ;
#112301 = CARTESIAN_POINT ( 'NONE',  ( 13.89961937509977652, -13.97604488694527269, 93.12390960531436690 ) ) ;
#112302 = CARTESIAN_POINT ( 'NONE',  ( 5.719274019375991003, -21.55341960407610458, 62.70724293864769550 ) ) ;
#112303 = CARTESIAN_POINT ( 'NONE',  ( 8.314922557960818139, 14.29746914071049879, 94.58224293864769550 ) ) ;
#112304 = CARTESIAN_POINT ( 'NONE',  ( 0.05219959533909260263, 19.03943276465977164, 69.99890960531435269 ) ) ;
#112305 = CARTESIAN_POINT ( 'NONE',  ( -0.05219959533909027116, -19.03943276465977164, 22.49890960531436690 ) ) ;
#112306 = CARTESIAN_POINT ( 'NONE',  ( -10.72451020669870658, -18.67979575497194134, 34.58442372801900433 ) ) ;
#112307 = CARTESIAN_POINT ( 'NONE',  ( 21.52544592524334988, 5.823673210054432836, 76.45942372801901854 ) ) ;
#112308 = CARTESIAN_POINT ( 'NONE',  ( -16.46253265017160317, 9.564922557960807481, 60.83224293864769550 ) ) ;
#112309 = CARTESIAN_POINT ( 'NONE',  ( -8.314922557961024197, 14.29746914071037800, 77.91775706135231871 ) ) ;
#112310 = CARTESIAN_POINT ( 'NONE',  ( 18.62759615963255655, 10.81492255796105972, 26.66775706135235424 ) ) ;
#112311 = CARTESIAN_POINT ( 'NONE',  ( -5.719274019375665041, -21.55341960407619695, 24.79275706135235779 ) ) ;
#112313 = CARTESIAN_POINT ( 'NONE',  ( 19.05341960407611168, 5.049401038298154454, 73.95724293864768129 ) ) ;
#112312 = CARTESIAN_POINT ( 'NONE',  ( -13.97604488694547697, 13.89961937509957934, 58.12609039468566863 ) ) ;
#112314 = CARTESIAN_POINT ( 'NONE',  ( -5.153800228976607833, 19.02544592524334988, 32.70942372801899722 ) ) ;
#112315 = CARTESIAN_POINT ( 'NONE',  ( -15.80617190586768217, 15.72974639402176855, 78.12609039468570415 ) ) ;
#112316 = CARTESIAN_POINT ( 'NONE',  ( 10.72451020669898902, -18.67979575497178502, 67.91557627198102409 ) ) ;
#112317 = CARTESIAN_POINT ( 'NONE',  ( 4.379528057220339221, -16.55341960407611168, 52.70724293864769550 ) ) ;
#112319 = CARTESIAN_POINT ( 'NONE',  ( -13.89961937509957401, -13.97604488694547875, 24.37609039468565442 ) ) ;
#112318 = CARTESIAN_POINT ( 'NONE',  ( -21.53943276465977519, -0.05219959533937600094, 88.75109039468567573 ) ) ;
#112320 = CARTESIAN_POINT ( 'NONE',  ( 0.05219959533910956823, 16.53943276465976808, 64.99890960531435269 ) ) ;
#112321 = CARTESIAN_POINT ( 'NONE',  ( -16.51473224551069308, -9.474510206698971260, 21.66557627198102765 ) ) ;
#112322 = CARTESIAN_POINT ( 'NONE',  ( -16.51473224551082808, 9.474510206698731452, 68.33442372801900433 ) ) ;
#112323 = CARTESIAN_POINT ( 'NONE',  ( -0.05219959533910754901, -16.53943276465976808, 37.49890960531436690 ) ) ;
#112324 = CARTESIAN_POINT ( 'NONE',  ( 15.72974639402176855, 15.80617190586768217, 76.87609039468567573 ) ) ;
#112325 = CARTESIAN_POINT ( 'NONE',  ( 13.89961937509977652, -13.97604488694527269, 73.12390960531436690 ) ) ;
#112326 = CARTESIAN_POINT ( 'NONE',  ( -0.05219959533936034679, 19.03943276465977164, 47.50109039468566863 ) ) ;
#112327 = CARTESIAN_POINT ( 'NONE',  ( 10.72451020669898902, -18.67979575497178502, 52.91557627198103830 ) ) ;
#112328 = CARTESIAN_POINT ( 'NONE',  ( -15.72974639402176322, -15.80617190586768395, 39.37609039468567573 ) ) ;
#112329 = CARTESIAN_POINT ( 'NONE',  ( -10.81492255796078084, -18.62759615963271287, 97.08224293864770971 ) ) ;
#112330 = CARTESIAN_POINT ( 'NONE',  ( -14.29746914071037622, -8.314922557961029526, 19.16775706135234714 ) ) ;
#112331 = CARTESIAN_POINT ( 'NONE',  ( -12.06949235617739369, -12.14591786802326823, 69.37609039468567573 ) ) ;
#112333 = CARTESIAN_POINT ( 'NONE',  ( -15.80617190586745835, -15.72974639402198527, 101.8739096053143811 ) ) ;
#112332 = CARTESIAN_POINT ( 'NONE',  ( 17.50000000000000000, 5.500000000000013323, 63.78230962303565832 ) ) ;
#112334 = CARTESIAN_POINT ( 'NONE',  ( -0.05219959533910754901, -16.53943276465976808, 107.4989096053143669 ) ) ;
#112335 = FACE_OUTER_BOUND ( 'NONE', #71340, .T. ) ;
#112336 = CARTESIAN_POINT ( 'NONE',  ( -4.483927247898782831, 16.52544592524335698, 32.70942372801900433 ) ) ;
#112337 = CARTESIAN_POINT ( 'NONE',  ( -21.53943276465977519, 0.05219959533907696930, 66.24890960531436690 ) ) ;
#112338 = CARTESIAN_POINT ( 'NONE',  ( -16.55341960407617563, 4.379528057220093196, 108.5427570613523756 ) ) ;
#112339 = CARTESIAN_POINT ( 'NONE',  ( 13.89961937509977652, -13.97604488694527269, 33.12390960531434558 ) ) ;
#112340 = CARTESIAN_POINT ( 'NONE',  ( 16.55341960407618274, -4.379528057220086978, 66.04275706135236135 ) ) ;
#112341 = CARTESIAN_POINT ( 'NONE',  ( 9.474510206698729675, 16.51473224551082808, 62.08442372801899722 ) ) ;
#112342 = CARTESIAN_POINT ( 'NONE',  ( 5.719274019375673035, 21.55341960407619339, 37.29275706135235424 ) ) ;
#112343 = CARTESIAN_POINT ( 'NONE',  ( -18.67979575497178146, -10.72451020669898902, 61.66557627198103120 ) ) ;
#112344 = CARTESIAN_POINT ( 'NONE',  ( 16.52544592524335698, 4.483927247898782831, 96.45942372801901854 ) ) ;
#112345 = CARTESIAN_POINT ( 'NONE',  ( -5.719274019375665041, -21.55341960407619695, 64.79275706135234714 ) ) ;
#112346 = CARTESIAN_POINT ( 'NONE',  ( 21.52544592524344225, -5.823673210054117533, 48.54057627198103120 ) ) ;
#112347 = CARTESIAN_POINT ( 'NONE',  ( 21.55341960407610458, 5.719274019375980345, 33.95724293864769550 ) ) ;
#112348 = EDGE_LOOP ( 'NONE', ( #156592, #141283, #73285, #191194 ) ) ;
#112349 = EDGE_LOOP ( 'NONE', ( #191536, #81613, #131867, #104003 ) ) ;
#112350 = CARTESIAN_POINT ( 'NONE',  ( -14.29746914071037622, -8.314922557961029526, 79.16775706135234714 ) ) ;
#112351 = CARTESIAN_POINT ( 'NONE',  ( -15.80617190586745835, -15.72974639402198527, 26.87390960531435979 ) ) ;
#112352 = ORIENTED_EDGE ( 'NONE', *, *, #138165, .T. ) ;
#112353 = CARTESIAN_POINT ( 'NONE',  ( 13.89961937509977652, -13.97604488694527269, 93.12390960531436690 ) ) ;
#112354 = CARTESIAN_POINT ( 'NONE',  ( -8.314922557960811034, -14.29746914071050412, 22.08224293864769194 ) ) ;
#112355 = FACE_OUTER_BOUND ( 'NONE', #128122, .T. ) ;
#112356 = CARTESIAN_POINT ( 'NONE',  ( 4.483927247898545687, 16.52544592524342804, 104.7905762719810241 ) ) ;
#112357 = CARTESIAN_POINT ( 'NONE',  ( -18.62759615963270932, 10.81492255796079327, 55.83224293864770260 ) ) ;
#112358 = CARTESIAN_POINT ( 'NONE',  ( 14.29746914071037800, 8.314922557961029526, 96.66775706135234714 ) ) ;
#112359 = CARTESIAN_POINT ( 'NONE',  ( 10.72451020669871369, 18.67979575497193778, 52.08442372801901854 ) ) ;
#112360 = CARTESIAN_POINT ( 'NONE',  ( 9.474510206698729675, 16.51473224551082808, 102.0844237280190043 ) ) ;
#112361 = CARTESIAN_POINT ( 'NONE',  ( 16.52544592524342804, -4.483927247898539470, 98.54057627198105251 ) ) ;
#112362 = CARTESIAN_POINT ( 'NONE',  ( -19.03943276465977164, -0.05219959533935918106, 113.7510903946856757 ) ) ;
#112363 = CARTESIAN_POINT ( 'NONE',  ( -19.02544592524342804, 5.153800228976336051, 31.04057627198102409 ) ) ;
#112364 = CYLINDRICAL_SURFACE ( 'NONE', #34927, 28.82186960331498682 ) ;
#112365 = CARTESIAN_POINT ( 'NONE',  ( 13.89961937509977652, -13.97604488694527269, 88.12390960531438111 ) ) ;
#112366 = CARTESIAN_POINT ( 'NONE',  ( 16.55341960407618274, -4.379528057220086978, 71.04275706135234714 ) ) ;
#112367 = CARTESIAN_POINT ( 'NONE',  ( 21.55341960407619695, -5.719274019375665929, 111.0427570613523613 ) ) ;
#112368 = CARTESIAN_POINT ( 'NONE',  ( 5.719274019375991003, -21.55341960407610458, 62.70724293864769550 ) ) ;
#112369 = CARTESIAN_POINT ( 'NONE',  ( -12.06949235617739369, -12.14591786802326823, 89.37609039468568994 ) ) ;
#112370 = CARTESIAN_POINT ( 'NONE',  ( -9.474510206698720793, -16.51473224551083518, 79.58442372801899012 ) ) ;
#112371 = CARTESIAN_POINT ( 'NONE',  ( -9.564922557960796823, -16.46253265017161027, 32.08224293864769550 ) ) ;
#112372 = CARTESIAN_POINT ( 'NONE',  ( -19.03943276465977164, 0.05219959533909376836, 76.24890960531435269 ) ) ;
#112373 = CARTESIAN_POINT ( 'NONE',  ( -5.153800228976328057, -19.02544592524343514, 27.29057627198103120 ) ) ;
#112374 = CARTESIAN_POINT ( 'NONE',  ( 19.02544592524334988, 5.153800228976608722, 66.45942372801899012 ) ) ;
#112375 = CARTESIAN_POINT ( 'NONE',  ( 25.55222625260920921, -11.31436996698924879, 166.3494238031457257 ) ) ;
#112376 = CARTESIAN_POINT ( 'NONE',  ( 13.89961937509977652, -13.97604488694527269, 98.12390960531433848 ) ) ;
#112377 = CARTESIAN_POINT ( 'NONE',  ( -12.06949235617756955, 12.14591786802309770, 45.62390960531436690 ) ) ;
#112378 = CARTESIAN_POINT ( 'NONE',  ( -10.72451020669898014, 18.67979575497178502, 65.41557627198102409 ) ) ;
#112379 = DIRECTION ( 'NONE',  ( 0.000000000000000000, 0.000000000000000000, 1.000000000000000000 ) ) ;
#112380 = CARTESIAN_POINT ( 'NONE',  ( -9.474510206698720793, -16.51473224551083518, 29.58442372801900433 ) ) ;
#112381 = CYLINDRICAL_SURFACE ( 'NONE', #186507, 1.500000000000001332 ) ;
#112383 = CARTESIAN_POINT ( 'NONE',  ( 13.89961937509977652, -13.97604488694527269, 73.12390960531436690 ) ) ;
#112382 = CARTESIAN_POINT ( 'NONE',  ( 5.153800228976335163, 19.02544592524342804, 49.79057627198100988 ) ) ;
#112384 = CARTESIAN_POINT ( 'NONE',  ( -8.314922557961024197, 14.29746914071037800, 37.91775706135235424 ) ) ;
#112385 = CARTESIAN_POINT ( 'NONE',  ( -19.25918095147779852, -5.499999999999535483, 99.45284276293932635 ) ) ;
#112386 = CARTESIAN_POINT ( 'NONE',  ( -0.6913667201904812876, -37.16948018716584556, -7.999999999999996447 ) ) ;
#112387 = CARTESIAN_POINT ( 'NONE',  ( -0.05219959533934338120, 16.53943276465976808, 82.50109039468568994 ) ) ;
#112389 = EDGE_CURVE ( 'NONE', #24708, #114881, #123583, .T. ) ;
#112388 = CARTESIAN_POINT ( 'NONE',  ( -21.52544592524343514, 5.823673210054127303, 96.04057627198102409 ) ) ;
#112390 = CARTESIAN_POINT ( 'NONE',  ( -16.53943276465976808, -0.05219959533934237506, 43.75109039468568284 ) ) ;
#112392 = DIRECTION ( 'NONE',  ( 0.000000000000000000, 0.000000000000000000, -1.000000000000000000 ) ) ;
#112391 = CARTESIAN_POINT ( 'NONE',  ( 9.564922557960805705, 16.46253265017160317, 44.58224293864769550 ) ) ;
#112393 = CARTESIAN_POINT ( 'NONE',  ( 5.823673210054444382, -21.52544592524334988, 50.20942372801901854 ) ) ;
#112394 = CARTESIAN_POINT ( 'NONE',  ( 19.02544592524334988, 5.153800228976608722, 56.45942372801898301 ) ) ;
#112395 = CARTESIAN_POINT ( 'NONE',  ( -5.719274019375665041, -21.55341960407619695, 99.79275706135234714 ) ) ;
#112396 = CARTESIAN_POINT ( 'NONE',  ( 16.20579543436678449, 7.371946100355102338, 98.06520834171875833 ) ) ;
#112397 = PLANE ( 'NONE',  #143267 ) ;
#112398 = CARTESIAN_POINT ( 'NONE',  ( -21.53943276465977519, 0.05219959533907696930, 51.24890960531436690 ) ) ;
#112399 = CARTESIAN_POINT ( 'NONE',  ( 13.89961937509977652, -13.97604488694527269, 98.12390960531433848 ) ) ;
#112400 = CARTESIAN_POINT ( 'NONE',  ( -8.314922557960811034, -14.29746914071050412, 102.0822429386476955 ) ) ;
#112401 = CARTESIAN_POINT ( 'NONE',  ( 4.379528057220092307, 16.55341960407617563, 22.29275706135235069 ) ) ;
#112402 = CARTESIAN_POINT ( 'NONE',  ( 16.53943276465976808, 0.05219959533934440121, 106.2510903946856757 ) ) ;
#112403 = VERTEX_POINT ( 'NONE', #9084 ) ;
#112404 = CARTESIAN_POINT ( 'NONE',  ( -21.53943276465977519, 0.05219959533907696930, 96.24890960531435269 ) ) ;
#112406 = CARTESIAN_POINT ( 'NONE',  ( -38.00000000000000711, 2.428612866367529932E-14, -10.00000000000000000 ) ) ;
#112405 = CARTESIAN_POINT ( 'NONE',  ( 16.52544592524342804, -4.483927247898539470, 33.54057627198102409 ) ) ;
#112407 = CARTESIAN_POINT ( 'NONE',  ( -13.97604488694547697, 13.89961937509957934, 88.12609039468563310 ) ) ;
#112408 = CARTESIAN_POINT ( 'NONE',  ( -0.05219959533937732626, 21.53943276465977519, 107.5010903946856899 ) ) ;
#112409 = CARTESIAN_POINT ( 'NONE',  ( -16.53943276465976808, 0.05219959533911058130, 31.24890960531435979 ) ) ;
#112410 = CARTESIAN_POINT ( 'NONE',  ( -21.52544592524343514, 5.823673210054127303, 91.04057627198103830 ) ) ;
#112411 = CARTESIAN_POINT ( 'NONE',  ( -21.53943276465977519, 0.05219959533907696930, 46.24890960531435979 ) ) ;
#112412 = CARTESIAN_POINT ( 'NONE',  ( -19.05341960407611168, -5.049401038298163336, 61.45724293864769550 ) ) ;
#112413 = CARTESIAN_POINT ( 'NONE',  ( 14.29746914071049879, -8.314922557960816363, 38.33224293864768839 ) ) ;
#112414 = CARTESIAN_POINT ( 'NONE',  ( -9.474510206698964154, 16.51473224551069663, 95.41557627198102409 ) ) ;
#112415 = ORIENTED_EDGE ( 'NONE', *, *, #102808, .T. ) ;
#112416 = CARTESIAN_POINT ( 'NONE',  ( 19.25918095147780917, 5.499999999999578115, 56.95284276293935477 ) ) ;
#112417 = CARTESIAN_POINT ( 'NONE',  ( 5.049401038297881783, 19.05341960407617563, 42.29275706135234003 ) ) ;
#112418 = CARTESIAN_POINT ( 'NONE',  ( -15.72974639402197994, 15.80617190586746368, 85.62390960531436690 ) ) ;
#112419 = CARTESIAN_POINT ( 'NONE',  ( 16.53943276465976808, -0.05219959533910856209, 93.74890960531436690 ) ) ;
#112420 = CARTESIAN_POINT ( 'NONE',  ( -18.67979575497193778, 10.72451020669871902, 43.33442372801901143 ) ) ;
#112421 = AXIS2_PLACEMENT_3D ( 'NONE', #106968, #168642, #30141 ) ;
#112422 = CARTESIAN_POINT ( 'NONE',  ( -17.14385361876520619, 23.59649016807275856, 142.5750000027312012 ) ) ;
#112423 = CARTESIAN_POINT ( 'NONE',  ( -14.29746914071037622, -8.314922557961029526, 109.1677570613523613 ) ) ;
#112424 = CARTESIAN_POINT ( 'NONE',  ( 19.03943276465977164, -0.05219959533909143690, 33.74890960531435979 ) ) ;
#112425 = CARTESIAN_POINT ( 'NONE',  ( -9.474510206698964154, 16.51473224551069663, 85.41557627198102409 ) ) ;
#112426 = CARTESIAN_POINT ( 'NONE',  ( 17.60769864724390388, -5.499999999999974243, 71.15024842019164453 ) ) ;
#112427 = CARTESIAN_POINT ( 'NONE',  ( 16.51473224551069308, 9.474510206698969483, 29.16557627198103475 ) ) ;
#112428 = CARTESIAN_POINT ( 'NONE',  ( 4.483927247898545687, 16.52544592524342804, 49.79057627198102409 ) ) ;
#112429 = AXIS2_PLACEMENT_3D ( 'NONE', #194471, #164138, #117619 ) ;
#112430 = CARTESIAN_POINT ( 'NONE',  ( 10.72451020669871369, 18.67979575497193778, 67.08442372801901854 ) ) ;
#112432 = CARTESIAN_POINT ( 'NONE',  ( -16.52544592524335698, -4.483927247898792601, 68.95942372801901854 ) ) ;
#112431 = CARTESIAN_POINT ( 'NONE',  ( 25.53334702086191754, -27.44079366658231578, -18.45201707416872239 ) ) ;
#112433 = CARTESIAN_POINT ( 'NONE',  ( -16.51473224551069308, -9.474510206698971260, 56.66557627198103120 ) ) ;
#112434 = CARTESIAN_POINT ( 'NONE',  ( 9.474510206698971260, -16.51473224551069308, 47.91557627198102409 ) ) ;
#112435 = EDGE_LOOP ( 'NONE', ( #77656, #20439, #104504, #117892, #9419, #151815 ) ) ;
#112436 = CARTESIAN_POINT ( 'NONE',  ( 5.719274019375673035, 21.55341960407619339, 107.2927570613523471 ) ) ;
#112437 = CARTESIAN_POINT ( 'NONE',  ( -8.224510206698735004, -14.34966873604973081, 64.58442372801900433 ) ) ;
#112438 = CARTESIAN_POINT ( 'NONE',  ( 15.72974639402176855, 15.80617190586768217, 101.8760903946857042 ) ) ;
#112439 = CARTESIAN_POINT ( 'NONE',  ( 5.823673210054125526, 21.52544592524343514, 29.79057627198102409 ) ) ;
#112440 = CARTESIAN_POINT ( 'NONE',  ( -13.97604488694547697, 13.89961937509957934, 113.1260903946856757 ) ) ;
#112441 = CARTESIAN_POINT ( 'NONE',  ( -0.05219959533937732626, 21.53943276465977519, 72.50109039468568994 ) ) ;
#112442 = CARTESIAN_POINT ( 'NONE',  ( 8.314922557961029526, -14.29746914071037800, 45.41775706135234003 ) ) ;
#112443 = CARTESIAN_POINT ( 'NONE',  ( -21.53943276465977519, 0.05219959533907696930, 96.24890960531435269 ) ) ;
#112444 = CARTESIAN_POINT ( 'NONE',  ( 19.05341960407617918, -5.049401038297876454, 101.0427570613523045 ) ) ;
#112445 = CARTESIAN_POINT ( 'NONE',  ( -0.05219959533909027116, -19.03943276465977164, 62.49890960531435979 ) ) ;
#112446 = CARTESIAN_POINT ( 'NONE',  ( 14.34966873604972726, -8.224510206698740333, 20.83442372801901143 ) ) ;
#112447 = CARTESIAN_POINT ( 'NONE',  ( 13.97604488694548053, -13.89961937509957401, 105.6260903946856757 ) ) ;
#112448 = CARTESIAN_POINT ( 'NONE',  ( -16.53943276465976808, 0.05219959533911058130, 66.24890960531436690 ) ) ;
#112449 = CARTESIAN_POINT ( 'NONE',  ( 16.55341960407618274, -4.379528057220086978, 76.04275706135237556 ) ) ;
#112451 = CARTESIAN_POINT ( 'NONE',  ( -13.97604488694527625, -13.89961937509977652, 51.87390960531436690 ) ) ;
#112450 = CARTESIAN_POINT ( 'NONE',  ( 5.823673210054125526, 21.52544592524343514, 114.7905762719810383 ) ) ;
#112452 = CARTESIAN_POINT ( 'NONE',  ( 19.03943276465977164, -0.05219959533909143690, 53.74890960531436690 ) ) ;
#112453 = CARTESIAN_POINT ( 'NONE',  ( -4.483927247898782831, 16.52544592524335698, 72.70942372801901854 ) ) ;
#112454 = CARTESIAN_POINT ( 'NONE',  ( -17.14385361876520264, -23.59649016807271593, 145.6750000027311671 ) ) ;
#112455 = CARTESIAN_POINT ( 'NONE',  ( 28.82186960331498327, 2.781578969918950771E-14, 147.2500000054623683 ) ) ;
#112456 = CARTESIAN_POINT ( 'NONE',  ( 5.719274019375673035, 21.55341960407619339, 112.2927570613523471 ) ) ;
#112457 = CARTESIAN_POINT ( 'NONE',  ( 11.45643923738960446, -4.999999999999992895, -15.00000000000000000 ) ) ;
#112458 = CARTESIAN_POINT ( 'NONE',  ( -8.224510206698735004, -14.34966873604973081, 19.58442372801901143 ) ) ;
#112459 = CARTESIAN_POINT ( 'NONE',  ( 10.72451020669898902, -18.67979575497178502, 47.91557627198102409 ) ) ;
#112461 = CARTESIAN_POINT ( 'NONE',  ( -0.05219959533934338120, 16.53943276465976808, 32.50109039468568284 ) ) ;
#112460 = CARTESIAN_POINT ( 'NONE',  ( 16.46253265017146816, 9.564922557961045513, 46.66775706135233293 ) ) ;
#112462 = CARTESIAN_POINT ( 'NONE',  ( 9.564922557960805705, 16.46253265017160317, 49.58224293864770260 ) ) ;
#112463 = CARTESIAN_POINT ( 'NONE',  ( 19.02544592524343514, -5.153800228976328945, 48.54057627198103120 ) ) ;
#112464 = CARTESIAN_POINT ( 'NONE',  ( -10.81492255796078084, -18.62759615963271287, 82.08224293864768129 ) ) ;
#112465 = CARTESIAN_POINT ( 'NONE',  ( 13.89961937509977652, -13.97604488694527269, 108.1239096053143669 ) ) ;
#112466 = CARTESIAN_POINT ( 'NONE',  ( -19.05341960407611168, -5.049401038298163336, 46.45724293864768129 ) ) ;
#112467 = CARTESIAN_POINT ( 'NONE',  ( 17.14385361876520264, 23.59649016807275856, 148.6750000027311387 ) ) ;
#112468 = CARTESIAN_POINT ( 'NONE',  ( 0.05219959533936267826, -19.03943276465977164, 100.0010903946856757 ) ) ;
#112469 = CARTESIAN_POINT ( 'NONE',  ( 0.05219959533910956823, 16.53943276465976808, 64.99890960531435269 ) ) ;
#112470 = CARTESIAN_POINT ( 'NONE',  ( 16.46253265017146816, 9.564922557961045513, 26.66775706135234003 ) ) ;
#112471 = CARTESIAN_POINT ( 'NONE',  ( 18.62759615963271287, -10.81492255796078972, 98.33224293864769550 ) ) ;
#112472 = CARTESIAN_POINT ( 'NONE',  ( 15.80617190586769283, -15.72974639402175789, 80.62609039468567573 ) ) ;
#112473 = CARTESIAN_POINT ( 'NONE',  ( -5.049401038298153566, 19.05341960407611168, 25.20724293864768484 ) ) ;
#112474 = CARTESIAN_POINT ( 'NONE',  ( -21.53943276465977519, -0.05219959533937600094, 73.75109039468567573 ) ) ;
#112476 = CARTESIAN_POINT ( 'NONE',  ( 18.62759615963255655, 10.81492255796105972, 81.66775706135236135 ) ) ;
#112475 = CARTESIAN_POINT ( 'NONE',  ( 16.52544592524342804, -4.483927247898539470, 23.54057627198102765 ) ) ;
#112477 = CARTESIAN_POINT ( 'NONE',  ( 16.51473224551069308, 9.474510206698969483, 69.16557627198102409 ) ) ;
#112478 = CARTESIAN_POINT ( 'NONE',  ( 5.823673210054444382, -21.52544592524334988, 45.20942372801901854 ) ) ;
#112479 = CARTESIAN_POINT ( 'NONE',  ( 13.97604488694527802, 13.89961937509977652, 84.37390960531433848 ) ) ;
#112480 = CARTESIAN_POINT ( 'NONE',  ( 12.14591786802309770, 12.06949235617756955, 99.37390960531436690 ) ) ;
#112481 = CARTESIAN_POINT ( 'NONE',  ( -12.14591786802309592, -12.06949235617757132, 61.87390960531436690 ) ) ;
#112482 = CARTESIAN_POINT ( 'NONE',  ( -5.823673210054116645, -21.52544592524344225, 67.29057627198103830 ) ) ;
#112483 = CARTESIAN_POINT ( 'NONE',  ( -9.474510206698964154, 16.51473224551069663, 80.41557627198103830 ) ) ;
#112484 = CARTESIAN_POINT ( 'NONE',  ( -5.719274019375978568, 21.55341960407610458, 85.20724293864770971 ) ) ;
#112485 = CARTESIAN_POINT ( 'NONE',  ( -19.02544592524334988, -5.153800228976617603, 63.95942372801899012 ) ) ;
#112487 = CARTESIAN_POINT ( 'NONE',  ( 16.53943276465976808, -0.05219959533910856209, 73.74890960531433848 ) ) ;
#112486 = CARTESIAN_POINT ( 'NONE',  ( 0.05219959533936267826, -19.03943276465977164, 35.00109039468566863 ) ) ;
#112488 = CARTESIAN_POINT ( 'NONE',  ( 15.80617190586746368, 15.72974639402197994, 59.37390960531436690 ) ) ;
#112489 = CARTESIAN_POINT ( 'NONE',  ( 3.735172737399431091E-16, 6.100000000000006750, -62.50719930893269805 ) ) ;
#112491 = CARTESIAN_POINT ( 'NONE',  ( -22.44159573604009950, -16.30477369853688430, 147.5750000027312012 ) ) ;
#112490 = CARTESIAN_POINT ( 'NONE',  ( 4.379528057220092307, 16.55341960407617563, 92.29275706135236135 ) ) ;
#112492 = CARTESIAN_POINT ( 'NONE',  ( -19.03943276465977164, -0.05219959533935918106, 98.75109039468567573 ) ) ;
#112493 = CARTESIAN_POINT ( 'NONE',  ( 8.224510206698953496, -14.34966873604960469, 62.91557627198102409 ) ) ;
#112494 = CARTESIAN_POINT ( 'NONE',  ( -17.50000000000002132, 3.471454075611629442, 34.48332581144360631 ) ) ;
#112495 = CARTESIAN_POINT ( 'NONE',  ( -19.02544592524342804, 5.153800228976336051, 66.04057627198103830 ) ) ;
#112496 = CARTESIAN_POINT ( 'NONE',  ( -14.29746914071049879, 8.314922557960819915, 50.83224293864770971 ) ) ;
#112497 = CARTESIAN_POINT ( 'NONE',  ( 19.02544592524343514, -5.153800228976328945, 98.54057627198100988 ) ) ;
#112499 = CARTESIAN_POINT ( 'NONE',  ( 19.02544592524343514, -5.153800228976328945, 68.54057627198103830 ) ) ;
#112498 = CARTESIAN_POINT ( 'NONE',  ( -9.474510206698720793, -16.51473224551083518, 79.58442372801899012 ) ) ;
#112500 = CARTESIAN_POINT ( 'NONE',  ( 9.474510206698971260, -16.51473224551069308, 82.91557627198103830 ) ) ;
#112501 = CARTESIAN_POINT ( 'NONE',  ( -5.049401038298153566, 19.05341960407611168, 80.20724293864769550 ) ) ;
#112502 = CARTESIAN_POINT ( 'NONE',  ( -15.80617190586745835, -15.72974639402198527, 56.87390960531436690 ) ) ;
#112503 = CARTESIAN_POINT ( 'NONE',  ( 16.53943276465976808, 0.05219959533934440121, 51.25109039468568994 ) ) ;
#112504 = CARTESIAN_POINT ( 'NONE',  ( 17.72662750342729510, 5.499999999999959144, 98.90179492283746754 ) ) ;
#112505 = CARTESIAN_POINT ( 'NONE',  ( -16.46253265017160317, 9.564922557960807481, 55.83224293864769550 ) ) ;
#112506 = CARTESIAN_POINT ( 'NONE',  ( 5.719274019375991003, -21.55341960407610458, 57.70724293864770260 ) ) ;
#112507 = CARTESIAN_POINT ( 'NONE',  ( -0.05219959533936034679, 19.03943276465977164, 92.50109039468566152 ) ) ;
#112509 = CARTESIAN_POINT ( 'NONE',  ( 15.72974639402176855, 15.80617190586768217, 51.87609039468568284 ) ) ;
#112508 = CARTESIAN_POINT ( 'NONE',  ( -4.483927247898539470, -16.52544592524342804, 27.29057627198103120 ) ) ;
#112510 = EDGE_CURVE ( 'NONE', #41998, #35005, #54576, .T. ) ;
#112511 = CARTESIAN_POINT ( 'NONE',  ( -5.049401038297874678, -19.05341960407617918, 34.79275706135233293 ) ) ;
#112513 = CARTESIAN_POINT ( 'NONE',  ( -4.379528057220086978, -16.55341960407618274, 94.79275706135234714 ) ) ;
#112512 = CARTESIAN_POINT ( 'NONE',  ( -16.53943276465976808, -0.05219959533934237506, 53.75109039468568994 ) ) ;
#112514 = CARTESIAN_POINT ( 'NONE',  ( -18.22780087662122028, 5.500000000000031086, 53.51540105326106556 ) ) ;
#112515 = CARTESIAN_POINT ( 'NONE',  ( 0.05219959533934541429, -16.53943276465976808, 75.00109039468568994 ) ) ;
#112516 = CARTESIAN_POINT ( 'NONE',  ( 0.05219959533934541429, -16.53943276465976808, 35.00109039468568284 ) ) ;
#112517 = CARTESIAN_POINT ( 'NONE',  ( 19.02544592524343514, -5.153800228976328945, 43.54057627198103120 ) ) ;
#112518 = CARTESIAN_POINT ( 'NONE',  ( -16.46253265017160317, 9.564922557960807481, 45.83224293864769550 ) ) ;
#112519 = CARTESIAN_POINT ( 'NONE',  ( -16.46253265017160317, 9.564922557960807481, 65.83224293864769550 ) ) ;
#112520 = CARTESIAN_POINT ( 'NONE',  ( 10.81492255796106328, -18.62759615963255655, 35.41775706135234003 ) ) ;
#112521 = CARTESIAN_POINT ( 'NONE',  ( 8.224510206698742110, 14.34966873604972548, 52.08442372801901854 ) ) ;
#112522 = CARTESIAN_POINT ( 'NONE',  ( 4.379528057220092307, 16.55341960407617563, 107.2927570613523471 ) ) ;
#112523 = CARTESIAN_POINT ( 'NONE',  ( 9.564922557960805705, 16.46253265017160317, 29.58224293864769550 ) ) ;
#112524 = CARTESIAN_POINT ( 'NONE',  ( -18.67979575497193778, 10.72451020669871902, 108.3344237280190185 ) ) ;
#112525 = CARTESIAN_POINT ( 'NONE',  ( 9.564922557961047289, -16.46253265017146816, 105.4177570613523471 ) ) ;
#112526 = CARTESIAN_POINT ( 'NONE',  ( -19.02544592524334988, -5.153800228976617603, 63.95942372801899012 ) ) ;
#112527 = CARTESIAN_POINT ( 'NONE',  ( 16.53943276465976808, -0.05219959533910856209, 73.74890960531433848 ) ) ;
#112528 = CARTESIAN_POINT ( 'NONE',  ( -5.153800228976328057, -19.02544592524343514, 42.29057627198101699 ) ) ;
#112530 = CARTESIAN_POINT ( 'NONE',  ( 16.79531203550648399, -7.028104445595605654, 91.24755011779559766 ) ) ;
#112529 = CARTESIAN_POINT ( 'NONE',  ( -16.51473224551082808, 9.474510206698731452, 73.33442372801900433 ) ) ;
#112531 = CARTESIAN_POINT ( 'NONE',  ( 10.81492255796106328, -18.62759615963255655, 75.41775706135233293 ) ) ;
#112532 = CARTESIAN_POINT ( 'NONE',  ( 16.52544592524335698, 4.483927247898782831, 36.45942372801901143 ) ) ;
#112533 = CARTESIAN_POINT ( 'NONE',  ( 16.29526858892878494, 7.335722546919996034, 38.29670597800206622 ) ) ;
#112534 = CARTESIAN_POINT ( 'NONE',  ( -10.81492255796078084, -18.62759615963271287, 32.08224293864769550 ) ) ;
#112535 = CARTESIAN_POINT ( 'NONE',  ( 4.483927247898790824, -16.52544592524335698, 20.20942372801900788 ) ) ;
#112536 = CARTESIAN_POINT ( 'NONE',  ( -0.05219959533909027116, -19.03943276465977164, 22.49890960531436690 ) ) ;
#112537 = CARTESIAN_POINT ( 'NONE',  ( -13.89961937509957401, -13.97604488694547875, 29.37609039468565797 ) ) ;
#112538 = DIRECTION ( 'NONE',  ( -1.000000000000000000, 0.000000000000000000, 0.000000000000000000 ) ) ;
#112539 = CARTESIAN_POINT ( 'NONE',  ( 13.89961937509977652, -13.97604488694527269, 33.12390960531434558 ) ) ;
#112540 = CARTESIAN_POINT ( 'NONE',  ( 5.049401038297881783, 19.05341960407617918, 57.29275706135232582 ) ) ;
#112541 = CARTESIAN_POINT ( 'NONE',  ( 9.474510206698971260, -16.51473224551069308, 67.91557627198102409 ) ) ;
#112542 = CARTESIAN_POINT ( 'NONE',  ( -19.20446147854528718, -5.499999999999912959, 54.38999695167677828 ) ) ;
#112543 = CARTESIAN_POINT ( 'NONE',  ( -13.89961937509957401, -13.97604488694547875, 19.37609039468566507 ) ) ;
#112544 = CARTESIAN_POINT ( 'NONE',  ( 16.53943276465976808, 0.05219959533934440121, 111.2510903946856899 ) ) ;
#112545 = CARTESIAN_POINT ( 'NONE',  ( 19.02544592524343514, -5.153800228976328945, 33.54057627198102409 ) ) ;
#112546 = CARTESIAN_POINT ( 'NONE',  ( -16.51473224551069308, -9.474510206698971260, 86.66557627198102409 ) ) ;
#112547 = CARTESIAN_POINT ( 'NONE',  ( -0.05219959533937732626, 21.53943276465977519, 67.50109039468568994 ) ) ;
#112548 = CARTESIAN_POINT ( 'NONE',  ( -13.97604488694527625, -13.89961937509977652, 46.87390960531435979 ) ) ;
#112549 = CARTESIAN_POINT ( 'NONE',  ( 21.55341960407619695, -5.719274019375665929, 61.04275706135234714 ) ) ;
#112551 = CARTESIAN_POINT ( 'NONE',  ( 10.81492255796078972, 18.62759615963270932, 24.58224293864768839 ) ) ;
#112550 = CARTESIAN_POINT ( 'NONE',  ( 9.474510206698729675, 16.51473224551082808, 92.08442372801900433 ) ) ;
#112552 = CARTESIAN_POINT ( 'NONE',  ( 16.51473224551069308, 9.474510206698969483, 39.16557627198103120 ) ) ;
#112553 = CARTESIAN_POINT ( 'NONE',  ( -21.52544592524334988, -5.823673210054445271, 18.95942372801901143 ) ) ;
#112554 = CARTESIAN_POINT ( 'NONE',  ( -0.05219959533936034679, 19.03943276465977164, 37.50109039468567573 ) ) ;
#112555 = CARTESIAN_POINT ( 'NONE',  ( -14.34966873604960291, -8.224510206698953496, 111.6655762719810525 ) ) ;
#112556 = CARTESIAN_POINT ( 'NONE',  ( 0.05219959533909260263, 19.03943276465977164, 64.99890960531436690 ) ) ;
#112557 = CARTESIAN_POINT ( 'NONE',  ( -5.153800228976607833, 19.02544592524334988, 112.7094237280190043 ) ) ;
#112558 = CARTESIAN_POINT ( 'NONE',  ( 12.06949235617757843, -12.14591786802309237, 73.12390960531436690 ) ) ;
#112559 = CARTESIAN_POINT ( 'NONE',  ( 18.67979575497178502, 10.72451020669898547, 24.16557627198103120 ) ) ;
#112560 = CARTESIAN_POINT ( 'NONE',  ( 9.564922557961047289, -16.46253265017146816, 85.41775706135233293 ) ) ;
#112561 = CARTESIAN_POINT ( 'NONE',  ( -18.62759615963270932, 10.81492255796079327, 95.83224293864770971 ) ) ;
#112562 = CARTESIAN_POINT ( 'NONE',  ( -21.55341960407619339, 5.719274019375674811, 63.54275706135234003 ) ) ;
#112563 = CARTESIAN_POINT ( 'NONE',  ( 16.55341960407618274, -4.379528057220086978, 56.04275706135235424 ) ) ;
#112565 = CARTESIAN_POINT ( 'NONE',  ( -15.72974639402176322, -15.80617190586768395, 54.37609039468568994 ) ) ;
#112564 = CARTESIAN_POINT ( 'NONE',  ( 4.379528057220092307, 16.55341960407617563, 52.29275706135236135 ) ) ;
#112566 = CARTESIAN_POINT ( 'NONE',  ( -21.53943276465977519, 0.05219959533907696930, 51.24890960531436690 ) ) ;
#112567 = CARTESIAN_POINT ( 'NONE',  ( 16.46253265017160672, -9.564922557960803928, 53.33224293864768839 ) ) ;
#112568 = CARTESIAN_POINT ( 'NONE',  ( 23.48529157249600630, -32.32473071737749137, -3.049999994537627490 ) ) ;
#112569 = CARTESIAN_POINT ( 'NONE',  ( 4.483927247898790824, -16.52544592524335698, 80.20942372801901854 ) ) ;
#112570 = AXIS2_PLACEMENT_3D ( 'NONE', #65203, #126862, #186595 ) ;
#112571 = CARTESIAN_POINT ( 'NONE',  ( 5.719274019375991003, -21.55341960407610458, 102.7072429386476955 ) ) ;
#112572 = CARTESIAN_POINT ( 'NONE',  ( 16.52544592524342804, -4.483927247898539470, 53.54057627198103120 ) ) ;
#112573 = CARTESIAN_POINT ( 'NONE',  ( 12.06949235617739724, 12.14591786802326823, 61.87609039468568284 ) ) ;
#112574 = CARTESIAN_POINT ( 'NONE',  ( -19.05341960407617563, 5.049401038297882671, 98.54275706135233293 ) ) ;
#112575 = CARTESIAN_POINT ( 'NONE',  ( -0.05219959533907301413, -21.53943276465977519, 102.4989096053143811 ) ) ;
#112576 = CARTESIAN_POINT ( 'NONE',  ( 4.483927247898545687, 16.52544592524342804, 44.79057627198103120 ) ) ;
#112577 = ORIENTED_EDGE ( 'NONE', *, *, #189500, .T. ) ;
#112578 = CARTESIAN_POINT ( 'NONE',  ( -17.50000000000001421, 5.622605283950874444, 73.68792689403892382 ) ) ;
#112579 = CARTESIAN_POINT ( 'NONE',  ( 15.80617190586746368, 15.72974639402197994, 74.37390960531436690 ) ) ;
#112580 = CARTESIAN_POINT ( 'NONE',  ( -12.06949235617756955, 12.14591786802309770, 30.62390960531436335 ) ) ;
#112581 = ORIENTED_EDGE ( 'NONE', *, *, #115218, .F. ) ;
#112582 = CARTESIAN_POINT ( 'NONE',  ( -16.31925111598459566, -7.325300261831489301, 54.83575461032751264 ) ) ;
#112583 = CARTESIAN_POINT ( 'NONE',  ( -10.72451020669898014, 18.67979575497178502, 95.41557627198102409 ) ) ;
#112584 = CARTESIAN_POINT ( 'NONE',  ( -18.62759615963255300, -10.81492255796106328, 24.16775706135235424 ) ) ;
#112585 = CARTESIAN_POINT ( 'NONE',  ( -0.05219959533910754901, -16.53943276465976808, 42.49890960531435979 ) ) ;
#112586 = CARTESIAN_POINT ( 'NONE',  ( 14.29746914071037800, 8.314922557961029526, 46.66775706135234714 ) ) ;
#112587 = CARTESIAN_POINT ( 'NONE',  ( -5.153800228976328057, -19.02544592524343514, 52.29057627198100988 ) ) ;
#112588 = CARTESIAN_POINT ( 'NONE',  ( -0.05219959533909027116, -19.03943276465977164, 77.49890960531435269 ) ) ;
#112589 = EDGE_LOOP ( 'NONE', ( #95298, #182725, #71984, #155588, #137832, #150184, #118355, #47328 ) ) ;
#112590 = ADVANCED_FACE ( 'NONE', ( #160756 ), #70753, .T. ) ;
#112591 = CARTESIAN_POINT ( 'NONE',  ( -5.823673210054116645, -21.52544592524344225, 32.29057627198102409 ) ) ;
#112592 = CARTESIAN_POINT ( 'NONE',  ( -26.89045226410910061, -26.45365283846046367, -20.38637362918493423 ) ) ;
#112593 = CARTESIAN_POINT ( 'NONE',  ( 12.14591786802327356, -12.06949235617739191, 25.62609039468567929 ) ) ;
#112594 = CARTESIAN_POINT ( 'NONE',  ( -16.51473224551082808, 9.474510206698731452, 53.33442372801900433 ) ) ;
#112595 = CARTESIAN_POINT ( 'NONE',  ( 21.55341960407610458, 5.719274019375980345, 103.9572429386476813 ) ) ;
#112596 = CARTESIAN_POINT ( 'NONE',  ( 14.29746914071049879, -8.314922557960816363, 33.33224293864769550 ) ) ;
#112597 = CARTESIAN_POINT ( 'NONE',  ( -19.02544592524342804, 5.153800228976336051, 81.04057627198103830 ) ) ;
#112598 = CARTESIAN_POINT ( 'NONE',  ( 21.55341960407610458, 5.719274019375980345, 63.95724293864770260 ) ) ;
#112600 = CARTESIAN_POINT ( 'NONE',  ( -0.05219959533934338120, 16.53943276465976808, 27.50109039468567929 ) ) ;
#112599 = CARTESIAN_POINT ( 'NONE',  ( -10.72451020669898014, 18.67979575497178502, 75.41557627198102409 ) ) ;
#112601 = CARTESIAN_POINT ( 'NONE',  ( -5.823673210054116645, -21.52544592524344225, 27.29057627198103120 ) ) ;
#112602 = CARTESIAN_POINT ( 'NONE',  ( 21.53943276465977519, 0.05219959533937863772, 81.25109039468568994 ) ) ;
#112604 = ADVANCED_FACE ( 'NONE', ( #22247 ), #55598, .T. ) ;
#112603 = CARTESIAN_POINT ( 'NONE',  ( -19.02544592524342804, 5.153800228976336051, 71.04057627198099567 ) ) ;
#112605 = CARTESIAN_POINT ( 'NONE',  ( 19.03943276465977164, -0.05219959533909143690, 23.74890960531435269 ) ) ;
#112606 = CARTESIAN_POINT ( 'NONE',  ( -19.03943276465977164, 0.05219959533909376836, 81.24890960531436690 ) ) ;
#112607 = CARTESIAN_POINT ( 'NONE',  ( 4.379528057220339221, -16.55341960407611168, 87.70724293864769550 ) ) ;
#112608 = VERTEX_POINT ( 'NONE', #125925 ) ;
#112609 = CARTESIAN_POINT ( 'NONE',  ( -13.89961937509957401, -13.97604488694547875, 99.37609039468567573 ) ) ;
#112610 = FACE_OUTER_BOUND ( 'NONE', #123706, .T. ) ;
#112611 = CARTESIAN_POINT ( 'NONE',  ( -0.05219959533909027116, -19.03943276465977164, 67.49890960531436690 ) ) ;
#112613 = CARTESIAN_POINT ( 'NONE',  ( -21.53943276465977519, 0.05219959533907696930, 21.24890960531436690 ) ) ;
#112612 = CARTESIAN_POINT ( 'NONE',  ( -21.55341960407619339, 5.719274019375674811, 98.54275706135234714 ) ) ;
#112614 = CARTESIAN_POINT ( 'NONE',  ( 8.224510206698742110, 14.34966873604972548, 77.08442372801901854 ) ) ;
#112615 = CARTESIAN_POINT ( 'NONE',  ( -17.50000000000002842, -5.499999999999952927, 76.28230962303568674 ) ) ;
#112616 = CARTESIAN_POINT ( 'NONE',  ( 19.05341960407617918, -5.049401038297876454, 56.04275706135234714 ) ) ;
#112617 = CARTESIAN_POINT ( 'NONE',  ( 18.62759615963255655, 10.81492255796105972, 106.6677570613523756 ) ) ;
#112618 = CARTESIAN_POINT ( 'NONE',  ( 37.19778934971984796, 4.370295695334257324, 41.64163531972153720 ) ) ;
#112619 = CARTESIAN_POINT ( 'NONE',  ( -16.51473224551069308, -9.474510206698971260, 31.66557627198102054 ) ) ;
#112620 = CARTESIAN_POINT ( 'NONE',  ( 12.06949235617739724, 12.14591786802326823, 111.8760903946856615 ) ) ;
#112621 = CARTESIAN_POINT ( 'NONE',  ( -35.50125023021173121, -3.320518091344054401, 38.27062242752714383 ) ) ;
#112622 = CARTESIAN_POINT ( 'NONE',  ( -4.379528057220086978, -16.55341960407618274, 104.7927570613523898 ) ) ;
#112623 = CARTESIAN_POINT ( 'NONE',  ( -19.34837522270366250, -5.499999999999857003, 85.86337684832578532 ) ) ;
#112624 = CARTESIAN_POINT ( 'NONE',  ( 14.29746914071037800, 8.314922557961029526, 86.66775706135234714 ) ) ;
#112625 = CARTESIAN_POINT ( 'NONE',  ( 16.51473224551069308, 9.474510206698969483, 29.16557627198103475 ) ) ;
#112626 = CARTESIAN_POINT ( 'NONE',  ( -15.80617190586768217, 15.72974639402176855, 88.12609039468570415 ) ) ;
#112627 = CARTESIAN_POINT ( 'NONE',  ( -0.05219959533936034679, 19.03943276465977164, 107.5010903946856615 ) ) ;
#112628 = CARTESIAN_POINT ( 'NONE',  ( -5.823673210054431948, 21.52544592524334988, 62.70942372801902565 ) ) ;
#112629 = CARTESIAN_POINT ( 'NONE',  ( -0.05219959533936034679, 19.03943276465977164, 42.50109039468566152 ) ) ;
#112630 = CARTESIAN_POINT ( 'NONE',  ( 9.474510206698971260, -16.51473224551069308, 77.91557627198103830 ) ) ;
#112631 = CARTESIAN_POINT ( 'NONE',  ( -13.97604488694527625, -13.89961937509977652, 71.87390960531433848 ) ) ;
#112632 = CARTESIAN_POINT ( 'NONE',  ( -10.31942656230733313, -38.65189766944586580, -12.74745618418806536 ) ) ;
#112633 = CARTESIAN_POINT ( 'NONE',  ( -21.55341960407610458, -5.719274019375992779, 46.45724293864769550 ) ) ;
#112634 = CARTESIAN_POINT ( 'NONE',  ( 9.564922557960805705, 16.46253265017160317, 44.58224293864769550 ) ) ;
#112635 = CARTESIAN_POINT ( 'NONE',  ( -12.14591786802326823, 12.06949235617739902, 78.12609039468570415 ) ) ;
#112636 = UNCERTAINTY_MEASURE_WITH_UNIT (LENGTH_MEASURE( 1.000000000000000082E-05 ), #14220, 'distance_accuracy_value', 'NONE');
#112637 = EDGE_LOOP ( 'NONE', ( #41842, #129033, #196625, #116492, #186829 ) ) ;
#112639 = CARTESIAN_POINT ( 'NONE',  ( -11.40812507854755609, 35.11059874428196537, -3.024999997268813523 ) ) ;
#112638 = CARTESIAN_POINT ( 'NONE',  ( -4.379528057220328563, 16.55341960407611168, 85.20724293864770971 ) ) ;
#112640 = CARTESIAN_POINT ( 'NONE',  ( -4.379528057220086978, -16.55341960407618274, 34.79275706135235424 ) ) ;
#112641 = CARTESIAN_POINT ( 'NONE',  ( 4.483927247898545687, 16.52544592524342804, 109.7905762719810383 ) ) ;
#112642 = CARTESIAN_POINT ( 'NONE',  ( 16.46253265017146816, 9.564922557961045513, 61.66775706135234003 ) ) ;
#112643 = CARTESIAN_POINT ( 'NONE',  ( -0.05219959533910754901, -16.53943276465976808, 77.49890960531433848 ) ) ;
#112644 = CARTESIAN_POINT ( 'NONE',  ( -21.53943276465977519, -0.05219959533937600094, 28.75109039468567929 ) ) ;
#112646 = CARTESIAN_POINT ( 'NONE',  ( -21.52544592524343514, 5.823673210054127303, 91.04057627198103830 ) ) ;
#112645 = CARTESIAN_POINT ( 'NONE',  ( -15.49999999999999822, -5.500000000000000888, 120.0000000000000142 ) ) ;
#112647 = CARTESIAN_POINT ( 'NONE',  ( 13.89961937509977652, -13.97604488694527269, 103.1239096053143527 ) ) ;
#112648 = CARTESIAN_POINT ( 'NONE',  ( 16.53943276465976808, -0.05219959533910856209, 78.74890960531436690 ) ) ;
#112649 = CARTESIAN_POINT ( 'NONE',  ( 27.99776551637609856, -28.30561827218008375, -16.93438536460889310 ) ) ;
#112650 = CARTESIAN_POINT ( 'NONE',  ( -16.46253265017160317, 9.564922557960807481, 50.83224293864770260 ) ) ;
#112651 = AXIS2_PLACEMENT_3D ( 'NONE', #53708, #113366, #158873 ) ;
#112652 = CARTESIAN_POINT ( 'NONE',  ( 36.91746824999999887, -11.99521256947793546, -3.724999997268813257 ) ) ;
#112653 = CARTESIAN_POINT ( 'NONE',  ( 16.46253265017146816, 9.564922557961045513, 81.66775706135233293 ) ) ;
#112654 = CARTESIAN_POINT ( 'NONE',  ( 10.72451020669871369, 18.67979575497193778, 22.08442372801901143 ) ) ;
#112655 = CARTESIAN_POINT ( 'NONE',  ( -16.51473224551069308, -9.474510206698971260, 76.66557627198103830 ) ) ;
#112656 = CARTESIAN_POINT ( 'NONE',  ( 0.05219959533936267826, -19.03943276465977164, 50.00109039468566863 ) ) ;
#112657 = CARTESIAN_POINT ( 'NONE',  ( -16.46253265017160317, 9.564922557960807481, 50.83224293864770260 ) ) ;
#112658 = CARTESIAN_POINT ( 'NONE',  ( -4.379528057220328563, 16.55341960407611168, 65.20724293864768129 ) ) ;
#112659 = CARTESIAN_POINT ( 'NONE',  ( 8.314922557960818139, 14.29746914071049879, 49.58224293864769550 ) ) ;
#112660 = CARTESIAN_POINT ( 'NONE',  ( 13.97604488694527802, 13.89961937509977652, 74.37390960531436690 ) ) ;
#112661 = CARTESIAN_POINT ( 'NONE',  ( -10.81492255796078084, -18.62759615963271287, 82.08224293864768129 ) ) ;
#112662 = CARTESIAN_POINT ( 'NONE',  ( -19.02544592524342804, 5.153800228976336051, 71.04057627198099567 ) ) ;
#112663 = CARTESIAN_POINT ( 'NONE',  ( 18.62759615963271287, -10.81492255796078972, 73.33224293864769550 ) ) ;
#112664 = CARTESIAN_POINT ( 'NONE',  ( -19.05341960407617563, 5.049401038297882671, 23.54275706135233648 ) ) ;
#112667 = CARTESIAN_POINT ( 'NONE',  ( -8.314922557960811034, -14.29746914071050412, 92.08224293864769550 ) ) ;
#112666 = CARTESIAN_POINT ( 'NONE',  ( 16.52544592524342804, -4.483927247898539470, 23.54057627198102765 ) ) ;
#112665 = CARTESIAN_POINT ( 'NONE',  ( -0.05219959533909027116, -19.03943276465977164, 22.49890960531436690 ) ) ;
#112668 = CARTESIAN_POINT ( 'NONE',  ( -13.89961937509957401, -13.97604488694547875, 109.3760903946856331 ) ) ;
#112669 = ORIENTED_EDGE ( 'NONE', *, *, #94539, .F. ) ;
#112670 = CARTESIAN_POINT ( 'NONE',  ( -15.72974639402197994, 15.80617190586746368, 115.6239096053143669 ) ) ;
#112671 = CARTESIAN_POINT ( 'NONE',  ( 5.049401038297881783, 19.05341960407617563, 52.29275706135234003 ) ) ;
#112672 = CARTESIAN_POINT ( 'NONE',  ( -0.05219959533910754901, -16.53943276465976808, 27.49890960531435269 ) ) ;
#112673 = CARTESIAN_POINT ( 'NONE',  ( -10.81492255796078084, -18.62759615963271287, 72.08224293864769550 ) ) ;
#112674 = CARTESIAN_POINT ( 'NONE',  ( 5.049401038298161559, -19.05341960407611168, 97.70724293864766707 ) ) ;
#112675 = CARTESIAN_POINT ( 'NONE',  ( -4.483927247898539470, -16.52544592524342804, 57.29057627198103120 ) ) ;
#112676 = LINE ( 'NONE', #174368, #79929 ) ;
#112677 = CARTESIAN_POINT ( 'NONE',  ( -9.564922557960796823, -16.46253265017161027, 37.08224293864768839 ) ) ;
#112678 = CARTESIAN_POINT ( 'NONE',  ( -10.81492255796105439, 18.62759615963255655, 102.9177570613523756 ) ) ;
#112679 = CARTESIAN_POINT ( 'NONE',  ( -12.14591786802326823, 12.06949235617739902, 93.12609039468568994 ) ) ;
#112680 = CARTESIAN_POINT ( 'NONE',  ( 15.80617190586769283, -15.72974639402175789, 45.62609039468567573 ) ) ;
#112681 = CARTESIAN_POINT ( 'NONE',  ( -16.52544592524335698, -4.483927247898792601, 43.95942372801902565 ) ) ;
#112682 = CARTESIAN_POINT ( 'NONE',  ( -5.823673210054116645, -21.52544592524344225, 27.29057627198103120 ) ) ;
#112683 = CARTESIAN_POINT ( 'NONE',  ( 19.05341960407611168, 5.049401038298154454, 58.95724293864768129 ) ) ;
#112684 = CARTESIAN_POINT ( 'NONE',  ( -5.049401038298153566, 19.05341960407611168, 60.20724293864768129 ) ) ;
#112685 = CARTESIAN_POINT ( 'NONE',  ( 16.52544592524335698, 4.483927247898782831, 51.45942372801901854 ) ) ;
#112686 = CARTESIAN_POINT ( 'NONE',  ( -12.06949235617756955, 12.14591786802309770, 105.6239096053143669 ) ) ;
#112687 = CARTESIAN_POINT ( 'NONE',  ( 8.224510206698953496, -14.34966873604960469, 27.91557627198103830 ) ) ;
#112688 = CARTESIAN_POINT ( 'NONE',  ( 18.22780087662121673, 5.500000000000056843, 48.98459894673892023 ) ) ;
#112691 = CARTESIAN_POINT ( 'NONE',  ( -0.05219959533909027116, -19.03943276465977164, 77.49890960531435269 ) ) ;
#112690 = CARTESIAN_POINT ( 'NONE',  ( 0.05219959533909260263, 19.03943276465977164, 89.99890960531436690 ) ) ;
#112689 = CARTESIAN_POINT ( 'NONE',  ( 5.719274019375673035, 21.55341960407619339, 62.29275706135236845 ) ) ;
#112692 = CARTESIAN_POINT ( 'NONE',  ( -9.564922557960796823, -16.46253265017161027, 102.0822429386477097 ) ) ;
#112693 = CARTESIAN_POINT ( 'NONE',  ( 16.55341960407611168, 4.379528057220329451, 48.95724293864770971 ) ) ;
#112694 = EDGE_CURVE ( 'NONE', #115498, #42832, #910, .T. ) ;
#112695 = CARTESIAN_POINT ( 'NONE',  ( -8.224510206698735004, -14.34966873604973081, 109.5844237280190328 ) ) ;
#112696 = CARTESIAN_POINT ( 'NONE',  ( -8.314922557960811034, -14.29746914071050412, 37.08224293864768129 ) ) ;
#112697 = CARTESIAN_POINT ( 'NONE',  ( -14.62203461105304036, -16.12203461105356794, -56.14925526931841659 ) ) ;
#112698 = CARTESIAN_POINT ( 'NONE',  ( -0.05219959533936034679, 19.03943276465977164, 37.50109039468567573 ) ) ;
#112699 = CARTESIAN_POINT ( 'NONE',  ( -19.03943276465977164, 0.05219959533909376836, 71.24890960531435269 ) ) ;
#112700 = CARTESIAN_POINT ( 'NONE',  ( -19.03943276465977164, -0.05219959533935918106, 53.75109039468566863 ) ) ;
#112701 = CARTESIAN_POINT ( 'NONE',  ( -11.40812507854754720, -35.11059874428192273, -10.72499999726881548 ) ) ;
#112702 = CARTESIAN_POINT ( 'NONE',  ( 13.89961937509978007, -13.97604488694527269, 68.12390960531436690 ) ) ;
#112704 = CARTESIAN_POINT ( 'NONE',  ( -14.29746914071037622, -8.314922557961029526, 64.16775706135234714 ) ) ;
#112703 = CARTESIAN_POINT ( 'NONE',  ( -19.03943276465977164, -0.05219959533935918106, 78.75109039468567573 ) ) ;
#112705 = CARTESIAN_POINT ( 'NONE',  ( 16.79531203550646268, 7.028104445595615424, 93.75244988220441655 ) ) ;
#112706 = CARTESIAN_POINT ( 'NONE',  ( 9.564922557960805705, 16.46253265017160317, 109.5822429386476955 ) ) ;
#112707 = CARTESIAN_POINT ( 'NONE',  ( 0.05219959533937995610, -21.53943276465977519, 25.00109039468567218 ) ) ;
#112708 = CARTESIAN_POINT ( 'NONE',  ( 16.51473224551083163, -9.474510206698727899, 90.83442372801900433 ) ) ;
#112710 = CARTESIAN_POINT ( 'NONE',  ( 13.89961937509977652, -13.97604488694527269, 43.12390960531434558 ) ) ;
#112709 = CARTESIAN_POINT ( 'NONE',  ( -19.03943276465977164, 0.05219959533909376836, 116.2489096053143669 ) ) ;
#112711 = CARTESIAN_POINT ( 'NONE',  ( -16.51473224551069308, -9.474510206698971260, 91.66557627198103830 ) ) ;
#112713 = CARTESIAN_POINT ( 'NONE',  ( -19.05341960407611168, -5.049401038298163336, 51.45724293864770260 ) ) ;
#112712 = CARTESIAN_POINT ( 'NONE',  ( 12.06949235617757843, -12.14591786802309237, 43.12390960531435269 ) ) ;
#112714 = CARTESIAN_POINT ( 'NONE',  ( 9.474510206698729675, 16.51473224551082808, 62.08442372801899722 ) ) ;
#112715 = CARTESIAN_POINT ( 'NONE',  ( 19.05341960407617918, -5.049401038297876454, 36.04275706135234003 ) ) ;
#112716 = CARTESIAN_POINT ( 'NONE',  ( 19.02544592524343514, -5.153800228976328945, 68.54057627198103830 ) ) ;
#112717 = CARTESIAN_POINT ( 'NONE',  ( 15.80617190586746368, 15.72974639402197994, 59.37390960531436690 ) ) ;
#112719 = CARTESIAN_POINT ( 'NONE',  ( 18.62759615963255655, 10.81492255796105972, 111.6677570613523613 ) ) ;
#112718 = CARTESIAN_POINT ( 'NONE',  ( -8.224510206698948167, 14.34966873604960824, 65.41557627198102409 ) ) ;
#112720 = CARTESIAN_POINT ( 'NONE',  ( 0.000000000000000000, 0.000000000000000000, -63.95112321872120731 ) ) ;
#112721 = CARTESIAN_POINT ( 'NONE',  ( 5.719274019375991003, -21.55341960407610458, 32.70724293864770260 ) ) ;
#112722 = CARTESIAN_POINT ( 'NONE',  ( -16.46253265017160317, 9.564922557960807481, 50.83224293864770260 ) ) ;
#112723 = CARTESIAN_POINT ( 'NONE',  ( 16.51473224551069308, 9.474510206698969483, 34.16557627198102409 ) ) ;
#112724 = CARTESIAN_POINT ( 'NONE',  ( -16.55341960407611168, -4.379528057220339221, 96.45724293864770971 ) ) ;
#112725 = CARTESIAN_POINT ( 'NONE',  ( 15.72974639402199770, -15.80617190586745480, 113.1239096053143953 ) ) ;
#112726 = DIRECTION ( 'NONE',  ( -0.000000000000000000, -0.000000000000000000, 1.000000000000000000 ) ) ;
#112727 = CARTESIAN_POINT ( 'NONE',  ( -5.823673210054431948, 21.52544592524334988, 32.70942372801900433 ) ) ;
#112728 = CARTESIAN_POINT ( 'NONE',  ( 19.02544592524343514, -5.153800228976328945, 98.54057627198100988 ) ) ;
#112729 = CARTESIAN_POINT ( 'NONE',  ( -13.97604488694527625, -13.89961937509977652, 21.87390960531435979 ) ) ;
#112730 = CARTESIAN_POINT ( 'NONE',  ( 5.719274019375673035, 21.55341960407619339, 77.29275706135234714 ) ) ;
#112731 = CARTESIAN_POINT ( 'NONE',  ( 5.823673210054125526, 21.52544592524343514, 99.79057627198103830 ) ) ;
#112732 = CARTESIAN_POINT ( 'NONE',  ( 0.000000000000000000, 0.000000000000000000, -62.91767397929362460 ) ) ;
#112733 = DIRECTION ( 'NONE',  ( -1.000000000000000000, 0.000000000000000000, -0.000000000000000000 ) ) ;
#112734 = FACE_OUTER_BOUND ( 'NONE', #53997, .T. ) ;
#112735 = CARTESIAN_POINT ( 'NONE',  ( 12.14591786802327356, -12.06949235617739191, 50.62609039468568994 ) ) ;
#112736 = CARTESIAN_POINT ( 'NONE',  ( -4.483927247898539470, -16.52544592524342804, 107.2905762719810525 ) ) ;
#112737 = CARTESIAN_POINT ( 'NONE',  ( 33.85315667487628133, 2.428612866512670557E-14, 100.5000000000010232 ) ) ;
#112738 = CARTESIAN_POINT ( 'NONE',  ( -16.51473224551069308, -9.474510206698971260, 56.66557627198103120 ) ) ;
#112739 = CARTESIAN_POINT ( 'NONE',  ( -14.29746914071049879, 8.314922557960819915, 90.83224293864769550 ) ) ;
#112740 = CARTESIAN_POINT ( 'NONE',  ( -21.52544592524343514, 5.823673210054127303, 51.04057627198103120 ) ) ;
#112741 = CARTESIAN_POINT ( 'NONE',  ( 16.53943276465976808, -0.05219959533910856209, 68.74890960531435269 ) ) ;
#112742 = CARTESIAN_POINT ( 'NONE',  ( 9.564922557961047289, -16.46253265017146816, 110.4177570613523471 ) ) ;
#112743 = CARTESIAN_POINT ( 'NONE',  ( -10.72451020669870658, -18.67979575497194134, 89.58442372801901854 ) ) ;
#112744 = CARTESIAN_POINT ( 'NONE',  ( 16.18388926212238488, -7.379444403734518154, 77.06046848633846480 ) ) ;
#112745 = CARTESIAN_POINT ( 'NONE',  ( -16.53943276465976808, -0.05219959533934237506, 93.75109039468567573 ) ) ;
#112746 = CARTESIAN_POINT ( 'NONE',  ( 14.34966873604960469, 8.224510206698951720, 39.16557627198102409 ) ) ;
#112747 = CARTESIAN_POINT ( 'NONE',  ( 19.03943276465977164, -0.05219959533909143690, 43.74890960531435979 ) ) ;
#112748 = CARTESIAN_POINT ( 'NONE',  ( -19.03943276465977164, 0.05219959533909376836, 91.24890960531436690 ) ) ;
#112749 = CARTESIAN_POINT ( 'NONE',  ( 15.80617190586746368, 15.72974639402197994, 94.37390960531436690 ) ) ;
#112750 = CARTESIAN_POINT ( 'NONE',  ( -16.52544592524335698, -4.483927247898792601, 43.95942372801902565 ) ) ;
#112752 = CARTESIAN_POINT ( 'NONE',  ( -18.62759615963255300, -10.81492255796106328, 89.16775706135236135 ) ) ;
#112751 = CARTESIAN_POINT ( 'NONE',  ( -12.14591786802309592, -12.06949235617757132, 66.87390960531436690 ) ) ;
#112753 = ADVANCED_FACE ( 'NONE', ( #140087 ), #14780, .F. ) ;
#112754 = CARTESIAN_POINT ( 'NONE',  ( -14.34966873604972548, 8.224510206698743886, 98.33442372801901854 ) ) ;
#112755 = CARTESIAN_POINT ( 'NONE',  ( 17.50000000000000000, 5.499999999999997335, 26.70309617465829888 ) ) ;
#112756 = CARTESIAN_POINT ( 'NONE',  ( 0.3535533905931707022, -30.00000000000000711, 4.646446609406720718 ) ) ;
#112757 = CARTESIAN_POINT ( 'NONE',  ( 16.53943276465976808, -0.05219959533910856209, 28.74890960531435624 ) ) ;
#112758 = CARTESIAN_POINT ( 'NONE',  ( -12.06949235617739369, -12.14591786802326823, 79.37609039468567573 ) ) ;
#112759 = CARTESIAN_POINT ( 'NONE',  ( 16.51473224551069308, 9.474510206698969483, 79.16557627198103830 ) ) ;
#112760 = CARTESIAN_POINT ( 'NONE',  ( -5.153800228976328057, -19.02544592524343514, 102.2905762719810383 ) ) ;
#112761 = CARTESIAN_POINT ( 'NONE',  ( -0.05219959533937732626, 21.53943276465977519, 87.50109039468568994 ) ) ;
#112762 = CARTESIAN_POINT ( 'NONE',  ( 14.34966873604972726, -8.224510206698740333, 95.83442372801903275 ) ) ;
#112763 = CARTESIAN_POINT ( 'NONE',  ( -12.14591786802309592, -12.06949235617757132, 61.87390960531436690 ) ) ;
#112764 = CARTESIAN_POINT ( 'NONE',  ( 16.51473224551069308, 9.474510206698969483, 64.16557627198102409 ) ) ;
#112765 = ORIENTED_EDGE ( 'NONE', *, *, #30682, .T. ) ;
#112766 = CARTESIAN_POINT ( 'NONE',  ( -13.89961937509957401, -13.97604488694547875, 104.3760903946856757 ) ) ;
#112767 = CARTESIAN_POINT ( 'NONE',  ( 16.51473224551069308, 9.474510206698969483, 24.16557627198102765 ) ) ;
#112768 = CARTESIAN_POINT ( 'NONE',  ( -5.153800228976328057, -19.02544592524343514, 72.29057627198102409 ) ) ;
#112770 = CARTESIAN_POINT ( 'NONE',  ( -38.00000000000001421, 12.34694845685046438, -0.09999999999999989453 ) ) ;
#112769 = CARTESIAN_POINT ( 'NONE',  ( 13.97604488694548053, -13.89961937509957401, 110.6260903946856615 ) ) ;
#112771 = CARTESIAN_POINT ( 'NONE',  ( 0.05219959533936267826, -19.03943276465977164, 20.00109039468567218 ) ) ;
#112772 = CARTESIAN_POINT ( 'NONE',  ( 12.14591786802327356, -12.06949235617739191, 85.62609039468568994 ) ) ;
#112773 = CARTESIAN_POINT ( 'NONE',  ( -13.97604488694547697, 13.89961937509957934, 108.1260903946856331 ) ) ;
#112774 = CARTESIAN_POINT ( 'NONE',  ( 12.14591786802309770, 12.06949235617756955, 114.3739096053143527 ) ) ;
#112775 = CARTESIAN_POINT ( 'NONE',  ( 12.06949235617739724, 12.14591786802326823, 66.87609039468568994 ) ) ;
#112776 = CARTESIAN_POINT ( 'NONE',  ( -16.55341960407617563, 4.379528057220093196, 53.54275706135234714 ) ) ;
#112777 = CARTESIAN_POINT ( 'NONE',  ( -13.89961937509977652, 13.97604488694528158, 25.62390960531434558 ) ) ;
#112778 = CARTESIAN_POINT ( 'NONE',  ( 19.03943276465977164, 0.05219959533936151252, 66.25109039468567573 ) ) ;
#112779 = CARTESIAN_POINT ( 'NONE',  ( 5.153800228976615827, -19.02544592524334988, 20.20942372801899722 ) ) ;
#112780 = CARTESIAN_POINT ( 'NONE',  ( 0.05219959533909260263, 19.03943276465977164, 29.99890960531435979 ) ) ;
#112781 = CARTESIAN_POINT ( 'NONE',  ( -9.474510206698964154, 16.51473224551069663, 75.41557627198103830 ) ) ;
#112782 = CARTESIAN_POINT ( 'NONE',  ( -16.53943276465976808, 0.05219959533911058130, 76.24890960531435269 ) ) ;
#112783 = EDGE_CURVE ( 'NONE', #131569, #130647, #97875, .T. ) ;
#112784 = CARTESIAN_POINT ( 'NONE',  ( 16.46253265017146816, 9.564922557961045513, 46.66775706135233293 ) ) ;
#112785 = CARTESIAN_POINT ( 'NONE',  ( -0.05219959533907301413, -21.53943276465977519, 37.49890960531436690 ) ) ;
#112786 = CARTESIAN_POINT ( 'NONE',  ( 19.05341960407617918, -5.049401038297876454, 21.04275706135232582 ) ) ;
#112787 = CARTESIAN_POINT ( 'NONE',  ( -5.049401038298153566, 19.05341960407611168, 95.20724293864770971 ) ) ;
#112788 = CARTESIAN_POINT ( 'NONE',  ( 21.52544592524334988, 5.823673210054432836, 101.4594237280190185 ) ) ;
#112789 = CARTESIAN_POINT ( 'NONE',  ( -15.80617190586745835, -15.72974639402198527, 66.87390960531436690 ) ) ;
#112790 = CARTESIAN_POINT ( 'NONE',  ( 9.474510206698971260, -16.51473224551069308, 92.91557627198103830 ) ) ;
#112791 = CARTESIAN_POINT ( 'NONE',  ( -9.474510206698720793, -16.51473224551083518, 94.58442372801900433 ) ) ;
#112792 = CARTESIAN_POINT ( 'NONE',  ( -9.474510206698964154, 16.51473224551069663, 100.4155762719810241 ) ) ;
#112793 = CARTESIAN_POINT ( 'NONE',  ( 5.153800228976615827, -19.02544592524334988, 100.2094237280190043 ) ) ;
#112794 = CARTESIAN_POINT ( 'NONE',  ( -16.55341960407611168, -4.379528057220339221, 111.4572429386476813 ) ) ;
#112795 = CARTESIAN_POINT ( 'NONE',  ( -5.153800228976328057, -19.02544592524343514, 87.29057627198103830 ) ) ;
#112796 = CARTESIAN_POINT ( 'NONE',  ( 10.81492255796078972, 18.62759615963270932, 64.58224293864769550 ) ) ;
#112797 = AXIS2_PLACEMENT_3D ( 'NONE', #108769, #97546, #16767 ) ;
#112798 = CARTESIAN_POINT ( 'NONE',  ( -14.34966873604972548, 8.224510206698743886, 38.33442372801900433 ) ) ;
#112799 = CARTESIAN_POINT ( 'NONE',  ( -10.81492255796105439, 18.62759615963255655, 42.91775706135235424 ) ) ;
#112800 = CARTESIAN_POINT ( 'NONE',  ( -0.05219959533937732626, 21.53943276465977519, 97.50109039468567573 ) ) ;
#112801 = CARTESIAN_POINT ( 'NONE',  ( 8.224510206698742110, 14.34966873604972548, 97.08442372801904696 ) ) ;
#112802 = CARTESIAN_POINT ( 'NONE',  ( 19.05341960407611168, 5.049401038298154454, 83.95724293864766707 ) ) ;
#112803 = CARTESIAN_POINT ( 'NONE',  ( -12.06949235617756955, 12.14591786802309770, 85.62390960531436690 ) ) ;
#112804 = CARTESIAN_POINT ( 'NONE',  ( 14.29746914071049879, -8.314922557960816363, 23.33224293864769194 ) ) ;
#112805 = CARTESIAN_POINT ( 'NONE',  ( 19.03943276465977164, 0.05219959533936151252, 71.25109039468566152 ) ) ;
#112806 = CARTESIAN_POINT ( 'NONE',  ( -21.53943276465977519, -0.05219959533937600094, 48.75109039468568284 ) ) ;
#112807 = CARTESIAN_POINT ( 'NONE',  ( -14.29746914071049879, 8.314922557960819915, 90.83224293864769550 ) ) ;
#112808 = CARTESIAN_POINT ( 'NONE',  ( 21.53943276465977519, -0.05219959533907433946, 23.74890960531435269 ) ) ;
#112809 = CARTESIAN_POINT ( 'NONE',  ( 0.05219959533910956823, 16.53943276465976808, 24.99890960531435624 ) ) ;
#112810 = CARTESIAN_POINT ( 'NONE',  ( -15.80617190586768217, 15.72974639402176855, 83.12609039468568994 ) ) ;
#112811 = CARTESIAN_POINT ( 'NONE',  ( -16.52544592524335698, -4.483927247898792601, 48.95942372801902565 ) ) ;
#112812 = CARTESIAN_POINT ( 'NONE',  ( -21.55341960407619339, 5.719274019375674811, 38.54275706135234714 ) ) ;
#112813 = VERTEX_POINT ( 'NONE', #61265 ) ;
#112814 = CARTESIAN_POINT ( 'NONE',  ( -5.719274019375978568, 21.55341960407610458, 115.2072429386476955 ) ) ;
#112815 = CARTESIAN_POINT ( 'NONE',  ( -14.29746914071049879, 8.314922557960819915, 90.83224293864769550 ) ) ;
#112816 = CARTESIAN_POINT ( 'NONE',  ( -19.20446147854529428, -5.499999999999913847, 49.38999695167678539 ) ) ;
#112817 = CARTESIAN_POINT ( 'NONE',  ( -16.55341960407611168, -4.379528057220339221, 61.45724293864770260 ) ) ;
#112818 = CARTESIAN_POINT ( 'NONE',  ( 9.474510206698971260, -16.51473224551069308, 62.91557627198102409 ) ) ;
#112819 = CARTESIAN_POINT ( 'NONE',  ( -12.14591786802326823, 12.06949235617739902, 103.1260903946856757 ) ) ;
#112820 = CARTESIAN_POINT ( 'NONE',  ( 9.474510206698971260, -16.51473224551069308, 37.91557627198102409 ) ) ;
#112821 = CARTESIAN_POINT ( 'NONE',  ( 15.72974639402199770, -15.80617190586745480, 48.12390960531436690 ) ) ;
#112822 = CARTESIAN_POINT ( 'NONE',  ( 12.14591786802309770, 12.06949235617756955, 84.37390960531438111 ) ) ;
#112823 = VECTOR ( 'NONE', #4843, 1000.000000000000000 ) ;
#112824 = CARTESIAN_POINT ( 'NONE',  ( -21.53943276465977519, 0.05219959533907696930, 81.24890960531436690 ) ) ;
#112825 = CARTESIAN_POINT ( 'NONE',  ( 9.474510206698971260, -16.51473224551069308, 82.91557627198103830 ) ) ;
#112827 = CARTESIAN_POINT ( 'NONE',  ( -0.05219959533936034679, 19.03943276465977164, 87.50109039468567573 ) ) ;
#112826 = CARTESIAN_POINT ( 'NONE',  ( -16.51473224551069308, -9.474510206698971260, 36.66557627198102409 ) ) ;
#112828 = CARTESIAN_POINT ( 'NONE',  ( 5.823673210054125526, 21.52544592524343514, 39.79057627198103830 ) ) ;
#112829 = CARTESIAN_POINT ( 'NONE',  ( -15.72974639402176322, -15.80617190586768395, 69.37609039468567573 ) ) ;
#112830 = CARTESIAN_POINT ( 'NONE',  ( 19.03943276465977164, -0.05219959533909143690, 53.74890960531436690 ) ) ;
#112831 = CARTESIAN_POINT ( 'NONE',  ( -13.97604488694527625, -13.89961937509977652, 81.87390960531436690 ) ) ;
#112832 = ORIENTED_EDGE ( 'NONE', *, *, #10604, .F. ) ;
#112833 = CARTESIAN_POINT ( 'NONE',  ( 8.224510206698742110, 14.34966873604972548, 67.08442372801901854 ) ) ;
#112834 = CARTESIAN_POINT ( 'NONE',  ( 18.62759615963255655, 10.81492255796105972, 46.66775706135234714 ) ) ;
#112835 = CARTESIAN_POINT ( 'NONE',  ( 10.72451020669871369, 18.67979575497193778, 67.08442372801901854 ) ) ;
#112836 = CARTESIAN_POINT ( 'NONE',  ( 21.53943276465977519, -0.05219959533907433946, 28.74890960531435624 ) ) ;
#112837 = CARTESIAN_POINT ( 'NONE',  ( 5.719274019375991003, -21.55341960407610458, 97.70724293864772392 ) ) ;
#112839 = CARTESIAN_POINT ( 'NONE',  ( 14.29746914071037800, 8.314922557961029526, 61.66775706135235424 ) ) ;
#112838 = CARTESIAN_POINT ( 'NONE',  ( 21.55341960407619695, -5.719274019375665929, 41.04275706135236135 ) ) ;
#112840 = CARTESIAN_POINT ( 'NONE',  ( -0.05219959533907301413, -21.53943276465977519, 57.49890960531435979 ) ) ;
#112841 = CARTESIAN_POINT ( 'NONE',  ( -0.05219959533936034679, 19.03943276465977164, 27.50109039468566507 ) ) ;
#112843 = CARTESIAN_POINT ( 'NONE',  ( -14.34966873604972548, 8.224510206698743886, 98.33442372801901854 ) ) ;
#112842 = CARTESIAN_POINT ( 'NONE',  ( 13.97604488694527802, 13.89961937509977652, 64.37390960531436690 ) ) ;
#112844 = CARTESIAN_POINT ( 'NONE',  ( -17.50000000000001776, -4.658240926743213883, 106.0552958218320185 ) ) ;
#112845 = SHAPE_REPRESENTATION ( 'tip', ( #82054 ), #166266 ) ;
#112846 = CARTESIAN_POINT ( 'NONE',  ( 19.05341960407611168, 5.049401038298154454, 98.95724293864766707 ) ) ;
#112847 = CARTESIAN_POINT ( 'NONE',  ( 20.03432139805449808, 21.88112277201184952, -48.74685162679677575 ) ) ;
#112848 = CARTESIAN_POINT ( 'NONE',  ( 9.564922557961047289, -16.46253265017146816, 75.41775706135234714 ) ) ;
#112849 = CARTESIAN_POINT ( 'NONE',  ( 10.81492255796078972, 18.62759615963270932, 59.58224293864770260 ) ) ;
#112850 = CARTESIAN_POINT ( 'NONE',  ( -4.483927247898539470, -16.52544592524342804, 32.29057627198102409 ) ) ;
#112851 = CARTESIAN_POINT ( 'NONE',  ( 13.97604488694548053, -13.89961937509957401, 105.6260903946856757 ) ) ;
#112852 = CARTESIAN_POINT ( 'NONE',  ( 5.153800228976335163, 19.02544592524342804, 24.79057627198102765 ) ) ;
#112853 = CARTESIAN_POINT ( 'NONE',  ( 5.049401038297881783, 19.05341960407617563, 102.2927570613523045 ) ) ;
#112855 = CARTESIAN_POINT ( 'NONE',  ( 19.02544592524334988, 5.153800228976608722, 56.45942372801898301 ) ) ;
#112854 = CARTESIAN_POINT ( 'NONE',  ( 10.72451020669898902, -18.67979575497178502, 82.91557627198103830 ) ) ;
#112856 = LINE ( 'NONE', #8691, #124208 ) ;
#112857 = CARTESIAN_POINT ( 'NONE',  ( 5.153800228976335163, 19.02544592524342804, 69.79057627198103830 ) ) ;
#112858 = CARTESIAN_POINT ( 'NONE',  ( -14.29746914071049879, 8.314922557960819915, 60.83224293864769550 ) ) ;
#112859 = CARTESIAN_POINT ( 'NONE',  ( 9.474510206698971260, -16.51473224551069308, 42.91557627198103120 ) ) ;
#112860 = CARTESIAN_POINT ( 'NONE',  ( 4.379528057220339221, -16.55341960407611168, 47.70724293864770260 ) ) ;
#112861 = CARTESIAN_POINT ( 'NONE',  ( -5.153800228976328057, -19.02544592524343514, 22.29057627198102765 ) ) ;
#112862 = CARTESIAN_POINT ( 'NONE',  ( 31.45337032948814482, -4.959272002022362180, 100.6317495573355671 ) ) ;
#112863 = CARTESIAN_POINT ( 'NONE',  ( 0.05219959533910956823, 16.53943276465976808, 34.99890960531435979 ) ) ;
#112864 = CARTESIAN_POINT ( 'NONE',  ( 0.05219959533909260263, 19.03943276465977164, 69.99890960531435269 ) ) ;
#112865 = FACE_OUTER_BOUND ( 'NONE', #46322, .T. ) ;
#112866 = CARTESIAN_POINT ( 'NONE',  ( -19.02544592524334988, -5.153800228976617603, 33.95942372801897591 ) ) ;
#112867 = CARTESIAN_POINT ( 'NONE',  ( -14.34966873604972548, 8.224510206698743886, 43.33442372801901143 ) ) ;
#112868 = CARTESIAN_POINT ( 'NONE',  ( -18.62759615963270932, 10.81492255796079327, 45.83224293864769550 ) ) ;
#112869 = CARTESIAN_POINT ( 'NONE',  ( -21.53943276465977519, -0.05219959533937600094, 108.7510903946857042 ) ) ;
#112870 = CARTESIAN_POINT ( 'NONE',  ( 19.05341960407611168, 5.049401038298154454, 78.95724293864769550 ) ) ;
#112871 = DIRECTION ( 'NONE',  ( 0.000000000000000000, 0.000000000000000000, 1.000000000000000000 ) ) ;
#112872 = CARTESIAN_POINT ( 'NONE',  ( -13.89961937509977652, 13.97604488694528158, 110.6239096053143243 ) ) ;
#112873 = CARTESIAN_POINT ( 'NONE',  ( -15.80617190586768217, 15.72974639402176855, 38.12609039468567573 ) ) ;
#112874 = CARTESIAN_POINT ( 'NONE',  ( 16.53943276465976808, -0.05219959533910856209, 93.74890960531436690 ) ) ;
#112877 = DIRECTION ( 'NONE',  ( -0.1178549842436473205, -0.9930308165857339997, 6.133374237849950220E-17 ) ) ;
#112876 = CARTESIAN_POINT ( 'NONE',  ( 13.89961937509977652, -13.97604488694527269, 78.12390960531433848 ) ) ;
#112875 = CARTESIAN_POINT ( 'NONE',  ( 21.55341960407610458, 5.719274019375980345, 93.95724293864770971 ) ) ;
#112878 = CARTESIAN_POINT ( 'NONE',  ( -9.474510206698964154, 16.51473224551069663, 85.41557627198102409 ) ) ;
#112879 = CARTESIAN_POINT ( 'NONE',  ( -21.53943276465977519, -0.05219959533937600094, 28.75109039468567929 ) ) ;
#112880 = ORIENTED_EDGE ( 'NONE', *, *, #176690, .T. ) ;
#112881 = CARTESIAN_POINT ( 'NONE',  ( 0.05219959533909260263, 19.03943276465977164, 89.99890960531436690 ) ) ;
#112882 = CARTESIAN_POINT ( 'NONE',  ( 19.01533133064923931, -5.499999999999436007, 81.26586590595741200 ) ) ;
#112884 = CARTESIAN_POINT ( 'NONE',  ( -5.153800228976328057, -19.02544592524343514, 37.29057627198102409 ) ) ;
#112883 = CARTESIAN_POINT ( 'NONE',  ( 16.46253265017160672, -9.564922557960803928, 28.33224293864769550 ) ) ;
#112885 = CARTESIAN_POINT ( 'NONE',  ( 19.03943276465977164, 0.05219959533936151252, 111.2510903946856757 ) ) ;
#112886 = CARTESIAN_POINT ( 'NONE',  ( -11.40812507854754720, -35.11059874428192273, -6.724999997268813701 ) ) ;
#112887 = CARTESIAN_POINT ( 'NONE',  ( -14.29746914071049879, 8.314922557960819915, 115.8322429386477097 ) ) ;
#112888 = CARTESIAN_POINT ( 'NONE',  ( 21.55341960407619695, -5.719274019375665929, 81.04275706135236135 ) ) ;
#112890 = CARTESIAN_POINT ( 'NONE',  ( 15.72974639402176855, 15.80617190586768217, 26.87609039468567218 ) ) ;
#112889 = CARTESIAN_POINT ( 'NONE',  ( -5.049401038298153566, 19.05341960407611168, 60.20724293864768129 ) ) ;
#112891 = CARTESIAN_POINT ( 'NONE',  ( -18.62759615963270932, 10.81492255796079327, 105.8322429386476955 ) ) ;
#112892 = CARTESIAN_POINT ( 'NONE',  ( 8.906447517083050158, 27.41122689804195645, 147.4000000000000057 ) ) ;
#112893 = CARTESIAN_POINT ( 'NONE',  ( -9.564922557960796823, -16.46253265017161027, 87.08224293864769550 ) ) ;
#112894 = DIRECTION ( 'NONE',  ( -0.000000000000000000, -0.000000000000000000, 1.000000000000000000 ) ) ;
#112896 = CARTESIAN_POINT ( 'NONE',  ( 21.55341960407610458, 5.719274019375980345, 48.95724293864770971 ) ) ;
#112895 = CARTESIAN_POINT ( 'NONE',  ( 8.314922557961029526, -14.29746914071037800, 20.41775706135234714 ) ) ;
#112897 = CARTESIAN_POINT ( 'NONE',  ( 10.81492255796106328, -18.62759615963255655, 60.41775706135235424 ) ) ;
#112898 = CARTESIAN_POINT ( 'NONE',  ( -13.97604488694527625, -13.89961937509977652, 106.8739096053143669 ) ) ;
#112899 = CARTESIAN_POINT ( 'NONE',  ( 13.89961937509957401, 13.97604488694547697, 91.87609039468567573 ) ) ;
#112900 = CARTESIAN_POINT ( 'NONE',  ( 9.474510206698971260, -16.51473224551069308, 57.91557627198103120 ) ) ;
#112901 = CARTESIAN_POINT ( 'NONE',  ( -16.51473224551069308, -9.474510206698971260, 86.66557627198102409 ) ) ;
#112902 = CARTESIAN_POINT ( 'NONE',  ( 0.05219959533910956823, 16.53943276465976808, 94.99890960531436690 ) ) ;
#112903 = CARTESIAN_POINT ( 'NONE',  ( 12.06949235617757843, -12.14591786802309237, 88.12390960531436690 ) ) ;
#112904 = CARTESIAN_POINT ( 'NONE',  ( 19.05341960407611168, 5.049401038298154454, 108.9572429386477097 ) ) ;
#112906 = CARTESIAN_POINT ( 'NONE',  ( 16.46253265017160672, -9.564922557960803928, 43.33224293864769550 ) ) ;
#112905 = CARTESIAN_POINT ( 'NONE',  ( -8.224510206698948167, 14.34966873604960824, 50.41557627198103120 ) ) ;
#112907 = CARTESIAN_POINT ( 'NONE',  ( -15.72974639402176322, -15.80617190586768395, 74.37609039468568994 ) ) ;
#112908 = CARTESIAN_POINT ( 'NONE',  ( 16.46253265017146816, 9.564922557961045513, 96.66775706135233293 ) ) ;
#112909 = CARTESIAN_POINT ( 'NONE',  ( -14.34966873604960291, -8.224510206698953496, 56.66557627198103830 ) ) ;
#112910 = CARTESIAN_POINT ( 'NONE',  ( 10.81492255796078972, 18.62759615963270932, 114.5822429386477097 ) ) ;
#112911 = CARTESIAN_POINT ( 'NONE',  ( 21.53943276465977519, -0.05219959533907433946, 48.74890960531435979 ) ) ;
#112912 = CARTESIAN_POINT ( 'NONE',  ( 19.39720447994795549, 5.499999999999970690, 72.16317477297177163 ) ) ;
#112913 = CARTESIAN_POINT ( 'NONE',  ( -17.81289503416611097, -24.51734667627696496, 140.5500000054623513 ) ) ;
#112914 = CARTESIAN_POINT ( 'NONE',  ( -9.564922557960796823, -16.46253265017161027, 62.08224293864769550 ) ) ;
#112915 = CARTESIAN_POINT ( 'NONE',  ( 16.55341960407611168, 4.379528057220329451, 38.95724293864768839 ) ) ;
#112916 = CARTESIAN_POINT ( 'NONE',  ( 16.53943276465976808, 0.05219959533934440121, 101.2510903946856757 ) ) ;
#112917 = CARTESIAN_POINT ( 'NONE',  ( 14.34966873604972726, -8.224510206698740333, 80.83442372801901854 ) ) ;
#112918 = CARTESIAN_POINT ( 'NONE',  ( 5.049401038297881783, 19.05341960407617563, 37.29275706135232582 ) ) ;
#112919 = CARTESIAN_POINT ( 'NONE',  ( 27.91311885011353411, 2.428612866367529932E-14, 155.0000000000000000 ) ) ;
#112920 = CARTESIAN_POINT ( 'NONE',  ( 0.05219959533909260263, 19.03943276465977164, 94.99890960531436690 ) ) ;
#112921 = CARTESIAN_POINT ( 'NONE',  ( -16.51473224551069308, -9.474510206698971260, 46.66557627198102409 ) ) ;
#112922 = CARTESIAN_POINT ( 'NONE',  ( 16.55341960407611168, 4.379528057220329451, 63.95724293864770260 ) ) ;
#112924 = CARTESIAN_POINT ( 'NONE',  ( 21.55341960407610458, 5.719274019375980345, 28.95724293864769905 ) ) ;
#112923 = CARTESIAN_POINT ( 'NONE',  ( 17.50000000000000000, -5.499999999999992895, 101.2176903769643559 ) ) ;
#112925 = CARTESIAN_POINT ( 'NONE',  ( -10.72451020669898014, 18.67979575497178502, 35.41557627198102409 ) ) ;
#112926 = CARTESIAN_POINT ( 'NONE',  ( -4.379528057220328563, 16.55341960407611168, 80.20724293864769550 ) ) ;
#112927 = CARTESIAN_POINT ( 'NONE',  ( 16.55341960407618274, -4.379528057220086978, 36.04275706135234714 ) ) ;
#112928 = EDGE_CURVE ( 'NONE', #101016, #88472, #1402, .T. ) ;
#112929 = CARTESIAN_POINT ( 'NONE',  ( -8.314922557960811034, -14.29746914071050412, 82.08224293864768129 ) ) ;
#112930 = CARTESIAN_POINT ( 'NONE',  ( 26.24776304279840389, 7.664901067105983401, 169.1545021717930126 ) ) ;
#112931 = CARTESIAN_POINT ( 'NONE',  ( 0.05219959533936267826, -19.03943276465977164, 80.00109039468567573 ) ) ;
#112932 = CARTESIAN_POINT ( 'NONE',  ( -5.823673210054116645, -21.52544592524344225, 22.29057627198102765 ) ) ;
#112933 = CARTESIAN_POINT ( 'NONE',  ( -11.40812507854755609, 35.11059874428196537, -3.524999997268813523 ) ) ;
#112934 = DIRECTION ( 'NONE',  ( 0.000000000000000000, 0.000000000000000000, -1.000000000000000000 ) ) ;
#112935 = CIRCLE ( 'NONE', #19422, 37.99626262588765968 ) ;
#112937 = CARTESIAN_POINT ( 'NONE',  ( -8.314922557960811034, -14.29746914071050412, 22.08224293864769194 ) ) ;
#112936 = CARTESIAN_POINT ( 'NONE',  ( -16.52544592524335698, -4.483927247898792601, 23.95942372801901143 ) ) ;
#112938 = CARTESIAN_POINT ( 'NONE',  ( 9.564922557961047289, -16.46253265017146816, 65.41775706135233293 ) ) ;
#112939 = CARTESIAN_POINT ( 'NONE',  ( 18.62759615963271287, -10.81492255796078972, 48.33224293864770260 ) ) ;
#112940 = CARTESIAN_POINT ( 'NONE',  ( 15.72974639402176855, 15.80617190586768217, 61.87609039468568284 ) ) ;
#112941 = DIRECTION ( 'NONE',  ( 0.000000000000000000, 0.000000000000000000, -1.000000000000000000 ) ) ;
#112942 = CARTESIAN_POINT ( 'NONE',  ( -12.06949235617739369, -12.14591786802326823, 29.37609039468568284 ) ) ;
#112944 = CARTESIAN_POINT ( 'NONE',  ( 16.46253265017160672, -9.564922557960803928, 93.33224293864769550 ) ) ;
#112943 = CARTESIAN_POINT ( 'NONE',  ( 5.049401038298161559, -19.05341960407611168, 22.70724293864769194 ) ) ;
#112945 = CARTESIAN_POINT ( 'NONE',  ( 19.02544592524343514, -5.153800228976328945, 28.54057627198102409 ) ) ;
#112946 = CARTESIAN_POINT ( 'NONE',  ( 12.06949235617757843, -12.14591786802309237, 88.12390960531436690 ) ) ;
#112947 = CONTEXT_DEPENDENT_SHAPE_REPRESENTATION ( #81636, #124404 ) ;
#112948 = CARTESIAN_POINT ( 'NONE',  ( -16.51473224551069308, -9.474510206698971260, 96.66557627198102409 ) ) ;
#112949 = ORIENTED_EDGE ( 'NONE', *, *, #133407, .F. ) ;
#112950 = CARTESIAN_POINT ( 'NONE',  ( 13.97604488694548053, -13.89961937509957401, 100.6260903946856615 ) ) ;
#112951 = CARTESIAN_POINT ( 'NONE',  ( 5.719274019375991003, -21.55341960407610458, 72.70724293864769550 ) ) ;
#112952 = CARTESIAN_POINT ( 'NONE',  ( 0.05219959533909260263, 19.03943276465977164, 44.99890960531435979 ) ) ;
#112954 = CARTESIAN_POINT ( 'NONE',  ( 10.81492255796078972, 18.62759615963270932, 114.5822429386477097 ) ) ;
#112953 = CARTESIAN_POINT ( 'NONE',  ( -0.05219959533936034679, 19.03943276465977164, 67.50109039468566152 ) ) ;
#112955 = CARTESIAN_POINT ( 'NONE',  ( -19.05341960407611168, -5.049401038298163336, 71.45724293864766707 ) ) ;
#112956 = CARTESIAN_POINT ( 'NONE',  ( 5.153800228976335163, 19.02544592524342804, 104.7905762719809957 ) ) ;
#112957 = ORIENTED_EDGE ( 'NONE', *, *, #83145, .F. ) ;
#112958 = CARTESIAN_POINT ( 'NONE',  ( -8.224510206698735004, -14.34966873604973081, 34.58442372801900433 ) ) ;
#112959 = CARTESIAN_POINT ( 'NONE',  ( -0.05219959533907301413, -21.53943276465977519, 97.49890960531436690 ) ) ;
#112962 = CARTESIAN_POINT ( 'NONE',  ( 13.89961937509957401, 13.97604488694547697, 56.87609039468564731 ) ) ;
#112961 = CARTESIAN_POINT ( 'NONE',  ( 5.153800228976335163, 19.02544592524342804, 89.79057627198102409 ) ) ;
#112960 = CARTESIAN_POINT ( 'NONE',  ( -16.55341960407611168, -4.379528057220339221, 111.4572429386476813 ) ) ;
#112963 = CARTESIAN_POINT ( 'NONE',  ( 5.823673210054125526, 21.52544592524343514, 89.79057627198103830 ) ) ;
#112964 = CARTESIAN_POINT ( 'NONE',  ( -12.14591786802309592, -12.06949235617757132, 51.87390960531437401 ) ) ;
#112965 = CARTESIAN_POINT ( 'NONE',  ( -19.03943276465977164, -0.05219959533935918106, 23.75109039468566152 ) ) ;
#112966 = CARTESIAN_POINT ( 'NONE',  ( 4.483927247898790824, -16.52544592524335698, 60.20942372801902565 ) ) ;
#112967 = CARTESIAN_POINT ( 'NONE',  ( -19.03943276465977164, 0.05219959533909376836, 96.24890960531436690 ) ) ;
#112968 = CARTESIAN_POINT ( 'NONE',  ( 13.89961937509977652, -13.97604488694527269, 43.12390960531434558 ) ) ;
#112969 = VECTOR ( 'NONE', #132334, 1000.000000000000000 ) ;
#112970 = CARTESIAN_POINT ( 'NONE',  ( -5.719274019375665041, -21.55341960407619695, 49.79275706135234714 ) ) ;
#112971 = CARTESIAN_POINT ( 'NONE',  ( -21.55341960407619339, 5.719274019375674811, 68.54275706135234714 ) ) ;
#112972 = CARTESIAN_POINT ( 'NONE',  ( 9.474510206698971260, -16.51473224551069308, 57.91557627198103120 ) ) ;
#112973 = CARTESIAN_POINT ( 'NONE',  ( -21.52544592524334988, -5.823673210054445271, 33.95942372801901143 ) ) ;
#112974 = CARTESIAN_POINT ( 'NONE',  ( -16.51473224551082808, 9.474510206698731452, 78.33442372801900433 ) ) ;
#112975 = CARTESIAN_POINT ( 'NONE',  ( -9.474510206698964154, 16.51473224551069663, 40.41557627198103120 ) ) ;
#112976 = CARTESIAN_POINT ( 'NONE',  ( -0.05219959533934338120, 16.53943276465976808, 87.50109039468568994 ) ) ;
#112977 = CARTESIAN_POINT ( 'NONE',  ( 19.05341960407611168, 5.049401038298154454, 58.95724293864768129 ) ) ;
#112978 = CARTESIAN_POINT ( 'NONE',  ( -0.05219959533909027116, -19.03943276465977164, 22.49890960531436690 ) ) ;
#112979 = CARTESIAN_POINT ( 'NONE',  ( -6.019987952026119621E-15, 39.95163481335720235, -2.247842220587802586 ) ) ;
#112980 = CARTESIAN_POINT ( 'NONE',  ( -19.02544592524342804, 5.153800228976336051, 36.04057627198100988 ) ) ;
#112981 = CARTESIAN_POINT ( 'NONE',  ( -15.80617190586745835, -15.72974639402198527, 86.87390960531438111 ) ) ;
#112982 = CARTESIAN_POINT ( 'NONE',  ( 0.05219959533934541429, -16.53943276465976808, 80.00109039468568994 ) ) ;
#112983 = CARTESIAN_POINT ( 'NONE',  ( 30.00000000000000000, 5.499999999999992895, 37.50000000000000000 ) ) ;
#112984 = CARTESIAN_POINT ( 'NONE',  ( 13.89961937509957401, 13.97604488694547697, 26.87609039468566507 ) ) ;
#112985 = CARTESIAN_POINT ( 'NONE',  ( -5.153800228976328057, -19.02544592524343514, 52.29057627198100988 ) ) ;
#112986 = CARTESIAN_POINT ( 'NONE',  ( -8.314922557960811034, -14.29746914071050412, 47.08224293864770260 ) ) ;
#112987 = CARTESIAN_POINT ( 'NONE',  ( -8.224510206698948167, 14.34966873604960824, 75.41557627198102409 ) ) ;
#112988 = CARTESIAN_POINT ( 'NONE',  ( -16.46253265017160317, 9.564922557960807481, 100.8322429386477097 ) ) ;
#112989 = CARTESIAN_POINT ( 'NONE',  ( -13.97604488694527625, -13.89961937509977652, 81.87390960531436690 ) ) ;
#112990 = CARTESIAN_POINT ( 'NONE',  ( 18.67979575497194134, -10.72451020669871369, 50.83442372801901143 ) ) ;
#112991 = CARTESIAN_POINT ( 'NONE',  ( 16.46253265017160672, -9.564922557960803928, 93.33224293864769550 ) ) ;
#112992 = CARTESIAN_POINT ( 'NONE',  ( -10.72451020669870658, -18.67979575497194134, 94.58442372801901854 ) ) ;
#112993 = CARTESIAN_POINT ( 'NONE',  ( 0.05219959533934541429, -16.53943276465976808, 80.00109039468568994 ) ) ;
#112994 = CARTESIAN_POINT ( 'NONE',  ( -5.719274019375665041, -21.55341960407619695, 29.79275706135234358 ) ) ;
#112995 = CARTESIAN_POINT ( 'NONE',  ( -21.52544592524343514, 5.823673210054127303, 101.0405762719810383 ) ) ;
#112996 = CARTESIAN_POINT ( 'NONE',  ( -16.55341960407611168, -4.379528057220339221, 46.45724293864769550 ) ) ;
#112997 = CARTESIAN_POINT ( 'NONE',  ( -19.03943276465977164, 0.05219959533909376836, 36.24890960531436690 ) ) ;
#112998 = CARTESIAN_POINT ( 'NONE',  ( -4.483927247898539470, -16.52544592524342804, 67.29057627198103830 ) ) ;
#112999 = CARTESIAN_POINT ( 'NONE',  ( 5.719274019375991003, -21.55341960407610458, 27.70724293864769905 ) ) ;
#113000 = CARTESIAN_POINT ( 'NONE',  ( -16.46253265017146816, -9.564922557961047289, 24.16775706135233648 ) ) ;
#113001 = CARTESIAN_POINT ( 'NONE',  ( -8.224510206698948167, 14.34966873604960824, 105.4155762719810383 ) ) ;
#113002 = VERTEX_POINT ( 'NONE', #143065 ) ;
#113003 = CARTESIAN_POINT ( 'NONE',  ( 12.06949235617739724, 12.14591786802326823, 71.87609039468568994 ) ) ;
#113004 = CARTESIAN_POINT ( 'NONE',  ( 9.564922557960805705, 16.46253265017160317, 74.58224293864769550 ) ) ;
#113005 = CARTESIAN_POINT ( 'NONE',  ( -16.88471381081837208, -5.722258574975401579, 20.56778223399915007 ) ) ;
#113006 = CARTESIAN_POINT ( 'NONE',  ( 4.379528057220339221, -16.55341960407611168, 92.70724293864770971 ) ) ;
#113007 = CARTESIAN_POINT ( 'NONE',  ( 5.719274019375991003, -21.55341960407610458, 42.70724293864770260 ) ) ;
#113008 = CARTESIAN_POINT ( 'NONE',  ( -16.52544592524335698, -4.483927247898792601, 88.95942372801901854 ) ) ;
#113009 = CARTESIAN_POINT ( 'NONE',  ( 19.05341960407617918, -5.049401038297876454, 111.0427570613523329 ) ) ;
#113010 = CARTESIAN_POINT ( 'NONE',  ( 10.81492255796106328, -18.62759615963255655, 80.41775706135234714 ) ) ;
#113011 = CARTESIAN_POINT ( 'NONE',  ( 19.02544592524343514, -5.153800228976328945, 68.54057627198103830 ) ) ;
#113012 = CARTESIAN_POINT ( 'NONE',  ( -0.05219959533907301413, -21.53943276465977519, 107.4989096053143669 ) ) ;
#113013 = CARTESIAN_POINT ( 'NONE',  ( -16.53943276465976808, -0.05219959533934237506, 53.75109039468568994 ) ) ;
#113014 = CARTESIAN_POINT ( 'NONE',  ( -14.29746914071049879, 8.314922557960819915, 115.8322429386477097 ) ) ;
#113015 = CARTESIAN_POINT ( 'NONE',  ( -19.05341960407617563, 5.049401038297882671, 113.5427570613523471 ) ) ;
#113016 = EDGE_CURVE ( 'NONE', #78253, #85061, #12741, .T. ) ;
#113017 = CARTESIAN_POINT ( 'NONE',  ( 13.89961937509957401, 13.97604488694547697, 86.87609039468567573 ) ) ;
#113018 = CARTESIAN_POINT ( 'NONE',  ( -15.72974639402197994, 15.80617190586746368, 70.62390960531436690 ) ) ;
#113019 = CARTESIAN_POINT ( 'NONE',  ( 16.51473224551083163, -9.474510206698727899, 60.83442372801900433 ) ) ;
#113020 = DIRECTION ( 'NONE',  ( 0.000000000000000000, 0.9396926207859095381, -0.3420201433256656043 ) ) ;
#113021 = CARTESIAN_POINT ( 'NONE',  ( -0.05219959533907301413, -21.53943276465977519, 102.4989096053143811 ) ) ;
#113022 = CARTESIAN_POINT ( 'NONE',  ( -17.44279575226822843, 5.990770900252458731, 85.83557567514317554 ) ) ;
#113023 = CARTESIAN_POINT ( 'NONE',  ( -5.153800228976328057, -19.02544592524343514, 72.29057627198102409 ) ) ;
#113024 = DIRECTION ( 'NONE',  ( 1.000000000000000000, 0.000000000000000000, 0.000000000000000000 ) ) ;
#113025 = CARTESIAN_POINT ( 'NONE',  ( -14.34966873604972548, 8.224510206698743886, 28.33442372801902209 ) ) ;
#113026 = CARTESIAN_POINT ( 'NONE',  ( 36.99122028029233178, -5.215067209438918994, 43.21662174228440989 ) ) ;
#113028 = CARTESIAN_POINT ( 'NONE',  ( 8.224510206698953496, -14.34966873604960469, 67.91557627198102409 ) ) ;
#113027 = CARTESIAN_POINT ( 'NONE',  ( 10.81492255796078972, 18.62759615963270932, 109.5822429386476955 ) ) ;
#113029 = CARTESIAN_POINT ( 'NONE',  ( 9.564922557960805705, 16.46253265017160317, 74.58224293864769550 ) ) ;
#113030 = CARTESIAN_POINT ( 'NONE',  ( -5.719274019375665041, -21.55341960407619695, 89.79275706135236135 ) ) ;
#113032 = CARTESIAN_POINT ( 'NONE',  ( -5.153800228976607833, 19.02544592524334988, 42.70942372801901143 ) ) ;
#113031 = CARTESIAN_POINT ( 'NONE',  ( 16.52544592524335698, 4.483927247898782831, 31.45942372801901854 ) ) ;
#113033 = CARTESIAN_POINT ( 'NONE',  ( 10.72451020669871369, 18.67979575497193778, 52.08442372801901854 ) ) ;
#113034 = CARTESIAN_POINT ( 'NONE',  ( -5.823673210054116645, -21.52544592524344225, 57.29057627198103120 ) ) ;
#113035 = CARTESIAN_POINT ( 'NONE',  ( -5.049401038297874678, -19.05341960407617918, 104.7927570613523471 ) ) ;
#113036 = CARTESIAN_POINT ( 'NONE',  ( -16.46253265017160317, 9.564922557960807481, 60.83224293864769550 ) ) ;
#113037 = CARTESIAN_POINT ( 'NONE',  ( 9.474510206698729675, 16.51473224551082808, 87.08442372801900433 ) ) ;
#113038 = CARTESIAN_POINT ( 'NONE',  ( 18.67979575497194134, -10.72451020669871369, 90.83442372801901854 ) ) ;
#113039 = CARTESIAN_POINT ( 'NONE',  ( -0.05219959533936034679, 19.03943276465977164, 62.50109039468566863 ) ) ;
#113040 = CARTESIAN_POINT ( 'NONE',  ( -9.564922557960796823, -16.46253265017161027, 37.08224293864768839 ) ) ;
#113041 = CARTESIAN_POINT ( 'NONE',  ( 21.55341960407610458, 5.719274019375980345, 58.95724293864770971 ) ) ;
#113042 = CARTESIAN_POINT ( 'NONE',  ( -14.34966873604960291, -8.224510206698953496, 66.66557627198102409 ) ) ;
#113043 = CARTESIAN_POINT ( 'NONE',  ( -17.49999999999998579, -5.499999999999973355, 101.2823096230356583 ) ) ;
#113044 = CARTESIAN_POINT ( 'NONE',  ( 5.153800228976615827, -19.02544592524334988, 30.20942372801900433 ) ) ;
#113045 = CARTESIAN_POINT ( 'NONE',  ( -0.05219959533934338120, 16.53943276465976808, 97.50109039468567573 ) ) ;
#113046 = CARTESIAN_POINT ( 'NONE',  ( 14.34966873604960469, 8.224510206698951720, 54.16557627198103120 ) ) ;
#113047 = CARTESIAN_POINT ( 'NONE',  ( 15.80617190586769283, -15.72974639402175789, 90.62609039468567573 ) ) ;
#113048 = CARTESIAN_POINT ( 'NONE',  ( 10.72451020669871369, 18.67979575497193778, 87.08442372801901854 ) ) ;
#113049 = CARTESIAN_POINT ( 'NONE',  ( -21.52544592524343514, 5.823673210054127303, 96.04057627198102409 ) ) ;
#113050 = CARTESIAN_POINT ( 'NONE',  ( -16.51473224551069308, -9.474510206698971260, 51.66557627198102409 ) ) ;
#113051 = CARTESIAN_POINT ( 'NONE',  ( 10.81492255796106328, -18.62759615963255655, 75.41775706135233293 ) ) ;
#113052 = CARTESIAN_POINT ( 'NONE',  ( -19.02544592524342804, 5.153800228976336051, 41.04057627198103120 ) ) ;
#113053 = CARTESIAN_POINT ( 'NONE',  ( -13.89961937509977652, 13.97604488694528158, 60.62390960531436690 ) ) ;
#113054 = CARTESIAN_POINT ( 'NONE',  ( -16.52544592524342804, 4.483927247898546575, 101.0405762719810383 ) ) ;
#113055 = CARTESIAN_POINT ( 'NONE',  ( -13.97604488694527625, -13.89961937509977652, 101.8739096053143811 ) ) ;
#113056 = CARTESIAN_POINT ( 'NONE',  ( 8.314922557960818139, 14.29746914071049879, 59.58224293864770260 ) ) ;
#113057 = CARTESIAN_POINT ( 'NONE',  ( 8.224510206698953496, -14.34966873604960469, 112.9155762719810383 ) ) ;
#113058 = CARTESIAN_POINT ( 'NONE',  ( 10.81492255796078972, 18.62759615963270932, 79.58224293864769550 ) ) ;
#113059 = CARTESIAN_POINT ( 'NONE',  ( -18.67979575497193778, 10.72451020669871902, 38.33442372801900433 ) ) ;
#113060 = CARTESIAN_POINT ( 'NONE',  ( 27.67867608143718527, -7.698234437107398520, 161.8893175680481704 ) ) ;
#113061 = CARTESIAN_POINT ( 'NONE',  ( 12.06949235617739724, 12.14591786802326823, 36.87609039468568994 ) ) ;
#113062 = CARTESIAN_POINT ( 'NONE',  ( 15.72974639402199770, -15.80617190586745480, 88.12390960531436690 ) ) ;
#113063 = CARTESIAN_POINT ( 'NONE',  ( 5.719274019375673035, 21.55341960407619339, 102.2927570613523613 ) ) ;
#113064 = CARTESIAN_POINT ( 'NONE',  ( 13.97604488694527802, 13.89961937509977652, 99.37390960531436690 ) ) ;
#113065 = CARTESIAN_POINT ( 'NONE',  ( 10.81492255796106328, -18.62759615963255655, 30.41775706135234358 ) ) ;
#113066 = CARTESIAN_POINT ( 'NONE',  ( 18.62759615963271287, -10.81492255796078972, 28.33224293864769550 ) ) ;
#113067 = CARTESIAN_POINT ( 'NONE',  ( -16.52544592524335698, -4.483927247898792601, 103.9594237280190185 ) ) ;
#113069 = CARTESIAN_POINT ( 'NONE',  ( -21.55341960407619339, 5.719274019375674811, 83.54275706135234714 ) ) ;
#113068 = CARTESIAN_POINT ( 'NONE',  ( -15.80617190586768217, 15.72974639402176855, 48.12609039468568284 ) ) ;
#113070 = CARTESIAN_POINT ( 'NONE',  ( -13.89961937509957401, -13.97604488694547875, 24.37609039468565442 ) ) ;
#113071 = CARTESIAN_POINT ( 'NONE',  ( 16.53943276465976808, 0.05219959533934440121, 81.25109039468568994 ) ) ;
#113072 = CARTESIAN_POINT ( 'NONE',  ( 10.81492255796106328, -18.62759615963255655, 40.41775706135234714 ) ) ;
#113073 = CARTESIAN_POINT ( 'NONE',  ( -5.049401038298153566, 19.05341960407611168, 35.20724293864768839 ) ) ;
#113074 = CARTESIAN_POINT ( 'NONE',  ( 15.72974639402176855, 15.80617190586768217, 96.87609039468568994 ) ) ;
#113075 = CARTESIAN_POINT ( 'NONE',  ( -9.474510206698964154, 16.51473224551069663, 105.4155762719810383 ) ) ;
#113076 = CARTESIAN_POINT ( 'NONE',  ( 21.55341960407610458, 5.719274019375980345, 108.9572429386476955 ) ) ;
#113078 = CARTESIAN_POINT ( 'NONE',  ( -21.53943276465977519, 0.05219959533907696930, 66.24890960531436690 ) ) ;
#113077 = CARTESIAN_POINT ( 'NONE',  ( 18.09805431107524498, -5.499999999999975131, 88.51606229291890315 ) ) ;
#113080 = CARTESIAN_POINT ( 'NONE',  ( 4.483927247898545687, 16.52544592524342804, 49.79057627198102409 ) ) ;
#113079 = CARTESIAN_POINT ( 'NONE',  ( -4.483927247898782831, 16.52544592524335698, 47.70942372801902565 ) ) ;
#113081 = CARTESIAN_POINT ( 'NONE',  ( 28.79475375365584711, -9.355982642739206767, 147.1656553485623533 ) ) ;
#113082 = CARTESIAN_POINT ( 'NONE',  ( -5.049401038297874678, -19.05341960407617918, 84.79275706135233293 ) ) ;
#113083 = CYLINDRICAL_SURFACE ( 'NONE', #170162, 1.999999999999998224 ) ;
#113084 = CARTESIAN_POINT ( 'NONE',  ( -16.52544592524335698, -4.483927247898792601, 23.95942372801901143 ) ) ;
#113085 = CARTESIAN_POINT ( 'NONE',  ( 5.823673210054125526, 21.52544592524343514, 99.79057627198103830 ) ) ;
#113086 = CARTESIAN_POINT ( 'NONE',  ( -21.53943276465977519, 0.05219959533907696930, 71.24890960531435269 ) ) ;
#113087 = CARTESIAN_POINT ( 'NONE',  ( 5.049401038298161559, -19.05341960407611168, 107.7072429386476955 ) ) ;
#113088 = CARTESIAN_POINT ( 'NONE',  ( 8.224510206698742110, 14.34966873604972548, 42.08442372801901854 ) ) ;
#113089 = CARTESIAN_POINT ( 'NONE',  ( -19.05341960407611168, -5.049401038298163336, 61.45724293864769550 ) ) ;
#113091 = CARTESIAN_POINT ( 'NONE',  ( -16.51473224551082808, 9.474510206698731452, 93.33442372801900433 ) ) ;
#113090 = CARTESIAN_POINT ( 'NONE',  ( 5.823673210054444382, -21.52544592524334988, 25.20942372801901854 ) ) ;
#113092 = CARTESIAN_POINT ( 'NONE',  ( -13.89961937509977652, 13.97604488694528158, 105.6239096053143527 ) ) ;
#113093 =( BOUNDED_SURFACE ( )  B_SPLINE_SURFACE ( 3, 2, ( 
 ( #101777, #72452, #150300, #166465, #42123, #71447, #163465, #136112, #56274, #164468, #26961, #179648, #196808, #41118, #195816, #102782, #57288, #25962, #149291, #134127, #118964, #103785, #73460, #58275, #12780, #119944, #74446, #197788, #182622, #123894, #18734, #199772, #108743, #187601, #171420, #2554, #156239, #106754, #168429, #183614, #76415, #141069, #169416, #154257, #107735, #138091, #60249, #140064, #64236, #92569, #79398, #170419, #139077, #95553, #32906, #155250, #49070, #62226, #29925, #157240, #153252, #31911, #91564, #14754, #110726, #77407, #555, #93564, #1555, #172407, #185593, #30921, #78388, #15748, #125902, #47082, #33896, #186608, #137097, #198783, #121920, #16739, #94560, #45097, #63231, #124910, #61239, #48080, #122911, #184599, #46080, #109736, #17741, #192563, #144044, #69205, #177408, #83363, #3539, #159206, #81358, #129853, #145039, #65217, #130873, #97519, #38879, #52039, #54046, #111725, #189577, #100536, #6521, #126877, #143042, #68200, #191551, #115720, #112711, #162215, #53028, #173411, #114709, #51049, #176402, #174404, #142053, #84359, #20700, #37877, #80381, #99535, #161217, #188583, #35873, #34882, #50064, #19716, #22712, #96537, #158226, #5526, #4520, #66213, #146037, #127873, #82356, #67206, #7521, #128864, #190564, #113695, #175391, #36859, #98526, #160219, #21709, #132877, #182384, #150053, #8538, #86372, #11559, #73225, #197550, #56036, #59018, #88360, #116710, #134896, #194566, #26721, #117714, #85362, #27722, #120685, #102548, #118724, #196573, #10547, #178400, #131883, #166221, #43862, #179410, #195576, #9548, #58043, #105527, #25728, #74211, #87374, #40875, #147054, #164232, #39864, #23714, #149059, #72211, #119713, #133885, #57049, #70216, #180412, #41884, #193568, #148057, #103551, #135879, #181397, #89365, #42875, #55040, #101530, #163222, #24723, #151054, #165226, #104540, #12545, #71214, #90346, #170175, #32659, #122670, #109489, #138834, #169169, #125657, #1303, #185346, #79145, #92326, #136854, #187354, #183373, #314, #60010, #121677, #17488, #107492, #30673, #61982, #31668, #140817, #154012, #137848, #108496, #184359, #94313, #15507, #155991, #16499, #167213, #2306, #28710, #152032, #13517, #62982, #77164, #45840, #44854, #123648, #63987, #124661, #186357, #171172, #48824, #93318, #106510, #46836, #78147, #76168, #155002, #139816, #47837, #199529, #75182, #198539, #168187, #29684, #14506, #91316, #153007, #60998, #64972, #175143, #97274, #37621, #111476, #99283, #20453, #3300, #114450, #160970, #22464, #36611, #96296, #6277, #130620, #157982, #51791, #127631, #19473, #190314, #144794, #82103, #158962, #110477, #173161, #98267, #33645, #172160, #128621, #159969, #34636, #52781, #84112, #21456, #65960, #143795, #83117, #50808, #5278, #66960, #191305, #81119, #49811, #95306, #142799, #113450, #67955, #189331, #7274, #4280, #112466, #129610, #176151, #141807, #174159, #126631, #188333, #192316, #145791, #35629, #68958, #156990, #18489, #80137, #12305, #119473, #104295, #164982, #103303, #55793, #117465, #150809, #26477, #149804, #181156, #42632, #194325, #178156, #87128, #11309, #86126, #165977, #41638, #88119, #89121, #39621, #85113, #69968, #177160, #147817, #195325, #27478, #25486, #72979, #146797, #115471, #73971, #38633, #100290, #134648, #118479, #161968, #135640, #70969, #53796, #148813, #23464, #8290, #162971, #131634, #180169, #193318, #116467, #196334, #57802, #54792, #9303, #101281, #24476, #132637, #179163, #40631, #56805, #102300, #163989, #10303, #71960, #133634, #92079, #108255, #184120, #151792, #105283, #139579, #170928, #167951, #168926, #183129, #74, #94074, #199288, #47595, #60755, #29450, #120442, #14261, #90108, #17251, #152769, #45602, #185105, #137605, #75930, #78904, #153768, #107255, #197310, #59768, #30432, #109248, #31426, #62739, #16261, #166971, #28474, #43619, #136610, #1064, #91082, #122428, #15263, #198291 ),
 ( #58774, #13283, #76921, #74947, #121436, #32419, #138592, #61744, #123412, #46595, #155753, #169935, #93079, #154763, #77912, #124419, #186115, #182136, #44612, #106267, #52549, #2071, #19246, #174913, #22225, #143558, #5041, #125424, #96066, #171925, #140581, #79908, #128387, #160733, #114210, #4049, #129380, #37386, #66727, #63750, #80893, #141579, #99043, #190083, #36377, #6044, #67722, #142570, #64744, #173927, #98031, #172929, #191076, #51559, #113223, #175915, #126406, #33414, #156761, #187120, #34408, #81867, #48592, #112237, #159728, #95073, #110243, #18255, #3067, #188102, #49575, #111238, #21224, #50577, #157755, #65726, #97047, #127395, #82880, #144558, #189104, #35396, #158729, #20219, #70735, #133396, #193082, #162734, #56568, #40394, #54557, #72743, #83874, #24242, #117231, #131394, #104062, #102065, #7034, #38393, #148576, #132402, #11065, #84874, #134414, #194095, #176922, #87881, #196100, #57570, #10066, #69726, #179933, #165743, #116230, #25250, #101049, #177921, #163750, #118242, #55557, #178924, #145556, #146551, #71726, #68716, #130373, #86892, #195086, #8047, #26242, #119240, #41400, #39389, #103065, #164747, #85891, #149569, #180924, #42399, #147579, #23230, #192071, #9065, #53552, #115231, #100049, #161735, #89884, #74723, #141099, #95586, #58550, #47114, #181906, #43385, #50096, #124942, #105057, #48110, #3571, #1587, #18766, #188615, #157270, #80413, #2586, #79428, #31942, #93596, #136386, #111756, #156271, #12077, #151567, #17773, #64266, #65249, #59529, #126909, #94593, #120216, #125932, #198063, #32938, #121207, #88886, #33928, #27237, #108773, #186639, #187631, #16772, #166741, #135412, #172440, #150578, #182898, #63262, #13056, #49101, #73740, #155282, #142085, #78420, #170451, #197083, #140096, #28244, #109766, #171450, #110759, #161249, #113728, #190595, #193601, #129884, #160252, #55073, #35904, #145071, #23748, #7553, #38910, #192595, #143074, #4552, #19747, #112741, #177440, #5558, #52072, #144077, #174434, #96569, #176435, #100567, #128896, #115752, #6553, #175425, #131917, #69239, #191584, #85397, #98558, #66245, #173445, #189607, #68231, #127905, #51081, #147090, #36893, #21742, #53062, #37909, #8574, #83394, #67237, #114741, #99568, #162249, #22743, #70249, #84392, #34913, #158257, #81388, #146068, #130905, #97550, #54078, #159238, #20732, #82389, #86406, #116743, #194599, #73259, #120717, #74243, #133921, #12578, #197583, #150087, #39901, #149093, #56071, #134928, #11591, #163257, #135912, #10583, #59050, #180447, #178433, #71248, #196605, #58076, #101566, #72244, #24759, #181429, #179444, #104573, #195612, #119746, #57084, #148091, #9582, #132912, #42907, #166255, #117751, #27755, #118758, #87408, #40910, #102583, #88394, #89398, #165260, #164267, #25762, #41919, #103585, #26754, #151087, #20380, #114376, #190242, #117392, #52712, #84043, #85039, #37549, #176080, #179091, #53725, #145722, #97204, #159897, #68887, #147743, #131561, #162896, #116390, #66884, #128545, #143723, #36538, #101207, #129538, #99212, #67885, #98194, #82027, #100217, #24405, #160900, #39548, #130547, #22393, #55720, #193245, #115401, #9230, #7203, #51719, #158890, #113382, #192244, #175072, #21386, #70897, #177089, #38561, #161898, #23393, #132564, #146720, #191238, #8217, #69893, #86054, #54718, #194253, #178080, #5203, #83044, #144719, #6205, #74878, #122354, #43548, #105214, #25414, #196263, #71889, #40560, #180098, #28401, #60679, #152696, #104223, #29379, #137530, #166901, #163918, #119402, #41566, #90040, #151722, #87056, #91010, #57732, #199212, #12237, #14185, #133559, #149732, #102229, #13215, #148741, #103229, #198221, #183057, #44541, #136540, #164911, #27402, #59693, #11233, #181085, #121364, #197241, #72907, #75854, #10229, #42560, #73899, #88044, #195250, #58702, #56734, #118404, #106196, #89047, #167880, #26405, #134576, #150737, #165904, #135569, #120372, #182065 ),
 ( #157677, #16184, #19167, #48518, #76847, #33339, #154689, #187048, #77839, #45526, #188028, #80816, #62663, #78830, #94999, #170856, #138518, #91998, #126331, #142494, #139506, #155681, #169858, #110172, #3972, #186038, #34331, #47521, #989, #107180, #124343, #30717, #65652, #109177, #32347, #171851, #94000, #17176, #184043, #140508, #1997, #168851, #46518, #63676, #95992, #18179, #49499, #2991, #153692, #15188, #30356, #123338, #111161, #125351, #156685, #79836, #185031, #61669, #141506, #172850, #64669, #108177, #31352, #93003, #81165, #19520, #52829, #22511, #67008, #68003, #188381, #157039, #130670, #18536, #80183, #141855, #3346, #129655, #5324, #50855, #49858, #51839, #7320, #114498, #65021, #174206, #96342, #144839, #160017, #126677, #145838, #112513, #53847, #128667, #69004, #111524, #4326, #115521, #21504, #173209, #158029, #83165, #6323, #192364, #127678, #177209, #191351, #34685, #176200, #66010, #98317, #189378, #142847, #99334, #95354, #35674, #190363, #37669, #82149, #97322, #159008, #161017, #20501, #143845, #113498, #175193, #84158, #36659, #40677, #89166, #102347, #9351, #162017, #55839, #131684, #58821, #194372, #25534, #26521, #179210, #117513, #120489, #195372, #87178, #38682, #101329, #10350, #150858, #73025, #104341, #57849, #8340, #70015, #85160, #178203, #42680, #71016, #164036, #132684, #39667, #23513, #41685, #166025, #148859, #181203, #72007, #134697, #86175, #100338, #119521, #12352, #133680, #193365, #146846, #54841, #56851, #116516, #163017, #74015, #118526, #180215, #103349, #165028, #135685, #88166, #149850, #11354, #196380, #27525, #197357, #24524, #147865, #182180, #94119, #43665, #60799, #16304, #63797, #185148, #46638, #167015, #137647, #13325, #105327, #121481, #169977, #2115, #155798, #45645, #170973, #78950, #108298, #77954, #153811, #30473, #28516, #44657, #31469, #90152, #151835, #117, #93121, #106310, #124464, #17296, #154806, #199334, #15306, #139621, #122472, #76965, #168968, #62783, #167996, #183175, #74990, #29492, #123456, #138636, #184163, #140625, #91125, #152815, #1109, #47642, #136654, #107296, #198335, #59811, #14307, #61786, #75974, #186161, #92123, #109294, #32466, #83922, #191122, #175962, #36419, #174956, #127440, #189146, #22271, #98075, #21268, #52596, #114257, #65771, #49621, #158773, #82925, #157799, #37431, #113264, #159773, #160783, #111283, #156807, #35438, #172973, #34452, #144603, #99091, #97090, #6088, #18299, #187166, #145603, #48637, #110289, #171971, #33459, #67767, #20262, #80937, #79955, #81908, #7082, #129424, #125469, #95117, #141624, #190125, #64789, #112280, #3113, #96111, #4092, #126450, #143601, #19290, #188148, #142613, #50619, #5085, #173970, #66767, #128428, #51600, #23275, #133440, #55600, #196141, #69770, #57613, #178968, #161780, #72786, #119281, #180964, #195130, #54598, #164790, #88930, #116272, #10110, #85933, #177962, #148619, #147622, #27284, #40435, #42441, #100096, #39430, #150622, #56611, #53601, #131438, #118285, #179976, #104104, #101090, #165787, #41444, #84919, #103109, #162776, #71770, #24284, #130421, #134456, #68763, #9110, #163792, #26284, #117274, #146599, #176971, #11111, #192119, #70776, #102107, #132445, #87926, #115277, #194136, #38440, #25294, #86936, #8092, #149613, #193124, #32232, #167765, #199094, #200088, #152580, #29263, #93890, #168736, #60561, #12118, #74764, #183927, #62551, #46400, #77728, #31238, #181947, #43430, #58590, #151607, #16070, #44425, #90894, #182942, #13099, #135454, #15071, #139394, #14070, #154574, #45412, #108059, #59573, #73782, #92887, #124227, #137413, #105099, #197123, #28286, #107065, #166785, #89926, #185923, #75737, #122237, #30240, #76732, #47408, #91883, #106079, #153574, #138408, #876, #61556, #109064, #123225, #120256, #170742, #136426, #184916, #169743, #198107, #121248, #158546, #140393, #111051, #186934, #155568, #94889, #143361, #175717, #67531 ),
 ( #79723, #97844, #129189, #4853, #172739, #127200, #81678, #95882, #188914, #142383, #36190, #141392, #156573, #17063, #2880, #96862, #112052, #34220, #52363, #18068, #64559, #66538, #21031, #48404, #157565, #110061, #171741, #37196, #50392, #33230, #173740, #190887, #35209, #144368, #114020, #82684, #5855, #128202, #189899, #19058, #80705, #78717, #51374, #113035, #1881, #63562, #3861, #126223, #20036, #174727, #187919, #125236, #159532, #49388, #65541, #23039, #130183, #8872, #84684, #146364, #56366, #26048, #70539, #71535, #191879, #160548, #134221, #22038, #83689, #145367, #6849, #133201, #132208, #54370, #53363, #55363, #10874, #118049, #179739, #41209, #102870, #163553, #38206, #85697, #148380, #7851, #177731, #194892, #117033, #69538, #87693, #98853, #39200, #193899, #131202, #119055, #178728, #68528, #115040, #25053, #147384, #149378, #99862, #72544, #40190, #176733, #164555, #195907, #57382, #86696, #192892, #180737, #161546, #116042, #101870, #100856, #162538, #9875, #24042, #13844, #90677, #42213, #104866, #168520, #165554, #103873, #45191, #136201, #27051, #46173, #139170, #121013, #137184, #153345, #29037, #196897, #150393, #184689, #15841, #12871, #75511, #28054, #106845, #647, #44196, #92659, #105855, #74536, #88697, #59344, #135225, #62317, #197876, #152359, #30018, #182711, #167542, #123987, #198872, #60339, #11889, #166555, #122013, #154348, #76509, #107826, #61332, #73552, #58364, #120031, #181716, #169510, #183704, #91656, #14846, #43199, #89695, #138185, #31010, #199868, #77500, #123003, #151381, #33002, #5622, #66308, #97612, #110823, #155346, #67301, #1651, #18831, #78486, #140159, #35965, #125996, #187694, #157336, #188680, #159301, #49164, #156336, #126972, #141163, #112805, #172505, #174498, #34980, #185685, #20797, #47175, #64329, #19809, #108834, #50160, #111819, #170514, #2652, #16835, #32004, #125007, #173507, #93661, #82452, #33992, #144140, #63329, #96633, #186702, #95648, #48173, #158321, #81450, #109830, #171513, #80476, #94656, #142149, #17836, #79494, #3633, #65312, #143137, #4616, #127968, #189671, #51144, #102649, #161315, #164334, #193667, #21806, #178500, #99633, #40980, #190660, #7619, #163327, #10650, #131982, #55138, #113793, #84455, #160316, #128960, #68298, #116808, #149160, #25828, #192659, #117819, #87473, #39966, #52136, #69303, #129949, #101636, #24823, #175488, #179512, #146133, #36960, #100632, #98622, #83458, #37975, #145136, #86472, #6619, #191649, #148157, #9649, #53128, #22809, #114806, #71315, #176499, #132978, #130969, #194668, #54142, #115816, #56138, #177506, #38975, #23814, #162313, #85464, #147153, #8641, #70313, #45939, #42976, #43964, #58145, #75285, #169272, #74313, #122770, #135980, #104641, #195680, #89467, #165330, #95156, #27825, #59117, #60111, #12646, #151156, #156844, #28810, #120783, #72312, #134997, #105626, #184459, #106614, #137947, #91421, #41986, #103652, #118829, #11660, #76269, #166328, #197651, #182483, #73326, #57151, #136956, #199630, #167314, #14612, #90451, #168289, #119813, #133989, #153108, #107594, #152135, #26822, #180513, #88463, #13618, #150159, #196676, #33497, #198645, #121779, #183472, #44957, #181498, #29785, #61097, #159815, #174009, #145643, #143641, #7123, #67810, #18339, #79994, #130464, #141662, #97129, #52637, #100137, #21310, #82967, #3154, #35480, #49659, #64827, #157839, #6127, #38480, #192162, #81949, #68805, #115319, #144644, #126489, #158813, #19330, #129465, #191164, #188187, #53642, #20301, #177011, #190165, #111323, #173013, #127480, #34492, #114302, #96150, #80978, #176004, #37473, #142653, #50658, #4132, #99134, #65811, #160824, #189185, #22312, #112319, #5124, #83963, #66806, #128469, #113305, #51641, #174996, #36461, #98118, #104145, #135494, #132485, #133478, #147662, #164830, #58630, #163832, #12159, #25334, #194174, #84957, #179007, #54636, #181989, #117311, #148662, #149654 ),
 ( #11152, #57654, #27324, #88971, #102147, #85972, #195170, #119320, #55638, #73824, #72826, #134495, #197164, #9149, #193164, #71810, #70816, #40475, #181007, #150661, #56651, #196182, #116311, #23313, #120296, #146639, #8132, #69810, #131477, #42482, #118324, #86975, #178000, #180017, #43471, #165827, #161818, #39467, #101128, #26326, #162814, #10150, #103149, #41484, #24323, #87966, #93928, #154612, #105139, #17102, #166825, #183964, #139432, #186973, #108097, #169782, #89965, #60601, #136465, #28326, #44465, #92926, #125276, #78754, #168775, #155607, #1921, #31275, #151645, #45451, #106119, #16107, #77765, #13140, #140431, #122276, #63600, #76772, #74802, #198145, #14110, #59615, #914, #121288, #167803, #62588, #124266, #182981, #137455, #29303, #185961, #90933, #47446, #75777, #109102, #199134, #152619, #170781, #107105, #30277, #200125, #32271, #91923, #153615, #15111, #138444, #61594, #123263, #184954, #46438, #51409, #145401, #50430, #98888, #112089, #19094, #171779, #65580, #141431, #68561, #3900, #35245, #36227, #188953, #127239, #130218, #4890, #96899, #48443, #111088, #20072, #160582, #82724, #114058, #67567, #18106, #79760, #94926, #187957, #52399, #80743, #173779, #142421, #49427, #33267, #113069, #175755, #158583, #190922, #81716, #144405, #95918, #110100, #129225, #22071, #143401, #2918, #156611, #64596, #66572, #126260, #172778, #83722, #128237, #189934, #174761, #97879, #6883, #159570, #21068, #5891, #37232, #34259, #157603, #163586, #178762, #72580, #116075, #131237, #53397, #39232, #133234, #148414, #147418, #88731, #54403, #100888, #102904, #57415, #23072, #8905, #146396, #7885, #11921, #86729, #69571, #9909, #165587, #25087, #180770, #150426, #119088, #42245, #164588, #41242, #193933, #55396, #73585, #26082, #87726, #103906, #27085, #132241, #177763, #71569, #149411, #24075, #191913, #179773, #10907, #115075, #162572, #84718, #101904, #85730, #70573, #134254, #176767, #194926, #195941, #192925, #38239, #99894, #161579, #117066, #40227, #56401, #118083, #45220, #90707, #89728, #91687, #47206, #92690, #154378, #77530, #139202, #199898, #74566, #122044, #184719, #44230, #13876, #107857, #153377, #105887, #124018, #135257, #75543, #168548, #182745, #155375, #14879, #58397, #151414, #61362, #183734, #62348, #136234, #185715, #106875, #28088, #677, #108865, #170544, #123033, #121050, #31041, #16864, #167574, #76540, #152390, #29068, #138216, #169542, #30046, #46203, #196929, #197908, #15872, #120063, #181751, #32035, #93692, #59378, #43233, #104899, #137217, #198904, #166588, #12902, #60372, #128990, #66337, #127998, #113820, #2681, #109857, #188709, #64358, #126027, #35993, #5651, #50191, #51174, #171542, #140189, #175515, #1681, #63359, #125036, #186732, #112834, #111848, #34022, #33030, #35007, #190688, #97640, #159329, #20825, #82482, #143166, #17867, #65341, #189701, #187723, #157366, #174526, #96662, #49194, #67328, #78515, #18860, #173538, #110852, #98651, #158349, #48203, #94685, #4646, #127001, #52163, #79522, #36989, #19838, #156364, #144166, #160345, #141192, #172536, #95680, #80506, #142179, #3663, #81479, #39002, #7646, #101663, #56165, #193695, #70341, #21834, #84483, #148183, #145164, #83486, #39992, #71342, #146160, #164360, #195707, #133005, #177533, #55164, #9677, #162340, #116834, #8668, #102675, #69330, #161344, #6648, #130996, #163354, #178525, #100658, #118856, #192688, #54171, #194695, #87499, #53156, #23841, #176529, #38005, #42013, #24850, #99660, #86499, #57179, #117846, #10676, #180539, #149187, #72340, #179539, #41008, #85490, #147179, #103677, #25855, #134015, #68326, #129976, #132008, #191676, #114835, #22836, #115844, #121804, #152159, #46966, #27852, #136980, #15633, #199657, #30804, #184487, #135026, #196701, #11687, #104669, #169298, #197675, #182509, #136004, #166354, #88491, #168315, #92453, #120810, #107620, #198669, #61123, #12671, #185476 ),
 ( #29811, #138960, #105650, #59140, #106642, #43989, #154141, #90477, #77290, #14638, #165356, #439, #26850, #167339, #122797, #150186, #91447, #153135, #73353, #28836, #58171, #119838, #89493, #76297, #181523, #62114, #13642, #123777, #43002, #137975, #151183, #75309, #74338, #45966, #60136, #183498, #44982, #125784, #67091, #80264, #159089, #139946, #17621, #128750, #34767, #93445, #171303, #96424, #158110, #82236, #140950, #143926, #173293, #1436, #19602, #79280, #111608, #2437, #170303, #112595, #5407, #187486, #3425, #81244, #95437, #63114, #16625, #50937, #190447, #64119, #141934, #94441, #142925, #108625, #110605, #20584, #172287, #48952, #31796, #33777, #124792, #155132, #157121, #78273, #65101, #186491, #47967, #18617, #109619, #4407, #32789, #156122, #66092, #127758, #126759, #188462, #49943, #189459, #174287, #35757, #97402, #54925, #145921, #113581, #55922, #148945, #130755, #146936, #163104, #38763, #6404, #160101, #194451, #25616, #22594, #23598, #37756, #116597, #10435, #53929, #102431, #115604, #84242, #175275, #69088, #144922, #72093, #7404, #100421, #39749, #192447, #177293, #133767, #8426, #162102, #51922, #114587, #85245, #164118, #86256, #117597, #71097, #21588, #83246, #98405, #191434, #179298, #70098, #131767, #193449, #52911, #36741, #178286, #40762, #101412, #87260, #24608, #147946, #99417, #68085, #132764, #129737, #9432, #176284, #161099, #11441, #28600, #88249, #149934, #45733, #135771, #197442, #167099, #198424, #169057, #58908, #166111, #136740, #150945, #122561, #120575, #184251, #44742, #195462, #107385, #56937, #74101, #29577, #77053, #59899, #121567, #180301, #12439, #26606, #118611, #134782, #183261, #15396, #30564, #182269, #92215, #153901, #106398, #41769, #43752, #196464, #168080, #91208, #103434, #165114, #105415, #90238, #152898, #73112, #57934, #119605, #181288, #42766, #104428, #27613, #14395, #151921, #13410, #89253, #75074, #76061, #137736, #199420, #60884, #81024, #3199, #78040, #125555, #188233, #47729, #17382, #111372, #95205, #109382, #127528, #138724, #79038, #172056, #186251, #158861, #156892, #61874, #93210, #64873, #187252, #65857, #139709, #189232, #48721, #31559, #142700, #50710, #112368, #126534, #124554, #34538, #20350, #171062, #80039, #155885, #32552, #18388, #173061, #110374, #33543, #205, #1196, #49706, #123544, #185237, #141708, #96197, #62873, #4179, #174059, #157886, #94205, #19375, #35528, #140713, #97176, #46729, #108391, #2203, #63884, #170068, #154895, #16393, #68857, #191211, #162866, #159866, #144691, #100187, #193214, #51692, #52686, #113354, #175046, #24374, #7174, #36511, #130516, #39518, #145692, #54688, #88761, #116361, #178050, #161869, #38531, #176054, #37521, #101178, #23363, #85009, #81998, #143691, #99183, #6176, #192212, #146689, #114349, #5173, #8185, #69861, #66856, #67856, #98166, #53695, #129511, #160872, #128518, #190213, #21359, #131530, #83016, #22362, #84014, #115372, #177061, #187894, #32208, #82656, #78691, #95855, #155543, #17037, #113007, #2853, #64531, #34194, #65514, #36164, #126198, #33204, #3835, #18042, #189872, #49361, #51347, #112025, #62525, #174700, #124198, #141366, #96837, #144340, #127175, #188885, #47383, #79696, #93865, #185898, #1855, #50366, #109038, #97816, #111024, #159505, #21001, #173714, #170717, #172710, #63537, #35182, #158521, #140368, #125212, #157539, #186908, #19033, #48379, #110036, #171714, #94862, #20009, #156543, #80679, #81652, #143336, #142355, #4823, #66511, #128173, #101582, #58089, #179458, #11604, #102596, #67504, #12593, #105571, #87421, #103598, #119759, #195625, #163270, #116756, #151101, #182430, #40923, #180460, #194612, #73272, #167257, #10596, #59063, #72257, #164282, #129161, #25775, #24772, #28756, #149106, #57098, #196619, #133935, #118772, #90393, #165273, #41932, #5828, #71261, #26767, #120730, #42921, #74257, #27769, #178447, #39914, #52335 ),
 ( #43909, #88407, #150103, #190858, #134942, #86419, #148105, #181443, #104586, #166271, #89412, #135927, #9596, #197597, #132925, #56084, #117765, #123693, #2352, #186405, #17534, #171217, #121723, #183415, #198587, #91362, #156037, #184404, #169214, #122714, #153053, #75229, #155049, #79194, #107538, #94358, #185391, #47882, #199573, #172206, #32706, #64033, #77209, #44899, #33691, #168233, #46882, #106556, #29729, #125703, #92370, #154056, #108542, #16544, #187402, #15551, #45885, #93362, #30723, #140863, #138878, #48870, #1350, #152077, #110525, #13562, #358, #109535, #136900, #78191, #139861, #60055, #62028, #14555, #76213, #137892, #63030, #61042, #170221, #31714, #124707, #138579, #140570, #156751, #189093, #59, #111227, #157744, #19234, #33403, #93065, #3057, #127382, #154752, #48580, #124409, #16249, #187110, #141569, #78891, #155742, #107242, #169922, #95062, #30418, #168912, #125413, #18245, #31414, #49563, #80882, #79898, #62726, #2060, #64734, #47584, #63739, #94063, #188092, #77901, #46581, #92066, #139568, #110233, #171914, #126395, #153754, #61732, #172919, #17239, #123400, #34398, #96056, #15249, #185092, #142559, #4037, #65715, #76908, #1052, #108243, #186103, #109236, #170915, #32408, #36365, #130359, #84860, #22212, #99030, #50566, #113211, #176909, #173916, #112226, #68703, #100036, #174900, #193067, #24225, #161722, #6030, #83861, #38380, #191063, #145543, #37372, #131379, #98017, #190071, #35385, #159712, #192057, #7021, #67709, #147564, #21210, #82867, #23217, #116216, #81853, #129367, #5029, #66714, #70719, #53539, #128375, #115216, #85876, #146537, #39375, #9049, #177907, #101034, #8031, #69712, #52536, #114196, #132387, #54543, #162719, #97037, #158717, #175901, #144545, #20207, #143543, #160720, #51547, #181891, #43369, #29207, #118226, #25235, #104046, #179917, #41384, #151551, #121191, #165726, #166725, #86876, #55543, #90841, #117215, #178908, #40376, #102050, #28229, #27222, #149553, #148560, #150563, #106024, #13041, #74708, #136371, #198048, #58535, #133379, #180908, #105041, #103049, #72724, #89869, #12062, #164731, #182884, #194080, #134397, #88870, #26225, #14013, #163735, #10051, #71711, #195069, #59514, #73724, #11048, #56549, #135397, #167711, #44367, #152526, #75679, #87865, #120201, #196084, #42383, #57554, #119224, #197068, #110001, #93832, #108001, #126166, #137358, #16015, #170687, #184861, #157507, #155512, #60507, #91827, #1824, #124165, #168684, #32176, #186877, #19001, #30185, #141334, #187861, #49330, #63506, #123173, #33171, #199037, #46344, #78659, #154518, #169687, #17007, #171682, #109008, #185867, #122182, #200036, #125181, #183874, #45359, #140334, #48347, #61504, #79663, #110991, #94830, #92833, #156508, #18009, #77672, #2821, #47353, #64499, #31182, #76678, #107011, #139341, #172676, #34161, #820, #95822, #62494, #153520, #15017, #138354, #111991, #97785, #35148, #96804, #100794, #175659, #158490, #98793, #54310, #52303, #69475, #39139, #146303, #131141, #191820, #130123, #82625, #144307, #177671, #53300, #176672, #7792, #192829, #20968, #4789, #113960, #38148, #112975, #115982, #68468, #114979, #162477, #66479, #173681, #190827, #128141, #189841, #99802, #80647, #37133, #161488, #19977, #142323, #3803, #65481, #127143, #188850, #159474, #22976, #50334, #83629, #145306, #81620, #36133, #143303, #51314, #174668, #84625, #5797, #67470, #129129, #160487, #21977, #6789, #10813, #102812, #24993, #73489, #88633, #8810, #74474, #41149, #182649, #195844, #136139, #55302, #133141, #44133, #150329, #70479, #86637, #11824, #135162, #197815, #56305, #59280, #196835, #116974, #58303, #194832, #26988, #117987, #85635, #27991, #120950, #164497, #118993, #119970, #72483, #178666, #132145, #166493, #105792, #179677, #57317, #9815, #181656, #23979, #25990, #147322, #87633, #149319, #193838, #134156, #40129, #101807, #180676, #42152, #43135, #103812 ) ),
 .UNSPECIFIED., .T., .F., .T. ) 
 B_SPLINE_SURFACE_WITH_KNOTS ( ( 4, 3, 4 ),
 ( 3, 2, 2, 2, 2, 2, 2, 2, 2, 2, 2, 2, 2, 2, 2, 2, 2, 2, 2, 2, 2, 2, 2, 2, 2, 2, 2, 2, 2, 2, 2, 2, 2, 2, 2, 2, 2, 2, 2, 2, 2, 2, 2, 2, 2, 2, 2, 2, 2, 2, 2, 2, 2, 2, 2, 2, 2, 2, 2, 2, 2, 2, 2, 2, 2, 2, 2, 2, 2, 2, 2, 2, 2, 2, 2, 2, 2, 2, 2, 2, 2, 2, 2, 2, 2, 2, 2, 2, 2, 2, 2, 2, 2, 2, 2, 2, 2, 2, 2, 2, 2, 2, 2, 2, 2, 2, 2, 2, 2, 2, 2, 2, 2, 2, 2, 2, 2, 2, 2, 2, 2, 2, 2, 2, 2, 2, 2, 2, 2, 2, 2, 2, 2, 2, 2, 2, 2, 2, 2, 2, 2, 2, 2, 2, 2, 2, 2, 2, 2, 2, 2, 2, 2, 2, 2, 2, 2, 2, 2, 2, 2, 2, 2, 2, 2, 2, 2, 2, 2, 2, 2, 2, 2, 2, 2, 2, 2, 2, 2, 2, 2, 2, 2, 2, 2, 2, 2, 2, 2, 2, 2, 2, 2, 2, 2, 2, 2, 2, 2, 2, 2, 2, 2, 2, 2, 2, 2, 2, 2, 2, 2, 2, 2, 2, 2, 2, 2, 2, 2, 2, 2, 2, 2, 2, 2, 2, 2, 2, 3 ),
 ( 0.000000000000000000, 0.5000000000000000000, 1.000000000000000000 ),
 ( 0.000000000000000000, 0.004385964912280701511, 0.008771929824561403022, 0.01315789473684210453, 0.01754385964912280604, 0.02192982456140350755, 0.02631578947368420907, 0.03070175438596491058, 0.03508771929824561209, 0.03947368421052631360, 0.04385964912280701511, 0.04824561403508771662, 0.05263157894736841813, 0.05701754385964911964, 0.06140350877192982115, 0.06578947368421052266, 0.07017543859649122417, 0.07456140350877192569, 0.07894736842105262720, 0.08333333333333332871, 0.08771929824561403022, 0.09210526315789473173, 0.09649122807017543324, 0.1008771929824561348, 0.1052631578947368363, 0.1096491228070175378, 0.1140350877192982393, 0.1184210526315789408, 0.1228070175438596423, 0.1271929824561403577, 0.1315789473684210453, 0.1359649122807017607, 0.1403508771929824483, 0.1447368421052631637, 0.1491228070175438514, 0.1535087719298245668, 0.1578947368421052544, 0.1622807017543859698, 0.1666666666666666574, 0.1710526315789473728, 0.1754385964912280604, 0.1798245614035087758, 0.1842105263157894635, 0.1885964912280701788, 0.1929824561403508665, 0.1973684210526315819, 0.2017543859649122695, 0.2061403508771929849, 0.2105263157894736725, 0.2149122807017543879, 0.2192982456140350755, 0.2236842105263157909, 0.2280701754385964786, 0.2324561403508771940, 0.2368421052631578816, 0.2412280701754385970, 0.2456140350877192846, 0.2500000000000000000, 0.2543859649122807154, 0.2587719298245614308, 0.2631578947368420907, 0.2675438596491228060, 0.2719298245614035214, 0.2763157894736842368, 0.2807017543859648967, 0.2850877192982456121, 0.2894736842105263275, 0.2938596491228070429, 0.2982456140350877027, 0.3026315789473684181, 0.3070175438596491335, 0.3114035087719298489, 0.3157894736842105088, 0.3201754385964912242, 0.3245614035087719396, 0.3289473684210526550, 0.3333333333333333148, 0.3377192982456140302, 0.3421052631578947456, 0.3464912280701754610, 0.3508771929824561209, 0.3552631578947368363, 0.3596491228070175517, 0.3640350877192982670, 0.3684210526315789269, 0.3728070175438596423, 0.3771929824561403577, 0.3815789473684210731, 0.3859649122807017330, 0.3903508771929824483, 0.3947368421052631637, 0.3991228070175438791, 0.4035087719298245390, 0.4078947368421052544, 0.4122807017543859698, 0.4166666666666666852, 0.4210526315789473450, 0.4254385964912280604, 0.4298245614035087758, 0.4342105263157894912, 0.4385964912280701511, 0.4429824561403508665, 0.4473684210526315819, 0.4517543859649122973, 0.4561403508771929571, 0.4605263157894736725, 0.4649122807017543879, 0.4692982456140351033, 0.4736842105263157632, 0.4780701754385964786, 0.4824561403508771940, 0.4868421052631579093, 0.4912280701754385692, 0.4956140350877192846, 0.5000000000000000000, 0.5043859649122807154, 0.5087719298245614308, 0.5131578947368421462, 0.5175438596491228616, 0.5219298245614034659, 0.5263157894736841813, 0.5307017543859648967, 0.5350877192982456121, 0.5394736842105263275, 0.5438596491228070429, 0.5482456140350877583, 0.5526315789473684736, 0.5570175438596490780, 0.5614035087719297934, 0.5657894736842105088, 0.5701754385964912242, 0.5745614035087719396, 0.5789473684210526550, 0.5833333333333333703, 0.5877192982456140857, 0.5921052631578946901, 0.5964912280701754055, 0.6008771929824561209, 0.6052631578947368363, 0.6096491228070175517, 0.6140350877192982670, 0.6184210526315789824, 0.6228070175438596978, 0.6271929824561403022, 0.6315789473684210176, 0.6359649122807017330, 0.6403508771929824483, 0.6447368421052631637, 0.6491228070175438791, 0.6535087719298245945, 0.6578947368421053099, 0.6622807017543859143, 0.6666666666666666297, 0.6710526315789473450, 0.6754385964912280604, 0.6798245614035087758, 0.6842105263157894912, 0.6885964912280702066, 0.6929824561403509220, 0.6973684210526315264, 0.7017543859649122417, 0.7061403508771929571, 0.7105263157894736725, 0.7149122807017543879, 0.7192982456140351033, 0.7236842105263158187, 0.7280701754385965341, 0.7324561403508771384, 0.7368421052631578538, 0.7412280701754385692, 0.7456140350877192846, 0.7500000000000000000, 0.7543859649122807154, 0.7587719298245614308, 0.7631578947368421462, 0.7675438596491228616, 0.7719298245614034659, 0.7763157894736841813, 0.7807017543859648967, 0.7850877192982456121, 0.7894736842105263275, 0.7938596491228070429, 0.7982456140350877583, 0.8026315789473684736, 0.8070175438596490780, 0.8114035087719297934, 0.8157894736842105088, 0.8201754385964912242, 0.8245614035087719396, 0.8289473684210526550, 0.8333333333333333703, 0.8377192982456140857, 0.8421052631578946901, 0.8464912280701754055, 0.8508771929824561209, 0.8552631578947368363, 0.8596491228070175517, 0.8640350877192982670, 0.8684210526315789824, 0.8728070175438596978, 0.8771929824561403022, 0.8815789473684210176, 0.8859649122807017330, 0.8903508771929824483, 0.8947368421052631637, 0.8991228070175438791, 0.9035087719298245945, 0.9078947368421053099, 0.9122807017543859143, 0.9166666666666666297, 0.9210526315789473450, 0.9254385964912280604, 0.9298245614035087758, 0.9342105263157894912, 0.9385964912280702066, 0.9429824561403509220, 0.9473684210526315264, 0.9517543859649122417, 0.9561403508771929571, 0.9605263157894736725, 0.9649122807017543879, 0.9692982456140351033, 0.9736842105263158187, 0.9780701754385965341, 0.9824561403508771384, 0.9868421052631578538, 0.9912280701754385692, 0.9956140350877192846, 1.000000000000000000 ),
 .UNSPECIFIED. ) 
 GEOMETRIC_REPRESENTATION_ITEM ( )  RATIONAL_B_SPLINE_SURFACE ( (
 ( 1.000000000000000000, 0.9659258262890683122, 1.000000000000000000, 0.9659258262890683122, 1.000000000000000000, 0.9659258262890683122, 1.000000000000000000, 0.9659258262890683122, 1.000000000000000000, 0.9659258262890683122, 1.000000000000000000, 0.9659258262890683122, 1.000000000000000000, 0.9659258262890683122, 1.000000000000000000, 0.9659258262890683122, 1.000000000000000000, 0.9659258262890683122, 1.000000000000000000, 0.9659258262890683122, 1.000000000000000000, 0.9659258262890683122, 1.000000000000000000, 0.9659258262890683122, 1.000000000000000000, 0.9659258262890683122, 1.000000000000000000, 0.9659258262890683122, 1.000000000000000000, 0.9659258262890683122, 1.000000000000000000, 0.9659258262890683122, 1.000000000000000000, 0.9659258262890683122, 1.000000000000000000, 0.9659258262890683122, 1.000000000000000000, 0.9659258262890683122, 1.000000000000000000, 0.9659258262890683122, 1.000000000000000000, 0.9659258262890683122, 1.000000000000000000, 0.9659258262890683122, 1.000000000000000000, 0.9659258262890683122, 1.000000000000000000, 0.9659258262890683122, 1.000000000000000000, 0.9659258262890683122, 1.000000000000000000, 0.9659258262890683122, 1.000000000000000000, 0.9659258262890683122, 1.000000000000000000, 0.9659258262890683122, 1.000000000000000000, 0.9659258262890683122, 1.000000000000000000, 0.9659258262890683122, 1.000000000000000000, 0.9659258262890683122, 1.000000000000000000, 0.9659258262890683122, 1.000000000000000000, 0.9659258262890683122, 1.000000000000000000, 0.9659258262890683122, 1.000000000000000000, 0.9659258262890683122, 1.000000000000000000, 0.9659258262890683122, 1.000000000000000000, 0.9659258262890683122, 1.000000000000000000, 0.9659258262890683122, 1.000000000000000000, 0.9659258262890683122, 1.000000000000000000, 0.9659258262890683122, 1.000000000000000000, 0.9659258262890683122, 1.000000000000000000, 0.9659258262890683122, 1.000000000000000000, 0.9659258262890683122, 1.000000000000000000, 0.9659258262890683122, 1.000000000000000000, 0.9659258262890683122, 1.000000000000000000, 0.9659258262890683122, 1.000000000000000000, 0.9659258262890683122, 1.000000000000000000, 0.9659258262890683122, 1.000000000000000000, 0.9659258262890683122, 1.000000000000000000, 0.9659258262890683122, 1.000000000000000000, 0.9659258262890683122, 1.000000000000000000, 0.9659258262890683122, 1.000000000000000000, 0.9659258262890683122, 1.000000000000000000, 0.9659258262890683122, 1.000000000000000000, 0.9659258262890683122, 1.000000000000000000, 0.9659258262890683122, 1.000000000000000000, 0.9659258262890683122, 1.000000000000000000, 0.9659258262890683122, 1.000000000000000000, 0.9659258262890683122, 1.000000000000000000, 0.9659258262890683122, 1.000000000000000000, 0.9659258262890683122, 1.000000000000000000, 0.9659258262890683122, 1.000000000000000000, 0.9659258262890683122, 1.000000000000000000, 0.9659258262890683122, 1.000000000000000000, 0.9659258262890683122, 1.000000000000000000, 0.9659258262890683122, 1.000000000000000000, 0.9659258262890683122, 1.000000000000000000, 0.9659258262890683122, 1.000000000000000000, 0.9659258262890683122, 1.000000000000000000, 0.9659258262890683122, 1.000000000000000000, 0.9659258262890683122, 1.000000000000000000, 0.9659258262890683122, 1.000000000000000000, 0.9659258262890683122, 1.000000000000000000, 0.9659258262890683122, 1.000000000000000000, 0.9659258262890683122, 1.000000000000000000, 0.9659258262890683122, 1.000000000000000000, 0.9659258262890683122, 1.000000000000000000, 0.9659258262890683122, 1.000000000000000000, 0.9659258262890683122, 1.000000000000000000, 0.9659258262890683122, 1.000000000000000000, 0.9659258262890683122, 1.000000000000000000, 0.9659258262890683122, 1.000000000000000000, 0.9659258262890683122, 1.000000000000000000, 0.9659258262890683122, 1.000000000000000000, 0.9659258262890683122, 1.000000000000000000, 0.9659258262890683122, 1.000000000000000000, 0.9659258262890683122, 1.000000000000000000, 0.9659258262890683122, 1.000000000000000000, 0.9659258262890683122, 1.000000000000000000, 0.9659258262890683122, 1.000000000000000000, 0.9659258262890683122, 1.000000000000000000, 0.9659258262890683122, 1.000000000000000000, 0.9659258262890683122, 1.000000000000000000, 0.9659258262890683122, 1.000000000000000000, 0.9659258262890683122, 1.000000000000000000, 0.9659258262890683122, 1.000000000000000000, 0.9659258262890683122, 1.000000000000000000, 0.9659258262890683122, 1.000000000000000000, 0.9659258262890683122, 1.000000000000000000, 0.9659258262890683122, 1.000000000000000000, 0.9659258262890683122, 1.000000000000000000, 0.9659258262890683122, 1.000000000000000000, 0.9659258262890683122, 1.000000000000000000, 0.9659258262890683122, 1.000000000000000000, 0.9659258262890683122, 1.000000000000000000, 0.9659258262890683122, 1.000000000000000000, 0.9659258262890683122, 1.000000000000000000, 0.9659258262890683122, 1.000000000000000000, 0.9659258262890683122, 1.000000000000000000, 0.9659258262890683122, 1.000000000000000000, 0.9659258262890683122, 1.000000000000000000, 0.9659258262890683122, 1.000000000000000000, 0.9659258262890683122, 1.000000000000000000, 0.9659258262890683122, 1.000000000000000000, 0.9659258262890683122, 1.000000000000000000, 0.9659258262890683122, 1.000000000000000000, 0.9659258262890683122, 1.000000000000000000, 0.9659258262890683122, 1.000000000000000000, 0.9659258262890683122, 1.000000000000000000, 0.9659258262890683122, 1.000000000000000000, 0.9659258262890683122, 1.000000000000000000, 0.9659258262890683122, 1.000000000000000000, 0.9659258262890683122, 1.000000000000000000, 0.9659258262890683122, 1.000000000000000000, 0.9659258262890683122, 1.000000000000000000, 0.9659258262890683122, 1.000000000000000000, 0.9659258262890683122, 1.000000000000000000, 0.9659258262890683122, 1.000000000000000000, 0.9659258262890683122, 1.000000000000000000, 0.9659258262890683122, 1.000000000000000000, 0.9659258262890683122, 1.000000000000000000, 0.9659258262890683122, 1.000000000000000000, 0.9659258262890683122, 1.000000000000000000, 0.9659258262890683122, 1.000000000000000000, 0.9659258262890683122, 1.000000000000000000, 0.9659258262890683122, 1.000000000000000000, 0.9659258262890683122, 1.000000000000000000, 0.9659258262890683122, 1.000000000000000000, 0.9659258262890683122, 1.000000000000000000, 0.9659258262890683122, 1.000000000000000000, 0.9659258262890683122, 1.000000000000000000, 0.9659258262890683122, 1.000000000000000000, 0.9659258262890683122, 1.000000000000000000, 0.9659258262890683122, 1.000000000000000000, 0.9659258262890683122, 1.000000000000000000, 0.9659258262890683122, 1.000000000000000000, 0.9659258262890683122, 1.000000000000000000, 0.9659258262890683122, 1.000000000000000000, 0.9659258262890683122, 1.000000000000000000, 0.9659258262890683122, 1.000000000000000000, 0.9659258262890683122, 1.000000000000000000, 0.9659258262890683122, 1.000000000000000000, 0.9659258262890683122, 1.000000000000000000, 0.9659258262890683122, 1.000000000000000000, 0.9659258262890683122, 1.000000000000000000, 0.9659258262890683122, 1.000000000000000000, 0.9659258262890683122, 1.000000000000000000, 0.9659258262890683122, 1.000000000000000000, 0.9659258262890683122, 1.000000000000000000, 0.9659258262890683122, 1.000000000000000000, 0.9659258262890683122, 1.000000000000000000, 0.9659258262890683122, 1.000000000000000000, 0.9659258262890683122, 1.000000000000000000, 0.9659258262890683122, 1.000000000000000000, 0.9659258262890683122, 1.000000000000000000, 0.9659258262890683122, 1.000000000000000000, 0.9659258262890683122, 1.000000000000000000, 0.9659258262890683122, 1.000000000000000000, 0.9659258262890683122, 1.000000000000000000, 0.9659258262890683122, 1.000000000000000000, 0.9659258262890683122, 1.000000000000000000, 0.9659258262890683122, 1.000000000000000000, 0.9659258262890683122, 1.000000000000000000, 0.9659258262890683122, 1.000000000000000000, 0.9659258262890683122, 1.000000000000000000, 0.9659258262890683122, 1.000000000000000000, 0.9659258262890683122, 1.000000000000000000, 0.9659258262890683122, 1.000000000000000000, 0.9659258262890683122, 1.000000000000000000, 0.9659258262890683122, 1.000000000000000000, 0.9659258262890683122, 1.000000000000000000, 0.9659258262890683122, 1.000000000000000000, 0.9659258262890683122, 1.000000000000000000, 0.9659258262890683122, 1.000000000000000000, 0.9659258262890683122, 1.000000000000000000, 0.9659258262890683122, 1.000000000000000000, 0.9659258262890683122, 1.000000000000000000, 0.9659258262890683122, 1.000000000000000000, 0.9659258262890683122, 1.000000000000000000, 0.9659258262890683122, 1.000000000000000000, 0.9659258262890683122, 1.000000000000000000, 0.9659258262890683122, 1.000000000000000000, 0.9659258262890683122, 1.000000000000000000, 0.9659258262890683122, 1.000000000000000000, 0.9659258262890683122, 1.000000000000000000, 0.9659258262890683122, 1.000000000000000000, 0.9659258262890683122, 1.000000000000000000, 0.9659258262890683122, 1.000000000000000000, 0.9659258262890683122, 1.000000000000000000, 0.9659258262890683122, 1.000000000000000000, 0.9659258262890683122, 1.000000000000000000, 0.9659258262890683122, 1.000000000000000000, 0.9659258262890683122, 1.000000000000000000, 0.9659258262890683122, 1.000000000000000000, 0.9659258262890683122, 1.000000000000000000, 0.9659258262890683122, 1.000000000000000000, 0.9659258262890683122, 1.000000000000000000, 0.9659258262890683122, 1.000000000000000000, 0.9659258262890683122, 1.000000000000000000, 0.9659258262890683122, 1.000000000000000000, 0.9659258262890683122, 1.000000000000000000, 0.9659258262890683122, 1.000000000000000000, 0.9659258262890683122, 1.000000000000000000, 0.9659258262890683122, 1.000000000000000000, 0.9659258262890683122, 1.000000000000000000, 0.9659258262890683122, 1.000000000000000000, 0.9659258262890683122, 1.000000000000000000, 0.9659258262890683122, 1.000000000000000000, 0.9659258262890683122, 1.000000000000000000, 0.9659258262890683122, 1.000000000000000000, 0.9659258262890683122, 1.000000000000000000, 0.9659258262890683122, 1.000000000000000000, 0.9659258262890683122, 1.000000000000000000, 0.9659258262890683122, 1.000000000000000000, 0.9659258262890683122, 1.000000000000000000, 0.9659258262890683122, 1.000000000000000000, 0.9659258262890683122, 1.000000000000000000, 0.9659258262890683122, 1.000000000000000000),
 ( 0.3333333333333333703, 0.3219752754296894559, 0.3333333333333333703, 0.3219752754296894559, 0.3333333333333333703, 0.3219752754296894559, 0.3333333333333333703, 0.3219752754296894559, 0.3333333333333333703, 0.3219752754296894559, 0.3333333333333333703, 0.3219752754296894559, 0.3333333333333333703, 0.3219752754296894559, 0.3333333333333333703, 0.3219752754296894559, 0.3333333333333333703, 0.3219752754296894559, 0.3333333333333333703, 0.3219752754296894559, 0.3333333333333333703, 0.3219752754296894559, 0.3333333333333333703, 0.3219752754296894559, 0.3333333333333333703, 0.3219752754296894559, 0.3333333333333333703, 0.3219752754296894559, 0.3333333333333333703, 0.3219752754296894559, 0.3333333333333333703, 0.3219752754296894559, 0.3333333333333333703, 0.3219752754296894559, 0.3333333333333333703, 0.3219752754296894559, 0.3333333333333333703, 0.3219752754296894559, 0.3333333333333333703, 0.3219752754296894559, 0.3333333333333333703, 0.3219752754296894559, 0.3333333333333333703, 0.3219752754296894559, 0.3333333333333333703, 0.3219752754296894559, 0.3333333333333333703, 0.3219752754296894559, 0.3333333333333333703, 0.3219752754296894559, 0.3333333333333333703, 0.3219752754296894559, 0.3333333333333333703, 0.3219752754296894559, 0.3333333333333333703, 0.3219752754296894559, 0.3333333333333333703, 0.3219752754296894559, 0.3333333333333333703, 0.3219752754296894559, 0.3333333333333333703, 0.3219752754296894559, 0.3333333333333333703, 0.3219752754296894559, 0.3333333333333333703, 0.3219752754296894559, 0.3333333333333333703, 0.3219752754296894559, 0.3333333333333333703, 0.3219752754296894559, 0.3333333333333333703, 0.3219752754296894559, 0.3333333333333333703, 0.3219752754296894559, 0.3333333333333333703, 0.3219752754296894559, 0.3333333333333333703, 0.3219752754296894559, 0.3333333333333333703, 0.3219752754296894559, 0.3333333333333333703, 0.3219752754296894559, 0.3333333333333333703, 0.3219752754296894559, 0.3333333333333333703, 0.3219752754296894559, 0.3333333333333333703, 0.3219752754296894559, 0.3333333333333333703, 0.3219752754296894559, 0.3333333333333333703, 0.3219752754296894559, 0.3333333333333333703, 0.3219752754296894559, 0.3333333333333333703, 0.3219752754296894559, 0.3333333333333333703, 0.3219752754296894559, 0.3333333333333333703, 0.3219752754296894559, 0.3333333333333333703, 0.3219752754296894559, 0.3333333333333333703, 0.3219752754296894559, 0.3333333333333333703, 0.3219752754296894559, 0.3333333333333333703, 0.3219752754296894559, 0.3333333333333333703, 0.3219752754296894559, 0.3333333333333333703, 0.3219752754296894559, 0.3333333333333333703, 0.3219752754296894559, 0.3333333333333333703, 0.3219752754296894559, 0.3333333333333333703, 0.3219752754296894559, 0.3333333333333333703, 0.3219752754296894559, 0.3333333333333333703, 0.3219752754296894559, 0.3333333333333333703, 0.3219752754296894559, 0.3333333333333333703, 0.3219752754296894559, 0.3333333333333333703, 0.3219752754296894559, 0.3333333333333333703, 0.3219752754296894559, 0.3333333333333333703, 0.3219752754296894559, 0.3333333333333333703, 0.3219752754296894559, 0.3333333333333333703, 0.3219752754296894559, 0.3333333333333333703, 0.3219752754296894559, 0.3333333333333333703, 0.3219752754296894559, 0.3333333333333333703, 0.3219752754296894559, 0.3333333333333333703, 0.3219752754296894559, 0.3333333333333333703, 0.3219752754296894559, 0.3333333333333333703, 0.3219752754296894559, 0.3333333333333333703, 0.3219752754296894559, 0.3333333333333333703, 0.3219752754296894559, 0.3333333333333333703, 0.3219752754296894559, 0.3333333333333333703, 0.3219752754296894559, 0.3333333333333333703, 0.3219752754296894559, 0.3333333333333333703, 0.3219752754296894559, 0.3333333333333333703, 0.3219752754296894559, 0.3333333333333333703, 0.3219752754296894559, 0.3333333333333333703, 0.3219752754296894559, 0.3333333333333333703, 0.3219752754296894559, 0.3333333333333333703, 0.3219752754296894559, 0.3333333333333333703, 0.3219752754296894559, 0.3333333333333333703, 0.3219752754296894559, 0.3333333333333333703, 0.3219752754296894559, 0.3333333333333333703, 0.3219752754296894559, 0.3333333333333333703, 0.3219752754296894559, 0.3333333333333333703, 0.3219752754296894559, 0.3333333333333333703, 0.3219752754296894559, 0.3333333333333333703, 0.3219752754296894559, 0.3333333333333333703, 0.3219752754296894559, 0.3333333333333333703, 0.3219752754296894559, 0.3333333333333333703, 0.3219752754296894559, 0.3333333333333333703, 0.3219752754296894559, 0.3333333333333333703, 0.3219752754296894559, 0.3333333333333333703, 0.3219752754296894559, 0.3333333333333333703, 0.3219752754296894559, 0.3333333333333333703, 0.3219752754296894559, 0.3333333333333333703, 0.3219752754296894559, 0.3333333333333333703, 0.3219752754296894559, 0.3333333333333333703, 0.3219752754296894559, 0.3333333333333333703, 0.3219752754296894559, 0.3333333333333333703, 0.3219752754296894559, 0.3333333333333333703, 0.3219752754296894559, 0.3333333333333333703, 0.3219752754296894559, 0.3333333333333333703, 0.3219752754296894559, 0.3333333333333333703, 0.3219752754296894559, 0.3333333333333333703, 0.3219752754296894559, 0.3333333333333333703, 0.3219752754296894559, 0.3333333333333333703, 0.3219752754296894559, 0.3333333333333333703, 0.3219752754296894559, 0.3333333333333333703, 0.3219752754296894559, 0.3333333333333333703, 0.3219752754296894559, 0.3333333333333333703, 0.3219752754296894559, 0.3333333333333333703, 0.3219752754296894559, 0.3333333333333333703, 0.3219752754296894559, 0.3333333333333333703, 0.3219752754296894559, 0.3333333333333333703, 0.3219752754296894559, 0.3333333333333333703, 0.3219752754296894559, 0.3333333333333333703, 0.3219752754296894559, 0.3333333333333333703, 0.3219752754296894559, 0.3333333333333333703, 0.3219752754296894559, 0.3333333333333333703, 0.3219752754296894559, 0.3333333333333333703, 0.3219752754296894559, 0.3333333333333333703, 0.3219752754296894559, 0.3333333333333333703, 0.3219752754296894559, 0.3333333333333333703, 0.3219752754296894559, 0.3333333333333333703, 0.3219752754296894559, 0.3333333333333333703, 0.3219752754296894559, 0.3333333333333333703, 0.3219752754296894559, 0.3333333333333333703, 0.3219752754296894559, 0.3333333333333333703, 0.3219752754296894559, 0.3333333333333333703, 0.3219752754296894559, 0.3333333333333333703, 0.3219752754296894559, 0.3333333333333333703, 0.3219752754296894559, 0.3333333333333333703, 0.3219752754296894559, 0.3333333333333333703, 0.3219752754296894559, 0.3333333333333333703, 0.3219752754296894559, 0.3333333333333333703, 0.3219752754296894559, 0.3333333333333333703, 0.3219752754296894559, 0.3333333333333333703, 0.3219752754296894559, 0.3333333333333333703, 0.3219752754296894559, 0.3333333333333333703, 0.3219752754296894559, 0.3333333333333333703, 0.3219752754296894559, 0.3333333333333333703, 0.3219752754296894559, 0.3333333333333333703, 0.3219752754296894559, 0.3333333333333333703, 0.3219752754296894559, 0.3333333333333333703, 0.3219752754296894559, 0.3333333333333333703, 0.3219752754296894559, 0.3333333333333333703, 0.3219752754296894559, 0.3333333333333333703, 0.3219752754296894559, 0.3333333333333333703, 0.3219752754296894559, 0.3333333333333333703, 0.3219752754296894559, 0.3333333333333333703, 0.3219752754296894559, 0.3333333333333333703, 0.3219752754296894559, 0.3333333333333333703, 0.3219752754296894559, 0.3333333333333333703, 0.3219752754296894559, 0.3333333333333333703, 0.3219752754296894559, 0.3333333333333333703, 0.3219752754296894559, 0.3333333333333333703, 0.3219752754296894559, 0.3333333333333333703, 0.3219752754296894559, 0.3333333333333333703, 0.3219752754296894559, 0.3333333333333333703, 0.3219752754296894559, 0.3333333333333333703, 0.3219752754296894559, 0.3333333333333333703, 0.3219752754296894559, 0.3333333333333333703, 0.3219752754296894559, 0.3333333333333333703, 0.3219752754296894559, 0.3333333333333333703, 0.3219752754296894559, 0.3333333333333333703, 0.3219752754296894559, 0.3333333333333333703, 0.3219752754296894559, 0.3333333333333333703, 0.3219752754296894559, 0.3333333333333333703, 0.3219752754296894559, 0.3333333333333333703, 0.3219752754296894559, 0.3333333333333333703, 0.3219752754296894559, 0.3333333333333333703, 0.3219752754296894559, 0.3333333333333333703, 0.3219752754296894559, 0.3333333333333333703, 0.3219752754296894559, 0.3333333333333333703, 0.3219752754296894559, 0.3333333333333333703, 0.3219752754296894559, 0.3333333333333333703, 0.3219752754296894559, 0.3333333333333333703, 0.3219752754296894559, 0.3333333333333333703, 0.3219752754296894559, 0.3333333333333333703, 0.3219752754296894559, 0.3333333333333333703, 0.3219752754296894559, 0.3333333333333333703, 0.3219752754296894559, 0.3333333333333333703, 0.3219752754296894559, 0.3333333333333333703, 0.3219752754296894559, 0.3333333333333333703, 0.3219752754296894559, 0.3333333333333333703, 0.3219752754296894559, 0.3333333333333333703, 0.3219752754296894559, 0.3333333333333333703, 0.3219752754296894559, 0.3333333333333333703, 0.3219752754296894559, 0.3333333333333333703, 0.3219752754296894559, 0.3333333333333333703, 0.3219752754296894559, 0.3333333333333333703, 0.3219752754296894559, 0.3333333333333333703, 0.3219752754296894559, 0.3333333333333333703, 0.3219752754296894559, 0.3333333333333333703, 0.3219752754296894559, 0.3333333333333333703, 0.3219752754296894559, 0.3333333333333333703, 0.3219752754296894559, 0.3333333333333333703, 0.3219752754296894559, 0.3333333333333333703, 0.3219752754296894559, 0.3333333333333333703, 0.3219752754296894559, 0.3333333333333333703, 0.3219752754296894559, 0.3333333333333333703, 0.3219752754296894559, 0.3333333333333333703, 0.3219752754296894559, 0.3333333333333333703, 0.3219752754296894559, 0.3333333333333333703, 0.3219752754296894559, 0.3333333333333333703, 0.3219752754296894559, 0.3333333333333333703, 0.3219752754296894559, 0.3333333333333333703, 0.3219752754296894559, 0.3333333333333333703, 0.3219752754296894559, 0.3333333333333333703, 0.3219752754296894559, 0.3333333333333333703, 0.3219752754296894559, 0.3333333333333333703, 0.3219752754296894559, 0.3333333333333333703, 0.3219752754296894559, 0.3333333333333333703, 0.3219752754296894559, 0.3333333333333333703, 0.3219752754296894559, 0.3333333333333333703, 0.3219752754296894559, 0.3333333333333333703, 0.3219752754296894559, 0.3333333333333333703, 0.3219752754296894559, 0.3333333333333333703, 0.3219752754296894559, 0.3333333333333333703, 0.3219752754296894559, 0.3333333333333333703, 0.3219752754296894559, 0.3333333333333333703, 0.3219752754296894559, 0.3333333333333333703),
 ( 0.3333333333333333703, 0.3219752754296894559, 0.3333333333333333703, 0.3219752754296894559, 0.3333333333333333703, 0.3219752754296894559, 0.3333333333333333703, 0.3219752754296894559, 0.3333333333333333703, 0.3219752754296894559, 0.3333333333333333703, 0.3219752754296894559, 0.3333333333333333703, 0.3219752754296894559, 0.3333333333333333703, 0.3219752754296894559, 0.3333333333333333703, 0.3219752754296894559, 0.3333333333333333703, 0.3219752754296894559, 0.3333333333333333703, 0.3219752754296894559, 0.3333333333333333703, 0.3219752754296894559, 0.3333333333333333703, 0.3219752754296894559, 0.3333333333333333703, 0.3219752754296894559, 0.3333333333333333703, 0.3219752754296894559, 0.3333333333333333703, 0.3219752754296894559, 0.3333333333333333703, 0.3219752754296894559, 0.3333333333333333703, 0.3219752754296894559, 0.3333333333333333703, 0.3219752754296894559, 0.3333333333333333703, 0.3219752754296894559, 0.3333333333333333703, 0.3219752754296894559, 0.3333333333333333703, 0.3219752754296894559, 0.3333333333333333703, 0.3219752754296894559, 0.3333333333333333703, 0.3219752754296894559, 0.3333333333333333703, 0.3219752754296894559, 0.3333333333333333703, 0.3219752754296894559, 0.3333333333333333703, 0.3219752754296894559, 0.3333333333333333703, 0.3219752754296894559, 0.3333333333333333703, 0.3219752754296894559, 0.3333333333333333703, 0.3219752754296894559, 0.3333333333333333703, 0.3219752754296894559, 0.3333333333333333703, 0.3219752754296894559, 0.3333333333333333703, 0.3219752754296894559, 0.3333333333333333703, 0.3219752754296894559, 0.3333333333333333703, 0.3219752754296894559, 0.3333333333333333703, 0.3219752754296894559, 0.3333333333333333703, 0.3219752754296894559, 0.3333333333333333703, 0.3219752754296894559, 0.3333333333333333703, 0.3219752754296894559, 0.3333333333333333703, 0.3219752754296894559, 0.3333333333333333703, 0.3219752754296894559, 0.3333333333333333703, 0.3219752754296894559, 0.3333333333333333703, 0.3219752754296894559, 0.3333333333333333703, 0.3219752754296894559, 0.3333333333333333703, 0.3219752754296894559, 0.3333333333333333703, 0.3219752754296894559, 0.3333333333333333703, 0.3219752754296894559, 0.3333333333333333703, 0.3219752754296894559, 0.3333333333333333703, 0.3219752754296894559, 0.3333333333333333703, 0.3219752754296894559, 0.3333333333333333703, 0.3219752754296894559, 0.3333333333333333703, 0.3219752754296894559, 0.3333333333333333703, 0.3219752754296894559, 0.3333333333333333703, 0.3219752754296894559, 0.3333333333333333703, 0.3219752754296894559, 0.3333333333333333703, 0.3219752754296894559, 0.3333333333333333703, 0.3219752754296894559, 0.3333333333333333703, 0.3219752754296894559, 0.3333333333333333703, 0.3219752754296894559, 0.3333333333333333703, 0.3219752754296894559, 0.3333333333333333703, 0.3219752754296894559, 0.3333333333333333703, 0.3219752754296894559, 0.3333333333333333703, 0.3219752754296894559, 0.3333333333333333703, 0.3219752754296894559, 0.3333333333333333703, 0.3219752754296894559, 0.3333333333333333703, 0.3219752754296894559, 0.3333333333333333703, 0.3219752754296894559, 0.3333333333333333703, 0.3219752754296894559, 0.3333333333333333703, 0.3219752754296894559, 0.3333333333333333703, 0.3219752754296894559, 0.3333333333333333703, 0.3219752754296894559, 0.3333333333333333703, 0.3219752754296894559, 0.3333333333333333703, 0.3219752754296894559, 0.3333333333333333703, 0.3219752754296894559, 0.3333333333333333703, 0.3219752754296894559, 0.3333333333333333703, 0.3219752754296894559, 0.3333333333333333703, 0.3219752754296894559, 0.3333333333333333703, 0.3219752754296894559, 0.3333333333333333703, 0.3219752754296894559, 0.3333333333333333703, 0.3219752754296894559, 0.3333333333333333703, 0.3219752754296894559, 0.3333333333333333703, 0.3219752754296894559, 0.3333333333333333703, 0.3219752754296894559, 0.3333333333333333703, 0.3219752754296894559, 0.3333333333333333703, 0.3219752754296894559, 0.3333333333333333703, 0.3219752754296894559, 0.3333333333333333703, 0.3219752754296894559, 0.3333333333333333703, 0.3219752754296894559, 0.3333333333333333703, 0.3219752754296894559, 0.3333333333333333703, 0.3219752754296894559, 0.3333333333333333703, 0.3219752754296894559, 0.3333333333333333703, 0.3219752754296894559, 0.3333333333333333703, 0.3219752754296894559, 0.3333333333333333703, 0.3219752754296894559, 0.3333333333333333703, 0.3219752754296894559, 0.3333333333333333703, 0.3219752754296894559, 0.3333333333333333703, 0.3219752754296894559, 0.3333333333333333703, 0.3219752754296894559, 0.3333333333333333703, 0.3219752754296894559, 0.3333333333333333703, 0.3219752754296894559, 0.3333333333333333703, 0.3219752754296894559, 0.3333333333333333703, 0.3219752754296894559, 0.3333333333333333703, 0.3219752754296894559, 0.3333333333333333703, 0.3219752754296894559, 0.3333333333333333703, 0.3219752754296894559, 0.3333333333333333703, 0.3219752754296894559, 0.3333333333333333703, 0.3219752754296894559, 0.3333333333333333703, 0.3219752754296894559, 0.3333333333333333703, 0.3219752754296894559, 0.3333333333333333703, 0.3219752754296894559, 0.3333333333333333703, 0.3219752754296894559, 0.3333333333333333703, 0.3219752754296894559, 0.3333333333333333703, 0.3219752754296894559, 0.3333333333333333703, 0.3219752754296894559, 0.3333333333333333703, 0.3219752754296894559, 0.3333333333333333703, 0.3219752754296894559, 0.3333333333333333703, 0.3219752754296894559, 0.3333333333333333703, 0.3219752754296894559, 0.3333333333333333703, 0.3219752754296894559, 0.3333333333333333703, 0.3219752754296894559, 0.3333333333333333703, 0.3219752754296894559, 0.3333333333333333703, 0.3219752754296894559, 0.3333333333333333703, 0.3219752754296894559, 0.3333333333333333703, 0.3219752754296894559, 0.3333333333333333703, 0.3219752754296894559, 0.3333333333333333703, 0.3219752754296894559, 0.3333333333333333703, 0.3219752754296894559, 0.3333333333333333703, 0.3219752754296894559, 0.3333333333333333703, 0.3219752754296894559, 0.3333333333333333703, 0.3219752754296894559, 0.3333333333333333703, 0.3219752754296894559, 0.3333333333333333703, 0.3219752754296894559, 0.3333333333333333703, 0.3219752754296894559, 0.3333333333333333703, 0.3219752754296894559, 0.3333333333333333703, 0.3219752754296894559, 0.3333333333333333703, 0.3219752754296894559, 0.3333333333333333703, 0.3219752754296894559, 0.3333333333333333703, 0.3219752754296894559, 0.3333333333333333703, 0.3219752754296894559, 0.3333333333333333703, 0.3219752754296894559, 0.3333333333333333703, 0.3219752754296894559, 0.3333333333333333703, 0.3219752754296894559, 0.3333333333333333703, 0.3219752754296894559, 0.3333333333333333703, 0.3219752754296894559, 0.3333333333333333703, 0.3219752754296894559, 0.3333333333333333703, 0.3219752754296894559, 0.3333333333333333703, 0.3219752754296894559, 0.3333333333333333703, 0.3219752754296894559, 0.3333333333333333703, 0.3219752754296894559, 0.3333333333333333703, 0.3219752754296894559, 0.3333333333333333703, 0.3219752754296894559, 0.3333333333333333703, 0.3219752754296894559, 0.3333333333333333703, 0.3219752754296894559, 0.3333333333333333703, 0.3219752754296894559, 0.3333333333333333703, 0.3219752754296894559, 0.3333333333333333703, 0.3219752754296894559, 0.3333333333333333703, 0.3219752754296894559, 0.3333333333333333703, 0.3219752754296894559, 0.3333333333333333703, 0.3219752754296894559, 0.3333333333333333703, 0.3219752754296894559, 0.3333333333333333703, 0.3219752754296894559, 0.3333333333333333703, 0.3219752754296894559, 0.3333333333333333703, 0.3219752754296894559, 0.3333333333333333703, 0.3219752754296894559, 0.3333333333333333703, 0.3219752754296894559, 0.3333333333333333703, 0.3219752754296894559, 0.3333333333333333703, 0.3219752754296894559, 0.3333333333333333703, 0.3219752754296894559, 0.3333333333333333703, 0.3219752754296894559, 0.3333333333333333703, 0.3219752754296894559, 0.3333333333333333703, 0.3219752754296894559, 0.3333333333333333703, 0.3219752754296894559, 0.3333333333333333703, 0.3219752754296894559, 0.3333333333333333703, 0.3219752754296894559, 0.3333333333333333703, 0.3219752754296894559, 0.3333333333333333703, 0.3219752754296894559, 0.3333333333333333703, 0.3219752754296894559, 0.3333333333333333703, 0.3219752754296894559, 0.3333333333333333703, 0.3219752754296894559, 0.3333333333333333703, 0.3219752754296894559, 0.3333333333333333703, 0.3219752754296894559, 0.3333333333333333703, 0.3219752754296894559, 0.3333333333333333703, 0.3219752754296894559, 0.3333333333333333703, 0.3219752754296894559, 0.3333333333333333703, 0.3219752754296894559, 0.3333333333333333703, 0.3219752754296894559, 0.3333333333333333703, 0.3219752754296894559, 0.3333333333333333703, 0.3219752754296894559, 0.3333333333333333703, 0.3219752754296894559, 0.3333333333333333703, 0.3219752754296894559, 0.3333333333333333703, 0.3219752754296894559, 0.3333333333333333703, 0.3219752754296894559, 0.3333333333333333703, 0.3219752754296894559, 0.3333333333333333703, 0.3219752754296894559, 0.3333333333333333703, 0.3219752754296894559, 0.3333333333333333703, 0.3219752754296894559, 0.3333333333333333703, 0.3219752754296894559, 0.3333333333333333703, 0.3219752754296894559, 0.3333333333333333703, 0.3219752754296894559, 0.3333333333333333703, 0.3219752754296894559, 0.3333333333333333703, 0.3219752754296894559, 0.3333333333333333703, 0.3219752754296894559, 0.3333333333333333703, 0.3219752754296894559, 0.3333333333333333703, 0.3219752754296894559, 0.3333333333333333703, 0.3219752754296894559, 0.3333333333333333703, 0.3219752754296894559, 0.3333333333333333703, 0.3219752754296894559, 0.3333333333333333703, 0.3219752754296894559, 0.3333333333333333703, 0.3219752754296894559, 0.3333333333333333703, 0.3219752754296894559, 0.3333333333333333703, 0.3219752754296894559, 0.3333333333333333703, 0.3219752754296894559, 0.3333333333333333703, 0.3219752754296894559, 0.3333333333333333703, 0.3219752754296894559, 0.3333333333333333703, 0.3219752754296894559, 0.3333333333333333703, 0.3219752754296894559, 0.3333333333333333703, 0.3219752754296894559, 0.3333333333333333703, 0.3219752754296894559, 0.3333333333333333703, 0.3219752754296894559, 0.3333333333333333703, 0.3219752754296894559, 0.3333333333333333703, 0.3219752754296894559, 0.3333333333333333703, 0.3219752754296894559, 0.3333333333333333703, 0.3219752754296894559, 0.3333333333333333703, 0.3219752754296894559, 0.3333333333333333703, 0.3219752754296894559, 0.3333333333333333703, 0.3219752754296894559, 0.3333333333333333703, 0.3219752754296894559, 0.3333333333333333703, 0.3219752754296894559, 0.3333333333333333703),
 ( 1.000000000000000000, 0.9659258262890683122, 1.000000000000000000, 0.9659258262890683122, 1.000000000000000000, 0.9659258262890683122, 1.000000000000000000, 0.9659258262890683122, 1.000000000000000000, 0.9659258262890683122, 1.000000000000000000, 0.9659258262890683122, 1.000000000000000000, 0.9659258262890683122, 1.000000000000000000, 0.9659258262890683122, 1.000000000000000000, 0.9659258262890683122, 1.000000000000000000, 0.9659258262890683122, 1.000000000000000000, 0.9659258262890683122, 1.000000000000000000, 0.9659258262890683122, 1.000000000000000000, 0.9659258262890683122, 1.000000000000000000, 0.9659258262890683122, 1.000000000000000000, 0.9659258262890683122, 1.000000000000000000, 0.9659258262890683122, 1.000000000000000000, 0.9659258262890683122, 1.000000000000000000, 0.9659258262890683122, 1.000000000000000000, 0.9659258262890683122, 1.000000000000000000, 0.9659258262890683122, 1.000000000000000000, 0.9659258262890683122, 1.000000000000000000, 0.9659258262890683122, 1.000000000000000000, 0.9659258262890683122, 1.000000000000000000, 0.9659258262890683122, 1.000000000000000000, 0.9659258262890683122, 1.000000000000000000, 0.9659258262890683122, 1.000000000000000000, 0.9659258262890683122, 1.000000000000000000, 0.9659258262890683122, 1.000000000000000000, 0.9659258262890683122, 1.000000000000000000, 0.9659258262890683122, 1.000000000000000000, 0.9659258262890683122, 1.000000000000000000, 0.9659258262890683122, 1.000000000000000000, 0.9659258262890683122, 1.000000000000000000, 0.9659258262890683122, 1.000000000000000000, 0.9659258262890683122, 1.000000000000000000, 0.9659258262890683122, 1.000000000000000000, 0.9659258262890683122, 1.000000000000000000, 0.9659258262890683122, 1.000000000000000000, 0.9659258262890683122, 1.000000000000000000, 0.9659258262890683122, 1.000000000000000000, 0.9659258262890683122, 1.000000000000000000, 0.9659258262890683122, 1.000000000000000000, 0.9659258262890683122, 1.000000000000000000, 0.9659258262890683122, 1.000000000000000000, 0.9659258262890683122, 1.000000000000000000, 0.9659258262890683122, 1.000000000000000000, 0.9659258262890683122, 1.000000000000000000, 0.9659258262890683122, 1.000000000000000000, 0.9659258262890683122, 1.000000000000000000, 0.9659258262890683122, 1.000000000000000000, 0.9659258262890683122, 1.000000000000000000, 0.9659258262890683122, 1.000000000000000000, 0.9659258262890683122, 1.000000000000000000, 0.9659258262890683122, 1.000000000000000000, 0.9659258262890683122, 1.000000000000000000, 0.9659258262890683122, 1.000000000000000000, 0.9659258262890683122, 1.000000000000000000, 0.9659258262890683122, 1.000000000000000000, 0.9659258262890683122, 1.000000000000000000, 0.9659258262890683122, 1.000000000000000000, 0.9659258262890683122, 1.000000000000000000, 0.9659258262890683122, 1.000000000000000000, 0.9659258262890683122, 1.000000000000000000, 0.9659258262890683122, 1.000000000000000000, 0.9659258262890683122, 1.000000000000000000, 0.9659258262890683122, 1.000000000000000000, 0.9659258262890683122, 1.000000000000000000, 0.9659258262890683122, 1.000000000000000000, 0.9659258262890683122, 1.000000000000000000, 0.9659258262890683122, 1.000000000000000000, 0.9659258262890683122, 1.000000000000000000, 0.9659258262890683122, 1.000000000000000000, 0.9659258262890683122, 1.000000000000000000, 0.9659258262890683122, 1.000000000000000000, 0.9659258262890683122, 1.000000000000000000, 0.9659258262890683122, 1.000000000000000000, 0.9659258262890683122, 1.000000000000000000, 0.9659258262890683122, 1.000000000000000000, 0.9659258262890683122, 1.000000000000000000, 0.9659258262890683122, 1.000000000000000000, 0.9659258262890683122, 1.000000000000000000, 0.9659258262890683122, 1.000000000000000000, 0.9659258262890683122, 1.000000000000000000, 0.9659258262890683122, 1.000000000000000000, 0.9659258262890683122, 1.000000000000000000, 0.9659258262890683122, 1.000000000000000000, 0.9659258262890683122, 1.000000000000000000, 0.9659258262890683122, 1.000000000000000000, 0.9659258262890683122, 1.000000000000000000, 0.9659258262890683122, 1.000000000000000000, 0.9659258262890683122, 1.000000000000000000, 0.9659258262890683122, 1.000000000000000000, 0.9659258262890683122, 1.000000000000000000, 0.9659258262890683122, 1.000000000000000000, 0.9659258262890683122, 1.000000000000000000, 0.9659258262890683122, 1.000000000000000000, 0.9659258262890683122, 1.000000000000000000, 0.9659258262890683122, 1.000000000000000000, 0.9659258262890683122, 1.000000000000000000, 0.9659258262890683122, 1.000000000000000000, 0.9659258262890683122, 1.000000000000000000, 0.9659258262890683122, 1.000000000000000000, 0.9659258262890683122, 1.000000000000000000, 0.9659258262890683122, 1.000000000000000000, 0.9659258262890683122, 1.000000000000000000, 0.9659258262890683122, 1.000000000000000000, 0.9659258262890683122, 1.000000000000000000, 0.9659258262890683122, 1.000000000000000000, 0.9659258262890683122, 1.000000000000000000, 0.9659258262890683122, 1.000000000000000000, 0.9659258262890683122, 1.000000000000000000, 0.9659258262890683122, 1.000000000000000000, 0.9659258262890683122, 1.000000000000000000, 0.9659258262890683122, 1.000000000000000000, 0.9659258262890683122, 1.000000000000000000, 0.9659258262890683122, 1.000000000000000000, 0.9659258262890683122, 1.000000000000000000, 0.9659258262890683122, 1.000000000000000000, 0.9659258262890683122, 1.000000000000000000, 0.9659258262890683122, 1.000000000000000000, 0.9659258262890683122, 1.000000000000000000, 0.9659258262890683122, 1.000000000000000000, 0.9659258262890683122, 1.000000000000000000, 0.9659258262890683122, 1.000000000000000000, 0.9659258262890683122, 1.000000000000000000, 0.9659258262890683122, 1.000000000000000000, 0.9659258262890683122, 1.000000000000000000, 0.9659258262890683122, 1.000000000000000000, 0.9659258262890683122, 1.000000000000000000, 0.9659258262890683122, 1.000000000000000000, 0.9659258262890683122, 1.000000000000000000, 0.9659258262890683122, 1.000000000000000000, 0.9659258262890683122, 1.000000000000000000, 0.9659258262890683122, 1.000000000000000000, 0.9659258262890683122, 1.000000000000000000, 0.9659258262890683122, 1.000000000000000000, 0.9659258262890683122, 1.000000000000000000, 0.9659258262890683122, 1.000000000000000000, 0.9659258262890683122, 1.000000000000000000, 0.9659258262890683122, 1.000000000000000000, 0.9659258262890683122, 1.000000000000000000, 0.9659258262890683122, 1.000000000000000000, 0.9659258262890683122, 1.000000000000000000, 0.9659258262890683122, 1.000000000000000000, 0.9659258262890683122, 1.000000000000000000, 0.9659258262890683122, 1.000000000000000000, 0.9659258262890683122, 1.000000000000000000, 0.9659258262890683122, 1.000000000000000000, 0.9659258262890683122, 1.000000000000000000, 0.9659258262890683122, 1.000000000000000000, 0.9659258262890683122, 1.000000000000000000, 0.9659258262890683122, 1.000000000000000000, 0.9659258262890683122, 1.000000000000000000, 0.9659258262890683122, 1.000000000000000000, 0.9659258262890683122, 1.000000000000000000, 0.9659258262890683122, 1.000000000000000000, 0.9659258262890683122, 1.000000000000000000, 0.9659258262890683122, 1.000000000000000000, 0.9659258262890683122, 1.000000000000000000, 0.9659258262890683122, 1.000000000000000000, 0.9659258262890683122, 1.000000000000000000, 0.9659258262890683122, 1.000000000000000000, 0.9659258262890683122, 1.000000000000000000, 0.9659258262890683122, 1.000000000000000000, 0.9659258262890683122, 1.000000000000000000, 0.9659258262890683122, 1.000000000000000000, 0.9659258262890683122, 1.000000000000000000, 0.9659258262890683122, 1.000000000000000000, 0.9659258262890683122, 1.000000000000000000, 0.9659258262890683122, 1.000000000000000000, 0.9659258262890683122, 1.000000000000000000, 0.9659258262890683122, 1.000000000000000000, 0.9659258262890683122, 1.000000000000000000, 0.9659258262890683122, 1.000000000000000000, 0.9659258262890683122, 1.000000000000000000, 0.9659258262890683122, 1.000000000000000000, 0.9659258262890683122, 1.000000000000000000, 0.9659258262890683122, 1.000000000000000000, 0.9659258262890683122, 1.000000000000000000, 0.9659258262890683122, 1.000000000000000000, 0.9659258262890683122, 1.000000000000000000, 0.9659258262890683122, 1.000000000000000000, 0.9659258262890683122, 1.000000000000000000, 0.9659258262890683122, 1.000000000000000000, 0.9659258262890683122, 1.000000000000000000, 0.9659258262890683122, 1.000000000000000000, 0.9659258262890683122, 1.000000000000000000, 0.9659258262890683122, 1.000000000000000000, 0.9659258262890683122, 1.000000000000000000, 0.9659258262890683122, 1.000000000000000000, 0.9659258262890683122, 1.000000000000000000, 0.9659258262890683122, 1.000000000000000000, 0.9659258262890683122, 1.000000000000000000, 0.9659258262890683122, 1.000000000000000000, 0.9659258262890683122, 1.000000000000000000, 0.9659258262890683122, 1.000000000000000000, 0.9659258262890683122, 1.000000000000000000, 0.9659258262890683122, 1.000000000000000000, 0.9659258262890683122, 1.000000000000000000, 0.9659258262890683122, 1.000000000000000000, 0.9659258262890683122, 1.000000000000000000, 0.9659258262890683122, 1.000000000000000000, 0.9659258262890683122, 1.000000000000000000, 0.9659258262890683122, 1.000000000000000000, 0.9659258262890683122, 1.000000000000000000, 0.9659258262890683122, 1.000000000000000000, 0.9659258262890683122, 1.000000000000000000, 0.9659258262890683122, 1.000000000000000000, 0.9659258262890683122, 1.000000000000000000, 0.9659258262890683122, 1.000000000000000000, 0.9659258262890683122, 1.000000000000000000, 0.9659258262890683122, 1.000000000000000000, 0.9659258262890683122, 1.000000000000000000, 0.9659258262890683122, 1.000000000000000000, 0.9659258262890683122, 1.000000000000000000, 0.9659258262890683122, 1.000000000000000000, 0.9659258262890683122, 1.000000000000000000, 0.9659258262890683122, 1.000000000000000000, 0.9659258262890683122, 1.000000000000000000, 0.9659258262890683122, 1.000000000000000000, 0.9659258262890683122, 1.000000000000000000, 0.9659258262890683122, 1.000000000000000000, 0.9659258262890683122, 1.000000000000000000, 0.9659258262890683122, 1.000000000000000000, 0.9659258262890683122, 1.000000000000000000, 0.9659258262890683122, 1.000000000000000000, 0.9659258262890683122, 1.000000000000000000, 0.9659258262890683122, 1.000000000000000000),
 ( 0.3333333333333333703, 0.3219752754296894559, 0.3333333333333333703, 0.3219752754296894559, 0.3333333333333333703, 0.3219752754296894559, 0.3333333333333333703, 0.3219752754296894559, 0.3333333333333333703, 0.3219752754296894559, 0.3333333333333333703, 0.3219752754296894559, 0.3333333333333333703, 0.3219752754296894559, 0.3333333333333333703, 0.3219752754296894559, 0.3333333333333333703, 0.3219752754296894559, 0.3333333333333333703, 0.3219752754296894559, 0.3333333333333333703, 0.3219752754296894559, 0.3333333333333333703, 0.3219752754296894559, 0.3333333333333333703, 0.3219752754296894559, 0.3333333333333333703, 0.3219752754296894559, 0.3333333333333333703, 0.3219752754296894559, 0.3333333333333333703, 0.3219752754296894559, 0.3333333333333333703, 0.3219752754296894559, 0.3333333333333333703, 0.3219752754296894559, 0.3333333333333333703, 0.3219752754296894559, 0.3333333333333333703, 0.3219752754296894559, 0.3333333333333333703, 0.3219752754296894559, 0.3333333333333333703, 0.3219752754296894559, 0.3333333333333333703, 0.3219752754296894559, 0.3333333333333333703, 0.3219752754296894559, 0.3333333333333333703, 0.3219752754296894559, 0.3333333333333333703, 0.3219752754296894559, 0.3333333333333333703, 0.3219752754296894559, 0.3333333333333333703, 0.3219752754296894559, 0.3333333333333333703, 0.3219752754296894559, 0.3333333333333333703, 0.3219752754296894559, 0.3333333333333333703, 0.3219752754296894559, 0.3333333333333333703, 0.3219752754296894559, 0.3333333333333333703, 0.3219752754296894559, 0.3333333333333333703, 0.3219752754296894559, 0.3333333333333333703, 0.3219752754296894559, 0.3333333333333333703, 0.3219752754296894559, 0.3333333333333333703, 0.3219752754296894559, 0.3333333333333333703, 0.3219752754296894559, 0.3333333333333333703, 0.3219752754296894559, 0.3333333333333333703, 0.3219752754296894559, 0.3333333333333333703, 0.3219752754296894559, 0.3333333333333333703, 0.3219752754296894559, 0.3333333333333333703, 0.3219752754296894559, 0.3333333333333333703, 0.3219752754296894559, 0.3333333333333333703, 0.3219752754296894559, 0.3333333333333333703, 0.3219752754296894559, 0.3333333333333333703, 0.3219752754296894559, 0.3333333333333333703, 0.3219752754296894559, 0.3333333333333333703, 0.3219752754296894559, 0.3333333333333333703, 0.3219752754296894559, 0.3333333333333333703, 0.3219752754296894559, 0.3333333333333333703, 0.3219752754296894559, 0.3333333333333333703, 0.3219752754296894559, 0.3333333333333333703, 0.3219752754296894559, 0.3333333333333333703, 0.3219752754296894559, 0.3333333333333333703, 0.3219752754296894559, 0.3333333333333333703, 0.3219752754296894559, 0.3333333333333333703, 0.3219752754296894559, 0.3333333333333333703, 0.3219752754296894559, 0.3333333333333333703, 0.3219752754296894559, 0.3333333333333333703, 0.3219752754296894559, 0.3333333333333333703, 0.3219752754296894559, 0.3333333333333333703, 0.3219752754296894559, 0.3333333333333333703, 0.3219752754296894559, 0.3333333333333333703, 0.3219752754296894559, 0.3333333333333333703, 0.3219752754296894559, 0.3333333333333333703, 0.3219752754296894559, 0.3333333333333333703, 0.3219752754296894559, 0.3333333333333333703, 0.3219752754296894559, 0.3333333333333333703, 0.3219752754296894559, 0.3333333333333333703, 0.3219752754296894559, 0.3333333333333333703, 0.3219752754296894559, 0.3333333333333333703, 0.3219752754296894559, 0.3333333333333333703, 0.3219752754296894559, 0.3333333333333333703, 0.3219752754296894559, 0.3333333333333333703, 0.3219752754296894559, 0.3333333333333333703, 0.3219752754296894559, 0.3333333333333333703, 0.3219752754296894559, 0.3333333333333333703, 0.3219752754296894559, 0.3333333333333333703, 0.3219752754296894559, 0.3333333333333333703, 0.3219752754296894559, 0.3333333333333333703, 0.3219752754296894559, 0.3333333333333333703, 0.3219752754296894559, 0.3333333333333333703, 0.3219752754296894559, 0.3333333333333333703, 0.3219752754296894559, 0.3333333333333333703, 0.3219752754296894559, 0.3333333333333333703, 0.3219752754296894559, 0.3333333333333333703, 0.3219752754296894559, 0.3333333333333333703, 0.3219752754296894559, 0.3333333333333333703, 0.3219752754296894559, 0.3333333333333333703, 0.3219752754296894559, 0.3333333333333333703, 0.3219752754296894559, 0.3333333333333333703, 0.3219752754296894559, 0.3333333333333333703, 0.3219752754296894559, 0.3333333333333333703, 0.3219752754296894559, 0.3333333333333333703, 0.3219752754296894559, 0.3333333333333333703, 0.3219752754296894559, 0.3333333333333333703, 0.3219752754296894559, 0.3333333333333333703, 0.3219752754296894559, 0.3333333333333333703, 0.3219752754296894559, 0.3333333333333333703, 0.3219752754296894559, 0.3333333333333333703, 0.3219752754296894559, 0.3333333333333333703, 0.3219752754296894559, 0.3333333333333333703, 0.3219752754296894559, 0.3333333333333333703, 0.3219752754296894559, 0.3333333333333333703, 0.3219752754296894559, 0.3333333333333333703, 0.3219752754296894559, 0.3333333333333333703, 0.3219752754296894559, 0.3333333333333333703, 0.3219752754296894559, 0.3333333333333333703, 0.3219752754296894559, 0.3333333333333333703, 0.3219752754296894559, 0.3333333333333333703, 0.3219752754296894559, 0.3333333333333333703, 0.3219752754296894559, 0.3333333333333333703, 0.3219752754296894559, 0.3333333333333333703, 0.3219752754296894559, 0.3333333333333333703, 0.3219752754296894559, 0.3333333333333333703, 0.3219752754296894559, 0.3333333333333333703, 0.3219752754296894559, 0.3333333333333333703, 0.3219752754296894559, 0.3333333333333333703, 0.3219752754296894559, 0.3333333333333333703, 0.3219752754296894559, 0.3333333333333333703, 0.3219752754296894559, 0.3333333333333333703, 0.3219752754296894559, 0.3333333333333333703, 0.3219752754296894559, 0.3333333333333333703, 0.3219752754296894559, 0.3333333333333333703, 0.3219752754296894559, 0.3333333333333333703, 0.3219752754296894559, 0.3333333333333333703, 0.3219752754296894559, 0.3333333333333333703, 0.3219752754296894559, 0.3333333333333333703, 0.3219752754296894559, 0.3333333333333333703, 0.3219752754296894559, 0.3333333333333333703, 0.3219752754296894559, 0.3333333333333333703, 0.3219752754296894559, 0.3333333333333333703, 0.3219752754296894559, 0.3333333333333333703, 0.3219752754296894559, 0.3333333333333333703, 0.3219752754296894559, 0.3333333333333333703, 0.3219752754296894559, 0.3333333333333333703, 0.3219752754296894559, 0.3333333333333333703, 0.3219752754296894559, 0.3333333333333333703, 0.3219752754296894559, 0.3333333333333333703, 0.3219752754296894559, 0.3333333333333333703, 0.3219752754296894559, 0.3333333333333333703, 0.3219752754296894559, 0.3333333333333333703, 0.3219752754296894559, 0.3333333333333333703, 0.3219752754296894559, 0.3333333333333333703, 0.3219752754296894559, 0.3333333333333333703, 0.3219752754296894559, 0.3333333333333333703, 0.3219752754296894559, 0.3333333333333333703, 0.3219752754296894559, 0.3333333333333333703, 0.3219752754296894559, 0.3333333333333333703, 0.3219752754296894559, 0.3333333333333333703, 0.3219752754296894559, 0.3333333333333333703, 0.3219752754296894559, 0.3333333333333333703, 0.3219752754296894559, 0.3333333333333333703, 0.3219752754296894559, 0.3333333333333333703, 0.3219752754296894559, 0.3333333333333333703, 0.3219752754296894559, 0.3333333333333333703, 0.3219752754296894559, 0.3333333333333333703, 0.3219752754296894559, 0.3333333333333333703, 0.3219752754296894559, 0.3333333333333333703, 0.3219752754296894559, 0.3333333333333333703, 0.3219752754296894559, 0.3333333333333333703, 0.3219752754296894559, 0.3333333333333333703, 0.3219752754296894559, 0.3333333333333333703, 0.3219752754296894559, 0.3333333333333333703, 0.3219752754296894559, 0.3333333333333333703, 0.3219752754296894559, 0.3333333333333333703, 0.3219752754296894559, 0.3333333333333333703, 0.3219752754296894559, 0.3333333333333333703, 0.3219752754296894559, 0.3333333333333333703, 0.3219752754296894559, 0.3333333333333333703, 0.3219752754296894559, 0.3333333333333333703, 0.3219752754296894559, 0.3333333333333333703, 0.3219752754296894559, 0.3333333333333333703, 0.3219752754296894559, 0.3333333333333333703, 0.3219752754296894559, 0.3333333333333333703, 0.3219752754296894559, 0.3333333333333333703, 0.3219752754296894559, 0.3333333333333333703, 0.3219752754296894559, 0.3333333333333333703, 0.3219752754296894559, 0.3333333333333333703, 0.3219752754296894559, 0.3333333333333333703, 0.3219752754296894559, 0.3333333333333333703, 0.3219752754296894559, 0.3333333333333333703, 0.3219752754296894559, 0.3333333333333333703, 0.3219752754296894559, 0.3333333333333333703, 0.3219752754296894559, 0.3333333333333333703, 0.3219752754296894559, 0.3333333333333333703, 0.3219752754296894559, 0.3333333333333333703, 0.3219752754296894559, 0.3333333333333333703, 0.3219752754296894559, 0.3333333333333333703, 0.3219752754296894559, 0.3333333333333333703, 0.3219752754296894559, 0.3333333333333333703, 0.3219752754296894559, 0.3333333333333333703, 0.3219752754296894559, 0.3333333333333333703, 0.3219752754296894559, 0.3333333333333333703, 0.3219752754296894559, 0.3333333333333333703, 0.3219752754296894559, 0.3333333333333333703, 0.3219752754296894559, 0.3333333333333333703, 0.3219752754296894559, 0.3333333333333333703, 0.3219752754296894559, 0.3333333333333333703, 0.3219752754296894559, 0.3333333333333333703, 0.3219752754296894559, 0.3333333333333333703, 0.3219752754296894559, 0.3333333333333333703, 0.3219752754296894559, 0.3333333333333333703, 0.3219752754296894559, 0.3333333333333333703, 0.3219752754296894559, 0.3333333333333333703, 0.3219752754296894559, 0.3333333333333333703, 0.3219752754296894559, 0.3333333333333333703, 0.3219752754296894559, 0.3333333333333333703, 0.3219752754296894559, 0.3333333333333333703, 0.3219752754296894559, 0.3333333333333333703, 0.3219752754296894559, 0.3333333333333333703, 0.3219752754296894559, 0.3333333333333333703, 0.3219752754296894559, 0.3333333333333333703, 0.3219752754296894559, 0.3333333333333333703, 0.3219752754296894559, 0.3333333333333333703, 0.3219752754296894559, 0.3333333333333333703, 0.3219752754296894559, 0.3333333333333333703, 0.3219752754296894559, 0.3333333333333333703, 0.3219752754296894559, 0.3333333333333333703, 0.3219752754296894559, 0.3333333333333333703, 0.3219752754296894559, 0.3333333333333333703, 0.3219752754296894559, 0.3333333333333333703, 0.3219752754296894559, 0.3333333333333333703, 0.3219752754296894559, 0.3333333333333333703, 0.3219752754296894559, 0.3333333333333333703, 0.3219752754296894559, 0.3333333333333333703, 0.3219752754296894559, 0.3333333333333333703),
 ( 0.3333333333333333703, 0.3219752754296894559, 0.3333333333333333703, 0.3219752754296894559, 0.3333333333333333703, 0.3219752754296894559, 0.3333333333333333703, 0.3219752754296894559, 0.3333333333333333703, 0.3219752754296894559, 0.3333333333333333703, 0.3219752754296894559, 0.3333333333333333703, 0.3219752754296894559, 0.3333333333333333703, 0.3219752754296894559, 0.3333333333333333703, 0.3219752754296894559, 0.3333333333333333703, 0.3219752754296894559, 0.3333333333333333703, 0.3219752754296894559, 0.3333333333333333703, 0.3219752754296894559, 0.3333333333333333703, 0.3219752754296894559, 0.3333333333333333703, 0.3219752754296894559, 0.3333333333333333703, 0.3219752754296894559, 0.3333333333333333703, 0.3219752754296894559, 0.3333333333333333703, 0.3219752754296894559, 0.3333333333333333703, 0.3219752754296894559, 0.3333333333333333703, 0.3219752754296894559, 0.3333333333333333703, 0.3219752754296894559, 0.3333333333333333703, 0.3219752754296894559, 0.3333333333333333703, 0.3219752754296894559, 0.3333333333333333703, 0.3219752754296894559, 0.3333333333333333703, 0.3219752754296894559, 0.3333333333333333703, 0.3219752754296894559, 0.3333333333333333703, 0.3219752754296894559, 0.3333333333333333703, 0.3219752754296894559, 0.3333333333333333703, 0.3219752754296894559, 0.3333333333333333703, 0.3219752754296894559, 0.3333333333333333703, 0.3219752754296894559, 0.3333333333333333703, 0.3219752754296894559, 0.3333333333333333703, 0.3219752754296894559, 0.3333333333333333703, 0.3219752754296894559, 0.3333333333333333703, 0.3219752754296894559, 0.3333333333333333703, 0.3219752754296894559, 0.3333333333333333703, 0.3219752754296894559, 0.3333333333333333703, 0.3219752754296894559, 0.3333333333333333703, 0.3219752754296894559, 0.3333333333333333703, 0.3219752754296894559, 0.3333333333333333703, 0.3219752754296894559, 0.3333333333333333703, 0.3219752754296894559, 0.3333333333333333703, 0.3219752754296894559, 0.3333333333333333703, 0.3219752754296894559, 0.3333333333333333703, 0.3219752754296894559, 0.3333333333333333703, 0.3219752754296894559, 0.3333333333333333703, 0.3219752754296894559, 0.3333333333333333703, 0.3219752754296894559, 0.3333333333333333703, 0.3219752754296894559, 0.3333333333333333703, 0.3219752754296894559, 0.3333333333333333703, 0.3219752754296894559, 0.3333333333333333703, 0.3219752754296894559, 0.3333333333333333703, 0.3219752754296894559, 0.3333333333333333703, 0.3219752754296894559, 0.3333333333333333703, 0.3219752754296894559, 0.3333333333333333703, 0.3219752754296894559, 0.3333333333333333703, 0.3219752754296894559, 0.3333333333333333703, 0.3219752754296894559, 0.3333333333333333703, 0.3219752754296894559, 0.3333333333333333703, 0.3219752754296894559, 0.3333333333333333703, 0.3219752754296894559, 0.3333333333333333703, 0.3219752754296894559, 0.3333333333333333703, 0.3219752754296894559, 0.3333333333333333703, 0.3219752754296894559, 0.3333333333333333703, 0.3219752754296894559, 0.3333333333333333703, 0.3219752754296894559, 0.3333333333333333703, 0.3219752754296894559, 0.3333333333333333703, 0.3219752754296894559, 0.3333333333333333703, 0.3219752754296894559, 0.3333333333333333703, 0.3219752754296894559, 0.3333333333333333703, 0.3219752754296894559, 0.3333333333333333703, 0.3219752754296894559, 0.3333333333333333703, 0.3219752754296894559, 0.3333333333333333703, 0.3219752754296894559, 0.3333333333333333703, 0.3219752754296894559, 0.3333333333333333703, 0.3219752754296894559, 0.3333333333333333703, 0.3219752754296894559, 0.3333333333333333703, 0.3219752754296894559, 0.3333333333333333703, 0.3219752754296894559, 0.3333333333333333703, 0.3219752754296894559, 0.3333333333333333703, 0.3219752754296894559, 0.3333333333333333703, 0.3219752754296894559, 0.3333333333333333703, 0.3219752754296894559, 0.3333333333333333703, 0.3219752754296894559, 0.3333333333333333703, 0.3219752754296894559, 0.3333333333333333703, 0.3219752754296894559, 0.3333333333333333703, 0.3219752754296894559, 0.3333333333333333703, 0.3219752754296894559, 0.3333333333333333703, 0.3219752754296894559, 0.3333333333333333703, 0.3219752754296894559, 0.3333333333333333703, 0.3219752754296894559, 0.3333333333333333703, 0.3219752754296894559, 0.3333333333333333703, 0.3219752754296894559, 0.3333333333333333703, 0.3219752754296894559, 0.3333333333333333703, 0.3219752754296894559, 0.3333333333333333703, 0.3219752754296894559, 0.3333333333333333703, 0.3219752754296894559, 0.3333333333333333703, 0.3219752754296894559, 0.3333333333333333703, 0.3219752754296894559, 0.3333333333333333703, 0.3219752754296894559, 0.3333333333333333703, 0.3219752754296894559, 0.3333333333333333703, 0.3219752754296894559, 0.3333333333333333703, 0.3219752754296894559, 0.3333333333333333703, 0.3219752754296894559, 0.3333333333333333703, 0.3219752754296894559, 0.3333333333333333703, 0.3219752754296894559, 0.3333333333333333703, 0.3219752754296894559, 0.3333333333333333703, 0.3219752754296894559, 0.3333333333333333703, 0.3219752754296894559, 0.3333333333333333703, 0.3219752754296894559, 0.3333333333333333703, 0.3219752754296894559, 0.3333333333333333703, 0.3219752754296894559, 0.3333333333333333703, 0.3219752754296894559, 0.3333333333333333703, 0.3219752754296894559, 0.3333333333333333703, 0.3219752754296894559, 0.3333333333333333703, 0.3219752754296894559, 0.3333333333333333703, 0.3219752754296894559, 0.3333333333333333703, 0.3219752754296894559, 0.3333333333333333703, 0.3219752754296894559, 0.3333333333333333703, 0.3219752754296894559, 0.3333333333333333703, 0.3219752754296894559, 0.3333333333333333703, 0.3219752754296894559, 0.3333333333333333703, 0.3219752754296894559, 0.3333333333333333703, 0.3219752754296894559, 0.3333333333333333703, 0.3219752754296894559, 0.3333333333333333703, 0.3219752754296894559, 0.3333333333333333703, 0.3219752754296894559, 0.3333333333333333703, 0.3219752754296894559, 0.3333333333333333703, 0.3219752754296894559, 0.3333333333333333703, 0.3219752754296894559, 0.3333333333333333703, 0.3219752754296894559, 0.3333333333333333703, 0.3219752754296894559, 0.3333333333333333703, 0.3219752754296894559, 0.3333333333333333703, 0.3219752754296894559, 0.3333333333333333703, 0.3219752754296894559, 0.3333333333333333703, 0.3219752754296894559, 0.3333333333333333703, 0.3219752754296894559, 0.3333333333333333703, 0.3219752754296894559, 0.3333333333333333703, 0.3219752754296894559, 0.3333333333333333703, 0.3219752754296894559, 0.3333333333333333703, 0.3219752754296894559, 0.3333333333333333703, 0.3219752754296894559, 0.3333333333333333703, 0.3219752754296894559, 0.3333333333333333703, 0.3219752754296894559, 0.3333333333333333703, 0.3219752754296894559, 0.3333333333333333703, 0.3219752754296894559, 0.3333333333333333703, 0.3219752754296894559, 0.3333333333333333703, 0.3219752754296894559, 0.3333333333333333703, 0.3219752754296894559, 0.3333333333333333703, 0.3219752754296894559, 0.3333333333333333703, 0.3219752754296894559, 0.3333333333333333703, 0.3219752754296894559, 0.3333333333333333703, 0.3219752754296894559, 0.3333333333333333703, 0.3219752754296894559, 0.3333333333333333703, 0.3219752754296894559, 0.3333333333333333703, 0.3219752754296894559, 0.3333333333333333703, 0.3219752754296894559, 0.3333333333333333703, 0.3219752754296894559, 0.3333333333333333703, 0.3219752754296894559, 0.3333333333333333703, 0.3219752754296894559, 0.3333333333333333703, 0.3219752754296894559, 0.3333333333333333703, 0.3219752754296894559, 0.3333333333333333703, 0.3219752754296894559, 0.3333333333333333703, 0.3219752754296894559, 0.3333333333333333703, 0.3219752754296894559, 0.3333333333333333703, 0.3219752754296894559, 0.3333333333333333703, 0.3219752754296894559, 0.3333333333333333703, 0.3219752754296894559, 0.3333333333333333703, 0.3219752754296894559, 0.3333333333333333703, 0.3219752754296894559, 0.3333333333333333703, 0.3219752754296894559, 0.3333333333333333703, 0.3219752754296894559, 0.3333333333333333703, 0.3219752754296894559, 0.3333333333333333703, 0.3219752754296894559, 0.3333333333333333703, 0.3219752754296894559, 0.3333333333333333703, 0.3219752754296894559, 0.3333333333333333703, 0.3219752754296894559, 0.3333333333333333703, 0.3219752754296894559, 0.3333333333333333703, 0.3219752754296894559, 0.3333333333333333703, 0.3219752754296894559, 0.3333333333333333703, 0.3219752754296894559, 0.3333333333333333703, 0.3219752754296894559, 0.3333333333333333703, 0.3219752754296894559, 0.3333333333333333703, 0.3219752754296894559, 0.3333333333333333703, 0.3219752754296894559, 0.3333333333333333703, 0.3219752754296894559, 0.3333333333333333703, 0.3219752754296894559, 0.3333333333333333703, 0.3219752754296894559, 0.3333333333333333703, 0.3219752754296894559, 0.3333333333333333703, 0.3219752754296894559, 0.3333333333333333703, 0.3219752754296894559, 0.3333333333333333703, 0.3219752754296894559, 0.3333333333333333703, 0.3219752754296894559, 0.3333333333333333703, 0.3219752754296894559, 0.3333333333333333703, 0.3219752754296894559, 0.3333333333333333703, 0.3219752754296894559, 0.3333333333333333703, 0.3219752754296894559, 0.3333333333333333703, 0.3219752754296894559, 0.3333333333333333703, 0.3219752754296894559, 0.3333333333333333703, 0.3219752754296894559, 0.3333333333333333703, 0.3219752754296894559, 0.3333333333333333703, 0.3219752754296894559, 0.3333333333333333703, 0.3219752754296894559, 0.3333333333333333703, 0.3219752754296894559, 0.3333333333333333703, 0.3219752754296894559, 0.3333333333333333703, 0.3219752754296894559, 0.3333333333333333703, 0.3219752754296894559, 0.3333333333333333703, 0.3219752754296894559, 0.3333333333333333703, 0.3219752754296894559, 0.3333333333333333703, 0.3219752754296894559, 0.3333333333333333703, 0.3219752754296894559, 0.3333333333333333703, 0.3219752754296894559, 0.3333333333333333703, 0.3219752754296894559, 0.3333333333333333703, 0.3219752754296894559, 0.3333333333333333703, 0.3219752754296894559, 0.3333333333333333703, 0.3219752754296894559, 0.3333333333333333703, 0.3219752754296894559, 0.3333333333333333703, 0.3219752754296894559, 0.3333333333333333703, 0.3219752754296894559, 0.3333333333333333703, 0.3219752754296894559, 0.3333333333333333703, 0.3219752754296894559, 0.3333333333333333703, 0.3219752754296894559, 0.3333333333333333703, 0.3219752754296894559, 0.3333333333333333703, 0.3219752754296894559, 0.3333333333333333703, 0.3219752754296894559, 0.3333333333333333703, 0.3219752754296894559, 0.3333333333333333703, 0.3219752754296894559, 0.3333333333333333703, 0.3219752754296894559, 0.3333333333333333703, 0.3219752754296894559, 0.3333333333333333703),
 ( 1.000000000000000000, 0.9659258262890683122, 1.000000000000000000, 0.9659258262890683122, 1.000000000000000000, 0.9659258262890683122, 1.000000000000000000, 0.9659258262890683122, 1.000000000000000000, 0.9659258262890683122, 1.000000000000000000, 0.9659258262890683122, 1.000000000000000000, 0.9659258262890683122, 1.000000000000000000, 0.9659258262890683122, 1.000000000000000000, 0.9659258262890683122, 1.000000000000000000, 0.9659258262890683122, 1.000000000000000000, 0.9659258262890683122, 1.000000000000000000, 0.9659258262890683122, 1.000000000000000000, 0.9659258262890683122, 1.000000000000000000, 0.9659258262890683122, 1.000000000000000000, 0.9659258262890683122, 1.000000000000000000, 0.9659258262890683122, 1.000000000000000000, 0.9659258262890683122, 1.000000000000000000, 0.9659258262890683122, 1.000000000000000000, 0.9659258262890683122, 1.000000000000000000, 0.9659258262890683122, 1.000000000000000000, 0.9659258262890683122, 1.000000000000000000, 0.9659258262890683122, 1.000000000000000000, 0.9659258262890683122, 1.000000000000000000, 0.9659258262890683122, 1.000000000000000000, 0.9659258262890683122, 1.000000000000000000, 0.9659258262890683122, 1.000000000000000000, 0.9659258262890683122, 1.000000000000000000, 0.9659258262890683122, 1.000000000000000000, 0.9659258262890683122, 1.000000000000000000, 0.9659258262890683122, 1.000000000000000000, 0.9659258262890683122, 1.000000000000000000, 0.9659258262890683122, 1.000000000000000000, 0.9659258262890683122, 1.000000000000000000, 0.9659258262890683122, 1.000000000000000000, 0.9659258262890683122, 1.000000000000000000, 0.9659258262890683122, 1.000000000000000000, 0.9659258262890683122, 1.000000000000000000, 0.9659258262890683122, 1.000000000000000000, 0.9659258262890683122, 1.000000000000000000, 0.9659258262890683122, 1.000000000000000000, 0.9659258262890683122, 1.000000000000000000, 0.9659258262890683122, 1.000000000000000000, 0.9659258262890683122, 1.000000000000000000, 0.9659258262890683122, 1.000000000000000000, 0.9659258262890683122, 1.000000000000000000, 0.9659258262890683122, 1.000000000000000000, 0.9659258262890683122, 1.000000000000000000, 0.9659258262890683122, 1.000000000000000000, 0.9659258262890683122, 1.000000000000000000, 0.9659258262890683122, 1.000000000000000000, 0.9659258262890683122, 1.000000000000000000, 0.9659258262890683122, 1.000000000000000000, 0.9659258262890683122, 1.000000000000000000, 0.9659258262890683122, 1.000000000000000000, 0.9659258262890683122, 1.000000000000000000, 0.9659258262890683122, 1.000000000000000000, 0.9659258262890683122, 1.000000000000000000, 0.9659258262890683122, 1.000000000000000000, 0.9659258262890683122, 1.000000000000000000, 0.9659258262890683122, 1.000000000000000000, 0.9659258262890683122, 1.000000000000000000, 0.9659258262890683122, 1.000000000000000000, 0.9659258262890683122, 1.000000000000000000, 0.9659258262890683122, 1.000000000000000000, 0.9659258262890683122, 1.000000000000000000, 0.9659258262890683122, 1.000000000000000000, 0.9659258262890683122, 1.000000000000000000, 0.9659258262890683122, 1.000000000000000000, 0.9659258262890683122, 1.000000000000000000, 0.9659258262890683122, 1.000000000000000000, 0.9659258262890683122, 1.000000000000000000, 0.9659258262890683122, 1.000000000000000000, 0.9659258262890683122, 1.000000000000000000, 0.9659258262890683122, 1.000000000000000000, 0.9659258262890683122, 1.000000000000000000, 0.9659258262890683122, 1.000000000000000000, 0.9659258262890683122, 1.000000000000000000, 0.9659258262890683122, 1.000000000000000000, 0.9659258262890683122, 1.000000000000000000, 0.9659258262890683122, 1.000000000000000000, 0.9659258262890683122, 1.000000000000000000, 0.9659258262890683122, 1.000000000000000000, 0.9659258262890683122, 1.000000000000000000, 0.9659258262890683122, 1.000000000000000000, 0.9659258262890683122, 1.000000000000000000, 0.9659258262890683122, 1.000000000000000000, 0.9659258262890683122, 1.000000000000000000, 0.9659258262890683122, 1.000000000000000000, 0.9659258262890683122, 1.000000000000000000, 0.9659258262890683122, 1.000000000000000000, 0.9659258262890683122, 1.000000000000000000, 0.9659258262890683122, 1.000000000000000000, 0.9659258262890683122, 1.000000000000000000, 0.9659258262890683122, 1.000000000000000000, 0.9659258262890683122, 1.000000000000000000, 0.9659258262890683122, 1.000000000000000000, 0.9659258262890683122, 1.000000000000000000, 0.9659258262890683122, 1.000000000000000000, 0.9659258262890683122, 1.000000000000000000, 0.9659258262890683122, 1.000000000000000000, 0.9659258262890683122, 1.000000000000000000, 0.9659258262890683122, 1.000000000000000000, 0.9659258262890683122, 1.000000000000000000, 0.9659258262890683122, 1.000000000000000000, 0.9659258262890683122, 1.000000000000000000, 0.9659258262890683122, 1.000000000000000000, 0.9659258262890683122, 1.000000000000000000, 0.9659258262890683122, 1.000000000000000000, 0.9659258262890683122, 1.000000000000000000, 0.9659258262890683122, 1.000000000000000000, 0.9659258262890683122, 1.000000000000000000, 0.9659258262890683122, 1.000000000000000000, 0.9659258262890683122, 1.000000000000000000, 0.9659258262890683122, 1.000000000000000000, 0.9659258262890683122, 1.000000000000000000, 0.9659258262890683122, 1.000000000000000000, 0.9659258262890683122, 1.000000000000000000, 0.9659258262890683122, 1.000000000000000000, 0.9659258262890683122, 1.000000000000000000, 0.9659258262890683122, 1.000000000000000000, 0.9659258262890683122, 1.000000000000000000, 0.9659258262890683122, 1.000000000000000000, 0.9659258262890683122, 1.000000000000000000, 0.9659258262890683122, 1.000000000000000000, 0.9659258262890683122, 1.000000000000000000, 0.9659258262890683122, 1.000000000000000000, 0.9659258262890683122, 1.000000000000000000, 0.9659258262890683122, 1.000000000000000000, 0.9659258262890683122, 1.000000000000000000, 0.9659258262890683122, 1.000000000000000000, 0.9659258262890683122, 1.000000000000000000, 0.9659258262890683122, 1.000000000000000000, 0.9659258262890683122, 1.000000000000000000, 0.9659258262890683122, 1.000000000000000000, 0.9659258262890683122, 1.000000000000000000, 0.9659258262890683122, 1.000000000000000000, 0.9659258262890683122, 1.000000000000000000, 0.9659258262890683122, 1.000000000000000000, 0.9659258262890683122, 1.000000000000000000, 0.9659258262890683122, 1.000000000000000000, 0.9659258262890683122, 1.000000000000000000, 0.9659258262890683122, 1.000000000000000000, 0.9659258262890683122, 1.000000000000000000, 0.9659258262890683122, 1.000000000000000000, 0.9659258262890683122, 1.000000000000000000, 0.9659258262890683122, 1.000000000000000000, 0.9659258262890683122, 1.000000000000000000, 0.9659258262890683122, 1.000000000000000000, 0.9659258262890683122, 1.000000000000000000, 0.9659258262890683122, 1.000000000000000000, 0.9659258262890683122, 1.000000000000000000, 0.9659258262890683122, 1.000000000000000000, 0.9659258262890683122, 1.000000000000000000, 0.9659258262890683122, 1.000000000000000000, 0.9659258262890683122, 1.000000000000000000, 0.9659258262890683122, 1.000000000000000000, 0.9659258262890683122, 1.000000000000000000, 0.9659258262890683122, 1.000000000000000000, 0.9659258262890683122, 1.000000000000000000, 0.9659258262890683122, 1.000000000000000000, 0.9659258262890683122, 1.000000000000000000, 0.9659258262890683122, 1.000000000000000000, 0.9659258262890683122, 1.000000000000000000, 0.9659258262890683122, 1.000000000000000000, 0.9659258262890683122, 1.000000000000000000, 0.9659258262890683122, 1.000000000000000000, 0.9659258262890683122, 1.000000000000000000, 0.9659258262890683122, 1.000000000000000000, 0.9659258262890683122, 1.000000000000000000, 0.9659258262890683122, 1.000000000000000000, 0.9659258262890683122, 1.000000000000000000, 0.9659258262890683122, 1.000000000000000000, 0.9659258262890683122, 1.000000000000000000, 0.9659258262890683122, 1.000000000000000000, 0.9659258262890683122, 1.000000000000000000, 0.9659258262890683122, 1.000000000000000000, 0.9659258262890683122, 1.000000000000000000, 0.9659258262890683122, 1.000000000000000000, 0.9659258262890683122, 1.000000000000000000, 0.9659258262890683122, 1.000000000000000000, 0.9659258262890683122, 1.000000000000000000, 0.9659258262890683122, 1.000000000000000000, 0.9659258262890683122, 1.000000000000000000, 0.9659258262890683122, 1.000000000000000000, 0.9659258262890683122, 1.000000000000000000, 0.9659258262890683122, 1.000000000000000000, 0.9659258262890683122, 1.000000000000000000, 0.9659258262890683122, 1.000000000000000000, 0.9659258262890683122, 1.000000000000000000, 0.9659258262890683122, 1.000000000000000000, 0.9659258262890683122, 1.000000000000000000, 0.9659258262890683122, 1.000000000000000000, 0.9659258262890683122, 1.000000000000000000, 0.9659258262890683122, 1.000000000000000000, 0.9659258262890683122, 1.000000000000000000, 0.9659258262890683122, 1.000000000000000000, 0.9659258262890683122, 1.000000000000000000, 0.9659258262890683122, 1.000000000000000000, 0.9659258262890683122, 1.000000000000000000, 0.9659258262890683122, 1.000000000000000000, 0.9659258262890683122, 1.000000000000000000, 0.9659258262890683122, 1.000000000000000000, 0.9659258262890683122, 1.000000000000000000, 0.9659258262890683122, 1.000000000000000000, 0.9659258262890683122, 1.000000000000000000, 0.9659258262890683122, 1.000000000000000000, 0.9659258262890683122, 1.000000000000000000, 0.9659258262890683122, 1.000000000000000000, 0.9659258262890683122, 1.000000000000000000, 0.9659258262890683122, 1.000000000000000000, 0.9659258262890683122, 1.000000000000000000, 0.9659258262890683122, 1.000000000000000000, 0.9659258262890683122, 1.000000000000000000, 0.9659258262890683122, 1.000000000000000000, 0.9659258262890683122, 1.000000000000000000, 0.9659258262890683122, 1.000000000000000000, 0.9659258262890683122, 1.000000000000000000, 0.9659258262890683122, 1.000000000000000000, 0.9659258262890683122, 1.000000000000000000, 0.9659258262890683122, 1.000000000000000000, 0.9659258262890683122, 1.000000000000000000, 0.9659258262890683122, 1.000000000000000000, 0.9659258262890683122, 1.000000000000000000, 0.9659258262890683122, 1.000000000000000000, 0.9659258262890683122, 1.000000000000000000, 0.9659258262890683122, 1.000000000000000000, 0.9659258262890683122, 1.000000000000000000, 0.9659258262890683122, 1.000000000000000000) ) ) 
 REPRESENTATION_ITEM ( '' )  SURFACE ( )  );
#113094 = CARTESIAN_POINT ( 'NONE',  ( -9.474510206698964154, 16.51473224551069663, 90.41557627198103830 ) ) ;
#113095 = CARTESIAN_POINT ( 'NONE',  ( 10.81492255796078972, 18.62759615963270932, 94.58224293864769550 ) ) ;
#113096 = CARTESIAN_POINT ( 'NONE',  ( -16.46253265017160317, 9.564922557960807481, 65.83224293864769550 ) ) ;
#113097 = CARTESIAN_POINT ( 'NONE',  ( -17.44270441346514033, -5.991230190323104665, 61.36335079264229364 ) ) ;
#113098 = CARTESIAN_POINT ( 'NONE',  ( 4.483927247898545687, 16.52544592524342804, 74.79057627198105251 ) ) ;
#113099 = CARTESIAN_POINT ( 'NONE',  ( 16.46253265017160672, -9.564922557960803928, 113.3322429386476955 ) ) ;
#113100 = CARTESIAN_POINT ( 'NONE',  ( -28.91687668646899922, 0.2552802045325772706, -52.63629878241253124 ) ) ;
#113101 = CARTESIAN_POINT ( 'NONE',  ( 21.52544592524344225, -5.823673210054117533, 88.54057627198103830 ) ) ;
#113102 = CARTESIAN_POINT ( 'NONE',  ( -13.97604488694547697, 13.89961937509957934, 48.12609039468566863 ) ) ;
#113103 = CARTESIAN_POINT ( 'NONE',  ( -5.153800228976328057, -19.02544592524343514, 112.2905762719810099 ) ) ;
#113104 = LINE ( 'NONE', #189969, #63000 ) ;
#113105 = CARTESIAN_POINT ( 'NONE',  ( -5.823673210054116645, -21.52544592524344225, 52.29057627198102409 ) ) ;
#113106 = AXIS2_PLACEMENT_3D ( 'NONE', #172208, #70768, #53593 ) ;
#113107 = CARTESIAN_POINT ( 'NONE',  ( -5.049401038298153566, 19.05341960407611168, 80.20724293864769550 ) ) ;
#113108 = CARTESIAN_POINT ( 'NONE',  ( 10.81492255796106328, -18.62759615963255655, 80.41775706135234714 ) ) ;
#113109 = CARTESIAN_POINT ( 'NONE',  ( 19.02544592524343514, -5.153800228976328945, 38.54057627198103120 ) ) ;
#113110 = CARTESIAN_POINT ( 'NONE',  ( -12.14591786802309592, -12.06949235617757132, 76.87390960531439532 ) ) ;
#113111 = CARTESIAN_POINT ( 'NONE',  ( 4.379528057220092307, 16.55341960407617563, 22.29275706135235069 ) ) ;
#113112 = CARTESIAN_POINT ( 'NONE',  ( -15.80617190586768217, 15.72974639402176855, 63.12609039468568994 ) ) ;
#113113 = ORIENTED_EDGE ( 'NONE', *, *, #93672, .T. ) ;
#113114 = CARTESIAN_POINT ( 'NONE',  ( -5.153800228976607833, 19.02544592524334988, 27.70942372801899722 ) ) ;
#113115 = CARTESIAN_POINT ( 'NONE',  ( 13.97604488694548053, -13.89961937509957401, 75.62609039468564731 ) ) ;
#113116 = CARTESIAN_POINT ( 'NONE',  ( 23.48529157249599564, 32.32473071737754111, -6.449999994537626513 ) ) ;
#113117 = CARTESIAN_POINT ( 'NONE',  ( -5.719274019375665041, -21.55341960407619695, 29.79275706135234358 ) ) ;
#113118 = ADVANCED_FACE ( 'NONE', ( #66237 ), #128887, .T. ) ;
#113119 = CARTESIAN_POINT ( 'NONE',  ( -18.89770734986052148, -5.499999999999912070, 44.10214472496640070 ) ) ;
#113120 = CARTESIAN_POINT ( 'NONE',  ( -21.52544592524334988, -5.823673210054445271, 108.9594237280190185 ) ) ;
#113121 = CARTESIAN_POINT ( 'NONE',  ( -0.05219959533909027116, -19.03943276465977164, 52.49890960531436690 ) ) ;
#113122 = CARTESIAN_POINT ( 'NONE',  ( -13.97604488694547697, 13.89961937509957934, 33.12609039468566863 ) ) ;
#113123 = CARTESIAN_POINT ( 'NONE',  ( -0.05219959533934338120, 16.53943276465976808, 97.50109039468567573 ) ) ;
#113125 = CARTESIAN_POINT ( 'NONE',  ( 18.62759615963255655, 10.81492255796105972, 76.66775706135234714 ) ) ;
#113124 = CARTESIAN_POINT ( 'NONE',  ( 16.51473224551069308, 9.474510206698969483, 104.1655762719810241 ) ) ;
#113126 = CARTESIAN_POINT ( 'NONE',  ( -22.81625015709509441, -31.40387420917324590, -6.324999997268815122 ) ) ;
#113127 = CARTESIAN_POINT ( 'NONE',  ( 30.00000000000000000, -5.510910596163089556E-15, 45.00000000000000000 ) ) ;
#113128 = CARTESIAN_POINT ( 'NONE',  ( 0.05219959533937995610, -21.53943276465977519, 80.00109039468568994 ) ) ;
#113129 = CARTESIAN_POINT ( 'NONE',  ( -18.67979575497193778, 10.72451020669871902, 103.3344237280190043 ) ) ;
#113130 = DIRECTION ( 'NONE',  ( 1.000000000000000000, 0.000000000000000000, 0.000000000000000000 ) ) ;
#113131 = CARTESIAN_POINT ( 'NONE',  ( -9.474510206698964154, 16.51473224551069663, 105.4155762719810383 ) ) ;
#113132 = CARTESIAN_POINT ( 'NONE',  ( -16.46253265017146816, -9.564922557961047289, 29.16775706135232937 ) ) ;
#113133 = ADVANCED_FACE ( 'NONE', ( #21733 ), #51072, .T. ) ;
#113134 = CARTESIAN_POINT ( 'NONE',  ( -29.15849868437705439, -5.438282248597753110, 174.2683007571264113 ) ) ;
#113135 = CARTESIAN_POINT ( 'NONE',  ( 5.153800228976335163, 19.02544592524342804, 44.79057627198103830 ) ) ;
#113136 = CARTESIAN_POINT ( 'NONE',  ( -21.52544592524343514, 5.823673210054127303, 61.04057627198103120 ) ) ;
#113137 = CARTESIAN_POINT ( 'NONE',  ( 8.224510206698953496, -14.34966873604960469, 22.91557627198102765 ) ) ;
#113139 = CARTESIAN_POINT ( 'NONE',  ( 5.049401038298161559, -19.05341960407611168, 82.70724293864770971 ) ) ;
#113138 = CARTESIAN_POINT ( 'NONE',  ( -16.52544592524342804, 4.483927247898546575, 91.04057627198103830 ) ) ;
#113140 = CARTESIAN_POINT ( 'NONE',  ( -18.62759615963255300, -10.81492255796106328, 99.16775706135234714 ) ) ;
#113141 = CARTESIAN_POINT ( 'NONE',  ( 13.89961937509977652, -13.97604488694527269, 43.12390960531434558 ) ) ;
#113142 = CARTESIAN_POINT ( 'NONE',  ( 14.34966873604960469, 8.224510206698951720, 104.1655762719810241 ) ) ;
#113143 = CARTESIAN_POINT ( 'NONE',  ( 10.72451020669871369, 18.67979575497193778, 57.08442372801901854 ) ) ;
#113144 = CARTESIAN_POINT ( 'NONE',  ( 18.62759615963271287, -10.81492255796078972, 88.33224293864769550 ) ) ;
#113145 = CARTESIAN_POINT ( 'NONE',  ( -16.46253265017146816, -9.564922557961047289, 54.16775706135234003 ) ) ;
#113146 = CARTESIAN_POINT ( 'NONE',  ( -18.25439838449807795, -35.60454171183379657, -12.00154358691121637 ) ) ;
#113147 = CARTESIAN_POINT ( 'NONE',  ( 16.51473224551069308, 9.474510206698969483, 104.1655762719810241 ) ) ;
#113148 = CARTESIAN_POINT ( 'NONE',  ( 8.314922557960818139, 14.29746914071049879, 74.58224293864768129 ) ) ;
#113149 = CARTESIAN_POINT ( 'NONE',  ( -16.46253265017146816, -9.564922557961047289, 39.16775706135234003 ) ) ;
#113150 = CARTESIAN_POINT ( 'NONE',  ( 16.46253265017160672, -9.564922557960803928, 68.33224293864770971 ) ) ;
#113151 = CARTESIAN_POINT ( 'NONE',  ( -16.55341960407611168, -4.379528057220339221, 56.45724293864768839 ) ) ;
#113152 = CARTESIAN_POINT ( 'NONE',  ( 5.153800228976615827, -19.02544592524334988, 80.20942372801901854 ) ) ;
#113153 = CARTESIAN_POINT ( 'NONE',  ( -16.46253265017146816, -9.564922557961047289, 89.16775706135234714 ) ) ;
#113154 = CARTESIAN_POINT ( 'NONE',  ( -5.719274019375978568, 21.55341960407610458, 30.20724293864769550 ) ) ;
#113155 = CARTESIAN_POINT ( 'NONE',  ( -4.379528057220328563, 16.55341960407611168, 105.2072429386477097 ) ) ;
#113156 = CARTESIAN_POINT ( 'NONE',  ( 2.310831529832237923E-15, -71.74905152827281540, -14.99410988490250496 ) ) ;
#113158 = CARTESIAN_POINT ( 'NONE',  ( 5.823673210054125526, 21.52544592524343514, 64.79057627198103830 ) ) ;
#113157 = CARTESIAN_POINT ( 'NONE',  ( -13.89961937509977652, 13.97604488694528158, 55.62390960531434558 ) ) ;
#113159 = CARTESIAN_POINT ( 'NONE',  ( -5.153800228976328057, -19.02544592524343514, 27.29057627198103120 ) ) ;
#113161 = CARTESIAN_POINT ( 'NONE',  ( 5.049401038298161559, -19.05341960407611168, 62.70724293864769550 ) ) ;
#113160 = CARTESIAN_POINT ( 'NONE',  ( 4.483927247898790824, -16.52544592524335698, 75.20942372801901854 ) ) ;
#113163 = EDGE_CURVE ( 'NONE', #175994, #180473, #78562, .T. ) ;
#113162 = CARTESIAN_POINT ( 'NONE',  ( 19.05341960407617918, -5.049401038297876454, 56.04275706135234714 ) ) ;
#113164 = CARTESIAN_POINT ( 'NONE',  ( -18.62759615963255300, -10.81492255796106328, 64.16775706135234714 ) ) ;
#113165 = CARTESIAN_POINT ( 'NONE',  ( 5.823673210054125526, 21.52544592524343514, 49.79057627198102409 ) ) ;
#113166 = AXIS2_PLACEMENT_3D ( 'NONE', #126778, #93465, #139965 ) ;
#113167 = CARTESIAN_POINT ( 'NONE',  ( 8.314922557960818139, 14.29746914071049879, 114.5822429386477097 ) ) ;
#113168 = CARTESIAN_POINT ( 'NONE',  ( -4.483927247898782831, 16.52544592524335698, 87.70942372801901854 ) ) ;
#113169 = CARTESIAN_POINT ( 'NONE',  ( 5.049401038297881783, 19.05341960407617563, 107.2927570613523187 ) ) ;
#113170 = CARTESIAN_POINT ( 'NONE',  ( -18.22780087662122384, -5.500000000000025757, 96.48459894673894155 ) ) ;
#113171 = PLANE ( 'NONE',  #199074 ) ;
#113172 = CARTESIAN_POINT ( 'NONE',  ( -18.67979575497193778, 10.72451020669871902, 98.33442372801901854 ) ) ;
#113173 = CARTESIAN_POINT ( 'NONE',  ( 12.06949235617757843, -12.14591786802309237, 53.12390960531436690 ) ) ;
#113174 = CARTESIAN_POINT ( 'NONE',  ( -8.224510206698948167, 14.34966873604960824, 55.41557627198102409 ) ) ;
#113175 = CARTESIAN_POINT ( 'NONE',  ( 15.80617190586746368, 15.72974639402197994, 94.37390960531436690 ) ) ;
#113176 = CARTESIAN_POINT ( 'NONE',  ( 15.72974639402199770, -15.80617190586745480, 88.12390960531436690 ) ) ;
#113177 = CARTESIAN_POINT ( 'NONE',  ( -1.408284774589554589, -29.87692619418718820, -48.43935853184043339 ) ) ;
#113178 = CARTESIAN_POINT ( 'NONE',  ( 18.62759615963271287, -10.81492255796078972, 33.33224293864769550 ) ) ;
#113179 = CARTESIAN_POINT ( 'NONE',  ( 12.06949235617739724, 12.14591786802326823, 66.87609039468568994 ) ) ;
#113180 = CARTESIAN_POINT ( 'NONE',  ( 4.483927247898545687, 16.52544592524342804, 74.79057627198105251 ) ) ;
#113181 = CARTESIAN_POINT ( 'NONE',  ( 5.153800228976335163, 19.02544592524342804, 49.79057627198100988 ) ) ;
#113182 = SURFACE_SIDE_STYLE ('',( #67681 ) ) ;
#113183 = CARTESIAN_POINT ( 'NONE',  ( 34.48175918554795061, -5.660046887242162761, 49.94512835368023218 ) ) ;
#113184 = ORIENTED_EDGE ( 'NONE', *, *, #80571, .F. ) ;
#113185 = CARTESIAN_POINT ( 'NONE',  ( -0.05219959533934338120, 16.53943276465976808, 92.50109039468567573 ) ) ;
#113186 = CARTESIAN_POINT ( 'NONE',  ( 21.53943276465977519, 0.05219959533937863772, 26.25109039468567573 ) ) ;
#113187 = CARTESIAN_POINT ( 'NONE',  ( -5.153800228976328057, -19.02544592524343514, 82.29057627198103830 ) ) ;
#113188 = CARTESIAN_POINT ( 'NONE',  ( -18.67979575497193778, 10.72451020669871902, 48.33442372801902565 ) ) ;
#113189 = CARTESIAN_POINT ( 'NONE',  ( -9.564922557960796823, -16.46253265017161027, 112.0822429386476955 ) ) ;
#113190 = CARTESIAN_POINT ( 'NONE',  ( -19.77856019328939396, -34.75272400654478844, -21.53639161264155533 ) ) ;
#113191 = ORIENTED_EDGE ( 'NONE', *, *, #43597, .T. ) ;
#113192 = CARTESIAN_POINT ( 'NONE',  ( 18.62759615963255655, 10.81492255796105972, 46.66775706135234714 ) ) ;
#113194 = CARTESIAN_POINT ( 'NONE',  ( 9.474510206698971260, -16.51473224551069308, 112.9155762719810383 ) ) ;
#113193 = CARTESIAN_POINT ( 'NONE',  ( -0.05219959533909027116, -19.03943276465977164, 32.49890960531435979 ) ) ;
#113195 = CARTESIAN_POINT ( 'NONE',  ( -19.02544592524334988, -5.153800228976617603, 58.95942372801900433 ) ) ;
#113196 = CARTESIAN_POINT ( 'NONE',  ( -18.67979575497193778, 10.72451020669871902, 33.33442372801900433 ) ) ;
#113197 = CARTESIAN_POINT ( 'NONE',  ( -0.05219959533936034679, 19.03943276465977164, 52.50109039468566863 ) ) ;
#113198 = CARTESIAN_POINT ( 'NONE',  ( 16.51473224551069308, 9.474510206698969483, 24.16557627198102765 ) ) ;
#113199 = CARTESIAN_POINT ( 'NONE',  ( 12.06949235617739724, 12.14591786802326823, 91.87609039468568994 ) ) ;
#113200 = CARTESIAN_POINT ( 'NONE',  ( -5.153800228976607833, 19.02544592524334988, 67.70942372801900433 ) ) ;
#113201 = CARTESIAN_POINT ( 'NONE',  ( 4.483927247898790824, -16.52544592524335698, 100.2094237280190043 ) ) ;
#113202 = CARTESIAN_POINT ( 'NONE',  ( 2.400000000000000799, 0.000000000000000000, 0.000000000000000000 ) ) ;
#113203 = CARTESIAN_POINT ( 'NONE',  ( 19.03943276465977164, -0.05219959533909143690, 88.74890960531436690 ) ) ;
#113204 = CARTESIAN_POINT ( 'NONE',  ( 5.719274019375673035, 21.55341960407619339, 97.29275706135234714 ) ) ;
#113205 = PRODUCT ( 'Rear Air Intake Grille & Cap', 'Rear Air Intake Grille & Cap', '', ( #3776 ) ) ;
#113206 = CARTESIAN_POINT ( 'NONE',  ( -5.719274019375665041, -21.55341960407619695, 104.7927570613523898 ) ) ;
#113207 = CARTESIAN_POINT ( 'NONE',  ( 23.48298174826589246, 32.32155151706776053, -4.702157773949823927 ) ) ;
#113208 = CARTESIAN_POINT ( 'NONE',  ( 16.51473224551069308, 9.474510206698969483, 104.1655762719810241 ) ) ;
#113209 = CARTESIAN_POINT ( 'NONE',  ( -5.823673210054431948, 21.52544592524334988, 72.70942372801901854 ) ) ;
#113210 = CARTESIAN_POINT ( 'NONE',  ( -12.06949235617739369, -12.14591786802326823, 24.37609039468567573 ) ) ;
#113211 = CARTESIAN_POINT ( 'NONE',  ( 5.153800228976335163, 19.02544592524342804, 84.79057627198099567 ) ) ;
#113212 = CARTESIAN_POINT ( 'NONE',  ( 21.55341960407610458, 5.719274019375980345, 33.95724293864769550 ) ) ;
#113213 = CARTESIAN_POINT ( 'NONE',  ( 19.02544592524343514, -5.153800228976328945, 93.54057627198102409 ) ) ;
#113214 = CARTESIAN_POINT ( 'NONE',  ( -5.359611314223446995E-15, 29.16686587814335496, 140.3750000027311842 ) ) ;
#113215 = CARTESIAN_POINT ( 'NONE',  ( -19.05341960407611168, -5.049401038298163336, 71.45724293864766707 ) ) ;
#113216 = CARTESIAN_POINT ( 'NONE',  ( -14.34966873604960291, -8.224510206698953496, 26.66557627198103475 ) ) ;
#113217 = CARTESIAN_POINT ( 'NONE',  ( 0.000000000000000000, 0.000000000000000000, -65.00100000000003320 ) ) ;
#113218 = CARTESIAN_POINT ( 'NONE',  ( -13.89961937509957401, -13.97604488694547875, 74.37609039468566152 ) ) ;
#113219 = CARTESIAN_POINT ( 'NONE',  ( -19.03943276465977164, 0.05219959533909376836, 96.24890960531436690 ) ) ;
#113220 = CARTESIAN_POINT ( 'NONE',  ( 12.06949235617757843, -12.14591786802309237, 88.12390960531436690 ) ) ;
#113221 = CARTESIAN_POINT ( 'NONE',  ( 21.53943276465977519, -0.05219959533907433946, 43.74890960531435979 ) ) ;
#113222 = CARTESIAN_POINT ( 'NONE',  ( -21.53943276465977519, 0.05219959533907696930, 26.24890960531435624 ) ) ;
#113223 = CARTESIAN_POINT ( 'NONE',  ( 0.05219959533910956823, 16.53943276465976808, 104.9989096053143669 ) ) ;
#113224 = CARTESIAN_POINT ( 'NONE',  ( -17.49999999999999289, 5.500000000000034639, 55.79690382534172954 ) ) ;
#113225 = CARTESIAN_POINT ( 'NONE',  ( 16.51473224551083163, -9.474510206698727899, 50.83442372801899722 ) ) ;
#113226 = CARTESIAN_POINT ( 'NONE',  ( 16.55341960407611168, 4.379528057220329451, 28.95724293864769905 ) ) ;
#113227 = CARTESIAN_POINT ( 'NONE',  ( 16.51473224551069308, 9.474510206698969483, 99.16557627198102409 ) ) ;
#113228 = CARTESIAN_POINT ( 'NONE',  ( -15.80617190586768217, 15.72974639402176855, 68.12609039468567573 ) ) ;
#113229 = CARTESIAN_POINT ( 'NONE',  ( 15.72974639402199770, -15.80617190586745480, 53.12390960531436690 ) ) ;
#113230 = CARTESIAN_POINT ( 'NONE',  ( -5.823673210054431948, 21.52544592524334988, 42.70942372801901854 ) ) ;
#113231 = CARTESIAN_POINT ( 'NONE',  ( 0.05219959533907565091, 21.53943276465977519, 94.99890960531436690 ) ) ;
#113232 = CARTESIAN_POINT ( 'NONE',  ( 15.80617190586769283, -15.72974639402175789, 40.62609039468567573 ) ) ;
#113233 = CARTESIAN_POINT ( 'NONE',  ( -4.483927247898539470, -16.52544592524342804, 107.2905762719810525 ) ) ;
#113234 = CARTESIAN_POINT ( 'NONE',  ( 19.05341960407617918, -5.049401038297876454, 76.04275706135230450 ) ) ;
#113235 = CARTESIAN_POINT ( 'NONE',  ( 16.51473224551069308, 9.474510206698969483, 64.16557627198102409 ) ) ;
#113236 = CARTESIAN_POINT ( 'NONE',  ( -16.53943276465976808, 0.05219959533911058130, 106.2489096053143811 ) ) ;
#113237 = CARTESIAN_POINT ( 'NONE',  ( -0.05219959533909027116, -19.03943276465977164, 112.4989096053143669 ) ) ;
#113238 = CARTESIAN_POINT ( 'NONE',  ( -4.483927247898539470, -16.52544592524342804, 42.29057627198103120 ) ) ;
#113239 = CARTESIAN_POINT ( 'NONE',  ( -12.06949235617739369, -12.14591786802326823, 109.3760903946857042 ) ) ;
#113240 = CARTESIAN_POINT ( 'NONE',  ( 13.97604488694527802, 13.89961937509977652, 59.37390960531434558 ) ) ;
#113241 = CARTESIAN_POINT ( 'NONE',  ( 16.52544592524342804, -4.483927247898539470, 113.5405762719810383 ) ) ;
#113242 = CARTESIAN_POINT ( 'NONE',  ( 19.03943276465977164, 0.05219959533936151252, 31.25109039468566863 ) ) ;
#113244 = CARTESIAN_POINT ( 'NONE',  ( -16.55341960407611168, -4.379528057220339221, 31.45724293864769550 ) ) ;
#113243 = CARTESIAN_POINT ( 'NONE',  ( -16.88567814943164791, -6.947325034625598583, 41.29001122652586986 ) ) ;
#113245 = CARTESIAN_POINT ( 'NONE',  ( -15.72974639402176322, -15.80617190586768395, 44.37609039468567573 ) ) ;
#113246 = ADVANCED_FACE ( 'NONE', ( #158249 ), #19739, .F. ) ;
#113247 = CARTESIAN_POINT ( 'NONE',  ( -4.295634330582060123, -37.01983766409437493, -32.60000000000000142 ) ) ;
#113248 = CARTESIAN_POINT ( 'NONE',  ( -12.14591786802326823, 12.06949235617739902, 58.12609039468568994 ) ) ;
#113249 = CARTESIAN_POINT ( 'NONE',  ( -4.483927247898539470, -16.52544592524342804, 27.29057627198103120 ) ) ;
#113250 = CARTESIAN_POINT ( 'NONE',  ( 0.05219959533934541429, -16.53943276465976808, 110.0010903946856757 ) ) ;
#113251 = CARTESIAN_POINT ( 'NONE',  ( -9.564922557960796823, -16.46253265017161027, 32.08224293864769550 ) ) ;
#113252 = CARTESIAN_POINT ( 'NONE',  ( -9.564922557960796823, -16.46253265017161027, 52.08224293864768839 ) ) ;
#113253 = CARTESIAN_POINT ( 'NONE',  ( -5.153800228976328057, -19.02544592524343514, 32.29057627198102409 ) ) ;
#113254 = CARTESIAN_POINT ( 'NONE',  ( -15.80617190586768217, 15.72974639402176855, 38.12609039468567573 ) ) ;
#113255 = CARTESIAN_POINT ( 'NONE',  ( 9.474510206698971260, -16.51473224551069308, 42.91557627198103120 ) ) ;
#113256 = LINE ( 'NONE', #141616, #45170 ) ;
#113257 = CARTESIAN_POINT ( 'NONE',  ( 5.153800228976335163, 19.02544592524342804, 34.79057627198102409 ) ) ;
#113258 = CARTESIAN_POINT ( 'NONE',  ( -21.53943276465977519, 0.05219959533907696930, 26.24890960531435624 ) ) ;
#113260 = CARTESIAN_POINT ( 'NONE',  ( 12.06949235617757843, -12.14591786802309237, 108.1239096053143811 ) ) ;
#113259 = CARTESIAN_POINT ( 'NONE',  ( 18.67979575497194134, -10.72451020669871369, 45.83442372801901854 ) ) ;
#113261 = CARTESIAN_POINT ( 'NONE',  ( 13.97604488694527802, 13.89961937509977652, 114.3739096053143669 ) ) ;
#113262 = CARTESIAN_POINT ( 'NONE',  ( -16.52544592524335698, -4.483927247898792601, 83.95942372801900433 ) ) ;
#113263 = CARTESIAN_POINT ( 'NONE',  ( 21.52544592524334988, 5.823673210054432836, 96.45942372801901854 ) ) ;
#113264 = CARTESIAN_POINT ( 'NONE',  ( 14.29746914071037800, 8.314922557961029526, 56.66775706135235424 ) ) ;
#113265 = CARTESIAN_POINT ( 'NONE',  ( 5.153800228976335163, 19.02544592524342804, 94.79057627198103830 ) ) ;
#113266 = CARTESIAN_POINT ( 'NONE',  ( -0.05219959533934338120, 16.53943276465976808, 42.50109039468567573 ) ) ;
#113267 = CARTESIAN_POINT ( 'NONE',  ( 14.34966873604972726, -8.224510206698740333, 30.83442372801902209 ) ) ;
#113268 = CARTESIAN_POINT ( 'NONE',  ( -16.52544592524335698, -4.483927247898792601, 78.95942372801901854 ) ) ;
#113269 = CARTESIAN_POINT ( 'NONE',  ( -5.153800228976607833, 19.02544592524334988, 107.7094237280189759 ) ) ;
#113270 = CARTESIAN_POINT ( 'NONE',  ( 5.049401038298161559, -19.05341960407611168, 82.70724293864770971 ) ) ;
#113271 = CARTESIAN_POINT ( 'NONE',  ( -18.62759615963270932, 10.81492255796079327, 95.83224293864770971 ) ) ;
#113273 = CARTESIAN_POINT ( 'NONE',  ( -19.05341960407617563, 5.049401038297882671, 103.5427570613523329 ) ) ;
#113272 = CARTESIAN_POINT ( 'NONE',  ( -12.06949235617756955, 12.14591786802309770, 100.6239096053143811 ) ) ;
#113274 = CARTESIAN_POINT ( 'NONE',  ( 16.53943276465976808, 0.05219959533934440121, 71.25109039468568994 ) ) ;
#113275 = CARTESIAN_POINT ( 'NONE',  ( 23.14613071126502675, 10.96668486446926138, 168.1016194467927392 ) ) ;
#113277 = EDGE_CURVE ( 'NONE', #142969, #33072, #10770, .T. ) ;
#113276 = CARTESIAN_POINT ( 'NONE',  ( 13.89961937509957401, 13.97604488694547697, 76.87609039468566152 ) ) ;
#113278 = CARTESIAN_POINT ( 'NONE',  ( -8.314922557960811034, -14.29746914071050412, 52.08224293864768839 ) ) ;
#113279 = CARTESIAN_POINT ( 'NONE',  ( -4.483927247898539470, -16.52544592524342804, 97.29057627198105251 ) ) ;
#113281 = CARTESIAN_POINT ( 'NONE',  ( -17.49999999999999645, -5.500000000000000888, 120.0000000000000142 ) ) ;
#113280 = CARTESIAN_POINT ( 'NONE',  ( -16.51473224551082808, 9.474510206698731452, 38.33442372801899722 ) ) ;
#113282 = CARTESIAN_POINT ( 'NONE',  ( -21.53943276465977519, -0.05219959533937600094, 43.75109039468568284 ) ) ;
#113283 = CARTESIAN_POINT ( 'NONE',  ( 19.05341960407617918, -5.049401038297876454, 101.0427570613523045 ) ) ;
#113284 = CARTESIAN_POINT ( 'NONE',  ( 0.05219959533909260263, 19.03943276465977164, 114.9989096053143669 ) ) ;
#113285 = CARTESIAN_POINT ( 'NONE',  ( 13.89961937509977652, -13.97604488694527269, 98.12390960531433848 ) ) ;
#113286 = CARTESIAN_POINT ( 'NONE',  ( -21.55341960407619339, 5.719274019375674811, 108.5427570613523756 ) ) ;
#113287 = CARTESIAN_POINT ( 'NONE',  ( -19.03943276465977164, 0.05219959533909376836, 86.24890960531436690 ) ) ;
#113288 = CARTESIAN_POINT ( 'NONE',  ( 5.719274019375991003, -21.55341960407610458, 37.70724293864769550 ) ) ;
#113289 = CARTESIAN_POINT ( 'NONE',  ( 14.29746914071049879, -8.314922557960816363, 93.33224293864769550 ) ) ;
#113290 = CARTESIAN_POINT ( 'NONE',  ( -16.46253265017160317, 9.564922557960807481, 60.83224293864769550 ) ) ;
#113291 = CARTESIAN_POINT ( 'NONE',  ( 12.06949235617757843, -12.14591786802309237, 113.1239096053143953 ) ) ;
#113292 = CARTESIAN_POINT ( 'NONE',  ( 21.52544592524334988, 5.823673210054432836, 26.45942372801901854 ) ) ;
#113293 = CARTESIAN_POINT ( 'NONE',  ( 15.72974639402176855, 15.80617190586768217, 76.87609039468567573 ) ) ;
#113294 = CARTESIAN_POINT ( 'NONE',  ( -9.474510206698964154, 16.51473224551069663, 40.41557627198103120 ) ) ;
#113295 = CARTESIAN_POINT ( 'NONE',  ( 0.05219959533934541429, -16.53943276465976808, 80.00109039468568994 ) ) ;
#113296 = CARTESIAN_POINT ( 'NONE',  ( -21.53943276465977519, -0.05219959533937600094, 18.75109039468568639 ) ) ;
#113297 = CARTESIAN_POINT ( 'NONE',  ( 0.05219959533937995610, -21.53943276465977519, 25.00109039468567218 ) ) ;
#113299 = CARTESIAN_POINT ( 'NONE',  ( -19.03943276465977164, 0.05219959533909376836, 71.24890960531435269 ) ) ;
#113298 = CARTESIAN_POINT ( 'NONE',  ( 9.474510206698729675, 16.51473224551082808, 52.08442372801900433 ) ) ;
#113300 = CARTESIAN_POINT ( 'NONE',  ( 16.51473224551083163, -9.474510206698727899, 25.83442372801900078 ) ) ;
#113301 = CARTESIAN_POINT ( 'NONE',  ( -21.55341960407619339, 5.719274019375674811, 83.54275706135234714 ) ) ;
#113302 = CARTESIAN_POINT ( 'NONE',  ( -21.52544592524343514, 5.823673210054127303, 76.04057627198102409 ) ) ;
#113303 = CARTESIAN_POINT ( 'NONE',  ( -4.483927247898539470, -16.52544592524342804, 52.29057627198102409 ) ) ;
#113305 = CARTESIAN_POINT ( 'NONE',  ( -16.51473224551082808, 9.474510206698731452, 23.33442372801900078 ) ) ;
#113304 = CARTESIAN_POINT ( 'NONE',  ( 10.72451020669871369, 18.67979575497193778, 92.08442372801901854 ) ) ;
#113306 = CARTESIAN_POINT ( 'NONE',  ( 4.483927247898545687, 16.52544592524342804, 74.79057627198105251 ) ) ;
#113307 = CARTESIAN_POINT ( 'NONE',  ( -13.97604488694527625, -13.89961937509977652, 21.87390960531435979 ) ) ;
#113308 = CARTESIAN_POINT ( 'NONE',  ( -13.89961937509957401, -13.97604488694547875, 59.37609039468566863 ) ) ;
#113309 = CARTESIAN_POINT ( 'NONE',  ( -0.05219959533910754901, -16.53943276465976808, 27.49890960531435269 ) ) ;
#113310 = CARTESIAN_POINT ( 'NONE',  ( 5.719274019375673035, 21.55341960407619339, 87.29275706135236135 ) ) ;
#113311 = CARTESIAN_POINT ( 'NONE',  ( -16.46253265017160317, 9.564922557960807481, 75.83224293864769550 ) ) ;
#113312 = CARTESIAN_POINT ( 'NONE',  ( -9.474510206698720793, -16.51473224551083518, 44.58442372801900433 ) ) ;
#113313 = CARTESIAN_POINT ( 'NONE',  ( -18.62759615963270932, 10.81492255796079327, 45.83224293864769550 ) ) ;
#113314 = CARTESIAN_POINT ( 'NONE',  ( 21.53943276465977519, 0.05219959533937863772, 46.25109039468567573 ) ) ;
#113315 = CARTESIAN_POINT ( 'NONE',  ( -18.67979575497178146, -10.72451020669898902, 106.6655762719810383 ) ) ;
#113316 = CARTESIAN_POINT ( 'NONE',  ( -13.97604488694547697, 13.89961937509957934, 93.12609039468566152 ) ) ;
#113317 = CARTESIAN_POINT ( 'NONE',  ( 14.34966873604972726, -8.224510206698740333, 60.83442372801901854 ) ) ;
#113319 = CARTESIAN_POINT ( 'NONE',  ( 21.52544592524344225, -5.823673210054117533, 108.5405762719810241 ) ) ;
#113318 = CYLINDRICAL_SURFACE ( 'NONE', #93484, 8.000000000000000000 ) ;
#113320 = CARTESIAN_POINT ( 'NONE',  ( -16.55341960407611168, -4.379528057220339221, 96.45724293864770971 ) ) ;
#113321 = CARTESIAN_POINT ( 'NONE',  ( -17.49999999999999645, 5.499999999999997335, 120.0000000000000142 ) ) ;
#113322 = CARTESIAN_POINT ( 'NONE',  ( -4.379528057220086978, -16.55341960407618274, 29.79275706135234358 ) ) ;
#113323 = CARTESIAN_POINT ( 'NONE',  ( -21.53943276465977519, 0.05219959533907696930, 61.24890960531435979 ) ) ;
#113324 = CARTESIAN_POINT ( 'NONE',  ( -8.224510206698735004, -14.34966873604973081, 94.58442372801901854 ) ) ;
#113325 = CARTESIAN_POINT ( 'NONE',  ( -5.153800228976328057, -19.02544592524343514, 27.29057627198103120 ) ) ;
#113326 = CARTESIAN_POINT ( 'NONE',  ( -8.224510206698735004, -14.34966873604973081, 69.58442372801900433 ) ) ;
#113327 = CARTESIAN_POINT ( 'NONE',  ( 19.02544592524334988, 5.153800228976608722, 61.45942372801900433 ) ) ;
#113328 = CARTESIAN_POINT ( 'NONE',  ( 5.719274019375673035, 21.55341960407619339, 47.29275706135234003 ) ) ;
#113329 = CARTESIAN_POINT ( 'NONE',  ( 0.05219959533907565091, 21.53943276465977519, 64.99890960531435269 ) ) ;
#113330 = CARTESIAN_POINT ( 'NONE',  ( -0.05219959533934338120, 16.53943276465976808, 82.50109039468568994 ) ) ;
#113331 = CARTESIAN_POINT ( 'NONE',  ( 5.719274019375673035, 21.55341960407619339, 67.29275706135234714 ) ) ;
#113332 = CARTESIAN_POINT ( 'NONE',  ( 10.81492255796078972, 18.62759615963270932, 54.58224293864769550 ) ) ;
#113333 = CARTESIAN_POINT ( 'NONE',  ( -15.72974639402197994, 15.80617190586746368, 35.62390960531437401 ) ) ;
#113334 = ORIENTED_EDGE ( 'NONE', *, *, #161468, .T. ) ;
#113335 = CARTESIAN_POINT ( 'NONE',  ( 4.379528057220092307, 16.55341960407617563, 67.29275706135234714 ) ) ;
#113336 = CARTESIAN_POINT ( 'NONE',  ( -10.81492255796078084, -18.62759615963271287, 27.08224293864769550 ) ) ;
#113337 = ORIENTED_EDGE ( 'NONE', *, *, #36547, .T. ) ;
#113338 = CARTESIAN_POINT ( 'NONE',  ( 13.97604488694527802, 13.89961937509977652, 104.3739096053143385 ) ) ;
#113339 = CARTESIAN_POINT ( 'NONE',  ( -0.05219959533934338120, 16.53943276465976808, 107.5010903946856899 ) ) ;
#113340 = FACE_OUTER_BOUND ( 'NONE', #40366, .T. ) ;
#113341 = CARTESIAN_POINT ( 'NONE',  ( 12.06949235617757843, -12.14591786802309237, 103.1239096053143811 ) ) ;
#113342 = CARTESIAN_POINT ( 'NONE',  ( -18.62759615963270932, 10.81492255796079327, 60.83224293864769550 ) ) ;
#113343 = CARTESIAN_POINT ( 'NONE',  ( -16.46253265017160317, 9.564922557960807481, 50.83224293864770260 ) ) ;
#113344 = CARTESIAN_POINT ( 'NONE',  ( 12.14591786802327356, -12.06949235617739191, 95.62609039468568994 ) ) ;
#113345 = CARTESIAN_POINT ( 'NONE',  ( -18.67979575497193778, 10.72451020669871902, 33.33442372801900433 ) ) ;
#113346 = CARTESIAN_POINT ( 'NONE',  ( 13.89961937509957401, 13.97604488694547697, 101.8760903946856331 ) ) ;
#113347 = CARTESIAN_POINT ( 'NONE',  ( -14.34966873604960291, -8.224510206698953496, 101.6655762719810383 ) ) ;
#113348 = CARTESIAN_POINT ( 'NONE',  ( 0.05219959533909260263, 19.03943276465977164, 54.99890960531435979 ) ) ;
#113349 = CARTESIAN_POINT ( 'NONE',  ( -9.564922557960796823, -16.46253265017161027, 22.08224293864768839 ) ) ;
#113350 = CARTESIAN_POINT ( 'NONE',  ( 17.48847506799968698, -5.747544572773780835, 38.32697437843281563 ) ) ;
#113351 = CARTESIAN_POINT ( 'NONE',  ( -9.474510206698964154, 16.51473224551069663, 90.41557627198103830 ) ) ;
#113352 = CARTESIAN_POINT ( 'NONE',  ( 8.224510206698742110, 14.34966873604972548, 77.08442372801901854 ) ) ;
#113353 = CARTESIAN_POINT ( 'NONE',  ( 5.823673210054444382, -21.52544592524334988, 105.2094237280190328 ) ) ;
#113354 = CARTESIAN_POINT ( 'NONE',  ( 18.62759615963271287, -10.81492255796078972, 53.33224293864769550 ) ) ;
#113355 = CARTESIAN_POINT ( 'NONE',  ( -8.314922557961024197, 14.29746914071037800, 77.91775706135231871 ) ) ;
#113356 = CARTESIAN_POINT ( 'NONE',  ( 9.474510206698729675, 16.51473224551082808, 77.08442372801900433 ) ) ;
#113357 = ORIENTED_EDGE ( 'NONE', *, *, #20248, .T. ) ;
#113358 = CARTESIAN_POINT ( 'NONE',  ( 16.46253265017160672, -9.564922557960803928, 38.33224293864768839 ) ) ;
#113359 = CARTESIAN_POINT ( 'NONE',  ( 16.51473224551069308, 9.474510206698969483, 79.16557627198103830 ) ) ;
#113360 = CARTESIAN_POINT ( 'NONE',  ( -16.51473224551069308, -9.474510206698971260, 36.66557627198102409 ) ) ;
#113361 = CARTESIAN_POINT ( 'NONE',  ( -5.153800228976607833, 19.02544592524334988, 77.70942372801900433 ) ) ;
#113362 = CARTESIAN_POINT ( 'NONE',  ( -19.02544592524342804, 5.153800228976336051, 116.0405762719810383 ) ) ;
#113363 = CARTESIAN_POINT ( 'NONE',  ( -0.05219959533909027116, -19.03943276465977164, 92.49890960531436690 ) ) ;
#113364 = CARTESIAN_POINT ( 'NONE',  ( -8.314922557960811034, -14.29746914071050412, 47.08224293864770260 ) ) ;
#113365 = CARTESIAN_POINT ( 'NONE',  ( 15.80617190586746368, 15.72974639402197994, 44.37390960531435979 ) ) ;
#113366 = DIRECTION ( 'NONE',  ( -0.000000000000000000, -0.000000000000000000, 1.000000000000000000 ) ) ;
#113367 = CARTESIAN_POINT ( 'NONE',  ( -13.97604488694547697, 13.89961937509957934, 33.12609039468566863 ) ) ;
#113368 = CARTESIAN_POINT ( 'NONE',  ( -16.20579543436678449, -7.371946100355090792, 80.56520834171877254 ) ) ;
#113369 = CARTESIAN_POINT ( 'NONE',  ( -13.89961937509977652, 13.97604488694528158, 50.62390960531435979 ) ) ;
#113370 = CARTESIAN_POINT ( 'NONE',  ( -14.29746914071037622, -8.314922557961029526, 44.16775706135234714 ) ) ;
#113371 = CARTESIAN_POINT ( 'NONE',  ( -19.39720447994794128, -5.500000000000030198, 99.66317477297174321 ) ) ;
#113372 = CARTESIAN_POINT ( 'NONE',  ( -16.61371651742600974, 7.165104196376152146, 108.8541506999299884 ) ) ;
#113373 = CARTESIAN_POINT ( 'NONE',  ( 0.05219959533934541429, -16.53943276465976808, 80.00109039468568994 ) ) ;
#113374 = CARTESIAN_POINT ( 'NONE',  ( 21.53943276465977519, -0.05219959533907433946, 93.74890960531436690 ) ) ;
#113375 = CARTESIAN_POINT ( 'NONE',  ( -4.483927247898782831, 16.52544592524335698, 47.70942372801902565 ) ) ;
#113377 = DIRECTION ( 'NONE',  ( 0.000000000000000000, 0.000000000000000000, 1.000000000000000000 ) ) ;
#113376 = CARTESIAN_POINT ( 'NONE',  ( 19.03943276465977164, -0.05219959533909143690, 38.74890960531436690 ) ) ;
#113378 = CARTESIAN_POINT ( 'NONE',  ( -15.80617190586768217, 15.72974639402176855, 43.12609039468568284 ) ) ;
#113379 = CARTESIAN_POINT ( 'NONE',  ( 9.474510206698729675, 16.51473224551082808, 47.08442372801900433 ) ) ;
#113380 = CARTESIAN_POINT ( 'NONE',  ( -5.719274019375665041, -21.55341960407619695, 94.79275706135234714 ) ) ;
#113381 = CARTESIAN_POINT ( 'NONE',  ( 17.44279575226823198, 5.990770900252457842, 96.66442432485682446 ) ) ;
#113382 = CARTESIAN_POINT ( 'NONE',  ( 16.55341960407611168, 4.379528057220329451, 38.95724293864768839 ) ) ;
#113383 = CARTESIAN_POINT ( 'NONE',  ( -15.01195240492205762, 1.500078752102993240, -59.87740586969341905 ) ) ;
#113384 = CARTESIAN_POINT ( 'NONE',  ( -21.52544592524343514, 5.823673210054127303, 51.04057627198103120 ) ) ;
#113385 = CARTESIAN_POINT ( 'NONE',  ( -4.500000000000000888, -139.5000000000000000, 21.32407087589995953 ) ) ;
#113386 = CARTESIAN_POINT ( 'NONE',  ( 16.46253265017160672, -9.564922557960803928, 103.3322429386476955 ) ) ;
#113387 = CARTESIAN_POINT ( 'NONE',  ( -0.05219959533910754901, -16.53943276465976808, 102.4989096053143811 ) ) ;
#113388 = CARTESIAN_POINT ( 'NONE',  ( -16.51473224551082808, 9.474510206698731452, 113.3344237280190043 ) ) ;
#113389 = CARTESIAN_POINT ( 'NONE',  ( -12.14591786802326823, 12.06949235617739902, 108.1260903946856757 ) ) ;
#113390 = EDGE_LOOP ( 'NONE', ( #31021, #198315, #192195, #77626, #23960 ) ) ;
#113392 = CARTESIAN_POINT ( 'NONE',  ( -21.53943276465977519, 0.05219959533907696930, 106.2489096053143811 ) ) ;
#113391 = CARTESIAN_POINT ( 'NONE',  ( 0.05219959533909260263, 19.03943276465977164, 99.99890960531436690 ) ) ;
#113394 = CARTESIAN_POINT ( 'NONE',  ( 13.97604488694527802, 13.89961937509977652, 99.37390960531436690 ) ) ;
#113393 = CARTESIAN_POINT ( 'NONE',  ( 8.314922557960818139, 14.29746914071049879, 24.58224293864768839 ) ) ;
#113395 = CARTESIAN_POINT ( 'NONE',  ( -5.153800228976607833, 19.02544592524334988, 97.70942372801900433 ) ) ;
#113396 = CARTESIAN_POINT ( 'NONE',  ( 21.55341960407619695, -5.719274019375665929, 111.0427570613523613 ) ) ;
#113397 = CARTESIAN_POINT ( 'NONE',  ( 0.05219959533907565091, 21.53943276465977519, 84.99890960531436690 ) ) ;
#113398 = CARTESIAN_POINT ( 'NONE',  ( -0.05219959533907301413, -21.53943276465977519, 52.49890960531435979 ) ) ;
#113399 = CARTESIAN_POINT ( 'NONE',  ( -16.46253265017160317, 9.564922557960807481, 65.83224293864769550 ) ) ;
#113400 = CARTESIAN_POINT ( 'NONE',  ( 16.55341960407611168, 4.379528057220329451, 33.95724293864769550 ) ) ;
#113401 = CARTESIAN_POINT ( 'NONE',  ( -16.46253265017160317, 9.564922557960807481, 70.83224293864770971 ) ) ;
#113402 = CARTESIAN_POINT ( 'NONE',  ( 18.89770734986052503, 5.499999999999904077, 56.60214472496641491 ) ) ;
#113403 = CARTESIAN_POINT ( 'NONE',  ( -9.564922557961040184, 16.46253265017147172, 37.91775706135233293 ) ) ;
#113404 = CARTESIAN_POINT ( 'NONE',  ( 15.72974639402199770, -15.80617190586745480, 83.12390960531436690 ) ) ;
#113405 = CARTESIAN_POINT ( 'NONE',  ( 12.06949235617757843, -12.14591786802309237, 88.12390960531436690 ) ) ;
#113406 = CARTESIAN_POINT ( 'NONE',  ( -15.80617190586768217, 15.72974639402176855, 38.12609039468567573 ) ) ;
#113407 = CARTESIAN_POINT ( 'NONE',  ( -27.73933785331498925, 2.428612866367529932E-14, 149.3750000027311842 ) ) ;
#113408 = CARTESIAN_POINT ( 'NONE',  ( 4.379528057220092307, 16.55341960407617563, 112.2927570613523471 ) ) ;
#113409 = CARTESIAN_POINT ( 'NONE',  ( -5.153800228976328057, -19.02544592524343514, 27.29057627198103120 ) ) ;
#113410 = CARTESIAN_POINT ( 'NONE',  ( -13.89961937509977652, 13.97604488694528158, 85.62390960531433848 ) ) ;
#113411 = DIRECTION ( 'NONE',  ( 0.000000000000000000, 0.000000000000000000, 1.000000000000000000 ) ) ;
#113412 = CARTESIAN_POINT ( 'NONE',  ( -0.05219959533910754901, -16.53943276465976808, 42.49890960531435979 ) ) ;
#113413 = CARTESIAN_POINT ( 'NONE',  ( -18.67979575497193778, 10.72451020669871902, 58.33442372801901143 ) ) ;
#113414 = CARTESIAN_POINT ( 'NONE',  ( 25.73110857337021784, -27.25168951599283673, -18.43918238434275736 ) ) ;
#113415 = CARTESIAN_POINT ( 'NONE',  ( 5.049401038298161559, -19.05341960407611168, 37.70724293864768839 ) ) ;
#113416 = CARTESIAN_POINT ( 'NONE',  ( -16.46253265017160317, 9.564922557960807481, 45.83224293864769550 ) ) ;
#113417 = ORIENTED_EDGE ( 'NONE', *, *, #13111, .F. ) ;
#113418 = CARTESIAN_POINT ( 'NONE',  ( -5.823673210054431948, 21.52544592524334988, 102.7094237280190185 ) ) ;
#113419 = CARTESIAN_POINT ( 'NONE',  ( 14.29746914071037800, 8.314922557961029526, 66.66775706135234714 ) ) ;
#113420 = CARTESIAN_POINT ( 'NONE',  ( 15.80617190586769283, -15.72974639402175789, 90.62609039468567573 ) ) ;
#113421 = CARTESIAN_POINT ( 'NONE',  ( 19.02544592524343514, -5.153800228976328945, 113.5405762719810241 ) ) ;
#113422 = CARTESIAN_POINT ( 'NONE',  ( -13.97604488694547697, 13.89961937509957934, 88.12609039468563310 ) ) ;
#113423 = CARTESIAN_POINT ( 'NONE',  ( 10.72451020669871369, 18.67979575497193778, 67.08442372801901854 ) ) ;
#113424 = CARTESIAN_POINT ( 'NONE',  ( 8.224510206698742110, 14.34966873604972548, 32.08442372801901854 ) ) ;
#113425 = CARTESIAN_POINT ( 'NONE',  ( -5.719274019375978568, 21.55341960407610458, 90.20724293864770971 ) ) ;
#113426 = CARTESIAN_POINT ( 'NONE',  ( -13.97604488694547697, 13.89961937509957934, 98.12609039468566152 ) ) ;
#113427 = CARTESIAN_POINT ( 'NONE',  ( 9.474510206698971260, -16.51473224551069308, 62.91557627198102409 ) ) ;
#113428 = CARTESIAN_POINT ( 'NONE',  ( 0.05219959533936267826, -19.03943276465977164, 105.0010903946856615 ) ) ;
#113429 = CARTESIAN_POINT ( 'NONE',  ( -5.049401038297874678, -19.05341960407617918, 99.79275706135234714 ) ) ;
#113430 = CARTESIAN_POINT ( 'NONE',  ( 12.06949235617757843, -12.14591786802309237, 58.12390960531435979 ) ) ;
#113431 = CARTESIAN_POINT ( 'NONE',  ( -9.564922557961040184, 16.46253265017147172, 72.91775706135233293 ) ) ;
#113432 = CARTESIAN_POINT ( 'NONE',  ( -16.55341960407617563, 4.379528057220093196, 78.54275706135236135 ) ) ;
#113434 = CARTESIAN_POINT ( 'NONE',  ( -19.05341960407611168, -5.049401038298163336, 36.45724293864766707 ) ) ;
#113433 = CARTESIAN_POINT ( 'NONE',  ( -5.823673210054116645, -21.52544592524344225, 112.2905762719810241 ) ) ;
#113435 = CARTESIAN_POINT ( 'NONE',  ( -16.46253265017160317, 9.564922557960807481, 50.83224293864770260 ) ) ;
#113436 = CARTESIAN_POINT ( 'NONE',  ( -8.314922557961024197, 14.29746914071037800, 52.91775706135235424 ) ) ;
#113437 = CARTESIAN_POINT ( 'NONE',  ( -22.44159573604009950, -16.30477369853688430, 139.5750000027311728 ) ) ;
#113438 = CARTESIAN_POINT ( 'NONE',  ( 28.82186960331498327, 2.781578969918950771E-14, 143.2500000054623683 ) ) ;
#113439 = CARTESIAN_POINT ( 'NONE',  ( -19.05341960407611168, -5.049401038298163336, 111.4572429386476671 ) ) ;
#113440 = DIRECTION ( 'NONE',  ( 0.7071067811865485719, 0.000000000000000000, 0.7071067811865465735 ) ) ;
#113441 = VERTEX_POINT ( 'NONE', #35896 ) ;
#113442 = CARTESIAN_POINT ( 'NONE',  ( 16.51473224551083163, -9.474510206698727899, 110.8344237280190043 ) ) ;
#113443 = CARTESIAN_POINT ( 'NONE',  ( -0.05219959533907301413, -21.53943276465977519, 47.49890960531435979 ) ) ;
#113445 = CARTESIAN_POINT ( 'NONE',  ( 14.34966873604972726, -8.224510206698740333, 30.83442372801902209 ) ) ;
#113444 = CARTESIAN_POINT ( 'NONE',  ( 0.05219959533936267826, -19.03943276465977164, 45.00109039468566863 ) ) ;
#113446 = CARTESIAN_POINT ( 'NONE',  ( -5.049401038298153566, 19.05341960407611168, 30.20724293864768839 ) ) ;
#113447 = CARTESIAN_POINT ( 'NONE',  ( 9.564922557960805705, 16.46253265017160317, 54.58224293864769550 ) ) ;
#113448 = CARTESIAN_POINT ( 'NONE',  ( -21.52544592524343514, 5.823673210054127303, 86.04057627198102409 ) ) ;
#113449 = CARTESIAN_POINT ( 'NONE',  ( -16.46253265017160317, 9.564922557960807481, 105.8322429386476955 ) ) ;
#113450 = CARTESIAN_POINT ( 'NONE',  ( -0.05219959533909027116, -19.03943276465977164, 47.49890960531435979 ) ) ;
#113451 = CARTESIAN_POINT ( 'NONE',  ( -17.60769864724391098, 5.499999999999985789, 93.65024842019165874 ) ) ;
#113452 = CARTESIAN_POINT ( 'NONE',  ( -5.049401038297874678, -19.05341960407617918, 89.79275706135230450 ) ) ;
#113453 = CARTESIAN_POINT ( 'NONE',  ( -14.34966873604960291, -8.224510206698953496, 61.66557627198103120 ) ) ;
#113454 = CARTESIAN_POINT ( 'NONE',  ( -15.80617190586768217, 15.72974639402176855, 103.1260903946856757 ) ) ;
#113455 = CARTESIAN_POINT ( 'NONE',  ( -10.81492255796078084, -18.62759615963271287, 92.08224293864769550 ) ) ;
#113456 = CARTESIAN_POINT ( 'NONE',  ( -21.52544592524334988, -5.823673210054445271, 88.95942372801901854 ) ) ;
#113457 = CARTESIAN_POINT ( 'NONE',  ( -19.05341960407611168, -5.049401038298163336, 21.45724293864768839 ) ) ;
#113458 = CARTESIAN_POINT ( 'NONE',  ( 21.53943276465977519, 0.05219959533937863772, 76.25109039468568994 ) ) ;
#113459 = CARTESIAN_POINT ( 'NONE',  ( 19.05341960407611168, 5.049401038298154454, 103.9572429386476671 ) ) ;
#113461 = CARTESIAN_POINT ( 'NONE',  ( 0.05219959533937995610, -21.53943276465977519, 75.00109039468568994 ) ) ;
#113460 = CARTESIAN_POINT ( 'NONE',  ( 16.52544592524342804, -4.483927247898539470, 33.54057627198102409 ) ) ;
#113462 = CARTESIAN_POINT ( 'NONE',  ( 13.89961937509977652, -13.97604488694527269, 63.12390960531435979 ) ) ;
#113463 = CARTESIAN_POINT ( 'NONE',  ( 10.81492255796106328, -18.62759615963255655, 45.41775706135234003 ) ) ;
#113464 = CARTESIAN_POINT ( 'NONE',  ( -19.05341960407611168, -5.049401038298163336, 86.45724293864769550 ) ) ;
#113465 = CARTESIAN_POINT ( 'NONE',  ( 4.483927247898545687, 16.52544592524342804, 94.79057627198105251 ) ) ;
#113466 = CARTESIAN_POINT ( 'NONE',  ( 0.05219959533910956823, 16.53943276465976808, 64.99890960531435269 ) ) ;
#113467 = CARTESIAN_POINT ( 'NONE',  ( 18.67979575497178502, 10.72451020669898547, 74.16557627198102409 ) ) ;
#113468 = CARTESIAN_POINT ( 'NONE',  ( -16.46253265017160317, 9.564922557960807481, 65.83224293864769550 ) ) ;
#113469 = CARTESIAN_POINT ( 'NONE',  ( -15.80617190586745835, -15.72974639402198527, 71.87390960531438111 ) ) ;
#113470 = CARTESIAN_POINT ( 'NONE',  ( 0.05219959533936267826, -19.03943276465977164, 60.00109039468566863 ) ) ;
#113472 = CARTESIAN_POINT ( 'NONE',  ( -0.05219959533910754901, -16.53943276465976808, 77.49890960531433848 ) ) ;
#113471 = CARTESIAN_POINT ( 'NONE',  ( 0.05219959533936267826, -19.03943276465977164, 30.00109039468566863 ) ) ;
#113473 = CARTESIAN_POINT ( 'NONE',  ( -18.67979575497178146, -10.72451020669898902, 46.66557627198102409 ) ) ;
#113474 = EDGE_CURVE ( 'NONE', #187814, #72196, #23746, .T. ) ;
#113475 = DIRECTION ( 'NONE',  ( -0.5150380737757255245, 0.000000000000000000, 0.8571673013836856869 ) ) ;
#113477 = CARTESIAN_POINT ( 'NONE',  ( -8.571926809382608425, 26.38167802310805854, 144.9750000027312069 ) ) ;
#113476 = CARTESIAN_POINT ( 'NONE',  ( 14.34966873604972726, -8.224510206698740333, 100.8344237280190185 ) ) ;
#113478 = CARTESIAN_POINT ( 'NONE',  ( -13.97604488694547697, 13.89961937509957934, 98.12609039468566152 ) ) ;
#113479 = CARTESIAN_POINT ( 'NONE',  ( -14.29746914071049879, 8.314922557960819915, 70.83224293864770971 ) ) ;
#113480 = SPHERICAL_SURFACE ( 'NONE', #122612, 4.324969328314201888 ) ;
#113481 = CARTESIAN_POINT ( 'NONE',  ( 19.05341960407611168, 5.049401038298154454, 63.95724293864769550 ) ) ;
#113482 = CARTESIAN_POINT ( 'NONE',  ( 12.14591786802309770, 12.06949235617756955, 54.37390960531435979 ) ) ;
#113483 = CARTESIAN_POINT ( 'NONE',  ( 9.474510206698971260, -16.51473224551069308, 102.9155762719810241 ) ) ;
#113485 = CARTESIAN_POINT ( 'NONE',  ( -9.474510206698964154, 16.51473224551069663, 65.41557627198102409 ) ) ;
#113484 = CARTESIAN_POINT ( 'NONE',  ( 19.03943276465977164, 0.05219959533936151252, 81.25109039468567573 ) ) ;
#113486 = CARTESIAN_POINT ( 'NONE',  ( 5.153800228976335163, 19.02544592524342804, 89.79057627198102409 ) ) ;
#113487 = CARTESIAN_POINT ( 'NONE',  ( 9.474510206698971260, -16.51473224551069308, 67.91557627198102409 ) ) ;
#113488 = CARTESIAN_POINT ( 'NONE',  ( -10.72451020669898014, 18.67979575497178502, 65.41557627198102409 ) ) ;
#113489 = CARTESIAN_POINT ( 'NONE',  ( -12.14591786802326823, 12.06949235617739902, 58.12609039468568994 ) ) ;
#113490 = CARTESIAN_POINT ( 'NONE',  ( 2.300691058039425752, -7.143419655154876757, 1.353258418600857382 ) ) ;
#113491 = CARTESIAN_POINT ( 'NONE',  ( 16.51473224551069308, 9.474510206698969483, 54.16557627198103120 ) ) ;
#113492 = CARTESIAN_POINT ( 'NONE',  ( 15.72974639402199770, -15.80617190586745480, 48.12390960531436690 ) ) ;
#113493 = CARTESIAN_POINT ( 'NONE',  ( -5.153800228976607833, 19.02544592524334988, 82.70942372801897591 ) ) ;
#113495 = CARTESIAN_POINT ( 'NONE',  ( -15.72974639402176322, -15.80617190586768395, 34.37609039468568284 ) ) ;
#113494 = CARTESIAN_POINT ( 'NONE',  ( 14.29746914071049879, -8.314922557960816363, 28.33224293864769550 ) ) ;
#113496 = CARTESIAN_POINT ( 'NONE',  ( 5.153800228976615827, -19.02544592524334988, 40.20942372801898301 ) ) ;
#113498 = CARTESIAN_POINT ( 'NONE',  ( -8.314922557961024197, 14.29746914071037800, 87.91775706135234714 ) ) ;
#113497 = CARTESIAN_POINT ( 'NONE',  ( -16.52544592524335698, -4.483927247898792601, 63.95942372801901854 ) ) ;
#113499 = CARTESIAN_POINT ( 'NONE',  ( -193.3062444957834884, -155.7167183371838064, -15.00000000000000178 ) ) ;
#113500 = CARTESIAN_POINT ( 'NONE',  ( -0.05219959533934338120, 16.53943276465976808, 77.50109039468567573 ) ) ;
#113502 = CARTESIAN_POINT ( 'NONE',  ( 16.55341960407618274, -4.379528057220086978, 31.04275706135234714 ) ) ;
#113501 = CARTESIAN_POINT ( 'NONE',  ( 18.67979575497178502, 10.72451020669898547, 24.16557627198103120 ) ) ;
#113503 = CARTESIAN_POINT ( 'NONE',  ( 5.153800228976335163, 19.02544592524342804, 44.79057627198103830 ) ) ;
#113504 = CARTESIAN_POINT ( 'NONE',  ( -13.89961937509977652, 13.97604488694528158, 55.62390960531434558 ) ) ;
#113505 = CARTESIAN_POINT ( 'NONE',  ( 13.89961937509977652, -13.97604488694527269, 58.12390960531436690 ) ) ;
#113506 = CARTESIAN_POINT ( 'NONE',  ( 18.62759615963255655, 10.81492255796105972, 36.66775706135234714 ) ) ;
#113507 = CARTESIAN_POINT ( 'NONE',  ( 14.34966873604972726, -8.224510206698740333, 45.83442372801901854 ) ) ;
#113508 = CARTESIAN_POINT ( 'NONE',  ( -12.14591786802326823, 12.06949235617739902, 113.1260903946856899 ) ) ;
#113509 = CARTESIAN_POINT ( 'NONE',  ( 9.474510206698971260, -16.51473224551069308, 27.91557627198103120 ) ) ;
#113510 = CARTESIAN_POINT ( 'NONE',  ( 21.53943276465977519, 0.05219959533937863772, 111.2510903946856899 ) ) ;
#113512 = ADVANCED_FACE ( 'NONE', ( #176427 ), #38902, .T. ) ;
#113511 = CARTESIAN_POINT ( 'NONE',  ( -19.02544592524334988, -5.153800228976617603, 103.9594237280190043 ) ) ;
#113513 = CARTESIAN_POINT ( 'NONE',  ( -19.05341960407617563, 5.049401038297882671, 63.54275706135234003 ) ) ;
#113514 = CARTESIAN_POINT ( 'NONE',  ( -4.379528057220328563, 16.55341960407611168, 70.20724293864769550 ) ) ;
#113515 = CARTESIAN_POINT ( 'NONE',  ( -13.97604488694527625, -13.89961937509977652, 31.87390960531435979 ) ) ;
#113517 = DIRECTION ( 'NONE',  ( 0.000000000000000000, 0.000000000000000000, -1.000000000000000000 ) ) ;
#113516 = CARTESIAN_POINT ( 'NONE',  ( -16.51473224551082808, 9.474510206698731452, 78.33442372801900433 ) ) ;
#113518 = CARTESIAN_POINT ( 'NONE',  ( 10.72451020669871369, 18.67979575497193778, 77.08442372801901854 ) ) ;
#113519 = CARTESIAN_POINT ( 'NONE',  ( -12.06949235617739369, -12.14591786802326823, 44.37609039468567573 ) ) ;
#113520 = CARTESIAN_POINT ( 'NONE',  ( 17.50000000000000000, 5.499999999999992895, 38.78230962303566542 ) ) ;
#113521 = CARTESIAN_POINT ( 'NONE',  ( -18.62759615963270932, 10.81492255796079327, 40.83224293864769550 ) ) ;
#113522 = CARTESIAN_POINT ( 'NONE',  ( 12.14591786802327356, -12.06949235617739191, 30.62609039468567929 ) ) ;
#113523 = CARTESIAN_POINT ( 'NONE',  ( -19.05341960407611168, -5.049401038298164224, 21.45724293864768839 ) ) ;
#113524 = CARTESIAN_POINT ( 'NONE',  ( 5.153800228976615827, -19.02544592524334988, 35.20942372801899722 ) ) ;
#113525 = CARTESIAN_POINT ( 'NONE',  ( 9.243954752495790572, 10.58667710475866564, -60.30599866924266905 ) ) ;
#113526 = CARTESIAN_POINT ( 'NONE',  ( 9.474510206698971260, -16.51473224551069308, 32.91557627198102409 ) ) ;
#113527 = DIRECTION ( 'NONE',  ( 0.000000000000000000, 0.000000000000000000, 1.000000000000000000 ) ) ;
#113528 = CARTESIAN_POINT ( 'NONE',  ( 9.474510206698971260, -16.51473224551069308, 57.91557627198103120 ) ) ;
#113529 = CARTESIAN_POINT ( 'NONE',  ( -18.87075004821569024, 5.499999999999997335, 98.67408112101047379 ) ) ;
#113530 = CARTESIAN_POINT ( 'NONE',  ( -0.05219959533936034679, 19.03943276465977164, 22.50109039468566152 ) ) ;
#113531 = CARTESIAN_POINT ( 'NONE',  ( 16.55341960407618274, -4.379528057220086978, 111.0427570613523613 ) ) ;
#113532 = CARTESIAN_POINT ( 'NONE',  ( -13.97604488694527625, -13.89961937509977652, 26.87390960531434558 ) ) ;
#113533 = CARTESIAN_POINT ( 'NONE',  ( -19.03943276465977164, 0.05219959533909376836, 91.24890960531436690 ) ) ;
#113534 = CARTESIAN_POINT ( 'NONE',  ( -18.62759615963255300, -10.81492255796106328, 64.16775706135234714 ) ) ;
#113535 = CARTESIAN_POINT ( 'NONE',  ( 5.049401038298161559, -19.05341960407611168, 37.70724293864768839 ) ) ;
#113536 = CARTESIAN_POINT ( 'NONE',  ( -5.823673210054431948, 21.52544592524334988, 72.70942372801901854 ) ) ;
#113538 = CARTESIAN_POINT ( 'NONE',  ( -9.564922557960796823, -16.46253265017161027, 102.0822429386477097 ) ) ;
#113537 = CARTESIAN_POINT ( 'NONE',  ( -19.02544592524334988, -5.153800228976617603, 93.95942372801900433 ) ) ;
#113539 = CARTESIAN_POINT ( 'NONE',  ( 13.97604488694527802, 13.89961937509977652, 39.37390960531435269 ) ) ;
#113540 = CARTESIAN_POINT ( 'NONE',  ( -5.719274019375978568, 21.55341960407610458, 110.2072429386477239 ) ) ;
#113541 = CARTESIAN_POINT ( 'NONE',  ( -5.153800228976607833, 19.02544592524334988, 37.70942372801899722 ) ) ;
#113542 = CARTESIAN_POINT ( 'NONE',  ( -8.224510206698948167, 14.34966873604960824, 115.4155762719810241 ) ) ;
#113543 = CARTESIAN_POINT ( 'NONE',  ( -16.51473224551069308, -9.474510206698971260, 61.66557627198103120 ) ) ;
#113544 = CARTESIAN_POINT ( 'NONE',  ( 5.049401038297881783, 19.05341960407617563, 92.29275706135234714 ) ) ;
#113545 = CARTESIAN_POINT ( 'NONE',  ( -16.53943276465976808, 0.05219959533911058130, 71.24890960531435269 ) ) ;
#113546 = CARTESIAN_POINT ( 'NONE',  ( 21.55341960407610458, 5.719274019375980345, 28.95724293864769905 ) ) ;
#113547 = CARTESIAN_POINT ( 'NONE',  ( 9.474510206698729675, 16.51473224551082808, 82.08442372801899012 ) ) ;
#113548 = CARTESIAN_POINT ( 'NONE',  ( -21.55341960407610458, -5.719274019375992779, 86.45724293864770971 ) ) ;
#113549 = CARTESIAN_POINT ( 'NONE',  ( -10.81492255796105439, 18.62759615963255655, 37.91775706135235424 ) ) ;
#113550 = CARTESIAN_POINT ( 'NONE',  ( -16.53943276465976808, -0.05219959533934237506, 48.75109039468568284 ) ) ;
#113552 = CARTESIAN_POINT ( 'NONE',  ( -21.53943276465977519, -0.05219959533937600094, 53.75109039468568994 ) ) ;
#113551 = CARTESIAN_POINT ( 'NONE',  ( 8.224510206698742110, 14.34966873604972548, 52.08442372801901854 ) ) ;
#113553 = CARTESIAN_POINT ( 'NONE',  ( -10.81492255796078084, -18.62759615963271287, 57.08224293864769550 ) ) ;
#113554 = CARTESIAN_POINT ( 'NONE',  ( 0.05219959533909260263, 19.03943276465977164, 44.99890960531435979 ) ) ;
#113555 = CARTESIAN_POINT ( 'NONE',  ( -38.00000000000001421, -12.34694845685042708, -5.649999994537625803 ) ) ;
#113556 = CARTESIAN_POINT ( 'NONE',  ( 8.224510206698742110, 14.34966873604972548, 77.08442372801901854 ) ) ;
#113557 = CARTESIAN_POINT ( 'NONE',  ( -18.67979575497178146, -10.72451020669898902, 96.66557627198102409 ) ) ;
#113558 = CARTESIAN_POINT ( 'NONE',  ( 4.483927247898545687, 16.52544592524342804, 34.79057627198103120 ) ) ;
#113559 = CARTESIAN_POINT ( 'NONE',  ( 16.52544592524335698, 4.483927247898782831, 66.45942372801903275 ) ) ;
#113560 = CARTESIAN_POINT ( 'NONE',  ( 16.46253265017146816, 9.564922557961045513, 101.6677570613523329 ) ) ;
#113561 = CARTESIAN_POINT ( 'NONE',  ( 21.53943276465977519, -0.05219959533907433946, 103.7489096053143669 ) ) ;
#113562 = CARTESIAN_POINT ( 'NONE',  ( 14.29746914071049879, -8.314922557960816363, 48.33224293864770260 ) ) ;
#113563 = EDGE_LOOP ( 'NONE', ( #49544, #172759, #173515, #199403, #36160 ) ) ;
#113564 = CARTESIAN_POINT ( 'NONE',  ( -16.55341960407617563, 4.379528057220093196, 73.54275706135234714 ) ) ;
#113565 = CARTESIAN_POINT ( 'NONE',  ( 19.36337904590691394, -5.500000000000039080, 92.91494137495617167 ) ) ;
#113566 = CARTESIAN_POINT ( 'NONE',  ( -21.52544592524343514, 5.823673210054127303, 71.04057627198103830 ) ) ;
#113567 = CARTESIAN_POINT ( 'NONE',  ( 16.55341960407611168, 4.379528057220329451, 23.95724293864769550 ) ) ;
#113568 = VERTEX_POINT ( 'NONE', #36884 ) ;
#113569 = CARTESIAN_POINT ( 'NONE',  ( -17.48847506799969054, -5.747544572773812810, 54.17302562156721280 ) ) ;
#113570 = CARTESIAN_POINT ( 'NONE',  ( 5.823673210054125526, 21.52544592524343514, 99.79057627198103830 ) ) ;
#113571 = CARTESIAN_POINT ( 'NONE',  ( 15.80617190586746368, 15.72974639402197994, 109.3739096053143811 ) ) ;
#113572 = CARTESIAN_POINT ( 'NONE',  ( 4.483927247898545687, 16.52544592524342804, 39.79057627198103830 ) ) ;
#113573 = CARTESIAN_POINT ( 'NONE',  ( 16.52544592524335698, 4.483927247898782831, 46.45942372801901854 ) ) ;
#113574 = CARTESIAN_POINT ( 'NONE',  ( 9.564922557960805705, 16.46253265017160317, 49.58224293864770260 ) ) ;
#113575 = CARTESIAN_POINT ( 'NONE',  ( -13.97604488694527625, -13.89961937509977652, 71.87390960531433848 ) ) ;
#113576 = VERTEX_POINT ( 'NONE', #161241 ) ;
#113577 = CARTESIAN_POINT ( 'NONE',  ( 15.80617190586746368, 15.72974639402197994, 24.37390960531435979 ) ) ;
#113578 = CARTESIAN_POINT ( 'NONE',  ( -25.73110857336972046, -27.25168951599382794, -18.43918238433846213 ) ) ;
#113579 = CARTESIAN_POINT ( 'NONE',  ( 13.97604488694548053, -13.89961937509957401, 100.6260903946856615 ) ) ;
#113580 = CARTESIAN_POINT ( 'NONE',  ( -13.89961937509957401, -13.97604488694547875, 54.37609039468565442 ) ) ;
#113581 = CARTESIAN_POINT ( 'NONE',  ( 5.823673210054125526, 21.52544592524343514, 94.79057627198105251 ) ) ;
#113582 = CARTESIAN_POINT ( 'NONE',  ( -16.52544592524335698, -4.483927247898792601, 108.9594237280190185 ) ) ;
#113583 = VECTOR ( 'NONE', #31417, 1000.000000000000000 ) ;
#113584 = CARTESIAN_POINT ( 'NONE',  ( -13.89961937509977652, 13.97604488694528158, 75.62390960531438111 ) ) ;
#113585 = CARTESIAN_POINT ( 'NONE',  ( -18.62759615963270932, 10.81492255796079327, 40.83224293864769550 ) ) ;
#113587 = CARTESIAN_POINT ( 'NONE',  ( -16.52544592524335698, -4.483927247898792601, 28.95942372801902209 ) ) ;
#113586 = CARTESIAN_POINT ( 'NONE',  ( 21.53943276465977519, -0.05219959533907433946, 78.74890960531436690 ) ) ;
#113588 = CARTESIAN_POINT ( 'NONE',  ( 15.72974639402199770, -15.80617190586745480, 28.12390960531435979 ) ) ;
#113589 = CARTESIAN_POINT ( 'NONE',  ( 10.81492255796106328, -18.62759615963255655, 80.41775706135234714 ) ) ;
#113590 = CARTESIAN_POINT ( 'NONE',  ( 9.564922557960805705, 16.46253265017160317, 74.58224293864769550 ) ) ;
#113591 = CARTESIAN_POINT ( 'NONE',  ( 9.474510206698971260, -16.51473224551069308, 22.91557627198102765 ) ) ;
#113592 = CARTESIAN_POINT ( 'NONE',  ( 19.05341960407611168, 5.049401038298154454, 88.95724293864769550 ) ) ;
#113593 = CARTESIAN_POINT ( 'NONE',  ( 14.34966873604960469, 8.224510206698951720, 89.16557627198102409 ) ) ;
#113594 = ORIENTED_EDGE ( 'NONE', *, *, #183262, .F. ) ;
#113595 = CARTESIAN_POINT ( 'NONE',  ( 16.51473224551083163, -9.474510206698727899, 100.8344237280190043 ) ) ;
#113596 = SPHERICAL_SURFACE ( 'NONE', #108514, 8.000000000000000000 ) ;
#113597 = CARTESIAN_POINT ( 'NONE',  ( -19.03943276465977164, 0.05219959533909376836, 76.24890960531435269 ) ) ;
#113599 = CARTESIAN_POINT ( 'NONE',  ( -9.564922557960796823, -16.46253265017161027, 102.0822429386477097 ) ) ;
#113598 = CARTESIAN_POINT ( 'NONE',  ( 5.823673210054444382, -21.52544592524334988, 80.20942372801901854 ) ) ;
#113600 = CARTESIAN_POINT ( 'NONE',  ( 4.379528057220092307, 16.55341960407617563, 77.29275706135234714 ) ) ;
#113601 = CARTESIAN_POINT ( 'NONE',  ( -28.91886483090992144, 0.2690448904511072437, -49.65045026909250936 ) ) ;
#113602 = CARTESIAN_POINT ( 'NONE',  ( 16.46253265017146816, 9.564922557961045513, 51.66775706135233293 ) ) ;
#113603 = CARTESIAN_POINT ( 'NONE',  ( 16.51473224551083163, -9.474510206698727899, 20.83442372801899722 ) ) ;
#113604 = CARTESIAN_POINT ( 'NONE',  ( 5.759383325533893760, 6.837149423127133474, -63.98874707071207268 ) ) ;
#113605 = CARTESIAN_POINT ( 'NONE',  ( -32.00000000000000000, -5.186379194389042044E-15, 42.35000000000000853 ) ) ;
#113606 = CARTESIAN_POINT ( 'NONE',  ( 22.81625015709510151, -31.40387420917324590, -4.424999997268812990 ) ) ;
#113607 = CARTESIAN_POINT ( 'NONE',  ( -14.34966873604960291, -8.224510206698953496, 21.66557627198102409 ) ) ;
#113608 = CARTESIAN_POINT ( 'NONE',  ( -17.49999999999999645, 5.499999999999992895, 102.5000000000000142 ) ) ;
#113609 = CARTESIAN_POINT ( 'NONE',  ( 8.224510206698742110, 14.34966873604972548, 112.0844237280190185 ) ) ;
#113610 = CARTESIAN_POINT ( 'NONE',  ( 28.79475375365674239, 9.355982642738014832, 145.3656553485623419 ) ) ;
#113611 = CARTESIAN_POINT ( 'NONE',  ( -16.52544592524335698, -4.483927247898792601, 78.95942372801901854 ) ) ;
#113612 = CARTESIAN_POINT ( 'NONE',  ( -21.52544592524334988, -5.823673210054445271, 93.95942372801903275 ) ) ;
#113613 = CARTESIAN_POINT ( 'NONE',  ( -16.46253265017146816, -9.564922557961047289, 99.16775706135233293 ) ) ;
#113614 = CARTESIAN_POINT ( 'NONE',  ( -10.72451020669870658, -18.67979575497194134, 69.58442372801900433 ) ) ;
#113615 = CARTESIAN_POINT ( 'NONE',  ( 16.51473224551083163, -9.474510206698727899, 40.83442372801900433 ) ) ;
#113616 = CARTESIAN_POINT ( 'NONE',  ( -16.51473224551069308, -9.474510206698971260, 76.66557627198103830 ) ) ;
#113617 = CARTESIAN_POINT ( 'NONE',  ( -16.51473224551069308, -9.474510206698971260, 56.66557627198103120 ) ) ;
#113618 = CARTESIAN_POINT ( 'NONE',  ( -12.85938658117095912, -37.87800364893588068, -12.00565553424693022 ) ) ;
#113619 = CARTESIAN_POINT ( 'NONE',  ( 15.72974639402199770, -15.80617190586745480, 98.12390960531436690 ) ) ;
#113620 = CARTESIAN_POINT ( 'NONE',  ( 0.05219959533907565091, 21.53943276465977519, 49.99890960531437401 ) ) ;
#113621 = CARTESIAN_POINT ( 'NONE',  ( 13.97604488694527802, 13.89961937509977652, 49.37390960531434558 ) ) ;
#113622 = CARTESIAN_POINT ( 'NONE',  ( 8.314922557961029526, -14.29746914071037800, 60.41775706135235424 ) ) ;
#113623 = ORIENTED_EDGE ( 'NONE', *, *, #48581, .T. ) ;
#113624 = CARTESIAN_POINT ( 'NONE',  ( 15.80617190586769283, -15.72974639402175789, 50.62609039468568994 ) ) ;
#113626 = CARTESIAN_POINT ( 'NONE',  ( -22.81625015709509441, -31.40387420917324590, -2.324999997268813789 ) ) ;
#113625 = CARTESIAN_POINT ( 'NONE',  ( -14.29746914071049879, 8.314922557960819915, 65.83224293864769550 ) ) ;
#113627 = CARTESIAN_POINT ( 'NONE',  ( -12.14591786802326823, 12.06949235617739902, 38.12609039468567573 ) ) ;
#113628 = CARTESIAN_POINT ( 'NONE',  ( 12.06949235617757843, -12.14591786802309237, 98.12390960531436690 ) ) ;
#113629 = CARTESIAN_POINT ( 'NONE',  ( -9.564922557961040184, 16.46253265017147172, 47.91775706135233293 ) ) ;
#113630 = CARTESIAN_POINT ( 'NONE',  ( 0.05219959533910956823, 16.53943276465976808, 64.99890960531435269 ) ) ;
#113631 = CARTESIAN_POINT ( 'NONE',  ( 21.53943276465977519, 0.05219959533937863772, 36.25109039468567573 ) ) ;
#113633 = CARTESIAN_POINT ( 'NONE',  ( 5.823673210054125526, 21.52544592524343514, 89.79057627198103830 ) ) ;
#113632 = CARTESIAN_POINT ( 'NONE',  ( -13.89961937509977652, 13.97604488694528158, 25.62390960531434558 ) ) ;
#113634 = CARTESIAN_POINT ( 'NONE',  ( 16.51473224551069308, 9.474510206698969483, 104.1655762719810241 ) ) ;
#113635 = CARTESIAN_POINT ( 'NONE',  ( 8.224510206698953496, -14.34966873604960469, 72.91557627198103830 ) ) ;
#113636 = CARTESIAN_POINT ( 'NONE',  ( 28.30573922537810816, -27.84595035627268800, -20.14355118860781957 ) ) ;
#113637 = CARTESIAN_POINT ( 'NONE',  ( 11.40812507854755253, -35.11059874428192273, -4.024999997268814411 ) ) ;
#113638 = CARTESIAN_POINT ( 'NONE',  ( 0.05219959533936267826, -19.03943276465977164, 80.00109039468567573 ) ) ;
#113639 = CARTESIAN_POINT ( 'NONE',  ( 15.80617190586769283, -15.72974639402175789, 20.62609039468568639 ) ) ;
#113640 = CARTESIAN_POINT ( 'NONE',  ( -13.97604488694527625, -13.89961937509977652, 71.87390960531433848 ) ) ;
#113641 = CARTESIAN_POINT ( 'NONE',  ( -5.049401038297874678, -19.05341960407617918, 54.79275706135234003 ) ) ;
#113642 = CARTESIAN_POINT ( 'NONE',  ( -13.97604488694527625, -13.89961937509977652, 36.87390960531436690 ) ) ;
#113643 = ADVANCED_FACE ( 'NONE', ( #146060 ), #162238, .F. ) ;
#113644 = CARTESIAN_POINT ( 'NONE',  ( -16.52544592524342804, 4.483927247898546575, 66.04057627198103830 ) ) ;
#113645 = CARTESIAN_POINT ( 'NONE',  ( -8.314922557960811034, -14.29746914071050412, 52.08224293864768839 ) ) ;
#113646 = CARTESIAN_POINT ( 'NONE',  ( -9.564922557960796823, -16.46253265017161027, 82.08224293864768129 ) ) ;
#113647 = CARTESIAN_POINT ( 'NONE',  ( -5.719274019375978568, 21.55341960407610458, 90.20724293864770971 ) ) ;
#113648 = CARTESIAN_POINT ( 'NONE',  ( 9.474510206698971260, -16.51473224551069308, 57.91557627198103120 ) ) ;
#113649 = CARTESIAN_POINT ( 'NONE',  ( -21.55341960407610458, -5.719274019375992779, 81.45724293864769550 ) ) ;
#113650 = CARTESIAN_POINT ( 'NONE',  ( -5.049401038297874678, -19.05341960407617918, 19.79275706135233293 ) ) ;
#113653 = CARTESIAN_POINT ( 'NONE',  ( -12.14591786802309592, -12.06949235617757132, 101.8739096053143811 ) ) ;
#113652 = CARTESIAN_POINT ( 'NONE',  ( -0.05219959533934338120, 16.53943276465976808, 107.5010903946856899 ) ) ;
#113651 = CARTESIAN_POINT ( 'NONE',  ( 9.564922557960805705, 16.46253265017160317, 29.58224293864769550 ) ) ;
#113654 = CARTESIAN_POINT ( 'NONE',  ( 9.474510206698729675, 16.51473224551082808, 92.08442372801900433 ) ) ;
#113655 = ORIENTED_EDGE ( 'NONE', *, *, #185853, .F. ) ;
#113656 = CARTESIAN_POINT ( 'NONE',  ( 21.52544592524344225, -5.823673210054117533, 113.5405762719810383 ) ) ;
#113657 = CARTESIAN_POINT ( 'NONE',  ( -19.03943276465977164, -0.05219959533935918106, 58.75109039468566863 ) ) ;
#113658 = CARTESIAN_POINT ( 'NONE',  ( 4.483927247898790824, -16.52544592524335698, 105.2094237280190328 ) ) ;
#113659 = CARTESIAN_POINT ( 'NONE',  ( -19.05341960407617563, 5.049401038297882671, 43.54275706135232582 ) ) ;
#113660 = CARTESIAN_POINT ( 'NONE',  ( 16.46253265017160672, -9.564922557960803928, 108.3322429386476955 ) ) ;
#113661 = CARTESIAN_POINT ( 'NONE',  ( -15.72974639402197994, 15.80617190586746368, 55.62390960531436690 ) ) ;
#113662 = FACE_OUTER_BOUND ( 'NONE', #174361, .T. ) ;
#113663 = CARTESIAN_POINT ( 'NONE',  ( 5.049401038298161559, -19.05341960407611168, 32.70724293864768129 ) ) ;
#113664 = CARTESIAN_POINT ( 'NONE',  ( 15.72974639402176855, 15.80617190586768217, 106.8760903946856899 ) ) ;
#113665 = CARTESIAN_POINT ( 'NONE',  ( -8.224510206698735004, -14.34966873604973081, 79.58442372801903275 ) ) ;
#113666 = CARTESIAN_POINT ( 'NONE',  ( -10.72451020669870658, -18.67979575497194134, 29.58442372801901854 ) ) ;
#113667 = CARTESIAN_POINT ( 'NONE',  ( -16.53943276465976808, -0.05219959533934237506, 48.75109039468568284 ) ) ;
#113668 = CARTESIAN_POINT ( 'NONE',  ( -19.02544592524342804, 5.153800228976336051, 111.0405762719810099 ) ) ;
#113669 = CARTESIAN_POINT ( 'NONE',  ( 13.97604488694527802, 13.89961937509977652, 49.37390960531434558 ) ) ;
#113670 = CARTESIAN_POINT ( 'NONE',  ( 13.89961937509977652, -13.97604488694527269, 68.12390960531436690 ) ) ;
#113671 = CARTESIAN_POINT ( 'NONE',  ( -16.53943276465976808, -0.05219959533934237506, 43.75109039468568284 ) ) ;
#113672 = CARTESIAN_POINT ( 'NONE',  ( 8.224510206698953496, -14.34966873604960469, 107.9155762719810241 ) ) ;
#113673 = CARTESIAN_POINT ( 'NONE',  ( 16.55341960407618274, -4.379528057220086978, 111.0427570613523613 ) ) ;
#113674 = DIRECTION ( 'NONE',  ( 1.000000000000000000, 0.000000000000000000, -0.000000000000000000 ) ) ;
#113677 = CARTESIAN_POINT ( 'NONE',  ( 5.153800228976335163, 19.02544592524342804, 64.79057627198100988 ) ) ;
#113676 = CARTESIAN_POINT ( 'NONE',  ( 16.46253265017160672, -9.564922557960803928, 98.33224293864769550 ) ) ;
#113675 = CARTESIAN_POINT ( 'NONE',  ( -0.05219959533937732626, 21.53943276465977519, 62.50109039468568284 ) ) ;
#113678 = CARTESIAN_POINT ( 'NONE',  ( 9.474510206698971260, -16.51473224551069308, 97.91557627198102409 ) ) ;
#113679 = CARTESIAN_POINT ( 'NONE',  ( 4.483927247898545687, 16.52544592524342804, 49.79057627198102409 ) ) ;
#113680 = CARTESIAN_POINT ( 'NONE',  ( 14.29746914071037800, 8.314922557961029526, 106.6677570613523756 ) ) ;
#113681 = CARTESIAN_POINT ( 'NONE',  ( -4.483927247898539470, -16.52544592524342804, 37.29057627198102409 ) ) ;
#113682 = CARTESIAN_POINT ( 'NONE',  ( 17.50000000000000000, 5.499999999999997335, 120.0000000000000142 ) ) ;
#113683 = CARTESIAN_POINT ( 'NONE',  ( 5.049401038298161559, -19.05341960407611168, 62.70724293864769550 ) ) ;
#113684 = CARTESIAN_POINT ( 'NONE',  ( -5.153800228976607833, 19.02544592524334988, 42.70942372801901143 ) ) ;
#113685 = CARTESIAN_POINT ( 'NONE',  ( -36.91746825000001309, -11.99521256947794789, -9.024999997268812635 ) ) ;
#113686 = CARTESIAN_POINT ( 'NONE',  ( -9.564922557960796823, -16.46253265017161027, 67.08224293864769550 ) ) ;
#113688 = CARTESIAN_POINT ( 'NONE',  ( -16.53943276465976808, -0.05219959533934237506, 73.75109039468567573 ) ) ;
#113687 = CARTESIAN_POINT ( 'NONE',  ( 19.05341960407617918, -5.049401038297876454, 91.04275706135234714 ) ) ;
#113689 = CARTESIAN_POINT ( 'NONE',  ( 16.18388926212238488, 7.379444403734540359, 92.93953151366149257 ) ) ;
#113690 = CARTESIAN_POINT ( 'NONE',  ( -16.51473224551069308, -9.474510206698971260, 86.66557627198102409 ) ) ;
#113691 = CARTESIAN_POINT ( 'NONE',  ( 10.72451020669871369, 18.67979575497193778, 32.08442372801901854 ) ) ;
#113692 = CARTESIAN_POINT ( 'NONE',  ( 13.97604488694548053, -13.89961937509957401, 85.62609039468568994 ) ) ;
#113694 = CARTESIAN_POINT ( 'NONE',  ( -13.97604488694527625, -13.89961937509977652, 46.87390960531435979 ) ) ;
#113693 = CARTESIAN_POINT ( 'NONE',  ( 16.20579543436678094, 7.371946100355120102, 88.06520834171882939 ) ) ;
#113695 = CARTESIAN_POINT ( 'NONE',  ( 5.153800228976335163, 19.02544592524342804, 84.79057627198099567 ) ) ;
#113697 = CARTESIAN_POINT ( 'NONE',  ( -19.02544592524342804, 5.153800228976336051, 51.04057627198103120 ) ) ;
#113696 = CARTESIAN_POINT ( 'NONE',  ( -14.34966873604960291, -8.224510206698953496, 41.66557627198103120 ) ) ;
#113698 = CARTESIAN_POINT ( 'NONE',  ( 5.153800228976615827, -19.02544592524334988, 60.20942372801899012 ) ) ;
#113699 = VERTEX_POINT ( 'NONE', #181419 ) ;
#113700 = CARTESIAN_POINT ( 'NONE',  ( 12.14591786802309770, 12.06949235617756955, 84.37390960531438111 ) ) ;
#113701 = CARTESIAN_POINT ( 'NONE',  ( -9.564922557961040184, 16.46253265017147172, 32.91775706135233293 ) ) ;
#113702 = CARTESIAN_POINT ( 'NONE',  ( 5.049401038298161559, -19.05341960407611168, 62.70724293864769550 ) ) ;
#113703 = CARTESIAN_POINT ( 'NONE',  ( 21.55341960407610458, 5.719274019375980345, 58.95724293864770971 ) ) ;
#113705 = CARTESIAN_POINT ( 'NONE',  ( 5.153800228976615827, -19.02544592524334988, 25.20942372801900433 ) ) ;
#113704 = CARTESIAN_POINT ( 'NONE',  ( -14.34966873604960291, -8.224510206698953496, 61.66557627198103120 ) ) ;
#113706 = CARTESIAN_POINT ( 'NONE',  ( 13.89961937509977652, -13.97604488694527269, 103.1239096053143527 ) ) ;
#113707 = CARTESIAN_POINT ( 'NONE',  ( -15.80617190586745835, -15.72974639402198527, 26.87390960531435979 ) ) ;
#113708 = CARTESIAN_POINT ( 'NONE',  ( 13.97604488694527802, 13.89961937509977652, 59.37390960531434558 ) ) ;
#113709 = CARTESIAN_POINT ( 'NONE',  ( -13.89961937509977652, 13.97604488694528158, 45.62390960531433848 ) ) ;
#113710 = CARTESIAN_POINT ( 'NONE',  ( -14.34966873604960291, -8.224510206698953496, 101.6655762719810383 ) ) ;
#113711 = CARTESIAN_POINT ( 'NONE',  ( -0.05219959533907301413, -21.53943276465977519, 112.4989096053143669 ) ) ;
#113712 = CARTESIAN_POINT ( 'NONE',  ( -13.89961937509977652, 13.97604488694528158, 95.62390960531436690 ) ) ;
#113713 = CARTESIAN_POINT ( 'NONE',  ( -10.81492255796105439, 18.62759615963255655, 22.91775706135235069 ) ) ;
#113714 = CARTESIAN_POINT ( 'NONE',  ( 16.51473224551069308, 9.474510206698969483, 104.1655762719810241 ) ) ;
#113715 = CARTESIAN_POINT ( 'NONE',  ( 19.03943276465977164, -0.05219959533909143690, 23.74890960531435269 ) ) ;
#113716 = CARTESIAN_POINT ( 'NONE',  ( 21.55341960407619695, -5.719274019375665929, 81.04275706135236135 ) ) ;
#113717 = CARTESIAN_POINT ( 'NONE',  ( -15.80617190586745835, -15.72974639402198527, 96.87390960531436690 ) ) ;
#113718 = EDGE_CURVE ( 'NONE', #84042, #123524, #150076, .T. ) ;
#113719 = CARTESIAN_POINT ( 'NONE',  ( -17.49999999999999645, 5.499999999999997335, 120.0000000000000142 ) ) ;
#113720 = CARTESIAN_POINT ( 'NONE',  ( 13.89961937509978007, -13.97604488694527269, 53.12390960531435269 ) ) ;
#113721 = CARTESIAN_POINT ( 'NONE',  ( 29.32058373238547588, -1.046637022530830574, -52.18867397238361150 ) ) ;
#113722 = CARTESIAN_POINT ( 'NONE',  ( 14.34966873604972726, -8.224510206698740333, 50.83442372801901143 ) ) ;
#113723 = CARTESIAN_POINT ( 'NONE',  ( 16.55341960407611168, 4.379528057220329451, 113.9572429386477239 ) ) ;
#113724 = CARTESIAN_POINT ( 'NONE',  ( 0.000000000000000000, -165.0000000000000000, 12.00000000000000355 ) ) ;
#113725 = CARTESIAN_POINT ( 'NONE',  ( 9.474510206698971260, -16.51473224551069308, 62.91557627198102409 ) ) ;
#113726 = CARTESIAN_POINT ( 'NONE',  ( 4.379528057220339221, -16.55341960407611168, 92.70724293864770971 ) ) ;
#113727 = CARTESIAN_POINT ( 'NONE',  ( 0.05219959533907565091, 21.53943276465977519, 49.99890960531437401 ) ) ;
#113728 = CARTESIAN_POINT ( 'NONE',  ( -12.14591786802309592, -12.06949235617757132, 71.87390960531438111 ) ) ;
#113729 = CARTESIAN_POINT ( 'NONE',  ( -8.224510206698735004, -14.34966873604973081, 24.58442372801901499 ) ) ;
#113730 = CARTESIAN_POINT ( 'NONE',  ( 10.72451020669871369, 18.67979575497193778, 77.08442372801901854 ) ) ;
#113731 = CARTESIAN_POINT ( 'NONE',  ( -16.51473224551082808, 9.474510206698731452, 63.33442372801900433 ) ) ;
#113732 = CARTESIAN_POINT ( 'NONE',  ( -8.314922557961024197, 14.29746914071037800, 92.91775706135236135 ) ) ;
#113733 = CARTESIAN_POINT ( 'NONE',  ( -14.34966873604960291, -8.224510206698953496, 41.66557627198103120 ) ) ;
#113734 = CARTESIAN_POINT ( 'NONE',  ( 9.564922557960805705, 16.46253265017160317, 39.58224293864768839 ) ) ;
#113735 = CARTESIAN_POINT ( 'NONE',  ( 19.02544592524343514, -5.153800228976328945, 93.54057627198102409 ) ) ;
#113736 = CARTESIAN_POINT ( 'NONE',  ( 21.52544592524344225, -5.823673210054117533, 88.54057627198103830 ) ) ;
#113737 = CARTESIAN_POINT ( 'NONE',  ( 12.06949235617739724, 12.14591786802326823, 36.87609039468568994 ) ) ;
#113739 = CARTESIAN_POINT ( 'NONE',  ( -15.80617190586768217, 15.72974639402176855, 73.12609039468567573 ) ) ;
#113738 = CARTESIAN_POINT ( 'NONE',  ( -16.55341960407611168, -4.379528057220339221, 71.45724293864769550 ) ) ;
#113740 = EDGE_CURVE ( 'NONE', #26356, #177652, #59235, .T. ) ;
#113741 = CARTESIAN_POINT ( 'NONE',  ( -16.55341960407617563, 4.379528057220093196, 103.5427570613523613 ) ) ;
#113742 = CARTESIAN_POINT ( 'NONE',  ( -28.79475375365586842, 2.428612866367529932E-14, 140.2656553485623760 ) ) ;
#113743 = CARTESIAN_POINT ( 'NONE',  ( -21.49604614807110536, 21.49604614807103786, -65.00100000000003320 ) ) ;
#113744 = CARTESIAN_POINT ( 'NONE',  ( 16.53943276465976808, -0.05219959533910856209, 23.74890960531435269 ) ) ;
#113745 = CARTESIAN_POINT ( 'NONE',  ( -8.224510206698735004, -14.34966873604973081, 69.58442372801900433 ) ) ;
#113746 = CARTESIAN_POINT ( 'NONE',  ( -19.02544592524342804, 5.153800228976336051, 91.04057627198100988 ) ) ;
#113747 = CARTESIAN_POINT ( 'NONE',  ( -19.05341960407611168, -5.049401038298163336, 106.4572429386476955 ) ) ;
#113748 = CARTESIAN_POINT ( 'NONE',  ( -21.53943276465977519, -0.05219959533937600094, 88.75109039468567573 ) ) ;
#113749 = CARTESIAN_POINT ( 'NONE',  ( 12.14591786802327356, -12.06949235617739191, 95.62609039468568994 ) ) ;
#113750 = CARTESIAN_POINT ( 'NONE',  ( -16.53943276465976808, 0.05219959533911058130, 61.24890960531435979 ) ) ;
#113751 = CARTESIAN_POINT ( 'NONE',  ( 19.05341960407611168, 5.049401038298154454, 73.95724293864768129 ) ) ;
#113752 = ORIENTED_EDGE ( 'NONE', *, *, #45027, .F. ) ;
#113753 = CARTESIAN_POINT ( 'NONE',  ( 13.97604488694548053, -13.89961937509957401, 110.6260903946856615 ) ) ;
#113754 = CARTESIAN_POINT ( 'NONE',  ( 12.14591786802309770, 12.06949235617756955, 109.3739096053143811 ) ) ;
#113755 = CARTESIAN_POINT ( 'NONE',  ( -19.05341960407611168, -5.049401038298163336, 81.45724293864769550 ) ) ;
#113757 = CARTESIAN_POINT ( 'NONE',  ( 23.48529157249599919, 32.32473071737754111, -0.6999999999999998446 ) ) ;
#113756 = CARTESIAN_POINT ( 'NONE',  ( 0.05219959533934541429, -16.53943276465976808, 20.00109039468568639 ) ) ;
#113758 = CARTESIAN_POINT ( 'NONE',  ( -15.80617190586768217, 15.72974639402176855, 113.1260903946856899 ) ) ;
#113759 = CARTESIAN_POINT ( 'NONE',  ( 16.55341960407618274, -4.379528057220086978, 86.04275706135236135 ) ) ;
#113760 = CARTESIAN_POINT ( 'NONE',  ( -19.05341960407617563, 5.049401038297882671, 103.5427570613523329 ) ) ;
#113761 = CARTESIAN_POINT ( 'NONE',  ( -8.224510206698948167, 14.34966873604960824, 115.4155762719810241 ) ) ;
#113762 = CARTESIAN_POINT ( 'NONE',  ( -0.05219959533934338120, 16.53943276465976808, 72.50109039468568994 ) ) ;
#113763 = CARTESIAN_POINT ( 'NONE',  ( -8.314922557961024197, 14.29746914071037800, 57.91775706135234714 ) ) ;
#113764 = CARTESIAN_POINT ( 'NONE',  ( 27.53984522711021299, -29.01046520254151773, -5.289306513719187031 ) ) ;
#113765 = CARTESIAN_POINT ( 'NONE',  ( -19.02544592524334988, -5.153800228976617603, 68.95942372801896170 ) ) ;
#113766 = CARTESIAN_POINT ( 'NONE',  ( 21.55341960407619695, -5.719274019375665929, 101.0427570613523756 ) ) ;
#113767 = CARTESIAN_POINT ( 'NONE',  ( 19.03943276465977164, -0.05219959533909143690, 28.74890960531435624 ) ) ;
#113768 = CARTESIAN_POINT ( 'NONE',  ( 19.03943276465977164, -0.05219959533909143690, 78.74890960531436690 ) ) ;
#113769 = CARTESIAN_POINT ( 'NONE',  ( -4.379528057220328563, 16.55341960407611168, 75.20724293864769550 ) ) ;
#113770 = CARTESIAN_POINT ( 'NONE',  ( -5.823673210054431948, 21.52544592524334988, 92.70942372801901854 ) ) ;
#113771 = CARTESIAN_POINT ( 'NONE',  ( 9.474510206698729675, 16.51473224551082808, 42.08442372801900433 ) ) ;
#113772 = CARTESIAN_POINT ( 'NONE',  ( -18.67979575497178146, -10.72451020669898902, 31.66557627198102054 ) ) ;
#113773 = CARTESIAN_POINT ( 'NONE',  ( 5.719274019375673035, 21.55341960407619339, 107.2927570613523471 ) ) ;
#113774 = CARTESIAN_POINT ( 'NONE',  ( 9.564922557960805705, 16.46253265017160317, 79.58224293864769550 ) ) ;
#113775 = CARTESIAN_POINT ( 'NONE',  ( 5.823673210054444382, -21.52544592524334988, 100.2094237280190043 ) ) ;
#113776 = CARTESIAN_POINT ( 'NONE',  ( 18.67979575497178502, 10.72451020669898547, 69.16557627198102409 ) ) ;
#113777 = CARTESIAN_POINT ( 'NONE',  ( 16.51473224551069308, 9.474510206698969483, 99.16557627198102409 ) ) ;
#113778 = CARTESIAN_POINT ( 'NONE',  ( 5.049401038297881783, 19.05341960407617563, 72.29275706135234714 ) ) ;
#113779 = CARTESIAN_POINT ( 'NONE',  ( 5.153800228976335163, 19.02544592524342804, 99.79057627198102409 ) ) ;
#113780 = CARTESIAN_POINT ( 'NONE',  ( 19.05341960407617918, -5.049401038297876454, 91.04275706135234714 ) ) ;
#113781 = CARTESIAN_POINT ( 'NONE',  ( -16.53943276465976808, -0.05219959533934237506, 58.75109039468568994 ) ) ;
#113782 = CARTESIAN_POINT ( 'NONE',  ( -9.564922557960796823, -16.46253265017161027, 22.08224293864768839 ) ) ;
#113783 = CARTESIAN_POINT ( 'NONE',  ( -16.51473224551069308, -9.474510206698971260, 86.66557627198102409 ) ) ;
#113785 = B_SPLINE_CURVE_WITH_KNOTS ( 'NONE', 3,
 ( #174972, #187183, #175978, #48654, #142629, #172990, #22287, #51616, #110306, #188165, #36436, #98091, #160799, #96127, #83938, #159789, #18316, #21284, #34468, #82941, #19306, #144619, #80954, #35455, #67783, #65787, #97106, #112296, #191139, #111301, #3131, #171988 ),
 .UNSPECIFIED., .F., .F.,
 ( 4, 2, 2, 2, 2, 2, 2, 2, 2, 2, 2, 2, 2, 2, 2, 4 ),
 ( 2.367436813247750825E-17, 0.0003712461730037028783, 0.0007424923460073820126, 0.001113738519011061310, 0.001484984692014740390, 0.002227477038022091828, 0.002598723211025753561, 0.002969969384029413993, 0.003341215557033075725, 0.003712461730036736591, 0.004083707903040397456, 0.004454954076044058756, 0.004826200249047720922, 0.005197446422051382221, 0.005568692595055043520, 0.005939938768058704820 ),
 .UNSPECIFIED. ) ;
#113784 = CARTESIAN_POINT ( 'NONE',  ( -5.719274019375978568, 21.55341960407610458, 65.20724293864768129 ) ) ;
#113786 = CARTESIAN_POINT ( 'NONE',  ( 0.05219959533934541429, -16.53943276465976808, 35.00109039468568284 ) ) ;
#113787 = CARTESIAN_POINT ( 'NONE',  ( -5.719274019375665041, -21.55341960407619695, 29.79275706135234358 ) ) ;
#113788 = CARTESIAN_POINT ( 'NONE',  ( 18.62759615963255655, 10.81492255796105972, 81.66775706135236135 ) ) ;
#113789 = CARTESIAN_POINT ( 'NONE',  ( -8.314922557961024197, 14.29746914071037800, 87.91775706135234714 ) ) ;
#113790 = CARTESIAN_POINT ( 'NONE',  ( -19.05341960407611168, -5.049401038298163336, 81.45724293864769550 ) ) ;
#113791 = CARTESIAN_POINT ( 'NONE',  ( -16.52544592524342804, 4.483927247898546575, 76.04057627198102409 ) ) ;
#113792 = CARTESIAN_POINT ( 'NONE',  ( 4.379528057220339221, -16.55341960407611168, 22.70724293864769194 ) ) ;
#113793 = CARTESIAN_POINT ( 'NONE',  ( -13.89961937509957401, -13.97604488694547875, 59.37609039468566863 ) ) ;
#113794 = CARTESIAN_POINT ( 'NONE',  ( 18.67979575497194134, -10.72451020669871369, 40.83442372801901854 ) ) ;
#113795 = CARTESIAN_POINT ( 'NONE',  ( 16.53943276465976808, -0.05219959533910856209, 88.74890960531436690 ) ) ;
#113796 = CARTESIAN_POINT ( 'NONE',  ( -21.55341960407610458, -5.719274019375992779, 21.45724293864769550 ) ) ;
#113797 = CARTESIAN_POINT ( 'NONE',  ( 14.34966873604972726, -8.224510206698740333, 105.8344237280190328 ) ) ;
#113798 = CARTESIAN_POINT ( 'NONE',  ( -0.05219959533937732626, 21.53943276465977519, 82.50109039468568994 ) ) ;
#113799 = CARTESIAN_POINT ( 'NONE',  ( -12.06949235617739369, -12.14591786802326823, 39.37609039468567573 ) ) ;
#113800 = CARTESIAN_POINT ( 'NONE',  ( 5.719274019375673035, 21.55341960407619339, 37.29275706135235424 ) ) ;
#113801 = EDGE_LOOP ( 'NONE', ( #148302, #12713 ) ) ;
#113802 = CARTESIAN_POINT ( 'NONE',  ( 15.80617190586769283, -15.72974639402175789, 20.62609039468568639 ) ) ;
#113803 = CARTESIAN_POINT ( 'NONE',  ( -14.29746914071049879, 8.314922557960819915, 95.83224293864770971 ) ) ;
#113804 = DIRECTION ( 'NONE',  ( 1.000000000000000000, 0.000000000000000000, 0.000000000000000000 ) ) ;
#113805 = CARTESIAN_POINT ( 'NONE',  ( -12.06949235617756955, 12.14591786802309770, 60.62390960531437401 ) ) ;
#113806 = CARTESIAN_POINT ( 'NONE',  ( -16.55341960407617563, 4.379528057220093196, 93.54275706135234714 ) ) ;
#113807 = CARTESIAN_POINT ( 'NONE',  ( -13.89961937509977652, 13.97604488694528158, 45.62390960531433848 ) ) ;
#113808 = CARTESIAN_POINT ( 'NONE',  ( -18.62759615963270932, 10.81492255796079327, 45.83224293864769550 ) ) ;
#113809 = CARTESIAN_POINT ( 'NONE',  ( -14.29746914071049879, 8.314922557960819915, 80.83224293864769550 ) ) ;
#113810 = CARTESIAN_POINT ( 'NONE',  ( -21.52544592524343514, 5.823673210054127303, 76.04057627198102409 ) ) ;
#113811 = CARTESIAN_POINT ( 'NONE',  ( -0.05219959533909027116, -19.03943276465977164, 82.49890960531436690 ) ) ;
#113813 = CARTESIAN_POINT ( 'NONE',  ( -19.05341960407617563, 5.049401038297882671, 93.54275706135234714 ) ) ;
#113812 = CARTESIAN_POINT ( 'NONE',  ( -5.049401038298153566, 19.05341960407611168, 45.20724293864769550 ) ) ;
#113814 = CARTESIAN_POINT ( 'NONE',  ( 15.80617190586746368, 15.72974639402197994, 29.37390960531435269 ) ) ;
#113815 = CARTESIAN_POINT ( 'NONE',  ( 5.719274019375673035, 21.55341960407619339, 57.29275706135234714 ) ) ;
#113816 = CARTESIAN_POINT ( 'NONE',  ( 0.05219959533909260263, 19.03943276465977164, 59.99890960531436690 ) ) ;
#113817 = CARTESIAN_POINT ( 'NONE',  ( -16.46253265017160317, 9.564922557960807481, 85.83224293864769550 ) ) ;
#113818 = ORIENTED_EDGE ( 'NONE', *, *, #113474, .F. ) ;
#113819 = CARTESIAN_POINT ( 'NONE',  ( -0.05219959533934338120, 16.53943276465976808, 47.50109039468568994 ) ) ;
#113820 = CARTESIAN_POINT ( 'NONE',  ( 5.823673210054444382, -21.52544592524334988, 50.20942372801901854 ) ) ;
#113821 = CARTESIAN_POINT ( 'NONE',  ( -21.55341960407619339, 5.719274019375674811, 78.54275706135236135 ) ) ;
#113822 = CARTESIAN_POINT ( 'NONE',  ( -18.67979575497178146, -10.72451020669898902, 21.66557627198102409 ) ) ;
#113823 = CARTESIAN_POINT ( 'NONE',  ( 21.53943276465977519, -0.05219959533907433946, 83.74890960531435269 ) ) ;
#113825 = CARTESIAN_POINT ( 'NONE',  ( -12.06949235617739369, -12.14591786802326823, 59.37609039468568284 ) ) ;
#113824 = CARTESIAN_POINT ( 'NONE',  ( 15.80617190586769283, -15.72974639402175789, 20.62609039468568639 ) ) ;
#113826 = CARTESIAN_POINT ( 'NONE',  ( 15.80617190586746368, 15.72974639402197994, 69.37390960531436690 ) ) ;
#113827 = CARTESIAN_POINT ( 'NONE',  ( -19.03943276465977164, -0.05219959533935918106, 18.75109039468567218 ) ) ;
#113829 = CARTESIAN_POINT ( 'NONE',  ( -16.53943276465976808, -0.05219959533934237506, 103.7510903946857042 ) ) ;
#113828 = CARTESIAN_POINT ( 'NONE',  ( 5.049401038298161559, -19.05341960407611168, 62.70724293864769550 ) ) ;
#113830 = CYLINDRICAL_SURFACE ( 'NONE', #85369, 37.99626262588765968 ) ;
#113831 = CARTESIAN_POINT ( 'NONE',  ( 5.153800228976335163, 19.02544592524342804, 84.79057627198099567 ) ) ;
#113832 = CARTESIAN_POINT ( 'NONE',  ( -17.59860650958993844, 7.585241751806885979, 53.42337014262493966 ) ) ;
#113833 = CARTESIAN_POINT ( 'NONE',  ( -5.049401038297874678, -19.05341960407617918, 84.79275706135233293 ) ) ;
#113834 = CARTESIAN_POINT ( 'NONE',  ( -15.72974639402197994, 15.80617190586746368, 55.62390960531436690 ) ) ;
#113835 = CARTESIAN_POINT ( 'NONE',  ( -12.14591786802326823, 12.06949235617739902, 113.1260903946856899 ) ) ;
#113836 = CARTESIAN_POINT ( 'NONE',  ( 16.51473224551083163, -9.474510206698727899, 105.8344237280190043 ) ) ;
#113837 = FACE_OUTER_BOUND ( 'NONE', #14286, .T. ) ;
#113838 = CARTESIAN_POINT ( 'NONE',  ( 5.153800228976615827, -19.02544592524334988, 100.2094237280190043 ) ) ;
#113840 = CARTESIAN_POINT ( 'NONE',  ( -9.564922557961040184, 16.46253265017147172, 57.91775706135233293 ) ) ;
#113839 = CARTESIAN_POINT ( 'NONE',  ( 18.67979575497178502, 10.72451020669898547, 89.16557627198102409 ) ) ;
#113841 = CARTESIAN_POINT ( 'NONE',  ( -35.00000000000000000, -3.889087296526017479, 8.181980515339454030 ) ) ;
#113842 = CARTESIAN_POINT ( 'NONE',  ( 19.05341960407611168, 5.049401038298154454, 48.95724293864768129 ) ) ;
#113843 = CARTESIAN_POINT ( 'NONE',  ( -4.483927247898539470, -16.52544592524342804, 57.29057627198103120 ) ) ;
#113844 = CARTESIAN_POINT ( 'NONE',  ( -5.153800228976328057, -19.02544592524343514, 47.29057627198102409 ) ) ;
#113845 = CARTESIAN_POINT ( 'NONE',  ( -16.52544592524342804, 4.483927247898546575, 51.04057627198103120 ) ) ;
#113846 = CARTESIAN_POINT ( 'NONE',  ( -27.98120534312124974, -28.16303873514637957, -20.10652275068721195 ) ) ;
#113847 = CARTESIAN_POINT ( 'NONE',  ( 32.53128430053961750, -2.419343514923771199, 87.89668391837237493 ) ) ;
#113848 = CARTESIAN_POINT ( 'NONE',  ( -4.483927247898539470, -16.52544592524342804, 32.29057627198102409 ) ) ;
#113849 = CARTESIAN_POINT ( 'NONE',  ( -0.05219959533909027116, -19.03943276465977164, 62.49890960531435979 ) ) ;
#113850 = CARTESIAN_POINT ( 'NONE',  ( 5.049401038297881783, 19.05341960407617918, 72.29275706135233293 ) ) ;
#113851 = CARTESIAN_POINT ( 'NONE',  ( 13.89961937509957401, 13.97604488694547697, 41.87609039468566152 ) ) ;
#113852 = CARTESIAN_POINT ( 'NONE',  ( 16.55341960407618274, -4.379528057220086978, 46.04275706135234714 ) ) ;
#113853 = CARTESIAN_POINT ( 'NONE',  ( -21.55341960407610458, -5.719274019375992779, 56.45724293864768839 ) ) ;
#113854 = CARTESIAN_POINT ( 'NONE',  ( -15.80617190586768217, 15.72974639402176855, 108.1260903946856757 ) ) ;
#113855 = CARTESIAN_POINT ( 'NONE',  ( 9.474510206698971260, -16.51473224551069308, 77.91557627198103830 ) ) ;
#113856 = DIRECTION ( 'NONE',  ( -0.000000000000000000, -0.000000000000000000, 1.000000000000000000 ) ) ;
#113857 = CARTESIAN_POINT ( 'NONE',  ( -19.05341960407611168, -5.049401038298163336, 91.45724293864766707 ) ) ;
#113858 = CARTESIAN_POINT ( 'NONE',  ( -22.81625015709509441, -31.40387420917324590, -2.324999997268813345 ) ) ;
#113859 = CARTESIAN_POINT ( 'NONE',  ( 15.72974639402176855, 15.80617190586768217, 31.87609039468567929 ) ) ;
#113860 = CARTESIAN_POINT ( 'NONE',  ( -4.483927247898539470, -16.52544592524342804, 97.29057627198105251 ) ) ;
#113862 = CARTESIAN_POINT ( 'NONE',  ( -5.153800228976328057, -19.02544592524343514, 87.29057627198103830 ) ) ;
#113861 = CARTESIAN_POINT ( 'NONE',  ( 10.72451020669898902, -18.67979575497178502, 92.91557627198103830 ) ) ;
#113863 = CARTESIAN_POINT ( 'NONE',  ( -5.049401038298153566, 19.05341960407611168, 85.20724293864766707 ) ) ;
#113864 = CARTESIAN_POINT ( 'NONE',  ( 0.05219959533907565091, 21.53943276465977519, 109.9989096053143527 ) ) ;
#113865 = ORIENTED_EDGE ( 'NONE', *, *, #17662, .T. ) ;
#113866 = CARTESIAN_POINT ( 'NONE',  ( 9.474510206698971260, -16.51473224551069308, 72.91557627198102409 ) ) ;
#113867 = CARTESIAN_POINT ( 'NONE',  ( -32.09281931051391012, -20.34824190692417289, -24.99999999999999289 ) ) ;
#113869 = CARTESIAN_POINT ( 'NONE',  ( -19.05341960407611168, -5.049401038298163336, 31.45724293864769550 ) ) ;
#113868 = CARTESIAN_POINT ( 'NONE',  ( -16.52544592524342804, 4.483927247898546575, 116.0405762719810383 ) ) ;
#113870 = CARTESIAN_POINT ( 'NONE',  ( -16.46253265017146816, -9.564922557961047289, 89.16775706135234714 ) ) ;
#113871 = CARTESIAN_POINT ( 'NONE',  ( -19.03943276465977164, 0.05219959533909376836, 21.24890960531436335 ) ) ;
#113872 = CARTESIAN_POINT ( 'NONE',  ( -10.81492255796105439, 18.62759615963255655, 67.91775706135234714 ) ) ;
#113874 = CARTESIAN_POINT ( 'NONE',  ( -21.53943276465977519, -0.05219959533937600094, 33.75109039468568284 ) ) ;
#113873 = CARTESIAN_POINT ( 'NONE',  ( -9.474510206698964154, 16.51473224551069663, 60.41557627198102409 ) ) ;
#113875 = CARTESIAN_POINT ( 'NONE',  ( 21.53943276465977519, -0.05219959533907433946, 113.7489096053143527 ) ) ;
#113876 = CARTESIAN_POINT ( 'NONE',  ( -28.82186960331499392, 9.364793116373565596, 147.8999999999999488 ) ) ;
#113877 = CARTESIAN_POINT ( 'NONE',  ( 13.97604488694527802, 13.89961937509977652, 89.37390960531436690 ) ) ;
#113878 = CARTESIAN_POINT ( 'NONE',  ( 27.20512408147139993, 7.754361572990046803, 164.3878212768029243 ) ) ;
#113880 = CARTESIAN_POINT ( 'NONE',  ( -18.62759615963270932, 10.81492255796079327, 25.83224293864769194 ) ) ;
#113879 = CARTESIAN_POINT ( 'NONE',  ( 16.52544592524335698, 4.483927247898782831, 31.45942372801901854 ) ) ;
#113881 = CARTESIAN_POINT ( 'NONE',  ( 21.55341960407619695, -5.719274019375665929, 61.04275706135234714 ) ) ;
#113882 = CARTESIAN_POINT ( 'NONE',  ( -9.474510206698720793, -16.51473224551083518, 99.58442372801900433 ) ) ;
#113883 = CARTESIAN_POINT ( 'NONE',  ( 16.46253265017160672, -9.564922557960803928, 43.33224293864769550 ) ) ;
#113884 = CARTESIAN_POINT ( 'NONE',  ( -19.03943276465977164, 0.05219959533909376836, 81.24890960531436690 ) ) ;
#113885 = EDGE_CURVE ( 'NONE', #80788, #167413, #182406, .T. ) ;
#113886 = CARTESIAN_POINT ( 'NONE',  ( -4.483927247898539470, -16.52544592524342804, 92.29057627198103830 ) ) ;
#113887 = CARTESIAN_POINT ( 'NONE',  ( 16.51473224551069308, 9.474510206698969483, 114.1655762719810241 ) ) ;
#113888 = CARTESIAN_POINT ( 'NONE',  ( -4.379528057220328563, 16.55341960407611168, 95.20724293864769550 ) ) ;
#113889 = CARTESIAN_POINT ( 'NONE',  ( -19.03943276465977164, 0.05219959533909376836, 106.2489096053143669 ) ) ;
#113891 = CARTESIAN_POINT ( 'NONE',  ( 5.153800228976335163, 19.02544592524342804, 39.79057627198100988 ) ) ;
#113890 = CARTESIAN_POINT ( 'NONE',  ( 16.55341960407611168, 4.379528057220329451, 58.95724293864770971 ) ) ;
#113892 = CARTESIAN_POINT ( 'NONE',  ( -18.67979575497193778, 10.72451020669871902, 58.33442372801901143 ) ) ;
#113893 = CARTESIAN_POINT ( 'NONE',  ( 5.153800228976615827, -19.02544592524334988, 90.20942372801900433 ) ) ;
#113894 = CARTESIAN_POINT ( 'NONE',  ( 12.06949235617757843, -12.14591786802309237, 48.12390960531436690 ) ) ;
#113895 = CARTESIAN_POINT ( 'NONE',  ( 5.823673210054125526, 21.52544592524343514, 109.7905762719810383 ) ) ;
#113896 = CARTESIAN_POINT ( 'NONE',  ( 21.52544592524344225, -5.823673210054117533, 53.54057627198103120 ) ) ;
#113897 = CARTESIAN_POINT ( 'NONE',  ( -0.05219959533909027116, -19.03943276465977164, 107.4989096053143527 ) ) ;
#113898 = CARTESIAN_POINT ( 'NONE',  ( 8.906447517083057264, -27.41122689804191026, 138.8500000054623911 ) ) ;
#113899 = CARTESIAN_POINT ( 'NONE',  ( -0.05219959533909027116, -19.03943276465977164, 52.49890960531436690 ) ) ;
#113900 = CARTESIAN_POINT ( 'NONE',  ( 4.379528057220092307, 16.55341960407617563, 112.2927570613523471 ) ) ;
#113901 = CARTESIAN_POINT ( 'NONE',  ( 14.34966873604972726, -8.224510206698740333, 95.83442372801903275 ) ) ;
#113902 = CARTESIAN_POINT ( 'NONE',  ( -8.224510206698735004, -14.34966873604973081, 89.58442372801901854 ) ) ;
#113903 = CARTESIAN_POINT ( 'NONE',  ( -9.564922557961040184, 16.46253265017147172, 32.91775706135233293 ) ) ;
#113904 = CARTESIAN_POINT ( 'NONE',  ( -17.05587630539786659, 6.762274262135695935, 70.74180309037316761 ) ) ;
#113905 = CARTESIAN_POINT ( 'NONE',  ( -19.03943276465977164, 0.05219959533909376836, 96.24890960531436690 ) ) ;
#113906 = CARTESIAN_POINT ( 'NONE',  ( 19.05341960407611168, 5.049401038298154454, 53.95724293864770260 ) ) ;
#113907 = CARTESIAN_POINT ( 'NONE',  ( -16.52544592524342804, 4.483927247898546575, 56.04057627198102409 ) ) ;
#113909 = CARTESIAN_POINT ( 'NONE',  ( 15.72974639402199770, -15.80617190586745480, 28.12390960531435979 ) ) ;
#113908 = CARTESIAN_POINT ( 'NONE',  ( 16.88567814943161949, -6.947325034625689177, 101.2099887734741515 ) ) ;
#113910 = CARTESIAN_POINT ( 'NONE',  ( 21.53943276465977519, -0.05219959533907433946, 38.74890960531435979 ) ) ;
#113911 = CARTESIAN_POINT ( 'NONE',  ( 4.483927247898545687, 16.52544592524342804, 79.79057627198102409 ) ) ;
#113912 = CARTESIAN_POINT ( 'NONE',  ( 0.05219959533934541429, -16.53943276465976808, 40.00109039468567573 ) ) ;
#113913 = CIRCLE ( 'NONE', #117258, 10.00000000000000000 ) ;
#113914 = CARTESIAN_POINT ( 'NONE',  ( -4.483927247898539470, -16.52544592524342804, 82.29057627198103830 ) ) ;
#113915 = CARTESIAN_POINT ( 'NONE',  ( 25.82491430096449747, 7.758527484246121375, 169.9682266581730232 ) ) ;
#113916 = CARTESIAN_POINT ( 'NONE',  ( 9.564922557961047289, -16.46253265017146816, 80.41775706135234714 ) ) ;
#113917 = CARTESIAN_POINT ( 'NONE',  ( 9.474510206698971260, -16.51473224551069308, 107.9155762719810383 ) ) ;
#113918 = CARTESIAN_POINT ( 'NONE',  ( 29.86685920354754487, 21.69954338932564752, -3.924999997268812990 ) ) ;
#113919 = CARTESIAN_POINT ( 'NONE',  ( -20.43538597629128262, 20.43538597629122222, -52.65483682830182488 ) ) ;
#113921 = CARTESIAN_POINT ( 'NONE',  ( 0.05219959533934541429, -16.53943276465976808, 110.0010903946856757 ) ) ;
#113920 = CARTESIAN_POINT ( 'NONE',  ( -12.06949235617739369, -12.14591786802326823, 29.37609039468568284 ) ) ;
#113922 = CARTESIAN_POINT ( 'NONE',  ( 0.05219959533936267826, -19.03943276465977164, 65.00109039468567573 ) ) ;
#113923 = CARTESIAN_POINT ( 'NONE',  ( 10.72451020669898902, -18.67979575497178502, 32.91557627198102409 ) ) ;
#113924 = CARTESIAN_POINT ( 'NONE',  ( 18.67979575497194134, -10.72451020669871369, 65.83442372801900433 ) ) ;
#113925 = CARTESIAN_POINT ( 'NONE',  ( -22.65770943308886487, -11.99324031494455589, 167.9410816520763206 ) ) ;
#113926 = CARTESIAN_POINT ( 'NONE',  ( 4.483927247898790824, -16.52544592524335698, 35.20942372801901854 ) ) ;
#113928 = CARTESIAN_POINT ( 'NONE',  ( -13.89961937509977652, 13.97604488694528158, 85.62390960531433848 ) ) ;
#113927 = LINE ( 'NONE', #143273, #196167 ) ;
#113929 = CARTESIAN_POINT ( 'NONE',  ( 17.01743274722963051, 17.33027132694079242, -56.78176416808769034 ) ) ;
#113930 = CARTESIAN_POINT ( 'NONE',  ( 16.52544592524342804, -4.483927247898539470, 83.54057627198102409 ) ) ;
#113931 = PRODUCT_CONTEXT ( 'NONE', #172025, 'mechanical' ) ;
#113932 = CARTESIAN_POINT ( 'NONE',  ( -5.153800228976328057, -19.02544592524343514, 82.29057627198103830 ) ) ;
#113933 = ORIENTED_EDGE ( 'NONE', *, *, #94568, .F. ) ;
#113934 = CARTESIAN_POINT ( 'NONE',  ( 19.05341960407617918, -5.049401038297876454, 111.0427570613523329 ) ) ;
#113935 = CARTESIAN_POINT ( 'NONE',  ( -18.67979575497178146, -10.72451020669898902, 71.66557627198100988 ) ) ;
#113936 = CARTESIAN_POINT ( 'NONE',  ( 16.51473224551069308, 9.474510206698969483, 39.16557627198103120 ) ) ;
#113938 = CARTESIAN_POINT ( 'NONE',  ( -15.72974639402197994, 15.80617190586746368, 115.6239096053143669 ) ) ;
#113937 = CARTESIAN_POINT ( 'NONE',  ( 13.89961937509957401, 13.97604488694547697, 66.87609039468567573 ) ) ;
#113939 = CARTESIAN_POINT ( 'NONE',  ( 13.97604488694527802, 13.89961937509977652, 74.37390960531436690 ) ) ;
#113940 = CARTESIAN_POINT ( 'NONE',  ( -9.564922557960796823, -16.46253265017161027, 112.0822429386476955 ) ) ;
#113941 = ORIENTED_EDGE ( 'NONE', *, *, #181196, .T. ) ;
#113942 = CARTESIAN_POINT ( 'NONE',  ( 16.55341960407618274, -4.379528057220086978, 31.04275706135234714 ) ) ;
#113943 = CARTESIAN_POINT ( 'NONE',  ( 21.55341960407610458, 5.719274019375980345, 108.9572429386476955 ) ) ;
#113946 = CARTESIAN_POINT ( 'NONE',  ( -9.564922557961040184, 16.46253265017147172, 67.91775706135233293 ) ) ;
#113945 = CARTESIAN_POINT ( 'NONE',  ( 9.474510206698971260, -16.51473224551069308, 87.91557627198102409 ) ) ;
#113944 = CARTESIAN_POINT ( 'NONE',  ( -12.14591786802309592, -12.06949235617757132, 101.8739096053143811 ) ) ;
#113947 = CARTESIAN_POINT ( 'NONE',  ( -15.80617190586745835, -15.72974639402198527, 86.87390960531438111 ) ) ;
#113948 = CARTESIAN_POINT ( 'NONE',  ( -16.53943276465976808, 0.05219959533911058130, 46.24890960531435979 ) ) ;
#113949 = CARTESIAN_POINT ( 'NONE',  ( 13.97604488694548053, -13.89961937509957401, 25.62609039468566507 ) ) ;
#113950 = CARTESIAN_POINT ( 'NONE',  ( -4.379528057220086978, -16.55341960407618274, 64.79275706135234714 ) ) ;
#113951 = CARTESIAN_POINT ( 'NONE',  ( 19.02544592524343514, -5.153800228976328945, 93.54057627198102409 ) ) ;
#113952 = CARTESIAN_POINT ( 'NONE',  ( -13.97604488694527625, -13.89961937509977652, 41.87390960531435979 ) ) ;
#113953 = CARTESIAN_POINT ( 'NONE',  ( -10.72451020669870658, -18.67979575497194134, 49.58442372801901143 ) ) ;
#113954 = CARTESIAN_POINT ( 'NONE',  ( 10.72451020669871369, 18.67979575497193778, 72.08442372801899012 ) ) ;
#113955 = CARTESIAN_POINT ( 'NONE',  ( -16.51473224551069308, -9.474510206698971260, 66.66557627198102409 ) ) ;
#113956 = CARTESIAN_POINT ( 'NONE',  ( -15.80617190586768217, 15.72974639402176855, 38.12609039468567573 ) ) ;
#113957 = ADVANCED_FACE ( 'NONE', ( #40900 ), #196595, .T. ) ;
#113958 = CARTESIAN_POINT ( 'NONE',  ( -13.97604488694547697, 13.89961937509957934, 73.12609039468568994 ) ) ;
#113959 = CARTESIAN_POINT ( 'NONE',  ( 5.049401038297881783, 19.05341960407617563, 67.29275706135234714 ) ) ;
#113960 = CARTESIAN_POINT ( 'NONE',  ( -16.46253265017160317, 9.564922557960807481, 40.83224293864769550 ) ) ;
#113961 = CARTESIAN_POINT ( 'NONE',  ( -16.53943276465976808, -0.05219959533934237506, 88.75109039468567573 ) ) ;
#113962 = CARTESIAN_POINT ( 'NONE',  ( -19.05341960407611168, -5.049401038298163336, 46.45724293864768129 ) ) ;
#113963 = CARTESIAN_POINT ( 'NONE',  ( 19.49401214000073779, -12.39993551617566503, 167.9999999999999716 ) ) ;
#113964 = CARTESIAN_POINT ( 'NONE',  ( -16.51473224551069308, -9.474510206698971260, 96.66557627198102409 ) ) ;
#113965 = CARTESIAN_POINT ( 'NONE',  ( -19.05341960407611168, -5.049401038298163336, 36.45724293864766707 ) ) ;
#113966 = CARTESIAN_POINT ( 'NONE',  ( 15.72974639402199770, -15.80617190586745480, 88.12390960531436690 ) ) ;
#113967 = CARTESIAN_POINT ( 'NONE',  ( -16.55341960407617563, 4.379528057220093196, 58.54275706135235424 ) ) ;
#113968 = CARTESIAN_POINT ( 'NONE',  ( 16.46253265017146816, 9.564922557961045513, 36.66775706135233293 ) ) ;
#113969 = ADVANCED_FACE ( 'NONE', ( #148081 ), #135902, .T. ) ;
#113970 = CARTESIAN_POINT ( 'NONE',  ( 9.564922557960805705, 16.46253265017160317, 54.58224293864769550 ) ) ;
#113971 = CARTESIAN_POINT ( 'NONE',  ( 16.53943276465976808, -0.05219959533910856209, 48.74890960531435979 ) ) ;
#113972 = CARTESIAN_POINT ( 'NONE',  ( 12.14591786802309770, 12.06949235617756955, 84.37390960531438111 ) ) ;
#113973 = CARTESIAN_POINT ( 'NONE',  ( 13.89961937509977652, -13.97604488694527269, 83.12390960531436690 ) ) ;
#113974 = CARTESIAN_POINT ( 'NONE',  ( 9.474510206698971260, -16.51473224551069308, 77.91557627198103830 ) ) ;
#113975 = CARTESIAN_POINT ( 'NONE',  ( 10.72451020669871369, 18.67979575497193778, 42.08442372801901854 ) ) ;
#113976 = CARTESIAN_POINT ( 'NONE',  ( 5.153800228976335163, 19.02544592524342804, 94.79057627198103830 ) ) ;
#113977 = CARTESIAN_POINT ( 'NONE',  ( -18.62759615963255300, -10.81492255796106328, 94.16775706135237556 ) ) ;
#113978 = CARTESIAN_POINT ( 'NONE',  ( 12.06949235617739724, 12.14591786802326823, 81.87609039468568994 ) ) ;
#113979 = CARTESIAN_POINT ( 'NONE',  ( 21.55341960407619695, -5.719274019375665929, 31.04275706135234714 ) ) ;
#113980 = CARTESIAN_POINT ( 'NONE',  ( -15.72974639402197994, 15.80617190586746368, 95.62390960531436690 ) ) ;
#113981 = CARTESIAN_POINT ( 'NONE',  ( 16.52544592524342804, -4.483927247898539470, 43.54057627198103830 ) ) ;
#113982 = CARTESIAN_POINT ( 'NONE',  ( 16.46253265017160672, -9.564922557960803928, 43.33224293864769550 ) ) ;
#113983 = CARTESIAN_POINT ( 'NONE',  ( 16.55341960407611168, 4.379528057220329451, 68.95724293864769550 ) ) ;
#113984 = CARTESIAN_POINT ( 'NONE',  ( 21.55341960407610458, 5.719274019375980345, 33.95724293864769550 ) ) ;
#113985 = CARTESIAN_POINT ( 'NONE',  ( 19.03943276465977164, 0.05219959533936151252, 31.25109039468566863 ) ) ;
#113986 = CARTESIAN_POINT ( 'NONE',  ( -16.52544592524342804, 4.483927247898546575, 96.04057627198102409 ) ) ;
#113987 = CARTESIAN_POINT ( 'NONE',  ( -9.474510206698964154, 16.51473224551069663, 110.4155762719810383 ) ) ;
#113988 = ORIENTED_EDGE ( 'NONE', *, *, #161100, .F. ) ;
#113989 = CARTESIAN_POINT ( 'NONE',  ( 14.34966873604972726, -8.224510206698740333, 50.83442372801901143 ) ) ;
#113990 = CARTESIAN_POINT ( 'NONE',  ( -16.51473224551069308, -9.474510206698971260, 56.66557627198103120 ) ) ;
#113991 = CARTESIAN_POINT ( 'NONE',  ( -17.49999999999999645, -5.500000000000000888, 120.0000000000000142 ) ) ;
#113992 = CARTESIAN_POINT ( 'NONE',  ( -12.14591786802326823, 12.06949235617739902, 98.12609039468570415 ) ) ;
#113993 = CARTESIAN_POINT ( 'NONE',  ( -19.05341960407617563, 5.049401038297882671, 108.5427570613523187 ) ) ;
#113994 = CARTESIAN_POINT ( 'NONE',  ( -10.72451020669870658, -18.67979575497194134, 84.58442372801903275 ) ) ;
#113995 = CARTESIAN_POINT ( 'NONE',  ( 16.51473224551069308, 9.474510206698969483, 69.16557627198102409 ) ) ;
#113996 = CARTESIAN_POINT ( 'NONE',  ( 10.72451020669898902, -18.67979575497178502, 107.9155762719810241 ) ) ;
#113997 = CARTESIAN_POINT ( 'NONE',  ( -16.52544592524335698, -4.483927247898792601, 58.95942372801902565 ) ) ;
#113998 = CARTESIAN_POINT ( 'NONE',  ( 12.06949235617757843, -12.14591786802309237, 108.1239096053143811 ) ) ;
#113999 = CARTESIAN_POINT ( 'NONE',  ( -16.52544592524335698, -4.483927247898792601, 23.95942372801901143 ) ) ;
#114000 = CARTESIAN_POINT ( 'NONE',  ( -13.97604488694547697, 13.89961937509957934, 83.12609039468564731 ) ) ;
#114001 = CARTESIAN_POINT ( 'NONE',  ( -21.55341960407610458, -5.719274019375992779, 81.45724293864769550 ) ) ;
#114002 = CARTESIAN_POINT ( 'NONE',  ( 13.89961937509957401, 13.97604488694547697, 56.87609039468564731 ) ) ;
#114003 = CARTESIAN_POINT ( 'NONE',  ( 0.000000000000000000, -105.0000000000000000, 12.00000000000000355 ) ) ;
#114004 = CARTESIAN_POINT ( 'NONE',  ( 15.72974639402199770, -15.80617190586745480, 103.1239096053143811 ) ) ;
#114005 = CARTESIAN_POINT ( 'NONE',  ( 17.50000000000002132, 3.471454075611646761, 28.01667418855641856 ) ) ;
#114006 = CARTESIAN_POINT ( 'NONE',  ( -5.049401038298153566, 19.05341960407611168, 70.20724293864769550 ) ) ;
#114007 = CARTESIAN_POINT ( 'NONE',  ( -11.29706596393373985, -12.15234863546621646, -59.18655785247093348 ) ) ;
#114008 = CARTESIAN_POINT ( 'NONE',  ( 12.06949235617739724, 12.14591786802326823, 21.87609039468567573 ) ) ;
#114009 = CARTESIAN_POINT ( 'NONE',  ( 36.82872320124401000, -3.359544971329622598, 49.36946820683672854 ) ) ;
#114011 = CARTESIAN_POINT ( 'NONE',  ( -16.53943276465976808, 0.05219959533911058130, 61.24890960531435979 ) ) ;
#114010 = CARTESIAN_POINT ( 'NONE',  ( 18.62759615963271287, -10.81492255796078972, 103.3322429386476955 ) ) ;
#114012 = CARTESIAN_POINT ( 'NONE',  ( 5.049401038298161559, -19.05341960407611168, 67.70724293864769550 ) ) ;
#114013 = CARTESIAN_POINT ( 'NONE',  ( -21.53943276465977519, -0.05219959533937600094, 68.75109039468568994 ) ) ;
#114016 = CARTESIAN_POINT ( 'NONE',  ( -9.474510206698720793, -16.51473224551083518, 44.58442372801900433 ) ) ;
#114015 = CARTESIAN_POINT ( 'NONE',  ( 8.224510206698742110, 14.34966873604972548, 22.08442372801901143 ) ) ;
#114014 =( BOUNDED_SURFACE ( )  B_SPLINE_SURFACE ( 3, 2, ( 
 ( #37277, #149454, #10950, #7932, #69616, #102948, #22116, #130262, #193980, #38284, #160625, #71613, #98934, #131282, #192970, #129272, #190966, #55442, #162619, #177808, #116119, #191958, #100935, #24125, #114101, #117113, #133279, #145446, #85777, #101950, #147464, #178807, #40277, #194970, #6928, #175804, #163631, #8954, #25134, #148461, #9954, #56449, #53444, #115119, #61407, #27127, #59420, #43274, #74608, #135297, #89771, #105929, #57458, #195985, #28131, #122087, #183778, #14924, #151456, #103949, #119130, #75585, #76584, #152431, #12943, #197950, #166629, #137264, #153426, #31088, #104943, #182788, #123078, #184764, #91730, #30089, #180811, #60414, #169590, #198947, #90748, #136275, #106918, #121094, #88774, #42290, #92736, #120104, #46249, #13919, #165628, #72624, #107903, #154424, #73627, #45264, #29110, #134299, #138260, #150467, #11962, #168591, #196969, #199943, #167614, #58437, #181794, #44271, #97689, #155419, #109903, #80551, #35052, #32081, #124065, #96706, #77576, #185766, #79568, #724, #2726, #174574, #81525, #139248, #141235, #64403, #112881, #19884, #111895, #47254, #36040, #65387, #173583, #143211, #126072, #15918, #33075, #187768, #62395, #110896, #93738, #17912, #49238, #158395, #172581, #34068, #95726, #156410, #171587, #157412, #16909, #18905, #4693, #108911, #125081, #50239, #142225, #170591, #78561, #140235, #63404, #128046, #3709, #1728, #186779, #189748, #48249, #94730, #127047, #188754, #66384, #51220, #117893, #41054, #100703, #37039, #55210, #54217, #56211, #163399, #101709, #159379, #98699, #53205, #23885, #178571, #175562, #67376, #40035, #20875, #129034, #22882, #144215, #146205, #179583, #24896, #82533, #84528, #7691, #5699, #86544, #116879, #190735, #52208, #8716, #148228, #9722, #69375, #113866, #176576, #131045, #160393, #115888, #21882, #161390, #192735, #71386, #177578, #39045, #162383, #99706, #114882, #85537, #83532, #147225, #133050, #145211, #68371, #6693, #70385, #132053, #193742, #194740, #130022, #191721, #38050, #61170, #75354, #135069, #43044, #167385, #44037, #105698, #196745, #74380, #91493, #57226, #89539, #73398, #104710, #165402, #119881, #136045, #87544, #25899, #58212, #152203, #13687, #45029, #181566, #134061, #149231, #28881, #106687, #182555, #166400, #27896, #151225, #90521, #183543, #122842, #12714, #197720, #153180, #14683, #121850, #60181, #10722, #137024, #199704, #198714, #120855, #59186, #168360, #29856, #76345, #138022, #184530, #102718, #164407, #72385, #180584, #195752, #118899, #42058, #11731, #103722, #26895, #88538, #150235, #98191, #172331, #52709, #15677, #7199, #21382, #78317, #186536, #110650, #187530, #48995, #139990, #17664, #37545, #484, #32833, #16668, #48009, #108670, #63157, #79323, #30851, #169342, #1478, #159894, #83041, #191235, #124836, #77337, #92498, #36535, #114373, #125827, #109665, #171345, #94484, #144716, #129535, #68883, #156166, #140993, #99209, #160897, #67882, #6202, #154187, #176077, #145718, #22389, #64162, #2481, #84039, #130543, #62157, #139004, #46010, #93491, #107665, #123821, #185519, #47011, #170348, #31840, #155177, #56731, #148738, #192241, #11230, #150734, #73896, #133556, #69888, #88041, #87053, #89044, #196260, #134573, #53721, #131557, #86051, #118401, #72904, #8213, #100214, #57729, #115398, #161894, #55717, #177086, #179088, #12234, #119399, #38557, #117389, #40557, #23390, #181082, #149729, #85036, #146717, #41563, #42557, #104220, #102226, #193242, #9227, #163915, #54715, #10226, #116387, #194250, #178077, #39544, #180095, #71886, #101203, #165901, #162893, #24402, #195247, #147740, #27399, #103226, #70894, #132561, #25411, #164908, #26402, #29376, #56566, #154686, #151719, #43545, #16181, #197238, #105211, #199209, #120369, #122351, #93997, #986, #58699, #60676, #184040, #32344, #139503, #31349, #166898, #155678, #185028, #93000, #62661, #45523, #17173, #152693, #107177, #135566 ),
 ( #77836, #182062, #44538, #28398, #168848, #108174, #30353, #46515, #61666, #124340, #90037, #13212, #169855, #167877, #75851, #123335, #76844, #138515, #91007, #91995, #186036, #74875, #153689, #106193, #137527, #198218, #14182, #15185, #136537, #59690, #47518, #109174, #170853, #121361, #183054, #110169, #125348, #81787, #21140, #158651, #95990, #3970, #172848, #143474, #159644, #37303, #49497, #189023, #129298, #190994, #97952, #36297, #1994, #66643, #175830, #4958, #96970, #34329, #113142, #142492, #33336, #187045, #98962, #126328, #52470, #20142, #171848, #78827, #114129, #111159, #80814, #141503, #157675, #112161, #63673, #48515, #19165, #128306, #190006, #82795, #65650, #94996, #156682, #51480, #144477, #174832, #127312, #50497, #173850, #5961, #67639, #160652, #35316, #140505, #18176, #79833, #2988, #64666, #188025, #9986, #119160, #148495, #40308, #116149, #56480, #85809, #176842, #130291, #180843, #69646, #134331, #163665, #53472, #22144, #196015, #103981, #23148, #86809, #178840, #83794, #41319, #42320, #145474, #25167, #99968, #118158, #117145, #6955, #26160, #164664, #68635, #161652, #177840, #71646, #102979, #38313, #191985, #87801, #115149, #84792, #147495, #146471, #8986, #7963, #149487, #131312, #70654, #132320, #193002, #10983, #179848, #54479, #39308, #133313, #72656, #57491, #194012, #100967, #162652, #55475, #24158, #101984, #195002, #167646, #29142, #46280, #90779, #152463, #183807, #105961, #59452, #75615, #43306, #13949, #61437, #62427, #74641, #135330, #137294, #138291, #198976, #14953, #91761, #169622, #197003, #124099, #199972, #197982, #60443, #30120, #106947, #168620, #121125, #122118, #154457, #120136, #45295, #153455, #76613, #123109, #184794, #104974, #182820, #12977, #185798, #107936, #31119, #58469, #11995, #92767, #15949, #77608, #47286, #139279, #756, #165660, #181827, #27158, #166661, #73658, #88805, #150498, #28162, #89804, #151486, #136307, #44302, #2756, #64432, #159408, #20903, #140267, #190762, #3739, #66412, #126102, #35082, #48281, #109936, #96735, #158424, #143240, #49267, #187798, #1759, #142255, #110925, #93769, #50268, #94762, #36069, #82561, #141266, #189777, #111926, #172611, #127077, #34098, #188785, #18936, #171618, #157441, #63437, #129061, #97718, #79597, #144243, #125113, #4723, #65416, #155450, #108942, #33106, #173612, #19912, #5727, #156444, #95756, #81554, #80581, #16940, #128074, #51249, #67406, #170623, #32112, #112909, #78594, #174603, #186811, #17943, #193772, #87573, #102748, #6721, #55241, #84556, #85569, #38078, #177607, #134093, #161418, #160421, #175592, #56242, #71414, #164436, #147255, #21910, #149260, #10752, #146234, #192762, #41085, #145240, #191751, #116909, #22910, #83561, #194768, #68399, #131073, #115917, #72416, #52237, #37068, #39075, #113894, #117923, #98727, #100732, #162413, #130051, #179612, #148257, #53234, #114910, #101742, #9750, #25930, #23915, #176604, #69407, #8746, #99734, #70416, #7721, #54245, #132083, #133078, #178602, #40065, #163430, #24928, #86573, #105729, #73428, #44069, #91525, #92531, #104741, #165432, #167416, #168392, #120887, #45060, #121882, #199735, #26927, #154220, #29887, #27927, #136077, #60212, #137057, #198747, #89570, #28912, #184561, #150267, #182586, #166432, #197751, #58243, #12746, #90552, #180615, #118930, #151256, #106718, #153212, #138054, #74411, #88569, #42088, #183575, #61201, #75385, #59218, #152234, #13719, #14717, #76377, #15710, #122873, #46042, #107697, #169376, #30884, #77370, #103753, #195783, #57256, #11761, #135099, #196775, #119911, #181597, #43074, #47046, #97480, #186570, #51011, #80341, #170382, #139038, #112672, #20661, #140025, #3502, #95514, #518, #158188, #159166, #62190, #142013, #16701, #34843, #33854, #35834, #143003, #81320, #123854, #78351, #32868, #65178, #19678, #155212, #108703, #4481, #185552, #31873, #2515, #96498, #157200, #93527, #66171 ),
 ( #64195, #18694, #141028, #1514, #172364, #127833, #174364, #63191, #124871, #125862, #189539, #49029, #48043, #94518, #126837, #109699, #171381, #156200, #188543, #17700, #50021, #79357, #187562, #110684, #111686, #173373, #5486, #86334, #101492, #132840, #177369, #190525, #117677, #40836, #176363, #22673, #71176, #175352, #21669, #147015, #191512, #113658, #24685, #51999, #161176, #145999, #102509, #164193, #85323, #115681, #130833, #69166, #83323, #37836, #129813, #82315, #8500, #148021, #36820, #128826, #9510, #84320, #194527, #144005, #38840, #192524, #7482, #98486, #67169, #160179, #145000, #54007, #100498, #6481, #55999, #162177, #68161, #23675, #99496, #70177, #179374, #52989, #114667, #131845, #193528, #39826, #55002, #116671, #178362, #163181, #151996, #13482, #59973, #166187, #104506, #57011, #58983, #27688, #10510, #167176, #11520, #152971, #137810, #58009, #106472, #28675, #119679, #43826, #181362, #105490, #135846, #199494, #42841, #168151, #90310, #89329, #75147, #151021, #136818, #197515, #165189, #74176, #180376, #45806, #14470, #196539, #76132, #118684, #121640, #182348, #72172, #107457, #26684, #120650, #198502, #60960, #88324, #12512, #183335, #44817, #133847, #29648, #91280, #122634, #25691, #184324, #87336, #149022, #195537, #41846, #103513, #150014, #73190, #134861, #123615, #110446, #1268, #2271, #154966, #94278, #50777, #78111, #77129, #92291, #173131, #188302, #19442, #63954, #138798, #4248, #127601, #62945, #109452, #157951, #61948, #108460, #33613, #139780, #279, #111444, #185310, #47802, #32624, #189300, #169133, #172127, #125623, #17453, #155956, #170137, #124625, #16462, #30638, #95276, #34606, #46801, #15472, #96265, #171135, #81090, #153975, #187321, #79109, #140782, #31632, #93281, #186320, #48792, #156959, #18456, #80107, #142768, #141775, #3269, #64941, #126600, #49779, #65928, #162938, #143763, #194294, #7242, #69937, #129577, #38601, #51758, #113419, #100257, #161938, #36579, #5244, #70937, #159937, #24445, #53765, #66924, #112437, #86094, #174126, #6245, #67924, #147785, #9271, #128588, #35597, #68927, #131601, #191274, #23433, #175111, #98234, #85080, #146764, #190282, #130589, #132605, #21424, #145760, #52749, #97243, #115439, #83084, #39590, #158931, #144760, #193286, #177130, #114418, #192284, #176119, #8257, #22431, #37590, #160939, #99252, #20420, #101249, #84081, #82070, #54760, #116434, #178122, #102271, #140303, #195292, #91795, #200005, #93802, #56773, #119442, #138323, #57772, #163959, #153489, #790, #32145, #55760, #155482, #181127, #108976, #165947, #47321, #11275, #61471, #16974, #170657, #10271, #123142, #88087, #14985, #41607, #42601, #117434, #164952, #25457, #179132, #62462, #77642, #78628, #76645, #87097, #40600, #148782, #149773, #196302, #71930, #133600, #118446, #184829, #26445, #180138, #124135, #103272, #134618, #104265, #72948, #27447, #46315, #107970, #169657, #31153, #92801, #154489, #15983, #139311, #185834, #144274, #94797, #48315, #5761, #142291, #67437, #83593, #35115, #188817, #65448, #171649, #160452, #17977, #109970, #3771, #111957, #64468, #129094, #96767, #1794, #81586, #143272, #18968, #127110, #95789, #66444, #82592, #21943, #172642, #173646, #52268, #113926, #20935, #159440, #125147, #189809, #98759, #128105, #19945, #157475, #33139, #50300, #126135, #156476, #63472, #49299, #175626, #4755, #79631, #186846, #37100, #141299, #2789, #51281, #158456, #187830, #190794, #110958, #34130, #112942, #80614, #97752, #174635, #36100, #149288, #87602, #26958, #84589, #39107, #9782, #164465, #161452, #53266, #25959, #6754, #114944, #8777, #130086, #132112, #103782, #10782, #68433, #70446, #193805, #42120, #72449, #41114, #176637, #165462, #194798, #102778, #134124, #55271, #145273, #162445, #116940, #191785, #40096, #22943, #147287, #178633, #195813, #101774, #163461, #24959, #85600, #100763, #86605, #146269, #148288, #57285 ),
 ( #71444, #133109, #56271, #117954, #177640, #179645, #118959, #99767, #180645, #115950, #38112, #7755, #23946, #69439, #131107, #192795, #54277, #138088, #199769, #30918, #105762, #119941, #135130, #91561, #92566, #153249, #107731, #104774, #196804, #169413, #150297, #58272, #152267, #73457, #75420, #47079, #154254, #11793, #13752, #137094, #185589, #15745, #184596, #181626, #108740, #61236, #46077, #77404, #198780, #170416, #167448, #60246, #88601, #183610, #166462, #90586, #121917, #139074, #45094, #106751, #168426, #28945, #182619, #29921, #27959, #14751, #552, #43106, #197785, #89600, #76412, #122908, #62223, #123891, #151288, #12777, #74442, #136109, #59251, #120920, #44104, #96533, #173408, #34879, #64233, #3537, #20697, #186605, #18730, #2551, #33893, #94557, #49067, #65214, #16737, #155247, #187598, #81355, #143039, #174400, #110723, #63227, #78385, #158223, #35870, #111722, #172404, #157237, #125898, #19713, #112708, #190561, #95550, #142050, #82353, #144041, #51046, #189574, #140061, #4517, #128861, #66210, #50061, #80378, #124907, #126874, #156236, #48077, #52035, #79395, #5523, #127870, #109733, #31908, #67203, #113692, #32903, #97516, #188580, #93561, #159203, #1552, #171417, #17738, #141065, #71211, #70213, #72208, #179407, #117711, #57046, #114706, #69202, #85358, #53025, #23711, #132874, #133882, #84356, #145036, #147051, #148054, #100533, #24720, #101527, #40871, #6518, #195573, #9545, #7517, #115717, #39861, #116707, #178397, #130870, #8534, #164228, #129849, #162212, #146034, #177405, #37874, #192560, #131880, #160216, #98523, #54043, #86369, #194563, #102545, #38876, #68197, #21706, #163218, #25725, #55037, #193565, #56033, #87371, #149056, #10544, #175388, #36856, #83360, #191548, #176399, #99532, #161214, #22709, #75179, #199526, #136851, #167210, #166218, #88357, #135876, #119710, #150050, #60994, #181394, #76165, #90343, #11556, #118720, #137845, #180409, #42872, #198536, #28707, #41881, #29680, #103548, #165223, #60007, #104537, #91312, #152028, #26718, #184356, #122668, #73222, #151051, #43859, #153004, #134893, #89362, #27719, #196569, #12542, #74207, #13514, #197547, #121674, #58040, #59015, #182381, #120682, #105524, #183369, #44851, #106507, #168184, #14503, #148712, #56702, #103201, #86026, #119373, #116363, #9203, #196235, #194225, #177063, #101180, #162868, #180069, #24376, #147715, #117364, #39520, #193216, #70868, #132536, #68859, #57704, #115374, #145694, #55690, #179060, #161871, #164882, #40529, #99185, #102200, #54690, #178052, #149704, #11202, #130518, #181056, #163888, #118375, #25385, #87027, #38533, #100189, #10200, #71860, #23365, #133529, #160874, #192214, #195221, #41537, #84016, #26377, #85011, #88016, #72878, #131532, #134546, #22364, #7176, #53697, #146691, #8187, #69863, #182038, #90981, #197213, #62639, #31325, #13187, #169832, #73872, #76821, #199184, #89019, #124315, #43520, #75826, #184017, #77812, #105186, #106169, #122325, #44513, #150710, #137504, #185004, #16158, #42532, #139481, #167852, #92977, #152668, #154662, #198194, #45499, #963, #104195, #58676, #107154, #74850, #60652, #28374, #29352, #165876, #151696, #12209, #27372, #46488, #61643, #135542, #168824, #120343, #166873, #90012, #136513, #183030, #59664, #121337, #14158, #30329, #91971, #153665, #108148, #15161, #138492, #200174, #123311, #67611, #188997, #19138, #34303, #172823, #125325, #79807, #33313, #144450, #50473, #128281, #78804, #32323, #189978, #126305, #51453, #186013, #80789, #141479, #94973, #5935, #112133, #113114, #140482, #93976, #174804, #188001, #36270, #47495, #142467, #95965, #49471, #155656, #109152, #1970, #17151, #111134, #157649, #48492, #97925, #3945, #170831, #65624, #2963, #64643, #159618, #21114, #63650, #187022, #127284, #143448, #173825, #35289, #110146, #171825, #96945, #158626, #156657, #20117, #82769, #18153, #81761, #4934, #66617, #147891, #24551 ),
 ( #89191, #57875, #39693, #196405, #100364, #103376, #25561, #115547, #150884, #8366, #102373, #10377, #104367, #70041, #132709, #148886, #71042, #177235, #164062, #11380, #42706, #69031, #166051, #194397, #119547, #179237, #181230, #86201, #72034, #27551, #130696, #23539, #133707, #101355, #87205, #54867, #55865, #192390, #178229, #38707, #53873, #73050, #88191, #162043, #195399, #85185, #146874, #131710, #163044, #9377, #193391, #116541, #117539, #56877, #40703, #118551, #134722, #180242, #41711, #165054, #26547, #149875, #15334, #45672, #60825, #199360, #151861, #107323, #170005, #29518, #138663, #13352, #75016, #144, #61813, #28542, #168996, #112067, #43691, #30500, #152841, #197383, #12379, #106336, #182207, #105353, #44683, #93149, #76992, #168022, #92151, #91152, #153837, #122499, #136681, #184190, #167040, #35223, #3877, #183201, #142398, #90178, #46666, #123483, #58848, #96876, #198363, #185175, #108325, #50407, #59838, #76000, #31496, #14335, #120515, #154833, #16332, #188929, #74041, #173755, #137674, #65556, #80720, #127215, #135712, #121507, #193911, #8884, #113048, #99874, #190900, #191891, #144381, #83701, #40203, #67544, #66551, #81692, #162550, #177743, #70552, #53375, #128215, #55375, #117045, #52376, #98865, #147396, #51387, #97857, #23051, #129202, #189912, #100868, #174740, #37209, #22050, #178740, #158559, #161558, #115053, #6861, #145379, #159546, #114033, #5868, #20049, #84696, #24054, #36203, #4866, #85710, #160560, #132219, #143374, #176745, #68540, #130195, #21044, #82697, #175730, #38218, #146376, #7863, #69550, #131214, #192905, #54382, #116054, #39212, #195918, #152370, #13855, #133213, #183715, #44207, #42224, #105866, #101883, #135236, #88708, #165565, #71547, #60350, #118061, #148393, #103885, #11900, #164567, #167553, #196908, #163565, #181729, #57393, #119066, #75522, #137197, #194904, #25065, #58375, #59356, #180748, #28065, #41221, #102882, #89706, #151392, #179751, #120042, #198883, #56378, #43210, #27062, #86708, #9887, #150404, #26061, #87704, #134233, #182722, #104877, #73563, #166566, #12882, #74547, #136212, #149389, #197887, #10885, #122024, #90688, #72555, #29048, #121025, #79503, #1662, #91666, #126980, #184699, #78496, #186713, #80485, #46183, #108844, #125017, #47185, #153356, #140169, #187703, #18840, #45201, #142159, #170525, #95657, #155356, #34001, #657, #48183, #3643, #157345, #199878, #109839, #77510, #63340, #31020, #32014, #106855, #154358, #14858, #168530, #49173, #64338, #65321, #171522, #76519, #30028, #138195, #139181, #185695, #61342, #123013, #107836, #33011, #15851, #169520, #110832, #92670, #123997, #93671, #62327, #16846, #94666, #156345, #17845, #141172, #2661, #126007, #172516, #147160, #191656, #130976, #81458, #34987, #145143, #85471, #19817, #21814, #128967, #173514, #188689, #82459, #158328, #143144, #20804, #69310, #53135, #144147, #6626, #5631, #68305, #98629, #127976, #36968, #4624, #8648, #177513, #159309, #115823, #66315, #22816, #129956, #96640, #70322, #189679, #83466, #114814, #23821, #51151, #52143, #176506, #190667, #112812, #37983, #192667, #162320, #50169, #111826, #113800, #38983, #160323, #100639, #67308, #99640, #174505, #35972, #97619, #161323, #175495, #84462, #146140, #7626, #54150, #40988, #39973, #55145, #135987, #151165, #182490, #26829, #101643, #167322, #90458, #25836, #72320, #120790, #24830, #71322, #196683, #102656, #163334, #74320, #86480, #10657, #195687, #152142, #13625, #135005, #165337, #180520, #118837, #132985, #87480, #179519, #131989, #58152, #197658, #148165, #178507, #59124, #133996, #43971, #193674, #88470, #41993, #57158, #9656, #116816, #194676, #56145, #103659, #150167, #117826, #105633, #11667, #164341, #73333, #149167, #119820, #28818, #181505, #42983, #104648, #166335, #89474, #27833, #12653, #14619, #76276, #1413, #124771, #91428, #172266, #184467, #44964, #123755, #47946, #418 ),
 ( #64095, #29792, #62092, #45946, #77269, #137954, #92432, #108604, #60118, #198652, #30785, #186469, #109597, #17598, #154119, #106622, #121786, #78251, #79257, #155110, #15612, #185454, #169279, #139924, #156100, #33756, #107601, #46944, #125763, #187463, #94420, #32768, #183480, #63092, #95415, #171280, #93423, #138938, #168296, #170281, #199638, #153115, #157100, #122777, #48931, #16604, #61104, #31775, #140929, #2415, #110585, #75292, #136963, #18596, #37734, #177272, #100401, #160080, #96403, #114566, #113561, #115584, #22574, #161079, #80244, #158090, #112575, #83227, #99396, #34744, #126738, #84221, #141914, #188441, #82215, #3405, #5388, #38743, #145900, #65080, #143906, #67071, #49920, #7384, #176263, #111585, #173270, #68064, #69068, #130735, #128730, #19582, #35737, #190426, #81225, #175255, #142906, #20564, #51902, #192427, #36721, #98383, #21567, #159070, #174269, #144902, #4387, #6385, #53909, #66072, #127738, #189440, #50917, #129718, #97384, #191415, #52891, #27591, #85224, #25597, #148924, #58886, #166088, #57912, #131747, #120552, #11419, #119584, #89229, #10413, #182245, #179276, #72071, #43730, #56914, #39730, #164098, #87241, #42744, #133744, #195439, #180279, #102411, #55903, #118589, #101391, #41749, #181267, #162082, #71078, #193429, #103413, #134760, #165091, #73089, #88228, #150923, #54905, #23576, #196442, #194432, #26585, #149912, #104406, #12416, #117576, #74078, #135749, #116578, #197420, #132744, #146915, #24588, #40741, #8404, #70079, #178267, #163084, #86236, #147926, #9412, #122536, #136719, #151899, #108365, #47706, #185212, #184227, #30538, #199397, #170043, #186225, #63859, #76038, #15372, #155860, #17358, #124530, #62846, #28580, #93186, #2179, #31533, #123519, #60861, #198400, #169032, #29555, #59878, #125530, #152877, #79013, #46703, #90216, #45708, #107359, #121544, #106376, #154871, #61850, #105392, #109356, #187227, #167078, #16368, #183239, #1171, #182, #13389, #171038, #32529, #75053, #44720, #92190, #78016, #94181, #168058, #153874, #91188, #14372, #139685, #140687, #137713, #77028, #138700, #142676, #113329, #129488, #7146, #19353, #158837, #99157, #160846, #67832, #6152, #172032, #36485, #145665, #175022, #66831, #4155, #80017, #112343, #173037, #141686, #68830, #96173, #22335, #190190, #33520, #127504, #65834, #64850, #49682, #98141, #5149, #48698, #191186, #130489, #110350, #51665, #126512, #144667, #143668, #95182, #52662, #114324, #156868, #188210, #189208, #159840, #176027, #111347, #18364, #37495, #3177, #34515, #174033, #157863, #35504, #81002, #83986, #50686, #97154, #20325, #81974, #128495, #21333, #82991, #150683, #41510, #149677, #196206, #179031, #12181, #9173, #102170, #88992, #86998, #69833, #194197, #55662, #72850, #117336, #40498, #10173, #132508, #85997, #163858, #131500, #25357, #87989, #73845, #101151, #161842, #148685, #164853, #71833, #103173, #118347, #57678, #23336, #192185, #26349, #24346, #133502, #56674, #195194, #180041, #147686, #11175, #181030, #146662, #134520, #162838, #119346, #54660, #70840, #42504, #177034, #115344, #104168, #165850, #27346, #53666, #38504, #100160, #84980, #8157, #193187, #116334, #178023, #39491, #136486, #199155, #15131, #137475, #43494, #168796, #77783, #109123, #17123, #170801, #60622, #185983, #45471, #124286, #90953, #76793, #32293, #47466, #89986, #138464, #167824, #30300, #121310, #122296, #135516, #44486, #105160, #58651, #139452, #154633, #93949, #91943, #166846, #155627, #197187, #29323, #75797, #120317, #28348, #74825, #200145, #106142, #151667, #933, #13161, #14130, #183986, #182011, #198166, #61615, #153636, #107125, #123283, #59636, #152640, #183002, #184974, #46459, #62607, #108119, #169802, #31295, #92947, #16128, #160600, #112107, #65599, #142441, #48463, #37250, #94946, #125297, #80763, #188972, #141452, #82743, #173798, #78775, #158601, #172797, #34278, #129244, #190940, #110120 ),
 ( #126279, #52417, #20091, #1941, #157623, #95937, #156630, #79780, #143421, #35264, #140451, #97898, #98907, #63621, #81735, #18125, #174779, #96919, #175776, #144423, #21086, #186993, #2937, #19113, #171798, #33286, #111108, #159589, #4908, #3919, #66591, #127259, #128255, #50448, #64617, #189953, #187976, #49445, #67586, #51427, #5909, #113087, #36245, #114075, #68580, #106651, #161597, #55415, #163605, #60145, #23091, #85750, #101923, #24096, #130236, #117086, #167348, #198678, #22090, #121813, #147437, #75318, #132261, #13651, #177781, #25106, #183508, #136989, #176785, #86750, #54423, #178781, #7905, #8925, #83740, #131256, #191932, #145419, #28845, #43999, #44991, #40249, #53416, #6901, #115093, #116093, #162591, #38258, #99912, #84736, #148433, #192944, #146414, #90486, #69589, #100907, #70593, #39251, #193952, #9928, #71587, #133253, #197684, #59149, #120819, #182519, #105661, #152168, #110614, #61132, #14646, #172296, #108633, #33785, #49952, #1444, #155141, #31804, #137984, #126767, #184495, #76306, #170311, #78281, #30812, #95445, #63122, #168323, #47975, #62122, #123785, #18625, #80272, #199667, #29820, #124801, #125792, #185484, #94450, #107628, #169306, #156130, #17629, #45974, #186499, #65109, #122805, #109627, #93453, #153144, #91456, #16634, #92461, #77299, #154149, #15641, #157129, #187494, #141942, #171311, #138969, #3433, #188471, #46974, #139954, #447, #32798, #79288, #140958, #2445, #64127, #48960, #81252, #190455, #175284, #131774, #193456, #114594, #144930, #160109, #98413, #50945, #5416, #159098, #70105, #176291, #53936, #4415, #158118, #115611, #51930, #177300, #111616, #6411, #21597, #36749, #142934, #173301, #127767, #19610, #113590, #83255, #174295, #38771, #68092, #34775, #191442, #67099, #128758, #162109, #23606, #66101, #96432, #129745, #69095, #52918, #37763, #112603, #35765, #99425, #161107, #189467, #22602, #8433, #97411, #84249, #145929, #20592, #82244, #7412, #143935, #130762, #192454, #100428, #85252, #146943, #73120, #10441, #134789, #165120, #194458, #103440, #9439, #75080, #43758, #25622, #182277, #86263, #89260, #11448, #101420, #136747, #55929, #88255, #196471, #90244, #117604, #118617, #57941, #56943, #163112, #149942, #197449, #28606, #54932, #151927, #180307, #105422, #26612, #167105, #72101, #119612, #13416, #116605, #71104, #181295, #87266, #42773, #40768, #41775, #148951, #104435, #179304, #133774, #166119, #39757, #178293, #195468, #27621, #150952, #58915, #12446, #147953, #24615, #74108, #120583, #135778, #132771, #102437, #164124, #62880, #79045, #156898, #169064, #108397, #48727, #110380, #17389, #155891, #121573, #186257, #95212, #124560, #16400, #92221, #29583, #61880, #122567, #91214, #18394, #45739, #172063, #139715, #183268, #77059, #153907, #14402, #199426, #47735, #154901, #198432, #140719, #80045, #59905, #1203, #76067, #94212, #93216, #44748, #2209, #63890, #106404, #137742, #15402, #109388, #125561, #60891, #168086, #187258, #152905, #184257, #123550, #107391, #185244, #30570, #33550, #138731, #46736, #170074, #211, #31565, #78046, #171068, #32558, #191217, #99190, #145698, #128524, #161876, #158867, #51697, #38538, #36516, #19380, #143698, #5180, #22369, #66861, #190218, #159873, #82004, #35533, #113360, #81029, #175052, #37527, #100194, #50715, #111378, #98171, #114355, #21364, #52691, #67862, #7180, #173066, #23370, #176060, #174065, #83022, #6182, #144696, #129517, #97181, #160878, #130523, #96202, #142705, #84020, #68864, #192220, #49713, #53702, #115379, #177067, #141714, #3204, #64878, #126539, #188238, #34543, #20356, #157891, #4184, #65863, #127535, #189237, #112373, #118379, #70873, #10205, #166877, #194229, #193221, #8193, #89023, #104199, #135546, #180073, #54695, #120347, #43525, #179065, #25390, #73876, #178056, #24381, #149708, #55695, #116368, #27377, #39524, #163894, #148717, #105190, #85015, #88020 ) ),
 .UNSPECIFIED., .T., .F., .T. ) 
 B_SPLINE_SURFACE_WITH_KNOTS ( ( 4, 3, 4 ),
 ( 3, 2, 2, 2, 2, 2, 2, 2, 2, 2, 2, 2, 2, 2, 2, 2, 2, 2, 2, 2, 2, 2, 2, 2, 2, 2, 2, 2, 2, 2, 2, 2, 2, 2, 2, 2, 2, 2, 2, 2, 2, 2, 2, 2, 2, 2, 2, 2, 2, 2, 2, 2, 2, 2, 2, 2, 2, 2, 2, 2, 2, 2, 2, 2, 2, 2, 2, 2, 2, 2, 2, 2, 2, 2, 2, 2, 2, 2, 2, 2, 2, 2, 2, 2, 2, 2, 2, 2, 2, 2, 2, 2, 2, 2, 2, 2, 2, 2, 2, 2, 2, 2, 2, 2, 2, 2, 2, 2, 2, 2, 2, 2, 2, 2, 2, 2, 2, 2, 2, 2, 2, 2, 2, 2, 2, 2, 2, 2, 2, 2, 2, 2, 2, 2, 2, 2, 2, 2, 2, 2, 2, 2, 2, 2, 2, 2, 2, 2, 2, 2, 2, 2, 2, 2, 2, 2, 2, 2, 2, 2, 2, 2, 2, 2, 2, 2, 2, 2, 2, 2, 2, 2, 2, 2, 2, 2, 2, 2, 2, 2, 2, 2, 2, 2, 2, 2, 2, 2, 2, 2, 2, 2, 2, 2, 2, 2, 2, 2, 2, 2, 2, 2, 2, 2, 2, 2, 2, 2, 2, 2, 2, 2, 2, 2, 2, 2, 2, 2, 2, 2, 2, 2, 2, 2, 2, 2, 2, 2, 3 ),
 ( 0.000000000000000000, 0.5000000000000000000, 1.000000000000000000 ),
 ( 0.000000000000000000, 0.004385964912280701511, 0.008771929824561403022, 0.01315789473684210453, 0.01754385964912280604, 0.02192982456140350755, 0.02631578947368420907, 0.03070175438596491058, 0.03508771929824561209, 0.03947368421052631360, 0.04385964912280701511, 0.04824561403508771662, 0.05263157894736841813, 0.05701754385964911964, 0.06140350877192982115, 0.06578947368421052266, 0.07017543859649122417, 0.07456140350877192569, 0.07894736842105262720, 0.08333333333333332871, 0.08771929824561403022, 0.09210526315789473173, 0.09649122807017543324, 0.1008771929824561348, 0.1052631578947368363, 0.1096491228070175378, 0.1140350877192982393, 0.1184210526315789408, 0.1228070175438596423, 0.1271929824561403577, 0.1315789473684210453, 0.1359649122807017607, 0.1403508771929824483, 0.1447368421052631637, 0.1491228070175438514, 0.1535087719298245668, 0.1578947368421052544, 0.1622807017543859698, 0.1666666666666666574, 0.1710526315789473728, 0.1754385964912280604, 0.1798245614035087758, 0.1842105263157894635, 0.1885964912280701788, 0.1929824561403508665, 0.1973684210526315819, 0.2017543859649122695, 0.2061403508771929849, 0.2105263157894736725, 0.2149122807017543879, 0.2192982456140350755, 0.2236842105263157909, 0.2280701754385964786, 0.2324561403508771940, 0.2368421052631578816, 0.2412280701754385970, 0.2456140350877192846, 0.2500000000000000000, 0.2543859649122807154, 0.2587719298245614308, 0.2631578947368420907, 0.2675438596491228060, 0.2719298245614035214, 0.2763157894736842368, 0.2807017543859648967, 0.2850877192982456121, 0.2894736842105263275, 0.2938596491228070429, 0.2982456140350877027, 0.3026315789473684181, 0.3070175438596491335, 0.3114035087719298489, 0.3157894736842105088, 0.3201754385964912242, 0.3245614035087719396, 0.3289473684210526550, 0.3333333333333333148, 0.3377192982456140302, 0.3421052631578947456, 0.3464912280701754610, 0.3508771929824561209, 0.3552631578947368363, 0.3596491228070175517, 0.3640350877192982670, 0.3684210526315789269, 0.3728070175438596423, 0.3771929824561403577, 0.3815789473684210731, 0.3859649122807017330, 0.3903508771929824483, 0.3947368421052631637, 0.3991228070175438791, 0.4035087719298245390, 0.4078947368421052544, 0.4122807017543859698, 0.4166666666666666852, 0.4210526315789473450, 0.4254385964912280604, 0.4298245614035087758, 0.4342105263157894912, 0.4385964912280701511, 0.4429824561403508665, 0.4473684210526315819, 0.4517543859649122973, 0.4561403508771929571, 0.4605263157894736725, 0.4649122807017543879, 0.4692982456140351033, 0.4736842105263157632, 0.4780701754385964786, 0.4824561403508771940, 0.4868421052631579093, 0.4912280701754385692, 0.4956140350877192846, 0.5000000000000000000, 0.5043859649122807154, 0.5087719298245614308, 0.5131578947368421462, 0.5175438596491228616, 0.5219298245614034659, 0.5263157894736841813, 0.5307017543859648967, 0.5350877192982456121, 0.5394736842105263275, 0.5438596491228070429, 0.5482456140350877583, 0.5526315789473684736, 0.5570175438596490780, 0.5614035087719297934, 0.5657894736842105088, 0.5701754385964912242, 0.5745614035087719396, 0.5789473684210526550, 0.5833333333333333703, 0.5877192982456140857, 0.5921052631578946901, 0.5964912280701754055, 0.6008771929824561209, 0.6052631578947368363, 0.6096491228070175517, 0.6140350877192982670, 0.6184210526315789824, 0.6228070175438596978, 0.6271929824561403022, 0.6315789473684210176, 0.6359649122807017330, 0.6403508771929824483, 0.6447368421052631637, 0.6491228070175438791, 0.6535087719298245945, 0.6578947368421053099, 0.6622807017543859143, 0.6666666666666666297, 0.6710526315789473450, 0.6754385964912280604, 0.6798245614035087758, 0.6842105263157894912, 0.6885964912280702066, 0.6929824561403509220, 0.6973684210526315264, 0.7017543859649122417, 0.7061403508771929571, 0.7105263157894736725, 0.7149122807017543879, 0.7192982456140351033, 0.7236842105263158187, 0.7280701754385965341, 0.7324561403508771384, 0.7368421052631578538, 0.7412280701754385692, 0.7456140350877192846, 0.7500000000000000000, 0.7543859649122807154, 0.7587719298245614308, 0.7631578947368421462, 0.7675438596491228616, 0.7719298245614034659, 0.7763157894736841813, 0.7807017543859648967, 0.7850877192982456121, 0.7894736842105263275, 0.7938596491228070429, 0.7982456140350877583, 0.8026315789473684736, 0.8070175438596490780, 0.8114035087719297934, 0.8157894736842105088, 0.8201754385964912242, 0.8245614035087719396, 0.8289473684210526550, 0.8333333333333333703, 0.8377192982456140857, 0.8421052631578946901, 0.8464912280701754055, 0.8508771929824561209, 0.8552631578947368363, 0.8596491228070175517, 0.8640350877192982670, 0.8684210526315789824, 0.8728070175438596978, 0.8771929824561403022, 0.8815789473684210176, 0.8859649122807017330, 0.8903508771929824483, 0.8947368421052631637, 0.8991228070175438791, 0.9035087719298245945, 0.9078947368421053099, 0.9122807017543859143, 0.9166666666666666297, 0.9210526315789473450, 0.9254385964912280604, 0.9298245614035087758, 0.9342105263157894912, 0.9385964912280702066, 0.9429824561403509220, 0.9473684210526315264, 0.9517543859649122417, 0.9561403508771929571, 0.9605263157894736725, 0.9649122807017543879, 0.9692982456140351033, 0.9736842105263158187, 0.9780701754385965341, 0.9824561403508771384, 0.9868421052631578538, 0.9912280701754385692, 0.9956140350877192846, 1.000000000000000000 ),
 .UNSPECIFIED. ) 
 GEOMETRIC_REPRESENTATION_ITEM ( )  RATIONAL_B_SPLINE_SURFACE ( (
 ( 1.000000000000000000, 0.9659258262890683122, 1.000000000000000000, 0.9659258262890683122, 1.000000000000000000, 0.9659258262890683122, 1.000000000000000000, 0.9659258262890683122, 1.000000000000000000, 0.9659258262890683122, 1.000000000000000000, 0.9659258262890683122, 1.000000000000000000, 0.9659258262890683122, 1.000000000000000000, 0.9659258262890683122, 1.000000000000000000, 0.9659258262890683122, 1.000000000000000000, 0.9659258262890683122, 1.000000000000000000, 0.9659258262890683122, 1.000000000000000000, 0.9659258262890683122, 1.000000000000000000, 0.9659258262890683122, 1.000000000000000000, 0.9659258262890683122, 1.000000000000000000, 0.9659258262890683122, 1.000000000000000000, 0.9659258262890683122, 1.000000000000000000, 0.9659258262890683122, 1.000000000000000000, 0.9659258262890683122, 1.000000000000000000, 0.9659258262890683122, 1.000000000000000000, 0.9659258262890683122, 1.000000000000000000, 0.9659258262890683122, 1.000000000000000000, 0.9659258262890683122, 1.000000000000000000, 0.9659258262890683122, 1.000000000000000000, 0.9659258262890683122, 1.000000000000000000, 0.9659258262890683122, 1.000000000000000000, 0.9659258262890683122, 1.000000000000000000, 0.9659258262890683122, 1.000000000000000000, 0.9659258262890683122, 1.000000000000000000, 0.9659258262890683122, 1.000000000000000000, 0.9659258262890683122, 1.000000000000000000, 0.9659258262890683122, 1.000000000000000000, 0.9659258262890683122, 1.000000000000000000, 0.9659258262890683122, 1.000000000000000000, 0.9659258262890683122, 1.000000000000000000, 0.9659258262890683122, 1.000000000000000000, 0.9659258262890683122, 1.000000000000000000, 0.9659258262890683122, 1.000000000000000000, 0.9659258262890683122, 1.000000000000000000, 0.9659258262890683122, 1.000000000000000000, 0.9659258262890683122, 1.000000000000000000, 0.9659258262890683122, 1.000000000000000000, 0.9659258262890683122, 1.000000000000000000, 0.9659258262890683122, 1.000000000000000000, 0.9659258262890683122, 1.000000000000000000, 0.9659258262890683122, 1.000000000000000000, 0.9659258262890683122, 1.000000000000000000, 0.9659258262890683122, 1.000000000000000000, 0.9659258262890683122, 1.000000000000000000, 0.9659258262890683122, 1.000000000000000000, 0.9659258262890683122, 1.000000000000000000, 0.9659258262890683122, 1.000000000000000000, 0.9659258262890683122, 1.000000000000000000, 0.9659258262890683122, 1.000000000000000000, 0.9659258262890683122, 1.000000000000000000, 0.9659258262890683122, 1.000000000000000000, 0.9659258262890683122, 1.000000000000000000, 0.9659258262890683122, 1.000000000000000000, 0.9659258262890683122, 1.000000000000000000, 0.9659258262890683122, 1.000000000000000000, 0.9659258262890683122, 1.000000000000000000, 0.9659258262890683122, 1.000000000000000000, 0.9659258262890683122, 1.000000000000000000, 0.9659258262890683122, 1.000000000000000000, 0.9659258262890683122, 1.000000000000000000, 0.9659258262890683122, 1.000000000000000000, 0.9659258262890683122, 1.000000000000000000, 0.9659258262890683122, 1.000000000000000000, 0.9659258262890683122, 1.000000000000000000, 0.9659258262890683122, 1.000000000000000000, 0.9659258262890683122, 1.000000000000000000, 0.9659258262890683122, 1.000000000000000000, 0.9659258262890683122, 1.000000000000000000, 0.9659258262890683122, 1.000000000000000000, 0.9659258262890683122, 1.000000000000000000, 0.9659258262890683122, 1.000000000000000000, 0.9659258262890683122, 1.000000000000000000, 0.9659258262890683122, 1.000000000000000000, 0.9659258262890683122, 1.000000000000000000, 0.9659258262890683122, 1.000000000000000000, 0.9659258262890683122, 1.000000000000000000, 0.9659258262890683122, 1.000000000000000000, 0.9659258262890683122, 1.000000000000000000, 0.9659258262890683122, 1.000000000000000000, 0.9659258262890683122, 1.000000000000000000, 0.9659258262890683122, 1.000000000000000000, 0.9659258262890683122, 1.000000000000000000, 0.9659258262890683122, 1.000000000000000000, 0.9659258262890683122, 1.000000000000000000, 0.9659258262890683122, 1.000000000000000000, 0.9659258262890683122, 1.000000000000000000, 0.9659258262890683122, 1.000000000000000000, 0.9659258262890683122, 1.000000000000000000, 0.9659258262890683122, 1.000000000000000000, 0.9659258262890683122, 1.000000000000000000, 0.9659258262890683122, 1.000000000000000000, 0.9659258262890683122, 1.000000000000000000, 0.9659258262890683122, 1.000000000000000000, 0.9659258262890683122, 1.000000000000000000, 0.9659258262890683122, 1.000000000000000000, 0.9659258262890683122, 1.000000000000000000, 0.9659258262890683122, 1.000000000000000000, 0.9659258262890683122, 1.000000000000000000, 0.9659258262890683122, 1.000000000000000000, 0.9659258262890683122, 1.000000000000000000, 0.9659258262890683122, 1.000000000000000000, 0.9659258262890683122, 1.000000000000000000, 0.9659258262890683122, 1.000000000000000000, 0.9659258262890683122, 1.000000000000000000, 0.9659258262890683122, 1.000000000000000000, 0.9659258262890683122, 1.000000000000000000, 0.9659258262890683122, 1.000000000000000000, 0.9659258262890683122, 1.000000000000000000, 0.9659258262890683122, 1.000000000000000000, 0.9659258262890683122, 1.000000000000000000, 0.9659258262890683122, 1.000000000000000000, 0.9659258262890683122, 1.000000000000000000, 0.9659258262890683122, 1.000000000000000000, 0.9659258262890683122, 1.000000000000000000, 0.9659258262890683122, 1.000000000000000000, 0.9659258262890683122, 1.000000000000000000, 0.9659258262890683122, 1.000000000000000000, 0.9659258262890683122, 1.000000000000000000, 0.9659258262890683122, 1.000000000000000000, 0.9659258262890683122, 1.000000000000000000, 0.9659258262890683122, 1.000000000000000000, 0.9659258262890683122, 1.000000000000000000, 0.9659258262890683122, 1.000000000000000000, 0.9659258262890683122, 1.000000000000000000, 0.9659258262890683122, 1.000000000000000000, 0.9659258262890683122, 1.000000000000000000, 0.9659258262890683122, 1.000000000000000000, 0.9659258262890683122, 1.000000000000000000, 0.9659258262890683122, 1.000000000000000000, 0.9659258262890683122, 1.000000000000000000, 0.9659258262890683122, 1.000000000000000000, 0.9659258262890683122, 1.000000000000000000, 0.9659258262890683122, 1.000000000000000000, 0.9659258262890683122, 1.000000000000000000, 0.9659258262890683122, 1.000000000000000000, 0.9659258262890683122, 1.000000000000000000, 0.9659258262890683122, 1.000000000000000000, 0.9659258262890683122, 1.000000000000000000, 0.9659258262890683122, 1.000000000000000000, 0.9659258262890683122, 1.000000000000000000, 0.9659258262890683122, 1.000000000000000000, 0.9659258262890683122, 1.000000000000000000, 0.9659258262890683122, 1.000000000000000000, 0.9659258262890683122, 1.000000000000000000, 0.9659258262890683122, 1.000000000000000000, 0.9659258262890683122, 1.000000000000000000, 0.9659258262890683122, 1.000000000000000000, 0.9659258262890683122, 1.000000000000000000, 0.9659258262890683122, 1.000000000000000000, 0.9659258262890683122, 1.000000000000000000, 0.9659258262890683122, 1.000000000000000000, 0.9659258262890683122, 1.000000000000000000, 0.9659258262890683122, 1.000000000000000000, 0.9659258262890683122, 1.000000000000000000, 0.9659258262890683122, 1.000000000000000000, 0.9659258262890683122, 1.000000000000000000, 0.9659258262890683122, 1.000000000000000000, 0.9659258262890683122, 1.000000000000000000, 0.9659258262890683122, 1.000000000000000000, 0.9659258262890683122, 1.000000000000000000, 0.9659258262890683122, 1.000000000000000000, 0.9659258262890683122, 1.000000000000000000, 0.9659258262890683122, 1.000000000000000000, 0.9659258262890683122, 1.000000000000000000, 0.9659258262890683122, 1.000000000000000000, 0.9659258262890683122, 1.000000000000000000, 0.9659258262890683122, 1.000000000000000000, 0.9659258262890683122, 1.000000000000000000, 0.9659258262890683122, 1.000000000000000000, 0.9659258262890683122, 1.000000000000000000, 0.9659258262890683122, 1.000000000000000000, 0.9659258262890683122, 1.000000000000000000, 0.9659258262890683122, 1.000000000000000000, 0.9659258262890683122, 1.000000000000000000, 0.9659258262890683122, 1.000000000000000000, 0.9659258262890683122, 1.000000000000000000, 0.9659258262890683122, 1.000000000000000000, 0.9659258262890683122, 1.000000000000000000, 0.9659258262890683122, 1.000000000000000000, 0.9659258262890683122, 1.000000000000000000, 0.9659258262890683122, 1.000000000000000000, 0.9659258262890683122, 1.000000000000000000, 0.9659258262890683122, 1.000000000000000000, 0.9659258262890683122, 1.000000000000000000, 0.9659258262890683122, 1.000000000000000000, 0.9659258262890683122, 1.000000000000000000, 0.9659258262890683122, 1.000000000000000000, 0.9659258262890683122, 1.000000000000000000, 0.9659258262890683122, 1.000000000000000000, 0.9659258262890683122, 1.000000000000000000, 0.9659258262890683122, 1.000000000000000000, 0.9659258262890683122, 1.000000000000000000, 0.9659258262890683122, 1.000000000000000000, 0.9659258262890683122, 1.000000000000000000, 0.9659258262890683122, 1.000000000000000000, 0.9659258262890683122, 1.000000000000000000, 0.9659258262890683122, 1.000000000000000000, 0.9659258262890683122, 1.000000000000000000, 0.9659258262890683122, 1.000000000000000000, 0.9659258262890683122, 1.000000000000000000, 0.9659258262890683122, 1.000000000000000000, 0.9659258262890683122, 1.000000000000000000, 0.9659258262890683122, 1.000000000000000000, 0.9659258262890683122, 1.000000000000000000, 0.9659258262890683122, 1.000000000000000000, 0.9659258262890683122, 1.000000000000000000, 0.9659258262890683122, 1.000000000000000000, 0.9659258262890683122, 1.000000000000000000, 0.9659258262890683122, 1.000000000000000000, 0.9659258262890683122, 1.000000000000000000, 0.9659258262890683122, 1.000000000000000000, 0.9659258262890683122, 1.000000000000000000, 0.9659258262890683122, 1.000000000000000000, 0.9659258262890683122, 1.000000000000000000, 0.9659258262890683122, 1.000000000000000000, 0.9659258262890683122, 1.000000000000000000, 0.9659258262890683122, 1.000000000000000000, 0.9659258262890683122, 1.000000000000000000, 0.9659258262890683122, 1.000000000000000000, 0.9659258262890683122, 1.000000000000000000, 0.9659258262890683122, 1.000000000000000000, 0.9659258262890683122, 1.000000000000000000, 0.9659258262890683122, 1.000000000000000000, 0.9659258262890683122, 1.000000000000000000),
 ( 0.3333333333333333703, 0.3219752754296894559, 0.3333333333333333703, 0.3219752754296894559, 0.3333333333333333703, 0.3219752754296894559, 0.3333333333333333703, 0.3219752754296894559, 0.3333333333333333703, 0.3219752754296894559, 0.3333333333333333703, 0.3219752754296894559, 0.3333333333333333703, 0.3219752754296894559, 0.3333333333333333703, 0.3219752754296894559, 0.3333333333333333703, 0.3219752754296894559, 0.3333333333333333703, 0.3219752754296894559, 0.3333333333333333703, 0.3219752754296894559, 0.3333333333333333703, 0.3219752754296894559, 0.3333333333333333703, 0.3219752754296894559, 0.3333333333333333703, 0.3219752754296894559, 0.3333333333333333703, 0.3219752754296894559, 0.3333333333333333703, 0.3219752754296894559, 0.3333333333333333703, 0.3219752754296894559, 0.3333333333333333703, 0.3219752754296894559, 0.3333333333333333703, 0.3219752754296894559, 0.3333333333333333703, 0.3219752754296894559, 0.3333333333333333703, 0.3219752754296894559, 0.3333333333333333703, 0.3219752754296894559, 0.3333333333333333703, 0.3219752754296894559, 0.3333333333333333703, 0.3219752754296894559, 0.3333333333333333703, 0.3219752754296894559, 0.3333333333333333703, 0.3219752754296894559, 0.3333333333333333703, 0.3219752754296894559, 0.3333333333333333703, 0.3219752754296894559, 0.3333333333333333703, 0.3219752754296894559, 0.3333333333333333703, 0.3219752754296894559, 0.3333333333333333703, 0.3219752754296894559, 0.3333333333333333703, 0.3219752754296894559, 0.3333333333333333703, 0.3219752754296894559, 0.3333333333333333703, 0.3219752754296894559, 0.3333333333333333703, 0.3219752754296894559, 0.3333333333333333703, 0.3219752754296894559, 0.3333333333333333703, 0.3219752754296894559, 0.3333333333333333703, 0.3219752754296894559, 0.3333333333333333703, 0.3219752754296894559, 0.3333333333333333703, 0.3219752754296894559, 0.3333333333333333703, 0.3219752754296894559, 0.3333333333333333703, 0.3219752754296894559, 0.3333333333333333703, 0.3219752754296894559, 0.3333333333333333703, 0.3219752754296894559, 0.3333333333333333703, 0.3219752754296894559, 0.3333333333333333703, 0.3219752754296894559, 0.3333333333333333703, 0.3219752754296894559, 0.3333333333333333703, 0.3219752754296894559, 0.3333333333333333703, 0.3219752754296894559, 0.3333333333333333703, 0.3219752754296894559, 0.3333333333333333703, 0.3219752754296894559, 0.3333333333333333703, 0.3219752754296894559, 0.3333333333333333703, 0.3219752754296894559, 0.3333333333333333703, 0.3219752754296894559, 0.3333333333333333703, 0.3219752754296894559, 0.3333333333333333703, 0.3219752754296894559, 0.3333333333333333703, 0.3219752754296894559, 0.3333333333333333703, 0.3219752754296894559, 0.3333333333333333703, 0.3219752754296894559, 0.3333333333333333703, 0.3219752754296894559, 0.3333333333333333703, 0.3219752754296894559, 0.3333333333333333703, 0.3219752754296894559, 0.3333333333333333703, 0.3219752754296894559, 0.3333333333333333703, 0.3219752754296894559, 0.3333333333333333703, 0.3219752754296894559, 0.3333333333333333703, 0.3219752754296894559, 0.3333333333333333703, 0.3219752754296894559, 0.3333333333333333703, 0.3219752754296894559, 0.3333333333333333703, 0.3219752754296894559, 0.3333333333333333703, 0.3219752754296894559, 0.3333333333333333703, 0.3219752754296894559, 0.3333333333333333703, 0.3219752754296894559, 0.3333333333333333703, 0.3219752754296894559, 0.3333333333333333703, 0.3219752754296894559, 0.3333333333333333703, 0.3219752754296894559, 0.3333333333333333703, 0.3219752754296894559, 0.3333333333333333703, 0.3219752754296894559, 0.3333333333333333703, 0.3219752754296894559, 0.3333333333333333703, 0.3219752754296894559, 0.3333333333333333703, 0.3219752754296894559, 0.3333333333333333703, 0.3219752754296894559, 0.3333333333333333703, 0.3219752754296894559, 0.3333333333333333703, 0.3219752754296894559, 0.3333333333333333703, 0.3219752754296894559, 0.3333333333333333703, 0.3219752754296894559, 0.3333333333333333703, 0.3219752754296894559, 0.3333333333333333703, 0.3219752754296894559, 0.3333333333333333703, 0.3219752754296894559, 0.3333333333333333703, 0.3219752754296894559, 0.3333333333333333703, 0.3219752754296894559, 0.3333333333333333703, 0.3219752754296894559, 0.3333333333333333703, 0.3219752754296894559, 0.3333333333333333703, 0.3219752754296894559, 0.3333333333333333703, 0.3219752754296894559, 0.3333333333333333703, 0.3219752754296894559, 0.3333333333333333703, 0.3219752754296894559, 0.3333333333333333703, 0.3219752754296894559, 0.3333333333333333703, 0.3219752754296894559, 0.3333333333333333703, 0.3219752754296894559, 0.3333333333333333703, 0.3219752754296894559, 0.3333333333333333703, 0.3219752754296894559, 0.3333333333333333703, 0.3219752754296894559, 0.3333333333333333703, 0.3219752754296894559, 0.3333333333333333703, 0.3219752754296894559, 0.3333333333333333703, 0.3219752754296894559, 0.3333333333333333703, 0.3219752754296894559, 0.3333333333333333703, 0.3219752754296894559, 0.3333333333333333703, 0.3219752754296894559, 0.3333333333333333703, 0.3219752754296894559, 0.3333333333333333703, 0.3219752754296894559, 0.3333333333333333703, 0.3219752754296894559, 0.3333333333333333703, 0.3219752754296894559, 0.3333333333333333703, 0.3219752754296894559, 0.3333333333333333703, 0.3219752754296894559, 0.3333333333333333703, 0.3219752754296894559, 0.3333333333333333703, 0.3219752754296894559, 0.3333333333333333703, 0.3219752754296894559, 0.3333333333333333703, 0.3219752754296894559, 0.3333333333333333703, 0.3219752754296894559, 0.3333333333333333703, 0.3219752754296894559, 0.3333333333333333703, 0.3219752754296894559, 0.3333333333333333703, 0.3219752754296894559, 0.3333333333333333703, 0.3219752754296894559, 0.3333333333333333703, 0.3219752754296894559, 0.3333333333333333703, 0.3219752754296894559, 0.3333333333333333703, 0.3219752754296894559, 0.3333333333333333703, 0.3219752754296894559, 0.3333333333333333703, 0.3219752754296894559, 0.3333333333333333703, 0.3219752754296894559, 0.3333333333333333703, 0.3219752754296894559, 0.3333333333333333703, 0.3219752754296894559, 0.3333333333333333703, 0.3219752754296894559, 0.3333333333333333703, 0.3219752754296894559, 0.3333333333333333703, 0.3219752754296894559, 0.3333333333333333703, 0.3219752754296894559, 0.3333333333333333703, 0.3219752754296894559, 0.3333333333333333703, 0.3219752754296894559, 0.3333333333333333703, 0.3219752754296894559, 0.3333333333333333703, 0.3219752754296894559, 0.3333333333333333703, 0.3219752754296894559, 0.3333333333333333703, 0.3219752754296894559, 0.3333333333333333703, 0.3219752754296894559, 0.3333333333333333703, 0.3219752754296894559, 0.3333333333333333703, 0.3219752754296894559, 0.3333333333333333703, 0.3219752754296894559, 0.3333333333333333703, 0.3219752754296894559, 0.3333333333333333703, 0.3219752754296894559, 0.3333333333333333703, 0.3219752754296894559, 0.3333333333333333703, 0.3219752754296894559, 0.3333333333333333703, 0.3219752754296894559, 0.3333333333333333703, 0.3219752754296894559, 0.3333333333333333703, 0.3219752754296894559, 0.3333333333333333703, 0.3219752754296894559, 0.3333333333333333703, 0.3219752754296894559, 0.3333333333333333703, 0.3219752754296894559, 0.3333333333333333703, 0.3219752754296894559, 0.3333333333333333703, 0.3219752754296894559, 0.3333333333333333703, 0.3219752754296894559, 0.3333333333333333703, 0.3219752754296894559, 0.3333333333333333703, 0.3219752754296894559, 0.3333333333333333703, 0.3219752754296894559, 0.3333333333333333703, 0.3219752754296894559, 0.3333333333333333703, 0.3219752754296894559, 0.3333333333333333703, 0.3219752754296894559, 0.3333333333333333703, 0.3219752754296894559, 0.3333333333333333703, 0.3219752754296894559, 0.3333333333333333703, 0.3219752754296894559, 0.3333333333333333703, 0.3219752754296894559, 0.3333333333333333703, 0.3219752754296894559, 0.3333333333333333703, 0.3219752754296894559, 0.3333333333333333703, 0.3219752754296894559, 0.3333333333333333703, 0.3219752754296894559, 0.3333333333333333703, 0.3219752754296894559, 0.3333333333333333703, 0.3219752754296894559, 0.3333333333333333703, 0.3219752754296894559, 0.3333333333333333703, 0.3219752754296894559, 0.3333333333333333703, 0.3219752754296894559, 0.3333333333333333703, 0.3219752754296894559, 0.3333333333333333703, 0.3219752754296894559, 0.3333333333333333703, 0.3219752754296894559, 0.3333333333333333703, 0.3219752754296894559, 0.3333333333333333703, 0.3219752754296894559, 0.3333333333333333703, 0.3219752754296894559, 0.3333333333333333703, 0.3219752754296894559, 0.3333333333333333703, 0.3219752754296894559, 0.3333333333333333703, 0.3219752754296894559, 0.3333333333333333703, 0.3219752754296894559, 0.3333333333333333703, 0.3219752754296894559, 0.3333333333333333703, 0.3219752754296894559, 0.3333333333333333703, 0.3219752754296894559, 0.3333333333333333703, 0.3219752754296894559, 0.3333333333333333703, 0.3219752754296894559, 0.3333333333333333703, 0.3219752754296894559, 0.3333333333333333703, 0.3219752754296894559, 0.3333333333333333703, 0.3219752754296894559, 0.3333333333333333703, 0.3219752754296894559, 0.3333333333333333703, 0.3219752754296894559, 0.3333333333333333703, 0.3219752754296894559, 0.3333333333333333703, 0.3219752754296894559, 0.3333333333333333703, 0.3219752754296894559, 0.3333333333333333703, 0.3219752754296894559, 0.3333333333333333703, 0.3219752754296894559, 0.3333333333333333703, 0.3219752754296894559, 0.3333333333333333703, 0.3219752754296894559, 0.3333333333333333703, 0.3219752754296894559, 0.3333333333333333703, 0.3219752754296894559, 0.3333333333333333703, 0.3219752754296894559, 0.3333333333333333703, 0.3219752754296894559, 0.3333333333333333703, 0.3219752754296894559, 0.3333333333333333703, 0.3219752754296894559, 0.3333333333333333703, 0.3219752754296894559, 0.3333333333333333703, 0.3219752754296894559, 0.3333333333333333703, 0.3219752754296894559, 0.3333333333333333703, 0.3219752754296894559, 0.3333333333333333703, 0.3219752754296894559, 0.3333333333333333703, 0.3219752754296894559, 0.3333333333333333703, 0.3219752754296894559, 0.3333333333333333703, 0.3219752754296894559, 0.3333333333333333703, 0.3219752754296894559, 0.3333333333333333703, 0.3219752754296894559, 0.3333333333333333703, 0.3219752754296894559, 0.3333333333333333703, 0.3219752754296894559, 0.3333333333333333703, 0.3219752754296894559, 0.3333333333333333703, 0.3219752754296894559, 0.3333333333333333703, 0.3219752754296894559, 0.3333333333333333703, 0.3219752754296894559, 0.3333333333333333703, 0.3219752754296894559, 0.3333333333333333703, 0.3219752754296894559, 0.3333333333333333703),
 ( 0.3333333333333333703, 0.3219752754296894559, 0.3333333333333333703, 0.3219752754296894559, 0.3333333333333333703, 0.3219752754296894559, 0.3333333333333333703, 0.3219752754296894559, 0.3333333333333333703, 0.3219752754296894559, 0.3333333333333333703, 0.3219752754296894559, 0.3333333333333333703, 0.3219752754296894559, 0.3333333333333333703, 0.3219752754296894559, 0.3333333333333333703, 0.3219752754296894559, 0.3333333333333333703, 0.3219752754296894559, 0.3333333333333333703, 0.3219752754296894559, 0.3333333333333333703, 0.3219752754296894559, 0.3333333333333333703, 0.3219752754296894559, 0.3333333333333333703, 0.3219752754296894559, 0.3333333333333333703, 0.3219752754296894559, 0.3333333333333333703, 0.3219752754296894559, 0.3333333333333333703, 0.3219752754296894559, 0.3333333333333333703, 0.3219752754296894559, 0.3333333333333333703, 0.3219752754296894559, 0.3333333333333333703, 0.3219752754296894559, 0.3333333333333333703, 0.3219752754296894559, 0.3333333333333333703, 0.3219752754296894559, 0.3333333333333333703, 0.3219752754296894559, 0.3333333333333333703, 0.3219752754296894559, 0.3333333333333333703, 0.3219752754296894559, 0.3333333333333333703, 0.3219752754296894559, 0.3333333333333333703, 0.3219752754296894559, 0.3333333333333333703, 0.3219752754296894559, 0.3333333333333333703, 0.3219752754296894559, 0.3333333333333333703, 0.3219752754296894559, 0.3333333333333333703, 0.3219752754296894559, 0.3333333333333333703, 0.3219752754296894559, 0.3333333333333333703, 0.3219752754296894559, 0.3333333333333333703, 0.3219752754296894559, 0.3333333333333333703, 0.3219752754296894559, 0.3333333333333333703, 0.3219752754296894559, 0.3333333333333333703, 0.3219752754296894559, 0.3333333333333333703, 0.3219752754296894559, 0.3333333333333333703, 0.3219752754296894559, 0.3333333333333333703, 0.3219752754296894559, 0.3333333333333333703, 0.3219752754296894559, 0.3333333333333333703, 0.3219752754296894559, 0.3333333333333333703, 0.3219752754296894559, 0.3333333333333333703, 0.3219752754296894559, 0.3333333333333333703, 0.3219752754296894559, 0.3333333333333333703, 0.3219752754296894559, 0.3333333333333333703, 0.3219752754296894559, 0.3333333333333333703, 0.3219752754296894559, 0.3333333333333333703, 0.3219752754296894559, 0.3333333333333333703, 0.3219752754296894559, 0.3333333333333333703, 0.3219752754296894559, 0.3333333333333333703, 0.3219752754296894559, 0.3333333333333333703, 0.3219752754296894559, 0.3333333333333333703, 0.3219752754296894559, 0.3333333333333333703, 0.3219752754296894559, 0.3333333333333333703, 0.3219752754296894559, 0.3333333333333333703, 0.3219752754296894559, 0.3333333333333333703, 0.3219752754296894559, 0.3333333333333333703, 0.3219752754296894559, 0.3333333333333333703, 0.3219752754296894559, 0.3333333333333333703, 0.3219752754296894559, 0.3333333333333333703, 0.3219752754296894559, 0.3333333333333333703, 0.3219752754296894559, 0.3333333333333333703, 0.3219752754296894559, 0.3333333333333333703, 0.3219752754296894559, 0.3333333333333333703, 0.3219752754296894559, 0.3333333333333333703, 0.3219752754296894559, 0.3333333333333333703, 0.3219752754296894559, 0.3333333333333333703, 0.3219752754296894559, 0.3333333333333333703, 0.3219752754296894559, 0.3333333333333333703, 0.3219752754296894559, 0.3333333333333333703, 0.3219752754296894559, 0.3333333333333333703, 0.3219752754296894559, 0.3333333333333333703, 0.3219752754296894559, 0.3333333333333333703, 0.3219752754296894559, 0.3333333333333333703, 0.3219752754296894559, 0.3333333333333333703, 0.3219752754296894559, 0.3333333333333333703, 0.3219752754296894559, 0.3333333333333333703, 0.3219752754296894559, 0.3333333333333333703, 0.3219752754296894559, 0.3333333333333333703, 0.3219752754296894559, 0.3333333333333333703, 0.3219752754296894559, 0.3333333333333333703, 0.3219752754296894559, 0.3333333333333333703, 0.3219752754296894559, 0.3333333333333333703, 0.3219752754296894559, 0.3333333333333333703, 0.3219752754296894559, 0.3333333333333333703, 0.3219752754296894559, 0.3333333333333333703, 0.3219752754296894559, 0.3333333333333333703, 0.3219752754296894559, 0.3333333333333333703, 0.3219752754296894559, 0.3333333333333333703, 0.3219752754296894559, 0.3333333333333333703, 0.3219752754296894559, 0.3333333333333333703, 0.3219752754296894559, 0.3333333333333333703, 0.3219752754296894559, 0.3333333333333333703, 0.3219752754296894559, 0.3333333333333333703, 0.3219752754296894559, 0.3333333333333333703, 0.3219752754296894559, 0.3333333333333333703, 0.3219752754296894559, 0.3333333333333333703, 0.3219752754296894559, 0.3333333333333333703, 0.3219752754296894559, 0.3333333333333333703, 0.3219752754296894559, 0.3333333333333333703, 0.3219752754296894559, 0.3333333333333333703, 0.3219752754296894559, 0.3333333333333333703, 0.3219752754296894559, 0.3333333333333333703, 0.3219752754296894559, 0.3333333333333333703, 0.3219752754296894559, 0.3333333333333333703, 0.3219752754296894559, 0.3333333333333333703, 0.3219752754296894559, 0.3333333333333333703, 0.3219752754296894559, 0.3333333333333333703, 0.3219752754296894559, 0.3333333333333333703, 0.3219752754296894559, 0.3333333333333333703, 0.3219752754296894559, 0.3333333333333333703, 0.3219752754296894559, 0.3333333333333333703, 0.3219752754296894559, 0.3333333333333333703, 0.3219752754296894559, 0.3333333333333333703, 0.3219752754296894559, 0.3333333333333333703, 0.3219752754296894559, 0.3333333333333333703, 0.3219752754296894559, 0.3333333333333333703, 0.3219752754296894559, 0.3333333333333333703, 0.3219752754296894559, 0.3333333333333333703, 0.3219752754296894559, 0.3333333333333333703, 0.3219752754296894559, 0.3333333333333333703, 0.3219752754296894559, 0.3333333333333333703, 0.3219752754296894559, 0.3333333333333333703, 0.3219752754296894559, 0.3333333333333333703, 0.3219752754296894559, 0.3333333333333333703, 0.3219752754296894559, 0.3333333333333333703, 0.3219752754296894559, 0.3333333333333333703, 0.3219752754296894559, 0.3333333333333333703, 0.3219752754296894559, 0.3333333333333333703, 0.3219752754296894559, 0.3333333333333333703, 0.3219752754296894559, 0.3333333333333333703, 0.3219752754296894559, 0.3333333333333333703, 0.3219752754296894559, 0.3333333333333333703, 0.3219752754296894559, 0.3333333333333333703, 0.3219752754296894559, 0.3333333333333333703, 0.3219752754296894559, 0.3333333333333333703, 0.3219752754296894559, 0.3333333333333333703, 0.3219752754296894559, 0.3333333333333333703, 0.3219752754296894559, 0.3333333333333333703, 0.3219752754296894559, 0.3333333333333333703, 0.3219752754296894559, 0.3333333333333333703, 0.3219752754296894559, 0.3333333333333333703, 0.3219752754296894559, 0.3333333333333333703, 0.3219752754296894559, 0.3333333333333333703, 0.3219752754296894559, 0.3333333333333333703, 0.3219752754296894559, 0.3333333333333333703, 0.3219752754296894559, 0.3333333333333333703, 0.3219752754296894559, 0.3333333333333333703, 0.3219752754296894559, 0.3333333333333333703, 0.3219752754296894559, 0.3333333333333333703, 0.3219752754296894559, 0.3333333333333333703, 0.3219752754296894559, 0.3333333333333333703, 0.3219752754296894559, 0.3333333333333333703, 0.3219752754296894559, 0.3333333333333333703, 0.3219752754296894559, 0.3333333333333333703, 0.3219752754296894559, 0.3333333333333333703, 0.3219752754296894559, 0.3333333333333333703, 0.3219752754296894559, 0.3333333333333333703, 0.3219752754296894559, 0.3333333333333333703, 0.3219752754296894559, 0.3333333333333333703, 0.3219752754296894559, 0.3333333333333333703, 0.3219752754296894559, 0.3333333333333333703, 0.3219752754296894559, 0.3333333333333333703, 0.3219752754296894559, 0.3333333333333333703, 0.3219752754296894559, 0.3333333333333333703, 0.3219752754296894559, 0.3333333333333333703, 0.3219752754296894559, 0.3333333333333333703, 0.3219752754296894559, 0.3333333333333333703, 0.3219752754296894559, 0.3333333333333333703, 0.3219752754296894559, 0.3333333333333333703, 0.3219752754296894559, 0.3333333333333333703, 0.3219752754296894559, 0.3333333333333333703, 0.3219752754296894559, 0.3333333333333333703, 0.3219752754296894559, 0.3333333333333333703, 0.3219752754296894559, 0.3333333333333333703, 0.3219752754296894559, 0.3333333333333333703, 0.3219752754296894559, 0.3333333333333333703, 0.3219752754296894559, 0.3333333333333333703, 0.3219752754296894559, 0.3333333333333333703, 0.3219752754296894559, 0.3333333333333333703, 0.3219752754296894559, 0.3333333333333333703, 0.3219752754296894559, 0.3333333333333333703, 0.3219752754296894559, 0.3333333333333333703, 0.3219752754296894559, 0.3333333333333333703, 0.3219752754296894559, 0.3333333333333333703, 0.3219752754296894559, 0.3333333333333333703, 0.3219752754296894559, 0.3333333333333333703, 0.3219752754296894559, 0.3333333333333333703, 0.3219752754296894559, 0.3333333333333333703, 0.3219752754296894559, 0.3333333333333333703, 0.3219752754296894559, 0.3333333333333333703, 0.3219752754296894559, 0.3333333333333333703, 0.3219752754296894559, 0.3333333333333333703, 0.3219752754296894559, 0.3333333333333333703, 0.3219752754296894559, 0.3333333333333333703, 0.3219752754296894559, 0.3333333333333333703, 0.3219752754296894559, 0.3333333333333333703, 0.3219752754296894559, 0.3333333333333333703, 0.3219752754296894559, 0.3333333333333333703, 0.3219752754296894559, 0.3333333333333333703, 0.3219752754296894559, 0.3333333333333333703, 0.3219752754296894559, 0.3333333333333333703, 0.3219752754296894559, 0.3333333333333333703, 0.3219752754296894559, 0.3333333333333333703, 0.3219752754296894559, 0.3333333333333333703, 0.3219752754296894559, 0.3333333333333333703, 0.3219752754296894559, 0.3333333333333333703, 0.3219752754296894559, 0.3333333333333333703, 0.3219752754296894559, 0.3333333333333333703, 0.3219752754296894559, 0.3333333333333333703, 0.3219752754296894559, 0.3333333333333333703, 0.3219752754296894559, 0.3333333333333333703, 0.3219752754296894559, 0.3333333333333333703, 0.3219752754296894559, 0.3333333333333333703, 0.3219752754296894559, 0.3333333333333333703, 0.3219752754296894559, 0.3333333333333333703, 0.3219752754296894559, 0.3333333333333333703, 0.3219752754296894559, 0.3333333333333333703, 0.3219752754296894559, 0.3333333333333333703, 0.3219752754296894559, 0.3333333333333333703, 0.3219752754296894559, 0.3333333333333333703, 0.3219752754296894559, 0.3333333333333333703, 0.3219752754296894559, 0.3333333333333333703, 0.3219752754296894559, 0.3333333333333333703, 0.3219752754296894559, 0.3333333333333333703, 0.3219752754296894559, 0.3333333333333333703, 0.3219752754296894559, 0.3333333333333333703),
 ( 1.000000000000000000, 0.9659258262890683122, 1.000000000000000000, 0.9659258262890683122, 1.000000000000000000, 0.9659258262890683122, 1.000000000000000000, 0.9659258262890683122, 1.000000000000000000, 0.9659258262890683122, 1.000000000000000000, 0.9659258262890683122, 1.000000000000000000, 0.9659258262890683122, 1.000000000000000000, 0.9659258262890683122, 1.000000000000000000, 0.9659258262890683122, 1.000000000000000000, 0.9659258262890683122, 1.000000000000000000, 0.9659258262890683122, 1.000000000000000000, 0.9659258262890683122, 1.000000000000000000, 0.9659258262890683122, 1.000000000000000000, 0.9659258262890683122, 1.000000000000000000, 0.9659258262890683122, 1.000000000000000000, 0.9659258262890683122, 1.000000000000000000, 0.9659258262890683122, 1.000000000000000000, 0.9659258262890683122, 1.000000000000000000, 0.9659258262890683122, 1.000000000000000000, 0.9659258262890683122, 1.000000000000000000, 0.9659258262890683122, 1.000000000000000000, 0.9659258262890683122, 1.000000000000000000, 0.9659258262890683122, 1.000000000000000000, 0.9659258262890683122, 1.000000000000000000, 0.9659258262890683122, 1.000000000000000000, 0.9659258262890683122, 1.000000000000000000, 0.9659258262890683122, 1.000000000000000000, 0.9659258262890683122, 1.000000000000000000, 0.9659258262890683122, 1.000000000000000000, 0.9659258262890683122, 1.000000000000000000, 0.9659258262890683122, 1.000000000000000000, 0.9659258262890683122, 1.000000000000000000, 0.9659258262890683122, 1.000000000000000000, 0.9659258262890683122, 1.000000000000000000, 0.9659258262890683122, 1.000000000000000000, 0.9659258262890683122, 1.000000000000000000, 0.9659258262890683122, 1.000000000000000000, 0.9659258262890683122, 1.000000000000000000, 0.9659258262890683122, 1.000000000000000000, 0.9659258262890683122, 1.000000000000000000, 0.9659258262890683122, 1.000000000000000000, 0.9659258262890683122, 1.000000000000000000, 0.9659258262890683122, 1.000000000000000000, 0.9659258262890683122, 1.000000000000000000, 0.9659258262890683122, 1.000000000000000000, 0.9659258262890683122, 1.000000000000000000, 0.9659258262890683122, 1.000000000000000000, 0.9659258262890683122, 1.000000000000000000, 0.9659258262890683122, 1.000000000000000000, 0.9659258262890683122, 1.000000000000000000, 0.9659258262890683122, 1.000000000000000000, 0.9659258262890683122, 1.000000000000000000, 0.9659258262890683122, 1.000000000000000000, 0.9659258262890683122, 1.000000000000000000, 0.9659258262890683122, 1.000000000000000000, 0.9659258262890683122, 1.000000000000000000, 0.9659258262890683122, 1.000000000000000000, 0.9659258262890683122, 1.000000000000000000, 0.9659258262890683122, 1.000000000000000000, 0.9659258262890683122, 1.000000000000000000, 0.9659258262890683122, 1.000000000000000000, 0.9659258262890683122, 1.000000000000000000, 0.9659258262890683122, 1.000000000000000000, 0.9659258262890683122, 1.000000000000000000, 0.9659258262890683122, 1.000000000000000000, 0.9659258262890683122, 1.000000000000000000, 0.9659258262890683122, 1.000000000000000000, 0.9659258262890683122, 1.000000000000000000, 0.9659258262890683122, 1.000000000000000000, 0.9659258262890683122, 1.000000000000000000, 0.9659258262890683122, 1.000000000000000000, 0.9659258262890683122, 1.000000000000000000, 0.9659258262890683122, 1.000000000000000000, 0.9659258262890683122, 1.000000000000000000, 0.9659258262890683122, 1.000000000000000000, 0.9659258262890683122, 1.000000000000000000, 0.9659258262890683122, 1.000000000000000000, 0.9659258262890683122, 1.000000000000000000, 0.9659258262890683122, 1.000000000000000000, 0.9659258262890683122, 1.000000000000000000, 0.9659258262890683122, 1.000000000000000000, 0.9659258262890683122, 1.000000000000000000, 0.9659258262890683122, 1.000000000000000000, 0.9659258262890683122, 1.000000000000000000, 0.9659258262890683122, 1.000000000000000000, 0.9659258262890683122, 1.000000000000000000, 0.9659258262890683122, 1.000000000000000000, 0.9659258262890683122, 1.000000000000000000, 0.9659258262890683122, 1.000000000000000000, 0.9659258262890683122, 1.000000000000000000, 0.9659258262890683122, 1.000000000000000000, 0.9659258262890683122, 1.000000000000000000, 0.9659258262890683122, 1.000000000000000000, 0.9659258262890683122, 1.000000000000000000, 0.9659258262890683122, 1.000000000000000000, 0.9659258262890683122, 1.000000000000000000, 0.9659258262890683122, 1.000000000000000000, 0.9659258262890683122, 1.000000000000000000, 0.9659258262890683122, 1.000000000000000000, 0.9659258262890683122, 1.000000000000000000, 0.9659258262890683122, 1.000000000000000000, 0.9659258262890683122, 1.000000000000000000, 0.9659258262890683122, 1.000000000000000000, 0.9659258262890683122, 1.000000000000000000, 0.9659258262890683122, 1.000000000000000000, 0.9659258262890683122, 1.000000000000000000, 0.9659258262890683122, 1.000000000000000000, 0.9659258262890683122, 1.000000000000000000, 0.9659258262890683122, 1.000000000000000000, 0.9659258262890683122, 1.000000000000000000, 0.9659258262890683122, 1.000000000000000000, 0.9659258262890683122, 1.000000000000000000, 0.9659258262890683122, 1.000000000000000000, 0.9659258262890683122, 1.000000000000000000, 0.9659258262890683122, 1.000000000000000000, 0.9659258262890683122, 1.000000000000000000, 0.9659258262890683122, 1.000000000000000000, 0.9659258262890683122, 1.000000000000000000, 0.9659258262890683122, 1.000000000000000000, 0.9659258262890683122, 1.000000000000000000, 0.9659258262890683122, 1.000000000000000000, 0.9659258262890683122, 1.000000000000000000, 0.9659258262890683122, 1.000000000000000000, 0.9659258262890683122, 1.000000000000000000, 0.9659258262890683122, 1.000000000000000000, 0.9659258262890683122, 1.000000000000000000, 0.9659258262890683122, 1.000000000000000000, 0.9659258262890683122, 1.000000000000000000, 0.9659258262890683122, 1.000000000000000000, 0.9659258262890683122, 1.000000000000000000, 0.9659258262890683122, 1.000000000000000000, 0.9659258262890683122, 1.000000000000000000, 0.9659258262890683122, 1.000000000000000000, 0.9659258262890683122, 1.000000000000000000, 0.9659258262890683122, 1.000000000000000000, 0.9659258262890683122, 1.000000000000000000, 0.9659258262890683122, 1.000000000000000000, 0.9659258262890683122, 1.000000000000000000, 0.9659258262890683122, 1.000000000000000000, 0.9659258262890683122, 1.000000000000000000, 0.9659258262890683122, 1.000000000000000000, 0.9659258262890683122, 1.000000000000000000, 0.9659258262890683122, 1.000000000000000000, 0.9659258262890683122, 1.000000000000000000, 0.9659258262890683122, 1.000000000000000000, 0.9659258262890683122, 1.000000000000000000, 0.9659258262890683122, 1.000000000000000000, 0.9659258262890683122, 1.000000000000000000, 0.9659258262890683122, 1.000000000000000000, 0.9659258262890683122, 1.000000000000000000, 0.9659258262890683122, 1.000000000000000000, 0.9659258262890683122, 1.000000000000000000, 0.9659258262890683122, 1.000000000000000000, 0.9659258262890683122, 1.000000000000000000, 0.9659258262890683122, 1.000000000000000000, 0.9659258262890683122, 1.000000000000000000, 0.9659258262890683122, 1.000000000000000000, 0.9659258262890683122, 1.000000000000000000, 0.9659258262890683122, 1.000000000000000000, 0.9659258262890683122, 1.000000000000000000, 0.9659258262890683122, 1.000000000000000000, 0.9659258262890683122, 1.000000000000000000, 0.9659258262890683122, 1.000000000000000000, 0.9659258262890683122, 1.000000000000000000, 0.9659258262890683122, 1.000000000000000000, 0.9659258262890683122, 1.000000000000000000, 0.9659258262890683122, 1.000000000000000000, 0.9659258262890683122, 1.000000000000000000, 0.9659258262890683122, 1.000000000000000000, 0.9659258262890683122, 1.000000000000000000, 0.9659258262890683122, 1.000000000000000000, 0.9659258262890683122, 1.000000000000000000, 0.9659258262890683122, 1.000000000000000000, 0.9659258262890683122, 1.000000000000000000, 0.9659258262890683122, 1.000000000000000000, 0.9659258262890683122, 1.000000000000000000, 0.9659258262890683122, 1.000000000000000000, 0.9659258262890683122, 1.000000000000000000, 0.9659258262890683122, 1.000000000000000000, 0.9659258262890683122, 1.000000000000000000, 0.9659258262890683122, 1.000000000000000000, 0.9659258262890683122, 1.000000000000000000, 0.9659258262890683122, 1.000000000000000000, 0.9659258262890683122, 1.000000000000000000, 0.9659258262890683122, 1.000000000000000000, 0.9659258262890683122, 1.000000000000000000, 0.9659258262890683122, 1.000000000000000000, 0.9659258262890683122, 1.000000000000000000, 0.9659258262890683122, 1.000000000000000000, 0.9659258262890683122, 1.000000000000000000, 0.9659258262890683122, 1.000000000000000000, 0.9659258262890683122, 1.000000000000000000, 0.9659258262890683122, 1.000000000000000000, 0.9659258262890683122, 1.000000000000000000, 0.9659258262890683122, 1.000000000000000000, 0.9659258262890683122, 1.000000000000000000, 0.9659258262890683122, 1.000000000000000000, 0.9659258262890683122, 1.000000000000000000, 0.9659258262890683122, 1.000000000000000000, 0.9659258262890683122, 1.000000000000000000, 0.9659258262890683122, 1.000000000000000000, 0.9659258262890683122, 1.000000000000000000, 0.9659258262890683122, 1.000000000000000000, 0.9659258262890683122, 1.000000000000000000, 0.9659258262890683122, 1.000000000000000000, 0.9659258262890683122, 1.000000000000000000, 0.9659258262890683122, 1.000000000000000000, 0.9659258262890683122, 1.000000000000000000, 0.9659258262890683122, 1.000000000000000000, 0.9659258262890683122, 1.000000000000000000, 0.9659258262890683122, 1.000000000000000000, 0.9659258262890683122, 1.000000000000000000, 0.9659258262890683122, 1.000000000000000000, 0.9659258262890683122, 1.000000000000000000, 0.9659258262890683122, 1.000000000000000000, 0.9659258262890683122, 1.000000000000000000, 0.9659258262890683122, 1.000000000000000000, 0.9659258262890683122, 1.000000000000000000, 0.9659258262890683122, 1.000000000000000000, 0.9659258262890683122, 1.000000000000000000, 0.9659258262890683122, 1.000000000000000000, 0.9659258262890683122, 1.000000000000000000, 0.9659258262890683122, 1.000000000000000000, 0.9659258262890683122, 1.000000000000000000, 0.9659258262890683122, 1.000000000000000000, 0.9659258262890683122, 1.000000000000000000, 0.9659258262890683122, 1.000000000000000000, 0.9659258262890683122, 1.000000000000000000),
 ( 0.3333333333333333703, 0.3219752754296894559, 0.3333333333333333703, 0.3219752754296894559, 0.3333333333333333703, 0.3219752754296894559, 0.3333333333333333703, 0.3219752754296894559, 0.3333333333333333703, 0.3219752754296894559, 0.3333333333333333703, 0.3219752754296894559, 0.3333333333333333703, 0.3219752754296894559, 0.3333333333333333703, 0.3219752754296894559, 0.3333333333333333703, 0.3219752754296894559, 0.3333333333333333703, 0.3219752754296894559, 0.3333333333333333703, 0.3219752754296894559, 0.3333333333333333703, 0.3219752754296894559, 0.3333333333333333703, 0.3219752754296894559, 0.3333333333333333703, 0.3219752754296894559, 0.3333333333333333703, 0.3219752754296894559, 0.3333333333333333703, 0.3219752754296894559, 0.3333333333333333703, 0.3219752754296894559, 0.3333333333333333703, 0.3219752754296894559, 0.3333333333333333703, 0.3219752754296894559, 0.3333333333333333703, 0.3219752754296894559, 0.3333333333333333703, 0.3219752754296894559, 0.3333333333333333703, 0.3219752754296894559, 0.3333333333333333703, 0.3219752754296894559, 0.3333333333333333703, 0.3219752754296894559, 0.3333333333333333703, 0.3219752754296894559, 0.3333333333333333703, 0.3219752754296894559, 0.3333333333333333703, 0.3219752754296894559, 0.3333333333333333703, 0.3219752754296894559, 0.3333333333333333703, 0.3219752754296894559, 0.3333333333333333703, 0.3219752754296894559, 0.3333333333333333703, 0.3219752754296894559, 0.3333333333333333703, 0.3219752754296894559, 0.3333333333333333703, 0.3219752754296894559, 0.3333333333333333703, 0.3219752754296894559, 0.3333333333333333703, 0.3219752754296894559, 0.3333333333333333703, 0.3219752754296894559, 0.3333333333333333703, 0.3219752754296894559, 0.3333333333333333703, 0.3219752754296894559, 0.3333333333333333703, 0.3219752754296894559, 0.3333333333333333703, 0.3219752754296894559, 0.3333333333333333703, 0.3219752754296894559, 0.3333333333333333703, 0.3219752754296894559, 0.3333333333333333703, 0.3219752754296894559, 0.3333333333333333703, 0.3219752754296894559, 0.3333333333333333703, 0.3219752754296894559, 0.3333333333333333703, 0.3219752754296894559, 0.3333333333333333703, 0.3219752754296894559, 0.3333333333333333703, 0.3219752754296894559, 0.3333333333333333703, 0.3219752754296894559, 0.3333333333333333703, 0.3219752754296894559, 0.3333333333333333703, 0.3219752754296894559, 0.3333333333333333703, 0.3219752754296894559, 0.3333333333333333703, 0.3219752754296894559, 0.3333333333333333703, 0.3219752754296894559, 0.3333333333333333703, 0.3219752754296894559, 0.3333333333333333703, 0.3219752754296894559, 0.3333333333333333703, 0.3219752754296894559, 0.3333333333333333703, 0.3219752754296894559, 0.3333333333333333703, 0.3219752754296894559, 0.3333333333333333703, 0.3219752754296894559, 0.3333333333333333703, 0.3219752754296894559, 0.3333333333333333703, 0.3219752754296894559, 0.3333333333333333703, 0.3219752754296894559, 0.3333333333333333703, 0.3219752754296894559, 0.3333333333333333703, 0.3219752754296894559, 0.3333333333333333703, 0.3219752754296894559, 0.3333333333333333703, 0.3219752754296894559, 0.3333333333333333703, 0.3219752754296894559, 0.3333333333333333703, 0.3219752754296894559, 0.3333333333333333703, 0.3219752754296894559, 0.3333333333333333703, 0.3219752754296894559, 0.3333333333333333703, 0.3219752754296894559, 0.3333333333333333703, 0.3219752754296894559, 0.3333333333333333703, 0.3219752754296894559, 0.3333333333333333703, 0.3219752754296894559, 0.3333333333333333703, 0.3219752754296894559, 0.3333333333333333703, 0.3219752754296894559, 0.3333333333333333703, 0.3219752754296894559, 0.3333333333333333703, 0.3219752754296894559, 0.3333333333333333703, 0.3219752754296894559, 0.3333333333333333703, 0.3219752754296894559, 0.3333333333333333703, 0.3219752754296894559, 0.3333333333333333703, 0.3219752754296894559, 0.3333333333333333703, 0.3219752754296894559, 0.3333333333333333703, 0.3219752754296894559, 0.3333333333333333703, 0.3219752754296894559, 0.3333333333333333703, 0.3219752754296894559, 0.3333333333333333703, 0.3219752754296894559, 0.3333333333333333703, 0.3219752754296894559, 0.3333333333333333703, 0.3219752754296894559, 0.3333333333333333703, 0.3219752754296894559, 0.3333333333333333703, 0.3219752754296894559, 0.3333333333333333703, 0.3219752754296894559, 0.3333333333333333703, 0.3219752754296894559, 0.3333333333333333703, 0.3219752754296894559, 0.3333333333333333703, 0.3219752754296894559, 0.3333333333333333703, 0.3219752754296894559, 0.3333333333333333703, 0.3219752754296894559, 0.3333333333333333703, 0.3219752754296894559, 0.3333333333333333703, 0.3219752754296894559, 0.3333333333333333703, 0.3219752754296894559, 0.3333333333333333703, 0.3219752754296894559, 0.3333333333333333703, 0.3219752754296894559, 0.3333333333333333703, 0.3219752754296894559, 0.3333333333333333703, 0.3219752754296894559, 0.3333333333333333703, 0.3219752754296894559, 0.3333333333333333703, 0.3219752754296894559, 0.3333333333333333703, 0.3219752754296894559, 0.3333333333333333703, 0.3219752754296894559, 0.3333333333333333703, 0.3219752754296894559, 0.3333333333333333703, 0.3219752754296894559, 0.3333333333333333703, 0.3219752754296894559, 0.3333333333333333703, 0.3219752754296894559, 0.3333333333333333703, 0.3219752754296894559, 0.3333333333333333703, 0.3219752754296894559, 0.3333333333333333703, 0.3219752754296894559, 0.3333333333333333703, 0.3219752754296894559, 0.3333333333333333703, 0.3219752754296894559, 0.3333333333333333703, 0.3219752754296894559, 0.3333333333333333703, 0.3219752754296894559, 0.3333333333333333703, 0.3219752754296894559, 0.3333333333333333703, 0.3219752754296894559, 0.3333333333333333703, 0.3219752754296894559, 0.3333333333333333703, 0.3219752754296894559, 0.3333333333333333703, 0.3219752754296894559, 0.3333333333333333703, 0.3219752754296894559, 0.3333333333333333703, 0.3219752754296894559, 0.3333333333333333703, 0.3219752754296894559, 0.3333333333333333703, 0.3219752754296894559, 0.3333333333333333703, 0.3219752754296894559, 0.3333333333333333703, 0.3219752754296894559, 0.3333333333333333703, 0.3219752754296894559, 0.3333333333333333703, 0.3219752754296894559, 0.3333333333333333703, 0.3219752754296894559, 0.3333333333333333703, 0.3219752754296894559, 0.3333333333333333703, 0.3219752754296894559, 0.3333333333333333703, 0.3219752754296894559, 0.3333333333333333703, 0.3219752754296894559, 0.3333333333333333703, 0.3219752754296894559, 0.3333333333333333703, 0.3219752754296894559, 0.3333333333333333703, 0.3219752754296894559, 0.3333333333333333703, 0.3219752754296894559, 0.3333333333333333703, 0.3219752754296894559, 0.3333333333333333703, 0.3219752754296894559, 0.3333333333333333703, 0.3219752754296894559, 0.3333333333333333703, 0.3219752754296894559, 0.3333333333333333703, 0.3219752754296894559, 0.3333333333333333703, 0.3219752754296894559, 0.3333333333333333703, 0.3219752754296894559, 0.3333333333333333703, 0.3219752754296894559, 0.3333333333333333703, 0.3219752754296894559, 0.3333333333333333703, 0.3219752754296894559, 0.3333333333333333703, 0.3219752754296894559, 0.3333333333333333703, 0.3219752754296894559, 0.3333333333333333703, 0.3219752754296894559, 0.3333333333333333703, 0.3219752754296894559, 0.3333333333333333703, 0.3219752754296894559, 0.3333333333333333703, 0.3219752754296894559, 0.3333333333333333703, 0.3219752754296894559, 0.3333333333333333703, 0.3219752754296894559, 0.3333333333333333703, 0.3219752754296894559, 0.3333333333333333703, 0.3219752754296894559, 0.3333333333333333703, 0.3219752754296894559, 0.3333333333333333703, 0.3219752754296894559, 0.3333333333333333703, 0.3219752754296894559, 0.3333333333333333703, 0.3219752754296894559, 0.3333333333333333703, 0.3219752754296894559, 0.3333333333333333703, 0.3219752754296894559, 0.3333333333333333703, 0.3219752754296894559, 0.3333333333333333703, 0.3219752754296894559, 0.3333333333333333703, 0.3219752754296894559, 0.3333333333333333703, 0.3219752754296894559, 0.3333333333333333703, 0.3219752754296894559, 0.3333333333333333703, 0.3219752754296894559, 0.3333333333333333703, 0.3219752754296894559, 0.3333333333333333703, 0.3219752754296894559, 0.3333333333333333703, 0.3219752754296894559, 0.3333333333333333703, 0.3219752754296894559, 0.3333333333333333703, 0.3219752754296894559, 0.3333333333333333703, 0.3219752754296894559, 0.3333333333333333703, 0.3219752754296894559, 0.3333333333333333703, 0.3219752754296894559, 0.3333333333333333703, 0.3219752754296894559, 0.3333333333333333703, 0.3219752754296894559, 0.3333333333333333703, 0.3219752754296894559, 0.3333333333333333703, 0.3219752754296894559, 0.3333333333333333703, 0.3219752754296894559, 0.3333333333333333703, 0.3219752754296894559, 0.3333333333333333703, 0.3219752754296894559, 0.3333333333333333703, 0.3219752754296894559, 0.3333333333333333703, 0.3219752754296894559, 0.3333333333333333703, 0.3219752754296894559, 0.3333333333333333703, 0.3219752754296894559, 0.3333333333333333703, 0.3219752754296894559, 0.3333333333333333703, 0.3219752754296894559, 0.3333333333333333703, 0.3219752754296894559, 0.3333333333333333703, 0.3219752754296894559, 0.3333333333333333703, 0.3219752754296894559, 0.3333333333333333703, 0.3219752754296894559, 0.3333333333333333703, 0.3219752754296894559, 0.3333333333333333703, 0.3219752754296894559, 0.3333333333333333703, 0.3219752754296894559, 0.3333333333333333703, 0.3219752754296894559, 0.3333333333333333703, 0.3219752754296894559, 0.3333333333333333703, 0.3219752754296894559, 0.3333333333333333703, 0.3219752754296894559, 0.3333333333333333703, 0.3219752754296894559, 0.3333333333333333703, 0.3219752754296894559, 0.3333333333333333703, 0.3219752754296894559, 0.3333333333333333703, 0.3219752754296894559, 0.3333333333333333703, 0.3219752754296894559, 0.3333333333333333703, 0.3219752754296894559, 0.3333333333333333703, 0.3219752754296894559, 0.3333333333333333703, 0.3219752754296894559, 0.3333333333333333703, 0.3219752754296894559, 0.3333333333333333703, 0.3219752754296894559, 0.3333333333333333703, 0.3219752754296894559, 0.3333333333333333703, 0.3219752754296894559, 0.3333333333333333703, 0.3219752754296894559, 0.3333333333333333703, 0.3219752754296894559, 0.3333333333333333703, 0.3219752754296894559, 0.3333333333333333703, 0.3219752754296894559, 0.3333333333333333703, 0.3219752754296894559, 0.3333333333333333703, 0.3219752754296894559, 0.3333333333333333703, 0.3219752754296894559, 0.3333333333333333703, 0.3219752754296894559, 0.3333333333333333703, 0.3219752754296894559, 0.3333333333333333703, 0.3219752754296894559, 0.3333333333333333703),
 ( 0.3333333333333333703, 0.3219752754296894559, 0.3333333333333333703, 0.3219752754296894559, 0.3333333333333333703, 0.3219752754296894559, 0.3333333333333333703, 0.3219752754296894559, 0.3333333333333333703, 0.3219752754296894559, 0.3333333333333333703, 0.3219752754296894559, 0.3333333333333333703, 0.3219752754296894559, 0.3333333333333333703, 0.3219752754296894559, 0.3333333333333333703, 0.3219752754296894559, 0.3333333333333333703, 0.3219752754296894559, 0.3333333333333333703, 0.3219752754296894559, 0.3333333333333333703, 0.3219752754296894559, 0.3333333333333333703, 0.3219752754296894559, 0.3333333333333333703, 0.3219752754296894559, 0.3333333333333333703, 0.3219752754296894559, 0.3333333333333333703, 0.3219752754296894559, 0.3333333333333333703, 0.3219752754296894559, 0.3333333333333333703, 0.3219752754296894559, 0.3333333333333333703, 0.3219752754296894559, 0.3333333333333333703, 0.3219752754296894559, 0.3333333333333333703, 0.3219752754296894559, 0.3333333333333333703, 0.3219752754296894559, 0.3333333333333333703, 0.3219752754296894559, 0.3333333333333333703, 0.3219752754296894559, 0.3333333333333333703, 0.3219752754296894559, 0.3333333333333333703, 0.3219752754296894559, 0.3333333333333333703, 0.3219752754296894559, 0.3333333333333333703, 0.3219752754296894559, 0.3333333333333333703, 0.3219752754296894559, 0.3333333333333333703, 0.3219752754296894559, 0.3333333333333333703, 0.3219752754296894559, 0.3333333333333333703, 0.3219752754296894559, 0.3333333333333333703, 0.3219752754296894559, 0.3333333333333333703, 0.3219752754296894559, 0.3333333333333333703, 0.3219752754296894559, 0.3333333333333333703, 0.3219752754296894559, 0.3333333333333333703, 0.3219752754296894559, 0.3333333333333333703, 0.3219752754296894559, 0.3333333333333333703, 0.3219752754296894559, 0.3333333333333333703, 0.3219752754296894559, 0.3333333333333333703, 0.3219752754296894559, 0.3333333333333333703, 0.3219752754296894559, 0.3333333333333333703, 0.3219752754296894559, 0.3333333333333333703, 0.3219752754296894559, 0.3333333333333333703, 0.3219752754296894559, 0.3333333333333333703, 0.3219752754296894559, 0.3333333333333333703, 0.3219752754296894559, 0.3333333333333333703, 0.3219752754296894559, 0.3333333333333333703, 0.3219752754296894559, 0.3333333333333333703, 0.3219752754296894559, 0.3333333333333333703, 0.3219752754296894559, 0.3333333333333333703, 0.3219752754296894559, 0.3333333333333333703, 0.3219752754296894559, 0.3333333333333333703, 0.3219752754296894559, 0.3333333333333333703, 0.3219752754296894559, 0.3333333333333333703, 0.3219752754296894559, 0.3333333333333333703, 0.3219752754296894559, 0.3333333333333333703, 0.3219752754296894559, 0.3333333333333333703, 0.3219752754296894559, 0.3333333333333333703, 0.3219752754296894559, 0.3333333333333333703, 0.3219752754296894559, 0.3333333333333333703, 0.3219752754296894559, 0.3333333333333333703, 0.3219752754296894559, 0.3333333333333333703, 0.3219752754296894559, 0.3333333333333333703, 0.3219752754296894559, 0.3333333333333333703, 0.3219752754296894559, 0.3333333333333333703, 0.3219752754296894559, 0.3333333333333333703, 0.3219752754296894559, 0.3333333333333333703, 0.3219752754296894559, 0.3333333333333333703, 0.3219752754296894559, 0.3333333333333333703, 0.3219752754296894559, 0.3333333333333333703, 0.3219752754296894559, 0.3333333333333333703, 0.3219752754296894559, 0.3333333333333333703, 0.3219752754296894559, 0.3333333333333333703, 0.3219752754296894559, 0.3333333333333333703, 0.3219752754296894559, 0.3333333333333333703, 0.3219752754296894559, 0.3333333333333333703, 0.3219752754296894559, 0.3333333333333333703, 0.3219752754296894559, 0.3333333333333333703, 0.3219752754296894559, 0.3333333333333333703, 0.3219752754296894559, 0.3333333333333333703, 0.3219752754296894559, 0.3333333333333333703, 0.3219752754296894559, 0.3333333333333333703, 0.3219752754296894559, 0.3333333333333333703, 0.3219752754296894559, 0.3333333333333333703, 0.3219752754296894559, 0.3333333333333333703, 0.3219752754296894559, 0.3333333333333333703, 0.3219752754296894559, 0.3333333333333333703, 0.3219752754296894559, 0.3333333333333333703, 0.3219752754296894559, 0.3333333333333333703, 0.3219752754296894559, 0.3333333333333333703, 0.3219752754296894559, 0.3333333333333333703, 0.3219752754296894559, 0.3333333333333333703, 0.3219752754296894559, 0.3333333333333333703, 0.3219752754296894559, 0.3333333333333333703, 0.3219752754296894559, 0.3333333333333333703, 0.3219752754296894559, 0.3333333333333333703, 0.3219752754296894559, 0.3333333333333333703, 0.3219752754296894559, 0.3333333333333333703, 0.3219752754296894559, 0.3333333333333333703, 0.3219752754296894559, 0.3333333333333333703, 0.3219752754296894559, 0.3333333333333333703, 0.3219752754296894559, 0.3333333333333333703, 0.3219752754296894559, 0.3333333333333333703, 0.3219752754296894559, 0.3333333333333333703, 0.3219752754296894559, 0.3333333333333333703, 0.3219752754296894559, 0.3333333333333333703, 0.3219752754296894559, 0.3333333333333333703, 0.3219752754296894559, 0.3333333333333333703, 0.3219752754296894559, 0.3333333333333333703, 0.3219752754296894559, 0.3333333333333333703, 0.3219752754296894559, 0.3333333333333333703, 0.3219752754296894559, 0.3333333333333333703, 0.3219752754296894559, 0.3333333333333333703, 0.3219752754296894559, 0.3333333333333333703, 0.3219752754296894559, 0.3333333333333333703, 0.3219752754296894559, 0.3333333333333333703, 0.3219752754296894559, 0.3333333333333333703, 0.3219752754296894559, 0.3333333333333333703, 0.3219752754296894559, 0.3333333333333333703, 0.3219752754296894559, 0.3333333333333333703, 0.3219752754296894559, 0.3333333333333333703, 0.3219752754296894559, 0.3333333333333333703, 0.3219752754296894559, 0.3333333333333333703, 0.3219752754296894559, 0.3333333333333333703, 0.3219752754296894559, 0.3333333333333333703, 0.3219752754296894559, 0.3333333333333333703, 0.3219752754296894559, 0.3333333333333333703, 0.3219752754296894559, 0.3333333333333333703, 0.3219752754296894559, 0.3333333333333333703, 0.3219752754296894559, 0.3333333333333333703, 0.3219752754296894559, 0.3333333333333333703, 0.3219752754296894559, 0.3333333333333333703, 0.3219752754296894559, 0.3333333333333333703, 0.3219752754296894559, 0.3333333333333333703, 0.3219752754296894559, 0.3333333333333333703, 0.3219752754296894559, 0.3333333333333333703, 0.3219752754296894559, 0.3333333333333333703, 0.3219752754296894559, 0.3333333333333333703, 0.3219752754296894559, 0.3333333333333333703, 0.3219752754296894559, 0.3333333333333333703, 0.3219752754296894559, 0.3333333333333333703, 0.3219752754296894559, 0.3333333333333333703, 0.3219752754296894559, 0.3333333333333333703, 0.3219752754296894559, 0.3333333333333333703, 0.3219752754296894559, 0.3333333333333333703, 0.3219752754296894559, 0.3333333333333333703, 0.3219752754296894559, 0.3333333333333333703, 0.3219752754296894559, 0.3333333333333333703, 0.3219752754296894559, 0.3333333333333333703, 0.3219752754296894559, 0.3333333333333333703, 0.3219752754296894559, 0.3333333333333333703, 0.3219752754296894559, 0.3333333333333333703, 0.3219752754296894559, 0.3333333333333333703, 0.3219752754296894559, 0.3333333333333333703, 0.3219752754296894559, 0.3333333333333333703, 0.3219752754296894559, 0.3333333333333333703, 0.3219752754296894559, 0.3333333333333333703, 0.3219752754296894559, 0.3333333333333333703, 0.3219752754296894559, 0.3333333333333333703, 0.3219752754296894559, 0.3333333333333333703, 0.3219752754296894559, 0.3333333333333333703, 0.3219752754296894559, 0.3333333333333333703, 0.3219752754296894559, 0.3333333333333333703, 0.3219752754296894559, 0.3333333333333333703, 0.3219752754296894559, 0.3333333333333333703, 0.3219752754296894559, 0.3333333333333333703, 0.3219752754296894559, 0.3333333333333333703, 0.3219752754296894559, 0.3333333333333333703, 0.3219752754296894559, 0.3333333333333333703, 0.3219752754296894559, 0.3333333333333333703, 0.3219752754296894559, 0.3333333333333333703, 0.3219752754296894559, 0.3333333333333333703, 0.3219752754296894559, 0.3333333333333333703, 0.3219752754296894559, 0.3333333333333333703, 0.3219752754296894559, 0.3333333333333333703, 0.3219752754296894559, 0.3333333333333333703, 0.3219752754296894559, 0.3333333333333333703, 0.3219752754296894559, 0.3333333333333333703, 0.3219752754296894559, 0.3333333333333333703, 0.3219752754296894559, 0.3333333333333333703, 0.3219752754296894559, 0.3333333333333333703, 0.3219752754296894559, 0.3333333333333333703, 0.3219752754296894559, 0.3333333333333333703, 0.3219752754296894559, 0.3333333333333333703, 0.3219752754296894559, 0.3333333333333333703, 0.3219752754296894559, 0.3333333333333333703, 0.3219752754296894559, 0.3333333333333333703, 0.3219752754296894559, 0.3333333333333333703, 0.3219752754296894559, 0.3333333333333333703, 0.3219752754296894559, 0.3333333333333333703, 0.3219752754296894559, 0.3333333333333333703, 0.3219752754296894559, 0.3333333333333333703, 0.3219752754296894559, 0.3333333333333333703, 0.3219752754296894559, 0.3333333333333333703, 0.3219752754296894559, 0.3333333333333333703, 0.3219752754296894559, 0.3333333333333333703, 0.3219752754296894559, 0.3333333333333333703, 0.3219752754296894559, 0.3333333333333333703, 0.3219752754296894559, 0.3333333333333333703, 0.3219752754296894559, 0.3333333333333333703, 0.3219752754296894559, 0.3333333333333333703, 0.3219752754296894559, 0.3333333333333333703, 0.3219752754296894559, 0.3333333333333333703, 0.3219752754296894559, 0.3333333333333333703, 0.3219752754296894559, 0.3333333333333333703, 0.3219752754296894559, 0.3333333333333333703, 0.3219752754296894559, 0.3333333333333333703, 0.3219752754296894559, 0.3333333333333333703, 0.3219752754296894559, 0.3333333333333333703, 0.3219752754296894559, 0.3333333333333333703, 0.3219752754296894559, 0.3333333333333333703, 0.3219752754296894559, 0.3333333333333333703, 0.3219752754296894559, 0.3333333333333333703, 0.3219752754296894559, 0.3333333333333333703, 0.3219752754296894559, 0.3333333333333333703, 0.3219752754296894559, 0.3333333333333333703, 0.3219752754296894559, 0.3333333333333333703, 0.3219752754296894559, 0.3333333333333333703, 0.3219752754296894559, 0.3333333333333333703, 0.3219752754296894559, 0.3333333333333333703, 0.3219752754296894559, 0.3333333333333333703, 0.3219752754296894559, 0.3333333333333333703, 0.3219752754296894559, 0.3333333333333333703, 0.3219752754296894559, 0.3333333333333333703, 0.3219752754296894559, 0.3333333333333333703, 0.3219752754296894559, 0.3333333333333333703, 0.3219752754296894559, 0.3333333333333333703),
 ( 1.000000000000000000, 0.9659258262890683122, 1.000000000000000000, 0.9659258262890683122, 1.000000000000000000, 0.9659258262890683122, 1.000000000000000000, 0.9659258262890683122, 1.000000000000000000, 0.9659258262890683122, 1.000000000000000000, 0.9659258262890683122, 1.000000000000000000, 0.9659258262890683122, 1.000000000000000000, 0.9659258262890683122, 1.000000000000000000, 0.9659258262890683122, 1.000000000000000000, 0.9659258262890683122, 1.000000000000000000, 0.9659258262890683122, 1.000000000000000000, 0.9659258262890683122, 1.000000000000000000, 0.9659258262890683122, 1.000000000000000000, 0.9659258262890683122, 1.000000000000000000, 0.9659258262890683122, 1.000000000000000000, 0.9659258262890683122, 1.000000000000000000, 0.9659258262890683122, 1.000000000000000000, 0.9659258262890683122, 1.000000000000000000, 0.9659258262890683122, 1.000000000000000000, 0.9659258262890683122, 1.000000000000000000, 0.9659258262890683122, 1.000000000000000000, 0.9659258262890683122, 1.000000000000000000, 0.9659258262890683122, 1.000000000000000000, 0.9659258262890683122, 1.000000000000000000, 0.9659258262890683122, 1.000000000000000000, 0.9659258262890683122, 1.000000000000000000, 0.9659258262890683122, 1.000000000000000000, 0.9659258262890683122, 1.000000000000000000, 0.9659258262890683122, 1.000000000000000000, 0.9659258262890683122, 1.000000000000000000, 0.9659258262890683122, 1.000000000000000000, 0.9659258262890683122, 1.000000000000000000, 0.9659258262890683122, 1.000000000000000000, 0.9659258262890683122, 1.000000000000000000, 0.9659258262890683122, 1.000000000000000000, 0.9659258262890683122, 1.000000000000000000, 0.9659258262890683122, 1.000000000000000000, 0.9659258262890683122, 1.000000000000000000, 0.9659258262890683122, 1.000000000000000000, 0.9659258262890683122, 1.000000000000000000, 0.9659258262890683122, 1.000000000000000000, 0.9659258262890683122, 1.000000000000000000, 0.9659258262890683122, 1.000000000000000000, 0.9659258262890683122, 1.000000000000000000, 0.9659258262890683122, 1.000000000000000000, 0.9659258262890683122, 1.000000000000000000, 0.9659258262890683122, 1.000000000000000000, 0.9659258262890683122, 1.000000000000000000, 0.9659258262890683122, 1.000000000000000000, 0.9659258262890683122, 1.000000000000000000, 0.9659258262890683122, 1.000000000000000000, 0.9659258262890683122, 1.000000000000000000, 0.9659258262890683122, 1.000000000000000000, 0.9659258262890683122, 1.000000000000000000, 0.9659258262890683122, 1.000000000000000000, 0.9659258262890683122, 1.000000000000000000, 0.9659258262890683122, 1.000000000000000000, 0.9659258262890683122, 1.000000000000000000, 0.9659258262890683122, 1.000000000000000000, 0.9659258262890683122, 1.000000000000000000, 0.9659258262890683122, 1.000000000000000000, 0.9659258262890683122, 1.000000000000000000, 0.9659258262890683122, 1.000000000000000000, 0.9659258262890683122, 1.000000000000000000, 0.9659258262890683122, 1.000000000000000000, 0.9659258262890683122, 1.000000000000000000, 0.9659258262890683122, 1.000000000000000000, 0.9659258262890683122, 1.000000000000000000, 0.9659258262890683122, 1.000000000000000000, 0.9659258262890683122, 1.000000000000000000, 0.9659258262890683122, 1.000000000000000000, 0.9659258262890683122, 1.000000000000000000, 0.9659258262890683122, 1.000000000000000000, 0.9659258262890683122, 1.000000000000000000, 0.9659258262890683122, 1.000000000000000000, 0.9659258262890683122, 1.000000000000000000, 0.9659258262890683122, 1.000000000000000000, 0.9659258262890683122, 1.000000000000000000, 0.9659258262890683122, 1.000000000000000000, 0.9659258262890683122, 1.000000000000000000, 0.9659258262890683122, 1.000000000000000000, 0.9659258262890683122, 1.000000000000000000, 0.9659258262890683122, 1.000000000000000000, 0.9659258262890683122, 1.000000000000000000, 0.9659258262890683122, 1.000000000000000000, 0.9659258262890683122, 1.000000000000000000, 0.9659258262890683122, 1.000000000000000000, 0.9659258262890683122, 1.000000000000000000, 0.9659258262890683122, 1.000000000000000000, 0.9659258262890683122, 1.000000000000000000, 0.9659258262890683122, 1.000000000000000000, 0.9659258262890683122, 1.000000000000000000, 0.9659258262890683122, 1.000000000000000000, 0.9659258262890683122, 1.000000000000000000, 0.9659258262890683122, 1.000000000000000000, 0.9659258262890683122, 1.000000000000000000, 0.9659258262890683122, 1.000000000000000000, 0.9659258262890683122, 1.000000000000000000, 0.9659258262890683122, 1.000000000000000000, 0.9659258262890683122, 1.000000000000000000, 0.9659258262890683122, 1.000000000000000000, 0.9659258262890683122, 1.000000000000000000, 0.9659258262890683122, 1.000000000000000000, 0.9659258262890683122, 1.000000000000000000, 0.9659258262890683122, 1.000000000000000000, 0.9659258262890683122, 1.000000000000000000, 0.9659258262890683122, 1.000000000000000000, 0.9659258262890683122, 1.000000000000000000, 0.9659258262890683122, 1.000000000000000000, 0.9659258262890683122, 1.000000000000000000, 0.9659258262890683122, 1.000000000000000000, 0.9659258262890683122, 1.000000000000000000, 0.9659258262890683122, 1.000000000000000000, 0.9659258262890683122, 1.000000000000000000, 0.9659258262890683122, 1.000000000000000000, 0.9659258262890683122, 1.000000000000000000, 0.9659258262890683122, 1.000000000000000000, 0.9659258262890683122, 1.000000000000000000, 0.9659258262890683122, 1.000000000000000000, 0.9659258262890683122, 1.000000000000000000, 0.9659258262890683122, 1.000000000000000000, 0.9659258262890683122, 1.000000000000000000, 0.9659258262890683122, 1.000000000000000000, 0.9659258262890683122, 1.000000000000000000, 0.9659258262890683122, 1.000000000000000000, 0.9659258262890683122, 1.000000000000000000, 0.9659258262890683122, 1.000000000000000000, 0.9659258262890683122, 1.000000000000000000, 0.9659258262890683122, 1.000000000000000000, 0.9659258262890683122, 1.000000000000000000, 0.9659258262890683122, 1.000000000000000000, 0.9659258262890683122, 1.000000000000000000, 0.9659258262890683122, 1.000000000000000000, 0.9659258262890683122, 1.000000000000000000, 0.9659258262890683122, 1.000000000000000000, 0.9659258262890683122, 1.000000000000000000, 0.9659258262890683122, 1.000000000000000000, 0.9659258262890683122, 1.000000000000000000, 0.9659258262890683122, 1.000000000000000000, 0.9659258262890683122, 1.000000000000000000, 0.9659258262890683122, 1.000000000000000000, 0.9659258262890683122, 1.000000000000000000, 0.9659258262890683122, 1.000000000000000000, 0.9659258262890683122, 1.000000000000000000, 0.9659258262890683122, 1.000000000000000000, 0.9659258262890683122, 1.000000000000000000, 0.9659258262890683122, 1.000000000000000000, 0.9659258262890683122, 1.000000000000000000, 0.9659258262890683122, 1.000000000000000000, 0.9659258262890683122, 1.000000000000000000, 0.9659258262890683122, 1.000000000000000000, 0.9659258262890683122, 1.000000000000000000, 0.9659258262890683122, 1.000000000000000000, 0.9659258262890683122, 1.000000000000000000, 0.9659258262890683122, 1.000000000000000000, 0.9659258262890683122, 1.000000000000000000, 0.9659258262890683122, 1.000000000000000000, 0.9659258262890683122, 1.000000000000000000, 0.9659258262890683122, 1.000000000000000000, 0.9659258262890683122, 1.000000000000000000, 0.9659258262890683122, 1.000000000000000000, 0.9659258262890683122, 1.000000000000000000, 0.9659258262890683122, 1.000000000000000000, 0.9659258262890683122, 1.000000000000000000, 0.9659258262890683122, 1.000000000000000000, 0.9659258262890683122, 1.000000000000000000, 0.9659258262890683122, 1.000000000000000000, 0.9659258262890683122, 1.000000000000000000, 0.9659258262890683122, 1.000000000000000000, 0.9659258262890683122, 1.000000000000000000, 0.9659258262890683122, 1.000000000000000000, 0.9659258262890683122, 1.000000000000000000, 0.9659258262890683122, 1.000000000000000000, 0.9659258262890683122, 1.000000000000000000, 0.9659258262890683122, 1.000000000000000000, 0.9659258262890683122, 1.000000000000000000, 0.9659258262890683122, 1.000000000000000000, 0.9659258262890683122, 1.000000000000000000, 0.9659258262890683122, 1.000000000000000000, 0.9659258262890683122, 1.000000000000000000, 0.9659258262890683122, 1.000000000000000000, 0.9659258262890683122, 1.000000000000000000, 0.9659258262890683122, 1.000000000000000000, 0.9659258262890683122, 1.000000000000000000, 0.9659258262890683122, 1.000000000000000000, 0.9659258262890683122, 1.000000000000000000, 0.9659258262890683122, 1.000000000000000000, 0.9659258262890683122, 1.000000000000000000, 0.9659258262890683122, 1.000000000000000000, 0.9659258262890683122, 1.000000000000000000, 0.9659258262890683122, 1.000000000000000000, 0.9659258262890683122, 1.000000000000000000, 0.9659258262890683122, 1.000000000000000000, 0.9659258262890683122, 1.000000000000000000, 0.9659258262890683122, 1.000000000000000000, 0.9659258262890683122, 1.000000000000000000, 0.9659258262890683122, 1.000000000000000000, 0.9659258262890683122, 1.000000000000000000, 0.9659258262890683122, 1.000000000000000000, 0.9659258262890683122, 1.000000000000000000, 0.9659258262890683122, 1.000000000000000000, 0.9659258262890683122, 1.000000000000000000, 0.9659258262890683122, 1.000000000000000000, 0.9659258262890683122, 1.000000000000000000, 0.9659258262890683122, 1.000000000000000000, 0.9659258262890683122, 1.000000000000000000, 0.9659258262890683122, 1.000000000000000000, 0.9659258262890683122, 1.000000000000000000, 0.9659258262890683122, 1.000000000000000000, 0.9659258262890683122, 1.000000000000000000, 0.9659258262890683122, 1.000000000000000000, 0.9659258262890683122, 1.000000000000000000, 0.9659258262890683122, 1.000000000000000000, 0.9659258262890683122, 1.000000000000000000, 0.9659258262890683122, 1.000000000000000000, 0.9659258262890683122, 1.000000000000000000, 0.9659258262890683122, 1.000000000000000000, 0.9659258262890683122, 1.000000000000000000, 0.9659258262890683122, 1.000000000000000000, 0.9659258262890683122, 1.000000000000000000, 0.9659258262890683122, 1.000000000000000000, 0.9659258262890683122, 1.000000000000000000, 0.9659258262890683122, 1.000000000000000000, 0.9659258262890683122, 1.000000000000000000, 0.9659258262890683122, 1.000000000000000000, 0.9659258262890683122, 1.000000000000000000, 0.9659258262890683122, 1.000000000000000000, 0.9659258262890683122, 1.000000000000000000) ) ) 
 REPRESENTATION_ITEM ( '' )  SURFACE ( )  );
#114017 = CARTESIAN_POINT ( 'NONE',  ( 21.55341960407619695, -5.719274019375665929, 56.04275706135235424 ) ) ;
#114018 = CARTESIAN_POINT ( 'NONE',  ( 5.823673210054125526, 21.52544592524343514, 109.7905762719810383 ) ) ;
#114019 = CARTESIAN_POINT ( 'NONE',  ( -21.55341960407610458, -5.719274019375992779, 56.45724293864768839 ) ) ;
#114020 = CARTESIAN_POINT ( 'NONE',  ( 16.46253265017146816, 9.564922557961045513, 106.6677570613523471 ) ) ;
#114021 = CARTESIAN_POINT ( 'NONE',  ( 16.46253265017160672, -9.564922557960803928, 48.33224293864769550 ) ) ;
#114022 = CARTESIAN_POINT ( 'NONE',  ( -19.05341960407617563, 5.049401038297882671, 73.54275706135233293 ) ) ;
#114023 = CARTESIAN_POINT ( 'NONE',  ( 5.719274019375673035, 21.55341960407619339, 87.29275706135236135 ) ) ;
#114024 = CARTESIAN_POINT ( 'NONE',  ( -9.474510206698720793, -16.51473224551083518, 59.58442372801900433 ) ) ;
#114025 = CARTESIAN_POINT ( 'NONE',  ( -16.51473224551069308, -9.474510206698971260, 41.66557627198103120 ) ) ;
#114026 = CARTESIAN_POINT ( 'NONE',  ( 15.72974639402199770, -15.80617190586745480, 58.12390960531435979 ) ) ;
#114027 = CARTESIAN_POINT ( 'NONE',  ( -14.34966873604960291, -8.224510206698953496, 46.66557627198102409 ) ) ;
#114028 = DIRECTION ( 'NONE',  ( 1.000000000000000000, 0.000000000000000000, 0.000000000000000000 ) ) ;
#114029 = CARTESIAN_POINT ( 'NONE',  ( -5.153800228976607833, 19.02544592524334988, 32.70942372801899722 ) ) ;
#114030 = CARTESIAN_POINT ( 'NONE',  ( 8.224510206698742110, 14.34966873604972548, 82.08442372801901854 ) ) ;
#114031 = CARTESIAN_POINT ( 'NONE',  ( 4.483927247898545687, 16.52544592524342804, 59.79057627198103120 ) ) ;
#114032 = CARTESIAN_POINT ( 'NONE',  ( 18.62759615963255655, 10.81492255796105972, 86.66775706135234714 ) ) ;
#114033 = CARTESIAN_POINT ( 'NONE',  ( -10.72451020669870658, -18.67979575497194134, 79.58442372801903275 ) ) ;
#114034 = CARTESIAN_POINT ( 'NONE',  ( -21.53943276465977519, 0.05219959533907696930, 86.24890960531436690 ) ) ;
#114035 = CARTESIAN_POINT ( 'NONE',  ( -16.46253265017160317, 9.564922557960807481, 55.83224293864769550 ) ) ;
#114036 = CARTESIAN_POINT ( 'NONE',  ( -10.81492255796105439, 18.62759615963255655, 52.91775706135235424 ) ) ;
#114037 = CARTESIAN_POINT ( 'NONE',  ( -19.03943276465977164, 0.05219959533909376836, 41.24890960531435269 ) ) ;
#114038 = ORIENTED_EDGE ( 'NONE', *, *, #168074, .F. ) ;
#114039 = CARTESIAN_POINT ( 'NONE',  ( -16.46253265017160317, 9.564922557960807481, 55.83224293864769550 ) ) ;
#114040 = CARTESIAN_POINT ( 'NONE',  ( 14.34966873604960469, 8.224510206698951720, 104.1655762719810241 ) ) ;
#114041 = CARTESIAN_POINT ( 'NONE',  ( 5.049401038298161559, -19.05341960407611168, 97.70724293864766707 ) ) ;
#114042 = CARTESIAN_POINT ( 'NONE',  ( -4.483927247898539470, -16.52544592524342804, 52.29057627198102409 ) ) ;
#114043 = CARTESIAN_POINT ( 'NONE',  ( -16.55341960407611168, -4.379528057220339221, 106.4572429386477097 ) ) ;
#114044 = CARTESIAN_POINT ( 'NONE',  ( -15.80617190586745835, -15.72974639402198527, 81.87390960531435269 ) ) ;
#114045 = CARTESIAN_POINT ( 'NONE',  ( -5.719274019375978568, 21.55341960407610458, 115.2072429386476955 ) ) ;
#114046 = DIRECTION ( 'NONE',  ( -0.000000000000000000, -0.000000000000000000, -1.000000000000000000 ) ) ;
#114047 = CARTESIAN_POINT ( 'NONE',  ( 14.29746914071037800, 8.314922557961029526, 41.66775706135235424 ) ) ;
#114048 = ORIENTED_EDGE ( 'NONE', *, *, #75628, .F. ) ;
#114049 = CARTESIAN_POINT ( 'NONE',  ( 21.55341960407610458, 5.719274019375980345, 73.95724293864769550 ) ) ;
#114050 = CARTESIAN_POINT ( 'NONE',  ( -0.05219959533937732626, 21.53943276465977519, 112.5010903946857042 ) ) ;
#114051 = CARTESIAN_POINT ( 'NONE',  ( 5.153800228976335163, 19.02544592524342804, 99.79057627198102409 ) ) ;
#114052 = CARTESIAN_POINT ( 'NONE',  ( 18.62759615963255655, 10.81492255796105972, 26.66775706135235424 ) ) ;
#114053 = ADVANCED_FACE ( 'NONE', ( #87398 ), #178424, .T. ) ;
#114054 = AXIS2_PLACEMENT_3D ( 'NONE', #140840, #79169, #110500 ) ;
#114055 = CARTESIAN_POINT ( 'NONE',  ( -18.67979575497178146, -10.72451020669898902, 31.66557627198102054 ) ) ;
#114056 = CARTESIAN_POINT ( 'NONE',  ( -14.34966873604972548, 8.224510206698743886, 103.3344237280190043 ) ) ;
#114058 = CARTESIAN_POINT ( 'NONE',  ( 21.55341960407619695, -5.719274019375665929, 86.04275706135236135 ) ) ;
#114057 = CARTESIAN_POINT ( 'NONE',  ( 18.67979575497194134, -10.72451020669871369, 50.83442372801901143 ) ) ;
#114059 = CARTESIAN_POINT ( 'NONE',  ( 5.823673210054444382, -21.52544592524334988, 110.2094237280190185 ) ) ;
#114060 = CARTESIAN_POINT ( 'NONE',  ( 12.14591786802327356, -12.06949235617739191, 75.62609039468567573 ) ) ;
#114061 = CARTESIAN_POINT ( 'NONE',  ( 15.80617190586769283, -15.72974639402175789, 35.62609039468568994 ) ) ;
#114062 = CARTESIAN_POINT ( 'NONE',  ( -5.153800228976328057, -19.02544592524343514, 37.29057627198102409 ) ) ;
#114063 = CARTESIAN_POINT ( 'NONE',  ( -21.53943276465977519, -0.05219959533937600094, 108.7510903946857042 ) ) ;
#114064 = CARTESIAN_POINT ( 'NONE',  ( 19.02544592524343514, -5.153800228976328945, 103.5405762719809957 ) ) ;
#114065 = CARTESIAN_POINT ( 'NONE',  ( 10.72451020669898902, -18.67979575497178502, 102.9155762719810383 ) ) ;
#114067 = CARTESIAN_POINT ( 'NONE',  ( 21.55341960407610458, 5.719274019375980345, 63.95724293864770260 ) ) ;
#114066 = CARTESIAN_POINT ( 'NONE',  ( -27.05641397906351742, 2.428612866367529932E-14, 169.9999999999999716 ) ) ;
#114069 = CARTESIAN_POINT ( 'NONE',  ( 4.379528057220339221, -16.55341960407611168, 52.70724293864769550 ) ) ;
#114068 = CARTESIAN_POINT ( 'NONE',  ( -4.483927247898782831, 16.52544592524335698, 52.70942372801902565 ) ) ;
#114070 = CARTESIAN_POINT ( 'NONE',  ( -5.049401038297874678, -19.05341960407617918, 74.79275706135231871 ) ) ;
#114071 = CARTESIAN_POINT ( 'NONE',  ( 11.30153831258470731, -190.0000000000000000, -15.00000000000000178 ) ) ;
#114072 = CARTESIAN_POINT ( 'NONE',  ( 16.52544592524335698, 4.483927247898782831, 26.45942372801901854 ) ) ;
#114073 = CARTESIAN_POINT ( 'NONE',  ( 18.67979575497178502, 10.72451020669898547, 104.1655762719810241 ) ) ;
#114074 = CARTESIAN_POINT ( 'NONE',  ( -16.55341960407611168, -4.379528057220339221, 61.45724293864770260 ) ) ;
#114075 = CARTESIAN_POINT ( 'NONE',  ( -5.153800228976328057, -19.02544592524343514, 107.2905762719810383 ) ) ;
#114076 = CARTESIAN_POINT ( 'NONE',  ( -14.34966873604972548, 8.224510206698743886, 43.33442372801901143 ) ) ;
#114077 = CARTESIAN_POINT ( 'NONE',  ( -16.51473224551069308, -9.474510206698971260, 56.66557627198103120 ) ) ;
#114079 = CARTESIAN_POINT ( 'NONE',  ( 5.049401038297881783, 19.05341960407617563, 97.29275706135233293 ) ) ;
#114078 = CARTESIAN_POINT ( 'NONE',  ( 0.05219959533937995610, -21.53943276465977519, 25.00109039468567218 ) ) ;
#114080 = CARTESIAN_POINT ( 'NONE',  ( 9.564922557960805705, 16.46253265017160317, 109.5822429386476955 ) ) ;
#114081 = CARTESIAN_POINT ( 'NONE',  ( -9.564922557960796823, -16.46253265017161027, 87.08224293864769550 ) ) ;
#114082 = CARTESIAN_POINT ( 'NONE',  ( -10.72451020669898014, 18.67979575497178502, 95.41557627198102409 ) ) ;
#114083 = CARTESIAN_POINT ( 'NONE',  ( 9.474510206698971260, -16.51473224551069308, 62.91557627198102409 ) ) ;
#114084 = CARTESIAN_POINT ( 'NONE',  ( 4.500000000000000888, -126.1226662136678272, 7.981152457036389869 ) ) ;
#114085 = CARTESIAN_POINT ( 'NONE',  ( -4.483927247898539470, -16.52544592524342804, 67.29057627198103830 ) ) ;
#114086 = CARTESIAN_POINT ( 'NONE',  ( 16.46253265017160672, -9.564922557960803928, 98.33224293864769550 ) ) ;
#114087 = DIRECTION ( 'NONE',  ( 0.8571673007021135549, 0.000000000000000000, 0.5150380749100520461 ) ) ;
#114088 = CARTESIAN_POINT ( 'NONE',  ( -13.97604488694547697, 13.89961937509957934, 78.12609039468567573 ) ) ;
#114089 = CARTESIAN_POINT ( 'NONE',  ( -0.05219959533907301413, -21.53943276465977519, 97.49890960531436690 ) ) ;
#114090 = CARTESIAN_POINT ( 'NONE',  ( -5.049401038297874678, -19.05341960407617918, 54.79275706135234003 ) ) ;
#114091 = CARTESIAN_POINT ( 'NONE',  ( -13.89961937509977652, 13.97604488694528158, 115.6239096053143669 ) ) ;
#114092 = CARTESIAN_POINT ( 'NONE',  ( 18.22780087662122739, 5.500000000000000888, 76.48236817873106475 ) ) ;
#114093 = CARTESIAN_POINT ( 'NONE',  ( -21.52544592524343514, 5.823673210054127303, 51.04057627198103120 ) ) ;
#114094 = CARTESIAN_POINT ( 'NONE',  ( 19.05341960407611168, 5.049401038298154454, 88.95724293864769550 ) ) ;
#114095 = CARTESIAN_POINT ( 'NONE',  ( 0.05219959533937995610, -21.53943276465977519, 75.00109039468568994 ) ) ;
#114096 = CARTESIAN_POINT ( 'NONE',  ( -19.05341960407611168, -5.049401038298163336, 36.45724293864766707 ) ) ;
#114097 = CARTESIAN_POINT ( 'NONE',  ( -4.379528057220328563, 16.55341960407611168, 75.20724293864769550 ) ) ;
#114098 = CARTESIAN_POINT ( 'NONE',  ( -4.379528057220086978, -16.55341960407618274, 19.79275706135235069 ) ) ;
#114099 = CARTESIAN_POINT ( 'NONE',  ( 21.53943276465977519, 0.05219959533937863772, 66.25109039468567573 ) ) ;
#114100 = EDGE_LOOP ( 'NONE', ( #106627, #117828, #159806 ) ) ;
#114101 = CARTESIAN_POINT ( 'NONE',  ( -19.03943276465977164, 0.05219959533909376836, 111.2489096053143669 ) ) ;
#114102 = CARTESIAN_POINT ( 'NONE',  ( -19.03943276465977164, -0.05219959533935918106, 73.75109039468566152 ) ) ;
#114103 = DIRECTION ( 'NONE',  ( -1.000000000000000000, 0.000000000000000000, 6.938893903907234689E-15 ) ) ;
#114104 = CARTESIAN_POINT ( 'NONE',  ( 21.53943276465977519, 0.05219959533937863772, 26.25109039468567573 ) ) ;
#114105 = CARTESIAN_POINT ( 'NONE',  ( 3.766062262543149401E-15, -39.95556452105413570, -3.249999994537627224 ) ) ;
#114106 = CARTESIAN_POINT ( 'NONE',  ( 19.02544592524334988, 5.153800228976608722, 21.45942372801899012 ) ) ;
#114107 = CARTESIAN_POINT ( 'NONE',  ( -5.049401038298153566, 19.05341960407611168, 60.20724293864768129 ) ) ;
#114108 = CARTESIAN_POINT ( 'NONE',  ( 5.719274019375673035, 21.55341960407619339, 107.2927570613523471 ) ) ;
#114109 = CARTESIAN_POINT ( 'NONE',  ( 12.14591786802327356, -12.06949235617739191, 105.6260903946856899 ) ) ;
#114111 = CARTESIAN_POINT ( 'NONE',  ( -5.719274019375665041, -21.55341960407619695, 79.79275706135236135 ) ) ;
#114110 = CARTESIAN_POINT ( 'NONE',  ( 19.03943276465977164, -0.05219959533909143690, 98.74890960531436690 ) ) ;
#114112 = CARTESIAN_POINT ( 'NONE',  ( -5.950531402560715689E-15, 38.81732327939063509, -3.124999997268813168 ) ) ;
#114113 = LINE ( 'NONE', #48504, #119188 ) ;
#114114 = CARTESIAN_POINT ( 'NONE',  ( 21.55341960407619695, -5.719274019375665929, 66.04275706135236135 ) ) ;
#114115 = CARTESIAN_POINT ( 'NONE',  ( -21.52544592524334988, -5.823673210054445271, 98.95942372801903275 ) ) ;
#114116 = VECTOR ( 'NONE', #152672, 1000.000000000000000 ) ;
#114117 = FACE_OUTER_BOUND ( 'NONE', #179899, .T. ) ;
#114118 = CARTESIAN_POINT ( 'NONE',  ( 19.02544592524343514, -5.153800228976328945, 93.54057627198102409 ) ) ;
#114119 = CARTESIAN_POINT ( 'NONE',  ( -19.02544592524334988, -5.153800228976617603, 28.95942372801900433 ) ) ;
#114120 = CARTESIAN_POINT ( 'NONE',  ( 20.53360937444653445, -31.96911244174550149, -23.96531494639225812 ) ) ;
#114121 = CARTESIAN_POINT ( 'NONE',  ( -19.03943276465977164, 0.05219959533909376836, 36.24890960531436690 ) ) ;
#114122 = CARTESIAN_POINT ( 'NONE',  ( 10.81492255796078972, 18.62759615963270932, 54.58224293864769550 ) ) ;
#114123 = CARTESIAN_POINT ( 'NONE',  ( -12.14591786802326823, 12.06949235617739902, 103.1260903946856757 ) ) ;
#114125 = CARTESIAN_POINT ( 'NONE',  ( -13.97604488694527625, -13.89961937509977652, 76.87390960531433848 ) ) ;
#114124 = CARTESIAN_POINT ( 'NONE',  ( -4.379528057220328563, 16.55341960407611168, 95.20724293864769550 ) ) ;
#114126 = CARTESIAN_POINT ( 'NONE',  ( 10.81492255796106328, -18.62759615963255655, 100.4177570613523471 ) ) ;
#114127 = ADVANCED_FACE ( 'NONE', ( #26744 ), #11581, .T. ) ;
#114128 = CARTESIAN_POINT ( 'NONE',  ( -19.03943276465977164, 0.05219959533909376836, 31.24890960531435979 ) ) ;
#114129 = CARTESIAN_POINT ( 'NONE',  ( -8.314922557960811034, -14.29746914071050412, 102.0822429386476955 ) ) ;
#114130 = CARTESIAN_POINT ( 'NONE',  ( 10.81492255796106328, -18.62759615963255655, 55.41775706135234714 ) ) ;
#114131 = CARTESIAN_POINT ( 'NONE',  ( -10.72451020669898014, 18.67979575497178502, 90.41557627198103830 ) ) ;
#114132 = CARTESIAN_POINT ( 'NONE',  ( 5.049401038297881783, 19.05341960407617563, 47.29275706135231161 ) ) ;
#114133 = CARTESIAN_POINT ( 'NONE',  ( 16.46253265017160672, -9.564922557960803928, 48.33224293864769550 ) ) ;
#114134 = CARTESIAN_POINT ( 'NONE',  ( 19.03943276465977164, -0.05219959533909143690, 93.74890960531435269 ) ) ;
#114135 = CARTESIAN_POINT ( 'NONE',  ( -4.379528057220328563, 16.55341960407611168, 75.20724293864769550 ) ) ;
#114136 = CARTESIAN_POINT ( 'NONE',  ( -19.03943276465977164, -0.05219959533935918106, 43.75109039468566863 ) ) ;
#114137 = CARTESIAN_POINT ( 'NONE',  ( -19.05341960407611168, -5.049401038298163336, 61.45724293864769550 ) ) ;
#114138 = CARTESIAN_POINT ( 'NONE',  ( 4.483927247898545687, 16.52544592524342804, 44.79057627198103120 ) ) ;
#114139 = CARTESIAN_POINT ( 'NONE',  ( 9.564922557961047289, -16.46253265017146816, 85.41775706135233293 ) ) ;
#114140 = CARTESIAN_POINT ( 'NONE',  ( -17.58332526062526213, -7.635886036038624702, 89.07665040441536064 ) ) ;
#114141 = CARTESIAN_POINT ( 'NONE',  ( 10.81492255796078972, 18.62759615963270932, 39.58224293864769550 ) ) ;
#114142 = EDGE_CURVE ( 'NONE', #135989, #65463, #197573, .T. ) ;
#114143 = CARTESIAN_POINT ( 'NONE',  ( -16.52544592524342804, 4.483927247898546575, 106.0405762719810525 ) ) ;
#114144 = CARTESIAN_POINT ( 'NONE',  ( -17.50000000000015277, -3.417042746627028560, 24.82619603767517447 ) ) ;
#114146 = CARTESIAN_POINT ( 'NONE',  ( -10.72451020669898014, 18.67979575497178502, 65.41557627198102409 ) ) ;
#114145 = CARTESIAN_POINT ( 'NONE',  ( 9.564922557960805705, 16.46253265017160317, 54.58224293864769550 ) ) ;
#114147 = CARTESIAN_POINT ( 'NONE',  ( 19.03943276465977164, -0.05219959533909143690, 28.74890960531435624 ) ) ;
#114149 = CARTESIAN_POINT ( 'NONE',  ( 19.03943276465977164, -0.05219959533909143690, 63.74890960531435979 ) ) ;
#114148 = CARTESIAN_POINT ( 'NONE',  ( 16.52544592524335698, 4.483927247898782831, 76.45942372801901854 ) ) ;
#114150 = CARTESIAN_POINT ( 'NONE',  ( 9.564922557961047289, -16.46253265017146816, 60.41775706135233293 ) ) ;
#114151 = CARTESIAN_POINT ( 'NONE',  ( -21.53943276465977519, -0.05219959533937600094, 63.75109039468568284 ) ) ;
#114152 = CARTESIAN_POINT ( 'NONE',  ( 5.719274019375991003, -21.55341960407610458, 52.70724293864769550 ) ) ;
#114153 = CARTESIAN_POINT ( 'NONE',  ( 13.89961937509977652, -13.97604488694527269, 28.12390960531435624 ) ) ;
#114154 = CARTESIAN_POINT ( 'NONE',  ( 0.05219959533934541429, -16.53943276465976808, 85.00109039468568994 ) ) ;
#114155 = CARTESIAN_POINT ( 'NONE',  ( -19.02544592524334988, -5.153800228976617603, 98.95942372801900433 ) ) ;
#114156 = CARTESIAN_POINT ( 'NONE',  ( 13.97604488694527802, 13.89961937509977652, 24.37390960531435624 ) ) ;
#114158 = CARTESIAN_POINT ( 'NONE',  ( -5.823673210054116645, -21.52544592524344225, 52.29057627198102409 ) ) ;
#114157 = DIRECTION ( 'NONE',  ( 0.000000000000000000, 0.000000000000000000, 1.000000000000000000 ) ) ;
#114159 = CARTESIAN_POINT ( 'NONE',  ( 18.62759615963255655, 10.81492255796105972, 86.66775706135234714 ) ) ;
#114160 = CARTESIAN_POINT ( 'NONE',  ( -0.05219959533910754901, -16.53943276465976808, 47.49890960531435979 ) ) ;
#114161 = CARTESIAN_POINT ( 'NONE',  ( 0.05219959533910956823, 16.53943276465976808, 49.99890960531437401 ) ) ;
#114162 = CARTESIAN_POINT ( 'NONE',  ( 0.05219959533907565091, 21.53943276465977519, 79.99890960531435269 ) ) ;
#114163 = CARTESIAN_POINT ( 'NONE',  ( 15.80617190586746368, 15.72974639402197994, 84.37390960531438111 ) ) ;
#114164 = DIRECTION ( 'NONE',  ( 1.000000000000000000, 0.000000000000000000, 0.000000000000000000 ) ) ;
#114165 = CARTESIAN_POINT ( 'NONE',  ( 0.05219959533907565091, 21.53943276465977519, 34.99890960531435979 ) ) ;
#114166 = CARTESIAN_POINT ( 'NONE',  ( 0.05219959533934541429, -16.53943276465976808, 65.00109039468568994 ) ) ;
#114167 = CARTESIAN_POINT ( 'NONE',  ( 14.34966873604960469, 8.224510206698951720, 79.16557627198103830 ) ) ;
#114168 = CARTESIAN_POINT ( 'NONE',  ( 5.049401038298161559, -19.05341960407611168, 37.70724293864768839 ) ) ;
#114169 = PRESENTATION_STYLE_ASSIGNMENT (( #129339 ) ) ;
#114170 = DIRECTION ( 'NONE',  ( -0.5150380737757255245, 1.049727191973305394E-16, -0.8571673013836856869 ) ) ;
#114171 = CARTESIAN_POINT ( 'NONE',  ( 0.05219959533934541429, -16.53943276465976808, 100.0010903946857042 ) ) ;
#114172 = CARTESIAN_POINT ( 'NONE',  ( -21.55341960407610458, -5.719274019375992779, 111.4572429386476813 ) ) ;
#114173 = CARTESIAN_POINT ( 'NONE',  ( -13.97604488694527625, -13.89961937509977652, 76.87390960531433848 ) ) ;
#114174 = CARTESIAN_POINT ( 'NONE',  ( -10.81492255796105439, 18.62759615963255655, 47.91775706135234714 ) ) ;
#114175 = CARTESIAN_POINT ( 'NONE',  ( 13.89961937509977652, -13.97604488694527269, 113.1239096053143527 ) ) ;
#114176 = CARTESIAN_POINT ( 'NONE',  ( -5.136056113502131204, -40.38396894447051721, -25.53196577691469926 ) ) ;
#114177 = EDGE_LOOP ( 'NONE', ( #172361, #74196, #14923, #193552 ) ) ;
#114178 = CARTESIAN_POINT ( 'NONE',  ( 21.52544592524334988, 5.823673210054432836, 41.45942372801901143 ) ) ;
#114180 = CARTESIAN_POINT ( 'NONE',  ( -5.153800228976328057, -19.02544592524343514, 97.29057627198099567 ) ) ;
#114179 = CARTESIAN_POINT ( 'NONE',  ( -9.474510206698964154, 16.51473224551069663, 35.41557627198102409 ) ) ;
#114181 = CARTESIAN_POINT ( 'NONE',  ( -16.46253265017146816, -9.564922557961047289, 49.16775706135233293 ) ) ;
#114182 = CARTESIAN_POINT ( 'NONE',  ( 21.53943276465977519, 0.05219959533937863772, 31.25109039468568639 ) ) ;
#114183 = CARTESIAN_POINT ( 'NONE',  ( 5.153800228976615827, -19.02544592524334988, 50.20942372801897591 ) ) ;
#114184 = CARTESIAN_POINT ( 'NONE',  ( 19.05341960407611168, 5.049401038298154454, 23.95724293864769194 ) ) ;
#114185 = CARTESIAN_POINT ( 'NONE',  ( -14.29746914071037622, -8.314922557961029526, 94.16775706135237556 ) ) ;
#114186 = CARTESIAN_POINT ( 'NONE',  ( -9.474510206698720793, -16.51473224551083518, 59.58442372801900433 ) ) ;
#114187 = CARTESIAN_POINT ( 'NONE',  ( 14.34966873604972726, -8.224510206698740333, 100.8344237280190185 ) ) ;
#114188 = CARTESIAN_POINT ( 'NONE',  ( 31.79999999999932214, 1.011436372600181938E-12, 97.70000000000020179 ) ) ;
#114189 = CARTESIAN_POINT ( 'NONE',  ( 16.51473224551069308, 9.474510206698969483, 79.16557627198103830 ) ) ;
#114190 = CARTESIAN_POINT ( 'NONE',  ( -10.81492255796105439, 18.62759615963255655, 92.91775706135236135 ) ) ;
#114191 = CARTESIAN_POINT ( 'NONE',  ( 21.52544592524334988, 5.823673210054432836, 101.4594237280190185 ) ) ;
#114192 = CARTESIAN_POINT ( 'NONE',  ( -13.97604488694527625, -13.89961937509977652, 21.87390960531435979 ) ) ;
#114193 = CARTESIAN_POINT ( 'NONE',  ( -16.46253265017160317, 9.564922557960807481, 95.83224293864769550 ) ) ;
#114194 = CARTESIAN_POINT ( 'NONE',  ( -21.52544592524334988, -5.823673210054445271, 78.95942372801901854 ) ) ;
#114195 = CARTESIAN_POINT ( 'NONE',  ( 4.379528057220092307, 16.55341960407617563, 22.29275706135235069 ) ) ;
#114196 = CARTESIAN_POINT ( 'NONE',  ( -5.049401038298153566, 19.05341960407611168, 75.20724293864769550 ) ) ;
#114197 = CARTESIAN_POINT ( 'NONE',  ( -18.67979575497178146, -10.72451020669898902, 26.66557627198103475 ) ) ;
#114198 = AXIS2_PLACEMENT_3D ( 'NONE', #84395, #6556, #69242 ) ;
#114199 = CARTESIAN_POINT ( 'NONE',  ( 5.153800228976335163, 19.02544592524342804, 89.79057627198102409 ) ) ;
#114200 = LINE ( 'NONE', #145546, #17610 ) ;
#114201 = CARTESIAN_POINT ( 'NONE',  ( 19.03943276465977164, -0.05219959533909143690, 73.74890960531435269 ) ) ;
#114202 = CARTESIAN_POINT ( 'NONE',  ( 16.46253265017160672, -9.564922557960803928, 68.33224293864770971 ) ) ;
#114203 = CARTESIAN_POINT ( 'NONE',  ( 16.55341960407618274, -4.379528057220086978, 96.04275706135236135 ) ) ;
#114204 = DIRECTION ( 'NONE',  ( 1.000000000000000000, 0.000000000000000000, 0.000000000000000000 ) ) ;
#114205 = CARTESIAN_POINT ( 'NONE',  ( -0.05219959533936034679, 19.03943276465977164, 77.50109039468566152 ) ) ;
#114206 = CARTESIAN_POINT ( 'NONE',  ( -9.474510206698964154, 16.51473224551069663, 95.41557627198102409 ) ) ;
#114207 = CARTESIAN_POINT ( 'NONE',  ( -12.14591786802309592, -12.06949235617757132, 81.87390960531435269 ) ) ;
#114208 = CARTESIAN_POINT ( 'NONE',  ( -5.719274019375978568, 21.55341960407610458, 40.20724293864769550 ) ) ;
#114209 = CARTESIAN_POINT ( 'NONE',  ( -18.67979575497178146, -10.72451020669898902, 21.66557627198102409 ) ) ;
#114210 = CARTESIAN_POINT ( 'NONE',  ( 14.34966873604960469, 8.224510206698951720, 109.1655762719810383 ) ) ;
#114211 = CARTESIAN_POINT ( 'NONE',  ( -16.52216118717207749, 7.221426719304497865, 53.92400978953007495 ) ) ;
#114212 = CARTESIAN_POINT ( 'NONE',  ( 16.46253265017146816, 9.564922557961045513, 46.66775706135233293 ) ) ;
#114213 = CARTESIAN_POINT ( 'NONE',  ( 4.379528057220339221, -16.55341960407611168, 32.70724293864770260 ) ) ;
#114214 = CARTESIAN_POINT ( 'NONE',  ( 19.05341960407611168, 5.049401038298154454, 98.95724293864766707 ) ) ;
#114215 = CARTESIAN_POINT ( 'NONE',  ( 15.80617190586769283, -15.72974639402175789, 60.62609039468567573 ) ) ;
#114216 = CARTESIAN_POINT ( 'NONE',  ( 0.05219959533907565091, 21.53943276465977519, 54.99890960531435269 ) ) ;
#114217 = CARTESIAN_POINT ( 'NONE',  ( -21.55341960407619339, 5.719274019375674811, 28.54275706135234358 ) ) ;
#114218 = CARTESIAN_POINT ( 'NONE',  ( -18.62759615963270932, 10.81492255796079327, 80.83224293864769550 ) ) ;
#114219 = CARTESIAN_POINT ( 'NONE',  ( -5.823673210054431948, 21.52544592524334988, 37.70942372801900433 ) ) ;
#114220 = CARTESIAN_POINT ( 'NONE',  ( 16.55341960407611168, 4.379528057220329451, 113.9572429386477239 ) ) ;
#114221 = CARTESIAN_POINT ( 'NONE',  ( 16.51473224551083163, -9.474510206698727899, 70.83442372801900433 ) ) ;
#114222 = CARTESIAN_POINT ( 'NONE',  ( 5.049401038298161559, -19.05341960407611168, 47.70724293864770260 ) ) ;
#114224 = CARTESIAN_POINT ( 'NONE',  ( -13.89961937509977652, 13.97604488694528158, 100.6239096053143669 ) ) ;
#114223 = CARTESIAN_POINT ( 'NONE',  ( -4.379528057220328563, 16.55341960407611168, 95.20724293864769550 ) ) ;
#114225 = CARTESIAN_POINT ( 'NONE',  ( -5.153800228976328057, -19.02544592524343514, 112.2905762719810099 ) ) ;
#114226 = CARTESIAN_POINT ( 'NONE',  ( -9.564922557960796823, -16.46253265017161027, 32.08224293864769550 ) ) ;
#114227 = CARTESIAN_POINT ( 'NONE',  ( 14.34966873604960469, 8.224510206698951720, 44.16557627198103120 ) ) ;
#114228 = CARTESIAN_POINT ( 'NONE',  ( -4.483927247898782831, 16.52544592524335698, 97.70942372801904696 ) ) ;
#114229 = CARTESIAN_POINT ( 'NONE',  ( 13.89961937509977652, -13.97604488694527269, 53.12390960531434558 ) ) ;
#114230 = CARTESIAN_POINT ( 'NONE',  ( 4.379528057220339221, -16.55341960407611168, 112.7072429386476955 ) ) ;
#114231 = CARTESIAN_POINT ( 'NONE',  ( 19.02544592524334988, 5.153800228976608722, 26.45942372801899722 ) ) ;
#114233 = CARTESIAN_POINT ( 'NONE',  ( -12.14591786802309592, -12.06949235617757132, 21.87390960531436690 ) ) ;
#114232 = CARTESIAN_POINT ( 'NONE',  ( 19.05341960407611168, 5.049401038298154454, 108.9572429386477097 ) ) ;
#114234 = CARTESIAN_POINT ( 'NONE',  ( 21.53943276465977519, 0.05219959533937863772, 41.25109039468568284 ) ) ;
#114235 = CARTESIAN_POINT ( 'NONE',  ( 5.049401038298161559, -19.05341960407611168, 112.7072429386476813 ) ) ;
#114236 = CARTESIAN_POINT ( 'NONE',  ( -12.14591786802326823, 12.06949235617739902, 63.12609039468568994 ) ) ;
#114237 = CARTESIAN_POINT ( 'NONE',  ( -14.29746914071049879, 8.314922557960819915, 30.83224293864770260 ) ) ;
#114238 = CARTESIAN_POINT ( 'NONE',  ( -8.314922557961024197, 14.29746914071037800, 107.9177570613523471 ) ) ;
#114239 = CARTESIAN_POINT ( 'NONE',  ( 0.05219959533934541429, -16.53943276465976808, 25.00109039468567218 ) ) ;
#114240 = CARTESIAN_POINT ( 'NONE',  ( 19.02544592524343514, -5.153800228976328945, 43.54057627198103120 ) ) ;
#114241 = CARTESIAN_POINT ( 'NONE',  ( 14.29746914071049879, -8.314922557960816363, 108.3322429386477097 ) ) ;
#114242 = CARTESIAN_POINT ( 'NONE',  ( -21.53943276465977519, -0.05219959533937600094, 23.75109039468567929 ) ) ;
#114243 = CARTESIAN_POINT ( 'NONE',  ( 0.05219959533909260263, 19.03943276465977164, 49.99890960531435979 ) ) ;
#114244 = DIRECTION ( 'NONE',  ( 0.000000000000000000, 0.000000000000000000, -1.000000000000000000 ) ) ;
#114245 = CARTESIAN_POINT ( 'NONE',  ( -9.564922557960796823, -16.46253265017161027, 27.08224293864769550 ) ) ;
#114246 = EDGE_CURVE ( 'NONE', #158282, #131752, #41909, .T. ) ;
#114247 = CARTESIAN_POINT ( 'NONE',  ( -9.564922557960796823, -16.46253265017161027, 112.0822429386476955 ) ) ;
#114248 = CARTESIAN_POINT ( 'NONE',  ( -17.50000000000001776, -5.622605283950791843, 36.31207310596109750 ) ) ;
#114249 = CARTESIAN_POINT ( 'NONE',  ( -9.474510206698964154, 16.51473224551069663, 95.41557627198102409 ) ) ;
#114251 = CARTESIAN_POINT ( 'NONE',  ( 14.29746914071049879, -8.314922557960816363, 103.3322429386476955 ) ) ;
#114250 = CARTESIAN_POINT ( 'NONE',  ( -5.823673210054431948, 21.52544592524334988, 42.70942372801901854 ) ) ;
#114252 = CARTESIAN_POINT ( 'NONE',  ( 19.03943276465977164, -0.05219959533909143690, 113.7489096053143669 ) ) ;
#114253 = CARTESIAN_POINT ( 'NONE',  ( -27.94727380668284056, -6.976214527057364556, 161.4607934398989642 ) ) ;
#114254 = VECTOR ( 'NONE', #154178, 1000.000000000000000 ) ;
#114255 = CARTESIAN_POINT ( 'NONE',  ( -12.06949235617739369, -12.14591786802326823, 84.37609039468570415 ) ) ;
#114256 = CARTESIAN_POINT ( 'NONE',  ( 21.52544592524334988, 5.823673210054432836, 91.45942372801901854 ) ) ;
#114257 = CARTESIAN_POINT ( 'NONE',  ( -12.14591786802326823, 12.06949235617739902, 58.12609039468568994 ) ) ;
#114258 = CARTESIAN_POINT ( 'NONE',  ( -0.05219959533909027116, -19.03943276465977164, 92.49890960531436690 ) ) ;
#114259 = EDGE_CURVE ( 'NONE', #66692, #189536, #174941, .T. ) ;
#114260 = CARTESIAN_POINT ( 'NONE',  ( 16.53943276465976808, 0.05219959533934440121, 46.25109039468567573 ) ) ;
#114261 = CARTESIAN_POINT ( 'NONE',  ( 5.153800228976615827, -19.02544592524334988, 105.2094237280190185 ) ) ;
#114262 = CARTESIAN_POINT ( 'NONE',  ( 4.379528057220092307, 16.55341960407617563, 77.29275706135234714 ) ) ;
#114263 = CARTESIAN_POINT ( 'NONE',  ( -19.05341960407617563, 5.049401038297882671, 98.54275706135233293 ) ) ;
#114264 = CARTESIAN_POINT ( 'NONE',  ( -16.51473224551069308, -9.474510206698971260, 71.66557627198102409 ) ) ;
#114265 = CARTESIAN_POINT ( 'NONE',  ( -0.05219959533907301413, -21.53943276465977519, 97.49890960531436690 ) ) ;
#114267 = CARTESIAN_POINT ( 'NONE',  ( -19.03943276465977164, -0.05219959533935918106, 108.7510903946856615 ) ) ;
#114266 = CARTESIAN_POINT ( 'NONE',  ( -16.52544592524342804, 4.483927247898546575, 106.0405762719810525 ) ) ;
#114268 = CARTESIAN_POINT ( 'NONE',  ( -14.34966873604972548, 8.224510206698743886, 73.33442372801901854 ) ) ;
#114269 = CARTESIAN_POINT ( 'NONE',  ( 23.63516320021127370, 9.722623904420892416, 168.4908852323012809 ) ) ;
#114270 = CARTESIAN_POINT ( 'NONE',  ( -5.153800228976607833, 19.02544592524334988, 72.70942372801900433 ) ) ;
#114271 = CARTESIAN_POINT ( 'NONE',  ( -8.314922557960811034, -14.29746914071050412, 37.08224293864768129 ) ) ;
#114272 = CARTESIAN_POINT ( 'NONE',  ( -12.06949235617756955, 12.14591786802309770, 90.62390960531436690 ) ) ;
#114274 = CARTESIAN_POINT ( 'NONE',  ( -40.00200000000003087, -5.510910596163089556E-15, 45.00000000000000000 ) ) ;
#114273 = CARTESIAN_POINT ( 'NONE',  ( 5.153800228976615827, -19.02544592524334988, 30.20942372801900433 ) ) ;
#114275 = CARTESIAN_POINT ( 'NONE',  ( 21.52544592524334988, 5.823673210054432836, 31.45942372801901854 ) ) ;
#114276 = CARTESIAN_POINT ( 'NONE',  ( -9.564922557961040184, 16.46253265017147172, 92.91775706135233293 ) ) ;
#114277 =( BOUNDED_CURVE ( )  B_SPLINE_CURVE ( 3, ( #9574, #181421, #25754, #73250 ),
 .UNSPECIFIED., .F., .T. ) 
 B_SPLINE_CURVE_WITH_KNOTS ( ( 4, 4 ),
 ( 2.008945357379066987, 2.115944711806982070 ),
 .UNSPECIFIED. ) 
 CURVE ( )  GEOMETRIC_REPRESENTATION_ITEM ( )  RATIONAL_B_SPLINE_CURVE ( ( 1.000000000000000000, 0.9990461557208837329, 0.9990461557208837329, 1.000000000000000000 ) ) 
 REPRESENTATION_ITEM ( '' )  );
#114278 = CARTESIAN_POINT ( 'NONE',  ( -5.049401038298153566, 19.05341960407611168, 115.2072429386477097 ) ) ;
#114279 = CARTESIAN_POINT ( 'NONE',  ( 5.049401038298161559, -19.05341960407611168, 87.70724293864769550 ) ) ;
#114280 = CARTESIAN_POINT ( 'NONE',  ( -10.72451020669870658, -18.67979575497194134, 94.58442372801901854 ) ) ;
#114281 = CARTESIAN_POINT ( 'NONE',  ( 5.153800228976335163, 19.02544592524342804, 74.79057627198103830 ) ) ;
#114282 = CARTESIAN_POINT ( 'NONE',  ( -5.823673210054116645, -21.52544592524344225, 37.29057627198102409 ) ) ;
#114283 = CARTESIAN_POINT ( 'NONE',  ( -14.34966873604960291, -8.224510206698953496, 91.66557627198103830 ) ) ;
#114284 = CARTESIAN_POINT ( 'NONE',  ( 9.474510206698971260, -16.51473224551069308, 57.91557627198103120 ) ) ;
#114285 = CARTESIAN_POINT ( 'NONE',  ( -13.97604488694527625, -13.89961937509977652, 21.87390960531435979 ) ) ;
#114286 = VECTOR ( 'NONE', #6836, 1000.000000000000000 ) ;
#114287 = CARTESIAN_POINT ( 'NONE',  ( 15.80617190586769283, -15.72974639402175789, 30.62609039468567929 ) ) ;
#114288 = CARTESIAN_POINT ( 'NONE',  ( 10.81492255796106328, -18.62759615963255655, 60.41775706135235424 ) ) ;
#114289 = CARTESIAN_POINT ( 'NONE',  ( -5.049401038298153566, 19.05341960407611168, 50.20724293864770260 ) ) ;
#114290 = CARTESIAN_POINT ( 'NONE',  ( -14.29746914071037622, -8.314922557961029526, 79.16775706135234714 ) ) ;
#114291 = CARTESIAN_POINT ( 'NONE',  ( 5.823673210054125526, 21.52544592524343514, 109.7905762719810383 ) ) ;
#114292 = ORIENTED_EDGE ( 'NONE', *, *, #168721, .T. ) ;
#114293 = CARTESIAN_POINT ( 'NONE',  ( 10.81492255796106328, -18.62759615963255655, 25.41775706135235779 ) ) ;
#114295 = CARTESIAN_POINT ( 'NONE',  ( -19.05341960407611168, -5.049401038298163336, 61.45724293864769550 ) ) ;
#114294 = CARTESIAN_POINT ( 'NONE',  ( 0.05219959533936267826, -19.03943276465977164, 50.00109039468566863 ) ) ;
#114296 = CARTESIAN_POINT ( 'NONE',  ( -13.89961937509957401, -13.97604488694547875, 34.37609039468566863 ) ) ;
#114297 = CARTESIAN_POINT ( 'NONE',  ( 15.72974639402176855, 15.80617190586768217, 76.87609039468567573 ) ) ;
#114298 = EDGE_CURVE ( 'NONE', #85078, #38003, #34922, .T. ) ;
#114299 = CARTESIAN_POINT ( 'NONE',  ( 18.62759615963271287, -10.81492255796078972, 73.33224293864769550 ) ) ;
#114300 = CARTESIAN_POINT ( 'NONE',  ( -16.55341960407611168, -4.379528057220339221, 56.45724293864768839 ) ) ;
#114302 = CARTESIAN_POINT ( 'NONE',  ( 9.474510206698729675, 16.51473224551082808, 27.08442372801900433 ) ) ;
#114301 = CARTESIAN_POINT ( 'NONE',  ( -10.81492255796105439, 18.62759615963255655, 92.91775706135236135 ) ) ;
#114303 = CARTESIAN_POINT ( 'NONE',  ( -14.34966873604960291, -8.224510206698953496, 66.66557627198102409 ) ) ;
#114304 = CARTESIAN_POINT ( 'NONE',  ( -14.29746914071049879, 8.314922557960819915, 115.8322429386477097 ) ) ;
#114305 = CARTESIAN_POINT ( 'NONE',  ( -19.03943276465977164, -0.05219959533935918106, 53.75109039468566863 ) ) ;
#114306 = CARTESIAN_POINT ( 'NONE',  ( 4.379528057220339221, -16.55341960407611168, 27.70724293864769905 ) ) ;
#114307 = CARTESIAN_POINT ( 'NONE',  ( 18.62759615963255655, 10.81492255796105972, 76.66775706135234714 ) ) ;
#114308 = CARTESIAN_POINT ( 'NONE',  ( -19.05341960407617563, 5.049401038297882671, 43.54275706135232582 ) ) ;
#114309 = CARTESIAN_POINT ( 'NONE',  ( 10.72451020669898902, -18.67979575497178502, 57.91557627198103120 ) ) ;
#114310 = CARTESIAN_POINT ( 'NONE',  ( -0.05219959533937732626, 21.53943276465977519, 47.50109039468568994 ) ) ;
#114311 = CARTESIAN_POINT ( 'NONE',  ( -15.72974639402197994, 15.80617190586746368, 95.62390960531436690 ) ) ;
#114312 = CARTESIAN_POINT ( 'NONE',  ( 13.89961937509957401, 13.97604488694547697, 101.8760903946856331 ) ) ;
#114313 = CARTESIAN_POINT ( 'NONE',  ( 0.05219959533934541429, -16.53943276465976808, 65.00109039468568994 ) ) ;
#114315 = CARTESIAN_POINT ( 'NONE',  ( 15.72974639402199770, -15.80617190586745480, 103.1239096053143811 ) ) ;
#114314 = CARTESIAN_POINT ( 'NONE',  ( -38.00000000000000711, 2.428612866367529932E-14, -5.999999999999999112 ) ) ;
#114316 = CARTESIAN_POINT ( 'NONE',  ( 14.34966873604960469, 8.224510206698951720, 84.16557627198103830 ) ) ;
#114317 = CARTESIAN_POINT ( 'NONE',  ( 36.91746825000000598, -11.99521256947793546, -10.22499999726881548 ) ) ;
#114318 = CARTESIAN_POINT ( 'NONE',  ( 16.52544592524335698, 4.483927247898782831, 36.45942372801901143 ) ) ;
#114319 = CARTESIAN_POINT ( 'NONE',  ( -21.55341960407610458, -5.719274019375992779, 51.45724293864770260 ) ) ;
#114320 = CARTESIAN_POINT ( 'NONE',  ( -12.14591786802326823, 12.06949235617739902, 93.12609039468568994 ) ) ;
#114321 = CARTESIAN_POINT ( 'NONE',  ( -13.97604488694527625, -13.89961937509977652, 21.87390960531435979 ) ) ;
#114322 = CARTESIAN_POINT ( 'NONE',  ( 14.29746914071037800, 8.314922557961029526, 71.66775706135234714 ) ) ;
#114323 = CARTESIAN_POINT ( 'NONE',  ( -0.05219959533937732626, 21.53943276465977519, 42.50109039468567573 ) ) ;
#114324 = CARTESIAN_POINT ( 'NONE',  ( -18.67979575497178146, -10.72451020669898902, 56.66557627198103830 ) ) ;
#114325 = CARTESIAN_POINT ( 'NONE',  ( 12.14591786802327356, -12.06949235617739191, 90.62609039468567573 ) ) ;
#114326 = CARTESIAN_POINT ( 'NONE',  ( -10.72451020669870658, -18.67979575497194134, 74.58442372801901854 ) ) ;
#114327 = CARTESIAN_POINT ( 'NONE',  ( 18.62759615963271287, -10.81492255796078972, 48.33224293864770260 ) ) ;
#114328 = CARTESIAN_POINT ( 'NONE',  ( 0.05219959533907565091, 21.53943276465977519, 34.99890960531435979 ) ) ;
#114329 = ORIENTED_EDGE ( 'NONE', *, *, #121851, .T. ) ;
#114330 = CARTESIAN_POINT ( 'NONE',  ( -12.14591786802326823, 12.06949235617739902, 68.12609039468567573 ) ) ;
#114331 = CARTESIAN_POINT ( 'NONE',  ( 18.67979575497178502, 10.72451020669898547, 39.16557627198102409 ) ) ;
#114332 = ORIENTED_EDGE ( 'NONE', *, *, #135116, .T. ) ;
#114333 = CARTESIAN_POINT ( 'NONE',  ( -16.51473224551069308, -9.474510206698971260, 101.6655762719810241 ) ) ;
#114334 = CARTESIAN_POINT ( 'NONE',  ( -8.314922557961024197, 14.29746914071037800, 112.9177570613523329 ) ) ;
#114335 = CARTESIAN_POINT ( 'NONE',  ( 17.36633513277089236, -35.95409897417799527, -27.53902325179317856 ) ) ;
#114336 = CARTESIAN_POINT ( 'NONE',  ( 8.224510206698953496, -14.34966873604960469, 112.9155762719810383 ) ) ;
#114337 = CARTESIAN_POINT ( 'NONE',  ( -10.72451020669898014, 18.67979575497178502, 45.41557627198103830 ) ) ;
#114338 = CARTESIAN_POINT ( 'NONE',  ( 13.89961937509977652, -13.97604488694527269, 48.12390960531435979 ) ) ;
#114339 = CARTESIAN_POINT ( 'NONE',  ( -14.34966873604972548, 8.224510206698743886, 93.33442372801901854 ) ) ;
#114340 = CARTESIAN_POINT ( 'NONE',  ( -18.62759615963255300, -10.81492255796106328, 29.16775706135234003 ) ) ;
#114341 = CARTESIAN_POINT ( 'NONE',  ( 13.97604488694548053, -13.89961937509957401, 95.62609039468563310 ) ) ;
#114342 = CARTESIAN_POINT ( 'NONE',  ( 4.483927247898545687, 16.52544592524342804, 99.79057627198103830 ) ) ;
#114343 = CARTESIAN_POINT ( 'NONE',  ( -16.51473224551069308, -9.474510206698971260, 56.66557627198103120 ) ) ;
#114344 = CARTESIAN_POINT ( 'NONE',  ( 16.46253265017160672, -9.564922557960803928, 28.33224293864769550 ) ) ;
#114345 = DIRECTION ( 'NONE',  ( 1.000000000000000000, -0.000000000000000000, -0.000000000000000000 ) ) ;
#114346 = CARTESIAN_POINT ( 'NONE',  ( 5.049401038298161559, -19.05341960407611168, 72.70724293864768129 ) ) ;
#114347 = CARTESIAN_POINT ( 'NONE',  ( 16.53943276465976808, 0.05219959533934440121, 66.25109039468567573 ) ) ;
#114348 = CARTESIAN_POINT ( 'NONE',  ( -18.62759615963255300, -10.81492255796106328, 109.1677570613523613 ) ) ;
#114349 = CARTESIAN_POINT ( 'NONE',  ( 15.72974639402199770, -15.80617190586745480, 48.12390960531436690 ) ) ;
#114350 = CARTESIAN_POINT ( 'NONE',  ( 8.224510206698742110, 14.34966873604972548, 72.08442372801899012 ) ) ;
#114351 = CARTESIAN_POINT ( 'NONE',  ( 5.153800228976615827, -19.02544592524334988, 70.20942372801899012 ) ) ;
#114352 = ORIENTED_EDGE ( 'NONE', *, *, #70168, .T. ) ;
#114353 = CARTESIAN_POINT ( 'NONE',  ( -15.80617190586768217, 15.72974639402176855, 63.12609039468568994 ) ) ;
#114354 = CARTESIAN_POINT ( 'NONE',  ( 13.97604488694527802, 13.89961937509977652, 64.37390960531436690 ) ) ;
#114355 = CARTESIAN_POINT ( 'NONE',  ( 0.05219959533909260263, 19.03943276465977164, 34.99890960531435979 ) ) ;
#114356 = CARTESIAN_POINT ( 'NONE',  ( -13.97604488694547697, 13.89961937509957934, 58.12609039468566863 ) ) ;
#114357 = CARTESIAN_POINT ( 'NONE',  ( 16.51473224551069308, 9.474510206698969483, 109.1655762719810383 ) ) ;
#114358 = CARTESIAN_POINT ( 'NONE',  ( -5.153800228976328057, -19.02544592524343514, 102.2905762719810383 ) ) ;
#114359 = CARTESIAN_POINT ( 'NONE',  ( 4.379528057220339221, -16.55341960407611168, 52.70724293864769550 ) ) ;
#114360 = CARTESIAN_POINT ( 'NONE',  ( 5.823673210054125526, 21.52544592524343514, 49.79057627198102409 ) ) ;
#114361 = CARTESIAN_POINT ( 'NONE',  ( -17.50000000000002132, 4.658240926743188126, 103.9447041781680667 ) ) ;
#114362 = CARTESIAN_POINT ( 'NONE',  ( 16.51473224551083163, -9.474510206698727899, 25.83442372801900078 ) ) ;
#114363 = CARTESIAN_POINT ( 'NONE',  ( -19.03943276465977164, 0.05219959533909376836, 56.24890960531435979 ) ) ;
#114364 = CARTESIAN_POINT ( 'NONE',  ( -18.89770734986049305, -5.499999999999956479, 99.10214472496639360 ) ) ;
#114365 = DIRECTION ( 'NONE',  ( 0.000000000000000000, 0.000000000000000000, -1.000000000000000000 ) ) ;
#114366 = CARTESIAN_POINT ( 'NONE',  ( -4.483927247898782831, 16.52544592524335698, 77.70942372801900433 ) ) ;
#114367 = CARTESIAN_POINT ( 'NONE',  ( 21.53943276465977519, -0.05219959533907433946, 98.74890960531438111 ) ) ;
#114368 = VECTOR ( 'NONE', #5141, 1000.000000000000000 ) ;
#114370 = FACE_OUTER_BOUND ( 'NONE', #99959, .T. ) ;
#114369 = CARTESIAN_POINT ( 'NONE',  ( -19.05341960407611168, -5.049401038298163336, 46.45724293864768129 ) ) ;
#114371 = CARTESIAN_POINT ( 'NONE',  ( -5.719274019375665041, -21.55341960407619695, 39.79275706135235424 ) ) ;
#114372 = CARTESIAN_POINT ( 'NONE',  ( 16.46253265017146816, 9.564922557961045513, 51.66775706135233293 ) ) ;
#114373 = CARTESIAN_POINT ( 'NONE',  ( -5.153800228976328057, -19.02544592524343514, 47.29057627198102409 ) ) ;
#114374 = CARTESIAN_POINT ( 'NONE',  ( 5.823673210054444382, -21.52544592524334988, 95.20942372801903275 ) ) ;
#114375 = CARTESIAN_POINT ( 'NONE',  ( 16.21995358207304250, 7.366697692864176972, 97.56448998487843483 ) ) ;
#114376 = CARTESIAN_POINT ( 'NONE',  ( -0.05219959533910754901, -16.53943276465976808, 47.49890960531435979 ) ) ;
#114377 = FACE_BOUND ( 'NONE', #176269, .T. ) ;
#114378 = CARTESIAN_POINT ( 'NONE',  ( 5.823673210054125526, 21.52544592524343514, 39.79057627198103830 ) ) ;
#114379 = CARTESIAN_POINT ( 'NONE',  ( 8.571926809382603096, -26.38167802310801235, 141.4750000027312069 ) ) ;
#114380 = CARTESIAN_POINT ( 'NONE',  ( 19.02544592524343514, -5.153800228976328945, 103.5405762719809957 ) ) ;
#114381 = CARTESIAN_POINT ( 'NONE',  ( 16.53943276465976808, -0.05219959533910856209, 88.74890960531436690 ) ) ;
#114382 = CARTESIAN_POINT ( 'NONE',  ( -4.379528057220086978, -16.55341960407618274, 29.79275706135234358 ) ) ;
#114383 = CARTESIAN_POINT ( 'NONE',  ( -14.29746914071037622, -8.314922557961029526, 104.1677570613523471 ) ) ;
#114384 = EDGE_LOOP ( 'NONE', ( #30881, #123581, #23400, #31597 ) ) ;
#114385 = EDGE_CURVE ( 'NONE', #181921, #70413, #59283, .T. ) ;
#114386 = B_SPLINE_CURVE_WITH_KNOTS ( 'NONE', 3,
 ( #120603, #148972, #197468, #133795, #181314, #106421, #121591, #195487, #182297, #43777, #103462, #164146, #180327, #183286, #56962, #165141, #28626, #44768, #26632, #168102, #102458, #25643, #42793, #87288, #88275, #118635, #149963, #104455, #167126, #11469, #73140, #134810 ),
 .UNSPECIFIED., .F., .F.,
 ( 4, 2, 2, 2, 2, 2, 2, 2, 2, 2, 2, 2, 2, 2, 2, 4 ),
 ( 1.346507514538369289E-17, 0.0003712461730036875911, 0.0007424923460073617381, 0.001113738519011035939, 0.001484984692014710032, 0.002227477038022060603, 0.002598723211025738382, 0.002969969384029416595, 0.003341215557033094807, 0.003712461730036773020, 0.004083707903040451233, 0.004454954076044129879, 0.004826200249047807658, 0.005197446422051485437, 0.005568692595055164084, 0.005939938768058842730 ),
 .UNSPECIFIED. ) ;
#114388 = CARTESIAN_POINT ( 'NONE',  ( 10.72451020669898902, -18.67979575497178502, 107.9155762719810241 ) ) ;
#114387 = CARTESIAN_POINT ( 'NONE',  ( -19.02544592524342804, 5.153800228976336051, 96.04057627198103830 ) ) ;
#114390 = CARTESIAN_POINT ( 'NONE',  ( -19.02544592524342804, 5.153800228976336051, 96.04057627198103830 ) ) ;
#114389 = CARTESIAN_POINT ( 'NONE',  ( -14.34966873604972548, 8.224510206698743886, 113.3344237280190328 ) ) ;
#114391 = CARTESIAN_POINT ( 'NONE',  ( -19.03943276465977164, -0.05219959533935918106, 98.75109039468567573 ) ) ;
#114392 = CARTESIAN_POINT ( 'NONE',  ( -5.823673210054431948, 21.52544592524334988, 112.7094237280190328 ) ) ;
#114393 = CARTESIAN_POINT ( 'NONE',  ( -15.72974639402197994, 15.80617190586746368, 90.62390960531436690 ) ) ;
#114394 = CARTESIAN_POINT ( 'NONE',  ( 18.62759615963271287, -10.81492255796078972, 48.33224293864770260 ) ) ;
#114395 = COLOUR_RGB ( '', 0.09019608, 0.27058824, 0.51372549) ;
#114396 = CARTESIAN_POINT ( 'NONE',  ( 5.153800228976335163, 19.02544592524342804, 59.79057627198100988 ) ) ;
#114397 = CARTESIAN_POINT ( 'NONE',  ( 4.379528057220339221, -16.55341960407611168, 37.70724293864769550 ) ) ;
#114398 = CARTESIAN_POINT ( 'NONE',  ( -9.564922557960796823, -16.46253265017161027, 72.08224293864770971 ) ) ;
#114399 = ORIENTED_EDGE ( 'NONE', *, *, #38764, .T. ) ;
#114400 = CARTESIAN_POINT ( 'NONE',  ( 19.02130022317636104, -5.499999999999802824, 63.28188669246573284 ) ) ;
#114401 = CARTESIAN_POINT ( 'NONE',  ( 16.51473224551083163, -9.474510206698727899, 40.83442372801900433 ) ) ;
#114402 = CARTESIAN_POINT ( 'NONE',  ( 14.29746914071049879, -8.314922557960816363, 88.33224293864769550 ) ) ;
#114403 = CARTESIAN_POINT ( 'NONE',  ( -21.52544592524334988, -5.823673210054445271, 28.95942372801902209 ) ) ;
#114404 = CARTESIAN_POINT ( 'NONE',  ( -17.14385361876520619, 23.59649016807275856, 145.0750000027311728 ) ) ;
#114405 = CARTESIAN_POINT ( 'NONE',  ( -8.314922557961024197, 14.29746914071037800, 107.9177570613523471 ) ) ;
#114406 = CARTESIAN_POINT ( 'NONE',  ( 14.29746914071049879, -8.314922557960816363, 113.3322429386476955 ) ) ;
#114407 = CARTESIAN_POINT ( 'NONE',  ( -19.05341960407611168, -5.049401038298163336, 66.45724293864769550 ) ) ;
#114408 = CARTESIAN_POINT ( 'NONE',  ( -7.284589286804265207, -1.784589286804211916, 1.818019484660534424 ) ) ;
#114409 = CARTESIAN_POINT ( 'NONE',  ( 12.14591786802309770, 12.06949235617756955, 49.37390960531436690 ) ) ;
#114410 = ADVANCED_FACE ( 'NONE', ( #136877 ), #93340, .F. ) ;
#114411 = CARTESIAN_POINT ( 'NONE',  ( -10.81492255796105439, 18.62759615963255655, 62.91775706135236135 ) ) ;
#114412 = CARTESIAN_POINT ( 'NONE',  ( 31.84446081652115978, -20.74826690461661372, -24.63985244029811739 ) ) ;
#114413 = CARTESIAN_POINT ( 'NONE',  ( 5.823673210054444382, -21.52544592524334988, 90.20942372801903275 ) ) ;
#114414 = CARTESIAN_POINT ( 'NONE',  ( -0.05219959533909027116, -19.03943276465977164, 37.49890960531436690 ) ) ;
#114415 = CARTESIAN_POINT ( 'NONE',  ( -13.89961937509977652, 13.97604488694528158, 45.62390960531433848 ) ) ;
#114416 = ORIENTED_EDGE ( 'NONE', *, *, #46491, .F. ) ;
#114417 = CARTESIAN_POINT ( 'NONE',  ( 0.05219959533937995610, -21.53943276465977519, 90.00109039468567573 ) ) ;
#114418 = CARTESIAN_POINT ( 'NONE',  ( -12.14591786802326823, 12.06949235617739902, 58.12609039468568994 ) ) ;
#114419 = CARTESIAN_POINT ( 'NONE',  ( 10.81492255796106328, -18.62759615963255655, 85.41775706135236135 ) ) ;
#114420 = CARTESIAN_POINT ( 'NONE',  ( 10.72451020669898902, -18.67979575497178502, 27.91557627198103830 ) ) ;
#114421 = CARTESIAN_POINT ( 'NONE',  ( -19.02544592524334988, -5.153800228976617603, 98.95942372801900433 ) ) ;
#114422 = CARTESIAN_POINT ( 'NONE',  ( -5.719274019375665041, -21.55341960407619695, 64.79275706135234714 ) ) ;
#114423 = CARTESIAN_POINT ( 'NONE',  ( -12.06949235617739369, -12.14591786802326823, 39.37609039468567573 ) ) ;
#114424 = CARTESIAN_POINT ( 'NONE',  ( 15.72974639402199770, -15.80617190586745480, 88.12390960531436690 ) ) ;
#114425 = CARTESIAN_POINT ( 'NONE',  ( 19.03943276465977164, 0.05219959533936151252, 101.2510903946856757 ) ) ;
#114426 = CARTESIAN_POINT ( 'NONE',  ( -16.51473224551069308, -9.474510206698971260, 61.66557627198103120 ) ) ;
#114427 = CARTESIAN_POINT ( 'NONE',  ( 16.51473224551083163, -9.474510206698727899, 100.8344237280190043 ) ) ;
#114428 = AXIS2_PLACEMENT_3D ( 'NONE', #178912, #117218, #161725 ) ;
#114429 = CARTESIAN_POINT ( 'NONE',  ( 16.46253265017146816, 9.564922557961045513, 96.66775706135233293 ) ) ;
#114430 = CARTESIAN_POINT ( 'NONE',  ( -8.314922557960811034, -14.29746914071050412, 57.08224293864769550 ) ) ;
#114431 = CARTESIAN_POINT ( 'NONE',  ( 13.89961937509957401, 13.97604488694547697, 71.87609039468567573 ) ) ;
#114432 = CARTESIAN_POINT ( 'NONE',  ( 16.55341960407618274, -4.379528057220086978, 66.04275706135236135 ) ) ;
#114434 = CARTESIAN_POINT ( 'NONE',  ( 9.564922557960805705, 16.46253265017160317, 39.58224293864768839 ) ) ;
#114433 = CARTESIAN_POINT ( 'NONE',  ( -21.52544592524343514, 5.823673210054127303, 116.0405762719810383 ) ) ;
#114435 = CARTESIAN_POINT ( 'NONE',  ( 9.474510206698971260, -16.51473224551069308, 57.91557627198103120 ) ) ;
#114436 = CARTESIAN_POINT ( 'NONE',  ( 12.14591786802327356, -12.06949235617739191, 65.62609039468568994 ) ) ;
#114437 = CARTESIAN_POINT ( 'NONE',  ( 67.00000000000000000, -1.163414459189985801E-14, 89.49999999999897682 ) ) ;
#114438 = CARTESIAN_POINT ( 'NONE',  ( 8.906447517083050158, 27.41122689804195645, 147.6500000054623740 ) ) ;
#114439 = CARTESIAN_POINT ( 'NONE',  ( 9.564922557960805705, 16.46253265017160317, 109.5822429386476955 ) ) ;
#114440 = CARTESIAN_POINT ( 'NONE',  ( -19.05341960407611168, -5.049401038298163336, 21.45724293864768839 ) ) ;
#114441 = ORIENTED_EDGE ( 'NONE', *, *, #142029, .T. ) ;
#114442 = CARTESIAN_POINT ( 'NONE',  ( -9.564922557961040184, 16.46253265017147172, 112.9177570613523329 ) ) ;
#114443 = CARTESIAN_POINT ( 'NONE',  ( -21.52544592524343514, 5.823673210054127303, 41.04057627198103120 ) ) ;
#114445 = CARTESIAN_POINT ( 'NONE',  ( -16.53943276465976808, -0.05219959533934237506, 33.75109039468568284 ) ) ;
#114444 = CARTESIAN_POINT ( 'NONE',  ( 16.46253265017146816, 9.564922557961045513, 26.66775706135234003 ) ) ;
#114446 = CARTESIAN_POINT ( 'NONE',  ( -5.153800228976328057, -19.02544592524343514, 32.29057627198102409 ) ) ;
#114447 = CARTESIAN_POINT ( 'NONE',  ( -16.51473224551069308, -9.474510206698971260, 46.66557627198102409 ) ) ;
#114448 = CARTESIAN_POINT ( 'NONE',  ( -18.67979575497178146, -10.72451020669898902, 81.66557627198103830 ) ) ;
#114449 = CARTESIAN_POINT ( 'NONE',  ( 19.03943276465977164, -0.05219959533909143690, 98.74890960531436690 ) ) ;
#114450 = CARTESIAN_POINT ( 'NONE',  ( -5.049401038298153566, 19.05341960407611168, 55.20724293864769550 ) ) ;
#114451 = CARTESIAN_POINT ( 'NONE',  ( 22.44159573604009239, 16.30477369853692693, 140.5750000027311728 ) ) ;
#114452 = CARTESIAN_POINT ( 'NONE',  ( 5.049401038297881783, 19.05341960407617563, 82.29275706135229029 ) ) ;
#114453 = CARTESIAN_POINT ( 'NONE',  ( 12.06949235617757843, -12.14591786802309237, 73.12390960531436690 ) ) ;
#114454 = CARTESIAN_POINT ( 'NONE',  ( 15.80617190586769283, -15.72974639402175789, 100.6260903946857184 ) ) ;
#114455 = CARTESIAN_POINT ( 'NONE',  ( 15.72974639402199770, -15.80617190586745480, 103.1239096053143811 ) ) ;
#114456 = CARTESIAN_POINT ( 'NONE',  ( -15.72974639402176322, -15.80617190586768395, 79.37609039468567573 ) ) ;
#114457 = CARTESIAN_POINT ( 'NONE',  ( 21.55341960407619695, -5.719274019375665929, 76.04275706135237556 ) ) ;
#114458 = CARTESIAN_POINT ( 'NONE',  ( -16.51473224551069308, -9.474510206698971260, 111.6655762719810383 ) ) ;
#114460 = CARTESIAN_POINT ( 'NONE',  ( 10.72451020669871369, 18.67979575497193778, 82.08442372801901854 ) ) ;
#114459 = CARTESIAN_POINT ( 'NONE',  ( -16.53943276465976808, -0.05219959533934237506, 108.7510903946857042 ) ) ;
#114461 = CARTESIAN_POINT ( 'NONE',  ( -16.46253265017160317, 9.564922557960807481, 60.83224293864769550 ) ) ;
#114462 = CARTESIAN_POINT ( 'NONE',  ( -21.52544592524334988, -5.823673210054445271, 48.95942372801902565 ) ) ;
#114463 = CARTESIAN_POINT ( 'NONE',  ( -13.97604488694527625, -13.89961937509977652, 86.87390960531436690 ) ) ;
#114464 = CARTESIAN_POINT ( 'NONE',  ( -8.224510206698948167, 14.34966873604960824, 75.41557627198102409 ) ) ;
#114465 = CARTESIAN_POINT ( 'NONE',  ( 16.52544592524342804, -4.483927247898539470, 53.54057627198103120 ) ) ;
#114466 = CARTESIAN_POINT ( 'NONE',  ( -10.72451020669898014, 18.67979575497178502, 55.41557627198102409 ) ) ;
#114467 = CARTESIAN_POINT ( 'NONE',  ( -5.049401038298153566, 19.05341960407611168, 55.20724293864769550 ) ) ;
#114468 = CARTESIAN_POINT ( 'NONE',  ( 10.72451020669898902, -18.67979575497178502, 67.91557627198102409 ) ) ;
#114469 = CARTESIAN_POINT ( 'NONE',  ( 9.474510206698729675, 16.51473224551082808, 67.08442372801900433 ) ) ;
#114471 = CARTESIAN_POINT ( 'NONE',  ( -16.55341960407611168, -4.379528057220339221, 71.45724293864769550 ) ) ;
#114470 = CARTESIAN_POINT ( 'NONE',  ( 0.2500000000000002220, 0.000000000000000000, 0.000000000000000000 ) ) ;
#114472 = CARTESIAN_POINT ( 'NONE',  ( 21.55341960407610458, 5.719274019375980345, 58.95724293864770971 ) ) ;
#114473 = VERTEX_POINT ( 'NONE', #76191 ) ;
#114474 = DIRECTION ( 'NONE',  ( -1.000000000000000000, -0.000000000000000000, -0.000000000000000000 ) ) ;
#114476 = CARTESIAN_POINT ( 'NONE',  ( -22.44159573604010305, 16.30477369853692338, 147.1750000027311671 ) ) ;
#114475 = CARTESIAN_POINT ( 'NONE',  ( -4.483927247898782831, 16.52544592524335698, 102.7094237280190185 ) ) ;
#114477 = CARTESIAN_POINT ( 'NONE',  ( 16.46253265017146816, 9.564922557961045513, 91.66775706135234714 ) ) ;
#114478 = CARTESIAN_POINT ( 'NONE',  ( 4.483927247898545687, 16.52544592524342804, 64.79057627198103830 ) ) ;
#114479 = DIRECTION ( 'NONE',  ( 0.8660254037844391517, -0.000000000000000000, -0.4999999999999991673 ) ) ;
#114480 = CARTESIAN_POINT ( 'NONE',  ( 19.02544592524343514, -5.153800228976328945, 58.54057627198102409 ) ) ;
#114481 = CARTESIAN_POINT ( 'NONE',  ( 8.314922557960818139, 14.29746914071049879, 59.58224293864770260 ) ) ;
#114482 = CARTESIAN_POINT ( 'NONE',  ( 9.564922557960805705, 16.46253265017160317, 89.58224293864769550 ) ) ;
#114483 = AXIS2_PLACEMENT_3D ( 'NONE', #15264, #103304, #43620 ) ;
#114485 = CARTESIAN_POINT ( 'NONE',  ( -9.474510206698964154, 16.51473224551069663, 55.41557627198103120 ) ) ;
#114484 = CARTESIAN_POINT ( 'NONE',  ( -5.153800228976607833, 19.02544592524334988, 77.70942372801900433 ) ) ;
#114486 = CARTESIAN_POINT ( 'NONE',  ( 5.153800228976335163, 19.02544592524342804, 84.79057627198099567 ) ) ;
#114487 = CARTESIAN_POINT ( 'NONE',  ( -9.564922557960796823, -16.46253265017161027, 67.08224293864769550 ) ) ;
#114488 = EDGE_CURVE ( 'NONE', #19226, #166399, #78169, .T. ) ;
#114489 = CARTESIAN_POINT ( 'NONE',  ( -18.62759615963270932, 10.81492255796079327, 60.83224293864769550 ) ) ;
#114490 = CARTESIAN_POINT ( 'NONE',  ( -12.06949235617739369, -12.14591786802326823, 64.37609039468568994 ) ) ;
#114491 = CARTESIAN_POINT ( 'NONE',  ( -6.856101608890801443E-16, -67.16067257189654072, -22.99988689144064580 ) ) ;
#114492 = CARTESIAN_POINT ( 'NONE',  ( 5.153800228976335163, 19.02544592524342804, 54.79057627198103120 ) ) ;
#114493 = CARTESIAN_POINT ( 'NONE',  ( -10.81492255796078084, -18.62759615963271287, 57.08224293864769550 ) ) ;
#114494 = CARTESIAN_POINT ( 'NONE',  ( 5.153800228976615827, -19.02544592524334988, 75.20942372801896170 ) ) ;
#114495 = CARTESIAN_POINT ( 'NONE',  ( -8.224510206698948167, 14.34966873604960824, 30.41557627198101699 ) ) ;
#114496 = CARTESIAN_POINT ( 'NONE',  ( -16.46253265017146816, -9.564922557961047289, 39.16775706135234003 ) ) ;
#114498 = CARTESIAN_POINT ( 'NONE',  ( 16.52544592524335698, 4.483927247898782831, 96.45942372801901854 ) ) ;
#114497 = CARTESIAN_POINT ( 'NONE',  ( -14.34966873604972548, 8.224510206698743886, 58.33442372801901143 ) ) ;
#114499 = CARTESIAN_POINT ( 'NONE',  ( -18.10062525802553424, 5.500000000000031086, 53.51383468041920111 ) ) ;
#114500 = CARTESIAN_POINT ( 'NONE',  ( 14.34966873604972726, -8.224510206698740333, 85.83442372801901854 ) ) ;
#114501 = CARTESIAN_POINT ( 'NONE',  ( 5.823673210054125526, 21.52544592524343514, 24.79057627198103120 ) ) ;
#114502 = CARTESIAN_POINT ( 'NONE',  ( -5.049401038298153566, 19.05341960407611168, 40.20724293864768839 ) ) ;
#114503 = CARTESIAN_POINT ( 'NONE',  ( -16.46253265017160317, 9.564922557960807481, 50.83224293864770260 ) ) ;
#114504 = CARTESIAN_POINT ( 'NONE',  ( -19.05341960407611168, -5.049401038298163336, 41.45724293864769550 ) ) ;
#114505 = CARTESIAN_POINT ( 'NONE',  ( -18.62759615963255300, -10.81492255796106328, 34.16775706135234714 ) ) ;
#114506 = CARTESIAN_POINT ( 'NONE',  ( -4.379528057220086978, -16.55341960407618274, 54.79275706135235424 ) ) ;
#114507 = CARTESIAN_POINT ( 'NONE',  ( 16.55341960407618274, -4.379528057220086978, 111.0427570613523613 ) ) ;
#114508 = CARTESIAN_POINT ( 'NONE',  ( -9.474510206698964154, 16.51473224551069663, 25.41557627198103120 ) ) ;
#114509 = CARTESIAN_POINT ( 'NONE',  ( -19.02544592524334988, -5.153800228976617603, 18.95942372801899722 ) ) ;
#114510 = CARTESIAN_POINT ( 'NONE',  ( -16.51473224551082808, 9.474510206698731452, 108.3344237280190043 ) ) ;
#114511 = VECTOR ( 'NONE', #179724, 1000.000000000000114 ) ;
#114512 = CARTESIAN_POINT ( 'NONE',  ( 13.97604488694548053, -13.89961937509957401, 70.62609039468567573 ) ) ;
#114513 = CARTESIAN_POINT ( 'NONE',  ( -16.52544592524342804, 4.483927247898546575, 66.04057627198103830 ) ) ;
#114514 = CARTESIAN_POINT ( 'NONE',  ( -19.02544592524342804, 5.153800228976336051, 41.04057627198103120 ) ) ;
#114516 = DIRECTION ( 'NONE',  ( -0.000000000000000000, -0.000000000000000000, -1.000000000000000000 ) ) ;
#114515 = CARTESIAN_POINT ( 'NONE',  ( -19.05341960407617563, 5.049401038297882671, 78.54275706135233293 ) ) ;
#114517 = CARTESIAN_POINT ( 'NONE',  ( -0.05219959533937732626, 21.53943276465977519, 72.50109039468568994 ) ) ;
#114518 = CARTESIAN_POINT ( 'NONE',  ( 8.224510206698742110, 14.34966873604972548, 47.08442372801901854 ) ) ;
#114519 = CARTESIAN_POINT ( 'NONE',  ( 18.87075004821571156, -5.499999999999887201, 56.17408112101048800 ) ) ;
#114520 = CARTESIAN_POINT ( 'NONE',  ( -18.67979575497178146, -10.72451020669898902, 36.66557627198103120 ) ) ;
#114521 = CARTESIAN_POINT ( 'NONE',  ( 16.55341960407618274, -4.379528057220086978, 31.04275706135234714 ) ) ;
#114522 = CARTESIAN_POINT ( 'NONE',  ( -38.00373040315628970, 1.963201398428686990E-14, -0.1220970790697140096 ) ) ;
#114523 = CARTESIAN_POINT ( 'NONE',  ( 5.153800228976615827, -19.02544592524334988, 20.20942372801899722 ) ) ;
#114524 = CARTESIAN_POINT ( 'NONE',  ( -24.86475712555796491, 11.37215039200969002, 169.9824823118007657 ) ) ;
#114525 = CARTESIAN_POINT ( 'NONE',  ( -0.05219959533909027116, -19.03943276465977164, 42.49890960531435269 ) ) ;
#114526 = CARTESIAN_POINT ( 'NONE',  ( 16.46253265017146816, 9.564922557961045513, 56.66775706135233293 ) ) ;
#114527 = CARTESIAN_POINT ( 'NONE',  ( -0.05219959533909027116, -19.03943276465977164, 62.49890960531435979 ) ) ;
#114528 = CARTESIAN_POINT ( 'NONE',  ( -15.72974639402176322, -15.80617190586768395, 69.37609039468567573 ) ) ;
#114529 = CARTESIAN_POINT ( 'NONE',  ( 16.51473224551083163, -9.474510206698727899, 20.83442372801899722 ) ) ;
#114530 = CARTESIAN_POINT ( 'NONE',  ( -4.379528057220328563, 16.55341960407611168, 25.20724293864769550 ) ) ;
#114531 = CARTESIAN_POINT ( 'NONE',  ( -5.049401038298153566, 19.05341960407611168, 30.20724293864768839 ) ) ;
#114532 = CIRCLE ( 'NONE', #11244, 37.23224409030433435 ) ;
#114533 = CARTESIAN_POINT ( 'NONE',  ( 19.05341960407611168, 5.049401038298154454, 88.95724293864769550 ) ) ;
#114534 = CARTESIAN_POINT ( 'NONE',  ( 21.52544592524334988, 5.823673210054432836, 56.45942372801902565 ) ) ;
#114535 = CARTESIAN_POINT ( 'NONE',  ( 19.05341960407611168, 5.049401038298154454, 43.95724293864769550 ) ) ;
#114536 = CARTESIAN_POINT ( 'NONE',  ( -15.80617190586768217, 15.72974639402176855, 68.12609039468567573 ) ) ;
#114538 = CARTESIAN_POINT ( 'NONE',  ( -5.049401038298153566, 19.05341960407611168, 105.2072429386476671 ) ) ;
#114537 = CARTESIAN_POINT ( 'NONE',  ( 19.03943276465977164, 0.05219959533936151252, 91.25109039468566152 ) ) ;
#114539 = CARTESIAN_POINT ( 'NONE',  ( 8.224510206698953496, -14.34966873604960469, 112.9155762719810383 ) ) ;
#114540 = CARTESIAN_POINT ( 'NONE',  ( -10.72451020669898014, 18.67979575497178502, 110.4155762719810383 ) ) ;
#114541 = CARTESIAN_POINT ( 'NONE',  ( 9.564922557961047289, -16.46253265017146816, 40.41775706135234003 ) ) ;
#114542 = CARTESIAN_POINT ( 'NONE',  ( -16.53943276465976808, 0.05219959533911058130, 111.2489096053143669 ) ) ;
#114543 = CARTESIAN_POINT ( 'NONE',  ( 19.03943276465977164, -0.05219959533909143690, 58.74890960531435979 ) ) ;
#114545 = VECTOR ( 'NONE', #28735, 1000.000000000000000 ) ;
#114544 = CARTESIAN_POINT ( 'NONE',  ( -16.51473224551082808, 9.474510206698731452, 103.3344237280190043 ) ) ;
#114546 = CARTESIAN_POINT ( 'NONE',  ( -14.29746914071049879, 8.314922557960819915, 60.83224293864769550 ) ) ;
#114547 = CARTESIAN_POINT ( 'NONE',  ( 5.153800228976615827, -19.02544592524334988, 25.20942372801900433 ) ) ;
#114548 = CARTESIAN_POINT ( 'NONE',  ( -9.474510206698964154, 16.51473224551069663, 115.4155762719810241 ) ) ;
#114549 = CARTESIAN_POINT ( 'NONE',  ( 0.05219959533936267826, -19.03943276465977164, 90.00109039468567573 ) ) ;
#114550 = CARTESIAN_POINT ( 'NONE',  ( -5.719274019375978568, 21.55341960407610458, 95.20724293864769550 ) ) ;
#114551 = CARTESIAN_POINT ( 'NONE',  ( 10.72451020669871369, 18.67979575497193778, 47.08442372801901854 ) ) ;
#114553 = CARTESIAN_POINT ( 'NONE',  ( 14.34966873604972726, -8.224510206698740333, 40.83442372801901854 ) ) ;
#114552 = B_SPLINE_CURVE_WITH_KNOTS ( 'NONE', 3,
 ( #19268, #81887, #157777, #36397, #190104, #155774 ),
 .UNSPECIFIED., .F., .F.,
 ( 4, 2, 4 ),
 ( 0.003989672132298030700, 0.004372778065220456548, 0.004755883998142883262 ),
 .UNSPECIFIED. ) ;
#114554 = CARTESIAN_POINT ( 'NONE',  ( -16.53943276465976808, -0.05219959533934237506, 108.7510903946857042 ) ) ;
#114556 = CARTESIAN_POINT ( 'NONE',  ( -5.719274019375665041, -21.55341960407619695, 44.79275706135234714 ) ) ;
#114555 = CARTESIAN_POINT ( 'NONE',  ( 16.55341960407618274, -4.379528057220086978, 41.04275706135236135 ) ) ;
#114557 = CARTESIAN_POINT ( 'NONE',  ( -10.72451020669898014, 18.67979575497178502, 55.41557627198102409 ) ) ;
#114558 = MECHANICAL_DESIGN_GEOMETRIC_PRESENTATION_REPRESENTATION (  '', ( #88743 ), #192069 ) ;
#114559 = CARTESIAN_POINT ( 'NONE',  ( 13.97604488694527802, 13.89961937509977652, 39.37390960531435269 ) ) ;
#114560 = CARTESIAN_POINT ( 'NONE',  ( 30.74264578624800137, -22.33583958711395212, -2.949999994537626957 ) ) ;
#114561 = CARTESIAN_POINT ( 'NONE',  ( -16.55341960407617563, 4.379528057220093196, 73.54275706135234714 ) ) ;
#114562 = CARTESIAN_POINT ( 'NONE',  ( -21.55341960407610458, -5.719274019375992779, 91.45724293864769550 ) ) ;
#114563 = CARTESIAN_POINT ( 'NONE',  ( -4.379528057220328563, 16.55341960407611168, 35.20724293864768839 ) ) ;
#114564 = CARTESIAN_POINT ( 'NONE',  ( -8.224510206698735004, -14.34966873604973081, 64.58442372801900433 ) ) ;
#114565 = CARTESIAN_POINT ( 'NONE',  ( 0.05219959533936267826, -19.03943276465977164, 105.0010903946856615 ) ) ;
#114566 = CARTESIAN_POINT ( 'NONE',  ( 21.55341960407610458, 5.719274019375980345, 103.9572429386476813 ) ) ;
#114567 = CARTESIAN_POINT ( 'NONE',  ( -14.29746914071049879, 8.314922557960819915, 25.83224293864769194 ) ) ;
#114568 = VERTEX_POINT ( 'NONE', #156014 ) ;
#114569 = CARTESIAN_POINT ( 'NONE',  ( -4.379528057220086978, -16.55341960407618274, 84.79275706135234714 ) ) ;
#114570 = FACE_OUTER_BOUND ( 'NONE', #85524, .T. ) ;
#114571 = CARTESIAN_POINT ( 'NONE',  ( 18.62759615963271287, -10.81492255796078972, 73.33224293864769550 ) ) ;
#114572 = CARTESIAN_POINT ( 'NONE',  ( 14.34966873604972726, -8.224510206698740333, 100.8344237280190185 ) ) ;
#114573 = EDGE_LOOP ( 'NONE', ( #132080, #160855, #51392, #181181, #81285 ) ) ;
#114574 = CARTESIAN_POINT ( 'NONE',  ( 19.19724070472095434, 5.499999999999968026, 88.56193348274382515 ) ) ;
#114575 = CARTESIAN_POINT ( 'NONE',  ( -15.72974639402197994, 15.80617190586746368, 105.6239096053143669 ) ) ;
#114576 = CARTESIAN_POINT ( 'NONE',  ( -10.81492255796078084, -18.62759615963271287, 112.0822429386477097 ) ) ;
#114577 = CARTESIAN_POINT ( 'NONE',  ( -16.53943276465976808, 0.05219959533911058130, 36.24890960531435979 ) ) ;
#114579 = CARTESIAN_POINT ( 'NONE',  ( 4.379528057220092307, 16.55341960407617563, 32.29275706135235424 ) ) ;
#114578 = CIRCLE ( 'NONE', #66227, 2.500000000000002220 ) ;
#114580 = CARTESIAN_POINT ( 'NONE',  ( 13.89961937509977652, -13.97604488694527269, 43.12390960531434558 ) ) ;
#114581 = CARTESIAN_POINT ( 'NONE',  ( -19.03943276465977164, 0.05219959533909376836, 61.24890960531436690 ) ) ;
#114582 = ORIENTED_EDGE ( 'NONE', *, *, #178148, .T. ) ;
#114583 = CARTESIAN_POINT ( 'NONE',  ( 21.52544592524344225, -5.823673210054117533, 23.54057627198102765 ) ) ;
#114584 = DIRECTION ( 'NONE',  ( -1.000000000000000000, -0.000000000000000000, 0.000000000000000000 ) ) ;
#114585 = CARTESIAN_POINT ( 'NONE',  ( -19.03943276465977164, -0.05219959533935918106, 103.7510903946856757 ) ) ;
#114586 = CARTESIAN_POINT ( 'NONE',  ( 19.03943276465977164, 0.05219959533936151252, 56.25109039468566863 ) ) ;
#114587 = CARTESIAN_POINT ( 'NONE',  ( 10.72451020669898902, -18.67979575497178502, 87.91557627198103830 ) ) ;
#114588 = CARTESIAN_POINT ( 'NONE',  ( -12.14591786802326823, 12.06949235617739902, 108.1260903946856757 ) ) ;
#114589 = CARTESIAN_POINT ( 'NONE',  ( -18.62759615963270932, 10.81492255796079327, 45.83224293864769550 ) ) ;
#114591 = CARTESIAN_POINT ( 'NONE',  ( 19.05341960407617918, -5.049401038297876454, 101.0427570613523045 ) ) ;
#114590 = CARTESIAN_POINT ( 'NONE',  ( -15.72974639402197994, 15.80617190586746368, 80.62390960531438111 ) ) ;
#114592 = CARTESIAN_POINT ( 'NONE',  ( 21.53943276465977519, -0.05219959533907433946, 28.74890960531435624 ) ) ;
#114593 = CARTESIAN_POINT ( 'NONE',  ( 15.72974639402176855, 15.80617190586768217, 76.87609039468567573 ) ) ;
#114594 = CARTESIAN_POINT ( 'NONE',  ( 13.97604488694527802, 13.89961937509977652, 79.37390960531435269 ) ) ;
#114595 = DIRECTION ( 'NONE',  ( -0.000000000000000000, -0.000000000000000000, -1.000000000000000000 ) ) ;
#114596 = CARTESIAN_POINT ( 'NONE',  ( 19.05341960407611168, 5.049401038298154454, 68.95724293864769550 ) ) ;
#114597 = CARTESIAN_POINT ( 'NONE',  ( -12.14591786802309592, -12.06949235617757132, 86.87390960531438111 ) ) ;
#114598 = ORIENTED_EDGE ( 'NONE', *, *, #90799, .T. ) ;
#114599 = CARTESIAN_POINT ( 'NONE',  ( -13.89961937509957401, -13.97604488694547875, 109.3760903946856331 ) ) ;
#114600 = CARTESIAN_POINT ( 'NONE',  ( -11.30153831258471975, -180.0000000000000000, -15.00000000000000178 ) ) ;
#114601 = CARTESIAN_POINT ( 'NONE',  ( 9.474510206698971260, -16.51473224551069308, 77.91557627198103830 ) ) ;
#114603 = CARTESIAN_POINT ( 'NONE',  ( 13.97604488694527802, 13.89961937509977652, 94.37390960531436690 ) ) ;
#114602 = CARTESIAN_POINT ( 'NONE',  ( 10.81492255796106328, -18.62759615963255655, 90.41775706135236135 ) ) ;
#114604 = CARTESIAN_POINT ( 'NONE',  ( -0.05219959533934338120, 16.53943276465976808, 82.50109039468568994 ) ) ;
#114605 = CARTESIAN_POINT ( 'NONE',  ( -31.88110949919180470, 0.2682394567897747883, -45.67705988491092484 ) ) ;
#114606 = CARTESIAN_POINT ( 'NONE',  ( -13.97604488694547697, 13.89961937509957934, 63.12609039468566152 ) ) ;
#114607 = CARTESIAN_POINT ( 'NONE',  ( -19.02544592524334988, -5.153800228976617603, 23.95942372801900078 ) ) ;
#114608 = CARTESIAN_POINT ( 'NONE',  ( 8.898068258721473001, -27.38543819252872069, 144.5843446568999866 ) ) ;
#114609 = CARTESIAN_POINT ( 'NONE',  ( 36.91746824999999887, 11.99521256947799053, -2.024999997268813523 ) ) ;
#114610 = CARTESIAN_POINT ( 'NONE',  ( -14.34966873604972548, 8.224510206698743886, 113.3344237280190328 ) ) ;
#114611 = CARTESIAN_POINT ( 'NONE',  ( -17.49999999999999645, -5.500000000000000000, 111.2823096230356725 ) ) ;
#114612 = CARTESIAN_POINT ( 'NONE',  ( 8.224510206698742110, 14.34966873604972548, 107.0844237280190043 ) ) ;
#114613 = CARTESIAN_POINT ( 'NONE',  ( 17.48853670773247515, 5.747243402303057636, 68.83328700250008580 ) ) ;
#114614 = CARTESIAN_POINT ( 'NONE',  ( 16.53943276465976808, 0.05219959533934440121, 81.25109039468568994 ) ) ;
#114615 = CARTESIAN_POINT ( 'NONE',  ( -21.52544592524334988, -5.823673210054445271, 78.95942372801901854 ) ) ;
#114616 = CARTESIAN_POINT ( 'NONE',  ( -5.153800228976607833, 19.02544592524334988, 87.70942372801897591 ) ) ;
#114617 = CARTESIAN_POINT ( 'NONE',  ( -5.049401038297874678, -19.05341960407617918, 44.79275706135232582 ) ) ;
#114618 = AXIS2_PLACEMENT_3D ( 'NONE', #118598, #145908, #101399 ) ;
#114619 = CARTESIAN_POINT ( 'NONE',  ( -19.03943276465977164, 0.05219959533909376836, 81.24890960531436690 ) ) ;
#114620 = CARTESIAN_POINT ( 'NONE',  ( 0.05219959533909260263, 19.03943276465977164, 59.99890960531436690 ) ) ;
#114621 = CARTESIAN_POINT ( 'NONE',  ( 18.22780087662114212, -5.499999999999987566, 41.01540105326107977 ) ) ;
#114622 = CARTESIAN_POINT ( 'NONE',  ( -21.52544592524343514, 5.823673210054127303, 101.0405762719810383 ) ) ;
#114623 = EDGE_CURVE ( 'NONE', #82599, #9179, #148459, .T. ) ;
#114624 = CARTESIAN_POINT ( 'NONE',  ( 10.72451020669898902, -18.67979575497178502, 52.91557627198103830 ) ) ;
#114625 = CARTESIAN_POINT ( 'NONE',  ( 9.564922557960805705, 16.46253265017160317, 34.58224293864770260 ) ) ;
#114626 = CARTESIAN_POINT ( 'NONE',  ( 4.483927247898790824, -16.52544592524335698, 60.20942372801902565 ) ) ;
#114627 = UNCERTAINTY_MEASURE_WITH_UNIT (LENGTH_MEASURE( 1.000000000000000082E-05 ), #101239, 'distance_accuracy_value', 'NONE');
#114628 = VERTEX_POINT ( 'NONE', #77186 ) ;
#114629 = CARTESIAN_POINT ( 'NONE',  ( -21.53943276465977519, -0.05219959533937600094, 43.75109039468568284 ) ) ;
#114631 = CARTESIAN_POINT ( 'NONE',  ( 38.00000000000000000, 12.34694845685046616, -0.9000000000000000222 ) ) ;
#114630 = CARTESIAN_POINT ( 'NONE',  ( -4.483927247898539470, -16.52544592524342804, 72.29057627198102409 ) ) ;
#114632 = CARTESIAN_POINT ( 'NONE',  ( -14.29746914071037622, -8.314922557961029526, 39.16775706135235424 ) ) ;
#114633 = CARTESIAN_POINT ( 'NONE',  ( -12.14591786802309592, -12.06949235617757132, 96.87390960531436690 ) ) ;
#114634 = CARTESIAN_POINT ( 'NONE',  ( -16.51473224551082808, 9.474510206698731452, 48.33442372801900433 ) ) ;
#114635 = CARTESIAN_POINT ( 'NONE',  ( 16.52544592524342804, -4.483927247898539470, 58.54057627198103120 ) ) ;
#114636 = CARTESIAN_POINT ( 'NONE',  ( -18.62759615963255300, -10.81492255796106328, 34.16775706135234714 ) ) ;
#114637 = EDGE_CURVE ( 'NONE', #144727, #170830, #27804, .T. ) ;
#114639 = CARTESIAN_POINT ( 'NONE',  ( 0.05219959533907565091, 21.53943276465977519, 84.99890960531436690 ) ) ;
#114638 = CARTESIAN_POINT ( 'NONE',  ( 4.500000000000000888, -139.5000000000000000, 21.32407087589996664 ) ) ;
#114640 = CARTESIAN_POINT ( 'NONE',  ( -19.03943276465977164, 0.05219959533909376836, 106.2489096053143669 ) ) ;
#114641 = CARTESIAN_POINT ( 'NONE',  ( 14.34966873604960469, 8.224510206698951720, 79.16557627198103830 ) ) ;
#114642 = CARTESIAN_POINT ( 'NONE',  ( 32.63354670693964721, -22.83594557638339850, -20.39123836177202520 ) ) ;
#114643 = CARTESIAN_POINT ( 'NONE',  ( -22.81625015709510507, 31.40387420917330275, -2.924999997268813434 ) ) ;
#114644 = CARTESIAN_POINT ( 'NONE',  ( -13.97604488694547697, 13.89961937509957934, 88.12609039468563310 ) ) ;
#114645 = CARTESIAN_POINT ( 'NONE',  ( 18.67979575497194134, -10.72451020669871369, 20.83442372801901143 ) ) ;
#114646 = CARTESIAN_POINT ( 'NONE',  ( 0.05219959533909260263, 19.03943276465977164, 74.99890960531435269 ) ) ;
#114647 = CARTESIAN_POINT ( 'NONE',  ( 19.02544592524334988, 5.153800228976608722, 61.45942372801900433 ) ) ;
#114648 = CARTESIAN_POINT ( 'NONE',  ( 5.049401038298161559, -19.05341960407611168, 37.70724293864768839 ) ) ;
#114649 = CARTESIAN_POINT ( 'NONE',  ( -15.72974639402176322, -15.80617190586768395, 79.37609039468567573 ) ) ;
#114650 = DIRECTION ( 'NONE',  ( 0.000000000000000000, 0.000000000000000000, 1.000000000000000000 ) ) ;
#114651 = CARTESIAN_POINT ( 'NONE',  ( -12.06949235617756955, 12.14591786802309770, 60.62390960531437401 ) ) ;
#114652 = CARTESIAN_POINT ( 'NONE',  ( -19.05341960407611168, -5.049401038298163336, 66.45724293864769550 ) ) ;
#114653 = AXIS2_PLACEMENT_3D ( 'NONE', #110773, #124957, #184645 ) ;
#114654 = CARTESIAN_POINT ( 'NONE',  ( -10.72451020669898014, 18.67979575497178502, 85.41557627198102409 ) ) ;
#114655 = CARTESIAN_POINT ( 'NONE',  ( 16.51473224551069308, 9.474510206698969483, 54.16557627198103120 ) ) ;
#114656 = VERTEX_POINT ( 'NONE', #31691 ) ;
#114657 = CARTESIAN_POINT ( 'NONE',  ( -5.719274019375978568, 21.55341960407610458, 75.20724293864769550 ) ) ;
#114658 = EDGE_CURVE ( 'NONE', #137960, #138821, #22490, .T. ) ;
#114659 = CARTESIAN_POINT ( 'NONE',  ( 15.72974639402176855, 15.80617190586768217, 96.87609039468568994 ) ) ;
#114662 = CARTESIAN_POINT ( 'NONE',  ( 8.314922557960818139, 14.29746914071049879, 99.58224293864770971 ) ) ;
#114661 = CARTESIAN_POINT ( 'NONE',  ( 8.314922557961029526, -14.29746914071037800, 95.41775706135234714 ) ) ;
#114660 = CARTESIAN_POINT ( 'NONE',  ( 16.46253265017160672, -9.564922557960803928, 23.33224293864769194 ) ) ;
#114663 = CARTESIAN_POINT ( 'NONE',  ( 19.03943276465977164, 0.05219959533936151252, 91.25109039468566152 ) ) ;
#114664 = EDGE_LOOP ( 'NONE', ( #92785, #12605, #58893, #110444, #43846 ) ) ;
#114665 = CARTESIAN_POINT ( 'NONE',  ( 21.55341960407610458, 5.719274019375980345, 108.9572429386476955 ) ) ;
#114666 = CARTESIAN_POINT ( 'NONE',  ( -16.46253265017146816, -9.564922557961047289, 54.16775706135234003 ) ) ;
#114667 = CARTESIAN_POINT ( 'NONE',  ( 14.29746914071037800, 8.314922557961029526, 96.66775706135234714 ) ) ;
#114668 = CARTESIAN_POINT ( 'NONE',  ( 5.049401038297881783, 19.05341960407617563, 32.29275706135233293 ) ) ;
#114669 = CARTESIAN_POINT ( 'NONE',  ( 0.05219959533909260263, 19.03943276465977164, 99.99890960531436690 ) ) ;
#114670 = CARTESIAN_POINT ( 'NONE',  ( 21.55341960407610458, 5.719274019375980345, 58.95724293864770971 ) ) ;
#114671 = CARTESIAN_POINT ( 'NONE',  ( -26.47577687012306313, 8.223210953690959002, 167.6032987643051229 ) ) ;
#114672 = CARTESIAN_POINT ( 'NONE',  ( 19.03943276465977164, -0.05219959533909143690, 28.74890960531435624 ) ) ;
#114673 = CARTESIAN_POINT ( 'NONE',  ( 21.52544592524334988, 5.823673210054432836, 106.4594237280190328 ) ) ;
#114674 = CARTESIAN_POINT ( 'NONE',  ( 12.06949235617739724, 12.14591786802326823, 71.87609039468568994 ) ) ;
#114675 = CARTESIAN_POINT ( 'NONE',  ( -21.53943276465977519, -0.05219959533937600094, 23.75109039468567929 ) ) ;
#114676 = CARTESIAN_POINT ( 'NONE',  ( 14.29746914071037800, 8.314922557961029526, 46.66775706135234714 ) ) ;
#114677 = CARTESIAN_POINT ( 'NONE',  ( 0.05219959533909260263, 19.03943276465977164, 99.99890960531436690 ) ) ;
#114678 = CARTESIAN_POINT ( 'NONE',  ( 9.474510206698971260, -16.51473224551069308, 42.91557627198103120 ) ) ;
#114679 = CARTESIAN_POINT ( 'NONE',  ( 5.049401038298161559, -19.05341960407611168, 62.70724293864769550 ) ) ;
#114680 = CIRCLE ( 'NONE', #33868, 1.250000000000006439 ) ;
#114681 = CARTESIAN_POINT ( 'NONE',  ( 16.52544592524335698, 4.483927247898782831, 46.45942372801901854 ) ) ;
#114682 = CARTESIAN_POINT ( 'NONE',  ( 8.314922557960818139, 14.29746914071049879, 94.58224293864769550 ) ) ;
#114683 = CARTESIAN_POINT ( 'NONE',  ( 16.53943276465976808, 0.05219959533934440121, 101.2510903946856757 ) ) ;
#114684 = CYLINDRICAL_SURFACE ( 'NONE', #102375, 1.500000000000001332 ) ;
#114687 = CARTESIAN_POINT ( 'NONE',  ( 13.97604488694527802, 13.89961937509977652, 69.37390960531436690 ) ) ;
#114686 = CARTESIAN_POINT ( 'NONE',  ( -5.153800228976328057, -19.02544592524343514, 82.29057627198103830 ) ) ;
#114685 = CARTESIAN_POINT ( 'NONE',  ( -21.55341960407619339, 5.719274019375674811, 53.54275706135234714 ) ) ;
#114688 = CARTESIAN_POINT ( 'NONE',  ( 13.97604488694527802, 13.89961937509977652, 89.37390960531436690 ) ) ;
#114689 = CARTESIAN_POINT ( 'NONE',  ( -14.34966873604960291, -8.224510206698953496, 51.66557627198102409 ) ) ;
#114690 = CARTESIAN_POINT ( 'NONE',  ( 16.55341960407618274, -4.379528057220086978, 101.0427570613523756 ) ) ;
#114691 = CARTESIAN_POINT ( 'NONE',  ( -0.05219959533910754901, -16.53943276465976808, 22.49890960531436335 ) ) ;
#114692 = ORIENTED_EDGE ( 'NONE', *, *, #24537, .T. ) ;
#114693 = CARTESIAN_POINT ( 'NONE',  ( 19.02544592524334988, 5.153800228976608722, 46.45942372801899012 ) ) ;
#114695 = CIRCLE ( 'NONE', #27569, 2.041999999999999815 ) ;
#114694 = CARTESIAN_POINT ( 'NONE',  ( -5.049401038298153566, 19.05341960407611168, 115.2072429386477097 ) ) ;
#114696 = CARTESIAN_POINT ( 'NONE',  ( -13.97604488694527625, -13.89961937509977652, 61.87390960531435979 ) ) ;
#114697 = CARTESIAN_POINT ( 'NONE',  ( -13.97604488694547697, 13.89961937509957934, 43.12609039468566152 ) ) ;
#114698 = CARTESIAN_POINT ( 'NONE',  ( -36.91746825000001309, -11.99521256947794789, -2.524999997268813523 ) ) ;
#114699 = CARTESIAN_POINT ( 'NONE',  ( -3.573655867282028392E-15, 2.428612866367529932E-14, 155.0000000000000000 ) ) ;
#114700 = AXIS2_PLACEMENT_3D ( 'NONE', #125340, #170847, #32338 ) ;
#114702 = CARTESIAN_POINT ( 'NONE',  ( -16.55341960407617563, 4.379528057220093196, 73.54275706135234714 ) ) ;
#114701 = CARTESIAN_POINT ( 'NONE',  ( -9.474510206698720793, -16.51473224551083518, 84.58442372801900433 ) ) ;
#114703 = CARTESIAN_POINT ( 'NONE',  ( 16.81555441253553695, 7.025013491695490941, 91.86314554665746357 ) ) ;
#114704 = CARTESIAN_POINT ( 'NONE',  ( -19.05341960407611168, -5.049401038298163336, 96.45724293864769550 ) ) ;
#114705 = CARTESIAN_POINT ( 'NONE',  ( -10.81492255796105439, 18.62759615963255655, 22.91775706135235069 ) ) ;
#114706 = CARTESIAN_POINT ( 'NONE',  ( 5.049401038297881783, 19.05341960407617563, 82.29275706135229029 ) ) ;
#114708 = CARTESIAN_POINT ( 'NONE',  ( -13.89961937509977652, 13.97604488694528158, 45.62390960531433848 ) ) ;
#114707 = CARTESIAN_POINT ( 'NONE',  ( 16.38665767535054130, 7.295008042176063690, 87.23599135785460135 ) ) ;
#114709 = CARTESIAN_POINT ( 'NONE',  ( -16.46253265017160317, 9.564922557960807481, 90.83224293864769550 ) ) ;
#114711 = CARTESIAN_POINT ( 'NONE',  ( -5.049401038298153566, 19.05341960407611168, 40.20724293864768839 ) ) ;
#114710 = CARTESIAN_POINT ( 'NONE',  ( 4.483927247898545687, 16.52544592524342804, 44.79057627198103120 ) ) ;
#114712 = CARTESIAN_POINT ( 'NONE',  ( -9.474510206698720793, -16.51473224551083518, 49.58442372801899722 ) ) ;
#114713 = VERTEX_POINT ( 'NONE', #160995 ) ;
#114714 = CARTESIAN_POINT ( 'NONE',  ( -14.34966873604960291, -8.224510206698953496, 91.66557627198103830 ) ) ;
#114715 = CARTESIAN_POINT ( 'NONE',  ( -19.03943276465977164, -0.05219959533935918106, 33.75109039468566863 ) ) ;
#114716 = CARTESIAN_POINT ( 'NONE',  ( 19.03943276465977164, -0.05219959533909143690, 63.74890960531435979 ) ) ;
#114717 = CARTESIAN_POINT ( 'NONE',  ( -18.67979575497178146, -10.72451020669898902, 66.66557627198102409 ) ) ;
#114719 = CARTESIAN_POINT ( 'NONE',  ( -19.03943276465977164, -0.05219959533935918106, 18.75109039468567218 ) ) ;
#114718 = CARTESIAN_POINT ( 'NONE',  ( 14.29746914071049879, -8.314922557960816363, 53.33224293864769550 ) ) ;
#114720 = CARTESIAN_POINT ( 'NONE',  ( -5.153800228976328057, -19.02544592524343514, 112.2905762719810099 ) ) ;
#114721 = CARTESIAN_POINT ( 'NONE',  ( 21.53943276465977519, -0.05219959533907433946, 23.74890960531435269 ) ) ;
#114722 = CARTESIAN_POINT ( 'NONE',  ( 5.049401038298161559, -19.05341960407611168, 57.70724293864769550 ) ) ;
#114723 = CARTESIAN_POINT ( 'NONE',  ( 13.97604488694527802, 13.89961937509977652, 24.37390960531435624 ) ) ;
#114724 = CARTESIAN_POINT ( 'NONE',  ( -14.34966873604960291, -8.224510206698953496, 96.66557627198102409 ) ) ;
#114725 = CARTESIAN_POINT ( 'NONE',  ( -10.81492255796078084, -18.62759615963271287, 107.0822429386476955 ) ) ;
#114726 = CARTESIAN_POINT ( 'NONE',  ( 19.03943276465977164, -0.05219959533909143690, 98.74890960531436690 ) ) ;
#114727 = CARTESIAN_POINT ( 'NONE',  ( -15.80617190586745835, -15.72974639402198527, 106.8739096053143811 ) ) ;
#114728 = CARTESIAN_POINT ( 'NONE',  ( 9.474510206698971260, -16.51473224551069308, 97.91557627198102409 ) ) ;
#114729 = CARTESIAN_POINT ( 'NONE',  ( -12.14591786802309592, -12.06949235617757132, 111.8739096053143669 ) ) ;
#114730 = CARTESIAN_POINT ( 'NONE',  ( -21.52544592524334988, -5.823673210054445271, 78.95942372801901854 ) ) ;
#114731 = CARTESIAN_POINT ( 'NONE',  ( 10.81492255796078972, 18.62759615963270932, 89.58224293864768129 ) ) ;
#114732 = CARTESIAN_POINT ( 'NONE',  ( 17.44270441346516520, -5.991230190323040716, 106.1366492073577064 ) ) ;
#114733 = DIRECTION ( 'NONE',  ( 0.000000000000000000, 0.000000000000000000, -1.000000000000000000 ) ) ;
#114734 = CARTESIAN_POINT ( 'NONE',  ( 11.95117975717237080, -11.66618673445833920, -61.34707691135563579 ) ) ;
#114735 = CARTESIAN_POINT ( 'NONE',  ( 14.34966873604972726, -8.224510206698740333, 40.83442372801901854 ) ) ;
#114736 = CARTESIAN_POINT ( 'NONE',  ( 16.55341960407611168, 4.379528057220329451, 103.9572429386476813 ) ) ;
#114737 = CARTESIAN_POINT ( 'NONE',  ( 19.24578484527059175, -180.9428398739492820, -15.00000000000000000 ) ) ;
#114738 = CARTESIAN_POINT ( 'NONE',  ( 9.564922557960805705, 16.46253265017160317, 64.58224293864769550 ) ) ;
#114739 = CARTESIAN_POINT ( 'NONE',  ( 12.14591786802309770, 12.06949235617756955, 99.37390960531436690 ) ) ;
#114740 = CARTESIAN_POINT ( 'NONE',  ( 18.62759615963271287, -10.81492255796078972, 38.33224293864768839 ) ) ;
#114741 = CARTESIAN_POINT ( 'NONE',  ( -8.314922557960811034, -14.29746914071050412, 62.08224293864769550 ) ) ;
#114742 = CARTESIAN_POINT ( 'NONE',  ( 5.049401038297881783, 19.05341960407617563, 112.2927570613523471 ) ) ;
#114743 = CARTESIAN_POINT ( 'NONE',  ( -15.72974639402176322, -15.80617190586768395, 79.37609039468567573 ) ) ;
#114744 = CARTESIAN_POINT ( 'NONE',  ( -18.22780087662122028, 5.500000000000031086, 63.51540105326107266 ) ) ;
#114745 = CARTESIAN_POINT ( 'NONE',  ( -14.34966873604972548, 8.224510206698743886, 93.33442372801901854 ) ) ;
#114746 = CARTESIAN_POINT ( 'NONE',  ( 14.29746914071049879, -8.314922557960816363, 38.33224293864768839 ) ) ;
#114747 = CARTESIAN_POINT ( 'NONE',  ( 5.049401038298161559, -19.05341960407611168, 32.70724293864768129 ) ) ;
#114748 = CARTESIAN_POINT ( 'NONE',  ( 9.564922557960805705, 16.46253265017160317, 94.58224293864769550 ) ) ;
#114749 = CARTESIAN_POINT ( 'NONE',  ( 21.55341960407610458, 5.719274019375980345, 93.95724293864770971 ) ) ;
#114750 = CARTESIAN_POINT ( 'NONE',  ( 8.314922557961029526, -14.29746914071037800, 20.41775706135234714 ) ) ;
#114752 = CARTESIAN_POINT ( 'NONE',  ( -21.52544592524334988, -5.823673210054445271, 68.95942372801901854 ) ) ;
#114751 = CARTESIAN_POINT ( 'NONE',  ( -4.379528057220328563, 16.55341960407611168, 60.20724293864768839 ) ) ;
#114753 = CARTESIAN_POINT ( 'NONE',  ( 12.14591786802327356, -12.06949235617739191, 105.6260903946856899 ) ) ;
#114754 = CARTESIAN_POINT ( 'NONE',  ( 17.05587630539785948, 6.762274262135715475, 26.75819690962688924 ) ) ;
#114755 = CARTESIAN_POINT ( 'NONE',  ( -19.49671883438228193, -5.499999999999979572, 64.89279849105683695 ) ) ;
#114756 = CARTESIAN_POINT ( 'NONE',  ( -8.224510206698948167, 14.34966873604960824, 30.41557627198101699 ) ) ;
#114757 = CARTESIAN_POINT ( 'NONE',  ( 16.55341960407618274, -4.379528057220086978, 71.04275706135234714 ) ) ;
#114758 = CARTESIAN_POINT ( 'NONE',  ( 9.474510206698971260, -16.51473224551069308, 82.91557627198103830 ) ) ;
#114759 = CARTESIAN_POINT ( 'NONE',  ( -9.564922557960796823, -16.46253265017161027, 82.08224293864768129 ) ) ;
#114760 = CARTESIAN_POINT ( 'NONE',  ( -5.823673210054431948, 21.52544592524334988, 87.70942372801901854 ) ) ;
#114761 = CARTESIAN_POINT ( 'NONE',  ( -16.52544592524335698, -4.483927247898792601, 88.95942372801901854 ) ) ;
#114762 = CARTESIAN_POINT ( 'NONE',  ( 12.14591786802309770, 12.06949235617756955, 59.37390960531436690 ) ) ;
#114763 = CARTESIAN_POINT ( 'NONE',  ( -19.05341960407611168, -5.049401038298163336, 71.45724293864766707 ) ) ;
#114764 = VERTEX_POINT ( 'NONE', #142823 ) ;
#114765 = CARTESIAN_POINT ( 'NONE',  ( 5.049401038297881783, 19.05341960407617563, 107.2927570613523187 ) ) ;
#114766 = CARTESIAN_POINT ( 'NONE',  ( -12.14591786802309592, -12.06949235617757132, 111.8739096053143669 ) ) ;
#114767 = CARTESIAN_POINT ( 'NONE',  ( 0.05219959533909260263, 19.03943276465977164, 79.99890960531436690 ) ) ;
#114769 = CARTESIAN_POINT ( 'NONE',  ( 22.81625015709510151, -31.40387420917324590, -9.924999997268814766 ) ) ;
#114768 = CARTESIAN_POINT ( 'NONE',  ( 5.153800228976615827, -19.02544592524334988, 110.2094237280189901 ) ) ;
#114770 = CARTESIAN_POINT ( 'NONE',  ( 5.153800228976615827, -19.02544592524334988, 25.20942372801900433 ) ) ;
#114771 = CARTESIAN_POINT ( 'NONE',  ( 14.29746914071037800, 8.314922557961029526, 86.66775706135234714 ) ) ;
#114772 = CARTESIAN_POINT ( 'NONE',  ( 19.02544592524334988, 5.153800228976608722, 96.45942372801897591 ) ) ;
#114773 = CARTESIAN_POINT ( 'NONE',  ( -8.314922557960811034, -14.29746914071050412, 112.0822429386477097 ) ) ;
#114774 = CARTESIAN_POINT ( 'NONE',  ( 4.379528057220092307, 16.55341960407617563, 62.29275706135236845 ) ) ;
#114775 = CARTESIAN_POINT ( 'NONE',  ( 14.29746914071037800, 8.314922557961029526, 56.66775706135235424 ) ) ;
#114776 = CARTESIAN_POINT ( 'NONE',  ( -5.049401038298153566, 19.05341960407611168, 25.20724293864768484 ) ) ;
#114777 = CARTESIAN_POINT ( 'NONE',  ( 13.97604488694548053, -13.89961937509957401, 50.62609039468566152 ) ) ;
#114778 = AXIS2_PLACEMENT_3D ( 'NONE', #5635, #6631, #113804 ) ;
#114779 = CARTESIAN_POINT ( 'NONE',  ( 15.72974639402176855, 15.80617190586768217, 91.87609039468568994 ) ) ;
#114780 = CARTESIAN_POINT ( 'NONE',  ( 13.89961937509977652, -13.97604488694527269, 28.12390960531435624 ) ) ;
#114781 = CARTESIAN_POINT ( 'NONE',  ( -19.03943276465977164, 0.05219959533909376836, 81.24890960531436690 ) ) ;
#114782 = CARTESIAN_POINT ( 'NONE',  ( 16.53943276465976808, -0.05219959533910856209, 78.74890960531436690 ) ) ;
#114783 = CARTESIAN_POINT ( 'NONE',  ( -0.05219959533937732626, 21.53943276465977519, 87.50109039468568994 ) ) ;
#114784 = CARTESIAN_POINT ( 'NONE',  ( -5.049401038297874678, -19.05341960407617918, 59.79275706135231871 ) ) ;
#114785 = CARTESIAN_POINT ( 'NONE',  ( -13.89961937509957401, -13.97604488694547875, 39.37609039468566152 ) ) ;
#114786 = CARTESIAN_POINT ( 'NONE',  ( 21.55341960407610458, 5.719274019375980345, 33.95724293864769550 ) ) ;
#114787 = CARTESIAN_POINT ( 'NONE',  ( 10.72451020669871369, 18.67979575497193778, 92.08442372801901854 ) ) ;
#114788 = CARTESIAN_POINT ( 'NONE',  ( -19.03943276465977164, 0.05219959533909376836, 71.24890960531435269 ) ) ;
#114789 = CARTESIAN_POINT ( 'NONE',  ( 5.719274019375673035, 21.55341960407619339, 112.2927570613523471 ) ) ;
#114790 = CARTESIAN_POINT ( 'NONE',  ( -15.72974639402197994, 15.80617190586746368, 55.62390960531436690 ) ) ;
#114791 = CARTESIAN_POINT ( 'NONE',  ( 5.049401038298161559, -19.05341960407611168, 97.70724293864766707 ) ) ;
#114792 = CARTESIAN_POINT ( 'NONE',  ( -5.153800228976607833, 19.02544592524334988, 77.70942372801900433 ) ) ;
#114793 = CARTESIAN_POINT ( 'NONE',  ( -19.05341960407611168, -5.049401038298163336, 106.4572429386476955 ) ) ;
#114794 = CARTESIAN_POINT ( 'NONE',  ( 0.05219959533936267826, -19.03943276465977164, 100.0010903946856757 ) ) ;
#114795 = CARTESIAN_POINT ( 'NONE',  ( 4.483927247898790824, -16.52544592524335698, 40.20942372801901854 ) ) ;
#114796 = CARTESIAN_POINT ( 'NONE',  ( 12.06949235617757843, -12.14591786802309237, 108.1239096053143811 ) ) ;
#114797 = CARTESIAN_POINT ( 'NONE',  ( 5.049401038298161559, -19.05341960407611168, 77.70724293864765286 ) ) ;
#114798 = CARTESIAN_POINT ( 'NONE',  ( 10.81492255796078972, 18.62759615963270932, 69.58224293864769550 ) ) ;
#114799 = CARTESIAN_POINT ( 'NONE',  ( -16.55341960407617563, 4.379528057220093196, 38.54275706135234714 ) ) ;
#114800 = CARTESIAN_POINT ( 'NONE',  ( 10.81492255796106328, -18.62759615963255655, 40.41775706135234714 ) ) ;
#114801 = CARTESIAN_POINT ( 'NONE',  ( 15.72974639402176855, 15.80617190586768217, 86.87609039468568994 ) ) ;
#114802 = CARTESIAN_POINT ( 'NONE',  ( -4.379528057220086978, -16.55341960407618274, 79.79275706135236135 ) ) ;
#114803 = CARTESIAN_POINT ( 'NONE',  ( 9.564922557960805705, 16.46253265017160317, 74.58224293864769550 ) ) ;
#114804 = CARTESIAN_POINT ( 'NONE',  ( -4.379528057220328563, 16.55341960407611168, 75.20724293864769550 ) ) ;
#114805 = CARTESIAN_POINT ( 'NONE',  ( 12.06949235617757843, -12.14591786802309237, 23.12390960531436335 ) ) ;
#114806 = CARTESIAN_POINT ( 'NONE',  ( -0.05219959533936034679, 19.03943276465977164, 52.50109039468566863 ) ) ;
#114807 = ADVANCED_FACE ( 'NONE', ( #158985 ), #4303, .F. ) ;
#114808 = CARTESIAN_POINT ( 'NONE',  ( -15.80617190586768217, 15.72974639402176855, 38.12609039468567573 ) ) ;
#114809 = CARTESIAN_POINT ( 'NONE',  ( 4.379528057220339221, -16.55341960407611168, 72.70724293864769550 ) ) ;
#114810 = CARTESIAN_POINT ( 'NONE',  ( -18.67979575497178146, -10.72451020669898902, 21.66557627198102409 ) ) ;
#114811 = CARTESIAN_POINT ( 'NONE',  ( -4.483927247898782831, 16.52544592524335698, 107.7094237280190328 ) ) ;
#114812 = CARTESIAN_POINT ( 'NONE',  ( -18.67979575497193778, 10.72451020669871902, 78.33442372801901854 ) ) ;
#114813 = CARTESIAN_POINT ( 'NONE',  ( 4.379528057220092307, 16.55341960407617563, 42.29275706135235424 ) ) ;
#114814 = CARTESIAN_POINT ( 'NONE',  ( -5.719274019375665041, -21.55341960407619695, 39.79275706135235424 ) ) ;
#114815 = ORIENTED_EDGE ( 'NONE', *, *, #53785, .T. ) ;
#114816 = CARTESIAN_POINT ( 'NONE',  ( -10.81492255796078084, -18.62759615963271287, 112.0822429386477097 ) ) ;
#114817 = CARTESIAN_POINT ( 'NONE',  ( -14.29746914071049879, 8.314922557960819915, 85.83224293864768129 ) ) ;
#114818 = CARTESIAN_POINT ( 'NONE',  ( 17.49999999999996803, -3.512728167237031407, 27.72809995181124521 ) ) ;
#114819 = CARTESIAN_POINT ( 'NONE',  ( -0.05219959533910754901, -16.53943276465976808, 47.49890960531435979 ) ) ;
#114820 = CARTESIAN_POINT ( 'NONE',  ( -0.05219959533934338120, 16.53943276465976808, 92.50109039468567573 ) ) ;
#114821 = CARTESIAN_POINT ( 'NONE',  ( -16.46253265017160317, 9.564922557960807481, 40.83224293864769550 ) ) ;
#114822 = CARTESIAN_POINT ( 'NONE',  ( 5.719274019375991003, -21.55341960407610458, 47.70724293864770260 ) ) ;
#114823 = CARTESIAN_POINT ( 'NONE',  ( 16.53943276465976808, -0.05219959533910856209, 78.74890960531436690 ) ) ;
#114824 = CARTESIAN_POINT ( 'NONE',  ( 15.80617190586746368, 15.72974639402197994, 84.37390960531438111 ) ) ;
#114825 = CARTESIAN_POINT ( 'NONE',  ( -16.51473224551069308, -9.474510206698971260, 81.66557627198103830 ) ) ;
#114827 = CARTESIAN_POINT ( 'NONE',  ( 5.153800228976615827, -19.02544592524334988, 90.20942372801900433 ) ) ;
#114826 = CARTESIAN_POINT ( 'NONE',  ( 13.89961937509977652, -13.97604488694527269, 33.12390960531434558 ) ) ;
#114828 = CARTESIAN_POINT ( 'NONE',  ( -21.52544592524343514, 5.823673210054127303, 26.04057627198103475 ) ) ;
#114830 = CARTESIAN_POINT ( 'NONE',  ( -0.05219959533907301413, -21.53943276465977519, 57.49890960531435979 ) ) ;
#114829 = CARTESIAN_POINT ( 'NONE',  ( 21.53943276465977519, 0.05219959533937863772, 51.25109039468568994 ) ) ;
#114831 = CARTESIAN_POINT ( 'NONE',  ( -9.474510206698964154, 16.51473224551069663, 55.41557627198103120 ) ) ;
#114832 = CARTESIAN_POINT ( 'NONE',  ( -13.89961937509977652, 13.97604488694528158, 75.62390960531438111 ) ) ;
#114833 = VERTEX_POINT ( 'NONE', #53824 ) ;
#114834 = CARTESIAN_POINT ( 'NONE',  ( -8.224510206698735004, -14.34966873604973081, 44.58442372801901854 ) ) ;
#114835 = CARTESIAN_POINT ( 'NONE',  ( -5.719274019375665041, -21.55341960407619695, 24.79275706135235779 ) ) ;
#114836 = CARTESIAN_POINT ( 'NONE',  ( -5.719274019375665041, -21.55341960407619695, 79.79275706135236135 ) ) ;
#114837 = CARTESIAN_POINT ( 'NONE',  ( 19.02544592524343514, -5.153800228976328945, 113.5405762719810241 ) ) ;
#114838 = CARTESIAN_POINT ( 'NONE',  ( -0.05219959533907301413, -21.53943276465977519, 82.49890960531436690 ) ) ;
#114840 = CARTESIAN_POINT ( 'NONE',  ( 4.379528057220092307, 16.55341960407617563, 67.29275706135234714 ) ) ;
#114839 = CARTESIAN_POINT ( 'NONE',  ( 21.55341960407619695, -5.719274019375665929, 26.04275706135235779 ) ) ;
#114841 = CARTESIAN_POINT ( 'NONE',  ( -5.719274019375978568, 21.55341960407610458, 65.20724293864768129 ) ) ;
#114842 = CARTESIAN_POINT ( 'NONE',  ( 19.03943276465977164, 0.05219959533936151252, 21.25109039468565797 ) ) ;
#114843 = CARTESIAN_POINT ( 'NONE',  ( -0.05219959533909027116, -19.03943276465977164, 57.49890960531435979 ) ) ;
#114844 = CARTESIAN_POINT ( 'NONE',  ( 5.049401038298161559, -19.05341960407611168, 107.7072429386476955 ) ) ;
#114845 = CARTESIAN_POINT ( 'NONE',  ( -9.474510206698964154, 16.51473224551069663, 95.41557627198102409 ) ) ;
#114846 = CARTESIAN_POINT ( 'NONE',  ( 17.50000000000000355, 3.203707223489912881, 102.7268034735096904 ) ) ;
#114847 = CARTESIAN_POINT ( 'NONE',  ( -19.03943276465977164, -0.05219959533935918106, 68.75109039468566152 ) ) ;
#114848 = CARTESIAN_POINT ( 'NONE',  ( -21.55341960407610458, -5.719274019375992779, 46.45724293864769550 ) ) ;
#114849 = CARTESIAN_POINT ( 'NONE',  ( -14.34966873604972548, 8.224510206698743886, 113.3344237280190328 ) ) ;
#114850 = CARTESIAN_POINT ( 'NONE',  ( -5.049401038297874678, -19.05341960407617918, 99.79275706135234714 ) ) ;
#114851 = CARTESIAN_POINT ( 'NONE',  ( 9.564922557960805705, 16.46253265017160317, 24.58224293864769194 ) ) ;
#114852 = CARTESIAN_POINT ( 'NONE',  ( 9.564922557961047289, -16.46253265017146816, 20.41775706135233293 ) ) ;
#114853 = CARTESIAN_POINT ( 'NONE',  ( 9.564922557961047289, -16.46253265017146816, 90.41775706135234714 ) ) ;
#114855 = CARTESIAN_POINT ( 'NONE',  ( -13.89961937509957401, -13.97604488694547875, 59.37609039468566863 ) ) ;
#114854 = CARTESIAN_POINT ( 'NONE',  ( 10.72451020669898902, -18.67979575497178502, 87.91557627198103830 ) ) ;
#114856 = CARTESIAN_POINT ( 'NONE',  ( 16.38665767535055195, 7.295008042176104546, 107.2359913578545587 ) ) ;
#114857 = CARTESIAN_POINT ( 'NONE',  ( 19.05341960407611168, 5.049401038298154454, 58.95724293864768129 ) ) ;
#114858 = CARTESIAN_POINT ( 'NONE',  ( 12.06949235617757843, -12.14591786802309237, 68.12390960531436690 ) ) ;
#114859 = CARTESIAN_POINT ( 'NONE',  ( -9.474510206698964154, 16.51473224551069663, 50.41557627198102409 ) ) ;
#114860 = CARTESIAN_POINT ( 'NONE',  ( 4.483927247898545687, 16.52544592524342804, 49.79057627198102409 ) ) ;
#114861 = CYLINDRICAL_SURFACE ( 'NONE', #100088, 2.000000000000001776 ) ;
#114862 = CARTESIAN_POINT ( 'NONE',  ( -8.314922557960811034, -14.29746914071050412, 32.08224293864769550 ) ) ;
#114863 = CARTESIAN_POINT ( 'NONE',  ( 19.05341960407611168, 5.049401038298154454, 63.95724293864769550 ) ) ;
#114864 = CARTESIAN_POINT ( 'NONE',  ( 16.51473224551083163, -9.474510206698727899, 20.83442372801899722 ) ) ;
#114865 = CARTESIAN_POINT ( 'NONE',  ( 8.314922557961029526, -14.29746914071037800, 30.41775706135234358 ) ) ;
#114866 = CARTESIAN_POINT ( 'NONE',  ( 10.81492255796078972, 18.62759615963270932, 49.58224293864769550 ) ) ;
#114868 = ORIENTED_EDGE ( 'NONE', *, *, #12204, .T. ) ;
#114867 = CARTESIAN_POINT ( 'NONE',  ( -18.62759615963255300, -10.81492255796106328, 99.16775706135234714 ) ) ;
#114869 = CARTESIAN_POINT ( 'NONE',  ( 19.05341960407611168, 5.049401038298154454, 58.95724293864768129 ) ) ;
#114870 = CARTESIAN_POINT ( 'NONE',  ( 2.649999999999999911, -165.0000000000000000, -15.00000000000000000 ) ) ;
#114871 = CARTESIAN_POINT ( 'NONE',  ( 13.89961937509977652, -13.97604488694527269, 93.12390960531436690 ) ) ;
#114872 = CARTESIAN_POINT ( 'NONE',  ( -29.86685920354755197, -21.69954338932560134, -4.424999997268812990 ) ) ;
#114873 = CARTESIAN_POINT ( 'NONE',  ( -21.52544592524334988, -5.823673210054445271, 23.95942372801901143 ) ) ;
#114874 = AXIS2_PLACEMENT_3D ( 'NONE', #36756, #162116, #19615 ) ;
#114875 = CARTESIAN_POINT ( 'NONE',  ( -12.14591786802309592, -12.06949235617757132, 91.87390960531436690 ) ) ;
#114876 = EDGE_CURVE ( 'NONE', #29557, #81477, #4363, .T. ) ;
#114878 = CARTESIAN_POINT ( 'NONE',  ( -9.474510206698964154, 16.51473224551069663, 65.41557627198102409 ) ) ;
#114877 = CARTESIAN_POINT ( 'NONE',  ( -18.67979575497178146, -10.72451020669898902, 91.66557627198103830 ) ) ;
#114879 = CARTESIAN_POINT ( 'NONE',  ( 0.05219959533909260263, 19.03943276465977164, 89.99890960531436690 ) ) ;
#114880 = CARTESIAN_POINT ( 'NONE',  ( 5.823673210054125526, 21.52544592524343514, 104.7905762719810241 ) ) ;
#114881 = VERTEX_POINT ( 'NONE', #95329 ) ;
#114882 = CARTESIAN_POINT ( 'NONE',  ( -5.049401038298153566, 19.05341960407611168, 70.20724293864769550 ) ) ;
#114883 = CARTESIAN_POINT ( 'NONE',  ( 19.35633801406909171, -5.499999999999674039, 96.63373818172770768 ) ) ;
#114885 = DIRECTION ( 'NONE',  ( -1.000000000000000000, -0.000000000000000000, -0.000000000000000000 ) ) ;
#114884 = CARTESIAN_POINT ( 'NONE',  ( -8.314922557960811034, -14.29746914071050412, 102.0822429386476955 ) ) ;
#114886 = CARTESIAN_POINT ( 'NONE',  ( -19.05341960407617563, 5.049401038297882671, 98.54275706135233293 ) ) ;
#114887 = CARTESIAN_POINT ( 'NONE',  ( -19.05341960407611168, -5.049401038298163336, 21.45724293864768839 ) ) ;
#114888 = CARTESIAN_POINT ( 'NONE',  ( 15.80617190586769283, -15.72974639402175789, 65.62609039468568994 ) ) ;
#114890 = CARTESIAN_POINT ( 'NONE',  ( 21.53943276465977519, 0.05219959533937863772, 36.25109039468567573 ) ) ;
#114889 = CARTESIAN_POINT ( 'NONE',  ( 19.02544592524343514, -5.153800228976328945, 68.54057627198103830 ) ) ;
#114891 = CARTESIAN_POINT ( 'NONE',  ( 10.81492255796078972, 18.62759615963270932, 104.5822429386477097 ) ) ;
#114892 = CARTESIAN_POINT ( 'NONE',  ( 23.31738231874054890, -16.94106989632523508, 142.7999999999999829 ) ) ;
#114893 = CARTESIAN_POINT ( 'NONE',  ( 19.03943276465977164, -0.05219959533909143690, 68.74890960531436690 ) ) ;
#114894 = CARTESIAN_POINT ( 'NONE',  ( -34.52594549653173317, 2.005792002353502844E-14, 89.49999999999897682 ) ) ;
#114896 = CARTESIAN_POINT ( 'NONE',  ( -21.52544592524343514, 5.823673210054127303, 26.04057627198103475 ) ) ;
#114895 = CARTESIAN_POINT ( 'NONE',  ( 14.29746914071037800, 8.314922557961029526, 21.66775706135235069 ) ) ;
#114897 = CARTESIAN_POINT ( 'NONE',  ( 21.52544592524334988, 5.823673210054432836, 56.45942372801902565 ) ) ;
#114898 = CARTESIAN_POINT ( 'NONE',  ( 5.049401038298161559, -19.05341960407611168, 112.7072429386476813 ) ) ;
#114899 = CARTESIAN_POINT ( 'NONE',  ( 0.05219959533936267826, -19.03943276465977164, 90.00109039468567573 ) ) ;
#114900 = CARTESIAN_POINT ( 'NONE',  ( 5.049401038298161559, -19.05341960407611168, 52.70724293864767418 ) ) ;
#114901 = CARTESIAN_POINT ( 'NONE',  ( -5.153800228976328057, -19.02544592524343514, 67.29057627198102409 ) ) ;
#114902 = CARTESIAN_POINT ( 'NONE',  ( 0.05219959533910956823, 16.53943276465976808, 99.99890960531436690 ) ) ;
#114903 = CARTESIAN_POINT ( 'NONE',  ( -13.97604488694527625, -13.89961937509977652, 106.8739096053143669 ) ) ;
#114904 = CARTESIAN_POINT ( 'NONE',  ( 8.224510206698953496, -14.34966873604960469, 87.91557627198103830 ) ) ;
#114905 = CARTESIAN_POINT ( 'NONE',  ( -19.02544592524342804, 5.153800228976336051, 101.0405762719810241 ) ) ;
#114907 = CARTESIAN_POINT ( 'NONE',  ( -9.564922557960796823, -16.46253265017161027, 47.08224293864769550 ) ) ;
#114906 = CARTESIAN_POINT ( 'NONE',  ( -0.05219959533910754901, -16.53943276465976808, 57.49890960531435979 ) ) ;
#114908 = CARTESIAN_POINT ( 'NONE',  ( -10.81492255796105439, 18.62759615963255655, 52.91775706135235424 ) ) ;
#114909 = CARTESIAN_POINT ( 'NONE',  ( 13.89961937509957401, 13.97604488694547697, 91.87609039468567573 ) ) ;
#114910 = CARTESIAN_POINT ( 'NONE',  ( -16.53943276465976808, 0.05219959533911058130, 46.24890960531435979 ) ) ;
#114911 = CARTESIAN_POINT ( 'NONE',  ( -21.53943276465977519, 0.05219959533907696930, 96.24890960531435269 ) ) ;
#114912 = CARTESIAN_POINT ( 'NONE',  ( 10.72451020669898902, -18.67979575497178502, 47.91557627198102409 ) ) ;
#114915 = CARTESIAN_POINT ( 'NONE',  ( -16.52544592524342804, 4.483927247898546575, 81.04057627198102409 ) ) ;
#114914 = CARTESIAN_POINT ( 'NONE',  ( -9.474510206698964154, 16.51473224551069663, 110.4155762719810383 ) ) ;
#114913 = AXIS2_PLACEMENT_3D ( 'NONE', #42699, #27544, #74034 ) ;
#114916 = CARTESIAN_POINT ( 'NONE',  ( -28.82186960331499392, -9.364793116373526516, 138.3500000054623911 ) ) ;
#114917 = CARTESIAN_POINT ( 'NONE',  ( -19.02544592524342804, 5.153800228976336051, 56.04057627198100988 ) ) ;
#114918 = CARTESIAN_POINT ( 'NONE',  ( 4.483927247898790824, -16.52544592524335698, 110.2094237280190185 ) ) ;
#114919 = CARTESIAN_POINT ( 'NONE',  ( 4.483927247898790824, -16.52544592524335698, 95.20942372801903275 ) ) ;
#114920 = CARTESIAN_POINT ( 'NONE',  ( -12.14591786802326823, 12.06949235617739902, 78.12609039468570415 ) ) ;
#114921 = CARTESIAN_POINT ( 'NONE',  ( 0.05219959533936267826, -19.03943276465977164, 40.00109039468566152 ) ) ;
#114923 = CARTESIAN_POINT ( 'NONE',  ( 0.05219959533909260263, 19.03943276465977164, 109.9989096053143669 ) ) ;
#114922 = CARTESIAN_POINT ( 'NONE',  ( -16.81555441253551919, 7.025013491695477619, 70.63685445334257906 ) ) ;
#114924 = CARTESIAN_POINT ( 'NONE',  ( 5.153800228976335163, 19.02544592524342804, 89.79057627198102409 ) ) ;
#114925 = CARTESIAN_POINT ( 'NONE',  ( -19.03943276465977164, 0.05219959533909376836, 36.24890960531436690 ) ) ;
#114926 = CARTESIAN_POINT ( 'NONE',  ( -16.53943276465976808, 0.05219959533911058130, 46.24890960531435979 ) ) ;
#114928 = CARTESIAN_POINT ( 'NONE',  ( 0.05219959533909260263, 19.03943276465977164, 109.9989096053143669 ) ) ;
#114927 =( NAMED_UNIT ( * ) PLANE_ANGLE_UNIT ( ) SI_UNIT ( $, .RADIAN. ) );
#114929 = CARTESIAN_POINT ( 'NONE',  ( -15.80617190586745835, -15.72974639402198527, 36.87390960531435979 ) ) ;
#114930 = CARTESIAN_POINT ( 'NONE',  ( -16.53943276465976808, 0.05219959533911058130, 91.24890960531436690 ) ) ;
#114931 = CARTESIAN_POINT ( 'NONE',  ( -0.05219959533934338120, 16.53943276465976808, 42.50109039468567573 ) ) ;
#114932 = CARTESIAN_POINT ( 'NONE',  ( 8.314922557960818139, 14.29746914071049879, 74.58224293864768129 ) ) ;
#114933 = CARTESIAN_POINT ( 'NONE',  ( -18.87075004821570801, 5.499999999999902300, 63.67408112101044537 ) ) ;
#114934 = CARTESIAN_POINT ( 'NONE',  ( 19.05341960407617918, -5.049401038297876454, 61.04275706135232582 ) ) ;
#114935 = CARTESIAN_POINT ( 'NONE',  ( 9.474510206698971260, -16.51473224551069308, 102.9155762719810241 ) ) ;
#114936 = CARTESIAN_POINT ( 'NONE',  ( -5.153800228976607833, 19.02544592524334988, 72.70942372801900433 ) ) ;
#114937 = CARTESIAN_POINT ( 'NONE',  ( 1.993301997531345686E-15, -30.30510711980685556, 142.5000000000000000 ) ) ;
#114939 = CARTESIAN_POINT ( 'NONE',  ( -14.34966873604960291, -8.224510206698953496, 21.66557627198102409 ) ) ;
#114938 = CARTESIAN_POINT ( 'NONE',  ( 8.314922557961029526, -14.29746914071037800, 30.41775706135234358 ) ) ;
#114940 = CARTESIAN_POINT ( 'NONE',  ( -13.97604488694547697, 13.89961937509957934, 68.12609039468563310 ) ) ;
#114941 = CARTESIAN_POINT ( 'NONE',  ( 18.62759615963271287, -10.81492255796078972, 33.33224293864769550 ) ) ;
#114942 = CARTESIAN_POINT ( 'NONE',  ( 0.05219959533937995610, -21.53943276465977519, 70.00109039468568994 ) ) ;
#114943 = CARTESIAN_POINT ( 'NONE',  ( 18.93472913878450825, 5.499999999999855227, 38.78010116131535767 ) ) ;
#114944 = CARTESIAN_POINT ( 'NONE',  ( 16.55341960407618274, -4.379528057220086978, 26.04275706135235779 ) ) ;
#114946 = CARTESIAN_POINT ( 'NONE',  ( 5.049401038298161559, -19.05341960407611168, 92.70724293864769550 ) ) ;
#114945 = CARTESIAN_POINT ( 'NONE',  ( -19.03943276465977164, 0.05219959533909376836, 26.24890960531435624 ) ) ;
#114947 = CARTESIAN_POINT ( 'NONE',  ( 14.67883866103747970, 15.69994562750269473, -58.73507448357032246 ) ) ;
#114949 = CARTESIAN_POINT ( 'NONE',  ( -16.46253265017160317, 9.564922557960807481, 85.83224293864769550 ) ) ;
#114948 = CARTESIAN_POINT ( 'NONE',  ( -0.05219959533910754901, -16.53943276465976808, 87.49890960531436690 ) ) ;
#114950 = PRODUCT_CONTEXT ( 'NONE', #68669, 'mechanical' ) ;
#114951 = CARTESIAN_POINT ( 'NONE',  ( 9.564922557960805705, 16.46253265017160317, 89.58224293864769550 ) ) ;
#114952 = ORIENTED_EDGE ( 'NONE', *, *, #56474, .F. ) ;
#114953 = CARTESIAN_POINT ( 'NONE',  ( -5.049401038297874678, -19.05341960407617918, 84.79275706135233293 ) ) ;
#114954 = CARTESIAN_POINT ( 'NONE',  ( -18.67979575497178146, -10.72451020669898902, 76.66557627198103830 ) ) ;
#114955 = CARTESIAN_POINT ( 'NONE',  ( 0.05219959533909260263, 19.03943276465977164, 29.99890960531435979 ) ) ;
#114957 = CARTESIAN_POINT ( 'NONE',  ( 0.05219959533907565091, 21.53943276465977519, 114.9989096053143669 ) ) ;
#114956 = CARTESIAN_POINT ( 'NONE',  ( 0.05219959533936267826, -19.03943276465977164, 70.00109039468566152 ) ) ;
#114958 = CARTESIAN_POINT ( 'NONE',  ( 13.89961937509977652, -13.97604488694527269, 68.12390960531436690 ) ) ;
#114959 = CARTESIAN_POINT ( 'NONE',  ( -5.153800228976328057, -19.02544592524343514, 102.2905762719810383 ) ) ;
#114960 = ORIENTED_EDGE ( 'NONE', *, *, #123771, .F. ) ;
#114961 = CARTESIAN_POINT ( 'NONE',  ( -21.55341960407610458, -5.719274019375992779, 101.4572429386476955 ) ) ;
#114964 = CARTESIAN_POINT ( 'NONE',  ( -0.05219959533936034679, 19.03943276465977164, 62.50109039468566863 ) ) ;
#114963 = CARTESIAN_POINT ( 'NONE',  ( -5.153800228976328057, -19.02544592524343514, 82.29057627198103830 ) ) ;
#114962 = CARTESIAN_POINT ( 'NONE',  ( 14.34966873604960469, 8.224510206698951720, 104.1655762719810241 ) ) ;
#114965 = CARTESIAN_POINT ( 'NONE',  ( 21.53943276465977519, -0.05219959533907433946, 88.74890960531436690 ) ) ;
#114966 = CARTESIAN_POINT ( 'NONE',  ( -18.62759615963270932, 10.81492255796079327, 75.83224293864769550 ) ) ;
#114967 = CARTESIAN_POINT ( 'NONE',  ( -14.34966873604960291, -8.224510206698953496, 41.66557627198103120 ) ) ;
#114968 = CARTESIAN_POINT ( 'NONE',  ( 5.719274019375673035, 21.55341960407619339, 112.2927570613523471 ) ) ;
#114970 = VECTOR ( 'NONE', #75534, 1000.000000000000114 ) ;
#114969 = CARTESIAN_POINT ( 'NONE',  ( -16.55341960407617563, 4.379528057220093196, 68.54275706135234714 ) ) ;
#114971 = CARTESIAN_POINT ( 'NONE',  ( -9.564922557960796823, -16.46253265017161027, 92.08224293864769550 ) ) ;
#114972 = CARTESIAN_POINT ( 'NONE',  ( -5.153800228976328057, -19.02544592524343514, 47.29057627198102409 ) ) ;
#114973 = CARTESIAN_POINT ( 'NONE',  ( -21.52544592524334988, -5.823673210054445271, 53.95942372801900433 ) ) ;
#114974 = CARTESIAN_POINT ( 'NONE',  ( 18.62759615963255655, 10.81492255796105972, 56.66775706135235424 ) ) ;
#114975 = CARTESIAN_POINT ( 'NONE',  ( -16.51473224551069308, -9.474510206698971260, 61.66557627198103120 ) ) ;
#114976 = CARTESIAN_POINT ( 'NONE',  ( 15.80617190586769283, -15.72974639402175789, 35.62609039468568994 ) ) ;
#114977 = CARTESIAN_POINT ( 'NONE',  ( 5.049401038297881783, 19.05341960407617563, 72.29275706135234714 ) ) ;
#114978 = CARTESIAN_POINT ( 'NONE',  ( -5.049401038297874678, -19.05341960407617918, 74.79275706135231871 ) ) ;
#114979 = CARTESIAN_POINT ( 'NONE',  ( 5.153800228976335163, 19.02544592524342804, 39.79057627198100988 ) ) ;
#114980 = CARTESIAN_POINT ( 'NONE',  ( 14.34966873604972726, -8.224510206698740333, 80.83442372801901854 ) ) ;
#114981 = CARTESIAN_POINT ( 'NONE',  ( -19.03943276465977164, 0.05219959533909376836, 51.24890960531436690 ) ) ;
#114982 = CARTESIAN_POINT ( 'NONE',  ( 21.04946095171255394, -10.24435024061060950, 168.3368280404224606 ) ) ;
#114983 = CARTESIAN_POINT ( 'NONE',  ( 5.153800228976335163, 19.02544592524342804, 94.79057627198103830 ) ) ;
#114984 = CARTESIAN_POINT ( 'NONE',  ( 19.03943276465977164, -0.05219959533909143690, 43.74890960531435979 ) ) ;
#114985 = CARTESIAN_POINT ( 'NONE',  ( 5.823673210054125526, 21.52544592524343514, 84.79057627198102409 ) ) ;
#114986 = CARTESIAN_POINT ( 'NONE',  ( 8.224510206698742110, 14.34966873604972548, 62.08442372801901143 ) ) ;
#114987 = CARTESIAN_POINT ( 'NONE',  ( 18.62759615963255655, 10.81492255796105972, 106.6677570613523756 ) ) ;
#114988 = CARTESIAN_POINT ( 'NONE',  ( 16.46253265017160672, -9.564922557960803928, 53.33224293864768839 ) ) ;
#114989 = CARTESIAN_POINT ( 'NONE',  ( 16.52544592524342804, -4.483927247898539470, 43.54057627198103830 ) ) ;
#114990 = CARTESIAN_POINT ( 'NONE',  ( 14.34966873604960469, 8.224510206698951720, 84.16557627198103830 ) ) ;
#114991 = CARTESIAN_POINT ( 'NONE',  ( 0.05219959533909260263, 19.03943276465977164, 74.99890960531435269 ) ) ;
#114992 = CARTESIAN_POINT ( 'NONE',  ( -21.52544592524334988, -5.823673210054445271, 33.95942372801901143 ) ) ;
#114993 = CARTESIAN_POINT ( 'NONE',  ( 9.564922557960805705, 16.46253265017160317, 89.58224293864769550 ) ) ;
#114994 = CARTESIAN_POINT ( 'NONE',  ( 5.823673210054444382, -21.52544592524334988, 100.2094237280190043 ) ) ;
#114995 = CARTESIAN_POINT ( 'NONE',  ( 16.52544592524335698, 4.483927247898782831, 66.45942372801903275 ) ) ;
#114996 = CARTESIAN_POINT ( 'NONE',  ( -21.53943276465977519, -0.05219959533937600094, 28.75109039468567929 ) ) ;
#114997 = CARTESIAN_POINT ( 'NONE',  ( -5.049401038298153566, 19.05341960407611168, 110.2072429386476671 ) ) ;
#114998 = ADVANCED_FACE ( 'NONE', ( #143820 ), #162569, .T. ) ;
#114999 = CARTESIAN_POINT ( 'NONE',  ( -21.52544592524343514, 5.823673210054127303, 91.04057627198103830 ) ) ;
#115000 = CARTESIAN_POINT ( 'NONE',  ( 12.06949235617757843, -12.14591786802309237, 48.12390960531436690 ) ) ;
#115001 = CARTESIAN_POINT ( 'NONE',  ( -0.05219959533909027116, -19.03943276465977164, 47.49890960531435979 ) ) ;
#115002 = CARTESIAN_POINT ( 'NONE',  ( 8.314922557960818139, 14.29746914071049879, 64.58224293864769550 ) ) ;
#115003 = CARTESIAN_POINT ( 'NONE',  ( 15.80617190586746368, 15.72974639402197994, 34.37390960531435979 ) ) ;
#115004 = CARTESIAN_POINT ( 'NONE',  ( 5.049401038297881783, 19.05341960407617563, 32.29275706135233293 ) ) ;
#115005 = CARTESIAN_POINT ( 'NONE',  ( -12.06949235617756955, 12.14591786802309770, 100.6239096053143811 ) ) ;
#115006 = CARTESIAN_POINT ( 'NONE',  ( 16.46253265017160672, -9.564922557960803928, 113.3322429386476955 ) ) ;
#115007 = ORIENTED_EDGE ( 'NONE', *, *, #182492, .T. ) ;
#115008 = CARTESIAN_POINT ( 'NONE',  ( -14.34966873604972548, 8.224510206698743886, 53.33442372801901854 ) ) ;
#115009 = CARTESIAN_POINT ( 'NONE',  ( -16.46253265017160317, 9.564922557960807481, 50.83224293864770260 ) ) ;
#115010 = CARTESIAN_POINT ( 'NONE',  ( -27.86273085795037829, -28.69962071417356242, 0.000000000000000000 ) ) ;
#115011 = CARTESIAN_POINT ( 'NONE',  ( -0.05219959533934338120, 16.53943276465976808, 87.50109039468568994 ) ) ;
#115012 = CARTESIAN_POINT ( 'NONE',  ( 12.14591786802327356, -12.06949235617739191, 20.62609039468568639 ) ) ;
#115013 = CARTESIAN_POINT ( 'NONE',  ( -5.719274019375665041, -21.55341960407619695, 74.79275706135234714 ) ) ;
#115014 = CARTESIAN_POINT ( 'NONE',  ( 5.153800228976335163, 19.02544592524342804, 74.79057627198103830 ) ) ;
#115015 = CARTESIAN_POINT ( 'NONE',  ( 21.52544592524344225, -5.823673210054117533, 88.54057627198103830 ) ) ;
#115016 = CARTESIAN_POINT ( 'NONE',  ( -0.05219959533934338120, 16.53943276465976808, 47.50109039468568994 ) ) ;
#115017 = CARTESIAN_POINT ( 'NONE',  ( -16.53943276465976808, 0.05219959533911058130, 116.2489096053143669 ) ) ;
#115018 = AXIS2_PLACEMENT_3D ( 'NONE', #88176, #54851, #87189 ) ;
#115019 = CARTESIAN_POINT ( 'NONE',  ( 8.224510206698742110, 14.34966873604972548, 22.08442372801901143 ) ) ;
#115020 = CARTESIAN_POINT ( 'NONE',  ( -0.05219959533936034679, 19.03943276465977164, 82.50109039468567573 ) ) ;
#115021 = CARTESIAN_POINT ( 'NONE',  ( -21.53943276465977519, 0.05219959533907696930, 76.24890960531435269 ) ) ;
#115022 = CARTESIAN_POINT ( 'NONE',  ( -9.474510206698720793, -16.51473224551083518, 49.58442372801899722 ) ) ;
#115023 = CARTESIAN_POINT ( 'NONE',  ( 19.52851543214744012, 5.499999999999982236, 97.89357721762578990 ) ) ;
#115024 = CARTESIAN_POINT ( 'NONE',  ( 18.67979575497178502, 10.72451020669898547, 89.16557627198102409 ) ) ;
#115025 = CARTESIAN_POINT ( 'NONE',  ( 17.97058386085787873, 5.500000000000054179, 61.50390968646219392 ) ) ;
#115026 = CARTESIAN_POINT ( 'NONE',  ( 13.89961937509977652, -13.97604488694527269, 63.12390960531435979 ) ) ;
#115027 = CARTESIAN_POINT ( 'NONE',  ( 3.766062262543149401E-15, -39.95556452105413570, -11.24999999453762456 ) ) ;
#115028 = CARTESIAN_POINT ( 'NONE',  ( -19.03943276465977164, -0.05219959533935918106, 108.7510903946856615 ) ) ;
#115029 = CARTESIAN_POINT ( 'NONE',  ( 14.64477982082356533, -37.22763889967101392, -11.21824398509625986 ) ) ;
#115030 = CARTESIAN_POINT ( 'NONE',  ( -10.81492255796105439, 18.62759615963255655, 52.91775706135235424 ) ) ;
#115032 = CARTESIAN_POINT ( 'NONE',  ( 16.53943276465976808, -0.05219959533910856209, 58.74890960531436690 ) ) ;
#115031 = CARTESIAN_POINT ( 'NONE',  ( -10.72451020669898014, 18.67979575497178502, 105.4155762719810383 ) ) ;
#115033 = CARTESIAN_POINT ( 'NONE',  ( 16.46253265017160672, -9.564922557960803928, 73.33224293864769550 ) ) ;
#115034 = CARTESIAN_POINT ( 'NONE',  ( -0.05219959533937732626, 21.53943276465977519, 67.50109039468568994 ) ) ;
#115036 = CARTESIAN_POINT ( 'NONE',  ( -9.474510206698720793, -16.51473224551083518, 29.58442372801900433 ) ) ;
#115035 = CARTESIAN_POINT ( 'NONE',  ( -14.29746914071037622, -8.314922557961029526, 19.16775706135234714 ) ) ;
#115037 = CARTESIAN_POINT ( 'NONE',  ( -18.67979575497193778, 10.72451020669871902, 43.33442372801901143 ) ) ;
#115038 = CARTESIAN_POINT ( 'NONE',  ( 10.72451020669898902, -18.67979575497178502, 107.9155762719810241 ) ) ;
#115039 = CARTESIAN_POINT ( 'NONE',  ( -15.80617190586745835, -15.72974639402198527, 56.87390960531436690 ) ) ;
#115040 = CARTESIAN_POINT ( 'NONE',  ( -16.51473224551082808, 9.474510206698731452, 93.33442372801900433 ) ) ;
#115041 = EDGE_CURVE ( 'NONE', #658, #138021, #18100, .T. ) ;
#115042 = CARTESIAN_POINT ( 'NONE',  ( -19.03943276465977164, -0.05219959533935918106, 63.75109039468566863 ) ) ;
#115043 = CARTESIAN_POINT ( 'NONE',  ( 21.55341960407619695, -5.719274019375665929, 86.04275706135236135 ) ) ;
#115044 = CARTESIAN_POINT ( 'NONE',  ( -5.049401038297874678, -19.05341960407617918, 59.79275706135231871 ) ) ;
#115045 = CARTESIAN_POINT ( 'NONE',  ( 19.03943276465977164, -0.05219959533909143690, 23.74890960531435269 ) ) ;
#115046 = CARTESIAN_POINT ( 'NONE',  ( -15.72974639402197994, 15.80617190586746368, 60.62390960531437401 ) ) ;
#115047 = CARTESIAN_POINT ( 'NONE',  ( -0.05219959533910754901, -16.53943276465976808, 52.49890960531435979 ) ) ;
#115048 = CARTESIAN_POINT ( 'NONE',  ( -19.99999999999998224, -188.0000000000000000, -4.999999999999999112 ) ) ;
#115049 = CARTESIAN_POINT ( 'NONE',  ( -13.89961937509957401, -13.97604488694547875, 34.37609039468566863 ) ) ;
#115050 = CARTESIAN_POINT ( 'NONE',  ( -8.314922557961024197, 14.29746914071037800, 87.91775706135234714 ) ) ;
#115051 = CARTESIAN_POINT ( 'NONE',  ( 8.224510206698953496, -14.34966873604960469, 37.91557627198102409 ) ) ;
#115052 = CARTESIAN_POINT ( 'NONE',  ( 21.55341960407619695, -5.719274019375665929, 81.04275706135236135 ) ) ;
#115053 = CARTESIAN_POINT ( 'NONE',  ( 10.81492255796106328, -18.62759615963255655, 80.41775706135234714 ) ) ;
#115054 = CARTESIAN_POINT ( 'NONE',  ( -10.81492255796078084, -18.62759615963271287, 87.08224293864769550 ) ) ;
#115055 = CARTESIAN_POINT ( 'NONE',  ( -19.02544592524342804, 5.153800228976336051, 41.04057627198103120 ) ) ;
#115056 = CARTESIAN_POINT ( 'NONE',  ( -5.823673210054431948, 21.52544592524334988, 52.70942372801902565 ) ) ;
#115057 = CARTESIAN_POINT ( 'NONE',  ( -19.02544592524342804, 5.153800228976336051, 31.04057627198102409 ) ) ;
#115058 = CARTESIAN_POINT ( 'NONE',  ( -19.03943276465977164, 0.05219959533909376836, 46.24890960531435979 ) ) ;
#115059 = CARTESIAN_POINT ( 'NONE',  ( -4.483927247898539470, -16.52544592524342804, 87.29057627198103830 ) ) ;
#115060 = CARTESIAN_POINT ( 'NONE',  ( -16.51473224551069308, -9.474510206698971260, 101.6655762719810241 ) ) ;
#115061 = VECTOR ( 'NONE', #191142, 1000.000000000000000 ) ;
#115062 = CARTESIAN_POINT ( 'NONE',  ( -12.06949235617756955, 12.14591786802309770, 40.62390960531435269 ) ) ;
#115063 = CARTESIAN_POINT ( 'NONE',  ( -8.224510206698948167, 14.34966873604960824, 115.4155762719810241 ) ) ;
#115064 = CARTESIAN_POINT ( 'NONE',  ( 0.05219959533907565091, 21.53943276465977519, 79.99890960531435269 ) ) ;
#115065 = CIRCLE ( 'NONE', #128038, 59.99999999999998579 ) ;
#115066 = CARTESIAN_POINT ( 'NONE',  ( 21.55341960407619695, -5.719274019375665929, 26.04275706135235779 ) ) ;
#115067 = CARTESIAN_POINT ( 'NONE',  ( 0.000000000000000000, 2.357898499370431722, -2.818925648462311528E-15 ) ) ;
#115068 = CARTESIAN_POINT ( 'NONE',  ( 8.224510206698742110, 14.34966873604972548, 32.08442372801901854 ) ) ;
#115069 = CARTESIAN_POINT ( 'NONE',  ( 5.823673210054125526, 21.52544592524343514, 64.79057627198103830 ) ) ;
#115070 = CARTESIAN_POINT ( 'NONE',  ( -15.72974639402176322, -15.80617190586768395, 99.37609039468568994 ) ) ;
#115071 = CARTESIAN_POINT ( 'NONE',  ( -16.51473224551069308, -9.474510206698971260, 96.66557627198102409 ) ) ;
#115072 = CARTESIAN_POINT ( 'NONE',  ( -10.72451020669870658, -18.67979575497194134, 29.58442372801901854 ) ) ;
#115073 = CARTESIAN_POINT ( 'NONE',  ( -10.72451020669898014, 18.67979575497178502, 25.41557627198103120 ) ) ;
#115074 = CARTESIAN_POINT ( 'NONE',  ( 8.224510206698742110, 14.34966873604972548, 87.08442372801901854 ) ) ;
#115075 = CARTESIAN_POINT ( 'NONE',  ( -10.81492255796105439, 18.62759615963255655, 67.91775706135234714 ) ) ;
#115076 = CARTESIAN_POINT ( 'NONE',  ( 5.719274019375673035, 21.55341960407619339, 112.2927570613523471 ) ) ;
#115077 = CARTESIAN_POINT ( 'NONE',  ( -12.14591786802326823, 12.06949235617739902, 73.12609039468567573 ) ) ;
#115078 = CARTESIAN_POINT ( 'NONE',  ( -18.62759615963255300, -10.81492255796106328, 24.16775706135235424 ) ) ;
#115079 = CARTESIAN_POINT ( 'NONE',  ( 9.474510206698971260, -16.51473224551069308, 32.91557627198102409 ) ) ;
#115080 = CARTESIAN_POINT ( 'NONE',  ( -21.52544592524334988, -5.823673210054445271, 103.9594237280190185 ) ) ;
#115081 = CARTESIAN_POINT ( 'NONE',  ( 13.97604488694527802, 13.89961937509977652, 109.3739096053143669 ) ) ;
#115082 = CARTESIAN_POINT ( 'NONE',  ( -10.81492255796078084, -18.62759615963271287, 102.0822429386476955 ) ) ;
#115084 = CARTESIAN_POINT ( 'NONE',  ( 21.52544592524344225, -5.823673210054117533, 68.54057627198103830 ) ) ;
#115083 = CARTESIAN_POINT ( 'NONE',  ( -4.347827484049745728, -37.01609572856843045, -32.59999999897104317 ) ) ;
#115086 = CARTESIAN_POINT ( 'NONE',  ( -16.55341960407611168, -4.379528057220339221, 46.45724293864769550 ) ) ;
#115085 = CARTESIAN_POINT ( 'NONE',  ( -16.55341960407617563, 4.379528057220093196, 53.54275706135234714 ) ) ;
#115087 = FACE_OUTER_BOUND ( 'NONE', #181269, .T. ) ;
#115088 = CARTESIAN_POINT ( 'NONE',  ( 16.46253265017146816, 9.564922557961045513, 81.66775706135233293 ) ) ;
#115089 = CARTESIAN_POINT ( 'NONE',  ( -16.79531203550646268, 7.028104445595631411, 103.7475501177956261 ) ) ;
#115090 = CARTESIAN_POINT ( 'NONE',  ( 8.224510206698742110, 14.34966873604972548, 27.08442372801901854 ) ) ;
#115091 = CARTESIAN_POINT ( 'NONE',  ( -5.719274019375978568, 21.55341960407610458, 90.20724293864770971 ) ) ;
#115092 = CARTESIAN_POINT ( 'NONE',  ( 8.224510206698953496, -14.34966873604960469, 62.91557627198102409 ) ) ;
#115093 = CARTESIAN_POINT ( 'NONE',  ( 19.03943276465977164, -0.05219959533909143690, 98.74890960531436690 ) ) ;
#115094 = CARTESIAN_POINT ( 'NONE',  ( 14.29746914071037800, 8.314922557961029526, 46.66775706135234714 ) ) ;
#115095 = CARTESIAN_POINT ( 'NONE',  ( 13.97604488694527802, 13.89961937509977652, 54.37390960531435979 ) ) ;
#115097 = CARTESIAN_POINT ( 'NONE',  ( 19.05341960407617918, -5.049401038297876454, 101.0427570613523045 ) ) ;
#115096 = CARTESIAN_POINT ( 'NONE',  ( -15.80617190586768217, 15.72974639402176855, 33.12609039468569705 ) ) ;
#115098 = CARTESIAN_POINT ( 'NONE',  ( -19.02544592524342804, 5.153800228976336051, 96.04057627198103830 ) ) ;
#115099 = CARTESIAN_POINT ( 'NONE',  ( -16.51473224551069308, -9.474510206698971260, 91.66557627198103830 ) ) ;
#115100 = CARTESIAN_POINT ( 'NONE',  ( -15.80617190586745835, -15.72974639402198527, 86.87390960531438111 ) ) ;
#115101 = CARTESIAN_POINT ( 'NONE',  ( 13.89961937509977652, -13.97604488694527269, 48.12390960531435979 ) ) ;
#115102 = CARTESIAN_POINT ( 'NONE',  ( -16.20579543436681291, -7.371946100354976217, 60.56520834171877254 ) ) ;
#115103 = CARTESIAN_POINT ( 'NONE',  ( -14.29746914071049879, 8.314922557960819915, 65.83224293864769550 ) ) ;
#115104 = CARTESIAN_POINT ( 'NONE',  ( 13.97604488694527802, 13.89961937509977652, 109.3739096053143669 ) ) ;
#115105 = CYLINDRICAL_SURFACE ( 'NONE', #173526, 28.79475375365586487 ) ;
#115106 = CARTESIAN_POINT ( 'NONE',  ( -13.89961937509957401, -13.97604488694547875, 69.37609039468564731 ) ) ;
#115107 = CARTESIAN_POINT ( 'NONE',  ( 15.80617190586746368, 15.72974639402197994, 84.37390960531438111 ) ) ;
#115108 = CARTESIAN_POINT ( 'NONE',  ( -19.05341960407617563, 5.049401038297882671, 43.54275706135232582 ) ) ;
#115109 = CARTESIAN_POINT ( 'NONE',  ( 0.05219959533909260263, 19.03943276465977164, 99.99890960531436690 ) ) ;
#115110 = CARTESIAN_POINT ( 'NONE',  ( -15.72974639402197994, 15.80617190586746368, 40.62390960531435269 ) ) ;
#115111 = CARTESIAN_POINT ( 'NONE',  ( -16.46253265017160317, 9.564922557960807481, 85.83224293864769550 ) ) ;
#115112 = CARTESIAN_POINT ( 'NONE',  ( -21.52544592524334988, -5.823673210054445271, 63.95942372801901854 ) ) ;
#115113 = CARTESIAN_POINT ( 'NONE',  ( 9.474510206698971260, -16.51473224551069308, 32.91557627198102409 ) ) ;
#115114 = EDGE_CURVE ( 'NONE', #658, #193741, #7299, .T. ) ;
#115115 = CARTESIAN_POINT ( 'NONE',  ( -4.379528057220328563, 16.55341960407611168, 70.20724293864769550 ) ) ;
#115116 = CARTESIAN_POINT ( 'NONE',  ( 14.29746914071037800, 8.314922557961029526, 26.66775706135235424 ) ) ;
#115117 = CARTESIAN_POINT ( 'NONE',  ( -15.72974639402176322, -15.80617190586768395, 54.37609039468568994 ) ) ;
#115118 = ORIENTED_EDGE ( 'NONE', *, *, #24178, .T. ) ;
#115119 = CARTESIAN_POINT ( 'NONE',  ( -5.153800228976328057, -19.02544592524343514, 107.2905762719810383 ) ) ;
#115120 = CARTESIAN_POINT ( 'NONE',  ( -19.03943276465977164, -0.05219959533935918106, 68.75109039468566152 ) ) ;
#115121 = DIRECTION ( 'NONE',  ( 0.000000000000000000, 0.000000000000000000, -1.000000000000000000 ) ) ;
#115122 = CARTESIAN_POINT ( 'NONE',  ( 5.823673210054444382, -21.52544592524334988, 25.20942372801901854 ) ) ;
#115123 = CARTESIAN_POINT ( 'NONE',  ( -38.00000000000001421, -12.34694845685042708, -7.649999994537626691 ) ) ;
#115124 = CARTESIAN_POINT ( 'NONE',  ( -19.02544592524334988, -5.153800228976617603, 18.95942372801899722 ) ) ;
#115125 = CARTESIAN_POINT ( 'NONE',  ( -9.564922557960796823, -16.46253265017161027, 52.08224293864768839 ) ) ;
#115126 = CARTESIAN_POINT ( 'NONE',  ( 5.049401038297881783, 19.05341960407617563, 22.29275706135233648 ) ) ;
#115127 = CARTESIAN_POINT ( 'NONE',  ( -16.53943276465976808, -0.05219959533934237506, 103.7510903946857042 ) ) ;
#115128 = EDGE_CURVE ( 'NONE', #164406, #40349, #130648, .T. ) ;
#115130 = CARTESIAN_POINT ( 'NONE',  ( 21.52544592524334988, 5.823673210054432836, 76.45942372801901854 ) ) ;
#115129 = CARTESIAN_POINT ( 'NONE',  ( -5.049401038298153566, 19.05341960407611168, 105.2072429386476671 ) ) ;
#115131 = CARTESIAN_POINT ( 'NONE',  ( 0.000000000000000000, 0.000000000000000000, -54.21489346206828230 ) ) ;
#115132 = DIRECTION ( 'NONE',  ( 1.000000000000000000, 0.000000000000000000, 0.000000000000000000 ) ) ;
#115133 = CARTESIAN_POINT ( 'NONE',  ( 24.45434260692612227, 5.907237110200220798, 169.8064932912610345 ) ) ;
#115135 = CARTESIAN_POINT ( 'NONE',  ( 10.72451020669871369, 18.67979575497193778, 67.08442372801901854 ) ) ;
#115134 = CARTESIAN_POINT ( 'NONE',  ( -8.314922557961024197, 14.29746914071037800, 67.91775706135234714 ) ) ;
#115136 = CARTESIAN_POINT ( 'NONE',  ( -21.52544592524334988, -5.823673210054445271, 108.9594237280190185 ) ) ;
#115137 = LINE ( 'NONE', #189012, #15305 ) ;
#115138 = CARTESIAN_POINT ( 'NONE',  ( -16.51473224551069308, -9.474510206698971260, 81.66557627198103830 ) ) ;
#115139 = CARTESIAN_POINT ( 'NONE',  ( -13.89961937509977652, 13.97604488694528158, 110.6239096053143243 ) ) ;
#115140 = ORIENTED_EDGE ( 'NONE', *, *, #152109, .F. ) ;
#115141 = DIRECTION ( 'NONE',  ( 1.000000000000000000, -0.000000000000000000, -0.000000000000000000 ) ) ;
#115142 = CARTESIAN_POINT ( 'NONE',  ( -5.049401038298153566, 19.05341960407611168, 40.20724293864768839 ) ) ;
#115143 = CARTESIAN_POINT ( 'NONE',  ( 5.823673210054125526, 21.52544592524343514, 44.79057627198103120 ) ) ;
#115144 = CARTESIAN_POINT ( 'NONE',  ( 16.55341960407618274, -4.379528057220086978, 111.0427570613523613 ) ) ;
#115146 = CARTESIAN_POINT ( 'NONE',  ( -19.02544592524342804, 5.153800228976336051, 86.04057627198103830 ) ) ;
#115145 = CARTESIAN_POINT ( 'NONE',  ( -12.06949235617756955, 12.14591786802309770, 100.6239096053143811 ) ) ;
#115147 = CARTESIAN_POINT ( 'NONE',  ( 5.823673210054444382, -21.52544592524334988, 110.2094237280190185 ) ) ;
#115148 = CARTESIAN_POINT ( 'NONE',  ( -13.89961937509977652, 13.97604488694528158, 35.62390960531435269 ) ) ;
#115149 = CARTESIAN_POINT ( 'NONE',  ( -0.05219959533910754901, -16.53943276465976808, 87.49890960531436690 ) ) ;
#115150 = CARTESIAN_POINT ( 'NONE',  ( -21.55341960407619339, 5.719274019375674811, 48.54275706135234714 ) ) ;
#115151 = CARTESIAN_POINT ( 'NONE',  ( -15.72974639402197994, 15.80617190586746368, 85.62390960531436690 ) ) ;
#115152 = CARTESIAN_POINT ( 'NONE',  ( 16.51473224551083163, -9.474510206698727899, 45.83442372801900433 ) ) ;
#115153 = CARTESIAN_POINT ( 'NONE',  ( -16.51473224551069308, -9.474510206698971260, 46.66557627198102409 ) ) ;
#115154 = CARTESIAN_POINT ( 'NONE',  ( -13.89961937509977652, 13.97604488694528158, 100.6239096053143669 ) ) ;
#115155 = CARTESIAN_POINT ( 'NONE',  ( -8.224510206698948167, 14.34966873604960824, 65.41557627198102409 ) ) ;
#115157 = CARTESIAN_POINT ( 'NONE',  ( 19.03943276465977164, 0.05219959533936151252, 46.25109039468566863 ) ) ;
#115156 = CIRCLE ( 'NONE', #179717, 8.000000000000000000 ) ;
#115158 = CARTESIAN_POINT ( 'NONE',  ( 8.314922557960818139, 14.29746914071049879, 49.58224293864769550 ) ) ;
#115159 = CARTESIAN_POINT ( 'NONE',  ( -9.474510206698720793, -16.51473224551083518, 79.58442372801899012 ) ) ;
#115160 = CARTESIAN_POINT ( 'NONE',  ( -9.474510206698720793, -16.51473224551083518, 89.58442372801900433 ) ) ;
#115161 = CARTESIAN_POINT ( 'NONE',  ( -10.72451020669898014, 18.67979575497178502, 30.41557627198101699 ) ) ;
#115162 = CARTESIAN_POINT ( 'NONE',  ( -16.55341960407611168, -4.379528057220339221, 96.45724293864770971 ) ) ;
#115163 = CARTESIAN_POINT ( 'NONE',  ( -3.791881235938239776E-15, -78.65691688641813073, -15.00000000000000000 ) ) ;
#115165 = CARTESIAN_POINT ( 'NONE',  ( 10.81492255796078972, 18.62759615963270932, 54.58224293864769550 ) ) ;
#115164 = CARTESIAN_POINT ( 'NONE',  ( 19.02544592524343514, -5.153800228976328945, 48.54057627198103120 ) ) ;
#115166 = CARTESIAN_POINT ( 'NONE',  ( 16.46253265017160672, -9.564922557960803928, 28.33224293864769550 ) ) ;
#115168 = CARTESIAN_POINT ( 'NONE',  ( 9.474510206698971260, -16.51473224551069308, 62.91557627198102409 ) ) ;
#115167 = CARTESIAN_POINT ( 'NONE',  ( -8.224510206698735004, -14.34966873604973081, 79.58442372801903275 ) ) ;
#115169 = CARTESIAN_POINT ( 'NONE',  ( 13.89961937509957401, 13.97604488694547697, 36.87609039468565442 ) ) ;
#115170 = CARTESIAN_POINT ( 'NONE',  ( -5.719274019375665041, -21.55341960407619695, 64.79275706135234714 ) ) ;
#115171 = CARTESIAN_POINT ( 'NONE',  ( -5.823673210054116645, -21.52544592524344225, 47.29057627198103120 ) ) ;
#115172 = CARTESIAN_POINT ( 'NONE',  ( 9.474510206698971260, -16.51473224551069308, 22.91557627198102765 ) ) ;
#115173 = CARTESIAN_POINT ( 'NONE',  ( 19.05341960407617918, -5.049401038297876454, 101.0427570613523045 ) ) ;
#115174 = CARTESIAN_POINT ( 'NONE',  ( 27.18966431762751412, 4.276553394868218838, 168.7322077152536508 ) ) ;
#115176 = CARTESIAN_POINT ( 'NONE',  ( -18.67979575497178146, -10.72451020669898902, 41.66557627198103120 ) ) ;
#115175 = DIRECTION ( 'NONE',  ( 0.000000000000000000, 0.000000000000000000, 1.000000000000000000 ) ) ;
#115177 = CARTESIAN_POINT ( 'NONE',  ( 16.79531203550645913, -7.028104445595738881, 66.24755011779559766 ) ) ;
#115178 = CARTESIAN_POINT ( 'NONE',  ( -21.53943276465977519, -0.05219959533937600094, 88.75109039468567573 ) ) ;
#115179 = CARTESIAN_POINT ( 'NONE',  ( -0.05219959533910754901, -16.53943276465976808, 42.49890960531435979 ) ) ;
#115180 = CARTESIAN_POINT ( 'NONE',  ( -16.52544592524342804, 4.483927247898546575, 61.04057627198103120 ) ) ;
#115181 = CARTESIAN_POINT ( 'NONE',  ( 10.72451020669898902, -18.67979575497178502, 87.91557627198103830 ) ) ;
#115182 = CARTESIAN_POINT ( 'NONE',  ( -15.72974639402197994, 15.80617190586746368, 80.62390960531438111 ) ) ;
#115183 = CARTESIAN_POINT ( 'NONE',  ( -11.45643923738960446, -4.999999999999992895, -18.00000000000000000 ) ) ;
#115184 = CARTESIAN_POINT ( 'NONE',  ( 18.62759615963271287, -10.81492255796078972, 38.33224293864768839 ) ) ;
#115185 = CARTESIAN_POINT ( 'NONE',  ( -4.483927247898782831, 16.52544592524335698, 52.70942372801902565 ) ) ;
#115186 = CARTESIAN_POINT ( 'NONE',  ( -4.483927247898539470, -16.52544592524342804, 82.29057627198103830 ) ) ;
#115187 = CARTESIAN_POINT ( 'NONE',  ( -13.97604488694527625, -13.89961937509977652, 66.87390960531436690 ) ) ;
#115188 = CARTESIAN_POINT ( 'NONE',  ( -19.03943276465977164, 0.05219959533909376836, 26.24890960531435624 ) ) ;
#115189 = DIRECTION ( 'NONE',  ( -1.000000000000000000, 0.000000000000000000, -0.000000000000000000 ) ) ;
#115190 = VERTEX_POINT ( 'NONE', #192342 ) ;
#115191 = CARTESIAN_POINT ( 'NONE',  ( -8.314922557961024197, 14.29746914071037800, 77.91775706135231871 ) ) ;
#115192 = CARTESIAN_POINT ( 'NONE',  ( 5.823673210054125526, 21.52544592524343514, 114.7905762719810383 ) ) ;
#115193 = CARTESIAN_POINT ( 'NONE',  ( 13.97604488694527802, 13.89961937509977652, 84.37390960531433848 ) ) ;
#115194 = CARTESIAN_POINT ( 'NONE',  ( 10.72451020669871369, 18.67979575497193778, 52.08442372801901854 ) ) ;
#115195 = CARTESIAN_POINT ( 'NONE',  ( 16.46253265017160672, -9.564922557960803928, 108.3322429386476955 ) ) ;
#115196 = CARTESIAN_POINT ( 'NONE',  ( -8.400629636141269785, -38.44252190851295836, -32.19688134020307047 ) ) ;
#115197 = VERTEX_POINT ( 'NONE', #141831 ) ;
#115198 = CARTESIAN_POINT ( 'NONE',  ( 10.81492255796106328, -18.62759615963255655, 40.41775706135234714 ) ) ;
#115200 = CARTESIAN_POINT ( 'NONE',  ( -9.564922557960796823, -16.46253265017161027, 102.0822429386477097 ) ) ;
#115199 = CARTESIAN_POINT ( 'NONE',  ( 16.46253265017160672, -9.564922557960803928, 38.33224293864768839 ) ) ;
#115201 = CARTESIAN_POINT ( 'NONE',  ( 5.153800228976615827, -19.02544592524334988, 50.20942372801897591 ) ) ;
#115202 = CARTESIAN_POINT ( 'NONE',  ( -21.52544592524343514, 5.823673210054127303, 116.0405762719810383 ) ) ;
#115203 = CARTESIAN_POINT ( 'NONE',  ( 13.89961937509957401, 13.97604488694547697, 41.87609039468566152 ) ) ;
#115204 = CARTESIAN_POINT ( 'NONE',  ( -19.05341960407611168, -5.049401038298163336, 26.45724293864769550 ) ) ;
#115205 = CARTESIAN_POINT ( 'NONE',  ( 8.224510206698742110, 14.34966873604972548, 97.08442372801904696 ) ) ;
#115206 = CARTESIAN_POINT ( 'NONE',  ( 13.89961937509957401, 13.97604488694547697, 56.87609039468564731 ) ) ;
#115207 = CARTESIAN_POINT ( 'NONE',  ( -8.224510206698735004, -14.34966873604973081, 104.5844237280190185 ) ) ;
#115208 = CARTESIAN_POINT ( 'NONE',  ( 9.252314257645119611, 10.97407593764238598, -62.33638803020407693 ) ) ;
#115209 = CARTESIAN_POINT ( 'NONE',  ( -16.51473224551069308, -9.474510206698971260, 81.66557627198103830 ) ) ;
#115210 = CARTESIAN_POINT ( 'NONE',  ( 18.67979575497194134, -10.72451020669871369, 90.83442372801901854 ) ) ;
#115211 = CARTESIAN_POINT ( 'NONE',  ( 0.05219959533937995610, -21.53943276465977519, 110.0010903946856757 ) ) ;
#115212 = CARTESIAN_POINT ( 'NONE',  ( -19.05341960407611168, -5.049401038298163336, 21.45724293864768839 ) ) ;
#115213 = CARTESIAN_POINT ( 'NONE',  ( 9.474510206698971260, -16.51473224551069308, 102.9155762719810241 ) ) ;
#115214 = CARTESIAN_POINT ( 'NONE',  ( -5.823673210054431948, 21.52544592524334988, 77.70942372801900433 ) ) ;
#115215 = CARTESIAN_POINT ( 'NONE',  ( 4.483927247898790824, -16.52544592524335698, 25.20942372801901854 ) ) ;
#115216 = CARTESIAN_POINT ( 'NONE',  ( -5.153800228976328057, -19.02544592524343514, 77.29057627198099567 ) ) ;
#115218 = EDGE_CURVE ( 'NONE', #69935, #168486, #130215, .T. ) ;
#115217 = CARTESIAN_POINT ( 'NONE',  ( -21.52544592524343514, 5.823673210054127303, 36.04057627198102409 ) ) ;
#115219 = CARTESIAN_POINT ( 'NONE',  ( -16.51473224551069308, -9.474510206698971260, 86.66557627198102409 ) ) ;
#115220 = CARTESIAN_POINT ( 'NONE',  ( -16.21995358207303894, -7.366697692864244473, 90.06448998487844904 ) ) ;
#115221 = CARTESIAN_POINT ( 'NONE',  ( -0.05219959533909027116, -19.03943276465977164, 82.49890960531436690 ) ) ;
#115222 = CARTESIAN_POINT ( 'NONE',  ( -9.474510206698964154, 16.51473224551069663, 60.41557627198102409 ) ) ;
#115223 = CARTESIAN_POINT ( 'NONE',  ( -4.483927247898782831, 16.52544592524335698, 97.70942372801904696 ) ) ;
#115224 = CARTESIAN_POINT ( 'NONE',  ( -17.12812012977049747, 6.668231424565647991, 98.64051240676855059 ) ) ;
#115225 = CARTESIAN_POINT ( 'NONE',  ( 19.03943276465977164, 0.05219959533936151252, 61.25109039468566863 ) ) ;
#115226 = CARTESIAN_POINT ( 'NONE',  ( 0.05219959533909260263, 19.03943276465977164, 94.99890960531436690 ) ) ;
#115227 = CARTESIAN_POINT ( 'NONE',  ( 14.34966873604960469, 8.224510206698951720, 79.16557627198103830 ) ) ;
#115228 = CARTESIAN_POINT ( 'NONE',  ( -10.81492255796078084, -18.62759615963271287, 37.08224293864768129 ) ) ;
#115229 =( BOUNDED_CURVE ( )  B_SPLINE_CURVE ( 2, ( #30745, #75252, #197620, #108566, #63052, #91387, #154080, #15574, #13585, #139884, #199598, #60078, #151123, #45908, #61065, #59085, #122737, #123718, #105593, #120752, #77232, #46906, #184428, #27793, #167279, #62053, #138901, #170244, #31738, #28777, #1373, #186429, #166297, #12616, #74280, #135950, #90416, #190388, #68026, #144863, #20525, #188404, #36682, #191375, #4349, #67032, #126700, #98342, #49882, #111547, #96365, #35699, #143869, #173232, #34708, #80207, #65044, #158053, #19543, #50878, #95377, #109559, #175217, #141878, #125727, #82173, #128691, #140887, #81188, #51863, #48894, #2377, #5348, #187426, #142870, #66034, #127701, #189401, #112536, #97346, #172230, #110549, #160041, #113523, #171240 ),
 .UNSPECIFIED., .F., .F. ) 
 B_SPLINE_CURVE_WITH_KNOTS ( ( 3, 2, 2, 2, 2, 2, 2, 2, 2, 2, 2, 2, 2, 2, 2, 2, 2, 2, 2, 2, 2, 2, 2, 2, 2, 2, 2, 2, 2, 2, 2, 2, 2, 2, 2, 2, 2, 2, 2, 2, 2, 2, 3 ),
 ( 0.8182199101112557216, 0.8201754385964912242, 0.8245614035087719396, 0.8289473684210526550, 0.8333333333333333703, 0.8377192982456140857, 0.8421052631578946901, 0.8464912280701754055, 0.8508771929824561209, 0.8552631578947368363, 0.8596491228070175517, 0.8640350877192982670, 0.8684210526315789824, 0.8728070175438596978, 0.8771929824561403022, 0.8815789473684210176, 0.8859649122807017330, 0.8903508771929824483, 0.8947368421052631637, 0.8991228070175438791, 0.9035087719298245945, 0.9078947368421053099, 0.9122807017543859143, 0.9166666666666666297, 0.9210526315789473450, 0.9254385964912280604, 0.9298245614035087758, 0.9342105263157894912, 0.9385964912280702066, 0.9429824561403509220, 0.9473684210526315264, 0.9517543859649122417, 0.9561403508771929571, 0.9605263157894736725, 0.9649122807017543879, 0.9692982456140351033, 0.9736842105263158187, 0.9780701754385965341, 0.9824561403508771384, 0.9868421052631578538, 0.9912280701754385692, 0.9956140350877192846, 1.000000000000000000 ),
 .UNSPECIFIED. ) 
 CURVE ( )  GEOMETRIC_REPRESENTATION_ITEM ( )  RATIONAL_B_SPLINE_CURVE ( ( 0.9831626618144007068, 0.9848076720550096308, 1.000000000000000000, 0.9659258262890683122, 1.000000000000000000, 0.9659258262890683122, 1.000000000000000000, 0.9659258262890683122, 1.000000000000000000, 0.9659258262890683122, 1.000000000000000000, 0.9659258262890683122, 1.000000000000000000, 0.9659258262890683122, 1.000000000000000000, 0.9659258262890683122, 1.000000000000000000, 0.9659258262890683122, 1.000000000000000000, 0.9659258262890683122, 1.000000000000000000, 0.9659258262890683122, 1.000000000000000000, 0.9659258262890683122, 1.000000000000000000, 0.9659258262890683122, 1.000000000000000000, 0.9659258262890683122, 1.000000000000000000, 0.9659258262890683122, 1.000000000000000000, 0.9659258262890683122, 1.000000000000000000, 0.9659258262890683122, 1.000000000000000000, 0.9659258262890683122, 1.000000000000000000, 0.9659258262890683122, 1.000000000000000000, 0.9659258262890683122, 1.000000000000000000, 0.9659258262890683122, 1.000000000000000000, 0.9659258262890683122, 1.000000000000000000, 0.9659258262890683122, 1.000000000000000000, 0.9659258262890683122, 1.000000000000000000, 0.9659258262890683122, 1.000000000000000000, 0.9659258262890683122, 1.000000000000000000, 0.9659258262890683122, 1.000000000000000000, 0.9659258262890683122, 1.000000000000000000, 0.9659258262890683122, 1.000000000000000000, 0.9659258262890683122, 1.000000000000000000, 0.9659258262890683122, 1.000000000000000000, 0.9659258262890683122, 1.000000000000000000, 0.9659258262890683122, 1.000000000000000000, 0.9659258262890683122, 1.000000000000000000, 0.9659258262890683122, 1.000000000000000000, 0.9659258262890683122, 1.000000000000000000, 0.9659258262890683122, 1.000000000000000000, 0.9659258262890683122, 1.000000000000000000, 0.9659258262890683122, 1.000000000000000000, 0.9659258262890683122, 1.000000000000000000, 0.9659258262890683122, 1.000000000000000000, 0.9659258262890683122, 1.000000000000000000 ) ) 
 REPRESENTATION_ITEM ( '' )  );
#115230 = CARTESIAN_POINT ( 'NONE',  ( 0.05219959533907565091, 21.53943276465977519, 24.99890960531435624 ) ) ;
#115231 = CARTESIAN_POINT ( 'NONE',  ( -16.52544592524342804, 4.483927247898546575, 86.04057627198102409 ) ) ;
#115232 = CARTESIAN_POINT ( 'NONE',  ( -17.48847506799969054, 5.747544572773785276, 55.82697437843281563 ) ) ;
#115233 = CARTESIAN_POINT ( 'NONE',  ( -9.474510206698720793, -16.51473224551083518, 39.58442372801899722 ) ) ;
#115234 = CARTESIAN_POINT ( 'NONE',  ( -12.14591786802309592, -12.06949235617757132, 21.87390960531436690 ) ) ;
#115235 = CARTESIAN_POINT ( 'NONE',  ( 19.03943276465977164, -0.05219959533909143690, 103.7489096053143669 ) ) ;
#115236 = CARTESIAN_POINT ( 'NONE',  ( 21.55341960407619695, -5.719274019375665929, 66.04275706135236135 ) ) ;
#115237 = CARTESIAN_POINT ( 'NONE',  ( -18.67979575497178146, -10.72451020669898902, 56.66557627198103830 ) ) ;
#115238 = CARTESIAN_POINT ( 'NONE',  ( -10.81492255796105439, 18.62759615963255655, 32.91775706135234714 ) ) ;
#115239 = CARTESIAN_POINT ( 'NONE',  ( 21.55341960407610458, 5.719274019375980345, 88.95724293864769550 ) ) ;
#115240 = CARTESIAN_POINT ( 'NONE',  ( 0.05219959533937995610, -21.53943276465977519, 35.00109039468568284 ) ) ;
#115241 = CARTESIAN_POINT ( 'NONE',  ( -14.34966873604960291, -8.224510206698953496, 106.6655762719810383 ) ) ;
#115242 = CARTESIAN_POINT ( 'NONE',  ( -5.153800228976607833, 19.02544592524334988, 72.70942372801900433 ) ) ;
#115243 = CARTESIAN_POINT ( 'NONE',  ( 16.46253265017160672, -9.564922557960803928, 43.33224293864769550 ) ) ;
#115245 = CARTESIAN_POINT ( 'NONE',  ( -16.46253265017160317, 9.564922557960807481, 90.83224293864769550 ) ) ;
#115244 = CARTESIAN_POINT ( 'NONE',  ( -16.55341960407611168, -4.379528057220339221, 91.45724293864769550 ) ) ;
#115246 = CARTESIAN_POINT ( 'NONE',  ( -9.474510206698964154, 16.51473224551069663, 90.41557627198103830 ) ) ;
#115247 = CARTESIAN_POINT ( 'NONE',  ( 4.379528057220339221, -16.55341960407611168, 107.7072429386476955 ) ) ;
#115248 = CARTESIAN_POINT ( 'NONE',  ( -14.29746914071049879, 8.314922557960819915, 35.83224293864768839 ) ) ;
#115249 = CARTESIAN_POINT ( 'NONE',  ( -4.379528057220086978, -16.55341960407618274, 104.7927570613523898 ) ) ;
#115250 = CARTESIAN_POINT ( 'NONE',  ( 9.564922557960805705, 16.46253265017160317, 54.58224293864769550 ) ) ;
#115251 = CARTESIAN_POINT ( 'NONE',  ( 14.34966873604960469, 8.224510206698951720, 114.1655762719810383 ) ) ;
#115252 = CARTESIAN_POINT ( 'NONE',  ( 19.03943276465977164, 0.05219959533936151252, 26.25109039468566507 ) ) ;
#115254 = CARTESIAN_POINT ( 'NONE',  ( -14.34966873604960291, -8.224510206698953496, 21.66557627198102409 ) ) ;
#115253 = CARTESIAN_POINT ( 'NONE',  ( 16.51473224551069308, 9.474510206698969483, 109.1655762719810383 ) ) ;
#115255 = CARTESIAN_POINT ( 'NONE',  ( 5.823673210054444382, -21.52544592524334988, 40.20942372801901854 ) ) ;
#115256 = CARTESIAN_POINT ( 'NONE',  ( 9.474510206698971260, -16.51473224551069308, 107.9155762719810383 ) ) ;
#115257 = CARTESIAN_POINT ( 'NONE',  ( -8.314922557961024197, 14.29746914071037800, 47.91775706135234714 ) ) ;
#115258 = CARTESIAN_POINT ( 'NONE',  ( 4.379528057220092307, 16.55341960407617563, 107.2927570613523471 ) ) ;
#115259 = CARTESIAN_POINT ( 'NONE',  ( -13.89961937509977652, 13.97604488694528158, 45.62390960531433848 ) ) ;
#115260 = CARTESIAN_POINT ( 'NONE',  ( -16.53943276465976808, -0.05219959533934237506, 93.75109039468567573 ) ) ;
#115261 = CARTESIAN_POINT ( 'NONE',  ( 8.314922557961029526, -14.29746914071037800, 20.41775706135234714 ) ) ;
#115262 = CARTESIAN_POINT ( 'NONE',  ( -13.97604488694527625, -13.89961937509977652, 46.87390960531435979 ) ) ;
#115263 = CARTESIAN_POINT ( 'NONE',  ( -0.05219959533910754901, -16.53943276465976808, 107.4989096053143669 ) ) ;
#115264 = CARTESIAN_POINT ( 'NONE',  ( -18.62759615963270932, 10.81492255796079327, 110.8322429386476955 ) ) ;
#115265 = CARTESIAN_POINT ( 'NONE',  ( 16.46253265017160672, -9.564922557960803928, 33.33224293864770260 ) ) ;
#115266 = CARTESIAN_POINT ( 'NONE',  ( -9.474510206698964154, 16.51473224551069663, 100.4155762719810241 ) ) ;
#115267 = CARTESIAN_POINT ( 'NONE',  ( -13.89961937509977652, 13.97604488694528158, 35.62390960531435269 ) ) ;
#115268 = CARTESIAN_POINT ( 'NONE',  ( 5.153800228976335163, 19.02544592524342804, 99.79057627198102409 ) ) ;
#115269 = CARTESIAN_POINT ( 'NONE',  ( -16.62475595723697808, -7.163666690055197073, 34.47286648189534475 ) ) ;
#115270 = CARTESIAN_POINT ( 'NONE',  ( 9.564922557960805705, 16.46253265017160317, 94.58224293864769550 ) ) ;
#115272 = CARTESIAN_POINT ( 'NONE',  ( -14.34966873604960291, -8.224510206698953496, 101.6655762719810383 ) ) ;
#115271 = CARTESIAN_POINT ( 'NONE',  ( -21.55341960407619339, 5.719274019375674811, 43.54275706135235424 ) ) ;
#115273 = CARTESIAN_POINT ( 'NONE',  ( -0.05219959533909027116, -19.03943276465977164, 107.4989096053143527 ) ) ;
#115274 = CARTESIAN_POINT ( 'NONE',  ( 17.60769864724391098, -5.499999999999974243, 96.15024842019167295 ) ) ;
#115275 = CARTESIAN_POINT ( 'NONE',  ( -16.52544592524335698, -4.483927247898792601, 63.95942372801901854 ) ) ;
#115276 = CARTESIAN_POINT ( 'NONE',  ( -10.72451020669870658, -18.67979575497194134, 94.58442372801901854 ) ) ;
#115277 = CARTESIAN_POINT ( 'NONE',  ( 8.314922557961029526, -14.29746914071037800, 35.41775706135234003 ) ) ;
#115279 = EDGE_CURVE ( 'NONE', #170287, #150779, #115499, .T. ) ;
#115278 = CARTESIAN_POINT ( 'NONE',  ( 5.153800228976335163, 19.02544592524342804, 84.79057627198099567 ) ) ;
#115280 = CARTESIAN_POINT ( 'NONE',  ( -9.564922557961040184, 16.46253265017147172, 112.9177570613523329 ) ) ;
#115281 = CARTESIAN_POINT ( 'NONE',  ( 12.14591786802327356, -12.06949235617739191, 85.62609039468568994 ) ) ;
#115282 = CARTESIAN_POINT ( 'NONE',  ( -19.02544592524334988, -5.153800228976617603, 88.95942372801897591 ) ) ;
#115283 = CARTESIAN_POINT ( 'NONE',  ( 9.474510206698971260, -16.51473224551069308, 72.91557627198102409 ) ) ;
#115284 = CARTESIAN_POINT ( 'NONE',  ( -15.72974639402197994, 15.80617190586746368, 100.6239096053143811 ) ) ;
#115286 = CARTESIAN_POINT ( 'NONE',  ( -13.97604488694547697, 13.89961937509957934, 88.12609039468563310 ) ) ;
#115285 = CARTESIAN_POINT ( 'NONE',  ( -8.314922557960811034, -14.29746914071050412, 92.08224293864769550 ) ) ;
#115287 = CARTESIAN_POINT ( 'NONE',  ( 16.52544592524335698, 4.483927247898782831, 76.45942372801901854 ) ) ;
#115288 = CARTESIAN_POINT ( 'NONE',  ( 21.36928693577338834, 5.431965077040404211, 174.3311293403526179 ) ) ;
#115289 = CARTESIAN_POINT ( 'NONE',  ( 9.474510206698729675, 16.51473224551082808, 72.08442372801900433 ) ) ;
#115290 = CARTESIAN_POINT ( 'NONE',  ( 16.52544592524342804, -4.483927247898539470, 28.54057627198103120 ) ) ;
#115291 = CARTESIAN_POINT ( 'NONE',  ( 14.34966873604960469, 8.224510206698951720, 94.16557627198103830 ) ) ;
#115293 = CARTESIAN_POINT ( 'NONE',  ( -19.02130022317638591, 5.499999999999807265, 90.78188669246574705 ) ) ;
#115292 = CARTESIAN_POINT ( 'NONE',  ( -16.46253265017146816, -9.564922557961047289, 24.16775706135233648 ) ) ;
#115294 = CARTESIAN_POINT ( 'NONE',  ( -21.55341960407619339, 5.719274019375674811, 28.54275706135234358 ) ) ;
#115295 = FACE_OUTER_BOUND ( 'NONE', #75407, .T. ) ;
#115296 = CARTESIAN_POINT ( 'NONE',  ( -5.049401038298153566, 19.05341960407611168, 75.20724293864769550 ) ) ;
#115297 = CARTESIAN_POINT ( 'NONE',  ( -21.55341960407619339, 5.719274019375674811, 98.54275706135234714 ) ) ;
#115298 = CARTESIAN_POINT ( 'NONE',  ( -16.46253265017160317, 9.564922557960807481, 70.83224293864770971 ) ) ;
#115299 = CARTESIAN_POINT ( 'NONE',  ( 5.719274019375991003, -21.55341960407610458, 42.70724293864770260 ) ) ;
#115300 = CARTESIAN_POINT ( 'NONE',  ( 12.14591786802309770, 12.06949235617756955, 74.37390960531436690 ) ) ;
#115301 = CARTESIAN_POINT ( 'NONE',  ( 9.564922557960805705, 16.46253265017160317, 54.58224293864769550 ) ) ;
#115302 = CARTESIAN_POINT ( 'NONE',  ( -8.314922557960811034, -14.29746914071050412, 107.0822429386476955 ) ) ;
#115303 = CIRCLE ( 'NONE', #157160, 59.99999999999998579 ) ;
#115304 = CARTESIAN_POINT ( 'NONE',  ( 15.72974639402176855, 15.80617190586768217, 31.87609039468567929 ) ) ;
#115305 = CARTESIAN_POINT ( 'NONE',  ( -10.81492255796105439, 18.62759615963255655, 57.91775706135234714 ) ) ;
#115306 = CARTESIAN_POINT ( 'NONE',  ( 16.51473224551069308, 9.474510206698969483, 44.16557627198103120 ) ) ;
#115307 = CARTESIAN_POINT ( 'NONE',  ( -12.06949235617739369, -12.14591786802326823, 74.37609039468568994 ) ) ;
#115308 = EDGE_CURVE ( 'NONE', #57298, #60581, #14053, .T. ) ;
#115309 = CARTESIAN_POINT ( 'NONE',  ( 15.72974639402199770, -15.80617190586745480, 108.1239096053143811 ) ) ;
#115310 = VERTEX_POINT ( 'NONE', #21481 ) ;
#115311 = CARTESIAN_POINT ( 'NONE',  ( 15.80617190586746368, 15.72974639402197994, 114.3739096053143527 ) ) ;
#115313 = CARTESIAN_POINT ( 'NONE',  ( -0.05219959533909027116, -19.03943276465977164, 62.49890960531435979 ) ) ;
#115312 = CARTESIAN_POINT ( 'NONE',  ( 0.05219959533936267826, -19.03943276465977164, 40.00109039468566152 ) ) ;
#115314 = CARTESIAN_POINT ( 'NONE',  ( 9.564922557961047289, -16.46253265017146816, 30.41775706135232937 ) ) ;
#115315 = CARTESIAN_POINT ( 'NONE',  ( 18.62759615963255655, 10.81492255796105972, 71.66775706135234714 ) ) ;
#115316 = CARTESIAN_POINT ( 'NONE',  ( -21.55341960407610458, -5.719274019375992779, 66.45724293864768129 ) ) ;
#115317 = CARTESIAN_POINT ( 'NONE',  ( -16.52544592524342804, 4.483927247898546575, 36.04057627198102409 ) ) ;
#115319 = CARTESIAN_POINT ( 'NONE',  ( 9.564922557961047289, -16.46253265017146816, 30.41775706135232937 ) ) ;
#115318 = CARTESIAN_POINT ( 'NONE',  ( -21.53943276465977519, -0.05219959533937600094, 83.75109039468568994 ) ) ;
#115320 = CARTESIAN_POINT ( 'NONE',  ( 16.52544592524342804, -4.483927247898539470, 58.54057627198103120 ) ) ;
#115321 = CARTESIAN_POINT ( 'NONE',  ( 14.34966873604960469, 8.224510206698951720, 109.1655762719810383 ) ) ;
#115322 = CARTESIAN_POINT ( 'NONE',  ( -19.03943276465977164, -0.05219959533935918106, 58.75109039468566863 ) ) ;
#115323 = CARTESIAN_POINT ( 'NONE',  ( -14.34966873604972548, 8.224510206698743886, 108.3344237280190185 ) ) ;
#115324 = AXIS2_PLACEMENT_3D ( 'NONE', #166599, #43244, #149425 ) ;
#115325 = CARTESIAN_POINT ( 'NONE',  ( 10.81492255796106328, -18.62759615963255655, 65.41775706135234714 ) ) ;
#115326 = CARTESIAN_POINT ( 'NONE',  ( 9.564922557960805705, 16.46253265017160317, 69.58224293864770971 ) ) ;
#115327 = CARTESIAN_POINT ( 'NONE',  ( -19.05341960407617563, 5.049401038297882671, 53.54275706135231871 ) ) ;
#115328 = CARTESIAN_POINT ( 'NONE',  ( -18.62759615963270932, 10.81492255796079327, 50.83224293864770971 ) ) ;
#115329 = CARTESIAN_POINT ( 'NONE',  ( 10.72451020669871369, 18.67979575497193778, 47.08442372801901854 ) ) ;
#115330 = CARTESIAN_POINT ( 'NONE',  ( -0.05219959533907301413, -21.53943276465977519, 102.4989096053143811 ) ) ;
#115331 = CARTESIAN_POINT ( 'NONE',  ( 9.474510206698729675, 16.51473224551082808, 97.08442372801900433 ) ) ;
#115332 = CARTESIAN_POINT ( 'NONE',  ( -16.53943276465976808, -0.05219959533934237506, 63.75109039468568284 ) ) ;
#115334 = CARTESIAN_POINT ( 'NONE',  ( 10.81492255796078972, 18.62759615963270932, 109.5822429386476955 ) ) ;
#115333 = FACE_OUTER_BOUND ( 'NONE', #174300, .T. ) ;
#115335 = CARTESIAN_POINT ( 'NONE',  ( -16.52544592524342804, 4.483927247898546575, 91.04057627198103830 ) ) ;
#115336 = CARTESIAN_POINT ( 'NONE',  ( -16.38665767535054130, -7.295008042176132079, 99.73599135785453029 ) ) ;
#115337 = CARTESIAN_POINT ( 'NONE',  ( -12.14591786802326823, 12.06949235617739902, 23.12609039468567573 ) ) ;
#115338 = PRODUCT_DEFINITION ( 'UNKNOWN', '', #188910, #127232 ) ;
#115339 = CARTESIAN_POINT ( 'NONE',  ( 5.823673210054125526, 21.52544592524343514, 44.79057627198103120 ) ) ;
#115340 = CARTESIAN_POINT ( 'NONE',  ( -14.34966873604972548, 8.224510206698743886, 93.33442372801901854 ) ) ;
#115341 = CARTESIAN_POINT ( 'NONE',  ( 35.73712089830454630, -9.569067683169670602, -7.999999999999996447 ) ) ;
#115342 = CARTESIAN_POINT ( 'NONE',  ( -4.379528057220086978, -16.55341960407618274, 64.79275706135234714 ) ) ;
#115343 = CARTESIAN_POINT ( 'NONE',  ( 5.823673210054444382, -21.52544592524334988, 35.20942372801901854 ) ) ;
#115344 = CARTESIAN_POINT ( 'NONE',  ( -21.53943276465977519, 0.05219959533907696930, 41.24890960531435269 ) ) ;
#115345 = CARTESIAN_POINT ( 'NONE',  ( -16.52544592524335698, -4.483927247898792601, 83.95942372801900433 ) ) ;
#115346 = CARTESIAN_POINT ( 'NONE',  ( -5.153800228976328057, -19.02544592524343514, 92.29057627198099567 ) ) ;
#115347 = CARTESIAN_POINT ( 'NONE',  ( 18.62759615963255655, 10.81492255796105972, 66.66775706135234714 ) ) ;
#115348 = CARTESIAN_POINT ( 'NONE',  ( 0.05219959533907565091, 21.53943276465977519, 34.99890960531435979 ) ) ;
#115349 = CARTESIAN_POINT ( 'NONE',  ( 18.67979575497178502, 10.72451020669898547, 39.16557627198102409 ) ) ;
#115350 = ORIENTED_EDGE ( 'NONE', *, *, #95040, .T. ) ;
#115351 = CARTESIAN_POINT ( 'NONE',  ( -19.02544592524334988, -5.153800228976617603, 48.95942372801900433 ) ) ;
#115352 = CARTESIAN_POINT ( 'NONE',  ( -8.314922557961024197, 14.29746914071037800, 67.91775706135234714 ) ) ;
#115353 = CARTESIAN_POINT ( 'NONE',  ( -21.52544592524343514, 5.823673210054127303, 36.04057627198102409 ) ) ;
#115354 = ORIENTED_EDGE ( 'NONE', *, *, #102120, .T. ) ;
#115355 = CARTESIAN_POINT ( 'NONE',  ( -5.049401038298153566, 19.05341960407611168, 90.20724293864766707 ) ) ;
#115356 = CARTESIAN_POINT ( 'NONE',  ( 14.29746914071037800, 8.314922557961029526, 111.6677570613523613 ) ) ;
#115357 = CARTESIAN_POINT ( 'NONE',  ( 8.231229499107000080, -38.47007264976928553, -32.24440875978786636 ) ) ;
#115358 = CARTESIAN_POINT ( 'NONE',  ( 8.224510206698953496, -14.34966873604960469, 107.9155762719810241 ) ) ;
#115359 = CARTESIAN_POINT ( 'NONE',  ( -15.80617190586745835, -15.72974639402198527, 51.87390960531437401 ) ) ;
#115360 = CARTESIAN_POINT ( 'NONE',  ( -9.474510206698964154, 16.51473224551069663, 45.41557627198103120 ) ) ;
#115361 = CARTESIAN_POINT ( 'NONE',  ( 12.06949235617739724, 12.14591786802326823, 86.87609039468568994 ) ) ;
#115362 = CARTESIAN_POINT ( 'NONE',  ( 21.53943276465977519, 0.05219959533937863772, 36.25109039468567573 ) ) ;
#115363 = CARTESIAN_POINT ( 'NONE',  ( -9.474510206698720793, -16.51473224551083518, 89.58442372801900433 ) ) ;
#115364 = CARTESIAN_POINT ( 'NONE',  ( 16.52544592524342804, -4.483927247898539470, 88.54057627198103830 ) ) ;
#115365 = CARTESIAN_POINT ( 'NONE',  ( 5.049401038298161559, -19.05341960407611168, 57.70724293864769550 ) ) ;
#115366 = VECTOR ( 'NONE', #196955, 1000.000000000000000 ) ;
#115367 = CARTESIAN_POINT ( 'NONE',  ( -0.05219959533909027116, -19.03943276465977164, 27.49890960531435624 ) ) ;
#115368 = CARTESIAN_POINT ( 'NONE',  ( 18.67979575497194134, -10.72451020669871369, 105.8344237280190328 ) ) ;
#115369 = CARTESIAN_POINT ( 'NONE',  ( -19.05341960407611168, -5.049401038298163336, 81.45724293864769550 ) ) ;
#115370 = CARTESIAN_POINT ( 'NONE',  ( -12.06949235617739369, -12.14591786802326823, 64.37609039468568994 ) ) ;
#115371 = CARTESIAN_POINT ( 'NONE',  ( -21.55341960407619339, 5.719274019375674811, 88.54275706135236135 ) ) ;
#115372 = CARTESIAN_POINT ( 'NONE',  ( 10.81492255796078972, 18.62759615963270932, 44.58224293864769550 ) ) ;
#115373 = CARTESIAN_POINT ( 'NONE',  ( -16.52544592524335698, -4.483927247898792601, 68.95942372801901854 ) ) ;
#115374 = CARTESIAN_POINT ( 'NONE',  ( -13.89961937509957401, -13.97604488694547875, 54.37609039468565442 ) ) ;
#115375 = CARTESIAN_POINT ( 'NONE',  ( 13.97604488694548053, -13.89961937509957401, 65.62609039468567573 ) ) ;
#115376 = VERTEX_POINT ( 'NONE', #83142 ) ;
#115377 = CARTESIAN_POINT ( 'NONE',  ( -18.67979575497193778, 10.72451020669871902, 58.33442372801901143 ) ) ;
#115378 = CARTESIAN_POINT ( 'NONE',  ( -13.89961937509977652, 13.97604488694528158, 65.62390960531436690 ) ) ;
#115379 = CARTESIAN_POINT ( 'NONE',  ( -5.049401038298153566, 19.05341960407611168, 30.20724293864768839 ) ) ;
#115380 = CARTESIAN_POINT ( 'NONE',  ( -16.51473224551082808, 9.474510206698731452, 53.33442372801900433 ) ) ;
#115381 = CARTESIAN_POINT ( 'NONE',  ( 0.05219959533909260263, 19.03943276465977164, 109.9989096053143669 ) ) ;
#115382 = CARTESIAN_POINT ( 'NONE',  ( 0.05219959533909260263, 19.03943276465977164, 94.99890960531436690 ) ) ;
#115383 = CARTESIAN_POINT ( 'NONE',  ( 0.05219959533910956823, 16.53943276465976808, 49.99890960531437401 ) ) ;
#115384 = CARTESIAN_POINT ( 'NONE',  ( -18.67979575497178146, -10.72451020669898902, 41.66557627198103120 ) ) ;
#115385 = CARTESIAN_POINT ( 'NONE',  ( 17.72696623605163424, -5.499999999999958256, 91.09811031808420978 ) ) ;
#115386 = CARTESIAN_POINT ( 'NONE',  ( 0.05219959533936267826, -19.03943276465977164, 20.00109039468567218 ) ) ;
#115387 = CARTESIAN_POINT ( 'NONE',  ( -16.18388926212238133, -7.379444403734535918, 80.43953151366153520 ) ) ;
#115388 = CARTESIAN_POINT ( 'NONE',  ( -16.51473224551069308, -9.474510206698971260, 51.66557627198102409 ) ) ;
#115389 = CARTESIAN_POINT ( 'NONE',  ( -19.39056639909674473, -5.500000000000012434, 100.7894878107434238 ) ) ;
#115390 = CARTESIAN_POINT ( 'NONE',  ( -17.26058549869090797, 6.457015423128533271, 108.6225416252393359 ) ) ;
#115391 = CARTESIAN_POINT ( 'NONE',  ( -4.379528057220086978, -16.55341960407618274, 79.79275706135236135 ) ) ;
#115392 = CARTESIAN_POINT ( 'NONE',  ( 21.52544592524344225, -5.823673210054117533, 93.54057627198103830 ) ) ;
#115393 = CARTESIAN_POINT ( 'NONE',  ( -4.483927247898539470, -16.52544592524342804, 47.29057627198103120 ) ) ;
#115395 = CARTESIAN_POINT ( 'NONE',  ( -7.500000000000001776, -1.104226503365435486, 6.811333284551973399 ) ) ;
#115394 = CARTESIAN_POINT ( 'NONE',  ( -5.049401038298153566, 19.05341960407611168, 35.20724293864768839 ) ) ;
#115396 = CARTESIAN_POINT ( 'NONE',  ( -0.05219959533937732626, 21.53943276465977519, 42.50109039468567573 ) ) ;
#115397 = CARTESIAN_POINT ( 'NONE',  ( -5.049401038297874678, -19.05341960407617918, 54.79275706135234003 ) ) ;
#115398 = CARTESIAN_POINT ( 'NONE',  ( -19.02544592524342804, 5.153800228976336051, 36.04057627198100988 ) ) ;
#115399 = CARTESIAN_POINT ( 'NONE',  ( 18.62759615963255655, 10.81492255796105972, 91.66775706135234714 ) ) ;
#115400 = CARTESIAN_POINT ( 'NONE',  ( -19.03943276465977164, 0.05219959533909376836, 21.24890960531436335 ) ) ;
#115401 = CARTESIAN_POINT ( 'NONE',  ( 0.05219959533910956823, 16.53943276465976808, 39.99890960531436690 ) ) ;
#115402 = DIRECTION ( 'NONE',  ( -0.000000000000000000, 0.000000000000000000, 1.000000000000000000 ) ) ;
#115403 = CARTESIAN_POINT ( 'NONE',  ( -15.72974639402197994, 15.80617190586746368, 35.62390960531437401 ) ) ;
#115404 = CARTESIAN_POINT ( 'NONE',  ( 27.73933785331498925, -9.013057229001034898, 143.7750000027311614 ) ) ;
#115405 = CARTESIAN_POINT ( 'NONE',  ( -9.564922557960796823, -16.46253265017161027, 107.0822429386476955 ) ) ;
#115406 = CARTESIAN_POINT ( 'NONE',  ( -16.53943276465976808, 0.05219959533911058130, 91.24890960531436690 ) ) ;
#115407 = CARTESIAN_POINT ( 'NONE',  ( 12.14591786802327356, -12.06949235617739191, 25.62609039468567929 ) ) ;
#115408 = CARTESIAN_POINT ( 'NONE',  ( -14.34966873604972548, 8.224510206698743886, 113.3344237280190328 ) ) ;
#115409 = ORIENTED_EDGE ( 'NONE', *, *, #59945, .F. ) ;
#115411 = CARTESIAN_POINT ( 'NONE',  ( -10.72451020669898014, 18.67979575497178502, 90.41557627198103830 ) ) ;
#115410 = CARTESIAN_POINT ( 'NONE',  ( 19.05341960407611168, 5.049401038298154454, 98.95724293864766707 ) ) ;
#115413 = CARTESIAN_POINT ( 'NONE',  ( -19.05341960407611168, -5.049401038298163336, 106.4572429386476955 ) ) ;
#115412 = CARTESIAN_POINT ( 'NONE',  ( -8.314922557960811034, -14.29746914071050412, 27.08224293864769550 ) ) ;
#115414 = CARTESIAN_POINT ( 'NONE',  ( 13.89961937509957401, 13.97604488694547697, 81.87609039468564731 ) ) ;
#115415 = CARTESIAN_POINT ( 'NONE',  ( -0.05219959533937732626, 21.53943276465977519, 112.5010903946857042 ) ) ;
#115416 = CARTESIAN_POINT ( 'NONE',  ( 21.55341960407610458, 5.719274019375980345, 93.95724293864770971 ) ) ;
#115417 = CARTESIAN_POINT ( 'NONE',  ( -15.72974639402197994, 15.80617190586746368, 40.62390960531435269 ) ) ;
#115418 = CARTESIAN_POINT ( 'NONE',  ( 9.564922557960805705, 16.46253265017160317, 64.58224293864769550 ) ) ;
#115419 = CARTESIAN_POINT ( 'NONE',  ( 16.52544592524342804, -4.483927247898539470, 33.54057627198102409 ) ) ;
#115420 = CARTESIAN_POINT ( 'NONE',  ( -5.153800228976328057, -19.02544592524343514, 77.29057627198099567 ) ) ;
#115421 = ORIENTED_EDGE ( 'NONE', *, *, #138961, .T. ) ;
#115422 = CARTESIAN_POINT ( 'NONE',  ( -31.23842136418743820, -7.314639034718686261, 96.67538241540150068 ) ) ;
#115423 = CARTESIAN_POINT ( 'NONE',  ( 19.03943276465977164, 0.05219959533936151252, 31.25109039468566863 ) ) ;
#115424 = CARTESIAN_POINT ( 'NONE',  ( -12.14591786802309592, -12.06949235617757132, 86.87390960531438111 ) ) ;
#115425 = CARTESIAN_POINT ( 'NONE',  ( 10.72451020669871369, 18.67979575497193778, 27.08442372801901854 ) ) ;
#115426 = CARTESIAN_POINT ( 'NONE',  ( 27.73933785331498925, -9.013057229001033122, 144.2750000027311899 ) ) ;
#115427 = CARTESIAN_POINT ( 'NONE',  ( -8.224510206698735004, -14.34966873604973081, 89.58442372801901854 ) ) ;
#115428 = CARTESIAN_POINT ( 'NONE',  ( -16.55341960407611168, -4.379528057220339221, 111.4572429386476813 ) ) ;
#115429 = CARTESIAN_POINT ( 'NONE',  ( -16.51473224551069308, -9.474510206698971260, 71.66557627198102409 ) ) ;
#115430 = CARTESIAN_POINT ( 'NONE',  ( -37.99626262588766679, 2.428612866367529932E-14, -5.747842220587803475 ) ) ;
#115431 = CARTESIAN_POINT ( 'NONE',  ( 4.379528057220339221, -16.55341960407611168, 27.70724293864769905 ) ) ;
#115432 = CARTESIAN_POINT ( 'NONE',  ( 21.55341960407619695, -5.719274019375665929, 61.04275706135234714 ) ) ;
#115433 = CARTESIAN_POINT ( 'NONE',  ( 31.20004872165405985, -21.37828431676117802, -20.08970689225314032 ) ) ;
#115434 = CARTESIAN_POINT ( 'NONE',  ( -15.80617190586768217, 15.72974639402176855, 93.12609039468568994 ) ) ;
#115435 = CARTESIAN_POINT ( 'NONE',  ( 13.89961937509977652, -13.97604488694527269, 43.12390960531434558 ) ) ;
#115436 = CARTESIAN_POINT ( 'NONE',  ( 13.97604488694527802, 13.89961937509977652, 54.37390960531435979 ) ) ;
#115437 = ORIENTED_EDGE ( 'NONE', *, *, #134940, .F. ) ;
#115438 = CARTESIAN_POINT ( 'NONE',  ( 10.72451020669871369, 18.67979575497193778, 97.08442372801904696 ) ) ;
#115439 = CARTESIAN_POINT ( 'NONE',  ( -8.224510206698735004, -14.34966873604973081, 59.58442372801901854 ) ) ;
#115440 = CARTESIAN_POINT ( 'NONE',  ( 15.72974639402176855, 15.80617190586768217, 81.87609039468568994 ) ) ;
#115441 = CARTESIAN_POINT ( 'NONE',  ( -5.153800228976328057, -19.02544592524343514, 112.2905762719810099 ) ) ;
#115442 = CARTESIAN_POINT ( 'NONE',  ( -9.474510206698720793, -16.51473224551083518, 99.58442372801900433 ) ) ;
#115443 = CARTESIAN_POINT ( 'NONE',  ( 5.823673210054444382, -21.52544592524334988, 70.20942372801904696 ) ) ;
#115444 = CARTESIAN_POINT ( 'NONE',  ( 8.224510206698742110, 14.34966873604972548, 37.08442372801901143 ) ) ;
#115445 = CARTESIAN_POINT ( 'NONE',  ( 18.67979575497178502, 10.72451020669898547, 89.16557627198102409 ) ) ;
#115446 = CARTESIAN_POINT ( 'NONE',  ( -5.049401038297874678, -19.05341960407617918, 89.79275706135230450 ) ) ;
#115447 = CARTESIAN_POINT ( 'NONE',  ( 13.97604488694527802, 13.89961937509977652, 59.37390960531434558 ) ) ;
#115448 = CARTESIAN_POINT ( 'NONE',  ( 19.02544592524334988, 5.153800228976608722, 96.45942372801897591 ) ) ;
#115449 = AXIS2_PLACEMENT_3D ( 'NONE', #84840, #112206, #116198 ) ;
#115450 = CARTESIAN_POINT ( 'NONE',  ( -16.51473224551082808, 9.474510206698731452, 108.3344237280190043 ) ) ;
#115451 = CARTESIAN_POINT ( 'NONE',  ( 16.52544592524342804, -4.483927247898539470, 58.54057627198103120 ) ) ;
#115452 = CARTESIAN_POINT ( 'NONE',  ( -5.153800228976607833, 19.02544592524334988, 77.70942372801900433 ) ) ;
#115453 = CARTESIAN_POINT ( 'NONE',  ( 14.29746914071037800, 8.314922557961029526, 61.66775706135235424 ) ) ;
#115454 = CARTESIAN_POINT ( 'NONE',  ( 16.46253265017160672, -9.564922557960803928, 43.33224293864769550 ) ) ;
#115455 = CARTESIAN_POINT ( 'NONE',  ( -16.46253265017160317, 9.564922557960807481, 60.83224293864769550 ) ) ;
#115456 = CARTESIAN_POINT ( 'NONE',  ( 14.29746914071037800, 8.314922557961029526, 61.66775706135235424 ) ) ;
#115457 = CARTESIAN_POINT ( 'NONE',  ( -18.22780087662119541, 5.500000000000102141, 46.01763182126894947 ) ) ;
#115458 = EDGE_CURVE ( 'NONE', #52978, #55466, #158006, .T. ) ;
#115459 = CARTESIAN_POINT ( 'NONE',  ( 17.81289503416610742, 24.51734667627700404, 139.5500000054623229 ) ) ;
#115460 = CARTESIAN_POINT ( 'NONE',  ( -16.51473224551069308, -9.474510206698971260, 111.6655762719810383 ) ) ;
#115461 = CARTESIAN_POINT ( 'NONE',  ( -69.65682714487590488, -71.74905178543390605, -15.00000000000000000 ) ) ;
#115462 = ORIENTED_EDGE ( 'NONE', *, *, #97283, .F. ) ;
#115463 = CARTESIAN_POINT ( 'NONE',  ( -16.51473224551082808, 9.474510206698731452, 113.3344237280190043 ) ) ;
#115464 = CARTESIAN_POINT ( 'NONE',  ( -0.05219959533907301413, -21.53943276465977519, 32.49890960531435979 ) ) ;
#115466 = CARTESIAN_POINT ( 'NONE',  ( 9.564922557961047289, -16.46253265017146816, 105.4177570613523471 ) ) ;
#115465 = CARTESIAN_POINT ( 'NONE',  ( 0.05219959533936267826, -19.03943276465977164, 30.00109039468566863 ) ) ;
#115467 = CARTESIAN_POINT ( 'NONE',  ( 5.049401038298161559, -19.05341960407611168, 27.70724293864769550 ) ) ;
#115468 = CARTESIAN_POINT ( 'NONE',  ( -19.03943276465977164, 0.05219959533909376836, 51.24890960531436690 ) ) ;
#115469 = CARTESIAN_POINT ( 'NONE',  ( 10.81492255796078972, 18.62759615963270932, 74.58224293864768129 ) ) ;
#115470 = CARTESIAN_POINT ( 'NONE',  ( -19.02544592524342804, 5.153800228976336051, 96.04057627198103830 ) ) ;
#115471 = CARTESIAN_POINT ( 'NONE',  ( -9.564922557960796823, -16.46253265017161027, 37.08224293864768839 ) ) ;
#115472 = CARTESIAN_POINT ( 'NONE',  ( -17.14385361876520264, -23.59649016807271238, 145.6750000027311671 ) ) ;
#115473 = CARTESIAN_POINT ( 'NONE',  ( 5.153800228976615827, -19.02544592524334988, 85.20942372801900433 ) ) ;
#115475 = VECTOR ( 'NONE', #11216, 1000.000000000000000 ) ;
#115474 = CARTESIAN_POINT ( 'NONE',  ( 8.224510206698953496, -14.34966873604960469, 72.91557627198103830 ) ) ;
#115476 = CARTESIAN_POINT ( 'NONE',  ( 15.80617190586746368, 15.72974639402197994, 49.37390960531436690 ) ) ;
#115477 = CARTESIAN_POINT ( 'NONE',  ( 21.53943276465977519, 0.05219959533937863772, 111.2510903946856899 ) ) ;
#115478 = CARTESIAN_POINT ( 'NONE',  ( 0.05219959533907565091, 21.53943276465977519, 94.99890960531436690 ) ) ;
#115479 = CARTESIAN_POINT ( 'NONE',  ( -21.55341960407619339, 5.719274019375674811, 78.54275706135236135 ) ) ;
#115480 = CARTESIAN_POINT ( 'NONE',  ( 21.53943276465977519, 0.05219959533937863772, 81.25109039468568994 ) ) ;
#115481 = CARTESIAN_POINT ( 'NONE',  ( -19.02544592524342804, 5.153800228976336051, 106.0405762719810241 ) ) ;
#115483 = CARTESIAN_POINT ( 'NONE',  ( -15.80617190586768217, 15.72974639402176855, 83.12609039468568994 ) ) ;
#115482 = CARTESIAN_POINT ( 'NONE',  ( 8.314922557961029526, -14.29746914071037800, 105.4177570613523613 ) ) ;
#115484 = CARTESIAN_POINT ( 'NONE',  ( 16.46253265017160672, -9.564922557960803928, 68.33224293864770971 ) ) ;
#115485 = CARTESIAN_POINT ( 'NONE',  ( 19.03943276465977164, 0.05219959533936151252, 31.25109039468566863 ) ) ;
#115486 = CARTESIAN_POINT ( 'NONE',  ( -21.55341960407619339, 5.719274019375674811, 28.54275706135234358 ) ) ;
#115487 = CARTESIAN_POINT ( 'NONE',  ( -13.89961937509977652, 13.97604488694528158, 70.62390960531432427 ) ) ;
#115488 = CARTESIAN_POINT ( 'NONE',  ( 8.224510206698953496, -14.34966873604960469, 82.91557627198103830 ) ) ;
#115489 = CARTESIAN_POINT ( 'NONE',  ( 12.06949235617757843, -12.14591786802309237, 48.12390960531436690 ) ) ;
#115490 = CARTESIAN_POINT ( 'NONE',  ( -18.62759615963270932, 10.81492255796079327, 60.83224293864769550 ) ) ;
#115491 = CARTESIAN_POINT ( 'NONE',  ( 9.564922557960805705, 16.46253265017160317, 59.58224293864769550 ) ) ;
#115492 = CARTESIAN_POINT ( 'NONE',  ( -5.823673210054116645, -21.52544592524344225, 77.29057627198102409 ) ) ;
#115493 = CARTESIAN_POINT ( 'NONE',  ( -5.049401038297874678, -19.05341960407617918, 59.79275706135231871 ) ) ;
#115495 = CARTESIAN_POINT ( 'NONE',  ( -0.05219959533910754901, -16.53943276465976808, 67.49890960531436690 ) ) ;
#115494 = CARTESIAN_POINT ( 'NONE',  ( 19.05341960407618274, -5.049401038297876454, 26.04275706135233648 ) ) ;
#115496 = VECTOR ( 'NONE', #163614, 1000.000000000000000 ) ;
#115497 = CARTESIAN_POINT ( 'NONE',  ( -18.67979575497178146, -10.72451020669898902, 36.66557627198103120 ) ) ;
#115498 = VERTEX_POINT ( 'NONE', #188357 ) ;
#115499 = LINE ( 'NONE', #177186, #101219 ) ;
#115501 = CARTESIAN_POINT ( 'NONE',  ( 0.2000162670639714646, 6.100000000000010303, -64.53213882399991519 ) ) ;
#115500 = CARTESIAN_POINT ( 'NONE',  ( 16.52544592524335698, 4.483927247898782831, 91.45942372801901854 ) ) ;
#115502 = CARTESIAN_POINT ( 'NONE',  ( -9.474510206698720793, -16.51473224551083518, 84.58442372801900433 ) ) ;
#115503 = CARTESIAN_POINT ( 'NONE',  ( 12.06949235617757843, -12.14591786802309237, 68.12390960531436690 ) ) ;
#115504 = CYLINDRICAL_SURFACE ( 'NONE', #167811, 38.00000000000000000 ) ;
#115505 = CARTESIAN_POINT ( 'NONE',  ( -16.51473224551069308, -9.474510206698971260, 56.66557627198103120 ) ) ;
#115506 = CARTESIAN_POINT ( 'NONE',  ( 16.55341960407611168, 4.379528057220329451, 43.95724293864769550 ) ) ;
#115507 = CARTESIAN_POINT ( 'NONE',  ( -13.97604488694527625, -13.89961937509977652, 81.87390960531436690 ) ) ;
#115509 = CARTESIAN_POINT ( 'NONE',  ( 16.51473224551069308, 9.474510206698969483, 49.16557627198102409 ) ) ;
#115508 = CARTESIAN_POINT ( 'NONE',  ( -0.05219959533936034679, 19.03943276465977164, 72.50109039468566152 ) ) ;
#115510 = CARTESIAN_POINT ( 'NONE',  ( 18.67979575497194134, -10.72451020669871369, 65.83442372801900433 ) ) ;
#115511 = CARTESIAN_POINT ( 'NONE',  ( 9.474510206698971260, -16.51473224551069308, 87.91557627198102409 ) ) ;
#115512 = CARTESIAN_POINT ( 'NONE',  ( -5.153800228976328057, -19.02544592524343514, 27.29057627198103120 ) ) ;
#115513 = CARTESIAN_POINT ( 'NONE',  ( -16.46253265017160317, 9.564922557960807481, 75.83224293864769550 ) ) ;
#115514 = CARTESIAN_POINT ( 'NONE',  ( -0.05219959533907301413, -21.53943276465977519, 47.49890960531435979 ) ) ;
#115515 = CARTESIAN_POINT ( 'NONE',  ( 16.51473224551069308, 9.474510206698969483, 44.16557627198103120 ) ) ;
#115516 = CARTESIAN_POINT ( 'NONE',  ( 0.05219959533907565091, 21.53943276465977519, 49.99890960531437401 ) ) ;
#115517 = CARTESIAN_POINT ( 'NONE',  ( 19.05341960407617918, -5.049401038297876454, 86.04275706135233293 ) ) ;
#115518 = CARTESIAN_POINT ( 'NONE',  ( 12.14591786802327356, -12.06949235617739191, 100.6260903946857184 ) ) ;
#115519 = CARTESIAN_POINT ( 'NONE',  ( 0.05219959533936267826, -19.03943276465977164, 35.00109039468566863 ) ) ;
#115521 = CARTESIAN_POINT ( 'NONE',  ( -16.55341960407617563, 4.379528057220093196, 93.54275706135234714 ) ) ;
#115520 = CARTESIAN_POINT ( 'NONE',  ( 12.14591786802327356, -12.06949235617739191, 65.62609039468568994 ) ) ;
#115522 = CARTESIAN_POINT ( 'NONE',  ( 18.22780087662122384, 5.500000000000018652, 98.98459894673892734 ) ) ;
#115523 = CARTESIAN_POINT ( 'NONE',  ( 14.34966873604972726, -8.224510206698740333, 80.83442372801901854 ) ) ;
#115524 = CARTESIAN_POINT ( 'NONE',  ( 5.719274019375991003, -21.55341960407610458, 32.70724293864770260 ) ) ;
#115525 = CARTESIAN_POINT ( 'NONE',  ( -19.05341960407611168, -5.049401038298163336, 36.45724293864766707 ) ) ;
#115526 = CARTESIAN_POINT ( 'NONE',  ( 4.379528057220092307, 16.55341960407617563, 32.29275706135235424 ) ) ;
#115527 = CARTESIAN_POINT ( 'NONE',  ( -16.51473224551069308, -9.474510206698971260, 51.66557627198102409 ) ) ;
#115528 = CARTESIAN_POINT ( 'NONE',  ( 5.823673210054444382, -21.52544592524334988, 45.20942372801901854 ) ) ;
#115529 = CARTESIAN_POINT ( 'NONE',  ( -16.53943276465976808, -0.05219959533934237506, 38.75109039468567573 ) ) ;
#115530 = CARTESIAN_POINT ( 'NONE',  ( -16.55341960407611168, -4.379528057220339221, 26.45724293864768839 ) ) ;
#115531 = CARTESIAN_POINT ( 'NONE',  ( -19.03943276465977164, 0.05219959533909376836, 26.24890960531435624 ) ) ;
#115532 = CARTESIAN_POINT ( 'NONE',  ( -16.46253265017146816, -9.564922557961047289, 19.16775706135233293 ) ) ;
#115533 = CARTESIAN_POINT ( 'NONE',  ( -19.05341960407617563, 5.049401038297882671, 113.5427570613523471 ) ) ;
#115534 = CARTESIAN_POINT ( 'NONE',  ( -0.05219959533936034679, 19.03943276465977164, 67.50109039468566152 ) ) ;
#115535 = CARTESIAN_POINT ( 'NONE',  ( -16.53943276465976808, 0.05219959533911058130, 71.24890960531435269 ) ) ;
#115536 = CARTESIAN_POINT ( 'NONE',  ( 9.474510206698971260, -16.51473224551069308, 37.91557627198102409 ) ) ;
#115538 = CARTESIAN_POINT ( 'NONE',  ( 17.26172910966779028, -6.454744622555846689, 93.30646908649222837 ) ) ;
#115537 = CARTESIAN_POINT ( 'NONE',  ( 13.97604488694548053, -13.89961937509957401, 70.62609039468567573 ) ) ;
#115539 = CARTESIAN_POINT ( 'NONE',  ( 10.81492255796106328, -18.62759615963255655, 60.41775706135235424 ) ) ;
#115540 = CARTESIAN_POINT ( 'NONE',  ( 0.05219959533934541429, -16.53943276465976808, 45.00109039468568284 ) ) ;
#115541 = CARTESIAN_POINT ( 'NONE',  ( 18.56197773271730256, -5.499999999999888090, 56.05066217314453070 ) ) ;
#115542 = CARTESIAN_POINT ( 'NONE',  ( -21.52544592524343514, 5.823673210054127303, 41.04057627198103120 ) ) ;
#115543 = CARTESIAN_POINT ( 'NONE',  ( 4.379528057220092307, 16.55341960407617563, 22.29275706135235069 ) ) ;
#115544 = CARTESIAN_POINT ( 'NONE',  ( 16.51473224551069308, 9.474510206698969483, 114.1655762719810241 ) ) ;
#115545 = CARTESIAN_POINT ( 'NONE',  ( -24.06609220500515178, 14.38661408136930575, 165.8682408874382475 ) ) ;
#115546 = CARTESIAN_POINT ( 'NONE',  ( -16.51473224551069308, -9.474510206698971260, 41.66557627198103120 ) ) ;
#115547 = CARTESIAN_POINT ( 'NONE',  ( 5.719274019375673035, 21.55341960407619339, 112.2927570613523471 ) ) ;
#115548 = CARTESIAN_POINT ( 'NONE',  ( -5.153800228976328057, -19.02544592524343514, 62.29057627198100988 ) ) ;
#115549 = CARTESIAN_POINT ( 'NONE',  ( -18.62759615963255300, -10.81492255796106328, 59.16775706135234714 ) ) ;
#115550 = CARTESIAN_POINT ( 'NONE',  ( 5.823673210054444382, -21.52544592524334988, 100.2094237280190043 ) ) ;
#115551 = CARTESIAN_POINT ( 'NONE',  ( 12.06949235617757843, -12.14591786802309237, 28.12390960531435979 ) ) ;
#115552 = CARTESIAN_POINT ( 'NONE',  ( -0.05219959533909027116, -19.03943276465977164, 27.49890960531435624 ) ) ;
#115553 = ADVANCED_FACE ( 'NONE', ( #49835 ), #36635, .T. ) ;
#115554 = CARTESIAN_POINT ( 'NONE',  ( -19.03943276465977164, 0.05219959533909376836, 86.24890960531436690 ) ) ;
#115555 = CARTESIAN_POINT ( 'NONE',  ( 21.53943276465977519, 0.05219959533937863772, 51.25109039468568994 ) ) ;
#115556 = CARTESIAN_POINT ( 'NONE',  ( -5.153800228976328057, -19.02544592524343514, 37.29057627198102409 ) ) ;
#115557 = CARTESIAN_POINT ( 'NONE',  ( -21.55341960407619339, 5.719274019375674811, 58.54275706135235424 ) ) ;
#115559 = CARTESIAN_POINT ( 'NONE',  ( -16.46253265017160317, 9.564922557960807481, 100.8322429386477097 ) ) ;
#115558 = CARTESIAN_POINT ( 'NONE',  ( 19.05341960407617918, -5.049401038297876454, 91.04275706135234714 ) ) ;
#115560 = CARTESIAN_POINT ( 'NONE',  ( 16.46253265017160672, -9.564922557960803928, 28.33224293864769550 ) ) ;
#115561 = CARTESIAN_POINT ( 'NONE',  ( -15.72974639402197994, 15.80617190586746368, 115.6239096053143669 ) ) ;
#115562 = CARTESIAN_POINT ( 'NONE',  ( 0.05219959533936267826, -19.03943276465977164, 30.00109039468566863 ) ) ;
#115563 = CARTESIAN_POINT ( 'NONE',  ( 0.05219959533910956823, 16.53943276465976808, 104.9989096053143669 ) ) ;
#115564 = CARTESIAN_POINT ( 'NONE',  ( 16.51473224551069308, 9.474510206698969483, 44.16557627198103120 ) ) ;
#115565 = CARTESIAN_POINT ( 'NONE',  ( -9.564922557961040184, 16.46253265017147172, 92.91775706135233293 ) ) ;
#115566 = CARTESIAN_POINT ( 'NONE',  ( 12.06949235617757843, -12.14591786802309237, 63.12390960531435979 ) ) ;
#115567 = CARTESIAN_POINT ( 'NONE',  ( -10.72451020669870658, -18.67979575497194134, 109.5844237280190328 ) ) ;
#115568 = CARTESIAN_POINT ( 'NONE',  ( -10.72451020669898014, 18.67979575497178502, 25.41557627198103120 ) ) ;
#115569 = CARTESIAN_POINT ( 'NONE',  ( -16.46253265017146816, -9.564922557961047289, 89.16775706135234714 ) ) ;
#115570 = CARTESIAN_POINT ( 'NONE',  ( 10.81492255796078972, 18.62759615963270932, 94.58224293864769550 ) ) ;
#115571 = CARTESIAN_POINT ( 'NONE',  ( -0.05219959533937732626, 21.53943276465977519, 37.50109039468568284 ) ) ;
#115572 = CARTESIAN_POINT ( 'NONE',  ( -16.52544592524335698, -4.483927247898792601, 43.95942372801902565 ) ) ;
#115573 = CARTESIAN_POINT ( 'NONE',  ( 16.52544592524335698, 4.483927247898782831, 106.4594237280190328 ) ) ;
#115575 = CARTESIAN_POINT ( 'NONE',  ( -5.823673210054431948, 21.52544592524334988, 52.70942372801902565 ) ) ;
#115574 = CARTESIAN_POINT ( 'NONE',  ( 16.55341960407618274, -4.379528057220086978, 46.04275706135234714 ) ) ;
#115576 = CARTESIAN_POINT ( 'NONE',  ( 5.823673210054125526, 21.52544592524343514, 49.79057627198102409 ) ) ;
#115577 = CARTESIAN_POINT ( 'NONE',  ( -19.03943276465977164, 0.05219959533909376836, 36.24890960531436690 ) ) ;
#115578 = CARTESIAN_POINT ( 'NONE',  ( -23.48529157249599919, -32.32473071737750558, -3.449999994537626957 ) ) ;
#115579 = CARTESIAN_POINT ( 'NONE',  ( -16.53943276465976808, -0.05219959533934237506, 63.75109039468568284 ) ) ;
#115580 = CARTESIAN_POINT ( 'NONE',  ( -5.823673210054116645, -21.52544592524344225, 87.29057627198103830 ) ) ;
#115581 = CARTESIAN_POINT ( 'NONE',  ( 14.34966873604960469, 8.224510206698951720, 44.16557627198103120 ) ) ;
#115582 = CARTESIAN_POINT ( 'NONE',  ( -0.05219959533934338120, 16.53943276465976808, 57.50109039468568994 ) ) ;
#115583 = CARTESIAN_POINT ( 'NONE',  ( -0.05219959533936034679, 19.03943276465977164, 97.50109039468567573 ) ) ;
#115584 = CARTESIAN_POINT ( 'NONE',  ( 21.52544592524344225, -5.823673210054117533, 103.5405762719810383 ) ) ;
#115585 = CARTESIAN_POINT ( 'NONE',  ( -8.314922557960811034, -14.29746914071050412, 37.08224293864768129 ) ) ;
#115586 = ORIENTED_EDGE ( 'NONE', *, *, #88498, .T. ) ;
#115587 = CARTESIAN_POINT ( 'NONE',  ( 4.379528057220092307, 16.55341960407617563, 72.29275706135236135 ) ) ;
#115588 = CARTESIAN_POINT ( 'NONE',  ( 26.73207562759453992, 6.543912086049501475, 168.7462576975894422 ) ) ;
#115589 = CARTESIAN_POINT ( 'NONE',  ( 5.719274019375991003, -21.55341960407610458, 72.70724293864769550 ) ) ;
#115590 = CARTESIAN_POINT ( 'NONE',  ( -8.314922557961024197, 14.29746914071037800, 107.9177570613523471 ) ) ;
#115591 = ORIENTED_EDGE ( 'NONE', *, *, #44038, .F. ) ;
#115592 = CARTESIAN_POINT ( 'NONE',  ( 37.99999999999999289, 2.428612866367529932E-14, -18.00000000000000000 ) ) ;
#115593 = CARTESIAN_POINT ( 'NONE',  ( -5.719274019375978568, 21.55341960407610458, 85.20724293864770971 ) ) ;
#115594 = CARTESIAN_POINT ( 'NONE',  ( 18.62759615963271287, -10.81492255796078972, 113.3322429386476955 ) ) ;
#115595 = CARTESIAN_POINT ( 'NONE',  ( 14.34966873604960469, 8.224510206698951720, 39.16557627198102409 ) ) ;
#115596 = CARTESIAN_POINT ( 'NONE',  ( 8.224510206698742110, 14.34966873604972548, 37.08442372801901143 ) ) ;
#115597 = VECTOR ( 'NONE', #71180, 1000.000000000000114 ) ;
#115598 = CARTESIAN_POINT ( 'NONE',  ( 19.03943276465977164, -0.05219959533909143690, 48.74890960531435979 ) ) ;
#115599 = CARTESIAN_POINT ( 'NONE',  ( 19.02544592524343514, -5.153800228976328945, 73.54057627198103830 ) ) ;
#115600 = CARTESIAN_POINT ( 'NONE',  ( 16.46253265017160672, -9.564922557960803928, 113.3322429386476955 ) ) ;
#115601 = CARTESIAN_POINT ( 'NONE',  ( -16.46253265017160317, 9.564922557960807481, 115.8322429386477097 ) ) ;
#115602 = CARTESIAN_POINT ( 'NONE',  ( -19.05341960407617563, 5.049401038297882671, 108.5427570613523187 ) ) ;
#115603 = CARTESIAN_POINT ( 'NONE',  ( 19.03943276465977164, 0.05219959533936151252, 46.25109039468566863 ) ) ;
#115604 = CARTESIAN_POINT ( 'NONE',  ( -21.52544592524343514, 5.823673210054127303, 91.04057627198103830 ) ) ;
#115605 = CARTESIAN_POINT ( 'NONE',  ( 8.314922557960818139, 14.29746914071049879, 24.58224293864768839 ) ) ;
#115606 = CARTESIAN_POINT ( 'NONE',  ( -5.823673210054116645, -21.52544592524344225, 42.29057627198103120 ) ) ;
#115608 = CARTESIAN_POINT ( 'NONE',  ( -0.05219959533936034679, 19.03943276465977164, 107.5010903946856615 ) ) ;
#115607 = CARTESIAN_POINT ( 'NONE',  ( -21.55341960407610458, -5.719274019375992779, 81.45724293864769550 ) ) ;
#115609 = CARTESIAN_POINT ( 'NONE',  ( 5.153800228976335163, 19.02544592524342804, 99.79057627198102409 ) ) ;
#115610 = CARTESIAN_POINT ( 'NONE',  ( -21.53943276465977519, -0.05219959533937600094, 73.75109039468567573 ) ) ;
#115611 = CARTESIAN_POINT ( 'NONE',  ( -13.97604488694527625, -13.89961937509977652, 76.87390960531433848 ) ) ;
#115612 = CARTESIAN_POINT ( 'NONE',  ( -16.53943276465976808, 0.05219959533911058130, 101.2489096053143669 ) ) ;
#115613 = CARTESIAN_POINT ( 'NONE',  ( 31.80025110837587832, 6.358902984670138814, 91.01589400111390660 ) ) ;
#115614 = CARTESIAN_POINT ( 'NONE',  ( 19.02544592524343514, -5.153800228976328945, 73.54057627198103830 ) ) ;
#115615 = CARTESIAN_POINT ( 'NONE',  ( -8.314922557960811034, -14.29746914071050412, 92.08224293864769550 ) ) ;
#115616 = VERTEX_POINT ( 'NONE', #67979 ) ;
#115617 = CARTESIAN_POINT ( 'NONE',  ( -16.46253265017146816, -9.564922557961047289, 109.1677570613523471 ) ) ;
#115618 = CARTESIAN_POINT ( 'NONE',  ( 5.000000000000000000, -125.7396439921083555, 8.159758652193112027 ) ) ;
#115619 = CARTESIAN_POINT ( 'NONE',  ( -13.89961937509977652, 13.97604488694528158, 55.62390960531434558 ) ) ;
#115620 = CIRCLE ( 'NONE', #5764, 10.00000000000000000 ) ;
#115622 = CARTESIAN_POINT ( 'NONE',  ( 16.46253265017160672, -9.564922557960803928, 103.3322429386476955 ) ) ;
#115621 = CARTESIAN_POINT ( 'NONE',  ( -21.55341960407619339, 5.719274019375674811, 83.54275706135234714 ) ) ;
#115623 = CARTESIAN_POINT ( 'NONE',  ( -0.05219959533934338120, 16.53943276465976808, 72.50109039468568994 ) ) ;
#115624 = DIRECTION ( 'NONE',  ( -0.9945218953682734009, 0.000000000000000000, 0.1045284632676537068 ) ) ;
#115625 = CARTESIAN_POINT ( 'NONE',  ( -5.049401038297874678, -19.05341960407617918, 59.79275706135231871 ) ) ;
#115626 = CARTESIAN_POINT ( 'NONE',  ( -18.62759615963255300, -10.81492255796106328, 94.16775706135237556 ) ) ;
#115627 = CARTESIAN_POINT ( 'NONE',  ( 28.79475375365599987, -9.355982642738995381, 144.8843446568999980 ) ) ;
#115628 = FACE_OUTER_BOUND ( 'NONE', #107361, .T. ) ;
#115629 = CARTESIAN_POINT ( 'NONE',  ( 16.55341960407611168, 4.379528057220329451, 28.95724293864769905 ) ) ;
#115630 = CARTESIAN_POINT ( 'NONE',  ( -17.58332526062526213, -7.635886036038624702, 74.07665040441536064 ) ) ;
#115631 = CARTESIAN_POINT ( 'NONE',  ( -4.379528057220086978, -16.55341960407618274, 89.79275706135236135 ) ) ;
#115632 = DIRECTION ( 'NONE',  ( 0.000000000000000000, -0.7071067811865483499, 0.7071067811865465735 ) ) ;
#115633 = CARTESIAN_POINT ( 'NONE',  ( 12.06949235617739724, 12.14591786802326823, 71.87609039468568994 ) ) ;
#115634 = CARTESIAN_POINT ( 'NONE',  ( -5.719274019375665041, -21.55341960407619695, 84.79275706135234714 ) ) ;
#115635 = CARTESIAN_POINT ( 'NONE',  ( 16.51473224551083163, -9.474510206698727899, 85.83442372801900433 ) ) ;
#115636 = CARTESIAN_POINT ( 'NONE',  ( -9.564922557961040184, 16.46253265017147172, 42.91775706135234003 ) ) ;
#115637 = CARTESIAN_POINT ( 'NONE',  ( -19.03943276465977164, 0.05219959533909376836, 71.24890960531435269 ) ) ;
#115638 = CARTESIAN_POINT ( 'NONE',  ( 19.02544592524343514, -5.153800228976328945, 63.54057627198103830 ) ) ;
#115639 = CARTESIAN_POINT ( 'NONE',  ( -7.284589286804255437, 1.784589286804319386, 8.181980515339454030 ) ) ;
#115640 = CARTESIAN_POINT ( 'NONE',  ( -15.72974639402197994, 15.80617190586746368, 85.62390960531436690 ) ) ;
#115641 = CARTESIAN_POINT ( 'NONE',  ( 21.55341960407610458, 5.719274019375980345, 53.95724293864770260 ) ) ;
#115642 = CARTESIAN_POINT ( 'NONE',  ( 9.564922557960805705, 16.46253265017160317, 39.58224293864768839 ) ) ;
#115643 = CARTESIAN_POINT ( 'NONE',  ( 8.224510206698742110, 14.34966873604972548, 67.08442372801901854 ) ) ;
#115644 = VERTEX_POINT ( 'NONE', #112489 ) ;
#115645 = CARTESIAN_POINT ( 'NONE',  ( 15.72974639402176855, 15.80617190586768217, 46.87609039468568994 ) ) ;
#115647 = CARTESIAN_POINT ( 'NONE',  ( -29.86685920354755197, -21.69954338932560134, -8.424999997268812990 ) ) ;
#115646 = CARTESIAN_POINT ( 'NONE',  ( 12.14591786802309770, 12.06949235617756955, 59.37390960531436690 ) ) ;
#115648 = CARTESIAN_POINT ( 'NONE',  ( -16.53943276465976808, -0.05219959533934237506, 33.75109039468568284 ) ) ;
#115649 = CARTESIAN_POINT ( 'NONE',  ( -0.05219959533936034679, 19.03943276465977164, 47.50109039468566863 ) ) ;
#115650 = CARTESIAN_POINT ( 'NONE',  ( -8.314922557960811034, -14.29746914071050412, 62.08224293864769550 ) ) ;
#115652 = EDGE_CURVE ( 'NONE', #30365, #99459, #138762, .T. ) ;
#115651 = CARTESIAN_POINT ( 'NONE',  ( -15.72974639402176322, -15.80617190586768395, 29.37609039468568284 ) ) ;
#115654 = CARTESIAN_POINT ( 'NONE',  ( 15.80617190586746368, 15.72974639402197994, 84.37390960531438111 ) ) ;
#115653 = FACE_OUTER_BOUND ( 'NONE', #51528, .T. ) ;
#115655 = CARTESIAN_POINT ( 'NONE',  ( -19.02544592524342804, 5.153800228976336051, 106.0405762719810241 ) ) ;
#115656 = CARTESIAN_POINT ( 'NONE',  ( 4.379528057220339221, -16.55341960407611168, 77.70724293864770971 ) ) ;
#115657 = CARTESIAN_POINT ( 'NONE',  ( -19.02544592524342804, 5.153800228976336051, 111.0405762719810099 ) ) ;
#115658 = CARTESIAN_POINT ( 'NONE',  ( -37.57676386873053076, 0.7175261378074869745, 39.53500980800841802 ) ) ;
#115659 = CARTESIAN_POINT ( 'NONE',  ( -19.02544592524334988, -5.153800228976617603, 73.95942372801900433 ) ) ;
#115660 = CARTESIAN_POINT ( 'NONE',  ( 0.05219959533907565091, 21.53943276465977519, 114.9989096053143669 ) ) ;
#115661 = CARTESIAN_POINT ( 'NONE',  ( 0.05219959533909260263, 19.03943276465977164, 59.99890960531436690 ) ) ;
#115662 = CARTESIAN_POINT ( 'NONE',  ( -5.153800228976607833, 19.02544592524334988, 42.70942372801901143 ) ) ;
#115663 = CARTESIAN_POINT ( 'NONE',  ( -19.02544592524342804, 5.153800228976336051, 31.04057627198102409 ) ) ;
#115664 = CARTESIAN_POINT ( 'NONE',  ( 10.72451020669871369, 18.67979575497193778, 67.08442372801901854 ) ) ;
#115665 = CARTESIAN_POINT ( 'NONE',  ( -16.62475595723696742, -7.163666690055377373, 69.47286648189532343 ) ) ;
#115666 = EDGE_CURVE ( 'NONE', #120193, #182543, #146824, .T. ) ;
#115667 = CARTESIAN_POINT ( 'NONE',  ( -16.53943276465976808, 0.05219959533911058130, 51.24890960531436690 ) ) ;
#115668 = CARTESIAN_POINT ( 'NONE',  ( -13.97604488694527625, -13.89961937509977652, 66.87390960531436690 ) ) ;
#115669 = CARTESIAN_POINT ( 'NONE',  ( 5.823673210054125526, 21.52544592524343514, 89.79057627198103830 ) ) ;
#115670 = CARTESIAN_POINT ( 'NONE',  ( -13.97604488694527625, -13.89961937509977652, 51.87390960531436690 ) ) ;
#115671 = ORIENTED_EDGE ( 'NONE', *, *, #72464, .T. ) ;
#115672 = CARTESIAN_POINT ( 'NONE',  ( -10.81492255796078084, -18.62759615963271287, 82.08224293864768129 ) ) ;
#115673 = CARTESIAN_POINT ( 'NONE',  ( -18.62759615963255300, -10.81492255796106328, 104.1677570613523471 ) ) ;
#115676 = CARTESIAN_POINT ( 'NONE',  ( 0.05219959533910956823, 16.53943276465976808, 79.99890960531435269 ) ) ;
#115675 = CARTESIAN_POINT ( 'NONE',  ( -4.483927247898782831, 16.52544592524335698, 102.7094237280190185 ) ) ;
#115674 = CARTESIAN_POINT ( 'NONE',  ( 9.564922557960805705, 16.46253265017160317, 24.58224293864769194 ) ) ;
#115677 = CARTESIAN_POINT ( 'NONE',  ( -13.97604488694547697, 13.89961937509957934, 93.12609039468566152 ) ) ;
#115678 = ORIENTED_EDGE ( 'NONE', *, *, #65894, .F. ) ;
#115679 = CARTESIAN_POINT ( 'NONE',  ( -10.72451020669898014, 18.67979575497178502, 115.4155762719810241 ) ) ;
#115680 = CARTESIAN_POINT ( 'NONE',  ( -16.46253265017146816, -9.564922557961047289, 39.16775706135234003 ) ) ;
#115681 = CARTESIAN_POINT ( 'NONE',  ( -16.55341960407617563, 4.379528057220093196, 103.5427570613523613 ) ) ;
#115682 = CARTESIAN_POINT ( 'NONE',  ( -19.03943276465977164, -0.05219959533935918106, 33.75109039468566863 ) ) ;
#115683 = CARTESIAN_POINT ( 'NONE',  ( -9.474510206698964154, 16.51473224551069663, 90.41557627198103830 ) ) ;
#115684 = CARTESIAN_POINT ( 'NONE',  ( -5.823673210054116645, -21.52544592524344225, 57.29057627198103120 ) ) ;
#115685 = CARTESIAN_POINT ( 'NONE',  ( -19.35633801406903487, 5.499999999999766409, 49.13373818172757979 ) ) ;
#115686 = CARTESIAN_POINT ( 'NONE',  ( -14.29746914071049879, 8.314922557960819915, 115.8322429386477097 ) ) ;
#115687 = CARTESIAN_POINT ( 'NONE',  ( 21.55341960407619695, -5.719274019375665929, 106.0427570613523471 ) ) ;
#115688 = CARTESIAN_POINT ( 'NONE',  ( 8.314922557961029526, -14.29746914071037800, 75.41775706135233293 ) ) ;
#115689 = CARTESIAN_POINT ( 'NONE',  ( 10.72451020669871369, 18.67979575497193778, 22.08442372801901143 ) ) ;
#115690 = CARTESIAN_POINT ( 'NONE',  ( -12.14591786802326823, 12.06949235617739902, 33.12609039468569705 ) ) ;
#115691 = CARTESIAN_POINT ( 'NONE',  ( 5.153800228976335163, 19.02544592524342804, 109.7905762719810099 ) ) ;
#115692 = CARTESIAN_POINT ( 'NONE',  ( 19.05341960407611168, 5.049401038298154454, 38.95724293864767418 ) ) ;
#115693 = CARTESIAN_POINT ( 'NONE',  ( 13.97604488694527802, 13.89961937509977652, 69.37390960531436690 ) ) ;
#115694 = CARTESIAN_POINT ( 'NONE',  ( -8.314922557961024197, 14.29746914071037800, 42.91775706135235424 ) ) ;
#115695 = CARTESIAN_POINT ( 'NONE',  ( -14.34966873604960291, -8.224510206698953496, 86.66557627198102409 ) ) ;
#115696 = CARTESIAN_POINT ( 'NONE',  ( -12.06949235617739369, -12.14591786802326823, 104.3760903946856899 ) ) ;
#115699 = CARTESIAN_POINT ( 'NONE',  ( 13.97604488694527802, 13.89961937509977652, 59.37390960531434558 ) ) ;
#115698 = CARTESIAN_POINT ( 'NONE',  ( 9.474510206698971260, -16.51473224551069308, 82.91557627198103830 ) ) ;
#115697 = CARTESIAN_POINT ( 'NONE',  ( 5.719274019375673035, 21.55341960407619339, 57.29275706135234714 ) ) ;
#115700 = CARTESIAN_POINT ( 'NONE',  ( -13.97604488694527625, -13.89961937509977652, 101.8739096053143811 ) ) ;
#115701 = CARTESIAN_POINT ( 'NONE',  ( 0.05219959533910956823, 16.53943276465976808, 39.99890960531436690 ) ) ;
#115702 = CARTESIAN_POINT ( 'NONE',  ( -12.14591786802326823, 12.06949235617739902, 103.1260903946856757 ) ) ;
#115703 = EDGE_CURVE ( 'NONE', #99310, #100403, #148839, .T. ) ;
#115704 = VERTEX_POINT ( 'NONE', #58801 ) ;
#115705 = CARTESIAN_POINT ( 'NONE',  ( -13.97604488694547697, 13.89961937509957934, 43.12609039468566152 ) ) ;
#115706 = CARTESIAN_POINT ( 'NONE',  ( 13.89961937509977652, -13.97604488694527269, 113.1239096053143527 ) ) ;
#115707 = CARTESIAN_POINT ( 'NONE',  ( 19.03943276465977164, -0.05219959533909143690, 63.74890960531435979 ) ) ;
#115708 = CARTESIAN_POINT ( 'NONE',  ( -16.46253265017146816, -9.564922557961047289, 44.16775706135232582 ) ) ;
#115709 = CARTESIAN_POINT ( 'NONE',  ( 36.91746824999999887, 11.99521256947799053, -9.524999997268812635 ) ) ;
#115710 = CARTESIAN_POINT ( 'NONE',  ( -17.12812012977023812, -6.668231424566064547, 66.35948759323143520 ) ) ;
#115711 = CARTESIAN_POINT ( 'NONE',  ( -14.34966873604972548, 8.224510206698743886, 53.33442372801901854 ) ) ;
#115713 = CARTESIAN_POINT ( 'NONE',  ( 8.224510206698742110, 14.34966873604972548, 67.08442372801901854 ) ) ;
#115712 = CARTESIAN_POINT ( 'NONE',  ( 19.02544592524334988, 5.153800228976608722, 66.45942372801899012 ) ) ;
#115714 = CARTESIAN_POINT ( 'NONE',  ( 17.48853670773245383, 5.747243402303094051, 93.83328700250011423 ) ) ;
#115715 = CARTESIAN_POINT ( 'NONE',  ( -9.564922557960796823, -16.46253265017161027, 97.08224293864769550 ) ) ;
#115716 = CARTESIAN_POINT ( 'NONE',  ( 10.72451020669898902, -18.67979575497178502, 107.9155762719810241 ) ) ;
#115717 = CARTESIAN_POINT ( 'NONE',  ( -16.51473224551082808, 9.474510206698731452, 78.33442372801900433 ) ) ;
#115719 = CARTESIAN_POINT ( 'NONE',  ( -5.049401038298153566, 19.05341960407611168, 35.20724293864768839 ) ) ;
#115718 = CARTESIAN_POINT ( 'NONE',  ( 13.97604488694527802, 13.89961937509977652, 104.3739096053143385 ) ) ;
#115720 = CARTESIAN_POINT ( 'NONE',  ( -13.97604488694527625, -13.89961937509977652, 91.87390960531432427 ) ) ;
#115722 = CARTESIAN_POINT ( 'NONE',  ( 13.97604488694527802, 13.89961937509977652, 34.37390960531436690 ) ) ;
#115721 = CARTESIAN_POINT ( 'NONE',  ( 14.34966873604960469, 8.224510206698951720, 54.16557627198103120 ) ) ;
#115723 = CARTESIAN_POINT ( 'NONE',  ( 5.153800228976615827, -19.02544592524334988, 45.20942372801901143 ) ) ;
#115724 = ORIENTED_EDGE ( 'NONE', *, *, #186744, .F. ) ;
#115725 = CARTESIAN_POINT ( 'NONE',  ( -0.05219959533910754901, -16.53943276465976808, 92.49890960531436690 ) ) ;
#115726 = CARTESIAN_POINT ( 'NONE',  ( -0.05219959533937732626, 21.53943276465977519, 112.5010903946857042 ) ) ;
#115727 = CARTESIAN_POINT ( 'NONE',  ( -5.153800228976328057, -19.02544592524343514, 52.29057627198100988 ) ) ;
#115728 = CARTESIAN_POINT ( 'NONE',  ( 18.62759615963271287, -10.81492255796078972, 68.33224293864769550 ) ) ;
#115730 = CARTESIAN_POINT ( 'NONE',  ( -21.55341960407619339, 5.719274019375674811, 113.5427570613523756 ) ) ;
#115729 = CARTESIAN_POINT ( 'NONE',  ( 16.53943276465976808, -0.05219959533910856209, 48.74890960531435979 ) ) ;
#115731 = CARTESIAN_POINT ( 'NONE',  ( -19.02544592524342804, 5.153800228976336051, 101.0405762719810241 ) ) ;
#115732 = CARTESIAN_POINT ( 'NONE',  ( 16.46253265017160672, -9.564922557960803928, 108.3322429386476955 ) ) ;
#115733 = CARTESIAN_POINT ( 'NONE',  ( 13.89961937509977652, -13.97604488694527269, 58.12390960531436690 ) ) ;
#115734 = CARTESIAN_POINT ( 'NONE',  ( -9.564922557960796823, -16.46253265017161027, 22.08224293864768839 ) ) ;
#115735 = CARTESIAN_POINT ( 'NONE',  ( 4.483927247898545687, 16.52544592524342804, 84.79057627198102409 ) ) ;
#115736 = CARTESIAN_POINT ( 'NONE',  ( -5.823673210054116645, -21.52544592524344225, 92.29057627198103830 ) ) ;
#115737 = CARTESIAN_POINT ( 'NONE',  ( -5.049401038298153566, 19.05341960407611168, 100.2072429386476955 ) ) ;
#115738 = CARTESIAN_POINT ( 'NONE',  ( -21.53943276465977519, 0.05219959533907696930, 111.2489096053143669 ) ) ;
#115739 = CARTESIAN_POINT ( 'NONE',  ( -5.153800228976328057, -19.02544592524343514, 102.2905762719810383 ) ) ;
#115740 = CARTESIAN_POINT ( 'NONE',  ( 8.224510206698953496, -14.34966873604960469, 97.91557627198103830 ) ) ;
#115741 = CARTESIAN_POINT ( 'NONE',  ( -21.52544592524334988, -5.823673210054445271, 73.95942372801901854 ) ) ;
#115742 = CARTESIAN_POINT ( 'NONE',  ( -15.72974639402197994, 15.80617190586746368, 95.62390960531436690 ) ) ;
#115743 = CARTESIAN_POINT ( 'NONE',  ( 17.05116617787824396, -6.768360034955795967, 106.1567555325920011 ) ) ;
#115744 = DIRECTION ( 'NONE',  ( 6.718897857320949450E-15, -0.9991276842514722478, 0.04175967627138119087 ) ) ;
#115745 = DIRECTION ( 'NONE',  ( 0.000000000000000000, 0.000000000000000000, 1.000000000000000000 ) ) ;
#115746 = CARTESIAN_POINT ( 'NONE',  ( -16.55341960407617563, 4.379528057220093196, 28.54275706135234358 ) ) ;
#115747 = CARTESIAN_POINT ( 'NONE',  ( 8.224510206698953496, -14.34966873604960469, 112.9155762719810383 ) ) ;
#115748 = CARTESIAN_POINT ( 'NONE',  ( 0.000000000000000000, 0.000000000000000000, -64.92279855667830191 ) ) ;
#115749 = CARTESIAN_POINT ( 'NONE',  ( 0.05219959533909260263, 19.03943276465977164, 64.99890960531436690 ) ) ;
#115750 = CARTESIAN_POINT ( 'NONE',  ( -4.483927247898539470, -16.52544592524342804, 92.29057627198103830 ) ) ;
#115751 = CARTESIAN_POINT ( 'NONE',  ( 21.53943276465977519, -0.05219959533907433946, 33.74890960531436690 ) ) ;
#115752 = CARTESIAN_POINT ( 'NONE',  ( -14.34966873604960291, -8.224510206698953496, 66.66557627198102409 ) ) ;
#115753 = CARTESIAN_POINT ( 'NONE',  ( -4.379528057220086978, -16.55341960407618274, 24.79275706135235779 ) ) ;
#115754 = CARTESIAN_POINT ( 'NONE',  ( -15.80617190586768217, 15.72974639402176855, 73.12609039468567573 ) ) ;
#115755 = LINE ( 'NONE', #100570, #101362 ) ;
#115756 = CARTESIAN_POINT ( 'NONE',  ( 13.89961937509977652, -13.97604488694527269, 113.1239096053143527 ) ) ;
#115757 = CARTESIAN_POINT ( 'NONE',  ( 12.06949235617739724, 12.14591786802326823, 101.8760903946857042 ) ) ;
#115758 = CARTESIAN_POINT ( 'NONE',  ( -19.05341960407611168, -5.049401038298163336, 36.45724293864766707 ) ) ;
#115759 = CARTESIAN_POINT ( 'NONE',  ( 19.03943276465977164, -0.05219959533909143690, 88.74890960531436690 ) ) ;
#115760 = CARTESIAN_POINT ( 'NONE',  ( 15.72974639402199770, -15.80617190586745480, 93.12390960531436690 ) ) ;
#115761 = CARTESIAN_POINT ( 'NONE',  ( -12.14591786802326823, 12.06949235617739902, 28.12609039468568284 ) ) ;
#115763 = CARTESIAN_POINT ( 'NONE',  ( -10.81492255796105439, 18.62759615963255655, 67.91775706135234714 ) ) ;
#115762 = CARTESIAN_POINT ( 'NONE',  ( -16.52544592524342804, 4.483927247898546575, 61.04057627198103120 ) ) ;
#115764 = CIRCLE ( 'NONE', #44756, 2.649999999999999911 ) ;
#115765 = CARTESIAN_POINT ( 'NONE',  ( 14.34966873604972726, -8.224510206698740333, 95.83442372801903275 ) ) ;
#115766 = CARTESIAN_POINT ( 'NONE',  ( 17.26172910966717211, -6.454744622556960465, 48.30646908649207205 ) ) ;
#115767 = CARTESIAN_POINT ( 'NONE',  ( 4.483927247898545687, 16.52544592524342804, 34.79057627198103120 ) ) ;
#115768 = CARTESIAN_POINT ( 'NONE',  ( -16.55341960407617563, 4.379528057220093196, 58.54275706135235424 ) ) ;
#115769 = CARTESIAN_POINT ( 'NONE',  ( 16.51473224551069308, 9.474510206698969483, 69.16557627198102409 ) ) ;
#115770 = CARTESIAN_POINT ( 'NONE',  ( 19.05341960407611168, 5.049401038298154454, 88.95724293864769550 ) ) ;
#115771 = CARTESIAN_POINT ( 'NONE',  ( -5.719274019375665041, -21.55341960407619695, 84.79275706135234714 ) ) ;
#115772 = CARTESIAN_POINT ( 'NONE',  ( -4.379528057220086978, -16.55341960407618274, 89.79275706135236135 ) ) ;
#115773 = CARTESIAN_POINT ( 'NONE',  ( 8.314922557960818139, 14.29746914071049879, 54.58224293864769550 ) ) ;
#115774 = CARTESIAN_POINT ( 'NONE',  ( -9.564922557960796823, -16.46253265017161027, 72.08224293864770971 ) ) ;
#115775 = ORIENTED_EDGE ( 'NONE', *, *, #105651, .F. ) ;
#115776 = CARTESIAN_POINT ( 'NONE',  ( -12.06949235617739369, -12.14591786802326823, 19.37609039468568639 ) ) ;
#115777 = CARTESIAN_POINT ( 'NONE',  ( -0.05219959533910754901, -16.53943276465976808, 112.4989096053143669 ) ) ;
#115778 = CARTESIAN_POINT ( 'NONE',  ( 13.89961937509977652, -13.97604488694527269, 83.12390960531436690 ) ) ;
#115780 = CARTESIAN_POINT ( 'NONE',  ( 22.81625015709510151, -31.40387420917324590, -5.924999997268812990 ) ) ;
#115779 = CARTESIAN_POINT ( 'NONE',  ( -4.379528057220086978, -16.55341960407618274, 24.79275706135235779 ) ) ;
#115781 = CARTESIAN_POINT ( 'NONE',  ( 5.823673210054444382, -21.52544592524334988, 110.2094237280190185 ) ) ;
#115782 = CARTESIAN_POINT ( 'NONE',  ( 8.224510206698742110, 14.34966873604972548, 77.08442372801901854 ) ) ;
#115783 = CARTESIAN_POINT ( 'NONE',  ( 16.46253265017146816, 9.564922557961045513, 86.66775706135233293 ) ) ;
#115784 = CARTESIAN_POINT ( 'NONE',  ( -14.29746914071049879, 8.314922557960819915, 115.8322429386477097 ) ) ;
#115785 = CARTESIAN_POINT ( 'NONE',  ( -14.34966873604972548, 8.224510206698743886, 63.33442372801900433 ) ) ;
#115786 = DIRECTION ( 'NONE',  ( -1.000000000000000000, -0.000000000000000000, -0.000000000000000000 ) ) ;
#115787 = CARTESIAN_POINT ( 'NONE',  ( -9.474510206698720793, -16.51473224551083518, 49.58442372801899722 ) ) ;
#115788 = CARTESIAN_POINT ( 'NONE',  ( 15.80617190586769283, -15.72974639402175789, 95.62609039468568994 ) ) ;
#115789 = CARTESIAN_POINT ( 'NONE',  ( 19.05341960407611168, 5.049401038298154454, 38.95724293864767418 ) ) ;
#115790 = CARTESIAN_POINT ( 'NONE',  ( -16.46253265017160317, 9.564922557960807481, 80.83224293864769550 ) ) ;
#115791 = CARTESIAN_POINT ( 'NONE',  ( -14.34966873604960291, -8.224510206698953496, 66.66557627198102409 ) ) ;
#115792 = CARTESIAN_POINT ( 'NONE',  ( 21.53943276465977519, 0.05219959533937863772, 96.25109039468568994 ) ) ;
#115793 = CARTESIAN_POINT ( 'NONE',  ( -19.05341960407617563, 5.049401038297882671, 48.54275706135233293 ) ) ;
#115794 = CARTESIAN_POINT ( 'NONE',  ( 19.02544592524334988, 5.153800228976608722, 41.45942372801900433 ) ) ;
#115795 = CARTESIAN_POINT ( 'NONE',  ( -21.55341960407610458, -5.719274019375992779, 41.45724293864769550 ) ) ;
#115796 = CARTESIAN_POINT ( 'NONE',  ( -10.72451020669870658, -18.67979575497194134, 99.58442372801900433 ) ) ;
#115797 = CARTESIAN_POINT ( 'NONE',  ( 9.474510206698971260, -16.51473224551069308, 77.91557627198103830 ) ) ;
#115798 = CARTESIAN_POINT ( 'NONE',  ( 18.67979575497194134, -10.72451020669871369, 90.83442372801901854 ) ) ;
#115799 = CARTESIAN_POINT ( 'NONE',  ( -15.80617190586745835, -15.72974639402198527, 51.87390960531437401 ) ) ;
#115800 = CARTESIAN_POINT ( 'NONE',  ( -5.049401038298153566, 19.05341960407611168, 100.2072429386476955 ) ) ;
#115801 = CARTESIAN_POINT ( 'NONE',  ( 0.05219959533936267826, -19.03943276465977164, 70.00109039468566152 ) ) ;
#115802 = CARTESIAN_POINT ( 'NONE',  ( 9.564922557960805705, 16.46253265017160317, 104.5822429386476955 ) ) ;
#115803 = CARTESIAN_POINT ( 'NONE',  ( 0.05219959533936267826, -19.03943276465977164, 95.00109039468567573 ) ) ;
#115804 = CARTESIAN_POINT ( 'NONE',  ( -12.14591786802326823, 12.06949235617739902, 48.12609039468568284 ) ) ;
#115805 = CARTESIAN_POINT ( 'NONE',  ( 14.29746914071049879, -8.314922557960816363, 98.33224293864769550 ) ) ;
#115806 = CARTESIAN_POINT ( 'NONE',  ( -5.049401038298153566, 19.05341960407611168, 70.20724293864769550 ) ) ;
#115807 = CARTESIAN_POINT ( 'NONE',  ( 21.53943276465977519, -0.05219959533907433946, 63.74890960531435979 ) ) ;
#115808 = B_SPLINE_CURVE_WITH_KNOTS ( 'NONE', 3,
 ( #101496, #98490, #114671, #178366, #176367, #20665, #68165, #37840, #116676, #99500, #161181, #146003, #7486, #175356 ),
 .UNSPECIFIED., .F., .F.,
 ( 4, 2, 2, 2, 2, 2, 4 ),
 ( -0.0006136969902427322687, 0.0004464899733162382622, 0.001506676936875208685, 0.003627050863993181839, 0.004687237827552175572, 0.005747424791111170606, 0.007867798718229164143 ),
 .UNSPECIFIED. ) ;
#115809 = CARTESIAN_POINT ( 'NONE',  ( 16.52544592524335698, 4.483927247898782831, 36.45942372801901143 ) ) ;
#115810 = CARTESIAN_POINT ( 'NONE',  ( -5.823673210054431948, 21.52544592524334988, 37.70942372801900433 ) ) ;
#115811 = CARTESIAN_POINT ( 'NONE',  ( -10.81492255796105439, 18.62759615963255655, 87.91775706135234714 ) ) ;
#115812 = CARTESIAN_POINT ( 'NONE',  ( 8.314922557961029526, -14.29746914071037800, 85.41775706135236135 ) ) ;
#115813 = CARTESIAN_POINT ( 'NONE',  ( 5.153800228976335163, 19.02544592524342804, 69.79057627198103830 ) ) ;
#115814 = CARTESIAN_POINT ( 'NONE',  ( -0.05219959533910754901, -16.53943276465976808, 72.49890960531435269 ) ) ;
#115815 = CARTESIAN_POINT ( 'NONE',  ( 8.314922557960818139, 14.29746914071049879, 29.58224293864769905 ) ) ;
#115816 = CARTESIAN_POINT ( 'NONE',  ( 19.05341960407617918, -5.049401038297876454, 51.04275706135231871 ) ) ;
#115817 = CARTESIAN_POINT ( 'NONE',  ( 15.72974639402176855, 15.80617190586768217, 31.87609039468567929 ) ) ;
#115818 = CARTESIAN_POINT ( 'NONE',  ( 4.483927247898545687, 16.52544592524342804, 79.79057627198102409 ) ) ;
#115819 = CARTESIAN_POINT ( 'NONE',  ( 9.564922557960805705, 16.46253265017160317, 99.58224293864770971 ) ) ;
#115820 = CARTESIAN_POINT ( 'NONE',  ( 14.29746914071037800, 8.314922557961029526, 106.6677570613523756 ) ) ;
#115821 = CARTESIAN_POINT ( 'NONE',  ( 21.52544592524334988, 5.823673210054432836, 71.45942372801901854 ) ) ;
#115822 = CARTESIAN_POINT ( 'NONE',  ( -16.55341960407617563, 4.379528057220093196, 48.54275706135234714 ) ) ;
#115823 = CARTESIAN_POINT ( 'NONE',  ( 21.52544592524334988, 5.823673210054432836, 41.45942372801901143 ) ) ;
#115824 = CARTESIAN_POINT ( 'NONE',  ( -4.379528057220328563, 16.55341960407611168, 65.20724293864768129 ) ) ;
#115825 = EDGE_CURVE ( 'NONE', #34604, #69503, #119501, .T. ) ;
#115826 = ORIENTED_EDGE ( 'NONE', *, *, #130089, .T. ) ;
#115827 = CARTESIAN_POINT ( 'NONE',  ( -5.719274019375665041, -21.55341960407619695, 19.79275706135235069 ) ) ;
#115828 = CARTESIAN_POINT ( 'NONE',  ( 17.49999999999999645, -4.013004640162636250, 27.94605720994409737 ) ) ;
#115829 = CARTESIAN_POINT ( 'NONE',  ( 12.14591786802309770, 12.06949235617756955, 54.37390960531435979 ) ) ;
#115830 = CARTESIAN_POINT ( 'NONE',  ( 0.05219959533909260263, 19.03943276465977164, 24.99890960531435269 ) ) ;
#115831 = CARTESIAN_POINT ( 'NONE',  ( 21.55341960407610458, 5.719274019375980345, 38.95724293864768839 ) ) ;
#115832 = CARTESIAN_POINT ( 'NONE',  ( 16.55341960407611168, 4.379528057220329451, 78.95724293864769550 ) ) ;
#115833 = EDGE_CURVE ( 'NONE', #41082, #42510, #62396, .T. ) ;
#115834 = CARTESIAN_POINT ( 'NONE',  ( 18.62759615963271287, -10.81492255796078972, 83.33224293864769550 ) ) ;
#115835 = CARTESIAN_POINT ( 'NONE',  ( -19.02544592524342804, 5.153800228976336051, 86.04057627198103830 ) ) ;
#115837 = CARTESIAN_POINT ( 'NONE',  ( 19.02544592524334988, 5.153800228976608722, 81.45942372801897591 ) ) ;
#115836 = CARTESIAN_POINT ( 'NONE',  ( -5.049401038298153566, 19.05341960407611168, 35.20724293864768839 ) ) ;
#115839 = CARTESIAN_POINT ( 'NONE',  ( -5.823673210054116645, -21.52544592524344225, 57.29057627198103120 ) ) ;
#115838 = CARTESIAN_POINT ( 'NONE',  ( -21.55341960407619339, 5.719274019375674811, 58.54275706135235424 ) ) ;
#115840 = CARTESIAN_POINT ( 'NONE',  ( 19.05341960407611168, 5.049401038298154454, 38.95724293864767418 ) ) ;
#115841 = CARTESIAN_POINT ( 'NONE',  ( 9.564922557960805705, 16.46253265017160317, 69.58224293864770971 ) ) ;
#115842 = EDGE_LOOP ( 'NONE', ( #97573, #44722, #55523, #21766, #73700 ) ) ;
#115843 = CARTESIAN_POINT ( 'NONE',  ( -12.14591786802326823, 12.06949235617739902, 53.12609039468568284 ) ) ;
#115844 = CARTESIAN_POINT ( 'NONE',  ( -15.72974639402176322, -15.80617190586768395, 24.37609039468567573 ) ) ;
#115845 = CARTESIAN_POINT ( 'NONE',  ( -10.81492255796105439, 18.62759615963255655, 67.91775706135234714 ) ) ;
#115846 = CARTESIAN_POINT ( 'NONE',  ( 16.46253265017160672, -9.564922557960803928, 98.33224293864769550 ) ) ;
#115847 = CARTESIAN_POINT ( 'NONE',  ( -5.719274019375978568, 21.55341960407610458, 85.20724293864770971 ) ) ;
#115849 = CARTESIAN_POINT ( 'NONE',  ( -4.379528057220086978, -16.55341960407618274, 54.79275706135235424 ) ) ;
#115848 = CARTESIAN_POINT ( 'NONE',  ( 15.80617190586769283, -15.72974639402175789, 30.62609039468567929 ) ) ;
#115850 = CARTESIAN_POINT ( 'NONE',  ( 15.80617190586746368, 15.72974639402197994, 49.37390960531436690 ) ) ;
#115851 = CARTESIAN_POINT ( 'NONE',  ( 5.153800228976615827, -19.02544592524334988, 25.20942372801900433 ) ) ;
#115852 = CARTESIAN_POINT ( 'NONE',  ( -19.05341960407611168, -5.049401038298163336, 51.45724293864770260 ) ) ;
#115853 = CARTESIAN_POINT ( 'NONE',  ( 0.05219959533909260263, 19.03943276465977164, 114.9989096053143669 ) ) ;
#115854 = CARTESIAN_POINT ( 'NONE',  ( 5.049401038298161559, -19.05341960407611168, 87.70724293864769550 ) ) ;
#115855 = CARTESIAN_POINT ( 'NONE',  ( 18.22780087662126647, 5.499999999999818812, 51.48236817873107896 ) ) ;
#115856 = CARTESIAN_POINT ( 'NONE',  ( 9.474510206698729675, 16.51473224551082808, 62.08442372801899722 ) ) ;
#115857 = CARTESIAN_POINT ( 'NONE',  ( -5.823673210054116645, -21.52544592524344225, 47.29057627198103120 ) ) ;
#115858 = CARTESIAN_POINT ( 'NONE',  ( -8.224510206698948167, 14.34966873604960824, 25.41557627198103120 ) ) ;
#115859 = CARTESIAN_POINT ( 'NONE',  ( 19.05341960407617918, -5.049401038297876454, 101.0427570613523045 ) ) ;
#115860 = PLANE ( 'NONE',  #85310 ) ;
#115861 = CARTESIAN_POINT ( 'NONE',  ( 0.05219959533936267826, -19.03943276465977164, 20.00109039468567218 ) ) ;
#115862 = CARTESIAN_POINT ( 'NONE',  ( 9.564922557961047289, -16.46253265017146816, 95.41775706135233293 ) ) ;
#115864 = CARTESIAN_POINT ( 'NONE',  ( -9.474510206698720793, -16.51473224551083518, 59.58442372801900433 ) ) ;
#115863 = CARTESIAN_POINT ( 'NONE',  ( -0.05219959533907301413, -21.53943276465977519, 77.49890960531433848 ) ) ;
#115865 = CARTESIAN_POINT ( 'NONE',  ( 24.99734946672222335, -12.60193342193096555, 166.0696721667194993 ) ) ;
#115866 = CARTESIAN_POINT ( 'NONE',  ( 19.03943276465977164, -0.05219959533909143690, 53.74890960531436690 ) ) ;
#115867 = CARTESIAN_POINT ( 'NONE',  ( 8.224510206698953496, -14.34966873604960469, 62.91557627198102409 ) ) ;
#115868 = CARTESIAN_POINT ( 'NONE',  ( 19.02544592524343514, -5.153800228976328945, 38.54057627198103120 ) ) ;
#115869 = CARTESIAN_POINT ( 'NONE',  ( -0.05219959533910754901, -16.53943276465976808, 37.49890960531436690 ) ) ;
#115870 = CARTESIAN_POINT ( 'NONE',  ( -27.19095269391954517, -10.02149780027903780, 149.7954620931811291 ) ) ;
#115871 = CARTESIAN_POINT ( 'NONE',  ( -16.55341960407617563, 4.379528057220093196, 103.5427570613523613 ) ) ;
#115872 = CARTESIAN_POINT ( 'NONE',  ( -0.05219959533909027116, -19.03943276465977164, 67.49890960531436690 ) ) ;
#115873 = CARTESIAN_POINT ( 'NONE',  ( 19.03943276465977164, 0.05219959533936151252, 21.25109039468565797 ) ) ;
#115874 = CARTESIAN_POINT ( 'NONE',  ( -16.55341960407617563, 4.379528057220093196, 33.54275706135234714 ) ) ;
#115875 = CARTESIAN_POINT ( 'NONE',  ( 5.823673210054125526, 21.52544592524343514, 54.79057627198104541 ) ) ;
#115876 = CARTESIAN_POINT ( 'NONE',  ( 5.823673210054444382, -21.52544592524334988, 110.2094237280190185 ) ) ;
#115877 = CARTESIAN_POINT ( 'NONE',  ( -19.03943276465977164, 0.05219959533909376836, 61.24890960531436690 ) ) ;
#115878 = CARTESIAN_POINT ( 'NONE',  ( 17.49999999999999289, 5.500000000000009770, 43.78230962303566542 ) ) ;
#115879 = CARTESIAN_POINT ( 'NONE',  ( 19.03943276465977164, -0.05219959533909143690, 103.7489096053143669 ) ) ;
#115880 = DIRECTION ( 'NONE',  ( 0.000000000000000000, 0.9945218953682734009, 0.1045284632676537068 ) ) ;
#115881 = CARTESIAN_POINT ( 'NONE',  ( 21.55341960407619695, -5.719274019375665929, 26.04275706135235779 ) ) ;
#115882 = CARTESIAN_POINT ( 'NONE',  ( 8.224510206698953496, -14.34966873604960469, 92.91557627198103830 ) ) ;
#115884 = CARTESIAN_POINT ( 'NONE',  ( 16.46253265017160672, -9.564922557960803928, 63.33224293864769550 ) ) ;
#115883 = CARTESIAN_POINT ( 'NONE',  ( 15.72974639402199770, -15.80617190586745480, 88.12390960531436690 ) ) ;
#115885 = CARTESIAN_POINT ( 'NONE',  ( 5.049401038298161559, -19.05341960407611168, 67.70724293864769550 ) ) ;
#115886 = CARTESIAN_POINT ( 'NONE',  ( 10.72451020669898902, -18.67979575497178502, 107.9155762719810241 ) ) ;
#115887 = EDGE_LOOP ( 'NONE', ( #41995, #194728, #145934, #180658 ) ) ;
#115888 = CARTESIAN_POINT ( 'NONE',  ( -9.564922557960796823, -16.46253265017161027, 72.08224293864770971 ) ) ;
#115889 = CARTESIAN_POINT ( 'NONE',  ( -31.67087737765754341, -20.99984420384768313, -23.45156215417600265 ) ) ;
#115891 = CARTESIAN_POINT ( 'NONE',  ( -13.97604488694527625, -13.89961937509977652, 26.87390960531434558 ) ) ;
#115890 = CARTESIAN_POINT ( 'NONE',  ( 16.53943276465976808, -0.05219959533910856209, 103.7489096053143669 ) ) ;
#115892 = CARTESIAN_POINT ( 'NONE',  ( -9.564922557961040184, 16.46253265017147172, 87.91775706135233293 ) ) ;
#115893 = CARTESIAN_POINT ( 'NONE',  ( 14.29746914071049879, -8.314922557960816363, 103.3322429386476955 ) ) ;
#115894 = CARTESIAN_POINT ( 'NONE',  ( 21.53943276465977519, 0.05219959533937863772, 71.25109039468568994 ) ) ;
#115896 = CARTESIAN_POINT ( 'NONE',  ( 5.823673210054444382, -21.52544592524334988, 30.20942372801902565 ) ) ;
#115895 = CARTESIAN_POINT ( 'NONE',  ( 19.03943276465977164, -0.05219959533909143690, 58.74890960531435979 ) ) ;
#115897 = CARTESIAN_POINT ( 'NONE',  ( -0.05219959533907301413, -21.53943276465977519, 112.4989096053143669 ) ) ;
#115898 = CARTESIAN_POINT ( 'NONE',  ( 28.82186960331498327, 9.364793116373570925, 145.1000000000000227 ) ) ;
#115899 = CARTESIAN_POINT ( 'NONE',  ( -19.05341960407611168, -5.049401038298163336, 71.45724293864766707 ) ) ;
#115900 = CARTESIAN_POINT ( 'NONE',  ( 27.96111904526279091, 7.044650443041771126, 161.2906300811259541 ) ) ;
#115902 = CARTESIAN_POINT ( 'NONE',  ( -5.823673210054116645, -21.52544592524344225, 27.29057627198103120 ) ) ;
#115901 = CARTESIAN_POINT ( 'NONE',  ( 14.29746914071037800, 8.314922557961029526, 26.66775706135235424 ) ) ;
#115903 = CARTESIAN_POINT ( 'NONE',  ( -21.53943276465977519, -0.05219959533937600094, 58.75109039468568994 ) ) ;
#115904 = CARTESIAN_POINT ( 'NONE',  ( 0.05219959533909260263, 19.03943276465977164, 104.9989096053143669 ) ) ;
#115905 = CARTESIAN_POINT ( 'NONE',  ( 13.89961937509957401, 13.97604488694547697, 101.8760903946856331 ) ) ;
#115906 = CARTESIAN_POINT ( 'NONE',  ( -13.89961937509977652, 13.97604488694528158, 50.62390960531435979 ) ) ;
#115907 = CARTESIAN_POINT ( 'NONE',  ( -19.02544592524342804, 5.153800228976336051, 71.04057627198099567 ) ) ;
#115908 = CARTESIAN_POINT ( 'NONE',  ( 12.14591786802309770, 12.06949235617756955, 94.37390960531436690 ) ) ;
#115909 = CARTESIAN_POINT ( 'NONE',  ( -13.97604488694527625, -13.89961937509977652, 101.8739096053143811 ) ) ;
#115910 = CARTESIAN_POINT ( 'NONE',  ( -12.06949235617756955, 12.14591786802309770, 95.62390960531436690 ) ) ;
#115911 = CARTESIAN_POINT ( 'NONE',  ( -5.049401038298153566, 19.05341960407611168, 95.20724293864770971 ) ) ;
#115913 = CARTESIAN_POINT ( 'NONE',  ( -9.564922557960796823, -16.46253265017161027, 37.08224293864768839 ) ) ;
#115912 = CARTESIAN_POINT ( 'NONE',  ( 12.14591786802309770, 12.06949235617756955, 44.37390960531435979 ) ) ;
#115914 = ORIENTED_EDGE ( 'NONE', *, *, #147079, .T. ) ;
#115915 = CARTESIAN_POINT ( 'NONE',  ( -5.823673210054431948, 21.52544592524334988, 57.70942372801901143 ) ) ;
#115916 = CARTESIAN_POINT ( 'NONE',  ( -13.89961937509957401, -13.97604488694547875, 84.37609039468567573 ) ) ;
#115917 = CARTESIAN_POINT ( 'NONE',  ( 14.34966873604960469, 8.224510206698951720, 49.16557627198102409 ) ) ;
#115918 = CARTESIAN_POINT ( 'NONE',  ( -21.52544592524343514, 5.823673210054127303, 101.0405762719810383 ) ) ;
#115919 = CARTESIAN_POINT ( 'NONE',  ( -15.80617190586745835, -15.72974639402198527, 41.87390960531435979 ) ) ;
#115921 = CARTESIAN_POINT ( 'NONE',  ( 14.29746914071049879, -8.314922557960816363, 78.33224293864770971 ) ) ;
#115920 = CARTESIAN_POINT ( 'NONE',  ( -5.049401038298153566, 19.05341960407611168, 110.2072429386476671 ) ) ;
#115922 = CARTESIAN_POINT ( 'NONE',  ( 13.97604488694527802, 13.89961937509977652, 59.37390960531434558 ) ) ;
#115923 = CARTESIAN_POINT ( 'NONE',  ( 14.29746914071049879, -8.314922557960816363, 28.33224293864769550 ) ) ;
#115924 = CARTESIAN_POINT ( 'NONE',  ( -14.29746914071037622, -8.314922557961029526, 104.1677570613523471 ) ) ;
#115925 = CARTESIAN_POINT ( 'NONE',  ( 0.05219959533934541429, -16.53943276465976808, 70.00109039468568994 ) ) ;
#115926 = CARTESIAN_POINT ( 'NONE',  ( -19.05341960407617563, 5.049401038297882671, 23.54275706135233648 ) ) ;
#115928 = CARTESIAN_POINT ( 'NONE',  ( -16.51473224551069308, -9.474510206698971260, 111.6655762719810383 ) ) ;
#115927 = FACE_OUTER_BOUND ( 'NONE', #131754, .T. ) ;
#115929 = CARTESIAN_POINT ( 'NONE',  ( 5.049401038298161559, -19.05341960407611168, 72.70724293864768129 ) ) ;
#115930 = CARTESIAN_POINT ( 'NONE',  ( 13.89961937509977652, -13.97604488694527269, 38.12390960531436690 ) ) ;
#115931 = CARTESIAN_POINT ( 'NONE',  ( 8.224510206698953496, -14.34966873604960469, 47.91557627198102409 ) ) ;
#115933 = CARTESIAN_POINT ( 'NONE',  ( -16.51473224551069308, -9.474510206698971260, 101.6655762719810241 ) ) ;
#115932 = CARTESIAN_POINT ( 'NONE',  ( -0.05219959533909027116, -19.03943276465977164, 112.4989096053143669 ) ) ;
#115934 = CARTESIAN_POINT ( 'NONE',  ( -18.67979575497178146, -10.72451020669898902, 41.66557627198103120 ) ) ;
#115935 = CARTESIAN_POINT ( 'NONE',  ( -8.314922557960811034, -14.29746914071050412, 82.08224293864768129 ) ) ;
#115936 = CARTESIAN_POINT ( 'NONE',  ( 4.483927247898790824, -16.52544592524335698, 45.20942372801901854 ) ) ;
#115937 = CARTESIAN_POINT ( 'NONE',  ( 16.55341960407611168, 4.379528057220329451, 58.95724293864770971 ) ) ;
#115938 = CARTESIAN_POINT ( 'NONE',  ( -16.70000000000002061, 1.759457951533292443E-13, -64.92279855667830191 ) ) ;
#115939 = CARTESIAN_POINT ( 'NONE',  ( 5.153800228976615827, -19.02544592524334988, 60.20942372801899012 ) ) ;
#115940 = CARTESIAN_POINT ( 'NONE',  ( -5.153800228976328057, -19.02544592524343514, 102.2905762719810383 ) ) ;
#115941 = CARTESIAN_POINT ( 'NONE',  ( 5.153800228976615827, -19.02544592524334988, 85.20942372801900433 ) ) ;
#115942 = B_SPLINE_CURVE_WITH_KNOTS ( 'NONE', 3,
 ( #133026, #194716, #56186, #117869, #44014, #119859, #165378, #25876 ),
 .UNSPECIFIED., .F., .F.,
 ( 4, 2, 2, 4 ),
 ( 2.784207231387392883E-07, 0.0003066998903876386857, 0.0006131213600521387115, 0.001225964299381153508 ),
 .UNSPECIFIED. ) ;
#115943 = CARTESIAN_POINT ( 'NONE',  ( 5.153800228976617603, -19.02544592524335343, 95.20942372801899012 ) ) ;
#115945 = CARTESIAN_POINT ( 'NONE',  ( 8.224510206698953496, -14.34966873604960469, 22.91557627198102765 ) ) ;
#115944 = CARTESIAN_POINT ( 'NONE',  ( 13.97604488694548053, -13.89961937509957401, 110.6260903946856615 ) ) ;
#115946 = CARTESIAN_POINT ( 'NONE',  ( -16.46253265017146816, -9.564922557961047289, 69.16775706135233293 ) ) ;
#115947 = CARTESIAN_POINT ( 'NONE',  ( -0.05219959533907301413, -21.53943276465977519, 32.49890960531435979 ) ) ;
#115948 = CARTESIAN_POINT ( 'NONE',  ( -10.72451020669870658, -18.67979575497194134, 64.58442372801900433 ) ) ;
#115949 = CARTESIAN_POINT ( 'NONE',  ( -8.906447517083053711, -27.41122689804191026, 146.6500000054623740 ) ) ;
#115950 = CARTESIAN_POINT ( 'NONE',  ( 13.89961937509957401, 13.97604488694547697, 111.8760903946856757 ) ) ;
#115952 = CARTESIAN_POINT ( 'NONE',  ( -9.564922557960796823, -16.46253265017161027, 77.08224293864769550 ) ) ;
#115951 = CARTESIAN_POINT ( 'NONE',  ( -13.97604488694527625, -13.89961937509977652, 26.87390960531434558 ) ) ;
#115953 = CARTESIAN_POINT ( 'NONE',  ( 5.049401038298161559, -19.05341960407611168, 22.70724293864769194 ) ) ;
#115955 = CARTESIAN_POINT ( 'NONE',  ( -16.51473224551069308, -9.474510206698971260, 81.66557627198103830 ) ) ;
#115954 = CARTESIAN_POINT ( 'NONE',  ( -8.224510206698948167, 14.34966873604960824, 90.41557627198103830 ) ) ;
#115956 = CARTESIAN_POINT ( 'NONE',  ( -13.89961937509977652, 13.97604488694528158, 85.62390960531433848 ) ) ;
#115957 = ORIENTED_EDGE ( 'NONE', *, *, #55329, .T. ) ;
#115958 = CARTESIAN_POINT ( 'NONE',  ( -16.46253265017146816, -9.564922557961047289, 94.16775706135233293 ) ) ;
#115959 = CARTESIAN_POINT ( 'NONE',  ( -10.81492255796078084, -18.62759615963271287, 77.08224293864769550 ) ) ;
#115960 = CARTESIAN_POINT ( 'NONE',  ( -13.89961937509977652, 13.97604488694528158, 25.62390960531434558 ) ) ;
#115961 = CARTESIAN_POINT ( 'NONE',  ( 19.02544592524334988, 5.153800228976608722, 76.45942372801897591 ) ) ;
#115962 = CARTESIAN_POINT ( 'NONE',  ( -16.51473224551069308, -9.474510206698971260, 66.66557627198102409 ) ) ;
#115963 = CARTESIAN_POINT ( 'NONE',  ( -5.153800228976328057, -19.02544592524343514, 97.29057627198099567 ) ) ;
#115964 = VERTEX_POINT ( 'NONE', #85139 ) ;
#115965 = CARTESIAN_POINT ( 'NONE',  ( 21.53943276465977519, -0.05219959533907433946, 103.7489096053143669 ) ) ;
#115968 = CARTESIAN_POINT ( 'NONE',  ( 13.89961937509957401, 13.97604488694547697, 61.87609039468566863 ) ) ;
#115967 = CARTESIAN_POINT ( 'NONE',  ( -16.46253265017160317, 9.564922557960807481, 80.83224293864769550 ) ) ;
#115966 = CARTESIAN_POINT ( 'NONE',  ( -4.483927247898539470, -16.52544592524342804, 92.29057627198103830 ) ) ;
#115969 = CARTESIAN_POINT ( 'NONE',  ( 18.67979575497178502, 10.72451020669898547, 94.16557627198103830 ) ) ;
#115970 = CARTESIAN_POINT ( 'NONE',  ( -15.72974639402197994, 15.80617190586746368, 70.62390960531436690 ) ) ;
#115971 = CARTESIAN_POINT ( 'NONE',  ( 16.52544592524342804, -4.483927247898539470, 48.54057627198103120 ) ) ;
#115972 = CARTESIAN_POINT ( 'NONE',  ( -15.72974639402176322, -15.80617190586768395, 109.3760903946857042 ) ) ;
#115973 = CARTESIAN_POINT ( 'NONE',  ( 4.483927247898790824, -16.52544592524335698, 65.20942372801901854 ) ) ;
#115974 = CARTESIAN_POINT ( 'NONE',  ( -9.474510206698964154, 16.51473224551069663, 95.41557627198102409 ) ) ;
#115975 = CARTESIAN_POINT ( 'NONE',  ( -19.03943276465977164, 0.05219959533909376836, 31.24890960531435979 ) ) ;
#115976 = CARTESIAN_POINT ( 'NONE',  ( -18.62759615963255300, -10.81492255796106328, 44.16775706135234714 ) ) ;
#115977 = CARTESIAN_POINT ( 'NONE',  ( -5.719274019375665041, -21.55341960407619695, 59.79275706135234714 ) ) ;
#115978 = CARTESIAN_POINT ( 'NONE',  ( 16.51473224551069308, 9.474510206698969483, 59.16557627198102409 ) ) ;
#115979 = CARTESIAN_POINT ( 'NONE',  ( 21.53943276465977519, 0.05219959533937863772, 41.25109039468568284 ) ) ;
#115980 = CARTESIAN_POINT ( 'NONE',  ( 5.153800228976615827, -19.02544592524334988, 75.20942372801896170 ) ) ;
#115981 = CARTESIAN_POINT ( 'NONE',  ( 16.46253265017146816, 9.564922557961045513, 76.66775706135234714 ) ) ;
#115982 = CARTESIAN_POINT ( 'NONE',  ( -5.049401038298153566, 19.05341960407611168, 40.20724293864768839 ) ) ;
#115983 = CARTESIAN_POINT ( 'NONE',  ( 4.379528057220092307, 16.55341960407617563, 72.29275706135236135 ) ) ;
#115984 = CARTESIAN_POINT ( 'NONE',  ( -0.05219959533909027116, -19.03943276465977164, 52.49890960531436690 ) ) ;
#115985 = CARTESIAN_POINT ( 'NONE',  ( 24.30454888808799296, -2.781629622375088928, 174.5654150192188183 ) ) ;
#115986 = CARTESIAN_POINT ( 'NONE',  ( -0.05219959533909027116, -19.03943276465977164, 97.49890960531436690 ) ) ;
#115987 = CARTESIAN_POINT ( 'NONE',  ( -16.51473224551069308, -9.474510206698971260, 41.66557627198103120 ) ) ;
#115988 = CARTESIAN_POINT ( 'NONE',  ( 18.67979575497178502, 10.72451020669898547, 69.16557627198102409 ) ) ;
#115989 = CARTESIAN_POINT ( 'NONE',  ( 0.05219959533934541429, -16.53943276465976808, 60.00109039468568284 ) ) ;
#115990 = CARTESIAN_POINT ( 'NONE',  ( -9.474510206698720793, -16.51473224551083518, 19.58442372801899722 ) ) ;
#115991 = CARTESIAN_POINT ( 'NONE',  ( 13.89961937509977652, -13.97604488694527269, 53.12390960531434558 ) ) ;
#115992 = CARTESIAN_POINT ( 'NONE',  ( -0.05219959533910754901, -16.53943276465976808, 42.49890960531435979 ) ) ;
#115993 = CARTESIAN_POINT ( 'NONE',  ( 8.224510206698953496, -14.34966873604960469, 87.91557627198103830 ) ) ;
#115994 = CARTESIAN_POINT ( 'NONE',  ( -16.51473224551069308, -9.474510206698971260, 81.66557627198103830 ) ) ;
#115995 = CARTESIAN_POINT ( 'NONE',  ( -15.72974639402176322, -15.80617190586768395, 39.37609039468567573 ) ) ;
#115996 = CARTESIAN_POINT ( 'NONE',  ( 0.05219959533909260263, 19.03943276465977164, 89.99890960531436690 ) ) ;
#115997 = CARTESIAN_POINT ( 'NONE',  ( -10.72451020669870658, -18.67979575497194134, 104.5844237280190185 ) ) ;
#115998 = CARTESIAN_POINT ( 'NONE',  ( 8.224510206698742110, 14.34966873604972548, 62.08442372801901143 ) ) ;
#115999 = CARTESIAN_POINT ( 'NONE',  ( -9.564922557960796823, -16.46253265017161027, 107.0822429386476955 ) ) ;
#116000 = CARTESIAN_POINT ( 'NONE',  ( 15.72974639402199770, -15.80617190586745480, 83.12390960531436690 ) ) ;
#116001 = CARTESIAN_POINT ( 'NONE',  ( -16.55341960407611168, -4.379528057220339221, 51.45724293864770260 ) ) ;
#116002 = CARTESIAN_POINT ( 'NONE',  ( 5.049401038298161559, -19.05341960407611168, 42.70724293864767418 ) ) ;
#116003 = CARTESIAN_POINT ( 'NONE',  ( -8.314922557960811034, -14.29746914071050412, 62.08224293864769550 ) ) ;
#116004 = CARTESIAN_POINT ( 'NONE',  ( -21.53943276465977519, 0.05219959533907696930, 26.24890960531435624 ) ) ;
#116005 = CARTESIAN_POINT ( 'NONE',  ( -21.53943276465977519, 0.05219959533907696930, 26.24890960531435624 ) ) ;
#116006 = CARTESIAN_POINT ( 'NONE',  ( 13.89961937509957401, 13.97604488694547697, 31.87609039468566863 ) ) ;
#116007 = CARTESIAN_POINT ( 'NONE',  ( -8.314922557960811034, -14.29746914071050412, 97.08224293864770971 ) ) ;
#116008 = CARTESIAN_POINT ( 'NONE',  ( 13.97604488694527802, 13.89961937509977652, 104.3739096053143385 ) ) ;
#116009 = VERTEX_POINT ( 'NONE', #71985 ) ;
#116010 = CARTESIAN_POINT ( 'NONE',  ( 12.06949235617739724, 12.14591786802326823, 51.87609039468568284 ) ) ;
#116011 = CARTESIAN_POINT ( 'NONE',  ( 13.89961937509977652, -13.97604488694527269, 58.12390960531436690 ) ) ;
#116012 = CARTESIAN_POINT ( 'NONE',  ( 1.784210473542230573E-15, -29.16686587814331588, 139.3750000027311842 ) ) ;
#116013 = CARTESIAN_POINT ( 'NONE',  ( 16.46253265017146816, 9.564922557961045513, 66.66775706135233293 ) ) ;
#116014 = CARTESIAN_POINT ( 'NONE',  ( -4.483927247898782831, 16.52544592524335698, 92.70942372801901854 ) ) ;
#116015 = CARTESIAN_POINT ( 'NONE',  ( -16.51473224551082808, 9.474510206698731452, 93.33442372801900433 ) ) ;
#116016 = CARTESIAN_POINT ( 'NONE',  ( 5.823673210054444382, -21.52544592524334988, 70.20942372801904696 ) ) ;
#116017 = CARTESIAN_POINT ( 'NONE',  ( -9.474510206698964154, 16.51473224551069663, 80.41557627198103830 ) ) ;
#116018 = CARTESIAN_POINT ( 'NONE',  ( 15.72974639402199770, -15.80617190586745480, 93.12390960531436690 ) ) ;
#116019 = CARTESIAN_POINT ( 'NONE',  ( -19.03943276465977164, 0.05219959533909376836, 21.24890960531436335 ) ) ;
#116020 = VECTOR ( 'NONE', #186214, 1000.000000000000000 ) ;
#116021 = CARTESIAN_POINT ( 'NONE',  ( -19.05341960407617563, 5.049401038297882671, 78.54275706135233293 ) ) ;
#116022 = CARTESIAN_POINT ( 'NONE',  ( 18.62759615963271287, -10.81492255796078972, 73.33224293864769550 ) ) ;
#116023 = CARTESIAN_POINT ( 'NONE',  ( 19.02544592524334988, 5.153800228976608722, 46.45942372801899012 ) ) ;
#116024 = DIRECTION ( 'NONE',  ( -0.000000000000000000, -0.000000000000000000, 1.000000000000000000 ) ) ;
#116025 = CARTESIAN_POINT ( 'NONE',  ( -18.62759615963270932, 10.81492255796079327, 90.83224293864769550 ) ) ;
#116026 = CARTESIAN_POINT ( 'NONE',  ( 17.50000000000003553, 3.850315288878739750, 28.23370869396553573 ) ) ;
#116027 = CARTESIAN_POINT ( 'NONE',  ( 9.564922557960805705, 16.46253265017160317, 69.58224293864770971 ) ) ;
#116028 = DIRECTION ( 'NONE',  ( 0.000000000000000000, 0.000000000000000000, 1.000000000000000000 ) ) ;
#116029 = CARTESIAN_POINT ( 'NONE',  ( 4.379528057220092307, 16.55341960407617563, 22.29275706135235069 ) ) ;
#116030 = CARTESIAN_POINT ( 'NONE',  ( 36.88736642480385086, -1.774289666830916490, 50.21844423102493948 ) ) ;
#116031 = CARTESIAN_POINT ( 'NONE',  ( 9.474510206698971260, -16.51473224551069308, 42.91557627198103120 ) ) ;
#116033 = CARTESIAN_POINT ( 'NONE',  ( -8.224510206698948167, 14.34966873604960824, 55.41557627198102409 ) ) ;
#116032 = CARTESIAN_POINT ( 'NONE',  ( -21.52544592524343514, 5.823673210054127303, 106.0405762719810525 ) ) ;
#116034 = CARTESIAN_POINT ( 'NONE',  ( 5.153800228976335163, 19.02544592524342804, 59.79057627198100988 ) ) ;
#116035 = CARTESIAN_POINT ( 'NONE',  ( -15.80617190586768217, 15.72974639402176855, 78.12609039468570415 ) ) ;
#116037 = CARTESIAN_POINT ( 'NONE',  ( -13.89961937509957401, -13.97604488694547875, 24.37609039468565442 ) ) ;
#116036 = CARTESIAN_POINT ( 'NONE',  ( -16.52544592524335698, -4.483927247898792601, 23.95942372801901143 ) ) ;
#116038 = CARTESIAN_POINT ( 'NONE',  ( 4.483927247898545687, 16.52544592524342804, 24.79057627198103120 ) ) ;
#116039 = CARTESIAN_POINT ( 'NONE',  ( 5.823673210054444382, -21.52544592524334988, 35.20942372801901854 ) ) ;
#116040 = CARTESIAN_POINT ( 'NONE',  ( 18.67979575497194134, -10.72451020669871369, 20.83442372801901143 ) ) ;
#116041 = CARTESIAN_POINT ( 'NONE',  ( 21.52544592524344225, -5.823673210054117533, 53.54057627198103120 ) ) ;
#116042 = CARTESIAN_POINT ( 'NONE',  ( 5.153800228976615827, -19.02544592524334988, 90.20942372801900433 ) ) ;
#116043 = CARTESIAN_POINT ( 'NONE',  ( 9.564922557961047289, -16.46253265017146816, 75.41775706135234714 ) ) ;
#116044 = CARTESIAN_POINT ( 'NONE',  ( -18.62759615963255300, -10.81492255796106328, 69.16775706135234714 ) ) ;
#116045 = CARTESIAN_POINT ( 'NONE',  ( 9.474510206698729675, 16.51473224551082808, 52.08442372801900433 ) ) ;
#116046 = CARTESIAN_POINT ( 'NONE',  ( 13.89961937509977652, -13.97604488694527269, 23.12390960531436335 ) ) ;
#116047 = CARTESIAN_POINT ( 'NONE',  ( -15.80617190586745835, -15.72974639402198527, 46.87390960531435979 ) ) ;
#116048 = CARTESIAN_POINT ( 'NONE',  ( 4.483927247898545687, 16.52544592524342804, 49.79057627198102409 ) ) ;
#116049 = CARTESIAN_POINT ( 'NONE',  ( -19.25663599770060586, 5.499999999999445777, 93.99419308057203182 ) ) ;
#116050 = CARTESIAN_POINT ( 'NONE',  ( -18.67979575497193778, 10.72451020669871902, 108.3344237280190185 ) ) ;
#116051 = CARTESIAN_POINT ( 'NONE',  ( 8.314922557961029526, -14.29746914071037800, 90.41775706135236135 ) ) ;
#116052 = CARTESIAN_POINT ( 'NONE',  ( -8.224510206698948167, 14.34966873604960824, 40.41557627198103120 ) ) ;
#116053 = CARTESIAN_POINT ( 'NONE',  ( 21.52544592524334988, 5.823673210054432836, 81.45942372801900433 ) ) ;
#116054 = CARTESIAN_POINT ( 'NONE',  ( -10.72451020669870658, -18.67979575497194134, 74.58442372801901854 ) ) ;
#116055 = CARTESIAN_POINT ( 'NONE',  ( -15.80617190586745835, -15.72974639402198527, 86.87390960531438111 ) ) ;
#116056 = ADVANCED_FACE ( 'NONE', ( #131662 ), #56830, .F. ) ;
#116057 = CARTESIAN_POINT ( 'NONE',  ( 19.02544592524343514, -5.153800228976328945, 33.54057627198102409 ) ) ;
#116058 = CARTESIAN_POINT ( 'NONE',  ( 18.67979575497194134, -10.72451020669871369, 60.83442372801901854 ) ) ;
#116059 = CARTESIAN_POINT ( 'NONE',  ( -9.474510206698964154, 16.51473224551069663, 30.41557627198102054 ) ) ;
#116060 = CARTESIAN_POINT ( 'NONE',  ( 9.474510206698971260, -16.51473224551069308, 52.91557627198102409 ) ) ;
#116061 = CARTESIAN_POINT ( 'NONE',  ( -0.05219959533910754901, -16.53943276465976808, 92.49890960531436690 ) ) ;
#116062 = CARTESIAN_POINT ( 'NONE',  ( -19.05341960407611168, -5.049401038298163336, 101.4572429386476955 ) ) ;
#116063 = CARTESIAN_POINT ( 'NONE',  ( 16.55341960407611168, 4.379528057220329451, 33.95724293864769550 ) ) ;
#116064 = CARTESIAN_POINT ( 'NONE',  ( -5.153800228976328057, -19.02544592524343514, 22.29057627198102765 ) ) ;
#116065 = CARTESIAN_POINT ( 'NONE',  ( 5.823673210054125526, 21.52544592524343514, 79.79057627198102409 ) ) ;
#116066 = CARTESIAN_POINT ( 'NONE',  ( 0.05219959533937995610, -21.53943276465977519, 25.00109039468567218 ) ) ;
#116067 = DIRECTION ( 'NONE',  ( 0.000000000000000000, 0.000000000000000000, 1.000000000000000000 ) ) ;
#116068 = CARTESIAN_POINT ( 'NONE',  ( -16.52544592524335698, -4.483927247898792601, 28.95942372801902209 ) ) ;
#116069 = CARTESIAN_POINT ( 'NONE',  ( -21.52544592524343514, 5.823673210054127303, 71.04057627198103830 ) ) ;
#116070 = CARTESIAN_POINT ( 'NONE',  ( -5.823673210054431948, 21.52544592524334988, 97.70942372801904696 ) ) ;
#116071 = CARTESIAN_POINT ( 'NONE',  ( 0.05219959533909260263, 19.03943276465977164, 79.99890960531436690 ) ) ;
#116072 = CARTESIAN_POINT ( 'NONE',  ( 15.72974639402176855, 15.80617190586768217, 36.87609039468568994 ) ) ;
#116073 = CARTESIAN_POINT ( 'NONE',  ( -5.153800228976328057, -19.02544592524343514, 112.2905762719810099 ) ) ;
#116074 = CARTESIAN_POINT ( 'NONE',  ( 16.52544592524335698, 4.483927247898782831, 86.45942372801901854 ) ) ;
#116075 = CARTESIAN_POINT ( 'NONE',  ( 15.72974639402176855, 15.80617190586768217, 76.87609039468567573 ) ) ;
#116076 = CARTESIAN_POINT ( 'NONE',  ( -19.02544592524334988, -5.153800228976617603, 18.95942372801899722 ) ) ;
#116077 = CARTESIAN_POINT ( 'NONE',  ( 12.06949235617739724, 12.14591786802326823, 71.87609039468568994 ) ) ;
#116078 = CARTESIAN_POINT ( 'NONE',  ( 15.72974639402176855, 15.80617190586768217, 26.87609039468567218 ) ) ;
#116079 = CARTESIAN_POINT ( 'NONE',  ( 19.03943276465977164, -0.05219959533909143690, 38.74890960531436690 ) ) ;
#116080 = CARTESIAN_POINT ( 'NONE',  ( 15.72974639402176855, 15.80617190586768217, 86.87609039468568994 ) ) ;
#116081 = CARTESIAN_POINT ( 'NONE',  ( 16.51473224551069308, 9.474510206698969483, 89.16557627198103830 ) ) ;
#116082 = CARTESIAN_POINT ( 'NONE',  ( 15.72974639402199770, -15.80617190586745480, 93.12390960531436690 ) ) ;
#116084 = CARTESIAN_POINT ( 'NONE',  ( 0.05219959533907565091, 21.53943276465977519, 49.99890960531437401 ) ) ;
#116083 = CARTESIAN_POINT ( 'NONE',  ( 19.25918095147779496, 5.499999999999574563, 81.95284276293932635 ) ) ;
#116086 = CARTESIAN_POINT ( 'NONE',  ( -4.379528057220328563, 16.55341960407611168, 45.20724293864769550 ) ) ;
#116085 = CARTESIAN_POINT ( 'NONE',  ( -13.97604488694527625, -13.89961937509977652, 96.87390960531433848 ) ) ;
#116087 = CARTESIAN_POINT ( 'NONE',  ( 11.48731001631952253, -9.434891085173717329, -62.13554135533229328 ) ) ;
#116088 = CARTESIAN_POINT ( 'NONE',  ( -13.89961937509957401, -13.97604488694547875, 74.37609039468566152 ) ) ;
#116089 = CARTESIAN_POINT ( 'NONE',  ( -17.31747979337946219, 6.344076630961073882, 103.6205513193481949 ) ) ;
#116090 = CARTESIAN_POINT ( 'NONE',  ( -13.89961937509957401, -13.97604488694547875, 104.3760903946856757 ) ) ;
#116091 = CARTESIAN_POINT ( 'NONE',  ( -10.81492255796078084, -18.62759615963271287, 87.08224293864769550 ) ) ;
#116092 = CARTESIAN_POINT ( 'NONE',  ( 14.29746914071049879, -8.314922557960816363, 63.33224293864770260 ) ) ;
#116093 = CARTESIAN_POINT ( 'NONE',  ( 19.02544592524343514, -5.153800228976328945, 98.54057627198100988 ) ) ;
#116094 = CARTESIAN_POINT ( 'NONE',  ( 12.06949235617739724, 12.14591786802326823, 46.87609039468568994 ) ) ;
#116095 = CARTESIAN_POINT ( 'NONE',  ( 13.89961937509977652, -13.97604488694527269, 63.12390960531435979 ) ) ;
#116097 = CARTESIAN_POINT ( 'NONE',  ( -9.474510206698720793, -16.51473224551083518, 99.58442372801900433 ) ) ;
#116096 = CARTESIAN_POINT ( 'NONE',  ( 21.55341960407619695, -5.719274019375665929, 31.04275706135234714 ) ) ;
#116098 = CARTESIAN_POINT ( 'NONE',  ( -19.03943276465977164, 0.05219959533909376836, 96.24890960531436690 ) ) ;
#116099 = CARTESIAN_POINT ( 'NONE',  ( -16.51473224551069308, -9.474510206698971260, 86.66557627198102409 ) ) ;
#116100 = CARTESIAN_POINT ( 'NONE',  ( 18.67979575497178502, 10.72451020669898547, 94.16557627198103830 ) ) ;
#116101 = CARTESIAN_POINT ( 'NONE',  ( 0.05219959533909260263, 19.03943276465977164, 39.99890960531436690 ) ) ;
#116102 = CARTESIAN_POINT ( 'NONE',  ( -17.13100169013299379, -6.664070546373172199, 59.23210164300151348 ) ) ;
#116103 = CARTESIAN_POINT ( 'NONE',  ( -0.05219959533910754901, -16.53943276465976808, 67.49890960531436690 ) ) ;
#116104 = CARTESIAN_POINT ( 'NONE',  ( -19.02544592524342804, 5.153800228976336051, 101.0405762719810241 ) ) ;
#116105 = LINE ( 'NONE', #129257, #199362 ) ;
#116106 = CARTESIAN_POINT ( 'NONE',  ( -13.89961937509957401, -13.97604488694547875, 59.37609039468566863 ) ) ;
#116107 = CARTESIAN_POINT ( 'NONE',  ( -18.62759615963270932, 10.81492255796079327, 90.83224293864769550 ) ) ;
#116108 = CARTESIAN_POINT ( 'NONE',  ( -0.05219959533936034679, 19.03943276465977164, 47.50109039468566863 ) ) ;
#116109 = CARTESIAN_POINT ( 'NONE',  ( -9.564922557960796823, -16.46253265017161027, 107.0822429386476955 ) ) ;
#116110 = CARTESIAN_POINT ( 'NONE',  ( 18.87255363501903105, 5.499999999999943157, 68.82513748171827217 ) ) ;
#116111 = CARTESIAN_POINT ( 'NONE',  ( -10.81492255796078084, -18.62759615963271287, 47.08224293864770260 ) ) ;
#116112 = CARTESIAN_POINT ( 'NONE',  ( 19.02544592524343514, -5.153800228976328945, 88.54057627198102409 ) ) ;
#116113 = CARTESIAN_POINT ( 'NONE',  ( 5.719274019375673035, 21.55341960407619339, 62.29275706135236845 ) ) ;
#116114 = CARTESIAN_POINT ( 'NONE',  ( 16.46253265017160672, -9.564922557960803928, 38.33224293864768839 ) ) ;
#116115 = CARTESIAN_POINT ( 'NONE',  ( 16.53943276465976808, -0.05219959533910856209, 68.74890960531435269 ) ) ;
#116116 = CARTESIAN_POINT ( 'NONE',  ( 8.224510206698742110, 14.34966873604972548, 27.08442372801901854 ) ) ;
#116117 = CARTESIAN_POINT ( 'NONE',  ( -18.62759615963255300, -10.81492255796106328, 49.16775706135234003 ) ) ;
#116118 = ORIENTED_EDGE ( 'NONE', *, *, #74851, .T. ) ;
#116119 = CARTESIAN_POINT ( 'NONE',  ( -9.564922557960796823, -16.46253265017161027, 112.0822429386476955 ) ) ;
#116120 = CARTESIAN_POINT ( 'NONE',  ( 9.564922557961047289, -16.46253265017146816, 60.41775706135233293 ) ) ;
#116121 = FACE_OUTER_BOUND ( 'NONE', #150689, .T. ) ;
#116122 = CARTESIAN_POINT ( 'NONE',  ( -5.719274019375665041, -21.55341960407619695, 19.79275706135235069 ) ) ;
#116123 = CARTESIAN_POINT ( 'NONE',  ( -13.89961937509977652, 13.97604488694528158, 55.62390960531434558 ) ) ;
#116124 = CARTESIAN_POINT ( 'NONE',  ( 30.74264578624800137, -22.33583958711395212, -8.949999994537627401 ) ) ;
#116125 = CARTESIAN_POINT ( 'NONE',  ( 13.97604488694548053, -13.89961937509957401, 20.62609039468567573 ) ) ;
#116126 = CARTESIAN_POINT ( 'NONE',  ( 9.474510206698971260, -16.51473224551069308, 47.91557627198102409 ) ) ;
#116127 = CARTESIAN_POINT ( 'NONE',  ( 18.67979575497194134, -10.72451020669871369, 105.8344237280190328 ) ) ;
#116128 = CARTESIAN_POINT ( 'NONE',  ( -12.14591786802326823, 12.06949235617739902, 88.12609039468570415 ) ) ;
#116130 = CARTESIAN_POINT ( 'NONE',  ( -0.05219959533937732626, 21.53943276465977519, 77.50109039468567573 ) ) ;
#116129 = CARTESIAN_POINT ( 'NONE',  ( -5.153800228976328057, -19.02544592524343514, 102.2905762719810383 ) ) ;
#116131 = AXIS2_PLACEMENT_3D ( 'NONE', #83148, #39652, #191334 ) ;
#116132 = CARTESIAN_POINT ( 'NONE',  ( 19.05341960407611168, 5.049401038298154454, 108.9572429386477097 ) ) ;
#116133 = CARTESIAN_POINT ( 'NONE',  ( 24.71161622716358153, 5.993525217005513994, 168.9855167950506143 ) ) ;
#116135 = CARTESIAN_POINT ( 'NONE',  ( 5.823673210054444382, -21.52544592524334988, 65.20942372801901854 ) ) ;
#116134 = CARTESIAN_POINT ( 'NONE',  ( -8.224510206698735004, -14.34966873604973081, 64.58442372801900433 ) ) ;
#116136 = CARTESIAN_POINT ( 'NONE',  ( -18.62759615963255300, -10.81492255796106328, 109.1677570613523613 ) ) ;
#116137 = CYLINDRICAL_SURFACE ( 'NONE', #70315, 5.000000000000000000 ) ;
#116138 = CARTESIAN_POINT ( 'NONE',  ( -9.474510206698964154, 16.51473224551069663, 80.41557627198103830 ) ) ;
#116139 = CARTESIAN_POINT ( 'NONE',  ( -16.46253265017160317, 9.564922557960807481, 110.8322429386476955 ) ) ;
#116140 = ORIENTED_EDGE ( 'NONE', *, *, #26049, .T. ) ;
#116141 = DIRECTION ( 'NONE',  ( -1.000000000000000000, -0.000000000000000000, -0.000000000000000000 ) ) ;
#116142 = CARTESIAN_POINT ( 'NONE',  ( 9.564922557960805705, 16.46253265017160317, 44.58224293864769550 ) ) ;
#116143 = CARTESIAN_POINT ( 'NONE',  ( -5.823673210054116645, -21.52544592524344225, 37.29057627198102409 ) ) ;
#116144 = CARTESIAN_POINT ( 'NONE',  ( 4.379528057220092307, 16.55341960407617563, 107.2927570613523471 ) ) ;
#116146 = CARTESIAN_POINT ( 'NONE',  ( 5.049401038298161559, -19.05341960407611168, 77.70724293864765286 ) ) ;
#116145 = CARTESIAN_POINT ( 'NONE',  ( 16.53943276465976808, -0.05219959533910856209, 83.74890960531435269 ) ) ;
#116147 = CARTESIAN_POINT ( 'NONE',  ( 5.719274019375673035, 21.55341960407619339, 107.2927570613523471 ) ) ;
#116148 = CARTESIAN_POINT ( 'NONE',  ( 5.049401038298161559, -19.05341960407611168, 37.70724293864768839 ) ) ;
#116149 = CARTESIAN_POINT ( 'NONE',  ( 4.483927247898545687, 16.52544592524342804, 94.79057627198105251 ) ) ;
#116150 = CARTESIAN_POINT ( 'NONE',  ( 21.53943276465977519, 0.05219959533937863772, 46.25109039468567573 ) ) ;
#116151 = CARTESIAN_POINT ( 'NONE',  ( -0.05219959533907301413, -21.53943276465977519, 92.49890960531436690 ) ) ;
#116152 = CARTESIAN_POINT ( 'NONE',  ( 13.97604488694548053, -13.89961937509957401, 50.62609039468566152 ) ) ;
#116153 = DIRECTION ( 'NONE',  ( -0.000000000000000000, -0.000000000000000000, 1.000000000000000000 ) ) ;
#116154 = CARTESIAN_POINT ( 'NONE',  ( -16.46253265017160317, 9.564922557960807481, 95.83224293864769550 ) ) ;
#116155 = CARTESIAN_POINT ( 'NONE',  ( 16.52544592524342804, -4.483927247898539470, 63.54057627198103830 ) ) ;
#116156 = TOROIDAL_SURFACE ( 'NONE', #12984, 48.98979485566358250, 12.00000000000000000 ) ;
#116157 = CARTESIAN_POINT ( 'NONE',  ( 4.483927247898545687, 16.52544592524342804, 54.79057627198104541 ) ) ;
#116158 = CARTESIAN_POINT ( 'NONE',  ( -14.34966873604960291, -8.224510206698953496, 31.66557627198102054 ) ) ;
#116159 = CARTESIAN_POINT ( 'NONE',  ( 19.05341960407617918, -5.049401038297876454, 81.04275706135231871 ) ) ;
#116160 = CARTESIAN_POINT ( 'NONE',  ( -18.39635199886970440, 5.499999999999980460, 86.01967076360000419 ) ) ;
#116161 = CARTESIAN_POINT ( 'NONE',  ( 21.55341960407610458, 5.719274019375980345, 28.95724293864769905 ) ) ;
#116162 = CARTESIAN_POINT ( 'NONE',  ( 14.29746914071049879, -8.314922557960816363, 88.33224293864769550 ) ) ;
#116163 = DIRECTION ( 'NONE',  ( 0.9930308165857338887, 0.1178549842436489581, 0.000000000000000000 ) ) ;
#116165 = CARTESIAN_POINT ( 'NONE',  ( -5.719274019375978568, 21.55341960407610458, 45.20724293864769550 ) ) ;
#116164 = CARTESIAN_POINT ( 'NONE',  ( -16.46253265017160317, 9.564922557960807481, 50.83224293864770260 ) ) ;
#116166 = CARTESIAN_POINT ( 'NONE',  ( 5.049401038298161559, -19.05341960407611168, 32.70724293864768129 ) ) ;
#116168 = CARTESIAN_POINT ( 'NONE',  ( 13.89961937509977652, -13.97604488694527269, 63.12390960531435979 ) ) ;
#116167 = CARTESIAN_POINT ( 'NONE',  ( -4.483927247898782831, 16.52544592524335698, 72.70942372801901854 ) ) ;
#116169 = CARTESIAN_POINT ( 'NONE',  ( -9.564922557961040184, 16.46253265017147172, 42.91775706135234003 ) ) ;
#116170 = CARTESIAN_POINT ( 'NONE',  ( 21.55341960407619695, -5.719274019375665929, 66.04275706135236135 ) ) ;
#116171 = CARTESIAN_POINT ( 'NONE',  ( -10.72451020669898014, 18.67979575497178502, 30.41557627198101699 ) ) ;
#116172 = CARTESIAN_POINT ( 'NONE',  ( -4.379528057220328563, 16.55341960407611168, 105.2072429386477097 ) ) ;
#116173 = CARTESIAN_POINT ( 'NONE',  ( 19.03943276465977164, 0.05219959533936151252, 91.25109039468566152 ) ) ;
#116174 = CARTESIAN_POINT ( 'NONE',  ( 22.81625015709510151, -31.40387420917324590, -2.424999997268812990 ) ) ;
#116176 = CARTESIAN_POINT ( 'NONE',  ( 0.05219959533907565091, 21.53943276465977519, 49.99890960531437401 ) ) ;
#116175 = CARTESIAN_POINT ( 'NONE',  ( -1.337618122189682346, -23.50300173439381624, -57.33987540012262230 ) ) ;
#116177 = CARTESIAN_POINT ( 'NONE',  ( -0.05219959533909027116, -19.03943276465977164, 27.49890960531435624 ) ) ;
#116178 = CARTESIAN_POINT ( 'NONE',  ( -10.72451020669870658, -18.67979575497194134, 84.58442372801903275 ) ) ;
#116179 = CARTESIAN_POINT ( 'NONE',  ( -4.483927247898539470, -16.52544592524342804, 52.29057627198102409 ) ) ;
#116181 = CARTESIAN_POINT ( 'NONE',  ( -0.05219959533910754901, -16.53943276465976808, 62.49890960531436690 ) ) ;
#116180 = CARTESIAN_POINT ( 'NONE',  ( -16.53943276465976808, -0.05219959533934237506, 68.75109039468568994 ) ) ;
#116182 = CARTESIAN_POINT ( 'NONE',  ( 18.67979575497178502, 10.72451020669898547, 79.16557627198103830 ) ) ;
#116183 = CARTESIAN_POINT ( 'NONE',  ( -21.53943276465977519, 0.05219959533907696930, 76.24890960531435269 ) ) ;
#116184 = DIRECTION ( 'NONE',  ( -0.000000000000000000, -0.000000000000000000, 1.000000000000000000 ) ) ;
#116186 = EDGE_CURVE ( 'NONE', #191800, #81477, #133660, .T. ) ;
#116185 = CARTESIAN_POINT ( 'NONE',  ( 21.52544592524344225, -5.823673210054117533, 33.54057627198102409 ) ) ;
#116187 = CARTESIAN_POINT ( 'NONE',  ( 16.52544592524335698, 4.483927247898782831, 51.45942372801901854 ) ) ;
#116188 = CARTESIAN_POINT ( 'NONE',  ( 16.52544592524342804, -4.483927247898539470, 83.54057627198102409 ) ) ;
#116189 = CARTESIAN_POINT ( 'NONE',  ( 19.03943276465977164, -0.05219959533909143690, 63.74890960531435979 ) ) ;
#116190 = CARTESIAN_POINT ( 'NONE',  ( 9.474510206698971260, -16.51473224551069308, 32.91557627198102409 ) ) ;
#116191 =( NAMED_UNIT ( * ) PLANE_ANGLE_UNIT ( ) SI_UNIT ( $, .RADIAN. ) );
#116192 = CARTESIAN_POINT ( 'NONE',  ( 24.81835880841864039, -6.052260367207979996, 168.4265213779230521 ) ) ;
#116193 = CARTESIAN_POINT ( 'NONE',  ( 16.53943276465976808, 0.05219959533934440121, 81.25109039468568994 ) ) ;
#116194 = CARTESIAN_POINT ( 'NONE',  ( 10.72451020669871369, 18.67979575497193778, 22.08442372801901143 ) ) ;
#116195 = CARTESIAN_POINT ( 'NONE',  ( 5.049401038298161559, -19.05341960407611168, 67.70724293864769550 ) ) ;
#116196 = CARTESIAN_POINT ( 'NONE',  ( 10.81492255796106328, -18.62759615963255655, 50.41775706135235424 ) ) ;
#116197 = CARTESIAN_POINT ( 'NONE',  ( 16.51473224551069308, 9.474510206698969483, 114.1655762719810241 ) ) ;
#116198 = DIRECTION ( 'NONE',  ( 1.000000000000000000, 0.000000000000000000, 0.000000000000000000 ) ) ;
#116199 = ORIENTED_EDGE ( 'NONE', *, *, #19937, .T. ) ;
#116200 = CARTESIAN_POINT ( 'NONE',  ( 10.72451020669871369, 18.67979575497193778, 47.08442372801901854 ) ) ;
#116202 = CARTESIAN_POINT ( 'NONE',  ( -5.153800228976328057, -19.02544592524343514, 107.2905762719810383 ) ) ;
#116201 = CARTESIAN_POINT ( 'NONE',  ( 9.564922557960805705, 16.46253265017160317, 114.5822429386476955 ) ) ;
#116203 = CARTESIAN_POINT ( 'NONE',  ( -19.05341960407617563, 5.049401038297882671, 53.54275706135231871 ) ) ;
#116204 = CARTESIAN_POINT ( 'NONE',  ( 0.05219959533907565091, 21.53943276465977519, 109.9989096053143527 ) ) ;
#116205 = CARTESIAN_POINT ( 'NONE',  ( -9.474510206698720793, -16.51473224551083518, 49.58442372801899722 ) ) ;
#116206 = CARTESIAN_POINT ( 'NONE',  ( -9.564922557961040184, 16.46253265017147172, 42.91775706135234003 ) ) ;
#116207 = CARTESIAN_POINT ( 'NONE',  ( 14.34966873604972726, -8.224510206698740333, 105.8344237280190328 ) ) ;
#116208 = CARTESIAN_POINT ( 'NONE',  ( 9.391041506135660910, 10.10090423873401733, -62.54717694538948791 ) ) ;
#116209 = CARTESIAN_POINT ( 'NONE',  ( -16.51473224551069308, -9.474510206698971260, 91.66557627198103830 ) ) ;
#116210 = CARTESIAN_POINT ( 'NONE',  ( -21.53943276465977519, -0.05219959533937600094, 93.75109039468567573 ) ) ;
#116211 = CARTESIAN_POINT ( 'NONE',  ( -18.67979575497193778, 10.72451020669871902, 88.33442372801901854 ) ) ;
#116212 = DIRECTION ( 'NONE',  ( -0.000000000000000000, -1.000000000000000000, -0.000000000000000000 ) ) ;
#116213 = CARTESIAN_POINT ( 'NONE',  ( 9.564922557960805705, 16.46253265017160317, 99.58224293864770971 ) ) ;
#116214 = CARTESIAN_POINT ( 'NONE',  ( 5.719274019375673035, 21.55341960407619339, 72.29275706135236135 ) ) ;
#116215 = CARTESIAN_POINT ( 'NONE',  ( -8.224510206698735004, -14.34966873604973081, 24.58442372801901499 ) ) ;
#116216 = CARTESIAN_POINT ( 'NONE',  ( 19.05341960407611168, 5.049401038298154454, 78.95724293864769550 ) ) ;
#116217 = CARTESIAN_POINT ( 'NONE',  ( 21.55341960407610458, 5.719274019375980345, 28.95724293864769905 ) ) ;
#116218 = CARTESIAN_POINT ( 'NONE',  ( -9.564922557960796823, -16.46253265017161027, 92.08224293864769550 ) ) ;
#116219 = DIRECTION ( 'NONE',  ( -0.000000000000000000, -0.000000000000000000, 1.000000000000000000 ) ) ;
#116220 = CARTESIAN_POINT ( 'NONE',  ( 16.46253265017160672, -9.564922557960803928, 73.33224293864769550 ) ) ;
#116221 = CARTESIAN_POINT ( 'NONE',  ( -19.03943276465977164, 0.05219959533909376836, 66.24890960531436690 ) ) ;
#116222 = CARTESIAN_POINT ( 'NONE',  ( -10.72451020669898014, 18.67979575497178502, 115.4155762719810241 ) ) ;
#116223 = CARTESIAN_POINT ( 'NONE',  ( 16.52544592524335698, 4.483927247898782831, 96.45942372801901854 ) ) ;
#116224 = CARTESIAN_POINT ( 'NONE',  ( -16.29526858892910823, 7.335722546919979159, 99.20329402199730850 ) ) ;
#116225 = CARTESIAN_POINT ( 'NONE',  ( -0.05219959533936034679, 19.03943276465977164, 52.50109039468566863 ) ) ;
#116226 = CARTESIAN_POINT ( 'NONE',  ( 19.03943276465977164, -0.05219959533909143690, 88.74890960531436690 ) ) ;
#116227 = CARTESIAN_POINT ( 'NONE',  ( 16.53943276465976808, -0.05219959533910856209, 78.74890960531436690 ) ) ;
#116228 = CARTESIAN_POINT ( 'NONE',  ( -10.81492255796078084, -18.62759615963271287, 32.08224293864769550 ) ) ;
#116229 = CARTESIAN_POINT ( 'NONE',  ( 5.823673210054125526, 21.52544592524343514, 29.79057627198102409 ) ) ;
#116230 = CARTESIAN_POINT ( 'NONE',  ( -0.05219959533910754901, -16.53943276465976808, 92.49890960531436690 ) ) ;
#116231 = CARTESIAN_POINT ( 'NONE',  ( -16.21995358207306381, 7.366697692864088154, 54.93551001512158649 ) ) ;
#116232 = CARTESIAN_POINT ( 'NONE',  ( 5.153800228976615827, -19.02544592524334988, 40.20942372801898301 ) ) ;
#116233 = CARTESIAN_POINT ( 'NONE',  ( 16.55341960407618274, -4.379528057220086978, 106.0427570613523471 ) ) ;
#116234 = CARTESIAN_POINT ( 'NONE',  ( -16.46253265017160317, 9.564922557960807481, 85.83224293864769550 ) ) ;
#116235 = CARTESIAN_POINT ( 'NONE',  ( -10.81492255796105439, 18.62759615963255655, 72.91775706135234714 ) ) ;
#116236 = CARTESIAN_POINT ( 'NONE',  ( 18.62759615963271287, -10.81492255796078972, 58.33224293864768839 ) ) ;
#116237 = CARTESIAN_POINT ( 'NONE',  ( -15.80617190586768217, 15.72974639402176855, 28.12609039468568284 ) ) ;
#116238 = CARTESIAN_POINT ( 'NONE',  ( 15.72974639402199770, -15.80617190586745480, 83.12390960531436690 ) ) ;
#116239 = CARTESIAN_POINT ( 'NONE',  ( -16.52544592524342804, 4.483927247898546575, 106.0405762719810525 ) ) ;
#116240 = CARTESIAN_POINT ( 'NONE',  ( 0.05219959533936267826, -19.03943276465977164, 70.00109039468566152 ) ) ;
#116241 = CARTESIAN_POINT ( 'NONE',  ( -5.049401038298153566, 19.05341960407611168, 45.20724293864769550 ) ) ;
#116242 = CARTESIAN_POINT ( 'NONE',  ( 5.049401038298161559, -19.05341960407611168, 97.70724293864766707 ) ) ;
#116243 = CARTESIAN_POINT ( 'NONE',  ( -0.05219959533909027116, -19.03943276465977164, 92.49890960531436690 ) ) ;
#116244 = CARTESIAN_POINT ( 'NONE',  ( -13.97604488694527625, -13.89961937509977652, 21.87390960531435979 ) ) ;
#116245 = CARTESIAN_POINT ( 'NONE',  ( 8.314922557960818139, 14.29746914071049879, 39.58224293864769550 ) ) ;
#116246 = CARTESIAN_POINT ( 'NONE',  ( 14.29746914071037800, 8.314922557961029526, 41.66775706135235424 ) ) ;
#116247 = CARTESIAN_POINT ( 'NONE',  ( -18.67979575497193778, 10.72451020669871902, 108.3344237280190185 ) ) ;
#116249 = CARTESIAN_POINT ( 'NONE',  ( -4.379528057220086978, -16.55341960407618274, 109.7927570613523613 ) ) ;
#116248 = CARTESIAN_POINT ( 'NONE',  ( 19.03943276465977164, -0.05219959533909143690, 113.7489096053143669 ) ) ;
#116250 = CARTESIAN_POINT ( 'NONE',  ( -15.72974639402176322, -15.80617190586768395, 29.37609039468568284 ) ) ;
#116251 = CARTESIAN_POINT ( 'NONE',  ( 19.05341960407611168, 5.049401038298154454, 98.95724293864766707 ) ) ;
#116252 = ADVANCED_FACE ( 'NONE', ( #162997 ), #178182, .T. ) ;
#116253 = CARTESIAN_POINT ( 'NONE',  ( 12.06949235617739724, 12.14591786802326823, 101.8760903946857042 ) ) ;
#116254 = CARTESIAN_POINT ( 'NONE',  ( 16.53943276465976808, 0.05219959533934440121, 91.25109039468568994 ) ) ;
#116255 = CARTESIAN_POINT ( 'NONE',  ( -14.34966873604972548, 8.224510206698743886, 28.33442372801902209 ) ) ;
#116256 = CARTESIAN_POINT ( 'NONE',  ( 19.05341960407611168, 5.049401038298154454, 48.95724293864768129 ) ) ;
#116257 = CARTESIAN_POINT ( 'NONE',  ( -16.53943276465976808, 0.05219959533911058130, 111.2489096053143669 ) ) ;
#116258 = CARTESIAN_POINT ( 'NONE',  ( -21.52544592524334988, -5.823673210054445271, 18.95942372801901143 ) ) ;
#116259 = CARTESIAN_POINT ( 'NONE',  ( 19.03943276465977164, -0.05219959533909143690, 38.74890960531436690 ) ) ;
#116260 = CARTESIAN_POINT ( 'NONE',  ( 19.03943276465977164, -0.05219959533909143690, 98.74890960531436690 ) ) ;
#116261 = CARTESIAN_POINT ( 'NONE',  ( -16.46253265017160317, 9.564922557960807481, 30.83224293864769550 ) ) ;
#116262 = CARTESIAN_POINT ( 'NONE',  ( -13.89961937509977652, 13.97604488694528158, 100.6239096053143669 ) ) ;
#116263 = CARTESIAN_POINT ( 'NONE',  ( 17.49999999999999645, 5.500000000000010658, 88.78230962303567253 ) ) ;
#116264 = AXIS2_PLACEMENT_3D ( 'NONE', #181549, #150216, #59169 ) ;
#116265 = CARTESIAN_POINT ( 'NONE',  ( 19.05341960407611168, 5.049401038298154454, 103.9572429386476671 ) ) ;
#116267 = CARTESIAN_POINT ( 'NONE',  ( -16.55341960407611168, -4.379528057220339221, 86.45724293864770971 ) ) ;
#116266 = CARTESIAN_POINT ( 'NONE',  ( 10.81492255796106328, -18.62759615963255655, 50.41775706135235424 ) ) ;
#116268 = CARTESIAN_POINT ( 'NONE',  ( 5.049401038298161559, -19.05341960407611168, 97.70724293864766707 ) ) ;
#116269 = CARTESIAN_POINT ( 'NONE',  ( -27.20512408146884908, -7.754361572989796336, 164.3878212768171920 ) ) ;
#116270 = CARTESIAN_POINT ( 'NONE',  ( 16.55341960407618274, -4.379528057220086978, 71.04275706135234714 ) ) ;
#116271 = CARTESIAN_POINT ( 'NONE',  ( -18.62759615963255300, -10.81492255796106328, 79.16775706135234714 ) ) ;
#116272 = CARTESIAN_POINT ( 'NONE',  ( -16.52544592524335698, -4.483927247898792601, 43.95942372801902565 ) ) ;
#116273 = CARTESIAN_POINT ( 'NONE',  ( -13.97604488694527625, -13.89961937509977652, 86.87390960531436690 ) ) ;
#116274 = CARTESIAN_POINT ( 'NONE',  ( -16.51473224551082808, 9.474510206698731452, 108.3344237280190043 ) ) ;
#116275 = CARTESIAN_POINT ( 'NONE',  ( -8.314922557961024197, 14.29746914071037800, 87.91775706135234714 ) ) ;
#116276 = CARTESIAN_POINT ( 'NONE',  ( -16.46253265017146816, -9.564922557961047289, 89.16775706135234714 ) ) ;
#116277 = CARTESIAN_POINT ( 'NONE',  ( -0.05219959533909027116, -19.03943276465977164, 57.49890960531435979 ) ) ;
#116278 = CARTESIAN_POINT ( 'NONE',  ( -15.80617190586745835, -15.72974639402198527, 96.87390960531436690 ) ) ;
#116280 = CARTESIAN_POINT ( 'NONE',  ( 19.05341960407617918, -5.049401038297876454, 91.04275706135234714 ) ) ;
#116279 = CARTESIAN_POINT ( 'NONE',  ( -16.52544592524342804, 4.483927247898546575, 91.04057627198103830 ) ) ;
#116281 = CARTESIAN_POINT ( 'NONE',  ( -0.05219959533934338120, 16.53943276465976808, 57.50109039468568994 ) ) ;
#116282 = CARTESIAN_POINT ( 'NONE',  ( 17.31728774477275934, -6.344390552232301417, 63.31906651689320142 ) ) ;
#116283 = CARTESIAN_POINT ( 'NONE',  ( -9.564922557961040184, 16.46253265017147172, 52.91775706135233293 ) ) ;
#116284 = CARTESIAN_POINT ( 'NONE',  ( -8.224510206698948167, 14.34966873604960824, 30.41557627198101699 ) ) ;
#116285 = CARTESIAN_POINT ( 'NONE',  ( 16.55341960407611168, 4.379528057220329451, 73.95724293864769550 ) ) ;
#116287 = CARTESIAN_POINT ( 'NONE',  ( -17.50000000000000711, 5.622605283950841581, 38.68792689403890961 ) ) ;
#116286 = CARTESIAN_POINT ( 'NONE',  ( 15.72974639402176855, 15.80617190586768217, 111.8760903946856615 ) ) ;
#116288 = CARTESIAN_POINT ( 'NONE',  ( 0.05219959533907565091, 21.53943276465977519, 114.9989096053143669 ) ) ;
#116289 = CARTESIAN_POINT ( 'NONE',  ( -37.99626262588766679, 2.428612866367529932E-14, 2.000000000000000000 ) ) ;
#116290 = CARTESIAN_POINT ( 'NONE',  ( -16.46253265017160317, 9.564922557960807481, 75.83224293864769550 ) ) ;
#116291 = CARTESIAN_POINT ( 'NONE',  ( -0.05219959533937732626, 21.53943276465977519, 92.50109039468567573 ) ) ;
#116292 = CARTESIAN_POINT ( 'NONE',  ( -13.89961937509977652, 13.97604488694528158, 70.62390960531432427 ) ) ;
#116293 = CARTESIAN_POINT ( 'NONE',  ( 5.719274019375991003, -21.55341960407610458, 47.70724293864770260 ) ) ;
#116294 = CARTESIAN_POINT ( 'NONE',  ( 0.05219959533910956823, 16.53943276465976808, 84.99890960531436690 ) ) ;
#116295 = CARTESIAN_POINT ( 'NONE',  ( 16.46253265017160672, -9.564922557960803928, 53.33224293864768839 ) ) ;
#116296 = CARTESIAN_POINT ( 'NONE',  ( -19.03943276465977164, 0.05219959533909376836, 21.24890960531436335 ) ) ;
#116297 = CARTESIAN_POINT ( 'NONE',  ( -18.67979575497193778, 10.72451020669871902, 23.33442372801901499 ) ) ;
#116298 = VECTOR ( 'NONE', #199327, 1000.000000000000000 ) ;
#116299 = CARTESIAN_POINT ( 'NONE',  ( 15.80617190586769283, -15.72974639402175789, 55.62609039468568284 ) ) ;
#116300 = CARTESIAN_POINT ( 'NONE',  ( 13.97604488694527802, 13.89961937509977652, 44.37390960531435269 ) ) ;
#116301 = CARTESIAN_POINT ( 'NONE',  ( 12.14591786802327356, -12.06949235617739191, 70.62609039468567573 ) ) ;
#116302 = CARTESIAN_POINT ( 'NONE',  ( 15.80617190586746368, 15.72974639402197994, 114.3739096053143527 ) ) ;
#116303 = CARTESIAN_POINT ( 'NONE',  ( 18.67979575497178502, 10.72451020669898547, 114.1655762719810383 ) ) ;
#116305 = CARTESIAN_POINT ( 'NONE',  ( 9.564922557960805705, 16.46253265017160317, 69.58224293864770971 ) ) ;
#116304 = CARTESIAN_POINT ( 'NONE',  ( -16.46253265017146816, -9.564922557961047289, 34.16775706135233293 ) ) ;
#116306 = FACE_OUTER_BOUND ( 'NONE', #156346, .T. ) ;
#116307 = CARTESIAN_POINT ( 'NONE',  ( 5.823673210054444382, -21.52544592524334988, 70.20942372801904696 ) ) ;
#116308 = CARTESIAN_POINT ( 'NONE',  ( -10.72451020669898014, 18.67979575497178502, 50.41557627198103120 ) ) ;
#116309 = CARTESIAN_POINT ( 'NONE',  ( -0.05219959533910754901, -16.53943276465976808, 32.49890960531435979 ) ) ;
#116311 = CARTESIAN_POINT ( 'NONE',  ( -18.62759615963255300, -10.81492255796106328, 109.1677570613523613 ) ) ;
#116310 = CARTESIAN_POINT ( 'NONE',  ( 18.62759615963255655, 10.81492255796105972, 91.66775706135234714 ) ) ;
#116312 = CARTESIAN_POINT ( 'NONE',  ( -16.52544592524342804, 4.483927247898546575, 61.04057627198103120 ) ) ;
#116313 = CARTESIAN_POINT ( 'NONE',  ( -8.224510206698948167, 14.34966873604960824, 105.4155762719810383 ) ) ;
#116314 = CARTESIAN_POINT ( 'NONE',  ( 13.97604488694548053, -13.89961937509957401, 60.62609039468564731 ) ) ;
#116315 = CARTESIAN_POINT ( 'NONE',  ( -4.483927247898782831, 16.52544592524335698, 112.7094237280190328 ) ) ;
#116316 = CARTESIAN_POINT ( 'NONE',  ( -18.67979575497193778, 10.72451020669871902, 68.33442372801900433 ) ) ;
#116317 = CARTESIAN_POINT ( 'NONE',  ( -16.46253265017160317, 9.564922557960807481, 70.83224293864770971 ) ) ;
#116318 = CARTESIAN_POINT ( 'NONE',  ( 16.51473224551083163, -9.474510206698727899, 30.83442372801900433 ) ) ;
#116319 = CARTESIAN_POINT ( 'NONE',  ( 21.52544592524344225, -5.823673210054117533, 48.54057627198103120 ) ) ;
#116320 = CARTESIAN_POINT ( 'NONE',  ( 21.53943276465977519, 0.05219959533937863772, 51.25109039468568994 ) ) ;
#116321 = CARTESIAN_POINT ( 'NONE',  ( 5.719274019375991003, -21.55341960407610458, 102.7072429386476955 ) ) ;
#116322 = CARTESIAN_POINT ( 'NONE',  ( -19.05341960407617563, 5.049401038297882671, 93.54275706135234714 ) ) ;
#116323 = CARTESIAN_POINT ( 'NONE',  ( 8.314922557961029526, -14.29746914071037800, 50.41775706135235424 ) ) ;
#116325 = CARTESIAN_POINT ( 'NONE',  ( -5.719274019375978568, 21.55341960407610458, 100.2072429386476955 ) ) ;
#116324 = DIRECTION ( 'NONE',  ( 1.000000000000000000, 0.000000000000000000, 0.000000000000000000 ) ) ;
#116326 = CARTESIAN_POINT ( 'NONE',  ( -4.379528057220328563, 16.55341960407611168, 85.20724293864770971 ) ) ;
#116327 = CARTESIAN_POINT ( 'NONE',  ( -25.65937876999938894, -27.64914803190709591, -20.38451907593472612 ) ) ;
#116328 = CARTESIAN_POINT ( 'NONE',  ( 5.049401038297881783, 19.05341960407617563, 112.2927570613523471 ) ) ;
#116329 = CARTESIAN_POINT ( 'NONE',  ( -10.72451020669898014, 18.67979575497178502, 45.41557627198103830 ) ) ;
#116330 = CARTESIAN_POINT ( 'NONE',  ( 16.55341960407618274, -4.379528057220086978, 86.04275706135236135 ) ) ;
#116331 = CARTESIAN_POINT ( 'NONE',  ( 35.74560708664564856, 9.537923430963926918, -7.999999999999994671 ) ) ;
#116332 = CARTESIAN_POINT ( 'NONE',  ( -8.224510206698735004, -14.34966873604973081, 54.58442372801901143 ) ) ;
#116333 = CARTESIAN_POINT ( 'NONE',  ( 15.72974639402176855, 15.80617190586768217, 21.87609039468567573 ) ) ;
#116334 = CARTESIAN_POINT ( 'NONE',  ( 18.67979575497178502, 10.72451020669898547, 39.16557627198102409 ) ) ;
#116335 = CARTESIAN_POINT ( 'NONE',  ( 0.05219959533934541429, -16.53943276465976808, 80.00109039468568994 ) ) ;
#116336 = CARTESIAN_POINT ( 'NONE',  ( 9.564922557960805705, 16.46253265017160317, 104.5822429386476955 ) ) ;
#116337 = CARTESIAN_POINT ( 'NONE',  ( -18.67979575497193778, 10.72451020669871902, 68.33442372801900433 ) ) ;
#116338 = CARTESIAN_POINT ( 'NONE',  ( -15.72974639402197994, 15.80617190586746368, 35.62390960531437401 ) ) ;
#116339 = CARTESIAN_POINT ( 'NONE',  ( 5.823673210054125526, 21.52544592524343514, 24.79057627198103120 ) ) ;
#116340 = ORIENTED_EDGE ( 'NONE', *, *, #123873, .T. ) ;
#116341 = CARTESIAN_POINT ( 'NONE',  ( 19.03943276465977164, 0.05219959533936151252, 51.25109039468567573 ) ) ;
#116342 = CARTESIAN_POINT ( 'NONE',  ( -4.379528057220086978, -16.55341960407618274, 69.79275706135234714 ) ) ;
#116343 = CARTESIAN_POINT ( 'NONE',  ( -0.05219959533907301413, -21.53943276465977519, 27.49890960531435269 ) ) ;
#116344 = ORIENTED_EDGE ( 'NONE', *, *, #13078, .F. ) ;
#116345 = CARTESIAN_POINT ( 'NONE',  ( 5.153800228976335163, 19.02544592524342804, 84.79057627198099567 ) ) ;
#116346 = CARTESIAN_POINT ( 'NONE',  ( -16.52544592524335698, -4.483927247898792601, 108.9594237280190185 ) ) ;
#116347 = CARTESIAN_POINT ( 'NONE',  ( 19.82991159619255228, -34.74521775907860643, -25.51696690232491349 ) ) ;
#116348 = CARTESIAN_POINT ( 'NONE',  ( -14.34966873604960291, -8.224510206698953496, 111.6655762719810525 ) ) ;
#116349 = CARTESIAN_POINT ( 'NONE',  ( -21.55341960407610458, -5.719274019375992779, 46.45724293864769550 ) ) ;
#116350 = CARTESIAN_POINT ( 'NONE',  ( 9.474510206698971260, -16.51473224551069308, 42.91557627198103120 ) ) ;
#116351 = CARTESIAN_POINT ( 'NONE',  ( -0.05219959533934338120, 16.53943276465976808, 82.50109039468568994 ) ) ;
#116352 = CARTESIAN_POINT ( 'NONE',  ( -18.67979575497193778, 10.72451020669871902, 38.33442372801900433 ) ) ;
#116353 = CARTESIAN_POINT ( 'NONE',  ( 9.474510206698729675, 16.51473224551082808, 92.08442372801900433 ) ) ;
#116354 = CARTESIAN_POINT ( 'NONE',  ( 8.224510206698953496, -14.34966873604960469, 92.91557627198103830 ) ) ;
#116355 = CARTESIAN_POINT ( 'NONE',  ( 19.02544592524343514, -5.153800228976328945, 58.54057627198102409 ) ) ;
#116356 = CARTESIAN_POINT ( 'NONE',  ( -5.153800228976328057, -19.02544592524343514, 32.29057627198102409 ) ) ;
#116357 = CARTESIAN_POINT ( 'NONE',  ( -21.52544592524334988, -5.823673210054445271, 98.95942372801903275 ) ) ;
#116358 = CARTESIAN_POINT ( 'NONE',  ( -19.02544592524342804, 5.153800228976336051, 81.04057627198103830 ) ) ;
#116359 = CARTESIAN_POINT ( 'NONE',  ( 8.224510206698742110, 14.34966873604972548, 67.08442372801901854 ) ) ;
#116360 = CARTESIAN_POINT ( 'NONE',  ( 21.55341960407619695, -5.719274019375665929, 91.04275706135236135 ) ) ;
#116361 = CARTESIAN_POINT ( 'NONE',  ( -21.53943276465977519, 0.05219959533907696930, 51.24890960531436690 ) ) ;
#116362 = CARTESIAN_POINT ( 'NONE',  ( -16.55341960407617563, 4.379528057220093196, 73.54275706135234714 ) ) ;
#116363 = CARTESIAN_POINT ( 'NONE',  ( -9.564922557961040184, 16.46253265017147172, 57.91775706135233293 ) ) ;
#116364 = CARTESIAN_POINT ( 'NONE',  ( -19.02544592524334988, -5.153800228976617603, 68.95942372801896170 ) ) ;
#116365 = EDGE_LOOP ( 'NONE', ( #192619, #8791, #132006, #10180 ) ) ;
#116366 = CARTESIAN_POINT ( 'NONE',  ( -0.05219959533937732626, 21.53943276465977519, 62.50109039468568284 ) ) ;
#116367 = CARTESIAN_POINT ( 'NONE',  ( 0.05219959533909260263, 19.03943276465977164, 69.99890960531435269 ) ) ;
#116368 = CARTESIAN_POINT ( 'NONE',  ( 5.049401038298161559, -19.05341960407611168, 22.70724293864769194 ) ) ;
#116369 = CARTESIAN_POINT ( 'NONE',  ( 9.474510206698729675, 16.51473224551082808, 57.08442372801900433 ) ) ;
#116370 = CARTESIAN_POINT ( 'NONE',  ( -25.90244409532896697, 6.509810826857618693, 161.8457455760362222 ) ) ;
#116371 = CARTESIAN_POINT ( 'NONE',  ( 5.153800228976335163, 19.02544592524342804, 99.79057627198102409 ) ) ;
#116372 = CARTESIAN_POINT ( 'NONE',  ( 14.34966873604960469, 8.224510206698951720, 54.16557627198103120 ) ) ;
#116373 = CARTESIAN_POINT ( 'NONE',  ( 21.55341960407610458, 5.719274019375980345, 43.95724293864769550 ) ) ;
#116374 = CARTESIAN_POINT ( 'NONE',  ( 6.874011537017776341, -5.374011537017756801, -64.03675147074802965 ) ) ;
#116375 = CARTESIAN_POINT ( 'NONE',  ( -5.823673210054431948, 21.52544592524334988, 112.7094237280190328 ) ) ;
#116376 = CARTESIAN_POINT ( 'NONE',  ( 19.02544592524343514, -5.153800228976328945, 53.54057627198102409 ) ) ;
#116377 = CARTESIAN_POINT ( 'NONE',  ( -13.89961937509977652, 13.97604488694528158, 25.62390960531434558 ) ) ;
#116378 = CARTESIAN_POINT ( 'NONE',  ( -10.27157327577100254, -12.17763598328338936, -59.49962702345104049 ) ) ;
#116379 = CARTESIAN_POINT ( 'NONE',  ( -36.89467761628205267, -8.593610866466510956, -7.999999999999994671 ) ) ;
#116380 = CARTESIAN_POINT ( 'NONE',  ( -12.06949235617739369, -12.14591786802326823, 59.37609039468568284 ) ) ;
#116381 = CARTESIAN_POINT ( 'NONE',  ( -10.81492255796078084, -18.62759615963271287, 82.08224293864768129 ) ) ;
#116382 = CARTESIAN_POINT ( 'NONE',  ( -16.52544592524342804, 4.483927247898546575, 56.04057627198102409 ) ) ;
#116384 = CARTESIAN_POINT ( 'NONE',  ( 11.74264578624800315, -36.14014761921581709, -5.149999994537626691 ) ) ;
#116383 = CARTESIAN_POINT ( 'NONE',  ( 16.51473224551069308, 9.474510206698969483, 44.16557627198103120 ) ) ;
#116385 = CARTESIAN_POINT ( 'NONE',  ( 15.80617190586769283, -15.72974639402175789, 40.62609039468567573 ) ) ;
#116386 = CARTESIAN_POINT ( 'NONE',  ( 5.049401038297881783, 19.05341960407617563, 47.29275706135231161 ) ) ;
#116387 = CARTESIAN_POINT ( 'NONE',  ( -19.02544592524342804, 5.153800228976336051, 31.04057627198102409 ) ) ;
#116388 = CARTESIAN_POINT ( 'NONE',  ( 10.81492255796106328, -18.62759615963255655, 85.41775706135236135 ) ) ;
#116389 = CARTESIAN_POINT ( 'NONE',  ( 17.05587630539788080, 6.762274262135702152, 96.75819690962687503 ) ) ;
#116390 = CARTESIAN_POINT ( 'NONE',  ( 16.55341960407611168, 4.379528057220329451, 43.95724293864769550 ) ) ;
#116391 = CARTESIAN_POINT ( 'NONE',  ( 1.697796032038702219, -7.741785448087965094, 5.990689250852171632 ) ) ;
#116392 = CARTESIAN_POINT ( 'NONE',  ( 21.52544592524344225, -5.823673210054117533, 38.54057627198103120 ) ) ;
#116393 = ORIENTED_EDGE ( 'NONE', *, *, #199792, .T. ) ;
#116394 = CARTESIAN_POINT ( 'NONE',  ( 27.73933785331498569, 2.768321779492822058E-14, 143.8750000027311842 ) ) ;
#116395 = CARTESIAN_POINT ( 'NONE',  ( 9.474510206698971260, -16.51473224551069308, 92.91557627198103830 ) ) ;
#116396 = CARTESIAN_POINT ( 'NONE',  ( -4.483927247898539470, -16.52544592524342804, 82.29057627198103830 ) ) ;
#116397 = CARTESIAN_POINT ( 'NONE',  ( -8.224510206698735004, -14.34966873604973081, 24.58442372801901499 ) ) ;
#116398 = CARTESIAN_POINT ( 'NONE',  ( 8.224510206698742110, 14.34966873604972548, 107.0844237280190043 ) ) ;
#116399 = ORIENTED_EDGE ( 'NONE', *, *, #141236, .T. ) ;
#116400 = CARTESIAN_POINT ( 'NONE',  ( -0.05219959533909027116, -19.03943276465977164, 37.49890960531436690 ) ) ;
#116402 = CARTESIAN_POINT ( 'NONE',  ( 5.719274019375991003, -21.55341960407610458, 87.70724293864769550 ) ) ;
#116401 = CARTESIAN_POINT ( 'NONE',  ( -16.46253265017160317, 9.564922557960807481, 85.83224293864769550 ) ) ;
#116404 = CARTESIAN_POINT ( 'NONE',  ( -5.153800228976328057, -19.02544592524343514, 102.2905762719810383 ) ) ;
#116403 = CARTESIAN_POINT ( 'NONE',  ( 8.224510206698953496, -14.34966873604960469, 27.91557627198103830 ) ) ;
#116405 = CARTESIAN_POINT ( 'NONE',  ( -5.049401038297874678, -19.05341960407617918, 79.79275706135233293 ) ) ;
#116406 = CARTESIAN_POINT ( 'NONE',  ( -18.67979575497193778, 10.72451020669871902, 108.3344237280190185 ) ) ;
#116407 = CARTESIAN_POINT ( 'NONE',  ( -18.62759615963270932, 10.81492255796079327, 90.83224293864769550 ) ) ;
#116408 = CARTESIAN_POINT ( 'NONE',  ( -15.80617190586745835, -15.72974639402198527, 31.87390960531435979 ) ) ;
#116409 = CARTESIAN_POINT ( 'NONE',  ( -19.03943276465977164, 0.05219959533909376836, 66.24890960531436690 ) ) ;
#116410 = CARTESIAN_POINT ( 'NONE',  ( 14.34966873604960469, 8.224510206698951720, 24.16557627198103120 ) ) ;
#116411 = CARTESIAN_POINT ( 'NONE',  ( -5.153800228976328057, -19.02544592524343514, 82.29057627198103830 ) ) ;
#116412 = EDGE_LOOP ( 'NONE', ( #120884, #72621, #71140, #172517 ) ) ;
#116413 = CARTESIAN_POINT ( 'NONE',  ( -32.57158834789616009, -1.949426887445991685, 87.75361764676915755 ) ) ;
#116414 = CARTESIAN_POINT ( 'NONE',  ( 5.049401038297881783, 19.05341960407617563, 22.29275706135233648 ) ) ;
#116415 = CARTESIAN_POINT ( 'NONE',  ( -8.224510206698948167, 14.34966873604960824, 90.41557627198103830 ) ) ;
#116416 =( BOUNDED_SURFACE ( )  B_SPLINE_SURFACE ( 3, 2, ( 
 ( #112709, #173409, #22710, #65215, #83361, #84357, #129850, #146035, #144042, #7518, #111723, #5524, #34880, #174401, #96534, #158224, #19714, #52036, #143040, #159204, #190562, #102546, #85359, #134894, #192561, #178398, #42873, #164229, #163219, #195574, #11557, #24721, #118721, #89363, #133883, #73223, #23712, #41882, #147052, #40872, #87372, #9546, #149057, #10545, #57047, #86370, #130871, #8535, #181395, #132875, #25726, #193566, #196570, #72209, #54044, #180410, #148055, #115718, #119711, #71212, #58041, #12543, #103549, #88358, #194564, #165224, #70214, #131881, #26719, #150051, #104538, #56034, #117712, #55038, #166219, #27720, #162213, #151052, #116708, #177406, #38877, #100534, #179408, #39862, #101528, #92324, #29681, #154009, #184357, #120683, #198537, #74208, #32657, #182382, #16496, #122669, #121675, #43860, #45838, #170173, #62979, #13515, #107489, #15505, #109487, #169167, #312, #199527, #105525, #78145, #60995, #183370, #137846, #31666, #46834, #30671, #60008, #77162, #124659, #91313, #138832, #171170, #186355, #61980, #155000, #94311, #155989, #185343, #47835, #135877, #93316, #139813, #197548, #123646, #59016, #108494, #1301, #168185, #167211, #28708, #90344, #152029, #75180, #136852, #14504, #44852, #106508, #153005, #76166, #102054, #21214, #192061, #70724, #125655, #39379, #178913, #17486, #161726, #63985, #8035, #117219, #191067, #115221, #132391, #23221, #162724, #101038, #100040, #84864, #53543, #187352, #24229, #79143, #48822, #85880, #146542, #69716, #131383, #147568, #110475, #40380, #172157, #160724, #194084, #9053, #6034, #140814, #193072, #177911, #55546, #7025, #2304, #37377, #130364, #33643, #176913, #98022, #22216, #159717, #82871, #144549, #67713, #38384, #83865, #114201, #54547, #116220, #129371, #52540, #175905, #99034, #145547, #68707, #136375, #88874, #13045, #89873, #167714, #104050, #57558, #14017, #122186, #182888, #43373, #121195, #181895, #41388, #71715, #164735, #73728, #150567, #134401, #165730, #26230, #133383, #197072, #44371, #105045, #25239, #179921, #198052, #196088, #42387, #12066, #87869, #163739, #106028, #166729, #180912, #135401, #119228, #75683, #86880, #103053, #28233, #27226, #58539, #120205, #59518, #183878, #29211, #10055, #72728, #195074, #151555, #90845, #74712, #152530, #137362, #199041, #60511, #45363, #148565, #56553, #118230, #149557, #11053, #125185, #184865, #15021, #108005, #17011, #93836, #77676, #109012, #169691, #76682, #140338, #126170, #186881, #168688, #123177, #141338, #139345, #185871, #32180, #31185, #107015, #49333, #48351, #124169, #155516, #824, #171686, #187865, #65485, #142327, #18013, #95826, #30189, #110995, #64503, #91831, #94834, #3807, #33175, #110005, #62498, #2825, #170691, #61508, #138358, #78663, #172680, #47357, #79667, #200039, #153524, #19005, #188854, #92837, #1828, #157511, #46348, #34165, #127147, #154522, #156512, #16019, #80651, #63510, #20973, #145311, #162482, #53305, #192834, #131146, #130128, #114984, #83634, #158494, #69480, #111995, #19981, #54315, #191825, #176677, #161493, #115987, #143307, #147327, #4793, #190832, #23984, #39144, #36138, #8814, #99807, #7797, #177676, #37138, #70484, #67475, #160492, #132150, #6794, #128145, #52308, #100799, #82630, #50338, #189845, #85640, #113965, #21982, #112980, #173685, #68473, #35152, #38153, #144312, #96808, #81624, #129134, #66483, #51318, #22981, #174673, #175664, #84630, #97790, #159479, #146308, #5802, #98798, #134161, #72488, #133146, #89635, #58307, #24998, #135167, #179682, #120955, #105797, #178671, #87638, #194837, #10818, #11829, #149324, #73494, #103817, #40134, #117992, #193843, #152302, #101812, #136144, #42157, #41154, #163500, #165497, #151323, #182654, #56310, #26993, #196840, #28978, #88638, #119975, #118998, #86642, #197820, #180681, #102817, #57322, #12812, #166498, #150334, #164502, #181661, #44138, #195849, #43140, #90620, #167483 ),
 ( #104809, #13786, #27996, #74479, #55307, #59286, #75453, #148325, #25995, #116979, #9820, #71481, #79426, #108771, #91595, #141097, #198814, #184628, #49099, #170449, #169449, #1585, #17770, #30951, #124940, #95583, #140093, #2584, #29957, #48108, #153285, #47112, #93594, #15778, #155280, #16769, #63260, #110756, #31940, #92598, #186637, #64264, #154288, #109764, #157268, #171448, #125930, #14786, #32935, #76446, #78417, #94590, #77437, #156269, #187629, #172438, #139109, #137127, #138123, #33926, #583, #18764, #199804, #60279, #121952, #183645, #45127, #62254, #106785, #168460, #123923, #61271, #122941, #46110, #107764, #185622, #6550, #19745, #81386, #68229, #129882, #114739, #20730, #159235, #143071, #176433, #145069, #111754, #21740, #66243, #7550, #192593, #65247, #174432, #4550, #97548, #98556, #35902, #160250, #190593, #126907, #127903, #80411, #38908, #188613, #22741, #128893, #189605, #50094, #52069, #37907, #69237, #51078, #113726, #83392, #115750, #175422, #191581, #5556, #173442, #84389, #67235, #112739, #144075, #99566, #53060, #36891, #82387, #161247, #130903, #146066, #54076, #177438, #100565, #34911, #162245, #142083, #3569, #96567, #158255, #9580, #27753, #193599, #196603, #89396, #42905, #74241, #118756, #182414, #150085, #180445, #23745, #164265, #12575, #116741, #163255, #88391, #132910, #55071, #166253, #195609, #178431, #151084, #85395, #71246, #135910, #43894, #104570, #103583, #181427, #41917, #101564, #25760, #39896, #147088, #105557, #26752, #197581, #24757, #134926, #86404, #133919, #165258, #102581, #11589, #73256, #58074, #56068, #8572, #148089, #59048, #87406, #57082, #194597, #120714, #119744, #70247, #131915, #117748, #179442, #40908, #149091, #10581, #72242, #62012, #124693, #184389, #93348, #106541, #168218, #155034, #16529, #1334, #107523, #45870, #29715, #63014, #31699, #198571, #108527, #153038, #94343, #79177, #152063, #61028, #91347, #169199, #185375, #122700, #46866, #77195, #13548, #14538, #167243, #125687, #75214, #109520, #15537, #76199, #136885, #138864, #186390, #156022, #137878, #344, #170206, #2337, #123677, #78176, #92356, #60041, #171202, #154042, #199559, #30706, #47867, #139845, #32692, #17519, #140848, #64018, #187385, #48854, #28741, #90378, #121709, #183402, #44885, #143828, #96326, #35658, #158013, #114481, #80167, #83150, #176184, #129640, #161003, #5308, #68991, #36642, #66992, #110509, #50839, #99319, #3330, #49842, #175176, #19504, #141839, #52814, #82134, #65993, #51822, #145823, #22497, #65003, #113482, #142830, #128651, #81149, #97306, #4310, #37654, #126661, #144824, #84144, #191336, #7306, #190346, #130655, #98299, #160001, #172190, #112496, #192349, #188365, #111506, #21489, #127662, #173192, #33675, #6308, #34668, #95337, #157022, #189362, #18520, #67986, #174190, #158992, #20484, #146831, #53831, #12337, #56837, #196366, #8325, #165014, #70000, #164023, #10337, #132671, #71993, #133667, #180202, #86161, #115506, #131669, #104327, #55826, #25519, #116501, #57834, #87164, #177194, #195357, #147851, #38667, #42665, #194359, #181188, #135671, #148846, #11340, #71003, #41671, #193351, #54827, #103335, #26508, #88151, #117499, #179196, #178189, #149836, #118512, #85145, #73011, #39654, #166011, #27511, #100322, #9337, #101315, #40664, #134680, #102333, #119507, #89152, #162001, #163004, #23497, #74001, #24511, #150841, #45631, #44644, #167001, #107283, #93107, #186146, #136639, #30460, #138621, #32452, #168954, #123440, #122457, #105314, #1093, #184150, #106296, #60786, #154792, #169962, #153796, #183160, #92108, #47625, #94105, #185133, #15291, #91111, #31454, #76951, #151822, #28503, #102, #62769, #137634, #108284, #90137, #197343, #109279, #78935, #198321, #61772, #170958, #13311, #16290, #155784, #58806, #46624, #43651, #77940, #17281, #167982, #139607, #120474, #124450, #182166, #74977, #59798, #121468, #29480, #152801 ),
 ( #14293, #75960, #199321, #50605, #129407, #96096, #81894, #175944, #191104, #95103, #143587, #172959, #173956, #126436, #65756, #188134, #144585, #110275, #113250, #6071, #159757, #52578, #35423, #99074, #66753, #97076, #140611, #80922, #114238, #33444, #79940, #5070, #49605, #171956, #82907, #112264, #156792, #67749, #2101, #111268, #37414, #158757, #34437, #174940, #142598, #18285, #63782, #160764, #128414, #22254, #141610, #51585, #3097, #20246, #190110, #19275, #36403, #98057, #21252, #157785, #125454, #64774, #187150, #4078, #48623, #127425, #189133, #117255, #83903, #163774, #177945, #145586, #72768, #162757, #11091, #165767, #178947, #41424, #101072, #132426, #56593, #9090, #133421, #10092, #87907, #24266, #39412, #134438, #42422, #103090, #25275, #164771, #102089, #85915, #38422, #194118, #115260, #70758, #54581, #147603, #146581, #53583, #40418, #26266, #86917, #7064, #100078, #118267, #116254, #55581, #148600, #84901, #68745, #149594, #71752, #195110, #179957, #196123, #57593, #119263, #104085, #180946, #130403, #192101, #176953, #161763, #23258, #8075, #69751, #131420, #193107, #48144, #123958, #64300, #93632, #184664, #138159, #78456, #95620, #170485, #141133, #61307, #27262, #142120, #111790, #30984, #1621, #80447, #199840, #49136, #188651, #88911, #171484, #76482, #17807, #126943, #620, #124977, #3605, #32973, #172475, #110794, #109801, #94627, #63297, #122977, #33962, #150603, #46146, #157305, #156306, #79464, #2623, #18802, #107800, #50130, #169484, #31976, #65284, #14821, #15812, #92632, #125967, #187666, #154323, #16806, #77473, #47148, #140130, #139143, #186674, #62291, #155317, #185656, #108806, #96603, #51116, #191617, #113762, #67271, #83427, #146102, #193635, #69272, #19781, #82422, #143108, #38943, #66280, #70283, #127939, #175458, #147123, #162282, #159271, #131951, #22777, #130938, #177474, #160285, #55107, #190630, #145104, #173478, #68266, #112775, #36929, #192629, #85432, #158292, #174468, #53096, #98591, #128929, #6587, #7586, #34951, #54111, #81422, #144111, #4587, #21776, #115785, #129917, #84425, #99602, #100600, #114774, #52105, #23782, #189641, #8610, #176468, #35937, #37942, #161282, #97583, #20767, #5591, #103621, #87443, #118795, #179481, #86441, #150126, #135949, #134965, #178468, #132948, #151122, #149128, #195648, #41955, #117787, #116777, #59084, #196643, #133957, #165297, #10619, #181466, #197619, #75251, #152100, #27792, #105592, #39935, #120751, #74279, #101604, #104608, #13584, #42944, #58112, #72280, #12615, #180484, #71283, #24793, #26790, #182450, #57121, #89434, #148127, #163293, #28776, #198609, #40946, #88432, #167278, #9618, #43930, #136922, #194636, #119782, #56106, #166296, #102618, #11627, #73295, #90415, #164304, #25797, #140886, #139883, #124730, #93385, #168255, #79217, #121745, #29751, #64056, #1372, #63051, #171239, #186428, #95376, #31737, #47904, #185414, #91386, #125726, #46905, #169238, #123717, #17557, #32728, #16566, #45907, #170243, #48893, #15573, #109558, #157061, #110548, #14577, #94380, #92392, #155071, #107560, #108565, #30744, #187425, #153075, #156060, #172229, #2376, #33714, #78213, #18558, #80206, #141877, #60077, #380, #183437, #76235, #199597, #44922, #154079, #137915, #106578, #61064, #122736, #184427, #77231, #138900, #62052, #36681, #35698, #176222, #5347, #96364, #3368, #162039, #6345, #145860, #158052, #114521, #19542, #113522, #160040, #82172, #21527, #83188, #129676, #97345, #65043, #81187, #53869, #67031, #175216, #66033, #7342, #98341, #126699, #144862, #159031, #188403, #192386, #143868, #130692, #85181, #68025, #161039, #20524, #191374, #142869, #4348, #52850, #37691, #99356, #128690, #190387, #127700, #22533, #84180, #34707, #69027, #189400, #115543, #177231, #49881, #51862, #50877, #38703, #100360, #23535, #111546, #173231, #112535, #174229, #146870, #105349, #54863, #89188, #195395, #194394 ),
 ( #116537, #56873, #42702, #135708, #86197, #180238, #88187, #182202, #118548, #73046, #72030, #178225, #150880, #133703, #55861, #10373, #104363, #119543, #103372, #132705, #41707, #197379, #102369, #149871, #43687, #58844, #101351, #11376, #179233, #165050, #117535, #26543, #40699, #12374, #39689, #181226, #74037, #166047, #120511, #134718, #167036, #196401, #57871, #8362, #87201, #28538, #163040, #147887, #27547, #164058, #24547, #70037, #131706, #9373, #193387, #71038, #25557, #148882, #15329, #137669, #31492, #184186, #121503, #90174, #94142, #123479, #1132, #183197, #93144, #44679, #153833, #140, #45668, #61809, #138659, #46662, #199356, #151857, #168018, #109317, #168992, #76988, #152837, #62806, #185171, #13348, #108321, #107319, #136677, #170996, #30496, #47665, #75012, #170001, #124488, #92147, #154829, #14331, #75996, #16327, #77977, #186184, #139644, #32489, #60821, #155821, #198359, #29514, #59833, #106332, #91148, #122495, #55512, #164700, #10022, #87835, #88839, #26196, #150531, #180879, #117182, #72691, #42354, #133348, #74675, #104016, #70690, #12031, #149521, #132356, #59486, #11018, #198017, #152495, #165694, #28197, #134366, #197037, #71681, #195039, #58504, #120170, #105008, #196050, #57525, #56516, #166694, #135366, #102019, #73694, #118194, #121160, #182853, #178877, #119194, #179885, #27192, #181861, #43340, #89839, #151520, #40344, #41353, #194048, #29176, #163702, #13011, #136342, #103017, #25204, #44336, #105993, #167679, #90812, #86846, #148531, #98042, #55567, #100061, #146564, #85902, #113234, #117241, #174925, #160744, #194105, #9075, #6055, #178934, #69736, #177932, #24252, #7045, #40404, #37397, #130385, #102075, #115242, #159739, #22236, #39399, #132413, #143570, #21236, #38404, #83885, #114221, #192082, #193092, #20230, #116240, #66738, #129391, #190095, #68727, #54568, #145567, #131404, #8059, #147590, #53564, #175926, #70745, #81878, #101059, #161746, #162744, #23241, #99056, #36388, #176934, #51570, #84885, #191087, #5052, #82891, #144569, #128398, #67733, #52561, #25260, #179943, #198073, #134424, #42409, #88896, #164757, #163760, #133406, #136396, #167733, #182908, #14037, #58560, #122205, #89894, #120226, #86903, #104072, #152549, #56578, #103075, #28255, #72753, #195095, #106047, #135422, #118252, #29231, #148586, #11075, #75702, #197093, #196110, #59539, #165754, #41410, #10078, #183897, #166751, #90864, #26252, #74732, #87893, #73750, #181916, #27247, #43396, #105067, #151577, #57580, #71736, #149579, #137382, #150588, #13066, #119250, #199061, #121218, #180934, #44392, #12087, #60530, #45382, #185892, #34187, #188877, #1848, #64524, #124191, #33196, #46368, #108026, #94855, #156536, #141359, #47377, #109032, #169713, #2846, #171707, #138378, #48372, #92857, #95848, #19026, #91851, #846, #31206, #170711, #125205, #62519, #186901, #17030, #153544, #154544, #107035, #65507, #15041, #49354, #155535, #16039, #76702, #78684, #126191, #157532, #77697, #140360, #110029, #142348, #80672, #18035, #79689, #187887, #111016, #32202, #139365, #93858, #172703, #3828, #63530, #127168, #168707, #30209, #200058, #61527, #123196, #184886, #4816, #191844, #82650, #83654, #36158, #175683, #97810, #54335, #8836, #158514, #192856, #98817, #159499, #20002, #160511, #146327, #39163, #189866, #145332, #53325, #85661, #162504, #176698, #115004, #38172, #116006, #37158, #20995, #113985, #7816, #23004, #6814, #144332, #22001, #100821, #5821, #99827, #147348, #24005, #66503, #161512, #67497, #68492, #129154, #130147, #190851, #177695, #81645, #84650, #70504, #69500, #132172, #131166, #50359, #112018, #173707, #35175, #52328, #96830, #143329, #51340, #128166, #113000, #174694, #136168, #165521, #148345, #197843, #55328, #41174, #105820, #27017, #26016, #166521, #195873, #86661, #193863, #152324, #196864, #59309, #9841, #104832, #71500, #103840, #150357, #72511, #11854, #73519, #119998 ),
 ( #28019, #182676, #116999, #12836, #151347, #178694, #181684, #90642, #43165, #135190, #87660, #89661, #57346, #133167, #101832, #42180, #120978, #134186, #74502, #25018, #40156, #167507, #75476, #194858, #88661, #44160, #163519, #29002, #13810, #56331, #58330, #118013, #179702, #102837, #164523, #149345, #10841, #119021, #180704, #156292, #95606, #18788, #78442, #183667, #124963, #33948, #107786, #31962, #49122, #140116, #79449, #17793, #16792, #1607, #170472, #45152, #141119, #198837, #106808, #14808, #172461, #63283, #186660, #2609, #29980, #157291, #91619, #77459, #110779, #125953, #122964, #137149, #48130, #94613, #64286, #123945, #60301, #154310, #47135, #121975, #93617, #76469, #139130, #187651, #168482, #153307, #138146, #155302, #607, #30972, #108793, #109787, #199826, #32958, #61294, #46133, #184651, #185643, #171470, #62277, #169471, #92619, #15799, #20753, #174454, #130924, #38929, #99587, #160271, #37927, #98577, #97569, #34937, #128915, #111776, #67257, #51101, #82408, #143094, #50116, #113748, #161268, #21761, #142106, #96589, #114760, #112761, #159257, #5577, #81408, #80433, #22762, #83413, #144096, #190616, #35923, #145090, #84411, #100586, #115771, #191603, #69258, #3591, #146088, #7572, #65269, #68252, #177459, #6573, #129903, #52091, #176454, #175444, #158278, #188636, #36914, #192615, #53082, #54097, #173464, #126929, #162268, #19767, #4573, #66265, #127925, #189627, #9603, #185142, #73279, #181450, #27776, #10603, #46633, #40931, #133942, #123450, #118779, #101590, #25782, #42928, #138631, #147109, #163278, #41939, #164289, #117772, #195632, #196627, #108293, #119766, #70269, #132932, #193621, #72265, #58096, #149113, #134949, #150110, #92118, #87428, #179466, #76960, #23768, #104592, #103605, #166278, #165281, #102603, #178454, #57105, #55092, #180467, #194620, #26774, #86426, #116763, #88415, #153806, #11611, #85418, #39921, #15300, #56091, #112, #61781, #24779, #8595, #131937, #148112, #71268, #95112, #63791, #34446, #50614, #128423, #5080, #80932, #158768, #169972, #189141, #127435, #93116, #157794, #66762, #96105, #188143, #125464, #4087, #33453, #124459, #77949, #18294, #35433, #110284, #142608, #1102, #31464, #81903, #51595, #170968, #141619, #20257, #139616, #112273, #190119, #154801, #111278, #16299, #19285, #62778, #140620, #64784, #143596, #172968, #173965, #97085, #49615, #65765, #3108, #186156, #47635, #109289, #32461, #94114, #155793, #17290, #78944, #2110, #187161, #48632, #126445, #171966, #156801, #79949, #71764, #195123, #54592, #159768, #101084, #10104, #83915, #8086, #25287, #116266, #55593, #194130, #193118, #177956, #146592, #21263, #132439, #174951, #82919, #191116, #148613, #39424, #162769, #178961, #6082, #133434, #67761, #53595, #86930, #102101, #99085, #113259, #24278, #70770, #117268, #100090, #36414, #130414, #23269, #98068, #69763, #52590, #115271, #40430, #144596, #129418, #114250, #131432, #176964, #7076, #84913, #85927, #175956, #9103, #37425, #22265, #160776, #161774, #147616, #38434, #163786, #145597, #68757, #192113, #150616, #107059, #15065, #75731, #136420, #14064, #74758, #73775, #11105, #105093, #87920, #43424, #27276, #58584, #119275, #26278, #89919, #137407, #198100, #118279, #72780, #90888, #88924, #135448, #181941, #57606, #56605, #199087, #59566, #197117, #166779, #12112, #121241, #60555, #76726, #91876, #167758, #45406, #179970, #122230, #183921, #41436, #44418, #153568, #182935, #106071, #120250, #152574, #28280, #134450, #164784, #151601, #168730, #13092, #29256, #149607, #103103, #30234, #138401, #180958, #196135, #42435, #104098, #165781, #109058, #31232, #142376, #171735, #154568, #3855, #61550, #47402, #112046, #33223, #32226, #172732, #1875, #92881, #200082, #158540, #2874, #65534, #16064, #111045, #77722, #110055, #156564, #78711, #18062, #79717, #126217, #93884, #123219, #139388, #50386, #63556, #94883, #62545 ),
 ( #187913, #870, #124220, #49382, #34213, #95876, #140387, #125230, #185917, #157559, #64553, #170735, #141386, #155562, #127194, #173734, #184909, #17056, #186928, #48398, #19052, #80699, #188906, #35203, #46394, #96856, #108052, #20030, #169737, #81672, #191870, #190878, #113027, #53353, #39189, #132199, #82676, #176724, #84675, #178720, #55355, #69527, #146354, #7841, #147374, #68519, #52354, #6840, #100847, #116032, #99853, #129180, #115031, #193890, #98844, #131192, #40182, #117025, #97836, #192882, #175708, #38197, #114010, #130173, #37186, #8863, #174719, #177721, #70530, #162529, #101861, #161537, #163545, #54360, #23030, #143355, #83680, #21021, #145358, #24033, #25045, #66530, #144360, #85687, #4844, #160539, #128193, #189891, #51366, #36182, #159524, #22028, #5847, #67523, #59336, #11882, #136194, #12864, #90670, #27044, #180730, #137177, #45183, #105848, #166548, #44189, #104859, #103866, #41201, #135218, #118040, #73545, #57375, #88690, #149371, #56358, #120024, #167535, #28047, #148372, #102863, #121006, #119048, #165547, #196890, #87686, #86688, #29030, #89688, #150386, #58357, #42206, #151373, #152352, #106837, #122006, #197869, #75503, #9867, #13837, #198865, #71526, #74529, #183697, #182704, #60332, #181709, #168512, #43190, #164548, #194884, #133193, #179731, #26041, #10867, #72537, #134213, #195900, #111811, #31001, #1642, #80467, #138177, #49156, #188672, #30010, #171505, #76501, #17828, #126963, #638, #124999, #142141, #32994, #172497, #110814, #109822, #94648, #63319, #199858, #33984, #91648, #61324, #107818, #65304, #156328, #79486, #95640, #122995, #50152, #184681, #170504, #3625, #18823, #15831, #153337, #141155, #187686, #157328, #16826, #14838, #47166, #140150, #46164, #186694, #169502, #48164, #2644, #92650, #154339, #64320, #125988, #77491, #139161, #155337, #62308, #93652, #123978, #185676, #108825, #31994, #78477, #162305, #128951, #114798, #8633, #23805, #127960, #176491, #5614, #6611, #159292, #98614, #20789, #177497, #143128, #146125, #38967, #192651, #85456, #68290, #131974, #99625, #129941, #173499, #113784, #147145, #66300, #112796, #37967, #82444, #4608, #115807, #145127, #189663, #100623, #34972, #144132, #70305, #191640, #67293, #7610, #175480, #51136, #96624, #193658, #161306, #55130, #174490, #84447, #35957, #83450, #53120, #52128, #22801, #69295, #130961, #190652, #158313, #97604, #19801, #36952, #54134, #160308, #81442, #21798, #116800, #196668, #10643, #178491, #105618, #195673, #43956, #198636, #11652, #74304, #133982, #42968, #56130, #117812, #104631, #166320, #151147, #57144, #118821, #179505, #12638, #181490, #148150, #58136, #102642, #167306, #28802, #101629, #72304, #40972, #180506, #134989, #41978, #119805, #26815, #163319, #164327, #39958, #75277, #24816, #59109, #165323, #25820, #86465, #88455, #135972, #90441, #120774, #9641, #89458, #182475, #197643, #152127, #73318, #136947, #27817, #13609, #71308, #103645, #132971, #194661, #87466, #149153, #150151, #91412, #2400, #31760, #14604, #64079, #121770, #107586, #172252, #93409, #92417, #32754, #62076, #153100, #60102, #18582, #63078, #125749, #76260, #171266, #137938, #170266, #16589, #138923, #78237, #139908, #186453, #154103, #183463, #199622, #110571, #123741, #155095, #122761, #187449, #1398, #44949, #124757, #15597, #106604, #48917, #404, #33740, #141900, #47929, #17583, #77255, #109583, #61089, #184451, #94405, #156086, #79243, #185440, #46930, #45931, #140914, #95400, #169264, #157086, #30770, #80229, #168280, #29777, #108589, #142891, #20549, #21552, #159055, #83212, #113546, #49905, #127724, #3391, #162063, #111571, #145884, #51887, #50901, #173255, #175240, #99380, #192411, #4373, #36705, #144887, #38727, #115568, #129702, #6369, #68049, #7367, #128714, #112559, #67056, #161063, #176247, #160065, #189426, #98367, #53893, #82199, #191399, #100385, #177255, #158075, #52876, #35722 ),
 ( #188427, #97369, #66057, #143891, #114548, #5372, #37718, #22558, #34730, #174254, #65066, #23559, #96388, #69052, #84204, #190411, #19566, #130718, #85207, #126723, #81210, #180260, #88209, #182227, #58868, #73069, #149893, #11400, #150904, #72052, #55885, #10395, #104387, #119565, #103394, #132727, #56896, #135731, #102392, #134741, #43712, #197402, #101374, #196423, #179258, #41730, #194415, #133726, #117558, #12398, #116561, #165072, #87223, #40723, #118570, #181248, #167060, #42725, #193412, #164080, #178250, #195418, #166070, #26566, #57893, #27572, #74060, #148905, #25579, #120534, #105373, #89211, #28561, #146896, #8387, #70062, #163064, #131730, #39711, #54887, #24570, #86219, #9395, #147909, #71061, #109339, #108345, #151881, #106356, #124512, #60843, #169014, #15354, #91170, #90198, #32512, #170025, #107341, #77010, #184208, #154853, #171021, #48681, #125513, #1154, #78996, #13371, #94164, #47689, #75035, #77999, #187210, #16351, #31515, #45690, #186208, #153856, #44702, #198382, #140670, #110333, #155843, #93168, #17340, #139666, #30518, #168040, #138682, #121526, #163, #122518, #92170, #152859, #59859, #123501, #2162, #62829, #136701, #29537, #63841, #61831, #185194, #46685, #14354, #183221, #172014, #76019, #137694, #199379, #127486, #98124, #117058, #194917, #71561, #144650, #25078, #33503, #55388, #193925, #156850, #21316, #133226, #159821, #51647, #189191, #70565, #97136, #188193, #141669, #81955, #101896, #174015, #8897, #64833, #95162, #148406, #118074, #34498, #5130, #86721, #3160, #178753, #56392, #18345, #175003, #80000, #82974, #126495, #4138, #128475, #9901, #36467, #40217, #163578, #113311, #132233, #66813, #49665, #111329, #173019, #96156, #157845, #19337, #80984, #142659, #65817, #50665, #112325, #35486, #158819, #20307, #143647, #190171, #138209, #29060, #137210, #183727, #166581, #199891, #196922, #89721, #76533, #74559, #57407, #181743, #43225, #60365, #104892, #28081, #197901, #120056, #73577, #151406, #152383, #61355, #75535, #26074, #88723, #149403, #12895, #13868, #136226, #90700, #105880, #45213, #59370, #135250, #58389, #106867, #179765, #121042, #198897, #182738, #167567, #119079, #180761, #122037, #168541, #30039, #44222, #91678, #42237, #153370, #14872, #10898, #41234, #165579, #102895, #164580, #87718, #72571, #103898, #134246, #195932, #27077, #150419, #11914, #169534, #47198, #123026, #81471, #31034, #65334, #171535, #170537, #92683, #33023, #18853, #111840, #62340, #156357, #64351, #158341, #34999, #49187, #126020, #187716, #126994, #48196, #32027, #186725, #80499, #95672, #79515, #108858, #94678, #173529, #78508, #110845, #19830, #96654, #77523, #172529, #155368, #17859, #93685, #109850, #4638, #16857, #154371, #46196, #188701, #142172, #143158, #141185, #184711, #34015, #2674, #107849, #63352, #15865, #139195, #124010, #157359, #140181, #670, #50183, #3656, #185708, #1674, #125029, #113812, #178517, #99651, #98643, #38994, #68317, #159321, #66329, #24842, #69322, #8660, #20817, #177525, #82473, #176520, #22827, #145156, #84473, #146151, #192680, #160337, #127990, #144158, #116826, #129968, #37996, #128981, #70333, #161335, #189693, #7638, #21826, #51165, #55156, #175507, #39983, #130988, #83478, #100650, #191668, #5643, #112826, #86491, #54163, #132000, #67320, #162331, #190679, #115836, #23832, #6639, #85482, #147171, #193688, #53147, #174518, #52155, #101654, #114826, #163346, #36981, #148176, #35985, #97632, #119832, #118849, #71334, #105644, #42006, #182503, #75303, #135018, #135999, #180532, #166348, #25849, #87492, #104663, #27846, #12665, #103671, #165349, #149181, #74333, #89487, #179531, #181517, #10669, #43983, #167333, #132996, #26843, #72333, #88484, #42996, #150179, #151177, #11680, #194687, #134008, #9669, #56157, #164353, #28829, #58165, #73345, #195699, #197670, #120803, #152153, #57171, #59135, #90470, #117838, #41001, #13636 ) ),
 .UNSPECIFIED., .T., .F., .T. ) 
 B_SPLINE_SURFACE_WITH_KNOTS ( ( 4, 3, 4 ),
 ( 3, 2, 2, 2, 2, 2, 2, 2, 2, 2, 2, 2, 2, 2, 2, 2, 2, 2, 2, 2, 2, 2, 2, 2, 2, 2, 2, 2, 2, 2, 2, 2, 2, 2, 2, 2, 2, 2, 2, 2, 2, 2, 2, 2, 2, 2, 2, 2, 2, 2, 2, 2, 2, 2, 2, 2, 2, 2, 2, 2, 2, 2, 2, 2, 2, 2, 2, 2, 2, 2, 2, 2, 2, 2, 2, 2, 2, 2, 2, 2, 2, 2, 2, 2, 2, 2, 2, 2, 2, 2, 2, 2, 2, 2, 2, 2, 2, 2, 2, 2, 2, 2, 2, 2, 2, 2, 2, 2, 2, 2, 2, 2, 2, 2, 2, 2, 2, 2, 2, 2, 2, 2, 2, 2, 2, 2, 2, 2, 2, 2, 2, 2, 2, 2, 2, 2, 2, 2, 2, 2, 2, 2, 2, 2, 2, 2, 2, 2, 2, 2, 2, 2, 2, 2, 2, 2, 2, 2, 2, 2, 2, 2, 2, 2, 2, 2, 2, 2, 2, 2, 2, 2, 2, 2, 2, 2, 2, 2, 2, 2, 2, 2, 2, 2, 2, 2, 2, 2, 2, 2, 2, 2, 2, 2, 2, 2, 2, 2, 2, 2, 2, 2, 2, 2, 2, 2, 2, 2, 2, 2, 2, 2, 2, 2, 2, 2, 2, 2, 2, 2, 2, 2, 2, 2, 2, 2, 2, 2, 3 ),
 ( 0.000000000000000000, 0.5000000000000000000, 1.000000000000000000 ),
 ( 0.000000000000000000, 0.004385964912280701511, 0.008771929824561403022, 0.01315789473684210453, 0.01754385964912280604, 0.02192982456140350755, 0.02631578947368420907, 0.03070175438596491058, 0.03508771929824561209, 0.03947368421052631360, 0.04385964912280701511, 0.04824561403508771662, 0.05263157894736841813, 0.05701754385964911964, 0.06140350877192982115, 0.06578947368421052266, 0.07017543859649122417, 0.07456140350877192569, 0.07894736842105262720, 0.08333333333333332871, 0.08771929824561403022, 0.09210526315789473173, 0.09649122807017543324, 0.1008771929824561348, 0.1052631578947368363, 0.1096491228070175378, 0.1140350877192982393, 0.1184210526315789408, 0.1228070175438596423, 0.1271929824561403577, 0.1315789473684210453, 0.1359649122807017607, 0.1403508771929824483, 0.1447368421052631637, 0.1491228070175438514, 0.1535087719298245668, 0.1578947368421052544, 0.1622807017543859698, 0.1666666666666666574, 0.1710526315789473728, 0.1754385964912280604, 0.1798245614035087758, 0.1842105263157894635, 0.1885964912280701788, 0.1929824561403508665, 0.1973684210526315819, 0.2017543859649122695, 0.2061403508771929849, 0.2105263157894736725, 0.2149122807017543879, 0.2192982456140350755, 0.2236842105263157909, 0.2280701754385964786, 0.2324561403508771940, 0.2368421052631578816, 0.2412280701754385970, 0.2456140350877192846, 0.2500000000000000000, 0.2543859649122807154, 0.2587719298245614308, 0.2631578947368420907, 0.2675438596491228060, 0.2719298245614035214, 0.2763157894736842368, 0.2807017543859648967, 0.2850877192982456121, 0.2894736842105263275, 0.2938596491228070429, 0.2982456140350877027, 0.3026315789473684181, 0.3070175438596491335, 0.3114035087719298489, 0.3157894736842105088, 0.3201754385964912242, 0.3245614035087719396, 0.3289473684210526550, 0.3333333333333333148, 0.3377192982456140302, 0.3421052631578947456, 0.3464912280701754610, 0.3508771929824561209, 0.3552631578947368363, 0.3596491228070175517, 0.3640350877192982670, 0.3684210526315789269, 0.3728070175438596423, 0.3771929824561403577, 0.3815789473684210731, 0.3859649122807017330, 0.3903508771929824483, 0.3947368421052631637, 0.3991228070175438791, 0.4035087719298245390, 0.4078947368421052544, 0.4122807017543859698, 0.4166666666666666852, 0.4210526315789473450, 0.4254385964912280604, 0.4298245614035087758, 0.4342105263157894912, 0.4385964912280701511, 0.4429824561403508665, 0.4473684210526315819, 0.4517543859649122973, 0.4561403508771929571, 0.4605263157894736725, 0.4649122807017543879, 0.4692982456140351033, 0.4736842105263157632, 0.4780701754385964786, 0.4824561403508771940, 0.4868421052631579093, 0.4912280701754385692, 0.4956140350877192846, 0.5000000000000000000, 0.5043859649122807154, 0.5087719298245614308, 0.5131578947368421462, 0.5175438596491228616, 0.5219298245614034659, 0.5263157894736841813, 0.5307017543859648967, 0.5350877192982456121, 0.5394736842105263275, 0.5438596491228070429, 0.5482456140350877583, 0.5526315789473684736, 0.5570175438596490780, 0.5614035087719297934, 0.5657894736842105088, 0.5701754385964912242, 0.5745614035087719396, 0.5789473684210526550, 0.5833333333333333703, 0.5877192982456140857, 0.5921052631578946901, 0.5964912280701754055, 0.6008771929824561209, 0.6052631578947368363, 0.6096491228070175517, 0.6140350877192982670, 0.6184210526315789824, 0.6228070175438596978, 0.6271929824561403022, 0.6315789473684210176, 0.6359649122807017330, 0.6403508771929824483, 0.6447368421052631637, 0.6491228070175438791, 0.6535087719298245945, 0.6578947368421053099, 0.6622807017543859143, 0.6666666666666666297, 0.6710526315789473450, 0.6754385964912280604, 0.6798245614035087758, 0.6842105263157894912, 0.6885964912280702066, 0.6929824561403509220, 0.6973684210526315264, 0.7017543859649122417, 0.7061403508771929571, 0.7105263157894736725, 0.7149122807017543879, 0.7192982456140351033, 0.7236842105263158187, 0.7280701754385965341, 0.7324561403508771384, 0.7368421052631578538, 0.7412280701754385692, 0.7456140350877192846, 0.7500000000000000000, 0.7543859649122807154, 0.7587719298245614308, 0.7631578947368421462, 0.7675438596491228616, 0.7719298245614034659, 0.7763157894736841813, 0.7807017543859648967, 0.7850877192982456121, 0.7894736842105263275, 0.7938596491228070429, 0.7982456140350877583, 0.8026315789473684736, 0.8070175438596490780, 0.8114035087719297934, 0.8157894736842105088, 0.8201754385964912242, 0.8245614035087719396, 0.8289473684210526550, 0.8333333333333333703, 0.8377192982456140857, 0.8421052631578946901, 0.8464912280701754055, 0.8508771929824561209, 0.8552631578947368363, 0.8596491228070175517, 0.8640350877192982670, 0.8684210526315789824, 0.8728070175438596978, 0.8771929824561403022, 0.8815789473684210176, 0.8859649122807017330, 0.8903508771929824483, 0.8947368421052631637, 0.8991228070175438791, 0.9035087719298245945, 0.9078947368421053099, 0.9122807017543859143, 0.9166666666666666297, 0.9210526315789473450, 0.9254385964912280604, 0.9298245614035087758, 0.9342105263157894912, 0.9385964912280702066, 0.9429824561403509220, 0.9473684210526315264, 0.9517543859649122417, 0.9561403508771929571, 0.9605263157894736725, 0.9649122807017543879, 0.9692982456140351033, 0.9736842105263158187, 0.9780701754385965341, 0.9824561403508771384, 0.9868421052631578538, 0.9912280701754385692, 0.9956140350877192846, 1.000000000000000000 ),
 .UNSPECIFIED. ) 
 GEOMETRIC_REPRESENTATION_ITEM ( )  RATIONAL_B_SPLINE_SURFACE ( (
 ( 1.000000000000000000, 0.9659258262890683122, 1.000000000000000000, 0.9659258262890683122, 1.000000000000000000, 0.9659258262890683122, 1.000000000000000000, 0.9659258262890683122, 1.000000000000000000, 0.9659258262890683122, 1.000000000000000000, 0.9659258262890683122, 1.000000000000000000, 0.9659258262890683122, 1.000000000000000000, 0.9659258262890683122, 1.000000000000000000, 0.9659258262890683122, 1.000000000000000000, 0.9659258262890683122, 1.000000000000000000, 0.9659258262890683122, 1.000000000000000000, 0.9659258262890683122, 1.000000000000000000, 0.9659258262890683122, 1.000000000000000000, 0.9659258262890683122, 1.000000000000000000, 0.9659258262890683122, 1.000000000000000000, 0.9659258262890683122, 1.000000000000000000, 0.9659258262890683122, 1.000000000000000000, 0.9659258262890683122, 1.000000000000000000, 0.9659258262890683122, 1.000000000000000000, 0.9659258262890683122, 1.000000000000000000, 0.9659258262890683122, 1.000000000000000000, 0.9659258262890683122, 1.000000000000000000, 0.9659258262890683122, 1.000000000000000000, 0.9659258262890683122, 1.000000000000000000, 0.9659258262890683122, 1.000000000000000000, 0.9659258262890683122, 1.000000000000000000, 0.9659258262890683122, 1.000000000000000000, 0.9659258262890683122, 1.000000000000000000, 0.9659258262890683122, 1.000000000000000000, 0.9659258262890683122, 1.000000000000000000, 0.9659258262890683122, 1.000000000000000000, 0.9659258262890683122, 1.000000000000000000, 0.9659258262890683122, 1.000000000000000000, 0.9659258262890683122, 1.000000000000000000, 0.9659258262890683122, 1.000000000000000000, 0.9659258262890683122, 1.000000000000000000, 0.9659258262890683122, 1.000000000000000000, 0.9659258262890683122, 1.000000000000000000, 0.9659258262890683122, 1.000000000000000000, 0.9659258262890683122, 1.000000000000000000, 0.9659258262890683122, 1.000000000000000000, 0.9659258262890683122, 1.000000000000000000, 0.9659258262890683122, 1.000000000000000000, 0.9659258262890683122, 1.000000000000000000, 0.9659258262890683122, 1.000000000000000000, 0.9659258262890683122, 1.000000000000000000, 0.9659258262890683122, 1.000000000000000000, 0.9659258262890683122, 1.000000000000000000, 0.9659258262890683122, 1.000000000000000000, 0.9659258262890683122, 1.000000000000000000, 0.9659258262890683122, 1.000000000000000000, 0.9659258262890683122, 1.000000000000000000, 0.9659258262890683122, 1.000000000000000000, 0.9659258262890683122, 1.000000000000000000, 0.9659258262890683122, 1.000000000000000000, 0.9659258262890683122, 1.000000000000000000, 0.9659258262890683122, 1.000000000000000000, 0.9659258262890683122, 1.000000000000000000, 0.9659258262890683122, 1.000000000000000000, 0.9659258262890683122, 1.000000000000000000, 0.9659258262890683122, 1.000000000000000000, 0.9659258262890683122, 1.000000000000000000, 0.9659258262890683122, 1.000000000000000000, 0.9659258262890683122, 1.000000000000000000, 0.9659258262890683122, 1.000000000000000000, 0.9659258262890683122, 1.000000000000000000, 0.9659258262890683122, 1.000000000000000000, 0.9659258262890683122, 1.000000000000000000, 0.9659258262890683122, 1.000000000000000000, 0.9659258262890683122, 1.000000000000000000, 0.9659258262890683122, 1.000000000000000000, 0.9659258262890683122, 1.000000000000000000, 0.9659258262890683122, 1.000000000000000000, 0.9659258262890683122, 1.000000000000000000, 0.9659258262890683122, 1.000000000000000000, 0.9659258262890683122, 1.000000000000000000, 0.9659258262890683122, 1.000000000000000000, 0.9659258262890683122, 1.000000000000000000, 0.9659258262890683122, 1.000000000000000000, 0.9659258262890683122, 1.000000000000000000, 0.9659258262890683122, 1.000000000000000000, 0.9659258262890683122, 1.000000000000000000, 0.9659258262890683122, 1.000000000000000000, 0.9659258262890683122, 1.000000000000000000, 0.9659258262890683122, 1.000000000000000000, 0.9659258262890683122, 1.000000000000000000, 0.9659258262890683122, 1.000000000000000000, 0.9659258262890683122, 1.000000000000000000, 0.9659258262890683122, 1.000000000000000000, 0.9659258262890683122, 1.000000000000000000, 0.9659258262890683122, 1.000000000000000000, 0.9659258262890683122, 1.000000000000000000, 0.9659258262890683122, 1.000000000000000000, 0.9659258262890683122, 1.000000000000000000, 0.9659258262890683122, 1.000000000000000000, 0.9659258262890683122, 1.000000000000000000, 0.9659258262890683122, 1.000000000000000000, 0.9659258262890683122, 1.000000000000000000, 0.9659258262890683122, 1.000000000000000000, 0.9659258262890683122, 1.000000000000000000, 0.9659258262890683122, 1.000000000000000000, 0.9659258262890683122, 1.000000000000000000, 0.9659258262890683122, 1.000000000000000000, 0.9659258262890683122, 1.000000000000000000, 0.9659258262890683122, 1.000000000000000000, 0.9659258262890683122, 1.000000000000000000, 0.9659258262890683122, 1.000000000000000000, 0.9659258262890683122, 1.000000000000000000, 0.9659258262890683122, 1.000000000000000000, 0.9659258262890683122, 1.000000000000000000, 0.9659258262890683122, 1.000000000000000000, 0.9659258262890683122, 1.000000000000000000, 0.9659258262890683122, 1.000000000000000000, 0.9659258262890683122, 1.000000000000000000, 0.9659258262890683122, 1.000000000000000000, 0.9659258262890683122, 1.000000000000000000, 0.9659258262890683122, 1.000000000000000000, 0.9659258262890683122, 1.000000000000000000, 0.9659258262890683122, 1.000000000000000000, 0.9659258262890683122, 1.000000000000000000, 0.9659258262890683122, 1.000000000000000000, 0.9659258262890683122, 1.000000000000000000, 0.9659258262890683122, 1.000000000000000000, 0.9659258262890683122, 1.000000000000000000, 0.9659258262890683122, 1.000000000000000000, 0.9659258262890683122, 1.000000000000000000, 0.9659258262890683122, 1.000000000000000000, 0.9659258262890683122, 1.000000000000000000, 0.9659258262890683122, 1.000000000000000000, 0.9659258262890683122, 1.000000000000000000, 0.9659258262890683122, 1.000000000000000000, 0.9659258262890683122, 1.000000000000000000, 0.9659258262890683122, 1.000000000000000000, 0.9659258262890683122, 1.000000000000000000, 0.9659258262890683122, 1.000000000000000000, 0.9659258262890683122, 1.000000000000000000, 0.9659258262890683122, 1.000000000000000000, 0.9659258262890683122, 1.000000000000000000, 0.9659258262890683122, 1.000000000000000000, 0.9659258262890683122, 1.000000000000000000, 0.9659258262890683122, 1.000000000000000000, 0.9659258262890683122, 1.000000000000000000, 0.9659258262890683122, 1.000000000000000000, 0.9659258262890683122, 1.000000000000000000, 0.9659258262890683122, 1.000000000000000000, 0.9659258262890683122, 1.000000000000000000, 0.9659258262890683122, 1.000000000000000000, 0.9659258262890683122, 1.000000000000000000, 0.9659258262890683122, 1.000000000000000000, 0.9659258262890683122, 1.000000000000000000, 0.9659258262890683122, 1.000000000000000000, 0.9659258262890683122, 1.000000000000000000, 0.9659258262890683122, 1.000000000000000000, 0.9659258262890683122, 1.000000000000000000, 0.9659258262890683122, 1.000000000000000000, 0.9659258262890683122, 1.000000000000000000, 0.9659258262890683122, 1.000000000000000000, 0.9659258262890683122, 1.000000000000000000, 0.9659258262890683122, 1.000000000000000000, 0.9659258262890683122, 1.000000000000000000, 0.9659258262890683122, 1.000000000000000000, 0.9659258262890683122, 1.000000000000000000, 0.9659258262890683122, 1.000000000000000000, 0.9659258262890683122, 1.000000000000000000, 0.9659258262890683122, 1.000000000000000000, 0.9659258262890683122, 1.000000000000000000, 0.9659258262890683122, 1.000000000000000000, 0.9659258262890683122, 1.000000000000000000, 0.9659258262890683122, 1.000000000000000000, 0.9659258262890683122, 1.000000000000000000, 0.9659258262890683122, 1.000000000000000000, 0.9659258262890683122, 1.000000000000000000, 0.9659258262890683122, 1.000000000000000000, 0.9659258262890683122, 1.000000000000000000, 0.9659258262890683122, 1.000000000000000000, 0.9659258262890683122, 1.000000000000000000, 0.9659258262890683122, 1.000000000000000000, 0.9659258262890683122, 1.000000000000000000, 0.9659258262890683122, 1.000000000000000000, 0.9659258262890683122, 1.000000000000000000, 0.9659258262890683122, 1.000000000000000000, 0.9659258262890683122, 1.000000000000000000, 0.9659258262890683122, 1.000000000000000000, 0.9659258262890683122, 1.000000000000000000, 0.9659258262890683122, 1.000000000000000000, 0.9659258262890683122, 1.000000000000000000, 0.9659258262890683122, 1.000000000000000000, 0.9659258262890683122, 1.000000000000000000, 0.9659258262890683122, 1.000000000000000000, 0.9659258262890683122, 1.000000000000000000, 0.9659258262890683122, 1.000000000000000000, 0.9659258262890683122, 1.000000000000000000, 0.9659258262890683122, 1.000000000000000000, 0.9659258262890683122, 1.000000000000000000, 0.9659258262890683122, 1.000000000000000000, 0.9659258262890683122, 1.000000000000000000, 0.9659258262890683122, 1.000000000000000000, 0.9659258262890683122, 1.000000000000000000, 0.9659258262890683122, 1.000000000000000000, 0.9659258262890683122, 1.000000000000000000, 0.9659258262890683122, 1.000000000000000000, 0.9659258262890683122, 1.000000000000000000, 0.9659258262890683122, 1.000000000000000000, 0.9659258262890683122, 1.000000000000000000, 0.9659258262890683122, 1.000000000000000000, 0.9659258262890683122, 1.000000000000000000, 0.9659258262890683122, 1.000000000000000000, 0.9659258262890683122, 1.000000000000000000, 0.9659258262890683122, 1.000000000000000000, 0.9659258262890683122, 1.000000000000000000, 0.9659258262890683122, 1.000000000000000000, 0.9659258262890683122, 1.000000000000000000, 0.9659258262890683122, 1.000000000000000000, 0.9659258262890683122, 1.000000000000000000, 0.9659258262890683122, 1.000000000000000000, 0.9659258262890683122, 1.000000000000000000, 0.9659258262890683122, 1.000000000000000000, 0.9659258262890683122, 1.000000000000000000, 0.9659258262890683122, 1.000000000000000000, 0.9659258262890683122, 1.000000000000000000, 0.9659258262890683122, 1.000000000000000000, 0.9659258262890683122, 1.000000000000000000, 0.9659258262890683122, 1.000000000000000000, 0.9659258262890683122, 1.000000000000000000, 0.9659258262890683122, 1.000000000000000000, 0.9659258262890683122, 1.000000000000000000, 0.9659258262890683122, 1.000000000000000000, 0.9659258262890683122, 1.000000000000000000),
 ( 0.3333333333333333703, 0.3219752754296894559, 0.3333333333333333703, 0.3219752754296894559, 0.3333333333333333703, 0.3219752754296894559, 0.3333333333333333703, 0.3219752754296894559, 0.3333333333333333703, 0.3219752754296894559, 0.3333333333333333703, 0.3219752754296894559, 0.3333333333333333703, 0.3219752754296894559, 0.3333333333333333703, 0.3219752754296894559, 0.3333333333333333703, 0.3219752754296894559, 0.3333333333333333703, 0.3219752754296894559, 0.3333333333333333703, 0.3219752754296894559, 0.3333333333333333703, 0.3219752754296894559, 0.3333333333333333703, 0.3219752754296894559, 0.3333333333333333703, 0.3219752754296894559, 0.3333333333333333703, 0.3219752754296894559, 0.3333333333333333703, 0.3219752754296894559, 0.3333333333333333703, 0.3219752754296894559, 0.3333333333333333703, 0.3219752754296894559, 0.3333333333333333703, 0.3219752754296894559, 0.3333333333333333703, 0.3219752754296894559, 0.3333333333333333703, 0.3219752754296894559, 0.3333333333333333703, 0.3219752754296894559, 0.3333333333333333703, 0.3219752754296894559, 0.3333333333333333703, 0.3219752754296894559, 0.3333333333333333703, 0.3219752754296894559, 0.3333333333333333703, 0.3219752754296894559, 0.3333333333333333703, 0.3219752754296894559, 0.3333333333333333703, 0.3219752754296894559, 0.3333333333333333703, 0.3219752754296894559, 0.3333333333333333703, 0.3219752754296894559, 0.3333333333333333703, 0.3219752754296894559, 0.3333333333333333703, 0.3219752754296894559, 0.3333333333333333703, 0.3219752754296894559, 0.3333333333333333703, 0.3219752754296894559, 0.3333333333333333703, 0.3219752754296894559, 0.3333333333333333703, 0.3219752754296894559, 0.3333333333333333703, 0.3219752754296894559, 0.3333333333333333703, 0.3219752754296894559, 0.3333333333333333703, 0.3219752754296894559, 0.3333333333333333703, 0.3219752754296894559, 0.3333333333333333703, 0.3219752754296894559, 0.3333333333333333703, 0.3219752754296894559, 0.3333333333333333703, 0.3219752754296894559, 0.3333333333333333703, 0.3219752754296894559, 0.3333333333333333703, 0.3219752754296894559, 0.3333333333333333703, 0.3219752754296894559, 0.3333333333333333703, 0.3219752754296894559, 0.3333333333333333703, 0.3219752754296894559, 0.3333333333333333703, 0.3219752754296894559, 0.3333333333333333703, 0.3219752754296894559, 0.3333333333333333703, 0.3219752754296894559, 0.3333333333333333703, 0.3219752754296894559, 0.3333333333333333703, 0.3219752754296894559, 0.3333333333333333703, 0.3219752754296894559, 0.3333333333333333703, 0.3219752754296894559, 0.3333333333333333703, 0.3219752754296894559, 0.3333333333333333703, 0.3219752754296894559, 0.3333333333333333703, 0.3219752754296894559, 0.3333333333333333703, 0.3219752754296894559, 0.3333333333333333703, 0.3219752754296894559, 0.3333333333333333703, 0.3219752754296894559, 0.3333333333333333703, 0.3219752754296894559, 0.3333333333333333703, 0.3219752754296894559, 0.3333333333333333703, 0.3219752754296894559, 0.3333333333333333703, 0.3219752754296894559, 0.3333333333333333703, 0.3219752754296894559, 0.3333333333333333703, 0.3219752754296894559, 0.3333333333333333703, 0.3219752754296894559, 0.3333333333333333703, 0.3219752754296894559, 0.3333333333333333703, 0.3219752754296894559, 0.3333333333333333703, 0.3219752754296894559, 0.3333333333333333703, 0.3219752754296894559, 0.3333333333333333703, 0.3219752754296894559, 0.3333333333333333703, 0.3219752754296894559, 0.3333333333333333703, 0.3219752754296894559, 0.3333333333333333703, 0.3219752754296894559, 0.3333333333333333703, 0.3219752754296894559, 0.3333333333333333703, 0.3219752754296894559, 0.3333333333333333703, 0.3219752754296894559, 0.3333333333333333703, 0.3219752754296894559, 0.3333333333333333703, 0.3219752754296894559, 0.3333333333333333703, 0.3219752754296894559, 0.3333333333333333703, 0.3219752754296894559, 0.3333333333333333703, 0.3219752754296894559, 0.3333333333333333703, 0.3219752754296894559, 0.3333333333333333703, 0.3219752754296894559, 0.3333333333333333703, 0.3219752754296894559, 0.3333333333333333703, 0.3219752754296894559, 0.3333333333333333703, 0.3219752754296894559, 0.3333333333333333703, 0.3219752754296894559, 0.3333333333333333703, 0.3219752754296894559, 0.3333333333333333703, 0.3219752754296894559, 0.3333333333333333703, 0.3219752754296894559, 0.3333333333333333703, 0.3219752754296894559, 0.3333333333333333703, 0.3219752754296894559, 0.3333333333333333703, 0.3219752754296894559, 0.3333333333333333703, 0.3219752754296894559, 0.3333333333333333703, 0.3219752754296894559, 0.3333333333333333703, 0.3219752754296894559, 0.3333333333333333703, 0.3219752754296894559, 0.3333333333333333703, 0.3219752754296894559, 0.3333333333333333703, 0.3219752754296894559, 0.3333333333333333703, 0.3219752754296894559, 0.3333333333333333703, 0.3219752754296894559, 0.3333333333333333703, 0.3219752754296894559, 0.3333333333333333703, 0.3219752754296894559, 0.3333333333333333703, 0.3219752754296894559, 0.3333333333333333703, 0.3219752754296894559, 0.3333333333333333703, 0.3219752754296894559, 0.3333333333333333703, 0.3219752754296894559, 0.3333333333333333703, 0.3219752754296894559, 0.3333333333333333703, 0.3219752754296894559, 0.3333333333333333703, 0.3219752754296894559, 0.3333333333333333703, 0.3219752754296894559, 0.3333333333333333703, 0.3219752754296894559, 0.3333333333333333703, 0.3219752754296894559, 0.3333333333333333703, 0.3219752754296894559, 0.3333333333333333703, 0.3219752754296894559, 0.3333333333333333703, 0.3219752754296894559, 0.3333333333333333703, 0.3219752754296894559, 0.3333333333333333703, 0.3219752754296894559, 0.3333333333333333703, 0.3219752754296894559, 0.3333333333333333703, 0.3219752754296894559, 0.3333333333333333703, 0.3219752754296894559, 0.3333333333333333703, 0.3219752754296894559, 0.3333333333333333703, 0.3219752754296894559, 0.3333333333333333703, 0.3219752754296894559, 0.3333333333333333703, 0.3219752754296894559, 0.3333333333333333703, 0.3219752754296894559, 0.3333333333333333703, 0.3219752754296894559, 0.3333333333333333703, 0.3219752754296894559, 0.3333333333333333703, 0.3219752754296894559, 0.3333333333333333703, 0.3219752754296894559, 0.3333333333333333703, 0.3219752754296894559, 0.3333333333333333703, 0.3219752754296894559, 0.3333333333333333703, 0.3219752754296894559, 0.3333333333333333703, 0.3219752754296894559, 0.3333333333333333703, 0.3219752754296894559, 0.3333333333333333703, 0.3219752754296894559, 0.3333333333333333703, 0.3219752754296894559, 0.3333333333333333703, 0.3219752754296894559, 0.3333333333333333703, 0.3219752754296894559, 0.3333333333333333703, 0.3219752754296894559, 0.3333333333333333703, 0.3219752754296894559, 0.3333333333333333703, 0.3219752754296894559, 0.3333333333333333703, 0.3219752754296894559, 0.3333333333333333703, 0.3219752754296894559, 0.3333333333333333703, 0.3219752754296894559, 0.3333333333333333703, 0.3219752754296894559, 0.3333333333333333703, 0.3219752754296894559, 0.3333333333333333703, 0.3219752754296894559, 0.3333333333333333703, 0.3219752754296894559, 0.3333333333333333703, 0.3219752754296894559, 0.3333333333333333703, 0.3219752754296894559, 0.3333333333333333703, 0.3219752754296894559, 0.3333333333333333703, 0.3219752754296894559, 0.3333333333333333703, 0.3219752754296894559, 0.3333333333333333703, 0.3219752754296894559, 0.3333333333333333703, 0.3219752754296894559, 0.3333333333333333703, 0.3219752754296894559, 0.3333333333333333703, 0.3219752754296894559, 0.3333333333333333703, 0.3219752754296894559, 0.3333333333333333703, 0.3219752754296894559, 0.3333333333333333703, 0.3219752754296894559, 0.3333333333333333703, 0.3219752754296894559, 0.3333333333333333703, 0.3219752754296894559, 0.3333333333333333703, 0.3219752754296894559, 0.3333333333333333703, 0.3219752754296894559, 0.3333333333333333703, 0.3219752754296894559, 0.3333333333333333703, 0.3219752754296894559, 0.3333333333333333703, 0.3219752754296894559, 0.3333333333333333703, 0.3219752754296894559, 0.3333333333333333703, 0.3219752754296894559, 0.3333333333333333703, 0.3219752754296894559, 0.3333333333333333703, 0.3219752754296894559, 0.3333333333333333703, 0.3219752754296894559, 0.3333333333333333703, 0.3219752754296894559, 0.3333333333333333703, 0.3219752754296894559, 0.3333333333333333703, 0.3219752754296894559, 0.3333333333333333703, 0.3219752754296894559, 0.3333333333333333703, 0.3219752754296894559, 0.3333333333333333703, 0.3219752754296894559, 0.3333333333333333703, 0.3219752754296894559, 0.3333333333333333703, 0.3219752754296894559, 0.3333333333333333703, 0.3219752754296894559, 0.3333333333333333703, 0.3219752754296894559, 0.3333333333333333703, 0.3219752754296894559, 0.3333333333333333703, 0.3219752754296894559, 0.3333333333333333703, 0.3219752754296894559, 0.3333333333333333703, 0.3219752754296894559, 0.3333333333333333703, 0.3219752754296894559, 0.3333333333333333703, 0.3219752754296894559, 0.3333333333333333703, 0.3219752754296894559, 0.3333333333333333703, 0.3219752754296894559, 0.3333333333333333703, 0.3219752754296894559, 0.3333333333333333703, 0.3219752754296894559, 0.3333333333333333703, 0.3219752754296894559, 0.3333333333333333703, 0.3219752754296894559, 0.3333333333333333703, 0.3219752754296894559, 0.3333333333333333703, 0.3219752754296894559, 0.3333333333333333703, 0.3219752754296894559, 0.3333333333333333703, 0.3219752754296894559, 0.3333333333333333703, 0.3219752754296894559, 0.3333333333333333703, 0.3219752754296894559, 0.3333333333333333703, 0.3219752754296894559, 0.3333333333333333703, 0.3219752754296894559, 0.3333333333333333703, 0.3219752754296894559, 0.3333333333333333703, 0.3219752754296894559, 0.3333333333333333703, 0.3219752754296894559, 0.3333333333333333703, 0.3219752754296894559, 0.3333333333333333703, 0.3219752754296894559, 0.3333333333333333703, 0.3219752754296894559, 0.3333333333333333703, 0.3219752754296894559, 0.3333333333333333703, 0.3219752754296894559, 0.3333333333333333703, 0.3219752754296894559, 0.3333333333333333703, 0.3219752754296894559, 0.3333333333333333703, 0.3219752754296894559, 0.3333333333333333703, 0.3219752754296894559, 0.3333333333333333703, 0.3219752754296894559, 0.3333333333333333703, 0.3219752754296894559, 0.3333333333333333703, 0.3219752754296894559, 0.3333333333333333703, 0.3219752754296894559, 0.3333333333333333703, 0.3219752754296894559, 0.3333333333333333703, 0.3219752754296894559, 0.3333333333333333703, 0.3219752754296894559, 0.3333333333333333703, 0.3219752754296894559, 0.3333333333333333703, 0.3219752754296894559, 0.3333333333333333703, 0.3219752754296894559, 0.3333333333333333703),
 ( 0.3333333333333333703, 0.3219752754296894559, 0.3333333333333333703, 0.3219752754296894559, 0.3333333333333333703, 0.3219752754296894559, 0.3333333333333333703, 0.3219752754296894559, 0.3333333333333333703, 0.3219752754296894559, 0.3333333333333333703, 0.3219752754296894559, 0.3333333333333333703, 0.3219752754296894559, 0.3333333333333333703, 0.3219752754296894559, 0.3333333333333333703, 0.3219752754296894559, 0.3333333333333333703, 0.3219752754296894559, 0.3333333333333333703, 0.3219752754296894559, 0.3333333333333333703, 0.3219752754296894559, 0.3333333333333333703, 0.3219752754296894559, 0.3333333333333333703, 0.3219752754296894559, 0.3333333333333333703, 0.3219752754296894559, 0.3333333333333333703, 0.3219752754296894559, 0.3333333333333333703, 0.3219752754296894559, 0.3333333333333333703, 0.3219752754296894559, 0.3333333333333333703, 0.3219752754296894559, 0.3333333333333333703, 0.3219752754296894559, 0.3333333333333333703, 0.3219752754296894559, 0.3333333333333333703, 0.3219752754296894559, 0.3333333333333333703, 0.3219752754296894559, 0.3333333333333333703, 0.3219752754296894559, 0.3333333333333333703, 0.3219752754296894559, 0.3333333333333333703, 0.3219752754296894559, 0.3333333333333333703, 0.3219752754296894559, 0.3333333333333333703, 0.3219752754296894559, 0.3333333333333333703, 0.3219752754296894559, 0.3333333333333333703, 0.3219752754296894559, 0.3333333333333333703, 0.3219752754296894559, 0.3333333333333333703, 0.3219752754296894559, 0.3333333333333333703, 0.3219752754296894559, 0.3333333333333333703, 0.3219752754296894559, 0.3333333333333333703, 0.3219752754296894559, 0.3333333333333333703, 0.3219752754296894559, 0.3333333333333333703, 0.3219752754296894559, 0.3333333333333333703, 0.3219752754296894559, 0.3333333333333333703, 0.3219752754296894559, 0.3333333333333333703, 0.3219752754296894559, 0.3333333333333333703, 0.3219752754296894559, 0.3333333333333333703, 0.3219752754296894559, 0.3333333333333333703, 0.3219752754296894559, 0.3333333333333333703, 0.3219752754296894559, 0.3333333333333333703, 0.3219752754296894559, 0.3333333333333333703, 0.3219752754296894559, 0.3333333333333333703, 0.3219752754296894559, 0.3333333333333333703, 0.3219752754296894559, 0.3333333333333333703, 0.3219752754296894559, 0.3333333333333333703, 0.3219752754296894559, 0.3333333333333333703, 0.3219752754296894559, 0.3333333333333333703, 0.3219752754296894559, 0.3333333333333333703, 0.3219752754296894559, 0.3333333333333333703, 0.3219752754296894559, 0.3333333333333333703, 0.3219752754296894559, 0.3333333333333333703, 0.3219752754296894559, 0.3333333333333333703, 0.3219752754296894559, 0.3333333333333333703, 0.3219752754296894559, 0.3333333333333333703, 0.3219752754296894559, 0.3333333333333333703, 0.3219752754296894559, 0.3333333333333333703, 0.3219752754296894559, 0.3333333333333333703, 0.3219752754296894559, 0.3333333333333333703, 0.3219752754296894559, 0.3333333333333333703, 0.3219752754296894559, 0.3333333333333333703, 0.3219752754296894559, 0.3333333333333333703, 0.3219752754296894559, 0.3333333333333333703, 0.3219752754296894559, 0.3333333333333333703, 0.3219752754296894559, 0.3333333333333333703, 0.3219752754296894559, 0.3333333333333333703, 0.3219752754296894559, 0.3333333333333333703, 0.3219752754296894559, 0.3333333333333333703, 0.3219752754296894559, 0.3333333333333333703, 0.3219752754296894559, 0.3333333333333333703, 0.3219752754296894559, 0.3333333333333333703, 0.3219752754296894559, 0.3333333333333333703, 0.3219752754296894559, 0.3333333333333333703, 0.3219752754296894559, 0.3333333333333333703, 0.3219752754296894559, 0.3333333333333333703, 0.3219752754296894559, 0.3333333333333333703, 0.3219752754296894559, 0.3333333333333333703, 0.3219752754296894559, 0.3333333333333333703, 0.3219752754296894559, 0.3333333333333333703, 0.3219752754296894559, 0.3333333333333333703, 0.3219752754296894559, 0.3333333333333333703, 0.3219752754296894559, 0.3333333333333333703, 0.3219752754296894559, 0.3333333333333333703, 0.3219752754296894559, 0.3333333333333333703, 0.3219752754296894559, 0.3333333333333333703, 0.3219752754296894559, 0.3333333333333333703, 0.3219752754296894559, 0.3333333333333333703, 0.3219752754296894559, 0.3333333333333333703, 0.3219752754296894559, 0.3333333333333333703, 0.3219752754296894559, 0.3333333333333333703, 0.3219752754296894559, 0.3333333333333333703, 0.3219752754296894559, 0.3333333333333333703, 0.3219752754296894559, 0.3333333333333333703, 0.3219752754296894559, 0.3333333333333333703, 0.3219752754296894559, 0.3333333333333333703, 0.3219752754296894559, 0.3333333333333333703, 0.3219752754296894559, 0.3333333333333333703, 0.3219752754296894559, 0.3333333333333333703, 0.3219752754296894559, 0.3333333333333333703, 0.3219752754296894559, 0.3333333333333333703, 0.3219752754296894559, 0.3333333333333333703, 0.3219752754296894559, 0.3333333333333333703, 0.3219752754296894559, 0.3333333333333333703, 0.3219752754296894559, 0.3333333333333333703, 0.3219752754296894559, 0.3333333333333333703, 0.3219752754296894559, 0.3333333333333333703, 0.3219752754296894559, 0.3333333333333333703, 0.3219752754296894559, 0.3333333333333333703, 0.3219752754296894559, 0.3333333333333333703, 0.3219752754296894559, 0.3333333333333333703, 0.3219752754296894559, 0.3333333333333333703, 0.3219752754296894559, 0.3333333333333333703, 0.3219752754296894559, 0.3333333333333333703, 0.3219752754296894559, 0.3333333333333333703, 0.3219752754296894559, 0.3333333333333333703, 0.3219752754296894559, 0.3333333333333333703, 0.3219752754296894559, 0.3333333333333333703, 0.3219752754296894559, 0.3333333333333333703, 0.3219752754296894559, 0.3333333333333333703, 0.3219752754296894559, 0.3333333333333333703, 0.3219752754296894559, 0.3333333333333333703, 0.3219752754296894559, 0.3333333333333333703, 0.3219752754296894559, 0.3333333333333333703, 0.3219752754296894559, 0.3333333333333333703, 0.3219752754296894559, 0.3333333333333333703, 0.3219752754296894559, 0.3333333333333333703, 0.3219752754296894559, 0.3333333333333333703, 0.3219752754296894559, 0.3333333333333333703, 0.3219752754296894559, 0.3333333333333333703, 0.3219752754296894559, 0.3333333333333333703, 0.3219752754296894559, 0.3333333333333333703, 0.3219752754296894559, 0.3333333333333333703, 0.3219752754296894559, 0.3333333333333333703, 0.3219752754296894559, 0.3333333333333333703, 0.3219752754296894559, 0.3333333333333333703, 0.3219752754296894559, 0.3333333333333333703, 0.3219752754296894559, 0.3333333333333333703, 0.3219752754296894559, 0.3333333333333333703, 0.3219752754296894559, 0.3333333333333333703, 0.3219752754296894559, 0.3333333333333333703, 0.3219752754296894559, 0.3333333333333333703, 0.3219752754296894559, 0.3333333333333333703, 0.3219752754296894559, 0.3333333333333333703, 0.3219752754296894559, 0.3333333333333333703, 0.3219752754296894559, 0.3333333333333333703, 0.3219752754296894559, 0.3333333333333333703, 0.3219752754296894559, 0.3333333333333333703, 0.3219752754296894559, 0.3333333333333333703, 0.3219752754296894559, 0.3333333333333333703, 0.3219752754296894559, 0.3333333333333333703, 0.3219752754296894559, 0.3333333333333333703, 0.3219752754296894559, 0.3333333333333333703, 0.3219752754296894559, 0.3333333333333333703, 0.3219752754296894559, 0.3333333333333333703, 0.3219752754296894559, 0.3333333333333333703, 0.3219752754296894559, 0.3333333333333333703, 0.3219752754296894559, 0.3333333333333333703, 0.3219752754296894559, 0.3333333333333333703, 0.3219752754296894559, 0.3333333333333333703, 0.3219752754296894559, 0.3333333333333333703, 0.3219752754296894559, 0.3333333333333333703, 0.3219752754296894559, 0.3333333333333333703, 0.3219752754296894559, 0.3333333333333333703, 0.3219752754296894559, 0.3333333333333333703, 0.3219752754296894559, 0.3333333333333333703, 0.3219752754296894559, 0.3333333333333333703, 0.3219752754296894559, 0.3333333333333333703, 0.3219752754296894559, 0.3333333333333333703, 0.3219752754296894559, 0.3333333333333333703, 0.3219752754296894559, 0.3333333333333333703, 0.3219752754296894559, 0.3333333333333333703, 0.3219752754296894559, 0.3333333333333333703, 0.3219752754296894559, 0.3333333333333333703, 0.3219752754296894559, 0.3333333333333333703, 0.3219752754296894559, 0.3333333333333333703, 0.3219752754296894559, 0.3333333333333333703, 0.3219752754296894559, 0.3333333333333333703, 0.3219752754296894559, 0.3333333333333333703, 0.3219752754296894559, 0.3333333333333333703, 0.3219752754296894559, 0.3333333333333333703, 0.3219752754296894559, 0.3333333333333333703, 0.3219752754296894559, 0.3333333333333333703, 0.3219752754296894559, 0.3333333333333333703, 0.3219752754296894559, 0.3333333333333333703, 0.3219752754296894559, 0.3333333333333333703, 0.3219752754296894559, 0.3333333333333333703, 0.3219752754296894559, 0.3333333333333333703, 0.3219752754296894559, 0.3333333333333333703, 0.3219752754296894559, 0.3333333333333333703, 0.3219752754296894559, 0.3333333333333333703, 0.3219752754296894559, 0.3333333333333333703, 0.3219752754296894559, 0.3333333333333333703, 0.3219752754296894559, 0.3333333333333333703, 0.3219752754296894559, 0.3333333333333333703, 0.3219752754296894559, 0.3333333333333333703, 0.3219752754296894559, 0.3333333333333333703, 0.3219752754296894559, 0.3333333333333333703, 0.3219752754296894559, 0.3333333333333333703, 0.3219752754296894559, 0.3333333333333333703, 0.3219752754296894559, 0.3333333333333333703, 0.3219752754296894559, 0.3333333333333333703, 0.3219752754296894559, 0.3333333333333333703, 0.3219752754296894559, 0.3333333333333333703, 0.3219752754296894559, 0.3333333333333333703, 0.3219752754296894559, 0.3333333333333333703, 0.3219752754296894559, 0.3333333333333333703, 0.3219752754296894559, 0.3333333333333333703, 0.3219752754296894559, 0.3333333333333333703, 0.3219752754296894559, 0.3333333333333333703, 0.3219752754296894559, 0.3333333333333333703, 0.3219752754296894559, 0.3333333333333333703, 0.3219752754296894559, 0.3333333333333333703, 0.3219752754296894559, 0.3333333333333333703, 0.3219752754296894559, 0.3333333333333333703, 0.3219752754296894559, 0.3333333333333333703, 0.3219752754296894559, 0.3333333333333333703, 0.3219752754296894559, 0.3333333333333333703, 0.3219752754296894559, 0.3333333333333333703, 0.3219752754296894559, 0.3333333333333333703, 0.3219752754296894559, 0.3333333333333333703, 0.3219752754296894559, 0.3333333333333333703, 0.3219752754296894559, 0.3333333333333333703, 0.3219752754296894559, 0.3333333333333333703, 0.3219752754296894559, 0.3333333333333333703, 0.3219752754296894559, 0.3333333333333333703),
 ( 1.000000000000000000, 0.9659258262890683122, 1.000000000000000000, 0.9659258262890683122, 1.000000000000000000, 0.9659258262890683122, 1.000000000000000000, 0.9659258262890683122, 1.000000000000000000, 0.9659258262890683122, 1.000000000000000000, 0.9659258262890683122, 1.000000000000000000, 0.9659258262890683122, 1.000000000000000000, 0.9659258262890683122, 1.000000000000000000, 0.9659258262890683122, 1.000000000000000000, 0.9659258262890683122, 1.000000000000000000, 0.9659258262890683122, 1.000000000000000000, 0.9659258262890683122, 1.000000000000000000, 0.9659258262890683122, 1.000000000000000000, 0.9659258262890683122, 1.000000000000000000, 0.9659258262890683122, 1.000000000000000000, 0.9659258262890683122, 1.000000000000000000, 0.9659258262890683122, 1.000000000000000000, 0.9659258262890683122, 1.000000000000000000, 0.9659258262890683122, 1.000000000000000000, 0.9659258262890683122, 1.000000000000000000, 0.9659258262890683122, 1.000000000000000000, 0.9659258262890683122, 1.000000000000000000, 0.9659258262890683122, 1.000000000000000000, 0.9659258262890683122, 1.000000000000000000, 0.9659258262890683122, 1.000000000000000000, 0.9659258262890683122, 1.000000000000000000, 0.9659258262890683122, 1.000000000000000000, 0.9659258262890683122, 1.000000000000000000, 0.9659258262890683122, 1.000000000000000000, 0.9659258262890683122, 1.000000000000000000, 0.9659258262890683122, 1.000000000000000000, 0.9659258262890683122, 1.000000000000000000, 0.9659258262890683122, 1.000000000000000000, 0.9659258262890683122, 1.000000000000000000, 0.9659258262890683122, 1.000000000000000000, 0.9659258262890683122, 1.000000000000000000, 0.9659258262890683122, 1.000000000000000000, 0.9659258262890683122, 1.000000000000000000, 0.9659258262890683122, 1.000000000000000000, 0.9659258262890683122, 1.000000000000000000, 0.9659258262890683122, 1.000000000000000000, 0.9659258262890683122, 1.000000000000000000, 0.9659258262890683122, 1.000000000000000000, 0.9659258262890683122, 1.000000000000000000, 0.9659258262890683122, 1.000000000000000000, 0.9659258262890683122, 1.000000000000000000, 0.9659258262890683122, 1.000000000000000000, 0.9659258262890683122, 1.000000000000000000, 0.9659258262890683122, 1.000000000000000000, 0.9659258262890683122, 1.000000000000000000, 0.9659258262890683122, 1.000000000000000000, 0.9659258262890683122, 1.000000000000000000, 0.9659258262890683122, 1.000000000000000000, 0.9659258262890683122, 1.000000000000000000, 0.9659258262890683122, 1.000000000000000000, 0.9659258262890683122, 1.000000000000000000, 0.9659258262890683122, 1.000000000000000000, 0.9659258262890683122, 1.000000000000000000, 0.9659258262890683122, 1.000000000000000000, 0.9659258262890683122, 1.000000000000000000, 0.9659258262890683122, 1.000000000000000000, 0.9659258262890683122, 1.000000000000000000, 0.9659258262890683122, 1.000000000000000000, 0.9659258262890683122, 1.000000000000000000, 0.9659258262890683122, 1.000000000000000000, 0.9659258262890683122, 1.000000000000000000, 0.9659258262890683122, 1.000000000000000000, 0.9659258262890683122, 1.000000000000000000, 0.9659258262890683122, 1.000000000000000000, 0.9659258262890683122, 1.000000000000000000, 0.9659258262890683122, 1.000000000000000000, 0.9659258262890683122, 1.000000000000000000, 0.9659258262890683122, 1.000000000000000000, 0.9659258262890683122, 1.000000000000000000, 0.9659258262890683122, 1.000000000000000000, 0.9659258262890683122, 1.000000000000000000, 0.9659258262890683122, 1.000000000000000000, 0.9659258262890683122, 1.000000000000000000, 0.9659258262890683122, 1.000000000000000000, 0.9659258262890683122, 1.000000000000000000, 0.9659258262890683122, 1.000000000000000000, 0.9659258262890683122, 1.000000000000000000, 0.9659258262890683122, 1.000000000000000000, 0.9659258262890683122, 1.000000000000000000, 0.9659258262890683122, 1.000000000000000000, 0.9659258262890683122, 1.000000000000000000, 0.9659258262890683122, 1.000000000000000000, 0.9659258262890683122, 1.000000000000000000, 0.9659258262890683122, 1.000000000000000000, 0.9659258262890683122, 1.000000000000000000, 0.9659258262890683122, 1.000000000000000000, 0.9659258262890683122, 1.000000000000000000, 0.9659258262890683122, 1.000000000000000000, 0.9659258262890683122, 1.000000000000000000, 0.9659258262890683122, 1.000000000000000000, 0.9659258262890683122, 1.000000000000000000, 0.9659258262890683122, 1.000000000000000000, 0.9659258262890683122, 1.000000000000000000, 0.9659258262890683122, 1.000000000000000000, 0.9659258262890683122, 1.000000000000000000, 0.9659258262890683122, 1.000000000000000000, 0.9659258262890683122, 1.000000000000000000, 0.9659258262890683122, 1.000000000000000000, 0.9659258262890683122, 1.000000000000000000, 0.9659258262890683122, 1.000000000000000000, 0.9659258262890683122, 1.000000000000000000, 0.9659258262890683122, 1.000000000000000000, 0.9659258262890683122, 1.000000000000000000, 0.9659258262890683122, 1.000000000000000000, 0.9659258262890683122, 1.000000000000000000, 0.9659258262890683122, 1.000000000000000000, 0.9659258262890683122, 1.000000000000000000, 0.9659258262890683122, 1.000000000000000000, 0.9659258262890683122, 1.000000000000000000, 0.9659258262890683122, 1.000000000000000000, 0.9659258262890683122, 1.000000000000000000, 0.9659258262890683122, 1.000000000000000000, 0.9659258262890683122, 1.000000000000000000, 0.9659258262890683122, 1.000000000000000000, 0.9659258262890683122, 1.000000000000000000, 0.9659258262890683122, 1.000000000000000000, 0.9659258262890683122, 1.000000000000000000, 0.9659258262890683122, 1.000000000000000000, 0.9659258262890683122, 1.000000000000000000, 0.9659258262890683122, 1.000000000000000000, 0.9659258262890683122, 1.000000000000000000, 0.9659258262890683122, 1.000000000000000000, 0.9659258262890683122, 1.000000000000000000, 0.9659258262890683122, 1.000000000000000000, 0.9659258262890683122, 1.000000000000000000, 0.9659258262890683122, 1.000000000000000000, 0.9659258262890683122, 1.000000000000000000, 0.9659258262890683122, 1.000000000000000000, 0.9659258262890683122, 1.000000000000000000, 0.9659258262890683122, 1.000000000000000000, 0.9659258262890683122, 1.000000000000000000, 0.9659258262890683122, 1.000000000000000000, 0.9659258262890683122, 1.000000000000000000, 0.9659258262890683122, 1.000000000000000000, 0.9659258262890683122, 1.000000000000000000, 0.9659258262890683122, 1.000000000000000000, 0.9659258262890683122, 1.000000000000000000, 0.9659258262890683122, 1.000000000000000000, 0.9659258262890683122, 1.000000000000000000, 0.9659258262890683122, 1.000000000000000000, 0.9659258262890683122, 1.000000000000000000, 0.9659258262890683122, 1.000000000000000000, 0.9659258262890683122, 1.000000000000000000, 0.9659258262890683122, 1.000000000000000000, 0.9659258262890683122, 1.000000000000000000, 0.9659258262890683122, 1.000000000000000000, 0.9659258262890683122, 1.000000000000000000, 0.9659258262890683122, 1.000000000000000000, 0.9659258262890683122, 1.000000000000000000, 0.9659258262890683122, 1.000000000000000000, 0.9659258262890683122, 1.000000000000000000, 0.9659258262890683122, 1.000000000000000000, 0.9659258262890683122, 1.000000000000000000, 0.9659258262890683122, 1.000000000000000000, 0.9659258262890683122, 1.000000000000000000, 0.9659258262890683122, 1.000000000000000000, 0.9659258262890683122, 1.000000000000000000, 0.9659258262890683122, 1.000000000000000000, 0.9659258262890683122, 1.000000000000000000, 0.9659258262890683122, 1.000000000000000000, 0.9659258262890683122, 1.000000000000000000, 0.9659258262890683122, 1.000000000000000000, 0.9659258262890683122, 1.000000000000000000, 0.9659258262890683122, 1.000000000000000000, 0.9659258262890683122, 1.000000000000000000, 0.9659258262890683122, 1.000000000000000000, 0.9659258262890683122, 1.000000000000000000, 0.9659258262890683122, 1.000000000000000000, 0.9659258262890683122, 1.000000000000000000, 0.9659258262890683122, 1.000000000000000000, 0.9659258262890683122, 1.000000000000000000, 0.9659258262890683122, 1.000000000000000000, 0.9659258262890683122, 1.000000000000000000, 0.9659258262890683122, 1.000000000000000000, 0.9659258262890683122, 1.000000000000000000, 0.9659258262890683122, 1.000000000000000000, 0.9659258262890683122, 1.000000000000000000, 0.9659258262890683122, 1.000000000000000000, 0.9659258262890683122, 1.000000000000000000, 0.9659258262890683122, 1.000000000000000000, 0.9659258262890683122, 1.000000000000000000, 0.9659258262890683122, 1.000000000000000000, 0.9659258262890683122, 1.000000000000000000, 0.9659258262890683122, 1.000000000000000000, 0.9659258262890683122, 1.000000000000000000, 0.9659258262890683122, 1.000000000000000000, 0.9659258262890683122, 1.000000000000000000, 0.9659258262890683122, 1.000000000000000000, 0.9659258262890683122, 1.000000000000000000, 0.9659258262890683122, 1.000000000000000000, 0.9659258262890683122, 1.000000000000000000, 0.9659258262890683122, 1.000000000000000000, 0.9659258262890683122, 1.000000000000000000, 0.9659258262890683122, 1.000000000000000000, 0.9659258262890683122, 1.000000000000000000, 0.9659258262890683122, 1.000000000000000000, 0.9659258262890683122, 1.000000000000000000, 0.9659258262890683122, 1.000000000000000000, 0.9659258262890683122, 1.000000000000000000, 0.9659258262890683122, 1.000000000000000000, 0.9659258262890683122, 1.000000000000000000, 0.9659258262890683122, 1.000000000000000000, 0.9659258262890683122, 1.000000000000000000, 0.9659258262890683122, 1.000000000000000000, 0.9659258262890683122, 1.000000000000000000, 0.9659258262890683122, 1.000000000000000000, 0.9659258262890683122, 1.000000000000000000, 0.9659258262890683122, 1.000000000000000000, 0.9659258262890683122, 1.000000000000000000, 0.9659258262890683122, 1.000000000000000000, 0.9659258262890683122, 1.000000000000000000, 0.9659258262890683122, 1.000000000000000000, 0.9659258262890683122, 1.000000000000000000, 0.9659258262890683122, 1.000000000000000000, 0.9659258262890683122, 1.000000000000000000, 0.9659258262890683122, 1.000000000000000000, 0.9659258262890683122, 1.000000000000000000, 0.9659258262890683122, 1.000000000000000000, 0.9659258262890683122, 1.000000000000000000, 0.9659258262890683122, 1.000000000000000000, 0.9659258262890683122, 1.000000000000000000, 0.9659258262890683122, 1.000000000000000000, 0.9659258262890683122, 1.000000000000000000),
 ( 0.3333333333333333703, 0.3219752754296894559, 0.3333333333333333703, 0.3219752754296894559, 0.3333333333333333703, 0.3219752754296894559, 0.3333333333333333703, 0.3219752754296894559, 0.3333333333333333703, 0.3219752754296894559, 0.3333333333333333703, 0.3219752754296894559, 0.3333333333333333703, 0.3219752754296894559, 0.3333333333333333703, 0.3219752754296894559, 0.3333333333333333703, 0.3219752754296894559, 0.3333333333333333703, 0.3219752754296894559, 0.3333333333333333703, 0.3219752754296894559, 0.3333333333333333703, 0.3219752754296894559, 0.3333333333333333703, 0.3219752754296894559, 0.3333333333333333703, 0.3219752754296894559, 0.3333333333333333703, 0.3219752754296894559, 0.3333333333333333703, 0.3219752754296894559, 0.3333333333333333703, 0.3219752754296894559, 0.3333333333333333703, 0.3219752754296894559, 0.3333333333333333703, 0.3219752754296894559, 0.3333333333333333703, 0.3219752754296894559, 0.3333333333333333703, 0.3219752754296894559, 0.3333333333333333703, 0.3219752754296894559, 0.3333333333333333703, 0.3219752754296894559, 0.3333333333333333703, 0.3219752754296894559, 0.3333333333333333703, 0.3219752754296894559, 0.3333333333333333703, 0.3219752754296894559, 0.3333333333333333703, 0.3219752754296894559, 0.3333333333333333703, 0.3219752754296894559, 0.3333333333333333703, 0.3219752754296894559, 0.3333333333333333703, 0.3219752754296894559, 0.3333333333333333703, 0.3219752754296894559, 0.3333333333333333703, 0.3219752754296894559, 0.3333333333333333703, 0.3219752754296894559, 0.3333333333333333703, 0.3219752754296894559, 0.3333333333333333703, 0.3219752754296894559, 0.3333333333333333703, 0.3219752754296894559, 0.3333333333333333703, 0.3219752754296894559, 0.3333333333333333703, 0.3219752754296894559, 0.3333333333333333703, 0.3219752754296894559, 0.3333333333333333703, 0.3219752754296894559, 0.3333333333333333703, 0.3219752754296894559, 0.3333333333333333703, 0.3219752754296894559, 0.3333333333333333703, 0.3219752754296894559, 0.3333333333333333703, 0.3219752754296894559, 0.3333333333333333703, 0.3219752754296894559, 0.3333333333333333703, 0.3219752754296894559, 0.3333333333333333703, 0.3219752754296894559, 0.3333333333333333703, 0.3219752754296894559, 0.3333333333333333703, 0.3219752754296894559, 0.3333333333333333703, 0.3219752754296894559, 0.3333333333333333703, 0.3219752754296894559, 0.3333333333333333703, 0.3219752754296894559, 0.3333333333333333703, 0.3219752754296894559, 0.3333333333333333703, 0.3219752754296894559, 0.3333333333333333703, 0.3219752754296894559, 0.3333333333333333703, 0.3219752754296894559, 0.3333333333333333703, 0.3219752754296894559, 0.3333333333333333703, 0.3219752754296894559, 0.3333333333333333703, 0.3219752754296894559, 0.3333333333333333703, 0.3219752754296894559, 0.3333333333333333703, 0.3219752754296894559, 0.3333333333333333703, 0.3219752754296894559, 0.3333333333333333703, 0.3219752754296894559, 0.3333333333333333703, 0.3219752754296894559, 0.3333333333333333703, 0.3219752754296894559, 0.3333333333333333703, 0.3219752754296894559, 0.3333333333333333703, 0.3219752754296894559, 0.3333333333333333703, 0.3219752754296894559, 0.3333333333333333703, 0.3219752754296894559, 0.3333333333333333703, 0.3219752754296894559, 0.3333333333333333703, 0.3219752754296894559, 0.3333333333333333703, 0.3219752754296894559, 0.3333333333333333703, 0.3219752754296894559, 0.3333333333333333703, 0.3219752754296894559, 0.3333333333333333703, 0.3219752754296894559, 0.3333333333333333703, 0.3219752754296894559, 0.3333333333333333703, 0.3219752754296894559, 0.3333333333333333703, 0.3219752754296894559, 0.3333333333333333703, 0.3219752754296894559, 0.3333333333333333703, 0.3219752754296894559, 0.3333333333333333703, 0.3219752754296894559, 0.3333333333333333703, 0.3219752754296894559, 0.3333333333333333703, 0.3219752754296894559, 0.3333333333333333703, 0.3219752754296894559, 0.3333333333333333703, 0.3219752754296894559, 0.3333333333333333703, 0.3219752754296894559, 0.3333333333333333703, 0.3219752754296894559, 0.3333333333333333703, 0.3219752754296894559, 0.3333333333333333703, 0.3219752754296894559, 0.3333333333333333703, 0.3219752754296894559, 0.3333333333333333703, 0.3219752754296894559, 0.3333333333333333703, 0.3219752754296894559, 0.3333333333333333703, 0.3219752754296894559, 0.3333333333333333703, 0.3219752754296894559, 0.3333333333333333703, 0.3219752754296894559, 0.3333333333333333703, 0.3219752754296894559, 0.3333333333333333703, 0.3219752754296894559, 0.3333333333333333703, 0.3219752754296894559, 0.3333333333333333703, 0.3219752754296894559, 0.3333333333333333703, 0.3219752754296894559, 0.3333333333333333703, 0.3219752754296894559, 0.3333333333333333703, 0.3219752754296894559, 0.3333333333333333703, 0.3219752754296894559, 0.3333333333333333703, 0.3219752754296894559, 0.3333333333333333703, 0.3219752754296894559, 0.3333333333333333703, 0.3219752754296894559, 0.3333333333333333703, 0.3219752754296894559, 0.3333333333333333703, 0.3219752754296894559, 0.3333333333333333703, 0.3219752754296894559, 0.3333333333333333703, 0.3219752754296894559, 0.3333333333333333703, 0.3219752754296894559, 0.3333333333333333703, 0.3219752754296894559, 0.3333333333333333703, 0.3219752754296894559, 0.3333333333333333703, 0.3219752754296894559, 0.3333333333333333703, 0.3219752754296894559, 0.3333333333333333703, 0.3219752754296894559, 0.3333333333333333703, 0.3219752754296894559, 0.3333333333333333703, 0.3219752754296894559, 0.3333333333333333703, 0.3219752754296894559, 0.3333333333333333703, 0.3219752754296894559, 0.3333333333333333703, 0.3219752754296894559, 0.3333333333333333703, 0.3219752754296894559, 0.3333333333333333703, 0.3219752754296894559, 0.3333333333333333703, 0.3219752754296894559, 0.3333333333333333703, 0.3219752754296894559, 0.3333333333333333703, 0.3219752754296894559, 0.3333333333333333703, 0.3219752754296894559, 0.3333333333333333703, 0.3219752754296894559, 0.3333333333333333703, 0.3219752754296894559, 0.3333333333333333703, 0.3219752754296894559, 0.3333333333333333703, 0.3219752754296894559, 0.3333333333333333703, 0.3219752754296894559, 0.3333333333333333703, 0.3219752754296894559, 0.3333333333333333703, 0.3219752754296894559, 0.3333333333333333703, 0.3219752754296894559, 0.3333333333333333703, 0.3219752754296894559, 0.3333333333333333703, 0.3219752754296894559, 0.3333333333333333703, 0.3219752754296894559, 0.3333333333333333703, 0.3219752754296894559, 0.3333333333333333703, 0.3219752754296894559, 0.3333333333333333703, 0.3219752754296894559, 0.3333333333333333703, 0.3219752754296894559, 0.3333333333333333703, 0.3219752754296894559, 0.3333333333333333703, 0.3219752754296894559, 0.3333333333333333703, 0.3219752754296894559, 0.3333333333333333703, 0.3219752754296894559, 0.3333333333333333703, 0.3219752754296894559, 0.3333333333333333703, 0.3219752754296894559, 0.3333333333333333703, 0.3219752754296894559, 0.3333333333333333703, 0.3219752754296894559, 0.3333333333333333703, 0.3219752754296894559, 0.3333333333333333703, 0.3219752754296894559, 0.3333333333333333703, 0.3219752754296894559, 0.3333333333333333703, 0.3219752754296894559, 0.3333333333333333703, 0.3219752754296894559, 0.3333333333333333703, 0.3219752754296894559, 0.3333333333333333703, 0.3219752754296894559, 0.3333333333333333703, 0.3219752754296894559, 0.3333333333333333703, 0.3219752754296894559, 0.3333333333333333703, 0.3219752754296894559, 0.3333333333333333703, 0.3219752754296894559, 0.3333333333333333703, 0.3219752754296894559, 0.3333333333333333703, 0.3219752754296894559, 0.3333333333333333703, 0.3219752754296894559, 0.3333333333333333703, 0.3219752754296894559, 0.3333333333333333703, 0.3219752754296894559, 0.3333333333333333703, 0.3219752754296894559, 0.3333333333333333703, 0.3219752754296894559, 0.3333333333333333703, 0.3219752754296894559, 0.3333333333333333703, 0.3219752754296894559, 0.3333333333333333703, 0.3219752754296894559, 0.3333333333333333703, 0.3219752754296894559, 0.3333333333333333703, 0.3219752754296894559, 0.3333333333333333703, 0.3219752754296894559, 0.3333333333333333703, 0.3219752754296894559, 0.3333333333333333703, 0.3219752754296894559, 0.3333333333333333703, 0.3219752754296894559, 0.3333333333333333703, 0.3219752754296894559, 0.3333333333333333703, 0.3219752754296894559, 0.3333333333333333703, 0.3219752754296894559, 0.3333333333333333703, 0.3219752754296894559, 0.3333333333333333703, 0.3219752754296894559, 0.3333333333333333703, 0.3219752754296894559, 0.3333333333333333703, 0.3219752754296894559, 0.3333333333333333703, 0.3219752754296894559, 0.3333333333333333703, 0.3219752754296894559, 0.3333333333333333703, 0.3219752754296894559, 0.3333333333333333703, 0.3219752754296894559, 0.3333333333333333703, 0.3219752754296894559, 0.3333333333333333703, 0.3219752754296894559, 0.3333333333333333703, 0.3219752754296894559, 0.3333333333333333703, 0.3219752754296894559, 0.3333333333333333703, 0.3219752754296894559, 0.3333333333333333703, 0.3219752754296894559, 0.3333333333333333703, 0.3219752754296894559, 0.3333333333333333703, 0.3219752754296894559, 0.3333333333333333703, 0.3219752754296894559, 0.3333333333333333703, 0.3219752754296894559, 0.3333333333333333703, 0.3219752754296894559, 0.3333333333333333703, 0.3219752754296894559, 0.3333333333333333703, 0.3219752754296894559, 0.3333333333333333703, 0.3219752754296894559, 0.3333333333333333703, 0.3219752754296894559, 0.3333333333333333703, 0.3219752754296894559, 0.3333333333333333703, 0.3219752754296894559, 0.3333333333333333703, 0.3219752754296894559, 0.3333333333333333703, 0.3219752754296894559, 0.3333333333333333703, 0.3219752754296894559, 0.3333333333333333703, 0.3219752754296894559, 0.3333333333333333703, 0.3219752754296894559, 0.3333333333333333703, 0.3219752754296894559, 0.3333333333333333703, 0.3219752754296894559, 0.3333333333333333703, 0.3219752754296894559, 0.3333333333333333703, 0.3219752754296894559, 0.3333333333333333703, 0.3219752754296894559, 0.3333333333333333703, 0.3219752754296894559, 0.3333333333333333703, 0.3219752754296894559, 0.3333333333333333703, 0.3219752754296894559, 0.3333333333333333703, 0.3219752754296894559, 0.3333333333333333703, 0.3219752754296894559, 0.3333333333333333703, 0.3219752754296894559, 0.3333333333333333703, 0.3219752754296894559, 0.3333333333333333703, 0.3219752754296894559, 0.3333333333333333703, 0.3219752754296894559, 0.3333333333333333703, 0.3219752754296894559, 0.3333333333333333703, 0.3219752754296894559, 0.3333333333333333703, 0.3219752754296894559, 0.3333333333333333703, 0.3219752754296894559, 0.3333333333333333703),
 ( 0.3333333333333333703, 0.3219752754296894559, 0.3333333333333333703, 0.3219752754296894559, 0.3333333333333333703, 0.3219752754296894559, 0.3333333333333333703, 0.3219752754296894559, 0.3333333333333333703, 0.3219752754296894559, 0.3333333333333333703, 0.3219752754296894559, 0.3333333333333333703, 0.3219752754296894559, 0.3333333333333333703, 0.3219752754296894559, 0.3333333333333333703, 0.3219752754296894559, 0.3333333333333333703, 0.3219752754296894559, 0.3333333333333333703, 0.3219752754296894559, 0.3333333333333333703, 0.3219752754296894559, 0.3333333333333333703, 0.3219752754296894559, 0.3333333333333333703, 0.3219752754296894559, 0.3333333333333333703, 0.3219752754296894559, 0.3333333333333333703, 0.3219752754296894559, 0.3333333333333333703, 0.3219752754296894559, 0.3333333333333333703, 0.3219752754296894559, 0.3333333333333333703, 0.3219752754296894559, 0.3333333333333333703, 0.3219752754296894559, 0.3333333333333333703, 0.3219752754296894559, 0.3333333333333333703, 0.3219752754296894559, 0.3333333333333333703, 0.3219752754296894559, 0.3333333333333333703, 0.3219752754296894559, 0.3333333333333333703, 0.3219752754296894559, 0.3333333333333333703, 0.3219752754296894559, 0.3333333333333333703, 0.3219752754296894559, 0.3333333333333333703, 0.3219752754296894559, 0.3333333333333333703, 0.3219752754296894559, 0.3333333333333333703, 0.3219752754296894559, 0.3333333333333333703, 0.3219752754296894559, 0.3333333333333333703, 0.3219752754296894559, 0.3333333333333333703, 0.3219752754296894559, 0.3333333333333333703, 0.3219752754296894559, 0.3333333333333333703, 0.3219752754296894559, 0.3333333333333333703, 0.3219752754296894559, 0.3333333333333333703, 0.3219752754296894559, 0.3333333333333333703, 0.3219752754296894559, 0.3333333333333333703, 0.3219752754296894559, 0.3333333333333333703, 0.3219752754296894559, 0.3333333333333333703, 0.3219752754296894559, 0.3333333333333333703, 0.3219752754296894559, 0.3333333333333333703, 0.3219752754296894559, 0.3333333333333333703, 0.3219752754296894559, 0.3333333333333333703, 0.3219752754296894559, 0.3333333333333333703, 0.3219752754296894559, 0.3333333333333333703, 0.3219752754296894559, 0.3333333333333333703, 0.3219752754296894559, 0.3333333333333333703, 0.3219752754296894559, 0.3333333333333333703, 0.3219752754296894559, 0.3333333333333333703, 0.3219752754296894559, 0.3333333333333333703, 0.3219752754296894559, 0.3333333333333333703, 0.3219752754296894559, 0.3333333333333333703, 0.3219752754296894559, 0.3333333333333333703, 0.3219752754296894559, 0.3333333333333333703, 0.3219752754296894559, 0.3333333333333333703, 0.3219752754296894559, 0.3333333333333333703, 0.3219752754296894559, 0.3333333333333333703, 0.3219752754296894559, 0.3333333333333333703, 0.3219752754296894559, 0.3333333333333333703, 0.3219752754296894559, 0.3333333333333333703, 0.3219752754296894559, 0.3333333333333333703, 0.3219752754296894559, 0.3333333333333333703, 0.3219752754296894559, 0.3333333333333333703, 0.3219752754296894559, 0.3333333333333333703, 0.3219752754296894559, 0.3333333333333333703, 0.3219752754296894559, 0.3333333333333333703, 0.3219752754296894559, 0.3333333333333333703, 0.3219752754296894559, 0.3333333333333333703, 0.3219752754296894559, 0.3333333333333333703, 0.3219752754296894559, 0.3333333333333333703, 0.3219752754296894559, 0.3333333333333333703, 0.3219752754296894559, 0.3333333333333333703, 0.3219752754296894559, 0.3333333333333333703, 0.3219752754296894559, 0.3333333333333333703, 0.3219752754296894559, 0.3333333333333333703, 0.3219752754296894559, 0.3333333333333333703, 0.3219752754296894559, 0.3333333333333333703, 0.3219752754296894559, 0.3333333333333333703, 0.3219752754296894559, 0.3333333333333333703, 0.3219752754296894559, 0.3333333333333333703, 0.3219752754296894559, 0.3333333333333333703, 0.3219752754296894559, 0.3333333333333333703, 0.3219752754296894559, 0.3333333333333333703, 0.3219752754296894559, 0.3333333333333333703, 0.3219752754296894559, 0.3333333333333333703, 0.3219752754296894559, 0.3333333333333333703, 0.3219752754296894559, 0.3333333333333333703, 0.3219752754296894559, 0.3333333333333333703, 0.3219752754296894559, 0.3333333333333333703, 0.3219752754296894559, 0.3333333333333333703, 0.3219752754296894559, 0.3333333333333333703, 0.3219752754296894559, 0.3333333333333333703, 0.3219752754296894559, 0.3333333333333333703, 0.3219752754296894559, 0.3333333333333333703, 0.3219752754296894559, 0.3333333333333333703, 0.3219752754296894559, 0.3333333333333333703, 0.3219752754296894559, 0.3333333333333333703, 0.3219752754296894559, 0.3333333333333333703, 0.3219752754296894559, 0.3333333333333333703, 0.3219752754296894559, 0.3333333333333333703, 0.3219752754296894559, 0.3333333333333333703, 0.3219752754296894559, 0.3333333333333333703, 0.3219752754296894559, 0.3333333333333333703, 0.3219752754296894559, 0.3333333333333333703, 0.3219752754296894559, 0.3333333333333333703, 0.3219752754296894559, 0.3333333333333333703, 0.3219752754296894559, 0.3333333333333333703, 0.3219752754296894559, 0.3333333333333333703, 0.3219752754296894559, 0.3333333333333333703, 0.3219752754296894559, 0.3333333333333333703, 0.3219752754296894559, 0.3333333333333333703, 0.3219752754296894559, 0.3333333333333333703, 0.3219752754296894559, 0.3333333333333333703, 0.3219752754296894559, 0.3333333333333333703, 0.3219752754296894559, 0.3333333333333333703, 0.3219752754296894559, 0.3333333333333333703, 0.3219752754296894559, 0.3333333333333333703, 0.3219752754296894559, 0.3333333333333333703, 0.3219752754296894559, 0.3333333333333333703, 0.3219752754296894559, 0.3333333333333333703, 0.3219752754296894559, 0.3333333333333333703, 0.3219752754296894559, 0.3333333333333333703, 0.3219752754296894559, 0.3333333333333333703, 0.3219752754296894559, 0.3333333333333333703, 0.3219752754296894559, 0.3333333333333333703, 0.3219752754296894559, 0.3333333333333333703, 0.3219752754296894559, 0.3333333333333333703, 0.3219752754296894559, 0.3333333333333333703, 0.3219752754296894559, 0.3333333333333333703, 0.3219752754296894559, 0.3333333333333333703, 0.3219752754296894559, 0.3333333333333333703, 0.3219752754296894559, 0.3333333333333333703, 0.3219752754296894559, 0.3333333333333333703, 0.3219752754296894559, 0.3333333333333333703, 0.3219752754296894559, 0.3333333333333333703, 0.3219752754296894559, 0.3333333333333333703, 0.3219752754296894559, 0.3333333333333333703, 0.3219752754296894559, 0.3333333333333333703, 0.3219752754296894559, 0.3333333333333333703, 0.3219752754296894559, 0.3333333333333333703, 0.3219752754296894559, 0.3333333333333333703, 0.3219752754296894559, 0.3333333333333333703, 0.3219752754296894559, 0.3333333333333333703, 0.3219752754296894559, 0.3333333333333333703, 0.3219752754296894559, 0.3333333333333333703, 0.3219752754296894559, 0.3333333333333333703, 0.3219752754296894559, 0.3333333333333333703, 0.3219752754296894559, 0.3333333333333333703, 0.3219752754296894559, 0.3333333333333333703, 0.3219752754296894559, 0.3333333333333333703, 0.3219752754296894559, 0.3333333333333333703, 0.3219752754296894559, 0.3333333333333333703, 0.3219752754296894559, 0.3333333333333333703, 0.3219752754296894559, 0.3333333333333333703, 0.3219752754296894559, 0.3333333333333333703, 0.3219752754296894559, 0.3333333333333333703, 0.3219752754296894559, 0.3333333333333333703, 0.3219752754296894559, 0.3333333333333333703, 0.3219752754296894559, 0.3333333333333333703, 0.3219752754296894559, 0.3333333333333333703, 0.3219752754296894559, 0.3333333333333333703, 0.3219752754296894559, 0.3333333333333333703, 0.3219752754296894559, 0.3333333333333333703, 0.3219752754296894559, 0.3333333333333333703, 0.3219752754296894559, 0.3333333333333333703, 0.3219752754296894559, 0.3333333333333333703, 0.3219752754296894559, 0.3333333333333333703, 0.3219752754296894559, 0.3333333333333333703, 0.3219752754296894559, 0.3333333333333333703, 0.3219752754296894559, 0.3333333333333333703, 0.3219752754296894559, 0.3333333333333333703, 0.3219752754296894559, 0.3333333333333333703, 0.3219752754296894559, 0.3333333333333333703, 0.3219752754296894559, 0.3333333333333333703, 0.3219752754296894559, 0.3333333333333333703, 0.3219752754296894559, 0.3333333333333333703, 0.3219752754296894559, 0.3333333333333333703, 0.3219752754296894559, 0.3333333333333333703, 0.3219752754296894559, 0.3333333333333333703, 0.3219752754296894559, 0.3333333333333333703, 0.3219752754296894559, 0.3333333333333333703, 0.3219752754296894559, 0.3333333333333333703, 0.3219752754296894559, 0.3333333333333333703, 0.3219752754296894559, 0.3333333333333333703, 0.3219752754296894559, 0.3333333333333333703, 0.3219752754296894559, 0.3333333333333333703, 0.3219752754296894559, 0.3333333333333333703, 0.3219752754296894559, 0.3333333333333333703, 0.3219752754296894559, 0.3333333333333333703, 0.3219752754296894559, 0.3333333333333333703, 0.3219752754296894559, 0.3333333333333333703, 0.3219752754296894559, 0.3333333333333333703, 0.3219752754296894559, 0.3333333333333333703, 0.3219752754296894559, 0.3333333333333333703, 0.3219752754296894559, 0.3333333333333333703, 0.3219752754296894559, 0.3333333333333333703, 0.3219752754296894559, 0.3333333333333333703, 0.3219752754296894559, 0.3333333333333333703, 0.3219752754296894559, 0.3333333333333333703, 0.3219752754296894559, 0.3333333333333333703, 0.3219752754296894559, 0.3333333333333333703, 0.3219752754296894559, 0.3333333333333333703, 0.3219752754296894559, 0.3333333333333333703, 0.3219752754296894559, 0.3333333333333333703, 0.3219752754296894559, 0.3333333333333333703, 0.3219752754296894559, 0.3333333333333333703, 0.3219752754296894559, 0.3333333333333333703, 0.3219752754296894559, 0.3333333333333333703, 0.3219752754296894559, 0.3333333333333333703, 0.3219752754296894559, 0.3333333333333333703, 0.3219752754296894559, 0.3333333333333333703, 0.3219752754296894559, 0.3333333333333333703, 0.3219752754296894559, 0.3333333333333333703, 0.3219752754296894559, 0.3333333333333333703, 0.3219752754296894559, 0.3333333333333333703, 0.3219752754296894559, 0.3333333333333333703, 0.3219752754296894559, 0.3333333333333333703, 0.3219752754296894559, 0.3333333333333333703, 0.3219752754296894559, 0.3333333333333333703, 0.3219752754296894559, 0.3333333333333333703, 0.3219752754296894559, 0.3333333333333333703, 0.3219752754296894559, 0.3333333333333333703, 0.3219752754296894559, 0.3333333333333333703, 0.3219752754296894559, 0.3333333333333333703, 0.3219752754296894559, 0.3333333333333333703, 0.3219752754296894559, 0.3333333333333333703, 0.3219752754296894559, 0.3333333333333333703),
 ( 1.000000000000000000, 0.9659258262890683122, 1.000000000000000000, 0.9659258262890683122, 1.000000000000000000, 0.9659258262890683122, 1.000000000000000000, 0.9659258262890683122, 1.000000000000000000, 0.9659258262890683122, 1.000000000000000000, 0.9659258262890683122, 1.000000000000000000, 0.9659258262890683122, 1.000000000000000000, 0.9659258262890683122, 1.000000000000000000, 0.9659258262890683122, 1.000000000000000000, 0.9659258262890683122, 1.000000000000000000, 0.9659258262890683122, 1.000000000000000000, 0.9659258262890683122, 1.000000000000000000, 0.9659258262890683122, 1.000000000000000000, 0.9659258262890683122, 1.000000000000000000, 0.9659258262890683122, 1.000000000000000000, 0.9659258262890683122, 1.000000000000000000, 0.9659258262890683122, 1.000000000000000000, 0.9659258262890683122, 1.000000000000000000, 0.9659258262890683122, 1.000000000000000000, 0.9659258262890683122, 1.000000000000000000, 0.9659258262890683122, 1.000000000000000000, 0.9659258262890683122, 1.000000000000000000, 0.9659258262890683122, 1.000000000000000000, 0.9659258262890683122, 1.000000000000000000, 0.9659258262890683122, 1.000000000000000000, 0.9659258262890683122, 1.000000000000000000, 0.9659258262890683122, 1.000000000000000000, 0.9659258262890683122, 1.000000000000000000, 0.9659258262890683122, 1.000000000000000000, 0.9659258262890683122, 1.000000000000000000, 0.9659258262890683122, 1.000000000000000000, 0.9659258262890683122, 1.000000000000000000, 0.9659258262890683122, 1.000000000000000000, 0.9659258262890683122, 1.000000000000000000, 0.9659258262890683122, 1.000000000000000000, 0.9659258262890683122, 1.000000000000000000, 0.9659258262890683122, 1.000000000000000000, 0.9659258262890683122, 1.000000000000000000, 0.9659258262890683122, 1.000000000000000000, 0.9659258262890683122, 1.000000000000000000, 0.9659258262890683122, 1.000000000000000000, 0.9659258262890683122, 1.000000000000000000, 0.9659258262890683122, 1.000000000000000000, 0.9659258262890683122, 1.000000000000000000, 0.9659258262890683122, 1.000000000000000000, 0.9659258262890683122, 1.000000000000000000, 0.9659258262890683122, 1.000000000000000000, 0.9659258262890683122, 1.000000000000000000, 0.9659258262890683122, 1.000000000000000000, 0.9659258262890683122, 1.000000000000000000, 0.9659258262890683122, 1.000000000000000000, 0.9659258262890683122, 1.000000000000000000, 0.9659258262890683122, 1.000000000000000000, 0.9659258262890683122, 1.000000000000000000, 0.9659258262890683122, 1.000000000000000000, 0.9659258262890683122, 1.000000000000000000, 0.9659258262890683122, 1.000000000000000000, 0.9659258262890683122, 1.000000000000000000, 0.9659258262890683122, 1.000000000000000000, 0.9659258262890683122, 1.000000000000000000, 0.9659258262890683122, 1.000000000000000000, 0.9659258262890683122, 1.000000000000000000, 0.9659258262890683122, 1.000000000000000000, 0.9659258262890683122, 1.000000000000000000, 0.9659258262890683122, 1.000000000000000000, 0.9659258262890683122, 1.000000000000000000, 0.9659258262890683122, 1.000000000000000000, 0.9659258262890683122, 1.000000000000000000, 0.9659258262890683122, 1.000000000000000000, 0.9659258262890683122, 1.000000000000000000, 0.9659258262890683122, 1.000000000000000000, 0.9659258262890683122, 1.000000000000000000, 0.9659258262890683122, 1.000000000000000000, 0.9659258262890683122, 1.000000000000000000, 0.9659258262890683122, 1.000000000000000000, 0.9659258262890683122, 1.000000000000000000, 0.9659258262890683122, 1.000000000000000000, 0.9659258262890683122, 1.000000000000000000, 0.9659258262890683122, 1.000000000000000000, 0.9659258262890683122, 1.000000000000000000, 0.9659258262890683122, 1.000000000000000000, 0.9659258262890683122, 1.000000000000000000, 0.9659258262890683122, 1.000000000000000000, 0.9659258262890683122, 1.000000000000000000, 0.9659258262890683122, 1.000000000000000000, 0.9659258262890683122, 1.000000000000000000, 0.9659258262890683122, 1.000000000000000000, 0.9659258262890683122, 1.000000000000000000, 0.9659258262890683122, 1.000000000000000000, 0.9659258262890683122, 1.000000000000000000, 0.9659258262890683122, 1.000000000000000000, 0.9659258262890683122, 1.000000000000000000, 0.9659258262890683122, 1.000000000000000000, 0.9659258262890683122, 1.000000000000000000, 0.9659258262890683122, 1.000000000000000000, 0.9659258262890683122, 1.000000000000000000, 0.9659258262890683122, 1.000000000000000000, 0.9659258262890683122, 1.000000000000000000, 0.9659258262890683122, 1.000000000000000000, 0.9659258262890683122, 1.000000000000000000, 0.9659258262890683122, 1.000000000000000000, 0.9659258262890683122, 1.000000000000000000, 0.9659258262890683122, 1.000000000000000000, 0.9659258262890683122, 1.000000000000000000, 0.9659258262890683122, 1.000000000000000000, 0.9659258262890683122, 1.000000000000000000, 0.9659258262890683122, 1.000000000000000000, 0.9659258262890683122, 1.000000000000000000, 0.9659258262890683122, 1.000000000000000000, 0.9659258262890683122, 1.000000000000000000, 0.9659258262890683122, 1.000000000000000000, 0.9659258262890683122, 1.000000000000000000, 0.9659258262890683122, 1.000000000000000000, 0.9659258262890683122, 1.000000000000000000, 0.9659258262890683122, 1.000000000000000000, 0.9659258262890683122, 1.000000000000000000, 0.9659258262890683122, 1.000000000000000000, 0.9659258262890683122, 1.000000000000000000, 0.9659258262890683122, 1.000000000000000000, 0.9659258262890683122, 1.000000000000000000, 0.9659258262890683122, 1.000000000000000000, 0.9659258262890683122, 1.000000000000000000, 0.9659258262890683122, 1.000000000000000000, 0.9659258262890683122, 1.000000000000000000, 0.9659258262890683122, 1.000000000000000000, 0.9659258262890683122, 1.000000000000000000, 0.9659258262890683122, 1.000000000000000000, 0.9659258262890683122, 1.000000000000000000, 0.9659258262890683122, 1.000000000000000000, 0.9659258262890683122, 1.000000000000000000, 0.9659258262890683122, 1.000000000000000000, 0.9659258262890683122, 1.000000000000000000, 0.9659258262890683122, 1.000000000000000000, 0.9659258262890683122, 1.000000000000000000, 0.9659258262890683122, 1.000000000000000000, 0.9659258262890683122, 1.000000000000000000, 0.9659258262890683122, 1.000000000000000000, 0.9659258262890683122, 1.000000000000000000, 0.9659258262890683122, 1.000000000000000000, 0.9659258262890683122, 1.000000000000000000, 0.9659258262890683122, 1.000000000000000000, 0.9659258262890683122, 1.000000000000000000, 0.9659258262890683122, 1.000000000000000000, 0.9659258262890683122, 1.000000000000000000, 0.9659258262890683122, 1.000000000000000000, 0.9659258262890683122, 1.000000000000000000, 0.9659258262890683122, 1.000000000000000000, 0.9659258262890683122, 1.000000000000000000, 0.9659258262890683122, 1.000000000000000000, 0.9659258262890683122, 1.000000000000000000, 0.9659258262890683122, 1.000000000000000000, 0.9659258262890683122, 1.000000000000000000, 0.9659258262890683122, 1.000000000000000000, 0.9659258262890683122, 1.000000000000000000, 0.9659258262890683122, 1.000000000000000000, 0.9659258262890683122, 1.000000000000000000, 0.9659258262890683122, 1.000000000000000000, 0.9659258262890683122, 1.000000000000000000, 0.9659258262890683122, 1.000000000000000000, 0.9659258262890683122, 1.000000000000000000, 0.9659258262890683122, 1.000000000000000000, 0.9659258262890683122, 1.000000000000000000, 0.9659258262890683122, 1.000000000000000000, 0.9659258262890683122, 1.000000000000000000, 0.9659258262890683122, 1.000000000000000000, 0.9659258262890683122, 1.000000000000000000, 0.9659258262890683122, 1.000000000000000000, 0.9659258262890683122, 1.000000000000000000, 0.9659258262890683122, 1.000000000000000000, 0.9659258262890683122, 1.000000000000000000, 0.9659258262890683122, 1.000000000000000000, 0.9659258262890683122, 1.000000000000000000, 0.9659258262890683122, 1.000000000000000000, 0.9659258262890683122, 1.000000000000000000, 0.9659258262890683122, 1.000000000000000000, 0.9659258262890683122, 1.000000000000000000, 0.9659258262890683122, 1.000000000000000000, 0.9659258262890683122, 1.000000000000000000, 0.9659258262890683122, 1.000000000000000000, 0.9659258262890683122, 1.000000000000000000, 0.9659258262890683122, 1.000000000000000000, 0.9659258262890683122, 1.000000000000000000, 0.9659258262890683122, 1.000000000000000000, 0.9659258262890683122, 1.000000000000000000, 0.9659258262890683122, 1.000000000000000000, 0.9659258262890683122, 1.000000000000000000, 0.9659258262890683122, 1.000000000000000000, 0.9659258262890683122, 1.000000000000000000, 0.9659258262890683122, 1.000000000000000000, 0.9659258262890683122, 1.000000000000000000, 0.9659258262890683122, 1.000000000000000000, 0.9659258262890683122, 1.000000000000000000, 0.9659258262890683122, 1.000000000000000000, 0.9659258262890683122, 1.000000000000000000, 0.9659258262890683122, 1.000000000000000000, 0.9659258262890683122, 1.000000000000000000, 0.9659258262890683122, 1.000000000000000000, 0.9659258262890683122, 1.000000000000000000, 0.9659258262890683122, 1.000000000000000000, 0.9659258262890683122, 1.000000000000000000, 0.9659258262890683122, 1.000000000000000000, 0.9659258262890683122, 1.000000000000000000, 0.9659258262890683122, 1.000000000000000000, 0.9659258262890683122, 1.000000000000000000, 0.9659258262890683122, 1.000000000000000000, 0.9659258262890683122, 1.000000000000000000, 0.9659258262890683122, 1.000000000000000000, 0.9659258262890683122, 1.000000000000000000, 0.9659258262890683122, 1.000000000000000000, 0.9659258262890683122, 1.000000000000000000, 0.9659258262890683122, 1.000000000000000000, 0.9659258262890683122, 1.000000000000000000, 0.9659258262890683122, 1.000000000000000000, 0.9659258262890683122, 1.000000000000000000, 0.9659258262890683122, 1.000000000000000000, 0.9659258262890683122, 1.000000000000000000, 0.9659258262890683122, 1.000000000000000000, 0.9659258262890683122, 1.000000000000000000, 0.9659258262890683122, 1.000000000000000000, 0.9659258262890683122, 1.000000000000000000, 0.9659258262890683122, 1.000000000000000000, 0.9659258262890683122, 1.000000000000000000, 0.9659258262890683122, 1.000000000000000000, 0.9659258262890683122, 1.000000000000000000, 0.9659258262890683122, 1.000000000000000000, 0.9659258262890683122, 1.000000000000000000, 0.9659258262890683122, 1.000000000000000000, 0.9659258262890683122, 1.000000000000000000) ) ) 
 REPRESENTATION_ITEM ( '' )  SURFACE ( )  );
#116417 = CARTESIAN_POINT ( 'NONE',  ( 18.62759615963255655, 10.81492255796105972, 21.66775706135235069 ) ) ;
#116418 = CARTESIAN_POINT ( 'NONE',  ( 27.73933785331498569, 2.768321779492822058E-14, 144.3750000027311842 ) ) ;
#116420 = EDGE_CURVE ( 'NONE', #193461, #71928, #55924, .T. ) ;
#116419 = CARTESIAN_POINT ( 'NONE',  ( -15.80617190586745835, -15.72974639402198527, 71.87390960531438111 ) ) ;
#116421 = CARTESIAN_POINT ( 'NONE',  ( -16.52544592524335698, -4.483927247898792601, 88.95942372801901854 ) ) ;
#116422 = CARTESIAN_POINT ( 'NONE',  ( -9.564922557960796823, -16.46253265017161027, 27.08224293864769550 ) ) ;
#116423 = CARTESIAN_POINT ( 'NONE',  ( -13.97604488694527625, -13.89961937509977652, 66.87390960531436690 ) ) ;
#116424 = CARTESIAN_POINT ( 'NONE',  ( 17.97182807773872426, -5.500000000000046185, 71.03038844047286204 ) ) ;
#116425 = DIRECTION ( 'NONE',  ( -0.000000000000000000, -0.000000000000000000, 1.000000000000000000 ) ) ;
#116426 = CARTESIAN_POINT ( 'NONE',  ( -8.224510206698948167, 14.34966873604960824, 30.41557627198101699 ) ) ;
#116427 = CARTESIAN_POINT ( 'NONE',  ( 10.72451020669871369, 18.67979575497193778, 57.08442372801901854 ) ) ;
#116428 = CARTESIAN_POINT ( 'NONE',  ( -5.049401038298153566, 19.05341960407611168, 105.2072429386476671 ) ) ;
#116429 = CARTESIAN_POINT ( 'NONE',  ( 18.67979575497194134, -10.72451020669871369, 95.83442372801903275 ) ) ;
#116430 = CARTESIAN_POINT ( 'NONE',  ( -13.89961937509977652, 13.97604488694528158, 45.62390960531433848 ) ) ;
#116431 = CARTESIAN_POINT ( 'NONE',  ( 16.46253265017160672, -9.564922557960803928, 53.33224293864768839 ) ) ;
#116432 = EDGE_LOOP ( 'NONE', ( #187058, #192341, #165913, #160701, #53204, #116627, #3411, #128737, #58981, #87334 ) ) ;
#116433 = CARTESIAN_POINT ( 'NONE',  ( -5.823673210054431948, 21.52544592524334988, 92.70942372801901854 ) ) ;
#116434 = CARTESIAN_POINT ( 'NONE',  ( 8.314922557961029526, -14.29746914071037800, 55.41775706135234714 ) ) ;
#116435 = CARTESIAN_POINT ( 'NONE',  ( 0.05219959533937995610, -21.53943276465977519, 80.00109039468568994 ) ) ;
#116436 = CARTESIAN_POINT ( 'NONE',  ( 21.55341960407610458, 5.719274019375980345, 23.95724293864769550 ) ) ;
#116437 = CARTESIAN_POINT ( 'NONE',  ( 13.97604488694548053, -13.89961937509957401, 95.62609039468563310 ) ) ;
#116438 = CARTESIAN_POINT ( 'NONE',  ( 15.72974639402176855, 15.80617190586768217, 51.87609039468568284 ) ) ;
#116439 = CARTESIAN_POINT ( 'NONE',  ( -8.314922557961024197, 14.29746914071037800, 32.91775706135234714 ) ) ;
#116440 = CARTESIAN_POINT ( 'NONE',  ( 15.80617190586746368, 15.72974639402197994, 89.37390960531435269 ) ) ;
#116441 = CARTESIAN_POINT ( 'NONE',  ( 5.153800228976615827, -19.02544592524334988, 90.20942372801900433 ) ) ;
#116442 = CARTESIAN_POINT ( 'NONE',  ( -16.46253265017160317, 9.564922557960807481, 70.83224293864770971 ) ) ;
#116443 = CARTESIAN_POINT ( 'NONE',  ( -19.03943276465977164, -0.05219959533935918106, 93.75109039468566152 ) ) ;
#116444 = AXIS2_PLACEMENT_3D ( 'NONE', #47884, #45887, #109537 ) ;
#116445 = CARTESIAN_POINT ( 'NONE',  ( 5.049401038297881783, 19.05341960407617563, 97.29275706135233293 ) ) ;
#116446 = CARTESIAN_POINT ( 'NONE',  ( -16.53943276465976808, 0.05219959533911058130, 56.24890960531436690 ) ) ;
#116447 = CARTESIAN_POINT ( 'NONE',  ( 16.46253265017146816, 9.564922557961045513, 81.66775706135233293 ) ) ;
#116448 = CARTESIAN_POINT ( 'NONE',  ( -12.06949235617739369, -12.14591786802326823, 64.37609039468568994 ) ) ;
#116449 = CARTESIAN_POINT ( 'NONE',  ( 9.564922557961047289, -16.46253265017146816, 40.41775706135234003 ) ) ;
#116450 = CARTESIAN_POINT ( 'NONE',  ( -9.474510206698964154, 16.51473224551069663, 40.41557627198103120 ) ) ;
#116452 = EDGE_CURVE ( 'NONE', #164406, #38283, #159236, .T. ) ;
#116451 = CARTESIAN_POINT ( 'NONE',  ( -9.474510206698964154, 16.51473224551069663, 45.41557627198103120 ) ) ;
#116453 = CARTESIAN_POINT ( 'NONE',  ( -16.52544592524335698, -4.483927247898792601, 63.95942372801901854 ) ) ;
#116454 = CARTESIAN_POINT ( 'NONE',  ( -18.09805431107519880, 5.500000000000101252, 46.01606229291888894 ) ) ;
#116455 = CARTESIAN_POINT ( 'NONE',  ( -28.82186960331499392, -9.364793116373526516, 140.3500000054623627 ) ) ;
#116456 = CARTESIAN_POINT ( 'NONE',  ( 19.05341960407611168, 5.049401038298154454, 108.9572429386477097 ) ) ;
#116457 = CARTESIAN_POINT ( 'NONE',  ( 16.51473224551069308, 9.474510206698969483, 24.16557627198102765 ) ) ;
#116458 = VERTEX_POINT ( 'NONE', #70996 ) ;
#116459 = CARTESIAN_POINT ( 'NONE',  ( -16.51473224551082808, 9.474510206698731452, 98.33442372801900433 ) ) ;
#116460 = CARTESIAN_POINT ( 'NONE',  ( 21.53943276465977519, -0.05219959533907433946, 33.74890960531436690 ) ) ;
#116462 = CARTESIAN_POINT ( 'NONE',  ( -5.153800228976607833, 19.02544592524334988, 107.7094237280189759 ) ) ;
#116461 = CARTESIAN_POINT ( 'NONE',  ( 19.02544592524334988, 5.153800228976608722, 31.45942372801900433 ) ) ;
#116463 = CARTESIAN_POINT ( 'NONE',  ( 16.46253265017160672, -9.564922557960803928, 28.33224293864769550 ) ) ;
#116464 = CARTESIAN_POINT ( 'NONE',  ( 5.049401038298161559, -19.05341960407611168, 52.70724293864767418 ) ) ;
#116465 = CARTESIAN_POINT ( 'NONE',  ( -10.81492255796078084, -18.62759615963271287, 72.08224293864769550 ) ) ;
#116466 = CARTESIAN_POINT ( 'NONE',  ( 19.03943276465977164, -0.05219959533909143690, 103.7489096053143669 ) ) ;
#116467 = CARTESIAN_POINT ( 'NONE',  ( 19.02544592524343514, -5.153800228976328945, 33.54057627198102409 ) ) ;
#116468 = CARTESIAN_POINT ( 'NONE',  ( -8.571926809382608425, 26.38167802310805854, 144.9750000027312069 ) ) ;
#116469 = CARTESIAN_POINT ( 'NONE',  ( -19.03943276465977164, -0.05219959533935918106, 78.75109039468567573 ) ) ;
#116470 = CARTESIAN_POINT ( 'NONE',  ( -12.14591786802309592, -12.06949235617757132, 51.87390960531437401 ) ) ;
#116471 = CARTESIAN_POINT ( 'NONE',  ( -0.05219959533907301413, -21.53943276465977519, 37.49890960531436690 ) ) ;
#116472 = CARTESIAN_POINT ( 'NONE',  ( -15.80617190586768217, 15.72974639402176855, 108.1260903946856757 ) ) ;
#116473 = CARTESIAN_POINT ( 'NONE',  ( -15.72974639402197994, 15.80617190586746368, 95.62390960531436690 ) ) ;
#116474 = CARTESIAN_POINT ( 'NONE',  ( 21.53943276465977519, 0.05219959533937863772, 76.25109039468568994 ) ) ;
#116475 = CARTESIAN_POINT ( 'NONE',  ( -10.72451020669870658, -18.67979575497194134, 74.58442372801901854 ) ) ;
#116476 = CARTESIAN_POINT ( 'NONE',  ( -9.474510206698964154, 16.51473224551069663, 115.4155762719810241 ) ) ;
#116478 = CARTESIAN_POINT ( 'NONE',  ( -21.55341960407619339, 5.719274019375674811, 58.54275706135235424 ) ) ;
#116477 = CARTESIAN_POINT ( 'NONE',  ( 12.06949235617739724, 12.14591786802326823, 111.8760903946856615 ) ) ;
#116479 = CARTESIAN_POINT ( 'NONE',  ( 13.89961937509977652, -13.97604488694527269, 73.12390960531436690 ) ) ;
#116480 = CARTESIAN_POINT ( 'NONE',  ( -13.89961937509957401, -13.97604488694547875, 39.37609039468566152 ) ) ;
#116481 = CARTESIAN_POINT ( 'NONE',  ( -10.72451020669870658, -18.67979575497194134, 34.58442372801900433 ) ) ;
#116482 = CARTESIAN_POINT ( 'NONE',  ( 9.564922557960805705, 16.46253265017160317, 64.58224293864769550 ) ) ;
#116483 = CARTESIAN_POINT ( 'NONE',  ( 16.52544592524342804, -4.483927247898539470, 78.54057627198103830 ) ) ;
#116484 = CARTESIAN_POINT ( 'NONE',  ( 16.53943276465976808, -0.05219959533910856209, 53.74890960531437401 ) ) ;
#116485 = CARTESIAN_POINT ( 'NONE',  ( 21.52544592524344225, -5.823673210054117533, 58.54057627198103120 ) ) ;
#116486 = CARTESIAN_POINT ( 'NONE',  ( -0.05219959533909027116, -19.03943276465977164, 57.49890960531435979 ) ) ;
#116487 = CARTESIAN_POINT ( 'NONE',  ( -0.05219959533907301413, -21.53943276465977519, 67.49890960531436690 ) ) ;
#116488 = CARTESIAN_POINT ( 'NONE',  ( 5.153800228976615827, -19.02544592524334988, 65.20942372801900433 ) ) ;
#116490 = CARTESIAN_POINT ( 'NONE',  ( -16.55341960407611168, -4.379528057220339221, 61.45724293864770260 ) ) ;
#116489 = CARTESIAN_POINT ( 'NONE',  ( 9.474510206698729675, 16.51473224551082808, 22.08442372801899722 ) ) ;
#116491 = CARTESIAN_POINT ( 'NONE',  ( -15.72974639402197994, 15.80617190586746368, 45.62390960531436690 ) ) ;
#116492 = ORIENTED_EDGE ( 'NONE', *, *, #121295, .F. ) ;
#116493 = CARTESIAN_POINT ( 'NONE',  ( 16.88567814943161949, 6.947325034625699836, 103.7900112265258770 ) ) ;
#116495 = CARTESIAN_POINT ( 'NONE',  ( 1.424896265312427746, 7.121249343341831128, -64.33531891713909090 ) ) ;
#116494 = CARTESIAN_POINT ( 'NONE',  ( -14.29746914071037622, -8.314922557961029526, 79.16775706135234714 ) ) ;
#116496 = EDGE_CURVE ( 'NONE', #19675, #141549, #134674, .T. ) ;
#116497 = CARTESIAN_POINT ( 'NONE',  ( -5.049401038297874678, -19.05341960407617918, 84.79275706135233293 ) ) ;
#116498 = CARTESIAN_POINT ( 'NONE',  ( 8.314922557960818139, 14.29746914071049879, 59.58224293864770260 ) ) ;
#116499 = DIRECTION ( 'NONE',  ( 1.000000000000000000, 0.000000000000000000, -0.000000000000000000 ) ) ;
#116500 = CARTESIAN_POINT ( 'NONE',  ( -19.02544592524342804, 5.153800228976336051, 46.04057627198101699 ) ) ;
#116501 = CARTESIAN_POINT ( 'NONE',  ( 8.224510206698953496, -14.34966873604960469, 42.91557627198103120 ) ) ;
#116502 = CARTESIAN_POINT ( 'NONE',  ( 16.46253265017160672, -9.564922557960803928, 93.33224293864769550 ) ) ;
#116503 = CARTESIAN_POINT ( 'NONE',  ( 19.05341960407611168, 5.049401038298154454, 53.95724293864770260 ) ) ;
#116504 = CARTESIAN_POINT ( 'NONE',  ( 15.80617190586769283, -15.72974639402175789, 65.62609039468568994 ) ) ;
#116505 = CARTESIAN_POINT ( 'NONE',  ( -16.46253265017160317, 9.564922557960807481, 65.83224293864769550 ) ) ;
#116506 = FACE_OUTER_BOUND ( 'NONE', #128502, .T. ) ;
#116507 = CARTESIAN_POINT ( 'NONE',  ( -9.564922557960796823, -16.46253265017161027, 72.08224293864770971 ) ) ;
#116508 = CARTESIAN_POINT ( 'NONE',  ( 21.55341960407610458, 5.719274019375980345, 48.95724293864770971 ) ) ;
#116509 = CARTESIAN_POINT ( 'NONE',  ( -16.46253265017160317, 9.564922557960807481, 50.83224293864770260 ) ) ;
#116510 = CARTESIAN_POINT ( 'NONE',  ( 21.55341960407610458, 5.719274019375980345, 53.95724293864770260 ) ) ;
#116511 = CARTESIAN_POINT ( 'NONE',  ( -9.474510206698720793, -16.51473224551083518, 79.58442372801899012 ) ) ;
#116512 =( REPRESENTATION_RELATIONSHIP ('NONE','NONE', #154205, #9542 ) REPRESENTATION_RELATIONSHIP_WITH_TRANSFORMATION ( #68439 )SHAPE_REPRESENTATION_RELATIONSHIP( ) );
#116513 = CARTESIAN_POINT ( 'NONE',  ( -16.52544592524335698, -4.483927247898792601, 98.95942372801903275 ) ) ;
#116514 = CARTESIAN_POINT ( 'NONE',  ( -19.02544592524334988, -5.153800228976617603, 23.95942372801900078 ) ) ;
#116516 = CARTESIAN_POINT ( 'NONE',  ( 8.224510206698742110, 14.34966873604972548, 77.08442372801901854 ) ) ;
#116515 = CARTESIAN_POINT ( 'NONE',  ( -4.483927247898782831, 16.52544592524335698, 47.70942372801902565 ) ) ;
#116517 = CARTESIAN_POINT ( 'NONE',  ( -12.06949235617739369, -12.14591786802326823, 64.37609039468568994 ) ) ;
#116518 = CARTESIAN_POINT ( 'NONE',  ( -21.53943276465977519, 0.05219959533907696930, 26.24890960531435624 ) ) ;
#116519 = CARTESIAN_POINT ( 'NONE',  ( 16.51473224551069308, 9.474510206698969483, 34.16557627198102409 ) ) ;
#116520 = CARTESIAN_POINT ( 'NONE',  ( 16.55341960407618274, -4.379528057220086978, 41.04275706135236135 ) ) ;
#116521 = CARTESIAN_POINT ( 'NONE',  ( 9.474510206698971260, -16.51473224551069308, 42.91557627198103120 ) ) ;
#116522 = CARTESIAN_POINT ( 'NONE',  ( 15.72974639402176855, 15.80617190586768217, 36.87609039468568994 ) ) ;
#116523 = CARTESIAN_POINT ( 'NONE',  ( 14.34966873604972726, -8.224510206698740333, 35.83442372801901143 ) ) ;
#116524 = CARTESIAN_POINT ( 'NONE',  ( 14.34966873604972726, -8.224510206698740333, 100.8344237280190185 ) ) ;
#116525 = CARTESIAN_POINT ( 'NONE',  ( -19.03943276465977164, 0.05219959533909376836, 21.24890960531436335 ) ) ;
#116526 = CARTESIAN_POINT ( 'NONE',  ( -21.52544592524334988, -5.823673210054445271, 103.9594237280190185 ) ) ;
#116527 = CARTESIAN_POINT ( 'NONE',  ( -19.02544592524334988, -5.153800228976617603, 108.9594237280189759 ) ) ;
#116528 = CARTESIAN_POINT ( 'NONE',  ( 5.153800228976615827, -19.02544592524334988, 70.20942372801899012 ) ) ;
#116529 = CARTESIAN_POINT ( 'NONE',  ( -0.05219959533910754901, -16.53943276465976808, 67.49890960531436690 ) ) ;
#116530 = CARTESIAN_POINT ( 'NONE',  ( 9.564922557960805705, 16.46253265017160317, 29.58224293864769550 ) ) ;
#116532 = CARTESIAN_POINT ( 'NONE',  ( 16.52216118717246829, -7.221426719304367303, 56.42400978952971258 ) ) ;
#116531 = CARTESIAN_POINT ( 'NONE',  ( 5.049401038297881783, 19.05341960407617563, 62.29275706135234003 ) ) ;
#116533 = CARTESIAN_POINT ( 'NONE',  ( -10.72451020669870658, -18.67979575497194134, 64.58442372801900433 ) ) ;
#116534 = CARTESIAN_POINT ( 'NONE',  ( -8.314922557961024197, 14.29746914071037800, 27.91775706135234358 ) ) ;
#116535 = CARTESIAN_POINT ( 'NONE',  ( 19.52217212775657629, -5.500000000000104805, 57.43993709005260939 ) ) ;
#116536 = CARTESIAN_POINT ( 'NONE',  ( -21.53943276465977519, 0.05219959533907696930, 26.24890960531435624 ) ) ;
#116537 = CARTESIAN_POINT ( 'NONE',  ( -19.03943276465977164, -0.05219959533935918106, 113.7510903946856757 ) ) ;
#116538 = CARTESIAN_POINT ( 'NONE',  ( -19.02544592524342804, 5.153800228976336051, 111.0405762719810099 ) ) ;
#116539 = CARTESIAN_POINT ( 'NONE',  ( 4.500000000000000000, 0.000000000000000000, -20.00000000000000000 ) ) ;
#116540 = CARTESIAN_POINT ( 'NONE',  ( 5.153800228976335163, 19.02544592524342804, 24.79057627198102765 ) ) ;
#116541 = CARTESIAN_POINT ( 'NONE',  ( -15.80617190586768217, 15.72974639402176855, 103.1260903946856757 ) ) ;
#116542 = CARTESIAN_POINT ( 'NONE',  ( -9.474510206698964154, 16.51473224551069663, 50.41557627198102409 ) ) ;
#116543 = CARTESIAN_POINT ( 'NONE',  ( 5.719274019375673035, 21.55341960407619339, 62.29275706135236845 ) ) ;
#116544 = CARTESIAN_POINT ( 'NONE',  ( 10.72451020669871369, 18.67979575497193778, 102.0844237280190185 ) ) ;
#116545 = CARTESIAN_POINT ( 'NONE',  ( 8.224510206698953496, -14.34966873604960469, 22.91557627198102765 ) ) ;
#116546 = CARTESIAN_POINT ( 'NONE',  ( 0.05219959533909260263, 19.03943276465977164, 29.99890960531435979 ) ) ;
#116547 = CARTESIAN_POINT ( 'NONE',  ( 19.03943276465977164, -0.05219959533909143690, 73.74890960531435269 ) ) ;
#116548 = CARTESIAN_POINT ( 'NONE',  ( -21.53943276465977519, -0.05219959533937600094, 58.75109039468568994 ) ) ;
#116549 = CARTESIAN_POINT ( 'NONE',  ( 16.51473224551069308, 9.474510206698969483, 39.16557627198103120 ) ) ;
#116550 = CARTESIAN_POINT ( 'NONE',  ( 10.72451020669871369, 18.67979575497193778, 52.08442372801901854 ) ) ;
#116552 = CARTESIAN_POINT ( 'NONE',  ( -5.049401038298153566, 19.05341960407611168, 110.2072429386476671 ) ) ;
#116551 = CARTESIAN_POINT ( 'NONE',  ( -19.03943276465977164, -0.05219959533935918106, 78.75109039468567573 ) ) ;
#116553 = CARTESIAN_POINT ( 'NONE',  ( -5.049401038298153566, 19.05341960407611168, 25.20724293864768484 ) ) ;
#116554 = CARTESIAN_POINT ( 'NONE',  ( -10.81492255796078084, -18.62759615963271287, 107.0822429386476955 ) ) ;
#116555 = CARTESIAN_POINT ( 'NONE',  ( 16.46253265017146816, 9.564922557961045513, 36.66775706135233293 ) ) ;
#116556 = CARTESIAN_POINT ( 'NONE',  ( -12.06949235617756955, 12.14591786802309770, 95.62390960531436690 ) ) ;
#116557 = CARTESIAN_POINT ( 'NONE',  ( 19.05341960407611168, 5.049401038298154454, 43.95724293864769550 ) ) ;
#116558 = CARTESIAN_POINT ( 'NONE',  ( 13.89961937509957401, 13.97604488694547697, 96.87609039468566152 ) ) ;
#116559 = CARTESIAN_POINT ( 'NONE',  ( -0.05219959533910754901, -16.53943276465976808, 57.49890960531435979 ) ) ;
#116560 = CARTESIAN_POINT ( 'NONE',  ( 18.67979575497194134, -10.72451020669871369, 105.8344237280190328 ) ) ;
#116561 = CARTESIAN_POINT ( 'NONE',  ( -16.46253265017160317, 9.564922557960807481, 105.8322429386476955 ) ) ;
#116562 = CARTESIAN_POINT ( 'NONE',  ( -19.02544592524334988, -5.153800228976617603, 88.95942372801897591 ) ) ;
#116563 = CARTESIAN_POINT ( 'NONE',  ( -21.52544592524343514, 5.823673210054127303, 91.04057627198103830 ) ) ;
#116564 = CARTESIAN_POINT ( 'NONE',  ( -21.55341960407619339, 5.719274019375674811, 38.54275706135234714 ) ) ;
#116565 = CARTESIAN_POINT ( 'NONE',  ( -16.52544592524335698, -4.483927247898792601, 48.95942372801902565 ) ) ;
#116566 = CARTESIAN_POINT ( 'NONE',  ( 0.05219959533934541429, -16.53943276465976808, 110.0010903946856757 ) ) ;
#116568 = CARTESIAN_POINT ( 'NONE',  ( 5.719274019375673035, 21.55341960407619339, 47.29275706135234003 ) ) ;
#116567 = CARTESIAN_POINT ( 'NONE',  ( 8.224510206698742110, 14.34966873604972548, 47.08442372801901854 ) ) ;
#116569 = CARTESIAN_POINT ( 'NONE',  ( 0.05219959533907565091, 21.53943276465977519, 44.99890960531435979 ) ) ;
#116570 = CARTESIAN_POINT ( 'NONE',  ( -16.46253265017160317, 9.564922557960807481, 30.83224293864769550 ) ) ;
#116571 = CARTESIAN_POINT ( 'NONE',  ( 11.74264578624799427, 36.14014761921585972, -10.34999999453762598 ) ) ;
#116572 = CARTESIAN_POINT ( 'NONE',  ( 12.14591786802327356, -12.06949235617739191, 60.62609039468567573 ) ) ;
#116573 = CARTESIAN_POINT ( 'NONE',  ( 21.52544592524344225, -5.823673210054117533, 93.54057627198103830 ) ) ;
#116574 = CARTESIAN_POINT ( 'NONE',  ( -4.379528057220328563, 16.55341960407611168, 45.20724293864769550 ) ) ;
#116575 = CARTESIAN_POINT ( 'NONE',  ( -16.55341960407617563, 4.379528057220093196, 68.54275706135234714 ) ) ;
#116576 = CARTESIAN_POINT ( 'NONE',  ( -0.05219959533909027116, -19.03943276465977164, 57.49890960531435979 ) ) ;
#116577 = CARTESIAN_POINT ( 'NONE',  ( 19.03943276465977164, 0.05219959533936151252, 106.2510903946856615 ) ) ;
#116578 = CARTESIAN_POINT ( 'NONE',  ( -21.53943276465977519, 0.05219959533907696930, 81.24890960531436690 ) ) ;
#116579 = CARTESIAN_POINT ( 'NONE',  ( -0.05219959533910754901, -16.53943276465976808, 32.49890960531435979 ) ) ;
#116580 = VERTEX_POINT ( 'NONE', #181182 ) ;
#116581 = CARTESIAN_POINT ( 'NONE',  ( 20.14845677604831664, 11.85354687992394496, 170.0217845860066745 ) ) ;
#116582 = CARTESIAN_POINT ( 'NONE',  ( 21.53943276465977519, -0.05219959533907433946, 78.74890960531436690 ) ) ;
#116583 = CARTESIAN_POINT ( 'NONE',  ( -12.14591786802326823, 12.06949235617739902, 108.1260903946856757 ) ) ;
#116584 = ORIENTED_EDGE ( 'NONE', *, *, #68983, .F. ) ;
#116585 = CARTESIAN_POINT ( 'NONE',  ( 17.50000000000000711, -4.119547552397547108, 102.9808761550738296 ) ) ;
#116586 = CARTESIAN_POINT ( 'NONE',  ( 18.67979575497178502, 10.72451020669898547, 89.16557627198102409 ) ) ;
#116587 = CARTESIAN_POINT ( 'NONE',  ( 21.53943276465977519, -0.05219959533907433946, 103.7489096053143669 ) ) ;
#116588 = CARTESIAN_POINT ( 'NONE',  ( 4.483927247898545687, 16.52544592524342804, 29.79057627198102409 ) ) ;
#116589 = CARTESIAN_POINT ( 'NONE',  ( 16.53943276465976808, 0.05219959533934440121, 31.25109039468568639 ) ) ;
#116590 = CARTESIAN_POINT ( 'NONE',  ( 16.51473224551069308, 9.474510206698969483, 29.16557627198103475 ) ) ;
#116591 = CARTESIAN_POINT ( 'NONE',  ( 16.51473224551069308, 9.474510206698969483, 64.16557627198102409 ) ) ;
#116592 = CARTESIAN_POINT ( 'NONE',  ( 17.81289503416611453, -24.51734667627695785, 146.6999999999999886 ) ) ;
#116593 = CARTESIAN_POINT ( 'NONE',  ( -21.55341960407610458, -5.719274019375992779, 21.45724293864769550 ) ) ;
#116594 = CARTESIAN_POINT ( 'NONE',  ( -4.647474457565486646E-15, 28.90000000000004476, -52.65483682830183199 ) ) ;
#116595 = CARTESIAN_POINT ( 'NONE',  ( -16.51473224551082808, 9.474510206698731452, 103.3344237280190043 ) ) ;
#116596 = CARTESIAN_POINT ( 'NONE',  ( -19.02544592524334988, -5.153800228976617603, 33.95942372801897591 ) ) ;
#116597 = CARTESIAN_POINT ( 'NONE',  ( -15.80617190586745835, -15.72974639402198527, 91.87390960531436690 ) ) ;
#116598 = EDGE_CURVE ( 'NONE', #116009, #184761, #139899, .T. ) ;
#116599 = CARTESIAN_POINT ( 'NONE',  ( 4.379528057220092307, 16.55341960407617563, 112.2927570613523471 ) ) ;
#116600 = CARTESIAN_POINT ( 'NONE',  ( -21.52544592524343514, 5.823673210054127303, 46.04057627198103830 ) ) ;
#116602 = CARTESIAN_POINT ( 'NONE',  ( 5.153800228976615827, -19.02544592524334988, 100.2094237280190043 ) ) ;
#116601 = CARTESIAN_POINT ( 'NONE',  ( 21.55341960407610458, 5.719274019375980345, 78.95724293864769550 ) ) ;
#116603 = CARTESIAN_POINT ( 'NONE',  ( -19.05341960407611168, -5.049401038298163336, 106.4572429386476955 ) ) ;
#116604 = CARTESIAN_POINT ( 'NONE',  ( 0.05219959533937995610, -21.53943276465977519, 70.00109039468568994 ) ) ;
#116605 = CARTESIAN_POINT ( 'NONE',  ( 13.97604488694527802, 13.89961937509977652, 59.37390960531434558 ) ) ;
#116606 = CARTESIAN_POINT ( 'NONE',  ( -4.483927247898539470, -16.52544592524342804, 97.29057627198105251 ) ) ;
#116607 = CARTESIAN_POINT ( 'NONE',  ( 31.60134953801815172, 3.338644055332157468, 101.7340227041929950 ) ) ;
#116608 = CARTESIAN_POINT ( 'NONE',  ( -9.474510206698964154, 16.51473224551069663, 65.41557627198102409 ) ) ;
#116609 = CARTESIAN_POINT ( 'NONE',  ( -4.379528057220328563, 16.55341960407611168, 90.20724293864770971 ) ) ;
#116610 = ORIENTED_EDGE ( 'NONE', *, *, #113016, .F. ) ;
#116611 = CARTESIAN_POINT ( 'NONE',  ( -9.564922557961040184, 16.46253265017147172, 87.91775706135233293 ) ) ;
#116612 = CARTESIAN_POINT ( 'NONE',  ( 0.000000000000000000, 0.000000000000000000, -64.53213882399991519 ) ) ;
#116613 = CARTESIAN_POINT ( 'NONE',  ( -19.05341960407611168, -5.049401038298163336, 66.45724293864769550 ) ) ;
#116615 = CARTESIAN_POINT ( 'NONE',  ( 5.049401038298161559, -19.05341960407611168, 102.7072429386476955 ) ) ;
#116614 = CARTESIAN_POINT ( 'NONE',  ( -18.67979575497193778, 10.72451020669871902, 78.33442372801901854 ) ) ;
#116616 = CARTESIAN_POINT ( 'NONE',  ( 16.55341960407618274, -4.379528057220086978, 81.04275706135236135 ) ) ;
#116617 = CARTESIAN_POINT ( 'NONE',  ( -17.26172910966778318, -6.454744622555875999, 49.19353091350777873 ) ) ;
#116618 = CARTESIAN_POINT ( 'NONE',  ( 0.05219959533936267826, -19.03943276465977164, 40.00109039468566152 ) ) ;
#116619 = CARTESIAN_POINT ( 'NONE',  ( 10.81492255796106328, -18.62759615963255655, 95.41775706135234714 ) ) ;
#116620 = CARTESIAN_POINT ( 'NONE',  ( 6.293193206003583562, 6.576150211591589745, -63.95112321872120731 ) ) ;
#116621 = DIRECTION ( 'NONE',  ( -1.000000000000000000, -0.000000000000000000, -0.000000000000000000 ) ) ;
#116622 = CARTESIAN_POINT ( 'NONE',  ( -14.29746914071037622, -8.314922557961029526, 99.16775706135234714 ) ) ;
#116623 = CARTESIAN_POINT ( 'NONE',  ( -34.40736802160862595, -7.501760008519349654, 45.46231226804128767 ) ) ;
#116624 = CARTESIAN_POINT ( 'NONE',  ( 16.52544592524335698, 4.483927247898782831, 96.45942372801901854 ) ) ;
#116625 = CARTESIAN_POINT ( 'NONE',  ( 31.05781409862806797, -25.21364184384349727, -18.17652835081984009 ) ) ;
#116626 = CARTESIAN_POINT ( 'NONE',  ( -8.314922557961024197, 14.29746914071037800, 62.91775706135236135 ) ) ;
#116627 = ORIENTED_EDGE ( 'NONE', *, *, #36648, .F. ) ;
#116628 = CARTESIAN_POINT ( 'NONE',  ( 21.53943276465977519, 0.05219959533937863772, 76.25109039468568994 ) ) ;
#116629 = CARTESIAN_POINT ( 'NONE',  ( -13.89961937509957401, -13.97604488694547875, 84.37609039468567573 ) ) ;
#116630 = CARTESIAN_POINT ( 'NONE',  ( 0.05219959533936267826, -19.03943276465977164, 40.00109039468566152 ) ) ;
#116631 = CARTESIAN_POINT ( 'NONE',  ( -9.474510206698964154, 16.51473224551069663, 70.41557627198102409 ) ) ;
#116632 = CARTESIAN_POINT ( 'NONE',  ( -19.05341960407611168, -5.049401038298163336, 56.45724293864768129 ) ) ;
#116633 = CARTESIAN_POINT ( 'NONE',  ( -17.49999999999999645, 5.499999999999998224, 22.00000000000000711 ) ) ;
#116634 = CARTESIAN_POINT ( 'NONE',  ( -15.72974639402197994, 15.80617190586746368, 75.62390960531439532 ) ) ;
#116635 = CARTESIAN_POINT ( 'NONE',  ( 18.67979575497178502, 10.72451020669898547, 34.16557627198102409 ) ) ;
#116636 = CARTESIAN_POINT ( 'NONE',  ( -19.03943276465977164, 0.05219959533909376836, 36.24890960531436690 ) ) ;
#116637 = CARTESIAN_POINT ( 'NONE',  ( 4.379528057220092307, 16.55341960407617563, 62.29275706135236845 ) ) ;
#116638 = VERTEX_POINT ( 'NONE', #151817 ) ;
#116639 = CARTESIAN_POINT ( 'NONE',  ( 15.72974639402176855, 15.80617190586768217, 26.87609039468567218 ) ) ;
#116641 = CARTESIAN_POINT ( 'NONE',  ( -23.48529157249600985, 32.32473071737754111, -0.2999999999999999334 ) ) ;
#116640 = CARTESIAN_POINT ( 'NONE',  ( -4.379528057220328563, 16.55341960407611168, 70.20724293864769550 ) ) ;
#116642 = CARTESIAN_POINT ( 'NONE',  ( -0.05219959533934338120, 16.53943276465976808, 22.50109039468567573 ) ) ;
#116643 = CARTESIAN_POINT ( 'NONE',  ( 19.05341960407617918, -5.049401038297876454, 51.04275706135231871 ) ) ;
#116644 = CARTESIAN_POINT ( 'NONE',  ( -12.06949235617756955, 12.14591786802309770, 60.62390960531437401 ) ) ;
#116645 = CARTESIAN_POINT ( 'NONE',  ( -21.53943276465977519, -0.05219959533937600094, 33.75109039468568284 ) ) ;
#116647 = CARTESIAN_POINT ( 'NONE',  ( 18.67979575497178502, 10.72451020669898547, 84.16557627198103830 ) ) ;
#116646 = CARTESIAN_POINT ( 'NONE',  ( 5.153800228976335163, 19.02544592524342804, 99.79057627198102409 ) ) ;
#116648 = CARTESIAN_POINT ( 'NONE',  ( 19.05341960407611168, 5.049401038298154454, 108.9572429386477097 ) ) ;
#116649 = CARTESIAN_POINT ( 'NONE',  ( -4.379528057220328563, 16.55341960407611168, 80.20724293864769550 ) ) ;
#116650 = CARTESIAN_POINT ( 'NONE',  ( 23.76721391575371811, -30.09498488473221656, -7.911512314823321290 ) ) ;
#116651 = CARTESIAN_POINT ( 'NONE',  ( -13.89961937509957401, -13.97604488694547875, 69.37609039468564731 ) ) ;
#116652 = CARTESIAN_POINT ( 'NONE',  ( 0.05219959533907565091, 21.53943276465977519, 104.9989096053143669 ) ) ;
#116653 = CARTESIAN_POINT ( 'NONE',  ( -9.564922557960796823, -16.46253265017161027, 57.08224293864769550 ) ) ;
#116654 = CARTESIAN_POINT ( 'NONE',  ( 13.97604488694548053, -13.89961937509957401, 40.62609039468564731 ) ) ;
#116655 = CARTESIAN_POINT ( 'NONE',  ( 19.05341960407611168, 5.049401038298154454, 33.95724293864769550 ) ) ;
#116656 = CARTESIAN_POINT ( 'NONE',  ( -5.823673210054431948, 21.52544592524334988, 57.70942372801901143 ) ) ;
#116657 = CARTESIAN_POINT ( 'NONE',  ( -17.50000000000001421, -5.499999999999944045, 71.28230962303567253 ) ) ;
#116658 = CARTESIAN_POINT ( 'NONE',  ( -8.224510206698948167, 14.34966873604960824, 40.41557627198103120 ) ) ;
#116659 = CARTESIAN_POINT ( 'NONE',  ( -19.05341960407611168, -5.049401038298163336, 56.45724293864768129 ) ) ;
#116660 = CARTESIAN_POINT ( 'NONE',  ( -10.72451020669898014, 18.67979575497178502, 90.41557627198103830 ) ) ;
#116661 = CARTESIAN_POINT ( 'NONE',  ( -0.05219959533909027116, -19.03943276465977164, 57.49890960531435979 ) ) ;
#116662 = ORIENTED_EDGE ( 'NONE', *, *, #200059, .F. ) ;
#116663 = CARTESIAN_POINT ( 'NONE',  ( -18.62759615963270932, 10.81492255796079327, 60.83224293864769550 ) ) ;
#116664 = CARTESIAN_POINT ( 'NONE',  ( 21.53943276465977519, 0.05219959533937863772, 96.25109039468568994 ) ) ;
#116667 = CARTESIAN_POINT ( 'NONE',  ( 16.52544592524342804, -4.483927247898539470, 88.54057627198103830 ) ) ;
#116666 = CARTESIAN_POINT ( 'NONE',  ( 8.314922557961029526, -14.29746914071037800, 90.41775706135236135 ) ) ;
#116665 = FACE_BOUND ( 'NONE', #154639, .T. ) ;
#116668 = CARTESIAN_POINT ( 'NONE',  ( 19.02544592524334988, 5.153800228976608722, 91.45942372801900433 ) ) ;
#116669 = ORIENTED_EDGE ( 'NONE', *, *, #165696, .F. ) ;
#116670 = CARTESIAN_POINT ( 'NONE',  ( -13.89961937509957401, -13.97604488694547875, 39.37609039468566152 ) ) ;
#116671 = CARTESIAN_POINT ( 'NONE',  ( 12.14591786802327356, -12.06949235617739191, 95.62609039468568994 ) ) ;
#116672 = EDGE_CURVE ( 'NONE', #86619, #124248, #138614, .T. ) ;
#116673 = CARTESIAN_POINT ( 'NONE',  ( 19.05341960407617918, -5.049401038297876454, 31.04275706135232227 ) ) ;
#116674 = CARTESIAN_POINT ( 'NONE',  ( 5.153800228976335163, 19.02544592524342804, 84.79057627198099567 ) ) ;
#116675 = CARTESIAN_POINT ( 'NONE',  ( -0.05219959533907301413, -21.53943276465977519, 62.49890960531436690 ) ) ;
#116676 = CARTESIAN_POINT ( 'NONE',  ( -25.28116846732003964, 11.97242897402593442, 166.1912472719371863 ) ) ;
#116677 = CARTESIAN_POINT ( 'NONE',  ( 9.564922557960805705, 16.46253265017160317, 24.58224293864769194 ) ) ;
#116678 = CARTESIAN_POINT ( 'NONE',  ( -5.823673210054431948, 21.52544592524334988, 97.70942372801904696 ) ) ;
#116679 = CARTESIAN_POINT ( 'NONE',  ( -4.483927247898782831, 16.52544592524335698, 72.70942372801901854 ) ) ;
#116680 = CARTESIAN_POINT ( 'NONE',  ( -5.719274019375665041, -21.55341960407619695, 34.79275706135235424 ) ) ;
#116681 = CARTESIAN_POINT ( 'NONE',  ( 8.224510206698742110, 14.34966873604972548, 27.08442372801901854 ) ) ;
#116682 = CARTESIAN_POINT ( 'NONE',  ( 16.51473224551069308, 9.474510206698969483, 109.1655762719810383 ) ) ;
#116683 = CARTESIAN_POINT ( 'NONE',  ( 0.05219959533909260263, 19.03943276465977164, 34.99890960531435979 ) ) ;
#116684 = CARTESIAN_POINT ( 'NONE',  ( 13.89961937509977652, -13.97604488694527269, 53.12390960531434558 ) ) ;
#116685 = CARTESIAN_POINT ( 'NONE',  ( -14.34966873604972548, 8.224510206698743886, 43.33442372801901143 ) ) ;
#116686 = CARTESIAN_POINT ( 'NONE',  ( 4.483927247898545687, 16.52544592524342804, 89.79057627198103830 ) ) ;
#116687 = CARTESIAN_POINT ( 'NONE',  ( -14.29746914071037622, -8.314922557961029526, 94.16775706135237556 ) ) ;
#116690 = CARTESIAN_POINT ( 'NONE',  ( -19.05341960407611168, -5.049401038298163336, 66.45724293864769550 ) ) ;
#116689 = CARTESIAN_POINT ( 'NONE',  ( -13.97604488694527625, -13.89961937509977652, 71.87390960531433848 ) ) ;
#116688 = CARTESIAN_POINT ( 'NONE',  ( 18.67979575497194134, -10.72451020669871369, 45.83442372801901854 ) ) ;
#116692 = EDGE_CURVE ( 'NONE', #35595, #34840, #190457, .T. ) ;
#116691 = CARTESIAN_POINT ( 'NONE',  ( 19.03943276465977164, -0.05219959533909143690, 93.74890960531435269 ) ) ;
#116693 = CARTESIAN_POINT ( 'NONE',  ( -0.05219959533910754901, -16.53943276465976808, 37.49890960531436690 ) ) ;
#116694 = CARTESIAN_POINT ( 'NONE',  ( 12.14591786802327356, -12.06949235617739191, 100.6260903946857184 ) ) ;
#116695 = VERTEX_POINT ( 'NONE', #29475 ) ;
#116696 = CARTESIAN_POINT ( 'NONE',  ( 5.153800228976615827, -19.02544592524334988, 40.20942372801898301 ) ) ;
#116697 = CARTESIAN_POINT ( 'NONE',  ( -9.474510206698964154, 16.51473224551069663, 65.41557627198102409 ) ) ;
#116698 = CARTESIAN_POINT ( 'NONE',  ( 5.153800228976615827, -19.02544592524334988, 40.20942372801898301 ) ) ;
#116699 = CARTESIAN_POINT ( 'NONE',  ( -36.91746825000001309, -11.99521256947794789, -6.524999997268810858 ) ) ;
#116700 = CARTESIAN_POINT ( 'NONE',  ( 19.48894818550246555, -5.499999999999910294, 72.60307310435236161 ) ) ;
#116701 = CARTESIAN_POINT ( 'NONE',  ( -16.52544592524335698, -4.483927247898792601, 48.95942372801902565 ) ) ;
#116703 = CARTESIAN_POINT ( 'NONE',  ( 8.224510206698742110, 14.34966873604972548, 62.08442372801901143 ) ) ;
#116702 = CARTESIAN_POINT ( 'NONE',  ( 16.46253265017146816, 9.564922557961045513, 71.66775706135233293 ) ) ;
#116704 = CARTESIAN_POINT ( 'NONE',  ( -19.02544592524342804, 5.153800228976336051, 116.0405762719810383 ) ) ;
#116705 = CARTESIAN_POINT ( 'NONE',  ( 19.05341960407611168, 5.049401038298154454, 93.95724293864769550 ) ) ;
#116706 = CARTESIAN_POINT ( 'NONE',  ( 0.05219959533937995610, -21.53943276465977519, 20.00109039468568639 ) ) ;
#116707 = CARTESIAN_POINT ( 'NONE',  ( -9.564922557961040184, 16.46253265017147172, 77.91775706135234714 ) ) ;
#116709 = CARTESIAN_POINT ( 'NONE',  ( 16.46253265017160672, -9.564922557960803928, 33.33224293864770260 ) ) ;
#116708 = CARTESIAN_POINT ( 'NONE',  ( 0.05219959533909260263, 19.03943276465977164, 99.99890960531436690 ) ) ;
#116710 = CARTESIAN_POINT ( 'NONE',  ( -19.03943276465977164, 0.05219959533909376836, 81.24890960531436690 ) ) ;
#116712 = CARTESIAN_POINT ( 'NONE',  ( -19.02544592524342804, 5.153800228976336051, 36.04057627198100988 ) ) ;
#116711 = CARTESIAN_POINT ( 'NONE',  ( -16.53943276465976808, 0.05219959533911058130, 51.24890960531436690 ) ) ;
#116713 = CARTESIAN_POINT ( 'NONE',  ( -0.05219959533936034679, 19.03943276465977164, 57.50109039468566863 ) ) ;
#116714 = VERTEX_POINT ( 'NONE', #43645 ) ;
#116715 = CARTESIAN_POINT ( 'NONE',  ( -14.34966873604960291, -8.224510206698953496, 86.66557627198102409 ) ) ;
#116716 = CARTESIAN_POINT ( 'NONE',  ( 21.53943276465977519, 0.05219959533937863772, 106.2510903946856757 ) ) ;
#116717 = CARTESIAN_POINT ( 'NONE',  ( 9.474510206698971260, -16.51473224551069308, 57.91557627198103120 ) ) ;
#116718 = CARTESIAN_POINT ( 'NONE',  ( 18.62759615963271287, -10.81492255796078972, 53.33224293864769550 ) ) ;
#116720 = CARTESIAN_POINT ( 'NONE',  ( 5.153800228976615827, -19.02544592524334988, 20.20942372801899722 ) ) ;
#116719 = CARTESIAN_POINT ( 'NONE',  ( -14.29746914071049879, 8.314922557960819915, 55.83224293864770260 ) ) ;
#116721 = CARTESIAN_POINT ( 'NONE',  ( -16.46253265017160317, 9.564922557960807481, 100.8322429386477097 ) ) ;
#116722 = CARTESIAN_POINT ( 'NONE',  ( 5.153800228976335163, 19.02544592524342804, 114.7905762719810241 ) ) ;
#116723 = CARTESIAN_POINT ( 'NONE',  ( 5.153800228976335163, 19.02544592524342804, 34.79057627198102409 ) ) ;
#116724 = CARTESIAN_POINT ( 'NONE',  ( -0.05219959533909027116, -19.03943276465977164, 27.49890960531435624 ) ) ;
#116725 = CARTESIAN_POINT ( 'NONE',  ( 14.34966873604960469, 8.224510206698951720, 84.16557627198103830 ) ) ;
#116726 = CARTESIAN_POINT ( 'NONE',  ( -0.05219959533907301413, -21.53943276465977519, 97.49890960531436690 ) ) ;
#116727 = CARTESIAN_POINT ( 'NONE',  ( -5.153800228976328057, -19.02544592524343514, 102.2905762719810383 ) ) ;
#116728 = CARTESIAN_POINT ( 'NONE',  ( -15.72974639402197994, 15.80617190586746368, 110.6239096053143669 ) ) ;
#116729 = CARTESIAN_POINT ( 'NONE',  ( 13.89961937509977652, -13.97604488694527269, 103.1239096053143527 ) ) ;
#116731 = CARTESIAN_POINT ( 'NONE',  ( -8.314922557960811034, -14.29746914071050412, 102.0822429386476955 ) ) ;
#116730 = FACE_BOUND ( 'NONE', #140317, .T. ) ;
#116732 = CARTESIAN_POINT ( 'NONE',  ( 0.05219959533909260263, 19.03943276465977164, 64.99890960531436690 ) ) ;
#116733 = CARTESIAN_POINT ( 'NONE',  ( 15.72974639402199770, -15.80617190586745480, 78.12390960531436690 ) ) ;
#116734 = CARTESIAN_POINT ( 'NONE',  ( 16.31925111598456724, -7.325300261831551474, 107.6642453896725158 ) ) ;
#116735 = DIRECTION ( 'NONE',  ( 0.000000000000000000, 0.000000000000000000, -1.000000000000000000 ) ) ;
#116736 = CARTESIAN_POINT ( 'NONE',  ( 15.80617190586746368, 15.72974639402197994, 34.37390960531435979 ) ) ;
#116737 = CARTESIAN_POINT ( 'NONE',  ( -4.379528057220086978, -16.55341960407618274, 34.79275706135235424 ) ) ;
#116738 = CARTESIAN_POINT ( 'NONE',  ( 14.29746914071049879, -8.314922557960816363, 93.33224293864769550 ) ) ;
#116739 = DIRECTION ( 'NONE',  ( -0.000000000000000000, -0.000000000000000000, -1.000000000000000000 ) ) ;
#116740 = CARTESIAN_POINT ( 'NONE',  ( -19.03943276465977164, 0.05219959533909376836, 61.24890960531436690 ) ) ;
#116741 = CARTESIAN_POINT ( 'NONE',  ( 14.34966873604960469, 8.224510206698951720, 84.16557627198103830 ) ) ;
#116742 = CARTESIAN_POINT ( 'NONE',  ( -15.80617190586745835, -15.72974639402198527, 36.87390960531435979 ) ) ;
#116743 = CARTESIAN_POINT ( 'NONE',  ( 16.52544592524342804, -4.483927247898539470, 58.54057627198103120 ) ) ;
#116744 = CARTESIAN_POINT ( 'NONE',  ( 4.379528057220092307, 16.55341960407617563, 27.29275706135234358 ) ) ;
#116745 = CARTESIAN_POINT ( 'NONE',  ( 10.72451020669871369, 18.67979575497193778, 72.08442372801899012 ) ) ;
#116746 = CARTESIAN_POINT ( 'NONE',  ( -5.359611314223446995E-15, 29.16686587814335851, 148.3750000027311842 ) ) ;
#116747 = CARTESIAN_POINT ( 'NONE',  ( 16.46253265017160672, -9.564922557960803928, 113.3322429386476955 ) ) ;
#116748 = CARTESIAN_POINT ( 'NONE',  ( -16.52544592524335698, -4.483927247898792601, 78.95942372801901854 ) ) ;
#116749 = CARTESIAN_POINT ( 'NONE',  ( -19.02544592524342804, 5.153800228976336051, 26.04057627198103120 ) ) ;
#116750 = CARTESIAN_POINT ( 'NONE',  ( -5.153800228976328057, -19.02544592524343514, 87.29057627198103830 ) ) ;
#116751 = CARTESIAN_POINT ( 'NONE',  ( 18.62759615963271287, -10.81492255796078972, 93.33224293864769550 ) ) ;
#116752 = CARTESIAN_POINT ( 'NONE',  ( 16.53943276465976808, 0.05219959533934440121, 26.25109039468567573 ) ) ;
#116754 = CARTESIAN_POINT ( 'NONE',  ( 10.72451020669871369, 18.67979575497193778, 72.08442372801899012 ) ) ;
#116753 = CARTESIAN_POINT ( 'NONE',  ( -14.34966873604960291, -8.224510206698953496, 56.66557627198103830 ) ) ;
#116756 = CARTESIAN_POINT ( 'NONE',  ( 15.72974639402199770, -15.80617190586745480, 28.12390960531435979 ) ) ;
#116755 = CARTESIAN_POINT ( 'NONE',  ( 4.483927247898790824, -16.52544592524335698, 105.2094237280190328 ) ) ;
#116757 = CARTESIAN_POINT ( 'NONE',  ( 5.049401038298163336, -19.05341960407611168, 112.7072429386476813 ) ) ;
#116758 = CARTESIAN_POINT ( 'NONE',  ( 31.79999999999934346, 1.011436372600181938E-12, 95.00000000000021316 ) ) ;
#116759 = CARTESIAN_POINT ( 'NONE',  ( 4.483927247898790824, -16.52544592524335698, 110.2094237280190185 ) ) ;
#116760 = CARTESIAN_POINT ( 'NONE',  ( 14.34966873604972726, -8.224510206698740333, 60.83442372801901854 ) ) ;
#116761 = CARTESIAN_POINT ( 'NONE',  ( -5.153800228976328057, -19.02544592524343514, 67.29057627198102409 ) ) ;
#116762 = CARTESIAN_POINT ( 'NONE',  ( -16.51473224551069308, -9.474510206698971260, 86.66557627198102409 ) ) ;
#116763 = CARTESIAN_POINT ( 'NONE',  ( -21.53943276465977519, -0.05219959533937600094, 68.75109039468568994 ) ) ;
#116764 = CARTESIAN_POINT ( 'NONE',  ( -16.52544592524335698, -4.483927247898792601, 78.95942372801901854 ) ) ;
#116765 = CARTESIAN_POINT ( 'NONE',  ( -14.34966873604960291, -8.224510206698953496, 61.66557627198103120 ) ) ;
#116766 = CARTESIAN_POINT ( 'NONE',  ( -19.03943276465977164, 0.05219959533909376836, 61.24890960531436690 ) ) ;
#116767 = ORIENTED_EDGE ( 'NONE', *, *, #599, .F. ) ;
#116768 = CARTESIAN_POINT ( 'NONE',  ( 19.02544592524334988, 5.153800228976608722, 111.4594237280190043 ) ) ;
#116769 = CARTESIAN_POINT ( 'NONE',  ( -12.06949235617756955, 12.14591786802309770, 110.6239096053143669 ) ) ;
#116770 = CARTESIAN_POINT ( 'NONE',  ( 19.03943276465977164, -0.05219959533909143690, 83.74890960531436690 ) ) ;
#116772 = CARTESIAN_POINT ( 'NONE',  ( 38.00000000000000711, -12.34694845685040754, -7.100000000000000533 ) ) ;
#116771 = CARTESIAN_POINT ( 'NONE',  ( 13.89961937509957401, 13.97604488694547697, 96.87609039468566152 ) ) ;
#116773 = CARTESIAN_POINT ( 'NONE',  ( 5.823673210054444382, -21.52544592524334988, 105.2094237280190328 ) ) ;
#116774 = CARTESIAN_POINT ( 'NONE',  ( 12.14591786802327356, -12.06949235617739191, 80.62609039468567573 ) ) ;
#116775 = CARTESIAN_POINT ( 'NONE',  ( 19.02544592524334988, 5.153800228976608722, 91.45942372801900433 ) ) ;
#116776 = CARTESIAN_POINT ( 'NONE',  ( 21.52544592524344225, -5.823673210054117533, 58.54057627198103120 ) ) ;
#116777 = CARTESIAN_POINT ( 'NONE',  ( 14.29746914071037800, 8.314922557961029526, 56.66775706135235424 ) ) ;
#116778 = CARTESIAN_POINT ( 'NONE',  ( 7.052343178074679031, 2.552343178074557350, 1.110912703473986074 ) ) ;
#116779 = CARTESIAN_POINT ( 'NONE',  ( 0.05219959533936267826, -19.03943276465977164, 50.00109039468566863 ) ) ;
#116780 = CARTESIAN_POINT ( 'NONE',  ( 0.05219959533937995610, -21.53943276465977519, 95.00109039468568994 ) ) ;
#116781 = CARTESIAN_POINT ( 'NONE',  ( 13.89961937509977652, -13.97604488694527269, 38.12390960531436690 ) ) ;
#116782 = CARTESIAN_POINT ( 'NONE',  ( -13.97604488694527625, -13.89961937509977652, 71.87390960531433848 ) ) ;
#116783 = CARTESIAN_POINT ( 'NONE',  ( -12.14591786802309592, -12.06949235617757132, 61.87390960531436690 ) ) ;
#116784 = CARTESIAN_POINT ( 'NONE',  ( 5.823673210054444382, -21.52544592524334988, 90.20942372801903275 ) ) ;
#116785 = CARTESIAN_POINT ( 'NONE',  ( -5.153800228976607833, 19.02544592524334988, 47.70942372801900433 ) ) ;
#116786 = CARTESIAN_POINT ( 'NONE',  ( -13.97604488694547697, 13.89961937509957934, 48.12609039468566863 ) ) ;
#116787 = CARTESIAN_POINT ( 'NONE',  ( -15.80617190586745835, -15.72974639402198527, 31.87390960531435979 ) ) ;
#116788 = CARTESIAN_POINT ( 'NONE',  ( 15.80617190586769283, -15.72974639402175789, 100.6260903946857184 ) ) ;
#116789 = CARTESIAN_POINT ( 'NONE',  ( 19.02544592524343514, -5.153800228976328945, 78.54057627198099567 ) ) ;
#116790 = CARTESIAN_POINT ( 'NONE',  ( -0.05219959533937732626, 21.53943276465977519, 87.50109039468568994 ) ) ;
#116791 = CARTESIAN_POINT ( 'NONE',  ( 21.55341960407610458, 5.719274019375980345, 53.95724293864770260 ) ) ;
#116792 = CARTESIAN_POINT ( 'NONE',  ( 9.474510206698971260, -16.51473224551069308, 82.91557627198103830 ) ) ;
#116793 = CARTESIAN_POINT ( 'NONE',  ( -13.97604488694547697, 13.89961937509957934, 78.12609039468567573 ) ) ;
#116794 = CARTESIAN_POINT ( 'NONE',  ( 19.02544592524343514, -5.153800228976328945, 93.54057627198102409 ) ) ;
#116795 = EDGE_CURVE ( 'NONE', #111465, #56681, #62082, .T. ) ;
#116796 = CARTESIAN_POINT ( 'NONE',  ( -13.97604488694547697, 13.89961937509957934, 98.12609039468566152 ) ) ;
#116797 = CARTESIAN_POINT ( 'NONE',  ( -16.55341960407617563, 4.379528057220093196, 43.54275706135235424 ) ) ;
#116798 = CARTESIAN_POINT ( 'NONE',  ( 8.224510206698953496, -14.34966873604960469, 107.9155762719810241 ) ) ;
#116799 = CARTESIAN_POINT ( 'NONE',  ( 0.05219959533909260263, 19.03943276465977164, 74.99890960531435269 ) ) ;
#116800 = CARTESIAN_POINT ( 'NONE',  ( -18.67979575497178146, -10.72451020669898902, 56.66557627198103830 ) ) ;
#116801 = CARTESIAN_POINT ( 'NONE',  ( -16.52544592524335698, -4.483927247898792601, 28.95942372801902209 ) ) ;
#116802 = CARTESIAN_POINT ( 'NONE',  ( 21.55341960407619695, -5.719274019375665929, 31.04275706135234714 ) ) ;
#116803 = CARTESIAN_POINT ( 'NONE',  ( -5.823673210054431948, 21.52544592524334988, 77.70942372801900433 ) ) ;
#116804 = CARTESIAN_POINT ( 'NONE',  ( 0.05219959533934541429, -16.53943276465976808, 85.00109039468568994 ) ) ;
#116805 = CARTESIAN_POINT ( 'NONE',  ( -9.564922557960796823, -16.46253265017161027, 77.08224293864769550 ) ) ;
#116806 = CARTESIAN_POINT ( 'NONE',  ( -16.55341960407611168, -4.379528057220339221, 76.45724293864769550 ) ) ;
#116807 = CARTESIAN_POINT ( 'NONE',  ( -16.55341960407617563, 4.379528057220093196, 108.5427570613523756 ) ) ;
#116808 = CARTESIAN_POINT ( 'NONE',  ( -16.51473224551082808, 9.474510206698731452, 58.33442372801900433 ) ) ;
#116809 = CARTESIAN_POINT ( 'NONE',  ( 21.52544592524334988, 5.823673210054432836, 36.45942372801901143 ) ) ;
#116810 = EDGE_CURVE ( 'NONE', #77030, #146728, #125938, .T. ) ;
#116811 = CARTESIAN_POINT ( 'NONE',  ( 8.314922557960818139, 14.29746914071049879, 84.58224293864769550 ) ) ;
#116812 = CARTESIAN_POINT ( 'NONE',  ( -16.46253265017160317, 9.564922557960807481, 105.8322429386476955 ) ) ;
#116813 = CARTESIAN_POINT ( 'NONE',  ( -0.05219959533934338120, 16.53943276465976808, 97.50109039468567573 ) ) ;
#116814 = CARTESIAN_POINT ( 'NONE',  ( 18.67979575497194134, -10.72451020669871369, 75.83442372801900433 ) ) ;
#116815 = CARTESIAN_POINT ( 'NONE',  ( -12.06949235617739369, -12.14591786802326823, 49.37609039468569705 ) ) ;
#116816 = CARTESIAN_POINT ( 'NONE',  ( 0.05219959533937995610, -21.53943276465977519, 25.00109039468567218 ) ) ;
#116817 = CARTESIAN_POINT ( 'NONE',  ( 4.379528057220339221, -16.55341960407611168, 77.70724293864770971 ) ) ;
#116818 = ORIENTED_EDGE ( 'NONE', *, *, #42863, .T. ) ;
#116819 = CARTESIAN_POINT ( 'NONE',  ( 15.80617190586746368, 15.72974639402197994, 109.3739096053143811 ) ) ;
#116820 = CARTESIAN_POINT ( 'NONE',  ( -14.34966873604960291, -8.224510206698953496, 56.66557627198103830 ) ) ;
#116821 = CARTESIAN_POINT ( 'NONE',  ( -9.564922557960796823, -16.46253265017161027, 22.08224293864768839 ) ) ;
#116822 = CARTESIAN_POINT ( 'NONE',  ( 5.719274019375991003, -21.55341960407610458, 32.70724293864770260 ) ) ;
#116823 = CARTESIAN_POINT ( 'NONE',  ( -14.34966873604960291, -8.224510206698953496, 61.66557627198103120 ) ) ;
#116824 = CARTESIAN_POINT ( 'NONE',  ( 21.53943276465977519, -0.05219959533907433946, 83.74890960531435269 ) ) ;
#116825 = CARTESIAN_POINT ( 'NONE',  ( 5.049401038298161559, -19.05341960407611168, 72.70724293864768129 ) ) ;
#116827 = CARTESIAN_POINT ( 'NONE',  ( -0.05219959533936034679, 19.03943276465977164, 82.50109039468567573 ) ) ;
#116826 = CARTESIAN_POINT ( 'NONE',  ( -9.474510206698964154, 16.51473224551069663, 40.41557627198103120 ) ) ;
#116829 = CARTESIAN_POINT ( 'NONE',  ( -21.55341960407610458, -5.719274019375992779, 56.45724293864768839 ) ) ;
#116828 = CARTESIAN_POINT ( 'NONE',  ( 15.80617190586769283, -15.72974639402175789, 50.62609039468568994 ) ) ;
#116830 = CARTESIAN_POINT ( 'NONE',  ( -19.03943276465977164, 0.05219959533909376836, 46.24890960531435979 ) ) ;
#116831 = CARTESIAN_POINT ( 'NONE',  ( -5.153800228976328057, -19.02544592524343514, 72.29057627198102409 ) ) ;
#116832 = VERTEX_POINT ( 'NONE', #63777 ) ;
#116833 = CARTESIAN_POINT ( 'NONE',  ( -12.06949235617739369, -12.14591786802326823, 49.37609039468569705 ) ) ;
#116834 = CARTESIAN_POINT ( 'NONE',  ( -15.80617190586768217, 15.72974639402176855, 33.12609039468569705 ) ) ;
#116835 = EDGE_CURVE ( 'NONE', #60581, #57298, #135633, .T. ) ;
#116836 = CARTESIAN_POINT ( 'NONE',  ( 21.55341960407619695, -5.719274019375665929, 66.04275706135236135 ) ) ;
#116837 = CARTESIAN_POINT ( 'NONE',  ( -9.474510206698964154, 16.51473224551069663, 110.4155762719810383 ) ) ;
#116838 = CARTESIAN_POINT ( 'NONE',  ( 10.81492255796078972, 18.62759615963270932, 89.58224293864768129 ) ) ;
#116840 = CARTESIAN_POINT ( 'NONE',  ( -14.29746914071037622, -8.314922557961029526, 54.16775706135235424 ) ) ;
#116839 = CARTESIAN_POINT ( 'NONE',  ( 0.05219959533937995610, -21.53943276465977519, 20.00109039468568639 ) ) ;
#116841 = CARTESIAN_POINT ( 'NONE',  ( 5.823673210054125526, 21.52544592524343514, 44.79057627198103120 ) ) ;
#116842 = CARTESIAN_POINT ( 'NONE',  ( -10.81492255796105439, 18.62759615963255655, 112.9177570613523329 ) ) ;
#116843 = CARTESIAN_POINT ( 'NONE',  ( -19.03943276465977164, 0.05219959533909376836, 61.24890960531436690 ) ) ;
#116844 = CARTESIAN_POINT ( 'NONE',  ( 9.474510206698971260, -16.51473224551069308, 107.9155762719810383 ) ) ;
#116845 = CARTESIAN_POINT ( 'NONE',  ( -13.97604488694527625, -13.89961937509977652, 86.87390960531436690 ) ) ;
#116846 = CARTESIAN_POINT ( 'NONE',  ( 30.00000000000000355, 0.3535533905932735643, 4.646446609406718942 ) ) ;
#116847 = CARTESIAN_POINT ( 'NONE',  ( -5.049401038297874678, -19.05341960407617918, 74.79275706135231871 ) ) ;
#116848 = CARTESIAN_POINT ( 'NONE',  ( -0.05219959533907301413, -21.53943276465977519, 47.49890960531435979 ) ) ;
#116849 = CARTESIAN_POINT ( 'NONE',  ( -0.05219959533910754901, -16.53943276465976808, 22.49890960531436335 ) ) ;
#116850 = CARTESIAN_POINT ( 'NONE',  ( -5.153800228976607833, 19.02544592524334988, 87.70942372801897591 ) ) ;
#116851 = CARTESIAN_POINT ( 'NONE',  ( -13.97604488694527625, -13.89961937509977652, 21.87390960531435979 ) ) ;
#116852 = CARTESIAN_POINT ( 'NONE',  ( 10.72451020669871369, 18.67979575497193778, 112.0844237280190185 ) ) ;
#116853 = CARTESIAN_POINT ( 'NONE',  ( -9.474510206698720793, -16.51473224551083518, 99.58442372801900433 ) ) ;
#116854 = CARTESIAN_POINT ( 'NONE',  ( 5.049401038297881783, 19.05341960407617563, 42.29275706135234003 ) ) ;
#116855 = CARTESIAN_POINT ( 'NONE',  ( 23.64874990377911246, -15.04272038711346937, 165.8682408883346397 ) ) ;
#116856 = CARTESIAN_POINT ( 'NONE',  ( -5.049401038298153566, 19.05341960407611168, 50.20724293864770260 ) ) ;
#116857 = CARTESIAN_POINT ( 'NONE',  ( 14.34966873604960469, 8.224510206698951720, 64.16557627198102409 ) ) ;
#116858 = CARTESIAN_POINT ( 'NONE',  ( 9.564922557960805705, 16.46253265017160317, 34.58224293864770260 ) ) ;
#116859 = CARTESIAN_POINT ( 'NONE',  ( 14.34966873604960469, 8.224510206698951720, 34.16557627198102409 ) ) ;
#116860 = CARTESIAN_POINT ( 'NONE',  ( 17.72696623605163779, -5.499999999999864997, 56.09811031808416715 ) ) ;
#116861 = CARTESIAN_POINT ( 'NONE',  ( 8.224510206698742110, 14.34966873604972548, 102.0844237280190185 ) ) ;
#116862 = CARTESIAN_POINT ( 'NONE',  ( -5.153800228976328057, -19.02544592524343514, 57.29057627198103120 ) ) ;
#116863 = CARTESIAN_POINT ( 'NONE',  ( -9.564922557961040184, 16.46253265017147172, 27.91775706135232582 ) ) ;
#116864 = CARTESIAN_POINT ( 'NONE',  ( 8.224510206698742110, 14.34966873604972548, 27.08442372801901854 ) ) ;
#116865 = CARTESIAN_POINT ( 'NONE',  ( -21.55341960407610458, -5.719274019375992779, 41.45724293864769550 ) ) ;
#116867 = ORIENTED_EDGE ( 'NONE', *, *, #62255, .F. ) ;
#116866 = CARTESIAN_POINT ( 'NONE',  ( -18.62759615963255300, -10.81492255796106328, 109.1677570613523613 ) ) ;
#116868 = CARTESIAN_POINT ( 'NONE',  ( 9.564922557960805705, 16.46253265017160317, 64.58224293864769550 ) ) ;
#116869 = CARTESIAN_POINT ( 'NONE',  ( -19.05341960407611168, -5.049401038298163336, 106.4572429386476955 ) ) ;
#116870 = CARTESIAN_POINT ( 'NONE',  ( -19.05341960407611168, -5.049401038298163336, 101.4572429386476955 ) ) ;
#116871 = CARTESIAN_POINT ( 'NONE',  ( -36.91746825000000598, 11.99521256947798520, -4.724999997268811924 ) ) ;
#116872 = CARTESIAN_POINT ( 'NONE',  ( -21.52544592524334988, -5.823673210054445271, 28.95942372801902209 ) ) ;
#116873 = CARTESIAN_POINT ( 'NONE',  ( -16.55341960407611168, -4.379528057220339221, 96.45724293864770971 ) ) ;
#116875 = CARTESIAN_POINT ( 'NONE',  ( -5.153800228976328057, -19.02544592524343514, 72.29057627198102409 ) ) ;
#116874 = CARTESIAN_POINT ( 'NONE',  ( 21.52544592524344225, -5.823673210054117533, 73.54057627198102409 ) ) ;
#116876 = CARTESIAN_POINT ( 'NONE',  ( 0.05219959533909260263, 19.03943276465977164, 79.99890960531436690 ) ) ;
#116877 = CARTESIAN_POINT ( 'NONE',  ( -5.823673210054116645, -21.52544592524344225, 107.2905762719810525 ) ) ;
#116878 = ORIENTED_EDGE ( 'NONE', *, *, #33729, .F. ) ;
#116879 = CARTESIAN_POINT ( 'NONE',  ( 13.97604488694527802, 13.89961937509977652, 74.37390960531436690 ) ) ;
#116880 = LINE ( 'NONE', #132054, #94792 ) ;
#116882 = DIRECTION ( 'NONE',  ( 1.000000000000000000, 0.000000000000000000, -0.000000000000000000 ) ) ;
#116881 = CARTESIAN_POINT ( 'NONE',  ( -14.29746914071049879, 8.314922557960819915, 105.8322429386476955 ) ) ;
#116883 = CARTESIAN_POINT ( 'NONE',  ( 0.05219959533909260263, 19.03943276465977164, 64.99890960531436690 ) ) ;
#116884 = CARTESIAN_POINT ( 'NONE',  ( 16.51473224551083163, -9.474510206698727899, 90.83442372801900433 ) ) ;
#116885 = CARTESIAN_POINT ( 'NONE',  ( 16.53943276465976808, -0.05219959533910856209, 93.74890960531436690 ) ) ;
#116886 = CARTESIAN_POINT ( 'NONE',  ( 10.81492255796106328, -18.62759615963255655, 75.41775706135233293 ) ) ;
#116888 = CARTESIAN_POINT ( 'NONE',  ( -5.823673210054431948, 21.52544592524334988, 22.70942372801901499 ) ) ;
#116887 = CARTESIAN_POINT ( 'NONE',  ( -9.474510206698964154, 16.51473224551069663, 45.41557627198103120 ) ) ;
#116889 = CARTESIAN_POINT ( 'NONE',  ( 10.72451020669898902, -18.67979575497178502, 107.9155762719810241 ) ) ;
#116890 = CARTESIAN_POINT ( 'NONE',  ( 23.31738231874054534, 16.94106989632529192, 143.1999999999999886 ) ) ;
#116891 = CARTESIAN_POINT ( 'NONE',  ( -19.03943276465977164, 0.05219959533909376836, 66.24890960531436690 ) ) ;
#116892 = CARTESIAN_POINT ( 'NONE',  ( 17.44279575226824974, 5.990770900252419651, 111.6644243248568245 ) ) ;
#116894 = CARTESIAN_POINT ( 'NONE',  ( -15.80617190586745835, -15.72974639402198527, 36.87390960531435979 ) ) ;
#116893 = CARTESIAN_POINT ( 'NONE',  ( -5.153800228976607833, 19.02544592524334988, 102.7094237280189759 ) ) ;
#116895 = CARTESIAN_POINT ( 'NONE',  ( -21.55341960407619339, 5.719274019375674811, 58.54275706135235424 ) ) ;
#116896 = CARTESIAN_POINT ( 'NONE',  ( 9.564922557960805705, 16.46253265017160317, 94.58224293864769550 ) ) ;
#116897 = CARTESIAN_POINT ( 'NONE',  ( 16.51473224551083163, -9.474510206698727899, 80.83442372801899012 ) ) ;
#116898 = CARTESIAN_POINT ( 'NONE',  ( -0.05219959533909027116, -19.03943276465977164, 52.49890960531436690 ) ) ;
#116899 = CARTESIAN_POINT ( 'NONE',  ( 5.153800228976335163, 19.02544592524342804, 64.79057627198100988 ) ) ;
#116900 = CARTESIAN_POINT ( 'NONE',  ( -16.52544592524342804, 4.483927247898546575, 86.04057627198102409 ) ) ;
#116901 = CARTESIAN_POINT ( 'NONE',  ( -9.564922557960796823, -16.46253265017161027, 97.08224293864769550 ) ) ;
#116902 = CARTESIAN_POINT ( 'NONE',  ( 8.314922557960818139, 14.29746914071049879, 94.58224293864769550 ) ) ;
#116903 = CARTESIAN_POINT ( 'NONE',  ( -13.89961937509977652, 13.97604488694528158, 100.6239096053143669 ) ) ;
#116905 = CARTESIAN_POINT ( 'NONE',  ( -5.153800228976328057, -19.02544592524343514, 32.29057627198102409 ) ) ;
#116904 = CARTESIAN_POINT ( 'NONE',  ( -16.53943276465976808, 0.05219959533911058130, 41.24890960531435269 ) ) ;
#116906 = ORIENTED_EDGE ( 'NONE', *, *, #75822, .F. ) ;
#116907 = CARTESIAN_POINT ( 'NONE',  ( -21.52544592524334988, -5.823673210054445271, 53.95942372801900433 ) ) ;
#116908 = CARTESIAN_POINT ( 'NONE',  ( -13.89961937509957401, -13.97604488694547875, 74.37609039468566152 ) ) ;
#116909 = CARTESIAN_POINT ( 'NONE',  ( -8.224510206698948167, 14.34966873604960824, 50.41557627198103120 ) ) ;
#116910 = CARTESIAN_POINT ( 'NONE',  ( -18.67979575497178146, -10.72451020669898902, 101.6655762719810383 ) ) ;
#116911 = CARTESIAN_POINT ( 'NONE',  ( -15.80617190586745835, -15.72974639402198527, 31.87390960531435979 ) ) ;
#116912 = CARTESIAN_POINT ( 'NONE',  ( 12.06949235617757843, -12.14591786802309237, 88.12390960531436690 ) ) ;
#116913 = CARTESIAN_POINT ( 'NONE',  ( -5.049401038298153566, 19.05341960407611168, 55.20724293864769550 ) ) ;
#116914 = CARTESIAN_POINT ( 'NONE',  ( 0.05219959533910956823, 16.53943276465976808, 24.99890960531435624 ) ) ;
#116915 = CARTESIAN_POINT ( 'NONE',  ( -4.379528057220086978, -16.55341960407618274, 99.79275706135234714 ) ) ;
#116916 = CARTESIAN_POINT ( 'NONE',  ( 4.483927247898790824, -16.52544592524335698, 75.20942372801901854 ) ) ;
#116917 = CARTESIAN_POINT ( 'NONE',  ( 0.05219959533936267826, -19.03943276465977164, 20.00109039468567218 ) ) ;
#116918 = CARTESIAN_POINT ( 'NONE',  ( 5.153800228976335163, 19.02544592524342804, 99.79057627198102409 ) ) ;
#116919 = CARTESIAN_POINT ( 'NONE',  ( -13.97604488694527625, -13.89961937509977652, 76.87390960531433848 ) ) ;
#116920 = CARTESIAN_POINT ( 'NONE',  ( -16.46253265017160317, 9.564922557960807481, 40.83224293864769550 ) ) ;
#116921 = CARTESIAN_POINT ( 'NONE',  ( 16.53943276465976808, -0.05219959533910856209, 43.74890960531435979 ) ) ;
#116923 = CARTESIAN_POINT ( 'NONE',  ( 13.97604488694527802, 13.89961937509977652, 109.3739096053143669 ) ) ;
#116922 = CARTESIAN_POINT ( 'NONE',  ( 5.153800228976335163, 19.02544592524342804, 114.7905762719810241 ) ) ;
#116924 = CARTESIAN_POINT ( 'NONE',  ( 21.52544592524344225, -5.823673210054117533, 38.54057627198103120 ) ) ;
#116925 = CARTESIAN_POINT ( 'NONE',  ( 8.314922557960818139, 14.29746914071049879, 74.58224293864768129 ) ) ;
#116926 = CARTESIAN_POINT ( 'NONE',  ( 14.29746914071037800, 8.314922557961029526, 21.66775706135235069 ) ) ;
#116927 = EDGE_LOOP ( 'NONE', ( #11959, #135427, #197425, #47827, #38985, #97999 ) ) ;
#116928 = CARTESIAN_POINT ( 'NONE',  ( -16.55341960407611168, -4.379528057220339221, 61.45724293864770260 ) ) ;
#116929 = FACE_OUTER_BOUND ( 'NONE', #169156, .T. ) ;
#116930 = CARTESIAN_POINT ( 'NONE',  ( -19.02544592524334988, -5.153800228976617603, 58.95942372801900433 ) ) ;
#116931 = CARTESIAN_POINT ( 'NONE',  ( -9.564922557960796823, -16.46253265017161027, 102.0822429386477097 ) ) ;
#116932 = CARTESIAN_POINT ( 'NONE',  ( -0.05219959533936034679, 19.03943276465977164, 77.50109039468566152 ) ) ;
#116933 = CARTESIAN_POINT ( 'NONE',  ( 27.73933785331498214, 9.013057229001095294, 148.4750000027311785 ) ) ;
#116935 = CARTESIAN_POINT ( 'NONE',  ( 12.14591786802327356, -12.06949235617739191, 100.6260903946857184 ) ) ;
#116934 = CARTESIAN_POINT ( 'NONE',  ( 5.049401038297881783, 19.05341960407617563, 107.2927570613523187 ) ) ;
#116936 = CARTESIAN_POINT ( 'NONE',  ( -13.89961937509977652, 13.97604488694528158, 45.62390960531433848 ) ) ;
#116937 = CARTESIAN_POINT ( 'NONE',  ( -10.72451020669898014, 18.67979575497178502, 35.41557627198102409 ) ) ;
#116938 = CARTESIAN_POINT ( 'NONE',  ( -10.81492255796105439, 18.62759615963255655, 52.91775706135235424 ) ) ;
#116939 = CARTESIAN_POINT ( 'NONE',  ( 19.33860699428957375, 5.500000000000045297, 38.39890772129063379 ) ) ;
#116940 = CARTESIAN_POINT ( 'NONE',  ( 12.06949235617739724, 12.14591786802326823, 21.87609039468567573 ) ) ;
#116942 = CARTESIAN_POINT ( 'NONE',  ( 16.51473224551069308, 9.474510206698969483, 69.16557627198102409 ) ) ;
#116941 = CARTESIAN_POINT ( 'NONE',  ( 17.50000000000000000, 4.189786006557876696, 22.00000000000000711 ) ) ;
#116943 = CARTESIAN_POINT ( 'NONE',  ( -11.74149087413295511, 36.13659316521247433, -0.4021577739498228832 ) ) ;
#116945 = CARTESIAN_POINT ( 'NONE',  ( -9.474510206698964154, 16.51473224551069663, 80.41557627198103830 ) ) ;
#116944 = CARTESIAN_POINT ( 'NONE',  ( -12.14591786802309592, -12.06949235617757132, 86.87390960531438111 ) ) ;
#116946 = ITEM_DEFINED_TRANSFORMATION ( 'NONE', 'NONE', #153245,  #82054 ) ;
#116947 = CARTESIAN_POINT ( 'NONE',  ( 9.474510206698971260, -16.51473224551069308, 92.91557627198103830 ) ) ;
#116948 = ORIENTED_EDGE ( 'NONE', *, *, #169870, .T. ) ;
#116949 = CARTESIAN_POINT ( 'NONE',  ( 5.049401038297881783, 19.05341960407617563, 97.29275706135233293 ) ) ;
#116950 = CARTESIAN_POINT ( 'NONE',  ( 10.81492255796078972, 18.62759615963270932, 64.58224293864769550 ) ) ;
#116951 = CARTESIAN_POINT ( 'NONE',  ( -5.049401038298153566, 19.05341960407611168, 30.20724293864768839 ) ) ;
#116952 = CARTESIAN_POINT ( 'NONE',  ( -19.05341960407617563, 5.049401038297882671, 53.54275706135231871 ) ) ;
#116953 = CARTESIAN_POINT ( 'NONE',  ( 0.05219959533909260263, 19.03943276465977164, 49.99890960531435979 ) ) ;
#116955 = EDGE_CURVE ( 'NONE', #73688, #165524, #102396, .T. ) ;
#116954 = CARTESIAN_POINT ( 'NONE',  ( 13.97604488694527802, 13.89961937509977652, 99.37390960531436690 ) ) ;
#116956 = VERTEX_POINT ( 'NONE', #166996 ) ;
#116957 = CARTESIAN_POINT ( 'NONE',  ( -21.55341960407610458, -5.719274019375992779, 96.45724293864770971 ) ) ;
#116960 = CARTESIAN_POINT ( 'NONE',  ( 0.05219959533936267826, -19.03943276465977164, 60.00109039468566863 ) ) ;
#116959 = CARTESIAN_POINT ( 'NONE',  ( -19.02544592524342804, 5.153800228976336051, 86.04057627198103830 ) ) ;
#116958 = CARTESIAN_POINT ( 'NONE',  ( 12.14591786802309770, 12.06949235617756955, 89.37390960531435269 ) ) ;
#116961 = CARTESIAN_POINT ( 'NONE',  ( -21.55341960407610458, -5.719274019375992779, 86.45724293864770971 ) ) ;
#116962 = CARTESIAN_POINT ( 'NONE',  ( 15.80617190586746368, 15.72974639402197994, 79.37390960531436690 ) ) ;
#116963 = CARTESIAN_POINT ( 'NONE',  ( 8.314922557960818139, 14.29746914071049879, 29.58224293864769905 ) ) ;
#116964 = CARTESIAN_POINT ( 'NONE',  ( 10.81492255796106328, -18.62759615963255655, 110.4177570613523756 ) ) ;
#116965 = CARTESIAN_POINT ( 'NONE',  ( 12.06949235617739724, 12.14591786802326823, 51.87609039468568284 ) ) ;
#116966 = CARTESIAN_POINT ( 'NONE',  ( -19.02544592524342804, 5.153800228976336051, 86.04057627198103830 ) ) ;
#116967 = CARTESIAN_POINT ( 'NONE',  ( 19.02544592524343514, -5.153800228976328945, 28.54057627198102409 ) ) ;
#116968 = CARTESIAN_POINT ( 'NONE',  ( -10.81492255796105439, 18.62759615963255655, 32.91775706135234714 ) ) ;
#116969 = CARTESIAN_POINT ( 'NONE',  ( -18.62759615963255300, -10.81492255796106328, 54.16775706135235424 ) ) ;
#116970 = CARTESIAN_POINT ( 'NONE',  ( -19.03943276465977164, 0.05219959533909376836, 46.24890960531435979 ) ) ;
#116971 = CARTESIAN_POINT ( 'NONE',  ( -21.53943276465977519, -0.05219959533937600094, 18.75109039468568639 ) ) ;
#116972 = CARTESIAN_POINT ( 'NONE',  ( 9.564922557961047289, -16.46253265017146816, 55.41775706135234003 ) ) ;
#116973 = CARTESIAN_POINT ( 'NONE',  ( 19.05341960407617918, -5.049401038297876454, 71.04275706135234714 ) ) ;
#116974 = CARTESIAN_POINT ( 'NONE',  ( 9.474510206698971260, -16.51473224551069308, 27.91557627198103120 ) ) ;
#116975 = CARTESIAN_POINT ( 'NONE',  ( -4.483927247898782831, 16.52544592524335698, 77.70942372801900433 ) ) ;
#116976 = CARTESIAN_POINT ( 'NONE',  ( 5.153800228976335163, 19.02544592524342804, 49.79057627198100988 ) ) ;
#116977 = CARTESIAN_POINT ( 'NONE',  ( 24.81886791266633097, -6.075537473402710553, 168.3989613422507432 ) ) ;
#116978 = CARTESIAN_POINT ( 'NONE',  ( 5.049401038298161559, -19.05341960407611168, 92.70724293864769550 ) ) ;
#116979 = CARTESIAN_POINT ( 'NONE',  ( 12.14591786802309770, 12.06949235617756955, 114.3739096053143527 ) ) ;
#116980 = CARTESIAN_POINT ( 'NONE',  ( 21.55341960407610458, 5.719274019375980345, 78.95724293864769550 ) ) ;
#116981 = CARTESIAN_POINT ( 'NONE',  ( 0.05219959533934541429, -16.53943276465976808, 55.00109039468568284 ) ) ;
#116982 = CARTESIAN_POINT ( 'NONE',  ( 19.05341960407617918, -5.049401038297876454, 21.04275706135232582 ) ) ;
#116983 = CARTESIAN_POINT ( 'NONE',  ( -0.05219959533909027116, -19.03943276465977164, 47.49890960531435979 ) ) ;
#116984 = CARTESIAN_POINT ( 'NONE',  ( 4.379528057220339221, -16.55341960407611168, 32.70724293864770260 ) ) ;
#116985 = CARTESIAN_POINT ( 'NONE',  ( 8.224510206698953496, -14.34966873604960469, 67.91557627198102409 ) ) ;
#116986 = CARTESIAN_POINT ( 'NONE',  ( 5.153800228976335163, 19.02544592524342804, 79.79057627198102409 ) ) ;
#116987 = CARTESIAN_POINT ( 'NONE',  ( -18.67979575497193778, 10.72451020669871902, 43.33442372801901143 ) ) ;
#116988 = CARTESIAN_POINT ( 'NONE',  ( 13.89961937509977652, -13.97604488694527269, 93.12390960531436690 ) ) ;
#116989 = CARTESIAN_POINT ( 'NONE',  ( 5.823673210054444382, -21.52544592524334988, 85.20942372801901854 ) ) ;
#116990 = CARTESIAN_POINT ( 'NONE',  ( -16.53943276465976808, -0.05219959533934237506, 68.75109039468568994 ) ) ;
#116991 = CARTESIAN_POINT ( 'NONE',  ( -5.153800228976328057, -19.02544592524343514, 112.2905762719810099 ) ) ;
#116992 = CARTESIAN_POINT ( 'NONE',  ( 5.823673210054125526, 21.52544592524343514, 89.79057627198103830 ) ) ;
#116993 = CARTESIAN_POINT ( 'NONE',  ( 14.29746914071049879, -8.314922557960816363, 43.33224293864769550 ) ) ;
#116994 = CARTESIAN_POINT ( 'NONE',  ( -9.474510206698964154, 16.51473224551069663, 30.41557627198102054 ) ) ;
#116995 = CARTESIAN_POINT ( 'NONE',  ( -16.52544592524335698, -4.483927247898792601, 53.95942372801900433 ) ) ;
#116996 = CARTESIAN_POINT ( 'NONE',  ( 12.06949235617757843, -12.14591786802309237, 68.12390960531436690 ) ) ;
#116997 = CARTESIAN_POINT ( 'NONE',  ( 0.05219959533909260263, 19.03943276465977164, 109.9989096053143669 ) ) ;
#116998 = CARTESIAN_POINT ( 'NONE',  ( -15.80617190586745835, -15.72974639402198527, 36.87390960531435979 ) ) ;
#116999 = CARTESIAN_POINT ( 'NONE',  ( -18.67979575497193778, 10.72451020669871902, 113.3344237280190328 ) ) ;
#117000 = CARTESIAN_POINT ( 'NONE',  ( -8.314922557960811034, -14.29746914071050412, 102.0822429386476955 ) ) ;
#117001 = CARTESIAN_POINT ( 'NONE',  ( 19.02544592524343514, -5.153800228976328945, 103.5405762719809957 ) ) ;
#117002 = VERTEX_POINT ( 'NONE', #97 ) ;
#117003 = CARTESIAN_POINT ( 'NONE',  ( 16.52544592524335698, 4.483927247898782831, 56.45942372801902565 ) ) ;
#117004 = CARTESIAN_POINT ( 'NONE',  ( -9.564922557960796823, -16.46253265017161027, 57.08224293864769550 ) ) ;
#117005 = FACE_OUTER_BOUND ( 'NONE', #21341, .T. ) ;
#117006 = CARTESIAN_POINT ( 'NONE',  ( 19.02544592524334988, 5.153800228976608722, 51.45942372801900433 ) ) ;
#117007 = CARTESIAN_POINT ( 'NONE',  ( 14.29746914071037800, 8.314922557961029526, 96.66775706135234714 ) ) ;
#117008 = CARTESIAN_POINT ( 'NONE',  ( -9.564922557961040184, 16.46253265017147172, 92.91775706135233293 ) ) ;
#117009 = CARTESIAN_POINT ( 'NONE',  ( 21.55341960407619695, -5.719274019375665929, 61.04275706135234714 ) ) ;
#117010 = CARTESIAN_POINT ( 'NONE',  ( -5.049401038298153566, 19.05341960407611168, 75.20724293864769550 ) ) ;
#117011 = CARTESIAN_POINT ( 'NONE',  ( 10.81492255796078972, 18.62759615963270932, 89.58224293864768129 ) ) ;
#117012 = CARTESIAN_POINT ( 'NONE',  ( -16.52544592524342804, 4.483927247898546575, 106.0405762719810525 ) ) ;
#117013 = CARTESIAN_POINT ( 'NONE',  ( -19.03943276465977164, -0.05219959533935918106, 78.75109039468567573 ) ) ;
#117014 = CARTESIAN_POINT ( 'NONE',  ( 5.719274019375991003, -21.55341960407610458, 77.70724293864770971 ) ) ;
#117015 = CARTESIAN_POINT ( 'NONE',  ( -0.05219959533936034679, 19.03943276465977164, 37.50109039468567573 ) ) ;
#117016 = CARTESIAN_POINT ( 'NONE',  ( 4.500000000000000888, -120.9454340326537505, 15.08688922109887187 ) ) ;
#117017 = CARTESIAN_POINT ( 'NONE',  ( -10.72451020669898014, 18.67979575497178502, 85.41557627198102409 ) ) ;
#117018 = CARTESIAN_POINT ( 'NONE',  ( -19.52217212775657984, 5.500000000000115463, 54.93993709005259518 ) ) ;
#117019 = CARTESIAN_POINT ( 'NONE',  ( 19.02544592524343514, -5.153800228976328945, 68.54057627198103830 ) ) ;
#117020 = CARTESIAN_POINT ( 'NONE',  ( -17.59860650958991002, -7.585241751807008548, 91.57662985737506744 ) ) ;
#117021 = CARTESIAN_POINT ( 'NONE',  ( 19.05341960407617918, -5.049401038297876454, 111.0427570613523329 ) ) ;
#117022 = CARTESIAN_POINT ( 'NONE',  ( -16.51473224551082808, 9.474510206698731452, 98.33442372801900433 ) ) ;
#117023 = CARTESIAN_POINT ( 'NONE',  ( 9.564922557960805705, 16.46253265017160317, 44.58224293864769550 ) ) ;
#117024 = CARTESIAN_POINT ( 'NONE',  ( -5.823673210054116645, -21.52544592524344225, 22.29057627198102765 ) ) ;
#117026 = CARTESIAN_POINT ( 'NONE',  ( 0.05219959533910956823, 16.53943276465976808, 44.99890960531435979 ) ) ;
#117025 = CARTESIAN_POINT ( 'NONE',  ( 15.80617190586746368, 15.72974639402197994, 104.3739096053143669 ) ) ;
#117027 = CARTESIAN_POINT ( 'NONE',  ( -21.55341960407619339, 5.719274019375674811, 78.54275706135236135 ) ) ;
#117029 = CARTESIAN_POINT ( 'NONE',  ( 13.89961937509957401, 13.97604488694547697, 31.87609039468566863 ) ) ;
#117028 = CARTESIAN_POINT ( 'NONE',  ( 14.29746914071037800, 8.314922557961029526, 26.66775706135235424 ) ) ;
#117030 = CARTESIAN_POINT ( 'NONE',  ( -16.53943276465976808, 0.05219959533911058130, 31.24890960531435979 ) ) ;
#117031 = CARTESIAN_POINT ( 'NONE',  ( 15.80617190586769283, -15.72974639402175789, 20.62609039468568639 ) ) ;
#117032 = CARTESIAN_POINT ( 'NONE',  ( 12.14591786802309770, 12.06949235617756955, 44.37390960531435979 ) ) ;
#117033 = CARTESIAN_POINT ( 'NONE',  ( 9.564922557961047289, -16.46253265017146816, 95.41775706135233293 ) ) ;
#117034 = CARTESIAN_POINT ( 'NONE',  ( -19.05341960407617563, 5.049401038297882671, 68.54275706135230450 ) ) ;
#117035 = CARTESIAN_POINT ( 'NONE',  ( -21.53943276465977519, -0.05219959533937600094, 73.75109039468567573 ) ) ;
#117036 = CARTESIAN_POINT ( 'NONE',  ( 16.46253265017146816, 9.564922557961045513, 51.66775706135233293 ) ) ;
#117037 = CARTESIAN_POINT ( 'NONE',  ( -5.153800228976328057, -19.02544592524343514, 27.29057627198103120 ) ) ;
#117038 = CARTESIAN_POINT ( 'NONE',  ( -10.72451020669898014, 18.67979575497178502, 40.41557627198103120 ) ) ;
#117039 = CARTESIAN_POINT ( 'NONE',  ( -4.379528057220328563, 16.55341960407611168, 45.20724293864769550 ) ) ;
#117040 = CARTESIAN_POINT ( 'NONE',  ( -18.87580814761077264, 5.499999999999961808, 95.87172394265761000 ) ) ;
#117041 = CARTESIAN_POINT ( 'NONE',  ( 5.153800228976615827, -19.02544592524334988, 20.20942372801899722 ) ) ;
#117042 = CARTESIAN_POINT ( 'NONE',  ( 14.34966873604972726, -8.224510206698740333, 80.83442372801901854 ) ) ;
#117043 = CARTESIAN_POINT ( 'NONE',  ( -16.52544592524342804, 4.483927247898546575, 46.04057627198103830 ) ) ;
#117044 = CARTESIAN_POINT ( 'NONE',  ( -15.80617190586768217, 15.72974639402176855, 78.12609039468570415 ) ) ;
#117045 = CARTESIAN_POINT ( 'NONE',  ( -21.53943276465977519, -0.05219959533937600094, 83.75109039468568994 ) ) ;
#117046 = CARTESIAN_POINT ( 'NONE',  ( 18.67979575497178502, 10.72451020669898547, 79.16557627198103830 ) ) ;
#117047 = CARTESIAN_POINT ( 'NONE',  ( -16.51473224551069308, -9.474510206698971260, 31.66557627198102054 ) ) ;
#117048 = CARTESIAN_POINT ( 'NONE',  ( 15.80617190586769283, -15.72974639402175789, 55.62609039468568284 ) ) ;
#117049 = CARTESIAN_POINT ( 'NONE',  ( -9.474510206698964154, 16.51473224551069663, 40.41557627198103120 ) ) ;
#117050 = CARTESIAN_POINT ( 'NONE',  ( -16.51473224551069308, -9.474510206698971260, 56.66557627198103120 ) ) ;
#117051 = CARTESIAN_POINT ( 'NONE',  ( -8.224510206698948167, 14.34966873604960824, 95.41557627198102409 ) ) ;
#117052 = CARTESIAN_POINT ( 'NONE',  ( 19.05341960407611168, 5.049401038298154454, 93.95724293864769550 ) ) ;
#117053 = CARTESIAN_POINT ( 'NONE',  ( 4.483927247898545687, 16.52544592524342804, 44.79057627198103120 ) ) ;
#117054 = CARTESIAN_POINT ( 'NONE',  ( 12.06949235617757843, -12.14591786802309237, 108.1239096053143811 ) ) ;
#117055 = CARTESIAN_POINT ( 'NONE',  ( -10.72451020669898014, 18.67979575497178502, 85.41557627198102409 ) ) ;
#117056 = CARTESIAN_POINT ( 'NONE',  ( -18.67979575497193778, 10.72451020669871902, 23.33442372801901499 ) ) ;
#117057 = CARTESIAN_POINT ( 'NONE',  ( -17.31327599691207197, 15.19344129729072712, -55.22348155082431020 ) ) ;
#117059 = CARTESIAN_POINT ( 'NONE',  ( -19.03943276465977164, -0.05219959533935918106, 113.7510903946856757 ) ) ;
#117058 = CARTESIAN_POINT ( 'NONE',  ( 5.153800228976335163, 19.02544592524342804, 84.79057627198099567 ) ) ;
#117060 = CARTESIAN_POINT ( 'NONE',  ( -18.62759615963270932, 10.81492255796079327, 70.83224293864770971 ) ) ;
#117061 = CARTESIAN_POINT ( 'NONE',  ( -21.55341960407619339, 5.719274019375674811, 93.54275706135234714 ) ) ;
#117062 = CARTESIAN_POINT ( 'NONE',  ( 19.02544592524343514, -5.153800228976328945, 78.54057627198099567 ) ) ;
#117063 = CARTESIAN_POINT ( 'NONE',  ( -21.53943276465977519, -0.05219959533937600094, 28.75109039468567929 ) ) ;
#117064 = CARTESIAN_POINT ( 'NONE',  ( 19.05341960407611168, 5.049401038298154454, 113.9572429386477097 ) ) ;
#117065 = CARTESIAN_POINT ( 'NONE',  ( -8.314922557961024197, 14.29746914071037800, 92.91775706135236135 ) ) ;
#117066 = CARTESIAN_POINT ( 'NONE',  ( 0.05219959533937995610, -21.53943276465977519, 65.00109039468568994 ) ) ;
#117067 = CARTESIAN_POINT ( 'NONE',  ( 18.67979575497194134, -10.72451020669871369, 100.8344237280190185 ) ) ;
#117068 = CARTESIAN_POINT ( 'NONE',  ( -14.29746914071037622, -8.314922557961029526, 79.16775706135234714 ) ) ;
#117069 = CARTESIAN_POINT ( 'NONE',  ( -15.72974639402176322, -15.80617190586768395, 34.37609039468568284 ) ) ;
#117070 = CARTESIAN_POINT ( 'NONE',  ( 5.049401038298161559, -19.05341960407611168, 22.70724293864769194 ) ) ;
#117071 = CARTESIAN_POINT ( 'NONE',  ( 21.53943276465977519, 0.05219959533937863772, 96.25109039468568994 ) ) ;
#117072 = CARTESIAN_POINT ( 'NONE',  ( 19.03943276465977164, -0.05219959533909143690, 88.74890960531436690 ) ) ;
#117073 = CARTESIAN_POINT ( 'NONE',  ( 0.05219959533907565091, 21.53943276465977519, 84.99890960531436690 ) ) ;
#117074 = CARTESIAN_POINT ( 'NONE',  ( 16.51473224551083163, -9.474510206698727899, 65.83442372801900433 ) ) ;
#117076 = CARTESIAN_POINT ( 'NONE',  ( -0.05219959533907301413, -21.53943276465977519, 47.49890960531435979 ) ) ;
#117075 = CARTESIAN_POINT ( 'NONE',  ( 19.25176906914650488, 5.499999999999744205, 83.49927264242278113 ) ) ;
#117079 = B_SPLINE_CURVE_WITH_KNOTS ( 'NONE', 3,
 ( #164012, #93, #198311, #59789, #119495, #122448 ),
 .UNSPECIFIED., .F., .F.,
 ( 4, 2, 4 ),
 ( 0.0003734705499822683190, 0.004296280022385642362, 0.008219089494789017653 ),
 .UNSPECIFIED. ) ;
#117078 = CARTESIAN_POINT ( 'NONE',  ( -16.53943276465976808, 0.05219959533911058130, 46.24890960531435979 ) ) ;
#117077 = CARTESIAN_POINT ( 'NONE',  ( -0.05219959533909027116, -19.03943276465977164, 97.49890960531436690 ) ) ;
#117080 = CARTESIAN_POINT ( 'NONE',  ( 8.906447517083050158, 27.41122689804195645, 145.4000000000000057 ) ) ;
#117081 = CARTESIAN_POINT ( 'NONE',  ( 0.05219959533936267826, -19.03943276465977164, 80.00109039468567573 ) ) ;
#117082 = CARTESIAN_POINT ( 'NONE',  ( -17.49999999999999645, 5.500000000000001776, 103.7176903769643701 ) ) ;
#117083 = CARTESIAN_POINT ( 'NONE',  ( -19.03943276465977164, -0.05219959533935918106, 108.7510903946856615 ) ) ;
#117084 = CARTESIAN_POINT ( 'NONE',  ( 21.52544592524344225, -5.823673210054117533, 88.54057627198103830 ) ) ;
#117085 = CARTESIAN_POINT ( 'NONE',  ( -12.06949235617756955, 12.14591786802309770, 70.62390960531436690 ) ) ;
#117086 = CARTESIAN_POINT ( 'NONE',  ( 5.153800228976335163, 19.02544592524342804, 104.7905762719809957 ) ) ;
#117087 = CARTESIAN_POINT ( 'NONE',  ( 8.314922557961029526, -14.29746914071037800, 50.41775706135235424 ) ) ;
#117088 = CARTESIAN_POINT ( 'NONE',  ( -5.153800228976328057, -19.02544592524343514, 57.29057627198103120 ) ) ;
#117090 = CARTESIAN_POINT ( 'NONE',  ( 0.05219959533936267826, -19.03943276465977164, 80.00109039468567573 ) ) ;
#117089 = CARTESIAN_POINT ( 'NONE',  ( 18.67979575497194134, -10.72451020669871369, 20.83442372801901143 ) ) ;
#117091 = CARTESIAN_POINT ( 'NONE',  ( -0.05219959533909027116, -19.03943276465977164, 97.49890960531436690 ) ) ;
#117092 = CARTESIAN_POINT ( 'NONE',  ( 0.05219959533909260263, 19.03943276465977164, 74.99890960531435269 ) ) ;
#117093 = CARTESIAN_POINT ( 'NONE',  ( -18.67979575497178146, -10.72451020669898902, 81.66557627198103830 ) ) ;
#117094 = CARTESIAN_POINT ( 'NONE',  ( -16.46253265017160317, 9.564922557960807481, 50.83224293864770260 ) ) ;
#117095 = CARTESIAN_POINT ( 'NONE',  ( 13.06108300879906103, 35.02243372997630644, -7.999999999999996447 ) ) ;
#117096 = CARTESIAN_POINT ( 'NONE',  ( -12.14591786802309592, -12.06949235617757132, 51.87390960531437401 ) ) ;
#117097 = CARTESIAN_POINT ( 'NONE',  ( -16.46253265017160317, 9.564922557960807481, 105.8322429386476955 ) ) ;
#117098 = CARTESIAN_POINT ( 'NONE',  ( 23.31738231874054890, -16.94106989632523508, 144.7999999999999829 ) ) ;
#117099 = CARTESIAN_POINT ( 'NONE',  ( 19.02544592524334988, 5.153800228976608722, 66.45942372801899012 ) ) ;
#117100 = CARTESIAN_POINT ( 'NONE',  ( -18.67979575497178146, -10.72451020669898902, 91.66557627198103830 ) ) ;
#117101 = CARTESIAN_POINT ( 'NONE',  ( 19.02544592524334988, 5.153800228976608722, 56.45942372801898301 ) ) ;
#117102 = CARTESIAN_POINT ( 'NONE',  ( 19.05341960407611168, 5.049401038298154454, 103.9572429386476671 ) ) ;
#117103 = CARTESIAN_POINT ( 'NONE',  ( -17.49999999999999289, 3.850315288878790376, 114.2662913060345176 ) ) ;
#117104 = CARTESIAN_POINT ( 'NONE',  ( -10.72451020669898014, 18.67979575497178502, 40.41557627198103120 ) ) ;
#117105 = CARTESIAN_POINT ( 'NONE',  ( -5.049401038298153566, 19.05341960407611168, 70.20724293864769550 ) ) ;
#117106 = CARTESIAN_POINT ( 'NONE',  ( 5.823673210054444382, -21.52544592524334988, 60.20942372801902565 ) ) ;
#117107 = CARTESIAN_POINT ( 'NONE',  ( -5.049401038298153566, 19.05341960407611168, 35.20724293864768839 ) ) ;
#117109 = ORIENTED_EDGE ( 'NONE', *, *, #122840, .F. ) ;
#117108 = CARTESIAN_POINT ( 'NONE',  ( 14.29746914071049879, -8.314922557960816363, 68.33224293864769550 ) ) ;
#117110 = CARTESIAN_POINT ( 'NONE',  ( 0.05219959533934541429, -16.53943276465976808, 20.00109039468568639 ) ) ;
#117111 = CARTESIAN_POINT ( 'NONE',  ( -10.72451020669870658, -18.67979575497194134, 54.58442372801901143 ) ) ;
#117112 = VERTEX_POINT ( 'NONE', #105308 ) ;
#117113 = CARTESIAN_POINT ( 'NONE',  ( -19.02544592524342804, 5.153800228976336051, 111.0405762719810099 ) ) ;
#117114 = CARTESIAN_POINT ( 'NONE',  ( -13.97604488694547697, 13.89961937509957934, 63.12609039468566152 ) ) ;
#117115 = LINE ( 'NONE', #53446, #156885 ) ;
#117116 = CARTESIAN_POINT ( 'NONE',  ( 21.52544592524334988, 5.823673210054432836, 26.45942372801901854 ) ) ;
#117117 = CARTESIAN_POINT ( 'NONE',  ( 0.05219959533909260263, 19.03943276465977164, 54.99890960531435979 ) ) ;
#117118 = CARTESIAN_POINT ( 'NONE',  ( -12.06949235617739369, -12.14591786802326823, 34.37609039468568284 ) ) ;
#117119 = CARTESIAN_POINT ( 'NONE',  ( -30.74264578624800492, 22.33583958711400186, -7.949999994537626513 ) ) ;
#117120 = CARTESIAN_POINT ( 'NONE',  ( -5.049401038297874678, -19.05341960407617918, 24.79275706135233648 ) ) ;
#117121 = CARTESIAN_POINT ( 'NONE',  ( -19.02544592524342804, 5.153800228976336051, 41.04057627198103120 ) ) ;
#117122 = CARTESIAN_POINT ( 'NONE',  ( 16.51473224551083163, -9.474510206698727899, 20.83442372801899722 ) ) ;
#117123 = CARTESIAN_POINT ( 'NONE',  ( 0.05219959533934541429, -16.53943276465976808, 90.00109039468567573 ) ) ;
#117125 = CARTESIAN_POINT ( 'NONE',  ( -21.53943276465977519, -0.05219959533937600094, 73.75109039468567573 ) ) ;
#117124 = CARTESIAN_POINT ( 'NONE',  ( 0.05219959533909260263, 19.03943276465977164, 89.99890960531436690 ) ) ;
#117126 = CARTESIAN_POINT ( 'NONE',  ( 4.944490673674106773, -3.929198865016385156, -62.47179825203327397 ) ) ;
#117127 = CARTESIAN_POINT ( 'NONE',  ( -19.05341960407611168, -5.049401038298163336, 106.4572429386476955 ) ) ;
#117128 = CARTESIAN_POINT ( 'NONE',  ( -28.82186960331499037, 2.428612866367529932E-14, 144.0000000000000000 ) ) ;
#117130 = CARTESIAN_POINT ( 'NONE',  ( -5.823673210054431948, 21.52544592524334988, 77.70942372801900433 ) ) ;
#117129 = CARTESIAN_POINT ( 'NONE',  ( 12.14591786802327356, -12.06949235617739191, 50.62609039468568994 ) ) ;
#117131 = CARTESIAN_POINT ( 'NONE',  ( 5.719274019375673035, 21.55341960407619339, 97.29275706135234714 ) ) ;
#117132 = CARTESIAN_POINT ( 'NONE',  ( -11.16651649332244212, 9.304348965730380172, -60.11051939825532031 ) ) ;
#117133 = CARTESIAN_POINT ( 'NONE',  ( -8.224510206698735004, -14.34966873604973081, 29.58442372801901854 ) ) ;
#117134 = CARTESIAN_POINT ( 'NONE',  ( 5.153800228976335163, 19.02544592524342804, 84.79057627198099567 ) ) ;
#117135 = CARTESIAN_POINT ( 'NONE',  ( 5.153800228976335163, 19.02544592524342804, 114.7905762719810241 ) ) ;
#117136 = EDGE_LOOP ( 'NONE', ( #76331, #192859, #167739, #28068 ) ) ;
#117137 = CARTESIAN_POINT ( 'NONE',  ( 17.31747979337947640, 6.344076630961015262, 43.87944868065184068 ) ) ;
#117138 = CARTESIAN_POINT ( 'NONE',  ( 9.474510206698971260, -16.51473224551069308, 32.91557627198102409 ) ) ;
#117139 = CARTESIAN_POINT ( 'NONE',  ( -10.72451020669898014, 18.67979575497178502, 45.41557627198103830 ) ) ;
#117140 = CARTESIAN_POINT ( 'NONE',  ( -8.224510206698735004, -14.34966873604973081, 104.5844237280190185 ) ) ;
#117142 = CARTESIAN_POINT ( 'NONE',  ( -19.02544592524342804, 5.153800228976336051, 71.04057627198099567 ) ) ;
#117141 = CARTESIAN_POINT ( 'NONE',  ( 14.34966873604960469, 8.224510206698951720, 79.16557627198103830 ) ) ;
#117143 = CARTESIAN_POINT ( 'NONE',  ( -15.72974639402176322, -15.80617190586768395, 99.37609039468568994 ) ) ;
#117144 = CARTESIAN_POINT ( 'NONE',  ( -12.06949235617739369, -12.14591786802326823, 19.37609039468568639 ) ) ;
#117145 = CARTESIAN_POINT ( 'NONE',  ( 0.05219959533910956823, 16.53943276465976808, 89.99890960531438111 ) ) ;
#117146 = CARTESIAN_POINT ( 'NONE',  ( -21.55341960407619339, 5.719274019375674811, 43.54275706135235424 ) ) ;
#117147 = CARTESIAN_POINT ( 'NONE',  ( 10.72451020669898902, -18.67979575497178502, 77.91557627198102409 ) ) ;
#117148 = CARTESIAN_POINT ( 'NONE',  ( -0.05219959533936034679, 19.03943276465977164, 47.50109039468566863 ) ) ;
#117149 = CARTESIAN_POINT ( 'NONE',  ( -35.24576003106574973, 4.949822944371127242, 39.34410620168027606 ) ) ;
#117150 = CARTESIAN_POINT ( 'NONE',  ( -19.02544592524342804, 5.153800228976336051, 96.04057627198103830 ) ) ;
#117151 = CARTESIAN_POINT ( 'NONE',  ( 16.53943276465976808, -0.05219959533910856209, 63.74890960531435979 ) ) ;
#117152 = CARTESIAN_POINT ( 'NONE',  ( 12.06949235617757843, -12.14591786802309237, 53.12390960531436690 ) ) ;
#117153 = CARTESIAN_POINT ( 'NONE',  ( 8.224510206698742110, 14.34966873604972548, 107.0844237280190043 ) ) ;
#117154 = CARTESIAN_POINT ( 'NONE',  ( 9.474510206698729675, 16.51473224551082808, 67.08442372801900433 ) ) ;
#117155 = DIRECTION ( 'NONE',  ( 1.000000000000000000, 0.000000000000000000, 0.000000000000000000 ) ) ;
#117156 = CARTESIAN_POINT ( 'NONE',  ( 5.049401038298161559, -19.05341960407611168, 112.7072429386476813 ) ) ;
#117157 = CARTESIAN_POINT ( 'NONE',  ( -8.224510206698948167, 14.34966873604960824, 85.41557627198102409 ) ) ;
#117158 = CARTESIAN_POINT ( 'NONE',  ( -3.573655867282028392E-15, 2.428612866367529932E-14, 2.000000000000000000 ) ) ;
#117160 = CARTESIAN_POINT ( 'NONE',  ( -15.72974639402197994, 15.80617190586746368, 55.62390960531436690 ) ) ;
#117159 = CARTESIAN_POINT ( 'NONE',  ( -13.89961937509977652, 13.97604488694528158, 45.62390960531433848 ) ) ;
#117161 = CARTESIAN_POINT ( 'NONE',  ( 5.719274019375991003, -21.55341960407610458, 77.70724293864770971 ) ) ;
#117162 = CARTESIAN_POINT ( 'NONE',  ( 0.05219959533909260263, 19.03943276465977164, 34.99890960531435979 ) ) ;
#117164 = CARTESIAN_POINT ( 'NONE',  ( 19.03943276465977164, -0.05219959533909143690, 58.74890960531435979 ) ) ;
#117163 = CARTESIAN_POINT ( 'NONE',  ( -14.29746914071037622, -8.314922557961029526, 64.16775706135234714 ) ) ;
#117165 = CARTESIAN_POINT ( 'NONE',  ( 16.51473224551083163, -9.474510206698727899, 40.83442372801900433 ) ) ;
#117166 = CARTESIAN_POINT ( 'NONE',  ( -18.62759615963255300, -10.81492255796106328, 49.16775706135234003 ) ) ;
#117167 = CARTESIAN_POINT ( 'NONE',  ( -15.80617190586745835, -15.72974639402198527, 36.87390960531435979 ) ) ;
#117168 = CARTESIAN_POINT ( 'NONE',  ( -16.53943276465976808, 0.05219959533911058130, 106.2489096053143811 ) ) ;
#117170 = CARTESIAN_POINT ( 'NONE',  ( -16.46253265017146816, -9.564922557961047289, 94.16775706135233293 ) ) ;
#117169 = ADVANCED_BREP_SHAPE_REPRESENTATION ( '', ( #79223, #82054 ), #65912 ) ;
#117171 = CARTESIAN_POINT ( 'NONE',  ( 36.91746824999999887, -11.99521256947793546, -4.224999997268813701 ) ) ;
#117173 = CARTESIAN_POINT ( 'NONE',  ( 21.55341960407610458, 5.719274019375980345, 48.95724293864770971 ) ) ;
#117172 = CARTESIAN_POINT ( 'NONE',  ( 17.50000000000000711, 3.427582784589808362, 37.32655242534940498 ) ) ;
#117174 = CARTESIAN_POINT ( 'NONE',  ( -16.46253265017160317, 9.564922557960807481, 25.83224293864769194 ) ) ;
#117175 = CARTESIAN_POINT ( 'NONE',  ( -10.81492255796105439, 18.62759615963255655, 82.91775706135234714 ) ) ;
#117176 = CARTESIAN_POINT ( 'NONE',  ( -0.05219959533910754901, -16.53943276465976808, 27.49890960531435269 ) ) ;
#117178 = CARTESIAN_POINT ( 'NONE',  ( 8.224510206698953496, -14.34966873604960469, 52.91557627198103830 ) ) ;
#117177 = CARTESIAN_POINT ( 'NONE',  ( 0.05219959533934541429, -16.53943276465976808, 60.00109039468568284 ) ) ;
#117179 = CARTESIAN_POINT ( 'NONE',  ( 15.72974639402199770, -15.80617190586745480, 78.12390960531436690 ) ) ;
#117180 = CARTESIAN_POINT ( 'NONE',  ( -15.80617190586745835, -15.72974639402198527, 76.87390960531439532 ) ) ;
#117181 = CARTESIAN_POINT ( 'NONE',  ( -40.00000000000000711, 2.918471586026471156E-14, 0.000000000000000000 ) ) ;
#117183 = CARTESIAN_POINT ( 'NONE',  ( 10.81492255796078972, 18.62759615963270932, 24.58224293864768839 ) ) ;
#117182 = CARTESIAN_POINT ( 'NONE',  ( -19.03943276465977164, -0.05219959533935918106, 88.75109039468567573 ) ) ;
#117185 = CARTESIAN_POINT ( 'NONE',  ( 19.05341960407611168, 5.049401038298154454, 68.95724293864769550 ) ) ;
#117184 = B_SPLINE_CURVE_WITH_KNOTS ( 'NONE', 3,
 ( #46596, #157756, #108256, #155754, #109249, #154764, #33415, #65727, #31427, #78905, #19247, #173928, #34409, #35397, #125425, #18256, #81868, #93080, #48593, #140582, #3068, #95074 ),
 .UNSPECIFIED., .F., .F.,
 ( 4, 2, 2, 2, 2, 2, 2, 2, 2, 2, 4 ),
 ( 1.970604705270169680E-07, 0.0003054521314110711003, 0.0006107072023516151114, 0.001221217344232706928, 0.001831727486113798962, 0.002136982557054344870, 0.002442237627994890779, 0.003052747769875995172, 0.003663257911757099566, 0.004273768053638204827, 0.004884278195519306184 ),
 .UNSPECIFIED. ) ;
#117186 = CARTESIAN_POINT ( 'NONE',  ( 9.564922557960805705, 16.46253265017160317, 34.58224293864770260 ) ) ;
#117187 = PRESENTATION_STYLE_ASSIGNMENT (( #72695 ) ) ;
#117188 = CARTESIAN_POINT ( 'NONE',  ( -30.00000000000000000, -5.510910596163089556E-15, 45.00000000000000000 ) ) ;
#117189 = ORIENTED_EDGE ( 'NONE', *, *, #164677, .F. ) ;
#117190 = CARTESIAN_POINT ( 'NONE',  ( -0.05219959533934338120, 16.53943276465976808, 82.50109039468568994 ) ) ;
#117191 = CARTESIAN_POINT ( 'NONE',  ( -5.719274019375978568, 21.55341960407610458, 115.2072429386476955 ) ) ;
#117192 = CARTESIAN_POINT ( 'NONE',  ( 16.46253265017160672, -9.564922557960803928, 73.33224293864769550 ) ) ;
#117193 = CARTESIAN_POINT ( 'NONE',  ( -15.72974639402176322, -15.80617190586768395, 49.37609039468569705 ) ) ;
#117194 = CARTESIAN_POINT ( 'NONE',  ( -16.51473224551069308, -9.474510206698971260, 96.66557627198102409 ) ) ;
#117196 = EDGE_CURVE ( 'NONE', #82312, #122086, #33382, .T. ) ;
#117195 = CARTESIAN_POINT ( 'NONE',  ( -24.80109738229592509, -30.87060611836150059, -19.02242571537068017 ) ) ;
#117197 = VERTEX_POINT ( 'NONE', #74972 ) ;
#117198 = CARTESIAN_POINT ( 'NONE',  ( 10.72451020669871369, 18.67979575497193778, 42.08442372801901854 ) ) ;
#117200 = CARTESIAN_POINT ( 'NONE',  ( 9.474510206698971260, -16.51473224551069308, 102.9155762719810241 ) ) ;
#117199 = CARTESIAN_POINT ( 'NONE',  ( 13.89961937509977652, -13.97604488694527269, 23.12390960531436335 ) ) ;
#117201 = CARTESIAN_POINT ( 'NONE',  ( -13.89961937509957401, -13.97604488694547875, 54.37609039468565442 ) ) ;
#117202 = CARTESIAN_POINT ( 'NONE',  ( 10.81492255796078972, 18.62759615963270932, 109.5822429386476955 ) ) ;
#117203 = CARTESIAN_POINT ( 'NONE',  ( -19.05341960407617563, 5.049401038297882671, 43.54275706135232582 ) ) ;
#117204 = CARTESIAN_POINT ( 'NONE',  ( -9.474510206698720793, -16.51473224551083518, 49.58442372801899722 ) ) ;
#117206 = ORIENTED_EDGE ( 'NONE', *, *, #68789, .F. ) ;
#117205 = CARTESIAN_POINT ( 'NONE',  ( 8.224510206698742110, 14.34966873604972548, 107.0844237280190043 ) ) ;
#117207 = CARTESIAN_POINT ( 'NONE',  ( -21.38418241377623374, -5.438282248597753110, 174.2683007571264113 ) ) ;
#117208 = CARTESIAN_POINT ( 'NONE',  ( -13.89961937509977652, 13.97604488694528158, 70.62390960531432427 ) ) ;
#117209 = CARTESIAN_POINT ( 'NONE',  ( -5.719274019375665041, -21.55341960407619695, 74.79275706135234714 ) ) ;
#117210 = CARTESIAN_POINT ( 'NONE',  ( -5.823673210054431948, 21.52544592524334988, 92.70942372801901854 ) ) ;
#117211 = CARTESIAN_POINT ( 'NONE',  ( 21.36119649488921013, -0.4379334789936405459, -56.42482690868973094 ) ) ;
#117212 = CARTESIAN_POINT ( 'NONE',  ( -16.51473224551069308, -9.474510206698971260, 81.66557627198103830 ) ) ;
#117213 = CARTESIAN_POINT ( 'NONE',  ( -10.72451020669870658, -18.67979575497194134, 59.58442372801901854 ) ) ;
#117214 = CARTESIAN_POINT ( 'NONE',  ( -19.02544592524334988, -5.153800228976617603, 108.9594237280189759 ) ) ;
#117215 = CARTESIAN_POINT ( 'NONE',  ( 9.564922557960805705, 16.46253265017160317, 69.58224293864770971 ) ) ;
#117216 = CARTESIAN_POINT ( 'NONE',  ( 13.97604488694527802, 13.89961937509977652, 109.3739096053143669 ) ) ;
#117217 = CARTESIAN_POINT ( 'NONE',  ( -13.97604488694527625, -13.89961937509977652, 91.87390960531432427 ) ) ;
#117218 = DIRECTION ( 'NONE',  ( 0.5000000000000002220, 0.4999999999999985012, -0.7071067811865483499 ) ) ;
#117219 = CARTESIAN_POINT ( 'NONE',  ( 9.474510206698971260, -16.51473224551069308, 82.91557627198103830 ) ) ;
#117220 = CARTESIAN_POINT ( 'NONE',  ( 0.05219959533909260263, 19.03943276465977164, 64.99890960531436690 ) ) ;
#117221 = CARTESIAN_POINT ( 'NONE',  ( -0.05219959533907301413, -21.53943276465977519, 112.4989096053143669 ) ) ;
#117222 = CARTESIAN_POINT ( 'NONE',  ( -16.52544592524335698, -4.483927247898792601, 103.9594237280190185 ) ) ;
#117223 = CARTESIAN_POINT ( 'NONE',  ( 0.000000000000000000, 0.000000000000000000, -65.00100000000003320 ) ) ;
#117224 = CARTESIAN_POINT ( 'NONE',  ( -5.153800228976607833, 19.02544592524334988, 62.70942372801899722 ) ) ;
#117225 = CARTESIAN_POINT ( 'NONE',  ( 16.46253265017160672, -9.564922557960803928, 98.33224293864769550 ) ) ;
#117226 = CARTESIAN_POINT ( 'NONE',  ( -16.53943276465976808, 0.05219959533911058130, 86.24890960531436690 ) ) ;
#117227 = CARTESIAN_POINT ( 'NONE',  ( -16.52544592524342804, 4.483927247898546575, 106.0405762719810525 ) ) ;
#117228 = CARTESIAN_POINT ( 'NONE',  ( 18.67979575497178502, 10.72451020669898547, 39.16557627198102409 ) ) ;
#117229 = CARTESIAN_POINT ( 'NONE',  ( -10.81492255796078084, -18.62759615963271287, 27.08224293864769550 ) ) ;
#117230 = CIRCLE ( 'NONE', #62360, 9.100000000000001421 ) ;
#117231 = CARTESIAN_POINT ( 'NONE',  ( -14.34966873604960291, -8.224510206698953496, 96.66557627198102409 ) ) ;
#117232 = CARTESIAN_POINT ( 'NONE',  ( -0.3968392070109439951, -6.139906835403845520, -62.49911542708239409 ) ) ;
#117233 = CARTESIAN_POINT ( 'NONE',  ( -19.05341960407617563, 5.049401038297882671, 38.54275706135233293 ) ) ;
#117234 = CARTESIAN_POINT ( 'NONE',  ( -14.29746914071037622, -8.314922557961029526, 109.1677570613523613 ) ) ;
#117235 = CARTESIAN_POINT ( 'NONE',  ( -16.51473224551069308, -9.474510206698971260, 91.66557627198103830 ) ) ;
#117236 = CARTESIAN_POINT ( 'NONE',  ( -21.52544592524334988, -5.823673210054445271, 63.95942372801901854 ) ) ;
#117237 = CARTESIAN_POINT ( 'NONE',  ( -15.80617190586745835, -15.72974639402198527, 41.87390960531435979 ) ) ;
#117238 = CARTESIAN_POINT ( 'NONE',  ( 15.72974639402176855, 15.80617190586768217, 26.87609039468567218 ) ) ;
#117239 = CARTESIAN_POINT ( 'NONE',  ( 15.72974639402199770, -15.80617190586745480, 88.12390960531436690 ) ) ;
#117240 = CARTESIAN_POINT ( 'NONE',  ( 8.224510206698953496, -14.34966873604960469, 102.9155762719810383 ) ) ;
#117241 = CARTESIAN_POINT ( 'NONE',  ( 16.51473224551083163, -9.474510206698727899, 75.83442372801900433 ) ) ;
#117242 = CARTESIAN_POINT ( 'NONE',  ( 5.153800228976335163, 19.02544592524342804, 39.79057627198100988 ) ) ;
#117243 =( BOUNDED_CURVE ( )  B_SPLINE_CURVE ( 3, ( #54842, #103350, #165029, #25535 ),
 .UNSPECIFIED., .F., .F. ) 
 B_SPLINE_CURVE_WITH_KNOTS ( ( 4, 4 ),
 ( 1.025647941782811046, 2.008945357379067431 ),
 .UNSPECIFIED. ) 
 CURVE ( )  GEOMETRIC_REPRESENTATION_ITEM ( )  RATIONAL_B_SPLINE_CURVE ( ( 1.000000000000000000, 0.9210371567966664230, 0.9210371567966664230, 1.000000000000000000 ) ) 
 REPRESENTATION_ITEM ( '' )  );
#117244 = CARTESIAN_POINT ( 'NONE',  ( 5.153800228976335163, 19.02544592524342804, 99.79057627198102409 ) ) ;
#117245 = CARTESIAN_POINT ( 'NONE',  ( -16.51473224551069308, -9.474510206698971260, 101.6655762719810241 ) ) ;
#117246 = CARTESIAN_POINT ( 'NONE',  ( 9.564922557960805705, 16.46253265017160317, 24.58224293864769194 ) ) ;
#117247 = CARTESIAN_POINT ( 'NONE',  ( -12.06949235617756955, 12.14591786802309770, 40.62390960531435269 ) ) ;
#117248 = CARTESIAN_POINT ( 'NONE',  ( 16.52544592524335698, 4.483927247898782831, 46.45942372801901854 ) ) ;
#117249 = CARTESIAN_POINT ( 'NONE',  ( 21.52544592524334988, 5.823673210054432836, 101.4594237280190185 ) ) ;
#117251 = CARTESIAN_POINT ( 'NONE',  ( 4.483927247898545687, 16.52544592524342804, 29.79057627198102409 ) ) ;
#117250 = CARTESIAN_POINT ( 'NONE',  ( -19.03943276465977164, 0.05219959533909376836, 116.2489096053143669 ) ) ;
#117252 = CARTESIAN_POINT ( 'NONE',  ( -21.53943276465977519, -0.05219959533937600094, 33.75109039468568284 ) ) ;
#117253 = CARTESIAN_POINT ( 'NONE',  ( -16.46253265017160317, 9.564922557960807481, 100.8322429386477097 ) ) ;
#117254 = CARTESIAN_POINT ( 'NONE',  ( 0.05219959533934541429, -16.53943276465976808, 105.0010903946856757 ) ) ;
#117255 = CARTESIAN_POINT ( 'NONE',  ( -4.379528057220086978, -16.55341960407618274, 99.79275706135234714 ) ) ;
#117256 = CARTESIAN_POINT ( 'NONE',  ( -12.14591786802326823, 12.06949235617739902, 28.12609039468568284 ) ) ;
#117257 = CARTESIAN_POINT ( 'NONE',  ( -16.46253265017160317, 9.564922557960807481, 45.83224293864769550 ) ) ;
#117258 = AXIS2_PLACEMENT_3D ( 'NONE', #181415, #104558, #51322 ) ;
#117259 = CARTESIAN_POINT ( 'NONE',  ( 12.14591786802309770, 12.06949235617756955, 104.3739096053143669 ) ) ;
#117260 = CARTESIAN_POINT ( 'NONE',  ( 18.67979575497178502, 10.72451020669898547, 114.1655762719810383 ) ) ;
#117261 = CARTESIAN_POINT ( 'NONE',  ( -19.03943276465977164, 0.05219959533909376836, 26.24890960531435624 ) ) ;
#117262 = CARTESIAN_POINT ( 'NONE',  ( 13.97604488694527802, 13.89961937509977652, 109.3739096053143669 ) ) ;
#117263 = CARTESIAN_POINT ( 'NONE',  ( -15.80617190586768217, 15.72974639402176855, 38.12609039468567573 ) ) ;
#117264 = CARTESIAN_POINT ( 'NONE',  ( 13.97604488694527802, 13.89961937509977652, 39.37390960531435269 ) ) ;
#117265 = CARTESIAN_POINT ( 'NONE',  ( -5.049401038298153566, 19.05341960407611168, 110.2072429386476671 ) ) ;
#117266 = CARTESIAN_POINT ( 'NONE',  ( -17.49999999999999645, -5.500000000000000888, 34.20309617465829177 ) ) ;
#117267 = CARTESIAN_POINT ( 'NONE',  ( 0.05219959533909260263, 19.03943276465977164, 94.99890960531436690 ) ) ;
#117269 = CARTESIAN_POINT ( 'NONE',  ( -12.06949235617756955, 12.14591786802309770, 95.62390960531436690 ) ) ;
#117268 = CARTESIAN_POINT ( 'NONE',  ( 5.823673210054444382, -21.52544592524334988, 45.20942372801901854 ) ) ;
#117270 = CARTESIAN_POINT ( 'NONE',  ( -19.03943276465977164, 0.05219959533909376836, 91.24890960531436690 ) ) ;
#117271 = LINE ( 'NONE', #144599, #138502 ) ;
#117272 = CARTESIAN_POINT ( 'NONE',  ( -16.52544592524335698, -4.483927247898792601, 68.95942372801901854 ) ) ;
#117273 = CARTESIAN_POINT ( 'NONE',  ( 0.05219959533937995610, -21.53943276465977519, 80.00109039468568994 ) ) ;
#117274 = CARTESIAN_POINT ( 'NONE',  ( 4.379528057220092307, 16.55341960407617563, 37.29275706135235424 ) ) ;
#117275 = CARTESIAN_POINT ( 'NONE',  ( -0.05219959533909027116, -19.03943276465977164, 87.49890960531436690 ) ) ;
#117276 = CARTESIAN_POINT ( 'NONE',  ( 0.05219959533936267826, -19.03943276465977164, 105.0010903946856615 ) ) ;
#117277 = CARTESIAN_POINT ( 'NONE',  ( -16.55341960407617563, 4.379528057220093196, 73.54275706135234714 ) ) ;
#117278 = CARTESIAN_POINT ( 'NONE',  ( 13.97604488694548053, -13.89961937509957401, 95.62609039468563310 ) ) ;
#117279 = CARTESIAN_POINT ( 'NONE',  ( 9.474510206698971260, -16.51473224551069308, 57.91557627198103120 ) ) ;
#117280 = CARTESIAN_POINT ( 'NONE',  ( -5.719274019375978568, 21.55341960407610458, 85.20724293864770971 ) ) ;
#117282 = CARTESIAN_POINT ( 'NONE',  ( -19.05341960407617563, 5.049401038297882671, 93.54275706135234714 ) ) ;
#117281 = CARTESIAN_POINT ( 'NONE',  ( 16.52544592524342804, -4.483927247898539470, 88.54057627198103830 ) ) ;
#117283 = CARTESIAN_POINT ( 'NONE',  ( 14.34966873604972726, -8.224510206698740333, 65.83442372801900433 ) ) ;
#117284 = CARTESIAN_POINT ( 'NONE',  ( 17.05587630539788080, -6.762274262135622216, 63.24180309037315340 ) ) ;
#117285 = CARTESIAN_POINT ( 'NONE',  ( 13.89961937509957401, 13.97604488694547697, 56.87609039468564731 ) ) ;
#117286 = CARTESIAN_POINT ( 'NONE',  ( 8.314922557960818139, 14.29746914071049879, 34.58224293864770260 ) ) ;
#117287 = CARTESIAN_POINT ( 'NONE',  ( 14.34966873604960469, 8.224510206698951720, 79.16557627198103830 ) ) ;
#117289 = CARTESIAN_POINT ( 'NONE',  ( -18.22780087662126647, -5.499999999999827693, 43.98236817873107185 ) ) ;
#117288 = CARTESIAN_POINT ( 'NONE',  ( -19.02544592524334988, -5.153800228976617603, 18.95942372801899722 ) ) ;
#117290 = CARTESIAN_POINT ( 'NONE',  ( 0.05219959533937995610, -21.53943276465977519, 20.00109039468568639 ) ) ;
#117291 = CARTESIAN_POINT ( 'NONE',  ( 19.02544592524343514, -5.153800228976328945, 78.54057627198099567 ) ) ;
#117292 = CARTESIAN_POINT ( 'NONE',  ( 21.52544592524334988, 5.823673210054432836, 91.45942372801901854 ) ) ;
#117293 = CARTESIAN_POINT ( 'NONE',  ( -16.46253265017160317, 9.564922557960807481, 80.83224293864769550 ) ) ;
#117294 = CARTESIAN_POINT ( 'NONE',  ( 21.53943276465977519, -0.05219959533907433946, 43.74890960531435979 ) ) ;
#117295 = CARTESIAN_POINT ( 'NONE',  ( -4.483927247898539470, -16.52544592524342804, 77.29057627198102409 ) ) ;
#117296 = CARTESIAN_POINT ( 'NONE',  ( 9.474510206698971260, -16.51473224551069308, 62.91557627198102409 ) ) ;
#117297 = CARTESIAN_POINT ( 'NONE',  ( -8.314922557960811034, -14.29746914071050412, 92.08224293864769550 ) ) ;
#117298 = CARTESIAN_POINT ( 'NONE',  ( -10.72451020669870658, -18.67979575497194134, 19.58442372801901143 ) ) ;
#117299 = CARTESIAN_POINT ( 'NONE',  ( 10.72451020669871369, 18.67979575497193778, 62.08442372801901143 ) ) ;
#117300 = CARTESIAN_POINT ( 'NONE',  ( 5.049401038298161559, -19.05341960407611168, 37.70724293864768839 ) ) ;
#117301 = CARTESIAN_POINT ( 'NONE',  ( -4.483927247898782831, 16.52544592524335698, 62.70942372801902565 ) ) ;
#117302 = CARTESIAN_POINT ( 'NONE',  ( 18.67979575497178502, 10.72451020669898547, 109.1655762719810383 ) ) ;
#117303 = CARTESIAN_POINT ( 'NONE',  ( -15.80617190586745835, -15.72974639402198527, 111.8739096053143669 ) ) ;
#117305 = CARTESIAN_POINT ( 'NONE',  ( 13.89961937509977652, -13.97604488694527269, 68.12390960531436690 ) ) ;
#117304 = CARTESIAN_POINT ( 'NONE',  ( 9.564922557961047289, -16.46253265017146816, 45.41775706135232582 ) ) ;
#117306 = LINE ( 'NONE', #196177, #124985 ) ;
#117307 = CARTESIAN_POINT ( 'NONE',  ( -5.719274019375665041, -21.55341960407619695, 74.79275706135234714 ) ) ;
#117308 = CARTESIAN_POINT ( 'NONE',  ( 21.55341960407610458, 5.719274019375980345, 53.95724293864770260 ) ) ;
#117309 = CARTESIAN_POINT ( 'NONE',  ( -4.379528057220328563, 16.55341960407611168, 35.20724293864768839 ) ) ;
#117311 = CARTESIAN_POINT ( 'NONE',  ( -16.46253265017146816, -9.564922557961047289, 19.16775706135233293 ) ) ;
#117310 = CARTESIAN_POINT ( 'NONE',  ( -18.67979575497193778, 10.72451020669871902, 83.33442372801903275 ) ) ;
#117312 = CARTESIAN_POINT ( 'NONE',  ( -12.06949235617756955, 12.14591786802309770, 60.62390960531437401 ) ) ;
#117313 = CARTESIAN_POINT ( 'NONE',  ( 4.483927247898545687, 16.52544592524342804, 104.7905762719810241 ) ) ;
#117314 = CARTESIAN_POINT ( 'NONE',  ( -0.05219959533936034679, 19.03943276465977164, 57.50109039468566863 ) ) ;
#117315 = CARTESIAN_POINT ( 'NONE',  ( 16.52544592524335698, 4.483927247898782831, 111.4594237280190328 ) ) ;
#117316 = CARTESIAN_POINT ( 'NONE',  ( 21.53943276465977519, 0.05219959533937863772, 66.25109039468567573 ) ) ;
#117317 = CARTESIAN_POINT ( 'NONE',  ( 13.97604488694527802, 13.89961937509977652, 54.37390960531435979 ) ) ;
#117318 = CARTESIAN_POINT ( 'NONE',  ( -9.564922557961040184, 16.46253265017147172, 37.91775706135233293 ) ) ;
#117319 = CARTESIAN_POINT ( 'NONE',  ( -15.80617190586745835, -15.72974639402198527, 36.87390960531435979 ) ) ;
#117320 = CARTESIAN_POINT ( 'NONE',  ( -10.81492255796105439, 18.62759615963255655, 37.91775706135235424 ) ) ;
#117321 = CARTESIAN_POINT ( 'NONE',  ( 21.53943276465977519, -0.05219959533907433946, 93.74890960531436690 ) ) ;
#117322 = CARTESIAN_POINT ( 'NONE',  ( -16.51473224551082808, 9.474510206698731452, 83.33442372801899012 ) ) ;
#117323 = CARTESIAN_POINT ( 'NONE',  ( -14.29746914071037622, -8.314922557961029526, 54.16775706135235424 ) ) ;
#117325 = CARTESIAN_POINT ( 'NONE',  ( 10.81492255796078972, 18.62759615963270932, 89.58224293864768129 ) ) ;
#117324 = CARTESIAN_POINT ( 'NONE',  ( -16.92372544712134541, -17.40010620954080522, -56.79388978676514910 ) ) ;
#117326 = CARTESIAN_POINT ( 'NONE',  ( 16.52544592524342804, -4.483927247898539470, 83.54057627198102409 ) ) ;
#117327 = CARTESIAN_POINT ( 'NONE',  ( -27.48145228890726699, -25.86941904439673223, -20.55877432051689624 ) ) ;
#117328 = CARTESIAN_POINT ( 'NONE',  ( -9.564922557961040184, 16.46253265017147172, 112.9177570613523329 ) ) ;
#117329 = VECTOR ( 'NONE', #127289, 1000.000000000000000 ) ;
#117330 = EDGE_CURVE ( 'NONE', #144387, #53443, #183154, .T. ) ;
#117331 = CARTESIAN_POINT ( 'NONE',  ( 10.72451020669898902, -18.67979575497178502, 52.91557627198103830 ) ) ;
#117332 = CARTESIAN_POINT ( 'NONE',  ( -16.52544592524335698, -4.483927247898792601, 93.95942372801903275 ) ) ;
#117333 = CARTESIAN_POINT ( 'NONE',  ( 5.153800228976335163, 19.02544592524342804, 24.79057627198102765 ) ) ;
#117334 = CARTESIAN_POINT ( 'NONE',  ( -12.06949235617739369, -12.14591786802326823, 49.37609039468569705 ) ) ;
#117335 = CARTESIAN_POINT ( 'NONE',  ( -15.72974639402176322, -15.80617190586768395, 24.37609039468567573 ) ) ;
#117336 = CARTESIAN_POINT ( 'NONE',  ( 21.55341960407610458, 5.719274019375980345, 48.95724293864770971 ) ) ;
#117337 = CARTESIAN_POINT ( 'NONE',  ( -16.52544592524335698, -4.483927247898792601, 88.95942372801901854 ) ) ;
#117338 = CARTESIAN_POINT ( 'NONE',  ( -5.153800228976328057, -19.02544592524343514, 97.29057627198099567 ) ) ;
#117339 = CARTESIAN_POINT ( 'NONE',  ( -10.81492255796105439, 18.62759615963255655, 62.91775706135236135 ) ) ;
#117340 = CARTESIAN_POINT ( 'NONE',  ( -0.05219959533907301413, -21.53943276465977519, 42.49890960531435979 ) ) ;
#117341 = CARTESIAN_POINT ( 'NONE',  ( -16.46253265017160317, 9.564922557960807481, 110.8322429386476955 ) ) ;
#117342 = ORIENTED_EDGE ( 'NONE', *, *, #52301, .T. ) ;
#117343 = CARTESIAN_POINT ( 'NONE',  ( -5.049401038297874678, -19.05341960407617918, 34.79275706135233293 ) ) ;
#117344 = CARTESIAN_POINT ( 'NONE',  ( 14.29746914071037800, 8.314922557961029526, 71.66775706135234714 ) ) ;
#117345 = CARTESIAN_POINT ( 'NONE',  ( -5.153800228976328057, -19.02544592524343514, 112.2905762719810099 ) ) ;
#117346 = EDGE_LOOP ( 'NONE', ( #69129, #134531, #37224, #86570 ) ) ;
#117347 = CARTESIAN_POINT ( 'NONE',  ( 0.05219959533909260263, 19.03943276465977164, 79.99890960531436690 ) ) ;
#117348 = CARTESIAN_POINT ( 'NONE',  ( 12.14591786802327356, -12.06949235617739191, 105.6260903946856899 ) ) ;
#117349 = CARTESIAN_POINT ( 'NONE',  ( -17.97161686093727795, 5.499999999999980460, 85.99637206859166838 ) ) ;
#117350 = CARTESIAN_POINT ( 'NONE',  ( -16.53943276465976808, 0.05219959533911058130, 96.24890960531435269 ) ) ;
#117351 = CARTESIAN_POINT ( 'NONE',  ( -18.62759615963270932, 10.81492255796079327, 45.83224293864769550 ) ) ;
#117352 = CARTESIAN_POINT ( 'NONE',  ( 0.05219959533909260263, 19.03943276465977164, 34.99890960531435979 ) ) ;
#117353 = CARTESIAN_POINT ( 'NONE',  ( -16.52544592524335698, -4.483927247898792601, 83.95942372801900433 ) ) ;
#117354 = CARTESIAN_POINT ( 'NONE',  ( -21.52544592524334988, -5.823673210054445271, 28.95942372801902209 ) ) ;
#117355 = CARTESIAN_POINT ( 'NONE',  ( -16.46253265017146816, -9.564922557961047289, 89.16775706135234714 ) ) ;
#117356 = CARTESIAN_POINT ( 'NONE',  ( 0.05219959533910956823, 16.53943276465976808, 89.99890960531438111 ) ) ;
#117357 = CARTESIAN_POINT ( 'NONE',  ( 16.51473224551069308, 9.474510206698969483, 59.16557627198102409 ) ) ;
#117358 = CARTESIAN_POINT ( 'NONE',  ( 19.03943276465977164, -0.05219959533909143690, 108.7489096053143527 ) ) ;
#117359 = CARTESIAN_POINT ( 'NONE',  ( 21.53943276465977519, 0.05219959533937863772, 106.2510903946856757 ) ) ;
#117360 = CARTESIAN_POINT ( 'NONE',  ( 19.02544592524343514, -5.153800228976328945, 73.54057627198103830 ) ) ;
#117361 = CARTESIAN_POINT ( 'NONE',  ( -0.05219959533934338120, 16.53943276465976808, 67.50109039468568994 ) ) ;
#117362 = CARTESIAN_POINT ( 'NONE',  ( -10.81492255796105439, 18.62759615963255655, 87.91775706135234714 ) ) ;
#117363 = CARTESIAN_POINT ( 'NONE',  ( -0.05219959533934338120, 16.53943276465976808, 67.50109039468568994 ) ) ;
#117364 = CARTESIAN_POINT ( 'NONE',  ( 16.51473224551083163, -9.474510206698727899, 55.83442372801899722 ) ) ;
#117365 = CARTESIAN_POINT ( 'NONE',  ( 9.474510206698729675, 16.51473224551082808, 72.08442372801900433 ) ) ;
#117366 = CARTESIAN_POINT ( 'NONE',  ( 18.67979575497194134, -10.72451020669871369, 60.83442372801901854 ) ) ;
#117367 = CARTESIAN_POINT ( 'NONE',  ( 19.05341960407611168, 5.049401038298154454, 68.95724293864769550 ) ) ;
#117368 = CARTESIAN_POINT ( 'NONE',  ( -9.564922557960796823, -16.46253265017161027, 57.08224293864769550 ) ) ;
#117369 = CARTESIAN_POINT ( 'NONE',  ( 19.02544592524334988, 5.153800228976608722, 61.45942372801900433 ) ) ;
#117370 = CARTESIAN_POINT ( 'NONE',  ( -13.97604488694527625, -13.89961937509977652, 111.8739096053143243 ) ) ;
#117371 = CARTESIAN_POINT ( 'NONE',  ( 16.51473224551069308, 9.474510206698969483, 89.16557627198103830 ) ) ;
#117372 = CARTESIAN_POINT ( 'NONE',  ( -8.224510206698948167, 14.34966873604960824, 35.41557627198102409 ) ) ;
#117373 = CARTESIAN_POINT ( 'NONE',  ( 0.05219959533907565091, 21.53943276465977519, 44.99890960531435979 ) ) ;
#117374 = CARTESIAN_POINT ( 'NONE',  ( -23.29544513554941076, 16.92513159979227666, 141.7843446568999752 ) ) ;
#117375 = CARTESIAN_POINT ( 'NONE',  ( 21.52544592524334988, 5.823673210054432836, 106.4594237280190328 ) ) ;
#117376 = CARTESIAN_POINT ( 'NONE',  ( -16.31925111598456368, -7.325300261831607429, 79.83575461032749843 ) ) ;
#117377 = CARTESIAN_POINT ( 'NONE',  ( -0.05219959533909027116, -19.03943276465977164, 32.49890960531435979 ) ) ;
#117378 = CARTESIAN_POINT ( 'NONE',  ( 13.97604488694527802, 13.89961937509977652, 24.37390960531435624 ) ) ;
#117379 = CARTESIAN_POINT ( 'NONE',  ( -34.25242159400493591, -3.629837513186700892, 90.85215659754989304 ) ) ;
#117380 = CARTESIAN_POINT ( 'NONE',  ( -21.55341960407619339, 5.719274019375674811, 63.54275706135234003 ) ) ;
#117381 = CARTESIAN_POINT ( 'NONE',  ( -23.43257786332091186, -29.32469887945705622, -7.999999999999994671 ) ) ;
#117382 = CARTESIAN_POINT ( 'NONE',  ( -0.05219959533934338120, 16.53943276465976808, 62.50109039468568284 ) ) ;
#117383 = CARTESIAN_POINT ( 'NONE',  ( -0.05219959533907301413, -21.53943276465977519, 82.49890960531436690 ) ) ;
#117384 = CARTESIAN_POINT ( 'NONE',  ( 16.52544592524342804, -4.483927247898539470, 48.54057627198103120 ) ) ;
#117386 = CARTESIAN_POINT ( 'NONE',  ( 2.500000000000000000, 0.000000000000000000, 0.000000000000000000 ) ) ;
#117385 = CARTESIAN_POINT ( 'NONE',  ( 19.03943276465977164, -0.05219959533909143690, 28.74890960531435624 ) ) ;
#117387 = CARTESIAN_POINT ( 'NONE',  ( 18.62759615963255655, 10.81492255796105972, 41.66775706135235424 ) ) ;
#117388 = CARTESIAN_POINT ( 'NONE',  ( 19.03943276465977164, 0.05219959533936151252, 46.25109039468566863 ) ) ;
#117389 = CARTESIAN_POINT ( 'NONE',  ( 13.97604488694527802, 13.89961937509977652, 34.37390960531436690 ) ) ;
#117390 = CARTESIAN_POINT ( 'NONE',  ( 10.72451020669871369, 18.67979575497193778, 87.08442372801901854 ) ) ;
#117391 = CARTESIAN_POINT ( 'NONE',  ( 22.00000000000000000, -5.510910596163089556E-15, 42.49999999999999289 ) ) ;
#117392 = CARTESIAN_POINT ( 'NONE',  ( -8.314922557960811034, -14.29746914071050412, 47.08224293864770260 ) ) ;
#117393 = CARTESIAN_POINT ( 'NONE',  ( 22.81625015709510151, -31.40387420917324590, -2.424999997268812990 ) ) ;
#117394 = CARTESIAN_POINT ( 'NONE',  ( 21.52544592524344225, -5.823673210054117533, 43.54057627198103830 ) ) ;
#117395 = CARTESIAN_POINT ( 'NONE',  ( 1.300000000000000044, -0.7216878364870319418, 1.249999999999999778 ) ) ;
#117396 = CARTESIAN_POINT ( 'NONE',  ( -13.97604488694527625, -13.89961937509977652, 91.87390960531432427 ) ) ;
#117397 = CARTESIAN_POINT ( 'NONE',  ( 4.379528057220339221, -16.55341960407611168, 82.70724293864770971 ) ) ;
#117398 = CARTESIAN_POINT ( 'NONE',  ( -13.97604488694547697, 13.89961937509957934, 103.1260903946856473 ) ) ;
#117399 = EDGE_CURVE ( 'NONE', #102413, #2480, #48451, .T. ) ;
#117400 = CARTESIAN_POINT ( 'NONE',  ( 15.80617190586746368, 15.72974639402197994, 59.37390960531436690 ) ) ;
#117401 = ORIENTED_EDGE ( 'NONE', *, *, #57096, .T. ) ;
#117402 = CARTESIAN_POINT ( 'NONE',  ( 13.97604488694527802, 13.89961937509977652, 34.37390960531436690 ) ) ;
#117404 = CARTESIAN_POINT ( 'NONE',  ( 18.62759615963271287, -10.81492255796078972, 83.33224293864769550 ) ) ;
#117403 = CARTESIAN_POINT ( 'NONE',  ( 16.51473224551069308, 9.474510206698969483, 79.16557627198103830 ) ) ;
#117405 = VECTOR ( 'NONE', #197338, 1000.000000000000000 ) ;
#117407 = CARTESIAN_POINT ( 'NONE',  ( -19.03943276465977164, 0.05219959533909376836, 101.2489096053143669 ) ) ;
#117406 = CARTESIAN_POINT ( 'NONE',  ( 8.314922557960818139, 14.29746914071049879, 29.58224293864769905 ) ) ;
#117408 = CARTESIAN_POINT ( 'NONE',  ( 19.03943276465977164, 0.05219959533936151252, 81.25109039468567573 ) ) ;
#117409 = CARTESIAN_POINT ( 'NONE',  ( -15.72974639402176322, -15.80617190586768395, 89.37609039468568994 ) ) ;
#117410 = CARTESIAN_POINT ( 'NONE',  ( -15.72974639402197994, 15.80617190586746368, 80.62390960531438111 ) ) ;
#117411 = CARTESIAN_POINT ( 'NONE',  ( -18.62759615963270932, 10.81492255796079327, 35.83224293864768839 ) ) ;
#117412 = CARTESIAN_POINT ( 'NONE',  ( 13.97604488694527802, 13.89961937509977652, 54.37390960531435979 ) ) ;
#117413 = CARTESIAN_POINT ( 'NONE',  ( 14.34966873604972726, -8.224510206698740333, 110.8344237280190043 ) ) ;
#117414 = CARTESIAN_POINT ( 'NONE',  ( -19.02544592524342804, 5.153800228976336051, 71.04057627198099567 ) ) ;
#117415 = ORIENTED_EDGE ( 'NONE', *, *, #130264, .F. ) ;
#117416 = CARTESIAN_POINT ( 'NONE',  ( -31.37911219714120037, -7.435064219939695462, 93.98466263399197373 ) ) ;
#117417 = CARTESIAN_POINT ( 'NONE',  ( -19.05341960407617563, 5.049401038297882671, 33.54275706135231871 ) ) ;
#117418 = CARTESIAN_POINT ( 'NONE',  ( -14.29746914071049879, 8.314922557960819915, 80.83224293864769550 ) ) ;
#117419 = CARTESIAN_POINT ( 'NONE',  ( 0.05219959533937995610, -21.53943276465977519, 30.00109039468568284 ) ) ;
#117420 = CARTESIAN_POINT ( 'NONE',  ( -22.44159573604010305, 16.30477369853692338, 145.1750000027311671 ) ) ;
#117421 = CARTESIAN_POINT ( 'NONE',  ( -18.62759615963270932, 10.81492255796079327, 55.83224293864770260 ) ) ;
#117422 = CARTESIAN_POINT ( 'NONE',  ( -16.53943276465976808, -0.05219959533934237506, 93.75109039468567573 ) ) ;
#117423 = CARTESIAN_POINT ( 'NONE',  ( 13.89961937509977652, -13.97604488694527269, 23.12390960531436335 ) ) ;
#117424 = CARTESIAN_POINT ( 'NONE',  ( 16.51473224551069308, 9.474510206698969483, 69.16557627198102409 ) ) ;
#117425 = CYLINDRICAL_SURFACE ( 'NONE', #173793, 59.99999999999998579 ) ;
#117426 = CARTESIAN_POINT ( 'NONE',  ( 14.29746914071049879, -8.314922557960816363, 33.33224293864769550 ) ) ;
#117427 = CARTESIAN_POINT ( 'NONE',  ( 15.80617190586769283, -15.72974639402175789, 65.62609039468568994 ) ) ;
#117428 = CARTESIAN_POINT ( 'NONE',  ( -13.89961937509977652, 13.97604488694528158, 105.6239096053143527 ) ) ;
#117429 = CARTESIAN_POINT ( 'NONE',  ( -18.62759615963255300, -10.81492255796106328, 89.16775706135236135 ) ) ;
#117430 = CARTESIAN_POINT ( 'NONE',  ( -16.46253265017160317, 9.564922557960807481, 25.83224293864769194 ) ) ;
#117431 = CARTESIAN_POINT ( 'NONE',  ( -13.89961937509977652, 13.97604488694528158, 35.62390960531435269 ) ) ;
#117432 = VERTEX_POINT ( 'NONE', #31449 ) ;
#117433 = CARTESIAN_POINT ( 'NONE',  ( 15.72974639402176855, 15.80617190586768217, 96.87609039468568994 ) ) ;
#117434 = CARTESIAN_POINT ( 'NONE',  ( -16.53943276465976808, -0.05219959533934237506, 48.75109039468568284 ) ) ;
#117435 = CARTESIAN_POINT ( 'NONE',  ( 21.52544592524334988, 5.823673210054432836, 91.45942372801901854 ) ) ;
#117436 = CARTESIAN_POINT ( 'NONE',  ( -13.97604488694527625, -13.89961937509977652, 111.8739096053143243 ) ) ;
#117437 = CARTESIAN_POINT ( 'NONE',  ( 9.564922557961047289, -16.46253265017146816, 90.41775706135234714 ) ) ;
#117438 = CARTESIAN_POINT ( 'NONE',  ( 15.80617190586769283, -15.72974639402175789, 55.62609039468568284 ) ) ;
#117439 = CARTESIAN_POINT ( 'NONE',  ( 12.06949235617739724, 12.14591786802326823, 21.87609039468567573 ) ) ;
#117440 = CARTESIAN_POINT ( 'NONE',  ( -13.89961937509957401, -13.97604488694547875, 79.37609039468567573 ) ) ;
#117441 = CARTESIAN_POINT ( 'NONE',  ( -9.564922557960796823, -16.46253265017161027, 52.08224293864768839 ) ) ;
#117442 = CARTESIAN_POINT ( 'NONE',  ( -19.05341960407617563, 5.049401038297882671, 98.54275706135233293 ) ) ;
#117443 = CARTESIAN_POINT ( 'NONE',  ( -19.03943276465977164, -0.05219959533935918106, 88.75109039468567573 ) ) ;
#117444 = CARTESIAN_POINT ( 'NONE',  ( 14.34966873604960469, 8.224510206698951720, 54.16557627198103120 ) ) ;
#117445 = CARTESIAN_POINT ( 'NONE',  ( 19.03943276465977164, 0.05219959533936151252, 71.25109039468566152 ) ) ;
#117446 = CARTESIAN_POINT ( 'NONE',  ( -8.224510206698735004, -14.34966873604973081, 54.58442372801901143 ) ) ;
#117447 = CARTESIAN_POINT ( 'NONE',  ( -21.55341960407619339, 5.719274019375674811, 113.5427570613523756 ) ) ;
#117448 = CARTESIAN_POINT ( 'NONE',  ( 9.474510206698971260, -16.51473224551069308, 32.91557627198102409 ) ) ;
#117449 = CARTESIAN_POINT ( 'NONE',  ( 0.05219959533909260263, 19.03943276465977164, 44.99890960531435979 ) ) ;
#117450 = CARTESIAN_POINT ( 'NONE',  ( 12.06949235617739724, 12.14591786802326823, 56.87609039468568994 ) ) ;
#117451 = CARTESIAN_POINT ( 'NONE',  ( -17.60728821187776205, 5.500000000000042633, 45.86690927743608626 ) ) ;
#117452 = CARTESIAN_POINT ( 'NONE',  ( -8.906447517083060816, 27.41122689804195645, 141.8500000054623911 ) ) ;
#117453 = CARTESIAN_POINT ( 'NONE',  ( 13.97604488694527802, 13.89961937509977652, 109.3739096053143669 ) ) ;
#117454 = CARTESIAN_POINT ( 'NONE',  ( -18.22780087662124160, -5.499999999999927169, 83.98236817873107896 ) ) ;
#117455 = EDGE_LOOP ( 'NONE', ( #24467, #166152, #161623, #109603 ) ) ;
#117456 = CARTESIAN_POINT ( 'NONE',  ( 5.049401038297881783, 19.05341960407617563, 92.29275706135234714 ) ) ;
#117457 = CARTESIAN_POINT ( 'NONE',  ( 21.55341960407610458, 5.719274019375980345, 33.95724293864769550 ) ) ;
#117459 = CARTESIAN_POINT ( 'NONE',  ( -0.05219959533936034679, 19.03943276465977164, 107.5010903946856615 ) ) ;
#117458 = CARTESIAN_POINT ( 'NONE',  ( -16.46253265017146816, -9.564922557961047289, 29.16775706135232937 ) ) ;
#117460 = CARTESIAN_POINT ( 'NONE',  ( -19.05341960407611168, -5.049401038298163336, 36.45724293864766707 ) ) ;
#117461 = CARTESIAN_POINT ( 'NONE',  ( -13.97604488694527625, -13.89961937509977652, 36.87390960531436690 ) ) ;
#117462 = CARTESIAN_POINT ( 'NONE',  ( -5.719274019375978568, 21.55341960407610458, 70.20724293864769550 ) ) ;
#117463 = CARTESIAN_POINT ( 'NONE',  ( -9.564922557960796823, -16.46253265017161027, 102.0822429386477097 ) ) ;
#117464 = CIRCLE ( 'NONE', #188477, 38.00000000000000000 ) ;
#117465 = CARTESIAN_POINT ( 'NONE',  ( -5.153800228976328057, -19.02544592524343514, 42.29057627198101699 ) ) ;
#117466 = CARTESIAN_POINT ( 'NONE',  ( -27.73933785331498925, 9.013057229001088189, 143.2750000027311899 ) ) ;
#117467 = CARTESIAN_POINT ( 'NONE',  ( -0.05219959533936034679, 19.03943276465977164, 87.50109039468567573 ) ) ;
#117468 = CARTESIAN_POINT ( 'NONE',  ( 4.379528057220339221, -16.55341960407611168, 57.70724293864770260 ) ) ;
#117469 = CARTESIAN_POINT ( 'NONE',  ( 18.67979575497178502, 10.72451020669898547, 39.16557627198102409 ) ) ;
#117470 = CARTESIAN_POINT ( 'NONE',  ( -0.05219959533937732626, 21.53943276465977519, 107.5010903946856899 ) ) ;
#117471 = CARTESIAN_POINT ( 'NONE',  ( 15.80617190586746368, 15.72974639402197994, 79.37390960531436690 ) ) ;
#117472 = CARTESIAN_POINT ( 'NONE',  ( -21.52544592524334988, -5.823673210054445271, 73.95942372801901854 ) ) ;
#117473 = CARTESIAN_POINT ( 'NONE',  ( 18.62759615963255655, 10.81492255796105972, 66.66775706135234714 ) ) ;
#117474 = CARTESIAN_POINT ( 'NONE',  ( -0.05219959533909027116, -19.03943276465977164, 112.4989096053143669 ) ) ;
#117476 = CARTESIAN_POINT ( 'NONE',  ( 21.53943276465977519, 0.05219959533937863772, 66.25109039468567573 ) ) ;
#117475 = CARTESIAN_POINT ( 'NONE',  ( -12.06949235617739369, -12.14591786802326823, 109.3760903946857042 ) ) ;
#117477 = CARTESIAN_POINT ( 'NONE',  ( -16.51473224551069308, -9.474510206698971260, 56.66557627198103120 ) ) ;
#117478 = CARTESIAN_POINT ( 'NONE',  ( -19.05341960407617563, 5.049401038297882671, 33.54275706135231871 ) ) ;
#117479 = CARTESIAN_POINT ( 'NONE',  ( -18.62759615963255300, -10.81492255796106328, 24.16775706135235424 ) ) ;
#117480 = CARTESIAN_POINT ( 'NONE',  ( 9.474510206698971260, -16.51473224551069308, 72.91557627198102409 ) ) ;
#117481 = CARTESIAN_POINT ( 'NONE',  ( -0.05219959533910754901, -16.53943276465976808, 77.49890960531433848 ) ) ;
#117482 = CARTESIAN_POINT ( 'NONE',  ( -12.14591786802309592, -12.06949235617757132, 51.87390960531437401 ) ) ;
#117483 = CARTESIAN_POINT ( 'NONE',  ( 5.719274019375991003, -21.55341960407610458, 57.70724293864770260 ) ) ;
#117484 = CARTESIAN_POINT ( 'NONE',  ( -5.049401038298153566, 19.05341960407611168, 65.20724293864765286 ) ) ;
#117485 = CARTESIAN_POINT ( 'NONE',  ( -18.62759615963270932, 10.81492255796079327, 75.83224293864769550 ) ) ;
#117487 = CIRCLE ( 'NONE', #101451, 61.99999999999998579 ) ;
#117486 = CARTESIAN_POINT ( 'NONE',  ( -13.89961937509957401, -13.97604488694547875, 54.37609039468565442 ) ) ;
#117489 = CARTESIAN_POINT ( 'NONE',  ( 16.55341960407611168, 4.379528057220329451, 63.95724293864770260 ) ) ;
#117488 = PLANE ( 'NONE',  #84904 ) ;
#117490 = CARTESIAN_POINT ( 'NONE',  ( -21.53943276465977519, 0.05219959533907696930, 41.24890960531435269 ) ) ;
#117491 = EDGE_LOOP ( 'NONE', ( #167510, #159675, #168298, #135754, #128823 ) ) ;
#117492 = CARTESIAN_POINT ( 'NONE',  ( 16.31925111598457434, 7.325300261831544368, 102.3357546103274984 ) ) ;
#117494 = CARTESIAN_POINT ( 'NONE',  ( -8.571926809382608425, 26.38167802310805854, 140.9750000027312069 ) ) ;
#117493 = CARTESIAN_POINT ( 'NONE',  ( -4.483927247898782831, 16.52544592524335698, 87.70942372801901854 ) ) ;
#117495 = CARTESIAN_POINT ( 'NONE',  ( 0.05219959533936267826, -19.03943276465977164, 95.00109039468567573 ) ) ;
#117496 = CARTESIAN_POINT ( 'NONE',  ( -4.379528057220328563, 16.55341960407611168, 50.20724293864769550 ) ) ;
#117497 = LINE ( 'NONE', #52812, #135502 ) ;
#117498 = CARTESIAN_POINT ( 'NONE',  ( 19.05341960407611168, 5.049401038298154454, 48.95724293864768129 ) ) ;
#117499 = CARTESIAN_POINT ( 'NONE',  ( 16.53943276465976808, -0.05219959533910856209, 38.74890960531435979 ) ) ;
#117500 = CARTESIAN_POINT ( 'NONE',  ( 19.05341960407611168, 5.049401038298154454, 83.95724293864766707 ) ) ;
#117501 = CARTESIAN_POINT ( 'NONE',  ( -9.474510206698964154, 16.51473224551069663, 50.41557627198102409 ) ) ;
#117502 = CARTESIAN_POINT ( 'NONE',  ( -21.53943276465977519, -0.05219959533937600094, 58.75109039468568994 ) ) ;
#117503 = CARTESIAN_POINT ( 'NONE',  ( -13.89961937509977652, 13.97604488694528158, 70.62390960531432427 ) ) ;
#117504 = CARTESIAN_POINT ( 'NONE',  ( 16.46253265017160672, -9.564922557960803928, 28.33224293864769550 ) ) ;
#117505 = CARTESIAN_POINT ( 'NONE',  ( -5.049401038298153566, 19.05341960407611168, 70.20724293864769550 ) ) ;
#117506 = CARTESIAN_POINT ( 'NONE',  ( 15.80617190586746368, 15.72974639402197994, 49.37390960531436690 ) ) ;
#117507 = CARTESIAN_POINT ( 'NONE',  ( 9.474510206698971260, -16.51473224551069308, 37.91557627198102409 ) ) ;
#117508 = CARTESIAN_POINT ( 'NONE',  ( -5.719274019375978568, 21.55341960407610458, 35.20724293864768839 ) ) ;
#117509 = CARTESIAN_POINT ( 'NONE',  ( -12.06949235617739369, -12.14591786802326823, 109.3760903946857042 ) ) ;
#117510 = CARTESIAN_POINT ( 'NONE',  ( -9.474510206698720793, -16.51473224551083518, 29.58442372801900433 ) ) ;
#117511 = EDGE_CURVE ( 'NONE', #183244, #45951, #77935, .T. ) ;
#117513 = CARTESIAN_POINT ( 'NONE',  ( -8.224510206698735004, -14.34966873604973081, 84.58442372801903275 ) ) ;
#117512 = CARTESIAN_POINT ( 'NONE',  ( -16.52544592524335698, -4.483927247898792601, 43.95942372801902565 ) ) ;
#117514 = CARTESIAN_POINT ( 'NONE',  ( -13.89961937509977652, 13.97604488694528158, 115.6239096053143669 ) ) ;
#117515 = CARTESIAN_POINT ( 'NONE',  ( 12.06949235617739724, 12.14591786802326823, 61.87609039468568284 ) ) ;
#117516 = CARTESIAN_POINT ( 'NONE',  ( 19.05341960407611168, 5.049401038298154454, 108.9572429386477097 ) ) ;
#117517 = CARTESIAN_POINT ( 'NONE',  ( -16.51473224551069308, -9.474510206698971260, 36.66557627198102409 ) ) ;
#117518 = CARTESIAN_POINT ( 'NONE',  ( -16.55341960407617563, 4.379528057220093196, 33.54275706135234714 ) ) ;
#117519 = CARTESIAN_POINT ( 'NONE',  ( 13.97604488694527802, 13.89961937509977652, 44.37390960531435269 ) ) ;
#117520 = CARTESIAN_POINT ( 'NONE',  ( -21.52544592524334988, -5.823673210054445271, 23.95942372801901143 ) ) ;
#117521 = CARTESIAN_POINT ( 'NONE',  ( 16.52544592524335698, 4.483927247898782831, 36.45942372801901143 ) ) ;
#117522 = CARTESIAN_POINT ( 'NONE',  ( 8.224510206698742110, 14.34966873604972548, 102.0844237280190185 ) ) ;
#117523 = CARTESIAN_POINT ( 'NONE',  ( -21.46320343559653665, -25.04568634023494056, 8.240304736541402164 ) ) ;
#117524 = CARTESIAN_POINT ( 'NONE',  ( 0.05219959533937995610, -21.53943276465977519, 95.00109039468568994 ) ) ;
#117525 = CARTESIAN_POINT ( 'NONE',  ( 19.03943276465977164, 0.05219959533936151252, 101.2510903946856757 ) ) ;
#117526 = CARTESIAN_POINT ( 'NONE',  ( -5.049401038297874678, -19.05341960407617918, 59.79275706135231871 ) ) ;
#117527 = CARTESIAN_POINT ( 'NONE',  ( -8.314922557960811034, -14.29746914071050412, 62.08224293864769550 ) ) ;
#117528 = CARTESIAN_POINT ( 'NONE',  ( 12.14591786802309770, 12.06949235617756955, 114.3739096053143527 ) ) ;
#117530 = CARTESIAN_POINT ( 'NONE',  ( 16.36317988757057762, 7.306389748694939179, 78.40210391636777842 ) ) ;
#117529 = CARTESIAN_POINT ( 'NONE',  ( 19.02544592524334988, 5.153800228976608722, 61.45942372801900433 ) ) ;
#117531 = CARTESIAN_POINT ( 'NONE',  ( -21.52544592524334988, -5.823673210054445271, 63.95942372801901854 ) ) ;
#117532 = CARTESIAN_POINT ( 'NONE',  ( -4.483927247898782831, 16.52544592524335698, 22.70942372801901499 ) ) ;
#117533 = FACE_OUTER_BOUND ( 'NONE', #181148, .T. ) ;
#117534 = CARTESIAN_POINT ( 'NONE',  ( 15.80617190586746368, 15.72974639402197994, 24.37390960531435979 ) ) ;
#117535 = CARTESIAN_POINT ( 'NONE',  ( -0.05219959533936034679, 19.03943276465977164, 107.5010903946856615 ) ) ;
#117536 = CARTESIAN_POINT ( 'NONE',  ( -40.00200000000003087, -1.163414459189985801E-14, 87.50000000000000000 ) ) ;
#117537 = CARTESIAN_POINT ( 'NONE',  ( -21.84611564451296672, 9.363109600221495299, 171.0247306346272751 ) ) ;
#117538 = CARTESIAN_POINT ( 'NONE',  ( -16.46253265017160317, 9.564922557960807481, 25.83224293864769194 ) ) ;
#117539 = CARTESIAN_POINT ( 'NONE',  ( -10.81492255796105439, 18.62759615963255655, 102.9177570613523756 ) ) ;
#117540 = CARTESIAN_POINT ( 'NONE',  ( 19.02544592524343514, -5.153800228976328945, 53.54057627198102409 ) ) ;
#117541 = CARTESIAN_POINT ( 'NONE',  ( 0.05219959533937995610, -21.53943276465977519, 65.00109039468568994 ) ) ;
#117542 = CARTESIAN_POINT ( 'NONE',  ( 21.52544592524334988, 5.823673210054432836, 101.4594237280190185 ) ) ;
#117543 = CARTESIAN_POINT ( 'NONE',  ( -8.314922557961024197, 14.29746914071037800, 97.91775706135236135 ) ) ;
#117544 = CARTESIAN_POINT ( 'NONE',  ( 16.46253265017160672, -9.564922557960803928, 73.33224293864769550 ) ) ;
#117545 = CARTESIAN_POINT ( 'NONE',  ( -21.52544592524334988, -5.823673210054445271, 58.95942372801902565 ) ) ;
#117546 = AXIS2_PLACEMENT_3D ( 'NONE', #150091, #104576, #149096 ) ;
#117547 = CARTESIAN_POINT ( 'NONE',  ( -18.62759615963255300, -10.81492255796106328, 54.16775706135235424 ) ) ;
#117549 = CARTESIAN_POINT ( 'NONE',  ( 9.564922557960805705, 16.46253265017160317, 104.5822429386476955 ) ) ;
#117548 = CARTESIAN_POINT ( 'NONE',  ( -13.89961937509957401, -13.97604488694547875, 79.37609039468567573 ) ) ;
#117550 = CARTESIAN_POINT ( 'NONE',  ( -0.05219959533910754901, -16.53943276465976808, 112.4989096053143669 ) ) ;
#117551 = CARTESIAN_POINT ( 'NONE',  ( -18.67979575497178146, -10.72451020669898902, 96.66557627198102409 ) ) ;
#117552 = CARTESIAN_POINT ( 'NONE',  ( 13.97604488694548053, -13.89961937509957401, 20.62609039468567573 ) ) ;
#117553 = CARTESIAN_POINT ( 'NONE',  ( -16.55341960407611168, -4.379528057220339221, 96.45724293864770971 ) ) ;
#117554 = CARTESIAN_POINT ( 'NONE',  ( 19.02544592524343514, -5.153800228976328945, 53.54057627198102409 ) ) ;
#117555 = CARTESIAN_POINT ( 'NONE',  ( 9.474510206698729675, 16.51473224551082808, 102.0844237280190043 ) ) ;
#117556 = CARTESIAN_POINT ( 'NONE',  ( -0.05219959533910754901, -16.53943276465976808, 67.49890960531436690 ) ) ;
#117557 = CARTESIAN_POINT ( 'NONE',  ( 21.52544592524334988, 5.823673210054432836, 111.4594237280190328 ) ) ;
#117558 = CARTESIAN_POINT ( 'NONE',  ( -19.03943276465977164, 0.05219959533909376836, 106.2489096053143669 ) ) ;
#117559 = CARTESIAN_POINT ( 'NONE',  ( -0.05219959533936034679, 19.03943276465977164, 72.50109039468566152 ) ) ;
#117560 = CARTESIAN_POINT ( 'NONE',  ( 18.62759615963271287, -10.81492255796078972, 83.33224293864769550 ) ) ;
#117561 = CARTESIAN_POINT ( 'NONE',  ( 10.81492255796106328, -18.62759615963255655, 50.41775706135235424 ) ) ;
#117562 = CARTESIAN_POINT ( 'NONE',  ( -8.314922557961024197, 14.29746914071037800, 37.91775706135235424 ) ) ;
#117563 = CARTESIAN_POINT ( 'NONE',  ( -16.55341960407617563, 4.379528057220093196, 93.54275706135234714 ) ) ;
#117565 = CARTESIAN_POINT ( 'NONE',  ( 21.52544592524334988, 5.823673210054432836, 36.45942372801901143 ) ) ;
#117564 = CARTESIAN_POINT ( 'NONE',  ( -4.379528057220086978, -16.55341960407618274, 39.79275706135235424 ) ) ;
#117566 = CARTESIAN_POINT ( 'NONE',  ( -10.81492255796078084, -18.62759615963271287, 42.08224293864769550 ) ) ;
#117567 = CARTESIAN_POINT ( 'NONE',  ( -9.474510206698964154, 16.51473224551069663, 40.41557627198103120 ) ) ;
#117568 = CARTESIAN_POINT ( 'NONE',  ( 30.74264578624799782, 22.33583958711400541, -10.54999999453762705 ) ) ;
#117569 = CARTESIAN_POINT ( 'NONE',  ( 16.55341960407618274, -4.379528057220086978, 66.04275706135236135 ) ) ;
#117570 = EDGE_CURVE ( 'NONE', #72196, #37464, #164644, .T. ) ;
#117571 = CARTESIAN_POINT ( 'NONE',  ( 0.05219959533907565091, 21.53943276465977519, 89.99890960531438111 ) ) ;
#117572 = CARTESIAN_POINT ( 'NONE',  ( -12.06949235617756955, 12.14591786802309770, 40.62390960531435269 ) ) ;
#117573 = CARTESIAN_POINT ( 'NONE',  ( -14.29746914071037622, -8.314922557961029526, 54.16775706135235424 ) ) ;
#117574 = CARTESIAN_POINT ( 'NONE',  ( 19.03943276465977164, -0.05219959533909143690, 58.74890960531435979 ) ) ;
#117575 = CARTESIAN_POINT ( 'NONE',  ( -9.564922557961040184, 16.46253265017147172, 82.91775706135233293 ) ) ;
#117576 = CARTESIAN_POINT ( 'NONE',  ( -15.80617190586745835, -15.72974639402198527, 81.87390960531435269 ) ) ;
#117577 = CARTESIAN_POINT ( 'NONE',  ( -4.379528057220328563, 16.55341960407611168, 30.20724293864769550 ) ) ;
#117578 = ORIENTED_EDGE ( 'NONE', *, *, #89522, .F. ) ;
#117579 = CARTESIAN_POINT ( 'NONE',  ( 25.62062145120080103, 9.171473787276196887, 171.1688781158127028 ) ) ;
#117580 = AXIS2_PLACEMENT_3D ( 'NONE', #42318, #60441, #89802 ) ;
#117581 = CARTESIAN_POINT ( 'NONE',  ( -15.72974639402197994, 15.80617190586746368, 55.62390960531436690 ) ) ;
#117582 = CARTESIAN_POINT ( 'NONE',  ( 0.05219959533934541429, -16.53943276465976808, 105.0010903946856757 ) ) ;
#117583 = ORIENTED_EDGE ( 'NONE', *, *, #131422, .T. ) ;
#117584 = CARTESIAN_POINT ( 'NONE',  ( 18.39639308325437028, 5.500000000000035527, 88.98252246182197212 ) ) ;
#117585 = CARTESIAN_POINT ( 'NONE',  ( 10.81492255796078972, 18.62759615963270932, 84.58224293864769550 ) ) ;
#117586 = CARTESIAN_POINT ( 'NONE',  ( -4.483927247898539470, -16.52544592524342804, 22.29057627198102765 ) ) ;
#117587 = CARTESIAN_POINT ( 'NONE',  ( 4.483927247898790824, -16.52544592524335698, 30.20942372801902565 ) ) ;
#117588 = CARTESIAN_POINT ( 'NONE',  ( 5.049401038298161559, -19.05341960407611168, 32.70724293864768129 ) ) ;
#117589 = CARTESIAN_POINT ( 'NONE',  ( 19.03943276465977164, -0.05219959533909143690, 68.74890960531436690 ) ) ;
#117590 = CARTESIAN_POINT ( 'NONE',  ( 8.906447517083057264, -27.41122689804191026, 148.5999999999999943 ) ) ;
#117591 = CARTESIAN_POINT ( 'NONE',  ( -21.55341960407610458, -5.719274019375992779, 26.45724293864768839 ) ) ;
#117592 = CARTESIAN_POINT ( 'NONE',  ( 18.09918380851993192, 5.500000000000035527, 78.98618307335611632 ) ) ;
#117593 = AXIS2_PLACEMENT_3D ( 'NONE', #34819, #95490, #43297 ) ;
#117594 = CARTESIAN_POINT ( 'NONE',  ( -12.14591786802326823, 12.06949235617739902, 98.12609039468570415 ) ) ;
#117595 = CARTESIAN_POINT ( 'NONE',  ( 13.97604488694548053, -13.89961937509957401, 105.6260903946856757 ) ) ;
#117596 = CARTESIAN_POINT ( 'NONE',  ( 19.02544592524334988, 5.153800228976608722, 31.45942372801900433 ) ) ;
#117597 = CARTESIAN_POINT ( 'NONE',  ( -10.81492255796078084, -18.62759615963271287, 87.08224293864769550 ) ) ;
#117598 = CARTESIAN_POINT ( 'NONE',  ( -16.53943276465976808, 0.05219959533911058130, 21.24890960531436690 ) ) ;
#117599 = CARTESIAN_POINT ( 'NONE',  ( 21.55341960407610458, 5.719274019375980345, 48.95724293864770971 ) ) ;
#117600 = CARTESIAN_POINT ( 'NONE',  ( -16.46253265017146816, -9.564922557961047289, 109.1677570613523471 ) ) ;
#117602 = CLOSED_SHELL ( 'NONE', ( #184481, #38662, #22207, #47032, #64370, #67491, #30330, #45643, #140183, #165578, #191364, #27705, #1779, #13777, #136809, #162076, #92282, #173652, #114127, #129217, #100839, #197994, #89653, #21634, #70806, #42424, #36421, #90878, #153015, #171965, #114998, #127422, #191910, #87717, #156285, #170129, #181717, #154536, #148251, #84984, #42332, #59345, #130630, #88416, #195013, #172668, #133971, #101406, #26137, #127217, #180603, #50685, #108149, #150543, #163464, #101656, #127617, #52761, #83017, #12349, #51269 ) ) ;
#117601 = CARTESIAN_POINT ( 'NONE',  ( 16.51473224551069308, 9.474510206698969483, 99.16557627198102409 ) ) ;
#117603 = CARTESIAN_POINT ( 'NONE',  ( -21.52544592524334988, -5.823673210054445271, 63.95942372801901854 ) ) ;
#117604 = CARTESIAN_POINT ( 'NONE',  ( 9.474510206698971260, -16.51473224551069308, 62.91557627198102409 ) ) ;
#117605 = CARTESIAN_POINT ( 'NONE',  ( -16.52544592524342804, 4.483927247898546575, 96.04057627198102409 ) ) ;
#117606 = CARTESIAN_POINT ( 'NONE',  ( 31.48310541436861243, 7.250236049019784801, 93.01911755558080586 ) ) ;
#117607 = CARTESIAN_POINT ( 'NONE',  ( -9.564922557960796823, -16.46253265017161027, 72.08224293864770971 ) ) ;
#117608 = CARTESIAN_POINT ( 'NONE',  ( 16.55341960407611168, 4.379528057220329451, 78.95724293864769550 ) ) ;
#117609 = ORIENTED_EDGE ( 'NONE', *, *, #137956, .T. ) ;
#117610 = CARTESIAN_POINT ( 'NONE',  ( 13.89961937509957401, 13.97604488694547697, 86.87609039468567573 ) ) ;
#117611 = STYLED_ITEM ( 'NONE', ( #148772 ), #35157 ) ;
#117612 =( BOUNDED_CURVE ( )  B_SPLINE_CURVE ( 3, ( #184964, #142430, #155617, #172787 ),
 .UNSPECIFIED., .F., .F. ) 
 B_SPLINE_CURVE_WITH_KNOTS ( ( 4, 4 ),
 ( 5.150538010968860547, 5.257537365396776075 ),
 .UNSPECIFIED. ) 
 CURVE ( )  GEOMETRIC_REPRESENTATION_ITEM ( )  RATIONAL_B_SPLINE_CURVE ( ( 1.000000000000000000, 0.9990461557208837329, 0.9990461557208837329, 1.000000000000000000 ) ) 
 REPRESENTATION_ITEM ( '' )  );
#117613 = CARTESIAN_POINT ( 'NONE',  ( 19.39056639909674473, 5.500000000000001776, 93.28948781074345220 ) ) ;
#117614 = CARTESIAN_POINT ( 'NONE',  ( -0.05219959533909027116, -19.03943276465977164, 57.49890960531435979 ) ) ;
#117615 = CARTESIAN_POINT ( 'NONE',  ( 32.57158834789613877, -1.949426887446015888, 87.75361764676912912 ) ) ;
#117617 = CARTESIAN_POINT ( 'NONE',  ( -5.049401038298153566, 19.05341960407611168, 105.2072429386476671 ) ) ;
#117616 = CARTESIAN_POINT ( 'NONE',  ( -5.153800228976328057, -19.02544592524343514, 72.29057627198102409 ) ) ;
#117618 = CARTESIAN_POINT ( 'NONE',  ( -16.52544592524335698, -4.483927247898792601, 68.95942372801901854 ) ) ;
#117619 = DIRECTION ( 'NONE',  ( -1.000000000000000000, 0.000000000000000000, 0.000000000000000000 ) ) ;
#117620 = CARTESIAN_POINT ( 'NONE',  ( -5.153800228976607833, 19.02544592524334988, 47.70942372801900433 ) ) ;
#117621 = CARTESIAN_POINT ( 'NONE',  ( -5.719274019375665041, -21.55341960407619695, 99.79275706135234714 ) ) ;
#117622 = CARTESIAN_POINT ( 'NONE',  ( 30.00000000000000355, 0.3535533905932755627, 4.646446609406720718 ) ) ;
#117623 = DIRECTION ( 'NONE',  ( 1.000000000000000000, 0.000000000000000000, 0.000000000000000000 ) ) ;
#117624 = CARTESIAN_POINT ( 'NONE',  ( -0.05219959533934338120, 16.53943276465976808, 97.50109039468567573 ) ) ;
#117625 = CARTESIAN_POINT ( 'NONE',  ( 13.97604488694548053, -13.89961937509957401, 75.62609039468566152 ) ) ;
#117626 = CARTESIAN_POINT ( 'NONE',  ( 14.29746914071037800, 8.314922557961029526, 86.66775706135234714 ) ) ;
#117627 = CARTESIAN_POINT ( 'NONE',  ( 16.29526858892874230, 7.335722546920140807, 68.29670597800208043 ) ) ;
#117628 = CARTESIAN_POINT ( 'NONE',  ( 16.53943276465976808, 0.05219959533934440121, 71.25109039468568994 ) ) ;
#117629 = ORIENTED_EDGE ( 'NONE', *, *, #12667, .F. ) ;
#117630 = CARTESIAN_POINT ( 'NONE',  ( 21.52544592524334988, 5.823673210054432836, 76.45942372801901854 ) ) ;
#117631 = CARTESIAN_POINT ( 'NONE',  ( -16.51473224551082808, 9.474510206698731452, 93.33442372801900433 ) ) ;
#117632 = CARTESIAN_POINT ( 'NONE',  ( -16.46253265017146816, -9.564922557961047289, 24.16775706135233648 ) ) ;
#117633 = CARTESIAN_POINT ( 'NONE',  ( 5.049401038298161559, -19.05341960407611168, 62.70724293864769550 ) ) ;
#117634 = CARTESIAN_POINT ( 'NONE',  ( -5.049401038298153566, 19.05341960407611168, 60.20724293864768129 ) ) ;
#117635 = CARTESIAN_POINT ( 'NONE',  ( -18.50634305796425849, -35.46236190392534837, -8.314214632502698876 ) ) ;
#117636 = CARTESIAN_POINT ( 'NONE',  ( -21.52544592524343514, 5.823673210054127303, 81.04057627198102409 ) ) ;
#117637 = CIRCLE ( 'NONE', #191812, 2.000000000000001776 ) ;
#117638 = CARTESIAN_POINT ( 'NONE',  ( 15.80617190586746368, 15.72974639402197994, 29.37390960531435269 ) ) ;
#117639 = CARTESIAN_POINT ( 'NONE',  ( -9.474510206698964154, 16.51473224551069663, 35.41557627198102409 ) ) ;
#117640 = CARTESIAN_POINT ( 'NONE',  ( -14.34966873604972548, 8.224510206698743886, 63.33442372801900433 ) ) ;
#117641 = EDGE_CURVE ( 'NONE', #159190, #103419, #124445, .T. ) ;
#117642 = ORIENTED_EDGE ( 'NONE', *, *, #94206, .F. ) ;
#117643 = CARTESIAN_POINT ( 'NONE',  ( 15.72974639402176855, 15.80617190586768217, 31.87609039468567929 ) ) ;
#117645 = CARTESIAN_POINT ( 'NONE',  ( -29.86685920354755552, 21.69954338932564397, -6.824999997268814234 ) ) ;
#117644 = CARTESIAN_POINT ( 'NONE',  ( -0.05219959533910754901, -16.53943276465976808, 62.49890960531436690 ) ) ;
#117646 = CARTESIAN_POINT ( 'NONE',  ( 4.483927247898790824, -16.52544592524335698, 20.20942372801900788 ) ) ;
#117647 = CARTESIAN_POINT ( 'NONE',  ( -19.02544592524334988, -5.153800228976617603, 58.95942372801900433 ) ) ;
#117648 = CARTESIAN_POINT ( 'NONE',  ( -14.29746914071049879, 8.314922557960819915, 60.83224293864769550 ) ) ;
#117649 = CARTESIAN_POINT ( 'NONE',  ( -21.52544592524334988, -5.823673210054445271, 23.95942372801901143 ) ) ;
#117651 = CARTESIAN_POINT ( 'NONE',  ( 15.72974639402199770, -15.80617190586745480, 83.12390960531436690 ) ) ;
#117650 = CARTESIAN_POINT ( 'NONE',  ( 13.97604488694527802, 13.89961937509977830, 99.37390960531436690 ) ) ;
#117652 = CARTESIAN_POINT ( 'NONE',  ( 9.474510206698971260, -16.51473224551069308, 92.91557627198103830 ) ) ;
#117653 = CARTESIAN_POINT ( 'NONE',  ( -12.14591786802309592, -12.06949235617757132, 56.87390960531436690 ) ) ;
#117654 = CARTESIAN_POINT ( 'NONE',  ( 27.83073679762881980, -28.30972371524019948, -20.09501658340476737 ) ) ;
#117655 = LINE ( 'NONE', #177348, #98876 ) ;
#117656 = CARTESIAN_POINT ( 'NONE',  ( 5.049401038297881783, 19.05341960407617563, 72.29275706135234714 ) ) ;
#117657 = CARTESIAN_POINT ( 'NONE',  ( 21.52544592524344225, -5.823673210054117533, 108.5405762719810241 ) ) ;
#117658 = CARTESIAN_POINT ( 'NONE',  ( 19.03943276465977164, -0.05219959533909143690, 58.74890960531435979 ) ) ;
#117659 = CARTESIAN_POINT ( 'NONE',  ( -13.89961937509957401, -13.97604488694547875, 39.37609039468566152 ) ) ;
#117660 = CARTESIAN_POINT ( 'NONE',  ( -9.564922557960796823, -16.46253265017161027, 37.08224293864768839 ) ) ;
#117661 = CARTESIAN_POINT ( 'NONE',  ( -0.05219959533937732626, 21.53943276465977519, 62.50109039468568284 ) ) ;
#117662 = DIRECTION ( 'NONE',  ( 0.000000000000000000, 0.000000000000000000, -1.000000000000000000 ) ) ;
#117663 = CARTESIAN_POINT ( 'NONE',  ( -16.55341960407611168, -4.379528057220339221, 41.45724293864769550 ) ) ;
#117665 = CIRCLE ( 'NONE', #75655, 214.0437394197456911 ) ;
#117664 = CARTESIAN_POINT ( 'NONE',  ( 16.46253265017160672, -9.564922557960803928, 58.33224293864769550 ) ) ;
#117666 = CARTESIAN_POINT ( 'NONE',  ( -21.53943276465977519, 0.05219959533907696930, 71.24890960531435269 ) ) ;
#117667 = CARTESIAN_POINT ( 'NONE',  ( 19.02544592524343514, -5.153800228976328945, 58.54057627198102409 ) ) ;
#117668 = ORIENTED_EDGE ( 'NONE', *, *, #143629, .F. ) ;
#117669 = CARTESIAN_POINT ( 'NONE',  ( 10.72451020669898902, -18.67979575497178502, 62.91557627198102409 ) ) ;
#117670 = CARTESIAN_POINT ( 'NONE',  ( 10.81492255796106328, -18.62759615963255655, 95.41775706135234714 ) ) ;
#117673 = CARTESIAN_POINT ( 'NONE',  ( -0.05219959533910754901, -16.53943276465976808, 82.49890960531436690 ) ) ;
#117672 = CARTESIAN_POINT ( 'NONE',  ( 14.34966873604972726, -8.224510206698740333, 95.83442372801903275 ) ) ;
#117671 = DIRECTION ( 'NONE',  ( 0.000000000000000000, 0.000000000000000000, -1.000000000000000000 ) ) ;
#117674 = CARTESIAN_POINT ( 'NONE',  ( -13.89961937509957401, -13.97604488694547875, 89.37609039468563310 ) ) ;
#117675 = ORIENTED_EDGE ( 'NONE', *, *, #182333, .F. ) ;
#117676 = CARTESIAN_POINT ( 'NONE',  ( -9.564922557961040184, 16.46253265017147172, 37.91775706135233293 ) ) ;
#117677 = CARTESIAN_POINT ( 'NONE',  ( 8.224510206698742110, 14.34966873604972548, 107.0844237280190043 ) ) ;
#117678 = CARTESIAN_POINT ( 'NONE',  ( -5.153800228976607833, 19.02544592524334988, 27.70942372801899722 ) ) ;
#117679 = CARTESIAN_POINT ( 'NONE',  ( 19.03943276465977164, -0.05219959533909143690, 88.74890960531436690 ) ) ;
#117680 = CARTESIAN_POINT ( 'NONE',  ( -21.53943276465977519, 0.05219959533907696930, 66.24890960531436690 ) ) ;
#117681 = DIRECTION ( 'NONE',  ( -0.7071067811865463515, 0.7071067811865487940, -0.000000000000000000 ) ) ;
#117682 = CARTESIAN_POINT ( 'NONE',  ( -16.51473224551069308, -9.474510206698971260, 21.66557627198102765 ) ) ;
#117683 = CARTESIAN_POINT ( 'NONE',  ( 0.05219959533937995610, -21.53943276465977519, 90.00109039468567573 ) ) ;
#117684 = CARTESIAN_POINT ( 'NONE',  ( -14.29746914071037622, -8.314922557961029526, 74.16775706135231871 ) ) ;
#117685 = CARTESIAN_POINT ( 'NONE',  ( 5.719274019375673035, 21.55341960407619339, 27.29275706135234358 ) ) ;
#117686 = CARTESIAN_POINT ( 'NONE',  ( -12.06949235617739369, -12.14591786802326823, 34.37609039468568284 ) ) ;
#117687 = CARTESIAN_POINT ( 'NONE',  ( -19.03943276465977164, 0.05219959533909376836, 106.2489096053143669 ) ) ;
#117688 = CARTESIAN_POINT ( 'NONE',  ( 19.03943276465977164, -0.05219959533909143690, 33.74890960531435979 ) ) ;
#117689 = CARTESIAN_POINT ( 'NONE',  ( -19.03943276465977164, 0.05219959533909376836, 51.24890960531436690 ) ) ;
#117690 = CARTESIAN_POINT ( 'NONE',  ( 16.52544592524335698, 4.483927247898782831, 31.45942372801901854 ) ) ;
#117691 = CARTESIAN_POINT ( 'NONE',  ( -16.53943276465976808, 0.05219959533911058130, 91.24890960531436690 ) ) ;
#117692 = CARTESIAN_POINT ( 'NONE',  ( -8.224510206698735004, -14.34966873604973081, 104.5844237280190185 ) ) ;
#117695 = CARTESIAN_POINT ( 'NONE',  ( 19.02544592524343514, -5.153800228976328945, 68.54057627198103830 ) ) ;
#117694 = CARTESIAN_POINT ( 'NONE',  ( -16.51473224551069308, -9.474510206698971260, 76.66557627198103830 ) ) ;
#117693 = CARTESIAN_POINT ( 'NONE',  ( -5.823673210054431948, 21.52544592524334988, 37.70942372801900433 ) ) ;
#117696 = CARTESIAN_POINT ( 'NONE',  ( 16.46253265017160672, -9.564922557960803928, 83.33224293864768129 ) ) ;
#117697 = CARTESIAN_POINT ( 'NONE',  ( 16.55341960407611168, 4.379528057220329451, 33.95724293864769550 ) ) ;
#117698 = CARTESIAN_POINT ( 'NONE',  ( -0.05219959533934338120, 16.53943276465976808, 102.5010903946856899 ) ) ;
#117699 = ORIENTED_EDGE ( 'NONE', *, *, #1307, .F. ) ;
#117700 = CARTESIAN_POINT ( 'NONE',  ( -5.153800228976607833, 19.02544592524334988, 47.70942372801900433 ) ) ;
#117701 = CARTESIAN_POINT ( 'NONE',  ( -19.05341960407611168, -5.049401038298163336, 106.4572429386476955 ) ) ;
#117702 = CARTESIAN_POINT ( 'NONE',  ( 0.05219959533909260263, 19.03943276465977164, 54.99890960531435979 ) ) ;
#117703 = CARTESIAN_POINT ( 'NONE',  ( 5.153800228976615827, -19.02544592524334988, 45.20942372801901143 ) ) ;
#117704 = CARTESIAN_POINT ( 'NONE',  ( -11.40812507854754720, -35.11059874428192273, -8.224999997268813701 ) ) ;
#117705 = CARTESIAN_POINT ( 'NONE',  ( -12.06949235617739369, -12.14591786802326823, 39.37609039468567573 ) ) ;
#117707 = CARTESIAN_POINT ( 'NONE',  ( 16.52544592524335698, 4.483927247898782831, 56.45942372801902565 ) ) ;
#117706 = CARTESIAN_POINT ( 'NONE',  ( 13.97604488694548053, -13.89961937509957401, 70.62609039468567573 ) ) ;
#117708 = CARTESIAN_POINT ( 'NONE',  ( 19.03943276465977164, -0.05219959533909143690, 113.7489096053143669 ) ) ;
#117709 = CARTESIAN_POINT ( 'NONE',  ( 5.153800228976335163, 19.02544592524342804, 89.79057627198102409 ) ) ;
#117710 = CARTESIAN_POINT ( 'NONE',  ( 18.67979575497178502, 10.72451020669898547, 109.1655762719810383 ) ) ;
#117711 = CARTESIAN_POINT ( 'NONE',  ( -5.153800228976607833, 19.02544592524334988, 82.70942372801897591 ) ) ;
#117713 = CARTESIAN_POINT ( 'NONE',  ( 19.05341960407611168, 5.049401038298154454, 33.95724293864769550 ) ) ;
#117712 = CARTESIAN_POINT ( 'NONE',  ( -19.03943276465977164, 0.05219959533909376836, 101.2489096053143669 ) ) ;
#117714 = CARTESIAN_POINT ( 'NONE',  ( -9.474510206698964154, 16.51473224551069663, 80.41557627198103830 ) ) ;
#117716 = CARTESIAN_POINT ( 'NONE',  ( 5.049401038298161559, -19.05341960407611168, 32.70724293864768129 ) ) ;
#117715 = CARTESIAN_POINT ( 'NONE',  ( -4.483927247898539470, -16.52544592524342804, 37.29057627198102409 ) ) ;
#117717 = CARTESIAN_POINT ( 'NONE',  ( -19.02544592524334988, -5.153800228976617603, 48.95942372801900433 ) ) ;
#117718 = CARTESIAN_POINT ( 'NONE',  ( -4.379528057220328563, 16.55341960407611168, 85.20724293864770971 ) ) ;
#117719 = CARTESIAN_POINT ( 'NONE',  ( -5.153800228976607833, 19.02544592524334988, 22.70942372801899012 ) ) ;
#117720 = CARTESIAN_POINT ( 'NONE',  ( -9.564922557960796823, -16.46253265017161027, 47.08224293864769550 ) ) ;
#117721 = AXIS2_PLACEMENT_3D ( 'NONE', #15187, #63675, #124342 ) ;
#117722 = CARTESIAN_POINT ( 'NONE',  ( 21.55341960407610458, 5.719274019375980345, 43.95724293864769550 ) ) ;
#117724 = CARTESIAN_POINT ( 'NONE',  ( 10.72451020669871369, 18.67979575497193778, 97.08442372801904696 ) ) ;
#117723 = CARTESIAN_POINT ( 'NONE',  ( 14.29746914071049879, -8.314922557960816363, 58.33224293864768839 ) ) ;
#117725 = CARTESIAN_POINT ( 'NONE',  ( 19.03943276465977164, -0.05219959533909143690, 103.7489096053143669 ) ) ;
#117726 = CARTESIAN_POINT ( 'NONE',  ( -13.97604488694527625, -13.89961937509977652, 106.8739096053143669 ) ) ;
#117727 = CARTESIAN_POINT ( 'NONE',  ( 0.05219959533909260263, 19.03943276465977164, 34.99890960531435979 ) ) ;
#117728 = CARTESIAN_POINT ( 'NONE',  ( -19.02544592524342804, 5.153800228976336051, 31.04057627198102409 ) ) ;
#117729 = CARTESIAN_POINT ( 'NONE',  ( -16.52544592524342804, 4.483927247898546575, 81.04057627198102409 ) ) ;
#117730 = CARTESIAN_POINT ( 'NONE',  ( 15.72974639402199770, -15.80617190586745480, 93.12390960531436690 ) ) ;
#117731 = CARTESIAN_POINT ( 'NONE',  ( 16.51473224551069308, 9.474510206698969483, 104.1655762719810241 ) ) ;
#117732 = CARTESIAN_POINT ( 'NONE',  ( 0.05219959533937995610, -21.53943276465977519, 20.00109039468568639 ) ) ;
#117733 = CARTESIAN_POINT ( 'NONE',  ( -13.97604488694527625, -13.89961937509977652, 96.87390960531433848 ) ) ;
#117735 = CARTESIAN_POINT ( 'NONE',  ( 4.483927247898545687, 16.52544592524342804, 99.79057627198103830 ) ) ;
#117734 = CARTESIAN_POINT ( 'NONE',  ( 30.00000000000000000, 5.499999999999992895, 102.5000000000000142 ) ) ;
#117736 = CARTESIAN_POINT ( 'NONE',  ( -19.03943276465977164, 0.05219959533909376836, 76.24890960531435269 ) ) ;
#117737 = CARTESIAN_POINT ( 'NONE',  ( 15.80617190586746368, 15.72974639402197994, 74.37390960531436690 ) ) ;
#117738 = CARTESIAN_POINT ( 'NONE',  ( -32.15509708611487127, 4.949069787320341973, 89.34338315600297165 ) ) ;
#117739 = CARTESIAN_POINT ( 'NONE',  ( -21.27717364736663797, -9.815017990598716935, 168.4818444780605375 ) ) ;
#117741 = CARTESIAN_POINT ( 'NONE',  ( 5.000000000000000000, 0.000000000000000000, -18.00000000000000000 ) ) ;
#117740 = CARTESIAN_POINT ( 'NONE',  ( 5.719274019375991003, -21.55341960407610458, 32.70724293864770260 ) ) ;
#117742 = CARTESIAN_POINT ( 'NONE',  ( -16.55341960407617563, 4.379528057220093196, 33.54275706135234714 ) ) ;
#117744 = CIRCLE ( 'NONE', #72574, 5.000000000000000888 ) ;
#117743 = CARTESIAN_POINT ( 'NONE',  ( -12.06949235617756955, 12.14591786802309770, 95.62390960531436690 ) ) ;
#117745 = DIRECTION ( 'NONE',  ( 1.000000000000000000, 0.000000000000000000, 0.000000000000000000 ) ) ;
#117746 = CARTESIAN_POINT ( 'NONE',  ( -16.46253265017160317, 9.564922557960807481, 90.83224293864769550 ) ) ;
#117747 = CARTESIAN_POINT ( 'NONE',  ( 19.05341960407611168, 5.049401038298154454, 48.95724293864768129 ) ) ;
#117749 = EDGE_CURVE ( 'NONE', #181556, #42534, #12955, .T. ) ;
#117748 = CARTESIAN_POINT ( 'NONE',  ( 0.05219959533910956823, 16.53943276465976808, 74.99890960531435269 ) ) ;
#117750 = CARTESIAN_POINT ( 'NONE',  ( 18.62759615963271287, -10.81492255796078972, 28.33224293864769550 ) ) ;
#117751 = CARTESIAN_POINT ( 'NONE',  ( -14.29746914071049879, 8.314922557960819915, 50.83224293864770971 ) ) ;
#117752 = CARTESIAN_POINT ( 'NONE',  ( 13.89961937509957401, 13.97604488694547697, 106.8760903946856757 ) ) ;
#117753 = CARTESIAN_POINT ( 'NONE',  ( -15.72974639402176322, -15.80617190586768395, 69.37609039468567573 ) ) ;
#117754 = VECTOR ( 'NONE', #171898, 1000.000000000000000 ) ;
#117755 = CARTESIAN_POINT ( 'NONE',  ( -22.44159573604009950, -16.30477369853688430, 145.0750000027311728 ) ) ;
#117756 = CARTESIAN_POINT ( 'NONE',  ( -13.97604488694527625, -13.89961937509977652, 111.8739096053143243 ) ) ;
#117757 = CARTESIAN_POINT ( 'NONE',  ( -12.14591786802326823, 12.06949235617739902, 83.12609039468568994 ) ) ;
#117758 = CARTESIAN_POINT ( 'NONE',  ( 19.05341960407611168, 5.049401038298154454, 28.95724293864769550 ) ) ;
#117759 = CARTESIAN_POINT ( 'NONE',  ( 9.474510206698971260, -16.51473224551069308, 77.91557627198103830 ) ) ;
#117760 = CARTESIAN_POINT ( 'NONE',  ( -5.719274019375978568, 21.55341960407610458, 80.20724293864769550 ) ) ;
#117761 = CARTESIAN_POINT ( 'NONE',  ( 0.05219959533934541429, -16.53943276465976808, 30.00109039468568284 ) ) ;
#117763 = CARTESIAN_POINT ( 'NONE',  ( 15.80617190586769283, -15.72974639402175789, 70.62609039468567573 ) ) ;
#117762 = CARTESIAN_POINT ( 'NONE',  ( -0.05219959533910754901, -16.53943276465976808, 57.49890960531435979 ) ) ;
#117765 = CARTESIAN_POINT ( 'NONE',  ( 9.474510206698971260, -16.51473224551069308, 112.9155762719810383 ) ) ;
#117764 = CARTESIAN_POINT ( 'NONE',  ( 12.06949235617739724, 12.14591786802326823, 86.87609039468568994 ) ) ;
#117766 = CARTESIAN_POINT ( 'NONE',  ( -5.049401038298153566, 19.05341960407611168, 115.2072429386477097 ) ) ;
#117767 = DIRECTION ( 'NONE',  ( -0.000000000000000000, -1.000000000000000000, -0.000000000000000000 ) ) ;
#117768 = CARTESIAN_POINT ( 'NONE',  ( -14.29746914071037622, -8.314922557961029526, 104.1677570613523471 ) ) ;
#117769 = CARTESIAN_POINT ( 'NONE',  ( 4.379528057220092307, 16.55341960407617563, 57.29275706135234714 ) ) ;
#117770 = CARTESIAN_POINT ( 'NONE',  ( 16.46253265017160672, -9.564922557960803928, 73.33224293864769550 ) ) ;
#117771 = CARTESIAN_POINT ( 'NONE',  ( 19.02544592524343514, -5.153800228976328945, 83.54057627198100988 ) ) ;
#117772 = CARTESIAN_POINT ( 'NONE',  ( 0.05219959533937995610, -21.53943276465977519, 75.00109039468568994 ) ) ;
#117773 = CARTESIAN_POINT ( 'NONE',  ( 4.483927247898790824, -16.52544592524335698, 80.20942372801901854 ) ) ;
#117774 = CARTESIAN_POINT ( 'NONE',  ( -16.53943276465976808, 0.05219959533911058130, 41.24890960531435269 ) ) ;
#117775 = CARTESIAN_POINT ( 'NONE',  ( 19.05341960407611168, 5.049401038298154454, 48.95724293864768129 ) ) ;
#117776 = CARTESIAN_POINT ( 'NONE',  ( 19.02544592524343514, -5.153800228976328945, 43.54057627198103120 ) ) ;
#117777 = VERTEX_POINT ( 'NONE', #99070 ) ;
#117778 = CARTESIAN_POINT ( 'NONE',  ( 5.049401038297881783, 19.05341960407617563, 97.29275706135233293 ) ) ;
#117779 = CARTESIAN_POINT ( 'NONE',  ( -8.224510206698948167, 14.34966873604960824, 115.4155762719810241 ) ) ;
#117780 = CARTESIAN_POINT ( 'NONE',  ( 9.564922557960805705, 16.46253265017160317, 64.58224293864769550 ) ) ;
#117782 = CARTESIAN_POINT ( 'NONE',  ( 11.74264578624799427, 36.14014761921585972, -4.599999999999999645 ) ) ;
#117781 = CARTESIAN_POINT ( 'NONE',  ( -5.049401038297874678, -19.05341960407617918, 104.7927570613523471 ) ) ;
#117783 = CARTESIAN_POINT ( 'NONE',  ( 10.81492255796106328, -18.62759615963255655, 105.4177570613523613 ) ) ;
#117784 = CARTESIAN_POINT ( 'NONE',  ( -16.52544592524335698, -4.483927247898792601, 63.95942372801901854 ) ) ;
#117785 = CARTESIAN_POINT ( 'NONE',  ( -19.02544592524334988, -5.153800228976617603, 98.95942372801900433 ) ) ;
#117786 = CARTESIAN_POINT ( 'NONE',  ( -15.80617190586745835, -15.72974639402198527, 56.87390960531436690 ) ) ;
#117787 = CARTESIAN_POINT ( 'NONE',  ( 12.06949235617739724, 12.14591786802326823, 56.87609039468568994 ) ) ;
#117788 = DIRECTION ( 'NONE',  ( 0.000000000000000000, 0.000000000000000000, -1.000000000000000000 ) ) ;
#117789 = CARTESIAN_POINT ( 'NONE',  ( 19.02544592524334988, 5.153800228976608722, 61.45942372801900433 ) ) ;
#117790 = CARTESIAN_POINT ( 'NONE',  ( 21.53943276465977519, 0.05219959533937863772, 96.25109039468568994 ) ) ;
#117791 = CARTESIAN_POINT ( 'NONE',  ( -8.314922557960811034, -14.29746914071050412, 112.0822429386477097 ) ) ;
#117792 = CARTESIAN_POINT ( 'NONE',  ( 19.05341960407611168, 5.049401038298154454, 63.95724293864769550 ) ) ;
#117794 = EDGE_CURVE ( 'NONE', #186058, #110081, #172435, .T. ) ;
#117793 = CARTESIAN_POINT ( 'NONE',  ( -4.379528057220328563, 16.55341960407611168, 55.20724293864770260 ) ) ;
#117795 = CIRCLE ( 'NONE', #66083, 1.249999999999999778 ) ;
#117796 = CARTESIAN_POINT ( 'NONE',  ( 10.81492255796106328, -18.62759615963255655, 95.41775706135234714 ) ) ;
#117797 = CARTESIAN_POINT ( 'NONE',  ( 9.474510206698729675, 16.51473224551082808, 52.08442372801900433 ) ) ;
#117798 = CARTESIAN_POINT ( 'NONE',  ( -19.02544592524334988, -5.153800228976617603, 33.95942372801897591 ) ) ;
#117799 = CARTESIAN_POINT ( 'NONE',  ( 15.72974639402199770, -15.80617190586745480, 23.12390960531436335 ) ) ;
#117800 = CARTESIAN_POINT ( 'NONE',  ( -0.05219959533937732626, 21.53943276465977519, 92.50109039468567573 ) ) ;
#117801 = CARTESIAN_POINT ( 'NONE',  ( 19.02544592524343514, -5.153800228976328945, 73.54057627198103830 ) ) ;
#117802 = CARTESIAN_POINT ( 'NONE',  ( 21.53943276465977519, 0.05219959533937863772, 91.25109039468568994 ) ) ;
#117803 = CARTESIAN_POINT ( 'NONE',  ( 5.823673210054125526, 21.52544592524343514, 54.79057627198104541 ) ) ;
#117804 = CARTESIAN_POINT ( 'NONE',  ( -9.564922557960796823, -16.46253265017161027, 77.08224293864769550 ) ) ;
#117805 = CARTESIAN_POINT ( 'NONE',  ( -5.049401038297874678, -19.05341960407617918, 59.79275706135231871 ) ) ;
#117806 = CARTESIAN_POINT ( 'NONE',  ( -5.153800228976328057, -19.02544592524343514, 37.29057627198102409 ) ) ;
#117807 = CARTESIAN_POINT ( 'NONE',  ( -0.05219959533909027116, -19.03943276465977164, 92.49890960531436690 ) ) ;
#117808 = CARTESIAN_POINT ( 'NONE',  ( -13.89961937509957401, -13.97604488694547875, 84.37609039468567573 ) ) ;
#117809 = CARTESIAN_POINT ( 'NONE',  ( 4.379528057220092307, 16.55341960407617563, 47.29275706135234003 ) ) ;
#117810 = CARTESIAN_POINT ( 'NONE',  ( 8.314922557960818139, 14.29746914071049879, 104.5822429386477097 ) ) ;
#117811 = CARTESIAN_POINT ( 'NONE',  ( -19.02544592524342804, 5.153800228976336051, 66.04057627198103830 ) ) ;
#117812 = CARTESIAN_POINT ( 'NONE',  ( 21.55341960407610458, 5.719274019375980345, 53.95724293864770260 ) ) ;
#117813 = CARTESIAN_POINT ( 'NONE',  ( 4.483927247898790824, -16.52544592524335698, 25.20942372801901854 ) ) ;
#117814 = CARTESIAN_POINT ( 'NONE',  ( -10.81492255796105439, 18.62759615963255655, 37.91775706135235424 ) ) ;
#117815 = CARTESIAN_POINT ( 'NONE',  ( -21.52544592524334988, -5.823673210054445271, 88.95942372801901854 ) ) ;
#117816 = CARTESIAN_POINT ( 'NONE',  ( 16.52544592524335698, 4.483927247898782831, 86.45942372801901854 ) ) ;
#117817 = CARTESIAN_POINT ( 'NONE',  ( 9.564922557960805705, 16.46253265017160317, 79.58224293864769550 ) ) ;
#117818 = CARTESIAN_POINT ( 'NONE',  ( -14.29746914071037622, -8.314922557961029526, 99.16775706135234714 ) ) ;
#117819 = CARTESIAN_POINT ( 'NONE',  ( -0.05219959533936034679, 19.03943276465977164, 57.50109039468566863 ) ) ;
#117820 = CARTESIAN_POINT ( 'NONE',  ( -21.55341960407619339, 5.719274019375674811, 28.54275706135234358 ) ) ;
#117821 = CARTESIAN_POINT ( 'NONE',  ( 12.14591786802309770, 12.06949235617756955, 79.37390960531436690 ) ) ;
#117822 = CARTESIAN_POINT ( 'NONE',  ( -19.02544592524342804, 5.153800228976336051, 96.04057627198103830 ) ) ;
#117823 = CARTESIAN_POINT ( 'NONE',  ( -16.55341960407617563, 4.379528057220093196, 103.5427570613523613 ) ) ;
#117824 = CARTESIAN_POINT ( 'NONE',  ( 18.62759615963255655, 10.81492255796105972, 71.66775706135234714 ) ) ;
#117825 = CARTESIAN_POINT ( 'NONE',  ( -0.05219959533934338120, 16.53943276465976808, 32.50109039468568284 ) ) ;
#117826 = CARTESIAN_POINT ( 'NONE',  ( -21.52544592524334988, -5.823673210054445271, 23.95942372801901143 ) ) ;
#117827 = CARTESIAN_POINT ( 'NONE',  ( -16.52544592524342804, 4.483927247898546575, 76.04057627198102409 ) ) ;
#117828 = ORIENTED_EDGE ( 'NONE', *, *, #127970, .T. ) ;
#117829 = CARTESIAN_POINT ( 'NONE',  ( -15.72974639402197994, 15.80617190586746368, 105.6239096053143669 ) ) ;
#117830 = CARTESIAN_POINT ( 'NONE',  ( -16.52544592524342804, 4.483927247898546575, 51.04057627198103120 ) ) ;
#117831 = ORIENTED_EDGE ( 'NONE', *, *, #127434, .T. ) ;
#117832 = CARTESIAN_POINT ( 'NONE',  ( 16.51473224551069308, 9.474510206698969483, 29.16557627198103475 ) ) ;
#117833 = CARTESIAN_POINT ( 'NONE',  ( -21.55341960407610458, -5.719274019375992779, 26.45724293864768839 ) ) ;
#117834 = CARTESIAN_POINT ( 'NONE',  ( -15.72974639402176322, -15.80617190586768395, 54.37609039468568994 ) ) ;
#117835 = CARTESIAN_POINT ( 'NONE',  ( 14.34966873604960469, 8.224510206698951720, 59.16557627198103120 ) ) ;
#117836 = CARTESIAN_POINT ( 'NONE',  ( -18.67979575497178146, -10.72451020669898902, 71.66557627198100988 ) ) ;
#117837 = CARTESIAN_POINT ( 'NONE',  ( -0.05219959533909027116, -19.03943276465977164, 72.49890960531435269 ) ) ;
#117839 = CARTESIAN_POINT ( 'NONE',  ( -19.05341960407617563, 5.049401038297882671, 83.54275706135233293 ) ) ;
#117838 = CARTESIAN_POINT ( 'NONE',  ( -16.51473224551069308, -9.474510206698971260, 21.66557627198102765 ) ) ;
#117840 = EDGE_CURVE ( 'NONE', #19028, #89236, #129079, .T. ) ;
#117842 = CARTESIAN_POINT ( 'NONE',  ( -18.62759615963270932, 10.81492255796079327, 55.83224293864770260 ) ) ;
#117841 = CARTESIAN_POINT ( 'NONE',  ( 15.72974639402176855, 15.80617190586768217, 51.87609039468568284 ) ) ;
#117843 = CARTESIAN_POINT ( 'NONE',  ( 19.05341960407611168, 5.049401038298154454, 43.95724293864769550 ) ) ;
#117844 = CARTESIAN_POINT ( 'NONE',  ( -16.51473224551069308, -9.474510206698971260, 66.66557627198102409 ) ) ;
#117845 = CARTESIAN_POINT ( 'NONE',  ( 12.06949235617739724, 12.14591786802326823, 56.87609039468568994 ) ) ;
#117846 = CARTESIAN_POINT ( 'NONE',  ( -15.80617190586768217, 15.72974639402176855, 28.12609039468568284 ) ) ;
#117847 = CARTESIAN_POINT ( 'NONE',  ( -5.823673210054431948, 21.52544592524334988, 57.70942372801901143 ) ) ;
#117848 = CARTESIAN_POINT ( 'NONE',  ( 19.05341960407611168, 5.049401038298154454, 103.9572429386476671 ) ) ;
#117849 = CARTESIAN_POINT ( 'NONE',  ( 10.81492255796078972, 18.62759615963270932, 79.58224293864769550 ) ) ;
#117851 = CARTESIAN_POINT ( 'NONE',  ( -16.52544592524335698, -4.483927247898792601, 53.95942372801900433 ) ) ;
#117850 = CARTESIAN_POINT ( 'NONE',  ( -5.719274019375665041, -21.55341960407619695, 24.79275706135235779 ) ) ;
#117852 = CARTESIAN_POINT ( 'NONE',  ( -18.62759615963270932, 10.81492255796079327, 55.83224293864770260 ) ) ;
#117853 = CARTESIAN_POINT ( 'NONE',  ( -13.97604488694547697, 13.89961937509957934, 23.12609039468565442 ) ) ;
#117854 = CARTESIAN_POINT ( 'NONE',  ( 0.05219959533909260263, 19.03943276465977164, 59.99890960531436690 ) ) ;
#117855 = CARTESIAN_POINT ( 'NONE',  ( 16.51473224551069308, 9.474510206698969483, 109.1655762719810383 ) ) ;
#117856 = B_SPLINE_CURVE_WITH_KNOTS ( 'NONE', 3,
 ( #114092, #6919, #100924, #68597, #23108, #162609 ),
 .UNSPECIFIED., .F., .F.,
 ( 4, 2, 4 ),
 ( 0.003989672132298186825, 0.004372778065220602264, 0.004755883998143018571 ),
 .UNSPECIFIED. ) ;
#117857 = CARTESIAN_POINT ( 'NONE',  ( 0.05219959533909260263, 19.03943276465977164, 94.99890960531436690 ) ) ;
#117858 = PRODUCT_DEFINITION ( 'UNKNOWN', '', #169553, #82716 ) ;
#117859 = CARTESIAN_POINT ( 'NONE',  ( -6.017829804060265353, -47.35862344248571532, -22.79591852006818087 ) ) ;
#117860 = CARTESIAN_POINT ( 'NONE',  ( -16.51473224551082808, 9.474510206698731452, 68.33442372801900433 ) ) ;
#117861 = CARTESIAN_POINT ( 'NONE',  ( -5.719274019375978568, 21.55341960407610458, 45.20724293864769550 ) ) ;
#117862 = CARTESIAN_POINT ( 'NONE',  ( 8.224510206698953496, -14.34966873604960469, 27.91557627198103830 ) ) ;
#117863 = CARTESIAN_POINT ( 'NONE',  ( -13.97604488694547697, 13.89961937509957934, 83.12609039468564731 ) ) ;
#117864 = CARTESIAN_POINT ( 'NONE',  ( -17.48853670773243252, 5.747243402303157112, 58.66671299749990709 ) ) ;
#117865 = VECTOR ( 'NONE', #22062, 1000.000000000000114 ) ;
#117866 = CARTESIAN_POINT ( 'NONE',  ( 19.05341960407617918, -5.049401038297876454, 26.04275706135233293 ) ) ;
#117867 = CARTESIAN_POINT ( 'NONE',  ( 19.05341960407617918, -5.049401038297876454, 81.04275706135231871 ) ) ;
#117868 = CARTESIAN_POINT ( 'NONE',  ( 19.05341960407617918, -5.049401038297876454, 51.04275706135231871 ) ) ;
#117869 = CARTESIAN_POINT ( 'NONE',  ( -14.81258577508671515, -15.38338031094985325, -56.43166240502930719 ) ) ;
#117870 = CARTESIAN_POINT ( 'NONE',  ( -9.474510206698964154, 16.51473224551069663, 60.41557627198102409 ) ) ;
#117871 = CARTESIAN_POINT ( 'NONE',  ( -12.14591786802309592, -12.06949235617757132, 51.87390960531437401 ) ) ;
#117872 = CARTESIAN_POINT ( 'NONE',  ( 5.153800228976335163, 19.02544592524342804, 39.79057627198100988 ) ) ;
#117873 = CARTESIAN_POINT ( 'NONE',  ( -16.52544592524342804, 4.483927247898546575, 46.04057627198103830 ) ) ;
#117874 = CARTESIAN_POINT ( 'NONE',  ( 18.22780087662123805, 5.499999999999960032, 101.4823681787310647 ) ) ;
#117875 = CARTESIAN_POINT ( 'NONE',  ( -14.34966873604960291, -8.224510206698953496, 21.66557627198102409 ) ) ;
#117876 = CARTESIAN_POINT ( 'NONE',  ( -16.51473224551069308, -9.474510206698971260, 56.66557627198103120 ) ) ;
#117877 = CARTESIAN_POINT ( 'NONE',  ( 13.89961937509957401, 13.97604488694547697, 26.87609039468566507 ) ) ;
#117878 = CARTESIAN_POINT ( 'NONE',  ( -0.05219959533934338120, 16.53943276465976808, 32.50109039468568284 ) ) ;
#117879 = CARTESIAN_POINT ( 'NONE',  ( -5.719274019375978568, 21.55341960407610458, 40.20724293864769550 ) ) ;
#117880 = CARTESIAN_POINT ( 'NONE',  ( 21.53943276465977519, 0.05219959533937863772, 96.25109039468568994 ) ) ;
#117881 = CARTESIAN_POINT ( 'NONE',  ( 5.049401038298161559, -19.05341960407611168, 62.70724293864769550 ) ) ;
#117882 = CARTESIAN_POINT ( 'NONE',  ( 16.51473224551069308, 9.474510206698969483, 109.1655762719810383 ) ) ;
#117883 = CARTESIAN_POINT ( 'NONE',  ( 16.46253265017160672, -9.564922557960803928, 98.33224293864769550 ) ) ;
#117884 = CARTESIAN_POINT ( 'NONE',  ( -36.91746825000000598, 2.428612866367529932E-14, -10.62499999726881406 ) ) ;
#117885 = CARTESIAN_POINT ( 'NONE',  ( 18.62759615963255655, 10.81492255796105972, 26.66775706135235424 ) ) ;
#117886 = VECTOR ( 'NONE', #37027, 1000.000000000000000 ) ;
#117887 = CARTESIAN_POINT ( 'NONE',  ( -8.224510206698948167, 14.34966873604960824, 75.41557627198102409 ) ) ;
#117889 = CARTESIAN_POINT ( 'NONE',  ( 19.03943276465977164, -0.05219959533909143690, 73.74890960531435269 ) ) ;
#117888 = CARTESIAN_POINT ( 'NONE',  ( -15.72974639402197994, 15.80617190586746368, 70.62390960531436690 ) ) ;
#117890 = CARTESIAN_POINT ( 'NONE',  ( 5.153800228976335163, 19.02544592524342804, 74.79057627198103830 ) ) ;
#117891 = CARTESIAN_POINT ( 'NONE',  ( 21.52544592524344225, -5.823673210054117533, 113.5405762719810383 ) ) ;
#117892 = ORIENTED_EDGE ( 'NONE', *, *, #123771, .T. ) ;
#117893 = CARTESIAN_POINT ( 'NONE',  ( -9.474510206698964154, 16.51473224551069663, 80.41557627198103830 ) ) ;
#117895 = CARTESIAN_POINT ( 'NONE',  ( -13.89961937509977652, 13.97604488694528158, 25.62390960531434558 ) ) ;
#117894 = CARTESIAN_POINT ( 'NONE',  ( 4.483927247898545687, 16.52544592524342804, 109.7905762719810383 ) ) ;
#117896 = CARTESIAN_POINT ( 'NONE',  ( 19.05341960407611168, 5.049401038298154454, 58.95724293864768129 ) ) ;
#117897 = CARTESIAN_POINT ( 'NONE',  ( -5.153800228976607833, 19.02544592524334988, 87.70942372801897591 ) ) ;
#117898 = AXIS2_PLACEMENT_3D ( 'NONE', #83660, #173712, #36163 ) ;
#117899 = CARTESIAN_POINT ( 'NONE',  ( -16.55341960407611168, -4.379528057220339221, 101.4572429386476955 ) ) ;
#117900 = CARTESIAN_POINT ( 'NONE',  ( -0.05219959533937732626, 21.53943276465977519, 72.50109039468568994 ) ) ;
#117902 = CARTESIAN_POINT ( 'NONE',  ( 5.823673210054125526, 21.52544592524343514, 114.7905762719810383 ) ) ;
#117901 = CARTESIAN_POINT ( 'NONE',  ( 19.02544592524343514, -5.153800228976328945, 43.54057627198103120 ) ) ;
#117903 = CARTESIAN_POINT ( 'NONE',  ( -14.29746914071049879, 8.314922557960819915, 95.83224293864770971 ) ) ;
#117904 = CARTESIAN_POINT ( 'NONE',  ( 28.82186960331499392, -9.364793116373510529, 142.9000000000000057 ) ) ;
#117905 = CARTESIAN_POINT ( 'NONE',  ( 16.51473224551069308, 9.474510206698969483, 69.16557627198102409 ) ) ;
#117906 = AXIS2_PLACEMENT_3D ( 'NONE', #174078, #83034, #6194 ) ;
#117908 = CARTESIAN_POINT ( 'NONE',  ( 21.53943276465977519, -0.05219959533907433946, 33.74890960531436690 ) ) ;
#117907 = CARTESIAN_POINT ( 'NONE',  ( -5.049401038297874678, -19.05341960407617918, 109.7927570613523187 ) ) ;
#117909 = CARTESIAN_POINT ( 'NONE',  ( -15.72974639402176322, -15.80617190586768395, 49.37609039468569705 ) ) ;
#117910 = CARTESIAN_POINT ( 'NONE',  ( 13.97604488694527802, 13.89961937509977652, 99.37390960531436690 ) ) ;
#117911 = CARTESIAN_POINT ( 'NONE',  ( -0.05219959533936034679, 19.03943276465977164, 77.50109039468566152 ) ) ;
#117912 = CARTESIAN_POINT ( 'NONE',  ( -16.51473224551069308, -9.474510206698971260, 76.66557627198103830 ) ) ;
#117913 = CARTESIAN_POINT ( 'NONE',  ( 12.06949235617757843, -12.14591786802309237, 78.12390960531436690 ) ) ;
#117914 = CARTESIAN_POINT ( 'NONE',  ( 13.89961937509977652, -13.97604488694527269, 98.12390960531433848 ) ) ;
#117915 = CARTESIAN_POINT ( 'NONE',  ( 8.224510206698953496, -14.34966873604960469, 72.91557627198103830 ) ) ;
#117916 = CARTESIAN_POINT ( 'NONE',  ( -16.51473224551069308, -9.474510206698971260, 101.6655762719810241 ) ) ;
#117919 = CARTESIAN_POINT ( 'NONE',  ( 16.51473224551069308, 9.474510206698969483, 29.16557627198103475 ) ) ;
#117918 = CARTESIAN_POINT ( 'NONE',  ( 4.483927247898545687, 16.52544592524342804, 49.79057627198102409 ) ) ;
#117917 = CARTESIAN_POINT ( 'NONE',  ( -19.03943276465977164, 0.05219959533909376836, 51.24890960531436690 ) ) ;
#117920 = ORIENTED_EDGE ( 'NONE', *, *, #180435, .T. ) ;
#117921 = CARTESIAN_POINT ( 'NONE',  ( -10.72451020669870658, -18.67979575497194134, 59.58442372801901854 ) ) ;
#117922 = CARTESIAN_POINT ( 'NONE',  ( -19.03943276465977164, -0.05219959533935918106, 83.75109039468567573 ) ) ;
#117923 = CARTESIAN_POINT ( 'NONE',  ( 8.224510206698953496, -14.34966873604960469, 47.91557627198102409 ) ) ;
#117924 = CARTESIAN_POINT ( 'NONE',  ( 18.62759615963271287, -10.81492255796078972, 93.33224293864769550 ) ) ;
#117925 = CARTESIAN_POINT ( 'NONE',  ( 0.05219959533907565091, 21.53943276465977519, 39.99890960531436690 ) ) ;
#117926 = CARTESIAN_POINT ( 'NONE',  ( 14.34966873604960469, 8.224510206698951720, 89.16557627198102409 ) ) ;
#117927 = CARTESIAN_POINT ( 'NONE',  ( 16.46253265017160672, -9.564922557960803928, 38.33224293864768839 ) ) ;
#117928 = CARTESIAN_POINT ( 'NONE',  ( -16.55341960407617563, 4.379528057220093196, 113.5427570613523756 ) ) ;
#117929 = AXIS2_PLACEMENT_3D ( 'NONE', #106930, #140249, #185780 ) ;
#117930 = CARTESIAN_POINT ( 'NONE',  ( -14.34966873604972548, 8.224510206698743886, 93.33442372801901854 ) ) ;
#117931 = CARTESIAN_POINT ( 'NONE',  ( 16.55341960407618274, -4.379528057220086978, 66.04275706135236135 ) ) ;
#117932 = CARTESIAN_POINT ( 'NONE',  ( 19.03943276465977164, 0.05219959533936151252, 21.25109039468565797 ) ) ;
#117933 = CARTESIAN_POINT ( 'NONE',  ( -5.049401038298153566, 19.05341960407611168, 90.20724293864766707 ) ) ;
#117934 = CARTESIAN_POINT ( 'NONE',  ( 19.05341960407611168, 5.049401038298154454, 83.95724293864766707 ) ) ;
#117935 = CARTESIAN_POINT ( 'NONE',  ( -16.55341960407617563, 4.379528057220093196, 88.54275706135236135 ) ) ;
#117936 = CARTESIAN_POINT ( 'NONE',  ( 0.05219959533909260263, 19.03943276465977164, 39.99890960531436690 ) ) ;
#117937 = CARTESIAN_POINT ( 'NONE',  ( -14.34966873604960291, -8.224510206698953496, 46.66557627198102409 ) ) ;
#117939 = CARTESIAN_POINT ( 'NONE',  ( -19.02544592524342804, 5.153800228976336051, 111.0405762719810099 ) ) ;
#117938 = DIRECTION ( 'NONE',  ( -1.000000000000000000, -0.000000000000000000, -0.000000000000000000 ) ) ;
#117940 = CARTESIAN_POINT ( 'NONE',  ( -0.05219959533907301413, -21.53943276465977519, 32.49890960531435979 ) ) ;
#117941 = CARTESIAN_POINT ( 'NONE',  ( 14.29746914071049879, -8.314922557960816363, 73.33224293864769550 ) ) ;
#117942 = ORIENTED_EDGE ( 'NONE', *, *, #106542, .T. ) ;
#117943 = CARTESIAN_POINT ( 'NONE',  ( 8.314922557960818139, 14.29746914071049879, 64.58224293864769550 ) ) ;
#117944 = LINE ( 'NONE', #115938, #144746 ) ;
#117945 = CARTESIAN_POINT ( 'NONE',  ( 19.05341960407617918, -5.049401038297876454, 66.04275706135233293 ) ) ;
#117946 = CARTESIAN_POINT ( 'NONE',  ( -16.46253265017160317, 9.564922557960807481, 105.8322429386476955 ) ) ;
#117947 = CARTESIAN_POINT ( 'NONE',  ( 0.05219959533936267826, -19.03943276465977164, 80.00109039468567573 ) ) ;
#117948 = CARTESIAN_POINT ( 'NONE',  ( -27.73933785331498925, -9.013057229001049109, 147.4750000027311785 ) ) ;
#117950 = CARTESIAN_POINT ( 'NONE',  ( 16.52544592524335698, 4.483927247898782831, 91.45942372801901854 ) ) ;
#117949 = CARTESIAN_POINT ( 'NONE',  ( 19.03943276465977164, 0.05219959533936151252, 106.2510903946856615 ) ) ;
#117951 = CARTESIAN_POINT ( 'NONE',  ( 19.05341960407611168, 5.049401038298154454, 33.95724293864769550 ) ) ;
#117952 = CARTESIAN_POINT ( 'NONE',  ( -18.67979575497178146, -10.72451020669898902, 41.66557627198103120 ) ) ;
#117953 = CARTESIAN_POINT ( 'NONE',  ( 5.823673210054444382, -21.52544592524334988, 60.20942372801902565 ) ) ;
#117954 = CARTESIAN_POINT ( 'NONE',  ( -13.97604488694547697, 13.89961937509957934, 113.1260903946856757 ) ) ;
#117956 = CARTESIAN_POINT ( 'NONE',  ( 5.049401038298161559, -19.05341960407611168, 72.70724293864768129 ) ) ;
#117955 = CARTESIAN_POINT ( 'NONE',  ( 17.49999999999996803, 3.285415412585594996, 22.44365530742415160 ) ) ;
#117957 = CARTESIAN_POINT ( 'NONE',  ( 23.48298174826589246, 32.32155151706776053, -0.7021577739498228166 ) ) ;
#117959 = CARTESIAN_POINT ( 'NONE',  ( -19.02544592524342804, 5.153800228976336051, 81.04057627198103830 ) ) ;
#117958 = CARTESIAN_POINT ( 'NONE',  ( -4.379528057220328563, 16.55341960407611168, 80.20724293864769550 ) ) ;
#117960 = CARTESIAN_POINT ( 'NONE',  ( -9.564922557960796823, -16.46253265017161027, 87.08224293864769550 ) ) ;
#117961 = VERTEX_POINT ( 'NONE', #175941 ) ;
#117962 = CARTESIAN_POINT ( 'NONE',  ( -13.97604488694547697, 13.89961937509957934, 88.12609039468563310 ) ) ;
#117963 = CARTESIAN_POINT ( 'NONE',  ( -5.823673210054116645, -21.52544592524344225, 62.29057627198102409 ) ) ;
#117964 = CARTESIAN_POINT ( 'NONE',  ( -9.564922557960796823, -16.46253265017161027, 32.08224293864769550 ) ) ;
#117965 = CARTESIAN_POINT ( 'NONE',  ( 13.89961937509957401, 13.97604488694547697, 56.87609039468564731 ) ) ;
#117966 = CARTESIAN_POINT ( 'NONE',  ( -5.049401038298153566, 19.05341960407611168, 60.20724293864768129 ) ) ;
#117967 = CARTESIAN_POINT ( 'NONE',  ( -5.049401038298153566, 19.05341960407611168, 95.20724293864770971 ) ) ;
#117968 = ORIENTED_EDGE ( 'NONE', *, *, #84475, .F. ) ;
#117969 = CARTESIAN_POINT ( 'NONE',  ( -18.62759615963270932, 10.81492255796079327, 90.83224293864769550 ) ) ;
#117971 = CARTESIAN_POINT ( 'NONE',  ( -13.97604488694547697, 13.89961937509957934, 53.12609039468565442 ) ) ;
#117970 = CARTESIAN_POINT ( 'NONE',  ( 12.14591786802309770, 12.06949235617756955, 99.37390960531436690 ) ) ;
#117972 = CARTESIAN_POINT ( 'NONE',  ( -15.72974639402197994, 15.80617190586746368, 95.62390960531436690 ) ) ;
#117973 = CARTESIAN_POINT ( 'NONE',  ( 5.823673210054125526, 21.52544592524343514, 69.79057627198102409 ) ) ;
#117974 = AXIS2_PLACEMENT_3D ( 'NONE', #186476, #79264, #97391 ) ;
#117975 = CARTESIAN_POINT ( 'NONE',  ( -16.55341960407611168, -4.379528057220339221, 26.45724293864768839 ) ) ;
#117976 = CARTESIAN_POINT ( 'NONE',  ( 21.53943276465977519, 0.05219959533937863772, 106.2510903946856757 ) ) ;
#117977 = CARTESIAN_POINT ( 'NONE',  ( -4.483927247898782831, 16.52544592524335698, 47.70942372801902565 ) ) ;
#117978 = CARTESIAN_POINT ( 'NONE',  ( -0.05219959533909027116, -19.03943276465977164, 77.49890960531435269 ) ) ;
#117979 = CARTESIAN_POINT ( 'NONE',  ( 19.03943276465977164, -0.05219959533909143690, 33.74890960531435979 ) ) ;
#117980 = CARTESIAN_POINT ( 'NONE',  ( -18.67979575497193778, 10.72451020669871902, 43.33442372801901143 ) ) ;
#117981 = CARTESIAN_POINT ( 'NONE',  ( 10.72451020669871369, 18.67979575497193778, 57.08442372801901854 ) ) ;
#117982 = CARTESIAN_POINT ( 'NONE',  ( -0.05219959533909027116, -19.03943276465977164, 52.49890960531436690 ) ) ;
#117983 = CARTESIAN_POINT ( 'NONE',  ( 5.823673210054125526, 21.52544592524343514, 114.7905762719810383 ) ) ;
#117984 = CARTESIAN_POINT ( 'NONE',  ( 16.51473224551083163, -9.474510206698727899, 65.83442372801900433 ) ) ;
#117985 = CARTESIAN_POINT ( 'NONE',  ( -9.564922557961040184, 16.46253265017147172, 77.91775706135234714 ) ) ;
#117986 = CARTESIAN_POINT ( 'NONE',  ( 12.06949235617739724, 12.14591786802326823, 26.87609039468567218 ) ) ;
#117987 = CARTESIAN_POINT ( 'NONE',  ( -9.564922557960796823, -16.46253265017161027, 27.08224293864769550 ) ) ;
#117988 = CARTESIAN_POINT ( 'NONE',  ( 12.14591786802327356, -12.06949235617739191, 75.62609039468567573 ) ) ;
#117989 = CARTESIAN_POINT ( 'NONE',  ( 5.153800228976335163, 19.02544592524342804, 39.79057627198100988 ) ) ;
#117990 = CARTESIAN_POINT ( 'NONE',  ( 21.96844466259035400, -7.174710485416647465, 170.3366942299255413 ) ) ;
#117991 = CARTESIAN_POINT ( 'NONE',  ( -9.474510206698964154, 16.51473224551069663, 105.4155762719810383 ) ) ;
#117993 = ADVANCED_FACE ( 'NONE', ( #18280 ), #159754, .F. ) ;
#117992 = CARTESIAN_POINT ( 'NONE',  ( 9.474510206698971260, -16.51473224551069308, 27.91557627198103120 ) ) ;
#117994 = CARTESIAN_POINT ( 'NONE',  ( -15.80617190586745835, -15.72974639402198527, 76.87390960531439532 ) ) ;
#117995 = CARTESIAN_POINT ( 'NONE',  ( 16.53943276465976808, 0.05219959533934440121, 66.25109039468567573 ) ) ;
#117996 = CARTESIAN_POINT ( 'NONE',  ( 15.72974639402176855, 15.80617190586768217, 111.8760903946856615 ) ) ;
#117997 = CARTESIAN_POINT ( 'NONE',  ( 19.05341960407611168, 5.049401038298154454, 38.95724293864767418 ) ) ;
#117998 = CARTESIAN_POINT ( 'NONE',  ( -8.314922557960811034, -14.29746914071050412, 37.08224293864768129 ) ) ;
#117999 = CARTESIAN_POINT ( 'NONE',  ( -14.34966873604960291, -8.224510206698953496, 61.66557627198103120 ) ) ;
#118000 = CARTESIAN_POINT ( 'NONE',  ( 19.03943276465977164, -0.05219959533909143690, 68.74890960531436690 ) ) ;
#118001 = CARTESIAN_POINT ( 'NONE',  ( 15.80617190586769283, -15.72974639402175789, 105.6260903946856899 ) ) ;
#118002 = CARTESIAN_POINT ( 'NONE',  ( 5.719274019375673035, 21.55341960407619339, 32.29275706135235424 ) ) ;
#118003 = CARTESIAN_POINT ( 'NONE',  ( 13.97604488694527802, 13.89961937509977652, 74.37390960531436690 ) ) ;
#118004 = CARTESIAN_POINT ( 'NONE',  ( 21.55341960407619695, -5.719274019375665929, 91.04275706135236135 ) ) ;
#118005 = CARTESIAN_POINT ( 'NONE',  ( 16.53943276465976808, 0.05219959533934440121, 66.25109039468567573 ) ) ;
#118006 = CARTESIAN_POINT ( 'NONE',  ( 13.89961937509977652, -13.97604488694527269, 103.1239096053143527 ) ) ;
#118007 = CARTESIAN_POINT ( 'NONE',  ( 12.14591786802309770, 12.06949235617756955, 29.37390960531435269 ) ) ;
#118008 = CARTESIAN_POINT ( 'NONE',  ( -5.153800228976328057, -19.02544592524343514, 27.29057627198103120 ) ) ;
#118009 = CARTESIAN_POINT ( 'NONE',  ( -14.29746914071037622, -8.314922557961029526, 59.16775706135234714 ) ) ;
#118010 = CARTESIAN_POINT ( 'NONE',  ( -16.55341960407611168, -4.379528057220339221, 61.45724293864770260 ) ) ;
#118011 = CARTESIAN_POINT ( 'NONE',  ( -19.05341960407611168, -5.049401038298163336, 111.4572429386476671 ) ) ;
#118012 = CARTESIAN_POINT ( 'NONE',  ( 21.52544592524344225, -5.823673210054117533, 33.54057627198102409 ) ) ;
#118013 = CARTESIAN_POINT ( 'NONE',  ( 5.719274019375673035, 21.55341960407619339, 107.2927570613523471 ) ) ;
#118014 = CARTESIAN_POINT ( 'NONE',  ( 14.34966873604960469, 8.224510206698951720, 89.16557627198102409 ) ) ;
#118015 = CARTESIAN_POINT ( 'NONE',  ( -19.02544592524342804, 5.153800228976336051, 96.04057627198103830 ) ) ;
#118016 = ORIENTED_EDGE ( 'NONE', *, *, #43597, .F. ) ;
#118017 = CARTESIAN_POINT ( 'NONE',  ( -8.224510206698735004, -14.34966873604973081, 54.58442372801901143 ) ) ;
#118018 = CARTESIAN_POINT ( 'NONE',  ( -19.02544592524342804, 5.153800228976336051, 51.04057627198103120 ) ) ;
#118019 = LINE ( 'NONE', #149351, #11397 ) ;
#118020 = CARTESIAN_POINT ( 'NONE',  ( 0.05219959533936267826, -19.03943276465977164, 45.00109039468566863 ) ) ;
#118021 = CARTESIAN_POINT ( 'NONE',  ( -4.379528057220086978, -16.55341960407618274, 84.79275706135234714 ) ) ;
#118022 = CARTESIAN_POINT ( 'NONE',  ( -19.05341960407617563, 5.049401038297882671, 98.54275706135233293 ) ) ;
#118023 = CARTESIAN_POINT ( 'NONE',  ( -10.81492255796105439, 18.62759615963255655, 67.91775706135234714 ) ) ;
#118024 = CARTESIAN_POINT ( 'NONE',  ( 5.049401038298161559, -19.05341960407611168, 67.70724293864769550 ) ) ;
#118025 = CARTESIAN_POINT ( 'NONE',  ( -5.823673210054116645, -21.52544592524344225, 92.29057627198103830 ) ) ;
#118027 = VECTOR ( 'NONE', #57489, 1000.000000000000000 ) ;
#118026 = CARTESIAN_POINT ( 'NONE',  ( 8.224510206698953496, -14.34966873604960469, 102.9155762719810383 ) ) ;
#118028 = CARTESIAN_POINT ( 'NONE',  ( 0.05219959533936267826, -19.03943276465977164, 70.00109039468566152 ) ) ;
#118029 = CARTESIAN_POINT ( 'NONE',  ( -15.72974639402197994, 15.80617190586746368, 60.62390960531437401 ) ) ;
#118030 = CARTESIAN_POINT ( 'NONE',  ( -5.049401038297874678, -19.05341960407617918, 39.79275706135232582 ) ) ;
#118031 = CARTESIAN_POINT ( 'NONE',  ( 19.05341960407611168, 5.049401038298154454, 113.9572429386477097 ) ) ;
#118032 = CARTESIAN_POINT ( 'NONE',  ( -15.80617190586745835, -15.72974639402198527, 91.87390960531436690 ) ) ;
#118033 = CARTESIAN_POINT ( 'NONE',  ( -19.26498983726238023, 5.499999999999602096, 55.55319577422003618 ) ) ;
#118034 = FACE_OUTER_BOUND ( 'NONE', #121551, .T. ) ;
#118035 = CARTESIAN_POINT ( 'NONE',  ( -9.474510206698720793, -16.51473224551083518, 109.5844237280190043 ) ) ;
#118036 = CARTESIAN_POINT ( 'NONE',  ( -19.02130022317637525, 5.499999999999600320, 60.78188669246576836 ) ) ;
#118037 = CARTESIAN_POINT ( 'NONE',  ( 12.14591786802327356, -12.06949235617739191, 30.62609039468567929 ) ) ;
#118038 = CARTESIAN_POINT ( 'NONE',  ( 9.564922557960805705, 16.46253265017160317, 49.58224293864770260 ) ) ;
#118039 = CARTESIAN_POINT ( 'NONE',  ( 13.89961937509977652, -13.97604488694527269, 108.1239096053143669 ) ) ;
#118041 = CARTESIAN_POINT ( 'NONE',  ( 14.34966873604960469, 8.224510206698951720, 54.16557627198103120 ) ) ;
#118040 = CARTESIAN_POINT ( 'NONE',  ( 18.62759615963271287, -10.81492255796078972, 93.33224293864769550 ) ) ;
#118042 = VECTOR ( 'NONE', #157176, 1000.000000000000000 ) ;
#118043 = CARTESIAN_POINT ( 'NONE',  ( 10.81492255796106328, -18.62759615963255655, 75.41775706135233293 ) ) ;
#118045 = CARTESIAN_POINT ( 'NONE',  ( -13.89961937509957401, -13.97604488694547875, 29.37609039468565797 ) ) ;
#118044 = CARTESIAN_POINT ( 'NONE',  ( 4.379528057220092307, 16.55341960407617563, 22.29275706135235069 ) ) ;
#118046 = CARTESIAN_POINT ( 'NONE',  ( 4.483927247898545687, 16.52544592524342804, 34.79057627198103120 ) ) ;
#118047 = CARTESIAN_POINT ( 'NONE',  ( 21.55341960407610458, 5.719274019375980345, 108.9572429386476955 ) ) ;
#118048 = CARTESIAN_POINT ( 'NONE',  ( -12.14591786802309592, -12.06949235617757132, 46.87390960531435979 ) ) ;
#118049 = CARTESIAN_POINT ( 'NONE',  ( -5.153800228976607833, 19.02544592524334988, 97.70942372801900433 ) ) ;
#118050 = CARTESIAN_POINT ( 'NONE',  ( 19.03943276465977164, 0.05219959533936151252, 61.25109039468566863 ) ) ;
#118051 = CARTESIAN_POINT ( 'NONE',  ( 15.72974639402176855, 15.80617190586768217, 71.87609039468568994 ) ) ;
#118052 = CARTESIAN_POINT ( 'NONE',  ( 9.474510206698729675, 16.51473224551082808, 57.08442372801900433 ) ) ;
#118053 = CARTESIAN_POINT ( 'NONE',  ( 16.51473224551069308, 9.474510206698969483, 29.16557627198103475 ) ) ;
#118054 = CARTESIAN_POINT ( 'NONE',  ( 21.52544592524344225, -5.823673210054117533, 38.54057627198103120 ) ) ;
#118055 = CARTESIAN_POINT ( 'NONE',  ( -8.314922557960811034, -14.29746914071050412, 52.08224293864768839 ) ) ;
#118056 = CARTESIAN_POINT ( 'NONE',  ( -19.46398650005389186, 5.499999999999950262, 95.18269651486369298 ) ) ;
#118057 = CARTESIAN_POINT ( 'NONE',  ( 19.02544592524334988, 5.153800228976608722, 21.45942372801899012 ) ) ;
#118058 = CARTESIAN_POINT ( 'NONE',  ( -0.05219959533934338120, 16.53943276465976808, 87.50109039468568994 ) ) ;
#118059 = CARTESIAN_POINT ( 'NONE',  ( -14.34966873604960291, -8.224510206698953496, 41.66557627198103120 ) ) ;
#118060 = CARTESIAN_POINT ( 'NONE',  ( -10.72451020669870658, -18.67979575497194134, 74.58442372801901854 ) ) ;
#118061 = CARTESIAN_POINT ( 'NONE',  ( 21.53943276465977519, 0.05219959533937863772, 71.25109039468568994 ) ) ;
#118062 = CARTESIAN_POINT ( 'NONE',  ( -18.67979575497178146, -10.72451020669898902, 76.66557627198103830 ) ) ;
#118063 = CARTESIAN_POINT ( 'NONE',  ( -13.89961937509977652, 13.97604488694528158, 40.62390960531435979 ) ) ;
#118064 = CARTESIAN_POINT ( 'NONE',  ( 15.72974639402176855, 15.80617190586768217, 56.87609039468568994 ) ) ;
#118065 = CARTESIAN_POINT ( 'NONE',  ( 9.564922557960805705, 16.46253265017160317, 29.58224293864769550 ) ) ;
#118066 = CARTESIAN_POINT ( 'NONE',  ( -16.51473224551069308, -9.474510206698971260, 51.66557627198102409 ) ) ;
#118067 = CARTESIAN_POINT ( 'NONE',  ( -16.55341960407611168, -4.379528057220339221, 91.45724293864769550 ) ) ;
#118068 = CARTESIAN_POINT ( 'NONE',  ( -9.474510206698964154, 16.51473224551069663, 85.41557627198102409 ) ) ;
#118069 = CARTESIAN_POINT ( 'NONE',  ( -8.314922557960811034, -14.29746914071050412, 42.08224293864769550 ) ) ;
#118070 = CARTESIAN_POINT ( 'NONE',  ( 8.314922557960818139, 14.29746914071049879, 99.58224293864770971 ) ) ;
#118071 = CARTESIAN_POINT ( 'NONE',  ( -10.81492255796078084, -18.62759615963271287, 72.08224293864769550 ) ) ;
#118072 = CARTESIAN_POINT ( 'NONE',  ( -18.67979575497193778, 10.72451020669871902, 28.33442372801902209 ) ) ;
#118073 = CARTESIAN_POINT ( 'NONE',  ( 13.89961937509977652, -13.97604488694527269, 113.1239096053143527 ) ) ;
#118075 = CARTESIAN_POINT ( 'NONE',  ( 8.224510206698742110, 14.34966873604972548, 27.08442372801901854 ) ) ;
#118074 = CARTESIAN_POINT ( 'NONE',  ( 9.564922557960805705, 16.46253265017160317, 79.58224293864769550 ) ) ;
#118076 = ADVANCED_FACE ( 'NONE', ( #19271 ), #69768, .T. ) ;
#118077 = CARTESIAN_POINT ( 'NONE',  ( -21.53943276465977519, 0.05219959533907696930, 71.24890960531435269 ) ) ;
#118078 = CARTESIAN_POINT ( 'NONE',  ( -18.62759615963255300, -10.81492255796106328, 94.16775706135237556 ) ) ;
#118079 = CARTESIAN_POINT ( 'NONE',  ( 19.05341960407611168, 5.049401038298154454, 73.95724293864768129 ) ) ;
#118080 = CARTESIAN_POINT ( 'NONE',  ( 21.52544592524344225, -5.823673210054117533, 108.5405762719810241 ) ) ;
#118081 = CARTESIAN_POINT ( 'NONE',  ( -13.97604488694527625, -13.89961937509977652, 111.8739096053143243 ) ) ;
#118082 = CARTESIAN_POINT ( 'NONE',  ( -4.379528057220086978, -16.55341960407618274, 89.79275706135236135 ) ) ;
#118083 = CARTESIAN_POINT ( 'NONE',  ( -15.72974639402176322, -15.80617190586768395, 64.37609039468568994 ) ) ;
#118084 = CARTESIAN_POINT ( 'NONE',  ( -21.55341960407619339, 5.719274019375674811, 93.54275706135234714 ) ) ;
#118085 = CARTESIAN_POINT ( 'NONE',  ( 16.52544592524335698, 4.483927247898782831, 56.45942372801902565 ) ) ;
#118086 = CARTESIAN_POINT ( 'NONE',  ( -21.53943276465977519, -0.05219959533937600094, 28.75109039468567929 ) ) ;
#118087 = CARTESIAN_POINT ( 'NONE',  ( 13.89961937509977652, -13.97604488694527269, 113.1239096053143527 ) ) ;
#118088 = CARTESIAN_POINT ( 'NONE',  ( 5.823673210054444382, -21.52544592524334988, 90.20942372801903275 ) ) ;
#118089 = CARTESIAN_POINT ( 'NONE',  ( -16.51473224551069308, -9.474510206698971260, 96.66557627198102409 ) ) ;
#118090 = CARTESIAN_POINT ( 'NONE',  ( 18.62759615963271287, -10.81492255796078972, 93.33224293864769550 ) ) ;
#118091 = CARTESIAN_POINT ( 'NONE',  ( 9.474510206698729675, 16.51473224551082808, 57.08442372801900433 ) ) ;
#118092 = CARTESIAN_POINT ( 'NONE',  ( 5.719274019375991003, -21.55341960407610458, 52.70724293864769550 ) ) ;
#118094 = CARTESIAN_POINT ( 'NONE',  ( -4.483927247898539470, -16.52544592524342804, 42.29057627198103120 ) ) ;
#118093 = CARTESIAN_POINT ( 'NONE',  ( -19.02544592524342804, 5.153800228976336051, 96.04057627198103830 ) ) ;
#118095 = CARTESIAN_POINT ( 'NONE',  ( 11.09110223580025689, -9.259486913381270057, -62.30073625427280604 ) ) ;
#118096 = CARTESIAN_POINT ( 'NONE',  ( 19.02544592524334988, 5.153800228976608722, 71.45942372801900433 ) ) ;
#118097 = CARTESIAN_POINT ( 'NONE',  ( -0.2045547421925955622, -16.68945015508927199, -61.35148950497489295 ) ) ;
#118098 = CARTESIAN_POINT ( 'NONE',  ( 5.153800228976615827, -19.02544592524334988, 110.2094237280189901 ) ) ;
#118099 = CARTESIAN_POINT ( 'NONE',  ( -5.719274019375978568, 21.55341960407610458, 85.20724293864770971 ) ) ;
#118100 = CARTESIAN_POINT ( 'NONE',  ( -16.53943276465976808, 0.05219959533911058130, 66.24890960531436690 ) ) ;
#118101 = CARTESIAN_POINT ( 'NONE',  ( 14.29746914071037800, 8.314922557961029526, 36.66775706135234714 ) ) ;
#118102 = CARTESIAN_POINT ( 'NONE',  ( -0.05219959533909027116, -19.03943276465977164, 47.49890960531435979 ) ) ;
#118104 = CARTESIAN_POINT ( 'NONE',  ( -5.153800228976607833, 19.02544592524334988, 87.70942372801897591 ) ) ;
#118103 = CARTESIAN_POINT ( 'NONE',  ( 5.823673210054125526, 21.52544592524343514, 114.7905762719810383 ) ) ;
#118105 = EDGE_CURVE ( 'NONE', #130010, #153137, #54053, .T. ) ;
#118106 = CARTESIAN_POINT ( 'NONE',  ( -9.474510206698964154, 16.51473224551069663, 90.41557627198103830 ) ) ;
#118107 = CARTESIAN_POINT ( 'NONE',  ( 19.02544592524343514, -5.153800228976328945, 68.54057627198103830 ) ) ;
#118108 = CARTESIAN_POINT ( 'NONE',  ( 18.62759615963271287, -10.81492255796078972, 73.33224293864769550 ) ) ;
#118109 = CARTESIAN_POINT ( 'NONE',  ( -5.049401038298153566, 19.05341960407611168, 45.20724293864769550 ) ) ;
#118110 = DIRECTION ( 'NONE',  ( -0.000000000000000000, -0.000000000000000000, 1.000000000000000000 ) ) ;
#118111 = CARTESIAN_POINT ( 'NONE',  ( 14.34966873604960469, 8.224510206698951720, 49.16557627198102409 ) ) ;
#118112 = CARTESIAN_POINT ( 'NONE',  ( 19.05341960407611168, 5.049401038298154454, 108.9572429386477097 ) ) ;
#118113 = CARTESIAN_POINT ( 'NONE',  ( -17.81289503416611097, -24.51734667627696496, 144.2999999999999829 ) ) ;
#118114 = CARTESIAN_POINT ( 'NONE',  ( 19.05341960407617918, -5.049401038297876454, 66.04275706135233293 ) ) ;
#118115 = CIRCLE ( 'NONE', #114778, 16.70000000000002061 ) ;
#118116 = CARTESIAN_POINT ( 'NONE',  ( -15.80617190586745835, -15.72974639402198527, 81.87390960531435269 ) ) ;
#118117 = CARTESIAN_POINT ( 'NONE',  ( 19.03943276465977164, 0.05219959533936151252, 31.25109039468566863 ) ) ;
#118118 = CARTESIAN_POINT ( 'NONE',  ( -9.474510206698964154, 16.51473224551069663, 100.4155762719810241 ) ) ;
#118119 = CARTESIAN_POINT ( 'NONE',  ( 12.22610943951276319, -10.45445179612737086, -59.42747105264538732 ) ) ;
#118120 = CARTESIAN_POINT ( 'NONE',  ( 18.62759615963271287, -10.81492255796078972, 43.33224293864769550 ) ) ;
#118121 = CARTESIAN_POINT ( 'NONE',  ( 13.97604488694527802, 13.89961937509977652, 74.37390960531436690 ) ) ;
#118122 = CARTESIAN_POINT ( 'NONE',  ( 0.05219959533937995610, -21.53943276465977519, 70.00109039468568994 ) ) ;
#118123 = CARTESIAN_POINT ( 'NONE',  ( 13.89961937509977652, -13.97604488694527269, 28.12390960531435624 ) ) ;
#118125 = VERTEX_POINT ( 'NONE', #95759 ) ;
#118124 = CARTESIAN_POINT ( 'NONE',  ( -0.05219959533937732626, 21.53943276465977519, 22.50109039468567573 ) ) ;
#118126 = CARTESIAN_POINT ( 'NONE',  ( 15.80617190586769283, -15.72974639402175789, 50.62609039468568994 ) ) ;
#118127 = VERTEX_POINT ( 'NONE', #108945 ) ;
#118128 = CARTESIAN_POINT ( 'NONE',  ( -26.81441202005693114, -10.25421135757314950, 139.9999999999999716 ) ) ;
#118129 = CARTESIAN_POINT ( 'NONE',  ( 19.03943276465977164, 0.05219959533936151252, 66.25109039468567573 ) ) ;
#118130 = CARTESIAN_POINT ( 'NONE',  ( -17.18269478283327345, -17.18269478283298568, -54.21489346206828230 ) ) ;
#118131 = CARTESIAN_POINT ( 'NONE',  ( 15.80617190586746368, 15.72974639402197994, 114.3739096053143527 ) ) ;
#118132 = CARTESIAN_POINT ( 'NONE',  ( 5.049401038298161559, -19.05341960407611168, 62.70724293864769550 ) ) ;
#118133 = CARTESIAN_POINT ( 'NONE',  ( -16.55341960407617563, 4.379528057220093196, 43.54275706135235424 ) ) ;
#118134 = CARTESIAN_POINT ( 'NONE',  ( 30.74264578624800137, -22.33583958711395212, -4.949999994537626513 ) ) ;
#118135 = CARTESIAN_POINT ( 'NONE',  ( 21.55341960407619695, -5.719274019375665929, 101.0427570613523756 ) ) ;
#118136 = CARTESIAN_POINT ( 'NONE',  ( -0.05219959533909027116, -19.03943276465977164, 42.49890960531435269 ) ) ;
#118137 = CARTESIAN_POINT ( 'NONE',  ( 5.719274019375673035, 21.55341960407619339, 112.2927570613523471 ) ) ;
#118139 = CARTESIAN_POINT ( 'NONE',  ( 15.80617190586769283, -15.72974639402175789, 60.62609039468567573 ) ) ;
#118138 = CARTESIAN_POINT ( 'NONE',  ( -19.02544592524342804, 5.153800228976336051, 91.04057627198100988 ) ) ;
#118140 = CARTESIAN_POINT ( 'NONE',  ( -13.89961937509977652, 13.97604488694528158, 115.6239096053143669 ) ) ;
#118141 = CARTESIAN_POINT ( 'NONE',  ( -2.300691058039380454, 7.143419655154890968, 1.353258418600854274 ) ) ;
#118143 = CARTESIAN_POINT ( 'NONE',  ( -0.05219959533937732626, 21.53943276465977519, 72.50109039468568994 ) ) ;
#118142 = CARTESIAN_POINT ( 'NONE',  ( -8.314922557961024197, 14.29746914071037800, 47.91775706135234714 ) ) ;
#118144 = CARTESIAN_POINT ( 'NONE',  ( 10.81492255796106328, -18.62759615963255655, 95.41775706135234714 ) ) ;
#118145 = CARTESIAN_POINT ( 'NONE',  ( -10.10305183197212742, 9.389996629557172625, -60.40856999928715254 ) ) ;
#118146 = CARTESIAN_POINT ( 'NONE',  ( -16.53943276465976808, -0.05219959533934237506, 23.75109039468567929 ) ) ;
#118147 = CARTESIAN_POINT ( 'NONE',  ( -19.05341960407611168, -5.049401038298163336, 86.45724293864769550 ) ) ;
#118148 = CARTESIAN_POINT ( 'NONE',  ( 5.049401038298161559, -19.05341960407611168, 107.7072429386476955 ) ) ;
#118149 = ORIENTED_EDGE ( 'NONE', *, *, #150015, .T. ) ;
#118150 = CARTESIAN_POINT ( 'NONE',  ( 17.26172910966777252, 6.454744622555864453, 41.69353091350778584 ) ) ;
#118151 = CARTESIAN_POINT ( 'NONE',  ( -19.05341960407611168, -5.049401038298163336, 31.45724293864769550 ) ) ;
#118152 = CARTESIAN_POINT ( 'NONE',  ( 0.05219959533907565091, 21.53943276465977519, 39.99890960531436690 ) ) ;
#118153 = CARTESIAN_POINT ( 'NONE',  ( 4.483927247898790824, -16.52544592524335698, 110.2094237280190185 ) ) ;
#118155 = CARTESIAN_POINT ( 'NONE',  ( 16.51473224551069308, 9.474510206698969483, 69.16557627198102409 ) ) ;
#118154 = CARTESIAN_POINT ( 'NONE',  ( 16.55341960407611168, 4.379528057220329451, 88.95724293864769550 ) ) ;
#118156 = CARTESIAN_POINT ( 'NONE',  ( 10.81492255796106328, -18.62759615963255655, 85.41775706135236135 ) ) ;
#118157 = CARTESIAN_POINT ( 'NONE',  ( -14.34966873604972548, 8.224510206698743886, 23.33442372801901499 ) ) ;
#118158 = CARTESIAN_POINT ( 'NONE',  ( -4.379528057220328563, 16.55341960407611168, 90.20724293864770971 ) ) ;
#118159 = CARTESIAN_POINT ( 'NONE',  ( 15.72974639402176855, 15.80617190586768217, 46.87609039468568994 ) ) ;
#118160 = CARTESIAN_POINT ( 'NONE',  ( -10.72451020669898014, 18.67979575497178502, 80.41557627198103830 ) ) ;
#118161 = CARTESIAN_POINT ( 'NONE',  ( 9.564922557961047289, -16.46253265017146816, 40.41775706135234003 ) ) ;
#118162 = CARTESIAN_POINT ( 'NONE',  ( -34.61352925372423783, 7.251504142776767914, 43.02394063628852194 ) ) ;
#118163 = CARTESIAN_POINT ( 'NONE',  ( -19.03943276465977164, 0.05219959533909376836, 101.2489096053143669 ) ) ;
#118164 = CARTESIAN_POINT ( 'NONE',  ( -12.06949235617756955, 12.14591786802309770, 60.62390960531437401 ) ) ;
#118165 = CARTESIAN_POINT ( 'NONE',  ( -4.379528057220328563, 16.55341960407611168, 35.20724293864768839 ) ) ;
#118166 = CARTESIAN_POINT ( 'NONE',  ( 8.314922557961029526, -14.29746914071037800, 110.4177570613523756 ) ) ;
#118167 = CARTESIAN_POINT ( 'NONE',  ( -9.564922557961040184, 16.46253265017147172, 67.91775706135233293 ) ) ;
#118168 = CARTESIAN_POINT ( 'NONE',  ( 18.39639308325435962, 5.500000000000037303, 53.98252246182195790 ) ) ;
#118169 = CARTESIAN_POINT ( 'NONE',  ( -13.89961937509977652, 13.97604488694528158, 115.6239096053143669 ) ) ;
#118170 = CARTESIAN_POINT ( 'NONE',  ( -16.53943276465976808, 0.05219959533911058130, 91.24890960531436690 ) ) ;
#118171 = DIRECTION ( 'NONE',  ( -5.392603844284257652E-33, -1.000000000000000000, -0.000000000000000000 ) ) ;
#118173 = CARTESIAN_POINT ( 'NONE',  ( 18.62759615963271287, -10.81492255796078972, 48.33224293864770260 ) ) ;
#118172 = CARTESIAN_POINT ( 'NONE',  ( -16.46253265017160317, 9.564922557960807481, 40.83224293864769550 ) ) ;
#118174 = CARTESIAN_POINT ( 'NONE',  ( -21.52544592524343514, 5.823673210054127303, 81.04057627198102409 ) ) ;
#118175 = CARTESIAN_POINT ( 'NONE',  ( 16.52544592524342804, -4.483927247898539470, 113.5405762719810383 ) ) ;
#118177 = CARTESIAN_POINT ( 'NONE',  ( 5.153800228976335163, 19.02544592524342804, 49.79057627198100988 ) ) ;
#118176 = CARTESIAN_POINT ( 'NONE',  ( 12.14591786802327356, -12.06949235617739191, 70.62609039468567573 ) ) ;
#118178 = CARTESIAN_POINT ( 'NONE',  ( 16.46253265017146816, 9.564922557961045513, 41.66775706135234003 ) ) ;
#118179 = CARTESIAN_POINT ( 'NONE',  ( -21.55341960407619339, 5.719274019375674811, 58.54275706135235424 ) ) ;
#118180 = CARTESIAN_POINT ( 'NONE',  ( 14.29746914071049879, -8.314922557960816363, 108.3322429386477097 ) ) ;
#118181 = EDGE_CURVE ( 'NONE', #30166, #50977, #3742, .T. ) ;
#118182 = CARTESIAN_POINT ( 'NONE',  ( 19.05341960407617918, -5.049401038297876454, 86.04275706135233293 ) ) ;
#118183 = CARTESIAN_POINT ( 'NONE',  ( -22.81625015709509441, -31.40387420917324590, -6.824999997268814234 ) ) ;
#118185 = CARTESIAN_POINT ( 'NONE',  ( -15.72974639402197994, 15.80617190586746368, 45.62390960531436690 ) ) ;
#118184 = CYLINDRICAL_SURFACE ( 'NONE', #79704, 214.0437394197456342 ) ;
#118186 = CARTESIAN_POINT ( 'NONE',  ( -19.05341960407611168, -5.049401038298163336, 21.45724293864768839 ) ) ;
#118187 = CARTESIAN_POINT ( 'NONE',  ( -10.81492255796105439, 18.62759615963255655, 87.91775706135234714 ) ) ;
#118188 = CARTESIAN_POINT ( 'NONE',  ( 0.05219959533910956823, 16.53943276465976808, 29.99890960531435979 ) ) ;
#118190 = CARTESIAN_POINT ( 'NONE',  ( -12.06949235617756955, 12.14591786802309770, 40.62390960531435269 ) ) ;
#118189 = CARTESIAN_POINT ( 'NONE',  ( 12.06949235617739724, 12.14591786802326823, 51.87609039468568284 ) ) ;
#118191 = CARTESIAN_POINT ( 'NONE',  ( -21.53943276465977519, 0.05219959533907696930, 86.24890960531436690 ) ) ;
#118192 = CARTESIAN_POINT ( 'NONE',  ( -0.05219959533907301413, -21.53943276465977519, 72.49890960531435269 ) ) ;
#118193 = CARTESIAN_POINT ( 'NONE',  ( -21.35096542554161658, -10.43949311476039554, 170.3901443614043671 ) ) ;
#118195 = CARTESIAN_POINT ( 'NONE',  ( -5.153800228976328057, -19.02544592524343514, 112.2905762719810099 ) ) ;
#118194 = CARTESIAN_POINT ( 'NONE',  ( -0.05219959533936034679, 19.03943276465977164, 82.50109039468567573 ) ) ;
#118196 = CARTESIAN_POINT ( 'NONE',  ( -5.153800228976328057, -19.02544592524343514, 52.29057627198100988 ) ) ;
#118198 = EDGE_CURVE ( 'NONE', #160176, #166994, #154945, .T. ) ;
#118197 = CARTESIAN_POINT ( 'NONE',  ( -13.97604488694527625, -13.89961937509977652, 31.87390960531435979 ) ) ;
#118199 =( NAMED_UNIT ( * ) SI_UNIT ( $, .STERADIAN. ) SOLID_ANGLE_UNIT ( ) );
#118200 = DIRECTION ( 'NONE',  ( 1.000000000000000000, -4.336808689942018352E-17, 0.000000000000000000 ) ) ;
#118201 = EDGE_LOOP ( 'NONE', ( #145989, #69959, #22366, #108908, #17911, #167198, #3407, #129546, #125080, #24198, #164920, #89327, #93375 ) ) ;
#118202 = CARTESIAN_POINT ( 'NONE',  ( -4.483927247898782831, 16.52544592524335698, 87.70942372801901854 ) ) ;
#118203 = CARTESIAN_POINT ( 'NONE',  ( -10.72451020669898014, 18.67979575497178502, 105.4155762719810383 ) ) ;
#118204 = CARTESIAN_POINT ( 'NONE',  ( 19.05341960407611168, 5.049401038298154454, 68.95724293864769550 ) ) ;
#118205 = CARTESIAN_POINT ( 'NONE',  ( 15.80617190586769283, -15.72974639402175789, 45.62609039468567573 ) ) ;
#118206 = CARTESIAN_POINT ( 'NONE',  ( -19.03943276465977164, 0.05219959533909376836, 96.24890960531436690 ) ) ;
#118207 = CARTESIAN_POINT ( 'NONE',  ( -27.53771902582940001, -28.32105632907237691, -18.50180672658962777 ) ) ;
#118208 = ORIENTED_EDGE ( 'NONE', *, *, #130640, .F. ) ;
#118209 = CARTESIAN_POINT ( 'NONE',  ( -5.823673210054431948, 21.52544592524334988, 27.70942372801901854 ) ) ;
#118211 = CARTESIAN_POINT ( 'NONE',  ( -9.474510206698964154, 16.51473224551069663, 100.4155762719810241 ) ) ;
#118210 = CARTESIAN_POINT ( 'NONE',  ( 5.049401038298161559, -19.05341960407611168, 22.70724293864769194 ) ) ;
#118212 = CARTESIAN_POINT ( 'NONE',  ( 5.153800228976615827, -19.02544592524334988, 35.20942372801899722 ) ) ;
#118213 = CARTESIAN_POINT ( 'NONE',  ( 5.823673210054125526, 21.52544592524343514, 109.7905762719810383 ) ) ;
#118214 = CARTESIAN_POINT ( 'NONE',  ( -9.474510206698720793, -16.51473224551083518, 44.58442372801900433 ) ) ;
#118215 = CARTESIAN_POINT ( 'NONE',  ( 5.153800228976615827, -19.02544592524334988, 55.20942372801899722 ) ) ;
#118216 = CARTESIAN_POINT ( 'NONE',  ( 12.14591786802327356, -12.06949235617739191, 95.62609039468568994 ) ) ;
#118217 = CARTESIAN_POINT ( 'NONE',  ( 21.98685479826775335, -13.98560643873835652, 165.5209445330007441 ) ) ;
#118218 = CARTESIAN_POINT ( 'NONE',  ( 9.474510206698971260, -16.51473224551069308, 77.91557627198103830 ) ) ;
#118219 = AXIS2_PLACEMENT_3D ( 'NONE', #183273, #97927, #67613 ) ;
#118220 = CARTESIAN_POINT ( 'NONE',  ( -21.52544592524334988, -5.823673210054445271, 73.95942372801901854 ) ) ;
#118221 = CARTESIAN_POINT ( 'NONE',  ( -21.52544592524334988, -5.823673210054445271, 88.95942372801901854 ) ) ;
#118222 = DIRECTION ( 'NONE',  ( -0.000000000000000000, -0.000000000000000000, 1.000000000000000000 ) ) ;
#118223 = CARTESIAN_POINT ( 'NONE',  ( -9.564922557960796823, -16.46253265017161027, 92.08224293864769550 ) ) ;
#118224 = CARTESIAN_POINT ( 'NONE',  ( 10.72451020669871369, 18.67979575497193778, 62.08442372801901143 ) ) ;
#118225 = CARTESIAN_POINT ( 'NONE',  ( -9.564922557961040184, 16.46253265017147172, 97.91775706135233293 ) ) ;
#118226 = CARTESIAN_POINT ( 'NONE',  ( -9.564922557960796823, -16.46253265017161027, 72.08224293864770971 ) ) ;
#118227 = CARTESIAN_POINT ( 'NONE',  ( -16.46253265017160317, 9.564922557960807481, 105.8322429386476955 ) ) ;
#118228 = CARTESIAN_POINT ( 'NONE',  ( 16.51473224551069308, 9.474510206698969483, 84.16557627198102409 ) ) ;
#118229 = CARTESIAN_POINT ( 'NONE',  ( -0.05219959533936034679, 19.03943276465977164, 87.50109039468567573 ) ) ;
#118230 = CARTESIAN_POINT ( 'NONE',  ( 16.51473224551069308, 9.474510206698969483, 59.16557627198102409 ) ) ;
#118231 = CARTESIAN_POINT ( 'NONE',  ( -5.049401038298153566, 19.05341960407611168, 50.20724293864770260 ) ) ;
#118232 = CARTESIAN_POINT ( 'NONE',  ( 0.05219959533907565091, 21.53943276465977519, 114.9989096053143669 ) ) ;
#118233 = CARTESIAN_POINT ( 'NONE',  ( -16.53943276465976808, -0.05219959533934237506, 103.7510903946857042 ) ) ;
#118234 = CARTESIAN_POINT ( 'NONE',  ( 22.49873734152911453, -26.99873734152921045, 1.110912703473986074 ) ) ;
#118235 = CARTESIAN_POINT ( 'NONE',  ( 6.404328268737250696, -0.9271017399331602515, -64.47359807031668311 ) ) ;
#118236 = CARTESIAN_POINT ( 'NONE',  ( -0.05219959533936034679, 19.03943276465977164, 57.50109039468566863 ) ) ;
#118237 = CARTESIAN_POINT ( 'NONE',  ( -19.03943276465977164, 0.05219959533909376836, 86.24890960531436690 ) ) ;
#118238 = CARTESIAN_POINT ( 'NONE',  ( -14.29746914071049879, 8.314922557960819915, 65.83224293864769550 ) ) ;
#118239 = CARTESIAN_POINT ( 'NONE',  ( 0.05219959533910956823, 16.53943276465976808, 104.9989096053143669 ) ) ;
#118240 = CARTESIAN_POINT ( 'NONE',  ( 10.72451020669898902, -18.67979575497178502, 27.91557627198103830 ) ) ;
#118241 = CARTESIAN_POINT ( 'NONE',  ( -13.89961937509977652, 13.97604488694528158, 110.6239096053143243 ) ) ;
#118242 = CARTESIAN_POINT ( 'NONE',  ( -16.55341960407611168, -4.379528057220339221, 91.45724293864769550 ) ) ;
#118243 = CARTESIAN_POINT ( 'NONE',  ( 19.02544592524343514, -5.153800228976328945, 113.5405762719810241 ) ) ;
#118244 = CARTESIAN_POINT ( 'NONE',  ( -19.02544592524334988, -5.153800228976617603, 33.95942372801897591 ) ) ;
#118245 = CARTESIAN_POINT ( 'NONE',  ( -0.05219959533934338120, 16.53943276465976808, 112.5010903946857042 ) ) ;
#118246 = CARTESIAN_POINT ( 'NONE',  ( 9.474510206698971260, -16.51473224551069308, 92.91557627198103830 ) ) ;
#118247 = CARTESIAN_POINT ( 'NONE',  ( -10.81492255796105439, 18.62759615963255655, 47.91775706135234714 ) ) ;
#118248 = CARTESIAN_POINT ( 'NONE',  ( 15.80617190586746368, 15.72974639402197994, 44.37390960531435979 ) ) ;
#118249 = CARTESIAN_POINT ( 'NONE',  ( -10.72451020669870658, -18.67979575497194134, 34.58442372801900433 ) ) ;
#118250 = CARTESIAN_POINT ( 'NONE',  ( 10.72451020669898902, -18.67979575497178502, 87.91557627198103830 ) ) ;
#118251 = CARTESIAN_POINT ( 'NONE',  ( 16.53943276465976808, -0.05219959533910856209, 93.74890960531436690 ) ) ;
#118252 = CARTESIAN_POINT ( 'NONE',  ( -13.97604488694547697, 13.89961937509957934, 58.12609039468566863 ) ) ;
#118253 = CARTESIAN_POINT ( 'NONE',  ( 9.564922557960805705, 16.46253265017160317, 29.58224293864769550 ) ) ;
#118254 = CARTESIAN_POINT ( 'NONE',  ( -19.03943276465977164, 0.05219959533909376836, 91.24890960531436690 ) ) ;
#118255 = CARTESIAN_POINT ( 'NONE',  ( 5.049401038298161559, -19.05341960407611168, 92.70724293864769550 ) ) ;
#118256 = CARTESIAN_POINT ( 'NONE',  ( -12.06949235617756955, 12.14591786802309770, 110.6239096053143669 ) ) ;
#118257 = CIRCLE ( 'NONE', #163433, 61.99999999999998579 ) ;
#118258 = CARTESIAN_POINT ( 'NONE',  ( 16.52544592524342804, -4.483927247898539470, 28.54057627198103120 ) ) ;
#118259 = CARTESIAN_POINT ( 'NONE',  ( -16.52544592524335698, -4.483927247898792601, 43.95942372801902565 ) ) ;
#118260 = CARTESIAN_POINT ( 'NONE',  ( 21.53943276465977519, 0.05219959533937863772, 101.2510903946856757 ) ) ;
#118262 = CARTESIAN_POINT ( 'NONE',  ( 8.314922557961029526, -14.29746914071037800, 110.4177570613523756 ) ) ;
#118261 = CARTESIAN_POINT ( 'NONE',  ( 5.153800228976335163, 19.02544592524342804, 114.7905762719810241 ) ) ;
#118263 = CARTESIAN_POINT ( 'NONE',  ( 21.55341960407619695, -5.719274019375665929, 36.04275706135234714 ) ) ;
#118264 = CARTESIAN_POINT ( 'NONE',  ( -5.153800228976328057, -19.02544592524343514, 37.29057627198102409 ) ) ;
#118265 = CARTESIAN_POINT ( 'NONE',  ( -12.14591786802326823, 12.06949235617739902, 38.12609039468567573 ) ) ;
#118266 = CARTESIAN_POINT ( 'NONE',  ( -14.29746914071037622, -8.314922557961029526, 109.1677570613523613 ) ) ;
#118267 = CARTESIAN_POINT ( 'NONE',  ( 16.52544592524335698, 4.483927247898782831, 91.45942372801901854 ) ) ;
#118268 = CARTESIAN_POINT ( 'NONE',  ( 5.049401038297881783, 19.05341960407617563, 102.2927570613523045 ) ) ;
#118269 = CARTESIAN_POINT ( 'NONE',  ( 0.05219959533909260263, 19.03943276465977164, 29.99890960531435979 ) ) ;
#118270 = CARTESIAN_POINT ( 'NONE',  ( -16.55341960407611168, -4.379528057220339221, 111.4572429386476813 ) ) ;
#118271 = CARTESIAN_POINT ( 'NONE',  ( -21.55341960407619339, 5.719274019375674811, 23.54275706135235424 ) ) ;
#118272 = CARTESIAN_POINT ( 'NONE',  ( -19.05341960407611168, -5.049401038298163336, 31.45724293864769550 ) ) ;
#118273 = CARTESIAN_POINT ( 'NONE',  ( 16.46253265017160672, -9.564922557960803928, 103.3322429386476955 ) ) ;
#118274 = CARTESIAN_POINT ( 'NONE',  ( -10.81492255796105439, 18.62759615963255655, 37.91775706135235424 ) ) ;
#118275 = CARTESIAN_POINT ( 'NONE',  ( 5.049401038298161559, -19.05341960407611168, 22.70724293864769194 ) ) ;
#118276 = CARTESIAN_POINT ( 'NONE',  ( 0.05219959533909260263, 19.03943276465977164, 104.9989096053143669 ) ) ;
#118277 = CARTESIAN_POINT ( 'NONE',  ( 23.29544513554940366, -16.92513159979222337, 142.7843446568999752 ) ) ;
#118278 = CARTESIAN_POINT ( 'NONE',  ( 19.03943276465977164, -0.05219959533909143690, 93.74890960531435269 ) ) ;
#118280 = CARTESIAN_POINT ( 'NONE',  ( 14.29746914071049879, -8.314922557960816363, 93.33224293864769550 ) ) ;
#118279 = CARTESIAN_POINT ( 'NONE',  ( 0.05219959533937995610, -21.53943276465977519, 35.00109039468568284 ) ) ;
#118281 = CARTESIAN_POINT ( 'NONE',  ( -9.474510206698964154, 16.51473224551069663, 95.41557627198102409 ) ) ;
#118282 = CARTESIAN_POINT ( 'NONE',  ( -27.89898386897531068, -7.496946767028572545, 160.9847407630206817 ) ) ;
#118283 = CARTESIAN_POINT ( 'NONE',  ( -4.379528057220086978, -16.55341960407618274, 64.79275706135234714 ) ) ;
#118284 = CARTESIAN_POINT ( 'NONE',  ( -10.72451020669870658, -18.67979575497194134, 79.58442372801903275 ) ) ;
#118285 = CARTESIAN_POINT ( 'NONE',  ( 14.34966873604972726, -8.224510206698740333, 40.83442372801901854 ) ) ;
#118286 = CARTESIAN_POINT ( 'NONE',  ( -13.89961937509977652, 13.97604488694528158, 85.62390960531433848 ) ) ;
#118287 = CARTESIAN_POINT ( 'NONE',  ( 13.97604488694548053, -13.89961937509957401, 105.6260903946856757 ) ) ;
#118288 = CARTESIAN_POINT ( 'NONE',  ( 4.379528057220092307, 16.55341960407617563, 67.29275706135234714 ) ) ;
#118289 = CARTESIAN_POINT ( 'NONE',  ( -21.55341960407619339, 5.719274019375674811, 113.5427570613523756 ) ) ;
#118290 = CARTESIAN_POINT ( 'NONE',  ( -0.05219959533936034679, 19.03943276465977164, 97.50109039468567573 ) ) ;
#118291 = CARTESIAN_POINT ( 'NONE',  ( -19.02544592524342804, 5.153800228976336051, 66.04057627198103830 ) ) ;
#118292 = CARTESIAN_POINT ( 'NONE',  ( 15.72974639402199770, -15.80617190586745480, 83.12390960531436690 ) ) ;
#118294 = CARTESIAN_POINT ( 'NONE',  ( 19.02544592524334988, 5.153800228976608722, 91.45942372801900433 ) ) ;
#118293 = CARTESIAN_POINT ( 'NONE',  ( -16.55341960407611168, -4.379528057220339221, 86.45724293864770971 ) ) ;
#118295 = CARTESIAN_POINT ( 'NONE',  ( 16.52544592524335698, 4.483927247898782831, 56.45942372801902565 ) ) ;
#118296 = CARTESIAN_POINT ( 'NONE',  ( 24.27995301597489686, 6.552671593954989326, 171.1165850637242443 ) ) ;
#118297 = CARTESIAN_POINT ( 'NONE',  ( 19.03943276465977164, 0.05219959533936151252, 61.25109039468566863 ) ) ;
#118298 = CARTESIAN_POINT ( 'NONE',  ( -12.14591786802309592, -12.06949235617757132, 26.87390960531435979 ) ) ;
#118299 = CARTESIAN_POINT ( 'NONE',  ( 12.14591786802309770, 12.06949235617756955, 84.37390960531438111 ) ) ;
#118301 = CARTESIAN_POINT ( 'NONE',  ( -19.46398650005392028, 5.499999999999953815, 90.18269651486369298 ) ) ;
#118300 = CARTESIAN_POINT ( 'NONE',  ( 16.51473224551083163, -9.474510206698727899, 20.83442372801899722 ) ) ;
#118302 = CARTESIAN_POINT ( 'NONE',  ( -15.80617190586768217, 15.72974639402176855, 28.12609039468568284 ) ) ;
#118303 = CARTESIAN_POINT ( 'NONE',  ( 9.564922557960805705, 16.46253265017160317, 99.58224293864770971 ) ) ;
#118304 = CARTESIAN_POINT ( 'NONE',  ( 9.564922557960805705, 16.46253265017160317, 74.58224293864769550 ) ) ;
#118305 = CARTESIAN_POINT ( 'NONE',  ( -5.823673210054431948, 21.52544592524334988, 102.7094237280190185 ) ) ;
#118306 = CARTESIAN_POINT ( 'NONE',  ( 13.89961937509977652, -13.97604488694527269, 73.12390960531436690 ) ) ;
#118307 = CARTESIAN_POINT ( 'NONE',  ( -18.67979575497178146, -10.72451020669898902, 31.66557627198102054 ) ) ;
#118308 = CARTESIAN_POINT ( 'NONE',  ( -12.14591786802309592, -12.06949235617757132, 86.87390960531438111 ) ) ;
#118309 = CARTESIAN_POINT ( 'NONE',  ( 5.153800228976335163, 19.02544592524342804, 49.79057627198100988 ) ) ;
#118310 = CARTESIAN_POINT ( 'NONE',  ( 16.55341960407611168, 4.379528057220329451, 98.95724293864770971 ) ) ;
#118311 = CARTESIAN_POINT ( 'NONE',  ( -5.823673210054116645, -21.52544592524344225, 107.2905762719810525 ) ) ;
#118312 = CARTESIAN_POINT ( 'NONE',  ( -21.55341960407619339, 5.719274019375674811, 58.54275706135235424 ) ) ;
#118313 = CARTESIAN_POINT ( 'NONE',  ( -0.05219959533909027116, -19.03943276465977164, 32.49890960531435979 ) ) ;
#118314 = CARTESIAN_POINT ( 'NONE',  ( 0.05219959533934541429, -16.53943276465976808, 65.00109039468568994 ) ) ;
#118315 = CARTESIAN_POINT ( 'NONE',  ( -21.52544592524343514, 5.823673210054127303, 101.0405762719810383 ) ) ;
#118316 = CARTESIAN_POINT ( 'NONE',  ( -15.72974639402197994, 15.80617190586746368, 105.6239096053143669 ) ) ;
#118318 = CARTESIAN_POINT ( 'NONE',  ( 13.97604488694527802, 13.89961937509977652, 54.37390960531435979 ) ) ;
#118317 = CARTESIAN_POINT ( 'NONE',  ( 9.474510206698729675, 16.51473224551082808, 42.08442372801900433 ) ) ;
#118319 = CARTESIAN_POINT ( 'NONE',  ( 0.05219959533909260263, 19.03943276465977164, 114.9989096053143669 ) ) ;
#118320 = CARTESIAN_POINT ( 'NONE',  ( -0.05219959533937732626, 21.53943276465977519, 52.50109039468567573 ) ) ;
#118321 = CARTESIAN_POINT ( 'NONE',  ( -21.52544592524343514, 5.823673210054127303, 51.04057627198103120 ) ) ;
#118322 = CARTESIAN_POINT ( 'NONE',  ( 12.06949235617757843, -12.14591786802309237, 43.12390960531435269 ) ) ;
#118324 = CARTESIAN_POINT ( 'NONE',  ( -0.05219959533937732626, 21.53943276465977519, 107.5010903946856899 ) ) ;
#118323 = CARTESIAN_POINT ( 'NONE',  ( 21.52544592524334988, 5.823673210054432836, 81.45942372801900433 ) ) ;
#118325 = CARTESIAN_POINT ( 'NONE',  ( 12.06949235617757843, -12.14591786802309237, 53.12390960531436690 ) ) ;
#118326 = CARTESIAN_POINT ( 'NONE',  ( -16.55341960407611168, -4.379528057220339221, 111.4572429386476813 ) ) ;
#118327 = CARTESIAN_POINT ( 'NONE',  ( -13.97604488694547697, 13.89961937509957934, 43.12609039468566152 ) ) ;
#118328 = CARTESIAN_POINT ( 'NONE',  ( -0.05219959533934338120, 16.53943276465976808, 102.5010903946856899 ) ) ;
#118329 = CARTESIAN_POINT ( 'NONE',  ( -21.55341960407619339, 5.719274019375674811, 73.54275706135234714 ) ) ;
#118330 = CARTESIAN_POINT ( 'NONE',  ( -13.89961937509977652, 13.97604488694528158, 60.62390960531436690 ) ) ;
#118331 = CARTESIAN_POINT ( 'NONE',  ( -9.474510206698720793, -16.51473224551083518, 39.58442372801899722 ) ) ;
#118332 = CARTESIAN_POINT ( 'NONE',  ( -21.53943276465977519, 0.05219959533907696930, 36.24890960531435979 ) ) ;
#118333 = CARTESIAN_POINT ( 'NONE',  ( 18.62759615963255655, 10.81492255796105972, 31.66775706135234358 ) ) ;
#118334 = CARTESIAN_POINT ( 'NONE',  ( -18.67979575497178146, -10.72451020669898902, 86.66557627198102409 ) ) ;
#118335 = CARTESIAN_POINT ( 'NONE',  ( -13.97604488694547697, 13.89961937509957934, 88.12609039468563310 ) ) ;
#118336 = CARTESIAN_POINT ( 'NONE',  ( -8.314922557961024197, 14.29746914071037800, 57.91775706135234714 ) ) ;
#118338 = CARTESIAN_POINT ( 'NONE',  ( -5.719274019375978568, 21.55341960407610458, 95.20724293864769550 ) ) ;
#118337 = DIRECTION ( 'NONE',  ( 0.000000000000000000, -1.000000000000000000, 0.000000000000000000 ) ) ;
#118339 = CARTESIAN_POINT ( 'NONE',  ( 12.06949235617757843, -12.14591786802309237, 73.12390960531436690 ) ) ;
#118340 = CARTESIAN_POINT ( 'NONE',  ( 1.370007243092780325, 31.03250612061568248, -46.89016925620975229 ) ) ;
#118341 = CARTESIAN_POINT ( 'NONE',  ( -16.53943276465976808, -0.05219959533934237506, 18.75109039468568639 ) ) ;
#118342 = CARTESIAN_POINT ( 'NONE',  ( 18.67979575497178502, 10.72451020669898547, 44.16557627198103120 ) ) ;
#118343 = CARTESIAN_POINT ( 'NONE',  ( -0.05219959533934338120, 16.53943276465976808, 77.50109039468567573 ) ) ;
#118344 = CARTESIAN_POINT ( 'NONE',  ( 17.50000000000000000, -5.500000000000000888, 120.0000000000000142 ) ) ;
#118345 = CARTESIAN_POINT ( 'NONE',  ( -14.29746914071037622, -8.314922557961029526, 54.16775706135235424 ) ) ;
#118346 = CARTESIAN_POINT ( 'NONE',  ( 0.05219959533937995610, -21.53943276465977519, 25.00109039468567218 ) ) ;
#118347 = CARTESIAN_POINT ( 'NONE',  ( -15.72974639402197994, 15.80617190586746368, 45.62390960531436690 ) ) ;
#118348 = CARTESIAN_POINT ( 'NONE',  ( -14.29746914071037622, -8.314922557961029526, 74.16775706135231871 ) ) ;
#118349 = CARTESIAN_POINT ( 'NONE',  ( -19.02544592524342804, 5.153800228976336051, 96.04057627198103830 ) ) ;
#118351 = CARTESIAN_POINT ( 'NONE',  ( 19.02544592524343514, -5.153800228976328945, 33.54057627198102409 ) ) ;
#118350 = CARTESIAN_POINT ( 'NONE',  ( 21.55341960407619695, -5.719274019375665929, 56.04275706135235424 ) ) ;
#118352 = EDGE_CURVE ( 'NONE', #87358, #42462, #172614, .T. ) ;
#118353 = CARTESIAN_POINT ( 'NONE',  ( -5.823673210054116645, -21.52544592524344225, 42.29057627198103120 ) ) ;
#118354 = CARTESIAN_POINT ( 'NONE',  ( 18.62759615963271287, -10.81492255796078972, 23.33224293864769194 ) ) ;
#118355 = ORIENTED_EDGE ( 'NONE', *, *, #59958, .F. ) ;
#118356 = CARTESIAN_POINT ( 'NONE',  ( -9.564922557961040184, 16.46253265017147172, 32.91775706135233293 ) ) ;
#118357 = CARTESIAN_POINT ( 'NONE',  ( 16.52544592524335698, 4.483927247898782831, 46.45942372801901854 ) ) ;
#118358 = CARTESIAN_POINT ( 'NONE',  ( 13.97604488694527802, 13.89961937509977652, 109.3739096053143669 ) ) ;
#118359 = EDGE_LOOP ( 'NONE', ( #48758, #167613 ) ) ;
#118360 = CARTESIAN_POINT ( 'NONE',  ( 19.05341960407611168, 5.049401038298154454, 83.95724293864766707 ) ) ;
#118361 = CARTESIAN_POINT ( 'NONE',  ( -8.224510206698735004, -14.34966873604973081, 99.58442372801900433 ) ) ;
#118362 = CARTESIAN_POINT ( 'NONE',  ( 0.000000000000000000, 0.000000000000000000, -64.92279855667830191 ) ) ;
#118363 = CARTESIAN_POINT ( 'NONE',  ( 4.483927247898545687, 16.52544592524342804, 89.79057627198103830 ) ) ;
#118364 = CARTESIAN_POINT ( 'NONE',  ( 0.05219959533907565091, 21.53943276465977519, 49.99890960531437401 ) ) ;
#118365 = CARTESIAN_POINT ( 'NONE',  ( -5.153800228976328057, -19.02544592524343514, 27.29057627198103120 ) ) ;
#118366 = CARTESIAN_POINT ( 'NONE',  ( 8.314922557961029526, -14.29746914071037800, 75.41775706135233293 ) ) ;
#118367 = CARTESIAN_POINT ( 'NONE',  ( 18.67979575497194134, -10.72451020669871369, 25.83442372801901499 ) ) ;
#118368 = CARTESIAN_POINT ( 'NONE',  ( 19.02544592524334988, 5.153800228976608722, 91.45942372801900433 ) ) ;
#118369 = CARTESIAN_POINT ( 'NONE',  ( 5.153800228976335163, 19.02544592524342804, 44.79057627198103830 ) ) ;
#118370 = CARTESIAN_POINT ( 'NONE',  ( 0.05219959533909260263, 19.03943276465977164, 109.9989096053143669 ) ) ;
#118371 = CARTESIAN_POINT ( 'NONE',  ( -10.72451020669870658, -18.67979575497194134, 104.5844237280190185 ) ) ;
#118372 = CARTESIAN_POINT ( 'NONE',  ( 16.46253265017160672, -9.564922557960803928, 78.33224293864769550 ) ) ;
#118373 = CARTESIAN_POINT ( 'NONE',  ( 8.224510206698742110, 14.34966873604972548, 57.08442372801901854 ) ) ;
#118374 = CARTESIAN_POINT ( 'NONE',  ( 5.823673210054444382, -21.52544592524334988, 90.20942372801903275 ) ) ;
#118375 = CARTESIAN_POINT ( 'NONE',  ( 19.05341960407617918, -5.049401038297876454, 51.04275706135231871 ) ) ;
#118376 = CARTESIAN_POINT ( 'NONE',  ( 16.46253265017146816, 9.564922557961045513, 71.66775706135233293 ) ) ;
#118377 = ORIENTED_EDGE ( 'NONE', *, *, #106236, .F. ) ;
#118378 = CARTESIAN_POINT ( 'NONE',  ( -10.72451020669870658, -18.67979575497194134, 69.58442372801900433 ) ) ;
#118379 = CARTESIAN_POINT ( 'NONE',  ( -9.564922557960796823, -16.46253265017161027, 27.08224293864769550 ) ) ;
#118380 = CARTESIAN_POINT ( 'NONE',  ( 16.51473224551083163, -9.474510206698727899, 55.83442372801899722 ) ) ;
#118381 = CARTESIAN_POINT ( 'NONE',  ( -19.03943276465977164, 0.05219959533909376836, 101.2489096053143669 ) ) ;
#118382 = CARTESIAN_POINT ( 'NONE',  ( 13.89961937509977652, -13.97604488694527269, 88.12390960531438111 ) ) ;
#118383 = CARTESIAN_POINT ( 'NONE',  ( -4.379528057220328563, 16.55341960407611168, 40.20724293864769550 ) ) ;
#118384 = CARTESIAN_POINT ( 'NONE',  ( -15.80617190586745835, -15.72974639402198527, 31.87390960531435979 ) ) ;
#118385 = CARTESIAN_POINT ( 'NONE',  ( -36.91746825000001309, 11.99521256947798342, -1.224999997268813035 ) ) ;
#118386 = CARTESIAN_POINT ( 'NONE',  ( 20.33413869251837980, 22.45862007004985728, -51.11888769873470295 ) ) ;
#118387 = CARTESIAN_POINT ( 'NONE',  ( -15.80617190586768217, 15.72974639402176855, 113.1260903946856899 ) ) ;
#118388 = CARTESIAN_POINT ( 'NONE',  ( -27.40223502306384873, 7.751740014893099051, 163.3164180876359524 ) ) ;
#118389 = CARTESIAN_POINT ( 'NONE',  ( -9.564922557960796823, -16.46253265017161027, 42.08224293864769550 ) ) ;
#118390 = CARTESIAN_POINT ( 'NONE',  ( -13.89961937509977830, 13.97604488694528158, 85.62390960531435269 ) ) ;
#118391 = CARTESIAN_POINT ( 'NONE',  ( -17.72517630440434289, 5.499999999999979572, 80.92175719257211597 ) ) ;
#118392 = CARTESIAN_POINT ( 'NONE',  ( 21.55341960407619695, -5.719274019375665929, 71.04275706135234714 ) ) ;
#118393 = CARTESIAN_POINT ( 'NONE',  ( -33.98078611207405686, -16.46121673129812990, -8.000000000000001776 ) ) ;
#118394 = CARTESIAN_POINT ( 'NONE',  ( -12.06949235617739369, -12.14591786802326823, 64.37609039468568994 ) ) ;
#118395 = CARTESIAN_POINT ( 'NONE',  ( -21.53943276465977519, 0.05219959533907696930, 81.24890960531436690 ) ) ;
#118396 = CARTESIAN_POINT ( 'NONE',  ( 16.53943276465976808, -0.05219959533910856209, 58.74890960531436690 ) ) ;
#118398 = CARTESIAN_POINT ( 'NONE',  ( -5.153800228976328057, -19.02544592524343514, 102.2905762719810383 ) ) ;
#118397 = CARTESIAN_POINT ( 'NONE',  ( 13.89961937509977652, -13.97604488694527269, 23.12390960531436335 ) ) ;
#118399 = CARTESIAN_POINT ( 'NONE',  ( 18.67979575497194134, -10.72451020669871369, 25.83442372801901499 ) ) ;
#118400 = CARTESIAN_POINT ( 'NONE',  ( 19.03943276465977164, 0.05219959533936151252, 31.25109039468566863 ) ) ;
#118401 = CARTESIAN_POINT ( 'NONE',  ( -9.564922557960796823, -16.46253265017161027, 37.08224293864768839 ) ) ;
#118402 = CARTESIAN_POINT ( 'NONE',  ( -0.05219959533937732626, 21.53943276465977519, 82.50109039468568994 ) ) ;
#118403 = CARTESIAN_POINT ( 'NONE',  ( 31.90000000000003411, 0.000000000000000000, -49.13275782002545355 ) ) ;
#118404 = CARTESIAN_POINT ( 'NONE',  ( 14.29746914071049879, -8.314922557960816363, 23.33224293864769194 ) ) ;
#118405 = DIRECTION ( 'NONE',  ( 1.000000000000000000, 0.000000000000000000, -0.000000000000000000 ) ) ;
#118406 = CARTESIAN_POINT ( 'NONE',  ( 21.53943276465977519, -0.05219959533907433946, 38.74890960531435979 ) ) ;
#118407 = CARTESIAN_POINT ( 'NONE',  ( 16.53943276465976808, -0.05219959533910856209, 98.74890960531438111 ) ) ;
#118408 = CARTESIAN_POINT ( 'NONE',  ( 18.36170132746700645, -35.61590944478783172, -18.35554273634629752 ) ) ;
#118409 = AXIS2_PLACEMENT_3D ( 'NONE', #187072, #65678, #155705 ) ;
#118410 = CARTESIAN_POINT ( 'NONE',  ( -13.89961937509977652, 13.97604488694528158, 90.62390960531432427 ) ) ;
#118411 = CARTESIAN_POINT ( 'NONE',  ( -14.29746914071049879, 8.314922557960819915, 90.83224293864769550 ) ) ;
#118412 = CARTESIAN_POINT ( 'NONE',  ( -13.89961937509957401, -13.97604488694547875, 104.3760903946856757 ) ) ;
#118413 = CARTESIAN_POINT ( 'NONE',  ( -15.80617190586745835, -15.72974639402198527, 66.87390960531436690 ) ) ;
#118414 = ORIENTED_EDGE ( 'NONE', *, *, #48810, .F. ) ;
#118415 = CARTESIAN_POINT ( 'NONE',  ( -16.51473224551069308, -9.474510206698971260, 26.66557627198103120 ) ) ;
#118417 = CARTESIAN_POINT ( 'NONE',  ( 5.823673210054125526, 21.52544592524343514, 94.79057627198105251 ) ) ;
#118416 = CARTESIAN_POINT ( 'NONE',  ( -19.05341960407611168, -5.049401038298163336, 86.45724293864769550 ) ) ;
#118419 = CARTESIAN_POINT ( 'NONE',  ( -5.153800228976328057, -19.02544592524343514, 82.29057627198103830 ) ) ;
#118418 = CARTESIAN_POINT ( 'NONE',  ( -16.52544592524335698, -4.483927247898792601, 103.9594237280190185 ) ) ;
#118420 = CARTESIAN_POINT ( 'NONE',  ( 19.02544592524334988, 5.153800228976608722, 86.45942372801900433 ) ) ;
#118421 = CARTESIAN_POINT ( 'NONE',  ( 18.67979575497194134, -10.72451020669871369, 95.83442372801903275 ) ) ;
#118422 = CARTESIAN_POINT ( 'NONE',  ( 15.72974639402199770, -15.80617190586745480, 73.12390960531436690 ) ) ;
#118423 = CARTESIAN_POINT ( 'NONE',  ( -10.81492255796078084, -18.62759615963271287, 37.08224293864768129 ) ) ;
#118424 = CARTESIAN_POINT ( 'NONE',  ( -5.049401038298153566, 19.05341960407611168, 45.20724293864769550 ) ) ;
#118425 = CARTESIAN_POINT ( 'NONE',  ( -0.05219959533934338120, 16.53943276465976808, 107.5010903946856899 ) ) ;
#118426 = CARTESIAN_POINT ( 'NONE',  ( 9.564922557960805705, 16.46253265017160317, 64.58224293864769550 ) ) ;
#118427 = ORIENTED_EDGE ( 'NONE', *, *, #43889, .F. ) ;
#118428 = CARTESIAN_POINT ( 'NONE',  ( -31.26372923869873688, -6.750542664803635518, 98.30470173274466106 ) ) ;
#118429 = CARTESIAN_POINT ( 'NONE',  ( -13.97604488694547697, 13.89961937509957934, 23.12609039468565442 ) ) ;
#118430 = CARTESIAN_POINT ( 'NONE',  ( 8.224510206698953496, -14.34966873604960469, 67.91557627198102409 ) ) ;
#118431 = CARTESIAN_POINT ( 'NONE',  ( -5.719274019375665041, -21.55341960407619695, 29.79275706135234358 ) ) ;
#118432 = CARTESIAN_POINT ( 'NONE',  ( 27.73933785331498925, -9.013057229001033122, 142.2750000027311899 ) ) ;
#118433 = CARTESIAN_POINT ( 'NONE',  ( 21.55341960407610458, 5.719274019375980345, 53.95724293864770260 ) ) ;
#118434 = CARTESIAN_POINT ( 'NONE',  ( -4.483927247898782831, 16.52544592524335698, 92.70942372801901854 ) ) ;
#118435 = CARTESIAN_POINT ( 'NONE',  ( 0.05219959533910956823, 16.53943276465976808, 104.9989096053143669 ) ) ;
#118436 = CARTESIAN_POINT ( 'NONE',  ( 0.05219959533909260263, 19.03943276465977164, 69.99890960531435269 ) ) ;
#118437 = CARTESIAN_POINT ( 'NONE',  ( 14.29746914071049879, -8.314922557960816363, 28.33224293864769550 ) ) ;
#118438 = CARTESIAN_POINT ( 'NONE',  ( -10.81492255796105439, 18.62759615963255655, 52.91775706135235424 ) ) ;
#118439 = CARTESIAN_POINT ( 'NONE',  ( 16.46253265017160672, -9.564922557960803928, 113.3322429386476955 ) ) ;
#118440 = CARTESIAN_POINT ( 'NONE',  ( 10.72451020669871369, 18.67979575497193778, 77.08442372801901854 ) ) ;
#118441 = CARTESIAN_POINT ( 'NONE',  ( 9.564922557960805705, 16.46253265017160317, 24.58224293864769194 ) ) ;
#118442 = CARTESIAN_POINT ( 'NONE',  ( -19.03943276465977164, 0.05219959533909376836, 36.24890960531436690 ) ) ;
#118443 =( BOUNDED_CURVE ( )  B_SPLINE_CURVE ( 2, ( #85269, #146960, #128773, #71122, #193472, #190472, #38788, #147970, #21613, #51945, #84265 ),
 .UNSPECIFIED., .F., .T. ) 
 B_SPLINE_CURVE_WITH_KNOTS ( ( 3, 2, 2, 2, 2, 3 ),
 ( 0.5000000000000001110, 0.5200000000000001288, 0.5400000000000001465, 0.5600000000000001643, 0.5800000000000000711, 0.6000000000000000888 ),
 .UNSPECIFIED. ) 
 CURVE ( )  GEOMETRIC_REPRESENTATION_ITEM ( )  RATIONAL_B_SPLINE_CURVE ( ( 0.9999999999999997780, 0.9510565162951537532, 1.000000000000000000, 0.9510565162951535312, 1.000000000000000000, 0.9510565162951535312, 1.000000000000000000, 0.9510565162951535312, 1.000000000000000000, 0.9510565162951533091, 1.000000000000000222 ) ) 
 REPRESENTATION_ITEM ( '' )  );
#118444 = ORIENTED_EDGE ( 'NONE', *, *, #166889, .T. ) ;
#118445 = CARTESIAN_POINT ( 'NONE',  ( 21.52544592524334988, 5.823673210054432836, 96.45942372801901854 ) ) ;
#118446 = CARTESIAN_POINT ( 'NONE',  ( 12.14591786802327356, -12.06949235617739191, 45.62609039468567573 ) ) ;
#118447 = CARTESIAN_POINT ( 'NONE',  ( -0.05219959533937732626, 21.53943276465977519, 72.50109039468568994 ) ) ;
#118448 = CARTESIAN_POINT ( 'NONE',  ( -5.153800228976328057, -19.02544592524343514, 107.2905762719810383 ) ) ;
#118449 = ORIENTED_EDGE ( 'NONE', *, *, #89522, .T. ) ;
#118450 = CARTESIAN_POINT ( 'NONE',  ( -19.03943276465977164, -0.05219959533935918106, 83.75109039468567573 ) ) ;
#118451 = CARTESIAN_POINT ( 'NONE',  ( -10.72451020669870658, -18.67979575497194134, 49.58442372801901143 ) ) ;
#118452 = CARTESIAN_POINT ( 'NONE',  ( -0.05219959533936034679, 19.03943276465977164, 112.5010903946856757 ) ) ;
#118453 = CARTESIAN_POINT ( 'NONE',  ( 16.46253265017146816, 9.564922557961045513, 81.66775706135233293 ) ) ;
#118454 = CARTESIAN_POINT ( 'NONE',  ( -19.02544592524342804, 5.153800228976336051, 46.04057627198101699 ) ) ;
#118455 = CARTESIAN_POINT ( 'NONE',  ( -13.97604488694547697, 13.89961937509957934, 93.12609039468566152 ) ) ;
#118456 = CARTESIAN_POINT ( 'NONE',  ( -0.05219959533934338120, 16.53943276465976808, 112.5010903946857042 ) ) ;
#118457 = CARTESIAN_POINT ( 'NONE',  ( -16.51473224551082808, 9.474510206698731452, 83.33442372801899012 ) ) ;
#118458 = CARTESIAN_POINT ( 'NONE',  ( 8.314922557960818139, 14.29746914071049879, 44.58224293864769550 ) ) ;
#118459 = CARTESIAN_POINT ( 'NONE',  ( -19.05341960407617563, 5.049401038297882671, 58.54275706135234003 ) ) ;
#118460 = CARTESIAN_POINT ( 'NONE',  ( -0.05219959533934338120, 16.53943276465976808, 47.50109039468568994 ) ) ;
#118461 = CARTESIAN_POINT ( 'NONE',  ( -10.81492255796105439, 18.62759615963255655, 112.9177570613523329 ) ) ;
#118462 = CARTESIAN_POINT ( 'NONE',  ( 16.46253265017160672, -9.564922557960803928, 28.33224293864769550 ) ) ;
#118463 = CARTESIAN_POINT ( 'NONE',  ( 0.05219959533909260263, 19.03943276465977164, 39.99890960531436690 ) ) ;
#118464 = CARTESIAN_POINT ( 'NONE',  ( -14.29746914071037622, -8.314922557961029526, 49.16775706135234003 ) ) ;
#118465 = LINE ( 'NONE', #27466, #82184 ) ;
#118466 = CARTESIAN_POINT ( 'NONE',  ( 17.14385361876520264, -23.59649016807271238, 147.5750000027311444 ) ) ;
#118467 = CARTESIAN_POINT ( 'NONE',  ( 9.564922557960805705, 16.46253265017160317, 89.58224293864769550 ) ) ;
#118468 = PLANE ( 'NONE',  #16770 ) ;
#118469 = ORIENTED_EDGE ( 'NONE', *, *, #54562, .F. ) ;
#118470 = CARTESIAN_POINT ( 'NONE',  ( -9.474510206698720793, -16.51473224551083518, 94.58442372801900433 ) ) ;
#118471 = B_SPLINE_CURVE_WITH_KNOTS ( 'NONE', 3,
 ( #109553, #168250, #125721, #171234, #110543, #68020, #115538, #36676, #98336, #18553, #189395, #65038, #33709, #173226, #21522, #53864, #145855, #97340, #22528, #37686, #66028, #112530, #34702, #83183, #160035, #80201, #84175, #50872, #192381, #5342, #7337, #126694 ),
 .UNSPECIFIED., .F., .F.,
 ( 4, 2, 2, 2, 2, 2, 2, 2, 2, 2, 2, 2, 2, 2, 2, 4 ),
 ( 2.195984522899319715E-17, 0.0003712461730036815196, 0.0007424923460073411382, 0.001113738519011000594, 0.001484984692014660159, 0.002227477038021986010, 0.002598723211025666391, 0.002969969384029346772, 0.003341215557033026719, 0.003712461730036707968, 0.004083707903040387915, 0.004454954076044069164, 0.004826200249047748678, 0.005197446422051429926, 0.005568692595055110307, 0.005939938768058790688 ),
 .UNSPECIFIED. ) ;
#118472 = CARTESIAN_POINT ( 'NONE',  ( 18.67979575497178502, 10.72451020669898547, 34.16557627198102409 ) ) ;
#118474 = CARTESIAN_POINT ( 'NONE',  ( -13.89961937509957401, -13.97604488694547875, 109.3760903946856331 ) ) ;
#118473 = CARTESIAN_POINT ( 'NONE',  ( -0.05219959533936034679, 19.03943276465977164, 37.50109039468567573 ) ) ;
#118475 = CARTESIAN_POINT ( 'NONE',  ( 16.55341960407611168, 4.379528057220329451, 113.9572429386477239 ) ) ;
#118476 = CARTESIAN_POINT ( 'NONE',  ( 5.049401038298161559, -19.05341960407611168, 42.70724293864767418 ) ) ;
#118477 = CARTESIAN_POINT ( 'NONE',  ( 18.62759615963271287, -10.81492255796078972, 73.33224293864769550 ) ) ;
#118478 = ADVANCED_FACE ( 'NONE', ( #184797 ), #158263, .F. ) ;
#118479 = CARTESIAN_POINT ( 'NONE',  ( -19.02544592524342804, 5.153800228976336051, 36.04057627198100988 ) ) ;
#118480 = CARTESIAN_POINT ( 'NONE',  ( 22.44159573604009239, 16.30477369853692693, 142.5750000027311728 ) ) ;
#118481 = CARTESIAN_POINT ( 'NONE',  ( 9.564922557961047289, -16.46253265017146816, 65.41775706135233293 ) ) ;
#118482 = CARTESIAN_POINT ( 'NONE',  ( 4.483927247898545687, 16.52544592524342804, 59.79057627198103120 ) ) ;
#118483 = CARTESIAN_POINT ( 'NONE',  ( 15.72974639402199770, -15.80617190586745480, 33.12390960531435979 ) ) ;
#118484 = CARTESIAN_POINT ( 'NONE',  ( 21.53943276465977519, 0.05219959533937863772, 91.25109039468568994 ) ) ;
#118485 = CARTESIAN_POINT ( 'NONE',  ( 18.62759615963271287, -10.81492255796078972, 78.33224293864770971 ) ) ;
#118486 = CARTESIAN_POINT ( 'NONE',  ( -0.05219959533937732626, 21.53943276465977519, 72.50109039468568994 ) ) ;
#118487 = CARTESIAN_POINT ( 'NONE',  ( -18.62759615963255300, -10.81492255796106328, 59.16775706135234714 ) ) ;
#118488 = CARTESIAN_POINT ( 'NONE',  ( -13.89961937509977652, 13.97604488694528158, 95.62390960531436690 ) ) ;
#118490 = CARTESIAN_POINT ( 'NONE',  ( -18.67979575497193778, 10.72451020669871902, 63.33442372801900433 ) ) ;
#118489 = CARTESIAN_POINT ( 'NONE',  ( 4.483927247898790824, -16.52544592524335698, 110.2094237280190185 ) ) ;
#118491 = CARTESIAN_POINT ( 'NONE',  ( -0.05219959533909027116, -19.03943276465977164, 52.49890960531436690 ) ) ;
#118492 = CARTESIAN_POINT ( 'NONE',  ( -5.823673210054431948, 21.52544592524334988, 27.70942372801901854 ) ) ;
#118493 = CARTESIAN_POINT ( 'NONE',  ( 9.474510206698971260, -16.51473224551069308, 62.91557627198102409 ) ) ;
#118494 = CARTESIAN_POINT ( 'NONE',  ( -12.14591786802309592, -12.06949235617757132, 76.87390960531439532 ) ) ;
#118495 = CARTESIAN_POINT ( 'NONE',  ( 0.05219959533910956823, 16.53943276465976808, 44.99890960531435979 ) ) ;
#118496 = CARTESIAN_POINT ( 'NONE',  ( -15.72974639402197994, 15.80617190586746368, 55.62390960531436690 ) ) ;
#118497 = CARTESIAN_POINT ( 'NONE',  ( 9.474510206698971260, -16.51473224551069308, 42.91557627198103120 ) ) ;
#118498 = CARTESIAN_POINT ( 'NONE',  ( 18.62759615963271287, -10.81492255796078972, 53.33224293864769550 ) ) ;
#118499 = CARTESIAN_POINT ( 'NONE',  ( 16.51473224551083163, -9.474510206698727899, 50.83442372801899722 ) ) ;
#118502 = CARTESIAN_POINT ( 'NONE',  ( -16.52544592524342804, 4.483927247898546575, 61.04057627198103120 ) ) ;
#118501 = CARTESIAN_POINT ( 'NONE',  ( -4.273745901508164025, -6.674792076160507293, 5.990689250852175185 ) ) ;
#118500 = CIRCLE ( 'NONE', #12003, 27.29906736325805028 ) ;
#118503 = CARTESIAN_POINT ( 'NONE',  ( -18.67979575497178146, -10.72451020669898902, 41.66557627198103120 ) ) ;
#118504 = ORIENTED_EDGE ( 'NONE', *, *, #37374, .T. ) ;
#118505 = DIRECTION ( 'NONE',  ( 1.000000000000000000, 0.000000000000000000, 0.000000000000000000 ) ) ;
#118507 = CARTESIAN_POINT ( 'NONE',  ( 17.14385361876520264, -23.59649016807270883, 140.0750000027311728 ) ) ;
#118506 = CARTESIAN_POINT ( 'NONE',  ( 12.06949235617739724, 12.14591786802326823, 91.87609039468568994 ) ) ;
#118508 = CARTESIAN_POINT ( 'NONE',  ( 9.564922557961047289, -16.46253265017146816, 85.41775706135233293 ) ) ;
#118509 = CARTESIAN_POINT ( 'NONE',  ( -4.379528057220328563, 16.55341960407611168, 60.20724293864768839 ) ) ;
#118510 = DIRECTION ( 'NONE',  ( -0.000000000000000000, -0.000000000000000000, 1.000000000000000000 ) ) ;
#118511 = CARTESIAN_POINT ( 'NONE',  ( 5.153800228976335163, 19.02544592524342804, 49.79057627198100988 ) ) ;
#118512 = CARTESIAN_POINT ( 'NONE',  ( 8.224510206698953496, -14.34966873604960469, 37.91557627198102409 ) ) ;
#118513 = CARTESIAN_POINT ( 'NONE',  ( 5.153800228976335163, 19.02544592524342804, 89.79057627198102409 ) ) ;
#118514 = CARTESIAN_POINT ( 'NONE',  ( 13.97604488694527802, 13.89961937509977652, 59.37390960531434558 ) ) ;
#118515 = CARTESIAN_POINT ( 'NONE',  ( 10.81492255796106328, -18.62759615963255655, 55.41775706135234714 ) ) ;
#118516 = CARTESIAN_POINT ( 'NONE',  ( 16.51473224551069308, 9.474510206698969483, 69.16557627198102409 ) ) ;
#118517 = CARTESIAN_POINT ( 'NONE',  ( -19.03943276465977164, 0.05219959533909376836, 31.24890960531435979 ) ) ;
#118518 = CIRCLE ( 'NONE', #99139, 0.2000000000000000944 ) ;
#118519 = CARTESIAN_POINT ( 'NONE',  ( -0.05219959533909027116, -19.03943276465977164, 62.49890960531435979 ) ) ;
#118520 = CARTESIAN_POINT ( 'NONE',  ( -5.719274019375978568, 21.55341960407610458, 50.20724293864769550 ) ) ;
#118521 = CARTESIAN_POINT ( 'NONE',  ( 9.564922557960805705, 16.46253265017160317, 29.58224293864769550 ) ) ;
#118522 = CARTESIAN_POINT ( 'NONE',  ( 10.72451020669898902, -18.67979575497178502, 42.91557627198103120 ) ) ;
#118523 = CARTESIAN_POINT ( 'NONE',  ( -4.483927247898782831, 16.52544592524335698, 107.7094237280190328 ) ) ;
#118524 = CARTESIAN_POINT ( 'NONE',  ( -13.97604488694547697, 13.89961937509957934, 28.12609039468565797 ) ) ;
#118526 = CARTESIAN_POINT ( 'NONE',  ( 16.52544592524335698, 4.483927247898782831, 76.45942372801901854 ) ) ;
#118525 = CARTESIAN_POINT ( 'NONE',  ( -12.06949235617739369, -12.14591786802326823, 49.37609039468569705 ) ) ;
#118527 = LINE ( 'NONE', #41686, #163021 ) ;
#118528 = CARTESIAN_POINT ( 'NONE',  ( -8.224510206698735004, -14.34966873604973081, 69.58442372801900433 ) ) ;
#118529 = CARTESIAN_POINT ( 'NONE',  ( 16.55341960407618274, -4.379528057220086978, 51.04275706135234714 ) ) ;
#118530 = CARTESIAN_POINT ( 'NONE',  ( -19.05341960407611168, -5.049401038298163336, 106.4572429386476955 ) ) ;
#118531 = CARTESIAN_POINT ( 'NONE',  ( 0.05219959533909260263, 19.03943276465977164, 29.99890960531435979 ) ) ;
#118532 = CARTESIAN_POINT ( 'NONE',  ( 12.14591786802327356, -12.06949235617739191, 40.62609039468567573 ) ) ;
#118533 = CARTESIAN_POINT ( 'NONE',  ( 19.02544592524343514, -5.153800228976328945, 53.54057627198102409 ) ) ;
#118534 = CARTESIAN_POINT ( 'NONE',  ( -15.80617190586768217, 15.72974639402176855, 23.12609039468567573 ) ) ;
#118535 = CARTESIAN_POINT ( 'NONE',  ( -8.224510206698735004, -14.34966873604973081, 39.58442372801901143 ) ) ;
#118536 = CARTESIAN_POINT ( 'NONE',  ( -8.224510206698735004, -14.34966873604973081, 104.5844237280190185 ) ) ;
#118537 = CARTESIAN_POINT ( 'NONE',  ( -11.30153831258470731, -188.0000000000000000, 0.000000000000000000 ) ) ;
#118538 = CARTESIAN_POINT ( 'NONE',  ( 15.72974639402176855, 15.80617190586768217, 101.8760903946857042 ) ) ;
#118539 = CARTESIAN_POINT ( 'NONE',  ( -16.51473224551082808, 9.474510206698731452, 103.3344237280190043 ) ) ;
#118540 = CARTESIAN_POINT ( 'NONE',  ( -16.52544592524342804, 4.483927247898546575, 56.04057627198102409 ) ) ;
#118541 = CARTESIAN_POINT ( 'NONE',  ( 5.153800228976335163, 19.02544592524342804, 29.79057627198102409 ) ) ;
#118543 = CARTESIAN_POINT ( 'NONE',  ( 16.62475595723611121, -7.163666690055877417, 58.02713351810401576 ) ) ;
#118542 = CARTESIAN_POINT ( 'NONE',  ( 13.97604488694548053, -13.89961937509957401, 65.62609039468567573 ) ) ;
#118544 = CARTESIAN_POINT ( 'NONE',  ( 10.81492255796106328, -18.62759615963255655, 70.41775706135236135 ) ) ;
#118545 = CARTESIAN_POINT ( 'NONE',  ( 4.379528057220092307, 16.55341960407617563, 27.29275706135234358 ) ) ;
#118546 = CARTESIAN_POINT ( 'NONE',  ( -17.72696623605163424, 5.499999999999875655, 63.59811031808420978 ) ) ;
#118547 = CARTESIAN_POINT ( 'NONE',  ( 0.05219959533909260263, 19.03943276465977164, 114.9989096053143669 ) ) ;
#118548 = CARTESIAN_POINT ( 'NONE',  ( 9.474510206698729675, 16.51473224551082808, 112.0844237280190043 ) ) ;
#118549 = CARTESIAN_POINT ( 'NONE',  ( -19.03943276465977164, 0.05219959533909376836, 116.2489096053143669 ) ) ;
#118550 = CARTESIAN_POINT ( 'NONE',  ( 13.89961937509977652, -13.97604488694527269, 23.12390960531436335 ) ) ;
#118551 = CARTESIAN_POINT ( 'NONE',  ( 5.719274019375673035, 21.55341960407619339, 102.2927570613523613 ) ) ;
#118552 = CARTESIAN_POINT ( 'NONE',  ( 19.02544592524343514, -5.153800228976328945, 38.54057627198103120 ) ) ;
#118554 = CARTESIAN_POINT ( 'NONE',  ( 18.67979575497194134, -10.72451020669871369, 70.83442372801901854 ) ) ;
#118553 = AXIS2_PLACEMENT_3D ( 'NONE', #114188, #100026, #177897 ) ;
#118555 = CARTESIAN_POINT ( 'NONE',  ( 0.05219959533937995610, -21.53943276465977519, 105.0010903946856757 ) ) ;
#118556 = CARTESIAN_POINT ( 'NONE',  ( 4.483927247898790824, -16.52544592524335698, 100.2094237280190043 ) ) ;
#118557 = CARTESIAN_POINT ( 'NONE',  ( 16.46253265017160672, -9.564922557960803928, 83.33224293864768129 ) ) ;
#118558 = CARTESIAN_POINT ( 'NONE',  ( 5.719274019375673035, 21.55341960407619339, 62.29275706135236845 ) ) ;
#118559 = CARTESIAN_POINT ( 'NONE',  ( 5.719274019375673035, 21.55341960407619339, 57.29275706135234714 ) ) ;
#118561 = CARTESIAN_POINT ( 'NONE',  ( -13.89961937509977652, 13.97604488694528158, 95.62390960531436690 ) ) ;
#118560 = CARTESIAN_POINT ( 'NONE',  ( -16.46253265017146816, -9.564922557961047289, 74.16775706135234714 ) ) ;
#118562 = CARTESIAN_POINT ( 'NONE',  ( 13.97604488694527802, 13.89961937509977652, 24.37390960531435624 ) ) ;
#118563 = CARTESIAN_POINT ( 'NONE',  ( 5.719274019375991003, -21.55341960407610458, 97.70724293864772392 ) ) ;
#118564 = CARTESIAN_POINT ( 'NONE',  ( -0.05219959533937732626, 21.53943276465977519, 112.5010903946857042 ) ) ;
#118565 = CARTESIAN_POINT ( 'NONE',  ( 12.06949235617757843, -12.14591786802309237, 103.1239096053143811 ) ) ;
#118566 = CARTESIAN_POINT ( 'NONE',  ( 19.05341960407611168, 5.049401038298154454, 53.95724293864770260 ) ) ;
#118567 = CARTESIAN_POINT ( 'NONE',  ( -19.03943276465977164, -0.05219959533935918106, 78.75109039468567573 ) ) ;
#118568 = CARTESIAN_POINT ( 'NONE',  ( -4.483927247898539470, -16.52544592524342804, 57.29057627198103120 ) ) ;
#118569 = CARTESIAN_POINT ( 'NONE',  ( 18.67979575497194134, -10.72451020669871369, 110.8344237280190043 ) ) ;
#118570 = CARTESIAN_POINT ( 'NONE',  ( 0.05219959533909260263, 19.03943276465977164, 104.9989096053143669 ) ) ;
#118571 = CARTESIAN_POINT ( 'NONE',  ( 19.02544592524334988, 5.153800228976608722, 76.45942372801897591 ) ) ;
#118572 = CARTESIAN_POINT ( 'NONE',  ( 10.81492255796078972, 18.62759615963270932, 84.58224293864769550 ) ) ;
#118573 = CARTESIAN_POINT ( 'NONE',  ( 21.55341960407619695, -5.719274019375665929, 26.04275706135235779 ) ) ;
#118574 = CARTESIAN_POINT ( 'NONE',  ( -14.34966873604972548, 8.224510206698743886, 23.33442372801901499 ) ) ;
#118575 = CARTESIAN_POINT ( 'NONE',  ( 14.34966873604972726, -8.224510206698740333, 95.83442372801903275 ) ) ;
#118577 = CARTESIAN_POINT ( 'NONE',  ( -10.81492255796105439, 18.62759615963255655, 32.91775706135234714 ) ) ;
#118576 = CARTESIAN_POINT ( 'NONE',  ( -16.55341960407617563, 4.379528057220093196, 43.54275706135235424 ) ) ;
#118578 = CARTESIAN_POINT ( 'NONE',  ( 10.81492255796078972, 18.62759615963270932, 39.58224293864769550 ) ) ;
#118579 = CARTESIAN_POINT ( 'NONE',  ( 16.51473224551069308, 9.474510206698969483, 34.16557627198102409 ) ) ;
#118580 = CARTESIAN_POINT ( 'NONE',  ( 36.91746824999999177, 2.880721459617395097E-14, -2.124999997268813168 ) ) ;
#118581 = CARTESIAN_POINT ( 'NONE',  ( 14.29746914071037800, 8.314922557961029526, 56.66775706135235424 ) ) ;
#118582 = CARTESIAN_POINT ( 'NONE',  ( -16.52544592524342804, 4.483927247898546575, 91.04057627198103830 ) ) ;
#118583 = CARTESIAN_POINT ( 'NONE',  ( 21.53943276465977519, -0.05219959533907433946, 88.74890960531436690 ) ) ;
#118584 = CARTESIAN_POINT ( 'NONE',  ( -16.55341960407611168, -4.379528057220339221, 26.45724293864768839 ) ) ;
#118585 = CARTESIAN_POINT ( 'NONE',  ( -8.314922557961024197, 14.29746914071037800, 42.91775706135235424 ) ) ;
#118586 = CARTESIAN_POINT ( 'NONE',  ( 19.02544592524343514, -5.153800228976328945, 53.54057627198102409 ) ) ;
#118587 = CARTESIAN_POINT ( 'NONE',  ( -12.14591786802326823, 12.06949235617739902, 88.12609039468570415 ) ) ;
#118588 = CARTESIAN_POINT ( 'NONE',  ( 0.05219959533936267826, -19.03943276465977164, 90.00109039468567573 ) ) ;
#118589 = CARTESIAN_POINT ( 'NONE',  ( -21.53943276465977519, 0.05219959533907696930, 86.24890960531436690 ) ) ;
#118590 = CARTESIAN_POINT ( 'NONE',  ( 12.06949235617739724, 12.14591786802326823, 106.8760903946856899 ) ) ;
#118591 = ORIENTED_EDGE ( 'NONE', *, *, #131511, .T. ) ;
#118592 = FACE_OUTER_BOUND ( 'NONE', #189074, .T. ) ;
#118593 = EDGE_CURVE ( 'NONE', #91492, #147765, #165309, .T. ) ;
#118594 = CARTESIAN_POINT ( 'NONE',  ( -10.81492255796078084, -18.62759615963271287, 67.08224293864770971 ) ) ;
#118595 = CARTESIAN_POINT ( 'NONE',  ( -0.05219959533934338120, 16.53943276465976808, 97.50109039468567573 ) ) ;
#118596 = ORIENTED_EDGE ( 'NONE', *, *, #37272, .T. ) ;
#118597 = CARTESIAN_POINT ( 'NONE',  ( -15.72974639402197994, 15.80617190586746368, 25.62390960531435624 ) ) ;
#118598 = CARTESIAN_POINT ( 'NONE',  ( 0.000000000000000000, 0.000000000000000000, -18.00000000000000000 ) ) ;
#118599 = CARTESIAN_POINT ( 'NONE',  ( -15.80617190586745835, -15.72974639402198527, 81.87390960531435269 ) ) ;
#118600 = CARTESIAN_POINT ( 'NONE',  ( 12.14591786802309770, 12.06949235617756955, 29.37390960531435269 ) ) ;
#118601 = CARTESIAN_POINT ( 'NONE',  ( 8.224510206698742110, 14.34966873604972548, 32.08442372801901854 ) ) ;
#118602 = CARTESIAN_POINT ( 'NONE',  ( -9.564922557960796823, -16.46253265017161027, 37.08224293864768839 ) ) ;
#118603 = CARTESIAN_POINT ( 'NONE',  ( 14.34966873604972726, -8.224510206698740333, 25.83442372801901499 ) ) ;
#118604 = CARTESIAN_POINT ( 'NONE',  ( -19.02544592524342804, 5.153800228976336051, 51.04057627198103120 ) ) ;
#118605 = CARTESIAN_POINT ( 'NONE',  ( -8.906447517083060816, 27.41122689804195645, 149.5999999999999943 ) ) ;
#118606 = CARTESIAN_POINT ( 'NONE',  ( 5.049401038298161559, -19.05341960407611168, 107.7072429386476955 ) ) ;
#118607 = CARTESIAN_POINT ( 'NONE',  ( 18.22780087662121673, 5.500000000000056843, 78.98459894673892734 ) ) ;
#118608 = CARTESIAN_POINT ( 'NONE',  ( -14.29746914071037622, -8.314922557961029526, 104.1677570613523471 ) ) ;
#118609 = CARTESIAN_POINT ( 'NONE',  ( -5.049401038297874678, -19.05341960407617918, 89.79275706135230450 ) ) ;
#118610 = CARTESIAN_POINT ( 'NONE',  ( 9.564922557961047289, -16.46253265017146816, 35.41775706135233293 ) ) ;
#118611 = CARTESIAN_POINT ( 'NONE',  ( -18.62759615963270932, 10.81492255796079327, 75.83224293864769550 ) ) ;
#118612 = CARTESIAN_POINT ( 'NONE',  ( 16.55341960407618274, -4.379528057220086978, 106.0427570613523471 ) ) ;
#118613 = CARTESIAN_POINT ( 'NONE',  ( 21.52544592524344225, -5.823673210054117533, 38.54057627198103120 ) ) ;
#118614 = CARTESIAN_POINT ( 'NONE',  ( 9.474510206698729675, 16.51473224551082808, 102.0844237280190043 ) ) ;
#118615 = CARTESIAN_POINT ( 'NONE',  ( 0.05219959533909260263, 19.03943276465977164, 104.9989096053143669 ) ) ;
#118616 = CARTESIAN_POINT ( 'NONE',  ( 21.55341960407619695, -5.719274019375665929, 61.04275706135234714 ) ) ;
#118617 = CARTESIAN_POINT ( 'NONE',  ( 5.049401038298161559, -19.05341960407611168, 62.70724293864769550 ) ) ;
#118618 = CARTESIAN_POINT ( 'NONE',  ( 4.379528057220339221, -16.55341960407611168, 102.7072429386476955 ) ) ;
#118619 = CARTESIAN_POINT ( 'NONE',  ( -69.65682714487590488, -71.74905178543390605, -15.00000000000000178 ) ) ;
#118620 = CARTESIAN_POINT ( 'NONE',  ( -12.14591786802309592, -12.06949235617757132, 71.87390960531438111 ) ) ;
#118621 = ORIENTED_EDGE ( 'NONE', *, *, #58626, .F. ) ;
#118622 = CARTESIAN_POINT ( 'NONE',  ( 19.02544592524334988, 5.153800228976608722, 86.45942372801900433 ) ) ;
#118623 = CARTESIAN_POINT ( 'NONE',  ( 19.19724070472096855, 5.500000000000033751, 93.56193348274381094 ) ) ;
#118624 = CARTESIAN_POINT ( 'NONE',  ( -19.05341960407611168, -5.049401038298163336, 61.45724293864769550 ) ) ;
#118625 = CARTESIAN_POINT ( 'NONE',  ( 16.18388926212248435, -7.379444403734418678, 72.06046848633769741 ) ) ;
#118627 = CARTESIAN_POINT ( 'NONE',  ( -16.51473224551069308, -9.474510206698971260, 91.66557627198103830 ) ) ;
#118626 = CARTESIAN_POINT ( 'NONE',  ( 13.89961937509977652, -13.97604488694527269, 73.12390960531436690 ) ) ;
#118628 = CARTESIAN_POINT ( 'NONE',  ( 4.483927247898790824, -16.52544592524335698, 70.20942372801904696 ) ) ;
#118629 = CARTESIAN_POINT ( 'NONE',  ( -17.44279575226822132, -5.990770900252485376, 49.16442432485681024 ) ) ;
#118630 = CARTESIAN_POINT ( 'NONE',  ( 16.51473224551083163, -9.474510206698727899, 40.83442372801900433 ) ) ;
#118631 = CARTESIAN_POINT ( 'NONE',  ( 36.76795047837062924, 4.947931209100013383, 47.42876213711300437 ) ) ;
#118632 = CARTESIAN_POINT ( 'NONE',  ( 19.05341960407611168, 5.049401038298154454, 108.9572429386477097 ) ) ;
#118633 = CARTESIAN_POINT ( 'NONE',  ( 12.14591786802327356, -12.06949235617739191, 105.6260903946856899 ) ) ;
#118634 = CARTESIAN_POINT ( 'NONE',  ( 12.14591786802327356, -12.06949235617739191, 95.62609039468568994 ) ) ;
#118635 = CARTESIAN_POINT ( 'NONE',  ( -17.26058549869089020, 6.457015423128606102, 28.62254162523932521 ) ) ;
#118636 = CARTESIAN_POINT ( 'NONE',  ( 16.55341960407618274, -4.379528057220086978, 66.04275706135236135 ) ) ;
#118637 = CARTESIAN_POINT ( 'NONE',  ( -3.573655867282028392E-15, 2.428612866367529932E-14, 0.000000000000000000 ) ) ;
#118638 = CARTESIAN_POINT ( 'NONE',  ( -18.67979575497193778, 10.72451020669871902, 68.33442372801900433 ) ) ;
#118639 = CARTESIAN_POINT ( 'NONE',  ( 13.97604488694548053, -13.89961937509957401, 85.62609039468568994 ) ) ;
#118640 = CARTESIAN_POINT ( 'NONE',  ( 9.474510206698729675, 16.51473224551082808, 32.08442372801900433 ) ) ;
#118641 = CARTESIAN_POINT ( 'NONE',  ( -9.474510206698964154, 16.51473224551069663, 60.41557627198102409 ) ) ;
#118642 = CARTESIAN_POINT ( 'NONE',  ( -0.05219959533909027116, -19.03943276465977164, 42.49890960531435269 ) ) ;
#118643 = CARTESIAN_POINT ( 'NONE',  ( 16.51128444969438291, 7.226502650581850595, 22.09735981835456542 ) ) ;
#118644 = CARTESIAN_POINT ( 'NONE',  ( -0.05219959533907301413, -21.53943276465977519, 87.49890960531436690 ) ) ;
#118645 = AXIS2_PLACEMENT_3D ( 'NONE', #151929, #45740, #107392 ) ;
#118646 = CARTESIAN_POINT ( 'NONE',  ( -10.81492255796078084, -18.62759615963271287, 32.08224293864769550 ) ) ;
#118647 = CARTESIAN_POINT ( 'NONE',  ( -16.46253265017160317, 9.564922557960807481, 30.83224293864769550 ) ) ;
#118648 = CARTESIAN_POINT ( 'NONE',  ( 4.483927247898790824, -16.52544592524335698, 55.20942372801902565 ) ) ;
#118649 = ORIENTED_EDGE ( 'NONE', *, *, #140094, .F. ) ;
#118650 = CARTESIAN_POINT ( 'NONE',  ( 15.80617190586769283, -15.72974639402175789, 25.62609039468567929 ) ) ;
#118652 = CARTESIAN_POINT ( 'NONE',  ( 29.86685920354754842, -21.69954338932559068, -9.824999997268813345 ) ) ;
#118651 = CARTESIAN_POINT ( 'NONE',  ( 16.52544592524342804, -4.483927247898539470, 53.54057627198103120 ) ) ;
#118653 = CARTESIAN_POINT ( 'NONE',  ( -16.55341960407617563, 4.379528057220093196, 23.54275706135235424 ) ) ;
#118654 = CARTESIAN_POINT ( 'NONE',  ( 9.564922557961047289, -16.46253265017146816, 40.41775706135234003 ) ) ;
#118655 = CARTESIAN_POINT ( 'NONE',  ( 16.52544592524342804, -4.483927247898539470, 53.54057627198103120 ) ) ;
#118656 = CARTESIAN_POINT ( 'NONE',  ( 18.62759615963271287, -10.81492255796078972, 113.3322429386476955 ) ) ;
#118658 = CARTESIAN_POINT ( 'NONE',  ( 18.67979575497178502, 10.72451020669898547, 74.16557627198102409 ) ) ;
#118657 = FACE_OUTER_BOUND ( 'NONE', #4933, .T. ) ;
#118659 = CARTESIAN_POINT ( 'NONE',  ( -9.564922557960796823, -16.46253265017161027, 92.08224293864769550 ) ) ;
#118660 = CARTESIAN_POINT ( 'NONE',  ( -4.483927247898539470, -16.52544592524342804, 62.29057627198102409 ) ) ;
#118661 = CARTESIAN_POINT ( 'NONE',  ( 5.049401038298161559, -19.05341960407611168, 102.7072429386476955 ) ) ;
#118662 = DIRECTION ( 'NONE',  ( 0.7071067811865467956, 0.000000000000000000, 0.7071067811865483499 ) ) ;
#118663 = CARTESIAN_POINT ( 'NONE',  ( 9.474510206698729675, 16.51473224551082808, 67.08442372801900433 ) ) ;
#118664 = CARTESIAN_POINT ( 'NONE',  ( -10.72451020669898014, 18.67979575497178502, 110.4155762719810383 ) ) ;
#118665 = CARTESIAN_POINT ( 'NONE',  ( -0.05219959533909027116, -19.03943276465977164, 62.49890960531435979 ) ) ;
#118666 = CARTESIAN_POINT ( 'NONE',  ( -5.153800228976607833, 19.02544592524334988, 47.70942372801900433 ) ) ;
#118667 = CARTESIAN_POINT ( 'NONE',  ( 14.29746914071049879, -8.314922557960816363, 108.3322429386477097 ) ) ;
#118668 = CARTESIAN_POINT ( 'NONE',  ( 21.55341960407619695, -5.719274019375665929, 61.04275706135234714 ) ) ;
#118669 = CIRCLE ( 'NONE', #183174, 0.5000000000000012212 ) ;
#118670 = CARTESIAN_POINT ( 'NONE',  ( -16.29526858892877073, -7.335722546920126597, 70.79670597800213727 ) ) ;
#118671 = CARTESIAN_POINT ( 'NONE',  ( -8.224510206698948167, 14.34966873604960824, 45.41557627198103830 ) ) ;
#118672 = CARTESIAN_POINT ( 'NONE',  ( 16.46253265017160672, -9.564922557960803928, 53.33224293864768839 ) ) ;
#118673 = CARTESIAN_POINT ( 'NONE',  ( -0.05219959533907301413, -21.53943276465977519, 77.49890960531433848 ) ) ;
#118674 = CARTESIAN_POINT ( 'NONE',  ( -27.73933785331498925, 2.428612866367529932E-14, 142.8750000027311842 ) ) ;
#118675 = CARTESIAN_POINT ( 'NONE',  ( 9.474510206698971260, -16.51473224551069308, 47.91557627198102409 ) ) ;
#118676 = CARTESIAN_POINT ( 'NONE',  ( -10.72451020669898014, 18.67979575497178502, 70.41557627198102409 ) ) ;
#118677 = CARTESIAN_POINT ( 'NONE',  ( -5.719274019375665041, -21.55341960407619695, 104.7927570613523898 ) ) ;
#118680 = CARTESIAN_POINT ( 'NONE',  ( 8.314922557960818139, 14.29746914071049879, 89.58224293864768129 ) ) ;
#118679 = CARTESIAN_POINT ( 'NONE',  ( -12.06949235617739369, -12.14591786802326823, 94.37609039468568994 ) ) ;
#118678 = CARTESIAN_POINT ( 'NONE',  ( 18.09918380851993192, 5.500000000000036415, 53.98618307335611632 ) ) ;
#118681 = CARTESIAN_POINT ( 'NONE',  ( 19.05341960407611168, 5.049401038298154454, 73.95724293864768129 ) ) ;
#118682 = ORIENTED_EDGE ( 'NONE', *, *, #177665, .T. ) ;
#118683 = CARTESIAN_POINT ( 'NONE',  ( -16.51473224551082808, 9.474510206698731452, 33.33442372801899722 ) ) ;
#118684 = CARTESIAN_POINT ( 'NONE',  ( 4.379528057220092307, 16.55341960407617563, 87.29275706135236135 ) ) ;
#118685 = CARTESIAN_POINT ( 'NONE',  ( 13.89961937509957401, 13.97604488694547697, 26.87609039468566507 ) ) ;
#118686 = CARTESIAN_POINT ( 'NONE',  ( 13.97604488694527802, 13.89961937509977652, 89.37390960531436690 ) ) ;
#118687 = CARTESIAN_POINT ( 'NONE',  ( -10.81492255796078084, -18.62759615963271287, 52.08224293864768839 ) ) ;
#118688 = FACE_OUTER_BOUND ( 'NONE', #181883, .T. ) ;
#118689 = CARTESIAN_POINT ( 'NONE',  ( -13.89961937509977652, 13.97604488694528158, 25.62390960531434558 ) ) ;
#118690 = CARTESIAN_POINT ( 'NONE',  ( -15.72974639402176322, -15.80617190586768395, 89.37609039468568994 ) ) ;
#118691 = CARTESIAN_POINT ( 'NONE',  ( 8.314922557961029526, -14.29746914071037800, 60.41775706135235424 ) ) ;
#118692 = CARTESIAN_POINT ( 'NONE',  ( 18.62759615963255655, 10.81492255796105972, 21.66775706135235069 ) ) ;
#118693 = CARTESIAN_POINT ( 'NONE',  ( 16.55341960407618274, -4.379528057220086978, 31.04275706135234714 ) ) ;
#118694 = CARTESIAN_POINT ( 'NONE',  ( 16.51473224551069308, 9.474510206698969483, 94.16557627198103830 ) ) ;
#118695 = CARTESIAN_POINT ( 'NONE',  ( 5.153800228976335163, 19.02544592524342804, 39.79057627198100988 ) ) ;
#118696 = CARTESIAN_POINT ( 'NONE',  ( 19.05341960407611168, 5.049401038298154454, 58.95724293864768129 ) ) ;
#118697 = CIRCLE ( 'NONE', #121843, 5.500000000000032863 ) ;
#118698 = CARTESIAN_POINT ( 'NONE',  ( 16.55341960407618274, -4.379528057220086978, 31.04275706135234714 ) ) ;
#118699 = CARTESIAN_POINT ( 'NONE',  ( 12.06949235617757843, -12.14591786802309237, 98.12390960531436690 ) ) ;
#118700 = CARTESIAN_POINT ( 'NONE',  ( -0.05219959533934338120, 16.53943276465976808, 97.50109039468567573 ) ) ;
#118703 = CARTESIAN_POINT ( 'NONE',  ( -0.05219959533909027116, -19.03943276465977164, 52.49890960531436690 ) ) ;
#118702 = CARTESIAN_POINT ( 'NONE',  ( 16.51473224551069308, 9.474510206698969483, 69.16557627198102409 ) ) ;
#118701 = CARTESIAN_POINT ( 'NONE',  ( -21.53943276465977519, -0.05219959533937600094, 43.75109039468568284 ) ) ;
#118704 = CARTESIAN_POINT ( 'NONE',  ( -19.02544592524342804, 5.153800228976336051, 81.04057627198103830 ) ) ;
#118705 = CARTESIAN_POINT ( 'NONE',  ( 14.29746914071049879, -8.314922557960816363, 38.33224293864768839 ) ) ;
#118706 = CARTESIAN_POINT ( 'NONE',  ( -14.34966873604972548, 8.224510206698743886, 103.3344237280190043 ) ) ;
#118707 = ORIENTED_EDGE ( 'NONE', *, *, #195934, .T. ) ;
#118708 = CARTESIAN_POINT ( 'NONE',  ( 9.474510206698729675, 16.51473224551082808, 47.08442372801900433 ) ) ;
#118709 = CARTESIAN_POINT ( 'NONE',  ( -16.46253265017160317, 9.564922557960807481, 110.8322429386476955 ) ) ;
#118710 = CARTESIAN_POINT ( 'NONE',  ( 16.46253265017160672, -9.564922557960803928, 43.33224293864769550 ) ) ;
#118711 = CARTESIAN_POINT ( 'NONE',  ( 9.474510206698729675, 16.51473224551082808, 32.08442372801900433 ) ) ;
#118712 = CARTESIAN_POINT ( 'NONE',  ( 22.81625015709509441, 31.40387420917330275, -9.324999997268813345 ) ) ;
#118713 = CARTESIAN_POINT ( 'NONE',  ( 8.314922557961029526, -14.29746914071037800, 45.41775706135234003 ) ) ;
#118714 = B_SPLINE_CURVE_WITH_KNOTS ( 'NONE', 3,
 ( #85017, #116370, #102207, #101186, #21366, #146698, #70875, #69870 ),
 .UNSPECIFIED., .F., .F.,
 ( 4, 2, 2, 4 ),
 ( 0.03534151991400969611, 0.03926041079282524549, 0.04121985623223305140, 0.04317930167164086425 ),
 .UNSPECIFIED. ) ;
#118716 = CARTESIAN_POINT ( 'NONE',  ( 12.06949235617739724, 12.14591786802326823, 56.87609039468568994 ) ) ;
#118715 = CARTESIAN_POINT ( 'NONE',  ( -19.02544592524334988, -5.153800228976617603, 68.95942372801896170 ) ) ;
#118717 = DIRECTION ( 'NONE',  ( 1.000000000000000000, -4.336808689942017120E-17, 0.000000000000000000 ) ) ;
#118718 = CARTESIAN_POINT ( 'NONE',  ( 0.05219959533909260263, 19.03943276465977164, 74.99890960531435269 ) ) ;
#118719 = CARTESIAN_POINT ( 'NONE',  ( -18.62759615963270932, 10.81492255796079327, 115.8322429386477097 ) ) ;
#118720 = CARTESIAN_POINT ( 'NONE',  ( 5.049401038297881783, 19.05341960407617563, 67.29275706135234714 ) ) ;
#118722 = CARTESIAN_POINT ( 'NONE',  ( 13.89961937509977652, -13.97604488694527269, 38.12390960531436690 ) ) ;
#118721 = CARTESIAN_POINT ( 'NONE',  ( 9.564922557960805705, 16.46253265017160317, 109.5822429386476955 ) ) ;
#118723 = EDGE_CURVE ( 'NONE', #178804, #67326, #182121, .T. ) ;
#118724 = CARTESIAN_POINT ( 'NONE',  ( 13.97604488694527802, 13.89961937509977652, 79.37390960531435269 ) ) ;
#118726 = CARTESIAN_POINT ( 'NONE',  ( 16.51473224551069308, 9.474510206698969483, 34.16557627198102409 ) ) ;
#118725 = CARTESIAN_POINT ( 'NONE',  ( 12.06949235617757843, -12.14591786802309237, 28.12390960531435979 ) ) ;
#118727 = CARTESIAN_POINT ( 'NONE',  ( -5.153800228976607833, 19.02544592524334988, 57.70942372801899012 ) ) ;
#118728 = CARTESIAN_POINT ( 'NONE',  ( -16.55341960407611168, -4.379528057220339221, 76.45724293864769550 ) ) ;
#118729 = CARTESIAN_POINT ( 'NONE',  ( -5.823673210054431948, 21.52544592524334988, 112.7094237280190328 ) ) ;
#118730 = CARTESIAN_POINT ( 'NONE',  ( -19.05341960407611168, -5.049401038298163336, 51.45724293864770260 ) ) ;
#118731 = CARTESIAN_POINT ( 'NONE',  ( 0.05219959533907565091, 21.53943276465977519, 44.99890960531435979 ) ) ;
#118733 = CARTESIAN_POINT ( 'NONE',  ( -0.05219959533937732626, 21.53943276465977519, 107.5010903946856899 ) ) ;
#118732 = CARTESIAN_POINT ( 'NONE',  ( -14.29746914071049879, 8.314922557960819915, 50.83224293864770971 ) ) ;
#118734 = CARTESIAN_POINT ( 'NONE',  ( -19.02544592524342804, 5.153800228976336051, 91.04057627198100988 ) ) ;
#118735 = CARTESIAN_POINT ( 'NONE',  ( -9.474510206698964154, 16.51473224551069663, 105.4155762719810383 ) ) ;
#118736 = CARTESIAN_POINT ( 'NONE',  ( 19.02544592524343514, -5.153800228976328945, 33.54057627198102409 ) ) ;
#118737 = CARTESIAN_POINT ( 'NONE',  ( -9.564922557960796823, -16.46253265017161027, 32.08224293864769550 ) ) ;
#118738 = CARTESIAN_POINT ( 'NONE',  ( 14.34966873604960469, 8.224510206698951720, 89.16557627198102409 ) ) ;
#118739 = CARTESIAN_POINT ( 'NONE',  ( 18.67979575497178502, 10.72451020669898547, 99.16557627198100988 ) ) ;
#118740 = CARTESIAN_POINT ( 'NONE',  ( -9.564922557960796823, -16.46253265017161027, 87.08224293864769550 ) ) ;
#118741 = CARTESIAN_POINT ( 'NONE',  ( -5.719274019375978568, 21.55341960407610458, 110.2072429386477239 ) ) ;
#118742 = CARTESIAN_POINT ( 'NONE',  ( -19.03943276465977164, 0.05219959533909376836, 86.24890960531436690 ) ) ;
#118744 = CARTESIAN_POINT ( 'NONE',  ( -12.14591786802309592, -12.06949235617757132, 96.87390960531436690 ) ) ;
#118743 = CARTESIAN_POINT ( 'NONE',  ( -4.622231866529366047E-30, -105.0000000000000000, -15.00000000000000000 ) ) ;
#118745 = CARTESIAN_POINT ( 'NONE',  ( -5.049401038298153566, 19.05341960407611168, 75.20724293864769550 ) ) ;
#118746 = CARTESIAN_POINT ( 'NONE',  ( -0.05219959533907301413, -21.53943276465977519, 82.49890960531436690 ) ) ;
#118747 = CARTESIAN_POINT ( 'NONE',  ( -31.68361083058365679, 1.948458647159044155, 102.2466786067743101 ) ) ;
#118748 = CARTESIAN_POINT ( 'NONE',  ( -19.49401214000074489, -12.39993551617566503, 167.9999999999999716 ) ) ;
#118750 = CARTESIAN_POINT ( 'NONE',  ( 18.39443945427639804, -5.500000000000021316, 66.01745347608652992 ) ) ;
#118749 = CARTESIAN_POINT ( 'NONE',  ( 15.72974639402199770, -15.80617190586745480, 23.12390960531436335 ) ) ;
#118751 = CARTESIAN_POINT ( 'NONE',  ( -0.05219959533934338120, 16.53943276465976808, 32.50109039468568284 ) ) ;
#118752 = CARTESIAN_POINT ( 'NONE',  ( 16.53943276465976808, -0.05219959533910856209, 93.74890960531436690 ) ) ;
#118753 = CARTESIAN_POINT ( 'NONE',  ( -17.05587630539785238, -6.762274262135695935, 94.25819690962687503 ) ) ;
#118754 = CARTESIAN_POINT ( 'NONE',  ( 13.89961937509977652, -13.97604488694527269, 93.12390960531436690 ) ) ;
#118755 = CARTESIAN_POINT ( 'NONE',  ( -19.05341960407611168, -5.049401038298163336, 41.45724293864769550 ) ) ;
#118756 = CARTESIAN_POINT ( 'NONE',  ( -12.06949235617756955, 12.14591786802309770, 85.62390960531436690 ) ) ;
#118757 = CARTESIAN_POINT ( 'NONE',  ( 5.823673210054125526, 21.52544592524343514, 29.79057627198102409 ) ) ;
#118758 = CARTESIAN_POINT ( 'NONE',  ( -8.224510206698948167, 14.34966873604960824, 50.41557627198103120 ) ) ;
#118759 = CARTESIAN_POINT ( 'NONE',  ( -13.97604488694547697, 13.89961937509957934, 98.12609039468566152 ) ) ;
#118760 = CARTESIAN_POINT ( 'NONE',  ( 15.72974639402176855, 15.80617190586768217, 61.87609039468568284 ) ) ;
#118761 = CARTESIAN_POINT ( 'NONE',  ( -27.73933785331498925, 2.428612866367529932E-14, 146.8750000027311842 ) ) ;
#118762 = CARTESIAN_POINT ( 'NONE',  ( -19.02544592524342804, 5.153800228976336051, 96.04057627198103830 ) ) ;
#118763 = CARTESIAN_POINT ( 'NONE',  ( 4.483927247898790824, -16.52544592524335698, 90.20942372801903275 ) ) ;
#118764 = CARTESIAN_POINT ( 'NONE',  ( -13.89961937509977652, 13.97604488694528158, 30.62390960531435269 ) ) ;
#118765 = CARTESIAN_POINT ( 'NONE',  ( 13.89961937509977652, -13.97604488694527269, 78.12390960531433848 ) ) ;
#118766 = CARTESIAN_POINT ( 'NONE',  ( -21.52544592524343514, 5.823673210054127303, 76.04057627198102409 ) ) ;
#118767 = CARTESIAN_POINT ( 'NONE',  ( 12.06949235617739724, 12.14591786802326823, 21.87609039468567573 ) ) ;
#118769 = CARTESIAN_POINT ( 'NONE',  ( -21.52544592524334988, -5.823673210054445271, 63.95942372801901854 ) ) ;
#118768 = CARTESIAN_POINT ( 'NONE',  ( 12.14591786802309770, 12.06949235617756955, 54.37390960531435979 ) ) ;
#118770 = B_SPLINE_CURVE_WITH_KNOTS ( 'NONE', 3,
 ( #41784, #183275, #135786, #75088, #13424, #134798, #136755, #198440, #106411, #150960, #59912, #60899, #56951, #30577, #92228, #118625, #120591, #58923, #72109, #165129, #168092, #121580, #57949, #26621, #122574, #180316, #182286, #29590, #149952, #88264, #197457, #11457 ),
 .UNSPECIFIED., .F., .F.,
 ( 4, 2, 2, 2, 2, 2, 2, 2, 2, 2, 2, 2, 2, 2, 2, 4 ),
 ( 1.644815183373819107E-15, 0.0003712461730052133888, 0.0007424923460087820429, 0.001113738519012350426, 0.001484984692015919134, 0.002227477038023074982, 0.002598723211026649979, 0.002969969384030225409, 0.003341215557033800406, 0.003712461730037375836, 0.004083707903040949966, 0.004454954076044525396, 0.004826200249048100827, 0.005197446422051676257, 0.005568692595055250820, 0.005939938768058826250 ),
 .UNSPECIFIED. ) ;
#118772 = CARTESIAN_POINT ( 'NONE',  ( 21.55341960407610458, 5.719274019375980345, 23.95724293864769550 ) ) ;
#118771 = CARTESIAN_POINT ( 'NONE',  ( 12.06949235617739724, 12.14591786802326823, 81.87609039468568994 ) ) ;
#118773 = CARTESIAN_POINT ( 'NONE',  ( 24.99788752995426577, 12.60079600866962046, 166.0698618172138481 ) ) ;
#118774 = CARTESIAN_POINT ( 'NONE',  ( -17.31728774477273447, 6.344390552232389346, 80.81906651689321563 ) ) ;
#118775 = CARTESIAN_POINT ( 'NONE',  ( 14.29746914071037800, 8.314922557961029526, 106.6677570613523756 ) ) ;
#118776 = CARTESIAN_POINT ( 'NONE',  ( 14.29746914071037800, 8.314922557961029526, 61.66775706135235424 ) ) ;
#118777 = CARTESIAN_POINT ( 'NONE',  ( 5.049401038298161559, -19.05341960407611168, 77.70724293864765286 ) ) ;
#118778 = CARTESIAN_POINT ( 'NONE',  ( 5.049401038298161559, -19.05341960407611168, 87.70724293864769550 ) ) ;
#118779 = CARTESIAN_POINT ( 'NONE',  ( 15.72974639402176855, 15.80617190586768217, 76.87609039468567573 ) ) ;
#118780 = CARTESIAN_POINT ( 'NONE',  ( 12.14591786802327356, -12.06949235617739191, 70.62609039468567573 ) ) ;
#118781 = CARTESIAN_POINT ( 'NONE',  ( -4.379528057220328563, 16.55341960407611168, 40.20724293864769550 ) ) ;
#118782 = CARTESIAN_POINT ( 'NONE',  ( 19.02544592524343514, -5.153800228976328945, 58.54057627198102409 ) ) ;
#118783 = CARTESIAN_POINT ( 'NONE',  ( -16.51473224551069308, -9.474510206698971260, 41.66557627198103120 ) ) ;
#118785 = VERTEX_POINT ( 'NONE', #19915 ) ;
#118784 = CARTESIAN_POINT ( 'NONE',  ( -16.52544592524335698, -4.483927247898792601, 38.95942372801901854 ) ) ;
#118786 = CARTESIAN_POINT ( 'NONE',  ( -16.51473224551082808, 9.474510206698731452, 98.33442372801900433 ) ) ;
#118787 = CARTESIAN_POINT ( 'NONE',  ( -0.05219959533910754901, -16.53943276465976808, 92.49890960531436690 ) ) ;
#118788 = CARTESIAN_POINT ( 'NONE',  ( 19.03943276465977164, -0.05219959533909143690, 58.74890960531435979 ) ) ;
#118790 = CARTESIAN_POINT ( 'NONE',  ( 11.74264578624799427, 36.14014761921585972, -2.600000000000000533 ) ) ;
#118789 = CARTESIAN_POINT ( 'NONE',  ( 5.153800228976615827, -19.02544592524334988, 105.2094237280190185 ) ) ;
#118791 = CARTESIAN_POINT ( 'NONE',  ( 5.719274019375673035, 21.55341960407619339, 107.2927570613523471 ) ) ;
#118792 = CARTESIAN_POINT ( 'NONE',  ( -14.29746914071037622, -8.314922557961029526, 64.16775706135234714 ) ) ;
#118793 = CARTESIAN_POINT ( 'NONE',  ( -19.99999999999998224, -180.0000000000000000, -15.00000000000000178 ) ) ;
#118794 = CARTESIAN_POINT ( 'NONE',  ( 21.55341960407610458, 5.719274019375980345, 58.95724293864770971 ) ) ;
#118795 = CARTESIAN_POINT ( 'NONE',  ( -12.06949235617739369, -12.14591786802326823, 59.37609039468568284 ) ) ;
#118796 = DIRECTION ( 'NONE',  ( 0.000000000000000000, -0.5601916035752839695, -0.8283630648959138254 ) ) ;
#118797 = CARTESIAN_POINT ( 'NONE',  ( 9.474510206698729675, 16.51473224551082808, 52.08442372801900433 ) ) ;
#118798 = CARTESIAN_POINT ( 'NONE',  ( -16.46253265017160317, 9.564922557960807481, 85.83224293864769550 ) ) ;
#118799 = CARTESIAN_POINT ( 'NONE',  ( -8.224510206698948167, 14.34966873604960824, 110.4155762719810383 ) ) ;
#118800 = CARTESIAN_POINT ( 'NONE',  ( -19.03943276465977164, 0.05219959533909376836, 61.24890960531436690 ) ) ;
#118801 = CARTESIAN_POINT ( 'NONE',  ( 16.55341960407611168, 4.379528057220329451, 53.95724293864770260 ) ) ;
#118802 = AXIS2_PLACEMENT_3D ( 'NONE', #178882, #11022, #130331 ) ;
#118803 = CARTESIAN_POINT ( 'NONE',  ( 10.81492255796106328, -18.62759615963255655, 80.41775706135234714 ) ) ;
#118804 = ADVANCED_FACE ( 'NONE', ( #51252 ), #6562, .T. ) ;
#118805 = CARTESIAN_POINT ( 'NONE',  ( -19.05341960407617563, 5.049401038297882671, 53.54275706135231871 ) ) ;
#118806 = CARTESIAN_POINT ( 'NONE',  ( -19.03943276465977164, -0.05219959533935918106, 28.75109039468566507 ) ) ;
#118807 = CARTESIAN_POINT ( 'NONE',  ( -21.55341960407610458, -5.719274019375992779, 21.45724293864769550 ) ) ;
#118808 = CARTESIAN_POINT ( 'NONE',  ( 21.53943276465977519, 0.05219959533937863772, 96.25109039468568994 ) ) ;
#118809 = CARTESIAN_POINT ( 'NONE',  ( 16.51473224551069308, 9.474510206698969483, 59.16557627198102409 ) ) ;
#118810 = CARTESIAN_POINT ( 'NONE',  ( 15.72974639402176855, 15.80617190586768217, 96.87609039468568994 ) ) ;
#118811 = CARTESIAN_POINT ( 'NONE',  ( -15.72974639402197994, 15.80617190586746368, 45.62390960531436690 ) ) ;
#118812 = CARTESIAN_POINT ( 'NONE',  ( -19.05341960407611168, -5.049401038298163336, 86.45724293864769550 ) ) ;
#118813 = CARTESIAN_POINT ( 'NONE',  ( 13.89961937509957401, 13.97604488694547697, 61.87609039468566863 ) ) ;
#118814 = CARTESIAN_POINT ( 'NONE',  ( -19.05341960407611168, -5.049401038298163336, 36.45724293864766707 ) ) ;
#118815 = CARTESIAN_POINT ( 'NONE',  ( -16.46253265017160317, 9.564922557960807481, 90.83224293864769550 ) ) ;
#118816 = CARTESIAN_POINT ( 'NONE',  ( -16.46253265017146816, -9.564922557961047289, 89.16775706135234714 ) ) ;
#118817 = CARTESIAN_POINT ( 'NONE',  ( 8.224510206698742110, 14.34966873604972548, 47.08442372801901854 ) ) ;
#118818 = CARTESIAN_POINT ( 'NONE',  ( -0.05219959533910754901, -16.53943276465976808, 97.49890960531436690 ) ) ;
#118819 = CARTESIAN_POINT ( 'NONE',  ( -9.474510206698964154, 16.51473224551069663, 75.41557627198103830 ) ) ;
#118820 = EDGE_CURVE ( 'NONE', #103419, #18224, #160115, .T. ) ;
#118821 = CARTESIAN_POINT ( 'NONE',  ( 10.72451020669898902, -18.67979575497178502, 52.91557627198103830 ) ) ;
#118822 = CARTESIAN_POINT ( 'NONE',  ( -19.05341960407617563, 5.049401038297882671, 108.5427570613523187 ) ) ;
#118823 = CARTESIAN_POINT ( 'NONE',  ( 15.80617190586746368, 15.72974639402197994, 114.3739096053143527 ) ) ;
#118824 = CARTESIAN_POINT ( 'NONE',  ( 10.72451020669871369, 18.67979575497193778, 67.08442372801901854 ) ) ;
#118825 = CARTESIAN_POINT ( 'NONE',  ( 16.53943276465976808, 0.05219959533934440121, 76.25109039468568994 ) ) ;
#118826 =( BOUNDED_CURVE ( )  B_SPLINE_CURVE ( 2, ( #102104, #163789, #160779, #53598, #25290, #41439, #82922, #22268, #83918, #23272, #145600, #7079, #38437 ),
 .UNSPECIFIED., .F., .T. ) 
 B_SPLINE_CURVE_WITH_KNOTS ( ( 3, 2, 2, 2, 2, 2, 3 ),
 ( 0.4498445373017669335, 0.4517543859649122973, 0.4561403508771929571, 0.4605263157894736725, 0.4649122807017543879, 0.4692982456140351033, 0.4712537740992707724 ),
 .UNSPECIFIED. ) 
 CURVE ( )  GEOMETRIC_REPRESENTATION_ITEM ( )  RATIONAL_B_SPLINE_CURVE ( ( 0.9832469066685285419, 0.9851625545550100060, 1.000000000000000000, 0.9659258262890683122, 1.000000000000000000, 0.9659258262890683122, 1.000000000000000000, 0.9659258262890683122, 1.000000000000000000, 0.9659258262890683122, 1.000000000000000000, 0.9848076720550081875, 0.9831626618144004848 ) ) 
 REPRESENTATION_ITEM ( '' )  );
#118827 = CARTESIAN_POINT ( 'NONE',  ( -16.51473224551069308, -9.474510206698971260, 71.66557627198102409 ) ) ;
#118828 = CARTESIAN_POINT ( 'NONE',  ( -16.52544592524335698, -4.483927247898792601, 103.9594237280190185 ) ) ;
#118829 = CARTESIAN_POINT ( 'NONE',  ( -0.05219959533936034679, 19.03943276465977164, 42.50109039468566152 ) ) ;
#118830 = VECTOR ( 'NONE', #46268, 1000.000000000000000 ) ;
#118831 = CARTESIAN_POINT ( 'NONE',  ( -15.80617190586768217, 15.72974639402176855, 33.12609039468569705 ) ) ;
#118832 = CARTESIAN_POINT ( 'NONE',  ( -12.14591786802309592, -12.06949235617757132, 76.87390960531439532 ) ) ;
#118833 = CARTESIAN_POINT ( 'NONE',  ( -19.05341960407611168, -5.049401038298163336, 96.45724293864769550 ) ) ;
#118834 = CARTESIAN_POINT ( 'NONE',  ( -4.483927247898782831, 16.52544592524335698, 92.70942372801901854 ) ) ;
#118835 = CARTESIAN_POINT ( 'NONE',  ( -18.67979575497193778, 10.72451020669871902, 68.33442372801900433 ) ) ;
#118836 = CARTESIAN_POINT ( 'NONE',  ( -4.483927247898782831, 16.52544592524335698, 27.70942372801901854 ) ) ;
#118837 = CARTESIAN_POINT ( 'NONE',  ( -21.55341960407619339, 5.719274019375674811, 28.54275706135234358 ) ) ;
#118838 = CARTESIAN_POINT ( 'NONE',  ( -16.53943276465976808, 0.05219959533911058130, 71.24890960531435269 ) ) ;
#118839 = ORIENTED_EDGE ( 'NONE', *, *, #145712, .F. ) ;
#118840 = CARTESIAN_POINT ( 'NONE',  ( 18.67979575497178502, 10.72451020669898547, 99.16557627198100988 ) ) ;
#118841 = CARTESIAN_POINT ( 'NONE',  ( -4.379528057220328563, 16.55341960407611168, 50.20724293864769550 ) ) ;
#118842 = ORIENTED_EDGE ( 'NONE', *, *, #21468, .T. ) ;
#118843 = CARTESIAN_POINT ( 'NONE',  ( -9.564922557960796823, -16.46253265017161027, 27.08224293864769550 ) ) ;
#118844 = CARTESIAN_POINT ( 'NONE',  ( -15.80617190586745835, -15.72974639402198527, 31.87390960531435979 ) ) ;
#118845 = CARTESIAN_POINT ( 'NONE',  ( -0.05219959533937732626, 21.53943276465977519, 42.50109039468567573 ) ) ;
#118846 = CARTESIAN_POINT ( 'NONE',  ( 16.55341960407611168, 4.379528057220329451, 63.95724293864770260 ) ) ;
#118847 = CARTESIAN_POINT ( 'NONE',  ( -15.80617190586745835, -15.72974639402198527, 66.87390960531436690 ) ) ;
#118848 = CARTESIAN_POINT ( 'NONE',  ( 13.97604488694527802, 13.89961937509977652, 74.37390960531436690 ) ) ;
#118850 = CARTESIAN_POINT ( 'NONE',  ( 13.97604488694548053, -13.89961937509957401, 80.62609039468567573 ) ) ;
#118849 = CARTESIAN_POINT ( 'NONE',  ( -16.51473224551069308, -9.474510206698971260, 31.66557627198102054 ) ) ;
#118851 = CARTESIAN_POINT ( 'NONE',  ( -15.80617190586745835, -15.72974639402198527, 61.87390960531436690 ) ) ;
#118852 = CARTESIAN_POINT ( 'NONE',  ( -19.03943276465977164, 0.05219959533909376836, 36.24890960531436690 ) ) ;
#118853 = CARTESIAN_POINT ( 'NONE',  ( 5.153800228976335163, 19.02544592524342804, 69.79057627198103830 ) ) ;
#118854 = ORIENTED_EDGE ( 'NONE', *, *, #113885, .F. ) ;
#118855 = CARTESIAN_POINT ( 'NONE',  ( -4.483927247898782831, 16.52544592524335698, 32.70942372801900433 ) ) ;
#118856 = CARTESIAN_POINT ( 'NONE',  ( 21.55341960407619695, -5.719274019375665929, 31.04275706135234714 ) ) ;
#118857 = CARTESIAN_POINT ( 'NONE',  ( 21.52544592524334988, 5.823673210054432836, 66.45942372801903275 ) ) ;
#118858 = CARTESIAN_POINT ( 'NONE',  ( -19.03943276465977164, 0.05219959533909376836, 106.2489096053143669 ) ) ;
#118859 = CARTESIAN_POINT ( 'NONE',  ( 10.72451020669898902, -18.67979575497178502, 67.91557627198102409 ) ) ;
#118861 = CARTESIAN_POINT ( 'NONE',  ( 8.224510206698742110, 14.34966873604972548, 57.08442372801901854 ) ) ;
#118860 = CARTESIAN_POINT ( 'NONE',  ( -21.53943276465977519, 0.05219959533907696930, 106.2489096053143811 ) ) ;
#118862 = CARTESIAN_POINT ( 'NONE',  ( 10.72451020669898902, -18.67979575497178502, 52.91557627198103830 ) ) ;
#118863 = CARTESIAN_POINT ( 'NONE',  ( -21.52544592524334988, -5.823673210054445271, 103.9594237280190185 ) ) ;
#118864 = CARTESIAN_POINT ( 'NONE',  ( -5.153800228976328057, -19.02544592524343514, 57.29057627198103120 ) ) ;
#118865 = CARTESIAN_POINT ( 'NONE',  ( 5.153800228976335163, 19.02544592524342804, 104.7905762719809957 ) ) ;
#118866 = CARTESIAN_POINT ( 'NONE',  ( 19.03943276465977164, -0.05219959533909143690, 78.74890960531436690 ) ) ;
#118867 = CARTESIAN_POINT ( 'NONE',  ( 16.79531203550681440, -7.028104445595344529, 86.24755011779544134 ) ) ;
#118868 = CARTESIAN_POINT ( 'NONE',  ( -9.474510206698720793, -16.51473224551083518, 64.58442372801900433 ) ) ;
#118870 = CARTESIAN_POINT ( 'NONE',  ( 18.67979575497178502, 10.72451020669898547, 44.16557627198103120 ) ) ;
#118869 = CARTESIAN_POINT ( 'NONE',  ( 0.05219959533937995610, -21.53943276465977519, 110.0010903946856757 ) ) ;
#118871 = CARTESIAN_POINT ( 'NONE',  ( -12.06949235617739369, -12.14591786802326823, 99.37609039468568994 ) ) ;
#118872 = CARTESIAN_POINT ( 'NONE',  ( -9.564922557961040184, 16.46253265017147172, 87.91775706135233293 ) ) ;
#118873 = LINE ( 'NONE', #180557, #87361 ) ;
#118874 = CARTESIAN_POINT ( 'NONE',  ( 5.049401038297881783, 19.05341960407617563, 27.29275706135232937 ) ) ;
#118875 = CARTESIAN_POINT ( 'NONE',  ( -16.51473224551082808, 9.474510206698731452, 88.33442372801900433 ) ) ;
#118876 = CARTESIAN_POINT ( 'NONE',  ( -13.89961937509957401, -13.97604488694547875, 49.37609039468567573 ) ) ;
#118877 = DIRECTION ( 'NONE',  ( 0.000000000000000000, 0.000000000000000000, 1.000000000000000000 ) ) ;
#118878 = CARTESIAN_POINT ( 'NONE',  ( -13.89961937509977652, 13.97604488694528158, 45.62390960531433848 ) ) ;
#118879 = CARTESIAN_POINT ( 'NONE',  ( -16.53943276465976808, 0.05219959533911058130, 51.24890960531436690 ) ) ;
#118880 = CARTESIAN_POINT ( 'NONE',  ( -13.89961937509977652, 13.97604488694528158, 35.62390960531435269 ) ) ;
#118881 = CARTESIAN_POINT ( 'NONE',  ( 16.55341960407611168, 4.379528057220329451, 38.95724293864768839 ) ) ;
#118882 = CARTESIAN_POINT ( 'NONE',  ( -15.49999999999999822, -7.500000000000000888, 120.0000000000000142 ) ) ;
#118883 = CARTESIAN_POINT ( 'NONE',  ( -0.05219959533934338120, 16.53943276465976808, 107.5010903946856899 ) ) ;
#118884 = CARTESIAN_POINT ( 'NONE',  ( 13.97604488694527802, 13.89961937509977652, 44.37390960531435269 ) ) ;
#118885 = CARTESIAN_POINT ( 'NONE',  ( -13.97604488694547697, 13.89961937509957934, 28.12609039468565797 ) ) ;
#118886 = CARTESIAN_POINT ( 'NONE',  ( 0.05219959533934541429, -16.53943276465976808, 30.00109039468568284 ) ) ;
#118887 = CARTESIAN_POINT ( 'NONE',  ( -15.80617190586745835, -15.72974639402198527, 36.87390960531435979 ) ) ;
#118888 = CARTESIAN_POINT ( 'NONE',  ( -21.52544592524334988, -5.823673210054445271, 93.95942372801903275 ) ) ;
#118889 = CARTESIAN_POINT ( 'NONE',  ( -0.05219959533909027116, -19.03943276465977164, 107.4989096053143527 ) ) ;
#118890 = CARTESIAN_POINT ( 'NONE',  ( -0.05219959533909027116, -19.03943276465977164, 77.49890960531435269 ) ) ;
#118891 = CARTESIAN_POINT ( 'NONE',  ( 29.86685920354754842, -21.69954338932559068, -9.824999997268813345 ) ) ;
#118892 = CARTESIAN_POINT ( 'NONE',  ( -21.53943276465977519, 0.05219959533907696930, 111.2489096053143669 ) ) ;
#118893 = CARTESIAN_POINT ( 'NONE',  ( -12.06949235617756955, 12.14591786802309770, 85.62390960531436690 ) ) ;
#118895 = CARTESIAN_POINT ( 'NONE',  ( 5.153800228976335163, 19.02544592524342804, 69.79057627198103830 ) ) ;
#118894 = CARTESIAN_POINT ( 'NONE',  ( 21.53943276465977519, -0.05219959533907433946, 78.74890960531436690 ) ) ;
#118896 = CARTESIAN_POINT ( 'NONE',  ( -19.05341960407611168, -5.049401038298163336, 71.45724293864766707 ) ) ;
#118897 = CARTESIAN_POINT ( 'NONE',  ( -18.67979575497178146, -10.72451020669898902, 96.66557627198102409 ) ) ;
#118898 = EDGE_LOOP ( 'NONE', ( #86612, #150986, #182251, #130855, #9476 ) ) ;
#118899 = CARTESIAN_POINT ( 'NONE',  ( -5.049401038298153566, 19.05341960407611168, 55.20724293864769550 ) ) ;
#118900 = EDGE_CURVE ( 'NONE', #3247, #45202, #128025, .T. ) ;
#118902 = CARTESIAN_POINT ( 'NONE',  ( -0.05219959533909027116, -19.03943276465977164, 22.49890960531436690 ) ) ;
#118901 = CARTESIAN_POINT ( 'NONE',  ( -16.55341960407611168, -4.379528057220339221, 111.4572429386476813 ) ) ;
#118903 = CARTESIAN_POINT ( 'NONE',  ( -5.049401038298153566, 19.05341960407611168, 60.20724293864768129 ) ) ;
#118904 = CARTESIAN_POINT ( 'NONE',  ( -9.474510206698720793, -16.51473224551083518, 84.58442372801900433 ) ) ;
#118905 = CARTESIAN_POINT ( 'NONE',  ( 12.06949235617757843, -12.14591786802309237, 93.12390960531436690 ) ) ;
#118906 = CARTESIAN_POINT ( 'NONE',  ( -15.80617190586768217, 15.72974639402176855, 58.12609039468568994 ) ) ;
#118908 = CARTESIAN_POINT ( 'NONE',  ( -21.52544592524343514, 5.823673210054127303, 111.0405762719810525 ) ) ;
#118907 = CARTESIAN_POINT ( 'NONE',  ( -13.89961937509977652, 13.97604488694528158, 50.62390960531435979 ) ) ;
#118909 = CARTESIAN_POINT ( 'NONE',  ( 4.483927247898545687, 16.52544592524342804, 94.79057627198105251 ) ) ;
#118910 = CARTESIAN_POINT ( 'NONE',  ( 1.993301997531345292E-15, -30.30510711980685912, 142.4999999999999716 ) ) ;
#118911 = CARTESIAN_POINT ( 'NONE',  ( -13.89961937509977652, 13.97604488694528158, 75.62390960531438111 ) ) ;
#118912 = CARTESIAN_POINT ( 'NONE',  ( 23.31738231874054534, 16.94106989632529192, 143.4500000054623854 ) ) ;
#118914 = CARTESIAN_POINT ( 'NONE',  ( -18.67979575497178146, -10.72451020669898902, 21.66557627198102409 ) ) ;
#118913 = CARTESIAN_POINT ( 'NONE',  ( -0.05219959533936034679, 19.03943276465977164, 107.5010903946856615 ) ) ;
#118915 = CARTESIAN_POINT ( 'NONE',  ( -21.52544592524334988, -5.823673210054445271, 53.95942372801900433 ) ) ;
#118916 = CARTESIAN_POINT ( 'NONE',  ( 16.46253265017160672, -9.564922557960803928, 93.33224293864769550 ) ) ;
#118917 = CARTESIAN_POINT ( 'NONE',  ( -19.02544592524334988, -5.153800228976617603, 78.95942372801900433 ) ) ;
#118918 = CARTESIAN_POINT ( 'NONE',  ( 13.97604488694527802, 13.89961937509977652, 74.37390960531436690 ) ) ;
#118919 = CARTESIAN_POINT ( 'NONE',  ( -14.34966873604960291, -8.224510206698953496, 76.66557627198103830 ) ) ;
#118920 = CARTESIAN_POINT ( 'NONE',  ( 9.474510206698971260, -16.51473224551069308, 102.9155762719810241 ) ) ;
#118921 = CARTESIAN_POINT ( 'NONE',  ( 12.14591786802309770, 12.06949235617756955, 84.37390960531438111 ) ) ;
#118922 = CARTESIAN_POINT ( 'NONE',  ( -16.51473224551069308, -9.474510206698971260, 91.66557627198103830 ) ) ;
#118923 = CARTESIAN_POINT ( 'NONE',  ( 5.153800228976615827, -19.02544592524334988, 40.20942372801898301 ) ) ;
#118926 = CARTESIAN_POINT ( 'NONE',  ( -0.05219959533909027116, -19.03943276465977164, 27.49890960531435624 ) ) ;
#118925 = CARTESIAN_POINT ( 'NONE',  ( 16.53943276465976808, -0.05219959533910856209, 38.74890960531435979 ) ) ;
#118924 = CARTESIAN_POINT ( 'NONE',  ( 0.05219959533909260263, 19.03943276465977164, 44.99890960531435979 ) ) ;
#118927 = ORIENTED_EDGE ( 'NONE', *, *, #92889, .T. ) ;
#118928 = CARTESIAN_POINT ( 'NONE',  ( 10.72451020669871369, 18.67979575497193778, 47.08442372801901854 ) ) ;
#118929 = CARTESIAN_POINT ( 'NONE',  ( 19.02544592524334988, 5.153800228976608722, 86.45942372801900433 ) ) ;
#118930 = CARTESIAN_POINT ( 'NONE',  ( -12.06949235617756955, 12.14591786802309770, 35.62390960531437401 ) ) ;
#118931 = CARTESIAN_POINT ( 'NONE',  ( 5.719274019375991003, -21.55341960407610458, 97.70724293864772392 ) ) ;
#118932 = CARTESIAN_POINT ( 'NONE',  ( 5.719274019375991003, -21.55341960407610458, 37.70724293864769550 ) ) ;
#118933 = CARTESIAN_POINT ( 'NONE',  ( -14.29746914071049879, 8.314922557960819915, 80.83224293864769550 ) ) ;
#118934 = CARTESIAN_POINT ( 'NONE',  ( -9.564922557960796823, -16.46253265017161027, 37.08224293864768839 ) ) ;
#118935 = CARTESIAN_POINT ( 'NONE',  ( 16.52544592524335698, 4.483927247898782831, 101.4594237280190185 ) ) ;
#118936 = CARTESIAN_POINT ( 'NONE',  ( 12.06949235617739724, 12.14591786802326823, 86.87609039468568994 ) ) ;
#118937 = CARTESIAN_POINT ( 'NONE',  ( 0.05219959533934541429, -16.53943276465976808, 65.00109039468568994 ) ) ;
#118938 = CARTESIAN_POINT ( 'NONE',  ( -16.46253265017146816, -9.564922557961047289, 29.16775706135232937 ) ) ;
#118939 = CARTESIAN_POINT ( 'NONE',  ( 19.03943276465977164, -0.05219959533909143690, 93.74890960531435269 ) ) ;
#118940 = CARTESIAN_POINT ( 'NONE',  ( -9.564922557960796823, -16.46253265017161027, 77.08224293864769550 ) ) ;
#118941 = CARTESIAN_POINT ( 'NONE',  ( 16.53943276465976808, 0.05219959533934440121, 71.25109039468568994 ) ) ;
#118942 = CARTESIAN_POINT ( 'NONE',  ( 19.02544592524343514, -5.153800228976328945, 33.54057627198102409 ) ) ;
#118943 = CARTESIAN_POINT ( 'NONE',  ( 4.379528057220339221, -16.55341960407611168, 47.70724293864770260 ) ) ;
#118945 = CARTESIAN_POINT ( 'NONE',  ( 5.153800228976335163, 19.02544592524342804, 94.79057627198103830 ) ) ;
#118944 = CARTESIAN_POINT ( 'NONE',  ( 19.02544592524343514, -5.153800228976328945, 113.5405762719810241 ) ) ;
#118946 = CARTESIAN_POINT ( 'NONE',  ( -10.81492255796078084, -18.62759615963271287, 32.08224293864769550 ) ) ;
#118947 = CARTESIAN_POINT ( 'NONE',  ( -8.224510206698948167, 14.34966873604960824, 65.41557627198102409 ) ) ;
#118948 = CARTESIAN_POINT ( 'NONE',  ( -14.29746914071049879, 8.314922557960819915, 60.83224293864769550 ) ) ;
#118949 = DIRECTION ( 'NONE',  ( 1.000000000000000000, 0.000000000000000000, 0.000000000000000000 ) ) ;
#118950 = CARTESIAN_POINT ( 'NONE',  ( -16.46253265017146816, -9.564922557961047289, 64.16775706135233293 ) ) ;
#118951 = CARTESIAN_POINT ( 'NONE',  ( -19.02544592524342804, 5.153800228976336051, 96.04057627198103830 ) ) ;
#118952 = CARTESIAN_POINT ( 'NONE',  ( 5.049401038297881783, 19.05341960407617563, 67.29275706135234714 ) ) ;
#118953 = CARTESIAN_POINT ( 'NONE',  ( -13.89961937509957401, -13.97604488694547697, 39.37609039468566152 ) ) ;
#118955 = CARTESIAN_POINT ( 'NONE',  ( 12.06949235617739724, 12.14591786802326823, 96.87609039468568994 ) ) ;
#118954 = CARTESIAN_POINT ( 'NONE',  ( 13.89961937509957401, 13.97604488694547697, 111.8760903946856757 ) ) ;
#118956 = CARTESIAN_POINT ( 'NONE',  ( 16.46253265017160672, -9.564922557960803928, 43.33224293864769550 ) ) ;
#118957 = CARTESIAN_POINT ( 'NONE',  ( -15.80617190586745835, -15.72974639402198527, 26.87390960531435979 ) ) ;
#118958 = CARTESIAN_POINT ( 'NONE',  ( 10.72451020669871369, 18.67979575497193778, 52.08442372801901854 ) ) ;
#118959 = CARTESIAN_POINT ( 'NONE',  ( -0.05219959533936034679, 19.03943276465977164, 112.5010903946856757 ) ) ;
#118961 = CARTESIAN_POINT ( 'NONE',  ( -5.153800228976328057, -19.02544592524343514, 77.29057627198099567 ) ) ;
#118960 = CARTESIAN_POINT ( 'NONE',  ( -3.573655867282028392E-15, 2.428612866367529932E-14, 169.9999999999999716 ) ) ;
#118962 = CIRCLE ( 'NONE', #31768, 10.00000000000000000 ) ;
#118963 = EDGE_CURVE ( 'NONE', #169284, #49756, #97668, .T. ) ;
#118964 = CARTESIAN_POINT ( 'NONE',  ( -9.564922557960796823, -16.46253265017161027, 112.0822429386476955 ) ) ;
#118966 = CARTESIAN_POINT ( 'NONE',  ( 13.89961937509977652, -13.97604488694527269, 78.12390960531433848 ) ) ;
#118965 = CARTESIAN_POINT ( 'NONE',  ( -8.224510206698948167, 14.34966873604960824, 70.41557627198102409 ) ) ;
#118967 = ITEM_DEFINED_TRANSFORMATION ( 'NONE', 'NONE', #101576,  #82054 ) ;
#118968 = CARTESIAN_POINT ( 'NONE',  ( 16.51473224551069308, 9.474510206698969483, 74.16557627198103830 ) ) ;
#118969 = CARTESIAN_POINT ( 'NONE',  ( -9.564922557961040184, 16.46253265017147172, 92.91775706135233293 ) ) ;
#118970 = CARTESIAN_POINT ( 'NONE',  ( -5.719274019375978568, 21.55341960407610458, 70.20724293864769550 ) ) ;
#118971 = CARTESIAN_POINT ( 'NONE',  ( 13.89961937509977652, -13.97604488694527269, 33.12390960531434558 ) ) ;
#118972 = CARTESIAN_POINT ( 'NONE',  ( -19.03943276465977164, -0.05219959533935918106, 58.75109039468566863 ) ) ;
#118973 = CARTESIAN_POINT ( 'NONE',  ( -0.05219959533909027116, -19.03943276465977164, 52.49890960531436690 ) ) ;
#118974 = CARTESIAN_POINT ( 'NONE',  ( 13.97604488694527802, 13.89961937509977652, 89.37390960531436690 ) ) ;
#118975 = VERTEX_POINT ( 'NONE', #159357 ) ;
#118976 = CARTESIAN_POINT ( 'NONE',  ( -21.52544592524343514, 5.823673210054127303, 91.04057627198103830 ) ) ;
#118978 = CARTESIAN_POINT ( 'NONE',  ( 5.153800228976615827, -19.02544592524334988, 45.20942372801901143 ) ) ;
#118977 = CARTESIAN_POINT ( 'NONE',  ( -16.55341960407611168, -4.379528057220339221, 96.45724293864770971 ) ) ;
#118979 = CARTESIAN_POINT ( 'NONE',  ( -18.67979575497178146, -10.72451020669898902, 91.66557627198103830 ) ) ;
#118980 = CARTESIAN_POINT ( 'NONE',  ( 5.823673210054125526, 21.52544592524343514, 79.79057627198102409 ) ) ;
#118981 = CARTESIAN_POINT ( 'NONE',  ( 4.379528057220339221, -16.55341960407611168, 32.70724293864770260 ) ) ;
#118982 = CARTESIAN_POINT ( 'NONE',  ( -21.53943276465977519, -0.05219959533937600094, 103.7510903946857042 ) ) ;
#118983 = CARTESIAN_POINT ( 'NONE',  ( 19.02544592524343514, -5.153800228976328945, 73.54057627198103830 ) ) ;
#118984 = CARTESIAN_POINT ( 'NONE',  ( -16.51473224551069308, -9.474510206698971260, 31.66557627198102054 ) ) ;
#118985 = CARTESIAN_POINT ( 'NONE',  ( 10.81492255796106328, -18.62759615963255655, 45.41775706135234003 ) ) ;
#118986 = CARTESIAN_POINT ( 'NONE',  ( 15.80617190586769283, -15.72974639402175789, 55.62609039468568284 ) ) ;
#118987 = CARTESIAN_POINT ( 'NONE',  ( -9.564922557960796823, -16.46253265017161027, 52.08224293864768839 ) ) ;
#118988 = CARTESIAN_POINT ( 'NONE',  ( 5.719274019375673035, 21.55341960407619339, 27.29275706135234358 ) ) ;
#118989 = CARTESIAN_POINT ( 'NONE',  ( 5.153800228976615827, -19.02544592524334988, 65.20942372801900433 ) ) ;
#118990 = EDGE_CURVE ( 'NONE', #139926, #167341, #16889, .T. ) ;
#118991 = CARTESIAN_POINT ( 'NONE',  ( 19.05341960407611168, 5.049401038298154454, 33.95724293864769550 ) ) ;
#118992 = CARTESIAN_POINT ( 'NONE',  ( -8.314922557961024197, 14.29746914071037800, 22.91775706135235069 ) ) ;
#118993 = CARTESIAN_POINT ( 'NONE',  ( -19.02544592524342804, 5.153800228976336051, 26.04057627198103120 ) ) ;
#118994 = CARTESIAN_POINT ( 'NONE',  ( -16.55341960407617563, 4.379528057220093196, 78.54275706135236135 ) ) ;
#118995 = CARTESIAN_POINT ( 'NONE',  ( 0.05219959533909260263, 19.03943276465977164, 34.99890960531435979 ) ) ;
#118996 = CARTESIAN_POINT ( 'NONE',  ( 23.84827716990776381, -9.022217638662555217, 168.8513102586128696 ) ) ;
#118997 = CARTESIAN_POINT ( 'NONE',  ( 19.02544592524343514, -5.153800228976328945, 88.54057627198102409 ) ) ;
#118998 = CARTESIAN_POINT ( 'NONE',  ( 13.97604488694527802, 13.89961937509977652, 24.37390960531435624 ) ) ;
#118999 = CARTESIAN_POINT ( 'NONE',  ( 5.719274019375991003, -21.55341960407610458, 77.70724293864770971 ) ) ;
#119000 = CARTESIAN_POINT ( 'NONE',  ( 14.34966873604972726, -8.224510206698740333, 40.83442372801901854 ) ) ;
#119001 = CARTESIAN_POINT ( 'NONE',  ( 19.03943276465977164, 0.05219959533936151252, 21.25109039468565797 ) ) ;
#119002 = CARTESIAN_POINT ( 'NONE',  ( 13.89961937509977652, -13.97604488694527269, 33.12390960531434558 ) ) ;
#119003 = CARTESIAN_POINT ( 'NONE',  ( -16.53943276465976808, 0.05219959533911058130, 31.24890960531435979 ) ) ;
#119004 = CARTESIAN_POINT ( 'NONE',  ( -16.53943276465976808, 0.05219959533911058130, 66.24890960531436690 ) ) ;
#119005 = CARTESIAN_POINT ( 'NONE',  ( -19.05341960407611168, -5.049401038298163336, 66.45724293864769550 ) ) ;
#119006 = CARTESIAN_POINT ( 'NONE',  ( 21.55341960407619695, -5.719274019375665929, 106.0427570613523471 ) ) ;
#119007 = CARTESIAN_POINT ( 'NONE',  ( 0.05219959533907565091, 21.53943276465977519, 114.9989096053143669 ) ) ;
#119008 = CARTESIAN_POINT ( 'NONE',  ( 19.05341960407611168, 5.049401038298154454, 73.95724293864768129 ) ) ;
#119009 = CARTESIAN_POINT ( 'NONE',  ( 18.62759615963255655, 10.81492255796105972, 91.66775706135234714 ) ) ;
#119010 = CARTESIAN_POINT ( 'NONE',  ( -16.53943276465976808, -0.05219959533934237506, 63.75109039468568284 ) ) ;
#119011 = CARTESIAN_POINT ( 'NONE',  ( 8.224510206698742110, 14.34966873604972548, 27.08442372801901854 ) ) ;
#119013 = CARTESIAN_POINT ( 'NONE',  ( 19.03943276465977164, -0.05219959533909143690, 103.7489096053143669 ) ) ;
#119012 = CARTESIAN_POINT ( 'NONE',  ( -16.53943276465976808, 0.05219959533911058130, 96.24890960531435269 ) ) ;
#119014 = CARTESIAN_POINT ( 'NONE',  ( 4.379528057220339221, -16.55341960407611168, 27.70724293864769905 ) ) ;
#119015 = CARTESIAN_POINT ( 'NONE',  ( 19.03943276465977164, -0.05219959533909143690, 28.74890960531435624 ) ) ;
#119016 = CARTESIAN_POINT ( 'NONE',  ( 16.53943276465976808, 0.05219959533934440121, 51.25109039468568994 ) ) ;
#119017 = CARTESIAN_POINT ( 'NONE',  ( 14.34966873604960469, 8.224510206698951720, 49.16557627198102409 ) ) ;
#119018 = CARTESIAN_POINT ( 'NONE',  ( 16.55341960407618274, -4.379528057220086978, 106.0427570613523471 ) ) ;
#119019 = CARTESIAN_POINT ( 'NONE',  ( -16.46253265017160317, 9.564922557960807481, 110.8322429386476955 ) ) ;
#119020 = CARTESIAN_POINT ( 'NONE',  ( 15.72974639402199770, -15.80617190586745480, 28.12390960531435979 ) ) ;
#119021 = CARTESIAN_POINT ( 'NONE',  ( 21.55341960407619695, -5.719274019375665929, 106.0427570613523471 ) ) ;
#119022 = CARTESIAN_POINT ( 'NONE',  ( -16.52544592524342804, 4.483927247898546575, 81.04057627198102409 ) ) ;
#119023 = CARTESIAN_POINT ( 'NONE',  ( 13.97604488694527802, 13.89961937509977652, 89.37390960531436690 ) ) ;
#119024 = ORIENTED_EDGE ( 'NONE', *, *, #130470, .F. ) ;
#119025 = CARTESIAN_POINT ( 'NONE',  ( -14.29746914071037622, -8.314922557961029526, 34.16775706135234714 ) ) ;
#119026 = CARTESIAN_POINT ( 'NONE',  ( 5.049401038298161559, -19.05341960407611168, 42.70724293864767418 ) ) ;
#119028 = FILL_AREA_STYLE_COLOUR ( '', #137220 ) ;
#119027 = CARTESIAN_POINT ( 'NONE',  ( 0.05219959533934541429, -16.53943276465976808, 40.00109039468567573 ) ) ;
#119029 = CARTESIAN_POINT ( 'NONE',  ( -5.153800228976607833, 19.02544592524334988, 47.70942372801900433 ) ) ;
#119030 = CARTESIAN_POINT ( 'NONE',  ( -5.049401038298153566, 19.05341960407611168, 50.20724293864770260 ) ) ;
#119031 = CARTESIAN_POINT ( 'NONE',  ( -8.314922557961024197, 14.29746914071037800, 82.91775706135234714 ) ) ;
#119032 = CARTESIAN_POINT ( 'NONE',  ( 9.564922557961047289, -16.46253265017146816, 90.41775706135234714 ) ) ;
#119033 = CARTESIAN_POINT ( 'NONE',  ( 19.02544592524343514, -5.153800228976328945, 63.54057627198103830 ) ) ;
#119034 = CARTESIAN_POINT ( 'NONE',  ( 21.55341960407610458, 5.719274019375980345, 93.95724293864770971 ) ) ;
#119035 = CARTESIAN_POINT ( 'NONE',  ( -4.379528057220328563, 16.55341960407611168, 95.20724293864769550 ) ) ;
#119036 = EDGE_CURVE ( 'NONE', #156928, #150928, #148611, .T. ) ;
#119037 = CARTESIAN_POINT ( 'NONE',  ( -19.03943276465977164, -0.05219959533935918106, 68.75109039468566152 ) ) ;
#119038 = CARTESIAN_POINT ( 'NONE',  ( -15.72974639402197994, 15.80617190586746368, 65.62390960531436690 ) ) ;
#119039 = CARTESIAN_POINT ( 'NONE',  ( 0.05219959533936267826, -19.03943276465977164, 40.00109039468566152 ) ) ;
#119040 = CARTESIAN_POINT ( 'NONE',  ( -30.82560697742735911, 1.994931101954655383E-14, 150.0000000000000000 ) ) ;
#119041 = CARTESIAN_POINT ( 'NONE',  ( 21.53943276465977519, -0.05219959533907433946, 88.74890960531436690 ) ) ;
#119042 = CARTESIAN_POINT ( 'NONE',  ( -17.49999999999999645, 5.499999999999992895, 83.71769037696435589 ) ) ;
#119043 = CARTESIAN_POINT ( 'NONE',  ( -5.049401038297874678, -19.05341960407617918, 104.7927570613523471 ) ) ;
#119044 = CARTESIAN_POINT ( 'NONE',  ( -17.60691670004650788, -5.500000000000026645, 99.13333313366442212 ) ) ;
#119045 = CARTESIAN_POINT ( 'NONE',  ( -12.06949235617739369, -12.14591786802326823, 29.37609039468568284 ) ) ;
#119046 = CARTESIAN_POINT ( 'NONE',  ( -0.05219959533909027116, -19.03943276465977164, 47.49890960531435979 ) ) ;
#119047 = CARTESIAN_POINT ( 'NONE',  ( 16.51473224551069308, 9.474510206698969483, 109.1655762719810383 ) ) ;
#119048 = CARTESIAN_POINT ( 'NONE',  ( -18.62759615963270932, 10.81492255796079327, 90.83224293864769550 ) ) ;
#119049 = CARTESIAN_POINT ( 'NONE',  ( -21.52544592524334988, -5.823673210054445271, 58.95942372801902565 ) ) ;
#119051 = CARTESIAN_POINT ( 'NONE',  ( 0.05219959533937995610, -21.53943276465977519, 110.0010903946856757 ) ) ;
#119050 = CARTESIAN_POINT ( 'NONE',  ( 5.049401038297881783, 19.05341960407617563, 112.2927570613523471 ) ) ;
#119052 = CARTESIAN_POINT ( 'NONE',  ( 8.314922557960818139, 14.29746914071049879, 34.58224293864770260 ) ) ;
#119053 = CARTESIAN_POINT ( 'NONE',  ( -10.81492255796078084, -18.62759615963271287, 102.0822429386476955 ) ) ;
#119054 = CARTESIAN_POINT ( 'NONE',  ( 8.314922557960818139, 14.29746914071049879, 49.58224293864769550 ) ) ;
#119055 = CARTESIAN_POINT ( 'NONE',  ( -19.02544592524334988, -5.153800228976617603, 93.95942372801900433 ) ) ;
#119056 = CARTESIAN_POINT ( 'NONE',  ( 16.46253265017146816, 9.564922557961045513, 51.66775706135233293 ) ) ;
#119057 = CARTESIAN_POINT ( 'NONE',  ( -0.05219959533937732626, 21.53943276465977519, 67.50109039468568994 ) ) ;
#119058 = CARTESIAN_POINT ( 'NONE',  ( 5.153800228976615827, -19.02544592524334988, 45.20942372801901143 ) ) ;
#119059 = CARTESIAN_POINT ( 'NONE',  ( -8.224510206698948167, 14.34966873604960824, 115.4155762719810241 ) ) ;
#119060 = CARTESIAN_POINT ( 'NONE',  ( 10.81492255796078972, 18.62759615963270932, 49.58224293864769550 ) ) ;
#119061 = CARTESIAN_POINT ( 'NONE',  ( 4.379528057220339221, -16.55341960407611168, 42.70724293864770260 ) ) ;
#119062 = CARTESIAN_POINT ( 'NONE',  ( -10.81492255796105439, 18.62759615963255655, 107.9177570613523471 ) ) ;
#119063 = CARTESIAN_POINT ( 'NONE',  ( -12.14591786802326823, 12.06949235617739902, 73.12609039468567573 ) ) ;
#119064 = CARTESIAN_POINT ( 'NONE',  ( -12.06949235617756955, 12.14591786802309770, 45.62390960531436690 ) ) ;
#119065 = CARTESIAN_POINT ( 'NONE',  ( 10.81492255796106328, -18.62759615963255655, 70.41775706135236135 ) ) ;
#119066 = CARTESIAN_POINT ( 'NONE',  ( -18.62759615963255300, -10.81492255796106328, 69.16775706135234714 ) ) ;
#119067 = CARTESIAN_POINT ( 'NONE',  ( -18.67979575497178146, -10.72451020669898902, 61.66557627198103120 ) ) ;
#119068 = CARTESIAN_POINT ( 'NONE',  ( 16.51473224551069308, 9.474510206698969483, 34.16557627198102409 ) ) ;
#119069 = CARTESIAN_POINT ( 'NONE',  ( -21.53943276465977519, -0.05219959533937600094, 38.75109039468567573 ) ) ;
#119070 = CARTESIAN_POINT ( 'NONE',  ( 16.55341960407611168, 4.379528057220329451, 113.9572429386477239 ) ) ;
#119071 = CARTESIAN_POINT ( 'NONE',  ( 5.049401038298161559, -19.05341960407611168, 37.70724293864768839 ) ) ;
#119072 = CARTESIAN_POINT ( 'NONE',  ( 8.224510206698953496, -14.34966873604960469, 87.91557627198103830 ) ) ;
#119073 = CARTESIAN_POINT ( 'NONE',  ( 5.153800228976335163, 19.02544592524342804, 84.79057627198099567 ) ) ;
#119074 = CARTESIAN_POINT ( 'NONE',  ( -16.53943276465976808, 0.05219959533911058130, 46.24890960531435979 ) ) ;
#119075 = CARTESIAN_POINT ( 'NONE',  ( -16.53943276465976808, 0.05219959533911058130, 101.2489096053143669 ) ) ;
#119076 = CARTESIAN_POINT ( 'NONE',  ( -10.72451020669898014, 18.67979575497178502, 75.41557627198102409 ) ) ;
#119077 = CARTESIAN_POINT ( 'NONE',  ( -21.53943276465977519, 0.05219959533907696930, 111.2489096053143669 ) ) ;
#119078 = CARTESIAN_POINT ( 'NONE',  ( -19.05341960407611168, -5.049401038298163336, 111.4572429386476671 ) ) ;
#119080 = CARTESIAN_POINT ( 'NONE',  ( 4.483927247898790824, -16.52544592524335698, 25.20942372801901854 ) ) ;
#119079 = CARTESIAN_POINT ( 'NONE',  ( 16.46253265017160672, -9.564922557960803928, 63.33224293864769550 ) ) ;
#119081 = CARTESIAN_POINT ( 'NONE',  ( -5.719274019375978568, 21.55341960407610458, 55.20724293864770260 ) ) ;
#119082 = CARTESIAN_POINT ( 'NONE',  ( 5.823673210054444382, -21.52544592524334988, 90.20942372801903275 ) ) ;
#119083 = B_SPLINE_CURVE_WITH_KNOTS ( 'NONE', 3,
 ( #106669, #151209, #166382, #72367, #165384, #75337 ),
 .UNSPECIFIED., .F., .F.,
 ( 4, 2, 4 ),
 ( 0.003239945802372208323, 0.003620412082092052709, 0.004000878361811896662 ),
 .UNSPECIFIED. ) ;
#119084 = CARTESIAN_POINT ( 'NONE',  ( -5.153800228976328057, -19.02544592524343514, 82.29057627198103830 ) ) ;
#119085 = CARTESIAN_POINT ( 'NONE',  ( -10.72451020669898014, 18.67979575497178502, 115.4155762719810241 ) ) ;
#119086 = CARTESIAN_POINT ( 'NONE',  ( 9.474510206698971260, -16.51473224551069308, 112.9155762719810383 ) ) ;
#119087 = CARTESIAN_POINT ( 'NONE',  ( 0.05219959533934541429, -16.53943276465976808, 95.00109039468568994 ) ) ;
#119088 = CARTESIAN_POINT ( 'NONE',  ( 15.72974639402176855, 15.80617190586768217, 71.87609039468568994 ) ) ;
#119089 = CARTESIAN_POINT ( 'NONE',  ( -5.823673210054431948, 21.52544592524334988, 97.70942372801904696 ) ) ;
#119090 = CARTESIAN_POINT ( 'NONE',  ( -16.52544592524335698, -4.483927247898792601, 58.95942372801902565 ) ) ;
#119091 = CARTESIAN_POINT ( 'NONE',  ( -18.67979575497178146, -10.72451020669898902, 106.6655762719810383 ) ) ;
#119092 = CARTESIAN_POINT ( 'NONE',  ( -16.46253265017160317, 9.564922557960807481, 110.8322429386476955 ) ) ;
#119093 = CARTESIAN_POINT ( 'NONE',  ( 15.80617190586769283, -15.72974639402175789, 85.62609039468568994 ) ) ;
#119094 = CARTESIAN_POINT ( 'NONE',  ( -21.55341960407610458, -5.719274019375992779, 91.45724293864769550 ) ) ;
#119095 = CARTESIAN_POINT ( 'NONE',  ( 5.049401038297881783, 19.05341960407617563, 52.29275706135234003 ) ) ;
#119096 = CARTESIAN_POINT ( 'NONE',  ( 10.72451020669898902, -18.67979575497178502, 57.91557627198103120 ) ) ;
#119098 = CARTESIAN_POINT ( 'NONE',  ( 14.29746914071049879, -8.314922557960816363, 33.33224293864769550 ) ) ;
#119097 = CARTESIAN_POINT ( 'NONE',  ( 19.03943276465977164, -0.05219959533909143690, 98.74890960531436690 ) ) ;
#119099 = CARTESIAN_POINT ( 'NONE',  ( 12.08042635477516846, -10.04444949571651158, -61.78581196890001337 ) ) ;
#119100 = CARTESIAN_POINT ( 'NONE',  ( 16.46253265017146816, 9.564922557961045513, 66.66775706135233293 ) ) ;
#119101 = CARTESIAN_POINT ( 'NONE',  ( 18.22780087662122384, -5.500000000000022204, 91.01540105326107266 ) ) ;
#119102 = CARTESIAN_POINT ( 'NONE',  ( -19.05341960407617563, 5.049401038297882671, 103.5427570613523329 ) ) ;
#119103 = CARTESIAN_POINT ( 'NONE',  ( -10.81492255796078084, -18.62759615963271287, 82.08224293864768129 ) ) ;
#119104 = CARTESIAN_POINT ( 'NONE',  ( -4.379528057220328563, 16.55341960407611168, 50.20724293864769550 ) ) ;
#119105 = CARTESIAN_POINT ( 'NONE',  ( 8.224510206698742110, 14.34966873604972548, 37.08442372801901143 ) ) ;
#119106 = CARTESIAN_POINT ( 'NONE',  ( 5.153800228976335163, 19.02544592524342804, 39.79057627198100988 ) ) ;
#119108 = CARTESIAN_POINT ( 'NONE',  ( 16.46253265017146816, 9.564922557961045513, 86.66775706135233293 ) ) ;
#119107 = CARTESIAN_POINT ( 'NONE',  ( 0.05219959533907565091, 21.53943276465977519, 109.9989096053143527 ) ) ;
#119109 = CARTESIAN_POINT ( 'NONE',  ( 5.153800228976335163, 19.02544592524342804, 79.79057627198102409 ) ) ;
#119110 = CARTESIAN_POINT ( 'NONE',  ( -9.474510206698964154, 16.51473224551069663, 70.41557627198102409 ) ) ;
#119111 = CARTESIAN_POINT ( 'NONE',  ( -21.53943276465977519, 0.05219959533907696930, 81.24890960531436690 ) ) ;
#119112 = CARTESIAN_POINT ( 'NONE',  ( -16.51473224551069308, -9.474510206698971260, 51.66557627198102409 ) ) ;
#119113 = CARTESIAN_POINT ( 'NONE',  ( 20.47950280166127968, 31.12035828766152790, -8.000000000000000000 ) ) ;
#119114 = CARTESIAN_POINT ( 'NONE',  ( -4.379528057220328563, 16.55341960407611168, 60.20724293864768839 ) ) ;
#119115 = CARTESIAN_POINT ( 'NONE',  ( 5.153800228976335163, 19.02544592524342804, 89.79057627198102409 ) ) ;
#119116 = DIRECTION ( 'NONE',  ( 0.000000000000000000, 0.000000000000000000, 1.000000000000000000 ) ) ;
#119117 = CARTESIAN_POINT ( 'NONE',  ( -19.03943276465977164, -0.05219959533935918106, 63.75109039468566863 ) ) ;
#119118 = CARTESIAN_POINT ( 'NONE',  ( -21.53943276465977519, 0.05219959533907696930, 71.24890960531435269 ) ) ;
#119119 = CARTESIAN_POINT ( 'NONE',  ( 16.46253265017146816, 9.564922557961045513, 36.66775706135233293 ) ) ;
#119120 = CARTESIAN_POINT ( 'NONE',  ( -5.153800228976328057, -19.02544592524343514, 97.29057627198099567 ) ) ;
#119121 = CARTESIAN_POINT ( 'NONE',  ( 22.49873734152949112, 26.99873734152889782, 8.889087296526001936 ) ) ;
#119122 = CARTESIAN_POINT ( 'NONE',  ( -18.62759615963270932, 10.81492255796079327, 35.83224293864768839 ) ) ;
#119123 = CARTESIAN_POINT ( 'NONE',  ( -0.05219959533909027116, -19.03943276465977164, 72.49890960531435269 ) ) ;
#119124 = CARTESIAN_POINT ( 'NONE',  ( -5.823673210054431948, 21.52544592524334988, 67.70942372801901854 ) ) ;
#119125 = CARTESIAN_POINT ( 'NONE',  ( 9.474510206698971260, -16.51473224551069308, 22.91557627198102765 ) ) ;
#119127 = ORIENTED_EDGE ( 'NONE', *, *, #114246, .T. ) ;
#119126 = CARTESIAN_POINT ( 'NONE',  ( 15.72974639402199770, -15.80617190586745480, 108.1239096053143811 ) ) ;
#119128 = CARTESIAN_POINT ( 'NONE',  ( -21.55341960407619339, 5.719274019375674811, 58.54275706135235424 ) ) ;
#119129 = VERTEX_POINT ( 'NONE', #108891 ) ;
#119130 = CARTESIAN_POINT ( 'NONE',  ( 19.03943276465977164, -0.05219959533909143690, 103.7489096053143669 ) ) ;
#119131 = EDGE_CURVE ( 'NONE', #100590, #101588, #170570, .T. ) ;
#119132 = CARTESIAN_POINT ( 'NONE',  ( 13.97604488694527802, 13.89961937509977830, 89.37390960531435269 ) ) ;
#119133 = CARTESIAN_POINT ( 'NONE',  ( 5.719274019375991003, -21.55341960407610458, 102.7072429386476955 ) ) ;
#119134 = CARTESIAN_POINT ( 'NONE',  ( 19.03943276465977164, -0.05219959533909143690, 58.74890960531435979 ) ) ;
#119135 = CARTESIAN_POINT ( 'NONE',  ( 14.29746914071037800, 8.314922557961029526, 36.66775706135234714 ) ) ;
#119136 = CARTESIAN_POINT ( 'NONE',  ( -38.00000000000001421, 12.34694845685046438, -5.849999994537627757 ) ) ;
#119137 = CARTESIAN_POINT ( 'NONE',  ( 18.62759615963255655, 10.81492255796105972, 101.6677570613523613 ) ) ;
#119138 = CARTESIAN_POINT ( 'NONE',  ( -16.51473224551069308, -9.474510206698971260, 41.66557627198103120 ) ) ;
#119139 = CARTESIAN_POINT ( 'NONE',  ( -15.72974639402176322, -15.80617190586768395, 104.3760903946856899 ) ) ;
#119141 = CARTESIAN_POINT ( 'NONE',  ( -21.53943276465977519, -0.05219959533937600094, 58.75109039468568994 ) ) ;
#119140 = CARTESIAN_POINT ( 'NONE',  ( -9.564922557960796823, -16.46253265017161027, 92.08224293864769550 ) ) ;
#119142 = CARTESIAN_POINT ( 'NONE',  ( 4.539240849104785980, -4.118817879080736155, -62.50270742379689182 ) ) ;
#119143 = CARTESIAN_POINT ( 'NONE',  ( -9.474510206698964154, 16.51473224551069663, 115.4155762719810241 ) ) ;
#119144 = CARTESIAN_POINT ( 'NONE',  ( 18.22780087662126647, 5.499999999999818812, 46.48236817873107185 ) ) ;
#119146 = CARTESIAN_POINT ( 'NONE',  ( -15.72974639402176322, -15.80617190586768395, 54.37609039468568994 ) ) ;
#119145 = CARTESIAN_POINT ( 'NONE',  ( 14.29746914071037800, 8.314922557961029526, 46.66775706135234714 ) ) ;
#119147 = CARTESIAN_POINT ( 'NONE',  ( -18.67979575497193778, 10.72451020669871902, 88.33442372801901854 ) ) ;
#119148 = CARTESIAN_POINT ( 'NONE',  ( -11.25730316407969234, 9.333912919581832668, -60.07366171483953110 ) ) ;
#119149 = CARTESIAN_POINT ( 'NONE',  ( -0.05219959533934338120, 16.53943276465976808, 27.50109039468567929 ) ) ;
#119150 = CARTESIAN_POINT ( 'NONE',  ( 9.474510206698971260, -16.51473224551069308, 67.91557627198102409 ) ) ;
#119151 = CARTESIAN_POINT ( 'NONE',  ( -5.049401038298153566, 19.05341960407611168, 110.2072429386476671 ) ) ;
#119152 = CARTESIAN_POINT ( 'NONE',  ( 16.29526858892879915, 7.335722546919997811, 43.29670597800208043 ) ) ;
#119153 = CARTESIAN_POINT ( 'NONE',  ( 5.049401038298161559, -19.05341960407611168, 22.70724293864769194 ) ) ;
#119154 = CARTESIAN_POINT ( 'NONE',  ( -15.80617190586745835, -15.72974639402198527, 41.87390960531435979 ) ) ;
#119155 = CARTESIAN_POINT ( 'NONE',  ( 12.14591786802327356, -12.06949235617739191, 95.62609039468568994 ) ) ;
#119157 = CARTESIAN_POINT ( 'NONE',  ( 16.51473224551069308, 9.474510206698969483, 64.16557627198102409 ) ) ;
#119156 = CARTESIAN_POINT ( 'NONE',  ( 8.314922557960818139, 14.29746914071049879, 79.58224293864769550 ) ) ;
#119158 = CARTESIAN_POINT ( 'NONE',  ( 10.81492255796106328, -18.62759615963255655, 95.41775706135234714 ) ) ;
#119159 = CARTESIAN_POINT ( 'NONE',  ( -14.29746914071037622, -8.314922557961029526, 24.16775706135235424 ) ) ;
#119160 = CARTESIAN_POINT ( 'NONE',  ( -8.224510206698948167, 14.34966873604960824, 95.41557627198102409 ) ) ;
#119161 = CARTESIAN_POINT ( 'NONE',  ( 10.72451020669871369, 18.67979575497193778, 37.08442372801901143 ) ) ;
#119162 = CARTESIAN_POINT ( 'NONE',  ( -18.62759615963270932, 10.81492255796079327, 70.83224293864770971 ) ) ;
#119163 = CARTESIAN_POINT ( 'NONE',  ( -13.97604488694547697, 13.89961937509957934, 43.12609039468566152 ) ) ;
#119164 = CARTESIAN_POINT ( 'NONE',  ( -34.75593525676444528, 1.707450833175019334, 52.30717240064831230 ) ) ;
#119165 = CARTESIAN_POINT ( 'NONE',  ( -0.05219959533909027116, -19.03943276465977164, 87.49890960531436690 ) ) ;
#119166 = CARTESIAN_POINT ( 'NONE',  ( 14.34966873604960469, 8.224510206698951720, 59.16557627198103120 ) ) ;
#119167 = CARTESIAN_POINT ( 'NONE',  ( -8.314922557960811034, -14.29746914071050412, 32.08224293864769550 ) ) ;
#119168 = CARTESIAN_POINT ( 'NONE',  ( 12.14591786802309770, 12.06949235617756955, 24.37390960531435979 ) ) ;
#119169 = CARTESIAN_POINT ( 'NONE',  ( 19.03943276465977164, 0.05219959533936151252, 71.25109039468566152 ) ) ;
#119170 = CARTESIAN_POINT ( 'NONE',  ( 17.26172910966777607, 6.454744622555865341, 46.69353091350776452 ) ) ;
#119171 = CARTESIAN_POINT ( 'NONE',  ( -0.05219959533907301413, -21.53943276465977519, 22.49890960531436335 ) ) ;
#119172 = CARTESIAN_POINT ( 'NONE',  ( 8.224510206698953496, -14.34966873604960469, 87.91557627198103830 ) ) ;
#119173 = DIRECTION ( 'NONE',  ( 1.000000000000000000, 0.000000000000000000, 0.000000000000000000 ) ) ;
#119175 = CARTESIAN_POINT ( 'NONE',  ( -5.823673210054116645, -21.52544592524344225, 47.29057627198103120 ) ) ;
#119174 = CARTESIAN_POINT ( 'NONE',  ( -13.97604488694527625, -13.89961937509977652, 51.87390960531436690 ) ) ;
#119176 = CARTESIAN_POINT ( 'NONE',  ( -21.53943276465977519, 0.05219959533907696930, 66.24890960531436690 ) ) ;
#119177 = CARTESIAN_POINT ( 'NONE',  ( -14.29746914071049879, 8.314922557960819915, 105.8322429386476955 ) ) ;
#119179 = CARTESIAN_POINT ( 'NONE',  ( 9.564922557960805705, 16.46253265017160317, 49.58224293864770260 ) ) ;
#119178 = CARTESIAN_POINT ( 'NONE',  ( -14.29746914071037622, -8.314922557961029526, 59.16775706135234714 ) ) ;
#119180 = CARTESIAN_POINT ( 'NONE',  ( 5.719274019375673035, 21.55341960407619339, 52.29275706135236135 ) ) ;
#119181 = CARTESIAN_POINT ( 'NONE',  ( 12.06949235617757843, -12.14591786802309237, 108.1239096053143811 ) ) ;
#119182 = CARTESIAN_POINT ( 'NONE',  ( 19.03943276465977164, 0.05219959533936151252, 96.25109039468567573 ) ) ;
#119183 = CARTESIAN_POINT ( 'NONE',  ( 29.86685920354754487, 21.69954338932564752, -1.924999997268813212 ) ) ;
#119185 = CARTESIAN_POINT ( 'NONE',  ( 5.823673210054125526, 21.52544592524343514, 29.79057627198102409 ) ) ;
#119184 = DIRECTION ( 'NONE',  ( 0.8164965809277249242, 0.000000000000000000, -0.5773502691896271743 ) ) ;
#119186 = CARTESIAN_POINT ( 'NONE',  ( 5.153800228976335163, 19.02544592524342804, 24.79057627198102765 ) ) ;
#119187 = CARTESIAN_POINT ( 'NONE',  ( -5.719274019375665041, -21.55341960407619695, 74.79275706135234714 ) ) ;
#119188 = VECTOR ( 'NONE', #171837, 1000.000000000000000 ) ;
#119190 = CARTESIAN_POINT ( 'NONE',  ( -8.314922557960811034, -14.29746914071050412, 47.08224293864770260 ) ) ;
#119189 = CARTESIAN_POINT ( 'NONE',  ( -16.52544592524335698, -4.483927247898792601, 53.95942372801900433 ) ) ;
#119191 = CARTESIAN_POINT ( 'NONE',  ( 18.67979575497178502, 10.72451020669898547, 64.16557627198102409 ) ) ;
#119192 = CARTESIAN_POINT ( 'NONE',  ( -18.62759615963270932, 10.81492255796079327, 75.83224293864769550 ) ) ;
#119193 = DIRECTION ( 'NONE',  ( 0.000000000000000000, 0.000000000000000000, 1.000000000000000000 ) ) ;
#119195 = CARTESIAN_POINT ( 'NONE',  ( 21.52544592524344225, -5.823673210054117533, 23.54057627198102765 ) ) ;
#119194 = CARTESIAN_POINT ( 'NONE',  ( 16.46253265017146816, 9.564922557961045513, 81.66775706135233293 ) ) ;
#119196 = CARTESIAN_POINT ( 'NONE',  ( -5.049401038298153566, 19.05341960407611168, 45.20724293864769550 ) ) ;
#119197 = CARTESIAN_POINT ( 'NONE',  ( -14.29746914071049879, 8.314922557960819915, 110.8322429386476955 ) ) ;
#119198 = CARTESIAN_POINT ( 'NONE',  ( 13.89961937509977652, -13.97604488694527269, 113.1239096053143527 ) ) ;
#119199 = ORIENTED_EDGE ( 'NONE', *, *, #981, .F. ) ;
#119200 = CARTESIAN_POINT ( 'NONE',  ( -16.53943276465976808, -0.05219959533934237506, 78.75109039468568994 ) ) ;
#119201 = CARTESIAN_POINT ( 'NONE',  ( -15.72974639402197994, 15.80617190586746368, 100.6239096053143811 ) ) ;
#119202 = CARTESIAN_POINT ( 'NONE',  ( 9.564922557960805705, 16.46253265017160317, 64.58224293864769550 ) ) ;
#119203 = CARTESIAN_POINT ( 'NONE',  ( -10.81492255796105439, 18.62759615963255655, 37.91775706135235424 ) ) ;
#119204 = CARTESIAN_POINT ( 'NONE',  ( -5.153800228976328057, -19.02544592524343514, 97.29057627198099567 ) ) ;
#119205 = CARTESIAN_POINT ( 'NONE',  ( -25.17999522921142841, -30.53243704067310560, -18.89073929087953374 ) ) ;
#119206 = ORIENTED_EDGE ( 'NONE', *, *, #86135, .F. ) ;
#119207 = CARTESIAN_POINT ( 'NONE',  ( -5.823673210054431948, 21.52544592524334988, 37.70942372801900433 ) ) ;
#119209 = CARTESIAN_POINT ( 'NONE',  ( -9.564922557961040184, 16.46253265017147172, 92.91775706135233293 ) ) ;
#119208 = CARTESIAN_POINT ( 'NONE',  ( 13.97604488694527802, 13.89961937509977652, 24.37390960531435624 ) ) ;
#119210 = CARTESIAN_POINT ( 'NONE',  ( -16.46253265017146816, -9.564922557961047289, 34.16775706135233293 ) ) ;
#119211 = CARTESIAN_POINT ( 'NONE',  ( 5.719274019375991003, -21.55341960407610458, 112.7072429386476955 ) ) ;
#119212 = CARTESIAN_POINT ( 'NONE',  ( -9.564922557961040184, 16.46253265017147172, 27.91775706135232582 ) ) ;
#119213 = CARTESIAN_POINT ( 'NONE',  ( -13.89961937509957401, -13.97604488694547875, 54.37609039468565442 ) ) ;
#119214 = CARTESIAN_POINT ( 'NONE',  ( -0.05219959533934338120, 16.53943276465976808, 87.50109039468568994 ) ) ;
#119215 = CARTESIAN_POINT ( 'NONE',  ( 22.40075113267181450, -13.33491755757044572, 165.5209445330007441 ) ) ;
#119216 = CARTESIAN_POINT ( 'NONE',  ( -5.153800228976328057, -19.02544592524343514, 77.29057627198099567 ) ) ;
#119217 = CARTESIAN_POINT ( 'NONE',  ( -21.53943276465977519, -0.05219959533937600094, 73.75109039468567573 ) ) ;
#119218 = CARTESIAN_POINT ( 'NONE',  ( -15.80617190586768217, 15.72974639402176855, 98.12609039468570415 ) ) ;
#119219 = CARTESIAN_POINT ( 'NONE',  ( 22.62812085840269560, -1.500606516337551044, -55.49205433527804843 ) ) ;
#119220 = CARTESIAN_POINT ( 'NONE',  ( -13.97604488694527625, -13.89961937509977652, 86.87390960531436690 ) ) ;
#119221 = CARTESIAN_POINT ( 'NONE',  ( 15.80617190586769283, -15.72974639402175789, 60.62609039468567573 ) ) ;
#119222 = CARTESIAN_POINT ( 'NONE',  ( 16.46253265017146816, 9.564922557961045513, 101.6677570613523329 ) ) ;
#119223 = EDGE_CURVE ( 'NONE', #87857, #69935, #38772, .T. ) ;
#119224 = CARTESIAN_POINT ( 'NONE',  ( 5.153800228976335163, 19.02544592524342804, 59.79057627198100988 ) ) ;
#119225 = CARTESIAN_POINT ( 'NONE',  ( 19.05341960407611168, 5.049401038298154454, 113.9572429386477097 ) ) ;
#119226 = CARTESIAN_POINT ( 'NONE',  ( 19.03943276465977164, -0.05219959533909143690, 83.74890960531436690 ) ) ;
#119227 = CARTESIAN_POINT ( 'NONE',  ( -18.22780087662123094, -5.499999999999984901, 76.48459894673894155 ) ) ;
#119228 = CARTESIAN_POINT ( 'NONE',  ( 16.51473224551069308, 9.474510206698969483, 64.16557627198102409 ) ) ;
#119229 = CARTESIAN_POINT ( 'NONE',  ( -19.03943276465977164, 0.05219959533909376836, 51.24890960531436690 ) ) ;
#119230 = CARTESIAN_POINT ( 'NONE',  ( 0.05219959533937995610, -21.53943276465977519, 20.00109039468568639 ) ) ;
#119231 = CARTESIAN_POINT ( 'NONE',  ( -4.483927247898782831, 16.52544592524335698, 92.70942372801901854 ) ) ;
#119232 = CARTESIAN_POINT ( 'NONE',  ( -18.89770734986051437, -5.499999999999909406, 39.10214472496640781 ) ) ;
#119233 = DIRECTION ( 'NONE',  ( -0.000000000000000000, -0.000000000000000000, 1.000000000000000000 ) ) ;
#119234 = CARTESIAN_POINT ( 'NONE',  ( -16.51473224551082808, 9.474510206698731452, 58.33442372801900433 ) ) ;
#119235 = CARTESIAN_POINT ( 'NONE',  ( -5.049401038298153566, 19.05341960407611168, 75.20724293864769550 ) ) ;
#119236 = CARTESIAN_POINT ( 'NONE',  ( 16.55341960407611168, 4.379528057220329451, 68.95724293864769550 ) ) ;
#119237 = CARTESIAN_POINT ( 'NONE',  ( -4.483927247898539470, -16.52544592524342804, 102.2905762719810383 ) ) ;
#119238 = CARTESIAN_POINT ( 'NONE',  ( 13.97604488694527802, 13.89961937509977652, 109.3739096053143669 ) ) ;
#119239 = CARTESIAN_POINT ( 'NONE',  ( 19.03943276465977164, -0.05219959533909143690, 108.7489096053143527 ) ) ;
#119240 = CARTESIAN_POINT ( 'NONE',  ( 16.55341960407611168, 4.379528057220329451, 88.95724293864769550 ) ) ;
#119241 = CARTESIAN_POINT ( 'NONE',  ( -17.59860650958991002, -7.585241751807008548, 81.57662985737506744 ) ) ;
#119242 = CARTESIAN_POINT ( 'NONE',  ( -13.97604488694547697, 13.89961937509957934, 33.12609039468566863 ) ) ;
#119243 = CARTESIAN_POINT ( 'NONE',  ( 16.52544592524335698, 4.483927247898782831, 101.4594237280190185 ) ) ;
#119244 = CARTESIAN_POINT ( 'NONE',  ( -13.97604488694527625, -13.89961937509977652, 91.87390960531432427 ) ) ;
#119245 = CARTESIAN_POINT ( 'NONE',  ( -5.719274019375665041, -21.55341960407619695, 59.79275706135234714 ) ) ;
#119246 = CARTESIAN_POINT ( 'NONE',  ( -0.05219959533907301413, -21.53943276465977519, 47.49890960531435979 ) ) ;
#119247 = CARTESIAN_POINT ( 'NONE',  ( -18.67979575497193778, 10.72451020669871902, 23.33442372801901499 ) ) ;
#119248 = CARTESIAN_POINT ( 'NONE',  ( -15.72974639402197994, 15.80617190586746368, 75.62390960531439532 ) ) ;
#119249 = CARTESIAN_POINT ( 'NONE',  ( 14.29746914071049879, -8.314922557960816363, 98.33224293864769550 ) ) ;
#119250 = CARTESIAN_POINT ( 'NONE',  ( 9.474510206698729675, 16.51473224551082808, 52.08442372801900433 ) ) ;
#119251 = CARTESIAN_POINT ( 'NONE',  ( 13.89961937509977652, -13.97604488694527269, 28.12390960531435624 ) ) ;
#119252 = CARTESIAN_POINT ( 'NONE',  ( -19.05341960407611168, -5.049401038298163336, 86.45724293864769550 ) ) ;
#119253 = CARTESIAN_POINT ( 'NONE',  ( 5.049401038298161559, -19.05341960407611168, 97.70724293864766707 ) ) ;
#119254 = CARTESIAN_POINT ( 'NONE',  ( -12.06949235617756955, 12.14591786802309770, 115.6239096053143669 ) ) ;
#119255 = CARTESIAN_POINT ( 'NONE',  ( -16.53943276465976808, 0.05219959533911058130, 21.24890960531436690 ) ) ;
#119256 = CARTESIAN_POINT ( 'NONE',  ( -12.06949235617739369, -12.14591786802326823, 34.37609039468568284 ) ) ;
#119257 = CARTESIAN_POINT ( 'NONE',  ( -10.81492255796105439, 18.62759615963255655, 107.9177570613523471 ) ) ;
#119258 = CARTESIAN_POINT ( 'NONE',  ( -13.89961937509977652, 13.97604488694528158, 100.6239096053143669 ) ) ;
#119259 = CARTESIAN_POINT ( 'NONE',  ( 21.53943276465977519, 0.05219959533937863772, 31.25109039468568639 ) ) ;
#119260 = CARTESIAN_POINT ( 'NONE',  ( -9.474510206698964154, 16.51473224551069663, 50.41557627198102409 ) ) ;
#119261 = CARTESIAN_POINT ( 'NONE',  ( 16.52544592524335698, 4.483927247898782831, 41.45942372801901143 ) ) ;
#119262 = CARTESIAN_POINT ( 'NONE',  ( -4.483927247898782831, 16.52544592524335698, 112.7094237280190328 ) ) ;
#119263 = CARTESIAN_POINT ( 'NONE',  ( -16.52544592524335698, -4.483927247898792601, 88.95942372801901854 ) ) ;
#119264 = CARTESIAN_POINT ( 'NONE',  ( -19.03943276465977164, -0.05219959533935918106, 108.7510903946856615 ) ) ;
#119265 = CARTESIAN_POINT ( 'NONE',  ( -13.89961937509977652, 13.97604488694528158, 30.62390960531435269 ) ) ;
#119266 = CARTESIAN_POINT ( 'NONE',  ( 16.55341960407611168, 4.379528057220329451, 98.95724293864770971 ) ) ;
#119267 = CARTESIAN_POINT ( 'NONE',  ( -10.72451020669898014, 18.67979575497178502, 100.4155762719810241 ) ) ;
#119268 = CARTESIAN_POINT ( 'NONE',  ( 16.51473224551069308, 9.474510206698969483, 29.16557627198103475 ) ) ;
#119269 = CARTESIAN_POINT ( 'NONE',  ( -13.97604488694527625, -13.89961937509977652, 111.8739096053143243 ) ) ;
#119270 = CARTESIAN_POINT ( 'NONE',  ( -21.55341960407619339, 5.719274019375674811, 33.54275706135234714 ) ) ;
#119271 = CARTESIAN_POINT ( 'NONE',  ( 19.05341960407611168, 5.049401038298154454, 23.95724293864769194 ) ) ;
#119272 = CARTESIAN_POINT ( 'NONE',  ( -16.46253265017160317, 9.564922557960807481, 100.8322429386477097 ) ) ;
#119273 = LINE ( 'NONE', #42433, #71290 ) ;
#119274 = CARTESIAN_POINT ( 'NONE',  ( -9.564922557960796823, -16.46253265017161027, 87.08224293864769550 ) ) ;
#119276 = CARTESIAN_POINT ( 'NONE',  ( 14.29746914071049879, -8.314922557960816363, 88.33224293864769550 ) ) ;
#119275 = CARTESIAN_POINT ( 'NONE',  ( 21.55341960407619695, -5.719274019375665929, 36.04275706135234714 ) ) ;
#119277 = CARTESIAN_POINT ( 'NONE',  ( 19.05341960407611168, 5.049401038298154454, 93.95724293864769550 ) ) ;
#119278 = CARTESIAN_POINT ( 'NONE',  ( -19.02544592524334988, -5.153800228976617603, 23.95942372801900078 ) ) ;
#119279 = CARTESIAN_POINT ( 'NONE',  ( 0.05219959533934541429, -16.53943276465976808, 65.00109039468568994 ) ) ;
#119280 = CARTESIAN_POINT ( 'NONE',  ( 18.67979575497194134, -10.72451020669871369, 75.83442372801900433 ) ) ;
#119281 = CARTESIAN_POINT ( 'NONE',  ( 4.483927247898790824, -16.52544592524335698, 45.20942372801901854 ) ) ;
#119282 = CARTESIAN_POINT ( 'NONE',  ( 19.02544592524343514, -5.153800228976328945, 78.54057627198099567 ) ) ;
#119283 = CARTESIAN_POINT ( 'NONE',  ( -9.564922557961040184, 16.46253265017147172, 97.91775706135233293 ) ) ;
#119284 = CARTESIAN_POINT ( 'NONE',  ( -4.379528057220086978, -16.55341960407618274, 69.79275706135234714 ) ) ;
#119285 = CARTESIAN_POINT ( 'NONE',  ( 10.72451020669871369, 18.67979575497193778, 112.0844237280190185 ) ) ;
#119286 = CARTESIAN_POINT ( 'NONE',  ( -16.46253265017146816, -9.564922557961047289, 84.16775706135233293 ) ) ;
#119287 = CARTESIAN_POINT ( 'NONE',  ( -19.05341960407611168, -5.049401038298163336, 61.45724293864769550 ) ) ;
#119288 = CARTESIAN_POINT ( 'NONE',  ( -15.72974639402197994, 15.80617190586746368, 80.62390960531438111 ) ) ;
#119290 = CARTESIAN_POINT ( 'NONE',  ( 5.049401038297881783, 19.05341960407617563, 92.29275706135234714 ) ) ;
#119289 = CARTESIAN_POINT ( 'NONE',  ( 8.314922557960818139, 14.29746914071049879, 74.58224293864768129 ) ) ;
#119291 = CARTESIAN_POINT ( 'NONE',  ( 16.55341960407618274, -4.379528057220086978, 56.04275706135235424 ) ) ;
#119292 = CARTESIAN_POINT ( 'NONE',  ( 21.97054992548844865, 7.027819292989578415, 170.5066066589220100 ) ) ;
#119293 = CARTESIAN_POINT ( 'NONE',  ( 9.564922557961047289, -16.46253265017146816, 60.41775706135233293 ) ) ;
#119294 = CARTESIAN_POINT ( 'NONE',  ( -8.314922557961024197, 14.29746914071037800, 112.9177570613523329 ) ) ;
#119295 = CARTESIAN_POINT ( 'NONE',  ( -4.379528057220328563, 16.55341960407611168, 80.20724293864769550 ) ) ;
#119297 = CARTESIAN_POINT ( 'NONE',  ( -16.79531203550682150, 7.028104445595347194, 38.74755011779544134 ) ) ;
#119296 = CARTESIAN_POINT ( 'NONE',  ( -19.03943276465977164, -0.05219959533935918106, 18.75109039468567218 ) ) ;
#119298 = CARTESIAN_POINT ( 'NONE',  ( -21.53943276465977519, 0.05219959533907696930, 106.2489096053143811 ) ) ;
#119299 = CARTESIAN_POINT ( 'NONE',  ( -13.97604488694527625, -13.89961937509977652, 101.8739096053143811 ) ) ;
#119300 = CARTESIAN_POINT ( 'NONE',  ( -0.05219959533909027116, -19.03943276465977164, 82.49890960531436690 ) ) ;
#119301 = CARTESIAN_POINT ( 'NONE',  ( 18.62759615963255655, 10.81492255796105972, 86.66775706135234714 ) ) ;
#119302 = CARTESIAN_POINT ( 'NONE',  ( 16.46253265017160672, -9.564922557960803928, 58.33224293864769550 ) ) ;
#119303 = CARTESIAN_POINT ( 'NONE',  ( 10.72451020669898902, -18.67979575497178502, 27.91557627198103830 ) ) ;
#119304 = CARTESIAN_POINT ( 'NONE',  ( 14.34966873604960469, 8.224510206698951720, 74.16557627198102409 ) ) ;
#119305 = CARTESIAN_POINT ( 'NONE',  ( -5.153800228976328057, -19.02544592524343514, 37.29057627198102409 ) ) ;
#119306 = CARTESIAN_POINT ( 'NONE',  ( -14.34966873604960291, -8.224510206698953496, 96.66557627198102409 ) ) ;
#119307 = CARTESIAN_POINT ( 'NONE',  ( 21.55341960407610458, 5.719274019375980345, 103.9572429386476813 ) ) ;
#119308 = CARTESIAN_POINT ( 'NONE',  ( -5.719274019375665041, -21.55341960407619695, 54.79275706135235424 ) ) ;
#119309 = CARTESIAN_POINT ( 'NONE',  ( 5.049401038298161559, -19.05341960407611168, 32.70724293864768129 ) ) ;
#119310 = CARTESIAN_POINT ( 'NONE',  ( 8.314922557961029526, -14.29746914071037800, 65.41775706135234714 ) ) ;
#119311 = CARTESIAN_POINT ( 'NONE',  ( -15.72974639402197994, 15.80617190586746368, 105.6239096053143669 ) ) ;
#119312 = CARTESIAN_POINT ( 'NONE',  ( -10.81492255796078084, -18.62759615963271287, 97.08224293864770971 ) ) ;
#119314 = CARTESIAN_POINT ( 'NONE',  ( -9.474510206698964154, 16.51473224551069663, 50.41557627198102409 ) ) ;
#119313 = CARTESIAN_POINT ( 'NONE',  ( 9.564922557961047289, -16.46253265017146816, 35.41775706135233293 ) ) ;
#119315 = CARTESIAN_POINT ( 'NONE',  ( -19.02544592524342804, 5.153800228976336051, 116.0405762719810383 ) ) ;
#119316 = CARTESIAN_POINT ( 'NONE',  ( -18.62759615963255300, -10.81492255796106328, 54.16775706135235424 ) ) ;
#119317 = CARTESIAN_POINT ( 'NONE',  ( 18.62759615963271287, -10.81492255796078972, 63.33224293864770260 ) ) ;
#119318 = CARTESIAN_POINT ( 'NONE',  ( -16.53943276465976808, 0.05219959533911058130, 31.24890960531435979 ) ) ;
#119320 = CARTESIAN_POINT ( 'NONE',  ( 5.719274019375673035, 21.55341960407619339, 112.2927570613523471 ) ) ;
#119319 = CARTESIAN_POINT ( 'NONE',  ( -10.81492255796105439, 18.62759615963255655, 82.91775706135234714 ) ) ;
#119321 = CARTESIAN_POINT ( 'NONE',  ( 0.05219959533910956823, 16.53943276465976808, 59.99890960531436690 ) ) ;
#119322 = CARTESIAN_POINT ( 'NONE',  ( 8.314922557960818139, 14.29746914071049879, 109.5822429386476955 ) ) ;
#119323 = CARTESIAN_POINT ( 'NONE',  ( -13.97604488694547697, 13.89961937509957934, 38.12609039468566152 ) ) ;
#119324 = CARTESIAN_POINT ( 'NONE',  ( 16.55341960407618274, -4.379528057220086978, 96.04275706135236135 ) ) ;
#119326 = ADVANCED_FACE ( 'NONE', ( #171567, #33056, #94711 ), #17893, .T. ) ;
#119325 = CARTESIAN_POINT ( 'NONE',  ( -15.72974639402176322, -15.80617190586768395, 69.37609039468567573 ) ) ;
#119327 = CARTESIAN_POINT ( 'NONE',  ( -0.05219959533909027116, -19.03943276465977164, 62.49890960531435979 ) ) ;
#119328 = CARTESIAN_POINT ( 'NONE',  ( 19.05341960407617918, -5.049401038297876454, 31.04275706135232227 ) ) ;
#119329 = CARTESIAN_POINT ( 'NONE',  ( 21.52544592524344225, -5.823673210054117533, 38.54057627198103120 ) ) ;
#119330 = CARTESIAN_POINT ( 'NONE',  ( 5.719274019375673035, 21.55341960407619339, 37.29275706135235424 ) ) ;
#119331 = CARTESIAN_POINT ( 'NONE',  ( 18.62759615963271287, -10.81492255796078972, 88.33224293864769550 ) ) ;
#119332 = CARTESIAN_POINT ( 'NONE',  ( -19.02544592524334988, -5.153800228976617603, 83.95942372801901854 ) ) ;
#119333 = CARTESIAN_POINT ( 'NONE',  ( 4.483927247898790824, -16.52544592524335698, 55.20942372801902565 ) ) ;
#119335 = CARTESIAN_POINT ( 'NONE',  ( -18.62759615963270932, 10.81492255796079327, 95.83224293864770971 ) ) ;
#119334 = CARTESIAN_POINT ( 'NONE',  ( 17.50000000000000000, -5.499999999999992895, 36.21769037696435589 ) ) ;
#119337 = CARTESIAN_POINT ( 'NONE',  ( -16.55341960407611168, -4.379528057220339221, 71.45724293864769550 ) ) ;
#119336 = CARTESIAN_POINT ( 'NONE',  ( 16.53943276465976808, 0.05219959533934440121, 76.25109039468568994 ) ) ;
#119338 = CARTESIAN_POINT ( 'NONE',  ( -1.221313414957698099E-14, 31.90000000000003411, -45.64921306006598201 ) ) ;
#119339 = CARTESIAN_POINT ( 'NONE',  ( -8.224510206698735004, -14.34966873604973081, 24.58442372801901499 ) ) ;
#119340 = CARTESIAN_POINT ( 'NONE',  ( 10.81492255796078972, 18.62759615963270932, 39.58224293864769550 ) ) ;
#119341 = CARTESIAN_POINT ( 'NONE',  ( 12.14591786802327356, -12.06949235617739191, 75.62609039468567573 ) ) ;
#119342 = LINE ( 'NONE', #123280, #183443 ) ;
#119343 = EDGE_CURVE ( 'NONE', #188321, #147696, #98073, .T. ) ;
#119344 = CARTESIAN_POINT ( 'NONE',  ( 14.34966873604972726, -8.224510206698740333, 50.83442372801901143 ) ) ;
#119345 = CARTESIAN_POINT ( 'NONE',  ( 5.719274019375673035, 21.55341960407619339, 27.29275706135234358 ) ) ;
#119346 = CARTESIAN_POINT ( 'NONE',  ( -5.823673210054116645, -21.52544592524344225, 42.29057627198103120 ) ) ;
#119347 = CARTESIAN_POINT ( 'NONE',  ( -8.224510206698735004, -14.34966873604973081, 64.58442372801900433 ) ) ;
#119348 = CARTESIAN_POINT ( 'NONE',  ( -19.02544592524342804, 5.153800228976336051, 86.04057627198103830 ) ) ;
#119350 = CARTESIAN_POINT ( 'NONE',  ( -0.05219959533909027116, -19.03943276465977164, 27.49890960531435624 ) ) ;
#119349 = CARTESIAN_POINT ( 'NONE',  ( 15.80617190586769283, -15.72974639402175789, 60.62609039468567573 ) ) ;
#119351 = CARTESIAN_POINT ( 'NONE',  ( -18.67979575497178146, -10.72451020669898902, 36.66557627198103120 ) ) ;
#119352 = VERTEX_POINT ( 'NONE', #160371 ) ;
#119353 = CARTESIAN_POINT ( 'NONE',  ( -19.03943276465977164, -0.05219959533935918106, 43.75109039468566863 ) ) ;
#119354 = CARTESIAN_POINT ( 'NONE',  ( 12.14591786802327356, -12.06949235617739191, 50.62609039468568994 ) ) ;
#119355 = CARTESIAN_POINT ( 'NONE',  ( -18.62759615963270932, 10.81492255796079327, 25.83224293864769194 ) ) ;
#119356 = ORIENTED_EDGE ( 'NONE', *, *, #82183, .T. ) ;
#119357 = CARTESIAN_POINT ( 'NONE',  ( 19.05341960407611168, 5.049401038298154454, 88.95724293864769550 ) ) ;
#119358 = CARTESIAN_POINT ( 'NONE',  ( 16.52544592524335698, 4.483927247898782831, 106.4594237280190328 ) ) ;
#119359 = FACE_OUTER_BOUND ( 'NONE', #182247, .T. ) ;
#119360 = CARTESIAN_POINT ( 'NONE',  ( -16.52544592524342804, 4.483927247898546575, 101.0405762719810383 ) ) ;
#119361 = CARTESIAN_POINT ( 'NONE',  ( -18.62759615963270932, 10.81492255796079327, 30.83224293864770260 ) ) ;
#119362 = CARTESIAN_POINT ( 'NONE',  ( -19.05341960407611168, -5.049401038298163336, 26.45724293864769550 ) ) ;
#119363 = CARTESIAN_POINT ( 'NONE',  ( 16.55341960407618274, -4.379528057220086978, 76.04275706135237556 ) ) ;
#119364 = CARTESIAN_POINT ( 'NONE',  ( -18.62759615963255300, -10.81492255796106328, 19.16775706135234714 ) ) ;
#119365 = CARTESIAN_POINT ( 'NONE',  ( 13.89961937509957401, 13.97604488694547697, 71.87609039468567573 ) ) ;
#119366 = CARTESIAN_POINT ( 'NONE',  ( 0.05219959533909260263, 19.03943276465977164, 34.99890960531435979 ) ) ;
#119367 = CIRCLE ( 'NONE', #70861, 38.00000000000000000 ) ;
#119368 = CARTESIAN_POINT ( 'NONE',  ( -9.564922557960796823, -16.46253265017161027, 112.0822429386476955 ) ) ;
#119369 = CARTESIAN_POINT ( 'NONE',  ( -5.823673210054431948, 21.52544592524334988, 107.7094237280190328 ) ) ;
#119370 = CARTESIAN_POINT ( 'NONE',  ( -9.564922557960796823, -16.46253265017161027, 67.08224293864769550 ) ) ;
#119371 = CARTESIAN_POINT ( 'NONE',  ( -16.52544592524335698, -4.483927247898792601, 53.95942372801900433 ) ) ;
#119372 = CARTESIAN_POINT ( 'NONE',  ( -15.72974639402176322, -15.80617190586768395, 94.37609039468568994 ) ) ;
#119373 = CARTESIAN_POINT ( 'NONE',  ( -13.97604488694547697, 13.89961937509957934, 58.12609039468566863 ) ) ;
#119374 = EDGE_CURVE ( 'NONE', #179892, #66839, #164922, .T. ) ;
#119375 = CARTESIAN_POINT ( 'NONE',  ( 19.03943276465977164, 0.05219959533936151252, 51.25109039468567573 ) ) ;
#119376 = ORIENTED_EDGE ( 'NONE', *, *, #3003, .T. ) ;
#119377 = CARTESIAN_POINT ( 'NONE',  ( 21.52544592524334988, 5.823673210054432836, 46.45942372801901854 ) ) ;
#119378 = CARTESIAN_POINT ( 'NONE',  ( -18.22780087662119897, 5.500000000000102141, 56.01763182126894947 ) ) ;
#119379 = CARTESIAN_POINT ( 'NONE',  ( -9.474510206698720793, -16.51473224551083518, 39.58442372801899722 ) ) ;
#119380 = CARTESIAN_POINT ( 'NONE',  ( -5.049401038298153566, 19.05341960407611168, 95.20724293864770971 ) ) ;
#119381 = CARTESIAN_POINT ( 'NONE',  ( 9.564922557960805705, 16.46253265017160317, 84.58224293864769550 ) ) ;
#119382 = CARTESIAN_POINT ( 'NONE',  ( -16.52544592524342804, 4.483927247898546575, 41.04057627198103120 ) ) ;
#119383 = CARTESIAN_POINT ( 'NONE',  ( 5.719274019375991003, -21.55341960407610458, 27.70724293864769905 ) ) ;
#119384 = CARTESIAN_POINT ( 'NONE',  ( 22.81625015709509441, 31.40387420917330275, -3.824999997268813345 ) ) ;
#119385 = CARTESIAN_POINT ( 'NONE',  ( 21.53952979013940094, 22.99870628207707668, -49.63989001790915978 ) ) ;
#119386 = CARTESIAN_POINT ( 'NONE',  ( -10.81492255796105439, 18.62759615963255655, 112.9177570613523329 ) ) ;
#119387 = DIRECTION ( 'NONE',  ( 1.000000000000000000, 0.000000000000000000, 0.000000000000000000 ) ) ;
#119388 = CARTESIAN_POINT ( 'NONE',  ( -16.46253265017160317, 9.564922557960807481, 30.83224293864769550 ) ) ;
#119389 = CARTESIAN_POINT ( 'NONE',  ( -0.05219959533909027116, -19.03943276465977164, 27.49890960531435624 ) ) ;
#119390 = CARTESIAN_POINT ( 'NONE',  ( -34.52594549653173317, 2.005792002353502844E-14, 89.49999999999897682 ) ) ;
#119391 = CARTESIAN_POINT ( 'NONE',  ( -11.25158478316796185, -35.59826842325142593, -8.000000000000005329 ) ) ;
#119392 = CARTESIAN_POINT ( 'NONE',  ( 0.05219959533934541429, -16.53943276465976808, 60.00109039468568284 ) ) ;
#119393 = CARTESIAN_POINT ( 'NONE',  ( -5.823673210054116645, -21.52544592524344225, 82.29057627198103830 ) ) ;
#119394 = CARTESIAN_POINT ( 'NONE',  ( 8.224510206698953496, -14.34966873604960469, 42.91557627198103120 ) ) ;
#119396 = CARTESIAN_POINT ( 'NONE',  ( -16.46253265017160317, 9.564922557960807481, 110.8322429386476955 ) ) ;
#119395 = CARTESIAN_POINT ( 'NONE',  ( -13.89961937509977652, 13.97604488694528158, 30.62390960531435269 ) ) ;
#119397 = CARTESIAN_POINT ( 'NONE',  ( -21.55341960407619339, 5.719274019375674811, 33.54275706135234714 ) ) ;
#119398 = CARTESIAN_POINT ( 'NONE',  ( 9.564922557961047289, -16.46253265017146816, 30.41775706135232937 ) ) ;
#119399 = CARTESIAN_POINT ( 'NONE',  ( 5.153800228976335163, 19.02544592524342804, 34.79057627198102409 ) ) ;
#119400 = CARTESIAN_POINT ( 'NONE',  ( -15.80617190586768217, 15.72974639402176855, 78.12609039468570415 ) ) ;
#119401 = CARTESIAN_POINT ( 'NONE',  ( 16.52216118717208815, -7.221426719304489872, 31.42400978953010338 ) ) ;
#119402 = CARTESIAN_POINT ( 'NONE',  ( -14.29746914071049879, 8.314922557960819915, 30.83224293864770260 ) ) ;
#119403 = CARTESIAN_POINT ( 'NONE',  ( 22.73749492396215288, -155.7167183371838064, -4.999999999999999112 ) ) ;
#119404 = CARTESIAN_POINT ( 'NONE',  ( -21.52544592524343514, 5.823673210054127303, 31.04057627198102409 ) ) ;
#119405 = CARTESIAN_POINT ( 'NONE',  ( 16.52544592524342804, -4.483927247898539470, 108.5405762719810241 ) ) ;
#119406 = CARTESIAN_POINT ( 'NONE',  ( -6.328346318964374717, -6.540997098630797701, -63.95112321872120731 ) ) ;
#119407 = CARTESIAN_POINT ( 'NONE',  ( 16.51473224551069308, 9.474510206698969483, 84.16557627198102409 ) ) ;
#119408 = CARTESIAN_POINT ( 'NONE',  ( 16.53943276465976808, -0.05219959533910856209, 78.74890960531436690 ) ) ;
#119409 = CARTESIAN_POINT ( 'NONE',  ( 5.153800228976615827, -19.02544592524334988, 100.2094237280190043 ) ) ;
#119410 = CARTESIAN_POINT ( 'NONE',  ( 10.72451020669898902, -18.67979575497178502, 57.91557627198103120 ) ) ;
#119411 = ORIENTED_EDGE ( 'NONE', *, *, #150161, .T. ) ;
#119412 = CARTESIAN_POINT ( 'NONE',  ( 13.97604488694527802, 13.89961937509977652, 39.37390960531435269 ) ) ;
#119414 = CARTESIAN_POINT ( 'NONE',  ( 5.719274019375991003, -21.55341960407610458, 92.70724293864770971 ) ) ;
#119413 = CARTESIAN_POINT ( 'NONE',  ( -9.564922557960796823, -16.46253265017161027, 82.08224293864768129 ) ) ;
#119416 = CARTESIAN_POINT ( 'NONE',  ( 9.474510206698971260, -16.51473224551069308, 92.91557627198103830 ) ) ;
#119415 = CARTESIAN_POINT ( 'NONE',  ( 0.05219959533934541429, -16.53943276465976808, 100.0010903946857042 ) ) ;
#119417 = CARTESIAN_POINT ( 'NONE',  ( -19.05341960407617563, 5.049401038297882671, 78.54275706135233293 ) ) ;
#119418 = CARTESIAN_POINT ( 'NONE',  ( -21.55341960407619339, 5.719274019375674811, 88.54275706135236135 ) ) ;
#119419 = CARTESIAN_POINT ( 'NONE',  ( 18.67979575497178502, 10.72451020669898547, 79.16557627198103830 ) ) ;
#119420 = CARTESIAN_POINT ( 'NONE',  ( 15.72974639402199770, -15.80617190586745480, 33.12390960531435979 ) ) ;
#119421 = CARTESIAN_POINT ( 'NONE',  ( -19.05341960407611168, -5.049401038298163336, 56.45724293864768129 ) ) ;
#119422 = CARTESIAN_POINT ( 'NONE',  ( 16.55341960407611168, 4.379528057220329451, 23.95724293864769550 ) ) ;
#119423 = CARTESIAN_POINT ( 'NONE',  ( 9.564922557960805705, 16.46253265017160317, 59.58224293864769550 ) ) ;
#119424 = CARTESIAN_POINT ( 'NONE',  ( -32.58888545195123498, -1.708444646721626770, 87.69298048441147841 ) ) ;
#119425 = CARTESIAN_POINT ( 'NONE',  ( -16.46253265017146816, -9.564922557961047289, 34.16775706135233293 ) ) ;
#119426 = CARTESIAN_POINT ( 'NONE',  ( -14.34966873604960291, -8.224510206698953496, 71.66557627198100988 ) ) ;
#119427 = CARTESIAN_POINT ( 'NONE',  ( 5.719274019375991003, -21.55341960407610458, 112.7072429386476955 ) ) ;
#119428 = CARTESIAN_POINT ( 'NONE',  ( 0.05219959533937995610, -21.53943276465977519, 20.00109039468568639 ) ) ;
#119429 = CARTESIAN_POINT ( 'NONE',  ( -6.565813341170984252, 4.458020396767564009, -64.20492216656604967 ) ) ;
#119430 = CARTESIAN_POINT ( 'NONE',  ( -21.52544592524343514, 5.823673210054127303, 61.04057627198103120 ) ) ;
#119431 = CARTESIAN_POINT ( 'NONE',  ( 8.224510206698742110, 14.34966873604972548, 97.08442372801904696 ) ) ;
#119432 = CARTESIAN_POINT ( 'NONE',  ( 14.29746914071049879, -8.314922557960816363, 108.3322429386477097 ) ) ;
#119433 = CARTESIAN_POINT ( 'NONE',  ( -0.05219959533909027116, -19.03943276465977164, 57.49890960531435979 ) ) ;
#119434 = CARTESIAN_POINT ( 'NONE',  ( 0.05219959533910956823, 16.53943276465976808, 29.99890960531435979 ) ) ;
#119435 = CARTESIAN_POINT ( 'NONE',  ( -21.52544592524334988, -5.823673210054445271, 43.95942372801902565 ) ) ;
#119436 = CARTESIAN_POINT ( 'NONE',  ( -9.564922557960796823, -16.46253265017161027, 107.0822429386476955 ) ) ;
#119437 = CARTESIAN_POINT ( 'NONE',  ( 0.05219959533937995610, -21.53943276465977519, 80.00109039468568994 ) ) ;
#119438 = CARTESIAN_POINT ( 'NONE',  ( 19.02544592524343514, -5.153800228976328945, 28.54057627198102409 ) ) ;
#119439 = CARTESIAN_POINT ( 'NONE',  ( 16.46253265017160672, -9.564922557960803928, 38.33224293864768839 ) ) ;
#119440 = ORIENTED_EDGE ( 'NONE', *, *, #50976, .F. ) ;
#119441 = CARTESIAN_POINT ( 'NONE',  ( 21.53943276465977519, 0.05219959533937863772, 81.25109039468568994 ) ) ;
#119442 = CARTESIAN_POINT ( 'NONE',  ( -16.55341960407617563, 4.379528057220093196, 53.54275706135234714 ) ) ;
#119443 = CARTESIAN_POINT ( 'NONE',  ( -10.72451020669870658, -18.67979575497194134, 69.58442372801900433 ) ) ;
#119444 = CARTESIAN_POINT ( 'NONE',  ( -19.05341960407611168, -5.049401038298163336, 106.4572429386476955 ) ) ;
#119445 = CARTESIAN_POINT ( 'NONE',  ( -9.564922557961040184, 16.46253265017147172, 82.91775706135233293 ) ) ;
#119446 = CARTESIAN_POINT ( 'NONE',  ( 21.55341960407619695, -5.719274019375665929, 61.04275706135234714 ) ) ;
#119447 = CARTESIAN_POINT ( 'NONE',  ( -16.55341960407617563, 4.379528057220093196, 28.54275706135234358 ) ) ;
#119448 = CARTESIAN_POINT ( 'NONE',  ( -0.05219959533936034679, 19.03943276465977164, 72.50109039468566152 ) ) ;
#119449 = CARTESIAN_POINT ( 'NONE',  ( -9.474510206698964154, 16.51473224551069663, 55.41557627198103120 ) ) ;
#119450 = CARTESIAN_POINT ( 'NONE',  ( -19.05341960407617563, 5.049401038297882671, 88.54275706135230450 ) ) ;
#119451 = CARTESIAN_POINT ( 'NONE',  ( -14.29746914071049879, 8.314922557960819915, 30.83224293864770260 ) ) ;
#119452 = CARTESIAN_POINT ( 'NONE',  ( -19.03943276465977164, -0.05219959533935918106, 93.75109039468566152 ) ) ;
#119453 = CARTESIAN_POINT ( 'NONE',  ( -4.379528057220328563, 16.55341960407611168, 35.20724293864768839 ) ) ;
#119454 = EDGE_CURVE ( 'NONE', #1233, #171664, #10577, .T. ) ;
#119455 = CARTESIAN_POINT ( 'NONE',  ( 13.89961937509957401, 13.97604488694547697, 61.87609039468566863 ) ) ;
#119456 = CARTESIAN_POINT ( 'NONE',  ( -4.379528057220086978, -16.55341960407618274, 49.79275706135234714 ) ) ;
#119457 = CARTESIAN_POINT ( 'NONE',  ( 13.89961937509957401, 13.97604488694547697, 21.87609039468566152 ) ) ;
#119458 = CARTESIAN_POINT ( 'NONE',  ( -5.049401038298153566, 19.05341960407611168, 45.20724293864769550 ) ) ;
#119459 = CARTESIAN_POINT ( 'NONE',  ( 16.55341960407618274, -4.379528057220086978, 41.04275706135236135 ) ) ;
#119460 = CARTESIAN_POINT ( 'NONE',  ( -23.96320343559627375, 18.46320343559663257, 8.181980515339454030 ) ) ;
#119461 = CARTESIAN_POINT ( 'NONE',  ( 8.906447517083057264, -27.41122689804191026, 142.8500000054623911 ) ) ;
#119462 = CARTESIAN_POINT ( 'NONE',  ( -19.02544592524342804, 5.153800228976336051, 86.04057627198103830 ) ) ;
#119463 = CARTESIAN_POINT ( 'NONE',  ( 5.000000000000003553, -4.999999999999996447, -15.00000000000000000 ) ) ;
#119464 = VERTEX_POINT ( 'NONE', #99687 ) ;
#119465 = CARTESIAN_POINT ( 'NONE',  ( 13.89961937509957401, 13.97604488694547697, 91.87609039468567573 ) ) ;
#119467 = CARTESIAN_POINT ( 'NONE',  ( 21.52544592524344225, -5.823673210054117533, 23.54057627198102765 ) ) ;
#119466 = VECTOR ( 'NONE', #30832, 1000.000000000000000 ) ;
#119469 = CARTESIAN_POINT ( 'NONE',  ( -19.05341960407617563, 5.049401038297882671, 113.5427570613523471 ) ) ;
#119468 = CARTESIAN_POINT ( 'NONE',  ( -18.67979575497193778, 10.72451020669871902, 108.3344237280190185 ) ) ;
#119470 = CARTESIAN_POINT ( 'NONE',  ( -14.29746914071049879, 8.314922557960819915, 105.8322429386476955 ) ) ;
#119471 = CARTESIAN_POINT ( 'NONE',  ( -16.51473224551069308, -9.474510206698971260, 41.66557627198103120 ) ) ;
#119472 = CARTESIAN_POINT ( 'NONE',  ( -10.81492255796078084, -18.62759615963271287, 77.08224293864769550 ) ) ;
#119473 = CARTESIAN_POINT ( 'NONE',  ( 16.46253265017160672, -9.564922557960803928, 43.33224293864769550 ) ) ;
#119474 = CARTESIAN_POINT ( 'NONE',  ( -13.97604488694547520, 13.89961937509957934, 48.12609039468566863 ) ) ;
#119475 = CARTESIAN_POINT ( 'NONE',  ( -9.564922557961040184, 16.46253265017147172, 67.91775706135233293 ) ) ;
#119476 = CARTESIAN_POINT ( 'NONE',  ( 0.05219959533910956823, 16.53943276465976808, 59.99890960531436690 ) ) ;
#119477 = CARTESIAN_POINT ( 'NONE',  ( -10.81492255796078084, -18.62759615963271287, 32.08224293864769550 ) ) ;
#119478 = CARTESIAN_POINT ( 'NONE',  ( 18.62759615963255655, 10.81492255796105972, 96.66775706135234714 ) ) ;
#119479 = CARTESIAN_POINT ( 'NONE',  ( 21.53943276465977519, -0.05219959533907433946, 88.74890960531436690 ) ) ;
#119480 = CARTESIAN_POINT ( 'NONE',  ( 21.55341960407619695, -5.719274019375665929, 71.04275706135234714 ) ) ;
#119481 = CARTESIAN_POINT ( 'NONE',  ( -21.52544592524334988, -5.823673210054445271, 68.95942372801901854 ) ) ;
#119482 = EDGE_CURVE ( 'NONE', #48307, #127799, #191702, .T. ) ;
#119483 = CARTESIAN_POINT ( 'NONE',  ( -0.05219959533909027116, -19.03943276465977164, 102.4989096053143669 ) ) ;
#119485 = CARTESIAN_POINT ( 'NONE',  ( -21.55341960407619339, 5.719274019375674811, 68.54275706135234714 ) ) ;
#119484 = CARTESIAN_POINT ( 'NONE',  ( -12.14591786802326823, 12.06949235617739902, 88.12609039468570415 ) ) ;
#119486 = CARTESIAN_POINT ( 'NONE',  ( -9.564922557960796823, -16.46253265017161027, 52.08224293864768839 ) ) ;
#119487 = CARTESIAN_POINT ( 'NONE',  ( 16.51473224551069308, 9.474510206698969483, 29.16557627198103475 ) ) ;
#119488 = CARTESIAN_POINT ( 'NONE',  ( -13.97604488694527625, -13.89961937509977652, 71.87390960531433848 ) ) ;
#119489 = CARTESIAN_POINT ( 'NONE',  ( -16.53943276465976808, 0.05219959533911058130, 71.24890960531435269 ) ) ;
#119490 = CARTESIAN_POINT ( 'NONE',  ( -14.34966873604960291, -8.224510206698953496, 36.66557627198103120 ) ) ;
#119491 = CARTESIAN_POINT ( 'NONE',  ( -5.719274019375978568, 21.55341960407610458, 50.20724293864769550 ) ) ;
#119492 = CARTESIAN_POINT ( 'NONE',  ( -16.51473224551069308, -9.474510206698971260, 41.66557627198103120 ) ) ;
#119493 = CARTESIAN_POINT ( 'NONE',  ( 0.05219959533907565091, 21.53943276465977519, 64.99890960531435269 ) ) ;
#119494 = CARTESIAN_POINT ( 'NONE',  ( -9.564922557961040184, 16.46253265017147172, 52.91775706135233293 ) ) ;
#119496 = CARTESIAN_POINT ( 'NONE',  ( 14.29746914071049879, -8.314922557960816363, 63.33224293864770260 ) ) ;
#119495 = CARTESIAN_POINT ( 'NONE',  ( 25.90238458237720565, 6.509645158105397122, 161.8463118039489643 ) ) ;
#119498 = CIRCLE ( 'NONE', #6440, 5.500000000000032863 ) ;
#119497 = CARTESIAN_POINT ( 'NONE',  ( 21.55341960407610458, 5.719274019375980345, 43.95724293864769550 ) ) ;
#119499 = VERTEX_POINT ( 'NONE', #24876 ) ;
#119500 = EDGE_LOOP ( 'NONE', ( #75060, #6214 ) ) ;
#119501 = LINE ( 'NONE', #89147, #30224 ) ;
#119502 = CARTESIAN_POINT ( 'NONE',  ( 16.53943276465976808, 0.05219959533934440121, 86.25109039468568994 ) ) ;
#119503 = CARTESIAN_POINT ( 'NONE',  ( 16.51473224551083163, -9.474510206698727899, 80.83442372801899012 ) ) ;
#119504 = CARTESIAN_POINT ( 'NONE',  ( 0.05219959533910956823, 16.53943276465976808, 49.99890960531437401 ) ) ;
#119505 = DIRECTION ( 'NONE',  ( -1.000000000000000000, 0.000000000000000000, 0.000000000000000000 ) ) ;
#119506 = CARTESIAN_POINT ( 'NONE',  ( 9.564922557960805705, 16.46253265017160317, 49.58224293864770260 ) ) ;
#119507 = CARTESIAN_POINT ( 'NONE',  ( -8.224510206698948167, 14.34966873604960824, 35.41557627198102409 ) ) ;
#119508 = CARTESIAN_POINT ( 'NONE',  ( 9.474510206698971260, -16.51473224551069308, 52.91557627198102409 ) ) ;
#119509 = CARTESIAN_POINT ( 'NONE',  ( -0.05219959533909027116, -19.03943276465977164, 77.49890960531435269 ) ) ;
#119510 = CARTESIAN_POINT ( 'NONE',  ( -0.05219959533909027116, -19.03943276465977164, 37.49890960531436690 ) ) ;
#119511 = CARTESIAN_POINT ( 'NONE',  ( -0.05219959533937732626, 21.53943276465977519, 42.50109039468567573 ) ) ;
#119512 = CARTESIAN_POINT ( 'NONE',  ( -5.049401038298153566, 19.05341960407611168, 70.20724293864769550 ) ) ;
#119513 = CARTESIAN_POINT ( 'NONE',  ( 5.049401038298161559, -19.05341960407611168, 22.70724293864769194 ) ) ;
#119514 = CARTESIAN_POINT ( 'NONE',  ( -5.049401038298153566, 19.05341960407611168, 65.20724293864765286 ) ) ;
#119515 = CARTESIAN_POINT ( 'NONE',  ( -18.62759615963270932, 10.81492255796079327, 45.83224293864769550 ) ) ;
#119516 = CARTESIAN_POINT ( 'NONE',  ( 19.03943276465977164, -0.05219959533909143690, 38.74890960531436690 ) ) ;
#119517 = CARTESIAN_POINT ( 'NONE',  ( -10.81492255796078084, -18.62759615963271287, 42.08224293864769550 ) ) ;
#119518 = CARTESIAN_POINT ( 'NONE',  ( 14.29746914071037800, 8.314922557961029526, 106.6677570613523756 ) ) ;
#119519 = CARTESIAN_POINT ( 'NONE',  ( -19.05341960407617563, 5.049401038297882671, 28.54275706135232937 ) ) ;
#119521 = CARTESIAN_POINT ( 'NONE',  ( -16.55341960407617563, 4.379528057220093196, 78.54275706135236135 ) ) ;
#119520 = CARTESIAN_POINT ( 'NONE',  ( -4.483927247898782831, 16.52544592524335698, 52.70942372801902565 ) ) ;
#119522 = CARTESIAN_POINT ( 'NONE',  ( -29.15849868437705439, -10.00000000000000000, 150.0000000000000000 ) ) ;
#119523 = CARTESIAN_POINT ( 'NONE',  ( -16.53943276465976808, -0.05219959533934237506, 63.75109039468568284 ) ) ;
#119524 = CARTESIAN_POINT ( 'NONE',  ( -12.06949235617739369, -12.14591786802326823, 39.37609039468567573 ) ) ;
#119525 = CARTESIAN_POINT ( 'NONE',  ( 9.564922557960805705, 16.46253265017160317, 104.5822429386476955 ) ) ;
#119526 = CARTESIAN_POINT ( 'NONE',  ( 16.53943276465976808, 0.05219959533934440121, 41.25109039468568284 ) ) ;
#119527 = CARTESIAN_POINT ( 'NONE',  ( -9.474510206698964154, 16.51473224551069663, 30.41557627198102054 ) ) ;
#119528 = CARTESIAN_POINT ( 'NONE',  ( 0.05219959533937995610, -21.53943276465977519, 25.00109039468567218 ) ) ;
#119529 = CARTESIAN_POINT ( 'NONE',  ( 16.55341960407618274, -4.379528057220086978, 31.04275706135234714 ) ) ;
#119530 = CARTESIAN_POINT ( 'NONE',  ( -4.483927247898782831, 16.52544592524335698, 102.7094237280190185 ) ) ;
#119531 = FACE_OUTER_BOUND ( 'NONE', #3292, .T. ) ;
#119532 = CARTESIAN_POINT ( 'NONE',  ( -21.53943276465977519, -0.05219959533937600094, 103.7510903946857042 ) ) ;
#119533 = CARTESIAN_POINT ( 'NONE',  ( 19.03943276465977164, 0.05219959533936151252, 96.25109039468567573 ) ) ;
#119534 = CARTESIAN_POINT ( 'NONE',  ( 4.483927247898545687, 16.52544592524342804, 59.79057627198103120 ) ) ;
#119535 = CARTESIAN_POINT ( 'NONE',  ( -16.51473224551069308, -9.474510206698971260, 21.66557627198102765 ) ) ;
#119537 = CARTESIAN_POINT ( 'NONE',  ( 16.19135201231351218, -7.376712067592053224, 57.31319145947882987 ) ) ;
#119536 = CARTESIAN_POINT ( 'NONE',  ( 13.89961937509957401, 13.97604488694547697, 66.87609039468567573 ) ) ;
#119538 = CARTESIAN_POINT ( 'NONE',  ( 0.05219959533937995610, -21.53943276465977519, 60.00109039468568284 ) ) ;
#119539 = CARTESIAN_POINT ( 'NONE',  ( 0.05219959533934541429, -16.53943276465976808, 30.00109039468568284 ) ) ;
#119540 = CARTESIAN_POINT ( 'NONE',  ( 38.00373040315627549, 2.428612866367529932E-14, -0.1220970790697140096 ) ) ;
#119541 = CARTESIAN_POINT ( 'NONE',  ( 19.03943276465977164, -0.05219959533909143690, 113.7489096053143669 ) ) ;
#119542 = CARTESIAN_POINT ( 'NONE',  ( -5.719274019375978568, 21.55341960407610458, 75.20724293864769550 ) ) ;
#119543 = CARTESIAN_POINT ( 'NONE',  ( 5.153800228976615827, -19.02544592524334988, 110.2094237280189901 ) ) ;
#119544 = CARTESIAN_POINT ( 'NONE',  ( 9.564922557960805705, 16.46253265017160317, 104.5822429386476955 ) ) ;
#119545 = CARTESIAN_POINT ( 'NONE',  ( -26.26139018963108285, 3.005588016160658071, 174.9127113745526572 ) ) ;
#119546 = CARTESIAN_POINT ( 'NONE',  ( -9.474510206698964154, 16.51473224551069663, 25.41557627198103120 ) ) ;
#119547 = CARTESIAN_POINT ( 'NONE',  ( -21.53943276465977519, -0.05219959533937600094, 108.7510903946857042 ) ) ;
#119548 = CARTESIAN_POINT ( 'NONE',  ( 5.153800228976335163, 19.02544592524342804, 44.79057627198103830 ) ) ;
#119549 = CARTESIAN_POINT ( 'NONE',  ( -18.62759615963255300, -10.81492255796106328, 54.16775706135235424 ) ) ;
#119550 = CARTESIAN_POINT ( 'NONE',  ( 18.62759615963255655, 10.81492255796105972, 96.66775706135234714 ) ) ;
#119551 = CARTESIAN_POINT ( 'NONE',  ( -16.53943276465976808, -0.05219959533934237506, 108.7510903946857042 ) ) ;
#119552 = CARTESIAN_POINT ( 'NONE',  ( 0.05219959533909260263, 19.03943276465977164, 84.99890960531436690 ) ) ;
#119553 = CARTESIAN_POINT ( 'NONE',  ( -18.67979575497193778, 10.72451020669871902, 43.33442372801901143 ) ) ;
#119554 = CARTESIAN_POINT ( 'NONE',  ( 15.80617190586769283, -15.72974639402175789, 55.62609039468568284 ) ) ;
#119556 = CARTESIAN_POINT ( 'NONE',  ( 9.474510206698971260, -16.51473224551069308, 87.91557627198102409 ) ) ;
#119555 = CARTESIAN_POINT ( 'NONE',  ( 13.97604488694548053, -13.89961937509957401, 80.62609039468567573 ) ) ;
#119557 = CARTESIAN_POINT ( 'NONE',  ( 16.52544592524342804, -4.483927247898539470, 98.54057627198105251 ) ) ;
#119558 = CARTESIAN_POINT ( 'NONE',  ( 0.05219959533907565091, 21.53943276465977519, 94.99890960531436690 ) ) ;
#119559 = CARTESIAN_POINT ( 'NONE',  ( 15.72974639402176855, 15.80617190586768217, 111.8760903946856615 ) ) ;
#119560 = CARTESIAN_POINT ( 'NONE',  ( -12.14591786802309592, -12.06949235617757132, 91.87390960531436690 ) ) ;
#119561 = CARTESIAN_POINT ( 'NONE',  ( 19.05341960407611168, 5.049401038298154454, 48.95724293864768129 ) ) ;
#119562 = CARTESIAN_POINT ( 'NONE',  ( 19.03943276465977164, 0.05219959533936151252, 81.25109039468567573 ) ) ;
#119563 = CARTESIAN_POINT ( 'NONE',  ( 14.29746914071049879, -8.314922557960816363, 43.33224293864769550 ) ) ;
#119564 = CARTESIAN_POINT ( 'NONE',  ( 15.72974639402176855, 15.80617190586768217, 101.8760903946857042 ) ) ;
#119565 = CARTESIAN_POINT ( 'NONE',  ( 13.97604488694527802, 13.89961937509977652, 109.3739096053143669 ) ) ;
#119566 = CARTESIAN_POINT ( 'NONE',  ( -9.474510206698720793, -16.51473224551083518, 69.58442372801901854 ) ) ;
#119567 = CARTESIAN_POINT ( 'NONE',  ( 21.52544592524344225, -5.823673210054117533, 73.54057627198102409 ) ) ;
#119568 = CARTESIAN_POINT ( 'NONE',  ( 18.67979575497194134, -10.72451020669871369, 35.83442372801901143 ) ) ;
#119569 = CARTESIAN_POINT ( 'NONE',  ( 16.52544592524335698, 4.483927247898782831, 31.45942372801901854 ) ) ;
#119570 = CARTESIAN_POINT ( 'NONE',  ( -8.224510206698735004, -14.34966873604973081, 94.58442372801901854 ) ) ;
#119572 = CARTESIAN_POINT ( 'NONE',  ( -18.67979575497193778, 10.72451020669871902, 38.33442372801900433 ) ) ;
#119571 = CARTESIAN_POINT ( 'NONE',  ( 5.153800228976335163, 19.02544592524342804, 29.79057627198102409 ) ) ;
#119573 = CARTESIAN_POINT ( 'NONE',  ( 10.72451020669898902, -18.67979575497178502, 37.91557627198102409 ) ) ;
#119574 = CARTESIAN_POINT ( 'NONE',  ( -13.97604488694527625, -13.89961937509977652, 21.87390960531435979 ) ) ;
#119575 = CARTESIAN_POINT ( 'NONE',  ( -30.74264578624800492, -22.33583958711396278, -11.54999999453762527 ) ) ;
#119576 = CARTESIAN_POINT ( 'NONE',  ( 12.06949235617739724, 12.14591786802326823, 56.87609039468568994 ) ) ;
#119577 = CARTESIAN_POINT ( 'NONE',  ( 14.34966873604960469, 8.224510206698951720, 94.16557627198103830 ) ) ;
#119578 = CARTESIAN_POINT ( 'NONE',  ( 0.05219959533907565091, 21.53943276465977519, 69.99890960531435269 ) ) ;
#119579 = CARTESIAN_POINT ( 'NONE',  ( -8.314922557960811034, -14.29746914071050412, 27.08224293864769550 ) ) ;
#119580 = CARTESIAN_POINT ( 'NONE',  ( -14.34966873604972548, 8.224510206698743886, 43.33442372801901143 ) ) ;
#119581 = CARTESIAN_POINT ( 'NONE',  ( -16.51473224551069308, -9.474510206698971260, 46.66557627198102409 ) ) ;
#119582 = CARTESIAN_POINT ( 'NONE',  ( 4.379528057220092307, 16.55341960407617563, 97.29275706135234714 ) ) ;
#119583 = CARTESIAN_POINT ( 'NONE',  ( 16.46253265017146816, 9.564922557961045513, 81.66775706135233293 ) ) ;
#119584 = CARTESIAN_POINT ( 'NONE',  ( 5.823673210054125526, 21.52544592524343514, 89.79057627198103830 ) ) ;
#119585 = CARTESIAN_POINT ( 'NONE',  ( 8.314922557961029526, -14.29746914071037800, 105.4177570613523613 ) ) ;
#119586 = ORIENTED_EDGE ( 'NONE', *, *, #140816, .F. ) ;
#119587 = CARTESIAN_POINT ( 'NONE',  ( 21.73861122199407347, 7.688394669363296963, 173.2969830217476499 ) ) ;
#119588 = CARTESIAN_POINT ( 'NONE',  ( 18.67979575497178502, 10.72451020669898547, 64.16557627198102409 ) ) ;
#119589 = CARTESIAN_POINT ( 'NONE',  ( -0.05219959533934338120, 16.53943276465976808, 87.50109039468568994 ) ) ;
#119590 = ORIENTED_EDGE ( 'NONE', *, *, #106006, .F. ) ;
#119591 = CARTESIAN_POINT ( 'NONE',  ( -21.55341960407610458, -5.719274019375992779, 31.45724293864769550 ) ) ;
#119592 = LINE ( 'NONE', #60870, #156644 ) ;
#119593 = CARTESIAN_POINT ( 'NONE',  ( -15.80617190586745835, -15.72974639402198527, 91.87390960531436690 ) ) ;
#119594 = CARTESIAN_POINT ( 'NONE',  ( 0.05219959533910956823, 16.53943276465976808, 29.99890960531435979 ) ) ;
#119595 = CARTESIAN_POINT ( 'NONE',  ( 5.153800228976615827, -19.02544592524334988, 110.2094237280189901 ) ) ;
#119596 = CARTESIAN_POINT ( 'NONE',  ( -16.46253265017160317, 9.564922557960807481, 35.83224293864768839 ) ) ;
#119597 = CARTESIAN_POINT ( 'NONE',  ( -16.55341960407617563, 4.379528057220093196, 23.54275706135235424 ) ) ;
#119598 = CARTESIAN_POINT ( 'NONE',  ( 9.474510206698971260, -16.51473224551069308, 47.91557627198102409 ) ) ;
#119599 = CARTESIAN_POINT ( 'NONE',  ( -8.906447517083053711, -27.41122689804191026, 146.4000000000000057 ) ) ;
#119600 = CARTESIAN_POINT ( 'NONE',  ( 19.05341960407611168, 5.049401038298154454, 103.9572429386476671 ) ) ;
#119601 = CARTESIAN_POINT ( 'NONE',  ( 16.51473224551069308, 9.474510206698969483, 104.1655762719810241 ) ) ;
#119602 = CARTESIAN_POINT ( 'NONE',  ( 8.224510206698742110, 14.34966873604972548, 92.08442372801901854 ) ) ;
#119603 = CARTESIAN_POINT ( 'NONE',  ( -13.89961937509957401, -13.97604488694547875, 89.37609039468563310 ) ) ;
#119604 = CARTESIAN_POINT ( 'NONE',  ( -5.153800228976607833, 19.02544592524334988, 37.70942372801899722 ) ) ;
#119605 = CARTESIAN_POINT ( 'NONE',  ( -21.55341960407610458, -5.719274019375992779, 71.45724293864769550 ) ) ;
#119606 = CARTESIAN_POINT ( 'NONE',  ( -8.314922557961024197, 14.29746914071037800, 97.91775706135236135 ) ) ;
#119607 = CARTESIAN_POINT ( 'NONE',  ( -21.52544592524343514, 5.823673210054127303, 36.04057627198102409 ) ) ;
#119608 = CARTESIAN_POINT ( 'NONE',  ( 5.049401038297881783, 19.05341960407617563, 87.29275706135234714 ) ) ;
#119609 = CARTESIAN_POINT ( 'NONE',  ( -19.03943276465977164, 0.05219959533909376836, 51.24890960531436690 ) ) ;
#119610 = CARTESIAN_POINT ( 'NONE',  ( 19.05341960407611168, 5.049401038298154454, 93.95724293864769550 ) ) ;
#119611 = CARTESIAN_POINT ( 'NONE',  ( 0.05219959533937995610, -21.53943276465977519, 65.00109039468568994 ) ) ;
#119612 = CARTESIAN_POINT ( 'NONE',  ( 5.153800228976335163, 19.02544592524342804, 59.79057627198100988 ) ) ;
#119613 = CARTESIAN_POINT ( 'NONE',  ( -16.55341960407611168, -4.379528057220339221, 101.4572429386476955 ) ) ;
#119614 = CARTESIAN_POINT ( 'NONE',  ( -17.40861289039003879, -6.110651285853240466, 86.37232470827434838 ) ) ;
#119615 = CARTESIAN_POINT ( 'NONE',  ( -8.314922557960811034, -14.29746914071050412, 82.08224293864768129 ) ) ;
#119616 = CARTESIAN_POINT ( 'NONE',  ( 21.52544592524344225, -5.823673210054117533, 68.54057627198103830 ) ) ;
#119617 = CARTESIAN_POINT ( 'NONE',  ( -13.89961937509957401, -13.97604488694547875, 89.37609039468563310 ) ) ;
#119618 = DIRECTION ( 'NONE',  ( -0.000000000000000000, -0.000000000000000000, 1.000000000000000000 ) ) ;
#119619 = CARTESIAN_POINT ( 'NONE',  ( -16.51473224551069308, -9.474510206698971260, 56.66557627198103120 ) ) ;
#119620 = DIRECTION ( 'NONE',  ( 0.000000000000000000, 0.7071067811865483499, 0.7071067811865465735 ) ) ;
#119622 = CARTESIAN_POINT ( 'NONE',  ( -19.03943276465977164, 0.05219959533909376836, 86.24890960531436690 ) ) ;
#119621 = CARTESIAN_POINT ( 'NONE',  ( 19.05341960407611168, 5.049401038298154454, 73.95724293864768129 ) ) ;
#119623 = CARTESIAN_POINT ( 'NONE',  ( -14.29746914071037622, -8.314922557961029526, 69.16775706135234714 ) ) ;
#119624 = DIRECTION ( 'NONE',  ( 0.9526137857479310966, -0.3041824702427718408, 0.000000000000000000 ) ) ;
#119625 = CARTESIAN_POINT ( 'NONE',  ( -9.564922557961040184, 16.46253265017147172, 37.91775706135233293 ) ) ;
#119626 = CARTESIAN_POINT ( 'NONE',  ( 5.000000000000003553, -4.999999999999996447, -18.00000000000000000 ) ) ;
#119627 = CARTESIAN_POINT ( 'NONE',  ( 16.46253265017160672, -9.564922557960803928, 113.3322429386476955 ) ) ;
#119628 = CARTESIAN_POINT ( 'NONE',  ( -4.379528057220086978, -16.55341960407618274, 99.79275706135234714 ) ) ;
#119629 = CARTESIAN_POINT ( 'NONE',  ( -34.54531151325589633, -4.968019249220468225, 50.63996542006479729 ) ) ;
#119630 = CARTESIAN_POINT ( 'NONE',  ( 8.314922557961029526, -14.29746914071037800, 95.41775706135234714 ) ) ;
#119631 = DIRECTION ( 'NONE',  ( 1.000000000000000000, 0.000000000000000000, 0.000000000000000000 ) ) ;
#119632 = CARTESIAN_POINT ( 'NONE',  ( 8.314922557961029526, -14.29746914071037800, 65.41775706135234714 ) ) ;
#119633 = CARTESIAN_POINT ( 'NONE',  ( 4.000000000000000888, -165.0000000000000000, -23.00000000000000000 ) ) ;
#119634 = CARTESIAN_POINT ( 'NONE',  ( 21.55341960407619695, -5.719274019375665929, 66.04275706135236135 ) ) ;
#119635 = CARTESIAN_POINT ( 'NONE',  ( -16.46253265017146816, -9.564922557961047289, 74.16775706135234714 ) ) ;
#119636 = CARTESIAN_POINT ( 'NONE',  ( -5.049401038297874678, -19.05341960407617918, 29.79275706135232227 ) ) ;
#119637 = CARTESIAN_POINT ( 'NONE',  ( 5.153800228976335163, 19.02544592524342804, 59.79057627198100988 ) ) ;
#119638 = CARTESIAN_POINT ( 'NONE',  ( 19.05341960407611168, 5.049401038298154454, 38.95724293864767418 ) ) ;
#119639 = CARTESIAN_POINT ( 'NONE',  ( -19.99999999999998224, -180.0000000000000000, -15.00000000000000178 ) ) ;
#119640 = CARTESIAN_POINT ( 'NONE',  ( -0.05219959533907301413, -21.53943276465977519, 82.49890960531436690 ) ) ;
#119641 = AXIS2_PLACEMENT_3D ( 'NONE', #25777, #54092, #134944 ) ;
#119642 = CARTESIAN_POINT ( 'NONE',  ( 21.52544592524344225, -5.823673210054117533, 33.54057627198102409 ) ) ;
#119643 = CARTESIAN_POINT ( 'NONE',  ( 8.314922557960818139, 14.29746914071049879, 109.5822429386476955 ) ) ;
#119644 = CARTESIAN_POINT ( 'NONE',  ( 12.14591786802327356, -12.06949235617739191, 50.62609039468568994 ) ) ;
#119645 = ORIENTED_EDGE ( 'NONE', *, *, #15702, .T. ) ;
#119646 = CARTESIAN_POINT ( 'NONE',  ( 15.80617190586769283, -15.72974639402175789, 30.62609039468567929 ) ) ;
#119648 = CARTESIAN_POINT ( 'NONE',  ( 38.00000000000000000, 12.34694845685046616, -6.899999999999999467 ) ) ;
#119647 = CARTESIAN_POINT ( 'NONE',  ( -16.55341960407611168, -4.379528057220339221, 56.45724293864768839 ) ) ;
#119649 = CARTESIAN_POINT ( 'NONE',  ( 16.53943276465976808, 0.05219959533934440121, 26.25109039468567573 ) ) ;
#119650 = CARTESIAN_POINT ( 'NONE',  ( 13.89961937509957401, 13.97604488694547697, 36.87609039468565442 ) ) ;
#119651 = CARTESIAN_POINT ( 'NONE',  ( 0.05219959533910956823, 16.53943276465976808, 49.99890960531437401 ) ) ;
#119652 = CARTESIAN_POINT ( 'NONE',  ( -5.719274019375978568, 21.55341960407610458, 110.2072429386477239 ) ) ;
#119654 = CARTESIAN_POINT ( 'NONE',  ( 5.719274019375991003, -21.55341960407610458, 77.70724293864770971 ) ) ;
#119653 = CARTESIAN_POINT ( 'NONE',  ( 1.500000000000000888, 15.20000000000002061, -59.79525829764741474 ) ) ;
#119655 = CARTESIAN_POINT ( 'NONE',  ( -19.05341960407611168, -5.049401038298163336, 96.45724293864769550 ) ) ;
#119656 = CARTESIAN_POINT ( 'NONE',  ( 8.224510206698953496, -14.34966873604960469, 62.91557627198102409 ) ) ;
#119657 = CARTESIAN_POINT ( 'NONE',  ( 16.51473224551069308, 9.474510206698969483, 99.16557627198102409 ) ) ;
#119658 = CARTESIAN_POINT ( 'NONE',  ( -36.86305638906667781, 5.498848518248649064, 44.61989603102465196 ) ) ;
#119659 = CARTESIAN_POINT ( 'NONE',  ( 19.03943276465977164, 0.05219959533936151252, 66.25109039468567573 ) ) ;
#119660 = CARTESIAN_POINT ( 'NONE',  ( -18.67979575497178146, -10.72451020669898902, 106.6655762719810383 ) ) ;
#119661 = CARTESIAN_POINT ( 'NONE',  ( -9.474510206698964154, 16.51473224551069663, 55.41557627198103120 ) ) ;
#119662 = CARTESIAN_POINT ( 'NONE',  ( 5.049401038298161559, -19.05341960407611168, 22.70724293864769194 ) ) ;
#119663 = CARTESIAN_POINT ( 'NONE',  ( -10.72451020669870658, -18.67979575497194134, 49.58442372801901143 ) ) ;
#119664 = CARTESIAN_POINT ( 'NONE',  ( -27.73933785331498925, 9.013057229001089965, 146.7750000027312183 ) ) ;
#119665 = CARTESIAN_POINT ( 'NONE',  ( -0.05219959533910754901, -16.53943276465976808, 37.49890960531436690 ) ) ;
#119666 = CARTESIAN_POINT ( 'NONE',  ( -0.05219959533909027116, -19.03943276465977164, 52.49890960531436690 ) ) ;
#119667 = CARTESIAN_POINT ( 'NONE',  ( 5.153800228976335163, 19.02544592524342804, 109.7905762719810099 ) ) ;
#119668 = CARTESIAN_POINT ( 'NONE',  ( 18.62759615963271287, -10.81492255796078972, 68.33224293864769550 ) ) ;
#119669 = CARTESIAN_POINT ( 'NONE',  ( 8.571926809382597767, 26.38167802310806209, 142.2750000027311899 ) ) ;
#119670 = CARTESIAN_POINT ( 'NONE',  ( -16.46253265017160317, 9.564922557960807481, 50.83224293864770260 ) ) ;
#119671 = CARTESIAN_POINT ( 'NONE',  ( 18.67979575497178502, 10.72451020669898547, 69.16557627198102409 ) ) ;
#119672 = CARTESIAN_POINT ( 'NONE',  ( 15.72974639402176855, 15.80617190586768217, 86.87609039468568994 ) ) ;
#119675 = CARTESIAN_POINT ( 'NONE',  ( 16.52544592524342804, -4.483927247898539470, 83.54057627198102409 ) ) ;
#119674 = CARTESIAN_POINT ( 'NONE',  ( -16.53943276465976808, -0.05219959533934237506, 83.75109039468568994 ) ) ;
#119673 = CARTESIAN_POINT ( 'NONE',  ( 17.49999999999999645, 5.500000000000010658, 53.78230962303567964 ) ) ;
#119676 = CARTESIAN_POINT ( 'NONE',  ( -5.049401038298153566, 19.05341960407611168, 75.20724293864769550 ) ) ;
#119677 = ORIENTED_EDGE ( 'NONE', *, *, #20984, .F. ) ;
#119678 = CARTESIAN_POINT ( 'NONE',  ( -19.05341960407617563, 5.049401038297882671, 43.54275706135232582 ) ) ;
#119679 = CARTESIAN_POINT ( 'NONE',  ( 14.29746914071037800, 8.314922557961029526, 91.66775706135234714 ) ) ;
#119680 = CARTESIAN_POINT ( 'NONE',  ( -15.80617190586768217, 15.72974639402176855, 113.1260903946856899 ) ) ;
#119681 = CARTESIAN_POINT ( 'NONE',  ( -0.05219959533909027116, -19.03943276465977164, 92.49890960531436690 ) ) ;
#119682 = CARTESIAN_POINT ( 'NONE',  ( -5.719274019375978568, 21.55341960407610458, 45.20724293864769550 ) ) ;
#119683 = CARTESIAN_POINT ( 'NONE',  ( 15.72974639402176855, 15.80617190586768217, 96.87609039468568994 ) ) ;
#119684 = CARTESIAN_POINT ( 'NONE',  ( -14.29746914071037622, -8.314922557961029526, 59.16775706135234714 ) ) ;
#119685 = CARTESIAN_POINT ( 'NONE',  ( 21.53943276465977519, -0.05219959533907433946, 108.7489096053143669 ) ) ;
#119686 = CARTESIAN_POINT ( 'NONE',  ( 0.05219959533934541429, -16.53943276465976808, 30.00109039468568284 ) ) ;
#119687 = CARTESIAN_POINT ( 'NONE',  ( -9.474510206698964154, 16.51473224551069663, 90.41557627198103830 ) ) ;
#119688 = CARTESIAN_POINT ( 'NONE',  ( 16.55341960407618274, -4.379528057220086978, 31.04275706135234714 ) ) ;
#119689 = CARTESIAN_POINT ( 'NONE',  ( 9.474510206698971260, -16.51473224551069308, 52.91557627198102409 ) ) ;
#119690 = CARTESIAN_POINT ( 'NONE',  ( -8.314922557961024197, 14.29746914071037800, 27.91775706135234358 ) ) ;
#119691 = CARTESIAN_POINT ( 'NONE',  ( -4.483927247898539470, -16.52544592524342804, 82.29057627198103830 ) ) ;
#119692 = EDGE_CURVE ( 'NONE', #141411, #101229, #74305, .T. ) ;
#119693 = CARTESIAN_POINT ( 'NONE',  ( -14.34966873604972548, 8.224510206698743886, 93.33442372801901854 ) ) ;
#119695 = CARTESIAN_POINT ( 'NONE',  ( -19.05341960407611168, -5.049401038298163336, 71.45724293864766707 ) ) ;
#119694 = CARTESIAN_POINT ( 'NONE',  ( 10.81492255796106328, -18.62759615963255655, 40.41775706135234714 ) ) ;
#119696 = CARTESIAN_POINT ( 'NONE',  ( 16.46253265017160672, -9.564922557960803928, 88.33224293864769550 ) ) ;
#119697 = CARTESIAN_POINT ( 'NONE',  ( -16.52544592524342804, 4.483927247898546575, 36.04057627198102409 ) ) ;
#119698 = CARTESIAN_POINT ( 'NONE',  ( 14.29746914071037800, 8.314922557961029526, 81.66775706135236135 ) ) ;
#119699 = ORIENTED_EDGE ( 'NONE', *, *, #128937, .F. ) ;
#119700 = CARTESIAN_POINT ( 'NONE',  ( 16.46253265017146816, 9.564922557961045513, 26.66775706135234003 ) ) ;
#119701 = CARTESIAN_POINT ( 'NONE',  ( 19.03943276465977164, -0.05219959533909143690, 98.74890960531436690 ) ) ;
#119702 = CARTESIAN_POINT ( 'NONE',  ( 16.46253265017160672, -9.564922557960803928, 48.33224293864769550 ) ) ;
#119703 = CARTESIAN_POINT ( 'NONE',  ( -36.91746825000000598, 2.428612866367529932E-14, -4.624999997268814056 ) ) ;
#119704 = CARTESIAN_POINT ( 'NONE',  ( -12.14591786802326823, 12.06949235617739902, 43.12609039468568284 ) ) ;
#119706 = CARTESIAN_POINT ( 'NONE',  ( -12.14591786802326823, 12.06949235617739902, 58.12609039468568994 ) ) ;
#119705 = CARTESIAN_POINT ( 'NONE',  ( 19.02544592524334988, 5.153800228976608722, 71.45942372801900433 ) ) ;
#119707 = CARTESIAN_POINT ( 'NONE',  ( 13.89961937509977652, -13.97604488694527269, 113.1239096053143527 ) ) ;
#119708 = CARTESIAN_POINT ( 'NONE',  ( -9.564922557960796823, -16.46253265017161027, 72.08224293864770971 ) ) ;
#119709 = CARTESIAN_POINT ( 'NONE',  ( -10.81492255796078084, -18.62759615963271287, 112.0822429386477097 ) ) ;
#119710 = CARTESIAN_POINT ( 'NONE',  ( -19.03943276465977164, -0.05219959533935918106, 68.75109039468566152 ) ) ;
#119712 = CARTESIAN_POINT ( 'NONE',  ( -19.02544592524342804, 5.153800228976336051, 31.04057627198102409 ) ) ;
#119711 = CARTESIAN_POINT ( 'NONE',  ( 16.51473224551069308, 9.474510206698969483, 104.1655762719810241 ) ) ;
#119713 = CARTESIAN_POINT ( 'NONE',  ( 5.153800228976335163, 19.02544592524342804, 74.79057627198103830 ) ) ;
#119715 = LINE ( 'NONE', #89367, #79129 ) ;
#119714 = CARTESIAN_POINT ( 'NONE',  ( 8.224510206698953496, -14.34966873604960469, 32.91557627198102409 ) ) ;
#119716 = CARTESIAN_POINT ( 'NONE',  ( 5.153800228976615827, -19.02544592524334988, 35.20942372801899722 ) ) ;
#119717 = CARTESIAN_POINT ( 'NONE',  ( -12.06949235617756955, 12.14591786802309770, 70.62390960531436690 ) ) ;
#119718 = CARTESIAN_POINT ( 'NONE',  ( -10.81492255796105439, 18.62759615963255655, 107.9177570613523471 ) ) ;
#119719 = CARTESIAN_POINT ( 'NONE',  ( -0.05219959533909027116, -19.03943276465977164, 52.49890960531436690 ) ) ;
#119720 = EDGE_CURVE ( 'NONE', #11730, #96182, #184112, .T. ) ;
#119722 = CARTESIAN_POINT ( 'NONE',  ( -10.81492255796105439, 18.62759615963255655, 102.9177570613523756 ) ) ;
#119721 = CARTESIAN_POINT ( 'NONE',  ( -4.379528057220328563, 16.55341960407611168, 45.20724293864769550 ) ) ;
#119723 = CARTESIAN_POINT ( 'NONE',  ( 19.03943276465977164, -0.05219959533909143690, 88.74890960531436690 ) ) ;
#119724 = CARTESIAN_POINT ( 'NONE',  ( 19.02544592524343514, -5.153800228976328945, 113.5405762719810241 ) ) ;
#119725 = CARTESIAN_POINT ( 'NONE',  ( -13.89961937509977652, 13.97604488694528158, 40.62390960531435979 ) ) ;
#119726 = CARTESIAN_POINT ( 'NONE',  ( 16.52544592524342804, -4.483927247898539470, 103.5405762719810383 ) ) ;
#119727 = CARTESIAN_POINT ( 'NONE',  ( -16.52544592524342804, 4.483927247898546575, 91.04057627198103830 ) ) ;
#119728 = CARTESIAN_POINT ( 'NONE',  ( 10.72451020669898902, -18.67979575497178502, 92.91557627198103830 ) ) ;
#119729 = CARTESIAN_POINT ( 'NONE',  ( 9.474510206698971260, -16.51473224551069308, 87.91557627198102409 ) ) ;
#119730 = CARTESIAN_POINT ( 'NONE',  ( 18.67979575497178502, 10.72451020669898547, 94.16557627198103830 ) ) ;
#119731 = CARTESIAN_POINT ( 'NONE',  ( 0.05219959533909260263, 19.03943276465977164, 84.99890960531436690 ) ) ;
#119733 = CARTESIAN_POINT ( 'NONE',  ( -16.53943276465976808, 0.05219959533911058130, 106.2489096053143811 ) ) ;
#119732 = DIRECTION ( 'NONE',  ( 1.000000000000000000, -0.000000000000000000, -0.000000000000000000 ) ) ;
#119734 = CARTESIAN_POINT ( 'NONE',  ( 19.02544592524343514, -5.153800228976328945, 73.54057627198103830 ) ) ;
#119735 = CARTESIAN_POINT ( 'NONE',  ( 18.67979575497178502, 10.72451020669898547, 84.16557627198103830 ) ) ;
#119736 = DIRECTION ( 'NONE',  ( 1.000000000000000000, 0.000000000000000000, -0.000000000000000000 ) ) ;
#119738 = CARTESIAN_POINT ( 'NONE',  ( 19.52837319214027900, -5.499999999999893419, 67.10471352585541638 ) ) ;
#119737 = CARTESIAN_POINT ( 'NONE',  ( -5.823673210054116645, -21.52544592524344225, 27.29057627198103120 ) ) ;
#119739 = CARTESIAN_POINT ( 'NONE',  ( -16.52544592524335698, -4.483927247898792601, 33.95942372801901143 ) ) ;
#119740 = CARTESIAN_POINT ( 'NONE',  ( 4.483927247898545687, 16.52544592524342804, 89.79057627198103830 ) ) ;
#119741 = CARTESIAN_POINT ( 'NONE',  ( 18.22780087662123805, -5.499999999999989342, 53.51763182126895657 ) ) ;
#119742 = CARTESIAN_POINT ( 'NONE',  ( 13.97604488694527802, 13.89961937509977652, 89.37390960531436690 ) ) ;
#119743 = CARTESIAN_POINT ( 'NONE',  ( 5.153800228976335163, 19.02544592524342804, 39.79057627198100988 ) ) ;
#119744 = CARTESIAN_POINT ( 'NONE',  ( -12.06949235617756955, 12.14591786802309770, 75.62390960531439532 ) ) ;
#119745 = CARTESIAN_POINT ( 'NONE',  ( 5.719274019375991003, -21.55341960407610458, 22.70724293864769194 ) ) ;
#119746 = CARTESIAN_POINT ( 'NONE',  ( -4.483927247898539470, -16.52544592524342804, 52.29057627198102409 ) ) ;
#119747 = CARTESIAN_POINT ( 'NONE',  ( 19.03943276465977164, 0.05219959533936151252, 106.2510903946856615 ) ) ;
#119748 = CARTESIAN_POINT ( 'NONE',  ( 21.53943276465977519, 0.05219959533937863772, 56.25109039468568284 ) ) ;
#119749 = CARTESIAN_POINT ( 'NONE',  ( 17.50000000000000711, -5.499999999999978684, 41.21769037696436300 ) ) ;
#119750 = CARTESIAN_POINT ( 'NONE',  ( -9.474510206698964154, 16.51473224551069663, 100.4155762719810241 ) ) ;
#119751 = CARTESIAN_POINT ( 'NONE',  ( 12.14591786802327356, -12.06949235617739191, 80.62609039468567573 ) ) ;
#119752 = CARTESIAN_POINT ( 'NONE',  ( 16.51473224551069308, 9.474510206698969483, 29.16557627198103475 ) ) ;
#119753 = CARTESIAN_POINT ( 'NONE',  ( 9.564922557960805705, 16.46253265017160317, 74.58224293864769550 ) ) ;
#119754 = CARTESIAN_POINT ( 'NONE',  ( -0.05219959533907301413, -21.53943276465977519, 82.49890960531436690 ) ) ;
#119755 = CARTESIAN_POINT ( 'NONE',  ( 9.564922557961047289, -16.46253265017146816, 105.4177570613523471 ) ) ;
#119757 = CARTESIAN_POINT ( 'NONE',  ( -18.67979575497193778, 10.72451020669871902, 58.33442372801901143 ) ) ;
#119756 = CARTESIAN_POINT ( 'NONE',  ( -0.05219959533910754901, -16.53943276465976808, 47.49890960531435979 ) ) ;
#119759 = CARTESIAN_POINT ( 'NONE',  ( 21.53943276465977519, -0.05219959533907433946, 28.74890960531435624 ) ) ;
#119758 = CARTESIAN_POINT ( 'NONE',  ( -16.52544592524335698, -4.483927247898792601, 88.95942372801901854 ) ) ;
#119760 = CARTESIAN_POINT ( 'NONE',  ( 17.48853670773242541, 5.747243402303174875, 28.83328700250010712 ) ) ;
#119761 = DIRECTION ( 'NONE',  ( 0.000000000000000000, 0.000000000000000000, 1.000000000000000000 ) ) ;
#119762 = CARTESIAN_POINT ( 'NONE',  ( 4.379528057220092307, 16.55341960407617563, 107.2927570613523471 ) ) ;
#119763 = CARTESIAN_POINT ( 'NONE',  ( -8.224510206698735004, -14.34966873604973081, 59.58442372801901854 ) ) ;
#119764 = CARTESIAN_POINT ( 'NONE',  ( -19.03943276465977164, 0.05219959533909376836, 76.24890960531435269 ) ) ;
#119765 = CARTESIAN_POINT ( 'NONE',  ( 5.049401038298161559, -19.05341960407611168, 77.70724293864765286 ) ) ;
#119766 = CARTESIAN_POINT ( 'NONE',  ( -18.62759615963255300, -10.81492255796106328, 74.16775706135231871 ) ) ;
#119767 = CARTESIAN_POINT ( 'NONE',  ( -0.05219959533934338120, 16.53943276465976808, 72.50109039468568994 ) ) ;
#119768 = CARTESIAN_POINT ( 'NONE',  ( 14.29746914071049879, -8.314922557960816363, 48.33224293864770260 ) ) ;
#119769 = CARTESIAN_POINT ( 'NONE',  ( 5.153800228976335163, 19.02544592524342804, 54.79057627198103120 ) ) ;
#119770 = CARTESIAN_POINT ( 'NONE',  ( 9.564922557960805705, 16.46253265017160317, 54.58224293864769550 ) ) ;
#119772 = VERTEX_POINT ( 'NONE', #117874 ) ;
#119771 = CARTESIAN_POINT ( 'NONE',  ( -14.29746914071037622, -8.314922557961029526, 39.16775706135235424 ) ) ;
#119773 = CARTESIAN_POINT ( 'NONE',  ( 19.02544592524334988, 5.153800228976608722, 101.4594237280189759 ) ) ;
#119774 = CARTESIAN_POINT ( 'NONE',  ( -16.55341960407611168, -4.379528057220339221, 96.45724293864770971 ) ) ;
#119775 = CARTESIAN_POINT ( 'NONE',  ( 13.97604488694527802, 13.89961937509977652, 69.37390960531436690 ) ) ;
#119777 = CARTESIAN_POINT ( 'NONE',  ( -38.00000000000001421, 12.34694845685046438, -4.100000000000000533 ) ) ;
#119776 = CARTESIAN_POINT ( 'NONE',  ( 19.03943276465977164, 0.05219959533936151252, 106.2510903946856615 ) ) ;
#119778 = CARTESIAN_POINT ( 'NONE',  ( 18.62759615963255655, 10.81492255796105972, 101.6677570613523613 ) ) ;
#119779 = CARTESIAN_POINT ( 'NONE',  ( 16.53943276465976808, 0.05219959533934440121, 71.25109039468568994 ) ) ;
#119780 = CARTESIAN_POINT ( 'NONE',  ( 0.000000000000000000, 0.000000000000000000, 1.999999999999999112 ) ) ;
#119781 = CARTESIAN_POINT ( 'NONE',  ( -15.80617190586745835, -15.72974639402198527, 66.87390960531436690 ) ) ;
#119782 = CARTESIAN_POINT ( 'NONE',  ( -14.34966873604972548, 8.224510206698743886, 48.33442372801902565 ) ) ;
#119783 = CARTESIAN_POINT ( 'NONE',  ( -69.65682714487590488, -71.74905178543390605, -4.999999999999999112 ) ) ;
#119784 = CARTESIAN_POINT ( 'NONE',  ( 19.05341960407617918, -5.049401038297876454, 46.04275706135233293 ) ) ;
#119785 = CARTESIAN_POINT ( 'NONE',  ( 13.89961937509977652, -13.97604488694527269, 93.12390960531436690 ) ) ;
#119786 = CARTESIAN_POINT ( 'NONE',  ( 19.03943276465977164, -0.05219959533909143690, 23.74890960531435269 ) ) ;
#119787 = CARTESIAN_POINT ( 'NONE',  ( -13.89961937509977652, 13.97604488694528158, 65.62390960531436690 ) ) ;
#119788 = CARTESIAN_POINT ( 'NONE',  ( 21.53943276465977519, 0.05219959533937863772, 71.25109039468568994 ) ) ;
#119789 = CARTESIAN_POINT ( 'NONE',  ( 19.05341960407617918, -5.049401038297876454, 46.04275706135233293 ) ) ;
#119790 = CARTESIAN_POINT ( 'NONE',  ( -16.46253265017146816, -9.564922557961047289, 34.16775706135233293 ) ) ;
#119791 = CARTESIAN_POINT ( 'NONE',  ( 0.05219959533909260263, 19.03943276465977164, 49.99890960531435979 ) ) ;
#119792 = CARTESIAN_POINT ( 'NONE',  ( -21.53943276465977519, 0.05219959533907696930, 21.24890960531436690 ) ) ;
#119793 = CARTESIAN_POINT ( 'NONE',  ( -0.05219959533937732626, 21.53943276465977519, 77.50109039468567573 ) ) ;
#119794 = CARTESIAN_POINT ( 'NONE',  ( 19.02544592524343514, -5.153800228976328945, 63.54057627198103830 ) ) ;
#119795 = CARTESIAN_POINT ( 'NONE',  ( -15.80617190586768217, 15.72974639402176855, 93.12609039468568994 ) ) ;
#119796 = CARTESIAN_POINT ( 'NONE',  ( -0.05219959533907301413, -21.53943276465977519, 42.49890960531435979 ) ) ;
#119797 = CARTESIAN_POINT ( 'NONE',  ( 19.05341960407611168, 5.049401038298154454, 88.95724293864769550 ) ) ;
#119798 = CARTESIAN_POINT ( 'NONE',  ( -5.719274019375665041, -21.55341960407619695, 34.79275706135235424 ) ) ;
#119799 = CARTESIAN_POINT ( 'NONE',  ( 16.46253265017146816, 9.564922557961045513, 61.66775706135234003 ) ) ;
#119800 = CARTESIAN_POINT ( 'NONE',  ( -16.46253265017160317, 9.564922557960807481, 40.83224293864769550 ) ) ;
#119801 = CARTESIAN_POINT ( 'NONE',  ( -13.89961937509977652, 13.97604488694528158, 90.62390960531432427 ) ) ;
#119802 = CARTESIAN_POINT ( 'NONE',  ( 4.379528057220092307, 16.55341960407617563, 27.29275706135234358 ) ) ;
#119803 = CARTESIAN_POINT ( 'NONE',  ( -14.29746914071049879, 8.314922557960819915, 85.83224293864768129 ) ) ;
#119804 = CARTESIAN_POINT ( 'NONE',  ( 5.049401038298161559, -19.05341960407611168, 67.70724293864769550 ) ) ;
#119805 = CARTESIAN_POINT ( 'NONE',  ( 5.823673210054125526, 21.52544592524343514, 49.79057627198102409 ) ) ;
#119806 = CARTESIAN_POINT ( 'NONE',  ( -8.224510206698735004, -14.34966873604973081, 24.58442372801901499 ) ) ;
#119807 = CARTESIAN_POINT ( 'NONE',  ( 18.62759615963255655, 10.81492255796105972, 26.66775706135235424 ) ) ;
#119808 = CARTESIAN_POINT ( 'NONE',  ( -5.719274019375665041, -21.55341960407619695, 74.79275706135234714 ) ) ;
#119809 = CARTESIAN_POINT ( 'NONE',  ( -4.379528057220086978, -16.55341960407618274, 64.79275706135234714 ) ) ;
#119810 = CARTESIAN_POINT ( 'NONE',  ( -12.14591786802326823, 12.06949235617739902, 68.12609039468567573 ) ) ;
#119811 = CARTESIAN_POINT ( 'NONE',  ( 5.049401038298161559, -19.05341960407611168, 67.70724293864769550 ) ) ;
#119812 = CARTESIAN_POINT ( 'NONE',  ( 12.14591786802327356, -12.06949235617739191, 100.6260903946857184 ) ) ;
#119813 = CARTESIAN_POINT ( 'NONE',  ( -9.474510206698720793, -16.51473224551083518, 39.58442372801899722 ) ) ;
#119814 = CARTESIAN_POINT ( 'NONE',  ( 10.72451020669871369, 18.67979575497193778, 27.08442372801901854 ) ) ;
#119815 = CARTESIAN_POINT ( 'NONE',  ( -16.53943276465976808, 0.05219959533911058130, 61.24890960531435979 ) ) ;
#119816 = CARTESIAN_POINT ( 'NONE',  ( -9.564922557960796823, -16.46253265017161027, 102.0822429386477097 ) ) ;
#119817 = CARTESIAN_POINT ( 'NONE',  ( 8.224510206698742110, 14.34966873604972548, 87.08442372801901854 ) ) ;
#119818 = CARTESIAN_POINT ( 'NONE',  ( -5.719274019375665041, -21.55341960407619695, 59.79275706135234714 ) ) ;
#119819 = CARTESIAN_POINT ( 'NONE',  ( 12.14591786802327356, -12.06949235617739191, 25.62609039468567929 ) ) ;
#119820 = CARTESIAN_POINT ( 'NONE',  ( -5.823673210054431948, 21.52544592524334988, 22.70942372801901499 ) ) ;
#119821 = CARTESIAN_POINT ( 'NONE',  ( 0.05219959533910956823, 16.53943276465976808, 54.99890960531435269 ) ) ;
#119822 = EDGE_LOOP ( 'NONE', ( #125172, #195052, #122968, #65273 ) ) ;
#119823 = CARTESIAN_POINT ( 'NONE',  ( -0.05219959533907301413, -21.53943276465977519, 107.4989096053143669 ) ) ;
#119824 = CARTESIAN_POINT ( 'NONE',  ( 12.14591786802309770, 12.06949235617756955, 39.37390960531436690 ) ) ;
#119825 = ORIENTED_EDGE ( 'NONE', *, *, #107496, .T. ) ;
#119826 = CARTESIAN_POINT ( 'NONE',  ( 34.38590767368158652, 6.751198732549910986, 48.30327006964592584 ) ) ;
#119827 = CARTESIAN_POINT ( 'NONE',  ( 5.823673210054125526, 21.52544592524343514, 29.79057627198102409 ) ) ;
#119828 = CARTESIAN_POINT ( 'NONE',  ( 21.53943276465977519, 0.05219959533937863772, 31.25109039468568639 ) ) ;
#119829 = CARTESIAN_POINT ( 'NONE',  ( 12.14591786802309770, 12.06949235617756955, 64.37390960531435269 ) ) ;
#119830 = CARTESIAN_POINT ( 'NONE',  ( -5.719274019375978568, 21.55341960407610458, 60.20724293864768839 ) ) ;
#119831 = CARTESIAN_POINT ( 'NONE',  ( 19.05341960407611168, 5.049401038298154454, 78.95724293864769550 ) ) ;
#119833 = CARTESIAN_POINT ( 'NONE',  ( -13.97604488694547697, 13.89961937509957934, 73.12609039468568994 ) ) ;
#119832 = CARTESIAN_POINT ( 'NONE',  ( -13.97604488694527625, -13.89961937509977652, 31.87390960531435979 ) ) ;
#119834 = CARTESIAN_POINT ( 'NONE',  ( 10.72451020669898902, -18.67979575497178502, 42.91557627198103120 ) ) ;
#119835 = CARTESIAN_POINT ( 'NONE',  ( 9.564922557960805705, 16.46253265017160317, 64.58224293864769550 ) ) ;
#119836 = ORIENTED_EDGE ( 'NONE', *, *, #196650, .T. ) ;
#119837 = CARTESIAN_POINT ( 'NONE',  ( -14.34966873604972548, 8.224510206698743886, 43.33442372801901143 ) ) ;
#119838 = CARTESIAN_POINT ( 'NONE',  ( -15.80617190586745835, -15.72974639402198527, 111.8739096053143669 ) ) ;
#119839 = CARTESIAN_POINT ( 'NONE',  ( -0.05219959533910754901, -16.53943276465976808, 52.49890960531435979 ) ) ;
#119840 = CARTESIAN_POINT ( 'NONE',  ( -13.97604488694527625, -13.89961937509977652, 101.8739096053143811 ) ) ;
#119841 = CARTESIAN_POINT ( 'NONE',  ( -21.53943276465977519, 0.05219959533907696930, 76.24890960531435269 ) ) ;
#119843 = CARTESIAN_POINT ( 'NONE',  ( 16.55341960407618274, -4.379528057220086978, 36.04275706135234714 ) ) ;
#119842 = CARTESIAN_POINT ( 'NONE',  ( 15.80617190586746368, 15.72974639402197994, 109.3739096053143811 ) ) ;
#119844 = CARTESIAN_POINT ( 'NONE',  ( -21.55341960407610458, -5.719274019375992779, 46.45724293864769550 ) ) ;
#119845 = CARTESIAN_POINT ( 'NONE',  ( -0.05219959533937732626, 21.53943276465977519, 97.50109039468567573 ) ) ;
#119846 = CARTESIAN_POINT ( 'NONE',  ( -5.049401038298153566, 19.05341960407611168, 40.20724293864768839 ) ) ;
#119847 = CARTESIAN_POINT ( 'NONE',  ( -16.46253265017160317, 9.564922557960807481, 95.83224293864769550 ) ) ;
#119848 = CARTESIAN_POINT ( 'NONE',  ( 13.97604488694527802, 13.89961937509977652, 79.37390960531435269 ) ) ;
#119849 = CARTESIAN_POINT ( 'NONE',  ( 2.200000000000000622, 1.999999999999999112, 0.000000000000000000 ) ) ;
#119850 = ADVANCED_FACE ( 'NONE', ( #131025 ), #114861, .T. ) ;
#119851 = CARTESIAN_POINT ( 'NONE',  ( 19.02544592524334988, 5.153800228976608722, 56.45942372801898301 ) ) ;
#119853 = CARTESIAN_POINT ( 'NONE',  ( -10.81492255796078084, -18.62759615963271287, 32.08224293864769550 ) ) ;
#119852 = CARTESIAN_POINT ( 'NONE',  ( -15.80617190586768217, 15.72974639402176855, 108.1260903946856757 ) ) ;
#119854 = CARTESIAN_POINT ( 'NONE',  ( -16.55341960407617563, 4.379528057220093196, 98.54275706135234714 ) ) ;
#119855 = CARTESIAN_POINT ( 'NONE',  ( 19.03943276465977164, 0.05219959533936151252, 81.25109039468567573 ) ) ;
#119856 = CARTESIAN_POINT ( 'NONE',  ( -17.49999999999999645, 5.499999999999992895, 58.71769037696435589 ) ) ;
#119857 = CARTESIAN_POINT ( 'NONE',  ( -19.02544592524334988, -5.153800228976617603, 78.95942372801900433 ) ) ;
#119858 = CARTESIAN_POINT ( 'NONE',  ( 19.05341960407617918, -5.049401038297876454, 46.04275706135233293 ) ) ;
#119859 = CARTESIAN_POINT ( 'NONE',  ( -14.65603373305124357, -15.74840231007434355, -56.32459802048661857 ) ) ;
#119860 = CARTESIAN_POINT ( 'NONE',  ( 9.474510206698971260, -16.51473224551069308, 47.91557627198102409 ) ) ;
#119861 = CARTESIAN_POINT ( 'NONE',  ( -0.05219959533910754901, -16.53943276465976808, 47.49890960531435979 ) ) ;
#119862 = CARTESIAN_POINT ( 'NONE',  ( -19.02544592524342804, 5.153800228976336051, 41.04057627198103120 ) ) ;
#119863 = CARTESIAN_POINT ( 'NONE',  ( 12.14591786802309770, 12.06949235617756955, 39.37390960531436690 ) ) ;
#119864 = CARTESIAN_POINT ( 'NONE',  ( -35.00000000000000000, 3.181980515339468241, 1.110912703473986074 ) ) ;
#119865 = CARTESIAN_POINT ( 'NONE',  ( -16.53943276465976808, 0.05219959533911058130, 21.24890960531436690 ) ) ;
#119866 = CARTESIAN_POINT ( 'NONE',  ( 16.51473224551069308, 9.474510206698969483, 49.16557627198102409 ) ) ;
#119867 = CARTESIAN_POINT ( 'NONE',  ( -18.67979575497193778, 10.72451020669871902, 113.3344237280190328 ) ) ;
#119868 = CARTESIAN_POINT ( 'NONE',  ( 19.05341960407617918, -5.049401038297876454, 111.0427570613523329 ) ) ;
#119869 = CARTESIAN_POINT ( 'NONE',  ( -21.52544592524343514, 5.823673210054127303, 36.04057627198102409 ) ) ;
#119871 = EDGE_LOOP ( 'NONE', ( #149914, #150264 ) ) ;
#119870 = CARTESIAN_POINT ( 'NONE',  ( 21.52544592524334988, 5.823673210054432836, 86.45942372801901854 ) ) ;
#119872 = CARTESIAN_POINT ( 'NONE',  ( -19.03943276465977164, 0.05219959533909376836, 106.2489096053143669 ) ) ;
#119873 = CARTESIAN_POINT ( 'NONE',  ( -19.02544592524342804, 5.153800228976336051, 81.04057627198103830 ) ) ;
#119874 = CARTESIAN_POINT ( 'NONE',  ( 22.81625015709509441, 31.40387420917330275, -7.324999997268812457 ) ) ;
#119875 = CARTESIAN_POINT ( 'NONE',  ( -10.81492255796078084, -18.62759615963271287, 112.0822429386477097 ) ) ;
#119876 = CARTESIAN_POINT ( 'NONE',  ( -4.379528057220328563, 16.55341960407611168, 85.20724293864770971 ) ) ;
#119877 = CARTESIAN_POINT ( 'NONE',  ( -21.52544592524343514, 5.823673210054127303, 76.04057627198102409 ) ) ;
#119878 = CARTESIAN_POINT ( 'NONE',  ( 16.51473224551069308, 9.474510206698969483, 69.16557627198102409 ) ) ;
#119879 = CARTESIAN_POINT ( 'NONE',  ( 18.62759615963271287, -10.81492255796078972, 98.33224293864769550 ) ) ;
#119880 = ORIENTED_EDGE ( 'NONE', *, *, #164988, .F. ) ;
#119881 = CARTESIAN_POINT ( 'NONE',  ( 19.05341960407611168, 5.049401038298154454, 63.95724293864769550 ) ) ;
#119883 = CARTESIAN_POINT ( 'NONE',  ( 21.71408805923169183, -8.664832797227230543, 169.0754946983649631 ) ) ;
#119882 = CARTESIAN_POINT ( 'NONE',  ( -8.224510206698948167, 14.34966873604960824, 90.41557627198103830 ) ) ;
#119884 = CARTESIAN_POINT ( 'NONE',  ( 19.02544592524343514, -5.153800228976328945, 68.54057627198103830 ) ) ;
#119885 = CARTESIAN_POINT ( 'NONE',  ( 9.564922557961047289, -16.46253265017146816, 75.41775706135234714 ) ) ;
#119886 = CARTESIAN_POINT ( 'NONE',  ( -16.55341960407611168, -4.379528057220339221, 91.45724293864769550 ) ) ;
#119887 = CARTESIAN_POINT ( 'NONE',  ( -5.823673210054431948, 21.52544592524334988, 57.70942372801901143 ) ) ;
#119889 = CARTESIAN_POINT ( 'NONE',  ( 0.05219959533937995610, -21.53943276465977519, 25.00109039468567218 ) ) ;
#119888 = CARTESIAN_POINT ( 'NONE',  ( 5.049401038298161559, -19.05341960407611168, 47.70724293864770260 ) ) ;
#119890 = CARTESIAN_POINT ( 'NONE',  ( -12.06949235617756955, 12.14591786802309770, 100.6239096053143811 ) ) ;
#119891 = CARTESIAN_POINT ( 'NONE',  ( 10.44694540016481099, -45.05842955090996327, -23.63933302999445729 ) ) ;
#119892 = CARTESIAN_POINT ( 'NONE',  ( -19.03943276465977164, 0.05219959533909376836, 61.24890960531436690 ) ) ;
#119893 = DIRECTION ( 'NONE',  ( 1.000000000000000000, 0.000000000000000000, -0.000000000000000000 ) ) ;
#119895 = CARTESIAN_POINT ( 'NONE',  ( 19.05341960407611168, 5.049401038298154454, 108.9572429386477097 ) ) ;
#119894 = CARTESIAN_POINT ( 'NONE',  ( 0.05219959533936267826, -19.03943276465977164, 105.0010903946856615 ) ) ;
#119896 = CARTESIAN_POINT ( 'NONE',  ( -10.72451020669870658, -18.67979575497194134, 54.58442372801901143 ) ) ;
#119897 = CARTESIAN_POINT ( 'NONE',  ( -16.51473224551069308, -9.474510206698971260, 96.66557627198102409 ) ) ;
#119898 = CARTESIAN_POINT ( 'NONE',  ( -9.564922557961040184, 16.46253265017147172, 82.91775706135233293 ) ) ;
#119899 = CARTESIAN_POINT ( 'NONE',  ( 9.474510206698971260, -16.51473224551069308, 57.91557627198103120 ) ) ;
#119900 = CARTESIAN_POINT ( 'NONE',  ( 8.314922557960818139, 14.29746914071049879, 84.58224293864769550 ) ) ;
#119901 = CARTESIAN_POINT ( 'NONE',  ( 19.03943276465977164, -0.05219959533909143690, 88.74890960531436690 ) ) ;
#119902 = CARTESIAN_POINT ( 'NONE',  ( 14.29746914071049879, -8.314922557960816363, 83.33224293864769550 ) ) ;
#119903 = CARTESIAN_POINT ( 'NONE',  ( -16.46253265017160317, 9.564922557960807481, 85.83224293864769550 ) ) ;
#119904 = CARTESIAN_POINT ( 'NONE',  ( -16.51473224551082808, 9.474510206698731452, 28.33442372801900433 ) ) ;
#119907 = CARTESIAN_POINT ( 'NONE',  ( 5.049401038298161559, -19.05341960407611168, 22.70724293864769194 ) ) ;
#119906 = CARTESIAN_POINT ( 'NONE',  ( -14.29746914071049879, 8.314922557960819915, 40.83224293864769550 ) ) ;
#119905 = CARTESIAN_POINT ( 'NONE',  ( 19.02544592524343514, -5.153800228976328945, 43.54057627198103120 ) ) ;
#119908 = EDGE_LOOP ( 'NONE', ( #18841, #183153, #159102, #85566 ) ) ;
#119909 = CARTESIAN_POINT ( 'NONE',  ( -0.05219959533937732626, 21.53943276465977519, 47.50109039468568994 ) ) ;
#119910 = CARTESIAN_POINT ( 'NONE',  ( 13.89961937509957401, 13.97604488694547697, 81.87609039468564731 ) ) ;
#119911 = CARTESIAN_POINT ( 'NONE',  ( 8.314922557960818139, 14.29746914071049879, 29.58224293864769905 ) ) ;
#119912 = CARTESIAN_POINT ( 'NONE',  ( 21.53943276465977519, -0.05219959533907433946, 83.74890960531435269 ) ) ;
#119913 = CARTESIAN_POINT ( 'NONE',  ( 10.81492255796078972, 18.62759615963270932, 29.58224293864769905 ) ) ;
#119914 = CARTESIAN_POINT ( 'NONE',  ( 14.29746914071049879, -8.314922557960816363, 68.33224293864769550 ) ) ;
#119915 = CARTESIAN_POINT ( 'NONE',  ( 16.46253265017160672, -9.564922557960803928, 43.33224293864769550 ) ) ;
#119916 = CARTESIAN_POINT ( 'NONE',  ( 4.379528057220092307, 16.55341960407617563, 97.29275706135234714 ) ) ;
#119917 = CARTESIAN_POINT ( 'NONE',  ( -14.29746914071037622, -8.314922557961029526, 64.16775706135234714 ) ) ;
#119918 = CARTESIAN_POINT ( 'NONE',  ( -9.564922557961040184, 16.46253265017147172, 22.91775706135233648 ) ) ;
#119919 = CARTESIAN_POINT ( 'NONE',  ( -9.474510206698964154, 16.51473224551069663, 90.41557627198103830 ) ) ;
#119920 = CARTESIAN_POINT ( 'NONE',  ( 19.03943276465977164, -0.05219959533909143690, 73.74890960531435269 ) ) ;
#119921 = CARTESIAN_POINT ( 'NONE',  ( -12.14591786802326823, 12.06949235617739902, 68.12609039468567573 ) ) ;
#119922 = CARTESIAN_POINT ( 'NONE',  ( 19.03943276465977164, -0.05219959533909143690, 28.74890960531435624 ) ) ;
#119923 = ADVANCED_FACE ( 'NONE', ( #133031 ), #7672, .F. ) ;
#119924 = CARTESIAN_POINT ( 'NONE',  ( -14.34966873604960291, -8.224510206698953496, 31.66557627198102054 ) ) ;
#119926 = CARTESIAN_POINT ( 'NONE',  ( 9.564922557960805705, 16.46253265017160317, 84.58224293864769550 ) ) ;
#119925 = CARTESIAN_POINT ( 'NONE',  ( 5.153800228976335163, 19.02544592524342804, 99.79057627198102409 ) ) ;
#119927 = CARTESIAN_POINT ( 'NONE',  ( -18.67979575497178146, -10.72451020669898902, 31.66557627198102054 ) ) ;
#119928 = CARTESIAN_POINT ( 'NONE',  ( 14.34966873604960469, 8.224510206698951720, 74.16557627198102409 ) ) ;
#119929 = CARTESIAN_POINT ( 'NONE',  ( -14.34966873604960291, -8.224510206698953496, 66.66557627198102409 ) ) ;
#119931 = CARTESIAN_POINT ( 'NONE',  ( -16.46253265017146816, -9.564922557961047289, 59.16775706135233293 ) ) ;
#119930 = CARTESIAN_POINT ( 'NONE',  ( 16.53943276465976808, 0.05219959533934440121, 56.25109039468568284 ) ) ;
#119932 = CARTESIAN_POINT ( 'NONE',  ( -5.049401038297874678, -19.05341960407617918, 54.79275706135234003 ) ) ;
#119933 = CARTESIAN_POINT ( 'NONE',  ( 13.89961937509977652, -13.97604488694527269, 93.12390960531436690 ) ) ;
#119934 = CARTESIAN_POINT ( 'NONE',  ( -5.153800228976607833, 19.02544592524334988, 62.70942372801899722 ) ) ;
#119935 = CARTESIAN_POINT ( 'NONE',  ( 17.14385361876520264, 23.59649016807275856, 144.6750000027311671 ) ) ;
#119937 = CARTESIAN_POINT ( 'NONE',  ( -4.483927247898782831, 16.52544592524335698, 97.70942372801904696 ) ) ;
#119936 = CARTESIAN_POINT ( 'NONE',  ( -9.564922557961040184, 16.46253265017147172, 112.9177570613523329 ) ) ;
#119938 = CARTESIAN_POINT ( 'NONE',  ( -0.05219959533909027116, -19.03943276465977164, 37.49890960531436690 ) ) ;
#119939 = CARTESIAN_POINT ( 'NONE',  ( -16.46253265017160317, 9.564922557960807481, 115.8322429386477097 ) ) ;
#119940 = CARTESIAN_POINT ( 'NONE',  ( 15.80617190586769283, -15.72974639402175789, 60.62609039468567573 ) ) ;
#119941 = CARTESIAN_POINT ( 'NONE',  ( -13.89961937509957401, -13.97604488694547875, 109.3760903946856331 ) ) ;
#119943 = CARTESIAN_POINT ( 'NONE',  ( 9.474510206698971260, -16.51473224551069308, 72.91557627198102409 ) ) ;
#119942 = CARTESIAN_POINT ( 'NONE',  ( 6.651581668633990515E-13, -67.16384485484805111, -24.99989890117360503 ) ) ;
#119944 = CARTESIAN_POINT ( 'NONE',  ( -19.02544592524342804, 5.153800228976336051, 111.0405762719810099 ) ) ;
#119946 = CARTESIAN_POINT ( 'NONE',  ( 5.049401038298161559, -19.05341960407611168, 62.70724293864769550 ) ) ;
#119945 = CARTESIAN_POINT ( 'NONE',  ( -0.05219959533910754901, -16.53943276465976808, 72.49890960531435269 ) ) ;
#119947 = CARTESIAN_POINT ( 'NONE',  ( 19.03943276465977164, -0.05219959533909143690, 68.74890960531436690 ) ) ;
#119948 = CARTESIAN_POINT ( 'NONE',  ( -19.05341960407617563, 5.049401038297882671, 73.54275706135233293 ) ) ;
#119949 = CARTESIAN_POINT ( 'NONE',  ( -5.719274019375978568, 21.55341960407610458, 60.20724293864768839 ) ) ;
#119950 = CARTESIAN_POINT ( 'NONE',  ( -16.53943276465976808, 0.05219959533911058130, 111.2489096053143669 ) ) ;
#119951 = CARTESIAN_POINT ( 'NONE',  ( -19.05341960407617563, 5.049401038297882671, 58.54275706135234003 ) ) ;
#119952 = CARTESIAN_POINT ( 'NONE',  ( 0.05219959533909260263, 19.03943276465977164, 54.99890960531435979 ) ) ;
#119953 = CARTESIAN_POINT ( 'NONE',  ( -19.02544592524342804, 5.153800228976336051, 91.04057627198100988 ) ) ;
#119954 = CARTESIAN_POINT ( 'NONE',  ( -18.67979575497178146, -10.72451020669898902, 91.66557627198103830 ) ) ;
#119956 = CARTESIAN_POINT ( 'NONE',  ( -16.46253265017146816, -9.564922557961047289, 49.16775706135233293 ) ) ;
#119955 = CARTESIAN_POINT ( 'NONE',  ( 16.55341960407611168, 4.379528057220329451, 98.95724293864770971 ) ) ;
#119957 = CARTESIAN_POINT ( 'NONE',  ( -21.53943276465977519, 0.05219959533907696930, 76.24890960531435269 ) ) ;
#119958 = CARTESIAN_POINT ( 'NONE',  ( 21.55341960407610458, 5.719274019375980345, 53.95724293864770260 ) ) ;
#119959 = CARTESIAN_POINT ( 'NONE',  ( 8.224510206698953496, -14.34966873604960469, 37.91557627198102409 ) ) ;
#119960 = CARTESIAN_POINT ( 'NONE',  ( -10.72451020669870658, -18.67979575497194134, 109.5844237280190328 ) ) ;
#119961 = CARTESIAN_POINT ( 'NONE',  ( 9.564922557960805705, 16.46253265017160317, 74.58224293864769550 ) ) ;
#119962 = CARTESIAN_POINT ( 'NONE',  ( 19.03943276465977164, -0.05219959533909143690, 38.74890960531436690 ) ) ;
#119963 = CARTESIAN_POINT ( 'NONE',  ( -15.80617190586768217, 15.72974639402176855, 43.12609039468568284 ) ) ;
#119964 = CARTESIAN_POINT ( 'NONE',  ( -21.55341960407619339, 5.719274019375674811, 43.54275706135235424 ) ) ;
#119965 = CARTESIAN_POINT ( 'NONE',  ( -16.51473224551069308, -9.474510206698971260, 46.66557627198102409 ) ) ;
#119966 = CARTESIAN_POINT ( 'NONE',  ( 5.823673210054444382, -21.52544592524334988, 20.20942372801900788 ) ) ;
#119967 = CARTESIAN_POINT ( 'NONE',  ( -0.05219959533936034679, 19.03943276465977164, 67.50109039468566152 ) ) ;
#119968 = CARTESIAN_POINT ( 'NONE',  ( -9.474510206698964154, 16.51473224551069663, 30.41557627198102054 ) ) ;
#119969 = CARTESIAN_POINT ( 'NONE',  ( -4.483927247898782831, 16.52544592524335698, 32.70942372801900433 ) ) ;
#119970 = CARTESIAN_POINT ( 'NONE',  ( -16.46253265017160317, 9.564922557960807481, 25.83224293864769194 ) ) ;
#119971 = CARTESIAN_POINT ( 'NONE',  ( -12.06949235617739369, -12.14591786802326823, 79.37609039468567573 ) ) ;
#119972 = CARTESIAN_POINT ( 'NONE',  ( 16.46253265017160672, -9.564922557960803928, 33.33224293864770260 ) ) ;
#119973 = CARTESIAN_POINT ( 'NONE',  ( -21.84611564451295962, -9.363109600220301587, 171.0247306346281277 ) ) ;
#119974 = CARTESIAN_POINT ( 'NONE',  ( -5.049401038298153566, 19.05341960407611168, 90.20724293864766707 ) ) ;
#119975 = CARTESIAN_POINT ( 'NONE',  ( 9.564922557960805705, 16.46253265017160317, 24.58224293864769194 ) ) ;
#119976 = CARTESIAN_POINT ( 'NONE',  ( 18.67979575497178502, 10.72451020669898547, 79.16557627198103830 ) ) ;
#119977 = CARTESIAN_POINT ( 'NONE',  ( -8.224510206698735004, -14.34966873604973081, 44.58442372801901854 ) ) ;
#119978 = CARTESIAN_POINT ( 'NONE',  ( -0.05219959533937732626, 21.53943276465977519, 97.50109039468567573 ) ) ;
#119979 = CARTESIAN_POINT ( 'NONE',  ( -16.51473224551069308, -9.474510206698971260, 36.66557627198102409 ) ) ;
#119980 = CARTESIAN_POINT ( 'NONE',  ( 14.29746914071049879, -8.314922557960816363, 38.33224293864768839 ) ) ;
#119981 = CARTESIAN_POINT ( 'NONE',  ( 8.314922557960818139, 14.29746914071049879, 69.58224293864769550 ) ) ;
#119982 = CARTESIAN_POINT ( 'NONE',  ( -19.02544592524342804, 5.153800228976336051, 61.04057627198103120 ) ) ;
#119983 = CARTESIAN_POINT ( 'NONE',  ( -13.89961937509957401, -13.97604488694547875, 19.37609039468566507 ) ) ;
#119984 = CARTESIAN_POINT ( 'NONE',  ( -5.823673210054431948, 21.52544592524334988, 27.70942372801901854 ) ) ;
#119985 = CARTESIAN_POINT ( 'NONE',  ( -19.05341960407611168, -5.049401038298163336, 81.45724293864769550 ) ) ;
#119986 = CARTESIAN_POINT ( 'NONE',  ( 0.05219959533937995610, -21.53943276465977519, 80.00109039468568994 ) ) ;
#119987 = CARTESIAN_POINT ( 'NONE',  ( -4.483927247898782831, 16.52544592524335698, 52.70942372801902565 ) ) ;
#119988 = CARTESIAN_POINT ( 'NONE',  ( 0.05219959533934541429, -16.53943276465976808, 30.00109039468568284 ) ) ;
#119990 = CARTESIAN_POINT ( 'NONE',  ( 5.719274019375673035, 21.55341960407619339, 102.2927570613523613 ) ) ;
#119989 = CARTESIAN_POINT ( 'NONE',  ( 16.53943276465976808, -0.05219959533910856209, 88.74890960531436690 ) ) ;
#119991 = CARTESIAN_POINT ( 'NONE',  ( -8.224510206698948167, 14.34966873604960824, 35.41557627198102409 ) ) ;
#119992 = CARTESIAN_POINT ( 'NONE',  ( -19.03943276465977164, 0.05219959533909376836, 26.24890960531435624 ) ) ;
#119993 = CARTESIAN_POINT ( 'NONE',  ( 14.34966873604972726, -8.224510206698740333, 55.83442372801901854 ) ) ;
#119994 = CARTESIAN_POINT ( 'NONE',  ( 16.52544592524342804, -4.483927247898539470, 48.54057627198103120 ) ) ;
#119995 = CARTESIAN_POINT ( 'NONE',  ( -16.53943276465976808, -0.05219959533934237506, 103.7510903946857042 ) ) ;
#119996 = CARTESIAN_POINT ( 'NONE',  ( -9.474510206698964154, 16.51473224551069663, 115.4155762719810241 ) ) ;
#119997 = CARTESIAN_POINT ( 'NONE',  ( 15.80617190586746368, 15.72974639402197994, 29.37390960531435269 ) ) ;
#119998 = CARTESIAN_POINT ( 'NONE',  ( -19.03943276465977164, -0.05219959533935918106, 18.75109039468567218 ) ) ;
#119999 = CARTESIAN_POINT ( 'NONE',  ( -4.379528057220328563, 16.55341960407611168, 85.20724293864770971 ) ) ;
#120000 = CARTESIAN_POINT ( 'NONE',  ( -0.05219959533909027116, -19.03943276465977164, 97.49890960531436690 ) ) ;
#120001 = VERTEX_POINT ( 'NONE', #161371 ) ;
#120002 = CARTESIAN_POINT ( 'NONE',  ( -12.06949235617739369, -12.14591786802326823, 34.37609039468568284 ) ) ;
#120003 = CARTESIAN_POINT ( 'NONE',  ( 19.03943276465977164, -0.05219959533909143690, 43.74890960531435979 ) ) ;
#120005 = DIRECTION ( 'NONE',  ( 0.000000000000000000, 0.000000000000000000, -1.000000000000000000 ) ) ;
#120004 = CARTESIAN_POINT ( 'NONE',  ( -8.224510206698735004, -14.34966873604973081, 49.58442372801901143 ) ) ;
#120006 = CARTESIAN_POINT ( 'NONE',  ( 19.03943276465977164, 0.05219959533936151252, 46.25109039468566863 ) ) ;
#120007 = CARTESIAN_POINT ( 'NONE',  ( -16.51473224551069308, -9.474510206698971260, 46.66557627198102409 ) ) ;
#120008 = CARTESIAN_POINT ( 'NONE',  ( 12.14591786802327356, -12.06949235617739191, 75.62609039468567573 ) ) ;
#120009 = CARTESIAN_POINT ( 'NONE',  ( 19.03943276465977164, 0.05219959533936151252, 81.25109039468567573 ) ) ;
#120010 = CARTESIAN_POINT ( 'NONE',  ( 16.51473224551083163, -9.474510206698727899, 25.83442372801900078 ) ) ;
#120011 = CARTESIAN_POINT ( 'NONE',  ( 16.46253265017160672, -9.564922557960803928, 58.33224293864769550 ) ) ;
#120012 = CARTESIAN_POINT ( 'NONE',  ( -4.483927247898539470, -16.52544592524342804, 97.29057627198105251 ) ) ;
#120013 = CARTESIAN_POINT ( 'NONE',  ( -19.02544592524334988, -5.153800228976617603, 63.95942372801899012 ) ) ;
#120014 = CARTESIAN_POINT ( 'NONE',  ( 10.72451020669898902, -18.67979575497178502, 67.91557627198102409 ) ) ;
#120015 = CARTESIAN_POINT ( 'NONE',  ( -19.03943276465977164, -0.05219959533935918106, 38.75109039468566152 ) ) ;
#120016 = CARTESIAN_POINT ( 'NONE',  ( 19.03943276465977164, -0.05219959533909143690, 98.74890960531436690 ) ) ;
#120017 = CARTESIAN_POINT ( 'NONE',  ( 21.55341960407610458, 5.719274019375980345, 73.95724293864769550 ) ) ;
#120018 = CARTESIAN_POINT ( 'NONE',  ( -16.29526858892876007, 7.335722546920119491, 84.20329402199796220 ) ) ;
#120019 = CARTESIAN_POINT ( 'NONE',  ( 19.02544592524334988, 5.153800228976608722, 96.45942372801897591 ) ) ;
#120020 = CARTESIAN_POINT ( 'NONE',  ( 9.474510206698729675, 16.51473224551082808, 97.08442372801900433 ) ) ;
#120021 = CARTESIAN_POINT ( 'NONE',  ( -14.29746914071037622, -8.314922557961029526, 34.16775706135234714 ) ) ;
#120022 = CARTESIAN_POINT ( 'NONE',  ( -16.51473224551069308, -9.474510206698971260, 41.66557627198103120 ) ) ;
#120023 = CARTESIAN_POINT ( 'NONE',  ( -13.97604488694527625, -13.89961937509977652, 106.8739096053143669 ) ) ;
#120024 = CARTESIAN_POINT ( 'NONE',  ( -10.81492255796078084, -18.62759615963271287, 92.08224293864769550 ) ) ;
#120025 = CARTESIAN_POINT ( 'NONE',  ( 18.67979575497194134, -10.72451020669871369, 55.83442372801901854 ) ) ;
#120027 = CARTESIAN_POINT ( 'NONE',  ( 5.153800228976615827, -19.02544592524334988, 20.20942372801899722 ) ) ;
#120026 = CARTESIAN_POINT ( 'NONE',  ( -19.03943276465977164, -0.05219959533935918106, 103.7510903946856757 ) ) ;
#120028 = CARTESIAN_POINT ( 'NONE',  ( 4.483927247898790824, -16.52544592524335698, 105.2094237280190328 ) ) ;
#120029 = CARTESIAN_POINT ( 'NONE',  ( 18.67979575497178502, 10.72451020669898547, 94.16557627198103830 ) ) ;
#120030 = CARTESIAN_POINT ( 'NONE',  ( -16.55341960407611168, -4.379528057220339221, 46.45724293864769550 ) ) ;
#120031 = CARTESIAN_POINT ( 'NONE',  ( -19.05341960407617563, 5.049401038297882671, 78.54275706135233293 ) ) ;
#120032 = CARTESIAN_POINT ( 'NONE',  ( 13.97604488694548053, -13.89961937509957401, 60.62609039468564731 ) ) ;
#120033 = CARTESIAN_POINT ( 'NONE',  ( 21.52544592524334988, 5.823673210054432836, 76.45942372801901854 ) ) ;
#120034 = CARTESIAN_POINT ( 'NONE',  ( 13.89961937509957401, 13.97604488694547697, 41.87609039468566152 ) ) ;
#120035 = CARTESIAN_POINT ( 'NONE',  ( 14.34966873604960469, 8.224510206698951720, 109.1655762719810383 ) ) ;
#120036 = CARTESIAN_POINT ( 'NONE',  ( 21.53943276465977519, -0.05219959533907433946, 48.74890960531435979 ) ) ;
#120037 = CARTESIAN_POINT ( 'NONE',  ( -16.53943276465976808, 0.05219959533911058130, 41.24890960531435269 ) ) ;
#120038 = CARTESIAN_POINT ( 'NONE',  ( 18.67979575497194134, -10.72451020669871369, 105.8344237280190328 ) ) ;
#120039 = CARTESIAN_POINT ( 'NONE',  ( -12.14591786802326823, 12.06949235617739902, 78.12609039468570415 ) ) ;
#120040 = CARTESIAN_POINT ( 'NONE',  ( 0.05219959533910956823, 16.53943276465976808, 29.99890960531435979 ) ) ;
#120041 = CARTESIAN_POINT ( 'NONE',  ( -10.72451020669870658, -18.67979575497194134, 64.58442372801900433 ) ) ;
#120042 = CARTESIAN_POINT ( 'NONE',  ( 21.53943276465977519, 0.05219959533937863772, 66.25109039468567573 ) ) ;
#120043 = CARTESIAN_POINT ( 'NONE',  ( 10.81492255796078972, 18.62759615963270932, 69.58224293864769550 ) ) ;
#120044 = ORIENTED_EDGE ( 'NONE', *, *, #158416, .T. ) ;
#120045 = CARTESIAN_POINT ( 'NONE',  ( 19.03943276465977164, -0.05219959533909143690, 28.74890960531435624 ) ) ;
#120046 = CARTESIAN_POINT ( 'NONE',  ( 18.67979575497194134, -10.72451020669871369, 45.83442372801901854 ) ) ;
#120047 = CARTESIAN_POINT ( 'NONE',  ( -12.14591786802309592, -12.06949235617757132, 111.8739096053143669 ) ) ;
#120048 = CARTESIAN_POINT ( 'NONE',  ( -5.153800228976328057, -19.02544592524343514, 37.29057627198102409 ) ) ;
#120049 = CARTESIAN_POINT ( 'NONE',  ( 14.29746914071049879, -8.314922557960816363, 78.33224293864770971 ) ) ;
#120050 = CARTESIAN_POINT ( 'NONE',  ( -19.03943276465977164, 0.05219959533909376836, 86.24890960531436690 ) ) ;
#120051 = CARTESIAN_POINT ( 'NONE',  ( -14.34966873604960291, -8.224510206698953496, 26.66557627198103475 ) ) ;
#120052 = CARTESIAN_POINT ( 'NONE',  ( 4.483927247898545687, 16.52544592524342804, 104.7905762719810241 ) ) ;
#120053 = CARTESIAN_POINT ( 'NONE',  ( 15.80617190586746368, 15.72974639402197994, 74.37390960531436690 ) ) ;
#120054 = CARTESIAN_POINT ( 'NONE',  ( 21.52544592524344225, -5.823673210054117533, 108.5405762719810241 ) ) ;
#120055 = CARTESIAN_POINT ( 'NONE',  ( -17.18269478283316332, 17.18269478283309226, -54.21489346206828230 ) ) ;
#120057 = CARTESIAN_POINT ( 'NONE',  ( 16.53943276465976808, 0.05219959533934440121, 21.25109039468567218 ) ) ;
#120056 = CARTESIAN_POINT ( 'NONE',  ( 16.46253265017160672, -9.564922557960803928, 68.33224293864770971 ) ) ;
#120058 = CARTESIAN_POINT ( 'NONE',  ( 18.62759615963271287, -10.81492255796078972, 63.33224293864770260 ) ) ;
#120059 = CARTESIAN_POINT ( 'NONE',  ( 0.05219959533937995610, -21.53943276465977519, 80.00109039468568994 ) ) ;
#120060 = CARTESIAN_POINT ( 'NONE',  ( -13.97604488694527625, -13.89961937509977652, 81.87390960531436690 ) ) ;
#120061 = CARTESIAN_POINT ( 'NONE',  ( 16.46253265017160672, -9.564922557960803928, 108.3322429386476955 ) ) ;
#120062 = CARTESIAN_POINT ( 'NONE',  ( -14.34966873604972548, 8.224510206698743886, 83.33442372801903275 ) ) ;
#120063 = CARTESIAN_POINT ( 'NONE',  ( -18.67979575497193778, 10.72451020669871902, 53.33442372801901854 ) ) ;
#120064 = CARTESIAN_POINT ( 'NONE',  ( 0.05219959533937995610, -21.53943276465977519, 100.0010903946857042 ) ) ;
#120065 = CARTESIAN_POINT ( 'NONE',  ( -16.52544592524335698, -4.483927247898792601, 63.95942372801901854 ) ) ;
#120066 = CARTESIAN_POINT ( 'NONE',  ( 10.72451020669898902, -18.67979575497178502, 112.9155762719810383 ) ) ;
#120067 = FACE_OUTER_BOUND ( 'NONE', #53013, .T. ) ;
#120068 = CARTESIAN_POINT ( 'NONE',  ( -0.05219959533907301413, -21.53943276465977519, 92.49890960531436690 ) ) ;
#120069 = CARTESIAN_POINT ( 'NONE',  ( -13.97604488694547697, 13.89961937509957934, 43.12609039468566152 ) ) ;
#120070 = CARTESIAN_POINT ( 'NONE',  ( 18.62759615963271287, -10.81492255796078972, 53.33224293864769550 ) ) ;
#120072 = CARTESIAN_POINT ( 'NONE',  ( 0.05219959533910956823, 16.53943276465976808, 39.99890960531436690 ) ) ;
#120071 = CARTESIAN_POINT ( 'NONE',  ( 0.05219959533909260263, 19.03943276465977164, 99.99890960531436690 ) ) ;
#120073 = CARTESIAN_POINT ( 'NONE',  ( -17.50000000000001421, 5.622605283950871780, 63.68792689403893093 ) ) ;
#120074 = CARTESIAN_POINT ( 'NONE',  ( -26.99873734152928506, -22.49873734152901861, 1.110912703473986074 ) ) ;
#120075 = EDGE_CURVE ( 'NONE', #10845, #181921, #146187, .T. ) ;
#120076 = CARTESIAN_POINT ( 'NONE',  ( -13.97604488694547697, 13.89961937509957934, 98.12609039468566152 ) ) ;
#120077 = CARTESIAN_POINT ( 'NONE',  ( -10.81492255796078084, -18.62759615963271287, 72.08224293864769550 ) ) ;
#120078 = CARTESIAN_POINT ( 'NONE',  ( -12.06949235617756955, 12.14591786802309770, 55.62390960531436690 ) ) ;
#120079 = CARTESIAN_POINT ( 'NONE',  ( 14.34966873604972726, -8.224510206698740333, 35.83442372801901143 ) ) ;
#120080 = CARTESIAN_POINT ( 'NONE',  ( 19.05341960407611168, 5.049401038298154454, 43.95724293864769550 ) ) ;
#120082 = CARTESIAN_POINT ( 'NONE',  ( -19.02544592524334988, -5.153800228976617603, 88.95942372801897591 ) ) ;
#120081 = CARTESIAN_POINT ( 'NONE',  ( 15.80617190586746368, 15.72974639402197994, 109.3739096053143811 ) ) ;
#120083 = CARTESIAN_POINT ( 'NONE',  ( 16.46253265017160672, -9.564922557960803928, 78.33224293864769550 ) ) ;
#120084 = CARTESIAN_POINT ( 'NONE',  ( -5.049401038298153566, 19.05341960407611168, 80.20724293864769550 ) ) ;
#120085 = CARTESIAN_POINT ( 'NONE',  ( -0.05219959533907301413, -21.53943276465977519, 72.49890960531435269 ) ) ;
#120086 = CARTESIAN_POINT ( 'NONE',  ( 13.97604488694527802, 13.89961937509977652, 29.37390960531435979 ) ) ;
#120087 = CARTESIAN_POINT ( 'NONE',  ( 4.205191997947069993, 37.27545319588617190, -8.000000000000000000 ) ) ;
#120088 = CARTESIAN_POINT ( 'NONE',  ( 8.224510206698953496, -14.34966873604960469, 57.91557627198103120 ) ) ;
#120089 = CARTESIAN_POINT ( 'NONE',  ( -13.89961937509977652, 13.97604488694528158, 90.62390960531432427 ) ) ;
#120090 = CARTESIAN_POINT ( 'NONE',  ( 1.993301997531345686E-15, -30.30510711980685556, 140.7500000054623683 ) ) ;
#120091 = CARTESIAN_POINT ( 'NONE',  ( -19.02544592524334988, -5.153800228976617603, 53.95942372801898301 ) ) ;
#120092 = CARTESIAN_POINT ( 'NONE',  ( 21.55341960407610458, 5.719274019375980345, 78.95724293864769550 ) ) ;
#120093 = CARTESIAN_POINT ( 'NONE',  ( -19.03943276465977164, -0.05219959533935918106, 38.75109039468566152 ) ) ;
#120094 = CARTESIAN_POINT ( 'NONE',  ( 16.46253265017160672, -9.564922557960803928, 93.33224293864769550 ) ) ;
#120095 = DIRECTION ( 'NONE',  ( -1.000000000000000000, 0.000000000000000000, 0.000000000000000000 ) ) ;
#120096 = CARTESIAN_POINT ( 'NONE',  ( 15.72974639402199770, -15.80617190586745480, 28.12390960531435979 ) ) ;
#120097 = CARTESIAN_POINT ( 'NONE',  ( -19.02544592524342804, 5.153800228976336051, 76.04057627198102409 ) ) ;
#120098 = CARTESIAN_POINT ( 'NONE',  ( 5.719274019375673035, 21.55341960407619339, 52.29275706135236135 ) ) ;
#120099 = CARTESIAN_POINT ( 'NONE',  ( -13.97604488694527625, -13.89961937509977652, 21.87390960531435979 ) ) ;
#120101 = VERTEX_POINT ( 'NONE', #102700 ) ;
#120100 = CARTESIAN_POINT ( 'NONE',  ( -15.80617190586745835, -15.72974639402198527, 111.8739096053143669 ) ) ;
#120102 = CARTESIAN_POINT ( 'NONE',  ( 21.53943276465977519, 0.05219959533937863772, 41.25109039468568284 ) ) ;
#120103 = ORIENTED_EDGE ( 'NONE', *, *, #155138, .T. ) ;
#120104 = CARTESIAN_POINT ( 'NONE',  ( 13.89961937509977652, -13.97604488694527269, 98.12390960531433848 ) ) ;
#120105 = VECTOR ( 'NONE', #62, 1000.000000000000000 ) ;
#120106 = DIRECTION ( 'NONE',  ( -1.000000000000000000, -0.000000000000000000, -0.000000000000000000 ) ) ;
#120107 = CARTESIAN_POINT ( 'NONE',  ( 21.55341960407610458, 5.719274019375980345, 108.9572429386476955 ) ) ;
#120108 = CARTESIAN_POINT ( 'NONE',  ( 13.97604488694527802, 13.89961937509977652, 64.37390960531436690 ) ) ;
#120109 = CARTESIAN_POINT ( 'NONE',  ( -19.05341960407617563, 5.049401038297882671, 113.5427570613523471 ) ) ;
#120110 = CARTESIAN_POINT ( 'NONE',  ( 36.91746825000000598, -11.99521256947793546, -2.224999997268813701 ) ) ;
#120111 = CARTESIAN_POINT ( 'NONE',  ( 0.05219959533937995610, -21.53943276465977519, 105.0010903946856757 ) ) ;
#120112 = CARTESIAN_POINT ( 'NONE',  ( -9.564922557960796823, -16.46253265017161027, 42.08224293864769550 ) ) ;
#120113 = CARTESIAN_POINT ( 'NONE',  ( -5.719274019375665041, -21.55341960407619695, 94.79275706135234714 ) ) ;
#120115 = CARTESIAN_POINT ( 'NONE',  ( 0.05219959533937995610, -21.53943276465977519, 60.00109039468568284 ) ) ;
#120114 = CARTESIAN_POINT ( 'NONE',  ( -19.03943276465977164, 0.05219959533909376836, 86.24890960531436690 ) ) ;
#120116 = CARTESIAN_POINT ( 'NONE',  ( -27.73933785331498925, 9.013057229001089965, 143.2750000027311899 ) ) ;
#120117 = CARTESIAN_POINT ( 'NONE',  ( 9.474510206698971260, -16.51473224551069308, 102.9155762719810241 ) ) ;
#120118 = CARTESIAN_POINT ( 'NONE',  ( -17.49999999999999645, 3.471454075611625001, 29.48332581144368447 ) ) ;
#120121 = CARTESIAN_POINT ( 'NONE',  ( -5.719274019375665041, -21.55341960407619695, 54.79275706135235424 ) ) ;
#120120 = CARTESIAN_POINT ( 'NONE',  ( -12.06949235617739369, -12.14591786802326823, 69.37609039468567573 ) ) ;
#120119 = CARTESIAN_POINT ( 'NONE',  ( 8.224510206698742110, 14.34966873604972548, 57.08442372801901854 ) ) ;
#120122 = CARTESIAN_POINT ( 'NONE',  ( 5.823673210054444382, -21.52544592524334988, 90.20942372801903275 ) ) ;
#120123 = CARTESIAN_POINT ( 'NONE',  ( 25.12473289294614176, -7.795855283352525866, 170.9710361440363329 ) ) ;
#120124 = CARTESIAN_POINT ( 'NONE',  ( -12.06949235617739369, -12.14591786802326823, 34.37609039468568284 ) ) ;
#120125 = CARTESIAN_POINT ( 'NONE',  ( -19.02544592524342804, 5.153800228976336051, 71.04057627198099567 ) ) ;
#120126 = CARTESIAN_POINT ( 'NONE',  ( 0.05219959533909260263, 19.03943276465977164, 94.99890960531436690 ) ) ;
#120127 = CARTESIAN_POINT ( 'NONE',  ( 17.05587630539784527, 6.762274262135707481, 41.75819690962689634 ) ) ;
#120128 = CARTESIAN_POINT ( 'NONE',  ( -13.97604488694527625, -13.89961937509977652, 31.87390960531435979 ) ) ;
#120129 = CARTESIAN_POINT ( 'NONE',  ( 0.05219959533907565091, 21.53943276465977519, 24.99890960531435624 ) ) ;
#120130 = CARTESIAN_POINT ( 'NONE',  ( -14.29746914071037622, -8.314922557961029526, 89.16775706135236135 ) ) ;
#120132 = CARTESIAN_POINT ( 'NONE',  ( 16.51473224551069308, 9.474510206698969483, 74.16557627198103830 ) ) ;
#120131 = CARTESIAN_POINT ( 'NONE',  ( -12.06949235617756955, 12.14591786802309770, 85.62390960531436690 ) ) ;
#120133 = CARTESIAN_POINT ( 'NONE',  ( 5.823673210054444382, -21.52544592524334988, 90.20942372801903275 ) ) ;
#120134 = LINE ( 'NONE', #75613, #118027 ) ;
#120135 = CARTESIAN_POINT ( 'NONE',  ( -12.06949235617739369, -12.14591786802326823, 24.37609039468567573 ) ) ;
#120136 = CARTESIAN_POINT ( 'NONE',  ( -12.06949235617756955, 12.14591786802309770, 75.62390960531439532 ) ) ;
#120137 = CARTESIAN_POINT ( 'NONE',  ( -0.05219959533937732626, 21.53943276465977519, 37.50109039468568284 ) ) ;
#120138 = CARTESIAN_POINT ( 'NONE',  ( 0.05219959533907565091, 21.53943276465977519, 69.99890960531435269 ) ) ;
#120139 = CARTESIAN_POINT ( 'NONE',  ( 5.153800228976615827, -19.02544592524334988, 35.20942372801899722 ) ) ;
#120140 = CARTESIAN_POINT ( 'NONE',  ( 4.999999999999996447, 5.000000000000003553, -18.00000000000000000 ) ) ;
#120141 = CARTESIAN_POINT ( 'NONE',  ( 9.564922557960805705, 16.46253265017160317, 79.58224293864769550 ) ) ;
#120142 = CARTESIAN_POINT ( 'NONE',  ( -4.379528057220328563, 16.55341960407611168, 50.20724293864769550 ) ) ;
#120143 = CARTESIAN_POINT ( 'NONE',  ( 8.224510206698953496, -14.34966873604960469, 32.91557627198102409 ) ) ;
#120144 = CARTESIAN_POINT ( 'NONE',  ( 8.224510206698742110, 14.34966873604972548, 112.0844237280190185 ) ) ;
#120145 = CARTESIAN_POINT ( 'NONE',  ( -9.474510206698720793, -16.51473224551083518, 69.58442372801901854 ) ) ;
#120146 = CARTESIAN_POINT ( 'NONE',  ( 16.46253265017146816, 9.564922557961045513, 76.66775706135234714 ) ) ;
#120147 = CARTESIAN_POINT ( 'NONE',  ( -21.55341960407610458, -5.719274019375992779, 26.45724293864768839 ) ) ;
#120148 = EDGE_CURVE ( 'NONE', #185073, #38805, #96907, .T. ) ;
#120149 = CARTESIAN_POINT ( 'NONE',  ( -4.379528057220328563, 16.55341960407611168, 90.20724293864770971 ) ) ;
#120150 = DIRECTION ( 'NONE',  ( -1.000000000000000000, 5.392603844284257652E-33, 0.000000000000000000 ) ) ;
#120152 = CARTESIAN_POINT ( 'NONE',  ( -10.81492255796078084, -18.62759615963271287, 42.08224293864769550 ) ) ;
#120151 = CARTESIAN_POINT ( 'NONE',  ( 19.02544592524343514, -5.153800228976328945, 28.54057627198102409 ) ) ;
#120153 = CARTESIAN_POINT ( 'NONE',  ( -0.05219959533907301413, -21.53943276465977519, 62.49890960531436690 ) ) ;
#120154 = CARTESIAN_POINT ( 'NONE',  ( 14.34966873604960469, 8.224510206698951720, 114.1655762719810383 ) ) ;
#120156 = CARTESIAN_POINT ( 'NONE',  ( 5.049401038298161559, -19.05341960407611168, 47.70724293864770260 ) ) ;
#120155 = CARTESIAN_POINT ( 'NONE',  ( -16.55341960407617563, 4.379528057220093196, 68.54275706135234714 ) ) ;
#120157 = CARTESIAN_POINT ( 'NONE',  ( -15.80617190586768217, 15.72974639402176855, 58.12609039468568994 ) ) ;
#120158 = CARTESIAN_POINT ( 'NONE',  ( -16.52544592524342804, 4.483927247898546575, 111.0405762719810525 ) ) ;
#120159 = CARTESIAN_POINT ( 'NONE',  ( 9.564922557961047289, -16.46253265017146816, 95.41775706135233293 ) ) ;
#120160 = CARTESIAN_POINT ( 'NONE',  ( -22.81625015709509441, -31.40387420917324590, -2.824999997268812901 ) ) ;
#120162 = CARTESIAN_POINT ( 'NONE',  ( -0.05219959533907301413, -21.53943276465977519, 32.49890960531435979 ) ) ;
#120161 = DIRECTION ( 'NONE',  ( -1.000000000000000000, 0.000000000000000000, 0.000000000000000000 ) ) ;
#120163 = FACE_OUTER_BOUND ( 'NONE', #11300, .T. ) ;
#120164 = CARTESIAN_POINT ( 'NONE',  ( -5.719274019375665041, -21.55341960407619695, 64.79275706135234714 ) ) ;
#120166 = CARTESIAN_POINT ( 'NONE',  ( -12.14591786802309592, -12.06949235617757132, 41.87390960531435979 ) ) ;
#120165 = CARTESIAN_POINT ( 'NONE',  ( -4.379528057220086978, -16.55341960407618274, 49.79275706135234714 ) ) ;
#120167 = CARTESIAN_POINT ( 'NONE',  ( 10.81492255796078972, 18.62759615963270932, 69.58224293864769550 ) ) ;
#120168 = CARTESIAN_POINT ( 'NONE',  ( 18.62759615963271287, -10.81492255796078972, 63.33224293864770260 ) ) ;
#120169 = CARTESIAN_POINT ( 'NONE',  ( 32.09281931051394565, -20.34824190692416934, -24.99999999999997868 ) ) ;
#120171 = CARTESIAN_POINT ( 'NONE',  ( 0.05219959533909260263, 19.03943276465977164, 114.9989096053143669 ) ) ;
#120170 = CARTESIAN_POINT ( 'NONE',  ( -13.89961937509957401, -13.97604488694547875, 84.37609039468567573 ) ) ;
#120172 = CARTESIAN_POINT ( 'NONE',  ( 13.97604488694527802, 13.89961937509977652, 54.37390960531435979 ) ) ;
#120173 = CARTESIAN_POINT ( 'NONE',  ( 4.483927247898545687, 16.52544592524342804, 109.7905762719810383 ) ) ;
#120174 =( NAMED_UNIT ( * ) PLANE_ANGLE_UNIT ( ) SI_UNIT ( $, .RADIAN. ) );
#120175 = CARTESIAN_POINT ( 'NONE',  ( 19.02544592524343514, -5.153800228976328945, 108.5405762719810383 ) ) ;
#120176 = VERTEX_POINT ( 'NONE', #74363 ) ;
#120177 = CARTESIAN_POINT ( 'NONE',  ( 12.06949235617739724, 12.14591786802326823, 66.87609039468568994 ) ) ;
#120178 = CARTESIAN_POINT ( 'NONE',  ( 10.72451020669898902, -18.67979575497178502, 97.91557627198103830 ) ) ;
#120179 = CARTESIAN_POINT ( 'NONE',  ( -0.05219959533909027116, -19.03943276465977164, 67.49890960531436690 ) ) ;
#120180 = CARTESIAN_POINT ( 'NONE',  ( -10.81492255796105439, 18.62759615963255655, 42.91775706135235424 ) ) ;
#120181 = CARTESIAN_POINT ( 'NONE',  ( 19.02544592524343514, -5.153800228976328945, 98.54057627198100988 ) ) ;
#120182 = CARTESIAN_POINT ( 'NONE',  ( -24.61032826407718233, -31.32210114170946724, -21.33226357149971619 ) ) ;
#120183 = ORIENTED_EDGE ( 'NONE', *, *, #30184, .T. ) ;
#120184 = CARTESIAN_POINT ( 'NONE',  ( 0.05219959533937995610, -21.53943276465977519, 30.00109039468568284 ) ) ;
#120186 = CARTESIAN_POINT ( 'NONE',  ( 16.46253265017146816, 9.564922557961045513, 86.66775706135233293 ) ) ;
#120185 = CARTESIAN_POINT ( 'NONE',  ( -9.564922557960796823, -16.46253265017161027, 22.08224293864768839 ) ) ;
#120187 = CARTESIAN_POINT ( 'NONE',  ( 13.97604488694548053, -13.89961937509957401, 45.62609039468566863 ) ) ;
#120188 = CARTESIAN_POINT ( 'NONE',  ( 5.719274019375991003, -21.55341960407610458, 97.70724293864772392 ) ) ;
#120189 = CARTESIAN_POINT ( 'NONE',  ( 19.03943276465977164, 0.05219959533936151252, 31.25109039468566863 ) ) ;
#120190 = CARTESIAN_POINT ( 'NONE',  ( -5.049401038297874678, -19.05341960407617918, 54.79275706135234003 ) ) ;
#120191 = CARTESIAN_POINT ( 'NONE',  ( 4.379528057220092307, 16.55341960407617563, 87.29275706135236135 ) ) ;
#120193 = VERTEX_POINT ( 'NONE', #29838 ) ;
#120192 = CARTESIAN_POINT ( 'NONE',  ( 28.79475375365606737, -9.355982642738910116, 146.8843446568999980 ) ) ;
#120194 = CARTESIAN_POINT ( 'NONE',  ( 13.89961937509977652, -13.97604488694527269, 78.12390960531433848 ) ) ;
#120195 = CARTESIAN_POINT ( 'NONE',  ( 15.80617190586769283, -15.72974639402175789, 80.62609039468567573 ) ) ;
#120196 = CARTESIAN_POINT ( 'NONE',  ( 5.719274019375673035, 21.55341960407619339, 97.29275706135234714 ) ) ;
#120197 = DIRECTION ( 'NONE',  ( 0.5000000000000002220, 0.4999999999999985012, -0.7071067811865483499 ) ) ;
#120198 = CARTESIAN_POINT ( 'NONE',  ( 16.46253265017160672, -9.564922557960803928, 93.33224293864769550 ) ) ;
#120199 = CARTESIAN_POINT ( 'NONE',  ( 0.05219959533937995610, -21.53943276465977519, 60.00109039468568284 ) ) ;
#120200 = CARTESIAN_POINT ( 'NONE',  ( -13.89961937509957401, -13.97604488694547875, 99.37609039468567573 ) ) ;
#120201 = CARTESIAN_POINT ( 'NONE',  ( -13.89961937509977652, 13.97604488694528158, 60.62390960531436690 ) ) ;
#120202 = CARTESIAN_POINT ( 'NONE',  ( 15.72974639402199770, -15.80617190586745480, 23.12390960531436335 ) ) ;
#120203 = CARTESIAN_POINT ( 'NONE',  ( -9.564922557960796823, -16.46253265017161027, 77.08224293864769550 ) ) ;
#120204 = FACE_OUTER_BOUND ( 'NONE', #69262, .T. ) ;
#120205 = CARTESIAN_POINT ( 'NONE',  ( 5.049401038298161559, -19.05341960407611168, 62.70724293864769550 ) ) ;
#120206 = CARTESIAN_POINT ( 'NONE',  ( 0.05219959533909260263, 19.03943276465977164, 54.99890960531435979 ) ) ;
#120207 = CARTESIAN_POINT ( 'NONE',  ( 21.55341960407610458, 5.719274019375980345, 113.9572429386477239 ) ) ;
#120208 = CARTESIAN_POINT ( 'NONE',  ( 12.06949235617739724, 12.14591786802326823, 81.87609039468568994 ) ) ;
#120209 = DIRECTION ( 'NONE',  ( 0.000000000000000000, 0.000000000000000000, 1.000000000000000000 ) ) ;
#120210 = CARTESIAN_POINT ( 'NONE',  ( 16.46253265017146816, 9.564922557961045513, 46.66775706135233293 ) ) ;
#120211 = CARTESIAN_POINT ( 'NONE',  ( -13.97604488694527625, -13.89961937509977652, 81.87390960531436690 ) ) ;
#120212 = CARTESIAN_POINT ( 'NONE',  ( -8.314922557960811034, -14.29746914071050412, 67.08224293864770971 ) ) ;
#120213 = CARTESIAN_POINT ( 'NONE',  ( 16.53943276465976808, -0.05219959533910856209, 108.7489096053143669 ) ) ;
#120214 = CARTESIAN_POINT ( 'NONE',  ( 15.72974639402199770, -15.80617190586745480, 23.12390960531436335 ) ) ;
#120215 = CARTESIAN_POINT ( 'NONE',  ( -5.049401038298153566, 19.05341960407611168, 105.2072429386476671 ) ) ;
#120216 = CARTESIAN_POINT ( 'NONE',  ( 16.52544592524342804, -4.483927247898539470, 78.54057627198103830 ) ) ;
#120217 = CARTESIAN_POINT ( 'NONE',  ( 11.74149087413295156, -36.13659316521243881, -3.402157773949823216 ) ) ;
#120218 = CARTESIAN_POINT ( 'NONE',  ( 19.03943276465977164, 0.05219959533936151252, 36.25109039468567573 ) ) ;
#120219 = CARTESIAN_POINT ( 'NONE',  ( -4.379528057220086978, -16.55341960407618274, 99.79275706135234714 ) ) ;
#120220 = CARTESIAN_POINT ( 'NONE',  ( 19.05341960407611168, 5.049401038298154454, 88.95724293864769550 ) ) ;
#120221 = CARTESIAN_POINT ( 'NONE',  ( 15.72974639402176855, 15.80617190586768217, 56.87609039468568994 ) ) ;
#120222 = CARTESIAN_POINT ( 'NONE',  ( -10.81492255796078084, -18.62759615963271287, 42.08224293864769550 ) ) ;
#120223 = CARTESIAN_POINT ( 'NONE',  ( 0.05219959533907565091, 21.53943276465977519, 109.9989096053143527 ) ) ;
#120224 = CARTESIAN_POINT ( 'NONE',  ( -0.05219959533907301413, -21.53943276465977519, 72.49890960531435269 ) ) ;
#120225 = CARTESIAN_POINT ( 'NONE',  ( -12.06949235617756955, 12.14591786802309770, 100.6239096053143811 ) ) ;
#120226 = CARTESIAN_POINT ( 'NONE',  ( 9.564922557961047289, -16.46253265017146816, 60.41775706135233293 ) ) ;
#120227 = CARTESIAN_POINT ( 'NONE',  ( 5.049401038298161559, -19.05341960407611168, 32.70724293864768129 ) ) ;
#120228 = CARTESIAN_POINT ( 'NONE',  ( -0.05219959533909027116, -19.03943276465977164, 87.49890960531436690 ) ) ;
#120229 = CARTESIAN_POINT ( 'NONE',  ( -19.05341960407611168, -5.049401038298163336, 86.45724293864769550 ) ) ;
#120230 = CARTESIAN_POINT ( 'NONE',  ( -12.14591786802309592, -12.06949235617757132, 96.87390960531436690 ) ) ;
#120231 = CARTESIAN_POINT ( 'NONE',  ( 16.55341960407611168, 4.379528057220329451, 23.95724293864769550 ) ) ;
#120232 = CARTESIAN_POINT ( 'NONE',  ( -4.379528057220086978, -16.55341960407618274, 44.79275706135234714 ) ) ;
#120233 = CARTESIAN_POINT ( 'NONE',  ( 21.55341960407619695, -5.719274019375665929, 101.0427570613523756 ) ) ;
#120234 = CARTESIAN_POINT ( 'NONE',  ( 5.049401038298161559, -19.05341960407611168, 107.7072429386476955 ) ) ;
#120235 = CARTESIAN_POINT ( 'NONE',  ( -10.72451020669870658, -18.67979575497194134, 39.58442372801901143 ) ) ;
#120236 = CARTESIAN_POINT ( 'NONE',  ( -19.03943276465977164, 0.05219959533909376836, 41.24890960531435269 ) ) ;
#120237 = CARTESIAN_POINT ( 'NONE',  ( -8.224510206698735004, -14.34966873604973081, 39.58442372801901143 ) ) ;
#120238 = CARTESIAN_POINT ( 'NONE',  ( -19.03943276465977164, -0.05219959533935918106, 103.7510903946856757 ) ) ;
#120239 = EDGE_CURVE ( 'NONE', #9179, #123381, #57207, .T. ) ;
#120240 = CARTESIAN_POINT ( 'NONE',  ( 13.89961937509977652, -13.97604488694527269, 33.12390960531434558 ) ) ;
#120241 = CARTESIAN_POINT ( 'NONE',  ( -16.55341960407611168, -4.379528057220339221, 91.45724293864769550 ) ) ;
#120242 = CARTESIAN_POINT ( 'NONE',  ( 21.55341960407610458, 5.719274019375980345, 108.9572429386476955 ) ) ;
#120243 = CARTESIAN_POINT ( 'NONE',  ( 19.02544592524334988, 5.153800228976608722, 81.45942372801897591 ) ) ;
#120244 = CARTESIAN_POINT ( 'NONE',  ( 9.474510206698971260, -16.51473224551069308, 97.91557627198102409 ) ) ;
#120245 = CARTESIAN_POINT ( 'NONE',  ( 21.53943276465977519, 0.05219959533937863772, 36.25109039468567573 ) ) ;
#120246 = CARTESIAN_POINT ( 'NONE',  ( -37.99626262588766679, 2.428612866367529932E-14, -2.002157773949823305 ) ) ;
#120247 = CARTESIAN_POINT ( 'NONE',  ( -5.049401038298153566, 19.05341960407611168, 90.20724293864766707 ) ) ;
#120248 = CARTESIAN_POINT ( 'NONE',  ( 16.20579543436677739, -7.371946100355105003, 111.9347916582813269 ) ) ;
#120249 = CARTESIAN_POINT ( 'NONE',  ( 16.46253265017160672, -9.564922557960803928, 83.33224293864768129 ) ) ;
#120251 = CARTESIAN_POINT ( 'NONE',  ( 4.483927247898545687, 16.52544592524342804, 84.79057627198102409 ) ) ;
#120250 = CARTESIAN_POINT ( 'NONE',  ( -15.72974639402176322, -15.80617190586768395, 29.37609039468568284 ) ) ;
#120252 = CARTESIAN_POINT ( 'NONE',  ( -0.05219959533909027116, -19.03943276465977164, 102.4989096053143669 ) ) ;
#120253 = CARTESIAN_POINT ( 'NONE',  ( 19.03943276465977164, 0.05219959533936151252, 26.25109039468566507 ) ) ;
#120254 = CARTESIAN_POINT ( 'NONE',  ( 16.52544592524335698, 4.483927247898782831, 51.45942372801901854 ) ) ;
#120255 = CARTESIAN_POINT ( 'NONE',  ( 5.823673210054444382, -21.52544592524334988, 80.20942372801901854 ) ) ;
#120256 = CARTESIAN_POINT ( 'NONE',  ( 12.06949235617739724, 12.14591786802326823, 21.87609039468567573 ) ) ;
#120257 = CARTESIAN_POINT ( 'NONE',  ( -9.474510206698964154, 16.51473224551069663, 65.41557627198102409 ) ) ;
#120258 = CARTESIAN_POINT ( 'NONE',  ( 5.153800228976615827, -19.02544592524334988, 100.2094237280190043 ) ) ;
#120259 = CARTESIAN_POINT ( 'NONE',  ( -8.224510206698735004, -14.34966873604973081, 74.58442372801901854 ) ) ;
#120260 = CARTESIAN_POINT ( 'NONE',  ( -21.53943276465977519, -0.05219959533937600094, 113.7510903946856757 ) ) ;
#120261 = CARTESIAN_POINT ( 'NONE',  ( -19.05341960407617563, 5.049401038297882671, 83.54275706135233293 ) ) ;
#120262 = CARTESIAN_POINT ( 'NONE',  ( 19.05341960407611168, 5.049401038298154454, 63.95724293864769550 ) ) ;
#120263 = CARTESIAN_POINT ( 'NONE',  ( -18.67979575497178146, -10.72451020669898902, 81.66557627198103830 ) ) ;
#120265 = CARTESIAN_POINT ( 'NONE',  ( -19.03943276465977164, -0.05219959533935918106, 73.75109039468566152 ) ) ;
#120264 = CARTESIAN_POINT ( 'NONE',  ( 0.05219959533910956823, 16.53943276465976808, 69.99890960531435269 ) ) ;
#120266 = CARTESIAN_POINT ( 'NONE',  ( -19.20446147854526231, -5.500000000000011546, 69.38999695167682091 ) ) ;
#120267 = CARTESIAN_POINT ( 'NONE',  ( 19.05341960407617918, -5.049401038297876454, 51.04275706135231871 ) ) ;
#120268 = CARTESIAN_POINT ( 'NONE',  ( 14.29746914071049879, -8.314922557960816363, 23.33224293864769194 ) ) ;
#120269 = CARTESIAN_POINT ( 'NONE',  ( -4.379528057220328563, 16.55341960407611168, 85.20724293864770971 ) ) ;
#120271 = CARTESIAN_POINT ( 'NONE',  ( 17.14385361876520264, 23.59649016807275856, 144.1750000027311671 ) ) ;
#120270 = CARTESIAN_POINT ( 'NONE',  ( -21.53943276465977519, -0.05219959533937600094, 103.7510903946857042 ) ) ;
#120272 = CARTESIAN_POINT ( 'NONE',  ( 5.719274019375991003, -21.55341960407610458, 102.7072429386476955 ) ) ;
#120273 = CARTESIAN_POINT ( 'NONE',  ( 13.97604488694527802, 13.89961937509977652, 99.37390960531436690 ) ) ;
#120274 = CARTESIAN_POINT ( 'NONE',  ( 19.05341960407611168, 5.049401038298154454, 63.95724293864769550 ) ) ;
#120275 = CARTESIAN_POINT ( 'NONE',  ( -18.62759615963255300, -10.81492255796106328, 79.16775706135234714 ) ) ;
#120276 = CARTESIAN_POINT ( 'NONE',  ( 5.049401038298161559, -19.05341960407611168, 67.70724293864769550 ) ) ;
#120277 = ORIENTED_EDGE ( 'NONE', *, *, #47276, .F. ) ;
#120278 = CARTESIAN_POINT ( 'NONE',  ( 0.05219959533909260263, 19.03943276465977164, 39.99890960531436690 ) ) ;
#120279 = CARTESIAN_POINT ( 'NONE',  ( 18.62759615963271287, -10.81492255796078972, 33.33224293864769550 ) ) ;
#120280 = CARTESIAN_POINT ( 'NONE',  ( 4.483927247898545687, 16.52544592524342804, 69.79057627198102409 ) ) ;
#120281 = CARTESIAN_POINT ( 'NONE',  ( -9.564922557960796823, -16.46253265017161027, 42.08224293864769550 ) ) ;
#120282 = CARTESIAN_POINT ( 'NONE',  ( 12.14591786802309770, 12.06949235617756955, 104.3739096053143669 ) ) ;
#120283 = CARTESIAN_POINT ( 'NONE',  ( -5.719274019375978568, 21.55341960407610458, 115.2072429386476955 ) ) ;
#120284 = CARTESIAN_POINT ( 'NONE',  ( -15.72974639402176322, -15.80617190586768395, 44.37609039468567573 ) ) ;
#120285 = CARTESIAN_POINT ( 'NONE',  ( 9.564922557960805705, 16.46253265017160317, 29.58224293864769550 ) ) ;
#120286 = CARTESIAN_POINT ( 'NONE',  ( 8.314922557961029526, -14.29746914071037800, 70.41775706135236135 ) ) ;
#120287 = CARTESIAN_POINT ( 'NONE',  ( 21.55341960407610458, 5.719274019375980345, 103.9572429386476813 ) ) ;
#120288 = CARTESIAN_POINT ( 'NONE',  ( 5.719274019375991003, -21.55341960407610458, 102.7072429386476955 ) ) ;
#120290 = CARTESIAN_POINT ( 'NONE',  ( 19.03943276465977164, -0.05219959533909143690, 53.74890960531436690 ) ) ;
#120289 = CARTESIAN_POINT ( 'NONE',  ( 19.05341960407617918, -5.049401038297876454, 21.04275706135232582 ) ) ;
#120291 = CARTESIAN_POINT ( 'NONE',  ( -17.60728821187774429, 5.500000000000034639, 40.86690927743607205 ) ) ;
#120292 = CARTESIAN_POINT ( 'NONE',  ( 15.80617190586769283, -15.72974639402175789, 60.62609039468567573 ) ) ;
#120293 = CARTESIAN_POINT ( 'NONE',  ( -21.55341960407610458, -5.719274019375992779, 51.45724293864770260 ) ) ;
#120294 = CARTESIAN_POINT ( 'NONE',  ( 4.483927247898545687, 16.52544592524342804, 29.79057627198102409 ) ) ;
#120296 = CARTESIAN_POINT ( 'NONE',  ( -21.53943276465977519, -0.05219959533937600094, 108.7510903946857042 ) ) ;
#120295 = CARTESIAN_POINT ( 'NONE',  ( -21.53943276465977519, -0.05219959533937600094, 78.75109039468568994 ) ) ;
#120297 = CARTESIAN_POINT ( 'NONE',  ( -19.03943276465977164, -0.05219959533935918106, 48.75109039468566863 ) ) ;
#120298 = CARTESIAN_POINT ( 'NONE',  ( -16.53943276465976808, -0.05219959533934237506, 98.75109039468568994 ) ) ;
#120299 = CARTESIAN_POINT ( 'NONE',  ( 18.62759615963255655, 10.81492255796105972, 51.66775706135234714 ) ) ;
#120300 = CARTESIAN_POINT ( 'NONE',  ( -16.51473224551069308, -9.474510206698971260, 61.66557627198103120 ) ) ;
#120301 = CARTESIAN_POINT ( 'NONE',  ( 16.46253265017146816, 9.564922557961045513, 36.66775706135233293 ) ) ;
#120302 = CARTESIAN_POINT ( 'NONE',  ( 5.823673210054125526, 21.52544592524343514, 44.79057627198103120 ) ) ;
#120303 = CARTESIAN_POINT ( 'NONE',  ( -10.81492255796105439, 18.62759615963255655, 27.91775706135234358 ) ) ;
#120304 = CARTESIAN_POINT ( 'NONE',  ( -15.80617190586745835, -15.72974639402198527, 86.87390960531438111 ) ) ;
#120305 = CARTESIAN_POINT ( 'NONE',  ( 5.153800228976615827, -19.02544592524334988, 90.20942372801900433 ) ) ;
#120306 = CARTESIAN_POINT ( 'NONE',  ( -14.34966873604972548, 8.224510206698743886, 48.33442372801902565 ) ) ;
#120308 = CARTESIAN_POINT ( 'NONE',  ( 15.80617190586746368, 15.72974639402197994, 94.37390960531436690 ) ) ;
#120307 = CARTESIAN_POINT ( 'NONE',  ( -4.897001621108284297, 3.948440707545709749, -62.47584611210317007 ) ) ;
#120310 = CARTESIAN_POINT ( 'NONE',  ( -8.314922557960811034, -14.29746914071050412, 77.08224293864769550 ) ) ;
#120309 = CARTESIAN_POINT ( 'NONE',  ( -12.06949235617739369, -12.14591786802326823, 84.37609039468570415 ) ) ;
#120311 = CARTESIAN_POINT ( 'NONE',  ( -23.87356034986281728, -29.32389248808953397, -21.14071813158723856 ) ) ;
#120312 = CARTESIAN_POINT ( 'NONE',  ( -5.049401038297874678, -19.05341960407617918, 104.7927570613523471 ) ) ;
#120313 = CARTESIAN_POINT ( 'NONE',  ( -18.62759615963270932, 10.81492255796079327, 40.83224293864769550 ) ) ;
#120314 = CARTESIAN_POINT ( 'NONE',  ( -21.46320343559653665, -20.96320343559631638, 5.353553390593268624 ) ) ;
#120315 = CARTESIAN_POINT ( 'NONE',  ( -14.29746914071037622, -8.314922557961029526, 49.16775706135234003 ) ) ;
#120316 = CARTESIAN_POINT ( 'NONE',  ( -21.55341960407619339, 5.719274019375674811, 23.54275706135235424 ) ) ;
#120317 = CARTESIAN_POINT ( 'NONE',  ( -18.62759615963270932, 10.81492255796079327, 30.83224293864770260 ) ) ;
#120318 = CARTESIAN_POINT ( 'NONE',  ( -16.52544592524335698, -4.483927247898792601, 73.95942372801901854 ) ) ;
#120319 = CARTESIAN_POINT ( 'NONE',  ( 9.474510206698971260, -16.51473224551069308, 82.91557627198103830 ) ) ;
#120321 = CARTESIAN_POINT ( 'NONE',  ( 19.03943276465977164, -0.05219959533909143690, 28.74890960531435624 ) ) ;
#120320 = CARTESIAN_POINT ( 'NONE',  ( 18.67979575497194134, -10.72451020669871369, 50.83442372801901143 ) ) ;
#120322 = CARTESIAN_POINT ( 'NONE',  ( 18.62759615963271287, -10.81492255796078972, 28.33224293864769550 ) ) ;
#120323 = CARTESIAN_POINT ( 'NONE',  ( 13.97604488694548053, -13.89961937509957401, 35.62609039468567573 ) ) ;
#120324 = CARTESIAN_POINT ( 'NONE',  ( -8.314922557961024197, 14.29746914071037800, 52.91775706135235424 ) ) ;
#120325 = CARTESIAN_POINT ( 'NONE',  ( 0.05219959533909260263, 19.03943276465977164, 114.9989096053143669 ) ) ;
#120326 = CARTESIAN_POINT ( 'NONE',  ( 9.474510206698971260, -16.51473224551069308, 77.91557627198103830 ) ) ;
#120327 = CARTESIAN_POINT ( 'NONE',  ( 14.34966873604972726, -8.224510206698740333, 105.8344237280190328 ) ) ;
#120328 = CARTESIAN_POINT ( 'NONE',  ( -9.474510206698964154, 16.51473224551069663, 115.4155762719810241 ) ) ;
#120329 = CARTESIAN_POINT ( 'NONE',  ( 14.34966873604960469, 8.224510206698951720, 99.16557627198100988 ) ) ;
#120330 = CARTESIAN_POINT ( 'NONE',  ( 5.823673210054125526, 21.52544592524343514, 29.79057627198102409 ) ) ;
#120331 = CARTESIAN_POINT ( 'NONE',  ( 19.03943276465977164, -0.05219959533909143690, 28.74890960531435624 ) ) ;
#120332 = CARTESIAN_POINT ( 'NONE',  ( -14.29746914071037622, -8.314922557961029526, 64.16775706135234714 ) ) ;
#120333 = CARTESIAN_POINT ( 'NONE',  ( -21.52544592524343514, 5.823673210054127303, 111.0405762719810525 ) ) ;
#120334 = CARTESIAN_POINT ( 'NONE',  ( 5.049401038297881783, 19.05341960407617563, 82.29275706135229029 ) ) ;
#120335 = CARTESIAN_POINT ( 'NONE',  ( 9.564922557960805705, 16.46253265017160317, 39.58224293864768839 ) ) ;
#120336 = CARTESIAN_POINT ( 'NONE',  ( 21.52544592524344225, -5.823673210054117533, 68.54057627198103830 ) ) ;
#120337 = CARTESIAN_POINT ( 'NONE',  ( -13.97604488694527625, -13.89961937509977652, 111.8739096053143243 ) ) ;
#120338 = CARTESIAN_POINT ( 'NONE',  ( -18.67979575497193778, 10.72451020669871902, 88.33442372801901854 ) ) ;
#120339 = CARTESIAN_POINT ( 'NONE',  ( -16.46253265017160317, 9.564922557960807481, 70.83224293864770971 ) ) ;
#120340 = EDGE_CURVE ( 'NONE', #89770, #196867, #184513, .T. ) ;
#120341 = CARTESIAN_POINT ( 'NONE',  ( -16.55341960407617563, 4.379528057220093196, 48.54275706135234714 ) ) ;
#120342 = CARTESIAN_POINT ( 'NONE',  ( -21.53943276465977519, -0.05219959533937600094, 78.75109039468568994 ) ) ;
#120343 = CARTESIAN_POINT ( 'NONE',  ( 13.97604488694548053, -13.89961937509957401, 35.62609039468567573 ) ) ;
#120344 = CARTESIAN_POINT ( 'NONE',  ( 16.51473224551083163, -9.474510206698727899, 50.83442372801899722 ) ) ;
#120345 = ORIENTED_EDGE ( 'NONE', *, *, #166008, .F. ) ;
#120346 = CARTESIAN_POINT ( 'NONE',  ( -21.52544592524334988, -5.823673210054445271, 43.95942372801902565 ) ) ;
#120347 = CARTESIAN_POINT ( 'NONE',  ( 9.564922557960805705, 16.46253265017160317, 24.58224293864769194 ) ) ;
#120348 = CARTESIAN_POINT ( 'NONE',  ( 9.564922557961047289, -16.46253265017146816, 50.41775706135233293 ) ) ;
#120349 = CARTESIAN_POINT ( 'NONE',  ( 16.51473224551069308, 9.474510206698969483, 104.1655762719810241 ) ) ;
#120350 = CARTESIAN_POINT ( 'NONE',  ( -16.46253265017160317, 9.564922557960807481, 85.83224293864769550 ) ) ;
#120351 = CARTESIAN_POINT ( 'NONE',  ( 4.483927247898545687, 16.52544592524342804, 39.79057627198103830 ) ) ;
#120352 = CARTESIAN_POINT ( 'NONE',  ( 21.53943276465977519, -0.05219959533907433946, 33.74890960531436690 ) ) ;
#120353 = DIRECTION ( 'NONE',  ( -0.000000000000000000, -1.000000000000000000, -0.000000000000000000 ) ) ;
#120354 = CARTESIAN_POINT ( 'NONE',  ( 20.25409705915565794, 20.61667489342684689, -52.65483682830181777 ) ) ;
#120355 = B_SPLINE_CURVE_WITH_KNOTS ( 'NONE', 3,
 ( #173729, #191864, #38191, #51361, #83674, #188900, #53346, #99847, #22022, #69521, #131186, #130167, #161531, #160533, #54354, #114005, #192876, #116026, #177715, #145352, #37179, #39183 ),
 .UNSPECIFIED., .F., .F.,
 ( 4, 2, 2, 2, 2, 2, 2, 2, 2, 2, 4 ),
 ( 2.110382192020081394E-17, 0.001309639967555352707, 0.001964459951333019736, 0.002291869943221851082, 0.002455574939166262852, 0.002619279935110674622, 0.002782984931055086392, 0.002946689926999498162, 0.003274099918888322136, 0.003928919902665964879, 0.005238559870221252100 ),
 .UNSPECIFIED. ) ;
#120356 = CARTESIAN_POINT ( 'NONE',  ( 5.823673210054444382, -21.52544592524334988, 100.2094237280190043 ) ) ;
#120357 = DIRECTION ( 'NONE',  ( -1.000000000000000000, -0.000000000000000000, -0.000000000000000000 ) ) ;
#120359 = CARTESIAN_POINT ( 'NONE',  ( 19.02544592524343514, -5.153800228976328945, 38.54057627198103120 ) ) ;
#120358 = PRODUCT_RELATED_PRODUCT_CATEGORY ( 'part', '', ( #177482 ) ) ;
#120360 = CARTESIAN_POINT ( 'NONE',  ( -19.03943276465977164, 0.05219959533909376836, 116.2489096053143669 ) ) ;
#120361 = CARTESIAN_POINT ( 'NONE',  ( -37.99626262588766679, 2.428612866367529932E-14, -2.002157773949823305 ) ) ;
#120362 = CARTESIAN_POINT ( 'NONE',  ( 16.53943276465976808, 0.05219959533934440121, 56.25109039468568284 ) ) ;
#120363 = CARTESIAN_POINT ( 'NONE',  ( 21.52544592524344225, -5.823673210054117533, 78.54057627198103830 ) ) ;
#120364 = CARTESIAN_POINT ( 'NONE',  ( 0.05219959533910956823, 16.53943276465976808, 34.99890960531435979 ) ) ;
#120366 = CARTESIAN_POINT ( 'NONE',  ( -16.46253265017160317, 9.564922557960807481, 105.8322429386476955 ) ) ;
#120365 = CARTESIAN_POINT ( 'NONE',  ( -19.03943276465977164, 0.05219959533909376836, 31.24890960531435979 ) ) ;
#120367 = CARTESIAN_POINT ( 'NONE',  ( -21.53943276465977519, -0.05219959533937600094, 33.75109039468568284 ) ) ;
#120368 = CARTESIAN_POINT ( 'NONE',  ( -0.05219959533936034679, 19.03943276465977164, 37.50109039468567573 ) ) ;
#120369 = CARTESIAN_POINT ( 'NONE',  ( -5.049401038298153566, 19.05341960407611168, 25.20724293864768484 ) ) ;
#120370 = CARTESIAN_POINT ( 'NONE',  ( -0.05219959533937732626, 21.53943276465977519, 77.50109039468567573 ) ) ;
#120371 = LINE ( 'NONE', #183056, #66326 ) ;
#120372 = CARTESIAN_POINT ( 'NONE',  ( -16.55341960407611168, -4.379528057220339221, 21.45724293864769550 ) ) ;
#120373 = CARTESIAN_POINT ( 'NONE',  ( 17.50000000000000000, 5.499999999999997335, 111.7030961746582847 ) ) ;
#120374 = CARTESIAN_POINT ( 'NONE',  ( -5.823673210054116645, -21.52544592524344225, 22.29057627198102765 ) ) ;
#120375 = CARTESIAN_POINT ( 'NONE',  ( -16.55341960407611168, -4.379528057220339221, 91.45724293864769550 ) ) ;
#120376 = CARTESIAN_POINT ( 'NONE',  ( 26.33511944008831307, -27.18111610334192463, -16.53814760372662107 ) ) ;
#120377 = CARTESIAN_POINT ( 'NONE',  ( 19.05341960407611168, 5.049401038298154454, 73.95724293864768129 ) ) ;
#120378 = CARTESIAN_POINT ( 'NONE',  ( 8.314922557960818139, 14.29746914071049879, 74.58224293864768129 ) ) ;
#120379 = CARTESIAN_POINT ( 'NONE',  ( 19.02544592524334988, 5.153800228976608722, 111.4594237280190043 ) ) ;
#120380 = CARTESIAN_POINT ( 'NONE',  ( -21.52544592524343514, 5.823673210054127303, 66.04057627198103830 ) ) ;
#120381 = VERTEX_POINT ( 'NONE', #137007 ) ;
#120382 = CARTESIAN_POINT ( 'NONE',  ( -9.564922557960796823, -16.46253265017161027, 37.08224293864768839 ) ) ;
#120384 = CARTESIAN_POINT ( 'NONE',  ( -15.72974639402197994, 15.80617190586746368, 75.62390960531439532 ) ) ;
#120383 = CARTESIAN_POINT ( 'NONE',  ( 16.51473224551069308, 9.474510206698969483, 89.16557627198103830 ) ) ;
#120386 = CARTESIAN_POINT ( 'NONE',  ( 16.46253265017160672, -9.564922557960803928, 83.33224293864768129 ) ) ;
#120385 = CARTESIAN_POINT ( 'NONE',  ( 8.314922557961029526, -14.29746914071037800, 110.4177570613523756 ) ) ;
#120387 = CARTESIAN_POINT ( 'NONE',  ( 13.89961937509957401, 13.97604488694547697, 61.87609039468566863 ) ) ;
#120388 = CARTESIAN_POINT ( 'NONE',  ( -15.80617190586768217, 15.72974639402176855, 98.12609039468570415 ) ) ;
#120389 = CARTESIAN_POINT ( 'NONE',  ( 21.52544592524344225, -5.823673210054117533, 73.54057627198102409 ) ) ;
#120390 = CARTESIAN_POINT ( 'NONE',  ( -15.72974639402197994, 15.80617190586746368, 25.62390960531435624 ) ) ;
#120391 = CARTESIAN_POINT ( 'NONE',  ( -5.049401038298153566, 19.05341960407611168, 50.20724293864770260 ) ) ;
#120392 = CARTESIAN_POINT ( 'NONE',  ( 8.224510206698953496, -14.34966873604960469, 22.91557627198102765 ) ) ;
#120393 = CARTESIAN_POINT ( 'NONE',  ( 0.05219959533909260263, 19.03943276465977164, 64.99890960531436690 ) ) ;
#120394 = CARTESIAN_POINT ( 'NONE',  ( 17.48847506799968343, 5.747544572773805704, 51.67302562156721280 ) ) ;
#120395 = CARTESIAN_POINT ( 'NONE',  ( -19.02544592524334988, -5.153800228976617603, 18.95942372801899722 ) ) ;
#120396 = CARTESIAN_POINT ( 'NONE',  ( -16.53943276465976808, 0.05219959533911058130, 71.24890960531435269 ) ) ;
#120397 = AXIS2_PLACEMENT_3D ( 'NONE', #72388, #91495, #183545 ) ;
#120398 = CARTESIAN_POINT ( 'NONE',  ( -10.72451020669898014, 18.67979575497178502, 105.4155762719810383 ) ) ;
#120399 = CARTESIAN_POINT ( 'NONE',  ( -10.81492255796078084, -18.62759615963271287, 102.0822429386476955 ) ) ;
#120400 = DIRECTION ( 'NONE',  ( 0.000000000000000000, 0.000000000000000000, 1.000000000000000000 ) ) ;
#120401 = CARTESIAN_POINT ( 'NONE',  ( 0.05219959533907565091, 21.53943276465977519, 59.99890960531436690 ) ) ;
#120402 = CARTESIAN_POINT ( 'NONE',  ( -12.14591786802326823, 12.06949235617739902, 83.12609039468568994 ) ) ;
#120403 = CARTESIAN_POINT ( 'NONE',  ( 12.06949235617757843, -12.14591786802309237, 98.12390960531436690 ) ) ;
#120404 = CARTESIAN_POINT ( 'NONE',  ( -5.049401038298153566, 19.05341960407611168, 65.20724293864765286 ) ) ;
#120405 = CARTESIAN_POINT ( 'NONE',  ( -16.53943276465976808, -0.05219959533934237506, 108.7510903946857042 ) ) ;
#120406 = CARTESIAN_POINT ( 'NONE',  ( 5.823673210054444382, -21.52544592524334988, 40.20942372801901854 ) ) ;
#120407 = CARTESIAN_POINT ( 'NONE',  ( -5.153800228976328057, -19.02544592524343514, 112.2905762719810099 ) ) ;
#120408 = CARTESIAN_POINT ( 'NONE',  ( 15.72974639402176855, 15.80617190586768217, 81.87609039468568994 ) ) ;
#120409 = CARTESIAN_POINT ( 'NONE',  ( 19.05341960407611168, 5.049401038298154454, 28.95724293864769550 ) ) ;
#120410 = CARTESIAN_POINT ( 'NONE',  ( 13.89961937509977652, -13.97604488694527269, 38.12390960531436690 ) ) ;
#120411 = ORIENTED_EDGE ( 'NONE', *, *, #125821, .F. ) ;
#120412 = CARTESIAN_POINT ( 'NONE',  ( -18.62759615963255300, -10.81492255796106328, 79.16775706135234714 ) ) ;
#120413 = CARTESIAN_POINT ( 'NONE',  ( 0.05219959533937995610, -21.53943276465977519, 75.00109039468568994 ) ) ;
#120414 = CARTESIAN_POINT ( 'NONE',  ( 19.02544592524343514, -5.153800228976328945, 98.54057627198100988 ) ) ;
#120415 = CARTESIAN_POINT ( 'NONE',  ( -5.153800228976607833, 19.02544592524334988, 82.70942372801897591 ) ) ;
#120416 = CARTESIAN_POINT ( 'NONE',  ( 18.62759615963255655, 10.81492255796105972, 61.66775706135235424 ) ) ;
#120417 = CARTESIAN_POINT ( 'NONE',  ( -14.29746914071037622, -8.314922557961029526, 24.16775706135235424 ) ) ;
#120418 = CARTESIAN_POINT ( 'NONE',  ( 9.474510206698729675, 16.51473224551082808, 77.08442372801900433 ) ) ;
#120419 = CARTESIAN_POINT ( 'NONE',  ( -9.474510206698964154, 16.51473224551069663, 50.41557627198102409 ) ) ;
#120420 = CARTESIAN_POINT ( 'NONE',  ( 13.89961937509957401, 13.97604488694547697, 76.87609039468566152 ) ) ;
#120421 = CARTESIAN_POINT ( 'NONE',  ( -4.483927247898539470, -16.52544592524342804, 22.29057627198102765 ) ) ;
#120422 = CARTESIAN_POINT ( 'NONE',  ( -19.05341960407617563, 5.049401038297882671, 88.54275706135230450 ) ) ;
#120423 = CARTESIAN_POINT ( 'NONE',  ( -16.55341960407611168, -4.379528057220339221, 36.45724293864768839 ) ) ;
#120424 = CARTESIAN_POINT ( 'NONE',  ( -16.51473224551082808, 9.474510206698731452, 58.33442372801900433 ) ) ;
#120425 = CARTESIAN_POINT ( 'NONE',  ( -8.314922557961024197, 14.29746914071037800, 47.91775706135234714 ) ) ;
#120426 = CARTESIAN_POINT ( 'NONE',  ( 16.51473224551083163, -9.474510206698727899, 20.83442372801899722 ) ) ;
#120427 = CARTESIAN_POINT ( 'NONE',  ( 13.97604488694527802, 13.89961937509977652, 44.37390960531435269 ) ) ;
#120428 = CARTESIAN_POINT ( 'NONE',  ( -17.49999999999998934, -5.622605283950889543, 66.31207310596113302 ) ) ;
#120429 = CARTESIAN_POINT ( 'NONE',  ( -4.379528057220086978, -16.55341960407618274, 49.79275706135234714 ) ) ;
#120430 = CARTESIAN_POINT ( 'NONE',  ( -5.429308488886486681E-15, 30.30510711980690175, 139.7500000054623683 ) ) ;
#120431 = CIRCLE ( 'NONE', #68748, 10.00000000000000000 ) ;
#120432 = CARTESIAN_POINT ( 'NONE',  ( 1.784210473542230573E-15, -29.16686587814331588, 145.3750000027311842 ) ) ;
#120433 = CARTESIAN_POINT ( 'NONE',  ( -13.89961937509977652, 13.97604488694528158, 95.62390960531436690 ) ) ;
#120434 = DIRECTION ( 'NONE',  ( -0.000000000000000000, -0.000000000000000000, -1.000000000000000000 ) ) ;
#120435 = CARTESIAN_POINT ( 'NONE',  ( -16.46253265017146816, -9.564922557961047289, 99.16775706135233293 ) ) ;
#120436 = CARTESIAN_POINT ( 'NONE',  ( -9.474510206698964154, 16.51473224551069663, 115.4155762719810241 ) ) ;
#120438 = CARTESIAN_POINT ( 'NONE',  ( 9.564922557961047289, -16.46253265017146816, 100.4177570613523329 ) ) ;
#120437 = CARTESIAN_POINT ( 'NONE',  ( -10.81492255796105439, 18.62759615963255655, 107.9177570613523471 ) ) ;
#120439 = CARTESIAN_POINT ( 'NONE',  ( 12.14591786802309770, 12.06949235617756955, 114.3739096053143527 ) ) ;
#120440 = CARTESIAN_POINT ( 'NONE',  ( -19.03943276465977164, 0.05219959533909376836, 41.24890960531435269 ) ) ;
#120441 = CARTESIAN_POINT ( 'NONE',  ( -10.72451020669898014, 18.67979575497178502, 65.41557627198102409 ) ) ;
#120442 = CARTESIAN_POINT ( 'NONE',  ( -13.97604488694527625, -13.89961937509977652, 26.87390960531434558 ) ) ;
#120443 = CARTESIAN_POINT ( 'NONE',  ( 16.46253265017146816, 9.564922557961045513, 46.66775706135233293 ) ) ;
#120444 = CARTESIAN_POINT ( 'NONE',  ( 5.153800228976615827, -19.02544592524334988, 75.20942372801896170 ) ) ;
#120445 = CARTESIAN_POINT ( 'NONE',  ( -4.483927247898539470, -16.52544592524342804, 57.29057627198103120 ) ) ;
#120446 = CARTESIAN_POINT ( 'NONE',  ( 21.53943276465977519, -0.05219959533907433946, 33.74890960531436690 ) ) ;
#120447 = CARTESIAN_POINT ( 'NONE',  ( 5.719274019375673035, 21.55341960407619339, 92.29275706135236135 ) ) ;
#120448 = EDGE_CURVE ( 'NONE', #119129, #175270, #45993, .T. ) ;
#120449 = CARTESIAN_POINT ( 'NONE',  ( -15.80617190586745835, -15.72974639402198527, 81.87390960531435269 ) ) ;
#120450 = CARTESIAN_POINT ( 'NONE',  ( 0.05219959533937995610, -21.53943276465977519, 55.00109039468568284 ) ) ;
#120451 = CARTESIAN_POINT ( 'NONE',  ( -18.62759615963255300, -10.81492255796106328, 69.16775706135234714 ) ) ;
#120452 = CARTESIAN_POINT ( 'NONE',  ( 0.05219959533909260263, 19.03943276465977164, 89.99890960531436690 ) ) ;
#120454 = CARTESIAN_POINT ( 'NONE',  ( 18.62759615963255655, 10.81492255796105972, 61.66775706135235424 ) ) ;
#120453 = CARTESIAN_POINT ( 'NONE',  ( 16.52544592524335698, 4.483927247898782831, 86.45942372801901854 ) ) ;
#120455 = CARTESIAN_POINT ( 'NONE',  ( 9.564922557960805705, 16.46253265017160317, 59.58224293864769550 ) ) ;
#120456 = CARTESIAN_POINT ( 'NONE',  ( 19.02544592524343514, -5.153800228976328945, 28.54057627198102409 ) ) ;
#120457 = CARTESIAN_POINT ( 'NONE',  ( -16.46253265017160317, 9.564922557960807481, 50.83224293864770260 ) ) ;
#120458 = CARTESIAN_POINT ( 'NONE',  ( 12.06949235617757843, -12.14591786802309237, 63.12390960531435979 ) ) ;
#120459 = CARTESIAN_POINT ( 'NONE',  ( 0.05219959533910956823, 16.53943276465976808, 34.99890960531435979 ) ) ;
#120460 = CARTESIAN_POINT ( 'NONE',  ( -5.823673210054116645, -21.52544592524344225, 47.29057627198103120 ) ) ;
#120461 = CARTESIAN_POINT ( 'NONE',  ( -9.474510206698964154, 16.51473224551069663, 45.41557627198103120 ) ) ;
#120462 = CARTESIAN_POINT ( 'NONE',  ( -10.81492255796078084, -18.62759615963271287, 52.08224293864768839 ) ) ;
#120463 = CARTESIAN_POINT ( 'NONE',  ( 13.89961937509957401, 13.97604488694547697, 56.87609039468564731 ) ) ;
#120465 = CARTESIAN_POINT ( 'NONE',  ( 4.483927247898545687, 16.52544592524342804, 44.79057627198103120 ) ) ;
#120464 = CARTESIAN_POINT ( 'NONE',  ( -16.81555441253550498, -7.025013491695498047, 39.36314554665744936 ) ) ;
#120466 = CARTESIAN_POINT ( 'NONE',  ( 10.72451020669898902, -18.67979575497178502, 22.91557627198102765 ) ) ;
#120467 = EDGE_LOOP ( 'NONE', ( #124062, #112219, #159076, #67375 ) ) ;
#120468 = ORIENTED_EDGE ( 'NONE', *, *, #98300, .T. ) ;
#120469 = CARTESIAN_POINT ( 'NONE',  ( 26.46959431505284499, -27.26463967846488146, -25.00000000000000000 ) ) ;
#120470 = CARTESIAN_POINT ( 'NONE',  ( -16.53943276465976808, -0.05219959533934237506, 78.75109039468568994 ) ) ;
#120471 = CARTESIAN_POINT ( 'NONE',  ( 16.46253265017146816, 9.564922557961045513, 76.66775706135234714 ) ) ;
#120472 = CARTESIAN_POINT ( 'NONE',  ( 16.55341960407611168, 4.379528057220329451, 58.95724293864770971 ) ) ;
#120473 = CYLINDRICAL_SURFACE ( 'NONE', #93454, 2.649999999999999911 ) ;
#120474 = CARTESIAN_POINT ( 'NONE',  ( 4.379528057220339221, -16.55341960407611168, 22.70724293864769194 ) ) ;
#120475 = CARTESIAN_POINT ( 'NONE',  ( -19.02544592524342804, 5.153800228976336051, 56.04057627198100988 ) ) ;
#120476 = EDGE_CURVE ( 'NONE', #4163, #76856, #28864, .T. ) ;
#120477 = CARTESIAN_POINT ( 'NONE',  ( 0.05219959533909260263, 19.03943276465977164, 74.99890960531435269 ) ) ;
#120478 = CARTESIAN_POINT ( 'NONE',  ( 19.05341960407611168, 5.049401038298154454, 33.95724293864769550 ) ) ;
#120479 = CARTESIAN_POINT ( 'NONE',  ( -10.72451020669870658, -18.67979575497194134, 39.58442372801901143 ) ) ;
#120480 = CARTESIAN_POINT ( 'NONE',  ( -13.97604488694527625, -13.89961937509977652, 66.87390960531436690 ) ) ;
#120481 = LINE ( 'NONE', #43658, #116298 ) ;
#120482 = CARTESIAN_POINT ( 'NONE',  ( 16.46253265017160672, -9.564922557960803928, 53.33224293864768839 ) ) ;
#120483 = CARTESIAN_POINT ( 'NONE',  ( -21.53943276465977519, 0.05219959533907696930, 36.24890960531435979 ) ) ;
#120484 = CARTESIAN_POINT ( 'NONE',  ( 5.049401038298161559, -19.05341960407611168, 32.70724293864768129 ) ) ;
#120485 = CARTESIAN_POINT ( 'NONE',  ( 15.80617190586746368, 15.72974639402197994, 39.37390960531436690 ) ) ;
#120486 = CARTESIAN_POINT ( 'NONE',  ( -16.53943276465976808, -0.05219959533934237506, 93.75109039468567573 ) ) ;
#120487 = CARTESIAN_POINT ( 'NONE',  ( -5.049401038297874678, -19.05341960407617918, 24.79275706135233648 ) ) ;
#120489 = CARTESIAN_POINT ( 'NONE',  ( -12.06949235617739369, -12.14591786802326823, 84.37609039468570415 ) ) ;
#120488 = CARTESIAN_POINT ( 'NONE',  ( -12.06949235617739369, -12.14591786802326823, 44.37609039468567573 ) ) ;
#120490 = CARTESIAN_POINT ( 'NONE',  ( 13.89961937509977652, -13.97604488694527269, 103.1239096053143527 ) ) ;
#120491 = CARTESIAN_POINT ( 'NONE',  ( 16.55341960407618274, -4.379528057220086978, 66.04275706135236135 ) ) ;
#120492 = CARTESIAN_POINT ( 'NONE',  ( 12.14591786802327356, -12.06949235617739191, 35.62609039468568994 ) ) ;
#120493 = CARTESIAN_POINT ( 'NONE',  ( -16.46253265017160317, 9.564922557960807481, 105.8322429386476955 ) ) ;
#120494 = CARTESIAN_POINT ( 'NONE',  ( -8.224510206698735004, -14.34966873604973081, 29.58442372801901854 ) ) ;
#120495 = CARTESIAN_POINT ( 'NONE',  ( -19.03943276465977164, 0.05219959533909376836, 36.24890960531436690 ) ) ;
#120496 = CARTESIAN_POINT ( 'NONE',  ( -15.72974639402176322, -15.80617190586768395, 29.37609039468568284 ) ) ;
#120497 = CARTESIAN_POINT ( 'NONE',  ( -0.05219959533936034679, 19.03943276465977164, 112.5010903946856757 ) ) ;
#120498 = CARTESIAN_POINT ( 'NONE',  ( 16.53943276465976808, 0.05219959533934440121, 96.25109039468568994 ) ) ;
#120499 = CARTESIAN_POINT ( 'NONE',  ( 4.500000000000000888, -130.0000000000000000, 13.99999999999999822 ) ) ;
#120500 = CARTESIAN_POINT ( 'NONE',  ( 10.72451020669871369, 18.67979575497193778, 97.08442372801904696 ) ) ;
#120501 = CARTESIAN_POINT ( 'NONE',  ( 13.89961937509957401, 13.97604488694547697, 91.87609039468567573 ) ) ;
#120502 = CARTESIAN_POINT ( 'NONE',  ( -16.53943276465976808, 0.05219959533911058130, 61.24890960531435979 ) ) ;
#120503 = CARTESIAN_POINT ( 'NONE',  ( -19.02544592524342804, 5.153800228976336051, 26.04057627198103120 ) ) ;
#120505 = DIRECTION ( 'NONE',  ( -1.000000000000000000, -0.000000000000000000, 0.000000000000000000 ) ) ;
#120504 = CARTESIAN_POINT ( 'NONE',  ( 16.46253265017146816, 9.564922557961045513, 66.66775706135233293 ) ) ;
#120506 = CARTESIAN_POINT ( 'NONE',  ( -18.62759615963255300, -10.81492255796106328, 54.16775706135235424 ) ) ;
#120507 = CARTESIAN_POINT ( 'NONE',  ( -16.55341960407617563, 4.379528057220093196, 28.54275706135234358 ) ) ;
#120508 = CARTESIAN_POINT ( 'NONE',  ( 3.889087296526381632, 34.99999999999996447, 1.818019484660534424 ) ) ;
#120509 = CARTESIAN_POINT ( 'NONE',  ( -0.05219959533909027116, -19.03943276465977164, 112.4989096053143669 ) ) ;
#120510 = CARTESIAN_POINT ( 'NONE',  ( 5.823673210054125526, 21.52544592524343514, 74.79057627198105251 ) ) ;
#120511 = CARTESIAN_POINT ( 'NONE',  ( 16.51473224551083163, -9.474510206698727899, 105.8344237280190043 ) ) ;
#120512 = CARTESIAN_POINT ( 'NONE',  ( -9.564922557960796823, -16.46253265017161027, 97.08224293864769550 ) ) ;
#120513 = CARTESIAN_POINT ( 'NONE',  ( -13.35345327432327878, -24.89324389316316655, 139.9999999999999716 ) ) ;
#120514 = CARTESIAN_POINT ( 'NONE',  ( 19.05341960407611168, 5.049401038298154454, 28.95724293864769550 ) ) ;
#120515 = CARTESIAN_POINT ( 'NONE',  ( 0.05219959533937995610, -21.53943276465977519, 90.00109039468567573 ) ) ;
#120516 = CARTESIAN_POINT ( 'NONE',  ( 19.05341960407611168, 5.049401038298154454, 48.95724293864768129 ) ) ;
#120517 = CARTESIAN_POINT ( 'NONE',  ( 5.823673210054444382, -21.52544592524334988, 55.20942372801902565 ) ) ;
#120518 = CARTESIAN_POINT ( 'NONE',  ( -21.55341960407619339, 5.719274019375674811, 83.54275706135234714 ) ) ;
#120519 = CARTESIAN_POINT ( 'NONE',  ( -4.379528057220086978, -16.55341960407618274, 99.79275706135234714 ) ) ;
#120520 = CARTESIAN_POINT ( 'NONE',  ( 13.89961937509977652, -13.97604488694527269, 83.12390960531436690 ) ) ;
#120521 = CARTESIAN_POINT ( 'NONE',  ( 15.80617190586769283, -15.72974639402175789, 45.62609039468567573 ) ) ;
#120522 = CARTESIAN_POINT ( 'NONE',  ( 10.81492255796106328, -18.62759615963255655, 35.41775706135234003 ) ) ;
#120524 = CARTESIAN_POINT ( 'NONE',  ( -19.03943276465977164, 0.05219959533909376836, 91.24890960531436690 ) ) ;
#120523 = CARTESIAN_POINT ( 'NONE',  ( 13.89961937509957401, 13.97604488694547697, 81.87609039468564731 ) ) ;
#120525 = CARTESIAN_POINT ( 'NONE',  ( -16.52544592524342804, 4.483927247898546575, 101.0405762719810383 ) ) ;
#120526 = CARTESIAN_POINT ( 'NONE',  ( 5.719274019375991003, -21.55341960407610458, 102.7072429386476955 ) ) ;
#120527 = CARTESIAN_POINT ( 'NONE',  ( -14.34966873604960291, -8.224510206698953496, 81.66557627198103830 ) ) ;
#120528 = CARTESIAN_POINT ( 'NONE',  ( 0.05219959533936267826, -19.03943276465977164, 20.00109039468567218 ) ) ;
#120529 = CARTESIAN_POINT ( 'NONE',  ( 14.29746914071049879, -8.314922557960816363, 93.33224293864769550 ) ) ;
#120530 = CARTESIAN_POINT ( 'NONE',  ( -9.564922557960796823, -16.46253265017161027, 37.08224293864768839 ) ) ;
#120531 = CARTESIAN_POINT ( 'NONE',  ( 5.153800228976615827, -19.02544592524334988, 85.20942372801900433 ) ) ;
#120532 = CARTESIAN_POINT ( 'NONE',  ( 12.06949235617757843, -12.14591786802309237, 43.12390960531435269 ) ) ;
#120533 = CARTESIAN_POINT ( 'NONE',  ( 0.05219959533937995610, -21.53943276465977519, 95.00109039468568994 ) ) ;
#120534 = CARTESIAN_POINT ( 'NONE',  ( -13.97604488694527625, -13.89961937509977652, 101.8739096053143811 ) ) ;
#120535 = CARTESIAN_POINT ( 'NONE',  ( 19.02544592524334988, 5.153800228976608722, 71.45942372801900433 ) ) ;
#120536 = CARTESIAN_POINT ( 'NONE',  ( 15.80617190586746368, 15.72974639402197994, 84.37390960531438111 ) ) ;
#120537 = CARTESIAN_POINT ( 'NONE',  ( 15.72974639402176855, 15.80617190586768217, 26.87609039468567218 ) ) ;
#120538 = CARTESIAN_POINT ( 'NONE',  ( 8.224510206698742110, 14.34966873604972548, 32.08442372801901854 ) ) ;
#120539 = CARTESIAN_POINT ( 'NONE',  ( -4.379528057220086978, -16.55341960407618274, 89.79275706135236135 ) ) ;
#120541 = CARTESIAN_POINT ( 'NONE',  ( 0.05219959533937995610, -21.53943276465977519, 30.00109039468568284 ) ) ;
#120540 = CARTESIAN_POINT ( 'NONE',  ( 19.02544592524343514, -5.153800228976328945, 23.54057627198102054 ) ) ;
#120542 = CARTESIAN_POINT ( 'NONE',  ( -9.564922557960796823, -16.46253265017161027, 27.08224293864769550 ) ) ;
#120543 = CARTESIAN_POINT ( 'NONE',  ( -11.74264578624800670, 36.14014761921585972, -8.149999994537626691 ) ) ;
#120544 = CARTESIAN_POINT ( 'NONE',  ( -12.14591786802326823, 12.06949235617739902, 48.12609039468568284 ) ) ;
#120545 = CARTESIAN_POINT ( 'NONE',  ( -8.314922557960811034, -14.29746914071050412, 82.08224293864768129 ) ) ;
#120546 = CARTESIAN_POINT ( 'NONE',  ( -18.67979575497178146, -10.72451020669898902, 71.66557627198100988 ) ) ;
#120547 = CARTESIAN_POINT ( 'NONE',  ( -16.53943276465976808, -0.05219959533934237506, 113.7510903946856757 ) ) ;
#120548 = CARTESIAN_POINT ( 'NONE',  ( 0.05219959533934541429, -16.53943276465976808, 50.00109039468568994 ) ) ;
#120549 = CARTESIAN_POINT ( 'NONE',  ( -5.153800228976328057, -19.02544592524343514, 47.29057627198102409 ) ) ;
#120550 = CARTESIAN_POINT ( 'NONE',  ( 8.224510206698742110, 14.34966873604972548, 92.08442372801901854 ) ) ;
#120551 = CARTESIAN_POINT ( 'NONE',  ( -9.474510206698720793, -16.51473224551083518, 84.58442372801900433 ) ) ;
#120552 = CARTESIAN_POINT ( 'NONE',  ( -5.719274019375978568, 21.55341960407610458, 90.20724293864770971 ) ) ;
#120553 = CARTESIAN_POINT ( 'NONE',  ( 12.06949235617739724, 12.14591786802326823, 111.8760903946856615 ) ) ;
#120554 = ORIENTED_EDGE ( 'NONE', *, *, #169979, .T. ) ;
#120555 = CARTESIAN_POINT ( 'NONE',  ( 26.77313074627685197, 4.631999166354653141, 170.7390164845645870 ) ) ;
#120556 = CARTESIAN_POINT ( 'NONE',  ( 15.72974639402199770, -15.80617190586745480, 58.12390960531435979 ) ) ;
#120557 = ORIENTED_EDGE ( 'NONE', *, *, #8921, .T. ) ;
#120558 = CARTESIAN_POINT ( 'NONE',  ( 14.34966873604972726, -8.224510206698740333, 90.83442372801901854 ) ) ;
#120559 = ORIENTED_EDGE ( 'NONE', *, *, #20458, .F. ) ;
#120560 = CARTESIAN_POINT ( 'NONE',  ( -15.80617190586745835, -15.72974639402198527, 31.87390960531435979 ) ) ;
#120561 = CARTESIAN_POINT ( 'NONE',  ( 17.50000000000002842, 4.658240926743181909, 108.5552958218320043 ) ) ;
#120562 = CARTESIAN_POINT ( 'NONE',  ( -21.55341960407610458, -5.719274019375992779, 76.45724293864769550 ) ) ;
#120563 = CARTESIAN_POINT ( 'NONE',  ( -16.55341960407617563, 4.379528057220093196, 113.5427570613523756 ) ) ;
#120564 = CARTESIAN_POINT ( 'NONE',  ( 4.379528057220092307, 16.55341960407617563, 27.29275706135234358 ) ) ;
#120565 = CARTESIAN_POINT ( 'NONE',  ( 16.53943276465976808, -0.05219959533910856209, 113.7489096053143527 ) ) ;
#120566 = CARTESIAN_POINT ( 'NONE',  ( 12.14591786802327356, -12.06949235617739191, 30.62609039468567929 ) ) ;
#120567 = CARTESIAN_POINT ( 'NONE',  ( 0.05219959533909260263, 19.03943276465977164, 59.99890960531436690 ) ) ;
#120568 = CARTESIAN_POINT ( 'NONE',  ( -28.82186960331499037, 2.428612866367529932E-14, 148.0000000000000000 ) ) ;
#120569 = CARTESIAN_POINT ( 'NONE',  ( -16.46253265017160317, 9.564922557960807481, 105.8322429386476955 ) ) ;
#120570 = CARTESIAN_POINT ( 'NONE',  ( -16.46253265017160317, 9.564922557960807481, 100.8322429386477097 ) ) ;
#120571 = EDGE_CURVE ( 'NONE', #138821, #3778, #138002, .T. ) ;
#120572 = CARTESIAN_POINT ( 'NONE',  ( -8.224510206698735004, -14.34966873604973081, 84.58442372801903275 ) ) ;
#120573 = CARTESIAN_POINT ( 'NONE',  ( 9.564922557961047289, -16.46253265017146816, 95.41775706135233293 ) ) ;
#120574 = CARTESIAN_POINT ( 'NONE',  ( -0.05219959533936034679, 19.03943276465977164, 37.50109039468567573 ) ) ;
#120575 = CARTESIAN_POINT ( 'NONE',  ( 21.53943276465977519, -0.05219959533907433946, 78.74890960531436690 ) ) ;
#120576 = CARTESIAN_POINT ( 'NONE',  ( -12.14591786802326823, 12.06949235617739902, 98.12609039468570415 ) ) ;
#120577 = AXIS2_PLACEMENT_3D ( 'NONE', #174183, #189355, #64996 ) ;
#120578 = CARTESIAN_POINT ( 'NONE',  ( -18.62759615963270932, 10.81492255796079327, 35.83224293864768839 ) ) ;
#120579 = CARTESIAN_POINT ( 'NONE',  ( -19.05341960407617563, 5.049401038297882671, 93.54275706135234714 ) ) ;
#120580 = CARTESIAN_POINT ( 'NONE',  ( 9.564922557960805705, 16.46253265017160317, 44.58224293864769550 ) ) ;
#120581 = CARTESIAN_POINT ( 'NONE',  ( -19.05341960407611168, -5.049401038298163336, 96.45724293864769550 ) ) ;
#120582 = CARTESIAN_POINT ( 'NONE',  ( -21.53943276465977519, -0.05219959533937600094, 58.75109039468568994 ) ) ;
#120583 = CARTESIAN_POINT ( 'NONE',  ( 5.153800228976335163, 19.02544592524342804, 54.79057627198103120 ) ) ;
#120584 = CARTESIAN_POINT ( 'NONE',  ( -16.52544592524342804, 4.483927247898546575, 81.04057627198102409 ) ) ;
#120585 = CARTESIAN_POINT ( 'NONE',  ( -17.12812012977030918, -6.668231424565924215, 86.35948759323143520 ) ) ;
#120586 = CARTESIAN_POINT ( 'NONE',  ( 16.52544592524342804, -4.483927247898539470, 83.54057627198102409 ) ) ;
#120587 = CARTESIAN_POINT ( 'NONE',  ( -21.55341960407610458, -5.719274019375992779, 71.45724293864769550 ) ) ;
#120588 = CARTESIAN_POINT ( 'NONE',  ( -9.564922557961040184, 16.46253265017147172, 97.91775706135233293 ) ) ;
#120589 = CARTESIAN_POINT ( 'NONE',  ( 193.3062444957835453, -155.7167183371837496, -4.999999999999999112 ) ) ;
#120590 = CARTESIAN_POINT ( 'NONE',  ( -19.02544592524334988, -5.153800228976617603, 48.95942372801900433 ) ) ;
#120591 = CARTESIAN_POINT ( 'NONE',  ( 16.20579543436695502, -7.371946100355081022, 71.93479165828050270 ) ) ;
#120593 = CARTESIAN_POINT ( 'NONE',  ( 5.049401038298161559, -19.05341960407611168, 87.70724293864769550 ) ) ;
#120592 = CARTESIAN_POINT ( 'NONE',  ( 9.564922557960805705, 16.46253265017160317, 74.58224293864769550 ) ) ;
#120594 = CARTESIAN_POINT ( 'NONE',  ( -4.483927247898782831, 16.52544592524335698, 67.70942372801901854 ) ) ;
#120595 = CARTESIAN_POINT ( 'NONE',  ( -17.12812012977023457, -6.668231424566066323, 51.35948759323144230 ) ) ;
#120596 = CARTESIAN_POINT ( 'NONE',  ( 13.89961937509957401, 13.97604488694547697, 41.87609039468566152 ) ) ;
#120597 = CARTESIAN_POINT ( 'NONE',  ( 17.59990718697208223, -15.82923402486897579, -57.24447373837836039 ) ) ;
#120598 = CARTESIAN_POINT ( 'NONE',  ( 13.97604488694527802, 13.89961937509977652, 114.3739096053143669 ) ) ;
#120599 = CARTESIAN_POINT ( 'NONE',  ( 14.29746914071037800, 8.314922557961029526, 106.6677570613523756 ) ) ;
#120600 = EDGE_CURVE ( 'NONE', #188457, #184582, #119083, .T. ) ;
#120601 = CARTESIAN_POINT ( 'NONE',  ( -0.2247805922399719325, -21.31291730435233234, -56.45983593933051026 ) ) ;
#120602 = CARTESIAN_POINT ( 'NONE',  ( 8.314922557961029526, -14.29746914071037800, 75.41775706135233293 ) ) ;
#120603 = CARTESIAN_POINT ( 'NONE',  ( -17.49999999999999645, 5.499999999999997335, 30.79690382534172599 ) ) ;
#120604 = CARTESIAN_POINT ( 'NONE',  ( -14.29746914071037622, -8.314922557961029526, 49.16775706135234003 ) ) ;
#120605 = CARTESIAN_POINT ( 'NONE',  ( 0.000000000000000000, -165.0000000000000000, 12.00000000000000355 ) ) ;
#120606 = CARTESIAN_POINT ( 'NONE',  ( -15.80617190586768217, 15.72974639402176855, 73.12609039468567573 ) ) ;
#120607 = CARTESIAN_POINT ( 'NONE',  ( -16.51473224551082808, 9.474510206698731452, 78.33442372801900433 ) ) ;
#120608 = CARTESIAN_POINT ( 'NONE',  ( -0.05219959533936034679, 19.03943276465977164, 22.50109039468566152 ) ) ;
#120609 = CARTESIAN_POINT ( 'NONE',  ( 19.02544592524343514, -5.153800228976328945, 58.54057627198102409 ) ) ;
#120610 = CARTESIAN_POINT ( 'NONE',  ( -5.153800228976328057, -19.02544592524343514, 47.29057627198102409 ) ) ;
#120611 = CARTESIAN_POINT ( 'NONE',  ( 3.181980515339446924, -6.791538853603077186, 8.889087296526001936 ) ) ;
#120612 = CARTESIAN_POINT ( 'NONE',  ( -0.05219959533907301413, -21.53943276465977519, 67.49890960531436690 ) ) ;
#120613 = CARTESIAN_POINT ( 'NONE',  ( 10.81492255796078972, 18.62759615963270932, 29.58224293864769905 ) ) ;
#120614 = CARTESIAN_POINT ( 'NONE',  ( -14.34966873604960291, -8.224510206698953496, 111.6655762719810525 ) ) ;
#120615 = CARTESIAN_POINT ( 'NONE',  ( 16.53943276465976808, 0.05219959533934440121, 51.25109039468568994 ) ) ;
#120616 = VERTEX_POINT ( 'NONE', #27878 ) ;
#120617 = CARTESIAN_POINT ( 'NONE',  ( -18.67979575497193778, 10.72451020669871902, 28.33442372801902209 ) ) ;
#120619 = CARTESIAN_POINT ( 'NONE',  ( -38.00000000000001421, 12.34694845685046438, -6.099999999999999645 ) ) ;
#120618 = CARTESIAN_POINT ( 'NONE',  ( -8.314922557960811034, -14.29746914071050412, 47.08224293864770260 ) ) ;
#120620 = CARTESIAN_POINT ( 'NONE',  ( 4.379528057220092307, 16.55341960407617563, 27.29275706135234358 ) ) ;
#120621 = CARTESIAN_POINT ( 'NONE',  ( -9.564922557961040184, 16.46253265017147172, 37.91775706135233293 ) ) ;
#120622 = CARTESIAN_POINT ( 'NONE',  ( 12.06949235617757843, -12.14591786802309237, 43.12390960531435269 ) ) ;
#120623 = CARTESIAN_POINT ( 'NONE',  ( -15.72974639402176322, -15.80617190586768395, 19.37609039468568639 ) ) ;
#120625 = CARTESIAN_POINT ( 'NONE',  ( 5.719274019375991003, -21.55341960407610458, 72.70724293864769550 ) ) ;
#120624 = CARTESIAN_POINT ( 'NONE',  ( 17.44279575226822843, 5.990770900252485376, 31.66442432485683867 ) ) ;
#120626 = CARTESIAN_POINT ( 'NONE',  ( -19.03943276465977164, 0.05219959533909376836, 96.24890960531436690 ) ) ;
#120627 = CARTESIAN_POINT ( 'NONE',  ( 16.53943276465976808, -0.05219959533910856209, 63.74890960531435979 ) ) ;
#120628 = CARTESIAN_POINT ( 'NONE',  ( 9.564922557960805705, 16.46253265017160317, 109.5822429386476955 ) ) ;
#120629 = DIRECTION ( 'NONE',  ( 1.000000000000000000, 0.000000000000000000, 0.000000000000000000 ) ) ;
#120630 = CARTESIAN_POINT ( 'NONE',  ( 13.97604488694548053, -13.89961937509957401, 50.62609039468566152 ) ) ;
#120631 = CARTESIAN_POINT ( 'NONE',  ( 18.67979575497178502, 10.72451020669898547, 104.1655762719810241 ) ) ;
#120632 = CARTESIAN_POINT ( 'NONE',  ( 19.05341960407611168, 5.049401038298154454, 48.95724293864768129 ) ) ;
#120633 = CARTESIAN_POINT ( 'NONE',  ( 12.14591786802309770, 12.06949235617756955, 109.3739096053143811 ) ) ;
#120634 = VECTOR ( 'NONE', #64407, 1000.000000000000114 ) ;
#120635 = CARTESIAN_POINT ( 'NONE',  ( -10.72451020669870658, -18.67979575497194134, 54.58442372801901143 ) ) ;
#120636 = CARTESIAN_POINT ( 'NONE',  ( 8.314922557960818139, 14.29746914071049879, 34.58224293864770260 ) ) ;
#120637 = CARTESIAN_POINT ( 'NONE',  ( 9.474510206698971260, -16.51473224551069308, 42.91557627198103120 ) ) ;
#120638 = CARTESIAN_POINT ( 'NONE',  ( 19.03943276465977164, -0.05219959533909143690, 103.7489096053143669 ) ) ;
#120639 = CARTESIAN_POINT ( 'NONE',  ( 21.52544592524344225, -5.823673210054117533, 73.54057627198102409 ) ) ;
#120640 = CARTESIAN_POINT ( 'NONE',  ( -5.359611314223446995E-15, 29.16686587814335496, 142.3750000027311557 ) ) ;
#120641 = CARTESIAN_POINT ( 'NONE',  ( -13.89961937509977652, 13.97604488694528158, 45.62390960531433848 ) ) ;
#120642 = CARTESIAN_POINT ( 'NONE',  ( -5.823673210054116645, -21.52544592524344225, 57.29057627198103120 ) ) ;
#120643 = CARTESIAN_POINT ( 'NONE',  ( 5.719274019375673035, 21.55341960407619339, 87.29275706135236135 ) ) ;
#120646 = CARTESIAN_POINT ( 'NONE',  ( -4.379528057220328563, 16.55341960407611168, 65.20724293864768129 ) ) ;
#120645 = CARTESIAN_POINT ( 'NONE',  ( -16.55341960407617563, 4.379528057220093196, 78.54275706135236135 ) ) ;
#120644 = CARTESIAN_POINT ( 'NONE',  ( -67.00000000000000000, -1.163414459189985801E-14, 95.00000000000000000 ) ) ;
#120647 = CARTESIAN_POINT ( 'NONE',  ( 13.97604488694527802, 13.89961937509977652, 64.37390960531436690 ) ) ;
#120648 = VERTEX_POINT ( 'NONE', #154169 ) ;
#120649 = CARTESIAN_POINT ( 'NONE',  ( -16.51473224551082808, 9.474510206698731452, 28.33442372801900433 ) ) ;
#120650 = CARTESIAN_POINT ( 'NONE',  ( 16.55341960407618274, -4.379528057220086978, 86.04275706135236135 ) ) ;
#120651 = CARTESIAN_POINT ( 'NONE',  ( 18.67979575497194134, -10.72451020669871369, 105.8344237280190328 ) ) ;
#120652 = CARTESIAN_POINT ( 'NONE',  ( 19.02544592524343514, -5.153800228976328945, 73.54057627198103830 ) ) ;
#120653 = CARTESIAN_POINT ( 'NONE',  ( 21.52544592524344225, -5.823673210054117533, 48.54057627198103120 ) ) ;
#120654 = CARTESIAN_POINT ( 'NONE',  ( -14.29746914071037622, -8.314922557961029526, 19.16775706135234714 ) ) ;
#120655 = CARTESIAN_POINT ( 'NONE',  ( -18.67979575497193778, 10.72451020669871902, 98.33442372801901854 ) ) ;
#120656 = CARTESIAN_POINT ( 'NONE',  ( -4.483927247898782831, 16.52544592524335698, 67.70942372801901854 ) ) ;
#120657 = CARTESIAN_POINT ( 'NONE',  ( -21.53943276465977519, -0.05219959533937600094, 18.75109039468568639 ) ) ;
#120658 = CARTESIAN_POINT ( 'NONE',  ( -19.02544592524334988, -5.153800228976617603, 108.9594237280189759 ) ) ;
#120659 = CARTESIAN_POINT ( 'NONE',  ( -19.03943276465977164, 0.05219959533909376836, 96.24890960531436690 ) ) ;
#120660 = CARTESIAN_POINT ( 'NONE',  ( -16.55341960407617563, 4.379528057220093196, 23.54275706135235424 ) ) ;
#120661 = CARTESIAN_POINT ( 'NONE',  ( 9.564922557960805705, 16.46253265017160317, 54.58224293864769550 ) ) ;
#120662 = CARTESIAN_POINT ( 'NONE',  ( -16.52544592524335698, -4.483927247898792601, 38.95942372801901854 ) ) ;
#120663 = CARTESIAN_POINT ( 'NONE',  ( 12.14591786802309770, 12.06949235617756955, 74.37390960531436690 ) ) ;
#120664 = CARTESIAN_POINT ( 'NONE',  ( 8.314922557961029526, -14.29746914071037800, 90.41775706135236135 ) ) ;
#120666 = CARTESIAN_POINT ( 'NONE',  ( -19.03943276465977164, 0.05219959533909376836, 66.24890960531436690 ) ) ;
#120665 = CARTESIAN_POINT ( 'NONE',  ( 15.80617190586769283, -15.72974639402175789, 45.62609039468567573 ) ) ;
#120667 = CARTESIAN_POINT ( 'NONE',  ( 19.02544592524343514, -5.153800228976328945, 88.54057627198102409 ) ) ;
#120668 = CARTESIAN_POINT ( 'NONE',  ( -16.53943276465976808, -0.05219959533934237506, 88.75109039468567573 ) ) ;
#120669 = DIRECTION ( 'NONE',  ( 0.000000000000000000, 0.000000000000000000, -1.000000000000000000 ) ) ;
#120670 = VERTEX_POINT ( 'NONE', #134041 ) ;
#120671 = CARTESIAN_POINT ( 'NONE',  ( 16.46253265017146816, 9.564922557961045513, 36.66775706135233293 ) ) ;
#120672 = CARTESIAN_POINT ( 'NONE',  ( -16.51473224551069308, -9.474510206698971260, 101.6655762719810241 ) ) ;
#120673 = EDGE_CURVE ( 'NONE', #51008, #19818, #177633, .T. ) ;
#120674 = CARTESIAN_POINT ( 'NONE',  ( 19.03943276465977164, -0.05219959533909143690, 48.74890960531435979 ) ) ;
#120675 = CARTESIAN_POINT ( 'NONE',  ( 19.02544592524343514, -5.153800228976328945, 108.5405762719810383 ) ) ;
#120676 = CARTESIAN_POINT ( 'NONE',  ( -14.34966873604972548, 8.224510206698743886, 43.33442372801901143 ) ) ;
#120678 = CARTESIAN_POINT ( 'NONE',  ( 16.53943276465976808, 0.05219959533934440121, 61.25109039468567573 ) ) ;
#120677 = CARTESIAN_POINT ( 'NONE',  ( -13.97604488694547697, 13.89961937509957934, 63.12609039468566152 ) ) ;
#120679 = CARTESIAN_POINT ( 'NONE',  ( -19.05341960407611168, -5.049401038298163336, 106.4572429386476955 ) ) ;
#120680 = CARTESIAN_POINT ( 'NONE',  ( 9.564922557960805705, 16.46253265017160317, 79.58224293864769550 ) ) ;
#120681 = CARTESIAN_POINT ( 'NONE',  ( 21.52544592524344225, -5.823673210054117533, 98.54057627198105251 ) ) ;
#120682 = CARTESIAN_POINT ( 'NONE',  ( 9.564922557961047289, -16.46253265017146816, 60.41775706135233293 ) ) ;
#120684 = CARTESIAN_POINT ( 'NONE',  ( 16.51473224551069308, 9.474510206698969483, 24.16557627198102765 ) ) ;
#120683 = CARTESIAN_POINT ( 'NONE',  ( 5.049401038298161559, -19.05341960407611168, 97.70724293864766707 ) ) ;
#120685 = CARTESIAN_POINT ( 'NONE',  ( 5.153800228976335163, 19.02544592524342804, 79.79057627198102409 ) ) ;
#120687 = CARTESIAN_POINT ( 'NONE',  ( 16.51473224551069308, 9.474510206698969483, 29.16557627198103475 ) ) ;
#120686 = CARTESIAN_POINT ( 'NONE',  ( 14.34966873604960469, 8.224510206698951720, 39.16557627198102409 ) ) ;
#120688 = CARTESIAN_POINT ( 'NONE',  ( -0.05219959533936034679, 19.03943276465977164, 42.50109039468566152 ) ) ;
#120689 = CARTESIAN_POINT ( 'NONE',  ( 16.53943276465976808, -0.05219959533910856209, 68.74890960531435269 ) ) ;
#120690 = CARTESIAN_POINT ( 'NONE',  ( -10.81492255796105439, 18.62759615963255655, 102.9177570613523756 ) ) ;
#120691 = CARTESIAN_POINT ( 'NONE',  ( -13.89961937509977652, 13.97604488694528158, 45.62390960531433848 ) ) ;
#120693 = CARTESIAN_POINT ( 'NONE',  ( -0.05219959533937732626, 21.53943276465977519, 102.5010903946856899 ) ) ;
#120692 = CARTESIAN_POINT ( 'NONE',  ( 4.483927247898545687, 16.52544592524342804, 34.79057627198103120 ) ) ;
#120694 = CARTESIAN_POINT ( 'NONE',  ( -0.05219959533909027116, -19.03943276465977164, 92.49890960531436690 ) ) ;
#120695 = CARTESIAN_POINT ( 'NONE',  ( 13.97604488694527802, 13.89961937509977652, 89.37390960531436690 ) ) ;
#120696 = CARTESIAN_POINT ( 'NONE',  ( -5.153800228976328057, -19.02544592524343514, 27.29057627198103120 ) ) ;
#120697 = CARTESIAN_POINT ( 'NONE',  ( -16.55341960407611168, -4.379528057220339221, 101.4572429386476955 ) ) ;
#120698 = CARTESIAN_POINT ( 'NONE',  ( 4.483927247898545687, 16.52544592524342804, 74.79057627198105251 ) ) ;
#120699 = CARTESIAN_POINT ( 'NONE',  ( -5.719274019375978568, 21.55341960407610458, 80.20724293864769550 ) ) ;
#120700 = CARTESIAN_POINT ( 'NONE',  ( -5.049401038298153566, 19.05341960407611168, 90.20724293864766707 ) ) ;
#120701 = CARTESIAN_POINT ( 'NONE',  ( 0.05219959533907565091, 21.53943276465977519, 104.9989096053143669 ) ) ;
#120702 = CARTESIAN_POINT ( 'NONE',  ( 19.02544592524343514, -5.153800228976328945, 88.54057627198102409 ) ) ;
#120704 = CARTESIAN_POINT ( 'NONE',  ( -16.52544592524342804, 4.483927247898546575, 86.04057627198102409 ) ) ;
#120703 = LINE ( 'NONE', #124680, #42957 ) ;
#120705 = CARTESIAN_POINT ( 'NONE',  ( -16.46253265017160317, 9.564922557960807481, 65.83224293864769550 ) ) ;
#120706 = CARTESIAN_POINT ( 'NONE',  ( -5.823673210054116645, -21.52544592524344225, 62.29057627198102409 ) ) ;
#120707 = CARTESIAN_POINT ( 'NONE',  ( 22.00000000000000000, -1.132798289211302014E-14, 97.50000000000000000 ) ) ;
#120708 = CARTESIAN_POINT ( 'NONE',  ( -15.72974639402197994, 15.80617190586746368, 35.62390960531437401 ) ) ;
#120709 = CARTESIAN_POINT ( 'NONE',  ( -19.03943276465977164, -0.05219959533935918106, 108.7510903946856615 ) ) ;
#120710 = CARTESIAN_POINT ( 'NONE',  ( 14.29746914071049879, -8.314922557960816363, 98.33224293864769550 ) ) ;
#120711 = CARTESIAN_POINT ( 'NONE',  ( -17.26172910966778318, -6.454744622555851130, 94.19353091350778584 ) ) ;
#120712 = CARTESIAN_POINT ( 'NONE',  ( -9.564922557960796823, -16.46253265017161027, 87.08224293864769550 ) ) ;
#120713 = CARTESIAN_POINT ( 'NONE',  ( -5.153800228976328057, -19.02544592524343514, 42.29057627198101699 ) ) ;
#120714 = CARTESIAN_POINT ( 'NONE',  ( -14.29746914071049879, 8.314922557960819915, 75.83224293864769550 ) ) ;
#120715 = AXIS2_PLACEMENT_3D ( 'NONE', #71659, #151499, #103995 ) ;
#120716 = CARTESIAN_POINT ( 'NONE',  ( -0.05219959533909027116, -19.03943276465977164, 112.4989096053143669 ) ) ;
#120717 = CARTESIAN_POINT ( 'NONE',  ( 8.224510206698953496, -14.34966873604960469, 57.91557627198103120 ) ) ;
#120718 = CARTESIAN_POINT ( 'NONE',  ( -19.02544592524334988, -5.153800228976617603, 108.9594237280189759 ) ) ;
#120719 = CARTESIAN_POINT ( 'NONE',  ( 10.81492255796106328, -18.62759615963255655, 60.41775706135235424 ) ) ;
#120720 = CARTESIAN_POINT ( 'NONE',  ( 13.89961937509977652, -13.97604488694527269, 98.12390960531433848 ) ) ;
#120721 = CARTESIAN_POINT ( 'NONE',  ( -21.55341960407610458, -5.719274019375992779, 86.45724293864770971 ) ) ;
#120722 = CARTESIAN_POINT ( 'NONE',  ( 8.224510206698742110, 14.34966873604972548, 87.08442372801901854 ) ) ;
#120723 = CARTESIAN_POINT ( 'NONE',  ( -16.51473224551069308, -9.474510206698971260, 21.66557627198102765 ) ) ;
#120724 = CARTESIAN_POINT ( 'NONE',  ( -0.05219959533909027116, -19.03943276465977164, 77.49890960531435269 ) ) ;
#120725 = CARTESIAN_POINT ( 'NONE',  ( 18.67979575497178502, 10.72451020669898547, 79.16557627198103830 ) ) ;
#120726 = CARTESIAN_POINT ( 'NONE',  ( -19.05341960407617563, 5.049401038297882671, 103.5427570613523329 ) ) ;
#120728 = CARTESIAN_POINT ( 'NONE',  ( 10.72451020669871369, 18.67979575497193778, 62.08442372801901143 ) ) ;
#120727 = CARTESIAN_POINT ( 'NONE',  ( -16.53943276465976808, 0.05219959533911058130, 46.24890960531435979 ) ) ;
#120730 = CARTESIAN_POINT ( 'NONE',  ( -0.05219959533907301413, -21.53943276465977519, 22.49890960531436335 ) ) ;
#120729 = CARTESIAN_POINT ( 'NONE',  ( -14.29746914071037622, -8.314922557961029526, 89.16775706135236135 ) ) ;
#120731 = CARTESIAN_POINT ( 'NONE',  ( 17.44270441346512612, 5.991230190323099336, 28.86335079264228654 ) ) ;
#120732 = FACE_OUTER_BOUND ( 'NONE', #93426, .T. ) ;
#120733 = CARTESIAN_POINT ( 'NONE',  ( 4.379528057220092307, 16.55341960407617563, 102.2927570613523613 ) ) ;
#120734 = CARTESIAN_POINT ( 'NONE',  ( -14.34966873604972548, 8.224510206698743886, 43.33442372801901143 ) ) ;
#120735 = CARTESIAN_POINT ( 'NONE',  ( 0.05219959533909260263, 19.03943276465977164, 64.99890960531436690 ) ) ;
#120736 = CARTESIAN_POINT ( 'NONE',  ( 19.03943276465977164, -0.05219959533909143690, 73.74890960531435269 ) ) ;
#120737 = CARTESIAN_POINT ( 'NONE',  ( -12.06949235617739369, -12.14591786802326823, 79.37609039468567573 ) ) ;
#120738 = CARTESIAN_POINT ( 'NONE',  ( 4.379528057220339221, -16.55341960407611168, 42.70724293864770260 ) ) ;
#120739 = CARTESIAN_POINT ( 'NONE',  ( -9.474510206698964154, 16.51473224551069663, 50.41557627198102409 ) ) ;
#120740 = CARTESIAN_POINT ( 'NONE',  ( -19.02544592524342804, 5.153800228976336051, 51.04057627198103120 ) ) ;
#120741 = CARTESIAN_POINT ( 'NONE',  ( -0.05219959533934338120, 16.53943276465976808, 42.50109039468567573 ) ) ;
#120742 = CARTESIAN_POINT ( 'NONE',  ( 19.03943276465977164, 0.05219959533936151252, 91.25109039468566152 ) ) ;
#120743 = CARTESIAN_POINT ( 'NONE',  ( 14.29746914071049879, -8.314922557960816363, 98.33224293864769550 ) ) ;
#120744 = CARTESIAN_POINT ( 'NONE',  ( -0.05219959533909027116, -19.03943276465977164, 67.49890960531436690 ) ) ;
#120746 = CARTESIAN_POINT ( 'NONE',  ( -23.48529157249599919, -32.32473071737750558, -3.699999999999999734 ) ) ;
#120745 = CARTESIAN_POINT ( 'NONE',  ( 9.474510206698729675, 16.51473224551082808, 102.0844237280190043 ) ) ;
#120747 = CARTESIAN_POINT ( 'NONE',  ( 15.72974639402176855, 15.80617190586768217, 91.87609039468568994 ) ) ;
#120748 = CARTESIAN_POINT ( 'NONE',  ( 14.34966873604972726, -8.224510206698740333, 65.83442372801900433 ) ) ;
#120749 = DIRECTION ( 'NONE',  ( 1.000000000000000000, 0.000000000000000000, 0.000000000000000000 ) ) ;
#120750 = CARTESIAN_POINT ( 'NONE',  ( 21.55341960407610458, 5.719274019375980345, 63.95724293864770260 ) ) ;
#120751 = CARTESIAN_POINT ( 'NONE',  ( -16.52544592524335698, -4.483927247898792601, 53.95942372801900433 ) ) ;
#120752 = CARTESIAN_POINT ( 'NONE',  ( 5.153800228976335163, 19.02544592524342804, 34.79057627198102409 ) ) ;
#120753 = CARTESIAN_POINT ( 'NONE',  ( 16.46253265017146816, 9.564922557961045513, 36.66775706135233293 ) ) ;
#120754 = CARTESIAN_POINT ( 'NONE',  ( 9.564922557960805705, 16.46253265017160317, 94.58224293864769550 ) ) ;
#120755 = CARTESIAN_POINT ( 'NONE',  ( 4.483927247898545687, 16.52544592524342804, 114.7905762719810383 ) ) ;
#120756 = CARTESIAN_POINT ( 'NONE',  ( 13.89961937509977652, -13.97604488694527269, 68.12390960531436690 ) ) ;
#120757 = CARTESIAN_POINT ( 'NONE',  ( -18.67979575497193778, 10.72451020669871902, 83.33442372801903275 ) ) ;
#120758 = CARTESIAN_POINT ( 'NONE',  ( 16.51473224551083163, -9.474510206698727899, 35.83442372801899722 ) ) ;
#120759 = CARTESIAN_POINT ( 'NONE',  ( -13.97604488694547697, 13.89961937509957934, 23.12609039468565442 ) ) ;
#120760 = CARTESIAN_POINT ( 'NONE',  ( 16.51473224551069308, 9.474510206698969483, 59.16557627198102409 ) ) ;
#120761 = CARTESIAN_POINT ( 'NONE',  ( -10.72451020669898014, 18.67979575497178502, 30.41557627198101699 ) ) ;
#120762 = CARTESIAN_POINT ( 'NONE',  ( -15.72974639402176322, -15.80617190586768395, 84.37609039468570415 ) ) ;
#120763 = CARTESIAN_POINT ( 'NONE',  ( -13.89961937509977652, 13.97604488694528158, 65.62390960531436690 ) ) ;
#120764 = CARTESIAN_POINT ( 'NONE',  ( -10.72451020669870658, -18.67979575497194134, 74.58442372801901854 ) ) ;
#120765 = CARTESIAN_POINT ( 'NONE',  ( -5.719274019375978568, 21.55341960407610458, 40.20724293864769550 ) ) ;
#120766 = CARTESIAN_POINT ( 'NONE',  ( -16.46253265017160317, 9.564922557960807481, 80.83224293864769550 ) ) ;
#120767 = CARTESIAN_POINT ( 'NONE',  ( 21.55341960407619695, -5.719274019375665929, 36.04275706135234714 ) ) ;
#120768 = CARTESIAN_POINT ( 'NONE',  ( -13.89961937509957401, -13.97604488694547875, 59.37609039468566863 ) ) ;
#120769 = CARTESIAN_POINT ( 'NONE',  ( 0.05219959533909260263, 19.03943276465977164, 44.99890960531435979 ) ) ;
#120770 = CARTESIAN_POINT ( 'NONE',  ( 5.153800228976335163, 19.02544592524342804, 84.79057627198099567 ) ) ;
#120771 = CARTESIAN_POINT ( 'NONE',  ( 4.483927247898790824, -16.52544592524335698, 30.20942372801902565 ) ) ;
#120772 = CARTESIAN_POINT ( 'NONE',  ( 8.314922557960818139, 14.29746914071049879, 89.58224293864768129 ) ) ;
#120773 = CARTESIAN_POINT ( 'NONE',  ( 19.05341960407611168, 5.049401038298154454, 53.95724293864770260 ) ) ;
#120774 = CARTESIAN_POINT ( 'NONE',  ( -15.80617190586745835, -15.72974639402198527, 46.87390960531435979 ) ) ;
#120775 = CARTESIAN_POINT ( 'NONE',  ( 12.06949235617739724, 12.14591786802326823, 21.87609039468567573 ) ) ;
#120776 = CARTESIAN_POINT ( 'NONE',  ( 10.72451020669871369, 18.67979575497193778, 22.08442372801901143 ) ) ;
#120777 = CARTESIAN_POINT ( 'NONE',  ( -10.81492255796105439, 18.62759615963255655, 67.91775706135234714 ) ) ;
#120778 = CARTESIAN_POINT ( 'NONE',  ( -12.14591786802326823, 12.06949235617739902, 63.12609039468568994 ) ) ;
#120779 = CARTESIAN_POINT ( 'NONE',  ( 14.29746914071037800, 8.314922557961029526, 61.66775706135235424 ) ) ;
#120780 = AXIS2_PLACEMENT_3D ( 'NONE', #116633, #35794, #86292 ) ;
#120781 = CARTESIAN_POINT ( 'NONE',  ( 19.02544592524343514, -5.153800228976328945, 58.54057627198102409 ) ) ;
#120782 = CARTESIAN_POINT ( 'NONE',  ( 16.55341960407618274, -4.379528057220086978, 91.04275706135236135 ) ) ;
#120783 = CARTESIAN_POINT ( 'NONE',  ( -9.474510206698720793, -16.51473224551083518, 44.58442372801900433 ) ) ;
#120784 = CARTESIAN_POINT ( 'NONE',  ( -10.72451020669870658, -18.67979575497194134, 19.58442372801901143 ) ) ;
#120785 = CARTESIAN_POINT ( 'NONE',  ( 8.314922557960818139, 14.29746914071049879, 59.58224293864770260 ) ) ;
#120786 = CARTESIAN_POINT ( 'NONE',  ( -9.564922557960796823, -16.46253265017161027, 87.08224293864769550 ) ) ;
#120787 = CARTESIAN_POINT ( 'NONE',  ( 0.05219959533934541429, -16.53943276465976808, 90.00109039468567573 ) ) ;
#120788 = CARTESIAN_POINT ( 'NONE',  ( -5.823673210054431948, 21.52544592524334988, 52.70942372801902565 ) ) ;
#120789 = CARTESIAN_POINT ( 'NONE',  ( 14.34966873604972726, -8.224510206698740333, 35.83442372801901143 ) ) ;
#120790 = CARTESIAN_POINT ( 'NONE',  ( 18.62759615963255655, 10.81492255796105972, 31.66775706135234358 ) ) ;
#120791 = CARTESIAN_POINT ( 'NONE',  ( -14.34966873604960291, -8.224510206698953496, 51.66557627198102409 ) ) ;
#120792 = EDGE_LOOP ( 'NONE', ( #7644, #174124 ) ) ;
#120793 =( BOUNDED_CURVE ( )  B_SPLINE_CURVE ( 2, ( #45386, #107039, #162999, #168711, #84139, #24505, #69996, #179191, #85141, #86156, #193346, #147846, #9332, #70998, #132665, #102328, #164018, #25514, #154548, #187892, #157537, #200063, #50364, #46372, #63535, #123200, #184890, #80677, #170715, #32206, #1853, #33202, #3833, #93863, #850, #171712, #185896, #19031, #155541, #142353, #79694, #17035, #141364, #139369, #109036, #2851, #186906, #62523, #65512, #30213, #78689, #125210, #77702, #112023, #48377, #153548, #108031, #94860, #140366, #61531, #110034, #169717, #34192, #127173, #188883, #156541, #16043, #126196, #91856, #124196, #18040, #47381, #64529, #49359, #111022, #172708, #95853, #15045, #92861, #76706, #138382, #31210, #23010, #144339, #176704, #67503, #35180, #177702, #70510, #52334, #68498, #84656, #160517, #128171, #81650, #116012, #147354, #5827, #145338, #159504, #38178 ),
 .UNSPECIFIED., .F., .T. ) 
 B_SPLINE_CURVE_WITH_KNOTS ( ( 3, 2, 2, 2, 2, 2, 2, 2, 2, 2, 2, 2, 2, 2, 2, 2, 2, 2, 2, 2, 2, 2, 2, 2, 2, 2, 2, 2, 2, 2, 2, 2, 2, 2, 2, 2, 2, 2, 2, 2, 2, 2, 2, 2, 2, 2, 2, 2, 2, 2, 3 ),
 ( 0.000000000000000000, 0.02000000000000000042, 0.04000000000000000083, 0.05999999999999999778, 0.08000000000000000167, 0.1000000000000000056, 0.1199999999999999956, 0.1400000000000000133, 0.1600000000000000033, 0.1799999999999999933, 0.2000000000000000111, 0.2200000000000000011, 0.2399999999999999911, 0.2600000000000000089, 0.2800000000000000266, 0.2999999999999999889, 0.3200000000000000067, 0.3400000000000000244, 0.3599999999999999867, 0.3800000000000000044, 0.4000000000000000222, 0.4199999999999999845, 0.4400000000000000022, 0.4600000000000000200, 0.4799999999999999822, 0.5000000000000000000, 0.5200000000000000178, 0.5400000000000000355, 0.5600000000000000533, 0.5799999999999999600, 0.5999999999999999778, 0.6199999999999999956, 0.6400000000000000133, 0.6600000000000000311, 0.6800000000000000488, 0.6999999999999999556, 0.7199999999999999734, 0.7399999999999999911, 0.7600000000000000089, 0.7800000000000000266, 0.8000000000000000444, 0.8199999999999999512, 0.8399999999999999689, 0.8599999999999999867, 0.8800000000000000044, 0.9000000000000000222, 0.9200000000000000400, 0.9399999999999999467, 0.9599999999999999645, 0.9799999999999999822, 1.000000000000000000 ),
 .UNSPECIFIED. ) 
 CURVE ( )  GEOMETRIC_REPRESENTATION_ITEM ( )  RATIONAL_B_SPLINE_CURVE ( ( 1.000000000000000000, 0.9510565162951535312, 1.000000000000000000, 0.9510565162951535312, 1.000000000000000000, 0.9510565162951535312, 1.000000000000000000, 0.9510565162951535312, 1.000000000000000000, 0.9510565162951535312, 1.000000000000000000, 0.9510565162951535312, 1.000000000000000000, 0.9510565162951535312, 1.000000000000000000, 0.9510565162951535312, 1.000000000000000000, 0.9510565162951535312, 1.000000000000000000, 0.9510565162951535312, 1.000000000000000000, 0.9510565162951535312, 1.000000000000000000, 0.9510565162951535312, 1.000000000000000000, 0.9510565162951535312, 1.000000000000000000, 0.9510565162951535312, 1.000000000000000000, 0.9510565162951535312, 1.000000000000000000, 0.9510565162951535312, 1.000000000000000000, 0.9510565162951535312, 1.000000000000000000, 0.9510565162951535312, 1.000000000000000000, 0.9510565162951535312, 1.000000000000000000, 0.9510565162951535312, 1.000000000000000000, 0.9510565162951535312, 1.000000000000000000, 0.9510565162951535312, 1.000000000000000000, 0.9510565162951535312, 1.000000000000000000, 0.9510565162951535312, 1.000000000000000000, 0.9510565162951535312, 1.000000000000000000, 0.9510565162951535312, 1.000000000000000000, 0.9510565162951535312, 1.000000000000000000, 0.9510565162951535312, 1.000000000000000000, 0.9510565162951535312, 1.000000000000000000, 0.9510565162951535312, 1.000000000000000000, 0.9510565162951535312, 1.000000000000000000, 0.9510565162951535312, 1.000000000000000000, 0.9510565162951535312, 1.000000000000000000, 0.9510565162951535312, 1.000000000000000000, 0.9510565162951535312, 1.000000000000000000, 0.9510565162951535312, 1.000000000000000000, 0.9510565162951535312, 1.000000000000000000, 0.9510565162951535312, 1.000000000000000000, 0.9510565162951535312, 1.000000000000000000, 0.9510565162951535312, 1.000000000000000000, 0.9510565162951535312, 1.000000000000000000, 0.9510565162951535312, 1.000000000000000000, 0.9510565162951535312, 1.000000000000000000, 0.9510565162951535312, 1.000000000000000000, 0.9510565162951535312, 1.000000000000000000, 0.9510565162951535312, 1.000000000000000000, 0.9510565162951535312, 1.000000000000000000, 0.9510565162951535312, 1.000000000000000000, 0.9510565162951535312, 1.000000000000000000, 0.9510565162951535312, 1.000000000000000000 ) ) 
 REPRESENTATION_ITEM ( '' )  );
#120794 = CARTESIAN_POINT ( 'NONE',  ( 15.80617190586746368, 15.72974639402197994, 104.3739096053143669 ) ) ;
#120795 = CARTESIAN_POINT ( 'NONE',  ( 4.483927247898545687, 16.52544592524342804, 39.79057627198103830 ) ) ;
#120796 = VERTEX_POINT ( 'NONE', #199686 ) ;
#120797 = CARTESIAN_POINT ( 'NONE',  ( 34.45218533337745725, 5.971079431359537892, 49.56529461667047798 ) ) ;
#120798 = CARTESIAN_POINT ( 'NONE',  ( -5.823673210054116645, -21.52544592524344225, 27.29057627198103120 ) ) ;
#120799 = CARTESIAN_POINT ( 'NONE',  ( -18.62759615963255300, -10.81492255796106328, 34.16775706135234714 ) ) ;
#120800 = CARTESIAN_POINT ( 'NONE',  ( -4.379528057220328563, 16.55341960407611168, 60.20724293864768839 ) ) ;
#120801 = CIRCLE ( 'NONE', #65939, 8.000000000000007105 ) ;
#120802 = CARTESIAN_POINT ( 'NONE',  ( 5.153800228976335163, 19.02544592524342804, 74.79057627198103830 ) ) ;
#120804 = CARTESIAN_POINT ( 'NONE',  ( 16.46253265017146816, 9.564922557961045513, 71.66775706135233293 ) ) ;
#120803 = CARTESIAN_POINT ( 'NONE',  ( 5.049401038298161559, -19.05341960407611168, 22.70724293864769194 ) ) ;
#120805 = CARTESIAN_POINT ( 'NONE',  ( 18.62759615963271287, -10.81492255796078972, 48.33224293864770260 ) ) ;
#120806 = B_SPLINE_CURVE_WITH_KNOTS ( 'NONE', 3,
 ( #155621, #63614, #48457, #172791, #156624, #126273, #67580, #175768, #36239, #160594, #79774, #82736 ),
 .UNSPECIFIED., .F., .F.,
 ( 4, 2, 2, 2, 2, 4 ),
 ( 0.003927129849554318076, 0.005134622258946400924, 0.006342114668338482905, 0.007549607077730566621, 0.008153353282426611948, 0.008757099487122657275 ),
 .UNSPECIFIED. ) ;
#120807 = CARTESIAN_POINT ( 'NONE',  ( -21.18879603622789531, -31.24179269222070587, -19.75583340878099037 ) ) ;
#120808 = CARTESIAN_POINT ( 'NONE',  ( -19.02544592524342804, 5.153800228976336051, 61.04057627198103120 ) ) ;
#120809 = CARTESIAN_POINT ( 'NONE',  ( -16.53943276465976808, -0.05219959533934237506, 33.75109039468568284 ) ) ;
#120810 = CARTESIAN_POINT ( 'NONE',  ( -5.719274019375665041, -21.55341960407619695, 19.79275706135235069 ) ) ;
#120811 = CARTESIAN_POINT ( 'NONE',  ( 12.14591786802309770, 12.06949235617756955, 44.37390960531435979 ) ) ;
#120812 = ORIENTED_EDGE ( 'NONE', *, *, #57861, .F. ) ;
#120813 = CARTESIAN_POINT ( 'NONE',  ( -19.05341960407611168, -5.049401038298163336, 96.45724293864769550 ) ) ;
#120814 = CARTESIAN_POINT ( 'NONE',  ( -21.52544592524343514, 5.823673210054127303, 71.04057627198103830 ) ) ;
#120816 = CARTESIAN_POINT ( 'NONE',  ( -8.314922557961024197, 14.29746914071037800, 32.91775706135234714 ) ) ;
#120815 = CARTESIAN_POINT ( 'NONE',  ( -5.719274019375978568, 21.55341960407610458, 115.2072429386476955 ) ) ;
#120817 = CARTESIAN_POINT ( 'NONE',  ( -21.55341960407610458, -5.719274019375992779, 36.45724293864768839 ) ) ;
#120818 = CARTESIAN_POINT ( 'NONE',  ( 15.72974639402176855, 15.80617190586768217, 106.8760903946856899 ) ) ;
#120819 = CARTESIAN_POINT ( 'NONE',  ( 9.564922557960805705, 16.46253265017160317, 94.58224293864769550 ) ) ;
#120820 = CARTESIAN_POINT ( 'NONE',  ( -16.46253265017160317, 9.564922557960807481, 45.83224293864769550 ) ) ;
#120821 = CARTESIAN_POINT ( 'NONE',  ( -0.05219959533909027116, -19.03943276465977164, 92.49890960531436690 ) ) ;
#120822 = CARTESIAN_POINT ( 'NONE',  ( -13.97604488694527625, -13.89961937509977652, 76.87390960531433848 ) ) ;
#120823 = DIRECTION ( 'NONE',  ( 1.000000000000000000, 0.000000000000000000, 0.000000000000000000 ) ) ;
#120824 = CARTESIAN_POINT ( 'NONE',  ( 13.89961937509957401, 13.97604488694547697, 51.87609039468566863 ) ) ;
#120826 = CARTESIAN_POINT ( 'NONE',  ( -18.62759615963270932, 10.81492255796079327, 25.83224293864769194 ) ) ;
#120825 = CARTESIAN_POINT ( 'NONE',  ( -5.049401038297874678, -19.05341960407617918, 19.79275706135233293 ) ) ;
#120827 = CARTESIAN_POINT ( 'NONE',  ( 16.52544592524335698, 4.483927247898782831, 106.4594237280190328 ) ) ;
#120828 = CARTESIAN_POINT ( 'NONE',  ( -9.474510206698720793, -16.51473224551083518, 89.58442372801900433 ) ) ;
#120829 = CARTESIAN_POINT ( 'NONE',  ( -17.31747979337949772, 6.344076630960999275, 58.62055131934815222 ) ) ;
#120830 = CARTESIAN_POINT ( 'NONE',  ( -19.02544592524334988, -5.153800228976617603, 83.95942372801901854 ) ) ;
#120831 = CARTESIAN_POINT ( 'NONE',  ( -19.02544592524334988, -5.153800228976617603, 38.95942372801900433 ) ) ;
#120832 = CARTESIAN_POINT ( 'NONE',  ( 16.52216118717204907, 7.221426719304542274, 108.5759902104699250 ) ) ;
#120833 = CARTESIAN_POINT ( 'NONE',  ( 5.049401038298161559, -19.05341960407611168, 42.70724293864767418 ) ) ;
#120834 = CARTESIAN_POINT ( 'NONE',  ( -16.52544592524342804, 4.483927247898546575, 46.04057627198103830 ) ) ;
#120835 = EDGE_CURVE ( 'NONE', #198713, #29557, #103704, .T. ) ;
#120836 = CARTESIAN_POINT ( 'NONE',  ( -17.12812012977026654, -6.668231424565989052, 111.3594875932314636 ) ) ;
#120837 = CARTESIAN_POINT ( 'NONE',  ( 16.53943276465976808, -0.05219959533910856209, 28.74890960531435624 ) ) ;
#120838 = DIRECTION ( 'NONE',  ( 0.000000000000000000, 0.000000000000000000, -1.000000000000000000 ) ) ;
#120839 = CARTESIAN_POINT ( 'NONE',  ( -8.224510206698735004, -14.34966873604973081, 89.58442372801901854 ) ) ;
#120840 = CARTESIAN_POINT ( 'NONE',  ( -16.51473224551069308, -9.474510206698971260, 46.66557627198102409 ) ) ;
#120841 = CARTESIAN_POINT ( 'NONE',  ( 5.719274019375673035, 21.55341960407619339, 102.2927570613523613 ) ) ;
#120842 = CARTESIAN_POINT ( 'NONE',  ( -14.34966873604972548, 8.224510206698743886, 23.33442372801901499 ) ) ;
#120844 = ORIENTED_EDGE ( 'NONE', *, *, #68275, .T. ) ;
#120843 = CARTESIAN_POINT ( 'NONE',  ( 18.62759615963255655, 10.81492255796105972, 91.66775706135234714 ) ) ;
#120845 = CARTESIAN_POINT ( 'NONE',  ( 13.97604488694527802, 13.89961937509977652, 109.3739096053143669 ) ) ;
#120846 = CARTESIAN_POINT ( 'NONE',  ( 9.474510206698971260, -16.51473224551069308, 82.91557627198103830 ) ) ;
#120847 = CARTESIAN_POINT ( 'NONE',  ( 11.40812507854755253, -35.11059874428192273, -8.024999997268814411 ) ) ;
#120848 = CARTESIAN_POINT ( 'NONE',  ( 15.80617190586746368, 15.72974639402197994, 114.3739096053143527 ) ) ;
#120849 = CARTESIAN_POINT ( 'NONE',  ( -0.05219959533910754901, -16.53943276465976808, 77.49890960531433848 ) ) ;
#120850 = CARTESIAN_POINT ( 'NONE',  ( 0.05219959533907565091, 21.53943276465977519, 79.99890960531435269 ) ) ;
#120851 = CARTESIAN_POINT ( 'NONE',  ( 19.02544592524343514, -5.153800228976328945, 63.54057627198103830 ) ) ;
#120853 = CARTESIAN_POINT ( 'NONE',  ( -4.483927247898782831, 16.52544592524335698, 87.70942372801901854 ) ) ;
#120852 = CARTESIAN_POINT ( 'NONE',  ( -18.62759615963270932, 10.81492255796079327, 100.8322429386477097 ) ) ;
#120854 = ORIENTED_EDGE ( 'NONE', *, *, #160051, .F. ) ;
#120855 = CARTESIAN_POINT ( 'NONE',  ( 5.049401038298161559, -19.05341960407611168, 57.70724293864769550 ) ) ;
#120857 = CARTESIAN_POINT ( 'NONE',  ( 1.500000000000003553, 30.40000000000004476, -47.75060438757614634 ) ) ;
#120856 = CARTESIAN_POINT ( 'NONE',  ( -8.314922557960811034, -14.29746914071050412, 87.08224293864769550 ) ) ;
#120858 = CARTESIAN_POINT ( 'NONE',  ( 9.564922557960805705, 16.46253265017160317, 69.58224293864770971 ) ) ;
#120859 = CARTESIAN_POINT ( 'NONE',  ( 19.02544592524334988, 5.153800228976608722, 81.45942372801897591 ) ) ;
#120860 = CARTESIAN_POINT ( 'NONE',  ( -14.34966873604960291, -8.224510206698953496, 86.66557627198102409 ) ) ;
#120861 = CARTESIAN_POINT ( 'NONE',  ( 18.62759615963255655, 10.81492255796105972, 56.66775706135235424 ) ) ;
#120863 = CARTESIAN_POINT ( 'NONE',  ( 5.823673210054444382, -21.52544592524334988, 20.20942372801900788 ) ) ;
#120862 = CARTESIAN_POINT ( 'NONE',  ( 16.51473224551069308, 9.474510206698969483, 44.16557627198103120 ) ) ;
#120864 = CARTESIAN_POINT ( 'NONE',  ( 8.224510206698953496, -14.34966873604960469, 102.9155762719810383 ) ) ;
#120865 = DIRECTION ( 'NONE',  ( 1.000000000000000000, -0.000000000000000000, 0.000000000000000000 ) ) ;
#120866 = CARTESIAN_POINT ( 'NONE',  ( 13.97604488694527802, 13.89961937509977652, 54.37390960531435979 ) ) ;
#120867 = CARTESIAN_POINT ( 'NONE',  ( 28.82186960331498327, 2.781578969918950771E-14, 139.2500000054623683 ) ) ;
#120869 = CARTESIAN_POINT ( 'NONE',  ( 9.474510206698971260, -16.51473224551069308, 112.9155762719810383 ) ) ;
#120868 = CARTESIAN_POINT ( 'NONE',  ( 19.02544592524334988, 5.153800228976608722, 106.4594237280190185 ) ) ;
#120870 = CARTESIAN_POINT ( 'NONE',  ( 21.52544592524334988, 5.823673210054432836, 51.45942372801901854 ) ) ;
#120871 = CARTESIAN_POINT ( 'NONE',  ( -19.02544592524342804, 5.153800228976336051, 101.0405762719810241 ) ) ;
#120872 = CARTESIAN_POINT ( 'NONE',  ( -19.03943276465977164, -0.05219959533935918106, 83.75109039468567573 ) ) ;
#120873 = CARTESIAN_POINT ( 'NONE',  ( 5.153800228976335163, 19.02544592524342804, 54.79057627198103120 ) ) ;
#120874 = CARTESIAN_POINT ( 'NONE',  ( 8.314922557960818139, 14.29746914071049879, 74.58224293864768129 ) ) ;
#120875 = CARTESIAN_POINT ( 'NONE',  ( 14.29746914071049879, -8.314922557960816363, 83.33224293864769550 ) ) ;
#120876 = CARTESIAN_POINT ( 'NONE',  ( 9.564922557960805705, 16.46253265017160317, 84.58224293864769550 ) ) ;
#120877 = CARTESIAN_POINT ( 'NONE',  ( -4.483927247898539470, -16.52544592524342804, 82.29057627198103830 ) ) ;
#120878 = CARTESIAN_POINT ( 'NONE',  ( 0.05219959533909260263, 19.03943276465977164, 84.99890960531436690 ) ) ;
#120879 = AXIS2_PLACEMENT_3D ( 'NONE', #174773, #21080, #95931 ) ;
#120880 = CARTESIAN_POINT ( 'NONE',  ( 0.05219959533936267826, -19.03943276465977164, 25.00109039468566152 ) ) ;
#120883 = CARTESIAN_POINT ( 'NONE',  ( -13.89961937509977652, 13.97604488694528158, 30.62390960531435269 ) ) ;
#120882 = CARTESIAN_POINT ( 'NONE',  ( 4.379528057220339221, -16.55341960407611168, 27.70724293864769905 ) ) ;
#120881 = CARTESIAN_POINT ( 'NONE',  ( 16.51473224551069308, 9.474510206698969483, 54.16557627198103120 ) ) ;
#120884 = ORIENTED_EDGE ( 'NONE', *, *, #138817, .T. ) ;
#120885 = CARTESIAN_POINT ( 'NONE',  ( 10.72451020669871369, 18.67979575497193778, 42.08442372801901854 ) ) ;
#120886 = CARTESIAN_POINT ( 'NONE',  ( 19.03943276465977164, 0.05219959533936151252, 71.25109039468566152 ) ) ;
#120887 = CARTESIAN_POINT ( 'NONE',  ( -8.224510206698948167, 14.34966873604960824, 40.41557627198103120 ) ) ;
#120888 = CARTESIAN_POINT ( 'NONE',  ( -21.52544592524343514, 5.823673210054127303, 86.04057627198102409 ) ) ;
#120889 = CARTESIAN_POINT ( 'NONE',  ( -18.67979575497178146, -10.72451020669898902, 31.66557627198102054 ) ) ;
#120890 = CARTESIAN_POINT ( 'NONE',  ( -12.14591786802309592, -12.06949235617757132, 71.87390960531438111 ) ) ;
#120891 = CARTESIAN_POINT ( 'NONE',  ( 13.89961937509977652, -13.97604488694527269, 48.12390960531435979 ) ) ;
#120892 = CARTESIAN_POINT ( 'NONE',  ( 4.379528057220092307, 16.55341960407617563, 107.2927570613523471 ) ) ;
#120893 = CARTESIAN_POINT ( 'NONE',  ( 14.29746914071037800, 8.314922557961029526, 56.66775706135235424 ) ) ;
#120894 = CARTESIAN_POINT ( 'NONE',  ( -21.55341960407610458, -5.719274019375992779, 41.45724293864769550 ) ) ;
#120895 = CARTESIAN_POINT ( 'NONE',  ( 21.52544592524334988, 5.823673210054432836, 111.4594237280190328 ) ) ;
#120896 = CARTESIAN_POINT ( 'NONE',  ( -5.153800228976328057, -19.02544592524343514, 87.29057627198103830 ) ) ;
#120897 = CARTESIAN_POINT ( 'NONE',  ( -8.314922557961024197, 14.29746914071037800, 77.91775706135231871 ) ) ;
#120898 = CARTESIAN_POINT ( 'NONE',  ( 12.14591786802309770, 12.06949235617756955, 114.3739096053143527 ) ) ;
#120899 = CARTESIAN_POINT ( 'NONE',  ( -16.53943276465976808, 0.05219959533911058130, 31.24890960531435979 ) ) ;
#120901 = CARTESIAN_POINT ( 'NONE',  ( -0.05219959533909027116, -19.03943276465977164, 92.49890960531436690 ) ) ;
#120900 = CARTESIAN_POINT ( 'NONE',  ( 19.03943276465977164, -0.05219959533909143690, 108.7489096053143527 ) ) ;
#120902 = CARTESIAN_POINT ( 'NONE',  ( 15.80617190586746368, 15.72974639402197994, 29.37390960531435269 ) ) ;
#120903 = VECTOR ( 'NONE', #100276, 1000.000000000000000 ) ;
#120904 = CARTESIAN_POINT ( 'NONE',  ( -8.314922557960811034, -14.29746914071050412, 72.08224293864769550 ) ) ;
#120905 = ORIENTED_EDGE ( 'NONE', *, *, #157130, .F. ) ;
#120906 = CARTESIAN_POINT ( 'NONE',  ( 8.224510206698953496, -14.34966873604960469, 57.91557627198103120 ) ) ;
#120908 = DIRECTION ( 'NONE',  ( -0.000000000000000000, 0.8660254037844391517, 0.4999999999999991673 ) ) ;
#120907 = CARTESIAN_POINT ( 'NONE',  ( -4.483927247898782831, 16.52544592524335698, 57.70942372801901143 ) ) ;
#120909 = CARTESIAN_POINT ( 'NONE',  ( -19.02544592524334988, -5.153800228976617603, 48.95942372801900433 ) ) ;
#120910 = CARTESIAN_POINT ( 'NONE',  ( -9.474510206698964154, 16.51473224551069663, 85.41557627198102409 ) ) ;
#120911 = CARTESIAN_POINT ( 'NONE',  ( 16.46253265017146816, 9.564922557961045513, 66.66775706135233293 ) ) ;
#120912 = CARTESIAN_POINT ( 'NONE',  ( -17.14385361876520264, -23.59649016807271593, 141.6750000027311103 ) ) ;
#120913 = CARTESIAN_POINT ( 'NONE',  ( -16.46253265017146816, -9.564922557961047289, 54.16775706135234003 ) ) ;
#120915 = CARTESIAN_POINT ( 'NONE',  ( 8.314922557961029526, -14.29746914071037800, 95.41775706135234714 ) ) ;
#120914 = CARTESIAN_POINT ( 'NONE',  ( 16.51473224551083163, -9.474510206698727899, 100.8344237280190043 ) ) ;
#120916 = CARTESIAN_POINT ( 'NONE',  ( -17.14385361876520619, 23.59649016807275856, 145.0750000027311728 ) ) ;
#120917 = CARTESIAN_POINT ( 'NONE',  ( 5.153800228976335163, 19.02544592524342804, 44.79057627198103830 ) ) ;
#120918 = CARTESIAN_POINT ( 'NONE',  ( -19.05341960407611168, -5.049401038298163336, 111.4572429386476671 ) ) ;
#120919 = CARTESIAN_POINT ( 'NONE',  ( 10.81492255796106328, -18.62759615963255655, 55.41775706135234714 ) ) ;
#120920 = CARTESIAN_POINT ( 'NONE',  ( 5.049401038297881783, 19.05341960407617563, 97.29275706135233293 ) ) ;
#120922 = CARTESIAN_POINT ( 'NONE',  ( -16.46253265017160317, 9.564922557960807481, 55.83224293864769550 ) ) ;
#120921 = DIRECTION ( 'NONE',  ( 1.000000000000000000, 0.000000000000000000, 0.000000000000000000 ) ) ;
#120923 = CARTESIAN_POINT ( 'NONE',  ( -37.99626262588765968, 12.34573411038917179, -0.1021577739498228665 ) ) ;
#120925 = CARTESIAN_POINT ( 'NONE',  ( 13.89961937509977652, -13.97604488694527269, 63.12390960531435979 ) ) ;
#120924 = CARTESIAN_POINT ( 'NONE',  ( 4.483927247898545687, 16.52544592524342804, 79.79057627198102409 ) ) ;
#120926 = CARTESIAN_POINT ( 'NONE',  ( 19.05341960407611168, 5.049401038298154454, 78.95724293864769550 ) ) ;
#120927 = CARTESIAN_POINT ( 'NONE',  ( -16.46253265017146816, -9.564922557961047289, 79.16775706135234714 ) ) ;
#120928 = CARTESIAN_POINT ( 'NONE',  ( -18.62759615963270932, 10.81492255796079327, 70.83224293864770971 ) ) ;
#120929 = CARTESIAN_POINT ( 'NONE',  ( -16.52544592524342804, 4.483927247898546575, 116.0405762719810383 ) ) ;
#120930 = CARTESIAN_POINT ( 'NONE',  ( -5.153800228976607833, 19.02544592524334988, 42.70942372801901143 ) ) ;
#120931 = CARTESIAN_POINT ( 'NONE',  ( 16.51473224551069308, 9.474510206698969483, 49.16557627198102409 ) ) ;
#120932 = CARTESIAN_POINT ( 'NONE',  ( 19.05341960407611168, 5.049401038298154454, 78.95724293864769550 ) ) ;
#120933 = CARTESIAN_POINT ( 'NONE',  ( -0.05219959533907301413, -21.53943276465977519, 87.49890960531436690 ) ) ;
#120935 = CARTESIAN_POINT ( 'NONE',  ( 13.97604488694548053, -13.89961937509957401, 50.62609039468566152 ) ) ;
#120934 = CARTESIAN_POINT ( 'NONE',  ( 14.29746914071049879, -8.314922557960816363, 78.33224293864770971 ) ) ;
#120936 = CARTESIAN_POINT ( 'NONE',  ( -10.72451020669898014, 18.67979575497178502, 80.41557627198103830 ) ) ;
#120937 = CARTESIAN_POINT ( 'NONE',  ( -18.62759615963270932, 10.81492255796079327, 60.83224293864769550 ) ) ;
#120938 = CARTESIAN_POINT ( 'NONE',  ( 14.29746914071049879, -8.314922557960816363, 33.33224293864769550 ) ) ;
#120939 = CARTESIAN_POINT ( 'NONE',  ( 15.72974639402176855, 15.80617190586768217, 91.87609039468568994 ) ) ;
#120940 = CARTESIAN_POINT ( 'NONE',  ( 16.46253265017160672, -9.564922557960803928, 78.33224293864769550 ) ) ;
#120941 = CARTESIAN_POINT ( 'NONE',  ( 5.153800228976335163, 19.02544592524342804, 24.79057627198102765 ) ) ;
#120942 = AXIS2_PLACEMENT_3D ( 'NONE', #151040, #138819, #93301 ) ;
#120943 = CARTESIAN_POINT ( 'NONE',  ( -21.52544592524334988, -5.823673210054445271, 23.95942372801901143 ) ) ;
#120944 = CARTESIAN_POINT ( 'NONE',  ( -21.52544592524334988, -5.823673210054445271, 43.95942372801902565 ) ) ;
#120945 = CARTESIAN_POINT ( 'NONE',  ( 16.51473224551069308, 9.474510206698969483, 44.16557627198103120 ) ) ;
#120946 = CARTESIAN_POINT ( 'NONE',  ( 15.80617190586769283, -15.72974639402175789, 20.62609039468568639 ) ) ;
#120947 = CARTESIAN_POINT ( 'NONE',  ( 0.05219959533936267826, -19.03943276465977164, 60.00109039468566863 ) ) ;
#120948 = CARTESIAN_POINT ( 'NONE',  ( 19.03943276465977164, -0.05219959533909143690, 38.74890960531436690 ) ) ;
#120949 = CARTESIAN_POINT ( 'NONE',  ( -12.06949235617739369, -12.14591786802326823, 29.37609039468568284 ) ) ;
#120950 = CARTESIAN_POINT ( 'NONE',  ( -19.05341960407611168, -5.049401038298163336, 26.45724293864769550 ) ) ;
#120951 = CARTESIAN_POINT ( 'NONE',  ( 8.314922557961029526, -14.29746914071037800, 60.41775706135235424 ) ) ;
#120952 = CARTESIAN_POINT ( 'NONE',  ( -19.03943276465977164, 0.05219959533909376836, 41.24890960531435269 ) ) ;
#120953 = CARTESIAN_POINT ( 'NONE',  ( -25.75939503182733858, -8.559839547494508594, 171.7912139782359588 ) ) ;
#120954 = CARTESIAN_POINT ( 'NONE',  ( -16.46253265017160317, 9.564922557960807481, 85.83224293864769550 ) ) ;
#120955 = CARTESIAN_POINT ( 'NONE',  ( -5.049401038298153566, 19.05341960407611168, 30.20724293864768839 ) ) ;
#120956 = CARTESIAN_POINT ( 'NONE',  ( 5.719274019375991003, -21.55341960407610458, 57.70724293864770260 ) ) ;
#120957 = CARTESIAN_POINT ( 'NONE',  ( 4.379528057220092307, 16.55341960407617563, 52.29275706135236135 ) ) ;
#120958 = CARTESIAN_POINT ( 'NONE',  ( -21.53943276465977519, -0.05219959533937600094, 93.75109039468567573 ) ) ;
#120959 = CARTESIAN_POINT ( 'NONE',  ( 16.46253265017160672, -9.564922557960803928, 43.33224293864769550 ) ) ;
#120960 = CARTESIAN_POINT ( 'NONE',  ( 4.483927247898545687, 16.52544592524342804, 29.79057627198102409 ) ) ;
#120961 = CARTESIAN_POINT ( 'NONE',  ( 4.379528057220339221, -16.55341960407611168, 62.70724293864769550 ) ) ;
#120962 = CARTESIAN_POINT ( 'NONE',  ( -16.51473224551069308, -9.474510206698971260, 61.66557627198103120 ) ) ;
#120963 = CARTESIAN_POINT ( 'NONE',  ( 21.52544592524334988, 5.823673210054432836, 111.4594237280190328 ) ) ;
#120964 = CARTESIAN_POINT ( 'NONE',  ( -5.823673210054431948, 21.52544592524334988, 22.70942372801901499 ) ) ;
#120965 = CARTESIAN_POINT ( 'NONE',  ( -0.05219959533937732626, 21.53943276465977519, 92.50109039468567573 ) ) ;
#120966 = CARTESIAN_POINT ( 'NONE',  ( -16.52544592524335698, -4.483927247898792601, 48.95942372801902565 ) ) ;
#120967 = CARTESIAN_POINT ( 'NONE',  ( 4.483927247898790824, -16.52544592524335698, 25.20942372801901854 ) ) ;
#120968 = EDGE_CURVE ( 'NONE', #194969, #163715, #105680, .T. ) ;
#120970 = CARTESIAN_POINT ( 'NONE',  ( 10.81492255796106328, -18.62759615963255655, 95.41775706135234714 ) ) ;
#120969 = CARTESIAN_POINT ( 'NONE',  ( 8.224510206698953496, -14.34966873604960469, 97.91557627198103830 ) ) ;
#120971 = CARTESIAN_POINT ( 'NONE',  ( -4.379528057220328563, 16.55341960407611168, 40.20724293864769550 ) ) ;
#120972 = CARTESIAN_POINT ( 'NONE',  ( -0.05219959533909027116, -19.03943276465977164, 22.49890960531436690 ) ) ;
#120973 = CARTESIAN_POINT ( 'NONE',  ( 4.379528057220092307, 16.55341960407617563, 47.29275706135234003 ) ) ;
#120974 = CARTESIAN_POINT ( 'NONE',  ( -4.379528057220328563, 16.55341960407611168, 60.20724293864768839 ) ) ;
#120975 = CARTESIAN_POINT ( 'NONE',  ( -4.483927247898782831, 16.52544592524335698, 102.7094237280190185 ) ) ;
#120976 = CARTESIAN_POINT ( 'NONE',  ( -5.049401038298153566, 19.05341960407611168, 115.2072429386477097 ) ) ;
#120977 = CARTESIAN_POINT ( 'NONE',  ( -10.81492255796078084, -18.62759615963271287, 22.08224293864769194 ) ) ;
#120978 = CARTESIAN_POINT ( 'NONE',  ( 10.81492255796106328, -18.62759615963255655, 110.4177570613523756 ) ) ;
#120979 = CARTESIAN_POINT ( 'NONE',  ( 12.14591786802309770, 12.06949235617756955, 89.37390960531435269 ) ) ;
#120980 = CARTESIAN_POINT ( 'NONE',  ( 19.03943276465977164, -0.05219959533909143690, 93.74890960531435269 ) ) ;
#120981 = ORIENTED_EDGE ( 'NONE', *, *, #192276, .F. ) ;
#120982 = CARTESIAN_POINT ( 'NONE',  ( -14.29746914071037622, -8.314922557961029526, 44.16775706135234714 ) ) ;
#120983 = CARTESIAN_POINT ( 'NONE',  ( -13.89961937509977652, 13.97604488694528158, 40.62390960531435979 ) ) ;
#120984 = CARTESIAN_POINT ( 'NONE',  ( -0.05219959533909027116, -19.03943276465977164, 107.4989096053143527 ) ) ;
#120986 = DIRECTION ( 'NONE',  ( -1.000000000000000000, 0.000000000000000000, 0.000000000000000000 ) ) ;
#120985 = CARTESIAN_POINT ( 'NONE',  ( -8.224510206698735004, -14.34966873604973081, 44.58442372801901854 ) ) ;
#120987 = CARTESIAN_POINT ( 'NONE',  ( -16.51473224551082808, 9.474510206698731452, 53.33442372801900433 ) ) ;
#120988 = CARTESIAN_POINT ( 'NONE',  ( -0.05219959533909027116, -19.03943276465977164, 52.49890960531436690 ) ) ;
#120989 = CARTESIAN_POINT ( 'NONE',  ( 8.314922557961029526, -14.29746914071037800, 85.41775706135236135 ) ) ;
#120990 = CARTESIAN_POINT ( 'NONE',  ( 16.46253265017146816, 9.564922557961045513, 86.66775706135233293 ) ) ;
#120991 = CARTESIAN_POINT ( 'NONE',  ( 5.049401038297881783, 19.05341960407617563, 32.29275706135233293 ) ) ;
#120992 = CARTESIAN_POINT ( 'NONE',  ( -0.05219959533909027116, -19.03943276465977164, 62.49890960531435979 ) ) ;
#120993 = CARTESIAN_POINT ( 'NONE',  ( -8.224510206698948167, 14.34966873604960824, 105.4155762719810383 ) ) ;
#120994 = CARTESIAN_POINT ( 'NONE',  ( -19.05341960407617563, 5.049401038297882671, 68.54275706135230450 ) ) ;
#120995 = CARTESIAN_POINT ( 'NONE',  ( 15.72974639402199770, -15.80617190586745480, 63.12390960531435979 ) ) ;
#120996 = CARTESIAN_POINT ( 'NONE',  ( -19.02544592524334988, -5.153800228976617603, 23.95942372801900078 ) ) ;
#120997 = CARTESIAN_POINT ( 'NONE',  ( 9.474510206698971260, -16.51473224551069308, 97.91557627198102409 ) ) ;
#120998 = AXIS2_PLACEMENT_3D ( 'NONE', #140110, #153301, #155296 ) ;
#120999 = CARTESIAN_POINT ( 'NONE',  ( -21.53943276465977519, 0.05219959533907696930, 81.24890960531436690 ) ) ;
#121000 = CARTESIAN_POINT ( 'NONE',  ( -16.36317988757058828, 7.306389748694927633, 84.09789608363227842 ) ) ;
#121001 = CARTESIAN_POINT ( 'NONE',  ( 19.02544592524334988, 5.153800228976608722, 106.4594237280190185 ) ) ;
#121002 = CARTESIAN_POINT ( 'NONE',  ( -19.01533133064925707, 5.499999999999454658, 58.76586590595741910 ) ) ;
#121003 = CARTESIAN_POINT ( 'NONE',  ( 14.29746914071037800, 8.314922557961029526, 31.66775706135234358 ) ) ;
#121004 = CARTESIAN_POINT ( 'NONE',  ( 9.564922557960805705, 16.46253265017160317, 34.58224293864770260 ) ) ;
#121005 = CARTESIAN_POINT ( 'NONE',  ( 16.46253265017160672, -9.564922557960803928, 113.3322429386476955 ) ) ;
#121006 = CARTESIAN_POINT ( 'NONE',  ( -21.52544592524343514, 5.823673210054127303, 91.04057627198103830 ) ) ;
#121007 = CARTESIAN_POINT ( 'NONE',  ( -18.62759615963255300, -10.81492255796106328, 54.16775706135235424 ) ) ;
#121009 = CARTESIAN_POINT ( 'NONE',  ( 18.62759615963255655, 10.81492255796105972, 106.6677570613523756 ) ) ;
#121008 = CARTESIAN_POINT ( 'NONE',  ( -13.89961937509957401, -13.97604488694547875, 104.3760903946856757 ) ) ;
#121010 = CARTESIAN_POINT ( 'NONE',  ( -16.55341960407617563, 4.379528057220093196, 108.5427570613523756 ) ) ;
#121011 = CARTESIAN_POINT ( 'NONE',  ( 18.62759615963271287, -10.81492255796078972, 98.33224293864769550 ) ) ;
#121012 = CARTESIAN_POINT ( 'NONE',  ( 8.314922557960818139, 14.29746914071049879, 44.58224293864769550 ) ) ;
#121013 = CARTESIAN_POINT ( 'NONE',  ( 19.02544592524334988, 5.153800228976608722, 86.45942372801900433 ) ) ;
#121014 = CARTESIAN_POINT ( 'NONE',  ( 13.89961937509957401, 13.97604488694547697, 51.87609039468566863 ) ) ;
#121015 = CARTESIAN_POINT ( 'NONE',  ( -15.72974639402176322, -15.80617190586768395, 64.37609039468568994 ) ) ;
#121016 = CARTESIAN_POINT ( 'NONE',  ( -13.89961937509957401, -13.97604488694547875, 44.37609039468566863 ) ) ;
#121017 = CARTESIAN_POINT ( 'NONE',  ( 0.05219959533910956823, 16.53943276465976808, 99.99890960531436690 ) ) ;
#121018 = CARTESIAN_POINT ( 'NONE',  ( -15.80617190586745835, -15.72974639402198527, 36.87390960531435979 ) ) ;
#121019 = CARTESIAN_POINT ( 'NONE',  ( -4.379528057220328563, 16.55341960407611168, 35.20724293864768839 ) ) ;
#121020 = VECTOR ( 'NONE', #158030, 1000.000000000000000 ) ;
#121021 = CARTESIAN_POINT ( 'NONE',  ( -21.53943276465977519, -0.05219959533937600094, 103.7510903946857042 ) ) ;
#121022 = CARTESIAN_POINT ( 'NONE',  ( 12.14591786802327356, -12.06949235617739191, 75.62609039468567573 ) ) ;
#121023 = CARTESIAN_POINT ( 'NONE',  ( -12.14591786802309592, -12.06949235617757132, 21.87390960531436690 ) ) ;
#121024 = CARTESIAN_POINT ( 'NONE',  ( -21.55341960407619339, 5.719274019375674811, 63.54275706135234003 ) ) ;
#121025 = CARTESIAN_POINT ( 'NONE',  ( 21.55341960407619695, -5.719274019375665929, 61.04275706135234714 ) ) ;
#121026 = CARTESIAN_POINT ( 'NONE',  ( 21.53943276465977519, -0.05219959533907433946, 73.74890960531433848 ) ) ;
#121027 = EDGE_LOOP ( 'NONE', ( #165708, #68677, #126745 ) ) ;
#121028 = CARTESIAN_POINT ( 'NONE',  ( 17.58332526062529411, -7.635886036038503910, 63.42334959558468199 ) ) ;
#121029 = CARTESIAN_POINT ( 'NONE',  ( -5.823673210054431948, 21.52544592524334988, 47.70942372801902565 ) ) ;
#121030 = CARTESIAN_POINT ( 'NONE',  ( -19.03943276465977164, 0.05219959533909376836, 26.24890960531435624 ) ) ;
#121031 = CARTESIAN_POINT ( 'NONE',  ( 9.474510206698971260, -16.51473224551069308, 37.91557627198102409 ) ) ;
#121032 = CARTESIAN_POINT ( 'NONE',  ( -14.29746914071049879, 8.314922557960819915, 75.83224293864769550 ) ) ;
#121033 = CARTESIAN_POINT ( 'NONE',  ( 0.05219959533909260263, 19.03943276465977164, 84.99890960531436690 ) ) ;
#121034 = CARTESIAN_POINT ( 'NONE',  ( -0.05219959533910754901, -16.53943276465976808, 32.49890960531435979 ) ) ;
#121035 = CARTESIAN_POINT ( 'NONE',  ( -16.55341960407611168, -4.379528057220339221, 101.4572429386476955 ) ) ;
#121036 = CARTESIAN_POINT ( 'NONE',  ( -5.823673210054116645, -21.52544592524344225, 67.29057627198103830 ) ) ;
#121037 = CIRCLE ( 'NONE', #30692, 2.041999999999999815 ) ;
#121038 = CARTESIAN_POINT ( 'NONE',  ( 0.05219959533907565091, 21.53943276465977519, 99.99890960531436690 ) ) ;
#121040 = EDGE_CURVE ( 'NONE', #83313, #54292, #58137, .T. ) ;
#121039 = CARTESIAN_POINT ( 'NONE',  ( -5.049401038298153566, 19.05341960407611168, 115.2072429386477097 ) ) ;
#121041 = EDGE_CURVE ( 'NONE', #117112, #200018, #11713, .T. ) ;
#121043 = CARTESIAN_POINT ( 'NONE',  ( 0.05219959533936267826, -19.03943276465977164, 100.0010903946856757 ) ) ;
#121042 = CARTESIAN_POINT ( 'NONE',  ( 16.51473224551069308, 9.474510206698969483, 64.16557627198102409 ) ) ;
#121044 = CARTESIAN_POINT ( 'NONE',  ( 15.80617190586746368, 15.72974639402197994, 59.37390960531436690 ) ) ;
#121045 = CARTESIAN_POINT ( 'NONE',  ( 10.72451020669871369, 18.67979575497193778, 82.08442372801901854 ) ) ;
#121046 = CARTESIAN_POINT ( 'NONE',  ( -19.03943276465977164, 0.05219959533909376836, 61.24890960531436690 ) ) ;
#121047 = B_SPLINE_CURVE_WITH_KNOTS ( 'NONE', 3,
 ( #109345, #171027, #32518, #94170, #155849, #79002, #187216 ),
 .UNSPECIFIED., .F., .F.,
 ( 4, 3, 4 ),
 ( 0.006882574723720362095, 0.01376514944744072419, 0.01380547055123299352 ),
 .UNSPECIFIED. ) ;
#121048 = CARTESIAN_POINT ( 'NONE',  ( 19.05341960407611168, 5.049401038298154454, 98.95724293864766707 ) ) ;
#121049 = CARTESIAN_POINT ( 'NONE',  ( -16.55341960407617563, 4.379528057220093196, 83.54275706135234714 ) ) ;
#121050 = CARTESIAN_POINT ( 'NONE',  ( 21.53943276465977519, 0.05219959533937863772, 56.25109039468568284 ) ) ;
#121051 = CARTESIAN_POINT ( 'NONE',  ( 10.72451020669871369, 18.67979575497193778, 97.08442372801904696 ) ) ;
#121052 = CARTESIAN_POINT ( 'NONE',  ( 15.72974639402199770, -15.80617190586745480, 113.1239096053143953 ) ) ;
#121053 = AXIS2_PLACEMENT_3D ( 'NONE', #92387, #15568, #47899 ) ;
#121054 = CARTESIAN_POINT ( 'NONE',  ( 15.72974639402199770, -15.80617190586745480, 73.12390960531436690 ) ) ;
#121055 = CARTESIAN_POINT ( 'NONE',  ( 5.153800228976615827, -19.02544592524334988, 45.20942372801901143 ) ) ;
#121056 = CARTESIAN_POINT ( 'NONE',  ( 10.81492255796078972, 18.62759615963270932, 39.58224293864769550 ) ) ;
#121057 = AXIS2_PLACEMENT_3D ( 'NONE', #176305, #69110, #20606 ) ;
#121059 = CARTESIAN_POINT ( 'NONE',  ( 4.379528057220339221, -16.55341960407611168, 32.70724293864770260 ) ) ;
#121058 = CARTESIAN_POINT ( 'NONE',  ( -16.51473224551069308, -9.474510206698971260, 76.66557627198103830 ) ) ;
#121060 = DIRECTION ( 'NONE',  ( 0.000000000000000000, 0.000000000000000000, -1.000000000000000000 ) ) ;
#121061 = CARTESIAN_POINT ( 'NONE',  ( -19.25918095147780562, -5.499999999999485745, 79.45284276293931214 ) ) ;
#121062 = CARTESIAN_POINT ( 'NONE',  ( 5.049401038297881783, 19.05341960407617563, 92.29275706135234714 ) ) ;
#121063 = CARTESIAN_POINT ( 'NONE',  ( 18.62759615963271287, -10.81492255796078972, 78.33224293864770971 ) ) ;
#121064 = CARTESIAN_POINT ( 'NONE',  ( 16.52544592524342804, -4.483927247898539470, 58.54057627198103120 ) ) ;
#121065 = CARTESIAN_POINT ( 'NONE',  ( 4.379528057220092307, 16.55341960407617563, 32.29275706135235424 ) ) ;
#121066 = CARTESIAN_POINT ( 'NONE',  ( 13.97604488694527802, 13.89961937509977652, 44.37390960531435269 ) ) ;
#121068 = CARTESIAN_POINT ( 'NONE',  ( -19.02544592524334988, -5.153800228976617603, 83.95942372801901854 ) ) ;
#121067 = CARTESIAN_POINT ( 'NONE',  ( 5.719274019375991003, -21.55341960407610458, 107.7072429386476955 ) ) ;
#121069 = CARTESIAN_POINT ( 'NONE',  ( -16.51473224551069308, -9.474510206698971260, 81.66557627198103830 ) ) ;
#121070 = CARTESIAN_POINT ( 'NONE',  ( -12.06949235617756955, 12.14591786802309770, 90.62390960531436690 ) ) ;
#121071 = CARTESIAN_POINT ( 'NONE',  ( -19.05341960407611168, -5.049401038298163336, 76.45724293864769550 ) ) ;
#121072 = CARTESIAN_POINT ( 'NONE',  ( -14.34966873604960291, -8.224510206698953496, 61.66557627198103120 ) ) ;
#121073 = CARTESIAN_POINT ( 'NONE',  ( -16.51473224551069308, -9.474510206698971260, 26.66557627198103120 ) ) ;
#121074 = CARTESIAN_POINT ( 'NONE',  ( -17.22444507756011234, -5.345458043314972763, 20.98594102011676554 ) ) ;
#121075 = CARTESIAN_POINT ( 'NONE',  ( -14.34966873604960291, -8.224510206698953496, 51.66557627198102409 ) ) ;
#121076 = CARTESIAN_POINT ( 'NONE',  ( 19.02544592524343514, -5.153800228976328945, 88.54057627198102409 ) ) ;
#121077 = CARTESIAN_POINT ( 'NONE',  ( -17.49999999999999645, 5.499999999999997335, 120.0000000000000142 ) ) ;
#121078 = CARTESIAN_POINT ( 'NONE',  ( 19.02544592524334988, 5.153800228976608722, 56.45942372801898301 ) ) ;
#121079 = CARTESIAN_POINT ( 'NONE',  ( -8.224510206698735004, -14.34966873604973081, 64.58442372801900433 ) ) ;
#121080 = CARTESIAN_POINT ( 'NONE',  ( -21.53943276465977519, 0.05219959533907696930, 76.24890960531435269 ) ) ;
#121081 = CARTESIAN_POINT ( 'NONE',  ( 16.51473224551083163, -9.474510206698727899, 40.83442372801900433 ) ) ;
#121082 = CARTESIAN_POINT ( 'NONE',  ( -13.97604488694527625, -13.89961937509977652, 81.87390960531436690 ) ) ;
#121083 = CARTESIAN_POINT ( 'NONE',  ( -17.60691670004652920, -5.499999999999996447, 74.13333313366439370 ) ) ;
#121084 = CARTESIAN_POINT ( 'NONE',  ( -15.72974639402197994, 15.80617190586746368, 30.62390960531436335 ) ) ;
#121085 = CIRCLE ( 'NONE', #153416, 2.649999999999999911 ) ;
#121086 = CARTESIAN_POINT ( 'NONE',  ( -13.89961937509977652, 13.97604488694528158, 70.62390960531432427 ) ) ;
#121087 = CARTESIAN_POINT ( 'NONE',  ( -21.53943276465977519, -0.05219959533937600094, 53.75109039468568994 ) ) ;
#121088 = CARTESIAN_POINT ( 'NONE',  ( -19.03943276465977164, 0.05219959533909376836, 21.24890960531436335 ) ) ;
#121091 = VERTEX_POINT ( 'NONE', #196728 ) ;
#121090 = CARTESIAN_POINT ( 'NONE',  ( -16.46253265017160317, 9.564922557960807481, 90.83224293864769550 ) ) ;
#121089 = CARTESIAN_POINT ( 'NONE',  ( 0.05219959533907565091, 21.53943276465977519, 109.9989096053143527 ) ) ;
#121092 = CARTESIAN_POINT ( 'NONE',  ( 18.67979575497194134, -10.72451020669871369, 35.83442372801901143 ) ) ;
#121093 = VERTEX_POINT ( 'NONE', #60163 ) ;
#121094 = CARTESIAN_POINT ( 'NONE',  ( 19.05341960407611168, 5.049401038298154454, 98.95724293864766707 ) ) ;
#121095 = CARTESIAN_POINT ( 'NONE',  ( 1.040834085586084257E-14, -30.40000000000003766, -64.92279855667830191 ) ) ;
#121096 = CARTESIAN_POINT ( 'NONE',  ( 15.80617190586746368, 15.72974639402197994, 104.3739096053143669 ) ) ;
#121097 = CARTESIAN_POINT ( 'NONE',  ( -16.51473224551069308, -9.474510206698971260, 46.66557627198102409 ) ) ;
#121098 = CARTESIAN_POINT ( 'NONE',  ( -4.483927247898782831, 16.52544592524335698, 27.70942372801901854 ) ) ;
#121099 = CARTESIAN_POINT ( 'NONE',  ( -5.950531402560715689E-15, 38.81732327939063509, -5.624999997268812280 ) ) ;
#121100 = CARTESIAN_POINT ( 'NONE',  ( 15.80617190586769283, -15.72974639402175789, 100.6260903946857184 ) ) ;
#121101 = CARTESIAN_POINT ( 'NONE',  ( 19.02544592524343514, -5.153800228976328945, 33.54057627198102409 ) ) ;
#121102 = CARTESIAN_POINT ( 'NONE',  ( 10.81492255796106328, -18.62759615963255655, 105.4177570613523613 ) ) ;
#121104 = CARTESIAN_POINT ( 'NONE',  ( -21.55341960407619339, 5.719274019375674811, 63.54275706135234003 ) ) ;
#121103 = CARTESIAN_POINT ( 'NONE',  ( 9.564922557960805705, 16.46253265017160317, 84.58224293864769550 ) ) ;
#121105 = CARTESIAN_POINT ( 'NONE',  ( -27.73933785331498925, 9.013057229001089965, 141.2750000027311614 ) ) ;
#121106 = CARTESIAN_POINT ( 'NONE',  ( 5.153800228976335163, 19.02544592524342804, 99.79057627198102409 ) ) ;
#121107 = CARTESIAN_POINT ( 'NONE',  ( 17.60691670004650788, 5.500000000000060396, 46.63333313366440791 ) ) ;
#121110 = CARTESIAN_POINT ( 'NONE',  ( 18.62759615963255655, 10.81492255796105972, 51.66775706135234714 ) ) ;
#121109 = CARTESIAN_POINT ( 'NONE',  ( 8.224510206698742110, 14.34966873604972548, 62.08442372801901143 ) ) ;
#121108 = CARTESIAN_POINT ( 'NONE',  ( 14.34966873604972726, -8.224510206698740333, 55.83442372801901854 ) ) ;
#121111 = CARTESIAN_POINT ( 'NONE',  ( 18.67979575497194134, -10.72451020669871369, 95.83442372801903275 ) ) ;
#121112 = CARTESIAN_POINT ( 'NONE',  ( 4.500000000000000888, -120.9970989573719038, 14.58956564881029827 ) ) ;
#121113 = CARTESIAN_POINT ( 'NONE',  ( -16.55341960407617563, 4.379528057220093196, 28.54275706135234358 ) ) ;
#121114 = CARTESIAN_POINT ( 'NONE',  ( 19.05341960407611168, 5.049401038298154454, 78.95724293864769550 ) ) ;
#121115 = CARTESIAN_POINT ( 'NONE',  ( 19.05341960407611168, 5.049401038298154454, 93.95724293864769550 ) ) ;
#121116 = CARTESIAN_POINT ( 'NONE',  ( -19.03943276465977164, 0.05219959533909376836, 111.2489096053143669 ) ) ;
#121117 = CARTESIAN_POINT ( 'NONE',  ( -16.46253265017160317, 9.564922557960807481, 30.83224293864769550 ) ) ;
#121118 = CARTESIAN_POINT ( 'NONE',  ( -10.72451020669898014, 18.67979575497178502, 30.41557627198101699 ) ) ;
#121119 = CARTESIAN_POINT ( 'NONE',  ( 14.29746914071037800, 8.314922557961029526, 86.66775706135234714 ) ) ;
#121121 = CARTESIAN_POINT ( 'NONE',  ( -5.049401038298153566, 19.05341960407611168, 70.20724293864769550 ) ) ;
#121120 = CARTESIAN_POINT ( 'NONE',  ( -12.14591786802309592, -12.06949235617757132, 66.87390960531436690 ) ) ;
#121122 = CARTESIAN_POINT ( 'NONE',  ( -21.52544592524334988, -5.823673210054445271, 93.95942372801903275 ) ) ;
#121123 = CARTESIAN_POINT ( 'NONE',  ( -27.73933785331498925, 2.428612866367529932E-14, 148.8750000027311842 ) ) ;
#121124 = CARTESIAN_POINT ( 'NONE',  ( 0.05219959533934541429, -16.53943276465976808, 25.00109039468567218 ) ) ;
#121125 = CARTESIAN_POINT ( 'NONE',  ( -16.53943276465976808, 0.05219959533911058130, 76.24890960531435269 ) ) ;
#121126 = CARTESIAN_POINT ( 'NONE',  ( -15.80617190586768217, 15.72974639402176855, 28.12609039468568284 ) ) ;
#121127 = CARTESIAN_POINT ( 'NONE',  ( 5.719274019375991003, -21.55341960407610458, 72.70724293864769550 ) ) ;
#121129 = CARTESIAN_POINT ( 'NONE',  ( -5.153800228976607833, 19.02544592524334988, 32.70942372801899722 ) ) ;
#121128 = AXIS2_PLACEMENT_3D ( 'NONE', #84994, #39504, #22348 ) ;
#121130 = CARTESIAN_POINT ( 'NONE',  ( 8.906447517083050158, 27.41122689804195645, 147.6500000054623740 ) ) ;
#121131 = CARTESIAN_POINT ( 'NONE',  ( -19.02544592524342804, 5.153800228976336051, 81.04057627198103830 ) ) ;
#121132 = CARTESIAN_POINT ( 'NONE',  ( 16.52544592524342804, -4.483927247898539470, 43.54057627198103830 ) ) ;
#121133 = CARTESIAN_POINT ( 'NONE',  ( 4.483927247898545687, 16.52544592524342804, 39.79057627198103830 ) ) ;
#121134 = CARTESIAN_POINT ( 'NONE',  ( 12.14591786802327356, -12.06949235617739191, 110.6260903946857042 ) ) ;
#121135 = CARTESIAN_POINT ( 'NONE',  ( 16.46253265017146816, 9.564922557961045513, 61.66775706135234003 ) ) ;
#121136 = CARTESIAN_POINT ( 'NONE',  ( 19.20446147854530139, 5.499999999999909406, 51.88999695167680670 ) ) ;
#121137 = CARTESIAN_POINT ( 'NONE',  ( -9.474510206698964154, 16.51473224551069663, 100.4155762719810241 ) ) ;
#121138 = CARTESIAN_POINT ( 'NONE',  ( 4.379528057220339221, -16.55341960407611168, 77.70724293864770971 ) ) ;
#121139 = CARTESIAN_POINT ( 'NONE',  ( 24.13306144861383729, 5.795830589372933161, 190.0000000000000000 ) ) ;
#121141 = CARTESIAN_POINT ( 'NONE',  ( -10.81492255796078084, -18.62759615963271287, 32.08224293864769550 ) ) ;
#121140 = CARTESIAN_POINT ( 'NONE',  ( -16.51473224551069308, -9.474510206698971260, 26.66557627198103120 ) ) ;
#121142 = CARTESIAN_POINT ( 'NONE',  ( -21.55341960407610458, -5.719274019375992779, 71.45724293864769550 ) ) ;
#121143 = CARTESIAN_POINT ( 'NONE',  ( -4.483927247898539470, -16.52544592524342804, 112.2905762719810241 ) ) ;
#121145 = CARTESIAN_POINT ( 'NONE',  ( -19.03943276465977164, 0.05219959533909376836, 51.24890960531436690 ) ) ;
#121144 = CARTESIAN_POINT ( 'NONE',  ( 14.34966873604972726, -8.224510206698740333, 60.83442372801901854 ) ) ;
#121146 = AXIS2_PLACEMENT_3D ( 'NONE', #118234, #70728, #149561 ) ;
#121147 = CARTESIAN_POINT ( 'NONE',  ( 10.81492255796106328, -18.62759615963255655, 60.41775706135235424 ) ) ;
#121148 = CARTESIAN_POINT ( 'NONE',  ( 16.53943276465976808, -0.05219959533910856209, 93.74890960531436690 ) ) ;
#121149 = CARTESIAN_POINT ( 'NONE',  ( 16.36317988757058828, -7.306389748694915198, 36.59789608363225710 ) ) ;
#121150 = CARTESIAN_POINT ( 'NONE',  ( 22.81625015709509441, 31.40387420917330275, -9.824999997268811569 ) ) ;
#121151 = CARTESIAN_POINT ( 'NONE',  ( 10.72451020669898902, -18.67979575497178502, 32.91557627198102409 ) ) ;
#121152 = DIRECTION ( 'NONE',  ( 1.000000000000000000, 0.000000000000000000, 0.000000000000000000 ) ) ;
#121154 = CARTESIAN_POINT ( 'NONE',  ( -17.60769864724391098, 5.499999999999987566, 43.65024842019164453 ) ) ;
#121153 = CARTESIAN_POINT ( 'NONE',  ( -21.52544592524334988, -5.823673210054445271, 63.95942372801901854 ) ) ;
#121156 = CARTESIAN_POINT ( 'NONE',  ( -4.483927247898539470, -16.52544592524342804, 47.29057627198103120 ) ) ;
#121155 = CARTESIAN_POINT ( 'NONE',  ( 12.14591786802327356, -12.06949235617739191, 60.62609039468567573 ) ) ;
#121157 = CARTESIAN_POINT ( 'NONE',  ( 15.80617190586746368, 15.72974639402197994, 69.37390960531436690 ) ) ;
#121158 = CARTESIAN_POINT ( 'NONE',  ( -10.81492255796078084, -18.62759615963271287, 57.08224293864769550 ) ) ;
#121159 = CARTESIAN_POINT ( 'NONE',  ( -21.96410559793011785, -8.829621495424600397, 171.4826196141302717 ) ) ;
#121161 = CARTESIAN_POINT ( 'NONE',  ( 16.46253265017160672, -9.564922557960803928, 103.3322429386476955 ) ) ;
#121160 = CARTESIAN_POINT ( 'NONE',  ( 5.049401038297881783, 19.05341960407617563, 82.29275706135229029 ) ) ;
#121162 = ADVANCED_FACE ( 'NONE', ( #91475 ), #58196, .F. ) ;
#121163 = CARTESIAN_POINT ( 'NONE',  ( -9.474510206698964154, 16.51473224551069663, 45.41557627198103120 ) ) ;
#121164 = CARTESIAN_POINT ( 'NONE',  ( -12.14591786802309592, -12.06949235617757132, 111.8739096053143669 ) ) ;
#121165 = CARTESIAN_POINT ( 'NONE',  ( 19.05341960407611168, 5.049401038298154454, 108.9572429386477097 ) ) ;
#121166 = ORIENTED_EDGE ( 'NONE', *, *, #171652, .T. ) ;
#121167 = CARTESIAN_POINT ( 'NONE',  ( -14.34966873604972548, 8.224510206698743886, 63.33442372801900433 ) ) ;
#121168 = CARTESIAN_POINT ( 'NONE',  ( 18.67979575497178502, 10.72451020669898547, 104.1655762719810241 ) ) ;
#121169 = CARTESIAN_POINT ( 'NONE',  ( 19.05341960407611168, 5.049401038298154454, 58.95724293864768129 ) ) ;
#121170 = CARTESIAN_POINT ( 'NONE',  ( -5.823673210054431948, 21.52544592524334988, 47.70942372801902565 ) ) ;
#121171 = CARTESIAN_POINT ( 'NONE',  ( 5.049401038298161559, -19.05341960407611168, 92.70724293864769550 ) ) ;
#121172 = CARTESIAN_POINT ( 'NONE',  ( -27.19415581439709939, -28.92630772671082084, -20.12198987529475147 ) ) ;
#121173 = ORIENTED_EDGE ( 'NONE', *, *, #104106, .F. ) ;
#121174 = CARTESIAN_POINT ( 'NONE',  ( 5.719274019375673035, 21.55341960407619339, 37.29275706135235424 ) ) ;
#121176 = CARTESIAN_POINT ( 'NONE',  ( -13.89961937509957401, -13.97604488694547875, 84.37609039468567573 ) ) ;
#121175 = CARTESIAN_POINT ( 'NONE',  ( 5.049401038298161559, -19.05341960407611168, 102.7072429386476955 ) ) ;
#121177 = CARTESIAN_POINT ( 'NONE',  ( -0.05219959533936034679, 19.03943276465977164, 37.50109039468567573 ) ) ;
#121178 = CARTESIAN_POINT ( 'NONE',  ( 18.67979575497178502, 10.72451020669898547, 94.16557627198103830 ) ) ;
#121179 = CARTESIAN_POINT ( 'NONE',  ( -13.89961937509957401, -13.97604488694547875, 29.37609039468565797 ) ) ;
#121180 = CARTESIAN_POINT ( 'NONE',  ( -0.05219959533936034679, 19.03943276465977164, 37.50109039468567573 ) ) ;
#121181 = CARTESIAN_POINT ( 'NONE',  ( 16.52544592524335698, 4.483927247898782831, 86.45942372801901854 ) ) ;
#121182 = CARTESIAN_POINT ( 'NONE',  ( 5.153800228976335163, 19.02544592524342804, 114.7905762719810241 ) ) ;
#121183 = CARTESIAN_POINT ( 'NONE',  ( -19.02544592524342804, 5.153800228976336051, 66.04057627198103830 ) ) ;
#121184 = CIRCLE ( 'NONE', #147028, 4.999999999999998224 ) ;
#121185 = CARTESIAN_POINT ( 'NONE',  ( -21.55341960407619339, 5.719274019375674811, 63.54275706135234003 ) ) ;
#121186 = CARTESIAN_POINT ( 'NONE',  ( -15.72974639402176322, -15.80617190586768395, 74.37609039468568994 ) ) ;
#121187 = CARTESIAN_POINT ( 'NONE',  ( 38.00000000000000000, -12.34694845685040754, -10.84999999453762598 ) ) ;
#121188 = CARTESIAN_POINT ( 'NONE',  ( 5.153800228976335163, 19.02544592524342804, 89.79057627198102409 ) ) ;
#121189 = CARTESIAN_POINT ( 'NONE',  ( 18.62759615963255655, 10.81492255796105972, 66.66775706135234714 ) ) ;
#121190 = CARTESIAN_POINT ( 'NONE',  ( -13.89961937509957401, -13.97604488694547875, 104.3760903946856757 ) ) ;
#121191 = CARTESIAN_POINT ( 'NONE',  ( -16.46253265017160317, 9.564922557960807481, 70.83224293864770971 ) ) ;
#121192 = CARTESIAN_POINT ( 'NONE',  ( 16.46253265017160672, -9.564922557960803928, 113.3322429386476955 ) ) ;
#121193 = CARTESIAN_POINT ( 'NONE',  ( 13.89961937509977652, -13.97604488694527269, 83.12390960531436690 ) ) ;
#121194 = LINE ( 'NONE', #182887, #191950 ) ;
#121195 = CARTESIAN_POINT ( 'NONE',  ( 9.564922557960805705, 16.46253265017160317, 69.58224293864770971 ) ) ;
#121196 = CARTESIAN_POINT ( 'NONE',  ( -9.564922557960796823, -16.46253265017161027, 57.08224293864769550 ) ) ;
#121197 = CARTESIAN_POINT ( 'NONE',  ( 5.823673210054125526, 21.52544592524343514, 94.79057627198105251 ) ) ;
#121198 = CARTESIAN_POINT ( 'NONE',  ( 16.52544592524335698, 4.483927247898782831, 81.45942372801900433 ) ) ;
#121199 = CARTESIAN_POINT ( 'NONE',  ( -6.856101608890825108E-16, -71.74905178543389184, -12.99263613531267936 ) ) ;
#121200 = CARTESIAN_POINT ( 'NONE',  ( -19.05341960407617563, 5.049401038297882671, 43.54275706135232582 ) ) ;
#121201 = CARTESIAN_POINT ( 'NONE',  ( -16.46253265017160317, 9.564922557960807481, 75.83224293864769550 ) ) ;
#121202 = CARTESIAN_POINT ( 'NONE',  ( 12.14591786802309770, 12.06949235617756955, 74.37390960531436690 ) ) ;
#121204 = B_SPLINE_CURVE_WITH_KNOTS ( 'NONE', 3,
 ( #113043, #33240, #188923, #35217, #95891, #96870 ),
 .UNSPECIFIED., .F., .F.,
 ( 4, 2, 4 ),
 ( 0.007228050697041513671, 0.007608510107495006572, 0.007988969517948500340 ),
 .UNSPECIFIED. ) ;
#121203 = CARTESIAN_POINT ( 'NONE',  ( 16.55341960407611168, 4.379528057220329451, 113.9572429386477239 ) ) ;
#121205 = CARTESIAN_POINT ( 'NONE',  ( 19.02544592524343514, -5.153800228976328945, 108.5405762719810383 ) ) ;
#121206 = CARTESIAN_POINT ( 'NONE',  ( 9.564922557960805705, 16.46253265017160317, 109.5822429386476955 ) ) ;
#121207 = CARTESIAN_POINT ( 'NONE',  ( 4.379528057220339221, -16.55341960407611168, 77.70724293864770971 ) ) ;
#121208 = CARTESIAN_POINT ( 'NONE',  ( 18.22780087662123805, -5.499999999999976019, 83.51763182126896368 ) ) ;
#121209 = CARTESIAN_POINT ( 'NONE',  ( 5.049401038297881783, 19.05341960407617563, 32.29275706135233293 ) ) ;
#121210 = CARTESIAN_POINT ( 'NONE',  ( -16.53943276465976808, -0.05219959533934237506, 98.75109039468568994 ) ) ;
#121212 = EDGE_CURVE ( 'NONE', #15707, #144387, #198697, .T. ) ;
#121211 = CARTESIAN_POINT ( 'NONE',  ( -5.153800228976328057, -19.02544592524343514, 77.29057627198099567 ) ) ;
#121213 = CARTESIAN_POINT ( 'NONE',  ( 5.823673210054444382, -21.52544592524334988, 50.20942372801901854 ) ) ;
#121214 = CARTESIAN_POINT ( 'NONE',  ( 10.72451020669898902, -18.67979575497178502, 42.91557627198103120 ) ) ;
#121215 = CARTESIAN_POINT ( 'NONE',  ( -15.80617190586768217, 15.72974639402176855, 23.12609039468567573 ) ) ;
#121216 = CARTESIAN_POINT ( 'NONE',  ( 18.67979575497178502, 10.72451020669898547, 69.16557627198102409 ) ) ;
#121217 = CARTESIAN_POINT ( 'NONE',  ( -4.483927247898539470, -16.52544592524342804, 97.29057627198105251 ) ) ;
#121218 = CARTESIAN_POINT ( 'NONE',  ( 16.46253265017146816, 9.564922557961045513, 51.66775706135233293 ) ) ;
#121219 = CARTESIAN_POINT ( 'NONE',  ( -16.51473224551069308, -9.474510206698971260, 31.66557627198102054 ) ) ;
#121220 = CARTESIAN_POINT ( 'NONE',  ( 9.564922557960805705, 16.46253265017160317, 89.58224293864769550 ) ) ;
#121221 = CARTESIAN_POINT ( 'NONE',  ( -16.46253265017160317, 9.564922557960807481, 75.83224293864769550 ) ) ;
#121222 = CARTESIAN_POINT ( 'NONE',  ( -12.06949235617756955, 12.14591786802309770, 95.62390960531436690 ) ) ;
#121223 = ORIENTED_EDGE ( 'NONE', *, *, #59834, .T. ) ;
#121224 = CARTESIAN_POINT ( 'NONE',  ( 16.53943276465976808, -0.05219959533910856209, 23.74890960531435269 ) ) ;
#121225 = CARTESIAN_POINT ( 'NONE',  ( 14.34966873604972726, -8.224510206698740333, 25.83442372801901499 ) ) ;
#121226 = CARTESIAN_POINT ( 'NONE',  ( -15.72974639402176322, -15.80617190586768395, 94.37609039468568994 ) ) ;
#121227 = CARTESIAN_POINT ( 'NONE',  ( 5.153800228976335163, 19.02544592524342804, 99.79057627198102409 ) ) ;
#121228 = CARTESIAN_POINT ( 'NONE',  ( -21.52544592524343514, 5.823673210054127303, 116.0405762719810383 ) ) ;
#121229 = CARTESIAN_POINT ( 'NONE',  ( 9.564922557960805705, 16.46253265017160317, 44.58224293864769550 ) ) ;
#121230 = CARTESIAN_POINT ( 'NONE',  ( -4.483927247898782831, 16.52544592524335698, 42.70942372801901854 ) ) ;
#121231 = CARTESIAN_POINT ( 'NONE',  ( 5.049401038297881783, 19.05341960407617563, 107.2927570613523187 ) ) ;
#121232 = CARTESIAN_POINT ( 'NONE',  ( 19.05341960407611168, 5.049401038298154454, 33.95724293864769550 ) ) ;
#121233 = CARTESIAN_POINT ( 'NONE',  ( -12.14591786802309592, -12.06949235617757132, 96.87390960531436690 ) ) ;
#121234 = CARTESIAN_POINT ( 'NONE',  ( -15.80617190586745835, -15.72974639402198527, 101.8739096053143811 ) ) ;
#121235 = CARTESIAN_POINT ( 'NONE',  ( -19.02544592524334988, -5.153800228976617603, 68.95942372801896170 ) ) ;
#121236 = CARTESIAN_POINT ( 'NONE',  ( -0.05219959533907301413, -21.53943276465977519, 112.4989096053143669 ) ) ;
#121237 = CARTESIAN_POINT ( 'NONE',  ( 26.58496454516999563, 7.626754437231445749, 167.9682100371138915 ) ) ;
#121238 = CARTESIAN_POINT ( 'NONE',  ( -5.049401038298153566, 19.05341960407611168, 95.20724293864770971 ) ) ;
#121239 = CARTESIAN_POINT ( 'NONE',  ( 16.19135201231366494, -7.376712067591912003, 112.3131914594796825 ) ) ;
#121240 = CARTESIAN_POINT ( 'NONE',  ( -19.05341960407611168, -5.049401038298163336, 91.45724293864766707 ) ) ;
#121242 = CARTESIAN_POINT ( 'NONE',  ( 16.52544592524342804, -4.483927247898539470, 83.54057627198102409 ) ) ;
#121241 = CARTESIAN_POINT ( 'NONE',  ( 5.719274019375673035, 21.55341960407619339, 32.29275706135235424 ) ) ;
#121243 = CARTESIAN_POINT ( 'NONE',  ( 9.474510206698971260, -16.51473224551069308, 77.91557627198103830 ) ) ;
#121244 = CARTESIAN_POINT ( 'NONE',  ( -5.049401038297874678, -19.05341960407617918, 24.79275706135233648 ) ) ;
#121246 = CARTESIAN_POINT ( 'NONE',  ( 19.05341960407617918, -5.049401038297876454, 61.04275706135232582 ) ) ;
#121245 = CARTESIAN_POINT ( 'NONE',  ( -8.224510206698735004, -14.34966873604973081, 44.58442372801901854 ) ) ;
#121247 = CARTESIAN_POINT ( 'NONE',  ( -18.67979575497193778, 10.72451020669871902, 68.33442372801900433 ) ) ;
#121248 = CARTESIAN_POINT ( 'NONE',  ( 12.14591786802327356, -12.06949235617739191, 20.62609039468568639 ) ) ;
#121249 = CARTESIAN_POINT ( 'NONE',  ( -13.89961937509977652, 13.97604488694528158, 70.62390960531432427 ) ) ;
#121250 = CARTESIAN_POINT ( 'NONE',  ( 16.46253265017146816, 9.564922557961045513, 101.6677570613523329 ) ) ;
#121251 = CARTESIAN_POINT ( 'NONE',  ( 8.314922557961029526, -14.29746914071037800, 65.41775706135234714 ) ) ;
#121252 = CARTESIAN_POINT ( 'NONE',  ( 19.05341960407617918, -5.049401038297876454, 21.04275706135232582 ) ) ;
#121253 = CARTESIAN_POINT ( 'NONE',  ( -16.51473224551082808, 9.474510206698731452, 73.33442372801900433 ) ) ;
#121254 = CARTESIAN_POINT ( 'NONE',  ( -13.89961937509977652, 13.97604488694528158, 50.62390960531435979 ) ) ;
#121255 = CARTESIAN_POINT ( 'NONE',  ( 21.52544592524344225, -5.823673210054117533, 83.54057627198102409 ) ) ;
#121257 = CARTESIAN_POINT ( 'NONE',  ( 5.049401038297881783, 19.05341960407617563, 72.29275706135234714 ) ) ;
#121256 = CARTESIAN_POINT ( 'NONE',  ( 16.55341960407611168, 4.379528057220329451, 73.95724293864769550 ) ) ;
#121258 = DIRECTION ( 'NONE',  ( -1.000000000000000000, 0.000000000000000000, -8.673617379884026597E-16 ) ) ;
#121259 = CARTESIAN_POINT ( 'NONE',  ( -5.153800228976607833, 19.02544592524334988, 47.70942372801900433 ) ) ;
#121260 = CARTESIAN_POINT ( 'NONE',  ( -8.314922557961024197, 14.29746914071037800, 107.9177570613523471 ) ) ;
#121261 = CARTESIAN_POINT ( 'NONE',  ( 16.52544592524342804, -4.483927247898539470, 63.54057627198103830 ) ) ;
#121263 = CARTESIAN_POINT ( 'NONE',  ( 8.571926809382603096, -26.38167802310801235, 145.4750000027311785 ) ) ;
#121262 = CARTESIAN_POINT ( 'NONE',  ( -5.823673210054431948, 21.52544592524334988, 102.7094237280190185 ) ) ;
#121264 = CARTESIAN_POINT ( 'NONE',  ( -15.80617190586745835, -15.72974639402198527, 101.8739096053143811 ) ) ;
#121265 = CARTESIAN_POINT ( 'NONE',  ( -5.049401038298153566, 19.05341960407611168, 60.20724293864768129 ) ) ;
#121266 = CARTESIAN_POINT ( 'NONE',  ( 5.719274019375673035, 21.55341960407619339, 77.29275706135234714 ) ) ;
#121267 = CARTESIAN_POINT ( 'NONE',  ( 9.564922557960805705, 16.46253265017160317, 69.58224293864770971 ) ) ;
#121268 = ORIENTED_EDGE ( 'NONE', *, *, #48904, .T. ) ;
#121269 = CARTESIAN_POINT ( 'NONE',  ( 9.564922557960805705, 16.46253265017160317, 24.58224293864769194 ) ) ;
#121270 = CARTESIAN_POINT ( 'NONE',  ( -18.67979575497178146, -10.72451020669898902, 36.66557627198103120 ) ) ;
#121271 = CARTESIAN_POINT ( 'NONE',  ( 14.29746914071049879, -8.314922557960816363, 63.33224293864770260 ) ) ;
#121272 = CARTESIAN_POINT ( 'NONE',  ( 13.97604488694527802, 13.89961937509977652, 49.37390960531434558 ) ) ;
#121273 = CARTESIAN_POINT ( 'NONE',  ( -4.483927247898539470, -16.52544592524342804, 92.29057627198103830 ) ) ;
#121274 = CARTESIAN_POINT ( 'NONE',  ( 15.72974639402199770, -15.80617190586745480, 113.1239096053143953 ) ) ;
#121275 = CARTESIAN_POINT ( 'NONE',  ( 10.81492255796106328, -18.62759615963255655, 55.41775706135234714 ) ) ;
#121276 = CARTESIAN_POINT ( 'NONE',  ( -5.153800228976328057, -19.02544592524343514, 32.29057627198102409 ) ) ;
#121277 = EDGE_CURVE ( 'NONE', #186287, #152202, #142091, .T. ) ;
#121278 = CARTESIAN_POINT ( 'NONE',  ( -16.53943276465976808, -0.05219959533934237506, 63.75109039468568284 ) ) ;
#121279 = CARTESIAN_POINT ( 'NONE',  ( -10.81492255796078084, -18.62759615963271287, 107.0822429386476955 ) ) ;
#121280 = CARTESIAN_POINT ( 'NONE',  ( 10.72451020669898902, -18.67979575497178502, 97.91557627198103830 ) ) ;
#121282 = CARTESIAN_POINT ( 'NONE',  ( 13.89961937509977652, -13.97604488694527269, 58.12390960531436690 ) ) ;
#121281 = CARTESIAN_POINT ( 'NONE',  ( 9.564922557961047289, -16.46253265017146816, 20.41775706135233293 ) ) ;
#121283 = CARTESIAN_POINT ( 'NONE',  ( 9.474510206698971260, -16.51473224551069308, 102.9155762719810241 ) ) ;
#121284 = CARTESIAN_POINT ( 'NONE',  ( 21.55341960407619695, -5.719274019375665929, 61.04275706135234714 ) ) ;
#121285 = CARTESIAN_POINT ( 'NONE',  ( -21.52544592524343514, 5.823673210054127303, 41.04057627198103120 ) ) ;
#121286 = CARTESIAN_POINT ( 'NONE',  ( -14.34966873604972548, 8.224510206698743886, 113.3344237280190328 ) ) ;
#121288 = CARTESIAN_POINT ( 'NONE',  ( 21.52544592524334988, 5.823673210054432836, 96.45942372801901854 ) ) ;
#121287 = CARTESIAN_POINT ( 'NONE',  ( -18.62759615963255300, -10.81492255796106328, 59.16775706135234714 ) ) ;
#121289 = CARTESIAN_POINT ( 'NONE',  ( -19.02544592524334988, -5.153800228976617603, 48.95942372801900433 ) ) ;
#121290 = CARTESIAN_POINT ( 'NONE',  ( -12.06949235617739369, -12.14591786802326823, 104.3760903946856899 ) ) ;
#121291 = CARTESIAN_POINT ( 'NONE',  ( -10.72451020669870658, -18.67979575497194134, 49.58442372801901143 ) ) ;
#121292 = CARTESIAN_POINT ( 'NONE',  ( 16.51473224551069308, 9.474510206698969483, 64.16557627198102409 ) ) ;
#121293 = CARTESIAN_POINT ( 'NONE',  ( -9.474510206698720793, -16.51473224551083518, 19.58442372801899722 ) ) ;
#121294 = CARTESIAN_POINT ( 'NONE',  ( 18.62759615963271287, -10.81492255796078972, 33.33224293864769550 ) ) ;
#121295 = EDGE_CURVE ( 'NONE', #114764, #148642, #107241, .T. ) ;
#121296 = CARTESIAN_POINT ( 'NONE',  ( 5.823673210054444382, -21.52544592524334988, 30.20942372801902565 ) ) ;
#121297 = CARTESIAN_POINT ( 'NONE',  ( -18.62759615963270932, 10.81492255796079327, 90.83224293864769550 ) ) ;
#121298 = CARTESIAN_POINT ( 'NONE',  ( 5.049401038297881783, 19.05341960407617563, 87.29275706135234714 ) ) ;
#121299 = CARTESIAN_POINT ( 'NONE',  ( 16.52544592524335698, 4.483927247898782831, 41.45942372801901143 ) ) ;
#121301 = CARTESIAN_POINT ( 'NONE',  ( -10.81492255796078084, -18.62759615963271287, 77.08224293864769550 ) ) ;
#121300 = CARTESIAN_POINT ( 'NONE',  ( -4.313351365237961588, 4.313351365237934054, -62.50719930893269805 ) ) ;
#121303 = CARTESIAN_POINT ( 'NONE',  ( 16.53943276465976808, -0.05219959533910856209, 78.74890960531436690 ) ) ;
#121302 = CARTESIAN_POINT ( 'NONE',  ( -16.53943276465976808, -0.05219959533934237506, 63.75109039468568284 ) ) ;
#121304 = CARTESIAN_POINT ( 'NONE',  ( 0.1328615419017731281, 28.90000000000004476, -49.67367017693149478 ) ) ;
#121305 = CARTESIAN_POINT ( 'NONE',  ( 0.05219959533936267826, -19.03943276465977164, 105.0010903946856615 ) ) ;
#121306 = CARTESIAN_POINT ( 'NONE',  ( 5.823673210054125526, 21.52544592524343514, 39.79057627198103830 ) ) ;
#121307 = CARTESIAN_POINT ( 'NONE',  ( 9.564922557960805705, 16.46253265017160317, 94.58224293864769550 ) ) ;
#121308 = CARTESIAN_POINT ( 'NONE',  ( -12.14591786802326823, 12.06949235617739902, 38.12609039468567573 ) ) ;
#121309 = CARTESIAN_POINT ( 'NONE',  ( -5.823673210054116645, -21.52544592524344225, 107.2905762719810525 ) ) ;
#121310 = CARTESIAN_POINT ( 'NONE',  ( 21.55341960407610458, 5.719274019375980345, 33.95724293864769550 ) ) ;
#121311 = CARTESIAN_POINT ( 'NONE',  ( 12.14591786802327356, -12.06949235617739191, 65.62609039468568994 ) ) ;
#121312 = CARTESIAN_POINT ( 'NONE',  ( 16.46253265017160672, -9.564922557960803928, 83.33224293864768129 ) ) ;
#121314 = CARTESIAN_POINT ( 'NONE',  ( 5.153800228976335163, 19.02544592524342804, 34.79057627198102409 ) ) ;
#121313 = CARTESIAN_POINT ( 'NONE',  ( 5.823673210054444382, -21.52544592524334988, 55.20942372801902565 ) ) ;
#121315 = CARTESIAN_POINT ( 'NONE',  ( -19.02544592524342804, 5.153800228976336051, 116.0405762719810383 ) ) ;
#121316 = ORIENTED_EDGE ( 'NONE', *, *, #82044, .T. ) ;
#121317 = CARTESIAN_POINT ( 'NONE',  ( -16.46253265017146816, -9.564922557961047289, 44.16775706135232582 ) ) ;
#121318 = CARTESIAN_POINT ( 'NONE',  ( 16.53943276465976808, 0.05219959533934440121, 46.25109039468567573 ) ) ;
#121319 = CARTESIAN_POINT ( 'NONE',  ( -13.89961937509977652, 13.97604488694528158, 110.6239096053143243 ) ) ;
#121320 = CARTESIAN_POINT ( 'NONE',  ( -13.89961937509977652, 13.97604488694528158, 75.62390960531438111 ) ) ;
#121321 = CARTESIAN_POINT ( 'NONE',  ( -4.379528057220086978, -16.55341960407618274, 94.79275706135234714 ) ) ;
#121322 = CARTESIAN_POINT ( 'NONE',  ( 11.30153831258471797, -180.0000000000000000, -4.999999999999999112 ) ) ;
#121323 = CARTESIAN_POINT ( 'NONE',  ( 12.06949235617757843, -12.14591786802309237, 93.12390960531436690 ) ) ;
#121324 = CARTESIAN_POINT ( 'NONE',  ( 21.52544592524344225, -5.823673210054117533, 28.54057627198103120 ) ) ;
#121325 = CARTESIAN_POINT ( 'NONE',  ( -19.02544592524342804, 5.153800228976336051, 26.04057627198103120 ) ) ;
#121326 = CARTESIAN_POINT ( 'NONE',  ( 12.06949235617739724, 12.14591786802326823, 61.87609039468568284 ) ) ;
#121327 = CARTESIAN_POINT ( 'NONE',  ( 21.53943276465977519, 0.05219959533937863772, 21.25109039468567218 ) ) ;
#121328 = CARTESIAN_POINT ( 'NONE',  ( -19.02544592524334988, -5.153800228976617603, 73.95942372801900433 ) ) ;
#121329 = CARTESIAN_POINT ( 'NONE',  ( -13.89961937509977652, 13.97604488694528158, 40.62390960531435979 ) ) ;
#121330 = CARTESIAN_POINT ( 'NONE',  ( -21.55341960407610458, -5.719274019375992779, 66.45724293864768129 ) ) ;
#121331 = CARTESIAN_POINT ( 'NONE',  ( 16.51473224551069308, 9.474510206698969483, 114.1655762719810241 ) ) ;
#121332 = CARTESIAN_POINT ( 'NONE',  ( 21.52544592524334988, 5.823673210054432836, 96.45942372801901854 ) ) ;
#121333 = CARTESIAN_POINT ( 'NONE',  ( 0.05219959533909260263, 19.03943276465977164, 59.99890960531436690 ) ) ;
#121334 = CARTESIAN_POINT ( 'NONE',  ( 16.53943276465976808, 0.05219959533934440121, 46.25109039468567573 ) ) ;
#121335 = CARTESIAN_POINT ( 'NONE',  ( -13.97604488694527625, -13.89961937509977652, 61.87390960531435979 ) ) ;
#121336 = CARTESIAN_POINT ( 'NONE',  ( -18.67979575497193778, 10.72451020669871902, 78.33442372801901854 ) ) ;
#121337 = CARTESIAN_POINT ( 'NONE',  ( -13.89961937509957401, -13.97604488694547875, 34.37609039468566863 ) ) ;
#121338 = CARTESIAN_POINT ( 'NONE',  ( -19.02544592524334988, -5.153800228976617603, 48.95942372801900433 ) ) ;
#121339 = CARTESIAN_POINT ( 'NONE',  ( -18.62759615963255300, -10.81492255796106328, 54.16775706135235424 ) ) ;
#121340 = CARTESIAN_POINT ( 'NONE',  ( -8.348819774032568475, 1.314123079931817317, -62.04874212273342948 ) ) ;
#121341 = CARTESIAN_POINT ( 'NONE',  ( 19.03943276465977164, 0.05219959533936151252, 51.25109039468567573 ) ) ;
#121342 = CARTESIAN_POINT ( 'NONE',  ( 0.05219959533909260263, 19.03943276465977164, 99.99890960531436690 ) ) ;
#121343 = CARTESIAN_POINT ( 'NONE',  ( 19.02544592524343514, -5.153800228976328945, 88.54057627198102409 ) ) ;
#121344 = CARTESIAN_POINT ( 'NONE',  ( 16.55341960407611168, 4.379528057220329451, 33.95724293864769550 ) ) ;
#121346 = CARTESIAN_POINT ( 'NONE',  ( 5.823673210054444382, -21.52544592524334988, 100.2094237280190043 ) ) ;
#121345 = CARTESIAN_POINT ( 'NONE',  ( 10.81492255796078972, 18.62759615963270932, 34.58224293864770260 ) ) ;
#121347 = CARTESIAN_POINT ( 'NONE',  ( -5.950531402560715689E-15, 38.81732327939063509, -1.124999997268812946 ) ) ;
#121348 = CARTESIAN_POINT ( 'NONE',  ( 17.05116617787827238, 6.768360034955700044, 58.84324446740803438 ) ) ;
#121349 = CARTESIAN_POINT ( 'NONE',  ( 21.55341960407619695, -5.719274019375665929, 101.0427570613523756 ) ) ;
#121350 = CARTESIAN_POINT ( 'NONE',  ( -27.79722099587806028, 7.618187661584445713, 161.3616444162223900 ) ) ;
#121351 = CARTESIAN_POINT ( 'NONE',  ( -19.05341960407611168, -5.049401038298163336, 41.45724293864769550 ) ) ;
#121352 = CARTESIAN_POINT ( 'NONE',  ( 5.049401038298161559, -19.05341960407611168, 112.7072429386476813 ) ) ;
#121353 = CARTESIAN_POINT ( 'NONE',  ( 33.82491520367208437, 1.773434586730185503, 100.2093774297293720 ) ) ;
#121354 = CARTESIAN_POINT ( 'NONE',  ( 4.483927247898790824, -16.52544592524335698, 45.20942372801901854 ) ) ;
#121355 = CARTESIAN_POINT ( 'NONE',  ( 15.72974639402199770, -15.80617190586745480, 68.12390960531436690 ) ) ;
#121356 = CARTESIAN_POINT ( 'NONE',  ( 16.52544592524342804, -4.483927247898539470, 33.54057627198102409 ) ) ;
#121358 = CARTESIAN_POINT ( 'NONE',  ( -5.153800228976328057, -19.02544592524343514, 107.2905762719810383 ) ) ;
#121357 = CARTESIAN_POINT ( 'NONE',  ( 5.153800228976335163, 19.02544592524342804, 29.79057627198102409 ) ) ;
#121359 = CARTESIAN_POINT ( 'NONE',  ( -21.55341960407619339, 5.719274019375674811, 23.54275706135235424 ) ) ;
#121360 = CARTESIAN_POINT ( 'NONE',  ( 0.05219959533936267826, -19.03943276465977164, 35.00109039468566863 ) ) ;
#121361 = CARTESIAN_POINT ( 'NONE',  ( 12.14591786802309770, 12.06949235617756955, 109.3739096053143811 ) ) ;
#121362 = CARTESIAN_POINT ( 'NONE',  ( -15.80617190586768217, 15.72974639402176855, 63.12609039468568994 ) ) ;
#121363 = CARTESIAN_POINT ( 'NONE',  ( 17.12812012977025589, -6.668231424566045007, 31.14051240676858967 ) ) ;
#121364 = CARTESIAN_POINT ( 'NONE',  ( -12.06949235617756955, 12.14591786802309770, 25.62390960531435624 ) ) ;
#121365 = CARTESIAN_POINT ( 'NONE',  ( -18.22780087662122028, 5.500000000000031086, 68.51540105326107266 ) ) ;
#121366 = CARTESIAN_POINT ( 'NONE',  ( -5.823673210054116645, -21.52544592524344225, 32.29057627198102409 ) ) ;
#121367 = CARTESIAN_POINT ( 'NONE',  ( 8.314922557960818139, 14.29746914071049879, 84.58224293864769550 ) ) ;
#121369 = CARTESIAN_POINT ( 'NONE',  ( 20.28159948851302374, -33.49867931359608519, -17.64937754809732695 ) ) ;
#121368 = AXIS2_PLACEMENT_3D ( 'NONE', #121095, #74610, #122088 ) ;
#121370 = CARTESIAN_POINT ( 'NONE',  ( 16.46253265017160672, -9.564922557960803928, 73.33224293864769550 ) ) ;
#121371 = CARTESIAN_POINT ( 'NONE',  ( -14.29746914071049879, 8.314922557960819915, 75.83224293864769550 ) ) ;
#121372 = CARTESIAN_POINT ( 'NONE',  ( -16.51473224551082808, 9.474510206698731452, 108.3344237280190043 ) ) ;
#121373 = CARTESIAN_POINT ( 'NONE',  ( -18.62759615963270932, 10.81492255796079327, 65.83224293864769550 ) ) ;
#121374 = ORIENTED_EDGE ( 'NONE', *, *, #159302, .T. ) ;
#121375 = CARTESIAN_POINT ( 'NONE',  ( 16.51473224551069308, 9.474510206698969483, 24.16557627198102765 ) ) ;
#121376 = EDGE_CURVE ( 'NONE', #40349, #132603, #87121, .T. ) ;
#121378 = CARTESIAN_POINT ( 'NONE',  ( -10.72451020669898014, 18.67979575497178502, 75.41557627198102409 ) ) ;
#121377 = CARTESIAN_POINT ( 'NONE',  ( 0.05219959533909260263, 19.03943276465977164, 74.99890960531435269 ) ) ;
#121380 = CARTESIAN_POINT ( 'NONE',  ( 16.46253265017160672, -9.564922557960803928, 93.33224293864769550 ) ) ;
#121379 = CARTESIAN_POINT ( 'NONE',  ( 16.55341960407618274, -4.379528057220086978, 101.0427570613523756 ) ) ;
#121381 = CARTESIAN_POINT ( 'NONE',  ( 16.51473224551083163, -9.474510206698727899, 60.83442372801900433 ) ) ;
#121382 = CARTESIAN_POINT ( 'NONE',  ( 21.52544592524334988, 5.823673210054432836, 101.4594237280190185 ) ) ;
#121383 = CARTESIAN_POINT ( 'NONE',  ( -15.72974639402197994, 15.80617190586746368, 70.62390960531436690 ) ) ;
#121384 = CARTESIAN_POINT ( 'NONE',  ( 13.97604488694527802, 13.89961937509977652, 114.3739096053143669 ) ) ;
#121385 = CARTESIAN_POINT ( 'NONE',  ( 13.97604488694527802, 13.89961937509977652, 44.37390960531435269 ) ) ;
#121386 = CARTESIAN_POINT ( 'NONE',  ( -12.06949235617739369, -12.14591786802326823, 94.37609039468568994 ) ) ;
#121387 = CARTESIAN_POINT ( 'NONE',  ( -19.03943276465977164, 0.05219959533909376836, 66.24890960531436690 ) ) ;
#121388 = CARTESIAN_POINT ( 'NONE',  ( 8.224510206698742110, 14.34966873604972548, 27.08442372801901854 ) ) ;
#121389 = CARTESIAN_POINT ( 'NONE',  ( 17.05587630539785238, 6.762274262135711034, 51.75819690962690345 ) ) ;
#121390 = CARTESIAN_POINT ( 'NONE',  ( 10.72451020669871369, 18.67979575497193778, 112.0844237280190185 ) ) ;
#121391 = CARTESIAN_POINT ( 'NONE',  ( 8.314922557960818139, 14.29746914071049879, 74.58224293864768129 ) ) ;
#121392 = CARTESIAN_POINT ( 'NONE',  ( 15.72974639402199770, -15.80617190586745480, 113.1239096053143953 ) ) ;
#121393 = CARTESIAN_POINT ( 'NONE',  ( -0.05219959533907301413, -21.53943276465977519, 97.49890960531436690 ) ) ;
#121394 = CARTESIAN_POINT ( 'NONE',  ( -4.718528363748727840E-30, -105.0000000000000000, -13.00000000000000000 ) ) ;
#121395 = CARTESIAN_POINT ( 'NONE',  ( 21.53943276465977519, -0.05219959533907433946, 58.74890960531436690 ) ) ;
#121396 = CARTESIAN_POINT ( 'NONE',  ( -14.34966873604972548, 8.224510206698743886, 78.33442372801901854 ) ) ;
#121397 = CARTESIAN_POINT ( 'NONE',  ( 8.224510206698953496, -14.34966873604960469, 102.9155762719810383 ) ) ;
#121398 = CARTESIAN_POINT ( 'NONE',  ( -0.05219959533909027116, -19.03943276465977164, 62.49890960531435979 ) ) ;
#121399 = CARTESIAN_POINT ( 'NONE',  ( -8.224510206698735004, -14.34966873604973081, 109.5844237280190328 ) ) ;
#121400 = CARTESIAN_POINT ( 'NONE',  ( 21.55341960407619695, -5.719274019375665929, 51.04275706135234714 ) ) ;
#121401 = CARTESIAN_POINT ( 'NONE',  ( -9.474510206698964154, 16.51473224551069663, 95.41557627198102409 ) ) ;
#121402 = CARTESIAN_POINT ( 'NONE',  ( -10.81492255796105439, 18.62759615963255655, 82.91775706135234714 ) ) ;
#121403 = CARTESIAN_POINT ( 'NONE',  ( 0.05219959533909260263, 19.03943276465977164, 29.99890960531435979 ) ) ;
#121404 = CARTESIAN_POINT ( 'NONE',  ( -9.474510206698964154, 16.51473224551069663, 40.41557627198103120 ) ) ;
#121405 = ORIENTED_EDGE ( 'NONE', *, *, #76155, .T. ) ;
#121406 = CARTESIAN_POINT ( 'NONE',  ( -18.62759615963255300, -10.81492255796106328, 74.16775706135231871 ) ) ;
#121407 = CARTESIAN_POINT ( 'NONE',  ( 13.89961937509977652, -13.97604488694527269, 108.1239096053143669 ) ) ;
#121408 = CARTESIAN_POINT ( 'NONE',  ( 0.05219959533936267826, -19.03943276465977164, 85.00109039468567573 ) ) ;
#121409 = CARTESIAN_POINT ( 'NONE',  ( -21.53943276465977519, -0.05219959533937600094, 38.75109039468567573 ) ) ;
#121410 = CARTESIAN_POINT ( 'NONE',  ( -16.53943276465976808, -0.05219959533934237506, 18.75109039468568639 ) ) ;
#121411 = VECTOR ( 'NONE', #197014, 1000.000000000000000 ) ;
#121412 = CARTESIAN_POINT ( 'NONE',  ( -19.05341960407617563, 5.049401038297882671, 68.54275706135230450 ) ) ;
#121413 = CARTESIAN_POINT ( 'NONE',  ( -19.03943276465977164, 0.05219959533909376836, 51.24890960531436690 ) ) ;
#121414 = CARTESIAN_POINT ( 'NONE',  ( 16.51473224551083163, -9.474510206698727899, 85.83442372801900433 ) ) ;
#121415 = EDGE_CURVE ( 'NONE', #136724, #103711, #112935, .T. ) ;
#121416 = CARTESIAN_POINT ( 'NONE',  ( -12.14591786802309592, -12.06949235617757132, 31.87390960531435979 ) ) ;
#121417 = CARTESIAN_POINT ( 'NONE',  ( -5.049401038297874678, -19.05341960407617918, 84.79275706135233293 ) ) ;
#121418 = CARTESIAN_POINT ( 'NONE',  ( -8.224510206698948167, 14.34966873604960824, 35.41557627198102409 ) ) ;
#121419 = CARTESIAN_POINT ( 'NONE',  ( -0.05219959533936034679, 19.03943276465977164, 57.50109039468566863 ) ) ;
#121420 = CARTESIAN_POINT ( 'NONE',  ( -14.34966873604972548, 8.224510206698743886, 43.33442372801901143 ) ) ;
#121421 = CARTESIAN_POINT ( 'NONE',  ( -13.89961937509957401, -13.97604488694547875, 24.37609039468565442 ) ) ;
#121422 = CARTESIAN_POINT ( 'NONE',  ( -13.89961937509977652, 13.97604488694528158, 30.62390960531435269 ) ) ;
#121423 = CARTESIAN_POINT ( 'NONE',  ( -16.36317988757057762, -7.306389748694952502, 65.90210391636775000 ) ) ;
#121424 = CARTESIAN_POINT ( 'NONE',  ( -16.55341960407617563, 4.379528057220093196, 43.54275706135235424 ) ) ;
#121425 = CARTESIAN_POINT ( 'NONE',  ( -17.14385361876520619, 23.59649016807275856, 142.5750000027312012 ) ) ;
#121426 = CARTESIAN_POINT ( 'NONE',  ( -0.05219959533909027116, -19.03943276465977164, 92.49890960531436690 ) ) ;
#121427 = CARTESIAN_POINT ( 'NONE',  ( -17.60691670004653631, -5.500000000000000000, 69.13333313366437949 ) ) ;
#121428 = ORIENTED_EDGE ( 'NONE', *, *, #6906, .T. ) ;
#121429 = CARTESIAN_POINT ( 'NONE',  ( -16.46253265017146816, -9.564922557961047289, 89.16775706135234714 ) ) ;
#121430 = CARTESIAN_POINT ( 'NONE',  ( -5.719274019375978568, 21.55341960407610458, 25.20724293864769550 ) ) ;
#121432 = CARTESIAN_POINT ( 'NONE',  ( 9.474510206698729675, 16.51473224551082808, 102.0844237280190043 ) ) ;
#121431 = CARTESIAN_POINT ( 'NONE',  ( 0.05219959533936267826, -19.03943276465977164, 20.00109039468567218 ) ) ;
#121433 = CARTESIAN_POINT ( 'NONE',  ( -4.379528057220328563, 16.55341960407611168, 110.2072429386477239 ) ) ;
#121434 = CARTESIAN_POINT ( 'NONE',  ( -16.46253265017160317, 9.564922557960807481, 35.83224293864768839 ) ) ;
#121435 = CARTESIAN_POINT ( 'NONE',  ( 18.62759615963271287, -10.81492255796078972, 63.33224293864770260 ) ) ;
#121436 = CARTESIAN_POINT ( 'NONE',  ( -8.224510206698948167, 14.34966873604960824, 115.4155762719810241 ) ) ;
#121437 = CARTESIAN_POINT ( 'NONE',  ( 8.906447517083057264, -27.41122689804191026, 142.8500000054623911 ) ) ;
#121438 = CARTESIAN_POINT ( 'NONE',  ( -5.153800228976607833, 19.02544592524334988, 72.70942372801900433 ) ) ;
#121439 = CARTESIAN_POINT ( 'NONE',  ( 12.06949235617757843, -12.14591786802309237, 43.12390960531435269 ) ) ;
#121441 = EDGE_CURVE ( 'NONE', #125394, #66168, #186777, .T. ) ;
#121440 = CARTESIAN_POINT ( 'NONE',  ( -16.46253265017160317, 9.564922557960807481, 115.8322429386477097 ) ) ;
#121442 = CARTESIAN_POINT ( 'NONE',  ( -5.823673210054431948, 21.52544592524334988, 92.70942372801901854 ) ) ;
#121443 = CARTESIAN_POINT ( 'NONE',  ( 15.72974639402199770, -15.80617190586745480, 83.12390960531436690 ) ) ;
#121444 = CARTESIAN_POINT ( 'NONE',  ( 21.55341960407619695, -5.719274019375665929, 56.04275706135235424 ) ) ;
#121445 = CARTESIAN_POINT ( 'NONE',  ( -0.05219959533937732626, 21.53943276465977519, 62.50109039468568284 ) ) ;
#121446 = CARTESIAN_POINT ( 'NONE',  ( 16.46253265017160672, -9.564922557960803928, 93.33224293864769550 ) ) ;
#121448 = CARTESIAN_POINT ( 'NONE',  ( -5.719274019375665041, -21.55341960407619695, 54.79275706135235424 ) ) ;
#121447 = CARTESIAN_POINT ( 'NONE',  ( 4.379528057220092307, 16.55341960407617563, 97.29275706135234714 ) ) ;
#121449 = CARTESIAN_POINT ( 'NONE',  ( 16.52544592524342804, -4.483927247898539470, 113.5405762719810383 ) ) ;
#121450 = CARTESIAN_POINT ( 'NONE',  ( 16.52544592524342804, -4.483927247898539470, 73.54057627198102409 ) ) ;
#121451 = CARTESIAN_POINT ( 'NONE',  ( -16.55341960407611168, -4.379528057220339221, 31.45724293864769550 ) ) ;
#121452 = CARTESIAN_POINT ( 'NONE',  ( 21.55341960407610458, 5.719274019375980345, 48.95724293864770971 ) ) ;
#121453 = CARTESIAN_POINT ( 'NONE',  ( -9.564922557960796823, -16.46253265017161027, 62.08224293864769550 ) ) ;
#121454 = CARTESIAN_POINT ( 'NONE',  ( -13.97604488694527625, -13.89961937509977652, 46.87390960531435979 ) ) ;
#121455 = CARTESIAN_POINT ( 'NONE',  ( 0.05219959533907565091, 21.53943276465977519, 59.99890960531436690 ) ) ;
#121456 = CARTESIAN_POINT ( 'NONE',  ( -16.51473224551082808, 9.474510206698731452, 48.33442372801900433 ) ) ;
#121458 = CARTESIAN_POINT ( 'NONE',  ( -14.29746914071049879, 8.314922557960819915, 55.83224293864770260 ) ) ;
#121457 = CARTESIAN_POINT ( 'NONE',  ( -16.29526858892878494, -7.335722546919999587, 40.79670597800206622 ) ) ;
#121459 = CARTESIAN_POINT ( 'NONE',  ( -13.89961937509977652, 13.97604488694528158, 115.6239096053143669 ) ) ;
#121460 = ORIENTED_EDGE ( 'NONE', *, *, #110488, .F. ) ;
#121461 = EDGE_LOOP ( 'NONE', ( #51781, #32252, #18660, #62966 ) ) ;
#121462 = CARTESIAN_POINT ( 'NONE',  ( 28.79475375365590040, -9.355982642739126831, 140.8843446568999696 ) ) ;
#121463 = CARTESIAN_POINT ( 'NONE',  ( -0.05219959533934338120, 16.53943276465976808, 72.50109039468568994 ) ) ;
#121464 = CARTESIAN_POINT ( 'NONE',  ( 19.02544592524334988, 5.153800228976608722, 81.45942372801897591 ) ) ;
#121465 = EDGE_CURVE ( 'NONE', #151273, #66675, #25821, .T. ) ;
#121466 = CARTESIAN_POINT ( 'NONE',  ( 0.05219959533910956823, 16.53943276465976808, 39.99890960531436690 ) ) ;
#121467 = FACE_BOUND ( 'NONE', #29639, .T. ) ;
#121468 = CARTESIAN_POINT ( 'NONE',  ( -14.34966873604960291, -8.224510206698953496, 21.66557627198102409 ) ) ;
#121469 = CARTESIAN_POINT ( 'NONE',  ( -5.153800228976328057, -19.02544592524343514, 47.29057627198102409 ) ) ;
#121470 = CARTESIAN_POINT ( 'NONE',  ( -9.474510206698964154, 16.51473224551069663, 80.41557627198103830 ) ) ;
#121471 = CARTESIAN_POINT ( 'NONE',  ( 13.89961937509977652, -13.97604488694527269, 33.12390960531434558 ) ) ;
#121472 = CARTESIAN_POINT ( 'NONE',  ( -5.823673210054431948, 21.52544592524334988, 47.70942372801902565 ) ) ;
#121473 = CARTESIAN_POINT ( 'NONE',  ( 19.05341960407611168, 5.049401038298154454, 58.95724293864768129 ) ) ;
#121474 = CARTESIAN_POINT ( 'NONE',  ( 28.79475375365586132, 2.781246896534039337E-14, 155.0000000000000000 ) ) ;
#121475 = CARTESIAN_POINT ( 'NONE',  ( -5.049401038298153566, 19.05341960407611168, 55.20724293864769550 ) ) ;
#121476 = CARTESIAN_POINT ( 'NONE',  ( -18.62759615963270932, 10.81492255796079327, 40.83224293864769550 ) ) ;
#121477 = CARTESIAN_POINT ( 'NONE',  ( -4.379528057220328563, 16.55341960407611168, 115.2072429386476955 ) ) ;
#121478 = CARTESIAN_POINT ( 'NONE',  ( -0.05219959533907301413, -21.53943276465977519, 47.49890960531435979 ) ) ;
#121479 = CARTESIAN_POINT ( 'NONE',  ( 16.52544592524335698, 4.483927247898782831, 86.45942372801901854 ) ) ;
#121480 = CARTESIAN_POINT ( 'NONE',  ( -5.823673210054431948, 21.52544592524334988, 107.7094237280190328 ) ) ;
#121481 = CARTESIAN_POINT ( 'NONE',  ( 16.53943276465976808, 0.05219959533934440121, 71.25109039468568994 ) ) ;
#121482 = CARTESIAN_POINT ( 'NONE',  ( 19.05341960407611168, 5.049401038298154454, 113.9572429386477097 ) ) ;
#121483 = CARTESIAN_POINT ( 'NONE',  ( 12.06949235617739724, 12.14591786802326823, 56.87609039468568994 ) ) ;
#121484 = CARTESIAN_POINT ( 'NONE',  ( 0.05219959533934541429, -16.53943276465976808, 35.00109039468568284 ) ) ;
#121485 = CARTESIAN_POINT ( 'NONE',  ( 5.153800228976335163, 19.02544592524342804, 114.7905762719810241 ) ) ;
#121486 = CARTESIAN_POINT ( 'NONE',  ( -14.29746914071037622, -8.314922557961029526, 19.16775706135234714 ) ) ;
#121487 = CARTESIAN_POINT ( 'NONE',  ( 9.564922557960805705, 16.46253265017160317, 34.58224293864770260 ) ) ;
#121488 = CARTESIAN_POINT ( 'NONE',  ( -5.823673210054431948, 21.52544592524334988, 22.70942372801901499 ) ) ;
#121489 = CARTESIAN_POINT ( 'NONE',  ( -5.153800228976607833, 19.02544592524334988, 112.7094237280190043 ) ) ;
#121490 = CARTESIAN_POINT ( 'NONE',  ( -14.34966873604972548, 8.224510206698743886, 88.33442372801901854 ) ) ;
#121491 = CARTESIAN_POINT ( 'NONE',  ( 30.74264578624799782, 22.33583958711400541, -4.549999994537627046 ) ) ;
#121492 = CARTESIAN_POINT ( 'NONE',  ( -21.52544592524334988, -5.823673210054445271, 83.95942372801900433 ) ) ;
#121493 = CARTESIAN_POINT ( 'NONE',  ( 16.51473224551083163, -9.474510206698727899, 90.83442372801900433 ) ) ;
#121494 = CARTESIAN_POINT ( 'NONE',  ( 8.224510206698953496, -14.34966873604960469, 57.91557627198103120 ) ) ;
#121495 = CARTESIAN_POINT ( 'NONE',  ( -8.224510206698948167, 14.34966873604960824, 110.4155762719810383 ) ) ;
#121497 = CARTESIAN_POINT ( 'NONE',  ( -7.794767548047328631, 1.499903966022481994, -64.20498622968419511 ) ) ;
#121496 = CARTESIAN_POINT ( 'NONE',  ( -16.51473224551082808, 9.474510206698731452, 48.33442372801900433 ) ) ;
#121498 = CARTESIAN_POINT ( 'NONE',  ( -5.823673210054431948, 21.52544592524334988, 47.70942372801902565 ) ) ;
#121499 = CARTESIAN_POINT ( 'NONE',  ( -19.03943276465977164, -0.05219959533935918106, 108.7510903946856615 ) ) ;
#121500 = CARTESIAN_POINT ( 'NONE',  ( 16.79531203550644491, 7.028104445595627858, 83.75244988220441655 ) ) ;
#121501 = CARTESIAN_POINT ( 'NONE',  ( 9.564922557960805705, 16.46253265017160317, 104.5822429386476955 ) ) ;
#121502 = CARTESIAN_POINT ( 'NONE',  ( -21.53943276465977519, 0.05219959533907696930, 66.24890960531436690 ) ) ;
#121503 = CARTESIAN_POINT ( 'NONE',  ( 16.51473224551083163, -9.474510206698727899, 100.8344237280190043 ) ) ;
#121504 = CARTESIAN_POINT ( 'NONE',  ( -5.153800228976328057, -19.02544592524343514, 107.2905762719810383 ) ) ;
#121505 = CARTESIAN_POINT ( 'NONE',  ( 8.545215834362450025, -26.44289320400097409, 139.9999999999999716 ) ) ;
#121506 = CARTESIAN_POINT ( 'NONE',  ( -12.14591786802309592, -12.06949235617757132, 106.8739096053143811 ) ) ;
#121507 = CARTESIAN_POINT ( 'NONE',  ( -5.823673210054431948, 21.52544592524334988, 87.70942372801901854 ) ) ;
#121508 = CARTESIAN_POINT ( 'NONE',  ( -19.05341960407611168, -5.049401038298163336, 46.45724293864768129 ) ) ;
#121509 = CARTESIAN_POINT ( 'NONE',  ( -21.55341960407619339, 5.719274019375674811, 58.54275706135235424 ) ) ;
#121510 = CARTESIAN_POINT ( 'NONE',  ( -10.72451020669870658, -18.67979575497194134, 89.58442372801901854 ) ) ;
#121511 = CARTESIAN_POINT ( 'NONE',  ( -14.29746914071037622, -8.314922557961029526, 109.1677570613523613 ) ) ;
#121512 = CARTESIAN_POINT ( 'NONE',  ( 19.05341960407611168, 5.049401038298154454, 63.95724293864769550 ) ) ;
#121513 = CARTESIAN_POINT ( 'NONE',  ( -5.823673210054431948, 21.52544592524334988, 37.70942372801900433 ) ) ;
#121514 = CARTESIAN_POINT ( 'NONE',  ( -21.52544592524334988, -5.823673210054445271, 38.95942372801901854 ) ) ;
#121516 = CARTESIAN_POINT ( 'NONE',  ( -13.97604488694527625, -13.89961937509977652, 96.87390960531433848 ) ) ;
#121515 = CARTESIAN_POINT ( 'NONE',  ( 16.46253265017146816, 9.564922557961045513, 66.66775706135233293 ) ) ;
#121517 = CARTESIAN_POINT ( 'NONE',  ( -12.06949235617756955, 12.14591786802309770, 110.6239096053143669 ) ) ;
#121518 = CARTESIAN_POINT ( 'NONE',  ( 5.719274019375991003, -21.55341960407610458, 92.70724293864770971 ) ) ;
#121519 = CARTESIAN_POINT ( 'NONE',  ( 8.314922557960818139, 14.29746914071049879, 64.58224293864769550 ) ) ;
#121520 = CARTESIAN_POINT ( 'NONE',  ( 10.81492255796106328, -18.62759615963255655, 110.4177570613523756 ) ) ;
#121521 = CARTESIAN_POINT ( 'NONE',  ( -4.483927247898539470, -16.52544592524342804, 87.29057627198103830 ) ) ;
#121522 = CARTESIAN_POINT ( 'NONE',  ( -9.474510206698964154, 16.51473224551069663, 40.41557627198103120 ) ) ;
#121523 = CARTESIAN_POINT ( 'NONE',  ( 19.02544592524334988, 5.153800228976608722, 86.45942372801900433 ) ) ;
#121524 = CARTESIAN_POINT ( 'NONE',  ( 16.55341960407611168, 4.379528057220329451, 48.95724293864770971 ) ) ;
#121525 = CARTESIAN_POINT ( 'NONE',  ( -18.62759615963255300, -10.81492255796106328, 99.16775706135234714 ) ) ;
#121526 = CARTESIAN_POINT ( 'NONE',  ( 9.564922557960805705, 16.46253265017160317, 89.58224293864769550 ) ) ;
#121527 = CARTESIAN_POINT ( 'NONE',  ( -16.51473224551082808, 9.474510206698731452, 73.33442372801900433 ) ) ;
#121528 = CARTESIAN_POINT ( 'NONE',  ( 15.72974639402199770, -15.80617190586745480, 83.12390960531436690 ) ) ;
#121529 = CARTESIAN_POINT ( 'NONE',  ( 0.05219959533937995610, -21.53943276465977519, 25.00109039468567218 ) ) ;
#121530 = CARTESIAN_POINT ( 'NONE',  ( 8.314922557961029526, -14.29746914071037800, 35.41775706135234003 ) ) ;
#121531 = CARTESIAN_POINT ( 'NONE',  ( -16.55341960407617563, 4.379528057220093196, 88.54275706135236135 ) ) ;
#121533 = CARTESIAN_POINT ( 'NONE',  ( -18.62759615963255300, -10.81492255796106328, 24.16775706135235424 ) ) ;
#121532 = CARTESIAN_POINT ( 'NONE',  ( 0.05219959533909260263, 19.03943276465977164, 29.99890960531435979 ) ) ;
#121534 = CARTESIAN_POINT ( 'NONE',  ( -9.474510206698964154, 16.51473224551069663, 25.41557627198103120 ) ) ;
#121535 = CARTESIAN_POINT ( 'NONE',  ( 11.40812507854755253, -35.11059874428192273, -8.524999997268814411 ) ) ;
#121536 = CARTESIAN_POINT ( 'NONE',  ( -8.224510206698735004, -14.34966873604973081, 54.58442372801901143 ) ) ;
#121537 = CARTESIAN_POINT ( 'NONE',  ( -16.55341960407611168, -4.379528057220339221, 81.45724293864769550 ) ) ;
#121538 = CARTESIAN_POINT ( 'NONE',  ( 15.80617190586746368, 15.72974639402197994, 79.37390960531436690 ) ) ;
#121539 = CARTESIAN_POINT ( 'NONE',  ( -12.14591786802309592, -12.06949235617757132, 31.87390960531435979 ) ) ;
#121540 = CARTESIAN_POINT ( 'NONE',  ( 12.06949235617739724, 12.14591786802326823, 46.87609039468568994 ) ) ;
#121541 = CARTESIAN_POINT ( 'NONE',  ( -9.474510206698964154, 16.51473224551069663, 45.41557627198103120 ) ) ;
#121542 = CARTESIAN_POINT ( 'NONE',  ( 16.52544592524335698, 4.483927247898782831, 81.45942372801900433 ) ) ;
#121543 = CARTESIAN_POINT ( 'NONE',  ( -16.51473224551082808, 9.474510206698731452, 93.33442372801900433 ) ) ;
#121544 = CARTESIAN_POINT ( 'NONE',  ( -21.53943276465977519, 0.05219959533907696930, 71.24890960531435269 ) ) ;
#121545 = CARTESIAN_POINT ( 'NONE',  ( 14.29746914071049879, -8.314922557960816363, 23.33224293864769194 ) ) ;
#121546 = ORIENTED_EDGE ( 'NONE', *, *, #120673, .F. ) ;
#121547 = FACE_OUTER_BOUND ( 'NONE', #123851, .T. ) ;
#121548 = CARTESIAN_POINT ( 'NONE',  ( -18.67979575497178146, -10.72451020669898902, 61.66557627198103120 ) ) ;
#121549 = ORIENTED_EDGE ( 'NONE', *, *, #181196, .F. ) ;
#121550 = CARTESIAN_POINT ( 'NONE',  ( 12.14591786802327356, -12.06949235617739191, 85.62609039468568994 ) ) ;
#121551 = EDGE_LOOP ( 'NONE', ( #66074, #144518, #196558, #39732 ) ) ;
#121552 = CARTESIAN_POINT ( 'NONE',  ( 0.05219959533909260263, 19.03943276465977164, 114.9989096053143669 ) ) ;
#121553 = CARTESIAN_POINT ( 'NONE',  ( 17.50000000000014566, 3.292511757969701858, 107.4347972978946615 ) ) ;
#121554 = CARTESIAN_POINT ( 'NONE',  ( 18.67979575497178502, 10.72451020669898547, 69.16557627198102409 ) ) ;
#121555 = CARTESIAN_POINT ( 'NONE',  ( 8.314922557961029526, -14.29746914071037800, 105.4177570613523613 ) ) ;
#121556 = CARTESIAN_POINT ( 'NONE',  ( 8.224510206698742110, 14.34966873604972548, 22.08442372801901143 ) ) ;
#121557 = CARTESIAN_POINT ( 'NONE',  ( -14.29746914071049879, 8.314922557960819915, 115.8322429386477097 ) ) ;
#121558 = CARTESIAN_POINT ( 'NONE',  ( 12.14591786802327356, -12.06949235617739191, 25.62609039468567929 ) ) ;
#121559 = AXIS2_PLACEMENT_3D ( 'NONE', #77864, #62688, #165928 ) ;
#121560 = CARTESIAN_POINT ( 'NONE',  ( -19.05341960407611168, -5.049401038298163336, 56.45724293864768129 ) ) ;
#121561 = CARTESIAN_POINT ( 'NONE',  ( -8.906447517083060816, 27.41122689804195645, 141.5999999999999943 ) ) ;
#121562 = CARTESIAN_POINT ( 'NONE',  ( -9.474510206698964154, 16.51473224551069663, 105.4155762719810383 ) ) ;
#121564 = B_SPLINE_CURVE_WITH_KNOTS ( 'NONE', 3,
 ( #106408, #108402, #79051, #170079, #91218, #63896, #183272, #186263 ),
 .UNSPECIFIED., .F., .F.,
 ( 4, 2, 2, 4 ),
 ( 1.015220885719448636E-17, 0.002784256700436080808, 0.005568513400872152075, 0.01113702680174429374 ),
 .UNSPECIFIED. ) ;
#121563 = CARTESIAN_POINT ( 'NONE',  ( -16.53943276465976808, -0.05219959533934237506, 88.75109039468567573 ) ) ;
#121565 = CARTESIAN_POINT ( 'NONE',  ( 13.89961937509957401, 13.97604488694547697, 86.87609039468567573 ) ) ;
#121566 = CARTESIAN_POINT ( 'NONE',  ( -9.474510206698720793, -16.51473224551083518, 24.58442372801900078 ) ) ;
#121567 = CARTESIAN_POINT ( 'NONE',  ( -18.67979575497178146, -10.72451020669898902, 76.66557627198103830 ) ) ;
#121568 = CARTESIAN_POINT ( 'NONE',  ( 4.379528057220092307, 16.55341960407617563, 102.2927570613523613 ) ) ;
#121569 = CARTESIAN_POINT ( 'NONE',  ( -5.153800228976607833, 19.02544592524334988, 97.70942372801900433 ) ) ;
#121570 = CARTESIAN_POINT ( 'NONE',  ( 16.46253265017160672, -9.564922557960803928, 43.33224293864769550 ) ) ;
#121571 = CARTESIAN_POINT ( 'NONE',  ( 5.049401038298161559, -19.05341960407611168, 92.70724293864769550 ) ) ;
#121572 = CARTESIAN_POINT ( 'NONE',  ( 21.55341960407619695, -5.719274019375665929, 56.04275706135235424 ) ) ;
#121573 = CARTESIAN_POINT ( 'NONE',  ( -13.97604488694527625, -13.89961937509977652, 51.87390960531436690 ) ) ;
#121574 = CARTESIAN_POINT ( 'NONE',  ( -17.49999999999999645, -5.499999999999992895, 84.20309617465829888 ) ) ;
#121575 = CARTESIAN_POINT ( 'NONE',  ( -4.379528057220328563, 16.55341960407611168, 80.20724293864769550 ) ) ;
#121576 = CARTESIAN_POINT ( 'NONE',  ( -5.823673210054116645, -21.52544592524344225, 77.29057627198102409 ) ) ;
#121577 = DIRECTION ( 'NONE',  ( -0.000000000000000000, -0.000000000000000000, -1.000000000000000000 ) ) ;
#121578 = CARTESIAN_POINT ( 'NONE',  ( 17.44270441346518652, -5.991230190322965221, 81.13664920735772057 ) ) ;
#121579 = CARTESIAN_POINT ( 'NONE',  ( -9.564922557961040184, 16.46253265017147172, 37.91775706135233293 ) ) ;
#121580 = CARTESIAN_POINT ( 'NONE',  ( 16.79531203550682861, -7.028104445595347194, 71.24755011779539871 ) ) ;
#121582 = CARTESIAN_POINT ( 'NONE',  ( -19.03943276465977164, 0.05219959533909376836, 91.24890960531436690 ) ) ;
#121581 = CARTESIAN_POINT ( 'NONE',  ( 19.03943276465977164, -0.05219959533909143690, 78.74890960531436690 ) ) ;
#121583 = CARTESIAN_POINT ( 'NONE',  ( 12.06949235617739724, 12.14591786802326823, 61.87609039468568284 ) ) ;
#121584 = CARTESIAN_POINT ( 'NONE',  ( -8.906447517083060816, 27.41122689804195645, 143.5999999999999943 ) ) ;
#121585 = CARTESIAN_POINT ( 'NONE',  ( -19.05341960407617563, 5.049401038297882671, 28.54275706135232937 ) ) ;
#121586 = CARTESIAN_POINT ( 'NONE',  ( 36.78370799935940028, 4.380135692641565548, 48.34576877258189143 ) ) ;
#121587 = CARTESIAN_POINT ( 'NONE',  ( 0.05219959533909260263, 19.03943276465977164, 114.9989096053143669 ) ) ;
#121588 = CARTESIAN_POINT ( 'NONE',  ( 8.314922557961029526, -14.29746914071037800, 85.41775706135236135 ) ) ;
#121589 = FACE_OUTER_BOUND ( 'NONE', #47384, .T. ) ;
#121590 = CARTESIAN_POINT ( 'NONE',  ( -16.53943276465976808, -0.05219959533934237506, 73.75109039468567573 ) ) ;
#121591 = CARTESIAN_POINT ( 'NONE',  ( -17.26172910966779739, 6.454744622555852018, 30.80646908649224258 ) ) ;
#121592 = CARTESIAN_POINT ( 'NONE',  ( -16.53943276465976808, -0.05219959533934237506, 58.75109039468568994 ) ) ;
#121593 = DIRECTION ( 'NONE',  ( -1.000000000000000000, -0.000000000000000000, -0.000000000000000000 ) ) ;
#121594 = CARTESIAN_POINT ( 'NONE',  ( -5.823673210054431948, 21.52544592524334988, 72.70942372801901854 ) ) ;
#121595 = CARTESIAN_POINT ( 'NONE',  ( -5.049401038297874678, -19.05341960407617918, 79.79275706135233293 ) ) ;
#121596 = CARTESIAN_POINT ( 'NONE',  ( 9.564922557961047289, -16.46253265017146816, 25.41775706135234003 ) ) ;
#121597 = CARTESIAN_POINT ( 'NONE',  ( 5.153800228976335163, 19.02544592524342804, 49.79057627198100988 ) ) ;
#121598 = CARTESIAN_POINT ( 'NONE',  ( 0.05219959533909260263, 19.03943276465977164, 39.99890960531436690 ) ) ;
#121599 = CARTESIAN_POINT ( 'NONE',  ( -19.88080942482812929, -34.70959879495532618, -5.862652211910081235 ) ) ;
#121600 = CARTESIAN_POINT ( 'NONE',  ( 21.52544592524344225, -5.823673210054117533, 63.54057627198103830 ) ) ;
#121601 = CARTESIAN_POINT ( 'NONE',  ( 10.72451020669898902, -18.67979575497178502, 22.91557627198102765 ) ) ;
#121602 = CARTESIAN_POINT ( 'NONE',  ( 9.564922557960805705, 16.46253265017160317, 24.58224293864769194 ) ) ;
#121603 = CARTESIAN_POINT ( 'NONE',  ( 4.379528057220092307, 16.55341960407617563, 47.29275706135234003 ) ) ;
#121604 = EDGE_LOOP ( 'NONE', ( #50547, #67559, #64532, #26832, #184289, #70621, #180071, #95804, #71080, #145094, #74688, #134640, #150834, #150466, #3012, #68861, #16908, #35991, #103023, #102608, #129725, #149795, #15254, #69892, #177577, #193253, #111683, #37737, #178353, #63094, #94729, #68185, #172093, #90223, #73211, #58491, #102024, #131534, #16429, #20200, #117675, #165718, #39736, #49800 ) ) ;
#121605 = EDGE_CURVE ( 'NONE', #60482, #144727, #179631, .T. ) ;
#121606 = CARTESIAN_POINT ( 'NONE',  ( 21.55341960407619695, -5.719274019375665929, 21.04275706135234714 ) ) ;
#121608 = CARTESIAN_POINT ( 'NONE',  ( 30.74264578624800137, -22.33583958711395212, -5.200000000000001066 ) ) ;
#121607 = CARTESIAN_POINT ( 'NONE',  ( -0.05219959533910754901, -16.53943276465976808, 57.49890960531435979 ) ) ;
#121609 = CARTESIAN_POINT ( 'NONE',  ( 19.03943276465977164, 0.05219959533936151252, 106.2510903946856615 ) ) ;
#121610 = CARTESIAN_POINT ( 'NONE',  ( 19.02544592524334988, 5.153800228976608722, 36.45942372801900433 ) ) ;
#121611 = CARTESIAN_POINT ( 'NONE',  ( 8.314922557960818139, 14.29746914071049879, 44.58224293864769550 ) ) ;
#121612 = CARTESIAN_POINT ( 'NONE',  ( 0.05219959533937995610, -21.53943276465977519, 20.00109039468568639 ) ) ;
#121614 = CARTESIAN_POINT ( 'NONE',  ( -5.719274019375978568, 21.55341960407610458, 65.20724293864768129 ) ) ;
#121613 = CARTESIAN_POINT ( 'NONE',  ( 17.44270441346512612, 5.991230190323098448, 33.86335079264229364 ) ) ;
#121615 = CARTESIAN_POINT ( 'NONE',  ( 9.564922557960805705, 16.46253265017160317, 84.58224293864769550 ) ) ;
#121616 = CARTESIAN_POINT ( 'NONE',  ( 4.483927247898545687, 16.52544592524342804, 59.79057627198103120 ) ) ;
#121617 = CARTESIAN_POINT ( 'NONE',  ( 19.05341960407611168, 5.049401038298154454, 103.9572429386476671 ) ) ;
#121618 = LINE ( 'NONE', #45784, #40896 ) ;
#121619 = CARTESIAN_POINT ( 'NONE',  ( -19.05341960407617563, 5.049401038297882671, 48.54275706135233293 ) ) ;
#121620 = CARTESIAN_POINT ( 'NONE',  ( -18.67979575497178146, -10.72451020669898902, 96.66557627198102409 ) ) ;
#121621 = CARTESIAN_POINT ( 'NONE',  ( -5.153800228976328057, -19.02544592524343514, 47.29057627198102409 ) ) ;
#121622 = CARTESIAN_POINT ( 'NONE',  ( -8.224510206698948167, 14.34966873604960824, 115.4155762719810241 ) ) ;
#121623 = CARTESIAN_POINT ( 'NONE',  ( 18.67979575497194134, -10.72451020669871369, 45.83442372801901854 ) ) ;
#121624 = CARTESIAN_POINT ( 'NONE',  ( 27.73933785331498569, 2.768321779492822058E-14, 143.8750000027311842 ) ) ;
#121625 = CARTESIAN_POINT ( 'NONE',  ( 16.52544592524342804, -4.483927247898539470, 23.54057627198102765 ) ) ;
#121626 = CARTESIAN_POINT ( 'NONE',  ( 19.03943276465977164, -0.05219959533909143690, 53.74890960531436690 ) ) ;
#121627 = CARTESIAN_POINT ( 'NONE',  ( 16.46253265017160672, -9.564922557960803928, 93.33224293864769550 ) ) ;
#121628 = CARTESIAN_POINT ( 'NONE',  ( 0.05219959533907565091, 21.53943276465977519, 69.99890960531435269 ) ) ;
#121629 = CARTESIAN_POINT ( 'NONE',  ( -8.571926809382601320, -26.38167802310801591, 141.2750000027311899 ) ) ;
#121630 = CARTESIAN_POINT ( 'NONE',  ( 13.97604488694527802, 13.89961937509977652, 39.37390960531435269 ) ) ;
#121631 = CARTESIAN_POINT ( 'NONE',  ( -15.80617190586745835, -15.72974639402198527, 46.87390960531435979 ) ) ;
#121632 = VERTEX_POINT ( 'NONE', #171329 ) ;
#121633 = CARTESIAN_POINT ( 'NONE',  ( 21.53943276465977519, 0.05219959533937863772, 86.25109039468568994 ) ) ;
#121636 = CARTESIAN_POINT ( 'NONE',  ( -16.55341960407611168, -4.379528057220339221, 71.45724293864769550 ) ) ;
#121635 = CARTESIAN_POINT ( 'NONE',  ( 12.06949235617739724, 12.14591786802326823, 81.87609039468568994 ) ) ;
#121634 = LINE ( 'NONE', #42835, #180147 ) ;
#121637 = CARTESIAN_POINT ( 'NONE',  ( -16.51473224551069308, -9.474510206698971260, 66.66557627198102409 ) ) ;
#121638 = ORIENTED_EDGE ( 'NONE', *, *, #127302, .F. ) ;
#121639 = CARTESIAN_POINT ( 'NONE',  ( -13.97604488694547697, 13.89961937509957934, 23.12609039468565442 ) ) ;
#121640 = CARTESIAN_POINT ( 'NONE',  ( 8.224510206698742110, 14.34966873604972548, 87.08442372801901854 ) ) ;
#121641 = CARTESIAN_POINT ( 'NONE',  ( -10.81492255796105439, 18.62759615963255655, 107.9177570613523471 ) ) ;
#121642 = CARTESIAN_POINT ( 'NONE',  ( 13.97604488694527802, 13.89961937509977652, 69.37390960531436690 ) ) ;
#121643 = CARTESIAN_POINT ( 'NONE',  ( -15.72974639402197994, 15.80617190586746368, 45.62390960531436690 ) ) ;
#121644 = CARTESIAN_POINT ( 'NONE',  ( 4.379528057220092307, 16.55341960407617563, 27.29275706135234358 ) ) ;
#121645 = CARTESIAN_POINT ( 'NONE',  ( 21.55341960407619695, -5.719274019375665929, 81.04275706135236135 ) ) ;
#121646 = CARTESIAN_POINT ( 'NONE',  ( 12.14591786802327356, -12.06949235617739191, 65.62609039468568994 ) ) ;
#121647 = CARTESIAN_POINT ( 'NONE',  ( 18.62759615963271287, -10.81492255796078972, 113.3322429386476955 ) ) ;
#121648 = CARTESIAN_POINT ( 'NONE',  ( -0.05219959533936034679, 19.03943276465977164, 112.5010903946856757 ) ) ;
#121649 = CARTESIAN_POINT ( 'NONE',  ( -0.05219959533909027116, -19.03943276465977164, 97.49890960531436690 ) ) ;
#121650 = CARTESIAN_POINT ( 'NONE',  ( -16.52544592524335698, -4.483927247898792601, 33.95942372801901143 ) ) ;
#121651 = CARTESIAN_POINT ( 'NONE',  ( 16.51473224551069308, 9.474510206698969483, 44.16557627198103120 ) ) ;
#121652 = VECTOR ( 'NONE', #176223, 1000.000000000000114 ) ;
#121653 = CARTESIAN_POINT ( 'NONE',  ( 16.53943276465976808, 0.05219959533934440121, 36.25109039468567573 ) ) ;
#121654 = CARTESIAN_POINT ( 'NONE',  ( 4.379528057220339221, -16.55341960407611168, 82.70724293864770971 ) ) ;
#121655 = CARTESIAN_POINT ( 'NONE',  ( -8.314922557961024197, 14.29746914071037800, 87.91775706135234714 ) ) ;
#121657 = CARTESIAN_POINT ( 'NONE',  ( -19.05341960407611168, -5.049401038298163336, 61.45724293864769550 ) ) ;
#121656 = CARTESIAN_POINT ( 'NONE',  ( -10.72451020669870658, -18.67979575497194134, 24.58442372801901499 ) ) ;
#121658 = CARTESIAN_POINT ( 'NONE',  ( -5.153800228976328057, -19.02544592524343514, 87.29057627198103830 ) ) ;
#121659 = CARTESIAN_POINT ( 'NONE',  ( -8.314922557961024197, 14.29746914071037800, 82.91775706135234714 ) ) ;
#121661 = ORIENTED_EDGE ( 'NONE', *, *, #87165, .F. ) ;
#121660 = CARTESIAN_POINT ( 'NONE',  ( -23.91168844458710652, -8.792376985860583360, 168.9858545422750353 ) ) ;
#121662 = ORIENTED_EDGE ( 'NONE', *, *, #26122, .F. ) ;
#121663 = CARTESIAN_POINT ( 'NONE',  ( -0.05219959533936034679, 19.03943276465977164, 37.50109039468567573 ) ) ;
#121664 = CARTESIAN_POINT ( 'NONE',  ( 19.05341960407611168, 5.049401038298154454, 103.9572429386476671 ) ) ;
#121665 = CARTESIAN_POINT ( 'NONE',  ( 5.153800228976335163, 19.02544592524342804, 49.79057627198100988 ) ) ;
#121667 = ORIENTED_EDGE ( 'NONE', *, *, #28410, .T. ) ;
#121666 = CARTESIAN_POINT ( 'NONE',  ( 13.89961937509977652, -13.97604488694527269, 113.1239096053143527 ) ) ;
#121668 = CARTESIAN_POINT ( 'NONE',  ( 12.14591786802327356, -12.06949235617739191, 25.62609039468567929 ) ) ;
#121670 = CARTESIAN_POINT ( 'NONE',  ( 16.52544592524335698, 4.483927247898782831, 36.45942372801901143 ) ) ;
#121669 = CARTESIAN_POINT ( 'NONE',  ( 19.05341960407617918, -5.049401038297876454, 56.04275706135234714 ) ) ;
#121671 = CARTESIAN_POINT ( 'NONE',  ( -9.564922557960796823, -16.46253265017161027, 102.0822429386477097 ) ) ;
#121672 = CARTESIAN_POINT ( 'NONE',  ( 9.564922557960805705, 16.46253265017160317, 74.58224293864769550 ) ) ;
#121673 = CARTESIAN_POINT ( 'NONE',  ( -18.67979575497178146, -10.72451020669898902, 96.66557627198102409 ) ) ;
#121674 = CARTESIAN_POINT ( 'NONE',  ( 19.03943276465977164, 0.05219959533936151252, 61.25109039468566863 ) ) ;
#121676 = CARTESIAN_POINT ( 'NONE',  ( 17.50000000000000000, -3.456093896842488800, 22.00000000000000711 ) ) ;
#121675 = CARTESIAN_POINT ( 'NONE',  ( -19.03943276465977164, 0.05219959533909376836, 96.24890960531436690 ) ) ;
#121677 = CARTESIAN_POINT ( 'NONE',  ( -16.51473224551069308, -9.474510206698971260, 66.66557627198102409 ) ) ;
#121679 = CARTESIAN_POINT ( 'NONE',  ( 19.05341960407611168, 5.049401038298154454, 28.95724293864769550 ) ) ;
#121678 = CARTESIAN_POINT ( 'NONE',  ( -16.55341960407611168, -4.379528057220339221, 31.45724293864769550 ) ) ;
#121680 = CARTESIAN_POINT ( 'NONE',  ( 5.153800228976615827, -19.02544592524334988, 40.20942372801898301 ) ) ;
#121681 = CARTESIAN_POINT ( 'NONE',  ( 14.34966873604960469, 8.224510206698951720, 79.16557627198103830 ) ) ;
#121682 = CARTESIAN_POINT ( 'NONE',  ( 5.823673210054444382, -21.52544592524334988, 100.2094237280190043 ) ) ;
#121683 = CARTESIAN_POINT ( 'NONE',  ( 13.89961937509977652, -13.97604488694527269, 33.12390960531434558 ) ) ;
#121684 = CARTESIAN_POINT ( 'NONE',  ( 16.53943276465976808, 0.05219959533934440121, 56.25109039468568284 ) ) ;
#121686 = CARTESIAN_POINT ( 'NONE',  ( -15.80617190586768217, 15.72974639402176855, 98.12609039468570415 ) ) ;
#121685 = CARTESIAN_POINT ( 'NONE',  ( 14.34966873604960469, 8.224510206698951720, 34.16557627198102409 ) ) ;
#121687 = CARTESIAN_POINT ( 'NONE',  ( -13.89961937509977652, 13.97604488694528158, 90.62390960531432427 ) ) ;
#121688 = CARTESIAN_POINT ( 'NONE',  ( -16.46253265017160317, 9.564922557960807481, 95.83224293864769550 ) ) ;
#121689 = CARTESIAN_POINT ( 'NONE',  ( -4.483927247898539470, -16.52544592524342804, 102.2905762719810383 ) ) ;
#121690 = CARTESIAN_POINT ( 'NONE',  ( 16.55341960407611168, 4.379528057220329451, 68.95724293864769550 ) ) ;
#121691 = CARTESIAN_POINT ( 'NONE',  ( 21.52544592524344225, -5.823673210054117533, 78.54057627198103830 ) ) ;
#121692 = CARTESIAN_POINT ( 'NONE',  ( 9.564922557960805705, 16.46253265017160317, 84.58224293864769550 ) ) ;
#121693 = CARTESIAN_POINT ( 'NONE',  ( 15.80617190586746368, 15.72974639402197994, 99.37390960531436690 ) ) ;
#121694 = CARTESIAN_POINT ( 'NONE',  ( -16.51473224551069308, -9.474510206698971260, 96.66557627198102409 ) ) ;
#121696 = CARTESIAN_POINT ( 'NONE',  ( 16.53943276465976808, -0.05219959533910856209, 88.74890960531436690 ) ) ;
#121695 = CARTESIAN_POINT ( 'NONE',  ( 19.49149378614658090, -5.499999999999770850, 46.93757513605363130 ) ) ;
#121698 = CARTESIAN_POINT ( 'NONE',  ( -9.564922557960796823, -16.46253265017161027, 62.08224293864769550 ) ) ;
#121697 = CIRCLE ( 'NONE', #34532, 59.99999999999998579 ) ;
#121699 = CARTESIAN_POINT ( 'NONE',  ( 18.67979575497178502, 10.72451020669898547, 69.16557627198102409 ) ) ;
#121700 = CARTESIAN_POINT ( 'NONE',  ( 17.50000000000000000, -5.500000000000000888, 28.29690382534172244 ) ) ;
#121702 =( NAMED_UNIT ( * ) SI_UNIT ( $, .STERADIAN. ) SOLID_ANGLE_UNIT ( ) );
#121701 = CARTESIAN_POINT ( 'NONE',  ( 14.29746914071049879, -8.314922557960816363, 23.33224293864769194 ) ) ;
#121703 = CARTESIAN_POINT ( 'NONE',  ( 13.89961937509957401, 13.97604488694547697, 111.8760903946856757 ) ) ;
#121704 = EDGE_CURVE ( 'NONE', #23056, #69916, #42106, .T. ) ;
#121705 = CARTESIAN_POINT ( 'NONE',  ( 14.29746914071049879, -8.314922557960816363, 83.33224293864769550 ) ) ;
#121706 = CARTESIAN_POINT ( 'NONE',  ( -17.40805194822031865, -6.112264579159342404, 94.16628727489391792 ) ) ;
#121707 = CARTESIAN_POINT ( 'NONE',  ( 0.05219959533909260263, 19.03943276465977164, 74.99890960531435269 ) ) ;
#121708 = CARTESIAN_POINT ( 'NONE',  ( 13.97604488694527802, 13.89961937509977652, 44.37390960531435269 ) ) ;
#121709 = CARTESIAN_POINT ( 'NONE',  ( -16.52544592524342804, 4.483927247898546575, 61.04057627198103120 ) ) ;
#121710 = CARTESIAN_POINT ( 'NONE',  ( 16.51473224551069308, 9.474510206698969483, 109.1655762719810383 ) ) ;
#121711 = CARTESIAN_POINT ( 'NONE',  ( -13.89961937509957401, -13.97604488694547875, 104.3760903946856757 ) ) ;
#121712 = CARTESIAN_POINT ( 'NONE',  ( 16.46253265017160672, -9.564922557960803928, 98.33224293864769550 ) ) ;
#121713 = CARTESIAN_POINT ( 'NONE',  ( 10.81492255796078972, 18.62759615963270932, 74.58224293864768129 ) ) ;
#121714 = CARTESIAN_POINT ( 'NONE',  ( -4.483927247898782831, 16.52544592524335698, 72.70942372801901854 ) ) ;
#121715 = CARTESIAN_POINT ( 'NONE',  ( -17.05116617787849975, 6.768360034955466453, 93.65675553259190167 ) ) ;
#121716 = CARTESIAN_POINT ( 'NONE',  ( -9.474510206698964154, 16.51473224551069663, 70.41557627198102409 ) ) ;
#121717 = CARTESIAN_POINT ( 'NONE',  ( 18.62759615963271287, -10.81492255796078972, 78.33224293864770971 ) ) ;
#121718 =( BOUNDED_SURFACE ( )  B_SPLINE_SURFACE ( 3, 2, ( 
 ( #30571, #57943, #181297 ),
 ( #166121, #89262, #150954 ),
 ( #12448, #74110, #135780 ),
 ( #136749, #4186, #174067 ),
 ( #5182, #1204, #48729 ),
 ( #97183, #94214, #156900 ),
 ( #112375, #95214, #128526 ),
 ( #18396, #66863, #3206 ),
 ( #110383, #127537, #20358 ),
 ( #186259, #126541, #172065 ),
 ( #80047, #81031, #190220 ),
 ( #108398, #33552, #158869 ),
 ( #47737, #173068, #17391 ),
 ( #50717, #170075, #31566 ),
 ( #109390, #155893, #82006 ),
 ( #140721, #34545, #189239 ),
 ( #96204, #141716, #65865 ),
 ( #62881, #19382, #124562 ),
 ( #64880, #187260, #188240 ),
 ( #157893, #2211, #93217 ),
 ( #35536, #49715, #125563 ),
 ( #111380, #154902, #142707 ),
 ( #16401, #143700, #78047 ),
 ( #139716, #171070, #32560 ) ),
 .UNSPECIFIED., .F., .F., .F. ) 
 B_SPLINE_SURFACE_WITH_KNOTS ( ( 4, 2, 2, 2, 2, 2, 2, 2, 2, 2, 2, 4 ),
 ( 3, 3 ),
 ( 0.000000000000000000, 0.001899702839891691426, 0.002849554259837537139, 0.003799405679783382853, 0.005699108519675074279, 0.006648959939620920426, 0.007598811359566765705, 0.008548662779512610985, 0.009498514199458456264, 0.01139821703935014856, 0.01329791987924184085, 0.01519762271913353141 ),
 ( 0.000000000000000000, 1.000000000000000000 ),
 .UNSPECIFIED. ) 
 GEOMETRIC_REPRESENTATION_ITEM ( )  RATIONAL_B_SPLINE_SURFACE ( (
 ( 1.000000000000000000, 0.7660444431189777914, 1.000000000000000000),
 ( 1.000000000000000000, 0.7753720600381861505, 1.000000000000000000),
 ( 1.000000000000000000, 0.7832595754286625356, 1.000000000000000000),
 ( 1.000000000000000000, 0.7928595458705119947, 1.000000000000000000),
 ( 1.000000000000000000, 0.7956872332516093937, 1.000000000000000000),
 ( 1.000000000000000000, 0.8005750596157590326, 1.000000000000000000),
 ( 1.000000000000000000, 0.8026302056541338992, 1.000000000000000000),
 ( 1.000000000000000000, 0.8075080643849141815, 1.000000000000000000),
 ( 1.000000000000000000, 0.8091143015809389993, 1.000000000000000000),
 ( 1.000000000000000000, 0.8093067629633259319, 1.000000000000000000),
 ( 1.000000000000000000, 0.8089952915731264405, 1.000000000000000000),
 ( 1.000000000000000000, 0.8076919994862710173, 1.000000000000000000),
 ( 1.000000000000000000, 0.8067078407648710092, 1.000000000000000000),
 ( 1.000000000000000000, 0.8041786842467625318, 1.000000000000000000),
 ( 1.000000000000000000, 0.8026334674876911546, 1.000000000000000000),
 ( 1.000000000000000000, 0.7990747329469507498, 1.000000000000000000),
 ( 1.000000000000000000, 0.7970509760941782984, 1.000000000000000000),
 ( 1.000000000000000000, 0.7904793850863390814, 1.000000000000000000),
 ( 1.000000000000000000, 0.7855040224314148167, 1.000000000000000000),
 ( 1.000000000000000000, 0.7751942650507165355, 1.000000000000000000),
 ( 1.000000000000000000, 0.7698260778210667121, 1.000000000000000000),
 ( 1.000000000000000000, 0.7598259884961829913, 1.000000000000000000),
 ( 1.000000000000000000, 0.7551428682219649691, 1.000000000000000000),
 ( 1.000000000000000000, 0.7510191126010862250, 1.000000000000000000) ) ) 
 REPRESENTATION_ITEM ( '' )  SURFACE ( )  );
#121719 = CARTESIAN_POINT ( 'NONE',  ( 13.89961937509957401, 13.97604488694547697, 111.8760903946856757 ) ) ;
#121721 = CARTESIAN_POINT ( 'NONE',  ( -10.72451020669870658, -18.67979575497194134, 59.58442372801901854 ) ) ;
#121720 = CARTESIAN_POINT ( 'NONE',  ( -0.05219959533910754901, -16.53943276465976808, 42.49890960531435979 ) ) ;
#121723 = CARTESIAN_POINT ( 'NONE',  ( -16.51473224551069308, -9.474510206698971260, 111.6655762719810383 ) ) ;
#121722 = CARTESIAN_POINT ( 'NONE',  ( -16.53943276465976808, -0.05219959533934237506, 88.75109039468567573 ) ) ;
#121724 = CARTESIAN_POINT ( 'NONE',  ( 9.474510206698971260, -16.51473224551069308, 107.9155762719810383 ) ) ;
#121725 = CARTESIAN_POINT ( 'NONE',  ( 2.200000000000000622, 0.000000000000000000, 0.000000000000000000 ) ) ;
#121726 = CARTESIAN_POINT ( 'NONE',  ( -16.52544592524335698, -4.483927247898792601, 88.95942372801901854 ) ) ;
#121727 = CARTESIAN_POINT ( 'NONE',  ( 16.53943276465976808, 0.05219959533934440121, 41.25109039468568284 ) ) ;
#121728 = CARTESIAN_POINT ( 'NONE',  ( 16.51473224551069308, 9.474510206698969483, 64.16557627198102409 ) ) ;
#121729 = CARTESIAN_POINT ( 'NONE',  ( 9.564922557960805705, 16.46253265017160317, 79.58224293864769550 ) ) ;
#121730 = CARTESIAN_POINT ( 'NONE',  ( 10.72451020669871369, 18.67979575497193778, 72.08442372801899012 ) ) ;
#121731 = CARTESIAN_POINT ( 'NONE',  ( -16.53943276465976808, -0.05219959533934237506, 68.75109039468568994 ) ) ;
#121732 = CARTESIAN_POINT ( 'NONE',  ( 0.05219959533910956823, 16.53943276465976808, 29.99890960531435979 ) ) ;
#121733 = CARTESIAN_POINT ( 'NONE',  ( 5.049401038298161559, -19.05341960407611168, 42.70724293864767418 ) ) ;
#121734 = CARTESIAN_POINT ( 'NONE',  ( 19.05341960407611168, 5.049401038298154454, 48.95724293864768129 ) ) ;
#121735 = CARTESIAN_POINT ( 'NONE',  ( 16.52544592524335698, 4.483927247898782831, 46.45942372801901854 ) ) ;
#121736 = CARTESIAN_POINT ( 'NONE',  ( -0.05219959533936034679, 19.03943276465977164, 97.50109039468567573 ) ) ;
#121737 = CARTESIAN_POINT ( 'NONE',  ( 4.483927247898545687, 16.52544592524342804, 99.79057627198103830 ) ) ;
#121738 = CARTESIAN_POINT ( 'NONE',  ( 0.05219959533909260263, 19.03943276465977164, 64.99890960531436690 ) ) ;
#121740 = DIRECTION ( 'NONE',  ( 0.000000000000000000, 0.000000000000000000, 1.000000000000000000 ) ) ;
#121739 = CARTESIAN_POINT ( 'NONE',  ( 9.474510206698729675, 16.51473224551082808, 87.08442372801900433 ) ) ;
#121741 = CARTESIAN_POINT ( 'NONE',  ( -18.67979575497193778, 10.72451020669871902, 88.33442372801901854 ) ) ;
#121742 = CARTESIAN_POINT ( 'NONE',  ( 14.34966873604972726, -8.224510206698740333, 60.83442372801901854 ) ) ;
#121743 = CARTESIAN_POINT ( 'NONE',  ( -193.3062444957834884, -155.7167183371838064, -15.00000000000000178 ) ) ;
#121744 = CARTESIAN_POINT ( 'NONE',  ( 18.67979575497178502, 10.72451020669898547, 44.16557627198103120 ) ) ;
#121745 = CARTESIAN_POINT ( 'NONE',  ( 4.483927247898790824, -16.52544592524335698, 45.20942372801901854 ) ) ;
#121746 = CARTESIAN_POINT ( 'NONE',  ( -19.52217212775661537, 5.499999999999920064, 69.93993709005260939 ) ) ;
#121747 = CARTESIAN_POINT ( 'NONE',  ( -19.03943276465977164, -0.05219959533935918106, 43.75109039468566863 ) ) ;
#121748 = CARTESIAN_POINT ( 'NONE',  ( -13.89961937509977652, 13.97604488694528158, 85.62390960531433848 ) ) ;
#121749 = CARTESIAN_POINT ( 'NONE',  ( 0.05219959533909260263, 19.03943276465977164, 24.99890960531435269 ) ) ;
#121750 = CARTESIAN_POINT ( 'NONE',  ( 16.46253265017160672, -9.564922557960803928, 58.33224293864769550 ) ) ;
#121751 = DIRECTION ( 'NONE',  ( 1.000000000000000000, 1.776356839400250465E-15, 0.000000000000000000 ) ) ;
#121752 = CARTESIAN_POINT ( 'NONE',  ( 0.05219959533937995610, -21.53943276465977519, 75.00109039468568994 ) ) ;
#121753 = FACE_OUTER_BOUND ( 'NONE', #193218, .T. ) ;
#121754 = CARTESIAN_POINT ( 'NONE',  ( 16.46253265017146816, 9.564922557961045513, 31.66775706135232937 ) ) ;
#121755 = CARTESIAN_POINT ( 'NONE',  ( -15.72974639402176322, -15.80617190586768395, 109.3760903946857042 ) ) ;
#121756 = CARTESIAN_POINT ( 'NONE',  ( 14.29746914071049879, -8.314922557960816363, 48.33224293864770260 ) ) ;
#121757 = CARTESIAN_POINT ( 'NONE',  ( -9.564922557960796823, -16.46253265017161027, 52.08224293864768839 ) ) ;
#121758 = CARTESIAN_POINT ( 'NONE',  ( -5.049401038298153566, 19.05341960407611168, 115.2072429386477097 ) ) ;
#121759 = CARTESIAN_POINT ( 'NONE',  ( -15.80617190586768217, 15.72974639402176855, 88.12609039468570415 ) ) ;
#121760 = CARTESIAN_POINT ( 'NONE',  ( -19.05341960407611168, -5.049401038298163336, 61.45724293864769550 ) ) ;
#121761 = CARTESIAN_POINT ( 'NONE',  ( 5.823673210054444382, -21.52544592524334988, 75.20942372801901854 ) ) ;
#121762 = CARTESIAN_POINT ( 'NONE',  ( -0.05219959533907301413, -21.53943276465977519, 37.49890960531436690 ) ) ;
#121763 = CARTESIAN_POINT ( 'NONE',  ( 10.81492255796106328, -18.62759615963255655, 40.41775706135234714 ) ) ;
#121764 = CARTESIAN_POINT ( 'NONE',  ( -9.474510206698720793, -16.51473224551083518, 64.58442372801900433 ) ) ;
#121765 = CARTESIAN_POINT ( 'NONE',  ( -9.564922557960796823, -16.46253265017161027, 32.08224293864769550 ) ) ;
#121766 = CARTESIAN_POINT ( 'NONE',  ( 13.97604488694527802, 13.89961937509977652, 79.37390960531435269 ) ) ;
#121767 = CARTESIAN_POINT ( 'NONE',  ( 8.314922557961029526, -14.29746914071037800, 35.41775706135234003 ) ) ;
#121768 = CARTESIAN_POINT ( 'NONE',  ( 12.06949235617757843, -12.14591786802309237, 93.12390960531436690 ) ) ;
#121769 = CARTESIAN_POINT ( 'NONE',  ( -0.05219959533909027116, -19.03943276465977164, 57.49890960531435979 ) ) ;
#121770 = CARTESIAN_POINT ( 'NONE',  ( -5.823673210054116645, -21.52544592524344225, 42.29057627198103120 ) ) ;
#121771 = CARTESIAN_POINT ( 'NONE',  ( -16.52544592524335698, -4.483927247898792601, 23.95942372801901143 ) ) ;
#121772 = CARTESIAN_POINT ( 'NONE',  ( -5.719274019375665041, -21.55341960407619695, 19.79275706135235069 ) ) ;
#121773 = CARTESIAN_POINT ( 'NONE',  ( -21.55341960407619339, 5.719274019375674811, 68.54275706135234714 ) ) ;
#121774 = CARTESIAN_POINT ( 'NONE',  ( -4.483927247898782831, 16.52544592524335698, 67.70942372801901854 ) ) ;
#121775 = CARTESIAN_POINT ( 'NONE',  ( 8.224510206698742110, 14.34966873604972548, 72.08442372801899012 ) ) ;
#121776 = ORIENTED_EDGE ( 'NONE', *, *, #163633, .F. ) ;
#121777 = CARTESIAN_POINT ( 'NONE',  ( 19.03943276465977164, -0.05219959533909143690, 63.74890960531435979 ) ) ;
#121778 = CARTESIAN_POINT ( 'NONE',  ( 16.53943276465976808, 0.05219959533934440121, 86.25109039468568994 ) ) ;
#121779 = CARTESIAN_POINT ( 'NONE',  ( 13.89961937509957401, 13.97604488694547697, 36.87609039468565442 ) ) ;
#121780 = CARTESIAN_POINT ( 'NONE',  ( -21.52544592524343514, 5.823673210054127303, 116.0405762719810383 ) ) ;
#121781 = CARTESIAN_POINT ( 'NONE',  ( -16.55341960407611168, -4.379528057220339221, 71.45724293864769550 ) ) ;
#121782 = CARTESIAN_POINT ( 'NONE',  ( 0.05219959533909260263, 19.03943276465977164, 84.99890960531436690 ) ) ;
#121783 = CARTESIAN_POINT ( 'NONE',  ( -4.483927247898782831, 16.52544592524335698, 87.70942372801901854 ) ) ;
#121784 = CARTESIAN_POINT ( 'NONE',  ( 18.67979575497194134, -10.72451020669871369, 55.83442372801901854 ) ) ;
#121785 = CARTESIAN_POINT ( 'NONE',  ( 4.483927247898790824, -16.52544592524335698, 30.20942372801902565 ) ) ;
#121786 = CARTESIAN_POINT ( 'NONE',  ( 10.72451020669898902, -18.67979575497178502, 112.9155762719810383 ) ) ;
#121787 = CARTESIAN_POINT ( 'NONE',  ( -14.29746914071049879, 8.314922557960819915, 60.83224293864769550 ) ) ;
#121788 = ORIENTED_EDGE ( 'NONE', *, *, #50162, .T. ) ;
#121789 = CARTESIAN_POINT ( 'NONE',  ( -5.719274019375978568, 21.55341960407610458, 105.2072429386477097 ) ) ;
#121790 = CARTESIAN_POINT ( 'NONE',  ( -14.29746914071049879, 8.314922557960819915, 40.83224293864769550 ) ) ;
#121791 = ORIENTED_EDGE ( 'NONE', *, *, #127587, .T. ) ;
#121792 = CARTESIAN_POINT ( 'NONE',  ( 34.80630918731041845, 6.717782050307409492, 41.65621224074541828 ) ) ;
#121793 = CARTESIAN_POINT ( 'NONE',  ( 13.89961937509977652, -13.97604488694527269, 113.1239096053143527 ) ) ;
#121794 = CARTESIAN_POINT ( 'NONE',  ( 18.62759615963255655, 10.81492255796105972, 36.66775706135234714 ) ) ;
#121795 = CARTESIAN_POINT ( 'NONE',  ( -16.55341960407611168, -4.379528057220339221, 56.45724293864768839 ) ) ;
#121796 = AXIS2_PLACEMENT_3D ( 'NONE', #56945, #99426, #130763 ) ;
#121797 = CARTESIAN_POINT ( 'NONE',  ( 9.474510206698971260, -16.51473224551069308, 67.91557627198102409 ) ) ;
#121798 = CARTESIAN_POINT ( 'NONE',  ( 19.05341960407617918, -5.049401038297876454, 71.04275706135234714 ) ) ;
#121799 = CARTESIAN_POINT ( 'NONE',  ( 16.46253265017160672, -9.564922557960803928, 93.33224293864769550 ) ) ;
#121800 = CARTESIAN_POINT ( 'NONE',  ( -15.80617190586745835, -15.72974639402198527, 46.87390960531435979 ) ) ;
#121801 = CARTESIAN_POINT ( 'NONE',  ( -12.97112549081923660, -41.39484261838730816, -20.61933656601500076 ) ) ;
#121802 = CARTESIAN_POINT ( 'NONE',  ( 13.97604488694527802, 13.89961937509977652, 54.37390960531435979 ) ) ;
#121803 = CARTESIAN_POINT ( 'NONE',  ( 8.224510206698742110, 14.34966873604972548, 42.08442372801901854 ) ) ;
#121804 = CARTESIAN_POINT ( 'NONE',  ( -18.62759615963255300, -10.81492255796106328, 24.16775706135235424 ) ) ;
#121805 = CARTESIAN_POINT ( 'NONE',  ( 12.06949235617757843, -12.14591786802309237, 48.12390960531436690 ) ) ;
#121806 = CARTESIAN_POINT ( 'NONE',  ( -5.153800228976328057, -19.02544592524343514, 87.29057627198103830 ) ) ;
#121807 = CARTESIAN_POINT ( 'NONE',  ( -10.81492255796078084, -18.62759615963271287, 67.08224293864770971 ) ) ;
#121809 = CARTESIAN_POINT ( 'NONE',  ( -12.06949235617739369, -12.14591786802326823, 39.37609039468567573 ) ) ;
#121808 = CARTESIAN_POINT ( 'NONE',  ( -5.719274019375978568, 21.55341960407610458, 105.2072429386477097 ) ) ;
#121810 = EDGE_CURVE ( 'NONE', #99783, #113699, #65, .T. ) ;
#121811 = CARTESIAN_POINT ( 'NONE',  ( -15.72974639402197994, 15.80617190586746368, 40.62390960531435269 ) ) ;
#121812 = CARTESIAN_POINT ( 'NONE',  ( 15.80617190586769283, -15.72974639402175789, 100.6260903946857184 ) ) ;
#121813 = CARTESIAN_POINT ( 'NONE',  ( 19.05341960407611168, 5.049401038298154454, 103.9572429386476671 ) ) ;
#121814 = CARTESIAN_POINT ( 'NONE',  ( 19.03943276465977164, -0.05219959533909143690, 38.74890960531436690 ) ) ;
#121815 = CARTESIAN_POINT ( 'NONE',  ( -19.02544592524342804, 5.153800228976336051, 96.04057627198103830 ) ) ;
#121816 = CARTESIAN_POINT ( 'NONE',  ( -16.51473224551069308, -9.474510206698971260, 81.66557627198103830 ) ) ;
#121817 = CARTESIAN_POINT ( 'NONE',  ( -6.613545406318515951, -46.94410406412049497, -22.68594355512400540 ) ) ;
#121818 = CARTESIAN_POINT ( 'NONE',  ( 9.564922557961047289, -16.46253265017146816, 60.41775706135233293 ) ) ;
#121819 = AXIS2_PLACEMENT_3D ( 'NONE', #69876, #158875, #66869 ) ;
#121821 = CARTESIAN_POINT ( 'NONE',  ( -21.55341960407610458, -5.719274019375992779, 36.45724293864768839 ) ) ;
#121820 = CARTESIAN_POINT ( 'NONE',  ( 9.474510206698729675, 16.51473224551082808, 22.08442372801899722 ) ) ;
#121823 = ADVANCED_FACE ( 'NONE', ( #101441 ), #193476, .T. ) ;
#121822 = CARTESIAN_POINT ( 'NONE',  ( 4.483927247898790824, -16.52544592524335698, 105.2094237280190328 ) ) ;
#121824 = CARTESIAN_POINT ( 'NONE',  ( -17.40805194822032220, 6.112264579159342404, 60.83371272510612471 ) ) ;
#121825 = CARTESIAN_POINT ( 'NONE',  ( -19.05341960407617563, 5.049401038297882671, 88.54275706135230450 ) ) ;
#121826 = CARTESIAN_POINT ( 'NONE',  ( -5.049401038297874678, -19.05341960407617918, 29.79275706135232227 ) ) ;
#121827 = CARTESIAN_POINT ( 'NONE',  ( 37.99999999999999289, 2.428612866367529932E-14, -25.00000000000000000 ) ) ;
#121828 = CARTESIAN_POINT ( 'NONE',  ( -16.51473224551069308, -9.474510206698971260, 36.66557627198102409 ) ) ;
#121829 = CARTESIAN_POINT ( 'NONE',  ( 16.52544592524342804, -4.483927247898539470, 43.54057627198103830 ) ) ;
#121830 = CARTESIAN_POINT ( 'NONE',  ( -16.38665767535053774, -7.295008042176102769, 109.7359913578545303 ) ) ;
#121831 = CARTESIAN_POINT ( 'NONE',  ( -12.06949235617756955, 12.14591786802309770, 25.62390960531435624 ) ) ;
#121832 = CARTESIAN_POINT ( 'NONE',  ( 20.99598008017551365, -20.07891204798916007, -52.49574298665344685 ) ) ;
#121833 = CARTESIAN_POINT ( 'NONE',  ( 4.483927247898790824, -16.52544592524335698, 90.20942372801903275 ) ) ;
#121834 = CARTESIAN_POINT ( 'NONE',  ( -19.05341960407611168, -5.049401038298163336, 51.45724293864770260 ) ) ;
#121835 = CARTESIAN_POINT ( 'NONE',  ( -15.72974639402176322, -15.80617190586768395, 104.3760903946856899 ) ) ;
#121836 = CARTESIAN_POINT ( 'NONE',  ( -13.89961937509957401, -13.97604488694547875, 109.3760903946856331 ) ) ;
#121837 = CARTESIAN_POINT ( 'NONE',  ( 21.53943276465977519, 0.05219959533937863772, 91.25109039468568994 ) ) ;
#121838 = CARTESIAN_POINT ( 'NONE',  ( 9.474510206698729675, 16.51473224551082808, 62.08442372801899722 ) ) ;
#121839 = CARTESIAN_POINT ( 'NONE',  ( -13.89961937509977652, 13.97604488694528158, 90.62390960531432427 ) ) ;
#121840 = CARTESIAN_POINT ( 'NONE',  ( 19.03943276465977164, -0.05219959533909143690, 83.74890960531436690 ) ) ;
#121841 = CARTESIAN_POINT ( 'NONE',  ( -29.86685920354755552, 21.69954338932564397, -6.824999997268814234 ) ) ;
#121842 = CARTESIAN_POINT ( 'NONE',  ( 0.05219959533907565091, 21.53943276465977519, 109.9989096053143527 ) ) ;
#121843 = AXIS2_PLACEMENT_3D ( 'NONE', #134283, #70606, #58423 ) ;
#121844 = CARTESIAN_POINT ( 'NONE',  ( -12.14591786802309592, -12.06949235617757132, 81.87390960531435269 ) ) ;
#121845 = CARTESIAN_POINT ( 'NONE',  ( 10.72451020669898902, -18.67979575497178502, 57.91557627198103120 ) ) ;
#121846 = CARTESIAN_POINT ( 'NONE',  ( 19.05341960407611168, 5.049401038298154454, 58.95724293864768129 ) ) ;
#121848 = CARTESIAN_POINT ( 'NONE',  ( 4.379528057220092307, 16.55341960407617563, 92.29275706135236135 ) ) ;
#121847 = CARTESIAN_POINT ( 'NONE',  ( 10.81492255796078972, 18.62759615963270932, 94.58224293864769550 ) ) ;
#121849 = ORIENTED_EDGE ( 'NONE', *, *, #148013, .F. ) ;
#121850 = CARTESIAN_POINT ( 'NONE',  ( 19.05341960407611168, 5.049401038298154454, 58.95724293864768129 ) ) ;
#121851 = EDGE_CURVE ( 'NONE', #122599, #68306, #129233, .T. ) ;
#121853 = CARTESIAN_POINT ( 'NONE',  ( 15.50000000000000178, -7.500000000000000888, 118.0000000000000142 ) ) ;
#121852 = CARTESIAN_POINT ( 'NONE',  ( -12.06949235617756955, 12.14591786802309770, 95.62390960531436690 ) ) ;
#121854 = CARTESIAN_POINT ( 'NONE',  ( -19.05341960407611168, -5.049401038298163336, 56.45724293864768129 ) ) ;
#121855 = CARTESIAN_POINT ( 'NONE',  ( 13.97604488694548053, -13.89961937509957401, 80.62609039468567573 ) ) ;
#121856 = CARTESIAN_POINT ( 'NONE',  ( 12.06949235617757843, -12.14591786802309237, 83.12390960531436690 ) ) ;
#121857 = CARTESIAN_POINT ( 'NONE',  ( -0.05219959533937732626, 21.53943276465977519, 57.50109039468568994 ) ) ;
#121859 = CARTESIAN_POINT ( 'NONE',  ( 21.55341960407610458, 5.719274019375980345, 98.95724293864770971 ) ) ;
#121858 = CARTESIAN_POINT ( 'NONE',  ( -16.46253265017160317, 9.564922557960807481, 30.83224293864769550 ) ) ;
#121860 = CARTESIAN_POINT ( 'NONE',  ( -8.314922557960811034, -14.29746914071050412, 102.0822429386476955 ) ) ;
#121861 = CARTESIAN_POINT ( 'NONE',  ( 18.22780087662122384, 5.500000000000018652, 93.98459894673892734 ) ) ;
#121862 = CARTESIAN_POINT ( 'NONE',  ( -5.049401038298153566, 19.05341960407611168, 60.20724293864768129 ) ) ;
#121863 = CARTESIAN_POINT ( 'NONE',  ( -11.80868324581545714, -11.80868324581525997, -61.34707691135562868 ) ) ;
#121865 = CARTESIAN_POINT ( 'NONE',  ( -19.02544592524342804, 5.153800228976336051, 106.0405762719810241 ) ) ;
#121864 = CARTESIAN_POINT ( 'NONE',  ( 16.46253265017146816, 9.564922557961045513, 96.66775706135233293 ) ) ;
#121866 = CARTESIAN_POINT ( 'NONE',  ( 21.53943276465977519, 0.05219959533937863772, 56.25109039468568284 ) ) ;
#121867 = CARTESIAN_POINT ( 'NONE',  ( 5.049401038298161559, -19.05341960407611168, 87.70724293864769550 ) ) ;
#121868 = CARTESIAN_POINT ( 'NONE',  ( 19.05341960407617918, -5.049401038297876454, 71.04275706135234714 ) ) ;
#121869 = CARTESIAN_POINT ( 'NONE',  ( -13.97604488694527625, -13.89961937509977652, 61.87390960531435979 ) ) ;
#121870 = CARTESIAN_POINT ( 'NONE',  ( -14.34966873604960291, -8.224510206698953496, 81.66557627198103830 ) ) ;
#121871 = CARTESIAN_POINT ( 'NONE',  ( 4.483927247898545687, 16.52544592524342804, 64.79057627198103830 ) ) ;
#121872 = CARTESIAN_POINT ( 'NONE',  ( -5.049401038298153566, 19.05341960407611168, 95.20724293864770971 ) ) ;
#121873 = CARTESIAN_POINT ( 'NONE',  ( -8.314922557960811034, -14.29746914071050412, 82.08224293864768129 ) ) ;
#121874 = CARTESIAN_POINT ( 'NONE',  ( 0.05219959533909260263, 19.03943276465977164, 79.99890960531436690 ) ) ;
#121875 = CARTESIAN_POINT ( 'NONE',  ( -19.03943276465977164, -0.05219959533935918106, 28.75109039468566507 ) ) ;
#121878 = CARTESIAN_POINT ( 'NONE',  ( -16.53943276465976808, 0.05219959533911058130, 106.2489096053143811 ) ) ;
#121877 = CARTESIAN_POINT ( 'NONE',  ( 8.224510206698953496, -14.34966873604960469, 32.91557627198102409 ) ) ;
#121876 = CARTESIAN_POINT ( 'NONE',  ( 5.153800228976335163, 19.02544592524342804, 49.79057627198100988 ) ) ;
#121879 = ORIENTED_EDGE ( 'NONE', *, *, #183827, .F. ) ;
#121880 = CARTESIAN_POINT ( 'NONE',  ( -21.55341960407619339, 5.719274019375674811, 38.54275706135234714 ) ) ;
#121881 = CARTESIAN_POINT ( 'NONE',  ( -5.153800228976607833, 19.02544592524334988, 67.70942372801900433 ) ) ;
#121882 = CARTESIAN_POINT ( 'NONE',  ( 0.05219959533910956823, 16.53943276465976808, 39.99890960531436690 ) ) ;
#121883 = CARTESIAN_POINT ( 'NONE',  ( 10.81492255796078972, 18.62759615963270932, 79.58224293864769550 ) ) ;
#121884 = CARTESIAN_POINT ( 'NONE',  ( 5.719274019375991003, -21.55341960407610458, 22.70724293864769194 ) ) ;
#121885 = CARTESIAN_POINT ( 'NONE',  ( 4.379528057220339221, -16.55341960407611168, 72.70724293864769550 ) ) ;
#121886 = CARTESIAN_POINT ( 'NONE',  ( 16.51473224551069308, 9.474510206698969483, 39.16557627198103120 ) ) ;
#121887 = CARTESIAN_POINT ( 'NONE',  ( -13.97604488694547697, 13.89961937509957934, 43.12609039468566152 ) ) ;
#121888 = CARTESIAN_POINT ( 'NONE',  ( 8.314922557961029526, -14.29746914071037800, 100.4177570613523471 ) ) ;
#121889 = CARTESIAN_POINT ( 'NONE',  ( 8.314922557961029526, -14.29746914071037800, 60.41775706135235424 ) ) ;
#121890 = CARTESIAN_POINT ( 'NONE',  ( -21.55341960407610458, -5.719274019375992779, 31.45724293864769550 ) ) ;
#121891 = CARTESIAN_POINT ( 'NONE',  ( -21.52544592524334988, -5.823673210054445271, 103.9594237280190185 ) ) ;
#121892 = CARTESIAN_POINT ( 'NONE',  ( 16.46253265017160672, -9.564922557960803928, 88.33224293864769550 ) ) ;
#121893 = CARTESIAN_POINT ( 'NONE',  ( 0.05219959533934541429, -16.53943276465976808, 80.00109039468568994 ) ) ;
#121894 = CARTESIAN_POINT ( 'NONE',  ( 9.474510206698971260, -16.51473224551069308, 27.91557627198103120 ) ) ;
#121895 = CARTESIAN_POINT ( 'NONE',  ( 0.05219959533910956823, 16.53943276465976808, 34.99890960531435979 ) ) ;
#121897 = CARTESIAN_POINT ( 'NONE',  ( -13.89961937509977652, 13.97604488694528158, 95.62390960531436690 ) ) ;
#121896 = CARTESIAN_POINT ( 'NONE',  ( -19.03943276465977164, 0.05219959533909376836, 111.2489096053143669 ) ) ;
#121898 = CARTESIAN_POINT ( 'NONE',  ( 5.823673210054125526, 21.52544592524343514, 24.79057627198103120 ) ) ;
#121899 = CARTESIAN_POINT ( 'NONE',  ( 8.224510206698953496, -14.34966873604960469, 57.91557627198103120 ) ) ;
#121900 = CARTESIAN_POINT ( 'NONE',  ( 12.06949235617757843, -12.14591786802309237, 28.12390960531435979 ) ) ;
#121901 = B_SPLINE_CURVE_WITH_KNOTS ( 'NONE', 3,
 ( #146454, #7947, #109404, #33565, #156913, #69630 ),
 .UNSPECIFIED., .F., .F.,
 ( 4, 2, 4 ),
 ( 0.003989672132298142590, 0.004372778065220565835, 0.004755883998142989948 ),
 .UNSPECIFIED. ) ;
#121902 = CARTESIAN_POINT ( 'NONE',  ( 12.06949235617757843, -12.14591786802309237, 58.12390960531435979 ) ) ;
#121903 = ORIENTED_EDGE ( 'NONE', *, *, #139056, .T. ) ;
#121905 = CARTESIAN_POINT ( 'NONE',  ( 30.00000000000000355, -0.3535533905932729537, 5.353553390593267736 ) ) ;
#121904 = CARTESIAN_POINT ( 'NONE',  ( 14.34966873604972726, -8.224510206698740333, 50.83442372801901143 ) ) ;
#121906 = CARTESIAN_POINT ( 'NONE',  ( 19.05341960407617918, -5.049401038297876454, 51.04275706135231871 ) ) ;
#121907 = CARTESIAN_POINT ( 'NONE',  ( 0.05219959533909260263, 19.03943276465977164, 94.99890960531436690 ) ) ;
#121908 = CARTESIAN_POINT ( 'NONE',  ( -13.89961937509957401, -13.97604488694547875, 69.37609039468564731 ) ) ;
#121909 = CARTESIAN_POINT ( 'NONE',  ( 8.571926809382603096, -26.38167802310801235, 141.9750000027312069 ) ) ;
#121910 = CARTESIAN_POINT ( 'NONE',  ( -9.474510206698720793, -16.51473224551083518, 59.58442372801900433 ) ) ;
#121912 = CARTESIAN_POINT ( 'NONE',  ( -0.05219959533934338120, 16.53943276465976808, 87.50109039468568994 ) ) ;
#121911 = CARTESIAN_POINT ( 'NONE',  ( -19.05341960407617563, 5.049401038297882671, 93.54275706135234714 ) ) ;
#121913 = CARTESIAN_POINT ( 'NONE',  ( -22.44159573604010305, 16.30477369853692338, 145.1750000027311671 ) ) ;
#121914 = CARTESIAN_POINT ( 'NONE',  ( -19.02544592524342804, 5.153800228976336051, 31.04057627198102409 ) ) ;
#121915 = CARTESIAN_POINT ( 'NONE',  ( -21.55341960407610458, -5.719274019375992779, 26.45724293864768839 ) ) ;
#121916 = CARTESIAN_POINT ( 'NONE',  ( -15.72974639402176322, -15.80617190586768395, 44.37609039468567573 ) ) ;
#121917 = CARTESIAN_POINT ( 'NONE',  ( 9.474510206698729675, 16.51473224551082808, 102.0844237280190043 ) ) ;
#121919 = CARTESIAN_POINT ( 'NONE',  ( -9.564922557960796823, -16.46253265017161027, 62.08224293864769550 ) ) ;
#121918 = CARTESIAN_POINT ( 'NONE',  ( 17.50000000000000000, -3.565345528327946489, 106.9249448680647703 ) ) ;
#121920 = CARTESIAN_POINT ( 'NONE',  ( 9.564922557960805705, 16.46253265017160317, 99.58224293864770971 ) ) ;
#121922 = CARTESIAN_POINT ( 'NONE',  ( -19.05341960407611168, -5.049401038298163336, 61.45724293864769550 ) ) ;
#121921 = CARTESIAN_POINT ( 'NONE',  ( -16.52544592524342804, 4.483927247898546575, 71.04057627198103830 ) ) ;
#121923 = CARTESIAN_POINT ( 'NONE',  ( -9.474510206698964154, 16.51473224551069663, 75.41557627198103830 ) ) ;
#121924 = CARTESIAN_POINT ( 'NONE',  ( -19.03943276465977164, -0.05219959533935918106, 78.75109039468567573 ) ) ;
#121925 = CARTESIAN_POINT ( 'NONE',  ( -10.81492255796078084, -18.62759615963271287, 47.08224293864770260 ) ) ;
#121926 = CARTESIAN_POINT ( 'NONE',  ( 16.55341960407611168, 4.379528057220329451, 108.9572429386476955 ) ) ;
#121927 = CARTESIAN_POINT ( 'NONE',  ( -19.02544592524334988, -5.153800228976617603, 38.95942372801900433 ) ) ;
#121928 = CARTESIAN_POINT ( 'NONE',  ( 9.564922557960805705, 16.46253265017160317, 84.58224293864769550 ) ) ;
#121929 = CARTESIAN_POINT ( 'NONE',  ( -0.05219959533907301413, -21.53943276465977519, 77.49890960531433848 ) ) ;
#121931 = CARTESIAN_POINT ( 'NONE',  ( -19.03943276465977164, -0.05219959533935918106, 48.75109039468566863 ) ) ;
#121930 = CARTESIAN_POINT ( 'NONE',  ( -4.379528057220328563, 16.55341960407611168, 85.20724293864770971 ) ) ;
#121932 = CARTESIAN_POINT ( 'NONE',  ( 5.719274019375991003, -21.55341960407610458, 72.70724293864769550 ) ) ;
#121933 = CARTESIAN_POINT ( 'NONE',  ( -21.52544592524343514, 5.823673210054127303, 56.04057627198102409 ) ) ;
#121934 = CARTESIAN_POINT ( 'NONE',  ( -10.81492255796078084, -18.62759615963271287, 37.08224293864768129 ) ) ;
#121935 = CARTESIAN_POINT ( 'NONE',  ( -5.823673210054431948, 21.52544592524334988, 97.70942372801904696 ) ) ;
#121936 = CARTESIAN_POINT ( 'NONE',  ( -5.049401038298153566, 19.05341960407611168, 70.20724293864769550 ) ) ;
#121937 = CARTESIAN_POINT ( 'NONE',  ( -0.05219959533910754901, -16.53943276465976808, 112.4989096053143669 ) ) ;
#121938 = AXIS2_PLACEMENT_3D ( 'NONE', #43344, #182859, #139316 ) ;
#121939 = CARTESIAN_POINT ( 'NONE',  ( -5.719274019375665041, -21.55341960407619695, 19.79275706135235069 ) ) ;
#121940 = EDGE_CURVE ( 'NONE', #76043, #84310, #103441, .T. ) ;
#121941 = CARTESIAN_POINT ( 'NONE',  ( 15.80617190586769283, -15.72974639402175789, 40.62609039468567573 ) ) ;
#121942 = CARTESIAN_POINT ( 'NONE',  ( 19.02544592524343514, -5.153800228976328945, 28.54057627198102409 ) ) ;
#121943 = CARTESIAN_POINT ( 'NONE',  ( 15.72974639402199770, -15.80617190586745480, 113.1239096053143953 ) ) ;
#121944 = CARTESIAN_POINT ( 'NONE',  ( -5.153800228976607833, 19.02544592524334988, 52.70942372801900433 ) ) ;
#121945 = CARTESIAN_POINT ( 'NONE',  ( -19.02544592524342804, 5.153800228976336051, 41.04057627198103120 ) ) ;
#121946 = CARTESIAN_POINT ( 'NONE',  ( 16.46253265017160672, -9.564922557960803928, 23.33224293864769194 ) ) ;
#121947 = DIRECTION ( 'NONE',  ( -0.000000000000000000, -0.000000000000000000, 1.000000000000000000 ) ) ;
#121948 = CARTESIAN_POINT ( 'NONE',  ( -8.314922557961024197, 14.29746914071037800, 62.91775706135236135 ) ) ;
#121949 = CARTESIAN_POINT ( 'NONE',  ( 9.474510206698971260, -16.51473224551069308, 32.91557627198102409 ) ) ;
#121950 = CARTESIAN_POINT ( 'NONE',  ( -19.49401214000074489, -12.39993551617566325, 169.9999999999999716 ) ) ;
#121951 = CARTESIAN_POINT ( 'NONE',  ( -5.153800228976328057, -19.02544592524343514, 82.29057627198103830 ) ) ;
#121952 = CARTESIAN_POINT ( 'NONE',  ( 8.224510206698953496, -14.34966873604960469, 102.9155762719810383 ) ) ;
#121953 = CARTESIAN_POINT ( 'NONE',  ( 15.80617190586746368, 15.72974639402197994, 54.37390960531435979 ) ) ;
#121954 = CARTESIAN_POINT ( 'NONE',  ( 14.34966873604972726, -8.224510206698740333, 50.83442372801901143 ) ) ;
#121955 = CARTESIAN_POINT ( 'NONE',  ( -5.719274019375665041, -21.55341960407619695, 99.79275706135234714 ) ) ;
#121956 = CARTESIAN_POINT ( 'NONE',  ( 13.97604488694527802, 13.89961937509977652, 39.37390960531435269 ) ) ;
#121957 = CARTESIAN_POINT ( 'NONE',  ( 12.06949235617739724, 12.14591786802326823, 111.8760903946856615 ) ) ;
#121958 = CARTESIAN_POINT ( 'NONE',  ( 12.14591786802309770, 12.06949235617756955, 54.37390960531435979 ) ) ;
#121959 = CARTESIAN_POINT ( 'NONE',  ( 16.46253265017160672, -9.564922557960803928, 63.33224293864769550 ) ) ;
#121960 = CARTESIAN_POINT ( 'NONE',  ( -21.53943276465977519, -0.05219959533937600094, 108.7510903946857042 ) ) ;
#121961 = CARTESIAN_POINT ( 'NONE',  ( -5.719274019375978568, 21.55341960407610458, 115.2072429386476955 ) ) ;
#121962 = CARTESIAN_POINT ( 'NONE',  ( 21.55341960407619695, -5.719274019375665929, 71.04275706135234714 ) ) ;
#121963 = CARTESIAN_POINT ( 'NONE',  ( -14.34966873604972548, 8.224510206698743886, 53.33442372801901854 ) ) ;
#121964 = CARTESIAN_POINT ( 'NONE',  ( -16.55341960407617563, 4.379528057220093196, 33.54275706135234714 ) ) ;
#121966 = CARTESIAN_POINT ( 'NONE',  ( -10.72451020669870658, -18.67979575497194134, 104.5844237280190185 ) ) ;
#121965 = CARTESIAN_POINT ( 'NONE',  ( 14.29746914071049879, -8.314922557960816363, 78.33224293864770971 ) ) ;
#121967 = STYLED_ITEM ( 'NONE', ( #75724 ), #79223 ) ;
#121968 = CARTESIAN_POINT ( 'NONE',  ( 4.379528057220339221, -16.55341960407611168, 37.70724293864769550 ) ) ;
#121969 = CARTESIAN_POINT ( 'NONE',  ( -17.48847506799969054, 5.747544572773736427, 115.8269743784328654 ) ) ;
#121970 = CARTESIAN_POINT ( 'NONE',  ( -14.34966873604972548, 8.224510206698743886, 43.33442372801901143 ) ) ;
#121971 = CARTESIAN_POINT ( 'NONE',  ( -0.05219959533910754901, -16.53943276465976808, 52.49890960531435979 ) ) ;
#121972 = CARTESIAN_POINT ( 'NONE',  ( 0.05219959533934541429, -16.53943276465976808, 85.00109039468568994 ) ) ;
#121973 = CARTESIAN_POINT ( 'NONE',  ( 16.51473224551069308, 9.474510206698969483, 104.1655762719810241 ) ) ;
#121974 = CARTESIAN_POINT ( 'NONE',  ( -0.05219959533909027116, -19.03943276465977164, 112.4989096053143669 ) ) ;
#121975 = CARTESIAN_POINT ( 'NONE',  ( 5.719274019375673035, 21.55341960407619339, 97.29275706135234714 ) ) ;
#121976 = EDGE_CURVE ( 'NONE', #116714, #51008, #87908, .T. ) ;
#121977 = CARTESIAN_POINT ( 'NONE',  ( 16.52544592524335698, 4.483927247898782831, 101.4594237280190185 ) ) ;
#121978 = CARTESIAN_POINT ( 'NONE',  ( 14.29746914071049879, -8.314922557960816363, 93.33224293864769550 ) ) ;
#121979 = CARTESIAN_POINT ( 'NONE',  ( 16.51473224551069308, 9.474510206698969483, 94.16557627198103830 ) ) ;
#121980 = ORIENTED_EDGE ( 'NONE', *, *, #108116, .T. ) ;
#121982 =( BOUNDED_CURVE ( )  B_SPLINE_CURVE ( 2, ( #75208, #185369, #136879, #198565, #60035, #122694, #184383, #45864, #107517, #126656, #36637, #160997, #188359, #82129, #158008, #49837, #20479, #175171, #112491, #189357, #140842, #173187, #114476, #5303, #33669, #190341, #111501, #144819, #37649, #19499, #35653, #51817, #127657, #95331, #48848, #83144, #176179, #34663, #174185, #96321, #143822, #99313, #3325, #81144, #113477, #6303, #172184, #142825, #157016, #18514, #22492, #97301, #80161, #158987, #2331, #66987, #129635, #64012, #67981, #191331, #98294, #159996, #52809, #125681, #128646, #187379, #141833, #64998, #110502, #4305, #65987, #50834, #21483, #7301, #87159, #152553, #39649, #29235, #55821, #180197, #131664, #8320, #44397, #14041, #117494, #56832, #177188, #145818, #122210, #68986, #130650, #192344, #53826, #118507, #194353, #101310, #38661, #40659, #199065, #106051, #167737 ),
 .UNSPECIFIED., .F., .T. ) 
 B_SPLINE_CURVE_WITH_KNOTS ( ( 3, 2, 2, 2, 2, 2, 2, 2, 2, 2, 2, 2, 2, 2, 2, 2, 2, 2, 2, 2, 2, 2, 2, 2, 2, 2, 2, 2, 2, 2, 2, 2, 2, 2, 2, 2, 2, 2, 2, 2, 2, 2, 2, 2, 2, 2, 2, 2, 2, 2, 3 ),
 ( 0.000000000000000000, 0.02000000000000000042, 0.04000000000000000083, 0.05999999999999999778, 0.08000000000000000167, 0.1000000000000000056, 0.1199999999999999956, 0.1400000000000000133, 0.1600000000000000033, 0.1799999999999999933, 0.2000000000000000111, 0.2200000000000000011, 0.2399999999999999911, 0.2600000000000000089, 0.2800000000000000266, 0.2999999999999999889, 0.3200000000000000067, 0.3400000000000000244, 0.3599999999999999867, 0.3800000000000000044, 0.4000000000000000222, 0.4199999999999999845, 0.4400000000000000022, 0.4600000000000000200, 0.4799999999999999822, 0.5000000000000000000, 0.5200000000000000178, 0.5400000000000000355, 0.5600000000000000533, 0.5799999999999999600, 0.5999999999999999778, 0.6199999999999999956, 0.6400000000000000133, 0.6600000000000000311, 0.6800000000000000488, 0.6999999999999999556, 0.7199999999999999734, 0.7399999999999999911, 0.7600000000000000089, 0.7800000000000000266, 0.8000000000000000444, 0.8199999999999999512, 0.8399999999999999689, 0.8599999999999999867, 0.8800000000000000044, 0.9000000000000000222, 0.9200000000000000400, 0.9399999999999999467, 0.9599999999999999645, 0.9799999999999999822, 1.000000000000000000 ),
 .UNSPECIFIED. ) 
 CURVE ( )  GEOMETRIC_REPRESENTATION_ITEM ( )  RATIONAL_B_SPLINE_CURVE ( ( 1.000000000000000000, 0.9510565162951535312, 1.000000000000000000, 0.9510565162951535312, 1.000000000000000000, 0.9510565162951535312, 1.000000000000000000, 0.9510565162951535312, 1.000000000000000000, 0.9510565162951535312, 1.000000000000000000, 0.9510565162951535312, 1.000000000000000000, 0.9510565162951535312, 1.000000000000000000, 0.9510565162951535312, 1.000000000000000000, 0.9510565162951535312, 1.000000000000000000, 0.9510565162951535312, 1.000000000000000000, 0.9510565162951535312, 1.000000000000000000, 0.9510565162951535312, 1.000000000000000000, 0.9510565162951535312, 1.000000000000000000, 0.9510565162951535312, 1.000000000000000000, 0.9510565162951535312, 1.000000000000000000, 0.9510565162951535312, 1.000000000000000000, 0.9510565162951535312, 1.000000000000000000, 0.9510565162951535312, 1.000000000000000000, 0.9510565162951535312, 1.000000000000000000, 0.9510565162951535312, 1.000000000000000000, 0.9510565162951535312, 1.000000000000000000, 0.9510565162951535312, 1.000000000000000000, 0.9510565162951535312, 1.000000000000000000, 0.9510565162951535312, 1.000000000000000000, 0.9510565162951535312, 1.000000000000000000, 0.9510565162951535312, 1.000000000000000000, 0.9510565162951535312, 1.000000000000000000, 0.9510565162951535312, 1.000000000000000000, 0.9510565162951535312, 1.000000000000000000, 0.9510565162951535312, 1.000000000000000000, 0.9510565162951535312, 1.000000000000000000, 0.9510565162951535312, 1.000000000000000000, 0.9510565162951535312, 1.000000000000000000, 0.9510565162951535312, 1.000000000000000000, 0.9510565162951535312, 1.000000000000000000, 0.9510565162951535312, 1.000000000000000000, 0.9510565162951535312, 1.000000000000000000, 0.9510565162951535312, 1.000000000000000000, 0.9510565162951535312, 1.000000000000000000, 0.9510565162951535312, 1.000000000000000000, 0.9510565162951535312, 1.000000000000000000, 0.9510565162951535312, 1.000000000000000000, 0.9510565162951535312, 1.000000000000000000, 0.9510565162951535312, 1.000000000000000000, 0.9510565162951535312, 1.000000000000000000, 0.9510565162951535312, 1.000000000000000000, 0.9510565162951535312, 1.000000000000000000, 0.9510565162951535312, 1.000000000000000000, 0.9510565162951535312, 1.000000000000000000, 0.9510565162951535312, 1.000000000000000000 ) ) 
 REPRESENTATION_ITEM ( '' )  );
#121981 = CARTESIAN_POINT ( 'NONE',  ( 16.55341960407618274, -4.379528057220086978, 41.04275706135236135 ) ) ;
#121983 = CARTESIAN_POINT ( 'NONE',  ( 16.46253265017160672, -9.564922557960803928, 48.33224293864769550 ) ) ;
#121984 = CARTESIAN_POINT ( 'NONE',  ( -19.02544592524342804, 5.153800228976336051, 111.0405762719810099 ) ) ;
#121986 = CARTESIAN_POINT ( 'NONE',  ( 17.60779699588839975, 5.500000000000013323, 68.84981316670106821 ) ) ;
#121985 = CARTESIAN_POINT ( 'NONE',  ( -12.14591786802326823, 12.06949235617739902, 48.12609039468568284 ) ) ;
#121987 = CARTESIAN_POINT ( 'NONE',  ( 9.474510206698729675, 16.51473224551082808, 32.08442372801900433 ) ) ;
#121988 = CARTESIAN_POINT ( 'NONE',  ( 19.03943276465977164, -0.05219959533909143690, 43.74890960531435979 ) ) ;
#121989 = CARTESIAN_POINT ( 'NONE',  ( -16.53943276465976808, -0.05219959533934237506, 78.75109039468568994 ) ) ;
#121990 = CARTESIAN_POINT ( 'NONE',  ( 16.46253265017146816, 9.564922557961045513, 76.66775706135234714 ) ) ;
#121991 = CARTESIAN_POINT ( 'NONE',  ( -13.97604488694547697, 13.89961937509957934, 23.12609039468565442 ) ) ;
#121992 = CARTESIAN_POINT ( 'NONE',  ( 5.153800228976335163, 19.02544592524342804, 54.79057627198103120 ) ) ;
#121993 = EDGE_CURVE ( 'NONE', #109599, #131044, #27282, .T. ) ;
#121994 = CARTESIAN_POINT ( 'NONE',  ( -16.53943276465976808, 0.05219959533911058130, 96.24890960531435269 ) ) ;
#121995 = CARTESIAN_POINT ( 'NONE',  ( -16.51473224551082808, 9.474510206698731452, 63.33442372801900433 ) ) ;
#121996 = CARTESIAN_POINT ( 'NONE',  ( 10.72451020669898902, -18.67979575497178502, 62.91557627198102409 ) ) ;
#121997 = CARTESIAN_POINT ( 'NONE',  ( 0.05219959533936267826, -19.03943276465977164, 30.00109039468566863 ) ) ;
#121998 = CARTESIAN_POINT ( 'NONE',  ( 19.02544592524343514, -5.153800228976328945, 103.5405762719809957 ) ) ;
#121999 = CARTESIAN_POINT ( 'NONE',  ( -21.55341960407610458, -5.719274019375992779, 71.45724293864769550 ) ) ;
#122000 = CARTESIAN_POINT ( 'NONE',  ( 9.564922557960805705, 16.46253265017160317, 104.5822429386476955 ) ) ;
#122001 = CARTESIAN_POINT ( 'NONE',  ( 0.05219959533936267826, -19.03943276465977164, 100.0010903946856757 ) ) ;
#122002 = CARTESIAN_POINT ( 'NONE',  ( -16.46253265017160317, 9.564922557960807481, 110.8322429386476955 ) ) ;
#122003 = CARTESIAN_POINT ( 'NONE',  ( -8.224510206698735004, -14.34966873604973081, 24.58442372801901499 ) ) ;
#122004 = CARTESIAN_POINT ( 'NONE',  ( 13.89961937509977652, -13.97604488694527269, 38.12390960531436690 ) ) ;
#122005 = CARTESIAN_POINT ( 'NONE',  ( 13.89961937509977652, -13.97604488694527269, 103.1239096053143527 ) ) ;
#122006 = CARTESIAN_POINT ( 'NONE',  ( 15.72974639402199770, -15.80617190586745480, 88.12390960531436690 ) ) ;
#122007 = CARTESIAN_POINT ( 'NONE',  ( -18.67979575497193778, 10.72451020669871902, 63.33442372801900433 ) ) ;
#122009 = CARTESIAN_POINT ( 'NONE',  ( -5.049401038297874678, -19.05341960407617918, 19.79275706135233293 ) ) ;
#122008 = CARTESIAN_POINT ( 'NONE',  ( -9.564922557961040184, 16.46253265017147172, 107.9177570613523471 ) ) ;
#122010 = CARTESIAN_POINT ( 'NONE',  ( -16.52544592524335698, -4.483927247898792601, 108.9594237280190185 ) ) ;
#122011 = CARTESIAN_POINT ( 'NONE',  ( -15.72974639402197994, 15.80617190586746368, 95.62390960531436690 ) ) ;
#122012 = CARTESIAN_POINT ( 'NONE',  ( -4.379528057220328563, 16.55341960407611168, 30.20724293864769550 ) ) ;
#122013 = CARTESIAN_POINT ( 'NONE',  ( 0.05219959533936267826, -19.03943276465977164, 80.00109039468567573 ) ) ;
#122014 = CARTESIAN_POINT ( 'NONE',  ( -0.05219959533936034679, 19.03943276465977164, 57.50109039468566863 ) ) ;
#122015 = CARTESIAN_POINT ( 'NONE',  ( -18.62759615963255300, -10.81492255796106328, 54.16775706135235424 ) ) ;
#122016 = CARTESIAN_POINT ( 'NONE',  ( -13.89961937509957401, -13.97604488694547875, 39.37609039468566152 ) ) ;
#122017 = CARTESIAN_POINT ( 'NONE',  ( 16.53943276465976808, -0.05219959533910856209, 103.7489096053143669 ) ) ;
#122018 = CARTESIAN_POINT ( 'NONE',  ( 21.53943276465977519, -0.05219959533907433946, 33.74890960531436690 ) ) ;
#122019 = CARTESIAN_POINT ( 'NONE',  ( -0.05219959533910754901, -16.53943276465976808, 42.49890960531435979 ) ) ;
#122020 = CARTESIAN_POINT ( 'NONE',  ( -5.823673210054431948, 21.52544592524334988, 92.70942372801901854 ) ) ;
#122021 = CARTESIAN_POINT ( 'NONE',  ( 4.483927247898790824, -16.52544592524335698, 70.20942372801904696 ) ) ;
#122022 = CARTESIAN_POINT ( 'NONE',  ( -16.52544592524342804, 4.483927247898546575, 31.04057627198102409 ) ) ;
#122023 = CARTESIAN_POINT ( 'NONE',  ( -10.81492255796105439, 18.62759615963255655, 67.91775706135234714 ) ) ;
#122024 = CARTESIAN_POINT ( 'NONE',  ( 15.72974639402176855, 15.80617190586768217, 61.87609039468568284 ) ) ;
#122025 = CARTESIAN_POINT ( 'NONE',  ( 21.52544592524344225, -5.823673210054117533, 63.54057627198103830 ) ) ;
#122026 = VERTEX_POINT ( 'NONE', #161127 ) ;
#122027 = CARTESIAN_POINT ( 'NONE',  ( 16.51473224551069308, 9.474510206698969483, 24.16557627198102765 ) ) ;
#122028 = CARTESIAN_POINT ( 'NONE',  ( 15.80617190586769283, -15.72974639402175789, 45.62609039468567573 ) ) ;
#122029 = CARTESIAN_POINT ( 'NONE',  ( 16.46253265017160672, -9.564922557960803928, 28.33224293864769550 ) ) ;
#122030 = CARTESIAN_POINT ( 'NONE',  ( 13.97604488694527802, 13.89961937509977652, 44.37390960531435269 ) ) ;
#122031 = CARTESIAN_POINT ( 'NONE',  ( 0.05219959533910956823, 16.53943276465976808, 74.99890960531435269 ) ) ;
#122032 = CARTESIAN_POINT ( 'NONE',  ( 5.153800228976335163, 19.02544592524342804, 79.79057627198102409 ) ) ;
#122033 = CARTESIAN_POINT ( 'NONE',  ( -12.14591786802309592, -12.06949235617757132, 26.87390960531435979 ) ) ;
#122034 = CARTESIAN_POINT ( 'NONE',  ( 10.72451020669898902, -18.67979575497178502, 72.91557627198103830 ) ) ;
#122035 = CARTESIAN_POINT ( 'NONE',  ( -0.05219959533907301413, -21.53943276465977519, 112.4989096053143669 ) ) ;
#122036 = CARTESIAN_POINT ( 'NONE',  ( -16.51473224551069308, -9.474510206698971260, 101.6655762719810241 ) ) ;
#122038 = CARTESIAN_POINT ( 'NONE',  ( 16.46253265017146816, 9.564922557961045513, 101.6677570613523329 ) ) ;
#122037 = CARTESIAN_POINT ( 'NONE',  ( 9.474510206698971260, -16.51473224551069308, 62.91557627198102409 ) ) ;
#122039 = CARTESIAN_POINT ( 'NONE',  ( 10.81492255796078972, 18.62759615963270932, 59.58224293864770260 ) ) ;
#122040 = CARTESIAN_POINT ( 'NONE',  ( 15.80617190586769283, -15.72974639402175789, 75.62609039468567573 ) ) ;
#122041 = CARTESIAN_POINT ( 'NONE',  ( -5.049401038298153566, 19.05341960407611168, 60.20724293864768129 ) ) ;
#122042 = CARTESIAN_POINT ( 'NONE',  ( -0.05219959533909027116, -19.03943276465977164, 92.49890960531436690 ) ) ;
#122043 = CARTESIAN_POINT ( 'NONE',  ( -12.14591786802326823, 12.06949235617739902, 83.12609039468568994 ) ) ;
#122044 = CARTESIAN_POINT ( 'NONE',  ( 15.72974639402176855, 15.80617190586768217, 61.87609039468568284 ) ) ;
#122045 = CARTESIAN_POINT ( 'NONE',  ( 10.72451020669871369, 18.67979575497193778, 82.08442372801901854 ) ) ;
#122046 = CARTESIAN_POINT ( 'NONE',  ( -21.53943276465977519, -0.05219959533937600094, 18.75109039468568639 ) ) ;
#122047 = CARTESIAN_POINT ( 'NONE',  ( -21.53943276465977519, 0.05219959533907696930, 71.24890960531435269 ) ) ;
#122048 = CARTESIAN_POINT ( 'NONE',  ( -5.049401038297874678, -19.05341960407617918, 49.79275706135231871 ) ) ;
#122049 = CARTESIAN_POINT ( 'NONE',  ( 21.55341960407610458, 5.719274019375980345, 43.95724293864769550 ) ) ;
#122051 = CARTESIAN_POINT ( 'NONE',  ( 12.14591786802309770, 12.06949235617756955, 39.37390960531436690 ) ) ;
#122050 = CARTESIAN_POINT ( 'NONE',  ( 16.46253265017160672, -9.564922557960803928, 78.33224293864769550 ) ) ;
#122052 = CARTESIAN_POINT ( 'NONE',  ( -17.05116617787826883, 6.768360034955676952, 63.65675553259197983 ) ) ;
#122053 = CARTESIAN_POINT ( 'NONE',  ( -21.53943276465977519, 0.05219959533907696930, 26.24890960531435624 ) ) ;
#122054 = CARTESIAN_POINT ( 'NONE',  ( -18.22780087662123094, -5.499999999999984901, 81.48459894673892734 ) ) ;
#122055 = CARTESIAN_POINT ( 'NONE',  ( -5.049401038297874678, -19.05341960407617918, 89.79275706135230450 ) ) ;
#122056 = CARTESIAN_POINT ( 'NONE',  ( 21.53943276465977519, -0.05219959533907433946, 73.74890960531433848 ) ) ;
#122057 = CARTESIAN_POINT ( 'NONE',  ( 16.55341960407611168, 4.379528057220329451, 53.95724293864770260 ) ) ;
#122058 = CARTESIAN_POINT ( 'NONE',  ( -4.483927247898782831, 16.52544592524335698, 22.70942372801901499 ) ) ;
#122059 = CARTESIAN_POINT ( 'NONE',  ( 0.05219959533909260263, 19.03943276465977164, 49.99890960531435979 ) ) ;
#122061 = CARTESIAN_POINT ( 'NONE',  ( 19.05341960407617918, -5.049401038297876454, 66.04275706135233293 ) ) ;
#122060 = CARTESIAN_POINT ( 'NONE',  ( -18.62759615963270932, 10.81492255796079327, 105.8322429386476955 ) ) ;
#122062 = CARTESIAN_POINT ( 'NONE',  ( -19.05341960407611168, -5.049401038298163336, 81.45724293864769550 ) ) ;
#122063 = CARTESIAN_POINT ( 'NONE',  ( 14.34966873604960469, 8.224510206698951720, 89.16557627198102409 ) ) ;
#122064 = CARTESIAN_POINT ( 'NONE',  ( 13.89961937509977652, -13.97604488694527269, 58.12390960531436690 ) ) ;
#122065 = CARTESIAN_POINT ( 'NONE',  ( -16.52544592524342804, 4.483927247898546575, 71.04057627198103830 ) ) ;
#122066 = CARTESIAN_POINT ( 'NONE',  ( -13.89961937509977652, 13.97604488694528158, 35.62390960531435269 ) ) ;
#122067 = CARTESIAN_POINT ( 'NONE',  ( -17.04537478617065815, -5.419303508143405779, 20.72959544958357725 ) ) ;
#122068 = CARTESIAN_POINT ( 'NONE',  ( -14.29746914071049879, 8.314922557960819915, 45.83224293864769550 ) ) ;
#122069 = CARTESIAN_POINT ( 'NONE',  ( 5.153800228976335163, 19.02544592524342804, 84.79057627198099567 ) ) ;
#122070 = CARTESIAN_POINT ( 'NONE',  ( -1.455916144794658473, -15.57302527691883576, -59.63194581529845806 ) ) ;
#122071 = CARTESIAN_POINT ( 'NONE',  ( 5.153800228976615827, -19.02544592524334988, 50.20942372801897591 ) ) ;
#122072 = CARTESIAN_POINT ( 'NONE',  ( 12.06949235617739724, 12.14591786802326823, 56.87609039468568994 ) ) ;
#122073 = CARTESIAN_POINT ( 'NONE',  ( 18.67979575497178502, 10.72451020669898547, 79.16557627198103830 ) ) ;
#122074 = CARTESIAN_POINT ( 'NONE',  ( 19.02544592524334988, 5.153800228976608722, 41.45942372801900433 ) ) ;
#122075 = CARTESIAN_POINT ( 'NONE',  ( -0.05219959533909027116, -19.03943276465977164, 82.49890960531436690 ) ) ;
#122076 = DIRECTION ( 'NONE',  ( 1.000000000000000000, 0.000000000000000000, 0.000000000000000000 ) ) ;
#122077 = CARTESIAN_POINT ( 'NONE',  ( 10.81492255796078972, 18.62759615963270932, 34.58224293864770260 ) ) ;
#122078 = VECTOR ( 'NONE', #67829, 1000.000000000000000 ) ;
#122079 = CARTESIAN_POINT ( 'NONE',  ( 5.049401038298161559, -19.05341960407611168, 57.70724293864769550 ) ) ;
#122080 = CARTESIAN_POINT ( 'NONE',  ( -15.72974639402176322, -15.80617190586768395, 49.37609039468569705 ) ) ;
#122081 = CARTESIAN_POINT ( 'NONE',  ( -16.51473224551069308, -9.474510206698971260, 26.66557627198103120 ) ) ;
#122084 = VERTEX_POINT ( 'NONE', #84270 ) ;
#122083 = CARTESIAN_POINT ( 'NONE',  ( -9.474510206698964154, 16.51473224551069663, 95.41557627198102409 ) ) ;
#122082 = CARTESIAN_POINT ( 'NONE',  ( 5.823673210054444382, -21.52544592524334988, 20.20942372801900788 ) ) ;
#122085 = CARTESIAN_POINT ( 'NONE',  ( 21.53943276465977519, 0.05219959533937863772, 36.25109039468567573 ) ) ;
#122086 = VERTEX_POINT ( 'NONE', #69116 ) ;
#122087 = CARTESIAN_POINT ( 'NONE',  ( 5.153800228976335163, 19.02544592524342804, 104.7905762719809957 ) ) ;
#122088 = DIRECTION ( 'NONE',  ( 1.000000000000000000, 0.000000000000000000, 0.000000000000000000 ) ) ;
#122089 = CARTESIAN_POINT ( 'NONE',  ( -15.80617190586745835, -15.72974639402198527, 106.8739096053143811 ) ) ;
#122090 = CARTESIAN_POINT ( 'NONE',  ( -5.153800228976328057, -19.02544592524343514, 42.29057627198101699 ) ) ;
#122091 = CARTESIAN_POINT ( 'NONE',  ( 12.06949235617739724, 12.14591786802326823, 21.87609039468567573 ) ) ;
#122092 = CARTESIAN_POINT ( 'NONE',  ( 22.81625015709510151, -31.40387420917324590, -2.424999997268812546 ) ) ;
#122093 = CARTESIAN_POINT ( 'NONE',  ( -19.05341960407611168, -5.049401038298163336, 26.45724293864769550 ) ) ;
#122094 = CARTESIAN_POINT ( 'NONE',  ( 15.72974639402176855, 15.80617190586768217, 96.87609039468568994 ) ) ;
#122096 = CARTESIAN_POINT ( 'NONE',  ( -21.55341960407619339, 5.719274019375674811, 58.54275706135235424 ) ) ;
#122095 = CARTESIAN_POINT ( 'NONE',  ( -13.89961937509977652, 13.97604488694528158, 80.62390960531436690 ) ) ;
#122097 = CARTESIAN_POINT ( 'NONE',  ( -27.73933785331498925, 2.428612866367529932E-14, 143.3750000027311842 ) ) ;
#122098 = CARTESIAN_POINT ( 'NONE',  ( -19.02544592524342804, 5.153800228976336051, 96.04057627198103830 ) ) ;
#122099 = B_SPLINE_CURVE_WITH_KNOTS ( 'NONE', 3,
 ( #97963, #23159, #40317, #129309, #68646, #175841, #176853, #145486, #128319, #22155, #85819, #163675, #159655, #7972, #132331, #177850, #54488, #130302, #116160, #53482 ),
 .UNSPECIFIED., .F., .F.,
 ( 4, 2, 2, 2, 2, 2, 2, 2, 2, 4 ),
 ( 0.004000878361811996409, 0.004499404418915992424, 0.004997930476019988438, 0.005496456533123985320, 0.005994982590227981335, 0.006244245618779979343, 0.006493508647331977350, 0.006992034704435974232, 0.007490560761539970247, 0.007989086818643966262 ),
 .UNSPECIFIED. ) ;
#122100 = CARTESIAN_POINT ( 'NONE',  ( -7.950080215733696498, 27.42129086533356030, 140.0000000000000284 ) ) ;
#122103 = CARTESIAN_POINT ( 'NONE',  ( -10.72451020669870658, -18.67979575497194134, 64.58442372801900433 ) ) ;
#122102 = CARTESIAN_POINT ( 'NONE',  ( -12.06949235617739369, -12.14591786802326823, 74.37609039468568994 ) ) ;
#122101 = CARTESIAN_POINT ( 'NONE',  ( 8.224510206698742110, 14.34966873604972548, 42.08442372801901854 ) ) ;
#122104 = CARTESIAN_POINT ( 'NONE',  ( -18.62759615963255300, -10.81492255796106328, 89.16775706135236135 ) ) ;
#122105 = CARTESIAN_POINT ( 'NONE',  ( 4.619076279717888589, 6.673813065215385087, -62.12322917040970083 ) ) ;
#122106 = CARTESIAN_POINT ( 'NONE',  ( 13.97604488694548053, -13.89961937509957401, 105.6260903946856757 ) ) ;
#122107 = CARTESIAN_POINT ( 'NONE',  ( 0.05219959533909260263, 19.03943276465977164, 69.99890960531435269 ) ) ;
#122108 = CARTESIAN_POINT ( 'NONE',  ( -0.05219959533909027116, -19.03943276465977164, 92.49890960531436690 ) ) ;
#122109 = VECTOR ( 'NONE', #90802, 1000.000000000000000 ) ;
#122110 = CARTESIAN_POINT ( 'NONE',  ( 5.049401038298161559, -19.05341960407611168, 27.70724293864769550 ) ) ;
#122111 = CARTESIAN_POINT ( 'NONE',  ( 15.72974639402199770, -15.80617190586745480, 23.12390960531436335 ) ) ;
#122112 = CARTESIAN_POINT ( 'NONE',  ( -4.379528057220086978, -16.55341960407618274, 94.79275706135234714 ) ) ;
#122114 = CARTESIAN_POINT ( 'NONE',  ( -13.89961937509977652, 13.97604488694528158, 55.62390960531434558 ) ) ;
#122113 = CARTESIAN_POINT ( 'NONE',  ( 16.55341960407611168, 4.379528057220329451, 63.95724293864770260 ) ) ;
#122115 = CARTESIAN_POINT ( 'NONE',  ( 15.80617190586769283, -15.72974639402175789, 95.62609039468568994 ) ) ;
#122116 = CARTESIAN_POINT ( 'NONE',  ( 31.99999999999932143, 1.011436372600181938E-12, 97.70000000000020179 ) ) ;
#122117 = CARTESIAN_POINT ( 'NONE',  ( 19.03943276465977164, 0.05219959533936151252, 111.2510903946856757 ) ) ;
#122118 = CARTESIAN_POINT ( 'NONE',  ( -16.52544592524342804, 4.483927247898546575, 76.04057627198102409 ) ) ;
#122119 = CARTESIAN_POINT ( 'NONE',  ( -21.53943276465977519, -0.05219959533937600094, 28.75109039468567929 ) ) ;
#122120 = CARTESIAN_POINT ( 'NONE',  ( 15.80617190586746368, 15.72974639402197994, 59.37390960531436690 ) ) ;
#122121 = CARTESIAN_POINT ( 'NONE',  ( 9.474510206698729675, 16.51473224551082808, 37.08442372801899722 ) ) ;
#122122 = CARTESIAN_POINT ( 'NONE',  ( 28.82186960331498327, 9.364793116373570925, 145.3500000054623627 ) ) ;
#122123 = CARTESIAN_POINT ( 'NONE',  ( -19.02544592524342804, 5.153800228976336051, 86.04057627198103830 ) ) ;
#122124 = CARTESIAN_POINT ( 'NONE',  ( -16.55341960407611168, -4.379528057220339221, 56.45724293864768839 ) ) ;
#122125 = CARTESIAN_POINT ( 'NONE',  ( 14.29746914071049879, -8.314922557960816363, 38.33224293864768839 ) ) ;
#122126 = CARTESIAN_POINT ( 'NONE',  ( 12.06949235617739724, 12.14591786802326823, 101.8760903946857042 ) ) ;
#122127 = CARTESIAN_POINT ( 'NONE',  ( -19.05341960407617563, 5.049401038297882671, 48.54275706135233293 ) ) ;
#122128 = B_SPLINE_CURVE_WITH_KNOTS ( 'NONE', 3,
 ( #153192, #92511, #199716, #76358, #156180, #75366, #198727, #60193, #498, #48022, #138035, #93506, #32848, #79337, #123834, #2495, #122854, #184542, #107678, #169355 ),
 .UNSPECIFIED., .F., .F.,
 ( 4, 2, 2, 2, 2, 2, 2, 2, 2, 4 ),
 ( 0.000000000000000000, 0.0004987090165372409355, 0.0009974180330744818711, 0.001246772541343112856, 0.001496127049611744274, 0.001994836066149007110, 0.002493545082686269513, 0.002742899590954893559, 0.002992254099223517604, 0.003989672132298028098 ),
 .UNSPECIFIED. ) ;
#122129 = LINE ( 'NONE', #44312, #121411 ) ;
#122130 = CARTESIAN_POINT ( 'NONE',  ( 16.46253265017160672, -9.564922557960803928, 108.3322429386476955 ) ) ;
#122131 = CARTESIAN_POINT ( 'NONE',  ( 14.29746914071049879, -8.314922557960816363, 73.33224293864769550 ) ) ;
#122132 = CARTESIAN_POINT ( 'NONE',  ( 19.05341960407617918, -5.049401038297876454, 41.04275706135233293 ) ) ;
#122134 = CARTESIAN_POINT ( 'NONE',  ( 15.80617190586746368, 15.72974639402197994, 34.37390960531435979 ) ) ;
#122133 = CARTESIAN_POINT ( 'NONE',  ( -13.89961937509977652, 13.97604488694528158, 35.62390960531435269 ) ) ;
#122135 = CARTESIAN_POINT ( 'NONE',  ( 15.80617190586746368, 15.72974639402197994, 64.37390960531435269 ) ) ;
#122136 = CARTESIAN_POINT ( 'NONE',  ( 8.314922557960818139, 14.29746914071049879, 114.5822429386477097 ) ) ;
#122137 = CARTESIAN_POINT ( 'NONE',  ( -4.483927247898782831, 16.52544592524335698, 57.70942372801901143 ) ) ;
#122138 = CARTESIAN_POINT ( 'NONE',  ( -5.719274019375665041, -21.55341960407619695, 39.79275706135235424 ) ) ;
#122139 = CARTESIAN_POINT ( 'NONE',  ( 4.483927247898545687, 16.52544592524342804, 94.79057627198105251 ) ) ;
#122140 = DIRECTION ( 'NONE',  ( 0.000000000000000000, 0.000000000000000000, -1.000000000000000000 ) ) ;
#122141 = CARTESIAN_POINT ( 'NONE',  ( -16.62475595723696031, 7.163666690055234376, 50.52713351810466946 ) ) ;
#122142 = CARTESIAN_POINT ( 'NONE',  ( -15.72974639402197994, 15.80617190586746368, 35.62390960531437401 ) ) ;
#122143 = LINE ( 'NONE', #184820, #91357 ) ;
#122144 = CARTESIAN_POINT ( 'NONE',  ( 0.3917941432913279454, 9.051283227799057585, -63.96062768057055337 ) ) ;
#122146 = CARTESIAN_POINT ( 'NONE',  ( 14.29746914071049879, -8.314922557960816363, 38.33224293864768839 ) ) ;
#122145 = CARTESIAN_POINT ( 'NONE',  ( 12.06949235617739724, 12.14591786802326823, 41.87609039468568284 ) ) ;
#122147 = CARTESIAN_POINT ( 'NONE',  ( -5.823673210054116645, -21.52544592524344225, 72.29057627198102409 ) ) ;
#122148 = CARTESIAN_POINT ( 'NONE',  ( -9.564922557961040184, 16.46253265017147172, 82.91775706135233293 ) ) ;
#122149 = CARTESIAN_POINT ( 'NONE',  ( 10.72451020669898902, -18.67979575497178502, 62.91557627198102409 ) ) ;
#122150 = CARTESIAN_POINT ( 'NONE',  ( -20.74358237093910162, 11.24271120488109865, 170.1279846108370180 ) ) ;
#122152 = CARTESIAN_POINT ( 'NONE',  ( 13.89961937509977652, -13.97604488694527269, 103.1239096053143527 ) ) ;
#122151 = CARTESIAN_POINT ( 'NONE',  ( 19.03943276465977164, -0.05219959533909143690, 38.74890960531436690 ) ) ;
#122153 = CARTESIAN_POINT ( 'NONE',  ( 19.05341960407611168, 5.049401038298154454, 43.95724293864769550 ) ) ;
#122154 = CARTESIAN_POINT ( 'NONE',  ( 4.483927247898545687, 16.52544592524342804, 114.7905762719810383 ) ) ;
#122155 = APPLICATION_PROTOCOL_DEFINITION ( 'draft international standard', 'automotive_design', 1998, #174 ) ;
#122156 = CARTESIAN_POINT ( 'NONE',  ( 19.05341960407611168, 5.049401038298154454, 113.9572429386477097 ) ) ;
#122157 = VERTEX_POINT ( 'NONE', #130782 ) ;
#122158 = CARTESIAN_POINT ( 'NONE',  ( 4.483927247898790824, -16.52544592524335698, 70.20942372801904696 ) ) ;
#122159 = CARTESIAN_POINT ( 'NONE',  ( 15.80617190586746368, 15.72974639402197994, 109.3739096053143811 ) ) ;
#122160 = CARTESIAN_POINT ( 'NONE',  ( 16.51473224551069308, 9.474510206698969483, 54.16557627198103120 ) ) ;
#122161 = CARTESIAN_POINT ( 'NONE',  ( -15.80617190586768217, 15.72974639402176855, 28.12609039468568284 ) ) ;
#122162 = CARTESIAN_POINT ( 'NONE',  ( 16.51473224551069308, 9.474510206698969483, 89.16557627198103830 ) ) ;
#122163 = CARTESIAN_POINT ( 'NONE',  ( -28.79475375365586842, 2.428612866367529932E-14, 145.9843446568999923 ) ) ;
#122164 = ORIENTED_EDGE ( 'NONE', *, *, #16838, .T. ) ;
#122165 = CARTESIAN_POINT ( 'NONE',  ( -10.81492255796105439, 18.62759615963255655, 27.91775706135234358 ) ) ;
#122168 = CARTESIAN_POINT ( 'NONE',  ( 9.474510206698729675, 16.51473224551082808, 82.08442372801899012 ) ) ;
#122167 = CARTESIAN_POINT ( 'NONE',  ( 13.97604488694527802, 13.89961937509977652, 104.3739096053143385 ) ) ;
#122166 = CARTESIAN_POINT ( 'NONE',  ( 19.03943276465977164, -0.05219959533909143690, 23.74890960531435269 ) ) ;
#122169 = CARTESIAN_POINT ( 'NONE',  ( 19.05341960407617918, -5.049401038297876454, 36.04275706135234003 ) ) ;
#122170 = CARTESIAN_POINT ( 'NONE',  ( 21.55341960407610458, 5.719274019375980345, 103.9572429386476813 ) ) ;
#122171 = CARTESIAN_POINT ( 'NONE',  ( -9.564922557961040184, 16.46253265017147172, 32.91775706135233293 ) ) ;
#122172 = CARTESIAN_POINT ( 'NONE',  ( 13.97604488694548053, -13.89961937509957401, 40.62609039468564731 ) ) ;
#122173 = CARTESIAN_POINT ( 'NONE',  ( -16.53943276465976808, -0.05219959533934237506, 88.75109039468567573 ) ) ;
#122174 = CARTESIAN_POINT ( 'NONE',  ( -16.51473224551069308, -9.474510206698971260, 106.6655762719810383 ) ) ;
#122175 = CARTESIAN_POINT ( 'NONE',  ( 0.05219959533909260263, 19.03943276465977164, 64.99890960531436690 ) ) ;
#122176 = CARTESIAN_POINT ( 'NONE',  ( -5.823673210054431948, 21.52544592524334988, 62.70942372801902565 ) ) ;
#122177 = CARTESIAN_POINT ( 'NONE',  ( 18.62759615963255655, 10.81492255796105972, 86.66775706135234714 ) ) ;
#122178 = CARTESIAN_POINT ( 'NONE',  ( -5.049401038298153566, 19.05341960407611168, 115.2072429386477097 ) ) ;
#122179 = CARTESIAN_POINT ( 'NONE',  ( -19.03943276465977164, 0.05219959533909376836, 81.24890960531436690 ) ) ;
#122180 = CARTESIAN_POINT ( 'NONE',  ( -10.81492255796105439, 18.62759615963255655, 52.91775706135235424 ) ) ;
#122181 = CARTESIAN_POINT ( 'NONE',  ( -16.46253265017146816, -9.564922557961047289, 99.16775706135233293 ) ) ;
#122182 = CARTESIAN_POINT ( 'NONE',  ( -5.153800228976328057, -19.02544592524343514, 52.29057627198100988 ) ) ;
#122183 = CARTESIAN_POINT ( 'NONE',  ( -5.153800228976328057, -19.02544592524343514, 97.29057627198099567 ) ) ;
#122184 = CARTESIAN_POINT ( 'NONE',  ( 0.05219959533909260263, 19.03943276465977164, 79.99890960531436690 ) ) ;
#122185 = DIRECTION ( 'NONE',  ( 0.000000000000000000, 0.000000000000000000, 1.000000000000000000 ) ) ;
#122186 = CARTESIAN_POINT ( 'NONE',  ( -5.049401038298153566, 19.05341960407611168, 70.20724293864769550 ) ) ;
#122187 = CARTESIAN_POINT ( 'NONE',  ( 21.53943276465977519, -0.05219959533907433946, 98.74890960531438111 ) ) ;
#122188 = CARTESIAN_POINT ( 'NONE',  ( 4.483927247898790824, -16.52544592524335698, 85.20942372801901854 ) ) ;
#122189 = FACE_OUTER_BOUND ( 'NONE', #57177, .T. ) ;
#122190 = CARTESIAN_POINT ( 'NONE',  ( 0.05219959533936267826, -19.03943276465977164, 45.00109039468566863 ) ) ;
#122191 = CARTESIAN_POINT ( 'NONE',  ( 19.03943276465977164, -0.05219959533909143690, 73.74890960531435269 ) ) ;
#122192 = CARTESIAN_POINT ( 'NONE',  ( 16.52544592524342804, -4.483927247898539470, 73.54057627198102409 ) ) ;
#122193 = CARTESIAN_POINT ( 'NONE',  ( 8.314922557960818139, 14.29746914071049879, 99.58224293864770971 ) ) ;
#122194 = CARTESIAN_POINT ( 'NONE',  ( -15.80617190586745835, -15.72974639402198527, 21.87390960531436690 ) ) ;
#122195 = CARTESIAN_POINT ( 'NONE',  ( -19.05341960407611168, -5.049401038298163336, 101.4572429386476955 ) ) ;
#122196 = CARTESIAN_POINT ( 'NONE',  ( -13.89961937509977652, 13.97604488694528158, 115.6239096053143669 ) ) ;
#122197 = CARTESIAN_POINT ( 'NONE',  ( -0.05219959533936034679, 19.03943276465977164, 37.50109039468567573 ) ) ;
#122198 = CARTESIAN_POINT ( 'NONE',  ( 14.29746914071037800, 8.314922557961029526, 96.66775706135234714 ) ) ;
#122199 = CARTESIAN_POINT ( 'NONE',  ( -16.51473224551069308, -9.474510206698971260, 81.66557627198103830 ) ) ;
#122200 = CARTESIAN_POINT ( 'NONE',  ( 15.80617190586769283, -15.72974639402175789, 55.62609039468568284 ) ) ;
#122201 = CARTESIAN_POINT ( 'NONE',  ( -18.62759615963270932, 10.81492255796079327, 35.83224293864768839 ) ) ;
#122202 = CARTESIAN_POINT ( 'NONE',  ( 10.81492255796106328, -18.62759615963255655, 20.41775706135234714 ) ) ;
#122203 = CARTESIAN_POINT ( 'NONE',  ( -15.80617190586745835, -15.72974639402198527, 71.87390960531438111 ) ) ;
#122204 = CARTESIAN_POINT ( 'NONE',  ( 8.314922557960818139, 14.29746914071049879, 99.58224293864770971 ) ) ;
#122205 = CARTESIAN_POINT ( 'NONE',  ( 16.51473224551083163, -9.474510206698727899, 60.83442372801900433 ) ) ;
#122206 = ADVANCED_FACE ( 'NONE', ( #192474 ), #41795, .T. ) ;
#122207 = CARTESIAN_POINT ( 'NONE',  ( -0.05219959533909027116, -19.03943276465977164, 37.49890960531436690 ) ) ;
#122208 = CARTESIAN_POINT ( 'NONE',  ( 13.97604488694527802, 13.89961937509977652, 89.37390960531436690 ) ) ;
#122209 = CARTESIAN_POINT ( 'NONE',  ( 16.51473224551069308, 9.474510206698969483, 79.16557627198103830 ) ) ;
#122210 = CARTESIAN_POINT ( 'NONE',  ( 22.44159573604009239, 16.30477369853692693, 140.5750000027311728 ) ) ;
#122211 = CARTESIAN_POINT ( 'NONE',  ( -4.483927247898539470, -16.52544592524342804, 97.29057627198105251 ) ) ;
#122212 = ORIENTED_EDGE ( 'NONE', *, *, #122826, .T. ) ;
#122213 = CARTESIAN_POINT ( 'NONE',  ( -0.05219959533910754901, -16.53943276465976808, 22.49890960531436335 ) ) ;
#122214 = CARTESIAN_POINT ( 'NONE',  ( -12.14591786802326823, 12.06949235617739902, 23.12609039468567573 ) ) ;
#122215 = CARTESIAN_POINT ( 'NONE',  ( -15.80617190586768217, 15.72974639402176855, 88.12609039468570415 ) ) ;
#122216 = CARTESIAN_POINT ( 'NONE',  ( 13.97604488694527802, 13.89961937509977652, 99.37390960531436690 ) ) ;
#122217 = CARTESIAN_POINT ( 'NONE',  ( -10.81492255796078084, -18.62759615963271287, 112.0822429386477097 ) ) ;
#122218 = CARTESIAN_POINT ( 'NONE',  ( 13.97604488694527802, 13.89961937509977652, 49.37390960531434558 ) ) ;
#122219 = CARTESIAN_POINT ( 'NONE',  ( 14.29746914071037800, 8.314922557961029526, 46.66775706135234714 ) ) ;
#122220 = CARTESIAN_POINT ( 'NONE',  ( -5.153800228976607833, 19.02544592524334988, 107.7094237280189759 ) ) ;
#122221 = CARTESIAN_POINT ( 'NONE',  ( -4.379528057220328563, 16.55341960407611168, 95.20724293864769550 ) ) ;
#122222 = CARTESIAN_POINT ( 'NONE',  ( -21.53943276465977519, 0.05219959533907696930, 106.2489096053143811 ) ) ;
#122223 = CARTESIAN_POINT ( 'NONE',  ( -9.474510206698720793, -16.51473224551083518, 74.58442372801900433 ) ) ;
#122224 = CARTESIAN_POINT ( 'NONE',  ( -4.500000000000001776, -139.8289899283371653, 13.46984631039293845 ) ) ;
#122225 = CARTESIAN_POINT ( 'NONE',  ( -15.80617190586745835, -15.72974639402198527, 111.8739096053143669 ) ) ;
#122226 = DIRECTION ( 'NONE',  ( -1.000000000000000000, -0.000000000000000000, -0.000000000000000000 ) ) ;
#122227 = CARTESIAN_POINT ( 'NONE',  ( 0.05219959533909260263, 19.03943276465977164, 84.99890960531436690 ) ) ;
#122228 = CARTESIAN_POINT ( 'NONE',  ( 17.49999999999999645, -5.622605283950884214, 111.1879268940389096 ) ) ;
#122229 = CARTESIAN_POINT ( 'NONE',  ( 9.564922557960805705, 16.46253265017160317, 79.58224293864769550 ) ) ;
#122231 = CARTESIAN_POINT ( 'NONE',  ( -12.14591786802309592, -12.06949235617757132, 71.87390960531438111 ) ) ;
#122230 = CARTESIAN_POINT ( 'NONE',  ( 18.67979575497194134, -10.72451020669871369, 30.83442372801902209 ) ) ;
#122232 = CARTESIAN_POINT ( 'NONE',  ( 16.46253265017160672, -9.564922557960803928, 88.33224293864769550 ) ) ;
#122234 = CARTESIAN_POINT ( 'NONE',  ( 5.153800228976615827, -19.02544592524334988, 50.20942372801897591 ) ) ;
#122233 = CARTESIAN_POINT ( 'NONE',  ( -8.224510206698735004, -14.34966873604973081, 49.58442372801901143 ) ) ;
#122235 = CARTESIAN_POINT ( 'NONE',  ( 15.80617190586769283, -15.72974639402175789, 60.62609039468567573 ) ) ;
#122236 = AXIS2_PLACEMENT_3D ( 'NONE', #95201, #114345, #110369 ) ;
#122237 = CARTESIAN_POINT ( 'NONE',  ( -12.06949235617739369, -12.14591786802326823, 24.37609039468567573 ) ) ;
#122238 = CARTESIAN_POINT ( 'NONE',  ( 5.153800228976335163, 19.02544592524342804, 64.79057627198100988 ) ) ;
#122239 = CARTESIAN_POINT ( 'NONE',  ( 9.474510206698729675, 16.51473224551082808, 97.08442372801900433 ) ) ;
#122240 = CARTESIAN_POINT ( 'NONE',  ( -8.224510206698735004, -14.34966873604973081, 54.58442372801901143 ) ) ;
#122241 = CARTESIAN_POINT ( 'NONE',  ( 5.719274019375673035, 21.55341960407619339, 102.2927570613523613 ) ) ;
#122242 = CARTESIAN_POINT ( 'NONE',  ( -19.05341960407617563, 5.049401038297882671, 78.54275706135233293 ) ) ;
#122243 = CARTESIAN_POINT ( 'NONE',  ( -0.05219959533909027116, -19.03943276465977164, 47.49890960531435979 ) ) ;
#122244 = CARTESIAN_POINT ( 'NONE',  ( -21.55341960407610458, -5.719274019375992779, 76.45724293864769550 ) ) ;
#122246 = CARTESIAN_POINT ( 'NONE',  ( -19.02544592524334988, -5.153800228976617603, 73.95942372801900433 ) ) ;
#122245 = CARTESIAN_POINT ( 'NONE',  ( -16.52544592524342804, 4.483927247898546575, 81.04057627198102409 ) ) ;
#122247 = CARTESIAN_POINT ( 'NONE',  ( -19.49190055781011566, -5.499999999999970690, 70.56116087098779133 ) ) ;
#122248 = CARTESIAN_POINT ( 'NONE',  ( -19.03943276465977164, -0.05219959533935918106, 38.75109039468566152 ) ) ;
#122249 = CARTESIAN_POINT ( 'NONE',  ( 4.483927247898545687, 16.52544592524342804, 24.79057627198103120 ) ) ;
#122250 = CARTESIAN_POINT ( 'NONE',  ( -16.55341960407611168, -4.379528057220339221, 71.45724293864769550 ) ) ;
#122252 = CARTESIAN_POINT ( 'NONE',  ( -22.44159573604009950, -16.30477369853688430, 147.0750000027312012 ) ) ;
#122251 = CARTESIAN_POINT ( 'NONE',  ( 21.55341960407619695, -5.719274019375665929, 96.04275706135236135 ) ) ;
#122253 = CARTESIAN_POINT ( 'NONE',  ( 10.81492255796078972, 18.62759615963270932, 109.5822429386476955 ) ) ;
#122254 = CARTESIAN_POINT ( 'NONE',  ( -19.03943276465977164, 0.05219959533909376836, 66.24890960531436690 ) ) ;
#122255 = CARTESIAN_POINT ( 'NONE',  ( -0.05219959533937732626, 21.53943276465977519, 87.50109039468568994 ) ) ;
#122256 = CARTESIAN_POINT ( 'NONE',  ( -13.97604488694527625, -13.89961937509977652, 66.87390960531436690 ) ) ;
#122257 = EDGE_LOOP ( 'NONE', ( #117920, #176811, #179521, #50799, #61576 ) ) ;
#122258 = CARTESIAN_POINT ( 'NONE',  ( -12.06949235617756955, 12.14591786802309770, 115.6239096053143669 ) ) ;
#122259 = CARTESIAN_POINT ( 'NONE',  ( 18.62759615963271287, -10.81492255796078972, 28.33224293864769550 ) ) ;
#122260 = CARTESIAN_POINT ( 'NONE',  ( 14.34966873604960469, 8.224510206698951720, 64.16557627198102409 ) ) ;
#122261 = CARTESIAN_POINT ( 'NONE',  ( -5.049401038298153566, 19.05341960407611168, 50.20724293864770260 ) ) ;
#122262 = CARTESIAN_POINT ( 'NONE',  ( -14.34966873604960291, -8.224510206698953496, 86.66557627198102409 ) ) ;
#122263 = CARTESIAN_POINT ( 'NONE',  ( 18.67979575497178502, 10.72451020669898547, 114.1655762719810383 ) ) ;
#122264 = CARTESIAN_POINT ( 'NONE',  ( -18.62759615963255300, -10.81492255796106328, 54.16775706135235424 ) ) ;
#122265 = CARTESIAN_POINT ( 'NONE',  ( 0.05219959533909260263, 19.03943276465977164, 29.99890960531435979 ) ) ;
#122266 = CARTESIAN_POINT ( 'NONE',  ( 16.52544592524335698, 4.483927247898782831, 51.45942372801901854 ) ) ;
#122267 = CARTESIAN_POINT ( 'NONE',  ( 15.80617190586746368, 15.72974639402197994, 104.3739096053143669 ) ) ;
#122268 = CARTESIAN_POINT ( 'NONE',  ( -0.05219959533907301413, -21.53943276465977519, 92.49890960531436690 ) ) ;
#122270 = CARTESIAN_POINT ( 'NONE',  ( -5.153800228976328057, -19.02544592524343514, 52.29057627198100988 ) ) ;
#122269 = CARTESIAN_POINT ( 'NONE',  ( -9.564922557961040184, 16.46253265017147172, 27.91775706135232582 ) ) ;
#122271 = CARTESIAN_POINT ( 'NONE',  ( 16.51473224551069308, 9.474510206698969483, 104.1655762719810241 ) ) ;
#122272 = CARTESIAN_POINT ( 'NONE',  ( -18.67979575497193778, 10.72451020669871902, 58.33442372801901143 ) ) ;
#122273 = CARTESIAN_POINT ( 'NONE',  ( -21.55341960407610458, -5.719274019375992779, 41.45724293864769550 ) ) ;
#122274 = CARTESIAN_POINT ( 'NONE',  ( 12.06949235617757843, -12.14591786802309237, 23.12390960531436335 ) ) ;
#122276 = CARTESIAN_POINT ( 'NONE',  ( -15.80617190586768217, 15.72974639402176855, 98.12609039468570415 ) ) ;
#122275 = CARTESIAN_POINT ( 'NONE',  ( -0.05219959533937732626, 21.53943276465977519, 57.50109039468568994 ) ) ;
#122277 = CARTESIAN_POINT ( 'NONE',  ( 19.05341960407617918, -5.049401038297876454, 51.04275706135231871 ) ) ;
#122278 = CARTESIAN_POINT ( 'NONE',  ( 0.05219959533934541429, -16.53943276465976808, 100.0010903946857042 ) ) ;
#122279 = CARTESIAN_POINT ( 'NONE',  ( 0.05219959533937995610, -21.53943276465977519, 55.00109039468568284 ) ) ;
#122280 = CARTESIAN_POINT ( 'NONE',  ( -19.03943276465977164, 0.05219959533909376836, 41.24890960531435269 ) ) ;
#122281 = CARTESIAN_POINT ( 'NONE',  ( -21.55341960407619339, 5.719274019375674811, 113.5427570613523756 ) ) ;
#122282 = CARTESIAN_POINT ( 'NONE',  ( 21.53943276465977519, -0.05219959533907433946, 23.74890960531435269 ) ) ;
#122283 = CARTESIAN_POINT ( 'NONE',  ( 18.62759615963271287, -10.81492255796078972, 113.3322429386476955 ) ) ;
#122284 = CARTESIAN_POINT ( 'NONE',  ( -18.62759615963270932, 10.81492255796079327, 75.83224293864769550 ) ) ;
#122285 = CARTESIAN_POINT ( 'NONE',  ( -8.314922557961024197, 14.29746914071037800, 37.91775706135235424 ) ) ;
#122287 = CARTESIAN_POINT ( 'NONE',  ( 15.80617190586746368, 15.72974639402197994, 84.37390960531438111 ) ) ;
#122286 = CARTESIAN_POINT ( 'NONE',  ( -6.873421141834968218, 5.266531018137379228, -62.00040165901305755 ) ) ;
#122289 = CARTESIAN_POINT ( 'NONE',  ( -12.14591786802309592, -12.06949235617757132, 76.87390960531439532 ) ) ;
#122288 = CARTESIAN_POINT ( 'NONE',  ( -16.55341960407617563, 4.379528057220093196, 63.54275706135234003 ) ) ;
#122290 = CARTESIAN_POINT ( 'NONE',  ( -22.85886502250330210, 22.13519047554786567, -45.77314885760244323 ) ) ;
#122291 = CARTESIAN_POINT ( 'NONE',  ( 16.51473224551083163, -9.474510206698727899, 105.8344237280190043 ) ) ;
#122292 = CARTESIAN_POINT ( 'NONE',  ( -21.53943276465977519, 0.05219959533907696930, 31.24890960531435979 ) ) ;
#122293 = DIRECTION ( 'NONE',  ( 0.000000000000000000, 0.000000000000000000, 1.000000000000000000 ) ) ;
#122294 = CARTESIAN_POINT ( 'NONE',  ( -4.483927247898782831, 16.52544592524335698, 42.70942372801901854 ) ) ;
#122295 = CARTESIAN_POINT ( 'NONE',  ( 15.80617190586769283, -15.72974639402175789, 20.62609039468568639 ) ) ;
#122296 = CARTESIAN_POINT ( 'NONE',  ( 21.53943276465977519, -0.05219959533907433946, 33.74890960531436690 ) ) ;
#122297 = CARTESIAN_POINT ( 'NONE',  ( 0.05219959533934541429, -16.53943276465976808, 70.00109039468568994 ) ) ;
#122298 = CARTESIAN_POINT ( 'NONE',  ( 0.05219959533909260263, 19.03943276465977164, 79.99890960531436690 ) ) ;
#122300 = CARTESIAN_POINT ( 'NONE',  ( 19.05341960407611168, 5.049401038298154454, 23.95724293864769194 ) ) ;
#122299 = CARTESIAN_POINT ( 'NONE',  ( 5.823673210054444382, -21.52544592524334988, 40.20942372801901854 ) ) ;
#122301 = CARTESIAN_POINT ( 'NONE',  ( -18.67979575497178146, -10.72451020669898902, 31.66557627198102054 ) ) ;
#122302 = VERTEX_POINT ( 'NONE', #105441 ) ;
#122303 = CARTESIAN_POINT ( 'NONE',  ( -0.05219959533936034679, 19.03943276465977164, 22.50109039468566152 ) ) ;
#122304 = CARTESIAN_POINT ( 'NONE',  ( 8.314922557961029526, -14.29746914071037800, 50.41775706135235424 ) ) ;
#122305 = CARTESIAN_POINT ( 'NONE',  ( -5.153800228976328057, -19.02544592524343514, 97.29057627198099567 ) ) ;
#122306 = CARTESIAN_POINT ( 'NONE',  ( 10.72451020669898902, -18.67979575497178502, 102.9155762719810383 ) ) ;
#122307 = CARTESIAN_POINT ( 'NONE',  ( -0.05219959533909027116, -19.03943276465977164, 72.49890960531435269 ) ) ;
#122308 = CARTESIAN_POINT ( 'NONE',  ( -3.883653825558159411, -5.178020654986570825, -62.44482655153596795 ) ) ;
#122309 = CARTESIAN_POINT ( 'NONE',  ( 24.81835718235489807, 6.052279806424484931, 168.4265042179603142 ) ) ;
#122310 = CARTESIAN_POINT ( 'NONE',  ( -8.224510206698948167, 14.34966873604960824, 75.41557627198102409 ) ) ;
#122311 = CARTESIAN_POINT ( 'NONE',  ( -10.72451020669898014, 18.67979575497178502, 40.41557627198103120 ) ) ;
#122312 = CARTESIAN_POINT ( 'NONE',  ( 12.99999999999999822, 2.516649172247811061E-16, -2.055000000000000160 ) ) ;
#122313 = CARTESIAN_POINT ( 'NONE',  ( 8.224510206698742110, 14.34966873604972548, 62.08442372801901143 ) ) ;
#122314 = CARTESIAN_POINT ( 'NONE',  ( -21.53943276465977519, -0.05219959533937600094, 23.75109039468567929 ) ) ;
#122315 = CARTESIAN_POINT ( 'NONE',  ( -5.153800228976607833, 19.02544592524334988, 82.70942372801897591 ) ) ;
#122316 = CARTESIAN_POINT ( 'NONE',  ( -19.03943276465977164, 0.05219959533909376836, 26.24890960531435624 ) ) ;
#122317 = CARTESIAN_POINT ( 'NONE',  ( 15.72974639402199770, -15.80617190586745480, 63.12390960531435979 ) ) ;
#122318 = CARTESIAN_POINT ( 'NONE',  ( -5.153800228976328057, -19.02544592524343514, 102.2905762719810383 ) ) ;
#122319 = CARTESIAN_POINT ( 'NONE',  ( 5.823673210054444382, -21.52544592524334988, 95.20942372801903275 ) ) ;
#122320 = CARTESIAN_POINT ( 'NONE',  ( -0.05219959533909027116, -19.03943276465977164, 67.49890960531436690 ) ) ;
#122321 = CARTESIAN_POINT ( 'NONE',  ( 4.379528057220092307, 16.55341960407617563, 52.29275706135236135 ) ) ;
#122322 = CARTESIAN_POINT ( 'NONE',  ( -0.05219959533909027116, -19.03943276465977164, 57.49890960531435979 ) ) ;
#122323 = CARTESIAN_POINT ( 'NONE',  ( 15.72974639402176855, 15.80617190586768217, 81.87609039468568994 ) ) ;
#122324 = ORIENTED_EDGE ( 'NONE', *, *, #15986, .T. ) ;
#122325 = CARTESIAN_POINT ( 'NONE',  ( 13.89961937509957401, 13.97604488694547697, 41.87609039468566152 ) ) ;
#122326 = CARTESIAN_POINT ( 'NONE',  ( -13.97604488694547697, 13.89961937509957934, 58.12609039468566863 ) ) ;
#122327 = CARTESIAN_POINT ( 'NONE',  ( -15.80617190586768217, 15.72974639402176855, 53.12609039468568284 ) ) ;
#122328 = CARTESIAN_POINT ( 'NONE',  ( -8.945340038113732462, 0.6707077324888295333, -61.92615459704094150 ) ) ;
#122329 = CARTESIAN_POINT ( 'NONE',  ( 13.97604488694548053, -13.89961937509957401, 40.62609039468564731 ) ) ;
#122330 = CARTESIAN_POINT ( 'NONE',  ( -19.02544592524342804, 5.153800228976336051, 96.04057627198103830 ) ) ;
#122331 = CARTESIAN_POINT ( 'NONE',  ( -9.564922557960796823, -16.46253265017161027, 67.08224293864769550 ) ) ;
#122332 = CARTESIAN_POINT ( 'NONE',  ( -0.05219959533934338120, 16.53943276465976808, 112.5010903946857042 ) ) ;
#122334 = CARTESIAN_POINT ( 'NONE',  ( -18.67979575497193778, 10.72451020669871902, 103.3344237280190043 ) ) ;
#122333 = CARTESIAN_POINT ( 'NONE',  ( -15.72974639402197994, 15.80617190586746368, 40.62390960531435269 ) ) ;
#122335 = TOROIDAL_SURFACE ( 'NONE', #12679, 48.98979485566358250, 10.00000000000000000 ) ;
#122336 = CARTESIAN_POINT ( 'NONE',  ( 22.81625015709510151, -31.40387420917324590, -8.424999997268812990 ) ) ;
#122337 = CARTESIAN_POINT ( 'NONE',  ( -34.29436769411893238, 3.356737774573908872, 90.62828869849683144 ) ) ;
#122338 = CARTESIAN_POINT ( 'NONE',  ( 21.53943276465977519, 0.05219959533937863772, 101.2510903946856757 ) ) ;
#122339 = DIRECTION ( 'NONE',  ( 1.000000000000000000, 0.000000000000000000, 0.000000000000000000 ) ) ;
#122340 = CARTESIAN_POINT ( 'NONE',  ( 13.89961937509977652, -13.97604488694527269, 28.12390960531435624 ) ) ;
#122341 = CARTESIAN_POINT ( 'NONE',  ( -9.474510206698964154, 16.51473224551069663, 110.4155762719810383 ) ) ;
#122342 = ADVANCED_FACE ( 'NONE', ( #75099 ), #58934, .F. ) ;
#122343 = ADVANCED_FACE ( 'NONE', ( #196490 ), #135797, .F. ) ;
#122344 = CARTESIAN_POINT ( 'NONE',  ( 33.67954790872092730, 5.223285087354250678, 96.76001495611576786 ) ) ;
#122345 = CARTESIAN_POINT ( 'NONE',  ( -8.224510206698735004, -14.34966873604973081, 54.58442372801901143 ) ) ;
#122346 = CARTESIAN_POINT ( 'NONE',  ( -21.55341960407610458, -5.719274019375992779, 66.45724293864768129 ) ) ;
#122347 = CARTESIAN_POINT ( 'NONE',  ( -14.34966873604960291, -8.224510206698953496, 41.66557627198103120 ) ) ;
#122349 = CARTESIAN_POINT ( 'NONE',  ( 19.03943276465977164, -0.05219959533909143690, 103.7489096053143669 ) ) ;
#122348 = CARTESIAN_POINT ( 'NONE',  ( -12.14591786802309592, -12.06949235617757132, 106.8739096053143811 ) ) ;
#122350 = CARTESIAN_POINT ( 'NONE',  ( 9.564922557961047289, -16.46253265017146816, 35.41775706135233293 ) ) ;
#122351 = CARTESIAN_POINT ( 'NONE',  ( 0.05219959533909260263, 19.03943276465977164, 24.99890960531435269 ) ) ;
#122352 = CARTESIAN_POINT ( 'NONE',  ( -10.72451020669870658, -18.67979575497194134, 64.58442372801900433 ) ) ;
#122353 = CARTESIAN_POINT ( 'NONE',  ( -5.153800228976328057, -19.02544592524343514, 112.2905762719810099 ) ) ;
#122354 = CARTESIAN_POINT ( 'NONE',  ( 14.34966873604960469, 8.224510206698951720, 34.16557627198102409 ) ) ;
#122355 = FACE_OUTER_BOUND ( 'NONE', #155112, .T. ) ;
#122356 = CARTESIAN_POINT ( 'NONE',  ( -18.62759615963270932, 10.81492255796079327, 25.83224293864769194 ) ) ;
#122357 = CARTESIAN_POINT ( 'NONE',  ( 12.14591786802309770, 12.06949235617756955, 89.37390960531435269 ) ) ;
#122358 = CARTESIAN_POINT ( 'NONE',  ( 9.474510206698729675, 16.51473224551082808, 57.08442372801900433 ) ) ;
#122359 = CARTESIAN_POINT ( 'NONE',  ( -9.564922557960796823, -16.46253265017161027, 72.08224293864770971 ) ) ;
#122360 = CARTESIAN_POINT ( 'NONE',  ( -8.224510206698948167, 14.34966873604960824, 80.41557627198103830 ) ) ;
#122361 = CARTESIAN_POINT ( 'NONE',  ( 9.474510206698729675, 16.51473224551082808, 87.08442372801900433 ) ) ;
#122362 = CARTESIAN_POINT ( 'NONE',  ( -15.80617190586745835, -15.72974639402198527, 51.87390960531437401 ) ) ;
#122363 = ORIENTED_EDGE ( 'NONE', *, *, #154133, .T. ) ;
#122364 = CARTESIAN_POINT ( 'NONE',  ( 16.55341960407611168, 4.379528057220329451, 113.9572429386477239 ) ) ;
#122365 = FACE_OUTER_BOUND ( 'NONE', #121461, .T. ) ;
#122367 = CARTESIAN_POINT ( 'NONE',  ( 15.80617190586746368, 15.72974639402197994, 69.37390960531436690 ) ) ;
#122366 = CARTESIAN_POINT ( 'NONE',  ( 5.049401038298161559, -19.05341960407611168, 67.70724293864769550 ) ) ;
#122369 = CARTESIAN_POINT ( 'NONE',  ( 16.46253265017160672, -9.564922557960803928, 88.33224293864769550 ) ) ;
#122368 = CARTESIAN_POINT ( 'NONE',  ( 0.05219959533934541429, -16.53943276465976808, 110.0010903946856757 ) ) ;
#122370 = CARTESIAN_POINT ( 'NONE',  ( 19.02544592524334988, 5.153800228976608722, 71.45942372801900433 ) ) ;
#122371 = CARTESIAN_POINT ( 'NONE',  ( 5.823673210054444382, -21.52544592524334988, 80.20942372801901854 ) ) ;
#122372 = CARTESIAN_POINT ( 'NONE',  ( -5.823673210054116645, -21.52544592524344225, 62.29057627198102409 ) ) ;
#122373 = CARTESIAN_POINT ( 'NONE',  ( 21.55341960407610458, 5.719274019375980345, 23.95724293864769550 ) ) ;
#122374 = CARTESIAN_POINT ( 'NONE',  ( 5.049401038298161559, -19.05341960407611168, 42.70724293864767418 ) ) ;
#122375 = CARTESIAN_POINT ( 'NONE',  ( -14.29746914071037622, -8.314922557961029526, 94.16775706135237556 ) ) ;
#122376 = CARTESIAN_POINT ( 'NONE',  ( 19.02544592524343514, -5.153800228976328945, 63.54057627198103830 ) ) ;
#122377 = CARTESIAN_POINT ( 'NONE',  ( 19.02544592524334988, 5.153800228976608722, 111.4594237280190043 ) ) ;
#122378 = DIRECTION ( 'NONE',  ( -1.000000000000000000, 0.000000000000000000, 0.000000000000000000 ) ) ;
#122379 = CARTESIAN_POINT ( 'NONE',  ( -13.89961937509957401, -13.97604488694547875, 19.37609039468566507 ) ) ;
#122380 = CARTESIAN_POINT ( 'NONE',  ( 4.483927247898545687, 16.52544592524342804, 74.79057627198105251 ) ) ;
#122381 = CARTESIAN_POINT ( 'NONE',  ( 10.81492255796078972, 18.62759615963270932, 104.5822429386477097 ) ) ;
#122382 = CARTESIAN_POINT ( 'NONE',  ( -18.67979575497178146, -10.72451020669898902, 96.66557627198102409 ) ) ;
#122383 = CARTESIAN_POINT ( 'NONE',  ( 17.50000000000000000, -5.500000000000031086, 98.29690382534174375 ) ) ;
#122384 = CARTESIAN_POINT ( 'NONE',  ( -0.05219959533907301413, -21.53943276465977519, 47.49890960531435979 ) ) ;
#122385 = CARTESIAN_POINT ( 'NONE',  ( 8.224510206698742110, 14.34966873604972548, 77.08442372801901854 ) ) ;
#122386 = CARTESIAN_POINT ( 'NONE',  ( 12.14591786802309770, 12.06949235617756955, 109.3739096053143811 ) ) ;
#122387 = CARTESIAN_POINT ( 'NONE',  ( 0.05219959533909260263, 19.03943276465977164, 54.99890960531435979 ) ) ;
#122388 = SURFACE_SIDE_STYLE ('',( #124380 ) ) ;
#122389 = CARTESIAN_POINT ( 'NONE',  ( -15.64208950468055193, -40.81369178264755959, -21.33727593494802477 ) ) ;
#122390 = CARTESIAN_POINT ( 'NONE',  ( -0.05219959533934338120, 16.53943276465976808, 112.5010903946857042 ) ) ;
#122391 = CARTESIAN_POINT ( 'NONE',  ( 0.05219959533937995610, -21.53943276465977519, 45.00109039468568284 ) ) ;
#122392 = CARTESIAN_POINT ( 'NONE',  ( -16.51473224551069308, -9.474510206698971260, 101.6655762719810241 ) ) ;
#122393 = CARTESIAN_POINT ( 'NONE',  ( 21.53943276465977519, 0.05219959533937863772, 76.25109039468568994 ) ) ;
#122394 = LINE ( 'NONE', #169901, #153532 ) ;
#122395 = CARTESIAN_POINT ( 'NONE',  ( -5.153800228976328057, -19.02544592524343514, 22.29057627198102765 ) ) ;
#122396 = ORIENTED_EDGE ( 'NONE', *, *, #194696, .T. ) ;
#122397 = CARTESIAN_POINT ( 'NONE',  ( 5.719274019375673035, 21.55341960407619339, 67.29275706135234714 ) ) ;
#122398 = CARTESIAN_POINT ( 'NONE',  ( 19.02544592524343514, -5.153800228976328945, 53.54057627198102409 ) ) ;
#122399 = CARTESIAN_POINT ( 'NONE',  ( 13.97604488694527802, 13.89961937509977652, 109.3739096053143669 ) ) ;
#122400 = CARTESIAN_POINT ( 'NONE',  ( -0.05219959533936034679, 19.03943276465977164, 82.50109039468567573 ) ) ;
#122401 = CARTESIAN_POINT ( 'NONE',  ( -18.67979575497193778, 10.72451020669871902, 43.33442372801901143 ) ) ;
#122402 = CARTESIAN_POINT ( 'NONE',  ( -9.474510206698720793, -16.51473224551083518, 109.5844237280190043 ) ) ;
#122403 = CARTESIAN_POINT ( 'NONE',  ( 19.05341960407617918, -5.049401038297876454, 66.04275706135233293 ) ) ;
#122404 = CARTESIAN_POINT ( 'NONE',  ( 5.049401038298161559, -19.05341960407611168, 32.70724293864768129 ) ) ;
#122405 = CARTESIAN_POINT ( 'NONE',  ( 0.05219959533936267826, -19.03943276465977164, 90.00109039468567573 ) ) ;
#122406 = CARTESIAN_POINT ( 'NONE',  ( -16.53943276465976808, -0.05219959533934237506, 108.7510903946857042 ) ) ;
#122407 = CARTESIAN_POINT ( 'NONE',  ( 9.564922557961047289, -16.46253265017146816, 75.41775706135234714 ) ) ;
#122408 = CARTESIAN_POINT ( 'NONE',  ( 14.34966873604960469, 8.224510206698951720, 39.16557627198102409 ) ) ;
#122409 = CARTESIAN_POINT ( 'NONE',  ( 5.153800228976615827, -19.02544592524334988, 60.20942372801899012 ) ) ;
#122410 = CARTESIAN_POINT ( 'NONE',  ( 10.81492255796106328, -18.62759615963255655, 105.4177570613523613 ) ) ;
#122412 = EDGE_CURVE ( 'NONE', #177566, #17000, #114386, .T. ) ;
#122411 = CARTESIAN_POINT ( 'NONE',  ( -9.564922557961040184, 16.46253265017147172, 27.91775706135232582 ) ) ;
#122413 = CARTESIAN_POINT ( 'NONE',  ( 9.474510206698971260, -16.51473224551069308, 27.91557627198103120 ) ) ;
#122414 = CARTESIAN_POINT ( 'NONE',  ( -17.13100169013298668, -6.664070546373171311, 64.23210164300152769 ) ) ;
#122415 = CARTESIAN_POINT ( 'NONE',  ( 8.314922557961029526, -14.29746914071037800, 45.41775706135234003 ) ) ;
#122416 = CARTESIAN_POINT ( 'NONE',  ( 22.44159573604009239, 16.30477369853692693, 146.0750000027311728 ) ) ;
#122417 = CARTESIAN_POINT ( 'NONE',  ( 0.05219959533909260263, 19.03943276465977164, 94.99890960531436690 ) ) ;
#122418 = CARTESIAN_POINT ( 'NONE',  ( -18.22780087662123805, 5.499999999999981348, 96.01763182126897789 ) ) ;
#122419 = VERTEX_POINT ( 'NONE', #90263 ) ;
#122420 = CARTESIAN_POINT ( 'NONE',  ( 0.05219959533936267826, -19.03943276465977164, 80.00109039468567573 ) ) ;
#122421 = CARTESIAN_POINT ( 'NONE',  ( -21.55341960407610458, -5.719274019375992779, 26.45724293864768839 ) ) ;
#122423 = CARTESIAN_POINT ( 'NONE',  ( 16.51473224551083163, -9.474510206698727899, 95.83442372801900433 ) ) ;
#122422 = CARTESIAN_POINT ( 'NONE',  ( 18.62759615963255655, 10.81492255796105972, 111.6677570613523613 ) ) ;
#122424 = CARTESIAN_POINT ( 'NONE',  ( 14.29746914071049879, -8.314922557960816363, 108.3322429386477097 ) ) ;
#122425 = CARTESIAN_POINT ( 'NONE',  ( 13.89961937509977652, -13.97604488694527269, 28.12390960531435624 ) ) ;
#122426 = CARTESIAN_POINT ( 'NONE',  ( -15.72974639402197994, 15.80617190586746368, 65.62390960531436690 ) ) ;
#122427 = CARTESIAN_POINT ( 'NONE',  ( -21.53943276465977519, 0.05219959533907696930, 46.24890960531435979 ) ) ;
#122428 = CARTESIAN_POINT ( 'NONE',  ( -16.51473224551069308, -9.474510206698971260, 21.66557627198102765 ) ) ;
#122429 = DIRECTION ( 'NONE',  ( 1.000000000000000000, 0.000000000000000000, 0.000000000000000000 ) ) ;
#122430 = CARTESIAN_POINT ( 'NONE',  ( -19.02544592524334988, -5.153800228976617603, 68.95942372801896170 ) ) ;
#122431 = CARTESIAN_POINT ( 'NONE',  ( 16.53943276465976808, -0.05219959533910856209, 33.74890960531436690 ) ) ;
#122432 = CARTESIAN_POINT ( 'NONE',  ( -0.05219959533909027116, -19.03943276465977164, 112.4989096053143669 ) ) ;
#122433 = CARTESIAN_POINT ( 'NONE',  ( 0.05219959533937995610, -21.53943276465977519, 95.00109039468568994 ) ) ;
#122434 = CARTESIAN_POINT ( 'NONE',  ( -18.62759615963270932, 10.81492255796079327, 65.83224293864769550 ) ) ;
#122435 = CARTESIAN_POINT ( 'NONE',  ( -21.53943276465977519, -0.05219959533937600094, 53.75109039468568994 ) ) ;
#122436 = CARTESIAN_POINT ( 'NONE',  ( -10.81492255796105439, 18.62759615963255655, 47.91775706135234714 ) ) ;
#122437 = CARTESIAN_POINT ( 'NONE',  ( 13.97604488694527802, 13.89961937509977652, 99.37390960531436690 ) ) ;
#122439 = CARTESIAN_POINT ( 'NONE',  ( 18.67979575497194134, -10.72451020669871369, 45.83442372801901854 ) ) ;
#122438 = CARTESIAN_POINT ( 'NONE',  ( 4.379528057220092307, 16.55341960407617563, 92.29275706135236135 ) ) ;
#122440 = CARTESIAN_POINT ( 'NONE',  ( -13.89961937509977652, 13.97604488694528158, 25.62390960531434558 ) ) ;
#122441 = CARTESIAN_POINT ( 'NONE',  ( -32.57470439124678308, 1.954246231034509895, 87.74243420032608753 ) ) ;
#122442 = CARTESIAN_POINT ( 'NONE',  ( 4.379528057220339221, -16.55341960407611168, 67.70724293864769550 ) ) ;
#122443 = CARTESIAN_POINT ( 'NONE',  ( 14.34966873604960469, 8.224510206698951720, 29.16557627198103120 ) ) ;
#122444 = CARTESIAN_POINT ( 'NONE',  ( 9.474510206698971260, -16.51473224551069308, 67.91557627198102409 ) ) ;
#122445 = CARTESIAN_POINT ( 'NONE',  ( 13.97604488694527802, 13.89961937509977652, 44.37390960531435269 ) ) ;
#122446 = CARTESIAN_POINT ( 'NONE',  ( -10.72451020669898014, 18.67979575497178502, 60.41557627198102409 ) ) ;
#122447 = CARTESIAN_POINT ( 'NONE',  ( 5.049401038297881783, 19.05341960407617563, 37.29275706135232582 ) ) ;
#122449 = CARTESIAN_POINT ( 'NONE',  ( -0.05219959533910754901, -16.53943276465976808, 47.49890960531435979 ) ) ;
#122448 = CARTESIAN_POINT ( 'NONE',  ( 26.03370437638686852, 6.875205692009825675, 160.5968874236875195 ) ) ;
#122450 = CARTESIAN_POINT ( 'NONE',  ( -15.72974639402197994, 15.80617190586746368, 30.62390960531436335 ) ) ;
#122451 = ORIENTED_EDGE ( 'NONE', *, *, #58814, .F. ) ;
#122452 = CARTESIAN_POINT ( 'NONE',  ( -21.99873734152892268, 27.49873734152935967, 1.818019484660534424 ) ) ;
#122453 = CARTESIAN_POINT ( 'NONE',  ( 4.379528057220092307, 16.55341960407617563, 77.29275706135234714 ) ) ;
#122454 = CARTESIAN_POINT ( 'NONE',  ( -9.564922557961040184, 16.46253265017147172, 77.91775706135234714 ) ) ;
#122455 = CARTESIAN_POINT ( 'NONE',  ( 0.05219959533910956823, 16.53943276465976808, 44.99890960531435979 ) ) ;
#122456 = CARTESIAN_POINT ( 'NONE',  ( 17.26172910966781515, -6.454744622555777411, 53.30646908649224969 ) ) ;
#122457 = CARTESIAN_POINT ( 'NONE',  ( -16.53943276465976808, 0.05219959533911058130, 31.24890960531435979 ) ) ;
#122458 = CARTESIAN_POINT ( 'NONE',  ( -16.46253265017160317, 9.564922557960807481, 55.83224293864769550 ) ) ;
#122459 = CARTESIAN_POINT ( 'NONE',  ( -19.03943276465977164, 0.05219959533909376836, 81.24890960531436690 ) ) ;
#122460 = CARTESIAN_POINT ( 'NONE',  ( -19.05341960407611168, -5.049401038298163336, 41.45724293864769550 ) ) ;
#122461 = CARTESIAN_POINT ( 'NONE',  ( -21.55341960407619339, 5.719274019375674811, 43.54275706135235424 ) ) ;
#122462 = CARTESIAN_POINT ( 'NONE',  ( 9.474510206698971260, -16.51473224551069308, 52.91557627198102409 ) ) ;
#122463 = CARTESIAN_POINT ( 'NONE',  ( 32.00000000000000000, -5.510910596163089556E-15, 45.00000000000000000 ) ) ;
#122464 = CARTESIAN_POINT ( 'NONE',  ( -13.97604488694527625, -13.89961937509977652, 56.87390960531434558 ) ) ;
#122465 = CARTESIAN_POINT ( 'NONE',  ( 21.55341960407610458, 5.719274019375980345, 38.95724293864768839 ) ) ;
#122466 = VECTOR ( 'NONE', #146595, 1000.000000000000000 ) ;
#122467 = CARTESIAN_POINT ( 'NONE',  ( 13.89961937509977652, -13.97604488694527269, 23.12390960531436335 ) ) ;
#122468 = CARTESIAN_POINT ( 'NONE',  ( -15.80617190586745835, -15.72974639402198527, 31.87390960531435979 ) ) ;
#122469 = B_SPLINE_CURVE_WITH_KNOTS ( 'NONE', 3,
 ( #24545, #36679, #146868, #194392, #128688, #86195 ),
 .UNSPECIFIED., .F., .F.,
 ( 4, 2, 4 ),
 ( 0.000000000000000000, 0.0003837532665635277852, 0.0007675065331270555704 ),
 .UNSPECIFIED. ) ;
#122470 = CARTESIAN_POINT ( 'NONE',  ( -8.224510206698735004, -14.34966873604973081, 84.58442372801903275 ) ) ;
#122471 = CARTESIAN_POINT ( 'NONE',  ( -18.67979575497193778, 10.72451020669871902, 103.3344237280190043 ) ) ;
#122472 = CARTESIAN_POINT ( 'NONE',  ( 16.55341960407618274, -4.379528057220086978, 66.04275706135236135 ) ) ;
#122473 = CARTESIAN_POINT ( 'NONE',  ( -9.474510206698964154, 16.51473224551069663, 115.4155762719810241 ) ) ;
#122474 = CARTESIAN_POINT ( 'NONE',  ( 12.14591786802327356, -12.06949235617739191, 60.62609039468567573 ) ) ;
#122475 = CARTESIAN_POINT ( 'NONE',  ( 12.14591786802327356, -12.06949235617739191, 40.62609039468567573 ) ) ;
#122476 = CARTESIAN_POINT ( 'NONE',  ( -14.34966873604972548, 8.224510206698743886, 93.33442372801901854 ) ) ;
#122477 = CARTESIAN_POINT ( 'NONE',  ( -4.379528057220086978, -16.55341960407618274, 24.79275706135235779 ) ) ;
#122478 = CARTESIAN_POINT ( 'NONE',  ( -19.02544592524342804, 5.153800228976336051, 31.04057627198102409 ) ) ;
#122479 = CARTESIAN_POINT ( 'NONE',  ( 0.05219959533907565091, 21.53943276465977519, 104.9989096053143669 ) ) ;
#122480 = CARTESIAN_POINT ( 'NONE',  ( -14.34966873604972548, 8.224510206698743886, 28.33442372801902209 ) ) ;
#122481 = CARTESIAN_POINT ( 'NONE',  ( 12.14591786802327356, -12.06949235617739191, 80.62609039468567573 ) ) ;
#122482 = CARTESIAN_POINT ( 'NONE',  ( 2.500000000000000000, 0.000000000000000000, 0.000000000000000000 ) ) ;
#122483 = CARTESIAN_POINT ( 'NONE',  ( -21.55341960407619339, 5.719274019375674811, 83.54275706135234714 ) ) ;
#122484 = CARTESIAN_POINT ( 'NONE',  ( 13.97604488694548053, -13.89961937509957401, 85.62609039468568994 ) ) ;
#122485 = CARTESIAN_POINT ( 'NONE',  ( -4.483927247898539470, -16.52544592524342804, 57.29057627198103120 ) ) ;
#122486 = CARTESIAN_POINT ( 'NONE',  ( 8.314922557960818139, 14.29746914071049879, 49.58224293864769550 ) ) ;
#122487 = CARTESIAN_POINT ( 'NONE',  ( -12.14591786802309592, -12.06949235617757132, 101.8739096053143811 ) ) ;
#122489 = CARTESIAN_POINT ( 'NONE',  ( 18.09805431107250584, -5.499999999999988454, 53.51606229291888184 ) ) ;
#122488 = CARTESIAN_POINT ( 'NONE',  ( -5.153800228976607833, 19.02544592524334988, 42.70942372801901143 ) ) ;
#122490 = CARTESIAN_POINT ( 'NONE',  ( 21.52544592524334988, 5.823673210054432836, 46.45942372801901854 ) ) ;
#122491 = CARTESIAN_POINT ( 'NONE',  ( -13.97604488694547697, 13.89961937509957934, 103.1260903946856473 ) ) ;
#122492 = CARTESIAN_POINT ( 'NONE',  ( 17.44270441346518652, 5.991230190322986537, 83.86335079264230785 ) ) ;
#122493 = CARTESIAN_POINT ( 'NONE',  ( 5.153800228976335163, 19.02544592524342804, 99.79057627198102409 ) ) ;
#122494 = CARTESIAN_POINT ( 'NONE',  ( -18.62759615963270932, 10.81492255796079327, 70.83224293864770971 ) ) ;
#122495 = CARTESIAN_POINT ( 'NONE',  ( 13.97604488694548053, -13.89961937509957401, 90.62609039468567573 ) ) ;
#122496 = CARTESIAN_POINT ( 'NONE',  ( -13.97604488694527625, -13.89961937509977652, 106.8739096053143669 ) ) ;
#122497 = CARTESIAN_POINT ( 'NONE',  ( -2.002489259400932919, -27.92993298909506095, 139.9999999999999716 ) ) ;
#122498 = CARTESIAN_POINT ( 'NONE',  ( -4.483927247898539470, -16.52544592524342804, 107.2905762719810525 ) ) ;
#122499 = CARTESIAN_POINT ( 'NONE',  ( -15.72974639402176322, -15.80617190586768395, 94.37609039468568994 ) ) ;
#122500 = CARTESIAN_POINT ( 'NONE',  ( 13.89961937509977652, -13.97604488694527269, 38.12390960531436690 ) ) ;
#122501 = CARTESIAN_POINT ( 'NONE',  ( -18.67979575497193778, 10.72451020669871902, 48.33442372801902565 ) ) ;
#122502 = AXIS2_PLACEMENT_3D ( 'NONE', #62598, #124276, #185972 ) ;
#122503 = CARTESIAN_POINT ( 'NONE',  ( -21.55341960407619339, 5.719274019375674811, 88.54275706135236135 ) ) ;
#122504 = CARTESIAN_POINT ( 'NONE',  ( 16.52544592524335698, 4.483927247898782831, 96.45942372801901854 ) ) ;
#122505 = CARTESIAN_POINT ( 'NONE',  ( -10.72451020669870658, -18.67979575497194134, 39.58442372801901143 ) ) ;
#122506 = CARTESIAN_POINT ( 'NONE',  ( 15.80617190586769283, -15.72974639402175789, 40.62609039468567573 ) ) ;
#122508 = CARTESIAN_POINT ( 'NONE',  ( 9.564922557960805705, 16.46253265017160317, 89.58224293864769550 ) ) ;
#122507 = CARTESIAN_POINT ( 'NONE',  ( -9.564922557961040184, 16.46253265017147172, 67.91775706135233293 ) ) ;
#122509 = CARTESIAN_POINT ( 'NONE',  ( -8.224510206698948167, 14.34966873604960824, 105.4155762719810383 ) ) ;
#122510 = CARTESIAN_POINT ( 'NONE',  ( -5.719274019375978568, 21.55341960407610458, 80.20724293864769550 ) ) ;
#122511 = CARTESIAN_POINT ( 'NONE',  ( 12.06949235617757843, -12.14591786802309237, 68.12390960531436690 ) ) ;
#122512 = CARTESIAN_POINT ( 'NONE',  ( 0.05219959533937995610, -21.53943276465977519, 110.0010903946856757 ) ) ;
#122513 = CARTESIAN_POINT ( 'NONE',  ( -14.29746914071049879, 8.314922557960819915, 85.83224293864768129 ) ) ;
#122514 = CARTESIAN_POINT ( 'NONE',  ( -13.89961937509977652, 13.97604488694528158, 40.62390960531435979 ) ) ;
#122515 = CARTESIAN_POINT ( 'NONE',  ( 13.89961937509957401, 13.97604488694547697, 86.87609039468567573 ) ) ;
#122516 = CARTESIAN_POINT ( 'NONE',  ( 0.05219959533910956823, 16.53943276465976808, 54.99890960531435269 ) ) ;
#122517 = CARTESIAN_POINT ( 'NONE',  ( -18.62759615963255300, -10.81492255796106328, 89.16775706135236135 ) ) ;
#122518 = CARTESIAN_POINT ( 'NONE',  ( 16.51473224551069308, 9.474510206698969483, 89.16557627198103830 ) ) ;
#122519 = CARTESIAN_POINT ( 'NONE',  ( -5.153800228976607833, 19.02544592524334988, 57.70942372801899012 ) ) ;
#122520 = CARTESIAN_POINT ( 'NONE',  ( 18.67979575497178502, 10.72451020669898547, 59.16557627198103120 ) ) ;
#122521 = CARTESIAN_POINT ( 'NONE',  ( 21.53943276465977519, -0.05219959533907433946, 113.7489096053143527 ) ) ;
#122522 = CARTESIAN_POINT ( 'NONE',  ( 8.314922557961029526, -14.29746914071037800, 25.41775706135235779 ) ) ;
#122523 = CARTESIAN_POINT ( 'NONE',  ( 16.55341960407618274, -4.379528057220086978, 76.04275706135237556 ) ) ;
#122525 = CARTESIAN_POINT ( 'NONE',  ( 21.53943276465977519, -0.05219959533907433946, 113.7489096053143527 ) ) ;
#122524 = CARTESIAN_POINT ( 'NONE',  ( -19.05341960407611168, -5.049401038298163336, 21.45724293864768839 ) ) ;
#122526 = CARTESIAN_POINT ( 'NONE',  ( -16.51473224551069308, -9.474510206698971260, 21.66557627198102765 ) ) ;
#122527 = CARTESIAN_POINT ( 'NONE',  ( -36.91746825000001309, 11.99521256947798342, -9.224999997268813701 ) ) ;
#122528 = CARTESIAN_POINT ( 'NONE',  ( 16.55341960407618274, -4.379528057220086978, 46.04275706135234714 ) ) ;
#122529 = CARTESIAN_POINT ( 'NONE',  ( 14.34966873604960469, 8.224510206698951720, 84.16557627198103830 ) ) ;
#122530 = CARTESIAN_POINT ( 'NONE',  ( 10.72451020669898902, -18.67979575497178502, 77.91557627198102409 ) ) ;
#122531 = CARTESIAN_POINT ( 'NONE',  ( -16.53943276465976808, 0.05219959533911058130, 21.24890960531436690 ) ) ;
#122532 = CARTESIAN_POINT ( 'NONE',  ( -8.224510206698735004, -14.34966873604973081, 39.58442372801901143 ) ) ;
#122533 = CARTESIAN_POINT ( 'NONE',  ( 13.89961937509977652, -13.97604488694527269, 48.12390960531435979 ) ) ;
#122534 = CARTESIAN_POINT ( 'NONE',  ( 16.55341960407618274, -4.379528057220086978, 76.04275706135237556 ) ) ;
#122535 = CARTESIAN_POINT ( 'NONE',  ( 0.05219959533936267826, -19.03943276465977164, 80.00109039468567573 ) ) ;
#122536 = CARTESIAN_POINT ( 'NONE',  ( 21.52544592524344225, -5.823673210054117533, 78.54057627198103830 ) ) ;
#122537 = CARTESIAN_POINT ( 'NONE',  ( -16.55341960407617563, 4.379528057220093196, 113.5427570613523756 ) ) ;
#122538 = VERTEX_POINT ( 'NONE', #166138 ) ;
#122539 = CARTESIAN_POINT ( 'NONE',  ( 0.000000000000000000, 0.000000000000000000, -45.64921306006598201 ) ) ;
#122540 = CARTESIAN_POINT ( 'NONE',  ( 18.62759615963271287, -10.81492255796078972, 48.33224293864770260 ) ) ;
#122541 = VERTEX_POINT ( 'NONE', #89281 ) ;
#122542 = VERTEX_POINT ( 'NONE', #150971 ) ;
#122543 = CARTESIAN_POINT ( 'NONE',  ( -16.55341960407617563, 4.379528057220093196, 93.54275706135234714 ) ) ;
#122544 = CARTESIAN_POINT ( 'NONE',  ( 0.05219959533907565091, 21.53943276465977519, 39.99890960531436690 ) ) ;
#122545 = ORIENTED_EDGE ( 'NONE', *, *, #31673, .F. ) ;
#122546 = CARTESIAN_POINT ( 'NONE',  ( 5.153800228976335163, 19.02544592524342804, 109.7905762719810099 ) ) ;
#122547 = CARTESIAN_POINT ( 'NONE',  ( 17.49999999999999645, 3.209263204892610410, 107.7380317439373272 ) ) ;
#122548 = CARTESIAN_POINT ( 'NONE',  ( -16.53943276465976808, 0.05219959533911058130, 116.2489096053143669 ) ) ;
#122549 = CARTESIAN_POINT ( 'NONE',  ( -15.72974639402197994, 15.80617190586746368, 70.62390960531436690 ) ) ;
#122550 = CARTESIAN_POINT ( 'NONE',  ( 16.52544592524335698, 4.483927247898782831, 101.4594237280190185 ) ) ;
#122551 = CARTESIAN_POINT ( 'NONE',  ( -10.72451020669870658, -18.67979575497194134, 64.58442372801900433 ) ) ;
#122552 = CARTESIAN_POINT ( 'NONE',  ( 13.97604488694548053, -13.89961937509957401, 110.6260903946856615 ) ) ;
#122553 = CARTESIAN_POINT ( 'NONE',  ( -5.153800228976328057, -19.02544592524343514, 27.29057627198103120 ) ) ;
#122554 = CARTESIAN_POINT ( 'NONE',  ( -0.05219959533934338120, 16.53943276465976808, 22.50109039468567573 ) ) ;
#122555 = CARTESIAN_POINT ( 'NONE',  ( 16.46253265017160672, -9.564922557960803928, 53.33224293864768839 ) ) ;
#122556 = CARTESIAN_POINT ( 'NONE',  ( -28.82186960331499037, 2.428612866367529932E-14, 144.0000000000000000 ) ) ;
#122557 = CARTESIAN_POINT ( 'NONE',  ( -19.02544592524342804, 5.153800228976336051, 106.0405762719810241 ) ) ;
#122558 = CARTESIAN_POINT ( 'NONE',  ( 16.53943276465976808, 0.05219959533934440121, 86.25109039468568994 ) ) ;
#122559 = CARTESIAN_POINT ( 'NONE',  ( -0.05219959533936034679, 19.03943276465977164, 97.50109039468567573 ) ) ;
#122560 = CARTESIAN_POINT ( 'NONE',  ( -9.564922557961040184, 16.46253265017147172, 27.91775706135232582 ) ) ;
#122561 = CARTESIAN_POINT ( 'NONE',  ( 21.55341960407610458, 5.719274019375980345, 78.95724293864769550 ) ) ;
#122562 = CARTESIAN_POINT ( 'NONE',  ( 0.05219959533934541429, -16.53943276465976808, 105.0010903946856757 ) ) ;
#122563 = CARTESIAN_POINT ( 'NONE',  ( 19.02544592524334988, 5.153800228976608722, 91.45942372801900433 ) ) ;
#122564 = CARTESIAN_POINT ( 'NONE',  ( 16.51473224551069308, 9.474510206698969483, 54.16557627198103120 ) ) ;
#122565 = CARTESIAN_POINT ( 'NONE',  ( -13.97604488694527625, -13.89961937509977652, 91.87390960531432427 ) ) ;
#122566 = CARTESIAN_POINT ( 'NONE',  ( 5.823673210054444382, -21.52544592524334988, 55.20942372801902565 ) ) ;
#122567 = CARTESIAN_POINT ( 'NONE',  ( -5.049401038298153566, 19.05341960407611168, 50.20724293864770260 ) ) ;
#122568 = DIRECTION ( 'NONE',  ( 0.000000000000000000, 0.000000000000000000, -1.000000000000000000 ) ) ;
#122569 = CARTESIAN_POINT ( 'NONE',  ( 5.153800228976335163, 19.02544592524342804, 109.7905762719810099 ) ) ;
#122570 = CARTESIAN_POINT ( 'NONE',  ( -4.379528057220328563, 16.55341960407611168, 65.20724293864768129 ) ) ;
#122571 = CARTESIAN_POINT ( 'NONE',  ( -10.81492255796078084, -18.62759615963271287, 72.08224293864769550 ) ) ;
#122572 = CARTESIAN_POINT ( 'NONE',  ( 17.50000000000000000, -5.500000000000000888, 23.29690382534171889 ) ) ;
#122573 = CARTESIAN_POINT ( 'NONE',  ( -13.89961937509957401, -13.97604488694547875, 39.37609039468566152 ) ) ;
#122574 = CARTESIAN_POINT ( 'NONE',  ( 17.12812012977047615, -6.668231424565698617, 71.14051240676850796 ) ) ;
#122576 = CARTESIAN_POINT ( 'NONE',  ( 13.97604488694527802, 13.89961937509977652, 84.37390960531433848 ) ) ;
#122575 = CARTESIAN_POINT ( 'NONE',  ( 9.564922557960805705, 16.46253265017160317, 69.58224293864770971 ) ) ;
#122577 = ADVANCED_FACE ( 'NONE', ( #151946 ), #167673, .F. ) ;
#122578 = CARTESIAN_POINT ( 'NONE',  ( -4.379528057220086978, -16.55341960407618274, 49.79275706135234714 ) ) ;
#122579 = CARTESIAN_POINT ( 'NONE',  ( 24.26175155739902323, -32.05389003868042863, -17.42962289376370677 ) ) ;
#122580 = B_SPLINE_CURVE_WITH_KNOTS ( 'NONE', 3,
 ( #23176, #72684, #27185, #179877, #146499, #41345, #24186, #194040, #103007, #55504, #40336, #102011, #7990, #164692, #134359, #130319, #25195, #145503, #6984, #69673, #192016, #115177, #176870, #193028, #54505, #123134, #60468, #137320, #197030, #183831, #29169, #58497 ),
 .UNSPECIFIED., .F., .F.,
 ( 4, 2, 2, 2, 2, 2, 2, 2, 2, 2, 2, 2, 2, 2, 2, 4 ),
 ( 1.769077770938648657E-17, 0.0003712461730036916026, 0.0007424923460073655328, 0.001113738519011039409, 0.001484984692014713501, 0.002227477038022061036, 0.002598723211025738382, 0.002969969384029415727, 0.003341215557033093073, 0.003712461730036770418, 0.004083707903040446896, 0.004454954076044123808, 0.004826200249047801587, 0.005197446422051478498, 0.005568692595055156278, 0.005939938768058833189 ),
 .UNSPECIFIED. ) ;
#122581 = CARTESIAN_POINT ( 'NONE',  ( -5.049401038297874678, -19.05341960407617918, 34.79275706135233293 ) ) ;
#122582 = CARTESIAN_POINT ( 'NONE',  ( -8.906447517083060816, 27.41122689804195645, 145.8500000054623627 ) ) ;
#122583 = CARTESIAN_POINT ( 'NONE',  ( 14.34966873604972726, -8.224510206698740333, 90.83442372801901854 ) ) ;
#122584 = CARTESIAN_POINT ( 'NONE',  ( 15.66521691804239502, -1.429200727443413088, -59.59145728475414217 ) ) ;
#122585 = CARTESIAN_POINT ( 'NONE',  ( -14.34966873604972548, 8.224510206698743886, 78.33442372801901854 ) ) ;
#122586 = CARTESIAN_POINT ( 'NONE',  ( 16.55341960407618274, -4.379528057220086978, 61.04275706135234714 ) ) ;
#122588 = CARTESIAN_POINT ( 'NONE',  ( 17.59860650958989936, 7.585241751807028088, 74.07662985737508166 ) ) ;
#122587 = CARTESIAN_POINT ( 'NONE',  ( -13.89961937509977652, 13.97604488694528158, 50.62390960531435979 ) ) ;
#122589 = CARTESIAN_POINT ( 'NONE',  ( 21.52544592524334988, 5.823673210054432836, 61.45942372801901854 ) ) ;
#122590 = CARTESIAN_POINT ( 'NONE',  ( 19.03943276465977164, 0.05219959533936151252, 81.25109039468567573 ) ) ;
#122591 = CARTESIAN_POINT ( 'NONE',  ( 10.81492255796106328, -18.62759615963255655, 110.4177570613523756 ) ) ;
#122592 = CARTESIAN_POINT ( 'NONE',  ( 9.564922557960805705, 16.46253265017160317, 44.58224293864769550 ) ) ;
#122593 = CARTESIAN_POINT ( 'NONE',  ( 17.50000000000000000, 5.499999999999997335, 23.78230962303566542 ) ) ;
#122594 = CARTESIAN_POINT ( 'NONE',  ( 10.72451020669898902, -18.67979575497178502, 62.91557627198102409 ) ) ;
#122595 = CARTESIAN_POINT ( 'NONE',  ( 0.05219959533909260263, 19.03943276465977164, 109.9989096053143669 ) ) ;
#122596 = CARTESIAN_POINT ( 'NONE',  ( -9.564922557960796823, -16.46253265017161027, 22.08224293864768839 ) ) ;
#122597 = CARTESIAN_POINT ( 'NONE',  ( 4.483927247898790824, -16.52544592524335698, 45.20942372801901854 ) ) ;
#122598 = CARTESIAN_POINT ( 'NONE',  ( -4.483927247898539470, -16.52544592524342804, 32.29057627198102409 ) ) ;
#122599 = VERTEX_POINT ( 'NONE', #74126 ) ;
#122600 = CARTESIAN_POINT ( 'NONE',  ( 10.81492255796106328, -18.62759615963255655, 20.41775706135234714 ) ) ;
#122602 = CARTESIAN_POINT ( 'NONE',  ( -30.74264578624800492, 22.33583958711400186, -6.200000000000001066 ) ) ;
#122601 = CARTESIAN_POINT ( 'NONE',  ( -12.14591786802309592, -12.06949235617757132, 51.87390960531437401 ) ) ;
#122603 = CARTESIAN_POINT ( 'NONE',  ( 5.049401038297881783, 19.05341960407617563, 102.2927570613523045 ) ) ;
#122604 = CARTESIAN_POINT ( 'NONE',  ( 16.46253265017146816, 9.564922557961045513, 41.66775706135234003 ) ) ;
#122605 = CARTESIAN_POINT ( 'NONE',  ( 16.53943276465976808, -0.05219959533910856209, 43.74890960531435979 ) ) ;
#122606 = CARTESIAN_POINT ( 'NONE',  ( -15.80617190586745835, -15.72974639402198527, 101.8739096053143811 ) ) ;
#122608 = CARTESIAN_POINT ( 'NONE',  ( 15.72974639402199770, -15.80617190586745480, 68.12390960531436690 ) ) ;
#122607 = FACE_OUTER_BOUND ( 'NONE', #30602, .T. ) ;
#122609 = CARTESIAN_POINT ( 'NONE',  ( 13.97604488694527802, 13.89961937509977652, 74.37390960531436690 ) ) ;
#122610 = CARTESIAN_POINT ( 'NONE',  ( -4.483927247898539470, -16.52544592524342804, 47.29057627198103120 ) ) ;
#122611 = CARTESIAN_POINT ( 'NONE',  ( -9.474510206698964154, 16.51473224551069663, 100.4155762719810241 ) ) ;
#122612 = AXIS2_PLACEMENT_3D ( 'NONE', #163002, #36640, #8323 ) ;
#122613 = CARTESIAN_POINT ( 'NONE',  ( -69.65682714487590488, -71.74905178543390605, -4.999999999999999112 ) ) ;
#122614 = CARTESIAN_POINT ( 'NONE',  ( -19.05341960407617563, 5.049401038297882671, 58.54275706135234003 ) ) ;
#122615 = CARTESIAN_POINT ( 'NONE',  ( -5.719274019375978568, 21.55341960407610458, 90.20724293864770971 ) ) ;
#122616 = CARTESIAN_POINT ( 'NONE',  ( 16.46253265017160672, -9.564922557960803928, 48.33224293864769550 ) ) ;
#122617 = CARTESIAN_POINT ( 'NONE',  ( -8.314922557960811034, -14.29746914071050412, 112.0822429386477097 ) ) ;
#122618 = CARTESIAN_POINT ( 'NONE',  ( -5.719274019375665041, -21.55341960407619695, 54.79275706135235424 ) ) ;
#122619 = CARTESIAN_POINT ( 'NONE',  ( 17.14385361876520264, -23.59649016807271238, 143.5750000027312012 ) ) ;
#122620 = CARTESIAN_POINT ( 'NONE',  ( -16.53943276465976808, 0.05219959533911058130, 21.24890960531436690 ) ) ;
#122621 = CARTESIAN_POINT ( 'NONE',  ( 16.51473224551069308, 9.474510206698969483, 54.16557627198103120 ) ) ;
#122622 = CARTESIAN_POINT ( 'NONE',  ( -5.153800228976328057, -19.02544592524343514, 102.2905762719810383 ) ) ;
#122623 = CARTESIAN_POINT ( 'NONE',  ( -0.05219959533907301413, -21.53943276465977519, 62.49890960531436690 ) ) ;
#122624 = CARTESIAN_POINT ( 'NONE',  ( -8.571926809382601320, -26.38167802310801591, 147.2750000027311899 ) ) ;
#122625 = CARTESIAN_POINT ( 'NONE',  ( 0.05219959533909260263, 19.03943276465977164, 49.99890960531435979 ) ) ;
#122626 = CARTESIAN_POINT ( 'NONE',  ( 18.62759615963271287, -10.81492255796078972, 53.33224293864769550 ) ) ;
#122627 = CARTESIAN_POINT ( 'NONE',  ( -5.823673210054431948, 21.52544592524334988, 87.70942372801901854 ) ) ;
#122629 = CARTESIAN_POINT ( 'NONE',  ( -16.53943276465976808, -0.05219959533934237506, 78.75109039468568994 ) ) ;
#122628 = CARTESIAN_POINT ( 'NONE',  ( 9.524678007105494615, -44.64363251549367106, -21.91146642400599021 ) ) ;
#122630 = CARTESIAN_POINT ( 'NONE',  ( -4.483927247898782831, 16.52544592524335698, 87.70942372801901854 ) ) ;
#122631 = CARTESIAN_POINT ( 'NONE',  ( 13.97604488694527802, 13.89961937509977652, 74.37390960531436690 ) ) ;
#122632 = ORIENTED_EDGE ( 'NONE', *, *, #130384, .F. ) ;
#122633 = CARTESIAN_POINT ( 'NONE',  ( -19.02544592524334988, -5.153800228976617603, 23.95942372801900078 ) ) ;
#122634 = CARTESIAN_POINT ( 'NONE',  ( -16.52544592524335698, -4.483927247898792601, 83.95942372801900433 ) ) ;
#122635 = CARTESIAN_POINT ( 'NONE',  ( 19.03943276465977164, 0.05219959533936151252, 21.25109039468565797 ) ) ;
#122636 = CARTESIAN_POINT ( 'NONE',  ( -13.97604488694527625, -13.89961937509977652, 76.87390960531433848 ) ) ;
#122637 = CARTESIAN_POINT ( 'NONE',  ( 18.67979575497178502, 10.72451020669898547, 54.16557627198103120 ) ) ;
#122638 = CARTESIAN_POINT ( 'NONE',  ( -12.14591786802326823, 12.06949235617739902, 23.12609039468567573 ) ) ;
#122639 = CARTESIAN_POINT ( 'NONE',  ( 21.53943276465977519, 0.05219959533937863772, 76.25109039468568994 ) ) ;
#122640 = CARTESIAN_POINT ( 'NONE',  ( -8.224510206698735004, -14.34966873604973081, 64.58442372801900433 ) ) ;
#122641 = CARTESIAN_POINT ( 'NONE',  ( -18.67979575497178146, -10.72451020669898902, 111.6655762719810525 ) ) ;
#122642 = CARTESIAN_POINT ( 'NONE',  ( 0.05219959533936267826, -19.03943276465977164, 110.0010903946856757 ) ) ;
#122643 = CARTESIAN_POINT ( 'NONE',  ( 13.89961937509977652, -13.97604488694527269, 98.12390960531433848 ) ) ;
#122644 = CARTESIAN_POINT ( 'NONE',  ( -8.314922557961024197, 14.29746914071037800, 32.91775706135234714 ) ) ;
#122645 = CARTESIAN_POINT ( 'NONE',  ( 13.89961937509977652, -13.97604488694527269, 43.12390960531434558 ) ) ;
#122646 = CIRCLE ( 'NONE', #87155, 216.0437394197456342 ) ;
#122647 = CARTESIAN_POINT ( 'NONE',  ( 16.53943276465976808, 0.05219959533934440121, 21.25109039468567218 ) ) ;
#122648 = CARTESIAN_POINT ( 'NONE',  ( 4.483927247898545687, 16.52544592524342804, 79.79057627198102409 ) ) ;
#122649 = CARTESIAN_POINT ( 'NONE',  ( 12.14591786802327356, -12.06949235617739191, 85.62609039468568994 ) ) ;
#122650 = EDGE_CURVE ( 'NONE', #30636, #120670, #177959, .T. ) ;
#122652 = CARTESIAN_POINT ( 'NONE',  ( -16.46253265017160317, 9.564922557960807481, 60.83224293864769550 ) ) ;
#122651 = CARTESIAN_POINT ( 'NONE',  ( 18.67979575497194134, -10.72451020669871369, 30.83442372801902209 ) ) ;
#122653 = CARTESIAN_POINT ( 'NONE',  ( -16.46253265017160317, 9.564922557960807481, 70.83224293864770971 ) ) ;
#122654 = CARTESIAN_POINT ( 'NONE',  ( 16.53943276465976808, 0.05219959533934440121, 91.25109039468568994 ) ) ;
#122656 = ORIENTED_EDGE ( 'NONE', *, *, #20347, .F. ) ;
#122655 = CARTESIAN_POINT ( 'NONE',  ( -24.22576942085221674, -7.195495839723525577, 170.3116806589360124 ) ) ;
#122657 = ORIENTED_EDGE ( 'NONE', *, *, #61085, .T. ) ;
#122658 = CARTESIAN_POINT ( 'NONE',  ( -0.05219959533936034679, 19.03943276465977164, 27.50109039468566507 ) ) ;
#122659 = CARTESIAN_POINT ( 'NONE',  ( -13.89961937509977652, 13.97604488694528158, 40.62390960531435979 ) ) ;
#122661 = ORIENTED_EDGE ( 'NONE', *, *, #190681, .T. ) ;
#122660 = CARTESIAN_POINT ( 'NONE',  ( 15.50000000000000355, 7.499999999999998224, 120.0000000000000142 ) ) ;
#122662 = CARTESIAN_POINT ( 'NONE',  ( -12.06949235617739369, -12.14591786802326823, 24.37609039468567573 ) ) ;
#122664 = CARTESIAN_POINT ( 'NONE',  ( -14.34966873604972548, 8.224510206698743886, 43.33442372801901143 ) ) ;
#122663 = CARTESIAN_POINT ( 'NONE',  ( 19.03943276465977164, 0.05219959533936151252, 61.25109039468566863 ) ) ;
#122665 = CARTESIAN_POINT ( 'NONE',  ( -9.564922557960796823, -16.46253265017161027, 112.0822429386476955 ) ) ;
#122666 = CARTESIAN_POINT ( 'NONE',  ( -9.564922557960796823, -16.46253265017161027, 77.08224293864769550 ) ) ;
#122667 = CARTESIAN_POINT ( 'NONE',  ( 5.719274019375991003, -21.55341960407610458, 102.7072429386476955 ) ) ;
#122668 = CARTESIAN_POINT ( 'NONE',  ( -19.02544592524334988, -5.153800228976617603, 63.95942372801899012 ) ) ;
#122669 = CARTESIAN_POINT ( 'NONE',  ( -19.05341960407611168, -5.049401038298163336, 96.45724293864769550 ) ) ;
#122670 = CARTESIAN_POINT ( 'NONE',  ( 9.564922557960805705, 16.46253265017160317, 69.58224293864770971 ) ) ;
#122672 = CARTESIAN_POINT ( 'NONE',  ( -16.46253265017160317, 9.564922557960807481, 70.83224293864770971 ) ) ;
#122671 = CARTESIAN_POINT ( 'NONE',  ( -16.55341960407611168, -4.379528057220339221, 21.45724293864769550 ) ) ;
#122673 = CARTESIAN_POINT ( 'NONE',  ( 0.05219959533936267826, -19.03943276465977164, 35.00109039468566863 ) ) ;
#122674 = CARTESIAN_POINT ( 'NONE',  ( 14.34966873604960469, 8.224510206698951720, 69.16557627198102409 ) ) ;
#122675 = CARTESIAN_POINT ( 'NONE',  ( -5.823673210054431948, 21.52544592524334988, 97.70942372801904696 ) ) ;
#122676 = CARTESIAN_POINT ( 'NONE',  ( -13.89961937509977652, 13.97604488694528158, 35.62390960531435269 ) ) ;
#122677 = CARTESIAN_POINT ( 'NONE',  ( -4.379528057220086978, -16.55341960407618274, 49.79275706135234714 ) ) ;
#122679 = CARTESIAN_POINT ( 'NONE',  ( 15.72974639402176855, 15.80617190586768217, 86.87609039468568994 ) ) ;
#122678 = CARTESIAN_POINT ( 'NONE',  ( 0.05219959533910956823, 16.53943276465976808, 44.99890960531435979 ) ) ;
#122680 = CARTESIAN_POINT ( 'NONE',  ( 13.97604488694527802, 13.89961937509977652, 79.37390960531435269 ) ) ;
#122681 = CARTESIAN_POINT ( 'NONE',  ( -16.51473224551069308, -9.474510206698971260, 91.66557627198103830 ) ) ;
#122682 = CARTESIAN_POINT ( 'NONE',  ( -0.05219959533910754901, -16.53943276465976808, 112.4989096053143669 ) ) ;
#122683 = CARTESIAN_POINT ( 'NONE',  ( 16.55341960407611168, 4.379528057220329451, 78.95724293864769550 ) ) ;
#122684 = CARTESIAN_POINT ( 'NONE',  ( -5.823673210054116645, -21.52544592524344225, 77.29057627198102409 ) ) ;
#122685 = CARTESIAN_POINT ( 'NONE',  ( -5.049401038298153566, 19.05341960407611168, 85.20724293864766707 ) ) ;
#122686 = CARTESIAN_POINT ( 'NONE',  ( 5.719274019375991003, -21.55341960407610458, 97.70724293864772392 ) ) ;
#122687 = CARTESIAN_POINT ( 'NONE',  ( -16.46253265017146816, -9.564922557961047289, 74.16775706135234714 ) ) ;
#122689 = CARTESIAN_POINT ( 'NONE',  ( -16.55341960407611168, -4.379528057220339221, 91.45724293864769550 ) ) ;
#122688 = CARTESIAN_POINT ( 'NONE',  ( -13.89961937509957401, -13.97604488694547697, 64.37609039468567573 ) ) ;
#122690 = CARTESIAN_POINT ( 'NONE',  ( 5.049401038298161559, -19.05341960407611168, 52.70724293864767418 ) ) ;
#122691 = CARTESIAN_POINT ( 'NONE',  ( -5.719274019375978568, 21.55341960407610458, 60.20724293864768839 ) ) ;
#122692 = CARTESIAN_POINT ( 'NONE',  ( 16.81555441253552985, -7.025013491695481171, 28.13685445334258262 ) ) ;
#122694 = CARTESIAN_POINT ( 'NONE',  ( -5.359611314223446995E-15, 29.16686587814335851, 148.8750000027311842 ) ) ;
#122693 = CARTESIAN_POINT ( 'NONE',  ( 16.53943276465976808, 0.05219959533934440121, 106.2510903946856757 ) ) ;
#122695 = CARTESIAN_POINT ( 'NONE',  ( -0.05219959533936034679, 19.03943276465977164, 112.5010903946856757 ) ) ;
#122696 = CARTESIAN_POINT ( 'NONE',  ( -16.55341960407611168, -4.379528057220339221, 76.45724293864769550 ) ) ;
#122697 = DIRECTION ( 'NONE',  ( 1.000000000000000000, -0.000000000000000000, -0.000000000000000000 ) ) ;
#122698 = CARTESIAN_POINT ( 'NONE',  ( 16.51473224551069308, 9.474510206698969483, 69.16557627198102409 ) ) ;
#122699 = CARTESIAN_POINT ( 'NONE',  ( -16.46253265017160317, 9.564922557960807481, 30.83224293864769550 ) ) ;
#122700 = CARTESIAN_POINT ( 'NONE',  ( 16.53943276465976808, -0.05219959533910856209, 68.74890960531435269 ) ) ;
#122701 = CARTESIAN_POINT ( 'NONE',  ( -13.89961937509977652, 13.97604488694528158, 115.6239096053143669 ) ) ;
#122702 = CARTESIAN_POINT ( 'NONE',  ( -13.97604488694547697, 13.89961937509957934, 83.12609039468564731 ) ) ;
#122703 = CARTESIAN_POINT ( 'NONE',  ( 5.153800228976335163, 19.02544592524342804, 99.79057627198102409 ) ) ;
#122704 = CARTESIAN_POINT ( 'NONE',  ( -21.55341960407610458, -5.719274019375992779, 71.45724293864769550 ) ) ;
#122705 = CARTESIAN_POINT ( 'NONE',  ( 14.29746914071037800, 8.314922557961029526, 66.66775706135234714 ) ) ;
#122706 = CARTESIAN_POINT ( 'NONE',  ( 9.474510206698729675, 16.51473224551082808, 107.0844237280190043 ) ) ;
#122707 = CARTESIAN_POINT ( 'NONE',  ( 16.51473224551069308, 9.474510206698969483, 59.16557627198102409 ) ) ;
#122708 = CARTESIAN_POINT ( 'NONE',  ( -15.80617190586745835, -15.72974639402198527, 66.87390960531436690 ) ) ;
#122709 = CARTESIAN_POINT ( 'NONE',  ( 13.89961937509957401, 13.97604488694547697, 106.8760903946856757 ) ) ;
#122711 = CARTESIAN_POINT ( 'NONE',  ( 15.80617190586769283, -15.72974639402175789, 65.62609039468568994 ) ) ;
#122710 = CARTESIAN_POINT ( 'NONE',  ( 12.06949235617757843, -12.14591786802309237, 43.12390960531435269 ) ) ;
#122712 = CARTESIAN_POINT ( 'NONE',  ( 13.89961937509957579, 13.97604488694547520, 71.87609039468567573 ) ) ;
#122714 = CARTESIAN_POINT ( 'NONE',  ( -5.049401038298153566, 19.05341960407611168, 110.2072429386476671 ) ) ;
#122713 = CARTESIAN_POINT ( 'NONE',  ( -4.483927247898782831, 16.52544592524335698, 72.70942372801901854 ) ) ;
#122715 = DIRECTION ( 'NONE',  ( 1.000000000000000000, 0.000000000000000000, 0.000000000000000000 ) ) ;
#122716 = CARTESIAN_POINT ( 'NONE',  ( -17.40861289039002813, 6.110651285853254677, 78.62767529172566583 ) ) ;
#122717 = CARTESIAN_POINT ( 'NONE',  ( 0.05219959533934541429, -16.53943276465976808, 95.00109039468568994 ) ) ;
#122718 = CARTESIAN_POINT ( 'NONE',  ( 8.224510206698742110, 14.34966873604972548, 47.08442372801901854 ) ) ;
#122719 = CARTESIAN_POINT ( 'NONE',  ( -13.97604488694527625, -13.89961937509977652, 61.87390960531435979 ) ) ;
#122720 = CARTESIAN_POINT ( 'NONE',  ( -9.474510206698964154, 16.51473224551069663, 70.41557627198102409 ) ) ;
#122721 = CARTESIAN_POINT ( 'NONE',  ( -15.72974639402176322, -15.80617190586768395, 64.37609039468568994 ) ) ;
#122722 = CARTESIAN_POINT ( 'NONE',  ( -16.52544592524335698, -4.483927247898792601, 58.95942372801902565 ) ) ;
#122723 = CARTESIAN_POINT ( 'NONE',  ( 14.29746914071049879, -8.314922557960816363, 33.33224293864769550 ) ) ;
#122724 = CARTESIAN_POINT ( 'NONE',  ( 5.153800228976335163, 19.02544592524342804, 44.79057627198103830 ) ) ;
#122725 = CARTESIAN_POINT ( 'NONE',  ( 19.03943276465977164, -0.05219959533909143690, 33.74890960531435979 ) ) ;
#122726 = CARTESIAN_POINT ( 'NONE',  ( -14.34966873604972548, 8.224510206698743886, 23.33442372801901499 ) ) ;
#122727 = CARTESIAN_POINT ( 'NONE',  ( -19.03943276465977164, -0.05219959533935918106, 78.75109039468567573 ) ) ;
#122728 = CARTESIAN_POINT ( 'NONE',  ( 0.05219959533910956823, 16.53943276465976808, 99.99890960531436690 ) ) ;
#122729 = CARTESIAN_POINT ( 'NONE',  ( 13.97604488694527802, 13.89961937509977652, 49.37390960531434558 ) ) ;
#122731 = CARTESIAN_POINT ( 'NONE',  ( 38.00000000000000000, 12.34694845685046616, -8.899999999999996803 ) ) ;
#122730 = CARTESIAN_POINT ( 'NONE',  ( 13.97604488694548053, -13.89961937509957401, 90.62609039468567573 ) ) ;
#122732 = CARTESIAN_POINT ( 'NONE',  ( -5.823673210054431948, 21.52544592524334988, 92.70942372801901854 ) ) ;
#122733 = CARTESIAN_POINT ( 'NONE',  ( 14.29746914071037800, 8.314922557961029526, 56.66775706135235424 ) ) ;
#122734 = CARTESIAN_POINT ( 'NONE',  ( -17.49999999999999645, 5.499999999999997335, 25.79690382534172244 ) ) ;
#122735 = CARTESIAN_POINT ( 'NONE',  ( 15.72974639402199770, -15.80617190586745480, 43.12390960531435269 ) ) ;
#122736 = CARTESIAN_POINT ( 'NONE',  ( -14.29746914071037622, -8.314922557961029526, 34.16775706135234714 ) ) ;
#122737 = CARTESIAN_POINT ( 'NONE',  ( -9.474510206698964154, 16.51473224551069663, 35.41557627198102409 ) ) ;
#122738 = CARTESIAN_POINT ( 'NONE',  ( 9.474510206698729675, 16.51473224551082808, 47.08442372801900433 ) ) ;
#122739 = CARTESIAN_POINT ( 'NONE',  ( -13.97604488694527625, -13.89961937509977652, 86.87390960531436690 ) ) ;
#122740 = CARTESIAN_POINT ( 'NONE',  ( 9.564922557960805705, 16.46253265017160317, 49.58224293864770260 ) ) ;
#122741 = CARTESIAN_POINT ( 'NONE',  ( 14.79648886421078124, 15.41147372653644787, -56.42550976940269436 ) ) ;
#122742 = CARTESIAN_POINT ( 'NONE',  ( -10.81492255796105439, 18.62759615963255655, 72.91775706135234714 ) ) ;
#122743 = CARTESIAN_POINT ( 'NONE',  ( -9.100000000000001421, 9.789526074884739315E-14, -61.89430850415821794 ) ) ;
#122744 = CARTESIAN_POINT ( 'NONE',  ( 13.89961937509957401, 13.97604488694547697, 36.87609039468565442 ) ) ;
#122745 = CARTESIAN_POINT ( 'NONE',  ( 21.53943276465977519, 0.05219959533937863772, 106.2510903946856757 ) ) ;
#122746 = CARTESIAN_POINT ( 'NONE',  ( -12.14591786802309592, -12.06949235617757132, 56.87390960531436690 ) ) ;
#122747 = CARTESIAN_POINT ( 'NONE',  ( -19.02544592524342804, 5.153800228976336051, 56.04057627198100988 ) ) ;
#122748 = CARTESIAN_POINT ( 'NONE',  ( -5.153800228976328057, -19.02544592524343514, 107.2905762719810383 ) ) ;
#122749 = CARTESIAN_POINT ( 'NONE',  ( 5.719274019375673035, 21.55341960407619339, 87.29275706135236135 ) ) ;
#122750 = CARTESIAN_POINT ( 'NONE',  ( -19.03943276465977164, 0.05219959533909376836, 66.24890960531436690 ) ) ;
#122751 = EDGE_CURVE ( 'NONE', #46822, #129974, #117271, .T. ) ;
#122752 = CARTESIAN_POINT ( 'NONE',  ( -5.719274019375665041, -21.55341960407619695, 84.79275706135234714 ) ) ;
#122753 = CARTESIAN_POINT ( 'NONE',  ( -15.80617190586745835, -15.72974639402198527, 36.87390960531435979 ) ) ;
#122754 = CARTESIAN_POINT ( 'NONE',  ( -0.05219959533937732626, 21.53943276465977519, 27.50109039468567929 ) ) ;
#122755 = CARTESIAN_POINT ( 'NONE',  ( -9.564922557961040184, 16.46253265017147172, 52.91775706135233293 ) ) ;
#122756 = CARTESIAN_POINT ( 'NONE',  ( 5.153800228976335163, 19.02544592524342804, 34.79057627198102409 ) ) ;
#122757 = CARTESIAN_POINT ( 'NONE',  ( -5.049401038298153566, 19.05341960407611168, 70.20724293864769550 ) ) ;
#122758 = CARTESIAN_POINT ( 'NONE',  ( -0.05219959533934338120, 16.53943276465976808, 32.50109039468568284 ) ) ;
#122759 = CARTESIAN_POINT ( 'NONE',  ( 0.05219959533910956823, 16.53943276465976808, 84.99890960531436690 ) ) ;
#122760 = CARTESIAN_POINT ( 'NONE',  ( 13.89961937509977652, -13.97604488694527269, 53.12390960531434558 ) ) ;
#122761 = CARTESIAN_POINT ( 'NONE',  ( -18.67979575497178146, -10.72451020669898902, 36.66557627198103120 ) ) ;
#122762 = VECTOR ( 'NONE', #173615, 1000.000000000000000 ) ;
#122763 = CARTESIAN_POINT ( 'NONE',  ( 5.049401038297881783, 19.05341960407617563, 107.2927570613523187 ) ) ;
#122764 = CARTESIAN_POINT ( 'NONE',  ( -5.719274019375978568, 21.55341960407610458, 110.2072429386477239 ) ) ;
#122765 = CARTESIAN_POINT ( 'NONE',  ( 5.823673210054444382, -21.52544592524334988, 75.20942372801901854 ) ) ;
#122766 = CARTESIAN_POINT ( 'NONE',  ( 4.379528057220092307, 16.55341960407617563, 67.29275706135234714 ) ) ;
#122767 = CARTESIAN_POINT ( 'NONE',  ( 16.53943276465976808, 0.05219959533934440121, 66.25109039468567573 ) ) ;
#122768 = CARTESIAN_POINT ( 'NONE',  ( -5.153800228976328057, -19.02544592524343514, 62.29057627198100988 ) ) ;
#122769 = CARTESIAN_POINT ( 'NONE',  ( -12.06949235617739369, -12.14591786802326823, 94.37609039468568994 ) ) ;
#122770 = CARTESIAN_POINT ( 'NONE',  ( -0.05219959533936034679, 19.03943276465977164, 47.50109039468566863 ) ) ;
#122771 = CARTESIAN_POINT ( 'NONE',  ( -15.80617190586768217, 15.72974639402176855, 23.12609039468567573 ) ) ;
#122772 = CARTESIAN_POINT ( 'NONE',  ( 14.29746914071049879, -8.314922557960816363, 68.33224293864769550 ) ) ;
#122773 = CARTESIAN_POINT ( 'NONE',  ( -0.05219959533909027116, -19.03943276465977164, 82.49890960531436690 ) ) ;
#122774 = CARTESIAN_POINT ( 'NONE',  ( -4.483927247898782831, 16.52544592524335698, 72.70942372801901854 ) ) ;
#122775 = CARTESIAN_POINT ( 'NONE',  ( 18.62759615963255655, 10.81492255796105972, 56.66775706135235424 ) ) ;
#122776 = CARTESIAN_POINT ( 'NONE',  ( 13.89961937509957401, 13.97604488694547697, 111.8760903946856757 ) ) ;
#122777 = CARTESIAN_POINT ( 'NONE',  ( -5.823673210054116645, -21.52544592524344225, 107.2905762719810525 ) ) ;
#122778 = CARTESIAN_POINT ( 'NONE',  ( -16.52544592524342804, 4.483927247898546575, 56.04057627198102409 ) ) ;
#122779 = ORIENTED_EDGE ( 'NONE', *, *, #134567, .F. ) ;
#122780 = CARTESIAN_POINT ( 'NONE',  ( -5.719274019375978568, 21.55341960407610458, 90.20724293864770971 ) ) ;
#122781 = CARTESIAN_POINT ( 'NONE',  ( -16.55341960407611168, -4.379528057220339221, 41.45724293864769550 ) ) ;
#122782 = ORIENTED_EDGE ( 'NONE', *, *, #154620, .F. ) ;
#122783 = CARTESIAN_POINT ( 'NONE',  ( 34.51210051733096407, 7.446700168151136445, 43.98226744806001420 ) ) ;
#122784 = CARTESIAN_POINT ( 'NONE',  ( -5.719274019375665041, -21.55341960407619695, 19.79275706135235069 ) ) ;
#122785 = CARTESIAN_POINT ( 'NONE',  ( 13.97604488694527802, 13.89961937509977652, 114.3739096053143669 ) ) ;
#122786 = CARTESIAN_POINT ( 'NONE',  ( 5.719274019375673035, 21.55341960407619339, 32.29275706135235424 ) ) ;
#122787 = CARTESIAN_POINT ( 'NONE',  ( -16.52544592524342804, 4.483927247898546575, 46.04057627198103830 ) ) ;
#122788 = CIRCLE ( 'NONE', #164817, 2.199999999999999289 ) ;
#122789 = CARTESIAN_POINT ( 'NONE',  ( -0.05219959533909027116, -19.03943276465977164, 62.49890960531435979 ) ) ;
#122790 = CARTESIAN_POINT ( 'NONE',  ( 16.51473224551083163, -9.474510206698727899, 60.83442372801900433 ) ) ;
#122791 = CARTESIAN_POINT ( 'NONE',  ( 19.03943276465977164, -0.05219959533909143690, 98.74890960531436690 ) ) ;
#122792 = CARTESIAN_POINT ( 'NONE',  ( -0.05219959533907301413, -21.53943276465977519, 42.49890960531435979 ) ) ;
#122793 = CARTESIAN_POINT ( 'NONE',  ( -22.55660001725368247, -30.45235066354263509, -22.16622550485435994 ) ) ;
#122794 = CARTESIAN_POINT ( 'NONE',  ( 13.89961937509977652, -13.97604488694527269, 53.12390960531434558 ) ) ;
#122795 = CARTESIAN_POINT ( 'NONE',  ( 16.55341960407618274, -4.379528057220086978, 36.04275706135234714 ) ) ;
#122796 = CARTESIAN_POINT ( 'NONE',  ( -9.564922557961040184, 16.46253265017147172, 67.91775706135233293 ) ) ;
#122797 = CARTESIAN_POINT ( 'NONE',  ( 18.62759615963271287, -10.81492255796078972, 113.3322429386476955 ) ) ;
#122798 = CARTESIAN_POINT ( 'NONE',  ( -14.34966873604960291, -8.224510206698953496, 46.66557627198102409 ) ) ;
#122799 = CARTESIAN_POINT ( 'NONE',  ( -19.02544592524342804, 5.153800228976336051, 91.04057627198100988 ) ) ;
#122800 = CARTESIAN_POINT ( 'NONE',  ( -15.80617190586745835, -15.72974639402198527, 76.87390960531439532 ) ) ;
#122802 = CARTESIAN_POINT ( 'NONE',  ( -12.14591786802326823, 12.06949235617739902, 43.12609039468568284 ) ) ;
#122801 = CARTESIAN_POINT ( 'NONE',  ( 21.55341960407610458, 5.719274019375980345, 113.9572429386477239 ) ) ;
#122803 = CARTESIAN_POINT ( 'NONE',  ( -18.67979575497178146, -10.72451020669898902, 36.66557627198103120 ) ) ;
#122804 = CARTESIAN_POINT ( 'NONE',  ( -15.80617190586768217, 15.72974639402176855, 108.1260903946856757 ) ) ;
#122805 = CARTESIAN_POINT ( 'NONE',  ( -16.46253265017160317, 9.564922557960807481, 85.83224293864769550 ) ) ;
#122806 = CARTESIAN_POINT ( 'NONE',  ( 5.049401038298161559, -19.05341960407611168, 47.70724293864770260 ) ) ;
#122807 = CARTESIAN_POINT ( 'NONE',  ( 13.89961937509977652, -13.97604488694527269, 98.12390960531433848 ) ) ;
#122808 = CARTESIAN_POINT ( 'NONE',  ( -16.51473224551069308, -9.474510206698971260, 76.66557627198103830 ) ) ;
#122809 = CARTESIAN_POINT ( 'NONE',  ( -12.06949235617739369, -12.14591786802326823, 24.37609039468567573 ) ) ;
#122810 = CARTESIAN_POINT ( 'NONE',  ( 17.49999999999997513, 3.805241302050415442, 32.12647527217407628 ) ) ;
#122811 = CARTESIAN_POINT ( 'NONE',  ( -9.564922557961040184, 16.46253265017147172, 52.91775706135233293 ) ) ;
#122813 = CARTESIAN_POINT ( 'NONE',  ( 5.823673210054125526, 21.52544592524343514, 29.79057627198102409 ) ) ;
#122812 = CARTESIAN_POINT ( 'NONE',  ( -19.03943276465977164, -0.05219959533935918106, 18.75109039468567218 ) ) ;
#122814 = CARTESIAN_POINT ( 'NONE',  ( 4.483927247898790824, -16.52544592524335698, 100.2094237280190043 ) ) ;
#122815 = CARTESIAN_POINT ( 'NONE',  ( -2.649999999999999911, -105.0000000000000000, -13.00000000000000000 ) ) ;
#122816 = CARTESIAN_POINT ( 'NONE',  ( -13.89961937509957401, -13.97604488694547875, 69.37609039468564731 ) ) ;
#122817 = CARTESIAN_POINT ( 'NONE',  ( 19.05341960407617918, -5.049401038297876454, 26.04275706135233293 ) ) ;
#122818 = CARTESIAN_POINT ( 'NONE',  ( -16.79531203550650176, -7.028104445595492855, 46.25244988220443787 ) ) ;
#122819 = CARTESIAN_POINT ( 'NONE',  ( -9.474510206698964154, 16.51473224551069663, 35.41557627198102409 ) ) ;
#122820 = CARTESIAN_POINT ( 'NONE',  ( -16.52544592524342804, 4.483927247898546575, 31.04057627198102409 ) ) ;
#122821 = CARTESIAN_POINT ( 'NONE',  ( -16.18388926212238843, -7.379444403734516378, 110.4395315136615068 ) ) ;
#122822 = CARTESIAN_POINT ( 'NONE',  ( 12.14591786802309770, 12.06949235617756955, 29.37390960531435269 ) ) ;
#122823 = DIRECTION ( 'NONE',  ( -0.000000000000000000, -0.000000000000000000, 1.000000000000000000 ) ) ;
#122824 = CARTESIAN_POINT ( 'NONE',  ( -14.34966873604972548, 8.224510206698743886, 98.33442372801901854 ) ) ;
#122825 = CARTESIAN_POINT ( 'NONE',  ( 13.97604488694527802, 13.89961937509977652, 34.37390960531436690 ) ) ;
#122826 = EDGE_CURVE ( 'NONE', #115310, #169831, #131232, .T. ) ;
#122827 = CARTESIAN_POINT ( 'NONE',  ( -10.81492255796105439, 18.62759615963255655, 107.9177570613523471 ) ) ;
#122828 = CARTESIAN_POINT ( 'NONE',  ( -12.14591786802326823, 12.06949235617739902, 23.12609039468567573 ) ) ;
#122829 = CARTESIAN_POINT ( 'NONE',  ( -21.55341960407619339, 5.719274019375674811, 78.54275706135236135 ) ) ;
#122830 = CARTESIAN_POINT ( 'NONE',  ( -9.474510206698720793, -16.51473224551083518, 59.58442372801900433 ) ) ;
#122831 = CARTESIAN_POINT ( 'NONE',  ( 5.049401038298161559, -19.05341960407611168, 97.70724293864766707 ) ) ;
#122832 = CARTESIAN_POINT ( 'NONE',  ( -19.03943276465977164, 0.05219959533909376836, 81.24890960531436690 ) ) ;
#122833 = CYLINDRICAL_SURFACE ( 'NONE', #185293, 5.500000000000032863 ) ;
#122834 = CARTESIAN_POINT ( 'NONE',  ( -15.80617190586745835, -15.72974639402198527, 106.8739096053143811 ) ) ;
#122835 = CARTESIAN_POINT ( 'NONE',  ( 16.53943276465976808, -0.05219959533910856209, 63.74890960531435979 ) ) ;
#122836 = CARTESIAN_POINT ( 'NONE',  ( -21.53943276465977519, 0.05219959533907696930, 56.24890960531436690 ) ) ;
#122837 = CARTESIAN_POINT ( 'NONE',  ( 9.564922557960805705, 16.46253265017160317, 59.58224293864769550 ) ) ;
#122839 = CARTESIAN_POINT ( 'NONE',  ( -14.29746914071037622, -8.314922557961029526, 89.16775706135236135 ) ) ;
#122838 = CARTESIAN_POINT ( 'NONE',  ( -10.81492255796078084, -18.62759615963271287, 92.08224293864769550 ) ) ;
#122840 = EDGE_CURVE ( 'NONE', #35005, #171876, #130417, .T. ) ;
#122841 = ORIENTED_EDGE ( 'NONE', *, *, #19233, .T. ) ;
#122842 = CARTESIAN_POINT ( 'NONE',  ( 0.05219959533909260263, 19.03943276465977164, 59.99890960531436690 ) ) ;
#122844 = CARTESIAN_POINT ( 'NONE',  ( 39.99999999999999289, 2.428612866367529932E-14, -25.00000000000000000 ) ) ;
#122843 = CARTESIAN_POINT ( 'NONE',  ( -12.06949235617756955, 12.14591786802309770, 90.62390960531436690 ) ) ;
#122845 = CARTESIAN_POINT ( 'NONE',  ( -16.46253265017160317, 9.564922557960807481, 55.83224293864769550 ) ) ;
#122846 = CARTESIAN_POINT ( 'NONE',  ( -9.564922557961040184, 16.46253265017147172, 77.91775706135234714 ) ) ;
#122847 = CARTESIAN_POINT ( 'NONE',  ( 12.14591786802309770, 12.06949235617756955, 84.37390960531438111 ) ) ;
#122848 = CARTESIAN_POINT ( 'NONE',  ( 15.80617190586769283, -15.72974639402175789, 40.62609039468567573 ) ) ;
#122850 = CARTESIAN_POINT ( 'NONE',  ( -10.72451020669898014, 18.67979575497178502, 100.4155762719810241 ) ) ;
#122849 = CARTESIAN_POINT ( 'NONE',  ( -9.474510206698964154, 16.51473224551069663, 40.41557627198103120 ) ) ;
#122851 = CARTESIAN_POINT ( 'NONE',  ( 14.29746914071049879, -8.314922557960816363, 93.33224293864769550 ) ) ;
#122852 = CARTESIAN_POINT ( 'NONE',  ( 6.300487686722097358, -38.77208804323581859, -32.75369354554603518 ) ) ;
#122853 = CARTESIAN_POINT ( 'NONE',  ( -5.049401038298153566, 19.05341960407611168, 55.20724293864769550 ) ) ;
#122854 = CARTESIAN_POINT ( 'NONE',  ( 19.20446147854529073, 5.499999999999904965, 46.88999695167679960 ) ) ;
#122856 = CARTESIAN_POINT ( 'NONE',  ( 5.153800228976335163, 19.02544592524342804, 114.7905762719810241 ) ) ;
#122855 = CARTESIAN_POINT ( 'NONE',  ( 19.05341960407617918, -5.049401038297876454, 96.04275706135231871 ) ) ;
#122857 = CARTESIAN_POINT ( 'NONE',  ( -0.05219959533937732626, 21.53943276465977519, 37.50109039468568284 ) ) ;
#122858 = CARTESIAN_POINT ( 'NONE',  ( 16.51473224551069308, 9.474510206698969483, 84.16557627198102409 ) ) ;
#122859 = CARTESIAN_POINT ( 'NONE',  ( -13.89961937509957401, -13.97604488694547875, 64.37609039468567573 ) ) ;
#122860 = CARTESIAN_POINT ( 'NONE',  ( -16.51473224551069308, -9.474510206698971260, 56.66557627198103120 ) ) ;
#122861 = CARTESIAN_POINT ( 'NONE',  ( 4.379528057220339221, -16.55341960407611168, 77.70724293864770971 ) ) ;
#122862 = CARTESIAN_POINT ( 'NONE',  ( 8.224510206698953496, -14.34966873604960469, 62.91557627198102409 ) ) ;
#122863 = CARTESIAN_POINT ( 'NONE',  ( -19.03943276465977164, 0.05219959533909376836, 91.24890960531436690 ) ) ;
#122864 = CARTESIAN_POINT ( 'NONE',  ( 18.62759615963271287, -10.81492255796078972, 98.33224293864769550 ) ) ;
#122865 = CARTESIAN_POINT ( 'NONE',  ( 13.89961937509977652, -13.97604488694527269, 88.12390960531438111 ) ) ;
#122866 = CARTESIAN_POINT ( 'NONE',  ( 5.153800228976615827, -19.02544592524334988, 30.20942372801900433 ) ) ;
#122869 = CARTESIAN_POINT ( 'NONE',  ( 12.14591786802309770, 12.06949235617756955, 114.3739096053143527 ) ) ;
#122868 = CARTESIAN_POINT ( 'NONE',  ( -12.14591786802309592, -12.06949235617757132, 36.87390960531435979 ) ) ;
#122867 = CARTESIAN_POINT ( 'NONE',  ( -5.153800228976328057, -19.02544592524343514, 42.29057627198101699 ) ) ;
#122870 = ORIENTED_EDGE ( 'NONE', *, *, #156994, .T. ) ;
#122871 = CARTESIAN_POINT ( 'NONE',  ( -5.823673210054431948, 21.52544592524334988, 27.70942372801901854 ) ) ;
#122872 = CARTESIAN_POINT ( 'NONE',  ( 19.02544592524334988, 5.153800228976608722, 61.45942372801900433 ) ) ;
#122873 = CARTESIAN_POINT ( 'NONE',  ( -8.314922557960811034, -14.29746914071050412, 32.08224293864769550 ) ) ;
#122874 = CARTESIAN_POINT ( 'NONE',  ( -15.72974639402197994, 15.80617190586746368, 85.62390960531436690 ) ) ;
#122875 = CARTESIAN_POINT ( 'NONE',  ( -19.02544592524342804, 5.153800228976336051, 116.0405762719810383 ) ) ;
#122876 = CARTESIAN_POINT ( 'NONE',  ( 16.53943276465976808, -0.05219959533910856209, 73.74890960531433848 ) ) ;
#122877 = CARTESIAN_POINT ( 'NONE',  ( -13.97604488694527625, -13.89961937509977652, 31.87390960531435979 ) ) ;
#122878 = CARTESIAN_POINT ( 'NONE',  ( -13.89961937509957401, -13.97604488694547875, 24.37609039468565442 ) ) ;
#122879 = CARTESIAN_POINT ( 'NONE',  ( 16.55341960407618274, -4.379528057220086978, 106.0427570613523471 ) ) ;
#122880 = CARTESIAN_POINT ( 'NONE',  ( 16.55341960407618274, -4.379528057220086978, 56.04275706135235424 ) ) ;
#122881 = CARTESIAN_POINT ( 'NONE',  ( -21.52544592524343514, 5.823673210054127303, 41.04057627198103120 ) ) ;
#122882 = CARTESIAN_POINT ( 'NONE',  ( 21.53943276465977519, 0.05219959533937863772, 101.2510903946856757 ) ) ;
#122883 = CARTESIAN_POINT ( 'NONE',  ( -0.05219959533909027116, -19.03943276465977164, 77.49890960531435269 ) ) ;
#122884 = CARTESIAN_POINT ( 'NONE',  ( 4.379528057220092307, 16.55341960407617563, 77.29275706135234714 ) ) ;
#122885 = CARTESIAN_POINT ( 'NONE',  ( -13.97604488694527625, -13.89961937509977652, 21.87390960531435979 ) ) ;
#122886 = CARTESIAN_POINT ( 'NONE',  ( -16.53943276465976808, 0.05219959533911058130, 41.24890960531435269 ) ) ;
#122888 = CARTESIAN_POINT ( 'NONE',  ( 13.89961937509977652, -13.97604488694527269, 88.12390960531438111 ) ) ;
#122887 = CARTESIAN_POINT ( 'NONE',  ( 16.46253265017160672, -9.564922557960803928, 103.3322429386476955 ) ) ;
#122889 = CARTESIAN_POINT ( 'NONE',  ( -19.02544592524342804, 5.153800228976336051, 106.0405762719810241 ) ) ;
#122890 = CARTESIAN_POINT ( 'NONE',  ( -4.483927247898539470, -16.52544592524342804, 62.29057627198102409 ) ) ;
#122891 = CARTESIAN_POINT ( 'NONE',  ( 14.34966873604960469, 8.224510206698951720, 29.16557627198103120 ) ) ;
#122892 = ORIENTED_EDGE ( 'NONE', *, *, #97731, .F. ) ;
#122893 = CARTESIAN_POINT ( 'NONE',  ( 4.379528057220339221, -16.55341960407611168, 57.70724293864770260 ) ) ;
#122895 = CARTESIAN_POINT ( 'NONE',  ( 2.649999999999999911, -165.0000000000000000, -15.00000000000000000 ) ) ;
#122894 = CARTESIAN_POINT ( 'NONE',  ( 14.29746914071037800, 8.314922557961029526, 46.66775706135234714 ) ) ;
#122896 = CARTESIAN_POINT ( 'NONE',  ( 16.51473224551083163, -9.474510206698727899, 55.83442372801899722 ) ) ;
#122897 = CARTESIAN_POINT ( 'NONE',  ( 19.03943276465977164, -0.05219959533909143690, 88.74890960531436690 ) ) ;
#122898 = CARTESIAN_POINT ( 'NONE',  ( 9.564922557961047289, -16.46253265017146816, 70.41775706135233293 ) ) ;
#122899 = CARTESIAN_POINT ( 'NONE',  ( 27.73933785331498925, -9.013057229001033122, 144.2750000027311899 ) ) ;
#122900 = CARTESIAN_POINT ( 'NONE',  ( 13.97604488694548053, -13.89961937509957401, 60.62609039468564731 ) ) ;
#122902 = CARTESIAN_POINT ( 'NONE',  ( -12.06949235617739369, -12.14591786802326823, 84.37609039468570415 ) ) ;
#122901 = CARTESIAN_POINT ( 'NONE',  ( 9.474510206698729675, 16.51473224551082808, 92.08442372801900433 ) ) ;
#122903 = CARTESIAN_POINT ( 'NONE',  ( 8.571926809382597767, 26.38167802310806209, 144.7750000027311899 ) ) ;
#122904 = CARTESIAN_POINT ( 'NONE',  ( 16.46253265017160672, -9.564922557960803928, 28.33224293864769550 ) ) ;
#122905 =( BOUNDED_SURFACE ( )  B_SPLINE_SURFACE ( 3, 2, ( 
 ( #16987, #168665, #13995, #30165, #48328, #109983, #33152, #156489, #106005, #137339, #152506, #91809, #153501, #14998, #76658, #138337, #61484, #161467, #82606, #81601, #113940, #130102, #143285, #37113, #51295, #6769, #188831, #142305, #160466, #65462, #159453, #5776, #128120, #67451, #129109, #175639, #4771, #49312, #127125, #99782, #176652, #22957, #97766, #84605, #144287, #110972, #190808, #66458, #172656, #38128, #189823, #146284, #131121, #52282, #68448, #112956, #7771, #174649, #36114, #20949, #98772, #83607, #21957, #145286, #19959, #191799, #53280, #114959, #69454, #35130, #34144, #95803, #157489, #18982, #80628, #3785, #50315, #111971, #173663, #96782, #158471, #116954, #192809, #151301, #166474, #180657, #102792, #100775, #103794, #149301, #56285, #115963, #132125, #25972, #134137, #27972, #177651, #147301, #85614, #89612, #196817, #117967, #101787, #179658, #150309, #165474, #10795, #178646, #11806, #73470, #87615, #58284, #12790, #43118, #8790, #195826, #24972, #72463, #40109, #41128, #163475, #119953, #162458, #26970, #181638, #135143, #104786, #57297, #74455, #118974, #42133, #54291, #133122, #39119, #70460, #193818, #88613, #86618, #23959, #55283, #148301, #9795, #164478, #71457, #194811, #76423, #14762, #106762, #91572, #138099, #184607, #77415, #121928, #63237, #48086, #94567, #47089, #199780, #108750, #154265, #153260, #15756, #46088, #182631, #60257, #136121, #156246, #109742, #123901, #107743, #44115, #170426, #92577, #61247, #59263, #75431, #169424, #139085, #171426, #120932, #90597, #28956, #32913, #140071, #122919, #45105, #30929, #93572, #31918, #562, #183622, #155257, #16746, #62233, #1562, #17748, #186614, #152279, #185600, #168437, #78395, #29933, #124916, #197797, #105773, #167460, #13763, #137105, #198791, #129859, #174409, #37884, #5533, #35878, #79404, #19721, #68206, #172414, #18740, #144051, #188589, #110732, #21716, #161224, #2560, #83369, #80387, #126883, #191557, #112716, #111731, #67212, #160225, #173418, #128870, #81363, #36866, #142059, #33902, #190570, #95559, #189582, #97524, #158231, #159212, #20706, #52046, #34888, #141075, #157246, #53034, #6527, #114716, #127878, #176408, #82362, #64242, #113702, #96543, #125909, #99542, #143047, #187607, #49076, #175398, #98532, #4525, #3545, #66218, #65223, #145046, #50070, #51054, #148063, #23720, #22718, #41890, #104546, #26727, #196579, #116717, #87380, #103557, #181403, #58049, #133891, #11565, #84366, #165232, #180418, #146043, #10553, #149065, #131890, #195583, #192569, #57055, #86378, #177414, #130879, #134902, #55046, #179416, #7527, #54052, #69211, #119719, #115727, #88366, #178406, #38885, #118730, #150059, #42881, #100542, #164238, #162221, #72217, #85368, #193574, #40881, #147062, #8544, #70222, #9554, #73231, #25734, #39870, #101536, #163229, #24729, #71220, #117720, #132883, #194572, #56042, #102554, #59024, #62990, #120691, #106516, #139822, #155009, #152038, #14513, #45846, #1311, #15513, #153013, #186364, #183379, #76174, #124668, #61004, #43868, #168194, #185352, #78154, #89371, #105533, #184365, #29691, #60016, #137854, #138840, #47844, #61988, #12551, #75188, #135885, #199534, #320, #91322, #77170, #92332, #170182, #31676, #151060, #74217, #197556, #46843, #107499, #123654, #169175, #167219, #182390, #28716, #122676, #30680, #154018, #16506, #108502, #90353, #93325, #166227, #27728, #13523, #136860, #198546, #121683, #44861, #65968, #188340, #127638, #189338, #35636, #141814, #109497, #187362, #159976, #36618, #85888, #157989, #24238, #142807, #171179, #50816, #3307, #32667, #98275, #49819, #147576, #194092, #4287, #66968, #126638, #9062, #111483, #173168, #96303, #97281, #143802, #34644, #19480, #80144, #64980, #81126, #112473, #174166, #95313, #70732, #132399, #94320, #20461, #158969, #82111, #5285, #128628, #190321, #51798, #155998, #33652, #17494, #79152, #140823, #113457, #175150 ),
 ( #2312, #63993, #18496, #125664, #48831, #110484, #172167, #156998, #74720, #136383, #88883, #121203, #90852, #106035, #10063, #197080, #87878, #150575, #41397, #180921, #103062, #59526, #25247, #28241, #182895, #198060, #167721, #12074, #14024, #181903, #73736, #55554, #196097, #44379, #148573, #195083, #120213, #164744, #86888, #29219, #137369, #178921, #152537, #56563, #26239, #75690, #135409, #149566, #43381, #117227, #11062, #105053, #57567, #13053, #118239, #58547, #40389, #166737, #102062, #71723, #89881, #72738, #134411, #42396, #179930, #163747, #133392, #119237, #104059, #165739, #27234, #151564, #79674, #157518, #34173, #110012, #187872, #199048, #18021, #156521, #122193, #186888, #63517, #108013, #171693, #168695, #33182, #62506, #153531, #107023, #111002, #31192, #155523, #60518, #30196, #183885, #172688, #80658, #64510, #92844, #15028, #94841, #141345, #19012, #45370, #140347, #91838, #48358, #95834, #169698, #17018, #76689, #138365, #200046, #185878, #2832, #1835, #125192, #61515, #126177, #123184, #184873, #93844, #49340, #46355, #154529, #16026, #77684, #139352, #832, #124177, #47364, #109019, #170698, #32187, #78671, #115993, #191831, #129141, #162489, #159485, #52314, #39150, #37145, #19988, #144319, #161499, #54321, #65492, #81631, #160498, #82636, #36145, #113972, #114990, #23990, #38159, #188862, #51326, #112004, #190838, #176684, #67482, #53312, #68479, #146314, #7803, #127154, #50345, #173693, #22989, #21988, #99813, #83640, #143314, #35160, #4801, #175670, #98804, #6801, #192841, #130134, #96815, #3814, #158501, #145318, #131152, #66490, #84637, #69487, #128153, #100806, #189853, #5808, #177682, #142334, #112987, #174680, #97797, #20979, #135173, #72494, #105803, #102823, #195856, #182660, #180687, #163506, #87644, #104815, #197826, #8821, #25004, #103823, #26002, #179688, #57328, #58313, #167490, #181667, #132156, #194843, #55314, #134168, #119981, #10824, #196846, #11836, #89642, #151330, #70490, #193849, #116985, #166504, #165503, #43146, #26999, #86648, #178678, #148331, #119004, #42163, #150340, #136151, #73501, #40141, #88644, #28002, #12818, #147334, #101818, #74485, #56317, #164508, #59292, #9827, #85647, #120961, #71487, #44144, #133153, #41160, #117999, #149330, #187636, #64271, #140101, #17778, #28985, #48115, #186644, #152308, #16777, #93601, #138129, #1592, #198820, #63267, #92604, #183651, #137133, #141104, #61277, #185628, #90626, #60285, #13794, #2592, #110764, #94598, #122948, #45134, #124948, #109771, #49106, #75459, #170456, #121958, #78426, #125937, #199810, #47120, #106792, #168466, #29964, #15784, #171455, #31947, #155287, #91602, #32943, #153291, #156277, #14792, #184636, #79433, #76452, #46117, #107770, #169456, #30957, #154294, #77443, #139115, #591, #62262, #123930, #108778, #52077, #80418, #175430, #127910, #3576, #18771, #129889, #19752, #20738, #33933, #142090, #172445, #53068, #95591, #68236, #4558, #111761, #36899, #83398, #157275, #65254, #98563, #173450, #145076, #126914, #174439, #160257, #188620, #50101, #158262, #113733, #37913, #6558, #191589, #81393, #34918, #143079, #66250, #21747, #96574, #51086, #189612, #112746, #67242, #35909, #128901, #114746, #97555, #159243, #176440, #82394, #144082, #5563, #190600, #139744, #173097, #170102, #62911, #49742, #47766, #30601, #154930, #172092, #64907, #76096, #92254, #171098, #93245, #46767, #124591, #125589, #34574, #48757, #199456, #61910, #122598, #1232, #187286, #78075, #2237, #79076, #156927, #18424, #137771, #60924, #184288, #33579, #32590, #110410, #94243, #153938, #45769, #15433, #186286, #109419, #17419, #3233, #140749, #107421, #155923, #95242, #63920, #14433, #169094, #80074, #123580, #31596, #141743, #77091, #152934, #126568, #138760, #188267, #185275, #242, #111411, #108426, #16428, #38568, #35563, #143731, #8224, #129545, #128553, #160907, #177096, #190249, #84051, #98201 ),
 ( #97211, #96231, #115408, #178087, #100224, #69901, #51726, #22400, #161906, #54725, #131568, #7210, #85046, #157919, #23399, #53733, #19409, #145729, #68894, #5210, #130554, #65892, #192251, #159905, #50744, #4214, #193252, #113389, #52719, #81058, #127567, #142735, #116398, #189268, #146727, #175079, #112402, #174094, #158897, #20387, #82034, #37557, #66891, #36545, #21393, #83052, #114383, #144726, #6213, #67892, #191245, #176087, #99219, #49625, #121, #94123, #2119, #96115, #45649, #15310, #153815, #157803, #64793, #186165, #169982, #124468, #18303, #33463, #17300, #46642, #79959, #141628, #155802, #126454, #19294, #111287, #76969, #63801, #93125, #78954, #108302, #47647, #31473, #188152, #30477, #95121, #172977, #3118, #34456, #140629, #80942, #187170, #125474, #60803, #1113, #142617, #138640, #154810, #122476, #61790, #184167, #107300, #168972, #109298, #92128, #48641, #123460, #110293, #16308, #185152, #77958, #139625, #62787, #170977, #171975, #32470, #156811, #131441, #144607, #98079, #38443, #67771, #158778, #112284, #116275, #36424, #160787, #65775, #35442, #4096, #177965, #85936, #69773, #159777, #20266, #115281, #23278, #162779, #127444, #145607, #50623, #192124, #101093, #174960, #22275, #189150, #173974, #97094, #84922, #83926, #68767, #37435, #81912, #146602, #143605, #5089, #99095, #193128, #66771, #100099, #54601, #128432, #24287, #190129, #6092, #39433, #51604, #113268, #52600, #7086, #21272, #53605, #191126, #82929, #129428, #114262, #175966, #130425, #176974, #161783, #8095, #59577, #70780, #25297, #165790, #87929, #41447, #57616, #120259, #167768, #43433, #194139, #56614, #117277, #196144, #181951, #72789, #197126, #73785, #151610, #13102, #132448, #55603, #178971, #166788, #27287, #105102, #88933, #86939, #40438, #148623, #119284, #180967, #12121, #198110, #135457, #102110, #42444, #28289, #150625, #9113, #163795, #89929, #118288, #179979, #10113, #58593, #74767, #106082, #29266, #136429, #71773, #121251, #44428, #103112, #104108, #147625, #133443, #195133, #182945, #164793, #26288, #149616, #11114, #134459, #152583, #60564, #185926, #82441, #14073, #186937, #159289, #183930, #190649, #45415, #31241, #67290, #144129, #76735, #139397, #170746, #128948, #140396, #77731, #113781, #108062, #879, #52125, #47411, #168739, #92891, #110064, #5611, #75740, #30243, #109067, #154577, #184919, #62554, #63565, #175477, #48408, #137417, #200091, #122240, #124230, #125239, #16073, #1884, #17066, #97601, #20786, #199097, #107068, #91886, #171744, #32235, #33233, #93893, #153577, #15075, #138411, #155571, #78720, #90897, #61559, #123228, #46403, #169746, #56127, #55127, #98611, #53117, #71305, #7606, #115804, #162302, #37964, #36949, #117809, #118817, #40968, #10640, #130958, #101626, #179502, #195670, #72301, #148147, #25817, #160305, #102639, #194658, #21795, #24813, #133979, #163315, #116797, #192648, #132968, #100620, #191637, #145124, #149150, #69292, #193655, #83447, #68287, #6608, #57141, #129938, #164324, #86462, #114795, #9638, #178488, #54131, #87463, #23802, #176488, #99622, #161303, #177494, #39955, #22798, #84444, #146122, #38964, #85452, #147142, #8630, #70302, #131971, #199619, #138920, #62073, #121767, #26812, #168277, #77252, #151144, #136944, #180503, #41975, #165320, #61086, #60099, #44946, #13606, #88452, #122758, #103642, #150148, #75274, #169260, #11649, #76257, #45928, #73315, #401, #134986, #120771, #154100, #30767, #166317, #28799, #183460, #15594, #29774, #167303, #196664, #197640, #90438, #58133, #198633, #119802, #182472, #184448, #92414, #181487, #42965, #106601, #43953, #74300, #152124, #153097, #104628, #137935, #27814, #89455, #12635, #91409, #14601, #105615, #107583, #135969, #59106, #189424, #108587, #170264, #31758, #142889, #3389, #81208, #141898, #1395, #93407, #124755, #33737, #157084, #188425, #174252, #49902, #155093, #18580, #4371, #65064 ),
 ( #111569, #66054, #82196, #159053, #34728, #112557, #123738, #127722, #50899, #46927, #16587, #47927, #185437, #143889, #97367, #173253, #95398, #78235, #139906, #172250, #19564, #35720, #63076, #80227, #126721, #20547, #186451, #109581, #171264, #5370, #32752, #48915, #94403, #187447, #156084, #96386, #158073, #17580, #79241, #140912, #2398, #64077, #125747, #110569, #21550, #8384, #99377, #100382, #52873, #192408, #114544, #71058, #36703, #39708, #132724, #86216, #117555, #162060, #25576, #193409, #23556, #67054, #7364, #55882, #160063, #6367, #131727, #176244, #98364, #9392, #148902, #190409, #194412, #68047, #37715, #179254, #85204, #161060, #54884, #147906, #22555, #116558, #69049, #24567, #129699, #83210, #178247, #144885, #177252, #146892, #145881, #70059, #101371, #163060, #84201, #128712, #191396, #40720, #102389, #164077, #115565, #87220, #51885, #113544, #175238, #130714, #53890, #38724, #89208, #137691, #92167, #105370, #168037, #27568, #136698, #149890, #11396, #198379, #59856, #44699, #150901, #12395, #181245, #166067, #74057, #58865, #151878, #196420, #199376, #122515, #169011, #121523, #135728, #183218, #28558, #197399, #90195, #120531, #182224, #57890, #14351, #180257, #106353, #76016, #29534, #60840, #167057, #30515, #91167, #13368, #10392, #43708, #184205, #103391, #73066, #75032, #119562, #41727, #152856, #72049, #133723, #45687, #134738, #42722, #107338, #195415, #104384, #56893, #118567, #165069, #26563, #88206, #111326, #93165, #46682, #64830, #170022, #63837, #110330, #32509, #172011, #33500, #79997, #186204, #153853, #31512, #4135, #80981, #127483, #2159, #65814, #187207, #15351, #95159, #47686, #77007, #142656, #94161, #189188, #35483, #48678, #173016, #171018, #141665, #154850, #16347, #3157, #126492, #188190, #155840, #17337, #124509, #109336, #78993, #125510, #156847, #139663, #50661, #112322, #174012, #49662, #140667, #34495, #18342, #96153, #157842, #19333, #159, #77996, #138679, #61828, #123498, #185191, #108341, #1151, #62826, #145646, #193167, #85975, #36464, #130467, #38483, #132488, #81952, #51644, #190168, #194177, #101131, #22315, #6130, #160827, #54639, #69813, #53645, #82970, #116314, #178003, #192165, #162817, #55641, #147665, #113308, #100140, #129468, #115322, #144647, #70819, #191167, #161821, #39470, #117314, #179010, #8135, #9153, #97132, #24326, #158816, #20304, #84960, #143644, #23316, #177014, #52640, #131480, #83966, #174999, #5127, #66809, #114305, #146642, #128472, #98121, #159818, #21313, #67813, #176007, #37476, #99137, #7126, #68808, #199135, #122277, #181990, #86978, #28327, #137456, #11155, #197165, #40478, #102150, #25337, #121289, #120297, #105140, #73825, #148665, #59616, #163835, #10153, #135495, #29304, #71813, #136466, #106120, #133481, #60602, #195173, #181010, #14111, #90934, #26329, #88972, #43472, #75778, #89966, #27326, #56654, #57657, #150662, #118327, #58631, #180020, #42484, #182982, #152620, #41487, #103152, #166826, #104147, #134499, #12160, #13141, #164833, #198146, #87969, #149657, #72829, #151646, #74803, #165829, #44466, #167804, #196185, #119323, #168776, #30278, #91924, #2919, #63601, #141432, #1922, #61595, #153616, #184955, #93929, #17103, #48444, #34260, #110101, #15112, #78755, #64597, #125277, #45452, #200126, #18107, #154613, #62589, #109103, #46439, #183965, #126261, #65581, #187958, #142422, #94927, #124267, #156612, #186974, #139433, #171780, #155608, #76773, #108098, #107106, #3901, #157604, #33268, #140432, #138445, #123264, #32272, #79761, #172779, #169783, #49428, #111089, #19095, #31276, #92927, #16108, #80744, #95919, #170782, #77766, #47447, #915, #185962, #83723, #113070, #146397, #7886, #160583, #192926, #162573, #177764, #81717, #68562, #159571, #22072, #174762, #52400, #36228, #131238, #96900, #99895, #54404, #69572, #39233, #145402, #85732, #53398, #6884, #127240, #67568, #116076, #20073 ),
 ( #4891, #35247, #128238, #37233, #130219, #191914, #100889, #115076, #158584, #176768, #24076, #38240, #188954, #143402, #161580, #97880, #5892, #114059, #189935, #50431, #147419, #8906, #112090, #173780, #21069, #23074, #66573, #51410, #82725, #84719, #144406, #129226, #190923, #175756, #98889, #58398, #167575, #196930, #88732, #164589, #104900, #134255, #25088, #178763, #182746, #102905, #27086, #132242, #101905, #70574, #44231, #152391, #136235, #105888, #103907, #193934, #150427, #26083, #55397, #59379, #149412, #197909, #117067, #165588, #28089, #87727, #120064, #9910, #71570, #181752, #43234, #166589, #10908, #72581, #41243, #195942, #57416, #119089, #11922, #56402, #121051, #29069, #90708, #89729, #180771, #151415, #73586, #42246, #135258, #12903, #40228, #194927, #163587, #86730, #148415, #74567, #133235, #118084, #179774, #62349, #109858, #2682, #153378, #47207, #155376, #49195, #198905, #168549, #106876, #110853, #17868, #139203, #123034, #77531, #171543, #186733, #170545, #199899, #33031, #94687, #108866, #79523, #172538, #64359, #30047, #16865, #46204, #32036, #61363, #678, #184720, #141193, #183735, #48204, #126028, #156365, #187724, #93693, #34023, #140190, #78516, #13877, #154379, #95681, #91688, #14880, #1682, #107858, #45221, #75544, #137218, #60373, #122045, #76541, #169543, #138217, #63360, #31042, #125037, #92691, #15873, #124019, #185716, #114836, #96663, #50193, #68327, #173539, #67329, #113821, #35994, #175516, #36991, #83488, #189702, #157367, #35008, #7647, #84484, #130997, #5653, #177534, #174527, #128991, #54172, #52164, #158350, #159330, #176530, #69331, #80507, #19839, #98652, #97641, #51175, #190689, #129977, #39004, #53158, #3664, #66338, #127002, #160346, #191677, #82483, #6649, #145165, #161346, #22837, #142180, #65342, #188710, #38006, #21835, #99661, #146161, #81480, #111849, #143167, #192689, #115845, #18861, #4647, #128000, #112835, #20827, #144167, #118857, #162341, #116836, #137726, #71343, #179540, #25856, #101665, #100659, #122551, #185227, #107375, #77043, #194697, #165358, #184241, #61864, #138714, #14384, #92205, #23842, #45722, #60874, #85492, #88493, #195, #26852, #180540, #56166, #199410, #164361, #55165, #8669, #15386, #133006, #57180, #147180, #132009, #70342, #123533, #193696, #169047, #117847, #178526, #76050, #30553, #39993, #163355, #42014, #24851, #150190, #86500, #41009, #103679, #148184, #9678, #102676, #153889, #87500, #149188, #134016, #10677, #72342, #195708, #16383, #141699, #35519, #170057, #142690, #112359, #139699, #143682, #1185, #187241, #20340, #97167, #32542, #95195, #126525, #81989, #96188, #33533, #5163, #62862, #48711, #66846, #158852, #94195, #156881, #188224, #128509, #157877, #18378, #46718, #63874, #80030, #108381, #3190, #124544, #110364, #65848, #31548, #93200, #186241, #64863, #172046, #140702, #49697, #19366, #154885, #4170, #78030, #155875, #47719, #111362, #81015, #173051, #127518, #34528, #50700, #174050, #109370, #171052, #17372, #189222, #79027, #2192, #125545, #67847, #98156, #191202, #100178, #23354, #54678, #40518, #116352, #159856, #84999, #9192, #8175, #51683, #6167, #24364, #160863, #68848, #115362, #52677, #190204, #70857, #71852, #194215, #163877, #84005, #178041, #132526, #148704, #25376, #101169, #179050, #113345, #55680, #147704, #175037, #39509, #87018, #162857, #69851, #145683, #86015, #53685, #144682, #21349, #102189, #22353, #146680, #36502, #83007, #129502, #10192, #114340, #117354, #7165, #176043, #37511, #99173, #130507, #192203, #131519, #177052, #38522, #161860, #193205, #90003, #15148, #133521, #118367, #14148, #13177, #198183, #166863, #41529, #152658, #195213, #103192, #28365, #122314, #56693, #29342, #199173, #26368, #180060, #151685, #90971, #150701, #59653, #72869, #134538, #121327, #183019, #167841, #73864, #12199, #104186, #89010, #135533, #182028, #74840, #119364, #60640, #45488 ),
 ( #44503, #43511, #164873, #88008, #105177, #75815, #184005, #196226, #136503, #106159, #168813, #149696, #11194, #57696, #30317, #137493, #58667, #42523, #197204, #107143, #91960, #153653, #181048, #165868, #27364, #120333, #142454, #112120, #127272, #31311, #18140, #109138, #110134, #62624, #1957, #124302, #80776, #46476, #49459, #3932, #95952, #188986, #171813, #35277, #2951, #33301, #76810, #17138, #65612, #169820, #16145, #141467, #185999, #108136, #19126, #158614, #200162, #50461, #77800, #47481, #173812, #94960, #170817, #64630, #157637, #32309, #126292, #78790, #34291, #139469, #92964, #187989, #154650, #187008, #156645, #155643, #79794, #111121, #172811, #93963, #138481, #949, #96932, #61632, #123300, #125312, #184992, #140468, #63636, #48478, #114089, #81748, #8939, #98922, #147451, #36258, #54437, #190954, #160614, #145433, #21102, #20104, #39265, #101938, #24110, #193966, #175790, #84751, #100921, #178795, #55429, #131270, #70608, #143435, #162606, #177795, #4922, #7919, #117100, #146429, #38272, #37264, #116107, #83754, #174792, #128268, #132275, #52431, #176799, #66604, #51441, #189966, #40264, #113101, #85765, #22104, #97912, #192958, #159603, #82757, #144437, #161611, #5923, #69604, #67600, #6916, #99926, #129259, #68594, #130250, #191945, #23105, #53431, #115107, #71601, #182775, #25120, #133267, #58425, #152418, #86764, #59406, #29096, #56435, #60401, #118116, #103936, #137248, #13906, #149442, #11950, #43261, #198934, #12930, #150455, #183765, #180799, #73614, #122073, #120092, #41273, #165616, #44258, #75572, #148447, #102935, #181780, #27115, #57445, #135285, #136262, #45251, #121080, #9942, #72611, #194958, #196957, #197937, #88762, #74594, #89757, #167601, #90735, #179804, #164620, #26114, #105915, #104929, #163619, #166616, #87757, #10938, #134286, #28118, #151443, #195973, #119118, #42278, #76571, #140222, #126059, #125068, #168578, #157400, #34055, #80539, #155406, #18893, #1715, #106905, #186765, #710, #30076, #95713, #185751, #142213, #188742, #63391, #64391, #124052, #33063, #46236, #107890, #94718, #156396, #141223, #47240, #108898, #77563, #62382, #170577, #16896, #48235, #92722, #3696, #65375, #127035, #17900, #32068, #79555, #109890, #93724, #171574, #78547, #153411, #31075, #91717, #14910, #138246, #2714, #187756, #199930, #61393, #49226, #110884, #123065, #169577, #172569, #184751, #154411, #15905, #139235, #143199, #85522, #54203, #175549, #159364, #113853, #7677, #22867, #6679, #36026, #69361, #131030, #83519, #115875, #147210, #100688, #4680, #191707, #82518, #145196, #97675, #37024, #20861, #177564, #19872, #84514, #39033, #192719, #162370, #68357, #8701, #176561, #130008, #50227, #190722, #23871, #66372, #189734, #114866, #144200, #81512, #70371, #132039, #173571, #111881, #51207, #5686, #35040, #53191, #67362, #38036, #96694, #129021, #99692, #52195, #158383, #112868, #128032, #161376, #174559, #160378, #146192, #98685, #21869, #180571, #88525, #41039, #193728, #9708, #42045, #55196, #26882, #25886, #178556, #12702, #149218, #89525, #116865, #165389, #166387, #10709, #196733, #56196, #117879, #135057, #58201, #43033, #134046, #72372, #87531, #195739, #57212, #103709, #11718, #102705, #74368, #197708, #40022, #181554, #118887, #104699, #73385, #150221, #119869, #27883, #86530, #164393, #101695, #163384, #24881, #151214, #136034, #194726, #179569, #59174, #148214, #71372, #133036, #7323, #115524, #9354, #159011, #128670, #67011, #71019, #178206, #99337, #83168, #37672, #131687, #146849, #130673, #160020, #193368, #54844, #69007, #39670, #132687, #24527, #190366, #177212, #6326, #192367, #21507, #161020, #144842, #101332, #143848, #8343, #163020, #116518, #86178, #53850, #194375, #100341, #38685, #174209, #114501, #147868, #51842, #113501, #162020, #68006, #5327, #55842, #35677, #97325, #20504, #175196, #129658, #82152, #23516, #191354, #85162, #36661 ),
 ( #52832, #176203, #22514, #98320, #84161, #145841, #70018, #121485, #91129, #90156, #74019, #103354, #136659, #198339, #150862, #183179, #152819, #168000, #72011, #58826, #149854, #12356, #165032, #42684, #26525, #44661, #87182, #151839, #106314, #59815, #29496, #135689, #75978, #43669, #197361, #117516, #57853, #14312, #10354, #56855, #182184, #88170, #148863, #137651, #199338, #40680, #179213, #118530, #11358, #102350, #120493, #73029, #105331, #164039, #134701, #167019, #119525, #74994, #180219, #133684, #28520, #195376, #27529, #13329, #196384, #25538, #41689, #181208, #104345, #166029, #89170, #103916, #41252, #178773, #86740, #55407, #26092, #42254, #120071, #196937, #72590, #150434, #161589, #180779, #119097, #84728, #149421, #58405, #87736, #179783, #117077, #195951, #25098, #116085, #69581, #73593, #193944, #118093, #23083, #192936, #146406, #135266, #43241, #27094, #40239, #177773, #134264, #165596, #181759, #7896, #102914, #131247, #10917, #54413, #132253, #164598, #39243, #100899, #162583, #88740, #57424, #11929, #194937, #24087, #85742, #147429, #8916, #56413, #70584, #101915, #163597, #148425, #9920, #71579, #133245, #45228, #78522, #13882, #168555, #62356, #77538, #61369, #90713, #124026, #185725, #138223, #170552, #140196, #155382, #59384, #46210, #137225, #199905, #152396, #30053, #75549, #108872, #74572, #139210, #32042, #47214, #16871, #123040, #63366, #31048, #184726, #104908, #106882, #93699, #197914, #44236, #169550, #198910, #136240, #1690, #186739, #28096, #125043, #105893, #60378, #166596, #107864, #122050, #92697, #89735, #183741, #154385, #91694, #151421, #167580, #121058, #15880, #182752, #14886, #685, #153386, #12908, #29074, #76547, #80514, #48210, #126034, #98659, #50201, #158358, #110859, #52171, #81487, #109864, #128007, #142187, #171549, #36998, #127009, #175523, #129984, #143174, #5660, #65349, #174534, #187730, #49201, #36001, #97648, #82491, #188717, #111856, #18868, #3671, #173546, #96670, #189709, #34029, #160353, #21843, #6656, #159337, #35015, #20834, #66345, #19846, #51182, #4654, #94693, #172544, #33038, #68334, #83495, #144174, #112842, #156371, #17875, #67336, #128998, #145172, #95687, #190696, #113828, #79529, #141199, #2688, #64365, #157375, #195715, #116843, #57188, #10685, #42021, #86507, #150197, #117854, #148192, #191684, #132016, #180548, #84491, #131004, #56173, #100666, #22844, #134023, #73362, #114843, #118864, #192696, #39011, #103686, #24858, #23849, #179547, #72349, #85499, #41017, #193704, #149195, #54179, #146169, #102683, #7654, #101672, #9685, #70349, #71350, #133014, #164369, #147187, #53165, #69338, #165365, #55173, #163362, #115852, #26859, #194704, #176537, #25863, #8677, #38013, #88501, #178533, #11695, #99669, #87507, #161353, #40000, #177542, #162348, #136012, #61134, #122806, #169307, #75319, #13652, #105662, #90487, #136990, #183510, #76307, #120820, #62123, #46975, #93455, #45975, #198679, #107629, #153145, #152169, #14647, #44993, #181531, #59150, #135034, #155142, #108634, #184496, #106652, #43010, #104677, #168324, #30813, #123786, #74346, #29821, #137985, #170312, #119846, #89502, #27861, #31805, #138970, #60146, #44001, #121814, #92462, #154150, #91457, #182520, #15642, #77301, #199668, #448, #16635, #185485, #151191, #196710, #167349, #58179, #28847, #166364, #12680, #197685, #47976, #50946, #67100, #171312, #17630, #142935, #187495, #109629, #20593, #160110, #1445, #82245, #79290, #125793, #190458, #111617, #110615, #4416, #159099, #172297, #66102, #80273, #35766, #140959, #32799, #189468, #94451, #188472, #34777, #157131, #96433, #158120, #127768, #33786, #78282, #156131, #128759, #141944, #49953, #2446, #143936, #173302, #139955, #19611, #95446, #63123, #51931, #18626, #5417, #124802, #81253, #97412, #3434, #112605, #64128, #48961, #174297, #113591, #175285, #65110, #126768, #36750, #98414, #186500, #52919, #21598 ) ),
 .UNSPECIFIED., .T., .F., .F. ) 
 B_SPLINE_SURFACE_WITH_KNOTS ( ( 4, 3, 4 ),
 ( 3, 2, 2, 2, 2, 2, 2, 2, 2, 2, 2, 2, 2, 2, 2, 2, 2, 2, 2, 2, 2, 2, 2, 2, 2, 2, 2, 2, 2, 2, 2, 2, 2, 2, 2, 2, 2, 2, 2, 2, 2, 2, 2, 2, 2, 2, 2, 2, 2, 2, 2, 2, 2, 2, 2, 2, 2, 2, 2, 2, 2, 2, 2, 2, 2, 2, 2, 2, 2, 2, 2, 2, 2, 2, 2, 2, 2, 2, 2, 2, 2, 2, 2, 2, 2, 2, 2, 2, 2, 2, 2, 2, 2, 2, 2, 2, 2, 2, 2, 2, 2, 2, 2, 2, 2, 2, 2, 2, 2, 2, 2, 2, 2, 2, 2, 2, 2, 2, 2, 2, 2, 2, 2, 2, 2, 2, 2, 2, 2, 2, 2, 2, 2, 2, 2, 2, 2, 2, 2, 2, 2, 2, 2, 2, 2, 2, 2, 2, 2, 2, 2, 2, 2, 2, 2, 2, 2, 2, 2, 2, 2, 2, 2, 2, 2, 2, 2, 2, 2, 2, 2, 2, 2, 2, 2, 2, 2, 2, 2, 2, 2, 2, 2, 2, 2, 2, 2, 2, 2, 2, 2, 2, 2, 2, 2, 2, 2, 2, 2, 2, 2, 2, 2, 2, 2, 2, 2, 2, 2, 2, 2, 2, 2, 2, 2, 2, 2, 2, 2, 2, 2, 2, 2, 2, 2, 2, 2, 2, 3 ),
 ( 0.000000000000000000, 0.5000000000000000000, 1.000000000000000000 ),
 ( 0.000000000000000000, 0.004385964912280701511, 0.008771929824561403022, 0.01315789473684210453, 0.01754385964912280604, 0.02192982456140350755, 0.02631578947368420907, 0.03070175438596491058, 0.03508771929824561209, 0.03947368421052631360, 0.04385964912280701511, 0.04824561403508771662, 0.05263157894736841813, 0.05701754385964911964, 0.06140350877192982115, 0.06578947368421052266, 0.07017543859649122417, 0.07456140350877192569, 0.07894736842105262720, 0.08333333333333332871, 0.08771929824561403022, 0.09210526315789473173, 0.09649122807017543324, 0.1008771929824561348, 0.1052631578947368363, 0.1096491228070175378, 0.1140350877192982393, 0.1184210526315789408, 0.1228070175438596423, 0.1271929824561403577, 0.1315789473684210453, 0.1359649122807017607, 0.1403508771929824483, 0.1447368421052631637, 0.1491228070175438514, 0.1535087719298245668, 0.1578947368421052544, 0.1622807017543859698, 0.1666666666666666574, 0.1710526315789473728, 0.1754385964912280604, 0.1798245614035087758, 0.1842105263157894635, 0.1885964912280701788, 0.1929824561403508665, 0.1973684210526315819, 0.2017543859649122695, 0.2061403508771929849, 0.2105263157894736725, 0.2149122807017543879, 0.2192982456140350755, 0.2236842105263157909, 0.2280701754385964786, 0.2324561403508771940, 0.2368421052631578816, 0.2412280701754385970, 0.2456140350877192846, 0.2500000000000000000, 0.2543859649122807154, 0.2587719298245614308, 0.2631578947368420907, 0.2675438596491228060, 0.2719298245614035214, 0.2763157894736842368, 0.2807017543859648967, 0.2850877192982456121, 0.2894736842105263275, 0.2938596491228070429, 0.2982456140350877027, 0.3026315789473684181, 0.3070175438596491335, 0.3114035087719298489, 0.3157894736842105088, 0.3201754385964912242, 0.3245614035087719396, 0.3289473684210526550, 0.3333333333333333148, 0.3377192982456140302, 0.3421052631578947456, 0.3464912280701754610, 0.3508771929824561209, 0.3552631578947368363, 0.3596491228070175517, 0.3640350877192982670, 0.3684210526315789269, 0.3728070175438596423, 0.3771929824561403577, 0.3815789473684210731, 0.3859649122807017330, 0.3903508771929824483, 0.3947368421052631637, 0.3991228070175438791, 0.4035087719298245390, 0.4078947368421052544, 0.4122807017543859698, 0.4166666666666666852, 0.4210526315789473450, 0.4254385964912280604, 0.4298245614035087758, 0.4342105263157894912, 0.4385964912280701511, 0.4429824561403508665, 0.4473684210526315819, 0.4517543859649122973, 0.4561403508771929571, 0.4605263157894736725, 0.4649122807017543879, 0.4692982456140351033, 0.4736842105263157632, 0.4780701754385964786, 0.4824561403508771940, 0.4868421052631579093, 0.4912280701754385692, 0.4956140350877192846, 0.5000000000000000000, 0.5043859649122807154, 0.5087719298245614308, 0.5131578947368421462, 0.5175438596491228616, 0.5219298245614034659, 0.5263157894736841813, 0.5307017543859648967, 0.5350877192982456121, 0.5394736842105263275, 0.5438596491228070429, 0.5482456140350877583, 0.5526315789473684736, 0.5570175438596490780, 0.5614035087719297934, 0.5657894736842105088, 0.5701754385964912242, 0.5745614035087719396, 0.5789473684210526550, 0.5833333333333333703, 0.5877192982456140857, 0.5921052631578946901, 0.5964912280701754055, 0.6008771929824561209, 0.6052631578947368363, 0.6096491228070175517, 0.6140350877192982670, 0.6184210526315789824, 0.6228070175438596978, 0.6271929824561403022, 0.6315789473684210176, 0.6359649122807017330, 0.6403508771929824483, 0.6447368421052631637, 0.6491228070175438791, 0.6535087719298245945, 0.6578947368421053099, 0.6622807017543859143, 0.6666666666666666297, 0.6710526315789473450, 0.6754385964912280604, 0.6798245614035087758, 0.6842105263157894912, 0.6885964912280702066, 0.6929824561403509220, 0.6973684210526315264, 0.7017543859649122417, 0.7061403508771929571, 0.7105263157894736725, 0.7149122807017543879, 0.7192982456140351033, 0.7236842105263158187, 0.7280701754385965341, 0.7324561403508771384, 0.7368421052631578538, 0.7412280701754385692, 0.7456140350877192846, 0.7500000000000000000, 0.7543859649122807154, 0.7587719298245614308, 0.7631578947368421462, 0.7675438596491228616, 0.7719298245614034659, 0.7763157894736841813, 0.7807017543859648967, 0.7850877192982456121, 0.7894736842105263275, 0.7938596491228070429, 0.7982456140350877583, 0.8026315789473684736, 0.8070175438596490780, 0.8114035087719297934, 0.8157894736842105088, 0.8201754385964912242, 0.8245614035087719396, 0.8289473684210526550, 0.8333333333333333703, 0.8377192982456140857, 0.8421052631578946901, 0.8464912280701754055, 0.8508771929824561209, 0.8552631578947368363, 0.8596491228070175517, 0.8640350877192982670, 0.8684210526315789824, 0.8728070175438596978, 0.8771929824561403022, 0.8815789473684210176, 0.8859649122807017330, 0.8903508771929824483, 0.8947368421052631637, 0.8991228070175438791, 0.9035087719298245945, 0.9078947368421053099, 0.9122807017543859143, 0.9166666666666666297, 0.9210526315789473450, 0.9254385964912280604, 0.9298245614035087758, 0.9342105263157894912, 0.9385964912280702066, 0.9429824561403509220, 0.9473684210526315264, 0.9517543859649122417, 0.9561403508771929571, 0.9605263157894736725, 0.9649122807017543879, 0.9692982456140351033, 0.9736842105263158187, 0.9780701754385965341, 0.9824561403508771384, 0.9868421052631578538, 0.9912280701754385692, 0.9956140350877192846, 1.000000000000000000 ),
 .UNSPECIFIED. ) 
 GEOMETRIC_REPRESENTATION_ITEM ( )  RATIONAL_B_SPLINE_SURFACE ( (
 ( 1.000000000000000000, 0.9659258262890683122, 1.000000000000000000, 0.9659258262890683122, 1.000000000000000000, 0.9659258262890683122, 1.000000000000000000, 0.9659258262890683122, 1.000000000000000000, 0.9659258262890683122, 1.000000000000000000, 0.9659258262890683122, 1.000000000000000000, 0.9659258262890683122, 1.000000000000000000, 0.9659258262890683122, 1.000000000000000000, 0.9659258262890683122, 1.000000000000000000, 0.9659258262890683122, 1.000000000000000000, 0.9659258262890683122, 1.000000000000000000, 0.9659258262890683122, 1.000000000000000000, 0.9659258262890683122, 1.000000000000000000, 0.9659258262890683122, 1.000000000000000000, 0.9659258262890683122, 1.000000000000000000, 0.9659258262890683122, 1.000000000000000000, 0.9659258262890683122, 1.000000000000000000, 0.9659258262890683122, 1.000000000000000000, 0.9659258262890683122, 1.000000000000000000, 0.9659258262890683122, 1.000000000000000000, 0.9659258262890683122, 1.000000000000000000, 0.9659258262890683122, 1.000000000000000000, 0.9659258262890683122, 1.000000000000000000, 0.9659258262890683122, 1.000000000000000000, 0.9659258262890683122, 1.000000000000000000, 0.9659258262890683122, 1.000000000000000000, 0.9659258262890683122, 1.000000000000000000, 0.9659258262890683122, 1.000000000000000000, 0.9659258262890683122, 1.000000000000000000, 0.9659258262890683122, 1.000000000000000000, 0.9659258262890683122, 1.000000000000000000, 0.9659258262890683122, 1.000000000000000000, 0.9659258262890683122, 1.000000000000000000, 0.9659258262890683122, 1.000000000000000000, 0.9659258262890683122, 1.000000000000000000, 0.9659258262890683122, 1.000000000000000000, 0.9659258262890683122, 1.000000000000000000, 0.9659258262890683122, 1.000000000000000000, 0.9659258262890683122, 1.000000000000000000, 0.9659258262890683122, 1.000000000000000000, 0.9659258262890683122, 1.000000000000000000, 0.9659258262890683122, 1.000000000000000000, 0.9659258262890683122, 1.000000000000000000, 0.9659258262890683122, 1.000000000000000000, 0.9659258262890683122, 1.000000000000000000, 0.9659258262890683122, 1.000000000000000000, 0.9659258262890683122, 1.000000000000000000, 0.9659258262890683122, 1.000000000000000000, 0.9659258262890683122, 1.000000000000000000, 0.9659258262890683122, 1.000000000000000000, 0.9659258262890683122, 1.000000000000000000, 0.9659258262890683122, 1.000000000000000000, 0.9659258262890683122, 1.000000000000000000, 0.9659258262890683122, 1.000000000000000000, 0.9659258262890683122, 1.000000000000000000, 0.9659258262890683122, 1.000000000000000000, 0.9659258262890683122, 1.000000000000000000, 0.9659258262890683122, 1.000000000000000000, 0.9659258262890683122, 1.000000000000000000, 0.9659258262890683122, 1.000000000000000000, 0.9659258262890683122, 1.000000000000000000, 0.9659258262890683122, 1.000000000000000000, 0.9659258262890683122, 1.000000000000000000, 0.9659258262890683122, 1.000000000000000000, 0.9659258262890683122, 1.000000000000000000, 0.9659258262890683122, 1.000000000000000000, 0.9659258262890683122, 1.000000000000000000, 0.9659258262890683122, 1.000000000000000000, 0.9659258262890683122, 1.000000000000000000, 0.9659258262890683122, 1.000000000000000000, 0.9659258262890683122, 1.000000000000000000, 0.9659258262890683122, 1.000000000000000000, 0.9659258262890683122, 1.000000000000000000, 0.9659258262890683122, 1.000000000000000000, 0.9659258262890683122, 1.000000000000000000, 0.9659258262890683122, 1.000000000000000000, 0.9659258262890683122, 1.000000000000000000, 0.9659258262890683122, 1.000000000000000000, 0.9659258262890683122, 1.000000000000000000, 0.9659258262890683122, 1.000000000000000000, 0.9659258262890683122, 1.000000000000000000, 0.9659258262890683122, 1.000000000000000000, 0.9659258262890683122, 1.000000000000000000, 0.9659258262890683122, 1.000000000000000000, 0.9659258262890683122, 1.000000000000000000, 0.9659258262890683122, 1.000000000000000000, 0.9659258262890683122, 1.000000000000000000, 0.9659258262890683122, 1.000000000000000000, 0.9659258262890683122, 1.000000000000000000, 0.9659258262890683122, 1.000000000000000000, 0.9659258262890683122, 1.000000000000000000, 0.9659258262890683122, 1.000000000000000000, 0.9659258262890683122, 1.000000000000000000, 0.9659258262890683122, 1.000000000000000000, 0.9659258262890683122, 1.000000000000000000, 0.9659258262890683122, 1.000000000000000000, 0.9659258262890683122, 1.000000000000000000, 0.9659258262890683122, 1.000000000000000000, 0.9659258262890683122, 1.000000000000000000, 0.9659258262890683122, 1.000000000000000000, 0.9659258262890683122, 1.000000000000000000, 0.9659258262890683122, 1.000000000000000000, 0.9659258262890683122, 1.000000000000000000, 0.9659258262890683122, 1.000000000000000000, 0.9659258262890683122, 1.000000000000000000, 0.9659258262890683122, 1.000000000000000000, 0.9659258262890683122, 1.000000000000000000, 0.9659258262890683122, 1.000000000000000000, 0.9659258262890683122, 1.000000000000000000, 0.9659258262890683122, 1.000000000000000000, 0.9659258262890683122, 1.000000000000000000, 0.9659258262890683122, 1.000000000000000000, 0.9659258262890683122, 1.000000000000000000, 0.9659258262890683122, 1.000000000000000000, 0.9659258262890683122, 1.000000000000000000, 0.9659258262890683122, 1.000000000000000000, 0.9659258262890683122, 1.000000000000000000, 0.9659258262890683122, 1.000000000000000000, 0.9659258262890683122, 1.000000000000000000, 0.9659258262890683122, 1.000000000000000000, 0.9659258262890683122, 1.000000000000000000, 0.9659258262890683122, 1.000000000000000000, 0.9659258262890683122, 1.000000000000000000, 0.9659258262890683122, 1.000000000000000000, 0.9659258262890683122, 1.000000000000000000, 0.9659258262890683122, 1.000000000000000000, 0.9659258262890683122, 1.000000000000000000, 0.9659258262890683122, 1.000000000000000000, 0.9659258262890683122, 1.000000000000000000, 0.9659258262890683122, 1.000000000000000000, 0.9659258262890683122, 1.000000000000000000, 0.9659258262890683122, 1.000000000000000000, 0.9659258262890683122, 1.000000000000000000, 0.9659258262890683122, 1.000000000000000000, 0.9659258262890683122, 1.000000000000000000, 0.9659258262890683122, 1.000000000000000000, 0.9659258262890683122, 1.000000000000000000, 0.9659258262890683122, 1.000000000000000000, 0.9659258262890683122, 1.000000000000000000, 0.9659258262890683122, 1.000000000000000000, 0.9659258262890683122, 1.000000000000000000, 0.9659258262890683122, 1.000000000000000000, 0.9659258262890683122, 1.000000000000000000, 0.9659258262890683122, 1.000000000000000000, 0.9659258262890683122, 1.000000000000000000, 0.9659258262890683122, 1.000000000000000000, 0.9659258262890683122, 1.000000000000000000, 0.9659258262890683122, 1.000000000000000000, 0.9659258262890683122, 1.000000000000000000, 0.9659258262890683122, 1.000000000000000000, 0.9659258262890683122, 1.000000000000000000, 0.9659258262890683122, 1.000000000000000000, 0.9659258262890683122, 1.000000000000000000, 0.9659258262890683122, 1.000000000000000000, 0.9659258262890683122, 1.000000000000000000, 0.9659258262890683122, 1.000000000000000000, 0.9659258262890683122, 1.000000000000000000, 0.9659258262890683122, 1.000000000000000000, 0.9659258262890683122, 1.000000000000000000, 0.9659258262890683122, 1.000000000000000000, 0.9659258262890683122, 1.000000000000000000, 0.9659258262890683122, 1.000000000000000000, 0.9659258262890683122, 1.000000000000000000, 0.9659258262890683122, 1.000000000000000000, 0.9659258262890683122, 1.000000000000000000, 0.9659258262890683122, 1.000000000000000000, 0.9659258262890683122, 1.000000000000000000, 0.9659258262890683122, 1.000000000000000000, 0.9659258262890683122, 1.000000000000000000, 0.9659258262890683122, 1.000000000000000000, 0.9659258262890683122, 1.000000000000000000, 0.9659258262890683122, 1.000000000000000000, 0.9659258262890683122, 1.000000000000000000, 0.9659258262890683122, 1.000000000000000000, 0.9659258262890683122, 1.000000000000000000, 0.9659258262890683122, 1.000000000000000000, 0.9659258262890683122, 1.000000000000000000, 0.9659258262890683122, 1.000000000000000000, 0.9659258262890683122, 1.000000000000000000, 0.9659258262890683122, 1.000000000000000000, 0.9659258262890683122, 1.000000000000000000, 0.9659258262890683122, 1.000000000000000000, 0.9659258262890683122, 1.000000000000000000, 0.9659258262890683122, 1.000000000000000000, 0.9659258262890683122, 1.000000000000000000, 0.9659258262890683122, 1.000000000000000000, 0.9659258262890683122, 1.000000000000000000, 0.9659258262890683122, 1.000000000000000000, 0.9659258262890683122, 1.000000000000000000, 0.9659258262890683122, 1.000000000000000000, 0.9659258262890683122, 1.000000000000000000, 0.9659258262890683122, 1.000000000000000000, 0.9659258262890683122, 1.000000000000000000, 0.9659258262890683122, 1.000000000000000000, 0.9659258262890683122, 1.000000000000000000, 0.9659258262890683122, 1.000000000000000000, 0.9659258262890683122, 1.000000000000000000, 0.9659258262890683122, 1.000000000000000000, 0.9659258262890683122, 1.000000000000000000, 0.9659258262890683122, 1.000000000000000000, 0.9659258262890683122, 1.000000000000000000, 0.9659258262890683122, 1.000000000000000000, 0.9659258262890683122, 1.000000000000000000, 0.9659258262890683122, 1.000000000000000000, 0.9659258262890683122, 1.000000000000000000, 0.9659258262890683122, 1.000000000000000000, 0.9659258262890683122, 1.000000000000000000, 0.9659258262890683122, 1.000000000000000000, 0.9659258262890683122, 1.000000000000000000, 0.9659258262890683122, 1.000000000000000000, 0.9659258262890683122, 1.000000000000000000, 0.9659258262890683122, 1.000000000000000000, 0.9659258262890683122, 1.000000000000000000, 0.9659258262890683122, 1.000000000000000000, 0.9659258262890683122, 1.000000000000000000, 0.9659258262890683122, 1.000000000000000000, 0.9659258262890683122, 1.000000000000000000, 0.9659258262890683122, 1.000000000000000000, 0.9659258262890683122, 1.000000000000000000, 0.9659258262890683122, 1.000000000000000000, 0.9659258262890683122, 1.000000000000000000, 0.9659258262890683122, 1.000000000000000000, 0.9659258262890683122, 1.000000000000000000, 0.9659258262890683122, 1.000000000000000000, 0.9659258262890683122, 1.000000000000000000, 0.9659258262890683122, 1.000000000000000000, 0.9659258262890683122, 1.000000000000000000, 0.9659258262890683122, 1.000000000000000000),
 ( 0.3333333333333333703, 0.3219752754296894559, 0.3333333333333333703, 0.3219752754296894559, 0.3333333333333333703, 0.3219752754296894559, 0.3333333333333333703, 0.3219752754296894559, 0.3333333333333333703, 0.3219752754296894559, 0.3333333333333333703, 0.3219752754296894559, 0.3333333333333333703, 0.3219752754296894559, 0.3333333333333333703, 0.3219752754296894559, 0.3333333333333333703, 0.3219752754296894559, 0.3333333333333333703, 0.3219752754296894559, 0.3333333333333333703, 0.3219752754296894559, 0.3333333333333333703, 0.3219752754296894559, 0.3333333333333333703, 0.3219752754296894559, 0.3333333333333333703, 0.3219752754296894559, 0.3333333333333333703, 0.3219752754296894559, 0.3333333333333333703, 0.3219752754296894559, 0.3333333333333333703, 0.3219752754296894559, 0.3333333333333333703, 0.3219752754296894559, 0.3333333333333333703, 0.3219752754296894559, 0.3333333333333333703, 0.3219752754296894559, 0.3333333333333333703, 0.3219752754296894559, 0.3333333333333333703, 0.3219752754296894559, 0.3333333333333333703, 0.3219752754296894559, 0.3333333333333333703, 0.3219752754296894559, 0.3333333333333333703, 0.3219752754296894559, 0.3333333333333333703, 0.3219752754296894559, 0.3333333333333333703, 0.3219752754296894559, 0.3333333333333333703, 0.3219752754296894559, 0.3333333333333333703, 0.3219752754296894559, 0.3333333333333333703, 0.3219752754296894559, 0.3333333333333333703, 0.3219752754296894559, 0.3333333333333333703, 0.3219752754296894559, 0.3333333333333333703, 0.3219752754296894559, 0.3333333333333333703, 0.3219752754296894559, 0.3333333333333333703, 0.3219752754296894559, 0.3333333333333333703, 0.3219752754296894559, 0.3333333333333333703, 0.3219752754296894559, 0.3333333333333333703, 0.3219752754296894559, 0.3333333333333333703, 0.3219752754296894559, 0.3333333333333333703, 0.3219752754296894559, 0.3333333333333333703, 0.3219752754296894559, 0.3333333333333333703, 0.3219752754296894559, 0.3333333333333333703, 0.3219752754296894559, 0.3333333333333333703, 0.3219752754296894559, 0.3333333333333333703, 0.3219752754296894559, 0.3333333333333333703, 0.3219752754296894559, 0.3333333333333333703, 0.3219752754296894559, 0.3333333333333333703, 0.3219752754296894559, 0.3333333333333333703, 0.3219752754296894559, 0.3333333333333333703, 0.3219752754296894559, 0.3333333333333333703, 0.3219752754296894559, 0.3333333333333333703, 0.3219752754296894559, 0.3333333333333333703, 0.3219752754296894559, 0.3333333333333333703, 0.3219752754296894559, 0.3333333333333333703, 0.3219752754296894559, 0.3333333333333333703, 0.3219752754296894559, 0.3333333333333333703, 0.3219752754296894559, 0.3333333333333333703, 0.3219752754296894559, 0.3333333333333333703, 0.3219752754296894559, 0.3333333333333333703, 0.3219752754296894559, 0.3333333333333333703, 0.3219752754296894559, 0.3333333333333333703, 0.3219752754296894559, 0.3333333333333333703, 0.3219752754296894559, 0.3333333333333333703, 0.3219752754296894559, 0.3333333333333333703, 0.3219752754296894559, 0.3333333333333333703, 0.3219752754296894559, 0.3333333333333333703, 0.3219752754296894559, 0.3333333333333333703, 0.3219752754296894559, 0.3333333333333333703, 0.3219752754296894559, 0.3333333333333333703, 0.3219752754296894559, 0.3333333333333333703, 0.3219752754296894559, 0.3333333333333333703, 0.3219752754296894559, 0.3333333333333333703, 0.3219752754296894559, 0.3333333333333333703, 0.3219752754296894559, 0.3333333333333333703, 0.3219752754296894559, 0.3333333333333333703, 0.3219752754296894559, 0.3333333333333333703, 0.3219752754296894559, 0.3333333333333333703, 0.3219752754296894559, 0.3333333333333333703, 0.3219752754296894559, 0.3333333333333333703, 0.3219752754296894559, 0.3333333333333333703, 0.3219752754296894559, 0.3333333333333333703, 0.3219752754296894559, 0.3333333333333333703, 0.3219752754296894559, 0.3333333333333333703, 0.3219752754296894559, 0.3333333333333333703, 0.3219752754296894559, 0.3333333333333333703, 0.3219752754296894559, 0.3333333333333333703, 0.3219752754296894559, 0.3333333333333333703, 0.3219752754296894559, 0.3333333333333333703, 0.3219752754296894559, 0.3333333333333333703, 0.3219752754296894559, 0.3333333333333333703, 0.3219752754296894559, 0.3333333333333333703, 0.3219752754296894559, 0.3333333333333333703, 0.3219752754296894559, 0.3333333333333333703, 0.3219752754296894559, 0.3333333333333333703, 0.3219752754296894559, 0.3333333333333333703, 0.3219752754296894559, 0.3333333333333333703, 0.3219752754296894559, 0.3333333333333333703, 0.3219752754296894559, 0.3333333333333333703, 0.3219752754296894559, 0.3333333333333333703, 0.3219752754296894559, 0.3333333333333333703, 0.3219752754296894559, 0.3333333333333333703, 0.3219752754296894559, 0.3333333333333333703, 0.3219752754296894559, 0.3333333333333333703, 0.3219752754296894559, 0.3333333333333333703, 0.3219752754296894559, 0.3333333333333333703, 0.3219752754296894559, 0.3333333333333333703, 0.3219752754296894559, 0.3333333333333333703, 0.3219752754296894559, 0.3333333333333333703, 0.3219752754296894559, 0.3333333333333333703, 0.3219752754296894559, 0.3333333333333333703, 0.3219752754296894559, 0.3333333333333333703, 0.3219752754296894559, 0.3333333333333333703, 0.3219752754296894559, 0.3333333333333333703, 0.3219752754296894559, 0.3333333333333333703, 0.3219752754296894559, 0.3333333333333333703, 0.3219752754296894559, 0.3333333333333333703, 0.3219752754296894559, 0.3333333333333333703, 0.3219752754296894559, 0.3333333333333333703, 0.3219752754296894559, 0.3333333333333333703, 0.3219752754296894559, 0.3333333333333333703, 0.3219752754296894559, 0.3333333333333333703, 0.3219752754296894559, 0.3333333333333333703, 0.3219752754296894559, 0.3333333333333333703, 0.3219752754296894559, 0.3333333333333333703, 0.3219752754296894559, 0.3333333333333333703, 0.3219752754296894559, 0.3333333333333333703, 0.3219752754296894559, 0.3333333333333333703, 0.3219752754296894559, 0.3333333333333333703, 0.3219752754296894559, 0.3333333333333333703, 0.3219752754296894559, 0.3333333333333333703, 0.3219752754296894559, 0.3333333333333333703, 0.3219752754296894559, 0.3333333333333333703, 0.3219752754296894559, 0.3333333333333333703, 0.3219752754296894559, 0.3333333333333333703, 0.3219752754296894559, 0.3333333333333333703, 0.3219752754296894559, 0.3333333333333333703, 0.3219752754296894559, 0.3333333333333333703, 0.3219752754296894559, 0.3333333333333333703, 0.3219752754296894559, 0.3333333333333333703, 0.3219752754296894559, 0.3333333333333333703, 0.3219752754296894559, 0.3333333333333333703, 0.3219752754296894559, 0.3333333333333333703, 0.3219752754296894559, 0.3333333333333333703, 0.3219752754296894559, 0.3333333333333333703, 0.3219752754296894559, 0.3333333333333333703, 0.3219752754296894559, 0.3333333333333333703, 0.3219752754296894559, 0.3333333333333333703, 0.3219752754296894559, 0.3333333333333333703, 0.3219752754296894559, 0.3333333333333333703, 0.3219752754296894559, 0.3333333333333333703, 0.3219752754296894559, 0.3333333333333333703, 0.3219752754296894559, 0.3333333333333333703, 0.3219752754296894559, 0.3333333333333333703, 0.3219752754296894559, 0.3333333333333333703, 0.3219752754296894559, 0.3333333333333333703, 0.3219752754296894559, 0.3333333333333333703, 0.3219752754296894559, 0.3333333333333333703, 0.3219752754296894559, 0.3333333333333333703, 0.3219752754296894559, 0.3333333333333333703, 0.3219752754296894559, 0.3333333333333333703, 0.3219752754296894559, 0.3333333333333333703, 0.3219752754296894559, 0.3333333333333333703, 0.3219752754296894559, 0.3333333333333333703, 0.3219752754296894559, 0.3333333333333333703, 0.3219752754296894559, 0.3333333333333333703, 0.3219752754296894559, 0.3333333333333333703, 0.3219752754296894559, 0.3333333333333333703, 0.3219752754296894559, 0.3333333333333333703, 0.3219752754296894559, 0.3333333333333333703, 0.3219752754296894559, 0.3333333333333333703, 0.3219752754296894559, 0.3333333333333333703, 0.3219752754296894559, 0.3333333333333333703, 0.3219752754296894559, 0.3333333333333333703, 0.3219752754296894559, 0.3333333333333333703, 0.3219752754296894559, 0.3333333333333333703, 0.3219752754296894559, 0.3333333333333333703, 0.3219752754296894559, 0.3333333333333333703, 0.3219752754296894559, 0.3333333333333333703, 0.3219752754296894559, 0.3333333333333333703, 0.3219752754296894559, 0.3333333333333333703, 0.3219752754296894559, 0.3333333333333333703, 0.3219752754296894559, 0.3333333333333333703, 0.3219752754296894559, 0.3333333333333333703, 0.3219752754296894559, 0.3333333333333333703, 0.3219752754296894559, 0.3333333333333333703, 0.3219752754296894559, 0.3333333333333333703, 0.3219752754296894559, 0.3333333333333333703, 0.3219752754296894559, 0.3333333333333333703, 0.3219752754296894559, 0.3333333333333333703, 0.3219752754296894559, 0.3333333333333333703, 0.3219752754296894559, 0.3333333333333333703, 0.3219752754296894559, 0.3333333333333333703, 0.3219752754296894559, 0.3333333333333333703, 0.3219752754296894559, 0.3333333333333333703, 0.3219752754296894559, 0.3333333333333333703, 0.3219752754296894559, 0.3333333333333333703, 0.3219752754296894559, 0.3333333333333333703, 0.3219752754296894559, 0.3333333333333333703, 0.3219752754296894559, 0.3333333333333333703, 0.3219752754296894559, 0.3333333333333333703, 0.3219752754296894559, 0.3333333333333333703, 0.3219752754296894559, 0.3333333333333333703, 0.3219752754296894559, 0.3333333333333333703, 0.3219752754296894559, 0.3333333333333333703, 0.3219752754296894559, 0.3333333333333333703, 0.3219752754296894559, 0.3333333333333333703, 0.3219752754296894559, 0.3333333333333333703, 0.3219752754296894559, 0.3333333333333333703, 0.3219752754296894559, 0.3333333333333333703, 0.3219752754296894559, 0.3333333333333333703, 0.3219752754296894559, 0.3333333333333333703, 0.3219752754296894559, 0.3333333333333333703, 0.3219752754296894559, 0.3333333333333333703, 0.3219752754296894559, 0.3333333333333333703, 0.3219752754296894559, 0.3333333333333333703, 0.3219752754296894559, 0.3333333333333333703, 0.3219752754296894559, 0.3333333333333333703, 0.3219752754296894559, 0.3333333333333333703, 0.3219752754296894559, 0.3333333333333333703, 0.3219752754296894559, 0.3333333333333333703, 0.3219752754296894559, 0.3333333333333333703, 0.3219752754296894559, 0.3333333333333333703, 0.3219752754296894559, 0.3333333333333333703, 0.3219752754296894559, 0.3333333333333333703, 0.3219752754296894559, 0.3333333333333333703, 0.3219752754296894559, 0.3333333333333333703, 0.3219752754296894559, 0.3333333333333333703, 0.3219752754296894559, 0.3333333333333333703),
 ( 0.3333333333333333703, 0.3219752754296894559, 0.3333333333333333703, 0.3219752754296894559, 0.3333333333333333703, 0.3219752754296894559, 0.3333333333333333703, 0.3219752754296894559, 0.3333333333333333703, 0.3219752754296894559, 0.3333333333333333703, 0.3219752754296894559, 0.3333333333333333703, 0.3219752754296894559, 0.3333333333333333703, 0.3219752754296894559, 0.3333333333333333703, 0.3219752754296894559, 0.3333333333333333703, 0.3219752754296894559, 0.3333333333333333703, 0.3219752754296894559, 0.3333333333333333703, 0.3219752754296894559, 0.3333333333333333703, 0.3219752754296894559, 0.3333333333333333703, 0.3219752754296894559, 0.3333333333333333703, 0.3219752754296894559, 0.3333333333333333703, 0.3219752754296894559, 0.3333333333333333703, 0.3219752754296894559, 0.3333333333333333703, 0.3219752754296894559, 0.3333333333333333703, 0.3219752754296894559, 0.3333333333333333703, 0.3219752754296894559, 0.3333333333333333703, 0.3219752754296894559, 0.3333333333333333703, 0.3219752754296894559, 0.3333333333333333703, 0.3219752754296894559, 0.3333333333333333703, 0.3219752754296894559, 0.3333333333333333703, 0.3219752754296894559, 0.3333333333333333703, 0.3219752754296894559, 0.3333333333333333703, 0.3219752754296894559, 0.3333333333333333703, 0.3219752754296894559, 0.3333333333333333703, 0.3219752754296894559, 0.3333333333333333703, 0.3219752754296894559, 0.3333333333333333703, 0.3219752754296894559, 0.3333333333333333703, 0.3219752754296894559, 0.3333333333333333703, 0.3219752754296894559, 0.3333333333333333703, 0.3219752754296894559, 0.3333333333333333703, 0.3219752754296894559, 0.3333333333333333703, 0.3219752754296894559, 0.3333333333333333703, 0.3219752754296894559, 0.3333333333333333703, 0.3219752754296894559, 0.3333333333333333703, 0.3219752754296894559, 0.3333333333333333703, 0.3219752754296894559, 0.3333333333333333703, 0.3219752754296894559, 0.3333333333333333703, 0.3219752754296894559, 0.3333333333333333703, 0.3219752754296894559, 0.3333333333333333703, 0.3219752754296894559, 0.3333333333333333703, 0.3219752754296894559, 0.3333333333333333703, 0.3219752754296894559, 0.3333333333333333703, 0.3219752754296894559, 0.3333333333333333703, 0.3219752754296894559, 0.3333333333333333703, 0.3219752754296894559, 0.3333333333333333703, 0.3219752754296894559, 0.3333333333333333703, 0.3219752754296894559, 0.3333333333333333703, 0.3219752754296894559, 0.3333333333333333703, 0.3219752754296894559, 0.3333333333333333703, 0.3219752754296894559, 0.3333333333333333703, 0.3219752754296894559, 0.3333333333333333703, 0.3219752754296894559, 0.3333333333333333703, 0.3219752754296894559, 0.3333333333333333703, 0.3219752754296894559, 0.3333333333333333703, 0.3219752754296894559, 0.3333333333333333703, 0.3219752754296894559, 0.3333333333333333703, 0.3219752754296894559, 0.3333333333333333703, 0.3219752754296894559, 0.3333333333333333703, 0.3219752754296894559, 0.3333333333333333703, 0.3219752754296894559, 0.3333333333333333703, 0.3219752754296894559, 0.3333333333333333703, 0.3219752754296894559, 0.3333333333333333703, 0.3219752754296894559, 0.3333333333333333703, 0.3219752754296894559, 0.3333333333333333703, 0.3219752754296894559, 0.3333333333333333703, 0.3219752754296894559, 0.3333333333333333703, 0.3219752754296894559, 0.3333333333333333703, 0.3219752754296894559, 0.3333333333333333703, 0.3219752754296894559, 0.3333333333333333703, 0.3219752754296894559, 0.3333333333333333703, 0.3219752754296894559, 0.3333333333333333703, 0.3219752754296894559, 0.3333333333333333703, 0.3219752754296894559, 0.3333333333333333703, 0.3219752754296894559, 0.3333333333333333703, 0.3219752754296894559, 0.3333333333333333703, 0.3219752754296894559, 0.3333333333333333703, 0.3219752754296894559, 0.3333333333333333703, 0.3219752754296894559, 0.3333333333333333703, 0.3219752754296894559, 0.3333333333333333703, 0.3219752754296894559, 0.3333333333333333703, 0.3219752754296894559, 0.3333333333333333703, 0.3219752754296894559, 0.3333333333333333703, 0.3219752754296894559, 0.3333333333333333703, 0.3219752754296894559, 0.3333333333333333703, 0.3219752754296894559, 0.3333333333333333703, 0.3219752754296894559, 0.3333333333333333703, 0.3219752754296894559, 0.3333333333333333703, 0.3219752754296894559, 0.3333333333333333703, 0.3219752754296894559, 0.3333333333333333703, 0.3219752754296894559, 0.3333333333333333703, 0.3219752754296894559, 0.3333333333333333703, 0.3219752754296894559, 0.3333333333333333703, 0.3219752754296894559, 0.3333333333333333703, 0.3219752754296894559, 0.3333333333333333703, 0.3219752754296894559, 0.3333333333333333703, 0.3219752754296894559, 0.3333333333333333703, 0.3219752754296894559, 0.3333333333333333703, 0.3219752754296894559, 0.3333333333333333703, 0.3219752754296894559, 0.3333333333333333703, 0.3219752754296894559, 0.3333333333333333703, 0.3219752754296894559, 0.3333333333333333703, 0.3219752754296894559, 0.3333333333333333703, 0.3219752754296894559, 0.3333333333333333703, 0.3219752754296894559, 0.3333333333333333703, 0.3219752754296894559, 0.3333333333333333703, 0.3219752754296894559, 0.3333333333333333703, 0.3219752754296894559, 0.3333333333333333703, 0.3219752754296894559, 0.3333333333333333703, 0.3219752754296894559, 0.3333333333333333703, 0.3219752754296894559, 0.3333333333333333703, 0.3219752754296894559, 0.3333333333333333703, 0.3219752754296894559, 0.3333333333333333703, 0.3219752754296894559, 0.3333333333333333703, 0.3219752754296894559, 0.3333333333333333703, 0.3219752754296894559, 0.3333333333333333703, 0.3219752754296894559, 0.3333333333333333703, 0.3219752754296894559, 0.3333333333333333703, 0.3219752754296894559, 0.3333333333333333703, 0.3219752754296894559, 0.3333333333333333703, 0.3219752754296894559, 0.3333333333333333703, 0.3219752754296894559, 0.3333333333333333703, 0.3219752754296894559, 0.3333333333333333703, 0.3219752754296894559, 0.3333333333333333703, 0.3219752754296894559, 0.3333333333333333703, 0.3219752754296894559, 0.3333333333333333703, 0.3219752754296894559, 0.3333333333333333703, 0.3219752754296894559, 0.3333333333333333703, 0.3219752754296894559, 0.3333333333333333703, 0.3219752754296894559, 0.3333333333333333703, 0.3219752754296894559, 0.3333333333333333703, 0.3219752754296894559, 0.3333333333333333703, 0.3219752754296894559, 0.3333333333333333703, 0.3219752754296894559, 0.3333333333333333703, 0.3219752754296894559, 0.3333333333333333703, 0.3219752754296894559, 0.3333333333333333703, 0.3219752754296894559, 0.3333333333333333703, 0.3219752754296894559, 0.3333333333333333703, 0.3219752754296894559, 0.3333333333333333703, 0.3219752754296894559, 0.3333333333333333703, 0.3219752754296894559, 0.3333333333333333703, 0.3219752754296894559, 0.3333333333333333703, 0.3219752754296894559, 0.3333333333333333703, 0.3219752754296894559, 0.3333333333333333703, 0.3219752754296894559, 0.3333333333333333703, 0.3219752754296894559, 0.3333333333333333703, 0.3219752754296894559, 0.3333333333333333703, 0.3219752754296894559, 0.3333333333333333703, 0.3219752754296894559, 0.3333333333333333703, 0.3219752754296894559, 0.3333333333333333703, 0.3219752754296894559, 0.3333333333333333703, 0.3219752754296894559, 0.3333333333333333703, 0.3219752754296894559, 0.3333333333333333703, 0.3219752754296894559, 0.3333333333333333703, 0.3219752754296894559, 0.3333333333333333703, 0.3219752754296894559, 0.3333333333333333703, 0.3219752754296894559, 0.3333333333333333703, 0.3219752754296894559, 0.3333333333333333703, 0.3219752754296894559, 0.3333333333333333703, 0.3219752754296894559, 0.3333333333333333703, 0.3219752754296894559, 0.3333333333333333703, 0.3219752754296894559, 0.3333333333333333703, 0.3219752754296894559, 0.3333333333333333703, 0.3219752754296894559, 0.3333333333333333703, 0.3219752754296894559, 0.3333333333333333703, 0.3219752754296894559, 0.3333333333333333703, 0.3219752754296894559, 0.3333333333333333703, 0.3219752754296894559, 0.3333333333333333703, 0.3219752754296894559, 0.3333333333333333703, 0.3219752754296894559, 0.3333333333333333703, 0.3219752754296894559, 0.3333333333333333703, 0.3219752754296894559, 0.3333333333333333703, 0.3219752754296894559, 0.3333333333333333703, 0.3219752754296894559, 0.3333333333333333703, 0.3219752754296894559, 0.3333333333333333703, 0.3219752754296894559, 0.3333333333333333703, 0.3219752754296894559, 0.3333333333333333703, 0.3219752754296894559, 0.3333333333333333703, 0.3219752754296894559, 0.3333333333333333703, 0.3219752754296894559, 0.3333333333333333703, 0.3219752754296894559, 0.3333333333333333703, 0.3219752754296894559, 0.3333333333333333703, 0.3219752754296894559, 0.3333333333333333703, 0.3219752754296894559, 0.3333333333333333703, 0.3219752754296894559, 0.3333333333333333703, 0.3219752754296894559, 0.3333333333333333703, 0.3219752754296894559, 0.3333333333333333703, 0.3219752754296894559, 0.3333333333333333703, 0.3219752754296894559, 0.3333333333333333703, 0.3219752754296894559, 0.3333333333333333703, 0.3219752754296894559, 0.3333333333333333703, 0.3219752754296894559, 0.3333333333333333703, 0.3219752754296894559, 0.3333333333333333703, 0.3219752754296894559, 0.3333333333333333703, 0.3219752754296894559, 0.3333333333333333703, 0.3219752754296894559, 0.3333333333333333703, 0.3219752754296894559, 0.3333333333333333703, 0.3219752754296894559, 0.3333333333333333703, 0.3219752754296894559, 0.3333333333333333703, 0.3219752754296894559, 0.3333333333333333703, 0.3219752754296894559, 0.3333333333333333703, 0.3219752754296894559, 0.3333333333333333703, 0.3219752754296894559, 0.3333333333333333703, 0.3219752754296894559, 0.3333333333333333703, 0.3219752754296894559, 0.3333333333333333703, 0.3219752754296894559, 0.3333333333333333703, 0.3219752754296894559, 0.3333333333333333703, 0.3219752754296894559, 0.3333333333333333703, 0.3219752754296894559, 0.3333333333333333703, 0.3219752754296894559, 0.3333333333333333703, 0.3219752754296894559, 0.3333333333333333703, 0.3219752754296894559, 0.3333333333333333703, 0.3219752754296894559, 0.3333333333333333703, 0.3219752754296894559, 0.3333333333333333703, 0.3219752754296894559, 0.3333333333333333703, 0.3219752754296894559, 0.3333333333333333703, 0.3219752754296894559, 0.3333333333333333703, 0.3219752754296894559, 0.3333333333333333703, 0.3219752754296894559, 0.3333333333333333703, 0.3219752754296894559, 0.3333333333333333703, 0.3219752754296894559, 0.3333333333333333703, 0.3219752754296894559, 0.3333333333333333703, 0.3219752754296894559, 0.3333333333333333703, 0.3219752754296894559, 0.3333333333333333703, 0.3219752754296894559, 0.3333333333333333703),
 ( 1.000000000000000000, 0.9659258262890683122, 1.000000000000000000, 0.9659258262890683122, 1.000000000000000000, 0.9659258262890683122, 1.000000000000000000, 0.9659258262890683122, 1.000000000000000000, 0.9659258262890683122, 1.000000000000000000, 0.9659258262890683122, 1.000000000000000000, 0.9659258262890683122, 1.000000000000000000, 0.9659258262890683122, 1.000000000000000000, 0.9659258262890683122, 1.000000000000000000, 0.9659258262890683122, 1.000000000000000000, 0.9659258262890683122, 1.000000000000000000, 0.9659258262890683122, 1.000000000000000000, 0.9659258262890683122, 1.000000000000000000, 0.9659258262890683122, 1.000000000000000000, 0.9659258262890683122, 1.000000000000000000, 0.9659258262890683122, 1.000000000000000000, 0.9659258262890683122, 1.000000000000000000, 0.9659258262890683122, 1.000000000000000000, 0.9659258262890683122, 1.000000000000000000, 0.9659258262890683122, 1.000000000000000000, 0.9659258262890683122, 1.000000000000000000, 0.9659258262890683122, 1.000000000000000000, 0.9659258262890683122, 1.000000000000000000, 0.9659258262890683122, 1.000000000000000000, 0.9659258262890683122, 1.000000000000000000, 0.9659258262890683122, 1.000000000000000000, 0.9659258262890683122, 1.000000000000000000, 0.9659258262890683122, 1.000000000000000000, 0.9659258262890683122, 1.000000000000000000, 0.9659258262890683122, 1.000000000000000000, 0.9659258262890683122, 1.000000000000000000, 0.9659258262890683122, 1.000000000000000000, 0.9659258262890683122, 1.000000000000000000, 0.9659258262890683122, 1.000000000000000000, 0.9659258262890683122, 1.000000000000000000, 0.9659258262890683122, 1.000000000000000000, 0.9659258262890683122, 1.000000000000000000, 0.9659258262890683122, 1.000000000000000000, 0.9659258262890683122, 1.000000000000000000, 0.9659258262890683122, 1.000000000000000000, 0.9659258262890683122, 1.000000000000000000, 0.9659258262890683122, 1.000000000000000000, 0.9659258262890683122, 1.000000000000000000, 0.9659258262890683122, 1.000000000000000000, 0.9659258262890683122, 1.000000000000000000, 0.9659258262890683122, 1.000000000000000000, 0.9659258262890683122, 1.000000000000000000, 0.9659258262890683122, 1.000000000000000000, 0.9659258262890683122, 1.000000000000000000, 0.9659258262890683122, 1.000000000000000000, 0.9659258262890683122, 1.000000000000000000, 0.9659258262890683122, 1.000000000000000000, 0.9659258262890683122, 1.000000000000000000, 0.9659258262890683122, 1.000000000000000000, 0.9659258262890683122, 1.000000000000000000, 0.9659258262890683122, 1.000000000000000000, 0.9659258262890683122, 1.000000000000000000, 0.9659258262890683122, 1.000000000000000000, 0.9659258262890683122, 1.000000000000000000, 0.9659258262890683122, 1.000000000000000000, 0.9659258262890683122, 1.000000000000000000, 0.9659258262890683122, 1.000000000000000000, 0.9659258262890683122, 1.000000000000000000, 0.9659258262890683122, 1.000000000000000000, 0.9659258262890683122, 1.000000000000000000, 0.9659258262890683122, 1.000000000000000000, 0.9659258262890683122, 1.000000000000000000, 0.9659258262890683122, 1.000000000000000000, 0.9659258262890683122, 1.000000000000000000, 0.9659258262890683122, 1.000000000000000000, 0.9659258262890683122, 1.000000000000000000, 0.9659258262890683122, 1.000000000000000000, 0.9659258262890683122, 1.000000000000000000, 0.9659258262890683122, 1.000000000000000000, 0.9659258262890683122, 1.000000000000000000, 0.9659258262890683122, 1.000000000000000000, 0.9659258262890683122, 1.000000000000000000, 0.9659258262890683122, 1.000000000000000000, 0.9659258262890683122, 1.000000000000000000, 0.9659258262890683122, 1.000000000000000000, 0.9659258262890683122, 1.000000000000000000, 0.9659258262890683122, 1.000000000000000000, 0.9659258262890683122, 1.000000000000000000, 0.9659258262890683122, 1.000000000000000000, 0.9659258262890683122, 1.000000000000000000, 0.9659258262890683122, 1.000000000000000000, 0.9659258262890683122, 1.000000000000000000, 0.9659258262890683122, 1.000000000000000000, 0.9659258262890683122, 1.000000000000000000, 0.9659258262890683122, 1.000000000000000000, 0.9659258262890683122, 1.000000000000000000, 0.9659258262890683122, 1.000000000000000000, 0.9659258262890683122, 1.000000000000000000, 0.9659258262890683122, 1.000000000000000000, 0.9659258262890683122, 1.000000000000000000, 0.9659258262890683122, 1.000000000000000000, 0.9659258262890683122, 1.000000000000000000, 0.9659258262890683122, 1.000000000000000000, 0.9659258262890683122, 1.000000000000000000, 0.9659258262890683122, 1.000000000000000000, 0.9659258262890683122, 1.000000000000000000, 0.9659258262890683122, 1.000000000000000000, 0.9659258262890683122, 1.000000000000000000, 0.9659258262890683122, 1.000000000000000000, 0.9659258262890683122, 1.000000000000000000, 0.9659258262890683122, 1.000000000000000000, 0.9659258262890683122, 1.000000000000000000, 0.9659258262890683122, 1.000000000000000000, 0.9659258262890683122, 1.000000000000000000, 0.9659258262890683122, 1.000000000000000000, 0.9659258262890683122, 1.000000000000000000, 0.9659258262890683122, 1.000000000000000000, 0.9659258262890683122, 1.000000000000000000, 0.9659258262890683122, 1.000000000000000000, 0.9659258262890683122, 1.000000000000000000, 0.9659258262890683122, 1.000000000000000000, 0.9659258262890683122, 1.000000000000000000, 0.9659258262890683122, 1.000000000000000000, 0.9659258262890683122, 1.000000000000000000, 0.9659258262890683122, 1.000000000000000000, 0.9659258262890683122, 1.000000000000000000, 0.9659258262890683122, 1.000000000000000000, 0.9659258262890683122, 1.000000000000000000, 0.9659258262890683122, 1.000000000000000000, 0.9659258262890683122, 1.000000000000000000, 0.9659258262890683122, 1.000000000000000000, 0.9659258262890683122, 1.000000000000000000, 0.9659258262890683122, 1.000000000000000000, 0.9659258262890683122, 1.000000000000000000, 0.9659258262890683122, 1.000000000000000000, 0.9659258262890683122, 1.000000000000000000, 0.9659258262890683122, 1.000000000000000000, 0.9659258262890683122, 1.000000000000000000, 0.9659258262890683122, 1.000000000000000000, 0.9659258262890683122, 1.000000000000000000, 0.9659258262890683122, 1.000000000000000000, 0.9659258262890683122, 1.000000000000000000, 0.9659258262890683122, 1.000000000000000000, 0.9659258262890683122, 1.000000000000000000, 0.9659258262890683122, 1.000000000000000000, 0.9659258262890683122, 1.000000000000000000, 0.9659258262890683122, 1.000000000000000000, 0.9659258262890683122, 1.000000000000000000, 0.9659258262890683122, 1.000000000000000000, 0.9659258262890683122, 1.000000000000000000, 0.9659258262890683122, 1.000000000000000000, 0.9659258262890683122, 1.000000000000000000, 0.9659258262890683122, 1.000000000000000000, 0.9659258262890683122, 1.000000000000000000, 0.9659258262890683122, 1.000000000000000000, 0.9659258262890683122, 1.000000000000000000, 0.9659258262890683122, 1.000000000000000000, 0.9659258262890683122, 1.000000000000000000, 0.9659258262890683122, 1.000000000000000000, 0.9659258262890683122, 1.000000000000000000, 0.9659258262890683122, 1.000000000000000000, 0.9659258262890683122, 1.000000000000000000, 0.9659258262890683122, 1.000000000000000000, 0.9659258262890683122, 1.000000000000000000, 0.9659258262890683122, 1.000000000000000000, 0.9659258262890683122, 1.000000000000000000, 0.9659258262890683122, 1.000000000000000000, 0.9659258262890683122, 1.000000000000000000, 0.9659258262890683122, 1.000000000000000000, 0.9659258262890683122, 1.000000000000000000, 0.9659258262890683122, 1.000000000000000000, 0.9659258262890683122, 1.000000000000000000, 0.9659258262890683122, 1.000000000000000000, 0.9659258262890683122, 1.000000000000000000, 0.9659258262890683122, 1.000000000000000000, 0.9659258262890683122, 1.000000000000000000, 0.9659258262890683122, 1.000000000000000000, 0.9659258262890683122, 1.000000000000000000, 0.9659258262890683122, 1.000000000000000000, 0.9659258262890683122, 1.000000000000000000, 0.9659258262890683122, 1.000000000000000000, 0.9659258262890683122, 1.000000000000000000, 0.9659258262890683122, 1.000000000000000000, 0.9659258262890683122, 1.000000000000000000, 0.9659258262890683122, 1.000000000000000000, 0.9659258262890683122, 1.000000000000000000, 0.9659258262890683122, 1.000000000000000000, 0.9659258262890683122, 1.000000000000000000, 0.9659258262890683122, 1.000000000000000000, 0.9659258262890683122, 1.000000000000000000, 0.9659258262890683122, 1.000000000000000000, 0.9659258262890683122, 1.000000000000000000, 0.9659258262890683122, 1.000000000000000000, 0.9659258262890683122, 1.000000000000000000, 0.9659258262890683122, 1.000000000000000000, 0.9659258262890683122, 1.000000000000000000, 0.9659258262890683122, 1.000000000000000000, 0.9659258262890683122, 1.000000000000000000, 0.9659258262890683122, 1.000000000000000000, 0.9659258262890683122, 1.000000000000000000, 0.9659258262890683122, 1.000000000000000000, 0.9659258262890683122, 1.000000000000000000, 0.9659258262890683122, 1.000000000000000000, 0.9659258262890683122, 1.000000000000000000, 0.9659258262890683122, 1.000000000000000000, 0.9659258262890683122, 1.000000000000000000, 0.9659258262890683122, 1.000000000000000000, 0.9659258262890683122, 1.000000000000000000, 0.9659258262890683122, 1.000000000000000000, 0.9659258262890683122, 1.000000000000000000, 0.9659258262890683122, 1.000000000000000000, 0.9659258262890683122, 1.000000000000000000, 0.9659258262890683122, 1.000000000000000000, 0.9659258262890683122, 1.000000000000000000, 0.9659258262890683122, 1.000000000000000000, 0.9659258262890683122, 1.000000000000000000, 0.9659258262890683122, 1.000000000000000000, 0.9659258262890683122, 1.000000000000000000, 0.9659258262890683122, 1.000000000000000000, 0.9659258262890683122, 1.000000000000000000, 0.9659258262890683122, 1.000000000000000000, 0.9659258262890683122, 1.000000000000000000, 0.9659258262890683122, 1.000000000000000000, 0.9659258262890683122, 1.000000000000000000, 0.9659258262890683122, 1.000000000000000000, 0.9659258262890683122, 1.000000000000000000, 0.9659258262890683122, 1.000000000000000000, 0.9659258262890683122, 1.000000000000000000, 0.9659258262890683122, 1.000000000000000000, 0.9659258262890683122, 1.000000000000000000, 0.9659258262890683122, 1.000000000000000000, 0.9659258262890683122, 1.000000000000000000, 0.9659258262890683122, 1.000000000000000000),
 ( 0.3333333333333333703, 0.3219752754296894559, 0.3333333333333333703, 0.3219752754296894559, 0.3333333333333333703, 0.3219752754296894559, 0.3333333333333333703, 0.3219752754296894559, 0.3333333333333333703, 0.3219752754296894559, 0.3333333333333333703, 0.3219752754296894559, 0.3333333333333333703, 0.3219752754296894559, 0.3333333333333333703, 0.3219752754296894559, 0.3333333333333333703, 0.3219752754296894559, 0.3333333333333333703, 0.3219752754296894559, 0.3333333333333333703, 0.3219752754296894559, 0.3333333333333333703, 0.3219752754296894559, 0.3333333333333333703, 0.3219752754296894559, 0.3333333333333333703, 0.3219752754296894559, 0.3333333333333333703, 0.3219752754296894559, 0.3333333333333333703, 0.3219752754296894559, 0.3333333333333333703, 0.3219752754296894559, 0.3333333333333333703, 0.3219752754296894559, 0.3333333333333333703, 0.3219752754296894559, 0.3333333333333333703, 0.3219752754296894559, 0.3333333333333333703, 0.3219752754296894559, 0.3333333333333333703, 0.3219752754296894559, 0.3333333333333333703, 0.3219752754296894559, 0.3333333333333333703, 0.3219752754296894559, 0.3333333333333333703, 0.3219752754296894559, 0.3333333333333333703, 0.3219752754296894559, 0.3333333333333333703, 0.3219752754296894559, 0.3333333333333333703, 0.3219752754296894559, 0.3333333333333333703, 0.3219752754296894559, 0.3333333333333333703, 0.3219752754296894559, 0.3333333333333333703, 0.3219752754296894559, 0.3333333333333333703, 0.3219752754296894559, 0.3333333333333333703, 0.3219752754296894559, 0.3333333333333333703, 0.3219752754296894559, 0.3333333333333333703, 0.3219752754296894559, 0.3333333333333333703, 0.3219752754296894559, 0.3333333333333333703, 0.3219752754296894559, 0.3333333333333333703, 0.3219752754296894559, 0.3333333333333333703, 0.3219752754296894559, 0.3333333333333333703, 0.3219752754296894559, 0.3333333333333333703, 0.3219752754296894559, 0.3333333333333333703, 0.3219752754296894559, 0.3333333333333333703, 0.3219752754296894559, 0.3333333333333333703, 0.3219752754296894559, 0.3333333333333333703, 0.3219752754296894559, 0.3333333333333333703, 0.3219752754296894559, 0.3333333333333333703, 0.3219752754296894559, 0.3333333333333333703, 0.3219752754296894559, 0.3333333333333333703, 0.3219752754296894559, 0.3333333333333333703, 0.3219752754296894559, 0.3333333333333333703, 0.3219752754296894559, 0.3333333333333333703, 0.3219752754296894559, 0.3333333333333333703, 0.3219752754296894559, 0.3333333333333333703, 0.3219752754296894559, 0.3333333333333333703, 0.3219752754296894559, 0.3333333333333333703, 0.3219752754296894559, 0.3333333333333333703, 0.3219752754296894559, 0.3333333333333333703, 0.3219752754296894559, 0.3333333333333333703, 0.3219752754296894559, 0.3333333333333333703, 0.3219752754296894559, 0.3333333333333333703, 0.3219752754296894559, 0.3333333333333333703, 0.3219752754296894559, 0.3333333333333333703, 0.3219752754296894559, 0.3333333333333333703, 0.3219752754296894559, 0.3333333333333333703, 0.3219752754296894559, 0.3333333333333333703, 0.3219752754296894559, 0.3333333333333333703, 0.3219752754296894559, 0.3333333333333333703, 0.3219752754296894559, 0.3333333333333333703, 0.3219752754296894559, 0.3333333333333333703, 0.3219752754296894559, 0.3333333333333333703, 0.3219752754296894559, 0.3333333333333333703, 0.3219752754296894559, 0.3333333333333333703, 0.3219752754296894559, 0.3333333333333333703, 0.3219752754296894559, 0.3333333333333333703, 0.3219752754296894559, 0.3333333333333333703, 0.3219752754296894559, 0.3333333333333333703, 0.3219752754296894559, 0.3333333333333333703, 0.3219752754296894559, 0.3333333333333333703, 0.3219752754296894559, 0.3333333333333333703, 0.3219752754296894559, 0.3333333333333333703, 0.3219752754296894559, 0.3333333333333333703, 0.3219752754296894559, 0.3333333333333333703, 0.3219752754296894559, 0.3333333333333333703, 0.3219752754296894559, 0.3333333333333333703, 0.3219752754296894559, 0.3333333333333333703, 0.3219752754296894559, 0.3333333333333333703, 0.3219752754296894559, 0.3333333333333333703, 0.3219752754296894559, 0.3333333333333333703, 0.3219752754296894559, 0.3333333333333333703, 0.3219752754296894559, 0.3333333333333333703, 0.3219752754296894559, 0.3333333333333333703, 0.3219752754296894559, 0.3333333333333333703, 0.3219752754296894559, 0.3333333333333333703, 0.3219752754296894559, 0.3333333333333333703, 0.3219752754296894559, 0.3333333333333333703, 0.3219752754296894559, 0.3333333333333333703, 0.3219752754296894559, 0.3333333333333333703, 0.3219752754296894559, 0.3333333333333333703, 0.3219752754296894559, 0.3333333333333333703, 0.3219752754296894559, 0.3333333333333333703, 0.3219752754296894559, 0.3333333333333333703, 0.3219752754296894559, 0.3333333333333333703, 0.3219752754296894559, 0.3333333333333333703, 0.3219752754296894559, 0.3333333333333333703, 0.3219752754296894559, 0.3333333333333333703, 0.3219752754296894559, 0.3333333333333333703, 0.3219752754296894559, 0.3333333333333333703, 0.3219752754296894559, 0.3333333333333333703, 0.3219752754296894559, 0.3333333333333333703, 0.3219752754296894559, 0.3333333333333333703, 0.3219752754296894559, 0.3333333333333333703, 0.3219752754296894559, 0.3333333333333333703, 0.3219752754296894559, 0.3333333333333333703, 0.3219752754296894559, 0.3333333333333333703, 0.3219752754296894559, 0.3333333333333333703, 0.3219752754296894559, 0.3333333333333333703, 0.3219752754296894559, 0.3333333333333333703, 0.3219752754296894559, 0.3333333333333333703, 0.3219752754296894559, 0.3333333333333333703, 0.3219752754296894559, 0.3333333333333333703, 0.3219752754296894559, 0.3333333333333333703, 0.3219752754296894559, 0.3333333333333333703, 0.3219752754296894559, 0.3333333333333333703, 0.3219752754296894559, 0.3333333333333333703, 0.3219752754296894559, 0.3333333333333333703, 0.3219752754296894559, 0.3333333333333333703, 0.3219752754296894559, 0.3333333333333333703, 0.3219752754296894559, 0.3333333333333333703, 0.3219752754296894559, 0.3333333333333333703, 0.3219752754296894559, 0.3333333333333333703, 0.3219752754296894559, 0.3333333333333333703, 0.3219752754296894559, 0.3333333333333333703, 0.3219752754296894559, 0.3333333333333333703, 0.3219752754296894559, 0.3333333333333333703, 0.3219752754296894559, 0.3333333333333333703, 0.3219752754296894559, 0.3333333333333333703, 0.3219752754296894559, 0.3333333333333333703, 0.3219752754296894559, 0.3333333333333333703, 0.3219752754296894559, 0.3333333333333333703, 0.3219752754296894559, 0.3333333333333333703, 0.3219752754296894559, 0.3333333333333333703, 0.3219752754296894559, 0.3333333333333333703, 0.3219752754296894559, 0.3333333333333333703, 0.3219752754296894559, 0.3333333333333333703, 0.3219752754296894559, 0.3333333333333333703, 0.3219752754296894559, 0.3333333333333333703, 0.3219752754296894559, 0.3333333333333333703, 0.3219752754296894559, 0.3333333333333333703, 0.3219752754296894559, 0.3333333333333333703, 0.3219752754296894559, 0.3333333333333333703, 0.3219752754296894559, 0.3333333333333333703, 0.3219752754296894559, 0.3333333333333333703, 0.3219752754296894559, 0.3333333333333333703, 0.3219752754296894559, 0.3333333333333333703, 0.3219752754296894559, 0.3333333333333333703, 0.3219752754296894559, 0.3333333333333333703, 0.3219752754296894559, 0.3333333333333333703, 0.3219752754296894559, 0.3333333333333333703, 0.3219752754296894559, 0.3333333333333333703, 0.3219752754296894559, 0.3333333333333333703, 0.3219752754296894559, 0.3333333333333333703, 0.3219752754296894559, 0.3333333333333333703, 0.3219752754296894559, 0.3333333333333333703, 0.3219752754296894559, 0.3333333333333333703, 0.3219752754296894559, 0.3333333333333333703, 0.3219752754296894559, 0.3333333333333333703, 0.3219752754296894559, 0.3333333333333333703, 0.3219752754296894559, 0.3333333333333333703, 0.3219752754296894559, 0.3333333333333333703, 0.3219752754296894559, 0.3333333333333333703, 0.3219752754296894559, 0.3333333333333333703, 0.3219752754296894559, 0.3333333333333333703, 0.3219752754296894559, 0.3333333333333333703, 0.3219752754296894559, 0.3333333333333333703, 0.3219752754296894559, 0.3333333333333333703, 0.3219752754296894559, 0.3333333333333333703, 0.3219752754296894559, 0.3333333333333333703, 0.3219752754296894559, 0.3333333333333333703, 0.3219752754296894559, 0.3333333333333333703, 0.3219752754296894559, 0.3333333333333333703, 0.3219752754296894559, 0.3333333333333333703, 0.3219752754296894559, 0.3333333333333333703, 0.3219752754296894559, 0.3333333333333333703, 0.3219752754296894559, 0.3333333333333333703, 0.3219752754296894559, 0.3333333333333333703, 0.3219752754296894559, 0.3333333333333333703, 0.3219752754296894559, 0.3333333333333333703, 0.3219752754296894559, 0.3333333333333333703, 0.3219752754296894559, 0.3333333333333333703, 0.3219752754296894559, 0.3333333333333333703, 0.3219752754296894559, 0.3333333333333333703, 0.3219752754296894559, 0.3333333333333333703, 0.3219752754296894559, 0.3333333333333333703, 0.3219752754296894559, 0.3333333333333333703, 0.3219752754296894559, 0.3333333333333333703, 0.3219752754296894559, 0.3333333333333333703, 0.3219752754296894559, 0.3333333333333333703, 0.3219752754296894559, 0.3333333333333333703, 0.3219752754296894559, 0.3333333333333333703, 0.3219752754296894559, 0.3333333333333333703, 0.3219752754296894559, 0.3333333333333333703, 0.3219752754296894559, 0.3333333333333333703, 0.3219752754296894559, 0.3333333333333333703, 0.3219752754296894559, 0.3333333333333333703, 0.3219752754296894559, 0.3333333333333333703, 0.3219752754296894559, 0.3333333333333333703, 0.3219752754296894559, 0.3333333333333333703, 0.3219752754296894559, 0.3333333333333333703, 0.3219752754296894559, 0.3333333333333333703, 0.3219752754296894559, 0.3333333333333333703, 0.3219752754296894559, 0.3333333333333333703, 0.3219752754296894559, 0.3333333333333333703, 0.3219752754296894559, 0.3333333333333333703, 0.3219752754296894559, 0.3333333333333333703, 0.3219752754296894559, 0.3333333333333333703, 0.3219752754296894559, 0.3333333333333333703, 0.3219752754296894559, 0.3333333333333333703, 0.3219752754296894559, 0.3333333333333333703, 0.3219752754296894559, 0.3333333333333333703, 0.3219752754296894559, 0.3333333333333333703, 0.3219752754296894559, 0.3333333333333333703, 0.3219752754296894559, 0.3333333333333333703, 0.3219752754296894559, 0.3333333333333333703, 0.3219752754296894559, 0.3333333333333333703, 0.3219752754296894559, 0.3333333333333333703, 0.3219752754296894559, 0.3333333333333333703, 0.3219752754296894559, 0.3333333333333333703, 0.3219752754296894559, 0.3333333333333333703),
 ( 0.3333333333333333703, 0.3219752754296894559, 0.3333333333333333703, 0.3219752754296894559, 0.3333333333333333703, 0.3219752754296894559, 0.3333333333333333703, 0.3219752754296894559, 0.3333333333333333703, 0.3219752754296894559, 0.3333333333333333703, 0.3219752754296894559, 0.3333333333333333703, 0.3219752754296894559, 0.3333333333333333703, 0.3219752754296894559, 0.3333333333333333703, 0.3219752754296894559, 0.3333333333333333703, 0.3219752754296894559, 0.3333333333333333703, 0.3219752754296894559, 0.3333333333333333703, 0.3219752754296894559, 0.3333333333333333703, 0.3219752754296894559, 0.3333333333333333703, 0.3219752754296894559, 0.3333333333333333703, 0.3219752754296894559, 0.3333333333333333703, 0.3219752754296894559, 0.3333333333333333703, 0.3219752754296894559, 0.3333333333333333703, 0.3219752754296894559, 0.3333333333333333703, 0.3219752754296894559, 0.3333333333333333703, 0.3219752754296894559, 0.3333333333333333703, 0.3219752754296894559, 0.3333333333333333703, 0.3219752754296894559, 0.3333333333333333703, 0.3219752754296894559, 0.3333333333333333703, 0.3219752754296894559, 0.3333333333333333703, 0.3219752754296894559, 0.3333333333333333703, 0.3219752754296894559, 0.3333333333333333703, 0.3219752754296894559, 0.3333333333333333703, 0.3219752754296894559, 0.3333333333333333703, 0.3219752754296894559, 0.3333333333333333703, 0.3219752754296894559, 0.3333333333333333703, 0.3219752754296894559, 0.3333333333333333703, 0.3219752754296894559, 0.3333333333333333703, 0.3219752754296894559, 0.3333333333333333703, 0.3219752754296894559, 0.3333333333333333703, 0.3219752754296894559, 0.3333333333333333703, 0.3219752754296894559, 0.3333333333333333703, 0.3219752754296894559, 0.3333333333333333703, 0.3219752754296894559, 0.3333333333333333703, 0.3219752754296894559, 0.3333333333333333703, 0.3219752754296894559, 0.3333333333333333703, 0.3219752754296894559, 0.3333333333333333703, 0.3219752754296894559, 0.3333333333333333703, 0.3219752754296894559, 0.3333333333333333703, 0.3219752754296894559, 0.3333333333333333703, 0.3219752754296894559, 0.3333333333333333703, 0.3219752754296894559, 0.3333333333333333703, 0.3219752754296894559, 0.3333333333333333703, 0.3219752754296894559, 0.3333333333333333703, 0.3219752754296894559, 0.3333333333333333703, 0.3219752754296894559, 0.3333333333333333703, 0.3219752754296894559, 0.3333333333333333703, 0.3219752754296894559, 0.3333333333333333703, 0.3219752754296894559, 0.3333333333333333703, 0.3219752754296894559, 0.3333333333333333703, 0.3219752754296894559, 0.3333333333333333703, 0.3219752754296894559, 0.3333333333333333703, 0.3219752754296894559, 0.3333333333333333703, 0.3219752754296894559, 0.3333333333333333703, 0.3219752754296894559, 0.3333333333333333703, 0.3219752754296894559, 0.3333333333333333703, 0.3219752754296894559, 0.3333333333333333703, 0.3219752754296894559, 0.3333333333333333703, 0.3219752754296894559, 0.3333333333333333703, 0.3219752754296894559, 0.3333333333333333703, 0.3219752754296894559, 0.3333333333333333703, 0.3219752754296894559, 0.3333333333333333703, 0.3219752754296894559, 0.3333333333333333703, 0.3219752754296894559, 0.3333333333333333703, 0.3219752754296894559, 0.3333333333333333703, 0.3219752754296894559, 0.3333333333333333703, 0.3219752754296894559, 0.3333333333333333703, 0.3219752754296894559, 0.3333333333333333703, 0.3219752754296894559, 0.3333333333333333703, 0.3219752754296894559, 0.3333333333333333703, 0.3219752754296894559, 0.3333333333333333703, 0.3219752754296894559, 0.3333333333333333703, 0.3219752754296894559, 0.3333333333333333703, 0.3219752754296894559, 0.3333333333333333703, 0.3219752754296894559, 0.3333333333333333703, 0.3219752754296894559, 0.3333333333333333703, 0.3219752754296894559, 0.3333333333333333703, 0.3219752754296894559, 0.3333333333333333703, 0.3219752754296894559, 0.3333333333333333703, 0.3219752754296894559, 0.3333333333333333703, 0.3219752754296894559, 0.3333333333333333703, 0.3219752754296894559, 0.3333333333333333703, 0.3219752754296894559, 0.3333333333333333703, 0.3219752754296894559, 0.3333333333333333703, 0.3219752754296894559, 0.3333333333333333703, 0.3219752754296894559, 0.3333333333333333703, 0.3219752754296894559, 0.3333333333333333703, 0.3219752754296894559, 0.3333333333333333703, 0.3219752754296894559, 0.3333333333333333703, 0.3219752754296894559, 0.3333333333333333703, 0.3219752754296894559, 0.3333333333333333703, 0.3219752754296894559, 0.3333333333333333703, 0.3219752754296894559, 0.3333333333333333703, 0.3219752754296894559, 0.3333333333333333703, 0.3219752754296894559, 0.3333333333333333703, 0.3219752754296894559, 0.3333333333333333703, 0.3219752754296894559, 0.3333333333333333703, 0.3219752754296894559, 0.3333333333333333703, 0.3219752754296894559, 0.3333333333333333703, 0.3219752754296894559, 0.3333333333333333703, 0.3219752754296894559, 0.3333333333333333703, 0.3219752754296894559, 0.3333333333333333703, 0.3219752754296894559, 0.3333333333333333703, 0.3219752754296894559, 0.3333333333333333703, 0.3219752754296894559, 0.3333333333333333703, 0.3219752754296894559, 0.3333333333333333703, 0.3219752754296894559, 0.3333333333333333703, 0.3219752754296894559, 0.3333333333333333703, 0.3219752754296894559, 0.3333333333333333703, 0.3219752754296894559, 0.3333333333333333703, 0.3219752754296894559, 0.3333333333333333703, 0.3219752754296894559, 0.3333333333333333703, 0.3219752754296894559, 0.3333333333333333703, 0.3219752754296894559, 0.3333333333333333703, 0.3219752754296894559, 0.3333333333333333703, 0.3219752754296894559, 0.3333333333333333703, 0.3219752754296894559, 0.3333333333333333703, 0.3219752754296894559, 0.3333333333333333703, 0.3219752754296894559, 0.3333333333333333703, 0.3219752754296894559, 0.3333333333333333703, 0.3219752754296894559, 0.3333333333333333703, 0.3219752754296894559, 0.3333333333333333703, 0.3219752754296894559, 0.3333333333333333703, 0.3219752754296894559, 0.3333333333333333703, 0.3219752754296894559, 0.3333333333333333703, 0.3219752754296894559, 0.3333333333333333703, 0.3219752754296894559, 0.3333333333333333703, 0.3219752754296894559, 0.3333333333333333703, 0.3219752754296894559, 0.3333333333333333703, 0.3219752754296894559, 0.3333333333333333703, 0.3219752754296894559, 0.3333333333333333703, 0.3219752754296894559, 0.3333333333333333703, 0.3219752754296894559, 0.3333333333333333703, 0.3219752754296894559, 0.3333333333333333703, 0.3219752754296894559, 0.3333333333333333703, 0.3219752754296894559, 0.3333333333333333703, 0.3219752754296894559, 0.3333333333333333703, 0.3219752754296894559, 0.3333333333333333703, 0.3219752754296894559, 0.3333333333333333703, 0.3219752754296894559, 0.3333333333333333703, 0.3219752754296894559, 0.3333333333333333703, 0.3219752754296894559, 0.3333333333333333703, 0.3219752754296894559, 0.3333333333333333703, 0.3219752754296894559, 0.3333333333333333703, 0.3219752754296894559, 0.3333333333333333703, 0.3219752754296894559, 0.3333333333333333703, 0.3219752754296894559, 0.3333333333333333703, 0.3219752754296894559, 0.3333333333333333703, 0.3219752754296894559, 0.3333333333333333703, 0.3219752754296894559, 0.3333333333333333703, 0.3219752754296894559, 0.3333333333333333703, 0.3219752754296894559, 0.3333333333333333703, 0.3219752754296894559, 0.3333333333333333703, 0.3219752754296894559, 0.3333333333333333703, 0.3219752754296894559, 0.3333333333333333703, 0.3219752754296894559, 0.3333333333333333703, 0.3219752754296894559, 0.3333333333333333703, 0.3219752754296894559, 0.3333333333333333703, 0.3219752754296894559, 0.3333333333333333703, 0.3219752754296894559, 0.3333333333333333703, 0.3219752754296894559, 0.3333333333333333703, 0.3219752754296894559, 0.3333333333333333703, 0.3219752754296894559, 0.3333333333333333703, 0.3219752754296894559, 0.3333333333333333703, 0.3219752754296894559, 0.3333333333333333703, 0.3219752754296894559, 0.3333333333333333703, 0.3219752754296894559, 0.3333333333333333703, 0.3219752754296894559, 0.3333333333333333703, 0.3219752754296894559, 0.3333333333333333703, 0.3219752754296894559, 0.3333333333333333703, 0.3219752754296894559, 0.3333333333333333703, 0.3219752754296894559, 0.3333333333333333703, 0.3219752754296894559, 0.3333333333333333703, 0.3219752754296894559, 0.3333333333333333703, 0.3219752754296894559, 0.3333333333333333703, 0.3219752754296894559, 0.3333333333333333703, 0.3219752754296894559, 0.3333333333333333703, 0.3219752754296894559, 0.3333333333333333703, 0.3219752754296894559, 0.3333333333333333703, 0.3219752754296894559, 0.3333333333333333703, 0.3219752754296894559, 0.3333333333333333703, 0.3219752754296894559, 0.3333333333333333703, 0.3219752754296894559, 0.3333333333333333703, 0.3219752754296894559, 0.3333333333333333703, 0.3219752754296894559, 0.3333333333333333703, 0.3219752754296894559, 0.3333333333333333703, 0.3219752754296894559, 0.3333333333333333703, 0.3219752754296894559, 0.3333333333333333703, 0.3219752754296894559, 0.3333333333333333703, 0.3219752754296894559, 0.3333333333333333703, 0.3219752754296894559, 0.3333333333333333703, 0.3219752754296894559, 0.3333333333333333703, 0.3219752754296894559, 0.3333333333333333703, 0.3219752754296894559, 0.3333333333333333703, 0.3219752754296894559, 0.3333333333333333703, 0.3219752754296894559, 0.3333333333333333703, 0.3219752754296894559, 0.3333333333333333703, 0.3219752754296894559, 0.3333333333333333703, 0.3219752754296894559, 0.3333333333333333703, 0.3219752754296894559, 0.3333333333333333703, 0.3219752754296894559, 0.3333333333333333703, 0.3219752754296894559, 0.3333333333333333703, 0.3219752754296894559, 0.3333333333333333703, 0.3219752754296894559, 0.3333333333333333703, 0.3219752754296894559, 0.3333333333333333703, 0.3219752754296894559, 0.3333333333333333703, 0.3219752754296894559, 0.3333333333333333703, 0.3219752754296894559, 0.3333333333333333703, 0.3219752754296894559, 0.3333333333333333703, 0.3219752754296894559, 0.3333333333333333703, 0.3219752754296894559, 0.3333333333333333703, 0.3219752754296894559, 0.3333333333333333703, 0.3219752754296894559, 0.3333333333333333703, 0.3219752754296894559, 0.3333333333333333703, 0.3219752754296894559, 0.3333333333333333703, 0.3219752754296894559, 0.3333333333333333703, 0.3219752754296894559, 0.3333333333333333703, 0.3219752754296894559, 0.3333333333333333703, 0.3219752754296894559, 0.3333333333333333703, 0.3219752754296894559, 0.3333333333333333703, 0.3219752754296894559, 0.3333333333333333703, 0.3219752754296894559, 0.3333333333333333703, 0.3219752754296894559, 0.3333333333333333703, 0.3219752754296894559, 0.3333333333333333703),
 ( 1.000000000000000000, 0.9659258262890683122, 1.000000000000000000, 0.9659258262890683122, 1.000000000000000000, 0.9659258262890683122, 1.000000000000000000, 0.9659258262890683122, 1.000000000000000000, 0.9659258262890683122, 1.000000000000000000, 0.9659258262890683122, 1.000000000000000000, 0.9659258262890683122, 1.000000000000000000, 0.9659258262890683122, 1.000000000000000000, 0.9659258262890683122, 1.000000000000000000, 0.9659258262890683122, 1.000000000000000000, 0.9659258262890683122, 1.000000000000000000, 0.9659258262890683122, 1.000000000000000000, 0.9659258262890683122, 1.000000000000000000, 0.9659258262890683122, 1.000000000000000000, 0.9659258262890683122, 1.000000000000000000, 0.9659258262890683122, 1.000000000000000000, 0.9659258262890683122, 1.000000000000000000, 0.9659258262890683122, 1.000000000000000000, 0.9659258262890683122, 1.000000000000000000, 0.9659258262890683122, 1.000000000000000000, 0.9659258262890683122, 1.000000000000000000, 0.9659258262890683122, 1.000000000000000000, 0.9659258262890683122, 1.000000000000000000, 0.9659258262890683122, 1.000000000000000000, 0.9659258262890683122, 1.000000000000000000, 0.9659258262890683122, 1.000000000000000000, 0.9659258262890683122, 1.000000000000000000, 0.9659258262890683122, 1.000000000000000000, 0.9659258262890683122, 1.000000000000000000, 0.9659258262890683122, 1.000000000000000000, 0.9659258262890683122, 1.000000000000000000, 0.9659258262890683122, 1.000000000000000000, 0.9659258262890683122, 1.000000000000000000, 0.9659258262890683122, 1.000000000000000000, 0.9659258262890683122, 1.000000000000000000, 0.9659258262890683122, 1.000000000000000000, 0.9659258262890683122, 1.000000000000000000, 0.9659258262890683122, 1.000000000000000000, 0.9659258262890683122, 1.000000000000000000, 0.9659258262890683122, 1.000000000000000000, 0.9659258262890683122, 1.000000000000000000, 0.9659258262890683122, 1.000000000000000000, 0.9659258262890683122, 1.000000000000000000, 0.9659258262890683122, 1.000000000000000000, 0.9659258262890683122, 1.000000000000000000, 0.9659258262890683122, 1.000000000000000000, 0.9659258262890683122, 1.000000000000000000, 0.9659258262890683122, 1.000000000000000000, 0.9659258262890683122, 1.000000000000000000, 0.9659258262890683122, 1.000000000000000000, 0.9659258262890683122, 1.000000000000000000, 0.9659258262890683122, 1.000000000000000000, 0.9659258262890683122, 1.000000000000000000, 0.9659258262890683122, 1.000000000000000000, 0.9659258262890683122, 1.000000000000000000, 0.9659258262890683122, 1.000000000000000000, 0.9659258262890683122, 1.000000000000000000, 0.9659258262890683122, 1.000000000000000000, 0.9659258262890683122, 1.000000000000000000, 0.9659258262890683122, 1.000000000000000000, 0.9659258262890683122, 1.000000000000000000, 0.9659258262890683122, 1.000000000000000000, 0.9659258262890683122, 1.000000000000000000, 0.9659258262890683122, 1.000000000000000000, 0.9659258262890683122, 1.000000000000000000, 0.9659258262890683122, 1.000000000000000000, 0.9659258262890683122, 1.000000000000000000, 0.9659258262890683122, 1.000000000000000000, 0.9659258262890683122, 1.000000000000000000, 0.9659258262890683122, 1.000000000000000000, 0.9659258262890683122, 1.000000000000000000, 0.9659258262890683122, 1.000000000000000000, 0.9659258262890683122, 1.000000000000000000, 0.9659258262890683122, 1.000000000000000000, 0.9659258262890683122, 1.000000000000000000, 0.9659258262890683122, 1.000000000000000000, 0.9659258262890683122, 1.000000000000000000, 0.9659258262890683122, 1.000000000000000000, 0.9659258262890683122, 1.000000000000000000, 0.9659258262890683122, 1.000000000000000000, 0.9659258262890683122, 1.000000000000000000, 0.9659258262890683122, 1.000000000000000000, 0.9659258262890683122, 1.000000000000000000, 0.9659258262890683122, 1.000000000000000000, 0.9659258262890683122, 1.000000000000000000, 0.9659258262890683122, 1.000000000000000000, 0.9659258262890683122, 1.000000000000000000, 0.9659258262890683122, 1.000000000000000000, 0.9659258262890683122, 1.000000000000000000, 0.9659258262890683122, 1.000000000000000000, 0.9659258262890683122, 1.000000000000000000, 0.9659258262890683122, 1.000000000000000000, 0.9659258262890683122, 1.000000000000000000, 0.9659258262890683122, 1.000000000000000000, 0.9659258262890683122, 1.000000000000000000, 0.9659258262890683122, 1.000000000000000000, 0.9659258262890683122, 1.000000000000000000, 0.9659258262890683122, 1.000000000000000000, 0.9659258262890683122, 1.000000000000000000, 0.9659258262890683122, 1.000000000000000000, 0.9659258262890683122, 1.000000000000000000, 0.9659258262890683122, 1.000000000000000000, 0.9659258262890683122, 1.000000000000000000, 0.9659258262890683122, 1.000000000000000000, 0.9659258262890683122, 1.000000000000000000, 0.9659258262890683122, 1.000000000000000000, 0.9659258262890683122, 1.000000000000000000, 0.9659258262890683122, 1.000000000000000000, 0.9659258262890683122, 1.000000000000000000, 0.9659258262890683122, 1.000000000000000000, 0.9659258262890683122, 1.000000000000000000, 0.9659258262890683122, 1.000000000000000000, 0.9659258262890683122, 1.000000000000000000, 0.9659258262890683122, 1.000000000000000000, 0.9659258262890683122, 1.000000000000000000, 0.9659258262890683122, 1.000000000000000000, 0.9659258262890683122, 1.000000000000000000, 0.9659258262890683122, 1.000000000000000000, 0.9659258262890683122, 1.000000000000000000, 0.9659258262890683122, 1.000000000000000000, 0.9659258262890683122, 1.000000000000000000, 0.9659258262890683122, 1.000000000000000000, 0.9659258262890683122, 1.000000000000000000, 0.9659258262890683122, 1.000000000000000000, 0.9659258262890683122, 1.000000000000000000, 0.9659258262890683122, 1.000000000000000000, 0.9659258262890683122, 1.000000000000000000, 0.9659258262890683122, 1.000000000000000000, 0.9659258262890683122, 1.000000000000000000, 0.9659258262890683122, 1.000000000000000000, 0.9659258262890683122, 1.000000000000000000, 0.9659258262890683122, 1.000000000000000000, 0.9659258262890683122, 1.000000000000000000, 0.9659258262890683122, 1.000000000000000000, 0.9659258262890683122, 1.000000000000000000, 0.9659258262890683122, 1.000000000000000000, 0.9659258262890683122, 1.000000000000000000, 0.9659258262890683122, 1.000000000000000000, 0.9659258262890683122, 1.000000000000000000, 0.9659258262890683122, 1.000000000000000000, 0.9659258262890683122, 1.000000000000000000, 0.9659258262890683122, 1.000000000000000000, 0.9659258262890683122, 1.000000000000000000, 0.9659258262890683122, 1.000000000000000000, 0.9659258262890683122, 1.000000000000000000, 0.9659258262890683122, 1.000000000000000000, 0.9659258262890683122, 1.000000000000000000, 0.9659258262890683122, 1.000000000000000000, 0.9659258262890683122, 1.000000000000000000, 0.9659258262890683122, 1.000000000000000000, 0.9659258262890683122, 1.000000000000000000, 0.9659258262890683122, 1.000000000000000000, 0.9659258262890683122, 1.000000000000000000, 0.9659258262890683122, 1.000000000000000000, 0.9659258262890683122, 1.000000000000000000, 0.9659258262890683122, 1.000000000000000000, 0.9659258262890683122, 1.000000000000000000, 0.9659258262890683122, 1.000000000000000000, 0.9659258262890683122, 1.000000000000000000, 0.9659258262890683122, 1.000000000000000000, 0.9659258262890683122, 1.000000000000000000, 0.9659258262890683122, 1.000000000000000000, 0.9659258262890683122, 1.000000000000000000, 0.9659258262890683122, 1.000000000000000000, 0.9659258262890683122, 1.000000000000000000, 0.9659258262890683122, 1.000000000000000000, 0.9659258262890683122, 1.000000000000000000, 0.9659258262890683122, 1.000000000000000000, 0.9659258262890683122, 1.000000000000000000, 0.9659258262890683122, 1.000000000000000000, 0.9659258262890683122, 1.000000000000000000, 0.9659258262890683122, 1.000000000000000000, 0.9659258262890683122, 1.000000000000000000, 0.9659258262890683122, 1.000000000000000000, 0.9659258262890683122, 1.000000000000000000, 0.9659258262890683122, 1.000000000000000000, 0.9659258262890683122, 1.000000000000000000, 0.9659258262890683122, 1.000000000000000000, 0.9659258262890683122, 1.000000000000000000, 0.9659258262890683122, 1.000000000000000000, 0.9659258262890683122, 1.000000000000000000, 0.9659258262890683122, 1.000000000000000000, 0.9659258262890683122, 1.000000000000000000, 0.9659258262890683122, 1.000000000000000000, 0.9659258262890683122, 1.000000000000000000, 0.9659258262890683122, 1.000000000000000000, 0.9659258262890683122, 1.000000000000000000, 0.9659258262890683122, 1.000000000000000000, 0.9659258262890683122, 1.000000000000000000, 0.9659258262890683122, 1.000000000000000000, 0.9659258262890683122, 1.000000000000000000, 0.9659258262890683122, 1.000000000000000000, 0.9659258262890683122, 1.000000000000000000, 0.9659258262890683122, 1.000000000000000000, 0.9659258262890683122, 1.000000000000000000, 0.9659258262890683122, 1.000000000000000000, 0.9659258262890683122, 1.000000000000000000, 0.9659258262890683122, 1.000000000000000000, 0.9659258262890683122, 1.000000000000000000, 0.9659258262890683122, 1.000000000000000000, 0.9659258262890683122, 1.000000000000000000, 0.9659258262890683122, 1.000000000000000000, 0.9659258262890683122, 1.000000000000000000, 0.9659258262890683122, 1.000000000000000000, 0.9659258262890683122, 1.000000000000000000, 0.9659258262890683122, 1.000000000000000000, 0.9659258262890683122, 1.000000000000000000, 0.9659258262890683122, 1.000000000000000000, 0.9659258262890683122, 1.000000000000000000, 0.9659258262890683122, 1.000000000000000000, 0.9659258262890683122, 1.000000000000000000, 0.9659258262890683122, 1.000000000000000000, 0.9659258262890683122, 1.000000000000000000, 0.9659258262890683122, 1.000000000000000000, 0.9659258262890683122, 1.000000000000000000, 0.9659258262890683122, 1.000000000000000000, 0.9659258262890683122, 1.000000000000000000, 0.9659258262890683122, 1.000000000000000000, 0.9659258262890683122, 1.000000000000000000, 0.9659258262890683122, 1.000000000000000000, 0.9659258262890683122, 1.000000000000000000, 0.9659258262890683122, 1.000000000000000000, 0.9659258262890683122, 1.000000000000000000, 0.9659258262890683122, 1.000000000000000000, 0.9659258262890683122, 1.000000000000000000, 0.9659258262890683122, 1.000000000000000000, 0.9659258262890683122, 1.000000000000000000, 0.9659258262890683122, 1.000000000000000000) ) ) 
 REPRESENTATION_ITEM ( '' )  SURFACE ( )  );
#122906 = CARTESIAN_POINT ( 'NONE',  ( 21.52544592524344225, -5.823673210054117533, 23.54057627198102765 ) ) ;
#122907 = CARTESIAN_POINT ( 'NONE',  ( 21.55341960407619695, -5.719274019375665929, 36.04275706135234714 ) ) ;
#122908 = CARTESIAN_POINT ( 'NONE',  ( -19.02544592524334988, -5.153800228976617603, 98.95942372801900433 ) ) ;
#122910 = CARTESIAN_POINT ( 'NONE',  ( -19.02544592524342804, 5.153800228976336051, 66.04057627198103830 ) ) ;
#122909 = CARTESIAN_POINT ( 'NONE',  ( -11.74264578624800670, 36.14014761921585972, -2.400000000000000355 ) ) ;
#122911 = CARTESIAN_POINT ( 'NONE',  ( 9.474510206698971260, -16.51473224551069308, 97.91557627198102409 ) ) ;
#122913 = CARTESIAN_POINT ( 'NONE',  ( -13.97604488694527625, -13.89961937509977652, 61.87390960531435979 ) ) ;
#122912 = CARTESIAN_POINT ( 'NONE',  ( -0.05219959533910754901, -16.53943276465976808, 67.49890960531436690 ) ) ;
#122914 = CARTESIAN_POINT ( 'NONE',  ( 19.05341960407611168, 5.049401038298154454, 68.95724293864769550 ) ) ;
#122915 = CARTESIAN_POINT ( 'NONE',  ( 13.97604488694548053, -13.89961937509957401, 75.62609039468564731 ) ) ;
#122916 = CARTESIAN_POINT ( 'NONE',  ( -21.53943276465977519, 0.05219959533907696930, 56.24890960531436690 ) ) ;
#122917 = CARTESIAN_POINT ( 'NONE',  ( -16.51473224551069308, -9.474510206698971260, 21.66557627198102765 ) ) ;
#122918 = CARTESIAN_POINT ( 'NONE',  ( 0.05219959533936267826, -19.03943276465977164, 40.00109039468566152 ) ) ;
#122919 = CARTESIAN_POINT ( 'NONE',  ( 9.474510206698971260, -16.51473224551069308, 77.91557627198103830 ) ) ;
#122920 = CARTESIAN_POINT ( 'NONE',  ( -10.72451020669898014, 18.67979575497178502, 70.41557627198102409 ) ) ;
#122922 = CARTESIAN_POINT ( 'NONE',  ( 9.564922557961047289, -16.46253265017146816, 35.41775706135233293 ) ) ;
#122921 = CARTESIAN_POINT ( 'NONE',  ( 12.06949235617757843, -12.14591786802309237, 78.12390960531436690 ) ) ;
#122923 = CARTESIAN_POINT ( 'NONE',  ( -21.55341960407610458, -5.719274019375992779, 66.45724293864768129 ) ) ;
#122924 = CARTESIAN_POINT ( 'NONE',  ( -15.80617190586745835, -15.72974639402198527, 41.87390960531435979 ) ) ;
#122925 = CARTESIAN_POINT ( 'NONE',  ( 18.67979575497194134, -10.72451020669871369, 90.83442372801901854 ) ) ;
#122926 = CARTESIAN_POINT ( 'NONE',  ( -16.46253265017160317, 9.564922557960807481, 60.83224293864769550 ) ) ;
#122927 = CARTESIAN_POINT ( 'NONE',  ( -4.483927247898539470, -16.52544592524342804, 112.2905762719810241 ) ) ;
#122928 = CARTESIAN_POINT ( 'NONE',  ( 15.80617190586769283, -15.72974639402175789, 25.62609039468567929 ) ) ;
#122929 = CARTESIAN_POINT ( 'NONE',  ( 1.428746744957154258, 15.66666519715284522, -61.77668719748695736 ) ) ;
#122930 = CARTESIAN_POINT ( 'NONE',  ( -5.719274019375665041, -21.55341960407619695, 44.79275706135234714 ) ) ;
#122931 = CARTESIAN_POINT ( 'NONE',  ( 0.05219959533909260263, 19.03943276465977164, 39.99890960531436690 ) ) ;
#122932 = CARTESIAN_POINT ( 'NONE',  ( -0.05219959533907301413, -21.53943276465977519, 102.4989096053143811 ) ) ;
#122933 = CARTESIAN_POINT ( 'NONE',  ( 19.03943276465977164, 0.05219959533936151252, 41.25109039468566152 ) ) ;
#122934 = CARTESIAN_POINT ( 'NONE',  ( 16.46253265017160672, -9.564922557960803928, 38.33224293864768839 ) ) ;
#122935 = CARTESIAN_POINT ( 'NONE',  ( 19.02544592524343514, -5.153800228976328945, 23.54057627198102054 ) ) ;
#122936 = CARTESIAN_POINT ( 'NONE',  ( 17.31090126489389291, -5.922914322405134158, 21.23212116175356456 ) ) ;
#122937 = CARTESIAN_POINT ( 'NONE',  ( -8.224510206698735004, -14.34966873604973081, 64.58442372801900433 ) ) ;
#122938 = CARTESIAN_POINT ( 'NONE',  ( 19.03943276465977164, -0.05219959533909143690, 23.74890960531435269 ) ) ;
#122939 = CARTESIAN_POINT ( 'NONE',  ( -21.94905633995418270, -8.886455535326843957, 171.4390084046468132 ) ) ;
#122940 = CARTESIAN_POINT ( 'NONE',  ( -19.05341960407611168, -5.049401038298163336, 86.45724293864769550 ) ) ;
#122941 = CARTESIAN_POINT ( 'NONE',  ( -16.53943276465976808, 0.05219959533911058130, 101.2489096053143669 ) ) ;
#122942 = CARTESIAN_POINT ( 'NONE',  ( 21.55341960407610458, 5.719274019375980345, 53.95724293864770260 ) ) ;
#122943 = CARTESIAN_POINT ( 'NONE',  ( -12.06949235617739369, -12.14591786802326823, 44.37609039468567573 ) ) ;
#122944 = CARTESIAN_POINT ( 'NONE',  ( -10.72451020669870658, -18.67979575497194134, 94.58442372801901854 ) ) ;
#122945 = EDGE_CURVE ( 'NONE', #70413, #46062, #13079, .T. ) ;
#122946 = CARTESIAN_POINT ( 'NONE',  ( -16.46253265017160317, 9.564922557960807481, 30.83224293864769550 ) ) ;
#122947 = CARTESIAN_POINT ( 'NONE',  ( -16.53943276465976808, 0.05219959533911058130, 21.24890960531436690 ) ) ;
#122948 = CARTESIAN_POINT ( 'NONE',  ( -14.29746914071049879, 8.314922557960819915, 55.83224293864770260 ) ) ;
#122949 = CARTESIAN_POINT ( 'NONE',  ( -5.153800228976328057, -19.02544592524343514, 47.29057627198102409 ) ) ;
#122950 = CARTESIAN_POINT ( 'NONE',  ( 5.823673210054444382, -21.52544592524334988, 90.20942372801903275 ) ) ;
#122951 = CARTESIAN_POINT ( 'NONE',  ( 5.719274019375673035, 21.55341960407619339, 22.29275706135235069 ) ) ;
#122952 = CARTESIAN_POINT ( 'NONE',  ( 15.80617190586769283, -15.72974639402175789, 70.62609039468567573 ) ) ;
#122953 = CARTESIAN_POINT ( 'NONE',  ( -8.314922557961024197, 14.29746914071037800, 57.91775706135234714 ) ) ;
#122955 = CARTESIAN_POINT ( 'NONE',  ( -15.72974639402176322, -15.80617190586768395, 99.37609039468568994 ) ) ;
#122954 = CARTESIAN_POINT ( 'NONE',  ( 4.483927247898545687, 16.52544592524342804, 79.79057627198102409 ) ) ;
#122956 = EDGE_CURVE ( 'NONE', #163173, #78021, #118826, .T. ) ;
#122957 = CARTESIAN_POINT ( 'NONE',  ( 0.05219959533934541429, -16.53943276465976808, 110.0010903946856757 ) ) ;
#122958 = DIRECTION ( 'NONE',  ( 1.000000000000000000, 0.000000000000000000, 0.000000000000000000 ) ) ;
#122959 = CARTESIAN_POINT ( 'NONE',  ( 12.14591786802327356, -12.06949235617739191, 35.62609039468568994 ) ) ;
#122960 = CARTESIAN_POINT ( 'NONE',  ( -0.05219959533910754901, -16.53943276465976808, 37.49890960531436690 ) ) ;
#122961 = CARTESIAN_POINT ( 'NONE',  ( -12.06949235617739369, -12.14591786802326823, 84.37609039468570415 ) ) ;
#122962 = CARTESIAN_POINT ( 'NONE',  ( -5.153800228976328057, -19.02544592524343514, 102.2905762719810383 ) ) ;
#122963 = CARTESIAN_POINT ( 'NONE',  ( 5.719274019375991003, -21.55341960407610458, 22.70724293864769194 ) ) ;
#122964 = CARTESIAN_POINT ( 'NONE',  ( -18.62759615963255300, -10.81492255796106328, 99.16775706135234714 ) ) ;
#122965 = CARTESIAN_POINT ( 'NONE',  ( 12.14591786802327356, -12.06949235617739191, 100.6260903946857184 ) ) ;
#122966 = CARTESIAN_POINT ( 'NONE',  ( -8.224510206698948167, 14.34966873604960824, 70.41557627198102409 ) ) ;
#122967 = CARTESIAN_POINT ( 'NONE',  ( -9.474510206698964154, 16.51473224551069663, 80.41557627198103830 ) ) ;
#122968 = ORIENTED_EDGE ( 'NONE', *, *, #111223, .F. ) ;
#122969 = CARTESIAN_POINT ( 'NONE',  ( -4.379528057220086978, -16.55341960407618274, 34.79275706135235424 ) ) ;
#122970 = CARTESIAN_POINT ( 'NONE',  ( 16.51473224551069308, 9.474510206698969483, 39.16557627198103120 ) ) ;
#122971 = CARTESIAN_POINT ( 'NONE',  ( -16.51473224551069308, -9.474510206698971260, 91.66557627198103830 ) ) ;
#122973 = DIRECTION ( 'NONE',  ( -0.000000000000000000, -0.000000000000000000, 1.000000000000000000 ) ) ;
#122972 = CARTESIAN_POINT ( 'NONE',  ( 4.483927247898790824, -16.52544592524335698, 30.20942372801902565 ) ) ;
#122974 = CARTESIAN_POINT ( 'NONE',  ( -19.05341960407617563, 5.049401038297882671, 33.54275706135231871 ) ) ;
#122975 = CARTESIAN_POINT ( 'NONE',  ( -8.314922557961024197, 14.29746914071037800, 97.91775706135236135 ) ) ;
#122976 = CARTESIAN_POINT ( 'NONE',  ( 9.564922557960805705, 16.46253265017160317, 34.58224293864770260 ) ) ;
#122977 = CARTESIAN_POINT ( 'NONE',  ( -12.06949235617739369, -12.14591786802326823, 79.37609039468567573 ) ) ;
#122978 = CARTESIAN_POINT ( 'NONE',  ( 8.314922557961029526, -14.29746914071037800, 65.41775706135234714 ) ) ;
#122979 = CARTESIAN_POINT ( 'NONE',  ( -0.05219959533936034679, 19.03943276465977164, 82.50109039468567573 ) ) ;
#122980 = CARTESIAN_POINT ( 'NONE',  ( 13.89961937509957401, 13.97604488694547697, 26.87609039468566507 ) ) ;
#122981 = CARTESIAN_POINT ( 'NONE',  ( 9.564922557960805705, 16.46253265017160317, 54.58224293864769550 ) ) ;
#122982 = CARTESIAN_POINT ( 'NONE',  ( 14.34966873604960469, 8.224510206698951720, 89.16557627198102409 ) ) ;
#122983 = CARTESIAN_POINT ( 'NONE',  ( 5.049401038297881783, 19.05341960407617563, 57.29275706135231871 ) ) ;
#122984 = CARTESIAN_POINT ( 'NONE',  ( 21.53943276465977519, -0.05219959533907433946, 48.74890960531435979 ) ) ;
#122985 = CARTESIAN_POINT ( 'NONE',  ( -13.97604488694547697, 13.89961937509957934, 28.12609039468565797 ) ) ;
#122986 = CARTESIAN_POINT ( 'NONE',  ( -9.474510206698964154, 16.51473224551069663, 110.4155762719810383 ) ) ;
#122987 = EDGE_CURVE ( 'NONE', #68306, #139247, #35161, .T. ) ;
#122988 = CARTESIAN_POINT ( 'NONE',  ( -21.53943276465977519, 0.05219959533907696930, 76.24890960531435269 ) ) ;
#122989 = CARTESIAN_POINT ( 'NONE',  ( 13.97604488694527802, 13.89961937509977652, 114.3739096053143669 ) ) ;
#122990 = CARTESIAN_POINT ( 'NONE',  ( -0.05219959533936034679, 19.03943276465977164, 102.5010903946856757 ) ) ;
#122991 = CARTESIAN_POINT ( 'NONE',  ( -19.02544592524342804, 5.153800228976336051, 116.0405762719810383 ) ) ;
#122992 = CARTESIAN_POINT ( 'NONE',  ( 19.03943276465977164, 0.05219959533936151252, 111.2510903946856757 ) ) ;
#122993 = CARTESIAN_POINT ( 'NONE',  ( -19.03943276465977164, 0.05219959533909376836, 36.24890960531436690 ) ) ;
#122994 = CARTESIAN_POINT ( 'NONE',  ( -19.05341960407611168, -5.049401038298163336, 101.4572429386476955 ) ) ;
#122995 = CARTESIAN_POINT ( 'NONE',  ( -10.81492255796078084, -18.62759615963271287, 77.08224293864769550 ) ) ;
#122996 = CARTESIAN_POINT ( 'NONE',  ( -12.14591786802326823, 12.06949235617739902, 63.12609039468568994 ) ) ;
#122997 = CARTESIAN_POINT ( 'NONE',  ( -21.55341960407619339, 5.719274019375674811, 58.54275706135235424 ) ) ;
#122999 = CARTESIAN_POINT ( 'NONE',  ( 15.72974639402176855, 15.80617190586768217, 111.8760903946856615 ) ) ;
#122998 = CARTESIAN_POINT ( 'NONE',  ( 16.51473224551083163, -9.474510206698727899, 105.8344237280190043 ) ) ;
#123000 = CARTESIAN_POINT ( 'NONE',  ( -12.14591786802326823, 12.06949235617739902, 108.1260903946856757 ) ) ;
#123001 = CARTESIAN_POINT ( 'NONE',  ( 18.62759615963271287, -10.81492255796078972, 103.3322429386476955 ) ) ;
#123002 = CARTESIAN_POINT ( 'NONE',  ( -4.379528057220328563, 16.55341960407611168, 35.20724293864768839 ) ) ;
#123003 = CARTESIAN_POINT ( 'NONE',  ( 19.05341960407617918, -5.049401038297876454, 76.04275706135230450 ) ) ;
#123004 = CARTESIAN_POINT ( 'NONE',  ( -5.719274019375665041, -21.55341960407619695, 54.79275706135235424 ) ) ;
#123005 = CARTESIAN_POINT ( 'NONE',  ( -19.03943276465977164, -0.05219959533935918106, 33.75109039468566863 ) ) ;
#123006 = CARTESIAN_POINT ( 'NONE',  ( 12.06949235617757843, -12.14591786802309237, 103.1239096053143811 ) ) ;
#123007 = CARTESIAN_POINT ( 'NONE',  ( 0.05219959533907565091, 21.53943276465977519, 29.99890960531435979 ) ) ;
#123008 = CARTESIAN_POINT ( 'NONE',  ( 16.52544592524342804, -4.483927247898539470, 38.54057627198103120 ) ) ;
#123009 = CARTESIAN_POINT ( 'NONE',  ( -18.62759615963255300, -10.81492255796106328, 104.1677570613523471 ) ) ;
#123010 = CARTESIAN_POINT ( 'NONE',  ( -12.06949235617739369, -12.14591786802326823, 59.37609039468568284 ) ) ;
#123011 = CARTESIAN_POINT ( 'NONE',  ( -16.52544592524342804, 4.483927247898546575, 26.04057627198103475 ) ) ;
#123012 = CARTESIAN_POINT ( 'NONE',  ( -18.62759615963255300, -10.81492255796106328, 69.16775706135234714 ) ) ;
#123013 = CARTESIAN_POINT ( 'NONE',  ( 21.53943276465977519, 0.05219959533937863772, 51.25109039468568994 ) ) ;
#123014 = ORIENTED_EDGE ( 'NONE', *, *, #136319, .T. ) ;
#123015 = CARTESIAN_POINT ( 'NONE',  ( -19.05341960407611168, -5.049401038298163336, 21.45724293864768839 ) ) ;
#123016 = CARTESIAN_POINT ( 'NONE',  ( -10.81492255796105439, 18.62759615963255655, 47.91775706135234714 ) ) ;
#123017 = CARTESIAN_POINT ( 'NONE',  ( -12.06949235617756955, 12.14591786802309770, 110.6239096053143669 ) ) ;
#123018 = CARTESIAN_POINT ( 'NONE',  ( 19.02544592524343514, -5.153800228976328945, 43.54057627198103120 ) ) ;
#123019 = CARTESIAN_POINT ( 'NONE',  ( 4.379528057220339221, -16.55341960407611168, 82.70724293864770971 ) ) ;
#123020 = CARTESIAN_POINT ( 'NONE',  ( -16.51473224551069308, -9.474510206698971260, 71.66557627198102409 ) ) ;
#123021 = CARTESIAN_POINT ( 'NONE',  ( 12.06949235617757843, -12.14591786802309237, 28.12390960531435979 ) ) ;
#123022 = CARTESIAN_POINT ( 'NONE',  ( -21.55341960407610458, -5.719274019375992779, 56.45724293864768839 ) ) ;
#123023 = CARTESIAN_POINT ( 'NONE',  ( 0.05219959533910956823, 16.53943276465976808, 89.99890960531438111 ) ) ;
#123024 = CARTESIAN_POINT ( 'NONE',  ( 5.719274019375991003, -21.55341960407610458, 107.7072429386476955 ) ) ;
#123025 = CARTESIAN_POINT ( 'NONE',  ( -9.474510206698964154, 16.51473224551069663, 100.4155762719810241 ) ) ;
#123027 = CARTESIAN_POINT ( 'NONE',  ( 5.153800228976615827, -19.02544592524334988, 110.2094237280189901 ) ) ;
#123026 = CARTESIAN_POINT ( 'NONE',  ( 13.89961937509977652, -13.97604488694527269, 58.12390960531436690 ) ) ;
#123028 = CARTESIAN_POINT ( 'NONE',  ( 5.719274019375991003, -21.55341960407610458, 62.70724293864769550 ) ) ;
#123029 = CARTESIAN_POINT ( 'NONE',  ( 5.823673210054444382, -21.52544592524334988, 80.20942372801901854 ) ) ;
#123030 = CARTESIAN_POINT ( 'NONE',  ( 9.564922557960805705, 16.46253265017160317, 69.58224293864770971 ) ) ;
#123031 = CARTESIAN_POINT ( 'NONE',  ( -5.049401038298153566, 19.05341960407611168, 100.2072429386476955 ) ) ;
#123032 = CARTESIAN_POINT ( 'NONE',  ( -4.483927247898782831, 16.52544592524335698, 82.70942372801900433 ) ) ;
#123033 = CARTESIAN_POINT ( 'NONE',  ( 21.52544592524334988, 5.823673210054432836, 56.45942372801902565 ) ) ;
#123034 = CARTESIAN_POINT ( 'NONE',  ( 10.81492255796106328, -18.62759615963255655, 90.41775706135236135 ) ) ;
#123035 = CARTESIAN_POINT ( 'NONE',  ( -15.72974639402197994, 15.80617190586746368, 110.6239096053143669 ) ) ;
#123036 = CARTESIAN_POINT ( 'NONE',  ( -14.34966873604972548, 8.224510206698743886, 83.33442372801903275 ) ) ;
#123037 = CARTESIAN_POINT ( 'NONE',  ( -18.67979575497178146, -10.72451020669898902, 71.66557627198100988 ) ) ;
#123038 = CARTESIAN_POINT ( 'NONE',  ( -19.05341960407617563, 5.049401038297882671, 43.54275706135232582 ) ) ;
#123039 = CARTESIAN_POINT ( 'NONE',  ( 0.05219959533907565091, 21.53943276465977519, 44.99890960531435979 ) ) ;
#123041 = CARTESIAN_POINT ( 'NONE',  ( -16.53943276465976808, 0.05219959533911058130, 26.24890960531435624 ) ) ;
#123040 = CARTESIAN_POINT ( 'NONE',  ( -0.05219959533909027116, -19.03943276465977164, 82.49890960531436690 ) ) ;
#123042 = CARTESIAN_POINT ( 'NONE',  ( -16.19135201231369692, 7.376712067591781441, 64.81319145947969673 ) ) ;
#123043 = CARTESIAN_POINT ( 'NONE',  ( -9.564922557960796823, -16.46253265017161027, 112.0822429386476955 ) ) ;
#123044 = CARTESIAN_POINT ( 'NONE',  ( 18.22780087662122384, -5.500000000000022204, 46.01540105326107266 ) ) ;
#123045 = CARTESIAN_POINT ( 'NONE',  ( -19.05341960407617563, 5.049401038297882671, 88.54275706135230450 ) ) ;
#123046 = CARTESIAN_POINT ( 'NONE',  ( 18.62759615963271287, -10.81492255796078972, 73.33224293864769550 ) ) ;
#123047 = CARTESIAN_POINT ( 'NONE',  ( 14.29746914071049879, -8.314922557960816363, 48.33224293864770260 ) ) ;
#123048 = CARTESIAN_POINT ( 'NONE',  ( 13.89961937509957401, 13.97604488694547697, 111.8760903946856757 ) ) ;
#123049 = CARTESIAN_POINT ( 'NONE',  ( -16.46253265017160317, 9.564922557960807481, 35.83224293864768839 ) ) ;
#123050 = CARTESIAN_POINT ( 'NONE',  ( 16.51473224551083163, -9.474510206698727899, 105.8344237280190043 ) ) ;
#123052 = CARTESIAN_POINT ( 'NONE',  ( 5.153800228976615827, -19.02544592524334988, 65.20942372801900433 ) ) ;
#123051 = CARTESIAN_POINT ( 'NONE',  ( -5.823673210054116645, -21.52544592524344225, 102.2905762719810383 ) ) ;
#123053 = CARTESIAN_POINT ( 'NONE',  ( -14.29746914071037622, -8.314922557961029526, 74.16775706135231871 ) ) ;
#123054 = CARTESIAN_POINT ( 'NONE',  ( -19.05341960407611168, -5.049401038298163336, 86.45724293864769550 ) ) ;
#123055 = CARTESIAN_POINT ( 'NONE',  ( 8.314922557960818139, 14.29746914071049879, 74.58224293864768129 ) ) ;
#123056 = CARTESIAN_POINT ( 'NONE',  ( -13.97604488694527625, -13.89961937509977652, 56.87390960531434558 ) ) ;
#123057 = CARTESIAN_POINT ( 'NONE',  ( -16.55341960407611168, -4.379528057220339221, 71.45724293864769550 ) ) ;
#123058 = CARTESIAN_POINT ( 'NONE',  ( 16.51473224551069308, 9.474510206698969483, 29.16557627198103475 ) ) ;
#123059 = CARTESIAN_POINT ( 'NONE',  ( -36.86261346499077263, -5.499032313789903093, 44.62661474502114345 ) ) ;
#123060 = CARTESIAN_POINT ( 'NONE',  ( -16.55341960407611168, -4.379528057220339221, 46.45724293864769550 ) ) ;
#123061 = CARTESIAN_POINT ( 'NONE',  ( 9.564922557960805705, 16.46253265017160317, 89.58224293864769550 ) ) ;
#123062 = CARTESIAN_POINT ( 'NONE',  ( -3.573655867282028392E-15, 2.428612866367529932E-14, -8.000000000000000000 ) ) ;
#123063 = CARTESIAN_POINT ( 'NONE',  ( 5.153800228976615827, -19.02544592524334988, 55.20942372801899722 ) ) ;
#123064 = CARTESIAN_POINT ( 'NONE',  ( 12.06949235617739724, 12.14591786802326823, 61.87609039468568284 ) ) ;
#123065 = CARTESIAN_POINT ( 'NONE',  ( 21.55341960407610458, 5.719274019375980345, 58.95724293864770971 ) ) ;
#123066 = CARTESIAN_POINT ( 'NONE',  ( 19.02544592524334988, 5.153800228976608722, 26.45942372801899722 ) ) ;
#123067 = CARTESIAN_POINT ( 'NONE',  ( 9.474510206698971260, -16.51473224551069308, 92.91557627198103830 ) ) ;
#123068 = CARTESIAN_POINT ( 'NONE',  ( 0.3535533905931536602, -35.00000000000000000, 4.646446609406721606 ) ) ;
#123069 = CARTESIAN_POINT ( 'NONE',  ( -10.72451020669898014, 18.67979575497178502, 25.41557627198103120 ) ) ;
#123070 = CARTESIAN_POINT ( 'NONE',  ( -19.02544592524342804, 5.153800228976336051, 61.04057627198103120 ) ) ;
#123071 = CARTESIAN_POINT ( 'NONE',  ( 18.67979575497194134, -10.72451020669871369, 50.83442372801901143 ) ) ;
#123072 = CARTESIAN_POINT ( 'NONE',  ( 14.29746914071049879, -8.314922557960816363, 103.3322429386476955 ) ) ;
#123075 = VERTEX_POINT ( 'NONE', #84916 ) ;
#123074 = CARTESIAN_POINT ( 'NONE',  ( 5.153800228976335163, 19.02544592524342804, 99.79057627198102409 ) ) ;
#123073 = CARTESIAN_POINT ( 'NONE',  ( 10.81492255796078972, 18.62759615963270932, 104.5822429386477097 ) ) ;
#123076 = CARTESIAN_POINT ( 'NONE',  ( -5.719274019375665041, -21.55341960407619695, 34.79275706135235424 ) ) ;
#123077 = VERTEX_POINT ( 'NONE', #62885 ) ;
#123078 = CARTESIAN_POINT ( 'NONE',  ( -19.03943276465977164, 0.05219959533909376836, 101.2489096053143669 ) ) ;
#123079 = LINE ( 'NONE', #105930, #178682 ) ;
#123080 = CARTESIAN_POINT ( 'NONE',  ( 18.67979575497178502, 10.72451020669898547, 94.16557627198103830 ) ) ;
#123081 = CARTESIAN_POINT ( 'NONE',  ( -9.564922557960796823, -16.46253265017161027, 42.08224293864769550 ) ) ;
#123082 = CARTESIAN_POINT ( 'NONE',  ( -8.224510206698735004, -14.34966873604973081, 19.58442372801901143 ) ) ;
#123083 = CARTESIAN_POINT ( 'NONE',  ( 38.00000000000000711, -12.34694845685040754, -10.84999999453762598 ) ) ;
#123084 = CARTESIAN_POINT ( 'NONE',  ( 16.46253265017160672, -9.564922557960803928, 28.33224293864769550 ) ) ;
#123085 = CARTESIAN_POINT ( 'NONE',  ( 18.67979575497194134, -10.72451020669871369, 100.8344237280190185 ) ) ;
#123087 = CARTESIAN_POINT ( 'NONE',  ( -0.05219959533937732626, 21.53943276465977519, 47.50109039468568994 ) ) ;
#123086 = CARTESIAN_POINT ( 'NONE',  ( 16.51473224551069308, 9.474510206698969483, 74.16557627198103830 ) ) ;
#123088 = CARTESIAN_POINT ( 'NONE',  ( -0.05219959533937732626, 21.53943276465977519, 27.50109039468567929 ) ) ;
#123089 = CARTESIAN_POINT ( 'NONE',  ( 17.14385361876520264, 23.59649016807275856, 146.6750000027311671 ) ) ;
#123090 = CARTESIAN_POINT ( 'NONE',  ( 19.02544592524343514, -5.153800228976328945, 103.5405762719809957 ) ) ;
#123091 = CARTESIAN_POINT ( 'NONE',  ( -69.65682714487590488, -71.74905178543390605, -4.999999999999999112 ) ) ;
#123094 = CARTESIAN_POINT ( 'NONE',  ( -21.52544592524334988, -5.823673210054445271, 53.95942372801900433 ) ) ;
#123093 = CARTESIAN_POINT ( 'NONE',  ( 16.55341960407618274, -4.379528057220086978, 71.04275706135234714 ) ) ;
#123092 = CARTESIAN_POINT ( 'NONE',  ( -16.52544592524335698, -4.483927247898792601, 33.95942372801901143 ) ) ;
#123095 = CARTESIAN_POINT ( 'NONE',  ( 21.55341960407619695, -5.719274019375665929, 81.04275706135236135 ) ) ;
#123096 = CARTESIAN_POINT ( 'NONE',  ( 4.179973224035756552, 4.460769206500171613, -62.50518786092069945 ) ) ;
#123097 = CARTESIAN_POINT ( 'NONE',  ( -19.03943276465977164, -0.05219959533935918106, 103.7510903946856757 ) ) ;
#123098 = CARTESIAN_POINT ( 'NONE',  ( 19.05341960407611168, 5.049401038298154454, 73.95724293864768129 ) ) ;
#123099 = CARTESIAN_POINT ( 'NONE',  ( 19.03943276465977164, -0.05219959533909143690, 93.74890960531435269 ) ) ;
#123100 = CARTESIAN_POINT ( 'NONE',  ( 12.14591786802309770, 12.06949235617756955, 109.3739096053143811 ) ) ;
#123102 = EDGE_CURVE ( 'NONE', #123348, #114473, #121564, .T. ) ;
#123101 = CARTESIAN_POINT ( 'NONE',  ( -18.62759615963270932, 10.81492255796079327, 25.83224293864769194 ) ) ;
#123103 = CARTESIAN_POINT ( 'NONE',  ( 4.379528057220092307, 16.55341960407617563, 87.29275706135236135 ) ) ;
#123105 = CARTESIAN_POINT ( 'NONE',  ( -16.46253265017160317, 9.564922557960807481, 50.83224293864770260 ) ) ;
#123104 = CARTESIAN_POINT ( 'NONE',  ( 8.224510206698953496, -14.34966873604960469, 72.91557627198103830 ) ) ;
#123106 = CARTESIAN_POINT ( 'NONE',  ( -18.62759615963255300, -10.81492255796106328, 74.16775706135231871 ) ) ;
#123107 = CARTESIAN_POINT ( 'NONE',  ( 17.79613651744294245, -24.49428055684527550, 144.9656553485623647 ) ) ;
#123108 = CARTESIAN_POINT ( 'NONE',  ( -13.97604488694547697, 13.89961937509957934, 108.1260903946856331 ) ) ;
#123109 = CARTESIAN_POINT ( 'NONE',  ( 4.483927247898545687, 16.52544592524342804, 74.79057627198105251 ) ) ;
#123110 = CARTESIAN_POINT ( 'NONE',  ( 18.67979575497194134, -10.72451020669871369, 25.83442372801901499 ) ) ;
#123111 = CARTESIAN_POINT ( 'NONE',  ( 15.72974639402199770, -15.80617190586745480, 63.12390960531435979 ) ) ;
#123112 = CARTESIAN_POINT ( 'NONE',  ( -16.36317988757055630, -7.306389748694962272, 105.9021039163677358 ) ) ;
#123113 = CARTESIAN_POINT ( 'NONE',  ( -28.82186960331499037, 2.428612866367529932E-14, 144.2500000054623683 ) ) ;
#123114 = CARTESIAN_POINT ( 'NONE',  ( -19.05341960407611168, -5.049401038298163336, 86.45724293864769550 ) ) ;
#123115 = CARTESIAN_POINT ( 'NONE',  ( -14.29746914071049879, 8.314922557960819915, 50.83224293864770971 ) ) ;
#123116 = CARTESIAN_POINT ( 'NONE',  ( 12.14591786802309770, 12.06949235617756955, 24.37390960531435979 ) ) ;
#123117 = CARTESIAN_POINT ( 'NONE',  ( 4.483927247898790824, -16.52544592524335698, 95.20942372801903275 ) ) ;
#123118 = CARTESIAN_POINT ( 'NONE',  ( 5.049401038297881783, 19.05341960407617563, 52.29275706135234003 ) ) ;
#123119 = CARTESIAN_POINT ( 'NONE',  ( 11.74264578624799427, 36.14014761921585972, -8.599999999999999645 ) ) ;
#123120 = CARTESIAN_POINT ( 'NONE',  ( -13.89961937509977652, 13.97604488694528158, 105.6239096053143527 ) ) ;
#123121 = CARTESIAN_POINT ( 'NONE',  ( -16.53943276465976808, 0.05219959533911058130, 76.24890960531435269 ) ) ;
#123122 = CARTESIAN_POINT ( 'NONE',  ( -0.05219959533936034679, 19.03943276465977164, 37.50109039468567573 ) ) ;
#123124 = CARTESIAN_POINT ( 'NONE',  ( 18.62759615963271287, -10.81492255796078972, 33.33224293864769550 ) ) ;
#123123 = CARTESIAN_POINT ( 'NONE',  ( 9.564922557960805705, 16.46253265017160317, 34.58224293864770260 ) ) ;
#123126 = ORIENTED_EDGE ( 'NONE', *, *, #111802, .F. ) ;
#123125 = CARTESIAN_POINT ( 'NONE',  ( -21.53943276465977519, 0.05219959533907696930, 71.24890960531435269 ) ) ;
#123127 = CARTESIAN_POINT ( 'NONE',  ( 14.29746914071049879, -8.314922557960816363, 103.3322429386476955 ) ) ;
#123128 = CARTESIAN_POINT ( 'NONE',  ( -0.05219959533934338120, 16.53943276465976808, 47.50109039468568994 ) ) ;
#123129 = CARTESIAN_POINT ( 'NONE',  ( -21.55341960407619339, 5.719274019375674811, 43.54275706135235424 ) ) ;
#123130 = CARTESIAN_POINT ( 'NONE',  ( 16.52544592524342804, -4.483927247898539470, 98.54057627198105251 ) ) ;
#123131 = LINE ( 'NONE', #139299, #122109 ) ;
#123132 = CARTESIAN_POINT ( 'NONE',  ( -29.86685920354755197, -21.69954338932560134, -10.92499999726881299 ) ) ;
#123133 = CARTESIAN_POINT ( 'NONE',  ( -18.62759615963270932, 10.81492255796079327, 30.83224293864770260 ) ) ;
#123134 = CARTESIAN_POINT ( 'NONE',  ( 17.26058549869091507, -6.457015423128606102, 66.12254162523933587 ) ) ;
#123135 = CARTESIAN_POINT ( 'NONE',  ( 28.82186960331480208, -9.364793116373776982, 142.9000000000000057 ) ) ;
#123137 = CARTESIAN_POINT ( 'NONE',  ( 8.224510206698953496, -14.34966873604960469, 27.91557627198103830 ) ) ;
#123136 = CARTESIAN_POINT ( 'NONE',  ( -8.314922557961024197, 14.29746914071037800, 37.91775706135235424 ) ) ;
#123138 = CARTESIAN_POINT ( 'NONE',  ( -10.81492255796078084, -18.62759615963271287, 57.08224293864769550 ) ) ;
#123139 = CARTESIAN_POINT ( 'NONE',  ( 19.05341960407617918, -5.049401038297876454, 81.04275706135231871 ) ) ;
#123140 = CARTESIAN_POINT ( 'NONE',  ( 15.80617190586746368, 15.72974639402197994, 59.37390960531436690 ) ) ;
#123141 = DIRECTION ( 'NONE',  ( 1.000000000000000000, 0.000000000000000000, 0.000000000000000000 ) ) ;
#123142 = CARTESIAN_POINT ( 'NONE',  ( -4.379528057220086978, -16.55341960407618274, 49.79275706135234714 ) ) ;
#123144 = CARTESIAN_POINT ( 'NONE',  ( -9.474510206698964154, 16.51473224551069663, 105.4155762719810383 ) ) ;
#123143 = CARTESIAN_POINT ( 'NONE',  ( -0.05219959533909027116, -19.03943276465977164, 32.49890960531435979 ) ) ;
#123145 = CARTESIAN_POINT ( 'NONE',  ( -9.564922557960796823, -16.46253265017161027, 42.08224293864769550 ) ) ;
#123146 = CARTESIAN_POINT ( 'NONE',  ( -5.049401038298153566, 19.05341960407611168, 25.20724293864768484 ) ) ;
#123147 = CARTESIAN_POINT ( 'NONE',  ( 0.000000000000000000, 0.000000000000000000, 0.000000000000000000 ) ) ;
#123148 = CARTESIAN_POINT ( 'NONE',  ( -13.97604488694527625, -13.89961937509977652, 111.8739096053143243 ) ) ;
#123149 = ORIENTED_EDGE ( 'NONE', *, *, #183499, .F. ) ;
#123150 = CARTESIAN_POINT ( 'NONE',  ( 16.55341960407618274, -4.379528057220086978, 66.04275706135236135 ) ) ;
#123151 = CARTESIAN_POINT ( 'NONE',  ( 15.72974639402199770, -15.80617190586745480, 88.12390960531436690 ) ) ;
#123152 = CARTESIAN_POINT ( 'NONE',  ( -5.049401038298153566, 19.05341960407611168, 55.20724293864769550 ) ) ;
#123153 = CARTESIAN_POINT ( 'NONE',  ( -10.81492255796105439, 18.62759615963255655, 22.91775706135235069 ) ) ;
#123154 = CARTESIAN_POINT ( 'NONE',  ( -0.05219959533909027116, -19.03943276465977164, 82.49890960531436690 ) ) ;
#123155 = CARTESIAN_POINT ( 'NONE',  ( -34.17105881114489563, -20.77207671795436639, -21.54825371331532935 ) ) ;
#123156 = ORIENTED_EDGE ( 'NONE', *, *, #131013, .T. ) ;
#123157 = CARTESIAN_POINT ( 'NONE',  ( 0.05219959533907565091, 21.53943276465977519, 114.9989096053143669 ) ) ;
#123160 = CARTESIAN_POINT ( 'NONE',  ( -5.153800228976607833, 19.02544592524334988, 72.70942372801900433 ) ) ;
#123159 = CARTESIAN_POINT ( 'NONE',  ( -5.049401038298153566, 19.05341960407611168, 110.2072429386476671 ) ) ;
#123158 = CARTESIAN_POINT ( 'NONE',  ( 12.14591786802309770, 12.06949235617756955, 114.3739096053143527 ) ) ;
#123161 = CARTESIAN_POINT ( 'NONE',  ( 13.97604488694548053, -13.89961937509957401, 30.62609039468566863 ) ) ;
#123162 = CARTESIAN_POINT ( 'NONE',  ( -0.05219959533907301413, -21.53943276465977519, 97.49890960531436690 ) ) ;
#123163 = CARTESIAN_POINT ( 'NONE',  ( 5.049401038297881783, 19.05341960407617563, 37.29275706135232582 ) ) ;
#123164 = CARTESIAN_POINT ( 'NONE',  ( -12.14591786802326823, 12.06949235617739902, 83.12609039468568994 ) ) ;
#123165 = CARTESIAN_POINT ( 'NONE',  ( -19.05341960407611168, -5.049401038298163336, 106.4572429386476955 ) ) ;
#123166 = CARTESIAN_POINT ( 'NONE',  ( 16.46253265017160672, -9.564922557960803928, 53.33224293864768839 ) ) ;
#123167 = CARTESIAN_POINT ( 'NONE',  ( 21.55341960407619695, -5.719274019375665929, 61.04275706135234714 ) ) ;
#123168 = CARTESIAN_POINT ( 'NONE',  ( -21.52544592524334988, -5.823673210054445271, 78.95942372801901854 ) ) ;
#123169 = CARTESIAN_POINT ( 'NONE',  ( -18.09867054820433907, -5.499999999999827693, 53.98393025253585620 ) ) ;
#123170 = CARTESIAN_POINT ( 'NONE',  ( -19.05341960407611168, -5.049401038298163336, 71.45724293864766707 ) ) ;
#123171 = CARTESIAN_POINT ( 'NONE',  ( -5.719274019375665041, -21.55341960407619695, 44.79275706135234714 ) ) ;
#123172 = CARTESIAN_POINT ( 'NONE',  ( -13.89961937509957401, -13.97604488694547875, 89.37609039468563310 ) ) ;
#123173 = CARTESIAN_POINT ( 'NONE',  ( 9.564922557960805705, 16.46253265017160317, 54.58224293864769550 ) ) ;
#123174 = CARTESIAN_POINT ( 'NONE',  ( 9.474510206698971260, -16.51473224551069308, 92.91557627198103830 ) ) ;
#123175 = CARTESIAN_POINT ( 'NONE',  ( -5.049401038298153566, 19.05341960407611168, 60.20724293864768129 ) ) ;
#123176 = CARTESIAN_POINT ( 'NONE',  ( -17.26058549869094350, -6.457015423128473763, 91.37745837476069255 ) ) ;
#123177 = CARTESIAN_POINT ( 'NONE',  ( -13.89961937509977652, 13.97604488694528158, 55.62390960531434558 ) ) ;
#123178 = CARTESIAN_POINT ( 'NONE',  ( 21.52544592524344225, -5.823673210054117533, 103.5405762719810383 ) ) ;
#123179 = CARTESIAN_POINT ( 'NONE',  ( -0.05219959533934338120, 16.53943276465976808, 92.50109039468567573 ) ) ;
#123180 = CARTESIAN_POINT ( 'NONE',  ( -22.72581825106501796, 12.75361973299702534, 165.5645137041830139 ) ) ;
#123181 = CARTESIAN_POINT ( 'NONE',  ( 16.51473224551083163, -9.474510206698727899, 50.83442372801899722 ) ) ;
#123182 = CARTESIAN_POINT ( 'NONE',  ( -19.05341960407611168, -5.049401038298163336, 61.45724293864769550 ) ) ;
#123183 = CARTESIAN_POINT ( 'NONE',  ( 16.55341960407611168, 4.379528057220329451, 58.95724293864770971 ) ) ;
#123184 = CARTESIAN_POINT ( 'NONE',  ( -16.53943276465976808, 0.05219959533911058130, 91.24890960531436690 ) ) ;
#123185 = CARTESIAN_POINT ( 'NONE',  ( 10.72451020669898902, -18.67979575497178502, 22.91557627198102765 ) ) ;
#123186 = CARTESIAN_POINT ( 'NONE',  ( 13.89961937509977652, -13.97604488694527269, 98.12390960531433848 ) ) ;
#123187 = CARTESIAN_POINT ( 'NONE',  ( 19.05341960407611168, 5.049401038298154454, 103.9572429386476671 ) ) ;
#123188 = CARTESIAN_POINT ( 'NONE',  ( 0.05219959533936267826, -19.03943276465977164, 20.00109039468567218 ) ) ;
#123189 = CARTESIAN_POINT ( 'NONE',  ( -16.53943276465976808, -0.05219959533934237506, 88.75109039468567573 ) ) ;
#123190 = CARTESIAN_POINT ( 'NONE',  ( -13.97604488694527625, -13.89961937509977652, 71.87390960531433848 ) ) ;
#123191 = CARTESIAN_POINT ( 'NONE',  ( -18.67979575497193778, 10.72451020669871902, 38.33442372801900433 ) ) ;
#123192 = CARTESIAN_POINT ( 'NONE',  ( 5.719274019375991003, -21.55341960407610458, 27.70724293864769905 ) ) ;
#123193 = CARTESIAN_POINT ( 'NONE',  ( 15.72974639402199770, -15.80617190586745480, 113.1239096053143953 ) ) ;
#123194 = CARTESIAN_POINT ( 'NONE',  ( -5.823673210054116645, -21.52544592524344225, 72.29057627198102409 ) ) ;
#123195 = CARTESIAN_POINT ( 'NONE',  ( 14.29746914071049879, -8.314922557960816363, 78.33224293864770971 ) ) ;
#123196 = CARTESIAN_POINT ( 'NONE',  ( -0.05219959533936034679, 19.03943276465977164, 37.50109039468567573 ) ) ;
#123197 = CARTESIAN_POINT ( 'NONE',  ( 8.314922557960818139, 14.29746914071049879, 114.5822429386477097 ) ) ;
#123198 = CARTESIAN_POINT ( 'NONE',  ( -16.51473224551069308, -9.474510206698971260, 86.66557627198102409 ) ) ;
#123199 = CARTESIAN_POINT ( 'NONE',  ( 19.02544592524343514, -5.153800228976328945, 78.54057627198099567 ) ) ;
#123200 = CARTESIAN_POINT ( 'NONE',  ( -5.359611314223446995E-15, 29.16686587814335851, 146.3750000027311842 ) ) ;
#123201 = CARTESIAN_POINT ( 'NONE',  ( 0.05219959533910956823, 16.53943276465976808, 94.99890960531436690 ) ) ;
#123202 = ORIENTED_EDGE ( 'NONE', *, *, #48034, .F. ) ;
#123203 = CARTESIAN_POINT ( 'NONE',  ( -14.29746914071037622, -8.314922557961029526, 109.1677570613523613 ) ) ;
#123204 = CARTESIAN_POINT ( 'NONE',  ( 16.55341960407618274, -4.379528057220086978, 26.04275706135235779 ) ) ;
#123205 = CARTESIAN_POINT ( 'NONE',  ( 10.72451020669871369, 18.67979575497193778, 87.08442372801901854 ) ) ;
#123206 = CARTESIAN_POINT ( 'NONE',  ( -13.97604488694527625, -13.89961937509977652, 106.8739096053143669 ) ) ;
#123207 = CARTESIAN_POINT ( 'NONE',  ( 21.52544592524334988, 5.823673210054432836, 21.45942372801901499 ) ) ;
#123208 = CARTESIAN_POINT ( 'NONE',  ( 16.46253265017160672, -9.564922557960803928, 33.33224293864770260 ) ) ;
#123209 = CARTESIAN_POINT ( 'NONE',  ( -14.29746914071037622, -8.314922557961029526, 34.16775706135234714 ) ) ;
#123210 = CARTESIAN_POINT ( 'NONE',  ( -19.05341960407617563, 5.049401038297882671, 98.54275706135233293 ) ) ;
#123211 = CARTESIAN_POINT ( 'NONE',  ( -21.53943276465977519, 0.05219959533907696930, 91.24890960531436690 ) ) ;
#123212 = CARTESIAN_POINT ( 'NONE',  ( -19.03943276465977164, -0.05219959533935918106, 73.75109039468566152 ) ) ;
#123213 = CARTESIAN_POINT ( 'NONE',  ( 9.474510206698971260, -16.51473224551069308, 22.91557627198102765 ) ) ;
#123214 = CARTESIAN_POINT ( 'NONE',  ( -15.72974639402197994, 15.80617190586746368, 110.6239096053143669 ) ) ;
#123215 = LINE ( 'NONE', #187908, #62705 ) ;
#123216 = CARTESIAN_POINT ( 'NONE',  ( 13.97604488694527802, 13.89961937509977652, 89.37390960531436690 ) ) ;
#123217 = PLANE ( 'NONE',  #193971 ) ;
#123218 = CARTESIAN_POINT ( 'NONE',  ( -5.153800228976328057, -19.02544592524343514, 82.29057627198103830 ) ) ;
#123220 = CARTESIAN_POINT ( 'NONE',  ( -16.53943276465976808, 0.05219959533911058130, 81.24890960531436690 ) ) ;
#123219 = CARTESIAN_POINT ( 'NONE',  ( -5.719274019375665041, -21.55341960407619695, 19.79275706135235069 ) ) ;
#123221 = CARTESIAN_POINT ( 'NONE',  ( 5.049401038298161559, -19.05341960407611168, 82.70724293864770971 ) ) ;
#123223 = CARTESIAN_POINT ( 'NONE',  ( -16.51473224551082808, 9.474510206698731452, 53.33442372801900433 ) ) ;
#123222 = CARTESIAN_POINT ( 'NONE',  ( 4.379528057220092307, 16.55341960407617563, 52.29275706135236135 ) ) ;
#123224 = CARTESIAN_POINT ( 'NONE',  ( 15.72974639402176855, 15.80617190586768217, 61.87609039468568284 ) ) ;
#123225 = CARTESIAN_POINT ( 'NONE',  ( 8.224510206698742110, 14.34966873604972548, 22.08442372801901143 ) ) ;
#123226 = CARTESIAN_POINT ( 'NONE',  ( 5.153800228976335163, 19.02544592524342804, 74.79057627198103830 ) ) ;
#123227 = CARTESIAN_POINT ( 'NONE',  ( -5.049401038297874678, -19.05341960407617918, 89.79275706135230450 ) ) ;
#123228 = CARTESIAN_POINT ( 'NONE',  ( 0.05219959533934541429, -16.53943276465976808, 50.00109039468568994 ) ) ;
#123229 = CARTESIAN_POINT ( 'NONE',  ( 21.52544592524334988, 5.823673210054432836, 91.45942372801901854 ) ) ;
#123230 = CARTESIAN_POINT ( 'NONE',  ( 16.51473224551083163, -9.474510206698727899, 75.83442372801900433 ) ) ;
#123231 = CARTESIAN_POINT ( 'NONE',  ( -19.05341960407611168, -5.049401038298163336, 46.45724293864768129 ) ) ;
#123232 = CARTESIAN_POINT ( 'NONE',  ( 21.53943276465977519, -0.05219959533907433946, 73.74890960531433848 ) ) ;
#123234 = CARTESIAN_POINT ( 'NONE',  ( -13.97604488694547697, 13.89961937509957934, 83.12609039468564731 ) ) ;
#123233 = CARTESIAN_POINT ( 'NONE',  ( -14.34966873604960291, -8.224510206698953496, 71.66557627198100988 ) ) ;
#123235 = FACE_OUTER_BOUND ( 'NONE', #173045, .T. ) ;
#123236 = CARTESIAN_POINT ( 'NONE',  ( 9.474510206698729675, 16.51473224551082808, 42.08442372801900433 ) ) ;
#123237 = CARTESIAN_POINT ( 'NONE',  ( -8.314922557960811034, -14.29746914071050412, 22.08224293864769194 ) ) ;
#123238 = CARTESIAN_POINT ( 'NONE',  ( 12.14591786802309770, 12.06949235617756955, 69.37390960531436690 ) ) ;
#123240 = CARTESIAN_POINT ( 'NONE',  ( 17.14385361876520264, 23.59649016807275856, 146.1750000027311387 ) ) ;
#123239 = CARTESIAN_POINT ( 'NONE',  ( -18.67979575497193778, 10.72451020669871902, 108.3344237280190185 ) ) ;
#123241 = CARTESIAN_POINT ( 'NONE',  ( -10.81492255796078084, -18.62759615963271287, 107.0822429386476955 ) ) ;
#123242 = CARTESIAN_POINT ( 'NONE',  ( 19.03943276465977164, -0.05219959533909143690, 63.74890960531435979 ) ) ;
#123243 = CARTESIAN_POINT ( 'NONE',  ( 18.67979575497194134, -10.72451020669871369, 80.83442372801901854 ) ) ;
#123244 = CARTESIAN_POINT ( 'NONE',  ( 19.05341960407611168, 5.049401038298154454, 58.95724293864768129 ) ) ;
#123245 = ORIENTED_EDGE ( 'NONE', *, *, #53412, .F. ) ;
#123246 = CARTESIAN_POINT ( 'NONE',  ( -13.89961937509977652, 13.97604488694528158, 25.62390960531434558 ) ) ;
#123247 = CARTESIAN_POINT ( 'NONE',  ( -5.153800228976328057, -19.02544592524343514, 112.2905762719810099 ) ) ;
#123248 = CARTESIAN_POINT ( 'NONE',  ( 4.379528057220339221, -16.55341960407611168, 67.70724293864769550 ) ) ;
#123249 = CARTESIAN_POINT ( 'NONE',  ( 5.153800228976335163, 19.02544592524342804, 24.79057627198102765 ) ) ;
#123250 = CARTESIAN_POINT ( 'NONE',  ( -4.379528057220328563, 16.55341960407611168, 80.20724293864769550 ) ) ;
#123251 = CARTESIAN_POINT ( 'NONE',  ( -18.67979575497178146, -10.72451020669898902, 96.66557627198102409 ) ) ;
#123252 = CARTESIAN_POINT ( 'NONE',  ( -21.52544592524334988, -5.823673210054445271, 43.95942372801902565 ) ) ;
#123253 = CARTESIAN_POINT ( 'NONE',  ( 8.906447517083050158, 27.41122689804195645, 149.4000000000000057 ) ) ;
#123254 = CARTESIAN_POINT ( 'NONE',  ( 14.29746914071037800, 8.314922557961029526, 56.66775706135235424 ) ) ;
#123255 = CARTESIAN_POINT ( 'NONE',  ( 0.05219959533907565091, 21.53943276465977519, 94.99890960531436690 ) ) ;
#123256 = CARTESIAN_POINT ( 'NONE',  ( -9.564922557961040184, 16.46253265017147172, 22.91775706135233648 ) ) ;
#123257 = CARTESIAN_POINT ( 'NONE',  ( -16.46253265017160317, 9.564922557960807481, 100.8322429386477097 ) ) ;
#123258 = CARTESIAN_POINT ( 'NONE',  ( 21.52544592524334988, 5.823673210054432836, 41.45942372801901143 ) ) ;
#123259 = CARTESIAN_POINT ( 'NONE',  ( 18.62759615963271287, -10.81492255796078972, 38.33224293864768839 ) ) ;
#123260 = CARTESIAN_POINT ( 'NONE',  ( -16.55341960407611168, -4.379528057220339221, 26.45724293864768839 ) ) ;
#123261 = AXIS2_PLACEMENT_3D ( 'NONE', #51553, #143548, #114204 ) ;
#123263 = CARTESIAN_POINT ( 'NONE',  ( 21.52544592524334988, 5.823673210054432836, 91.45942372801901854 ) ) ;
#123262 = CARTESIAN_POINT ( 'NONE',  ( -15.72974639402176322, -15.80617190586768395, 64.37609039468568994 ) ) ;
#123264 = CARTESIAN_POINT ( 'NONE',  ( -16.51473224551082808, 9.474510206698731452, 28.33442372801900433 ) ) ;
#123265 = CARTESIAN_POINT ( 'NONE',  ( -4.483927247898782831, 16.52544592524335698, 87.70942372801901854 ) ) ;
#123266 = CARTESIAN_POINT ( 'NONE',  ( 21.52544592524334988, 5.823673210054432836, 56.45942372801902565 ) ) ;
#123267 = CARTESIAN_POINT ( 'NONE',  ( 5.049401038298161559, -19.05341960407611168, 42.70724293864767418 ) ) ;
#123268 = CARTESIAN_POINT ( 'NONE',  ( 9.474510206698729675, 16.51473224551082808, 27.08442372801900433 ) ) ;
#123269 = CARTESIAN_POINT ( 'NONE',  ( -21.52544592524343514, 5.823673210054127303, 31.04057627198102409 ) ) ;
#123270 = CARTESIAN_POINT ( 'NONE',  ( -10.72451020669870658, -18.67979575497194134, 19.58442372801901143 ) ) ;
#123271 = CARTESIAN_POINT ( 'NONE',  ( 15.72974639402199770, -15.80617190586745480, 73.12390960531436690 ) ) ;
#123272 = CARTESIAN_POINT ( 'NONE',  ( 8.224510206698742110, 14.34966873604972548, 37.08442372801901143 ) ) ;
#123274 = CARTESIAN_POINT ( 'NONE',  ( -15.80617190586745835, -15.72974639402198527, 86.87390960531438111 ) ) ;
#123273 = CARTESIAN_POINT ( 'NONE',  ( 29.43349580481983452, 2.428612866367529932E-14, 139.9999999999999716 ) ) ;
#123276 = CARTESIAN_POINT ( 'NONE',  ( -0.05219959533910754901, -16.53943276465976808, 57.49890960531435979 ) ) ;
#123275 = CARTESIAN_POINT ( 'NONE',  ( -0.05219959533934338120, 16.53943276465976808, 62.50109039468568284 ) ) ;
#123277 = CARTESIAN_POINT ( 'NONE',  ( 0.9142611263790301201, 29.18971664064655513, -49.31446279634770491 ) ) ;
#123278 = CARTESIAN_POINT ( 'NONE',  ( -13.89961937509957401, -13.97604488694547875, 99.37609039468567573 ) ) ;
#123279 = CARTESIAN_POINT ( 'NONE',  ( 21.52544592524344225, -5.823673210054117533, 33.54057627198102409 ) ) ;
#123280 = CARTESIAN_POINT ( 'NONE',  ( -26.46959431505283789, -27.26463967846487435, -25.00000000000000000 ) ) ;
#123281 = CARTESIAN_POINT ( 'NONE',  ( -8.224510206698735004, -14.34966873604973081, 44.58442372801901854 ) ) ;
#123282 = CARTESIAN_POINT ( 'NONE',  ( 21.52544592524344225, -5.823673210054117533, 108.5405762719810241 ) ) ;
#123283 = CARTESIAN_POINT ( 'NONE',  ( 5.719274019375991003, -21.55341960407610458, 27.70724293864769905 ) ) ;
#123284 = CARTESIAN_POINT ( 'NONE',  ( 8.314922557961029526, -14.29746914071037800, 60.41775706135235424 ) ) ;
#123285 = CARTESIAN_POINT ( 'NONE',  ( -9.474510206698964154, 16.51473224551069663, 85.41557627198102409 ) ) ;
#123287 = CARTESIAN_POINT ( 'NONE',  ( 19.02544592524334988, 5.153800228976608722, 111.4594237280190043 ) ) ;
#123286 = CARTESIAN_POINT ( 'NONE',  ( 18.62759615963255655, 10.81492255796105972, 36.66775706135234714 ) ) ;
#123288 = CARTESIAN_POINT ( 'NONE',  ( 10.72451020669898902, -18.67979575497178502, 32.91557627198102409 ) ) ;
#123289 = ORIENTED_EDGE ( 'NONE', *, *, #152109, .T. ) ;
#123290 = CARTESIAN_POINT ( 'NONE',  ( 19.03943276465977164, 0.05219959533936151252, 26.25109039468566507 ) ) ;
#123291 = CARTESIAN_POINT ( 'NONE',  ( 4.483927247898790824, -16.52544592524335698, 45.20942372801901854 ) ) ;
#123292 = CARTESIAN_POINT ( 'NONE',  ( 5.049401038298161559, -19.05341960407611168, 102.7072429386476955 ) ) ;
#123293 = CARTESIAN_POINT ( 'NONE',  ( -0.05219959533907301413, -21.53943276465977519, 107.4989096053143669 ) ) ;
#123294 = CARTESIAN_POINT ( 'NONE',  ( 9.564922557960805705, 16.46253265017160317, 74.58224293864769550 ) ) ;
#123295 = CARTESIAN_POINT ( 'NONE',  ( -16.52216118717207749, 7.221426719304501418, 23.92400978953008917 ) ) ;
#123296 = CARTESIAN_POINT ( 'NONE',  ( -0.05219959533910754901, -16.53943276465976808, 82.49890960531436690 ) ) ;
#123297 = CARTESIAN_POINT ( 'NONE',  ( -15.72974639402197994, 15.80617190586746368, 35.62390960531437401 ) ) ;
#123298 = CARTESIAN_POINT ( 'NONE',  ( -17.50000000000000000, 5.622605283950870891, 33.68792689403888119 ) ) ;
#123299 = CARTESIAN_POINT ( 'NONE',  ( 4.379528057220092307, 16.55341960407617563, 62.29275706135236845 ) ) ;
#123300 = CARTESIAN_POINT ( 'NONE',  ( 21.53943276465977519, -0.05219959533907433946, 98.74890960531438111 ) ) ;
#123301 = CARTESIAN_POINT ( 'NONE',  ( -13.97604488694547697, 13.89961937509957934, 78.12609039468567573 ) ) ;
#123302 = CARTESIAN_POINT ( 'NONE',  ( -13.97604488694527625, -13.89961937509977652, 31.87390960531435979 ) ) ;
#123303 = CARTESIAN_POINT ( 'NONE',  ( -5.823673210054116645, -21.52544592524344225, 72.29057627198102409 ) ) ;
#123304 = CARTESIAN_POINT ( 'NONE',  ( 5.153800228976335163, 19.02544592524342804, 94.79057627198103830 ) ) ;
#123305 = CARTESIAN_POINT ( 'NONE',  ( 10.72451020669871369, 18.67979575497193778, 87.08442372801901854 ) ) ;
#123306 = CARTESIAN_POINT ( 'NONE',  ( 5.049401038298161559, -19.05341960407611168, 62.70724293864769550 ) ) ;
#123307 = CARTESIAN_POINT ( 'NONE',  ( -12.14591786802326823, 12.06949235617739902, 43.12609039468568284 ) ) ;
#123308 = CARTESIAN_POINT ( 'NONE',  ( -9.474510206698964154, 16.51473224551069663, 55.41557627198103120 ) ) ;
#123309 = CARTESIAN_POINT ( 'NONE',  ( -18.62759615963255300, -10.81492255796106328, 79.16775706135234714 ) ) ;
#123310 = ORIENTED_EDGE ( 'NONE', *, *, #88498, .F. ) ;
#123311 = CARTESIAN_POINT ( 'NONE',  ( -0.05219959533936034679, 19.03943276465977164, 32.50109039468566863 ) ) ;
#123312 = CARTESIAN_POINT ( 'NONE',  ( -9.474510206698720793, -16.51473224551083518, 39.58442372801899722 ) ) ;
#123313 = CARTESIAN_POINT ( 'NONE',  ( -10.81492255796105439, 18.62759615963255655, 47.91775706135234714 ) ) ;
#123314 = CARTESIAN_POINT ( 'NONE',  ( -9.099999999999999645, 0.1001428631147401743, -61.89430850415823215 ) ) ;
#123315 = CARTESIAN_POINT ( 'NONE',  ( 0.05219959533936267826, -19.03943276465977164, 50.00109039468566863 ) ) ;
#123316 = CARTESIAN_POINT ( 'NONE',  ( -19.05341960407611168, -5.049401038298163336, 86.45724293864769550 ) ) ;
#123317 = CARTESIAN_POINT ( 'NONE',  ( 13.97604488694527802, 13.89961937509977652, 64.37390960531436690 ) ) ;
#123318 = CARTESIAN_POINT ( 'NONE',  ( -8.314922557961024197, 14.29746914071037800, 112.9177570613523329 ) ) ;
#123320 = CARTESIAN_POINT ( 'NONE',  ( 5.823673210054444382, -21.52544592524334988, 90.20942372801903275 ) ) ;
#123319 = CARTESIAN_POINT ( 'NONE',  ( -15.72974639402197994, 15.80617190586746368, 25.62390960531435624 ) ) ;
#123321 = CARTESIAN_POINT ( 'NONE',  ( 3.556970738554033499E-15, -38.81732327939057825, -8.624999997268814056 ) ) ;
#123322 = DIRECTION ( 'NONE',  ( -1.000000000000000000, 0.000000000000000000, 0.000000000000000000 ) ) ;
#123323 = CARTESIAN_POINT ( 'NONE',  ( -21.52544592524334988, -5.823673210054445271, 98.95942372801903275 ) ) ;
#123324 = CARTESIAN_POINT ( 'NONE',  ( -11.74149087413294623, -36.13659316521243881, -3.347842220587804007 ) ) ;
#123325 = CARTESIAN_POINT ( 'NONE',  ( 0.05219959533909260263, 19.03943276465977164, 29.99890960531435979 ) ) ;
#123326 = CARTESIAN_POINT ( 'NONE',  ( -19.02544592524342804, 5.153800228976336051, 111.0405762719810099 ) ) ;
#123327 = CARTESIAN_POINT ( 'NONE',  ( 33.70615967800006985, 5.466638699193797635, 95.70352821367445983 ) ) ;
#123328 = CARTESIAN_POINT ( 'NONE',  ( 4.483927247898790824, -16.52544592524335698, 55.20942372801902565 ) ) ;
#123330 = ADVANCED_FACE ( 'NONE', ( #94218 ), #15407, .T. ) ;
#123329 = CARTESIAN_POINT ( 'NONE',  ( 18.67979575497178502, 10.72451020669898547, 64.16557627198102409 ) ) ;
#123331 = CARTESIAN_POINT ( 'NONE',  ( -8.314922557960811034, -14.29746914071050412, 37.08224293864768129 ) ) ;
#123333 = CARTESIAN_POINT ( 'NONE',  ( 19.03943276465977164, -0.05219959533909143690, 98.74890960531436690 ) ) ;
#123332 = CARTESIAN_POINT ( 'NONE',  ( 8.314922557960818139, 14.29746914071049879, 104.5822429386477097 ) ) ;
#123334 = CARTESIAN_POINT ( 'NONE',  ( 21.53943276465977519, 0.05219959533937863772, 111.2510903946856899 ) ) ;
#123335 = CARTESIAN_POINT ( 'NONE',  ( 12.06949235617757843, -12.14591786802309237, 113.1239096053143953 ) ) ;
#123336 = CARTESIAN_POINT ( 'NONE',  ( 0.05219959533937995610, -21.53943276465977519, 70.00109039468568994 ) ) ;
#123337 = CARTESIAN_POINT ( 'NONE',  ( -13.89961937509977652, 13.97604488694528158, 115.6239096053143669 ) ) ;
#123338 = CARTESIAN_POINT ( 'NONE',  ( -12.14591786802326823, 12.06949235617739902, 103.1260903946856757 ) ) ;
#123339 = CARTESIAN_POINT ( 'NONE',  ( -19.02544592524334988, -5.153800228976617603, 58.95942372801900433 ) ) ;
#123340 = CARTESIAN_POINT ( 'NONE',  ( -11.40812507854754720, -35.11059874428192273, -6.724999997268813701 ) ) ;
#123341 = CARTESIAN_POINT ( 'NONE',  ( -15.80617190586745835, -15.72974639402198527, 26.87390960531435979 ) ) ;
#123342 = CARTESIAN_POINT ( 'NONE',  ( 8.224510206698953496, -14.34966873604960469, 87.91557627198103830 ) ) ;
#123343 = CARTESIAN_POINT ( 'NONE',  ( -19.05341960407617563, 5.049401038297882671, 53.54275706135231871 ) ) ;
#123344 = CARTESIAN_POINT ( 'NONE',  ( -16.46253265017160317, 9.564922557960807481, 80.83224293864769550 ) ) ;
#123345 = CARTESIAN_POINT ( 'NONE',  ( 4.483927247898545687, 16.52544592524342804, 69.79057627198102409 ) ) ;
#123346 = CARTESIAN_POINT ( 'NONE',  ( -19.05341960407617563, 5.049401038297882671, 93.54275706135234714 ) ) ;
#123347 = CARTESIAN_POINT ( 'NONE',  ( 21.52544592524344225, -5.823673210054117533, 43.54057627198103830 ) ) ;
#123348 = VERTEX_POINT ( 'NONE', #124566 ) ;
#123349 = CARTESIAN_POINT ( 'NONE',  ( 14.34966873604960469, 8.224510206698951720, 114.1655762719810383 ) ) ;
#123350 = CARTESIAN_POINT ( 'NONE',  ( -17.31728774477272381, -6.344390552232408886, 29.18093348310683410 ) ) ;
#123352 = CARTESIAN_POINT ( 'NONE',  ( 18.62759615963271287, -10.81492255796078972, 78.33224293864770971 ) ) ;
#123351 = CARTESIAN_POINT ( 'NONE',  ( 16.46253265017160672, -9.564922557960803928, 73.33224293864769550 ) ) ;
#123354 = CARTESIAN_POINT ( 'NONE',  ( -19.03943276465977164, 0.05219959533909376836, 71.24890960531435269 ) ) ;
#123353 = CARTESIAN_POINT ( 'NONE',  ( 4.483927247898790824, -16.52544592524335698, 95.20942372801903275 ) ) ;
#123355 = CARTESIAN_POINT ( 'NONE',  ( 13.89961937509957401, 13.97604488694547697, 71.87609039468567573 ) ) ;
#123356 = CARTESIAN_POINT ( 'NONE',  ( -0.05219959533937732626, 21.53943276465977519, 77.50109039468567573 ) ) ;
#123357 = CARTESIAN_POINT ( 'NONE',  ( -10.81492255796078084, -18.62759615963271287, 62.08224293864769550 ) ) ;
#123358 = CARTESIAN_POINT ( 'NONE',  ( 21.52544592524344225, -5.823673210054117533, 28.54057627198103120 ) ) ;
#123359 = CARTESIAN_POINT ( 'NONE',  ( 13.89961937509977652, -13.97604488694527269, 43.12390960531434558 ) ) ;
#123360 = CARTESIAN_POINT ( 'NONE',  ( -4.483927247898782831, 16.52544592524335698, 102.7094237280190185 ) ) ;
#123361 = CARTESIAN_POINT ( 'NONE',  ( -19.05341960407611168, -5.049401038298163336, 51.45724293864770260 ) ) ;
#123362 = CARTESIAN_POINT ( 'NONE',  ( -8.314922557961024197, 14.29746914071037800, 27.91775706135234358 ) ) ;
#123363 = CARTESIAN_POINT ( 'NONE',  ( 18.22780087662122384, -5.500000000000022204, 101.0154010532610869 ) ) ;
#123364 = CARTESIAN_POINT ( 'NONE',  ( -9.474510206698720793, -16.51473224551083518, 19.58442372801899722 ) ) ;
#123365 = CARTESIAN_POINT ( 'NONE',  ( -16.52544592524342804, 4.483927247898546575, 56.04057627198102409 ) ) ;
#123366 = CARTESIAN_POINT ( 'NONE',  ( -5.823673210054116645, -21.52544592524344225, 102.2905762719810383 ) ) ;
#123367 = CARTESIAN_POINT ( 'NONE',  ( 21.52544592524344225, -5.823673210054117533, 98.54057627198105251 ) ) ;
#123368 = CARTESIAN_POINT ( 'NONE',  ( -4.460609718571558524, 4.180103257450054066, -64.53023439669115646 ) ) ;
#123369 = CARTESIAN_POINT ( 'NONE',  ( -18.62759615963270932, 10.81492255796079327, 45.83224293864769550 ) ) ;
#123370 = CARTESIAN_POINT ( 'NONE',  ( 16.52544592524335698, 4.483927247898782831, 86.45942372801901854 ) ) ;
#123371 = CARTESIAN_POINT ( 'NONE',  ( 12.06949235617757843, -12.14591786802309237, 93.12390960531436690 ) ) ;
#123372 = CARTESIAN_POINT ( 'NONE',  ( -19.03943276465977164, 0.05219959533909376836, 61.24890960531436690 ) ) ;
#123373 = FILL_AREA_STYLE ('',( #156723 ) ) ;
#123374 = CARTESIAN_POINT ( 'NONE',  ( -16.67568593663830256, -39.83563513005474732, -20.80532163689326097 ) ) ;
#123375 = CARTESIAN_POINT ( 'NONE',  ( 8.314922557961029526, -14.29746914071037800, 105.4177570613523613 ) ) ;
#123376 = CARTESIAN_POINT ( 'NONE',  ( -0.05219959533937732626, 21.53943276465977519, 32.50109039468568284 ) ) ;
#123377 = CARTESIAN_POINT ( 'NONE',  ( 0.05219959533909260263, 19.03943276465977164, 94.99890960531436690 ) ) ;
#123378 = CARTESIAN_POINT ( 'NONE',  ( 10.81492255796106328, -18.62759615963255655, 70.41775706135236135 ) ) ;
#123379 = DIRECTION ( 'NONE',  ( 0.000000000000000000, 0.000000000000000000, 1.000000000000000000 ) ) ;
#123380 = CARTESIAN_POINT ( 'NONE',  ( -19.02544592524342804, 5.153800228976336051, 26.04057627198103120 ) ) ;
#123381 = VERTEX_POINT ( 'NONE', #122572 ) ;
#123382 = CARTESIAN_POINT ( 'NONE',  ( -5.719274019375665041, -21.55341960407619695, 64.79275706135234714 ) ) ;
#123383 = CARTESIAN_POINT ( 'NONE',  ( -5.153800228976328057, -19.02544592524343514, 47.29057627198102409 ) ) ;
#123384 = CARTESIAN_POINT ( 'NONE',  ( 19.02544592524343514, -5.153800228976328945, 93.54057627198102409 ) ) ;
#123385 = CARTESIAN_POINT ( 'NONE',  ( -19.05341960407617563, 5.049401038297882671, 73.54275706135233293 ) ) ;
#123386 = CARTESIAN_POINT ( 'NONE',  ( 0.05219959533937995610, -21.53943276465977519, 40.00109039468567573 ) ) ;
#123387 = CARTESIAN_POINT ( 'NONE',  ( 0.05219959533936267826, -19.03943276465977164, 100.0010903946856757 ) ) ;
#123388 = CARTESIAN_POINT ( 'NONE',  ( -0.05219959533936034679, 19.03943276465977164, 77.50109039468566152 ) ) ;
#123389 = CARTESIAN_POINT ( 'NONE',  ( -16.46253265017160317, 9.564922557960807481, 40.83224293864769550 ) ) ;
#123390 = CARTESIAN_POINT ( 'NONE',  ( -5.153800228976607833, 19.02544592524334988, 82.70942372801897591 ) ) ;
#123391 = CARTESIAN_POINT ( 'NONE',  ( -4.379528057220086978, -16.55341960407618274, 109.7927570613523613 ) ) ;
#123392 = CARTESIAN_POINT ( 'NONE',  ( -13.89961937509957401, -13.97604488694547875, 79.37609039468567573 ) ) ;
#123393 = CARTESIAN_POINT ( 'NONE',  ( -0.05219959533910754901, -16.53943276465976808, 27.49890960531435269 ) ) ;
#123394 = CARTESIAN_POINT ( 'NONE',  ( -13.97604488694547697, 13.89961937509957934, 53.12609039468565442 ) ) ;
#123395 = CARTESIAN_POINT ( 'NONE',  ( 5.719274019375673035, 21.55341960407619339, 102.2927570613523613 ) ) ;
#123396 = CARTESIAN_POINT ( 'NONE',  ( -19.02544592524334988, -5.153800228976617603, 28.95942372801900433 ) ) ;
#123397 = CARTESIAN_POINT ( 'NONE',  ( -0.05219959533909027116, -19.03943276465977164, 27.49890960531435624 ) ) ;
#123398 = CARTESIAN_POINT ( 'NONE',  ( -10.72451020669870658, -18.67979575497194134, 89.58442372801901854 ) ) ;
#123399 = CARTESIAN_POINT ( 'NONE',  ( -14.29746914071037622, -8.314922557961029526, 29.16775706135234003 ) ) ;
#123400 = CARTESIAN_POINT ( 'NONE',  ( 16.51473224551069308, 9.474510206698969483, 89.16557627198103830 ) ) ;
#123401 = CARTESIAN_POINT ( 'NONE',  ( 27.73933785331498925, -9.013057229001033122, 141.7750000027311899 ) ) ;
#123402 = CARTESIAN_POINT ( 'NONE',  ( -19.03943276465977164, 0.05219959533909376836, 76.24890960531435269 ) ) ;
#123403 = CARTESIAN_POINT ( 'NONE',  ( 28.82186960331498327, 2.781578969918950771E-14, 141.0000000000000000 ) ) ;
#123404 = CARTESIAN_POINT ( 'NONE',  ( 5.153800228976615827, -19.02544592524334988, 80.20942372801901854 ) ) ;
#123405 = CARTESIAN_POINT ( 'NONE',  ( 21.53943276465977519, -0.05219959533907433946, 23.74890960531435269 ) ) ;
#123407 = CARTESIAN_POINT ( 'NONE',  ( -5.049401038297874678, -19.05341960407617918, 99.79275706135234714 ) ) ;
#123406 = CARTESIAN_POINT ( 'NONE',  ( -5.823673210054431948, 21.52544592524334988, 112.7094237280190328 ) ) ;
#123408 = CARTESIAN_POINT ( 'NONE',  ( 12.06949235617757843, -12.14591786802309237, 103.1239096053143811 ) ) ;
#123409 = CARTESIAN_POINT ( 'NONE',  ( -5.049401038298153566, 19.05341960407611168, 30.20724293864768839 ) ) ;
#123410 = CARTESIAN_POINT ( 'NONE',  ( 10.72451020669898902, -18.67979575497178502, 62.91557627198102409 ) ) ;
#123411 = CARTESIAN_POINT ( 'NONE',  ( -15.80617190586745835, -15.72974639402198527, 46.87390960531435979 ) ) ;
#123412 = CARTESIAN_POINT ( 'NONE',  ( 8.314922557960818139, 14.29746914071049879, 114.5822429386477097 ) ) ;
#123413 = CARTESIAN_POINT ( 'NONE',  ( -1.305043071815281008, -6.854124442542008033, -62.35408385982739077 ) ) ;
#123414 = CARTESIAN_POINT ( 'NONE',  ( -19.05341960407617563, 5.049401038297882671, 63.54275706135234003 ) ) ;
#123415 = CARTESIAN_POINT ( 'NONE',  ( -16.52544592524342804, 4.483927247898546575, 36.04057627198102409 ) ) ;
#123416 = CARTESIAN_POINT ( 'NONE',  ( -9.564922557960796823, -16.46253265017161027, 112.0822429386476955 ) ) ;
#123417 = CARTESIAN_POINT ( 'NONE',  ( -5.823673210054431948, 21.52544592524334988, 82.70942372801900433 ) ) ;
#123418 = CARTESIAN_POINT ( 'NONE',  ( 0.05219959533907565091, 21.53943276465977519, 64.99890960531435269 ) ) ;
#123419 = CARTESIAN_POINT ( 'NONE',  ( -10.81492255796105439, 18.62759615963255655, 57.91775706135234714 ) ) ;
#123420 = CARTESIAN_POINT ( 'NONE',  ( -5.719274019375665041, -21.55341960407619695, 44.79275706135234714 ) ) ;
#123421 = CARTESIAN_POINT ( 'NONE',  ( -9.564922557960796823, -16.46253265017161027, 82.08224293864768129 ) ) ;
#123422 = CARTESIAN_POINT ( 'NONE',  ( -16.53943276465976808, -0.05219959533934237506, 98.75109039468568994 ) ) ;
#123423 = CARTESIAN_POINT ( 'NONE',  ( 16.51473224551069308, 9.474510206698969483, 24.16557627198102765 ) ) ;
#123424 = CARTESIAN_POINT ( 'NONE',  ( -31.48310541436861953, 7.250236049019783913, 93.01911755558079165 ) ) ;
#123425 = CARTESIAN_POINT ( 'NONE',  ( 4.379528057220339221, -16.55341960407611168, 72.70724293864769550 ) ) ;
#123426 = CARTESIAN_POINT ( 'NONE',  ( 8.314922557960818139, 14.29746914071049879, 34.58224293864770260 ) ) ;
#123427 = CARTESIAN_POINT ( 'NONE',  ( -5.049401038298153566, 19.05341960407611168, 60.20724293864768129 ) ) ;
#123428 = CARTESIAN_POINT ( 'NONE',  ( 13.97604488694527802, 13.89961937509977652, 29.37390960531435979 ) ) ;
#123429 = CARTESIAN_POINT ( 'NONE',  ( -18.62759615963270932, 10.81492255796079327, 50.83224293864770971 ) ) ;
#123430 = CARTESIAN_POINT ( 'NONE',  ( 16.46253265017146816, 9.564922557961045513, 36.66775706135233293 ) ) ;
#123432 = CARTESIAN_POINT ( 'NONE',  ( -12.06949235617756955, 12.14591786802309770, 45.62390960531436690 ) ) ;
#123431 = DIRECTION ( 'NONE',  ( 0.000000000000000000, 0.000000000000000000, 1.000000000000000000 ) ) ;
#123433 = CARTESIAN_POINT ( 'NONE',  ( -21.52544592524343514, 5.823673210054127303, 26.04057627198103475 ) ) ;
#123434 = CARTESIAN_POINT ( 'NONE',  ( 9.687362902255726382, 9.687362902255699737, -64.92279855667830191 ) ) ;
#123435 = CARTESIAN_POINT ( 'NONE',  ( 16.52544592524335698, 4.483927247898782831, 71.45942372801901854 ) ) ;
#123436 = CARTESIAN_POINT ( 'NONE',  ( -19.05341960407617563, 5.049401038297882671, 78.54275706135233293 ) ) ;
#123437 = CARTESIAN_POINT ( 'NONE',  ( 8.224510206698953496, -14.34966873604960469, 47.91557627198102409 ) ) ;
#123438 = ORIENTED_EDGE ( 'NONE', *, *, #95827, .T. ) ;
#123439 = CARTESIAN_POINT ( 'NONE',  ( -18.56101223717332260, -5.500000000000062172, 76.44978406935678095 ) ) ;
#123440 = CARTESIAN_POINT ( 'NONE',  ( -16.55341960407611168, -4.379528057220339221, 31.45724293864769550 ) ) ;
#123441 = CARTESIAN_POINT ( 'NONE',  ( -9.564922557960796823, -16.46253265017161027, 52.08224293864768839 ) ) ;
#123442 = CARTESIAN_POINT ( 'NONE',  ( -19.05341960407611168, -5.049401038298163336, 81.45724293864769550 ) ) ;
#123443 = CARTESIAN_POINT ( 'NONE',  ( 5.153800228976335163, 19.02544592524342804, 44.79057627198103830 ) ) ;
#123444 = CARTESIAN_POINT ( 'NONE',  ( 15.80617190586769283, -15.72974639402175789, 40.62609039468567573 ) ) ;
#123445 = CARTESIAN_POINT ( 'NONE',  ( 9.474510206698971260, -16.51473224551069308, 62.91557627198102409 ) ) ;
#123446 = DIRECTION ( 'NONE',  ( 0.5367108174878536531, -0.8437662581494473901, 0.000000000000000000 ) ) ;
#123447 = CARTESIAN_POINT ( 'NONE',  ( 9.474510206698971260, -16.51473224551069308, 42.91557627198103120 ) ) ;
#123448 = CARTESIAN_POINT ( 'NONE',  ( -18.67979575497178146, -10.72451020669898902, 31.66557627198102054 ) ) ;
#123449 = B_SPLINE_CURVE_WITH_KNOTS ( 'NONE', 3,
 ( #94136, #122489, #91142, #61803, #184180, #109311 ),
 .UNSPECIFIED., .F., .F.,
 ( 4, 2, 4 ),
 ( 0.000000000000000000, 0.0003837532665634991623, 0.0007675065331269983245 ),
 .UNSPECIFIED. ) ;
#123451 = CARTESIAN_POINT ( 'NONE',  ( 19.03943276465977164, -0.05219959533909143690, 23.74890960531435269 ) ) ;
#123450 = CARTESIAN_POINT ( 'NONE',  ( 10.72451020669871369, 18.67979575497193778, 77.08442372801901854 ) ) ;
#123452 = CARTESIAN_POINT ( 'NONE',  ( 18.62759615963271287, -10.81492255796078972, 23.33224293864769194 ) ) ;
#123453 = CARTESIAN_POINT ( 'NONE',  ( 14.29746914071037800, 8.314922557961029526, 96.66775706135234714 ) ) ;
#123454 = EDGE_CURVE ( 'NONE', #28306, #50238, #1251, .T. ) ;
#123455 = CARTESIAN_POINT ( 'NONE',  ( 10.72451020669871369, 18.67979575497193778, 107.0844237280190043 ) ) ;
#123456 = CARTESIAN_POINT ( 'NONE',  ( -12.06949235617739369, -12.14591786802326823, 64.37609039468568994 ) ) ;
#123457 = CARTESIAN_POINT ( 'NONE',  ( -13.89961937509977652, 13.97604488694528158, 105.6239096053143527 ) ) ;
#123458 = CARTESIAN_POINT ( 'NONE',  ( 0.05219959533934541429, -16.53943276465976808, 60.00109039468568284 ) ) ;
#123459 = CARTESIAN_POINT ( 'NONE',  ( 14.29746914071037800, 8.314922557961029526, 41.66775706135235424 ) ) ;
#123460 = CARTESIAN_POINT ( 'NONE',  ( 14.29746914071037800, 8.314922557961029526, 91.66775706135234714 ) ) ;
#123461 = CARTESIAN_POINT ( 'NONE',  ( -18.67979575497193778, 10.72451020669871902, 48.33442372801902565 ) ) ;
#123462 = CARTESIAN_POINT ( 'NONE',  ( 12.06949235617739724, 12.14591786802326823, 26.87609039468567218 ) ) ;
#123463 = CARTESIAN_POINT ( 'NONE',  ( -10.72451020669898014, 18.67979575497178502, 115.4155762719810241 ) ) ;
#123464 = CARTESIAN_POINT ( 'NONE',  ( 8.224510206698742110, 14.34966873604972548, 22.08442372801901143 ) ) ;
#123465 = CARTESIAN_POINT ( 'NONE',  ( 12.06949235617739724, 12.14591786802326823, 81.87609039468568994 ) ) ;
#123466 = DIRECTION ( 'NONE',  ( -0.5000000000000014433, -0.4999999999999996114, -0.7071067811865467956 ) ) ;
#123467 = CARTESIAN_POINT ( 'NONE',  ( 18.62759615963255655, 10.81492255796105972, 81.66775706135236135 ) ) ;
#123468 = CARTESIAN_POINT ( 'NONE',  ( 0.05219959533936267826, -19.03943276465977164, 85.00109039468567573 ) ) ;
#123469 = CARTESIAN_POINT ( 'NONE',  ( -12.06949235617756955, 12.14591786802309770, 55.62390960531436690 ) ) ;
#123470 = CARTESIAN_POINT ( 'NONE',  ( 16.53943276465976808, -0.05219959533910856209, 38.74890960531435979 ) ) ;
#123471 = CARTESIAN_POINT ( 'NONE',  ( -14.34966873604960291, -8.224510206698953496, 111.6655762719810525 ) ) ;
#123473 = CARTESIAN_POINT ( 'NONE',  ( -6.691186640346280967, 1.197302953328974739, -64.41832325557876970 ) ) ;
#123472 = CARTESIAN_POINT ( 'NONE',  ( 0.05219959533936267826, -19.03943276465977164, 50.00109039468566863 ) ) ;
#123474 = CARTESIAN_POINT ( 'NONE',  ( -10.72451020669870658, -18.67979575497194134, 44.58442372801901854 ) ) ;
#123475 = CARTESIAN_POINT ( 'NONE',  ( -19.05341960407617563, 5.049401038297882671, 113.5427570613523471 ) ) ;
#123476 = FACE_OUTER_BOUND ( 'NONE', #186231, .T. ) ;
#123477 = CARTESIAN_POINT ( 'NONE',  ( -19.02544592524342804, 5.153800228976336051, 111.0405762719810099 ) ) ;
#123478 = CARTESIAN_POINT ( 'NONE',  ( 18.67979575497178502, 10.72451020669898547, 69.16557627198102409 ) ) ;
#123479 = CARTESIAN_POINT ( 'NONE',  ( 5.153800228976615827, -19.02544592524334988, 100.2094237280190043 ) ) ;
#123480 = CARTESIAN_POINT ( 'NONE',  ( 9.474510206698971260, -16.51473224551069308, 102.9155762719810241 ) ) ;
#123481 = CARTESIAN_POINT ( 'NONE',  ( -17.58332526062528345, -7.635886036038592728, 49.07665040441535353 ) ) ;
#123482 = CARTESIAN_POINT ( 'NONE',  ( -16.55341960407611168, -4.379528057220339221, 106.4572429386477097 ) ) ;
#123483 = CARTESIAN_POINT ( 'NONE',  ( 5.719274019375673035, 21.55341960407619339, 92.29275706135236135 ) ) ;
#123484 = CARTESIAN_POINT ( 'NONE',  ( 13.89961937509977652, -13.97604488694527269, 33.12390960531434558 ) ) ;
#123485 = CARTESIAN_POINT ( 'NONE',  ( -15.80617190586768217, 15.72974639402176855, 38.12609039468567573 ) ) ;
#123486 = CARTESIAN_POINT ( 'NONE',  ( -0.05219959533937732626, 21.53943276465977519, 92.50109039468567573 ) ) ;
#123487 = CARTESIAN_POINT ( 'NONE',  ( 16.55341960407618274, -4.379528057220086978, 86.04275706135236135 ) ) ;
#123488 = CARTESIAN_POINT ( 'NONE',  ( 18.62759615963255655, 10.81492255796105972, 36.66775706135234714 ) ) ;
#123489 = CARTESIAN_POINT ( 'NONE',  ( -18.62759615963255300, -10.81492255796106328, 34.16775706135234714 ) ) ;
#123491 = CARTESIAN_POINT ( 'NONE',  ( 5.049401038298161559, -19.05341960407611168, 77.70724293864765286 ) ) ;
#123490 = CARTESIAN_POINT ( 'NONE',  ( 13.89961937509957401, 13.97604488694547697, 66.87609039468567573 ) ) ;
#123492 = CARTESIAN_POINT ( 'NONE',  ( 16.55341960407611168, 4.379528057220329451, 98.95724293864770971 ) ) ;
#123493 = CARTESIAN_POINT ( 'NONE',  ( -21.53943276465977519, 0.05219959533907696930, 86.24890960531436690 ) ) ;
#123494 = CARTESIAN_POINT ( 'NONE',  ( -12.06949235617756955, 12.14591786802309770, 65.62390960531436690 ) ) ;
#123495 = CARTESIAN_POINT ( 'NONE',  ( 0.05219959533937995610, -21.53943276465977519, 105.0010903946856757 ) ) ;
#123496 = CARTESIAN_POINT ( 'NONE',  ( -16.52544592524342804, 4.483927247898546575, 86.04057627198102409 ) ) ;
#123497 = CARTESIAN_POINT ( 'NONE',  ( 19.02544592524343514, -5.153800228976328945, 38.54057627198103120 ) ) ;
#123498 = CARTESIAN_POINT ( 'NONE',  ( 13.97604488694548053, -13.89961937509957401, 65.62609039468567573 ) ) ;
#123499 = CARTESIAN_POINT ( 'NONE',  ( -16.55341960407611168, -4.379528057220339221, 46.45724293864769550 ) ) ;
#123500 = CARTESIAN_POINT ( 'NONE',  ( -10.72451020669870658, -18.67979575497194134, 99.58442372801900433 ) ) ;
#123501 = CARTESIAN_POINT ( 'NONE',  ( 16.46253265017160672, -9.564922557960803928, 88.33224293864769550 ) ) ;
#123502 = CARTESIAN_POINT ( 'NONE',  ( -5.049401038297874678, -19.05341960407617918, 64.79275706135233293 ) ) ;
#123503 = CARTESIAN_POINT ( 'NONE',  ( 0.05219959533907565091, 21.53943276465977519, 59.99890960531436690 ) ) ;
#123504 = CARTESIAN_POINT ( 'NONE',  ( -15.72974639402197994, 15.80617190586746368, 115.6239096053143669 ) ) ;
#123505 = CARTESIAN_POINT ( 'NONE',  ( -8.314922557961024197, 14.29746914071037800, 22.91775706135235069 ) ) ;
#123506 = CARTESIAN_POINT ( 'NONE',  ( 16.53943276465976808, 0.05219959533934440121, 76.25109039468568994 ) ) ;
#123508 = CARTESIAN_POINT ( 'NONE',  ( -0.05219959533937732626, 21.53943276465977519, 22.50109039468567573 ) ) ;
#123507 = DIRECTION ( 'NONE',  ( 0.000000000000000000, 0.000000000000000000, 1.000000000000000000 ) ) ;
#123509 = CARTESIAN_POINT ( 'NONE',  ( -5.153800228976328057, -19.02544592524343514, 27.29057627198103120 ) ) ;
#123510 = CARTESIAN_POINT ( 'NONE',  ( 11.40812507854754365, 35.11059874428196537, -5.724999997268812812 ) ) ;
#123511 = CARTESIAN_POINT ( 'NONE',  ( 14.29746914071037800, 8.314922557961029526, 51.66775706135234714 ) ) ;
#123512 = CARTESIAN_POINT ( 'NONE',  ( 8.224510206698953496, -14.34966873604960469, 82.91557627198103830 ) ) ;
#123513 = CARTESIAN_POINT ( 'NONE',  ( -21.55341960407610458, -5.719274019375992779, 81.45724293864769550 ) ) ;
#123514 = CARTESIAN_POINT ( 'NONE',  ( 12.14591786802327356, -12.06949235617739191, 110.6260903946857042 ) ) ;
#123515 = CARTESIAN_POINT ( 'NONE',  ( -12.14591786802326823, 12.06949235617739902, 38.12609039468567573 ) ) ;
#123516 = CARTESIAN_POINT ( 'NONE',  ( -19.03943276465977164, 0.05219959533909376836, 46.24890960531435979 ) ) ;
#123517 = CARTESIAN_POINT ( 'NONE',  ( 12.06949235617739724, 12.14591786802326823, 81.87609039468568994 ) ) ;
#123518 = CARTESIAN_POINT ( 'NONE',  ( -19.05341960407617563, 5.049401038297882671, 73.54275706135233293 ) ) ;
#123519 = CARTESIAN_POINT ( 'NONE',  ( 21.55341960407610458, 5.719274019375980345, 73.95724293864769550 ) ) ;
#123520 = CARTESIAN_POINT ( 'NONE',  ( -14.34966873604972548, 8.224510206698743886, 103.3344237280190043 ) ) ;
#123521 = CARTESIAN_POINT ( 'NONE',  ( -5.719274019375665041, -21.55341960407619695, 84.79275706135234714 ) ) ;
#123522 = CARTESIAN_POINT ( 'NONE',  ( 21.52544592524344225, -5.823673210054117533, 63.54057627198103830 ) ) ;
#123523 = CARTESIAN_POINT ( 'NONE',  ( 18.62759615963271287, -10.81492255796078972, 53.33224293864769550 ) ) ;
#123524 = VERTEX_POINT ( 'NONE', #109394 ) ;
#123525 = CARTESIAN_POINT ( 'NONE',  ( 16.53943276465976808, 0.05219959533934440121, 76.25109039468568994 ) ) ;
#123526 = CARTESIAN_POINT ( 'NONE',  ( 0.05219959533907565091, 21.53943276465977519, 49.99890960531437401 ) ) ;
#123527 = ORIENTED_EDGE ( 'NONE', *, *, #5609, .T. ) ;
#123528 = CARTESIAN_POINT ( 'NONE',  ( -0.05219959533909027116, -19.03943276465977164, 112.4989096053143669 ) ) ;
#123529 = CARTESIAN_POINT ( 'NONE',  ( -30.74264578624800492, 22.33583958711400186, -7.949999994537626513 ) ) ;
#123530 = CARTESIAN_POINT ( 'NONE',  ( 16.51473224551069308, 9.474510206698969483, 24.16557627198102765 ) ) ;
#123531 = CARTESIAN_POINT ( 'NONE',  ( 10.72451020669898902, -18.67979575497178502, 77.91557627198102409 ) ) ;
#123532 = CARTESIAN_POINT ( 'NONE',  ( 8.314922557961029526, -14.29746914071037800, 100.4177570613523471 ) ) ;
#123533 = CARTESIAN_POINT ( 'NONE',  ( -18.67979575497193778, 10.72451020669871902, 58.33442372801901143 ) ) ;
#123534 = CARTESIAN_POINT ( 'NONE',  ( 0.05219959533934541429, -16.53943276465976808, 25.00109039468567218 ) ) ;
#123535 = CARTESIAN_POINT ( 'NONE',  ( -16.51473224551069308, -9.474510206698971260, 26.66557627198103120 ) ) ;
#123536 = CARTESIAN_POINT ( 'NONE',  ( -5.153800228976607833, 19.02544592524334988, 112.7094237280190043 ) ) ;
#123537 = CARTESIAN_POINT ( 'NONE',  ( 5.153800228976335163, 19.02544592524342804, 34.79057627198102409 ) ) ;
#123538 = EDGE_CURVE ( 'NONE', #69189, #184349, #124086, .T. ) ;
#123539 = CARTESIAN_POINT ( 'NONE',  ( 23.31738231874054890, -16.94106989632523508, 142.7999999999999829 ) ) ;
#123540 = CARTESIAN_POINT ( 'NONE',  ( -19.02544592524342804, 5.153800228976336051, 111.0405762719810099 ) ) ;
#123541 = CARTESIAN_POINT ( 'NONE',  ( -16.55341960407617563, 4.379528057220093196, 83.54275706135234714 ) ) ;
#123542 = CARTESIAN_POINT ( 'NONE',  ( -16.46253265017146816, -9.564922557961047289, 79.16775706135234714 ) ) ;
#123543 = CARTESIAN_POINT ( 'NONE',  ( 13.97604488694548053, -13.89961937509957401, 30.62609039468566863 ) ) ;
#123544 = CARTESIAN_POINT ( 'NONE',  ( 15.80617190586746368, 15.72974639402197994, 59.37390960531436690 ) ) ;
#123545 = CARTESIAN_POINT ( 'NONE',  ( -8.314922557961024197, 14.29746914071037800, 87.91775706135234714 ) ) ;
#123546 = CARTESIAN_POINT ( 'NONE',  ( 9.564922557961047289, -16.46253265017146816, 95.41775706135233293 ) ) ;
#123547 = CARTESIAN_POINT ( 'NONE',  ( 5.153800228976335163, 19.02544592524342804, 49.79057627198100988 ) ) ;
#123548 = CARTESIAN_POINT ( 'NONE',  ( 16.46253265017160672, -9.564922557960803928, 88.33224293864769550 ) ) ;
#123549 = CARTESIAN_POINT ( 'NONE',  ( 15.80617190586769283, -15.72974639402175789, 50.62609039468568994 ) ) ;
#123550 = CARTESIAN_POINT ( 'NONE',  ( 13.89961937509977652, -13.97604488694527269, 43.12390960531434558 ) ) ;
#123551 = CARTESIAN_POINT ( 'NONE',  ( -17.48853670773246805, -5.747243402303014115, 86.33328700250008580 ) ) ;
#123552 = CARTESIAN_POINT ( 'NONE',  ( 19.05341960407611168, 5.049401038298154454, 108.9572429386477097 ) ) ;
#123553 = CARTESIAN_POINT ( 'NONE',  ( 16.53943276465976808, -0.05219959533910856209, 58.74890960531436690 ) ) ;
#123554 = CARTESIAN_POINT ( 'NONE',  ( 18.62759615963271287, -10.81492255796078972, 63.33224293864770260 ) ) ;
#123555 = DIRECTION ( 'NONE',  ( -6.938893903907222067E-15, 0.000000000000000000, -1.000000000000000000 ) ) ;
#123556 = CARTESIAN_POINT ( 'NONE',  ( 13.97604488694548053, -13.89961937509957401, 45.62609039468566863 ) ) ;
#123557 = DIRECTION ( 'NONE',  ( 1.000000000000000000, 0.000000000000000000, 0.000000000000000000 ) ) ;
#123559 = CARTESIAN_POINT ( 'NONE',  ( 13.97604488694527802, 13.89961937509977652, 74.37390960531436690 ) ) ;
#123558 = CARTESIAN_POINT ( 'NONE',  ( 16.51473224551069308, 9.474510206698969483, 69.16557627198102409 ) ) ;
#123560 = CARTESIAN_POINT ( 'NONE',  ( -12.06949235617739369, -12.14591786802326823, 54.37609039468568994 ) ) ;
#123561 = CARTESIAN_POINT ( 'NONE',  ( 0.000000000000000000, -3.784814030245899019, 190.0000000000000000 ) ) ;
#123562 = CARTESIAN_POINT ( 'NONE',  ( -19.02544592524334988, -5.153800228976617603, 28.95942372801900433 ) ) ;
#123563 = CARTESIAN_POINT ( 'NONE',  ( 21.99873734152911453, -27.49873734152921045, 1.818019484660534424 ) ) ;
#123564 = CARTESIAN_POINT ( 'NONE',  ( 14.34966873604972726, -8.224510206698740333, 85.83442372801901854 ) ) ;
#123565 = CARTESIAN_POINT ( 'NONE',  ( 16.70000000000002061, 0.000000000000000000, -59.13370768023891344 ) ) ;
#123566 = CARTESIAN_POINT ( 'NONE',  ( -14.29746914071037622, -8.314922557961029526, 79.16775706135234714 ) ) ;
#123567 = CARTESIAN_POINT ( 'NONE',  ( 14.29746914071037800, 8.314922557961029526, 51.66775706135234714 ) ) ;
#123568 = CARTESIAN_POINT ( 'NONE',  ( -0.05219959533936034679, 19.03943276465977164, 22.50109039468566152 ) ) ;
#123570 = CARTESIAN_POINT ( 'NONE',  ( -28.79475375365586842, 2.428612866367529932E-14, 155.0000000000000000 ) ) ;
#123569 = CARTESIAN_POINT ( 'NONE',  ( 13.97604488694527802, 13.89961937509977652, 59.37390960531434558 ) ) ;
#123571 = CARTESIAN_POINT ( 'NONE',  ( 15.80617190586769283, -15.72974639402175789, 60.62609039468567573 ) ) ;
#123572 = CARTESIAN_POINT ( 'NONE',  ( -0.05219959533936034679, 19.03943276465977164, 72.50109039468566152 ) ) ;
#123573 = CARTESIAN_POINT ( 'NONE',  ( -15.80617190586768217, 15.72974639402176855, 103.1260903946856757 ) ) ;
#123574 = CARTESIAN_POINT ( 'NONE',  ( 16.46253265017160672, -9.564922557960803928, 28.33224293864769550 ) ) ;
#123575 = CARTESIAN_POINT ( 'NONE',  ( -17.56609036915072153, 15.67660317299526085, -57.33766855040060051 ) ) ;
#123576 = CARTESIAN_POINT ( 'NONE',  ( -21.55341960407610458, -5.719274019375992779, 71.45724293864769550 ) ) ;
#123577 = CARTESIAN_POINT ( 'NONE',  ( -21.55341960407610458, -5.719274019375992779, 21.45724293864769550 ) ) ;
#123578 = CARTESIAN_POINT ( 'NONE',  ( 12.14591786802309770, 12.06949235617756955, 114.3739096053143527 ) ) ;
#123579 = CARTESIAN_POINT ( 'NONE',  ( -4.483927247898782831, 16.52544592524335698, 32.70942372801900433 ) ) ;
#123580 = CARTESIAN_POINT ( 'NONE',  ( -16.52544592524342804, 4.483927247898546575, 26.04057627198103475 ) ) ;
#123581 = ORIENTED_EDGE ( 'NONE', *, *, #118963, .T. ) ;
#123582 = CARTESIAN_POINT ( 'NONE',  ( 15.80617190586746368, 15.72974639402197994, 114.3739096053143527 ) ) ;
#123583 = CIRCLE ( 'NONE', #178620, 35.99626262588765258 ) ;
#123585 = CARTESIAN_POINT ( 'NONE',  ( -6.020228577223754586E-15, 39.95556452105416412, -4.500000000000000888 ) ) ;
#123584 = CARTESIAN_POINT ( 'NONE',  ( -8.224510206698948167, 14.34966873604960824, 45.41557627198103830 ) ) ;
#123586 = CARTESIAN_POINT ( 'NONE',  ( 13.89961937509957401, 13.97604488694547697, 106.8760903946856757 ) ) ;
#123587 = CARTESIAN_POINT ( 'NONE',  ( -9.564922557961040184, 16.46253265017147172, 22.91775706135233648 ) ) ;
#123588 = CARTESIAN_POINT ( 'NONE',  ( 14.34966873604960469, 8.224510206698951720, 44.16557627198103120 ) ) ;
#123589 = CARTESIAN_POINT ( 'NONE',  ( 5.719274019375991003, -21.55341960407610458, 97.70724293864772392 ) ) ;
#123591 = CARTESIAN_POINT ( 'NONE',  ( 15.80617190586746368, 15.72974639402197994, 69.37390960531436690 ) ) ;
#123590 = CARTESIAN_POINT ( 'NONE',  ( 17.50000000000000000, 5.624438216177605199, 31.68329655085357643 ) ) ;
#123592 = CARTESIAN_POINT ( 'NONE',  ( -16.51473224551069308, -9.474510206698971260, 76.66557627198103830 ) ) ;
#123593 = CARTESIAN_POINT ( 'NONE',  ( 16.52544592524342804, -4.483927247898539470, 48.54057627198103120 ) ) ;
#123594 = CARTESIAN_POINT ( 'NONE',  ( 13.89961937509977652, -13.97604488694527269, 93.12390960531436690 ) ) ;
#123595 = CARTESIAN_POINT ( 'NONE',  ( -21.23184647844206197, -181.1785498424364675, 1.787262988391354872E-28 ) ) ;
#123596 = CARTESIAN_POINT ( 'NONE',  ( -13.97604488694547697, 13.89961937509957934, 53.12609039468565442 ) ) ;
#123597 = CARTESIAN_POINT ( 'NONE',  ( 18.67979575497178502, 10.72451020669898547, 89.16557627198102409 ) ) ;
#123598 = CARTESIAN_POINT ( 'NONE',  ( -8.314922557960811034, -14.29746914071050412, 102.0822429386476955 ) ) ;
#123599 = CARTESIAN_POINT ( 'NONE',  ( -21.53943276465977519, -0.05219959533937600094, 53.75109039468568994 ) ) ;
#123600 = CARTESIAN_POINT ( 'NONE',  ( 27.73933785331498214, 9.013057229001095294, 145.9750000027311785 ) ) ;
#123601 = CARTESIAN_POINT ( 'NONE',  ( -14.34966873604960291, -8.224510206698953496, 31.66557627198102054 ) ) ;
#123602 = CARTESIAN_POINT ( 'NONE',  ( -19.05341960407611168, -5.049401038298163336, 41.45724293864769550 ) ) ;
#123603 = CARTESIAN_POINT ( 'NONE',  ( 16.46253265017160672, -9.564922557960803928, 98.33224293864769550 ) ) ;
#123604 = CARTESIAN_POINT ( 'NONE',  ( -5.719274019375978568, 21.55341960407610458, 55.20724293864770260 ) ) ;
#123605 = CARTESIAN_POINT ( 'NONE',  ( -27.73933785331498925, 9.013057229001089965, 140.7750000027311899 ) ) ;
#123606 = CARTESIAN_POINT ( 'NONE',  ( -19.03943276465977164, 0.05219959533909376836, 36.24890960531436690 ) ) ;
#123607 = CARTESIAN_POINT ( 'NONE',  ( -10.81492255796078084, -18.62759615963271287, 57.08224293864769550 ) ) ;
#123608 = CARTESIAN_POINT ( 'NONE',  ( -10.81492255796105439, 18.62759615963255655, 72.91775706135234714 ) ) ;
#123610 = CARTESIAN_POINT ( 'NONE',  ( -8.314922557961024197, 14.29746914071037800, 87.91775706135234714 ) ) ;
#123609 = CARTESIAN_POINT ( 'NONE',  ( 8.139631411198177346, -37.86970803904774385, -24.01681473739955663 ) ) ;
#123611 = CARTESIAN_POINT ( 'NONE',  ( -0.05219959533909027116, -19.03943276465977164, 57.49890960531435979 ) ) ;
#123612 = CARTESIAN_POINT ( 'NONE',  ( -9.474510206698964154, 16.51473224551069663, 60.41557627198102409 ) ) ;
#123613 = ORIENTED_EDGE ( 'NONE', *, *, #50743, .F. ) ;
#123614 = CARTESIAN_POINT ( 'NONE',  ( 19.02544592524334988, 5.153800228976608722, 31.45942372801900433 ) ) ;
#123615 = CARTESIAN_POINT ( 'NONE',  ( 14.29746914071037800, 8.314922557961029526, 81.66775706135236135 ) ) ;
#123616 = CARTESIAN_POINT ( 'NONE',  ( 21.53943276465977519, 0.05219959533937863772, 111.2510903946856899 ) ) ;
#123617 = CARTESIAN_POINT ( 'NONE',  ( -19.02544592524342804, 5.153800228976336051, 71.04057627198099567 ) ) ;
#123618 = CARTESIAN_POINT ( 'NONE',  ( -5.823673210054116645, -21.52544592524344225, 37.29057627198102409 ) ) ;
#123619 = CARTESIAN_POINT ( 'NONE',  ( -4.379528057220086978, -16.55341960407618274, 24.79275706135235779 ) ) ;
#123620 = CARTESIAN_POINT ( 'NONE',  ( 10.81492255796106328, -18.62759615963255655, 80.41775706135234714 ) ) ;
#123621 = CARTESIAN_POINT ( 'NONE',  ( 0.05219959533934541429, -16.53943276465976808, 50.00109039468568994 ) ) ;
#123622 = CARTESIAN_POINT ( 'NONE',  ( -18.67979575497178146, -10.72451020669898902, 96.66557627198102409 ) ) ;
#123623 = CARTESIAN_POINT ( 'NONE',  ( 19.02544592524334988, 5.153800228976608722, 111.4594237280190043 ) ) ;
#123624 = CARTESIAN_POINT ( 'NONE',  ( -13.89961937509977652, 13.97604488694528158, 80.62390960531436690 ) ) ;
#123625 = CARTESIAN_POINT ( 'NONE',  ( -12.06949235617739369, -12.14591786802326823, 24.37609039468567573 ) ) ;
#123626 = CARTESIAN_POINT ( 'NONE',  ( 19.02544592524343514, -5.153800228976328945, 43.54057627198103120 ) ) ;
#123627 = CARTESIAN_POINT ( 'NONE',  ( 8.314922557961029526, -14.29746914071037800, 25.41775706135235779 ) ) ;
#123628 = CARTESIAN_POINT ( 'NONE',  ( 16.52544592524342804, -4.483927247898539470, 73.54057627198102409 ) ) ;
#123629 = CARTESIAN_POINT ( 'NONE',  ( 14.34966873604972726, -8.224510206698740333, 85.83442372801901854 ) ) ;
#123631 = CARTESIAN_POINT ( 'NONE',  ( -5.153800228976328057, -19.02544592524343514, 47.29057627198102409 ) ) ;
#123630 = CARTESIAN_POINT ( 'NONE',  ( -18.62759615963255300, -10.81492255796106328, 34.16775706135234714 ) ) ;
#123632 = CARTESIAN_POINT ( 'NONE',  ( 9.474510206698971260, -16.51473224551069308, 62.91557627198102409 ) ) ;
#123633 = CARTESIAN_POINT ( 'NONE',  ( 8.224510206698742110, 14.34966873604972548, 92.08442372801901854 ) ) ;
#123634 = CARTESIAN_POINT ( 'NONE',  ( -21.96844466259036111, -7.174710485412877148, 170.3366942299294635 ) ) ;
#123635 = ORIENTED_EDGE ( 'NONE', *, *, #149591, .T. ) ;
#123636 = CARTESIAN_POINT ( 'NONE',  ( 19.02544592524334988, 5.153800228976608722, 31.45942372801900433 ) ) ;
#123637 = CARTESIAN_POINT ( 'NONE',  ( 0.05219959533909260263, 19.03943276465977164, 29.99890960531435979 ) ) ;
#123639 = ORIENTED_EDGE ( 'NONE', *, *, #99796, .T. ) ;
#123638 = CARTESIAN_POINT ( 'NONE',  ( 13.97604488694527802, 13.89961937509977652, 109.3739096053143669 ) ) ;
#123640 = CARTESIAN_POINT ( 'NONE',  ( 12.14591786802327356, -12.06949235617739191, 30.62609039468567929 ) ) ;
#123642 = CARTESIAN_POINT ( 'NONE',  ( 16.53943276465976808, 0.05219959533934440121, 41.25109039468568284 ) ) ;
#123641 = CARTESIAN_POINT ( 'NONE',  ( -13.97604488694547697, 13.89961937509957934, 58.12609039468566863 ) ) ;
#123643 = CARTESIAN_POINT ( 'NONE',  ( -19.05341960407611168, -5.049401038298163336, 101.4572429386476955 ) ) ;
#123644 = CARTESIAN_POINT ( 'NONE',  ( 5.153800228976335163, 19.02544592524342804, 64.79057627198100988 ) ) ;
#123645 = CARTESIAN_POINT ( 'NONE',  ( 5.719274019375991003, -21.55341960407610458, 97.70724293864772392 ) ) ;
#123647 = CARTESIAN_POINT ( 'NONE',  ( -16.51473224551069308, -9.474510206698971260, 26.66557627198103120 ) ) ;
#123646 = CARTESIAN_POINT ( 'NONE',  ( 19.02544592524343514, -5.153800228976328945, 88.54057627198102409 ) ) ;
#123648 = CARTESIAN_POINT ( 'NONE',  ( -16.51473224551069308, -9.474510206698971260, 61.66557627198103120 ) ) ;
#123650 = CARTESIAN_POINT ( 'NONE',  ( 13.97604488694527802, 13.89961937509977652, 29.37390960531435979 ) ) ;
#123649 = CARTESIAN_POINT ( 'NONE',  ( -16.53943276465976808, -0.05219959533934237506, 108.7510903946857042 ) ) ;
#123651 = CARTESIAN_POINT ( 'NONE',  ( 9.474510206698729675, 16.51473224551082808, 27.08442372801900433 ) ) ;
#123652 = CARTESIAN_POINT ( 'NONE',  ( -12.06949235617756955, 12.14591786802309770, 65.62390960531436690 ) ) ;
#123653 = CARTESIAN_POINT ( 'NONE',  ( 0.05219959533937995610, -21.53943276465977519, 105.0010903946856757 ) ) ;
#123654 = CARTESIAN_POINT ( 'NONE',  ( -16.51473224551069308, -9.474510206698971260, 36.66557627198102409 ) ) ;
#123655 = CARTESIAN_POINT ( 'NONE',  ( 16.52544592524335698, 4.483927247898782831, 56.45942372801902565 ) ) ;
#123657 = CARTESIAN_POINT ( 'NONE',  ( 0.05219959533937995610, -21.53943276465977519, 95.00109039468568994 ) ) ;
#123656 = CARTESIAN_POINT ( 'NONE',  ( -14.29746914071049879, 8.314922557960819915, 40.83224293864769550 ) ) ;
#123658 = CARTESIAN_POINT ( 'NONE',  ( -13.89961937509977652, 13.97604488694528158, 85.62390960531433848 ) ) ;
#123659 = CARTESIAN_POINT ( 'NONE',  ( -13.89961937509977652, 13.97604488694528158, 90.62390960531432427 ) ) ;
#123660 = CARTESIAN_POINT ( 'NONE',  ( 4.379528057220339221, -16.55341960407611168, 107.7072429386476955 ) ) ;
#123661 = CARTESIAN_POINT ( 'NONE',  ( -14.34966873604960291, -8.224510206698953496, 76.66557627198103830 ) ) ;
#123662 = CARTESIAN_POINT ( 'NONE',  ( 15.72974639402199770, -15.80617190586745480, 88.12390960531436690 ) ) ;
#123663 = CARTESIAN_POINT ( 'NONE',  ( -13.89961937509977652, 13.97604488694528158, 70.62390960531432427 ) ) ;
#123664 = CARTESIAN_POINT ( 'NONE',  ( 10.81492255796078972, 18.62759615963270932, 104.5822429386477097 ) ) ;
#123665 = CARTESIAN_POINT ( 'NONE',  ( 19.02544592524334988, 5.153800228976608722, 71.45942372801900433 ) ) ;
#123667 = CARTESIAN_POINT ( 'NONE',  ( 12.14591786802309770, 12.06949235617756955, 84.37390960531438111 ) ) ;
#123666 = CARTESIAN_POINT ( 'NONE',  ( 19.46398650005390252, -5.499999999999938716, 47.68269651486372851 ) ) ;
#123668 = CARTESIAN_POINT ( 'NONE',  ( -13.97604488694527625, -13.89961937509977652, 61.87390960531435979 ) ) ;
#123669 = CARTESIAN_POINT ( 'NONE',  ( 15.72974639402199770, -15.80617190586745480, 63.12390960531435979 ) ) ;
#123670 = CARTESIAN_POINT ( 'NONE',  ( 16.18388926212235290, -7.379444403734659375, 27.06046848633847901 ) ) ;
#123671 = CARTESIAN_POINT ( 'NONE',  ( 8.224510206698742110, 14.34966873604972548, 112.0844237280190185 ) ) ;
#123672 = CARTESIAN_POINT ( 'NONE',  ( 16.52544592524335698, 4.483927247898782831, 21.45942372801901499 ) ) ;
#123673 = CARTESIAN_POINT ( 'NONE',  ( 12.14591786802309770, 12.06949235617756955, 84.37390960531438111 ) ) ;
#123674 = CARTESIAN_POINT ( 'NONE',  ( -18.22780087662123805, -5.499999999999968026, 93.98236817873105053 ) ) ;
#123675 = CARTESIAN_POINT ( 'NONE',  ( 16.51473224551069308, 9.474510206698969483, 74.16557627198103830 ) ) ;
#123676 = CARTESIAN_POINT ( 'NONE',  ( -19.03943276465977164, 0.05219959533909376836, 31.24890960531435979 ) ) ;
#123677 = CARTESIAN_POINT ( 'NONE',  ( 4.483927247898545687, 16.52544592524342804, 64.79057627198103830 ) ) ;
#123678 = CARTESIAN_POINT ( 'NONE',  ( -19.03943276465977164, 0.05219959533909376836, 116.2489096053143669 ) ) ;
#123680 = CARTESIAN_POINT ( 'NONE',  ( -16.46253265017160317, 9.564922557960807481, 80.83224293864769550 ) ) ;
#123679 = CARTESIAN_POINT ( 'NONE',  ( 19.05341960407617918, -5.049401038297876454, 91.04275706135234714 ) ) ;
#123681 = CARTESIAN_POINT ( 'NONE',  ( 16.51473224551069308, 9.474510206698969483, 84.16557627198102409 ) ) ;
#123682 = CARTESIAN_POINT ( 'NONE',  ( 0.05219959533907565091, 21.53943276465977519, 69.99890960531435269 ) ) ;
#123683 = CARTESIAN_POINT ( 'NONE',  ( -0.05219959533934338120, 16.53943276465976808, 77.50109039468567573 ) ) ;
#123684 = CARTESIAN_POINT ( 'NONE',  ( 16.46253265017146816, 9.564922557961045513, 111.6677570613523329 ) ) ;
#123685 = CARTESIAN_POINT ( 'NONE',  ( -19.05341960407611168, -5.049401038298163336, 56.45724293864768129 ) ) ;
#123686 = CARTESIAN_POINT ( 'NONE',  ( -18.67979575497178146, -10.72451020669898902, 61.66557627198103120 ) ) ;
#123687 = CARTESIAN_POINT ( 'NONE',  ( -19.02544592524334988, -5.153800228976617603, 108.9594237280189759 ) ) ;
#123689 = CARTESIAN_POINT ( 'NONE',  ( -5.719274019375665041, -21.55341960407619695, 44.79275706135234714 ) ) ;
#123688 = CARTESIAN_POINT ( 'NONE',  ( 12.14591786802309770, 12.06949235617756955, 34.37390960531435979 ) ) ;
#123690 = EDGE_CURVE ( 'NONE', #53763, #98202, #61885, .T. ) ;
#123691 = DIRECTION ( 'NONE',  ( -1.000000000000000000, 0.000000000000000000, 0.000000000000000000 ) ) ;
#123693 = CARTESIAN_POINT ( 'NONE',  ( 5.049401038298161559, -19.05341960407611168, 112.7072429386476813 ) ) ;
#123692 = CARTESIAN_POINT ( 'NONE',  ( 4.379528057220092307, 16.55341960407617563, 72.29275706135236135 ) ) ;
#123694 = FACE_OUTER_BOUND ( 'NONE', #52893, .T. ) ;
#123695 = DIRECTION ( 'NONE',  ( 0.000000000000000000, -0.7071067811865467956, 0.7071067811865483499 ) ) ;
#123696 = CARTESIAN_POINT ( 'NONE',  ( 8.314922557961029526, -14.29746914071037800, 100.4177570613523471 ) ) ;
#123697 = CARTESIAN_POINT ( 'NONE',  ( 16.52544592524335698, 4.483927247898782831, 51.45942372801901854 ) ) ;
#123698 = CARTESIAN_POINT ( 'NONE',  ( -0.05219959533909027116, -19.03943276465977164, 57.49890960531435979 ) ) ;
#123699 = CARTESIAN_POINT ( 'NONE',  ( 13.97604488694527802, 13.89961937509977652, 69.37390960531436690 ) ) ;
#123700 = CARTESIAN_POINT ( 'NONE',  ( 21.55341960407619695, -5.719274019375665929, 51.04275706135234714 ) ) ;
#123701 = CARTESIAN_POINT ( 'NONE',  ( 4.483927247898790824, -16.52544592524335698, 65.20942372801901854 ) ) ;
#123702 = CARTESIAN_POINT ( 'NONE',  ( -14.34966873604960291, -8.224510206698953496, 36.66557627198103120 ) ) ;
#123703 = CARTESIAN_POINT ( 'NONE',  ( -13.89961937509977652, 13.97604488694528158, 35.62390960531435269 ) ) ;
#123704 = CARTESIAN_POINT ( 'NONE',  ( 5.153800228976335163, 19.02544592524342804, 39.79057627198100988 ) ) ;
#123706 = EDGE_LOOP ( 'NONE', ( #147544, #6011, #150712 ) ) ;
#123705 = CARTESIAN_POINT ( 'NONE',  ( -12.14591786802326823, 12.06949235617739902, 23.12609039468567573 ) ) ;
#123708 = CARTESIAN_POINT ( 'NONE',  ( -19.02544592524334988, -5.153800228976617603, 83.95942372801901854 ) ) ;
#123707 =( BOUNDED_CURVE ( )  B_SPLINE_CURVE ( 2, ( #171114, #105468, #28654, #151973, #66906, #189281, #2251, #188283, #142749, #63933, #37571, #49757, #126581 ),
 .UNSPECIFIED., .F., .F. ) 
 B_SPLINE_CURVE_WITH_KNOTS ( ( 3, 2, 2, 2, 2, 2, 3 ),
 ( 0.3708514890586240842, 0.3728070175438596423, 0.3771929824561403577, 0.3815789473684210731, 0.3859649122807017330, 0.3903508771929824483, 0.3922607258561279231 ),
 .UNSPECIFIED. ) 
 CURVE ( )  GEOMETRIC_REPRESENTATION_ITEM ( )  RATIONAL_B_SPLINE_CURVE ( ( 0.9831626618144004848, 0.9848076720550091867, 1.000000000000000000, 0.9659258262890683122, 1.000000000000000000, 0.9659258262890683122, 1.000000000000000000, 0.9659258262890683122, 1.000000000000000000, 0.9659258262890683122, 1.000000000000000000, 0.9851625545550091179, 0.9832469066685282089 ) ) 
 REPRESENTATION_ITEM ( '' )  );
#123709 = CARTESIAN_POINT ( 'NONE',  ( 12.14591786802309770, 12.06949235617756955, 84.37390960531438111 ) ) ;
#123710 = CARTESIAN_POINT ( 'NONE',  ( -19.02544592524342804, 5.153800228976336051, 56.04057627198100988 ) ) ;
#123712 = CARTESIAN_POINT ( 'NONE',  ( -30.74264578624800492, -22.33583958711396278, -9.799999999999998934 ) ) ;
#123711 = CARTESIAN_POINT ( 'NONE',  ( -19.03943276465977164, -0.05219959533935918106, 88.75109039468567573 ) ) ;
#123713 = CARTESIAN_POINT ( 'NONE',  ( 21.55341960407619695, -5.719274019375665929, 96.04275706135236135 ) ) ;
#123714 = CARTESIAN_POINT ( 'NONE',  ( -8.314922557961024197, 14.29746914071037800, 47.91775706135234714 ) ) ;
#123715 = CARTESIAN_POINT ( 'NONE',  ( 17.26172910966778673, 6.454744622555868894, 36.69353091350777163 ) ) ;
#123716 = CARTESIAN_POINT ( 'NONE',  ( -21.53943276465977519, 0.05219959533907696930, 51.24890960531436690 ) ) ;
#123717 = CARTESIAN_POINT ( 'NONE',  ( 8.224510206698742110, 14.34966873604972548, 42.08442372801901854 ) ) ;
#123718 = CARTESIAN_POINT ( 'NONE',  ( -5.049401038298153566, 19.05341960407611168, 35.20724293864768839 ) ) ;
#123719 = CARTESIAN_POINT ( 'NONE',  ( 5.153800228976615827, -19.02544592524334988, 45.20942372801901143 ) ) ;
#123720 = CARTESIAN_POINT ( 'NONE',  ( 0.05219959533909260263, 19.03943276465977164, 74.99890960531435269 ) ) ;
#123721 = CARTESIAN_POINT ( 'NONE',  ( -13.89961937509977652, 13.97604488694528158, 45.62390960531433848 ) ) ;
#123722 = DIRECTION ( 'NONE',  ( -0.1039620511844979306, -0.1039620511844979306, 0.9891328443778538704 ) ) ;
#123723 = CARTESIAN_POINT ( 'NONE',  ( 5.049401038298161559, -19.05341960407611168, 67.70724293864769550 ) ) ;
#123724 = CARTESIAN_POINT ( 'NONE',  ( -27.88129983271673851, -6.733757357603135318, 162.1517353552107750 ) ) ;
#123725 = CARTESIAN_POINT ( 'NONE',  ( 19.03943276465977164, 0.05219959533936151252, 36.25109039468567573 ) ) ;
#123726 = CARTESIAN_POINT ( 'NONE',  ( -18.62759615963255300, -10.81492255796106328, 104.1677570613523471 ) ) ;
#123727 = CARTESIAN_POINT ( 'NONE',  ( 16.52544592524342804, -4.483927247898539470, 43.54057627198103830 ) ) ;
#123728 = CARTESIAN_POINT ( 'NONE',  ( 0.05219959533909260263, 19.03943276465977164, 44.99890960531435979 ) ) ;
#123729 = CARTESIAN_POINT ( 'NONE',  ( -9.474510206698964154, 16.51473224551069663, 105.4155762719810383 ) ) ;
#123730 = CARTESIAN_POINT ( 'NONE',  ( -5.823673210054431948, 21.52544592524334988, 87.70942372801901854 ) ) ;
#123731 = CARTESIAN_POINT ( 'NONE',  ( 5.049401038298161559, -19.05341960407611168, 52.70724293864767418 ) ) ;
#123732 = CARTESIAN_POINT ( 'NONE',  ( -15.72974639402176322, -15.80617190586768395, 84.37609039468570415 ) ) ;
#123733 = CARTESIAN_POINT ( 'NONE',  ( 5.719274019375991003, -21.55341960407610458, 42.70724293864770260 ) ) ;
#123734 = CARTESIAN_POINT ( 'NONE',  ( 21.55341960407619695, -5.719274019375665929, 21.04275706135234714 ) ) ;
#123735 = CARTESIAN_POINT ( 'NONE',  ( -16.46253265017146816, -9.564922557961047289, 54.16775706135234003 ) ) ;
#123736 = CARTESIAN_POINT ( 'NONE',  ( -19.03943276465977164, 0.05219959533909376836, 26.24890960531435624 ) ) ;
#123737 = CARTESIAN_POINT ( 'NONE',  ( -13.89961937509977652, 13.97604488694528158, 80.62390960531436690 ) ) ;
#123738 = CARTESIAN_POINT ( 'NONE',  ( -0.05219959533936034679, 19.03943276465977164, 112.5010903946856757 ) ) ;
#123739 = CARTESIAN_POINT ( 'NONE',  ( 16.55341960407611168, 4.379528057220329451, 88.95724293864769550 ) ) ;
#123740 = CARTESIAN_POINT ( 'NONE',  ( 16.51473224551069308, 9.474510206698969483, 54.16557627198103120 ) ) ;
#123741 = CARTESIAN_POINT ( 'NONE',  ( -10.81492255796078084, -18.62759615963271287, 37.08224293864768129 ) ) ;
#123742 = CARTESIAN_POINT ( 'NONE',  ( 19.03943276465977164, 0.05219959533936151252, 96.25109039468567573 ) ) ;
#123743 = CARTESIAN_POINT ( 'NONE',  ( -15.80617190586745835, -15.72974639402198527, 101.8739096053143811 ) ) ;
#123744 = CARTESIAN_POINT ( 'NONE',  ( 5.719274019375673035, 21.55341960407619339, 52.29275706135236135 ) ) ;
#123745 = CARTESIAN_POINT ( 'NONE',  ( 4.483927247898790824, -16.52544592524335698, 60.20942372801902565 ) ) ;
#123746 = CARTESIAN_POINT ( 'NONE',  ( -16.55341960407617563, 4.379528057220093196, 73.54275706135234714 ) ) ;
#123747 = CARTESIAN_POINT ( 'NONE',  ( -0.05219959533909027116, -19.03943276465977164, 57.49890960531435979 ) ) ;
#123748 = CARTESIAN_POINT ( 'NONE',  ( -4.379528057220086978, -16.55341960407618274, 89.79275706135236135 ) ) ;
#123749 = CARTESIAN_POINT ( 'NONE',  ( 18.67979575497194134, -10.72451020669871369, 20.83442372801901143 ) ) ;
#123750 = CARTESIAN_POINT ( 'NONE',  ( 16.53943276465976808, -0.05219959533910856209, 68.74890960531435269 ) ) ;
#123751 = CARTESIAN_POINT ( 'NONE',  ( 19.02544592524343514, -5.153800228976328945, 83.54057627198100988 ) ) ;
#123752 = CARTESIAN_POINT ( 'NONE',  ( -12.14591786802326823, 12.06949235617739902, 73.12609039468567573 ) ) ;
#123753 = CARTESIAN_POINT ( 'NONE',  ( -15.80617190586768217, 15.72974639402176855, 53.12609039468568284 ) ) ;
#123754 = CARTESIAN_POINT ( 'NONE',  ( -16.53943276465976808, -0.05219959533934237506, 18.75109039468568639 ) ) ;
#123755 = CARTESIAN_POINT ( 'NONE',  ( -18.62759615963255300, -10.81492255796106328, 19.16775706135234714 ) ) ;
#123756 = CARTESIAN_POINT ( 'NONE',  ( -8.224510206698948167, 14.34966873604960824, 60.41557627198102409 ) ) ;
#123757 = VERTEX_POINT ( 'NONE', #46741 ) ;
#123758 = CARTESIAN_POINT ( 'NONE',  ( -17.44279575226823553, 5.990770900252460507, 75.83557567514316133 ) ) ;
#123759 = CARTESIAN_POINT ( 'NONE',  ( 5.719274019375991003, -21.55341960407610458, 82.70724293864770971 ) ) ;
#123760 = CARTESIAN_POINT ( 'NONE',  ( -16.52544592524342804, 4.483927247898546575, 46.04057627198103830 ) ) ;
#123761 = VERTEX_POINT ( 'NONE', #29587 ) ;
#123762 = CARTESIAN_POINT ( 'NONE',  ( 34.75593525676444528, 1.707450833175044425, 52.30717240064831941 ) ) ;
#123763 = CARTESIAN_POINT ( 'NONE',  ( -15.72974639402197994, 15.80617190586746368, 110.6239096053143669 ) ) ;
#123764 = CARTESIAN_POINT ( 'NONE',  ( 19.02544592524343514, -5.153800228976328945, 113.5405762719810241 ) ) ;
#123765 = CARTESIAN_POINT ( 'NONE',  ( 10.72451020669871369, 18.67979575497193778, 27.08442372801901854 ) ) ;
#123766 = CARTESIAN_POINT ( 'NONE',  ( -4.483927247898539470, -16.52544592524342804, 57.29057627198103120 ) ) ;
#123767 = CARTESIAN_POINT ( 'NONE',  ( -16.55341960407617563, 4.379528057220093196, 58.54275706135235424 ) ) ;
#123768 = CARTESIAN_POINT ( 'NONE',  ( 13.89961937509977652, -13.97604488694527269, 63.12390960531435979 ) ) ;
#123769 = CARTESIAN_POINT ( 'NONE',  ( 16.46253265017146816, 9.564922557961045513, 66.66775706135233293 ) ) ;
#123770 = CARTESIAN_POINT ( 'NONE',  ( -9.474510206698964154, 16.51473224551069663, 75.41557627198103830 ) ) ;
#123771 = EDGE_CURVE ( 'NONE', #88998, #49922, #78051, .T. ) ;
#123772 = CARTESIAN_POINT ( 'NONE',  ( 0.05219959533907565091, 21.53943276465977519, 54.99890960531435269 ) ) ;
#123773 = CARTESIAN_POINT ( 'NONE',  ( -12.11826072628013584, -36.49684537641458348, -23.43927118308474178 ) ) ;
#123774 = CARTESIAN_POINT ( 'NONE',  ( -5.049401038298153566, 19.05341960407611168, 60.20724293864768129 ) ) ;
#123775 = CARTESIAN_POINT ( 'NONE',  ( -14.29746914071037622, -8.314922557961029526, 29.16775706135234003 ) ) ;
#123776 = CARTESIAN_POINT ( 'NONE',  ( 5.153800228976615827, -19.02544592524334988, 65.20942372801900433 ) ) ;
#123777 = CARTESIAN_POINT ( 'NONE',  ( -15.72974639402197994, 15.80617190586746368, 110.6239096053143669 ) ) ;
#123778 = CARTESIAN_POINT ( 'NONE',  ( 14.34966873604960469, 8.224510206698951720, 49.16557627198102409 ) ) ;
#123779 = CARTESIAN_POINT ( 'NONE',  ( 0.05219959533909260263, 19.03943276465977164, 94.99890960531436690 ) ) ;
#123780 = CARTESIAN_POINT ( 'NONE',  ( 15.72974639402199770, -15.80617190586745480, 58.12390960531435979 ) ) ;
#123782 = CARTESIAN_POINT ( 'NONE',  ( -0.05219959533934338120, 16.53943276465976808, 42.50109039468567573 ) ) ;
#123781 = CARTESIAN_POINT ( 'NONE',  ( -0.05219959533907301413, -21.53943276465977519, 92.49890960531436690 ) ) ;
#123783 = CARTESIAN_POINT ( 'NONE',  ( 5.823673210054125526, 21.52544592524343514, 34.79057627198103120 ) ) ;
#123784 = CARTESIAN_POINT ( 'NONE',  ( 18.62759615963255655, 10.81492255796105972, 86.66775706135234714 ) ) ;
#123785 = CARTESIAN_POINT ( 'NONE',  ( 16.51473224551069308, 9.474510206698969483, 89.16557627198103830 ) ) ;
#123786 = CARTESIAN_POINT ( 'NONE',  ( -19.03943276465977164, 0.05219959533909376836, 41.24890960531435269 ) ) ;
#123787 = CARTESIAN_POINT ( 'NONE',  ( -19.03943276465977164, 0.05219959533909376836, 91.24890960531436690 ) ) ;
#123788 = CARTESIAN_POINT ( 'NONE',  ( 12.06949235617757843, -12.14591786802309237, 103.1239096053143811 ) ) ;
#123789 = CARTESIAN_POINT ( 'NONE',  ( 9.564922557960805705, 16.46253265017160317, 69.58224293864770971 ) ) ;
#123790 = CARTESIAN_POINT ( 'NONE',  ( 14.34966873604972726, -8.224510206698740333, 25.83442372801901499 ) ) ;
#123791 = VECTOR ( 'NONE', #109155, 1000.000000000000000 ) ;
#123792 = CARTESIAN_POINT ( 'NONE',  ( 17.50000000000003197, 4.658240926743142829, 33.55529582183199722 ) ) ;
#123794 = CARTESIAN_POINT ( 'NONE',  ( 21.53943276465977519, -0.05219959533907433946, 28.74890960531435624 ) ) ;
#123793 = CARTESIAN_POINT ( 'NONE',  ( -15.72974639402176322, -15.80617190586768395, 104.3760903946856899 ) ) ;
#123795 = CARTESIAN_POINT ( 'NONE',  ( 4.379528057220092307, 16.55341960407617563, 87.29275706135236135 ) ) ;
#123796 = FACE_OUTER_BOUND ( 'NONE', #50236, .T. ) ;
#123797 = CARTESIAN_POINT ( 'NONE',  ( 16.46253265017146816, 9.564922557961045513, 71.66775706135233293 ) ) ;
#123798 = CARTESIAN_POINT ( 'NONE',  ( 19.05341960407617918, -5.049401038297876454, 31.04275706135232227 ) ) ;
#123799 = DIRECTION ( 'NONE',  ( 0.000000000000000000, 0.000000000000000000, 1.000000000000000000 ) ) ;
#123800 = CARTESIAN_POINT ( 'NONE',  ( 19.02544592524343514, -5.153800228976328945, 33.54057627198102409 ) ) ;
#123801 = CARTESIAN_POINT ( 'NONE',  ( 8.224510206698953496, -14.34966873604960469, 32.91557627198102409 ) ) ;
#123802 = CARTESIAN_POINT ( 'NONE',  ( -16.88567814943161949, -6.947325034625689177, 111.2900112265258770 ) ) ;
#123803 = CARTESIAN_POINT ( 'NONE',  ( 16.52544592524342804, -4.483927247898539470, 28.54057627198103120 ) ) ;
#123804 = CARTESIAN_POINT ( 'NONE',  ( 17.49999999999999289, 5.624438216177599870, 66.68329655085355512 ) ) ;
#123805 = CARTESIAN_POINT ( 'NONE',  ( 16.52544592524335698, 4.483927247898782831, 91.45942372801901854 ) ) ;
#123806 = CARTESIAN_POINT ( 'NONE',  ( 19.05341960407611168, 5.049401038298154454, 33.95724293864769550 ) ) ;
#123807 = CARTESIAN_POINT ( 'NONE',  ( 15.80617190586769283, -15.72974639402175789, 110.6260903946857042 ) ) ;
#123808 = CARTESIAN_POINT ( 'NONE',  ( 16.52544592524335698, 4.483927247898782831, 21.45942372801901499 ) ) ;
#123809 = CARTESIAN_POINT ( 'NONE',  ( -15.72974639402176322, -15.80617190586768395, 79.37609039468567573 ) ) ;
#123810 = CARTESIAN_POINT ( 'NONE',  ( 16.46253265017146816, 9.564922557961045513, 51.66775706135233293 ) ) ;
#123811 = CARTESIAN_POINT ( 'NONE',  ( 19.03943276465977164, -0.05219959533909143690, 88.74890960531436690 ) ) ;
#123812 = CARTESIAN_POINT ( 'NONE',  ( -5.153800228976328057, -19.02544592524343514, 72.29057627198102409 ) ) ;
#123813 = CARTESIAN_POINT ( 'NONE',  ( -19.52837319214028255, 5.499999999999903189, 39.60471352585542348 ) ) ;
#123814 = CARTESIAN_POINT ( 'NONE',  ( -0.05219959533907301413, -21.53943276465977519, 92.49890960531436690 ) ) ;
#123815 = CARTESIAN_POINT ( 'NONE',  ( 4.379528057220339221, -16.55341960407611168, 62.70724293864769550 ) ) ;
#123816 = CARTESIAN_POINT ( 'NONE',  ( 5.719274019375991003, -21.55341960407610458, 62.70724293864769550 ) ) ;
#123817 = CARTESIAN_POINT ( 'NONE',  ( -5.049401038298153566, 19.05341960407611168, 65.20724293864765286 ) ) ;
#123819 = CARTESIAN_POINT ( 'NONE',  ( 12.14591786802327356, -12.06949235617739191, 80.62609039468567573 ) ) ;
#123818 = CARTESIAN_POINT ( 'NONE',  ( -10.81492255796078084, -18.62759615963271287, 87.08224293864769550 ) ) ;
#123820 = ORIENTED_EDGE ( 'NONE', *, *, #190234, .F. ) ;
#123821 = CARTESIAN_POINT ( 'NONE',  ( -16.51473224551069308, -9.474510206698971260, 41.66557627198103120 ) ) ;
#123823 = FACE_OUTER_BOUND ( 'NONE', #198260, .T. ) ;
#123822 = CARTESIAN_POINT ( 'NONE',  ( -12.14591786802309592, -12.06949235617757132, 76.87390960531439532 ) ) ;
#123824 = CARTESIAN_POINT ( 'NONE',  ( -5.049401038298153566, 19.05341960407611168, 55.20724293864769550 ) ) ;
#123825 = CARTESIAN_POINT ( 'NONE',  ( 16.53943276465976808, -0.05219959533910856209, 113.7489096053143527 ) ) ;
#123826 = CARTESIAN_POINT ( 'NONE',  ( 19.05341960407617918, -5.049401038297876454, 66.04275706135233293 ) ) ;
#123827 = CARTESIAN_POINT ( 'NONE',  ( 12.06949235617757843, -12.14591786802309237, 88.12390960531436690 ) ) ;
#123828 = CARTESIAN_POINT ( 'NONE',  ( 21.52544592524334988, 5.823673210054432836, 46.45942372801901854 ) ) ;
#123830 = CARTESIAN_POINT ( 'NONE',  ( 15.72974639402199770, -15.80617190586745480, 103.1239096053143811 ) ) ;
#123829 = CARTESIAN_POINT ( 'NONE',  ( 5.049401038298161559, -19.05341960407611168, 32.70724293864768129 ) ) ;
#123831 = CARTESIAN_POINT ( 'NONE',  ( 12.06949235617757843, -12.14591786802309237, 88.12390960531436690 ) ) ;
#123832 = CARTESIAN_POINT ( 'NONE',  ( 9.816778487193307257, -45.49549017958584329, -23.86159105743385211 ) ) ;
#123833 = CARTESIAN_POINT ( 'NONE',  ( 9.474510206698971260, -16.51473224551069308, 57.91557627198103120 ) ) ;
#123834 = CARTESIAN_POINT ( 'NONE',  ( 19.35543954521082100, 5.499999999999580780, 47.08901960356454452 ) ) ;
#123836 = CARTESIAN_POINT ( 'NONE',  ( -5.153800228976328057, -19.02544592524343514, 102.2905762719810383 ) ) ;
#123835 = CARTESIAN_POINT ( 'NONE',  ( -16.51473224551082808, 9.474510206698731452, 98.33442372801900433 ) ) ;
#123837 = CARTESIAN_POINT ( 'NONE',  ( -10.72451020669870658, -18.67979575497194134, 34.58442372801900433 ) ) ;
#123838 = CARTESIAN_POINT ( 'NONE',  ( -16.46253265017160317, 9.564922557960807481, 85.83224293864769550 ) ) ;
#123839 = CARTESIAN_POINT ( 'NONE',  ( -19.02544592524334988, -5.153800228976617603, 68.95942372801896170 ) ) ;
#123840 = CARTESIAN_POINT ( 'NONE',  ( 19.02544592524343514, -5.153800228976328945, 58.54057627198102409 ) ) ;
#123841 = CARTESIAN_POINT ( 'NONE',  ( 0.05219959533910956823, 16.53943276465976808, 79.99890960531435269 ) ) ;
#123842 = CARTESIAN_POINT ( 'NONE',  ( 12.14591786802309770, 12.06949235617756955, 64.37390960531435269 ) ) ;
#123843 = CARTESIAN_POINT ( 'NONE',  ( 19.05341960407611168, 5.049401038298154454, 83.95724293864766707 ) ) ;
#123844 = CARTESIAN_POINT ( 'NONE',  ( 10.72451020669898902, -18.67979575497178502, 97.91557627198103830 ) ) ;
#123845 = CARTESIAN_POINT ( 'NONE',  ( -13.89961937509977652, 13.97604488694528158, 80.62390960531436690 ) ) ;
#123846 = CARTESIAN_POINT ( 'NONE',  ( -0.05219959533936034679, 19.03943276465977164, 27.50109039468566507 ) ) ;
#123849 = CARTESIAN_POINT ( 'NONE',  ( 16.52544592524342804, -4.483927247898539470, 103.5405762719810383 ) ) ;
#123848 = CARTESIAN_POINT ( 'NONE',  ( 8.314922557960818139, 14.29746914071049879, 34.58224293864770260 ) ) ;
#123847 = CARTESIAN_POINT ( 'NONE',  ( -5.049401038298153566, 19.05341960407611168, 30.20724293864768839 ) ) ;
#123850 = CARTESIAN_POINT ( 'NONE',  ( 0.05219959533936267826, -19.03943276465977164, 105.0010903946856615 ) ) ;
#123851 = EDGE_LOOP ( 'NONE', ( #69843, #4872, #57827, #156696, #18602 ) ) ;
#123852 = CARTESIAN_POINT ( 'NONE',  ( -15.72974639402176322, -15.80617190586768395, 34.37609039468568284 ) ) ;
#123853 = CARTESIAN_POINT ( 'NONE',  ( -19.03943276465977164, -0.05219959533935918106, 68.75109039468566152 ) ) ;
#123854 = CARTESIAN_POINT ( 'NONE',  ( 14.34966873604960469, 8.224510206698951720, 24.16557627198103120 ) ) ;
#123855 = CARTESIAN_POINT ( 'NONE',  ( -0.05219959533907301413, -21.53943276465977519, 82.49890960531436690 ) ) ;
#123856 = CARTESIAN_POINT ( 'NONE',  ( 9.564922557960805705, 16.46253265017160317, 114.5822429386476955 ) ) ;
#123857 = CARTESIAN_POINT ( 'NONE',  ( -0.05219959533910754901, -16.53943276465976808, 67.49890960531436690 ) ) ;
#123858 = CARTESIAN_POINT ( 'NONE',  ( 19.02544592524343514, -5.153800228976328945, 23.54057627198102054 ) ) ;
#123859 = CARTESIAN_POINT ( 'NONE',  ( -0.05219959533936034679, 19.03943276465977164, 32.50109039468566863 ) ) ;
#123860 = CARTESIAN_POINT ( 'NONE',  ( 16.52544592524335698, 4.483927247898782831, 86.45942372801901854 ) ) ;
#123861 = CARTESIAN_POINT ( 'NONE',  ( 16.53943276465976808, 0.05219959533934440121, 61.25109039468567573 ) ) ;
#123862 = CARTESIAN_POINT ( 'NONE',  ( 16.46253265017160672, -9.564922557960803928, 113.3322429386476955 ) ) ;
#123863 = CARTESIAN_POINT ( 'NONE',  ( -21.53943276465977519, -0.05219959533937600094, 108.7510903946857042 ) ) ;
#123864 = CARTESIAN_POINT ( 'NONE',  ( 19.05341960407611168, 5.049401038298154454, 73.95724293864768129 ) ) ;
#123865 = CARTESIAN_POINT ( 'NONE',  ( -16.52544592524335698, -4.483927247898792601, 63.95942372801901854 ) ) ;
#123866 = CARTESIAN_POINT ( 'NONE',  ( -12.06949235617756955, 12.14591786802309770, 115.6239096053143669 ) ) ;
#123867 = CARTESIAN_POINT ( 'NONE',  ( 8.314922557960818139, 14.29746914071049879, 39.58224293864769550 ) ) ;
#123868 = CARTESIAN_POINT ( 'NONE',  ( -17.60728821186567217, 5.500000000000031086, 70.86690927743002533 ) ) ;
#123870 = CARTESIAN_POINT ( 'NONE',  ( 19.02544592524343514, -5.153800228976328945, 78.54057627198099567 ) ) ;
#123869 = CARTESIAN_POINT ( 'NONE',  ( 13.97604488694527802, 13.89961937509977652, 104.3739096053143385 ) ) ;
#123871 = CARTESIAN_POINT ( 'NONE',  ( -5.049401038298153566, 19.05341960407611168, 115.2072429386477097 ) ) ;
#123872 = CARTESIAN_POINT ( 'NONE',  ( 16.55341960407611168, 4.379528057220329451, 63.95724293864770260 ) ) ;
#123873 = EDGE_CURVE ( 'NONE', #188447, #38864, #93309, .T. ) ;
#123874 = CARTESIAN_POINT ( 'NONE',  ( -12.06949235617756955, 12.14591786802309770, 35.62390960531437401 ) ) ;
#123875 = ORIENTED_EDGE ( 'NONE', *, *, #136297, .T. ) ;
#123876 = CARTESIAN_POINT ( 'NONE',  ( -4.483927247898539470, -16.52544592524342804, 57.29057627198103120 ) ) ;
#123877 = ORIENTED_EDGE ( 'NONE', *, *, #74851, .F. ) ;
#123879 = CARTESIAN_POINT ( 'NONE',  ( -17.58332526062528345, -7.635886036038592728, 59.07665040441534643 ) ) ;
#123878 = CARTESIAN_POINT ( 'NONE',  ( -12.14591786802326823, 12.06949235617739902, 43.12609039468568284 ) ) ;
#123880 = CARTESIAN_POINT ( 'NONE',  ( 13.97604488694548053, -13.89961937509957401, 45.62609039468566863 ) ) ;
#123881 = CARTESIAN_POINT ( 'NONE',  ( -5.153800228976328057, -19.02544592524343514, 82.29057627198103830 ) ) ;
#123882 = CARTESIAN_POINT ( 'NONE',  ( 0.05219959533936267826, -19.03943276465977164, 50.00109039468566863 ) ) ;
#123883 = CARTESIAN_POINT ( 'NONE',  ( -17.14385361876520264, -23.59649016807271593, 145.6750000027311671 ) ) ;
#123884 = CARTESIAN_POINT ( 'NONE',  ( 13.97604488694548053, -13.89961937509957401, 55.62609039468566863 ) ) ;
#123886 = CARTESIAN_POINT ( 'NONE',  ( -14.34966873604972548, 8.224510206698743886, 78.33442372801901854 ) ) ;
#123885 = CARTESIAN_POINT ( 'NONE',  ( 9.564922557961047289, -16.46253265017146816, 95.41775706135233293 ) ) ;
#123887 = CARTESIAN_POINT ( 'NONE',  ( 27.73933785331498925, -9.013057229001033122, 148.2750000027311330 ) ) ;
#123888 = CARTESIAN_POINT ( 'NONE',  ( -9.474510206698964154, 16.51473224551069663, 25.41557627198103120 ) ) ;
#123889 = CARTESIAN_POINT ( 'NONE',  ( 13.97604488694527802, 13.89961937509977652, 104.3739096053143385 ) ) ;
#123890 = CARTESIAN_POINT ( 'NONE',  ( -0.05219959533937732626, 21.53943276465977519, 47.50109039468568994 ) ) ;
#123891 = CARTESIAN_POINT ( 'NONE',  ( -19.05341960407617563, 5.049401038297882671, 98.54275706135233293 ) ) ;
#123893 = CARTESIAN_POINT ( 'NONE',  ( -13.97604488694527625, -13.89961937509977652, 56.87390960531434558 ) ) ;
#123892 = CARTESIAN_POINT ( 'NONE',  ( 17.49999999999999645, 3.534425089339017223, 23.05531345578905800 ) ) ;
#123894 = CARTESIAN_POINT ( 'NONE',  ( -5.049401038298153566, 19.05341960407611168, 110.2072429386476671 ) ) ;
#123896 = CARTESIAN_POINT ( 'NONE',  ( 16.51473224551069308, 9.474510206698969483, 69.16557627198102409 ) ) ;
#123895 = CARTESIAN_POINT ( 'NONE',  ( 16.55341960407611168, 4.379528057220329451, 63.95724293864770260 ) ) ;
#123897 = CARTESIAN_POINT ( 'NONE',  ( -5.049401038298153566, 19.05341960407611168, 60.20724293864768129 ) ) ;
#123898 = CARTESIAN_POINT ( 'NONE',  ( -19.02544592524334988, -5.153800228976617603, 83.95942372801901854 ) ) ;
#123899 = CARTESIAN_POINT ( 'NONE',  ( 15.72974639402199770, -15.80617190586745480, 53.12390960531436690 ) ) ;
#123900 = CARTESIAN_POINT ( 'NONE',  ( 16.51473224551083163, -9.474510206698727899, 45.83442372801900433 ) ) ;
#123901 = CARTESIAN_POINT ( 'NONE',  ( -19.03943276465977164, 0.05219959533909376836, 81.24890960531436690 ) ) ;
#123902 = CARTESIAN_POINT ( 'NONE',  ( 0.05219959533907565091, 21.53943276465977519, 79.99890960531435269 ) ) ;
#123904 = CARTESIAN_POINT ( 'NONE',  ( -13.97604488694547697, 13.89961937509957934, 33.12609039468566863 ) ) ;
#123903 = CARTESIAN_POINT ( 'NONE',  ( -8.314922557960811034, -14.29746914071050412, 82.08224293864768129 ) ) ;
#123905 = CARTESIAN_POINT ( 'NONE',  ( 10.81492255796078972, 18.62759615963270932, 59.58224293864770260 ) ) ;
#123906 = CARTESIAN_POINT ( 'NONE',  ( -21.55341960407610458, -5.719274019375992779, 41.45724293864769550 ) ) ;
#123907 = CARTESIAN_POINT ( 'NONE',  ( 19.03943276465977164, -0.05219959533909143690, 63.74890960531435979 ) ) ;
#123908 = CARTESIAN_POINT ( 'NONE',  ( -0.05219959533909027116, -19.03943276465977164, 22.49890960531436690 ) ) ;
#123909 = ADVANCED_FACE ( 'NONE', ( #172069 ), #122335, .F. ) ;
#123910 = CARTESIAN_POINT ( 'NONE',  ( -5.719274019375665041, -21.55341960407619695, 29.79275706135234358 ) ) ;
#123911 = CARTESIAN_POINT ( 'NONE',  ( -19.05341960407611168, -5.049401038298163336, 111.4572429386476671 ) ) ;
#123912 = CARTESIAN_POINT ( 'NONE',  ( 15.72974639402176855, 15.80617190586768217, 41.87609039468568284 ) ) ;
#123913 = CARTESIAN_POINT ( 'NONE',  ( 16.51473224551069308, 9.474510206698969483, 39.16557627198103120 ) ) ;
#123914 = CARTESIAN_POINT ( 'NONE',  ( 21.53943276465977519, -0.05219959533907433946, 108.7489096053143669 ) ) ;
#123915 = CARTESIAN_POINT ( 'NONE',  ( -19.02544592524334988, -5.153800228976617603, 53.95942372801898301 ) ) ;
#123916 = DIRECTION ( 'NONE',  ( -0.000000000000000000, -0.000000000000000000, -1.000000000000000000 ) ) ;
#123917 = CARTESIAN_POINT ( 'NONE',  ( 19.49149378614661288, -5.499999999999571010, 76.93757513605359577 ) ) ;
#123918 = LINE ( 'NONE', #167478, #98365 ) ;
#123919 = CARTESIAN_POINT ( 'NONE',  ( -16.53943276465976808, -0.05219959533934237506, 58.75109039468568994 ) ) ;
#123920 = CARTESIAN_POINT ( 'NONE',  ( -19.03943276465977164, 0.05219959533909376836, 21.24890960531436335 ) ) ;
#123921 = CARTESIAN_POINT ( 'NONE',  ( -21.95653654802831412, -8.266568072468361450, 172.1684357517875412 ) ) ;
#123922 = CARTESIAN_POINT ( 'NONE',  ( 9.474510206698971260, -16.51473224551069308, 67.91557627198102409 ) ) ;
#123923 = CARTESIAN_POINT ( 'NONE',  ( -14.34966873604960291, -8.224510206698953496, 101.6655762719810383 ) ) ;
#123924 = B_SPLINE_CURVE_WITH_KNOTS ( 'NONE', 3,
 ( #127908, #99571, #161252, #8577, #22746, #162252, #36897, #160255, #19750, #7556, #81391, #21745, #189610, #51084, #20736, #112744, #70252, #130908, #129887, #192598, #23751, #174437, #85401, #97553, #35907, #131920, #82392, #5561, #67240, #128899, #190598, #101570 ),
 .UNSPECIFIED., .F., .F.,
 ( 4, 2, 2, 2, 2, 2, 2, 2, 2, 2, 2, 2, 2, 2, 2, 4 ),
 ( 1.599336020787782259E-17, 0.0003712461730036884584, 0.0007424923460073609791, 0.001113738519011033337, 0.001484984692014705912, 0.002227477038022050628, 0.002598723211025726672, 0.002969969384029402283, 0.003341215557033078327, 0.003712461730036753938, 0.004083707903040429549, 0.004454954076044104726, 0.004826200249047780770, 0.005197446422051455947, 0.005568692595055131991, 0.005939938768058808036 ),
 .UNSPECIFIED. ) ;
#123925 = CARTESIAN_POINT ( 'NONE',  ( -5.719274019375978568, 21.55341960407610458, 60.20724293864768839 ) ) ;
#123926 = CARTESIAN_POINT ( 'NONE',  ( -4.379528057220086978, -16.55341960407618274, 34.79275706135235424 ) ) ;
#123927 = CARTESIAN_POINT ( 'NONE',  ( -21.55341960407619339, 5.719274019375674811, 103.5427570613523613 ) ) ;
#123928 = CARTESIAN_POINT ( 'NONE',  ( 5.049401038298161559, -19.05341960407611168, 27.70724293864769550 ) ) ;
#123929 = CARTESIAN_POINT ( 'NONE',  ( -16.52544592524335698, -4.483927247898792601, 108.9594237280190185 ) ) ;
#123930 = CARTESIAN_POINT ( 'NONE',  ( 14.29746914071049879, -8.314922557960816363, 48.33224293864770260 ) ) ;
#123931 = CARTESIAN_POINT ( 'NONE',  ( 16.51473224551069308, 9.474510206698969483, 49.16557627198102409 ) ) ;
#123932 = CARTESIAN_POINT ( 'NONE',  ( -0.05219959533937732626, 21.53943276465977519, 92.50109039468567573 ) ) ;
#123933 = CARTESIAN_POINT ( 'NONE',  ( 15.80617190586746368, 15.72974639402197994, 109.3739096053143811 ) ) ;
#123934 = CARTESIAN_POINT ( 'NONE',  ( -15.80617190586768217, 15.72974639402176855, 68.12609039468567573 ) ) ;
#123935 = CARTESIAN_POINT ( 'NONE',  ( -8.314922557961024197, 14.29746914071037800, 52.91775706135235424 ) ) ;
#123937 = CARTESIAN_POINT ( 'NONE',  ( -21.53943276465977519, -0.05219959533937600094, 98.75109039468568994 ) ) ;
#123936 = CARTESIAN_POINT ( 'NONE',  ( -14.29746914071049879, 8.314922557960819915, 75.83224293864769550 ) ) ;
#123938 = CARTESIAN_POINT ( 'NONE',  ( 12.14591786802327356, -12.06949235617739191, 110.6260903946857042 ) ) ;
#123939 = CARTESIAN_POINT ( 'NONE',  ( -17.31728774477274513, 6.344390552232361813, 115.8190665168932156 ) ) ;
#123940 = CARTESIAN_POINT ( 'NONE',  ( 0.05219959533934541429, -16.53943276465976808, 35.00109039468568284 ) ) ;
#123941 = CARTESIAN_POINT ( 'NONE',  ( -12.14591786802309592, -12.06949235617757132, 36.87390960531435979 ) ) ;
#123942 = CARTESIAN_POINT ( 'NONE',  ( 12.14591786802327356, -12.06949235617739191, 80.62609039468567573 ) ) ;
#123943 = CARTESIAN_POINT ( 'NONE',  ( 19.05341960407611168, 5.049401038298154454, 93.95724293864769550 ) ) ;
#123944 = CARTESIAN_POINT ( 'NONE',  ( 19.05341960407611168, 5.049401038298154454, 108.9572429386477097 ) ) ;
#123945 = CARTESIAN_POINT ( 'NONE',  ( -15.80617190586768217, 15.72974639402176855, 98.12609039468570415 ) ) ;
#123946 = CARTESIAN_POINT ( 'NONE',  ( -16.53943276465976808, -0.05219959533934237506, 108.7510903946857042 ) ) ;
#123947 = CARTESIAN_POINT ( 'NONE',  ( 14.29746914071049879, -8.314922557960816363, 68.33224293864769550 ) ) ;
#123948 = CARTESIAN_POINT ( 'NONE',  ( -19.03943276465977164, 0.05219959533909376836, 76.24890960531435269 ) ) ;
#123949 = ORIENTED_EDGE ( 'NONE', *, *, #45027, .T. ) ;
#123950 = CARTESIAN_POINT ( 'NONE',  ( -0.05219959533934338120, 16.53943276465976808, 32.50109039468568284 ) ) ;
#123951 = CARTESIAN_POINT ( 'NONE',  ( 13.97604488694527802, 13.89961937509977652, 24.37390960531435624 ) ) ;
#123952 = CARTESIAN_POINT ( 'NONE',  ( -19.05341960407611168, -5.049401038298163336, 86.45724293864769550 ) ) ;
#123954 = CARTESIAN_POINT ( 'NONE',  ( -36.91746825000001309, -11.99521256947794789, -4.524999997268813523 ) ) ;
#123953 = CARTESIAN_POINT ( 'NONE',  ( -16.53943276465976808, -0.05219959533934237506, 33.75109039468568284 ) ) ;
#123955 = CARTESIAN_POINT ( 'NONE',  ( -13.97604488694547697, 13.89961937509957934, 33.12609039468566863 ) ) ;
#123956 = CARTESIAN_POINT ( 'NONE',  ( -4.483927247898782831, 16.52544592524335698, 92.70942372801901854 ) ) ;
#123957 = CARTESIAN_POINT ( 'NONE',  ( -0.05219959533909027116, -19.03943276465977164, 32.49890960531435979 ) ) ;
#123958 = CARTESIAN_POINT ( 'NONE',  ( 16.53943276465976808, 0.05219959533934440121, 86.25109039468568994 ) ) ;
#123959 = CARTESIAN_POINT ( 'NONE',  ( -8.314922557961024197, 14.29746914071037800, 72.91775706135234714 ) ) ;
#123960 = CARTESIAN_POINT ( 'NONE',  ( -5.153800228976607833, 19.02544592524334988, 82.70942372801897591 ) ) ;
#123961 = CARTESIAN_POINT ( 'NONE',  ( 0.05219959533936267826, -19.03943276465977164, 35.00109039468566863 ) ) ;
#123962 = CARTESIAN_POINT ( 'NONE',  ( -0.05219959533909027116, -19.03943276465977164, 42.49890960531435269 ) ) ;
#123963 = CARTESIAN_POINT ( 'NONE',  ( -13.97604488694527625, -13.89961937509977652, 96.87390960531433848 ) ) ;
#123964 = CARTESIAN_POINT ( 'NONE',  ( 8.314922557960818139, 14.29746914071049879, 84.58224293864769550 ) ) ;
#123965 = AXIS2_PLACEMENT_3D ( 'NONE', #126551, #64890, #66873 ) ;
#123966 = EDGE_CURVE ( 'NONE', #183542, #84042, #132157, .T. ) ;
#123967 = CARTESIAN_POINT ( 'NONE',  ( -9.474510206698720793, -16.51473224551083518, 54.58442372801899722 ) ) ;
#123968 = CARTESIAN_POINT ( 'NONE',  ( -5.719274019375978568, 21.55341960407610458, 45.20724293864769550 ) ) ;
#123969 = CARTESIAN_POINT ( 'NONE',  ( 13.89961937509957401, 13.97604488694547697, 31.87609039468566863 ) ) ;
#123970 = CARTESIAN_POINT ( 'NONE',  ( 5.049401038298161559, -19.05341960407611168, 102.7072429386476955 ) ) ;
#123971 = CARTESIAN_POINT ( 'NONE',  ( 15.80617190586746368, 15.72974639402197994, 74.37390960531436690 ) ) ;
#123972 = CARTESIAN_POINT ( 'NONE',  ( -9.474510206698964154, 16.51473224551069663, 110.4155762719810383 ) ) ;
#123973 = CARTESIAN_POINT ( 'NONE',  ( 9.564922557961047289, -16.46253265017146816, 85.41775706135233293 ) ) ;
#123974 = CARTESIAN_POINT ( 'NONE',  ( -17.49999999999999289, 5.068104630630373642, 110.7281840534002413 ) ) ;
#123975 = CARTESIAN_POINT ( 'NONE',  ( -16.51473224551082808, 9.474510206698731452, 108.3344237280190043 ) ) ;
#123976 = CARTESIAN_POINT ( 'NONE',  ( -13.89961937509977652, 13.97604488694528158, 35.62390960531435269 ) ) ;
#123977 = CARTESIAN_POINT ( 'NONE',  ( -16.51473224551069308, -9.474510206698971260, 91.66557627198103830 ) ) ;
#123978 = CARTESIAN_POINT ( 'NONE',  ( -21.52544592524343514, 5.823673210054127303, 71.04057627198103830 ) ) ;
#123979 = CARTESIAN_POINT ( 'NONE',  ( -12.14591786802326823, 12.06949235617739902, 48.12609039468568284 ) ) ;
#123980 = CARTESIAN_POINT ( 'NONE',  ( 21.52544592524334988, 5.823673210054432836, 51.45942372801901854 ) ) ;
#123982 = CARTESIAN_POINT ( 'NONE',  ( -15.72974639402176322, -15.80617190586768395, 94.37609039468568994 ) ) ;
#123981 = CARTESIAN_POINT ( 'NONE',  ( 0.05219959533936267826, -19.03943276465977164, 95.00109039468567573 ) ) ;
#123983 = CARTESIAN_POINT ( 'NONE',  ( 8.224510206698742110, 14.34966873604972548, 112.0844237280190185 ) ) ;
#123984 = CARTESIAN_POINT ( 'NONE',  ( 16.46253265017160672, -9.564922557960803928, 103.3322429386476955 ) ) ;
#123985 = CARTESIAN_POINT ( 'NONE',  ( 4.483927247898545687, 16.52544592524342804, 84.79057627198102409 ) ) ;
#123986 = CARTESIAN_POINT ( 'NONE',  ( -0.05219959533910754901, -16.53943276465976808, 42.49890960531435979 ) ) ;
#123987 = CARTESIAN_POINT ( 'NONE',  ( 19.05341960407617918, -5.049401038297876454, 81.04275706135231871 ) ) ;
#123988 = CARTESIAN_POINT ( 'NONE',  ( -10.81492255796105439, 18.62759615963255655, 57.91775706135234714 ) ) ;
#123989 = CARTESIAN_POINT ( 'NONE',  ( -19.02544592524334988, -5.153800228976617603, 28.95942372801900433 ) ) ;
#123990 = CARTESIAN_POINT ( 'NONE',  ( 12.14591786802309770, 12.06949235617756955, 104.3739096053143669 ) ) ;
#123991 = CARTESIAN_POINT ( 'NONE',  ( -0.05219959533907301413, -21.53943276465977519, 37.49890960531436690 ) ) ;
#123992 = CARTESIAN_POINT ( 'NONE',  ( -16.53943276465976808, 0.05219959533911058130, 21.24890960531436690 ) ) ;
#123993 = CARTESIAN_POINT ( 'NONE',  ( -21.52544592524334988, -5.823673210054445271, 98.95942372801903275 ) ) ;
#123994 = CARTESIAN_POINT ( 'NONE',  ( 0.05219959533934541429, -16.53943276465976808, 55.00109039468568284 ) ) ;
#123995 = CARTESIAN_POINT ( 'NONE',  ( -4.379528057220328563, 16.55341960407611168, 30.20724293864769550 ) ) ;
#123996 = CARTESIAN_POINT ( 'NONE',  ( -21.52544592524334988, -5.823673210054445271, 68.95942372801901854 ) ) ;
#123997 = CARTESIAN_POINT ( 'NONE',  ( -5.719274019375665041, -21.55341960407619695, 49.79275706135234714 ) ) ;
#123998 = VERTEX_POINT ( 'NONE', #60896 ) ;
#123999 = CARTESIAN_POINT ( 'NONE',  ( -9.564922557960796823, -16.46253265017161027, 22.08224293864768839 ) ) ;
#124000 = CARTESIAN_POINT ( 'NONE',  ( 15.80617190586769283, -15.72974639402175789, 35.62609039468568994 ) ) ;
#124001 = CARTESIAN_POINT ( 'NONE',  ( -14.29746914071049879, 8.314922557960819915, 100.8322429386477097 ) ) ;
#124002 = CARTESIAN_POINT ( 'NONE',  ( 16.51473224551069308, 9.474510206698969483, 29.16557627198103475 ) ) ;
#124003 = CARTESIAN_POINT ( 'NONE',  ( -8.314922557960811034, -14.29746914071050412, 82.08224293864768129 ) ) ;
#124004 = CARTESIAN_POINT ( 'NONE',  ( -13.89961937509977652, 13.97604488694528158, 75.62390960531438111 ) ) ;
#124005 = CARTESIAN_POINT ( 'NONE',  ( -14.34966873604960291, -8.224510206698953496, 31.66557627198102054 ) ) ;
#124006 = CARTESIAN_POINT ( 'NONE',  ( -21.53943276465977519, 0.05219959533907696930, 61.24890960531435979 ) ) ;
#124007 = CARTESIAN_POINT ( 'NONE',  ( -12.14591786802309592, -12.06949235617757132, 86.87390960531438111 ) ) ;
#124008 = CARTESIAN_POINT ( 'NONE',  ( -15.72974639402197994, 15.80617190586746368, 90.62390960531436690 ) ) ;
#124009 = CARTESIAN_POINT ( 'NONE',  ( 5.049401038298161559, -19.05341960407611168, 102.7072429386476955 ) ) ;
#124011 = CARTESIAN_POINT ( 'NONE',  ( 19.02544592524334988, 5.153800228976608722, 101.4594237280189759 ) ) ;
#124010 = CARTESIAN_POINT ( 'NONE',  ( -9.564922557960796823, -16.46253265017161027, 47.08224293864769550 ) ) ;
#124012 = CARTESIAN_POINT ( 'NONE',  ( -10.72451020669898014, 18.67979575497178502, 40.41557627198103120 ) ) ;
#124013 = CARTESIAN_POINT ( 'NONE',  ( 18.67979575497194134, -10.72451020669871369, 85.83442372801901854 ) ) ;
#124014 = CARTESIAN_POINT ( 'NONE',  ( -19.02544592524342804, 5.153800228976336051, 66.04057627198103830 ) ) ;
#124015 = CONICAL_SURFACE ( 'NONE', #11050, 2.055000000000000160, 0.7853981633974712606 ) ;
#124016 = CARTESIAN_POINT ( 'NONE',  ( -16.51473224551069308, -9.474510206698971260, 96.66557627198102409 ) ) ;
#124017 = CARTESIAN_POINT ( 'NONE',  ( -14.29746914071037622, -8.314922557961029526, 74.16775706135231871 ) ) ;
#124018 = CARTESIAN_POINT ( 'NONE',  ( 10.81492255796106328, -18.62759615963255655, 60.41775706135235424 ) ) ;
#124019 = CARTESIAN_POINT ( 'NONE',  ( 5.823673210054444382, -21.52544592524334988, 80.20942372801901854 ) ) ;
#124020 = CARTESIAN_POINT ( 'NONE',  ( 15.72974639402199770, -15.80617190586745480, 103.1239096053143811 ) ) ;
#124022 = CARTESIAN_POINT ( 'NONE',  ( 16.55341960407618274, -4.379528057220086978, 76.04275706135237556 ) ) ;
#124021 = CARTESIAN_POINT ( 'NONE',  ( 10.72451020669871369, 18.67979575497193778, 42.08442372801901854 ) ) ;
#124023 = CARTESIAN_POINT ( 'NONE',  ( 18.62759615963271287, -10.81492255796078972, 78.33224293864770971 ) ) ;
#124024 = CARTESIAN_POINT ( 'NONE',  ( 9.564922557961047289, -16.46253265017146816, 35.41775706135233293 ) ) ;
#124025 = CARTESIAN_POINT ( 'NONE',  ( -15.72974639402197994, 15.80617190586746368, 45.62390960531436690 ) ) ;
#124027 = CARTESIAN_POINT ( 'NONE',  ( -16.53943276465976808, -0.05219959533934237506, 113.7510903946856757 ) ) ;
#124026 = CARTESIAN_POINT ( 'NONE',  ( -19.05341960407611168, -5.049401038298163336, 86.45724293864769550 ) ) ;
#124028 = CARTESIAN_POINT ( 'NONE',  ( -13.70000000000001528, 1.443387660838688656E-13, -64.92279855667830191 ) ) ;
#124029 = CARTESIAN_POINT ( 'NONE',  ( -5.153800228976328057, -19.02544592524343514, 102.2905762719810383 ) ) ;
#124030 = FACE_OUTER_BOUND ( 'NONE', #11186, .T. ) ;
#124031 = CARTESIAN_POINT ( 'NONE',  ( -9.474510206698720793, -16.51473224551083518, 94.58442372801900433 ) ) ;
#124032 = CARTESIAN_POINT ( 'NONE',  ( -5.719274019375978568, 21.55341960407610458, 75.20724293864769550 ) ) ;
#124033 = CARTESIAN_POINT ( 'NONE',  ( 4.379528057220339221, -16.55341960407611168, 42.70724293864770260 ) ) ;
#124034 = CARTESIAN_POINT ( 'NONE',  ( 16.51473224551083163, -9.474510206698727899, 110.8344237280190043 ) ) ;
#124035 = CARTESIAN_POINT ( 'NONE',  ( -19.05341960407611168, -5.049401038298163336, 31.45724293864769550 ) ) ;
#124036 = CARTESIAN_POINT ( 'NONE',  ( -16.46253265017146816, -9.564922557961047289, 109.1677570613523471 ) ) ;
#124038 = CARTESIAN_POINT ( 'NONE',  ( -9.564922557961040184, 16.46253265017147172, 72.91775706135233293 ) ) ;
#124037 = CARTESIAN_POINT ( 'NONE',  ( -21.53943276465977519, 0.05219959533907696930, 106.2489096053143811 ) ) ;
#124039 = CARTESIAN_POINT ( 'NONE',  ( 16.53943276465976808, 0.05219959533934440121, 86.25109039468568994 ) ) ;
#124040 = CARTESIAN_POINT ( 'NONE',  ( 19.05341960407611168, 5.049401038298154454, 73.95724293864768129 ) ) ;
#124041 = CARTESIAN_POINT ( 'NONE',  ( -8.314922557960811034, -14.29746914071050412, 82.08224293864768129 ) ) ;
#124042 = CIRCLE ( 'NONE', #50180, 0.5000000000000004441 ) ;
#124043 = CARTESIAN_POINT ( 'NONE',  ( -9.474510206698964154, 16.51473224551069663, 60.41557627198102409 ) ) ;
#124044 = CARTESIAN_POINT ( 'NONE',  ( 12.14591786802309770, 12.06949235617756955, 64.37390960531435269 ) ) ;
#124045 = CARTESIAN_POINT ( 'NONE',  ( 13.97604488694527802, 13.89961937509977652, 34.37390960531436690 ) ) ;
#124046 = CARTESIAN_POINT ( 'NONE',  ( 17.61379574983714846, -16.30506298781205743, -54.46030667112336232 ) ) ;
#124047 = CARTESIAN_POINT ( 'NONE',  ( -4.379528057220328563, 16.55341960407611168, 40.20724293864769550 ) ) ;
#124048 = CARTESIAN_POINT ( 'NONE',  ( 5.049401038298161559, -19.05341960407611168, 72.70724293864768129 ) ) ;
#124049 = CARTESIAN_POINT ( 'NONE',  ( 1.667840370490710761E-14, -64.85621347262014069, -14.99999966871768642 ) ) ;
#124050 = CARTESIAN_POINT ( 'NONE',  ( 19.03943276465977164, 0.05219959533936151252, 46.25109039468566863 ) ) ;
#124051 = CARTESIAN_POINT ( 'NONE',  ( -16.55341960407617563, 4.379528057220093196, 58.54275706135235424 ) ) ;
#124052 = CARTESIAN_POINT ( 'NONE',  ( -21.55341960407610458, -5.719274019375992779, 66.45724293864768129 ) ) ;
#124053 = CARTESIAN_POINT ( 'NONE',  ( 16.46253265017146816, 9.564922557961045513, 26.66775706135234003 ) ) ;
#124054 = CARTESIAN_POINT ( 'NONE',  ( 9.474510206698971260, -16.51473224551069308, 82.91557627198103830 ) ) ;
#124055 = CARTESIAN_POINT ( 'NONE',  ( 17.50000000000000000, -5.500000000000000888, 118.0000000000000142 ) ) ;
#124056 = CARTESIAN_POINT ( 'NONE',  ( -0.05219959533907301413, -21.53943276465977519, 32.49890960531435979 ) ) ;
#124057 = CARTESIAN_POINT ( 'NONE',  ( -5.153800228976328057, -19.02544592524343514, 57.29057627198103120 ) ) ;
#124058 = CARTESIAN_POINT ( 'NONE',  ( -10.81492255796105439, 18.62759615963255655, 57.91775706135234714 ) ) ;
#124059 = CARTESIAN_POINT ( 'NONE',  ( 14.34966873604960469, 8.224510206698951720, 109.1655762719810383 ) ) ;
#124062 = ORIENTED_EDGE ( 'NONE', *, *, #64134, .T. ) ;
#124061 = CARTESIAN_POINT ( 'NONE',  ( -0.05219959533909027116, -19.03943276465977164, 92.49890960531436690 ) ) ;
#124060 = CARTESIAN_POINT ( 'NONE',  ( -5.719274019375978568, 21.55341960407610458, 105.2072429386477097 ) ) ;
#124063 = CARTESIAN_POINT ( 'NONE',  ( 15.80617190586769283, -15.72974639402175789, 40.62609039468567573 ) ) ;
#124064 = ORIENTED_EDGE ( 'NONE', *, *, #141141, .F. ) ;
#124065 = CARTESIAN_POINT ( 'NONE',  ( -0.05219959533909027116, -19.03943276465977164, 92.49890960531436690 ) ) ;
#124066 = CARTESIAN_POINT ( 'NONE',  ( 19.48894818550247265, -5.499999999999913847, 82.60307310435241845 ) ) ;
#124067 = CARTESIAN_POINT ( 'NONE',  ( 5.719274019375991003, -21.55341960407610458, 97.70724293864772392 ) ) ;
#124068 = CARTESIAN_POINT ( 'NONE',  ( 9.474510206698971260, -16.51473224551069308, 52.91557627198102409 ) ) ;
#124070 = EDGE_CURVE ( 'NONE', #142350, #74166, #96625, .T. ) ;
#124069 = CARTESIAN_POINT ( 'NONE',  ( -8.314922557961024197, 14.29746914071037800, 27.91775706135234358 ) ) ;
#124071 = CARTESIAN_POINT ( 'NONE',  ( -29.86685920354755552, 21.69954338932564397, -1.324999997268813345 ) ) ;
#124072 = CARTESIAN_POINT ( 'NONE',  ( -5.049401038298153566, 19.05341960407611168, 35.20724293864768839 ) ) ;
#124073 = CARTESIAN_POINT ( 'NONE',  ( -15.80617190586768217, 15.72974639402176855, 83.12609039468568994 ) ) ;
#124075 = CARTESIAN_POINT ( 'NONE',  ( -10.72451020669870658, -18.67979575497194134, 44.58442372801901854 ) ) ;
#124074 = CARTESIAN_POINT ( 'NONE',  ( 9.564922557960805705, 16.46253265017160317, 69.58224293864770971 ) ) ;
#124076 = CARTESIAN_POINT ( 'NONE',  ( -18.62759615963255300, -10.81492255796106328, 24.16775706135235424 ) ) ;
#124077 = CARTESIAN_POINT ( 'NONE',  ( 22.44159573604009239, 16.30477369853692693, 142.5750000027311728 ) ) ;
#124078 = CARTESIAN_POINT ( 'NONE',  ( -16.46253265017160317, 9.564922557960807481, 105.8322429386476955 ) ) ;
#124079 = CARTESIAN_POINT ( 'NONE',  ( -5.222609727149285952, 28.09897361876272726, 140.0000000000000284 ) ) ;
#124082 = CARTESIAN_POINT ( 'NONE',  ( -18.67979575497193778, 10.72451020669871902, 43.33442372801901143 ) ) ;
#124081 = CARTESIAN_POINT ( 'NONE',  ( -8.224510206698735004, -14.34966873604973081, 64.58442372801900433 ) ) ;
#124080 = CARTESIAN_POINT ( 'NONE',  ( -12.06949235617739369, -12.14591786802326823, 39.37609039468567573 ) ) ;
#124083 = CARTESIAN_POINT ( 'NONE',  ( -0.05219959533937732626, 21.53943276465977519, 72.50109039468568994 ) ) ;
#124084 = STYLED_ITEM ( 'NONE', ( #129568 ), #100331 ) ;
#124085 = CARTESIAN_POINT ( 'NONE',  ( 3.948440707545728845, 4.897001621108269198, -62.47584611210316297 ) ) ;
#124086 =( BOUNDED_CURVE ( )  B_SPLINE_CURVE ( 2, ( #136752, #32564, #198436, #59909, #187264, #48733, #31570, #93221, #216, #16405, #185250 ),
 .UNSPECIFIED., .F., .T. ) 
 B_SPLINE_CURVE_WITH_KNOTS ( ( 3, 2, 2, 2, 2, 3 ),
 ( 0.4000000000000031308, 0.4200000000000030931, 0.4400000000000031664, 0.4600000000000031841, 0.4800000000000032019, 0.5000000000000032196 ),
 .UNSPECIFIED. ) 
 CURVE ( )  GEOMETRIC_REPRESENTATION_ITEM ( )  RATIONAL_B_SPLINE_CURVE ( ( 0.9999999999999923395, 0.9510565162951611917, 1.000000000000000000, 0.9510565162951535312, 1.000000000000000000, 0.9510565162951535312, 1.000000000000000000, 0.9510565162951535312, 1.000000000000000000, 0.9510565162951456486, 1.000000000000007772 ) ) 
 REPRESENTATION_ITEM ( '' )  );
#124087 = CARTESIAN_POINT ( 'NONE',  ( -19.03943276465977164, -0.05219959533935918106, 113.7510903946856757 ) ) ;
#124088 = CARTESIAN_POINT ( 'NONE',  ( -16.46253265017160317, 9.564922557960807481, 60.83224293864769550 ) ) ;
#124089 = CARTESIAN_POINT ( 'NONE',  ( -5.049401038298153566, 19.05341960407611168, 95.20724293864770971 ) ) ;
#124090 = CARTESIAN_POINT ( 'NONE',  ( -4.483927247898539470, -16.52544592524342804, 112.2905762719810241 ) ) ;
#124091 = CARTESIAN_POINT ( 'NONE',  ( 16.55341960407611168, 4.379528057220329451, 98.95724293864770971 ) ) ;
#124092 = CARTESIAN_POINT ( 'NONE',  ( 18.67979575497178502, 10.72451020669898547, 29.16557627198103120 ) ) ;
#124093 = CARTESIAN_POINT ( 'NONE',  ( 16.55341960407618274, -4.379528057220086978, 81.04275706135236135 ) ) ;
#124095 = CARTESIAN_POINT ( 'NONE',  ( 9.564922557960805705, 16.46253265017160317, 49.58224293864770260 ) ) ;
#124094 = CARTESIAN_POINT ( 'NONE',  ( 8.314922557960818139, 14.29746914071049879, 69.58224293864769550 ) ) ;
#124096 = CARTESIAN_POINT ( 'NONE',  ( -5.719274019375665041, -21.55341960407619695, 79.79275706135236135 ) ) ;
#124097 = CARTESIAN_POINT ( 'NONE',  ( -21.53943276465977519, -0.05219959533937600094, 68.75109039468568994 ) ) ;
#124098 = CARTESIAN_POINT ( 'NONE',  ( -0.05219959533936034679, 19.03943276465977164, 112.5010903946856757 ) ) ;
#124099 = CARTESIAN_POINT ( 'NONE',  ( 4.379528057220339221, -16.55341960407611168, 77.70724293864770971 ) ) ;
#124100 = CARTESIAN_POINT ( 'NONE',  ( -21.53943276465977519, -0.05219959533937600094, 33.75109039468568284 ) ) ;
#124101 = CARTESIAN_POINT ( 'NONE',  ( -10.72451020669898014, 18.67979575497178502, 55.41557627198102409 ) ) ;
#124102 = CARTESIAN_POINT ( 'NONE',  ( -17.49999999999999645, -5.624438216177586547, 104.1832965508535693 ) ) ;
#124103 = CARTESIAN_POINT ( 'NONE',  ( -5.429308488886486681E-15, 30.30510711980690175, 143.7500000054623399 ) ) ;
#124104 = CARTESIAN_POINT ( 'NONE',  ( -9.474510206698964154, 16.51473224551069663, 75.41557627198103830 ) ) ;
#124105 = CARTESIAN_POINT ( 'NONE',  ( 4.379528057220339221, -16.55341960407611168, 47.70724293864770260 ) ) ;
#124106 = AXIS2_PLACEMENT_3D ( 'NONE', #189095, #186104, #50568 ) ;
#124107 = CARTESIAN_POINT ( 'NONE',  ( -8.224510206698948167, 14.34966873604960824, 25.41557627198103120 ) ) ;
#124108 = CARTESIAN_POINT ( 'NONE',  ( -4.483927247898782831, 16.52544592524335698, 102.7094237280190185 ) ) ;
#124109 = CARTESIAN_POINT ( 'NONE',  ( 16.46253265017146816, 9.564922557961045513, 51.66775706135233293 ) ) ;
#124110 = CARTESIAN_POINT ( 'NONE',  ( -24.39440776506090458, -8.562465606919657191, 166.7298475161185252 ) ) ;
#124111 = CARTESIAN_POINT ( 'NONE',  ( -19.03943276465977164, 0.05219959533909376836, 111.2489096053143669 ) ) ;
#124112 = CARTESIAN_POINT ( 'NONE',  ( -4.379528057220328563, 16.55341960407611168, 70.20724293864769550 ) ) ;
#124113 = CARTESIAN_POINT ( 'NONE',  ( 13.97604488694548053, -13.89961937509957401, 40.62609039468564731 ) ) ;
#124115 = CARTESIAN_POINT ( 'NONE',  ( -0.05219959533907301413, -21.53943276465977519, 42.49890960531435979 ) ) ;
#124114 = CARTESIAN_POINT ( 'NONE',  ( -5.153800228976328057, -19.02544592524343514, 32.29057627198102409 ) ) ;
#124117 = ORIENTED_EDGE ( 'NONE', *, *, #84711, .T. ) ;
#124116 = CARTESIAN_POINT ( 'NONE',  ( 5.719274019375991003, -21.55341960407610458, 52.70724293864769550 ) ) ;
#124118 = CARTESIAN_POINT ( 'NONE',  ( 12.14591786802309770, 12.06949235617756955, 99.37390960531436690 ) ) ;
#124119 = CARTESIAN_POINT ( 'NONE',  ( 12.06949235617739724, 12.14591786802326823, 46.87609039468568994 ) ) ;
#124120 = ADVANCED_FACE ( 'NONE', ( #107396 ), #169069, .F. ) ;
#124121 = CARTESIAN_POINT ( 'NONE',  ( 14.29746914071049879, -8.314922557960816363, 98.33224293864769550 ) ) ;
#124122 = CARTESIAN_POINT ( 'NONE',  ( 17.13100169013301510, -6.664070546373149107, 38.26789835699850073 ) ) ;
#124123 = CARTESIAN_POINT ( 'NONE',  ( 29.86685920354754842, -21.69954338932559068, -10.32499999726881335 ) ) ;
#124124 = CARTESIAN_POINT ( 'NONE',  ( 0.05219959533907565091, 21.53943276465977519, 24.99890960531435624 ) ) ;
#124125 = DIRECTION ( 'NONE',  ( -0.000000000000000000, 1.000000000000000000, -0.000000000000000000 ) ) ;
#124126 = CARTESIAN_POINT ( 'NONE',  ( 0.1000683901517948615, 9.099999999999999645, -63.95112321872117889 ) ) ;
#124127 = ORIENTED_EDGE ( 'NONE', *, *, #165748, .T. ) ;
#124129 = CARTESIAN_POINT ( 'NONE',  ( -14.29746914071049879, 8.314922557960819915, 35.83224293864768839 ) ) ;
#124128 = CARTESIAN_POINT ( 'NONE',  ( 16.52544592524335698, 4.483927247898782831, 36.45942372801901143 ) ) ;
#124130 = CARTESIAN_POINT ( 'NONE',  ( 5.823673210054125526, 21.52544592524343514, 54.79057627198104541 ) ) ;
#124131 = CARTESIAN_POINT ( 'NONE',  ( 19.05341960407617918, -5.049401038297876454, 91.04275706135234714 ) ) ;
#124132 = CARTESIAN_POINT ( 'NONE',  ( 15.72974639402199770, -15.80617190586745480, 68.12390960531436690 ) ) ;
#124133 = CARTESIAN_POINT ( 'NONE',  ( 15.80617190586769283, -15.72974639402175789, 85.62609039468568994 ) ) ;
#124134 = CARTESIAN_POINT ( 'NONE',  ( -10.58303160951406419, 9.244353370540759229, -62.45107349144919340 ) ) ;
#124135 = CARTESIAN_POINT ( 'NONE',  ( -4.379528057220086978, -16.55341960407618274, 44.79275706135234714 ) ) ;
#124137 = CARTESIAN_POINT ( 'NONE',  ( 16.51473224551069308, 9.474510206698969483, 99.16557627198102409 ) ) ;
#124136 = CARTESIAN_POINT ( 'NONE',  ( 19.05341960407611168, 5.049401038298154454, 33.95724293864769550 ) ) ;
#124138 = CARTESIAN_POINT ( 'NONE',  ( 0.05219959533909260263, 19.03943276465977164, 29.99890960531435979 ) ) ;
#124139 = CARTESIAN_POINT ( 'NONE',  ( -16.55341960407611168, -4.379528057220339221, 101.4572429386476955 ) ) ;
#124140 = DIRECTION ( 'NONE',  ( 0.000000000000000000, 0.000000000000000000, 1.000000000000000000 ) ) ;
#124141 = CARTESIAN_POINT ( 'NONE',  ( 9.564922557960805705, 16.46253265017160317, 99.58224293864770971 ) ) ;
#124142 = ORIENTED_EDGE ( 'NONE', *, *, #141815, .F. ) ;
#124143 = CARTESIAN_POINT ( 'NONE',  ( 16.52544592524335698, 4.483927247898782831, 61.45942372801901854 ) ) ;
#124144 = CARTESIAN_POINT ( 'NONE',  ( -21.52544592524343514, 5.823673210054127303, 86.04057627198102409 ) ) ;
#124145 = CARTESIAN_POINT ( 'NONE',  ( 13.89961937509977652, -13.97604488694527269, 63.12390960531435979 ) ) ;
#124146 = CARTESIAN_POINT ( 'NONE',  ( -18.67979575497193778, 10.72451020669871902, 28.33442372801902209 ) ) ;
#124147 = CARTESIAN_POINT ( 'NONE',  ( 19.05341960407611168, 5.049401038298154454, 88.95724293864769550 ) ) ;
#124148 = DIRECTION ( 'NONE',  ( -0.000000000000000000, 1.000000000000000000, -0.000000000000000000 ) ) ;
#124149 = ORIENTED_EDGE ( 'NONE', *, *, #128318, .T. ) ;
#124150 = CARTESIAN_POINT ( 'NONE',  ( -21.53943276465977519, 0.05219959533907696930, 111.2489096053143669 ) ) ;
#124153 = CARTESIAN_POINT ( 'NONE',  ( 16.51473224551083163, -9.474510206698727899, 80.83442372801899012 ) ) ;
#124152 = CARTESIAN_POINT ( 'NONE',  ( -19.03943276465977164, 0.05219959533909376836, 111.2489096053143669 ) ) ;
#124151 = CARTESIAN_POINT ( 'NONE',  ( 5.153800228976335163, 19.02544592524342804, 29.79057627198102409 ) ) ;
#124154 = CARTESIAN_POINT ( 'NONE',  ( 16.46253265017146816, 9.564922557961045513, 26.66775706135234003 ) ) ;
#124155 = CARTESIAN_POINT ( 'NONE',  ( 21.52544592524344225, -5.823673210054117533, 98.54057627198105251 ) ) ;
#124156 = CARTESIAN_POINT ( 'NONE',  ( 0.05219959533936267826, -19.03943276465977164, 40.00109039468566152 ) ) ;
#124157 = CARTESIAN_POINT ( 'NONE',  ( -14.29746914071037622, -8.314922557961029526, 74.16775706135231871 ) ) ;
#124158 = CARTESIAN_POINT ( 'NONE',  ( -16.46253265017160317, 9.564922557960807481, 110.8322429386476955 ) ) ;
#124159 = CARTESIAN_POINT ( 'NONE',  ( 13.97604488694527802, 13.89961937509977652, 59.37390960531434558 ) ) ;
#124160 = CARTESIAN_POINT ( 'NONE',  ( -18.62759615963255300, -10.81492255796106328, 69.16775706135234714 ) ) ;
#124161 = CARTESIAN_POINT ( 'NONE',  ( 21.52544592524334988, 5.823673210054432836, 81.45942372801900433 ) ) ;
#124162 = CARTESIAN_POINT ( 'NONE',  ( -19.02544592524342804, 5.153800228976336051, 81.04057627198103830 ) ) ;
#124163 = CARTESIAN_POINT ( 'NONE',  ( 5.719274019375673035, 21.55341960407619339, 42.29275706135235424 ) ) ;
#124164 = CARTESIAN_POINT ( 'NONE',  ( 19.02544592524334988, 5.153800228976608722, 86.45942372801900433 ) ) ;
#124165 = CARTESIAN_POINT ( 'NONE',  ( -16.51473224551069308, -9.474510206698971260, 56.66557627198103120 ) ) ;
#124166 = CARTESIAN_POINT ( 'NONE',  ( 9.474510206698971260, -16.51473224551069308, 97.91557627198102409 ) ) ;
#124167 = CARTESIAN_POINT ( 'NONE',  ( 13.89961937509977652, -13.97604488694527269, 63.12390960531435979 ) ) ;
#124168 = CARTESIAN_POINT ( 'NONE',  ( 9.564922557960805705, 16.46253265017160317, 109.5822429386476955 ) ) ;
#124169 = CARTESIAN_POINT ( 'NONE',  ( 19.03943276465977164, -0.05219959533909143690, 53.74890960531436690 ) ) ;
#124170 = VECTOR ( 'NONE', #98032, 1000.000000000000000 ) ;
#124171 = CARTESIAN_POINT ( 'NONE',  ( 5.823673210054125526, 21.52544592524343514, 104.7905762719810241 ) ) ;
#124172 = CARTESIAN_POINT ( 'NONE',  ( -4.483927247898782831, 16.52544592524335698, 67.70942372801901854 ) ) ;
#124173 = CARTESIAN_POINT ( 'NONE',  ( -24.27957997113400879, 6.290849861785950736, 171.5443985711291077 ) ) ;
#124174 = CARTESIAN_POINT ( 'NONE',  ( -5.153800228976607833, 19.02544592524334988, 42.70942372801901143 ) ) ;
#124175 = CARTESIAN_POINT ( 'NONE',  ( 5.049401038298161559, -19.05341960407611168, 67.70724293864769550 ) ) ;
#124176 = CARTESIAN_POINT ( 'NONE',  ( -12.14591786802309592, -12.06949235617757132, 56.87390960531436690 ) ) ;
#124177 = CARTESIAN_POINT ( 'NONE',  ( 14.34966873604960469, 8.224510206698951720, 89.16557627198102409 ) ) ;
#124178 = CARTESIAN_POINT ( 'NONE',  ( 19.03943276465977164, -0.05219959533909143690, 103.7489096053143669 ) ) ;
#124179 = CARTESIAN_POINT ( 'NONE',  ( -19.02544592524342804, 5.153800228976336051, 86.04057627198103830 ) ) ;
#124180 = CARTESIAN_POINT ( 'NONE',  ( 0.05219959533909260263, 19.03943276465977164, 109.9989096053143669 ) ) ;
#124181 = APPLICATION_CONTEXT ( 'automotive_design' ) ;
#124182 = CARTESIAN_POINT ( 'NONE',  ( 15.72974639402176855, 15.80617190586768217, 106.8760903946856899 ) ) ;
#124183 = CARTESIAN_POINT ( 'NONE',  ( 8.224510206698742110, 14.34966873604972548, 87.08442372801901854 ) ) ;
#124184 = CARTESIAN_POINT ( 'NONE',  ( -19.03943276465977164, 0.05219959533909376836, 81.24890960531436690 ) ) ;
#124185 = CARTESIAN_POINT ( 'NONE',  ( -21.52544592524334988, -5.823673210054445271, 38.95942372801901854 ) ) ;
#124186 = CARTESIAN_POINT ( 'NONE',  ( -10.81492255796078084, -18.62759615963271287, 37.08224293864768129 ) ) ;
#124187 = CARTESIAN_POINT ( 'NONE',  ( -5.719274019375978568, 21.55341960407610458, 100.2072429386476955 ) ) ;
#124188 = CARTESIAN_POINT ( 'NONE',  ( -8.314922557960811034, -14.29746914071050412, 62.08224293864769550 ) ) ;
#124189 = CARTESIAN_POINT ( 'NONE',  ( 5.153800228976335163, 19.02544592524342804, 54.79057627198103120 ) ) ;
#124190 = CARTESIAN_POINT ( 'NONE',  ( 12.14591786802309770, 12.06949235617756955, 79.37390960531436690 ) ) ;
#124191 = CARTESIAN_POINT ( 'NONE',  ( -13.89961937509957401, -13.97604488694547875, 49.37609039468567573 ) ) ;
#124192 = CIRCLE ( 'NONE', #137049, 3.799999999999999378 ) ;
#124193 = CARTESIAN_POINT ( 'NONE',  ( 14.29746914071049879, -8.314922557960816363, 108.3322429386477097 ) ) ;
#124194 = CARTESIAN_POINT ( 'NONE',  ( 12.14591786802327356, -12.06949235617739191, 65.62609039468568994 ) ) ;
#124195 = CARTESIAN_POINT ( 'NONE',  ( -16.51473224551069308, -9.474510206698971260, 81.66557627198103830 ) ) ;
#124196 = CARTESIAN_POINT ( 'NONE',  ( 27.73933785331498569, 9.013057229001093518, 141.9750000027311785 ) ) ;
#124197 = CARTESIAN_POINT ( 'NONE',  ( 16.53943276465976808, -0.05219959533910856209, 103.7489096053143669 ) ) ;
#124198 = CARTESIAN_POINT ( 'NONE',  ( 15.80617190586746368, 15.72974639402197994, 39.37390960531436690 ) ) ;
#124199 = EDGE_LOOP ( 'NONE', ( #178647, #126982 ) ) ;
#124200 = CARTESIAN_POINT ( 'NONE',  ( -8.314922557961024197, 14.29746914071037800, 102.9177570613523756 ) ) ;
#124201 = CARTESIAN_POINT ( 'NONE',  ( -16.55341960407617563, 4.379528057220093196, 33.54275706135234714 ) ) ;
#124202 = CARTESIAN_POINT ( 'NONE',  ( 18.67979575497194134, -10.72451020669871369, 90.83442372801901854 ) ) ;
#124203 = CARTESIAN_POINT ( 'NONE',  ( -19.05341960407611168, -5.049401038298163336, 86.45724293864769550 ) ) ;
#124204 = CARTESIAN_POINT ( 'NONE',  ( -10.72451020669870658, -18.67979575497194134, 24.58442372801901499 ) ) ;
#124205 = CARTESIAN_POINT ( 'NONE',  ( -13.89961937509977652, 13.97604488694528158, 35.62390960531435269 ) ) ;
#124206 = CARTESIAN_POINT ( 'NONE',  ( -12.06949235617739369, -12.14591786802326823, 29.37609039468568284 ) ) ;
#124207 = EDGE_CURVE ( 'NONE', #175270, #148926, #77064, .T. ) ;
#124208 = VECTOR ( 'NONE', #144188, 1000.000000000000000 ) ;
#124209 = CARTESIAN_POINT ( 'NONE',  ( 16.51473224551083163, -9.474510206698727899, 90.83442372801900433 ) ) ;
#124210 = CARTESIAN_POINT ( 'NONE',  ( -18.62759615963270932, 10.81492255796079327, 85.83224293864768129 ) ) ;
#124211 = CARTESIAN_POINT ( 'NONE',  ( 5.049401038297881783, 19.05341960407617563, 67.29275706135234714 ) ) ;
#124212 = SURFACE_STYLE_USAGE ( .BOTH. , #77715 ) ;
#124213 = CARTESIAN_POINT ( 'NONE',  ( -21.53943276465977519, -0.05219959533937600094, 23.75109039468567929 ) ) ;
#124214 = LINE ( 'NONE', #155557, #156386 ) ;
#124215 = CARTESIAN_POINT ( 'NONE',  ( -19.05341960407611168, -5.049401038298163336, 91.45724293864766707 ) ) ;
#124216 = PRESENTATION_LAYER_ASSIGNMENT (  '', '', ( #4699 ) ) ;
#124217 = CARTESIAN_POINT ( 'NONE',  ( 16.55341960407618274, -4.379528057220086978, 31.04275706135234714 ) ) ;
#124218 = CARTESIAN_POINT ( 'NONE',  ( -3.573655867282028392E-15, 2.428612866367529932E-14, 6.432029388270255055E-14 ) ) ;
#124219 = CARTESIAN_POINT ( 'NONE',  ( 16.46253265017146816, 9.564922557961045513, 66.66775706135233293 ) ) ;
#124221 = CARTESIAN_POINT ( 'NONE',  ( 12.14591786802309770, 12.06949235617756955, 84.37390960531438111 ) ) ;
#124220 = CARTESIAN_POINT ( 'NONE',  ( -18.62759615963270932, 10.81492255796079327, 115.8322429386477097 ) ) ;
#124222 = CARTESIAN_POINT ( 'NONE',  ( 19.03943276465977164, -0.05219959533909143690, 88.74890960531436690 ) ) ;
#124223 = AXIS2_PLACEMENT_3D ( 'NONE', #14990, #154494, #94802 ) ;
#124225 = CARTESIAN_POINT ( 'NONE',  ( 5.153800228976615827, -19.02544592524334988, 60.20942372801899012 ) ) ;
#124224 = CARTESIAN_POINT ( 'NONE',  ( -14.34966873604972548, 8.224510206698743886, 53.33442372801901854 ) ) ;
#124226 = CARTESIAN_POINT ( 'NONE',  ( 10.72451020669871369, 18.67979575497193778, 67.08442372801901854 ) ) ;
#124227 = CARTESIAN_POINT ( 'NONE',  ( 16.52544592524335698, 4.483927247898782831, 26.45942372801901854 ) ) ;
#124228 = CARTESIAN_POINT ( 'NONE',  ( 0.05219959533909260263, 19.03943276465977164, 74.99890960531435269 ) ) ;
#124229 = CARTESIAN_POINT ( 'NONE',  ( -5.049401038297874678, -19.05341960407617918, 84.79275706135233293 ) ) ;
#124230 = CARTESIAN_POINT ( 'NONE',  ( -12.06949235617739369, -12.14591786802326823, 54.37609039468568994 ) ) ;
#124231 = CARTESIAN_POINT ( 'NONE',  ( -18.62759615963255300, -10.81492255796106328, 104.1677570613523471 ) ) ;
#124232 = CARTESIAN_POINT ( 'NONE',  ( 13.97604488694548053, -13.89961937509957401, 65.62609039468567573 ) ) ;
#124233 = CARTESIAN_POINT ( 'NONE',  ( -16.51473224551069308, -9.474510206698971260, 51.66557627198102409 ) ) ;
#124234 = CARTESIAN_POINT ( 'NONE',  ( 21.53943276465977519, -0.05219959533907433946, 68.74890960531435269 ) ) ;
#124236 = CARTESIAN_POINT ( 'NONE',  ( 5.153800228976615827, -19.02544592524334988, 75.20942372801896170 ) ) ;
#124235 = CARTESIAN_POINT ( 'NONE',  ( -8.224510206698948167, 14.34966873604960824, 60.41557627198102409 ) ) ;
#124237 = DIRECTION ( 'NONE',  ( 8.673617379884027583E-16, 0.000000000000000000, -1.000000000000000000 ) ) ;
#124239 = ADVANCED_FACE ( 'NONE', ( #83028 ), #188244, .F. ) ;
#124238 = CARTESIAN_POINT ( 'NONE',  ( -9.564922557961040184, 16.46253265017147172, 37.91775706135233293 ) ) ;
#124240 = CARTESIAN_POINT ( 'NONE',  ( -0.05219959533934338120, 16.53943276465976808, 102.5010903946856899 ) ) ;
#124241 = CARTESIAN_POINT ( 'NONE',  ( -4.379528057220328563, 16.55341960407611168, 65.20724293864768129 ) ) ;
#124243 = CARTESIAN_POINT ( 'NONE',  ( -27.73933785331498925, -9.013057229001049109, 146.9750000027311785 ) ) ;
#124242 = CARTESIAN_POINT ( 'NONE',  ( -5.823673210054431948, 21.52544592524334988, 107.7094237280190328 ) ) ;
#124244 = CARTESIAN_POINT ( 'NONE',  ( -21.55341960407610458, -5.719274019375992779, 96.45724293864770971 ) ) ;
#124245 = CARTESIAN_POINT ( 'NONE',  ( -19.03943276465977164, 0.05219959533909376836, 61.24890960531436690 ) ) ;
#124246 = CARTESIAN_POINT ( 'NONE',  ( -0.05219959533937732626, 21.53943276465977519, 72.50109039468568994 ) ) ;
#124247 = CARTESIAN_POINT ( 'NONE',  ( 13.97604488694527802, 13.89961937509977652, 54.37390960531435979 ) ) ;
#124248 = VERTEX_POINT ( 'NONE', #174071 ) ;
#124249 = CARTESIAN_POINT ( 'NONE',  ( -9.474510206698964154, 16.51473224551069663, 25.41557627198103120 ) ) ;
#124250 = CARTESIAN_POINT ( 'NONE',  ( 5.153800228976335163, 19.02544592524342804, 109.7905762719810099 ) ) ;
#124251 = CARTESIAN_POINT ( 'NONE',  ( -12.14591786802309592, -12.06949235617757132, 71.87390960531438111 ) ) ;
#124252 = CARTESIAN_POINT ( 'NONE',  ( -13.89961937509977652, 13.97604488694528158, 35.62390960531435269 ) ) ;
#124253 = CARTESIAN_POINT ( 'NONE',  ( -8.314922557960811034, -14.29746914071050412, 82.08224293864768129 ) ) ;
#124254 = AXIS2_PLACEMENT_3D ( 'NONE', #106027, #134400, #151554 ) ;
#124255 = CARTESIAN_POINT ( 'NONE',  ( -18.62759615963270932, 10.81492255796079327, 90.83224293864769550 ) ) ;
#124256 = CARTESIAN_POINT ( 'NONE',  ( 18.67979575497194134, -10.72451020669871369, 35.83442372801901143 ) ) ;
#124257 = CARTESIAN_POINT ( 'NONE',  ( -0.05219959533909027116, -19.03943276465977164, 22.49890960531436690 ) ) ;
#124258 = CARTESIAN_POINT ( 'NONE',  ( 0.05219959533934541429, -16.53943276465976808, 55.00109039468568284 ) ) ;
#124259 = CARTESIAN_POINT ( 'NONE',  ( 21.53943276465977519, -0.05219959533907433946, 83.74890960531435269 ) ) ;
#124260 = CARTESIAN_POINT ( 'NONE',  ( 5.049401038297881783, 19.05341960407617563, 22.29275706135233648 ) ) ;
#124261 = CARTESIAN_POINT ( 'NONE',  ( -16.46253265017160317, 9.564922557960807481, 110.8322429386476955 ) ) ;
#124262 = CARTESIAN_POINT ( 'NONE',  ( 0.05219959533937995610, -21.53943276465977519, 40.00109039468567573 ) ) ;
#124263 = CARTESIAN_POINT ( 'NONE',  ( 21.55341960407610458, 5.719274019375980345, 38.95724293864768839 ) ) ;
#124264 = CARTESIAN_POINT ( 'NONE',  ( -4.379528057220328563, 16.55341960407611168, 25.20724293864769550 ) ) ;
#124266 = CARTESIAN_POINT ( 'NONE',  ( 18.67979575497194134, -10.72451020669871369, 95.83442372801903275 ) ) ;
#124265 = CARTESIAN_POINT ( 'NONE',  ( 18.67979575497194134, -10.72451020669871369, 65.83442372801900433 ) ) ;
#124267 = CARTESIAN_POINT ( 'NONE',  ( 19.03943276465977164, 0.05219959533936151252, 31.25109039468566863 ) ) ;
#124268 = CARTESIAN_POINT ( 'NONE',  ( 4.379528057220092307, 16.55341960407617563, 87.29275706135236135 ) ) ;
#124269 = CARTESIAN_POINT ( 'NONE',  ( -18.67979575497193778, 10.72451020669871902, 58.33442372801901143 ) ) ;
#124270 = CARTESIAN_POINT ( 'NONE',  ( -19.05341960407611168, -5.049401038298163336, 41.45724293864769550 ) ) ;
#124271 = CARTESIAN_POINT ( 'NONE',  ( 10.72451020669871369, 18.67979575497193778, 112.0844237280190185 ) ) ;
#124272 = CARTESIAN_POINT ( 'NONE',  ( 21.53943276465977519, -0.05219959533907433946, 28.74890960531435624 ) ) ;
#124273 = CARTESIAN_POINT ( 'NONE',  ( -15.72974639402176322, -15.80617190586768395, 24.37609039468567573 ) ) ;
#124274 = CARTESIAN_POINT ( 'NONE',  ( 0.05219959533907565091, 21.53943276465977519, 79.99890960531435269 ) ) ;
#124275 = CARTESIAN_POINT ( 'NONE',  ( 16.52544592524335698, 4.483927247898782831, 36.45942372801901143 ) ) ;
#124277 = CARTESIAN_POINT ( 'NONE',  ( 21.53943276465977519, -0.05219959533907433946, 83.74890960531435269 ) ) ;
#124276 = DIRECTION ( 'NONE',  ( 0.000000000000000000, 0.000000000000000000, 1.000000000000000000 ) ) ;
#124279 = CARTESIAN_POINT ( 'NONE',  ( -4.483927247898539470, -16.52544592524342804, 67.29057627198103830 ) ) ;
#124278 = CARTESIAN_POINT ( 'NONE',  ( -8.314922557961024197, 14.29746914071037800, 67.91775706135234714 ) ) ;
#124280 = FACE_BOUND ( 'NONE', #56704, .T. ) ;
#124281 = CARTESIAN_POINT ( 'NONE',  ( 0.05219959533936267826, -19.03943276465977164, 90.00109039468567573 ) ) ;
#124282 = DIRECTION ( 'NONE',  ( -7.855351589328939542E-15, 0.000000000000000000, 1.000000000000000000 ) ) ;
#124283 = CARTESIAN_POINT ( 'NONE',  ( 8.224510206698742110, 14.34966873604972548, 37.08442372801901143 ) ) ;
#124284 = CARTESIAN_POINT ( 'NONE',  ( -18.67979575497178146, -10.72451020669898902, 111.6655762719810525 ) ) ;
#124285 = CARTESIAN_POINT ( 'NONE',  ( -18.62759615963270932, 10.81492255796079327, 70.83224293864770971 ) ) ;
#124286 = CARTESIAN_POINT ( 'NONE',  ( -18.62759615963270932, 10.81492255796079327, 35.83224293864768839 ) ) ;
#124287 = CARTESIAN_POINT ( 'NONE',  ( -8.314922557961024197, 14.29746914071037800, 57.91775706135234714 ) ) ;
#124288 = CARTESIAN_POINT ( 'NONE',  ( 9.564922557960805705, 16.46253265017160317, 69.58224293864770971 ) ) ;
#124290 = CARTESIAN_POINT ( 'NONE',  ( 13.89961937509957401, 13.97604488694547697, 106.8760903946856757 ) ) ;
#124289 = CARTESIAN_POINT ( 'NONE',  ( 15.80617190586769283, -15.72974639402175789, 40.62609039468567573 ) ) ;
#124291 = CARTESIAN_POINT ( 'NONE',  ( 5.719274019375991003, -21.55341960407610458, 32.70724293864770260 ) ) ;
#124292 = CARTESIAN_POINT ( 'NONE',  ( 13.89961937509957401, 13.97604488694547697, 31.87609039468566863 ) ) ;
#124293 = CARTESIAN_POINT ( 'NONE',  ( 0.05219959533934541429, -16.53943276465976808, 45.00109039468568284 ) ) ;
#124294 = CARTESIAN_POINT ( 'NONE',  ( -13.89961937509977652, 13.97604488694528158, 105.6239096053143527 ) ) ;
#124295 = CARTESIAN_POINT ( 'NONE',  ( -5.823673210054116645, -21.52544592524344225, 107.2905762719810525 ) ) ;
#124296 = CARTESIAN_POINT ( 'NONE',  ( -5.049401038298153566, 19.05341960407611168, 75.20724293864769550 ) ) ;
#124297 = CARTESIAN_POINT ( 'NONE',  ( -16.81555441253552274, 7.025013491695479395, 25.63685445334257906 ) ) ;
#124298 = CARTESIAN_POINT ( 'NONE',  ( 12.06949235617757843, -12.14591786802309237, 78.12390960531436690 ) ) ;
#124299 = CARTESIAN_POINT ( 'NONE',  ( -21.52544592524343514, 5.823673210054127303, 26.04057627198103475 ) ) ;
#124300 = CARTESIAN_POINT ( 'NONE',  ( 18.22780087662122739, 5.500000000000000888, 71.48236817873106475 ) ) ;
#124301 = CARTESIAN_POINT ( 'NONE',  ( -16.52544592524335698, -4.483927247898792601, 68.95942372801901854 ) ) ;
#124302 = CARTESIAN_POINT ( 'NONE',  ( 21.55341960407610458, 5.719274019375980345, 108.9572429386476955 ) ) ;
#124303 = CARTESIAN_POINT ( 'NONE',  ( -13.89961937509957401, -13.97604488694547875, 69.37609039468564731 ) ) ;
#124304 = CARTESIAN_POINT ( 'NONE',  ( -21.55341960407610458, -5.719274019375992779, 26.45724293864768839 ) ) ;
#124305 = CARTESIAN_POINT ( 'NONE',  ( 0.05219959533909260263, 19.03943276465977164, 29.99890960531435979 ) ) ;
#124306 = CARTESIAN_POINT ( 'NONE',  ( -21.53943276465977519, 0.05219959533907696930, 71.24890960531435269 ) ) ;
#124307 = CARTESIAN_POINT ( 'NONE',  ( 19.03943276465977164, -0.05219959533909143690, 98.74890960531436690 ) ) ;
#124308 = CARTESIAN_POINT ( 'NONE',  ( -18.67979575497193778, 10.72451020669871902, 98.33442372801901854 ) ) ;
#124309 = CARTESIAN_POINT ( 'NONE',  ( 9.474510206698971260, -16.51473224551069308, 47.91557627198102409 ) ) ;
#124310 = CARTESIAN_POINT ( 'NONE',  ( 4.379528057220339221, -16.55341960407611168, 87.70724293864769550 ) ) ;
#124311 = CARTESIAN_POINT ( 'NONE',  ( -16.55341960407617563, 4.379528057220093196, 38.54275706135234714 ) ) ;
#124312 = CARTESIAN_POINT ( 'NONE',  ( -5.153800228976328057, -19.02544592524343514, 62.29057627198100988 ) ) ;
#124313 = CARTESIAN_POINT ( 'NONE',  ( -5.719274019375665041, -21.55341960407619695, 79.79275706135236135 ) ) ;
#124314 = ORIENTED_EDGE ( 'NONE', *, *, #141568, .F. ) ;
#124315 = CARTESIAN_POINT ( 'NONE',  ( -16.51473224551082808, 9.474510206698731452, 43.33442372801900433 ) ) ;
#124316 = CARTESIAN_POINT ( 'NONE',  ( -13.97604488694547697, 13.89961937509957934, 38.12609039468566152 ) ) ;
#124317 = CARTESIAN_POINT ( 'NONE',  ( -15.80617190586768217, 15.72974639402176855, 38.12609039468567573 ) ) ;
#124318 = EDGE_CURVE ( 'NONE', #69839, #165180, #199859, .T. ) ;
#124319 = DIRECTION ( 'NONE',  ( 1.000000000000000000, 0.000000000000000000, 0.000000000000000000 ) ) ;
#124320 = CARTESIAN_POINT ( 'NONE',  ( 13.89961937509957401, 13.97604488694547697, 31.87609039468566863 ) ) ;
#124321 = CARTESIAN_POINT ( 'NONE',  ( 9.564922557960805705, 16.46253265017160317, 89.58224293864769550 ) ) ;
#124322 = CARTESIAN_POINT ( 'NONE',  ( 19.02544592524343514, -5.153800228976328945, 63.54057627198103830 ) ) ;
#124323 = CARTESIAN_POINT ( 'NONE',  ( 8.314922557960818139, 14.29746914071049879, 29.58224293864769905 ) ) ;
#124325 = CARTESIAN_POINT ( 'NONE',  ( 21.52544592524334988, 5.823673210054432836, 91.45942372801901854 ) ) ;
#124324 = CARTESIAN_POINT ( 'NONE',  ( -10.81492255796078084, -18.62759615963271287, 22.08224293864769194 ) ) ;
#124326 = CARTESIAN_POINT ( 'NONE',  ( -11.40812507854754720, -35.11059874428192273, -2.224999997268813701 ) ) ;
#124327 = CARTESIAN_POINT ( 'NONE',  ( 16.31925111598457789, 7.325300261831481308, 57.33575461032751974 ) ) ;
#124328 = CARTESIAN_POINT ( 'NONE',  ( -0.05219959533937732626, 21.53943276465977519, 97.50109039468567573 ) ) ;
#124329 = CARTESIAN_POINT ( 'NONE',  ( 17.05587630539785238, -6.762274262135678171, 43.24180309037312497 ) ) ;
#124330 = CARTESIAN_POINT ( 'NONE',  ( 16.46253265017160672, -9.564922557960803928, 113.3322429386476955 ) ) ;
#124331 = EDGE_CURVE ( 'NONE', #180473, #170159, #159880, .T. ) ;
#124332 = DIRECTION ( 'NONE',  ( 0.000000000000000000, 0.000000000000000000, -1.000000000000000000 ) ) ;
#124333 = CIRCLE ( 'NONE', #95181, 2.500000000000000000 ) ;
#124334 = CARTESIAN_POINT ( 'NONE',  ( -4.379528057220086978, -16.55341960407618274, 54.79275706135235424 ) ) ;
#124335 = CARTESIAN_POINT ( 'NONE',  ( 18.67979575497178502, 10.72451020669898547, 74.16557627198102409 ) ) ;
#124336 = CARTESIAN_POINT ( 'NONE',  ( -16.55341960407611168, -4.379528057220339221, 26.45724293864768839 ) ) ;
#124338 = CARTESIAN_POINT ( 'NONE',  ( -16.51473224551069308, -9.474510206698971260, 96.66557627198102409 ) ) ;
#124337 = CARTESIAN_POINT ( 'NONE',  ( -4.379528057220328563, 16.55341960407611168, 110.2072429386477239 ) ) ;
#124339 = CARTESIAN_POINT ( 'NONE',  ( -13.89961937509957401, -13.97604488694547875, 24.37609039468565442 ) ) ;
#124340 = CARTESIAN_POINT ( 'NONE',  ( 12.14591786802309770, 12.06949235617756955, 114.3739096053143527 ) ) ;
#124341 = CARTESIAN_POINT ( 'NONE',  ( -18.62759615963255300, -10.81492255796106328, 64.16775706135234714 ) ) ;
#124342 = DIRECTION ( 'NONE',  ( 0.000000000000000000, 0.000000000000000000, 1.000000000000000000 ) ) ;
#124343 = CARTESIAN_POINT ( 'NONE',  ( -0.05219959533934338120, 16.53943276465976808, 107.5010903946856899 ) ) ;
#124344 = CARTESIAN_POINT ( 'NONE',  ( -16.46253265017146816, -9.564922557961047289, 64.16775706135233293 ) ) ;
#124345 = CARTESIAN_POINT ( 'NONE',  ( -13.97604488694547520, 13.89961937509957934, 68.12609039468566152 ) ) ;
#124346 = CARTESIAN_POINT ( 'NONE',  ( -5.153800228976328057, -19.02544592524343514, 112.2905762719810099 ) ) ;
#124347 = CARTESIAN_POINT ( 'NONE',  ( 4.379528057220339221, -16.55341960407611168, 92.70724293864770971 ) ) ;
#124348 = AXIS2_PLACEMENT_3D ( 'NONE', #170580, #79558, #169580 ) ;
#124349 = CARTESIAN_POINT ( 'NONE',  ( -9.474510206698720793, -16.51473224551083518, 64.58442372801900433 ) ) ;
#124350 = CARTESIAN_POINT ( 'NONE',  ( 19.05341960407611168, 5.049401038298154454, 78.95724293864769550 ) ) ;
#124351 = CARTESIAN_POINT ( 'NONE',  ( 0.05219959533910956823, 16.53943276465976808, 59.99890960531436690 ) ) ;
#124352 = CARTESIAN_POINT ( 'NONE',  ( 19.03943276465977164, 0.05219959533936151252, 91.25109039468566152 ) ) ;
#124353 = CARTESIAN_POINT ( 'NONE',  ( 21.52544592524344225, -5.823673210054117533, 53.54057627198103120 ) ) ;
#124354 = ORIENTED_EDGE ( 'NONE', *, *, #154702, .F. ) ;
#124355 = CARTESIAN_POINT ( 'NONE',  ( 14.29746914071049879, -8.314922557960816363, 113.3322429386476955 ) ) ;
#124356 = CARTESIAN_POINT ( 'NONE',  ( -17.12812012977023812, -6.668231424566067211, 31.35948759323143520 ) ) ;
#124358 = CARTESIAN_POINT ( 'NONE',  ( 10.81492255796078972, 18.62759615963270932, 74.58224293864768129 ) ) ;
#124357 = CARTESIAN_POINT ( 'NONE',  ( 16.51473224551069308, 9.474510206698969483, 69.16557627198102409 ) ) ;
#124360 = CARTESIAN_POINT ( 'NONE',  ( -9.564922557960796823, -16.46253265017161027, 77.08224293864769550 ) ) ;
#124359 = CARTESIAN_POINT ( 'NONE',  ( -12.14591786802326823, 12.06949235617739902, 88.12609039468570415 ) ) ;
#124361 = CARTESIAN_POINT ( 'NONE',  ( -19.05341960407617563, 5.049401038297882671, 63.54275706135234003 ) ) ;
#124362 = CARTESIAN_POINT ( 'NONE',  ( 5.719274019375673035, 21.55341960407619339, 87.29275706135236135 ) ) ;
#124363 = CARTESIAN_POINT ( 'NONE',  ( 21.55341960407610458, 5.719274019375980345, 68.95724293864769550 ) ) ;
#124364 = CARTESIAN_POINT ( 'NONE',  ( 0.05219959533907565091, 21.53943276465977519, 29.99890960531435979 ) ) ;
#124365 = STYLED_ITEM ( 'NONE', ( #87666 ), #9086 ) ;
#124366 = CARTESIAN_POINT ( 'NONE',  ( -13.97604488694527625, -13.89961937509977652, 41.87390960531435979 ) ) ;
#124367 = CARTESIAN_POINT ( 'NONE',  ( 16.55341960407618274, -4.379528057220086978, 101.0427570613523756 ) ) ;
#124368 = CARTESIAN_POINT ( 'NONE',  ( -9.564922557960796823, -16.46253265017161027, 52.08224293864768839 ) ) ;
#124369 = CARTESIAN_POINT ( 'NONE',  ( -16.52544592524335698, -4.483927247898792601, 18.95942372801901143 ) ) ;
#124370 = CARTESIAN_POINT ( 'NONE',  ( -16.51473224551082808, 9.474510206698731452, 83.33442372801899012 ) ) ;
#124371 = CARTESIAN_POINT ( 'NONE',  ( 19.05341960407617918, -5.049401038297876454, 21.04275706135232582 ) ) ;
#124372 = CARTESIAN_POINT ( 'NONE',  ( -16.53943276465976808, 0.05219959533911058130, 66.24890960531436690 ) ) ;
#124373 = CARTESIAN_POINT ( 'NONE',  ( -5.823673210054116645, -21.52544592524344225, 92.29057627198103830 ) ) ;
#124374 = CARTESIAN_POINT ( 'NONE',  ( 0.05219959533907565091, 21.53943276465977519, 99.99890960531436690 ) ) ;
#124375 = CARTESIAN_POINT ( 'NONE',  ( -17.79613651744294600, 24.49428055684532524, 149.6843446568999809 ) ) ;
#124376 = CARTESIAN_POINT ( 'NONE',  ( -15.80617190586745835, -15.72974639402198527, 51.87390960531437401 ) ) ;
#124377 = CARTESIAN_POINT ( 'NONE',  ( 8.314922557961029526, -14.29746914071037800, 80.41775706135234714 ) ) ;
#124378 = CARTESIAN_POINT ( 'NONE',  ( -16.55341960407611168, -4.379528057220339221, 96.45724293864770971 ) ) ;
#124379 = CARTESIAN_POINT ( 'NONE',  ( -9.474510206698964154, 16.51473224551069663, 45.41557627198103120 ) ) ;
#124380 = SURFACE_STYLE_FILL_AREA ( #123373 ) ;
#124381 = CARTESIAN_POINT ( 'NONE',  ( -13.50000934768029026, -42.70547949999481574, -22.37447973961943504 ) ) ;
#124382 = CARTESIAN_POINT ( 'NONE',  ( -12.14591786802326823, 12.06949235617739902, 103.1260903946856757 ) ) ;
#124383 = CARTESIAN_POINT ( 'NONE',  ( 10.72451020669871369, 18.67979575497193778, 27.08442372801901854 ) ) ;
#124384 = CARTESIAN_POINT ( 'NONE',  ( 19.05341960407611168, 5.049401038298154454, 98.95724293864766707 ) ) ;
#124385 = CARTESIAN_POINT ( 'NONE',  ( -10.72451020669870658, -18.67979575497194134, 69.58442372801900433 ) ) ;
#124386 = CARTESIAN_POINT ( 'NONE',  ( 37.99626262588765258, 2.893932880411085066E-14, -1.002157773949823083 ) ) ;
#124387 = CARTESIAN_POINT ( 'NONE',  ( -16.46253265017160317, 9.564922557960807481, 25.83224293864769194 ) ) ;
#124388 = ORIENTED_EDGE ( 'NONE', *, *, #62981, .F. ) ;
#124389 = CARTESIAN_POINT ( 'NONE',  ( 5.823673210054444382, -21.52544592524334988, 55.20942372801902565 ) ) ;
#124391 = CARTESIAN_POINT ( 'NONE',  ( -5.049401038298153566, 19.05341960407611168, 25.20724293864768484 ) ) ;
#124390 = CARTESIAN_POINT ( 'NONE',  ( 16.51473224551069308, 9.474510206698969483, 54.16557627198103120 ) ) ;
#124392 = CARTESIAN_POINT ( 'NONE',  ( -0.05219959533909027116, -19.03943276465977164, 87.49890960531436690 ) ) ;
#124393 = CARTESIAN_POINT ( 'NONE',  ( -9.474510206698720793, -16.51473224551083518, 69.58442372801901854 ) ) ;
#124394 = CARTESIAN_POINT ( 'NONE',  ( -21.52544592524334988, -5.823673210054445271, 48.95942372801902565 ) ) ;
#124395 = CARTESIAN_POINT ( 'NONE',  ( -13.97604488694547697, 13.89961937509957934, 98.12609039468566152 ) ) ;
#124396 = CARTESIAN_POINT ( 'NONE',  ( 19.05341960407617918, -5.049401038297876454, 61.04275706135232582 ) ) ;
#124397 = CARTESIAN_POINT ( 'NONE',  ( -13.97604488694527625, -13.89961937509977652, 31.87390960531435979 ) ) ;
#124398 = VECTOR ( 'NONE', #165414, 1000.000000000000000 ) ;
#124399 = CARTESIAN_POINT ( 'NONE',  ( 4.379528057220092307, 16.55341960407617563, 102.2927570613523613 ) ) ;
#124400 = CARTESIAN_POINT ( 'NONE',  ( 16.51473224551083163, -9.474510206698727899, 75.83442372801900433 ) ) ;
#124401 = CARTESIAN_POINT ( 'NONE',  ( 14.29746914071049879, -8.314922557960816363, 23.33224293864769194 ) ) ;
#124402 = CARTESIAN_POINT ( 'NONE',  ( 19.02544592524334988, 5.153800228976608722, 46.45942372801899012 ) ) ;
#124403 = CARTESIAN_POINT ( 'NONE',  ( 5.719274019375673035, 21.55341960407619339, 107.2927570613523471 ) ) ;
#124404 = PRODUCT_DEFINITION_SHAPE ( 'NONE', 'NONE',  #200197 ) ;
#124405 = CARTESIAN_POINT ( 'NONE',  ( -19.03943276465977164, -0.05219959533935918106, 28.75109039468566507 ) ) ;
#124406 = CARTESIAN_POINT ( 'NONE',  ( -5.049401038298153566, 19.05341960407611168, 25.20724293864768484 ) ) ;
#124407 = CARTESIAN_POINT ( 'NONE',  ( -10.72451020669870658, -18.67979575497194134, 84.58442372801903275 ) ) ;
#124408 = CARTESIAN_POINT ( 'NONE',  ( -4.379528057220086978, -16.55341960407618274, 34.79275706135235424 ) ) ;
#124409 = CARTESIAN_POINT ( 'NONE',  ( -19.05341960407611168, -5.049401038298163336, 96.45724293864769550 ) ) ;
#124410 = CARTESIAN_POINT ( 'NONE',  ( -27.12243378312306064, 3.972435522077925718, 169.3718635229811298 ) ) ;
#124411 = CARTESIAN_POINT ( 'NONE',  ( 19.03943276465977164, -0.05219959533909143690, 78.74890960531436690 ) ) ;
#124412 = CARTESIAN_POINT ( 'NONE',  ( -16.62475595723611477, 7.163666690055877417, 100.5271335181040371 ) ) ;
#124413 = CARTESIAN_POINT ( 'NONE',  ( 19.05341960407617918, -5.049401038297876454, 81.04275706135231871 ) ) ;
#124414 = CARTESIAN_POINT ( 'NONE',  ( -9.564922557960796823, -16.46253265017161027, 107.0822429386476955 ) ) ;
#124415 = CARTESIAN_POINT ( 'NONE',  ( -15.80617190586768217, 15.72974639402176855, 98.12609039468570415 ) ) ;
#124416 = CARTESIAN_POINT ( 'NONE',  ( -8.224510206698948167, 14.34966873604960824, 100.4155762719810241 ) ) ;
#124417 = CARTESIAN_POINT ( 'NONE',  ( 5.719274019375991003, -21.55341960407610458, 57.70724293864770260 ) ) ;
#124418 = CARTESIAN_POINT ( 'NONE',  ( 21.53943276465977519, -0.05219959533907433946, 38.74890960531435979 ) ) ;
#124419 = CARTESIAN_POINT ( 'NONE',  ( 12.06949235617757843, -12.14591786802309237, 113.1239096053143953 ) ) ;
#124420 = CARTESIAN_POINT ( 'NONE',  ( -0.7571601631681732503, -8.898623008803074441, -61.93576936796790022 ) ) ;
#124421 = CARTESIAN_POINT ( 'NONE',  ( 19.03943276465977164, 0.05219959533936151252, 51.25109039468567573 ) ) ;
#124422 = CARTESIAN_POINT ( 'NONE',  ( 12.14591786802309770, 12.06949235617756955, 39.37390960531436690 ) ) ;
#124423 = CARTESIAN_POINT ( 'NONE',  ( 21.53943276465977519, -0.05219959533907433946, 23.74890960531435269 ) ) ;
#124424 = CARTESIAN_POINT ( 'NONE',  ( 21.52544592524334988, 5.823673210054432836, 76.45942372801901854 ) ) ;
#124425 = CARTESIAN_POINT ( 'NONE',  ( 10.72451020669898902, -18.67979575497178502, 67.91557627198102409 ) ) ;
#124426 = CARTESIAN_POINT ( 'NONE',  ( 21.53943276465977519, 0.05219959533937863772, 46.25109039468567573 ) ) ;
#124427 = CARTESIAN_POINT ( 'NONE',  ( 5.719274019375991003, -21.55341960407610458, 102.7072429386476955 ) ) ;
#124428 = CARTESIAN_POINT ( 'NONE',  ( -5.719274019375665041, -21.55341960407619695, 54.79275706135235424 ) ) ;
#124429 = CARTESIAN_POINT ( 'NONE',  ( 19.05341960407611168, 5.049401038298154454, 28.95724293864769550 ) ) ;
#124430 = CARTESIAN_POINT ( 'NONE',  ( -16.51473224551069308, -9.474510206698971260, 76.66557627198103830 ) ) ;
#124431 = CARTESIAN_POINT ( 'NONE',  ( 16.55341960407618274, -4.379528057220086978, 86.04275706135236135 ) ) ;
#124432 = CARTESIAN_POINT ( 'NONE',  ( 8.314922557960818139, 14.29746914071049879, 109.5822429386476955 ) ) ;
#124433 = CARTESIAN_POINT ( 'NONE',  ( -20.43538597629143538, -20.43538597629106945, -64.92279855667830191 ) ) ;
#124434 = CIRCLE ( 'NONE', #114618, 12.50000000000000000 ) ;
#124435 = CARTESIAN_POINT ( 'NONE',  ( 16.52544592524342804, -4.483927247898539470, 53.54057627198103120 ) ) ;
#124436 = CARTESIAN_POINT ( 'NONE',  ( 16.52544592524335698, 4.483927247898782831, 111.4594237280190328 ) ) ;
#124437 = CARTESIAN_POINT ( 'NONE',  ( -0.05219959533909027116, -19.03943276465977164, 72.49890960531435269 ) ) ;
#124438 = CARTESIAN_POINT ( 'NONE',  ( -16.46253265017160317, 9.564922557960807481, 30.83224293864769550 ) ) ;
#124439 = CARTESIAN_POINT ( 'NONE',  ( -21.52544592524343514, 5.823673210054127303, 41.04057627198103120 ) ) ;
#124440 = CARTESIAN_POINT ( 'NONE',  ( -5.153800228976607833, 19.02544592524334988, 42.70942372801901143 ) ) ;
#124442 = CARTESIAN_POINT ( 'NONE',  ( -14.34966873604960291, -8.224510206698953496, 46.66557627198102409 ) ) ;
#124441 = CARTESIAN_POINT ( 'NONE',  ( -37.99626262588766679, 2.428612866367529932E-14, 2.000000000000000000 ) ) ;
#124443 = CARTESIAN_POINT ( 'NONE',  ( 15.80617190586746368, 15.72974639402197994, 29.37390960531435269 ) ) ;
#124444 = CARTESIAN_POINT ( 'NONE',  ( 18.62759615963255655, 10.81492255796105972, 56.66775706135235424 ) ) ;
#124445 = LINE ( 'NONE', #122452, #171113 ) ;
#124446 = CARTESIAN_POINT ( 'NONE',  ( 8.224510206698742110, 14.34966873604972548, 67.08442372801901854 ) ) ;
#124447 = CARTESIAN_POINT ( 'NONE',  ( -16.46253265017146816, -9.564922557961047289, 59.16775706135233293 ) ) ;
#124448 = CARTESIAN_POINT ( 'NONE',  ( 4.379528057220339221, -16.55341960407611168, 47.70724293864770260 ) ) ;
#124449 = DIRECTION ( 'NONE',  ( -0.000000000000000000, 0.000000000000000000, 1.000000000000000000 ) ) ;
#124450 = CARTESIAN_POINT ( 'NONE',  ( -0.05219959533910754901, -16.53943276465976808, 22.49890960531436335 ) ) ;
#124451 = CARTESIAN_POINT ( 'NONE',  ( -19.02544592524342804, 5.153800228976336051, 41.04057627198103120 ) ) ;
#124452 = CARTESIAN_POINT ( 'NONE',  ( 16.51473224551069308, 9.474510206698969483, 59.16557627198102409 ) ) ;
#124453 = CARTESIAN_POINT ( 'NONE',  ( -14.29746914071049879, 8.314922557960819915, 115.8322429386477097 ) ) ;
#124454 = CARTESIAN_POINT ( 'NONE',  ( 0.05219959533937995610, -21.53943276465977519, 35.00109039468568284 ) ) ;
#124455 = CARTESIAN_POINT ( 'NONE',  ( 5.049401038298161559, -19.05341960407611168, 57.70724293864769550 ) ) ;
#124456 = CARTESIAN_POINT ( 'NONE',  ( -17.49999999999999645, -5.499999999999992895, 99.20309617465831309 ) ) ;
#124457 = CARTESIAN_POINT ( 'NONE',  ( -13.89961937509977652, 13.97604488694528158, 40.62390960531435979 ) ) ;
#124458 = CARTESIAN_POINT ( 'NONE',  ( -10.72451020669898014, 18.67979575497178502, 40.41557627198103120 ) ) ;
#124460 = CARTESIAN_POINT ( 'NONE',  ( -4.483927247898539470, -16.52544592524342804, 112.2905762719810241 ) ) ;
#124459 = CARTESIAN_POINT ( 'NONE',  ( 18.62759615963255655, 10.81492255796105972, 61.66775706135235424 ) ) ;
#124461 = CARTESIAN_POINT ( 'NONE',  ( -10.81492255796078084, -18.62759615963271287, 22.08224293864769194 ) ) ;
#124462 = CARTESIAN_POINT ( 'NONE',  ( 4.379528057220092307, 16.55341960407617563, 92.29275706135236135 ) ) ;
#124463 = CARTESIAN_POINT ( 'NONE',  ( 5.823673210054444382, -21.52544592524334988, 100.2094237280190043 ) ) ;
#124464 = CARTESIAN_POINT ( 'NONE',  ( 4.379528057220092307, 16.55341960407617563, 67.29275706135234714 ) ) ;
#124465 = CARTESIAN_POINT ( 'NONE',  ( -5.153800228976328057, -19.02544592524343514, 107.2905762719810383 ) ) ;
#124466 = CARTESIAN_POINT ( 'NONE',  ( 8.314922557961029526, -14.29746914071037800, 60.41775706135235424 ) ) ;
#124467 = CARTESIAN_POINT ( 'NONE',  ( 4.483927247898790824, -16.52544592524335698, 30.20942372801902565 ) ) ;
#124468 = CARTESIAN_POINT ( 'NONE',  ( 4.483927247898790824, -16.52544592524335698, 100.2094237280190043 ) ) ;
#124469 = CARTESIAN_POINT ( 'NONE',  ( -21.53943276465977519, -0.05219959533937600094, 53.75109039468568994 ) ) ;
#124470 = CARTESIAN_POINT ( 'NONE',  ( 4.483927247898790824, -16.52544592524335698, 30.20942372801902565 ) ) ;
#124471 = CARTESIAN_POINT ( 'NONE',  ( 10.81492255796078972, 18.62759615963270932, 104.5822429386477097 ) ) ;
#124472 = CARTESIAN_POINT ( 'NONE',  ( 4.483927247898790824, -16.52544592524335698, 20.20942372801900788 ) ) ;
#124473 = CARTESIAN_POINT ( 'NONE',  ( -0.05219959533934338120, 16.53943276465976808, 82.50109039468568994 ) ) ;
#124474 = CYLINDRICAL_SURFACE ( 'NONE', #47346, 1.500000000000001332 ) ;
#124475 = CARTESIAN_POINT ( 'NONE',  ( 15.72974639402176855, 15.80617190586768217, 91.87609039468568994 ) ) ;
#124477 = ADVANCED_FACE ( 'NONE', ( #111385 ), #192227, .F. ) ;
#124476 = CARTESIAN_POINT ( 'NONE',  ( 0.05219959533936267826, -19.03943276465977164, 90.00109039468567573 ) ) ;
#124478 = CARTESIAN_POINT ( 'NONE',  ( -4.483927247898539470, -16.52544592524342804, 42.29057627198103120 ) ) ;
#124479 = CARTESIAN_POINT ( 'NONE',  ( 12.14591786802309770, 12.06949235617756955, 49.37390960531436690 ) ) ;
#124480 = CARTESIAN_POINT ( 'NONE',  ( 8.224510206698953496, -14.34966873604960469, 102.9155762719810383 ) ) ;
#124482 = FACE_BOUND ( 'NONE', #24883, .T. ) ;
#124481 = CARTESIAN_POINT ( 'NONE',  ( -19.03943276465977164, -0.05219959533935918106, 48.75109039468566863 ) ) ;
#124483 = CARTESIAN_POINT ( 'NONE',  ( 21.55341960407619695, -5.719274019375665929, 56.04275706135235424 ) ) ;
#124484 = CARTESIAN_POINT ( 'NONE',  ( 19.02544592524334988, 5.153800228976608722, 106.4594237280190185 ) ) ;
#124485 = CARTESIAN_POINT ( 'NONE',  ( -19.23457310888357341, -35.06695140040310577, -26.03237767043702533 ) ) ;
#124486 = CARTESIAN_POINT ( 'NONE',  ( -19.02544592524342804, 5.153800228976336051, 106.0405762719810241 ) ) ;
#124487 = CARTESIAN_POINT ( 'NONE',  ( -21.53943276465977519, 0.05219959533907696930, 61.24890960531435979 ) ) ;
#124488 = CARTESIAN_POINT ( 'NONE',  ( -16.46253265017146816, -9.564922557961047289, 94.16775706135233293 ) ) ;
#124489 = CARTESIAN_POINT ( 'NONE',  ( -5.049401038298153566, 19.05341960407611168, 85.20724293864766707 ) ) ;
#124490 = CARTESIAN_POINT ( 'NONE',  ( 10.81492255796078972, 18.62759615963270932, 54.58224293864769550 ) ) ;
#124491 = CARTESIAN_POINT ( 'NONE',  ( -16.53943276465976808, 0.05219959533911058130, 111.2489096053143669 ) ) ;
#124492 = CARTESIAN_POINT ( 'NONE',  ( -9.564922557960796823, -16.46253265017161027, 67.08224293864769550 ) ) ;
#124493 = ADVANCED_FACE ( 'NONE', ( #98177 ), #161154, .T. ) ;
#124494 = CARTESIAN_POINT ( 'NONE',  ( 19.05341960407611168, 5.049401038298154454, 33.95724293864769550 ) ) ;
#124495 = AXIS2_PLACEMENT_3D ( 'NONE', #142063, #151547, #126887 ) ;
#124496 = CARTESIAN_POINT ( 'NONE',  ( -15.72974639402176322, -15.80617190586768395, 34.37609039468568284 ) ) ;
#124497 = CARTESIAN_POINT ( 'NONE',  ( 15.72974639402176855, 15.80617190586768217, 86.87609039468568994 ) ) ;
#124498 = CARTESIAN_POINT ( 'NONE',  ( -14.34966873604972548, 8.224510206698743886, 88.33442372801901854 ) ) ;
#124499 = CARTESIAN_POINT ( 'NONE',  ( 5.823673210054444382, -21.52544592524334988, 30.20942372801902565 ) ) ;
#124500 = CARTESIAN_POINT ( 'NONE',  ( 21.53943276465977519, 0.05219959533937863772, 36.25109039468567573 ) ) ;
#124502 = CARTESIAN_POINT ( 'NONE',  ( 5.049401038298161559, -19.05341960407611168, 72.70724293864768129 ) ) ;
#124501 = CARTESIAN_POINT ( 'NONE',  ( 5.049401038297881783, 19.05341960407617563, 72.29275706135234714 ) ) ;
#124503 = CARTESIAN_POINT ( 'NONE',  ( 18.62759615963255655, 10.81492255796105972, 86.66775706135234714 ) ) ;
#124504 = CARTESIAN_POINT ( 'NONE',  ( -5.823673210054116645, -21.52544592524344225, 87.29057627198103830 ) ) ;
#124505 = CARTESIAN_POINT ( 'NONE',  ( 8.314922557960818139, 14.29746914071049879, 69.58224293864769550 ) ) ;
#124506 = CARTESIAN_POINT ( 'NONE',  ( -5.719274019375665041, -21.55341960407619695, 104.7927570613523898 ) ) ;
#124507 = CARTESIAN_POINT ( 'NONE',  ( 8.314922557960818139, 14.29746914071049879, 89.58224293864768129 ) ) ;
#124508 = CARTESIAN_POINT ( 'NONE',  ( -19.05341960407611168, -5.049401038298163336, 36.45724293864766707 ) ) ;
#124509 = CARTESIAN_POINT ( 'NONE',  ( -5.049401038297874678, -19.05341960407617918, 69.79275706135233293 ) ) ;
#124510 = CARTESIAN_POINT ( 'NONE',  ( -16.55341960407611168, -4.379528057220339221, 41.45724293864769550 ) ) ;
#124511 = CARTESIAN_POINT ( 'NONE',  ( 15.80617190586769283, -15.72974639402175789, 95.62609039468568994 ) ) ;
#124512 = CARTESIAN_POINT ( 'NONE',  ( 5.049401038298161559, -19.05341960407611168, 97.70724293864766707 ) ) ;
#124513 = CARTESIAN_POINT ( 'NONE',  ( 5.153800228976615827, -19.02544592524334988, 65.20942372801900433 ) ) ;
#124514 = CARTESIAN_POINT ( 'NONE',  ( -21.55341960407610458, -5.719274019375992779, 61.45724293864770260 ) ) ;
#124515 = AXIS2_PLACEMENT_3D ( 'NONE', #39300, #162643, #49006 ) ;
#124516 = CARTESIAN_POINT ( 'NONE',  ( 18.62759615963255655, 10.81492255796105972, 21.66775706135235069 ) ) ;
#124517 = CARTESIAN_POINT ( 'NONE',  ( 13.97604488694548053, -13.89961937509957401, 105.6260903946856757 ) ) ;
#124518 = CARTESIAN_POINT ( 'NONE',  ( -14.34966873604972548, 8.224510206698743886, 83.33442372801903275 ) ) ;
#124520 = CARTESIAN_POINT ( 'NONE',  ( 21.55341960407619695, -5.719274019375665929, 21.04275706135234714 ) ) ;
#124519 = CARTESIAN_POINT ( 'NONE',  ( 30.00000000000000000, -5.499999999999992895, 37.50000000000000000 ) ) ;
#124521 = CARTESIAN_POINT ( 'NONE',  ( 12.06949235617757843, -12.14591786802309237, 108.1239096053143811 ) ) ;
#124522 = CARTESIAN_POINT ( 'NONE',  ( -29.86685920354755552, 21.69954338932564397, -7.324999997268814234 ) ) ;
#124523 = CARTESIAN_POINT ( 'NONE',  ( -8.314922557961024197, 14.29746914071037800, 42.91775706135235424 ) ) ;
#124524 = CARTESIAN_POINT ( 'NONE',  ( 18.67979575497178502, 10.72451020669898547, 59.16557627198103120 ) ) ;
#124525 = CARTESIAN_POINT ( 'NONE',  ( 0.05219959533934541429, -16.53943276465976808, 105.0010903946856757 ) ) ;
#124526 = CARTESIAN_POINT ( 'NONE',  ( 16.52544592524335698, 4.483927247898782831, 36.45942372801901143 ) ) ;
#124527 = CARTESIAN_POINT ( 'NONE',  ( -13.89961937509977652, 13.97604488694528158, 25.62390960531434558 ) ) ;
#124528 = CARTESIAN_POINT ( 'NONE',  ( 4.483927247898790824, -16.52544592524335698, 80.20942372801901854 ) ) ;
#124529 = CARTESIAN_POINT ( 'NONE',  ( -5.049401038297874678, -19.05341960407617918, 69.79275706135233293 ) ) ;
#124530 = CARTESIAN_POINT ( 'NONE',  ( -5.719274019375978568, 21.55341960407610458, 75.20724293864769550 ) ) ;
#124531 = CARTESIAN_POINT ( 'NONE',  ( 16.53943276465976808, 0.05219959533934440121, 91.25109039468568994 ) ) ;
#124532 = CARTESIAN_POINT ( 'NONE',  ( -21.52544592524334988, -5.823673210054445271, 78.95942372801901854 ) ) ;
#124533 = CARTESIAN_POINT ( 'NONE',  ( 10.72451020669898902, -18.67979575497178502, 62.91557627198102409 ) ) ;
#124534 = CARTESIAN_POINT ( 'NONE',  ( 15.80617190586746368, 15.72974639402197994, 49.37390960531436690 ) ) ;
#124535 = ORIENTED_EDGE ( 'NONE', *, *, #29998, .T. ) ;
#124536 = CARTESIAN_POINT ( 'NONE',  ( -4.379528057220086978, -16.55341960407618274, 79.79275706135236135 ) ) ;
#124537 = CARTESIAN_POINT ( 'NONE',  ( 18.62759615963271287, -10.81492255796078972, 43.33224293864769550 ) ) ;
#124538 = EDGE_LOOP ( 'NONE', ( #194519, #185331, #103750, #87247, #147224, #13989 ) ) ;
#124539 = CARTESIAN_POINT ( 'NONE',  ( 13.97604488694527802, 13.89961937509977652, 114.3739096053143669 ) ) ;
#124540 = CARTESIAN_POINT ( 'NONE',  ( -22.98342225928958982, -7.557218236066893802, 173.2415159841883394 ) ) ;
#124541 = CARTESIAN_POINT ( 'NONE',  ( 13.97604488694527802, 13.89961937509977652, 24.37390960531435624 ) ) ;
#124542 = CARTESIAN_POINT ( 'NONE',  ( -0.05219959533907301413, -21.53943276465977519, 57.49890960531435979 ) ) ;
#124543 = CARTESIAN_POINT ( 'NONE',  ( 16.55341960407618274, -4.379528057220086978, 106.0427570613523471 ) ) ;
#124544 = CARTESIAN_POINT ( 'NONE',  ( 21.55341960407619695, -5.719274019375665929, 46.04275706135234714 ) ) ;
#124545 = CARTESIAN_POINT ( 'NONE',  ( -9.564922557961040184, 16.46253265017147172, 102.9177570613523329 ) ) ;
#124546 = CARTESIAN_POINT ( 'NONE',  ( 9.564922557960805705, 16.46253265017160317, 24.58224293864769194 ) ) ;
#124547 = CARTESIAN_POINT ( 'NONE',  ( 19.05341960407617918, -5.049401038297876454, 106.0427570613523471 ) ) ;
#124548 = CARTESIAN_POINT ( 'NONE',  ( -9.474510206698964154, 16.51473224551069663, 45.41557627198103120 ) ) ;
#124549 = CARTESIAN_POINT ( 'NONE',  ( 28.82186960331498327, 9.364793116373570925, 145.1000000000000227 ) ) ;
#124550 = CARTESIAN_POINT ( 'NONE',  ( -9.564922557960796823, -16.46253265017161027, 97.08224293864769550 ) ) ;
#124551 = CARTESIAN_POINT ( 'NONE',  ( -12.06949235617739369, -12.14591786802326823, 69.37609039468567573 ) ) ;
#124552 = CARTESIAN_POINT ( 'NONE',  ( -13.89961937509957401, -13.97604488694547875, 79.37609039468567573 ) ) ;
#124553 = CARTESIAN_POINT ( 'NONE',  ( -9.474510206698720793, -16.51473224551083518, 29.58442372801900433 ) ) ;
#124554 = CARTESIAN_POINT ( 'NONE',  ( -5.823673210054116645, -21.52544592524344225, 62.29057627198102409 ) ) ;
#124555 = CARTESIAN_POINT ( 'NONE',  ( 14.29746914071037800, 8.314922557961029526, 81.66775706135236135 ) ) ;
#124556 = CARTESIAN_POINT ( 'NONE',  ( -16.46253265017146816, -9.564922557961047289, 84.16775706135233293 ) ) ;
#124557 = CARTESIAN_POINT ( 'NONE',  ( -16.46253265017160317, 9.564922557960807481, 35.83224293864768839 ) ) ;
#124558 = CARTESIAN_POINT ( 'NONE',  ( -9.564922557960796823, -16.46253265017161027, 82.08224293864768129 ) ) ;
#124559 = CARTESIAN_POINT ( 'NONE',  ( 0.05219959533937995610, -21.53943276465977519, 45.00109039468568284 ) ) ;
#124560 = CARTESIAN_POINT ( 'NONE',  ( -19.03943276465977164, 0.05219959533909376836, 51.24890960531436690 ) ) ;
#124561 = CARTESIAN_POINT ( 'NONE',  ( 0.05219959533936267826, -19.03943276465977164, 70.00109039468566152 ) ) ;
#124562 = CARTESIAN_POINT ( 'NONE',  ( 21.95653654802608301, -8.266568072468363226, 172.1684357517875412 ) ) ;
#124563 = CARTESIAN_POINT ( 'NONE',  ( 13.97604488694527802, 13.89961937509977652, 109.3739096053143669 ) ) ;
#124564 = CARTESIAN_POINT ( 'NONE',  ( -16.55341960407611168, -4.379528057220339221, 61.45724293864770260 ) ) ;
#124565 = CARTESIAN_POINT ( 'NONE',  ( 10.81492255796078972, 18.62759615963270932, 54.58224293864769550 ) ) ;
#124566 = CARTESIAN_POINT ( 'NONE',  ( 19.50973618000807264, -5.499999999999992895, 102.5000000000000142 ) ) ;
#124567 = CARTESIAN_POINT ( 'NONE',  ( 0.05219959533936267826, -19.03943276465977164, 40.00109039468566152 ) ) ;
#124568 = CARTESIAN_POINT ( 'NONE',  ( 21.94207162742805650, -8.184381772639680364, 172.2902002187019832 ) ) ;
#124570 = CARTESIAN_POINT ( 'NONE',  ( 9.474510206698971260, -16.51473224551069308, 67.91557627198102409 ) ) ;
#124569 = CARTESIAN_POINT ( 'NONE',  ( 19.03943276465977164, -0.05219959533909143690, 68.74890960531436690 ) ) ;
#124571 = CARTESIAN_POINT ( 'NONE',  ( 16.53943276465976808, 0.05219959533934440121, 46.25109039468567573 ) ) ;
#124572 = CARTESIAN_POINT ( 'NONE',  ( -5.049401038297874678, -19.05341960407618274, 79.79275706135233293 ) ) ;
#124573 = CARTESIAN_POINT ( 'NONE',  ( 30.00000000000000355, -3.889087296526014814, 1.818019484660534424 ) ) ;
#124574 = CARTESIAN_POINT ( 'NONE',  ( -14.34966873604972548, 8.224510206698743886, 83.33442372801903275 ) ) ;
#124575 = CARTESIAN_POINT ( 'NONE',  ( -1.470710558936382917, -22.45286902209804580, -55.62279185774873724 ) ) ;
#124576 = CARTESIAN_POINT ( 'NONE',  ( 8.314922557961029526, -14.29746914071037800, 70.41775706135236135 ) ) ;
#124577 = CARTESIAN_POINT ( 'NONE',  ( -8.224510206698735004, -14.34966873604973081, 54.58442372801901143 ) ) ;
#124578 = CARTESIAN_POINT ( 'NONE',  ( 19.05341960407617918, -5.049401038297876454, 26.04275706135233293 ) ) ;
#124580 = CARTESIAN_POINT ( 'NONE',  ( 17.47810363111204879, -16.77070589658688604, -56.83189886071843944 ) ) ;
#124579 = CARTESIAN_POINT ( 'NONE',  ( -9.474510206698964154, 16.51473224551069663, 60.41557627198102409 ) ) ;
#124581 = CARTESIAN_POINT ( 'NONE',  ( -21.55341960407619339, 5.719274019375674811, 53.54275706135234714 ) ) ;
#124582 = CARTESIAN_POINT ( 'NONE',  ( 19.02544592524334988, 5.153800228976608722, 66.45942372801899012 ) ) ;
#124583 = CARTESIAN_POINT ( 'NONE',  ( -15.80617190586768217, 15.72974639402176855, 108.1260903946856757 ) ) ;
#124584 = VECTOR ( 'NONE', #56871, 1000.000000000000000 ) ;
#124585 = CARTESIAN_POINT ( 'NONE',  ( 0.05219959533909260263, 19.03943276465977164, 34.99890960531435979 ) ) ;
#124586 = CARTESIAN_POINT ( 'NONE',  ( -17.62966412709571529, 16.24235425892366891, -57.02231465076383188 ) ) ;
#124587 = CARTESIAN_POINT ( 'NONE',  ( -21.52544592524343514, 5.823673210054127303, 66.04057627198103830 ) ) ;
#124588 = CARTESIAN_POINT ( 'NONE',  ( 5.049401038298161559, -19.05341960407611168, 112.7072429386476813 ) ) ;
#124589 = CARTESIAN_POINT ( 'NONE',  ( -4.379528057220328563, 16.55341960407611168, 100.2072429386476955 ) ) ;
#124590 = CARTESIAN_POINT ( 'NONE',  ( 16.52544592524335698, 4.483927247898782831, 31.45942372801901854 ) ) ;
#124591 = CARTESIAN_POINT ( 'NONE',  ( 16.52544592524342804, -4.483927247898539470, 33.54057627198102409 ) ) ;
#124592 = ORIENTED_EDGE ( 'NONE', *, *, #192356, .T. ) ;
#124593 = CARTESIAN_POINT ( 'NONE',  ( 5.719274019375991003, -21.55341960407610458, 112.7072429386476955 ) ) ;
#124595 = CARTESIAN_POINT ( 'NONE',  ( 5.153800228976335163, 19.02544592524342804, 109.7905762719810099 ) ) ;
#124594 = CARTESIAN_POINT ( 'NONE',  ( 16.55341960407611168, 4.379528057220329451, 38.95724293864768839 ) ) ;
#124596 = CARTESIAN_POINT ( 'NONE',  ( 16.51473224551083163, -9.474510206698727899, 105.8344237280190043 ) ) ;
#124597 = CARTESIAN_POINT ( 'NONE',  ( 5.049401038297881783, 19.05341960407617563, 27.29275706135232937 ) ) ;
#124598 = CARTESIAN_POINT ( 'NONE',  ( -0.05219959533910754901, -16.53943276465976808, 37.49890960531436690 ) ) ;
#124599 = CARTESIAN_POINT ( 'NONE',  ( 10.72451020669898902, -18.67979575497178502, 102.9155762719810383 ) ) ;
#124601 = CARTESIAN_POINT ( 'NONE',  ( -10.81492255796078084, -18.62759615963271287, 67.08224293864770971 ) ) ;
#124600 = CARTESIAN_POINT ( 'NONE',  ( 17.13100169013300444, 6.664070546373172199, 31.73210164300152414 ) ) ;
#124602 = CARTESIAN_POINT ( 'NONE',  ( -9.474510206698964154, 16.51473224551069663, 70.41557627198102409 ) ) ;
#124603 = CARTESIAN_POINT ( 'NONE',  ( -16.52544592524342804, 4.483927247898546575, 46.04057627198103830 ) ) ;
#124604 = CARTESIAN_POINT ( 'NONE',  ( 9.564922557960805705, 16.46253265017160317, 84.58224293864769550 ) ) ;
#124605 = CARTESIAN_POINT ( 'NONE',  ( 0.000000000000000000, 0.000000000000000000, -62.58071313852362039 ) ) ;
#124606 = CARTESIAN_POINT ( 'NONE',  ( -16.46253265017146816, -9.564922557961047289, 59.16775706135233293 ) ) ;
#124607 = CARTESIAN_POINT ( 'NONE',  ( 21.52544592524344225, -5.823673210054117533, 93.54057627198103830 ) ) ;
#124608 = CARTESIAN_POINT ( 'NONE',  ( 4.379528057220339221, -16.55341960407611168, 102.7072429386476955 ) ) ;
#124609 = CARTESIAN_POINT ( 'NONE',  ( -21.52544592524334988, -5.823673210054445271, 33.95942372801901143 ) ) ;
#124610 = CARTESIAN_POINT ( 'NONE',  ( -17.14385361876520619, 23.59649016807275856, 149.0750000027311728 ) ) ;
#124611 = CARTESIAN_POINT ( 'NONE',  ( -16.55341960407611168, -4.379528057220339221, 26.45724293864768839 ) ) ;
#124612 = CARTESIAN_POINT ( 'NONE',  ( 0.05219959533909260263, 19.03943276465977164, 34.99890960531435979 ) ) ;
#124613 = CARTESIAN_POINT ( 'NONE',  ( -13.97604488694527625, -13.89961937509977652, 86.87390960531436690 ) ) ;
#124614 = CARTESIAN_POINT ( 'NONE',  ( 15.72974639402199770, -15.80617190586745480, 63.12390960531435979 ) ) ;
#124615 = CARTESIAN_POINT ( 'NONE',  ( -18.56453257813360835, 5.500000000000041744, 45.99000423690687711 ) ) ;
#124616 = CARTESIAN_POINT ( 'NONE',  ( 5.049401038298161559, -19.05341960407611168, 27.70724293864769550 ) ) ;
#124617 = CARTESIAN_POINT ( 'NONE',  ( -15.80617190586745835, -15.72974639402198527, 51.87390960531437401 ) ) ;
#124618 = CARTESIAN_POINT ( 'NONE',  ( -10.72451020669870658, -18.67979575497194134, 69.58442372801900433 ) ) ;
#124620 = CARTESIAN_POINT ( 'NONE',  ( -8.314922557961024197, 14.29746914071037800, 67.91775706135234714 ) ) ;
#124619 = CARTESIAN_POINT ( 'NONE',  ( 20.12333042654781678, -32.04799867105307953, -20.24659421909878532 ) ) ;
#124621 = CARTESIAN_POINT ( 'NONE',  ( 16.51473224551069308, 9.474510206698969483, 54.16557627198103120 ) ) ;
#124622 = CARTESIAN_POINT ( 'NONE',  ( 19.05341960407611168, 5.049401038298154454, 58.95724293864768129 ) ) ;
#124623 = ORIENTED_EDGE ( 'NONE', *, *, #76459, .F. ) ;
#124624 = CARTESIAN_POINT ( 'NONE',  ( -19.05341960407617563, 5.049401038297882671, 28.54275706135232937 ) ) ;
#124625 = CARTESIAN_POINT ( 'NONE',  ( -14.29746914071037622, -8.314922557961029526, 74.16775706135231871 ) ) ;
#124626 = CARTESIAN_POINT ( 'NONE',  ( -21.55341960407619339, 5.719274019375674811, 93.54275706135234714 ) ) ;
#124627 = CARTESIAN_POINT ( 'NONE',  ( 19.02544592524343514, -5.153800228976328945, 78.54057627198099567 ) ) ;
#124628 = CARTESIAN_POINT ( 'NONE',  ( 10.81492255796078972, 18.62759615963270932, 39.58224293864769550 ) ) ;
#124629 = CARTESIAN_POINT ( 'NONE',  ( 19.05341960407617918, -5.049401038297876454, 106.0427570613523471 ) ) ;
#124630 = CARTESIAN_POINT ( 'NONE',  ( 15.80617190586769283, -15.72974639402175789, 85.62609039468568994 ) ) ;
#124631 = CARTESIAN_POINT ( 'NONE',  ( 4.379528057220092307, 16.55341960407617563, 47.29275706135234003 ) ) ;
#124632 = CARTESIAN_POINT ( 'NONE',  ( 21.55341960407610458, 5.719274019375980345, 103.9572429386476813 ) ) ;
#124634 = VECTOR ( 'NONE', #128886, 1000.000000000000000 ) ;
#124633 = CARTESIAN_POINT ( 'NONE',  ( 16.51473224551083163, -9.474510206698727899, 110.8344237280190043 ) ) ;
#124635 = CARTESIAN_POINT ( 'NONE',  ( 19.05341960407611168, 5.049401038298154454, 73.95724293864768129 ) ) ;
#124636 = CARTESIAN_POINT ( 'NONE',  ( 0.05219959533934541429, -16.53943276465976808, 20.00109039468568639 ) ) ;
#124637 = CARTESIAN_POINT ( 'NONE',  ( 5.049401038298161559, -19.05341960407611168, 42.70724293864767418 ) ) ;
#124638 = CARTESIAN_POINT ( 'NONE',  ( 4.483927247898790824, -16.52544592524335698, 20.20942372801900788 ) ) ;
#124639 = CARTESIAN_POINT ( 'NONE',  ( 16.52544592524342804, -4.483927247898539470, 68.54057627198103830 ) ) ;
#124640 = CARTESIAN_POINT ( 'NONE',  ( -14.34966873604972548, 8.224510206698743886, 78.33442372801901854 ) ) ;
#124642 = CARTESIAN_POINT ( 'NONE',  ( -0.05219959533909027116, -19.03943276465977164, 47.49890960531435979 ) ) ;
#124641 = CARTESIAN_POINT ( 'NONE',  ( 10.81492255796106328, -18.62759615963255655, 35.41775706135234003 ) ) ;
#124643 = CARTESIAN_POINT ( 'NONE',  ( 16.46253265017160672, -9.564922557960803928, 68.33224293864770971 ) ) ;
#124644 = CARTESIAN_POINT ( 'NONE',  ( 12.14591786802327356, -12.06949235617739191, 70.62609039468567573 ) ) ;
#124646 = EDGE_LOOP ( 'NONE', ( #139745, #199492, #130928, #177898, #136329, #82218, #198030, #191509 ) ) ;
#124645 = FACE_OUTER_BOUND ( 'NONE', #81817, .T. ) ;
#124647 = ORIENTED_EDGE ( 'NONE', *, *, #42468, .F. ) ;
#124648 = CARTESIAN_POINT ( 'NONE',  ( -9.474510206698720793, -16.51473224551083518, 19.58442372801899722 ) ) ;
#124649 = CARTESIAN_POINT ( 'NONE',  ( 13.97604488694527802, 13.89961937509977652, 39.37390960531435269 ) ) ;
#124651 = ORIENTED_EDGE ( 'NONE', *, *, #14709, .F. ) ;
#124650 = CARTESIAN_POINT ( 'NONE',  ( -11.40812507854754720, -35.11059874428192273, -10.22499999726881548 ) ) ;
#124652 = CARTESIAN_POINT ( 'NONE',  ( 12.14591786802327356, -12.06949235617739191, 35.62609039468568994 ) ) ;
#124654 = CARTESIAN_POINT ( 'NONE',  ( -16.53943276465976808, -0.05219959533934237506, 43.75109039468568284 ) ) ;
#124653 = CARTESIAN_POINT ( 'NONE',  ( 16.51473224551083163, -9.474510206698727899, 60.83442372801900433 ) ) ;
#124655 = CARTESIAN_POINT ( 'NONE',  ( -5.153800228976328057, -19.02544592524343514, 37.29057627198102409 ) ) ;
#124656 = CARTESIAN_POINT ( 'NONE',  ( -13.89961937509977652, 13.97604488694528158, 105.6239096053143527 ) ) ;
#124657 = CARTESIAN_POINT ( 'NONE',  ( 19.03943276465977164, -0.05219959533909143690, 58.74890960531435979 ) ) ;
#124658 = CARTESIAN_POINT ( 'NONE',  ( 0.05219959533907565091, 21.53943276465977519, 104.9989096053143669 ) ) ;
#124660 = CARTESIAN_POINT ( 'NONE',  ( -13.89961937509977652, 13.97604488694528158, 110.6239096053143243 ) ) ;
#124659 = CARTESIAN_POINT ( 'NONE',  ( -16.51473224551069308, -9.474510206698971260, 91.66557627198103830 ) ) ;
#124661 = CARTESIAN_POINT ( 'NONE',  ( -19.03943276465977164, 0.05219959533909376836, 61.24890960531436690 ) ) ;
#124663 = CARTESIAN_POINT ( 'NONE',  ( -17.14385361876520264, -23.59649016807271238, 147.6750000027311671 ) ) ;
#124662 = CARTESIAN_POINT ( 'NONE',  ( -12.14591786802326823, 12.06949235617739902, 113.1260903946856899 ) ) ;
#124664 = CARTESIAN_POINT ( 'NONE',  ( 5.153800228976615827, -19.02544592524334988, 100.2094237280190043 ) ) ;
#124665 = CARTESIAN_POINT ( 'NONE',  ( 5.049401038297881783, 19.05341960407617563, 22.29275706135233648 ) ) ;
#124666 = CARTESIAN_POINT ( 'NONE',  ( -4.379528057220328563, 16.55341960407611168, 55.20724293864770260 ) ) ;
#124667 = CARTESIAN_POINT ( 'NONE',  ( 15.72974639402176855, 15.80617190586768217, 96.87609039468568994 ) ) ;
#124668 = CARTESIAN_POINT ( 'NONE',  ( 9.474510206698971260, -16.51473224551069308, 42.91557627198103120 ) ) ;
#124670 = CARTESIAN_POINT ( 'NONE',  ( 10.72451020669871369, 18.67979575497193778, 92.08442372801901854 ) ) ;
#124669 = CARTESIAN_POINT ( 'NONE',  ( -14.34966873604960291, -8.224510206698953496, 21.66557627198102409 ) ) ;
#124671 = CARTESIAN_POINT ( 'NONE',  ( -19.05341960407611168, -5.049401038298163336, 76.45724293864769550 ) ) ;
#124672 = CARTESIAN_POINT ( 'NONE',  ( -9.564922557960796823, -16.46253265017161027, 97.08224293864769550 ) ) ;
#124673 = CARTESIAN_POINT ( 'NONE',  ( -16.52544592524342804, 4.483927247898546575, 96.04057627198102409 ) ) ;
#124674 = CARTESIAN_POINT ( 'NONE',  ( -16.52544592524342804, 4.483927247898546575, 71.04057627198103830 ) ) ;
#124675 = CARTESIAN_POINT ( 'NONE',  ( 21.55341960407610458, 5.719274019375980345, 63.95724293864770260 ) ) ;
#124676 = CARTESIAN_POINT ( 'NONE',  ( 9.564922557960805705, 16.46253265017160317, 74.58224293864769550 ) ) ;
#124677 = CARTESIAN_POINT ( 'NONE',  ( 21.53943276465977519, -0.05219959533907433946, 78.74890960531436690 ) ) ;
#124678 = CARTESIAN_POINT ( 'NONE',  ( -19.05341960407617563, 5.049401038297882671, 83.54275706135233293 ) ) ;
#124681 = CARTESIAN_POINT ( 'NONE',  ( 12.14591786802309770, 12.06949235617756955, 94.37390960531436690 ) ) ;
#124680 = CARTESIAN_POINT ( 'NONE',  ( -5.000000000000000000, -139.5000000000000000, 22.27940468532398910 ) ) ;
#124679 = VECTOR ( 'NONE', #90250, 1000.000000000000114 ) ;
#124682 = CARTESIAN_POINT ( 'NONE',  ( -13.97604488694527625, -13.89961937509977652, 56.87390960531434558 ) ) ;
#124683 = CARTESIAN_POINT ( 'NONE',  ( 10.81492255796078972, 18.62759615963270932, 69.58224293864769550 ) ) ;
#124684 = EDGE_CURVE ( 'NONE', #197049, #28823, #9489, .T. ) ;
#124685 = CARTESIAN_POINT ( 'NONE',  ( 17.49999999999999289, -5.624438216177594541, 28.31670344914645199 ) ) ;
#124687 = DIRECTION ( 'NONE',  ( 1.000000000000000000, 0.000000000000000000, 0.000000000000000000 ) ) ;
#124686 = CARTESIAN_POINT ( 'NONE',  ( -4.379528057220086978, -16.55341960407618274, 109.7927570613523613 ) ) ;
#124688 = CARTESIAN_POINT ( 'NONE',  ( 13.97604488694548053, -13.89961937509957401, 110.6260903946856615 ) ) ;
#124689 = CARTESIAN_POINT ( 'NONE',  ( 16.52544592524342804, -4.483927247898539470, 83.54057627198102409 ) ) ;
#124690 = CARTESIAN_POINT ( 'NONE',  ( 7.405410116723220249, -1.490485923554886405, -62.24175268741320366 ) ) ;
#124691 = CARTESIAN_POINT ( 'NONE',  ( -5.049401038298153566, 19.05341960407611168, 80.20724293864769550 ) ) ;
#124692 = CARTESIAN_POINT ( 'NONE',  ( 5.153800228976335163, 19.02544592524342804, 34.79057627198102409 ) ) ;
#124693 = CARTESIAN_POINT ( 'NONE',  ( 16.52544592524342804, -4.483927247898539470, 73.54057627198102409 ) ) ;
#124694 = CARTESIAN_POINT ( 'NONE',  ( -9.474510206698964154, 16.51473224551069663, 100.4155762719810241 ) ) ;
#124696 = CARTESIAN_POINT ( 'NONE',  ( 19.05341960407611168, 5.049401038298154454, 78.95724293864769550 ) ) ;
#124695 = CARTESIAN_POINT ( 'NONE',  ( -5.049401038297874678, -19.05341960407617918, 84.79275706135233293 ) ) ;
#124697 = CARTESIAN_POINT ( 'NONE',  ( -9.564922557960796823, -16.46253265017161027, 92.08224293864769550 ) ) ;
#124698 = CARTESIAN_POINT ( 'NONE',  ( -5.823673210054116645, -21.52544592524344225, 77.29057627198102409 ) ) ;
#124699 = CARTESIAN_POINT ( 'NONE',  ( 14.29746914071037800, 8.314922557961029526, 76.66775706135234714 ) ) ;
#124700 = CARTESIAN_POINT ( 'NONE',  ( 13.97604488694548053, -13.89961937509957401, 110.6260903946856757 ) ) ;
#124701 = CARTESIAN_POINT ( 'NONE',  ( -16.46253265017160317, 9.564922557960807481, 60.83224293864769550 ) ) ;
#124702 = CARTESIAN_POINT ( 'NONE',  ( -21.53943276465977519, 0.05219959533907696930, 66.24890960531436690 ) ) ;
#124703 = CARTESIAN_POINT ( 'NONE',  ( -13.89961937509957401, -13.97604488694547875, 99.37609039468567573 ) ) ;
#124705 = CARTESIAN_POINT ( 'NONE',  ( -5.719274019375665041, -21.55341960407619695, 39.79275706135235424 ) ) ;
#124704 = CARTESIAN_POINT ( 'NONE',  ( -14.34966873604960291, -8.224510206698953496, 41.66557627198103120 ) ) ;
#124707 = CARTESIAN_POINT ( 'NONE',  ( 9.564922557960805705, 16.46253265017160317, 99.58224293864770971 ) ) ;
#124706 = CARTESIAN_POINT ( 'NONE',  ( -4.379528057220086978, -16.55341960407618274, 74.79275706135234714 ) ) ;
#124708 = CARTESIAN_POINT ( 'NONE',  ( -20.43538597629128262, 20.43538597629122222, -52.65483682830182488 ) ) ;
#124709 = DIRECTION ( 'NONE',  ( 0.000000000000000000, 0.000000000000000000, 1.000000000000000000 ) ) ;
#124710 = CARTESIAN_POINT ( 'NONE',  ( -16.55341960407617563, 4.379528057220093196, 88.54275706135236135 ) ) ;
#124711 = CARTESIAN_POINT ( 'NONE',  ( 0.05219959533934541429, -16.53943276465976808, 50.00109039468568994 ) ) ;
#124712 = CARTESIAN_POINT ( 'NONE',  ( -19.03943276465977164, 0.05219959533909376836, 56.24890960531435979 ) ) ;
#124713 = CARTESIAN_POINT ( 'NONE',  ( -19.05341960407611168, -5.049401038298163336, 61.45724293864769550 ) ) ;
#124714 = CARTESIAN_POINT ( 'NONE',  ( -18.67979575497193778, 10.72451020669871902, 48.33442372801902565 ) ) ;
#124715 = CARTESIAN_POINT ( 'NONE',  ( 16.55341960407618274, -4.379528057220086978, 66.04275706135236135 ) ) ;
#124716 = CARTESIAN_POINT ( 'NONE',  ( 16.53943276465976808, -0.05219959533910856209, 28.74890960531435624 ) ) ;
#124717 = CARTESIAN_POINT ( 'NONE',  ( -19.05341960407611168, -5.049401038298163336, 46.45724293864768129 ) ) ;
#124718 = CARTESIAN_POINT ( 'NONE',  ( -19.05341960407611168, -5.049401038298163336, 31.45724293864769550 ) ) ;
#124720 = EDGE_CURVE ( 'NONE', #107790, #33383, #80051, .T. ) ;
#124719 = CARTESIAN_POINT ( 'NONE',  ( 4.483927247898790824, -16.52544592524335698, 30.20942372801902565 ) ) ;
#124721 = CARTESIAN_POINT ( 'NONE',  ( 16.46253265017146816, 9.564922557961045513, 81.66775706135233293 ) ) ;
#124722 = CARTESIAN_POINT ( 'NONE',  ( -12.06949235617756955, 12.14591786802309770, 80.62390960531438111 ) ) ;
#124723 = CARTESIAN_POINT ( 'NONE',  ( 0.05219959533909260263, 19.03943276465977164, 54.99890960531435979 ) ) ;
#124725 = CARTESIAN_POINT ( 'NONE',  ( -38.00000000000001421, 12.34694845685046438, -8.099999999999997868 ) ) ;
#124724 = CARTESIAN_POINT ( 'NONE',  ( 19.02544592524334988, 5.153800228976608722, 86.45942372801900433 ) ) ;
#124726 = CARTESIAN_POINT ( 'NONE',  ( -0.05219959533937732626, 21.53943276465977519, 87.50109039468568994 ) ) ;
#124727 = CARTESIAN_POINT ( 'NONE',  ( 16.55341960407618274, -4.379528057220086978, 51.04275706135234714 ) ) ;
#124728 = CARTESIAN_POINT ( 'NONE',  ( 17.49999999999999645, 5.624438216177604311, 36.68329655085356933 ) ) ;
#124729 = CARTESIAN_POINT ( 'NONE',  ( -21.55341960407610458, -5.719274019375992779, 51.45724293864770260 ) ) ;
#124730 = CARTESIAN_POINT ( 'NONE',  ( 16.55341960407618274, -4.379528057220086978, 46.04275706135234714 ) ) ;
#124731 = DIRECTION ( 'NONE',  ( -1.000000000000000000, -0.000000000000000000, -0.000000000000000000 ) ) ;
#124732 = CARTESIAN_POINT ( 'NONE',  ( 16.51473224551083163, -9.474510206698727899, 25.83442372801900078 ) ) ;
#124733 = AXIS2_PLACEMENT_3D ( 'NONE', #68782, #55617, #52615 ) ;
#124734 = CARTESIAN_POINT ( 'NONE',  ( -9.564922557960796823, -16.46253265017161027, 72.08224293864770971 ) ) ;
#124735 = CARTESIAN_POINT ( 'NONE',  ( 9.437681514439660191, 10.01085954718715598, -60.42207423661103860 ) ) ;
#124736 = CARTESIAN_POINT ( 'NONE',  ( 19.02544592524343514, -5.153800228976328945, 53.54057627198102409 ) ) ;
#124737 = CARTESIAN_POINT ( 'NONE',  ( -17.49999999999999645, -5.499999999999992895, 44.20309617465829888 ) ) ;
#124738 = CARTESIAN_POINT ( 'NONE',  ( 16.46253265017160672, -9.564922557960803928, 68.33224293864770971 ) ) ;
#124740 = CARTESIAN_POINT ( 'NONE',  ( -18.09805431107247387, 5.500000000000101252, 66.01606229291884631 ) ) ;
#124739 = AXIS2_PLACEMENT_3D ( 'NONE', #153952, #16442, #135824 ) ;
#124741 = CARTESIAN_POINT ( 'NONE',  ( 16.46253265017146816, 9.564922557961045513, 36.66775706135233293 ) ) ;
#124742 = CARTESIAN_POINT ( 'NONE',  ( -21.55341960407619339, 5.719274019375674811, 113.5427570613523756 ) ) ;
#124743 = CARTESIAN_POINT ( 'NONE',  ( 14.34966873604960469, 8.224510206698951720, 44.16557627198103120 ) ) ;
#124744 = CARTESIAN_POINT ( 'NONE',  ( -0.05219959533909027116, -19.03943276465977164, 42.49890960531435269 ) ) ;
#124745 = CARTESIAN_POINT ( 'NONE',  ( 19.02544592524343514, -5.153800228976328945, 103.5405762719809957 ) ) ;
#124746 = CARTESIAN_POINT ( 'NONE',  ( -5.823673210054431948, 21.52544592524334988, 72.70942372801901854 ) ) ;
#124747 = CARTESIAN_POINT ( 'NONE',  ( 5.153800228976335163, 19.02544592524342804, 49.79057627198100988 ) ) ;
#124748 = CARTESIAN_POINT ( 'NONE',  ( -10.81492255796105439, 18.62759615963255655, 82.91775706135234714 ) ) ;
#124749 = CARTESIAN_POINT ( 'NONE',  ( -21.52544592524343514, 5.823673210054127303, 26.04057627198103475 ) ) ;
#124750 = CARTESIAN_POINT ( 'NONE',  ( 5.153800228976335163, 19.02544592524342804, 34.79057627198102409 ) ) ;
#124751 = CARTESIAN_POINT ( 'NONE',  ( 5.823673210054444382, -21.52544592524334988, 25.20942372801901854 ) ) ;
#124752 = CARTESIAN_POINT ( 'NONE',  ( -5.049401038297874678, -19.05341960407617918, 49.79275706135231871 ) ) ;
#124753 = CARTESIAN_POINT ( 'NONE',  ( 5.049401038298161559, -19.05341960407611168, 27.70724293864769550 ) ) ;
#124754 = CARTESIAN_POINT ( 'NONE',  ( -9.474510206698964154, 16.51473224551069663, 75.41557627198103830 ) ) ;
#124755 = CARTESIAN_POINT ( 'NONE',  ( 12.14591786802327356, -12.06949235617739191, 20.62609039468568639 ) ) ;
#124756 = CARTESIAN_POINT ( 'NONE',  ( 4.483927247898545687, 16.52544592524342804, 79.79057627198102409 ) ) ;
#124757 = CARTESIAN_POINT ( 'NONE',  ( -18.62759615963270932, 10.81492255796079327, 35.83224293864768839 ) ) ;
#124758 = CARTESIAN_POINT ( 'NONE',  ( -0.05219959533936034679, 19.03943276465977164, 102.5010903946856757 ) ) ;
#124759 = CARTESIAN_POINT ( 'NONE',  ( 21.53943276465977519, -0.05219959533907433946, 98.74890960531438111 ) ) ;
#124760 = CARTESIAN_POINT ( 'NONE',  ( 21.55341960407619695, -5.719274019375665929, 61.04275706135234714 ) ) ;
#124761 = CARTESIAN_POINT ( 'NONE',  ( 14.29746914071037800, 8.314922557961029526, 51.66775706135234714 ) ) ;
#124762 = CARTESIAN_POINT ( 'NONE',  ( 16.52544592524335698, 4.483927247898782831, 61.45942372801901854 ) ) ;
#124763 = CARTESIAN_POINT ( 'NONE',  ( -0.05219959533909027116, -19.03943276465977164, 47.49890960531435979 ) ) ;
#124764 = CARTESIAN_POINT ( 'NONE',  ( 4.379528057220092307, 16.55341960407617563, 92.29275706135236135 ) ) ;
#124765 = CARTESIAN_POINT ( 'NONE',  ( 21.52544592524334988, 5.823673210054432836, 21.45942372801901499 ) ) ;
#124766 = CARTESIAN_POINT ( 'NONE',  ( 16.55341960407611168, 4.379528057220329451, 53.95724293864770260 ) ) ;
#124767 = CARTESIAN_POINT ( 'NONE',  ( -9.474510206698964154, 16.51473224551069663, 85.41557627198102409 ) ) ;
#124768 = CARTESIAN_POINT ( 'NONE',  ( -16.53943276465976808, -0.05219959533934237506, 73.75109039468567573 ) ) ;
#124769 = CARTESIAN_POINT ( 'NONE',  ( -15.80617190586768217, 15.72974639402176855, 43.12609039468568284 ) ) ;
#124770 = CARTESIAN_POINT ( 'NONE',  ( 9.474510206698729675, 16.51473224551082808, 107.0844237280190043 ) ) ;
#124771 = CARTESIAN_POINT ( 'NONE',  ( 5.823673210054444382, -21.52544592524334988, 20.20942372801900788 ) ) ;
#124772 = CARTESIAN_POINT ( 'NONE',  ( 16.55341960407611168, 4.379528057220329451, 43.95724293864769550 ) ) ;
#124773 = ORIENTED_EDGE ( 'NONE', *, *, #155029, .F. ) ;
#124774 = CARTESIAN_POINT ( 'NONE',  ( -16.21995358207303539, 7.366697692864240032, 74.93551001512157939 ) ) ;
#124775 = CARTESIAN_POINT ( 'NONE',  ( 18.67979575497178502, 10.72451020669898547, 94.16557627198103830 ) ) ;
#124776 = CARTESIAN_POINT ( 'NONE',  ( 16.52544592524342804, -4.483927247898539470, 23.54057627198102765 ) ) ;
#124777 = ORIENTED_EDGE ( 'NONE', *, *, #184979, .F. ) ;
#124778 = DIRECTION ( 'NONE',  ( 0.000000000000000000, 0.000000000000000000, 1.000000000000000000 ) ) ;
#124779 = CARTESIAN_POINT ( 'NONE',  ( -21.55341960407610458, -5.719274019375992779, 111.4572429386476813 ) ) ;
#124780 = CARTESIAN_POINT ( 'NONE',  ( 0.05219959533909260263, 19.03943276465977164, 114.9989096053143669 ) ) ;
#124781 = CARTESIAN_POINT ( 'NONE',  ( -15.72974639402176322, -15.80617190586768395, 19.37609039468568639 ) ) ;
#124782 = CARTESIAN_POINT ( 'NONE',  ( 8.314922557960818139, 14.29746914071049879, 49.58224293864769550 ) ) ;
#124783 = CARTESIAN_POINT ( 'NONE',  ( -4.483927247898782831, 16.52544592524335698, 67.70942372801901854 ) ) ;
#124784 = CARTESIAN_POINT ( 'NONE',  ( -16.51473224551069308, -9.474510206698971260, 61.66557627198103120 ) ) ;
#124785 = CARTESIAN_POINT ( 'NONE',  ( -13.89961937509957401, -13.97604488694547875, 59.37609039468566863 ) ) ;
#124786 = CARTESIAN_POINT ( 'NONE',  ( 19.05341960407611168, 5.049401038298154454, 73.95724293864768129 ) ) ;
#124787 = CARTESIAN_POINT ( 'NONE',  ( 0.05219959533907565091, 21.53943276465977519, 29.99890960531435979 ) ) ;
#124788 = CARTESIAN_POINT ( 'NONE',  ( -20.37447694477751980, -32.07477979233467380, -24.11443027215549506 ) ) ;
#124789 = CARTESIAN_POINT ( 'NONE',  ( -19.03943276465977164, 0.05219959533909376836, 41.24890960531435269 ) ) ;
#124790 = CARTESIAN_POINT ( 'NONE',  ( 14.34966873604972726, -8.224510206698740333, 20.83442372801901143 ) ) ;
#124791 = CARTESIAN_POINT ( 'NONE',  ( -19.03943276465977164, -0.05219959533935918106, 58.75109039468566863 ) ) ;
#124792 = CARTESIAN_POINT ( 'NONE',  ( 10.81492255796078972, 18.62759615963270932, 99.58224293864770971 ) ) ;
#124793 = CARTESIAN_POINT ( 'NONE',  ( 16.53943276465976808, -0.05219959533910856209, 33.74890960531436690 ) ) ;
#124794 = B_SPLINE_CURVE_WITH_KNOTS ( 'NONE', 3,
 ( #29759, #147369, #101856, #90423, #40177, #91394 ),
 .UNSPECIFIED., .F., .F.,
 ( 4, 2, 4 ),
 ( 0.003989672132298185958, 0.004372778065220619612, 0.004755883998143053265 ),
 .UNSPECIFIED. ) ;
#124795 = CARTESIAN_POINT ( 'NONE',  ( 19.03943276465977164, -0.05219959533909143690, 93.74890960531435269 ) ) ;
#124796 = CARTESIAN_POINT ( 'NONE',  ( 10.81492255796078972, 18.62759615963270932, 54.58224293864769550 ) ) ;
#124798 = CARTESIAN_POINT ( 'NONE',  ( 0.05219959533934541429, -16.53943276465976808, 25.00109039468567218 ) ) ;
#124797 = CARTESIAN_POINT ( 'NONE',  ( -21.55341960407610458, -5.719274019375992779, 96.45724293864770971 ) ) ;
#124799 = CARTESIAN_POINT ( 'NONE',  ( 5.823673210054125526, 21.52544592524343514, 39.79057627198103830 ) ) ;
#124800 = CARTESIAN_POINT ( 'NONE',  ( 10.72451020669871369, 18.67979575497193778, 92.08442372801901854 ) ) ;
#124801 = CARTESIAN_POINT ( 'NONE',  ( 13.89961937509977652, -13.97604488694527269, 88.12390960531438111 ) ) ;
#124802 = CARTESIAN_POINT ( 'NONE',  ( 9.564922557960805705, 16.46253265017160317, 24.58224293864769194 ) ) ;
#124803 = CARTESIAN_POINT ( 'NONE',  ( -5.153800228976328057, -19.02544592524343514, 87.29057627198103830 ) ) ;
#124804 = CARTESIAN_POINT ( 'NONE',  ( -4.379528057220328563, 16.55341960407611168, 105.2072429386477097 ) ) ;
#124805 = CARTESIAN_POINT ( 'NONE',  ( -19.03943276465977164, 0.05219959533909376836, 61.24890960531436690 ) ) ;
#124806 = CARTESIAN_POINT ( 'NONE',  ( -14.29746914071037622, -8.314922557961029526, 24.16775706135235424 ) ) ;
#124807 = DIRECTION ( 'NONE',  ( -1.000000000000000000, 0.000000000000000000, 0.000000000000000000 ) ) ;
#124809 = CARTESIAN_POINT ( 'NONE',  ( 9.474510206698971260, -16.51473224551069308, 107.9155762719810383 ) ) ;
#124808 = CARTESIAN_POINT ( 'NONE',  ( -15.80617190586768217, 15.72974639402176855, 98.12609039468570415 ) ) ;
#124810 = CARTESIAN_POINT ( 'NONE',  ( -4.379528057220086978, -16.55341960407618274, 84.79275706135234714 ) ) ;
#124811 = CARTESIAN_POINT ( 'NONE',  ( 22.85092056426274354, -20.84023149160054089, -47.08084238880162076 ) ) ;
#124812 = CARTESIAN_POINT ( 'NONE',  ( 9.564922557961047289, -16.46253265017146816, 70.41775706135233293 ) ) ;
#124813 = CARTESIAN_POINT ( 'NONE',  ( 19.02544592524334988, 5.153800228976608722, 36.45942372801900433 ) ) ;
#124814 = CARTESIAN_POINT ( 'NONE',  ( -17.50000000000000355, -5.622605283950894872, 46.31207310596113302 ) ) ;
#124815 = CARTESIAN_POINT ( 'NONE',  ( 19.03943276465977164, -0.05219959533909143690, 33.74890960531435979 ) ) ;
#124816 = CARTESIAN_POINT ( 'NONE',  ( 8.314922557960818139, 14.29746914071049879, 39.58224293864769550 ) ) ;
#124817 = CARTESIAN_POINT ( 'NONE',  ( -17.44270441346516876, -5.991230190323022953, 111.3633507926423079 ) ) ;
#124818 = CARTESIAN_POINT ( 'NONE',  ( -4.379528057220328563, 16.55341960407611168, 25.20724293864769550 ) ) ;
#124819 = CARTESIAN_POINT ( 'NONE',  ( -19.39720447994791286, -5.500000000000075495, 84.66317477297172900 ) ) ;
#124820 = CARTESIAN_POINT ( 'NONE',  ( 4.483927247898790824, -16.52544592524335698, 100.2094237280190043 ) ) ;
#124821 = CARTESIAN_POINT ( 'NONE',  ( -5.153800228976328057, -19.02544592524343514, 37.29057627198102409 ) ) ;
#124822 = CARTESIAN_POINT ( 'NONE',  ( -5.719274019375665041, -21.55341960407619695, 99.79275706135234714 ) ) ;
#124823 = CARTESIAN_POINT ( 'NONE',  ( 19.02544592524334988, 5.153800228976608722, 106.4594237280190185 ) ) ;
#124824 = CARTESIAN_POINT ( 'NONE',  ( -10.72451020669870658, -18.67979575497194134, 79.58442372801903275 ) ) ;
#124825 = CARTESIAN_POINT ( 'NONE',  ( 5.153800228976615827, -19.02544592524334988, 50.20942372801897591 ) ) ;
#124826 = CARTESIAN_POINT ( 'NONE',  ( -5.153800228976328057, -19.02544592524343514, 97.29057627198099567 ) ) ;
#124827 = CARTESIAN_POINT ( 'NONE',  ( 13.97604488694527802, 13.89961937509977652, 69.37390960531436690 ) ) ;
#124828 = CARTESIAN_POINT ( 'NONE',  ( 0.000000000000000000, 0.000000000000000000, -49.13275782002545355 ) ) ;
#124829 = AXIS2_PLACEMENT_3D ( 'NONE', #122482, #78961, #43675 ) ;
#124830 = CARTESIAN_POINT ( 'NONE',  ( -14.29746914071049879, 8.314922557960819915, 70.83224293864770971 ) ) ;
#124831 = CARTESIAN_POINT ( 'NONE',  ( 21.53943276465977519, -0.05219959533907433946, 63.74890960531435979 ) ) ;
#124832 = CARTESIAN_POINT ( 'NONE',  ( 16.46253265017160672, -9.564922557960803928, 63.33224293864769550 ) ) ;
#124834 = CARTESIAN_POINT ( 'NONE',  ( -0.05219959533934338120, 16.53943276465976808, 77.50109039468567573 ) ) ;
#124833 = CARTESIAN_POINT ( 'NONE',  ( -15.80617190586745835, -15.72974639402198527, 81.87390960531435269 ) ) ;
#124835 = ORIENTED_EDGE ( 'NONE', *, *, #32424, .T. ) ;
#124836 = CARTESIAN_POINT ( 'NONE',  ( 13.89961937509977652, -13.97604488694527269, 48.12390960531435979 ) ) ;
#124838 = CARTESIAN_POINT ( 'NONE',  ( 29.86685920354754842, -21.69954338932559068, -1.824999997268813345 ) ) ;
#124837 = CARTESIAN_POINT ( 'NONE',  ( 16.55341960407611168, 4.379528057220329451, 78.95724293864769550 ) ) ;
#124839 = CARTESIAN_POINT ( 'NONE',  ( 13.89961937509977652, -13.97604488694527269, 48.12390960531435979 ) ) ;
#124840 = CARTESIAN_POINT ( 'NONE',  ( -16.55341960407611168, -4.379528057220339221, 111.4572429386476813 ) ) ;
#124841 = CARTESIAN_POINT ( 'NONE',  ( -19.05341960407617563, 5.049401038297882671, 68.54275706135230450 ) ) ;
#124842 = CARTESIAN_POINT ( 'NONE',  ( -14.29746914071049879, 8.314922557960819915, 80.83224293864769550 ) ) ;
#124843 = CARTESIAN_POINT ( 'NONE',  ( 21.52544592524334988, 5.823673210054432836, 41.45942372801901143 ) ) ;
#124845 = CARTESIAN_POINT ( 'NONE',  ( -5.719274019375978568, 21.55341960407610458, 105.2072429386477097 ) ) ;
#124844 = CARTESIAN_POINT ( 'NONE',  ( 19.02544592524343514, -5.153800228976328945, 33.54057627198102409 ) ) ;
#124846 = DIRECTION ( 'NONE',  ( -1.000000000000000000, -0.000000000000000000, -0.000000000000000000 ) ) ;
#124847 = CARTESIAN_POINT ( 'NONE',  ( 12.06949235617757843, -12.14591786802309237, 83.12390960531436690 ) ) ;
#124848 = CARTESIAN_POINT ( 'NONE',  ( 26.35664240927018653, -29.91691629194446378, -17.00538226201184600 ) ) ;
#124849 = CARTESIAN_POINT ( 'NONE',  ( 0.05219959533909260263, 19.03943276465977164, 49.99890960531435979 ) ) ;
#124850 = CARTESIAN_POINT ( 'NONE',  ( -10.70657341253913231, -12.25455453777589554, -61.54064628990102648 ) ) ;
#124852 = CARTESIAN_POINT ( 'NONE',  ( 13.97604488694527802, 13.89961937509977652, 99.37390960531436690 ) ) ;
#124851 = CARTESIAN_POINT ( 'NONE',  ( -16.46253265017146816, -9.564922557961047289, 89.16775706135234714 ) ) ;
#124853 = CARTESIAN_POINT ( 'NONE',  ( 10.72451020669871369, 18.67979575497193778, 37.08442372801901143 ) ) ;
#124854 = CARTESIAN_POINT ( 'NONE',  ( 5.153800228976335163, 19.02544592524342804, 84.79057627198099567 ) ) ;
#124855 = CARTESIAN_POINT ( 'NONE',  ( 16.51473224551083163, -9.474510206698727899, 75.83442372801900433 ) ) ;
#124856 = CARTESIAN_POINT ( 'NONE',  ( 0.05219959533909260263, 19.03943276465977164, 39.99890960531436690 ) ) ;
#124857 = EDGE_CURVE ( 'NONE', #162507, #60180, #100200, .T. ) ;
#124858 = CARTESIAN_POINT ( 'NONE',  ( -12.14591786802309592, -12.06949235617757132, 81.87390960531435269 ) ) ;
#124859 = CARTESIAN_POINT ( 'NONE',  ( 8.314922557960818139, 14.29746914071049879, 64.58224293864769550 ) ) ;
#124860 = CARTESIAN_POINT ( 'NONE',  ( -16.46253265017160317, 9.564922557960807481, 80.83224293864769550 ) ) ;
#124861 = CARTESIAN_POINT ( 'NONE',  ( -15.80617190586745835, -15.72974639402198527, 106.8739096053143811 ) ) ;
#124862 = CARTESIAN_POINT ( 'NONE',  ( -0.05219959533909027116, -19.03943276465977164, 72.49890960531435269 ) ) ;
#124863 = CARTESIAN_POINT ( 'NONE',  ( 19.02544592524334988, 5.153800228976608722, 21.45942372801899012 ) ) ;
#124866 = CARTESIAN_POINT ( 'NONE',  ( 0.05219959533910956823, 16.53943276465976808, 104.9989096053143669 ) ) ;
#124865 = CARTESIAN_POINT ( 'NONE',  ( -16.52544592524342804, 4.483927247898546575, 36.04057627198102409 ) ) ;
#124864 = CARTESIAN_POINT ( 'NONE',  ( -13.89961937509977652, 13.97604488694528158, 35.62390960531435269 ) ) ;
#124867 = CARTESIAN_POINT ( 'NONE',  ( 5.153800228976615827, -19.02544592524334988, 105.2094237280190185 ) ) ;
#124868 = ORIENTED_EDGE ( 'NONE', *, *, #41146, .T. ) ;
#124869 = CARTESIAN_POINT ( 'NONE',  ( 10.81492255796106328, -18.62759615963255655, 25.41775706135235779 ) ) ;
#124870 = CARTESIAN_POINT ( 'NONE',  ( 13.89961937509957401, 13.97604488694547697, 66.87609039468567573 ) ) ;
#124871 = CARTESIAN_POINT ( 'NONE',  ( 8.224510206698742110, 14.34966873604972548, 112.0844237280190185 ) ) ;
#124872 = CARTESIAN_POINT ( 'NONE',  ( 5.719274019375991003, -21.55341960407610458, 67.70724293864769550 ) ) ;
#124873 = CARTESIAN_POINT ( 'NONE',  ( 13.97604488694527802, 13.89961937509977652, 109.3739096053143669 ) ) ;
#124874 = CARTESIAN_POINT ( 'NONE',  ( -0.05219959533910754901, -16.53943276465976808, 52.49890960531435979 ) ) ;
#124875 = CARTESIAN_POINT ( 'NONE',  ( 13.89961937509977652, -13.97604488694527269, 33.12390960531434558 ) ) ;
#124876 = CARTESIAN_POINT ( 'NONE',  ( -0.05219959533909027116, -19.03943276465977164, 52.49890960531436690 ) ) ;
#124877 = CARTESIAN_POINT ( 'NONE',  ( 19.02544592524334988, 5.153800228976608722, 31.45942372801900433 ) ) ;
#124878 = CARTESIAN_POINT ( 'NONE',  ( -16.55341960407617563, 4.379528057220093196, 83.54275706135234714 ) ) ;
#124879 = CARTESIAN_POINT ( 'NONE',  ( -12.14591786802326823, 12.06949235617739902, 53.12609039468568284 ) ) ;
#124880 = CARTESIAN_POINT ( 'NONE',  ( 15.80617190586746368, 15.72974639402197994, 24.37390960531435979 ) ) ;
#124881 = CARTESIAN_POINT ( 'NONE',  ( 15.72974639402176855, 15.80617190586768217, 106.8760903946856899 ) ) ;
#124882 = CARTESIAN_POINT ( 'NONE',  ( 19.02544592524343514, -5.153800228976328945, 78.54057627198099567 ) ) ;
#124883 = VECTOR ( 'NONE', #159704, 1000.000000000000000 ) ;
#124884 = CARTESIAN_POINT ( 'NONE',  ( -8.314922557961024197, 14.29746914071037800, 57.91775706135234714 ) ) ;
#124885 = CARTESIAN_POINT ( 'NONE',  ( -16.55341960407611168, -4.379528057220339221, 106.4572429386477097 ) ) ;
#124886 = CARTESIAN_POINT ( 'NONE',  ( -0.05219959533934338120, 16.53943276465976808, 112.5010903946857042 ) ) ;
#124887 = CARTESIAN_POINT ( 'NONE',  ( -17.49999999999999645, -5.500000000000000888, 120.0000000000000142 ) ) ;
#124890 = CARTESIAN_POINT ( 'NONE',  ( -9.474510206698964154, 16.51473224551069663, 80.41557627198103830 ) ) ;
#124889 = CARTESIAN_POINT ( 'NONE',  ( -16.51473224551069308, -9.474510206698971260, 96.66557627198102409 ) ) ;
#124888 = CARTESIAN_POINT ( 'NONE',  ( 21.52544592524334988, 5.823673210054432836, 66.45942372801903275 ) ) ;
#124891 = CARTESIAN_POINT ( 'NONE',  ( -16.46253265017160317, 9.564922557960807481, 115.8322429386477097 ) ) ;
#124892 = CARTESIAN_POINT ( 'NONE',  ( 8.314922557960818139, 14.29746914071049879, 54.58224293864769550 ) ) ;
#124893 = CARTESIAN_POINT ( 'NONE',  ( 12.06949235617739724, 12.14591786802326823, 106.8760903946856899 ) ) ;
#124894 = CARTESIAN_POINT ( 'NONE',  ( -8.314922557960811034, -14.29746914071050412, 47.08224293864770260 ) ) ;
#124896 = CARTESIAN_POINT ( 'NONE',  ( -5.000000000000000000, -120.9970989573719038, 14.58956564881029472 ) ) ;
#124895 = CARTESIAN_POINT ( 'NONE',  ( 14.34966873604972726, -8.224510206698740333, 35.83442372801901143 ) ) ;
#124897 = CARTESIAN_POINT ( 'NONE',  ( 9.474510206698729675, 16.51473224551082808, 37.08442372801899722 ) ) ;
#124898 = CARTESIAN_POINT ( 'NONE',  ( -13.89961937509977652, 13.97604488694528158, 75.62390960531438111 ) ) ;
#124899 = CARTESIAN_POINT ( 'NONE',  ( 9.564922557961047289, -16.46253265017146816, 50.41775706135233293 ) ) ;
#124900 = CARTESIAN_POINT ( 'NONE',  ( 16.46253265017146816, 9.564922557961045513, 61.66775706135234003 ) ) ;
#124902 = CARTESIAN_POINT ( 'NONE',  ( -4.483927247898782831, 16.52544592524335698, 87.70942372801901854 ) ) ;
#124901 = CARTESIAN_POINT ( 'NONE',  ( 19.03943276465977164, 0.05219959533936151252, 96.25109039468567573 ) ) ;
#124903 = CARTESIAN_POINT ( 'NONE',  ( -22.44159573604010305, 16.30477369853692338, 147.1750000027311671 ) ) ;
#124904 = CARTESIAN_POINT ( 'NONE',  ( 19.05341960407611168, 5.049401038298154454, 28.95724293864769550 ) ) ;
#124905 = CARTESIAN_POINT ( 'NONE',  ( 13.89961937509977652, -13.97604488694527269, 103.1239096053143527 ) ) ;
#124906 = CARTESIAN_POINT ( 'NONE',  ( 18.67979575497194134, -10.72451020669871369, 40.83442372801901854 ) ) ;
#124907 = CARTESIAN_POINT ( 'NONE',  ( -9.564922557961040184, 16.46253265017147172, 87.91775706135233293 ) ) ;
#124909 = CARTESIAN_POINT ( 'NONE',  ( -16.46253265017160317, 9.564922557960807481, 65.83224293864769550 ) ) ;
#124908 = CARTESIAN_POINT ( 'NONE',  ( 24.93942350307310107, -7.769968609432603479, 171.2173313942149377 ) ) ;
#124910 = CARTESIAN_POINT ( 'NONE',  ( 19.02544592524343514, -5.153800228976328945, 98.54057627198100988 ) ) ;
#124912 = CARTESIAN_POINT ( 'NONE',  ( 9.564922557960805705, 16.46253265017160317, 49.58224293864770260 ) ) ;
#124911 = CARTESIAN_POINT ( 'NONE',  ( -14.29746914071049879, 8.314922557960819915, 60.83224293864769550 ) ) ;
#124913 = CARTESIAN_POINT ( 'NONE',  ( -19.03943276465977164, 0.05219959533909376836, 66.24890960531436690 ) ) ;
#124914 = CARTESIAN_POINT ( 'NONE',  ( 19.03943276465977164, 0.05219959533936151252, 71.25109039468566152 ) ) ;
#124915 = CARTESIAN_POINT ( 'NONE',  ( -0.05219959533936034679, 19.03943276465977164, 37.50109039468567573 ) ) ;
#124916 = CARTESIAN_POINT ( 'NONE',  ( 16.51473224551069308, 9.474510206698969483, 74.16557627198103830 ) ) ;
#124917 =( BOUNDED_SURFACE ( )  B_SPLINE_SURFACE ( 3, 2, ( 
 ( #155515, #95825, #172679, #16018, #140337, #173684, #35151, #110004, #2824, #64502, #78662, #170690, #141337, #19004, #1827, #33174, #174672, #80650, #126169, #63509, #36137, #154521, #125184, #77675, #62497, #142326, #186880, #81623, #3806, #171685, #187864, #139344, #124168, #188853, #18012, #48350, #185870, #156511, #65484, #127146, #50337, #96807, #111994, #47356, #158493, #19980, #143306, #4792, #66482, #128144, #109011, #101811, #117991, #21981, #148324, #133145, #193842, #56309, #82629, #7796, #146307, #129133, #163499, #38152, #23983, #24997, #144311, #5801, #84629, #179681, #39143, #97789, #159478, #54314, #85639, #191824, #175663, #100798, #162481, #194836, #147326, #69479, #20972, #6793, #161492, #67474, #190831, #68472, #145310, #130127, #115986, #8813, #52307, #70483, #113964, #37137, #132149, #178670, #131145, #9819, #98797, #53304, #83633, #114983, #160491, #176676, #99806, #22980, #55306, #86641, #177675, #192833, #71480, #116978, #40133, #197819, #43139, #104808, #88637, #180680, #44137, #138122, #135166, #89634, #59285, #119974, #41153, #12811, #196839, #58306, #137126, #105796, #74478, #118997, #199803, #164501, #181660, #29956, #90619, #42156, #61270, #103816, #167482, #122940, #166497, #151322, #120954, #27995, #102816, #136143, #182653, #28977, #198813, #152301, #13785, #165496, #25994, #87637, #75452, #91594, #60278, #26992, #149323, #121951, #150333, #183644, #10817, #45126, #106784, #11828, #72487, #76445, #73493, #134160, #195848, #168459, #153284, #14785, #57321, #140092, #32934, #81385, #92597, #18763, #48107, #108770, #15777, #124939, #141096, #157267, #156268, #65246, #16768, #77436, #80410, #109763, #49098, #79425, #47111, #582, #78416, #188612, #4549, #170448, #34910, #19744, #142082, #143070, #169448, #94589, #17769, #139108, #50093, #186636, #110755, #111753, #30950, #154287, #171447, #66242, #125929, #184627, #46109, #2583, #172437, #1584, #62253, #187628, #33925, #107763, #95582, #64263, #123922, #93593, #3568, #185621, #31939, #155279, #63259, #126906, #173441, #96566, #158254, #38907, #20729, #9579, #115749, #8571, #114738, #39895, #127902, #21739, #52068, #83391, #189604, #190592, #113725, #86403, #85394, #193598, #7549, #144074, #55070, #97547, #116740, #84388, #129881, #191580, #175421, #37906, #100564, #178430, #101563, #69236, #163254, #177437, #162244, #51077, #145068, #36890, #98555, #160249, #24756, #6549, #5555, #176432, #112738, #146065, #174431, #70246, #82386, #22740, #130902, #192592, #148088, #35901, #67234, #23744, #53059, #99565, #159234, #54075, #128892, #147087, #68228, #161246, #131914, #135909, #153037, #56067, #102580, #181426, #13547, #132909, #194596, #167242, #43893, #40907, #136884, #73255, #166252, #29714, #149090, #117747, #42904, #41916, #196602, #197580, #28740, #179441, #150084, #152062, #58073, #151083, #182413, #11588, #27752, #164264, #12574, #105556, #104569, #71245, #134925, #10580, #183401, #121708, #57081, #89395, #72241, #198570, #74240, #25759, #59047, #133918, #87405, #120713, #90377, #195608, #103582, #118755, #75213, #60040, #165257, #180444, #44884, #26751, #88390, #119743, #106540, #168217, #91346, #156021, #37402, #1333, #47866, #172189, #107522, #185374, #92355, #154041, #76198, #48853, #15536, #94342, #171201, #137877, #343, #33674, #95336, #170205, #63013, #124692, #77194, #30705, #186389, #199558, #93347, #14537, #32691, #140847, #108526, #138863, #17518, #79176, #114226, #2336, #109519, #61027, #123676, #78175, #122699, #175931, #46865, #62011, #31698, #64017, #125686, #184388, #187384, #169198, #99061, #110508, #157021, #18519, #129395, #45869, #155033, #16528, #139844, #80166, #141838, #6059, #67737, #191091, #52566, #40408, #176939, #26256, #130390, #87897, #117246, #162748, #24256, #8063, #100066, #163764, #57584, #54572, #9079, #178938, #39403, #160749, #132417, #116244, #177936, #56582, #25264 ),
 ( #102079, #85906, #161751, #119254, #196114, #23246, #180938, #7050, #86907, #69740, #149583, #148590, #101063, #70749, #42413, #68732, #195100, #147594, #84890, #192087, #194109, #10082, #133411, #55572, #41414, #193096, #53569, #118256, #71740, #179947, #103080, #146569, #38409, #164761, #11081, #22241, #131409, #72757, #83890, #134428, #145573, #115247, #14042, #152554, #135426, #169718, #44398, #30214, #108032, #150592, #88902, #90869, #185897, #45387, #104076, #181920, #62524, #183902, #28259, #182912, #124197, #107040, #29236, #43401, #165758, #139370, #166756, #851, #12091, #168712, #13070, #31211, #91857, #59544, #75708, #27252, #73754, #138383, #167738, #89898, #197097, #106052, #60535, #76707, #137386, #184891, #136400, #58564, #200064, #199066, #153549, #122211, #151581, #120230, #198077, #92862, #105071, #74737, #154549, #121222, #61532, #15046, #123201, #46373, #16044, #77703, #20008, #141365, #142354, #158520, #93864, #170716, #126197, #113006, #19032, #47382, #109037, #80678, #127174, #2852, #186907, #3834, #65513, #32207, #112024, #157538, #17036, #79695, #172709, #78690, #155542, #64530, #187893, #49360, #50365, #173713, #48378, #81651, #110035, #140367, #143335, #189871, #188884, #1854, #63536, #34193, #111023, #95854, #125211, #35181, #96836, #171713, #33203, #94861, #66510, #4822, #156542, #128172, #18041, #51346, #29875, #91513, #75373, #167404, #30872, #124858, #121870, #76365, #184549, #106706, #27915, #199723, #183563, #45048, #123841, #92518, #61189, #105717, #186557, #151244, #168380, #16688, #77358, #28900, #139025, #122861, #153199, #90540, #78338, #74399, #12733, #136065, #138042, #62177, #31860, #169363, #48029, #14704, #46030, #185539, #120874, #198735, #152222, #13707, #89558, #47033, #137043, #107685, #154208, #197739, #60200, #108690, #170368, #15697, #505, #93513, #155199, #44057, #140012, #59205, #1500, #63178, #109686, #182574, #21655, #50997, #83308, #20647, #159151, #32855, #126823, #18680, #80327, #157186, #144985, #141999, #187549, #158173, #171367, #189525, #94505, #113644, #64182, #66156, #127819, #112658, #6466, #129798, #110671, #143991, #96484, #19664, #68147, #174349, #156187, #97466, #191497, #17686, #35820, #82300, #52973, #79344, #2502, #81305, #175338, #141015, #125848, #67155, #5472, #49016, #36805, #173359, #128812, #172351, #33840, #95500, #142989, #3487, #4467, #190511, #51985, #65164, #50006, #98471, #160164, #188529, #111672, #34829, #88696, #27050, #72543, #86695, #105854, #182710, #9874, #44195, #193898, #150392, #56365, #74535, #11888, #102869, #195906, #167541, #55362, #181715, #10873, #71534, #178727, #87692, #26047, #28053, #134220, #73551, #194891, #57381, #166554, #29036, #135224, #58363, #119054, #147382, #149377, #25052, #59343, #197875, #133200, #180736, #148379, #136200, #196896, #40189, #42212, #118048, #101869, #120030, #103872, #163552, #179738, #41208, #43198, #165553, #164554, #104865, #121012, #117032, #132207, #89694, #151380, #12870, #8871, #70538, #110822, #77499, #123986, #48172, #183703, #61331, #168519, #30017, #152358, #125006, #91655, #170513, #47174, #13843, #76508, #109829, #171512, #46172, #139169, #646, #153344, #106844, #62316, #75510, #169509, #185684, #63328, #17835, #141162, #32003, #2651, #140158, #78485, #137183, #107825, #138184, #199867, #123002, #64328, #184688, #14845, #108833, #90676, #93660, #198871, #33001, #45190, #155345, #16834, #1650, #125995, #49163, #31009, #186701, #15840, #94655, #187693, #156335, #60338, #79493, #172504, #122012, #92658, #154347, #115815, #18830, #65311, #144139, #176498, #95647, #157335, #129948, #6618, #3632, #99632, #35964, #128959, #192658, #111818, #80475, #5621, #4615, #159300, #98621, #191648, #142148, #173506, #126971, #67300, #66307, #20796, #160315, #53127, #188679, #112804, #114805, #82451, #113792, #81449, #190659, #37974, #54141, #175487, #145135, #52135 ),
 ( #68297, #97611, #158320, #50159, #174497, #36959, #34979, #21805, #127967, #96632, #22808, #19808, #143136, #189670, #83457, #161314, #84454, #146132, #33991, #7618, #69302, #130968, #51143, #148156, #55137, #116807, #38974, #11659, #178499, #57150, #133988, #100631, #163326, #196675, #58144, #132977, #25827, #87472, #39965, #193666, #164333, #162312, #56137, #149159, #150158, #104640, #27824, #118828, #89466, #26821, #165329, #23813, #194667, #24822, #86471, #9648, #151155, #71314, #101635, #10649, #177505, #195679, #85463, #119812, #70312, #72311, #180512, #41985, #12645, #135979, #117818, #73325, #102648, #103651, #74312, #88462, #147152, #134996, #197650, #8640, #181497, #42975, #59116, #131981, #179511, #166327, #40979, #182482, #43963, #16596, #93416, #90450, #186461, #122769, #15604, #79251, #105625, #30778, #169271, #152134, #47939, #61096, #46937, #124764, #167313, #28809, #107593, #2409, #62084, #120782, #13617, #77262, #108597, #14611, #198644, #123748, #185447, #17591, #170274, #92425, #75284, #29784, #184458, #136955, #140923, #91420, #168288, #153107, #138931, #31767, #60110, #155103, #121778, #183471, #78244, #1406, #154111, #32762, #44956, #76268, #106613, #137946, #199629, #45938, #411, #139916, #63085, #109591, #171274, #94414, #156094, #33750, #129713, #20559, #66067, #127733, #111579, #3399, #67066, #161074, #158084, #112569, #82210, #142900, #64088, #35732, #19576, #81219, #160075, #128724, #97379, #141908, #22569, #187457, #4382, #52886, #113556, #65074, #84215, #159065, #191410, #37729, #5383, #143901, #189435, #126732, #145895, #99391, #188435, #125757, #110579, #190421, #173263, #114561, #51897, #50911, #174264, #48925, #172260, #98378, #175250, #49914, #95408, #157094, #36715, #21562, #83222, #144897, #96396, #18590, #6379, #68059, #176258, #80237, #34738, #23570, #101385, #11411, #27583, #131741, #57904, #42736, #103405, #166080, #100396, #179270, #70073, #38738, #72063, #117569, #162074, #104398, #87234, #8398, #194426, #163078, #193423, #196434, #53904, #192422, #115579, #55896, #41741, #73080, #148917, #89221, #40734, #102404, #165083, #85218, #178261, #146909, #54898, #69063, #26577, #116572, #10406, #164091, #130730, #39722, #88220, #149904, #24581, #25590, #133737, #86230, #147920, #195431, #177267, #9406, #56907, #180271, #134752, #119576, #118581, #181259, #7378, #71072, #132738, #106367, #198392, #59869, #136711, #62839, #121536, #167070, #137704, #150914, #169024, #12408, #93178, #43722, #45700, #107351, #30529, #186218, #109349, #90208, #123511, #76029, #199389, #47699, #92182, #74070, #77020, #171031, #135741, #153866, #15364, #32522, #197412, #182237, #60853, #154863, #58878, #120544, #46695, #185204, #105383, #16361, #152869, #138692, #28571, #151891, #13381, #122528, #183231, #184218, #173, #108356, #75045, #29547, #31525, #61841, #170035, #44712, #78009, #139676, #168050, #1164, #124523, #91180, #14364, #34508, #172024, #6144, #144661, #80010, #4148, #33513, #21327, #97147, #191180, #188203, #142669, #50676, #173029, #94174, #65827, #49675, #111339, #190183, #158830, #127496, #95172, #52655, #17350, #96166, #82985, #143658, #156860, #114318, #189201, #159832, #67826, #35497, #174026, #19346, #18355, #176020, #129481, #141679, #155853, #140680, #20318, #3170, #79006, #81966, #157855, #112336, #2172, #63852, #128487, #80994, #64843, #125523, #187220, #5142, #66824, #51658, #175014, #126505, #48690, #113322, #36478, #98135, #110343, #100154, #53660, #131494, #41503, #57672, #161835, #87983, #72844, #133495, #196200, #22329, #147679, #85990, #68823, #103167, #178017, #163850, #164847, #83979, #145659, #24340, #119339, #179024, #37489, #99151, #194191, #25351, #193181, #115337, #40492, #102164, #134514, #86992, #9167, #160840, #146656, #101145, #7140, #130482, #8150, #84973, #69827, #55656, #148679, #192179, #10167, #177028, #38498, #71827, #118341 ),
 ( #23330, #26343, #54654, #149671, #117328, #39484, #162831, #116328, #70834, #195187, #132502, #56668, #180034, #11169, #42499, #76788, #153631, #150677, #46453, #182997, #75792, #139447, #58646, #104163, #90948, #151662, #106135, #45466, #138459, #165844, #59631, #61609, #167819, #60616, #28342, #29318, #200140, #929, #122291, #91938, #152635, #181025, #121305, #120312, #92941, #31290, #166841, #14125, #182005, #108113, #183980, #73840, #137470, #43488, #12175, #107120, #199150, #135511, #77779, #168791, #105155, #30293, #74819, #89981, #169797, #27341, #88987, #197181, #15126, #123278, #184969, #154629, #62603, #16124, #13156, #136481, #198161, #44480, #1936, #63615, #185977, #158596, #125290, #3914, #80758, #47461, #110115, #143415, #4903, #79775, #172792, #34273, #186987, #140446, #111102, #109117, #2932, #95932, #96913, #51422, #174774, #65594, #36240, #173792, #112102, #170796, #141445, #171793, #33281, #94940, #97892, #156625, #48458, #157617, #124281, #142435, #32288, #66586, #17118, #19108, #127254, #188967, #159584, #82737, #18120, #20085, #49440, #50443, #21081, #35259, #93943, #81730, #144418, #155622, #128250, #189947, #5904, #78769, #64611, #113082, #126274, #187971, #145414, #70587, #8919, #164601, #55410, #177776, #190935, #176780, #131250, #52412, #26095, #38252, #115088, #99907, #85745, #132256, #37245, #178776, #160595, #149424, #117081, #148428, #54416, #179786, #67581, #161592, #191926, #23086, #129239, #130231, #53410, #87739, #25101, #133248, #147432, #83735, #194940, #98901, #56416, #24090, #69584, #192939, #84731, #6896, #193947, #114070, #146409, #116088, #40242, #7899, #175769, #39246, #100902, #162586, #163600, #101918, #86743, #68574, #22084, #9923, #71582, #118096, #41255, #102917, #172286, #108624, #79279, #187485, #155131, #93444, #138959, #153134, #33776, #48951, #76296, #110604, #57427, #16624, #122796, #140949, #78272, #169297, #62113, #95436, #119100, #47966, #77289, #137974, #44981, #72593, #46965, #123776, #186490, #94440, #45965, #106641, #109618, #438, #139945, #170302, #199656, #29810, #107619, #17620, #10920, #61122, #64118, #134267, #171302, #195954, #183497, #185475, #31795, #168314, #2436, #154140, #1435, #125783, #91446, #14637, #63113, #184486, #124791, #30803, #92452, #15632, #32788, #156121, #191433, #161098, #98404, #177292, #143925, #190446, #114586, #49942, #127757, #34766, #96423, #18616, #52910, #158109, #36740, #113580, #80263, #142924, #176283, #37755, #112594, #5406, #67090, #19601, #173292, #128749, #141933, #35756, #51921, #129736, #84241, #7403, #160100, #69087, #6403, #144921, #3424, #174286, #4406, #66091, #189458, #130754, #50936, #81243, #175274, #157120, #21587, #65100, #99416, #111607, #83245, #68084, #22593, #192446, #115603, #97401, #145920, #82235, #53928, #38762, #126758, #188461, #159088, #20583, #162101, #56936, #165113, #182268, #85244, #131766, #10434, #42765, #23597, #146935, #196463, #73111, #70097, #166110, #102430, #195461, #58907, #178285, #8425, #72092, #71096, #25615, #26605, #57933, #193448, #179297, #181287, #87259, #180300, #147945, #148944, #119604, #120574, #41768, #11440, #133766, #100420, #40761, #39748, #12438, #150944, #86255, #118610, #101411, #27612, #103433, #54924, #88248, #163103, #116596, #149933, #134781, #24607, #197441, #104427, #9431, #89252, #194450, #132763, #74100, #55921, #117596, #164117, #135770, #183260, #123543, #204, #105414, #29576, #62872, #124553, #199419, #92214, #153900, #44741, #59898, #30563, #28599, #122560, #15395, #16392, #171061, #94204, #185236, #155884, #93209, #31558, #167098, #60883, #91207, #152897, #14394, #17381, #76060, #121566, #77052, #43751, #61873, #90237, #186250, #136739, #138723, #46728, #108390, #79037, #2202, #106397, #78039, #169056, #170067, #140712, #154894, #151920, #139708, #63883, #13409, #1195, #47728, #125554, #75073, #198423, #109381, #32551 ),
 ( #168079, #137735, #184250, #45732, #107384, #36510, #64872, #145691, #81997, #52685, #160871, #128517, #66855, #112367, #126533, #7173, #22361, #49705, #84013, #33542, #190212, #96196, #114348, #51691, #142699, #35527, #68856, #95204, #21358, #50709, #111371, #18387, #48720, #20349, #97175, #159865, #67855, #19374, #80038, #83015, #174058, #113353, #143690, #173060, #3198, #81023, #191210, #187251, #34537, #37520, #110373, #144690, #172055, #129510, #158860, #99182, #156891, #4178, #157885, #65856, #141707, #127527, #189231, #188232, #6175, #176053, #175045, #5172, #98165, #100186, #196234, #87026, #132534, #194223, #178049, #69860, #133528, #27371, #24373, #179058, #148711, #9201, #130515, #102198, #86024, #147713, #26376, #195220, #163886, #8184, #89018, #53694, #70866, #119372, #180068, #131529, #150709, #25383, #57703, #104194, #71859, #10199, #55688, #193213, #12208, #165875, #54687, #192211, #40527, #116360, #56701, #39517, #181055, #118374, #23362, #41536, #101177, #161868, #103200, #164881, #85008, #115371, #88015, #162865, #117362, #149703, #11201, #42531, #177060, #38530, #146688, #72877, #134545, #77810, #15159, #93974, #60650, #107152, #31323, #166872, #44512, #151695, #13186, #135541, #108146, #74849, #153663, #30327, #197212, #59663, #92975, #154660, #29351, #122323, #184015, #136512, #90011, #45497, #58675, #152667, #168822, #46486, #961, #124313, #76819, #186011, #123309, #61641, #120342, #90980, #121336, #183029, #106168, #47493, #167851, #198193, #91969, #73871, #138490, #182037, #43519, #169830, #14157, #200172, #185002, #105185, #75825, #16156, #139479, #137503, #62637, #109150, #199183, #170829, #32321, #28373, #155654, #127282, #189976, #144448, #67609, #96943, #129270, #66615, #4932, #78802, #172821, #64641, #126303, #2961, #190964, #187999, #33311, #3943, #17149, #35287, #140480, #159616, #110144, #112131, #173823, #158624, #52441, #175802, #156655, #51451, #142465, #65622, #114099, #20115, #1968, #143446, #37275, #63648, #81759, #128279, #98932, #125323, #48490, #188995, #21112, #187020, #171823, #113112, #174802, #94971, #82767, #19136, #36268, #18151, #79805, #141477, #50471, #49469, #97923, #5933, #111132, #34301, #95963, #157647, #80787, #40275, #7930, #85775, #179814, #119128, #101948, #71611, #132286, #160623, #177806, #25132, #146439, #70620, #69614, #193978, #38282, #87767, #163629, #53442, #55440, #23116, #191956, #86774, #117111, #115117, #57456, #148458, #161622, #147462, #54447, #84761, #149452, #6926, #145444, #68604, #8952, #194968, #164630, #9952, #180809, #178805, #133277, #118126, #176810, #131280, #99936, #192968, #10948, #56447, #116117, #42288, #41284, #26125, #134297, #102946, #72622, #195983, #39276, #22114, #83764, #130260, #100933, #162617, #24123, #12941, #31086, #168589, #59418, #152429, #721, #11960, #138258, #167612, #28129, #135295, #165626, #137262, #13917, #76582, #184762, #136273, #196967, #199941, #29108, #30087, #198945, #166627, #120102, #197948, #107901, #124063, #89769, #154422, #139246, #61405, #62393, #88772, #75583, #60412, #58435, #169588, #44269, #91728, #92734, #150465, #73625, #90746, #185764, #45262, #103947, #27125, #122085, #153424, #121092, #181792, #106916, #14922, #43272, #123076, #183776, #104941, #74606, #46247, #151454, #182786, #105927, #15916, #77574, #65385, #50237, #16907, #158393, #140233, #129032, #35050, #128044, #34065, #159377, #47252, #141233, #171585, #2724, #108909, #109901, #33073, #5697, #4690, #112879, #127045, #63402, #174572, #78558, #36038, #3707, #49236, #110894, #94728, #186776, #111892, #144213, #64401, #95724, #188752, #126070, #170589, #18903, #187766, #172579, #143209, #173581, #80549, #125079, #67373, #32079, #157410, #142223, #156406, #1726, #96704, #19882, #48247, #93736, #81523, #17910, #66382, #189745, #79566, #97687, #155417, #51218, #20873, #82531, #24894, #194738, #132051, #10720 ),
 ( #176574, #9720, #71384, #146203, #39043, #100700, #130020, #6691, #177576, #175560, #69373, #162381, #163397, #117891, #41052, #70383, #102716, #40033, #178568, #52206, #7689, #38048, #99704, #161388, #164405, #22879, #68369, #23883, #190733, #8714, #113864, #133048, #83530, #85535, #147223, #193740, #25897, #149229, #191719, #86542, #115886, #55208, #87542, #116877, #37036, #101707, #72383, #98697, #148226, #56208, #160391, #21880, #145208, #179581, #53203, #114880, #84526, #131043, #192733, #54215, #199701, #136043, #28878, #92495, #11728, #195750, #44034, #104708, #59183, #198711, #91490, #57224, #12712, #14680, #120852, #13684, #181564, #182552, #153177, #154184, #75351, #45025, #105695, #134058, #151223, #60178, #119879, #167381, #43042, #90518, #73396, #61167, #137021, #26893, #118897, #89536, #166398, #27894, #74378, #46007, #197718, #150233, #152200, #180582, #121847, #42056, #76342, #88536, #183540, #106684, #168357, #169339, #15674, #135067, #29853, #138018, #122838, #30848, #184527, #103720, #107662, #165400, #196743, #58210, #172328, #142966, #480, #185516, #79320, #126799, #139001, #62154, #80304, #18658, #47008, #188505, #32830, #64159, #19641, #31837, #123818, #140990, #63154, #156162, #33817, #141977, #108667, #109662, #65142, #17660, #187527, #139986, #2478, #3465, #81283, #48992, #157164, #125824, #77334, #110647, #49984, #171342, #95477, #94481, #111648, #124833, #170345, #173334, #186533, #34807, #96462, #1475, #158150, #93488, #48006, #155174, #16665, #78313, #44678, #151856, #58843, #46661, #104362, #42701, #166046, #106331, #92146, #61808, #199355, #77976, #168017, #91147, #15328, #150879, #28537, #135707, #197378, #119542, #153832, #120510, #137668, #14330, #181225, #43686, #76987, #138658, #13347, #29513, #152836, #182201, #74036, #75995, #27546, #136676, #60820, #30495, #185170, #108320, #122494, #170000, #107318, #45667, #168991, #12373, #139643, #139, #123478, #184185, #31491, #57870, #75011, #105348, #198358, #89187, #167035, #90173, #16326, #93143, #154828, #59832, #121502, #183196, #170995, #69537, #160547, #5854, #67530, #51373, #140648, #6848, #100855, #97843, #52362, #22036, #82683, #1131, #175716, #159531, #21030, #99861, #68527, #37195, #78973, #162537, #124487, #144367, #192891, #53362, #2138, #24041, #98852, #131201, #177730, #145366, #83688, #129188, #66537, #85696, #7850, #39199, #128201, #191878, #130182, #113034, #54369, #115039, #190886, #114019, #62805, #109316, #38205, #176732, #189898, #32488, #186183, #161545, #23038, #84683, #146363, #36189, #94141, #116041, #47664, #155820, #17318, #174726, #108374, #110357, #95188, #34521, #155868, #80023, #15379, #93193, #188, #61857, #184234, #156874, #123526, #2185, #79020, #45715, #170050, #141692, #3183, #78023, #171045, #32535, #185220, #138707, #109363, #107368, #1178, #94188, #18371, #49690, #173044, #63867, #96181, #172039, #33526, #169040, #139692, #31541, #154878, #16376, #157870, #62855, #46711, #17365, #124537, #4162, #186234, #47713, #81008, #64856, #188217, #125538, #140695, #111355, #92198, #19359, #187234, #48704, #126518, #142683, #122544, #30546, #153882, #77036, #114331, #22344, #144673, #65840, #37502, #21340, #82998, #161851, #68839, #99164, #143674, #24355, #189214, #6158, #54669, #115353, #5155, #86006, #160854, #131509, #39500, #7156, #145674, #191193, #66838, #147695, #69842, #101160, #128501, #53675, #130498, #175028, #193196, #192194, #67838, #176034, #162848, #174042, #100169, #129495, #190196, #97160, #127510, #83995, #177043, #38513, #146671, #98147, #158844, #23345, #52669, #84990, #8166, #51674, #50693, #81981, #116343, #178032, #113336, #112351, #35511, #20332, #36493, #159847, #119355, #57687, #40509, #74833, #149687, #135525, #13170, #55671, #194206, #196217, #90962, #150692, #9182, #70848, #165859, #197196, #103183, #87008, #12190, #73855, #106151, #58659, #181039 ),
 ( #27355, #132517, #151677, #102180, #104177, #89001, #120325, #44495, #163868, #182020, #42513, #25367, #167833, #43503, #10183, #105169, #164863, #71843, #198175, #117345, #179041, #148695, #166855, #28357, #195204, #89995, #136495, #121319, #59645, #183011, #133512, #180051, #56684, #118358, #41520, #29334, #26359, #87999, #11185, #72860, #134530, #171806, #33294, #108128, #941, #62616, #91952, #168805, #139461, #137484, #31303, #124294, #125305, #79787, #2944, #32302, #64623, #1950, #140460, #14139, #169812, #200154, #61624, #138473, #126285, #123292, #30309, #185991, #152649, #170809, #75806, #94953, #45479, #47474, #109131, #93957, #187982, #111114, #153645, #187001, #77792, #155636, #49452, #17131, #199164, #78783, #172803, #60631, #63629, #48471, #34284, #122305, #183996, #110128, #156637, #107135, #15140, #18133, #141460, #76802, #184984, #154642, #46468, #92956, #16137, #157630, #5915, #66597, #21092, #160606, #53422, #19119, #174785, #176791, #82749, #175782, #143428, #144429, #115099, #54429, #37256, #6908, #67592, #95944, #113094, #22096, #81741, #129251, #4914, #190946, #173805, #23097, #98914, #188978, #52423, #158607, #161603, #69595, #83746, #145425, #114081, #35270, #116099, #99918, #131262, #96925, #68586, #130242, #128261, #84744, #191938, #51434, #38264, #192950, #3925, #146420, #159595, #20097, #127265, #80769, #7911, #177787, #142447, #65605, #189959, #50454, #112113, #36251, #97904, #134277, #101929, #136253, #55421, #120084, #165608, #163611, #89748, #74585, #135277, #197929, #24102, #149434, #87749, #70600, #104921, #179796, #27107, #43253, #85756, #147443, #26106, #121071, #180791, #39257, #100913, #195965, #88753, #133259, #117092, #42270, #103928, #59397, #150446, #10930, #162598, #148439, #102927, #8931, #132267, #9934, #86756, #193958, #72603, #166608, #11942, #178787, #57437, #40256, #181772, #25112, #119110, #73606, #196949, #71593, #194950, #56427, #58417, #164612, #28110, #118107, #151434, #41265, #12921, #17891, #44249, #139226, #47230, #64382, #167592, #13897, #92713, #125059, #105906, #29087, #78538, #155397, #152409, #48226, #184742, #77554, #141215, #60392, #90726, #154402, #153402, #107881, #108889, #140213, #75563, #61384, #63382, #169568, #62373, #30067, #137239, #2705, #91708, #14900, #124043, #170568, #168569, #183756, #93715, #198924, #182765, #32059, #186756, #31065, #94709, #122064, #76562, #106896, #138237, #45242, #199921, #123056, #46227, #1706, #109881, #185742, #15896, #171565, #701, #33054, #16887, #156387, #79545, #173562, #65366, #129013, #22860, #19863, #174550, #82509, #4671, #126050, #97666, #81503, #143191, #21860, #190713, #159355, #3687, #84507, #49217, #66363, #114859, #175540, #127026, #146185, #20853, #191700, #99685, #67353, #5677, #51198, #188733, #7670, #130000, #161369, #50218, #113844, #52186, #35031, #53184, #37015, #128023, #36017, #187747, #34046, #160369, #189725, #111872, #157391, #110875, #144191, #98676, #83510, #6671, #158374, #18884, #145187, #112859, #68349, #176554, #96686, #172560, #142204, #38029, #95703, #80530, #119862, #104692, #165382, #27876, #54196, #179562, #117872, #100681, #135050, #9701, #195732, #73378, #115868, #177557, #56189, #151207, #10702, #69354, #131023, #25879, #57205, #163377, #147203, #72365, #134039, #166380, #118880, #41032, #192712, #178549, #133029, #116858, #149211, #180564, #55189, #70364, #42038, #162363, #39026, #103702, #150214, #102698, #181547, #23864, #24874, #193721, #86523, #85515, #132032, #40015, #89517, #26875, #196726, #88518, #8694, #58194, #101688, #43026, #87524, #71365, #194719, #148207, #164386, #11711, #109645, #106667, #61149, #169323, #91473, #12695, #184511, #168340, #29836, #108650, #15658, #45991, #90502, #171327, #136027, #153161, #1460, #62138, #152184, #32815, #107646, #78297, #186517, #154167, #92478, #138000, #13668, #94466, #16650, #47991, #75335, #463 ) ),
 .UNSPECIFIED., .T., .F., .F. ) 
 B_SPLINE_SURFACE_WITH_KNOTS ( ( 4, 3, 4 ),
 ( 3, 2, 2, 2, 2, 2, 2, 2, 2, 2, 2, 2, 2, 2, 2, 2, 2, 2, 2, 2, 2, 2, 2, 2, 2, 2, 2, 2, 2, 2, 2, 2, 2, 2, 2, 2, 2, 2, 2, 2, 2, 2, 2, 2, 2, 2, 2, 2, 2, 2, 2, 2, 2, 2, 2, 2, 2, 2, 2, 2, 2, 2, 2, 2, 2, 2, 2, 2, 2, 2, 2, 2, 2, 2, 2, 2, 2, 2, 2, 2, 2, 2, 2, 2, 2, 2, 2, 2, 2, 2, 2, 2, 2, 2, 2, 2, 2, 2, 2, 2, 2, 2, 2, 2, 2, 2, 2, 2, 2, 2, 2, 2, 2, 2, 2, 2, 2, 2, 2, 2, 2, 2, 2, 2, 2, 2, 2, 2, 2, 2, 2, 2, 2, 2, 2, 2, 2, 2, 2, 2, 2, 2, 2, 2, 2, 2, 2, 2, 2, 2, 2, 2, 2, 2, 2, 2, 2, 2, 2, 2, 2, 2, 2, 2, 2, 2, 2, 2, 2, 2, 2, 2, 2, 2, 2, 2, 2, 2, 2, 2, 2, 2, 2, 2, 2, 2, 2, 2, 2, 2, 2, 2, 2, 2, 2, 2, 2, 2, 2, 2, 2, 2, 2, 2, 2, 2, 2, 2, 2, 2, 2, 2, 2, 2, 2, 2, 2, 2, 2, 2, 2, 2, 2, 2, 2, 2, 2, 2, 3 ),
 ( 0.000000000000000000, 0.5000000000000000000, 1.000000000000000000 ),
 ( 0.000000000000000000, 0.004385964912280701511, 0.008771929824561403022, 0.01315789473684210453, 0.01754385964912280604, 0.02192982456140350755, 0.02631578947368420907, 0.03070175438596491058, 0.03508771929824561209, 0.03947368421052631360, 0.04385964912280701511, 0.04824561403508771662, 0.05263157894736841813, 0.05701754385964911964, 0.06140350877192982115, 0.06578947368421052266, 0.07017543859649122417, 0.07456140350877192569, 0.07894736842105262720, 0.08333333333333332871, 0.08771929824561403022, 0.09210526315789473173, 0.09649122807017543324, 0.1008771929824561348, 0.1052631578947368363, 0.1096491228070175378, 0.1140350877192982393, 0.1184210526315789408, 0.1228070175438596423, 0.1271929824561403577, 0.1315789473684210453, 0.1359649122807017607, 0.1403508771929824483, 0.1447368421052631637, 0.1491228070175438514, 0.1535087719298245668, 0.1578947368421052544, 0.1622807017543859698, 0.1666666666666666574, 0.1710526315789473728, 0.1754385964912280604, 0.1798245614035087758, 0.1842105263157894635, 0.1885964912280701788, 0.1929824561403508665, 0.1973684210526315819, 0.2017543859649122695, 0.2061403508771929849, 0.2105263157894736725, 0.2149122807017543879, 0.2192982456140350755, 0.2236842105263157909, 0.2280701754385964786, 0.2324561403508771940, 0.2368421052631578816, 0.2412280701754385970, 0.2456140350877192846, 0.2500000000000000000, 0.2543859649122807154, 0.2587719298245614308, 0.2631578947368420907, 0.2675438596491228060, 0.2719298245614035214, 0.2763157894736842368, 0.2807017543859648967, 0.2850877192982456121, 0.2894736842105263275, 0.2938596491228070429, 0.2982456140350877027, 0.3026315789473684181, 0.3070175438596491335, 0.3114035087719298489, 0.3157894736842105088, 0.3201754385964912242, 0.3245614035087719396, 0.3289473684210526550, 0.3333333333333333148, 0.3377192982456140302, 0.3421052631578947456, 0.3464912280701754610, 0.3508771929824561209, 0.3552631578947368363, 0.3596491228070175517, 0.3640350877192982670, 0.3684210526315789269, 0.3728070175438596423, 0.3771929824561403577, 0.3815789473684210731, 0.3859649122807017330, 0.3903508771929824483, 0.3947368421052631637, 0.3991228070175438791, 0.4035087719298245390, 0.4078947368421052544, 0.4122807017543859698, 0.4166666666666666852, 0.4210526315789473450, 0.4254385964912280604, 0.4298245614035087758, 0.4342105263157894912, 0.4385964912280701511, 0.4429824561403508665, 0.4473684210526315819, 0.4517543859649122973, 0.4561403508771929571, 0.4605263157894736725, 0.4649122807017543879, 0.4692982456140351033, 0.4736842105263157632, 0.4780701754385964786, 0.4824561403508771940, 0.4868421052631579093, 0.4912280701754385692, 0.4956140350877192846, 0.5000000000000000000, 0.5043859649122807154, 0.5087719298245614308, 0.5131578947368421462, 0.5175438596491228616, 0.5219298245614034659, 0.5263157894736841813, 0.5307017543859648967, 0.5350877192982456121, 0.5394736842105263275, 0.5438596491228070429, 0.5482456140350877583, 0.5526315789473684736, 0.5570175438596490780, 0.5614035087719297934, 0.5657894736842105088, 0.5701754385964912242, 0.5745614035087719396, 0.5789473684210526550, 0.5833333333333333703, 0.5877192982456140857, 0.5921052631578946901, 0.5964912280701754055, 0.6008771929824561209, 0.6052631578947368363, 0.6096491228070175517, 0.6140350877192982670, 0.6184210526315789824, 0.6228070175438596978, 0.6271929824561403022, 0.6315789473684210176, 0.6359649122807017330, 0.6403508771929824483, 0.6447368421052631637, 0.6491228070175438791, 0.6535087719298245945, 0.6578947368421053099, 0.6622807017543859143, 0.6666666666666666297, 0.6710526315789473450, 0.6754385964912280604, 0.6798245614035087758, 0.6842105263157894912, 0.6885964912280702066, 0.6929824561403509220, 0.6973684210526315264, 0.7017543859649122417, 0.7061403508771929571, 0.7105263157894736725, 0.7149122807017543879, 0.7192982456140351033, 0.7236842105263158187, 0.7280701754385965341, 0.7324561403508771384, 0.7368421052631578538, 0.7412280701754385692, 0.7456140350877192846, 0.7500000000000000000, 0.7543859649122807154, 0.7587719298245614308, 0.7631578947368421462, 0.7675438596491228616, 0.7719298245614034659, 0.7763157894736841813, 0.7807017543859648967, 0.7850877192982456121, 0.7894736842105263275, 0.7938596491228070429, 0.7982456140350877583, 0.8026315789473684736, 0.8070175438596490780, 0.8114035087719297934, 0.8157894736842105088, 0.8201754385964912242, 0.8245614035087719396, 0.8289473684210526550, 0.8333333333333333703, 0.8377192982456140857, 0.8421052631578946901, 0.8464912280701754055, 0.8508771929824561209, 0.8552631578947368363, 0.8596491228070175517, 0.8640350877192982670, 0.8684210526315789824, 0.8728070175438596978, 0.8771929824561403022, 0.8815789473684210176, 0.8859649122807017330, 0.8903508771929824483, 0.8947368421052631637, 0.8991228070175438791, 0.9035087719298245945, 0.9078947368421053099, 0.9122807017543859143, 0.9166666666666666297, 0.9210526315789473450, 0.9254385964912280604, 0.9298245614035087758, 0.9342105263157894912, 0.9385964912280702066, 0.9429824561403509220, 0.9473684210526315264, 0.9517543859649122417, 0.9561403508771929571, 0.9605263157894736725, 0.9649122807017543879, 0.9692982456140351033, 0.9736842105263158187, 0.9780701754385965341, 0.9824561403508771384, 0.9868421052631578538, 0.9912280701754385692, 0.9956140350877192846, 1.000000000000000000 ),
 .UNSPECIFIED. ) 
 GEOMETRIC_REPRESENTATION_ITEM ( )  RATIONAL_B_SPLINE_SURFACE ( (
 ( 1.000000000000000000, 0.9659258262890683122, 1.000000000000000000, 0.9659258262890683122, 1.000000000000000000, 0.9659258262890683122, 1.000000000000000000, 0.9659258262890683122, 1.000000000000000000, 0.9659258262890683122, 1.000000000000000000, 0.9659258262890683122, 1.000000000000000000, 0.9659258262890683122, 1.000000000000000000, 0.9659258262890683122, 1.000000000000000000, 0.9659258262890683122, 1.000000000000000000, 0.9659258262890683122, 1.000000000000000000, 0.9659258262890683122, 1.000000000000000000, 0.9659258262890683122, 1.000000000000000000, 0.9659258262890683122, 1.000000000000000000, 0.9659258262890683122, 1.000000000000000000, 0.9659258262890683122, 1.000000000000000000, 0.9659258262890683122, 1.000000000000000000, 0.9659258262890683122, 1.000000000000000000, 0.9659258262890683122, 1.000000000000000000, 0.9659258262890683122, 1.000000000000000000, 0.9659258262890683122, 1.000000000000000000, 0.9659258262890683122, 1.000000000000000000, 0.9659258262890683122, 1.000000000000000000, 0.9659258262890683122, 1.000000000000000000, 0.9659258262890683122, 1.000000000000000000, 0.9659258262890683122, 1.000000000000000000, 0.9659258262890683122, 1.000000000000000000, 0.9659258262890683122, 1.000000000000000000, 0.9659258262890683122, 1.000000000000000000, 0.9659258262890683122, 1.000000000000000000, 0.9659258262890683122, 1.000000000000000000, 0.9659258262890683122, 1.000000000000000000, 0.9659258262890683122, 1.000000000000000000, 0.9659258262890683122, 1.000000000000000000, 0.9659258262890683122, 1.000000000000000000, 0.9659258262890683122, 1.000000000000000000, 0.9659258262890683122, 1.000000000000000000, 0.9659258262890683122, 1.000000000000000000, 0.9659258262890683122, 1.000000000000000000, 0.9659258262890683122, 1.000000000000000000, 0.9659258262890683122, 1.000000000000000000, 0.9659258262890683122, 1.000000000000000000, 0.9659258262890683122, 1.000000000000000000, 0.9659258262890683122, 1.000000000000000000, 0.9659258262890683122, 1.000000000000000000, 0.9659258262890683122, 1.000000000000000000, 0.9659258262890683122, 1.000000000000000000, 0.9659258262890683122, 1.000000000000000000, 0.9659258262890683122, 1.000000000000000000, 0.9659258262890683122, 1.000000000000000000, 0.9659258262890683122, 1.000000000000000000, 0.9659258262890683122, 1.000000000000000000, 0.9659258262890683122, 1.000000000000000000, 0.9659258262890683122, 1.000000000000000000, 0.9659258262890683122, 1.000000000000000000, 0.9659258262890683122, 1.000000000000000000, 0.9659258262890683122, 1.000000000000000000, 0.9659258262890683122, 1.000000000000000000, 0.9659258262890683122, 1.000000000000000000, 0.9659258262890683122, 1.000000000000000000, 0.9659258262890683122, 1.000000000000000000, 0.9659258262890683122, 1.000000000000000000, 0.9659258262890683122, 1.000000000000000000, 0.9659258262890683122, 1.000000000000000000, 0.9659258262890683122, 1.000000000000000000, 0.9659258262890683122, 1.000000000000000000, 0.9659258262890683122, 1.000000000000000000, 0.9659258262890683122, 1.000000000000000000, 0.9659258262890683122, 1.000000000000000000, 0.9659258262890683122, 1.000000000000000000, 0.9659258262890683122, 1.000000000000000000, 0.9659258262890683122, 1.000000000000000000, 0.9659258262890683122, 1.000000000000000000, 0.9659258262890683122, 1.000000000000000000, 0.9659258262890683122, 1.000000000000000000, 0.9659258262890683122, 1.000000000000000000, 0.9659258262890683122, 1.000000000000000000, 0.9659258262890683122, 1.000000000000000000, 0.9659258262890683122, 1.000000000000000000, 0.9659258262890683122, 1.000000000000000000, 0.9659258262890683122, 1.000000000000000000, 0.9659258262890683122, 1.000000000000000000, 0.9659258262890683122, 1.000000000000000000, 0.9659258262890683122, 1.000000000000000000, 0.9659258262890683122, 1.000000000000000000, 0.9659258262890683122, 1.000000000000000000, 0.9659258262890683122, 1.000000000000000000, 0.9659258262890683122, 1.000000000000000000, 0.9659258262890683122, 1.000000000000000000, 0.9659258262890683122, 1.000000000000000000, 0.9659258262890683122, 1.000000000000000000, 0.9659258262890683122, 1.000000000000000000, 0.9659258262890683122, 1.000000000000000000, 0.9659258262890683122, 1.000000000000000000, 0.9659258262890683122, 1.000000000000000000, 0.9659258262890683122, 1.000000000000000000, 0.9659258262890683122, 1.000000000000000000, 0.9659258262890683122, 1.000000000000000000, 0.9659258262890683122, 1.000000000000000000, 0.9659258262890683122, 1.000000000000000000, 0.9659258262890683122, 1.000000000000000000, 0.9659258262890683122, 1.000000000000000000, 0.9659258262890683122, 1.000000000000000000, 0.9659258262890683122, 1.000000000000000000, 0.9659258262890683122, 1.000000000000000000, 0.9659258262890683122, 1.000000000000000000, 0.9659258262890683122, 1.000000000000000000, 0.9659258262890683122, 1.000000000000000000, 0.9659258262890683122, 1.000000000000000000, 0.9659258262890683122, 1.000000000000000000, 0.9659258262890683122, 1.000000000000000000, 0.9659258262890683122, 1.000000000000000000, 0.9659258262890683122, 1.000000000000000000, 0.9659258262890683122, 1.000000000000000000, 0.9659258262890683122, 1.000000000000000000, 0.9659258262890683122, 1.000000000000000000, 0.9659258262890683122, 1.000000000000000000, 0.9659258262890683122, 1.000000000000000000, 0.9659258262890683122, 1.000000000000000000, 0.9659258262890683122, 1.000000000000000000, 0.9659258262890683122, 1.000000000000000000, 0.9659258262890683122, 1.000000000000000000, 0.9659258262890683122, 1.000000000000000000, 0.9659258262890683122, 1.000000000000000000, 0.9659258262890683122, 1.000000000000000000, 0.9659258262890683122, 1.000000000000000000, 0.9659258262890683122, 1.000000000000000000, 0.9659258262890683122, 1.000000000000000000, 0.9659258262890683122, 1.000000000000000000, 0.9659258262890683122, 1.000000000000000000, 0.9659258262890683122, 1.000000000000000000, 0.9659258262890683122, 1.000000000000000000, 0.9659258262890683122, 1.000000000000000000, 0.9659258262890683122, 1.000000000000000000, 0.9659258262890683122, 1.000000000000000000, 0.9659258262890683122, 1.000000000000000000, 0.9659258262890683122, 1.000000000000000000, 0.9659258262890683122, 1.000000000000000000, 0.9659258262890683122, 1.000000000000000000, 0.9659258262890683122, 1.000000000000000000, 0.9659258262890683122, 1.000000000000000000, 0.9659258262890683122, 1.000000000000000000, 0.9659258262890683122, 1.000000000000000000, 0.9659258262890683122, 1.000000000000000000, 0.9659258262890683122, 1.000000000000000000, 0.9659258262890683122, 1.000000000000000000, 0.9659258262890683122, 1.000000000000000000, 0.9659258262890683122, 1.000000000000000000, 0.9659258262890683122, 1.000000000000000000, 0.9659258262890683122, 1.000000000000000000, 0.9659258262890683122, 1.000000000000000000, 0.9659258262890683122, 1.000000000000000000, 0.9659258262890683122, 1.000000000000000000, 0.9659258262890683122, 1.000000000000000000, 0.9659258262890683122, 1.000000000000000000, 0.9659258262890683122, 1.000000000000000000, 0.9659258262890683122, 1.000000000000000000, 0.9659258262890683122, 1.000000000000000000, 0.9659258262890683122, 1.000000000000000000, 0.9659258262890683122, 1.000000000000000000, 0.9659258262890683122, 1.000000000000000000, 0.9659258262890683122, 1.000000000000000000, 0.9659258262890683122, 1.000000000000000000, 0.9659258262890683122, 1.000000000000000000, 0.9659258262890683122, 1.000000000000000000, 0.9659258262890683122, 1.000000000000000000, 0.9659258262890683122, 1.000000000000000000, 0.9659258262890683122, 1.000000000000000000, 0.9659258262890683122, 1.000000000000000000, 0.9659258262890683122, 1.000000000000000000, 0.9659258262890683122, 1.000000000000000000, 0.9659258262890683122, 1.000000000000000000, 0.9659258262890683122, 1.000000000000000000, 0.9659258262890683122, 1.000000000000000000, 0.9659258262890683122, 1.000000000000000000, 0.9659258262890683122, 1.000000000000000000, 0.9659258262890683122, 1.000000000000000000, 0.9659258262890683122, 1.000000000000000000, 0.9659258262890683122, 1.000000000000000000, 0.9659258262890683122, 1.000000000000000000, 0.9659258262890683122, 1.000000000000000000, 0.9659258262890683122, 1.000000000000000000, 0.9659258262890683122, 1.000000000000000000, 0.9659258262890683122, 1.000000000000000000, 0.9659258262890683122, 1.000000000000000000, 0.9659258262890683122, 1.000000000000000000, 0.9659258262890683122, 1.000000000000000000, 0.9659258262890683122, 1.000000000000000000, 0.9659258262890683122, 1.000000000000000000, 0.9659258262890683122, 1.000000000000000000, 0.9659258262890683122, 1.000000000000000000, 0.9659258262890683122, 1.000000000000000000, 0.9659258262890683122, 1.000000000000000000, 0.9659258262890683122, 1.000000000000000000, 0.9659258262890683122, 1.000000000000000000, 0.9659258262890683122, 1.000000000000000000, 0.9659258262890683122, 1.000000000000000000, 0.9659258262890683122, 1.000000000000000000, 0.9659258262890683122, 1.000000000000000000, 0.9659258262890683122, 1.000000000000000000, 0.9659258262890683122, 1.000000000000000000, 0.9659258262890683122, 1.000000000000000000, 0.9659258262890683122, 1.000000000000000000, 0.9659258262890683122, 1.000000000000000000, 0.9659258262890683122, 1.000000000000000000, 0.9659258262890683122, 1.000000000000000000, 0.9659258262890683122, 1.000000000000000000, 0.9659258262890683122, 1.000000000000000000, 0.9659258262890683122, 1.000000000000000000, 0.9659258262890683122, 1.000000000000000000, 0.9659258262890683122, 1.000000000000000000, 0.9659258262890683122, 1.000000000000000000, 0.9659258262890683122, 1.000000000000000000, 0.9659258262890683122, 1.000000000000000000, 0.9659258262890683122, 1.000000000000000000, 0.9659258262890683122, 1.000000000000000000, 0.9659258262890683122, 1.000000000000000000, 0.9659258262890683122, 1.000000000000000000, 0.9659258262890683122, 1.000000000000000000, 0.9659258262890683122, 1.000000000000000000, 0.9659258262890683122, 1.000000000000000000, 0.9659258262890683122, 1.000000000000000000, 0.9659258262890683122, 1.000000000000000000, 0.9659258262890683122, 1.000000000000000000, 0.9659258262890683122, 1.000000000000000000, 0.9659258262890683122, 1.000000000000000000, 0.9659258262890683122, 1.000000000000000000, 0.9659258262890683122, 1.000000000000000000, 0.9659258262890683122, 1.000000000000000000),
 ( 0.3333333333333333703, 0.3219752754296894559, 0.3333333333333333703, 0.3219752754296894559, 0.3333333333333333703, 0.3219752754296894559, 0.3333333333333333703, 0.3219752754296894559, 0.3333333333333333703, 0.3219752754296894559, 0.3333333333333333703, 0.3219752754296894559, 0.3333333333333333703, 0.3219752754296894559, 0.3333333333333333703, 0.3219752754296894559, 0.3333333333333333703, 0.3219752754296894559, 0.3333333333333333703, 0.3219752754296894559, 0.3333333333333333703, 0.3219752754296894559, 0.3333333333333333703, 0.3219752754296894559, 0.3333333333333333703, 0.3219752754296894559, 0.3333333333333333703, 0.3219752754296894559, 0.3333333333333333703, 0.3219752754296894559, 0.3333333333333333703, 0.3219752754296894559, 0.3333333333333333703, 0.3219752754296894559, 0.3333333333333333703, 0.3219752754296894559, 0.3333333333333333703, 0.3219752754296894559, 0.3333333333333333703, 0.3219752754296894559, 0.3333333333333333703, 0.3219752754296894559, 0.3333333333333333703, 0.3219752754296894559, 0.3333333333333333703, 0.3219752754296894559, 0.3333333333333333703, 0.3219752754296894559, 0.3333333333333333703, 0.3219752754296894559, 0.3333333333333333703, 0.3219752754296894559, 0.3333333333333333703, 0.3219752754296894559, 0.3333333333333333703, 0.3219752754296894559, 0.3333333333333333703, 0.3219752754296894559, 0.3333333333333333703, 0.3219752754296894559, 0.3333333333333333703, 0.3219752754296894559, 0.3333333333333333703, 0.3219752754296894559, 0.3333333333333333703, 0.3219752754296894559, 0.3333333333333333703, 0.3219752754296894559, 0.3333333333333333703, 0.3219752754296894559, 0.3333333333333333703, 0.3219752754296894559, 0.3333333333333333703, 0.3219752754296894559, 0.3333333333333333703, 0.3219752754296894559, 0.3333333333333333703, 0.3219752754296894559, 0.3333333333333333703, 0.3219752754296894559, 0.3333333333333333703, 0.3219752754296894559, 0.3333333333333333703, 0.3219752754296894559, 0.3333333333333333703, 0.3219752754296894559, 0.3333333333333333703, 0.3219752754296894559, 0.3333333333333333703, 0.3219752754296894559, 0.3333333333333333703, 0.3219752754296894559, 0.3333333333333333703, 0.3219752754296894559, 0.3333333333333333703, 0.3219752754296894559, 0.3333333333333333703, 0.3219752754296894559, 0.3333333333333333703, 0.3219752754296894559, 0.3333333333333333703, 0.3219752754296894559, 0.3333333333333333703, 0.3219752754296894559, 0.3333333333333333703, 0.3219752754296894559, 0.3333333333333333703, 0.3219752754296894559, 0.3333333333333333703, 0.3219752754296894559, 0.3333333333333333703, 0.3219752754296894559, 0.3333333333333333703, 0.3219752754296894559, 0.3333333333333333703, 0.3219752754296894559, 0.3333333333333333703, 0.3219752754296894559, 0.3333333333333333703, 0.3219752754296894559, 0.3333333333333333703, 0.3219752754296894559, 0.3333333333333333703, 0.3219752754296894559, 0.3333333333333333703, 0.3219752754296894559, 0.3333333333333333703, 0.3219752754296894559, 0.3333333333333333703, 0.3219752754296894559, 0.3333333333333333703, 0.3219752754296894559, 0.3333333333333333703, 0.3219752754296894559, 0.3333333333333333703, 0.3219752754296894559, 0.3333333333333333703, 0.3219752754296894559, 0.3333333333333333703, 0.3219752754296894559, 0.3333333333333333703, 0.3219752754296894559, 0.3333333333333333703, 0.3219752754296894559, 0.3333333333333333703, 0.3219752754296894559, 0.3333333333333333703, 0.3219752754296894559, 0.3333333333333333703, 0.3219752754296894559, 0.3333333333333333703, 0.3219752754296894559, 0.3333333333333333703, 0.3219752754296894559, 0.3333333333333333703, 0.3219752754296894559, 0.3333333333333333703, 0.3219752754296894559, 0.3333333333333333703, 0.3219752754296894559, 0.3333333333333333703, 0.3219752754296894559, 0.3333333333333333703, 0.3219752754296894559, 0.3333333333333333703, 0.3219752754296894559, 0.3333333333333333703, 0.3219752754296894559, 0.3333333333333333703, 0.3219752754296894559, 0.3333333333333333703, 0.3219752754296894559, 0.3333333333333333703, 0.3219752754296894559, 0.3333333333333333703, 0.3219752754296894559, 0.3333333333333333703, 0.3219752754296894559, 0.3333333333333333703, 0.3219752754296894559, 0.3333333333333333703, 0.3219752754296894559, 0.3333333333333333703, 0.3219752754296894559, 0.3333333333333333703, 0.3219752754296894559, 0.3333333333333333703, 0.3219752754296894559, 0.3333333333333333703, 0.3219752754296894559, 0.3333333333333333703, 0.3219752754296894559, 0.3333333333333333703, 0.3219752754296894559, 0.3333333333333333703, 0.3219752754296894559, 0.3333333333333333703, 0.3219752754296894559, 0.3333333333333333703, 0.3219752754296894559, 0.3333333333333333703, 0.3219752754296894559, 0.3333333333333333703, 0.3219752754296894559, 0.3333333333333333703, 0.3219752754296894559, 0.3333333333333333703, 0.3219752754296894559, 0.3333333333333333703, 0.3219752754296894559, 0.3333333333333333703, 0.3219752754296894559, 0.3333333333333333703, 0.3219752754296894559, 0.3333333333333333703, 0.3219752754296894559, 0.3333333333333333703, 0.3219752754296894559, 0.3333333333333333703, 0.3219752754296894559, 0.3333333333333333703, 0.3219752754296894559, 0.3333333333333333703, 0.3219752754296894559, 0.3333333333333333703, 0.3219752754296894559, 0.3333333333333333703, 0.3219752754296894559, 0.3333333333333333703, 0.3219752754296894559, 0.3333333333333333703, 0.3219752754296894559, 0.3333333333333333703, 0.3219752754296894559, 0.3333333333333333703, 0.3219752754296894559, 0.3333333333333333703, 0.3219752754296894559, 0.3333333333333333703, 0.3219752754296894559, 0.3333333333333333703, 0.3219752754296894559, 0.3333333333333333703, 0.3219752754296894559, 0.3333333333333333703, 0.3219752754296894559, 0.3333333333333333703, 0.3219752754296894559, 0.3333333333333333703, 0.3219752754296894559, 0.3333333333333333703, 0.3219752754296894559, 0.3333333333333333703, 0.3219752754296894559, 0.3333333333333333703, 0.3219752754296894559, 0.3333333333333333703, 0.3219752754296894559, 0.3333333333333333703, 0.3219752754296894559, 0.3333333333333333703, 0.3219752754296894559, 0.3333333333333333703, 0.3219752754296894559, 0.3333333333333333703, 0.3219752754296894559, 0.3333333333333333703, 0.3219752754296894559, 0.3333333333333333703, 0.3219752754296894559, 0.3333333333333333703, 0.3219752754296894559, 0.3333333333333333703, 0.3219752754296894559, 0.3333333333333333703, 0.3219752754296894559, 0.3333333333333333703, 0.3219752754296894559, 0.3333333333333333703, 0.3219752754296894559, 0.3333333333333333703, 0.3219752754296894559, 0.3333333333333333703, 0.3219752754296894559, 0.3333333333333333703, 0.3219752754296894559, 0.3333333333333333703, 0.3219752754296894559, 0.3333333333333333703, 0.3219752754296894559, 0.3333333333333333703, 0.3219752754296894559, 0.3333333333333333703, 0.3219752754296894559, 0.3333333333333333703, 0.3219752754296894559, 0.3333333333333333703, 0.3219752754296894559, 0.3333333333333333703, 0.3219752754296894559, 0.3333333333333333703, 0.3219752754296894559, 0.3333333333333333703, 0.3219752754296894559, 0.3333333333333333703, 0.3219752754296894559, 0.3333333333333333703, 0.3219752754296894559, 0.3333333333333333703, 0.3219752754296894559, 0.3333333333333333703, 0.3219752754296894559, 0.3333333333333333703, 0.3219752754296894559, 0.3333333333333333703, 0.3219752754296894559, 0.3333333333333333703, 0.3219752754296894559, 0.3333333333333333703, 0.3219752754296894559, 0.3333333333333333703, 0.3219752754296894559, 0.3333333333333333703, 0.3219752754296894559, 0.3333333333333333703, 0.3219752754296894559, 0.3333333333333333703, 0.3219752754296894559, 0.3333333333333333703, 0.3219752754296894559, 0.3333333333333333703, 0.3219752754296894559, 0.3333333333333333703, 0.3219752754296894559, 0.3333333333333333703, 0.3219752754296894559, 0.3333333333333333703, 0.3219752754296894559, 0.3333333333333333703, 0.3219752754296894559, 0.3333333333333333703, 0.3219752754296894559, 0.3333333333333333703, 0.3219752754296894559, 0.3333333333333333703, 0.3219752754296894559, 0.3333333333333333703, 0.3219752754296894559, 0.3333333333333333703, 0.3219752754296894559, 0.3333333333333333703, 0.3219752754296894559, 0.3333333333333333703, 0.3219752754296894559, 0.3333333333333333703, 0.3219752754296894559, 0.3333333333333333703, 0.3219752754296894559, 0.3333333333333333703, 0.3219752754296894559, 0.3333333333333333703, 0.3219752754296894559, 0.3333333333333333703, 0.3219752754296894559, 0.3333333333333333703, 0.3219752754296894559, 0.3333333333333333703, 0.3219752754296894559, 0.3333333333333333703, 0.3219752754296894559, 0.3333333333333333703, 0.3219752754296894559, 0.3333333333333333703, 0.3219752754296894559, 0.3333333333333333703, 0.3219752754296894559, 0.3333333333333333703, 0.3219752754296894559, 0.3333333333333333703, 0.3219752754296894559, 0.3333333333333333703, 0.3219752754296894559, 0.3333333333333333703, 0.3219752754296894559, 0.3333333333333333703, 0.3219752754296894559, 0.3333333333333333703, 0.3219752754296894559, 0.3333333333333333703, 0.3219752754296894559, 0.3333333333333333703, 0.3219752754296894559, 0.3333333333333333703, 0.3219752754296894559, 0.3333333333333333703, 0.3219752754296894559, 0.3333333333333333703, 0.3219752754296894559, 0.3333333333333333703, 0.3219752754296894559, 0.3333333333333333703, 0.3219752754296894559, 0.3333333333333333703, 0.3219752754296894559, 0.3333333333333333703, 0.3219752754296894559, 0.3333333333333333703, 0.3219752754296894559, 0.3333333333333333703, 0.3219752754296894559, 0.3333333333333333703, 0.3219752754296894559, 0.3333333333333333703, 0.3219752754296894559, 0.3333333333333333703, 0.3219752754296894559, 0.3333333333333333703, 0.3219752754296894559, 0.3333333333333333703, 0.3219752754296894559, 0.3333333333333333703, 0.3219752754296894559, 0.3333333333333333703, 0.3219752754296894559, 0.3333333333333333703, 0.3219752754296894559, 0.3333333333333333703, 0.3219752754296894559, 0.3333333333333333703, 0.3219752754296894559, 0.3333333333333333703, 0.3219752754296894559, 0.3333333333333333703, 0.3219752754296894559, 0.3333333333333333703, 0.3219752754296894559, 0.3333333333333333703, 0.3219752754296894559, 0.3333333333333333703, 0.3219752754296894559, 0.3333333333333333703, 0.3219752754296894559, 0.3333333333333333703, 0.3219752754296894559, 0.3333333333333333703, 0.3219752754296894559, 0.3333333333333333703, 0.3219752754296894559, 0.3333333333333333703, 0.3219752754296894559, 0.3333333333333333703, 0.3219752754296894559, 0.3333333333333333703, 0.3219752754296894559, 0.3333333333333333703, 0.3219752754296894559, 0.3333333333333333703),
 ( 0.3333333333333333703, 0.3219752754296894559, 0.3333333333333333703, 0.3219752754296894559, 0.3333333333333333703, 0.3219752754296894559, 0.3333333333333333703, 0.3219752754296894559, 0.3333333333333333703, 0.3219752754296894559, 0.3333333333333333703, 0.3219752754296894559, 0.3333333333333333703, 0.3219752754296894559, 0.3333333333333333703, 0.3219752754296894559, 0.3333333333333333703, 0.3219752754296894559, 0.3333333333333333703, 0.3219752754296894559, 0.3333333333333333703, 0.3219752754296894559, 0.3333333333333333703, 0.3219752754296894559, 0.3333333333333333703, 0.3219752754296894559, 0.3333333333333333703, 0.3219752754296894559, 0.3333333333333333703, 0.3219752754296894559, 0.3333333333333333703, 0.3219752754296894559, 0.3333333333333333703, 0.3219752754296894559, 0.3333333333333333703, 0.3219752754296894559, 0.3333333333333333703, 0.3219752754296894559, 0.3333333333333333703, 0.3219752754296894559, 0.3333333333333333703, 0.3219752754296894559, 0.3333333333333333703, 0.3219752754296894559, 0.3333333333333333703, 0.3219752754296894559, 0.3333333333333333703, 0.3219752754296894559, 0.3333333333333333703, 0.3219752754296894559, 0.3333333333333333703, 0.3219752754296894559, 0.3333333333333333703, 0.3219752754296894559, 0.3333333333333333703, 0.3219752754296894559, 0.3333333333333333703, 0.3219752754296894559, 0.3333333333333333703, 0.3219752754296894559, 0.3333333333333333703, 0.3219752754296894559, 0.3333333333333333703, 0.3219752754296894559, 0.3333333333333333703, 0.3219752754296894559, 0.3333333333333333703, 0.3219752754296894559, 0.3333333333333333703, 0.3219752754296894559, 0.3333333333333333703, 0.3219752754296894559, 0.3333333333333333703, 0.3219752754296894559, 0.3333333333333333703, 0.3219752754296894559, 0.3333333333333333703, 0.3219752754296894559, 0.3333333333333333703, 0.3219752754296894559, 0.3333333333333333703, 0.3219752754296894559, 0.3333333333333333703, 0.3219752754296894559, 0.3333333333333333703, 0.3219752754296894559, 0.3333333333333333703, 0.3219752754296894559, 0.3333333333333333703, 0.3219752754296894559, 0.3333333333333333703, 0.3219752754296894559, 0.3333333333333333703, 0.3219752754296894559, 0.3333333333333333703, 0.3219752754296894559, 0.3333333333333333703, 0.3219752754296894559, 0.3333333333333333703, 0.3219752754296894559, 0.3333333333333333703, 0.3219752754296894559, 0.3333333333333333703, 0.3219752754296894559, 0.3333333333333333703, 0.3219752754296894559, 0.3333333333333333703, 0.3219752754296894559, 0.3333333333333333703, 0.3219752754296894559, 0.3333333333333333703, 0.3219752754296894559, 0.3333333333333333703, 0.3219752754296894559, 0.3333333333333333703, 0.3219752754296894559, 0.3333333333333333703, 0.3219752754296894559, 0.3333333333333333703, 0.3219752754296894559, 0.3333333333333333703, 0.3219752754296894559, 0.3333333333333333703, 0.3219752754296894559, 0.3333333333333333703, 0.3219752754296894559, 0.3333333333333333703, 0.3219752754296894559, 0.3333333333333333703, 0.3219752754296894559, 0.3333333333333333703, 0.3219752754296894559, 0.3333333333333333703, 0.3219752754296894559, 0.3333333333333333703, 0.3219752754296894559, 0.3333333333333333703, 0.3219752754296894559, 0.3333333333333333703, 0.3219752754296894559, 0.3333333333333333703, 0.3219752754296894559, 0.3333333333333333703, 0.3219752754296894559, 0.3333333333333333703, 0.3219752754296894559, 0.3333333333333333703, 0.3219752754296894559, 0.3333333333333333703, 0.3219752754296894559, 0.3333333333333333703, 0.3219752754296894559, 0.3333333333333333703, 0.3219752754296894559, 0.3333333333333333703, 0.3219752754296894559, 0.3333333333333333703, 0.3219752754296894559, 0.3333333333333333703, 0.3219752754296894559, 0.3333333333333333703, 0.3219752754296894559, 0.3333333333333333703, 0.3219752754296894559, 0.3333333333333333703, 0.3219752754296894559, 0.3333333333333333703, 0.3219752754296894559, 0.3333333333333333703, 0.3219752754296894559, 0.3333333333333333703, 0.3219752754296894559, 0.3333333333333333703, 0.3219752754296894559, 0.3333333333333333703, 0.3219752754296894559, 0.3333333333333333703, 0.3219752754296894559, 0.3333333333333333703, 0.3219752754296894559, 0.3333333333333333703, 0.3219752754296894559, 0.3333333333333333703, 0.3219752754296894559, 0.3333333333333333703, 0.3219752754296894559, 0.3333333333333333703, 0.3219752754296894559, 0.3333333333333333703, 0.3219752754296894559, 0.3333333333333333703, 0.3219752754296894559, 0.3333333333333333703, 0.3219752754296894559, 0.3333333333333333703, 0.3219752754296894559, 0.3333333333333333703, 0.3219752754296894559, 0.3333333333333333703, 0.3219752754296894559, 0.3333333333333333703, 0.3219752754296894559, 0.3333333333333333703, 0.3219752754296894559, 0.3333333333333333703, 0.3219752754296894559, 0.3333333333333333703, 0.3219752754296894559, 0.3333333333333333703, 0.3219752754296894559, 0.3333333333333333703, 0.3219752754296894559, 0.3333333333333333703, 0.3219752754296894559, 0.3333333333333333703, 0.3219752754296894559, 0.3333333333333333703, 0.3219752754296894559, 0.3333333333333333703, 0.3219752754296894559, 0.3333333333333333703, 0.3219752754296894559, 0.3333333333333333703, 0.3219752754296894559, 0.3333333333333333703, 0.3219752754296894559, 0.3333333333333333703, 0.3219752754296894559, 0.3333333333333333703, 0.3219752754296894559, 0.3333333333333333703, 0.3219752754296894559, 0.3333333333333333703, 0.3219752754296894559, 0.3333333333333333703, 0.3219752754296894559, 0.3333333333333333703, 0.3219752754296894559, 0.3333333333333333703, 0.3219752754296894559, 0.3333333333333333703, 0.3219752754296894559, 0.3333333333333333703, 0.3219752754296894559, 0.3333333333333333703, 0.3219752754296894559, 0.3333333333333333703, 0.3219752754296894559, 0.3333333333333333703, 0.3219752754296894559, 0.3333333333333333703, 0.3219752754296894559, 0.3333333333333333703, 0.3219752754296894559, 0.3333333333333333703, 0.3219752754296894559, 0.3333333333333333703, 0.3219752754296894559, 0.3333333333333333703, 0.3219752754296894559, 0.3333333333333333703, 0.3219752754296894559, 0.3333333333333333703, 0.3219752754296894559, 0.3333333333333333703, 0.3219752754296894559, 0.3333333333333333703, 0.3219752754296894559, 0.3333333333333333703, 0.3219752754296894559, 0.3333333333333333703, 0.3219752754296894559, 0.3333333333333333703, 0.3219752754296894559, 0.3333333333333333703, 0.3219752754296894559, 0.3333333333333333703, 0.3219752754296894559, 0.3333333333333333703, 0.3219752754296894559, 0.3333333333333333703, 0.3219752754296894559, 0.3333333333333333703, 0.3219752754296894559, 0.3333333333333333703, 0.3219752754296894559, 0.3333333333333333703, 0.3219752754296894559, 0.3333333333333333703, 0.3219752754296894559, 0.3333333333333333703, 0.3219752754296894559, 0.3333333333333333703, 0.3219752754296894559, 0.3333333333333333703, 0.3219752754296894559, 0.3333333333333333703, 0.3219752754296894559, 0.3333333333333333703, 0.3219752754296894559, 0.3333333333333333703, 0.3219752754296894559, 0.3333333333333333703, 0.3219752754296894559, 0.3333333333333333703, 0.3219752754296894559, 0.3333333333333333703, 0.3219752754296894559, 0.3333333333333333703, 0.3219752754296894559, 0.3333333333333333703, 0.3219752754296894559, 0.3333333333333333703, 0.3219752754296894559, 0.3333333333333333703, 0.3219752754296894559, 0.3333333333333333703, 0.3219752754296894559, 0.3333333333333333703, 0.3219752754296894559, 0.3333333333333333703, 0.3219752754296894559, 0.3333333333333333703, 0.3219752754296894559, 0.3333333333333333703, 0.3219752754296894559, 0.3333333333333333703, 0.3219752754296894559, 0.3333333333333333703, 0.3219752754296894559, 0.3333333333333333703, 0.3219752754296894559, 0.3333333333333333703, 0.3219752754296894559, 0.3333333333333333703, 0.3219752754296894559, 0.3333333333333333703, 0.3219752754296894559, 0.3333333333333333703, 0.3219752754296894559, 0.3333333333333333703, 0.3219752754296894559, 0.3333333333333333703, 0.3219752754296894559, 0.3333333333333333703, 0.3219752754296894559, 0.3333333333333333703, 0.3219752754296894559, 0.3333333333333333703, 0.3219752754296894559, 0.3333333333333333703, 0.3219752754296894559, 0.3333333333333333703, 0.3219752754296894559, 0.3333333333333333703, 0.3219752754296894559, 0.3333333333333333703, 0.3219752754296894559, 0.3333333333333333703, 0.3219752754296894559, 0.3333333333333333703, 0.3219752754296894559, 0.3333333333333333703, 0.3219752754296894559, 0.3333333333333333703, 0.3219752754296894559, 0.3333333333333333703, 0.3219752754296894559, 0.3333333333333333703, 0.3219752754296894559, 0.3333333333333333703, 0.3219752754296894559, 0.3333333333333333703, 0.3219752754296894559, 0.3333333333333333703, 0.3219752754296894559, 0.3333333333333333703, 0.3219752754296894559, 0.3333333333333333703, 0.3219752754296894559, 0.3333333333333333703, 0.3219752754296894559, 0.3333333333333333703, 0.3219752754296894559, 0.3333333333333333703, 0.3219752754296894559, 0.3333333333333333703, 0.3219752754296894559, 0.3333333333333333703, 0.3219752754296894559, 0.3333333333333333703, 0.3219752754296894559, 0.3333333333333333703, 0.3219752754296894559, 0.3333333333333333703, 0.3219752754296894559, 0.3333333333333333703, 0.3219752754296894559, 0.3333333333333333703, 0.3219752754296894559, 0.3333333333333333703, 0.3219752754296894559, 0.3333333333333333703, 0.3219752754296894559, 0.3333333333333333703, 0.3219752754296894559, 0.3333333333333333703, 0.3219752754296894559, 0.3333333333333333703, 0.3219752754296894559, 0.3333333333333333703, 0.3219752754296894559, 0.3333333333333333703, 0.3219752754296894559, 0.3333333333333333703, 0.3219752754296894559, 0.3333333333333333703, 0.3219752754296894559, 0.3333333333333333703, 0.3219752754296894559, 0.3333333333333333703, 0.3219752754296894559, 0.3333333333333333703, 0.3219752754296894559, 0.3333333333333333703, 0.3219752754296894559, 0.3333333333333333703, 0.3219752754296894559, 0.3333333333333333703, 0.3219752754296894559, 0.3333333333333333703, 0.3219752754296894559, 0.3333333333333333703, 0.3219752754296894559, 0.3333333333333333703, 0.3219752754296894559, 0.3333333333333333703, 0.3219752754296894559, 0.3333333333333333703, 0.3219752754296894559, 0.3333333333333333703, 0.3219752754296894559, 0.3333333333333333703, 0.3219752754296894559, 0.3333333333333333703, 0.3219752754296894559, 0.3333333333333333703, 0.3219752754296894559, 0.3333333333333333703, 0.3219752754296894559, 0.3333333333333333703, 0.3219752754296894559, 0.3333333333333333703, 0.3219752754296894559, 0.3333333333333333703, 0.3219752754296894559, 0.3333333333333333703),
 ( 1.000000000000000000, 0.9659258262890683122, 1.000000000000000000, 0.9659258262890683122, 1.000000000000000000, 0.9659258262890683122, 1.000000000000000000, 0.9659258262890683122, 1.000000000000000000, 0.9659258262890683122, 1.000000000000000000, 0.9659258262890683122, 1.000000000000000000, 0.9659258262890683122, 1.000000000000000000, 0.9659258262890683122, 1.000000000000000000, 0.9659258262890683122, 1.000000000000000000, 0.9659258262890683122, 1.000000000000000000, 0.9659258262890683122, 1.000000000000000000, 0.9659258262890683122, 1.000000000000000000, 0.9659258262890683122, 1.000000000000000000, 0.9659258262890683122, 1.000000000000000000, 0.9659258262890683122, 1.000000000000000000, 0.9659258262890683122, 1.000000000000000000, 0.9659258262890683122, 1.000000000000000000, 0.9659258262890683122, 1.000000000000000000, 0.9659258262890683122, 1.000000000000000000, 0.9659258262890683122, 1.000000000000000000, 0.9659258262890683122, 1.000000000000000000, 0.9659258262890683122, 1.000000000000000000, 0.9659258262890683122, 1.000000000000000000, 0.9659258262890683122, 1.000000000000000000, 0.9659258262890683122, 1.000000000000000000, 0.9659258262890683122, 1.000000000000000000, 0.9659258262890683122, 1.000000000000000000, 0.9659258262890683122, 1.000000000000000000, 0.9659258262890683122, 1.000000000000000000, 0.9659258262890683122, 1.000000000000000000, 0.9659258262890683122, 1.000000000000000000, 0.9659258262890683122, 1.000000000000000000, 0.9659258262890683122, 1.000000000000000000, 0.9659258262890683122, 1.000000000000000000, 0.9659258262890683122, 1.000000000000000000, 0.9659258262890683122, 1.000000000000000000, 0.9659258262890683122, 1.000000000000000000, 0.9659258262890683122, 1.000000000000000000, 0.9659258262890683122, 1.000000000000000000, 0.9659258262890683122, 1.000000000000000000, 0.9659258262890683122, 1.000000000000000000, 0.9659258262890683122, 1.000000000000000000, 0.9659258262890683122, 1.000000000000000000, 0.9659258262890683122, 1.000000000000000000, 0.9659258262890683122, 1.000000000000000000, 0.9659258262890683122, 1.000000000000000000, 0.9659258262890683122, 1.000000000000000000, 0.9659258262890683122, 1.000000000000000000, 0.9659258262890683122, 1.000000000000000000, 0.9659258262890683122, 1.000000000000000000, 0.9659258262890683122, 1.000000000000000000, 0.9659258262890683122, 1.000000000000000000, 0.9659258262890683122, 1.000000000000000000, 0.9659258262890683122, 1.000000000000000000, 0.9659258262890683122, 1.000000000000000000, 0.9659258262890683122, 1.000000000000000000, 0.9659258262890683122, 1.000000000000000000, 0.9659258262890683122, 1.000000000000000000, 0.9659258262890683122, 1.000000000000000000, 0.9659258262890683122, 1.000000000000000000, 0.9659258262890683122, 1.000000000000000000, 0.9659258262890683122, 1.000000000000000000, 0.9659258262890683122, 1.000000000000000000, 0.9659258262890683122, 1.000000000000000000, 0.9659258262890683122, 1.000000000000000000, 0.9659258262890683122, 1.000000000000000000, 0.9659258262890683122, 1.000000000000000000, 0.9659258262890683122, 1.000000000000000000, 0.9659258262890683122, 1.000000000000000000, 0.9659258262890683122, 1.000000000000000000, 0.9659258262890683122, 1.000000000000000000, 0.9659258262890683122, 1.000000000000000000, 0.9659258262890683122, 1.000000000000000000, 0.9659258262890683122, 1.000000000000000000, 0.9659258262890683122, 1.000000000000000000, 0.9659258262890683122, 1.000000000000000000, 0.9659258262890683122, 1.000000000000000000, 0.9659258262890683122, 1.000000000000000000, 0.9659258262890683122, 1.000000000000000000, 0.9659258262890683122, 1.000000000000000000, 0.9659258262890683122, 1.000000000000000000, 0.9659258262890683122, 1.000000000000000000, 0.9659258262890683122, 1.000000000000000000, 0.9659258262890683122, 1.000000000000000000, 0.9659258262890683122, 1.000000000000000000, 0.9659258262890683122, 1.000000000000000000, 0.9659258262890683122, 1.000000000000000000, 0.9659258262890683122, 1.000000000000000000, 0.9659258262890683122, 1.000000000000000000, 0.9659258262890683122, 1.000000000000000000, 0.9659258262890683122, 1.000000000000000000, 0.9659258262890683122, 1.000000000000000000, 0.9659258262890683122, 1.000000000000000000, 0.9659258262890683122, 1.000000000000000000, 0.9659258262890683122, 1.000000000000000000, 0.9659258262890683122, 1.000000000000000000, 0.9659258262890683122, 1.000000000000000000, 0.9659258262890683122, 1.000000000000000000, 0.9659258262890683122, 1.000000000000000000, 0.9659258262890683122, 1.000000000000000000, 0.9659258262890683122, 1.000000000000000000, 0.9659258262890683122, 1.000000000000000000, 0.9659258262890683122, 1.000000000000000000, 0.9659258262890683122, 1.000000000000000000, 0.9659258262890683122, 1.000000000000000000, 0.9659258262890683122, 1.000000000000000000, 0.9659258262890683122, 1.000000000000000000, 0.9659258262890683122, 1.000000000000000000, 0.9659258262890683122, 1.000000000000000000, 0.9659258262890683122, 1.000000000000000000, 0.9659258262890683122, 1.000000000000000000, 0.9659258262890683122, 1.000000000000000000, 0.9659258262890683122, 1.000000000000000000, 0.9659258262890683122, 1.000000000000000000, 0.9659258262890683122, 1.000000000000000000, 0.9659258262890683122, 1.000000000000000000, 0.9659258262890683122, 1.000000000000000000, 0.9659258262890683122, 1.000000000000000000, 0.9659258262890683122, 1.000000000000000000, 0.9659258262890683122, 1.000000000000000000, 0.9659258262890683122, 1.000000000000000000, 0.9659258262890683122, 1.000000000000000000, 0.9659258262890683122, 1.000000000000000000, 0.9659258262890683122, 1.000000000000000000, 0.9659258262890683122, 1.000000000000000000, 0.9659258262890683122, 1.000000000000000000, 0.9659258262890683122, 1.000000000000000000, 0.9659258262890683122, 1.000000000000000000, 0.9659258262890683122, 1.000000000000000000, 0.9659258262890683122, 1.000000000000000000, 0.9659258262890683122, 1.000000000000000000, 0.9659258262890683122, 1.000000000000000000, 0.9659258262890683122, 1.000000000000000000, 0.9659258262890683122, 1.000000000000000000, 0.9659258262890683122, 1.000000000000000000, 0.9659258262890683122, 1.000000000000000000, 0.9659258262890683122, 1.000000000000000000, 0.9659258262890683122, 1.000000000000000000, 0.9659258262890683122, 1.000000000000000000, 0.9659258262890683122, 1.000000000000000000, 0.9659258262890683122, 1.000000000000000000, 0.9659258262890683122, 1.000000000000000000, 0.9659258262890683122, 1.000000000000000000, 0.9659258262890683122, 1.000000000000000000, 0.9659258262890683122, 1.000000000000000000, 0.9659258262890683122, 1.000000000000000000, 0.9659258262890683122, 1.000000000000000000, 0.9659258262890683122, 1.000000000000000000, 0.9659258262890683122, 1.000000000000000000, 0.9659258262890683122, 1.000000000000000000, 0.9659258262890683122, 1.000000000000000000, 0.9659258262890683122, 1.000000000000000000, 0.9659258262890683122, 1.000000000000000000, 0.9659258262890683122, 1.000000000000000000, 0.9659258262890683122, 1.000000000000000000, 0.9659258262890683122, 1.000000000000000000, 0.9659258262890683122, 1.000000000000000000, 0.9659258262890683122, 1.000000000000000000, 0.9659258262890683122, 1.000000000000000000, 0.9659258262890683122, 1.000000000000000000, 0.9659258262890683122, 1.000000000000000000, 0.9659258262890683122, 1.000000000000000000, 0.9659258262890683122, 1.000000000000000000, 0.9659258262890683122, 1.000000000000000000, 0.9659258262890683122, 1.000000000000000000, 0.9659258262890683122, 1.000000000000000000, 0.9659258262890683122, 1.000000000000000000, 0.9659258262890683122, 1.000000000000000000, 0.9659258262890683122, 1.000000000000000000, 0.9659258262890683122, 1.000000000000000000, 0.9659258262890683122, 1.000000000000000000, 0.9659258262890683122, 1.000000000000000000, 0.9659258262890683122, 1.000000000000000000, 0.9659258262890683122, 1.000000000000000000, 0.9659258262890683122, 1.000000000000000000, 0.9659258262890683122, 1.000000000000000000, 0.9659258262890683122, 1.000000000000000000, 0.9659258262890683122, 1.000000000000000000, 0.9659258262890683122, 1.000000000000000000, 0.9659258262890683122, 1.000000000000000000, 0.9659258262890683122, 1.000000000000000000, 0.9659258262890683122, 1.000000000000000000, 0.9659258262890683122, 1.000000000000000000, 0.9659258262890683122, 1.000000000000000000, 0.9659258262890683122, 1.000000000000000000, 0.9659258262890683122, 1.000000000000000000, 0.9659258262890683122, 1.000000000000000000, 0.9659258262890683122, 1.000000000000000000, 0.9659258262890683122, 1.000000000000000000, 0.9659258262890683122, 1.000000000000000000, 0.9659258262890683122, 1.000000000000000000, 0.9659258262890683122, 1.000000000000000000, 0.9659258262890683122, 1.000000000000000000, 0.9659258262890683122, 1.000000000000000000, 0.9659258262890683122, 1.000000000000000000, 0.9659258262890683122, 1.000000000000000000, 0.9659258262890683122, 1.000000000000000000, 0.9659258262890683122, 1.000000000000000000, 0.9659258262890683122, 1.000000000000000000, 0.9659258262890683122, 1.000000000000000000, 0.9659258262890683122, 1.000000000000000000, 0.9659258262890683122, 1.000000000000000000, 0.9659258262890683122, 1.000000000000000000, 0.9659258262890683122, 1.000000000000000000, 0.9659258262890683122, 1.000000000000000000, 0.9659258262890683122, 1.000000000000000000, 0.9659258262890683122, 1.000000000000000000, 0.9659258262890683122, 1.000000000000000000, 0.9659258262890683122, 1.000000000000000000, 0.9659258262890683122, 1.000000000000000000, 0.9659258262890683122, 1.000000000000000000, 0.9659258262890683122, 1.000000000000000000, 0.9659258262890683122, 1.000000000000000000, 0.9659258262890683122, 1.000000000000000000, 0.9659258262890683122, 1.000000000000000000, 0.9659258262890683122, 1.000000000000000000, 0.9659258262890683122, 1.000000000000000000, 0.9659258262890683122, 1.000000000000000000, 0.9659258262890683122, 1.000000000000000000, 0.9659258262890683122, 1.000000000000000000, 0.9659258262890683122, 1.000000000000000000, 0.9659258262890683122, 1.000000000000000000, 0.9659258262890683122, 1.000000000000000000, 0.9659258262890683122, 1.000000000000000000, 0.9659258262890683122, 1.000000000000000000, 0.9659258262890683122, 1.000000000000000000, 0.9659258262890683122, 1.000000000000000000, 0.9659258262890683122, 1.000000000000000000),
 ( 0.3333333333333333703, 0.3219752754296894559, 0.3333333333333333703, 0.3219752754296894559, 0.3333333333333333703, 0.3219752754296894559, 0.3333333333333333703, 0.3219752754296894559, 0.3333333333333333703, 0.3219752754296894559, 0.3333333333333333703, 0.3219752754296894559, 0.3333333333333333703, 0.3219752754296894559, 0.3333333333333333703, 0.3219752754296894559, 0.3333333333333333703, 0.3219752754296894559, 0.3333333333333333703, 0.3219752754296894559, 0.3333333333333333703, 0.3219752754296894559, 0.3333333333333333703, 0.3219752754296894559, 0.3333333333333333703, 0.3219752754296894559, 0.3333333333333333703, 0.3219752754296894559, 0.3333333333333333703, 0.3219752754296894559, 0.3333333333333333703, 0.3219752754296894559, 0.3333333333333333703, 0.3219752754296894559, 0.3333333333333333703, 0.3219752754296894559, 0.3333333333333333703, 0.3219752754296894559, 0.3333333333333333703, 0.3219752754296894559, 0.3333333333333333703, 0.3219752754296894559, 0.3333333333333333703, 0.3219752754296894559, 0.3333333333333333703, 0.3219752754296894559, 0.3333333333333333703, 0.3219752754296894559, 0.3333333333333333703, 0.3219752754296894559, 0.3333333333333333703, 0.3219752754296894559, 0.3333333333333333703, 0.3219752754296894559, 0.3333333333333333703, 0.3219752754296894559, 0.3333333333333333703, 0.3219752754296894559, 0.3333333333333333703, 0.3219752754296894559, 0.3333333333333333703, 0.3219752754296894559, 0.3333333333333333703, 0.3219752754296894559, 0.3333333333333333703, 0.3219752754296894559, 0.3333333333333333703, 0.3219752754296894559, 0.3333333333333333703, 0.3219752754296894559, 0.3333333333333333703, 0.3219752754296894559, 0.3333333333333333703, 0.3219752754296894559, 0.3333333333333333703, 0.3219752754296894559, 0.3333333333333333703, 0.3219752754296894559, 0.3333333333333333703, 0.3219752754296894559, 0.3333333333333333703, 0.3219752754296894559, 0.3333333333333333703, 0.3219752754296894559, 0.3333333333333333703, 0.3219752754296894559, 0.3333333333333333703, 0.3219752754296894559, 0.3333333333333333703, 0.3219752754296894559, 0.3333333333333333703, 0.3219752754296894559, 0.3333333333333333703, 0.3219752754296894559, 0.3333333333333333703, 0.3219752754296894559, 0.3333333333333333703, 0.3219752754296894559, 0.3333333333333333703, 0.3219752754296894559, 0.3333333333333333703, 0.3219752754296894559, 0.3333333333333333703, 0.3219752754296894559, 0.3333333333333333703, 0.3219752754296894559, 0.3333333333333333703, 0.3219752754296894559, 0.3333333333333333703, 0.3219752754296894559, 0.3333333333333333703, 0.3219752754296894559, 0.3333333333333333703, 0.3219752754296894559, 0.3333333333333333703, 0.3219752754296894559, 0.3333333333333333703, 0.3219752754296894559, 0.3333333333333333703, 0.3219752754296894559, 0.3333333333333333703, 0.3219752754296894559, 0.3333333333333333703, 0.3219752754296894559, 0.3333333333333333703, 0.3219752754296894559, 0.3333333333333333703, 0.3219752754296894559, 0.3333333333333333703, 0.3219752754296894559, 0.3333333333333333703, 0.3219752754296894559, 0.3333333333333333703, 0.3219752754296894559, 0.3333333333333333703, 0.3219752754296894559, 0.3333333333333333703, 0.3219752754296894559, 0.3333333333333333703, 0.3219752754296894559, 0.3333333333333333703, 0.3219752754296894559, 0.3333333333333333703, 0.3219752754296894559, 0.3333333333333333703, 0.3219752754296894559, 0.3333333333333333703, 0.3219752754296894559, 0.3333333333333333703, 0.3219752754296894559, 0.3333333333333333703, 0.3219752754296894559, 0.3333333333333333703, 0.3219752754296894559, 0.3333333333333333703, 0.3219752754296894559, 0.3333333333333333703, 0.3219752754296894559, 0.3333333333333333703, 0.3219752754296894559, 0.3333333333333333703, 0.3219752754296894559, 0.3333333333333333703, 0.3219752754296894559, 0.3333333333333333703, 0.3219752754296894559, 0.3333333333333333703, 0.3219752754296894559, 0.3333333333333333703, 0.3219752754296894559, 0.3333333333333333703, 0.3219752754296894559, 0.3333333333333333703, 0.3219752754296894559, 0.3333333333333333703, 0.3219752754296894559, 0.3333333333333333703, 0.3219752754296894559, 0.3333333333333333703, 0.3219752754296894559, 0.3333333333333333703, 0.3219752754296894559, 0.3333333333333333703, 0.3219752754296894559, 0.3333333333333333703, 0.3219752754296894559, 0.3333333333333333703, 0.3219752754296894559, 0.3333333333333333703, 0.3219752754296894559, 0.3333333333333333703, 0.3219752754296894559, 0.3333333333333333703, 0.3219752754296894559, 0.3333333333333333703, 0.3219752754296894559, 0.3333333333333333703, 0.3219752754296894559, 0.3333333333333333703, 0.3219752754296894559, 0.3333333333333333703, 0.3219752754296894559, 0.3333333333333333703, 0.3219752754296894559, 0.3333333333333333703, 0.3219752754296894559, 0.3333333333333333703, 0.3219752754296894559, 0.3333333333333333703, 0.3219752754296894559, 0.3333333333333333703, 0.3219752754296894559, 0.3333333333333333703, 0.3219752754296894559, 0.3333333333333333703, 0.3219752754296894559, 0.3333333333333333703, 0.3219752754296894559, 0.3333333333333333703, 0.3219752754296894559, 0.3333333333333333703, 0.3219752754296894559, 0.3333333333333333703, 0.3219752754296894559, 0.3333333333333333703, 0.3219752754296894559, 0.3333333333333333703, 0.3219752754296894559, 0.3333333333333333703, 0.3219752754296894559, 0.3333333333333333703, 0.3219752754296894559, 0.3333333333333333703, 0.3219752754296894559, 0.3333333333333333703, 0.3219752754296894559, 0.3333333333333333703, 0.3219752754296894559, 0.3333333333333333703, 0.3219752754296894559, 0.3333333333333333703, 0.3219752754296894559, 0.3333333333333333703, 0.3219752754296894559, 0.3333333333333333703, 0.3219752754296894559, 0.3333333333333333703, 0.3219752754296894559, 0.3333333333333333703, 0.3219752754296894559, 0.3333333333333333703, 0.3219752754296894559, 0.3333333333333333703, 0.3219752754296894559, 0.3333333333333333703, 0.3219752754296894559, 0.3333333333333333703, 0.3219752754296894559, 0.3333333333333333703, 0.3219752754296894559, 0.3333333333333333703, 0.3219752754296894559, 0.3333333333333333703, 0.3219752754296894559, 0.3333333333333333703, 0.3219752754296894559, 0.3333333333333333703, 0.3219752754296894559, 0.3333333333333333703, 0.3219752754296894559, 0.3333333333333333703, 0.3219752754296894559, 0.3333333333333333703, 0.3219752754296894559, 0.3333333333333333703, 0.3219752754296894559, 0.3333333333333333703, 0.3219752754296894559, 0.3333333333333333703, 0.3219752754296894559, 0.3333333333333333703, 0.3219752754296894559, 0.3333333333333333703, 0.3219752754296894559, 0.3333333333333333703, 0.3219752754296894559, 0.3333333333333333703, 0.3219752754296894559, 0.3333333333333333703, 0.3219752754296894559, 0.3333333333333333703, 0.3219752754296894559, 0.3333333333333333703, 0.3219752754296894559, 0.3333333333333333703, 0.3219752754296894559, 0.3333333333333333703, 0.3219752754296894559, 0.3333333333333333703, 0.3219752754296894559, 0.3333333333333333703, 0.3219752754296894559, 0.3333333333333333703, 0.3219752754296894559, 0.3333333333333333703, 0.3219752754296894559, 0.3333333333333333703, 0.3219752754296894559, 0.3333333333333333703, 0.3219752754296894559, 0.3333333333333333703, 0.3219752754296894559, 0.3333333333333333703, 0.3219752754296894559, 0.3333333333333333703, 0.3219752754296894559, 0.3333333333333333703, 0.3219752754296894559, 0.3333333333333333703, 0.3219752754296894559, 0.3333333333333333703, 0.3219752754296894559, 0.3333333333333333703, 0.3219752754296894559, 0.3333333333333333703, 0.3219752754296894559, 0.3333333333333333703, 0.3219752754296894559, 0.3333333333333333703, 0.3219752754296894559, 0.3333333333333333703, 0.3219752754296894559, 0.3333333333333333703, 0.3219752754296894559, 0.3333333333333333703, 0.3219752754296894559, 0.3333333333333333703, 0.3219752754296894559, 0.3333333333333333703, 0.3219752754296894559, 0.3333333333333333703, 0.3219752754296894559, 0.3333333333333333703, 0.3219752754296894559, 0.3333333333333333703, 0.3219752754296894559, 0.3333333333333333703, 0.3219752754296894559, 0.3333333333333333703, 0.3219752754296894559, 0.3333333333333333703, 0.3219752754296894559, 0.3333333333333333703, 0.3219752754296894559, 0.3333333333333333703, 0.3219752754296894559, 0.3333333333333333703, 0.3219752754296894559, 0.3333333333333333703, 0.3219752754296894559, 0.3333333333333333703, 0.3219752754296894559, 0.3333333333333333703, 0.3219752754296894559, 0.3333333333333333703, 0.3219752754296894559, 0.3333333333333333703, 0.3219752754296894559, 0.3333333333333333703, 0.3219752754296894559, 0.3333333333333333703, 0.3219752754296894559, 0.3333333333333333703, 0.3219752754296894559, 0.3333333333333333703, 0.3219752754296894559, 0.3333333333333333703, 0.3219752754296894559, 0.3333333333333333703, 0.3219752754296894559, 0.3333333333333333703, 0.3219752754296894559, 0.3333333333333333703, 0.3219752754296894559, 0.3333333333333333703, 0.3219752754296894559, 0.3333333333333333703, 0.3219752754296894559, 0.3333333333333333703, 0.3219752754296894559, 0.3333333333333333703, 0.3219752754296894559, 0.3333333333333333703, 0.3219752754296894559, 0.3333333333333333703, 0.3219752754296894559, 0.3333333333333333703, 0.3219752754296894559, 0.3333333333333333703, 0.3219752754296894559, 0.3333333333333333703, 0.3219752754296894559, 0.3333333333333333703, 0.3219752754296894559, 0.3333333333333333703, 0.3219752754296894559, 0.3333333333333333703, 0.3219752754296894559, 0.3333333333333333703, 0.3219752754296894559, 0.3333333333333333703, 0.3219752754296894559, 0.3333333333333333703, 0.3219752754296894559, 0.3333333333333333703, 0.3219752754296894559, 0.3333333333333333703, 0.3219752754296894559, 0.3333333333333333703, 0.3219752754296894559, 0.3333333333333333703, 0.3219752754296894559, 0.3333333333333333703, 0.3219752754296894559, 0.3333333333333333703, 0.3219752754296894559, 0.3333333333333333703, 0.3219752754296894559, 0.3333333333333333703, 0.3219752754296894559, 0.3333333333333333703, 0.3219752754296894559, 0.3333333333333333703, 0.3219752754296894559, 0.3333333333333333703, 0.3219752754296894559, 0.3333333333333333703, 0.3219752754296894559, 0.3333333333333333703, 0.3219752754296894559, 0.3333333333333333703, 0.3219752754296894559, 0.3333333333333333703, 0.3219752754296894559, 0.3333333333333333703, 0.3219752754296894559, 0.3333333333333333703, 0.3219752754296894559, 0.3333333333333333703, 0.3219752754296894559, 0.3333333333333333703, 0.3219752754296894559, 0.3333333333333333703, 0.3219752754296894559, 0.3333333333333333703, 0.3219752754296894559, 0.3333333333333333703),
 ( 0.3333333333333333703, 0.3219752754296894559, 0.3333333333333333703, 0.3219752754296894559, 0.3333333333333333703, 0.3219752754296894559, 0.3333333333333333703, 0.3219752754296894559, 0.3333333333333333703, 0.3219752754296894559, 0.3333333333333333703, 0.3219752754296894559, 0.3333333333333333703, 0.3219752754296894559, 0.3333333333333333703, 0.3219752754296894559, 0.3333333333333333703, 0.3219752754296894559, 0.3333333333333333703, 0.3219752754296894559, 0.3333333333333333703, 0.3219752754296894559, 0.3333333333333333703, 0.3219752754296894559, 0.3333333333333333703, 0.3219752754296894559, 0.3333333333333333703, 0.3219752754296894559, 0.3333333333333333703, 0.3219752754296894559, 0.3333333333333333703, 0.3219752754296894559, 0.3333333333333333703, 0.3219752754296894559, 0.3333333333333333703, 0.3219752754296894559, 0.3333333333333333703, 0.3219752754296894559, 0.3333333333333333703, 0.3219752754296894559, 0.3333333333333333703, 0.3219752754296894559, 0.3333333333333333703, 0.3219752754296894559, 0.3333333333333333703, 0.3219752754296894559, 0.3333333333333333703, 0.3219752754296894559, 0.3333333333333333703, 0.3219752754296894559, 0.3333333333333333703, 0.3219752754296894559, 0.3333333333333333703, 0.3219752754296894559, 0.3333333333333333703, 0.3219752754296894559, 0.3333333333333333703, 0.3219752754296894559, 0.3333333333333333703, 0.3219752754296894559, 0.3333333333333333703, 0.3219752754296894559, 0.3333333333333333703, 0.3219752754296894559, 0.3333333333333333703, 0.3219752754296894559, 0.3333333333333333703, 0.3219752754296894559, 0.3333333333333333703, 0.3219752754296894559, 0.3333333333333333703, 0.3219752754296894559, 0.3333333333333333703, 0.3219752754296894559, 0.3333333333333333703, 0.3219752754296894559, 0.3333333333333333703, 0.3219752754296894559, 0.3333333333333333703, 0.3219752754296894559, 0.3333333333333333703, 0.3219752754296894559, 0.3333333333333333703, 0.3219752754296894559, 0.3333333333333333703, 0.3219752754296894559, 0.3333333333333333703, 0.3219752754296894559, 0.3333333333333333703, 0.3219752754296894559, 0.3333333333333333703, 0.3219752754296894559, 0.3333333333333333703, 0.3219752754296894559, 0.3333333333333333703, 0.3219752754296894559, 0.3333333333333333703, 0.3219752754296894559, 0.3333333333333333703, 0.3219752754296894559, 0.3333333333333333703, 0.3219752754296894559, 0.3333333333333333703, 0.3219752754296894559, 0.3333333333333333703, 0.3219752754296894559, 0.3333333333333333703, 0.3219752754296894559, 0.3333333333333333703, 0.3219752754296894559, 0.3333333333333333703, 0.3219752754296894559, 0.3333333333333333703, 0.3219752754296894559, 0.3333333333333333703, 0.3219752754296894559, 0.3333333333333333703, 0.3219752754296894559, 0.3333333333333333703, 0.3219752754296894559, 0.3333333333333333703, 0.3219752754296894559, 0.3333333333333333703, 0.3219752754296894559, 0.3333333333333333703, 0.3219752754296894559, 0.3333333333333333703, 0.3219752754296894559, 0.3333333333333333703, 0.3219752754296894559, 0.3333333333333333703, 0.3219752754296894559, 0.3333333333333333703, 0.3219752754296894559, 0.3333333333333333703, 0.3219752754296894559, 0.3333333333333333703, 0.3219752754296894559, 0.3333333333333333703, 0.3219752754296894559, 0.3333333333333333703, 0.3219752754296894559, 0.3333333333333333703, 0.3219752754296894559, 0.3333333333333333703, 0.3219752754296894559, 0.3333333333333333703, 0.3219752754296894559, 0.3333333333333333703, 0.3219752754296894559, 0.3333333333333333703, 0.3219752754296894559, 0.3333333333333333703, 0.3219752754296894559, 0.3333333333333333703, 0.3219752754296894559, 0.3333333333333333703, 0.3219752754296894559, 0.3333333333333333703, 0.3219752754296894559, 0.3333333333333333703, 0.3219752754296894559, 0.3333333333333333703, 0.3219752754296894559, 0.3333333333333333703, 0.3219752754296894559, 0.3333333333333333703, 0.3219752754296894559, 0.3333333333333333703, 0.3219752754296894559, 0.3333333333333333703, 0.3219752754296894559, 0.3333333333333333703, 0.3219752754296894559, 0.3333333333333333703, 0.3219752754296894559, 0.3333333333333333703, 0.3219752754296894559, 0.3333333333333333703, 0.3219752754296894559, 0.3333333333333333703, 0.3219752754296894559, 0.3333333333333333703, 0.3219752754296894559, 0.3333333333333333703, 0.3219752754296894559, 0.3333333333333333703, 0.3219752754296894559, 0.3333333333333333703, 0.3219752754296894559, 0.3333333333333333703, 0.3219752754296894559, 0.3333333333333333703, 0.3219752754296894559, 0.3333333333333333703, 0.3219752754296894559, 0.3333333333333333703, 0.3219752754296894559, 0.3333333333333333703, 0.3219752754296894559, 0.3333333333333333703, 0.3219752754296894559, 0.3333333333333333703, 0.3219752754296894559, 0.3333333333333333703, 0.3219752754296894559, 0.3333333333333333703, 0.3219752754296894559, 0.3333333333333333703, 0.3219752754296894559, 0.3333333333333333703, 0.3219752754296894559, 0.3333333333333333703, 0.3219752754296894559, 0.3333333333333333703, 0.3219752754296894559, 0.3333333333333333703, 0.3219752754296894559, 0.3333333333333333703, 0.3219752754296894559, 0.3333333333333333703, 0.3219752754296894559, 0.3333333333333333703, 0.3219752754296894559, 0.3333333333333333703, 0.3219752754296894559, 0.3333333333333333703, 0.3219752754296894559, 0.3333333333333333703, 0.3219752754296894559, 0.3333333333333333703, 0.3219752754296894559, 0.3333333333333333703, 0.3219752754296894559, 0.3333333333333333703, 0.3219752754296894559, 0.3333333333333333703, 0.3219752754296894559, 0.3333333333333333703, 0.3219752754296894559, 0.3333333333333333703, 0.3219752754296894559, 0.3333333333333333703, 0.3219752754296894559, 0.3333333333333333703, 0.3219752754296894559, 0.3333333333333333703, 0.3219752754296894559, 0.3333333333333333703, 0.3219752754296894559, 0.3333333333333333703, 0.3219752754296894559, 0.3333333333333333703, 0.3219752754296894559, 0.3333333333333333703, 0.3219752754296894559, 0.3333333333333333703, 0.3219752754296894559, 0.3333333333333333703, 0.3219752754296894559, 0.3333333333333333703, 0.3219752754296894559, 0.3333333333333333703, 0.3219752754296894559, 0.3333333333333333703, 0.3219752754296894559, 0.3333333333333333703, 0.3219752754296894559, 0.3333333333333333703, 0.3219752754296894559, 0.3333333333333333703, 0.3219752754296894559, 0.3333333333333333703, 0.3219752754296894559, 0.3333333333333333703, 0.3219752754296894559, 0.3333333333333333703, 0.3219752754296894559, 0.3333333333333333703, 0.3219752754296894559, 0.3333333333333333703, 0.3219752754296894559, 0.3333333333333333703, 0.3219752754296894559, 0.3333333333333333703, 0.3219752754296894559, 0.3333333333333333703, 0.3219752754296894559, 0.3333333333333333703, 0.3219752754296894559, 0.3333333333333333703, 0.3219752754296894559, 0.3333333333333333703, 0.3219752754296894559, 0.3333333333333333703, 0.3219752754296894559, 0.3333333333333333703, 0.3219752754296894559, 0.3333333333333333703, 0.3219752754296894559, 0.3333333333333333703, 0.3219752754296894559, 0.3333333333333333703, 0.3219752754296894559, 0.3333333333333333703, 0.3219752754296894559, 0.3333333333333333703, 0.3219752754296894559, 0.3333333333333333703, 0.3219752754296894559, 0.3333333333333333703, 0.3219752754296894559, 0.3333333333333333703, 0.3219752754296894559, 0.3333333333333333703, 0.3219752754296894559, 0.3333333333333333703, 0.3219752754296894559, 0.3333333333333333703, 0.3219752754296894559, 0.3333333333333333703, 0.3219752754296894559, 0.3333333333333333703, 0.3219752754296894559, 0.3333333333333333703, 0.3219752754296894559, 0.3333333333333333703, 0.3219752754296894559, 0.3333333333333333703, 0.3219752754296894559, 0.3333333333333333703, 0.3219752754296894559, 0.3333333333333333703, 0.3219752754296894559, 0.3333333333333333703, 0.3219752754296894559, 0.3333333333333333703, 0.3219752754296894559, 0.3333333333333333703, 0.3219752754296894559, 0.3333333333333333703, 0.3219752754296894559, 0.3333333333333333703, 0.3219752754296894559, 0.3333333333333333703, 0.3219752754296894559, 0.3333333333333333703, 0.3219752754296894559, 0.3333333333333333703, 0.3219752754296894559, 0.3333333333333333703, 0.3219752754296894559, 0.3333333333333333703, 0.3219752754296894559, 0.3333333333333333703, 0.3219752754296894559, 0.3333333333333333703, 0.3219752754296894559, 0.3333333333333333703, 0.3219752754296894559, 0.3333333333333333703, 0.3219752754296894559, 0.3333333333333333703, 0.3219752754296894559, 0.3333333333333333703, 0.3219752754296894559, 0.3333333333333333703, 0.3219752754296894559, 0.3333333333333333703, 0.3219752754296894559, 0.3333333333333333703, 0.3219752754296894559, 0.3333333333333333703, 0.3219752754296894559, 0.3333333333333333703, 0.3219752754296894559, 0.3333333333333333703, 0.3219752754296894559, 0.3333333333333333703, 0.3219752754296894559, 0.3333333333333333703, 0.3219752754296894559, 0.3333333333333333703, 0.3219752754296894559, 0.3333333333333333703, 0.3219752754296894559, 0.3333333333333333703, 0.3219752754296894559, 0.3333333333333333703, 0.3219752754296894559, 0.3333333333333333703, 0.3219752754296894559, 0.3333333333333333703, 0.3219752754296894559, 0.3333333333333333703, 0.3219752754296894559, 0.3333333333333333703, 0.3219752754296894559, 0.3333333333333333703, 0.3219752754296894559, 0.3333333333333333703, 0.3219752754296894559, 0.3333333333333333703, 0.3219752754296894559, 0.3333333333333333703, 0.3219752754296894559, 0.3333333333333333703, 0.3219752754296894559, 0.3333333333333333703, 0.3219752754296894559, 0.3333333333333333703, 0.3219752754296894559, 0.3333333333333333703, 0.3219752754296894559, 0.3333333333333333703, 0.3219752754296894559, 0.3333333333333333703, 0.3219752754296894559, 0.3333333333333333703, 0.3219752754296894559, 0.3333333333333333703, 0.3219752754296894559, 0.3333333333333333703, 0.3219752754296894559, 0.3333333333333333703, 0.3219752754296894559, 0.3333333333333333703, 0.3219752754296894559, 0.3333333333333333703, 0.3219752754296894559, 0.3333333333333333703, 0.3219752754296894559, 0.3333333333333333703, 0.3219752754296894559, 0.3333333333333333703, 0.3219752754296894559, 0.3333333333333333703, 0.3219752754296894559, 0.3333333333333333703, 0.3219752754296894559, 0.3333333333333333703, 0.3219752754296894559, 0.3333333333333333703, 0.3219752754296894559, 0.3333333333333333703, 0.3219752754296894559, 0.3333333333333333703, 0.3219752754296894559, 0.3333333333333333703, 0.3219752754296894559, 0.3333333333333333703, 0.3219752754296894559, 0.3333333333333333703, 0.3219752754296894559, 0.3333333333333333703, 0.3219752754296894559, 0.3333333333333333703),
 ( 1.000000000000000000, 0.9659258262890683122, 1.000000000000000000, 0.9659258262890683122, 1.000000000000000000, 0.9659258262890683122, 1.000000000000000000, 0.9659258262890683122, 1.000000000000000000, 0.9659258262890683122, 1.000000000000000000, 0.9659258262890683122, 1.000000000000000000, 0.9659258262890683122, 1.000000000000000000, 0.9659258262890683122, 1.000000000000000000, 0.9659258262890683122, 1.000000000000000000, 0.9659258262890683122, 1.000000000000000000, 0.9659258262890683122, 1.000000000000000000, 0.9659258262890683122, 1.000000000000000000, 0.9659258262890683122, 1.000000000000000000, 0.9659258262890683122, 1.000000000000000000, 0.9659258262890683122, 1.000000000000000000, 0.9659258262890683122, 1.000000000000000000, 0.9659258262890683122, 1.000000000000000000, 0.9659258262890683122, 1.000000000000000000, 0.9659258262890683122, 1.000000000000000000, 0.9659258262890683122, 1.000000000000000000, 0.9659258262890683122, 1.000000000000000000, 0.9659258262890683122, 1.000000000000000000, 0.9659258262890683122, 1.000000000000000000, 0.9659258262890683122, 1.000000000000000000, 0.9659258262890683122, 1.000000000000000000, 0.9659258262890683122, 1.000000000000000000, 0.9659258262890683122, 1.000000000000000000, 0.9659258262890683122, 1.000000000000000000, 0.9659258262890683122, 1.000000000000000000, 0.9659258262890683122, 1.000000000000000000, 0.9659258262890683122, 1.000000000000000000, 0.9659258262890683122, 1.000000000000000000, 0.9659258262890683122, 1.000000000000000000, 0.9659258262890683122, 1.000000000000000000, 0.9659258262890683122, 1.000000000000000000, 0.9659258262890683122, 1.000000000000000000, 0.9659258262890683122, 1.000000000000000000, 0.9659258262890683122, 1.000000000000000000, 0.9659258262890683122, 1.000000000000000000, 0.9659258262890683122, 1.000000000000000000, 0.9659258262890683122, 1.000000000000000000, 0.9659258262890683122, 1.000000000000000000, 0.9659258262890683122, 1.000000000000000000, 0.9659258262890683122, 1.000000000000000000, 0.9659258262890683122, 1.000000000000000000, 0.9659258262890683122, 1.000000000000000000, 0.9659258262890683122, 1.000000000000000000, 0.9659258262890683122, 1.000000000000000000, 0.9659258262890683122, 1.000000000000000000, 0.9659258262890683122, 1.000000000000000000, 0.9659258262890683122, 1.000000000000000000, 0.9659258262890683122, 1.000000000000000000, 0.9659258262890683122, 1.000000000000000000, 0.9659258262890683122, 1.000000000000000000, 0.9659258262890683122, 1.000000000000000000, 0.9659258262890683122, 1.000000000000000000, 0.9659258262890683122, 1.000000000000000000, 0.9659258262890683122, 1.000000000000000000, 0.9659258262890683122, 1.000000000000000000, 0.9659258262890683122, 1.000000000000000000, 0.9659258262890683122, 1.000000000000000000, 0.9659258262890683122, 1.000000000000000000, 0.9659258262890683122, 1.000000000000000000, 0.9659258262890683122, 1.000000000000000000, 0.9659258262890683122, 1.000000000000000000, 0.9659258262890683122, 1.000000000000000000, 0.9659258262890683122, 1.000000000000000000, 0.9659258262890683122, 1.000000000000000000, 0.9659258262890683122, 1.000000000000000000, 0.9659258262890683122, 1.000000000000000000, 0.9659258262890683122, 1.000000000000000000, 0.9659258262890683122, 1.000000000000000000, 0.9659258262890683122, 1.000000000000000000, 0.9659258262890683122, 1.000000000000000000, 0.9659258262890683122, 1.000000000000000000, 0.9659258262890683122, 1.000000000000000000, 0.9659258262890683122, 1.000000000000000000, 0.9659258262890683122, 1.000000000000000000, 0.9659258262890683122, 1.000000000000000000, 0.9659258262890683122, 1.000000000000000000, 0.9659258262890683122, 1.000000000000000000, 0.9659258262890683122, 1.000000000000000000, 0.9659258262890683122, 1.000000000000000000, 0.9659258262890683122, 1.000000000000000000, 0.9659258262890683122, 1.000000000000000000, 0.9659258262890683122, 1.000000000000000000, 0.9659258262890683122, 1.000000000000000000, 0.9659258262890683122, 1.000000000000000000, 0.9659258262890683122, 1.000000000000000000, 0.9659258262890683122, 1.000000000000000000, 0.9659258262890683122, 1.000000000000000000, 0.9659258262890683122, 1.000000000000000000, 0.9659258262890683122, 1.000000000000000000, 0.9659258262890683122, 1.000000000000000000, 0.9659258262890683122, 1.000000000000000000, 0.9659258262890683122, 1.000000000000000000, 0.9659258262890683122, 1.000000000000000000, 0.9659258262890683122, 1.000000000000000000, 0.9659258262890683122, 1.000000000000000000, 0.9659258262890683122, 1.000000000000000000, 0.9659258262890683122, 1.000000000000000000, 0.9659258262890683122, 1.000000000000000000, 0.9659258262890683122, 1.000000000000000000, 0.9659258262890683122, 1.000000000000000000, 0.9659258262890683122, 1.000000000000000000, 0.9659258262890683122, 1.000000000000000000, 0.9659258262890683122, 1.000000000000000000, 0.9659258262890683122, 1.000000000000000000, 0.9659258262890683122, 1.000000000000000000, 0.9659258262890683122, 1.000000000000000000, 0.9659258262890683122, 1.000000000000000000, 0.9659258262890683122, 1.000000000000000000, 0.9659258262890683122, 1.000000000000000000, 0.9659258262890683122, 1.000000000000000000, 0.9659258262890683122, 1.000000000000000000, 0.9659258262890683122, 1.000000000000000000, 0.9659258262890683122, 1.000000000000000000, 0.9659258262890683122, 1.000000000000000000, 0.9659258262890683122, 1.000000000000000000, 0.9659258262890683122, 1.000000000000000000, 0.9659258262890683122, 1.000000000000000000, 0.9659258262890683122, 1.000000000000000000, 0.9659258262890683122, 1.000000000000000000, 0.9659258262890683122, 1.000000000000000000, 0.9659258262890683122, 1.000000000000000000, 0.9659258262890683122, 1.000000000000000000, 0.9659258262890683122, 1.000000000000000000, 0.9659258262890683122, 1.000000000000000000, 0.9659258262890683122, 1.000000000000000000, 0.9659258262890683122, 1.000000000000000000, 0.9659258262890683122, 1.000000000000000000, 0.9659258262890683122, 1.000000000000000000, 0.9659258262890683122, 1.000000000000000000, 0.9659258262890683122, 1.000000000000000000, 0.9659258262890683122, 1.000000000000000000, 0.9659258262890683122, 1.000000000000000000, 0.9659258262890683122, 1.000000000000000000, 0.9659258262890683122, 1.000000000000000000, 0.9659258262890683122, 1.000000000000000000, 0.9659258262890683122, 1.000000000000000000, 0.9659258262890683122, 1.000000000000000000, 0.9659258262890683122, 1.000000000000000000, 0.9659258262890683122, 1.000000000000000000, 0.9659258262890683122, 1.000000000000000000, 0.9659258262890683122, 1.000000000000000000, 0.9659258262890683122, 1.000000000000000000, 0.9659258262890683122, 1.000000000000000000, 0.9659258262890683122, 1.000000000000000000, 0.9659258262890683122, 1.000000000000000000, 0.9659258262890683122, 1.000000000000000000, 0.9659258262890683122, 1.000000000000000000, 0.9659258262890683122, 1.000000000000000000, 0.9659258262890683122, 1.000000000000000000, 0.9659258262890683122, 1.000000000000000000, 0.9659258262890683122, 1.000000000000000000, 0.9659258262890683122, 1.000000000000000000, 0.9659258262890683122, 1.000000000000000000, 0.9659258262890683122, 1.000000000000000000, 0.9659258262890683122, 1.000000000000000000, 0.9659258262890683122, 1.000000000000000000, 0.9659258262890683122, 1.000000000000000000, 0.9659258262890683122, 1.000000000000000000, 0.9659258262890683122, 1.000000000000000000, 0.9659258262890683122, 1.000000000000000000, 0.9659258262890683122, 1.000000000000000000, 0.9659258262890683122, 1.000000000000000000, 0.9659258262890683122, 1.000000000000000000, 0.9659258262890683122, 1.000000000000000000, 0.9659258262890683122, 1.000000000000000000, 0.9659258262890683122, 1.000000000000000000, 0.9659258262890683122, 1.000000000000000000, 0.9659258262890683122, 1.000000000000000000, 0.9659258262890683122, 1.000000000000000000, 0.9659258262890683122, 1.000000000000000000, 0.9659258262890683122, 1.000000000000000000, 0.9659258262890683122, 1.000000000000000000, 0.9659258262890683122, 1.000000000000000000, 0.9659258262890683122, 1.000000000000000000, 0.9659258262890683122, 1.000000000000000000, 0.9659258262890683122, 1.000000000000000000, 0.9659258262890683122, 1.000000000000000000, 0.9659258262890683122, 1.000000000000000000, 0.9659258262890683122, 1.000000000000000000, 0.9659258262890683122, 1.000000000000000000, 0.9659258262890683122, 1.000000000000000000, 0.9659258262890683122, 1.000000000000000000, 0.9659258262890683122, 1.000000000000000000, 0.9659258262890683122, 1.000000000000000000, 0.9659258262890683122, 1.000000000000000000, 0.9659258262890683122, 1.000000000000000000, 0.9659258262890683122, 1.000000000000000000, 0.9659258262890683122, 1.000000000000000000, 0.9659258262890683122, 1.000000000000000000, 0.9659258262890683122, 1.000000000000000000, 0.9659258262890683122, 1.000000000000000000, 0.9659258262890683122, 1.000000000000000000, 0.9659258262890683122, 1.000000000000000000, 0.9659258262890683122, 1.000000000000000000, 0.9659258262890683122, 1.000000000000000000, 0.9659258262890683122, 1.000000000000000000, 0.9659258262890683122, 1.000000000000000000, 0.9659258262890683122, 1.000000000000000000, 0.9659258262890683122, 1.000000000000000000, 0.9659258262890683122, 1.000000000000000000, 0.9659258262890683122, 1.000000000000000000, 0.9659258262890683122, 1.000000000000000000, 0.9659258262890683122, 1.000000000000000000, 0.9659258262890683122, 1.000000000000000000, 0.9659258262890683122, 1.000000000000000000, 0.9659258262890683122, 1.000000000000000000, 0.9659258262890683122, 1.000000000000000000, 0.9659258262890683122, 1.000000000000000000, 0.9659258262890683122, 1.000000000000000000, 0.9659258262890683122, 1.000000000000000000, 0.9659258262890683122, 1.000000000000000000, 0.9659258262890683122, 1.000000000000000000, 0.9659258262890683122, 1.000000000000000000, 0.9659258262890683122, 1.000000000000000000, 0.9659258262890683122, 1.000000000000000000, 0.9659258262890683122, 1.000000000000000000, 0.9659258262890683122, 1.000000000000000000, 0.9659258262890683122, 1.000000000000000000, 0.9659258262890683122, 1.000000000000000000, 0.9659258262890683122, 1.000000000000000000, 0.9659258262890683122, 1.000000000000000000, 0.9659258262890683122, 1.000000000000000000, 0.9659258262890683122, 1.000000000000000000, 0.9659258262890683122, 1.000000000000000000) ) ) 
 REPRESENTATION_ITEM ( '' )  SURFACE ( )  );
#124918 = CARTESIAN_POINT ( 'NONE',  ( 15.80617190586746368, 15.72974639402197994, 79.37390960531436690 ) ) ;
#124920 = CARTESIAN_POINT ( 'NONE',  ( -5.049401038297874678, -19.05341960407617918, 39.79275706135232582 ) ) ;
#124919 = CARTESIAN_POINT ( 'NONE',  ( -12.06949235617756955, 12.14591786802309770, 60.62390960531437401 ) ) ;
#124921 = CARTESIAN_POINT ( 'NONE',  ( -5.719274019375978568, 21.55341960407610458, 45.20724293864769550 ) ) ;
#124922 = CARTESIAN_POINT ( 'NONE',  ( 21.53943276465977519, -0.05219959533907433946, 33.74890960531436690 ) ) ;
#124923 = CARTESIAN_POINT ( 'NONE',  ( 16.46253265017160672, -9.564922557960803928, 63.33224293864769550 ) ) ;
#124924 = CARTESIAN_POINT ( 'NONE',  ( -9.564922557960796823, -16.46253265017161027, 52.08224293864768839 ) ) ;
#124925 = CARTESIAN_POINT ( 'NONE',  ( 12.14591786802309770, 12.06949235617756955, 109.3739096053143811 ) ) ;
#124926 = CARTESIAN_POINT ( 'NONE',  ( 21.53943276465977519, 0.05219959533937863772, 21.25109039468567218 ) ) ;
#124927 = CARTESIAN_POINT ( 'NONE',  ( -5.049401038298153566, 19.05341960407611168, 110.2072429386476671 ) ) ;
#124928 = CARTESIAN_POINT ( 'NONE',  ( 18.67979575497194134, -10.72451020669871369, 30.83442372801902209 ) ) ;
#124929 = CARTESIAN_POINT ( 'NONE',  ( 16.51473224551069308, 9.474510206698969483, 29.16557627198103475 ) ) ;
#124930 = CARTESIAN_POINT ( 'NONE',  ( -21.55341960407610458, -5.719274019375992779, 101.4572429386476955 ) ) ;
#124931 = EDGE_CURVE ( 'NONE', #14227, #182496, #186386, .T. ) ;
#124932 = CARTESIAN_POINT ( 'NONE',  ( 19.02544592524334988, 5.153800228976608722, 51.45942372801900433 ) ) ;
#124933 = CARTESIAN_POINT ( 'NONE',  ( -11.30153831258470731, -190.0000000000000000, -15.00000000000000000 ) ) ;
#124934 = CARTESIAN_POINT ( 'NONE',  ( 19.05341960407611168, 5.049401038298154454, 28.95724293864769550 ) ) ;
#124935 = DIRECTION ( 'NONE',  ( 1.000000000000000000, -0.000000000000000000, -0.000000000000000000 ) ) ;
#124936 = CARTESIAN_POINT ( 'NONE',  ( 16.53943276465976808, 0.05219959533934440121, 61.25109039468567573 ) ) ;
#124937 = CARTESIAN_POINT ( 'NONE',  ( 13.97604488694527802, 13.89961937509977652, 29.37390960531435979 ) ) ;
#124938 = CARTESIAN_POINT ( 'NONE',  ( -26.45763050569073727, -3.219288925402985946, 173.6696415116520882 ) ) ;
#124939 = CARTESIAN_POINT ( 'NONE',  ( -5.153800228976328057, -19.02544592524343514, 77.29057627198099567 ) ) ;
#124940 = CARTESIAN_POINT ( 'NONE',  ( -16.53943276465976808, 0.05219959533911058130, 111.2489096053143669 ) ) ;
#124941 = CARTESIAN_POINT ( 'NONE',  ( -21.53943276465977519, 0.05219959533907696930, 61.24890960531435979 ) ) ;
#124942 = CARTESIAN_POINT ( 'NONE',  ( 16.52544592524342804, -4.483927247898539470, 83.54057627198102409 ) ) ;
#124943 = CARTESIAN_POINT ( 'NONE',  ( -12.14591786802326823, 12.06949235617739902, 28.12609039468568284 ) ) ;
#124944 = CARTESIAN_POINT ( 'NONE',  ( 10.72451020669871369, 18.67979575497193778, 87.08442372801901854 ) ) ;
#124945 = CARTESIAN_POINT ( 'NONE',  ( -9.564922557960796823, -16.46253265017161027, 32.08224293864769550 ) ) ;
#124946 = EDGE_CURVE ( 'NONE', #87433, #116956, #20362, .T. ) ;
#124947 = CARTESIAN_POINT ( 'NONE',  ( -12.14591786802326823, 12.06949235617739902, 113.1260903946856899 ) ) ;
#124948 = CARTESIAN_POINT ( 'NONE',  ( -8.224510206698948167, 14.34966873604960824, 55.41557627198102409 ) ) ;
#124949 = CARTESIAN_POINT ( 'NONE',  ( 19.03943276465977164, -0.05219959533909143690, 53.74890960531436690 ) ) ;
#124950 = CARTESIAN_POINT ( 'NONE',  ( -5.719274019375665041, -21.55341960407619695, 99.79275706135234714 ) ) ;
#124951 = CARTESIAN_POINT ( 'NONE',  ( 5.823673210054125526, 21.52544592524343514, 104.7905762719810241 ) ) ;
#124952 = CARTESIAN_POINT ( 'NONE',  ( -21.52544592524334988, -5.823673210054445271, 73.95942372801901854 ) ) ;
#124953 = CARTESIAN_POINT ( 'NONE',  ( -4.483927247898782831, 16.52544592524335698, 37.70942372801900433 ) ) ;
#124955 = CARTESIAN_POINT ( 'NONE',  ( -18.67979575497193778, 10.72451020669871902, 83.33442372801903275 ) ) ;
#124954 = CARTESIAN_POINT ( 'NONE',  ( 12.06949235617757843, -12.14591786802309237, 83.12390960531436690 ) ) ;
#124956 = CARTESIAN_POINT ( 'NONE',  ( 12.06949235617739724, 12.14591786802326823, 111.8760903946856615 ) ) ;
#124957 = DIRECTION ( 'NONE',  ( 0.5000000000000049960, 0.4999999999999962252, -0.7071067811865466846 ) ) ;
#124958 = CARTESIAN_POINT ( 'NONE',  ( -16.53943276465976808, -0.05219959533934237506, 38.75109039468567573 ) ) ;
#124959 = CARTESIAN_POINT ( 'NONE',  ( -0.05219959533910754901, -16.53943276465976808, 47.49890960531435979 ) ) ;
#124960 = CARTESIAN_POINT ( 'NONE',  ( -12.06949235617739369, -12.14591786802326823, 89.37609039468568994 ) ) ;
#124961 = CARTESIAN_POINT ( 'NONE',  ( 9.474510206698971260, -16.51473224551069308, 102.9155762719810241 ) ) ;
#124962 = CARTESIAN_POINT ( 'NONE',  ( -9.564922557960796823, -16.46253265017161027, 112.0822429386476955 ) ) ;
#124963 = CARTESIAN_POINT ( 'NONE',  ( -10.72451020669870658, -18.67979575497194134, 104.5844237280190185 ) ) ;
#124964 = CARTESIAN_POINT ( 'NONE',  ( -12.14591786802326823, 12.06949235617739902, 103.1260903946856757 ) ) ;
#124965 = CARTESIAN_POINT ( 'NONE',  ( 0.05219959533910956823, 16.53943276465976808, 74.99890960531435269 ) ) ;
#124966 = CARTESIAN_POINT ( 'NONE',  ( -5.153800228976328057, -19.02544592524343514, 82.29057627198103830 ) ) ;
#124967 = VERTEX_POINT ( 'NONE', #22375 ) ;
#124968 = CARTESIAN_POINT ( 'NONE',  ( -4.483927247898782831, 16.52544592524335698, 22.70942372801901499 ) ) ;
#124969 = CARTESIAN_POINT ( 'NONE',  ( 9.474510206698971260, -16.51473224551069308, 32.91557627198102409 ) ) ;
#124970 = CARTESIAN_POINT ( 'NONE',  ( -9.564922557960796823, -16.46253265017161027, 87.08224293864769550 ) ) ;
#124972 = CARTESIAN_POINT ( 'NONE',  ( 11.40812507854754365, 35.11059874428196537, -3.224999997268813701 ) ) ;
#124971 = CARTESIAN_POINT ( 'NONE',  ( -16.52544592524335698, -4.483927247898792601, 33.95942372801901143 ) ) ;
#124973 = CARTESIAN_POINT ( 'NONE',  ( -0.05219959533936034679, 19.03943276465977164, 37.50109039468567573 ) ) ;
#124974 = CARTESIAN_POINT ( 'NONE',  ( 12.06949235617739724, 12.14591786802326823, 96.87609039468568994 ) ) ;
#124975 = CARTESIAN_POINT ( 'NONE',  ( 19.05341960407617918, -5.049401038297876454, 111.0427570613523329 ) ) ;
#124976 = CARTESIAN_POINT ( 'NONE',  ( 9.474510206698971260, -16.51473224551069308, 27.91557627198103120 ) ) ;
#124977 = CARTESIAN_POINT ( 'NONE',  ( 16.55341960407618274, -4.379528057220086978, 81.04275706135236135 ) ) ;
#124978 = CARTESIAN_POINT ( 'NONE',  ( -16.52544592524335698, -4.483927247898792601, 68.95942372801901854 ) ) ;
#124979 = CARTESIAN_POINT ( 'NONE',  ( 5.153800228976335163, 19.02544592524342804, 34.79057627198102409 ) ) ;
#124980 = CARTESIAN_POINT ( 'NONE',  ( -13.89961937509957401, -13.97604488694547875, 64.37609039468567573 ) ) ;
#124981 = CARTESIAN_POINT ( 'NONE',  ( 10.72451020669871369, 18.67979575497193778, 107.0844237280190043 ) ) ;
#124982 = CARTESIAN_POINT ( 'NONE',  ( 19.05341960407611168, 5.049401038298154454, 48.95724293864768129 ) ) ;
#124983 = CARTESIAN_POINT ( 'NONE',  ( 0.05219959533909260263, 19.03943276465977164, 94.99890960531436690 ) ) ;
#124984 = CARTESIAN_POINT ( 'NONE',  ( -14.34966873604960291, -8.224510206698953496, 91.66557627198103830 ) ) ;
#124985 = VECTOR ( 'NONE', #179002, 1000.000000000000000 ) ;
#124986 = CARTESIAN_POINT ( 'NONE',  ( -16.46253265017146816, -9.564922557961047289, 49.16775706135233293 ) ) ;
#124987 = CARTESIAN_POINT ( 'NONE',  ( 5.823673210054125526, 21.52544592524343514, 54.79057627198104541 ) ) ;
#124988 = CARTESIAN_POINT ( 'NONE',  ( -19.05341960407617563, 5.049401038297882671, 23.54275706135233648 ) ) ;
#124989 = CARTESIAN_POINT ( 'NONE',  ( -5.153800228976328057, -19.02544592524343514, 87.29057627198103830 ) ) ;
#124990 = CARTESIAN_POINT ( 'NONE',  ( -16.46253265017146816, -9.564922557961047289, 24.16775706135233648 ) ) ;
#124991 = CARTESIAN_POINT ( 'NONE',  ( 18.62759615963271287, -10.81492255796078972, 63.33224293864770260 ) ) ;
#124992 = CARTESIAN_POINT ( 'NONE',  ( -19.05341960407611168, -5.049401038298163336, 106.4572429386476955 ) ) ;
#124993 = AXIS2_PLACEMENT_3D ( 'NONE', #94697, #185729, #50205 ) ;
#124994 = CARTESIAN_POINT ( 'NONE',  ( -16.46253265017146816, -9.564922557961047289, 94.16775706135233293 ) ) ;
#124995 = CARTESIAN_POINT ( 'NONE',  ( -13.89961937509977652, 13.97604488694528158, 110.6239096053143243 ) ) ;
#124996 = CARTESIAN_POINT ( 'NONE',  ( 13.97604488694548053, -13.89961937509957401, 110.6260903946856615 ) ) ;
#124997 = CARTESIAN_POINT ( 'NONE',  ( 16.53943276465976808, -0.05219959533910856209, 113.7489096053143527 ) ) ;
#124998 = CARTESIAN_POINT ( 'NONE',  ( -19.02544592524342804, 5.153800228976336051, 96.04057627198103830 ) ) ;
#124999 = CARTESIAN_POINT ( 'NONE',  ( -15.72974639402197994, 15.80617190586746368, 80.62390960531438111 ) ) ;
#125000 = CARTESIAN_POINT ( 'NONE',  ( 12.14591786802327356, -12.06949235617739191, 50.62609039468568994 ) ) ;
#125001 = CARTESIAN_POINT ( 'NONE',  ( -10.72451020669870658, -18.67979575497194134, 49.58442372801901143 ) ) ;
#125002 = CARTESIAN_POINT ( 'NONE',  ( -21.55341960407619339, 5.719274019375674811, 103.5427570613523613 ) ) ;
#125003 = CARTESIAN_POINT ( 'NONE',  ( 16.53943276465976808, 0.05219959533934440121, 91.25109039468568994 ) ) ;
#125004 = CARTESIAN_POINT ( 'NONE',  ( 13.89961937509977652, -13.97604488694527269, 88.12390960531438111 ) ) ;
#125005 = CARTESIAN_POINT ( 'NONE',  ( 12.14591786802309770, 12.06949235617756955, 84.37390960531438111 ) ) ;
#125006 = CARTESIAN_POINT ( 'NONE',  ( -16.52544592524342804, 4.483927247898546575, 41.04057627198103120 ) ) ;
#125007 = CARTESIAN_POINT ( 'NONE',  ( -9.564922557961040184, 16.46253265017147172, 67.91775706135233293 ) ) ;
#125008 = CARTESIAN_POINT ( 'NONE',  ( 15.72974639402176855, 15.80617190586768217, 51.87609039468568284 ) ) ;
#125009 = CARTESIAN_POINT ( 'NONE',  ( 0.05219959533936267826, -19.03943276465977164, 30.00109039468566863 ) ) ;
#125010 = CARTESIAN_POINT ( 'NONE',  ( 0.05219959533910956823, 16.53943276465976808, 94.99890960531436690 ) ) ;
#125011 = CARTESIAN_POINT ( 'NONE',  ( -15.80617190586745835, -15.72974639402198527, 26.87390960531435979 ) ) ;
#125012 = CARTESIAN_POINT ( 'NONE',  ( -0.05219959533910754901, -16.53943276465976808, 22.49890960531436335 ) ) ;
#125013 = CARTESIAN_POINT ( 'NONE',  ( 5.823673210054444382, -21.52544592524334988, 105.2094237280190328 ) ) ;
#125014 = CARTESIAN_POINT ( 'NONE',  ( 14.29746914071037800, 8.314922557961029526, 61.66775706135235424 ) ) ;
#125015 = CARTESIAN_POINT ( 'NONE',  ( 4.483927247898790824, -16.52544592524335698, 110.2094237280190185 ) ) ;
#125016 = CARTESIAN_POINT ( 'NONE',  ( -21.53943276465977519, -0.05219959533937600094, 48.75109039468568284 ) ) ;
#125017 = CARTESIAN_POINT ( 'NONE',  ( -21.53943276465977519, -0.05219959533937600094, 58.75109039468568994 ) ) ;
#125018 = EDGE_LOOP ( 'NONE', ( #87768, #87302, #101949 ) ) ;
#125019 = CARTESIAN_POINT ( 'NONE',  ( 10.81492255796106328, -18.62759615963255655, 30.41775706135234358 ) ) ;
#125020 = CARTESIAN_POINT ( 'NONE',  ( 16.55341960407611168, 4.379528057220329451, 98.95724293864770971 ) ) ;
#125021 = CARTESIAN_POINT ( 'NONE',  ( 5.153800228976335163, 19.02544592524342804, 24.79057627198102765 ) ) ;
#125022 = CARTESIAN_POINT ( 'NONE',  ( -4.483927247898539470, -16.52544592524342804, 67.29057627198103830 ) ) ;
#125023 = CARTESIAN_POINT ( 'NONE',  ( -16.46253265017160317, 9.564922557960807481, 70.83224293864770971 ) ) ;
#125024 = CARTESIAN_POINT ( 'NONE',  ( -12.14591786802326823, 12.06949235617739902, 108.1260903946856757 ) ) ;
#125025 = CARTESIAN_POINT ( 'NONE',  ( -18.62759615963270932, 10.81492255796079327, 60.83224293864769550 ) ) ;
#125026 = CARTESIAN_POINT ( 'NONE',  ( -16.53943276465976808, 0.05219959533911058130, 86.24890960531436690 ) ) ;
#125027 = CARTESIAN_POINT ( 'NONE',  ( -0.05219959533907301413, -21.53943276465977519, 97.49890960531436690 ) ) ;
#125028 = CARTESIAN_POINT ( 'NONE',  ( -19.03943276465977164, 0.05219959533909376836, 101.2489096053143669 ) ) ;
#125030 = CARTESIAN_POINT ( 'NONE',  ( 13.97604488694548053, -13.89961937509957401, 110.6260903946856615 ) ) ;
#125029 = CARTESIAN_POINT ( 'NONE',  ( -9.474510206698964154, 16.51473224551069663, 45.41557627198103120 ) ) ;
#125031 = CARTESIAN_POINT ( 'NONE',  ( 21.52544592524344225, -5.823673210054117533, 38.54057627198103120 ) ) ;
#125032 = CARTESIAN_POINT ( 'NONE',  ( -21.55341960407619339, 5.719274019375674811, 63.54275706135234003 ) ) ;
#125033 = CARTESIAN_POINT ( 'NONE',  ( -9.564922557960796823, -16.46253265017161027, 67.08224293864769550 ) ) ;
#125034 = CARTESIAN_POINT ( 'NONE',  ( -13.97604488694527625, -13.89961937509977652, 96.87390960531433848 ) ) ;
#125035 = CARTESIAN_POINT ( 'NONE',  ( -4.483927247898782831, 16.52544592524335698, 62.70942372801902565 ) ) ;
#125036 = CARTESIAN_POINT ( 'NONE',  ( 10.72451020669871369, 18.67979575497193778, 47.08442372801901854 ) ) ;
#125037 = CARTESIAN_POINT ( 'NONE',  ( 18.67979575497194134, -10.72451020669871369, 80.83442372801901854 ) ) ;
#125038 = CARTESIAN_POINT ( 'NONE',  ( -21.52544592524343514, 5.823673210054127303, 101.0405762719810383 ) ) ;
#125040 = CARTESIAN_POINT ( 'NONE',  ( -4.483927247898782831, 16.52544592524335698, 77.70942372801900433 ) ) ;
#125039 = CARTESIAN_POINT ( 'NONE',  ( -10.72451020669870658, -18.67979575497194134, 34.58442372801900433 ) ) ;
#125041 = CARTESIAN_POINT ( 'NONE',  ( -5.719274019375978568, 21.55341960407610458, 75.20724293864769550 ) ) ;
#125042 = CARTESIAN_POINT ( 'NONE',  ( -16.46253265017146816, -9.564922557961047289, 29.16775706135232937 ) ) ;
#125044 = CARTESIAN_POINT ( 'NONE',  ( 8.314922557960818139, 14.29746914071049879, 29.58224293864769905 ) ) ;
#125043 = CARTESIAN_POINT ( 'NONE',  ( 13.97604488694527802, 13.89961937509977652, 79.37390960531435269 ) ) ;
#125045 = CARTESIAN_POINT ( 'NONE',  ( 25.25560589046783022, 4.310829775027161581, 167.9999999999999716 ) ) ;
#125046 = CARTESIAN_POINT ( 'NONE',  ( 5.049401038298161559, -19.05341960407611168, 97.70724293864766707 ) ) ;
#125047 = DIRECTION ( 'NONE',  ( -1.000000000000000000, 0.000000000000000000, 0.000000000000000000 ) ) ;
#125048 = CARTESIAN_POINT ( 'NONE',  ( -19.03943276465977164, -0.05219959533935918106, 83.75109039468567573 ) ) ;
#125049 = CARTESIAN_POINT ( 'NONE',  ( 10.72451020669898902, -18.67979575497178502, 57.91557627198103120 ) ) ;
#125050 = CARTESIAN_POINT ( 'NONE',  ( 0.05219959533910956823, 16.53943276465976808, 44.99890960531435979 ) ) ;
#125051 = CARTESIAN_POINT ( 'NONE',  ( -0.05219959533936034679, 19.03943276465977164, 107.5010903946856615 ) ) ;
#125052 = CARTESIAN_POINT ( 'NONE',  ( -5.049401038298153566, 19.05341960407611168, 35.20724293864768839 ) ) ;
#125053 = CARTESIAN_POINT ( 'NONE',  ( -13.89961937509957401, -13.97604488694547875, 104.3760903946856757 ) ) ;
#125055 = CARTESIAN_POINT ( 'NONE',  ( 0.05219959533936267826, -19.03943276465977164, 70.00109039468566152 ) ) ;
#125054 = CARTESIAN_POINT ( 'NONE',  ( 21.52544592524344225, -5.823673210054117533, 103.5405762719810383 ) ) ;
#125056 = CARTESIAN_POINT ( 'NONE',  ( -0.05219959533934338120, 16.53943276465976808, 77.50109039468567573 ) ) ;
#125057 = CARTESIAN_POINT ( 'NONE',  ( -19.02544592524342804, 5.153800228976336051, 71.04057627198099567 ) ) ;
#125058 = CARTESIAN_POINT ( 'NONE',  ( 16.55341960407611168, 4.379528057220329451, 78.95724293864769550 ) ) ;
#125059 = CARTESIAN_POINT ( 'NONE',  ( -19.02544592524342804, 5.153800228976336051, 66.04057627198103830 ) ) ;
#125060 = CARTESIAN_POINT ( 'NONE',  ( -12.06949235617756955, 12.14591786802309770, 65.62390960531436690 ) ) ;
#125061 = CARTESIAN_POINT ( 'NONE',  ( -4.273745901508076983, 6.674792076160563248, 4.009310749147818598 ) ) ;
#125062 = CARTESIAN_POINT ( 'NONE',  ( -37.54768727782017379, -1.429952535790612433, 39.67699414429139892 ) ) ;
#125063 = CARTESIAN_POINT ( 'NONE',  ( 0.05219959533910956823, 16.53943276465976808, 44.99890960531435979 ) ) ;
#125064 = CARTESIAN_POINT ( 'NONE',  ( 16.46253265017160672, -9.564922557960803928, 73.33224293864769550 ) ) ;
#125065 = CARTESIAN_POINT ( 'NONE',  ( 2.310831529832237923E-15, -71.74905152827281540, -14.99410988490250496 ) ) ;
#125066 = CARTESIAN_POINT ( 'NONE',  ( -19.02544592524334988, -5.153800228976617603, 43.95942372801899012 ) ) ;
#125067 = CARTESIAN_POINT ( 'NONE',  ( -16.53943276465976808, -0.05219959533934237506, 63.75109039468568284 ) ) ;
#125068 = CARTESIAN_POINT ( 'NONE',  ( -5.719274019375978568, 21.55341960407610458, 70.20724293864769550 ) ) ;
#125069 = CARTESIAN_POINT ( 'NONE',  ( 13.97604488694548053, -13.89961937509957401, 20.62609039468567573 ) ) ;
#125070 = CARTESIAN_POINT ( 'NONE',  ( -19.05341960407611168, -5.049401038298163336, 71.45724293864766707 ) ) ;
#125071 = CARTESIAN_POINT ( 'NONE',  ( 1.468936857220423775, 22.44461420004035901, -58.07763101479264378 ) ) ;
#125072 = CARTESIAN_POINT ( 'NONE',  ( -9.474510206698964154, 16.51473224551069663, 110.4155762719810383 ) ) ;
#125073 = CARTESIAN_POINT ( 'NONE',  ( -5.049401038298153566, 19.05341960407611168, 60.20724293864768129 ) ) ;
#125074 = CARTESIAN_POINT ( 'NONE',  ( -21.52544592524334988, -5.823673210054445271, 43.95942372801902565 ) ) ;
#125075 = CARTESIAN_POINT ( 'NONE',  ( -8.314922557960811034, -14.29746914071050412, 102.0822429386476955 ) ) ;
#125078 = EDGE_LOOP ( 'NONE', ( #176117, #41129 ) ) ;
#125077 = CARTESIAN_POINT ( 'NONE',  ( -13.89961937509977652, 13.97604488694528158, 85.62390960531433848 ) ) ;
#125076 = CARTESIAN_POINT ( 'NONE',  ( -10.81492255796078084, -18.62759615963271287, 102.0822429386476955 ) ) ;
#125079 = CARTESIAN_POINT ( 'NONE',  ( -21.53943276465977519, -0.05219959533937600094, 23.75109039468567929 ) ) ;
#125080 = ORIENTED_EDGE ( 'NONE', *, *, #137780, .F. ) ;
#125081 = CARTESIAN_POINT ( 'NONE',  ( 16.51473224551069308, 9.474510206698969483, 84.16557627198102409 ) ) ;
#125082 = DIRECTION ( 'NONE',  ( -1.000000000000000000, 0.000000000000000000, 0.000000000000000000 ) ) ;
#125083 = CARTESIAN_POINT ( 'NONE',  ( 21.53943276465977519, -0.05219959533907433946, 98.74890960531438111 ) ) ;
#125084 = CARTESIAN_POINT ( 'NONE',  ( -0.05219959533909027116, -19.03943276465977164, 42.49890960531435269 ) ) ;
#125085 = CARTESIAN_POINT ( 'NONE',  ( 19.03943276465977164, 0.05219959533936151252, 101.2510903946856757 ) ) ;
#125086 = CARTESIAN_POINT ( 'NONE',  ( 3.556970738554033499E-15, -38.81732327939057825, -8.624999997268814056 ) ) ;
#125087 = CARTESIAN_POINT ( 'NONE',  ( -5.153800228976328057, -19.02544592524343514, 27.29057627198103120 ) ) ;
#125088 = CARTESIAN_POINT ( 'NONE',  ( 18.62759615963255655, 10.81492255796105972, 91.66775706135234714 ) ) ;
#125090 = CARTESIAN_POINT ( 'NONE',  ( -5.719274019375665041, -21.55341960407619695, 44.79275706135234714 ) ) ;
#125089 = CARTESIAN_POINT ( 'NONE',  ( -13.89961937509977652, 13.97604488694528158, 70.62390960531432427 ) ) ;
#125091 = CARTESIAN_POINT ( 'NONE',  ( -5.719274019375665041, -21.55341960407619695, 29.79275706135234358 ) ) ;
#125092 = CARTESIAN_POINT ( 'NONE',  ( -17.81289503416611097, -24.51734667627696496, 146.2999999999999829 ) ) ;
#125093 = CARTESIAN_POINT ( 'NONE',  ( -19.05341960407611168, -5.049401038298163336, 91.45724293864766707 ) ) ;
#125094 = CARTESIAN_POINT ( 'NONE',  ( 0.000000000000000000, -105.0000000000000000, 7.000000000000003553 ) ) ;
#125097 = CARTESIAN_POINT ( 'NONE',  ( -18.62759615963255300, -10.81492255796106328, 39.16775706135235424 ) ) ;
#125096 = CARTESIAN_POINT ( 'NONE',  ( -10.81492255796078084, -18.62759615963271287, 47.08224293864770260 ) ) ;
#125095 = CARTESIAN_POINT ( 'NONE',  ( 12.14591786802327356, -12.06949235617739191, 45.62609039468567573 ) ) ;
#125098 = CARTESIAN_POINT ( 'NONE',  ( -5.823673210054431948, 21.52544592524334988, 72.70942372801901854 ) ) ;
#125099 = CARTESIAN_POINT ( 'NONE',  ( 18.09873248133749257, -5.500000000000147438, 38.51607049666168336 ) ) ;
#125100 = CARTESIAN_POINT ( 'NONE',  ( -16.51473224551082808, 9.474510206698731452, 108.3344237280190043 ) ) ;
#125101 = CARTESIAN_POINT ( 'NONE',  ( 0.05219959533909260263, 19.03943276465977164, 54.99890960531435979 ) ) ;
#125102 = CARTESIAN_POINT ( 'NONE',  ( 9.564922557960805705, 16.46253265017160317, 84.58224293864769550 ) ) ;
#125103 = EDGE_CURVE ( 'NONE', #114833, #113576, #39177, .T. ) ;
#125104 = CARTESIAN_POINT ( 'NONE',  ( 8.314922557960818139, 14.29746914071049879, 104.5822429386477097 ) ) ;
#125105 = CARTESIAN_POINT ( 'NONE',  ( -4.483927247898539470, -16.52544592524342804, 102.2905762719810383 ) ) ;
#125106 = CARTESIAN_POINT ( 'NONE',  ( -19.03943276465977164, 0.05219959533909376836, 111.2489096053143669 ) ) ;
#125107 = CARTESIAN_POINT ( 'NONE',  ( -12.14591786802326823, 12.06949235617739902, 83.12609039468568994 ) ) ;
#125109 = CARTESIAN_POINT ( 'NONE',  ( -5.049401038298153566, 19.05341960407611168, 55.20724293864769550 ) ) ;
#125108 = CARTESIAN_POINT ( 'NONE',  ( 0.05219959533910956823, 16.53943276465976808, 74.99890960531435269 ) ) ;
#125110 = CARTESIAN_POINT ( 'NONE',  ( 21.53943276465977519, 0.05219959533937863772, 81.25109039468568994 ) ) ;
#125111 = CARTESIAN_POINT ( 'NONE',  ( 15.72974639402176855, 15.80617190586768217, 76.87609039468567573 ) ) ;
#125112 = CARTESIAN_POINT ( 'NONE',  ( 19.03943276465977164, 0.05219959533936151252, 106.2510903946856615 ) ) ;
#125113 = CARTESIAN_POINT ( 'NONE',  ( -12.06949235617756955, 12.14591786802309770, 60.62390960531437401 ) ) ;
#125114 = CARTESIAN_POINT ( 'NONE',  ( -18.67979575497193778, 10.72451020669871902, 28.33442372801902209 ) ) ;
#125115 = CARTESIAN_POINT ( 'NONE',  ( -10.81492255796078084, -18.62759615963271287, 62.08224293864769550 ) ) ;
#125116 = DIRECTION ( 'NONE',  ( 1.000000000000000000, -0.000000000000000000, -0.000000000000000000 ) ) ;
#125117 = CARTESIAN_POINT ( 'NONE',  ( 23.31738231874054534, 16.94106989632529192, 143.4500000054623854 ) ) ;
#125118 = CARTESIAN_POINT ( 'NONE',  ( 5.153800228976335163, 19.02544592524342804, 74.79057627198103830 ) ) ;
#125119 = CARTESIAN_POINT ( 'NONE',  ( -16.55341960407611168, -4.379528057220339221, 36.45724293864768839 ) ) ;
#125120 = AXIS2_PLACEMENT_3D ( 'NONE', #177302, #87269, #10443 ) ;
#125121 = CARTESIAN_POINT ( 'NONE',  ( -4.379528057220086978, -16.55341960407618274, 109.7927570613523613 ) ) ;
#125122 = CARTESIAN_POINT ( 'NONE',  ( 8.224510206698742110, 14.34966873604972548, 102.0844237280190185 ) ) ;
#125123 = CARTESIAN_POINT ( 'NONE',  ( -16.46253265017146816, -9.564922557961047289, 54.16775706135234003 ) ) ;
#125124 = CARTESIAN_POINT ( 'NONE',  ( 2.500000000000000000, -165.0000000000000000, 12.00000000000000355 ) ) ;
#125125 = CARTESIAN_POINT ( 'NONE',  ( 9.564922557960805705, 16.46253265017160317, 104.5822429386476955 ) ) ;
#125126 = EDGE_CURVE ( 'NONE', #93910, #140935, #11214, .T. ) ;
#125127 = CARTESIAN_POINT ( 'NONE',  ( -8.224510206698948167, 14.34966873604960824, 80.41557627198103830 ) ) ;
#125128 = CARTESIAN_POINT ( 'NONE',  ( -13.89961937509957401, -13.97604488694547875, 39.37609039468566152 ) ) ;
#125130 = CARTESIAN_POINT ( 'NONE',  ( 16.46253265017160672, -9.564922557960803928, 113.3322429386476955 ) ) ;
#125129 = CARTESIAN_POINT ( 'NONE',  ( 5.049401038298161559, -19.05341960407611168, 22.70724293864769194 ) ) ;
#125131 = CARTESIAN_POINT ( 'NONE',  ( -10.72451020669898014, 18.67979575497178502, 60.41557627198102409 ) ) ;
#125132 = CARTESIAN_POINT ( 'NONE',  ( -12.06949235617756955, 12.14591786802309770, 100.6239096053143811 ) ) ;
#125133 = CARTESIAN_POINT ( 'NONE',  ( -16.53943276465976808, -0.05219959533934237506, 48.75109039468568284 ) ) ;
#125134 = CARTESIAN_POINT ( 'NONE',  ( 8.224510206698953496, -14.34966873604960469, 87.91557627198103830 ) ) ;
#125135 = CARTESIAN_POINT ( 'NONE',  ( 16.31925111598458145, -7.325300261831445781, 37.66424538967251578 ) ) ;
#125136 = CARTESIAN_POINT ( 'NONE',  ( -16.36317988757059538, 7.306389748694931185, 49.09789608363226421 ) ) ;
#125137 = CARTESIAN_POINT ( 'NONE',  ( -18.62759615963270932, 10.81492255796079327, 25.83224293864769194 ) ) ;
#125138 = CARTESIAN_POINT ( 'NONE',  ( 3.556970738554033499E-15, -38.81732327939057825, -6.624999997268814056 ) ) ;
#125139 = CARTESIAN_POINT ( 'NONE',  ( 0.4292098674014996895, 24.24132924781739362, -56.81486547910376572 ) ) ;
#125141 = CARTESIAN_POINT ( 'NONE',  ( -12.06949235617756955, 12.14591786802309770, 25.62390960531435624 ) ) ;
#125140 = CARTESIAN_POINT ( 'NONE',  ( -14.34966873604972548, 8.224510206698743886, 43.33442372801901143 ) ) ;
#125142 = CARTESIAN_POINT ( 'NONE',  ( 10.81492255796078972, 18.62759615963270932, 54.58224293864769550 ) ) ;
#125143 = CARTESIAN_POINT ( 'NONE',  ( 19.03943276465977164, 0.05219959533936151252, 86.25109039468567573 ) ) ;
#125144 = CARTESIAN_POINT ( 'NONE',  ( -21.52544592524343514, 5.823673210054127303, 51.04057627198103120 ) ) ;
#125145 = CARTESIAN_POINT ( 'NONE',  ( 5.823673210054444382, -21.52544592524334988, 80.20942372801901854 ) ) ;
#125146 = CARTESIAN_POINT ( 'NONE',  ( 11.19179774862115018, -35.88147526272302912, -30.64906824478838843 ) ) ;
#125147 = CARTESIAN_POINT ( 'NONE',  ( -8.224510206698735004, -14.34966873604973081, 34.58442372801900433 ) ) ;
#125149 = CARTESIAN_POINT ( 'NONE',  ( -0.05219959533909027116, -19.03943276465977164, 97.49890960531436690 ) ) ;
#125148 = CARTESIAN_POINT ( 'NONE',  ( 19.05341960407611168, 5.049401038298154454, 43.95724293864769550 ) ) ;
#125150 = CARTESIAN_POINT ( 'NONE',  ( -13.89961937509977652, 13.97604488694528158, 35.62390960531435269 ) ) ;
#125151 = CARTESIAN_POINT ( 'NONE',  ( 8.314922557960818139, 14.29746914071049879, 99.58224293864770971 ) ) ;
#125152 = DIRECTION ( 'NONE',  ( 1.000000000000000000, 0.000000000000000000, 0.000000000000000000 ) ) ;
#125153 = CARTESIAN_POINT ( 'NONE',  ( 0.05219959533909260263, 19.03943276465977164, 94.99890960531436690 ) ) ;
#125154 = ORIENTED_EDGE ( 'NONE', *, *, #30441, .F. ) ;
#125155 = CARTESIAN_POINT ( 'NONE',  ( 14.34966873604972726, -8.224510206698740333, 50.83442372801901143 ) ) ;
#125156 = CARTESIAN_POINT ( 'NONE',  ( -0.05219959533907301413, -21.53943276465977519, 87.49890960531436690 ) ) ;
#125157 = CARTESIAN_POINT ( 'NONE',  ( -0.05219959533909027116, -19.03943276465977164, 62.49890960531435979 ) ) ;
#125158 = CARTESIAN_POINT ( 'NONE',  ( -21.53943276465977519, -0.05219959533937600094, 28.75109039468567929 ) ) ;
#125159 = CARTESIAN_POINT ( 'NONE',  ( -13.97604488694527625, -13.89961937509977652, 86.87390960531436690 ) ) ;
#125160 = CARTESIAN_POINT ( 'NONE',  ( -35.08666314276963760, -21.80769648729559407, -18.77091308352783017 ) ) ;
#125161 = ORIENTED_EDGE ( 'NONE', *, *, #5777, .F. ) ;
#125162 = CARTESIAN_POINT ( 'NONE',  ( 16.55341960407618274, -4.379528057220086978, 41.04275706135236135 ) ) ;
#125163 = CARTESIAN_POINT ( 'NONE',  ( -18.62759615963255300, -10.81492255796106328, 24.16775706135235424 ) ) ;
#125166 = CARTESIAN_POINT ( 'NONE',  ( -13.89961937509957401, -13.97604488694547875, 79.37609039468567573 ) ) ;
#125165 = CARTESIAN_POINT ( 'NONE',  ( -5.153800228976328057, -19.02544592524343514, 87.29057627198103830 ) ) ;
#125164 = CARTESIAN_POINT ( 'NONE',  ( 9.564922557960805705, 16.46253265017160317, 29.58224293864769550 ) ) ;
#125167 = CARTESIAN_POINT ( 'NONE',  ( -13.97604488694547697, 13.89961937509957934, 28.12609039468565797 ) ) ;
#125168 = CARTESIAN_POINT ( 'NONE',  ( -5.823673210054116645, -21.52544592524344225, 92.29057627198103830 ) ) ;
#125169 = CARTESIAN_POINT ( 'NONE',  ( -16.51473224551082808, 9.474510206698731452, 38.33442372801899722 ) ) ;
#125170 = CARTESIAN_POINT ( 'NONE',  ( -14.34966873604972548, 8.224510206698743886, 73.33442372801901854 ) ) ;
#125172 = ORIENTED_EDGE ( 'NONE', *, *, #43025, .T. ) ;
#125171 = CARTESIAN_POINT ( 'NONE',  ( -9.474510206698964154, 16.51473224551069663, 105.4155762719810383 ) ) ;
#125173 = CARTESIAN_POINT ( 'NONE',  ( -5.049401038298153566, 19.05341960407611168, 60.20724293864768129 ) ) ;
#125174 = CIRCLE ( 'NONE', #37993, 48.98979485566358250 ) ;
#125175 = CARTESIAN_POINT ( 'NONE',  ( 10.72451020669871369, 18.67979575497193778, 67.08442372801901854 ) ) ;
#125176 = CARTESIAN_POINT ( 'NONE',  ( -21.55341960407619339, 5.719274019375674811, 63.54275706135234003 ) ) ;
#125177 = CARTESIAN_POINT ( 'NONE',  ( -9.564922557960796823, -16.46253265017161027, 72.08224293864770971 ) ) ;
#125178 = CARTESIAN_POINT ( 'NONE',  ( -10.72451020669870658, -18.67979575497194134, 49.58442372801901143 ) ) ;
#125179 = EDGE_CURVE ( 'NONE', #180340, #185456, #99814, .T. ) ;
#125180 = CARTESIAN_POINT ( 'NONE',  ( 16.46253265017146816, 9.564922557961045513, 81.66775706135233293 ) ) ;
#125181 = CARTESIAN_POINT ( 'NONE',  ( -13.97604488694527625, -13.89961937509977652, 51.87390960531436690 ) ) ;
#125182 = CARTESIAN_POINT ( 'NONE',  ( -19.02544592524342804, 5.153800228976336051, 101.0405762719810241 ) ) ;
#125183 = CARTESIAN_POINT ( 'NONE',  ( -19.05341960407611168, -5.049401038298163336, 66.45724293864769550 ) ) ;
#125184 = CARTESIAN_POINT ( 'NONE',  ( -16.51473224551069308, -9.474510206698971260, 111.6655762719810383 ) ) ;
#125185 = CARTESIAN_POINT ( 'NONE',  ( 19.02544592524343514, -5.153800228976328945, 58.54057627198102409 ) ) ;
#125186 = CARTESIAN_POINT ( 'NONE',  ( -5.719274019375978568, 21.55341960407610458, 105.2072429386477097 ) ) ;
#125187 = CARTESIAN_POINT ( 'NONE',  ( 16.52544592524335698, 4.483927247898782831, 76.45942372801901854 ) ) ;
#125188 = CARTESIAN_POINT ( 'NONE',  ( -24.68411608548793268, 7.148172978119906595, 167.5704058020754701 ) ) ;
#125189 = CARTESIAN_POINT ( 'NONE',  ( -13.89961937509957401, -13.97604488694547875, 29.37609039468565797 ) ) ;
#125190 = CARTESIAN_POINT ( 'NONE',  ( 9.564922557960805705, 16.46253265017160317, 64.58224293864769550 ) ) ;
#125191 = CARTESIAN_POINT ( 'NONE',  ( 4.379528057220339221, -16.55341960407611168, 57.70724293864770260 ) ) ;
#125192 = CARTESIAN_POINT ( 'NONE',  ( -12.14591786802309592, -12.06949235617757132, 91.87390960531436690 ) ) ;
#125193 = CARTESIAN_POINT ( 'NONE',  ( -5.153800228976328057, -19.02544592524343514, 107.2905762719810383 ) ) ;
#125194 = CARTESIAN_POINT ( 'NONE',  ( 0.05219959533909260263, 19.03943276465977164, 94.99890960531436690 ) ) ;
#125195 = CARTESIAN_POINT ( 'NONE',  ( -0.05219959533909027116, -19.03943276465977164, 112.4989096053143669 ) ) ;
#125196 = CARTESIAN_POINT ( 'NONE',  ( 0.05219959533937995610, -21.53943276465977519, 110.0010903946856757 ) ) ;
#125197 = CARTESIAN_POINT ( 'NONE',  ( 0.05219959533934541429, -16.53943276465976808, 95.00109039468568994 ) ) ;
#125198 = CARTESIAN_POINT ( 'NONE',  ( -0.05219959533937732626, 21.53943276465977519, 42.50109039468567573 ) ) ;
#125199 = CARTESIAN_POINT ( 'NONE',  ( 18.67979575497178502, 10.72451020669898547, 34.16557627198102409 ) ) ;
#125200 = CARTESIAN_POINT ( 'NONE',  ( -0.05219959533907301413, -21.53943276465977519, 102.4989096053143811 ) ) ;
#125201 = CARTESIAN_POINT ( 'NONE',  ( 16.52544592524342804, -4.483927247898539470, 58.54057627198103120 ) ) ;
#125202 = CARTESIAN_POINT ( 'NONE',  ( 5.153800228976335163, 19.02544592524342804, 59.79057627198100988 ) ) ;
#125203 = CARTESIAN_POINT ( 'NONE',  ( 12.14591786802309770, 12.06949235617756955, 84.37390960531438111 ) ) ;
#125204 = CARTESIAN_POINT ( 'NONE',  ( 21.52544592524344225, -5.823673210054117533, 43.54057627198103830 ) ) ;
#125205 = CARTESIAN_POINT ( 'NONE',  ( 0.05219959533936267826, -19.03943276465977164, 45.00109039468566863 ) ) ;
#125206 = CARTESIAN_POINT ( 'NONE',  ( 4.379528057220339221, -16.55341960407611168, 107.7072429386476955 ) ) ;
#125207 = ORIENTED_EDGE ( 'NONE', *, *, #6551, .T. ) ;
#125208 = CARTESIAN_POINT ( 'NONE',  ( 16.53943276465976808, 0.05219959533934440121, 71.25109039468568994 ) ) ;
#125209 = CARTESIAN_POINT ( 'NONE',  ( -9.564922557960796823, -16.46253265017161027, 72.08224293864770971 ) ) ;
#125210 = CARTESIAN_POINT ( 'NONE',  ( 27.73933785331498925, -9.013057229001034898, 143.7750000027311614 ) ) ;
#125211 = CARTESIAN_POINT ( 'NONE',  ( -8.224510206698948167, 14.34966873604960824, 85.41557627198102409 ) ) ;
#125212 = CARTESIAN_POINT ( 'NONE',  ( 15.80617190586746368, 15.72974639402197994, 34.37390960531435979 ) ) ;
#125213 = CARTESIAN_POINT ( 'NONE',  ( 4.483927247898790824, -16.52544592524335698, 105.2094237280190328 ) ) ;
#125214 = CARTESIAN_POINT ( 'NONE',  ( -8.314922557961024197, 14.29746914071037800, 22.91775706135235069 ) ) ;
#125215 = CARTESIAN_POINT ( 'NONE',  ( 5.719274019375673035, 21.55341960407619339, 92.29275706135236135 ) ) ;
#125216 = CARTESIAN_POINT ( 'NONE',  ( 19.02544592524343514, -5.153800228976328945, 83.54057627198100988 ) ) ;
#125217 = CARTESIAN_POINT ( 'NONE',  ( -21.52544592524334988, -5.823673210054445271, 18.95942372801901143 ) ) ;
#125218 = CARTESIAN_POINT ( 'NONE',  ( -16.51473224551069308, -9.474510206698971260, 36.66557627198102409 ) ) ;
#125219 = CARTESIAN_POINT ( 'NONE',  ( -4.483927247898782831, 16.52544592524335698, 32.70942372801900433 ) ) ;
#125220 = CARTESIAN_POINT ( 'NONE',  ( -0.05219959533936034679, 19.03943276465977164, 92.50109039468566152 ) ) ;
#125221 = CARTESIAN_POINT ( 'NONE',  ( -21.53943276465977519, 0.05219959533907696930, 96.24890960531435269 ) ) ;
#125222 = CARTESIAN_POINT ( 'NONE',  ( 5.153800228976615827, -19.02544592524334988, 65.20942372801900433 ) ) ;
#125223 = LINE ( 'NONE', #67516, #151157 ) ;
#125224 = CARTESIAN_POINT ( 'NONE',  ( -10.72451020669870658, -18.67979575497194134, 24.58442372801901499 ) ) ;
#125225 = CARTESIAN_POINT ( 'NONE',  ( -6.100000000000006750, 6.426762577456935076E-14, -64.53213882399991519 ) ) ;
#125226 = CARTESIAN_POINT ( 'NONE',  ( -19.05341960407611168, -5.049401038298163336, 76.45724293864769550 ) ) ;
#125227 = CARTESIAN_POINT ( 'NONE',  ( 4.483927247898790824, -16.52544592524335698, 30.20942372801902565 ) ) ;
#125228 = PLANE ( 'NONE',  #58020 ) ;
#125229 = CARTESIAN_POINT ( 'NONE',  ( 0.05219959533936267826, -19.03943276465977164, 65.00109039468567573 ) ) ;
#125231 = CARTESIAN_POINT ( 'NONE',  ( -16.52544592524342804, 4.483927247898546575, 81.04057627198102409 ) ) ;
#125230 = CARTESIAN_POINT ( 'NONE',  ( 5.823673210054125526, 21.52544592524343514, 114.7905762719810383 ) ) ;
#125232 = CARTESIAN_POINT ( 'NONE',  ( 19.02544592524343514, -5.153800228976328945, 78.54057627198099567 ) ) ;
#125234 = CARTESIAN_POINT ( 'NONE',  ( 13.89961937509957401, 13.97604488694547697, 36.87609039468565442 ) ) ;
#125233 = CARTESIAN_POINT ( 'NONE',  ( -16.53943276465976808, -0.05219959533934237506, 33.75109039468568284 ) ) ;
#125235 = CARTESIAN_POINT ( 'NONE',  ( 5.719274019375673035, 21.55341960407619339, 62.29275706135236845 ) ) ;
#125236 = CARTESIAN_POINT ( 'NONE',  ( -13.97604488694547697, 13.89961937509957934, 103.1260903946856473 ) ) ;
#125237 = CARTESIAN_POINT ( 'NONE',  ( -19.02544592524342804, 5.153800228976336051, 56.04057627198100988 ) ) ;
#125238 = CARTESIAN_POINT ( 'NONE',  ( 13.89961937509957401, 13.97604488694547697, 86.87609039468567573 ) ) ;
#125239 = CARTESIAN_POINT ( 'NONE',  ( -14.29746914071037622, -8.314922557961029526, 54.16775706135235424 ) ) ;
#125240 = CARTESIAN_POINT ( 'NONE',  ( 18.67979575497194134, -10.72451020669871369, 100.8344237280190185 ) ) ;
#125241 = CARTESIAN_POINT ( 'NONE',  ( -16.51473224551082808, 9.474510206698731452, 63.33442372801900433 ) ) ;
#125242 = CARTESIAN_POINT ( 'NONE',  ( -13.97604488694527625, -13.89961937509977652, 46.87390960531435979 ) ) ;
#125243 = CARTESIAN_POINT ( 'NONE',  ( -21.52544592524343514, 5.823673210054127303, 76.04057627198102409 ) ) ;
#125245 = CARTESIAN_POINT ( 'NONE',  ( -13.97604488694547697, 13.89961937509957934, 63.12609039468566152 ) ) ;
#125244 = CARTESIAN_POINT ( 'NONE',  ( 8.224510206698953496, -14.34966873604960469, 67.91557627198102409 ) ) ;
#125246 = CARTESIAN_POINT ( 'NONE',  ( 21.35096542554163079, 10.43949311476039554, 170.3901443614043671 ) ) ;
#125247 = CARTESIAN_POINT ( 'NONE',  ( -9.564922557961040184, 16.46253265017147172, 42.91775706135234003 ) ) ;
#125248 = CARTESIAN_POINT ( 'NONE',  ( 4.483927247898790824, -16.52544592524335698, 95.20942372801903275 ) ) ;
#125249 = CARTESIAN_POINT ( 'NONE',  ( -16.55341960407611168, -4.379528057220339221, 61.45724293864770260 ) ) ;
#125251 = CARTESIAN_POINT ( 'NONE',  ( -22.44159573604009950, -16.30477369853688430, 139.0750000027311728 ) ) ;
#125250 = CARTESIAN_POINT ( 'NONE',  ( 21.52544592524334988, 5.823673210054432836, 91.45942372801901854 ) ) ;
#125252 = CARTESIAN_POINT ( 'NONE',  ( 18.67979575497178502, 10.72451020669898547, 99.16557627198100988 ) ) ;
#125253 = CARTESIAN_POINT ( 'NONE',  ( 9.474510206698971260, -16.51473224551069308, 57.91557627198103120 ) ) ;
#125254 = CARTESIAN_POINT ( 'NONE',  ( 21.52544592524334988, 5.823673210054432836, 71.45942372801901854 ) ) ;
#125255 = CARTESIAN_POINT ( 'NONE',  ( 9.564922557960805705, 16.46253265017160317, 49.58224293864770260 ) ) ;
#125256 = ORIENTED_EDGE ( 'NONE', *, *, #50192, .F. ) ;
#125257 = CARTESIAN_POINT ( 'NONE',  ( -9.564922557960796823, -16.46253265017161027, 62.08224293864769550 ) ) ;
#125258 = CARTESIAN_POINT ( 'NONE',  ( -0.05219959533909027116, -19.03943276465977164, 22.49890960531436690 ) ) ;
#125259 = CARTESIAN_POINT ( 'NONE',  ( -19.05341960407611168, -5.049401038298163336, 106.4572429386476955 ) ) ;
#125260 = CARTESIAN_POINT ( 'NONE',  ( 12.14591786802309770, 12.06949235617756955, 59.37390960531436690 ) ) ;
#125261 = CARTESIAN_POINT ( 'NONE',  ( 13.89961937509977652, -13.97604488694527269, 28.12390960531435624 ) ) ;
#125262 = CARTESIAN_POINT ( 'NONE',  ( -16.53943276465976808, 0.05219959533911058130, 91.24890960531436690 ) ) ;
#125263 = VECTOR ( 'NONE', #99002, 1000.000000000000000 ) ;
#125264 = CARTESIAN_POINT ( 'NONE',  ( 5.719274019375991003, -21.55341960407610458, 97.70724293864772392 ) ) ;
#125265 = CARTESIAN_POINT ( 'NONE',  ( 21.53943276465977519, 0.05219959533937863772, 41.25109039468568284 ) ) ;
#125266 = CARTESIAN_POINT ( 'NONE',  ( 20.96320343559639454, -21.46320343559646560, 5.353553390593270400 ) ) ;
#125267 = CARTESIAN_POINT ( 'NONE',  ( 16.53943276465976808, 0.05219959533934440121, 51.25109039468568994 ) ) ;
#125268 = CARTESIAN_POINT ( 'NONE',  ( 5.823673210054125526, 21.52544592524343514, 89.79057627198103830 ) ) ;
#125269 = CARTESIAN_POINT ( 'NONE',  ( 10.72451020669871369, 18.67979575497193778, 107.0844237280190043 ) ) ;
#125270 = CARTESIAN_POINT ( 'NONE',  ( -9.564922557960796823, -16.46253265017161027, 107.0822429386476955 ) ) ;
#125271 = CARTESIAN_POINT ( 'NONE',  ( -21.52544592524334988, -5.823673210054445271, 48.95942372801902565 ) ) ;
#125272 = EDGE_CURVE ( 'NONE', #156405, #164148, #181747, .T. ) ;
#125273 = CARTESIAN_POINT ( 'NONE',  ( -0.05219959533907301413, -21.53943276465977519, 47.49890960531435979 ) ) ;
#125274 = CARTESIAN_POINT ( 'NONE',  ( -12.06949235617739369, -12.14591786802326823, 99.37609039468568994 ) ) ;
#125276 = CARTESIAN_POINT ( 'NONE',  ( 18.67979575497194134, -10.72451020669871369, 100.8344237280190185 ) ) ;
#125275 = CARTESIAN_POINT ( 'NONE',  ( -0.05219959533937732626, 21.53943276465977519, 67.50109039468568994 ) ) ;
#125277 = CARTESIAN_POINT ( 'NONE',  ( -16.46253265017146816, -9.564922557961047289, 34.16775706135233293 ) ) ;
#125278 = CARTESIAN_POINT ( 'NONE',  ( -16.52544592524335698, -4.483927247898792601, 83.95942372801900433 ) ) ;
#125279 = CARTESIAN_POINT ( 'NONE',  ( 0.05219959533937995610, -21.53943276465977519, 40.00109039468567573 ) ) ;
#125280 = CARTESIAN_POINT ( 'NONE',  ( -16.51473224551069308, -9.474510206698971260, 46.66557627198102409 ) ) ;
#125281 = CARTESIAN_POINT ( 'NONE',  ( 9.474510206698729675, 16.51473224551082808, 22.08442372801899722 ) ) ;
#125282 = CARTESIAN_POINT ( 'NONE',  ( -10.81492255796078084, -18.62759615963271287, 22.08224293864769194 ) ) ;
#125283 = CARTESIAN_POINT ( 'NONE',  ( -18.67979575497193778, 10.72451020669871902, 23.33442372801901499 ) ) ;
#125284 = CARTESIAN_POINT ( 'NONE',  ( -15.80617190586745835, -15.72974639402198527, 71.87390960531438111 ) ) ;
#125286 = CARTESIAN_POINT ( 'NONE',  ( 10.81492255796078972, 18.62759615963270932, 84.58224293864769550 ) ) ;
#125285 = CARTESIAN_POINT ( 'NONE',  ( -17.49999999999999645, -7.500000000000000888, 37.49999999999999289 ) ) ;
#125288 = CARTESIAN_POINT ( 'NONE',  ( 16.53943276465976808, -0.05219959533910856209, 68.74890960531435269 ) ) ;
#125287 = CARTESIAN_POINT ( 'NONE',  ( 14.34966873604972726, -8.224510206698740333, 65.83442372801900433 ) ) ;
#125289 = DIRECTION ( 'NONE',  ( 0.5367108174878537641, 0.8437662581494472791, -0.000000000000000000 ) ) ;
#125290 = CARTESIAN_POINT ( 'NONE',  ( 16.46253265017146816, 9.564922557961045513, 96.66775706135233293 ) ) ;
#125291 =( BOUNDED_CURVE ( )  B_SPLINE_CURVE ( 3, ( #177402, #148051, #162209, #74204 ),
 .UNSPECIFIED., .F., .F. ) 
 B_SPLINE_CURVE_WITH_KNOTS ( ( 4, 4 ),
 ( 1.570796326794896558, 2.115944711806982959 ),
 .UNSPECIFIED. ) 
 CURVE ( )  GEOMETRIC_REPRESENTATION_ITEM ( )  RATIONAL_B_SPLINE_CURVE ( ( 1.000000000000000000, 0.9753873905749756990, 0.9753873905749756990, 1.000000000000000000 ) ) 
 REPRESENTATION_ITEM ( '' )  );
#125292 = AXIS2_PLACEMENT_3D ( 'NONE', #169608, #79584, #31106 ) ;
#125293 = CARTESIAN_POINT ( 'NONE',  ( -193.3062444957834884, -155.7167183371838064, -4.999999999999999112 ) ) ;
#125294 = CARTESIAN_POINT ( 'NONE',  ( 12.06949235617739724, 12.14591786802326823, 41.87609039468568284 ) ) ;
#125295 = CARTESIAN_POINT ( 'NONE',  ( -15.80617190586745835, -15.72974639402198527, 111.8739096053143669 ) ) ;
#125296 = CARTESIAN_POINT ( 'NONE',  ( 21.52544592524344225, -5.823673210054117533, 68.54057627198103830 ) ) ;
#125297 = CARTESIAN_POINT ( 'NONE',  ( 21.53943276465977519, -0.05219959533907433946, 23.74890960531435269 ) ) ;
#125298 = CARTESIAN_POINT ( 'NONE',  ( -14.29746914071037622, -8.314922557961029526, 59.16775706135234714 ) ) ;
#125299 = CARTESIAN_POINT ( 'NONE',  ( -19.05341960407611168, -5.049401038298163336, 66.45724293864769550 ) ) ;
#125301 = CARTESIAN_POINT ( 'NONE',  ( -14.29746914071037622, -8.314922557961029526, 19.16775706135234714 ) ) ;
#125300 = CARTESIAN_POINT ( 'NONE',  ( 18.62759615963255655, 10.81492255796105972, 41.66775706135235424 ) ) ;
#125302 = CARTESIAN_POINT ( 'NONE',  ( -19.02544592524342804, 5.153800228976336051, 111.0405762719810099 ) ) ;
#125303 = CARTESIAN_POINT ( 'NONE',  ( 9.564922557961047289, -16.46253265017146816, 25.41775706135234003 ) ) ;
#125304 = CARTESIAN_POINT ( 'NONE',  ( 4.379528057220092307, 16.55341960407617563, 42.29275706135235424 ) ) ;
#125305 = CARTESIAN_POINT ( 'NONE',  ( -9.474510206698964154, 16.51473224551069663, 105.4155762719810383 ) ) ;
#125306 = CARTESIAN_POINT ( 'NONE',  ( -21.52544592524343514, 5.823673210054127303, 106.0405762719810525 ) ) ;
#125307 = CARTESIAN_POINT ( 'NONE',  ( -16.51473224551069308, -9.474510206698971260, 61.66557627198103120 ) ) ;
#125308 = CARTESIAN_POINT ( 'NONE',  ( -17.26058549869089731, 6.457015423128606990, 23.62254162523932521 ) ) ;
#125309 = CARTESIAN_POINT ( 'NONE',  ( 4.379528057220339221, -16.55341960407611168, 77.70724293864770971 ) ) ;
#125310 = CARTESIAN_POINT ( 'NONE',  ( 10.81492255796078972, 18.62759615963270932, 24.58224293864768839 ) ) ;
#125311 = CARTESIAN_POINT ( 'NONE',  ( -17.48853670773242897, 5.747243402303157112, 33.66671299749992130 ) ) ;
#125312 = CARTESIAN_POINT ( 'NONE',  ( 21.52544592524344225, -5.823673210054117533, 98.54057627198105251 ) ) ;
#125313 = CARTESIAN_POINT ( 'NONE',  ( -0.05219959533936034679, 19.03943276465977164, 57.50109039468566863 ) ) ;
#125314 = CARTESIAN_POINT ( 'NONE',  ( 13.89961937509977652, -13.97604488694527269, 113.1239096053143527 ) ) ;
#125315 = CARTESIAN_POINT ( 'NONE',  ( -19.05341960407611168, -5.049401038298163336, 26.45724293864769550 ) ) ;
#125316 = CARTESIAN_POINT ( 'NONE',  ( -21.52544592524343514, 5.823673210054127303, 56.04057627198102409 ) ) ;
#125317 = CARTESIAN_POINT ( 'NONE',  ( 16.46253265017160672, -9.564922557960803928, 103.3322429386476955 ) ) ;
#125318 = CARTESIAN_POINT ( 'NONE',  ( -10.81492255796105439, 18.62759615963255655, 77.91775706135231871 ) ) ;
#125319 = CARTESIAN_POINT ( 'NONE',  ( 19.02544592524343514, -5.153800228976328945, 53.54057627198102409 ) ) ;
#125320 = CARTESIAN_POINT ( 'NONE',  ( 14.29746914071049879, -8.314922557960816363, 83.33224293864769550 ) ) ;
#125321 = CARTESIAN_POINT ( 'NONE',  ( -4.379528057220086978, -16.55341960407618274, 29.79275706135234358 ) ) ;
#125322 = CARTESIAN_POINT ( 'NONE',  ( 19.02544592524343514, -5.153800228976328945, 63.54057627198103830 ) ) ;
#125323 = CARTESIAN_POINT ( 'NONE',  ( -15.72974639402176322, -15.80617190586768395, 64.37609039468568994 ) ) ;
#125324 = ORIENTED_EDGE ( 'NONE', *, *, #173096, .F. ) ;
#125325 = CARTESIAN_POINT ( 'NONE',  ( 19.03943276465977164, 0.05219959533936151252, 31.25109039468566863 ) ) ;
#125326 = CARTESIAN_POINT ( 'NONE',  ( 9.564922557961047289, -16.46253265017146816, 40.41775706135234003 ) ) ;
#125327 = CARTESIAN_POINT ( 'NONE',  ( 193.3062444957835453, -155.7167183371837496, -15.00000000000000178 ) ) ;
#125328 = CARTESIAN_POINT ( 'NONE',  ( 21.55341960407619695, -5.719274019375665929, 41.04275706135236135 ) ) ;
#125329 = CARTESIAN_POINT ( 'NONE',  ( -17.79613651744294600, 24.49428055684532524, 143.6843446569000093 ) ) ;
#125330 = CARTESIAN_POINT ( 'NONE',  ( 16.51473224551083163, -9.474510206698727899, 30.83442372801900433 ) ) ;
#125331 = CARTESIAN_POINT ( 'NONE',  ( 19.05341960407611168, 5.049401038298154454, 68.95724293864769550 ) ) ;
#125332 = CARTESIAN_POINT ( 'NONE',  ( 8.224510206698953496, -14.34966873604960469, 22.91557627198102765 ) ) ;
#125334 = CARTESIAN_POINT ( 'NONE',  ( -5.823673210054431948, 21.52544592524334988, 92.70942372801901854 ) ) ;
#125333 = CARTESIAN_POINT ( 'NONE',  ( -5.153800228976328057, -19.02544592524343514, 112.2905762719810099 ) ) ;
#125335 = CARTESIAN_POINT ( 'NONE',  ( -22.81625015709510507, 31.40387420917330275, -8.924999997268814766 ) ) ;
#125336 = CARTESIAN_POINT ( 'NONE',  ( -28.79475375365586842, 2.428612866367529932E-14, 155.0000000000000000 ) ) ;
#125337 = CARTESIAN_POINT ( 'NONE',  ( 21.55341960407619695, -5.719274019375665929, 81.04275706135236135 ) ) ;
#125338 = DIRECTION ( 'NONE',  ( -0.000000000000000000, -0.000000000000000000, -1.000000000000000000 ) ) ;
#125339 = CARTESIAN_POINT ( 'NONE',  ( 13.89961937509977652, -13.97604488694527269, 98.12390960531433848 ) ) ;
#125340 = CARTESIAN_POINT ( 'NONE',  ( -32.00000000000000000, -1.163414459189985801E-14, 95.00000000000000000 ) ) ;
#125341 = CARTESIAN_POINT ( 'NONE',  ( -9.564922557960796823, -16.46253265017161027, 52.08224293864768839 ) ) ;
#125342 = CARTESIAN_POINT ( 'NONE',  ( -15.80617190586745835, -15.72974639402198527, 71.87390960531438111 ) ) ;
#125343 = CARTESIAN_POINT ( 'NONE',  ( -4.379528057220328563, 16.55341960407611168, 30.20724293864769550 ) ) ;
#125345 = CARTESIAN_POINT ( 'NONE',  ( 16.46253265017160672, -9.564922557960803928, 88.33224293864769550 ) ) ;
#125344 = CARTESIAN_POINT ( 'NONE',  ( -14.29746914071049879, 8.314922557960819915, 115.8322429386477097 ) ) ;
#125346 = CARTESIAN_POINT ( 'NONE',  ( 15.72974639402176855, 15.80617190586768217, 111.8760903946856615 ) ) ;
#125347 = EDGE_CURVE ( 'NONE', #143210, #56919, #151514, .T. ) ;
#125348 = CARTESIAN_POINT ( 'NONE',  ( 16.53943276465976808, -0.05219959533910856209, 108.7489096053143669 ) ) ;
#125349 = CARTESIAN_POINT ( 'NONE',  ( 10.81492255796106328, -18.62759615963255655, 70.41775706135236135 ) ) ;
#125350 = CARTESIAN_POINT ( 'NONE',  ( -5.049401038298153566, 19.05341960407611168, 110.2072429386476671 ) ) ;
#125351 = CARTESIAN_POINT ( 'NONE',  ( -4.483927247898782831, 16.52544592524335698, 102.7094237280190185 ) ) ;
#125352 = CARTESIAN_POINT ( 'NONE',  ( -5.153800228976607833, 19.02544592524334988, 62.70942372801899722 ) ) ;
#125353 = CARTESIAN_POINT ( 'NONE',  ( -36.91746825000000598, 11.99521256947798520, -7.224999997268813701 ) ) ;
#125354 = CARTESIAN_POINT ( 'NONE',  ( 13.89961937509977652, -13.97604488694527269, 103.1239096053143527 ) ) ;
#125355 = CARTESIAN_POINT ( 'NONE',  ( 16.53943276465976808, -0.05219959533910856209, 73.74890960531433848 ) ) ;
#125356 = CARTESIAN_POINT ( 'NONE',  ( -9.564922557961040184, 16.46253265017147172, 57.91775706135233293 ) ) ;
#125357 = CARTESIAN_POINT ( 'NONE',  ( -19.03943276465977164, 0.05219959533909376836, 61.24890960531436690 ) ) ;
#125358 = CARTESIAN_POINT ( 'NONE',  ( -8.314922557960811034, -14.29746914071050412, 62.08224293864769550 ) ) ;
#125359 = CARTESIAN_POINT ( 'NONE',  ( 16.51473224551083163, -9.474510206698727899, 95.83442372801900433 ) ) ;
#125360 = CARTESIAN_POINT ( 'NONE',  ( -10.72451020669898014, 18.67979575497178502, 45.41557627198103830 ) ) ;
#125361 = VERTEX_POINT ( 'NONE', #26388 ) ;
#125362 = EDGE_CURVE ( 'NONE', #134824, #163522, #2974, .T. ) ;
#125363 = CARTESIAN_POINT ( 'NONE',  ( 14.34966873604960469, 8.224510206698951720, 109.1655762719810383 ) ) ;
#125364 = CARTESIAN_POINT ( 'NONE',  ( -17.44270441346514033, -5.991230190323105553, 31.36335079264230430 ) ) ;
#125366 = CARTESIAN_POINT ( 'NONE',  ( 21.53943276465977519, -0.05219959533907433946, 68.74890960531435269 ) ) ;
#125365 = CARTESIAN_POINT ( 'NONE',  ( 19.02544592524343514, -5.153800228976328945, 73.54057627198103830 ) ) ;
#125368 = CARTESIAN_POINT ( 'NONE',  ( -16.51473224551069308, -9.474510206698971260, 71.66557627198102409 ) ) ;
#125367 = CARTESIAN_POINT ( 'NONE',  ( 14.29746914071037800, 8.314922557961029526, 91.66775706135234714 ) ) ;
#125369 = CARTESIAN_POINT ( 'NONE',  ( -13.89961937509957401, -13.97604488694547875, 59.37609039468566863 ) ) ;
#125370 = CARTESIAN_POINT ( 'NONE',  ( -21.55341960407619339, 5.719274019375674811, 78.54275706135236135 ) ) ;
#125371 = CARTESIAN_POINT ( 'NONE',  ( -15.72974639402197994, 15.80617190586746368, 65.62390960531436690 ) ) ;
#125372 = CARTESIAN_POINT ( 'NONE',  ( 9.474510206698971260, -16.51473224551069308, 107.9155762719810383 ) ) ;
#125373 = CARTESIAN_POINT ( 'NONE',  ( 0.05219959533909260263, 19.03943276465977164, 34.99890960531435979 ) ) ;
#125374 = CARTESIAN_POINT ( 'NONE',  ( 4.483927247898790824, -16.52544592524335698, 100.2094237280190043 ) ) ;
#125375 = CARTESIAN_POINT ( 'NONE',  ( 16.55341960407618274, -4.379528057220086978, 21.04275706135234714 ) ) ;
#125376 = CARTESIAN_POINT ( 'NONE',  ( 19.34837522270368382, 5.499999999999744205, 78.36337684832574269 ) ) ;
#125377 = CARTESIAN_POINT ( 'NONE',  ( 15.80617190586769283, -15.72974639402175789, 95.62609039468568994 ) ) ;
#125378 = CARTESIAN_POINT ( 'NONE',  ( 8.314922557960818139, 14.29746914071049879, 64.58224293864769550 ) ) ;
#125379 = CARTESIAN_POINT ( 'NONE',  ( 8.224510206698953496, -14.34966873604960469, 72.91557627198103830 ) ) ;
#125380 = CARTESIAN_POINT ( 'NONE',  ( 10.81492255796078972, 18.62759615963270932, 89.58224293864768129 ) ) ;
#125381 = CARTESIAN_POINT ( 'NONE',  ( -5.823673210054116645, -21.52544592524344225, 87.29057627198103830 ) ) ;
#125382 = CARTESIAN_POINT ( 'NONE',  ( -1.054302444749779077, -31.48176515315803670, -46.25693415911323569 ) ) ;
#125383 = CARTESIAN_POINT ( 'NONE',  ( 10.72451020669898902, -18.67979575497178502, 47.91557627198102409 ) ) ;
#125384 = CARTESIAN_POINT ( 'NONE',  ( -16.55341960407617563, 4.379528057220093196, 73.54275706135234714 ) ) ;
#125385 = CARTESIAN_POINT ( 'NONE',  ( 4.379528057220339221, -16.55341960407611168, 87.70724293864769550 ) ) ;
#125386 = CARTESIAN_POINT ( 'NONE',  ( 5.049401038298161559, -19.05341960407611168, 42.70724293864767418 ) ) ;
#125387 = CARTESIAN_POINT ( 'NONE',  ( 34.57969012852954904, -4.582005219005605312, 50.95785156492174650 ) ) ;
#125388 = CARTESIAN_POINT ( 'NONE',  ( 8.224510206698742110, 14.34966873604972548, 102.0844237280190185 ) ) ;
#125389 = CARTESIAN_POINT ( 'NONE',  ( -10.81492255796105439, 18.62759615963255655, 32.91775706135234714 ) ) ;
#125390 = CARTESIAN_POINT ( 'NONE',  ( -13.97604488694527625, -13.89961937509977652, 96.87390960531433848 ) ) ;
#125391 = CARTESIAN_POINT ( 'NONE',  ( -15.72974639402176322, -15.80617190586768395, 64.37609039468568994 ) ) ;
#125392 = DIRECTION ( 'NONE',  ( 0.9945218953682734009, 0.000000000000000000, 0.1045284632676537068 ) ) ;
#125393 = CARTESIAN_POINT ( 'NONE',  ( 19.03943276465977164, -0.05219959533909143690, 23.74890960531435269 ) ) ;
#125394 = VERTEX_POINT ( 'NONE', #116374 ) ;
#125395 = CARTESIAN_POINT ( 'NONE',  ( 5.823673210054444382, -21.52544592524334988, 65.20942372801901854 ) ) ;
#125397 = CARTESIAN_POINT ( 'NONE',  ( 13.97604488694527802, 13.89961937509977652, 24.37390960531435624 ) ) ;
#125396 = CARTESIAN_POINT ( 'NONE',  ( -13.89961937509977652, 13.97604488694528158, 45.62390960531433848 ) ) ;
#125398 = CARTESIAN_POINT ( 'NONE',  ( 19.05341960407611168, 5.049401038298154454, 93.95724293864769550 ) ) ;
#125399 = CARTESIAN_POINT ( 'NONE',  ( 19.03943276465977164, 0.05219959533936151252, 61.25109039468566863 ) ) ;
#125400 = CARTESIAN_POINT ( 'NONE',  ( 5.719274019375673035, 21.55341960407619339, 42.29275706135235424 ) ) ;
#125401 = CARTESIAN_POINT ( 'NONE',  ( 19.03943276465977164, 0.05219959533936151252, 56.25109039468566863 ) ) ;
#125402 = CARTESIAN_POINT ( 'NONE',  ( 9.564922557960805705, 16.46253265017160317, 44.58224293864769550 ) ) ;
#125403 = CARTESIAN_POINT ( 'NONE',  ( 4.483927247898790824, -16.52544592524335698, 110.2094237280190185 ) ) ;
#125404 = CARTESIAN_POINT ( 'NONE',  ( 16.46253265017146816, 9.564922557961045513, 81.66775706135233293 ) ) ;
#125405 = CARTESIAN_POINT ( 'NONE',  ( -16.52544592524342804, 4.483927247898546575, 26.04057627198103475 ) ) ;
#125406 = CARTESIAN_POINT ( 'NONE',  ( 5.049401038297881783, 19.05341960407617563, 52.29275706135234003 ) ) ;
#125407 = CARTESIAN_POINT ( 'NONE',  ( 19.03943276465977164, -0.05219959533909143690, 103.7489096053143669 ) ) ;
#125408 = CARTESIAN_POINT ( 'NONE',  ( -15.80617190586768217, 15.72974639402176855, 103.1260903946856757 ) ) ;
#125409 = CARTESIAN_POINT ( 'NONE',  ( -13.97604488694547697, 13.89961937509957934, 23.12609039468565442 ) ) ;
#125410 = CARTESIAN_POINT ( 'NONE',  ( 9.474510206698971260, -16.51473224551069308, 32.91557627198102409 ) ) ;
#125411 = CARTESIAN_POINT ( 'NONE',  ( -18.62759615963255300, -10.81492255796106328, 84.16775706135234714 ) ) ;
#125412 = CARTESIAN_POINT ( 'NONE',  ( -8.224510206698735004, -14.34966873604973081, 29.58442372801901854 ) ) ;
#125413 = CARTESIAN_POINT ( 'NONE',  ( 16.51473224551069308, 9.474510206698969483, 94.16557627198103830 ) ) ;
#125414 = CARTESIAN_POINT ( 'NONE',  ( -8.571926809382608425, 26.38167802310805854, 140.4750000027312069 ) ) ;
#125415 = CARTESIAN_POINT ( 'NONE',  ( 13.89961937509977652, -13.97604488694527269, 73.12390960531436690 ) ) ;
#125416 = CARTESIAN_POINT ( 'NONE',  ( -5.429308488886486681E-15, 30.30510711980690175, 141.5000000000000000 ) ) ;
#125417 = CARTESIAN_POINT ( 'NONE',  ( 5.049401038297881783, 19.05341960407617563, 87.29275706135234714 ) ) ;
#125418 = CARTESIAN_POINT ( 'NONE',  ( -5.153800228976328057, -19.02544592524343514, 102.2905762719810383 ) ) ;
#125419 = CARTESIAN_POINT ( 'NONE',  ( 21.55341960407619695, -5.719274019375665929, 106.0427570613523471 ) ) ;
#125420 = CARTESIAN_POINT ( 'NONE',  ( 8.314922557960818139, 14.29746914071049879, 104.5822429386477097 ) ) ;
#125421 = CARTESIAN_POINT ( 'NONE',  ( 19.83802472612679324, -12.02135855755840232, 167.9999999999999716 ) ) ;
#125422 = CARTESIAN_POINT ( 'NONE',  ( 10.81492255796078972, 18.62759615963270932, 49.58224293864769550 ) ) ;
#125423 = CARTESIAN_POINT ( 'NONE',  ( -21.55341960407610458, -5.719274019375992779, 41.45724293864769550 ) ) ;
#125424 = CARTESIAN_POINT ( 'NONE',  ( -12.06949235617756955, 12.14591786802309770, 110.6239096053143669 ) ) ;
#125425 = CARTESIAN_POINT ( 'NONE',  ( -14.82342540975555600, 1.464556741314251731, -62.12362001602809869 ) ) ;
#125426 = CARTESIAN_POINT ( 'NONE',  ( 19.03943276465977164, 0.05219959533936151252, 61.25109039468566863 ) ) ;
#125427 = CARTESIAN_POINT ( 'NONE',  ( -0.05219959533910754901, -16.53943276465976808, 37.49890960531436690 ) ) ;
#125428 = CARTESIAN_POINT ( 'NONE',  ( -5.049401038298153566, 19.05341960407611168, 115.2072429386477097 ) ) ;
#125429 = CARTESIAN_POINT ( 'NONE',  ( -21.52544592524334988, -5.823673210054445271, 83.95942372801900433 ) ) ;
#125430 = CARTESIAN_POINT ( 'NONE',  ( 5.823673210054125526, 21.52544592524343514, 69.79057627198102409 ) ) ;
#125431 = CARTESIAN_POINT ( 'NONE',  ( -21.55341960407619339, 5.719274019375674811, 43.54275706135235424 ) ) ;
#125432 = CARTESIAN_POINT ( 'NONE',  ( -10.81492255796078084, -18.62759615963271287, 92.08224293864769550 ) ) ;
#125433 = CARTESIAN_POINT ( 'NONE',  ( 21.52544592524334988, 5.823673210054432836, 51.45942372801901854 ) ) ;
#125434 = CARTESIAN_POINT ( 'NONE',  ( 19.05341960407611168, 5.049401038298154454, 23.95724293864769194 ) ) ;
#125435 = CARTESIAN_POINT ( 'NONE',  ( 19.03943276465977164, -0.05219959533909143690, 83.74890960531436690 ) ) ;
#125436 = CARTESIAN_POINT ( 'NONE',  ( 16.55341960407618274, -4.379528057220086978, 76.04275706135237556 ) ) ;
#125437 = CARTESIAN_POINT ( 'NONE',  ( 16.55341960407611168, 4.379528057220329451, 103.9572429386476813 ) ) ;
#125438 = CARTESIAN_POINT ( 'NONE',  ( -5.153800228976328057, -19.02544592524343514, 107.2905762719810383 ) ) ;
#125439 = CARTESIAN_POINT ( 'NONE',  ( 12.06949235617757843, -12.14591786802309237, 53.12390960531436690 ) ) ;
#125440 = CARTESIAN_POINT ( 'NONE',  ( 8.314922557960818139, 14.29746914071049879, 24.58224293864768839 ) ) ;
#125441 = CARTESIAN_POINT ( 'NONE',  ( -9.564922557960796823, -16.46253265017161027, 67.08224293864769550 ) ) ;
#125442 = CARTESIAN_POINT ( 'NONE',  ( -9.474510206698964154, 16.51473224551069663, 35.41557627198102409 ) ) ;
#125443 = CARTESIAN_POINT ( 'NONE',  ( 10.81492255796078972, 18.62759615963270932, 44.58224293864769550 ) ) ;
#125444 = CARTESIAN_POINT ( 'NONE',  ( -16.46253265017146816, -9.564922557961047289, 34.16775706135233293 ) ) ;
#125446 = CARTESIAN_POINT ( 'NONE',  ( -14.34966873604960291, -8.224510206698953496, 31.66557627198102054 ) ) ;
#125445 = FACE_OUTER_BOUND ( 'NONE', #82461, .T. ) ;
#125447 = CARTESIAN_POINT ( 'NONE',  ( 19.02544592524343514, -5.153800228976328945, 113.5405762719810241 ) ) ;
#125448 = CARTESIAN_POINT ( 'NONE',  ( 10.72451020669871369, 18.67979575497193778, 62.08442372801901143 ) ) ;
#125449 = CARTESIAN_POINT ( 'NONE',  ( 5.153800228976335163, 19.02544592524342804, 114.7905762719810241 ) ) ;
#125450 = CARTESIAN_POINT ( 'NONE',  ( 12.06949235617739724, 12.14591786802326823, 61.87609039468568284 ) ) ;
#125451 = CARTESIAN_POINT ( 'NONE',  ( 19.03943276465977164, 0.05219959533936151252, 56.25109039468566863 ) ) ;
#125452 = CARTESIAN_POINT ( 'NONE',  ( -12.14591786802309592, -12.06949235617757132, 41.87390960531435979 ) ) ;
#125453 = CARTESIAN_POINT ( 'NONE',  ( -18.87255363501902394, -5.500000000000063949, 76.32513748171827217 ) ) ;
#125454 = CARTESIAN_POINT ( 'NONE',  ( 16.53943276465976808, 0.05219959533934440121, 101.2510903946856757 ) ) ;
#125455 = CARTESIAN_POINT ( 'NONE',  ( 19.03943276465977164, -0.05219959533909143690, 38.74890960531436690 ) ) ;
#125456 = CARTESIAN_POINT ( 'NONE',  ( -0.05219959533909027116, -19.03943276465977164, 67.49890960531436690 ) ) ;
#125457 = CARTESIAN_POINT ( 'NONE',  ( 19.05341960407611168, 5.049401038298154454, 28.95724293864769550 ) ) ;
#125458 = CARTESIAN_POINT ( 'NONE',  ( 5.719274019375673035, 21.55341960407619339, 37.29275706135235424 ) ) ;
#125459 = CARTESIAN_POINT ( 'NONE',  ( -13.89961937509977652, 13.97604488694528158, 60.62390960531436690 ) ) ;
#125460 = CARTESIAN_POINT ( 'NONE',  ( 1.820000000000000062, 0.000000000000000000, 0.000000000000000000 ) ) ;
#125461 = CARTESIAN_POINT ( 'NONE',  ( 16.51473224551069308, 9.474510206698969483, 49.16557627198102409 ) ) ;
#125462 = EDGE_CURVE ( 'NONE', #168063, #127046, #38490, .T. ) ;
#125463 = CARTESIAN_POINT ( 'NONE',  ( 21.53943276465977519, -0.05219959533907433946, 23.74890960531435269 ) ) ;
#125465 = CARTESIAN_POINT ( 'NONE',  ( 16.51473224551069308, 9.474510206698969483, 29.16557627198103475 ) ) ;
#125464 = CARTESIAN_POINT ( 'NONE',  ( 5.719274019375673035, 21.55341960407619339, 62.29275706135236845 ) ) ;
#125466 = CARTESIAN_POINT ( 'NONE',  ( -0.05219959533907301413, -21.53943276465977519, 27.49890960531435269 ) ) ;
#125467 = CARTESIAN_POINT ( 'NONE',  ( -14.29746914071037622, -8.314922557961029526, 79.16775706135234714 ) ) ;
#125468 = CARTESIAN_POINT ( 'NONE',  ( -21.55341960407619339, 5.719274019375674811, 108.5427570613523756 ) ) ;
#125469 = CARTESIAN_POINT ( 'NONE',  ( 16.53943276465976808, 0.05219959533934440121, 51.25109039468568994 ) ) ;
#125470 = CARTESIAN_POINT ( 'NONE',  ( 13.89961937509977652, -13.97604488694527269, 93.12390960531436690 ) ) ;
#125471 = EDGE_CURVE ( 'NONE', #42510, #171133, #70879, .T. ) ;
#125472 = CARTESIAN_POINT ( 'NONE',  ( -8.314922557961024197, 14.29746914071037800, 47.91775706135234714 ) ) ;
#125473 = CARTESIAN_POINT ( 'NONE',  ( -16.55341960407617563, 4.379528057220093196, 23.54275706135235424 ) ) ;
#125474 = CARTESIAN_POINT ( 'NONE',  ( -8.224510206698735004, -14.34966873604973081, 94.58442372801901854 ) ) ;
#125475 = CARTESIAN_POINT ( 'NONE',  ( 0.05219959533937995610, -21.53943276465977519, 55.00109039468568284 ) ) ;
#125476 = CARTESIAN_POINT ( 'NONE',  ( -19.05341960407617563, 5.049401038297882671, 103.5427570613523329 ) ) ;
#125477 = CARTESIAN_POINT ( 'NONE',  ( -18.67979575497178146, -10.72451020669898902, 106.6655762719810383 ) ) ;
#125479 = CARTESIAN_POINT ( 'NONE',  ( 9.474510206698729675, 16.51473224551082808, 102.0844237280190043 ) ) ;
#125478 = CARTESIAN_POINT ( 'NONE',  ( 16.52544592524342804, -4.483927247898539470, 98.54057627198105251 ) ) ;
#125480 = CARTESIAN_POINT ( 'NONE',  ( 12.06949235617739724, 12.14591786802326823, 86.87609039468568994 ) ) ;
#125481 = DIRECTION ( 'NONE',  ( 0.8164965809277261455, -6.938893903907231336E-16, 0.5773502691896253980 ) ) ;
#125482 = CARTESIAN_POINT ( 'NONE',  ( -13.97604488694547697, 13.89961937509957934, 78.12609039468567573 ) ) ;
#125483 = CARTESIAN_POINT ( 'NONE',  ( 8.224510206698953496, -14.34966873604960469, 47.91557627198102409 ) ) ;
#125484 = CARTESIAN_POINT ( 'NONE',  ( -12.14591786802309592, -12.06949235617757132, 46.87390960531435979 ) ) ;
#125485 = CARTESIAN_POINT ( 'NONE',  ( 4.379528057220339221, -16.55341960407611168, 107.7072429386476955 ) ) ;
#125486 = CARTESIAN_POINT ( 'NONE',  ( -19.05341960407617563, 5.049401038297882671, 48.54275706135233293 ) ) ;
#125487 = CARTESIAN_POINT ( 'NONE',  ( 18.62759615963255655, 10.81492255796105972, 31.66775706135234358 ) ) ;
#125488 = CARTESIAN_POINT ( 'NONE',  ( 19.03943276465977164, 0.05219959533936151252, 106.2510903946856615 ) ) ;
#125489 = CARTESIAN_POINT ( 'NONE',  ( 3.889087296526082316, 6.412877669190294228, 1.818019484660534424 ) ) ;
#125490 = CARTESIAN_POINT ( 'NONE',  ( 13.89961937509977652, -13.97604488694527269, 108.1239096053143669 ) ) ;
#125491 = CARTESIAN_POINT ( 'NONE',  ( 13.97604488694527802, 13.89961937509977652, 94.37390960531436690 ) ) ;
#125492 = CARTESIAN_POINT ( 'NONE',  ( 10.72451020669898902, -18.67979575497178502, 52.91557627198103830 ) ) ;
#125493 = CARTESIAN_POINT ( 'NONE',  ( 12.06949235617757843, -12.14591786802309237, 108.1239096053143811 ) ) ;
#125494 = CARTESIAN_POINT ( 'NONE',  ( 16.51473224551069308, 9.474510206698969483, 74.16557627198103830 ) ) ;
#125495 = CARTESIAN_POINT ( 'NONE',  ( 5.153800228976335163, 19.02544592524342804, 34.79057627198102409 ) ) ;
#125496 = CARTESIAN_POINT ( 'NONE',  ( 18.67979575497194134, -10.72451020669871369, 35.83442372801901143 ) ) ;
#125497 = CARTESIAN_POINT ( 'NONE',  ( 5.823673210054444382, -21.52544592524334988, 75.20942372801901854 ) ) ;
#125498 = CARTESIAN_POINT ( 'NONE',  ( -8.314922557961024197, 14.29746914071037800, 92.91775706135236135 ) ) ;
#125499 = CARTESIAN_POINT ( 'NONE',  ( 10.72451020669871369, 18.67979575497193778, 27.08442372801901854 ) ) ;
#125500 = CARTESIAN_POINT ( 'NONE',  ( 18.67979575497194134, -10.72451020669871369, 25.83442372801901499 ) ) ;
#125502 = CARTESIAN_POINT ( 'NONE',  ( 19.03943276465977164, -0.05219959533909143690, 73.74890960531435269 ) ) ;
#125501 = CARTESIAN_POINT ( 'NONE',  ( -13.97604488694547697, 13.89961937509957934, 68.12609039468563310 ) ) ;
#125503 = CARTESIAN_POINT ( 'NONE',  ( 18.67979575497194134, -10.72451020669871369, 85.83442372801901854 ) ) ;
#125504 = EDGE_CURVE ( 'NONE', #122086, #162114, #72, .T. ) ;
#125505 = CARTESIAN_POINT ( 'NONE',  ( 18.67979575497178502, 10.72451020669898547, 89.16557627198102409 ) ) ;
#125506 = CARTESIAN_POINT ( 'NONE',  ( 4.483927247898545687, 16.52544592524342804, 64.79057627198103830 ) ) ;
#125507 = CARTESIAN_POINT ( 'NONE',  ( -15.80617190586768217, 15.72974639402176855, 98.12609039468570415 ) ) ;
#125508 = CARTESIAN_POINT ( 'NONE',  ( -4.379528057220328563, 16.55341960407611168, 80.20724293864769550 ) ) ;
#125509 = CARTESIAN_POINT ( 'NONE',  ( 9.474510206698971260, -16.51473224551069308, 22.91557627198102765 ) ) ;
#125510 = CARTESIAN_POINT ( 'NONE',  ( -16.46253265017146816, -9.564922557961047289, 69.16775706135233293 ) ) ;
#125511 = CARTESIAN_POINT ( 'NONE',  ( -4.379528057220328563, 16.55341960407611168, 30.20724293864769550 ) ) ;
#125512 = CARTESIAN_POINT ( 'NONE',  ( -18.62759615963255300, -10.81492255796106328, 79.16775706135234714 ) ) ;
#125513 = CARTESIAN_POINT ( 'NONE',  ( 5.153800228976335163, 19.02544592524342804, 94.79057627198103830 ) ) ;
#125514 = CARTESIAN_POINT ( 'NONE',  ( -16.51473224551082808, 9.474510206698731452, 58.33442372801900433 ) ) ;
#125515 = CARTESIAN_POINT ( 'NONE',  ( -0.05219959533907301413, -21.53943276465977519, 67.49890960531436690 ) ) ;
#125516 = CARTESIAN_POINT ( 'NONE',  ( 10.72451020669871369, 18.67979575497193778, 22.08442372801901143 ) ) ;
#125517 = CARTESIAN_POINT ( 'NONE',  ( -4.483927247898782831, 16.52544592524335698, 22.70942372801901499 ) ) ;
#125518 = CARTESIAN_POINT ( 'NONE',  ( -16.53943276465976808, -0.05219959533934237506, 83.75109039468568994 ) ) ;
#125520 = CARTESIAN_POINT ( 'NONE',  ( 5.719274019375673035, 21.55341960407619339, 22.29275706135235069 ) ) ;
#125519 = CARTESIAN_POINT ( 'NONE',  ( -22.00000000000000000, -1.132798289211302014E-14, 92.50000000000000000 ) ) ;
#125521 = CARTESIAN_POINT ( 'NONE',  ( 16.52544592524342804, -4.483927247898539470, 103.5405762719810383 ) ) ;
#125522 = CARTESIAN_POINT ( 'NONE',  ( 36.91746825000000598, -11.99521256947793546, -8.224999997268810148 ) ) ;
#125523 = CARTESIAN_POINT ( 'NONE',  ( 16.52544592524335698, 4.483927247898782831, 31.45942372801901854 ) ) ;
#125524 = CARTESIAN_POINT ( 'NONE',  ( 21.53943276465977519, -0.05219959533907433946, 68.74890960531435269 ) ) ;
#125525 = CARTESIAN_POINT ( 'NONE',  ( -14.34966873604972548, 8.224510206698743886, 108.3344237280190185 ) ) ;
#125526 = CARTESIAN_POINT ( 'NONE',  ( -14.29746914071037622, -8.314922557961029526, 39.16775706135235424 ) ) ;
#125527 = CARTESIAN_POINT ( 'NONE',  ( 13.97604488694527802, 13.89961937509977652, 29.37390960531435979 ) ) ;
#125528 = CARTESIAN_POINT ( 'NONE',  ( -0.05219959533934338120, 16.53943276465976808, 77.50109039468567573 ) ) ;
#125529 = CARTESIAN_POINT ( 'NONE',  ( 5.049401038297881783, 19.05341960407617563, 72.29275706135234714 ) ) ;
#125530 = CARTESIAN_POINT ( 'NONE',  ( 5.719274019375991003, -21.55341960407610458, 72.70724293864769550 ) ) ;
#125531 = CARTESIAN_POINT ( 'NONE',  ( -4.483927247898782831, 16.52544592524335698, 97.70942372801904696 ) ) ;
#125532 = CARTESIAN_POINT ( 'NONE',  ( -18.67979575497193778, 10.72451020669871902, 78.33442372801901854 ) ) ;
#125533 = CARTESIAN_POINT ( 'NONE',  ( 10.72451020669898902, -18.67979575497178502, 57.91557627198103120 ) ) ;
#125534 = CARTESIAN_POINT ( 'NONE',  ( 10.81492255796078972, 18.62759615963270932, 49.58224293864769550 ) ) ;
#125535 = EDGE_LOOP ( 'NONE', ( #125590, #152253, #64714, #198841, #6505 ) ) ;
#125536 = VERTEX_POINT ( 'NONE', #161882 ) ;
#125537 = CARTESIAN_POINT ( 'NONE',  ( -8.314922557961024197, 14.29746914071037800, 72.91775706135234714 ) ) ;
#125538 = CARTESIAN_POINT ( 'NONE',  ( -15.80617190586745835, -15.72974639402198527, 41.87390960531435979 ) ) ;
#125539 = ORIENTED_EDGE ( 'NONE', *, *, #186126, .F. ) ;
#125540 = CARTESIAN_POINT ( 'NONE',  ( -16.46253265017160317, 9.564922557960807481, 95.83224293864769550 ) ) ;
#125541 = CARTESIAN_POINT ( 'NONE',  ( 7.652493125987820832, -39.26116846142902261, -13.00000000000000000 ) ) ;
#125542 = CARTESIAN_POINT ( 'NONE',  ( -0.05219959533909027116, -19.03943276465977164, 22.49890960531436690 ) ) ;
#125543 = CARTESIAN_POINT ( 'NONE',  ( -21.52544592524343514, 5.823673210054127303, 61.04057627198103120 ) ) ;
#125544 = CARTESIAN_POINT ( 'NONE',  ( -14.34966873604972548, 8.224510206698743886, 98.33442372801901854 ) ) ;
#125545 = CARTESIAN_POINT ( 'NONE',  ( 0.05219959533937995610, -21.53943276465977519, 40.00109039468567573 ) ) ;
#125546 = CARTESIAN_POINT ( 'NONE',  ( -0.05219959533936034679, 19.03943276465977164, 102.5010903946856757 ) ) ;
#125547 = CARTESIAN_POINT ( 'NONE',  ( 8.314922557960818139, 14.29746914071049879, 109.5822429386476955 ) ) ;
#125548 = CARTESIAN_POINT ( 'NONE',  ( 9.474510206698729675, 16.51473224551082808, 112.0844237280190043 ) ) ;
#125549 = CARTESIAN_POINT ( 'NONE',  ( -19.03943276465977164, 0.05219959533909376836, 46.24890960531435979 ) ) ;
#125550 = CARTESIAN_POINT ( 'NONE',  ( -17.81289503416611097, -24.51734667627696496, 142.2999999999999829 ) ) ;
#125551 = CARTESIAN_POINT ( 'NONE',  ( -19.03943276465977164, 0.05219959533909376836, 86.24890960531436690 ) ) ;
#125552 = CARTESIAN_POINT ( 'NONE',  ( 4.483927247898790824, -16.52544592524335698, 70.20942372801904696 ) ) ;
#125553 = CARTESIAN_POINT ( 'NONE',  ( -19.02544592524334988, -5.153800228976617603, 78.95942372801900433 ) ) ;
#125554 = CARTESIAN_POINT ( 'NONE',  ( -9.474510206698720793, -16.51473224551083518, 19.58442372801899722 ) ) ;
#125555 = CARTESIAN_POINT ( 'NONE',  ( 10.72451020669898902, -18.67979575497178502, 67.91557627198102409 ) ) ;
#125556 = CARTESIAN_POINT ( 'NONE',  ( 8.314922557961029526, -14.29746914071037800, 90.41775706135236135 ) ) ;
#125557 = CARTESIAN_POINT ( 'NONE',  ( 9.564922557961047289, -16.46253265017146816, 85.41775706135233293 ) ) ;
#125558 = CARTESIAN_POINT ( 'NONE',  ( -19.05341960407611168, -5.049401038298163336, 31.45724293864769550 ) ) ;
#125559 = CARTESIAN_POINT ( 'NONE',  ( 19.03943276465977164, -0.05219959533909143690, 83.74890960531436690 ) ) ;
#125560 = CARTESIAN_POINT ( 'NONE',  ( 21.52544592524334988, 5.823673210054432836, 51.45942372801901854 ) ) ;
#125561 = CARTESIAN_POINT ( 'NONE',  ( 13.97604488694527802, 13.89961937509977652, 44.37390960531435269 ) ) ;
#125562 = CARTESIAN_POINT ( 'NONE',  ( 16.51473224551083163, -9.474510206698727899, 75.83442372801900433 ) ) ;
#125563 = CARTESIAN_POINT ( 'NONE',  ( 21.73861122199297569, -7.688394669363299627, 173.2969830217476215 ) ) ;
#125564 = CARTESIAN_POINT ( 'NONE',  ( -19.02544592524342804, 5.153800228976336051, 111.0405762719810099 ) ) ;
#125565 = CARTESIAN_POINT ( 'NONE',  ( -8.314922557960811034, -14.29746914071050412, 67.08224293864770971 ) ) ;
#125566 = CARTESIAN_POINT ( 'NONE',  ( 5.719274019375991003, -21.55341960407610458, 57.70724293864770260 ) ) ;
#125567 = CARTESIAN_POINT ( 'NONE',  ( -3.181980515339492221, -6.791538853603052317, 1.110912703473986074 ) ) ;
#125568 = CARTESIAN_POINT ( 'NONE',  ( 9.474510206698729675, 16.51473224551082808, 27.08442372801900433 ) ) ;
#125570 = CARTESIAN_POINT ( 'NONE',  ( 5.049401038298161559, -19.05341960407611168, 72.70724293864768129 ) ) ;
#125569 = CARTESIAN_POINT ( 'NONE',  ( -19.05341960407611168, -5.049401038298163336, 66.45724293864769550 ) ) ;
#125571 = CARTESIAN_POINT ( 'NONE',  ( -16.55341960407617563, 4.379528057220093196, 53.54275706135234714 ) ) ;
#125572 = CARTESIAN_POINT ( 'NONE',  ( 23.31738231874054534, 16.94106989632529192, 143.1999999999999886 ) ) ;
#125573 = CARTESIAN_POINT ( 'NONE',  ( 0.000000000000000000, 0.000000000000000000, -63.95112321872120731 ) ) ;
#125574 = CARTESIAN_POINT ( 'NONE',  ( -8.224510206698735004, -14.34966873604973081, 94.58442372801901854 ) ) ;
#125575 = DIRECTION ( 'NONE',  ( -1.000000000000000000, -8.921435019309295657E-15, 0.000000000000000000 ) ) ;
#125576 = CARTESIAN_POINT ( 'NONE',  ( -16.53943276465976808, -0.05219959533934237506, 63.75109039468568284 ) ) ;
#125577 = CARTESIAN_POINT ( 'NONE',  ( 16.53943276465976808, 0.05219959533934440121, 46.25109039468567573 ) ) ;
#125579 = SPHERICAL_SURFACE ( 'NONE', #85699, 38.00000000000002132 ) ;
#125578 = CARTESIAN_POINT ( 'NONE',  ( -9.564922557960796823, -16.46253265017161027, 57.08224293864769550 ) ) ;
#125580 = CARTESIAN_POINT ( 'NONE',  ( -15.72974639402176322, -15.80617190586768395, 49.37609039468569705 ) ) ;
#125581 = CARTESIAN_POINT ( 'NONE',  ( -19.05341960407617563, 5.049401038297882671, 68.54275706135230450 ) ) ;
#125582 = CARTESIAN_POINT ( 'NONE',  ( -0.05219959533937732626, 21.53943276465977519, 102.5010903946856899 ) ) ;
#125583 = CARTESIAN_POINT ( 'NONE',  ( 13.89961937509977652, -13.97604488694527269, 33.12390960531434558 ) ) ;
#125584 = CARTESIAN_POINT ( 'NONE',  ( 37.99626262588768100, -12.34573411038909008, -7.102157773949824282 ) ) ;
#125585 = CARTESIAN_POINT ( 'NONE',  ( 21.53943276465977519, -0.05219959533907433946, 53.74890960531437401 ) ) ;
#125586 = CARTESIAN_POINT ( 'NONE',  ( -10.81492255796078084, -18.62759615963271287, 27.08224293864769550 ) ) ;
#125587 = CARTESIAN_POINT ( 'NONE',  ( 16.55341960407611168, 4.379528057220329451, 103.9572429386476813 ) ) ;
#125588 = CARTESIAN_POINT ( 'NONE',  ( -8.224510206698735004, -14.34966873604973081, 39.58442372801901143 ) ) ;
#125589 = CARTESIAN_POINT ( 'NONE',  ( 14.29746914071049879, -8.314922557960816363, 33.33224293864769550 ) ) ;
#125590 = ORIENTED_EDGE ( 'NONE', *, *, #175617, .F. ) ;
#125591 = CARTESIAN_POINT ( 'NONE',  ( 5.719274019375673035, 21.55341960407619339, 22.29275706135235069 ) ) ;
#125593 = CARTESIAN_POINT ( 'NONE',  ( -38.00000000000001421, -12.34694845685042708, -9.899999999999998579 ) ) ;
#125592 = CARTESIAN_POINT ( 'NONE',  ( -16.52544592524342804, 4.483927247898546575, 41.04057627198103120 ) ) ;
#125594 = CARTESIAN_POINT ( 'NONE',  ( -19.05341960407617563, 5.049401038297882671, 98.54275706135233293 ) ) ;
#125595 = CARTESIAN_POINT ( 'NONE',  ( 16.46253265017146816, 9.564922557961045513, 26.66775706135234003 ) ) ;
#125596 = CARTESIAN_POINT ( 'NONE',  ( 8.314922557960818139, 14.29746914071049879, 34.58224293864770260 ) ) ;
#125597 = CARTESIAN_POINT ( 'NONE',  ( 10.81492255796078972, 18.62759615963270932, 104.5822429386477097 ) ) ;
#125598 = CARTESIAN_POINT ( 'NONE',  ( -21.52544592524343514, 5.823673210054127303, 66.04057627198103830 ) ) ;
#125599 = CARTESIAN_POINT ( 'NONE',  ( -19.02544592524342804, 5.153800228976336051, 81.04057627198103830 ) ) ;
#125600 = CARTESIAN_POINT ( 'NONE',  ( -8.314922557960811034, -14.29746914071050412, 42.08224293864769550 ) ) ;
#125601 = CARTESIAN_POINT ( 'NONE',  ( -0.05219959533909027116, -19.03943276465977164, 87.49890960531436690 ) ) ;
#125602 = CARTESIAN_POINT ( 'NONE',  ( 34.78522506798721992, 2.428612866353961525E-14, 52.50000000000000000 ) ) ;
#125603 = CARTESIAN_POINT ( 'NONE',  ( 19.02544592524334988, 5.153800228976608722, 36.45942372801900433 ) ) ;
#125604 = CARTESIAN_POINT ( 'NONE',  ( 21.53943276465977519, -0.05219959533907433946, 88.74890960531436690 ) ) ;
#125605 = CARTESIAN_POINT ( 'NONE',  ( -14.29746914071049879, 8.314922557960819915, 100.8322429386477097 ) ) ;
#125606 = CARTESIAN_POINT ( 'NONE',  ( -0.05219959533937732626, 21.53943276465977519, 32.50109039468568284 ) ) ;
#125607 = CARTESIAN_POINT ( 'NONE',  ( 1.784210473542230573E-15, -29.16686587814331588, 139.3750000027311842 ) ) ;
#125608 = CARTESIAN_POINT ( 'NONE',  ( -12.06949235617756955, 12.14591786802309770, 25.62390960531435624 ) ) ;
#125609 = CARTESIAN_POINT ( 'NONE',  ( 16.46253265017160672, -9.564922557960803928, 38.33224293864768839 ) ) ;
#125610 = CARTESIAN_POINT ( 'NONE',  ( -5.153800228976328057, -19.02544592524343514, 87.29057627198103830 ) ) ;
#125611 = CARTESIAN_POINT ( 'NONE',  ( -15.80617190586745835, -15.72974639402198527, 66.87390960531436690 ) ) ;
#125612 = CARTESIAN_POINT ( 'NONE',  ( -18.22780087662122028, 5.500000000000031086, 43.51540105326107977 ) ) ;
#125613 = CARTESIAN_POINT ( 'NONE',  ( 0.05219959533909260263, 19.03943276465977164, 24.99890960531435269 ) ) ;
#125614 = CARTESIAN_POINT ( 'NONE',  ( -14.34966873604960291, -8.224510206698953496, 41.66557627198103120 ) ) ;
#125615 = EDGE_CURVE ( 'NONE', #199942, #88260, #15199, .T. ) ;
#125616 = CARTESIAN_POINT ( 'NONE',  ( -15.80617190586768217, 15.72974639402176855, 68.12609039468567573 ) ) ;
#125618 = CARTESIAN_POINT ( 'NONE',  ( -16.55341960407617563, 4.379528057220093196, 63.54275706135234003 ) ) ;
#125617 = CARTESIAN_POINT ( 'NONE',  ( 10.65591991699549368, -43.63381331854910172, -21.52219975116264195 ) ) ;
#125619 = CARTESIAN_POINT ( 'NONE',  ( -13.89961937509977652, 13.97604488694528158, 60.62390960531436690 ) ) ;
#125620 = CARTESIAN_POINT ( 'NONE',  ( 5.153800228976335163, 19.02544592524342804, 69.79057627198103830 ) ) ;
#125621 = ORIENTED_EDGE ( 'NONE', *, *, #65973, .F. ) ;
#125622 = CARTESIAN_POINT ( 'NONE',  ( -10.72451020669870658, -18.67979575497194134, 109.5844237280190328 ) ) ;
#125623 = CARTESIAN_POINT ( 'NONE',  ( 0.05219959533934541429, -16.53943276465976808, 75.00109039468568994 ) ) ;
#125624 = CARTESIAN_POINT ( 'NONE',  ( 21.55341960407619695, -5.719274019375665929, 101.0427570613523756 ) ) ;
#125625 = CARTESIAN_POINT ( 'NONE',  ( 19.05341960407611168, 5.049401038298154454, 58.95724293864768129 ) ) ;
#125626 = CARTESIAN_POINT ( 'NONE',  ( 18.62759615963271287, -10.81492255796078972, 33.33224293864769550 ) ) ;
#125627 = CARTESIAN_POINT ( 'NONE',  ( 9.474510206698729675, 16.51473224551082808, 102.0844237280190043 ) ) ;
#125628 = CARTESIAN_POINT ( 'NONE',  ( -15.72974639402176322, -15.80617190586768395, 79.37609039468567573 ) ) ;
#125629 = CARTESIAN_POINT ( 'NONE',  ( 0.05219959533934541429, -16.53943276465976808, 55.00109039468568284 ) ) ;
#125630 = CARTESIAN_POINT ( 'NONE',  ( 18.67979575497178502, 10.72451020669898547, 99.16557627198100988 ) ) ;
#125631 = CARTESIAN_POINT ( 'NONE',  ( 9.564922557961047289, -16.46253265017146816, 100.4177570613523329 ) ) ;
#125633 = EDGE_CURVE ( 'NONE', #44638, #99775, #196083, .T. ) ;
#125632 = CARTESIAN_POINT ( 'NONE',  ( 16.51473224551069308, 9.474510206698969483, 79.16557627198103830 ) ) ;
#125634 = CARTESIAN_POINT ( 'NONE',  ( 13.89961937509957401, 13.97604488694547697, 106.8760903946856757 ) ) ;
#125635 = CARTESIAN_POINT ( 'NONE',  ( -0.05219959533909027116, -19.03943276465977164, 42.49890960531435269 ) ) ;
#125636 = CARTESIAN_POINT ( 'NONE',  ( -4.483927247898782831, 16.52544592524335698, 22.70942372801901499 ) ) ;
#125637 = CARTESIAN_POINT ( 'NONE',  ( -16.53943276465976808, 0.05219959533911058130, 61.24890960531435979 ) ) ;
#125638 = CARTESIAN_POINT ( 'NONE',  ( -16.52544592524335698, -4.483927247898792601, 68.95942372801901854 ) ) ;
#125640 = CARTESIAN_POINT ( 'NONE',  ( 19.03943276465977164, -0.05219959533909143690, 53.74890960531436690 ) ) ;
#125639 = CARTESIAN_POINT ( 'NONE',  ( 21.55341960407619695, -5.719274019375665929, 26.04275706135235779 ) ) ;
#125641 = CARTESIAN_POINT ( 'NONE',  ( -19.05341960407611168, -5.049401038298163336, 66.45724293864769550 ) ) ;
#125642 = CARTESIAN_POINT ( 'NONE',  ( -4.483927247898782831, 16.52544592524335698, 67.70942372801901854 ) ) ;
#125643 = CARTESIAN_POINT ( 'NONE',  ( 17.81289503416610742, 24.51734667627700404, 145.5500000054623513 ) ) ;
#125644 = ORIENTED_EDGE ( 'NONE', *, *, #35339, .T. ) ;
#125645 = CARTESIAN_POINT ( 'NONE',  ( 5.719274019375673035, 21.55341960407619339, 107.2927570613523471 ) ) ;
#125646 = CARTESIAN_POINT ( 'NONE',  ( -5.153800228976328057, -19.02544592524343514, 42.29057627198101699 ) ) ;
#125647 = VERTEX_POINT ( 'NONE', #106180 ) ;
#125648 = CARTESIAN_POINT ( 'NONE',  ( 14.34966873604972726, -8.224510206698740333, 25.83442372801901499 ) ) ;
#125649 = AXIS2_PLACEMENT_3D ( 'NONE', #25396, #131543, #165887 ) ;
#125651 = CARTESIAN_POINT ( 'NONE',  ( -8.224510206698735004, -14.34966873604973081, 39.58442372801901143 ) ) ;
#125650 = CARTESIAN_POINT ( 'NONE',  ( 13.89961937509957401, 13.97604488694547697, 46.87609039468565442 ) ) ;
#125652 = CARTESIAN_POINT ( 'NONE',  ( -9.474510206698964154, 16.51473224551069663, 40.41557627198103120 ) ) ;
#125653 = CARTESIAN_POINT ( 'NONE',  ( -9.474510206698964154, 16.51473224551069663, 70.41557627198102409 ) ) ;
#125654 = CARTESIAN_POINT ( 'NONE',  ( 21.55341960407610458, 5.719274019375980345, 83.95724293864770971 ) ) ;
#125656 = CARTESIAN_POINT ( 'NONE',  ( -19.02544592524342804, 5.153800228976336051, 111.0405762719810099 ) ) ;
#125655 = CARTESIAN_POINT ( 'NONE',  ( 13.97604488694527802, 13.89961937509977652, 84.37390960531433848 ) ) ;
#125657 = CARTESIAN_POINT ( 'NONE',  ( 19.03943276465977164, -0.05219959533909143690, 68.74890960531436690 ) ) ;
#125658 = CARTESIAN_POINT ( 'NONE',  ( -22.44159573604010305, 16.30477369853692338, 149.1750000027311671 ) ) ;
#125659 = CARTESIAN_POINT ( 'NONE',  ( 5.049401038297881783, 19.05341960407617563, 102.2927570613523045 ) ) ;
#125660 = CARTESIAN_POINT ( 'NONE',  ( -21.53943276465977519, 0.05219959533907696930, 71.24890960531435269 ) ) ;
#125661 = CARTESIAN_POINT ( 'NONE',  ( 0.05219959533936267826, -19.03943276465977164, 25.00109039468566152 ) ) ;
#125662 = CARTESIAN_POINT ( 'NONE',  ( -8.314922557960811034, -14.29746914071050412, 62.08224293864769550 ) ) ;
#125663 = CARTESIAN_POINT ( 'NONE',  ( 10.81492255796106328, -18.62759615963255655, 90.41775706135236135 ) ) ;
#125664 = CARTESIAN_POINT ( 'NONE',  ( -12.06949235617756955, 12.14591786802309770, 115.6239096053143669 ) ) ;
#125666 = CARTESIAN_POINT ( 'NONE',  ( -18.67979575497193778, 10.72451020669871902, 88.33442372801901854 ) ) ;
#125665 = CARTESIAN_POINT ( 'NONE',  ( -14.29746914071049879, 8.314922557960819915, 25.83224293864769194 ) ) ;
#125667 = CARTESIAN_POINT ( 'NONE',  ( -16.46253265017160317, 9.564922557960807481, 85.83224293864769550 ) ) ;
#125668 = CARTESIAN_POINT ( 'NONE',  ( -21.52544592524334988, -5.823673210054445271, 43.95942372801902565 ) ) ;
#125669 = CARTESIAN_POINT ( 'NONE',  ( -9.564922557960796823, -16.46253265017161027, 77.08224293864769550 ) ) ;
#125670 = CARTESIAN_POINT ( 'NONE',  ( -0.05219959533910754901, -16.53943276465976808, 92.49890960531436690 ) ) ;
#125671 = CARTESIAN_POINT ( 'NONE',  ( 16.53943276465976808, -0.05219959533910856209, 58.74890960531436690 ) ) ;
#125672 = CARTESIAN_POINT ( 'NONE',  ( 15.80617190586746368, 15.72974639402197994, 74.37390960531436690 ) ) ;
#125673 = CARTESIAN_POINT ( 'NONE',  ( -13.89961937509977652, 13.97604488694528158, 75.62390960531438111 ) ) ;
#125674 = CARTESIAN_POINT ( 'NONE',  ( 0.05219959533907565091, 21.53943276465977519, 89.99890960531438111 ) ) ;
#125675 = CARTESIAN_POINT ( 'NONE',  ( -19.03943276465977164, -0.05219959533935918106, 78.75109039468567573 ) ) ;
#125677 = CARTESIAN_POINT ( 'NONE',  ( -14.34966873604960291, -8.224510206698953496, 81.66557627198103830 ) ) ;
#125676 = CARTESIAN_POINT ( 'NONE',  ( 19.05341960407618274, -5.049401038297876454, 36.04275706135233293 ) ) ;
#125678 = CARTESIAN_POINT ( 'NONE',  ( -21.55341960407610458, -5.719274019375992779, 56.45724293864768839 ) ) ;
#125679 = CARTESIAN_POINT ( 'NONE',  ( 17.05587630539787369, -6.762274262135688829, 28.24180309037314274 ) ) ;
#125681 = CARTESIAN_POINT ( 'NONE',  ( -17.14385361876520975, 23.59649016807275856, 143.0750000027311444 ) ) ;
#125680 = CARTESIAN_POINT ( 'NONE',  ( 4.379528057220339221, -16.55341960407611168, 22.70724293864769194 ) ) ;
#125682 = CARTESIAN_POINT ( 'NONE',  ( -19.02544592524334988, -5.153800228976617603, 98.95942372801900433 ) ) ;
#125683 = CARTESIAN_POINT ( 'NONE',  ( -14.29746914071049879, 8.314922557960819915, 80.83224293864769550 ) ) ;
#125684 = CARTESIAN_POINT ( 'NONE',  ( -19.39720447994795194, -5.500000000000030198, 94.66317477297180005 ) ) ;
#125685 = CARTESIAN_POINT ( 'NONE',  ( -0.05219959533909027116, -19.03943276465977164, 77.49890960531435269 ) ) ;
#125686 = CARTESIAN_POINT ( 'NONE',  ( 9.564922557960805705, 16.46253265017160317, 29.58224293864769550 ) ) ;
#125687 = CARTESIAN_POINT ( 'NONE',  ( -0.05219959533910754901, -16.53943276465976808, 67.49890960531436690 ) ) ;
#125688 = CARTESIAN_POINT ( 'NONE',  ( 16.51473224551069308, 9.474510206698969483, 99.16557627198102409 ) ) ;
#125690 = CARTESIAN_POINT ( 'NONE',  ( -16.46253265017160317, 9.564922557960807481, 60.83224293864769550 ) ) ;
#125689 = CARTESIAN_POINT ( 'NONE',  ( -19.02544592524334988, -5.153800228976617603, 88.95942372801897591 ) ) ;
#125691 = CARTESIAN_POINT ( 'NONE',  ( -0.05219959533934338120, 16.53943276465976808, 27.50109039468567929 ) ) ;
#125692 = CARTESIAN_POINT ( 'NONE',  ( -5.153800228976328057, -19.02544592524343514, 82.29057627198103830 ) ) ;
#125693 = CARTESIAN_POINT ( 'NONE',  ( -21.52544592524343514, 5.823673210054127303, 81.04057627198102409 ) ) ;
#125694 = CARTESIAN_POINT ( 'NONE',  ( 16.53943276465976808, 0.05219959533934440121, 66.25109039468567573 ) ) ;
#125695 = CARTESIAN_POINT ( 'NONE',  ( -16.20579543436698344, 7.371946100355022402, 94.43479165828047428 ) ) ;
#125696 = CARTESIAN_POINT ( 'NONE',  ( 16.46253265017160672, -9.564922557960803928, 58.33224293864769550 ) ) ;
#125697 = CARTESIAN_POINT ( 'NONE',  ( 21.55341960407610458, 5.719274019375980345, 73.95724293864769550 ) ) ;
#125698 = CARTESIAN_POINT ( 'NONE',  ( -16.51473224551082808, 9.474510206698731452, 93.33442372801900433 ) ) ;
#125700 = CARTESIAN_POINT ( 'NONE',  ( 5.823673210054444382, -21.52544592524334988, 45.20942372801901854 ) ) ;
#125699 = CARTESIAN_POINT ( 'NONE',  ( -16.53943276465976808, 0.05219959533911058130, 31.24890960531435979 ) ) ;
#125701 = CARTESIAN_POINT ( 'NONE',  ( 69.65682714487590488, -71.74905178543389184, -13.00000000000000000 ) ) ;
#125703 = CARTESIAN_POINT ( 'NONE',  ( -19.02544592524342804, 5.153800228976336051, 106.0405762719810241 ) ) ;
#125702 = CARTESIAN_POINT ( 'NONE',  ( -0.05219959533934338120, 16.53943276465976808, 72.50109039468568994 ) ) ;
#125704 = CARTESIAN_POINT ( 'NONE',  ( 13.97604488694527802, 13.89961937509977830, 104.3739096053143527 ) ) ;
#125705 = CARTESIAN_POINT ( 'NONE',  ( -16.61371651742599909, -7.165104196376252510, 36.14584930007006847 ) ) ;
#125706 = CARTESIAN_POINT ( 'NONE',  ( -12.06949235617739369, -12.14591786802326823, 94.37609039468568994 ) ) ;
#125707 = CARTESIAN_POINT ( 'NONE',  ( 4.483927247898790824, -16.52544592524335698, 40.20942372801901854 ) ) ;
#125708 = CARTESIAN_POINT ( 'NONE',  ( 9.564922557960805705, 16.46253265017160317, 49.58224293864770260 ) ) ;
#125709 = CARTESIAN_POINT ( 'NONE',  ( 19.02544592524343514, -5.153800228976328945, 48.54057627198103120 ) ) ;
#125710 = CARTESIAN_POINT ( 'NONE',  ( 9.564922557960805705, 16.46253265017160317, 64.58224293864769550 ) ) ;
#125711 = CARTESIAN_POINT ( 'NONE',  ( -15.72974639402176322, -15.80617190586768395, 49.37609039468569705 ) ) ;
#125712 = CARTESIAN_POINT ( 'NONE',  ( 0.05219959533934541429, -16.53943276465976808, 60.00109039468568284 ) ) ;
#125713 = CARTESIAN_POINT ( 'NONE',  ( -16.52544592524342804, 4.483927247898546575, 36.04057627198102409 ) ) ;
#125714 = CARTESIAN_POINT ( 'NONE',  ( -0.05219959533909027116, -19.03943276465977164, 42.49890960531435269 ) ) ;
#125715 = CARTESIAN_POINT ( 'NONE',  ( -9.564922557960796823, -16.46253265017161027, 32.08224293864769550 ) ) ;
#125716 = CARTESIAN_POINT ( 'NONE',  ( -4.483927247898782831, 16.52544592524335698, 32.70942372801900433 ) ) ;
#125717 = CARTESIAN_POINT ( 'NONE',  ( 9.474510206698729675, 16.51473224551082808, 77.08442372801900433 ) ) ;
#125718 = CARTESIAN_POINT ( 'NONE',  ( 16.53943276465976808, -0.05219959533910856209, 88.74890960531436690 ) ) ;
#125719 = CARTESIAN_POINT ( 'NONE',  ( -5.049401038298153566, 19.05341960407611168, 50.20724293864770260 ) ) ;
#125721 = CARTESIAN_POINT ( 'NONE',  ( 17.48847506799967988, -5.747544572773779947, 93.32697437843278010 ) ) ;
#125720 = CARTESIAN_POINT ( 'NONE',  ( -0.05219959533936034679, 19.03943276465977164, 92.50109039468566152 ) ) ;
#125722 = CARTESIAN_POINT ( 'NONE',  ( 10.72451020669871369, 18.67979575497193778, 82.08442372801901854 ) ) ;
#125723 = CARTESIAN_POINT ( 'NONE',  ( -0.05219959533934338120, 16.53943276465976808, 52.50109039468567573 ) ) ;
#125724 = CARTESIAN_POINT ( 'NONE',  ( -17.50000000000144240, 3.254303733634824169, 25.02395893071417632 ) ) ;
#125725 = CARTESIAN_POINT ( 'NONE',  ( 21.53943276465977519, -0.05219959533907433946, 48.74890960531435979 ) ) ;
#125726 = CARTESIAN_POINT ( 'NONE',  ( -4.483927247898782831, 16.52544592524335698, 42.70942372801901854 ) ) ;
#125727 = CARTESIAN_POINT ( 'NONE',  ( -9.474510206698964154, 16.51473224551069663, 25.41557627198103120 ) ) ;
#125728 = CARTESIAN_POINT ( 'NONE',  ( 0.05219959533936267826, -19.03943276465977164, 35.00109039468566863 ) ) ;
#125729 = CARTESIAN_POINT ( 'NONE',  ( 9.822817408787017257, 11.94368209565400640, -59.71171441009363434 ) ) ;
#125730 = CARTESIAN_POINT ( 'NONE',  ( 13.97604488694527802, 13.89961937509977652, 49.37390960531434558 ) ) ;
#125731 = DIRECTION ( 'NONE',  ( -0.000000000000000000, -0.000000000000000000, -1.000000000000000000 ) ) ;
#125732 = CARTESIAN_POINT ( 'NONE',  ( -9.564922557960796823, -16.46253265017161027, 67.08224293864769550 ) ) ;
#125733 = CARTESIAN_POINT ( 'NONE',  ( 17.50000000000000711, -3.850315288878807696, 111.7662913060345034 ) ) ;
#125734 = CARTESIAN_POINT ( 'NONE',  ( -15.80617190586768217, 15.72974639402176855, 113.1260903946856899 ) ) ;
#125735 = CARTESIAN_POINT ( 'NONE',  ( -16.53943276465976808, 0.05219959533911058130, 36.24890960531435979 ) ) ;
#125736 = CARTESIAN_POINT ( 'NONE',  ( -5.049401038298153566, 19.05341960407611168, 40.20724293864768839 ) ) ;
#125737 = CARTESIAN_POINT ( 'NONE',  ( 5.049401038298161559, -19.05341960407611168, 102.7072429386476955 ) ) ;
#125738 = CARTESIAN_POINT ( 'NONE',  ( -18.67979575497193778, 10.72451020669871902, 68.33442372801900433 ) ) ;
#125739 = CARTESIAN_POINT ( 'NONE',  ( -19.05341960407611168, -5.049401038298163336, 51.45724293864770260 ) ) ;
#125740 = CARTESIAN_POINT ( 'NONE',  ( 21.53943276465977519, 0.05219959533937863772, 66.25109039468567573 ) ) ;
#125741 = CARTESIAN_POINT ( 'NONE',  ( -5.719274019375978568, 21.55341960407610458, 25.20724293864769550 ) ) ;
#125742 = CARTESIAN_POINT ( 'NONE',  ( -9.564922557960796823, -16.46253265017161027, 37.08224293864768839 ) ) ;
#125743 = CARTESIAN_POINT ( 'NONE',  ( -10.81492255796105439, 18.62759615963255655, 22.91775706135235069 ) ) ;
#125744 = CARTESIAN_POINT ( 'NONE',  ( -13.89961937509957401, -13.97604488694547875, 44.37609039468566863 ) ) ;
#125745 = CARTESIAN_POINT ( 'NONE',  ( -19.02544592524342804, 5.153800228976336051, 26.04057627198103120 ) ) ;
#125746 = CARTESIAN_POINT ( 'NONE',  ( -9.474510206698964154, 16.51473224551069663, 80.41557627198103830 ) ) ;
#125747 = CARTESIAN_POINT ( 'NONE',  ( 0.05219959533936267826, -19.03943276465977164, 105.0010903946856615 ) ) ;
#125748 = CARTESIAN_POINT ( 'NONE',  ( -14.29746914071049879, 8.314922557960819915, 80.83224293864769550 ) ) ;
#125749 = CARTESIAN_POINT ( 'NONE',  ( 0.05219959533907565091, 21.53943276465977519, 39.99890960531436690 ) ) ;
#125750 = CARTESIAN_POINT ( 'NONE',  ( -19.02544592524334988, -5.153800228976617603, 98.95942372801900433 ) ) ;
#125751 = CARTESIAN_POINT ( 'NONE',  ( 5.719274019375991003, -21.55341960407610458, 107.7072429386476955 ) ) ;
#125752 = CARTESIAN_POINT ( 'NONE',  ( 18.67979575497194134, -10.72451020669871369, 60.83442372801901854 ) ) ;
#125753 = CARTESIAN_POINT ( 'NONE',  ( 14.34966873604972726, -8.224510206698740333, 60.83442372801901854 ) ) ;
#125754 = CARTESIAN_POINT ( 'NONE',  ( -16.55341960407617563, 4.379528057220093196, 48.54275706135234714 ) ) ;
#125755 = CARTESIAN_POINT ( 'NONE',  ( 15.72974639402199770, -15.80617190586745480, 63.12390960531435979 ) ) ;
#125756 = CARTESIAN_POINT ( 'NONE',  ( 19.03943276465977164, -0.05219959533909143690, 48.74890960531435979 ) ) ;
#125757 = CARTESIAN_POINT ( 'NONE',  ( -12.06949235617739369, -12.14591786802326823, 74.37609039468568994 ) ) ;
#125758 = CARTESIAN_POINT ( 'NONE',  ( -5.719274019375978568, 21.55341960407610458, 100.2072429386476955 ) ) ;
#125759 = CARTESIAN_POINT ( 'NONE',  ( 12.06949235617757843, -12.14591786802309237, 53.12390960531436690 ) ) ;
#125760 = CARTESIAN_POINT ( 'NONE',  ( 13.97604488694527802, 13.89961937509977652, 74.37390960531436690 ) ) ;
#125761 = CARTESIAN_POINT ( 'NONE',  ( -4.379528057220086978, -16.55341960407618274, 74.79275706135234714 ) ) ;
#125762 = CARTESIAN_POINT ( 'NONE',  ( 4.483927247898790824, -16.52544592524335698, 20.20942372801900788 ) ) ;
#125763 = CARTESIAN_POINT ( 'NONE',  ( -10.72451020669898014, 18.67979575497178502, 110.4155762719810383 ) ) ;
#125764 = CARTESIAN_POINT ( 'NONE',  ( -14.29746914071049879, 8.314922557960819915, 50.83224293864770971 ) ) ;
#125765 = ORIENTED_EDGE ( 'NONE', *, *, #68000, .F. ) ;
#125766 = CARTESIAN_POINT ( 'NONE',  ( -17.48853670773247160, 5.747243402303039872, 73.66671299749992841 ) ) ;
#125767 = CARTESIAN_POINT ( 'NONE',  ( 18.67979575497178502, 10.72451020669898547, 89.16557627198102409 ) ) ;
#125768 = CARTESIAN_POINT ( 'NONE',  ( -12.14591786802309592, -12.06949235617757132, 31.87390960531435979 ) ) ;
#125769 = EDGE_LOOP ( 'NONE', ( #34746, #64908, #70959, #118208 ) ) ;
#125770 = CARTESIAN_POINT ( 'NONE',  ( -16.81555441253551919, -7.025013491695508705, 54.36314554665747778 ) ) ;
#125771 = CARTESIAN_POINT ( 'NONE',  ( -21.55341960407610458, -5.719274019375992779, 106.4572429386477097 ) ) ;
#125772 = CARTESIAN_POINT ( 'NONE',  ( -5.049401038298153566, 19.05341960407611168, 105.2072429386476671 ) ) ;
#125773 = CARTESIAN_POINT ( 'NONE',  ( -5.719274019375978568, 21.55341960407610458, 115.2072429386476955 ) ) ;
#125774 = CARTESIAN_POINT ( 'NONE',  ( -14.29746914071049879, 8.314922557960819915, 55.83224293864770260 ) ) ;
#125775 = CARTESIAN_POINT ( 'NONE',  ( -14.34966873604972548, 8.224510206698743886, 53.33442372801901854 ) ) ;
#125776 = CARTESIAN_POINT ( 'NONE',  ( 5.153800228976335163, 19.02544592524342804, 64.79057627198100988 ) ) ;
#125777 = CARTESIAN_POINT ( 'NONE',  ( 9.474510206698729675, 16.51473224551082808, 57.08442372801900433 ) ) ;
#125778 = CARTESIAN_POINT ( 'NONE',  ( -16.46253265017160317, 9.564922557960807481, 85.83224293864769550 ) ) ;
#125779 = CARTESIAN_POINT ( 'NONE',  ( -10.81492255796078084, -18.62759615963271287, 37.08224293864768129 ) ) ;
#125780 = CARTESIAN_POINT ( 'NONE',  ( -9.474510206698964154, 16.51473224551069663, 65.41557627198102409 ) ) ;
#125781 = CARTESIAN_POINT ( 'NONE',  ( 19.05341960407611168, 5.049401038298154454, 48.95724293864768129 ) ) ;
#125782 = CARTESIAN_POINT ( 'NONE',  ( -0.05219959533934338120, 16.53943276465976808, 22.50109039468567573 ) ) ;
#125783 = CARTESIAN_POINT ( 'NONE',  ( -5.049401038297874678, -19.05341960407617918, 59.79275706135231871 ) ) ;
#125784 = CARTESIAN_POINT ( 'NONE',  ( 21.52544592524344225, -5.823673210054117533, 108.5405762719810241 ) ) ;
#125785 = CARTESIAN_POINT ( 'NONE',  ( 8.224510206698953496, -14.34966873604960469, 32.91557627198102409 ) ) ;
#125786 = CARTESIAN_POINT ( 'NONE',  ( 13.89961937509977652, -13.97604488694527269, 83.12390960531436690 ) ) ;
#125787 = CARTESIAN_POINT ( 'NONE',  ( 10.72451020669898902, -18.67979575497178502, 57.91557627198103120 ) ) ;
#125789 = CARTESIAN_POINT ( 'NONE',  ( -12.14591786802326823, 12.06949235617739902, 23.12609039468567573 ) ) ;
#125788 = CARTESIAN_POINT ( 'NONE',  ( -10.72451020669898014, 18.67979575497178502, 100.4155762719810241 ) ) ;
#125790 = CARTESIAN_POINT ( 'NONE',  ( -5.719274019375978568, 21.55341960407610458, 25.20724293864769550 ) ) ;
#125791 = CARTESIAN_POINT ( 'NONE',  ( -15.72974639402176322, -15.80617190586768395, 84.37609039468570415 ) ) ;
#125792 = CARTESIAN_POINT ( 'NONE',  ( 9.474510206698971260, -16.51473224551069308, 87.91557627198102409 ) ) ;
#125793 = CARTESIAN_POINT ( 'NONE',  ( -9.564922557960796823, -16.46253265017161027, 32.08224293864769550 ) ) ;
#125794 = CARTESIAN_POINT ( 'NONE',  ( 16.51473224551069308, 9.474510206698969483, 79.16557627198103830 ) ) ;
#125795 = CARTESIAN_POINT ( 'NONE',  ( -4.379528057220328563, 16.55341960407611168, 110.2072429386477239 ) ) ;
#125796 = CARTESIAN_POINT ( 'NONE',  ( 16.51473224551069308, 9.474510206698969483, 69.16557627198102409 ) ) ;
#125797 = CARTESIAN_POINT ( 'NONE',  ( 16.53943276465976808, 0.05219959533934440121, 21.25109039468567218 ) ) ;
#125798 = CARTESIAN_POINT ( 'NONE',  ( 17.50000000000000000, 5.499999999999997335, 31.70309617465830243 ) ) ;
#125800 = CARTESIAN_POINT ( 'NONE',  ( -13.89961937509977652, 13.97604488694528158, 110.6239096053143243 ) ) ;
#125799 = CARTESIAN_POINT ( 'NONE',  ( -5.719274019375665041, -21.55341960407619695, 99.79275706135234714 ) ) ;
#125801 = CARTESIAN_POINT ( 'NONE',  ( 12.14591786802327356, -12.06949235617739191, 90.62609039468567573 ) ) ;
#125802 = CARTESIAN_POINT ( 'NONE',  ( 11.74264578624800315, -36.14014761921581709, -9.400000000000000355 ) ) ;
#125803 = CARTESIAN_POINT ( 'NONE',  ( 19.05341960407617918, -5.049401038297876454, 66.04275706135233293 ) ) ;
#125804 = CARTESIAN_POINT ( 'NONE',  ( 13.97604488694548053, -13.89961937509957401, 30.62609039468566863 ) ) ;
#125805 = CARTESIAN_POINT ( 'NONE',  ( 4.180103257450070942, 4.460609718571543425, -64.53023439669115646 ) ) ;
#125806 = CARTESIAN_POINT ( 'NONE',  ( -19.03943276465977164, 0.05219959533909376836, 26.24890960531435624 ) ) ;
#125807 = CARTESIAN_POINT ( 'NONE',  ( 14.29746914071049879, -8.314922557960816363, 38.33224293864768839 ) ) ;
#125808 = CYLINDRICAL_SURFACE ( 'NONE', #79072, 2.000000000000000000 ) ;
#125809 = CARTESIAN_POINT ( 'NONE',  ( -12.14591786802326823, 12.06949235617739902, 108.1260903946856757 ) ) ;
#125810 = CARTESIAN_POINT ( 'NONE',  ( 16.31925111598458145, 7.325300261831479531, 67.33575461032748422 ) ) ;
#125811 = CARTESIAN_POINT ( 'NONE',  ( -14.29746914071037622, -8.314922557961029526, 79.16775706135234714 ) ) ;
#125812 = CARTESIAN_POINT ( 'NONE',  ( 5.153800228976335163, 19.02544592524342804, 39.79057627198100988 ) ) ;
#125813 = CARTESIAN_POINT ( 'NONE',  ( -21.52544592524334988, -5.823673210054445271, 98.95942372801903275 ) ) ;
#125814 = CARTESIAN_POINT ( 'NONE',  ( -16.51473224551082808, 9.474510206698731452, 103.3344237280190043 ) ) ;
#125815 = CARTESIAN_POINT ( 'NONE',  ( 5.719274019375673035, 21.55341960407619339, 77.29275706135234714 ) ) ;
#125816 = CARTESIAN_POINT ( 'NONE',  ( -13.97604488694547697, 13.89961937509957934, 58.12609039468566863 ) ) ;
#125817 = CARTESIAN_POINT ( 'NONE',  ( -13.97604488694527625, -13.89961937509977652, 81.87390960531436690 ) ) ;
#125818 = CARTESIAN_POINT ( 'NONE',  ( 19.02544592524343514, -5.153800228976328945, 68.54057627198103830 ) ) ;
#125819 = LINE ( 'NONE', #172324, #114254 ) ;
#125821 = EDGE_CURVE ( 'NONE', #35378, #181866, #74862, .T. ) ;
#125820 = CARTESIAN_POINT ( 'NONE',  ( 0.05219959533910956823, 16.53943276465976808, 64.99890960531435269 ) ) ;
#125822 = CARTESIAN_POINT ( 'NONE',  ( 18.62759615963271287, -10.81492255796078972, 58.33224293864768839 ) ) ;
#125823 = CARTESIAN_POINT ( 'NONE',  ( -19.02544592524342804, 5.153800228976336051, 46.04057627198101699 ) ) ;
#125825 = CARTESIAN_POINT ( 'NONE',  ( -12.14591786802326823, 12.06949235617739902, 83.12609039468568994 ) ) ;
#125824 = CARTESIAN_POINT ( 'NONE',  ( 21.52544592524344225, -5.823673210054117533, 83.54057627198102409 ) ) ;
#125826 = ORIENTED_EDGE ( 'NONE', *, *, #197214, .T. ) ;
#125827 = CARTESIAN_POINT ( 'NONE',  ( -9.564922557960796823, -16.46253265017161027, 47.08224293864769550 ) ) ;
#125829 = CARTESIAN_POINT ( 'NONE',  ( -11.40812507854754720, -35.11059874428192273, -6.224999997268812812 ) ) ;
#125828 = CARTESIAN_POINT ( 'NONE',  ( 4.483927247898545687, 16.52544592524342804, 79.79057627198102409 ) ) ;
#125830 = CARTESIAN_POINT ( 'NONE',  ( -9.564922557960796823, -16.46253265017161027, 47.08224293864769550 ) ) ;
#125831 = CARTESIAN_POINT ( 'NONE',  ( -19.05341960407611168, -5.049401038298163336, 26.45724293864769550 ) ) ;
#125832 = CARTESIAN_POINT ( 'NONE',  ( 19.03943276465977164, 0.05219959533936151252, 66.25109039468567573 ) ) ;
#125833 = CARTESIAN_POINT ( 'NONE',  ( 4.483927247898545687, 16.52544592524342804, 69.79057627198102409 ) ) ;
#125834 = CARTESIAN_POINT ( 'NONE',  ( 21.53943276465977519, 0.05219959533937863772, 51.25109039468568994 ) ) ;
#125836 = CARTESIAN_POINT ( 'NONE',  ( 18.62759615963271287, -10.81492255796078972, 108.3322429386477097 ) ) ;
#125835 = CARTESIAN_POINT ( 'NONE',  ( 9.564922557960805705, 16.46253265017160317, 39.58224293864768839 ) ) ;
#125837 = CARTESIAN_POINT ( 'NONE',  ( 13.97604488694527802, 13.89961937509977652, 114.3739096053143669 ) ) ;
#125838 = CARTESIAN_POINT ( 'NONE',  ( 8.224510206698953496, -14.34966873604960469, 82.91557627198103830 ) ) ;
#125839 = CARTESIAN_POINT ( 'NONE',  ( 27.28412861566094350, -28.99984389462593271, -16.93987563810616592 ) ) ;
#125840 = CARTESIAN_POINT ( 'NONE',  ( -13.89961937509977652, 13.97604488694528158, 40.62390960531435979 ) ) ;
#125841 = CARTESIAN_POINT ( 'NONE',  ( -3.573655867282028392E-15, 2.428612866367529932E-14, 167.9999999999999716 ) ) ;
#125842 = CARTESIAN_POINT ( 'NONE',  ( 5.153800228976615827, -19.02544592524334988, 100.2094237280190043 ) ) ;
#125843 = CARTESIAN_POINT ( 'NONE',  ( -18.62759615963255300, -10.81492255796106328, 34.16775706135234714 ) ) ;
#125844 = CARTESIAN_POINT ( 'NONE',  ( 16.51473224551069308, 9.474510206698969483, 89.16557627198103830 ) ) ;
#125845 = SHAPE_REPRESENTATION ( 'Switch', ( #82054 ), #188624 ) ;
#125846 = CARTESIAN_POINT ( 'NONE',  ( 5.049401038297881783, 19.05341960407617563, 67.29275706135234714 ) ) ;
#125847 = CARTESIAN_POINT ( 'NONE',  ( 16.51473224551069308, 9.474510206698969483, 39.16557627198103120 ) ) ;
#125848 = CARTESIAN_POINT ( 'NONE',  ( -14.29746914071049879, 8.314922557960819915, 60.83224293864769550 ) ) ;
#125849 = CARTESIAN_POINT ( 'NONE',  ( 16.55341960407611168, 4.379528057220329451, 63.95724293864770260 ) ) ;
#125850 = CARTESIAN_POINT ( 'NONE',  ( -9.474510206698964154, 16.51473224551069663, 70.41557627198102409 ) ) ;
#125851 = CARTESIAN_POINT ( 'NONE',  ( -21.52544592524343514, 5.823673210054127303, 96.04057627198102409 ) ) ;
#125852 = CARTESIAN_POINT ( 'NONE',  ( -5.153800228976328057, -19.02544592524343514, 72.29057627198102409 ) ) ;
#125853 = EDGE_CURVE ( 'NONE', #140780, #196237, #190175, .T. ) ;
#125854 = CARTESIAN_POINT ( 'NONE',  ( -5.823673210054431948, 21.52544592524334988, 107.7094237280190328 ) ) ;
#125857 = CARTESIAN_POINT ( 'NONE',  ( 0.05219959533910956823, 16.53943276465976808, 114.9989096053143669 ) ) ;
#125856 = CARTESIAN_POINT ( 'NONE',  ( -16.55341960407617563, 4.379528057220093196, 108.5427570613523756 ) ) ;
#125855 = CARTESIAN_POINT ( 'NONE',  ( 19.05341960407611168, 5.049401038298154454, 33.95724293864769550 ) ) ;
#125858 = CARTESIAN_POINT ( 'NONE',  ( 19.02544592524334988, 5.153800228976608722, 111.4594237280190043 ) ) ;
#125859 = VERTEX_POINT ( 'NONE', #138504 ) ;
#125860 = CARTESIAN_POINT ( 'NONE',  ( 10.72451020669871369, 18.67979575497193778, 32.08442372801901854 ) ) ;
#125861 = CARTESIAN_POINT ( 'NONE',  ( 16.46253265017146816, 9.564922557961045513, 51.66775706135233293 ) ) ;
#125862 = CARTESIAN_POINT ( 'NONE',  ( 12.06949235617739724, 12.14591786802326823, 111.8760903946856615 ) ) ;
#125863 = CARTESIAN_POINT ( 'NONE',  ( -21.53943276465977519, 0.05219959533907696930, 76.24890960531435269 ) ) ;
#125864 = CARTESIAN_POINT ( 'NONE',  ( 16.51473224551069308, 9.474510206698969483, 114.1655762719810241 ) ) ;
#125865 = CARTESIAN_POINT ( 'NONE',  ( 14.29746914071049879, -8.314922557960816363, 53.33224293864769550 ) ) ;
#125866 = CARTESIAN_POINT ( 'NONE',  ( -16.51473224551069308, -9.474510206698971260, 26.66557627198103120 ) ) ;
#125867 = CARTESIAN_POINT ( 'NONE',  ( 13.97604488694527802, 13.89961937509977652, 34.37390960531436690 ) ) ;
#125868 = CARTESIAN_POINT ( 'NONE',  ( 9.564922557961047289, -16.46253265017146816, 30.41775706135232937 ) ) ;
#125869 = CARTESIAN_POINT ( 'NONE',  ( 0.05219959533934541429, -16.53943276465976808, 90.00109039468567573 ) ) ;
#125870 = CARTESIAN_POINT ( 'NONE',  ( -16.52544592524335698, -4.483927247898792601, 48.95942372801902565 ) ) ;
#125871 = CARTESIAN_POINT ( 'NONE',  ( -18.67979575497178146, -10.72451020669898902, 21.66557627198102409 ) ) ;
#125873 = CARTESIAN_POINT ( 'NONE',  ( -21.55341960407619339, 5.719274019375674811, 88.54275706135236135 ) ) ;
#125872 = CARTESIAN_POINT ( 'NONE',  ( -19.02544592524342804, 5.153800228976336051, 56.04057627198100988 ) ) ;
#125874 = CARTESIAN_POINT ( 'NONE',  ( 5.153800228976335163, 19.02544592524342804, 79.79057627198102409 ) ) ;
#125875 = CARTESIAN_POINT ( 'NONE',  ( 14.29746914071037800, 8.314922557961029526, 66.66775706135234714 ) ) ;
#125876 = CARTESIAN_POINT ( 'NONE',  ( -8.224510206698948167, 14.34966873604960824, 110.4155762719810383 ) ) ;
#125877 = CARTESIAN_POINT ( 'NONE',  ( -16.53943276465976808, 0.05219959533911058130, 26.24890960531435624 ) ) ;
#125878 = CARTESIAN_POINT ( 'NONE',  ( 31.99999999999968736, 4.791014396527177230E-13, 45.00000000000022027 ) ) ;
#125881 = CARTESIAN_POINT ( 'NONE',  ( -19.02544592524342804, 5.153800228976336051, 76.04057627198102409 ) ) ;
#125880 = CARTESIAN_POINT ( 'NONE',  ( -19.03943276465977164, 0.05219959533909376836, 86.24890960531436690 ) ) ;
#125879 = CARTESIAN_POINT ( 'NONE',  ( -21.53943276465977519, -0.05219959533937600094, 68.75109039468568994 ) ) ;
#125882 = CARTESIAN_POINT ( 'NONE',  ( 19.03943276465977164, -0.05219959533909143690, 108.7489096053143527 ) ) ;
#125883 = CARTESIAN_POINT ( 'NONE',  ( -12.06949235617756955, 12.14591786802309770, 60.62390960531437401 ) ) ;
#125884 = CARTESIAN_POINT ( 'NONE',  ( -16.52544592524335698, -4.483927247898792601, 108.9594237280190185 ) ) ;
#125885 = CARTESIAN_POINT ( 'NONE',  ( -16.53943276465976808, 0.05219959533911058130, 41.24890960531435269 ) ) ;
#125887 = CARTESIAN_POINT ( 'NONE',  ( -21.23184647844206197, -181.1785498424364675, -15.00000000000000000 ) ) ;
#125886 = CARTESIAN_POINT ( 'NONE',  ( -12.06949235617739369, -12.14591786802326823, 39.37609039468567573 ) ) ;
#125888 = CARTESIAN_POINT ( 'NONE',  ( 19.05341960407617918, -5.049401038297876454, 41.04275706135233293 ) ) ;
#125889 = CARTESIAN_POINT ( 'NONE',  ( -16.51473224551069308, -9.474510206698971260, 81.66557627198103830 ) ) ;
#125890 = CARTESIAN_POINT ( 'NONE',  ( -19.05341960407617563, 5.049401038297882671, 53.54275706135231871 ) ) ;
#125891 = CARTESIAN_POINT ( 'NONE',  ( 29.86685920354754487, 21.69954338932564752, -9.924999997268812990 ) ) ;
#125892 = CARTESIAN_POINT ( 'NONE',  ( 17.60779699588839975, 5.500000000000012434, 58.84981316670105400 ) ) ;
#125894 = CARTESIAN_POINT ( 'NONE',  ( -12.06949235617739369, -12.14591786802326823, 79.37609039468567573 ) ) ;
#125893 = CARTESIAN_POINT ( 'NONE',  ( 9.474510206698729675, 16.51473224551082808, 87.08442372801900433 ) ) ;
#125895 = CYLINDRICAL_SURFACE ( 'NONE', #107716, 1.500000000000001332 ) ;
#125896 = CARTESIAN_POINT ( 'NONE',  ( -16.51473224551069308, -9.474510206698971260, 106.6655762719810383 ) ) ;
#125897 = CARTESIAN_POINT ( 'NONE',  ( -10.72451020669870658, -18.67979575497194134, 44.58442372801901854 ) ) ;
#125898 = CARTESIAN_POINT ( 'NONE',  ( 19.03943276465977164, 0.05219959533936151252, 91.25109039468566152 ) ) ;
#125900 = CARTESIAN_POINT ( 'NONE',  ( 13.97604488694527802, 13.89961937509977652, 49.37390960531434558 ) ) ;
#125899 = CARTESIAN_POINT ( 'NONE',  ( 17.50000000000001421, 4.414220700528461272, 23.46024564252573796 ) ) ;
#125901 = B_SPLINE_CURVE_WITH_KNOTS ( 'NONE', 3,
 ( #91360, #108540, #107536, #169212, #139859, #14553 ),
 .UNSPECIFIED., .F., .F.,
 ( 4, 2, 4 ),
 ( 0.007228050697041581325, 0.007608510107495070757, 0.007988969517948561055 ),
 .UNSPECIFIED. ) ;
#125902 = CARTESIAN_POINT ( 'NONE',  ( -16.46253265017160317, 9.564922557960807481, 100.8322429386477097 ) ) ;
#125904 = CARTESIAN_POINT ( 'NONE',  ( 5.153800228976335163, 19.02544592524342804, 44.79057627198103830 ) ) ;
#125903 = CARTESIAN_POINT ( 'NONE',  ( 8.224510206698953496, -14.34966873604960469, 62.91557627198102409 ) ) ;
#125905 = CARTESIAN_POINT ( 'NONE',  ( -16.46253265017160317, 9.564922557960807481, 60.83224293864769550 ) ) ;
#125906 = CARTESIAN_POINT ( 'NONE',  ( -13.89961937509957401, -13.97604488694547875, 69.37609039468564731 ) ) ;
#125907 = EDGE_LOOP ( 'NONE', ( #82607, #195535, #8163, #118621 ) ) ;
#125908 = CARTESIAN_POINT ( 'NONE',  ( 5.153800228976615827, -19.02544592524334988, 30.20942372801900433 ) ) ;
#125909 = CARTESIAN_POINT ( 'NONE',  ( -5.153800228976328057, -19.02544592524343514, 62.29057627198100988 ) ) ;
#125910 = CARTESIAN_POINT ( 'NONE',  ( -21.53943276465977519, 0.05219959533907696930, 76.24890960531435269 ) ) ;
#125912 = CARTESIAN_POINT ( 'NONE',  ( -5.153800228976607833, 19.02544592524334988, 32.70942372801899722 ) ) ;
#125911 = CARTESIAN_POINT ( 'NONE',  ( -8.314922557960811034, -14.29746914071050412, 62.08224293864769550 ) ) ;
#125913 = CARTESIAN_POINT ( 'NONE',  ( 10.81492255796078972, 18.62759615963270932, 44.58224293864769550 ) ) ;
#125914 = CARTESIAN_POINT ( 'NONE',  ( -5.823673210054116645, -21.52544592524344225, 22.29057627198102765 ) ) ;
#125915 = CARTESIAN_POINT ( 'NONE',  ( -19.05341960407611168, -5.049401038298163336, 71.45724293864766707 ) ) ;
#125916 = CARTESIAN_POINT ( 'NONE',  ( 19.05341960407611168, 5.049401038298154454, 38.95724293864767418 ) ) ;
#125917 = CARTESIAN_POINT ( 'NONE',  ( -12.06949235617756955, 12.14591786802309770, 105.6239096053143669 ) ) ;
#125918 = CARTESIAN_POINT ( 'NONE',  ( 10.81492255796078972, 18.62759615963270932, 104.5822429386477097 ) ) ;
#125919 = CARTESIAN_POINT ( 'NONE',  ( 16.46253265017160672, -9.564922557960803928, 108.3322429386476955 ) ) ;
#125920 = CARTESIAN_POINT ( 'NONE',  ( -21.52544592524334988, -5.823673210054445271, 23.95942372801901143 ) ) ;
#125921 = CARTESIAN_POINT ( 'NONE',  ( 16.46253265017160672, -9.564922557960803928, 38.33224293864768839 ) ) ;
#125922 = CARTESIAN_POINT ( 'NONE',  ( -21.53943276465977519, 0.05219959533907696930, 106.2489096053143811 ) ) ;
#125923 = CARTESIAN_POINT ( 'NONE',  ( 19.05341960407617918, -5.049401038297876454, 46.04275706135233293 ) ) ;
#125924 = CARTESIAN_POINT ( 'NONE',  ( 13.89961937509977652, -13.97604488694527269, 23.12390960531436335 ) ) ;
#125925 = CARTESIAN_POINT ( 'NONE',  ( 17.50000000000001066, -3.242565516153302241, 102.5000000000090807 ) ) ;
#125926 = CARTESIAN_POINT ( 'NONE',  ( 16.55341960407618274, -4.379528057220086978, 46.04275706135234714 ) ) ;
#125927 = CARTESIAN_POINT ( 'NONE',  ( -13.89961937509977652, 13.97604488694528158, 25.62390960531434558 ) ) ;
#125928 = CARTESIAN_POINT ( 'NONE',  ( 34.42160027699925706, -2.272024392515961999, 89.98798656105708460 ) ) ;
#125929 = CARTESIAN_POINT ( 'NONE',  ( -9.474510206698964154, 16.51473224551069663, 70.41557627198102409 ) ) ;
#125930 = CARTESIAN_POINT ( 'NONE',  ( -14.34966873604960291, -8.224510206698953496, 106.6655762719810383 ) ) ;
#125931 = CARTESIAN_POINT ( 'NONE',  ( 10.72451020669898902, -18.67979575497178502, 52.91557627198103830 ) ) ;
#125932 = CARTESIAN_POINT ( 'NONE',  ( 14.29746914071049879, -8.314922557960816363, 78.33224293864770971 ) ) ;
#125933 = CARTESIAN_POINT ( 'NONE',  ( 4.379528057220092307, 16.55341960407617563, 37.29275706135235424 ) ) ;
#125934 = CARTESIAN_POINT ( 'NONE',  ( 15.80617190586769283, -15.72974639402175789, 80.62609039468567573 ) ) ;
#125935 = CARTESIAN_POINT ( 'NONE',  ( -16.46253265017160317, 9.564922557960807481, 25.83224293864769194 ) ) ;
#125936 = CARTESIAN_POINT ( 'NONE',  ( 4.483927247898790824, -16.52544592524335698, 110.2094237280190185 ) ) ;
#125937 = CARTESIAN_POINT ( 'NONE',  ( 16.55341960407611168, 4.379528057220329451, 53.95724293864770260 ) ) ;
#125938 = CIRCLE ( 'NONE', #54933, 1.500000000000001332 ) ;
#125939 = CARTESIAN_POINT ( 'NONE',  ( 13.89961937509977652, -13.97604488694527269, 58.12390960531436690 ) ) ;
#125940 = CARTESIAN_POINT ( 'NONE',  ( 15.72974639402176855, 15.80617190586768217, 91.87609039468568994 ) ) ;
#125941 = CARTESIAN_POINT ( 'NONE',  ( 15.72974639402199770, -15.80617190586745480, 108.1239096053143811 ) ) ;
#125942 = CARTESIAN_POINT ( 'NONE',  ( 0.05219959533937995610, -21.53943276465977519, 70.00109039468568994 ) ) ;
#125943 = CARTESIAN_POINT ( 'NONE',  ( 8.314922557961029526, -14.29746914071037800, 40.41775706135234714 ) ) ;
#125945 = CARTESIAN_POINT ( 'NONE',  ( -21.53943276465977519, -0.05219959533937600094, 88.75109039468567573 ) ) ;
#125944 = CARTESIAN_POINT ( 'NONE',  ( 16.53943276465976808, -0.05219959533910856209, 78.74890960531436690 ) ) ;
#125946 = CARTESIAN_POINT ( 'NONE',  ( -4.483927247898782831, 16.52544592524335698, 112.7094237280190328 ) ) ;
#125947 = CARTESIAN_POINT ( 'NONE',  ( 17.79613651744294245, -24.49428055684527550, 140.9656553485623363 ) ) ;
#125948 = CARTESIAN_POINT ( 'NONE',  ( -12.06949235617739369, -12.14591786802326823, 39.37609039468567573 ) ) ;
#125949 = CARTESIAN_POINT ( 'NONE',  ( -12.06949235617756955, 12.14591786802309770, 35.62390960531437401 ) ) ;
#125950 = CARTESIAN_POINT ( 'NONE',  ( 16.53943276465976808, 0.05219959533934440121, 91.25109039468568994 ) ) ;
#125951 = CARTESIAN_POINT ( 'NONE',  ( 5.049401038298161559, -19.05341960407611168, 102.7072429386476955 ) ) ;
#125952 = CARTESIAN_POINT ( 'NONE',  ( 13.97604488694527802, 13.89961937509977652, 94.37390960531436690 ) ) ;
#125953 = CARTESIAN_POINT ( 'NONE',  ( -15.72974639402176322, -15.80617190586768395, 99.37609039468568994 ) ) ;
#125954 = CARTESIAN_POINT ( 'NONE',  ( -16.52544592524335698, -4.483927247898792601, 108.9594237280190185 ) ) ;
#125955 = CARTESIAN_POINT ( 'NONE',  ( 12.06949235617757843, -12.14591786802309237, 68.12390960531436690 ) ) ;
#125956 = CARTESIAN_POINT ( 'NONE',  ( -9.564922557960796823, -16.46253265017161027, 82.08224293864768129 ) ) ;
#125957 = ORIENTED_EDGE ( 'NONE', *, *, #150678, .T. ) ;
#125958 = CARTESIAN_POINT ( 'NONE',  ( -12.06949235617739369, -12.14591786802326823, 24.37609039468567573 ) ) ;
#125959 = CARTESIAN_POINT ( 'NONE',  ( 9.564922557960805705, 16.46253265017160317, 29.58224293864769550 ) ) ;
#125960 = CARTESIAN_POINT ( 'NONE',  ( -9.474510206698964154, 16.51473224551069663, 90.41557627198103830 ) ) ;
#125962 = CARTESIAN_POINT ( 'NONE',  ( -5.950531402560715689E-15, 38.81732327939063509, -3.124999997268813168 ) ) ;
#125961 = CARTESIAN_POINT ( 'NONE',  ( 0.05219959533934541429, -16.53943276465976808, 35.00109039468568284 ) ) ;
#125963 = CARTESIAN_POINT ( 'NONE',  ( 13.97604488694548053, -13.89961937509957401, 40.62609039468564731 ) ) ;
#125964 = CARTESIAN_POINT ( 'NONE',  ( 16.53943276465976808, 0.05219959533934440121, 91.25109039468568994 ) ) ;
#125965 = CARTESIAN_POINT ( 'NONE',  ( 19.05341960407617918, -5.049401038297876454, 101.0427570613523045 ) ) ;
#125966 = CARTESIAN_POINT ( 'NONE',  ( 5.049401038298161559, -19.05341960407611168, 27.70724293864769550 ) ) ;
#125967 = CARTESIAN_POINT ( 'NONE',  ( 14.34966873604972726, -8.224510206698740333, 75.83442372801900433 ) ) ;
#125968 = CARTESIAN_POINT ( 'NONE',  ( 4.483927247898790824, -16.52544592524335698, 70.20942372801904696 ) ) ;
#125969 = CARTESIAN_POINT ( 'NONE',  ( 2.500000000000000000, 2.357898499370431722, -2.818925648462311528E-15 ) ) ;
#125970 = CARTESIAN_POINT ( 'NONE',  ( -19.05341960407617563, 5.049401038297882671, 63.54275706135234003 ) ) ;
#125971 = CARTESIAN_POINT ( 'NONE',  ( 18.67979575497194134, -10.72451020669871369, 110.8344237280190043 ) ) ;
#125972 = CARTESIAN_POINT ( 'NONE',  ( 9.564922557960805705, 16.46253265017160317, 44.58224293864769550 ) ) ;
#125973 = CARTESIAN_POINT ( 'NONE',  ( 9.474510206698971260, -16.51473224551069308, 87.91557627198102409 ) ) ;
#125974 = CARTESIAN_POINT ( 'NONE',  ( -16.55341960407611168, -4.379528057220339221, 81.45724293864769550 ) ) ;
#125975 = AXIS2_PLACEMENT_3D ( 'NONE', #54922, #145918, #55918 ) ;
#125976 = CARTESIAN_POINT ( 'NONE',  ( -16.51473224551082808, 9.474510206698731452, 58.33442372801900433 ) ) ;
#125977 = CARTESIAN_POINT ( 'NONE',  ( -15.80617190586745835, -15.72974639402198527, 51.87390960531437401 ) ) ;
#125978 = CARTESIAN_POINT ( 'NONE',  ( 15.72974639402176855, 15.80617190586768217, 106.8760903946856899 ) ) ;
#125979 = CARTESIAN_POINT ( 'NONE',  ( 9.474510206698971260, -16.51473224551069308, 92.91557627198103830 ) ) ;
#125980 = CARTESIAN_POINT ( 'NONE',  ( 5.153800228976615827, -19.02544592524334988, 30.20942372801900433 ) ) ;
#125981 = CARTESIAN_POINT ( 'NONE',  ( 0.05219959533907565091, 21.53943276465977519, 59.99890960531436690 ) ) ;
#125982 = CARTESIAN_POINT ( 'NONE',  ( 5.153800228976335163, 19.02544592524342804, 104.7905762719809957 ) ) ;
#125983 = CARTESIAN_POINT ( 'NONE',  ( -13.97604488694547697, 13.89961937509957934, 88.12609039468563310 ) ) ;
#125984 = CARTESIAN_POINT ( 'NONE',  ( -17.49999999999999645, 3.237210098469633923, 109.7123698737954243 ) ) ;
#125985 = CARTESIAN_POINT ( 'NONE',  ( -8.224510206698735004, -14.34966873604973081, 19.58442372801901143 ) ) ;
#125986 = CARTESIAN_POINT ( 'NONE',  ( 8.314922557960818139, 14.29746914071049879, 109.5822429386476955 ) ) ;
#125987 = CARTESIAN_POINT ( 'NONE',  ( -19.03943276465977164, 0.05219959533909376836, 96.24890960531436690 ) ) ;
#125988 = CARTESIAN_POINT ( 'NONE',  ( -5.823673210054116645, -21.52544592524344225, 72.29057627198102409 ) ) ;
#125989 = CARTESIAN_POINT ( 'NONE',  ( 4.483927247898790824, -16.52544592524335698, 50.20942372801901854 ) ) ;
#125990 = CARTESIAN_POINT ( 'NONE',  ( -5.719274019375665041, -21.55341960407619695, 49.79275706135234714 ) ) ;
#125991 = CARTESIAN_POINT ( 'NONE',  ( 5.719274019375673035, 21.55341960407619339, 97.29275706135234714 ) ) ;
#125992 = CARTESIAN_POINT ( 'NONE',  ( 4.483927247898790824, -16.52544592524335698, 100.2094237280190043 ) ) ;
#125993 = CARTESIAN_POINT ( 'NONE',  ( 0.05219959533909260263, 19.03943276465977164, 84.99890960531436690 ) ) ;
#125994 = CARTESIAN_POINT ( 'NONE',  ( 8.224510206698953496, -14.34966873604960469, 87.91557627198103830 ) ) ;
#125995 = CARTESIAN_POINT ( 'NONE',  ( -0.05219959533910754901, -16.53943276465976808, 32.49890960531435979 ) ) ;
#125996 = CARTESIAN_POINT ( 'NONE',  ( -13.97604488694547697, 13.89961937509957934, 73.12609039468568994 ) ) ;
#125997 = EDGE_CURVE ( 'NONE', #63582, #88085, #193503, .T. ) ;
#125998 = CARTESIAN_POINT ( 'NONE',  ( 15.80617190586769283, -15.72974639402175789, 50.62609039468568994 ) ) ;
#125999 = CARTESIAN_POINT ( 'NONE',  ( 13.89961937509957401, 13.97604488694547697, 31.87609039468566863 ) ) ;
#126000 = CARTESIAN_POINT ( 'NONE',  ( 16.52544592524342804, -4.483927247898539470, 88.54057627198103830 ) ) ;
#126001 = CARTESIAN_POINT ( 'NONE',  ( 13.97604488694527802, 13.89961937509977652, 109.3739096053143669 ) ) ;
#126002 = CARTESIAN_POINT ( 'NONE',  ( 4.483927247898545687, 16.52544592524342804, 24.79057627198103120 ) ) ;
#126004 = CARTESIAN_POINT ( 'NONE',  ( 10.72451020669871369, 18.67979575497193778, 87.08442372801901854 ) ) ;
#126003 = B_SPLINE_CURVE_WITH_KNOTS ( 'NONE', 3,
 ( #137488, #199168, #196221, #105172, #151680, #60635, #103187 ),
 .UNSPECIFIED., .F., .F.,
 ( 4, 3, 4 ),
 ( 0.006882574723720362095, 0.01376514944744072419, 0.01380547055123299352 ),
 .UNSPECIFIED. ) ;
#126005 = CARTESIAN_POINT ( 'NONE',  ( 8.224510206698742110, 14.34966873604972548, 62.08442372801901143 ) ) ;
#126006 = CARTESIAN_POINT ( 'NONE',  ( 8.224510206698742110, 14.34966873604972548, 102.0844237280190185 ) ) ;
#126007 = CARTESIAN_POINT ( 'NONE',  ( -10.81492255796105439, 18.62759615963255655, 47.91775706135234714 ) ) ;
#126008 = VERTEX_POINT ( 'NONE', #47507 ) ;
#126009 = CARTESIAN_POINT ( 'NONE',  ( 18.67979575497194134, -10.72451020669871369, 35.83442372801901143 ) ) ;
#126010 = CARTESIAN_POINT ( 'NONE',  ( 8.224510206698953496, -14.34966873604960469, 102.9155762719810383 ) ) ;
#126011 = CARTESIAN_POINT ( 'NONE',  ( 19.02544592524343514, -5.153800228976328945, 23.54057627198102054 ) ) ;
#126012 = CARTESIAN_POINT ( 'NONE',  ( 8.314922557960818139, 14.29746914071049879, 59.58224293864770260 ) ) ;
#126013 = CARTESIAN_POINT ( 'NONE',  ( -19.02544592524342804, 5.153800228976336051, 71.04057627198099567 ) ) ;
#126014 = CARTESIAN_POINT ( 'NONE',  ( 14.34966873604972726, -8.224510206698740333, 100.8344237280190185 ) ) ;
#126015 = CARTESIAN_POINT ( 'NONE',  ( -19.05341960407611168, -5.049401038298163336, 41.45724293864769550 ) ) ;
#126016 = CARTESIAN_POINT ( 'NONE',  ( -5.823673210054116645, -21.52544592524344225, 62.29057627198102409 ) ) ;
#126017 = CARTESIAN_POINT ( 'NONE',  ( 4.379528057220339221, -16.55341960407611168, 97.70724293864772392 ) ) ;
#126018 = CARTESIAN_POINT ( 'NONE',  ( 18.62759615963271287, -10.81492255796078972, 98.33224293864769550 ) ) ;
#126019 = CARTESIAN_POINT ( 'NONE',  ( 5.049401038298161559, -19.05341960407611168, 107.7072429386476955 ) ) ;
#126021 = CARTESIAN_POINT ( 'NONE',  ( 9.474510206698729675, 16.51473224551082808, 87.08442372801900433 ) ) ;
#126020 = CARTESIAN_POINT ( 'NONE',  ( 5.153800228976335163, 19.02544592524342804, 54.79057627198103120 ) ) ;
#126022 = CARTESIAN_POINT ( 'NONE',  ( -18.62759615963270932, 10.81492255796079327, 45.83224293864769550 ) ) ;
#126023 = CARTESIAN_POINT ( 'NONE',  ( -0.05219959533937732626, 21.53943276465977519, 67.50109039468568994 ) ) ;
#126024 = CARTESIAN_POINT ( 'NONE',  ( -13.97604488694527625, -13.89961937509977652, 56.87390960531434558 ) ) ;
#126025 = CARTESIAN_POINT ( 'NONE',  ( 19.03943276465977164, -0.05219959533909143690, 83.74890960531436690 ) ) ;
#126026 = CARTESIAN_POINT ( 'NONE',  ( -14.34966873604972548, 8.224510206698743886, 63.33442372801900433 ) ) ;
#126027 = CARTESIAN_POINT ( 'NONE',  ( -18.62759615963255300, -10.81492255796106328, 49.16775706135234003 ) ) ;
#126028 = CARTESIAN_POINT ( 'NONE',  ( 18.67979575497194134, -10.72451020669871369, 85.83442372801901854 ) ) ;
#126029 = CARTESIAN_POINT ( 'NONE',  ( -18.67979575497178146, -10.72451020669898902, 96.66557627198102409 ) ) ;
#126031 = CARTESIAN_POINT ( 'NONE',  ( -12.06949235617739369, -12.14591786802326823, 69.37609039468567573 ) ) ;
#126030 = CARTESIAN_POINT ( 'NONE',  ( 21.53943276465977519, 0.05219959533937863772, 31.25109039468568639 ) ) ;
#126032 = CARTESIAN_POINT ( 'NONE',  ( 18.62759615963271287, -10.81492255796078972, 58.33224293864768839 ) ) ;
#126033 = CARTESIAN_POINT ( 'NONE',  ( 19.05341960407617918, -5.049401038297876454, 31.04275706135232227 ) ) ;
#126035 = CARTESIAN_POINT ( 'NONE',  ( -16.55341960407611168, -4.379528057220339221, 21.45724293864769550 ) ) ;
#126034 = CARTESIAN_POINT ( 'NONE',  ( 13.97604488694527802, 13.89961937509977652, 74.37390960531436690 ) ) ;
#126036 = DIRECTION ( 'NONE',  ( -1.000000000000000000, 0.000000000000000000, 0.000000000000000000 ) ) ;
#126037 = CARTESIAN_POINT ( 'NONE',  ( 5.049401038298161559, -19.05341960407611168, 107.7072429386476955 ) ) ;
#126038 = FACE_BOUND ( 'NONE', #112435, .T. ) ;
#126039 = CARTESIAN_POINT ( 'NONE',  ( 16.51473224551083163, -9.474510206698727899, 80.83442372801899012 ) ) ;
#126040 = CARTESIAN_POINT ( 'NONE',  ( -0.05219959533907301413, -21.53943276465977519, 62.49890960531436690 ) ) ;
#126041 = CARTESIAN_POINT ( 'NONE',  ( 0.05219959533910956823, 16.53943276465976808, 34.99890960531435979 ) ) ;
#126042 = CARTESIAN_POINT ( 'NONE',  ( -14.29746914071037622, -8.314922557961029526, 24.16775706135235424 ) ) ;
#126043 = CARTESIAN_POINT ( 'NONE',  ( 9.474510206698971260, -16.51473224551069308, 27.91557627198103120 ) ) ;
#126044 = CARTESIAN_POINT ( 'NONE',  ( 5.049401038297881783, 19.05341960407617563, 112.2927570613523471 ) ) ;
#126046 = CARTESIAN_POINT ( 'NONE',  ( 19.02544592524334988, 5.153800228976608722, 66.45942372801899012 ) ) ;
#126045 = CARTESIAN_POINT ( 'NONE',  ( -5.823673210054116645, -21.52544592524344225, 107.2905762719810525 ) ) ;
#126047 = CARTESIAN_POINT ( 'NONE',  ( -8.314922557961024197, 14.29746914071037800, 77.91775706135231871 ) ) ;
#126048 = CARTESIAN_POINT ( 'NONE',  ( -0.05219959533909027116, -19.03943276465977164, 62.49890960531435979 ) ) ;
#126049 = CARTESIAN_POINT ( 'NONE',  ( 16.52544592524342804, -4.483927247898539470, 78.54057627198103830 ) ) ;
#126050 = CARTESIAN_POINT ( 'NONE',  ( 5.049401038298161559, -19.05341960407611168, 52.70724293864767418 ) ) ;
#126051 = CARTESIAN_POINT ( 'NONE',  ( -4.483927247898539470, -16.52544592524342804, 57.29057627198103120 ) ) ;
#126052 = CARTESIAN_POINT ( 'NONE',  ( -37.99626262588765968, 12.34573411038917179, -5.847842220587804896 ) ) ;
#126053 = CARTESIAN_POINT ( 'NONE',  ( 0.8267425368004359676, 21.53050622130930591, -56.30180790818311465 ) ) ;
#126054 = CARTESIAN_POINT ( 'NONE',  ( 4.483927247898545687, 16.52544592524342804, 24.79057627198103120 ) ) ;
#126055 = CARTESIAN_POINT ( 'NONE',  ( -9.474510206698964154, 16.51473224551069663, 70.41557627198102409 ) ) ;
#126056 = FACE_OUTER_BOUND ( 'NONE', #134794, .T. ) ;
#126057 = CARTESIAN_POINT ( 'NONE',  ( 16.51473224551083163, -9.474510206698727899, 35.83442372801899722 ) ) ;
#126058 = CARTESIAN_POINT ( 'NONE',  ( 12.06949235617739724, 12.14591786802326823, 46.87609039468568994 ) ) ;
#126059 = CARTESIAN_POINT ( 'NONE',  ( -10.72451020669898014, 18.67979575497178502, 70.41557627198102409 ) ) ;
#126060 = CARTESIAN_POINT ( 'NONE',  ( -13.89961937509957401, -13.97604488694547875, 19.37609039468566507 ) ) ;
#126061 = CARTESIAN_POINT ( 'NONE',  ( 13.97604488694527802, 13.89961937509977652, 69.37390960531436690 ) ) ;
#126062 = CARTESIAN_POINT ( 'NONE',  ( -22.22593230296001465, -22.81042121942878609, -45.72930070417675097 ) ) ;
#126063 = CARTESIAN_POINT ( 'NONE',  ( -9.474510206698964154, 16.51473224551069663, 115.4155762719810241 ) ) ;
#126064 = CARTESIAN_POINT ( 'NONE',  ( -21.55341960407619339, 5.719274019375674811, 43.54275706135235424 ) ) ;
#126065 = CARTESIAN_POINT ( 'NONE',  ( 4.379528057220339221, -16.55341960407611168, 112.7072429386476955 ) ) ;
#126066 = ADVANCED_FACE ( 'NONE', ( #13199 ), #136524, .F. ) ;
#126069 = CARTESIAN_POINT ( 'NONE',  ( 17.97161686093722466, -5.500000000000140332, 68.49637206859166838 ) ) ;
#126068 = CARTESIAN_POINT ( 'NONE',  ( 0.05219959533909260263, 19.03943276465977164, 79.99890960531436690 ) ) ;
#126067 = CARTESIAN_POINT ( 'NONE',  ( -10.72451020669898014, 18.67979575497178502, 95.41557627198102409 ) ) ;
#126070 = CARTESIAN_POINT ( 'NONE',  ( 10.81492255796106328, -18.62759615963255655, 25.41775706135235779 ) ) ;
#126071 = EDGE_LOOP ( 'NONE', ( #122451, #137054, #132805, #60628 ) ) ;
#126072 = CARTESIAN_POINT ( 'NONE',  ( 16.46253265017160672, -9.564922557960803928, 88.33224293864769550 ) ) ;
#126073 = CYLINDRICAL_SURFACE ( 'NONE', #198014, 28.90000000000004476 ) ;
#126074 = CARTESIAN_POINT ( 'NONE',  ( 9.474510206698971260, -16.51473224551069308, 27.91557627198103120 ) ) ;
#126075 = CARTESIAN_POINT ( 'NONE',  ( 5.153800228976615827, -19.02544592524334988, 100.2094237280190043 ) ) ;
#126076 = CARTESIAN_POINT ( 'NONE',  ( -2.500000000000000000, -105.0000000000000000, 7.000000000000003553 ) ) ;
#126077 = CARTESIAN_POINT ( 'NONE',  ( 14.34966873604960469, 8.224510206698951720, 114.1655762719810383 ) ) ;
#126078 = CARTESIAN_POINT ( 'NONE',  ( 18.62759615963255655, 10.81492255796105972, 81.66775706135236135 ) ) ;
#126080 = CARTESIAN_POINT ( 'NONE',  ( 18.62759615963255655, 10.81492255796105972, 41.66775706135235424 ) ) ;
#126079 = CARTESIAN_POINT ( 'NONE',  ( -16.46253265017160317, 9.564922557960807481, 80.83224293864769550 ) ) ;
#126081 = CARTESIAN_POINT ( 'NONE',  ( 5.823673210054444382, -21.52544592524334988, 30.20942372801902565 ) ) ;
#126082 = CARTESIAN_POINT ( 'NONE',  ( 8.906447517083050158, 27.41122689804195645, 145.4000000000000057 ) ) ;
#126083 = CARTESIAN_POINT ( 'NONE',  ( -16.46253265017160317, 9.564922557960807481, 85.83224293864769550 ) ) ;
#126084 = DIRECTION ( 'NONE',  ( -0.000000000000000000, -0.000000000000000000, -1.000000000000000000 ) ) ;
#126086 = CARTESIAN_POINT ( 'NONE',  ( 10.72451020669898902, -18.67979575497178502, 37.91557627198102409 ) ) ;
#126085 = CARTESIAN_POINT ( 'NONE',  ( -16.55341960407617563, 4.379528057220093196, 38.54275706135234714 ) ) ;
#126087 = CARTESIAN_POINT ( 'NONE',  ( -21.55341960407619339, 5.719274019375674811, 78.54275706135236135 ) ) ;
#126088 = CARTESIAN_POINT ( 'NONE',  ( 12.24802307403548518, -10.94040653594595724, -59.26855811195190427 ) ) ;
#126089 = CARTESIAN_POINT ( 'NONE',  ( 5.049401038297881783, 19.05341960407617563, 112.2927570613523471 ) ) ;
#126090 = CARTESIAN_POINT ( 'NONE',  ( 5.049401038298161559, -19.05341960407611168, 62.70724293864769550 ) ) ;
#126091 = CARTESIAN_POINT ( 'NONE',  ( -9.474510206698964154, 16.51473224551069663, 85.41557627198102409 ) ) ;
#126092 = CARTESIAN_POINT ( 'NONE',  ( 0.05219959533910956823, 16.53943276465976808, 104.9989096053143669 ) ) ;
#126093 = CARTESIAN_POINT ( 'NONE',  ( -14.34966873604960291, -8.224510206698953496, 111.6655762719810525 ) ) ;
#126094 = CARTESIAN_POINT ( 'NONE',  ( -19.03943276465977164, 0.05219959533909376836, 116.2489096053143669 ) ) ;
#126095 = CARTESIAN_POINT ( 'NONE',  ( -14.29746914071037622, -8.314922557961029526, 79.16775706135234714 ) ) ;
#126098 = CARTESIAN_POINT ( 'NONE',  ( -0.05219959533909027116, -19.03943276465977164, 57.49890960531435979 ) ) ;
#126097 =( BOUNDED_CURVE ( )  B_SPLINE_CURVE ( 2, ( #97833, #159521, #21018, #115027, #45914, #108573, #132194 ),
 .UNSPECIFIED., .F., .F. ) 
 B_SPLINE_CURVE_WITH_KNOTS ( ( 3, 2, 2, 3 ),
 ( 0.9255006513465138251, 0.9399999999999999467, 0.9599999999999999645, 0.9744993486534860860 ),
 .UNSPECIFIED. ) 
 CURVE ( )  GEOMETRIC_REPRESENTATION_ITEM ( )  RATIONAL_B_SPLINE_CURVE ( ( 0.9804823514139773266, 0.9645175682723605703, 1.000000000000000000, 0.9510565162951535312, 1.000000000000000000, 0.9645175682723607924, 0.9804823514139775487 ) ) 
 REPRESENTATION_ITEM ( '' )  );
#126096 = CARTESIAN_POINT ( 'NONE',  ( 12.06949235617757843, -12.14591786802309237, 53.12390960531436690 ) ) ;
#126099 = CARTESIAN_POINT ( 'NONE',  ( -5.823673210054431948, 21.52544592524334988, 82.70942372801900433 ) ) ;
#126100 = CARTESIAN_POINT ( 'NONE',  ( -15.72974639402176322, -15.80617190586768395, 69.37609039468567573 ) ) ;
#126101 = CARTESIAN_POINT ( 'NONE',  ( 9.474510206698729675, 16.51473224551082808, 107.0844237280190043 ) ) ;
#126102 = CARTESIAN_POINT ( 'NONE',  ( -4.483927247898539470, -16.52544592524342804, 67.29057627198103830 ) ) ;
#126103 = CARTESIAN_POINT ( 'NONE',  ( -18.62759615963270932, 10.81492255796079327, 115.8322429386477097 ) ) ;
#126104 = CARTESIAN_POINT ( 'NONE',  ( -18.67979575497178146, -10.72451020669898902, 66.66557627198102409 ) ) ;
#126105 = CARTESIAN_POINT ( 'NONE',  ( -8.906447517083053711, -27.41122689804191026, 140.4000000000000057 ) ) ;
#126106 = CARTESIAN_POINT ( 'NONE',  ( -17.81289503416611097, -24.51734667627696496, 142.5500000054623513 ) ) ;
#126107 = CARTESIAN_POINT ( 'NONE',  ( -5.049401038298153566, 19.05341960407611168, 70.20724293864769550 ) ) ;
#126108 = CARTESIAN_POINT ( 'NONE',  ( -16.55341960407611168, -4.379528057220339221, 31.45724293864769550 ) ) ;
#126109 = CIRCLE ( 'NONE', #84091, 12.50000000000000000 ) ;
#126110 = CARTESIAN_POINT ( 'NONE',  ( -14.34966873604960291, -8.224510206698953496, 21.66557627198102409 ) ) ;
#126111 = CARTESIAN_POINT ( 'NONE',  ( -0.05219959533934338120, 16.53943276465976808, 97.50109039468567573 ) ) ;
#126112 = CARTESIAN_POINT ( 'NONE',  ( 0.05219959533936267826, -19.03943276465977164, 55.00109039468566863 ) ) ;
#126113 = CARTESIAN_POINT ( 'NONE',  ( 16.38665767535053419, 7.295008042176043261, 47.23599135785458003 ) ) ;
#126114 = CARTESIAN_POINT ( 'NONE',  ( -19.03943276465977164, 0.05219959533909376836, 86.24890960531436690 ) ) ;
#126115 = CARTESIAN_POINT ( 'NONE',  ( -16.52544592524342804, 4.483927247898546575, 61.04057627198103120 ) ) ;
#126117 = CARTESIAN_POINT ( 'NONE',  ( -19.05341960407611168, -5.049401038298163336, 111.4572429386476671 ) ) ;
#126116 = CARTESIAN_POINT ( 'NONE',  ( 16.31925111598458855, -7.325300261831530158, 102.6642453896725726 ) ) ;
#126119 = ORIENTED_EDGE ( 'NONE', *, *, #110318, .F. ) ;
#126118 = CARTESIAN_POINT ( 'NONE',  ( 21.52544592524344225, -5.823673210054117533, 58.54057627198103120 ) ) ;
#126120 = CARTESIAN_POINT ( 'NONE',  ( 12.06949235617757843, -12.14591786802309237, 93.12390960531436690 ) ) ;
#126121 = CARTESIAN_POINT ( 'NONE',  ( -16.52544592524335698, -4.483927247898792601, 53.95942372801900433 ) ) ;
#126122 = CARTESIAN_POINT ( 'NONE',  ( -0.05219959533910754901, -16.53943276465976808, 82.49890960531436690 ) ) ;
#126123 = CARTESIAN_POINT ( 'NONE',  ( 28.82186960331498327, 2.781578969918950771E-14, 147.0000000000000000 ) ) ;
#126124 = CARTESIAN_POINT ( 'NONE',  ( -13.97604488694547697, 13.89961937509957934, 78.12609039468567573 ) ) ;
#126125 = CARTESIAN_POINT ( 'NONE',  ( -0.05219959533907301413, -21.53943276465977519, 22.49890960531436335 ) ) ;
#126126 = CARTESIAN_POINT ( 'NONE',  ( -22.81625015709509441, -31.40387420917324590, -6.824999997268814234 ) ) ;
#126127 = CARTESIAN_POINT ( 'NONE',  ( 19.50973618000807619, 5.499999999999992895, 102.5000000000000142 ) ) ;
#126129 = CARTESIAN_POINT ( 'NONE',  ( -16.55341960407611168, -4.379528057220339221, 26.45724293864768839 ) ) ;
#126128 = CARTESIAN_POINT ( 'NONE',  ( -14.29746914071037622, -8.314922557961029526, 44.16775706135234714 ) ) ;
#126130 = CARTESIAN_POINT ( 'NONE',  ( 10.72451020669898902, -18.67979575497178502, 57.91557627198103120 ) ) ;
#126131 = CARTESIAN_POINT ( 'NONE',  ( -5.153800228976607833, 19.02544592524334988, 87.70942372801897591 ) ) ;
#126132 = CARTESIAN_POINT ( 'NONE',  ( 21.55341960407610458, 5.719274019375980345, 43.95724293864769550 ) ) ;
#126133 = CARTESIAN_POINT ( 'NONE',  ( 10.72451020669871369, 18.67979575497193778, 77.08442372801901854 ) ) ;
#126134 = CARTESIAN_POINT ( 'NONE',  ( 0.000000000000000000, -1.178949249685218970, -2.041999999999998039 ) ) ;
#126135 = CARTESIAN_POINT ( 'NONE',  ( -8.314922557961024197, 14.29746914071037800, 32.91775706135234714 ) ) ;
#126137 = CARTESIAN_POINT ( 'NONE',  ( 16.51473224551069308, 9.474510206698969483, 89.16557627198103830 ) ) ;
#126136 = CARTESIAN_POINT ( 'NONE',  ( 16.46253265017160672, -9.564922557960803928, 43.33224293864769550 ) ) ;
#126138 = CARTESIAN_POINT ( 'NONE',  ( 5.049401038298161559, -19.05341960407611168, 37.70724293864768839 ) ) ;
#126139 = CARTESIAN_POINT ( 'NONE',  ( 0.05219959533910956823, 16.53943276465976808, 99.99890960531436690 ) ) ;
#126140 = CARTESIAN_POINT ( 'NONE',  ( -9.564922557960796823, -16.46253265017161027, 107.0822429386476955 ) ) ;
#126141 = EDGE_LOOP ( 'NONE', ( #148019, #145902, #13503, #42593, #196530, #85473, #797, #161563 ) ) ;
#126142 = CARTESIAN_POINT ( 'NONE',  ( 12.14591786802327356, -12.06949235617739191, 55.62609039468568284 ) ) ;
#126143 = CARTESIAN_POINT ( 'NONE',  ( -15.80617190586745835, -15.72974639402198527, 86.87390960531438111 ) ) ;
#126144 = CARTESIAN_POINT ( 'NONE',  ( -5.049401038298153566, 19.05341960407611168, 40.20724293864768839 ) ) ;
#126145 = CARTESIAN_POINT ( 'NONE',  ( 21.55341960407619695, -5.719274019375665929, 31.04275706135234714 ) ) ;
#126146 = CARTESIAN_POINT ( 'NONE',  ( -5.153800228976328057, -19.02544592524343514, 77.29057627198099567 ) ) ;
#126147 = CARTESIAN_POINT ( 'NONE',  ( -33.12942481080120416, -22.41379292486517016, -24.08540372093838045 ) ) ;
#126148 = ORIENTED_EDGE ( 'NONE', *, *, #120075, .F. ) ;
#126149 = CARTESIAN_POINT ( 'NONE',  ( 14.29746914071037800, 8.314922557961029526, 31.66775706135234358 ) ) ;
#126150 = CARTESIAN_POINT ( 'NONE',  ( -0.05219959533907301413, -21.53943276465977519, 112.4989096053143669 ) ) ;
#126153 = CARTESIAN_POINT ( 'NONE',  ( 0.05219959533936267826, -19.03943276465977164, 75.00109039468566152 ) ) ;
#126152 = CARTESIAN_POINT ( 'NONE',  ( 19.05341960407611168, 5.049401038298154454, 93.95724293864769550 ) ) ;
#126151 = CARTESIAN_POINT ( 'NONE',  ( 16.52544592524342804, -4.483927247898539470, 113.5405762719810383 ) ) ;
#126154 = CARTESIAN_POINT ( 'NONE',  ( 9.474510206698729675, 16.51473224551082808, 27.08442372801900433 ) ) ;
#126155 = CARTESIAN_POINT ( 'NONE',  ( -21.53943276465977519, 0.05219959533907696930, 81.24890960531436690 ) ) ;
#126156 = CARTESIAN_POINT ( 'NONE',  ( -9.474510206698720793, -16.51473224551083518, 24.58442372801900078 ) ) ;
#126157 = CARTESIAN_POINT ( 'NONE',  ( -12.06949235617739369, -12.14591786802326823, 84.37609039468570415 ) ) ;
#126159 = VERTEX_POINT ( 'NONE', #93987 ) ;
#126158 = CARTESIAN_POINT ( 'NONE',  ( -13.89961937509977652, 13.97604488694528158, 105.6239096053143527 ) ) ;
#126160 = CARTESIAN_POINT ( 'NONE',  ( 16.51473224551069308, 9.474510206698969483, 39.16557627198103120 ) ) ;
#126161 = CARTESIAN_POINT ( 'NONE',  ( 5.719274019375673035, 21.55341960407619339, 57.29275706135234714 ) ) ;
#126162 = CARTESIAN_POINT ( 'NONE',  ( 21.55341960407619695, -5.719274019375665929, 71.04275706135234714 ) ) ;
#126163 = CARTESIAN_POINT ( 'NONE',  ( -19.03943276465977164, 0.05219959533909376836, 76.24890960531435269 ) ) ;
#126164 = CARTESIAN_POINT ( 'NONE',  ( 21.53943276465977519, 0.05219959533937863772, 51.25109039468568994 ) ) ;
#126165 = CARTESIAN_POINT ( 'NONE',  ( -13.89961937509957401, -13.97604488694547875, 94.37609039468566152 ) ) ;
#126166 = CARTESIAN_POINT ( 'NONE',  ( 19.03943276465977164, -0.05219959533909143690, 58.74890960531435979 ) ) ;
#126167 = CARTESIAN_POINT ( 'NONE',  ( 19.05341960407611168, 5.049401038298154454, 93.95724293864769550 ) ) ;
#126168 = CARTESIAN_POINT ( 'NONE',  ( 13.89961937509977652, -13.97604488694527269, 68.12390960531436690 ) ) ;
#126169 = CARTESIAN_POINT ( 'NONE',  ( -0.05219959533909027116, -19.03943276465977164, 112.4989096053143669 ) ) ;
#126170 = CARTESIAN_POINT ( 'NONE',  ( -19.03943276465977164, 0.05219959533909376836, 56.24890960531435979 ) ) ;
#126171 = CARTESIAN_POINT ( 'NONE',  ( 10.72451020669898902, -18.67979575497178502, 82.91557627198103830 ) ) ;
#126172 = CARTESIAN_POINT ( 'NONE',  ( -16.55341960407617563, 4.379528057220093196, 68.54275706135234714 ) ) ;
#126173 = CARTESIAN_POINT ( 'NONE',  ( -20.14845677604832375, 11.63499142542279152, 168.0304984204094296 ) ) ;
#126174 = CARTESIAN_POINT ( 'NONE',  ( 9.474510206698729675, 16.51473224551082808, 32.08442372801900433 ) ) ;
#126175 = CARTESIAN_POINT ( 'NONE',  ( -9.564922557960796823, -16.46253265017161027, 62.08224293864769550 ) ) ;
#126176 = CARTESIAN_POINT ( 'NONE',  ( 8.314922557960818139, 14.29746914071049879, 59.58224293864770260 ) ) ;
#126177 = CARTESIAN_POINT ( 'NONE',  ( -16.55341960407611168, -4.379528057220339221, 91.45724293864769550 ) ) ;
#126178 = CARTESIAN_POINT ( 'NONE',  ( 19.05341960407611168, 5.049401038298154454, 98.95724293864766707 ) ) ;
#126179 = CARTESIAN_POINT ( 'NONE',  ( -5.049401038298153566, 19.05341960407611168, 90.20724293864766707 ) ) ;
#126180 = CARTESIAN_POINT ( 'NONE',  ( -10.72451020669870658, -18.67979575497194134, 44.58442372801901854 ) ) ;
#126181 = CARTESIAN_POINT ( 'NONE',  ( -19.05341960407611168, -5.049401038298163336, 101.4572429386476955 ) ) ;
#126182 = CARTESIAN_POINT ( 'NONE',  ( 13.97604488694548053, -13.89961937509957401, 20.62609039468567573 ) ) ;
#126183 = CARTESIAN_POINT ( 'NONE',  ( -4.379528057220086978, -16.55341960407618274, 79.79275706135236135 ) ) ;
#126184 = CARTESIAN_POINT ( 'NONE',  ( -18.62759615963255300, -10.81492255796106328, 44.16775706135234714 ) ) ;
#126185 = CARTESIAN_POINT ( 'NONE',  ( 10.81492255796078972, 18.62759615963270932, 24.58224293864768839 ) ) ;
#126186 = CARTESIAN_POINT ( 'NONE',  ( 10.81492255796078972, 18.62759615963270932, 104.5822429386477097 ) ) ;
#126187 = CARTESIAN_POINT ( 'NONE',  ( 4.483927247898545687, 16.52544592524342804, 54.79057627198104541 ) ) ;
#126188 = CARTESIAN_POINT ( 'NONE',  ( -13.89961937509977652, 13.97604488694528158, 60.62390960531436690 ) ) ;
#126189 = CARTESIAN_POINT ( 'NONE',  ( -8.314922557960811034, -14.29746914071050412, 82.08224293864768129 ) ) ;
#126190 = CARTESIAN_POINT ( 'NONE',  ( 15.72974639402199770, -15.80617190586745480, 38.12390960531436690 ) ) ;
#126191 = CARTESIAN_POINT ( 'NONE',  ( 9.474510206698729675, 16.51473224551082808, 42.08442372801900433 ) ) ;
#126192 = CARTESIAN_POINT ( 'NONE',  ( 16.53943276465976808, -0.05219959533910856209, 113.7489096053143527 ) ) ;
#126193 = ORIENTED_EDGE ( 'NONE', *, *, #148621, .F. ) ;
#126194 = CARTESIAN_POINT ( 'NONE',  ( -4.483927247898782831, 16.52544592524335698, 72.70942372801901854 ) ) ;
#126195 = CARTESIAN_POINT ( 'NONE',  ( -19.05341960407611168, -5.049401038298163336, 71.45724293864766707 ) ) ;
#126196 = CARTESIAN_POINT ( 'NONE',  ( 17.14385361876520264, 23.59649016807275856, 142.1750000027311671 ) ) ;
#126197 = CARTESIAN_POINT ( 'NONE',  ( 8.224510206698953496, -14.34966873604960469, 92.91557627198103830 ) ) ;
#126198 = CARTESIAN_POINT ( 'NONE',  ( -21.55341960407610458, -5.719274019375992779, 41.45724293864769550 ) ) ;
#126199 = CARTESIAN_POINT ( 'NONE',  ( -8.224510206698735004, -14.34966873604973081, 104.5844237280190185 ) ) ;
#126200 = CARTESIAN_POINT ( 'NONE',  ( 19.02544592524334988, 5.153800228976608722, 111.4594237280190043 ) ) ;
#126201 = CARTESIAN_POINT ( 'NONE',  ( -5.719274019375665041, -21.55341960407619695, 79.79275706135236135 ) ) ;
#126202 = CARTESIAN_POINT ( 'NONE',  ( -13.97604488694527625, -13.89961937509977652, 86.87390960531436690 ) ) ;
#126203 = CARTESIAN_POINT ( 'NONE',  ( 10.81492255796078972, 18.62759615963270932, 104.5822429386477097 ) ) ;
#126204 = CARTESIAN_POINT ( 'NONE',  ( 16.55341960407618274, -4.379528057220086978, 56.04275706135235424 ) ) ;
#126205 = CARTESIAN_POINT ( 'NONE',  ( -5.049401038298153566, 19.05341960407611168, 30.20724293864768839 ) ) ;
#126206 = CARTESIAN_POINT ( 'NONE',  ( 16.55341960407618274, -4.379528057220086978, 36.04275706135234714 ) ) ;
#126207 = CARTESIAN_POINT ( 'NONE',  ( 5.049401038297881783, 19.05341960407617563, 97.29275706135233293 ) ) ;
#126208 = CARTESIAN_POINT ( 'NONE',  ( 15.72974639402199770, -15.80617190586745480, 88.12390960531436690 ) ) ;
#126209 = CARTESIAN_POINT ( 'NONE',  ( -16.51473224551082808, 9.474510206698731452, 58.33442372801900433 ) ) ;
#126210 = FACE_OUTER_BOUND ( 'NONE', #101443, .T. ) ;
#126211 = CARTESIAN_POINT ( 'NONE',  ( 5.719274019375991003, -21.55341960407610458, 102.7072429386476955 ) ) ;
#126212 = CARTESIAN_POINT ( 'NONE',  ( -4.313351365237979351, -4.313351365237916291, -64.92279855667830191 ) ) ;
#126213 = CARTESIAN_POINT ( 'NONE',  ( -19.05341960407611168, -5.049401038298163336, 81.45724293864769550 ) ) ;
#126214 = CARTESIAN_POINT ( 'NONE',  ( -16.53943276465976808, -0.05219959533934237506, 38.75109039468567573 ) ) ;
#126215 = FACE_BOUND ( 'NONE', #105513, .T. ) ;
#126216 = CARTESIAN_POINT ( 'NONE',  ( 19.02544592524334988, 5.153800228976608722, 61.45942372801900433 ) ) ;
#126218 = CARTESIAN_POINT ( 'NONE',  ( -4.483927247898539470, -16.52544592524342804, 67.29057627198103830 ) ) ;
#126217 = CARTESIAN_POINT ( 'NONE',  ( 5.823673210054444382, -21.52544592524334988, 20.20942372801900788 ) ) ;
#126219 = CARTESIAN_POINT ( 'NONE',  ( -9.474510206698964154, 16.51473224551069663, 70.41557627198102409 ) ) ;
#126221 = CARTESIAN_POINT ( 'NONE',  ( 13.97604488694548053, -13.89961937509957401, 40.62609039468564731 ) ) ;
#126220 = CARTESIAN_POINT ( 'NONE',  ( -16.55341960407617563, 4.379528057220093196, 38.54275706135234714 ) ) ;
#126222 = CARTESIAN_POINT ( 'NONE',  ( 21.55341960407619695, -5.719274019375665929, 51.04275706135234714 ) ) ;
#126223 = CARTESIAN_POINT ( 'NONE',  ( -19.02544592524334988, -5.153800228976617603, 103.9594237280190043 ) ) ;
#126225 = EDGE_CURVE ( 'NONE', #58436, #9032, #145542, .T. ) ;
#126224 = CARTESIAN_POINT ( 'NONE',  ( 0.05219959533909260263, 19.03943276465977164, 49.99890960531435979 ) ) ;
#126226 = CARTESIAN_POINT ( 'NONE',  ( -5.049401038297874678, -19.05341960407617918, 79.79275706135233293 ) ) ;
#126227 = CARTESIAN_POINT ( 'NONE',  ( 5.823673210054444382, -21.52544592524334988, 90.20942372801903275 ) ) ;
#126228 = CARTESIAN_POINT ( 'NONE',  ( 0.05219959533936267826, -19.03943276465977164, 70.00109039468566152 ) ) ;
#126229 = CARTESIAN_POINT ( 'NONE',  ( 13.97604488694527802, 13.89961937509977652, 34.37390960531436690 ) ) ;
#126230 = CARTESIAN_POINT ( 'NONE',  ( -18.62759615963270932, 10.81492255796079327, 65.83224293864769550 ) ) ;
#126232 = CARTESIAN_POINT ( 'NONE',  ( -19.05341960407617563, 5.049401038297882671, 68.54275706135230450 ) ) ;
#126231 = CARTESIAN_POINT ( 'NONE',  ( 12.14591786802309770, 12.06949235617756955, 59.37390960531436690 ) ) ;
#126233 = CARTESIAN_POINT ( 'NONE',  ( 21.96410559793011075, 8.829621495424600397, 171.4826196141302717 ) ) ;
#126234 = CARTESIAN_POINT ( 'NONE',  ( -13.89961937509957401, -13.97604488694547875, 24.37609039468565442 ) ) ;
#126235 = CARTESIAN_POINT ( 'NONE',  ( -4.483927247898782831, 16.52544592524335698, 92.70942372801901854 ) ) ;
#126236 = CARTESIAN_POINT ( 'NONE',  ( -8.224510206698948167, 14.34966873604960824, 50.41557627198103120 ) ) ;
#126238 = CARTESIAN_POINT ( 'NONE',  ( 22.44159573604009239, 16.30477369853692693, 140.0750000027311728 ) ) ;
#126237 = CARTESIAN_POINT ( 'NONE',  ( -10.81492255796105439, 18.62759615963255655, 82.91775706135234714 ) ) ;
#126239 = CARTESIAN_POINT ( 'NONE',  ( 21.53943276465977519, -0.05219959533907433946, 93.74890960531436690 ) ) ;
#126240 = CARTESIAN_POINT ( 'NONE',  ( -0.05219959533909027116, -19.03943276465977164, 47.49890960531435979 ) ) ;
#126241 = CARTESIAN_POINT ( 'NONE',  ( -21.53943276465977519, -0.05219959533937600094, 68.75109039468568994 ) ) ;
#126242 = CARTESIAN_POINT ( 'NONE',  ( 19.02544592524343514, -5.153800228976328945, 53.54057627198102409 ) ) ;
#126243 = CARTESIAN_POINT ( 'NONE',  ( 16.46253265017160672, -9.564922557960803928, 68.33224293864770971 ) ) ;
#126244 = CARTESIAN_POINT ( 'NONE',  ( -8.314922557960811034, -14.29746914071050412, 107.0822429386476955 ) ) ;
#126245 = CARTESIAN_POINT ( 'NONE',  ( 19.05341960407611168, 5.049401038298154454, 108.9572429386477097 ) ) ;
#126246 = CARTESIAN_POINT ( 'NONE',  ( -16.53943276465976808, 0.05219959533911058130, 51.24890960531436690 ) ) ;
#126247 = CARTESIAN_POINT ( 'NONE',  ( -19.05341960407611168, -5.049401038298163336, 31.45724293864769550 ) ) ;
#126248 = CARTESIAN_POINT ( 'NONE',  ( -8.224510206698948167, 14.34966873604960824, 85.41557627198102409 ) ) ;
#126249 = CARTESIAN_POINT ( 'NONE',  ( -15.72974639402197994, 15.80617190586746368, 90.62390960531436690 ) ) ;
#126250 = CARTESIAN_POINT ( 'NONE',  ( 18.67979575497194134, -10.72451020669871369, 40.83442372801901854 ) ) ;
#126251 = CARTESIAN_POINT ( 'NONE',  ( -9.564922557960796823, -16.46253265017161027, 22.08224293864768839 ) ) ;
#126252 = CARTESIAN_POINT ( 'NONE',  ( 12.06949235617739724, 12.14591786802326823, 56.87609039468568994 ) ) ;
#126253 = CARTESIAN_POINT ( 'NONE',  ( -21.55341960407610458, -5.719274019375992779, 81.45724293864769550 ) ) ;
#126254 = CARTESIAN_POINT ( 'NONE',  ( -10.72451020669870658, -18.67979575497194134, 109.5844237280190328 ) ) ;
#126255 = CARTESIAN_POINT ( 'NONE',  ( 5.153800228976335163, 19.02544592524342804, 89.79057627198102409 ) ) ;
#126256 = CARTESIAN_POINT ( 'NONE',  ( 21.55341960407619695, -5.719274019375665929, 46.04275706135234714 ) ) ;
#126257 = CARTESIAN_POINT ( 'NONE',  ( 21.52544592524344225, -5.823673210054117533, 33.54057627198102409 ) ) ;
#126258 = CARTESIAN_POINT ( 'NONE',  ( -4.379528057220086978, -16.55341960407618274, 109.7927570613523613 ) ) ;
#126260 = CARTESIAN_POINT ( 'NONE',  ( 10.81492255796106328, -18.62759615963255655, 80.41775706135234714 ) ) ;
#126259 = CARTESIAN_POINT ( 'NONE',  ( -21.55341960407619339, 5.719274019375674811, 53.54275706135234714 ) ) ;
#126261 = CARTESIAN_POINT ( 'NONE',  ( 5.049401038297881783, 19.05341960407617563, 32.29275706135233293 ) ) ;
#126262 = CARTESIAN_POINT ( 'NONE',  ( -8.224510206698735004, -14.34966873604973081, 89.58442372801901854 ) ) ;
#126263 = CARTESIAN_POINT ( 'NONE',  ( 10.72451020669871369, 18.67979575497193778, 47.08442372801901854 ) ) ;
#126264 = CARTESIAN_POINT ( 'NONE',  ( -5.153800228976328057, -19.02544592524343514, 42.29057627198101699 ) ) ;
#126265 = CARTESIAN_POINT ( 'NONE',  ( 21.52544592524334988, 5.823673210054432836, 106.4594237280190328 ) ) ;
#126266 = CARTESIAN_POINT ( 'NONE',  ( 5.153800228976335163, 19.02544592524342804, 109.7905762719810099 ) ) ;
#126267 = CARTESIAN_POINT ( 'NONE',  ( 21.53943276465977519, -0.05219959533907433946, 113.7489096053143527 ) ) ;
#126268 = CARTESIAN_POINT ( 'NONE',  ( -5.719274019375978568, 21.55341960407610458, 80.20724293864769550 ) ) ;
#126270 = CARTESIAN_POINT ( 'NONE',  ( -10.81492255796078084, -18.62759615963271287, 67.08224293864770971 ) ) ;
#126269 = DIRECTION ( 'NONE',  ( -0.000000000000000000, -0.000000000000000000, -1.000000000000000000 ) ) ;
#126272 = CARTESIAN_POINT ( 'NONE',  ( -14.29746914071049879, 8.314922557960819915, 65.83224293864769550 ) ) ;
#126271 = CARTESIAN_POINT ( 'NONE',  ( 8.224510206698742110, 14.34966873604972548, 52.08442372801901854 ) ) ;
#126273 = CARTESIAN_POINT ( 'NONE',  ( 22.98342225928956850, 7.557218236066892914, 173.2415159841882542 ) ) ;
#126274 = CARTESIAN_POINT ( 'NONE',  ( -9.474510206698720793, -16.51473224551083518, 84.58442372801900433 ) ) ;
#126275 = DIRECTION ( 'NONE',  ( -0.9945218953682734009, 0.000000000000000000, 0.1045284632676530684 ) ) ;
#126276 = CARTESIAN_POINT ( 'NONE',  ( 12.06949235617739724, 12.14591786802326823, 21.87609039468567573 ) ) ;
#126277 = CARTESIAN_POINT ( 'NONE',  ( -21.55341960407610458, -5.719274019375992779, 96.45724293864770971 ) ) ;
#126278 = CARTESIAN_POINT ( 'NONE',  ( 21.55341960407610458, 5.719274019375980345, 68.95724293864769550 ) ) ;
#126279 = CARTESIAN_POINT ( 'NONE',  ( -19.03943276465977164, 0.05219959533909376836, 116.2489096053143669 ) ) ;
#126280 = CARTESIAN_POINT ( 'NONE',  ( -12.14591786802326823, 12.06949235617739902, 58.12609039468568994 ) ) ;
#126281 = CARTESIAN_POINT ( 'NONE',  ( 16.46253265017160672, -9.564922557960803928, 73.33224293864769550 ) ) ;
#126283 = CARTESIAN_POINT ( 'NONE',  ( -13.89961937509957401, -13.97604488694547875, 109.3760903946856331 ) ) ;
#126282 = CARTESIAN_POINT ( 'NONE',  ( -10.72451020669870658, -18.67979575497194134, 49.58442372801901143 ) ) ;
#126284 = CARTESIAN_POINT ( 'NONE',  ( 19.02544592524343514, -5.153800228976328945, 113.5405762719810241 ) ) ;
#126285 = CARTESIAN_POINT ( 'NONE',  ( 9.474510206698971260, -16.51473224551069308, 102.9155762719810241 ) ) ;
#126286 = CARTESIAN_POINT ( 'NONE',  ( 18.62759615963271287, -10.81492255796078972, 108.3322429386477097 ) ) ;
#126287 = CARTESIAN_POINT ( 'NONE',  ( -13.89961937509977652, 13.97604488694528158, 65.62390960531436690 ) ) ;
#126288 = CARTESIAN_POINT ( 'NONE',  ( -16.19135201231369692, 7.376712067591784994, 24.81319145947970028 ) ) ;
#126289 = CARTESIAN_POINT ( 'NONE',  ( 14.34966873604960469, 8.224510206698951720, 79.16557627198103830 ) ) ;
#126290 = CARTESIAN_POINT ( 'NONE',  ( 5.823673210054125526, 21.52544592524343514, 24.79057627198103120 ) ) ;
#126291 = CARTESIAN_POINT ( 'NONE',  ( -17.26058549869089376, 6.457015423128611431, 33.62254162523932166 ) ) ;
#126292 = CARTESIAN_POINT ( 'NONE',  ( -0.05219959533907301413, -21.53943276465977519, 102.4989096053143811 ) ) ;
#126293 = CARTESIAN_POINT ( 'NONE',  ( 0.05219959533936267826, -19.03943276465977164, 70.00109039468566152 ) ) ;
#126294 = CARTESIAN_POINT ( 'NONE',  ( 13.89961937509977652, -13.97604488694527269, 108.1239096053143669 ) ) ;
#126295 = CARTESIAN_POINT ( 'NONE',  ( 16.46253265017160672, -9.564922557960803928, 33.33224293864770260 ) ) ;
#126296 = CARTESIAN_POINT ( 'NONE',  ( 15.80617190586746368, 15.72974639402197994, 54.37390960531435979 ) ) ;
#126297 = CARTESIAN_POINT ( 'NONE',  ( -19.02544592524342804, 5.153800228976336051, 101.0405762719810241 ) ) ;
#126298 = CARTESIAN_POINT ( 'NONE',  ( -15.80617190586768217, 15.72974639402176855, 73.12609039468567573 ) ) ;
#126299 = CARTESIAN_POINT ( 'NONE',  ( 9.474510206698971260, -16.51473224551069308, 52.91557627198102409 ) ) ;
#126300 = EDGE_CURVE ( 'NONE', #103535, #134048, #196709, .T. ) ;
#126301 = CARTESIAN_POINT ( 'NONE',  ( 4.379528057220339221, -16.55341960407611168, 92.70724293864770971 ) ) ;
#126302 = CARTESIAN_POINT ( 'NONE',  ( -0.05219959533934338120, 16.53943276465976808, 42.50109039468567573 ) ) ;
#126303 = CARTESIAN_POINT ( 'NONE',  ( 10.81492255796106328, -18.62759615963255655, 70.41775706135236135 ) ) ;
#126304 = ORIENTED_EDGE ( 'NONE', *, *, #157314, .F. ) ;
#126305 = CARTESIAN_POINT ( 'NONE',  ( -13.89961937509957401, -13.97604488694547875, 29.37609039468565797 ) ) ;
#126306 = CARTESIAN_POINT ( 'NONE',  ( -9.564922557961040184, 16.46253265017147172, 82.91775706135233293 ) ) ;
#126307 = CARTESIAN_POINT ( 'NONE',  ( -9.564922557961040184, 16.46253265017147172, 42.91775706135234003 ) ) ;
#126308 = DIRECTION ( 'NONE',  ( -0.000000000000000000, -0.000000000000000000, 1.000000000000000000 ) ) ;
#126309 = CARTESIAN_POINT ( 'NONE',  ( -15.72974639402176322, -15.80617190586768395, 34.37609039468568284 ) ) ;
#126310 = FACE_OUTER_BOUND ( 'NONE', #111894, .T. ) ;
#126311 = CARTESIAN_POINT ( 'NONE',  ( -5.153800228976607833, 19.02544592524334988, 37.70942372801899722 ) ) ;
#126312 = CARTESIAN_POINT ( 'NONE',  ( 5.153800228976335163, 19.02544592524342804, 69.79057627198103830 ) ) ;
#126313 = CARTESIAN_POINT ( 'NONE',  ( -8.314922557960811034, -14.29746914071050412, 22.08224293864769194 ) ) ;
#126315 = CARTESIAN_POINT ( 'NONE',  ( 5.719274019375673035, 21.55341960407619339, 82.29275706135234714 ) ) ;
#126314 = CARTESIAN_POINT ( 'NONE',  ( -13.89961937509977652, 13.97604488694528158, 110.6239096053143243 ) ) ;
#126316 = CARTESIAN_POINT ( 'NONE',  ( -29.86685920354755197, -21.69954338932560134, -4.424999997268812990 ) ) ;
#126317 = CARTESIAN_POINT ( 'NONE',  ( -33.82491520367208437, 1.773434586730183060, 100.2093774297293862 ) ) ;
#126318 = CARTESIAN_POINT ( 'NONE',  ( -10.72451020669870658, -18.67979575497194134, 79.58442372801903275 ) ) ;
#126319 = CARTESIAN_POINT ( 'NONE',  ( 17.44279575226823198, -5.990770900252458731, 43.33557567514318976 ) ) ;
#126320 = CARTESIAN_POINT ( 'NONE',  ( -5.049401038298153566, 19.05341960407611168, 95.20724293864770971 ) ) ;
#126321 = CARTESIAN_POINT ( 'NONE',  ( 25.96435248595184220, -27.35529834266878524, -20.33897993952045979 ) ) ;
#126322 = CARTESIAN_POINT ( 'NONE',  ( -19.02544592524342804, 5.153800228976336051, 56.04057627198100988 ) ) ;
#126323 = CARTESIAN_POINT ( 'NONE',  ( 0.05219959533907565091, 21.53943276465977519, 59.99890960531436690 ) ) ;
#126324 = CARTESIAN_POINT ( 'NONE',  ( -14.34966873604960291, -8.224510206698953496, 26.66557627198103475 ) ) ;
#126326 = CARTESIAN_POINT ( 'NONE',  ( -13.89961937509977652, 13.97604488694528158, 100.6239096053143669 ) ) ;
#126325 = CARTESIAN_POINT ( 'NONE',  ( -16.53943276465976808, 0.05219959533911058130, 116.2489096053143669 ) ) ;
#126327 = CARTESIAN_POINT ( 'NONE',  ( -16.46253265017146816, -9.564922557961047289, 24.16775706135233648 ) ) ;
#126328 = CARTESIAN_POINT ( 'NONE',  ( 12.06949235617757843, -12.14591786802309237, 103.1239096053143811 ) ) ;
#126329 = CARTESIAN_POINT ( 'NONE',  ( -10.81492255796105439, 18.62759615963255655, 57.91775706135234714 ) ) ;
#126330 = CARTESIAN_POINT ( 'NONE',  ( 13.97604488694527802, 13.89961937509977652, 114.3739096053143669 ) ) ;
#126331 = CARTESIAN_POINT ( 'NONE',  ( 0.05219959533934541429, -16.53943276465976808, 110.0010903946856757 ) ) ;
#126332 = CARTESIAN_POINT ( 'NONE',  ( -19.02544592524334988, -5.153800228976617603, 63.95942372801899012 ) ) ;
#126333 = DIRECTION ( 'NONE',  ( 0.000000000000000000, 0.000000000000000000, -1.000000000000000000 ) ) ;
#126334 = CARTESIAN_POINT ( 'NONE',  ( 19.05341960407611168, 5.049401038298154454, 113.9572429386477097 ) ) ;
#126335 = CARTESIAN_POINT ( 'NONE',  ( -12.06949235617756955, 12.14591786802309770, 70.62390960531436690 ) ) ;
#126336 = CARTESIAN_POINT ( 'NONE',  ( 5.049401038297881783, 19.05341960407617563, 62.29275706135234003 ) ) ;
#126337 = CARTESIAN_POINT ( 'NONE',  ( 19.03943276465977164, -0.05219959533909143690, 58.74890960531435979 ) ) ;
#126338 = CARTESIAN_POINT ( 'NONE',  ( -12.06949235617756955, 12.14591786802309770, 55.62390960531436690 ) ) ;
#126339 = CARTESIAN_POINT ( 'NONE',  ( 13.97604488694548053, -13.89961937509957401, 90.62609039468567573 ) ) ;
#126340 = CARTESIAN_POINT ( 'NONE',  ( -18.67979575497178146, -10.72451020669898902, 36.66557627198103120 ) ) ;
#126341 = ORIENTED_EDGE ( 'NONE', *, *, #107092, .T. ) ;
#126342 = CARTESIAN_POINT ( 'NONE',  ( -14.29746914071049879, 8.314922557960819915, 105.8322429386476955 ) ) ;
#126343 = CARTESIAN_POINT ( 'NONE',  ( -13.89961937509957401, -13.97604488694547697, 99.37609039468567573 ) ) ;
#126345 = CARTESIAN_POINT ( 'NONE',  ( -10.72451020669898014, 18.67979575497178502, 60.41557627198102409 ) ) ;
#126344 = CARTESIAN_POINT ( 'NONE',  ( 13.97604488694527802, 13.89961937509977652, 64.37390960531436690 ) ) ;
#126346 = CARTESIAN_POINT ( 'NONE',  ( -19.05341960407611168, -5.049401038298163336, 46.45724293864768129 ) ) ;
#126348 = CARTESIAN_POINT ( 'NONE',  ( -5.153800228976328057, -19.02544592524343514, 72.29057627198102409 ) ) ;
#126347 = CARTESIAN_POINT ( 'NONE',  ( -12.06949235617739369, -12.14591786802326823, 89.37609039468568994 ) ) ;
#126349 = CARTESIAN_POINT ( 'NONE',  ( -13.89961937509957401, -13.97604488694547875, 49.37609039468567573 ) ) ;
#126350 = CARTESIAN_POINT ( 'NONE',  ( 5.719274019375673035, 21.55341960407619339, 82.29275706135234714 ) ) ;
#126351 = CARTESIAN_POINT ( 'NONE',  ( 21.55341960407610458, 5.719274019375980345, 48.95724293864770971 ) ) ;
#126352 = CARTESIAN_POINT ( 'NONE',  ( 19.02544592524343514, -5.153800228976328945, 108.5405762719810383 ) ) ;
#126353 = CARTESIAN_POINT ( 'NONE',  ( -0.05219959533909027116, -19.03943276465977164, 42.49890960531435269 ) ) ;
#126354 = CARTESIAN_POINT ( 'NONE',  ( 16.53943276465976808, 0.05219959533934440121, 86.25109039468568994 ) ) ;
#126355 = CARTESIAN_POINT ( 'NONE',  ( -13.97604488694547697, 13.89961937509957934, 108.1260903946856331 ) ) ;
#126356 = CARTESIAN_POINT ( 'NONE',  ( 19.02544592524343514, -5.153800228976328945, 23.54057627198102054 ) ) ;
#126357 = CARTESIAN_POINT ( 'NONE',  ( 18.87255363501903815, 5.499999999999945821, 78.82513748171830059 ) ) ;
#126358 = CARTESIAN_POINT ( 'NONE',  ( -0.05219959533937732626, 21.53943276465977519, 92.50109039468567573 ) ) ;
#126359 = EDGE_LOOP ( 'NONE', ( #72861, #197250, #90130, #11023 ) ) ;
#126360 = CARTESIAN_POINT ( 'NONE',  ( -16.52544592524342804, 4.483927247898546575, 61.04057627198103120 ) ) ;
#126361 = CARTESIAN_POINT ( 'NONE',  ( 16.53943276465976808, -0.05219959533910856209, 68.74890960531435269 ) ) ;
#126362 = CARTESIAN_POINT ( 'NONE',  ( -21.52544592524343514, 5.823673210054127303, 96.04057627198102409 ) ) ;
#126363 = CARTESIAN_POINT ( 'NONE',  ( 21.53943276465977519, -0.05219959533907433946, 83.74890960531435269 ) ) ;
#126364 = CARTESIAN_POINT ( 'NONE',  ( -8.898068258721474777, 27.38543819252877043, 149.5843446568999866 ) ) ;
#126365 = CARTESIAN_POINT ( 'NONE',  ( 18.67979575497178502, 10.72451020669898547, 44.16557627198103120 ) ) ;
#126366 = CARTESIAN_POINT ( 'NONE',  ( 14.34966873604972726, -8.224510206698740333, 60.83442372801901854 ) ) ;
#126367 = CARTESIAN_POINT ( 'NONE',  ( -14.34966873604960291, -8.224510206698953496, 86.66557627198102409 ) ) ;
#126368 = CARTESIAN_POINT ( 'NONE',  ( -19.05341960407611168, -5.049401038298163336, 41.45724293864769550 ) ) ;
#126369 = CARTESIAN_POINT ( 'NONE',  ( 31.99999999999968736, 4.791014396527177230E-13, 45.00000000000022027 ) ) ;
#126370 = CARTESIAN_POINT ( 'NONE',  ( 8.314922557961029526, -14.29746914071037800, 100.4177570613523471 ) ) ;
#126371 = CARTESIAN_POINT ( 'NONE',  ( -15.80617190586768217, 15.72974639402176855, 33.12609039468569705 ) ) ;
#126372 = CARTESIAN_POINT ( 'NONE',  ( 16.51473224551069308, 9.474510206698969483, 89.16557627198103830 ) ) ;
#126373 = CARTESIAN_POINT ( 'NONE',  ( 15.72974639402176855, 15.80617190586768217, 66.87609039468568994 ) ) ;
#126374 = CARTESIAN_POINT ( 'NONE',  ( -19.05341960407611168, -5.049401038298163336, 21.45724293864768839 ) ) ;
#126375 = CARTESIAN_POINT ( 'NONE',  ( -9.564922557960796823, -16.46253265017161027, 27.08224293864769550 ) ) ;
#126376 = VERTEX_POINT ( 'NONE', #98947 ) ;
#126377 = CARTESIAN_POINT ( 'NONE',  ( -21.52544592524334988, -5.823673210054445271, 58.95942372801902565 ) ) ;
#126379 = CARTESIAN_POINT ( 'NONE',  ( -0.05219959533909027116, -19.03943276465977164, 112.4989096053143669 ) ) ;
#126378 = CARTESIAN_POINT ( 'NONE',  ( 19.03943276465977164, -0.05219959533909143690, 33.74890960531435979 ) ) ;
#126380 = CARTESIAN_POINT ( 'NONE',  ( 9.474510206698971260, -16.51473224551069308, 87.91557627198102409 ) ) ;
#126381 = CARTESIAN_POINT ( 'NONE',  ( -13.89961937509957401, -13.97604488694547875, 64.37609039468567573 ) ) ;
#126382 = CARTESIAN_POINT ( 'NONE',  ( -0.05219959533937732626, 21.53943276465977519, 27.50109039468567929 ) ) ;
#126383 = CARTESIAN_POINT ( 'NONE',  ( -19.05341960407617563, 5.049401038297882671, 53.54275706135231871 ) ) ;
#126384 = CARTESIAN_POINT ( 'NONE',  ( 13.89961937509977652, -13.97604488694527269, 33.12390960531434558 ) ) ;
#126385 = CARTESIAN_POINT ( 'NONE',  ( -16.52544592524335698, -4.483927247898792601, 108.9594237280190185 ) ) ;
#126386 = CARTESIAN_POINT ( 'NONE',  ( -5.153800228976607833, 19.02544592524334988, 77.70942372801900433 ) ) ;
#126387 = CARTESIAN_POINT ( 'NONE',  ( 12.14591786802309770, 12.06949235617756955, 29.37390960531435269 ) ) ;
#126388 = CARTESIAN_POINT ( 'NONE',  ( 9.564922557961047289, -16.46253265017146816, 55.41775706135234003 ) ) ;
#126389 = CARTESIAN_POINT ( 'NONE',  ( 9.474510206698971260, -16.51473224551069308, 102.9155762719810241 ) ) ;
#126390 = CARTESIAN_POINT ( 'NONE',  ( -21.55341960407619339, 5.719274019375674811, 103.5427570613523613 ) ) ;
#126391 = CARTESIAN_POINT ( 'NONE',  ( -21.55341960407619339, 5.719274019375674811, 113.5427570613523756 ) ) ;
#126392 = CARTESIAN_POINT ( 'NONE',  ( -9.564922557960796823, -16.46253265017161027, 22.08224293864768839 ) ) ;
#126393 = CARTESIAN_POINT ( 'NONE',  ( 5.823673210054444382, -21.52544592524334988, 90.20942372801903275 ) ) ;
#126394 = CARTESIAN_POINT ( 'NONE',  ( 8.224510206698742110, 14.34966873604972548, 32.08442372801901854 ) ) ;
#126395 = CARTESIAN_POINT ( 'NONE',  ( -5.049401038298153566, 19.05341960407611168, 90.20724293864766707 ) ) ;
#126396 = EDGE_CURVE ( 'NONE', #95772, #90645, #154672, .T. ) ;
#126397 = CARTESIAN_POINT ( 'NONE',  ( -30.74264578624800492, -22.33583958711396278, -9.549999994537627046 ) ) ;
#126398 = CARTESIAN_POINT ( 'NONE',  ( 13.89961937509977652, -13.97604488694527269, 78.12390960531433848 ) ) ;
#126399 = CARTESIAN_POINT ( 'NONE',  ( 1.227931366032057224E-14, 24.30000000000003268, -65.00100000000003320 ) ) ;
#126400 = CARTESIAN_POINT ( 'NONE',  ( 19.02544592524334988, 5.153800228976608722, 76.45942372801897591 ) ) ;
#126401 = CARTESIAN_POINT ( 'NONE',  ( 19.02544592524343514, -5.153800228976328945, 103.5405762719809957 ) ) ;
#126402 = CARTESIAN_POINT ( 'NONE',  ( 18.67979575497194134, -10.72451020669871369, 100.8344237280190185 ) ) ;
#126403 = CARTESIAN_POINT ( 'NONE',  ( 14.34966873604960469, 8.224510206698951720, 94.16557627198103830 ) ) ;
#126404 = CARTESIAN_POINT ( 'NONE',  ( 15.80617190586746368, 15.72974639402197994, 44.37390960531435979 ) ) ;
#126405 = CARTESIAN_POINT ( 'NONE',  ( -5.719274019375978568, 21.55341960407610458, 30.20724293864769550 ) ) ;
#126406 = CARTESIAN_POINT ( 'NONE',  ( 8.314922557960818139, 14.29746914071049879, 104.5822429386477097 ) ) ;
#126407 = CARTESIAN_POINT ( 'NONE',  ( 18.22780087662126647, 5.499999999999818812, 46.48236817873107185 ) ) ;
#126408 = CARTESIAN_POINT ( 'NONE',  ( -0.05219959533936034679, 19.03943276465977164, 62.50109039468566863 ) ) ;
#126409 = CARTESIAN_POINT ( 'NONE',  ( -8.224510206698948167, 14.34966873604960824, 25.41557627198103120 ) ) ;
#126410 = CARTESIAN_POINT ( 'NONE',  ( 19.03943276465977164, -0.05219959533909143690, 98.74890960531436690 ) ) ;
#126411 = CARTESIAN_POINT ( 'NONE',  ( -21.53943276465977519, -0.05219959533937600094, 83.75109039468568994 ) ) ;
#126412 = CARTESIAN_POINT ( 'NONE',  ( 10.72451020669898902, -18.67979575497178502, 72.91557627198103830 ) ) ;
#126413 = CARTESIAN_POINT ( 'NONE',  ( -10.72451020669870658, -18.67979575497194134, 39.58442372801901143 ) ) ;
#126414 = CARTESIAN_POINT ( 'NONE',  ( -15.80617190586745835, -15.72974639402198527, 91.87390960531436690 ) ) ;
#126415 = CARTESIAN_POINT ( 'NONE',  ( -21.55341960407619339, 5.719274019375674811, 48.54275706135234714 ) ) ;
#126416 = CARTESIAN_POINT ( 'NONE',  ( -9.564922557960796823, -16.46253265017161027, 32.08224293864769550 ) ) ;
#126417 = CARTESIAN_POINT ( 'NONE',  ( -16.51473224551069308, -9.474510206698971260, 86.66557627198102409 ) ) ;
#126418 = CARTESIAN_POINT ( 'NONE',  ( 4.379528057220092307, 16.55341960407617563, 82.29275706135234714 ) ) ;
#126419 = CARTESIAN_POINT ( 'NONE',  ( -4.483927247898539470, -16.52544592524342804, 102.2905762719810383 ) ) ;
#126420 = CARTESIAN_POINT ( 'NONE',  ( 19.03943276465977164, -0.05219959533909143690, 103.7489096053143669 ) ) ;
#126421 = CARTESIAN_POINT ( 'NONE',  ( 12.06949235617757843, -12.14591786802309237, 58.12390960531435979 ) ) ;
#126422 = CARTESIAN_POINT ( 'NONE',  ( -14.34966873604960291, -8.224510206698953496, 21.66557627198102409 ) ) ;
#126423 = CARTESIAN_POINT ( 'NONE',  ( -9.564922557960796823, -16.46253265017161027, 57.08224293864769550 ) ) ;
#126424 = CARTESIAN_POINT ( 'NONE',  ( -9.564922557960796823, -16.46253265017161027, 37.08224293864768839 ) ) ;
#126425 = CARTESIAN_POINT ( 'NONE',  ( -5.719274019375978568, 21.55341960407610458, 40.20724293864769550 ) ) ;
#126426 = EDGE_CURVE ( 'NONE', #169038, #114713, #85007, .T. ) ;
#126427 = CARTESIAN_POINT ( 'NONE',  ( -9.564922557961040184, 16.46253265017147172, 27.91775706135232582 ) ) ;
#126429 = CARTESIAN_POINT ( 'NONE',  ( -14.34966873604960291, -8.224510206698953496, 36.66557627198103120 ) ) ;
#126428 = DIRECTION ( 'NONE',  ( -0.3041824702427683436, -0.9526137857479322069, 2.960637879548173518E-15 ) ) ;
#126430 = CARTESIAN_POINT ( 'NONE',  ( 5.719274019375673035, 21.55341960407619339, 47.29275706135234003 ) ) ;
#126431 = CARTESIAN_POINT ( 'NONE',  ( -17.10305700086924929, -33.88765926517217508, -26.94085628989254033 ) ) ;
#126432 = CARTESIAN_POINT ( 'NONE',  ( -12.14591786802326823, 12.06949235617739902, 53.12609039468568284 ) ) ;
#126433 = CARTESIAN_POINT ( 'NONE',  ( 9.564922557961047289, -16.46253265017146816, 55.41775706135234003 ) ) ;
#126434 = CARTESIAN_POINT ( 'NONE',  ( 8.314922557960818139, 14.29746914071049879, 24.58224293864768839 ) ) ;
#126435 = CARTESIAN_POINT ( 'NONE',  ( 16.52216118717208104, -7.221426719304427699, 51.42400978953011759 ) ) ;
#126436 = CARTESIAN_POINT ( 'NONE',  ( 16.55341960407618274, -4.379528057220086978, 111.0427570613523613 ) ) ;
#126437 = CARTESIAN_POINT ( 'NONE',  ( 5.153800228976335163, 19.02544592524342804, 34.79057627198102409 ) ) ;
#126438 = CARTESIAN_POINT ( 'NONE',  ( -16.51473224551069308, -9.474510206698971260, 66.66557627198102409 ) ) ;
#126439 = CARTESIAN_POINT ( 'NONE',  ( -16.46253265017160317, 9.564922557960807481, 25.83224293864769194 ) ) ;
#126440 = CARTESIAN_POINT ( 'NONE',  ( -5.823673210054431948, 21.52544592524334988, 37.70942372801900433 ) ) ;
#126441 = CARTESIAN_POINT ( 'NONE',  ( 0.05219959533909260263, 19.03943276465977164, 44.99890960531435979 ) ) ;
#126442 = CARTESIAN_POINT ( 'NONE',  ( -19.02544592524342804, 5.153800228976336051, 116.0405762719810383 ) ) ;
#126443 = CARTESIAN_POINT ( 'NONE',  ( -5.153800228976328057, -19.02544592524343514, 52.29057627198100988 ) ) ;
#126444 = CARTESIAN_POINT ( 'NONE',  ( -10.81492255796078084, -18.62759615963271287, 22.08224293864769194 ) ) ;
#126446 = CARTESIAN_POINT ( 'NONE',  ( 12.14591786802309770, 12.06949235617756955, 109.3739096053143811 ) ) ;
#126445 = CARTESIAN_POINT ( 'NONE',  ( -15.80617190586768217, 15.72974639402176855, 53.12609039468568284 ) ) ;
#126447 = CARTESIAN_POINT ( 'NONE',  ( 0.05219959533907565091, 21.53943276465977519, 24.99890960531435624 ) ) ;
#126448 = CARTESIAN_POINT ( 'NONE',  ( 16.52544592524335698, 4.483927247898782831, 71.45942372801901854 ) ) ;
#126449 = CARTESIAN_POINT ( 'NONE',  ( -21.55341960407619339, 5.719274019375674811, 93.54275706135234714 ) ) ;
#126450 = CARTESIAN_POINT ( 'NONE',  ( -12.06949235617739369, -12.14591786802326823, 49.37609039468569705 ) ) ;
#126451 = CARTESIAN_POINT ( 'NONE',  ( 13.97604488694527802, 13.89961937509977652, 89.37390960531436690 ) ) ;
#126452 = CARTESIAN_POINT ( 'NONE',  ( 8.224510206698742110, 14.34966873604972548, 42.08442372801901854 ) ) ;
#126453 = CARTESIAN_POINT ( 'NONE',  ( -14.34966873604972548, 8.224510206698743886, 23.33442372801901499 ) ) ;
#126454 = CARTESIAN_POINT ( 'NONE',  ( -16.55341960407617563, 4.379528057220093196, 98.54275706135234714 ) ) ;
#126455 = CARTESIAN_POINT ( 'NONE',  ( 15.72974639402176855, 15.80617190586768217, 51.87609039468568284 ) ) ;
#126456 = CARTESIAN_POINT ( 'NONE',  ( 16.51473224551083163, -9.474510206698727899, 100.8344237280190043 ) ) ;
#126457 = CARTESIAN_POINT ( 'NONE',  ( -5.719274019375978568, 21.55341960407610458, 110.2072429386477239 ) ) ;
#126459 = CARTESIAN_POINT ( 'NONE',  ( -9.474510206698720793, -16.51473224551083518, 104.5844237280190043 ) ) ;
#126458 = CARTESIAN_POINT ( 'NONE',  ( -0.05219959533910754901, -16.53943276465976808, 97.49890960531436690 ) ) ;
#126460 = CARTESIAN_POINT ( 'NONE',  ( -8.224510206698735004, -14.34966873604973081, 69.58442372801900433 ) ) ;
#126461 = CARTESIAN_POINT ( 'NONE',  ( 22.72581825106501086, 12.75361973299702001, 165.5645137041830139 ) ) ;
#126462 = CARTESIAN_POINT ( 'NONE',  ( -5.153800228976607833, 19.02544592524334988, 82.70942372801897591 ) ) ;
#126463 = CARTESIAN_POINT ( 'NONE',  ( 16.55341960407611168, 4.379528057220329451, 48.95724293864770971 ) ) ;
#126464 = CARTESIAN_POINT ( 'NONE',  ( 14.29746914071049879, -8.314922557960816363, 43.33224293864769550 ) ) ;
#126465 = CARTESIAN_POINT ( 'NONE',  ( 4.483927247898545687, 16.52544592524342804, 94.79057627198105251 ) ) ;
#126467 =( LENGTH_UNIT ( ) NAMED_UNIT ( * ) SI_UNIT ( .MILLI., .METRE. ) );
#126466 = CARTESIAN_POINT ( 'NONE',  ( -19.02544592524334988, -5.153800228976617603, 38.95942372801900433 ) ) ;
#126468 = CARTESIAN_POINT ( 'NONE',  ( 21.52544592524334988, 5.823673210054432836, 36.45942372801901143 ) ) ;
#126469 = CARTESIAN_POINT ( 'NONE',  ( 9.564922557961047289, -16.46253265017146816, 100.4177570613523329 ) ) ;
#126470 = DIRECTION ( 'NONE',  ( 0.000000000000000000, -1.000000000000000000, 0.000000000000000000 ) ) ;
#126471 = CARTESIAN_POINT ( 'NONE',  ( 13.89961937509977652, -13.97604488694527269, 88.12390960531438111 ) ) ;
#126472 = CARTESIAN_POINT ( 'NONE',  ( -13.89961937509977652, 13.97604488694528158, 90.62390960531432427 ) ) ;
#126473 = CARTESIAN_POINT ( 'NONE',  ( -18.67979575497178146, -10.72451020669898902, 51.66557627198102409 ) ) ;
#126474 = CARTESIAN_POINT ( 'NONE',  ( 16.52544592524342804, -4.483927247898539470, 93.54057627198103830 ) ) ;
#126475 = CARTESIAN_POINT ( 'NONE',  ( -16.51473224551069308, -9.474510206698971260, 71.66557627198102409 ) ) ;
#126476 = CARTESIAN_POINT ( 'NONE',  ( -5.049401038298153566, 19.05341960407611168, 35.20724293864768839 ) ) ;
#126477 = CARTESIAN_POINT ( 'NONE',  ( -21.55341960407619339, 5.719274019375674811, 38.54275706135234714 ) ) ;
#126478 = CARTESIAN_POINT ( 'NONE',  ( -18.62759615963255300, -10.81492255796106328, 69.16775706135234714 ) ) ;
#126479 = CARTESIAN_POINT ( 'NONE',  ( 8.224510206698742110, 14.34966873604972548, 87.08442372801901854 ) ) ;
#126480 = EDGE_CURVE ( 'NONE', #131506, #31781, #114113, .T. ) ;
#126481 = CARTESIAN_POINT ( 'NONE',  ( -5.823673210054431948, 21.52544592524334988, 32.70942372801900433 ) ) ;
#126482 = CARTESIAN_POINT ( 'NONE',  ( 18.62759615963255655, 10.81492255796105972, 21.66775706135235069 ) ) ;
#126484 = CARTESIAN_POINT ( 'NONE',  ( 19.05341960407611168, 5.049401038298154454, 78.95724293864769550 ) ) ;
#126483 = CARTESIAN_POINT ( 'NONE',  ( -16.46253265017146816, -9.564922557961047289, 54.16775706135234003 ) ) ;
#126485 = CARTESIAN_POINT ( 'NONE',  ( -5.719274019375665041, -21.55341960407619695, 84.79275706135234714 ) ) ;
#126486 = CARTESIAN_POINT ( 'NONE',  ( 18.67979575497178502, 10.72451020669898547, 79.16557627198103830 ) ) ;
#126487 = CARTESIAN_POINT ( 'NONE',  ( -8.224510206698948167, 14.34966873604960824, 50.41557627198103120 ) ) ;
#126489 = CARTESIAN_POINT ( 'NONE',  ( 0.05219959533936267826, -19.03943276465977164, 30.00109039468566863 ) ) ;
#126488 = CARTESIAN_POINT ( 'NONE',  ( 5.719274019375673035, 21.55341960407619339, 102.2927570613523613 ) ) ;
#126490 = CARTESIAN_POINT ( 'NONE',  ( 14.34966873604960469, 8.224510206698951720, 69.16557627198102409 ) ) ;
#126491 = CARTESIAN_POINT ( 'NONE',  ( 8.224510206698953496, -14.34966873604960469, 112.9155762719810383 ) ) ;
#126492 = CARTESIAN_POINT ( 'NONE',  ( 13.97604488694548053, -13.89961937509957401, 70.62609039468567573 ) ) ;
#126493 = CARTESIAN_POINT ( 'NONE',  ( -12.06949235617756955, 12.14591786802309770, 40.62390960531435269 ) ) ;
#126494 = CARTESIAN_POINT ( 'NONE',  ( -5.823673210054431948, 21.52544592524334988, 77.70942372801900433 ) ) ;
#126495 = CARTESIAN_POINT ( 'NONE',  ( -5.153800228976328057, -19.02544592524343514, 77.29057627198099567 ) ) ;
#126496 = CARTESIAN_POINT ( 'NONE',  ( -9.564922557961040184, 16.46253265017147172, 67.91775706135233293 ) ) ;
#126497 = CARTESIAN_POINT ( 'NONE',  ( 5.823673210054125526, 21.52544592524343514, 64.79057627198103830 ) ) ;
#126498 = CARTESIAN_POINT ( 'NONE',  ( 10.81492255796078972, 18.62759615963270932, 114.5822429386477097 ) ) ;
#126499 = CARTESIAN_POINT ( 'NONE',  ( -9.564922557961040184, 16.46253265017147172, 107.9177570613523471 ) ) ;
#126500 = CARTESIAN_POINT ( 'NONE',  ( 8.224510206698742110, 14.34966873604972548, 77.08442372801901854 ) ) ;
#126502 = CARTESIAN_POINT ( 'NONE',  ( 18.62759615963271287, -10.81492255796078972, 113.3322429386476955 ) ) ;
#126501 = CARTESIAN_POINT ( 'NONE',  ( 16.62475595723694965, 7.163666690055258357, 61.97286648189533764 ) ) ;
#126503 = CARTESIAN_POINT ( 'NONE',  ( 16.53943276465976808, -0.05219959533910856209, 98.74890960531438111 ) ) ;
#126504 = CARTESIAN_POINT ( 'NONE',  ( -17.49999999999998934, -3.512728167237066046, 29.77190004818872282 ) ) ;
#126505 = CARTESIAN_POINT ( 'NONE',  ( 4.483927247898790824, -16.52544592524335698, 30.20942372801902565 ) ) ;
#126506 = CARTESIAN_POINT ( 'NONE',  ( -5.823673210054116645, -21.52544592524344225, 67.29057627198103830 ) ) ;
#126507 = CARTESIAN_POINT ( 'NONE',  ( -14.34966873604972548, 8.224510206698743886, 98.33442372801901854 ) ) ;
#126508 = CARTESIAN_POINT ( 'NONE',  ( -16.51473224551069308, -9.474510206698971260, 36.66557627198102409 ) ) ;
#126509 = CARTESIAN_POINT ( 'NONE',  ( -16.55341960407617563, 4.379528057220093196, 68.54275706135234714 ) ) ;
#126510 = CARTESIAN_POINT ( 'NONE',  ( 5.153800228976615827, -19.02544592524334988, 55.20942372801899722 ) ) ;
#126511 = CARTESIAN_POINT ( 'NONE',  ( 15.80617190586769283, -15.72974639402175789, 45.62609039468567573 ) ) ;
#126512 = CARTESIAN_POINT ( 'NONE',  ( 5.719274019375991003, -21.55341960407610458, 57.70724293864770260 ) ) ;
#126513 = CARTESIAN_POINT ( 'NONE',  ( 12.14591786802327356, -12.06949235617739191, 100.6260903946857184 ) ) ;
#126514 = CARTESIAN_POINT ( 'NONE',  ( -21.53943276465977519, -0.05219959533937600094, 88.75109039468567573 ) ) ;
#126515 = CARTESIAN_POINT ( 'NONE',  ( 21.53943276465977519, -0.05219959533907433946, 48.74890960531435979 ) ) ;
#126516 = CARTESIAN_POINT ( 'NONE',  ( 10.81492255796078972, 18.62759615963270932, 44.58224293864769550 ) ) ;
#126517 = CARTESIAN_POINT ( 'NONE',  ( -16.52544592524335698, -4.483927247898792601, 83.95942372801900433 ) ) ;
#126518 = CARTESIAN_POINT ( 'NONE',  ( -10.72451020669898014, 18.67979575497178502, 40.41557627198103120 ) ) ;
#126519 = ORIENTED_EDGE ( 'NONE', *, *, #182922, .F. ) ;
#126520 = CARTESIAN_POINT ( 'NONE',  ( -9.564922557960796823, -16.46253265017161027, 102.0822429386477097 ) ) ;
#126521 = CARTESIAN_POINT ( 'NONE',  ( -11.30153831258471975, -180.0000000000000000, -15.00000000000000178 ) ) ;
#126522 = CARTESIAN_POINT ( 'NONE',  ( 9.474510206698971260, -16.51473224551069308, 32.91557627198102409 ) ) ;
#126523 = CARTESIAN_POINT ( 'NONE',  ( 10.81492255796078972, 18.62759615963270932, 59.58224293864770260 ) ) ;
#126524 = CARTESIAN_POINT ( 'NONE',  ( -8.224510206698735004, -14.34966873604973081, 89.58442372801901854 ) ) ;
#126525 = CARTESIAN_POINT ( 'NONE',  ( 5.823673210054444382, -21.52544592524334988, 50.20942372801901854 ) ) ;
#126526 = CARTESIAN_POINT ( 'NONE',  ( 5.153800228976615827, -19.02544592524334988, 105.2094237280190185 ) ) ;
#126527 = CARTESIAN_POINT ( 'NONE',  ( 14.29746914071049879, -8.314922557960816363, 98.33224293864769550 ) ) ;
#126528 = CARTESIAN_POINT ( 'NONE',  ( 4.379528057220092307, 16.55341960407617563, 22.29275706135235069 ) ) ;
#126529 = CARTESIAN_POINT ( 'NONE',  ( 5.049401038298161559, -19.05341960407611168, 37.70724293864768839 ) ) ;
#126530 = CARTESIAN_POINT ( 'NONE',  ( 14.82342540975558443, -1.464556741314153587, -62.12362001602809869 ) ) ;
#126531 = CARTESIAN_POINT ( 'NONE',  ( 5.049401038298161559, -19.05341960407611168, 97.70724293864766707 ) ) ;
#126532 = CARTESIAN_POINT ( 'NONE',  ( -8.314922557961024197, 14.29746914071037800, 72.91775706135234714 ) ) ;
#126533 = CARTESIAN_POINT ( 'NONE',  ( 18.67979575497194134, -10.72451020669871369, 110.8344237280190043 ) ) ;
#126534 = CARTESIAN_POINT ( 'NONE',  ( -0.05219959533907301413, -21.53943276465977519, 62.49890960531436690 ) ) ;
#126535 = CARTESIAN_POINT ( 'NONE',  ( -8.314922557961024197, 14.29746914071037800, 92.91775706135236135 ) ) ;
#126536 = CARTESIAN_POINT ( 'NONE',  ( 16.51473224551083163, -9.474510206698727899, 85.83442372801900433 ) ) ;
#126537 = CARTESIAN_POINT ( 'NONE',  ( -16.46253265017160317, 9.564922557960807481, 40.83224293864769550 ) ) ;
#126538 = CARTESIAN_POINT ( 'NONE',  ( -19.02544592524342804, 5.153800228976336051, 76.04057627198102409 ) ) ;
#126539 = CARTESIAN_POINT ( 'NONE',  ( 16.51473224551069308, 9.474510206698969483, 29.16557627198103475 ) ) ;
#126540 = CARTESIAN_POINT ( 'NONE',  ( 5.153800228976615827, -19.02544592524334988, 75.20942372801896170 ) ) ;
#126541 = CARTESIAN_POINT ( 'NONE',  ( 25.27727188472196573, -10.29814791481116920, 170.4127952078933674 ) ) ;
#126542 = CARTESIAN_POINT ( 'NONE',  ( -9.474510206698964154, 16.51473224551069663, 115.4155762719810241 ) ) ;
#126543 = CARTESIAN_POINT ( 'NONE',  ( 4.379528057220339221, -16.55341960407611168, 62.70724293864769550 ) ) ;
#126544 = CARTESIAN_POINT ( 'NONE',  ( 18.67979575497178502, 10.72451020669898547, 59.16557627198103120 ) ) ;
#126545 = CARTESIAN_POINT ( 'NONE',  ( -17.49999999999999645, 5.499999999999997335, 105.7969038253417153 ) ) ;
#126546 = CARTESIAN_POINT ( 'NONE',  ( -16.46253265017146816, -9.564922557961047289, 29.16775706135232937 ) ) ;
#126547 = CARTESIAN_POINT ( 'NONE',  ( 4.500000000000000888, -130.0000000000000000, 15.50000000000000000 ) ) ;
#126549 = CARTESIAN_POINT ( 'NONE',  ( -5.049401038298153566, 19.05341960407611168, 75.20724293864769550 ) ) ;
#126548 = CARTESIAN_POINT ( 'NONE',  ( 16.51473224551069308, 9.474510206698969483, 64.16557627198102409 ) ) ;
#126550 = CARTESIAN_POINT ( 'NONE',  ( 12.14591786802327356, -12.06949235617739191, 50.62609039468568994 ) ) ;
#126551 = CARTESIAN_POINT ( 'NONE',  ( -1.734723475976807094E-15, 15.20000000000001883, -65.00100000000003320 ) ) ;
#126552 = CARTESIAN_POINT ( 'NONE',  ( 24.43796699203919331, -7.704306453272278254, 171.8420650787744250 ) ) ;
#126553 = CARTESIAN_POINT ( 'NONE',  ( -8.314922557961024197, 14.29746914071037800, 72.91775706135234714 ) ) ;
#126554 = CARTESIAN_POINT ( 'NONE',  ( 24.55187747166651135, 5.935858836270472949, 169.5341757581197157 ) ) ;
#126555 = CARTESIAN_POINT ( 'NONE',  ( 12.14591786802327356, -12.06949235617739191, 60.62609039468567573 ) ) ;
#126556 = CARTESIAN_POINT ( 'NONE',  ( 8.314922557961029526, -14.29746914071037800, 35.41775706135234003 ) ) ;
#126558 = DIRECTION ( 'NONE',  ( -6.982962677686266711E-15, 0.000000000000000000, 1.000000000000000000 ) ) ;
#126557 = CARTESIAN_POINT ( 'NONE',  ( -16.51473224551069308, -9.474510206698971260, 61.66557627198103120 ) ) ;
#126559 = CARTESIAN_POINT ( 'NONE',  ( 21.53943276465977519, 0.05219959533937863772, 51.25109039468568994 ) ) ;
#126560 = CARTESIAN_POINT ( 'NONE',  ( -5.049401038297874678, -19.05341960407617918, 59.79275706135231871 ) ) ;
#126561 = CARTESIAN_POINT ( 'NONE',  ( 5.719274019375673035, 21.55341960407619339, 107.2927570613523471 ) ) ;
#126562 = CARTESIAN_POINT ( 'NONE',  ( -13.97604488694527625, -13.89961937509977652, 36.87390960531436690 ) ) ;
#126563 = CARTESIAN_POINT ( 'NONE',  ( 16.49949742642548856, 7.238363427225953828, 23.55948828841231446 ) ) ;
#126564 = CARTESIAN_POINT ( 'NONE',  ( 15.72974639402199770, -15.80617190586745480, 53.12390960531436690 ) ) ;
#126565 = CARTESIAN_POINT ( 'NONE',  ( 5.049401038298161559, -19.05341960407611168, 102.7072429386476955 ) ) ;
#126566 = CARTESIAN_POINT ( 'NONE',  ( -12.14591786802309592, -12.06949235617757132, 101.8739096053143811 ) ) ;
#126567 = CARTESIAN_POINT ( 'NONE',  ( -14.34966873604972548, 8.224510206698743886, 43.33442372801901143 ) ) ;
#126568 = CARTESIAN_POINT ( 'NONE',  ( 0.05219959533910956823, 16.53943276465976808, 24.99890960531435624 ) ) ;
#126569 = VERTEX_POINT ( 'NONE', #110158 ) ;
#126570 = CARTESIAN_POINT ( 'NONE',  ( 0.05219959533907565091, 21.53943276465977519, 104.9989096053143669 ) ) ;
#126572 = CARTESIAN_POINT ( 'NONE',  ( -19.99999999999998224, -188.0000000000000000, 0.000000000000000000 ) ) ;
#126571 = CARTESIAN_POINT ( 'NONE',  ( 14.34966873604960469, 8.224510206698951720, 44.16557627198103120 ) ) ;
#126573 = CARTESIAN_POINT ( 'NONE',  ( -5.049401038297874678, -19.05341960407617918, 89.79275706135230450 ) ) ;
#126574 = CARTESIAN_POINT ( 'NONE',  ( -16.51473224551082808, 9.474510206698731452, 23.33442372801900078 ) ) ;
#126575 = CARTESIAN_POINT ( 'NONE',  ( -8.314922557960811034, -14.29746914071050412, 27.08224293864769550 ) ) ;
#126576 = CARTESIAN_POINT ( 'NONE',  ( 0.05219959533907565091, 21.53943276465977519, 99.99890960531436690 ) ) ;
#126577 = CARTESIAN_POINT ( 'NONE',  ( 10.81492255796078972, 18.62759615963270932, 49.58224293864769550 ) ) ;
#126578 = CARTESIAN_POINT ( 'NONE',  ( -19.05341960407611168, -5.049401038298163336, 81.45724293864769550 ) ) ;
#126579 = CARTESIAN_POINT ( 'NONE',  ( 8.224510206698953496, -14.34966873604960469, 37.91557627198102409 ) ) ;
#126580 = CARTESIAN_POINT ( 'NONE',  ( -13.97604488694527625, -13.89961937509977652, 96.87390960531433848 ) ) ;
#126581 = CARTESIAN_POINT ( 'NONE',  ( 18.22780087662121673, 5.500000000000056843, 78.98459894673892734 ) ) ;
#126582 = CARTESIAN_POINT ( 'NONE',  ( 0.05219959533936267826, -19.03943276465977164, 35.00109039468566863 ) ) ;
#126583 = CARTESIAN_POINT ( 'NONE',  ( -21.55341960407610458, -5.719274019375992779, 76.45724293864769550 ) ) ;
#126584 = CARTESIAN_POINT ( 'NONE',  ( 16.52544592524342804, -4.483927247898539470, 103.5405762719810383 ) ) ;
#126585 = CARTESIAN_POINT ( 'NONE',  ( 18.67979575497194134, -10.72451020669871369, 30.83442372801902209 ) ) ;
#126586 = CARTESIAN_POINT ( 'NONE',  ( 27.73933785331498569, 2.768321779492822058E-14, 148.3750000027311842 ) ) ;
#126587 = CARTESIAN_POINT ( 'NONE',  ( 8.314922557961029526, -14.29746914071037800, 110.4177570613523756 ) ) ;
#126588 = CARTESIAN_POINT ( 'NONE',  ( 0.05219959533909260263, 19.03943276465977164, 39.99890960531436690 ) ) ;
#126589 = CARTESIAN_POINT ( 'NONE',  ( 13.89961937509977652, -13.97604488694527269, 88.12390960531438111 ) ) ;
#126590 = CARTESIAN_POINT ( 'NONE',  ( 22.44159573604009594, -16.30477369853687364, 139.6750000027311955 ) ) ;
#126591 = CARTESIAN_POINT ( 'NONE',  ( 13.97604488694527802, 13.89961937509977652, 34.37390960531436690 ) ) ;
#126592 = CARTESIAN_POINT ( 'NONE',  ( -12.06949235617756955, 12.14591786802309770, 45.62390960531436690 ) ) ;
#126593 = CARTESIAN_POINT ( 'NONE',  ( 5.823673210054444382, -21.52544592524334988, 75.20942372801901854 ) ) ;
#126595 = CARTESIAN_POINT ( 'NONE',  ( -14.34966873604972548, 8.224510206698743886, 68.33442372801900433 ) ) ;
#126594 = CARTESIAN_POINT ( 'NONE',  ( 28.03896471500612719, -25.30868469084780870, -20.82118626250830573 ) ) ;
#126596 = CARTESIAN_POINT ( 'NONE',  ( -19.03943276465977164, 0.05219959533909376836, 56.24890960531435979 ) ) ;
#126597 = CARTESIAN_POINT ( 'NONE',  ( -5.153800228976328057, -19.02544592524343514, 62.29057627198100988 ) ) ;
#126598 = ORIENTED_EDGE ( 'NONE', *, *, #82917, .T. ) ;
#126599 = CARTESIAN_POINT ( 'NONE',  ( 5.719274019375673035, 21.55341960407619339, 112.2927570613523471 ) ) ;
#126600 = CARTESIAN_POINT ( 'NONE',  ( -16.52544592524335698, -4.483927247898792601, 68.95942372801901854 ) ) ;
#126601 = CARTESIAN_POINT ( 'NONE',  ( 15.80617190586769283, -15.72974639402175789, 100.6260903946857184 ) ) ;
#126602 = CARTESIAN_POINT ( 'NONE',  ( 19.02544592524343514, -5.153800228976328945, 58.54057627198102409 ) ) ;
#126603 = CARTESIAN_POINT ( 'NONE',  ( -5.823673210054116645, -21.52544592524344225, 32.29057627198102409 ) ) ;
#126604 = CARTESIAN_POINT ( 'NONE',  ( 16.46253265017146816, 9.564922557961045513, 111.6677570613523329 ) ) ;
#126605 = CARTESIAN_POINT ( 'NONE',  ( -18.62759615963255300, -10.81492255796106328, 64.16775706135234714 ) ) ;
#126606 = CARTESIAN_POINT ( 'NONE',  ( 12.06949235617739724, 12.14591786802326823, 46.87609039468568994 ) ) ;
#126607 = CARTESIAN_POINT ( 'NONE',  ( -21.52544592524343514, 5.823673210054127303, 101.0405762719810383 ) ) ;
#126608 = CARTESIAN_POINT ( 'NONE',  ( 9.474510206698729675, 16.51473224551082808, 97.08442372801900433 ) ) ;
#126609 = CARTESIAN_POINT ( 'NONE',  ( 0.05219959533909260263, 19.03943276465977164, 79.99890960531436690 ) ) ;
#126610 = CARTESIAN_POINT ( 'NONE',  ( 5.049401038297881783, 19.05341960407617563, 107.2927570613523187 ) ) ;
#126611 = CARTESIAN_POINT ( 'NONE',  ( -19.05341960407617563, 5.049401038297882671, 113.5427570613523471 ) ) ;
#126612 = CARTESIAN_POINT ( 'NONE',  ( -4.379528057220328563, 16.55341960407611168, 60.20724293864768839 ) ) ;
#126613 = CARTESIAN_POINT ( 'NONE',  ( 4.483927247898790824, -16.52544592524335698, 70.20942372801904696 ) ) ;
#126615 = CARTESIAN_POINT ( 'NONE',  ( 0.05219959533909260263, 19.03943276465977164, 54.99890960531435979 ) ) ;
#126614 = CARTESIAN_POINT ( 'NONE',  ( 21.52544592524334988, 5.823673210054432836, 21.45942372801901499 ) ) ;
#126616 = CARTESIAN_POINT ( 'NONE',  ( 19.03943276465977164, -0.05219959533909143690, 73.74890960531435269 ) ) ;
#126617 = CARTESIAN_POINT ( 'NONE',  ( -16.52544592524335698, -4.483927247898792601, 68.95942372801901854 ) ) ;
#126618 = EDGE_CURVE ( 'NONE', #16989, #4215, #109379, .T. ) ;
#126619 = CARTESIAN_POINT ( 'NONE',  ( -17.81289503416611808, 24.51734667627700404, 147.9500000054623570 ) ) ;
#126620 = ORIENTED_EDGE ( 'NONE', *, *, #28653, .T. ) ;
#126621 = CARTESIAN_POINT ( 'NONE',  ( -0.05219959533937732626, 21.53943276465977519, 112.5010903946857042 ) ) ;
#126622 = CARTESIAN_POINT ( 'NONE',  ( -0.05219959533909027116, -19.03943276465977164, 42.49890960531435269 ) ) ;
#126623 = VERTEX_POINT ( 'NONE', #18165 ) ;
#126624 = CARTESIAN_POINT ( 'NONE',  ( 16.46253265017146816, 9.564922557961045513, 106.6677570613523471 ) ) ;
#126626 = CARTESIAN_POINT ( 'NONE',  ( -14.34966873604972548, 8.224510206698743886, 23.33442372801901499 ) ) ;
#126625 = CARTESIAN_POINT ( 'NONE',  ( -5.049401038297874678, -19.05341960407617918, 39.79275706135232582 ) ) ;
#126627 = CARTESIAN_POINT ( 'NONE',  ( 9.474510206698971260, -16.51473224551069308, 47.91557627198102409 ) ) ;
#126628 = CARTESIAN_POINT ( 'NONE',  ( -16.46253265017160317, 9.564922557960807481, 60.83224293864769550 ) ) ;
#126629 = CARTESIAN_POINT ( 'NONE',  ( -15.72974639402197994, 15.80617190586746368, 85.62390960531436690 ) ) ;
#126630 = CARTESIAN_POINT ( 'NONE',  ( -11.30153831258471975, -180.0000000000000000, -15.00000000000000178 ) ) ;
#126631 = CARTESIAN_POINT ( 'NONE',  ( -9.474510206698964154, 16.51473224551069663, 45.41557627198103120 ) ) ;
#126632 = CARTESIAN_POINT ( 'NONE',  ( 1.300000000000000044, 0.7216878364870328300, -1.250000000000000000 ) ) ;
#126633 = CARTESIAN_POINT ( 'NONE',  ( -19.05341960407617563, 5.049401038297882671, 93.54275706135234714 ) ) ;
#126634 = CARTESIAN_POINT ( 'NONE',  ( -4.379528057220328563, 16.55341960407611168, 70.20724293864769550 ) ) ;
#126635 = CARTESIAN_POINT ( 'NONE',  ( -5.049401038297874678, -19.05341960407617918, 24.79275706135233648 ) ) ;
#126636 = CARTESIAN_POINT ( 'NONE',  ( 14.34966873604960469, 8.224510206698951720, 59.16557627198103120 ) ) ;
#126637 = CARTESIAN_POINT ( 'NONE',  ( -21.52544592524334988, -5.823673210054445271, 83.95942372801900433 ) ) ;
#126638 = CARTESIAN_POINT ( 'NONE',  ( 5.049401038298161559, -19.05341960407611168, 27.70724293864769550 ) ) ;
#126639 = CARTESIAN_POINT ( 'NONE',  ( 10.72451020669871369, 18.67979575497193778, 87.08442372801901854 ) ) ;
#126641 = CARTESIAN_POINT ( 'NONE',  ( -15.72974639402176322, -15.80617190586768395, 79.37609039468567573 ) ) ;
#126640 = CARTESIAN_POINT ( 'NONE',  ( 12.06949235617757843, -12.14591786802309237, 28.12390960531435979 ) ) ;
#126642 = CARTESIAN_POINT ( 'NONE',  ( 0.05219959533909260263, 19.03943276465977164, 84.99890960531436690 ) ) ;
#126643 = CARTESIAN_POINT ( 'NONE',  ( -0.05219959533937732626, 21.53943276465977519, 37.50109039468568284 ) ) ;
#126644 = CARTESIAN_POINT ( 'NONE',  ( 19.02544592524343514, -5.153800228976328945, 83.54057627198100988 ) ) ;
#126645 = CARTESIAN_POINT ( 'NONE',  ( -8.314922557960811034, -14.29746914071050412, 97.08224293864770971 ) ) ;
#126646 = CARTESIAN_POINT ( 'NONE',  ( 16.55341960407611168, 4.379528057220329451, 58.95724293864770971 ) ) ;
#126647 = CARTESIAN_POINT ( 'NONE',  ( 0.05219959533907565091, 21.53943276465977519, 74.99890960531435269 ) ) ;
#126648 = CARTESIAN_POINT ( 'NONE',  ( -5.153800228976328057, -19.02544592524343514, 72.29057627198102409 ) ) ;
#126649 = CARTESIAN_POINT ( 'NONE',  ( -5.823673210054116645, -21.52544592524344225, 82.29057627198103830 ) ) ;
#126650 = CARTESIAN_POINT ( 'NONE',  ( -19.02544592524334988, -5.153800228976617603, 73.95942372801900433 ) ) ;
#126652 = CARTESIAN_POINT ( 'NONE',  ( 14.34966873604960469, 8.224510206698951720, 79.16557627198103830 ) ) ;
#126651 = CARTESIAN_POINT ( 'NONE',  ( -19.05341960407617918, 5.049401038297883559, 28.54275706135232937 ) ) ;
#126653 = CARTESIAN_POINT ( 'NONE',  ( -21.52544592524343514, 5.823673210054127303, 51.04057627198103120 ) ) ;
#126654 = CARTESIAN_POINT ( 'NONE',  ( -17.49999999999999645, -5.500000000000000888, 20.00000000000000000 ) ) ;
#126656 = CARTESIAN_POINT ( 'NONE',  ( 27.73933785331498569, 9.013057229001093518, 148.4750000027311785 ) ) ;
#126655 = CARTESIAN_POINT ( 'NONE',  ( 12.06949235617739724, 12.14591786802326823, 96.87609039468568994 ) ) ;
#126657 = CARTESIAN_POINT ( 'NONE',  ( 13.97604488694548053, -13.89961937509957401, 100.6260903946856615 ) ) ;
#126658 = CARTESIAN_POINT ( 'NONE',  ( 16.55341960407611168, 4.379528057220329451, 73.95724293864769550 ) ) ;
#126659 = CARTESIAN_POINT ( 'NONE',  ( 7.122238460089383771, -1.425225664899866684, -62.29949481927938137 ) ) ;
#126660 = CARTESIAN_POINT ( 'NONE',  ( 9.474510206698971260, -16.51473224551069308, 57.91557627198103120 ) ) ;
#126661 = CARTESIAN_POINT ( 'NONE',  ( 8.224510206698953496, -14.34966873604960469, 52.91557627198103830 ) ) ;
#126662 = CARTESIAN_POINT ( 'NONE',  ( -16.46253265017160317, 9.564922557960807481, 95.83224293864769550 ) ) ;
#126664 = CARTESIAN_POINT ( 'NONE',  ( -16.51473224551069308, -9.474510206698971260, 61.66557627198103120 ) ) ;
#126663 = CARTESIAN_POINT ( 'NONE',  ( 13.97604488694548053, -13.89961937509957401, 90.62609039468567573 ) ) ;
#126665 = CARTESIAN_POINT ( 'NONE',  ( -13.89961937509977652, 13.97604488694528158, 90.62390960531432427 ) ) ;
#126666 = CARTESIAN_POINT ( 'NONE',  ( 0.05219959533909260263, 19.03943276465977164, 84.99890960531436690 ) ) ;
#126667 = CARTESIAN_POINT ( 'NONE',  ( 0.05219959533907565091, 21.53943276465977519, 59.99890960531436690 ) ) ;
#126668 = CARTESIAN_POINT ( 'NONE',  ( 14.29746914071037800, 8.314922557961029526, 61.66775706135235424 ) ) ;
#126669 = CARTESIAN_POINT ( 'NONE',  ( 18.22780087662122384, 5.500000000000018652, 98.98459894673892734 ) ) ;
#126670 = CARTESIAN_POINT ( 'NONE',  ( 13.89961937509977652, -13.97604488694527269, 58.12390960531436690 ) ) ;
#126671 = CARTESIAN_POINT ( 'NONE',  ( -0.05219959533907301413, -21.53943276465977519, 67.49890960531436690 ) ) ;
#126672 = CARTESIAN_POINT ( 'NONE',  ( -16.51473224551082808, 9.474510206698731452, 98.33442372801900433 ) ) ;
#126674 = CARTESIAN_POINT ( 'NONE',  ( -21.53943276465977519, -0.05219959533937600094, 43.75109039468568284 ) ) ;
#126673 = CARTESIAN_POINT ( 'NONE',  ( 16.52544592524342804, -4.483927247898539470, 28.54057627198103120 ) ) ;
#126675 = DIRECTION ( 'NONE',  ( -1.000000000000000000, 0.000000000000000000, 0.000000000000000000 ) ) ;
#126677 = CARTESIAN_POINT ( 'NONE',  ( 4.483927247898790824, -16.52544592524335698, 95.20942372801903275 ) ) ;
#126676 = CARTESIAN_POINT ( 'NONE',  ( 14.29746914071037800, 8.314922557961029526, 76.66775706135234714 ) ) ;
#126678 = CARTESIAN_POINT ( 'NONE',  ( 17.79613651744293534, 24.49428055684532524, 147.5656553485623306 ) ) ;
#126679 = CARTESIAN_POINT ( 'NONE',  ( 16.53943276465976808, 0.05219959533934440121, 76.25109039468568994 ) ) ;
#126680 = CARTESIAN_POINT ( 'NONE',  ( 8.314922557961029526, -14.29746914071037800, 35.41775706135234003 ) ) ;
#126681 = CARTESIAN_POINT ( 'NONE',  ( -13.89961937509977652, 13.97604488694528158, 50.62390960531435979 ) ) ;
#126682 = CARTESIAN_POINT ( 'NONE',  ( -19.03943276465977164, 0.05219959533909376836, 51.24890960531436690 ) ) ;
#126683 = CARTESIAN_POINT ( 'NONE',  ( -9.564922557960796823, -16.46253265017161027, 57.08224293864769550 ) ) ;
#126684 = CARTESIAN_POINT ( 'NONE',  ( 15.72974639402176855, 15.80617190586768217, 51.87609039468568284 ) ) ;
#126685 = CARTESIAN_POINT ( 'NONE',  ( 14.34966873604972726, -8.224510206698740333, 55.83442372801901854 ) ) ;
#126686 = CARTESIAN_POINT ( 'NONE',  ( -8.224510206698948167, 14.34966873604960824, 25.41557627198103120 ) ) ;
#126687 = CARTESIAN_POINT ( 'NONE',  ( 19.03943276465977164, -0.05219959533909143690, 28.74890960531435624 ) ) ;
#126688 = CARTESIAN_POINT ( 'NONE',  ( 13.97604488694527802, 13.89961937509977652, 34.37390960531436690 ) ) ;
#126689 = CARTESIAN_POINT ( 'NONE',  ( 16.55341960407618274, -4.379528057220086978, 26.04275706135235779 ) ) ;
#126690 = CARTESIAN_POINT ( 'NONE',  ( -5.153800228976607833, 19.02544592524334988, 82.70942372801897591 ) ) ;
#126691 = CARTESIAN_POINT ( 'NONE',  ( 12.14591786802309770, 12.06949235617756955, 89.37390960531435269 ) ) ;
#126692 = CARTESIAN_POINT ( 'NONE',  ( -16.46253265017160317, 9.564922557960807481, 50.83224293864770260 ) ) ;
#126694 = CARTESIAN_POINT ( 'NONE',  ( 17.50000000000000000, -5.499999999999992895, 91.21769037696437010 ) ) ;
#126693 = CARTESIAN_POINT ( 'NONE',  ( -13.97604488694547697, 13.89961937509957934, 73.12609039468568994 ) ) ;
#126695 = CARTESIAN_POINT ( 'NONE',  ( 21.53943276465977519, 0.05219959533937863772, 76.25109039468568994 ) ) ;
#126696 = CARTESIAN_POINT ( 'NONE',  ( 12.14591786802327356, -12.06949235617739191, 50.62609039468568994 ) ) ;
#126697 = CARTESIAN_POINT ( 'NONE',  ( -17.50000000000000711, 5.076555817581202668, 23.82048507950227645 ) ) ;
#126698 = CARTESIAN_POINT ( 'NONE',  ( -10.81492255796078084, -18.62759615963271287, 42.08224293864769550 ) ) ;
#126699 = CARTESIAN_POINT ( 'NONE',  ( -0.05219959533934338120, 16.53943276465976808, 27.50109039468567929 ) ) ;
#126700 = CARTESIAN_POINT ( 'NONE',  ( 16.51473224551069308, 9.474510206698969483, 29.16557627198103475 ) ) ;
#126701 = CARTESIAN_POINT ( 'NONE',  ( 5.153800228976615827, -19.02544592524334988, 30.20942372801900433 ) ) ;
#126702 = CARTESIAN_POINT ( 'NONE',  ( 10.91206588261563759, 12.25194888441100716, -59.27621954310798458 ) ) ;
#126703 = CARTESIAN_POINT ( 'NONE',  ( -9.564922557960796823, -16.46253265017161027, 37.08224293864768839 ) ) ;
#126704 = CARTESIAN_POINT ( 'NONE',  ( 0.000000000000000000, 0.000000000000000000, -20.00000000000000000 ) ) ;
#126705 = CARTESIAN_POINT ( 'NONE',  ( -19.02544592524342804, 5.153800228976336051, 71.04057627198099567 ) ) ;
#126706 = CARTESIAN_POINT ( 'NONE',  ( -19.35543954521081744, -5.499999999999586109, 54.58901960356452321 ) ) ;
#126707 = CARTESIAN_POINT ( 'NONE',  ( 10.81492255796106328, -18.62759615963255655, 110.4177570613523756 ) ) ;
#126708 = CARTESIAN_POINT ( 'NONE',  ( -16.52544592524342804, 4.483927247898546575, 41.04057627198103120 ) ) ;
#126709 = CARTESIAN_POINT ( 'NONE',  ( -5.153800228976328057, -19.02544592524343514, 37.29057627198102409 ) ) ;
#126710 = EDGE_CURVE ( 'NONE', #128792, #15917, #38296, .T. ) ;
#126711 = CARTESIAN_POINT ( 'NONE',  ( 19.03943276465977164, -0.05219959533909143690, 93.74890960531435269 ) ) ;
#126712 = CARTESIAN_POINT ( 'NONE',  ( 0.05219959533937995610, -21.53943276465977519, 75.00109039468568994 ) ) ;
#126713 = CARTESIAN_POINT ( 'NONE',  ( -5.049401038298153566, 19.05341960407611168, 55.20724293864769550 ) ) ;
#126714 = CARTESIAN_POINT ( 'NONE',  ( 15.72974639402176855, 15.80617190586768217, 61.87609039468568284 ) ) ;
#126715 = CARTESIAN_POINT ( 'NONE',  ( -0.05219959533907301413, -21.53943276465977519, 27.49890960531435269 ) ) ;
#126716 = CARTESIAN_POINT ( 'NONE',  ( -5.049401038298153566, 19.05341960407611168, 30.20724293864768839 ) ) ;
#126717 = CARTESIAN_POINT ( 'NONE',  ( -10.72451020669870658, -18.67979575497194134, 29.58442372801901854 ) ) ;
#126718 = CARTESIAN_POINT ( 'NONE',  ( 9.474510206698729675, 16.51473224551082808, 42.08442372801900433 ) ) ;
#126719 = CARTESIAN_POINT ( 'NONE',  ( 0.05219959533910956823, 16.53943276465976808, 109.9989096053143527 ) ) ;
#126720 = CARTESIAN_POINT ( 'NONE',  ( 16.51473224551069308, 9.474510206698969483, 69.16557627198102409 ) ) ;
#126721 = CARTESIAN_POINT ( 'NONE',  ( -19.03943276465977164, -0.05219959533935918106, 108.7510903946856615 ) ) ;
#126722 = CARTESIAN_POINT ( 'NONE',  ( 0.05219959533910956823, 16.53943276465976808, 79.99890960531435269 ) ) ;
#126723 = CARTESIAN_POINT ( 'NONE',  ( -5.153800228976328057, -19.02544592524343514, 112.2905762719810099 ) ) ;
#126724 = CARTESIAN_POINT ( 'NONE',  ( -19.02544592524334988, -5.153800228976617603, 103.9594237280190043 ) ) ;
#126725 = CARTESIAN_POINT ( 'NONE',  ( 15.80617190586746368, 15.72974639402197994, 109.3739096053143811 ) ) ;
#126726 = CARTESIAN_POINT ( 'NONE',  ( -0.05219959533937732626, 21.53943276465977519, 52.50109039468567573 ) ) ;
#126728 = CARTESIAN_POINT ( 'NONE',  ( -14.29746914071037622, -8.314922557961029526, 54.16775706135235424 ) ) ;
#126727 = B_SPLINE_CURVE_WITH_KNOTS ( 'NONE', 3,
 ( #179094, #88048, #165908, #27406, #106200, #74882 ),
 .UNSPECIFIED., .F., .F.,
 ( 4, 2, 4 ),
 ( 0.003989672132298133049, 0.004372778065220572774, 0.004755883998143011632 ),
 .UNSPECIFIED. ) ;
#126729 = CARTESIAN_POINT ( 'NONE',  ( -16.53943276465976808, -0.05219959533934237506, 58.75109039468568994 ) ) ;
#126730 = CARTESIAN_POINT ( 'NONE',  ( -10.72451020669898014, 18.67979575497178502, 60.41557627198102409 ) ) ;
#126731 = CARTESIAN_POINT ( 'NONE',  ( 19.02544592524343514, -5.153800228976328945, 43.54057627198103120 ) ) ;
#126732 = CARTESIAN_POINT ( 'NONE',  ( 4.483927247898790824, -16.52544592524335698, 75.20942372801901854 ) ) ;
#126733 = CARTESIAN_POINT ( 'NONE',  ( -15.72974639402197994, 15.80617190586746368, 105.6239096053143669 ) ) ;
#126734 = CARTESIAN_POINT ( 'NONE',  ( 14.34966873604960469, 8.224510206698951720, 49.16557627198102409 ) ) ;
#126735 = CARTESIAN_POINT ( 'NONE',  ( -5.153800228976328057, -19.02544592524343514, 67.29057627198102409 ) ) ;
#126736 = CARTESIAN_POINT ( 'NONE',  ( 4.483927247898790824, -16.52544592524335698, 80.20942372801901854 ) ) ;
#126737 = CARTESIAN_POINT ( 'NONE',  ( 0.05219959533934541429, -16.53943276465976808, 25.00109039468567218 ) ) ;
#126738 = CARTESIAN_POINT ( 'NONE',  ( -18.67979575497178146, -10.72451020669898902, 101.6655762719810383 ) ) ;
#126739 = CARTESIAN_POINT ( 'NONE',  ( -12.06949235617756955, 12.14591786802309770, 45.62390960531436690 ) ) ;
#126740 = ADVANCED_FACE ( 'NONE', ( #25148 ), #73639, .F. ) ;
#126741 = ORIENTED_EDGE ( 'NONE', *, *, #74517, .T. ) ;
#126742 = CARTESIAN_POINT ( 'NONE',  ( -16.36317988757058828, 7.306389748694924080, 74.09789608363229263 ) ) ;
#126743 = CARTESIAN_POINT ( 'NONE',  ( 15.72974639402199770, -15.80617190586745480, 83.12390960531436690 ) ) ;
#126744 = CARTESIAN_POINT ( 'NONE',  ( -16.53943276465976808, -0.05219959533934237506, 113.7510903946856757 ) ) ;
#126745 = ORIENTED_EDGE ( 'NONE', *, *, #99054, .T. ) ;
#126746 = CARTESIAN_POINT ( 'NONE',  ( 17.18269478283314911, 17.18269478283310647, -54.21489346206828230 ) ) ;
#126747 = CARTESIAN_POINT ( 'NONE',  ( -5.719274019375978568, 21.55341960407610458, 100.2072429386476955 ) ) ;
#126748 = CARTESIAN_POINT ( 'NONE',  ( -13.89961937509977652, 13.97604488694528158, 100.6239096053143669 ) ) ;
#126749 = CARTESIAN_POINT ( 'NONE',  ( -18.62759615963255300, -10.81492255796106328, 19.16775706135234714 ) ) ;
#126750 = CARTESIAN_POINT ( 'NONE',  ( -14.34966873604960291, -8.224510206698953496, 41.66557627198103120 ) ) ;
#126751 = CARTESIAN_POINT ( 'NONE',  ( 14.34966873604972726, -8.224510206698740333, 50.83442372801901143 ) ) ;
#126752 = CARTESIAN_POINT ( 'NONE',  ( 5.049401038298161559, -19.05341960407611168, 42.70724293864767418 ) ) ;
#126753 = CARTESIAN_POINT ( 'NONE',  ( 9.474510206698729675, 16.51473224551082808, 52.08442372801900433 ) ) ;
#126754 = CARTESIAN_POINT ( 'NONE',  ( -19.03943276465977164, 0.05219959533909376836, 86.24890960531436690 ) ) ;
#126755 = CARTESIAN_POINT ( 'NONE',  ( -10.72451020669898014, 18.67979575497178502, 30.41557627198101699 ) ) ;
#126756 = CARTESIAN_POINT ( 'NONE',  ( -26.43919995774735554, -26.89423752947756441, -20.34026575423078853 ) ) ;
#126757 = CARTESIAN_POINT ( 'NONE',  ( 14.34966873604972726, -8.224510206698740333, 25.83442372801901499 ) ) ;
#126758 = CARTESIAN_POINT ( 'NONE',  ( 0.05219959533936267826, -19.03943276465977164, 45.00109039468566863 ) ) ;
#126759 = CARTESIAN_POINT ( 'NONE',  ( -18.67979575497178146, -10.72451020669898902, 96.66557627198102409 ) ) ;
#126760 = CARTESIAN_POINT ( 'NONE',  ( 16.52544592524342804, -4.483927247898539470, 33.54057627198102409 ) ) ;
#126761 = CARTESIAN_POINT ( 'NONE',  ( -13.97604488694527625, -13.89961937509977652, 76.87390960531433848 ) ) ;
#126762 = CARTESIAN_POINT ( 'NONE',  ( 21.52544592524344225, -5.823673210054117533, 58.54057627198103120 ) ) ;
#126764 = CARTESIAN_POINT ( 'NONE',  ( -16.55341960407617563, 4.379528057220093196, 28.54275706135234358 ) ) ;
#126763 = CARTESIAN_POINT ( 'NONE',  ( 0.05219959533907565091, 21.53943276465977519, 94.99890960531436690 ) ) ;
#126765 = CARTESIAN_POINT ( 'NONE',  ( -18.62759615963270932, 10.81492255796079327, 25.83224293864769194 ) ) ;
#126766 = CARTESIAN_POINT ( 'NONE',  ( 15.80617190586769283, -15.72974639402175789, 90.62609039468567573 ) ) ;
#126767 = CARTESIAN_POINT ( 'NONE',  ( -19.05341960407611168, -5.049401038298163336, 91.45724293864766707 ) ) ;
#126768 = CARTESIAN_POINT ( 'NONE',  ( -5.153800228976328057, -19.02544592524343514, 22.29057627198102765 ) ) ;
#126769 = CARTESIAN_POINT ( 'NONE',  ( 19.05341960407611168, 5.049401038298154454, 78.95724293864769550 ) ) ;
#126770 = CARTESIAN_POINT ( 'NONE',  ( 8.224510206698953496, -14.34966873604960469, 102.9155762719810383 ) ) ;
#126771 = CARTESIAN_POINT ( 'NONE',  ( -19.05341960407611168, -5.049401038298163336, 66.45724293864769550 ) ) ;
#126772 = CARTESIAN_POINT ( 'NONE',  ( -14.34966873604972548, 8.224510206698743886, 28.33442372801902209 ) ) ;
#126773 = CARTESIAN_POINT ( 'NONE',  ( 17.50000000000000000, 3.209263204892558896, 32.73803174393727744 ) ) ;
#126774 = CARTESIAN_POINT ( 'NONE',  ( -13.97604488694527625, -13.89961937509977652, 71.87390960531433848 ) ) ;
#126776 = CARTESIAN_POINT ( 'NONE',  ( -9.474510206698964154, 16.51473224551069663, 110.4155762719810383 ) ) ;
#126775 = CARTESIAN_POINT ( 'NONE',  ( -10.81492255796105439, 18.62759615963255655, 102.9177570613523756 ) ) ;
#126777 = CARTESIAN_POINT ( 'NONE',  ( -14.34966873604972548, 8.224510206698743886, 88.33442372801901854 ) ) ;
#126778 = CARTESIAN_POINT ( 'NONE',  ( 30.00000000000000000, 5.499999999999992895, 37.50000000000000000 ) ) ;
#126779 = CARTESIAN_POINT ( 'NONE',  ( 0.05219959533936267826, -19.03943276465977164, 65.00109039468567573 ) ) ;
#126780 = CARTESIAN_POINT ( 'NONE',  ( 21.55341960407619695, -5.719274019375665929, 111.0427570613523613 ) ) ;
#126781 = LINE ( 'NONE', #79302, #137224 ) ;
#126782 = CARTESIAN_POINT ( 'NONE',  ( 16.46253265017160672, -9.564922557960803928, 33.33224293864770260 ) ) ;
#126783 = CARTESIAN_POINT ( 'NONE',  ( 8.224510206698953496, -14.34966873604960469, 27.91557627198103830 ) ) ;
#126784 = DIRECTION ( 'NONE',  ( -0.000000000000000000, -0.000000000000000000, 1.000000000000000000 ) ) ;
#126785 = CARTESIAN_POINT ( 'NONE',  ( 14.34966873604972726, -8.224510206698740333, 100.8344237280190185 ) ) ;
#126786 = CARTESIAN_POINT ( 'NONE',  ( -19.19724070472097566, -5.499999999999895195, 86.06193348274379673 ) ) ;
#126787 = CARTESIAN_POINT ( 'NONE',  ( -4.483927247898782831, 16.52544592524335698, 77.70942372801900433 ) ) ;
#126788 = CARTESIAN_POINT ( 'NONE',  ( -0.05219959533909027116, -19.03943276465977164, 37.49890960531436690 ) ) ;
#126789 = CARTESIAN_POINT ( 'NONE',  ( -10.81492255796105439, 18.62759615963255655, 97.91775706135236135 ) ) ;
#126790 = CARTESIAN_POINT ( 'NONE',  ( -9.474510206698720793, -16.51473224551083518, 104.5844237280190043 ) ) ;
#126791 = CARTESIAN_POINT ( 'NONE',  ( 21.53943276465977519, 0.05219959533937863772, 76.25109039468568994 ) ) ;
#126792 = CARTESIAN_POINT ( 'NONE',  ( 13.89961937509957401, 13.97604488694547697, 56.87609039468564731 ) ) ;
#126793 = CARTESIAN_POINT ( 'NONE',  ( -13.89961937509977652, 13.97604488694528158, 80.62390960531436690 ) ) ;
#126794 = CARTESIAN_POINT ( 'NONE',  ( -9.564922557960796823, -16.46253265017161027, 67.08224293864769550 ) ) ;
#126795 = CARTESIAN_POINT ( 'NONE',  ( 17.31747979337950127, 6.344076630961023255, 73.87944868065186199 ) ) ;
#126796 = CARTESIAN_POINT ( 'NONE',  ( -0.05219959533910754901, -16.53943276465976808, 67.49890960531436690 ) ) ;
#126797 = CARTESIAN_POINT ( 'NONE',  ( -18.67979575497178146, -10.72451020669898902, 46.66557627198102409 ) ) ;
#126798 = CARTESIAN_POINT ( 'NONE',  ( 16.51473224551069308, 9.474510206698969483, 44.16557627198103120 ) ) ;
#126800 = CARTESIAN_POINT ( 'NONE',  ( 12.14591786802327356, -12.06949235617739191, 75.62609039468567573 ) ) ;
#126799 = CARTESIAN_POINT ( 'NONE',  ( 15.80617190586746368, 15.72974639402197994, 89.37390960531435269 ) ) ;
#126801 = ORIENTED_EDGE ( 'NONE', *, *, #21058, .F. ) ;
#126803 = CARTESIAN_POINT ( 'NONE',  ( 22.81625015709509441, 31.40387420917330275, -3.324999997268812901 ) ) ;
#126802 = CARTESIAN_POINT ( 'NONE',  ( 16.53943276465976808, -0.05219959533910856209, 83.74890960531435269 ) ) ;
#126804 = CARTESIAN_POINT ( 'NONE',  ( 16.52544592524335698, 4.483927247898782831, 36.45942372801901143 ) ) ;
#126805 = CARTESIAN_POINT ( 'NONE',  ( 9.474510206698971260, -16.51473224551069308, 22.91557627198102765 ) ) ;
#126806 = CARTESIAN_POINT ( 'NONE',  ( -9.474510206698720793, -16.51473224551083518, 64.58442372801900433 ) ) ;
#126807 = CARTESIAN_POINT ( 'NONE',  ( -12.14591786802309592, -12.06949235617757132, 66.87390960531436690 ) ) ;
#126809 = EDGE_CURVE ( 'NONE', #117002, #17032, #109480, .T. ) ;
#126808 = CARTESIAN_POINT ( 'NONE',  ( 15.72974639402176855, 15.80617190586768217, 51.87609039468568284 ) ) ;
#126811 = CARTESIAN_POINT ( 'NONE',  ( 5.719274019375991003, -21.55341960407610458, 92.70724293864770971 ) ) ;
#126810 = CARTESIAN_POINT ( 'NONE',  ( 5.049401038298161559, -19.05341960407611168, 27.70724293864769550 ) ) ;
#126812 = B_SPLINE_CURVE_WITH_KNOTS ( 'NONE', 3,
 ( #35320, #19169, #6959, #80818, #143478, #128310, #146475, #64671, #67643, #97956, #113146, #51484, #127316, #158655, #112165, #23152, #52474, #68639, #142496, #111163, #130295, #188030 ),
 .UNSPECIFIED., .F., .F.,
 ( 4, 2, 2, 2, 2, 2, 2, 2, 2, 2, 4 ),
 ( 0.008245893658555575323, 0.01147022081997697146, 0.01308238440068766953, 0.01469454798139836760, 0.01791887514281974986, 0.02114320230424113906, 0.02759185662708390011, 0.03081618378850527543, 0.03242834736921596656, 0.03323442915957131039, 0.03404051094992665422 ),
 .UNSPECIFIED. ) ;
#126813 = CARTESIAN_POINT ( 'NONE',  ( 9.474510206698971260, -16.51473224551069308, 112.9155762719810383 ) ) ;
#126814 = CARTESIAN_POINT ( 'NONE',  ( -16.53943276465976808, 0.05219959533911058130, 86.24890960531436690 ) ) ;
#126815 = CARTESIAN_POINT ( 'NONE',  ( 23.69010019207190965, -31.82897765506827881, -19.48018210901874525 ) ) ;
#126816 = CARTESIAN_POINT ( 'NONE',  ( 5.049401038298161559, -19.05341960407611168, 47.70724293864770260 ) ) ;
#126817 = CARTESIAN_POINT ( 'NONE',  ( -22.81625015709510507, 31.40387420917330275, -4.924999997268813878 ) ) ;
#126818 = CARTESIAN_POINT ( 'NONE',  ( -19.05341960407617563, 5.049401038297882671, 83.54275706135233293 ) ) ;
#126819 = CARTESIAN_POINT ( 'NONE',  ( 18.62759615963255655, 10.81492255796105972, 31.66775706135234358 ) ) ;
#126820 = CARTESIAN_POINT ( 'NONE',  ( 16.46253265017160672, -9.564922557960803928, 68.33224293864770971 ) ) ;
#126821 = CARTESIAN_POINT ( 'NONE',  ( 9.474510206698729675, 16.51473224551082808, 57.08442372801900433 ) ) ;
#126822 = CARTESIAN_POINT ( 'NONE',  ( 13.89961937509977652, -13.97604488694527269, 48.12390960531435979 ) ) ;
#126823 = CARTESIAN_POINT ( 'NONE',  ( 14.29746914071049879, -8.314922557960816363, 68.33224293864769550 ) ) ;
#126824 = CARTESIAN_POINT ( 'NONE',  ( -16.52544592524342804, 4.483927247898546575, 56.04057627198102409 ) ) ;
#126825 = CARTESIAN_POINT ( 'NONE',  ( -0.05219959533909027116, -19.03943276465977164, 72.49890960531435269 ) ) ;
#126826 = CARTESIAN_POINT ( 'NONE',  ( -15.80617190586745835, -15.72974639402198527, 101.8739096053143811 ) ) ;
#126827 = CARTESIAN_POINT ( 'NONE',  ( 16.51473224551069308, 9.474510206698969483, 74.16557627198103830 ) ) ;
#126828 = CARTESIAN_POINT ( 'NONE',  ( -21.53943276465977519, 0.05219959533907696930, 76.24890960531435269 ) ) ;
#126829 = CARTESIAN_POINT ( 'NONE',  ( -9.474510206698720793, -16.51473224551083518, 19.58442372801899722 ) ) ;
#126832 = CARTESIAN_POINT ( 'NONE',  ( -12.06949235617756955, 12.14591786802309770, 90.62390960531436690 ) ) ;
#126831 = CARTESIAN_POINT ( 'NONE',  ( -16.52544592524335698, -4.483927247898792601, 103.9594237280190185 ) ) ;
#126830 = CARTESIAN_POINT ( 'NONE',  ( -19.05341960407611168, -5.049401038298163336, 31.45724293864769550 ) ) ;
#126833 = CARTESIAN_POINT ( 'NONE',  ( -9.474510206698720793, -16.51473224551083518, 104.5844237280190043 ) ) ;
#126834 = VERTEX_POINT ( 'NONE', #41300 ) ;
#126835 = CARTESIAN_POINT ( 'NONE',  ( -5.719274019375665041, -21.55341960407619695, 34.79275706135235424 ) ) ;
#126836 = CARTESIAN_POINT ( 'NONE',  ( 19.03943276465977164, 0.05219959533936151252, 56.25109039468566863 ) ) ;
#126837 = CARTESIAN_POINT ( 'NONE',  ( 14.34966873604972726, -8.224510206698740333, 110.8344237280190043 ) ) ;
#126838 = CARTESIAN_POINT ( 'NONE',  ( -21.55341960407610458, -5.719274019375992779, 66.45724293864768129 ) ) ;
#126839 = CARTESIAN_POINT ( 'NONE',  ( 5.153800228976335163, 19.02544592524342804, 104.7905762719809957 ) ) ;
#126840 = CARTESIAN_POINT ( 'NONE',  ( -16.55341960407611168, -4.379528057220339221, 61.45724293864770260 ) ) ;
#126841 = CARTESIAN_POINT ( 'NONE',  ( 5.049401038298161559, -19.05341960407611168, 27.70724293864769550 ) ) ;
#126842 = CARTESIAN_POINT ( 'NONE',  ( -13.89961937509977652, 13.97604488694528158, 30.62390960531435269 ) ) ;
#126843 = CARTESIAN_POINT ( 'NONE',  ( -19.02544592524334988, -5.153800228976617603, 23.95942372801900078 ) ) ;
#126844 = CARTESIAN_POINT ( 'NONE',  ( -4.379528057220086978, -16.55341960407618274, 94.79275706135234714 ) ) ;
#126845 = CARTESIAN_POINT ( 'NONE',  ( 5.719274019375673035, 21.55341960407619339, 47.29275706135234003 ) ) ;
#126846 = CARTESIAN_POINT ( 'NONE',  ( -12.06949235617739369, -12.14591786802326823, 44.37609039468567573 ) ) ;
#126847 = CARTESIAN_POINT ( 'NONE',  ( 16.51473224551069308, 9.474510206698969483, 114.1655762719810241 ) ) ;
#126849 = CARTESIAN_POINT ( 'NONE',  ( 15.80617190586769283, -15.72974639402175789, 90.62609039468567573 ) ) ;
#126848 = CARTESIAN_POINT ( 'NONE',  ( -5.153800228976328057, -19.02544592524343514, 47.29057627198102409 ) ) ;
#126850 = CARTESIAN_POINT ( 'NONE',  ( 5.153800228976335163, 19.02544592524342804, 74.79057627198103830 ) ) ;
#126851 = CARTESIAN_POINT ( 'NONE',  ( 8.314922557961029526, -14.29746914071037800, 60.41775706135235424 ) ) ;
#126852 = CARTESIAN_POINT ( 'NONE',  ( 16.52544592524342804, -4.483927247898539470, 108.5405762719810241 ) ) ;
#126853 = CARTESIAN_POINT ( 'NONE',  ( -12.14591786802309592, -12.06949235617757132, 26.87390960531435979 ) ) ;
#126854 = CARTESIAN_POINT ( 'NONE',  ( -13.89961937509977830, 13.97604488694528158, 50.62390960531435979 ) ) ;
#126857 = CARTESIAN_POINT ( 'NONE',  ( 19.03943276465977164, -0.05219959533909143690, 83.74890960531436690 ) ) ;
#126856 = CARTESIAN_POINT ( 'NONE',  ( 19.03943276465977164, -0.05219959533909143690, 88.74890960531436690 ) ) ;
#126855 = CARTESIAN_POINT ( 'NONE',  ( 21.52544592524334988, 5.823673210054432836, 51.45942372801901854 ) ) ;
#126858 = CARTESIAN_POINT ( 'NONE',  ( -5.049401038298153566, 19.05341960407611168, 110.2072429386476671 ) ) ;
#126859 = CARTESIAN_POINT ( 'NONE',  ( -12.06949235617756955, 12.14591786802309770, 45.62390960531436690 ) ) ;
#126860 = CARTESIAN_POINT ( 'NONE',  ( -8.314922557960811034, -14.29746914071050412, 22.08224293864769194 ) ) ;
#126861 = CARTESIAN_POINT ( 'NONE',  ( -14.34966873604960291, -8.224510206698953496, 41.66557627198103120 ) ) ;
#126862 = DIRECTION ( 'NONE',  ( 0.000000000000000000, 0.000000000000000000, -1.000000000000000000 ) ) ;
#126863 = CARTESIAN_POINT ( 'NONE',  ( 5.049401038297881783, 19.05341960407617563, 32.29275706135233293 ) ) ;
#126864 = CARTESIAN_POINT ( 'NONE',  ( -5.153800228976328057, -19.02544592524343514, 77.29057627198099567 ) ) ;
#126865 = CARTESIAN_POINT ( 'NONE',  ( -19.05341960407617563, 5.049401038297882671, 58.54275706135234003 ) ) ;
#126866 = CARTESIAN_POINT ( 'NONE',  ( -36.91746825000001309, 11.99521256947798342, -0.7249999972688133676 ) ) ;
#126867 = DIRECTION ( 'NONE',  ( -0.000000000000000000, 0.000000000000000000, 1.000000000000000000 ) ) ;
#126869 = CARTESIAN_POINT ( 'NONE',  ( -4.483927247898782831, 16.52544592524335698, 72.70942372801901854 ) ) ;
#126868 = CARTESIAN_POINT ( 'NONE',  ( -16.46253265017146816, -9.564922557961047289, 79.16775706135234714 ) ) ;
#126870 = DIRECTION ( 'NONE',  ( -0.4999999999999967248, 0.5000000000000019984, 0.7071067811865485719 ) ) ;
#126871 = CARTESIAN_POINT ( 'NONE',  ( -5.049401038298153566, 19.05341960407611168, 110.2072429386476671 ) ) ;
#126872 = CARTESIAN_POINT ( 'NONE',  ( -5.823673210054431948, 21.52544592524334988, 22.70942372801901499 ) ) ;
#126873 = AXIS2_PLACEMENT_3D ( 'NONE', #198008, #76637, #199996 ) ;
#126874 = CARTESIAN_POINT ( 'NONE',  ( -5.153800228976607833, 19.02544592524334988, 87.70942372801897591 ) ) ;
#126876 = CARTESIAN_POINT ( 'NONE',  ( 0.05219959533909260263, 19.03943276465977164, 44.99890960531435979 ) ) ;
#126875 = CARTESIAN_POINT ( 'NONE',  ( 16.29526858892876007, 7.335722546920148801, 88.29670597800215148 ) ) ;
#126877 = CARTESIAN_POINT ( 'NONE',  ( 5.049401038298161559, -19.05341960407611168, 92.70724293864769550 ) ) ;
#126879 = CARTESIAN_POINT ( 'NONE',  ( 13.97604488694527802, 13.89961937509977652, 44.37390960531435269 ) ) ;
#126878 = CARTESIAN_POINT ( 'NONE',  ( 16.52544592524342804, -4.483927247898539470, 63.54057627198103830 ) ) ;
#126880 = CARTESIAN_POINT ( 'NONE',  ( -19.05341960407611168, -5.049401038298163336, 61.45724293864769550 ) ) ;
#126881 = CARTESIAN_POINT ( 'NONE',  ( -9.474510206698720793, -16.51473224551083518, 69.58442372801901854 ) ) ;
#126882 = CARTESIAN_POINT ( 'NONE',  ( 5.153800228976615827, -19.02544592524334988, 25.20942372801900433 ) ) ;
#126883 = CARTESIAN_POINT ( 'NONE',  ( 19.05341960407611168, 5.049401038298154454, 68.95724293864769550 ) ) ;
#126884 = CARTESIAN_POINT ( 'NONE',  ( -21.53943276465977519, 0.05219959533907696930, 66.24890960531436690 ) ) ;
#126886 = CARTESIAN_POINT ( 'NONE',  ( 19.05341960407617918, -5.049401038297876454, 41.04275706135233293 ) ) ;
#126885 = CARTESIAN_POINT ( 'NONE',  ( -12.14591786802309592, -12.06949235617757132, 71.87390960531438111 ) ) ;
#126887 = DIRECTION ( 'NONE',  ( 0.000000000000000000, 0.1045284632676537068, 0.9945218953682734009 ) ) ;
#126888 = CARTESIAN_POINT ( 'NONE',  ( -0.05219959533907301413, -21.53943276465977519, 47.49890960531435979 ) ) ;
#126889 = CARTESIAN_POINT ( 'NONE',  ( -15.72974639402197994, 15.80617190586746368, 25.62390960531435624 ) ) ;
#126890 = CARTESIAN_POINT ( 'NONE',  ( 16.46253265017160672, -9.564922557960803928, 58.33224293864769550 ) ) ;
#126891 = CARTESIAN_POINT ( 'NONE',  ( -9.564922557960796823, -16.46253265017161027, 37.08224293864768839 ) ) ;
#126892 = CARTESIAN_POINT ( 'NONE',  ( -8.314922557960811034, -14.29746914071050412, 102.0822429386476955 ) ) ;
#126893 = CARTESIAN_POINT ( 'NONE',  ( 5.719274019375991003, -21.55341960407610458, 107.7072429386476955 ) ) ;
#126894 = FACE_OUTER_BOUND ( 'NONE', #135389, .T. ) ;
#126895 = CARTESIAN_POINT ( 'NONE',  ( 15.72974639402176855, 15.80617190586768217, 31.87609039468567929 ) ) ;
#126896 = CARTESIAN_POINT ( 'NONE',  ( -14.29746914071049879, 8.314922557960819915, 110.8322429386476955 ) ) ;
#126897 = CARTESIAN_POINT ( 'NONE',  ( 18.67979575497194134, -10.72451020669871369, 80.83442372801901854 ) ) ;
#126898 = CARTESIAN_POINT ( 'NONE',  ( 18.62759615963271287, -10.81492255796078972, 98.33224293864769550 ) ) ;
#126899 = CARTESIAN_POINT ( 'NONE',  ( -19.02544592524334988, -5.153800228976617603, 38.95942372801900433 ) ) ;
#126900 = DIRECTION ( 'NONE',  ( -0.000000000000000000, -0.000000000000000000, -1.000000000000000000 ) ) ;
#126901 = DIRECTION ( 'NONE',  ( 1.000000000000000000, 0.000000000000000000, 0.000000000000000000 ) ) ;
#126902 = CARTESIAN_POINT ( 'NONE',  ( 38.00000000000000000, -12.34694845685040754, -1.099999999999999645 ) ) ;
#126903 = CARTESIAN_POINT ( 'NONE',  ( 14.29746914071037800, 8.314922557961029526, 46.66775706135234714 ) ) ;
#126904 = CARTESIAN_POINT ( 'NONE',  ( 16.52544592524342804, -4.483927247898539470, 108.5405762719810241 ) ) ;
#126905 = CARTESIAN_POINT ( 'NONE',  ( 33.76764775315835010, -5.498935319396520249, 94.62547034095169352 ) ) ;
#126906 = CARTESIAN_POINT ( 'NONE',  ( -19.05341960407611168, -5.049401038298163336, 66.45724293864769550 ) ) ;
#126907 = CARTESIAN_POINT ( 'NONE',  ( -8.224510206698948167, 14.34966873604960824, 95.41557627198102409 ) ) ;
#126908 = CARTESIAN_POINT ( 'NONE',  ( 10.72451020669898902, -18.67979575497178502, 47.91557627198102409 ) ) ;
#126909 = CARTESIAN_POINT ( 'NONE',  ( 16.55341960407611168, 4.379528057220329451, 78.95724293864769550 ) ) ;
#126910 = CARTESIAN_POINT ( 'NONE',  ( 14.34966873604972726, -8.224510206698740333, 30.83442372801902209 ) ) ;
#126911 = CARTESIAN_POINT ( 'NONE',  ( -5.823673210054431948, 21.52544592524334988, 82.70942372801900433 ) ) ;
#126912 = CARTESIAN_POINT ( 'NONE',  ( -16.51473224551069308, -9.474510206698971260, 26.66557627198103120 ) ) ;
#126913 = CARTESIAN_POINT ( 'NONE',  ( 8.224510206698742110, 14.34966873604972548, 92.08442372801901854 ) ) ;
#126914 = CARTESIAN_POINT ( 'NONE',  ( 8.224510206698953496, -14.34966873604960469, 42.91557627198103120 ) ) ;
#126915 = CARTESIAN_POINT ( 'NONE',  ( 5.049401038298161559, -19.05341960407611168, 57.70724293864769550 ) ) ;
#126916 = CARTESIAN_POINT ( 'NONE',  ( -21.55341960407619339, 5.719274019375674811, 93.54275706135234714 ) ) ;
#126917 = CARTESIAN_POINT ( 'NONE',  ( -21.53943276465977519, 0.05219959533907696930, 111.2489096053143669 ) ) ;
#126918 = CARTESIAN_POINT ( 'NONE',  ( 5.823673210054444382, -21.52544592524334988, 55.20942372801902565 ) ) ;
#126919 = CARTESIAN_POINT ( 'NONE',  ( -16.52544592524335698, -4.483927247898792601, 33.95942372801901143 ) ) ;
#126921 = CARTESIAN_POINT ( 'NONE',  ( -10.72451020669870658, -18.67979575497194134, 84.58442372801903275 ) ) ;
#126920 = CARTESIAN_POINT ( 'NONE',  ( 16.55341960407611168, 4.379528057220329451, 58.95724293864770971 ) ) ;
#126922 = CARTESIAN_POINT ( 'NONE',  ( 8.314922557961029526, -14.29746914071037800, 110.4177570613523756 ) ) ;
#126923 = CARTESIAN_POINT ( 'NONE',  ( 17.50000000000001421, -5.622605283950838029, 46.18792689403891671 ) ) ;
#126924 = DIRECTION ( 'NONE',  ( 0.000000000000000000, 0.000000000000000000, 1.000000000000000000 ) ) ;
#126925 = CARTESIAN_POINT ( 'NONE',  ( -8.314922557960811034, -14.29746914071050412, 22.08224293864769194 ) ) ;
#126926 = CARTESIAN_POINT ( 'NONE',  ( 12.06949235617739724, 12.14591786802326823, 76.87609039468567573 ) ) ;
#126927 = CARTESIAN_POINT ( 'NONE',  ( 13.97604488694527802, 13.89961937509977652, 89.37390960531436690 ) ) ;
#126928 = CARTESIAN_POINT ( 'NONE',  ( 9.564922557960805705, 16.46253265017160317, 99.58224293864770971 ) ) ;
#126929 = CARTESIAN_POINT ( 'NONE',  ( 10.81492255796106328, -18.62759615963255655, 80.41775706135234714 ) ) ;
#126930 = CARTESIAN_POINT ( 'NONE',  ( -12.14591786802326823, 12.06949235617739902, 88.12609039468570415 ) ) ;
#126931 = CARTESIAN_POINT ( 'NONE',  ( -12.14591786802309592, -12.06949235617757132, 66.87390960531436690 ) ) ;
#126932 = CARTESIAN_POINT ( 'NONE',  ( 19.05341960407611168, 5.049401038298154454, 68.95724293864769550 ) ) ;
#126933 = VERTEX_POINT ( 'NONE', #146453 ) ;
#126934 = CARTESIAN_POINT ( 'NONE',  ( 0.05219959533934541429, -16.53943276465976808, 25.00109039468567218 ) ) ;
#126935 = CARTESIAN_POINT ( 'NONE',  ( -16.46253265017160317, 9.564922557960807481, 25.83224293864769194 ) ) ;
#126936 = CARTESIAN_POINT ( 'NONE',  ( -9.474510206698964154, 16.51473224551069663, 95.41557627198102409 ) ) ;
#126938 = CARTESIAN_POINT ( 'NONE',  ( -29.86685920354755552, 21.69954338932564397, -6.824999997268814234 ) ) ;
#126937 = CARTESIAN_POINT ( 'NONE',  ( -12.06949235617739369, -12.14591786802326823, 29.37609039468568284 ) ) ;
#126939 = CARTESIAN_POINT ( 'NONE',  ( 15.80617190586769283, -15.72974639402175789, 110.6260903946857042 ) ) ;
#126940 = CARTESIAN_POINT ( 'NONE',  ( 14.34966873604972726, -8.224510206698740333, 95.83442372801903275 ) ) ;
#126941 = CARTESIAN_POINT ( 'NONE',  ( -0.05219959533936034679, 19.03943276465977164, 112.5010903946856757 ) ) ;
#126942 = CARTESIAN_POINT ( 'NONE',  ( -0.05219959533909027116, -19.03943276465977164, 37.49890960531436690 ) ) ;
#126943 = CARTESIAN_POINT ( 'NONE',  ( 16.52544592524335698, 4.483927247898782831, 81.45942372801900433 ) ) ;
#126944 = CARTESIAN_POINT ( 'NONE',  ( 14.34966873604972726, -8.224510206698740333, 60.83442372801901854 ) ) ;
#126945 = CARTESIAN_POINT ( 'NONE',  ( 26.55164451606355769, -29.92006817138308605, -6.154309889040165515 ) ) ;
#126946 = CARTESIAN_POINT ( 'NONE',  ( -19.03943276465977164, -0.05219959533935918106, 73.75109039468566152 ) ) ;
#126947 = CARTESIAN_POINT ( 'NONE',  ( -15.72974639402176322, -15.80617190586768395, 104.3760903946856899 ) ) ;
#126948 = CARTESIAN_POINT ( 'NONE',  ( 9.474510206698971260, -16.51473224551069308, 42.91557627198103120 ) ) ;
#126949 = CARTESIAN_POINT ( 'NONE',  ( -19.03943276465977164, 0.05219959533909376836, 91.24890960531436690 ) ) ;
#126950 = CARTESIAN_POINT ( 'NONE',  ( -16.52544592524342804, 4.483927247898546575, 81.04057627198102409 ) ) ;
#126951 = CARTESIAN_POINT ( 'NONE',  ( 19.02544592524334988, 5.153800228976608722, 56.45942372801898301 ) ) ;
#126952 = CARTESIAN_POINT ( 'NONE',  ( -21.53943276465977519, 0.05219959533907696930, 46.24890960531435979 ) ) ;
#126953 = CARTESIAN_POINT ( 'NONE',  ( 0.05219959533937995610, -21.53943276465977519, 110.0010903946856757 ) ) ;
#126954 = CARTESIAN_POINT ( 'NONE',  ( -13.97604488694527625, -13.89961937509977652, 91.87390960531432427 ) ) ;
#126955 = CARTESIAN_POINT ( 'NONE',  ( 15.72974639402176855, 15.80617190586768217, 111.8760903946856615 ) ) ;
#126956 = CARTESIAN_POINT ( 'NONE',  ( 21.53943276465977519, -0.05219959533907433946, 58.74890960531436690 ) ) ;
#126957 = CARTESIAN_POINT ( 'NONE',  ( -9.564922557960796823, -16.46253265017161027, 92.08224293864769550 ) ) ;
#126958 = CARTESIAN_POINT ( 'NONE',  ( 19.05341960407617918, -5.049401038297876454, 86.04275706135233293 ) ) ;
#126959 = CARTESIAN_POINT ( 'NONE',  ( 13.89961937509977652, -13.97604488694527269, 103.1239096053143527 ) ) ;
#126960 = CARTESIAN_POINT ( 'NONE',  ( 19.02544592524334988, 5.153800228976608722, 111.4594237280190043 ) ) ;
#126961 = CARTESIAN_POINT ( 'NONE',  ( -13.97604488694527625, -13.89961937509977652, 26.87390960531434558 ) ) ;
#126962 = CARTESIAN_POINT ( 'NONE',  ( 19.02544592524343514, -5.153800228976328945, 88.54057627198102409 ) ) ;
#126963 = CARTESIAN_POINT ( 'NONE',  ( -21.52544592524343514, 5.823673210054127303, 81.04057627198102409 ) ) ;
#126964 = CARTESIAN_POINT ( 'NONE',  ( 4.483927247898790824, -16.52544592524335698, 40.20942372801901854 ) ) ;
#126965 = CARTESIAN_POINT ( 'NONE',  ( -21.52544592524334988, -5.823673210054445271, 43.95942372801902565 ) ) ;
#126966 = CARTESIAN_POINT ( 'NONE',  ( 5.719274019375673035, 21.55341960407619339, 102.2927570613523613 ) ) ;
#126967 = CARTESIAN_POINT ( 'NONE',  ( -14.34966873604972548, 8.224510206698743886, 93.33442372801901854 ) ) ;
#126968 = AXIS2_PLACEMENT_3D ( 'NONE', #158055, #33717, #174232 ) ;
#126969 = CARTESIAN_POINT ( 'NONE',  ( 13.89961937509977652, -13.97604488694527269, 93.12390960531436690 ) ) ;
#126970 = CARTESIAN_POINT ( 'NONE',  ( -14.34966873604960291, -8.224510206698953496, 86.66557627198102409 ) ) ;
#126971 = CARTESIAN_POINT ( 'NONE',  ( 4.483927247898545687, 16.52544592524342804, 24.79057627198103120 ) ) ;
#126972 = CARTESIAN_POINT ( 'NONE',  ( 16.46253265017146816, 9.564922557961045513, 71.66775706135233293 ) ) ;
#126973 = CARTESIAN_POINT ( 'NONE',  ( -10.81492255796105439, 18.62759615963255655, 47.91775706135234714 ) ) ;
#126974 = CARTESIAN_POINT ( 'NONE',  ( -16.52544592524342804, 4.483927247898546575, 96.04057627198102409 ) ) ;
#126975 = CARTESIAN_POINT ( 'NONE',  ( -0.05219959533909027116, -19.03943276465977164, 112.4989096053143669 ) ) ;
#126976 = CARTESIAN_POINT ( 'NONE',  ( 14.34966873604960469, 8.224510206698951720, 29.16557627198103120 ) ) ;
#126977 = CARTESIAN_POINT ( 'NONE',  ( 5.823673210054444382, -21.52544592524334988, 80.20942372801901854 ) ) ;
#126978 = CARTESIAN_POINT ( 'NONE',  ( 0.05219959533934541429, -16.53943276465976808, 60.00109039468568284 ) ) ;
#126979 = CARTESIAN_POINT ( 'NONE',  ( 8.224510206698742110, 14.34966873604972548, 112.0844237280190185 ) ) ;
#126980 = CARTESIAN_POINT ( 'NONE',  ( 5.823673210054444382, -21.52544592524334988, 60.20942372801902565 ) ) ;
#126981 = ADVANCED_FACE ( 'NONE', ( #161636 ), #21939, .T. ) ;
#126982 = ORIENTED_EDGE ( 'NONE', *, *, #23933, .F. ) ;
#126983 = CARTESIAN_POINT ( 'NONE',  ( -10.72451020669870658, -18.67979575497194134, 24.58442372801901499 ) ) ;
#126984 = CARTESIAN_POINT ( 'NONE',  ( -16.52544592524342804, 4.483927247898546575, 101.0405762719810383 ) ) ;
#126985 = CARTESIAN_POINT ( 'NONE',  ( -9.564922557960796823, -16.46253265017161027, 27.08224293864769550 ) ) ;
#126986 = CARTESIAN_POINT ( 'NONE',  ( 16.53943276465976808, -0.05219959533910856209, 68.74890960531435269 ) ) ;
#126987 = CARTESIAN_POINT ( 'NONE',  ( -19.03943276465977164, 0.05219959533909376836, 76.24890960531435269 ) ) ;
#126988 = CARTESIAN_POINT ( 'NONE',  ( 8.314922557961029526, -14.29746914071037800, 100.4177570613523471 ) ) ;
#126989 = CARTESIAN_POINT ( 'NONE',  ( 9.564922557960805705, 16.46253265017160317, 39.58224293864768839 ) ) ;
#126990 = CARTESIAN_POINT ( 'NONE',  ( 21.52544592524344225, -5.823673210054117533, 38.54057627198103120 ) ) ;
#126991 = CARTESIAN_POINT ( 'NONE',  ( -8.224510206698948167, 14.34966873604960824, 85.41557627198102409 ) ) ;
#126992 = CARTESIAN_POINT ( 'NONE',  ( 10.72451020669898902, -18.67979575497178502, 92.91557627198103830 ) ) ;
#126993 = CARTESIAN_POINT ( 'NONE',  ( 13.97604488694527802, 13.89961937509977652, 89.37390960531436690 ) ) ;
#126995 = CARTESIAN_POINT ( 'NONE',  ( 19.05341960407617918, -5.049401038297876454, 86.04275706135233293 ) ) ;
#126994 = CARTESIAN_POINT ( 'NONE',  ( 13.97604488694527802, 13.89961937509977652, 54.37390960531435979 ) ) ;
#126996 = CARTESIAN_POINT ( 'NONE',  ( 18.67979575497178502, 10.72451020669898547, 39.16557627198102409 ) ) ;
#126997 = CARTESIAN_POINT ( 'NONE',  ( 15.72974639402176855, 15.80617190586768217, 66.87609039468568994 ) ) ;
#126998 = CARTESIAN_POINT ( 'NONE',  ( -13.89961937509977652, 13.97604488694528158, 50.62390960531435979 ) ) ;
#126999 = CARTESIAN_POINT ( 'NONE',  ( 5.153800228976335163, 19.02544592524342804, 79.79057627198102409 ) ) ;
#127000 = CARTESIAN_POINT ( 'NONE',  ( 14.34966873604972726, -8.224510206698740333, 60.83442372801901854 ) ) ;
#127001 = CARTESIAN_POINT ( 'NONE',  ( 15.80617190586769283, -15.72974639402175789, 40.62609039468567573 ) ) ;
#127002 = CARTESIAN_POINT ( 'NONE',  ( 15.72974639402176855, 15.80617190586768217, 71.87609039468568994 ) ) ;
#127003 = CARTESIAN_POINT ( 'NONE',  ( 5.719274019375991003, -21.55341960407610458, 27.70724293864769905 ) ) ;
#127004 = CARTESIAN_POINT ( 'NONE',  ( -0.05219959533907301413, -21.53943276465977519, 102.4989096053143811 ) ) ;
#127006 = CARTESIAN_POINT ( 'NONE',  ( -4.379528057220086978, -16.55341960407618274, 64.79275706135234714 ) ) ;
#127005 = CARTESIAN_POINT ( 'NONE',  ( 21.52544592524334988, 5.823673210054432836, 41.45942372801901143 ) ) ;
#127007 = CARTESIAN_POINT ( 'NONE',  ( 18.67979575497178502, 10.72451020669898547, 69.16557627198102409 ) ) ;
#127008 = CARTESIAN_POINT ( 'NONE',  ( 0.05219959533936267826, -19.03943276465977164, 35.00109039468566863 ) ) ;
#127010 = CARTESIAN_POINT ( 'NONE',  ( 8.224510206698953496, -14.34966873604960469, 27.91557627198103830 ) ) ;
#127009 = CARTESIAN_POINT ( 'NONE',  ( -13.97604488694527625, -13.89961937509977652, 71.87390960531433848 ) ) ;
#127011 = CARTESIAN_POINT ( 'NONE',  ( -17.49999999999998934, -4.013004640162571413, 104.5539427900559417 ) ) ;
#127012 =( BOUNDED_CURVE ( )  B_SPLINE_CURVE ( 2, ( #121365, #137531, #60680, #124345, #47523, #184044, #44542, #109179, #170858, #32349, #94002, #76848, #17178 ),
 .UNSPECIFIED., .F., .T. ) 
 B_SPLINE_CURVE_WITH_KNOTS ( ( 3, 2, 2, 2, 2, 2, 3 ),
 ( 0.4761603267754511148, 0.4780701754385964786, 0.4824561403508771940, 0.4868421052631579093, 0.4912280701754385692, 0.4956140350877192846, 0.4975695635729549537 ),
 .UNSPECIFIED. ) 
 CURVE ( )  GEOMETRIC_REPRESENTATION_ITEM ( )  RATIONAL_B_SPLINE_CURVE ( ( 0.9832469066685285419, 0.9851625545550100060, 1.000000000000000000, 0.9659258262890683122, 1.000000000000000000, 0.9659258262890683122, 1.000000000000000000, 0.9659258262890683122, 1.000000000000000000, 0.9659258262890683122, 1.000000000000000000, 0.9848076720550082985, 0.9831626618144002627 ) ) 
 REPRESENTATION_ITEM ( '' )  );
#127013 = CARTESIAN_POINT ( 'NONE',  ( 19.02544592524343514, -5.153800228976328945, 103.5405762719809957 ) ) ;
#127014 = CARTESIAN_POINT ( 'NONE',  ( 12.55500000000001748, 0.000000000000000000, 2.500000000000000444 ) ) ;
#127015 = CARTESIAN_POINT ( 'NONE',  ( 16.46253265017146816, 9.564922557961045513, 86.66775706135233293 ) ) ;
#127016 = CARTESIAN_POINT ( 'NONE',  ( -0.05219959533907301413, -21.53943276465977519, 52.49890960531435979 ) ) ;
#127017 = CARTESIAN_POINT ( 'NONE',  ( 16.53943276465976808, -0.05219959533910856209, 43.74890960531435979 ) ) ;
#127018 = CARTESIAN_POINT ( 'NONE',  ( 19.05341960407617918, -5.049401038297876454, 96.04275706135231871 ) ) ;
#127019 = CARTESIAN_POINT ( 'NONE',  ( 19.03943276465977164, -0.05219959533909143690, 28.74890960531435624 ) ) ;
#127020 = CARTESIAN_POINT ( 'NONE',  ( 9.474510206698729675, 16.51473224551082808, 112.0844237280190043 ) ) ;
#127022 = CARTESIAN_POINT ( 'NONE',  ( -0.05219959533936034679, 19.03943276465977164, 62.50109039468566863 ) ) ;
#127021 = CARTESIAN_POINT ( 'NONE',  ( -5.719274019375978568, 21.55341960407610458, 90.20724293864770971 ) ) ;
#127023 = CARTESIAN_POINT ( 'NONE',  ( -4.379528057220086978, -16.55341960407618274, 74.79275706135234714 ) ) ;
#127024 = CARTESIAN_POINT ( 'NONE',  ( -19.05341960407611168, -5.049401038298163336, 71.45724293864766707 ) ) ;
#127025 = CARTESIAN_POINT ( 'NONE',  ( 12.14591786802309770, 12.06949235617756955, 79.37390960531436690 ) ) ;
#127026 = CARTESIAN_POINT ( 'NONE',  ( 0.05219959533909260263, 19.03943276465977164, 49.99890960531435979 ) ) ;
#127027 = CARTESIAN_POINT ( 'NONE',  ( -14.29746914071049879, 8.314922557960819915, 50.83224293864770971 ) ) ;
#127028 = CARTESIAN_POINT ( 'NONE',  ( -193.3062444957834884, -155.7167183371838064, 0.000000000000000000 ) ) ;
#127029 = CARTESIAN_POINT ( 'NONE',  ( 0.4883415225378692215, 9.021730311186841433, -61.91042889546767469 ) ) ;
#127030 = CARTESIAN_POINT ( 'NONE',  ( 4.379528057220339221, -16.55341960407611168, 22.70724293864769194 ) ) ;
#127031 = CARTESIAN_POINT ( 'NONE',  ( 5.049401038298161559, -19.05341960407611168, 77.70724293864765286 ) ) ;
#127032 = CARTESIAN_POINT ( 'NONE',  ( 12.50000000000001066, -90.00000000000005684, 0.000000000000000000 ) ) ;
#127033 = CARTESIAN_POINT ( 'NONE',  ( 16.46253265017146816, 9.564922557961045513, 41.66775706135234003 ) ) ;
#127034 = CARTESIAN_POINT ( 'NONE',  ( -16.53943276465976808, -0.05219959533934237506, 43.75109039468568284 ) ) ;
#127035 = CARTESIAN_POINT ( 'NONE',  ( 10.72451020669898902, -18.67979575497178502, 62.91557627198102409 ) ) ;
#127036 = CARTESIAN_POINT ( 'NONE',  ( -21.55341960407619339, 5.719274019375674811, 113.5427570613523756 ) ) ;
#127037 = CARTESIAN_POINT ( 'NONE',  ( -9.474510206698964154, 16.51473224551069663, 75.41557627198103830 ) ) ;
#127038 = CARTESIAN_POINT ( 'NONE',  ( -19.02544592524342804, 5.153800228976336051, 116.0405762719810383 ) ) ;
#127039 = CARTESIAN_POINT ( 'NONE',  ( -19.02544592524342804, 5.153800228976336051, 116.0405762719810383 ) ) ;
#127040 = CARTESIAN_POINT ( 'NONE',  ( -18.62759615963255300, -10.81492255796106328, 39.16775706135235424 ) ) ;
#127041 = CARTESIAN_POINT ( 'NONE',  ( 12.06949235617757843, -12.14591786802309237, 108.1239096053143811 ) ) ;
#127044 = CYLINDRICAL_SURFACE ( 'NONE', #82498, 2.649999999999999911 ) ;
#127043 = CARTESIAN_POINT ( 'NONE',  ( -9.474510206698964154, 16.51473224551069663, 75.41557627198103830 ) ) ;
#127042 = CARTESIAN_POINT ( 'NONE',  ( 15.80617190586746368, 15.72974639402197994, 99.37390960531436690 ) ) ;
#127045 = CARTESIAN_POINT ( 'NONE',  ( -21.55341960407619339, 5.719274019375674811, 28.54275706135234358 ) ) ;
#127046 = VERTEX_POINT ( 'NONE', #196933 ) ;
#127047 = CARTESIAN_POINT ( 'NONE',  ( -19.03943276465977164, 0.05219959533909376836, 81.24890960531436690 ) ) ;
#127048 = AXIS2_PLACEMENT_3D ( 'NONE', #6301, #157014, #18512 ) ;
#127049 = DIRECTION ( 'NONE',  ( 1.000000000000000000, 0.000000000000000000, 0.000000000000000000 ) ) ;
#127051 = CARTESIAN_POINT ( 'NONE',  ( -5.153800228976328057, -19.02544592524343514, 27.29057627198103120 ) ) ;
#127050 = CARTESIAN_POINT ( 'NONE',  ( 5.049401038298161559, -19.05341960407611168, 22.70724293864769194 ) ) ;
#127052 = CARTESIAN_POINT ( 'NONE',  ( -13.89961937509957401, -13.97604488694547875, 104.3760903946856757 ) ) ;
#127053 = CARTESIAN_POINT ( 'NONE',  ( 11.40812507854755253, -35.11059874428192273, -8.524999997268814411 ) ) ;
#127054 = CARTESIAN_POINT ( 'NONE',  ( 16.55341960407611168, 4.379528057220329451, 113.9572429386477239 ) ) ;
#127055 = CARTESIAN_POINT ( 'NONE',  ( -21.52544592524334988, -5.823673210054445271, 83.95942372801900433 ) ) ;
#127057 = CARTESIAN_POINT ( 'NONE',  ( -0.05219959533937732626, 21.53943276465977519, 52.50109039468567573 ) ) ;
#127056 = CARTESIAN_POINT ( 'NONE',  ( -16.51473224551069308, -9.474510206698971260, 56.66557627198103120 ) ) ;
#127058 = CARTESIAN_POINT ( 'NONE',  ( 21.55341960407619695, -5.719274019375665929, 21.04275706135234714 ) ) ;
#127059 = CARTESIAN_POINT ( 'NONE',  ( 8.571926809382597767, 26.38167802310806209, 140.7750000027311899 ) ) ;
#127060 = CARTESIAN_POINT ( 'NONE',  ( -5.049401038298153566, 19.05341960407611168, 80.20724293864769550 ) ) ;
#127061 = DIRECTION ( 'NONE',  ( -0.7071067811865467956, 7.406550393246786959E-15, -0.7071067811865483499 ) ) ;
#127063 = CARTESIAN_POINT ( 'NONE',  ( 0.05219959533907565091, 21.53943276465977519, 44.99890960531435979 ) ) ;
#127062 = CARTESIAN_POINT ( 'NONE',  ( -8.314922557961024197, 14.29746914071037800, 27.91775706135234358 ) ) ;
#127064 = CARTESIAN_POINT ( 'NONE',  ( 5.823673210054444382, -21.52544592524334988, 70.20942372801904696 ) ) ;
#127065 = CARTESIAN_POINT ( 'NONE',  ( 13.97604488694527802, 13.89961937509977652, 114.3739096053143669 ) ) ;
#127066 = CARTESIAN_POINT ( 'NONE',  ( 19.03943276465977164, 0.05219959533936151252, 101.2510903946856757 ) ) ;
#127067 = CARTESIAN_POINT ( 'NONE',  ( -19.03943276465977164, 0.05219959533909376836, 61.24890960531436690 ) ) ;
#127068 = CARTESIAN_POINT ( 'NONE',  ( 9.564922557960805705, 16.46253265017160317, 89.58224293864769550 ) ) ;
#127069 = CARTESIAN_POINT ( 'NONE',  ( 16.55341960407611168, 4.379528057220329451, 113.9572429386477239 ) ) ;
#127070 = CARTESIAN_POINT ( 'NONE',  ( -0.05219959533910754901, -16.53943276465976808, 102.4989096053143811 ) ) ;
#127071 = CARTESIAN_POINT ( 'NONE',  ( -0.05219959533909027116, -19.03943276465977164, 112.4989096053143669 ) ) ;
#127072 = CARTESIAN_POINT ( 'NONE',  ( 16.53943276465976808, 0.05219959533934440121, 76.25109039468568994 ) ) ;
#127074 = CARTESIAN_POINT ( 'NONE',  ( -19.02544592524342804, 5.153800228976336051, 36.04057627198100988 ) ) ;
#127073 = CARTESIAN_POINT ( 'NONE',  ( -12.06949235617756955, 12.14591786802309770, 55.62390960531436690 ) ) ;
#127075 = CARTESIAN_POINT ( 'NONE',  ( 18.67979575497194134, -10.72451020669871369, 75.83442372801900433 ) ) ;
#127076 = CARTESIAN_POINT ( 'NONE',  ( -13.89961937509957401, -13.97604488694547875, 99.37609039468567573 ) ) ;
#127077 = CARTESIAN_POINT ( 'NONE',  ( 8.224510206698953496, -14.34966873604960469, 62.91557627198102409 ) ) ;
#127078 = CARTESIAN_POINT ( 'NONE',  ( 0.05219959533937995610, -21.53943276465977519, 20.00109039468568639 ) ) ;
#127079 = CARTESIAN_POINT ( 'NONE',  ( 15.80617190586746368, 15.72974639402197994, 49.37390960531436690 ) ) ;
#127080 = CARTESIAN_POINT ( 'NONE',  ( 1.993301997531345686E-15, -30.30510711980685556, 140.5000000000000000 ) ) ;
#127081 = CARTESIAN_POINT ( 'NONE',  ( -23.31738231874055245, -16.94106989632524574, 140.4500000054623854 ) ) ;
#127082 = CARTESIAN_POINT ( 'NONE',  ( -19.05341960407611168, -5.049401038298163336, 71.45724293864766707 ) ) ;
#127083 = CARTESIAN_POINT ( 'NONE',  ( -8.224510206698948167, 14.34966873604960824, 40.41557627198103120 ) ) ;
#127084 = CARTESIAN_POINT ( 'NONE',  ( 16.52544592524342804, -4.483927247898539470, 28.54057627198103120 ) ) ;
#127085 = CARTESIAN_POINT ( 'NONE',  ( 4.379528057220092307, 16.55341960407617563, 82.29275706135234714 ) ) ;
#127086 = CARTESIAN_POINT ( 'NONE',  ( 19.05341960407617918, -5.049401038297876454, 36.04275706135234003 ) ) ;
#127087 = DIRECTION ( 'NONE',  ( -0.000000000000000000, -0.000000000000000000, 1.000000000000000000 ) ) ;
#127088 = CARTESIAN_POINT ( 'NONE',  ( 13.89961937509977652, -13.97604488694527269, 88.12390960531438111 ) ) ;
#127089 = CARTESIAN_POINT ( 'NONE',  ( -12.06949235617756955, 12.14591786802309770, 55.62390960531436690 ) ) ;
#127091 = CARTESIAN_POINT ( 'NONE',  ( 16.51473224551069308, 9.474510206698969483, 114.1655762719810241 ) ) ;
#127090 = CARTESIAN_POINT ( 'NONE',  ( 16.29526858892874586, -7.335722546920107945, 101.7032940219979764 ) ) ;
#127093 = EDGE_LOOP ( 'NONE', ( #99187, #162199, #33074, #81522, #141916, #76278, #100027, #21575, #24206, #162642 ) ) ;
#127092 = CARTESIAN_POINT ( 'NONE',  ( 21.52544592524344225, -5.823673210054117533, 53.54057627198103120 ) ) ;
#127094 = CARTESIAN_POINT ( 'NONE',  ( 16.52544592524342804, -4.483927247898539470, 98.54057627198105251 ) ) ;
#127095 = CARTESIAN_POINT ( 'NONE',  ( -14.34966873604972548, 8.224510206698743886, 38.33442372801900433 ) ) ;
#127096 = CARTESIAN_POINT ( 'NONE',  ( -8.314922557960811034, -14.29746914071050412, 77.08224293864769550 ) ) ;
#127097 = CARTESIAN_POINT ( 'NONE',  ( 37.66961640367472341, 5.000000000000023981, -25.00000000000000000 ) ) ;
#127098 = CARTESIAN_POINT ( 'NONE',  ( 19.05341960407617918, -5.049401038297876454, 76.04275706135230450 ) ) ;
#127099 = CARTESIAN_POINT ( 'NONE',  ( -15.72974639402197994, 15.80617190586746368, 25.62390960531435624 ) ) ;
#127100 = CARTESIAN_POINT ( 'NONE',  ( 11.40812507854754365, 35.11059874428196537, -7.724999997268813701 ) ) ;
#127101 = CARTESIAN_POINT ( 'NONE',  ( 18.22780087662119897, -5.500000000000096811, 43.51763182126894236 ) ) ;
#127103 = CARTESIAN_POINT ( 'NONE',  ( -12.06949235617756955, 12.14591786802309770, 30.62390960531436335 ) ) ;
#127102 = CARTESIAN_POINT ( 'NONE',  ( 16.52544592524335698, 4.483927247898782831, 31.45942372801901854 ) ) ;
#127104 = CARTESIAN_POINT ( 'NONE',  ( -10.72451020669898014, 18.67979575497178502, 55.41557627198102409 ) ) ;
#127106 = CARTESIAN_POINT ( 'NONE',  ( 16.46253265017146816, 9.564922557961045513, 66.66775706135233293 ) ) ;
#127105 = AXIS2_PLACEMENT_3D ( 'NONE', #24162, #116153, #88810 ) ;
#127107 = CARTESIAN_POINT ( 'NONE',  ( -5.719274019375978568, 21.55341960407610458, 50.20724293864769550 ) ) ;
#127108 = CARTESIAN_POINT ( 'NONE',  ( -21.53943276465977519, -0.05219959533937600094, 68.75109039468568994 ) ) ;
#127109 = CARTESIAN_POINT ( 'NONE',  ( -3.889087296526037463, -6.412877669190318208, 1.818019484660534424 ) ) ;
#127110 = CARTESIAN_POINT ( 'NONE',  ( 12.06949235617739724, 12.14591786802326823, 36.87609039468568994 ) ) ;
#127113 = ADVANCED_FACE ( 'NONE', ( #120067 ), #20742, .T. ) ;
#127112 = CARTESIAN_POINT ( 'NONE',  ( 19.03943276465977164, -0.05219959533909143690, 83.74890960531436690 ) ) ;
#127111 = CARTESIAN_POINT ( 'NONE',  ( -5.049401038298153566, 19.05341960407611168, 30.20724293864768839 ) ) ;
#127114 = CARTESIAN_POINT ( 'NONE',  ( 16.51473224551069308, 9.474510206698969483, 34.16557627198102409 ) ) ;
#127115 = CARTESIAN_POINT ( 'NONE',  ( -14.29746914071049879, 8.314922557960819915, 100.8322429386477097 ) ) ;
#127116 = APPLICATION_PROTOCOL_DEFINITION ( 'draft international standard', 'automotive_design', 1998, #143659 ) ;
#127117 = CARTESIAN_POINT ( 'NONE',  ( 19.05341960407611168, 5.049401038298154454, 103.9572429386476671 ) ) ;
#127118 = ORIENTED_EDGE ( 'NONE', *, *, #87010, .F. ) ;
#127119 = CARTESIAN_POINT ( 'NONE',  ( 8.314922557961029526, -14.29746914071037800, 55.41775706135234714 ) ) ;
#127120 = CARTESIAN_POINT ( 'NONE',  ( 18.62759615963271287, -10.81492255796078972, 78.33224293864770971 ) ) ;
#127121 = CARTESIAN_POINT ( 'NONE',  ( 9.564922557960805705, 16.46253265017160317, 44.58224293864769550 ) ) ;
#127123 = CARTESIAN_POINT ( 'NONE',  ( 15.72974639402199770, -15.80617190586745480, 108.1239096053143811 ) ) ;
#127122 = CARTESIAN_POINT ( 'NONE',  ( -0.05219959533936034679, 19.03943276465977164, 72.50109039468566152 ) ) ;
#127124 = CARTESIAN_POINT ( 'NONE',  ( 13.97604488694527802, 13.89961937509977652, 69.37390960531436690 ) ) ;
#127125 = CARTESIAN_POINT ( 'NONE',  ( 16.46253265017160672, -9.564922557960803928, 108.3322429386476955 ) ) ;
#127126 = ORIENTED_EDGE ( 'NONE', *, *, #94442, .F. ) ;
#127127 = CARTESIAN_POINT ( 'NONE',  ( -12.06949235617739369, -12.14591786802326823, 39.37609039468567573 ) ) ;
#127128 = CARTESIAN_POINT ( 'NONE',  ( -15.72974639402176322, -15.80617190586768395, 24.37609039468567573 ) ) ;
#127131 = CARTESIAN_POINT ( 'NONE',  ( 19.03943276465977164, 0.05219959533936151252, 71.25109039468566152 ) ) ;
#127130 = CARTESIAN_POINT ( 'NONE',  ( 16.51473224551069308, 9.474510206698969483, 89.16557627198103830 ) ) ;
#127129 = CARTESIAN_POINT ( 'NONE',  ( -16.53943276465976808, 0.05219959533911058130, 101.2489096053143669 ) ) ;
#127132 = CARTESIAN_POINT ( 'NONE',  ( -18.67979575497178146, -10.72451020669898902, 81.66557627198103830 ) ) ;
#127133 = CARTESIAN_POINT ( 'NONE',  ( -4.483927247898539470, -16.52544592524342804, 52.29057627198102409 ) ) ;
#127134 = CARTESIAN_POINT ( 'NONE',  ( -5.153800228976607833, 19.02544592524334988, 22.70942372801899012 ) ) ;
#127135 = CARTESIAN_POINT ( 'NONE',  ( -16.55341960407617563, 4.379528057220093196, 73.54275706135234714 ) ) ;
#127136 = CARTESIAN_POINT ( 'NONE',  ( -13.97604488694527625, -13.89961937509977652, 91.87390960531432427 ) ) ;
#127137 = CARTESIAN_POINT ( 'NONE',  ( -19.05341960407611168, -5.049401038298163336, 46.45724293864768129 ) ) ;
#127138 = CARTESIAN_POINT ( 'NONE',  ( 21.55341960407619695, -5.719274019375665929, 51.04275706135234714 ) ) ;
#127139 = CARTESIAN_POINT ( 'NONE',  ( 5.719274019375673035, 21.55341960407619339, 62.29275706135236845 ) ) ;
#127140 = CARTESIAN_POINT ( 'NONE',  ( 9.474510206698971260, -16.51473224551069308, 62.91557627198102409 ) ) ;
#127141 = CARTESIAN_POINT ( 'NONE',  ( 5.823673210054444382, -21.52544592524334988, 35.20942372801901854 ) ) ;
#127142 = CARTESIAN_POINT ( 'NONE',  ( 9.564922557961047289, -16.46253265017146816, 85.41775706135233293 ) ) ;
#127143 = CARTESIAN_POINT ( 'NONE',  ( -16.51473224551069308, -9.474510206698971260, 36.66557627198102409 ) ) ;
#127144 = CARTESIAN_POINT ( 'NONE',  ( -14.29746914071037622, -8.314922557961029526, 89.16775706135236135 ) ) ;
#127145 = CARTESIAN_POINT ( 'NONE',  ( 5.049401038298161559, -19.05341960407611168, 72.70724293864768129 ) ) ;
#127146 = CARTESIAN_POINT ( 'NONE',  ( 13.89961937509977652, -13.97604488694527269, 108.1239096053143669 ) ) ;
#127147 = CARTESIAN_POINT ( 'NONE',  ( -19.05341960407611168, -5.049401038298163336, 46.45724293864768129 ) ) ;
#127148 = CARTESIAN_POINT ( 'NONE',  ( -21.53943276465977519, 0.05219959533907696930, 81.24890960531436690 ) ) ;
#127149 = CARTESIAN_POINT ( 'NONE',  ( -8.224510206698735004, -14.34966873604973081, 79.58442372801903275 ) ) ;
#127150 = CARTESIAN_POINT ( 'NONE',  ( -21.73861122199408058, 5.803778330637469729, 172.6157762304496828 ) ) ;
#127151 = CARTESIAN_POINT ( 'NONE',  ( 0.05219959533936267826, -19.03943276465977164, 35.00109039468566863 ) ) ;
#127152 = CARTESIAN_POINT ( 'NONE',  ( 19.03943276465977164, -0.05219959533909143690, 68.74890960531436690 ) ) ;
#127153 = CARTESIAN_POINT ( 'NONE',  ( 14.34966873604960469, 8.224510206698951720, 39.16557627198102409 ) ) ;
#127154 = CARTESIAN_POINT ( 'NONE',  ( -16.55341960407611168, -4.379528057220339221, 81.45724293864769550 ) ) ;
#127155 = CARTESIAN_POINT ( 'NONE',  ( -0.05219959533909027116, -19.03943276465977164, 107.4989096053143527 ) ) ;
#127156 = CARTESIAN_POINT ( 'NONE',  ( -19.02544592524342804, 5.153800228976336051, 91.04057627198100988 ) ) ;
#127157 = CARTESIAN_POINT ( 'NONE',  ( 5.719274019375673035, 21.55341960407619339, 52.29275706135236135 ) ) ;
#127158 = CARTESIAN_POINT ( 'NONE',  ( -5.049401038298153566, 19.05341960407611168, 110.2072429386476671 ) ) ;
#127159 = CARTESIAN_POINT ( 'NONE',  ( -15.72974639402176322, -15.80617190586768395, 109.3760903946857042 ) ) ;
#127160 = CARTESIAN_POINT ( 'NONE',  ( 14.34966873604972726, -8.224510206698740333, 80.83442372801901854 ) ) ;
#127161 = CARTESIAN_POINT ( 'NONE',  ( 5.719274019375673035, 21.55341960407619339, 27.29275706135234358 ) ) ;
#127162 = CARTESIAN_POINT ( 'NONE',  ( -19.02544592524342804, 5.153800228976336051, 116.0405762719810383 ) ) ;
#127163 = CARTESIAN_POINT ( 'NONE',  ( 21.53943276465977519, -0.05219959533907433946, 98.74890960531438111 ) ) ;
#127164 = CARTESIAN_POINT ( 'NONE',  ( 14.34966873604960469, 8.224510206698951720, 54.16557627198103120 ) ) ;
#127165 = CARTESIAN_POINT ( 'NONE',  ( 0.05219959533909260263, 19.03943276465977164, 59.99890960531436690 ) ) ;
#127166 = CARTESIAN_POINT ( 'NONE',  ( -12.14591786802309592, -12.06949235617757132, 76.87390960531439532 ) ) ;
#127167 = CARTESIAN_POINT ( 'NONE',  ( -15.72974639402197994, 15.80617190586746368, 35.62390960531437401 ) ) ;
#127168 = CARTESIAN_POINT ( 'NONE',  ( -19.05341960407617563, 5.049401038297882671, 38.54275706135233293 ) ) ;
#127169 = CARTESIAN_POINT ( 'NONE',  ( -12.06949235617756955, 12.14591786802309770, 115.6239096053143669 ) ) ;
#127170 = EDGE_LOOP ( 'NONE', ( #103912, #60489, #193059, #140234, #85488 ) ) ;
#127171 = CARTESIAN_POINT ( 'NONE',  ( -16.55341960407617563, 4.379528057220093196, 68.54275706135234714 ) ) ;
#127172 = CARTESIAN_POINT ( 'NONE',  ( -9.564922557960796823, -16.46253265017161027, 67.08224293864769550 ) ) ;
#127173 = CARTESIAN_POINT ( 'NONE',  ( -17.14385361876520975, 23.59649016807275856, 142.5750000027311728 ) ) ;
#127174 = CARTESIAN_POINT ( 'NONE',  ( -14.34966873604960291, -8.224510206698953496, 91.66557627198103830 ) ) ;
#127175 = CARTESIAN_POINT ( 'NONE',  ( 21.52544592524344225, -5.823673210054117533, 38.54057627198103120 ) ) ;
#127176 = CARTESIAN_POINT ( 'NONE',  ( 8.224510206698742110, 14.34966873604972548, 107.0844237280190043 ) ) ;
#127177 = CARTESIAN_POINT ( 'NONE',  ( -0.05219959533936034679, 19.03943276465977164, 107.5010903946856615 ) ) ;
#127178 = CARTESIAN_POINT ( 'NONE',  ( -15.72974639402176322, -15.80617190586768395, 84.37609039468570415 ) ) ;
#127179 = CARTESIAN_POINT ( 'NONE',  ( 13.89961937509977652, -13.97604488694527269, 83.12390960531436690 ) ) ;
#127180 = CARTESIAN_POINT ( 'NONE',  ( 21.53943276465977519, -0.05219959533907433946, 98.74890960531438111 ) ) ;
#127181 = CARTESIAN_POINT ( 'NONE',  ( -12.14591786802326823, 12.06949235617739902, 58.12609039468568994 ) ) ;
#127182 = CARTESIAN_POINT ( 'NONE',  ( -9.564922557960796823, -16.46253265017161027, 32.08224293864769550 ) ) ;
#127183 = CARTESIAN_POINT ( 'NONE',  ( 16.53943276465976808, 0.05219959533934440121, 31.25109039468568639 ) ) ;
#127184 = CARTESIAN_POINT ( 'NONE',  ( -9.474510206698720793, -16.51473224551083518, 94.58442372801900433 ) ) ;
#127185 = CARTESIAN_POINT ( 'NONE',  ( -21.52544592524343514, 5.823673210054127303, 91.04057627198103830 ) ) ;
#127186 = CARTESIAN_POINT ( 'NONE',  ( -0.05219959533936034679, 19.03943276465977164, 52.50109039468566863 ) ) ;
#127187 = FACE_OUTER_BOUND ( 'NONE', #101947, .T. ) ;
#127188 = CARTESIAN_POINT ( 'NONE',  ( 21.53943276465977519, -0.05219959533907433946, 103.7489096053143669 ) ) ;
#127189 = CARTESIAN_POINT ( 'NONE',  ( 3.181980515339365656, -30.00000000000001776, 8.889087296526001936 ) ) ;
#127190 = CARTESIAN_POINT ( 'NONE',  ( -16.46253265017160317, 9.564922557960807481, 80.83224293864769550 ) ) ;
#127191 = DIRECTION ( 'NONE',  ( 0.000000000000000000, 0.000000000000000000, 1.000000000000000000 ) ) ;
#127192 = CARTESIAN_POINT ( 'NONE',  ( 8.314922557961029526, -14.29746914071037800, 35.41775706135234003 ) ) ;
#127193 = FACE_BOUND ( 'NONE', #132838, .T. ) ;
#127195 = CARTESIAN_POINT ( 'NONE',  ( 8.314922557960818139, 14.29746914071049879, 64.58224293864769550 ) ) ;
#127194 = CARTESIAN_POINT ( 'NONE',  ( 18.62759615963271287, -10.81492255796078972, 113.3322429386476955 ) ) ;
#127196 = CARTESIAN_POINT ( 'NONE',  ( 19.03943276465977164, -0.05219959533909143690, 68.74890960531436690 ) ) ;
#127198 = CARTESIAN_POINT ( 'NONE',  ( 16.51473224551083163, -9.474510206698727899, 35.83442372801899722 ) ) ;
#127197 = CARTESIAN_POINT ( 'NONE',  ( -16.53943276465976808, -0.05219959533934237506, 38.75109039468567573 ) ) ;
#127199 = CARTESIAN_POINT ( 'NONE',  ( 5.719274019375673035, 21.55341960407619339, 52.29275706135236135 ) ) ;
#127200 = CARTESIAN_POINT ( 'NONE',  ( -5.153800228976607833, 19.02544592524334988, 112.7094237280190043 ) ) ;
#127201 = CARTESIAN_POINT ( 'NONE',  ( 13.89961937509977652, -13.97604488694527269, 58.12390960531436690 ) ) ;
#127202 = CARTESIAN_POINT ( 'NONE',  ( -0.05219959533936034679, 19.03943276465977164, 87.50109039468567573 ) ) ;
#127203 = CARTESIAN_POINT ( 'NONE',  ( -10.72451020669870658, -18.67979575497194134, 84.58442372801903275 ) ) ;
#127204 = CARTESIAN_POINT ( 'NONE',  ( 0.05219959533936267826, -19.03943276465977164, 65.00109039468567573 ) ) ;
#127205 = CARTESIAN_POINT ( 'NONE',  ( 9.474510206698971260, -16.51473224551069308, 42.91557627198103120 ) ) ;
#127206 = CARTESIAN_POINT ( 'NONE',  ( -10.81492255796078084, -18.62759615963271287, 62.08224293864769550 ) ) ;
#127208 = CARTESIAN_POINT ( 'NONE',  ( 5.153800228976615827, -19.02544592524334988, 70.20942372801899012 ) ) ;
#127207 = CARTESIAN_POINT ( 'NONE',  ( 16.52544592524342804, -4.483927247898539470, 63.54057627198103830 ) ) ;
#127209 = DIRECTION ( 'NONE',  ( 0.000000000000000000, 0.000000000000000000, 1.000000000000000000 ) ) ;
#127210 = CARTESIAN_POINT ( 'NONE',  ( -19.02544592524334988, -5.153800228976617603, 23.95942372801900078 ) ) ;
#127211 = CARTESIAN_POINT ( 'NONE',  ( 0.05219959533934541429, -16.53943276465976808, 105.0010903946856757 ) ) ;
#127212 = CARTESIAN_POINT ( 'NONE',  ( -4.483927247898539470, -16.52544592524342804, 47.29057627198103120 ) ) ;
#127214 = CARTESIAN_POINT ( 'NONE',  ( -27.73933785331498925, 2.428612866367529932E-14, 138.8750000027311842 ) ) ;
#127213 = CARTESIAN_POINT ( 'NONE',  ( -5.823673210054431948, 21.52544592524334988, 92.70942372801901854 ) ) ;
#127215 = CARTESIAN_POINT ( 'NONE',  ( -15.80617190586768217, 15.72974639402176855, 88.12609039468570415 ) ) ;
#127216 = CARTESIAN_POINT ( 'NONE',  ( -21.53943276465977519, 0.05219959533907696930, 91.24890960531436690 ) ) ;
#127217 = ADVANCED_FACE ( 'NONE', ( #2068 ), #166648, .F. ) ;
#127218 = CARTESIAN_POINT ( 'NONE',  ( -13.97604488694527625, -13.89961937509977652, 56.87390960531434558 ) ) ;
#127219 = CARTESIAN_POINT ( 'NONE',  ( -21.52544592524334988, -5.823673210054445271, 63.95942372801901854 ) ) ;
#127220 = CARTESIAN_POINT ( 'NONE',  ( -19.03943276465977164, 0.05219959533909376836, 56.24890960531435979 ) ) ;
#127221 = CARTESIAN_POINT ( 'NONE',  ( 16.51473224551069308, 9.474510206698969483, 64.16557627198102409 ) ) ;
#127222 = CARTESIAN_POINT ( 'NONE',  ( 14.29746914071049879, -8.314922557960816363, 103.3322429386476955 ) ) ;
#127223 = CARTESIAN_POINT ( 'NONE',  ( -5.049401038298153566, 19.05341960407611168, 110.2072429386476671 ) ) ;
#127224 = CARTESIAN_POINT ( 'NONE',  ( 8.314922557960818139, 14.29746914071049879, 49.58224293864769550 ) ) ;
#127225 = CARTESIAN_POINT ( 'NONE',  ( -19.05341960407611168, -5.049401038298163336, 26.45724293864769550 ) ) ;
#127226 = CARTESIAN_POINT ( 'NONE',  ( -14.29746914071049879, 8.314922557960819915, 70.83224293864770971 ) ) ;
#127227 = CARTESIAN_POINT ( 'NONE',  ( 21.55341960407610458, 5.719274019375980345, 93.95724293864770971 ) ) ;
#127228 = CARTESIAN_POINT ( 'NONE',  ( -21.55341960407619339, 5.719274019375674811, 33.54275706135234714 ) ) ;
#127229 = CARTESIAN_POINT ( 'NONE',  ( 5.049401038298161559, -19.05341960407611168, 22.70724293864769194 ) ) ;
#127230 = CARTESIAN_POINT ( 'NONE',  ( 4.483927247898790824, -16.52544592524335698, 35.20942372801901854 ) ) ;
#127231 = CARTESIAN_POINT ( 'NONE',  ( 21.53943276465977519, -0.05219959533907433946, 78.74890960531436690 ) ) ;
#127233 = CARTESIAN_POINT ( 'NONE',  ( -10.72451020669870658, -18.67979575497194134, 104.5844237280190185 ) ) ;
#127232 = PRODUCT_DEFINITION_CONTEXT ( 'detailed design', #50677, 'design' ) ;
#127234 = CARTESIAN_POINT ( 'NONE',  ( -0.05219959533909027116, -19.03943276465977164, 87.49890960531436690 ) ) ;
#127235 = CARTESIAN_POINT ( 'NONE',  ( -5.823673210054431948, 21.52544592524334988, 37.70942372801900433 ) ) ;
#127236 = CARTESIAN_POINT ( 'NONE',  ( 0.05219959533907565091, 21.53943276465977519, 24.99890960531435624 ) ) ;
#127237 = CARTESIAN_POINT ( 'NONE',  ( 8.314922557961029526, -14.29746914071037800, 100.4177570613523471 ) ) ;
#127239 = CARTESIAN_POINT ( 'NONE',  ( -10.81492255796105439, 18.62759615963255655, 87.91775706135234714 ) ) ;
#127238 = CARTESIAN_POINT ( 'NONE',  ( -21.52544592524334988, -5.823673210054445271, 48.95942372801902565 ) ) ;
#127240 = CARTESIAN_POINT ( 'NONE',  ( -13.89961937509957401, -13.97604488694547875, 19.37609039468566507 ) ) ;
#127241 = CARTESIAN_POINT ( 'NONE',  ( -14.29746914071037622, -8.314922557961029526, 89.16775706135236135 ) ) ;
#127242 = CARTESIAN_POINT ( 'NONE',  ( 15.80617190586769283, -15.72974639402175789, 40.62609039468567573 ) ) ;
#127243 = AXIS2_PLACEMENT_3D ( 'NONE', #178074, #191232, #9224 ) ;
#127244 = CARTESIAN_POINT ( 'NONE',  ( -5.153800228976328057, -19.02544592524343514, 27.29057627198103120 ) ) ;
#127245 = CARTESIAN_POINT ( 'NONE',  ( -15.80617190586768217, 15.72974639402176855, 103.1260903946856757 ) ) ;
#127246 = CARTESIAN_POINT ( 'NONE',  ( 0.05219959533909260263, 19.03943276465977164, 104.9989096053143669 ) ) ;
#127247 = CARTESIAN_POINT ( 'NONE',  ( 21.53943276465977519, -0.05219959533907433946, 98.74890960531438111 ) ) ;
#127248 = CARTESIAN_POINT ( 'NONE',  ( -5.719274019375978568, 21.55341960407610458, 65.20724293864768129 ) ) ;
#127250 = CARTESIAN_POINT ( 'NONE',  ( -15.80617190586745835, -15.72974639402198527, 71.87390960531438111 ) ) ;
#127249 = LINE ( 'NONE', #1931, #19174 ) ;
#127252 = CARTESIAN_POINT ( 'NONE',  ( -14.34966873604960291, -8.224510206698953496, 56.66557627198103830 ) ) ;
#127251 = CARTESIAN_POINT ( 'NONE',  ( 16.52544592524335698, 4.483927247898782831, 46.45942372801901854 ) ) ;
#127253 = CARTESIAN_POINT ( 'NONE',  ( -17.79613651744293890, -24.49428055684528260, 146.5656553485623306 ) ) ;
#127254 = CARTESIAN_POINT ( 'NONE',  ( -19.03943276465977164, -0.05219959533935918106, 88.75109039468567573 ) ) ;
#127255 = CARTESIAN_POINT ( 'NONE',  ( -28.79475375365586842, 2.428612866367529932E-14, 147.9843446568999923 ) ) ;
#127256 = CARTESIAN_POINT ( 'NONE',  ( 12.06949235617739724, 12.14591786802326823, 31.87609039468567929 ) ) ;
#127257 = CARTESIAN_POINT ( 'NONE',  ( 15.72974639402199770, -15.80617190586745480, 103.1239096053143811 ) ) ;
#127258 = CARTESIAN_POINT ( 'NONE',  ( 15.72974639402199770, -15.80617190586745480, 78.12390960531436690 ) ) ;
#127259 = CARTESIAN_POINT ( 'NONE',  ( 5.153800228976335163, 19.02544592524342804, 109.7905762719810099 ) ) ;
#127260 = CARTESIAN_POINT ( 'NONE',  ( 4.483927247898790824, -16.52544592524335698, 55.20942372801902565 ) ) ;
#127261 = CARTESIAN_POINT ( 'NONE',  ( -19.02544592524342804, 5.153800228976336051, 76.04057627198102409 ) ) ;
#127263 = CARTESIAN_POINT ( 'NONE',  ( -9.564922557961040184, 16.46253265017147172, 102.9177570613523329 ) ) ;
#127262 = CARTESIAN_POINT ( 'NONE',  ( 5.719274019375673035, 21.55341960407619339, 27.29275706135234358 ) ) ;
#127264 = CARTESIAN_POINT ( 'NONE',  ( 16.51473224551069308, 9.474510206698969483, 114.1655762719810241 ) ) ;
#127265 = CARTESIAN_POINT ( 'NONE',  ( 16.46253265017160672, -9.564922557960803928, 83.33224293864768129 ) ) ;
#127266 = CARTESIAN_POINT ( 'NONE',  ( 5.823673210054125526, 21.52544592524343514, 84.79057627198102409 ) ) ;
#127267 = CARTESIAN_POINT ( 'NONE',  ( 13.97604488694527802, 13.89961937509977652, 64.37390960531436690 ) ) ;
#127268 = CARTESIAN_POINT ( 'NONE',  ( -17.31747979337949417, -6.344076630961023255, 61.37944868065187620 ) ) ;
#127269 = CARTESIAN_POINT ( 'NONE',  ( 16.53943276465976808, -0.05219959533910856209, 63.74890960531435979 ) ) ;
#127270 = CARTESIAN_POINT ( 'NONE',  ( 0.05219959533909260263, 19.03943276465977164, 114.9989096053143669 ) ) ;
#127271 = DIRECTION ( 'NONE',  ( 0.000000000000000000, 0.000000000000000000, 1.000000000000000000 ) ) ;
#127272 = CARTESIAN_POINT ( 'NONE',  ( -10.72451020669898014, 18.67979575497178502, 110.4155762719810383 ) ) ;
#127273 = CARTESIAN_POINT ( 'NONE',  ( -13.97604488694547697, 13.89961937509957934, 58.12609039468566863 ) ) ;
#127274 = CARTESIAN_POINT ( 'NONE',  ( 0.05219959533907565091, 21.53943276465977519, 24.99890960531435624 ) ) ;
#127275 = CARTESIAN_POINT ( 'NONE',  ( 15.80617190586746368, 15.72974639402197994, 59.37390960531436690 ) ) ;
#127276 = CIRCLE ( 'NONE', #72330, 40.49999999999999289 ) ;
#127277 = CARTESIAN_POINT ( 'NONE',  ( -5.153800228976328057, -19.02544592524343514, 87.29057627198103830 ) ) ;
#127278 = CARTESIAN_POINT ( 'NONE',  ( -10.81492255796105439, 18.62759615963255655, 82.91775706135234714 ) ) ;
#127279 = CARTESIAN_POINT ( 'NONE',  ( 16.46253265017160672, -9.564922557960803928, 53.33224293864768839 ) ) ;
#127280 = CARTESIAN_POINT ( 'NONE',  ( 16.53943276465976808, -0.05219959533910856209, 93.74890960531436690 ) ) ;
#127281 = CARTESIAN_POINT ( 'NONE',  ( 16.52544592524335698, 4.483927247898782831, 36.45942372801901143 ) ) ;
#127282 = CARTESIAN_POINT ( 'NONE',  ( -5.823673210054431948, 21.52544592524334988, 72.70942372801901854 ) ) ;
#127283 = ORIENTED_EDGE ( 'NONE', *, *, #79968, .T. ) ;
#127284 = CARTESIAN_POINT ( 'NONE',  ( 9.474510206698729675, 16.51473224551082808, 22.08442372801899722 ) ) ;
#127285 = CARTESIAN_POINT ( 'NONE',  ( -19.02544592524334988, -5.153800228976617603, 83.95942372801901854 ) ) ;
#127286 = CARTESIAN_POINT ( 'NONE',  ( -13.97604488694547697, 13.89961937509957934, 43.12609039468566152 ) ) ;
#127287 = LINE ( 'NONE', #152910, #43880 ) ;
#127288 = CARTESIAN_POINT ( 'NONE',  ( -5.823673210054431948, 21.52544592524334988, 32.70942372801900433 ) ) ;
#127289 = DIRECTION ( 'NONE',  ( -0.000000000000000000, -0.000000000000000000, 1.000000000000000000 ) ) ;
#127290 = CARTESIAN_POINT ( 'NONE',  ( -5.153800228976607833, 19.02544592524334988, 27.70942372801899722 ) ) ;
#127291 = CARTESIAN_POINT ( 'NONE',  ( 5.153800228976335163, 19.02544592524342804, 59.79057627198100988 ) ) ;
#127292 = CARTESIAN_POINT ( 'NONE',  ( -19.03943276465977164, -0.05219959533935918106, 28.75109039468566507 ) ) ;
#127293 = CARTESIAN_POINT ( 'NONE',  ( -16.53943276465976808, -0.05219959533934237506, 98.75109039468568994 ) ) ;
#127295 = CARTESIAN_POINT ( 'NONE',  ( 15.72974639402176855, 15.80617190586768217, 81.87609039468568994 ) ) ;
#127294 = CARTESIAN_POINT ( 'NONE',  ( -21.53943276465977519, 0.05219959533907696930, 21.24890960531436690 ) ) ;
#127296 = CARTESIAN_POINT ( 'NONE',  ( -29.86685920354755197, -21.69954338932560134, -6.424999997268812990 ) ) ;
#127297 = CARTESIAN_POINT ( 'NONE',  ( -17.50000000000149569, -3.202012800152108873, 35.07177583972763557 ) ) ;
#127298 = CARTESIAN_POINT ( 'NONE',  ( -18.67979575497193778, 10.72451020669871902, 88.33442372801901854 ) ) ;
#127299 = DIRECTION ( 'NONE',  ( 1.000000000000000000, 0.000000000000000000, 0.000000000000000000 ) ) ;
#127300 = CARTESIAN_POINT ( 'NONE',  ( 9.564922557960805705, 16.46253265017160317, 94.58224293864769550 ) ) ;
#127301 = VERTEX_POINT ( 'NONE', #176675 ) ;
#127302 = EDGE_CURVE ( 'NONE', #193812, #163522, #177674, .T. ) ;
#127303 = CIRCLE ( 'NONE', #49816, 6.100000000000006750 ) ;
#127304 = DIRECTION ( 'NONE',  ( -1.000000000000000000, 0.000000000000000000, -0.000000000000000000 ) ) ;
#127305 = CARTESIAN_POINT ( 'NONE',  ( -19.03943276465977164, 0.05219959533909376836, 46.24890960531435979 ) ) ;
#127306 = CARTESIAN_POINT ( 'NONE',  ( 0.05219959533907565091, 21.53943276465977519, 54.99890960531435269 ) ) ;
#127307 = CARTESIAN_POINT ( 'NONE',  ( 16.52544592524342804, -4.483927247898539470, 28.54057627198103120 ) ) ;
#127309 = CARTESIAN_POINT ( 'NONE',  ( -5.049401038298153566, 19.05341960407611168, 100.2072429386476955 ) ) ;
#127308 = CARTESIAN_POINT ( 'NONE',  ( 12.14591786802309770, 12.06949235617756955, 94.37390960531436690 ) ) ;
#127310 = CARTESIAN_POINT ( 'NONE',  ( -0.05219959533936034679, 19.03943276465977164, 22.50109039468566152 ) ) ;
#127311 = CARTESIAN_POINT ( 'NONE',  ( -16.46253265017160317, 9.564922557960807481, 35.83224293864768839 ) ) ;
#127312 = CARTESIAN_POINT ( 'NONE',  ( 14.29746914071049879, -8.314922557960816363, 98.33224293864769550 ) ) ;
#127313 = CARTESIAN_POINT ( 'NONE',  ( 10.81492255796106328, -18.62759615963255655, 50.41775706135235424 ) ) ;
#127314 = CARTESIAN_POINT ( 'NONE',  ( -5.823673210054116645, -21.52544592524344225, 92.29057627198103830 ) ) ;
#127315 = CARTESIAN_POINT ( 'NONE',  ( -13.97604488694547697, 13.89961937509957934, 63.12609039468566152 ) ) ;
#127316 = CARTESIAN_POINT ( 'NONE',  ( -22.30831786103663816, -33.25057925659813662, -9.512335543930488413 ) ) ;
#127317 = CARTESIAN_POINT ( 'NONE',  ( -19.02544592524342804, 5.153800228976336051, 111.0405762719810099 ) ) ;
#127318 = CARTESIAN_POINT ( 'NONE',  ( 14.29746914071049879, -8.314922557960816363, 73.33224293864769550 ) ) ;
#127319 = CARTESIAN_POINT ( 'NONE',  ( -9.474510206698720793, -16.51473224551083518, 39.58442372801899722 ) ) ;
#127320 = CARTESIAN_POINT ( 'NONE',  ( -19.02544592524342804, 5.153800228976336051, 66.04057627198103830 ) ) ;
#127321 = CARTESIAN_POINT ( 'NONE',  ( 16.53943276465976808, -0.05219959533910856209, 58.74890960531436690 ) ) ;
#127322 = CARTESIAN_POINT ( 'NONE',  ( 9.474510206698729675, 16.51473224551082808, 82.08442372801899012 ) ) ;
#127323 = CARTESIAN_POINT ( 'NONE',  ( -21.53943276465977519, 0.05219959533907696930, 41.24890960531435269 ) ) ;
#127324 = EDGE_LOOP ( 'NONE', ( #182512, #77573, #140750, #32963 ) ) ;
#127325 = CARTESIAN_POINT ( 'NONE',  ( -8.224510206698948167, 14.34966873604960824, 100.4155762719810241 ) ) ;
#127326 = CARTESIAN_POINT ( 'NONE',  ( -3.573655867282028392E-15, 2.428612866367529932E-14, 155.0000000000000000 ) ) ;
#127328 = CARTESIAN_POINT ( 'NONE',  ( -21.53943276465977519, 0.05219959533907696930, 66.24890960531436690 ) ) ;
#127327 = CARTESIAN_POINT ( 'NONE',  ( 19.03943276465977164, -0.05219959533909143690, 53.74890960531436690 ) ) ;
#127329 = CARTESIAN_POINT ( 'NONE',  ( -16.51473224551069308, -9.474510206698971260, 46.66557627198102409 ) ) ;
#127331 = CARTESIAN_POINT ( 'NONE',  ( 16.51473224551069308, 9.474510206698969483, 74.16557627198103830 ) ) ;
#127330 = CARTESIAN_POINT ( 'NONE',  ( 8.314922557961029526, -14.29746914071037800, 80.41775706135234714 ) ) ;
#127332 = CARTESIAN_POINT ( 'NONE',  ( -5.153800228976607833, 19.02544592524334988, 57.70942372801899012 ) ) ;
#127333 = CARTESIAN_POINT ( 'NONE',  ( 10.81492255796106328, -18.62759615963255655, 65.41775706135234714 ) ) ;
#127334 = CARTESIAN_POINT ( 'NONE',  ( -15.72974639402197994, 15.80617190586746368, 55.62390960531436690 ) ) ;
#127335 = CARTESIAN_POINT ( 'NONE',  ( 0.05219959533909260263, 19.03943276465977164, 99.99890960531436690 ) ) ;
#127336 = CARTESIAN_POINT ( 'NONE',  ( 16.52544592524342804, -4.483927247898539470, 113.5405762719810383 ) ) ;
#127337 = CARTESIAN_POINT ( 'NONE',  ( 4.379528057220092307, 16.55341960407617563, 87.29275706135236135 ) ) ;
#127338 = CARTESIAN_POINT ( 'NONE',  ( -19.02544592524334988, -5.153800228976617603, 108.9594237280189759 ) ) ;
#127339 = CARTESIAN_POINT ( 'NONE',  ( -9.564922557960796823, -16.46253265017161027, 27.08224293864769550 ) ) ;
#127340 = DIRECTION ( 'NONE',  ( 1.000000000000000000, 0.000000000000000000, 0.000000000000000000 ) ) ;
#127341 = CARTESIAN_POINT ( 'NONE',  ( -5.823673210054431948, 21.52544592524334988, 92.70942372801901854 ) ) ;
#127342 = EDGE_LOOP ( 'NONE', ( #14468, #186235, #91190, #50472 ) ) ;
#127343 = CARTESIAN_POINT ( 'NONE',  ( -0.05219959533910754901, -16.53943276465976808, 57.49890960531435979 ) ) ;
#127344 = CARTESIAN_POINT ( 'NONE',  ( -16.55341960407611168, -4.379528057220339221, 66.45724293864768129 ) ) ;
#127345 = CARTESIAN_POINT ( 'NONE',  ( -0.05219959533907301413, -21.53943276465977519, 97.49890960531436690 ) ) ;
#127346 = CARTESIAN_POINT ( 'NONE',  ( -21.55341960407610458, -5.719274019375992779, 86.45724293864770971 ) ) ;
#127347 = CARTESIAN_POINT ( 'NONE',  ( -2.577820198429831642E-15, -9.100000000000001421, -63.95112321872120731 ) ) ;
#127349 = ADVANCED_FACE ( 'NONE', ( #147325 ), #158119, .F. ) ;
#127348 = CARTESIAN_POINT ( 'NONE',  ( 18.67979575497178502, 10.72451020669898547, 39.16557627198102409 ) ) ;
#127350 = CARTESIAN_POINT ( 'NONE',  ( 0.05219959533934541429, -16.53943276465976808, 70.00109039468568994 ) ) ;
#127351 = CARTESIAN_POINT ( 'NONE',  ( -14.34966873604960291, -8.224510206698953496, 96.66557627198102409 ) ) ;
#127352 = CARTESIAN_POINT ( 'NONE',  ( -13.89961937509977652, 13.97604488694528158, 45.62390960531433848 ) ) ;
#127353 =( LENGTH_UNIT ( ) NAMED_UNIT ( * ) SI_UNIT ( .MILLI., .METRE. ) );
#127354 = CARTESIAN_POINT ( 'NONE',  ( 34.38690502837283702, -7.455999864800775256, 45.95008414374197514 ) ) ;
#127355 = CARTESIAN_POINT ( 'NONE',  ( 12.14591786802327356, -12.06949235617739191, 100.6260903946857184 ) ) ;
#127356 = CARTESIAN_POINT ( 'NONE',  ( 18.62759615963255655, 10.81492255796105972, 31.66775706135234358 ) ) ;
#127357 = CARTESIAN_POINT ( 'NONE',  ( 9.474510206698971260, -16.51473224551069308, 82.91557627198103830 ) ) ;
#127358 = CARTESIAN_POINT ( 'NONE',  ( 5.719274019375673035, 21.55341960407619339, 72.29275706135236135 ) ) ;
#127359 = CARTESIAN_POINT ( 'NONE',  ( -19.03943276465977164, 0.05219959533909376836, 116.2489096053143669 ) ) ;
#127360 = CARTESIAN_POINT ( 'NONE',  ( -3.964304649048260742, -40.57928608015912175, -25.32305239478594672 ) ) ;
#127361 = CIRCLE ( 'NONE', #40205, 2.041999999999999815 ) ;
#127362 = EDGE_LOOP ( 'NONE', ( #181793, #121980, #138796, #124773 ) ) ;
#127363 = CARTESIAN_POINT ( 'NONE',  ( -10.72451020669870658, -18.67979575497194134, 59.58442372801901854 ) ) ;
#127365 = CARTESIAN_POINT ( 'NONE',  ( -13.97604488694527625, -13.89961937509977652, 21.87390960531435979 ) ) ;
#127364 = CARTESIAN_POINT ( 'NONE',  ( 13.97604488694527802, 13.89961937509977652, 44.37390960531435269 ) ) ;
#127366 = CARTESIAN_POINT ( 'NONE',  ( -19.03943276465977164, -0.05219959533935918106, 73.75109039468566152 ) ) ;
#127367 = CARTESIAN_POINT ( 'NONE',  ( -0.05219959533937732626, 21.53943276465977519, 22.50109039468567573 ) ) ;
#127368 = CARTESIAN_POINT ( 'NONE',  ( -9.564922557961040184, 16.46253265017147172, 62.91775706135233293 ) ) ;
#127369 = CARTESIAN_POINT ( 'NONE',  ( -0.05219959533909027116, -19.03943276465977164, 27.49890960531435624 ) ) ;
#127370 = CARTESIAN_POINT ( 'NONE',  ( -16.52544592524335698, -4.483927247898792601, 93.95942372801903275 ) ) ;
#127371 = CARTESIAN_POINT ( 'NONE',  ( -9.564922557961040184, 16.46253265017147172, 62.91775706135233293 ) ) ;
#127372 = CARTESIAN_POINT ( 'NONE',  ( -4.483927247898782831, 16.52544592524335698, 112.7094237280190328 ) ) ;
#127374 = EDGE_LOOP ( 'NONE', ( #110355, #184417, #138527, #84701 ) ) ;
#127373 = CARTESIAN_POINT ( 'NONE',  ( 13.89961937509957401, 13.97604488694547697, 51.87609039468566863 ) ) ;
#127375 = CARTESIAN_POINT ( 'NONE',  ( 13.97604488694527802, 13.89961937509977652, 89.37390960531436690 ) ) ;
#127376 = CARTESIAN_POINT ( 'NONE',  ( -5.719274019375665041, -21.55341960407619695, 89.79275706135236135 ) ) ;
#127377 = CARTESIAN_POINT ( 'NONE',  ( -5.823673210054431948, 21.52544592524334988, 107.7094237280190328 ) ) ;
#127378 = DIRECTION ( 'NONE',  ( 1.000000000000000000, 0.000000000000000000, 0.000000000000000000 ) ) ;
#127379 = CARTESIAN_POINT ( 'NONE',  ( -18.67979575497193778, 10.72451020669871902, 88.33442372801901854 ) ) ;
#127380 = CARTESIAN_POINT ( 'NONE',  ( -16.55341960407617563, 4.379528057220093196, 33.54275706135234714 ) ) ;
#127381 = CIRCLE ( 'NONE', #53057, 0.2000000000000000944 ) ;
#127382 = CARTESIAN_POINT ( 'NONE',  ( -9.564922557960796823, -16.46253265017161027, 97.08224293864769550 ) ) ;
#127383 = CARTESIAN_POINT ( 'NONE',  ( 10.72451020669898902, -18.67979575497178502, 32.91557627198102409 ) ) ;
#127384 = CARTESIAN_POINT ( 'NONE',  ( -28.79475375365586487, 2.428612866367529932E-14, 149.9843446568999923 ) ) ;
#127385 = CARTESIAN_POINT ( 'NONE',  ( 13.97604488694527802, 13.89961937509977652, 79.37390960531435269 ) ) ;
#127386 = CARTESIAN_POINT ( 'NONE',  ( -16.31925111598405920, 7.325300261831753978, 100.1642453896716489 ) ) ;
#127387 = VECTOR ( 'NONE', #16764, 1000.000000000000000 ) ;
#127388 = CARTESIAN_POINT ( 'NONE',  ( 16.51473224551083163, -9.474510206698727899, 65.83442372801900433 ) ) ;
#127389 = CARTESIAN_POINT ( 'NONE',  ( 19.02544592524343514, -5.153800228976328945, 108.5405762719810383 ) ) ;
#127390 = CARTESIAN_POINT ( 'NONE',  ( -21.55341960407619339, 5.719274019375674811, 103.5427570613523613 ) ) ;
#127391 = CARTESIAN_POINT ( 'NONE',  ( -14.29746914071049879, 8.314922557960819915, 100.8322429386477097 ) ) ;
#127392 = CARTESIAN_POINT ( 'NONE',  ( 18.67979575497178502, 10.72451020669898547, 44.16557627198103120 ) ) ;
#127393 = AXIS2_PLACEMENT_3D ( 'NONE', #48320, #30157, #60480 ) ;
#127394 = CARTESIAN_POINT ( 'NONE',  ( 0.05219959533907565091, 21.53943276465977519, 34.99890960531435979 ) ) ;
#127395 = CARTESIAN_POINT ( 'NONE',  ( -4.379528057220328563, 16.55341960407611168, 100.2072429386476955 ) ) ;
#127396 = DIRECTION ( 'NONE',  ( 1.000000000000000000, 0.000000000000000000, 0.000000000000000000 ) ) ;
#127397 = CARTESIAN_POINT ( 'NONE',  ( -9.564922557961040184, 16.46253265017147172, 52.91775706135233293 ) ) ;
#127398 = CARTESIAN_POINT ( 'NONE',  ( 14.29746914071049879, -8.314922557960816363, 33.33224293864769550 ) ) ;
#127399 = CARTESIAN_POINT ( 'NONE',  ( 16.46253265017160672, -9.564922557960803928, 103.3322429386476955 ) ) ;
#127400 = CARTESIAN_POINT ( 'NONE',  ( -15.72974639402176322, -15.80617190586768395, 79.37609039468567573 ) ) ;
#127401 = CARTESIAN_POINT ( 'NONE',  ( -10.72451020669898014, 18.67979575497178502, 60.41557627198102409 ) ) ;
#127402 = CARTESIAN_POINT ( 'NONE',  ( 0.05219959533937995610, -21.53943276465977519, 50.00109039468568994 ) ) ;
#127403 = CARTESIAN_POINT ( 'NONE',  ( -10.81492255796078084, -18.62759615963271287, 102.0822429386476955 ) ) ;
#127404 = CARTESIAN_POINT ( 'NONE',  ( -5.719274019375665041, -21.55341960407619695, 34.79275706135235424 ) ) ;
#127405 = CARTESIAN_POINT ( 'NONE',  ( -12.06949235617756955, 12.14591786802309770, 115.6239096053143669 ) ) ;
#127406 = CARTESIAN_POINT ( 'NONE',  ( 5.153800228976335163, 19.02544592524342804, 79.79057627198102409 ) ) ;
#127407 = CARTESIAN_POINT ( 'NONE',  ( 12.06949235617739724, 12.14591786802326823, 76.87609039468567573 ) ) ;
#127408 = CARTESIAN_POINT ( 'NONE',  ( -16.52544592524342804, 4.483927247898546575, 111.0405762719810525 ) ) ;
#127409 = CARTESIAN_POINT ( 'NONE',  ( -5.049401038298153566, 19.05341960407611168, 110.2072429386476671 ) ) ;
#127410 = CARTESIAN_POINT ( 'NONE',  ( -8.224510206698948167, 14.34966873604960824, 60.41557627198102409 ) ) ;
#127411 = CARTESIAN_POINT ( 'NONE',  ( 16.53943276465976808, 0.05219959533934440121, 111.2510903946856899 ) ) ;
#127412 = CARTESIAN_POINT ( 'NONE',  ( 13.97604488694527802, 13.89961937509977652, 54.37390960531435979 ) ) ;
#127413 = CARTESIAN_POINT ( 'NONE',  ( 9.474510206698971260, -16.51473224551069308, 22.91557627198102765 ) ) ;
#127414 = CARTESIAN_POINT ( 'NONE',  ( -5.719274019375978568, 21.55341960407610458, 45.20724293864769550 ) ) ;
#127416 = CIRCLE ( 'NONE', #56297, 16.70000000000002061 ) ;
#127415 = CARTESIAN_POINT ( 'NONE',  ( -19.02544592524334988, -5.153800228976617603, 23.95942372801900078 ) ) ;
#127418 = CARTESIAN_POINT ( 'NONE',  ( -16.52544592524342804, 4.483927247898546575, 36.04057627198102409 ) ) ;
#127417 = DIRECTION ( 'NONE',  ( -0.000000000000000000, -0.000000000000000000, 1.000000000000000000 ) ) ;
#127419 = CARTESIAN_POINT ( 'NONE',  ( -10.72451020669870658, -18.67979575497194134, 49.58442372801901143 ) ) ;
#127420 = CARTESIAN_POINT ( 'NONE',  ( 16.46253265017160672, -9.564922557960803928, 113.3322429386476955 ) ) ;
#127421 = CARTESIAN_POINT ( 'NONE',  ( -14.34966873604972548, 8.224510206698743886, 58.33442372801901143 ) ) ;
#127422 = ADVANCED_FACE ( 'NONE', ( #70482 ), #165459, .T. ) ;
#127423 = CARTESIAN_POINT ( 'NONE',  ( 19.03943276465977164, 0.05219959533936151252, 66.25109039468567573 ) ) ;
#127424 = CARTESIAN_POINT ( 'NONE',  ( 12.06949235617757843, -12.14591786802309237, 23.12390960531436335 ) ) ;
#127425 = CARTESIAN_POINT ( 'NONE',  ( 4.483927247898790824, -16.52544592524335698, 100.2094237280190043 ) ) ;
#127426 = CARTESIAN_POINT ( 'NONE',  ( -19.02544592524342804, 5.153800228976336051, 36.04057627198100988 ) ) ;
#127427 = CARTESIAN_POINT ( 'NONE',  ( 19.05341960407611168, 5.049401038298154454, 58.95724293864768129 ) ) ;
#127428 = CARTESIAN_POINT ( 'NONE',  ( 19.03943276465977164, -0.05219959533909143690, 23.74890960531435269 ) ) ;
#127429 = CARTESIAN_POINT ( 'NONE',  ( -10.81492255796105439, 18.62759615963255655, 27.91775706135234358 ) ) ;
#127430 = CARTESIAN_POINT ( 'NONE',  ( -13.89961937509977652, 13.97604488694528158, 45.62390960531433848 ) ) ;
#127431 = FACE_OUTER_BOUND ( 'NONE', #49691, .T. ) ;
#127432 = CARTESIAN_POINT ( 'NONE',  ( 0.05219959533909260263, 19.03943276465977164, 39.99890960531436690 ) ) ;
#127433 = CARTESIAN_POINT ( 'NONE',  ( 15.80617190586746368, 15.72974639402197994, 24.37390960531435979 ) ) ;
#127434 = EDGE_CURVE ( 'NONE', #177652, #57298, #196847, .T. ) ;
#127436 = CARTESIAN_POINT ( 'NONE',  ( 16.53943276465976808, -0.05219959533910856209, 103.7489096053143669 ) ) ;
#127435 = CARTESIAN_POINT ( 'NONE',  ( -21.55341960407619339, 5.719274019375674811, 63.54275706135234003 ) ) ;
#127437 = CARTESIAN_POINT ( 'NONE',  ( 16.46253265017160672, -9.564922557960803928, 108.3322429386476955 ) ) ;
#127438 = CARTESIAN_POINT ( 'NONE',  ( 8.314922557961029526, -14.29746914071037800, 80.41775706135234714 ) ) ;
#127439 = CARTESIAN_POINT ( 'NONE',  ( 21.52544592524334988, 5.823673210054432836, 86.45942372801901854 ) ) ;
#127440 = CARTESIAN_POINT ( 'NONE',  ( -12.06949235617739369, -12.14591786802326823, 59.37609039468568284 ) ) ;
#127441 = CARTESIAN_POINT ( 'NONE',  ( 9.564922557960805705, 16.46253265017160317, 94.58224293864769550 ) ) ;
#127442 = CARTESIAN_POINT ( 'NONE',  ( 4.483927247898790824, -16.52544592524335698, 35.20942372801901854 ) ) ;
#127443 = CARTESIAN_POINT ( 'NONE',  ( 8.224510206698742110, 14.34966873604972548, 27.08442372801901854 ) ) ;
#127444 = CARTESIAN_POINT ( 'NONE',  ( 0.05219959533934541429, -16.53943276465976808, 85.00109039468568994 ) ) ;
#127445 = CARTESIAN_POINT ( 'NONE',  ( 16.51473224551083163, -9.474510206698727899, 110.8344237280190043 ) ) ;
#127446 = CARTESIAN_POINT ( 'NONE',  ( 18.62759615963271287, -10.81492255796078972, 98.33224293864769550 ) ) ;
#127448 = CARTESIAN_POINT ( 'NONE',  ( -19.03943276465977164, -0.05219959533935918106, 98.75109039468567573 ) ) ;
#127447 = CARTESIAN_POINT ( 'NONE',  ( -8.314922557960811034, -14.29746914071050412, 97.08224293864770971 ) ) ;
#127449 = CARTESIAN_POINT ( 'NONE',  ( 4.379528057220092307, 16.55341960407617563, 67.29275706135234714 ) ) ;
#127450 = CARTESIAN_POINT ( 'NONE',  ( 20.56371838171434874, 11.04494471775294961, 168.1294998094270454 ) ) ;
#127451 = CARTESIAN_POINT ( 'NONE',  ( 0.05219959533936267826, -19.03943276465977164, 65.00109039468567573 ) ) ;
#127452 = CARTESIAN_POINT ( 'NONE',  ( -0.05219959533910754901, -16.53943276465976808, 42.49890960531435979 ) ) ;
#127453 = CARTESIAN_POINT ( 'NONE',  ( 14.29746914071049879, -8.314922557960816363, 28.33224293864769550 ) ) ;
#127454 = CARTESIAN_POINT ( 'NONE',  ( 0.05219959533910956823, 16.53943276465976808, 89.99890960531438111 ) ) ;
#127456 = DIRECTION ( 'NONE',  ( 0.000000000000000000, 0.000000000000000000, -1.000000000000000000 ) ) ;
#127455 = CARTESIAN_POINT ( 'NONE',  ( 0.05219959533936267826, -19.03943276465977164, 35.00109039468566863 ) ) ;
#127457 = CARTESIAN_POINT ( 'NONE',  ( -21.53943276465977519, -0.05219959533937600094, 33.75109039468568284 ) ) ;
#127458 = CARTESIAN_POINT ( 'NONE',  ( -0.05219959533936034679, 19.03943276465977164, 92.50109039468566152 ) ) ;
#127459 = CARTESIAN_POINT ( 'NONE',  ( -9.841528761215647236, -38.18405872352760611, -31.73089324721045656 ) ) ;
#127460 = CARTESIAN_POINT ( 'NONE',  ( -19.05341960407611168, -5.049401038298163336, 96.45724293864769550 ) ) ;
#127461 = CARTESIAN_POINT ( 'NONE',  ( 19.05341960407611168, 5.049401038298154454, 88.95724293864769550 ) ) ;
#127462 = CARTESIAN_POINT ( 'NONE',  ( -15.80617190586745835, -15.72974639402198527, 56.87390960531436690 ) ) ;
#127463 = CARTESIAN_POINT ( 'NONE',  ( 16.52544592524342804, -4.483927247898539470, 98.54057627198105251 ) ) ;
#127464 = CARTESIAN_POINT ( 'NONE',  ( 5.153800228976335163, 19.02544592524342804, 74.79057627198103830 ) ) ;
#127465 = CARTESIAN_POINT ( 'NONE',  ( -5.049401038298153566, 19.05341960407611168, 30.20724293864768839 ) ) ;
#127466 = CARTESIAN_POINT ( 'NONE',  ( 5.823673210054444382, -21.52544592524334988, 35.20942372801901854 ) ) ;
#127467 = CARTESIAN_POINT ( 'NONE',  ( 21.53943276465977519, 0.05219959533937863772, 76.25109039468568994 ) ) ;
#127468 = CARTESIAN_POINT ( 'NONE',  ( -19.05341960407611168, -5.049401038298163336, 56.45724293864768129 ) ) ;
#127469 = CARTESIAN_POINT ( 'NONE',  ( 14.29746914071037800, 8.314922557961029526, 76.66775706135234714 ) ) ;
#127470 = CARTESIAN_POINT ( 'NONE',  ( -15.72974639402176322, -15.80617190586768395, 29.37609039468568284 ) ) ;
#127471 = CARTESIAN_POINT ( 'NONE',  ( 10.72451020669871369, 18.67979575497193778, 32.08442372801901854 ) ) ;
#127473 = CARTESIAN_POINT ( 'NONE',  ( -13.89961937509977652, 13.97604488694528158, 75.62390960531438111 ) ) ;
#127472 = CARTESIAN_POINT ( 'NONE',  ( 5.049401038297881783, 19.05341960407617563, 47.29275706135231161 ) ) ;
#127474 = CARTESIAN_POINT ( 'NONE',  ( 16.46253265017146816, 9.564922557961045513, 31.66775706135232937 ) ) ;
#127475 = CARTESIAN_POINT ( 'NONE',  ( 5.823673210054444382, -21.52544592524334988, 80.20942372801901854 ) ) ;
#127476 = CIRCLE ( 'NONE', #4794, 1.249999999999999778 ) ;
#127477 = CARTESIAN_POINT ( 'NONE',  ( -15.72974639402197994, 15.80617190586746368, 75.62390960531439532 ) ) ;
#127478 = CARTESIAN_POINT ( 'NONE',  ( -16.53943276465976808, 0.05219959533911058130, 51.24890960531436690 ) ) ;
#127480 = CARTESIAN_POINT ( 'NONE',  ( -0.05219959533936034679, 19.03943276465977164, 27.50109039468566507 ) ) ;
#127479 = CARTESIAN_POINT ( 'NONE',  ( 15.72974639402176855, 15.80617190586768217, 96.87609039468568994 ) ) ;
#127481 = CARTESIAN_POINT ( 'NONE',  ( 8.224510206698953496, -14.34966873604960469, 67.91557627198102409 ) ) ;
#127482 = CARTESIAN_POINT ( 'NONE',  ( 19.05341960407611168, 5.049401038298154454, 23.95724293864769194 ) ) ;
#127483 = CARTESIAN_POINT ( 'NONE',  ( -9.474510206698720793, -16.51473224551083518, 74.58442372801900433 ) ) ;
#127484 = CARTESIAN_POINT ( 'NONE',  ( -14.29746914071049879, 8.314922557960819915, 40.83224293864769550 ) ) ;
#127485 = CARTESIAN_POINT ( 'NONE',  ( 18.67979575497194134, -10.72451020669871369, 85.83442372801901854 ) ) ;
#127486 = CARTESIAN_POINT ( 'NONE',  ( -5.049401038298153566, 19.05341960407611168, 85.20724293864766707 ) ) ;
#127487 = CARTESIAN_POINT ( 'NONE',  ( 19.02544592524334988, 5.153800228976608722, 51.45942372801900433 ) ) ;
#127488 = CARTESIAN_POINT ( 'NONE',  ( -0.05219959533907301413, -21.53943276465977519, 47.49890960531435979 ) ) ;
#127489 = CARTESIAN_POINT ( 'NONE',  ( 18.62759615963271287, -10.81492255796078972, 108.3322429386477097 ) ) ;
#127490 = CARTESIAN_POINT ( 'NONE',  ( 0.05219959533934541429, -16.53943276465976808, 20.00109039468568639 ) ) ;
#127491 = CARTESIAN_POINT ( 'NONE',  ( -4.483927247898782831, 16.52544592524335698, 67.70942372801901854 ) ) ;
#127493 = CARTESIAN_POINT ( 'NONE',  ( -18.62759615963270932, 10.81492255796079327, 105.8322429386476955 ) ) ;
#127492 = CARTESIAN_POINT ( 'NONE',  ( -11.30153831258470731, -180.0000000000000000, 1.787262988391354872E-28 ) ) ;
#127494 = CARTESIAN_POINT ( 'NONE',  ( 0.05219959533910956823, 16.53943276465976808, 104.9989096053143669 ) ) ;
#127495 = CARTESIAN_POINT ( 'NONE',  ( -17.49999999999999645, -5.500000000000005329, 31.28230962303567253 ) ) ;
#127496 = CARTESIAN_POINT ( 'NONE',  ( -12.14591786802326823, 12.06949235617739902, 38.12609039468567573 ) ) ;
#127497 = CARTESIAN_POINT ( 'NONE',  ( -21.52544592524343514, 5.823673210054127303, 61.04057627198103120 ) ) ;
#127498 = CARTESIAN_POINT ( 'NONE',  ( 8.224510206698742110, 14.34966873604972548, 107.0844237280190043 ) ) ;
#127499 = CARTESIAN_POINT ( 'NONE',  ( -19.05341960407611168, -5.049401038298163336, 31.45724293864769550 ) ) ;
#127500 = CARTESIAN_POINT ( 'NONE',  ( 0.05219959533934541429, -16.53943276465976808, 70.00109039468568994 ) ) ;
#127501 = CARTESIAN_POINT ( 'NONE',  ( 19.02544592524334988, 5.153800228976608722, 66.45942372801899012 ) ) ;
#127502 = CARTESIAN_POINT ( 'NONE',  ( 10.81492255796106328, -18.62759615963255655, 45.41775706135234003 ) ) ;
#127503 = CIRCLE ( 'NONE', #66159, 8.000000000000000000 ) ;
#127504 = CARTESIAN_POINT ( 'NONE',  ( 0.05219959533907565091, 21.53943276465977519, 59.99890960531436690 ) ) ;
#127505 = CARTESIAN_POINT ( 'NONE',  ( -14.34966873604972548, 8.224510206698743886, 93.33442372801901854 ) ) ;
#127506 = CARTESIAN_POINT ( 'NONE',  ( -10.81492255796105439, 18.62759615963255655, 87.91775706135234714 ) ) ;
#127507 = CARTESIAN_POINT ( 'NONE',  ( -5.823673210054116645, -21.52544592524344225, 57.29057627198103120 ) ) ;
#127508 = CARTESIAN_POINT ( 'NONE',  ( 21.55341960407610458, 5.719274019375980345, 28.95724293864769905 ) ) ;
#127509 = CARTESIAN_POINT ( 'NONE',  ( -14.34966873604972548, 8.224510206698743886, 83.33442372801903275 ) ) ;
#127510 = CARTESIAN_POINT ( 'NONE',  ( -10.72451020669898014, 18.67979575497178502, 30.41557627198101699 ) ) ;
#127511 = VERTEX_POINT ( 'NONE', #80409 ) ;
#127512 = CARTESIAN_POINT ( 'NONE',  ( 5.153800228976335163, 19.02544592524342804, 99.79057627198102409 ) ) ;
#127513 = CARTESIAN_POINT ( 'NONE',  ( 14.34966873604960469, 8.224510206698951720, 24.16557627198103120 ) ) ;
#127514 = DIRECTION ( 'NONE',  ( 0.000000000000000000, 0.000000000000000000, -1.000000000000000000 ) ) ;
#127515 = CARTESIAN_POINT ( 'NONE',  ( -0.05219959533910754901, -16.53943276465976808, 107.4989096053143669 ) ) ;
#127516 = CARTESIAN_POINT ( 'NONE',  ( -21.55341960407610458, -5.719274019375992779, 61.45724293864770260 ) ) ;
#127517 = CARTESIAN_POINT ( 'NONE',  ( 8.314922557961029526, -14.29746914071037800, 85.41775706135236135 ) ) ;
#127518 = CARTESIAN_POINT ( 'NONE',  ( 10.72451020669871369, 18.67979575497193778, 42.08442372801901854 ) ) ;
#127519 = CARTESIAN_POINT ( 'NONE',  ( -5.049401038297874678, -19.05341960407617918, 104.7927570613523471 ) ) ;
#127520 = CARTESIAN_POINT ( 'NONE',  ( 16.53943276465976808, -0.05219959533910856209, 98.74890960531438111 ) ) ;
#127521 = CARTESIAN_POINT ( 'NONE',  ( -5.153800228976607833, 19.02544592524334988, 107.7094237280189759 ) ) ;
#127522 = VECTOR ( 'NONE', #101756, 1000.000000000000000 ) ;
#127523 = CARTESIAN_POINT ( 'NONE',  ( 0.05219959533909260263, 19.03943276465977164, 44.99890960531435979 ) ) ;
#127524 = DIRECTION ( 'NONE',  ( 0.000000000000000000, 0.000000000000000000, -1.000000000000000000 ) ) ;
#127525 = CARTESIAN_POINT ( 'NONE',  ( 16.51473224551069308, 9.474510206698969483, 89.16557627198103830 ) ) ;
#127526 = CARTESIAN_POINT ( 'NONE',  ( -8.224510206698735004, -14.34966873604973081, 74.58442372801901854 ) ) ;
#127527 = CARTESIAN_POINT ( 'NONE',  ( 21.55341960407619695, -5.719274019375665929, 101.0427570613523756 ) ) ;
#127528 = CARTESIAN_POINT ( 'NONE',  ( -21.55341960407610458, -5.719274019375992779, 66.45724293864768129 ) ) ;
#127529 = EDGE_CURVE ( 'NONE', #163891, #70870, #143025, .T. ) ;
#127530 = CARTESIAN_POINT ( 'NONE',  ( 0.05219959533934541429, -16.53943276465976808, 85.00109039468568994 ) ) ;
#127531 = CARTESIAN_POINT ( 'NONE',  ( 19.05341960407617918, -5.049401038297876454, 81.04275706135231871 ) ) ;
#127532 = CARTESIAN_POINT ( 'NONE',  ( -16.46253265017160317, 9.564922557960807481, 30.83224293864769550 ) ) ;
#127534 = AXIS2_PLACEMENT_3D ( 'NONE', #11861, #136175, #197850 ) ;
#127533 = CARTESIAN_POINT ( 'NONE',  ( -5.049401038298153566, 19.05341960407611168, 80.20724293864769550 ) ) ;
#127535 = CARTESIAN_POINT ( 'NONE',  ( 5.049401038298161559, -19.05341960407611168, 27.70724293864769550 ) ) ;
#127536 = CARTESIAN_POINT ( 'NONE',  ( -19.05341960407617563, 5.049401038297882671, 73.54275706135233293 ) ) ;
#127537 = CARTESIAN_POINT ( 'NONE',  ( 25.04733094907550850, -10.92720321514008575, 170.1247377027657421 ) ) ;
#127538 = CARTESIAN_POINT ( 'NONE',  ( -13.97604488694527625, -13.89961937509977652, 101.8739096053143811 ) ) ;
#127539 = CARTESIAN_POINT ( 'NONE',  ( 14.29746914071049879, -8.314922557960816363, 48.33224293864770260 ) ) ;
#127540 = CARTESIAN_POINT ( 'NONE',  ( -21.53943276465977519, 0.05219959533907696930, 56.24890960531436690 ) ) ;
#127541 = AXIS2_PLACEMENT_3D ( 'NONE', #150211, #182532, #27873 ) ;
#127542 = CARTESIAN_POINT ( 'NONE',  ( -17.49999999999999645, 5.068104630630383411, 105.7281840534002981 ) ) ;
#127543 = PRODUCT_DEFINITION_FORMATION_WITH_SPECIFIED_SOURCE ( 'ANY', '', #159611, .NOT_KNOWN. ) ;
#127544 = CARTESIAN_POINT ( 'NONE',  ( 16.46253265017146816, 9.564922557961045513, 26.66775706135234003 ) ) ;
#127545 = DIRECTION ( 'NONE',  ( 0.000000000000000000, 0.000000000000000000, 1.000000000000000000 ) ) ;
#127547 = CARTESIAN_POINT ( 'NONE',  ( -9.474510206698964154, 16.51473224551069663, 70.41557627198102409 ) ) ;
#127546 = CARTESIAN_POINT ( 'NONE',  ( -19.03943276465977164, 0.05219959533909376836, 51.24890960531436690 ) ) ;
#127548 = CARTESIAN_POINT ( 'NONE',  ( 4.379528057220092307, 16.55341960407617563, 42.29275706135235424 ) ) ;
#127549 = CARTESIAN_POINT ( 'NONE',  ( -33.74160284725413561, -3.639722220971261191, 99.13931652913684900 ) ) ;
#127550 = CARTESIAN_POINT ( 'NONE',  ( 3.887666669675321707, -36.87873209731345270, -7.999999999999996447 ) ) ;
#127551 = CARTESIAN_POINT ( 'NONE',  ( -4.483927247898782831, 16.52544592524335698, 72.70942372801901854 ) ) ;
#127553 = CARTESIAN_POINT ( 'NONE',  ( 5.719274019375991003, -21.55341960407610458, 102.7072429386476955 ) ) ;
#127552 = CARTESIAN_POINT ( 'NONE',  ( 16.55341960407618274, -4.379528057220086978, 66.04275706135236135 ) ) ;
#127554 = CARTESIAN_POINT ( 'NONE',  ( 14.34966873604972726, -8.224510206698740333, 45.83442372801901854 ) ) ;
#127556 = FACE_BOUND ( 'NONE', #117491, .T. ) ;
#127555 = CARTESIAN_POINT ( 'NONE',  ( 9.474510206698971260, -16.51473224551069308, 47.91557627198102409 ) ) ;
#127557 = CARTESIAN_POINT ( 'NONE',  ( 5.719274019375673035, 21.55341960407619339, 57.29275706135234714 ) ) ;
#127558 = CARTESIAN_POINT ( 'NONE',  ( 13.89961937509957401, 13.97604488694547697, 61.87609039468566863 ) ) ;
#127559 = CARTESIAN_POINT ( 'NONE',  ( 21.52544592524334988, 5.823673210054432836, 96.45942372801901854 ) ) ;
#127560 = CARTESIAN_POINT ( 'NONE',  ( -5.049401038298153566, 19.05341960407611168, 30.20724293864768839 ) ) ;
#127561 = CARTESIAN_POINT ( 'NONE',  ( 37.66961640367472341, 5.000000000000023981, -15.00000000000000000 ) ) ;
#127562 = CARTESIAN_POINT ( 'NONE',  ( -10.81492255796078084, -18.62759615963271287, 57.08224293864769550 ) ) ;
#127563 = CIRCLE ( 'NONE', #172766, 5.000000000000000000 ) ;
#127564 = CARTESIAN_POINT ( 'NONE',  ( 9.564922557960805705, 16.46253265017160317, 109.5822429386476955 ) ) ;
#127565 = CARTESIAN_POINT ( 'NONE',  ( -12.06949235617756955, 12.14591786802309770, 105.6239096053143669 ) ) ;
#127566 = CARTESIAN_POINT ( 'NONE',  ( 12.06949235617739724, 12.14591786802326823, 41.87609039468568284 ) ) ;
#127567 = CARTESIAN_POINT ( 'NONE',  ( -0.05219959533934338120, 16.53943276465976808, 107.5010903946856899 ) ) ;
#127568 = VERTEX_POINT ( 'NONE', #189603 ) ;
#127569 = CARTESIAN_POINT ( 'NONE',  ( -18.62759615963270932, 10.81492255796079327, 105.8322429386476955 ) ) ;
#127571 = CARTESIAN_POINT ( 'NONE',  ( 0.05219959533909260263, 19.03943276465977164, 109.9989096053143669 ) ) ;
#127570 = CARTESIAN_POINT ( 'NONE',  ( -14.34966873604960291, -8.224510206698953496, 41.66557627198103120 ) ) ;
#127572 = CARTESIAN_POINT ( 'NONE',  ( -16.51473224551082808, 9.474510206698731452, 88.33442372801900433 ) ) ;
#127573 = CARTESIAN_POINT ( 'NONE',  ( -13.97604488694547697, 13.89961937509957934, 28.12609039468565797 ) ) ;
#127574 = CARTESIAN_POINT ( 'NONE',  ( 12.14591786802309770, 12.06949235617756955, 34.37390960531435979 ) ) ;
#127575 = CARTESIAN_POINT ( 'NONE',  ( 15.80617190586746368, 15.72974639402197994, 94.37390960531436690 ) ) ;
#127576 = CARTESIAN_POINT ( 'NONE',  ( 21.53943276465977519, -0.05219959533907433946, 48.74890960531435979 ) ) ;
#127577 = CARTESIAN_POINT ( 'NONE',  ( 13.97604488694527802, 13.89961937509977652, 69.37390960531436690 ) ) ;
#127578 = CARTESIAN_POINT ( 'NONE',  ( -8.314922557960811034, -14.29746914071050412, 37.08224293864768129 ) ) ;
#127579 = CARTESIAN_POINT ( 'NONE',  ( -19.05341960407611168, -5.049401038298163336, 86.45724293864769550 ) ) ;
#127580 = ORIENTED_EDGE ( 'NONE', *, *, #115128, .F. ) ;
#127581 = CARTESIAN_POINT ( 'NONE',  ( 19.52837319214023992, -5.500000000000092371, 62.10471352585538796 ) ) ;
#127582 = CARTESIAN_POINT ( 'NONE',  ( 5.153800228976615827, -19.02544592524334988, 45.20942372801901143 ) ) ;
#127583 = CARTESIAN_POINT ( 'NONE',  ( 15.80617190586746368, 15.72974639402197994, 84.37390960531438111 ) ) ;
#127584 = CARTESIAN_POINT ( 'NONE',  ( -8.314922557960811034, -14.29746914071050412, 97.08224293864770971 ) ) ;
#127585 = CARTESIAN_POINT ( 'NONE',  ( -10.81492255796105439, 18.62759615963255655, 42.91775706135235424 ) ) ;
#127586 = CARTESIAN_POINT ( 'NONE',  ( 27.73933785331498925, -9.013057229001033122, 148.2750000027311330 ) ) ;
#127587 = EDGE_CURVE ( 'NONE', #186347, #101009, #33924, .T. ) ;
#127588 = CARTESIAN_POINT ( 'NONE',  ( -16.53943276465976808, -0.05219959533934237506, 108.7510903946857042 ) ) ;
#127589 = CARTESIAN_POINT ( 'NONE',  ( 16.51473224551069308, 9.474510206698969483, 34.16557627198102409 ) ) ;
#127590 = CARTESIAN_POINT ( 'NONE',  ( 13.97604488694527802, 13.89961937509977652, 84.37390960531433848 ) ) ;
#127591 = SURFACE_STYLE_FILL_AREA ( #7232 ) ;
#127592 = CARTESIAN_POINT ( 'NONE',  ( -9.564922557960796823, -16.46253265017161027, 27.08224293864769550 ) ) ;
#127593 = CARTESIAN_POINT ( 'NONE',  ( -8.314922557960811034, -14.29746914071050412, 47.08224293864770260 ) ) ;
#127594 = CARTESIAN_POINT ( 'NONE',  ( 21.52544592524334988, 5.823673210054432836, 71.45942372801901854 ) ) ;
#127596 = CARTESIAN_POINT ( 'NONE',  ( 14.34966873604972726, -8.224510206698740333, 70.83442372801901854 ) ) ;
#127595 = CARTESIAN_POINT ( 'NONE',  ( 26.91739389984235942, -26.09363094301860642, -18.46721497145071211 ) ) ;
#127597 = CARTESIAN_POINT ( 'NONE',  ( 16.46253265017160672, -9.564922557960803928, 53.33224293864768839 ) ) ;
#127598 = CARTESIAN_POINT ( 'NONE',  ( -16.51473224551069308, -9.474510206698971260, 61.66557627198103120 ) ) ;
#127599 = ORIENTED_EDGE ( 'NONE', *, *, #86511, .T. ) ;
#127600 = CARTESIAN_POINT ( 'NONE',  ( -19.02544592524334988, -5.153800228976617603, 18.95942372801899722 ) ) ;
#127601 = CARTESIAN_POINT ( 'NONE',  ( -14.34966873604972548, 8.224510206698743886, 78.33442372801901854 ) ) ;
#127602 = CARTESIAN_POINT ( 'NONE',  ( 21.55341960407619695, -5.719274019375665929, 96.04275706135236135 ) ) ;
#127603 = CARTESIAN_POINT ( 'NONE',  ( -10.72451020669898014, 18.67979575497178502, 30.41557627198101699 ) ) ;
#127604 = CARTESIAN_POINT ( 'NONE',  ( -19.05341960407617563, 5.049401038297882671, 103.5427570613523329 ) ) ;
#127605 = CARTESIAN_POINT ( 'NONE',  ( -21.52544592524334988, -5.823673210054445271, 63.95942372801901854 ) ) ;
#127606 = CARTESIAN_POINT ( 'NONE',  ( -16.53943276465976808, -0.05219959533934237506, 48.75109039468568284 ) ) ;
#127607 = CARTESIAN_POINT ( 'NONE',  ( 18.67979575497178502, 10.72451020669898547, 104.1655762719810241 ) ) ;
#127608 = CARTESIAN_POINT ( 'NONE',  ( 13.97604488694548053, -13.89961937509957401, 105.6260903946856757 ) ) ;
#127609 = CARTESIAN_POINT ( 'NONE',  ( 9.564922557960805705, 16.46253265017160317, 74.58224293864769550 ) ) ;
#127610 = CARTESIAN_POINT ( 'NONE',  ( -16.51473224551082808, 9.474510206698731452, 113.3344237280190043 ) ) ;
#127611 = CARTESIAN_POINT ( 'NONE',  ( -0.05219959533936034679, 19.03943276465977164, 107.5010903946856615 ) ) ;
#127612 = CARTESIAN_POINT ( 'NONE',  ( 4.379528057220339221, -16.55341960407611168, 67.70724293864769550 ) ) ;
#127613 = CARTESIAN_POINT ( 'NONE',  ( 12.06949235617739724, 12.14591786802326823, 76.87609039468567573 ) ) ;
#127615 = CARTESIAN_POINT ( 'NONE',  ( -13.89961937509977652, 13.97604488694528158, 50.62390960531435979 ) ) ;
#127614 = CARTESIAN_POINT ( 'NONE',  ( -18.62759615963255300, -10.81492255796106328, 19.16775706135234714 ) ) ;
#127617 = ADVANCED_FACE ( 'NONE', ( #18762 ), #50092, .F. ) ;
#127616 = CARTESIAN_POINT ( 'NONE',  ( -13.97604488694527625, -13.89961937509977652, 56.87390960531434558 ) ) ;
#127618 = CARTESIAN_POINT ( 'NONE',  ( -16.55341960407617563, 4.379528057220093196, 73.54275706135234714 ) ) ;
#127619 = CARTESIAN_POINT ( 'NONE',  ( -23.31738231874055600, 16.94106989632528837, 144.0500000054623513 ) ) ;
#127620 = CARTESIAN_POINT ( 'NONE',  ( -21.53943276465977519, -0.05219959533937600094, 108.7510903946857042 ) ) ;
#127621 = FACE_OUTER_BOUND ( 'NONE', #52984, .T. ) ;
#127622 = VERTEX_POINT ( 'NONE', #10578 ) ;
#127623 = CARTESIAN_POINT ( 'NONE',  ( 0.05219959533936267826, -19.03943276465977164, 110.0010903946856757 ) ) ;
#127624 = CARTESIAN_POINT ( 'NONE',  ( -5.719274019375978568, 21.55341960407610458, 55.20724293864770260 ) ) ;
#127626 = CARTESIAN_POINT ( 'NONE',  ( -12.14591786802326823, 12.06949235617739902, 33.12609039468569705 ) ) ;
#127625 = CARTESIAN_POINT ( 'NONE',  ( -16.51473224551082808, 9.474510206698731452, 38.33442372801899722 ) ) ;
#127627 = CARTESIAN_POINT ( 'NONE',  ( -9.474510206698964154, 16.51473224551069663, 45.41557627198103120 ) ) ;
#127628 = CARTESIAN_POINT ( 'NONE',  ( 9.564922557960805705, 16.46253265017160317, 69.58224293864770971 ) ) ;
#127629 = CARTESIAN_POINT ( 'NONE',  ( 18.67979575497178502, 10.72451020669898547, 84.16557627198103830 ) ) ;
#127630 = CARTESIAN_POINT ( 'NONE',  ( -19.03943276465977164, 0.05219959533909376836, 111.2489096053143669 ) ) ;
#127631 = CARTESIAN_POINT ( 'NONE',  ( 16.46253265017160672, -9.564922557960803928, 53.33224293864768839 ) ) ;
#127632 = CARTESIAN_POINT ( 'NONE',  ( 8.571926809382597767, 26.38167802310806209, 148.7750000027311899 ) ) ;
#127633 = CARTESIAN_POINT ( 'NONE',  ( 13.97604488694548053, -13.89961937509957401, 95.62609039468563310 ) ) ;
#127634 = CARTESIAN_POINT ( 'NONE',  ( 12.14591786802309770, 12.06949235617756955, 69.37390960531436690 ) ) ;
#127635 = CARTESIAN_POINT ( 'NONE',  ( -16.46253265017146816, -9.564922557961047289, 29.16775706135232937 ) ) ;
#127636 = CARTESIAN_POINT ( 'NONE',  ( 12.06949235617757843, -12.14591786802309237, 63.12390960531435979 ) ) ;
#127637 = CARTESIAN_POINT ( 'NONE',  ( 21.53943276465977519, 0.05219959533937863772, 81.25109039468568994 ) ) ;
#127638 = CARTESIAN_POINT ( 'NONE',  ( -5.153800228976328057, -19.02544592524343514, 32.29057627198102409 ) ) ;
#127639 = CARTESIAN_POINT ( 'NONE',  ( -5.823673210054431948, 21.52544592524334988, 92.70942372801901854 ) ) ;
#127641 = CARTESIAN_POINT ( 'NONE',  ( -18.67979575497193778, 10.72451020669871902, 83.33442372801903275 ) ) ;
#127640 = CARTESIAN_POINT ( 'NONE',  ( 8.224510206698953496, -14.34966873604960469, 22.91557627198102765 ) ) ;
#127642 = CARTESIAN_POINT ( 'NONE',  ( -16.51473224551069308, -9.474510206698971260, 71.66557627198102409 ) ) ;
#127643 = CARTESIAN_POINT ( 'NONE',  ( 18.62759615963255655, 10.81492255796105972, 46.66775706135234714 ) ) ;
#127644 = CARTESIAN_POINT ( 'NONE',  ( 5.049401038298161559, -19.05341960407611168, 82.70724293864770971 ) ) ;
#127645 = CARTESIAN_POINT ( 'NONE',  ( 16.53943276465976808, -0.05219959533910856209, 93.74890960531436690 ) ) ;
#127646 = CARTESIAN_POINT ( 'NONE',  ( 12.06949235617757843, -12.14591786802309237, 63.12390960531435979 ) ) ;
#127647 = CARTESIAN_POINT ( 'NONE',  ( 5.719274019375991003, -21.55341960407610458, 72.70724293864769550 ) ) ;
#127648 = CARTESIAN_POINT ( 'NONE',  ( -0.05219959533909027116, -19.03943276465977164, 72.49890960531435269 ) ) ;
#127649 = CARTESIAN_POINT ( 'NONE',  ( 5.823673210054125526, 21.52544592524343514, 84.79057627198102409 ) ) ;
#127650 = AXIS2_PLACEMENT_3D ( 'NONE', #29203, #76674, #137354 ) ;
#127651 = CARTESIAN_POINT ( 'NONE',  ( -9.564922557961040184, 16.46253265017147172, 62.91775706135233293 ) ) ;
#127653 = CARTESIAN_POINT ( 'NONE',  ( -12.14591786802309592, -12.06949235617757132, 81.87390960531435269 ) ) ;
#127652 = CARTESIAN_POINT ( 'NONE',  ( -13.89961937509957401, -13.97604488694547697, 29.37609039468566152 ) ) ;
#127654 = CARTESIAN_POINT ( 'NONE',  ( 15.80617190586746368, 15.72974639402197994, 54.37390960531435979 ) ) ;
#127655 = DIRECTION ( 'NONE',  ( 1.000000000000000000, 0.000000000000000000, 0.000000000000000000 ) ) ;
#127657 = CARTESIAN_POINT ( 'NONE',  ( 22.44159573604009594, -16.30477369853687364, 146.1750000027311671 ) ) ;
#127656 = CARTESIAN_POINT ( 'NONE',  ( -0.05219959533934338120, 16.53943276465976808, 92.50109039468567573 ) ) ;
#127658 = CARTESIAN_POINT ( 'NONE',  ( 13.89961937509957401, 13.97604488694547697, 106.8760903946856757 ) ) ;
#127659 = CARTESIAN_POINT ( 'NONE',  ( -14.34966873604960291, -8.224510206698953496, 61.66557627198103120 ) ) ;
#127660 = CARTESIAN_POINT ( 'NONE',  ( 8.898623008803079770, -0.7571601631681817990, -61.93576936796788601 ) ) ;
#127661 = CARTESIAN_POINT ( 'NONE',  ( 0.05219959533909260263, 19.03943276465977164, 64.99890960531436690 ) ) ;
#127662 = CARTESIAN_POINT ( 'NONE',  ( 4.483927247898545687, 16.52544592524342804, 49.79057627198102409 ) ) ;
#127663 = CARTESIAN_POINT ( 'NONE',  ( -16.46253265017160317, 9.564922557960807481, 100.8322429386477097 ) ) ;
#127665 = CARTESIAN_POINT ( 'NONE',  ( 19.05341960407611168, 5.049401038298154454, 68.95724293864769550 ) ) ;
#127664 = CARTESIAN_POINT ( 'NONE',  ( 19.05341960407617918, -5.049401038297876454, 76.04275706135230450 ) ) ;
#127666 = CARTESIAN_POINT ( 'NONE',  ( -19.05341960407611168, -5.049401038298163336, 91.45724293864766707 ) ) ;
#127667 = CARTESIAN_POINT ( 'NONE',  ( -13.89961937509977652, 13.97604488694528158, 80.62390960531436690 ) ) ;
#127668 = CARTESIAN_POINT ( 'NONE',  ( -10.81492255796078084, -18.62759615963271287, 57.08224293864769550 ) ) ;
#127669 = CARTESIAN_POINT ( 'NONE',  ( -8.224510206698735004, -14.34966873604973081, 59.58442372801901854 ) ) ;
#127670 = AXIS2_PLACEMENT_3D ( 'NONE', #57482, #42311, #103972 ) ;
#127671 = CARTESIAN_POINT ( 'NONE',  ( -19.02544592524342804, 5.153800228976336051, 46.04057627198101699 ) ) ;
#127672 = CARTESIAN_POINT ( 'NONE',  ( -21.55341960407610458, -5.719274019375992779, 51.45724293864770260 ) ) ;
#127673 = CARTESIAN_POINT ( 'NONE',  ( 19.03943276465977164, 0.05219959533936151252, 101.2510903946856757 ) ) ;
#127675 = CARTESIAN_POINT ( 'NONE',  ( 15.80617190586769283, -15.72974639402175789, 45.62609039468567573 ) ) ;
#127674 = CARTESIAN_POINT ( 'NONE',  ( -0.05219959533910754901, -16.53943276465976808, 27.49890960531435269 ) ) ;
#127676 = CARTESIAN_POINT ( 'NONE',  ( 13.97604488694548053, -13.89961937509957401, 40.62609039468564731 ) ) ;
#127678 = CARTESIAN_POINT ( 'NONE',  ( 8.224510206698742110, 14.34966873604972548, 92.08442372801901854 ) ) ;
#127677 = CARTESIAN_POINT ( 'NONE',  ( -8.314922557961024197, 14.29746914071037800, 57.91775706135234714 ) ) ;
#127679 = CARTESIAN_POINT ( 'NONE',  ( 18.39635199886966532, -5.500000000000096811, 43.51967076359999709 ) ) ;
#127680 = CARTESIAN_POINT ( 'NONE',  ( 8.314922557961029526, -14.29746914071037800, 75.41775706135233293 ) ) ;
#127681 = CARTESIAN_POINT ( 'NONE',  ( 14.34966873604972726, -8.224510206698740333, 35.83442372801901143 ) ) ;
#127682 = CARTESIAN_POINT ( 'NONE',  ( -5.153800228976328057, -19.02544592524343514, 52.29057627198100988 ) ) ;
#127683 = CARTESIAN_POINT ( 'NONE',  ( 5.153800228976335163, 19.02544592524342804, 49.79057627198100988 ) ) ;
#127684 = CARTESIAN_POINT ( 'NONE',  ( -13.97604488694527625, -13.89961937509977652, 66.87390960531436690 ) ) ;
#127685 = CARTESIAN_POINT ( 'NONE',  ( -5.823673210054431948, 21.52544592524334988, 57.70942372801901143 ) ) ;
#127686 = CARTESIAN_POINT ( 'NONE',  ( -12.14591786802326823, 12.06949235617739902, 43.12609039468568284 ) ) ;
#127687 = CARTESIAN_POINT ( 'NONE',  ( -4.379528057220086978, -16.55341960407618274, 109.7927570613523613 ) ) ;
#127688 = CARTESIAN_POINT ( 'NONE',  ( -5.153800228976328057, -19.02544592524343514, 22.29057627198102765 ) ) ;
#127689 = CARTESIAN_POINT ( 'NONE',  ( -18.62759615963255300, -10.81492255796106328, 109.1677570613523613 ) ) ;
#127690 = CARTESIAN_POINT ( 'NONE',  ( 16.51473224551083163, -9.474510206698727899, 110.8344237280190043 ) ) ;
#127691 = CARTESIAN_POINT ( 'NONE',  ( -5.153800228976607833, 19.02544592524334988, 72.70942372801900433 ) ) ;
#127692 = CARTESIAN_POINT ( 'NONE',  ( 8.314922557960818139, 14.29746914071049879, 79.58224293864769550 ) ) ;
#127693 = CARTESIAN_POINT ( 'NONE',  ( 5.153800228976335163, 19.02544592524342804, 34.79057627198102409 ) ) ;
#127695 = LINE ( 'NONE', #188398, #140529 ) ;
#127694 = CARTESIAN_POINT ( 'NONE',  ( 13.97604488694548053, -13.89961937509957401, 75.62609039468564731 ) ) ;
#127696 = CARTESIAN_POINT ( 'NONE',  ( 18.67979575497194134, -10.72451020669871369, 80.83442372801901854 ) ) ;
#127697 = CARTESIAN_POINT ( 'NONE',  ( -14.29746914071037622, -8.314922557961029526, 39.16775706135235424 ) ) ;
#127698 = CYLINDRICAL_SURFACE ( 'NONE', #105122, 2.000000000000001776 ) ;
#127699 = CARTESIAN_POINT ( 'NONE',  ( -15.72974639402197994, 15.80617190586746368, 30.62390960531436335 ) ) ;
#127700 = CARTESIAN_POINT ( 'NONE',  ( -16.55341960407617563, 4.379528057220093196, 23.54275706135235424 ) ) ;
#127701 = CARTESIAN_POINT ( 'NONE',  ( 9.474510206698971260, -16.51473224551069308, 22.91557627198102765 ) ) ;
#127702 = CARTESIAN_POINT ( 'NONE',  ( -9.474510206698720793, -16.51473224551083518, 34.58442372801899722 ) ) ;
#127703 = FACE_OUTER_BOUND ( 'NONE', #32865, .T. ) ;
#127704 = CARTESIAN_POINT ( 'NONE',  ( 16.51473224551069308, 9.474510206698969483, 44.16557627198103120 ) ) ;
#127705 = DIRECTION ( 'NONE',  ( -1.000000000000000000, 0.000000000000000000, 0.000000000000000000 ) ) ;
#127706 = CARTESIAN_POINT ( 'NONE',  ( -0.05219959533909027116, -19.03943276465977164, 72.49890960531435269 ) ) ;
#127707 = CARTESIAN_POINT ( 'NONE',  ( -19.25663599770060586, 5.499999999999443112, 98.99419308057201761 ) ) ;
#127708 = CARTESIAN_POINT ( 'NONE',  ( -16.46253265017146816, -9.564922557961047289, 24.16775706135233648 ) ) ;
#127709 = CARTESIAN_POINT ( 'NONE',  ( 12.06949235617739724, 12.14591786802326823, 111.8760903946856615 ) ) ;
#127710 = CARTESIAN_POINT ( 'NONE',  ( 9.564922557960805705, 16.46253265017160317, 49.58224293864770260 ) ) ;
#127711 = CARTESIAN_POINT ( 'NONE',  ( -9.564922557960796823, -16.46253265017161027, 92.08224293864769550 ) ) ;
#127712 = CARTESIAN_POINT ( 'NONE',  ( 5.823673210054444382, -21.52544592524334988, 70.20942372801904696 ) ) ;
#127713 = CARTESIAN_POINT ( 'NONE',  ( 19.03943276465977164, -0.05219959533909143690, 53.74890960531436690 ) ) ;
#127714 = CARTESIAN_POINT ( 'NONE',  ( -0.05219959533937732626, 21.53943276465977519, 62.50109039468568284 ) ) ;
#127716 = CARTESIAN_POINT ( 'NONE',  ( 19.03943276465977164, -0.05219959533909143690, 113.7489096053143669 ) ) ;
#127715 = CARTESIAN_POINT ( 'NONE',  ( -16.46253265017146816, -9.564922557961047289, 99.16775706135233293 ) ) ;
#127717 = CARTESIAN_POINT ( 'NONE',  ( 16.51473224551069308, 9.474510206698969483, 29.16557627198103475 ) ) ;
#127718 = CARTESIAN_POINT ( 'NONE',  ( -15.72974639402197994, 15.80617190586746368, 110.6239096053143669 ) ) ;
#127719 = CARTESIAN_POINT ( 'NONE',  ( 5.049401038297881783, 19.05341960407617563, 37.29275706135232582 ) ) ;
#127720 = CARTESIAN_POINT ( 'NONE',  ( -16.52544592524342804, 4.483927247898546575, 106.0405762719810525 ) ) ;
#127721 = CARTESIAN_POINT ( 'NONE',  ( 13.89961937509977652, -13.97604488694527269, 68.12390960531436690 ) ) ;
#127722 = CARTESIAN_POINT ( 'NONE',  ( 5.049401038297881783, 19.05341960407617563, 112.2927570613523471 ) ) ;
#127723 = CARTESIAN_POINT ( 'NONE',  ( -4.379528057220328563, 16.55341960407611168, 80.20724293864769550 ) ) ;
#127724 = CARTESIAN_POINT ( 'NONE',  ( 21.52544592524344225, -5.823673210054117533, 28.54057627198103120 ) ) ;
#127725 = CARTESIAN_POINT ( 'NONE',  ( 13.97604488694548053, -13.89961937509957401, 85.62609039468568994 ) ) ;
#127726 = CARTESIAN_POINT ( 'NONE',  ( 5.823673210054125526, 21.52544592524343514, 89.79057627198103830 ) ) ;
#127727 = CARTESIAN_POINT ( 'NONE',  ( -0.05219959533937732626, 21.53943276465977519, 62.50109039468568284 ) ) ;
#127728 = CARTESIAN_POINT ( 'NONE',  ( -14.34966873604972548, 8.224510206698743886, 58.33442372801901143 ) ) ;
#127729 = CARTESIAN_POINT ( 'NONE',  ( -14.34966873604972548, 8.224510206698743886, 58.33442372801901143 ) ) ;
#127730 = CARTESIAN_POINT ( 'NONE',  ( -15.72974639402197994, 15.80617190586746368, 60.62390960531437401 ) ) ;
#127731 = CARTESIAN_POINT ( 'NONE',  ( -9.564922557960796823, -16.46253265017161027, 47.08224293864769550 ) ) ;
#127732 = CARTESIAN_POINT ( 'NONE',  ( 11.74264578624799427, 36.14014761921585972, -4.349999994537626868 ) ) ;
#127733 = CARTESIAN_POINT ( 'NONE',  ( 16.52544592524335698, 4.483927247898782831, 81.45942372801900433 ) ) ;
#127734 = CARTESIAN_POINT ( 'NONE',  ( -10.81492255796078084, -18.62759615963271287, 107.0822429386476955 ) ) ;
#127735 = CARTESIAN_POINT ( 'NONE',  ( 8.314922557960818139, 14.29746914071049879, 49.58224293864769550 ) ) ;
#127736 = CARTESIAN_POINT ( 'NONE',  ( -12.06949235617739369, -12.14591786802326823, 59.37609039468568284 ) ) ;
#127737 = CARTESIAN_POINT ( 'NONE',  ( 19.03943276465977164, 0.05219959533936151252, 101.2510903946856757 ) ) ;
#127738 = CARTESIAN_POINT ( 'NONE',  ( 18.62759615963271287, -10.81492255796078972, 93.33224293864769550 ) ) ;
#127739 = CARTESIAN_POINT ( 'NONE',  ( -8.224510206698948167, 14.34966873604960824, 40.41557627198103120 ) ) ;
#127740 = ORIENTED_EDGE ( 'NONE', *, *, #47203, .F. ) ;
#127741 = CARTESIAN_POINT ( 'NONE',  ( -16.79531203550648044, 7.028104445595610095, 68.74755011779559766 ) ) ;
#127742 = CARTESIAN_POINT ( 'NONE',  ( -21.52544592524343514, 5.823673210054127303, 81.04057627198102409 ) ) ;
#127743 = CARTESIAN_POINT ( 'NONE',  ( -12.14591786802326823, 12.06949235617739902, 113.1260903946856899 ) ) ;
#127744 = EDGE_LOOP ( 'NONE', ( #183099, #18037, #50170, #19178 ) ) ;
#127745 = CARTESIAN_POINT ( 'NONE',  ( -16.19135201231369692, -7.376712067591813415, 55.18680854052030327 ) ) ;
#127746 = CARTESIAN_POINT ( 'NONE',  ( -21.52544592524343514, 5.823673210054127303, 96.04057627198102409 ) ) ;
#127747 = VECTOR ( 'NONE', #89432, 1000.000000000000000 ) ;
#127748 = CARTESIAN_POINT ( 'NONE',  ( 10.72451020669871369, 18.67979575497193778, 22.08442372801901143 ) ) ;
#127749 = CARTESIAN_POINT ( 'NONE',  ( 8.224510206698953496, -14.34966873604960469, 32.91557627198102409 ) ) ;
#127750 = CARTESIAN_POINT ( 'NONE',  ( 4.483927247898790824, -16.52544592524335698, 50.20942372801901854 ) ) ;
#127751 = CARTESIAN_POINT ( 'NONE',  ( 9.474510206698971260, -16.51473224551069308, 42.91557627198103120 ) ) ;
#127752 = CARTESIAN_POINT ( 'NONE',  ( 13.89961937509977652, -13.97604488694527269, 83.12390960531436690 ) ) ;
#127753 = ORIENTED_EDGE ( 'NONE', *, *, #145835, .T. ) ;
#127754 = CARTESIAN_POINT ( 'NONE',  ( -18.62759615963270932, 10.81492255796079327, 40.83224293864769550 ) ) ;
#127755 = CARTESIAN_POINT ( 'NONE',  ( -28.83006054357406711, -24.83490584245891597, -16.72457388843617920 ) ) ;
#127756 = CARTESIAN_POINT ( 'NONE',  ( -8.224510206698735004, -14.34966873604973081, 24.58442372801901499 ) ) ;
#127757 = CARTESIAN_POINT ( 'NONE',  ( 16.51473224551083163, -9.474510206698727899, 55.83442372801899722 ) ) ;
#127758 = CARTESIAN_POINT ( 'NONE',  ( -15.80617190586745835, -15.72974639402198527, 96.87390960531436690 ) ) ;
#127759 = EDGE_CURVE ( 'NONE', #101645, #188707, #80606, .T. ) ;
#127760 = CARTESIAN_POINT ( 'NONE',  ( 8.224510206698953496, -14.34966873604960469, 37.91557627198102409 ) ) ;
#127761 = CARTESIAN_POINT ( 'NONE',  ( 19.02544592524343514, -5.153800228976328945, 83.54057627198100988 ) ) ;
#127762 = CARTESIAN_POINT ( 'NONE',  ( -10.81492255796078084, -18.62759615963271287, 57.08224293864769550 ) ) ;
#127764 = CARTESIAN_POINT ( 'NONE',  ( -8.314922557961024197, 14.29746914071037800, 22.91775706135235069 ) ) ;
#127763 = CARTESIAN_POINT ( 'NONE',  ( -21.52544592524343514, 5.823673210054127303, 96.04057627198102409 ) ) ;
#127765 = CARTESIAN_POINT ( 'NONE',  ( -0.05219959533909027116, -19.03943276465977164, 112.4989096053143669 ) ) ;
#127766 = CARTESIAN_POINT ( 'NONE',  ( -10.72451020669870658, -18.67979575497194134, 89.58442372801901854 ) ) ;
#127767 = CARTESIAN_POINT ( 'NONE',  ( 0.05219959533909260263, 19.03943276465977164, 74.99890960531435269 ) ) ;
#127768 = CARTESIAN_POINT ( 'NONE',  ( 13.89961937509977652, -13.97604488694527269, 28.12390960531435624 ) ) ;
#127769 = CARTESIAN_POINT ( 'NONE',  ( 9.474510206698971260, -16.51473224551069308, 87.91557627198102409 ) ) ;
#127770 = CARTESIAN_POINT ( 'NONE',  ( 16.55341960407611168, 4.379528057220329451, 98.95724293864770971 ) ) ;
#127771 = EDGE_LOOP ( 'NONE', ( #112149, #9789, #103025, #183596 ) ) ;
#127772 = CARTESIAN_POINT ( 'NONE',  ( -13.89961937509957401, -13.97604488694547875, 104.3760903946856757 ) ) ;
#127773 = DIRECTION ( 'NONE',  ( -0.000000000000000000, -0.000000000000000000, 1.000000000000000000 ) ) ;
#127774 = CARTESIAN_POINT ( 'NONE',  ( 19.05341960407611168, 5.049401038298154454, 73.95724293864768129 ) ) ;
#127776 = CARTESIAN_POINT ( 'NONE',  ( -5.049401038298153566, 19.05341960407611168, 110.2072429386476671 ) ) ;
#127775 = CARTESIAN_POINT ( 'NONE',  ( 21.53943276465977519, 0.05219959533937863772, 96.25109039468568994 ) ) ;
#127777 = CARTESIAN_POINT ( 'NONE',  ( 14.34966873604972726, -8.224510206698740333, 80.83442372801901854 ) ) ;
#127778 = CARTESIAN_POINT ( 'NONE',  ( -29.41559601785653655, 1.135674102528529295, -49.03020479230152517 ) ) ;
#127779 = CARTESIAN_POINT ( 'NONE',  ( -19.03943276465977164, -0.05219959533935918106, 58.75109039468566863 ) ) ;
#127780 = CARTESIAN_POINT ( 'NONE',  ( 10.72451020669871369, 18.67979575497193778, 107.0844237280190043 ) ) ;
#127781 = CARTESIAN_POINT ( 'NONE',  ( 37.36578165719732425, 3.357000025855910064, 40.62839678089417816 ) ) ;
#127782 = CARTESIAN_POINT ( 'NONE',  ( -19.02544592524342804, 5.153800228976336051, 31.04057627198102409 ) ) ;
#127783 = CARTESIAN_POINT ( 'NONE',  ( 14.34966873604960469, 8.224510206698951720, 24.16557627198103120 ) ) ;
#127784 = DIRECTION ( 'NONE',  ( 0.000000000000000000, 0.000000000000000000, -1.000000000000000000 ) ) ;
#127785 = CARTESIAN_POINT ( 'NONE',  ( -14.29746914071037622, -8.314922557961029526, 104.1677570613523471 ) ) ;
#127786 = CARTESIAN_POINT ( 'NONE',  ( -19.25176906914649777, -5.499999999999857003, 85.99927264242278113 ) ) ;
#127787 = CARTESIAN_POINT ( 'NONE',  ( -0.05219959533934338120, 16.53943276465976808, 77.50109039468567573 ) ) ;
#127788 = CARTESIAN_POINT ( 'NONE',  ( -0.05219959533909027116, -19.03943276465977164, 22.49890960531436690 ) ) ;
#127789 = CARTESIAN_POINT ( 'NONE',  ( -18.62759615963255300, -10.81492255796106328, 89.16775706135236135 ) ) ;
#127790 = CARTESIAN_POINT ( 'NONE',  ( -5.153800228976607833, 19.02544592524334988, 102.7094237280189759 ) ) ;
#127791 = CARTESIAN_POINT ( 'NONE',  ( -15.80617190586768217, 15.72974639402176855, 63.12609039468568994 ) ) ;
#127792 = CARTESIAN_POINT ( 'NONE',  ( -19.02544592524334988, -5.153800228976617603, 33.95942372801897591 ) ) ;
#127793 = CARTESIAN_POINT ( 'NONE',  ( 5.049401038298161559, -19.05341960407611168, 82.70724293864770971 ) ) ;
#127794 = CARTESIAN_POINT ( 'NONE',  ( 13.97604488694527802, 13.89961937509977652, 64.37390960531436690 ) ) ;
#127795 = CARTESIAN_POINT ( 'NONE',  ( -8.334442550624215684, -39.12824798328761489, -13.00000000000136957 ) ) ;
#127796 = CARTESIAN_POINT ( 'NONE',  ( -18.67979575497178146, -10.72451020669898902, 41.66557627198103120 ) ) ;
#127797 = CARTESIAN_POINT ( 'NONE',  ( -19.03943276465977164, 0.05219959533909376836, 51.24890960531436690 ) ) ;
#127798 = CARTESIAN_POINT ( 'NONE',  ( -12.06949235617739369, -12.14591786802326823, 74.37609039468568994 ) ) ;
#127799 = VERTEX_POINT ( 'NONE', #129880 ) ;
#127801 = CARTESIAN_POINT ( 'NONE',  ( 36.91746825000000598, -11.99521256947793546, -3.724999997268812812 ) ) ;
#127800 = CARTESIAN_POINT ( 'NONE',  ( 4.379528057220339221, -16.55341960407611168, 72.70724293864769550 ) ) ;
#127802 = CARTESIAN_POINT ( 'NONE',  ( 16.55341960407618274, -4.379528057220086978, 41.04275706135236135 ) ) ;
#127803 = CARTESIAN_POINT ( 'NONE',  ( 4.483927247898545687, 16.52544592524342804, 114.7905762719810383 ) ) ;
#127804 = CARTESIAN_POINT ( 'NONE',  ( -5.153800228976607833, 19.02544592524334988, 72.70942372801900433 ) ) ;
#127805 = CARTESIAN_POINT ( 'NONE',  ( 12.14591786802309770, 12.06949235617756955, 69.37390960531436690 ) ) ;
#127806 = CARTESIAN_POINT ( 'NONE',  ( -18.62759615963255300, -10.81492255796106328, 29.16775706135234003 ) ) ;
#127808 = CARTESIAN_POINT ( 'NONE',  ( -5.823673210054116645, -21.52544592524344225, 97.29057627198105251 ) ) ;
#127807 = CARTESIAN_POINT ( 'NONE',  ( 23.46320343559640165, -18.96320343559646204, 8.889087296526001936 ) ) ;
#127809 = CARTESIAN_POINT ( 'NONE',  ( -9.564922557960796823, -16.46253265017161027, 112.0822429386476955 ) ) ;
#127810 = CARTESIAN_POINT ( 'NONE',  ( 0.05219959533910956823, 16.53943276465976808, 69.99890960531435269 ) ) ;
#127811 = CARTESIAN_POINT ( 'NONE',  ( 27.05031264677070979, -29.22974442244436588, -16.95124367203838744 ) ) ;
#127812 = CARTESIAN_POINT ( 'NONE',  ( -13.97604488694527625, -13.89961937509977652, 51.87390960531436690 ) ) ;
#127813 = CARTESIAN_POINT ( 'NONE',  ( 36.91746824999999887, -11.99521256947793546, -5.724999997268813701 ) ) ;
#127814 = CARTESIAN_POINT ( 'NONE',  ( 5.153800228976615827, -19.02544592524334988, 75.20942372801896170 ) ) ;
#127815 = CARTESIAN_POINT ( 'NONE',  ( 21.55341960407619695, -5.719274019375665929, 21.04275706135234714 ) ) ;
#127816 = CARTESIAN_POINT ( 'NONE',  ( -19.02544592524342804, 5.153800228976336051, 76.04057627198102409 ) ) ;
#127817 = CARTESIAN_POINT ( 'NONE',  ( 19.05341960407617918, -5.049401038297876454, 61.04275706135232582 ) ) ;
#127818 = CARTESIAN_POINT ( 'NONE',  ( 0.05219959533909260263, 19.03943276465977164, 49.99890960531435979 ) ) ;
#127819 = CARTESIAN_POINT ( 'NONE',  ( -8.224510206698948167, 14.34966873604960824, 65.41557627198102409 ) ) ;
#127820 = CARTESIAN_POINT ( 'NONE',  ( 14.29746914071049879, -8.314922557960816363, 48.33224293864770260 ) ) ;
#127821 = CARTESIAN_POINT ( 'NONE',  ( -16.51473224551069308, -9.474510206698971260, 76.66557627198103830 ) ) ;
#127822 = CARTESIAN_POINT ( 'NONE',  ( 21.52544592524344225, -5.823673210054117533, 83.54057627198102409 ) ) ;
#127823 = CARTESIAN_POINT ( 'NONE',  ( -0.05219959533909027116, -19.03943276465977164, 77.49890960531435269 ) ) ;
#127824 = CARTESIAN_POINT ( 'NONE',  ( 10.81492255796078972, 18.62759615963270932, 74.58224293864768129 ) ) ;
#127825 = CARTESIAN_POINT ( 'NONE',  ( -19.02544592524334988, -5.153800228976617603, 23.95942372801900078 ) ) ;
#127828 = CARTESIAN_POINT ( 'NONE',  ( 14.29746914071049879, -8.314922557960816363, 98.33224293864769550 ) ) ;
#127827 = CARTESIAN_POINT ( 'NONE',  ( 4.483927247898790824, -16.52544592524335698, 110.2094237280190185 ) ) ;
#127826 = CARTESIAN_POINT ( 'NONE',  ( 5.049401038298161559, -19.05341960407611168, 27.70724293864769550 ) ) ;
#127829 = CARTESIAN_POINT ( 'NONE',  ( 16.51473224551083163, -9.474510206698727899, 110.8344237280190043 ) ) ;
#127830 = ORIENTED_EDGE ( 'NONE', *, *, #145930, .F. ) ;
#127831 = CARTESIAN_POINT ( 'NONE',  ( -15.72974639402197994, 15.80617190586746368, 110.6239096053143669 ) ) ;
#127832 = CARTESIAN_POINT ( 'NONE',  ( -13.89961937509957401, -13.97604488694547875, 54.37609039468565442 ) ) ;
#127833 = CARTESIAN_POINT ( 'NONE',  ( -4.483927247898782831, 16.52544592524335698, 112.7094237280190328 ) ) ;
#127834 = CARTESIAN_POINT ( 'NONE',  ( -0.05219959533907301413, -21.53943276465977519, 72.49890960531435269 ) ) ;
#127835 = CARTESIAN_POINT ( 'NONE',  ( -16.46253265017160317, 9.564922557960807481, 105.8322429386476955 ) ) ;
#127836 = CARTESIAN_POINT ( 'NONE',  ( 12.06949235617757843, -12.14591786802309237, 63.12390960531435979 ) ) ;
#127837 = CARTESIAN_POINT ( 'NONE',  ( -18.39443945427632343, 5.499999999999999112, 48.51745347608652992 ) ) ;
#127838 = CARTESIAN_POINT ( 'NONE',  ( -19.02544592524342804, 5.153800228976336051, 36.04057627198100988 ) ) ;
#127839 = CARTESIAN_POINT ( 'NONE',  ( -10.72451020669870658, -18.67979575497194134, 109.5844237280190328 ) ) ;
#127840 = CARTESIAN_POINT ( 'NONE',  ( -16.53943276465976808, -0.05219959533934237506, 93.75109039468567573 ) ) ;
#127841 = CARTESIAN_POINT ( 'NONE',  ( 21.55341960407619695, -5.719274019375665929, 46.04275706135234714 ) ) ;
#127842 = CARTESIAN_POINT ( 'NONE',  ( 16.55341960407618274, -4.379528057220086978, 46.04275706135234714 ) ) ;
#127843 = CARTESIAN_POINT ( 'NONE',  ( 5.719274019375991003, -21.55341960407610458, 27.70724293864769905 ) ) ;
#127844 = CARTESIAN_POINT ( 'NONE',  ( 19.03943276465977164, -0.05219959533909143690, 48.74890960531435979 ) ) ;
#127845 = CARTESIAN_POINT ( 'NONE',  ( 19.03943276465977164, -0.05219959533909143690, 63.74890960531435979 ) ) ;
#127846 = CIRCLE ( 'NONE', #31031, 4.999999999999999112 ) ;
#127847 = CARTESIAN_POINT ( 'NONE',  ( 14.34966873604972726, -8.224510206698740333, 55.83442372801901854 ) ) ;
#127848 = CARTESIAN_POINT ( 'NONE',  ( -14.34966873604960291, -8.224510206698953496, 106.6655762719810383 ) ) ;
#127849 = CARTESIAN_POINT ( 'NONE',  ( 0.05219959533910956823, 16.53943276465976808, 24.99890960531435624 ) ) ;
#127850 = CYLINDRICAL_SURFACE ( 'NONE', #5499, 24.30000000000003268 ) ;
#127853 = CARTESIAN_POINT ( 'NONE',  ( -9.564922557960796823, -16.46253265017161027, 77.08224293864769550 ) ) ;
#127852 = CARTESIAN_POINT ( 'NONE',  ( -5.153800228976328057, -19.02544592524343514, 97.29057627198099567 ) ) ;
#127851 = CARTESIAN_POINT ( 'NONE',  ( -10.81492255796105439, 18.62759615963255655, 62.91775706135236135 ) ) ;
#127855 = EDGE_CURVE ( 'NONE', #189743, #20330, #32031, .T. ) ;
#127854 = CARTESIAN_POINT ( 'NONE',  ( 5.049401038298161559, -19.05341960407611168, 97.70724293864766707 ) ) ;
#127856 = CARTESIAN_POINT ( 'NONE',  ( 16.55341960407611168, 4.379528057220329451, 43.95724293864769550 ) ) ;
#127857 = CARTESIAN_POINT ( 'NONE',  ( -4.483927247898782831, 16.52544592524335698, 107.7094237280190328 ) ) ;
#127858 = CARTESIAN_POINT ( 'NONE',  ( -8.224510206698948167, 14.34966873604960824, 40.41557627198103120 ) ) ;
#127859 = LINE ( 'NONE', #189563, #190087 ) ;
#127860 = CARTESIAN_POINT ( 'NONE',  ( 0.05219959533936267826, -19.03943276465977164, 40.00109039468566152 ) ) ;
#127861 = CARTESIAN_POINT ( 'NONE',  ( 19.02544592524343514, -5.153800228976328945, 78.54057627198099567 ) ) ;
#127862 = CARTESIAN_POINT ( 'NONE',  ( 9.564922557961047289, -16.46253265017146816, 55.41775706135234003 ) ) ;
#127863 = CARTESIAN_POINT ( 'NONE',  ( -22.81625015709510507, 31.40387420917330275, -9.424999997268812990 ) ) ;
#127864 = LINE ( 'NONE', #189568, #160480 ) ;
#127866 = CARTESIAN_POINT ( 'NONE',  ( 14.34966873604972726, -8.224510206698740333, 70.83442372801901854 ) ) ;
#127865 = CARTESIAN_POINT ( 'NONE',  ( -9.474510206698720793, -16.51473224551083518, 79.58442372801899012 ) ) ;
#127867 = CARTESIAN_POINT ( 'NONE',  ( -22.68041372103478182, 7.529096845820648198, 173.5090731399504875 ) ) ;
#127868 = CARTESIAN_POINT ( 'NONE',  ( 13.97604488694527802, 13.89961937509977652, 109.3739096053143669 ) ) ;
#127869 = CARTESIAN_POINT ( 'NONE',  ( 15.72974639402176855, 15.80617190586768217, 26.87609039468567218 ) ) ;
#127870 = CARTESIAN_POINT ( 'NONE',  ( 19.02544592524334988, 5.153800228976608722, 86.45942372801900433 ) ) ;
#127872 = CARTESIAN_POINT ( 'NONE',  ( 5.153800228976335163, 19.02544592524342804, 44.79057627198103830 ) ) ;
#127871 = CARTESIAN_POINT ( 'NONE',  ( 17.26058549869092928, 6.457015423128507514, 88.87745837476070676 ) ) ;
#127873 = CARTESIAN_POINT ( 'NONE',  ( -19.02544592524342804, 5.153800228976336051, 86.04057627198103830 ) ) ;
#127875 = CARTESIAN_POINT ( 'NONE',  ( 13.89961937509977652, -13.97604488694527269, 53.12390960531434558 ) ) ;
#127874 = CARTESIAN_POINT ( 'NONE',  ( 0.05219959533910956823, 16.53943276465976808, 49.99890960531437401 ) ) ;
#127876 = CARTESIAN_POINT ( 'NONE',  ( 19.03943276465977164, 0.05219959533936151252, 61.25109039468566863 ) ) ;
#127877 = CARTESIAN_POINT ( 'NONE',  ( -19.02544592524334988, -5.153800228976617603, 33.95942372801897591 ) ) ;
#127878 = CARTESIAN_POINT ( 'NONE',  ( 19.02544592524343514, -5.153800228976328945, 63.54057627198103830 ) ) ;
#127879 = CARTESIAN_POINT ( 'NONE',  ( 10.81492255796078972, 18.62759615963270932, 59.58224293864770260 ) ) ;
#127881 = CARTESIAN_POINT ( 'NONE',  ( -19.02544592524334988, -5.153800228976617603, 23.95942372801900078 ) ) ;
#127880 = CARTESIAN_POINT ( 'NONE',  ( -12.06949235617756955, 12.14591786802309770, 65.62390960531436690 ) ) ;
#127882 = FACE_OUTER_BOUND ( 'NONE', #146277, .T. ) ;
#127883 = AXIS2_PLACEMENT_3D ( 'NONE', #105526, #185344, #106509 ) ;
#127884 = CARTESIAN_POINT ( 'NONE',  ( -9.474510206698964154, 16.51473224551069663, 115.4155762719810241 ) ) ;
#127885 = CARTESIAN_POINT ( 'NONE',  ( -13.97604488694527625, -13.89961937509977652, 56.87390960531434558 ) ) ;
#127886 = CARTESIAN_POINT ( 'NONE',  ( 13.97604488694527802, 13.89961937509977652, 39.37390960531435269 ) ) ;
#127887 = CARTESIAN_POINT ( 'NONE',  ( 12.14591786802309770, 12.06949235617756955, 99.37390960531436690 ) ) ;
#127888 = CARTESIAN_POINT ( 'NONE',  ( 18.67979575497178502, 10.72451020669898547, 104.1655762719810241 ) ) ;
#127889 = FACE_OUTER_BOUND ( 'NONE', #139183, .T. ) ;
#127890 = CARTESIAN_POINT ( 'NONE',  ( 15.80617190586769283, -15.72974639402175789, 25.62609039468567929 ) ) ;
#127891 = CARTESIAN_POINT ( 'NONE',  ( 0.05219959533909260263, 19.03943276465977164, 104.9989096053143669 ) ) ;
#127892 = CARTESIAN_POINT ( 'NONE',  ( 9.564922557960805705, 16.46253265017160317, 24.58224293864769194 ) ) ;
#127893 = CARTESIAN_POINT ( 'NONE',  ( -5.719274019375665041, -21.55341960407619695, 79.79275706135236135 ) ) ;
#127894 = CARTESIAN_POINT ( 'NONE',  ( 10.72451020669898902, -18.67979575497178502, 97.91557627198103830 ) ) ;
#127895 = CARTESIAN_POINT ( 'NONE',  ( -13.97604488694547697, 13.89961937509957934, 33.12609039468566863 ) ) ;
#127896 = CARTESIAN_POINT ( 'NONE',  ( -30.00000000000000000, -40.00099999999999767, 37.49999999999999289 ) ) ;
#127897 = CARTESIAN_POINT ( 'NONE',  ( 17.58332526062529411, -7.635886036038503910, 53.42334959558467489 ) ) ;
#127898 = CARTESIAN_POINT ( 'NONE',  ( 31.90000000000004476, -0.1282610754044114509, -49.13275782002542513 ) ) ;
#127899 = CARTESIAN_POINT ( 'NONE',  ( 8.224510206698742110, 14.34966873604972548, 47.08442372801901854 ) ) ;
#127900 = CARTESIAN_POINT ( 'NONE',  ( -4.483927247898539470, -16.52544592524342804, 102.2905762719810383 ) ) ;
#127901 = CARTESIAN_POINT ( 'NONE',  ( 33.70211957050086937, -4.378872343537608458, 98.34732289368842828 ) ) ;
#127902 = CARTESIAN_POINT ( 'NONE',  ( 16.51473224551069308, 9.474510206698969483, 64.16557627198102409 ) ) ;
#127903 = CARTESIAN_POINT ( 'NONE',  ( -4.379528057220328563, 16.55341960407611168, 95.20724293864769550 ) ) ;
#127904 = CARTESIAN_POINT ( 'NONE',  ( -15.72974639402197994, 15.80617190586746368, 50.62390960531435979 ) ) ;
#127905 = CARTESIAN_POINT ( 'NONE',  ( 14.34966873604960469, 8.224510206698951720, 64.16557627198102409 ) ) ;
#127906 = CARTESIAN_POINT ( 'NONE',  ( 16.53943276465976808, 0.05219959533934440121, 36.25109039468567573 ) ) ;
#127907 = CARTESIAN_POINT ( 'NONE',  ( -0.05219959533937732626, 21.53943276465977519, 82.50109039468568994 ) ) ;
#127908 = CARTESIAN_POINT ( 'NONE',  ( 17.49999999999998934, -5.500000000000023981, 78.29690382534170112 ) ) ;
#127909 = CARTESIAN_POINT ( 'NONE',  ( -12.06949235617739369, -12.14591786802326823, 99.37609039468568994 ) ) ;
#127910 = CARTESIAN_POINT ( 'NONE',  ( -4.483927247898539470, -16.52544592524342804, 47.29057627198103120 ) ) ;
#127911 = CARTESIAN_POINT ( 'NONE',  ( 19.05341960407611168, 5.049401038298154454, 38.95724293864767418 ) ) ;
#127912 = CARTESIAN_POINT ( 'NONE',  ( -13.89961937509977652, 13.97604488694528158, 95.62390960531436690 ) ) ;
#127913 = CARTESIAN_POINT ( 'NONE',  ( -18.62759615963270932, 10.81492255796079327, 110.8322429386476955 ) ) ;
#127914 = CARTESIAN_POINT ( 'NONE',  ( -5.719274019375665041, -21.55341960407619695, 54.79275706135235424 ) ) ;
#127915 = CARTESIAN_POINT ( 'NONE',  ( 8.224510206698742110, 14.34966873604972548, 37.08442372801901143 ) ) ;
#127917 = CARTESIAN_POINT ( 'NONE',  ( 10.72451020669871369, 18.67979575497193778, 82.08442372801901854 ) ) ;
#127916 = CARTESIAN_POINT ( 'NONE',  ( 16.52544592524342804, -4.483927247898539470, 58.54057627198103120 ) ) ;
#127918 = CARTESIAN_POINT ( 'NONE',  ( 16.55341960407618274, -4.379528057220086978, 96.04275706135236135 ) ) ;
#127919 = CARTESIAN_POINT ( 'NONE',  ( 16.79531203550650176, 7.028104445595485750, 28.75244988220443076 ) ) ;
#127920 = FACE_OUTER_BOUND ( 'NONE', #180525, .T. ) ;
#127921 = CARTESIAN_POINT ( 'NONE',  ( -12.06949235617756955, 12.14591786802309770, 30.62390960531436335 ) ) ;
#127922 = CARTESIAN_POINT ( 'NONE',  ( -16.53943276465976808, -0.05219959533934237506, 78.75109039468568994 ) ) ;
#127923 = CARTESIAN_POINT ( 'NONE',  ( -19.02544592524342804, 5.153800228976336051, 86.04057627198103830 ) ) ;
#127924 = CARTESIAN_POINT ( 'NONE',  ( 16.51473224551069308, 9.474510206698969483, 99.16557627198102409 ) ) ;
#127925 = CARTESIAN_POINT ( 'NONE',  ( -15.72974639402176322, -15.80617190586768395, 79.37609039468567573 ) ) ;
#127926 = CARTESIAN_POINT ( 'NONE',  ( 8.314922557961029526, -14.29746914071037800, 95.41775706135234714 ) ) ;
#127927 = CARTESIAN_POINT ( 'NONE',  ( 8.224510206698953496, -14.34966873604960469, 57.91557627198103120 ) ) ;
#127928 = CARTESIAN_POINT ( 'NONE',  ( 16.51473224551069308, 9.474510206698969483, 74.16557627198103830 ) ) ;
#127929 = EDGE_LOOP ( 'NONE', ( #195441, #167384, #122363, #184811, #188282, #89538, #170664, #136840, #196358, #128609, #188832, #71897 ) ) ;
#127930 = CARTESIAN_POINT ( 'NONE',  ( 12.06949235617739724, 12.14591786802326823, 21.87609039468567573 ) ) ;
#127931 = CARTESIAN_POINT ( 'NONE',  ( 13.97604488694527802, 13.89961937509977652, 29.37390960531435979 ) ) ;
#127932 = CARTESIAN_POINT ( 'NONE',  ( 9.474510206698971260, -16.51473224551069308, 72.91557627198102409 ) ) ;
#127934 = CARTESIAN_POINT ( 'NONE',  ( -11.74264578624800670, 36.14014761921585972, -0.3999999999999999112 ) ) ;
#127933 = CARTESIAN_POINT ( 'NONE',  ( 5.049401038297881783, 19.05341960407617563, 112.2927570613523471 ) ) ;
#127935 = CARTESIAN_POINT ( 'NONE',  ( -16.51473224551082808, 9.474510206698731452, 23.33442372801900078 ) ) ;
#127936 = CARTESIAN_POINT ( 'NONE',  ( -16.53943276465976808, -0.05219959533934237506, 78.75109039468568994 ) ) ;
#127937 = CARTESIAN_POINT ( 'NONE',  ( 9.564922557961047289, -16.46253265017146816, 110.4177570613523471 ) ) ;
#127938 = CARTESIAN_POINT ( 'NONE',  ( 9.474510206698971260, -16.51473224551069308, 22.91557627198102765 ) ) ;
#127939 = CARTESIAN_POINT ( 'NONE',  ( 0.05219959533934541429, -16.53943276465976808, 70.00109039468568994 ) ) ;
#127940 = CARTESIAN_POINT ( 'NONE',  ( -14.34966873604972548, 8.224510206698743886, 53.33442372801901854 ) ) ;
#127941 = CARTESIAN_POINT ( 'NONE',  ( 16.46253265017160672, -9.564922557960803928, 23.33224293864769194 ) ) ;
#127942 = CARTESIAN_POINT ( 'NONE',  ( -13.97604488694547697, 13.89961937509957934, 73.12609039468568994 ) ) ;
#127943 = CARTESIAN_POINT ( 'NONE',  ( 5.719274019375673035, 21.55341960407619339, 107.2927570613523471 ) ) ;
#127944 = CARTESIAN_POINT ( 'NONE',  ( 5.153800228976335163, 19.02544592524342804, 39.79057627198100988 ) ) ;
#127945 = CARTESIAN_POINT ( 'NONE',  ( -13.97604488694527625, -13.89961937509977652, 81.87390960531436690 ) ) ;
#127946 = CARTESIAN_POINT ( 'NONE',  ( -4.483927247898539470, -16.52544592524342804, 72.29057627198102409 ) ) ;
#127947 = CARTESIAN_POINT ( 'NONE',  ( -19.05341960407617563, 5.049401038297882671, 38.54275706135233293 ) ) ;
#127948 = CARTESIAN_POINT ( 'NONE',  ( -18.62759615963270932, 10.81492255796079327, 40.83224293864769550 ) ) ;
#127949 = CARTESIAN_POINT ( 'NONE',  ( 5.719274019375673035, 21.55341960407619339, 112.2927570613523471 ) ) ;
#127950 = CARTESIAN_POINT ( 'NONE',  ( 19.03943276465977164, -0.05219959533909143690, 88.74890960531436690 ) ) ;
#127951 = CARTESIAN_POINT ( 'NONE',  ( 5.719274019375673035, 21.55341960407619339, 102.2927570613523613 ) ) ;
#127952 = CARTESIAN_POINT ( 'NONE',  ( 5.719274019375991003, -21.55341960407610458, 57.70724293864770260 ) ) ;
#127953 = CARTESIAN_POINT ( 'NONE',  ( 16.46253265017160672, -9.564922557960803928, 93.33224293864769550 ) ) ;
#127954 = CARTESIAN_POINT ( 'NONE',  ( -16.51473224551082808, 9.474510206698731452, 88.33442372801900433 ) ) ;
#127955 = CARTESIAN_POINT ( 'NONE',  ( -13.89961937509977652, 13.97604488694528158, 100.6239096053143669 ) ) ;
#127956 = ADVANCED_FACE ( 'NONE', ( #102578 ), #191579, .T. ) ;
#127957 = CARTESIAN_POINT ( 'NONE',  ( 19.03943276465977164, 0.05219959533936151252, 96.25109039468567573 ) ) ;
#127958 = CARTESIAN_POINT ( 'NONE',  ( 13.97604488694527802, 13.89961937509977652, 24.37390960531435624 ) ) ;
#127959 = CARTESIAN_POINT ( 'NONE',  ( -0.05219959533909027116, -19.03943276465977164, 82.49890960531436690 ) ) ;
#127960 = CARTESIAN_POINT ( 'NONE',  ( 21.55341960407610458, 5.719274019375980345, 68.95724293864769550 ) ) ;
#127961 = CARTESIAN_POINT ( 'NONE',  ( 12.14591786802327356, -12.06949235617739191, 30.62609039468567929 ) ) ;
#127962 = CARTESIAN_POINT ( 'NONE',  ( -10.72451020669870658, -18.67979575497194134, 44.58442372801901854 ) ) ;
#127963 = CARTESIAN_POINT ( 'NONE',  ( -18.67979575497193778, 10.72451020669871902, 93.33442372801901854 ) ) ;
#127964 = CARTESIAN_POINT ( 'NONE',  ( -4.379528057220086978, -16.55341960407618274, 94.79275706135234714 ) ) ;
#127965 = CARTESIAN_POINT ( 'NONE',  ( 16.46253265017160672, -9.564922557960803928, 88.33224293864769550 ) ) ;
#127966 = CARTESIAN_POINT ( 'NONE',  ( -14.29746914071049879, 8.314922557960819915, 90.83224293864769550 ) ) ;
#127967 = CARTESIAN_POINT ( 'NONE',  ( 8.224510206698742110, 14.34966873604972548, 112.0844237280190185 ) ) ;
#127968 = CARTESIAN_POINT ( 'NONE',  ( -9.564922557961040184, 16.46253265017147172, 62.91775706135233293 ) ) ;
#127969 = CARTESIAN_POINT ( 'NONE',  ( 0.05219959533937995610, -21.53943276465977519, 50.00109039468568994 ) ) ;
#127970 = EDGE_CURVE ( 'NONE', #76158, #182346, #38625, .T. ) ;
#127971 = CARTESIAN_POINT ( 'NONE',  ( 16.55341960407611168, 4.379528057220329451, 93.95724293864770971 ) ) ;
#127972 = CARTESIAN_POINT ( 'NONE',  ( -16.51473224551069308, -9.474510206698971260, 106.6655762719810383 ) ) ;
#127973 = CARTESIAN_POINT ( 'NONE',  ( -16.53943276465976808, 0.05219959533911058130, 26.24890960531435624 ) ) ;
#127974 = CARTESIAN_POINT ( 'NONE',  ( 21.55341960407619695, -5.719274019375665929, 91.04275706135236135 ) ) ;
#127975 = CARTESIAN_POINT ( 'NONE',  ( -16.55341960407617563, 4.379528057220093196, 38.54275706135234714 ) ) ;
#127976 = CARTESIAN_POINT ( 'NONE',  ( -5.823673210054431948, 21.52544592524334988, 42.70942372801901854 ) ) ;
#127977 = ORIENTED_EDGE ( 'NONE', *, *, #82288, .F. ) ;
#127978 = CARTESIAN_POINT ( 'NONE',  ( -18.62759615963255300, -10.81492255796106328, 19.16775706135234714 ) ) ;
#127979 = CARTESIAN_POINT ( 'NONE',  ( -12.14591786802309592, -12.06949235617757132, 91.87390960531436690 ) ) ;
#127980 = CARTESIAN_POINT ( 'NONE',  ( -5.153800228976328057, -19.02544592524343514, 27.29057627198103120 ) ) ;
#127981 = CARTESIAN_POINT ( 'NONE',  ( 4.379528057220339221, -16.55341960407611168, 67.70724293864769550 ) ) ;
#127982 = CARTESIAN_POINT ( 'NONE',  ( -19.03943276465977164, 0.05219959533909376836, 61.24890960531436690 ) ) ;
#127983 = CARTESIAN_POINT ( 'NONE',  ( -16.53943276465976808, -0.05219959533934237506, 103.7510903946857042 ) ) ;
#127984 = CARTESIAN_POINT ( 'NONE',  ( 5.153800228976335163, 19.02544592524342804, 44.79057627198103830 ) ) ;
#127985 = CARTESIAN_POINT ( 'NONE',  ( -21.53943276465977519, 0.05219959533907696930, 46.24890960531435979 ) ) ;
#127986 = CARTESIAN_POINT ( 'NONE',  ( -16.55341960407611168, -4.379528057220339221, 81.45724293864769550 ) ) ;
#127987 = AXIS2_PLACEMENT_3D ( 'NONE', #57691, #166858, #136498 ) ;
#127988 = CARTESIAN_POINT ( 'NONE',  ( -21.53943276465977519, 0.05219959533907696930, 96.24890960531435269 ) ) ;
#127989 = CARTESIAN_POINT ( 'NONE',  ( 16.46253265017160672, -9.564922557960803928, 93.33224293864769550 ) ) ;
#127991 = CARTESIAN_POINT ( 'NONE',  ( -16.51473224551082808, 9.474510206698731452, 93.33442372801900433 ) ) ;
#127990 = CARTESIAN_POINT ( 'NONE',  ( -16.46253265017160317, 9.564922557960807481, 40.83224293864769550 ) ) ;
#127992 = CARTESIAN_POINT ( 'NONE',  ( 21.53943276465977519, -0.05219959533907433946, 43.74890960531435979 ) ) ;
#127993 = CARTESIAN_POINT ( 'NONE',  ( 15.72974639402176855, 15.80617190586768217, 71.87609039468568994 ) ) ;
#127994 = CARTESIAN_POINT ( 'NONE',  ( 16.46253265017160672, -9.564922557960803928, 58.33224293864769550 ) ) ;
#127995 = CARTESIAN_POINT ( 'NONE',  ( -19.03943276465977164, 0.05219959533909376836, 81.24890960531436690 ) ) ;
#127996 = ORIENTED_EDGE ( 'NONE', *, *, #35339, .F. ) ;
#127997 = CARTESIAN_POINT ( 'NONE',  ( -12.06949235617739369, -12.14591786802326823, 59.37609039468568284 ) ) ;
#127998 = CARTESIAN_POINT ( 'NONE',  ( 10.81492255796106328, -18.62759615963255655, 50.41775706135235424 ) ) ;
#127999 = EDGE_CURVE ( 'NONE', #116009, #193478, #163252, .T. ) ;
#128000 = CARTESIAN_POINT ( 'NONE',  ( 5.719274019375673035, 21.55341960407619339, 67.29275706135234714 ) ) ;
#128001 = CARTESIAN_POINT ( 'NONE',  ( 15.72974639402199770, -15.80617190586745480, 23.12390960531436335 ) ) ;
#128002 = CARTESIAN_POINT ( 'NONE',  ( -10.72451020669898014, 18.67979575497178502, 105.4155762719810383 ) ) ;
#128004 = CARTESIAN_POINT ( 'NONE',  ( -8.314922557961024197, 14.29746914071037800, 62.91775706135236135 ) ) ;
#128003 = CARTESIAN_POINT ( 'NONE',  ( 18.62759615963255655, 10.81492255796105972, 31.66775706135234358 ) ) ;
#128005 = CARTESIAN_POINT ( 'NONE',  ( -18.67979575497178146, -10.72451020669898902, 66.66557627198102409 ) ) ;
#128006 = CARTESIAN_POINT ( 'NONE',  ( 19.02544592524334988, 5.153800228976608722, 36.45942372801900433 ) ) ;
#128008 = CARTESIAN_POINT ( 'NONE',  ( -8.314922557961024197, 14.29746914071037800, 107.9177570613523471 ) ) ;
#128007 = CARTESIAN_POINT ( 'NONE',  ( 5.049401038298161559, -19.05341960407611168, 72.70724293864768129 ) ) ;
#128009 = CARTESIAN_POINT ( 'NONE',  ( -30.00000000000000000, -5.510910596163089556E-15, 47.64999999999999147 ) ) ;
#128010 = CARTESIAN_POINT ( 'NONE',  ( 0.05219959533909260263, 19.03943276465977164, 99.99890960531436690 ) ) ;
#128011 = CARTESIAN_POINT ( 'NONE',  ( 21.81714873624722628, 22.96531869715549234, -45.99103957044146540 ) ) ;
#128012 = CARTESIAN_POINT ( 'NONE',  ( 13.97604488694548053, -13.89961937509957401, 85.62609039468568994 ) ) ;
#128013 = CARTESIAN_POINT ( 'NONE',  ( -18.67979575497178146, -10.72451020669898902, 61.66557627198103120 ) ) ;
#128014 = CARTESIAN_POINT ( 'NONE',  ( -12.06949235617756955, 12.14591786802309770, 35.62390960531437401 ) ) ;
#128015 = CARTESIAN_POINT ( 'NONE',  ( -16.51473224551082808, 9.474510206698731452, 93.33442372801900433 ) ) ;
#128016 = CARTESIAN_POINT ( 'NONE',  ( -3.573655867282028392E-15, 2.428612866367529932E-14, -25.00000000000000000 ) ) ;
#128017 = CARTESIAN_POINT ( 'NONE',  ( -19.05341960407617563, 5.049401038297882671, 98.54275706135233293 ) ) ;
#128019 = CARTESIAN_POINT ( 'NONE',  ( -5.153800228976607833, 19.02544592524334988, 52.70942372801900433 ) ) ;
#128018 = CARTESIAN_POINT ( 'NONE',  ( -18.67979575497178146, -10.72451020669898902, 81.66557627198103830 ) ) ;
#128020 = CARTESIAN_POINT ( 'NONE',  ( -30.00000000000000000, -5.510910596163089556E-15, 37.50000000000000000 ) ) ;
#128021 = CARTESIAN_POINT ( 'NONE',  ( -0.05219959533909027116, -19.03943276465977164, 67.49890960531436690 ) ) ;
#128022 = CARTESIAN_POINT ( 'NONE',  ( -8.314922557960811034, -14.29746914071050412, 62.08224293864769550 ) ) ;
#128023 = CARTESIAN_POINT ( 'NONE',  ( -19.03943276465977164, 0.05219959533909376836, 46.24890960531435979 ) ) ;
#128024 = CARTESIAN_POINT ( 'NONE',  ( -4.379528057220328563, 16.55341960407611168, 55.20724293864770260 ) ) ;
#128025 = LINE ( 'NONE', #186758, #67759 ) ;
#128026 = CARTESIAN_POINT ( 'NONE',  ( 32.42844225013696757, -3.321486864536503880, 88.27111922316778703 ) ) ;
#128027 = CARTESIAN_POINT ( 'NONE',  ( 16.52544592524342804, -4.483927247898539470, 33.54057627198102409 ) ) ;
#128028 = CARTESIAN_POINT ( 'NONE',  ( -9.564922557960796823, -16.46253265017161027, 62.08224293864769550 ) ) ;
#128029 = DIRECTION ( 'NONE',  ( 1.000000000000000000, -0.000000000000000000, -0.000000000000000000 ) ) ;
#128030 = CARTESIAN_POINT ( 'NONE',  ( -19.05341960407617563, 5.049401038297882671, 38.54275706135233293 ) ) ;
#128031 = CARTESIAN_POINT ( 'NONE',  ( -16.53943276465976808, -0.05219959533934237506, 48.75109039468568284 ) ) ;
#128032 = CARTESIAN_POINT ( 'NONE',  ( -15.72974639402197994, 15.80617190586746368, 45.62390960531436690 ) ) ;
#128033 = CARTESIAN_POINT ( 'NONE',  ( 21.55341960407619695, -5.719274019375665929, 101.0427570613523756 ) ) ;
#128034 = CARTESIAN_POINT ( 'NONE',  ( -5.153800228976328057, -19.02544592524343514, 77.29057627198099567 ) ) ;
#128035 = DIRECTION ( 'NONE',  ( 1.000000000000000000, 0.000000000000000000, 0.000000000000000000 ) ) ;
#128036 = CARTESIAN_POINT ( 'NONE',  ( 16.46253265017160672, -9.564922557960803928, 113.3322429386476955 ) ) ;
#128037 = CARTESIAN_POINT ( 'NONE',  ( 5.823673210054444382, -21.52544592524334988, 45.20942372801901854 ) ) ;
#128038 = AXIS2_PLACEMENT_3D ( 'NONE', #122613, #91257, #198479 ) ;
#128039 = CARTESIAN_POINT ( 'NONE',  ( -12.06949235617756955, 12.14591786802309770, 95.62390960531436690 ) ) ;
#128042 = ORIENTED_EDGE ( 'NONE', *, *, #150161, .F. ) ;
#128041 = CARTESIAN_POINT ( 'NONE',  ( 19.02544592524343514, -5.153800228976328945, 83.54057627198100988 ) ) ;
#128040 = CARTESIAN_POINT ( 'NONE',  ( -10.81492255796078084, -18.62759615963271287, 92.08224293864769550 ) ) ;
#128043 = CARTESIAN_POINT ( 'NONE',  ( 19.02544592524343514, -5.153800228976328945, 88.54057627198102409 ) ) ;
#128044 = CARTESIAN_POINT ( 'NONE',  ( 21.53943276465977519, 0.05219959533937863772, 31.25109039468568639 ) ) ;
#128045 = VERTEX_POINT ( 'NONE', #178429 ) ;
#128046 = CARTESIAN_POINT ( 'NONE',  ( 5.049401038298161559, -19.05341960407611168, 82.70724293864770971 ) ) ;
#128047 = CARTESIAN_POINT ( 'NONE',  ( 18.39635199886970796, -5.499999999999976019, 83.51967076360001840 ) ) ;
#128049 = CARTESIAN_POINT ( 'NONE',  ( 9.474510206698971260, -16.51473224551069308, 32.91557627198102409 ) ) ;
#128048 = CARTESIAN_POINT ( 'NONE',  ( 12.14591786802309770, 12.06949235617756955, 114.3739096053143527 ) ) ;
#128050 = CARTESIAN_POINT ( 'NONE',  ( 13.97604488694548053, -13.89961937509957401, 110.6260903946856615 ) ) ;
#128051 = CARTESIAN_POINT ( 'NONE',  ( 29.86685920354754487, 21.69954338932564752, -9.924999997268812990 ) ) ;
#128052 = CARTESIAN_POINT ( 'NONE',  ( -16.52544592524342804, 4.483927247898546575, 106.0405762719810525 ) ) ;
#128053 = CARTESIAN_POINT ( 'NONE',  ( 15.80617190586769283, -15.72974639402175789, 90.62609039468567573 ) ) ;
#128055 = CARTESIAN_POINT ( 'NONE',  ( 0.05219959533937995610, -21.53943276465977519, 30.00109039468568284 ) ) ;
#128054 = CARTESIAN_POINT ( 'NONE',  ( 13.89961937509977652, -13.97604488694527269, 68.12390960531436690 ) ) ;
#128056 = CARTESIAN_POINT ( 'NONE',  ( 10.81492255796078972, 18.62759615963270932, 109.5822429386476955 ) ) ;
#128057 = CARTESIAN_POINT ( 'NONE',  ( 23.31738231874054890, -16.94106989632523508, 148.7999999999999829 ) ) ;
#128058 = CARTESIAN_POINT ( 'NONE',  ( 19.05341960407611168, 5.049401038298154454, 88.95724293864769550 ) ) ;
#128059 = CARTESIAN_POINT ( 'NONE',  ( 27.88129983271499768, 6.733757357597986548, 162.1517353552272880 ) ) ;
#128061 = CARTESIAN_POINT ( 'NONE',  ( -15.80617190586745835, -15.72974639402198527, 41.87390960531435979 ) ) ;
#128060 = CARTESIAN_POINT ( 'NONE',  ( 16.52544592524335698, 4.483927247898782831, 21.45942372801901499 ) ) ;
#128062 = CARTESIAN_POINT ( 'NONE',  ( -15.72974639402176322, -15.80617190586768395, 69.37609039468567573 ) ) ;
#128063 = CARTESIAN_POINT ( 'NONE',  ( 16.46253265017160672, -9.564922557960803928, 108.3322429386476955 ) ) ;
#128064 = CARTESIAN_POINT ( 'NONE',  ( -19.02544592524334988, -5.153800228976617603, 93.95942372801900433 ) ) ;
#128065 = CARTESIAN_POINT ( 'NONE',  ( -13.89961937509977652, 13.97604488694528158, 60.62390960531436690 ) ) ;
#128066 = CARTESIAN_POINT ( 'NONE',  ( -9.564922557960796823, -16.46253265017161027, 82.08224293864768129 ) ) ;
#128067 = CARTESIAN_POINT ( 'NONE',  ( 4.483927247898545687, 16.52544592524342804, 89.79057627198103830 ) ) ;
#128068 = CARTESIAN_POINT ( 'NONE',  ( -8.224510206698948167, 14.34966873604960824, 100.4155762719810241 ) ) ;
#128069 = CARTESIAN_POINT ( 'NONE',  ( -13.89961937509977652, 13.97604488694528158, 115.6239096053143669 ) ) ;
#128071 = CARTESIAN_POINT ( 'NONE',  ( 5.153800228976335163, 19.02544592524342804, 34.79057627198102409 ) ) ;
#128070 = CARTESIAN_POINT ( 'NONE',  ( -16.53943276465976808, 0.05219959533911058130, 51.24890960531436690 ) ) ;
#128072 = CARTESIAN_POINT ( 'NONE',  ( -5.823673210054431948, 21.52544592524334988, 67.70942372801901854 ) ) ;
#128073 = CARTESIAN_POINT ( 'NONE',  ( 19.05341960407617918, -5.049401038297876454, 91.04275706135234714 ) ) ;
#128074 = CARTESIAN_POINT ( 'NONE',  ( 4.379528057220339221, -16.55341960407611168, 57.70724293864770260 ) ) ;
#128075 = CARTESIAN_POINT ( 'NONE',  ( 18.67979575497178502, 10.72451020669898547, 114.1655762719810383 ) ) ;
#128076 = CARTESIAN_POINT ( 'NONE',  ( -10.72451020669898014, 18.67979575497178502, 45.41557627198103830 ) ) ;
#128077 = CARTESIAN_POINT ( 'NONE',  ( 19.02544592524343514, -5.153800228976328945, 108.5405762719810383 ) ) ;
#128078 = CARTESIAN_POINT ( 'NONE',  ( 28.82186960331498327, 2.781578969918950771E-14, 143.2500000054623683 ) ) ;
#128079 = CARTESIAN_POINT ( 'NONE',  ( -13.89961937509977652, 13.97604488694528158, 65.62390960531436690 ) ) ;
#128080 = CARTESIAN_POINT ( 'NONE',  ( -16.52544592524342804, 4.483927247898546575, 36.04057627198102409 ) ) ;
#128081 = CARTESIAN_POINT ( 'NONE',  ( -16.53943276465976808, -0.05219959533934237506, 103.7510903946857042 ) ) ;
#128082 = CARTESIAN_POINT ( 'NONE',  ( -16.52544592524335698, -4.483927247898792601, 88.95942372801901854 ) ) ;
#128083 = CARTESIAN_POINT ( 'NONE',  ( 19.05341960407617918, -5.049401038297876454, 41.04275706135233293 ) ) ;
#128084 = CARTESIAN_POINT ( 'NONE',  ( -24.81835880841865816, 6.052260367207988878, 168.4265213779230521 ) ) ;
#128085 = CARTESIAN_POINT ( 'NONE',  ( 16.51473224551069308, 9.474510206698969483, 89.16557627198103830 ) ) ;
#128086 = CARTESIAN_POINT ( 'NONE',  ( 5.153800228976335163, 19.02544592524342804, 49.79057627198100988 ) ) ;
#128087 = CARTESIAN_POINT ( 'NONE',  ( -16.55341960407611168, -4.379528057220339221, 61.45724293864770260 ) ) ;
#128089 = CARTESIAN_POINT ( 'NONE',  ( 9.564922557960805705, 16.46253265017160317, 114.5822429386476955 ) ) ;
#128088 = CARTESIAN_POINT ( 'NONE',  ( 16.79531203550646268, -7.028104445595594107, 101.2475501177955977 ) ) ;
#128090 = CARTESIAN_POINT ( 'NONE',  ( 15.80617190586746368, 15.72974639402197994, 59.37390960531436690 ) ) ;
#128091 = CARTESIAN_POINT ( 'NONE',  ( 4.379528057220339221, -16.55341960407611168, 82.70724293864770971 ) ) ;
#128092 = CARTESIAN_POINT ( 'NONE',  ( 4.379528057220092307, 16.55341960407617563, 42.29275706135235424 ) ) ;
#128093 = CARTESIAN_POINT ( 'NONE',  ( -16.53943276465976808, 0.05219959533911058130, 76.24890960531435269 ) ) ;
#128094 = CARTESIAN_POINT ( 'NONE',  ( -19.26498983726237313, 5.499999999999599432, 65.55319577422002908 ) ) ;
#128095 = CARTESIAN_POINT ( 'NONE',  ( -19.03943276465977164, -0.05219959533935918106, 73.75109039468566152 ) ) ;
#128096 = CARTESIAN_POINT ( 'NONE',  ( 5.823673210054125526, 21.52544592524343514, 24.79057627198103120 ) ) ;
#128097 = CARTESIAN_POINT ( 'NONE',  ( -36.91746825000001309, 11.99521256947798342, -3.224999997268813257 ) ) ;
#128098 = CARTESIAN_POINT ( 'NONE',  ( 19.48255537605750831, 5.500000000000000888, 102.3528781528247293 ) ) ;
#128100 = CARTESIAN_POINT ( 'NONE',  ( 4.483927247898790824, -16.52544592524335698, 105.2094237280190328 ) ) ;
#128099 = CARTESIAN_POINT ( 'NONE',  ( -8.224510206698735004, -14.34966873604973081, 24.58442372801901499 ) ) ;
#128101 = CARTESIAN_POINT ( 'NONE',  ( 13.89961937509957401, 13.97604488694547697, 76.87609039468566152 ) ) ;
#128102 = CARTESIAN_POINT ( 'NONE',  ( -5.719274019375978568, 21.55341960407610458, 45.20724293864769550 ) ) ;
#128103 = CARTESIAN_POINT ( 'NONE',  ( -10.81492255796105439, 18.62759615963255655, 67.91775706135234714 ) ) ;
#128104 = CARTESIAN_POINT ( 'NONE',  ( 17.81289503416611453, -24.51734667627695785, 146.9500000054623854 ) ) ;
#128105 = CARTESIAN_POINT ( 'NONE',  ( -16.52544592524335698, -4.483927247898792601, 33.95942372801901143 ) ) ;
#128107 = CARTESIAN_POINT ( 'NONE',  ( 5.049401038298161559, -19.05341960407611168, 87.70724293864769550 ) ) ;
#128106 = CARTESIAN_POINT ( 'NONE',  ( 16.51473224551069308, 9.474510206698969483, 29.16557627198103475 ) ) ;
#128108 = CARTESIAN_POINT ( 'NONE',  ( -19.03943276465977164, 0.05219959533909376836, 21.24890960531436335 ) ) ;
#128109 = CARTESIAN_POINT ( 'NONE',  ( 4.379528057220339221, -16.55341960407611168, 87.70724293864769550 ) ) ;
#128110 = PRODUCT_CONTEXT ( 'NONE', #175865, 'mechanical' ) ;
#128111 = CARTESIAN_POINT ( 'NONE',  ( -9.564922557960796823, -16.46253265017161027, 97.08224293864769550 ) ) ;
#128112 = VERTEX_POINT ( 'NONE', #130901 ) ;
#128113 = CARTESIAN_POINT ( 'NONE',  ( 5.153800228976615827, -19.02544592524334988, 110.2094237280189901 ) ) ;
#128114 = B_SPLINE_CURVE_WITH_KNOTS ( 'NONE', 3,
 ( #84350, #146028, #44598, #162205, #7511, #69195, #23703, #85351, #147044, #8528, #55030, #116700, #178390, #39854, #101520, #163210, #27464, #89106, #150796, #89960 ),
 .UNSPECIFIED., .F., .F.,
 ( 4, 2, 2, 2, 2, 2, 2, 2, 2, 4 ),
 ( 0.004000878361812037175, 0.004499404418916065282, 0.004997930476020092522, 0.005496456533124120629, 0.005994982590228148736, 0.006244245618780140672, 0.006493508647332134343, 0.006992034704436119949, 0.007490560761540107290, 0.007989086818644092897 ),
 .UNSPECIFIED. ) ;
#128115 = CARTESIAN_POINT ( 'NONE',  ( 5.823673210054125526, 21.52544592524343514, 74.79057627198105251 ) ) ;
#128116 = CARTESIAN_POINT ( 'NONE',  ( -9.474510206698964154, 16.51473224551069663, 40.41557627198103120 ) ) ;
#128118 = CARTESIAN_POINT ( 'NONE',  ( 21.55341960407619695, -5.719274019375665929, 21.04275706135234714 ) ) ;
#128117 = CARTESIAN_POINT ( 'NONE',  ( 5.153800228976615827, -19.02544592524334988, 65.20942372801900433 ) ) ;
#128119 = CARTESIAN_POINT ( 'NONE',  ( -19.05341960407611168, -5.049401038298163336, 66.45724293864769550 ) ) ;
#128121 = ADVANCED_FACE ( 'NONE', ( #149088 ), #99564, .T. ) ;
#128120 = CARTESIAN_POINT ( 'NONE',  ( 9.564922557960805705, 16.46253265017160317, 109.5822429386476955 ) ) ;
#128122 = EDGE_LOOP ( 'NONE', ( #25131, #138470, #104174, #77367 ) ) ;
#128123 = CARTESIAN_POINT ( 'NONE',  ( -12.14591786802326823, 12.06949235617739902, 38.12609039468567573 ) ) ;
#128124 = CARTESIAN_POINT ( 'NONE',  ( 15.72974639402199770, -15.80617190586745480, 108.1239096053143811 ) ) ;
#128127 = CARTESIAN_POINT ( 'NONE',  ( 5.049401038297881783, 19.05341960407617563, 57.29275706135231871 ) ) ;
#128126 = CARTESIAN_POINT ( 'NONE',  ( -0.05219959533909027116, -19.03943276465977164, 92.49890960531436690 ) ) ;
#128125 = CARTESIAN_POINT ( 'NONE',  ( 12.06949235617757843, -12.14591786802309237, 113.1239096053143953 ) ) ;
#128128 = CARTESIAN_POINT ( 'NONE',  ( -10.72451020669898014, 18.67979575497178502, 85.41557627198102409 ) ) ;
#128129 = CARTESIAN_POINT ( 'NONE',  ( -0.05219959533910754901, -16.53943276465976808, 47.49890960531435979 ) ) ;
#128130 = CARTESIAN_POINT ( 'NONE',  ( 18.62759615963255655, 10.81492255796105972, 111.6677570613523613 ) ) ;
#128131 = CARTESIAN_POINT ( 'NONE',  ( 16.53943276465976808, 0.05219959533934440121, 61.25109039468567573 ) ) ;
#128132 = ADVANCED_FACE ( 'NONE', ( #8570 ), #70245, .F. ) ;
#128133 = CARTESIAN_POINT ( 'NONE',  ( 13.97604488694527802, 13.89961937509977652, 94.37390960531436690 ) ) ;
#128134 = CARTESIAN_POINT ( 'NONE',  ( -9.564922557960796823, -16.46253265017161027, 47.08224293864769550 ) ) ;
#128135 = VECTOR ( 'NONE', #83354, 1000.000000000000000 ) ;
#128136 = CARTESIAN_POINT ( 'NONE',  ( -21.55341960407619339, 5.719274019375674811, 53.54275706135234714 ) ) ;
#128137 = CARTESIAN_POINT ( 'NONE',  ( -18.62759615963255300, -10.81492255796106328, 74.16775706135231871 ) ) ;
#128138 = CARTESIAN_POINT ( 'NONE',  ( 16.46253265017160672, -9.564922557960803928, 63.33224293864769550 ) ) ;
#128139 = CARTESIAN_POINT ( 'NONE',  ( -10.72451020669870658, -18.67979575497194134, 29.58442372801901854 ) ) ;
#128140 = CARTESIAN_POINT ( 'NONE',  ( -19.03943276465977164, -0.05219959533935918106, 68.75109039468566152 ) ) ;
#128141 = CARTESIAN_POINT ( 'NONE',  ( 19.03943276465977164, -0.05219959533909143690, 38.74890960531436690 ) ) ;
#128142 = CARTESIAN_POINT ( 'NONE',  ( -14.34966873604972548, 8.224510206698743886, 83.33442372801903275 ) ) ;
#128143 = CARTESIAN_POINT ( 'NONE',  ( -16.51473224551069308, -9.474510206698971260, 51.66557627198102409 ) ) ;
#128144 = CARTESIAN_POINT ( 'NONE',  ( -19.02544592524342804, 5.153800228976336051, 106.0405762719810241 ) ) ;
#128145 = CARTESIAN_POINT ( 'NONE',  ( 9.474510206698971260, -16.51473224551069308, 37.91557627198102409 ) ) ;
#128146 = CARTESIAN_POINT ( 'NONE',  ( -18.62759615963270932, 10.81492255796079327, 80.83224293864769550 ) ) ;
#128147 = CARTESIAN_POINT ( 'NONE',  ( -12.14591786802326823, 12.06949235617739902, 68.12609039468567573 ) ) ;
#128149 = DIRECTION ( 'NONE',  ( 1.000000000000000000, 0.000000000000000000, 0.000000000000000000 ) ) ;
#128148 = AXIS2_PLACEMENT_3D ( 'NONE', #129240, #82739, #101919 ) ;
#128150 = CARTESIAN_POINT ( 'NONE',  ( 0.05219959533936267826, -19.03943276465977164, 30.00109039468566863 ) ) ;
#128151 = CARTESIAN_POINT ( 'NONE',  ( -0.05219959533909027116, -19.03943276465977164, 52.49890960531436690 ) ) ;
#128152 = CARTESIAN_POINT ( 'NONE',  ( 14.34966873604960469, 8.224510206698951720, 49.16557627198102409 ) ) ;
#128153 = CARTESIAN_POINT ( 'NONE',  ( -14.34966873604960291, -8.224510206698953496, 76.66557627198103830 ) ) ;
#128154 = CARTESIAN_POINT ( 'NONE',  ( 19.02544592524343514, -5.153800228976328945, 98.54057627198100988 ) ) ;
#128155 = CARTESIAN_POINT ( 'NONE',  ( 16.46253265017160672, -9.564922557960803928, 78.33224293864769550 ) ) ;
#128156 = CARTESIAN_POINT ( 'NONE',  ( 0.05219959533937995610, -21.53943276465977519, 50.00109039468568994 ) ) ;
#128157 = CARTESIAN_POINT ( 'NONE',  ( -5.049401038298153566, 19.05341960407611168, 95.20724293864770971 ) ) ;
#128158 = CARTESIAN_POINT ( 'NONE',  ( 21.55341960407619695, -5.719274019375665929, 106.0427570613523471 ) ) ;
#128159 = CARTESIAN_POINT ( 'NONE',  ( -16.52544592524335698, -4.483927247898792601, 78.95942372801901854 ) ) ;
#128160 = CARTESIAN_POINT ( 'NONE',  ( -21.53943276465977519, -0.05219959533937600094, 23.75109039468567929 ) ) ;
#128161 = CARTESIAN_POINT ( 'NONE',  ( 15.80617190586746368, 15.72974639402197994, 109.3739096053143811 ) ) ;
#128162 = CARTESIAN_POINT ( 'NONE',  ( -12.14591786802309592, -12.06949235617757132, 66.87390960531436690 ) ) ;
#128163 = CARTESIAN_POINT ( 'NONE',  ( -0.05219959533909027116, -19.03943276465977164, 37.49890960531436690 ) ) ;
#128164 = CARTESIAN_POINT ( 'NONE',  ( -0.05219959533910754901, -16.53943276465976808, 62.49890960531436690 ) ) ;
#128165 = CARTESIAN_POINT ( 'NONE',  ( 0.05219959533907565091, 21.53943276465977519, 34.99890960531435979 ) ) ;
#128166 = CARTESIAN_POINT ( 'NONE',  ( -13.89961937509957401, -13.97604488694547875, 24.37609039468565442 ) ) ;
#128167 = CARTESIAN_POINT ( 'NONE',  ( -0.05219959533910754901, -16.53943276465976808, 97.49890960531436690 ) ) ;
#128168 = EDGE_LOOP ( 'NONE', ( #32015, #123639, #136272, #64526, #112020 ) ) ;
#128169 = CARTESIAN_POINT ( 'NONE',  ( -12.14591786802326823, 12.06949235617739902, 63.12609039468568994 ) ) ;
#128170 = CARTESIAN_POINT ( 'NONE',  ( -19.02544592524342804, 5.153800228976336051, 66.04057627198103830 ) ) ;
#128171 = CARTESIAN_POINT ( 'NONE',  ( 17.14385361876520264, -23.59649016807270883, 139.5750000027311444 ) ) ;
#128172 = CARTESIAN_POINT ( 'NONE',  ( 16.52544592524342804, -4.483927247898539470, 83.54057627198102409 ) ) ;
#128173 = CARTESIAN_POINT ( 'NONE',  ( -21.52544592524343514, 5.823673210054127303, 31.04057627198102409 ) ) ;
#128174 = CARTESIAN_POINT ( 'NONE',  ( 4.483927247898790824, -16.52544592524335698, 95.20942372801903275 ) ) ;
#128175 = CARTESIAN_POINT ( 'NONE',  ( -9.564922557961040184, 16.46253265017147172, 112.9177570613523329 ) ) ;
#128176 = CARTESIAN_POINT ( 'NONE',  ( -18.67979575497193778, 10.72451020669871902, 78.33442372801901854 ) ) ;
#128177 = CARTESIAN_POINT ( 'NONE',  ( -19.05341960407611168, -5.049401038298163336, 91.45724293864766707 ) ) ;
#128178 = CARTESIAN_POINT ( 'NONE',  ( -15.80617190586745835, -15.72974639402198527, 106.8739096053143811 ) ) ;
#128179 = CARTESIAN_POINT ( 'NONE',  ( -12.14591786802326823, 12.06949235617739902, 53.12609039468568284 ) ) ;
#128180 = CARTESIAN_POINT ( 'NONE',  ( -12.14591786802309592, -12.06949235617757132, 106.8739096053143811 ) ) ;
#128181 = VECTOR ( 'NONE', #67185, 1000.000000000000000 ) ;
#128182 = CARTESIAN_POINT ( 'NONE',  ( -9.564922557961040184, 16.46253265017147172, 112.9177570613523329 ) ) ;
#128183 = CARTESIAN_POINT ( 'NONE',  ( 13.97604488694548053, -13.89961937509957401, 85.62609039468568994 ) ) ;
#128184 = CARTESIAN_POINT ( 'NONE',  ( 15.72974639402199770, -15.80617190586745480, 83.12390960531436690 ) ) ;
#128185 = CARTESIAN_POINT ( 'NONE',  ( 9.564922557961047289, -16.46253265017146816, 50.41775706135233293 ) ) ;
#128186 = CARTESIAN_POINT ( 'NONE',  ( 19.36337904590692460, -5.499999999999944933, 87.91494137495620009 ) ) ;
#128187 = CARTESIAN_POINT ( 'NONE',  ( 10.81492255796078972, 18.62759615963270932, 109.5822429386476955 ) ) ;
#128188 = CARTESIAN_POINT ( 'NONE',  ( -17.48847506799967988, 5.747544572773786165, 85.82697437843280852 ) ) ;
#128189 = CARTESIAN_POINT ( 'NONE',  ( -19.03943276465977164, 0.05219959533909376836, 81.24890960531436690 ) ) ;
#128190 = CARTESIAN_POINT ( 'NONE',  ( 15.50000000000000178, 5.499999999999998224, 118.0000000000000142 ) ) ;
#128191 = CARTESIAN_POINT ( 'NONE',  ( -16.52544592524335698, -4.483927247898792601, 28.95942372801902209 ) ) ;
#128192 = CARTESIAN_POINT ( 'NONE',  ( 36.87149605698873245, -2.274342727564266475, 50.01098105774816105 ) ) ;
#128194 = CARTESIAN_POINT ( 'NONE',  ( -14.29746914071049879, 8.314922557960819915, 70.83224293864770971 ) ) ;
#128193 = CARTESIAN_POINT ( 'NONE',  ( 18.62759615963271287, -10.81492255796078972, 98.33224293864769550 ) ) ;
#128195 = CARTESIAN_POINT ( 'NONE',  ( 16.51473224551069308, 9.474510206698969483, 64.16557627198102409 ) ) ;
#128196 = CARTESIAN_POINT ( 'NONE',  ( -15.80617190586768217, 15.72974639402176855, 88.12609039468570415 ) ) ;
#128199 = CARTESIAN_POINT ( 'NONE',  ( 13.89961937509957401, 13.97604488694547697, 46.87609039468565442 ) ) ;
#128198 =( BOUNDED_SURFACE ( )  B_SPLINE_SURFACE ( 3, 2, ( 
 ( #70350, #176538, #25864, #69339, #38014, #55174, #115853, #26860, #148193, #146170, #129985, #99670, #41018, #149196, #9686, #195716, #53166, #56174, #131005, #71351, #147188, #22845, #161354, #191685, #194705, #84492, #7655, #72350, #133015, #57189, #179548, #8678, #163363, #101673, #117855, #132017, #177543, #165366, #162349, #145173, #116844, #114844, #192697, #103687, #40001, #164370, #102684, #68335, #24859, #54180, #39012, #100667, #86508, #87508, #10686, #118865, #180549, #42022, #6657, #73363, #14648, #105663, #43011, #135035, #196711, #154151, #58180, #166365, #136013, #168325, #449, #76308, #77302, #106653, #170313, #104678, #60147, #27862, #107630, #184497, #198680, #137986, #181532, #89503, #15643, #199669, #138971, #122807, #167350, #29822, #44994, #61135, #28848, #59151, #108635, #90488, #88502, #121815, #119847, #151192, #46976, #152170, #169308, #91458, #11696, #75320, #12681, #197686, #74347, #44002, #182521, #45976, #13653, #136991, #120821, #92463, #183511, #30814, #153146, #62124, #123787, #185486, #150198, #1446, #109630, #79291, #111618, #143937, #19612, #20594, #49954, #113592, #47977, #3435, #186501, #50947, #127769, #141945, #81254, #124803, #34778, #4417, #31806, #139956, #93456, #78283, #32800, #51932, #64129, #173303, #80274, #188473, #16636, #171313, #94452, #67101, #96434, #142936, #63124, #158121, #156132, #157132, #155143, #159100, #17631, #66103, #189469, #140960, #112606, #2447, #174298, #35767, #97413, #82246, #5418, #128760, #190459, #65111, #125794, #126769, #110616, #187496, #48962, #18627, #172298, #33787, #95447, #55932, #99427, #68095, #85255, #145932, #59662, #178296, #176293, #160111, #129747, #71108, #179307, #39760, #164127, #83257, #86266, #161109, #101423, #115614, #52920, #191444, #21599, #144932, #8436, #24618, #117607, #147956, #40771, #25625, #9443, #23609, #7414, #69097, #146947, #130764, #163115, #6414, #70108, #192456, #132774, #114596, #131777, #87270, #98415, #194461, #37765, #193459, #102440, #175286, #148954, #22605, #84251, #54936, #136511, #177303, #53939, #13185, #116608, #74848, #38775, #100431, #162112, #198192, #36751, #183028, #46485, #125322, #170828, #44511, #153662, #78801, #187019, #124312, #108145, #121335, #91968, #31322, #107151, #137502, #169829, #15158, #106167, #960, #45496, #90979, #199182, #32320, #17148, #62636, #63647, #14156, #47492, #168821, #186010, #61640, #122322, #60649, #152666, #109149, #184014, #30326, #140479, #93973, #167850, #155653, #123308, #139478, #16155, #1967, #185001, #76818, #29350, #92974, #75824, #138489, #154659, #77809, #200171, #165530, #120988, #104840, #22253, #88671, #164530, #10850, #26023, #57356, #195882, #136177, #180713, #119030, #68744, #105830, #83902, #28028, #42189, #53582, #145585, #7063, #167517, #130402, #176952, #149353, #181692, #13820, #89669, #90652, #120007, #183679, #150367, #58339, #192100, #115259, #41182, #137159, #43173, #151356, #102845, #166531, #87668, #27026, #121988, #29012, #72519, #12845, #74511, #134194, #197852, #99073, #59319, #182686, #44171, #152334, #75486, #198848, #60312, #135200, #160763, #11863, #103849, #73528, #196872, #170484, #93631, #65283, #15811, #78455, #169483, #138158, #155316, #77472, #126942, #48143, #46145, #29992, #199839, #141132, #49135, #109800, #33961, #153319, #156305, #30983, #171483, #185655, #122976, #61306, #91631, #94626, #184663, #107799, #172474, #32972, #95619, #79463, #123957, #63296, #1620, #17806, #47147, #139142, #45164, #62289, #106820, #16805, #14820, #76481, #3604, #108805, #64299, #2622, #168494, #31975, #92631, #154322, #619, #140129, #124976, #125966, #186673, #187664, #110793, #157304, #18801, #80446, #142119, #143107, #34950, #96602, #54110, #158291, #66279, #35936, #68265, #100599, #176467, #177473, #6586, #70282, #4586, #160284, #127938, #7585, #84424, #98590, #37940, #81421, #191616, #161281, #188650 ),
 ( #36928, #67270, #115784, #173477, #113761, #21775, #8609, #159270, #83426, #112774, #189640, #145103, #20766, #50129, #53095, #51115, #19780, #174467, #146101, #192628, #114773, #38942, #97582, #99601, #82421, #22776, #128928, #144110, #5590, #190629, #69271, #52104, #175457, #162281, #130937, #23781, #85431, #129916, #147122, #111789, #11740, #91502, #28890, #44047, #90530, #74389, #43053, #150245, #89548, #12723, #60190, #165411, #56221, #103731, #59195, #197729, #152212, #106696, #102727, #151234, #166410, #87553, #45038, #42067, #120864, #26904, #27905, #137033, #121860, #75363, #72395, #149240, #180593, #104719, #182564, #119890, #73407, #179592, #13696, #41064, #164416, #25909, #136054, #105707, #198723, #167394, #183552, #168369, #29865, #58221, #88547, #135078, #181575, #196754, #9731, #194749, #71395, #133059, #117903, #10731, #134071, #195761, #57235, #118909, #46019, #186547, #18671, #34820, #80317, #107675, #122851, #171357, #111662, #93503, #108680, #188520, #32845, #156177, #92508, #155189, #62167, #16679, #153189, #141990, #169352, #184539, #94495, #173349, #78328, #170358, #49997, #17676, #79334, #154197, #140001, #123831, #1490, #141004, #14692, #48019, #76355, #95491, #138031, #31850, #126814, #199714, #187540, #61179, #30861, #33831, #63168, #64173, #15687, #77348, #109676, #139015, #494, #185529, #47021, #124847, #125838, #2492, #49007, #110662, #172342, #157177, #3478, #65155, #160156, #131821, #52964, #36797, #21647, #116649, #130808, #69141, #176339, #177345, #114641, #158163, #112648, #192499, #67146, #98462, #178339, #115656, #53983, #38816, #161152, #129789, #83300, #37811, #99472, #146989, #51977, #142980, #190503, #145975, #84296, #100474, #193501, #189515, #22649, #7457, #174340, #54979, #128804, #162153, #113635, #23649, #85297, #8476, #70151, #159142, #35810, #175330, #191486, #96475, #6457, #144976, #66147, #19655, #127810, #50988, #97456, #81296, #4458, #20639, #82292, #143983, #5464, #68138, #88300, #10486, #72146, #11494, #133822, #42817, #24660, #73165, #195513, #135822, #71151, #134835, #28651, #163157, #197492, #132817, #196514, #105466, #166164, #57984, #120627, #167152, #104480, #58959, #119656, #90287, #149988, #118660, #151971, #86309, #165165, #181338, #59949, #56986, #27665, #164170, #194503, #89305, #180351, #121616, #150997, #40813, #147998, #55976, #182324, #43803, #12489, #13459, #9487, #74150, #25668, #75123, #41819, #117653, #179350, #102483, #136791, #87313, #148997, #198477, #39801, #101466, #103487, #26658, #1244, #139757, #109431, #187297, #94255, #95253, #168127, #64918, #154943, #91255, #152946, #141754, #46779, #2248, #186298, #106446, #170114, #45782, #92266, #107434, #138773, #77104, #17430, #61923, #254, #14445, #48769, #29623, #171111, #123593, #137784, #76108, #199469, #110423, #60936, #122610, #30613, #62923, #156938, #32602, #172104, #124603, #183311, #184300, #16440, #169106, #63931, #79087, #93258, #155935, #153950, #47778, #140760, #44793, #15446, #185287, #108438, #31608, #3244, #78089, #125600, #33590, #18435, #80085, #81068, #19420, #161917, #144737, #176098, #34585, #191256, #96242, #51738, #146741, #53745, #157930, #52731, #99231, #112413, #6224, #126579, #114397, #188280, #173108, #127578, #8236, #158908, #67903, #175090, #83063, #111422, #142746, #4226, #23411, #129556, #37568, #65905, #160918, #189279, #113400, #49754, #115419, #50755, #22411, #84062, #174105, #145740, #35574, #7221, #68906, #130566, #192263, #177108, #38579, #100235, #159916, #85059, #36558, #5222, #97222, #20399, #98213, #21405, #82048, #143743, #66903, #128566, #190261, #180118, #40579, #151742, #72928, #70916, #54738, #24424, #165926, #73919, #134597, #58723, #178099, #181106, #194272, #196283, #10249, #147763, #86073, #116410, #119422, #162916, #9249, #197261, #57752, #120392, #104243, #148760, #88065, #26425, #42580, #135589, #27423, #182086 ),
 ( #89068, #166922, #132584, #149752, #11255, #55739, #105234, #102249, #150759, #163937, #12257, #43569, #28423, #90060, #117413, #179111, #25434, #164932, #69914, #41586, #133580, #39569, #131580, #101227, #87075, #71908, #103250, #193264, #195270, #56754, #118425, #2020, #62685, #61691, #184064, #45547, #106216, #93025, #169882, #91030, #48540, #107202, #1011, #168872, #31375, #140531, #63699, #78852, #75875, #152716, #30377, #108201, #186062, #123360, #76869, #183078, #32369, #44561, #167900, #29400, #46541, #124367, #94022, #47545, #155703, #125374, #109199, #185053, #92022, #153714, #154713, #15210, #16206, #198242, #77861, #138539, #170878, #14207, #139528, #187070, #136561, #17198, #137551, #110194, #171872, #95020, #33361, #199234, #60699, #13235, #74898, #17, #59714, #121386, #122375, #159669, #96016, #96995, #65675, #158678, #174856, #18202, #51506, #179624, #98987, #141528, #35344, #133089, #41096, #191019, #79860, #34355, #37328, #20167, #67666, #194779, #56253, #190032, #3016, #142517, #111184, #117935, #3995, #129323, #156709, #113168, #36322, #127337, #64693, #49521, #21165, #81812, #126354, #97976, #143500, #4984, #188051, #52494, #114154, #82821, #160676, #144502, #172874, #157701, #175856, #189049, #66670, #19191, #22168, #86585, #148269, #5986, #9761, #128333, #71425, #80840, #50524, #112186, #173874, #196785, #152245, #90563, #121893, #199746, #58253, #138065, #182597, #105740, #42098, #43085, #11774, #104752, #120897, #164447, #197761, #122884, #45071, #87584, #181607, #76389, #184572, #137068, #25941, #180626, #183586, #166442, #13730, #61212, #102760, #136087, #149271, #88579, #57267, #10763, #150277, #75396, #72427, #59228, #44082, #73438, #134105, #195795, #167427, #27938, #118941, #28923, #89580, #151266, #103763, #198758, #60224, #106729, #168403, #29898, #165442, #26937, #91536, #135109, #12756, #119921, #153223, #14728, #74421, #110698, #79371, #186582, #125875, #49043, #96511, #1525, #92543, #140036, #95528, #33869, #65192, #143016, #139049, #187575, #2528, #123865, #81333, #78362, #157215, #63204, #64208, #173386, #158201, #111700, #108715, #185563, #16712, #141042, #18708, #156213, #109711, #15721, #126851, #77381, #529, #62201, #172378, #80355, #188557, #142027, #50036, #34856, #3516, #94531, #124884, #48055, #17713, #171394, #19691, #30895, #4494, #32881, #66185, #47057, #127847, #46053, #169387, #107708, #170393, #154231, #31884, #93538, #155223, #144019, #159179, #7495, #148034, #129826, #9523, #131858, #174377, #68174, #163195, #71189, #23688, #112685, #67182, #70191, #191525, #100511, #24699, #86348, #22686, #35847, #175365, #5500, #189552, #36833, #162190, #51024, #84333, #69180, #98499, #97493, #82329, #54021, #53002, #20674, #146012, #114681, #176376, #128839, #85336, #147029, #130846, #193542, #192538, #190538, #52012, #8513, #160193, #37850, #113671, #55015, #116685, #178375, #115694, #177383, #99509, #38854, #39839, #101505, #145013, #21683, #83336, #6494, #161190, #152008, #29660, #25704, #12523, #89341, #10523, #168163, #165201, #120662, #26696, #151033, #59985, #183347, #152983, #90323, #13494, #72186, #180389, #74188, #44829, #182360, #121653, #135857, #14482, #149035, #104517, #87349, #75159, #28687, #42852, #43838, #133860, #197527, #105503, #132853, #40850, #194541, #179387, #195551, #56012, #88336, #58996, #181374, #167189, #117690, #57025, #118698, #91292, #136831, #198514, #102524, #106485, #164206, #58021, #41860, #103526, #150027, #11533, #73202, #134873, #196550, #119690, #166198, #27699, #32636, #156971, #141786, #140795, #172138, #96276, #33624, #95287, #153987, #123627, #155968, #188313, #63966, #64952, #94290, #157962, #92304, #47815, #30650, #18468, #80118, #186333, #125636, #169146, #79122, #48803, #76144, #184336, #137823, #122647, #77141, #199506, #108472, #17466, #124638, #2284, #60972, #15484, #138811, #111456, #187333, #110457 ),
 ( #3281, #126611, #49790, #173142, #34617, #45818, #109464, #107469, #171148, #154979, #291, #61960, #1281, #185323, #46813, #170151, #31644, #93293, #16474, #78123, #139792, #62957, #22442, #20430, #4260, #174136, #115450, #23443, #84092, #8268, #127611, #130600, #143773, #145770, #159947, #97253, #35608, #65940, #68937, #112447, #158941, #146775, #7252, #69947, #53775, #98245, #37600, #176130, #192296, #85090, #177140, #131612, #189310, #101259, #191284, #50788, #82081, #178133, #83095, #38611, #100267, #142779, #6255, #5254, #128598, #66936, #175121, #113429, #161948, #21434, #36589, #190292, #193296, #51769, #54771, #144770, #67935, #52759, #129588, #116445, #99263, #39600, #114429, #19454, #160949, #81101, #183109, #90089, #70946, #89099, #135619, #148792, #181137, #162949, #150790, #12286, #119452, #43599, #28453, #27458, #58753, #196313, #151771, #11286, #41617, #13264, #147796, #88097, #72959, #44591, #133610, #57782, #87106, #55769, #134628, #195304, #24455, #165957, #163968, #9281, #117443, #120422, #166950, #73951, #74927, #132616, #197290, #10282, #182113, #103282, #40610, #179142, #194303, #105264, #102280, #25466, #136590, #198270, #59747, #121417, #164962, #42611, #104275, #86104, #71940, #56785, #118457, #180149, #26455, #149783, #14237, #75909, #64724, #169914, #125404, #109228, #29429, #93057, #168904, #15241, #30410, #61724, #49, #140561, #185084, #123392, #137583, #110224, #91060, #32399, #46573, #60734, #77892, #126386, #63729, #187101, #184097, #153746, #186094, #18235, #94054, #95052, #124400, #188083, #122407, #139560, #45580, #48571, #2050, #16240, #155732, #199266, #170907, #78882, #106247, #107233, #167929, #152747, #92057, #76900, #138571, #47576, #154744, #62717, #108234, #31406, #156741, #171905, #1044, #17230, #33393, #79889, #141559, #3048, #161711, #34387, #131367, #21199, #157734, #19223, #8018, #113200, #68693, #52525, #172909, #36355, #112216, #158708, #173906, #5019, #143531, #83850, #128365, #66701, #80873, #53528, #96047, #175890, #190061, #4027, #82855, #69700, #7011, #130348, #127371, #97027, #129357, #23207, #37361, #38369, #67699, #49554, #65705, #144534, #189083, #192047, #145532, #159702, #99019, #142549, #114186, #22201, #111217, #50556, #35375, #20197, #81843, #51537, #174889, #191052, #98007, #6020, #160710, #115206, #176898, #84850, #100024, #146527, #101023, #57544, #162708, #118215, #13030, #120190, #24213, #119213, #165715, #178896, #11037, #193056, #180898, #42373, #149542, #73714, #58524, #104036, #88858, #26215, #181880, #41372, #71701, #43359, #177895, #179906, #103038, #74696, #163722, #87854, #117204, #85862, #164720, #25224, #54533, #196071, #194069, #39365, #147551, #150551, #197056, #27212, #105030, #9039, #12050, #40364, #135386, #133368, #70708, #132376, #55530, #166714, #102039, #86866, #28218, #89858, #72713, #134385, #148550, #10041, #195059, #151541, #116206, #56537, #44355, #811, #106014, #61493, #156498, #63494, #167700, #62484, #108997, #122172, #154509, #136361, #124156, #185856, #92823, #16996, #1815, #47342, #32166, #169677, #125169, #184851, #15006, #186868, #121180, #123163, #46335, #18000, #107001, #31173, #60496, #29197, #107991, #168674, #198037, #139332, #137347, #182874, #90831, #93823, #140325, #170678, #48337, #152515, #155503, #183862, #78650, #76666, #14003, #75670, #199027, #109992, #45349, #30174, #171672, #33161, #94820, #59505, #138345, #16005, #77663, #91817, #153509, #200025, #191808, #64489, #161477, #51304, #187852, #49321, #38138, #143294, #98782, #82615, #2811, #66468, #142314, #188840, #3794, #35139, #173672, #113949, #158480, #96791, #110981, #83618, #126156, #5786, #19968, #34152, #112965, #99791, #37123, #160476, #157498, #127134, #159462, #53290, #67460, #68458, #97775, #79653, #95812, #174658, #18991, #21967, #175648, #189832, #129118, #172666, #144296, #52292, #141322, #80637, #65471 ),
 ( #50325, #145296, #111980, #81610, #4780, #6779, #130112, #114968, #190817, #36123, #128130, #20958, #176661, #73478, #178655, #69464, #116964, #72472, #10803, #42141, #119960, #115972, #102800, #179666, #100784, #58291, #55292, #134146, #40117, #41136, #150319, #165482, #131130, #101796, #104793, #193827, #117976, #195834, #133130, #86626, #192818, #103802, #54300, #177660, #39129, #56293, #57306, #26978, #118982, #88621, #11814, #180665, #71465, #163483, #24980, #194821, #148309, #25980, #7780, #164486, #9803, #135151, #162467, #87623, #196824, #146293, #181646, #23968, #149309, #43125, #22966, #84614, #85624, #147310, #8799, #70469, #132135, #121935, #4288, #46094, #169431, #105781, #106769, #75438, #168444, #184613, #27980, #61255, #189339, #111484, #151308, #45112, #142808, #50817, #3308, #89619, #44122, #49820, #29940, #77421, #65969, #127639, #199787, #12797, #152286, #120939, #166482, #13770, #139093, #74462, #122925, #107749, #137112, #136128, #59270, #30936, #91579, #197804, #92583, #153268, #182639, #154271, #15762, #167468, #28963, #198799, #64981, #60264, #126639, #96304, #173169, #90604, #183630, #14770, #76430, #188341, #34645, #138106, #157990, #19481, #81127, #143803, #5286, #82112, #145799, #161976, #193326, #23472, #54800, #101289, #85121, #160978, #83125, #144801, #84120, #6284, #115480, #97282, #7282, #67963, #8298, #66969, #68966, #162979, #35637, #69976, #128629, #130629, #178164, #194333, #39629, #190322, #51799, #192324, #70977, #52788, #129617, #147826, #53805, #177168, #113458, #114457, #21463, #176159, #38641, #174167, #100298, #132645, #116475, #158970, #191312, #86134, #112474, #146805, #20462, #175151, #24484, #37629, #131644, #9312, #36619, #98276, #159977, #99292, #22472, #29458, #103311, #166979, #14269, #89129, #135648, #164991, #137613, #148821, #120451, #119481, #91090, #12314, #196342, #181164, #75938, #90116, #28482, #197318, #136618, #73979, #117473, #71968, #151800, #26485, #57810, #55801, #74955, #13291, #198299, #182144, #150817, #42641, #58782, #43628, #106274, #11317, #102308, #149811, #105291, #59776, #121445, #152777, #183137, #179171, #44621, #40639, #167959, #163997, #134656, #25494, #87137, #10311, #133642, #195333, #56813, #104303, #118487, #180178, #41646, #88127, #72987, #165986, #27486, #172938, #46603, #110253, #157765, #32429, #78913, #108263, #80902, #92087, #63759, #62748, #34417, #155762, #139588, #124428, #19255, #33423, #171934, #140590, #79917, #17260, #60764, #15271, #95082, #169943, #1073, #199297, #18264, #156770, #141589, #125433, #94083, #186124, #2080, #187129, #49584, #154772, #45611, #93088, #48601, #3077, #64753, #96076, #153776, #126415, #188112, #76931, #122436, #31434, #111247, #16269, #184128, #107263, #168934, #30440, #77921, #138600, #47604, #82, #61752, #109258, #170937, #123420, #185113, #112246, #173937, #50586, #67731, #160742, #130382, #22234, #192080, #38402, #83883, #82889, #128396, #190093, #6053, #51568, #175924, #65736, #129389, #113232, #7043, #35405, #191085, #176932, #4058, #145565, #97056, #52558, #53562, #8057, #100059, #158739, #20228, #114219, #84883, #36386, #174922, #161744, #37395, #99053, #81876, #98040, #66736, #159737, #68725, #21234, #115240, #127404, #23239, #144567, #146562, #143568, #142579, #189113, #5050, #18915, #15928, #156421, #188765, #4704, #50249, #77587, #92746, #141246, #81535, #63416, #78572, #158405, #2735, #126081, #62406, #125091, #32091, #186789, #64412, #184774, #17922, #143222, #65397, #107915, #1738, #96717, #123088, #157421, #46260, #734, #3720, #48260, #34077, #19894, #169600, #79577, #31098, #108921, #139258, #154434, #170601, #95735, #124076, #187777, #49247, #93748, #185777, #47264, #110905, #109913, #155429, #172591, #171597, #33085, #16919, #80560, #142235, #127058, #111905, #173593, #140246, #94741, #35062, #37049, #68380, #148237, #85548, #100712, #147234 ),
 ( #159390, #146214, #22891, #144225, #101720, #98708, #54226, #160402, #84537, #193752, #67386, #52218, #113875, #38059, #5709, #175572, #7702, #178581, #115897, #55220, #69385, #66394, #82543, #99715, #20885, #8726, #162392, #176585, #177587, #129043, #131054, #39054, #128056, #174585, #23895, #36050, #192744, #97699, #191731, #86553, #116889, #190744, #70395, #132063, #21891, #40046, #189758, #163410, #24906, #51230, #112891, #83541, #145220, #6702, #161399, #130032, #114891, #53213, #6282, #22470, #35634, #190319, #193324, #114455, #23470, #86132, #147824, #145797, #158967, #98273, #66966, #9310, #159974, #85119, #70975, #7280, #192322, #21461, #194331, #5283, #177166, #176157, #132643, #68964, #52786, #37627, #112471, #146803, #8296, #53803, #54798, #130626, #174164, #128626, #69974, #83123, #99290, #97279, #131642, #116473, #178162, #38639, #115478, #160976, #100296, #161974, #162977, #67960, #20459, #129615, #39627, #101287, #24482, #82109, #51796, #143800, #113455, #175148, #36616, #144799, #191310, #84118, #73977, #183135, #28480, #29456, #90114, #196340, #26483, #150815, #151798, #165984, #119479, #25492, #74953, #87135, #148819, #10309, #89127, #105289, #136616, #166977, #198297, #44619, #13289, #104301, #88125, #149809, #27484, #11315, #58780, #40637, #12312, #72985, #59774, #71966, #135646, #106272, #179169, #121443, #133640, #197316, #103309, #137611, #195331, #120449, #181162, #91088, #182142, #57808, #42639, #75936, #167957, #152775, #43626, #14267, #55799, #117471, #56811, #102306, #134654, #163995, #118485, #180176, #41644, #164989, #63756, #32426, #139585, #78910, #2077, #49581, #154770, #45608, #93086, #48598, #187126, #18261, #96072, #92085, #140587, #155759, #76929, #34414, #31432, #110250, #16267, #17257, #126412, #171931, #172935, #33420, #1070, #169941, #94080, #95079, #109255, #62745, #168932, #79914, #30438, #153774, #15269, #125430, #156767, #141586, #3074, #64750, #188109, #111244, #47601, #77918, #124425, #170934, #186121, #157762, #184126, #19252, #80899, #199295, #138598, #60762, #122434, #107261, #80, #61750, #123418, #185111, #46601, #108261, #97053, #112243, #160739, #101055, #82886, #98037, #177927, #22231, #145562, #81873, #144564, #51565, #6050, #83880, #4055, #37392, #162740, #84880, #127401, #7040, #67728, #36383, #52555, #65733, #20225, #23236, #129386, #53559, #116236, #39395, #175921, #189110, #128393, #158735, #24248, #190090, #115237, #142576, #99050, #146557, #176929, #54564, #50583, #173934, #114216, #35402, #143565, #5047, #191082, #161741, #68722, #66733, #130379, #113229, #174919, #159734, #21231, #192077, #38399, #100055, #8053, #69732, #131400, #193088, #12083, #103071, #40400, #86898, #71732, #133402, #57576, #163756, #195091, #165750, #198069, #73746, #74728, #104068, #167729, #102071, #119246, #25256, #105063, #181912, #196106, #135418, #178930, #88892, #58556, #85897, #194101, #147585, #132409, #148582, #106043, #118248, #27243, #134420, #42405, #70741, #10073, #56574, #121214, #150584, #197089, #55563, #120222, #117237, #11071, #9071, #13062, #179939, #43392, #166747, #41406, #28250, #164753, #89890, #151573, #136392, #59535, #182904, #44388, #26248, #180930, #87888, #149575, #72749, #48366, #79683, #124186, #77692, #49348, #200054, #62514, #153540, #122201, #139360, #61523, #111010, #32196, #30205, #14033, #183893, #125199, #33190, #93853, #18029, #137378, #140354, #15037, #155530, #169708, #107031, #45378, #75698, #78678, #168703, #91846, #156530, #17025, #141353, #63524, #108021, #47372, #185887, #1842, #186895, #110022, #29227, #199057, #90860, #60526, #76698, #152545, #123192, #109027, #841, #170706, #138374, #184881, #46363, #64518, #171701, #94849, #31201, #2840, #92852, #154538, #16034, #126185, #187881, #101571, #148095, #161253, #193605, #172696, #163261, #24763, #131921, #56075, #40914, #39905, #71252, #8578, #164271, #23752 ),
 ( #22747, #127162, #149097, #84396, #86410, #133926, #70253, #55077, #146072, #57088, #65501, #9586, #38914, #10587, #116747, #115756, #100571, #195616, #132916, #194603, #178437, #117756, #179448, #34181, #188870, #102587, #7557, #177444, #95842, #25766, #87412, #72248, #157526, #19020, #162253, #80666, #142342, #3822, #130909, #50353, #69243, #112012, #173701, #35169, #96824, #192599, #54082, #85402, #147094, #154045, #151091, #106545, #12582, #136890, #45873, #91350, #92359, #153042, #59053, #89402, #13552, #14542, #28746, #182419, #88398, #137881, #150092, #11595, #73263, #152067, #168221, #199562, #29718, #61031, #107526, #76202, #119750, #103589, #134932, #122703, #184393, #183405, #169203, #26758, #30710, #42911, #121712, #120720, #196609, #58080, #165264, #15540, #181433, #104577, #77198, #138867, #347, #118762, #197587, #198576, #75218, #44888, #180451, #41923, #166260, #27759, #74247, #90382, #135916, #43898, #105561, #167247, #60045, #65009, #185380, #48859, #124697, #171206, #186394, #17523, #156026, #96331, #140852, #79182, #31703, #65998, #46871, #188370, #2341, #16533, #63018, #47871, #109524, #33680, #139849, #32696, #141844, #174195, #49847, #50844, #80172, #143833, #78180, #95342, #1338, #81154, #158018, #172195, #111511, #155038, #126666, #34673, #62017, #170210, #123681, #108531, #94347, #82139, #64022, #3335, #110514, #18525, #93352, #125692, #187391, #97311, #173197, #19509, #157027, #142836, #4315, #127667, #189367, #112501, #35663, #158997, #20490, #191341, #23504, #5313, #193357, #131676, #162008, #86168, #71009, #70006, #101321, #38674, #194365, #53839, #9344, #24517, #55832, #100329, #115513, #25525, #176190, #85152, #129645, #98306, #177201, #37659, #87171, #8331, #147857, #102340, #160006, #146838, #54833, #83155, #40670, #99324, #116507, #161008, #178195, #132677, #39660, #179202, #163010, #145828, #22502, #117505, #164029, #66997, #68996, #175181, #128656, #36647, #21494, #144829, #190351, #51828, #113487, #6313, #67992, #52819, #114487, #84149, #7311, #130662, #192355, #181195, #151829, #133673, #182173, #119514, #44651, #180208, #43659, #137641, #71999, #106303, #41677, #105321, #14300, #30467, #75968, #103341, #118519, #167009, #107290, #89159, #104334, #184157, #28510, #13318, #88158, #150849, #57841, #12344, #90144, #10343, #74984, #168961, #91119, #195364, #136646, #74007, #42673, #58813, #56843, #26514, #29486, #135678, #59805, #122464, #45638, #198329, #165021, #134688, #149843, #148852, #196373, #121475, #11347, #183168, #167989, #166018, #73018, #27518, #152808, #197350, #120482, #199328, #60793, #155791, #112271, #126443, #64782, #171963, #172966, #110282, #153804, #108291, #188141, #62776, #94112, #173963, #111275, #49612, #34444, #156799, #125461, #32459, #33451, #95110, #142606, #47632, #138628, #186153, #141617, #79947, #4085, #76958, #92115, #63789, #109, #61779, #50612, #17288, #96103, #18292, #15298, #78942, #154799, #1100, #16297, #109287, #170965, #157792, #140618, #2108, #123447, #19282, #185140, #3104, #187158, #46631, #93114, #77947, #139614, #48630, #169969, #124457, #80929, #65763, #127432, #189139, #31462, #117264, #51592, #7072, #190117, #54588, #131428, #145593, #84909, #128421, #38429, #8082, #35430, #143594, #97083, #81901, #36410, #55589, #67756, #115267, #83910, #192108, #20255, #113257, #174949, #70766, #53591, #146588, #5077, #100085, #66760, #160771, #158765, #162764, #98065, #161770, #69758, #21259, #176960, #159764, #23265, #193114, #116261, #177952, #101079, #39420, #24274, #68753, #85923, #130410, #147611, #9099, #132434, #194126, #82914, #144592, #6078, #129414, #191112, #52586, #114245, #175952, #37421, #99081, #22261, #163782, #133430, #74753, #182931, #43419, #167754, #86926, #89915, #103098, #181937, #119271, #56601, #195118, #25283, #28276, #71760, #118275, #106068, #166775, #29252, #13088, #57602, #197113, #135444 ) ),
 .UNSPECIFIED., .T., .F., .F. ) 
 B_SPLINE_SURFACE_WITH_KNOTS ( ( 4, 3, 4 ),
 ( 3, 2, 2, 2, 2, 2, 2, 2, 2, 2, 2, 2, 2, 2, 2, 2, 2, 2, 2, 2, 2, 2, 2, 2, 2, 2, 2, 2, 2, 2, 2, 2, 2, 2, 2, 2, 2, 2, 2, 2, 2, 2, 2, 2, 2, 2, 2, 2, 2, 2, 2, 2, 2, 2, 2, 2, 2, 2, 2, 2, 2, 2, 2, 2, 2, 2, 2, 2, 2, 2, 2, 2, 2, 2, 2, 2, 2, 2, 2, 2, 2, 2, 2, 2, 2, 2, 2, 2, 2, 2, 2, 2, 2, 2, 2, 2, 2, 2, 2, 2, 2, 2, 2, 2, 2, 2, 2, 2, 2, 2, 2, 2, 2, 2, 2, 2, 2, 2, 2, 2, 2, 2, 2, 2, 2, 2, 2, 2, 2, 2, 2, 2, 2, 2, 2, 2, 2, 2, 2, 2, 2, 2, 2, 2, 2, 2, 2, 2, 2, 2, 2, 2, 2, 2, 2, 2, 2, 2, 2, 2, 2, 2, 2, 2, 2, 2, 2, 2, 2, 2, 2, 2, 2, 2, 2, 2, 2, 2, 2, 2, 2, 2, 2, 2, 2, 2, 2, 2, 2, 2, 2, 2, 2, 2, 2, 2, 2, 2, 2, 2, 2, 2, 2, 2, 2, 2, 2, 2, 2, 2, 2, 2, 2, 2, 2, 2, 2, 2, 2, 2, 2, 2, 2, 2, 2, 2, 2, 2, 3 ),
 ( 0.000000000000000000, 0.5000000000000000000, 1.000000000000000000 ),
 ( 0.000000000000000000, 0.004385964912280701511, 0.008771929824561403022, 0.01315789473684210453, 0.01754385964912280604, 0.02192982456140350755, 0.02631578947368420907, 0.03070175438596491058, 0.03508771929824561209, 0.03947368421052631360, 0.04385964912280701511, 0.04824561403508771662, 0.05263157894736841813, 0.05701754385964911964, 0.06140350877192982115, 0.06578947368421052266, 0.07017543859649122417, 0.07456140350877192569, 0.07894736842105262720, 0.08333333333333332871, 0.08771929824561403022, 0.09210526315789473173, 0.09649122807017543324, 0.1008771929824561348, 0.1052631578947368363, 0.1096491228070175378, 0.1140350877192982393, 0.1184210526315789408, 0.1228070175438596423, 0.1271929824561403577, 0.1315789473684210453, 0.1359649122807017607, 0.1403508771929824483, 0.1447368421052631637, 0.1491228070175438514, 0.1535087719298245668, 0.1578947368421052544, 0.1622807017543859698, 0.1666666666666666574, 0.1710526315789473728, 0.1754385964912280604, 0.1798245614035087758, 0.1842105263157894635, 0.1885964912280701788, 0.1929824561403508665, 0.1973684210526315819, 0.2017543859649122695, 0.2061403508771929849, 0.2105263157894736725, 0.2149122807017543879, 0.2192982456140350755, 0.2236842105263157909, 0.2280701754385964786, 0.2324561403508771940, 0.2368421052631578816, 0.2412280701754385970, 0.2456140350877192846, 0.2500000000000000000, 0.2543859649122807154, 0.2587719298245614308, 0.2631578947368420907, 0.2675438596491228060, 0.2719298245614035214, 0.2763157894736842368, 0.2807017543859648967, 0.2850877192982456121, 0.2894736842105263275, 0.2938596491228070429, 0.2982456140350877027, 0.3026315789473684181, 0.3070175438596491335, 0.3114035087719298489, 0.3157894736842105088, 0.3201754385964912242, 0.3245614035087719396, 0.3289473684210526550, 0.3333333333333333148, 0.3377192982456140302, 0.3421052631578947456, 0.3464912280701754610, 0.3508771929824561209, 0.3552631578947368363, 0.3596491228070175517, 0.3640350877192982670, 0.3684210526315789269, 0.3728070175438596423, 0.3771929824561403577, 0.3815789473684210731, 0.3859649122807017330, 0.3903508771929824483, 0.3947368421052631637, 0.3991228070175438791, 0.4035087719298245390, 0.4078947368421052544, 0.4122807017543859698, 0.4166666666666666852, 0.4210526315789473450, 0.4254385964912280604, 0.4298245614035087758, 0.4342105263157894912, 0.4385964912280701511, 0.4429824561403508665, 0.4473684210526315819, 0.4517543859649122973, 0.4561403508771929571, 0.4605263157894736725, 0.4649122807017543879, 0.4692982456140351033, 0.4736842105263157632, 0.4780701754385964786, 0.4824561403508771940, 0.4868421052631579093, 0.4912280701754385692, 0.4956140350877192846, 0.5000000000000000000, 0.5043859649122807154, 0.5087719298245614308, 0.5131578947368421462, 0.5175438596491228616, 0.5219298245614034659, 0.5263157894736841813, 0.5307017543859648967, 0.5350877192982456121, 0.5394736842105263275, 0.5438596491228070429, 0.5482456140350877583, 0.5526315789473684736, 0.5570175438596490780, 0.5614035087719297934, 0.5657894736842105088, 0.5701754385964912242, 0.5745614035087719396, 0.5789473684210526550, 0.5833333333333333703, 0.5877192982456140857, 0.5921052631578946901, 0.5964912280701754055, 0.6008771929824561209, 0.6052631578947368363, 0.6096491228070175517, 0.6140350877192982670, 0.6184210526315789824, 0.6228070175438596978, 0.6271929824561403022, 0.6315789473684210176, 0.6359649122807017330, 0.6403508771929824483, 0.6447368421052631637, 0.6491228070175438791, 0.6535087719298245945, 0.6578947368421053099, 0.6622807017543859143, 0.6666666666666666297, 0.6710526315789473450, 0.6754385964912280604, 0.6798245614035087758, 0.6842105263157894912, 0.6885964912280702066, 0.6929824561403509220, 0.6973684210526315264, 0.7017543859649122417, 0.7061403508771929571, 0.7105263157894736725, 0.7149122807017543879, 0.7192982456140351033, 0.7236842105263158187, 0.7280701754385965341, 0.7324561403508771384, 0.7368421052631578538, 0.7412280701754385692, 0.7456140350877192846, 0.7500000000000000000, 0.7543859649122807154, 0.7587719298245614308, 0.7631578947368421462, 0.7675438596491228616, 0.7719298245614034659, 0.7763157894736841813, 0.7807017543859648967, 0.7850877192982456121, 0.7894736842105263275, 0.7938596491228070429, 0.7982456140350877583, 0.8026315789473684736, 0.8070175438596490780, 0.8114035087719297934, 0.8157894736842105088, 0.8201754385964912242, 0.8245614035087719396, 0.8289473684210526550, 0.8333333333333333703, 0.8377192982456140857, 0.8421052631578946901, 0.8464912280701754055, 0.8508771929824561209, 0.8552631578947368363, 0.8596491228070175517, 0.8640350877192982670, 0.8684210526315789824, 0.8728070175438596978, 0.8771929824561403022, 0.8815789473684210176, 0.8859649122807017330, 0.8903508771929824483, 0.8947368421052631637, 0.8991228070175438791, 0.9035087719298245945, 0.9078947368421053099, 0.9122807017543859143, 0.9166666666666666297, 0.9210526315789473450, 0.9254385964912280604, 0.9298245614035087758, 0.9342105263157894912, 0.9385964912280702066, 0.9429824561403509220, 0.9473684210526315264, 0.9517543859649122417, 0.9561403508771929571, 0.9605263157894736725, 0.9649122807017543879, 0.9692982456140351033, 0.9736842105263158187, 0.9780701754385965341, 0.9824561403508771384, 0.9868421052631578538, 0.9912280701754385692, 0.9956140350877192846, 1.000000000000000000 ),
 .UNSPECIFIED. ) 
 GEOMETRIC_REPRESENTATION_ITEM ( )  RATIONAL_B_SPLINE_SURFACE ( (
 ( 1.000000000000000000, 0.9659258262890683122, 1.000000000000000000, 0.9659258262890683122, 1.000000000000000000, 0.9659258262890683122, 1.000000000000000000, 0.9659258262890683122, 1.000000000000000000, 0.9659258262890683122, 1.000000000000000000, 0.9659258262890683122, 1.000000000000000000, 0.9659258262890683122, 1.000000000000000000, 0.9659258262890683122, 1.000000000000000000, 0.9659258262890683122, 1.000000000000000000, 0.9659258262890683122, 1.000000000000000000, 0.9659258262890683122, 1.000000000000000000, 0.9659258262890683122, 1.000000000000000000, 0.9659258262890683122, 1.000000000000000000, 0.9659258262890683122, 1.000000000000000000, 0.9659258262890683122, 1.000000000000000000, 0.9659258262890683122, 1.000000000000000000, 0.9659258262890683122, 1.000000000000000000, 0.9659258262890683122, 1.000000000000000000, 0.9659258262890683122, 1.000000000000000000, 0.9659258262890683122, 1.000000000000000000, 0.9659258262890683122, 1.000000000000000000, 0.9659258262890683122, 1.000000000000000000, 0.9659258262890683122, 1.000000000000000000, 0.9659258262890683122, 1.000000000000000000, 0.9659258262890683122, 1.000000000000000000, 0.9659258262890683122, 1.000000000000000000, 0.9659258262890683122, 1.000000000000000000, 0.9659258262890683122, 1.000000000000000000, 0.9659258262890683122, 1.000000000000000000, 0.9659258262890683122, 1.000000000000000000, 0.9659258262890683122, 1.000000000000000000, 0.9659258262890683122, 1.000000000000000000, 0.9659258262890683122, 1.000000000000000000, 0.9659258262890683122, 1.000000000000000000, 0.9659258262890683122, 1.000000000000000000, 0.9659258262890683122, 1.000000000000000000, 0.9659258262890683122, 1.000000000000000000, 0.9659258262890683122, 1.000000000000000000, 0.9659258262890683122, 1.000000000000000000, 0.9659258262890683122, 1.000000000000000000, 0.9659258262890683122, 1.000000000000000000, 0.9659258262890683122, 1.000000000000000000, 0.9659258262890683122, 1.000000000000000000, 0.9659258262890683122, 1.000000000000000000, 0.9659258262890683122, 1.000000000000000000, 0.9659258262890683122, 1.000000000000000000, 0.9659258262890683122, 1.000000000000000000, 0.9659258262890683122, 1.000000000000000000, 0.9659258262890683122, 1.000000000000000000, 0.9659258262890683122, 1.000000000000000000, 0.9659258262890683122, 1.000000000000000000, 0.9659258262890683122, 1.000000000000000000, 0.9659258262890683122, 1.000000000000000000, 0.9659258262890683122, 1.000000000000000000, 0.9659258262890683122, 1.000000000000000000, 0.9659258262890683122, 1.000000000000000000, 0.9659258262890683122, 1.000000000000000000, 0.9659258262890683122, 1.000000000000000000, 0.9659258262890683122, 1.000000000000000000, 0.9659258262890683122, 1.000000000000000000, 0.9659258262890683122, 1.000000000000000000, 0.9659258262890683122, 1.000000000000000000, 0.9659258262890683122, 1.000000000000000000, 0.9659258262890683122, 1.000000000000000000, 0.9659258262890683122, 1.000000000000000000, 0.9659258262890683122, 1.000000000000000000, 0.9659258262890683122, 1.000000000000000000, 0.9659258262890683122, 1.000000000000000000, 0.9659258262890683122, 1.000000000000000000, 0.9659258262890683122, 1.000000000000000000, 0.9659258262890683122, 1.000000000000000000, 0.9659258262890683122, 1.000000000000000000, 0.9659258262890683122, 1.000000000000000000, 0.9659258262890683122, 1.000000000000000000, 0.9659258262890683122, 1.000000000000000000, 0.9659258262890683122, 1.000000000000000000, 0.9659258262890683122, 1.000000000000000000, 0.9659258262890683122, 1.000000000000000000, 0.9659258262890683122, 1.000000000000000000, 0.9659258262890683122, 1.000000000000000000, 0.9659258262890683122, 1.000000000000000000, 0.9659258262890683122, 1.000000000000000000, 0.9659258262890683122, 1.000000000000000000, 0.9659258262890683122, 1.000000000000000000, 0.9659258262890683122, 1.000000000000000000, 0.9659258262890683122, 1.000000000000000000, 0.9659258262890683122, 1.000000000000000000, 0.9659258262890683122, 1.000000000000000000, 0.9659258262890683122, 1.000000000000000000, 0.9659258262890683122, 1.000000000000000000, 0.9659258262890683122, 1.000000000000000000, 0.9659258262890683122, 1.000000000000000000, 0.9659258262890683122, 1.000000000000000000, 0.9659258262890683122, 1.000000000000000000, 0.9659258262890683122, 1.000000000000000000, 0.9659258262890683122, 1.000000000000000000, 0.9659258262890683122, 1.000000000000000000, 0.9659258262890683122, 1.000000000000000000, 0.9659258262890683122, 1.000000000000000000, 0.9659258262890683122, 1.000000000000000000, 0.9659258262890683122, 1.000000000000000000, 0.9659258262890683122, 1.000000000000000000, 0.9659258262890683122, 1.000000000000000000, 0.9659258262890683122, 1.000000000000000000, 0.9659258262890683122, 1.000000000000000000, 0.9659258262890683122, 1.000000000000000000, 0.9659258262890683122, 1.000000000000000000, 0.9659258262890683122, 1.000000000000000000, 0.9659258262890683122, 1.000000000000000000, 0.9659258262890683122, 1.000000000000000000, 0.9659258262890683122, 1.000000000000000000, 0.9659258262890683122, 1.000000000000000000, 0.9659258262890683122, 1.000000000000000000, 0.9659258262890683122, 1.000000000000000000, 0.9659258262890683122, 1.000000000000000000, 0.9659258262890683122, 1.000000000000000000, 0.9659258262890683122, 1.000000000000000000, 0.9659258262890683122, 1.000000000000000000, 0.9659258262890683122, 1.000000000000000000, 0.9659258262890683122, 1.000000000000000000, 0.9659258262890683122, 1.000000000000000000, 0.9659258262890683122, 1.000000000000000000, 0.9659258262890683122, 1.000000000000000000, 0.9659258262890683122, 1.000000000000000000, 0.9659258262890683122, 1.000000000000000000, 0.9659258262890683122, 1.000000000000000000, 0.9659258262890683122, 1.000000000000000000, 0.9659258262890683122, 1.000000000000000000, 0.9659258262890683122, 1.000000000000000000, 0.9659258262890683122, 1.000000000000000000, 0.9659258262890683122, 1.000000000000000000, 0.9659258262890683122, 1.000000000000000000, 0.9659258262890683122, 1.000000000000000000, 0.9659258262890683122, 1.000000000000000000, 0.9659258262890683122, 1.000000000000000000, 0.9659258262890683122, 1.000000000000000000, 0.9659258262890683122, 1.000000000000000000, 0.9659258262890683122, 1.000000000000000000, 0.9659258262890683122, 1.000000000000000000, 0.9659258262890683122, 1.000000000000000000, 0.9659258262890683122, 1.000000000000000000, 0.9659258262890683122, 1.000000000000000000, 0.9659258262890683122, 1.000000000000000000, 0.9659258262890683122, 1.000000000000000000, 0.9659258262890683122, 1.000000000000000000, 0.9659258262890683122, 1.000000000000000000, 0.9659258262890683122, 1.000000000000000000, 0.9659258262890683122, 1.000000000000000000, 0.9659258262890683122, 1.000000000000000000, 0.9659258262890683122, 1.000000000000000000, 0.9659258262890683122, 1.000000000000000000, 0.9659258262890683122, 1.000000000000000000, 0.9659258262890683122, 1.000000000000000000, 0.9659258262890683122, 1.000000000000000000, 0.9659258262890683122, 1.000000000000000000, 0.9659258262890683122, 1.000000000000000000, 0.9659258262890683122, 1.000000000000000000, 0.9659258262890683122, 1.000000000000000000, 0.9659258262890683122, 1.000000000000000000, 0.9659258262890683122, 1.000000000000000000, 0.9659258262890683122, 1.000000000000000000, 0.9659258262890683122, 1.000000000000000000, 0.9659258262890683122, 1.000000000000000000, 0.9659258262890683122, 1.000000000000000000, 0.9659258262890683122, 1.000000000000000000, 0.9659258262890683122, 1.000000000000000000, 0.9659258262890683122, 1.000000000000000000, 0.9659258262890683122, 1.000000000000000000, 0.9659258262890683122, 1.000000000000000000, 0.9659258262890683122, 1.000000000000000000, 0.9659258262890683122, 1.000000000000000000, 0.9659258262890683122, 1.000000000000000000, 0.9659258262890683122, 1.000000000000000000, 0.9659258262890683122, 1.000000000000000000, 0.9659258262890683122, 1.000000000000000000, 0.9659258262890683122, 1.000000000000000000, 0.9659258262890683122, 1.000000000000000000, 0.9659258262890683122, 1.000000000000000000, 0.9659258262890683122, 1.000000000000000000, 0.9659258262890683122, 1.000000000000000000, 0.9659258262890683122, 1.000000000000000000, 0.9659258262890683122, 1.000000000000000000, 0.9659258262890683122, 1.000000000000000000, 0.9659258262890683122, 1.000000000000000000, 0.9659258262890683122, 1.000000000000000000, 0.9659258262890683122, 1.000000000000000000, 0.9659258262890683122, 1.000000000000000000, 0.9659258262890683122, 1.000000000000000000, 0.9659258262890683122, 1.000000000000000000, 0.9659258262890683122, 1.000000000000000000, 0.9659258262890683122, 1.000000000000000000, 0.9659258262890683122, 1.000000000000000000, 0.9659258262890683122, 1.000000000000000000, 0.9659258262890683122, 1.000000000000000000, 0.9659258262890683122, 1.000000000000000000, 0.9659258262890683122, 1.000000000000000000, 0.9659258262890683122, 1.000000000000000000, 0.9659258262890683122, 1.000000000000000000, 0.9659258262890683122, 1.000000000000000000, 0.9659258262890683122, 1.000000000000000000, 0.9659258262890683122, 1.000000000000000000, 0.9659258262890683122, 1.000000000000000000, 0.9659258262890683122, 1.000000000000000000, 0.9659258262890683122, 1.000000000000000000, 0.9659258262890683122, 1.000000000000000000, 0.9659258262890683122, 1.000000000000000000, 0.9659258262890683122, 1.000000000000000000, 0.9659258262890683122, 1.000000000000000000, 0.9659258262890683122, 1.000000000000000000, 0.9659258262890683122, 1.000000000000000000, 0.9659258262890683122, 1.000000000000000000, 0.9659258262890683122, 1.000000000000000000, 0.9659258262890683122, 1.000000000000000000, 0.9659258262890683122, 1.000000000000000000, 0.9659258262890683122, 1.000000000000000000, 0.9659258262890683122, 1.000000000000000000, 0.9659258262890683122, 1.000000000000000000, 0.9659258262890683122, 1.000000000000000000, 0.9659258262890683122, 1.000000000000000000, 0.9659258262890683122, 1.000000000000000000, 0.9659258262890683122, 1.000000000000000000, 0.9659258262890683122, 1.000000000000000000, 0.9659258262890683122, 1.000000000000000000, 0.9659258262890683122, 1.000000000000000000, 0.9659258262890683122, 1.000000000000000000, 0.9659258262890683122, 1.000000000000000000, 0.9659258262890683122, 1.000000000000000000, 0.9659258262890683122, 1.000000000000000000),
 ( 0.3333333333333333703, 0.3219752754296894559, 0.3333333333333333703, 0.3219752754296894559, 0.3333333333333333703, 0.3219752754296894559, 0.3333333333333333703, 0.3219752754296894559, 0.3333333333333333703, 0.3219752754296894559, 0.3333333333333333703, 0.3219752754296894559, 0.3333333333333333703, 0.3219752754296894559, 0.3333333333333333703, 0.3219752754296894559, 0.3333333333333333703, 0.3219752754296894559, 0.3333333333333333703, 0.3219752754296894559, 0.3333333333333333703, 0.3219752754296894559, 0.3333333333333333703, 0.3219752754296894559, 0.3333333333333333703, 0.3219752754296894559, 0.3333333333333333703, 0.3219752754296894559, 0.3333333333333333703, 0.3219752754296894559, 0.3333333333333333703, 0.3219752754296894559, 0.3333333333333333703, 0.3219752754296894559, 0.3333333333333333703, 0.3219752754296894559, 0.3333333333333333703, 0.3219752754296894559, 0.3333333333333333703, 0.3219752754296894559, 0.3333333333333333703, 0.3219752754296894559, 0.3333333333333333703, 0.3219752754296894559, 0.3333333333333333703, 0.3219752754296894559, 0.3333333333333333703, 0.3219752754296894559, 0.3333333333333333703, 0.3219752754296894559, 0.3333333333333333703, 0.3219752754296894559, 0.3333333333333333703, 0.3219752754296894559, 0.3333333333333333703, 0.3219752754296894559, 0.3333333333333333703, 0.3219752754296894559, 0.3333333333333333703, 0.3219752754296894559, 0.3333333333333333703, 0.3219752754296894559, 0.3333333333333333703, 0.3219752754296894559, 0.3333333333333333703, 0.3219752754296894559, 0.3333333333333333703, 0.3219752754296894559, 0.3333333333333333703, 0.3219752754296894559, 0.3333333333333333703, 0.3219752754296894559, 0.3333333333333333703, 0.3219752754296894559, 0.3333333333333333703, 0.3219752754296894559, 0.3333333333333333703, 0.3219752754296894559, 0.3333333333333333703, 0.3219752754296894559, 0.3333333333333333703, 0.3219752754296894559, 0.3333333333333333703, 0.3219752754296894559, 0.3333333333333333703, 0.3219752754296894559, 0.3333333333333333703, 0.3219752754296894559, 0.3333333333333333703, 0.3219752754296894559, 0.3333333333333333703, 0.3219752754296894559, 0.3333333333333333703, 0.3219752754296894559, 0.3333333333333333703, 0.3219752754296894559, 0.3333333333333333703, 0.3219752754296894559, 0.3333333333333333703, 0.3219752754296894559, 0.3333333333333333703, 0.3219752754296894559, 0.3333333333333333703, 0.3219752754296894559, 0.3333333333333333703, 0.3219752754296894559, 0.3333333333333333703, 0.3219752754296894559, 0.3333333333333333703, 0.3219752754296894559, 0.3333333333333333703, 0.3219752754296894559, 0.3333333333333333703, 0.3219752754296894559, 0.3333333333333333703, 0.3219752754296894559, 0.3333333333333333703, 0.3219752754296894559, 0.3333333333333333703, 0.3219752754296894559, 0.3333333333333333703, 0.3219752754296894559, 0.3333333333333333703, 0.3219752754296894559, 0.3333333333333333703, 0.3219752754296894559, 0.3333333333333333703, 0.3219752754296894559, 0.3333333333333333703, 0.3219752754296894559, 0.3333333333333333703, 0.3219752754296894559, 0.3333333333333333703, 0.3219752754296894559, 0.3333333333333333703, 0.3219752754296894559, 0.3333333333333333703, 0.3219752754296894559, 0.3333333333333333703, 0.3219752754296894559, 0.3333333333333333703, 0.3219752754296894559, 0.3333333333333333703, 0.3219752754296894559, 0.3333333333333333703, 0.3219752754296894559, 0.3333333333333333703, 0.3219752754296894559, 0.3333333333333333703, 0.3219752754296894559, 0.3333333333333333703, 0.3219752754296894559, 0.3333333333333333703, 0.3219752754296894559, 0.3333333333333333703, 0.3219752754296894559, 0.3333333333333333703, 0.3219752754296894559, 0.3333333333333333703, 0.3219752754296894559, 0.3333333333333333703, 0.3219752754296894559, 0.3333333333333333703, 0.3219752754296894559, 0.3333333333333333703, 0.3219752754296894559, 0.3333333333333333703, 0.3219752754296894559, 0.3333333333333333703, 0.3219752754296894559, 0.3333333333333333703, 0.3219752754296894559, 0.3333333333333333703, 0.3219752754296894559, 0.3333333333333333703, 0.3219752754296894559, 0.3333333333333333703, 0.3219752754296894559, 0.3333333333333333703, 0.3219752754296894559, 0.3333333333333333703, 0.3219752754296894559, 0.3333333333333333703, 0.3219752754296894559, 0.3333333333333333703, 0.3219752754296894559, 0.3333333333333333703, 0.3219752754296894559, 0.3333333333333333703, 0.3219752754296894559, 0.3333333333333333703, 0.3219752754296894559, 0.3333333333333333703, 0.3219752754296894559, 0.3333333333333333703, 0.3219752754296894559, 0.3333333333333333703, 0.3219752754296894559, 0.3333333333333333703, 0.3219752754296894559, 0.3333333333333333703, 0.3219752754296894559, 0.3333333333333333703, 0.3219752754296894559, 0.3333333333333333703, 0.3219752754296894559, 0.3333333333333333703, 0.3219752754296894559, 0.3333333333333333703, 0.3219752754296894559, 0.3333333333333333703, 0.3219752754296894559, 0.3333333333333333703, 0.3219752754296894559, 0.3333333333333333703, 0.3219752754296894559, 0.3333333333333333703, 0.3219752754296894559, 0.3333333333333333703, 0.3219752754296894559, 0.3333333333333333703, 0.3219752754296894559, 0.3333333333333333703, 0.3219752754296894559, 0.3333333333333333703, 0.3219752754296894559, 0.3333333333333333703, 0.3219752754296894559, 0.3333333333333333703, 0.3219752754296894559, 0.3333333333333333703, 0.3219752754296894559, 0.3333333333333333703, 0.3219752754296894559, 0.3333333333333333703, 0.3219752754296894559, 0.3333333333333333703, 0.3219752754296894559, 0.3333333333333333703, 0.3219752754296894559, 0.3333333333333333703, 0.3219752754296894559, 0.3333333333333333703, 0.3219752754296894559, 0.3333333333333333703, 0.3219752754296894559, 0.3333333333333333703, 0.3219752754296894559, 0.3333333333333333703, 0.3219752754296894559, 0.3333333333333333703, 0.3219752754296894559, 0.3333333333333333703, 0.3219752754296894559, 0.3333333333333333703, 0.3219752754296894559, 0.3333333333333333703, 0.3219752754296894559, 0.3333333333333333703, 0.3219752754296894559, 0.3333333333333333703, 0.3219752754296894559, 0.3333333333333333703, 0.3219752754296894559, 0.3333333333333333703, 0.3219752754296894559, 0.3333333333333333703, 0.3219752754296894559, 0.3333333333333333703, 0.3219752754296894559, 0.3333333333333333703, 0.3219752754296894559, 0.3333333333333333703, 0.3219752754296894559, 0.3333333333333333703, 0.3219752754296894559, 0.3333333333333333703, 0.3219752754296894559, 0.3333333333333333703, 0.3219752754296894559, 0.3333333333333333703, 0.3219752754296894559, 0.3333333333333333703, 0.3219752754296894559, 0.3333333333333333703, 0.3219752754296894559, 0.3333333333333333703, 0.3219752754296894559, 0.3333333333333333703, 0.3219752754296894559, 0.3333333333333333703, 0.3219752754296894559, 0.3333333333333333703, 0.3219752754296894559, 0.3333333333333333703, 0.3219752754296894559, 0.3333333333333333703, 0.3219752754296894559, 0.3333333333333333703, 0.3219752754296894559, 0.3333333333333333703, 0.3219752754296894559, 0.3333333333333333703, 0.3219752754296894559, 0.3333333333333333703, 0.3219752754296894559, 0.3333333333333333703, 0.3219752754296894559, 0.3333333333333333703, 0.3219752754296894559, 0.3333333333333333703, 0.3219752754296894559, 0.3333333333333333703, 0.3219752754296894559, 0.3333333333333333703, 0.3219752754296894559, 0.3333333333333333703, 0.3219752754296894559, 0.3333333333333333703, 0.3219752754296894559, 0.3333333333333333703, 0.3219752754296894559, 0.3333333333333333703, 0.3219752754296894559, 0.3333333333333333703, 0.3219752754296894559, 0.3333333333333333703, 0.3219752754296894559, 0.3333333333333333703, 0.3219752754296894559, 0.3333333333333333703, 0.3219752754296894559, 0.3333333333333333703, 0.3219752754296894559, 0.3333333333333333703, 0.3219752754296894559, 0.3333333333333333703, 0.3219752754296894559, 0.3333333333333333703, 0.3219752754296894559, 0.3333333333333333703, 0.3219752754296894559, 0.3333333333333333703, 0.3219752754296894559, 0.3333333333333333703, 0.3219752754296894559, 0.3333333333333333703, 0.3219752754296894559, 0.3333333333333333703, 0.3219752754296894559, 0.3333333333333333703, 0.3219752754296894559, 0.3333333333333333703, 0.3219752754296894559, 0.3333333333333333703, 0.3219752754296894559, 0.3333333333333333703, 0.3219752754296894559, 0.3333333333333333703, 0.3219752754296894559, 0.3333333333333333703, 0.3219752754296894559, 0.3333333333333333703, 0.3219752754296894559, 0.3333333333333333703, 0.3219752754296894559, 0.3333333333333333703, 0.3219752754296894559, 0.3333333333333333703, 0.3219752754296894559, 0.3333333333333333703, 0.3219752754296894559, 0.3333333333333333703, 0.3219752754296894559, 0.3333333333333333703, 0.3219752754296894559, 0.3333333333333333703, 0.3219752754296894559, 0.3333333333333333703, 0.3219752754296894559, 0.3333333333333333703, 0.3219752754296894559, 0.3333333333333333703, 0.3219752754296894559, 0.3333333333333333703, 0.3219752754296894559, 0.3333333333333333703, 0.3219752754296894559, 0.3333333333333333703, 0.3219752754296894559, 0.3333333333333333703, 0.3219752754296894559, 0.3333333333333333703, 0.3219752754296894559, 0.3333333333333333703, 0.3219752754296894559, 0.3333333333333333703, 0.3219752754296894559, 0.3333333333333333703, 0.3219752754296894559, 0.3333333333333333703, 0.3219752754296894559, 0.3333333333333333703, 0.3219752754296894559, 0.3333333333333333703, 0.3219752754296894559, 0.3333333333333333703, 0.3219752754296894559, 0.3333333333333333703, 0.3219752754296894559, 0.3333333333333333703, 0.3219752754296894559, 0.3333333333333333703, 0.3219752754296894559, 0.3333333333333333703, 0.3219752754296894559, 0.3333333333333333703, 0.3219752754296894559, 0.3333333333333333703, 0.3219752754296894559, 0.3333333333333333703, 0.3219752754296894559, 0.3333333333333333703, 0.3219752754296894559, 0.3333333333333333703, 0.3219752754296894559, 0.3333333333333333703, 0.3219752754296894559, 0.3333333333333333703, 0.3219752754296894559, 0.3333333333333333703, 0.3219752754296894559, 0.3333333333333333703, 0.3219752754296894559, 0.3333333333333333703, 0.3219752754296894559, 0.3333333333333333703, 0.3219752754296894559, 0.3333333333333333703, 0.3219752754296894559, 0.3333333333333333703, 0.3219752754296894559, 0.3333333333333333703, 0.3219752754296894559, 0.3333333333333333703, 0.3219752754296894559, 0.3333333333333333703, 0.3219752754296894559, 0.3333333333333333703, 0.3219752754296894559, 0.3333333333333333703, 0.3219752754296894559, 0.3333333333333333703, 0.3219752754296894559, 0.3333333333333333703, 0.3219752754296894559, 0.3333333333333333703),
 ( 0.3333333333333333703, 0.3219752754296894559, 0.3333333333333333703, 0.3219752754296894559, 0.3333333333333333703, 0.3219752754296894559, 0.3333333333333333703, 0.3219752754296894559, 0.3333333333333333703, 0.3219752754296894559, 0.3333333333333333703, 0.3219752754296894559, 0.3333333333333333703, 0.3219752754296894559, 0.3333333333333333703, 0.3219752754296894559, 0.3333333333333333703, 0.3219752754296894559, 0.3333333333333333703, 0.3219752754296894559, 0.3333333333333333703, 0.3219752754296894559, 0.3333333333333333703, 0.3219752754296894559, 0.3333333333333333703, 0.3219752754296894559, 0.3333333333333333703, 0.3219752754296894559, 0.3333333333333333703, 0.3219752754296894559, 0.3333333333333333703, 0.3219752754296894559, 0.3333333333333333703, 0.3219752754296894559, 0.3333333333333333703, 0.3219752754296894559, 0.3333333333333333703, 0.3219752754296894559, 0.3333333333333333703, 0.3219752754296894559, 0.3333333333333333703, 0.3219752754296894559, 0.3333333333333333703, 0.3219752754296894559, 0.3333333333333333703, 0.3219752754296894559, 0.3333333333333333703, 0.3219752754296894559, 0.3333333333333333703, 0.3219752754296894559, 0.3333333333333333703, 0.3219752754296894559, 0.3333333333333333703, 0.3219752754296894559, 0.3333333333333333703, 0.3219752754296894559, 0.3333333333333333703, 0.3219752754296894559, 0.3333333333333333703, 0.3219752754296894559, 0.3333333333333333703, 0.3219752754296894559, 0.3333333333333333703, 0.3219752754296894559, 0.3333333333333333703, 0.3219752754296894559, 0.3333333333333333703, 0.3219752754296894559, 0.3333333333333333703, 0.3219752754296894559, 0.3333333333333333703, 0.3219752754296894559, 0.3333333333333333703, 0.3219752754296894559, 0.3333333333333333703, 0.3219752754296894559, 0.3333333333333333703, 0.3219752754296894559, 0.3333333333333333703, 0.3219752754296894559, 0.3333333333333333703, 0.3219752754296894559, 0.3333333333333333703, 0.3219752754296894559, 0.3333333333333333703, 0.3219752754296894559, 0.3333333333333333703, 0.3219752754296894559, 0.3333333333333333703, 0.3219752754296894559, 0.3333333333333333703, 0.3219752754296894559, 0.3333333333333333703, 0.3219752754296894559, 0.3333333333333333703, 0.3219752754296894559, 0.3333333333333333703, 0.3219752754296894559, 0.3333333333333333703, 0.3219752754296894559, 0.3333333333333333703, 0.3219752754296894559, 0.3333333333333333703, 0.3219752754296894559, 0.3333333333333333703, 0.3219752754296894559, 0.3333333333333333703, 0.3219752754296894559, 0.3333333333333333703, 0.3219752754296894559, 0.3333333333333333703, 0.3219752754296894559, 0.3333333333333333703, 0.3219752754296894559, 0.3333333333333333703, 0.3219752754296894559, 0.3333333333333333703, 0.3219752754296894559, 0.3333333333333333703, 0.3219752754296894559, 0.3333333333333333703, 0.3219752754296894559, 0.3333333333333333703, 0.3219752754296894559, 0.3333333333333333703, 0.3219752754296894559, 0.3333333333333333703, 0.3219752754296894559, 0.3333333333333333703, 0.3219752754296894559, 0.3333333333333333703, 0.3219752754296894559, 0.3333333333333333703, 0.3219752754296894559, 0.3333333333333333703, 0.3219752754296894559, 0.3333333333333333703, 0.3219752754296894559, 0.3333333333333333703, 0.3219752754296894559, 0.3333333333333333703, 0.3219752754296894559, 0.3333333333333333703, 0.3219752754296894559, 0.3333333333333333703, 0.3219752754296894559, 0.3333333333333333703, 0.3219752754296894559, 0.3333333333333333703, 0.3219752754296894559, 0.3333333333333333703, 0.3219752754296894559, 0.3333333333333333703, 0.3219752754296894559, 0.3333333333333333703, 0.3219752754296894559, 0.3333333333333333703, 0.3219752754296894559, 0.3333333333333333703, 0.3219752754296894559, 0.3333333333333333703, 0.3219752754296894559, 0.3333333333333333703, 0.3219752754296894559, 0.3333333333333333703, 0.3219752754296894559, 0.3333333333333333703, 0.3219752754296894559, 0.3333333333333333703, 0.3219752754296894559, 0.3333333333333333703, 0.3219752754296894559, 0.3333333333333333703, 0.3219752754296894559, 0.3333333333333333703, 0.3219752754296894559, 0.3333333333333333703, 0.3219752754296894559, 0.3333333333333333703, 0.3219752754296894559, 0.3333333333333333703, 0.3219752754296894559, 0.3333333333333333703, 0.3219752754296894559, 0.3333333333333333703, 0.3219752754296894559, 0.3333333333333333703, 0.3219752754296894559, 0.3333333333333333703, 0.3219752754296894559, 0.3333333333333333703, 0.3219752754296894559, 0.3333333333333333703, 0.3219752754296894559, 0.3333333333333333703, 0.3219752754296894559, 0.3333333333333333703, 0.3219752754296894559, 0.3333333333333333703, 0.3219752754296894559, 0.3333333333333333703, 0.3219752754296894559, 0.3333333333333333703, 0.3219752754296894559, 0.3333333333333333703, 0.3219752754296894559, 0.3333333333333333703, 0.3219752754296894559, 0.3333333333333333703, 0.3219752754296894559, 0.3333333333333333703, 0.3219752754296894559, 0.3333333333333333703, 0.3219752754296894559, 0.3333333333333333703, 0.3219752754296894559, 0.3333333333333333703, 0.3219752754296894559, 0.3333333333333333703, 0.3219752754296894559, 0.3333333333333333703, 0.3219752754296894559, 0.3333333333333333703, 0.3219752754296894559, 0.3333333333333333703, 0.3219752754296894559, 0.3333333333333333703, 0.3219752754296894559, 0.3333333333333333703, 0.3219752754296894559, 0.3333333333333333703, 0.3219752754296894559, 0.3333333333333333703, 0.3219752754296894559, 0.3333333333333333703, 0.3219752754296894559, 0.3333333333333333703, 0.3219752754296894559, 0.3333333333333333703, 0.3219752754296894559, 0.3333333333333333703, 0.3219752754296894559, 0.3333333333333333703, 0.3219752754296894559, 0.3333333333333333703, 0.3219752754296894559, 0.3333333333333333703, 0.3219752754296894559, 0.3333333333333333703, 0.3219752754296894559, 0.3333333333333333703, 0.3219752754296894559, 0.3333333333333333703, 0.3219752754296894559, 0.3333333333333333703, 0.3219752754296894559, 0.3333333333333333703, 0.3219752754296894559, 0.3333333333333333703, 0.3219752754296894559, 0.3333333333333333703, 0.3219752754296894559, 0.3333333333333333703, 0.3219752754296894559, 0.3333333333333333703, 0.3219752754296894559, 0.3333333333333333703, 0.3219752754296894559, 0.3333333333333333703, 0.3219752754296894559, 0.3333333333333333703, 0.3219752754296894559, 0.3333333333333333703, 0.3219752754296894559, 0.3333333333333333703, 0.3219752754296894559, 0.3333333333333333703, 0.3219752754296894559, 0.3333333333333333703, 0.3219752754296894559, 0.3333333333333333703, 0.3219752754296894559, 0.3333333333333333703, 0.3219752754296894559, 0.3333333333333333703, 0.3219752754296894559, 0.3333333333333333703, 0.3219752754296894559, 0.3333333333333333703, 0.3219752754296894559, 0.3333333333333333703, 0.3219752754296894559, 0.3333333333333333703, 0.3219752754296894559, 0.3333333333333333703, 0.3219752754296894559, 0.3333333333333333703, 0.3219752754296894559, 0.3333333333333333703, 0.3219752754296894559, 0.3333333333333333703, 0.3219752754296894559, 0.3333333333333333703, 0.3219752754296894559, 0.3333333333333333703, 0.3219752754296894559, 0.3333333333333333703, 0.3219752754296894559, 0.3333333333333333703, 0.3219752754296894559, 0.3333333333333333703, 0.3219752754296894559, 0.3333333333333333703, 0.3219752754296894559, 0.3333333333333333703, 0.3219752754296894559, 0.3333333333333333703, 0.3219752754296894559, 0.3333333333333333703, 0.3219752754296894559, 0.3333333333333333703, 0.3219752754296894559, 0.3333333333333333703, 0.3219752754296894559, 0.3333333333333333703, 0.3219752754296894559, 0.3333333333333333703, 0.3219752754296894559, 0.3333333333333333703, 0.3219752754296894559, 0.3333333333333333703, 0.3219752754296894559, 0.3333333333333333703, 0.3219752754296894559, 0.3333333333333333703, 0.3219752754296894559, 0.3333333333333333703, 0.3219752754296894559, 0.3333333333333333703, 0.3219752754296894559, 0.3333333333333333703, 0.3219752754296894559, 0.3333333333333333703, 0.3219752754296894559, 0.3333333333333333703, 0.3219752754296894559, 0.3333333333333333703, 0.3219752754296894559, 0.3333333333333333703, 0.3219752754296894559, 0.3333333333333333703, 0.3219752754296894559, 0.3333333333333333703, 0.3219752754296894559, 0.3333333333333333703, 0.3219752754296894559, 0.3333333333333333703, 0.3219752754296894559, 0.3333333333333333703, 0.3219752754296894559, 0.3333333333333333703, 0.3219752754296894559, 0.3333333333333333703, 0.3219752754296894559, 0.3333333333333333703, 0.3219752754296894559, 0.3333333333333333703, 0.3219752754296894559, 0.3333333333333333703, 0.3219752754296894559, 0.3333333333333333703, 0.3219752754296894559, 0.3333333333333333703, 0.3219752754296894559, 0.3333333333333333703, 0.3219752754296894559, 0.3333333333333333703, 0.3219752754296894559, 0.3333333333333333703, 0.3219752754296894559, 0.3333333333333333703, 0.3219752754296894559, 0.3333333333333333703, 0.3219752754296894559, 0.3333333333333333703, 0.3219752754296894559, 0.3333333333333333703, 0.3219752754296894559, 0.3333333333333333703, 0.3219752754296894559, 0.3333333333333333703, 0.3219752754296894559, 0.3333333333333333703, 0.3219752754296894559, 0.3333333333333333703, 0.3219752754296894559, 0.3333333333333333703, 0.3219752754296894559, 0.3333333333333333703, 0.3219752754296894559, 0.3333333333333333703, 0.3219752754296894559, 0.3333333333333333703, 0.3219752754296894559, 0.3333333333333333703, 0.3219752754296894559, 0.3333333333333333703, 0.3219752754296894559, 0.3333333333333333703, 0.3219752754296894559, 0.3333333333333333703, 0.3219752754296894559, 0.3333333333333333703, 0.3219752754296894559, 0.3333333333333333703, 0.3219752754296894559, 0.3333333333333333703, 0.3219752754296894559, 0.3333333333333333703, 0.3219752754296894559, 0.3333333333333333703, 0.3219752754296894559, 0.3333333333333333703, 0.3219752754296894559, 0.3333333333333333703, 0.3219752754296894559, 0.3333333333333333703, 0.3219752754296894559, 0.3333333333333333703, 0.3219752754296894559, 0.3333333333333333703, 0.3219752754296894559, 0.3333333333333333703, 0.3219752754296894559, 0.3333333333333333703, 0.3219752754296894559, 0.3333333333333333703, 0.3219752754296894559, 0.3333333333333333703, 0.3219752754296894559, 0.3333333333333333703, 0.3219752754296894559, 0.3333333333333333703, 0.3219752754296894559, 0.3333333333333333703, 0.3219752754296894559, 0.3333333333333333703, 0.3219752754296894559, 0.3333333333333333703, 0.3219752754296894559, 0.3333333333333333703, 0.3219752754296894559, 0.3333333333333333703, 0.3219752754296894559, 0.3333333333333333703, 0.3219752754296894559, 0.3333333333333333703),
 ( 1.000000000000000000, 0.9659258262890683122, 1.000000000000000000, 0.9659258262890683122, 1.000000000000000000, 0.9659258262890683122, 1.000000000000000000, 0.9659258262890683122, 1.000000000000000000, 0.9659258262890683122, 1.000000000000000000, 0.9659258262890683122, 1.000000000000000000, 0.9659258262890683122, 1.000000000000000000, 0.9659258262890683122, 1.000000000000000000, 0.9659258262890683122, 1.000000000000000000, 0.9659258262890683122, 1.000000000000000000, 0.9659258262890683122, 1.000000000000000000, 0.9659258262890683122, 1.000000000000000000, 0.9659258262890683122, 1.000000000000000000, 0.9659258262890683122, 1.000000000000000000, 0.9659258262890683122, 1.000000000000000000, 0.9659258262890683122, 1.000000000000000000, 0.9659258262890683122, 1.000000000000000000, 0.9659258262890683122, 1.000000000000000000, 0.9659258262890683122, 1.000000000000000000, 0.9659258262890683122, 1.000000000000000000, 0.9659258262890683122, 1.000000000000000000, 0.9659258262890683122, 1.000000000000000000, 0.9659258262890683122, 1.000000000000000000, 0.9659258262890683122, 1.000000000000000000, 0.9659258262890683122, 1.000000000000000000, 0.9659258262890683122, 1.000000000000000000, 0.9659258262890683122, 1.000000000000000000, 0.9659258262890683122, 1.000000000000000000, 0.9659258262890683122, 1.000000000000000000, 0.9659258262890683122, 1.000000000000000000, 0.9659258262890683122, 1.000000000000000000, 0.9659258262890683122, 1.000000000000000000, 0.9659258262890683122, 1.000000000000000000, 0.9659258262890683122, 1.000000000000000000, 0.9659258262890683122, 1.000000000000000000, 0.9659258262890683122, 1.000000000000000000, 0.9659258262890683122, 1.000000000000000000, 0.9659258262890683122, 1.000000000000000000, 0.9659258262890683122, 1.000000000000000000, 0.9659258262890683122, 1.000000000000000000, 0.9659258262890683122, 1.000000000000000000, 0.9659258262890683122, 1.000000000000000000, 0.9659258262890683122, 1.000000000000000000, 0.9659258262890683122, 1.000000000000000000, 0.9659258262890683122, 1.000000000000000000, 0.9659258262890683122, 1.000000000000000000, 0.9659258262890683122, 1.000000000000000000, 0.9659258262890683122, 1.000000000000000000, 0.9659258262890683122, 1.000000000000000000, 0.9659258262890683122, 1.000000000000000000, 0.9659258262890683122, 1.000000000000000000, 0.9659258262890683122, 1.000000000000000000, 0.9659258262890683122, 1.000000000000000000, 0.9659258262890683122, 1.000000000000000000, 0.9659258262890683122, 1.000000000000000000, 0.9659258262890683122, 1.000000000000000000, 0.9659258262890683122, 1.000000000000000000, 0.9659258262890683122, 1.000000000000000000, 0.9659258262890683122, 1.000000000000000000, 0.9659258262890683122, 1.000000000000000000, 0.9659258262890683122, 1.000000000000000000, 0.9659258262890683122, 1.000000000000000000, 0.9659258262890683122, 1.000000000000000000, 0.9659258262890683122, 1.000000000000000000, 0.9659258262890683122, 1.000000000000000000, 0.9659258262890683122, 1.000000000000000000, 0.9659258262890683122, 1.000000000000000000, 0.9659258262890683122, 1.000000000000000000, 0.9659258262890683122, 1.000000000000000000, 0.9659258262890683122, 1.000000000000000000, 0.9659258262890683122, 1.000000000000000000, 0.9659258262890683122, 1.000000000000000000, 0.9659258262890683122, 1.000000000000000000, 0.9659258262890683122, 1.000000000000000000, 0.9659258262890683122, 1.000000000000000000, 0.9659258262890683122, 1.000000000000000000, 0.9659258262890683122, 1.000000000000000000, 0.9659258262890683122, 1.000000000000000000, 0.9659258262890683122, 1.000000000000000000, 0.9659258262890683122, 1.000000000000000000, 0.9659258262890683122, 1.000000000000000000, 0.9659258262890683122, 1.000000000000000000, 0.9659258262890683122, 1.000000000000000000, 0.9659258262890683122, 1.000000000000000000, 0.9659258262890683122, 1.000000000000000000, 0.9659258262890683122, 1.000000000000000000, 0.9659258262890683122, 1.000000000000000000, 0.9659258262890683122, 1.000000000000000000, 0.9659258262890683122, 1.000000000000000000, 0.9659258262890683122, 1.000000000000000000, 0.9659258262890683122, 1.000000000000000000, 0.9659258262890683122, 1.000000000000000000, 0.9659258262890683122, 1.000000000000000000, 0.9659258262890683122, 1.000000000000000000, 0.9659258262890683122, 1.000000000000000000, 0.9659258262890683122, 1.000000000000000000, 0.9659258262890683122, 1.000000000000000000, 0.9659258262890683122, 1.000000000000000000, 0.9659258262890683122, 1.000000000000000000, 0.9659258262890683122, 1.000000000000000000, 0.9659258262890683122, 1.000000000000000000, 0.9659258262890683122, 1.000000000000000000, 0.9659258262890683122, 1.000000000000000000, 0.9659258262890683122, 1.000000000000000000, 0.9659258262890683122, 1.000000000000000000, 0.9659258262890683122, 1.000000000000000000, 0.9659258262890683122, 1.000000000000000000, 0.9659258262890683122, 1.000000000000000000, 0.9659258262890683122, 1.000000000000000000, 0.9659258262890683122, 1.000000000000000000, 0.9659258262890683122, 1.000000000000000000, 0.9659258262890683122, 1.000000000000000000, 0.9659258262890683122, 1.000000000000000000, 0.9659258262890683122, 1.000000000000000000, 0.9659258262890683122, 1.000000000000000000, 0.9659258262890683122, 1.000000000000000000, 0.9659258262890683122, 1.000000000000000000, 0.9659258262890683122, 1.000000000000000000, 0.9659258262890683122, 1.000000000000000000, 0.9659258262890683122, 1.000000000000000000, 0.9659258262890683122, 1.000000000000000000, 0.9659258262890683122, 1.000000000000000000, 0.9659258262890683122, 1.000000000000000000, 0.9659258262890683122, 1.000000000000000000, 0.9659258262890683122, 1.000000000000000000, 0.9659258262890683122, 1.000000000000000000, 0.9659258262890683122, 1.000000000000000000, 0.9659258262890683122, 1.000000000000000000, 0.9659258262890683122, 1.000000000000000000, 0.9659258262890683122, 1.000000000000000000, 0.9659258262890683122, 1.000000000000000000, 0.9659258262890683122, 1.000000000000000000, 0.9659258262890683122, 1.000000000000000000, 0.9659258262890683122, 1.000000000000000000, 0.9659258262890683122, 1.000000000000000000, 0.9659258262890683122, 1.000000000000000000, 0.9659258262890683122, 1.000000000000000000, 0.9659258262890683122, 1.000000000000000000, 0.9659258262890683122, 1.000000000000000000, 0.9659258262890683122, 1.000000000000000000, 0.9659258262890683122, 1.000000000000000000, 0.9659258262890683122, 1.000000000000000000, 0.9659258262890683122, 1.000000000000000000, 0.9659258262890683122, 1.000000000000000000, 0.9659258262890683122, 1.000000000000000000, 0.9659258262890683122, 1.000000000000000000, 0.9659258262890683122, 1.000000000000000000, 0.9659258262890683122, 1.000000000000000000, 0.9659258262890683122, 1.000000000000000000, 0.9659258262890683122, 1.000000000000000000, 0.9659258262890683122, 1.000000000000000000, 0.9659258262890683122, 1.000000000000000000, 0.9659258262890683122, 1.000000000000000000, 0.9659258262890683122, 1.000000000000000000, 0.9659258262890683122, 1.000000000000000000, 0.9659258262890683122, 1.000000000000000000, 0.9659258262890683122, 1.000000000000000000, 0.9659258262890683122, 1.000000000000000000, 0.9659258262890683122, 1.000000000000000000, 0.9659258262890683122, 1.000000000000000000, 0.9659258262890683122, 1.000000000000000000, 0.9659258262890683122, 1.000000000000000000, 0.9659258262890683122, 1.000000000000000000, 0.9659258262890683122, 1.000000000000000000, 0.9659258262890683122, 1.000000000000000000, 0.9659258262890683122, 1.000000000000000000, 0.9659258262890683122, 1.000000000000000000, 0.9659258262890683122, 1.000000000000000000, 0.9659258262890683122, 1.000000000000000000, 0.9659258262890683122, 1.000000000000000000, 0.9659258262890683122, 1.000000000000000000, 0.9659258262890683122, 1.000000000000000000, 0.9659258262890683122, 1.000000000000000000, 0.9659258262890683122, 1.000000000000000000, 0.9659258262890683122, 1.000000000000000000, 0.9659258262890683122, 1.000000000000000000, 0.9659258262890683122, 1.000000000000000000, 0.9659258262890683122, 1.000000000000000000, 0.9659258262890683122, 1.000000000000000000, 0.9659258262890683122, 1.000000000000000000, 0.9659258262890683122, 1.000000000000000000, 0.9659258262890683122, 1.000000000000000000, 0.9659258262890683122, 1.000000000000000000, 0.9659258262890683122, 1.000000000000000000, 0.9659258262890683122, 1.000000000000000000, 0.9659258262890683122, 1.000000000000000000, 0.9659258262890683122, 1.000000000000000000, 0.9659258262890683122, 1.000000000000000000, 0.9659258262890683122, 1.000000000000000000, 0.9659258262890683122, 1.000000000000000000, 0.9659258262890683122, 1.000000000000000000, 0.9659258262890683122, 1.000000000000000000, 0.9659258262890683122, 1.000000000000000000, 0.9659258262890683122, 1.000000000000000000, 0.9659258262890683122, 1.000000000000000000, 0.9659258262890683122, 1.000000000000000000, 0.9659258262890683122, 1.000000000000000000, 0.9659258262890683122, 1.000000000000000000, 0.9659258262890683122, 1.000000000000000000, 0.9659258262890683122, 1.000000000000000000, 0.9659258262890683122, 1.000000000000000000, 0.9659258262890683122, 1.000000000000000000, 0.9659258262890683122, 1.000000000000000000, 0.9659258262890683122, 1.000000000000000000, 0.9659258262890683122, 1.000000000000000000, 0.9659258262890683122, 1.000000000000000000, 0.9659258262890683122, 1.000000000000000000, 0.9659258262890683122, 1.000000000000000000, 0.9659258262890683122, 1.000000000000000000, 0.9659258262890683122, 1.000000000000000000, 0.9659258262890683122, 1.000000000000000000, 0.9659258262890683122, 1.000000000000000000, 0.9659258262890683122, 1.000000000000000000, 0.9659258262890683122, 1.000000000000000000, 0.9659258262890683122, 1.000000000000000000, 0.9659258262890683122, 1.000000000000000000, 0.9659258262890683122, 1.000000000000000000, 0.9659258262890683122, 1.000000000000000000, 0.9659258262890683122, 1.000000000000000000, 0.9659258262890683122, 1.000000000000000000, 0.9659258262890683122, 1.000000000000000000, 0.9659258262890683122, 1.000000000000000000, 0.9659258262890683122, 1.000000000000000000, 0.9659258262890683122, 1.000000000000000000, 0.9659258262890683122, 1.000000000000000000, 0.9659258262890683122, 1.000000000000000000, 0.9659258262890683122, 1.000000000000000000, 0.9659258262890683122, 1.000000000000000000),
 ( 0.3333333333333333703, 0.3219752754296894559, 0.3333333333333333703, 0.3219752754296894559, 0.3333333333333333703, 0.3219752754296894559, 0.3333333333333333703, 0.3219752754296894559, 0.3333333333333333703, 0.3219752754296894559, 0.3333333333333333703, 0.3219752754296894559, 0.3333333333333333703, 0.3219752754296894559, 0.3333333333333333703, 0.3219752754296894559, 0.3333333333333333703, 0.3219752754296894559, 0.3333333333333333703, 0.3219752754296894559, 0.3333333333333333703, 0.3219752754296894559, 0.3333333333333333703, 0.3219752754296894559, 0.3333333333333333703, 0.3219752754296894559, 0.3333333333333333703, 0.3219752754296894559, 0.3333333333333333703, 0.3219752754296894559, 0.3333333333333333703, 0.3219752754296894559, 0.3333333333333333703, 0.3219752754296894559, 0.3333333333333333703, 0.3219752754296894559, 0.3333333333333333703, 0.3219752754296894559, 0.3333333333333333703, 0.3219752754296894559, 0.3333333333333333703, 0.3219752754296894559, 0.3333333333333333703, 0.3219752754296894559, 0.3333333333333333703, 0.3219752754296894559, 0.3333333333333333703, 0.3219752754296894559, 0.3333333333333333703, 0.3219752754296894559, 0.3333333333333333703, 0.3219752754296894559, 0.3333333333333333703, 0.3219752754296894559, 0.3333333333333333703, 0.3219752754296894559, 0.3333333333333333703, 0.3219752754296894559, 0.3333333333333333703, 0.3219752754296894559, 0.3333333333333333703, 0.3219752754296894559, 0.3333333333333333703, 0.3219752754296894559, 0.3333333333333333703, 0.3219752754296894559, 0.3333333333333333703, 0.3219752754296894559, 0.3333333333333333703, 0.3219752754296894559, 0.3333333333333333703, 0.3219752754296894559, 0.3333333333333333703, 0.3219752754296894559, 0.3333333333333333703, 0.3219752754296894559, 0.3333333333333333703, 0.3219752754296894559, 0.3333333333333333703, 0.3219752754296894559, 0.3333333333333333703, 0.3219752754296894559, 0.3333333333333333703, 0.3219752754296894559, 0.3333333333333333703, 0.3219752754296894559, 0.3333333333333333703, 0.3219752754296894559, 0.3333333333333333703, 0.3219752754296894559, 0.3333333333333333703, 0.3219752754296894559, 0.3333333333333333703, 0.3219752754296894559, 0.3333333333333333703, 0.3219752754296894559, 0.3333333333333333703, 0.3219752754296894559, 0.3333333333333333703, 0.3219752754296894559, 0.3333333333333333703, 0.3219752754296894559, 0.3333333333333333703, 0.3219752754296894559, 0.3333333333333333703, 0.3219752754296894559, 0.3333333333333333703, 0.3219752754296894559, 0.3333333333333333703, 0.3219752754296894559, 0.3333333333333333703, 0.3219752754296894559, 0.3333333333333333703, 0.3219752754296894559, 0.3333333333333333703, 0.3219752754296894559, 0.3333333333333333703, 0.3219752754296894559, 0.3333333333333333703, 0.3219752754296894559, 0.3333333333333333703, 0.3219752754296894559, 0.3333333333333333703, 0.3219752754296894559, 0.3333333333333333703, 0.3219752754296894559, 0.3333333333333333703, 0.3219752754296894559, 0.3333333333333333703, 0.3219752754296894559, 0.3333333333333333703, 0.3219752754296894559, 0.3333333333333333703, 0.3219752754296894559, 0.3333333333333333703, 0.3219752754296894559, 0.3333333333333333703, 0.3219752754296894559, 0.3333333333333333703, 0.3219752754296894559, 0.3333333333333333703, 0.3219752754296894559, 0.3333333333333333703, 0.3219752754296894559, 0.3333333333333333703, 0.3219752754296894559, 0.3333333333333333703, 0.3219752754296894559, 0.3333333333333333703, 0.3219752754296894559, 0.3333333333333333703, 0.3219752754296894559, 0.3333333333333333703, 0.3219752754296894559, 0.3333333333333333703, 0.3219752754296894559, 0.3333333333333333703, 0.3219752754296894559, 0.3333333333333333703, 0.3219752754296894559, 0.3333333333333333703, 0.3219752754296894559, 0.3333333333333333703, 0.3219752754296894559, 0.3333333333333333703, 0.3219752754296894559, 0.3333333333333333703, 0.3219752754296894559, 0.3333333333333333703, 0.3219752754296894559, 0.3333333333333333703, 0.3219752754296894559, 0.3333333333333333703, 0.3219752754296894559, 0.3333333333333333703, 0.3219752754296894559, 0.3333333333333333703, 0.3219752754296894559, 0.3333333333333333703, 0.3219752754296894559, 0.3333333333333333703, 0.3219752754296894559, 0.3333333333333333703, 0.3219752754296894559, 0.3333333333333333703, 0.3219752754296894559, 0.3333333333333333703, 0.3219752754296894559, 0.3333333333333333703, 0.3219752754296894559, 0.3333333333333333703, 0.3219752754296894559, 0.3333333333333333703, 0.3219752754296894559, 0.3333333333333333703, 0.3219752754296894559, 0.3333333333333333703, 0.3219752754296894559, 0.3333333333333333703, 0.3219752754296894559, 0.3333333333333333703, 0.3219752754296894559, 0.3333333333333333703, 0.3219752754296894559, 0.3333333333333333703, 0.3219752754296894559, 0.3333333333333333703, 0.3219752754296894559, 0.3333333333333333703, 0.3219752754296894559, 0.3333333333333333703, 0.3219752754296894559, 0.3333333333333333703, 0.3219752754296894559, 0.3333333333333333703, 0.3219752754296894559, 0.3333333333333333703, 0.3219752754296894559, 0.3333333333333333703, 0.3219752754296894559, 0.3333333333333333703, 0.3219752754296894559, 0.3333333333333333703, 0.3219752754296894559, 0.3333333333333333703, 0.3219752754296894559, 0.3333333333333333703, 0.3219752754296894559, 0.3333333333333333703, 0.3219752754296894559, 0.3333333333333333703, 0.3219752754296894559, 0.3333333333333333703, 0.3219752754296894559, 0.3333333333333333703, 0.3219752754296894559, 0.3333333333333333703, 0.3219752754296894559, 0.3333333333333333703, 0.3219752754296894559, 0.3333333333333333703, 0.3219752754296894559, 0.3333333333333333703, 0.3219752754296894559, 0.3333333333333333703, 0.3219752754296894559, 0.3333333333333333703, 0.3219752754296894559, 0.3333333333333333703, 0.3219752754296894559, 0.3333333333333333703, 0.3219752754296894559, 0.3333333333333333703, 0.3219752754296894559, 0.3333333333333333703, 0.3219752754296894559, 0.3333333333333333703, 0.3219752754296894559, 0.3333333333333333703, 0.3219752754296894559, 0.3333333333333333703, 0.3219752754296894559, 0.3333333333333333703, 0.3219752754296894559, 0.3333333333333333703, 0.3219752754296894559, 0.3333333333333333703, 0.3219752754296894559, 0.3333333333333333703, 0.3219752754296894559, 0.3333333333333333703, 0.3219752754296894559, 0.3333333333333333703, 0.3219752754296894559, 0.3333333333333333703, 0.3219752754296894559, 0.3333333333333333703, 0.3219752754296894559, 0.3333333333333333703, 0.3219752754296894559, 0.3333333333333333703, 0.3219752754296894559, 0.3333333333333333703, 0.3219752754296894559, 0.3333333333333333703, 0.3219752754296894559, 0.3333333333333333703, 0.3219752754296894559, 0.3333333333333333703, 0.3219752754296894559, 0.3333333333333333703, 0.3219752754296894559, 0.3333333333333333703, 0.3219752754296894559, 0.3333333333333333703, 0.3219752754296894559, 0.3333333333333333703, 0.3219752754296894559, 0.3333333333333333703, 0.3219752754296894559, 0.3333333333333333703, 0.3219752754296894559, 0.3333333333333333703, 0.3219752754296894559, 0.3333333333333333703, 0.3219752754296894559, 0.3333333333333333703, 0.3219752754296894559, 0.3333333333333333703, 0.3219752754296894559, 0.3333333333333333703, 0.3219752754296894559, 0.3333333333333333703, 0.3219752754296894559, 0.3333333333333333703, 0.3219752754296894559, 0.3333333333333333703, 0.3219752754296894559, 0.3333333333333333703, 0.3219752754296894559, 0.3333333333333333703, 0.3219752754296894559, 0.3333333333333333703, 0.3219752754296894559, 0.3333333333333333703, 0.3219752754296894559, 0.3333333333333333703, 0.3219752754296894559, 0.3333333333333333703, 0.3219752754296894559, 0.3333333333333333703, 0.3219752754296894559, 0.3333333333333333703, 0.3219752754296894559, 0.3333333333333333703, 0.3219752754296894559, 0.3333333333333333703, 0.3219752754296894559, 0.3333333333333333703, 0.3219752754296894559, 0.3333333333333333703, 0.3219752754296894559, 0.3333333333333333703, 0.3219752754296894559, 0.3333333333333333703, 0.3219752754296894559, 0.3333333333333333703, 0.3219752754296894559, 0.3333333333333333703, 0.3219752754296894559, 0.3333333333333333703, 0.3219752754296894559, 0.3333333333333333703, 0.3219752754296894559, 0.3333333333333333703, 0.3219752754296894559, 0.3333333333333333703, 0.3219752754296894559, 0.3333333333333333703, 0.3219752754296894559, 0.3333333333333333703, 0.3219752754296894559, 0.3333333333333333703, 0.3219752754296894559, 0.3333333333333333703, 0.3219752754296894559, 0.3333333333333333703, 0.3219752754296894559, 0.3333333333333333703, 0.3219752754296894559, 0.3333333333333333703, 0.3219752754296894559, 0.3333333333333333703, 0.3219752754296894559, 0.3333333333333333703, 0.3219752754296894559, 0.3333333333333333703, 0.3219752754296894559, 0.3333333333333333703, 0.3219752754296894559, 0.3333333333333333703, 0.3219752754296894559, 0.3333333333333333703, 0.3219752754296894559, 0.3333333333333333703, 0.3219752754296894559, 0.3333333333333333703, 0.3219752754296894559, 0.3333333333333333703, 0.3219752754296894559, 0.3333333333333333703, 0.3219752754296894559, 0.3333333333333333703, 0.3219752754296894559, 0.3333333333333333703, 0.3219752754296894559, 0.3333333333333333703, 0.3219752754296894559, 0.3333333333333333703, 0.3219752754296894559, 0.3333333333333333703, 0.3219752754296894559, 0.3333333333333333703, 0.3219752754296894559, 0.3333333333333333703, 0.3219752754296894559, 0.3333333333333333703, 0.3219752754296894559, 0.3333333333333333703, 0.3219752754296894559, 0.3333333333333333703, 0.3219752754296894559, 0.3333333333333333703, 0.3219752754296894559, 0.3333333333333333703, 0.3219752754296894559, 0.3333333333333333703, 0.3219752754296894559, 0.3333333333333333703, 0.3219752754296894559, 0.3333333333333333703, 0.3219752754296894559, 0.3333333333333333703, 0.3219752754296894559, 0.3333333333333333703, 0.3219752754296894559, 0.3333333333333333703, 0.3219752754296894559, 0.3333333333333333703, 0.3219752754296894559, 0.3333333333333333703, 0.3219752754296894559, 0.3333333333333333703, 0.3219752754296894559, 0.3333333333333333703, 0.3219752754296894559, 0.3333333333333333703, 0.3219752754296894559, 0.3333333333333333703, 0.3219752754296894559, 0.3333333333333333703, 0.3219752754296894559, 0.3333333333333333703, 0.3219752754296894559, 0.3333333333333333703, 0.3219752754296894559, 0.3333333333333333703, 0.3219752754296894559, 0.3333333333333333703, 0.3219752754296894559, 0.3333333333333333703, 0.3219752754296894559, 0.3333333333333333703, 0.3219752754296894559, 0.3333333333333333703, 0.3219752754296894559, 0.3333333333333333703),
 ( 0.3333333333333333703, 0.3219752754296894559, 0.3333333333333333703, 0.3219752754296894559, 0.3333333333333333703, 0.3219752754296894559, 0.3333333333333333703, 0.3219752754296894559, 0.3333333333333333703, 0.3219752754296894559, 0.3333333333333333703, 0.3219752754296894559, 0.3333333333333333703, 0.3219752754296894559, 0.3333333333333333703, 0.3219752754296894559, 0.3333333333333333703, 0.3219752754296894559, 0.3333333333333333703, 0.3219752754296894559, 0.3333333333333333703, 0.3219752754296894559, 0.3333333333333333703, 0.3219752754296894559, 0.3333333333333333703, 0.3219752754296894559, 0.3333333333333333703, 0.3219752754296894559, 0.3333333333333333703, 0.3219752754296894559, 0.3333333333333333703, 0.3219752754296894559, 0.3333333333333333703, 0.3219752754296894559, 0.3333333333333333703, 0.3219752754296894559, 0.3333333333333333703, 0.3219752754296894559, 0.3333333333333333703, 0.3219752754296894559, 0.3333333333333333703, 0.3219752754296894559, 0.3333333333333333703, 0.3219752754296894559, 0.3333333333333333703, 0.3219752754296894559, 0.3333333333333333703, 0.3219752754296894559, 0.3333333333333333703, 0.3219752754296894559, 0.3333333333333333703, 0.3219752754296894559, 0.3333333333333333703, 0.3219752754296894559, 0.3333333333333333703, 0.3219752754296894559, 0.3333333333333333703, 0.3219752754296894559, 0.3333333333333333703, 0.3219752754296894559, 0.3333333333333333703, 0.3219752754296894559, 0.3333333333333333703, 0.3219752754296894559, 0.3333333333333333703, 0.3219752754296894559, 0.3333333333333333703, 0.3219752754296894559, 0.3333333333333333703, 0.3219752754296894559, 0.3333333333333333703, 0.3219752754296894559, 0.3333333333333333703, 0.3219752754296894559, 0.3333333333333333703, 0.3219752754296894559, 0.3333333333333333703, 0.3219752754296894559, 0.3333333333333333703, 0.3219752754296894559, 0.3333333333333333703, 0.3219752754296894559, 0.3333333333333333703, 0.3219752754296894559, 0.3333333333333333703, 0.3219752754296894559, 0.3333333333333333703, 0.3219752754296894559, 0.3333333333333333703, 0.3219752754296894559, 0.3333333333333333703, 0.3219752754296894559, 0.3333333333333333703, 0.3219752754296894559, 0.3333333333333333703, 0.3219752754296894559, 0.3333333333333333703, 0.3219752754296894559, 0.3333333333333333703, 0.3219752754296894559, 0.3333333333333333703, 0.3219752754296894559, 0.3333333333333333703, 0.3219752754296894559, 0.3333333333333333703, 0.3219752754296894559, 0.3333333333333333703, 0.3219752754296894559, 0.3333333333333333703, 0.3219752754296894559, 0.3333333333333333703, 0.3219752754296894559, 0.3333333333333333703, 0.3219752754296894559, 0.3333333333333333703, 0.3219752754296894559, 0.3333333333333333703, 0.3219752754296894559, 0.3333333333333333703, 0.3219752754296894559, 0.3333333333333333703, 0.3219752754296894559, 0.3333333333333333703, 0.3219752754296894559, 0.3333333333333333703, 0.3219752754296894559, 0.3333333333333333703, 0.3219752754296894559, 0.3333333333333333703, 0.3219752754296894559, 0.3333333333333333703, 0.3219752754296894559, 0.3333333333333333703, 0.3219752754296894559, 0.3333333333333333703, 0.3219752754296894559, 0.3333333333333333703, 0.3219752754296894559, 0.3333333333333333703, 0.3219752754296894559, 0.3333333333333333703, 0.3219752754296894559, 0.3333333333333333703, 0.3219752754296894559, 0.3333333333333333703, 0.3219752754296894559, 0.3333333333333333703, 0.3219752754296894559, 0.3333333333333333703, 0.3219752754296894559, 0.3333333333333333703, 0.3219752754296894559, 0.3333333333333333703, 0.3219752754296894559, 0.3333333333333333703, 0.3219752754296894559, 0.3333333333333333703, 0.3219752754296894559, 0.3333333333333333703, 0.3219752754296894559, 0.3333333333333333703, 0.3219752754296894559, 0.3333333333333333703, 0.3219752754296894559, 0.3333333333333333703, 0.3219752754296894559, 0.3333333333333333703, 0.3219752754296894559, 0.3333333333333333703, 0.3219752754296894559, 0.3333333333333333703, 0.3219752754296894559, 0.3333333333333333703, 0.3219752754296894559, 0.3333333333333333703, 0.3219752754296894559, 0.3333333333333333703, 0.3219752754296894559, 0.3333333333333333703, 0.3219752754296894559, 0.3333333333333333703, 0.3219752754296894559, 0.3333333333333333703, 0.3219752754296894559, 0.3333333333333333703, 0.3219752754296894559, 0.3333333333333333703, 0.3219752754296894559, 0.3333333333333333703, 0.3219752754296894559, 0.3333333333333333703, 0.3219752754296894559, 0.3333333333333333703, 0.3219752754296894559, 0.3333333333333333703, 0.3219752754296894559, 0.3333333333333333703, 0.3219752754296894559, 0.3333333333333333703, 0.3219752754296894559, 0.3333333333333333703, 0.3219752754296894559, 0.3333333333333333703, 0.3219752754296894559, 0.3333333333333333703, 0.3219752754296894559, 0.3333333333333333703, 0.3219752754296894559, 0.3333333333333333703, 0.3219752754296894559, 0.3333333333333333703, 0.3219752754296894559, 0.3333333333333333703, 0.3219752754296894559, 0.3333333333333333703, 0.3219752754296894559, 0.3333333333333333703, 0.3219752754296894559, 0.3333333333333333703, 0.3219752754296894559, 0.3333333333333333703, 0.3219752754296894559, 0.3333333333333333703, 0.3219752754296894559, 0.3333333333333333703, 0.3219752754296894559, 0.3333333333333333703, 0.3219752754296894559, 0.3333333333333333703, 0.3219752754296894559, 0.3333333333333333703, 0.3219752754296894559, 0.3333333333333333703, 0.3219752754296894559, 0.3333333333333333703, 0.3219752754296894559, 0.3333333333333333703, 0.3219752754296894559, 0.3333333333333333703, 0.3219752754296894559, 0.3333333333333333703, 0.3219752754296894559, 0.3333333333333333703, 0.3219752754296894559, 0.3333333333333333703, 0.3219752754296894559, 0.3333333333333333703, 0.3219752754296894559, 0.3333333333333333703, 0.3219752754296894559, 0.3333333333333333703, 0.3219752754296894559, 0.3333333333333333703, 0.3219752754296894559, 0.3333333333333333703, 0.3219752754296894559, 0.3333333333333333703, 0.3219752754296894559, 0.3333333333333333703, 0.3219752754296894559, 0.3333333333333333703, 0.3219752754296894559, 0.3333333333333333703, 0.3219752754296894559, 0.3333333333333333703, 0.3219752754296894559, 0.3333333333333333703, 0.3219752754296894559, 0.3333333333333333703, 0.3219752754296894559, 0.3333333333333333703, 0.3219752754296894559, 0.3333333333333333703, 0.3219752754296894559, 0.3333333333333333703, 0.3219752754296894559, 0.3333333333333333703, 0.3219752754296894559, 0.3333333333333333703, 0.3219752754296894559, 0.3333333333333333703, 0.3219752754296894559, 0.3333333333333333703, 0.3219752754296894559, 0.3333333333333333703, 0.3219752754296894559, 0.3333333333333333703, 0.3219752754296894559, 0.3333333333333333703, 0.3219752754296894559, 0.3333333333333333703, 0.3219752754296894559, 0.3333333333333333703, 0.3219752754296894559, 0.3333333333333333703, 0.3219752754296894559, 0.3333333333333333703, 0.3219752754296894559, 0.3333333333333333703, 0.3219752754296894559, 0.3333333333333333703, 0.3219752754296894559, 0.3333333333333333703, 0.3219752754296894559, 0.3333333333333333703, 0.3219752754296894559, 0.3333333333333333703, 0.3219752754296894559, 0.3333333333333333703, 0.3219752754296894559, 0.3333333333333333703, 0.3219752754296894559, 0.3333333333333333703, 0.3219752754296894559, 0.3333333333333333703, 0.3219752754296894559, 0.3333333333333333703, 0.3219752754296894559, 0.3333333333333333703, 0.3219752754296894559, 0.3333333333333333703, 0.3219752754296894559, 0.3333333333333333703, 0.3219752754296894559, 0.3333333333333333703, 0.3219752754296894559, 0.3333333333333333703, 0.3219752754296894559, 0.3333333333333333703, 0.3219752754296894559, 0.3333333333333333703, 0.3219752754296894559, 0.3333333333333333703, 0.3219752754296894559, 0.3333333333333333703, 0.3219752754296894559, 0.3333333333333333703, 0.3219752754296894559, 0.3333333333333333703, 0.3219752754296894559, 0.3333333333333333703, 0.3219752754296894559, 0.3333333333333333703, 0.3219752754296894559, 0.3333333333333333703, 0.3219752754296894559, 0.3333333333333333703, 0.3219752754296894559, 0.3333333333333333703, 0.3219752754296894559, 0.3333333333333333703, 0.3219752754296894559, 0.3333333333333333703, 0.3219752754296894559, 0.3333333333333333703, 0.3219752754296894559, 0.3333333333333333703, 0.3219752754296894559, 0.3333333333333333703, 0.3219752754296894559, 0.3333333333333333703, 0.3219752754296894559, 0.3333333333333333703, 0.3219752754296894559, 0.3333333333333333703, 0.3219752754296894559, 0.3333333333333333703, 0.3219752754296894559, 0.3333333333333333703, 0.3219752754296894559, 0.3333333333333333703, 0.3219752754296894559, 0.3333333333333333703, 0.3219752754296894559, 0.3333333333333333703, 0.3219752754296894559, 0.3333333333333333703, 0.3219752754296894559, 0.3333333333333333703, 0.3219752754296894559, 0.3333333333333333703, 0.3219752754296894559, 0.3333333333333333703, 0.3219752754296894559, 0.3333333333333333703, 0.3219752754296894559, 0.3333333333333333703, 0.3219752754296894559, 0.3333333333333333703, 0.3219752754296894559, 0.3333333333333333703, 0.3219752754296894559, 0.3333333333333333703, 0.3219752754296894559, 0.3333333333333333703, 0.3219752754296894559, 0.3333333333333333703, 0.3219752754296894559, 0.3333333333333333703, 0.3219752754296894559, 0.3333333333333333703, 0.3219752754296894559, 0.3333333333333333703, 0.3219752754296894559, 0.3333333333333333703, 0.3219752754296894559, 0.3333333333333333703, 0.3219752754296894559, 0.3333333333333333703, 0.3219752754296894559, 0.3333333333333333703, 0.3219752754296894559, 0.3333333333333333703, 0.3219752754296894559, 0.3333333333333333703, 0.3219752754296894559, 0.3333333333333333703, 0.3219752754296894559, 0.3333333333333333703, 0.3219752754296894559, 0.3333333333333333703, 0.3219752754296894559, 0.3333333333333333703, 0.3219752754296894559, 0.3333333333333333703, 0.3219752754296894559, 0.3333333333333333703, 0.3219752754296894559, 0.3333333333333333703, 0.3219752754296894559, 0.3333333333333333703, 0.3219752754296894559, 0.3333333333333333703, 0.3219752754296894559, 0.3333333333333333703, 0.3219752754296894559, 0.3333333333333333703, 0.3219752754296894559, 0.3333333333333333703, 0.3219752754296894559, 0.3333333333333333703, 0.3219752754296894559, 0.3333333333333333703, 0.3219752754296894559, 0.3333333333333333703, 0.3219752754296894559, 0.3333333333333333703, 0.3219752754296894559, 0.3333333333333333703, 0.3219752754296894559, 0.3333333333333333703, 0.3219752754296894559, 0.3333333333333333703, 0.3219752754296894559, 0.3333333333333333703, 0.3219752754296894559, 0.3333333333333333703),
 ( 1.000000000000000000, 0.9659258262890683122, 1.000000000000000000, 0.9659258262890683122, 1.000000000000000000, 0.9659258262890683122, 1.000000000000000000, 0.9659258262890683122, 1.000000000000000000, 0.9659258262890683122, 1.000000000000000000, 0.9659258262890683122, 1.000000000000000000, 0.9659258262890683122, 1.000000000000000000, 0.9659258262890683122, 1.000000000000000000, 0.9659258262890683122, 1.000000000000000000, 0.9659258262890683122, 1.000000000000000000, 0.9659258262890683122, 1.000000000000000000, 0.9659258262890683122, 1.000000000000000000, 0.9659258262890683122, 1.000000000000000000, 0.9659258262890683122, 1.000000000000000000, 0.9659258262890683122, 1.000000000000000000, 0.9659258262890683122, 1.000000000000000000, 0.9659258262890683122, 1.000000000000000000, 0.9659258262890683122, 1.000000000000000000, 0.9659258262890683122, 1.000000000000000000, 0.9659258262890683122, 1.000000000000000000, 0.9659258262890683122, 1.000000000000000000, 0.9659258262890683122, 1.000000000000000000, 0.9659258262890683122, 1.000000000000000000, 0.9659258262890683122, 1.000000000000000000, 0.9659258262890683122, 1.000000000000000000, 0.9659258262890683122, 1.000000000000000000, 0.9659258262890683122, 1.000000000000000000, 0.9659258262890683122, 1.000000000000000000, 0.9659258262890683122, 1.000000000000000000, 0.9659258262890683122, 1.000000000000000000, 0.9659258262890683122, 1.000000000000000000, 0.9659258262890683122, 1.000000000000000000, 0.9659258262890683122, 1.000000000000000000, 0.9659258262890683122, 1.000000000000000000, 0.9659258262890683122, 1.000000000000000000, 0.9659258262890683122, 1.000000000000000000, 0.9659258262890683122, 1.000000000000000000, 0.9659258262890683122, 1.000000000000000000, 0.9659258262890683122, 1.000000000000000000, 0.9659258262890683122, 1.000000000000000000, 0.9659258262890683122, 1.000000000000000000, 0.9659258262890683122, 1.000000000000000000, 0.9659258262890683122, 1.000000000000000000, 0.9659258262890683122, 1.000000000000000000, 0.9659258262890683122, 1.000000000000000000, 0.9659258262890683122, 1.000000000000000000, 0.9659258262890683122, 1.000000000000000000, 0.9659258262890683122, 1.000000000000000000, 0.9659258262890683122, 1.000000000000000000, 0.9659258262890683122, 1.000000000000000000, 0.9659258262890683122, 1.000000000000000000, 0.9659258262890683122, 1.000000000000000000, 0.9659258262890683122, 1.000000000000000000, 0.9659258262890683122, 1.000000000000000000, 0.9659258262890683122, 1.000000000000000000, 0.9659258262890683122, 1.000000000000000000, 0.9659258262890683122, 1.000000000000000000, 0.9659258262890683122, 1.000000000000000000, 0.9659258262890683122, 1.000000000000000000, 0.9659258262890683122, 1.000000000000000000, 0.9659258262890683122, 1.000000000000000000, 0.9659258262890683122, 1.000000000000000000, 0.9659258262890683122, 1.000000000000000000, 0.9659258262890683122, 1.000000000000000000, 0.9659258262890683122, 1.000000000000000000, 0.9659258262890683122, 1.000000000000000000, 0.9659258262890683122, 1.000000000000000000, 0.9659258262890683122, 1.000000000000000000, 0.9659258262890683122, 1.000000000000000000, 0.9659258262890683122, 1.000000000000000000, 0.9659258262890683122, 1.000000000000000000, 0.9659258262890683122, 1.000000000000000000, 0.9659258262890683122, 1.000000000000000000, 0.9659258262890683122, 1.000000000000000000, 0.9659258262890683122, 1.000000000000000000, 0.9659258262890683122, 1.000000000000000000, 0.9659258262890683122, 1.000000000000000000, 0.9659258262890683122, 1.000000000000000000, 0.9659258262890683122, 1.000000000000000000, 0.9659258262890683122, 1.000000000000000000, 0.9659258262890683122, 1.000000000000000000, 0.9659258262890683122, 1.000000000000000000, 0.9659258262890683122, 1.000000000000000000, 0.9659258262890683122, 1.000000000000000000, 0.9659258262890683122, 1.000000000000000000, 0.9659258262890683122, 1.000000000000000000, 0.9659258262890683122, 1.000000000000000000, 0.9659258262890683122, 1.000000000000000000, 0.9659258262890683122, 1.000000000000000000, 0.9659258262890683122, 1.000000000000000000, 0.9659258262890683122, 1.000000000000000000, 0.9659258262890683122, 1.000000000000000000, 0.9659258262890683122, 1.000000000000000000, 0.9659258262890683122, 1.000000000000000000, 0.9659258262890683122, 1.000000000000000000, 0.9659258262890683122, 1.000000000000000000, 0.9659258262890683122, 1.000000000000000000, 0.9659258262890683122, 1.000000000000000000, 0.9659258262890683122, 1.000000000000000000, 0.9659258262890683122, 1.000000000000000000, 0.9659258262890683122, 1.000000000000000000, 0.9659258262890683122, 1.000000000000000000, 0.9659258262890683122, 1.000000000000000000, 0.9659258262890683122, 1.000000000000000000, 0.9659258262890683122, 1.000000000000000000, 0.9659258262890683122, 1.000000000000000000, 0.9659258262890683122, 1.000000000000000000, 0.9659258262890683122, 1.000000000000000000, 0.9659258262890683122, 1.000000000000000000, 0.9659258262890683122, 1.000000000000000000, 0.9659258262890683122, 1.000000000000000000, 0.9659258262890683122, 1.000000000000000000, 0.9659258262890683122, 1.000000000000000000, 0.9659258262890683122, 1.000000000000000000, 0.9659258262890683122, 1.000000000000000000, 0.9659258262890683122, 1.000000000000000000, 0.9659258262890683122, 1.000000000000000000, 0.9659258262890683122, 1.000000000000000000, 0.9659258262890683122, 1.000000000000000000, 0.9659258262890683122, 1.000000000000000000, 0.9659258262890683122, 1.000000000000000000, 0.9659258262890683122, 1.000000000000000000, 0.9659258262890683122, 1.000000000000000000, 0.9659258262890683122, 1.000000000000000000, 0.9659258262890683122, 1.000000000000000000, 0.9659258262890683122, 1.000000000000000000, 0.9659258262890683122, 1.000000000000000000, 0.9659258262890683122, 1.000000000000000000, 0.9659258262890683122, 1.000000000000000000, 0.9659258262890683122, 1.000000000000000000, 0.9659258262890683122, 1.000000000000000000, 0.9659258262890683122, 1.000000000000000000, 0.9659258262890683122, 1.000000000000000000, 0.9659258262890683122, 1.000000000000000000, 0.9659258262890683122, 1.000000000000000000, 0.9659258262890683122, 1.000000000000000000, 0.9659258262890683122, 1.000000000000000000, 0.9659258262890683122, 1.000000000000000000, 0.9659258262890683122, 1.000000000000000000, 0.9659258262890683122, 1.000000000000000000, 0.9659258262890683122, 1.000000000000000000, 0.9659258262890683122, 1.000000000000000000, 0.9659258262890683122, 1.000000000000000000, 0.9659258262890683122, 1.000000000000000000, 0.9659258262890683122, 1.000000000000000000, 0.9659258262890683122, 1.000000000000000000, 0.9659258262890683122, 1.000000000000000000, 0.9659258262890683122, 1.000000000000000000, 0.9659258262890683122, 1.000000000000000000, 0.9659258262890683122, 1.000000000000000000, 0.9659258262890683122, 1.000000000000000000, 0.9659258262890683122, 1.000000000000000000, 0.9659258262890683122, 1.000000000000000000, 0.9659258262890683122, 1.000000000000000000, 0.9659258262890683122, 1.000000000000000000, 0.9659258262890683122, 1.000000000000000000, 0.9659258262890683122, 1.000000000000000000, 0.9659258262890683122, 1.000000000000000000, 0.9659258262890683122, 1.000000000000000000, 0.9659258262890683122, 1.000000000000000000, 0.9659258262890683122, 1.000000000000000000, 0.9659258262890683122, 1.000000000000000000, 0.9659258262890683122, 1.000000000000000000, 0.9659258262890683122, 1.000000000000000000, 0.9659258262890683122, 1.000000000000000000, 0.9659258262890683122, 1.000000000000000000, 0.9659258262890683122, 1.000000000000000000, 0.9659258262890683122, 1.000000000000000000, 0.9659258262890683122, 1.000000000000000000, 0.9659258262890683122, 1.000000000000000000, 0.9659258262890683122, 1.000000000000000000, 0.9659258262890683122, 1.000000000000000000, 0.9659258262890683122, 1.000000000000000000, 0.9659258262890683122, 1.000000000000000000, 0.9659258262890683122, 1.000000000000000000, 0.9659258262890683122, 1.000000000000000000, 0.9659258262890683122, 1.000000000000000000, 0.9659258262890683122, 1.000000000000000000, 0.9659258262890683122, 1.000000000000000000, 0.9659258262890683122, 1.000000000000000000, 0.9659258262890683122, 1.000000000000000000, 0.9659258262890683122, 1.000000000000000000, 0.9659258262890683122, 1.000000000000000000, 0.9659258262890683122, 1.000000000000000000, 0.9659258262890683122, 1.000000000000000000, 0.9659258262890683122, 1.000000000000000000, 0.9659258262890683122, 1.000000000000000000, 0.9659258262890683122, 1.000000000000000000, 0.9659258262890683122, 1.000000000000000000, 0.9659258262890683122, 1.000000000000000000, 0.9659258262890683122, 1.000000000000000000, 0.9659258262890683122, 1.000000000000000000, 0.9659258262890683122, 1.000000000000000000, 0.9659258262890683122, 1.000000000000000000, 0.9659258262890683122, 1.000000000000000000, 0.9659258262890683122, 1.000000000000000000, 0.9659258262890683122, 1.000000000000000000, 0.9659258262890683122, 1.000000000000000000, 0.9659258262890683122, 1.000000000000000000, 0.9659258262890683122, 1.000000000000000000, 0.9659258262890683122, 1.000000000000000000, 0.9659258262890683122, 1.000000000000000000, 0.9659258262890683122, 1.000000000000000000, 0.9659258262890683122, 1.000000000000000000, 0.9659258262890683122, 1.000000000000000000, 0.9659258262890683122, 1.000000000000000000, 0.9659258262890683122, 1.000000000000000000, 0.9659258262890683122, 1.000000000000000000, 0.9659258262890683122, 1.000000000000000000, 0.9659258262890683122, 1.000000000000000000, 0.9659258262890683122, 1.000000000000000000, 0.9659258262890683122, 1.000000000000000000, 0.9659258262890683122, 1.000000000000000000, 0.9659258262890683122, 1.000000000000000000, 0.9659258262890683122, 1.000000000000000000, 0.9659258262890683122, 1.000000000000000000, 0.9659258262890683122, 1.000000000000000000, 0.9659258262890683122, 1.000000000000000000, 0.9659258262890683122, 1.000000000000000000, 0.9659258262890683122, 1.000000000000000000, 0.9659258262890683122, 1.000000000000000000, 0.9659258262890683122, 1.000000000000000000, 0.9659258262890683122, 1.000000000000000000, 0.9659258262890683122, 1.000000000000000000, 0.9659258262890683122, 1.000000000000000000, 0.9659258262890683122, 1.000000000000000000, 0.9659258262890683122, 1.000000000000000000, 0.9659258262890683122, 1.000000000000000000) ) ) 
 REPRESENTATION_ITEM ( '' )  SURFACE ( )  );
#128197 = CARTESIAN_POINT ( 'NONE',  ( -16.52544592524335698, -4.483927247898792601, 38.95942372801901854 ) ) ;
#128200 = CARTESIAN_POINT ( 'NONE',  ( 18.67979575497194134, -10.72451020669871369, 55.83442372801901854 ) ) ;
#128201 = CARTESIAN_POINT ( 'NONE',  ( 10.72451020669898902, -18.67979575497178502, 57.91557627198103120 ) ) ;
#128202 = CARTESIAN_POINT ( 'NONE',  ( 19.05341960407617918, -5.049401038297876454, 106.0427570613523471 ) ) ;
#128203 = CARTESIAN_POINT ( 'NONE',  ( -5.153800228976328057, -19.02544592524343514, 52.29057627198100988 ) ) ;
#128204 = CARTESIAN_POINT ( 'NONE',  ( 0.05219959533936267826, -19.03943276465977164, 85.00109039468567573 ) ) ;
#128205 = CARTESIAN_POINT ( 'NONE',  ( -10.72451020669870658, -18.67979575497194134, 89.58442372801901854 ) ) ;
#128206 = CARTESIAN_POINT ( 'NONE',  ( 19.02544592524334988, 5.153800228976608722, 71.45942372801900433 ) ) ;
#128207 = CARTESIAN_POINT ( 'NONE',  ( -9.474510206698964154, 16.51473224551069663, 35.41557627198102409 ) ) ;
#128208 = CARTESIAN_POINT ( 'NONE',  ( -10.81492255796078084, -18.62759615963271287, 52.08224293864768839 ) ) ;
#128209 = CARTESIAN_POINT ( 'NONE',  ( -0.05219959533910754901, -16.53943276465976808, 57.49890960531435979 ) ) ;
#128210 = CARTESIAN_POINT ( 'NONE',  ( 21.49230439284897187, 7.461675232480832420, 174.1505469413571348 ) ) ;
#128211 = CARTESIAN_POINT ( 'NONE',  ( -16.51473224551082808, 9.474510206698731452, 28.33442372801900433 ) ) ;
#128212 = CARTESIAN_POINT ( 'NONE',  ( 16.55341960407618274, -4.379528057220086978, 96.04275706135236135 ) ) ;
#128213 = CARTESIAN_POINT ( 'NONE',  ( 0.05219959533910956823, 16.53943276465976808, 49.99890960531437401 ) ) ;
#128214 = CARTESIAN_POINT ( 'NONE',  ( 10.72451020669871369, 18.67979575497193778, 87.08442372801901854 ) ) ;
#128215 = CARTESIAN_POINT ( 'NONE',  ( -18.62759615963255300, -10.81492255796106328, 84.16775706135234714 ) ) ;
#128216 = CARTESIAN_POINT ( 'NONE',  ( 18.62759615963271287, -10.81492255796078972, 98.33224293864769550 ) ) ;
#128217 = CARTESIAN_POINT ( 'NONE',  ( -9.474510206698964154, 16.51473224551069663, 55.41557627198103120 ) ) ;
#128218 = CARTESIAN_POINT ( 'NONE',  ( -15.72974639402176322, -15.80617190586768395, 69.37609039468567573 ) ) ;
#128219 = CARTESIAN_POINT ( 'NONE',  ( 0.05219959533909260263, 19.03943276465977164, 44.99890960531435979 ) ) ;
#128220 = ORIENTED_EDGE ( 'NONE', *, *, #73153, .F. ) ;
#128221 = CARTESIAN_POINT ( 'NONE',  ( -19.02544592524342804, 5.153800228976336051, 61.04057627198103120 ) ) ;
#128222 = CARTESIAN_POINT ( 'NONE',  ( -14.29746914071049879, 8.314922557960819915, 100.8322429386477097 ) ) ;
#128223 = CARTESIAN_POINT ( 'NONE',  ( -16.51473224551069308, -9.474510206698971260, 96.66557627198102409 ) ) ;
#128224 = CARTESIAN_POINT ( 'NONE',  ( -16.52544592524342804, 4.483927247898546575, 51.04057627198103120 ) ) ;
#128225 = CARTESIAN_POINT ( 'NONE',  ( -12.14591786802309592, -12.06949235617757132, 106.8739096053143811 ) ) ;
#128226 = CARTESIAN_POINT ( 'NONE',  ( -21.53943276465977519, 0.05219959533907696930, 81.24890960531436690 ) ) ;
#128227 = CARTESIAN_POINT ( 'NONE',  ( 5.719274019375673035, 21.55341960407619339, 32.29275706135235424 ) ) ;
#128228 = LINE ( 'NONE', #83713, #20991 ) ;
#128229 = CARTESIAN_POINT ( 'NONE',  ( 12.14591786802327356, -12.06949235617739191, 30.62609039468567929 ) ) ;
#128230 = CARTESIAN_POINT ( 'NONE',  ( -18.67979575497178146, -10.72451020669898902, 81.66557627198103830 ) ) ;
#128231 = CARTESIAN_POINT ( 'NONE',  ( -0.05219959533937732626, 21.53943276465977519, 102.5010903946856899 ) ) ;
#128232 = CARTESIAN_POINT ( 'NONE',  ( 19.02544592524343514, -5.153800228976328945, 93.54057627198102409 ) ) ;
#128233 = CARTESIAN_POINT ( 'NONE',  ( -0.05219959533937732626, 21.53943276465977519, 32.50109039468568284 ) ) ;
#128234 = CARTESIAN_POINT ( 'NONE',  ( -15.72974639402197994, 15.80617190586746368, 35.62390960531437401 ) ) ;
#128235 = CARTESIAN_POINT ( 'NONE',  ( -4.379528057220086978, -16.55341960407618274, 104.7927570613523898 ) ) ;
#128237 = CARTESIAN_POINT ( 'NONE',  ( -5.719274019375665041, -21.55341960407619695, 79.79275706135236135 ) ) ;
#128236 = CARTESIAN_POINT ( 'NONE',  ( 21.52544592524334988, 5.823673210054432836, 56.45942372801902565 ) ) ;
#128238 = CARTESIAN_POINT ( 'NONE',  ( -18.67979575497193778, 10.72451020669871902, 113.3344237280190328 ) ) ;
#128239 = CARTESIAN_POINT ( 'NONE',  ( -8.224510206698735004, -14.34966873604973081, 69.58442372801900433 ) ) ;
#128240 = CARTESIAN_POINT ( 'NONE',  ( -10.72451020669870658, -18.67979575497194134, 44.58442372801901854 ) ) ;
#128241 = CARTESIAN_POINT ( 'NONE',  ( 16.51473224551069308, 9.474510206698969483, 39.16557627198103120 ) ) ;
#128242 = CARTESIAN_POINT ( 'NONE',  ( -15.80617190586768217, 15.72974639402176855, 108.1260903946856757 ) ) ;
#128243 = CARTESIAN_POINT ( 'NONE',  ( 5.049401038298161559, -19.05341960407611168, 107.7072429386476955 ) ) ;
#128244 = CARTESIAN_POINT ( 'NONE',  ( 21.53943276465977519, -0.05219959533907433946, 108.7489096053143669 ) ) ;
#128246 = CARTESIAN_POINT ( 'NONE',  ( -18.62759615963270932, 10.81492255796079327, 70.83224293864770971 ) ) ;
#128245 = CARTESIAN_POINT ( 'NONE',  ( 19.35543954521081389, 5.499999999999574563, 82.08901960356452321 ) ) ;
#128248 = CARTESIAN_POINT ( 'NONE',  ( 16.53943276465976808, -0.05219959533910856209, 53.74890960531437401 ) ) ;
#128247 = CARTESIAN_POINT ( 'NONE',  ( 14.34966873604972726, -8.224510206698740333, 45.83442372801901854 ) ) ;
#128249 = CARTESIAN_POINT ( 'NONE',  ( -28.79475375365672107, -9.355982642738018384, 146.3656553485623419 ) ) ;
#128250 = CARTESIAN_POINT ( 'NONE',  ( 16.51473224551083163, -9.474510206698727899, 85.83442372801900433 ) ) ;
#128251 = CARTESIAN_POINT ( 'NONE',  ( -26.46959431505279525, -27.26463967846491698, -11.49588912907431393 ) ) ;
#128252 = CARTESIAN_POINT ( 'NONE',  ( 12.14591786802327356, -12.06949235617739191, 30.62609039468567929 ) ) ;
#128253 = CARTESIAN_POINT ( 'NONE',  ( -15.72974639402197994, 15.80617190586746368, 100.6239096053143811 ) ) ;
#128254 = CARTESIAN_POINT ( 'NONE',  ( -5.719274019375978568, 21.55341960407610458, 80.20724293864769550 ) ) ;
#128255 = CARTESIAN_POINT ( 'NONE',  ( 9.564922557960805705, 16.46253265017160317, 109.5822429386476955 ) ) ;
#128256 = CARTESIAN_POINT ( 'NONE',  ( 8.314922557961029526, -14.29746914071037800, 45.41775706135234003 ) ) ;
#128257 = CARTESIAN_POINT ( 'NONE',  ( -9.474510206698964154, 16.51473224551069663, 75.41557627198103830 ) ) ;
#128259 = CARTESIAN_POINT ( 'NONE',  ( -13.97604488694547697, 13.89961937509957934, 93.12609039468566152 ) ) ;
#128258 = CARTESIAN_POINT ( 'NONE',  ( -21.52544592524334988, -5.823673210054445271, 23.95942372801901143 ) ) ;
#128260 = CARTESIAN_POINT ( 'NONE',  ( -5.153800228976328057, -19.02544592524343514, 112.2905762719810099 ) ) ;
#128261 = CARTESIAN_POINT ( 'NONE',  ( -9.474510206698964154, 16.51473224551069663, 85.41557627198102409 ) ) ;
#128262 = CARTESIAN_POINT ( 'NONE',  ( -5.719274019375978568, 21.55341960407610458, 95.20724293864769550 ) ) ;
#128263 = CARTESIAN_POINT ( 'NONE',  ( 9.564922557960805705, 16.46253265017160317, 59.58224293864769550 ) ) ;
#128264 = CARTESIAN_POINT ( 'NONE',  ( -16.21995358207306026, -7.366697692864123681, 60.06448998487844904 ) ) ;
#128265 = CARTESIAN_POINT ( 'NONE',  ( -8.314922557960811034, -14.29746914071050412, 62.08224293864769550 ) ) ;
#128266 = CARTESIAN_POINT ( 'NONE',  ( -10.72451020669898014, 18.67979575497178502, 25.41557627198103120 ) ) ;
#128267 = CARTESIAN_POINT ( 'NONE',  ( -17.49999999999998579, 5.500000000000032863, 60.79690382534172244 ) ) ;
#128268 = CARTESIAN_POINT ( 'NONE',  ( -5.719274019375978568, 21.55341960407610458, 90.20724293864770971 ) ) ;
#128269 = CARTESIAN_POINT ( 'NONE',  ( -13.97604488694547697, 13.89961937509957934, 63.12609039468566152 ) ) ;
#128270 = CARTESIAN_POINT ( 'NONE',  ( -5.049401038298153566, 19.05341960407611168, 115.2072429386477097 ) ) ;
#128271 = CARTESIAN_POINT ( 'NONE',  ( 19.35543954521079968, 5.499999999999572786, 67.08901960356450900 ) ) ;
#128272 = CARTESIAN_POINT ( 'NONE',  ( 18.67979575497178502, 10.72451020669898547, 54.16557627198103120 ) ) ;
#128273 = CIRCLE ( 'NONE', #28312, 4.000000000000000888 ) ;
#128274 = CARTESIAN_POINT ( 'NONE',  ( 19.02544592524343514, -5.153800228976328945, 83.54057627198100988 ) ) ;
#128275 = CARTESIAN_POINT ( 'NONE',  ( 10.81492255796106328, -18.62759615963255655, 75.41775706135233293 ) ) ;
#128276 = CARTESIAN_POINT ( 'NONE',  ( -5.153800228976328057, -19.02544592524343514, 57.29057627198103120 ) ) ;
#128277 = CARTESIAN_POINT ( 'NONE',  ( -0.05219959533910754901, -16.53943276465976808, 72.49890960531435269 ) ) ;
#128278 = CARTESIAN_POINT ( 'NONE',  ( -0.05219959533934338120, 16.53943276465976808, 32.50109039468568284 ) ) ;
#128279 = CARTESIAN_POINT ( 'NONE',  ( -5.719274019375665041, -21.55341960407619695, 64.79275706135234714 ) ) ;
#128280 = ORIENTED_EDGE ( 'NONE', *, *, #92125, .T. ) ;
#128281 = CARTESIAN_POINT ( 'NONE',  ( 5.153800228976615827, -19.02544592524334988, 30.20942372801900433 ) ) ;
#128282 = CARTESIAN_POINT ( 'NONE',  ( 0.05219959533936267826, -19.03943276465977164, 85.00109039468567573 ) ) ;
#128283 = CARTESIAN_POINT ( 'NONE',  ( 27.98120534312134922, -28.16303873514628364, -20.10652275068718708 ) ) ;
#128284 = CARTESIAN_POINT ( 'NONE',  ( 18.62759615963255655, 10.81492255796105972, 21.66775706135235069 ) ) ;
#128285 = CARTESIAN_POINT ( 'NONE',  ( 11.74264578624799427, 36.14014761921585972, -2.349999994537626868 ) ) ;
#128286 = CARTESIAN_POINT ( 'NONE',  ( 5.823673210054444382, -21.52544592524334988, 110.2094237280190185 ) ) ;
#128287 = CARTESIAN_POINT ( 'NONE',  ( 5.049401038298161559, -19.05341960407611168, 57.70724293864769550 ) ) ;
#128288 = CARTESIAN_POINT ( 'NONE',  ( 5.153800228976615827, -19.02544592524334988, 25.20942372801900433 ) ) ;
#128289 = CARTESIAN_POINT ( 'NONE',  ( -4.483927247898782831, 16.52544592524335698, 97.70942372801904696 ) ) ;
#128291 = CARTESIAN_POINT ( 'NONE',  ( 5.719274019375673035, 21.55341960407619339, 77.29275706135234714 ) ) ;
#128290 = CARTESIAN_POINT ( 'NONE',  ( 16.46253265017160672, -9.564922557960803928, 108.3322429386476955 ) ) ;
#128292 = CARTESIAN_POINT ( 'NONE',  ( -11.40812507854755609, 35.11059874428196537, -3.024999997268813523 ) ) ;
#128293 = CARTESIAN_POINT ( 'NONE',  ( -17.49999999999999289, -3.189878218039144731, 35.12948562571269662 ) ) ;
#128294 = CARTESIAN_POINT ( 'NONE',  ( -10.72451020669870658, -18.67979575497194134, 84.58442372801903275 ) ) ;
#128295 = CARTESIAN_POINT ( 'NONE',  ( 21.23184647844207618, -181.1785498424364675, -15.00000000000000178 ) ) ;
#128296 = CARTESIAN_POINT ( 'NONE',  ( -13.97604488694527625, -13.89961937509977652, 96.87390960531433848 ) ) ;
#128297 = CARTESIAN_POINT ( 'NONE',  ( 19.02544592524334988, 5.153800228976608722, 21.45942372801899012 ) ) ;
#128298 = LINE ( 'NONE', #113134, #53356 ) ;
#128299 = CARTESIAN_POINT ( 'NONE',  ( -13.89961937509977652, 13.97604488694528158, 45.62390960531433848 ) ) ;
#128300 = CARTESIAN_POINT ( 'NONE',  ( -10.81492255796078084, -18.62759615963271287, 62.08224293864769550 ) ) ;
#128301 = CARTESIAN_POINT ( 'NONE',  ( 16.53943276465976808, -0.05219959533910856209, 23.74890960531435269 ) ) ;
#128303 = CARTESIAN_POINT ( 'NONE',  ( -0.05219959533909027116, -19.03943276465977164, 82.49890960531436690 ) ) ;
#128302 = CARTESIAN_POINT ( 'NONE',  ( -16.55341960407611168, -4.379528057220339221, 91.45724293864769550 ) ) ;
#128304 = CARTESIAN_POINT ( 'NONE',  ( 21.53943276465977519, 0.05219959533937863772, 106.2510903946856757 ) ) ;
#128305 = CARTESIAN_POINT ( 'NONE',  ( -9.474510206698964154, 16.51473224551069663, 30.41557627198102054 ) ) ;
#128306 = CARTESIAN_POINT ( 'NONE',  ( -4.379528057220328563, 16.55341960407611168, 100.2072429386476955 ) ) ;
#128307 = CARTESIAN_POINT ( 'NONE',  ( -10.72451020669870658, -18.67979575497194134, 54.58442372801901143 ) ) ;
#128308 = CARTESIAN_POINT ( 'NONE',  ( 0.05219959533907565091, 21.53943276465977519, 89.99890960531438111 ) ) ;
#128309 = CARTESIAN_POINT ( 'NONE',  ( -5.153800228976607833, 19.02544592524334988, 57.70942372801899012 ) ) ;
#128310 = CARTESIAN_POINT ( 'NONE',  ( -12.73180063597635403, -37.92326222289558757, -14.26362963886643875 ) ) ;
#128311 = CARTESIAN_POINT ( 'NONE',  ( 0.05219959533909260263, 19.03943276465977164, 109.9989096053143669 ) ) ;
#128312 = CARTESIAN_POINT ( 'NONE',  ( -16.52544592524342804, 4.483927247898546575, 76.04057627198102409 ) ) ;
#128313 = CARTESIAN_POINT ( 'NONE',  ( 16.46253265017146816, 9.564922557961045513, 41.66775706135234003 ) ) ;
#128314 = VECTOR ( 'NONE', #60638, 1000.000000000000000 ) ;
#128315 = CARTESIAN_POINT ( 'NONE',  ( -9.474510206698964154, 16.51473224551069663, 60.41557627198102409 ) ) ;
#128316 = CARTESIAN_POINT ( 'NONE',  ( 8.314922557960818139, 14.29746914071049879, 59.58224293864770260 ) ) ;
#128318 = EDGE_CURVE ( 'NONE', #141920, #78253, #44226, .T. ) ;
#128317 = CARTESIAN_POINT ( 'NONE',  ( -13.97604488694547697, 13.89961937509957934, 73.12609039468568994 ) ) ;
#128319 = CARTESIAN_POINT ( 'NONE',  ( -19.52837319214028611, 5.499999999999899636, 84.60471352585540217 ) ) ;
#128320 = CARTESIAN_POINT ( 'NONE',  ( 15.80617190586746368, 15.72974639402197994, 39.37390960531436690 ) ) ;
#128321 = ORIENTED_EDGE ( 'NONE', *, *, #185673, .T. ) ;
#128322 = CARTESIAN_POINT ( 'NONE',  ( -12.06949235617756955, 12.14591786802309770, 100.6239096053143811 ) ) ;
#128323 = CARTESIAN_POINT ( 'NONE',  ( 2.995967610389833449E-15, -76.33425854457907178, -14.99989890116611768 ) ) ;
#128325 = CARTESIAN_POINT ( 'NONE',  ( 15.80617190586746368, 15.72974639402197994, 64.37390960531435269 ) ) ;
#128324 = CARTESIAN_POINT ( 'NONE',  ( -9.564922557960796823, -16.46253265017161027, 57.08224293864769550 ) ) ;
#128326 = CARTESIAN_POINT ( 'NONE',  ( 5.153800228976335163, 19.02544592524342804, 29.79057627198102409 ) ) ;
#128328 = CARTESIAN_POINT ( 'NONE',  ( -13.89961937509977652, 13.97604488694528158, 65.62390960531436690 ) ) ;
#128327 = CARTESIAN_POINT ( 'NONE',  ( -0.05219959533934338120, 16.53943276465976808, 82.50109039468568994 ) ) ;
#128329 = CARTESIAN_POINT ( 'NONE',  ( 16.51473224551083163, -9.474510206698727899, 55.83442372801899722 ) ) ;
#128330 = CARTESIAN_POINT ( 'NONE',  ( 21.52544592524334988, 5.823673210054432836, 71.45942372801901854 ) ) ;
#128331 = CARTESIAN_POINT ( 'NONE',  ( 21.55341960407610458, 5.719274019375980345, 43.95724293864769550 ) ) ;
#128332 = CARTESIAN_POINT ( 'NONE',  ( -9.564922557960796823, -16.46253265017161027, 27.08224293864769550 ) ) ;
#128333 = CARTESIAN_POINT ( 'NONE',  ( 12.06949235617739724, 12.14591786802326823, 81.87609039468568994 ) ) ;
#128334 = CARTESIAN_POINT ( 'NONE',  ( 0.05219959533936267826, -19.03943276465977164, 110.0010903946856757 ) ) ;
#128335 = FACE_OUTER_BOUND ( 'NONE', #10034, .T. ) ;
#128336 = CARTESIAN_POINT ( 'NONE',  ( 18.39639308325437383, 5.500000000000035527, 78.98252246182197212 ) ) ;
#128337 = CARTESIAN_POINT ( 'NONE',  ( -0.05219959533937732626, 21.53943276465977519, 97.50109039468567573 ) ) ;
#128338 = CARTESIAN_POINT ( 'NONE',  ( -16.52544592524342804, 4.483927247898546575, 46.04057627198103830 ) ) ;
#128339 = CARTESIAN_POINT ( 'NONE',  ( 8.314922557960818139, 14.29746914071049879, 54.58224293864769550 ) ) ;
#128340 = CARTESIAN_POINT ( 'NONE',  ( -21.52544592524343514, 5.823673210054127303, 101.0405762719810383 ) ) ;
#128341 = CARTESIAN_POINT ( 'NONE',  ( 18.67979575497178502, 10.72451020669898547, 94.16557627198103830 ) ) ;
#128342 = CARTESIAN_POINT ( 'NONE',  ( 17.44270441346516520, -5.991230190323020288, 96.13664920735770636 ) ) ;
#128343 = CARTESIAN_POINT ( 'NONE',  ( -5.823673210054116645, -21.52544592524344225, 32.29057627198102409 ) ) ;
#128344 = CARTESIAN_POINT ( 'NONE',  ( 14.29746914071037800, 8.314922557961029526, 71.66775706135234714 ) ) ;
#128345 = CARTESIAN_POINT ( 'NONE',  ( -16.53943276465976808, 0.05219959533911058130, 81.24890960531436690 ) ) ;
#128346 = CARTESIAN_POINT ( 'NONE',  ( -19.03943276465977164, 0.05219959533909376836, 51.24890960531436690 ) ) ;
#128347 = CARTESIAN_POINT ( 'NONE',  ( 35.68964480816959650, -0.9792624367684675812, 37.54765762180189625 ) ) ;
#128348 = EDGE_LOOP ( 'NONE', ( #65907, #44036 ) ) ;
#128349 = CARTESIAN_POINT ( 'NONE',  ( -16.52544592524335698, -4.483927247898792601, 98.95942372801903275 ) ) ;
#128350 = CARTESIAN_POINT ( 'NONE',  ( 10.81492255796078972, 18.62759615963270932, 114.5822429386477097 ) ) ;
#128351 = CARTESIAN_POINT ( 'NONE',  ( 9.564922557960805705, 16.46253265017160317, 89.58224293864769550 ) ) ;
#128352 = CARTESIAN_POINT ( 'NONE',  ( -21.53943276465977519, -0.05219959533937600094, 48.75109039468568284 ) ) ;
#128353 = CARTESIAN_POINT ( 'NONE',  ( 19.02544592524343514, -5.153800228976328945, 103.5405762719809957 ) ) ;
#128355 = EDGE_CURVE ( 'NONE', #191800, #198713, #199998, .T. ) ;
#128354 = CARTESIAN_POINT ( 'NONE',  ( -15.71981542752435423, -36.60361700297588072, -28.71911170261294899 ) ) ;
#128356 = ORIENTED_EDGE ( 'NONE', *, *, #85361, .F. ) ;
#128357 = CARTESIAN_POINT ( 'NONE',  ( 21.52544592524334988, 5.823673210054432836, 51.45942372801901854 ) ) ;
#128359 = CARTESIAN_POINT ( 'NONE',  ( 19.05341960407611168, 5.049401038298154454, 113.9572429386477097 ) ) ;
#128358 = CARTESIAN_POINT ( 'NONE',  ( 19.02544592524343514, -5.153800228976328945, 33.54057627198102409 ) ) ;
#128360 = CARTESIAN_POINT ( 'NONE',  ( -13.97604488694547697, 13.89961937509957934, 58.12609039468566863 ) ) ;
#128361 = CARTESIAN_POINT ( 'NONE',  ( -21.55341960407619339, 5.719274019375674811, 33.54275706135234714 ) ) ;
#128362 = CARTESIAN_POINT ( 'NONE',  ( 13.97604488694548053, -13.89961937509957401, 60.62609039468564731 ) ) ;
#128363 = CARTESIAN_POINT ( 'NONE',  ( -13.97604488694527625, -13.89961937509977652, 21.87390960531435979 ) ) ;
#128364 = CARTESIAN_POINT ( 'NONE',  ( -8.314922557961024197, 14.29746914071037800, 97.91775706135236135 ) ) ;
#128365 = CARTESIAN_POINT ( 'NONE',  ( 9.564922557961047289, -16.46253265017146816, 65.41775706135233293 ) ) ;
#128366 = CARTESIAN_POINT ( 'NONE',  ( 0.05219959533934541429, -16.53943276465976808, 105.0010903946856757 ) ) ;
#128367 = CARTESIAN_POINT ( 'NONE',  ( -28.28060372831499336, 2.428612866367529932E-14, 149.6875000013656063 ) ) ;
#128368 = CARTESIAN_POINT ( 'NONE',  ( -9.564922557960796823, -16.46253265017161027, 87.08224293864769550 ) ) ;
#128369 = CARTESIAN_POINT ( 'NONE',  ( -0.05219959533937732626, 21.53943276465977519, 92.50109039468567573 ) ) ;
#128370 = CARTESIAN_POINT ( 'NONE',  ( -0.05219959533937732626, 21.53943276465977519, 107.5010903946856899 ) ) ;
#128371 = CARTESIAN_POINT ( 'NONE',  ( 2.200000000000000178, 0.000000000000000000, 0.000000000000000000 ) ) ;
#128372 = CARTESIAN_POINT ( 'NONE',  ( -16.51473224551069308, -9.474510206698971260, 101.6655762719810241 ) ) ;
#128373 = CARTESIAN_POINT ( 'NONE',  ( 18.62759615963255655, 10.81492255796105972, 71.66775706135234714 ) ) ;
#128374 = CARTESIAN_POINT ( 'NONE',  ( -16.46253265017146816, -9.564922557961047289, 109.1677570613523471 ) ) ;
#128375 = CARTESIAN_POINT ( 'NONE',  ( -0.05219959533909027116, -19.03943276465977164, 77.49890960531435269 ) ) ;
#128376 = CARTESIAN_POINT ( 'NONE',  ( -21.55341960407610458, -5.719274019375992779, 31.45724293864769550 ) ) ;
#128377 = CARTESIAN_POINT ( 'NONE',  ( -9.474510206698964154, 16.51473224551069663, 95.41557627198102409 ) ) ;
#128378 = CARTESIAN_POINT ( 'NONE',  ( 27.73933785331498925, -9.013057229001033122, 139.7750000027311899 ) ) ;
#128379 = CARTESIAN_POINT ( 'NONE',  ( -0.05219959533909027116, -19.03943276465977164, 67.49890960531436690 ) ) ;
#128380 = CARTESIAN_POINT ( 'NONE',  ( 12.06949235617757843, -12.14591786802309237, 23.12390960531436335 ) ) ;
#128381 = CARTESIAN_POINT ( 'NONE',  ( -18.39639308325437028, -5.500000000000041744, 41.48252246182197212 ) ) ;
#128382 = CARTESIAN_POINT ( 'NONE',  ( 16.51473224551083163, -9.474510206698727899, 75.83442372801900433 ) ) ;
#128383 = CARTESIAN_POINT ( 'NONE',  ( -5.049401038298153566, 19.05341960407611168, 100.2072429386476955 ) ) ;
#128384 = CARTESIAN_POINT ( 'NONE',  ( 16.55341960407611168, 4.379528057220329451, 78.95724293864769550 ) ) ;
#128385 = CARTESIAN_POINT ( 'NONE',  ( -18.62759615963270932, 10.81492255796079327, 45.83224293864769550 ) ) ;
#128386 = CARTESIAN_POINT ( 'NONE',  ( -18.62759615963270932, 10.81492255796079327, 40.83224293864769550 ) ) ;
#128387 = CARTESIAN_POINT ( 'NONE',  ( 8.314922557960818139, 14.29746914071049879, 109.5822429386476955 ) ) ;
#128388 = CARTESIAN_POINT ( 'NONE',  ( -16.20579543436675252, 7.371946100355232900, 54.43479165828124167 ) ) ;
#128389 = CARTESIAN_POINT ( 'NONE',  ( 9.564922557961047289, -16.46253265017146816, 40.41775706135234003 ) ) ;
#128390 = CARTESIAN_POINT ( 'NONE',  ( -0.05219959533910754901, -16.53943276465976808, 22.49890960531436335 ) ) ;
#128391 = CARTESIAN_POINT ( 'NONE',  ( -5.153800228976328057, -19.02544592524343514, 102.2905762719810383 ) ) ;
#128392 = CARTESIAN_POINT ( 'NONE',  ( -10.72451020669870658, -18.67979575497194134, 69.58442372801900433 ) ) ;
#128393 = CARTESIAN_POINT ( 'NONE',  ( -0.05219959533907301413, -21.53943276465977519, 57.49890960531435979 ) ) ;
#128394 = CARTESIAN_POINT ( 'NONE',  ( -15.72974639402176322, -15.80617190586768395, 44.37609039468567573 ) ) ;
#128395 = CARTESIAN_POINT ( 'NONE',  ( 15.80617190586746368, 15.72974639402197994, 94.37390960531436690 ) ) ;
#128396 = CARTESIAN_POINT ( 'NONE',  ( 10.72451020669871369, 18.67979575497193778, 42.08442372801901854 ) ) ;
#128397 = CARTESIAN_POINT ( 'NONE',  ( -14.34966873604960291, -8.224510206698953496, 111.6655762719810525 ) ) ;
#128398 = CARTESIAN_POINT ( 'NONE',  ( -13.89961937509957401, -13.97604488694547875, 64.37609039468567573 ) ) ;
#128399 = CARTESIAN_POINT ( 'NONE',  ( -5.153800228976328057, -19.02544592524343514, 62.29057627198100988 ) ) ;
#128400 = CARTESIAN_POINT ( 'NONE',  ( -4.483927247898539470, -16.52544592524342804, 107.2905762719810525 ) ) ;
#128401 = CARTESIAN_POINT ( 'NONE',  ( 13.97604488694527802, 13.89961937509977652, 114.3739096053143669 ) ) ;
#128402 = CARTESIAN_POINT ( 'NONE',  ( -4.483927247898539470, -16.52544592524342804, 52.29057627198102409 ) ) ;
#128403 = CARTESIAN_POINT ( 'NONE',  ( -14.29746914071049879, 8.314922557960819915, 25.83224293864769194 ) ) ;
#128404 = CARTESIAN_POINT ( 'NONE',  ( -19.03943276465977164, 0.05219959533909376836, 46.24890960531435979 ) ) ;
#128405 = CARTESIAN_POINT ( 'NONE',  ( -12.06949235617756955, 12.14591786802309770, 115.6239096053143669 ) ) ;
#128406 = CARTESIAN_POINT ( 'NONE',  ( -19.03943276465977164, -0.05219959533935918106, 28.75109039468566507 ) ) ;
#128409 = CARTESIAN_POINT ( 'NONE',  ( 8.224510206698953496, -14.34966873604960469, 32.91557627198102409 ) ) ;
#128408 = CARTESIAN_POINT ( 'NONE',  ( -28.82186960331499037, 2.428612866367529932E-14, 140.2500000054623683 ) ) ;
#128407 = AXIS2_PLACEMENT_3D ( 'NONE', #23427, #36574, #97237 ) ;
#128410 = CARTESIAN_POINT ( 'NONE',  ( -0.05219959533937732626, 21.53943276465977519, 47.50109039468568994 ) ) ;
#128411 = CARTESIAN_POINT ( 'NONE',  ( 24.04960827311052540, -5.809912860844005600, 170.7323280178997891 ) ) ;
#128412 = CARTESIAN_POINT ( 'NONE',  ( -16.55341960407617563, 4.379528057220093196, 63.54275706135234003 ) ) ;
#128413 = CARTESIAN_POINT ( 'NONE',  ( -16.53943276465976808, 0.05219959533911058130, 31.24890960531435979 ) ) ;
#128414 = CARTESIAN_POINT ( 'NONE',  ( -16.53943276465976808, -0.05219959533934237506, 103.7510903946857042 ) ) ;
#128415 = CARTESIAN_POINT ( 'NONE',  ( -0.05219959533909027116, -19.03943276465977164, 32.49890960531435979 ) ) ;
#128416 = CARTESIAN_POINT ( 'NONE',  ( 5.049401038298161559, -19.05341960407611168, 57.70724293864769550 ) ) ;
#128417 = CARTESIAN_POINT ( 'NONE',  ( -9.474510206698964154, 16.51473224551069663, 30.41557627198102054 ) ) ;
#128418 = CARTESIAN_POINT ( 'NONE',  ( -10.81492255796105439, 18.62759615963255655, 32.91775706135234714 ) ) ;
#128419 = CARTESIAN_POINT ( 'NONE',  ( 5.153800228976335163, 19.02544592524342804, 49.79057627198100988 ) ) ;
#128420 = CARTESIAN_POINT ( 'NONE',  ( -5.374011537017778117, 5.374011537017756801, -65.00100000000003320 ) ) ;
#128421 = CARTESIAN_POINT ( 'NONE',  ( 5.049401038298161559, -19.05341960407611168, 37.70724293864768839 ) ) ;
#128422 = CARTESIAN_POINT ( 'NONE',  ( 16.51473224551069308, 9.474510206698969483, 114.1655762719810241 ) ) ;
#128424 = CARTESIAN_POINT ( 'NONE',  ( -12.06949235617756955, 12.14591786802309770, 105.6239096053143669 ) ) ;
#128423 = CARTESIAN_POINT ( 'NONE',  ( -5.719274019375665041, -21.55341960407619695, 64.79275706135234714 ) ) ;
#128425 = CARTESIAN_POINT ( 'NONE',  ( 16.46253265017160672, -9.564922557960803928, 113.3322429386476955 ) ) ;
#128426 = CARTESIAN_POINT ( 'NONE',  ( -16.53943276465976808, -0.05219959533934237506, 78.75109039468568994 ) ) ;
#128427 = CARTESIAN_POINT ( 'NONE',  ( 0.05219959533937995610, -21.53943276465977519, 90.00109039468567573 ) ) ;
#128428 = CARTESIAN_POINT ( 'NONE',  ( -0.05219959533934338120, 16.53943276465976808, 47.50109039468568994 ) ) ;
#128429 = CARTESIAN_POINT ( 'NONE',  ( -19.03943276465977164, 0.05219959533909376836, 91.24890960531436690 ) ) ;
#128430 = CARTESIAN_POINT ( 'NONE',  ( -12.06949235617739369, -12.14591786802326823, 34.37609039468568284 ) ) ;
#128431 = CARTESIAN_POINT ( 'NONE',  ( -16.53943276465976808, -0.05219959533934237506, 23.75109039468567929 ) ) ;
#128432 = CARTESIAN_POINT ( 'NONE',  ( 4.483927247898790824, -16.52544592524335698, 80.20942372801901854 ) ) ;
#128433 = CARTESIAN_POINT ( 'NONE',  ( 13.97604488694548053, -13.89961937509957401, 105.6260903946856757 ) ) ;
#128434 = CARTESIAN_POINT ( 'NONE',  ( 9.564922557960805705, 16.46253265017160317, 79.58224293864769550 ) ) ;
#128435 = CARTESIAN_POINT ( 'NONE',  ( 5.823673210054125526, 21.52544592524343514, 94.79057627198105251 ) ) ;
#128437 = CARTESIAN_POINT ( 'NONE',  ( 5.153800228976615827, -19.02544592524334988, 110.2094237280189901 ) ) ;
#128436 = CARTESIAN_POINT ( 'NONE',  ( -8.314922557960811034, -14.29746914071050412, 107.0822429386476955 ) ) ;
#128438 = CARTESIAN_POINT ( 'NONE',  ( 16.55341960407618274, -4.379528057220086978, 76.04275706135237556 ) ) ;
#128439 = CARTESIAN_POINT ( 'NONE',  ( 20.69372460268669300, 10.84650605405351875, 168.1714143675832247 ) ) ;
#128440 = CARTESIAN_POINT ( 'NONE',  ( -19.03943276465977164, -0.05219959533935918106, 63.75109039468566863 ) ) ;
#128441 = CARTESIAN_POINT ( 'NONE',  ( 8.314922557960818139, 14.29746914071049879, 44.58224293864769550 ) ) ;
#128442 = CARTESIAN_POINT ( 'NONE',  ( 14.34966873604960469, 8.224510206698951720, 89.16557627198102409 ) ) ;
#128444 = CARTESIAN_POINT ( 'NONE',  ( 69.65682714487590488, -71.74905178543389184, -25.00000000000000000 ) ) ;
#128443 = CARTESIAN_POINT ( 'NONE',  ( 13.89961937509957401, 13.97604488694547697, 31.87609039468566863 ) ) ;
#128445 = CARTESIAN_POINT ( 'NONE',  ( 10.81492255796106328, -18.62759615963255655, 40.41775706135234714 ) ) ;
#128446 = CARTESIAN_POINT ( 'NONE',  ( -19.03943276465977164, -0.05219959533935918106, 98.75109039468567573 ) ) ;
#128447 =( BOUNDED_SURFACE ( )  B_SPLINE_SURFACE ( 3, 2, ( 
 ( #127359, #7000, #69691, #159690, #146518, #175878, #100013, #51526, #24204, #84839, #116197, #129346, #173895, #85853, #130337, #114175, #145520, #189072, #131358, #191041, #113189, #8008, #68682, #177886, #144523, #174878, #192035, #21188, #193047, #52514, #54524, #53517, #4016, #39355, #65694, #82844, #38358, #50544, #115195, #176887, #112205, #6008, #36344, #160699, #22190, #101014, #35364, #162699, #67688, #97016, #158697, #97997, #37350, #99008, #5008, #161699, #23196, #20186, #83838, #81832, #143519, #128353, #190051, #178887, #56528, #106004, #73705, #132367, #10032, #135377, #26206, #42364, #87845, #55521, #9030, #165706, #197047, #71692, #148541, #58515, #134376, #104027, #179897, #27203, #89849, #120181, #57535, #133359, #195049, #105021, #74686, #119204, #181871, #40355, #117194, #72703, #118206, #88849, #136352, #150541, #12041, #41363, #103029, #102030, #43350, #59496, #166705, #28208, #151532, #13021, #198028, #86857, #196062, #121171, #164711, #149533, #182865, #44346, #11028, #167691, #147542, #180889, #194060, #163712, #29188, #70699, #25215, #45339, #155494, #77654, #122162, #124147, #140315, #172655, #183851, #94809, #141312, #2801, #75661, #137338, #139322, #125159, #76657, #32157, #107981, #138336, #170669, #186858, #62475, #802, #199018, #185846, #31164, #60487, #152505, #108988, #1805, #14997, #91808, #16986, #47333, #93814, #123154, #78640, #33151, #63483, #48327, #171662, #200016, #30164, #13994, #61483, #109982, #156488, #46327, #187842, #153500, #184842, #17990, #79643, #106991, #169669, #168664, #92814, #110971, #64479, #154501, #126146, #49311, #90822, #15996, #192808, #99781, #84604, #145285, #83606, #36113, #97765, #143284, #173662, #142304, #113939, #176651, #175638, #3784, #53279, #130101, #66457, #146283, #21956, #6768, #69453, #158470, #65461, #20948, #112955, #35129, #68447, #98771, #18981, #159452, #160465, #129108, #96781, #7770, #127124, #4770, #54290, #191798, #80627, #19958, #114958, #38127, #188830, #161466, #131120, #22956, #50314, #115962, #128119, #82605, #37112, #34143, #95802, #81600, #157488, #111970, #5775, #144286, #189822, #51294, #174648, #67450, #190807, #52281, #163474, #180656, #74454, #179657, #27971, #41127, #148300, #100774, #194810, #70459, #197796, #133121, #164477, #165473, #117966, #56284, #59262, #134136, #25971, #177650, #40108, #149300, #89611, #11805, #43117, #87614, #42132, #151300, #195825, #101786, #24971, #150308, #162457, #9794, #178645, #23958, #103793, #104785, #102791, #119952, #10794, #73469, #86617, #39118, #58283, #12789, #72462, #147300, #85613, #26969, #57296, #118973, #8789, #166473, #88612, #71456, #181637, #135142, #136120, #196816, #132124, #193817, #55282, #116953, #48819, #112462, #173157, #120931, #35625, #182630, #2300, #157978, #5274, #126627, #188328, #108490, #79139, #171166, #80133, #141803, #50804, #143791, #97270, #187349, #174154, #127627, #155985, #49807, #16492, #34632, #94307, #110472, #64968, #46830, #111472, #62975, #65956, #158958, #95302, #172154, #78141, #31662, #189327, #20448, #17482, #156986, #109483, #96291, #82099, #125652, #170169, #33640, #140810, #93312, #63982, #139809, #154996, #18484, #3296, #19470, #81115, #142795, #1297, #4275, #124655, #186351, #47831, #32653, #117460, #101276, #132633, #177156, #69964, #40627, #85107, #191301, #52777, #39617, #190310, #37617, #67951, #51786, #131630, #194321, #22460, #9299, #38629, #162966, #114446, #87125, #147813, #179159, #192312, #36606, #148810, #193314, #100286, #8286, #113446, #55789, #53792, #176147, #70965, #54788, #102297, #7269, #99279, #116463, #84108, #163986, #115467, #25483, #178152, #66955, #128617, #175139, #145787, #24472, #98263, #86122, #159965, #21452, #68953, #160966, #23460, #146793, #83113, #144790, #6273, #130616, #129605, #161964, #42628, #197307, #89118, #11306, #59765, #74944, #195322, #135637, #136607, #105280 ),
 ( #181153, #58771, #151789, #30428, #13280, #149800, #152765, #45598, #182132, #120439, #164979, #118475, #14255, #184116, #104292, #43616, #196331, #198287, #107251, #12302, #60751, #73968, #165973, #133630, #27475, #103300, #92075, #150806, #166968, #121433, #28470, #90105, #10300, #183126, #44609, #71957, #72976, #106264, #122424, #167948, #75926, #29446, #91078, #168922, #137601, #134645, #57799, #199284, #56802, #180165, #119470, #41635, #26474, #88116, #109244, #96063, #125420, #49572, #1060, #173924, #34405, #65723, #78899, #123408, #35393, #79905, #63746, #95070, #76917, #80890, #140577, #62734, #157751, #156758, #127391, #94070, #124416, #18252, #170924, #142567, #2067, #4046, #3064, #153764, #189101, #15259, #32415, #188099, #138588, #141576, #64741, #69, #155749, #186110, #110240, #171921, #50574, #61740, #112234, #17247, #185101, #19243, #47591, #187116, #48588, #154759, #126403, #111235, #46590, #33411, #172926, #108251, #16257, #169931, #31422, #93074, #77908, #139575, #81864, #159724, #23227, #177918, #51556, #39386, #9061, #161732, #190080, #146548, #6040, #55553, #84870, #143553, #21221, #8042, #101045, #113220, #162731, #70731, #69723, #174910, #131390, #67719, #22222, #38390, #117226, #100046, #36374, #24237, #132398, #68713, #83871, #98028, #5038, #85887, #194091, #129376, #130370, #82877, #193079, #178920, #99040, #147575, #160730, #191073, #20216, #114207, #144555, #97044, #52546, #145553, #54554, #37383, #175912, #158726, #53549, #7031, #66724, #192067, #115227, #128384, #116227, #176919, #150574, #43380, #14023, #58546, #164743, #26238, #13052, #163746, #11061, #41396, #25246, #105052, #106034, #196096, #182894, #12073, #136382, #87877, #60517, #121202, #152536, #165738, #10062, #122192, #166736, #73735, #181902, #86887, #167720, #27233, #149565, #44378, #28240, #75689, #180920, #72737, #89880, #57566, #29218, #88882, #90851, #151563, #40388, #137368, #102061, #119236, #74719, #148572, #198059, #59525, #71722, #42395, #134410, #197079, #120212, #199047, #133391, #195082, #104058, #56562, #118238, #135408, #179929, #103061, #184872, #33181, #48357, #168694, #109018, #110011, #78670, #46354, #34172, #15027, #156520, #76688, #153530, #170697, #154528, #63516, #111001, #186887, #140346, #92843, #139351, #138364, #1834, #95833, #141344, #2831, #126176, #187871, #171692, #123183, #32186, #94840, #16025, #62505, #18020, #125191, #77683, #172687, #183884, #124176, #30195, #91837, #79673, #108012, #107022, #200045, #64509, #93843, #61514, #17017, #49339, #65491, #169697, #157517, #19011, #80657, #31191, #831, #155522, #142333, #185877, #3813, #47363, #45369, #6800, #161498, #98803, #175669, #35159, #21987, #67481, #96814, #188861, #145317, #176683, #51325, #128152, #53311, #113971, #83639, #159484, #68478, #69486, #38158, #37144, #7802, #112986, #66489, #50344, #174679, #130133, #191830, #82635, #23989, #189852, #36144, #99812, #192840, #158500, #144318, #81630, #143313, #147332, #114989, #4800, #22988, #100805, #160497, #115992, #85646, #54320, #177681, #84636, #146313, #129140, #190837, #97796, #20978, #19987, #131151, #39149, #162488, #5807, #8820, #127153, #52313, #112003, #173692, #119980, #105802, #194842, #101817, #180686, #56316, #117998, #28001, #197825, #42162, #182659, #89641, #151329, #12817, #74484, #135172, #9825, #57327, #181666, #179687, #149329, #43145, #26998, #41159, #59291, #70489, #10823, #116984, #178677, #104814, #102822, #193848, #25003, #196845, #119003, #163505, #103822, #166503, #152307, #86647, #136150, #120960, #44143, #55313, #40140, #165502, #167489, #164507, #11835, #87643, #26001, #150339, #28984, #88643, #73500, #148330, #58312, #72493, #71486, #132155, #90625, #133152, #134167, #195855, #140100, #590, #170455, #46116, #93600, #156276, #63266, #62261, #94597, #138128, #153290, #75458, #61276, #155286, #31946, #169455, #110763, #76451, #122947 ),
 ( #172444, #79432, #64270, #124947, #186643, #15783, #77442, #184635, #14791, #121957, #16776, #17777, #78425, #183650, #32942, #109770, #107769, #125936, #1591, #48114, #49105, #199809, #45133, #123929, #30956, #92603, #171454, #141103, #185627, #2591, #106791, #168465, #139114, #154293, #187635, #33932, #95590, #13793, #47119, #108777, #29963, #137132, #198819, #60284, #91601, #35908, #158261, #6557, #21746, #142089, #82393, #83397, #52076, #19751, #7558, #188619, #66249, #115757, #145075, #3575, #81392, #68235, #37912, #111760, #99572, #69244, #129888, #50100, #191588, #127909, #144081, #98562, #177445, #160256, #96573, #161254, #192600, #128900, #5562, #173449, #65253, #22748, #130910, #189611, #190599, #143078, #53067, #54083, #159242, #38915, #20737, #51085, #80417, #174438, #34917, #157274, #112745, #67241, #114745, #97554, #113732, #18770, #175429, #36898, #126913, #4557, #176439, #84397, #146073, #166262, #10588, #103590, #74249, #118763, #24764, #86411, #73264, #23753, #71253, #101572, #85403, #165265, #27761, #56076, #42912, #72249, #196610, #148096, #120722, #181434, #12584, #25767, #70254, #182421, #26759, #133927, #41924, #147095, #89404, #87413, #9587, #104578, #88399, #135918, #40915, #132917, #150093, #117757, #151093, #149098, #197589, #11596, #100572, #59055, #162254, #179449, #134933, #8579, #58081, #119751, #131922, #102588, #194604, #57089, #180452, #193606, #55078, #116748, #164272, #178438, #39906, #195617, #163262, #76204, #123683, #186396, #93354, #30712, #124699, #168223, #183407, #105563, #91352, #185382, #349, #199564, #140854, #106547, #153044, #155040, #109526, #75220, #61033, #198578, #60047, #64024, #138869, #121714, #62019, #17525, #15542, #32698, #2343, #171208, #94349, #16535, #78182, #45875, #107528, #14544, #44890, #152069, #46873, #47873, #108533, #13554, #63020, #139851, #137883, #156028, #31705, #1340, #79184, #29720, #136892, #154047, #122705, #184395, #125694, #43900, #77200, #167249, #169205, #92361, #170212, #28748, #90384, #114490, #190353, #143835, #96333, #142838, #141846, #5315, #99326, #144831, #6315, #129647, #191343, #51830, #126668, #174197, #36650, #158020, #66000, #160008, #66999, #19511, #176192, #187393, #127669, #33682, #95344, #21496, #111513, #110516, #3337, #113489, #35665, #18527, #20492, #98308, #71749, #80174, #52821, #37661, #163772, #172197, #157029, #97313, #83157, #173199, #128658, #4317, #34675, #175183, #67994, #158999, #82141, #65011, #25273, #189369, #188372, #48861, #86915, #148598, #81156, #49849, #10090, #50846, #112503, #72766, #195108, #180945, #74744, #89905, #88910, #30222, #196121, #42421, #44406, #199075, #164769, #150602, #87905, #149592, #153557, #28267, #11089, #151588, #107048, #105080, #122219, #91864, #60544, #183910, #106060, #182923, #135434, #197105, #104084, #134436, #41422, #13077, #75716, #136407, #103088, #152561, #29244, #165766, #45395, #121230, #167746, #168720, #57591, #26264, #43409, #119261, #27261, #90877, #15055, #166766, #14050, #12099, #73762, #58572, #120237, #198085, #133419, #59552, #137394, #181928, #56591, #118265, #179955, #188894, #34202, #95865, #19041, #80688, #141375, #16053, #63545, #126206, #185906, #155551, #49371, #33212, #47392, #65523, #76715, #17045, #123209, #184899, #111033, #859, #200072, #31220, #2862, #125219, #108040, #110044, #187902, #158530, #169726, #142364, #127183, #50375, #61540, #46381, #186916, #172720, #62533, #18052, #93873, #124206, #156552, #157547, #48387, #171724, #92870, #94871, #78699, #154557, #138391, #79705, #3844, #109046, #77711, #64540, #112035, #173723, #170724, #35191, #96845, #139377, #32216, #140376, #1863, #67512, #174708, #113999, #191858, #82665, #68506, #144349, #36172, #81661, #159513, #66519, #115019, #21009, #5836, #37173, #129169, #190866, #20018, #175697, #52343, #143344, #97824, #98832, #53340, #145346, #4832, #160527, #22016 ),
 ( #83668, #113015, #6828, #130161, #128182, #189880, #51355, #172360, #173369, #93523, #170378, #125858, #171377, #80337, #127829, #3498, #157196, #109695, #156196, #155208, #18690, #112668, #158184, #19674, #142999, #4477, #65174, #140021, #187558, #50017, #32864, #79353, #34839, #142009, #94514, #189535, #514, #141024, #47042, #108699, #96494, #124867, #123850, #16697, #126833, #49025, #31869, #33850, #111682, #82311, #78347, #66167, #51007, #174360, #185548, #1510, #110680, #81316, #186566, #188539, #17696, #48039, #35830, #97476, #95510, #159162, #63187, #20657, #2511, #64191, #62186, #162173, #193524, #68157, #144996, #70173, #130829, #100494, #176359, #23671, #86331, #54999, #192520, #24682, #129809, #36816, #148018, #194524, #55996, #128822, #190521, #54003, #178359, #191508, #85319, #161172, #52985, #147011, #39823, #115677, #177365, #51995, #38836, #84316, #113654, #5482, #8496, #116668, #114663, #6477, #131841, #101489, #163178, #37832, #9507, #71173, #132837, #117674, #179371, #99492, #83319, #67165, #22669, #40833, #102506, #145995, #164190, #7478, #69162, #25688, #144001, #175348, #98482, #160175, #21665, #193795, #163453, #115941, #192786, #195806, #132104, #162437, #57278, #38104, #147279, #25952, #9774, #41107, #85592, #178625, #149281, #55263, #99759, #161443, #148281, #98751, #146261, #176629, #160444, #40088, #102771, #131098, #117947, #8769, #71438, #22935, #175616, #56264, #87595, #100755, #145264, #37092, #101766, #70438, #116932, #21934, #164458, #23938, #84581, #179637, #24951, #10776, #177631, #7745, #86598, #54269, #72441, #133102, #134117, #194791, #83585, #6746, #68425, #39099, #130077, #191776, #53258, #114936, #69431, #74433, #166455, #75411, #137083, #46068, #139065, #30909, #182610, #107722, #122898, #151280, #105753, #197776, #61227, #121908, #92557, #59242, #89593, #60237, #136100, #169403, #44095, #154245, #168417, #118952, #15736, #180638, #120911, #153239, #543, #183601, #45085, #103775, #167439, #27952, #198771, #106742, #77395, #42113, #165454, #28936, #26951, #184587, #12769, #90577, #152258, #119934, #29912, #91552, #88593, #13743, #14742, #76403, #181619, #150291, #11786, #138079, #73450, #199760, #135123, #43098, #196797, #58265, #104767, #4509, #174392, #126865, #155239, #111714, #32896, #187590, #3530, #82344, #65206, #1543, #66199, #97508, #33885, #49059, #16729, #170408, #127862, #35862, #94548, #95542, #48070, #188572, #159194, #64225, #112700, #125890, #156229, #185580, #79388, #50052, #20689, #17730, #80369, #173400, #2543, #141057, #144033, #18722, #110714, #62214, #124899, #157230, #123882, #96525, #189566, #172396, #34871, #47071, #142042, #186598, #109726, #158215, #108731, #19705, #63219, #31900, #81347, #51038, #143031, #93553, #78377, #140053, #171410, #25717, #86361, #117703, #130860, #175379, #87363, #131871, #115708, #147042, #128853, #132866, #192551, #114697, #146026, #113684, #67195, #23701, #55028, #129841, #6509, #193556, #54034, #162203, #37865, #85349, #148046, #116698, #177396, #9536, #191540, #145028, #190553, #53017, #8526, #70204, #161206, #102537, #68189, #176391, #178388, #71203, #36848, #22701, #100524, #38868, #163208, #5515, #83352, #39852, #179399, #101518, #194555, #164220, #56025, #40863, #24712, #52026, #7509, #69193, #99524, #84348, #98514, #160208, #21698, #93061, #118711, #170911, #47580, #184102, #2056, #139564, #1048, #187106, #75913, #180401, #61728, #137587, #199270, #109232, #78887, #123396, #124405, #41873, #103540, #76904, #122411, #31410, #140566, #154748, #108238, #60738, #107237, #165215, #169918, #63734, #32404, #94059, #155737, #17235, #16245, #88349, #138575, #62721, #45584, #30414, #186098, #77896, #168908, #125409, #149048, #92062, #195564, #57038, #48576, #153750, #72200, #26710, #110229, #54, #150042, #185088, #171910, #33398, #11547, #10536, #133874, #15245, #46577, #141564, #143537 ),
 ( #145537, #126391, #4033, #53534, #21205, #79894, #157740, #82862, #175895, #49559, #37367, #7016, #159707, #188088, #144539, #65711, #20203, #36360, #115211, #98012, #34394, #99025, #130353, #66708, #81849, #111222, #3053, #160715, #68698, #127377, #128370, #80878, #6025, #192052, #97032, #176904, #158713, #189088, #18241, #112222, #67704, #95057, #50562, #113206, #129362, #35381, #173912, #156747, #51542, #5024, #64730, #19229, #190066, #172915, #191058, #22206, #174894, #52530, #96052, #114191, #142555, #83856, #11043, #161717, #9044, #39370, #23212, #41378, #104041, #194075, #180903, #10046, #134392, #85870, #58530, #119218, #150558, #163729, #8025, #120196, #164726, #148555, #179912, #84855, #165721, #25230, #147559, #42378, #103044, #12057, #178903, #70714, #26220, #55538, #27217, #86871, #88865, #87860, #38375, #73719, #100030, #117210, #72719, #146532, #149548, #196078, #69707, #40371, #132382, #195064, #56544, #135392, #131374, #197062, #102045, #193062, #54538, #71706, #133374, #118221, #101029, #57549, #116211, #177901, #162714, #24220, #78655, #75675, #200031, #169683, #122177, #199033, #1820, #138350, #168679, #63501, #44362, #153515, #32172, #16011, #47348, #91822, #184856, #155508, #61499, #106019, #167706, #154514, #105036, #152520, #182879, #166720, #46340, #109004, #137353, #124161, #15012, #77668, #29202, #181886, #62490, #93828, #107006, #151546, #43364, #107996, #76673, #123168, #28224, #170683, #30179, #90836, #185862, #31178, #17003, #183869, #14008, #92829, #60502, #140330, #139337, #89864, #816, #13036, #74702, #136366, #45354, #198043, #59510, #121186, #128137, #109997, #80642, #172672, #81616, #143299, #52297, #145301, #37128, #188846, #113954, #129124, #157503, #111986, #3799, #126162, #174663, #189837, #171677, #50330, #51310, #19973, #187857, #175654, #156503, #34157, #83624, #112971, #33167, #49326, #36128, #5792, #79659, #67465, #98788, #97780, #18005, #159468, #95818, #173677, #66475, #6784, #20963, #64495, #190822, #160482, #96798, #35144, #141328, #94826, #21972, #125176, #18996, #158485, #110987, #82620, #186873, #127139, #48343, #4785, #142319, #2816, #65477, #144302, #150323, #71470, #133135, #53295, #23974, #115977, #24986, #86631, #195838, #88627, #180669, #132140, #57311, #72477, #100789, #55297, #147315, #69469, #117981, #194826, #114974, #193833, #56299, #163488, #131136, #118986, #85629, #25984, #103806, #148314, #102805, #40123, #116969, #176667, #9809, #8805, #38143, #130117, #179671, #41142, #192824, #54305, #164491, #178660, #87627, #162472, #149313, #10807, #134150, #101801, #42146, #177666, #7786, #191814, #39134, #165486, #26982, #70474, #68463, #99797, #161483, #22971, #84619, #146298, #28967, #106774, #198803, #169437, #11818, #89624, #29945, #185611, #183634, #572, #170438, #77427, #62243, #122930, #61260, #13774, #75442, #120944, #151312, #119964, #91583, #154277, #153274, #181650, #30941, #107754, #44127, #123912, #199793, #184617, #47100, #136132, #43129, #121941, #197808, #59274, #92588, #139098, #45116, #46099, #104798, #166487, #137117, #182643, #14775, #108761, #76435, #168449, #105786, #167472, #27985, #138112, #31929, #15767, #93583, #73483, #135155, #196828, #12801, #60268, #58296, #90609, #152290, #74467, #67223, #140082, #1574, #3557, #189593, #32924, #172426, #112727, #190581, #34900, #51066, #126895, #65235, #63249, #50082, #95572, #124928, #16758, #173430, #4537, #79416, #156257, #81374, #142071, #111742, #187618, #96555, #97536, #66230, #188601, #35889, #141086, #94579, #78406, #2572, #158242, #19733, #110745, #52057, #17760, #64253, #127890, #20718, #186626, #33915, #143059, #174420, #159223, #155269, #125920, #82375, #128881, #144063, #5544, #113713, #175410, #36878, #48097, #109753, #157258, #18753, #49088, #80399, #171437, #178417, #40892, #39881, #68218, #117732, #194583, #130891, #149076, #86390, #148074, #133903 ),
 ( #21727, #25745, #85380, #7538, #102565, #101548, #72228, #38896, #69223, #163240, #54064, #87391, #23731, #10564, #9565, #98544, #195594, #160237, #177425, #132894, #180429, #24740, #71231, #83380, #115738, #146054, #55057, #116728, #57066, #118741, #145057, #162232, #6538, #164250, #192581, #147073, #100553, #99553, #56053, #179427, #129870, #191568, #53047, #8557, #70233, #114727, #131901, #176420, #193585, #37895, #161235, #22729, #84377, #103568, #120701, #76184, #123664, #44871, #106527, #26737, #197567, #89381, #198556, #60026, #169185, #61998, #154028, #105543, #30691, #45856, #74227, #28727, #182400, #42891, #91332, #168204, #88376, #167229, #29701, #136871, #104556, #121693, #138850, #41902, #58059, #153024, #150070, #166238, #14523, #122686, #196589, #184375, #15523, #137864, #134912, #199544, #12561, #90364, #183389, #165243, #61014, #181413, #107509, #77180, #13534, #152049, #119730, #11575, #92342, #330, #135895, #75200, #27738, #73241, #151070, #43878, #59034, #187372, #156008, #108512, #2322, #49830, #82122, #79162, #3318, #173179, #125674, #64004, #5296, #141825, #172177, #66979, #47853, #157008, #35647, #19492, #50827, #95323, #188352, #158980, #64991, #109506, #171188, #158000, #170191, #17505, #186374, #31685, #111494, #112484, #140833, #127649, #18506, #81137, #32677, #185361, #65980, #97294, #110495, #155019, #46852, #34655, #80154, #126649, #93334, #174177, #33662, #94330, #78163, #16515, #96314, #48841, #142818, #20472, #4298, #189349, #143814, #139831, #1320, #62999, #124677, #86147, #147838, #70989, #132657, #193338, #67974, #115492, #178176, #37640, #7293, #101302, #85133, #99304, #117485, #128639, #68977, #175164, #36630, #162991, #52801, #51810, #83136, #54812, #177180, #159988, #161988, #39641, #10323, #21475, #194345, #179183, #40651, #113469, #98287, #38653, #24496, #6295, #145810, #9324, #164010, #8312, #55813, #100310, #23484, #144812, #146817, #130642, #129628, #190333, #69988, #102320, #114468, #191323, #116487, #131656, #25506, #160989, #87150, #148833, #176170, #22483, #84131, #192336, #53817, #133653, #119493, #13300, #28491, #27498, #168943, #134667, #181175, #183147, #137623, #103322, #89140, #166988, #58794, #29468, #71979, #149822, #90125, #45620, #43638, #60774, #30450, #199307, #122446, #44632, #121455, #73990, #135659, #42652, #11328, #180189, #151809, #14280, #74965, #41659, #91101, #167969, #104314, #184138, #59787, #106284, #107272, #196353, #165002, #182153, #57821, #165997, #152789, #92097, #105301, #75949, #153785, #26496, #195344, #56824, #136627, #88138, #118498, #150828, #197331, #198308, #72999, #12325, #120462, #157775, #50596, #187139, #2090, #169952, #123429, #19266, #189124, #186135, #48611, #1083, #18274, #112255, #17270, #65746, #78923, #47614, #138609, #32439, #79927, #173947, #109268, #33433, #3087, #155772, #94093, #35414, #171944, #63770, #97066, #77930, #110263, #127414, #49594, #80912, #125443, #141600, #15280, #95092, #139597, #62758, #188123, #91, #170947, #16278, #61761, #64763, #142589, #140600, #4068, #156781, #111257, #124439, #76940, #96086, #185122, #126425, #46612, #108274, #172949, #34427, #31443, #93097, #154781, #148344, #70503, #103839, #164522, #135189, #101831, #132171, #102836, #116998, #88660, #86660, #150356, #10840, #158748, #73518, #20237, #40155, #195872, #43164, #26015, #87659, #143577, #178693, #8835, #118012, #179701, #11853, #181683, #196863, #25017, #58329, #165520, #193862, #9840, #163518, #162503, #72510, #149344, #5060, #71499, #134185, #56330, #24004, #41173, #119997, #81885, #177694, #57345, #66745, #85660, #119020, #131165, #180703, #42179, #192855, #133166, #55327, #27016, #54334, #116005, #39162, #100820, #194857, #147347, #108792, #137148, #91618, #183666, #105819, #154309, #169470, #89660, #29979, #30971, #199825, #167506, #122963, #1606, #186659, #120977, #92618, #151346, #29001, #15798 ),
 ( #47134, #140115, #76468, #153306, #59308, #12835, #170471, #78441, #75475, #138145, #90641, #107785, #63282, #106807, #155301, #168481, #198836, #28018, #121974, #77458, #124962, #60300, #184650, #139129, #45151, #14807, #104831, #61293, #46132, #166520, #152323, #606, #16791, #62276, #31961, #123944, #185642, #74501, #93616, #13809, #136167, #197842, #182675, #44159, #49121, #171469, #51100, #113747, #3590, #190615, #19766, #144095, #95605, #68251, #128914, #160270, #173463, #17792, #129902, #174453, #158277, #189626, #32957, #175443, #34936, #157290, #52090, #112760, #21760, #188635, #18787, #35922, #65268, #36913, #96588, #98576, #97568, #48129, #83412, #109786, #126928, #82407, #127924, #145089, #159256, #81407, #6572, #172460, #187650, #94612, #80432, #20752, #4572, #50115, #156291, #110778, #142105, #5576, #79448, #141118, #111775, #143093, #66264, #67256, #2608, #125952, #64285, #33947, #163277, #180466, #150109, #57104, #41938, #102602, #40930, #193620, #55091, #100585, #130923, #99586, #71267, #133941, #132931, #161267, #10602, #87427, #23767, #103604, #179465, #164288, #26773, #115770, #22761, #101589, #177458, #38928, #149112, #118778, #24778, #25781, #84410, #146087, #116762, #162267, #194619, #165280, #56090, #148111, #85417, #147108, #7571, #9602, #88414, #72264, #195631, #11610, #73278, #117771, #192614, #178453, #191602, #8594, #70268, #53081, #114759, #131936, #176453, #37926, #39920, #69257, #54096, #86425, #59069, #58095, #89418, #199580, #121729, #166277, #168239, #184410, #16550, #27775, #138884, #185397, #46888, #119765, #181449, #183421, #169220, #12599, #152083, #92376, #170227, #14561, #30729, #106562, #44905, #42927, #29735, #75235, #104591, #196626, #153059, #45891, #120736, #135933, #61048, #91368, #76219, #167263, #77215, #137898, #154062, #182435, #155055, #15557, #108548, #60061, #151107, #134948, #122720, #107544, #364, #74263, #62035, #123699, #43915, #31720, #93368, #197603, #136906, #105577, #28762, #90399, #13568, #198593, #67015, #127684, #78197, #190371, #139867, #157045, #112519, #160024, #81171, #142853, #63035, #33697, #125710, #34691, #96348, #5331, #98324, #51846, #141861, #128674, #82156, #110532, #65027, #18542, #79201, #189384, #4332, #124713, #3352, #66016, #173215, #140870, #158035, #175200, #1356, #94364, #50861, #186411, #2359, #174213, #159015, #32712, #20508, #113505, #35681, #171223, #97329, #48877, #126683, #19526, #47888, #143852, #17540, #36665, #109541, #49864, #188387, #156043, #64040, #187409, #172213, #95360, #111530, #80189, #24530, #118533, #23519, #72014, #85165, #192370, #144846, #38688, #86181, #180222, #115527, #39673, #9357, #162023, #100344, #41692, #178209, #8346, #103357, #84164, #193371, #133687, #55845, #87185, #131690, #147871, #195380, #101335, #145844, #7326, #194378, #6329, #53853, #22517, #68009, #71022, #148866, #177215, #10357, #54847, #132690, #56858, #163024, #69010, #130676, #117519, #129661, #146853, #70021, #191357, #179217, #21511, #116521, #164042, #40683, #102353, #25541, #83172, #52835, #114504, #176206, #37675, #99340, #161023, #167021, #136661, #88172, #137653, #43671, #89172, #14315, #198342, #184169, #58828, #150864, #59817, #74021, #199340, #105333, #60805, #183181, #165035, #45651, #149856, #120495, #29498, #26528, #44663, #106316, #134703, #182186, #135691, #121487, #168002, #107302, #11361, #30479, #28522, #168974, #73031, #90158, #74996, #151841, #197363, #75980, #91131, #181210, #13331, #152821, #122478, #196386, #57855, #119527, #42686, #104347, #166031, #12358, #27531, #71673, #26187, #99995, #87827, #57518, #10013, #38339, #195031, #116177, #70682, #86837, #165687, #148523, #84820, #149513, #180871, #117174, #132348, #161680, #53500, #11010, #119186, #177867, #178869, #131340, #133340, #42347, #147526, #196043, #9014, #39336, #68664, #162680, #56508, #104009, #100995, #163693, #118186, #85836 ) ),
 .UNSPECIFIED., .T., .F., .T. ) 
 B_SPLINE_SURFACE_WITH_KNOTS ( ( 4, 3, 4 ),
 ( 3, 2, 2, 2, 2, 2, 2, 2, 2, 2, 2, 2, 2, 2, 2, 2, 2, 2, 2, 2, 2, 2, 2, 2, 2, 2, 2, 2, 2, 2, 2, 2, 2, 2, 2, 2, 2, 2, 2, 2, 2, 2, 2, 2, 2, 2, 2, 2, 2, 2, 2, 2, 2, 2, 2, 2, 2, 2, 2, 2, 2, 2, 2, 2, 2, 2, 2, 2, 2, 2, 2, 2, 2, 2, 2, 2, 2, 2, 2, 2, 2, 2, 2, 2, 2, 2, 2, 2, 2, 2, 2, 2, 2, 2, 2, 2, 2, 2, 2, 2, 2, 2, 2, 2, 2, 2, 2, 2, 2, 2, 2, 2, 2, 2, 2, 2, 2, 2, 2, 2, 2, 2, 2, 2, 2, 2, 2, 2, 2, 2, 2, 2, 2, 2, 2, 2, 2, 2, 2, 2, 2, 2, 2, 2, 2, 2, 2, 2, 2, 2, 2, 2, 2, 2, 2, 2, 2, 2, 2, 2, 2, 2, 2, 2, 2, 2, 2, 2, 2, 2, 2, 2, 2, 2, 2, 2, 2, 2, 2, 2, 2, 2, 2, 2, 2, 2, 2, 2, 2, 2, 2, 2, 2, 2, 2, 2, 2, 2, 2, 2, 2, 2, 2, 2, 2, 2, 2, 2, 2, 2, 2, 2, 2, 2, 2, 2, 2, 2, 2, 2, 2, 2, 2, 2, 2, 2, 2, 2, 3 ),
 ( 0.000000000000000000, 0.5000000000000000000, 1.000000000000000000 ),
 ( 0.000000000000000000, 0.004385964912280701511, 0.008771929824561403022, 0.01315789473684210453, 0.01754385964912280604, 0.02192982456140350755, 0.02631578947368420907, 0.03070175438596491058, 0.03508771929824561209, 0.03947368421052631360, 0.04385964912280701511, 0.04824561403508771662, 0.05263157894736841813, 0.05701754385964911964, 0.06140350877192982115, 0.06578947368421052266, 0.07017543859649122417, 0.07456140350877192569, 0.07894736842105262720, 0.08333333333333332871, 0.08771929824561403022, 0.09210526315789473173, 0.09649122807017543324, 0.1008771929824561348, 0.1052631578947368363, 0.1096491228070175378, 0.1140350877192982393, 0.1184210526315789408, 0.1228070175438596423, 0.1271929824561403577, 0.1315789473684210453, 0.1359649122807017607, 0.1403508771929824483, 0.1447368421052631637, 0.1491228070175438514, 0.1535087719298245668, 0.1578947368421052544, 0.1622807017543859698, 0.1666666666666666574, 0.1710526315789473728, 0.1754385964912280604, 0.1798245614035087758, 0.1842105263157894635, 0.1885964912280701788, 0.1929824561403508665, 0.1973684210526315819, 0.2017543859649122695, 0.2061403508771929849, 0.2105263157894736725, 0.2149122807017543879, 0.2192982456140350755, 0.2236842105263157909, 0.2280701754385964786, 0.2324561403508771940, 0.2368421052631578816, 0.2412280701754385970, 0.2456140350877192846, 0.2500000000000000000, 0.2543859649122807154, 0.2587719298245614308, 0.2631578947368420907, 0.2675438596491228060, 0.2719298245614035214, 0.2763157894736842368, 0.2807017543859648967, 0.2850877192982456121, 0.2894736842105263275, 0.2938596491228070429, 0.2982456140350877027, 0.3026315789473684181, 0.3070175438596491335, 0.3114035087719298489, 0.3157894736842105088, 0.3201754385964912242, 0.3245614035087719396, 0.3289473684210526550, 0.3333333333333333148, 0.3377192982456140302, 0.3421052631578947456, 0.3464912280701754610, 0.3508771929824561209, 0.3552631578947368363, 0.3596491228070175517, 0.3640350877192982670, 0.3684210526315789269, 0.3728070175438596423, 0.3771929824561403577, 0.3815789473684210731, 0.3859649122807017330, 0.3903508771929824483, 0.3947368421052631637, 0.3991228070175438791, 0.4035087719298245390, 0.4078947368421052544, 0.4122807017543859698, 0.4166666666666666852, 0.4210526315789473450, 0.4254385964912280604, 0.4298245614035087758, 0.4342105263157894912, 0.4385964912280701511, 0.4429824561403508665, 0.4473684210526315819, 0.4517543859649122973, 0.4561403508771929571, 0.4605263157894736725, 0.4649122807017543879, 0.4692982456140351033, 0.4736842105263157632, 0.4780701754385964786, 0.4824561403508771940, 0.4868421052631579093, 0.4912280701754385692, 0.4956140350877192846, 0.5000000000000000000, 0.5043859649122807154, 0.5087719298245614308, 0.5131578947368421462, 0.5175438596491228616, 0.5219298245614034659, 0.5263157894736841813, 0.5307017543859648967, 0.5350877192982456121, 0.5394736842105263275, 0.5438596491228070429, 0.5482456140350877583, 0.5526315789473684736, 0.5570175438596490780, 0.5614035087719297934, 0.5657894736842105088, 0.5701754385964912242, 0.5745614035087719396, 0.5789473684210526550, 0.5833333333333333703, 0.5877192982456140857, 0.5921052631578946901, 0.5964912280701754055, 0.6008771929824561209, 0.6052631578947368363, 0.6096491228070175517, 0.6140350877192982670, 0.6184210526315789824, 0.6228070175438596978, 0.6271929824561403022, 0.6315789473684210176, 0.6359649122807017330, 0.6403508771929824483, 0.6447368421052631637, 0.6491228070175438791, 0.6535087719298245945, 0.6578947368421053099, 0.6622807017543859143, 0.6666666666666666297, 0.6710526315789473450, 0.6754385964912280604, 0.6798245614035087758, 0.6842105263157894912, 0.6885964912280702066, 0.6929824561403509220, 0.6973684210526315264, 0.7017543859649122417, 0.7061403508771929571, 0.7105263157894736725, 0.7149122807017543879, 0.7192982456140351033, 0.7236842105263158187, 0.7280701754385965341, 0.7324561403508771384, 0.7368421052631578538, 0.7412280701754385692, 0.7456140350877192846, 0.7500000000000000000, 0.7543859649122807154, 0.7587719298245614308, 0.7631578947368421462, 0.7675438596491228616, 0.7719298245614034659, 0.7763157894736841813, 0.7807017543859648967, 0.7850877192982456121, 0.7894736842105263275, 0.7938596491228070429, 0.7982456140350877583, 0.8026315789473684736, 0.8070175438596490780, 0.8114035087719297934, 0.8157894736842105088, 0.8201754385964912242, 0.8245614035087719396, 0.8289473684210526550, 0.8333333333333333703, 0.8377192982456140857, 0.8421052631578946901, 0.8464912280701754055, 0.8508771929824561209, 0.8552631578947368363, 0.8596491228070175517, 0.8640350877192982670, 0.8684210526315789824, 0.8728070175438596978, 0.8771929824561403022, 0.8815789473684210176, 0.8859649122807017330, 0.8903508771929824483, 0.8947368421052631637, 0.8991228070175438791, 0.9035087719298245945, 0.9078947368421053099, 0.9122807017543859143, 0.9166666666666666297, 0.9210526315789473450, 0.9254385964912280604, 0.9298245614035087758, 0.9342105263157894912, 0.9385964912280702066, 0.9429824561403509220, 0.9473684210526315264, 0.9517543859649122417, 0.9561403508771929571, 0.9605263157894736725, 0.9649122807017543879, 0.9692982456140351033, 0.9736842105263158187, 0.9780701754385965341, 0.9824561403508771384, 0.9868421052631578538, 0.9912280701754385692, 0.9956140350877192846, 1.000000000000000000 ),
 .UNSPECIFIED. ) 
 GEOMETRIC_REPRESENTATION_ITEM ( )  RATIONAL_B_SPLINE_SURFACE ( (
 ( 1.000000000000000000, 0.9659258262890683122, 1.000000000000000000, 0.9659258262890683122, 1.000000000000000000, 0.9659258262890683122, 1.000000000000000000, 0.9659258262890683122, 1.000000000000000000, 0.9659258262890683122, 1.000000000000000000, 0.9659258262890683122, 1.000000000000000000, 0.9659258262890683122, 1.000000000000000000, 0.9659258262890683122, 1.000000000000000000, 0.9659258262890683122, 1.000000000000000000, 0.9659258262890683122, 1.000000000000000000, 0.9659258262890683122, 1.000000000000000000, 0.9659258262890683122, 1.000000000000000000, 0.9659258262890683122, 1.000000000000000000, 0.9659258262890683122, 1.000000000000000000, 0.9659258262890683122, 1.000000000000000000, 0.9659258262890683122, 1.000000000000000000, 0.9659258262890683122, 1.000000000000000000, 0.9659258262890683122, 1.000000000000000000, 0.9659258262890683122, 1.000000000000000000, 0.9659258262890683122, 1.000000000000000000, 0.9659258262890683122, 1.000000000000000000, 0.9659258262890683122, 1.000000000000000000, 0.9659258262890683122, 1.000000000000000000, 0.9659258262890683122, 1.000000000000000000, 0.9659258262890683122, 1.000000000000000000, 0.9659258262890683122, 1.000000000000000000, 0.9659258262890683122, 1.000000000000000000, 0.9659258262890683122, 1.000000000000000000, 0.9659258262890683122, 1.000000000000000000, 0.9659258262890683122, 1.000000000000000000, 0.9659258262890683122, 1.000000000000000000, 0.9659258262890683122, 1.000000000000000000, 0.9659258262890683122, 1.000000000000000000, 0.9659258262890683122, 1.000000000000000000, 0.9659258262890683122, 1.000000000000000000, 0.9659258262890683122, 1.000000000000000000, 0.9659258262890683122, 1.000000000000000000, 0.9659258262890683122, 1.000000000000000000, 0.9659258262890683122, 1.000000000000000000, 0.9659258262890683122, 1.000000000000000000, 0.9659258262890683122, 1.000000000000000000, 0.9659258262890683122, 1.000000000000000000, 0.9659258262890683122, 1.000000000000000000, 0.9659258262890683122, 1.000000000000000000, 0.9659258262890683122, 1.000000000000000000, 0.9659258262890683122, 1.000000000000000000, 0.9659258262890683122, 1.000000000000000000, 0.9659258262890683122, 1.000000000000000000, 0.9659258262890683122, 1.000000000000000000, 0.9659258262890683122, 1.000000000000000000, 0.9659258262890683122, 1.000000000000000000, 0.9659258262890683122, 1.000000000000000000, 0.9659258262890683122, 1.000000000000000000, 0.9659258262890683122, 1.000000000000000000, 0.9659258262890683122, 1.000000000000000000, 0.9659258262890683122, 1.000000000000000000, 0.9659258262890683122, 1.000000000000000000, 0.9659258262890683122, 1.000000000000000000, 0.9659258262890683122, 1.000000000000000000, 0.9659258262890683122, 1.000000000000000000, 0.9659258262890683122, 1.000000000000000000, 0.9659258262890683122, 1.000000000000000000, 0.9659258262890683122, 1.000000000000000000, 0.9659258262890683122, 1.000000000000000000, 0.9659258262890683122, 1.000000000000000000, 0.9659258262890683122, 1.000000000000000000, 0.9659258262890683122, 1.000000000000000000, 0.9659258262890683122, 1.000000000000000000, 0.9659258262890683122, 1.000000000000000000, 0.9659258262890683122, 1.000000000000000000, 0.9659258262890683122, 1.000000000000000000, 0.9659258262890683122, 1.000000000000000000, 0.9659258262890683122, 1.000000000000000000, 0.9659258262890683122, 1.000000000000000000, 0.9659258262890683122, 1.000000000000000000, 0.9659258262890683122, 1.000000000000000000, 0.9659258262890683122, 1.000000000000000000, 0.9659258262890683122, 1.000000000000000000, 0.9659258262890683122, 1.000000000000000000, 0.9659258262890683122, 1.000000000000000000, 0.9659258262890683122, 1.000000000000000000, 0.9659258262890683122, 1.000000000000000000, 0.9659258262890683122, 1.000000000000000000, 0.9659258262890683122, 1.000000000000000000, 0.9659258262890683122, 1.000000000000000000, 0.9659258262890683122, 1.000000000000000000, 0.9659258262890683122, 1.000000000000000000, 0.9659258262890683122, 1.000000000000000000, 0.9659258262890683122, 1.000000000000000000, 0.9659258262890683122, 1.000000000000000000, 0.9659258262890683122, 1.000000000000000000, 0.9659258262890683122, 1.000000000000000000, 0.9659258262890683122, 1.000000000000000000, 0.9659258262890683122, 1.000000000000000000, 0.9659258262890683122, 1.000000000000000000, 0.9659258262890683122, 1.000000000000000000, 0.9659258262890683122, 1.000000000000000000, 0.9659258262890683122, 1.000000000000000000, 0.9659258262890683122, 1.000000000000000000, 0.9659258262890683122, 1.000000000000000000, 0.9659258262890683122, 1.000000000000000000, 0.9659258262890683122, 1.000000000000000000, 0.9659258262890683122, 1.000000000000000000, 0.9659258262890683122, 1.000000000000000000, 0.9659258262890683122, 1.000000000000000000, 0.9659258262890683122, 1.000000000000000000, 0.9659258262890683122, 1.000000000000000000, 0.9659258262890683122, 1.000000000000000000, 0.9659258262890683122, 1.000000000000000000, 0.9659258262890683122, 1.000000000000000000, 0.9659258262890683122, 1.000000000000000000, 0.9659258262890683122, 1.000000000000000000, 0.9659258262890683122, 1.000000000000000000, 0.9659258262890683122, 1.000000000000000000, 0.9659258262890683122, 1.000000000000000000, 0.9659258262890683122, 1.000000000000000000, 0.9659258262890683122, 1.000000000000000000, 0.9659258262890683122, 1.000000000000000000, 0.9659258262890683122, 1.000000000000000000, 0.9659258262890683122, 1.000000000000000000, 0.9659258262890683122, 1.000000000000000000, 0.9659258262890683122, 1.000000000000000000, 0.9659258262890683122, 1.000000000000000000, 0.9659258262890683122, 1.000000000000000000, 0.9659258262890683122, 1.000000000000000000, 0.9659258262890683122, 1.000000000000000000, 0.9659258262890683122, 1.000000000000000000, 0.9659258262890683122, 1.000000000000000000, 0.9659258262890683122, 1.000000000000000000, 0.9659258262890683122, 1.000000000000000000, 0.9659258262890683122, 1.000000000000000000, 0.9659258262890683122, 1.000000000000000000, 0.9659258262890683122, 1.000000000000000000, 0.9659258262890683122, 1.000000000000000000, 0.9659258262890683122, 1.000000000000000000, 0.9659258262890683122, 1.000000000000000000, 0.9659258262890683122, 1.000000000000000000, 0.9659258262890683122, 1.000000000000000000, 0.9659258262890683122, 1.000000000000000000, 0.9659258262890683122, 1.000000000000000000, 0.9659258262890683122, 1.000000000000000000, 0.9659258262890683122, 1.000000000000000000, 0.9659258262890683122, 1.000000000000000000, 0.9659258262890683122, 1.000000000000000000, 0.9659258262890683122, 1.000000000000000000, 0.9659258262890683122, 1.000000000000000000, 0.9659258262890683122, 1.000000000000000000, 0.9659258262890683122, 1.000000000000000000, 0.9659258262890683122, 1.000000000000000000, 0.9659258262890683122, 1.000000000000000000, 0.9659258262890683122, 1.000000000000000000, 0.9659258262890683122, 1.000000000000000000, 0.9659258262890683122, 1.000000000000000000, 0.9659258262890683122, 1.000000000000000000, 0.9659258262890683122, 1.000000000000000000, 0.9659258262890683122, 1.000000000000000000, 0.9659258262890683122, 1.000000000000000000, 0.9659258262890683122, 1.000000000000000000, 0.9659258262890683122, 1.000000000000000000, 0.9659258262890683122, 1.000000000000000000, 0.9659258262890683122, 1.000000000000000000, 0.9659258262890683122, 1.000000000000000000, 0.9659258262890683122, 1.000000000000000000, 0.9659258262890683122, 1.000000000000000000, 0.9659258262890683122, 1.000000000000000000, 0.9659258262890683122, 1.000000000000000000, 0.9659258262890683122, 1.000000000000000000, 0.9659258262890683122, 1.000000000000000000, 0.9659258262890683122, 1.000000000000000000, 0.9659258262890683122, 1.000000000000000000, 0.9659258262890683122, 1.000000000000000000, 0.9659258262890683122, 1.000000000000000000, 0.9659258262890683122, 1.000000000000000000, 0.9659258262890683122, 1.000000000000000000, 0.9659258262890683122, 1.000000000000000000, 0.9659258262890683122, 1.000000000000000000, 0.9659258262890683122, 1.000000000000000000, 0.9659258262890683122, 1.000000000000000000, 0.9659258262890683122, 1.000000000000000000, 0.9659258262890683122, 1.000000000000000000, 0.9659258262890683122, 1.000000000000000000, 0.9659258262890683122, 1.000000000000000000, 0.9659258262890683122, 1.000000000000000000, 0.9659258262890683122, 1.000000000000000000, 0.9659258262890683122, 1.000000000000000000, 0.9659258262890683122, 1.000000000000000000, 0.9659258262890683122, 1.000000000000000000, 0.9659258262890683122, 1.000000000000000000, 0.9659258262890683122, 1.000000000000000000, 0.9659258262890683122, 1.000000000000000000, 0.9659258262890683122, 1.000000000000000000, 0.9659258262890683122, 1.000000000000000000, 0.9659258262890683122, 1.000000000000000000, 0.9659258262890683122, 1.000000000000000000, 0.9659258262890683122, 1.000000000000000000, 0.9659258262890683122, 1.000000000000000000, 0.9659258262890683122, 1.000000000000000000, 0.9659258262890683122, 1.000000000000000000, 0.9659258262890683122, 1.000000000000000000, 0.9659258262890683122, 1.000000000000000000, 0.9659258262890683122, 1.000000000000000000, 0.9659258262890683122, 1.000000000000000000, 0.9659258262890683122, 1.000000000000000000, 0.9659258262890683122, 1.000000000000000000, 0.9659258262890683122, 1.000000000000000000, 0.9659258262890683122, 1.000000000000000000, 0.9659258262890683122, 1.000000000000000000, 0.9659258262890683122, 1.000000000000000000, 0.9659258262890683122, 1.000000000000000000, 0.9659258262890683122, 1.000000000000000000, 0.9659258262890683122, 1.000000000000000000, 0.9659258262890683122, 1.000000000000000000, 0.9659258262890683122, 1.000000000000000000, 0.9659258262890683122, 1.000000000000000000, 0.9659258262890683122, 1.000000000000000000, 0.9659258262890683122, 1.000000000000000000, 0.9659258262890683122, 1.000000000000000000, 0.9659258262890683122, 1.000000000000000000, 0.9659258262890683122, 1.000000000000000000, 0.9659258262890683122, 1.000000000000000000, 0.9659258262890683122, 1.000000000000000000, 0.9659258262890683122, 1.000000000000000000, 0.9659258262890683122, 1.000000000000000000, 0.9659258262890683122, 1.000000000000000000, 0.9659258262890683122, 1.000000000000000000, 0.9659258262890683122, 1.000000000000000000, 0.9659258262890683122, 1.000000000000000000, 0.9659258262890683122, 1.000000000000000000),
 ( 0.3333333333333333703, 0.3219752754296894559, 0.3333333333333333703, 0.3219752754296894559, 0.3333333333333333703, 0.3219752754296894559, 0.3333333333333333703, 0.3219752754296894559, 0.3333333333333333703, 0.3219752754296894559, 0.3333333333333333703, 0.3219752754296894559, 0.3333333333333333703, 0.3219752754296894559, 0.3333333333333333703, 0.3219752754296894559, 0.3333333333333333703, 0.3219752754296894559, 0.3333333333333333703, 0.3219752754296894559, 0.3333333333333333703, 0.3219752754296894559, 0.3333333333333333703, 0.3219752754296894559, 0.3333333333333333703, 0.3219752754296894559, 0.3333333333333333703, 0.3219752754296894559, 0.3333333333333333703, 0.3219752754296894559, 0.3333333333333333703, 0.3219752754296894559, 0.3333333333333333703, 0.3219752754296894559, 0.3333333333333333703, 0.3219752754296894559, 0.3333333333333333703, 0.3219752754296894559, 0.3333333333333333703, 0.3219752754296894559, 0.3333333333333333703, 0.3219752754296894559, 0.3333333333333333703, 0.3219752754296894559, 0.3333333333333333703, 0.3219752754296894559, 0.3333333333333333703, 0.3219752754296894559, 0.3333333333333333703, 0.3219752754296894559, 0.3333333333333333703, 0.3219752754296894559, 0.3333333333333333703, 0.3219752754296894559, 0.3333333333333333703, 0.3219752754296894559, 0.3333333333333333703, 0.3219752754296894559, 0.3333333333333333703, 0.3219752754296894559, 0.3333333333333333703, 0.3219752754296894559, 0.3333333333333333703, 0.3219752754296894559, 0.3333333333333333703, 0.3219752754296894559, 0.3333333333333333703, 0.3219752754296894559, 0.3333333333333333703, 0.3219752754296894559, 0.3333333333333333703, 0.3219752754296894559, 0.3333333333333333703, 0.3219752754296894559, 0.3333333333333333703, 0.3219752754296894559, 0.3333333333333333703, 0.3219752754296894559, 0.3333333333333333703, 0.3219752754296894559, 0.3333333333333333703, 0.3219752754296894559, 0.3333333333333333703, 0.3219752754296894559, 0.3333333333333333703, 0.3219752754296894559, 0.3333333333333333703, 0.3219752754296894559, 0.3333333333333333703, 0.3219752754296894559, 0.3333333333333333703, 0.3219752754296894559, 0.3333333333333333703, 0.3219752754296894559, 0.3333333333333333703, 0.3219752754296894559, 0.3333333333333333703, 0.3219752754296894559, 0.3333333333333333703, 0.3219752754296894559, 0.3333333333333333703, 0.3219752754296894559, 0.3333333333333333703, 0.3219752754296894559, 0.3333333333333333703, 0.3219752754296894559, 0.3333333333333333703, 0.3219752754296894559, 0.3333333333333333703, 0.3219752754296894559, 0.3333333333333333703, 0.3219752754296894559, 0.3333333333333333703, 0.3219752754296894559, 0.3333333333333333703, 0.3219752754296894559, 0.3333333333333333703, 0.3219752754296894559, 0.3333333333333333703, 0.3219752754296894559, 0.3333333333333333703, 0.3219752754296894559, 0.3333333333333333703, 0.3219752754296894559, 0.3333333333333333703, 0.3219752754296894559, 0.3333333333333333703, 0.3219752754296894559, 0.3333333333333333703, 0.3219752754296894559, 0.3333333333333333703, 0.3219752754296894559, 0.3333333333333333703, 0.3219752754296894559, 0.3333333333333333703, 0.3219752754296894559, 0.3333333333333333703, 0.3219752754296894559, 0.3333333333333333703, 0.3219752754296894559, 0.3333333333333333703, 0.3219752754296894559, 0.3333333333333333703, 0.3219752754296894559, 0.3333333333333333703, 0.3219752754296894559, 0.3333333333333333703, 0.3219752754296894559, 0.3333333333333333703, 0.3219752754296894559, 0.3333333333333333703, 0.3219752754296894559, 0.3333333333333333703, 0.3219752754296894559, 0.3333333333333333703, 0.3219752754296894559, 0.3333333333333333703, 0.3219752754296894559, 0.3333333333333333703, 0.3219752754296894559, 0.3333333333333333703, 0.3219752754296894559, 0.3333333333333333703, 0.3219752754296894559, 0.3333333333333333703, 0.3219752754296894559, 0.3333333333333333703, 0.3219752754296894559, 0.3333333333333333703, 0.3219752754296894559, 0.3333333333333333703, 0.3219752754296894559, 0.3333333333333333703, 0.3219752754296894559, 0.3333333333333333703, 0.3219752754296894559, 0.3333333333333333703, 0.3219752754296894559, 0.3333333333333333703, 0.3219752754296894559, 0.3333333333333333703, 0.3219752754296894559, 0.3333333333333333703, 0.3219752754296894559, 0.3333333333333333703, 0.3219752754296894559, 0.3333333333333333703, 0.3219752754296894559, 0.3333333333333333703, 0.3219752754296894559, 0.3333333333333333703, 0.3219752754296894559, 0.3333333333333333703, 0.3219752754296894559, 0.3333333333333333703, 0.3219752754296894559, 0.3333333333333333703, 0.3219752754296894559, 0.3333333333333333703, 0.3219752754296894559, 0.3333333333333333703, 0.3219752754296894559, 0.3333333333333333703, 0.3219752754296894559, 0.3333333333333333703, 0.3219752754296894559, 0.3333333333333333703, 0.3219752754296894559, 0.3333333333333333703, 0.3219752754296894559, 0.3333333333333333703, 0.3219752754296894559, 0.3333333333333333703, 0.3219752754296894559, 0.3333333333333333703, 0.3219752754296894559, 0.3333333333333333703, 0.3219752754296894559, 0.3333333333333333703, 0.3219752754296894559, 0.3333333333333333703, 0.3219752754296894559, 0.3333333333333333703, 0.3219752754296894559, 0.3333333333333333703, 0.3219752754296894559, 0.3333333333333333703, 0.3219752754296894559, 0.3333333333333333703, 0.3219752754296894559, 0.3333333333333333703, 0.3219752754296894559, 0.3333333333333333703, 0.3219752754296894559, 0.3333333333333333703, 0.3219752754296894559, 0.3333333333333333703, 0.3219752754296894559, 0.3333333333333333703, 0.3219752754296894559, 0.3333333333333333703, 0.3219752754296894559, 0.3333333333333333703, 0.3219752754296894559, 0.3333333333333333703, 0.3219752754296894559, 0.3333333333333333703, 0.3219752754296894559, 0.3333333333333333703, 0.3219752754296894559, 0.3333333333333333703, 0.3219752754296894559, 0.3333333333333333703, 0.3219752754296894559, 0.3333333333333333703, 0.3219752754296894559, 0.3333333333333333703, 0.3219752754296894559, 0.3333333333333333703, 0.3219752754296894559, 0.3333333333333333703, 0.3219752754296894559, 0.3333333333333333703, 0.3219752754296894559, 0.3333333333333333703, 0.3219752754296894559, 0.3333333333333333703, 0.3219752754296894559, 0.3333333333333333703, 0.3219752754296894559, 0.3333333333333333703, 0.3219752754296894559, 0.3333333333333333703, 0.3219752754296894559, 0.3333333333333333703, 0.3219752754296894559, 0.3333333333333333703, 0.3219752754296894559, 0.3333333333333333703, 0.3219752754296894559, 0.3333333333333333703, 0.3219752754296894559, 0.3333333333333333703, 0.3219752754296894559, 0.3333333333333333703, 0.3219752754296894559, 0.3333333333333333703, 0.3219752754296894559, 0.3333333333333333703, 0.3219752754296894559, 0.3333333333333333703, 0.3219752754296894559, 0.3333333333333333703, 0.3219752754296894559, 0.3333333333333333703, 0.3219752754296894559, 0.3333333333333333703, 0.3219752754296894559, 0.3333333333333333703, 0.3219752754296894559, 0.3333333333333333703, 0.3219752754296894559, 0.3333333333333333703, 0.3219752754296894559, 0.3333333333333333703, 0.3219752754296894559, 0.3333333333333333703, 0.3219752754296894559, 0.3333333333333333703, 0.3219752754296894559, 0.3333333333333333703, 0.3219752754296894559, 0.3333333333333333703, 0.3219752754296894559, 0.3333333333333333703, 0.3219752754296894559, 0.3333333333333333703, 0.3219752754296894559, 0.3333333333333333703, 0.3219752754296894559, 0.3333333333333333703, 0.3219752754296894559, 0.3333333333333333703, 0.3219752754296894559, 0.3333333333333333703, 0.3219752754296894559, 0.3333333333333333703, 0.3219752754296894559, 0.3333333333333333703, 0.3219752754296894559, 0.3333333333333333703, 0.3219752754296894559, 0.3333333333333333703, 0.3219752754296894559, 0.3333333333333333703, 0.3219752754296894559, 0.3333333333333333703, 0.3219752754296894559, 0.3333333333333333703, 0.3219752754296894559, 0.3333333333333333703, 0.3219752754296894559, 0.3333333333333333703, 0.3219752754296894559, 0.3333333333333333703, 0.3219752754296894559, 0.3333333333333333703, 0.3219752754296894559, 0.3333333333333333703, 0.3219752754296894559, 0.3333333333333333703, 0.3219752754296894559, 0.3333333333333333703, 0.3219752754296894559, 0.3333333333333333703, 0.3219752754296894559, 0.3333333333333333703, 0.3219752754296894559, 0.3333333333333333703, 0.3219752754296894559, 0.3333333333333333703, 0.3219752754296894559, 0.3333333333333333703, 0.3219752754296894559, 0.3333333333333333703, 0.3219752754296894559, 0.3333333333333333703, 0.3219752754296894559, 0.3333333333333333703, 0.3219752754296894559, 0.3333333333333333703, 0.3219752754296894559, 0.3333333333333333703, 0.3219752754296894559, 0.3333333333333333703, 0.3219752754296894559, 0.3333333333333333703, 0.3219752754296894559, 0.3333333333333333703, 0.3219752754296894559, 0.3333333333333333703, 0.3219752754296894559, 0.3333333333333333703, 0.3219752754296894559, 0.3333333333333333703, 0.3219752754296894559, 0.3333333333333333703, 0.3219752754296894559, 0.3333333333333333703, 0.3219752754296894559, 0.3333333333333333703, 0.3219752754296894559, 0.3333333333333333703, 0.3219752754296894559, 0.3333333333333333703, 0.3219752754296894559, 0.3333333333333333703, 0.3219752754296894559, 0.3333333333333333703, 0.3219752754296894559, 0.3333333333333333703, 0.3219752754296894559, 0.3333333333333333703, 0.3219752754296894559, 0.3333333333333333703, 0.3219752754296894559, 0.3333333333333333703, 0.3219752754296894559, 0.3333333333333333703, 0.3219752754296894559, 0.3333333333333333703, 0.3219752754296894559, 0.3333333333333333703, 0.3219752754296894559, 0.3333333333333333703, 0.3219752754296894559, 0.3333333333333333703, 0.3219752754296894559, 0.3333333333333333703, 0.3219752754296894559, 0.3333333333333333703, 0.3219752754296894559, 0.3333333333333333703, 0.3219752754296894559, 0.3333333333333333703, 0.3219752754296894559, 0.3333333333333333703, 0.3219752754296894559, 0.3333333333333333703, 0.3219752754296894559, 0.3333333333333333703, 0.3219752754296894559, 0.3333333333333333703, 0.3219752754296894559, 0.3333333333333333703, 0.3219752754296894559, 0.3333333333333333703, 0.3219752754296894559, 0.3333333333333333703, 0.3219752754296894559, 0.3333333333333333703, 0.3219752754296894559, 0.3333333333333333703, 0.3219752754296894559, 0.3333333333333333703, 0.3219752754296894559, 0.3333333333333333703, 0.3219752754296894559, 0.3333333333333333703, 0.3219752754296894559, 0.3333333333333333703, 0.3219752754296894559, 0.3333333333333333703, 0.3219752754296894559, 0.3333333333333333703, 0.3219752754296894559, 0.3333333333333333703),
 ( 0.3333333333333333703, 0.3219752754296894559, 0.3333333333333333703, 0.3219752754296894559, 0.3333333333333333703, 0.3219752754296894559, 0.3333333333333333703, 0.3219752754296894559, 0.3333333333333333703, 0.3219752754296894559, 0.3333333333333333703, 0.3219752754296894559, 0.3333333333333333703, 0.3219752754296894559, 0.3333333333333333703, 0.3219752754296894559, 0.3333333333333333703, 0.3219752754296894559, 0.3333333333333333703, 0.3219752754296894559, 0.3333333333333333703, 0.3219752754296894559, 0.3333333333333333703, 0.3219752754296894559, 0.3333333333333333703, 0.3219752754296894559, 0.3333333333333333703, 0.3219752754296894559, 0.3333333333333333703, 0.3219752754296894559, 0.3333333333333333703, 0.3219752754296894559, 0.3333333333333333703, 0.3219752754296894559, 0.3333333333333333703, 0.3219752754296894559, 0.3333333333333333703, 0.3219752754296894559, 0.3333333333333333703, 0.3219752754296894559, 0.3333333333333333703, 0.3219752754296894559, 0.3333333333333333703, 0.3219752754296894559, 0.3333333333333333703, 0.3219752754296894559, 0.3333333333333333703, 0.3219752754296894559, 0.3333333333333333703, 0.3219752754296894559, 0.3333333333333333703, 0.3219752754296894559, 0.3333333333333333703, 0.3219752754296894559, 0.3333333333333333703, 0.3219752754296894559, 0.3333333333333333703, 0.3219752754296894559, 0.3333333333333333703, 0.3219752754296894559, 0.3333333333333333703, 0.3219752754296894559, 0.3333333333333333703, 0.3219752754296894559, 0.3333333333333333703, 0.3219752754296894559, 0.3333333333333333703, 0.3219752754296894559, 0.3333333333333333703, 0.3219752754296894559, 0.3333333333333333703, 0.3219752754296894559, 0.3333333333333333703, 0.3219752754296894559, 0.3333333333333333703, 0.3219752754296894559, 0.3333333333333333703, 0.3219752754296894559, 0.3333333333333333703, 0.3219752754296894559, 0.3333333333333333703, 0.3219752754296894559, 0.3333333333333333703, 0.3219752754296894559, 0.3333333333333333703, 0.3219752754296894559, 0.3333333333333333703, 0.3219752754296894559, 0.3333333333333333703, 0.3219752754296894559, 0.3333333333333333703, 0.3219752754296894559, 0.3333333333333333703, 0.3219752754296894559, 0.3333333333333333703, 0.3219752754296894559, 0.3333333333333333703, 0.3219752754296894559, 0.3333333333333333703, 0.3219752754296894559, 0.3333333333333333703, 0.3219752754296894559, 0.3333333333333333703, 0.3219752754296894559, 0.3333333333333333703, 0.3219752754296894559, 0.3333333333333333703, 0.3219752754296894559, 0.3333333333333333703, 0.3219752754296894559, 0.3333333333333333703, 0.3219752754296894559, 0.3333333333333333703, 0.3219752754296894559, 0.3333333333333333703, 0.3219752754296894559, 0.3333333333333333703, 0.3219752754296894559, 0.3333333333333333703, 0.3219752754296894559, 0.3333333333333333703, 0.3219752754296894559, 0.3333333333333333703, 0.3219752754296894559, 0.3333333333333333703, 0.3219752754296894559, 0.3333333333333333703, 0.3219752754296894559, 0.3333333333333333703, 0.3219752754296894559, 0.3333333333333333703, 0.3219752754296894559, 0.3333333333333333703, 0.3219752754296894559, 0.3333333333333333703, 0.3219752754296894559, 0.3333333333333333703, 0.3219752754296894559, 0.3333333333333333703, 0.3219752754296894559, 0.3333333333333333703, 0.3219752754296894559, 0.3333333333333333703, 0.3219752754296894559, 0.3333333333333333703, 0.3219752754296894559, 0.3333333333333333703, 0.3219752754296894559, 0.3333333333333333703, 0.3219752754296894559, 0.3333333333333333703, 0.3219752754296894559, 0.3333333333333333703, 0.3219752754296894559, 0.3333333333333333703, 0.3219752754296894559, 0.3333333333333333703, 0.3219752754296894559, 0.3333333333333333703, 0.3219752754296894559, 0.3333333333333333703, 0.3219752754296894559, 0.3333333333333333703, 0.3219752754296894559, 0.3333333333333333703, 0.3219752754296894559, 0.3333333333333333703, 0.3219752754296894559, 0.3333333333333333703, 0.3219752754296894559, 0.3333333333333333703, 0.3219752754296894559, 0.3333333333333333703, 0.3219752754296894559, 0.3333333333333333703, 0.3219752754296894559, 0.3333333333333333703, 0.3219752754296894559, 0.3333333333333333703, 0.3219752754296894559, 0.3333333333333333703, 0.3219752754296894559, 0.3333333333333333703, 0.3219752754296894559, 0.3333333333333333703, 0.3219752754296894559, 0.3333333333333333703, 0.3219752754296894559, 0.3333333333333333703, 0.3219752754296894559, 0.3333333333333333703, 0.3219752754296894559, 0.3333333333333333703, 0.3219752754296894559, 0.3333333333333333703, 0.3219752754296894559, 0.3333333333333333703, 0.3219752754296894559, 0.3333333333333333703, 0.3219752754296894559, 0.3333333333333333703, 0.3219752754296894559, 0.3333333333333333703, 0.3219752754296894559, 0.3333333333333333703, 0.3219752754296894559, 0.3333333333333333703, 0.3219752754296894559, 0.3333333333333333703, 0.3219752754296894559, 0.3333333333333333703, 0.3219752754296894559, 0.3333333333333333703, 0.3219752754296894559, 0.3333333333333333703, 0.3219752754296894559, 0.3333333333333333703, 0.3219752754296894559, 0.3333333333333333703, 0.3219752754296894559, 0.3333333333333333703, 0.3219752754296894559, 0.3333333333333333703, 0.3219752754296894559, 0.3333333333333333703, 0.3219752754296894559, 0.3333333333333333703, 0.3219752754296894559, 0.3333333333333333703, 0.3219752754296894559, 0.3333333333333333703, 0.3219752754296894559, 0.3333333333333333703, 0.3219752754296894559, 0.3333333333333333703, 0.3219752754296894559, 0.3333333333333333703, 0.3219752754296894559, 0.3333333333333333703, 0.3219752754296894559, 0.3333333333333333703, 0.3219752754296894559, 0.3333333333333333703, 0.3219752754296894559, 0.3333333333333333703, 0.3219752754296894559, 0.3333333333333333703, 0.3219752754296894559, 0.3333333333333333703, 0.3219752754296894559, 0.3333333333333333703, 0.3219752754296894559, 0.3333333333333333703, 0.3219752754296894559, 0.3333333333333333703, 0.3219752754296894559, 0.3333333333333333703, 0.3219752754296894559, 0.3333333333333333703, 0.3219752754296894559, 0.3333333333333333703, 0.3219752754296894559, 0.3333333333333333703, 0.3219752754296894559, 0.3333333333333333703, 0.3219752754296894559, 0.3333333333333333703, 0.3219752754296894559, 0.3333333333333333703, 0.3219752754296894559, 0.3333333333333333703, 0.3219752754296894559, 0.3333333333333333703, 0.3219752754296894559, 0.3333333333333333703, 0.3219752754296894559, 0.3333333333333333703, 0.3219752754296894559, 0.3333333333333333703, 0.3219752754296894559, 0.3333333333333333703, 0.3219752754296894559, 0.3333333333333333703, 0.3219752754296894559, 0.3333333333333333703, 0.3219752754296894559, 0.3333333333333333703, 0.3219752754296894559, 0.3333333333333333703, 0.3219752754296894559, 0.3333333333333333703, 0.3219752754296894559, 0.3333333333333333703, 0.3219752754296894559, 0.3333333333333333703, 0.3219752754296894559, 0.3333333333333333703, 0.3219752754296894559, 0.3333333333333333703, 0.3219752754296894559, 0.3333333333333333703, 0.3219752754296894559, 0.3333333333333333703, 0.3219752754296894559, 0.3333333333333333703, 0.3219752754296894559, 0.3333333333333333703, 0.3219752754296894559, 0.3333333333333333703, 0.3219752754296894559, 0.3333333333333333703, 0.3219752754296894559, 0.3333333333333333703, 0.3219752754296894559, 0.3333333333333333703, 0.3219752754296894559, 0.3333333333333333703, 0.3219752754296894559, 0.3333333333333333703, 0.3219752754296894559, 0.3333333333333333703, 0.3219752754296894559, 0.3333333333333333703, 0.3219752754296894559, 0.3333333333333333703, 0.3219752754296894559, 0.3333333333333333703, 0.3219752754296894559, 0.3333333333333333703, 0.3219752754296894559, 0.3333333333333333703, 0.3219752754296894559, 0.3333333333333333703, 0.3219752754296894559, 0.3333333333333333703, 0.3219752754296894559, 0.3333333333333333703, 0.3219752754296894559, 0.3333333333333333703, 0.3219752754296894559, 0.3333333333333333703, 0.3219752754296894559, 0.3333333333333333703, 0.3219752754296894559, 0.3333333333333333703, 0.3219752754296894559, 0.3333333333333333703, 0.3219752754296894559, 0.3333333333333333703, 0.3219752754296894559, 0.3333333333333333703, 0.3219752754296894559, 0.3333333333333333703, 0.3219752754296894559, 0.3333333333333333703, 0.3219752754296894559, 0.3333333333333333703, 0.3219752754296894559, 0.3333333333333333703, 0.3219752754296894559, 0.3333333333333333703, 0.3219752754296894559, 0.3333333333333333703, 0.3219752754296894559, 0.3333333333333333703, 0.3219752754296894559, 0.3333333333333333703, 0.3219752754296894559, 0.3333333333333333703, 0.3219752754296894559, 0.3333333333333333703, 0.3219752754296894559, 0.3333333333333333703, 0.3219752754296894559, 0.3333333333333333703, 0.3219752754296894559, 0.3333333333333333703, 0.3219752754296894559, 0.3333333333333333703, 0.3219752754296894559, 0.3333333333333333703, 0.3219752754296894559, 0.3333333333333333703, 0.3219752754296894559, 0.3333333333333333703, 0.3219752754296894559, 0.3333333333333333703, 0.3219752754296894559, 0.3333333333333333703, 0.3219752754296894559, 0.3333333333333333703, 0.3219752754296894559, 0.3333333333333333703, 0.3219752754296894559, 0.3333333333333333703, 0.3219752754296894559, 0.3333333333333333703, 0.3219752754296894559, 0.3333333333333333703, 0.3219752754296894559, 0.3333333333333333703, 0.3219752754296894559, 0.3333333333333333703, 0.3219752754296894559, 0.3333333333333333703, 0.3219752754296894559, 0.3333333333333333703, 0.3219752754296894559, 0.3333333333333333703, 0.3219752754296894559, 0.3333333333333333703, 0.3219752754296894559, 0.3333333333333333703, 0.3219752754296894559, 0.3333333333333333703, 0.3219752754296894559, 0.3333333333333333703, 0.3219752754296894559, 0.3333333333333333703, 0.3219752754296894559, 0.3333333333333333703, 0.3219752754296894559, 0.3333333333333333703, 0.3219752754296894559, 0.3333333333333333703, 0.3219752754296894559, 0.3333333333333333703, 0.3219752754296894559, 0.3333333333333333703, 0.3219752754296894559, 0.3333333333333333703, 0.3219752754296894559, 0.3333333333333333703, 0.3219752754296894559, 0.3333333333333333703, 0.3219752754296894559, 0.3333333333333333703, 0.3219752754296894559, 0.3333333333333333703, 0.3219752754296894559, 0.3333333333333333703, 0.3219752754296894559, 0.3333333333333333703, 0.3219752754296894559, 0.3333333333333333703, 0.3219752754296894559, 0.3333333333333333703, 0.3219752754296894559, 0.3333333333333333703, 0.3219752754296894559, 0.3333333333333333703, 0.3219752754296894559, 0.3333333333333333703, 0.3219752754296894559, 0.3333333333333333703, 0.3219752754296894559, 0.3333333333333333703),
 ( 1.000000000000000000, 0.9659258262890683122, 1.000000000000000000, 0.9659258262890683122, 1.000000000000000000, 0.9659258262890683122, 1.000000000000000000, 0.9659258262890683122, 1.000000000000000000, 0.9659258262890683122, 1.000000000000000000, 0.9659258262890683122, 1.000000000000000000, 0.9659258262890683122, 1.000000000000000000, 0.9659258262890683122, 1.000000000000000000, 0.9659258262890683122, 1.000000000000000000, 0.9659258262890683122, 1.000000000000000000, 0.9659258262890683122, 1.000000000000000000, 0.9659258262890683122, 1.000000000000000000, 0.9659258262890683122, 1.000000000000000000, 0.9659258262890683122, 1.000000000000000000, 0.9659258262890683122, 1.000000000000000000, 0.9659258262890683122, 1.000000000000000000, 0.9659258262890683122, 1.000000000000000000, 0.9659258262890683122, 1.000000000000000000, 0.9659258262890683122, 1.000000000000000000, 0.9659258262890683122, 1.000000000000000000, 0.9659258262890683122, 1.000000000000000000, 0.9659258262890683122, 1.000000000000000000, 0.9659258262890683122, 1.000000000000000000, 0.9659258262890683122, 1.000000000000000000, 0.9659258262890683122, 1.000000000000000000, 0.9659258262890683122, 1.000000000000000000, 0.9659258262890683122, 1.000000000000000000, 0.9659258262890683122, 1.000000000000000000, 0.9659258262890683122, 1.000000000000000000, 0.9659258262890683122, 1.000000000000000000, 0.9659258262890683122, 1.000000000000000000, 0.9659258262890683122, 1.000000000000000000, 0.9659258262890683122, 1.000000000000000000, 0.9659258262890683122, 1.000000000000000000, 0.9659258262890683122, 1.000000000000000000, 0.9659258262890683122, 1.000000000000000000, 0.9659258262890683122, 1.000000000000000000, 0.9659258262890683122, 1.000000000000000000, 0.9659258262890683122, 1.000000000000000000, 0.9659258262890683122, 1.000000000000000000, 0.9659258262890683122, 1.000000000000000000, 0.9659258262890683122, 1.000000000000000000, 0.9659258262890683122, 1.000000000000000000, 0.9659258262890683122, 1.000000000000000000, 0.9659258262890683122, 1.000000000000000000, 0.9659258262890683122, 1.000000000000000000, 0.9659258262890683122, 1.000000000000000000, 0.9659258262890683122, 1.000000000000000000, 0.9659258262890683122, 1.000000000000000000, 0.9659258262890683122, 1.000000000000000000, 0.9659258262890683122, 1.000000000000000000, 0.9659258262890683122, 1.000000000000000000, 0.9659258262890683122, 1.000000000000000000, 0.9659258262890683122, 1.000000000000000000, 0.9659258262890683122, 1.000000000000000000, 0.9659258262890683122, 1.000000000000000000, 0.9659258262890683122, 1.000000000000000000, 0.9659258262890683122, 1.000000000000000000, 0.9659258262890683122, 1.000000000000000000, 0.9659258262890683122, 1.000000000000000000, 0.9659258262890683122, 1.000000000000000000, 0.9659258262890683122, 1.000000000000000000, 0.9659258262890683122, 1.000000000000000000, 0.9659258262890683122, 1.000000000000000000, 0.9659258262890683122, 1.000000000000000000, 0.9659258262890683122, 1.000000000000000000, 0.9659258262890683122, 1.000000000000000000, 0.9659258262890683122, 1.000000000000000000, 0.9659258262890683122, 1.000000000000000000, 0.9659258262890683122, 1.000000000000000000, 0.9659258262890683122, 1.000000000000000000, 0.9659258262890683122, 1.000000000000000000, 0.9659258262890683122, 1.000000000000000000, 0.9659258262890683122, 1.000000000000000000, 0.9659258262890683122, 1.000000000000000000, 0.9659258262890683122, 1.000000000000000000, 0.9659258262890683122, 1.000000000000000000, 0.9659258262890683122, 1.000000000000000000, 0.9659258262890683122, 1.000000000000000000, 0.9659258262890683122, 1.000000000000000000, 0.9659258262890683122, 1.000000000000000000, 0.9659258262890683122, 1.000000000000000000, 0.9659258262890683122, 1.000000000000000000, 0.9659258262890683122, 1.000000000000000000, 0.9659258262890683122, 1.000000000000000000, 0.9659258262890683122, 1.000000000000000000, 0.9659258262890683122, 1.000000000000000000, 0.9659258262890683122, 1.000000000000000000, 0.9659258262890683122, 1.000000000000000000, 0.9659258262890683122, 1.000000000000000000, 0.9659258262890683122, 1.000000000000000000, 0.9659258262890683122, 1.000000000000000000, 0.9659258262890683122, 1.000000000000000000, 0.9659258262890683122, 1.000000000000000000, 0.9659258262890683122, 1.000000000000000000, 0.9659258262890683122, 1.000000000000000000, 0.9659258262890683122, 1.000000000000000000, 0.9659258262890683122, 1.000000000000000000, 0.9659258262890683122, 1.000000000000000000, 0.9659258262890683122, 1.000000000000000000, 0.9659258262890683122, 1.000000000000000000, 0.9659258262890683122, 1.000000000000000000, 0.9659258262890683122, 1.000000000000000000, 0.9659258262890683122, 1.000000000000000000, 0.9659258262890683122, 1.000000000000000000, 0.9659258262890683122, 1.000000000000000000, 0.9659258262890683122, 1.000000000000000000, 0.9659258262890683122, 1.000000000000000000, 0.9659258262890683122, 1.000000000000000000, 0.9659258262890683122, 1.000000000000000000, 0.9659258262890683122, 1.000000000000000000, 0.9659258262890683122, 1.000000000000000000, 0.9659258262890683122, 1.000000000000000000, 0.9659258262890683122, 1.000000000000000000, 0.9659258262890683122, 1.000000000000000000, 0.9659258262890683122, 1.000000000000000000, 0.9659258262890683122, 1.000000000000000000, 0.9659258262890683122, 1.000000000000000000, 0.9659258262890683122, 1.000000000000000000, 0.9659258262890683122, 1.000000000000000000, 0.9659258262890683122, 1.000000000000000000, 0.9659258262890683122, 1.000000000000000000, 0.9659258262890683122, 1.000000000000000000, 0.9659258262890683122, 1.000000000000000000, 0.9659258262890683122, 1.000000000000000000, 0.9659258262890683122, 1.000000000000000000, 0.9659258262890683122, 1.000000000000000000, 0.9659258262890683122, 1.000000000000000000, 0.9659258262890683122, 1.000000000000000000, 0.9659258262890683122, 1.000000000000000000, 0.9659258262890683122, 1.000000000000000000, 0.9659258262890683122, 1.000000000000000000, 0.9659258262890683122, 1.000000000000000000, 0.9659258262890683122, 1.000000000000000000, 0.9659258262890683122, 1.000000000000000000, 0.9659258262890683122, 1.000000000000000000, 0.9659258262890683122, 1.000000000000000000, 0.9659258262890683122, 1.000000000000000000, 0.9659258262890683122, 1.000000000000000000, 0.9659258262890683122, 1.000000000000000000, 0.9659258262890683122, 1.000000000000000000, 0.9659258262890683122, 1.000000000000000000, 0.9659258262890683122, 1.000000000000000000, 0.9659258262890683122, 1.000000000000000000, 0.9659258262890683122, 1.000000000000000000, 0.9659258262890683122, 1.000000000000000000, 0.9659258262890683122, 1.000000000000000000, 0.9659258262890683122, 1.000000000000000000, 0.9659258262890683122, 1.000000000000000000, 0.9659258262890683122, 1.000000000000000000, 0.9659258262890683122, 1.000000000000000000, 0.9659258262890683122, 1.000000000000000000, 0.9659258262890683122, 1.000000000000000000, 0.9659258262890683122, 1.000000000000000000, 0.9659258262890683122, 1.000000000000000000, 0.9659258262890683122, 1.000000000000000000, 0.9659258262890683122, 1.000000000000000000, 0.9659258262890683122, 1.000000000000000000, 0.9659258262890683122, 1.000000000000000000, 0.9659258262890683122, 1.000000000000000000, 0.9659258262890683122, 1.000000000000000000, 0.9659258262890683122, 1.000000000000000000, 0.9659258262890683122, 1.000000000000000000, 0.9659258262890683122, 1.000000000000000000, 0.9659258262890683122, 1.000000000000000000, 0.9659258262890683122, 1.000000000000000000, 0.9659258262890683122, 1.000000000000000000, 0.9659258262890683122, 1.000000000000000000, 0.9659258262890683122, 1.000000000000000000, 0.9659258262890683122, 1.000000000000000000, 0.9659258262890683122, 1.000000000000000000, 0.9659258262890683122, 1.000000000000000000, 0.9659258262890683122, 1.000000000000000000, 0.9659258262890683122, 1.000000000000000000, 0.9659258262890683122, 1.000000000000000000, 0.9659258262890683122, 1.000000000000000000, 0.9659258262890683122, 1.000000000000000000, 0.9659258262890683122, 1.000000000000000000, 0.9659258262890683122, 1.000000000000000000, 0.9659258262890683122, 1.000000000000000000, 0.9659258262890683122, 1.000000000000000000, 0.9659258262890683122, 1.000000000000000000, 0.9659258262890683122, 1.000000000000000000, 0.9659258262890683122, 1.000000000000000000, 0.9659258262890683122, 1.000000000000000000, 0.9659258262890683122, 1.000000000000000000, 0.9659258262890683122, 1.000000000000000000, 0.9659258262890683122, 1.000000000000000000, 0.9659258262890683122, 1.000000000000000000, 0.9659258262890683122, 1.000000000000000000, 0.9659258262890683122, 1.000000000000000000, 0.9659258262890683122, 1.000000000000000000, 0.9659258262890683122, 1.000000000000000000, 0.9659258262890683122, 1.000000000000000000, 0.9659258262890683122, 1.000000000000000000, 0.9659258262890683122, 1.000000000000000000, 0.9659258262890683122, 1.000000000000000000, 0.9659258262890683122, 1.000000000000000000, 0.9659258262890683122, 1.000000000000000000, 0.9659258262890683122, 1.000000000000000000, 0.9659258262890683122, 1.000000000000000000, 0.9659258262890683122, 1.000000000000000000, 0.9659258262890683122, 1.000000000000000000, 0.9659258262890683122, 1.000000000000000000, 0.9659258262890683122, 1.000000000000000000, 0.9659258262890683122, 1.000000000000000000, 0.9659258262890683122, 1.000000000000000000, 0.9659258262890683122, 1.000000000000000000, 0.9659258262890683122, 1.000000000000000000, 0.9659258262890683122, 1.000000000000000000, 0.9659258262890683122, 1.000000000000000000, 0.9659258262890683122, 1.000000000000000000, 0.9659258262890683122, 1.000000000000000000, 0.9659258262890683122, 1.000000000000000000, 0.9659258262890683122, 1.000000000000000000, 0.9659258262890683122, 1.000000000000000000, 0.9659258262890683122, 1.000000000000000000, 0.9659258262890683122, 1.000000000000000000, 0.9659258262890683122, 1.000000000000000000, 0.9659258262890683122, 1.000000000000000000, 0.9659258262890683122, 1.000000000000000000, 0.9659258262890683122, 1.000000000000000000, 0.9659258262890683122, 1.000000000000000000, 0.9659258262890683122, 1.000000000000000000, 0.9659258262890683122, 1.000000000000000000, 0.9659258262890683122, 1.000000000000000000, 0.9659258262890683122, 1.000000000000000000, 0.9659258262890683122, 1.000000000000000000),
 ( 0.3333333333333333703, 0.3219752754296894559, 0.3333333333333333703, 0.3219752754296894559, 0.3333333333333333703, 0.3219752754296894559, 0.3333333333333333703, 0.3219752754296894559, 0.3333333333333333703, 0.3219752754296894559, 0.3333333333333333703, 0.3219752754296894559, 0.3333333333333333703, 0.3219752754296894559, 0.3333333333333333703, 0.3219752754296894559, 0.3333333333333333703, 0.3219752754296894559, 0.3333333333333333703, 0.3219752754296894559, 0.3333333333333333703, 0.3219752754296894559, 0.3333333333333333703, 0.3219752754296894559, 0.3333333333333333703, 0.3219752754296894559, 0.3333333333333333703, 0.3219752754296894559, 0.3333333333333333703, 0.3219752754296894559, 0.3333333333333333703, 0.3219752754296894559, 0.3333333333333333703, 0.3219752754296894559, 0.3333333333333333703, 0.3219752754296894559, 0.3333333333333333703, 0.3219752754296894559, 0.3333333333333333703, 0.3219752754296894559, 0.3333333333333333703, 0.3219752754296894559, 0.3333333333333333703, 0.3219752754296894559, 0.3333333333333333703, 0.3219752754296894559, 0.3333333333333333703, 0.3219752754296894559, 0.3333333333333333703, 0.3219752754296894559, 0.3333333333333333703, 0.3219752754296894559, 0.3333333333333333703, 0.3219752754296894559, 0.3333333333333333703, 0.3219752754296894559, 0.3333333333333333703, 0.3219752754296894559, 0.3333333333333333703, 0.3219752754296894559, 0.3333333333333333703, 0.3219752754296894559, 0.3333333333333333703, 0.3219752754296894559, 0.3333333333333333703, 0.3219752754296894559, 0.3333333333333333703, 0.3219752754296894559, 0.3333333333333333703, 0.3219752754296894559, 0.3333333333333333703, 0.3219752754296894559, 0.3333333333333333703, 0.3219752754296894559, 0.3333333333333333703, 0.3219752754296894559, 0.3333333333333333703, 0.3219752754296894559, 0.3333333333333333703, 0.3219752754296894559, 0.3333333333333333703, 0.3219752754296894559, 0.3333333333333333703, 0.3219752754296894559, 0.3333333333333333703, 0.3219752754296894559, 0.3333333333333333703, 0.3219752754296894559, 0.3333333333333333703, 0.3219752754296894559, 0.3333333333333333703, 0.3219752754296894559, 0.3333333333333333703, 0.3219752754296894559, 0.3333333333333333703, 0.3219752754296894559, 0.3333333333333333703, 0.3219752754296894559, 0.3333333333333333703, 0.3219752754296894559, 0.3333333333333333703, 0.3219752754296894559, 0.3333333333333333703, 0.3219752754296894559, 0.3333333333333333703, 0.3219752754296894559, 0.3333333333333333703, 0.3219752754296894559, 0.3333333333333333703, 0.3219752754296894559, 0.3333333333333333703, 0.3219752754296894559, 0.3333333333333333703, 0.3219752754296894559, 0.3333333333333333703, 0.3219752754296894559, 0.3333333333333333703, 0.3219752754296894559, 0.3333333333333333703, 0.3219752754296894559, 0.3333333333333333703, 0.3219752754296894559, 0.3333333333333333703, 0.3219752754296894559, 0.3333333333333333703, 0.3219752754296894559, 0.3333333333333333703, 0.3219752754296894559, 0.3333333333333333703, 0.3219752754296894559, 0.3333333333333333703, 0.3219752754296894559, 0.3333333333333333703, 0.3219752754296894559, 0.3333333333333333703, 0.3219752754296894559, 0.3333333333333333703, 0.3219752754296894559, 0.3333333333333333703, 0.3219752754296894559, 0.3333333333333333703, 0.3219752754296894559, 0.3333333333333333703, 0.3219752754296894559, 0.3333333333333333703, 0.3219752754296894559, 0.3333333333333333703, 0.3219752754296894559, 0.3333333333333333703, 0.3219752754296894559, 0.3333333333333333703, 0.3219752754296894559, 0.3333333333333333703, 0.3219752754296894559, 0.3333333333333333703, 0.3219752754296894559, 0.3333333333333333703, 0.3219752754296894559, 0.3333333333333333703, 0.3219752754296894559, 0.3333333333333333703, 0.3219752754296894559, 0.3333333333333333703, 0.3219752754296894559, 0.3333333333333333703, 0.3219752754296894559, 0.3333333333333333703, 0.3219752754296894559, 0.3333333333333333703, 0.3219752754296894559, 0.3333333333333333703, 0.3219752754296894559, 0.3333333333333333703, 0.3219752754296894559, 0.3333333333333333703, 0.3219752754296894559, 0.3333333333333333703, 0.3219752754296894559, 0.3333333333333333703, 0.3219752754296894559, 0.3333333333333333703, 0.3219752754296894559, 0.3333333333333333703, 0.3219752754296894559, 0.3333333333333333703, 0.3219752754296894559, 0.3333333333333333703, 0.3219752754296894559, 0.3333333333333333703, 0.3219752754296894559, 0.3333333333333333703, 0.3219752754296894559, 0.3333333333333333703, 0.3219752754296894559, 0.3333333333333333703, 0.3219752754296894559, 0.3333333333333333703, 0.3219752754296894559, 0.3333333333333333703, 0.3219752754296894559, 0.3333333333333333703, 0.3219752754296894559, 0.3333333333333333703, 0.3219752754296894559, 0.3333333333333333703, 0.3219752754296894559, 0.3333333333333333703, 0.3219752754296894559, 0.3333333333333333703, 0.3219752754296894559, 0.3333333333333333703, 0.3219752754296894559, 0.3333333333333333703, 0.3219752754296894559, 0.3333333333333333703, 0.3219752754296894559, 0.3333333333333333703, 0.3219752754296894559, 0.3333333333333333703, 0.3219752754296894559, 0.3333333333333333703, 0.3219752754296894559, 0.3333333333333333703, 0.3219752754296894559, 0.3333333333333333703, 0.3219752754296894559, 0.3333333333333333703, 0.3219752754296894559, 0.3333333333333333703, 0.3219752754296894559, 0.3333333333333333703, 0.3219752754296894559, 0.3333333333333333703, 0.3219752754296894559, 0.3333333333333333703, 0.3219752754296894559, 0.3333333333333333703, 0.3219752754296894559, 0.3333333333333333703, 0.3219752754296894559, 0.3333333333333333703, 0.3219752754296894559, 0.3333333333333333703, 0.3219752754296894559, 0.3333333333333333703, 0.3219752754296894559, 0.3333333333333333703, 0.3219752754296894559, 0.3333333333333333703, 0.3219752754296894559, 0.3333333333333333703, 0.3219752754296894559, 0.3333333333333333703, 0.3219752754296894559, 0.3333333333333333703, 0.3219752754296894559, 0.3333333333333333703, 0.3219752754296894559, 0.3333333333333333703, 0.3219752754296894559, 0.3333333333333333703, 0.3219752754296894559, 0.3333333333333333703, 0.3219752754296894559, 0.3333333333333333703, 0.3219752754296894559, 0.3333333333333333703, 0.3219752754296894559, 0.3333333333333333703, 0.3219752754296894559, 0.3333333333333333703, 0.3219752754296894559, 0.3333333333333333703, 0.3219752754296894559, 0.3333333333333333703, 0.3219752754296894559, 0.3333333333333333703, 0.3219752754296894559, 0.3333333333333333703, 0.3219752754296894559, 0.3333333333333333703, 0.3219752754296894559, 0.3333333333333333703, 0.3219752754296894559, 0.3333333333333333703, 0.3219752754296894559, 0.3333333333333333703, 0.3219752754296894559, 0.3333333333333333703, 0.3219752754296894559, 0.3333333333333333703, 0.3219752754296894559, 0.3333333333333333703, 0.3219752754296894559, 0.3333333333333333703, 0.3219752754296894559, 0.3333333333333333703, 0.3219752754296894559, 0.3333333333333333703, 0.3219752754296894559, 0.3333333333333333703, 0.3219752754296894559, 0.3333333333333333703, 0.3219752754296894559, 0.3333333333333333703, 0.3219752754296894559, 0.3333333333333333703, 0.3219752754296894559, 0.3333333333333333703, 0.3219752754296894559, 0.3333333333333333703, 0.3219752754296894559, 0.3333333333333333703, 0.3219752754296894559, 0.3333333333333333703, 0.3219752754296894559, 0.3333333333333333703, 0.3219752754296894559, 0.3333333333333333703, 0.3219752754296894559, 0.3333333333333333703, 0.3219752754296894559, 0.3333333333333333703, 0.3219752754296894559, 0.3333333333333333703, 0.3219752754296894559, 0.3333333333333333703, 0.3219752754296894559, 0.3333333333333333703, 0.3219752754296894559, 0.3333333333333333703, 0.3219752754296894559, 0.3333333333333333703, 0.3219752754296894559, 0.3333333333333333703, 0.3219752754296894559, 0.3333333333333333703, 0.3219752754296894559, 0.3333333333333333703, 0.3219752754296894559, 0.3333333333333333703, 0.3219752754296894559, 0.3333333333333333703, 0.3219752754296894559, 0.3333333333333333703, 0.3219752754296894559, 0.3333333333333333703, 0.3219752754296894559, 0.3333333333333333703, 0.3219752754296894559, 0.3333333333333333703, 0.3219752754296894559, 0.3333333333333333703, 0.3219752754296894559, 0.3333333333333333703, 0.3219752754296894559, 0.3333333333333333703, 0.3219752754296894559, 0.3333333333333333703, 0.3219752754296894559, 0.3333333333333333703, 0.3219752754296894559, 0.3333333333333333703, 0.3219752754296894559, 0.3333333333333333703, 0.3219752754296894559, 0.3333333333333333703, 0.3219752754296894559, 0.3333333333333333703, 0.3219752754296894559, 0.3333333333333333703, 0.3219752754296894559, 0.3333333333333333703, 0.3219752754296894559, 0.3333333333333333703, 0.3219752754296894559, 0.3333333333333333703, 0.3219752754296894559, 0.3333333333333333703, 0.3219752754296894559, 0.3333333333333333703, 0.3219752754296894559, 0.3333333333333333703, 0.3219752754296894559, 0.3333333333333333703, 0.3219752754296894559, 0.3333333333333333703, 0.3219752754296894559, 0.3333333333333333703, 0.3219752754296894559, 0.3333333333333333703, 0.3219752754296894559, 0.3333333333333333703, 0.3219752754296894559, 0.3333333333333333703, 0.3219752754296894559, 0.3333333333333333703, 0.3219752754296894559, 0.3333333333333333703, 0.3219752754296894559, 0.3333333333333333703, 0.3219752754296894559, 0.3333333333333333703, 0.3219752754296894559, 0.3333333333333333703, 0.3219752754296894559, 0.3333333333333333703, 0.3219752754296894559, 0.3333333333333333703, 0.3219752754296894559, 0.3333333333333333703, 0.3219752754296894559, 0.3333333333333333703, 0.3219752754296894559, 0.3333333333333333703, 0.3219752754296894559, 0.3333333333333333703, 0.3219752754296894559, 0.3333333333333333703, 0.3219752754296894559, 0.3333333333333333703, 0.3219752754296894559, 0.3333333333333333703, 0.3219752754296894559, 0.3333333333333333703, 0.3219752754296894559, 0.3333333333333333703, 0.3219752754296894559, 0.3333333333333333703, 0.3219752754296894559, 0.3333333333333333703, 0.3219752754296894559, 0.3333333333333333703, 0.3219752754296894559, 0.3333333333333333703, 0.3219752754296894559, 0.3333333333333333703, 0.3219752754296894559, 0.3333333333333333703, 0.3219752754296894559, 0.3333333333333333703, 0.3219752754296894559, 0.3333333333333333703, 0.3219752754296894559, 0.3333333333333333703, 0.3219752754296894559, 0.3333333333333333703, 0.3219752754296894559, 0.3333333333333333703, 0.3219752754296894559, 0.3333333333333333703, 0.3219752754296894559, 0.3333333333333333703, 0.3219752754296894559, 0.3333333333333333703, 0.3219752754296894559, 0.3333333333333333703),
 ( 0.3333333333333333703, 0.3219752754296894559, 0.3333333333333333703, 0.3219752754296894559, 0.3333333333333333703, 0.3219752754296894559, 0.3333333333333333703, 0.3219752754296894559, 0.3333333333333333703, 0.3219752754296894559, 0.3333333333333333703, 0.3219752754296894559, 0.3333333333333333703, 0.3219752754296894559, 0.3333333333333333703, 0.3219752754296894559, 0.3333333333333333703, 0.3219752754296894559, 0.3333333333333333703, 0.3219752754296894559, 0.3333333333333333703, 0.3219752754296894559, 0.3333333333333333703, 0.3219752754296894559, 0.3333333333333333703, 0.3219752754296894559, 0.3333333333333333703, 0.3219752754296894559, 0.3333333333333333703, 0.3219752754296894559, 0.3333333333333333703, 0.3219752754296894559, 0.3333333333333333703, 0.3219752754296894559, 0.3333333333333333703, 0.3219752754296894559, 0.3333333333333333703, 0.3219752754296894559, 0.3333333333333333703, 0.3219752754296894559, 0.3333333333333333703, 0.3219752754296894559, 0.3333333333333333703, 0.3219752754296894559, 0.3333333333333333703, 0.3219752754296894559, 0.3333333333333333703, 0.3219752754296894559, 0.3333333333333333703, 0.3219752754296894559, 0.3333333333333333703, 0.3219752754296894559, 0.3333333333333333703, 0.3219752754296894559, 0.3333333333333333703, 0.3219752754296894559, 0.3333333333333333703, 0.3219752754296894559, 0.3333333333333333703, 0.3219752754296894559, 0.3333333333333333703, 0.3219752754296894559, 0.3333333333333333703, 0.3219752754296894559, 0.3333333333333333703, 0.3219752754296894559, 0.3333333333333333703, 0.3219752754296894559, 0.3333333333333333703, 0.3219752754296894559, 0.3333333333333333703, 0.3219752754296894559, 0.3333333333333333703, 0.3219752754296894559, 0.3333333333333333703, 0.3219752754296894559, 0.3333333333333333703, 0.3219752754296894559, 0.3333333333333333703, 0.3219752754296894559, 0.3333333333333333703, 0.3219752754296894559, 0.3333333333333333703, 0.3219752754296894559, 0.3333333333333333703, 0.3219752754296894559, 0.3333333333333333703, 0.3219752754296894559, 0.3333333333333333703, 0.3219752754296894559, 0.3333333333333333703, 0.3219752754296894559, 0.3333333333333333703, 0.3219752754296894559, 0.3333333333333333703, 0.3219752754296894559, 0.3333333333333333703, 0.3219752754296894559, 0.3333333333333333703, 0.3219752754296894559, 0.3333333333333333703, 0.3219752754296894559, 0.3333333333333333703, 0.3219752754296894559, 0.3333333333333333703, 0.3219752754296894559, 0.3333333333333333703, 0.3219752754296894559, 0.3333333333333333703, 0.3219752754296894559, 0.3333333333333333703, 0.3219752754296894559, 0.3333333333333333703, 0.3219752754296894559, 0.3333333333333333703, 0.3219752754296894559, 0.3333333333333333703, 0.3219752754296894559, 0.3333333333333333703, 0.3219752754296894559, 0.3333333333333333703, 0.3219752754296894559, 0.3333333333333333703, 0.3219752754296894559, 0.3333333333333333703, 0.3219752754296894559, 0.3333333333333333703, 0.3219752754296894559, 0.3333333333333333703, 0.3219752754296894559, 0.3333333333333333703, 0.3219752754296894559, 0.3333333333333333703, 0.3219752754296894559, 0.3333333333333333703, 0.3219752754296894559, 0.3333333333333333703, 0.3219752754296894559, 0.3333333333333333703, 0.3219752754296894559, 0.3333333333333333703, 0.3219752754296894559, 0.3333333333333333703, 0.3219752754296894559, 0.3333333333333333703, 0.3219752754296894559, 0.3333333333333333703, 0.3219752754296894559, 0.3333333333333333703, 0.3219752754296894559, 0.3333333333333333703, 0.3219752754296894559, 0.3333333333333333703, 0.3219752754296894559, 0.3333333333333333703, 0.3219752754296894559, 0.3333333333333333703, 0.3219752754296894559, 0.3333333333333333703, 0.3219752754296894559, 0.3333333333333333703, 0.3219752754296894559, 0.3333333333333333703, 0.3219752754296894559, 0.3333333333333333703, 0.3219752754296894559, 0.3333333333333333703, 0.3219752754296894559, 0.3333333333333333703, 0.3219752754296894559, 0.3333333333333333703, 0.3219752754296894559, 0.3333333333333333703, 0.3219752754296894559, 0.3333333333333333703, 0.3219752754296894559, 0.3333333333333333703, 0.3219752754296894559, 0.3333333333333333703, 0.3219752754296894559, 0.3333333333333333703, 0.3219752754296894559, 0.3333333333333333703, 0.3219752754296894559, 0.3333333333333333703, 0.3219752754296894559, 0.3333333333333333703, 0.3219752754296894559, 0.3333333333333333703, 0.3219752754296894559, 0.3333333333333333703, 0.3219752754296894559, 0.3333333333333333703, 0.3219752754296894559, 0.3333333333333333703, 0.3219752754296894559, 0.3333333333333333703, 0.3219752754296894559, 0.3333333333333333703, 0.3219752754296894559, 0.3333333333333333703, 0.3219752754296894559, 0.3333333333333333703, 0.3219752754296894559, 0.3333333333333333703, 0.3219752754296894559, 0.3333333333333333703, 0.3219752754296894559, 0.3333333333333333703, 0.3219752754296894559, 0.3333333333333333703, 0.3219752754296894559, 0.3333333333333333703, 0.3219752754296894559, 0.3333333333333333703, 0.3219752754296894559, 0.3333333333333333703, 0.3219752754296894559, 0.3333333333333333703, 0.3219752754296894559, 0.3333333333333333703, 0.3219752754296894559, 0.3333333333333333703, 0.3219752754296894559, 0.3333333333333333703, 0.3219752754296894559, 0.3333333333333333703, 0.3219752754296894559, 0.3333333333333333703, 0.3219752754296894559, 0.3333333333333333703, 0.3219752754296894559, 0.3333333333333333703, 0.3219752754296894559, 0.3333333333333333703, 0.3219752754296894559, 0.3333333333333333703, 0.3219752754296894559, 0.3333333333333333703, 0.3219752754296894559, 0.3333333333333333703, 0.3219752754296894559, 0.3333333333333333703, 0.3219752754296894559, 0.3333333333333333703, 0.3219752754296894559, 0.3333333333333333703, 0.3219752754296894559, 0.3333333333333333703, 0.3219752754296894559, 0.3333333333333333703, 0.3219752754296894559, 0.3333333333333333703, 0.3219752754296894559, 0.3333333333333333703, 0.3219752754296894559, 0.3333333333333333703, 0.3219752754296894559, 0.3333333333333333703, 0.3219752754296894559, 0.3333333333333333703, 0.3219752754296894559, 0.3333333333333333703, 0.3219752754296894559, 0.3333333333333333703, 0.3219752754296894559, 0.3333333333333333703, 0.3219752754296894559, 0.3333333333333333703, 0.3219752754296894559, 0.3333333333333333703, 0.3219752754296894559, 0.3333333333333333703, 0.3219752754296894559, 0.3333333333333333703, 0.3219752754296894559, 0.3333333333333333703, 0.3219752754296894559, 0.3333333333333333703, 0.3219752754296894559, 0.3333333333333333703, 0.3219752754296894559, 0.3333333333333333703, 0.3219752754296894559, 0.3333333333333333703, 0.3219752754296894559, 0.3333333333333333703, 0.3219752754296894559, 0.3333333333333333703, 0.3219752754296894559, 0.3333333333333333703, 0.3219752754296894559, 0.3333333333333333703, 0.3219752754296894559, 0.3333333333333333703, 0.3219752754296894559, 0.3333333333333333703, 0.3219752754296894559, 0.3333333333333333703, 0.3219752754296894559, 0.3333333333333333703, 0.3219752754296894559, 0.3333333333333333703, 0.3219752754296894559, 0.3333333333333333703, 0.3219752754296894559, 0.3333333333333333703, 0.3219752754296894559, 0.3333333333333333703, 0.3219752754296894559, 0.3333333333333333703, 0.3219752754296894559, 0.3333333333333333703, 0.3219752754296894559, 0.3333333333333333703, 0.3219752754296894559, 0.3333333333333333703, 0.3219752754296894559, 0.3333333333333333703, 0.3219752754296894559, 0.3333333333333333703, 0.3219752754296894559, 0.3333333333333333703, 0.3219752754296894559, 0.3333333333333333703, 0.3219752754296894559, 0.3333333333333333703, 0.3219752754296894559, 0.3333333333333333703, 0.3219752754296894559, 0.3333333333333333703, 0.3219752754296894559, 0.3333333333333333703, 0.3219752754296894559, 0.3333333333333333703, 0.3219752754296894559, 0.3333333333333333703, 0.3219752754296894559, 0.3333333333333333703, 0.3219752754296894559, 0.3333333333333333703, 0.3219752754296894559, 0.3333333333333333703, 0.3219752754296894559, 0.3333333333333333703, 0.3219752754296894559, 0.3333333333333333703, 0.3219752754296894559, 0.3333333333333333703, 0.3219752754296894559, 0.3333333333333333703, 0.3219752754296894559, 0.3333333333333333703, 0.3219752754296894559, 0.3333333333333333703, 0.3219752754296894559, 0.3333333333333333703, 0.3219752754296894559, 0.3333333333333333703, 0.3219752754296894559, 0.3333333333333333703, 0.3219752754296894559, 0.3333333333333333703, 0.3219752754296894559, 0.3333333333333333703, 0.3219752754296894559, 0.3333333333333333703, 0.3219752754296894559, 0.3333333333333333703, 0.3219752754296894559, 0.3333333333333333703, 0.3219752754296894559, 0.3333333333333333703, 0.3219752754296894559, 0.3333333333333333703, 0.3219752754296894559, 0.3333333333333333703, 0.3219752754296894559, 0.3333333333333333703, 0.3219752754296894559, 0.3333333333333333703, 0.3219752754296894559, 0.3333333333333333703, 0.3219752754296894559, 0.3333333333333333703, 0.3219752754296894559, 0.3333333333333333703, 0.3219752754296894559, 0.3333333333333333703, 0.3219752754296894559, 0.3333333333333333703, 0.3219752754296894559, 0.3333333333333333703, 0.3219752754296894559, 0.3333333333333333703, 0.3219752754296894559, 0.3333333333333333703, 0.3219752754296894559, 0.3333333333333333703, 0.3219752754296894559, 0.3333333333333333703, 0.3219752754296894559, 0.3333333333333333703, 0.3219752754296894559, 0.3333333333333333703, 0.3219752754296894559, 0.3333333333333333703, 0.3219752754296894559, 0.3333333333333333703, 0.3219752754296894559, 0.3333333333333333703, 0.3219752754296894559, 0.3333333333333333703, 0.3219752754296894559, 0.3333333333333333703, 0.3219752754296894559, 0.3333333333333333703, 0.3219752754296894559, 0.3333333333333333703, 0.3219752754296894559, 0.3333333333333333703, 0.3219752754296894559, 0.3333333333333333703, 0.3219752754296894559, 0.3333333333333333703, 0.3219752754296894559, 0.3333333333333333703, 0.3219752754296894559, 0.3333333333333333703, 0.3219752754296894559, 0.3333333333333333703, 0.3219752754296894559, 0.3333333333333333703, 0.3219752754296894559, 0.3333333333333333703, 0.3219752754296894559, 0.3333333333333333703, 0.3219752754296894559, 0.3333333333333333703, 0.3219752754296894559, 0.3333333333333333703, 0.3219752754296894559, 0.3333333333333333703, 0.3219752754296894559, 0.3333333333333333703, 0.3219752754296894559, 0.3333333333333333703, 0.3219752754296894559, 0.3333333333333333703, 0.3219752754296894559, 0.3333333333333333703, 0.3219752754296894559, 0.3333333333333333703, 0.3219752754296894559, 0.3333333333333333703, 0.3219752754296894559, 0.3333333333333333703),
 ( 1.000000000000000000, 0.9659258262890683122, 1.000000000000000000, 0.9659258262890683122, 1.000000000000000000, 0.9659258262890683122, 1.000000000000000000, 0.9659258262890683122, 1.000000000000000000, 0.9659258262890683122, 1.000000000000000000, 0.9659258262890683122, 1.000000000000000000, 0.9659258262890683122, 1.000000000000000000, 0.9659258262890683122, 1.000000000000000000, 0.9659258262890683122, 1.000000000000000000, 0.9659258262890683122, 1.000000000000000000, 0.9659258262890683122, 1.000000000000000000, 0.9659258262890683122, 1.000000000000000000, 0.9659258262890683122, 1.000000000000000000, 0.9659258262890683122, 1.000000000000000000, 0.9659258262890683122, 1.000000000000000000, 0.9659258262890683122, 1.000000000000000000, 0.9659258262890683122, 1.000000000000000000, 0.9659258262890683122, 1.000000000000000000, 0.9659258262890683122, 1.000000000000000000, 0.9659258262890683122, 1.000000000000000000, 0.9659258262890683122, 1.000000000000000000, 0.9659258262890683122, 1.000000000000000000, 0.9659258262890683122, 1.000000000000000000, 0.9659258262890683122, 1.000000000000000000, 0.9659258262890683122, 1.000000000000000000, 0.9659258262890683122, 1.000000000000000000, 0.9659258262890683122, 1.000000000000000000, 0.9659258262890683122, 1.000000000000000000, 0.9659258262890683122, 1.000000000000000000, 0.9659258262890683122, 1.000000000000000000, 0.9659258262890683122, 1.000000000000000000, 0.9659258262890683122, 1.000000000000000000, 0.9659258262890683122, 1.000000000000000000, 0.9659258262890683122, 1.000000000000000000, 0.9659258262890683122, 1.000000000000000000, 0.9659258262890683122, 1.000000000000000000, 0.9659258262890683122, 1.000000000000000000, 0.9659258262890683122, 1.000000000000000000, 0.9659258262890683122, 1.000000000000000000, 0.9659258262890683122, 1.000000000000000000, 0.9659258262890683122, 1.000000000000000000, 0.9659258262890683122, 1.000000000000000000, 0.9659258262890683122, 1.000000000000000000, 0.9659258262890683122, 1.000000000000000000, 0.9659258262890683122, 1.000000000000000000, 0.9659258262890683122, 1.000000000000000000, 0.9659258262890683122, 1.000000000000000000, 0.9659258262890683122, 1.000000000000000000, 0.9659258262890683122, 1.000000000000000000, 0.9659258262890683122, 1.000000000000000000, 0.9659258262890683122, 1.000000000000000000, 0.9659258262890683122, 1.000000000000000000, 0.9659258262890683122, 1.000000000000000000, 0.9659258262890683122, 1.000000000000000000, 0.9659258262890683122, 1.000000000000000000, 0.9659258262890683122, 1.000000000000000000, 0.9659258262890683122, 1.000000000000000000, 0.9659258262890683122, 1.000000000000000000, 0.9659258262890683122, 1.000000000000000000, 0.9659258262890683122, 1.000000000000000000, 0.9659258262890683122, 1.000000000000000000, 0.9659258262890683122, 1.000000000000000000, 0.9659258262890683122, 1.000000000000000000, 0.9659258262890683122, 1.000000000000000000, 0.9659258262890683122, 1.000000000000000000, 0.9659258262890683122, 1.000000000000000000, 0.9659258262890683122, 1.000000000000000000, 0.9659258262890683122, 1.000000000000000000, 0.9659258262890683122, 1.000000000000000000, 0.9659258262890683122, 1.000000000000000000, 0.9659258262890683122, 1.000000000000000000, 0.9659258262890683122, 1.000000000000000000, 0.9659258262890683122, 1.000000000000000000, 0.9659258262890683122, 1.000000000000000000, 0.9659258262890683122, 1.000000000000000000, 0.9659258262890683122, 1.000000000000000000, 0.9659258262890683122, 1.000000000000000000, 0.9659258262890683122, 1.000000000000000000, 0.9659258262890683122, 1.000000000000000000, 0.9659258262890683122, 1.000000000000000000, 0.9659258262890683122, 1.000000000000000000, 0.9659258262890683122, 1.000000000000000000, 0.9659258262890683122, 1.000000000000000000, 0.9659258262890683122, 1.000000000000000000, 0.9659258262890683122, 1.000000000000000000, 0.9659258262890683122, 1.000000000000000000, 0.9659258262890683122, 1.000000000000000000, 0.9659258262890683122, 1.000000000000000000, 0.9659258262890683122, 1.000000000000000000, 0.9659258262890683122, 1.000000000000000000, 0.9659258262890683122, 1.000000000000000000, 0.9659258262890683122, 1.000000000000000000, 0.9659258262890683122, 1.000000000000000000, 0.9659258262890683122, 1.000000000000000000, 0.9659258262890683122, 1.000000000000000000, 0.9659258262890683122, 1.000000000000000000, 0.9659258262890683122, 1.000000000000000000, 0.9659258262890683122, 1.000000000000000000, 0.9659258262890683122, 1.000000000000000000, 0.9659258262890683122, 1.000000000000000000, 0.9659258262890683122, 1.000000000000000000, 0.9659258262890683122, 1.000000000000000000, 0.9659258262890683122, 1.000000000000000000, 0.9659258262890683122, 1.000000000000000000, 0.9659258262890683122, 1.000000000000000000, 0.9659258262890683122, 1.000000000000000000, 0.9659258262890683122, 1.000000000000000000, 0.9659258262890683122, 1.000000000000000000, 0.9659258262890683122, 1.000000000000000000, 0.9659258262890683122, 1.000000000000000000, 0.9659258262890683122, 1.000000000000000000, 0.9659258262890683122, 1.000000000000000000, 0.9659258262890683122, 1.000000000000000000, 0.9659258262890683122, 1.000000000000000000, 0.9659258262890683122, 1.000000000000000000, 0.9659258262890683122, 1.000000000000000000, 0.9659258262890683122, 1.000000000000000000, 0.9659258262890683122, 1.000000000000000000, 0.9659258262890683122, 1.000000000000000000, 0.9659258262890683122, 1.000000000000000000, 0.9659258262890683122, 1.000000000000000000, 0.9659258262890683122, 1.000000000000000000, 0.9659258262890683122, 1.000000000000000000, 0.9659258262890683122, 1.000000000000000000, 0.9659258262890683122, 1.000000000000000000, 0.9659258262890683122, 1.000000000000000000, 0.9659258262890683122, 1.000000000000000000, 0.9659258262890683122, 1.000000000000000000, 0.9659258262890683122, 1.000000000000000000, 0.9659258262890683122, 1.000000000000000000, 0.9659258262890683122, 1.000000000000000000, 0.9659258262890683122, 1.000000000000000000, 0.9659258262890683122, 1.000000000000000000, 0.9659258262890683122, 1.000000000000000000, 0.9659258262890683122, 1.000000000000000000, 0.9659258262890683122, 1.000000000000000000, 0.9659258262890683122, 1.000000000000000000, 0.9659258262890683122, 1.000000000000000000, 0.9659258262890683122, 1.000000000000000000, 0.9659258262890683122, 1.000000000000000000, 0.9659258262890683122, 1.000000000000000000, 0.9659258262890683122, 1.000000000000000000, 0.9659258262890683122, 1.000000000000000000, 0.9659258262890683122, 1.000000000000000000, 0.9659258262890683122, 1.000000000000000000, 0.9659258262890683122, 1.000000000000000000, 0.9659258262890683122, 1.000000000000000000, 0.9659258262890683122, 1.000000000000000000, 0.9659258262890683122, 1.000000000000000000, 0.9659258262890683122, 1.000000000000000000, 0.9659258262890683122, 1.000000000000000000, 0.9659258262890683122, 1.000000000000000000, 0.9659258262890683122, 1.000000000000000000, 0.9659258262890683122, 1.000000000000000000, 0.9659258262890683122, 1.000000000000000000, 0.9659258262890683122, 1.000000000000000000, 0.9659258262890683122, 1.000000000000000000, 0.9659258262890683122, 1.000000000000000000, 0.9659258262890683122, 1.000000000000000000, 0.9659258262890683122, 1.000000000000000000, 0.9659258262890683122, 1.000000000000000000, 0.9659258262890683122, 1.000000000000000000, 0.9659258262890683122, 1.000000000000000000, 0.9659258262890683122, 1.000000000000000000, 0.9659258262890683122, 1.000000000000000000, 0.9659258262890683122, 1.000000000000000000, 0.9659258262890683122, 1.000000000000000000, 0.9659258262890683122, 1.000000000000000000, 0.9659258262890683122, 1.000000000000000000, 0.9659258262890683122, 1.000000000000000000, 0.9659258262890683122, 1.000000000000000000, 0.9659258262890683122, 1.000000000000000000, 0.9659258262890683122, 1.000000000000000000, 0.9659258262890683122, 1.000000000000000000, 0.9659258262890683122, 1.000000000000000000, 0.9659258262890683122, 1.000000000000000000, 0.9659258262890683122, 1.000000000000000000, 0.9659258262890683122, 1.000000000000000000, 0.9659258262890683122, 1.000000000000000000, 0.9659258262890683122, 1.000000000000000000, 0.9659258262890683122, 1.000000000000000000, 0.9659258262890683122, 1.000000000000000000, 0.9659258262890683122, 1.000000000000000000, 0.9659258262890683122, 1.000000000000000000, 0.9659258262890683122, 1.000000000000000000, 0.9659258262890683122, 1.000000000000000000, 0.9659258262890683122, 1.000000000000000000, 0.9659258262890683122, 1.000000000000000000, 0.9659258262890683122, 1.000000000000000000, 0.9659258262890683122, 1.000000000000000000, 0.9659258262890683122, 1.000000000000000000, 0.9659258262890683122, 1.000000000000000000, 0.9659258262890683122, 1.000000000000000000, 0.9659258262890683122, 1.000000000000000000, 0.9659258262890683122, 1.000000000000000000, 0.9659258262890683122, 1.000000000000000000, 0.9659258262890683122, 1.000000000000000000, 0.9659258262890683122, 1.000000000000000000, 0.9659258262890683122, 1.000000000000000000, 0.9659258262890683122, 1.000000000000000000, 0.9659258262890683122, 1.000000000000000000, 0.9659258262890683122, 1.000000000000000000, 0.9659258262890683122, 1.000000000000000000, 0.9659258262890683122, 1.000000000000000000, 0.9659258262890683122, 1.000000000000000000, 0.9659258262890683122, 1.000000000000000000, 0.9659258262890683122, 1.000000000000000000, 0.9659258262890683122, 1.000000000000000000, 0.9659258262890683122, 1.000000000000000000, 0.9659258262890683122, 1.000000000000000000, 0.9659258262890683122, 1.000000000000000000, 0.9659258262890683122, 1.000000000000000000, 0.9659258262890683122, 1.000000000000000000, 0.9659258262890683122, 1.000000000000000000, 0.9659258262890683122, 1.000000000000000000, 0.9659258262890683122, 1.000000000000000000, 0.9659258262890683122, 1.000000000000000000, 0.9659258262890683122, 1.000000000000000000, 0.9659258262890683122, 1.000000000000000000, 0.9659258262890683122, 1.000000000000000000, 0.9659258262890683122, 1.000000000000000000, 0.9659258262890683122, 1.000000000000000000, 0.9659258262890683122, 1.000000000000000000, 0.9659258262890683122, 1.000000000000000000, 0.9659258262890683122, 1.000000000000000000, 0.9659258262890683122, 1.000000000000000000, 0.9659258262890683122, 1.000000000000000000, 0.9659258262890683122, 1.000000000000000000) ) ) 
 REPRESENTATION_ITEM ( '' )  SURFACE ( )  );
#128448 = CARTESIAN_POINT ( 'NONE',  ( -1.697796032038755287, -7.741785448087954435, 4.009310749147816821 ) ) ;
#128449 = CARTESIAN_POINT ( 'NONE',  ( -0.05219959533909027116, -19.03943276465977164, 97.49890960531436690 ) ) ;
#128450 = CARTESIAN_POINT ( 'NONE',  ( -10.72451020669870658, -18.67979575497194134, 109.5844237280190328 ) ) ;
#128451 = CARTESIAN_POINT ( 'NONE',  ( 19.03943276465977164, -0.05219959533909143690, 88.74890960531436690 ) ) ;
#128452 = CARTESIAN_POINT ( 'NONE',  ( 15.72974639402199770, -15.80617190586745480, 63.12390960531435979 ) ) ;
#128453 = CARTESIAN_POINT ( 'NONE',  ( -4.483927247898539470, -16.52544592524342804, 87.29057627198103830 ) ) ;
#128454 = CARTESIAN_POINT ( 'NONE',  ( -19.02544592524342804, 5.153800228976336051, 56.04057627198100988 ) ) ;
#128455 = CARTESIAN_POINT ( 'NONE',  ( -0.05219959533910754901, -16.53943276465976808, 107.4989096053143669 ) ) ;
#128456 = CARTESIAN_POINT ( 'NONE',  ( -15.80617190586768217, 15.72974639402176855, 28.12609039468568284 ) ) ;
#128457 = CARTESIAN_POINT ( 'NONE',  ( -5.823673210054431948, 21.52544592524334988, 72.70942372801901854 ) ) ;
#128458 = CARTESIAN_POINT ( 'NONE',  ( -9.474510206698964154, 16.51473224551069663, 45.41557627198103120 ) ) ;
#128459 = CARTESIAN_POINT ( 'NONE',  ( 12.06949235617739724, 12.14591786802326823, 71.87609039468568994 ) ) ;
#128460 = CARTESIAN_POINT ( 'NONE',  ( -0.05219959533937732626, 21.53943276465977519, 27.50109039468567929 ) ) ;
#128461 = CARTESIAN_POINT ( 'NONE',  ( -15.80617190586768217, 15.72974639402176855, 33.12609039468569705 ) ) ;
#128463 = CARTESIAN_POINT ( 'NONE',  ( 0.05219959533909260263, 19.03943276465977164, 64.99890960531436690 ) ) ;
#128462 = CARTESIAN_POINT ( 'NONE',  ( 5.049401038297881783, 19.05341960407617563, 52.29275706135234003 ) ) ;
#128464 = CARTESIAN_POINT ( 'NONE',  ( 16.51473224551083163, -9.474510206698727899, 35.83442372801899722 ) ) ;
#128465 = CARTESIAN_POINT ( 'NONE',  ( 5.823673210054444382, -21.52544592524334988, 85.20942372801901854 ) ) ;
#128466 = CARTESIAN_POINT ( 'NONE',  ( -21.53943276465977519, 0.05219959533907696930, 71.24890960531435269 ) ) ;
#128467 = CARTESIAN_POINT ( 'NONE',  ( 14.34966873604960469, 8.224510206698951720, 49.16557627198102409 ) ) ;
#128469 = CARTESIAN_POINT ( 'NONE',  ( -19.05341960407617563, 5.049401038297882671, 23.54275706135233648 ) ) ;
#128468 = CARTESIAN_POINT ( 'NONE',  ( -5.823673210054431948, 21.52544592524334988, 92.70942372801901854 ) ) ;
#128470 = CARTESIAN_POINT ( 'NONE',  ( 8.224510206698953496, -14.34966873604960469, 72.91557627198103830 ) ) ;
#128471 = CARTESIAN_POINT ( 'NONE',  ( 16.46253265017160672, -9.564922557960803928, 28.33224293864769550 ) ) ;
#128472 = CARTESIAN_POINT ( 'NONE',  ( -16.51473224551082808, 9.474510206698731452, 53.33442372801900433 ) ) ;
#128473 = CARTESIAN_POINT ( 'NONE',  ( -14.29746914071037622, -8.314922557961029526, 109.1677570613523613 ) ) ;
#128474 = CARTESIAN_POINT ( 'NONE',  ( 0.05219959533937995610, -21.53943276465977519, 85.00109039468568994 ) ) ;
#128475 = CARTESIAN_POINT ( 'NONE',  ( -13.97604488694527625, -13.89961937509977652, 76.87390960531433848 ) ) ;
#128476 = CARTESIAN_POINT ( 'NONE',  ( -5.153800228976607833, 19.02544592524334988, 47.70942372801900433 ) ) ;
#128477 = CARTESIAN_POINT ( 'NONE',  ( -21.53943276465977519, 0.05219959533907696930, 46.24890960531435979 ) ) ;
#128478 = B_SPLINE_CURVE_WITH_KNOTS ( 'NONE', 3,
 ( #185265, #172082, #1222, #65882, #46757, #124580, #174083, #141733, #232, #78065 ),
 .UNSPECIFIED., .F., .F.,
 ( 4, 2, 2, 2, 4 ),
 ( 0.003992163664268632249, 0.004297753711354872219, 0.004603343758441113057, 0.004908933805527353894, 0.005214523852613593864 ),
 .UNSPECIFIED. ) ;
#128479 = CARTESIAN_POINT ( 'NONE',  ( 18.62759615963255655, 10.81492255796105972, 51.66775706135234714 ) ) ;
#128480 = CARTESIAN_POINT ( 'NONE',  ( -18.62759615963270932, 10.81492255796079327, 95.83224293864770971 ) ) ;
#128481 = CARTESIAN_POINT ( 'NONE',  ( -19.02544592524334988, -5.153800228976617603, 93.95942372801900433 ) ) ;
#128482 = CARTESIAN_POINT ( 'NONE',  ( 14.29746914071037800, 8.314922557961029526, 61.66775706135235424 ) ) ;
#128484 = CARTESIAN_POINT ( 'NONE',  ( -10.72451020669898014, 18.67979575497178502, 100.4155762719810241 ) ) ;
#128483 = CARTESIAN_POINT ( 'NONE',  ( -15.03002592745795774, -17.15945613581673257, -57.85847139087537983 ) ) ;
#128485 = CARTESIAN_POINT ( 'NONE',  ( 4.379528057220339221, -16.55341960407611168, 87.70724293864769550 ) ) ;
#128486 = CARTESIAN_POINT ( 'NONE',  ( -17.49999999999999289, -5.624438216177589211, 99.18329655085356933 ) ) ;
#128487 = CARTESIAN_POINT ( 'NONE',  ( 8.224510206698742110, 14.34966873604972548, 32.08442372801901854 ) ) ;
#128488 = EDGE_CURVE ( 'NONE', #68886, #44815, #174150, .T. ) ;
#128489 = CARTESIAN_POINT ( 'NONE',  ( -0.05219959533907301413, -21.53943276465977519, 62.49890960531436690 ) ) ;
#128490 = CARTESIAN_POINT ( 'NONE',  ( -0.05219959533934338120, 16.53943276465976808, 97.50109039468567573 ) ) ;
#128491 = CARTESIAN_POINT ( 'NONE',  ( 9.474510206698971260, -16.51473224551069308, 27.91557627198103120 ) ) ;
#128492 = CARTESIAN_POINT ( 'NONE',  ( 12.06949235617739724, 12.14591786802326823, 61.87609039468568284 ) ) ;
#128493 = CARTESIAN_POINT ( 'NONE',  ( -9.474510206698720793, -16.51473224551083518, 54.58442372801899722 ) ) ;
#128494 = CARTESIAN_POINT ( 'NONE',  ( 18.62759615963255655, 10.81492255796105972, 41.66775706135235424 ) ) ;
#128495 = CARTESIAN_POINT ( 'NONE',  ( -0.05219959533907301413, -21.53943276465977519, 52.49890960531435979 ) ) ;
#128496 = CARTESIAN_POINT ( 'NONE',  ( -4.379528057220086978, -16.55341960407618274, 84.79275706135234714 ) ) ;
#128497 = CARTESIAN_POINT ( 'NONE',  ( -5.719274019375665041, -21.55341960407619695, 69.79275706135234714 ) ) ;
#128498 = CARTESIAN_POINT ( 'NONE',  ( -21.52544592524343514, 5.823673210054127303, 56.04057627198102409 ) ) ;
#128499 = CARTESIAN_POINT ( 'NONE',  ( -10.81492255796078084, -18.62759615963271287, 37.08224293864768129 ) ) ;
#128500 = CARTESIAN_POINT ( 'NONE',  ( -12.06949235617739369, -12.14591786802326823, 69.37609039468567573 ) ) ;
#128501 = CARTESIAN_POINT ( 'NONE',  ( 18.62759615963271287, -10.81492255796078972, 33.33224293864769550 ) ) ;
#128502 = EDGE_LOOP ( 'NONE', ( #55905, #115409, #17451, #145742 ) ) ;
#128503 = CARTESIAN_POINT ( 'NONE',  ( -16.46253265017160317, 9.564922557960807481, 100.8322429386477097 ) ) ;
#128504 = CARTESIAN_POINT ( 'NONE',  ( -4.483927247898782831, 16.52544592524335698, 107.7094237280190328 ) ) ;
#128505 = CARTESIAN_POINT ( 'NONE',  ( -26.58496454517000629, 7.626754437231443084, 167.9682100371138915 ) ) ;
#128506 = CARTESIAN_POINT ( 'NONE',  ( -0.05219959533910754901, -16.53943276465976808, 102.4989096053143811 ) ) ;
#128507 = CARTESIAN_POINT ( 'NONE',  ( -21.53943276465977519, 0.05219959533907696930, 61.24890960531435979 ) ) ;
#128508 = CARTESIAN_POINT ( 'NONE',  ( -8.224510206698735004, -14.34966873604973081, 84.58442372801903275 ) ) ;
#128509 = CARTESIAN_POINT ( 'NONE',  ( -5.823673210054431948, 21.52544592524334988, 47.70942372801902565 ) ) ;
#128510 = CARTESIAN_POINT ( 'NONE',  ( 16.46253265017146816, 9.564922557961045513, 106.6677570613523471 ) ) ;
#128511 = CARTESIAN_POINT ( 'NONE',  ( 0.05219959533910956823, 16.53943276465976808, 104.9989096053143669 ) ) ;
#128512 = CARTESIAN_POINT ( 'NONE',  ( -13.89961937509977652, 13.97604488694528158, 55.62390960531434558 ) ) ;
#128513 = CARTESIAN_POINT ( 'NONE',  ( -16.46253265017160317, 9.564922557960807481, 30.83224293864769550 ) ) ;
#128514 = CYLINDRICAL_SURFACE ( 'NONE', #22085, 37.99626262588765968 ) ;
#128515 = CARTESIAN_POINT ( 'NONE',  ( -19.02544592524342804, 5.153800228976336051, 86.04057627198103830 ) ) ;
#128516 = CARTESIAN_POINT ( 'NONE',  ( -16.52544592524335698, -4.483927247898792601, 78.95942372801901854 ) ) ;
#128517 = CARTESIAN_POINT ( 'NONE',  ( 21.52544592524334988, 5.823673210054432836, 111.4594237280190328 ) ) ;
#128518 = CARTESIAN_POINT ( 'NONE',  ( -21.52544592524343514, 5.823673210054127303, 46.04057627198103830 ) ) ;
#128519 = CARTESIAN_POINT ( 'NONE',  ( -4.379528057220086978, -16.55341960407618274, 79.79275706135236135 ) ) ;
#128520 = CARTESIAN_POINT ( 'NONE',  ( -9.474510206698720793, -16.51473224551083518, 84.58442372801900433 ) ) ;
#128521 = VERTEX_POINT ( 'NONE', #151081 ) ;
#128522 = CARTESIAN_POINT ( 'NONE',  ( 13.97604488694527802, 13.89961937509977652, 34.37390960531436690 ) ) ;
#128523 = CARTESIAN_POINT ( 'NONE',  ( 9.474510206698971260, -16.51473224551069308, 77.91557627198103830 ) ) ;
#128524 = CARTESIAN_POINT ( 'NONE',  ( 5.153800228976335163, 19.02544592524342804, 39.79057627198100988 ) ) ;
#128525 = CARTESIAN_POINT ( 'NONE',  ( 16.46253265017146816, 9.564922557961045513, 71.66775706135233293 ) ) ;
#128526 = CARTESIAN_POINT ( 'NONE',  ( 21.04946095171200326, -10.86023174791519530, 170.2405914574445092 ) ) ;
#128527 = CARTESIAN_POINT ( 'NONE',  ( 19.02544592524343514, -5.153800228976328945, 98.54057627198100988 ) ) ;
#128528 = CARTESIAN_POINT ( 'NONE',  ( 16.53943276465976808, -0.05219959533910856209, 53.74890960531437401 ) ) ;
#128529 = CARTESIAN_POINT ( 'NONE',  ( -15.80617190586745835, -15.72974639402198527, 41.87390960531435979 ) ) ;
#128530 = CARTESIAN_POINT ( 'NONE',  ( -17.49999999999999645, 3.565345528327982016, 104.4249448680647419 ) ) ;
#128531 = CARTESIAN_POINT ( 'NONE',  ( -5.153800228976607833, 19.02544592524334988, 27.70942372801899722 ) ) ;
#128532 = CARTESIAN_POINT ( 'NONE',  ( 4.999999999999999112, 0.000000000000000000, 0.000000000000000000 ) ) ;
#128533 = CARTESIAN_POINT ( 'NONE',  ( -5.153800228976328057, -19.02544592524343514, 57.29057627198103120 ) ) ;
#128534 = CARTESIAN_POINT ( 'NONE',  ( -12.06949235617739369, -12.14591786802326823, 44.37609039468567573 ) ) ;
#128535 = CARTESIAN_POINT ( 'NONE',  ( -18.87255363501903105, -5.500000000000007105, 101.3251374817182437 ) ) ;
#128536 = CARTESIAN_POINT ( 'NONE',  ( -16.21995358207304960, 7.366697692864183189, 109.9355100151216220 ) ) ;
#128537 = CARTESIAN_POINT ( 'NONE',  ( -8.314922557961024197, 14.29746914071037800, 77.91775706135231871 ) ) ;
#128538 = CARTESIAN_POINT ( 'NONE',  ( -21.55341960407610458, -5.719274019375992779, 101.4572429386476955 ) ) ;
#128539 = CARTESIAN_POINT ( 'NONE',  ( -4.379528057220086978, -16.55341960407618274, 39.79275706135235424 ) ) ;
#128540 = CARTESIAN_POINT ( 'NONE',  ( -16.51473224551069308, -9.474510206698971260, 36.66557627198102409 ) ) ;
#128541 = CARTESIAN_POINT ( 'NONE',  ( 10.81492255796106328, -18.62759615963255655, 45.41775706135234003 ) ) ;
#128542 = CARTESIAN_POINT ( 'NONE',  ( 16.51473224551083163, -9.474510206698727899, 60.83442372801900433 ) ) ;
#128543 = CARTESIAN_POINT ( 'NONE',  ( -0.05219959533937732626, 21.53943276465977519, 92.50109039468567573 ) ) ;
#128544 = CARTESIAN_POINT ( 'NONE',  ( -17.60769864724388611, 5.499999999999981348, 48.65024842019164453 ) ) ;
#128545 = CARTESIAN_POINT ( 'NONE',  ( 16.52544592524342804, -4.483927247898539470, 43.54057627198103830 ) ) ;
#128546 = CARTESIAN_POINT ( 'NONE',  ( -16.49581645235992156, 0.7820921006974912437, -59.22453004090982631 ) ) ;
#128547 = CARTESIAN_POINT ( 'NONE',  ( 21.52544592524344225, -5.823673210054117533, 53.54057627198103120 ) ) ;
#128548 = DIRECTION ( 'NONE',  ( 0.000000000000000000, 0.000000000000000000, 1.000000000000000000 ) ) ;
#128549 = CARTESIAN_POINT ( 'NONE',  ( 5.153800228976335163, 19.02544592524342804, 104.7905762719809957 ) ) ;
#128550 = CARTESIAN_POINT ( 'NONE',  ( -14.34966873604960291, -8.224510206698953496, 106.6655762719810383 ) ) ;
#128551 = CARTESIAN_POINT ( 'NONE',  ( -8.224510206698735004, -14.34966873604973081, 29.58442372801901854 ) ) ;
#128552 = EDGE_CURVE ( 'NONE', #46712, #45827, #183972, .T. ) ;
#128553 = CARTESIAN_POINT ( 'NONE',  ( -4.483927247898539470, -16.52544592524342804, 22.29057627198102765 ) ) ;
#128554 = EDGE_LOOP ( 'NONE', ( #48184, #16957 ) ) ;
#128557 = CARTESIAN_POINT ( 'NONE',  ( -21.52544592524343514, 5.823673210054127303, 106.0405762719810525 ) ) ;
#128556 = B_SPLINE_CURVE_WITH_KNOTS ( 'NONE', 3,
 ( #146031, #50058, #127867, #5520, #54040, #4514, #18727, #67200 ),
 .UNSPECIFIED., .F., .F.,
 ( 4, 2, 2, 4 ),
 ( -1.451984513602681931E-05, 0.002415095736453747293, 0.003629903527248607049, 0.004844711318043467239 ),
 .UNSPECIFIED. ) ;
#128555 = CARTESIAN_POINT ( 'NONE',  ( -13.89961937509977652, 13.97604488694528158, 100.6239096053143669 ) ) ;
#128559 = CARTESIAN_POINT ( 'NONE',  ( 37.99999999999999289, 2.893978650043524126E-14, -9.000000000000001776 ) ) ;
#128558 = CARTESIAN_POINT ( 'NONE',  ( 14.29746914071049879, -8.314922557960816363, 28.33224293864769550 ) ) ;
#128560 = CARTESIAN_POINT ( 'NONE',  ( -5.153800228976607833, 19.02544592524334988, 92.70942372801901854 ) ) ;
#128561 = CARTESIAN_POINT ( 'NONE',  ( 10.72451020669871369, 18.67979575497193778, 102.0844237280190185 ) ) ;
#128562 = CARTESIAN_POINT ( 'NONE',  ( -16.55341960407611168, -4.379528057220339221, 36.45724293864768839 ) ) ;
#128563 = CARTESIAN_POINT ( 'NONE',  ( -21.55341960407610458, -5.719274019375992779, 86.45724293864770971 ) ) ;
#128564 = CARTESIAN_POINT ( 'NONE',  ( -0.05219959533907301413, -21.53943276465977519, 47.49890960531435979 ) ) ;
#128565 = CARTESIAN_POINT ( 'NONE',  ( -0.05219959533909027116, -19.03943276465977164, 62.49890960531435979 ) ) ;
#128566 = CARTESIAN_POINT ( 'NONE',  ( 14.29746914071049879, -8.314922557960816363, 28.33224293864769550 ) ) ;
#128567 = CARTESIAN_POINT ( 'NONE',  ( 16.46253265017160672, -9.564922557960803928, 73.33224293864769550 ) ) ;
#128568 = ORIENTED_EDGE ( 'NONE', *, *, #93805, .T. ) ;
#128569 = CARTESIAN_POINT ( 'NONE',  ( 19.34837522270365895, 5.499999999999732658, 58.36337684832577821 ) ) ;
#128570 = CARTESIAN_POINT ( 'NONE',  ( 13.97604488694548053, -13.89961937509957401, 45.62609039468566863 ) ) ;
#128571 = CARTESIAN_POINT ( 'NONE',  ( 5.823673210054125526, 21.52544592524343514, 84.79057627198102409 ) ) ;
#128572 = CARTESIAN_POINT ( 'NONE',  ( 16.52544592524342804, -4.483927247898539470, 83.54057627198102409 ) ) ;
#128573 = CARTESIAN_POINT ( 'NONE',  ( -5.719274019375665041, -21.55341960407619695, 39.79275706135235424 ) ) ;
#128574 = CIRCLE ( 'NONE', #80238, 6.100000000000006750 ) ;
#128575 = CARTESIAN_POINT ( 'NONE',  ( 1.784210473542230573E-15, -29.16686587814331588, 147.8750000027311273 ) ) ;
#128576 = CARTESIAN_POINT ( 'NONE',  ( -16.55341960407617563, 4.379528057220093196, 108.5427570613523756 ) ) ;
#128577 = CARTESIAN_POINT ( 'NONE',  ( 16.53943276465976808, -0.05219959533910856209, 113.7489096053143527 ) ) ;
#128578 = CARTESIAN_POINT ( 'NONE',  ( 19.03943276465977164, -0.05219959533909143690, 88.74890960531436690 ) ) ;
#128579 =( NAMED_UNIT ( * ) SI_UNIT ( $, .STERADIAN. ) SOLID_ANGLE_UNIT ( ) );
#128580 = CARTESIAN_POINT ( 'NONE',  ( -11.74149087413294623, -36.13659316521243881, -5.347842220587803119 ) ) ;
#128581 = CARTESIAN_POINT ( 'NONE',  ( -16.52544592524342804, 4.483927247898546575, 46.04057627198103830 ) ) ;
#128582 = CARTESIAN_POINT ( 'NONE',  ( 18.67979575497194134, -10.72451020669871369, 55.83442372801901854 ) ) ;
#128583 = CARTESIAN_POINT ( 'NONE',  ( 25.90290776672146222, -27.60635150542609750, -16.55190051048762001 ) ) ;
#128584 = CARTESIAN_POINT ( 'NONE',  ( 19.05341960407611168, 5.049401038298154454, 38.95724293864767418 ) ) ;
#128585 = CARTESIAN_POINT ( 'NONE',  ( -19.03943276465977164, 0.05219959533909376836, 56.24890960531435979 ) ) ;
#128586 = EDGE_LOOP ( 'NONE', ( #165627, #195205, #129456, #15615, #30086, #120981, #20443, #133278 ) ) ;
#128587 = CARTESIAN_POINT ( 'NONE',  ( 10.81492255796106328, -18.62759615963255655, 110.4177570613523756 ) ) ;
#128588 = CARTESIAN_POINT ( 'NONE',  ( -12.14591786802326823, 12.06949235617739902, 63.12609039468568994 ) ) ;
#128589 = CARTESIAN_POINT ( 'NONE',  ( 10.72451020669871369, 18.67979575497193778, 92.08442372801901854 ) ) ;
#128590 = CARTESIAN_POINT ( 'NONE',  ( -0.05219959533909027116, -19.03943276465977164, 112.4989096053143669 ) ) ;
#128591 = CARTESIAN_POINT ( 'NONE',  ( 16.51473224551083163, -9.474510206698727899, 110.8344237280190043 ) ) ;
#128592 = CARTESIAN_POINT ( 'NONE',  ( -0.05219959533937732626, 21.53943276465977519, 67.50109039468568994 ) ) ;
#128593 = CARTESIAN_POINT ( 'NONE',  ( 16.53943276465976808, 0.05219959533934440121, 31.25109039468568639 ) ) ;
#128594 = CARTESIAN_POINT ( 'NONE',  ( -10.81492255796078084, -18.62759615963271287, 82.08224293864768129 ) ) ;
#128595 = CARTESIAN_POINT ( 'NONE',  ( 5.049401038297881783, 19.05341960407617563, 97.29275706135233293 ) ) ;
#128596 = CARTESIAN_POINT ( 'NONE',  ( -9.564922557960796823, -16.46253265017161027, 62.08224293864769550 ) ) ;
#128597 = CARTESIAN_POINT ( 'NONE',  ( -13.97604488694547697, 13.89961937509957934, 108.1260903946856331 ) ) ;
#128598 = CARTESIAN_POINT ( 'NONE',  ( 9.564922557961047289, -16.46253265017146816, 100.4177570613523329 ) ) ;
#128599 = CARTESIAN_POINT ( 'NONE',  ( -4.379528057220328563, 16.55341960407611168, 70.20724293864769550 ) ) ;
#128601 = EDGE_LOOP ( 'NONE', ( #171404, #69312, #80550, #124835 ) ) ;
#128600 = CARTESIAN_POINT ( 'NONE',  ( -9.564922557961040184, 16.46253265017147172, 77.91775706135234714 ) ) ;
#128602 = CARTESIAN_POINT ( 'NONE',  ( -0.05219959533934338120, 16.53943276465976808, 72.50109039468568994 ) ) ;
#128604 = CARTESIAN_POINT ( 'NONE',  ( 13.89961937509977652, -13.97604488694527269, 43.12390960531434558 ) ) ;
#128603 = CARTESIAN_POINT ( 'NONE',  ( 15.72974639402199770, -15.80617190586745480, 113.1239096053143953 ) ) ;
#128605 = CARTESIAN_POINT ( 'NONE',  ( -13.97604488694527625, -13.89961937509977652, 61.87390960531435979 ) ) ;
#128606 = CARTESIAN_POINT ( 'NONE',  ( 16.53943276465976808, 0.05219959533934440121, 71.25109039468568994 ) ) ;
#128607 = CARTESIAN_POINT ( 'NONE',  ( -27.73933785331498925, 2.428612866367529932E-14, 139.3750000027311842 ) ) ;
#128608 = CARTESIAN_POINT ( 'NONE',  ( 23.31738231874054534, 16.94106989632529192, 143.4500000054623854 ) ) ;
#128609 = ORIENTED_EDGE ( 'NONE', *, *, #94539, .T. ) ;
#128610 = CARTESIAN_POINT ( 'NONE',  ( -19.03943276465977164, 0.05219959533909376836, 101.2489096053143669 ) ) ;
#128611 = CARTESIAN_POINT ( 'NONE',  ( -13.89961937509977652, 13.97604488694528158, 25.62390960531434558 ) ) ;
#128612 = ORIENTED_EDGE ( 'NONE', *, *, #15818, .T. ) ;
#128613 = CARTESIAN_POINT ( 'NONE',  ( -4.379528057220086978, -16.55341960407618274, 19.79275706135235069 ) ) ;
#128614 = CARTESIAN_POINT ( 'NONE',  ( 0.05219959533907565091, 21.53943276465977519, 44.99890960531435979 ) ) ;
#128616 = CARTESIAN_POINT ( 'NONE',  ( 4.379528057220092307, 16.55341960407617563, 32.29275706135235424 ) ) ;
#128615 = CARTESIAN_POINT ( 'NONE',  ( -16.51473224551082808, 9.474510206698731452, 48.33442372801900433 ) ) ;
#128617 = CARTESIAN_POINT ( 'NONE',  ( -13.97604488694527625, -13.89961937509977652, 26.87390960531434558 ) ) ;
#128618 = CARTESIAN_POINT ( 'NONE',  ( 19.03943276465977164, -0.05219959533909143690, 53.74890960531436690 ) ) ;
#128619 = CARTESIAN_POINT ( 'NONE',  ( -15.80617190586745835, -15.72974639402198527, 91.87390960531436690 ) ) ;
#128620 = CARTESIAN_POINT ( 'NONE',  ( 16.46253265017160672, -9.564922557960803928, 113.3322429386476955 ) ) ;
#128621 = CARTESIAN_POINT ( 'NONE',  ( -19.02544592524342804, 5.153800228976336051, 51.04057627198103120 ) ) ;
#128622 = CARTESIAN_POINT ( 'NONE',  ( 27.73933785331498569, 2.768321779492822058E-14, 148.3750000027311842 ) ) ;
#128623 = CARTESIAN_POINT ( 'NONE',  ( -9.474510206698720793, -16.51473224551083518, 94.58442372801900433 ) ) ;
#128624 = CARTESIAN_POINT ( 'NONE',  ( -4.379528057220328563, 16.55341960407611168, 60.20724293864768839 ) ) ;
#128625 = CARTESIAN_POINT ( 'NONE',  ( 10.72451020669871369, 18.67979575497193778, 102.0844237280190185 ) ) ;
#128626 = CARTESIAN_POINT ( 'NONE',  ( -15.80617190586745835, -15.72974639402198527, 96.87390960531436690 ) ) ;
#128627 = CARTESIAN_POINT ( 'NONE',  ( 21.55341960407619695, -5.719274019375665929, 91.04275706135236135 ) ) ;
#128628 = CARTESIAN_POINT ( 'NONE',  ( 13.89961937509977652, -13.97604488694527269, 23.12390960531436335 ) ) ;
#128629 = CARTESIAN_POINT ( 'NONE',  ( -18.62759615963255300, -10.81492255796106328, 79.16775706135234714 ) ) ;
#128631 = CARTESIAN_POINT ( 'NONE',  ( -21.55341960407619339, 5.719274019375674811, 73.54275706135234714 ) ) ;
#128630 = CARTESIAN_POINT ( 'NONE',  ( -8.314922557960811034, -14.29746914071050412, 27.08224293864769550 ) ) ;
#128632 = CARTESIAN_POINT ( 'NONE',  ( 19.05341960407611168, 5.049401038298154454, 68.95724293864769550 ) ) ;
#128633 = CARTESIAN_POINT ( 'NONE',  ( 15.72974639402176855, 15.80617190586768217, 46.87609039468568994 ) ) ;
#128634 = CARTESIAN_POINT ( 'NONE',  ( 9.474510206698971260, -16.51473224551069308, 82.91557627198103830 ) ) ;
#128635 = CARTESIAN_POINT ( 'NONE',  ( 8.314922557960818139, 14.29746914071049879, 94.58224293864769550 ) ) ;
#128636 = CARTESIAN_POINT ( 'NONE',  ( -12.14591786802309592, -12.06949235617757132, 66.87390960531436690 ) ) ;
#128637 = CARTESIAN_POINT ( 'NONE',  ( -21.55341960407610458, -5.719274019375992779, 66.45724293864768129 ) ) ;
#128638 = CARTESIAN_POINT ( 'NONE',  ( -13.97604488694527625, -13.89961937509977652, 66.87390960531436690 ) ) ;
#128639 = CARTESIAN_POINT ( 'NONE',  ( -15.72974639402197994, 15.80617190586746368, 75.62390960531439532 ) ) ;
#128640 = CARTESIAN_POINT ( 'NONE',  ( 16.51473224551083163, -9.474510206698727899, 70.83442372801900433 ) ) ;
#128642 = CARTESIAN_POINT ( 'NONE',  ( -4.483927247898539470, -16.52544592524342804, 82.29057627198103830 ) ) ;
#128641 = CARTESIAN_POINT ( 'NONE',  ( -13.97604488694547520, 13.89961937509957934, 38.12609039468566152 ) ) ;
#128643 = CARTESIAN_POINT ( 'NONE',  ( 5.719274019375991003, -21.55341960407610458, 57.70724293864770260 ) ) ;
#128644 = CARTESIAN_POINT ( 'NONE',  ( 17.50000000000000000, 5.624438216177590100, 101.6832965508535835 ) ) ;
#128646 = CARTESIAN_POINT ( 'NONE',  ( -8.571926809382608425, 26.38167802310805854, 142.9750000027312069 ) ) ;
#128645 = CARTESIAN_POINT ( 'NONE',  ( 16.53943276465976808, 0.05219959533934440121, 101.2510903946856757 ) ) ;
#128647 = CARTESIAN_POINT ( 'NONE',  ( 13.97604488694548053, -13.89961937509957401, 95.62609039468563310 ) ) ;
#128648 = CARTESIAN_POINT ( 'NONE',  ( 12.14591786802309770, 12.06949235617756955, 74.37390960531436690 ) ) ;
#128649 = CARTESIAN_POINT ( 'NONE',  ( -3.573655867282028392E-15, 2.428612866367529932E-14, 169.9999999999999716 ) ) ;
#128650 = CARTESIAN_POINT ( 'NONE',  ( -19.03943276465977164, 0.05219959533909376836, 56.24890960531435979 ) ) ;
#128651 = CARTESIAN_POINT ( 'NONE',  ( 16.55341960407611168, 4.379528057220329451, 53.95724293864770260 ) ) ;
#128652 = CARTESIAN_POINT ( 'NONE',  ( -13.97604488694527625, -13.89961937509977652, 106.8739096053143669 ) ) ;
#128654 = CARTESIAN_POINT ( 'NONE',  ( -16.51473224551069308, -9.474510206698971260, 66.66557627198102409 ) ) ;
#128653 = CARTESIAN_POINT ( 'NONE',  ( 5.049401038297881783, 19.05341960407617563, 72.29275706135234714 ) ) ;
#128655 = CARTESIAN_POINT ( 'NONE',  ( -19.03943276465977164, 0.05219959533909376836, 91.24890960531436690 ) ) ;
#128656 = CARTESIAN_POINT ( 'NONE',  ( 16.51473224551069308, 9.474510206698969483, 69.16557627198102409 ) ) ;
#128657 = CARTESIAN_POINT ( 'NONE',  ( -10.81492255796078084, -18.62759615963271287, 67.08224293864770971 ) ) ;
#128658 = CARTESIAN_POINT ( 'NONE',  ( 0.05219959533934541429, -16.53943276465976808, 55.00109039468568284 ) ) ;
#128659 = CARTESIAN_POINT ( 'NONE',  ( 17.60779699588841041, 5.499999999999981348, 98.84981316670102558 ) ) ;
#128660 = CARTESIAN_POINT ( 'NONE',  ( 9.564922557960805705, 16.46253265017160317, 49.58224293864770260 ) ) ;
#128661 = CARTESIAN_POINT ( 'NONE',  ( 21.55341960407610458, 5.719274019375980345, 48.95724293864770971 ) ) ;
#128662 = CARTESIAN_POINT ( 'NONE',  ( 19.02544592524334988, 5.153800228976608722, 91.45942372801900433 ) ) ;
#128664 = CARTESIAN_POINT ( 'NONE',  ( 0.05219959533937995610, -21.53943276465977519, 35.00109039468568284 ) ) ;
#128663 = CARTESIAN_POINT ( 'NONE',  ( 12.14591786802309770, 12.06949235617756955, 24.37390960531435979 ) ) ;
#128665 = CARTESIAN_POINT ( 'NONE',  ( 9.564922557961047289, -16.46253265017146816, 35.41775706135233293 ) ) ;
#128667 = CARTESIAN_POINT ( 'NONE',  ( -12.06949235617739369, -12.14591786802326823, 94.37609039468568994 ) ) ;
#128666 = CARTESIAN_POINT ( 'NONE',  ( 0.05219959533934541429, -16.53943276465976808, 65.00109039468568994 ) ) ;
#128668 = CARTESIAN_POINT ( 'NONE',  ( 23.29544513554940011, 16.92513159979228021, 147.4656553485623647 ) ) ;
#128669 = CARTESIAN_POINT ( 'NONE',  ( 8.314922557961029526, -14.29746914071037800, 80.41775706135234714 ) ) ;
#128671 = CARTESIAN_POINT ( 'NONE',  ( -14.29746914071037622, -8.314922557961029526, 29.16775706135234003 ) ) ;
#128670 = CARTESIAN_POINT ( 'NONE',  ( -10.81492255796078084, -18.62759615963271287, 32.08224293864769550 ) ) ;
#128672 = CARTESIAN_POINT ( 'NONE',  ( 16.51473224551069308, 9.474510206698969483, 39.16557627198103120 ) ) ;
#128673 = CARTESIAN_POINT ( 'NONE',  ( 0.05219959533909260263, 19.03943276465977164, 54.99890960531435979 ) ) ;
#128674 = CARTESIAN_POINT ( 'NONE',  ( 13.89961937509977652, -13.97604488694527269, 63.12390960531435979 ) ) ;
#128675 = CARTESIAN_POINT ( 'NONE',  ( 21.53943276465977519, 0.05219959533937863772, 41.25109039468568284 ) ) ;
#128676 = CARTESIAN_POINT ( 'NONE',  ( 12.14591786802327356, -12.06949235617739191, 55.62609039468568284 ) ) ;
#128677 = CARTESIAN_POINT ( 'NONE',  ( 16.53943276465976808, 0.05219959533934440121, 106.2510903946856757 ) ) ;
#128678 = CARTESIAN_POINT ( 'NONE',  ( -13.97604488694527625, -13.89961937509977652, 31.87390960531435979 ) ) ;
#128679 = CARTESIAN_POINT ( 'NONE',  ( -10.72451020669870658, -18.67979575497194134, 109.5844237280190328 ) ) ;
#128680 = CARTESIAN_POINT ( 'NONE',  ( -14.29746914071037622, -8.314922557961029526, 19.16775706135234714 ) ) ;
#128681 = CARTESIAN_POINT ( 'NONE',  ( 13.89961937509957401, 13.97604488694547697, 71.87609039468567573 ) ) ;
#128682 = CARTESIAN_POINT ( 'NONE',  ( 16.55341960407611168, 4.379528057220329451, 63.95724293864770260 ) ) ;
#128683 = CARTESIAN_POINT ( 'NONE',  ( -0.05219959533909027116, -19.03943276465977164, 32.49890960531435979 ) ) ;
#128685 = CARTESIAN_POINT ( 'NONE',  ( 17.50000000000000000, 5.499999999999992895, 76.70309617465829888 ) ) ;
#128684 = CARTESIAN_POINT ( 'NONE',  ( 19.02544592524334988, 5.153800228976608722, 71.45942372801900433 ) ) ;
#128686 = CARTESIAN_POINT ( 'NONE',  ( -5.823673210054431948, 21.52544592524334988, 77.70942372801900433 ) ) ;
#128687 = CARTESIAN_POINT ( 'NONE',  ( -8.224510206698735004, -14.34966873604973081, 34.58442372801900433 ) ) ;
#128688 = CARTESIAN_POINT ( 'NONE',  ( -17.60728821186565085, 5.500000000000021316, 90.86690927743005375 ) ) ;
#128689 = CARTESIAN_POINT ( 'NONE',  ( 0.05219959533907565091, 21.53943276465977519, 29.99890960531435979 ) ) ;
#128690 = CARTESIAN_POINT ( 'NONE',  ( -16.52544592524335698, -4.483927247898792601, 23.95942372801901143 ) ) ;
#128691 = CARTESIAN_POINT ( 'NONE',  ( 0.05219959533909260263, 19.03943276465977164, 24.99890960531435269 ) ) ;
#128692 = CARTESIAN_POINT ( 'NONE',  ( 19.02544592524334988, 5.153800228976608722, 31.45942372801900433 ) ) ;
#128693 = CARTESIAN_POINT ( 'NONE',  ( 9.389996629557208152, 10.10305183197209544, -60.40856999928715254 ) ) ;
#128694 = CARTESIAN_POINT ( 'NONE',  ( -5.153800228976328057, -19.02544592524343514, 42.29057627198101699 ) ) ;
#128695 = CARTESIAN_POINT ( 'NONE',  ( 28.79475375365586132, 2.781246896534039337E-14, 143.2656553485623760 ) ) ;
#128696 = CARTESIAN_POINT ( 'NONE',  ( 16.51473224551069308, 9.474510206698969483, 54.16557627198103120 ) ) ;
#128697 = CARTESIAN_POINT ( 'NONE',  ( -18.22780087662122028, 5.500000000000031086, 98.51540105326105845 ) ) ;
#128698 = CARTESIAN_POINT ( 'NONE',  ( -5.823673210054431948, 21.52544592524334988, 112.7094237280190328 ) ) ;
#128699 = CARTESIAN_POINT ( 'NONE',  ( -16.53943276465976808, 0.05219959533911058130, 21.24890960531436690 ) ) ;
#128700 = CARTESIAN_POINT ( 'NONE',  ( 5.049401038298161559, -19.05341960407611168, 27.70724293864769550 ) ) ;
#128701 = CARTESIAN_POINT ( 'NONE',  ( 19.05341960407611168, 5.049401038298154454, 93.95724293864769550 ) ) ;
#128702 = CARTESIAN_POINT ( 'NONE',  ( 0.05219959533937995610, -21.53943276465977519, 70.00109039468568994 ) ) ;
#128703 = CARTESIAN_POINT ( 'NONE',  ( -13.89961937509977652, 13.97604488694528158, 35.62390960531435269 ) ) ;
#128704 = CARTESIAN_POINT ( 'NONE',  ( -10.81492255796105439, 18.62759615963255655, 62.91775706135236135 ) ) ;
#128706 = CARTESIAN_POINT ( 'NONE',  ( 18.62759615963271287, -10.81492255796078972, 23.33224293864769194 ) ) ;
#128705 = CARTESIAN_POINT ( 'NONE',  ( -9.564922557961040184, 16.46253265017147172, 97.91775706135233293 ) ) ;
#128707 = CARTESIAN_POINT ( 'NONE',  ( 5.049401038298161559, -19.05341960407611168, 37.70724293864768839 ) ) ;
#128708 = CARTESIAN_POINT ( 'NONE',  ( -10.72451020669898014, 18.67979575497178502, 105.4155762719810383 ) ) ;
#128709 = CARTESIAN_POINT ( 'NONE',  ( -13.89961937509957401, -13.97604488694547875, 29.37609039468565797 ) ) ;
#128710 = CARTESIAN_POINT ( 'NONE',  ( 16.52544592524342804, -4.483927247898539470, 108.5405762719810241 ) ) ;
#128711 = CARTESIAN_POINT ( 'NONE',  ( -19.03943276465977164, 0.05219959533909376836, 66.24890960531436690 ) ) ;
#128712 = CARTESIAN_POINT ( 'NONE',  ( -19.02544592524334988, -5.153800228976617603, 93.95942372801900433 ) ) ;
#128713 = CARTESIAN_POINT ( 'NONE',  ( 8.224510206698953496, -14.34966873604960469, 72.91557627198103830 ) ) ;
#128714 = CARTESIAN_POINT ( 'NONE',  ( 15.80617190586746368, 15.72974639402197994, 24.37390960531435979 ) ) ;
#128715 = CARTESIAN_POINT ( 'NONE',  ( -5.153800228976607833, 19.02544592524334988, 82.70942372801897591 ) ) ;
#128716 = CARTESIAN_POINT ( 'NONE',  ( -15.80617190586745835, -15.72974639402198527, 86.87390960531438111 ) ) ;
#128717 = CARTESIAN_POINT ( 'NONE',  ( -0.05219959533937732626, 21.53943276465977519, 42.50109039468567573 ) ) ;
#128718 = CARTESIAN_POINT ( 'NONE',  ( -0.05219959533934338120, 16.53943276465976808, 47.50109039468568994 ) ) ;
#128720 = CARTESIAN_POINT ( 'NONE',  ( -10.72451020669870658, -18.67979575497194134, 54.58442372801901143 ) ) ;
#128719 = CARTESIAN_POINT ( 'NONE',  ( -14.29746914071037622, -8.314922557961029526, 49.16775706135234003 ) ) ;
#128721 = CARTESIAN_POINT ( 'NONE',  ( -21.55341960407610458, -5.719274019375992779, 61.45724293864770260 ) ) ;
#128722 = CARTESIAN_POINT ( 'NONE',  ( -19.05341960407611168, -5.049401038298163336, 46.45724293864768129 ) ) ;
#128723 = CARTESIAN_POINT ( 'NONE',  ( -23.48529157249600985, 32.32473071737754111, -2.049999994537626158 ) ) ;
#128724 = CARTESIAN_POINT ( 'NONE',  ( -16.55341960407617563, 4.379528057220093196, 78.54275706135236135 ) ) ;
#128725 = EDGE_CURVE ( 'NONE', #164433, #96037, #76196, .T. ) ;
#128726 = CARTESIAN_POINT ( 'NONE',  ( 21.52544592524344225, -5.823673210054117533, 98.54057627198105251 ) ) ;
#128727 = CARTESIAN_POINT ( 'NONE',  ( 16.52544592524342804, -4.483927247898539470, 58.54057627198103120 ) ) ;
#128728 = CARTESIAN_POINT ( 'NONE',  ( 12.14591786802327356, -12.06949235617739191, 65.62609039468568994 ) ) ;
#128729 = CARTESIAN_POINT ( 'NONE',  ( 5.153800228976615827, -19.02544592524334988, 100.2094237280190043 ) ) ;
#128730 = CARTESIAN_POINT ( 'NONE',  ( -0.05219959533907301413, -21.53943276465977519, 97.49890960531436690 ) ) ;
#128731 = CARTESIAN_POINT ( 'NONE',  ( -16.55341960407611168, -4.379528057220339221, 51.45724293864770260 ) ) ;
#128732 = ORIENTED_EDGE ( 'NONE', *, *, #42790, .T. ) ;
#128733 = CARTESIAN_POINT ( 'NONE',  ( -4.379528057220086978, -16.55341960407618274, 79.79275706135236135 ) ) ;
#128734 = CARTESIAN_POINT ( 'NONE',  ( 25.27727188472143283, 10.29814791481116032, 170.4127952078933674 ) ) ;
#128735 = CARTESIAN_POINT ( 'NONE',  ( 15.72974639402199770, -15.80617190586745480, 73.12390960531436690 ) ) ;
#128736 = CARTESIAN_POINT ( 'NONE',  ( 4.379528057220339221, -16.55341960407611168, 32.70724293864770260 ) ) ;
#128737 = ORIENTED_EDGE ( 'NONE', *, *, #182320, .F. ) ;
#128738 = CARTESIAN_POINT ( 'NONE',  ( -16.36317988757057407, -7.306389748694946285, 55.90210391636774290 ) ) ;
#128739 = CARTESIAN_POINT ( 'NONE',  ( -21.55341960407610458, -5.719274019375992779, 101.4572429386476955 ) ) ;
#128740 = CARTESIAN_POINT ( 'NONE',  ( -15.72974639402197994, 15.80617190586746368, 110.6239096053143669 ) ) ;
#128741 = CARTESIAN_POINT ( 'NONE',  ( -8.314922557960811034, -14.29746914071050412, 32.08224293864769550 ) ) ;
#128742 = CARTESIAN_POINT ( 'NONE',  ( 14.34966873604972726, -8.224510206698740333, 45.83442372801901854 ) ) ;
#128743 = CARTESIAN_POINT ( 'NONE',  ( -19.03943276465977164, 0.05219959533909376836, 51.24890960531436690 ) ) ;
#128744 = CARTESIAN_POINT ( 'NONE',  ( -16.51473224551069308, -9.474510206698971260, 66.66557627198102409 ) ) ;
#128745 = EDGE_LOOP ( 'NONE', ( #71910, #175561, #195044, #122657 ) ) ;
#128746 = CARTESIAN_POINT ( 'NONE',  ( -21.52544592524343514, 5.823673210054127303, 26.04057627198103475 ) ) ;
#128747 = CARTESIAN_POINT ( 'NONE',  ( -30.24683373042578083, -22.89668476416583687, -22.64123003232879228 ) ) ;
#128748 = CARTESIAN_POINT ( 'NONE',  ( 13.89961937509957401, 13.97604488694547697, 101.8760903946856331 ) ) ;
#128749 = CARTESIAN_POINT ( 'NONE',  ( 5.049401038297881783, 19.05341960407617563, 52.29275706135234003 ) ) ;
#128750 = CARTESIAN_POINT ( 'NONE',  ( -5.823673210054116645, -21.52544592524344225, 107.2905762719810525 ) ) ;
#128751 = CARTESIAN_POINT ( 'NONE',  ( 12.06949235617757843, -12.14591786802309237, 33.12390960531435979 ) ) ;
#128752 = CARTESIAN_POINT ( 'NONE',  ( 5.049401038298161559, -19.05341960407611168, 77.70724293864765286 ) ) ;
#128753 = CARTESIAN_POINT ( 'NONE',  ( -10.72451020669898014, 18.67979575497178502, 50.41557627198103120 ) ) ;
#128755 = CARTESIAN_POINT ( 'NONE',  ( 12.06949235617739724, 12.14591786802326823, 21.87609039468567573 ) ) ;
#128754 = CARTESIAN_POINT ( 'NONE',  ( -18.67979575497178146, -10.72451020669898902, 81.66557627198103830 ) ) ;
#128756 = CARTESIAN_POINT ( 'NONE',  ( 18.62759615963271287, -10.81492255796078972, 28.33224293864769550 ) ) ;
#128757 = CARTESIAN_POINT ( 'NONE',  ( 15.80617190586769283, -15.72974639402175789, 75.62609039468567573 ) ) ;
#128758 = CARTESIAN_POINT ( 'NONE',  ( 9.474510206698971260, -16.51473224551069308, 72.91557627198102409 ) ) ;
#128759 = CARTESIAN_POINT ( 'NONE',  ( -5.153800228976328057, -19.02544592524343514, 27.29057627198103120 ) ) ;
#128760 = CARTESIAN_POINT ( 'NONE',  ( 5.153800228976335163, 19.02544592524342804, 79.79057627198102409 ) ) ;
#128761 = CARTESIAN_POINT ( 'NONE',  ( -12.06949235617756955, 12.14591786802309770, 95.62390960531436690 ) ) ;
#128762 = ORIENTED_EDGE ( 'NONE', *, *, #174237, .T. ) ;
#128763 = CARTESIAN_POINT ( 'NONE',  ( -16.51473224551082808, 9.474510206698731452, 103.3344237280190043 ) ) ;
#128764 = CARTESIAN_POINT ( 'NONE',  ( 31.99999999999966604, 4.791014396527177230E-13, 47.70000000000022311 ) ) ;
#128765 = CARTESIAN_POINT ( 'NONE',  ( 19.05341960407611168, 5.049401038298154454, 78.95724293864769550 ) ) ;
#128767 = CARTESIAN_POINT ( 'NONE',  ( -5.823673210054116645, -21.52544592524344225, 22.29057627198102765 ) ) ;
#128766 = CARTESIAN_POINT ( 'NONE',  ( -0.05219959533937732626, 21.53943276465977519, 87.50109039468568994 ) ) ;
#128768 = CARTESIAN_POINT ( 'NONE',  ( 0.05219959533934541429, -16.53943276465976808, 75.00109039468568994 ) ) ;
#128769 = CARTESIAN_POINT ( 'NONE',  ( -28.98522958361496293, 0.5143648618589782284, -49.56847006845431025 ) ) ;
#128770 = CARTESIAN_POINT ( 'NONE',  ( 5.049401038297881783, 19.05341960407617563, 52.29275706135234003 ) ) ;
#128771 = CARTESIAN_POINT ( 'NONE',  ( -10.81492255796105439, 18.62759615963255655, 112.9177570613523329 ) ) ;
#128772 = DIRECTION ( 'NONE',  ( -0.000000000000000000, -0.000000000000000000, 1.000000000000000000 ) ) ;
#128773 = CARTESIAN_POINT ( 'NONE',  ( 30.74264578624800137, -22.33583958711395212, -6.949999994537627401 ) ) ;
#128774 = CARTESIAN_POINT ( 'NONE',  ( -11.40812507854755609, 35.11059874428196537, -1.524999997268813301 ) ) ;
#128775 = CARTESIAN_POINT ( 'NONE',  ( 4.483927247898545687, 16.52544592524342804, 29.79057627198102409 ) ) ;
#128776 = DIRECTION ( 'NONE',  ( -1.000000000000000000, 0.000000000000000000, 0.000000000000000000 ) ) ;
#128777 = CARTESIAN_POINT ( 'NONE',  ( -0.05219959533934338120, 16.53943276465976808, 102.5010903946856899 ) ) ;
#128778 = CARTESIAN_POINT ( 'NONE',  ( 33.78191506369888941, -21.41920200728860380, -24.99999999999997868 ) ) ;
#128779 = CARTESIAN_POINT ( 'NONE',  ( -16.55341960407617563, 4.379528057220093196, 83.54275706135234714 ) ) ;
#128780 = CARTESIAN_POINT ( 'NONE',  ( -18.67979575497193778, 10.72451020669871902, 98.33442372801901854 ) ) ;
#128781 = CARTESIAN_POINT ( 'NONE',  ( 19.05341960407617918, -5.049401038297876454, 101.0427570613523045 ) ) ;
#128782 = CARTESIAN_POINT ( 'NONE',  ( 10.81492255796106328, -18.62759615963255655, 70.41775706135236135 ) ) ;
#128783 = CARTESIAN_POINT ( 'NONE',  ( 13.97604488694548053, -13.89961937509957401, 35.62609039468567573 ) ) ;
#128784 = CARTESIAN_POINT ( 'NONE',  ( 13.89961937509977652, -13.97604488694527269, 83.12390960531436690 ) ) ;
#128785 = CARTESIAN_POINT ( 'NONE',  ( -5.153800228976328057, -19.02544592524343514, 62.29057627198100988 ) ) ;
#128786 = CARTESIAN_POINT ( 'NONE',  ( -11.92151346184467897, -38.18361175107895633, -12.32871365052710999 ) ) ;
#128787 = CARTESIAN_POINT ( 'NONE',  ( -10.72451020669898014, 18.67979575497178502, 90.41557627198103830 ) ) ;
#128788 = CARTESIAN_POINT ( 'NONE',  ( 21.52544592524344225, -5.823673210054117533, 48.54057627198103120 ) ) ;
#128789 = CARTESIAN_POINT ( 'NONE',  ( -9.564922557960796823, -16.46253265017161027, 42.08224293864769550 ) ) ;
#128790 = CARTESIAN_POINT ( 'NONE',  ( 0.05219959533934541429, -16.53943276465976808, 70.00109039468568994 ) ) ;
#128791 = EDGE_CURVE ( 'NONE', #186347, #65463, #45135, .T. ) ;
#128792 = VERTEX_POINT ( 'NONE', #30703 ) ;
#128793 = CARTESIAN_POINT ( 'NONE',  ( -5.823673210054431948, 21.52544592524334988, 47.70942372801902565 ) ) ;
#128795 = CARTESIAN_POINT ( 'NONE',  ( -29.86685920354755552, 21.69954338932564397, -0.8249999972688133454 ) ) ;
#128794 = CARTESIAN_POINT ( 'NONE',  ( 14.34966873604960469, 8.224510206698951720, 69.16557627198102409 ) ) ;
#128796 = CARTESIAN_POINT ( 'NONE',  ( 14.34966873604972726, -8.224510206698740333, 40.83442372801901854 ) ) ;
#128797 = CARTESIAN_POINT ( 'NONE',  ( 4.483927247898545687, 16.52544592524342804, 104.7905762719810241 ) ) ;
#128798 = CARTESIAN_POINT ( 'NONE',  ( 5.153800228976615827, -19.02544592524334988, 50.20942372801897591 ) ) ;
#128799 = CARTESIAN_POINT ( 'NONE',  ( -16.53943276465976808, 0.05219959533911058130, 76.24890960531435269 ) ) ;
#128800 = CARTESIAN_POINT ( 'NONE',  ( 10.81492255796106328, -18.62759615963255655, 35.41775706135234003 ) ) ;
#128802 = CARTESIAN_POINT ( 'NONE',  ( -21.55341960407610458, -5.719274019375992779, 91.45724293864769550 ) ) ;
#128801 = DIRECTION ( 'NONE',  ( -0.000000000000000000, -0.000000000000000000, -1.000000000000000000 ) ) ;
#128803 = CARTESIAN_POINT ( 'NONE',  ( -9.564922557960796823, -16.46253265017161027, 97.08224293864769550 ) ) ;
#128804 = CARTESIAN_POINT ( 'NONE',  ( 14.29746914071049879, -8.314922557960816363, 73.33224293864769550 ) ) ;
#128805 = CARTESIAN_POINT ( 'NONE',  ( 19.03943276465977164, -0.05219959533909143690, 113.7489096053143669 ) ) ;
#128806 = CARTESIAN_POINT ( 'NONE',  ( 3.556970738554034288E-15, -38.81732327939057114, -2.124999997268813168 ) ) ;
#128807 = CARTESIAN_POINT ( 'NONE',  ( 5.153800228976615827, -19.02544592524334988, 85.20942372801900433 ) ) ;
#128808 = CARTESIAN_POINT ( 'NONE',  ( 18.67979575497194134, -10.72451020669871369, 25.83442372801901499 ) ) ;
#128809 = CARTESIAN_POINT ( 'NONE',  ( -19.02544592524342804, 5.153800228976336051, 71.04057627198099567 ) ) ;
#128810 = CARTESIAN_POINT ( 'NONE',  ( 13.89961937509957401, 13.97604488694547697, 56.87609039468564731 ) ) ;
#128811 = CARTESIAN_POINT ( 'NONE',  ( 9.564922557960805705, 16.46253265017160317, 39.58224293864768839 ) ) ;
#128812 = CARTESIAN_POINT ( 'NONE',  ( 8.314922557960818139, 14.29746914071049879, 59.58224293864770260 ) ) ;
#128813 = CARTESIAN_POINT ( 'NONE',  ( -8.224510206698948167, 14.34966873604960824, 60.41557627198102409 ) ) ;
#128814 = CARTESIAN_POINT ( 'NONE',  ( 9.474510206698971260, -16.51473224551069308, 72.91557627198102409 ) ) ;
#128815 = CARTESIAN_POINT ( 'NONE',  ( 21.52544592524344225, -5.823673210054117533, 88.54057627198103830 ) ) ;
#128816 = CARTESIAN_POINT ( 'NONE',  ( -13.89961937509977652, 13.97604488694528158, 75.62390960531438111 ) ) ;
#128817 = CARTESIAN_POINT ( 'NONE',  ( 5.719274019375991003, -21.55341960407610458, 82.70724293864770971 ) ) ;
#128818 = CARTESIAN_POINT ( 'NONE',  ( -0.05219959533936034679, 19.03943276465977164, 22.50109039468566152 ) ) ;
#128821 = CARTESIAN_POINT ( 'NONE',  ( 12.06949235617757843, -12.14591786802309237, 93.12390960531436690 ) ) ;
#128820 = CARTESIAN_POINT ( 'NONE',  ( 0.05219959533934541429, -16.53943276465976808, 110.0010903946856757 ) ) ;
#128819 = DIRECTION ( 'NONE',  ( -1.000000000000000000, 0.000000000000000000, 0.000000000000000000 ) ) ;
#128822 = CARTESIAN_POINT ( 'NONE',  ( 5.153800228976615827, -19.02544592524334988, 95.20942372801897591 ) ) ;
#128823 = ORIENTED_EDGE ( 'NONE', *, *, #55964, .T. ) ;
#128824 = CARTESIAN_POINT ( 'NONE',  ( 21.55341960407619695, -5.719274019375665929, 21.04275706135234714 ) ) ;
#128825 = CARTESIAN_POINT ( 'NONE',  ( 0.05219959533936267826, -19.03943276465977164, 50.00109039468566863 ) ) ;
#128826 = CARTESIAN_POINT ( 'NONE',  ( 16.52544592524335698, 4.483927247898782831, 101.4594237280190185 ) ) ;
#128827 = CARTESIAN_POINT ( 'NONE',  ( 13.89961937509957401, 13.97604488694547697, 46.87609039468565442 ) ) ;
#128828 = CARTESIAN_POINT ( 'NONE',  ( 16.51473224551069308, 9.474510206698969483, 104.1655762719810241 ) ) ;
#128829 = CARTESIAN_POINT ( 'NONE',  ( 16.55341960407611168, 4.379528057220329451, 58.95724293864770971 ) ) ;
#128830 = CARTESIAN_POINT ( 'NONE',  ( -21.53032740501643261, 19.35460773160097503, 140.0335582641266683 ) ) ;
#128831 = CARTESIAN_POINT ( 'NONE',  ( -13.97604488694527625, -13.89961937509977652, 36.87390960531436690 ) ) ;
#128832 = CARTESIAN_POINT ( 'NONE',  ( -21.55341960407619339, 5.719274019375674811, 113.5427570613523756 ) ) ;
#128833 = CARTESIAN_POINT ( 'NONE',  ( -16.52544592524335698, -4.483927247898792601, 73.95942372801901854 ) ) ;
#128834 = CARTESIAN_POINT ( 'NONE',  ( -0.05219959533937732626, 21.53943276465977519, 37.50109039468568284 ) ) ;
#128835 = CARTESIAN_POINT ( 'NONE',  ( -8.314922557961024197, 14.29746914071037800, 37.91775706135235424 ) ) ;
#128836 = CARTESIAN_POINT ( 'NONE',  ( -16.46253265017160317, 9.564922557960807481, 110.8322429386476955 ) ) ;
#128837 = CARTESIAN_POINT ( 'NONE',  ( 9.474510206698971260, -16.51473224551069308, 52.91557627198102409 ) ) ;
#128838 = CARTESIAN_POINT ( 'NONE',  ( 13.97604488694527802, 13.89961937509977652, 64.37390960531436690 ) ) ;
#128839 = CARTESIAN_POINT ( 'NONE',  ( 16.55341960407618274, -4.379528057220086978, 46.04275706135234714 ) ) ;
#128840 = CARTESIAN_POINT ( 'NONE',  ( 14.34966873604960469, 8.224510206698951720, 109.1655762719810383 ) ) ;
#128841 = CARTESIAN_POINT ( 'NONE',  ( -16.53943276465976808, 0.05219959533911058130, 21.24890960531436690 ) ) ;
#128842 = CARTESIAN_POINT ( 'NONE',  ( -16.12203461105333702, 16.12203461105326951, -65.00100000000003320 ) ) ;
#128845 = CARTESIAN_POINT ( 'NONE',  ( 9.474510206698971260, -16.51473224551069308, 57.91557627198103120 ) ) ;
#128844 = CARTESIAN_POINT ( 'NONE',  ( 13.89961937509977652, -13.97604488694527269, 88.12390960531438111 ) ) ;
#128843 = CARTESIAN_POINT ( 'NONE',  ( -0.05219959533937732626, 21.53943276465977519, 57.50109039468568994 ) ) ;
#128846 = CARTESIAN_POINT ( 'NONE',  ( 13.89961937509977652, -13.97604488694527269, 93.12390960531436690 ) ) ;
#128847 = CARTESIAN_POINT ( 'NONE',  ( -4.379528057220328563, 16.55341960407611168, 45.20724293864769550 ) ) ;
#128848 = CARTESIAN_POINT ( 'NONE',  ( 16.52544592524342804, -4.483927247898539470, 23.54057627198102765 ) ) ;
#128849 = CARTESIAN_POINT ( 'NONE',  ( -14.34966873604960291, -8.224510206698953496, 36.66557627198103120 ) ) ;
#128850 = VERTEX_POINT ( 'NONE', #169196 ) ;
#128851 = CARTESIAN_POINT ( 'NONE',  ( 26.03370437638690049, -6.875205692009868308, 160.5968874236871784 ) ) ;
#128852 = CARTESIAN_POINT ( 'NONE',  ( -5.049401038298153566, 19.05341960407611168, 65.20724293864765286 ) ) ;
#128853 = CARTESIAN_POINT ( 'NONE',  ( -19.03943276465977164, -0.05219959533935918106, 43.75109039468566863 ) ) ;
#128854 = CARTESIAN_POINT ( 'NONE',  ( -36.91746825000000598, 2.428612866367529932E-14, -11.12499999726881228 ) ) ;
#128855 = CARTESIAN_POINT ( 'NONE',  ( 18.22780087662121673, 5.500000000000056843, 58.98459894673892023 ) ) ;
#128857 = CARTESIAN_POINT ( 'NONE',  ( 0.05219959533934541429, -16.53943276465976808, 65.00109039468568994 ) ) ;
#128856 = CARTESIAN_POINT ( 'NONE',  ( -5.153800228976607833, 19.02544592524334988, 82.70942372801897591 ) ) ;
#128858 = CARTESIAN_POINT ( 'NONE',  ( 16.31925111598456013, 7.325300261831534598, 92.33575461032747000 ) ) ;
#128859 = CARTESIAN_POINT ( 'NONE',  ( -13.97604488694527625, -13.89961937509977652, 91.87390960531432427 ) ) ;
#128860 = CARTESIAN_POINT ( 'NONE',  ( 15.72974639402176855, 15.80617190586768217, 21.87609039468567573 ) ) ;
#128861 = CARTESIAN_POINT ( 'NONE',  ( -19.03943276465977164, -0.05219959533935918106, 88.75109039468567573 ) ) ;
#128863 = CARTESIAN_POINT ( 'NONE',  ( 5.049401038298161559, -19.05341960407611168, 47.70724293864770260 ) ) ;
#128862 = CARTESIAN_POINT ( 'NONE',  ( 37.99999999999999289, 2.893978650043524126E-14, -2.749999994537626780 ) ) ;
#128864 = CARTESIAN_POINT ( 'NONE',  ( -5.049401038298153566, 19.05341960407611168, 85.20724293864766707 ) ) ;
#128866 = CARTESIAN_POINT ( 'NONE',  ( -19.02544592524342804, 5.153800228976336051, 56.04057627198100988 ) ) ;
#128865 = CARTESIAN_POINT ( 'NONE',  ( 16.55341960407611168, 4.379528057220329451, 53.95724293864770260 ) ) ;
#128867 = CARTESIAN_POINT ( 'NONE',  ( -13.89961937509957401, -13.97604488694547875, 64.37609039468567573 ) ) ;
#128868 = CARTESIAN_POINT ( 'NONE',  ( 12.06949235617757843, -12.14591786802309237, 88.12390960531436690 ) ) ;
#128869 = CARTESIAN_POINT ( 'NONE',  ( -19.05341960407617563, 5.049401038297882671, 23.54275706135233648 ) ) ;
#128870 = CARTESIAN_POINT ( 'NONE',  ( -0.05219959533909027116, -19.03943276465977164, 67.49890960531436690 ) ) ;
#128871 = CARTESIAN_POINT ( 'NONE',  ( -5.823673210054116645, -21.52544592524344225, 57.29057627198103120 ) ) ;
#128873 = CARTESIAN_POINT ( 'NONE',  ( 18.67979575497194134, -10.72451020669871369, 110.8344237280190043 ) ) ;
#128872 = CARTESIAN_POINT ( 'NONE',  ( 12.06949235617757843, -12.14591786802309237, 63.12390960531435979 ) ) ;
#128874 = CARTESIAN_POINT ( 'NONE',  ( 5.049401038298161559, -19.05341960407611168, 107.7072429386476955 ) ) ;
#128875 = CARTESIAN_POINT ( 'NONE',  ( -0.05219959533907301413, -21.53943276465977519, 27.49890960531435269 ) ) ;
#128876 = CARTESIAN_POINT ( 'NONE',  ( -9.564922557960796823, -16.46253265017161027, 47.08224293864769550 ) ) ;
#128877 = CARTESIAN_POINT ( 'NONE',  ( -0.05219959533909027116, -19.03943276465977164, 32.49890960531435979 ) ) ;
#128878 = CARTESIAN_POINT ( 'NONE',  ( -16.53943276465976808, 0.05219959533911058130, 106.2489096053143811 ) ) ;
#128879 = CARTESIAN_POINT ( 'NONE',  ( -21.52544592524334988, -5.823673210054445271, 18.95942372801901143 ) ) ;
#128880 = CARTESIAN_POINT ( 'NONE',  ( -16.51473224551069308, -9.474510206698971260, 96.66557627198102409 ) ) ;
#128881 = CARTESIAN_POINT ( 'NONE',  ( -21.55341960407619339, 5.719274019375674811, 23.54275706135235424 ) ) ;
#128882 = CARTESIAN_POINT ( 'NONE',  ( 9.564922557960805705, 16.46253265017160317, 109.5822429386476955 ) ) ;
#128883 = CARTESIAN_POINT ( 'NONE',  ( -19.03943276465977164, 0.05219959533909376836, 21.24890960531436335 ) ) ;
#128884 = CARTESIAN_POINT ( 'NONE',  ( -18.62759615963255300, -10.81492255796106328, 74.16775706135231871 ) ) ;
#128885 = CARTESIAN_POINT ( 'NONE',  ( -0.05219959533907301413, -21.53943276465977519, 92.49890960531436690 ) ) ;
#128886 = DIRECTION ( 'NONE',  ( 0.000000000000000000, 0.000000000000000000, -1.000000000000000000 ) ) ;
#128887 = CYLINDRICAL_SURFACE ( 'NONE', #181931, 5.000000000000000888 ) ;
#128888 = CARTESIAN_POINT ( 'NONE',  ( 3.766062262543149401E-15, -39.95556452105413570, -1.499999999999999778 ) ) ;
#128889 = CARTESIAN_POINT ( 'NONE',  ( 4.483927247898790824, -16.52544592524335698, 50.20942372801901854 ) ) ;
#128890 = CARTESIAN_POINT ( 'NONE',  ( -16.53943276465976808, 0.05219959533911058130, 111.2489096053143669 ) ) ;
#128891 = CARTESIAN_POINT ( 'NONE',  ( -21.56952297831670151, -7.512152360717307964, 173.9007003117370971 ) ) ;
#128892 = CARTESIAN_POINT ( 'NONE',  ( 16.46253265017160672, -9.564922557960803928, 53.33224293864768839 ) ) ;
#128894 = EDGE_CURVE ( 'NONE', #43824, #155176, #180442, .T. ) ;
#128893 = CARTESIAN_POINT ( 'NONE',  ( 14.34966873604960469, 8.224510206698951720, 94.16557627198103830 ) ) ;
#128895 = CARTESIAN_POINT ( 'NONE',  ( 5.719274019375991003, -21.55341960407610458, 42.70724293864770260 ) ) ;
#128896 = CARTESIAN_POINT ( 'NONE',  ( -12.14591786802309592, -12.06949235617757132, 66.87390960531436690 ) ) ;
#128897 = CARTESIAN_POINT ( 'NONE',  ( 8.224510206698742110, 14.34966873604972548, 22.08442372801901143 ) ) ;
#128898 = CARTESIAN_POINT ( 'NONE',  ( -15.72974639402176322, -15.80617190586768395, 84.37609039468570415 ) ) ;
#128899 = CARTESIAN_POINT ( 'NONE',  ( 17.48853670773243607, -5.747243402303152671, 76.16671299749989998 ) ) ;
#128900 = CARTESIAN_POINT ( 'NONE',  ( -4.483927247898782831, 16.52544592524335698, 97.70942372801904696 ) ) ;
#128901 = CARTESIAN_POINT ( 'NONE',  ( 16.52544592524342804, -4.483927247898539470, 38.54057627198103120 ) ) ;
#128902 = CARTESIAN_POINT ( 'NONE',  ( 5.153800228976335163, 19.02544592524342804, 34.79057627198102409 ) ) ;
#128903 = CARTESIAN_POINT ( 'NONE',  ( 5.153800228976335163, 19.02544592524342804, 84.79057627198099567 ) ) ;
#128904 = CARTESIAN_POINT ( 'NONE',  ( 5.823673210054125526, 21.52544592524343514, 89.79057627198103830 ) ) ;
#128905 = CARTESIAN_POINT ( 'NONE',  ( -8.314922557961024197, 14.29746914071037800, 32.91775706135234714 ) ) ;
#128907 = CARTESIAN_POINT ( 'NONE',  ( -21.52544592524334988, -5.823673210054445271, 88.95942372801901854 ) ) ;
#128906 = CARTESIAN_POINT ( 'NONE',  ( 14.34966873604960469, 8.224510206698951720, 69.16557627198102409 ) ) ;
#128908 = CARTESIAN_POINT ( 'NONE',  ( -14.29746914071037622, -8.314922557961029526, 94.16775706135237556 ) ) ;
#128909 = CARTESIAN_POINT ( 'NONE',  ( 16.29526858892907271, -7.335722546920040443, 46.70329402199735114 ) ) ;
#128910 = CARTESIAN_POINT ( 'NONE',  ( -19.52851543214741881, -5.500000000000036415, 65.39357721762580411 ) ) ;
#128911 = CARTESIAN_POINT ( 'NONE',  ( 4.379528057220339221, -16.55341960407611168, 32.70724293864770260 ) ) ;
#128912 = CARTESIAN_POINT ( 'NONE',  ( 8.224510206698742110, 14.34966873604972548, 72.08442372801899012 ) ) ;
#128913 = CARTESIAN_POINT ( 'NONE',  ( -13.97604488694527625, -13.89961937509977652, 91.87390960531432427 ) ) ;
#128914 = CARTESIAN_POINT ( 'NONE',  ( 0.05219959533909260263, 19.03943276465977164, 104.9989096053143669 ) ) ;
#128915 = CARTESIAN_POINT ( 'NONE',  ( 5.823673210054444382, -21.52544592524334988, 90.20942372801903275 ) ) ;
#128916 = CARTESIAN_POINT ( 'NONE',  ( 14.29746914071037800, 8.314922557961029526, 91.66775706135234714 ) ) ;
#128917 = CARTESIAN_POINT ( 'NONE',  ( 0.05219959533910956823, 16.53943276465976808, 64.99890960531435269 ) ) ;
#128918 = CARTESIAN_POINT ( 'NONE',  ( 9.474510206698971260, -16.51473224551069308, 62.91557627198102409 ) ) ;
#128919 = EDGE_LOOP ( 'NONE', ( #999, #103328, #46184, #182554 ) ) ;
#128920 = CARTESIAN_POINT ( 'NONE',  ( -19.05341960407617563, 5.049401038297882671, 103.5427570613523329 ) ) ;
#128921 = CARTESIAN_POINT ( 'NONE',  ( 14.29746914071049879, -8.314922557960816363, 108.3322429386477097 ) ) ;
#128922 = CARTESIAN_POINT ( 'NONE',  ( -13.97604488694527625, -13.89961937509977652, 71.87390960531433848 ) ) ;
#128924 = CARTESIAN_POINT ( 'NONE',  ( 22.81625015709510151, -31.40387420917324590, -7.924999997268812990 ) ) ;
#128923 = CARTESIAN_POINT ( 'NONE',  ( 19.02544592524334988, 5.153800228976608722, 111.4594237280190043 ) ) ;
#128925 = CARTESIAN_POINT ( 'NONE',  ( 10.72451020669871369, 18.67979575497193778, 112.0844237280190185 ) ) ;
#128926 = CARTESIAN_POINT ( 'NONE',  ( -14.34966873604972548, 8.224510206698743886, 78.33442372801901854 ) ) ;
#128927 = CARTESIAN_POINT ( 'NONE',  ( -13.89961937509957401, -13.97604488694547875, 104.3760903946856757 ) ) ;
#128928 = CARTESIAN_POINT ( 'NONE',  ( -14.29746914071049879, 8.314922557960819915, 110.8322429386476955 ) ) ;
#128929 = CARTESIAN_POINT ( 'NONE',  ( 4.483927247898790824, -16.52544592524335698, 65.20942372801901854 ) ) ;
#128930 = CARTESIAN_POINT ( 'NONE',  ( -4.483927247898782831, 16.52544592524335698, 47.70942372801902565 ) ) ;
#128931 = CARTESIAN_POINT ( 'NONE',  ( 9.474510206698971260, -16.51473224551069308, 27.91557627198103120 ) ) ;
#128932 = CARTESIAN_POINT ( 'NONE',  ( -5.153800228976607833, 19.02544592524334988, 67.70942372801900433 ) ) ;
#128933 = CARTESIAN_POINT ( 'NONE',  ( 19.03943276465977164, 0.05219959533936151252, 21.25109039468565797 ) ) ;
#128934 = CARTESIAN_POINT ( 'NONE',  ( -13.97604488694527625, -13.89961937509977652, 31.87390960531435979 ) ) ;
#128935 = CARTESIAN_POINT ( 'NONE',  ( 19.02544592524343514, -5.153800228976328945, 83.54057627198100988 ) ) ;
#128937 = EDGE_CURVE ( 'NONE', #188751, #178458, #179244, .T. ) ;
#128936 = CARTESIAN_POINT ( 'NONE',  ( -4.379528057220328563, 16.55341960407611168, 70.20724293864769550 ) ) ;
#128938 = CARTESIAN_POINT ( 'NONE',  ( 5.049401038297881783, 19.05341960407617563, 37.29275706135232582 ) ) ;
#128939 = CARTESIAN_POINT ( 'NONE',  ( 15.72974639402199770, -15.80617190586745480, 43.12390960531435269 ) ) ;
#128940 = CARTESIAN_POINT ( 'NONE',  ( 18.62759615963255655, 10.81492255796105972, 111.6677570613523613 ) ) ;
#128941 = CARTESIAN_POINT ( 'NONE',  ( -16.46253265017160317, 9.564922557960807481, 95.83224293864769550 ) ) ;
#128942 = CARTESIAN_POINT ( 'NONE',  ( -10.81492255796105439, 18.62759615963255655, 102.9177570613523756 ) ) ;
#128943 = CARTESIAN_POINT ( 'NONE',  ( -21.55341960407610458, -5.719274019375992779, 66.45724293864768129 ) ) ;
#128944 = CARTESIAN_POINT ( 'NONE',  ( -0.05219959533909027116, -19.03943276465977164, 102.4989096053143669 ) ) ;
#128945 = CARTESIAN_POINT ( 'NONE',  ( -5.049401038297874678, -19.05341960407617918, 79.79275706135233293 ) ) ;
#128946 = CARTESIAN_POINT ( 'NONE',  ( -13.89961937509977652, 13.97604488694528158, 105.6239096053143527 ) ) ;
#128947 = CARTESIAN_POINT ( 'NONE',  ( 5.049401038297881783, 19.05341960407617563, 102.2927570613523045 ) ) ;
#128948 = CARTESIAN_POINT ( 'NONE',  ( -12.06949235617739369, -12.14591786802326823, 59.37609039468568284 ) ) ;
#128949 = CARTESIAN_POINT ( 'NONE',  ( -16.51473224551069308, -9.474510206698971260, 26.66557627198103120 ) ) ;
#128950 = CARTESIAN_POINT ( 'NONE',  ( 19.03943276465977164, -0.05219959533909143690, 78.74890960531436690 ) ) ;
#128951 = CARTESIAN_POINT ( 'NONE',  ( 5.823673210054125526, 21.52544592524343514, 69.79057627198102409 ) ) ;
#128952 = AXIS2_PLACEMENT_3D ( 'NONE', #136638, #181186, #71991 ) ;
#128953 = CARTESIAN_POINT ( 'NONE',  ( -16.55341960407617563, 4.379528057220093196, 28.54275706135234358 ) ) ;
#128954 = CARTESIAN_POINT ( 'NONE',  ( 21.53943276465977519, 0.05219959533937863772, 36.25109039468567573 ) ) ;
#128955 = CARTESIAN_POINT ( 'NONE',  ( -0.05219959533937732626, 21.53943276465977519, 87.50109039468568994 ) ) ;
#128956 = CARTESIAN_POINT ( 'NONE',  ( 0.05219959533934541429, -16.53943276465976808, 95.00109039468568994 ) ) ;
#128957 = CARTESIAN_POINT ( 'NONE',  ( -16.51473224551069308, -9.474510206698971260, 91.66557627198103830 ) ) ;
#128958 = CARTESIAN_POINT ( 'NONE',  ( 12.14591786802309770, 12.06949235617756955, 74.37390960531436690 ) ) ;
#128959 = CARTESIAN_POINT ( 'NONE',  ( -8.314922557960811034, -14.29746914071050412, 27.08224293864769550 ) ) ;
#128960 = CARTESIAN_POINT ( 'NONE',  ( -19.03943276465977164, -0.05219959533935918106, 58.75109039468566863 ) ) ;
#128961 = CARTESIAN_POINT ( 'NONE',  ( -15.72974639402176322, -15.80617190586768395, 49.37609039468569705 ) ) ;
#128962 = CARTESIAN_POINT ( 'NONE',  ( 12.06949235617757843, -12.14591786802309237, 93.12390960531436690 ) ) ;
#128963 = CARTESIAN_POINT ( 'NONE',  ( -19.02544592524342804, 5.153800228976336051, 111.0405762719810099 ) ) ;
#128964 = CARTESIAN_POINT ( 'NONE',  ( -14.29746914071037622, -8.314922557961029526, 104.1677570613523471 ) ) ;
#128965 = CARTESIAN_POINT ( 'NONE',  ( -5.823673210054431948, 21.52544592524334988, 87.70942372801901854 ) ) ;
#128966 = CARTESIAN_POINT ( 'NONE',  ( 4.483927247898790824, -16.52544592524335698, 45.20942372801901854 ) ) ;
#128967 = CARTESIAN_POINT ( 'NONE',  ( 15.80617190586769283, -15.72974639402175789, 45.62609039468567573 ) ) ;
#128968 = ORIENTED_EDGE ( 'NONE', *, *, #192109, .T. ) ;
#128969 = CARTESIAN_POINT ( 'NONE',  ( 18.67979575497178502, 10.72451020669898547, 114.1655762719810383 ) ) ;
#128970 = CARTESIAN_POINT ( 'NONE',  ( -4.483927247898539470, -16.52544592524342804, 87.29057627198103830 ) ) ;
#128971 = EDGE_CURVE ( 'NONE', #56210, #199942, #41717, .T. ) ;
#128972 = CARTESIAN_POINT ( 'NONE',  ( -19.39056639909671986, -5.500000000000051514, 50.78948781074345931 ) ) ;
#128973 = CARTESIAN_POINT ( 'NONE',  ( -12.14591786802309592, -12.06949235617757132, 61.87390960531436690 ) ) ;
#128974 = CARTESIAN_POINT ( 'NONE',  ( -8.314922557961024197, 14.29746914071037800, 112.9177570613523329 ) ) ;
#128975 = CARTESIAN_POINT ( 'NONE',  ( -16.51473224551069308, -9.474510206698971260, 41.66557627198103120 ) ) ;
#128976 = CARTESIAN_POINT ( 'NONE',  ( -18.67979575497178146, -10.72451020669898902, 36.66557627198103120 ) ) ;
#128977 = CARTESIAN_POINT ( 'NONE',  ( -8.314922557960811034, -14.29746914071050412, 72.08224293864769550 ) ) ;
#128978 = VECTOR ( 'NONE', #46392, 1000.000000000000114 ) ;
#128979 = CARTESIAN_POINT ( 'NONE',  ( -15.72974639402197994, 15.80617190586746368, 80.62390960531438111 ) ) ;
#128980 = CARTESIAN_POINT ( 'NONE',  ( 5.049401038298161559, -19.05341960407611168, 82.70724293864770971 ) ) ;
#128982 = CARTESIAN_POINT ( 'NONE',  ( -13.97604488694547697, 13.89961937509957934, 93.12609039468566152 ) ) ;
#128981 = CARTESIAN_POINT ( 'NONE',  ( 5.153800228976335163, 19.02544592524342804, 39.79057627198100988 ) ) ;
#128983 = EDGE_CURVE ( 'NONE', #88260, #84227, #82477, .T. ) ;
#128984 = CARTESIAN_POINT ( 'NONE',  ( -18.67979575497178146, -10.72451020669898902, 31.66557627198102054 ) ) ;
#128985 = CARTESIAN_POINT ( 'NONE',  ( -21.53943276465977519, -0.05219959533937600094, 68.75109039468568994 ) ) ;
#128986 = CARTESIAN_POINT ( 'NONE',  ( -9.564922557960796823, -16.46253265017161027, 47.08224293864769550 ) ) ;
#128987 = CARTESIAN_POINT ( 'NONE',  ( 9.564922557960805705, 16.46253265017160317, 89.58224293864769550 ) ) ;
#128988 = EDGE_LOOP ( 'NONE', ( #72322, #103270, #160575, #54448 ) ) ;
#128989 = CARTESIAN_POINT ( 'NONE',  ( -14.29746914071037622, -8.314922557961029526, 64.16775706135234714 ) ) ;
#128990 = CARTESIAN_POINT ( 'NONE',  ( 18.67979575497194134, -10.72451020669871369, 50.83442372801901143 ) ) ;
#128991 = CARTESIAN_POINT ( 'NONE',  ( 15.80617190586769283, -15.72974639402175789, 75.62609039468567573 ) ) ;
#128992 = CARTESIAN_POINT ( 'NONE',  ( -21.52544592524343514, 5.823673210054127303, 26.04057627198103475 ) ) ;
#128993 = CARTESIAN_POINT ( 'NONE',  ( -18.67979575497178146, -10.72451020669898902, 86.66557627198102409 ) ) ;
#128995 = CARTESIAN_POINT ( 'NONE',  ( -12.14591786802326823, 12.06949235617739902, 68.12609039468567573 ) ) ;
#128994 = CARTESIAN_POINT ( 'NONE',  ( 10.72451020669871369, 18.67979575497193778, 27.08442372801901854 ) ) ;
#128996 = CARTESIAN_POINT ( 'NONE',  ( -18.62759615963270932, 10.81492255796079327, 65.83224293864769550 ) ) ;
#128997 = CARTESIAN_POINT ( 'NONE',  ( -16.51473224551082808, 9.474510206698731452, 23.33442372801900078 ) ) ;
#128999 = CARTESIAN_POINT ( 'NONE',  ( -16.53943276465976808, -0.05219959533934237506, 108.7510903946857042 ) ) ;
#128998 = CARTESIAN_POINT ( 'NONE',  ( 19.02544592524343514, -5.153800228976328945, 63.54057627198103830 ) ) ;
#129000 = CARTESIAN_POINT ( 'NONE',  ( -17.50000000000000000, -3.565345528328005997, 105.5750551319353576 ) ) ;
#129001 = CARTESIAN_POINT ( 'NONE',  ( -9.564922557960796823, -16.46253265017161027, 92.08224293864769550 ) ) ;
#129002 = CARTESIAN_POINT ( 'NONE',  ( 17.49999999999999645, 3.232540337672813902, 102.7809047999542003 ) ) ;
#129003 = CARTESIAN_POINT ( 'NONE',  ( 16.51473224551083163, -9.474510206698727899, 75.83442372801900433 ) ) ;
#129004 = CARTESIAN_POINT ( 'NONE',  ( 5.719274019375991003, -21.55341960407610458, 57.70724293864770260 ) ) ;
#129005 = CARTESIAN_POINT ( 'NONE',  ( -12.14591786802309592, -12.06949235617757132, 21.87390960531436690 ) ) ;
#129006 = CARTESIAN_POINT ( 'NONE',  ( 5.049401038297881783, 19.05341960407617563, 102.2927570613523045 ) ) ;
#129007 = CARTESIAN_POINT ( 'NONE',  ( 19.05341960407617918, -5.049401038297876454, 91.04275706135234714 ) ) ;
#129009 = CARTESIAN_POINT ( 'NONE',  ( 13.97604488694548053, -13.89961937509957401, 60.62609039468564731 ) ) ;
#129008 = CARTESIAN_POINT ( 'NONE',  ( -0.05219959533907301413, -21.53943276465977519, 92.49890960531436690 ) ) ;
#129010 = CARTESIAN_POINT ( 'NONE',  ( 17.50000000000000711, 5.624438216177583882, 106.6832965508535551 ) ) ;
#129011 = CARTESIAN_POINT ( 'NONE',  ( 13.97604488694527802, 13.89961937509977652, 49.37390960531434558 ) ) ;
#129012 = CARTESIAN_POINT ( 'NONE',  ( -16.52544592524342804, 4.483927247898546575, 61.04057627198103120 ) ) ;
#129013 = CARTESIAN_POINT ( 'NONE',  ( 19.05341960407611168, 5.049401038298154454, 53.95724293864770260 ) ) ;
#129014 = CARTESIAN_POINT ( 'NONE',  ( 16.52544592524342804, -4.483927247898539470, 58.54057627198103120 ) ) ;
#129015 = DIRECTION ( 'NONE',  ( 1.000000000000000000, 0.000000000000000000, 0.000000000000000000 ) ) ;
#129016 = CARTESIAN_POINT ( 'NONE',  ( 0.1121086616460852114, 21.30000000000003268, -56.46919128290400636 ) ) ;
#129017 = CARTESIAN_POINT ( 'NONE',  ( -16.52544592524342804, 4.483927247898546575, 31.04057627198102409 ) ) ;
#129018 = CARTESIAN_POINT ( 'NONE',  ( 9.474510206698971260, -16.51473224551069308, 57.91557627198103120 ) ) ;
#129019 = CARTESIAN_POINT ( 'NONE',  ( -16.46253265017146816, -9.564922557961047289, 39.16775706135234003 ) ) ;
#129020 = CARTESIAN_POINT ( 'NONE',  ( 16.53943276465976808, 0.05219959533934440121, 51.25109039468568994 ) ) ;
#129021 = CARTESIAN_POINT ( 'NONE',  ( -18.67979575497178146, -10.72451020669898902, 46.66557627198102409 ) ) ;
#129022 = CARTESIAN_POINT ( 'NONE',  ( -18.67979575497193778, 10.72451020669871902, 108.3344237280190185 ) ) ;
#129023 = CARTESIAN_POINT ( 'NONE',  ( 13.89961937509977652, -13.97604488694527269, 73.12390960531436690 ) ) ;
#129024 = CARTESIAN_POINT ( 'NONE',  ( 9.564922557960805705, 16.46253265017160317, 114.5822429386476955 ) ) ;
#129025 = CARTESIAN_POINT ( 'NONE',  ( 0.05219959533909260263, 19.03943276465977164, 114.9989096053143669 ) ) ;
#129026 = CARTESIAN_POINT ( 'NONE',  ( -17.97058386085787163, -5.500000000000054179, 44.00390968646217260 ) ) ;
#129027 = CARTESIAN_POINT ( 'NONE',  ( -10.72451020669870658, -18.67979575497194134, 34.58442372801900433 ) ) ;
#129028 = CARTESIAN_POINT ( 'NONE',  ( -8.314922557960811034, -14.29746914071050412, 87.08224293864769550 ) ) ;
#129030 = CARTESIAN_POINT ( 'NONE',  ( -9.474510206698964154, 16.51473224551069663, 80.41557627198103830 ) ) ;
#129029 = CARTESIAN_POINT ( 'NONE',  ( 5.823673210054125526, 21.52544592524343514, 89.79057627198103830 ) ) ;
#129031 = CARTESIAN_POINT ( 'NONE',  ( -5.049401038298153566, 19.05341960407611168, 80.20724293864769550 ) ) ;
#129032 = CARTESIAN_POINT ( 'NONE',  ( 18.62759615963255655, 10.81492255796105972, 31.66775706135234358 ) ) ;
#129033 = ORIENTED_EDGE ( 'NONE', *, *, #195501, .F. ) ;
#129034 = CARTESIAN_POINT ( 'NONE',  ( -16.51473224551069308, -9.474510206698971260, 76.66557627198103830 ) ) ;
#129035 = CARTESIAN_POINT ( 'NONE',  ( 18.56453257813367230, -5.499999999999956479, 98.49000423690687001 ) ) ;
#129037 = CARTESIAN_POINT ( 'NONE',  ( -5.049401038298153566, 19.05341960407611168, 30.20724293864768839 ) ) ;
#129036 = CARTESIAN_POINT ( 'NONE',  ( 5.153800228976335163, 19.02544592524342804, 29.79057627198102409 ) ) ;
#129038 = CARTESIAN_POINT ( 'NONE',  ( -16.46253265017146816, -9.564922557961047289, 104.1677570613523329 ) ) ;
#129039 = CARTESIAN_POINT ( 'NONE',  ( 0.05219959533910956823, 16.53943276465976808, 109.9989096053143527 ) ) ;
#129040 = CARTESIAN_POINT ( 'NONE',  ( 18.67979575497194134, -10.72451020669871369, 75.83442372801900433 ) ) ;
#129042 = CARTESIAN_POINT ( 'NONE',  ( -5.823673210054431948, 21.52544592524334988, 37.70942372801900433 ) ) ;
#129041 = CARTESIAN_POINT ( 'NONE',  ( -13.97604488694527625, -13.89961937509977652, 56.87390960531434558 ) ) ;
#129043 = CARTESIAN_POINT ( 'NONE',  ( -5.719274019375978568, 21.55341960407610458, 110.2072429386477239 ) ) ;
#129044 = CARTESIAN_POINT ( 'NONE',  ( -17.81289503416611097, -24.51734667627696496, 148.2999999999999545 ) ) ;
#129045 = CARTESIAN_POINT ( 'NONE',  ( 9.564922557960805705, 16.46253265017160317, 79.58224293864769550 ) ) ;
#129046 = LINE ( 'NONE', #6705, #108232 ) ;
#129048 = CARTESIAN_POINT ( 'NONE',  ( 5.719274019375991003, -21.55341960407610458, 37.70724293864769550 ) ) ;
#129047 = CARTESIAN_POINT ( 'NONE',  ( -12.14591786802326823, 12.06949235617739902, 28.12609039468568284 ) ) ;
#129049 = CARTESIAN_POINT ( 'NONE',  ( 5.719274019375673035, 21.55341960407619339, 62.29275706135236845 ) ) ;
#129050 = CARTESIAN_POINT ( 'NONE',  ( -5.049401038298153566, 19.05341960407611168, 115.2072429386477097 ) ) ;
#129051 = CARTESIAN_POINT ( 'NONE',  ( 9.564922557961047289, -16.46253265017146816, 95.41775706135233293 ) ) ;
#129052 = CARTESIAN_POINT ( 'NONE',  ( 9.474510206698971260, -16.51473224551069308, 47.91557627198102409 ) ) ;
#129053 = CARTESIAN_POINT ( 'NONE',  ( -16.51473224551069308, -9.474510206698971260, 81.66557627198103830 ) ) ;
#129054 = CARTESIAN_POINT ( 'NONE',  ( -4.483927247898539470, -16.52544592524342804, 97.29057627198105251 ) ) ;
#129055 = CARTESIAN_POINT ( 'NONE',  ( 4.483927247898545687, 16.52544592524342804, 89.79057627198103830 ) ) ;
#129056 = CARTESIAN_POINT ( 'NONE',  ( 9.474510206698971260, -16.51473224551069308, 107.9155762719810383 ) ) ;
#129058 = CARTESIAN_POINT ( 'NONE',  ( -13.97604488694527625, -13.89961937509977652, 36.87390960531436690 ) ) ;
#129057 = CARTESIAN_POINT ( 'NONE',  ( -4.483927247898539470, -16.52544592524342804, 57.29057627198103120 ) ) ;
#129059 = CARTESIAN_POINT ( 'NONE',  ( 15.72974639402176855, 15.80617190586768217, 61.87609039468568284 ) ) ;
#129060 = CARTESIAN_POINT ( 'NONE',  ( -5.153800228976607833, 19.02544592524334988, 97.70942372801900433 ) ) ;
#129061 = CARTESIAN_POINT ( 'NONE',  ( -16.55341960407611168, -4.379528057220339221, 61.45724293864770260 ) ) ;
#129062 = CARTESIAN_POINT ( 'NONE',  ( 10.81492255796078972, 18.62759615963270932, 109.5822429386476955 ) ) ;
#129063 = CARTESIAN_POINT ( 'NONE',  ( 5.719274019375991003, -21.55341960407610458, 52.70724293864769550 ) ) ;
#129064 = CARTESIAN_POINT ( 'NONE',  ( 19.49671883438228193, 5.499999999999968914, 72.39279849105680853 ) ) ;
#129065 = CARTESIAN_POINT ( 'NONE',  ( 17.81289503416611453, -24.51734667627695785, 140.9500000054623285 ) ) ;
#129066 = CARTESIAN_POINT ( 'NONE',  ( 13.97604488694527802, 13.89961937509977652, 54.37390960531435979 ) ) ;
#129067 = CARTESIAN_POINT ( 'NONE',  ( -14.29746914071049879, 8.314922557960819915, 40.83224293864769550 ) ) ;
#129068 = CARTESIAN_POINT ( 'NONE',  ( 16.52544592524335698, 4.483927247898782831, 96.45942372801901854 ) ) ;
#129069 = CARTESIAN_POINT ( 'NONE',  ( 8.224510206698742110, 14.34966873604972548, 87.08442372801901854 ) ) ;
#129070 = CARTESIAN_POINT ( 'NONE',  ( 16.46253265017146816, 9.564922557961045513, 41.66775706135234003 ) ) ;
#129071 = CARTESIAN_POINT ( 'NONE',  ( -69.65682714487590488, -71.74905178543390605, -15.00000000000000000 ) ) ;
#129072 = CARTESIAN_POINT ( 'NONE',  ( 19.02544592524343514, -5.153800228976328945, 88.54057627198102409 ) ) ;
#129073 = CARTESIAN_POINT ( 'NONE',  ( 0.05219959533909260263, 19.03943276465977164, 44.99890960531435979 ) ) ;
#129074 = CARTESIAN_POINT ( 'NONE',  ( -16.53943276465976808, 0.05219959533911058130, 66.24890960531436690 ) ) ;
#129076 = CARTESIAN_POINT ( 'NONE',  ( -21.55341960407610458, -5.719274019375992779, 21.45724293864769550 ) ) ;
#129075 = CARTESIAN_POINT ( 'NONE',  ( 17.50000000001358558, -5.500000000000039968, 48.29690382535059001 ) ) ;
#129077 = CARTESIAN_POINT ( 'NONE',  ( 21.55341960407610458, 5.719274019375980345, 43.95724293864769550 ) ) ;
#129078 = CARTESIAN_POINT ( 'NONE',  ( -16.55341960407611168, -4.379528057220339221, 86.45724293864770971 ) ) ;
#129079 = B_SPLINE_CURVE_WITH_KNOTS ( 'NONE', 3,
 ( #174937, #113247, #49599, #51582, #142594, #191101, #81890, #3092, #160759, #157781, #6068, #64769, #126431, #129404, #143583, #36400 ),
 .UNSPECIFIED., .F., .F.,
 ( 4, 2, 2, 2, 2, 2, 2, 4 ),
 ( 0.000000000000000000, 0.004834299366836557893, 0.006042874208545700836, 0.007251449050254843778, 0.009668598733673129664, 0.01450289810050969970, 0.01692004778392798212, 0.01933719746734626627 ),
 .UNSPECIFIED. ) ;
#129080 = CARTESIAN_POINT ( 'NONE',  ( 8.224510206698742110, 14.34966873604972548, 32.08442372801901854 ) ) ;
#129081 = CARTESIAN_POINT ( 'NONE',  ( 8.314922557960818139, 14.29746914071049879, 79.58224293864769550 ) ) ;
#129082 = EDGE_CURVE ( 'NONE', #74887, #22341, #159472, .T. ) ;
#129083 = DIRECTION ( 'NONE',  ( 0.000000000000000000, -1.000000000000000000, 0.000000000000000000 ) ) ;
#129084 = CARTESIAN_POINT ( 'NONE',  ( -0.05219959533936034679, 19.03943276465977164, 72.50109039468566152 ) ) ;
#129085 = CARTESIAN_POINT ( 'NONE',  ( 9.474510206698971260, -16.51473224551069308, 97.91557627198102409 ) ) ;
#129086 = CARTESIAN_POINT ( 'NONE',  ( -5.950531402560715689E-15, 38.81732327939063509, -5.624999997268812280 ) ) ;
#129087 = CARTESIAN_POINT ( 'NONE',  ( 7.992609269207028790E-30, -165.0000000000000000, -15.00000000000000000 ) ) ;
#129089 = CARTESIAN_POINT ( 'NONE',  ( -0.05219959533910754901, -16.53943276465976808, 22.49890960531436335 ) ) ;
#129088 = CARTESIAN_POINT ( 'NONE',  ( -14.29746914071037622, -8.314922557961029526, 34.16775706135234714 ) ) ;
#129090 = CARTESIAN_POINT ( 'NONE',  ( 9.474510206698729675, 16.51473224551082808, 67.08442372801900433 ) ) ;
#129091 = CARTESIAN_POINT ( 'NONE',  ( -21.53943276465977519, 0.05219959533907696930, 36.24890960531435979 ) ) ;
#129092 = CARTESIAN_POINT ( 'NONE',  ( 21.52544592524334988, 5.823673210054432836, 66.45942372801903275 ) ) ;
#129093 = DIRECTION ( 'NONE',  ( 0.000000000000000000, 0.000000000000000000, -1.000000000000000000 ) ) ;
#129094 = CARTESIAN_POINT ( 'NONE',  ( -12.14591786802326823, 12.06949235617739902, 38.12609039468567573 ) ) ;
#129096 = CARTESIAN_POINT ( 'NONE',  ( 16.51473224551069308, 9.474510206698969483, 94.16557627198103830 ) ) ;
#129095 = CARTESIAN_POINT ( 'NONE',  ( -5.049401038298153566, 19.05341960407611168, 25.20724293864768484 ) ) ;
#129097 = CARTESIAN_POINT ( 'NONE',  ( -5.153800228976328057, -19.02544592524343514, 22.29057627198102765 ) ) ;
#129099 = EDGE_CURVE ( 'NONE', #174275, #44164, #101848, .T. ) ;
#129098 = CARTESIAN_POINT ( 'NONE',  ( 14.29746914071049879, -8.314922557960816363, 93.33224293864769550 ) ) ;
#129100 = APPLICATION_PROTOCOL_DEFINITION ( 'draft international standard', 'automotive_design', 1998, #68669 ) ;
#129101 = CARTESIAN_POINT ( 'NONE',  ( 19.05341960407611168, 5.049401038298154454, 83.95724293864766707 ) ) ;
#129102 = EDGE_LOOP ( 'NONE', ( #3786, #76045, #184345, #10075, #92816 ) ) ;
#129103 = CARTESIAN_POINT ( 'NONE',  ( -16.51473224551082808, 9.474510206698731452, 108.3344237280190043 ) ) ;
#129104 = CARTESIAN_POINT ( 'NONE',  ( -10.72451020669898014, 18.67979575497178502, 75.41557627198102409 ) ) ;
#129105 = CARTESIAN_POINT ( 'NONE',  ( 19.02544592524343514, -5.153800228976328945, 48.54057627198103120 ) ) ;
#129107 = CARTESIAN_POINT ( 'NONE',  ( 21.53943276465977519, -0.05219959533907433946, 113.7489096053143527 ) ) ;
#129106 = CARTESIAN_POINT ( 'NONE',  ( -19.02544592524334988, -5.153800228976617603, 63.95942372801899012 ) ) ;
#129108 = CARTESIAN_POINT ( 'NONE',  ( 0.05219959533909260263, 19.03943276465977164, 69.99890960531435269 ) ) ;
#129109 = CARTESIAN_POINT ( 'NONE',  ( 16.51473224551069308, 9.474510206698969483, 109.1655762719810383 ) ) ;
#129110 = ORIENTED_EDGE ( 'NONE', *, *, #116420, .T. ) ;
#129111 = CARTESIAN_POINT ( 'NONE',  ( 4.483927247898790824, -16.52544592524335698, 30.20942372801902565 ) ) ;
#129112 = CARTESIAN_POINT ( 'NONE',  ( 10.72451020669898902, -18.67979575497178502, 102.9155762719810383 ) ) ;
#129115 = CARTESIAN_POINT ( 'NONE',  ( 13.97604488694548053, -13.89961937509957401, 65.62609039468567573 ) ) ;
#129114 = CARTESIAN_POINT ( 'NONE',  ( 5.049401038298161559, -19.05341960407611168, 97.70724293864766707 ) ) ;
#129113 = CARTESIAN_POINT ( 'NONE',  ( -8.314922557960811034, -14.29746914071050412, 102.0822429386476955 ) ) ;
#129116 = CARTESIAN_POINT ( 'NONE',  ( 18.62759615963271287, -10.81492255796078972, 83.33224293864769550 ) ) ;
#129117 = CARTESIAN_POINT ( 'NONE',  ( -14.29746914071049879, 8.314922557960819915, 50.83224293864770971 ) ) ;
#129118 = CARTESIAN_POINT ( 'NONE',  ( 0.05219959533936267826, -19.03943276465977164, 20.00109039468567218 ) ) ;
#129119 = CARTESIAN_POINT ( 'NONE',  ( 14.29746914071037800, 8.314922557961029526, 66.66775706135234714 ) ) ;
#129120 = CARTESIAN_POINT ( 'NONE',  ( -5.153800228976328057, -19.02544592524343514, 92.29057627198099567 ) ) ;
#129121 = CARTESIAN_POINT ( 'NONE',  ( 5.153800228976335163, 19.02544592524342804, 44.79057627198103830 ) ) ;
#129122 = VECTOR ( 'NONE', #87414, 1000.000000000000000 ) ;
#129123 = CARTESIAN_POINT ( 'NONE',  ( -18.67979575497193778, 10.72451020669871902, 58.33442372801901143 ) ) ;
#129124 = CARTESIAN_POINT ( 'NONE',  ( 15.72974639402176855, 15.80617190586768217, 71.87609039468568994 ) ) ;
#129125 = CARTESIAN_POINT ( 'NONE',  ( 0.05219959533909260263, 19.03943276465977164, 59.99890960531436690 ) ) ;
#129126 = CARTESIAN_POINT ( 'NONE',  ( 10.81492255796106328, -18.62759615963255655, 30.41775706135234358 ) ) ;
#129127 = CARTESIAN_POINT ( 'NONE',  ( -13.97604488694547697, 13.89961937509957934, 68.12609039468563310 ) ) ;
#129128 = CARTESIAN_POINT ( 'NONE',  ( 0.05219959533936267826, -19.03943276465977164, 70.00109039468566152 ) ) ;
#129129 = CARTESIAN_POINT ( 'NONE',  ( 19.02544592524343514, -5.153800228976328945, 33.54057627198102409 ) ) ;
#129130 = CARTESIAN_POINT ( 'NONE',  ( 4.379528057220092307, 16.55341960407617563, 87.29275706135236135 ) ) ;
#129131 = CARTESIAN_POINT ( 'NONE',  ( 19.05341960407611168, 5.049401038298154454, 48.95724293864768129 ) ) ;
#129132 = CARTESIAN_POINT ( 'NONE',  ( 9.564922557960805705, 16.46253265017160317, 24.58224293864769194 ) ) ;
#129133 = CARTESIAN_POINT ( 'NONE',  ( 19.02544592524343514, -5.153800228976328945, 103.5405762719809957 ) ) ;
#129135 = ADVANCED_FACE ( 'NONE', ( #175174 ), #6269, .T. ) ;
#129134 = CARTESIAN_POINT ( 'NONE',  ( 13.97604488694527802, 13.89961937509977652, 34.37390960531436690 ) ) ;
#129136 = CARTESIAN_POINT ( 'NONE',  ( 0.05219959533907565091, 21.53943276465977519, 84.99890960531436690 ) ) ;
#129137 = CARTESIAN_POINT ( 'NONE',  ( 14.29746914071037800, 8.314922557961029526, 56.66775706135235424 ) ) ;
#129138 = CARTESIAN_POINT ( 'NONE',  ( 16.46253265017146816, 9.564922557961045513, 31.66775706135232937 ) ) ;
#129139 = CARTESIAN_POINT ( 'NONE',  ( 13.89961937509977652, -13.97604488694527269, 58.12390960531436690 ) ) ;
#129140 = CARTESIAN_POINT ( 'NONE',  ( -16.53943276465976808, 0.05219959533911058130, 41.24890960531435269 ) ) ;
#129141 = CARTESIAN_POINT ( 'NONE',  ( -0.05219959533910754901, -16.53943276465976808, 87.49890960531436690 ) ) ;
#129142 = CARTESIAN_POINT ( 'NONE',  ( 13.97604488694527802, 13.89961937509977652, 84.37390960531433848 ) ) ;
#129143 = CARTESIAN_POINT ( 'NONE',  ( 0.05219959533909260263, 19.03943276465977164, 84.99890960531436690 ) ) ;
#129144 = CARTESIAN_POINT ( 'NONE',  ( 5.719274019375673035, 21.55341960407619339, 42.29275706135235424 ) ) ;
#129145 = CARTESIAN_POINT ( 'NONE',  ( 13.97604488694527802, 13.89961937509977652, 94.37390960531436690 ) ) ;
#129146 = CARTESIAN_POINT ( 'NONE',  ( -10.81492255796105439, 18.62759615963255655, 92.91775706135236135 ) ) ;
#129147 = CARTESIAN_POINT ( 'NONE',  ( -12.14591786802326823, 12.06949235617739902, 78.12609039468570415 ) ) ;
#129148 = CARTESIAN_POINT ( 'NONE',  ( 5.823673210054444382, -21.52544592524334988, 25.20942372801901854 ) ) ;
#129149 = CARTESIAN_POINT ( 'NONE',  ( -0.05219959533907301413, -21.53943276465977519, 87.49890960531436690 ) ) ;
#129150 = CARTESIAN_POINT ( 'NONE',  ( 8.314922557960818139, 14.29746914071049879, 44.58224293864769550 ) ) ;
#129151 = CARTESIAN_POINT ( 'NONE',  ( -13.89961937509977652, 13.97604488694528158, 40.62390960531435979 ) ) ;
#129152 = CARTESIAN_POINT ( 'NONE',  ( 14.29746914071049879, -8.314922557960816363, 68.33224293864769550 ) ) ;
#129153 = CARTESIAN_POINT ( 'NONE',  ( -21.53943276465977519, 0.05219959533907696930, 36.24890960531435979 ) ) ;
#129154 = CARTESIAN_POINT ( 'NONE',  ( -13.97604488694547697, 13.89961937509957934, 28.12609039468565797 ) ) ;
#129155 = CARTESIAN_POINT ( 'NONE',  ( -4.379528057220328563, 16.55341960407611168, 100.2072429386476955 ) ) ;
#129156 = CARTESIAN_POINT ( 'NONE',  ( 13.97604488694527802, 13.89961937509977652, 114.3739096053143669 ) ) ;
#129157 = ORIENTED_EDGE ( 'NONE', *, *, #63651, .T. ) ;
#129158 = CARTESIAN_POINT ( 'NONE',  ( 8.224510206698742110, 14.34966873604972548, 52.08442372801901854 ) ) ;
#129159 = CARTESIAN_POINT ( 'NONE',  ( -5.153800228976328057, -19.02544592524343514, 62.29057627198100988 ) ) ;
#129160 = CARTESIAN_POINT ( 'NONE',  ( -16.60570611055986490, -6.631713784153137503, 20.77476115285328717 ) ) ;
#129161 = CARTESIAN_POINT ( 'NONE',  ( -15.72974639402197994, 15.80617190586746368, 25.62390960531435624 ) ) ;
#129162 = CARTESIAN_POINT ( 'NONE',  ( -14.29746914071037622, -8.314922557961029526, 89.16775706135236135 ) ) ;
#129163 = CARTESIAN_POINT ( 'NONE',  ( 9.474510206698729675, 16.51473224551082808, 107.0844237280190043 ) ) ;
#129164 = CARTESIAN_POINT ( 'NONE',  ( 21.52544592524334988, 5.823673210054432836, 86.45942372801901854 ) ) ;
#129165 = CARTESIAN_POINT ( 'NONE',  ( 16.51473224551069308, 9.474510206698969483, 79.16557627198103830 ) ) ;
#129166 = CARTESIAN_POINT ( 'NONE',  ( 10.72451020669898902, -18.67979575497178502, 97.91557627198103830 ) ) ;
#129167 = CARTESIAN_POINT ( 'NONE',  ( 8.314922557961029526, -14.29746914071037800, 55.41775706135234714 ) ) ;
#129168 = CARTESIAN_POINT ( 'NONE',  ( -14.34966873604960291, -8.224510206698953496, 111.6655762719810525 ) ) ;
#129169 = CARTESIAN_POINT ( 'NONE',  ( 16.53943276465976808, 0.05219959533934440121, 21.25109039468567218 ) ) ;
#129170 = CARTESIAN_POINT ( 'NONE',  ( 19.02544592524334988, 5.153800228976608722, 86.45942372801900433 ) ) ;
#129171 = CARTESIAN_POINT ( 'NONE',  ( 21.55341960407610458, 5.719274019375980345, 73.95724293864769550 ) ) ;
#129172 = CARTESIAN_POINT ( 'NONE',  ( -13.97604488694547697, 13.89961937509957934, 58.12609039468566863 ) ) ;
#129173 = CYLINDRICAL_SURFACE ( 'NONE', #18779, 16.70000000000002061 ) ;
#129174 = CARTESIAN_POINT ( 'NONE',  ( -10.81492255796078084, -18.62759615963271287, 107.0822429386476955 ) ) ;
#129175 = CARTESIAN_POINT ( 'NONE',  ( -36.91746825000000598, 2.428612866367529932E-14, -0.6249999972688132788 ) ) ;
#129176 = CARTESIAN_POINT ( 'NONE',  ( -0.05219959533909027116, -19.03943276465977164, 82.49890960531436690 ) ) ;
#129177 = CARTESIAN_POINT ( 'NONE',  ( -32.00000000000000000, -1.163414459189985801E-14, 95.00000000000000000 ) ) ;
#129178 = CARTESIAN_POINT ( 'NONE',  ( -16.52544592524335698, -4.483927247898792601, 23.95942372801901143 ) ) ;
#129179 = CARTESIAN_POINT ( 'NONE',  ( 23.42531391676913088, 11.30614932247368642, 165.8025715494068493 ) ) ;
#129181 = CARTESIAN_POINT ( 'NONE',  ( -16.55341960407611168, -4.379528057220339221, 61.45724293864770260 ) ) ;
#129180 = CARTESIAN_POINT ( 'NONE',  ( -15.72974639402197994, 15.80617190586746368, 105.6239096053143669 ) ) ;
#129182 = CARTESIAN_POINT ( 'NONE',  ( -16.46253265017160317, 9.564922557960807481, 75.83224293864769550 ) ) ;
#129183 = CARTESIAN_POINT ( 'NONE',  ( 5.823673210054444382, -21.52544592524334988, 80.20942372801901854 ) ) ;
#129185 = CARTESIAN_POINT ( 'NONE',  ( 19.05341960407617918, -5.049401038297876454, 41.04275706135233293 ) ) ;
#129184 = CARTESIAN_POINT ( 'NONE',  ( -16.53943276465976808, -0.05219959533934237506, 23.75109039468567929 ) ) ;
#129186 = CARTESIAN_POINT ( 'NONE',  ( -21.55341960407619339, 5.719274019375674811, 58.54275706135235424 ) ) ;
#129187 = CARTESIAN_POINT ( 'NONE',  ( -15.72974639402176322, -15.80617190586768395, 19.37609039468568639 ) ) ;
#129188 = CARTESIAN_POINT ( 'NONE',  ( 21.55341960407610458, 5.719274019375980345, 58.95724293864770971 ) ) ;
#129189 = CARTESIAN_POINT ( 'NONE',  ( -16.51473224551082808, 9.474510206698731452, 113.3344237280190043 ) ) ;
#129190 = CARTESIAN_POINT ( 'NONE',  ( -9.474510206698964154, 16.51473224551069663, 60.41557627198102409 ) ) ;
#129191 = CARTESIAN_POINT ( 'NONE',  ( 5.153800228976615827, -19.02544592524334988, 70.20942372801899012 ) ) ;
#129192 = CARTESIAN_POINT ( 'NONE',  ( 21.53943276465977519, 0.05219959533937863772, 86.25109039468568994 ) ) ;
#129193 = CARTESIAN_POINT ( 'NONE',  ( -5.049401038297874678, -19.05341960407617918, 54.79275706135234003 ) ) ;
#129194 = CARTESIAN_POINT ( 'NONE',  ( 13.97604488694527802, 13.89961937509977652, 39.37390960531435269 ) ) ;
#129195 = CARTESIAN_POINT ( 'NONE',  ( -18.67979575497178146, -10.72451020669898902, 51.66557627198102409 ) ) ;
#129196 = CARTESIAN_POINT ( 'NONE',  ( 12.06949235617757843, -12.14591786802309237, 53.12390960531436690 ) ) ;
#129197 = CARTESIAN_POINT ( 'NONE',  ( 21.16473053983487418, 10.71450305990368967, 170.2845851188453992 ) ) ;
#129198 = CARTESIAN_POINT ( 'NONE',  ( 0.05219959533936267826, -19.03943276465977164, 30.00109039468566863 ) ) ;
#129199 = CARTESIAN_POINT ( 'NONE',  ( -12.14591786802326823, 12.06949235617739902, 83.12609039468568994 ) ) ;
#129200 = CARTESIAN_POINT ( 'NONE',  ( -4.379528057220328563, 16.55341960407611168, 50.20724293864769550 ) ) ;
#129201 = CARTESIAN_POINT ( 'NONE',  ( 21.53943276465977519, 0.05219959533937863772, 91.25109039468568994 ) ) ;
#129202 = CARTESIAN_POINT ( 'NONE',  ( 5.719274019375673035, 21.55341960407619339, 82.29275706135234714 ) ) ;
#129203 = CARTESIAN_POINT ( 'NONE',  ( 15.72974639402199770, -15.80617190586745480, 83.12390960531436690 ) ) ;
#129204 = CARTESIAN_POINT ( 'NONE',  ( -9.474510206698964154, 16.51473224551069663, 50.41557627198102409 ) ) ;
#129205 = CARTESIAN_POINT ( 'NONE',  ( 5.823673210054444382, -21.52544592524334988, 55.20942372801902565 ) ) ;
#129206 = CARTESIAN_POINT ( 'NONE',  ( -5.153800228976328057, -19.02544592524343514, 42.29057627198101699 ) ) ;
#129207 = CARTESIAN_POINT ( 'NONE',  ( -13.97604488694527625, -13.89961937509977652, 56.87390960531434558 ) ) ;
#129208 = CARTESIAN_POINT ( 'NONE',  ( 14.34966873604960469, 8.224510206698951720, 109.1655762719810383 ) ) ;
#129209 = CARTESIAN_POINT ( 'NONE',  ( -5.153800228976328057, -19.02544592524343514, 92.29057627198099567 ) ) ;
#129210 = CARTESIAN_POINT ( 'NONE',  ( -14.29746914071049879, 8.314922557960819915, 55.83224293864770260 ) ) ;
#129211 = CARTESIAN_POINT ( 'NONE',  ( 19.02544592524343514, -5.153800228976328945, 23.54057627198102054 ) ) ;
#129212 = CARTESIAN_POINT ( 'NONE',  ( 15.72974639402199770, -15.80617190586745480, 78.12390960531436690 ) ) ;
#129213 = CARTESIAN_POINT ( 'NONE',  ( -18.62759615963255300, -10.81492255796106328, 24.16775706135235424 ) ) ;
#129214 = CARTESIAN_POINT ( 'NONE',  ( -28.79475375365586842, 2.428612866367529932E-14, 142.2656553485623760 ) ) ;
#129215 = CARTESIAN_POINT ( 'NONE',  ( 4.483927247898790824, -16.52544592524335698, 40.20942372801901854 ) ) ;
#129216 = ORIENTED_EDGE ( 'NONE', *, *, #62612, .T. ) ;
#129217 = ADVANCED_FACE ( 'NONE', ( #54825 ), #164021, .T. ) ;
#129218 = CARTESIAN_POINT ( 'NONE',  ( 5.823673210054125526, 21.52544592524343514, 74.79057627198105251 ) ) ;
#129219 = CARTESIAN_POINT ( 'NONE',  ( 21.52544592524334988, 5.823673210054432836, 106.4594237280190328 ) ) ;
#129220 = CARTESIAN_POINT ( 'NONE',  ( 16.46253265017160672, -9.564922557960803928, 98.33224293864769550 ) ) ;
#129221 = CARTESIAN_POINT ( 'NONE',  ( -5.719274019375665041, -21.55341960407619695, 34.79275706135235424 ) ) ;
#129222 = CARTESIAN_POINT ( 'NONE',  ( -21.52544592524343514, 5.823673210054127303, 36.04057627198102409 ) ) ;
#129223 = CARTESIAN_POINT ( 'NONE',  ( 4.483927247898790824, -16.52544592524335698, 105.2094237280190328 ) ) ;
#129225 = CARTESIAN_POINT ( 'NONE',  ( 15.72974639402176855, 15.80617190586768217, 81.87609039468568994 ) ) ;
#129224 = CARTESIAN_POINT ( 'NONE',  ( 15.80617190586769283, -15.72974639402175789, 45.62609039468567573 ) ) ;
#129226 = CARTESIAN_POINT ( 'NONE',  ( 5.719274019375673035, 21.55341960407619339, 107.2927570613523471 ) ) ;
#129227 = CARTESIAN_POINT ( 'NONE',  ( 0.05219959533934541429, -16.53943276465976808, 80.00109039468568994 ) ) ;
#129228 = CARTESIAN_POINT ( 'NONE',  ( -0.05219959533937732626, 21.53943276465977519, 37.50109039468568284 ) ) ;
#129229 = CARTESIAN_POINT ( 'NONE',  ( 5.049401038298161559, -19.05341960407611168, 27.70724293864769550 ) ) ;
#129230 = CARTESIAN_POINT ( 'NONE',  ( -5.823673210054431948, 21.52544592524334988, 102.7094237280190185 ) ) ;
#129231 = CARTESIAN_POINT ( 'NONE',  ( -0.05219959533909027116, -19.03943276465977164, 107.4989096053143527 ) ) ;
#129232 = CARTESIAN_POINT ( 'NONE',  ( -21.55341960407610458, -5.719274019375992779, 106.4572429386477097 ) ) ;
#129233 = CIRCLE ( 'NONE', #51740, 25.62086810090349331 ) ;
#129235 = CARTESIAN_POINT ( 'NONE',  ( 18.67979575497178502, 10.72451020669898547, 69.16557627198102409 ) ) ;
#129234 = CARTESIAN_POINT ( 'NONE',  ( 19.52851543214742946, 5.500000000000031974, 82.89357721762580411 ) ) ;
#129237 = CARTESIAN_POINT ( 'NONE',  ( -16.53943276465976808, 0.05219959533911058130, 56.24890960531436690 ) ) ;
#129236 = CARTESIAN_POINT ( 'NONE',  ( 0.05219959533934541429, -16.53943276465976808, 55.00109039468568284 ) ) ;
#129238 = FACE_OUTER_BOUND ( 'NONE', #141123, .T. ) ;
#129239 = CARTESIAN_POINT ( 'NONE',  ( -16.51473224551082808, 9.474510206698731452, 78.33442372801900433 ) ) ;
#129240 = CARTESIAN_POINT ( 'NONE',  ( -11.30153831258470731, -180.0000000000000000, 0.000000000000000000 ) ) ;
#129241 = CARTESIAN_POINT ( 'NONE',  ( -8.224510206698735004, -14.34966873604973081, 29.58442372801901854 ) ) ;
#129242 = CARTESIAN_POINT ( 'NONE',  ( 21.53943276465977519, -0.05219959533907433946, 103.7489096053143669 ) ) ;
#129243 = CARTESIAN_POINT ( 'NONE',  ( 12.06949235617757843, -12.14591786802309237, 63.12390960531435979 ) ) ;
#129244 = CARTESIAN_POINT ( 'NONE',  ( -18.67979575497178146, -10.72451020669898902, 21.66557627198102409 ) ) ;
#129245 = CARTESIAN_POINT ( 'NONE',  ( 4.483927247898790824, -16.52544592524335698, 40.20942372801901854 ) ) ;
#129246 = CARTESIAN_POINT ( 'NONE',  ( 19.03943276465977164, -0.05219959533909143690, 53.74890960531436690 ) ) ;
#129248 = CARTESIAN_POINT ( 'NONE',  ( -19.05341960407617563, 5.049401038297882671, 93.54275706135234714 ) ) ;
#129247 = CARTESIAN_POINT ( 'NONE',  ( 15.80617190586769283, -15.72974639402175789, 25.62609039468567929 ) ) ;
#129249 = EDGE_CURVE ( 'NONE', #13448, #171876, #23495, .T. ) ;
#129250 = CARTESIAN_POINT ( 'NONE',  ( -0.05219959533909027116, -19.03943276465977164, 107.4989096053143527 ) ) ;
#129251 = CARTESIAN_POINT ( 'NONE',  ( 5.153800228976335163, 19.02544592524342804, 89.79057627198102409 ) ) ;
#129252 = CARTESIAN_POINT ( 'NONE',  ( 21.55341960407610458, 5.719274019375980345, 93.95724293864770971 ) ) ;
#129253 = CARTESIAN_POINT ( 'NONE',  ( 16.51473224551069308, 9.474510206698969483, 64.16557627198102409 ) ) ;
#129254 = CARTESIAN_POINT ( 'NONE',  ( -26.99873734152897242, 22.49873734152939520, 8.889087296526001936 ) ) ;
#129255 = CARTESIAN_POINT ( 'NONE',  ( 16.52544592524342804, -4.483927247898539470, 73.54057627198102409 ) ) ;
#129256 = CARTESIAN_POINT ( 'NONE',  ( -9.474510206698964154, 16.51473224551069663, 105.4155762719810383 ) ) ;
#129257 = CARTESIAN_POINT ( 'NONE',  ( 26.46959431505284499, -27.26463967846488146, -25.00000000000000000 ) ) ;
#129258 = CARTESIAN_POINT ( 'NONE',  ( -19.05341960407617563, 5.049401038297882671, 78.54275706135233293 ) ) ;
#129259 = CARTESIAN_POINT ( 'NONE',  ( -15.72974639402197994, 15.80617190586746368, 85.62390960531436690 ) ) ;
#129260 = CARTESIAN_POINT ( 'NONE',  ( 13.97604488694548053, -13.89961937509957401, 45.62609039468566863 ) ) ;
#129261 = CARTESIAN_POINT ( 'NONE',  ( 5.823673210054125526, 21.52544592524343514, 24.79057627198103120 ) ) ;
#129262 = CARTESIAN_POINT ( 'NONE',  ( 19.25176906914650843, 5.499999999999742428, 68.49927264242278113 ) ) ;
#129263 = CARTESIAN_POINT ( 'NONE',  ( 0.05219959533907565091, 21.53943276465977519, 54.99890960531435269 ) ) ;
#129264 = VECTOR ( 'NONE', #157286, 999.9999999999998863 ) ;
#129265 = CARTESIAN_POINT ( 'NONE',  ( 9.564922557960805705, 16.46253265017160317, 84.58224293864769550 ) ) ;
#129266 = CARTESIAN_POINT ( 'NONE',  ( 18.67979575497194134, -10.72451020669871369, 75.83442372801900433 ) ) ;
#129267 = CARTESIAN_POINT ( 'NONE',  ( 5.153800228976335163, 19.02544592524342804, 44.79057627198103830 ) ) ;
#129268 = CARTESIAN_POINT ( 'NONE',  ( 8.224510206698953496, -14.34966873604960469, 67.91557627198102409 ) ) ;
#129269 = CARTESIAN_POINT ( 'NONE',  ( -8.314922557961024197, 14.29746914071037800, 27.91775706135234358 ) ) ;
#129270 = CARTESIAN_POINT ( 'NONE',  ( 18.62759615963255655, 10.81492255796105972, 71.66775706135234714 ) ) ;
#129271 = ORIENTED_EDGE ( 'NONE', *, *, #20851, .T. ) ;
#129272 = CARTESIAN_POINT ( 'NONE',  ( 13.89961937509977652, -13.97604488694527269, 113.1239096053143527 ) ) ;
#129273 = CARTESIAN_POINT ( 'NONE',  ( -16.51473224551082808, 9.474510206698731452, 78.33442372801900433 ) ) ;
#129274 = CARTESIAN_POINT ( 'NONE',  ( 193.3062444957835453, -155.7167183371837496, 0.000000000000000000 ) ) ;
#129275 = CARTESIAN_POINT ( 'NONE',  ( -18.62759615963270932, 10.81492255796079327, 115.8322429386477097 ) ) ;
#129276 = CARTESIAN_POINT ( 'NONE',  ( 37.99626262588765258, 2.893932880411085066E-14, -2.747842220587803475 ) ) ;
#129277 = CARTESIAN_POINT ( 'NONE',  ( -21.55341960407619339, 5.719274019375674811, 113.5427570613523756 ) ) ;
#129278 = CARTESIAN_POINT ( 'NONE',  ( 9.564922557960805705, 16.46253265017160317, 54.58224293864769550 ) ) ;
#129279 = CARTESIAN_POINT ( 'NONE',  ( -15.80617190586768217, 15.72974639402176855, 108.1260903946856757 ) ) ;
#129280 = CARTESIAN_POINT ( 'NONE',  ( -8.314922557961024197, 14.29746914071037800, 102.9177570613523756 ) ) ;
#129282 = CARTESIAN_POINT ( 'NONE',  ( -15.80617190586768217, 15.72974639402176855, 78.12609039468570415 ) ) ;
#129281 = CARTESIAN_POINT ( 'NONE',  ( -19.05341960407611168, -5.049401038298163336, 96.45724293864769550 ) ) ;
#129283 = CARTESIAN_POINT ( 'NONE',  ( 22.81625015709510151, -31.40387420917324590, -7.924999997268812990 ) ) ;
#129284 = CARTESIAN_POINT ( 'NONE',  ( -33.84955102792977755, 0.7177882281432041989, 100.4649514046632248 ) ) ;
#129285 = CARTESIAN_POINT ( 'NONE',  ( -18.67979575497193778, 10.72451020669871902, 83.33442372801903275 ) ) ;
#129286 = CARTESIAN_POINT ( 'NONE',  ( -5.719274019375665041, -21.55341960407619695, 99.79275706135234714 ) ) ;
#129287 = DIRECTION ( 'NONE',  ( 0.000000000000000000, 0.000000000000000000, 1.000000000000000000 ) ) ;
#129288 = CARTESIAN_POINT ( 'NONE',  ( -19.05341960407611168, -5.049401038298163336, 101.4572429386476955 ) ) ;
#129289 = CARTESIAN_POINT ( 'NONE',  ( -19.03943276465977164, -0.05219959533935918106, 23.75109039468566152 ) ) ;
#129290 = CARTESIAN_POINT ( 'NONE',  ( 1.221313414957698099E-14, -31.90000000000003411, -49.13275782002545355 ) ) ;
#129291 = CARTESIAN_POINT ( 'NONE',  ( 16.51473224551069308, 9.474510206698969483, 34.16557627198102409 ) ) ;
#129292 = CARTESIAN_POINT ( 'NONE',  ( 5.719274019375991003, -21.55341960407610458, 57.70724293864770260 ) ) ;
#129293 = CARTESIAN_POINT ( 'NONE',  ( 0.05219959533934541429, -16.53943276465976808, 110.0010903946856757 ) ) ;
#129295 = CARTESIAN_POINT ( 'NONE',  ( 19.02544592524343514, -5.153800228976328945, 83.54057627198100988 ) ) ;
#129294 = CARTESIAN_POINT ( 'NONE',  ( -4.483927247898539470, -16.52544592524342804, 97.29057627198105251 ) ) ;
#129296 = CARTESIAN_POINT ( 'NONE',  ( -21.53943276465977519, -0.05219959533937600094, 98.75109039468568994 ) ) ;
#129297 = CARTESIAN_POINT ( 'NONE',  ( 19.03943276465977164, -0.05219959533909143690, 33.74890960531435979 ) ) ;
#129298 = CARTESIAN_POINT ( 'NONE',  ( -16.53943276465976808, 0.05219959533911058130, 106.2489096053143811 ) ) ;
#129299 = CARTESIAN_POINT ( 'NONE',  ( 10.72451020669871369, 18.67979575497193778, 52.08442372801901854 ) ) ;
#129300 = CARTESIAN_POINT ( 'NONE',  ( 15.72974639402199770, -15.80617190586745480, 83.12390960531436690 ) ) ;
#129301 = CARTESIAN_POINT ( 'NONE',  ( -19.05341960407617563, 5.049401038297882671, 48.54275706135233293 ) ) ;
#129302 = CARTESIAN_POINT ( 'NONE',  ( -35.00000000000000000, 3.181980515339468241, 1.110912703473986074 ) ) ;
#129303 = CARTESIAN_POINT ( 'NONE',  ( 5.153800228976335163, 19.02544592524342804, 99.79057627198102409 ) ) ;
#129304 = CARTESIAN_POINT ( 'NONE',  ( 4.379528057220339221, -16.55341960407611168, 82.70724293864770971 ) ) ;
#129305 = CARTESIAN_POINT ( 'NONE',  ( -9.564922557961040184, 16.46253265017147172, 47.91775706135233293 ) ) ;
#129306 = CARTESIAN_POINT ( 'NONE',  ( 9.474510206698971260, -16.51473224551069308, 67.91557627198102409 ) ) ;
#129307 = CARTESIAN_POINT ( 'NONE',  ( 4.483927247898545687, 16.52544592524342804, 49.79057627198102409 ) ) ;
#129308 = CARTESIAN_POINT ( 'NONE',  ( -19.02544592524334988, -5.153800228976617603, 78.95942372801900433 ) ) ;
#129309 = CARTESIAN_POINT ( 'NONE',  ( -18.87075004821571866, 5.499999999999900524, 83.67408112101044537 ) ) ;
#129310 = CARTESIAN_POINT ( 'NONE',  ( 18.67979575497178502, 10.72451020669898547, 34.16557627198102409 ) ) ;
#129311 = CARTESIAN_POINT ( 'NONE',  ( 4.483927247898545687, 16.52544592524342804, 104.7905762719810241 ) ) ;
#129312 = CARTESIAN_POINT ( 'NONE',  ( -17.49999999999999645, -5.500000000000000888, 24.20309617465829533 ) ) ;
#129314 = CARTESIAN_POINT ( 'NONE',  ( 21.52544592524344225, -5.823673210054117533, 68.54057627198103830 ) ) ;
#129313 = CARTESIAN_POINT ( 'NONE',  ( 19.05341960407611168, 5.049401038298154454, 58.95724293864768129 ) ) ;
#129315 = CARTESIAN_POINT ( 'NONE',  ( -16.51473224551069308, -9.474510206698971260, 26.66557627198103120 ) ) ;
#129317 = CARTESIAN_POINT ( 'NONE',  ( -5.049401038298153566, 19.05341960407611168, 55.20724293864769550 ) ) ;
#129316 = CARTESIAN_POINT ( 'NONE',  ( 4.379528057220092307, 16.55341960407617563, 72.29275706135236135 ) ) ;
#129318 = CARTESIAN_POINT ( 'NONE',  ( -13.97604488694547697, 13.89961937509957934, 53.12609039468565442 ) ) ;
#129319 = CARTESIAN_POINT ( 'NONE',  ( -15.80617190586768217, 15.72974639402176855, 68.12609039468567573 ) ) ;
#129320 = CARTESIAN_POINT ( 'NONE',  ( -18.62759615963270932, 10.81492255796079327, 45.83224293864769550 ) ) ;
#129321 = AXIS2_PLACEMENT_3D ( 'NONE', #170322, #78291, #140968 ) ;
#129322 = CARTESIAN_POINT ( 'NONE',  ( -12.06949235617756955, 12.14591786802309770, 115.6239096053143669 ) ) ;
#129323 = CARTESIAN_POINT ( 'NONE',  ( -12.14591786802326823, 12.06949235617739902, 88.12609039468570415 ) ) ;
#129324 = ADVANCED_FACE ( 'NONE', ( #143826 ), #194357, .T. ) ;
#129325 = CARTESIAN_POINT ( 'NONE',  ( 5.153800228976615827, -19.02544592524334988, 105.2094237280190185 ) ) ;
#129326 = CARTESIAN_POINT ( 'NONE',  ( -19.03943276465977164, 0.05219959533909376836, 26.24890960531435624 ) ) ;
#129328 = CARTESIAN_POINT ( 'NONE',  ( -21.52544592524343514, 5.823673210054127303, 56.04057627198102409 ) ) ;
#129327 = CARTESIAN_POINT ( 'NONE',  ( -38.00000000000000711, 2.893978650043524126E-14, -24.99999999999997868 ) ) ;
#129329 = CARTESIAN_POINT ( 'NONE',  ( -15.72974639402176322, -15.80617190586768395, 94.37609039468568994 ) ) ;
#129330 = CARTESIAN_POINT ( 'NONE',  ( -16.52544592524342804, 4.483927247898546575, 51.04057627198103120 ) ) ;
#129331 = CARTESIAN_POINT ( 'NONE',  ( -16.52544592524342804, 4.483927247898546575, 51.04057627198103120 ) ) ;
#129332 = CARTESIAN_POINT ( 'NONE',  ( -10.72451020669898014, 18.67979575497178502, 80.41557627198103830 ) ) ;
#129333 = CARTESIAN_POINT ( 'NONE',  ( 0.05219959533907565091, 21.53943276465977519, 84.99890960531436690 ) ) ;
#129334 = CARTESIAN_POINT ( 'NONE',  ( -0.8274645171313256276, -29.14368513529649007, -49.37167794572891921 ) ) ;
#129335 = CARTESIAN_POINT ( 'NONE',  ( -0.05219959533907301413, -21.53943276465977519, 37.49890960531436690 ) ) ;
#129336 = CARTESIAN_POINT ( 'NONE',  ( -12.06949235617739369, -12.14591786802326823, 69.37609039468567573 ) ) ;
#129337 = CARTESIAN_POINT ( 'NONE',  ( 12.06949235617757843, -12.14591786802309237, 83.12390960531436690 ) ) ;
#129338 = CARTESIAN_POINT ( 'NONE',  ( -16.46253265017160317, 9.564922557960807481, 30.83224293864769550 ) ) ;
#129339 = SURFACE_STYLE_USAGE ( .BOTH. , #113182 ) ;
#129340 = DIRECTION ( 'NONE',  ( 0.000000000000000000, -0.000000000000000000, -1.000000000000000000 ) ) ;
#129341 = ORIENTED_EDGE ( 'NONE', *, *, #122751, .T. ) ;
#129342 = CARTESIAN_POINT ( 'NONE',  ( 12.14591786802327356, -12.06949235617739191, 90.62609039468567573 ) ) ;
#129343 = CARTESIAN_POINT ( 'NONE',  ( -10.81492255796078084, -18.62759615963271287, 112.0822429386477097 ) ) ;
#129344 = CARTESIAN_POINT ( 'NONE',  ( -0.05219959533909027116, -19.03943276465977164, 77.49890960531435269 ) ) ;
#129345 = CARTESIAN_POINT ( 'NONE',  ( -10.72451020669870658, -18.67979575497194134, 49.58442372801901143 ) ) ;
#129346 = CARTESIAN_POINT ( 'NONE',  ( 19.05341960407611168, 5.049401038298154454, 113.9572429386477097 ) ) ;
#129347 = CARTESIAN_POINT ( 'NONE',  ( -11.26676076909002155, -37.89014424912453904, -31.17854569212617832 ) ) ;
#129348 = ORIENTED_EDGE ( 'NONE', *, *, #131623, .F. ) ;
#129349 = CARTESIAN_POINT ( 'NONE',  ( -21.53943276465977519, -0.05219959533937600094, 48.75109039468568284 ) ) ;
#129351 = CARTESIAN_POINT ( 'NONE',  ( 5.153800228976335163, 19.02544592524342804, 109.7905762719810099 ) ) ;
#129350 = CARTESIAN_POINT ( 'NONE',  ( 19.05341960407611168, 5.049401038298154454, 38.95724293864767418 ) ) ;
#129352 = CARTESIAN_POINT ( 'NONE',  ( 13.97604488694548053, -13.89961937509957401, 50.62609039468566152 ) ) ;
#129353 = CARTESIAN_POINT ( 'NONE',  ( -21.53943276465977519, -0.05219959533937600094, 33.75109039468568284 ) ) ;
#129354 = CARTESIAN_POINT ( 'NONE',  ( -16.46253265017146816, -9.564922557961047289, 39.16775706135234003 ) ) ;
#129355 = CARTESIAN_POINT ( 'NONE',  ( 5.153800228976335163, 19.02544592524342804, 29.79057627198102409 ) ) ;
#129356 = CARTESIAN_POINT ( 'NONE',  ( 4.483927247898790824, -16.52544592524335698, 90.20942372801903275 ) ) ;
#129357 = CARTESIAN_POINT ( 'NONE',  ( -0.05219959533936034679, 19.03943276465977164, 62.50109039468566863 ) ) ;
#129358 = CARTESIAN_POINT ( 'NONE',  ( -8.224510206698735004, -14.34966873604973081, 109.5844237280190328 ) ) ;
#129359 = CARTESIAN_POINT ( 'NONE',  ( 17.60691670004650788, 5.500000000000064837, 86.63333313366442212 ) ) ;
#129360 = CARTESIAN_POINT ( 'NONE',  ( 5.153800228976335163, 19.02544592524342804, 79.79057627198102409 ) ) ;
#129361 = CARTESIAN_POINT ( 'NONE',  ( -5.823673210054431948, 21.52544592524334988, 97.70942372801904696 ) ) ;
#129362 = CARTESIAN_POINT ( 'NONE',  ( -10.72451020669870658, -18.67979575497194134, 104.5844237280190185 ) ) ;
#129363 = CARTESIAN_POINT ( 'NONE',  ( 18.22780087662122739, 5.500000000000000888, 66.48236817873106475 ) ) ;
#129364 = CARTESIAN_POINT ( 'NONE',  ( -5.049401038298153566, 19.05341960407611168, 105.2072429386476671 ) ) ;
#129365 = CARTESIAN_POINT ( 'NONE',  ( -18.67979575497193778, 10.72451020669871902, 78.33442372801901854 ) ) ;
#129366 = CARTESIAN_POINT ( 'NONE',  ( -12.14591786802326823, 12.06949235617739902, 23.12609039468567573 ) ) ;
#129367 = CARTESIAN_POINT ( 'NONE',  ( 19.02544592524343514, -5.153800228976328945, 78.54057627198099567 ) ) ;
#129368 = CARTESIAN_POINT ( 'NONE',  ( -18.67979575497178146, -10.72451020669898902, 31.66557627198102054 ) ) ;
#129369 = CARTESIAN_POINT ( 'NONE',  ( 16.46253265017160672, -9.564922557960803928, 98.33224293864769550 ) ) ;
#129370 = CARTESIAN_POINT ( 'NONE',  ( 11.30153831258470731, -188.0000000000000000, -15.00000000000000000 ) ) ;
#129371 = CARTESIAN_POINT ( 'NONE',  ( 13.89961937509977652, -13.97604488694527269, 73.12390960531436690 ) ) ;
#129372 = CARTESIAN_POINT ( 'NONE',  ( 9.564922557960805705, 16.46253265017160317, 69.58224293864770971 ) ) ;
#129373 = CARTESIAN_POINT ( 'NONE',  ( 4.483927247898545687, 16.52544592524342804, 24.79057627198103120 ) ) ;
#129374 = CARTESIAN_POINT ( 'NONE',  ( 16.46253265017146816, 9.564922557961045513, 66.66775706135233293 ) ) ;
#129375 = CARTESIAN_POINT ( 'NONE',  ( 9.564922557960805705, 16.46253265017160317, 89.58224293864769550 ) ) ;
#129376 = CARTESIAN_POINT ( 'NONE',  ( 16.55341960407611168, 4.379528057220329451, 83.95724293864770971 ) ) ;
#129377 = CARTESIAN_POINT ( 'NONE',  ( -15.72974639402197994, 15.80617190586746368, 40.62390960531435269 ) ) ;
#129378 =( BOUNDED_CURVE ( )  B_SPLINE_CURVE ( 2, ( #107905, #152433, #183779, #199944, #154425, #45265, #43275, #103951, #76585, #119132, #136276, #31089, #168592 ),
 .UNSPECIFIED., .F., .F. ) 
 B_SPLINE_CURVE_WITH_KNOTS ( ( 3, 2, 2, 2, 2, 2, 3 ),
 ( 0.2655883311638872479, 0.2675438596491228060, 0.2719298245614035214, 0.2763157894736842368, 0.2807017543859648967, 0.2850877192982456121, 0.2869975679613910868 ),
 .UNSPECIFIED. ) 
 CURVE ( )  GEOMETRIC_REPRESENTATION_ITEM ( )  RATIONAL_B_SPLINE_CURVE ( ( 0.9831626618144004848, 0.9848076720550091867, 1.000000000000000000, 0.9659258262890683122, 1.000000000000000000, 0.9659258262890683122, 1.000000000000000000, 0.9659258262890683122, 1.000000000000000000, 0.9659258262890683122, 1.000000000000000000, 0.9851625545550091179, 0.9832469066685282089 ) ) 
 REPRESENTATION_ITEM ( '' )  );
#129379 = CARTESIAN_POINT ( 'NONE',  ( 15.72974639402199770, -15.80617190586745480, 28.12390960531435979 ) ) ;
#129380 = CARTESIAN_POINT ( 'NONE',  ( 16.53943276465976808, -0.05219959533910856209, 108.7489096053143669 ) ) ;
#129381 = DIRECTION ( 'NONE',  ( 0.000000000000000000, 0.000000000000000000, 1.000000000000000000 ) ) ;
#129382 = CARTESIAN_POINT ( 'NONE',  ( -13.97604488694547697, 13.89961937509957934, 38.12609039468566152 ) ) ;
#129383 = CARTESIAN_POINT ( 'NONE',  ( -16.52544592524342804, 4.483927247898546575, 26.04057627198103475 ) ) ;
#129384 = CARTESIAN_POINT ( 'NONE',  ( -13.97604488694527625, -13.89961937509977652, 96.87390960531433848 ) ) ;
#129385 = CARTESIAN_POINT ( 'NONE',  ( 5.823673210054444382, -21.52544592524334988, 70.20942372801904696 ) ) ;
#129386 = CARTESIAN_POINT ( 'NONE',  ( 21.53943276465977519, -0.05219959533907433946, 58.74890960531436690 ) ) ;
#129387 = CARTESIAN_POINT ( 'NONE',  ( 21.52544592524334988, 5.823673210054432836, 31.45942372801901854 ) ) ;
#129388 = CARTESIAN_POINT ( 'NONE',  ( 18.67979575497178502, 10.72451020669898547, 84.16557627198103830 ) ) ;
#129389 = CARTESIAN_POINT ( 'NONE',  ( 18.67979575497194134, -10.72451020669871369, 40.83442372801901854 ) ) ;
#129390 = CARTESIAN_POINT ( 'NONE',  ( 4.379528057220339221, -16.55341960407611168, 107.7072429386476955 ) ) ;
#129391 = CARTESIAN_POINT ( 'NONE',  ( -9.474510206698720793, -16.51473224551083518, 69.58442372801901854 ) ) ;
#129392 = CARTESIAN_POINT ( 'NONE',  ( 19.05341960407611168, 5.049401038298154454, 38.95724293864767418 ) ) ;
#129393 = CARTESIAN_POINT ( 'NONE',  ( -12.06949235617756955, 12.14591786802309770, 85.62390960531436690 ) ) ;
#129394 = CARTESIAN_POINT ( 'NONE',  ( 19.03943276465977164, -0.05219959533909143690, 113.7489096053143669 ) ) ;
#129395 = CARTESIAN_POINT ( 'NONE',  ( 9.474510206698971260, -16.51473224551069308, 27.91557627198103120 ) ) ;
#129396 = CARTESIAN_POINT ( 'NONE',  ( 4.379528057220339221, -16.55341960407611168, 37.70724293864769550 ) ) ;
#129397 = CARTESIAN_POINT ( 'NONE',  ( -12.06949235617739369, -12.14591786802326823, 94.37609039468568994 ) ) ;
#129398 = CARTESIAN_POINT ( 'NONE',  ( 0.05219959533909260263, 19.03943276465977164, 49.99890960531435979 ) ) ;
#129399 = CARTESIAN_POINT ( 'NONE',  ( -19.05341960407611168, -5.049401038298163336, 26.45724293864769550 ) ) ;
#129400 = CARTESIAN_POINT ( 'NONE',  ( 13.97604488694548053, -13.89961937509957401, 25.62609039468566507 ) ) ;
#129402 = CARTESIAN_POINT ( 'NONE',  ( -0.05219959533910754901, -16.53943276465976808, 42.49890960531435979 ) ) ;
#129401 = CARTESIAN_POINT ( 'NONE',  ( 1.300000000000000044, 0.7216878364870328300, 1.249999999999999778 ) ) ;
#129403 = CARTESIAN_POINT ( 'NONE',  ( -10.72451020669870658, -18.67979575497194134, 44.58442372801901854 ) ) ;
#129404 = CARTESIAN_POINT ( 'NONE',  ( -18.27284445343937236, -33.31360383038296646, -25.98075878691516039 ) ) ;
#129405 = CARTESIAN_POINT ( 'NONE',  ( -14.29746914071037622, -8.314922557961029526, 59.16775706135234714 ) ) ;
#129406 = CARTESIAN_POINT ( 'NONE',  ( -0.05219959533910754901, -16.53943276465976808, 27.49890960531435269 ) ) ;
#129407 = CARTESIAN_POINT ( 'NONE',  ( -8.314922557961024197, 14.29746914071037800, 112.9177570613523329 ) ) ;
#129408 = CARTESIAN_POINT ( 'NONE',  ( 4.379528057220092307, 16.55341960407617563, 32.29275706135235424 ) ) ;
#129409 = CARTESIAN_POINT ( 'NONE',  ( 5.153800228976335163, 19.02544592524342804, 54.79057627198103120 ) ) ;
#129410 = CARTESIAN_POINT ( 'NONE',  ( -16.53943276465976808, 0.05219959533911058130, 106.2489096053143811 ) ) ;
#129411 = CARTESIAN_POINT ( 'NONE',  ( 21.55341960407619695, -5.719274019375665929, 21.04275706135234714 ) ) ;
#129412 = CARTESIAN_POINT ( 'NONE',  ( -0.05219959533909027116, -19.03943276465977164, 42.49890960531435269 ) ) ;
#129413 = CARTESIAN_POINT ( 'NONE',  ( 0.05219959533909260263, 19.03943276465977164, 114.9989096053143669 ) ) ;
#129414 = CARTESIAN_POINT ( 'NONE',  ( 5.049401038298161559, -19.05341960407611168, 27.70724293864769550 ) ) ;
#129415 = CARTESIAN_POINT ( 'NONE',  ( -9.474510206698964154, 16.51473224551069663, 115.4155762719810241 ) ) ;
#129416 = CARTESIAN_POINT ( 'NONE',  ( -17.48853670773245028, -5.747243402303086945, 36.33328700250008580 ) ) ;
#129417 = CARTESIAN_POINT ( 'NONE',  ( 0.05219959533909260263, 19.03943276465977164, 99.99890960531436690 ) ) ;
#129419 = CARTESIAN_POINT ( 'NONE',  ( 4.483927247898545687, 16.52544592524342804, 99.79057627198103830 ) ) ;
#129418 = CARTESIAN_POINT ( 'NONE',  ( -10.81492255796105439, 18.62759615963255655, 42.91775706135235424 ) ) ;
#129420 = CARTESIAN_POINT ( 'NONE',  ( 19.05341960407611168, 5.049401038298154454, 103.9572429386476671 ) ) ;
#129421 = CARTESIAN_POINT ( 'NONE',  ( 17.97182807773873137, -5.499999999999949374, 96.03038844047289047 ) ) ;
#129422 = CARTESIAN_POINT ( 'NONE',  ( -16.52544592524335698, -4.483927247898792601, 73.95942372801901854 ) ) ;
#129423 = CARTESIAN_POINT ( 'NONE',  ( 18.67979575497194134, -10.72451020669871369, 90.83442372801901854 ) ) ;
#129424 = CARTESIAN_POINT ( 'NONE',  ( 16.52544592524335698, 4.483927247898782831, 51.45942372801901854 ) ) ;
#129425 = CARTESIAN_POINT ( 'NONE',  ( -9.564922557960796823, -16.46253265017161027, 102.0822429386477097 ) ) ;
#129426 = CARTESIAN_POINT ( 'NONE',  ( -4.379528057220086978, -16.55341960407618274, 39.79275706135235424 ) ) ;
#129427 = CARTESIAN_POINT ( 'NONE',  ( -5.153800228976607833, 19.02544592524334988, 102.7094237280189759 ) ) ;
#129428 = CARTESIAN_POINT ( 'NONE',  ( -0.05219959533934338120, 16.53943276465976808, 77.50109039468567573 ) ) ;
#129429 = CARTESIAN_POINT ( 'NONE',  ( 13.89961937509957401, 13.97604488694547697, 106.8760903946856757 ) ) ;
#129430 = CARTESIAN_POINT ( 'NONE',  ( 19.03943276465977164, -0.05219959533909143690, 73.74890960531435269 ) ) ;
#129431 = CARTESIAN_POINT ( 'NONE',  ( -21.53943276465977519, 0.05219959533907696930, 91.24890960531436690 ) ) ;
#129433 = CARTESIAN_POINT ( 'NONE',  ( -5.153800228976607833, 19.02544592524334988, 102.7094237280189759 ) ) ;
#129432 = CARTESIAN_POINT ( 'NONE',  ( 12.06949235617757843, -12.14591786802309237, 108.1239096053143811 ) ) ;
#129434 = CARTESIAN_POINT ( 'NONE',  ( 8.224510206698742110, 14.34966873604972548, 77.08442372801901854 ) ) ;
#129435 = CARTESIAN_POINT ( 'NONE',  ( -17.40861289039009208, 6.110651285853054837, 43.62767529172568715 ) ) ;
#129436 = CARTESIAN_POINT ( 'NONE',  ( 5.153800228976615827, -19.02544592524334988, 70.20942372801899012 ) ) ;
#129437 = CARTESIAN_POINT ( 'NONE',  ( 16.53943276465976808, -0.05219959533910856209, 33.74890960531436690 ) ) ;
#129438 = CARTESIAN_POINT ( 'NONE',  ( 8.314922557960818139, 14.29746914071049879, 89.58224293864768129 ) ) ;
#129440 = DIRECTION ( 'NONE',  ( -0.000000000000000000, -0.000000000000000000, 1.000000000000000000 ) ) ;
#129439 = CARTESIAN_POINT ( 'NONE',  ( 9.564922557961047289, -16.46253265017146816, 40.41775706135234003 ) ) ;
#129441 = CARTESIAN_POINT ( 'NONE',  ( -10.81492255796105439, 18.62759615963255655, 32.91775706135234714 ) ) ;
#129442 = CARTESIAN_POINT ( 'NONE',  ( 13.89961937509957401, 13.97604488694547697, 101.8760903946856331 ) ) ;
#129443 = CARTESIAN_POINT ( 'NONE',  ( 5.153800228976335163, 19.02544592524342804, 109.7905762719810099 ) ) ;
#129444 = CARTESIAN_POINT ( 'NONE',  ( 13.97604488694527802, 13.89961937509977652, 89.37390960531436690 ) ) ;
#129445 = CARTESIAN_POINT ( 'NONE',  ( 18.62759615963255655, 10.81492255796105972, 101.6677570613523613 ) ) ;
#129446 = CARTESIAN_POINT ( 'NONE',  ( -16.51473224551069308, -9.474510206698971260, 81.66557627198103830 ) ) ;
#129447 = CARTESIAN_POINT ( 'NONE',  ( 15.80617190586746368, 15.72974639402197994, 39.37390960531436690 ) ) ;
#129448 = CARTESIAN_POINT ( 'NONE',  ( -4.379528057220328563, 16.55341960407611168, 95.20724293864769550 ) ) ;
#129449 = CARTESIAN_POINT ( 'NONE',  ( 9.474510206698971260, -16.51473224551069308, 52.91557627198102409 ) ) ;
#129450 = CARTESIAN_POINT ( 'NONE',  ( -14.34966873604960291, -8.224510206698953496, 106.6655762719810383 ) ) ;
#129451 = CARTESIAN_POINT ( 'NONE',  ( 18.67979575497194134, -10.72451020669871369, 20.83442372801901143 ) ) ;
#129452 = CARTESIAN_POINT ( 'NONE',  ( 10.72451020669871369, 18.67979575497193778, 72.08442372801899012 ) ) ;
#129453 = CARTESIAN_POINT ( 'NONE',  ( -19.05341960407611168, -5.049401038298163336, 41.45724293864769550 ) ) ;
#129454 = CARTESIAN_POINT ( 'NONE',  ( 0.05219959533934541429, -16.53943276465976808, 75.00109039468568994 ) ) ;
#129455 = CARTESIAN_POINT ( 'NONE',  ( -15.72974639402197994, 15.80617190586746368, 115.6239096053143669 ) ) ;
#129456 = ORIENTED_EDGE ( 'NONE', *, *, #133810, .T. ) ;
#129457 = CARTESIAN_POINT ( 'NONE',  ( -10.72451020669870658, -18.67979575497194134, 29.58442372801901854 ) ) ;
#129459 = CARTESIAN_POINT ( 'NONE',  ( -5.153800228976328057, -19.02544592524343514, 62.29057627198100988 ) ) ;
#129458 = CARTESIAN_POINT ( 'NONE',  ( -0.05219959533936034679, 19.03943276465977164, 52.50109039468566863 ) ) ;
#129460 = CARTESIAN_POINT ( 'NONE',  ( -16.51473224551082808, 9.474510206698731452, 38.33442372801899722 ) ) ;
#129461 = CARTESIAN_POINT ( 'NONE',  ( 10.72451020669871369, 18.67979575497193778, 72.08442372801899012 ) ) ;
#129462 = CARTESIAN_POINT ( 'NONE',  ( 5.823673210054125526, 21.52544592524343514, 69.79057627198102409 ) ) ;
#129463 = CARTESIAN_POINT ( 'NONE',  ( -8.224510206698948167, 14.34966873604960824, 45.41557627198103830 ) ) ;
#129465 = CARTESIAN_POINT ( 'NONE',  ( -13.89961937509957401, -13.97604488694547875, 29.37609039468565797 ) ) ;
#129464 = CARTESIAN_POINT ( 'NONE',  ( 21.52544592524334988, 5.823673210054432836, 91.45942372801901854 ) ) ;
#129466 = CARTESIAN_POINT ( 'NONE',  ( 16.55341960407611168, 4.379528057220329451, 73.95724293864769550 ) ) ;
#129467 = CARTESIAN_POINT ( 'NONE',  ( 0.05219959533910956823, 16.53943276465976808, 114.9989096053143669 ) ) ;
#129468 = CARTESIAN_POINT ( 'NONE',  ( -19.02544592524334988, -5.153800228976617603, 58.95942372801900433 ) ) ;
#129469 = CARTESIAN_POINT ( 'NONE',  ( 8.224510206698742110, 14.34966873604972548, 112.0844237280190185 ) ) ;
#129470 = CARTESIAN_POINT ( 'NONE',  ( -10.72451020669870658, -18.67979575497194134, 84.58442372801903275 ) ) ;
#129471 = CARTESIAN_POINT ( 'NONE',  ( -19.02544592524334988, -5.153800228976617603, 48.95942372801900433 ) ) ;
#129472 = CARTESIAN_POINT ( 'NONE',  ( 21.55341960407610458, 5.719274019375980345, 53.95724293864770260 ) ) ;
#129473 = CARTESIAN_POINT ( 'NONE',  ( 18.67979575497194134, -10.72451020669871369, 40.83442372801901854 ) ) ;
#129474 = CARTESIAN_POINT ( 'NONE',  ( -10.72451020669898014, 18.67979575497178502, 105.4155762719810383 ) ) ;
#129475 = CARTESIAN_POINT ( 'NONE',  ( -0.05219959533936034679, 19.03943276465977164, 92.50109039468566152 ) ) ;
#129476 = CARTESIAN_POINT ( 'NONE',  ( 4.483927247898790824, -16.52544592524335698, 70.20942372801904696 ) ) ;
#129478 = CARTESIAN_POINT ( 'NONE',  ( 5.719274019375991003, -21.55341960407610458, 112.7072429386476955 ) ) ;
#129477 = LINE ( 'NONE', #37485, #164537 ) ;
#129479 = CARTESIAN_POINT ( 'NONE',  ( 16.52544592524342804, -4.483927247898539470, 88.54057627198103830 ) ) ;
#129480 = CARTESIAN_POINT ( 'NONE',  ( -17.49999999999999645, -3.850315288878745967, 30.73370869396548954 ) ) ;
#129481 = CARTESIAN_POINT ( 'NONE',  ( -8.224510206698735004, -14.34966873604973081, 34.58442372801900433 ) ) ;
#129482 = APPLICATION_CONTEXT ( 'automotive_design' ) ;
#129483 = CARTESIAN_POINT ( 'NONE',  ( 18.62759615963271287, -10.81492255796078972, 53.33224293864769550 ) ) ;
#129484 = CARTESIAN_POINT ( 'NONE',  ( -16.53943276465976808, -0.05219959533934237506, 88.75109039468567573 ) ) ;
#129485 = CARTESIAN_POINT ( 'NONE',  ( 19.03943276465977164, -0.05219959533909143690, 23.74890960531435269 ) ) ;
#129486 = CARTESIAN_POINT ( 'NONE',  ( 16.53943276465976808, 0.05219959533934440121, 71.25109039468568994 ) ) ;
#129487 = CARTESIAN_POINT ( 'NONE',  ( 18.62759615963255655, 10.81492255796105972, 46.66775706135234714 ) ) ;
#129488 = CARTESIAN_POINT ( 'NONE',  ( 5.823673210054125526, 21.52544592524343514, 64.79057627198103830 ) ) ;
#129489 = CARTESIAN_POINT ( 'NONE',  ( -14.29746914071037622, -8.314922557961029526, 79.16775706135234714 ) ) ;
#129490 = CARTESIAN_POINT ( 'NONE',  ( -10.81492255796105439, 18.62759615963255655, 67.91775706135234714 ) ) ;
#129491 = EDGE_CURVE ( 'NONE', #196218, #158096, #51464, .T. ) ;
#129492 = CARTESIAN_POINT ( 'NONE',  ( 10.72451020669898902, -18.67979575497178502, 52.91557627198103830 ) ) ;
#129493 = CARTESIAN_POINT ( 'NONE',  ( 10.81492255796078972, 18.62759615963270932, 39.58224293864769550 ) ) ;
#129494 = CARTESIAN_POINT ( 'NONE',  ( -14.29746914071037622, -8.314922557961029526, 59.16775706135234714 ) ) ;
#129495 = CARTESIAN_POINT ( 'NONE',  ( -21.52544592524343514, 5.823673210054127303, 31.04057627198102409 ) ) ;
#129496 = CARTESIAN_POINT ( 'NONE',  ( -13.97604488694527625, -13.89961937509977652, 101.8739096053143811 ) ) ;
#129497 = CARTESIAN_POINT ( 'NONE',  ( 4.483927247898545687, 16.52544592524342804, 24.79057627198103120 ) ) ;
#129498 = CARTESIAN_POINT ( 'NONE',  ( 12.06949235617757843, -12.14591786802309237, 113.1239096053143953 ) ) ;
#129499 = CARTESIAN_POINT ( 'NONE',  ( -21.53943276465977519, 0.05219959533907696930, 46.24890960531435979 ) ) ;
#129500 = CARTESIAN_POINT ( 'NONE',  ( -13.97604488694527625, -13.89961937509977652, 46.87390960531435979 ) ) ;
#129501 = CARTESIAN_POINT ( 'NONE',  ( -4.379528057220086978, -16.55341960407618274, 94.79275706135234714 ) ) ;
#129502 = CARTESIAN_POINT ( 'NONE',  ( -10.72451020669870658, -18.67979575497194134, 29.58442372801901854 ) ) ;
#129503 = CARTESIAN_POINT ( 'NONE',  ( -9.564922557961040184, 16.46253265017147172, 92.91775706135233293 ) ) ;
#129504 = CARTESIAN_POINT ( 'NONE',  ( -12.14591786802309592, -12.06949235617757132, 106.8739096053143811 ) ) ;
#129505 = CARTESIAN_POINT ( 'NONE',  ( -19.03943276465977164, 0.05219959533909376836, 56.24890960531435979 ) ) ;
#129506 = CARTESIAN_POINT ( 'NONE',  ( -0.05219959533909027116, -19.03943276465977164, 22.49890960531436690 ) ) ;
#129507 = FACE_OUTER_BOUND ( 'NONE', #181687, .T. ) ;
#129508 = CARTESIAN_POINT ( 'NONE',  ( 19.03943276465977164, -0.05219959533909143690, 78.74890960531436690 ) ) ;
#129509 = CARTESIAN_POINT ( 'NONE',  ( 0.05219959533934541429, -16.53943276465976808, 65.00109039468568994 ) ) ;
#129510 = CARTESIAN_POINT ( 'NONE',  ( -5.823673210054431948, 21.52544592524334988, 102.7094237280190185 ) ) ;
#129511 = CARTESIAN_POINT ( 'NONE',  ( -21.55341960407610458, -5.719274019375992779, 46.45724293864769550 ) ) ;
#129512 = CARTESIAN_POINT ( 'NONE',  ( -4.483927247898782831, 16.52544592524335698, 72.70942372801901854 ) ) ;
#129513 = CARTESIAN_POINT ( 'NONE',  ( -19.05341960407617563, 5.049401038297882671, 63.54275706135234003 ) ) ;
#129514 = ORIENTED_EDGE ( 'NONE', *, *, #189089, .T. ) ;
#129515 = CARTESIAN_POINT ( 'NONE',  ( 21.52544592524334988, 5.823673210054432836, 61.45942372801901854 ) ) ;
#129516 = CARTESIAN_POINT ( 'NONE',  ( 9.474510206698971260, -16.51473224551069308, 62.91557627198102409 ) ) ;
#129517 = CARTESIAN_POINT ( 'NONE',  ( -0.05219959533909027116, -19.03943276465977164, 32.49890960531435979 ) ) ;
#129518 = CARTESIAN_POINT ( 'NONE',  ( -19.03943276465977164, -0.05219959533935918106, 63.75109039468566863 ) ) ;
#129519 = CARTESIAN_POINT ( 'NONE',  ( 13.97604488694527802, 13.89961937509977652, 109.3739096053143669 ) ) ;
#129520 = CARTESIAN_POINT ( 'NONE',  ( 13.97604488694527802, 13.89961937509977652, 89.37390960531436690 ) ) ;
#129521 = CARTESIAN_POINT ( 'NONE',  ( 12.06949235617757843, -12.14591786802309237, 53.12390960531436690 ) ) ;
#129522 = CARTESIAN_POINT ( 'NONE',  ( -10.81492255796078084, -18.62759615963271287, 47.08224293864770260 ) ) ;
#129523 = CARTESIAN_POINT ( 'NONE',  ( -17.50000000000014211, 3.417042746626915761, 105.1738039623247545 ) ) ;
#129524 = CARTESIAN_POINT ( 'NONE',  ( -16.51473224551082808, 9.474510206698731452, 33.33442372801899722 ) ) ;
#129525 = CARTESIAN_POINT ( 'NONE',  ( -17.48847506799967988, -5.747544572773762184, 79.17302562156723411 ) ) ;
#129526 = CARTESIAN_POINT ( 'NONE',  ( 5.153800228976335163, 19.02544592524342804, 44.79057627198103830 ) ) ;
#129527 = CARTESIAN_POINT ( 'NONE',  ( -19.49190055781010500, -5.500000000000011546, 100.5611608709877913 ) ) ;
#129528 = CARTESIAN_POINT ( 'NONE',  ( 67.00000000000000000, -5.510910596163089556E-15, 45.00000000000000000 ) ) ;
#129529 = CARTESIAN_POINT ( 'NONE',  ( -14.29746914071037622, -8.314922557961029526, 79.16775706135234714 ) ) ;
#129530 = CARTESIAN_POINT ( 'NONE',  ( 15.80617190586746368, 15.72974639402197994, 94.37390960531436690 ) ) ;
#129532 = CARTESIAN_POINT ( 'NONE',  ( 3.766062262543149401E-15, -39.95556452105413570, -5.249999994537625447 ) ) ;
#129531 = CARTESIAN_POINT ( 'NONE',  ( -5.153800228976328057, -19.02544592524343514, 37.29057627198102409 ) ) ;
#129533 = CARTESIAN_POINT ( 'NONE',  ( 21.55341960407619695, -5.719274019375665929, 46.04275706135234714 ) ) ;
#129534 = CARTESIAN_POINT ( 'NONE',  ( 13.97604488694548053, -13.89961937509957401, 45.62609039468566863 ) ) ;
#129535 = CARTESIAN_POINT ( 'NONE',  ( -19.02544592524342804, 5.153800228976336051, 46.04057627198101699 ) ) ;
#129536 = CARTESIAN_POINT ( 'NONE',  ( -21.53943276465977519, -0.05219959533937600094, 98.75109039468568994 ) ) ;
#129537 = CARTESIAN_POINT ( 'NONE',  ( 16.29526858892875651, 7.335722546920131037, 98.29670597800206622 ) ) ;
#129538 = CARTESIAN_POINT ( 'NONE',  ( 4.379528057220339221, -16.55341960407611168, 42.70724293864770260 ) ) ;
#129539 = CARTESIAN_POINT ( 'NONE',  ( -16.70000000000002061, 0.1037895044724580218, -59.13370768023892055 ) ) ;
#129540 = CARTESIAN_POINT ( 'NONE',  ( -18.62759615963270932, 10.81492255796079327, 50.83224293864770971 ) ) ;
#129541 = CARTESIAN_POINT ( 'NONE',  ( -5.359611314223446995E-15, 29.16686587814335851, 140.3750000027311842 ) ) ;
#129542 = CARTESIAN_POINT ( 'NONE',  ( 0.05219959533909260263, 19.03943276465977164, 104.9989096053143669 ) ) ;
#129543 = CARTESIAN_POINT ( 'NONE',  ( 12.06949235617757843, -12.14591786802309237, 88.12390960531436690 ) ) ;
#129544 = CARTESIAN_POINT ( 'NONE',  ( -14.34966873604972548, 8.224510206698743886, 23.33442372801901499 ) ) ;
#129545 = CARTESIAN_POINT ( 'NONE',  ( -0.05219959533910754901, -16.53943276465976808, 22.49890960531436335 ) ) ;
#129546 = ORIENTED_EDGE ( 'NONE', *, *, #69017, .F. ) ;
#129548 = CARTESIAN_POINT ( 'NONE',  ( 21.53943276465977519, -0.05219959533907433946, 103.7489096053143669 ) ) ;
#129547 = CARTESIAN_POINT ( 'NONE',  ( -9.564922557960796823, -16.46253265017161027, 97.08224293864769550 ) ) ;
#129550 = CARTESIAN_POINT ( 'NONE',  ( -19.03943276465977164, 0.05219959533909376836, 106.2489096053143669 ) ) ;
#129549 = CARTESIAN_POINT ( 'NONE',  ( -16.53943276465976808, 0.05219959533911058130, 21.24890960531436690 ) ) ;
#129551 = CARTESIAN_POINT ( 'NONE',  ( 19.05341960407617918, -5.049401038297876454, 91.04275706135234714 ) ) ;
#129552 = CARTESIAN_POINT ( 'NONE',  ( 5.823673210054444382, -21.52544592524334988, 105.2094237280190328 ) ) ;
#129553 = CARTESIAN_POINT ( 'NONE',  ( 10.81492255796078972, 18.62759615963270932, 94.58224293864769550 ) ) ;
#129554 = CARTESIAN_POINT ( 'NONE',  ( 10.81492255796078972, 18.62759615963270932, 54.58224293864769550 ) ) ;
#129555 = CARTESIAN_POINT ( 'NONE',  ( 9.474510206698971260, -16.51473224551069308, 62.91557627198102409 ) ) ;
#129556 = CARTESIAN_POINT ( 'NONE',  ( 0.05219959533910956823, 16.53943276465976808, 34.99890960531435979 ) ) ;
#129557 = CARTESIAN_POINT ( 'NONE',  ( 9.474510206698971260, -16.51473224551069308, 77.91557627198103830 ) ) ;
#129558 = ORIENTED_EDGE ( 'NONE', *, *, #124318, .T. ) ;
#129559 = CARTESIAN_POINT ( 'NONE',  ( 19.01529144963332030, 5.500000000000158096, 58.73431955728438680 ) ) ;
#129560 = CARTESIAN_POINT ( 'NONE',  ( -9.564922557961040184, 16.46253265017147172, 47.91775706135233293 ) ) ;
#129561 = CARTESIAN_POINT ( 'NONE',  ( -21.55341960407610458, -5.719274019375992779, 86.45724293864770971 ) ) ;
#129562 = CARTESIAN_POINT ( 'NONE',  ( -4.379528057220328563, 16.55341960407611168, 80.20724293864769550 ) ) ;
#129563 = CARTESIAN_POINT ( 'NONE',  ( -5.823673210054431948, 21.52544592524334988, 27.70942372801901854 ) ) ;
#129564 = CARTESIAN_POINT ( 'NONE',  ( 1.784210473542230573E-15, -29.16686587814331588, 145.8750000027311273 ) ) ;
#129565 = CARTESIAN_POINT ( 'NONE',  ( 16.53943276465976808, 0.05219959533934440121, 111.2510903946856899 ) ) ;
#129566 = CARTESIAN_POINT ( 'NONE',  ( -13.97604488694527625, -13.89961937509977652, 26.87390960531434558 ) ) ;
#129567 = CARTESIAN_POINT ( 'NONE',  ( -5.153800228976328057, -19.02544592524343514, 67.29057627198102409 ) ) ;
#129568 = PRESENTATION_STYLE_ASSIGNMENT (( #67915 ) ) ;
#129569 = CARTESIAN_POINT ( 'NONE',  ( 23.48529157249599564, 32.32473071737754111, -10.44999999453762562 ) ) ;
#129570 = CARTESIAN_POINT ( 'NONE',  ( 0.05219959533910956823, 16.53943276465976808, 44.99890960531435979 ) ) ;
#129571 = CARTESIAN_POINT ( 'NONE',  ( 10.72451020669871369, 18.67979575497193778, 62.08442372801901143 ) ) ;
#129572 = CARTESIAN_POINT ( 'NONE',  ( 35.57212018829687139, -18.96864681236966277, -18.54270186059541814 ) ) ;
#129573 = CARTESIAN_POINT ( 'NONE',  ( -16.46253265017160317, 9.564922557960807481, 45.83224293864769550 ) ) ;
#129574 = CARTESIAN_POINT ( 'NONE',  ( 5.153800228976335163, 19.02544592524342804, 49.79057627198100988 ) ) ;
#129575 = ORIENTED_EDGE ( 'NONE', *, *, #43624, .F. ) ;
#129576 = CARTESIAN_POINT ( 'NONE',  ( -10.81492255796105439, 18.62759615963255655, 107.9177570613523471 ) ) ;
#129577 = CARTESIAN_POINT ( 'NONE',  ( 4.379528057220092307, 16.55341960407617563, 67.29275706135234714 ) ) ;
#129578 = CARTESIAN_POINT ( 'NONE',  ( 15.80617190586769283, -15.72974639402175789, 85.62609039468568994 ) ) ;
#129579 = CARTESIAN_POINT ( 'NONE',  ( -9.474510206698964154, 16.51473224551069663, 110.4155762719810383 ) ) ;
#129580 = EDGE_LOOP ( 'NONE', ( #120468, #28203, #32357, #15676 ) ) ;
#129581 = CARTESIAN_POINT ( 'NONE',  ( -9.564922557961040184, 16.46253265017147172, 92.91775706135233293 ) ) ;
#129582 = CARTESIAN_POINT ( 'NONE',  ( 21.52544592524334988, 5.823673210054432836, 71.45942372801901854 ) ) ;
#129583 = CARTESIAN_POINT ( 'NONE',  ( -4.483927247898782831, 16.52544592524335698, 37.70942372801900433 ) ) ;
#129584 = CARTESIAN_POINT ( 'NONE',  ( -15.80617190586745835, -15.72974639402198527, 91.87390960531436690 ) ) ;
#129585 = CARTESIAN_POINT ( 'NONE',  ( -13.97604488694547697, 13.89961937509957934, 103.1260903946856473 ) ) ;
#129586 = CARTESIAN_POINT ( 'NONE',  ( 16.51473224551069308, 9.474510206698969483, 64.16557627198102409 ) ) ;
#129587 = CARTESIAN_POINT ( 'NONE',  ( -13.97604488694547697, 13.89961937509957934, 103.1260903946856473 ) ) ;
#129588 = CARTESIAN_POINT ( 'NONE',  ( -0.05219959533936034679, 19.03943276465977164, 97.50109039468567573 ) ) ;
#129589 = CARTESIAN_POINT ( 'NONE',  ( -4.379528057220328563, 16.55341960407611168, 55.20724293864770260 ) ) ;
#129590 = CARTESIAN_POINT ( 'NONE',  ( -19.02544592524334988, -5.153800228976617603, 78.95942372801900433 ) ) ;
#129591 = CARTESIAN_POINT ( 'NONE',  ( -8.314922557961024197, 14.29746914071037800, 57.91775706135234714 ) ) ;
#129593 = CARTESIAN_POINT ( 'NONE',  ( -13.97604488694527625, -13.89961937509977652, 31.87390960531435979 ) ) ;
#129592 = CARTESIAN_POINT ( 'NONE',  ( 18.67979575497194134, -10.72451020669871369, 20.83442372801901143 ) ) ;
#129594 = CARTESIAN_POINT ( 'NONE',  ( 13.97604488694527802, 13.89961937509977652, 49.37390960531434558 ) ) ;
#129595 = CARTESIAN_POINT ( 'NONE',  ( -14.29746914071037622, -8.314922557961029526, 64.16775706135234714 ) ) ;
#129596 = CARTESIAN_POINT ( 'NONE',  ( -27.73933785331498925, -9.013057229001049109, 139.4750000027311785 ) ) ;
#129597 = CARTESIAN_POINT ( 'NONE',  ( -8.906447517083060816, 27.41122689804195645, 145.8500000054623627 ) ) ;
#129598 = CARTESIAN_POINT ( 'NONE',  ( 0.05219959533909260263, 19.03943276465977164, 99.99890960531436690 ) ) ;
#129599 = CARTESIAN_POINT ( 'NONE',  ( -5.153800228976328057, -19.02544592524343514, 27.29057627198103120 ) ) ;
#129600 = ORIENTED_EDGE ( 'NONE', *, *, #68789, .T. ) ;
#129601 = CARTESIAN_POINT ( 'NONE',  ( 5.153800228976615827, -19.02544592524334988, 110.2094237280189901 ) ) ;
#129602 = CARTESIAN_POINT ( 'NONE',  ( 15.72974639402199770, -15.80617190586745480, 43.12390960531435269 ) ) ;
#129604 = CARTESIAN_POINT ( 'NONE',  ( 4.483927247898790824, -16.52544592524335698, 25.20942372801901854 ) ) ;
#129603 = CARTESIAN_POINT ( 'NONE',  ( -16.46253265017146816, -9.564922557961047289, 49.16775706135233293 ) ) ;
#129605 = CARTESIAN_POINT ( 'NONE',  ( 19.02544592524343514, -5.153800228976328945, 23.54057627198102054 ) ) ;
#129606 = CARTESIAN_POINT ( 'NONE',  ( 16.51473224551069308, 9.474510206698969483, 54.16557627198103120 ) ) ;
#129607 = CARTESIAN_POINT ( 'NONE',  ( -18.67979575497178146, -10.72451020669898902, 91.66557627198103830 ) ) ;
#129608 = CARTESIAN_POINT ( 'NONE',  ( 13.89961937509977652, -13.97604488694527269, 98.12390960531433848 ) ) ;
#129609 = EDGE_CURVE ( 'NONE', #110145, #115498, #15975, .T. ) ;
#129610 = CARTESIAN_POINT ( 'NONE',  ( -19.03943276465977164, 0.05219959533909376836, 46.24890960531435979 ) ) ;
#129611 = CARTESIAN_POINT ( 'NONE',  ( -5.359611314223446995E-15, 29.16686587814335851, 140.8750000027311842 ) ) ;
#129612 = CARTESIAN_POINT ( 'NONE',  ( 13.89961937509957401, 13.97604488694547697, 81.87609039468564731 ) ) ;
#129613 = CARTESIAN_POINT ( 'NONE',  ( -12.06949235617756955, 12.14591786802309770, 70.62390960531436690 ) ) ;
#129614 = CARTESIAN_POINT ( 'NONE',  ( 10.81492255796106328, -18.62759615963255655, 100.4177570613523471 ) ) ;
#129615 = CARTESIAN_POINT ( 'NONE',  ( 21.52544592524344225, -5.823673210054117533, 93.54057627198103830 ) ) ;
#129616 = CARTESIAN_POINT ( 'NONE',  ( 21.52544592524334988, 5.823673210054432836, 81.45942372801900433 ) ) ;
#129617 = CARTESIAN_POINT ( 'NONE',  ( 10.72451020669871369, 18.67979575497193778, 77.08442372801901854 ) ) ;
#129618 = CARTESIAN_POINT ( 'NONE',  ( -5.049401038298153566, 19.05341960407611168, 115.2072429386477097 ) ) ;
#129620 = CARTESIAN_POINT ( 'NONE',  ( -18.62759615963255300, -10.81492255796106328, 74.16775706135231871 ) ) ;
#129619 = CARTESIAN_POINT ( 'NONE',  ( -8.224510206698735004, -14.34966873604973081, 109.5844237280190328 ) ) ;
#129621 = CARTESIAN_POINT ( 'NONE',  ( 19.02544592524343514, -5.153800228976328945, 68.54057627198103830 ) ) ;
#129622 = CARTESIAN_POINT ( 'NONE',  ( 21.52544592524334988, 5.823673210054432836, 46.45942372801901854 ) ) ;
#129623 = CARTESIAN_POINT ( 'NONE',  ( 5.153800228976335163, 19.02544592524342804, 79.79057627198102409 ) ) ;
#129624 = CARTESIAN_POINT ( 'NONE',  ( 16.55341960407611168, 4.379528057220329451, 78.95724293864769550 ) ) ;
#129625 = CARTESIAN_POINT ( 'NONE',  ( 4.379528057220339221, -16.55341960407611168, 42.70724293864770260 ) ) ;
#129626 = CARTESIAN_POINT ( 'NONE',  ( 10.72451020669898902, -18.67979575497178502, 57.91557627198103120 ) ) ;
#129627 = CARTESIAN_POINT ( 'NONE',  ( -16.46253265017160317, 9.564922557960807481, 60.83224293864769550 ) ) ;
#129628 = CARTESIAN_POINT ( 'NONE',  ( 21.53943276465977519, -0.05219959533907433946, 68.74890960531435269 ) ) ;
#129629 = CARTESIAN_POINT ( 'NONE',  ( -16.51473224551082808, 9.474510206698731452, 68.33442372801900433 ) ) ;
#129631 = CARTESIAN_POINT ( 'NONE',  ( 12.14591786802309770, 12.06949235617756955, 74.37390960531436690 ) ) ;
#129630 = CARTESIAN_POINT ( 'NONE',  ( -16.46253265017146816, -9.564922557961047289, 29.16775706135232937 ) ) ;
#129632 = CARTESIAN_POINT ( 'NONE',  ( 15.80617190586746368, 15.72974639402197994, 49.37390960531436690 ) ) ;
#129633 = DIRECTION ( 'NONE',  ( 0.000000000000000000, 0.000000000000000000, 1.000000000000000000 ) ) ;
#129635 = CARTESIAN_POINT ( 'NONE',  ( -8.571926809382601320, -26.38167802310801591, 143.7750000027311899 ) ) ;
#129634 = CARTESIAN_POINT ( 'NONE',  ( 4.483927247898790824, -16.52544592524335698, 95.20942372801903275 ) ) ;
#129636 = CARTESIAN_POINT ( 'NONE',  ( -19.03943276465977164, -0.05219959533935918106, 103.7510903946856757 ) ) ;
#129637 = CARTESIAN_POINT ( 'NONE',  ( 8.314922557960818139, 14.29746914071049879, 74.58224293864768129 ) ) ;
#129638 = CARTESIAN_POINT ( 'NONE',  ( -17.50000000000003197, 4.658240926743115295, 33.94470417816803121 ) ) ;
#129639 = CARTESIAN_POINT ( 'NONE',  ( -19.05341960407611168, -5.049401038298163336, 61.45724293864769550 ) ) ;
#129640 = CARTESIAN_POINT ( 'NONE',  ( 16.53943276465976808, -0.05219959533910856209, 58.74890960531436690 ) ) ;
#129641 = CARTESIAN_POINT ( 'NONE',  ( -19.03943276465977164, 0.05219959533909376836, 91.24890960531436690 ) ) ;
#129643 = CARTESIAN_POINT ( 'NONE',  ( 16.51473224551069308, 9.474510206698969483, 59.16557627198102409 ) ) ;
#129642 = CARTESIAN_POINT ( 'NONE',  ( 16.51473224551083163, -9.474510206698727899, 75.83442372801900433 ) ) ;
#129644 = CARTESIAN_POINT ( 'NONE',  ( -5.153800228976328057, -19.02544592524343514, 82.29057627198103830 ) ) ;
#129645 = CARTESIAN_POINT ( 'NONE',  ( 0.05219959533909260263, 19.03943276465977164, 74.99890960531435269 ) ) ;
#129646 = CARTESIAN_POINT ( 'NONE',  ( -15.80617190586745835, -15.72974639402198527, 66.87390960531436690 ) ) ;
#129647 = CARTESIAN_POINT ( 'NONE',  ( 4.379528057220092307, 16.55341960407617563, 62.29275706135236845 ) ) ;
#129648 = CARTESIAN_POINT ( 'NONE',  ( -13.97604488694547520, 13.89961937509957934, 103.1260903946856615 ) ) ;
#129649 = CARTESIAN_POINT ( 'NONE',  ( 19.05341960407611168, 5.049401038298154454, 43.95724293864769550 ) ) ;
#129650 = CARTESIAN_POINT ( 'NONE',  ( 21.53943276465977519, -0.05219959533907433946, 53.74890960531437401 ) ) ;
#129651 = CARTESIAN_POINT ( 'NONE',  ( 19.03943276465977164, 0.05219959533936151252, 86.25109039468567573 ) ) ;
#129652 = CARTESIAN_POINT ( 'NONE',  ( -14.34966873604960291, -8.224510206698953496, 31.66557627198102054 ) ) ;
#129653 = CARTESIAN_POINT ( 'NONE',  ( -9.474510206698720793, -16.51473224551083518, 39.58442372801899722 ) ) ;
#129655 = CARTESIAN_POINT ( 'NONE',  ( -4.483927247898782831, 16.52544592524335698, 97.70942372801904696 ) ) ;
#129654 = CARTESIAN_POINT ( 'NONE',  ( -8.314922557961024197, 14.29746914071037800, 62.91775706135236135 ) ) ;
#129656 = DIRECTION ( 'NONE',  ( 1.000000000000000000, 0.000000000000000000, 0.000000000000000000 ) ) ;
#129657 = CARTESIAN_POINT ( 'NONE',  ( -12.06949235617739369, -12.14591786802326823, 84.37609039468570415 ) ) ;
#129658 = CARTESIAN_POINT ( 'NONE',  ( -5.823673210054116645, -21.52544592524344225, 22.29057627198102765 ) ) ;
#129659 = CARTESIAN_POINT ( 'NONE',  ( -19.02544592524342804, 5.153800228976336051, 41.04057627198103120 ) ) ;
#129660 = CARTESIAN_POINT ( 'NONE',  ( -19.02544592524342804, 5.153800228976336051, 51.04057627198103120 ) ) ;
#129661 = CARTESIAN_POINT ( 'NONE',  ( 16.51473224551069308, 9.474510206698969483, 44.16557627198103120 ) ) ;
#129662 = CARTESIAN_POINT ( 'NONE',  ( -5.719274019375665041, -21.55341960407619695, 44.79275706135234714 ) ) ;
#129663 = CARTESIAN_POINT ( 'NONE',  ( 4.483927247898790824, -16.52544592524335698, 55.20942372801902565 ) ) ;
#129664 = CARTESIAN_POINT ( 'NONE',  ( 12.14591786802309770, 12.06949235617756955, 24.37390960531435979 ) ) ;
#129665 = CARTESIAN_POINT ( 'NONE',  ( 5.049401038298161559, -19.05341960407611168, 27.70724293864769550 ) ) ;
#129666 = CARTESIAN_POINT ( 'NONE',  ( 10.72451020669871369, 18.67979575497193778, 112.0844237280190185 ) ) ;
#129667 = CARTESIAN_POINT ( 'NONE',  ( 16.52544592524335698, 4.483927247898782831, 21.45942372801901499 ) ) ;
#129668 = CARTESIAN_POINT ( 'NONE',  ( -9.474510206698720793, -16.51473224551083518, 74.58442372801900433 ) ) ;
#129669 = CARTESIAN_POINT ( 'NONE',  ( 14.34966873604960469, 8.224510206698951720, 64.16557627198102409 ) ) ;
#129670 = CARTESIAN_POINT ( 'NONE',  ( -0.05219959533909027116, -19.03943276465977164, 37.49890960531436690 ) ) ;
#129671 = CARTESIAN_POINT ( 'NONE',  ( 5.153800228976615827, -19.02544592524334988, 80.20942372801901854 ) ) ;
#129672 = CARTESIAN_POINT ( 'NONE',  ( -10.81492255796105439, 18.62759615963255655, 77.91775706135231871 ) ) ;
#129673 = CARTESIAN_POINT ( 'NONE',  ( -0.05219959533934338120, 16.53943276465976808, 37.50109039468568284 ) ) ;
#129674 = CARTESIAN_POINT ( 'NONE',  ( -27.86273085795036408, -28.69962071417357663, -15.00000000000000178 ) ) ;
#129675 = CARTESIAN_POINT ( 'NONE',  ( -21.55341960407610458, -5.719274019375992779, 41.45724293864769550 ) ) ;
#129676 = CARTESIAN_POINT ( 'NONE',  ( -8.224510206698735004, -14.34966873604973081, 29.58442372801901854 ) ) ;
#129677 = CARTESIAN_POINT ( 'NONE',  ( 18.09918380851992836, 5.500000000000035527, 88.98618307335613054 ) ) ;
#129678 = CARTESIAN_POINT ( 'NONE',  ( -5.823673210054431948, 21.52544592524334988, 112.7094237280190328 ) ) ;
#129679 = CARTESIAN_POINT ( 'NONE',  ( -26.77293948118379063, 6.014770499723010033, 169.2063755025576199 ) ) ;
#129680 = CARTESIAN_POINT ( 'NONE',  ( 9.564922557960805705, 16.46253265017160317, 34.58224293864770260 ) ) ;
#129681 = CARTESIAN_POINT ( 'NONE',  ( 69.65682714487590488, -71.74905178543389184, -15.00000000000000178 ) ) ;
#129682 = CARTESIAN_POINT ( 'NONE',  ( -16.51473224551069308, -9.474510206698971260, 56.66557627198103120 ) ) ;
#129683 = CARTESIAN_POINT ( 'NONE',  ( 18.62759615963255655, 10.81492255796105972, 61.66775706135235424 ) ) ;
#129684 = ADVANCED_FACE ( 'NONE', ( #161001 ), #113480, .T. ) ;
#129685 = CARTESIAN_POINT ( 'NONE',  ( 9.474510206698729675, 16.51473224551082808, 22.08442372801899722 ) ) ;
#129686 = CARTESIAN_POINT ( 'NONE',  ( -12.06949235617756955, 12.14591786802309770, 30.62390960531436335 ) ) ;
#129687 = CARTESIAN_POINT ( 'NONE',  ( -13.89961937509977652, 13.97604488694528158, 25.62390960531434558 ) ) ;
#129688 = CARTESIAN_POINT ( 'NONE',  ( 0.05219959533909260263, 19.03943276465977164, 89.99890960531436690 ) ) ;
#129689 = CARTESIAN_POINT ( 'NONE',  ( 5.719274019375673035, 21.55341960407619339, 57.29275706135234714 ) ) ;
#129690 = CARTESIAN_POINT ( 'NONE',  ( 16.51473224551069308, 9.474510206698969483, 34.16557627198102409 ) ) ;
#129691 = CARTESIAN_POINT ( 'NONE',  ( 18.67979575497194134, -10.72451020669871369, 65.83442372801900433 ) ) ;
#129693 = CARTESIAN_POINT ( 'NONE',  ( -16.51473224551069308, -9.474510206698971260, 106.6655762719810383 ) ) ;
#129692 = CARTESIAN_POINT ( 'NONE',  ( -5.049401038297874678, -19.05341960407617918, 89.79275706135230450 ) ) ;
#129694 = CARTESIAN_POINT ( 'NONE',  ( -4.483927247898539470, -16.52544592524342804, 112.2905762719810241 ) ) ;
#129695 = CARTESIAN_POINT ( 'NONE',  ( 21.53943276465977519, -0.05219959533907433946, 113.7489096053143527 ) ) ;
#129696 = CARTESIAN_POINT ( 'NONE',  ( -13.97604488694547697, 13.89961937509957934, 38.12609039468566152 ) ) ;
#129697 = CARTESIAN_POINT ( 'NONE',  ( -4.483927247898539470, -16.52544592524342804, 107.2905762719810525 ) ) ;
#129698 = CARTESIAN_POINT ( 'NONE',  ( 16.51473224551069308, 9.474510206698969483, 59.16557627198102409 ) ) ;
#129699 = CARTESIAN_POINT ( 'NONE',  ( 19.03943276465977164, 0.05219959533936151252, 96.25109039468567573 ) ) ;
#129700 = CARTESIAN_POINT ( 'NONE',  ( 16.52544592524342804, -4.483927247898539470, 63.54057627198103830 ) ) ;
#129701 = CARTESIAN_POINT ( 'NONE',  ( -9.564922557961040184, 16.46253265017147172, 32.91775706135233293 ) ) ;
#129702 = CARTESIAN_POINT ( 'NONE',  ( -5.719274019375978568, 21.55341960407610458, 25.20724293864769550 ) ) ;
#129703 = B_SPLINE_CURVE_WITH_KNOTS ( 'NONE', 3,
 ( #65388, #173584, #19885, #2727, #36041, #94732 ),
 .UNSPECIFIED., .F., .F.,
 ( 4, 2, 4 ),
 ( 0.007228050697041655918, 0.007608510107495138411, 0.007988969517948621771 ),
 .UNSPECIFIED. ) ;
#129704 = CARTESIAN_POINT ( 'NONE',  ( -9.474510206698720793, -16.51473224551083518, 89.58442372801900433 ) ) ;
#129705 = CARTESIAN_POINT ( 'NONE',  ( -10.72451020669898014, 18.67979575497178502, 85.41557627198102409 ) ) ;
#129706 = CARTESIAN_POINT ( 'NONE',  ( -18.62759615963255300, -10.81492255796106328, 39.16775706135235424 ) ) ;
#129707 = CARTESIAN_POINT ( 'NONE',  ( 8.224510206698742110, 14.34966873604972548, 37.08442372801901143 ) ) ;
#129709 = CARTESIAN_POINT ( 'NONE',  ( 21.52544592524334988, 5.823673210054432836, 51.45942372801901854 ) ) ;
#129708 = CARTESIAN_POINT ( 'NONE',  ( -14.34966873604972548, 8.224510206698743886, 38.33442372801900433 ) ) ;
#129710 = CARTESIAN_POINT ( 'NONE',  ( -5.719274019375978568, 21.55341960407610458, 60.20724293864768839 ) ) ;
#129711 = CARTESIAN_POINT ( 'NONE',  ( 19.02544592524343514, -5.153800228976328945, 33.54057627198102409 ) ) ;
#129712 = CARTESIAN_POINT ( 'NONE',  ( -11.74264578624799782, -36.14014761921581709, -5.349999994537626868 ) ) ;
#129713 = CARTESIAN_POINT ( 'NONE',  ( 8.224510206698742110, 14.34966873604972548, 82.08442372801901854 ) ) ;
#129714 = CARTESIAN_POINT ( 'NONE',  ( 10.72451020669898902, -18.67979575497178502, 92.91557627198103830 ) ) ;
#129715 = CARTESIAN_POINT ( 'NONE',  ( -0.05219959533910754901, -16.53943276465976808, 42.49890960531435979 ) ) ;
#129716 = CARTESIAN_POINT ( 'NONE',  ( -4.379528057220086978, -16.55341960407618274, 59.79275706135234714 ) ) ;
#129717 = CARTESIAN_POINT ( 'NONE',  ( -13.97604488694547697, 13.89961937509957934, 103.1260903946856473 ) ) ;
#129718 = CARTESIAN_POINT ( 'NONE',  ( 5.719274019375991003, -21.55341960407610458, 92.70724293864770971 ) ) ;
#129719 = CARTESIAN_POINT ( 'NONE',  ( -8.314922557960811034, -14.29746914071050412, 32.08224293864769550 ) ) ;
#129720 = ORIENTED_EDGE ( 'NONE', *, *, #192515, .F. ) ;
#129721 = CARTESIAN_POINT ( 'NONE',  ( 4.379528057220092307, 16.55341960407617563, 77.29275706135234714 ) ) ;
#129722 = CARTESIAN_POINT ( 'NONE',  ( 25.11239783071223997, 12.35465959875007336, 166.1131185557730987 ) ) ;
#129723 = CARTESIAN_POINT ( 'NONE',  ( -15.72974639402197994, 15.80617190586746368, 80.62390960531438111 ) ) ;
#129724 = CARTESIAN_POINT ( 'NONE',  ( -12.06949235617739369, -12.14591786802326823, 109.3760903946857042 ) ) ;
#129725 = ORIENTED_EDGE ( 'NONE', *, *, #47442, .F. ) ;
#129726 = CARTESIAN_POINT ( 'NONE',  ( -26.03370437638690049, -6.875205692009850544, 160.5968874236872637 ) ) ;
#129727 = CARTESIAN_POINT ( 'NONE',  ( -10.72451020669898014, 18.67979575497178502, 100.4155762719810241 ) ) ;
#129728 = CARTESIAN_POINT ( 'NONE',  ( -21.52544592524343514, 5.823673210054127303, 106.0405762719810525 ) ) ;
#129729 = CARTESIAN_POINT ( 'NONE',  ( 14.34966873604960469, 8.224510206698951720, 34.16557627198102409 ) ) ;
#129730 = CARTESIAN_POINT ( 'NONE',  ( 14.29746914071037800, 8.314922557961029526, 41.66775706135235424 ) ) ;
#129731 = CARTESIAN_POINT ( 'NONE',  ( -0.05219959533909027116, -19.03943276465977164, 42.49890960531435269 ) ) ;
#129732 = CARTESIAN_POINT ( 'NONE',  ( -13.97604488694527625, -13.89961937509977652, 61.87390960531435979 ) ) ;
#129733 = CARTESIAN_POINT ( 'NONE',  ( -18.67979575497178146, -10.72451020669898902, 21.66557627198102409 ) ) ;
#129734 = CARTESIAN_POINT ( 'NONE',  ( -5.153800228976328057, -19.02544592524343514, 112.2905762719810099 ) ) ;
#129735 = CARTESIAN_POINT ( 'NONE',  ( -16.51473224551082808, 9.474510206698731452, 108.3344237280190043 ) ) ;
#129736 = CARTESIAN_POINT ( 'NONE',  ( 19.02544592524334988, 5.153800228976608722, 51.45942372801900433 ) ) ;
#129737 = CARTESIAN_POINT ( 'NONE',  ( 5.719274019375991003, -21.55341960407610458, 82.70724293864770971 ) ) ;
#129738 = CARTESIAN_POINT ( 'NONE',  ( -16.55341960407611168, -4.379528057220339221, 21.45724293864769550 ) ) ;
#129739 = VECTOR ( 'NONE', #9293, 1000.000000000000000 ) ;
#129740 = CARTESIAN_POINT ( 'NONE',  ( 15.80617190586746368, 15.72974639402197994, 44.37390960531435979 ) ) ;
#129742 = CARTESIAN_POINT ( 'NONE',  ( 13.97604488694548053, -13.89961937509957401, 110.6260903946856615 ) ) ;
#129741 = CARTESIAN_POINT ( 'NONE',  ( -18.67979575497178146, -10.72451020669898902, 86.66557627198102409 ) ) ;
#129743 = CARTESIAN_POINT ( 'NONE',  ( -10.72451020669898014, 18.67979575497178502, 25.41557627198103120 ) ) ;
#129744 = CARTESIAN_POINT ( 'NONE',  ( 18.62759615963255655, 10.81492255796105972, 71.66775706135234714 ) ) ;
#129745 = CARTESIAN_POINT ( 'NONE',  ( -13.97604488694527625, -13.89961937509977652, 71.87390960531433848 ) ) ;
#129746 = CARTESIAN_POINT ( 'NONE',  ( 28.90000000000004476, 0.000000000000000000, -49.67367017693150189 ) ) ;
#129747 = CARTESIAN_POINT ( 'NONE',  ( -9.474510206698964154, 16.51473224551069663, 75.41557627198103830 ) ) ;
#129748 = CARTESIAN_POINT ( 'NONE',  ( -12.06949235617756955, 12.14591786802309770, 85.62390960531436690 ) ) ;
#129749 = ORIENTED_EDGE ( 'NONE', *, *, #117794, .T. ) ;
#129750 = CARTESIAN_POINT ( 'NONE',  ( 9.564922557961047289, -16.46253265017146816, 105.4177570613523471 ) ) ;
#129751 = CARTESIAN_POINT ( 'NONE',  ( 17.31728774477273447, -6.344390552232386682, 83.31906651689317300 ) ) ;
#129752 = CARTESIAN_POINT ( 'NONE',  ( 16.46253265017160672, -9.564922557960803928, 73.33224293864769550 ) ) ;
#129754 = CARTESIAN_POINT ( 'NONE',  ( 19.03943276465977164, -0.05219959533909143690, 103.7489096053143669 ) ) ;
#129753 = CARTESIAN_POINT ( 'NONE',  ( 21.55341960407619695, -5.719274019375665929, 86.04275706135236135 ) ) ;
#129755 = CARTESIAN_POINT ( 'NONE',  ( -12.14591786802326823, 12.06949235617739902, 73.12609039468567573 ) ) ;
#129756 = DIRECTION ( 'NONE',  ( 0.1045284632676537068, 0.000000000000000000, 0.9945218953682734009 ) ) ;
#129757 = CARTESIAN_POINT ( 'NONE',  ( 16.46253265017146816, 9.564922557961045513, 61.66775706135234003 ) ) ;
#129758 = CARTESIAN_POINT ( 'NONE',  ( 9.474510206698729675, 16.51473224551082808, 22.08442372801899722 ) ) ;
#129759 = CARTESIAN_POINT ( 'NONE',  ( -28.79475375365586842, 2.428612866367529932E-14, 143.9843446568999923 ) ) ;
#129760 = FACE_OUTER_BOUND ( 'NONE', #10445, .T. ) ;
#129761 = CARTESIAN_POINT ( 'NONE',  ( 29.86685920354754842, -21.69954338932559068, -4.324999997268814234 ) ) ;
#129762 = CARTESIAN_POINT ( 'NONE',  ( 14.34966873604960469, 8.224510206698951720, 29.16557627198103120 ) ) ;
#129763 = CYLINDRICAL_SURFACE ( 'NONE', #101748, 0.5000000000000006661 ) ;
#129764 = CARTESIAN_POINT ( 'NONE',  ( -8.314922557961024197, 14.29746914071037800, 112.9177570613523329 ) ) ;
#129765 = CARTESIAN_POINT ( 'NONE',  ( 16.20579543436677739, 7.371946100355112996, 68.06520834171880097 ) ) ;
#129766 = CARTESIAN_POINT ( 'NONE',  ( -16.53943276465976808, -0.05219959533934237506, 78.75109039468568994 ) ) ;
#129767 = CARTESIAN_POINT ( 'NONE',  ( 5.823673210054444382, -21.52544592524334988, 85.20942372801901854 ) ) ;
#129768 = CARTESIAN_POINT ( 'NONE',  ( 16.46253265017146816, 9.564922557961045513, 91.66775706135234714 ) ) ;
#129769 = CARTESIAN_POINT ( 'NONE',  ( 19.02544592524334988, 5.153800228976608722, 46.45942372801899012 ) ) ;
#129770 = CARTESIAN_POINT ( 'NONE',  ( 19.03943276465977164, -0.05219959533909143690, 73.74890960531435269 ) ) ;
#129771 = CARTESIAN_POINT ( 'NONE',  ( -0.05219959533909027116, -19.03943276465977164, 52.49890960531436690 ) ) ;
#129772 = CARTESIAN_POINT ( 'NONE',  ( 17.60769864724390388, -5.499999999999978684, 41.15024842019165874 ) ) ;
#129773 = CARTESIAN_POINT ( 'NONE',  ( 10.81492255796078972, 18.62759615963270932, 89.58224293864768129 ) ) ;
#129774 = CARTESIAN_POINT ( 'NONE',  ( -5.719274019375978568, 21.55341960407610458, 45.20724293864769550 ) ) ;
#129775 = CARTESIAN_POINT ( 'NONE',  ( -16.51473224551069308, -9.474510206698971260, 51.66557627198102409 ) ) ;
#129776 = CARTESIAN_POINT ( 'NONE',  ( -8.314922557961024197, 14.29746914071037800, 67.91775706135234714 ) ) ;
#129777 = ORIENTED_EDGE ( 'NONE', *, *, #117749, .F. ) ;
#129778 = CARTESIAN_POINT ( 'NONE',  ( 21.53943276465977519, 0.05219959533937863772, 46.25109039468567573 ) ) ;
#129780 = CARTESIAN_POINT ( 'NONE',  ( -22.81625015709509441, -31.40387420917324590, -10.32499999726881157 ) ) ;
#129779 = CARTESIAN_POINT ( 'NONE',  ( 16.55341960407611168, 4.379528057220329451, 63.95724293864770260 ) ) ;
#129781 = CARTESIAN_POINT ( 'NONE',  ( -8.224510206698735004, -14.34966873604973081, 39.58442372801901143 ) ) ;
#129782 = CARTESIAN_POINT ( 'NONE',  ( 4.379528057220339221, -16.55341960407611168, 107.7072429386476955 ) ) ;
#129783 = CARTESIAN_POINT ( 'NONE',  ( 19.03943276465977164, 0.05219959533936151252, 56.25109039468566863 ) ) ;
#129784 = CARTESIAN_POINT ( 'NONE',  ( 8.224510206698953496, -14.34966873604960469, 67.91557627198102409 ) ) ;
#129785 = CARTESIAN_POINT ( 'NONE',  ( -10.72451020669870658, -18.67979575497194134, 29.58442372801901854 ) ) ;
#129787 = CARTESIAN_POINT ( 'NONE',  ( -21.53943276465977519, 0.05219959533907696930, 86.24890960531436690 ) ) ;
#129786 = CARTESIAN_POINT ( 'NONE',  ( 16.46253265017160672, -9.564922557960803928, 28.33224293864769550 ) ) ;
#129788 = CARTESIAN_POINT ( 'NONE',  ( 19.03943276465977164, -0.05219959533909143690, 103.7489096053143669 ) ) ;
#129789 = CARTESIAN_POINT ( 'NONE',  ( -12.14591786802309592, -12.06949235617757132, 76.87390960531439532 ) ) ;
#129790 = CARTESIAN_POINT ( 'NONE',  ( 13.89961937509977652, -13.97604488694527269, 113.1239096053143527 ) ) ;
#129791 = CARTESIAN_POINT ( 'NONE',  ( 29.86685920354754842, -21.69954338932559068, -5.824999997268813345 ) ) ;
#129792 = CARTESIAN_POINT ( 'NONE',  ( 9.564922557961047289, -16.46253265017146816, 80.41775706135234714 ) ) ;
#129793 = CARTESIAN_POINT ( 'NONE',  ( 5.719274019375673035, 21.55341960407619339, 27.29275706135234358 ) ) ;
#129794 = CARTESIAN_POINT ( 'NONE',  ( -5.049401038298153566, 19.05341960407611168, 65.20724293864765286 ) ) ;
#129795 = CARTESIAN_POINT ( 'NONE',  ( -5.153800228976607833, 19.02544592524334988, 52.70942372801900433 ) ) ;
#129796 = CARTESIAN_POINT ( 'NONE',  ( -9.474510206698964154, 16.51473224551069663, 30.41557627198102054 ) ) ;
#129797 = CARTESIAN_POINT ( 'NONE',  ( 18.67979575497194134, -10.72451020669871369, 75.83442372801900433 ) ) ;
#129798 = CARTESIAN_POINT ( 'NONE',  ( 4.483927247898545687, 16.52544592524342804, 64.79057627198103830 ) ) ;
#129799 = CARTESIAN_POINT ( 'NONE',  ( -16.53943276465976808, 0.05219959533911058130, 56.24890960531436690 ) ) ;
#129800 = CARTESIAN_POINT ( 'NONE',  ( 16.51473224551069308, 9.474510206698969483, 59.16557627198102409 ) ) ;
#129801 = CARTESIAN_POINT ( 'NONE',  ( 10.81492255796078972, 18.62759615963270932, 89.58224293864768129 ) ) ;
#129802 = CARTESIAN_POINT ( 'NONE',  ( 5.153800228976335163, 19.02544592524342804, 59.79057627198100988 ) ) ;
#129803 = VERTEX_POINT ( 'NONE', #5306 ) ;
#129804 = CARTESIAN_POINT ( 'NONE',  ( -15.72974639402197994, 15.80617190586746368, 75.62390960531439532 ) ) ;
#129805 = CARTESIAN_POINT ( 'NONE',  ( 10.81492255796106328, -18.62759615963255655, 105.4177570613523613 ) ) ;
#129808 = CARTESIAN_POINT ( 'NONE',  ( -12.14591786802309592, -12.06949235617757132, 91.87390960531436690 ) ) ;
#129807 = CARTESIAN_POINT ( 'NONE',  ( 16.53943276465976808, 0.05219959533934440121, 106.2510903946856757 ) ) ;
#129806 = CARTESIAN_POINT ( 'NONE',  ( 13.97604488694527802, 13.89961937509977652, 29.37390960531435979 ) ) ;
#129809 = CARTESIAN_POINT ( 'NONE',  ( 19.03943276465977164, 0.05219959533936151252, 96.25109039468567573 ) ) ;
#129810 = VERTEX_POINT ( 'NONE', #66990 ) ;
#129811 = CARTESIAN_POINT ( 'NONE',  ( 21.55341960407610458, 5.719274019375980345, 113.9572429386477239 ) ) ;
#129812 = CARTESIAN_POINT ( 'NONE',  ( -19.02544592524334988, -5.153800228976617603, 58.95942372801900433 ) ) ;
#129813 = CARTESIAN_POINT ( 'NONE',  ( -0.05219959533934338120, 16.53943276465976808, 102.5010903946856899 ) ) ;
#129814 = CARTESIAN_POINT ( 'NONE',  ( -19.02544592524334988, -5.153800228976617603, 33.95942372801897591 ) ) ;
#129815 = CARTESIAN_POINT ( 'NONE',  ( -9.564922557960796823, -16.46253265017161027, 107.0822429386476955 ) ) ;
#129816 = CARTESIAN_POINT ( 'NONE',  ( 18.62759615963271287, -10.81492255796078972, 63.33224293864770260 ) ) ;
#129817 = CYLINDRICAL_SURFACE ( 'NONE', #5599, 0.5000000000000004441 ) ;
#129818 = CARTESIAN_POINT ( 'NONE',  ( -19.02544592524342804, 5.153800228976336051, 31.04057627198102409 ) ) ;
#129819 = CARTESIAN_POINT ( 'NONE',  ( -0.05219959533937732626, 21.53943276465977519, 102.5010903946856899 ) ) ;
#129820 = CARTESIAN_POINT ( 'NONE',  ( 12.06949235617739724, 12.14591786802326823, 76.87609039468567573 ) ) ;
#129821 = CARTESIAN_POINT ( 'NONE',  ( -10.72451020669870658, -18.67979575497194134, 24.58442372801901499 ) ) ;
#129822 = CARTESIAN_POINT ( 'NONE',  ( -12.06949235617739369, -12.14591786802326823, 39.37609039468567573 ) ) ;
#129823 = CARTESIAN_POINT ( 'NONE',  ( 19.05341960407611168, 5.049401038298154454, 108.9572429386477097 ) ) ;
#129824 = CARTESIAN_POINT ( 'NONE',  ( -13.89961937509977652, 13.97604488694528158, 50.62390960531435979 ) ) ;
#129825 = CARTESIAN_POINT ( 'NONE',  ( 5.049401038298161559, -19.05341960407611168, 67.70724293864769550 ) ) ;
#129826 = CARTESIAN_POINT ( 'NONE',  ( -12.14591786802326823, 12.06949235617739902, 53.12609039468568284 ) ) ;
#129827 = CARTESIAN_POINT ( 'NONE',  ( -14.34966873604960291, -8.224510206698953496, 91.66557627198103830 ) ) ;
#129828 = CARTESIAN_POINT ( 'NONE',  ( -14.29746914071037622, -8.314922557961029526, 104.1677570613523471 ) ) ;
#129829 = CARTESIAN_POINT ( 'NONE',  ( -18.22780087662122028, 5.500000000000031086, 58.51540105326107977 ) ) ;
#129832 = CARTESIAN_POINT ( 'NONE',  ( 13.97604488694527802, 13.89961937509977652, 64.37390960531436690 ) ) ;
#129831 = CARTESIAN_POINT ( 'NONE',  ( 5.153800228976335163, 19.02544592524342804, 84.79057627198099567 ) ) ;
#129830 = CARTESIAN_POINT ( 'NONE',  ( -18.67979575497193778, 10.72451020669871902, 53.33442372801901854 ) ) ;
#129833 = CARTESIAN_POINT ( 'NONE',  ( -19.03943276465977164, 0.05219959533909376836, 91.24890960531436690 ) ) ;
#129834 = CARTESIAN_POINT ( 'NONE',  ( -8.314922557960811034, -14.29746914071050412, 42.08224293864769550 ) ) ;
#129835 = CARTESIAN_POINT ( 'NONE',  ( 0.05219959533934541429, -16.53943276465976808, 95.00109039468568994 ) ) ;
#129836 = CARTESIAN_POINT ( 'NONE',  ( -16.52544592524342804, 4.483927247898546575, 41.04057627198103120 ) ) ;
#129837 = ORIENTED_EDGE ( 'NONE', *, *, #46651, .F. ) ;
#129838 = CARTESIAN_POINT ( 'NONE',  ( 16.51473224551083163, -9.474510206698727899, 50.83442372801899722 ) ) ;
#129839 = CARTESIAN_POINT ( 'NONE',  ( -0.05219959533909027116, -19.03943276465977164, 107.4989096053143527 ) ) ;
#129840 = CARTESIAN_POINT ( 'NONE',  ( 19.02544592524343514, -5.153800228976328945, 58.54057627198102409 ) ) ;
#129841 = CARTESIAN_POINT ( 'NONE',  ( 13.89961937509957401, 13.97604488694547697, 41.87609039468566152 ) ) ;
#129842 = CARTESIAN_POINT ( 'NONE',  ( -36.91746825000000598, 2.428612866367529932E-14, -0.6249999972688132788 ) ) ;
#129843 = CARTESIAN_POINT ( 'NONE',  ( 17.49999999999999645, 5.500000000000009770, 58.78230962303567253 ) ) ;
#129845 = CARTESIAN_POINT ( 'NONE',  ( 14.34966873604972726, -8.224510206698740333, 75.83442372801900433 ) ) ;
#129844 = CARTESIAN_POINT ( 'NONE',  ( -19.02544592524334988, -5.153800228976617603, 88.95942372801897591 ) ) ;
#129846 = CARTESIAN_POINT ( 'NONE',  ( 16.19135201231366139, 7.376712067591940425, 92.68680854052028906 ) ) ;
#129847 = CARTESIAN_POINT ( 'NONE',  ( 9.564922557960805705, 16.46253265017160317, 94.58224293864769550 ) ) ;
#129848 = CARTESIAN_POINT ( 'NONE',  ( 18.67979575497194134, -10.72451020669871369, 30.83442372801902209 ) ) ;
#129849 = CARTESIAN_POINT ( 'NONE',  ( 13.89961937509957401, 13.97604488694547697, 76.87609039468566152 ) ) ;
#129851 = CARTESIAN_POINT ( 'NONE',  ( 9.474510206698971260, -16.51473224551069308, 52.91557627198102409 ) ) ;
#129850 = CARTESIAN_POINT ( 'NONE',  ( 0.05219959533909260263, 19.03943276465977164, 114.9989096053143669 ) ) ;
#129852 = EDGE_CURVE ( 'NONE', #196867, #69099, #177498, .T. ) ;
#129853 = CARTESIAN_POINT ( 'NONE',  ( -5.049401038298153566, 19.05341960407611168, 95.20724293864770971 ) ) ;
#129855 = CARTESIAN_POINT ( 'NONE',  ( 0.05219959533909260263, 19.03943276465977164, 39.99890960531436690 ) ) ;
#129854 = CARTESIAN_POINT ( 'NONE',  ( 4.379528057220339221, -16.55341960407611168, 52.70724293864769550 ) ) ;
#129856 = CARTESIAN_POINT ( 'NONE',  ( 19.05341960407617918, -5.049401038297876454, 56.04275706135234714 ) ) ;
#129857 = CARTESIAN_POINT ( 'NONE',  ( 14.34966873604960469, 8.224510206698951720, 84.16557627198103830 ) ) ;
#129858 = CARTESIAN_POINT ( 'NONE',  ( 16.46253265017146816, 9.564922557961045513, 36.66775706135233293 ) ) ;
#129859 = CARTESIAN_POINT ( 'NONE',  ( 5.049401038298161559, -19.05341960407611168, 72.70724293864768129 ) ) ;
#129860 = CARTESIAN_POINT ( 'NONE',  ( 21.53943276465977519, -0.05219959533907433946, 68.74890960531435269 ) ) ;
#129862 = CARTESIAN_POINT ( 'NONE',  ( 9.474510206698729675, 16.51473224551082808, 27.08442372801900433 ) ) ;
#129861 = CARTESIAN_POINT ( 'NONE',  ( -12.14591786802309592, -12.06949235617757132, 51.87390960531437401 ) ) ;
#129863 = CARTESIAN_POINT ( 'NONE',  ( -16.51473224551069308, -9.474510206698971260, 106.6655762719810383 ) ) ;
#129864 = CARTESIAN_POINT ( 'NONE',  ( -21.53943276465977519, 0.05219959533907696930, 31.24890960531435979 ) ) ;
#129865 = CARTESIAN_POINT ( 'NONE',  ( -19.05341960407611168, -5.049401038298163336, 46.45724293864768129 ) ) ;
#129866 = CARTESIAN_POINT ( 'NONE',  ( -13.97604488694527625, -13.89961937509977652, 41.87390960531435979 ) ) ;
#129867 = CARTESIAN_POINT ( 'NONE',  ( 16.53943276465976808, -0.05219959533910856209, 98.74890960531438111 ) ) ;
#129868 = CARTESIAN_POINT ( 'NONE',  ( 18.62759615963271287, -10.81492255796078972, 108.3322429386477097 ) ) ;
#129869 = CARTESIAN_POINT ( 'NONE',  ( -9.474510206698964154, 16.51473224551069663, 105.4155762719810383 ) ) ;
#129870 = CARTESIAN_POINT ( 'NONE',  ( 10.72451020669898902, -18.67979575497178502, 107.9155762719810241 ) ) ;
#129871 = CARTESIAN_POINT ( 'NONE',  ( 19.03943276465977164, -0.05219959533909143690, 98.74890960531436690 ) ) ;
#129872 = CARTESIAN_POINT ( 'NONE',  ( 4.379528057220339221, -16.55341960407611168, 112.7072429386476955 ) ) ;
#129873 = CARTESIAN_POINT ( 'NONE',  ( 15.80617190586769283, -15.72974639402175789, 80.62609039468567573 ) ) ;
#129874 = CARTESIAN_POINT ( 'NONE',  ( -5.719274019375978568, 21.55341960407610458, 90.20724293864770971 ) ) ;
#129875 = CARTESIAN_POINT ( 'NONE',  ( 16.61371651742600974, -7.165104196376164580, 106.3541506999299742 ) ) ;
#129876 = CARTESIAN_POINT ( 'NONE',  ( 0.3535533905931680931, -30.00000000000000355, 4.646446609406719830 ) ) ;
#129877 = CARTESIAN_POINT ( 'NONE',  ( 13.97604488694527802, 13.89961937509977830, 59.37390960531435979 ) ) ;
#129878 = CARTESIAN_POINT ( 'NONE',  ( -12.14591786802326823, 12.06949235617739902, 43.12609039468568284 ) ) ;
#129879 = CARTESIAN_POINT ( 'NONE',  ( -4.379528057220328563, 16.55341960407611168, 105.2072429386477097 ) ) ;
#129880 = CARTESIAN_POINT ( 'NONE',  ( -2.577820198429831642E-15, -9.100000000000001421, -61.89430850415821794 ) ) ;
#129881 = CARTESIAN_POINT ( 'NONE',  ( -16.46253265017160317, 9.564922557960807481, 60.83224293864769550 ) ) ;
#129882 = CARTESIAN_POINT ( 'NONE',  ( 8.314922557960818139, 14.29746914071049879, 99.58224293864770971 ) ) ;
#129883 = CARTESIAN_POINT ( 'NONE',  ( -10.72451020669898014, 18.67979575497178502, 30.41557627198101699 ) ) ;
#129884 = CARTESIAN_POINT ( 'NONE',  ( -16.53943276465976808, 0.05219959533911058130, 71.24890960531435269 ) ) ;
#129885 = CARTESIAN_POINT ( 'NONE',  ( -19.05341960407617563, 5.049401038297882671, 113.5427570613523471 ) ) ;
#129886 = CARTESIAN_POINT ( 'NONE',  ( -18.62759615963255300, -10.81492255796106328, 79.16775706135234714 ) ) ;
#129887 = CARTESIAN_POINT ( 'NONE',  ( 16.36317988757058117, -7.306389748694916975, 76.59789608363225000 ) ) ;
#129888 = CARTESIAN_POINT ( 'NONE',  ( 0.05219959533934541429, -16.53943276465976808, 100.0010903946857042 ) ) ;
#129889 = CARTESIAN_POINT ( 'NONE',  ( -14.34966873604960291, -8.224510206698953496, 46.66557627198102409 ) ) ;
#129890 = CARTESIAN_POINT ( 'NONE',  ( -0.05219959533909027116, -19.03943276465977164, 37.49890960531436690 ) ) ;
#129891 = CARTESIAN_POINT ( 'NONE',  ( -9.564922557960796823, -16.46253265017161027, 92.08224293864769550 ) ) ;
#129892 = CARTESIAN_POINT ( 'NONE',  ( 10.72451020669898902, -18.67979575497178502, 97.91557627198103830 ) ) ;
#129893 = CARTESIAN_POINT ( 'NONE',  ( 16.55341960407618274, -4.379528057220086978, 21.04275706135234714 ) ) ;
#129895 = CARTESIAN_POINT ( 'NONE',  ( -10.72451020669870658, -18.67979575497194134, 69.58442372801900433 ) ) ;
#129894 = CARTESIAN_POINT ( 'NONE',  ( -12.06949235617756955, 12.14591786802309770, 65.62390960531436690 ) ) ;
#129896 = CARTESIAN_POINT ( 'NONE',  ( 16.52544592524335698, 4.483927247898782831, 106.4594237280190328 ) ) ;
#129897 = CARTESIAN_POINT ( 'NONE',  ( 17.13100169013300444, 6.664070546373170423, 26.73210164300153835 ) ) ;
#129898 = LINE ( 'NONE', #37922, #177800 ) ;
#129899 = CARTESIAN_POINT ( 'NONE',  ( -16.55341960407611168, -4.379528057220339221, 31.45724293864769550 ) ) ;
#129900 = CARTESIAN_POINT ( 'NONE',  ( 16.52544592524335698, 4.483927247898782831, 71.45942372801901854 ) ) ;
#129901 = CARTESIAN_POINT ( 'NONE',  ( -5.049401038298153566, 19.05341960407611168, 85.20724293864766707 ) ) ;
#129902 = CARTESIAN_POINT ( 'NONE',  ( 16.51473224551069308, 9.474510206698969483, 104.1655762719810241 ) ) ;
#129903 = CARTESIAN_POINT ( 'NONE',  ( -5.823673210054431948, 21.52544592524334988, 82.70942372801900433 ) ) ;
#129904 = CARTESIAN_POINT ( 'NONE',  ( -4.483927247898782831, 16.52544592524335698, 92.70942372801901854 ) ) ;
#129905 = CARTESIAN_POINT ( 'NONE',  ( -12.06949235617756955, 12.14591786802309770, 65.62390960531436690 ) ) ;
#129906 = CARTESIAN_POINT ( 'NONE',  ( -13.97604488694527625, -13.89961937509977652, 66.87390960531436690 ) ) ;
#129907 = VERTEX_POINT ( 'NONE', #6306 ) ;
#129908 = CARTESIAN_POINT ( 'NONE',  ( 16.51473224551083163, -9.474510206698727899, 105.8344237280190043 ) ) ;
#129909 = CARTESIAN_POINT ( 'NONE',  ( 14.34966873604960469, 8.224510206698951720, 104.1655762719810241 ) ) ;
#129910 = CARTESIAN_POINT ( 'NONE',  ( 16.46253265017160672, -9.564922557960803928, 73.33224293864769550 ) ) ;
#129912 = CARTESIAN_POINT ( 'NONE',  ( 11.40812507854755253, -35.11059874428192273, -6.024999997268814411 ) ) ;
#129911 = CARTESIAN_POINT ( 'NONE',  ( 19.05341960407617918, -5.049401038297876454, 111.0427570613523329 ) ) ;
#129913 = CARTESIAN_POINT ( 'NONE',  ( 21.53943276465977519, 0.05219959533937863772, 111.2510903946856899 ) ) ;
#129914 = CARTESIAN_POINT ( 'NONE',  ( -4.379528057220086978, -16.55341960407618274, 74.79275706135234714 ) ) ;
#129915 = CARTESIAN_POINT ( 'NONE',  ( -16.46253265017146816, -9.564922557961047289, 99.16775706135233293 ) ) ;
#129916 = CARTESIAN_POINT ( 'NONE',  ( 16.52544592524342804, -4.483927247898539470, 108.5405762719810241 ) ) ;
#129917 = CARTESIAN_POINT ( 'NONE',  ( -12.14591786802326823, 12.06949235617739902, 63.12609039468568994 ) ) ;
#129918 = CARTESIAN_POINT ( 'NONE',  ( 0.05219959533934541429, -16.53943276465976808, 60.00109039468568284 ) ) ;
#129919 = CARTESIAN_POINT ( 'NONE',  ( 5.049401038298161559, -19.05341960407611168, 22.70724293864769194 ) ) ;
#129920 = CARTESIAN_POINT ( 'NONE',  ( 19.05341960407617918, -5.049401038297876454, 51.04275706135231871 ) ) ;
#129921 = CARTESIAN_POINT ( 'NONE',  ( 21.52544592524334988, 5.823673210054432836, 96.45942372801901854 ) ) ;
#129922 = CARTESIAN_POINT ( 'NONE',  ( 13.97604488694527802, 13.89961937509977652, 29.37390960531435979 ) ) ;
#129923 = CARTESIAN_POINT ( 'NONE',  ( -9.564922557960796823, -16.46253265017161027, 72.08224293864770971 ) ) ;
#129924 = CARTESIAN_POINT ( 'NONE',  ( 16.55341960407611168, 4.379528057220329451, 68.95724293864769550 ) ) ;
#129925 = CARTESIAN_POINT ( 'NONE',  ( -21.52544592524334988, -5.823673210054445271, 88.95942372801901854 ) ) ;
#129926 = EDGE_CURVE ( 'NONE', #198944, #35288, #164509, .T. ) ;
#129927 = CARTESIAN_POINT ( 'NONE',  ( 5.153800228976615827, -19.02544592524334988, 65.20942372801900433 ) ) ;
#129928 = CARTESIAN_POINT ( 'NONE',  ( -0.05219959533936034679, 19.03943276465977164, 42.50109039468566152 ) ) ;
#129929 = CARTESIAN_POINT ( 'NONE',  ( 21.52544592524344225, -5.823673210054117533, 43.54057627198103830 ) ) ;
#129930 = CARTESIAN_POINT ( 'NONE',  ( -5.719274019375665041, -21.55341960407619695, 104.7927570613523898 ) ) ;
#129931 = CARTESIAN_POINT ( 'NONE',  ( -19.05341960407611168, -5.049401038298163336, 71.45724293864766707 ) ) ;
#129932 = CARTESIAN_POINT ( 'NONE',  ( 10.81492255796106328, -18.62759615963255655, 100.4177570613523471 ) ) ;
#129933 = CARTESIAN_POINT ( 'NONE',  ( 5.823673210054125526, 21.52544592524343514, 44.79057627198103120 ) ) ;
#129934 = CARTESIAN_POINT ( 'NONE',  ( 0.05219959533909260263, 19.03943276465977164, 99.99890960531436690 ) ) ;
#129935 = CARTESIAN_POINT ( 'NONE',  ( -13.89961937509957401, -13.97604488694547875, 79.37609039468567573 ) ) ;
#129936 = CARTESIAN_POINT ( 'NONE',  ( 5.153800228976335163, 19.02544592524342804, 104.7905762719809957 ) ) ;
#129937 = CARTESIAN_POINT ( 'NONE',  ( 19.02544592524334988, 5.153800228976608722, 91.45942372801900433 ) ) ;
#129938 = CARTESIAN_POINT ( 'NONE',  ( 14.34966873604972726, -8.224510206698740333, 40.83442372801901854 ) ) ;
#129939 = CARTESIAN_POINT ( 'NONE',  ( 0.05219959533910956823, 16.53943276465976808, 104.9989096053143669 ) ) ;
#129940 = CARTESIAN_POINT ( 'NONE',  ( -19.02544592524342804, 5.153800228976336051, 86.04057627198103830 ) ) ;
#129941 = CARTESIAN_POINT ( 'NONE',  ( -15.72974639402197994, 15.80617190586746368, 65.62390960531436690 ) ) ;
#129942 = CARTESIAN_POINT ( 'NONE',  ( -0.05219959533934338120, 16.53943276465976808, 27.50109039468567929 ) ) ;
#129943 = CARTESIAN_POINT ( 'NONE',  ( -0.05219959533937732626, 21.53943276465977519, 27.50109039468567929 ) ) ;
#129944 = CARTESIAN_POINT ( 'NONE',  ( 21.53943276465977519, 0.05219959533937863772, 81.25109039468568994 ) ) ;
#129945 = CARTESIAN_POINT ( 'NONE',  ( 12.14591786802327356, -12.06949235617739191, 85.62609039468568994 ) ) ;
#129946 = CARTESIAN_POINT ( 'NONE',  ( 19.05341960407611168, 5.049401038298154454, 73.95724293864768129 ) ) ;
#129947 = CARTESIAN_POINT ( 'NONE',  ( 12.06949235617757843, -12.14591786802309237, 78.12390960531436690 ) ) ;
#129948 = CARTESIAN_POINT ( 'NONE',  ( 12.06949235617757843, -12.14591786802309237, 28.12390960531435979 ) ) ;
#129949 = CARTESIAN_POINT ( 'NONE',  ( 19.02544592524334988, 5.153800228976608722, 56.45942372801898301 ) ) ;
#129950 = CARTESIAN_POINT ( 'NONE',  ( 18.67979575497194134, -10.72451020669871369, 50.83442372801901143 ) ) ;
#129951 = CARTESIAN_POINT ( 'NONE',  ( 8.224510206698953496, -14.34966873604960469, 77.91557627198102409 ) ) ;
#129952 = CARTESIAN_POINT ( 'NONE',  ( 13.89961937509977652, -13.97604488694527269, 108.1239096053143669 ) ) ;
#129953 = CARTESIAN_POINT ( 'NONE',  ( 16.55341960407618274, -4.379528057220086978, 96.04275706135236135 ) ) ;
#129954 = CARTESIAN_POINT ( 'NONE',  ( 21.52544592524334988, 5.823673210054432836, 91.45942372801901854 ) ) ;
#129955 = CARTESIAN_POINT ( 'NONE',  ( 16.53943276465976808, 0.05219959533934440121, 46.25109039468567573 ) ) ;
#129956 = CARTESIAN_POINT ( 'NONE',  ( 18.67979575497194134, -10.72451020669871369, 40.83442372801901854 ) ) ;
#129957 = VERTEX_POINT ( 'NONE', #84142 ) ;
#129958 = CARTESIAN_POINT ( 'NONE',  ( 21.55341960407610458, 5.719274019375980345, 108.9572429386476955 ) ) ;
#129959 = CARTESIAN_POINT ( 'NONE',  ( -16.55341960407611168, -4.379528057220339221, 86.45724293864770971 ) ) ;
#129960 = CARTESIAN_POINT ( 'NONE',  ( 17.50000000000000000, -5.068104630630397622, 28.22818405340030168 ) ) ;
#129961 = CARTESIAN_POINT ( 'NONE',  ( -0.05219959533910754901, -16.53943276465976808, 57.49890960531435979 ) ) ;
#129962 = CARTESIAN_POINT ( 'NONE',  ( -12.14591786802326823, 12.06949235617739902, 93.12609039468568994 ) ) ;
#129963 = CARTESIAN_POINT ( 'NONE',  ( 13.97604488694527802, 13.89961937509977652, 44.37390960531435269 ) ) ;
#129964 = CARTESIAN_POINT ( 'NONE',  ( -10.72451020669898014, 18.67979575497178502, 40.41557627198103120 ) ) ;
#129965 = CARTESIAN_POINT ( 'NONE',  ( -16.55341960407611168, -4.379528057220339221, 76.45724293864769550 ) ) ;
#129966 = CARTESIAN_POINT ( 'NONE',  ( -21.55341960407610458, -5.719274019375992779, 76.45724293864769550 ) ) ;
#129967 = CARTESIAN_POINT ( 'NONE',  ( -16.46253265017160317, 9.564922557960807481, 85.83224293864769550 ) ) ;
#129969 = CARTESIAN_POINT ( 'NONE',  ( 13.89961937509957401, 13.97604488694547697, 91.87609039468567573 ) ) ;
#129968 = CARTESIAN_POINT ( 'NONE',  ( -5.049401038298153566, 19.05341960407611168, 40.20724293864768839 ) ) ;
#129970 = CARTESIAN_POINT ( 'NONE',  ( -21.55341960407610458, -5.719274019375992779, 26.45724293864768839 ) ) ;
#129971 = CARTESIAN_POINT ( 'NONE',  ( 18.62759615963255655, 10.81492255796105972, 51.66775706135234714 ) ) ;
#129972 = CARTESIAN_POINT ( 'NONE',  ( 9.474510206698971260, -16.51473224551069308, 47.91557627198102409 ) ) ;
#129973 = CARTESIAN_POINT ( 'NONE',  ( 9.564922557960805705, 16.46253265017160317, 84.58224293864769550 ) ) ;
#129974 = VERTEX_POINT ( 'NONE', #190344 ) ;
#129975 = CARTESIAN_POINT ( 'NONE',  ( 14.34966873604972726, -8.224510206698740333, 50.83442372801901143 ) ) ;
#129976 = CARTESIAN_POINT ( 'NONE',  ( 10.81492255796106328, -18.62759615963255655, 25.41775706135235779 ) ) ;
#129977 = CARTESIAN_POINT ( 'NONE',  ( -10.81492255796105439, 18.62759615963255655, 72.91775706135234714 ) ) ;
#129978 = CARTESIAN_POINT ( 'NONE',  ( -18.62759615963270932, 10.81492255796079327, 25.83224293864769194 ) ) ;
#129979 = CARTESIAN_POINT ( 'NONE',  ( -21.55341960407610458, -5.719274019375992779, 86.45724293864770971 ) ) ;
#129981 = CARTESIAN_POINT ( 'NONE',  ( 14.34966873604972726, -8.224510206698740333, 70.83442372801901854 ) ) ;
#129980 = CARTESIAN_POINT ( 'NONE',  ( -21.52544592524343514, 5.823673210054127303, 116.0405762719810383 ) ) ;
#129982 = CARTESIAN_POINT ( 'NONE',  ( -10.81492255796078084, -18.62759615963271287, 57.08224293864769550 ) ) ;
#129983 = CARTESIAN_POINT ( 'NONE',  ( 10.72451020669871369, 18.67979575497193778, 112.0844237280190185 ) ) ;
#129984 = CARTESIAN_POINT ( 'NONE',  ( -19.05341960407611168, -5.049401038298163336, 71.45724293864766707 ) ) ;
#129985 = CARTESIAN_POINT ( 'NONE',  ( 16.51473224551069308, 9.474510206698969483, 114.1655762719810241 ) ) ;
#129986 = CARTESIAN_POINT ( 'NONE',  ( -16.46253265017160317, 9.564922557960807481, 85.83224293864769550 ) ) ;
#129987 = CARTESIAN_POINT ( 'NONE',  ( 20.33951628977429849, 20.53125566280822056, -49.67367017693150189 ) ) ;
#129988 = CARTESIAN_POINT ( 'NONE',  ( -9.474510206698720793, -16.51473224551083518, 69.58442372801901854 ) ) ;
#129989 = CARTESIAN_POINT ( 'NONE',  ( -15.80617190586745835, -15.72974639402198527, 41.87390960531435979 ) ) ;
#129990 = CARTESIAN_POINT ( 'NONE',  ( 8.314922557960818139, 14.29746914071049879, 24.58224293864768839 ) ) ;
#129991 = CARTESIAN_POINT ( 'NONE',  ( -13.97604488694547697, 13.89961937509957934, 103.1260903946856473 ) ) ;
#129992 = DIRECTION ( 'NONE',  ( 1.000000000000000000, 0.000000000000000000, -0.000000000000000000 ) ) ;
#129993 = CARTESIAN_POINT ( 'NONE',  ( 21.52544592524334988, 5.823673210054432836, 111.4594237280190328 ) ) ;
#129994 = CARTESIAN_POINT ( 'NONE',  ( -9.564922557961040184, 16.46253265017147172, 97.91775706135233293 ) ) ;
#129996 = CARTESIAN_POINT ( 'NONE',  ( 13.89961937509957401, 13.97604488694547697, 51.87609039468566863 ) ) ;
#129995 = CARTESIAN_POINT ( 'NONE',  ( -5.823673210054116645, -21.52544592524344225, 87.29057627198103830 ) ) ;
#129997 = CARTESIAN_POINT ( 'NONE',  ( 1.300000000000000044, -0.7216878364870318308, 1.249999999999999778 ) ) ;
#129998 = CARTESIAN_POINT ( 'NONE',  ( 13.97604488694527802, 13.89961937509977652, 59.37390960531434558 ) ) ;
#129999 = CARTESIAN_POINT ( 'NONE',  ( -8.224510206698948167, 14.34966873604960824, 65.41557627198102409 ) ) ;
#130000 = CARTESIAN_POINT ( 'NONE',  ( 9.474510206698971260, -16.51473224551069308, 47.91557627198102409 ) ) ;
#130001 = CARTESIAN_POINT ( 'NONE',  ( 8.224510206698953496, -14.34966873604960469, 52.91557627198103830 ) ) ;
#130002 = CARTESIAN_POINT ( 'NONE',  ( -25.13006352617138006, -30.86725525062055553, -20.93759803324971713 ) ) ;
#130003 = CARTESIAN_POINT ( 'NONE',  ( -8.314922557960811034, -14.29746914071050412, 27.08224293864769550 ) ) ;
#130004 = CARTESIAN_POINT ( 'NONE',  ( -13.97604488694527625, -13.89961937509977652, 61.87390960531435979 ) ) ;
#130005 = CARTESIAN_POINT ( 'NONE',  ( -29.15849868437705439, -7.427326039334300134, 174.4773576836617224 ) ) ;
#130006 = CARTESIAN_POINT ( 'NONE',  ( -0.05219959533936034679, 19.03943276465977164, 22.50109039468566152 ) ) ;
#130007 = CARTESIAN_POINT ( 'NONE',  ( 14.29746914071037800, 8.314922557961029526, 41.66775706135235424 ) ) ;
#130008 = CARTESIAN_POINT ( 'NONE',  ( -18.62759615963270932, 10.81492255796079327, 50.83224293864770971 ) ) ;
#130010 = VERTEX_POINT ( 'NONE', #98297 ) ;
#130009 = CARTESIAN_POINT ( 'NONE',  ( -15.72974639402176322, -15.80617190586768395, 99.37609039468568994 ) ) ;
#130011 = CARTESIAN_POINT ( 'NONE',  ( -19.03943276465977164, 0.05219959533909376836, 66.24890960531436690 ) ) ;
#130012 = CARTESIAN_POINT ( 'NONE',  ( 0.000000000000000000, 0.000000000000000000, -58.85720012050612837 ) ) ;
#130013 = CARTESIAN_POINT ( 'NONE',  ( -5.049401038298153566, 19.05341960407611168, 95.20724293864770971 ) ) ;
#130014 = CARTESIAN_POINT ( 'NONE',  ( -29.86685920354755552, 21.69954338932564397, -0.8249999972688133454 ) ) ;
#130015 = CARTESIAN_POINT ( 'NONE',  ( 10.81492255796106328, -18.62759615963255655, 25.41775706135235779 ) ) ;
#130016 = CARTESIAN_POINT ( 'NONE',  ( -8.224510206698948167, 14.34966873604960824, 95.41557627198102409 ) ) ;
#130018 = CARTESIAN_POINT ( 'NONE',  ( -19.03943276465977164, 0.05219959533909376836, 71.24890960531435269 ) ) ;
#130017 = CARTESIAN_POINT ( 'NONE',  ( 21.55341960407610458, 5.719274019375980345, 83.95724293864770971 ) ) ;
#130019 = CARTESIAN_POINT ( 'NONE',  ( -16.51473224551069308, -9.474510206698971260, 91.66557627198103830 ) ) ;
#130020 = CARTESIAN_POINT ( 'NONE',  ( 0.05219959533907565091, 21.53943276465977519, 114.9989096053143669 ) ) ;
#130021 = ORIENTED_EDGE ( 'NONE', *, *, #82833, .T. ) ;
#130022 = CARTESIAN_POINT ( 'NONE',  ( 5.049401038298161559, -19.05341960407611168, 67.70724293864769550 ) ) ;
#130023 = ADVANCED_FACE ( 'NONE', ( #192347 ), #115504, .T. ) ;
#130024 = CARTESIAN_POINT ( 'NONE',  ( 19.52837319214026479, -5.499999999999990230, 97.10471352585543059 ) ) ;
#130026 = CARTESIAN_POINT ( 'NONE',  ( -5.049401038298153566, 19.05341960407611168, 35.20724293864768839 ) ) ;
#130025 = CARTESIAN_POINT ( 'NONE',  ( 12.14591786802309770, 12.06949235617756955, 109.3739096053143811 ) ) ;
#130027 = CARTESIAN_POINT ( 'NONE',  ( -19.03943276465977164, -0.05219959533935918106, 93.75109039468566152 ) ) ;
#130028 = CARTESIAN_POINT ( 'NONE',  ( 8.314922557960818139, 14.29746914071049879, 104.5822429386477097 ) ) ;
#130029 = CARTESIAN_POINT ( 'NONE',  ( -10.72451020669870658, -18.67979575497194134, 69.58442372801900433 ) ) ;
#130031 = CARTESIAN_POINT ( 'NONE',  ( 21.52544592524334988, 5.823673210054432836, 31.45942372801901854 ) ) ;
#130030 = CARTESIAN_POINT ( 'NONE',  ( 13.97604488694527802, 13.89961937509977652, 59.37390960531434558 ) ) ;
#130032 = CARTESIAN_POINT ( 'NONE',  ( 5.823673210054125526, 21.52544592524343514, 104.7905762719810241 ) ) ;
#130033 = CARTESIAN_POINT ( 'NONE',  ( 8.906447517083050158, 27.41122689804195645, 143.4000000000000057 ) ) ;
#130034 = CARTESIAN_POINT ( 'NONE',  ( 13.97604488694527802, 13.89961937509977652, 69.37390960531436690 ) ) ;
#130035 = CARTESIAN_POINT ( 'NONE',  ( 27.96625882250224393, 7.271219613198154796, 160.9431592986539101 ) ) ;
#130037 = CARTESIAN_POINT ( 'NONE',  ( -10.81492255796078084, -18.62759615963271287, 27.08224293864769550 ) ) ;
#130036 = CARTESIAN_POINT ( 'NONE',  ( -12.06949235617739369, -12.14591786802326823, 24.37609039468567573 ) ) ;
#130038 = CARTESIAN_POINT ( 'NONE',  ( -5.719274019375665041, -21.55341960407619695, 59.79275706135234714 ) ) ;
#130039 = CARTESIAN_POINT ( 'NONE',  ( 9.564922557960805705, 16.46253265017160317, 114.5822429386476955 ) ) ;
#130040 = CARTESIAN_POINT ( 'NONE',  ( 19.02544592524334988, 5.153800228976608722, 91.45942372801900433 ) ) ;
#130041 = CARTESIAN_POINT ( 'NONE',  ( -19.02544592524342804, 5.153800228976336051, 51.04057627198103120 ) ) ;
#130042 = CARTESIAN_POINT ( 'NONE',  ( -19.05341960407611168, -5.049401038298163336, 76.45724293864769550 ) ) ;
#130043 = CARTESIAN_POINT ( 'NONE',  ( -14.34966873604960291, -8.224510206698953496, 91.66557627198103830 ) ) ;
#130044 = CARTESIAN_POINT ( 'NONE',  ( 16.46253265017160672, -9.564922557960803928, 103.3322429386476955 ) ) ;
#130045 = CARTESIAN_POINT ( 'NONE',  ( -8.224510206698948167, 14.34966873604960824, 85.41557627198102409 ) ) ;
#130046 = CARTESIAN_POINT ( 'NONE',  ( 0.05219959533909260263, 19.03943276465977164, 94.99890960531436690 ) ) ;
#130048 = CARTESIAN_POINT ( 'NONE',  ( -9.474510206698964154, 16.51473224551069663, 35.41557627198102409 ) ) ;
#130047 = CARTESIAN_POINT ( 'NONE',  ( -4.483927247898539470, -16.52544592524342804, 62.29057627198102409 ) ) ;
#130049 = CARTESIAN_POINT ( 'NONE',  ( 0.05219959533937995610, -21.53943276465977519, 55.00109039468568284 ) ) ;
#130050 = CARTESIAN_POINT ( 'NONE',  ( -5.049401038297874678, -19.05341960407617918, 94.79275706135230450 ) ) ;
#130051 = CARTESIAN_POINT ( 'NONE',  ( -8.314922557960811034, -14.29746914071050412, 47.08224293864770260 ) ) ;
#130052 = CARTESIAN_POINT ( 'NONE',  ( 18.62759615963271287, -10.81492255796078972, 113.3322429386476955 ) ) ;
#130053 = CARTESIAN_POINT ( 'NONE',  ( -18.62759615963270932, 10.81492255796079327, 50.83224293864770971 ) ) ;
#130055 = CARTESIAN_POINT ( 'NONE',  ( 8.314922557960818139, 14.29746914071049879, 89.58224293864768129 ) ) ;
#130054 = CARTESIAN_POINT ( 'NONE',  ( 13.89961937509977652, -13.97604488694527269, 108.1239096053143669 ) ) ;
#130056 = CARTESIAN_POINT ( 'NONE',  ( 23.31738231874054890, -16.94106989632523508, 141.0500000054623513 ) ) ;
#130057 = CARTESIAN_POINT ( 'NONE',  ( -19.03943276465977164, 0.05219959533909376836, 61.24890960531436690 ) ) ;
#130058 = CARTESIAN_POINT ( 'NONE',  ( 12.14591786802327356, -12.06949235617739191, 110.6260903946857042 ) ) ;
#130059 = EDGE_CURVE ( 'NONE', #130796, #137721, #117497, .T. ) ;
#130060 = CARTESIAN_POINT ( 'NONE',  ( 14.29746914071037800, 8.314922557961029526, 106.6677570613523756 ) ) ;
#130061 = CARTESIAN_POINT ( 'NONE',  ( 8.224510206698742110, 14.34966873604972548, 82.08442372801901854 ) ) ;
#130062 = CARTESIAN_POINT ( 'NONE',  ( 9.564922557961047289, -16.46253265017146816, 40.41775706135234003 ) ) ;
#130063 = CARTESIAN_POINT ( 'NONE',  ( -17.13100169013300089, 6.664070546373152659, 70.76789835699851494 ) ) ;
#130064 = CARTESIAN_POINT ( 'NONE',  ( 9.474510206698971260, -16.51473224551069308, 92.91557627198103830 ) ) ;
#130065 = CARTESIAN_POINT ( 'NONE',  ( -9.474510206698964154, 16.51473224551069663, 45.41557627198103120 ) ) ;
#130066 = CARTESIAN_POINT ( 'NONE',  ( 8.224510206698953496, -14.34966873604960469, 67.91557627198102409 ) ) ;
#130068 = CARTESIAN_POINT ( 'NONE',  ( 13.89961937509977652, -13.97604488694527269, 108.1239096053143669 ) ) ;
#130067 =( LENGTH_UNIT ( ) NAMED_UNIT ( * ) SI_UNIT ( .MILLI., .METRE. ) );
#130069 = CARTESIAN_POINT ( 'NONE',  ( -21.52544592524343514, 5.823673210054127303, 41.04057627198103120 ) ) ;
#130070 = CARTESIAN_POINT ( 'NONE',  ( -14.29746914071049879, 8.314922557960819915, 85.83224293864768129 ) ) ;
#130071 = CARTESIAN_POINT ( 'NONE',  ( -12.06949235617739369, -12.14591786802326823, 44.37609039468567573 ) ) ;
#130072 = CIRCLE ( 'NONE', #155926, 4.000000000000000888 ) ;
#130073 = CARTESIAN_POINT ( 'NONE',  ( 0.05219959533910956823, 16.53943276465976808, 74.99890960531435269 ) ) ;
#130074 = CARTESIAN_POINT ( 'NONE',  ( -18.22780087662122028, 5.500000000000031086, 63.51540105326107266 ) ) ;
#130075 = CARTESIAN_POINT ( 'NONE',  ( -5.153800228976607833, 19.02544592524334988, 82.70942372801897591 ) ) ;
#130076 = CARTESIAN_POINT ( 'NONE',  ( -9.564922557960796823, -16.46253265017161027, 107.0822429386476955 ) ) ;
#130077 = CARTESIAN_POINT ( 'NONE',  ( -16.51473224551082808, 9.474510206698731452, 73.33442372801900433 ) ) ;
#130079 = CARTESIAN_POINT ( 'NONE',  ( -22.72511982729796287, 22.36433501015060799, -49.15411784021379304 ) ) ;
#130078 = B_SPLINE_CURVE_WITH_KNOTS ( 'NONE', 3,
 ( #45232, #106886, #164602, #165599, #196940, #198913, #60382, #72594, #30057, #134268 ),
 .UNSPECIFIED., .F., .F.,
 ( 4, 2, 2, 2, 4 ),
 ( 0.002455067421798150240, 0.003068445128277203469, 0.003681822834756256699, 0.004295200541235309928, 0.004908578247714363157 ),
 .UNSPECIFIED. ) ;
#130081 = CARTESIAN_POINT ( 'NONE',  ( -8.224510206698735004, -14.34966873604973081, 104.5844237280190185 ) ) ;
#130080 = CARTESIAN_POINT ( 'NONE',  ( 16.53943276465976808, 0.05219959533934440121, 36.25109039468567573 ) ) ;
#130082 = CARTESIAN_POINT ( 'NONE',  ( -5.153800228976607833, 19.02544592524334988, 77.70942372801900433 ) ) ;
#130083 = CARTESIAN_POINT ( 'NONE',  ( 18.62759615963271287, -10.81492255796078972, 38.33224293864768839 ) ) ;
#130084 = CARTESIAN_POINT ( 'NONE',  ( -18.62759615963255300, -10.81492255796106328, 74.16775706135231871 ) ) ;
#130085 = LINE ( 'NONE', #51280, #195156 ) ;
#130086 = CARTESIAN_POINT ( 'NONE',  ( 12.14591786802327356, -12.06949235617739191, 25.62609039468567929 ) ) ;
#130088 = CARTESIAN_POINT ( 'NONE',  ( 13.97604488694527802, 13.89961937509977652, 94.37390960531436690 ) ) ;
#130087 = CARTESIAN_POINT ( 'NONE',  ( 5.153800228976335163, 19.02544592524342804, 29.79057627198102409 ) ) ;
#130089 = EDGE_CURVE ( 'NONE', #199831, #113002, #138020, .T. ) ;
#130090 = LINE ( 'NONE', #160455, #78895 ) ;
#130092 = CARTESIAN_POINT ( 'NONE',  ( 13.97604488694527802, 13.89961937509977652, 89.37390960531436690 ) ) ;
#130091 = CARTESIAN_POINT ( 'NONE',  ( 16.52544592524342804, -4.483927247898539470, 88.54057627198103830 ) ) ;
#130093 = CONTEXT_DEPENDENT_SHAPE_REPRESENTATION ( #154011, #106587 ) ;
#130094 = CARTESIAN_POINT ( 'NONE',  ( -0.05219959533909027116, -19.03943276465977164, 92.49890960531436690 ) ) ;
#130095 = EDGE_LOOP ( 'NONE', ( #2899, #6875 ) ) ;
#130096 = CARTESIAN_POINT ( 'NONE',  ( -16.51473224551082808, 9.474510206698731452, 88.33442372801900433 ) ) ;
#130097 = CARTESIAN_POINT ( 'NONE',  ( 10.72451020669898902, -18.67979575497178502, 77.91557627198102409 ) ) ;
#130098 = CARTESIAN_POINT ( 'NONE',  ( 9.474510206698971260, -16.51473224551069308, 32.91557627198102409 ) ) ;
#130100 = CARTESIAN_POINT ( 'NONE',  ( -5.823673210054116645, -21.52544592524344225, 112.2905762719810241 ) ) ;
#130099 = CARTESIAN_POINT ( 'NONE',  ( 16.46253265017146816, 9.564922557961045513, 71.66775706135233293 ) ) ;
#130101 = CARTESIAN_POINT ( 'NONE',  ( 16.46253265017160672, -9.564922557960803928, 73.33224293864769550 ) ) ;
#130102 = CARTESIAN_POINT ( 'NONE',  ( -13.97604488694527625, -13.89961937509977652, 111.8739096053143243 ) ) ;
#130103 = ORIENTED_EDGE ( 'NONE', *, *, #68244, .F. ) ;
#130104 = CARTESIAN_POINT ( 'NONE',  ( -16.55341960407617563, 4.379528057220093196, 38.54275706135234714 ) ) ;
#130105 = CARTESIAN_POINT ( 'NONE',  ( 18.62759615963271287, -10.81492255796078972, 108.3322429386477097 ) ) ;
#130108 = CARTESIAN_POINT ( 'NONE',  ( -16.46253265017146816, -9.564922557961047289, 59.16775706135233293 ) ) ;
#130107 = CARTESIAN_POINT ( 'NONE',  ( -0.05219959533909027116, -19.03943276465977164, 82.49890960531436690 ) ) ;
#130106 = CARTESIAN_POINT ( 'NONE',  ( -16.53943276465976808, 0.05219959533911058130, 106.2489096053143811 ) ) ;
#130109 = CARTESIAN_POINT ( 'NONE',  ( -5.823673210054116645, -21.52544592524344225, 92.29057627198103830 ) ) ;
#130110 = CARTESIAN_POINT ( 'NONE',  ( 5.719274019375991003, -21.55341960407610458, 77.70724293864770971 ) ) ;
#130111 = CARTESIAN_POINT ( 'NONE',  ( 14.34966873604960469, 8.224510206698951720, 49.16557627198102409 ) ) ;
#130112 = CARTESIAN_POINT ( 'NONE',  ( -0.05219959533937732626, 21.53943276465977519, 112.5010903946857042 ) ) ;
#130113 = CARTESIAN_POINT ( 'NONE',  ( -8.224510206698735004, -14.34966873604973081, 64.58442372801900433 ) ) ;
#130114 = CARTESIAN_POINT ( 'NONE',  ( -16.46253265017160317, 9.564922557960807481, 95.83224293864769550 ) ) ;
#130115 = CARTESIAN_POINT ( 'NONE',  ( -19.02544592524342804, 5.153800228976336051, 41.04057627198103120 ) ) ;
#130116 = CARTESIAN_POINT ( 'NONE',  ( 15.72974639402176855, 15.80617190586768217, 46.87609039468568994 ) ) ;
#130117 = CARTESIAN_POINT ( 'NONE',  ( -15.80617190586768217, 15.72974639402176855, 53.12609039468568284 ) ) ;
#130118 = CARTESIAN_POINT ( 'NONE',  ( -0.05219959533909027116, -19.03943276465977164, 67.49890960531436690 ) ) ;
#130119 = CARTESIAN_POINT ( 'NONE',  ( 0.05219959533937995610, -21.53943276465977519, 35.00109039468568284 ) ) ;
#130120 = CARTESIAN_POINT ( 'NONE',  ( -0.05219959533936034679, 19.03943276465977164, 72.50109039468566152 ) ) ;
#130121 = EDGE_CURVE ( 'NONE', #26617, #134298, #48306, .T. ) ;
#130122 = CARTESIAN_POINT ( 'NONE',  ( 0.05219959533936267826, -19.03943276465977164, 75.00109039468566152 ) ) ;
#130123 = CARTESIAN_POINT ( 'NONE',  ( 9.474510206698971260, -16.51473224551069308, 42.91557627198103120 ) ) ;
#130124 = CARTESIAN_POINT ( 'NONE',  ( 16.53943276465976808, 0.05219959533934440121, 86.25109039468568994 ) ) ;
#130125 = CARTESIAN_POINT ( 'NONE',  ( -13.97604488694527625, -13.89961937509977652, 51.87390960531436690 ) ) ;
#130126 = CARTESIAN_POINT ( 'NONE',  ( 24.02130208662952171, -8.352503713170980504, 169.2769999910312890 ) ) ;
#130127 = CARTESIAN_POINT ( 'NONE',  ( 5.049401038298161559, -19.05341960407611168, 97.70724293864766707 ) ) ;
#130128 = CARTESIAN_POINT ( 'NONE',  ( 19.05341960407611168, 5.049401038298154454, 43.95724293864769550 ) ) ;
#130129 = CARTESIAN_POINT ( 'NONE',  ( -0.05219959533907301413, -21.53943276465977519, 82.49890960531436690 ) ) ;
#130130 = CARTESIAN_POINT ( 'NONE',  ( -14.34966873604972548, 8.224510206698743886, 63.33442372801900433 ) ) ;
#130131 = CARTESIAN_POINT ( 'NONE',  ( 10.72451020669871369, 18.67979575497193778, 107.0844237280190043 ) ) ;
#130132 = CARTESIAN_POINT ( 'NONE',  ( -19.05341960407611168, -5.049401038298163336, 46.45724293864768129 ) ) ;
#130133 = CARTESIAN_POINT ( 'NONE',  ( -16.53943276465976808, 0.05219959533911058130, 46.24890960531435979 ) ) ;
#130134 = CARTESIAN_POINT ( 'NONE',  ( 16.52544592524342804, -4.483927247898539470, 78.54057627198103830 ) ) ;
#130135 = CARTESIAN_POINT ( 'NONE',  ( -16.46253265017160317, 9.564922557960807481, 80.83224293864769550 ) ) ;
#130136 = CARTESIAN_POINT ( 'NONE',  ( 18.67979575497194134, -10.72451020669871369, 40.83442372801901854 ) ) ;
#130137 = CARTESIAN_POINT ( 'NONE',  ( -9.474510206698964154, 16.51473224551069663, 95.41557627198102409 ) ) ;
#130138 = CARTESIAN_POINT ( 'NONE',  ( 21.52544592524334988, 5.823673210054432836, 101.4594237280190185 ) ) ;
#130139 = CARTESIAN_POINT ( 'NONE',  ( -14.34966873604972548, 8.224510206698743886, 63.33442372801900433 ) ) ;
#130140 = CARTESIAN_POINT ( 'NONE',  ( 0.05219959533937995610, -21.53943276465977519, 30.00109039468568284 ) ) ;
#130141 = CARTESIAN_POINT ( 'NONE',  ( 0.05219959533909260263, 19.03943276465977164, 114.9989096053143669 ) ) ;
#130142 = CARTESIAN_POINT ( 'NONE',  ( 18.67979575497178502, 10.72451020669898547, 84.16557627198103830 ) ) ;
#130143 = CARTESIAN_POINT ( 'NONE',  ( -8.314922557960811034, -14.29746914071050412, 52.08224293864768839 ) ) ;
#130144 = CARTESIAN_POINT ( 'NONE',  ( 9.474510206698971260, -16.51473224551069308, 47.91557627198102409 ) ) ;
#130145 = CARTESIAN_POINT ( 'NONE',  ( 14.29746914071049879, -8.314922557960816363, 63.33224293864770260 ) ) ;
#130146 = CARTESIAN_POINT ( 'NONE',  ( -21.52544592524343514, 5.823673210054127303, 31.04057627198102409 ) ) ;
#130147 = CARTESIAN_POINT ( 'NONE',  ( -9.564922557961040184, 16.46253265017147172, 27.91775706135232582 ) ) ;
#130148 = CARTESIAN_POINT ( 'NONE',  ( 16.52544592524342804, -4.483927247898539470, 93.54057627198103830 ) ) ;
#130149 = CARTESIAN_POINT ( 'NONE',  ( 9.564922557960805705, 16.46253265017160317, 114.5822429386476955 ) ) ;
#130150 = ORIENTED_EDGE ( 'NONE', *, *, #177902, .T. ) ;
#130151 = CARTESIAN_POINT ( 'NONE',  ( 4.483927247898790824, -16.52544592524335698, 55.20942372801902565 ) ) ;
#130152 = CARTESIAN_POINT ( 'NONE',  ( -9.564922557960796823, -16.46253265017161027, 52.08224293864768839 ) ) ;
#130153 = CARTESIAN_POINT ( 'NONE',  ( 4.999999999999997335, 0.000000000000000000, -2.700000000000000622 ) ) ;
#130154 = CARTESIAN_POINT ( 'NONE',  ( -4.483927247898782831, 16.52544592524335698, 97.70942372801904696 ) ) ;
#130155 = CARTESIAN_POINT ( 'NONE',  ( 16.46253265017146816, 9.564922557961045513, 106.6677570613523471 ) ) ;
#130156 = CARTESIAN_POINT ( 'NONE',  ( 21.55341960407619695, -5.719274019375665929, 76.04275706135237556 ) ) ;
#130157 = CARTESIAN_POINT ( 'NONE',  ( 19.03943276465977164, -0.05219959533909143690, 68.74890960531436690 ) ) ;
#130158 = CARTESIAN_POINT ( 'NONE',  ( 5.823673210054125526, 21.52544592524343514, 109.7905762719810383 ) ) ;
#130159 = CARTESIAN_POINT ( 'NONE',  ( 16.52544592524335698, 4.483927247898782831, 41.45942372801901143 ) ) ;
#130160 = CARTESIAN_POINT ( 'NONE',  ( 8.314922557960818139, 14.29746914071049879, 114.5822429386477097 ) ) ;
#130161 = CARTESIAN_POINT ( 'NONE',  ( -13.97604488694547697, 13.89961937509957934, 113.1260903946856757 ) ) ;
#130162 = CARTESIAN_POINT ( 'NONE',  ( -0.05219959533936034679, 19.03943276465977164, 87.50109039468567573 ) ) ;
#130163 = CARTESIAN_POINT ( 'NONE',  ( -5.719274019375978568, 21.55341960407610458, 80.20724293864769550 ) ) ;
#130164 = CARTESIAN_POINT ( 'NONE',  ( 9.474510206698729675, 16.51473224551082808, 57.08442372801900433 ) ) ;
#130165 = CARTESIAN_POINT ( 'NONE',  ( -16.51473224551069308, -9.474510206698971260, 111.6655762719810383 ) ) ;
#130166 = CARTESIAN_POINT ( 'NONE',  ( 21.55341960407610458, 5.719274019375980345, 98.95724293864770971 ) ) ;
#130167 = CARTESIAN_POINT ( 'NONE',  ( 17.50000000000001421, 3.209263204892573995, 27.73803174393734494 ) ) ;
#130168 = CARTESIAN_POINT ( 'NONE',  ( 16.46253265017160672, -9.564922557960803928, 63.33224293864769550 ) ) ;
#130169 = LINE ( 'NONE', #24028, #136973 ) ;
#130170 = CARTESIAN_POINT ( 'NONE',  ( 0.05219959533936267826, -19.03943276465977164, 110.0010903946856757 ) ) ;
#130171 = CARTESIAN_POINT ( 'NONE',  ( 24.75981411741738825, 6.635778407391001110, 167.9383864321132194 ) ) ;
#130172 = CARTESIAN_POINT ( 'NONE',  ( 5.823673210054444382, -21.52544592524334988, 55.20942372801902565 ) ) ;
#130174 = CARTESIAN_POINT ( 'NONE',  ( -12.14591786802309592, -12.06949235617757132, 61.87390960531436690 ) ) ;
#130173 = CARTESIAN_POINT ( 'NONE',  ( 15.72974639402199770, -15.80617190586745480, 103.1239096053143811 ) ) ;
#130175 = CARTESIAN_POINT ( 'NONE',  ( 19.05341960407611168, 5.049401038298154454, 73.95724293864768129 ) ) ;
#130176 = CARTESIAN_POINT ( 'NONE',  ( -10.81492255796105439, 18.62759615963255655, 67.91775706135234714 ) ) ;
#130178 = CARTESIAN_POINT ( 'NONE',  ( -19.05341960407617563, 5.049401038297882671, 28.54275706135232937 ) ) ;
#130177 = CARTESIAN_POINT ( 'NONE',  ( -4.483927247898782831, 16.52544592524335698, 22.70942372801901499 ) ) ;
#130179 = AXIS2_PLACEMENT_3D ( 'NONE', #115461, #37611, #193308 ) ;
#130180 = CARTESIAN_POINT ( 'NONE',  ( -21.52544592524334988, -5.823673210054445271, 58.95942372801902565 ) ) ;
#130181 = CARTESIAN_POINT ( 'NONE',  ( 18.62759615963271287, -10.81492255796078972, 108.3322429386477097 ) ) ;
#130182 = CARTESIAN_POINT ( 'NONE',  ( -0.05219959533907301413, -21.53943276465977519, 57.49890960531435979 ) ) ;
#130183 = CARTESIAN_POINT ( 'NONE',  ( 9.474510206698729675, 16.51473224551082808, 102.0844237280190043 ) ) ;
#130184 = CARTESIAN_POINT ( 'NONE',  ( -16.46253265017146816, -9.564922557961047289, 64.16775706135233293 ) ) ;
#130185 = CARTESIAN_POINT ( 'NONE',  ( 10.81492255796106328, -18.62759615963255655, 85.41775706135236135 ) ) ;
#130186 = CARTESIAN_POINT ( 'NONE',  ( -13.97604488694547697, 13.89961937509957934, 53.12609039468565442 ) ) ;
#130187 = CARTESIAN_POINT ( 'NONE',  ( -0.05219959533909027116, -19.03943276465977164, 42.49890960531435269 ) ) ;
#130188 = CARTESIAN_POINT ( 'NONE',  ( -21.55341960407610458, -5.719274019375992779, 61.45724293864770260 ) ) ;
#130189 = CARTESIAN_POINT ( 'NONE',  ( 14.29746914071049879, -8.314922557960816363, 53.33224293864769550 ) ) ;
#130190 = DIRECTION ( 'NONE',  ( -1.000000000000000000, 0.000000000000000000, 0.000000000000000000 ) ) ;
#130191 = CARTESIAN_POINT ( 'NONE',  ( 13.89961937509957401, 13.97604488694547697, 36.87609039468565442 ) ) ;
#130192 = CARTESIAN_POINT ( 'NONE',  ( -16.53943276465976808, -0.05219959533934237506, 88.75109039468567573 ) ) ;
#130193 = CARTESIAN_POINT ( 'NONE',  ( 16.52544592524342804, -4.483927247898539470, 53.54057627198103120 ) ) ;
#130194 = CARTESIAN_POINT ( 'NONE',  ( 10.72451020669871369, 18.67979575497193778, 77.08442372801901854 ) ) ;
#130195 = CARTESIAN_POINT ( 'NONE',  ( 15.72974639402176855, 15.80617190586768217, 76.87609039468567573 ) ) ;
#130196 = CARTESIAN_POINT ( 'NONE',  ( -5.719274019375978568, 21.55341960407610458, 75.20724293864769550 ) ) ;
#130197 =( BOUNDED_CURVE ( )  B_SPLINE_CURVE ( 2, ( #110339, #33509, #53656, #68819, #23326, #193177, #160836, #144657, #69823, #8146, #163846 ),
 .UNSPECIFIED., .F., .F. ) 
 B_SPLINE_CURVE_WITH_KNOTS ( ( 3, 2, 2, 2, 2, 3 ),
 ( 0.4000000000000001332, 0.4200000000000001510, 0.4400000000000000022, 0.4600000000000000200, 0.4799999999999999822, 0.5000000000000000000 ),
 .UNSPECIFIED. ) 
 CURVE ( )  GEOMETRIC_REPRESENTATION_ITEM ( )  RATIONAL_B_SPLINE_CURVE ( ( 0.9999999999999997780, 0.9510565162951537532, 1.000000000000000000, 0.9510565162951535312, 1.000000000000000000, 0.9510565162951535312, 1.000000000000000000, 0.9510565162951535312, 1.000000000000000000, 0.9510565162951535312, 1.000000000000000000 ) ) 
 REPRESENTATION_ITEM ( '' )  );
#130198 = CARTESIAN_POINT ( 'NONE',  ( 5.153800228976335163, 19.02544592524342804, 39.79057627198100988 ) ) ;
#130199 = CARTESIAN_POINT ( 'NONE',  ( 21.55341960407619695, -5.719274019375665929, 51.04275706135234714 ) ) ;
#130200 = CARTESIAN_POINT ( 'NONE',  ( -13.97604488694527625, -13.89961937509977652, 31.87390960531435979 ) ) ;
#130201 = CARTESIAN_POINT ( 'NONE',  ( 13.89961937509977652, -13.97604488694527269, 58.12390960531436690 ) ) ;
#130202 = CARTESIAN_POINT ( 'NONE',  ( -8.224510206698948167, 14.34966873604960824, 100.4155762719810241 ) ) ;
#130203 = CARTESIAN_POINT ( 'NONE',  ( 19.05341960407611168, 5.049401038298154454, 103.9572429386476671 ) ) ;
#130204 = CARTESIAN_POINT ( 'NONE',  ( -14.34966873604960291, -8.224510206698953496, 46.66557627198102409 ) ) ;
#130205 = CARTESIAN_POINT ( 'NONE',  ( 4.379528057220339221, -16.55341960407611168, 112.7072429386476955 ) ) ;
#130206 = CARTESIAN_POINT ( 'NONE',  ( -0.05219959533907301413, -21.53943276465977519, 87.49890960531436690 ) ) ;
#130207 = CARTESIAN_POINT ( 'NONE',  ( -5.719274019375665041, -21.55341960407619695, 19.79275706135235069 ) ) ;
#130208 = CARTESIAN_POINT ( 'NONE',  ( 27.95290315088917055, -7.353483241874310572, 160.8982923760598567 ) ) ;
#130209 = CARTESIAN_POINT ( 'NONE',  ( 12.14591786802327356, -12.06949235617739191, 35.62609039468568994 ) ) ;
#130210 = ORIENTED_EDGE ( 'NONE', *, *, #108344, .T. ) ;
#130211 = CARTESIAN_POINT ( 'NONE',  ( -15.72974639402197994, 15.80617190586746368, 65.62390960531436690 ) ) ;
#130212 = CARTESIAN_POINT ( 'NONE',  ( 10.81492255796106328, -18.62759615963255655, 95.41775706135234714 ) ) ;
#130213 = CARTESIAN_POINT ( 'NONE',  ( -5.153800228976328057, -19.02544592524343514, 97.29057627198099567 ) ) ;
#130214 = CARTESIAN_POINT ( 'NONE',  ( 15.80617190586769283, -15.72974639402175789, 25.62609039468567929 ) ) ;
#130215 = CIRCLE ( 'NONE', #188417, 59.99999999999998579 ) ;
#130216 = CARTESIAN_POINT ( 'NONE',  ( -21.53943276465977519, 0.05219959533907696930, 26.24890960531435624 ) ) ;
#130217 = CARTESIAN_POINT ( 'NONE',  ( 4.483927247898790824, -16.52544592524335698, 85.20942372801901854 ) ) ;
#130218 = CARTESIAN_POINT ( 'NONE',  ( -5.823673210054431948, 21.52544592524334988, 87.70942372801901854 ) ) ;
#130219 = CARTESIAN_POINT ( 'NONE',  ( -10.81492255796105439, 18.62759615963255655, 112.9177570613523329 ) ) ;
#130220 = CARTESIAN_POINT ( 'NONE',  ( -8.224510206698735004, -14.34966873604973081, 79.58442372801903275 ) ) ;
#130221 = CARTESIAN_POINT ( 'NONE',  ( -15.80617190586768217, 15.72974639402176855, 23.12609039468567573 ) ) ;
#130222 = CARTESIAN_POINT ( 'NONE',  ( -13.89961937509977652, 13.97604488694528158, 30.62390960531435269 ) ) ;
#130223 = CARTESIAN_POINT ( 'NONE',  ( 10.72451020669871369, 18.67979575497193778, 102.0844237280190185 ) ) ;
#130224 = CARTESIAN_POINT ( 'NONE',  ( -13.97604488694527625, -13.89961937509977652, 111.8739096053143243 ) ) ;
#130225 = CARTESIAN_POINT ( 'NONE',  ( -15.80617190586745835, -15.72974639402198527, 106.8739096053143811 ) ) ;
#130227 = CARTESIAN_POINT ( 'NONE',  ( -21.55341960407610458, -5.719274019375992779, 61.45724293864770260 ) ) ;
#130226 = CARTESIAN_POINT ( 'NONE',  ( 19.20446147854523389, 5.500000000000087041, 81.88999695167674986 ) ) ;
#130229 = CARTESIAN_POINT ( 'NONE',  ( -14.29746914071049879, 8.314922557960819915, 50.83224293864770971 ) ) ;
#130228 = CARTESIAN_POINT ( 'NONE',  ( 12.14591786802327356, -12.06949235617739191, 50.62609039468568994 ) ) ;
#130230 = CARTESIAN_POINT ( 'NONE',  ( 0.000000000000000000, -78.67194367458512261, -25.00000000000000000 ) ) ;
#130231 = CARTESIAN_POINT ( 'NONE',  ( -13.97604488694547697, 13.89961937509957934, 78.12609039468567573 ) ) ;
#130232 = CARTESIAN_POINT ( 'NONE',  ( -17.26172910966780094, 6.454744622555846689, 105.8064690864922426 ) ) ;
#130233 = CARTESIAN_POINT ( 'NONE',  ( -8.224510206698735004, -14.34966873604973081, 24.58442372801901499 ) ) ;
#130234 = CARTESIAN_POINT ( 'NONE',  ( 15.72974639402199770, -15.80617190586745480, 83.12390960531436690 ) ) ;
#130235 = CARTESIAN_POINT ( 'NONE',  ( 16.53943276465976808, -0.05219959533910856209, 63.74890960531435979 ) ) ;
#130236 = CARTESIAN_POINT ( 'NONE',  ( 0.05219959533909260263, 19.03943276465977164, 104.9989096053143669 ) ) ;
#130237 = CARTESIAN_POINT ( 'NONE',  ( -4.483927247898782831, 16.52544592524335698, 47.70942372801902565 ) ) ;
#130238 = CARTESIAN_POINT ( 'NONE',  ( -13.97604488694527625, -13.89961937509977652, 51.87390960531436690 ) ) ;
#130240 = CARTESIAN_POINT ( 'NONE',  ( 16.46253265017146816, 9.564922557961045513, 101.6677570613523329 ) ) ;
#130239 = CARTESIAN_POINT ( 'NONE',  ( -0.05219959533937732626, 21.53943276465977519, 27.50109039468567929 ) ) ;
#130241 = CARTESIAN_POINT ( 'NONE',  ( -19.05341960407611168, -5.049401038298163336, 96.45724293864769550 ) ) ;
#130242 = CARTESIAN_POINT ( 'NONE',  ( -13.89961937509977652, 13.97604488694528158, 85.62390960531433848 ) ) ;
#130243 = CARTESIAN_POINT ( 'NONE',  ( -5.823673210054116645, -21.52544592524344225, 87.29057627198103830 ) ) ;
#130244 = CARTESIAN_POINT ( 'NONE',  ( 13.97604488694527802, 13.89961937509977652, 44.37390960531435269 ) ) ;
#130245 = CARTESIAN_POINT ( 'NONE',  ( -17.49999999999999645, -5.624438216177605199, 59.18329655085358354 ) ) ;
#130246 = CARTESIAN_POINT ( 'NONE',  ( 0.05219959533910956823, 16.53943276465976808, 69.99890960531435269 ) ) ;
#130247 = CARTESIAN_POINT ( 'NONE',  ( 5.049401038298161559, -19.05341960407611168, 107.7072429386476955 ) ) ;
#130248 = CARTESIAN_POINT ( 'NONE',  ( 15.77906466954398113, -14.65353482790562012, -56.31012573826036771 ) ) ;
#130249 = CARTESIAN_POINT ( 'NONE',  ( 19.02544592524334988, 5.153800228976608722, 76.45942372801897591 ) ) ;
#130250 = CARTESIAN_POINT ( 'NONE',  ( -5.719274019375978568, 21.55341960407610458, 85.20724293864770971 ) ) ;
#130251 = CARTESIAN_POINT ( 'NONE',  ( -19.02544592524334988, -5.153800228976617603, 43.95942372801899012 ) ) ;
#130252 = CARTESIAN_POINT ( 'NONE',  ( -13.89961937509977652, 13.97604488694528158, 100.6239096053143669 ) ) ;
#130253 =( NAMED_UNIT ( * ) PLANE_ANGLE_UNIT ( ) SI_UNIT ( $, .RADIAN. ) );
#130254 = CARTESIAN_POINT ( 'NONE',  ( -18.62759615963270932, 10.81492255796079327, 45.83224293864769550 ) ) ;
#130255 = CARTESIAN_POINT ( 'NONE',  ( 9.564922557960805705, 16.46253265017160317, 89.58224293864769550 ) ) ;
#130256 = CARTESIAN_POINT ( 'NONE',  ( 18.62759615963255655, 10.81492255796105972, 71.66775706135234714 ) ) ;
#130257 = CARTESIAN_POINT ( 'NONE',  ( 19.03943276465977164, -0.05219959533909143690, 33.74890960531435979 ) ) ;
#130258 = CARTESIAN_POINT ( 'NONE',  ( 14.29746914071049879, -8.314922557960816363, 73.33224293864769550 ) ) ;
#130259 = CARTESIAN_POINT ( 'NONE',  ( 16.53943276465976808, 0.05219959533934440121, 21.25109039468567218 ) ) ;
#130260 = CARTESIAN_POINT ( 'NONE',  ( 15.72974639402176855, 15.80617190586768217, 46.87609039468568994 ) ) ;
#130261 = ORIENTED_EDGE ( 'NONE', *, *, #56324, .T. ) ;
#130262 = CARTESIAN_POINT ( 'NONE',  ( 5.153800228976335163, 19.02544592524342804, 114.7905762719810241 ) ) ;
#130264 = EDGE_CURVE ( 'NONE', #102413, #165180, #13310, .T. ) ;
#130263 = CARTESIAN_POINT ( 'NONE',  ( -9.474510206698720793, -16.51473224551083518, 84.58442372801900433 ) ) ;
#130265 = DIRECTION ( 'NONE',  ( 1.000000000000000000, 0.000000000000000000, 0.000000000000000000 ) ) ;
#130266 = CARTESIAN_POINT ( 'NONE',  ( -21.53943276465977519, -0.05219959533937600094, 23.75109039468567929 ) ) ;
#130267 = CARTESIAN_POINT ( 'NONE',  ( -19.35543954521082100, -5.499999999999585221, 44.58901960356452321 ) ) ;
#130268 = CARTESIAN_POINT ( 'NONE',  ( 15.80617190586769283, -15.72974639402175789, 110.6260903946857042 ) ) ;
#130269 = CARTESIAN_POINT ( 'NONE',  ( 13.97604488694527802, 13.89961937509977652, 49.37390960531434558 ) ) ;
#130270 = CARTESIAN_POINT ( 'NONE',  ( 9.564922557961047289, -16.46253265017146816, 20.41775706135233293 ) ) ;
#130271 = CARTESIAN_POINT ( 'NONE',  ( -4.379528057220086978, -16.55341960407618274, 99.79275706135234714 ) ) ;
#130273 = CARTESIAN_POINT ( 'NONE',  ( -10.81492255796105439, 18.62759615963255655, 77.91775706135231871 ) ) ;
#130272 = CARTESIAN_POINT ( 'NONE',  ( -16.51473224551069308, -9.474510206698971260, 106.6655762719810383 ) ) ;
#130274 = CARTESIAN_POINT ( 'NONE',  ( -27.73933785331498925, 2.428612866367529932E-14, 149.3750000027311842 ) ) ;
#130275 = CARTESIAN_POINT ( 'NONE',  ( -33.67954790872092730, 5.223285087354250678, 96.76001495611576786 ) ) ;
#130276 = CARTESIAN_POINT ( 'NONE',  ( 21.77012268028601483, 5.483007391791947072, 173.8427694445095426 ) ) ;
#130277 = CARTESIAN_POINT ( 'NONE',  ( -18.67979575497193778, 10.72451020669871902, 73.33442372801901854 ) ) ;
#130278 = CARTESIAN_POINT ( 'NONE',  ( -5.823673210054431948, 21.52544592524334988, 97.70942372801904696 ) ) ;
#130279 = AXIS2_PLACEMENT_3D ( 'NONE', #171588, #80552, #174576 ) ;
#130280 = CARTESIAN_POINT ( 'NONE',  ( 17.44270441346513678, -5.991230190323081573, 41.13664920735773478 ) ) ;
#130281 = CARTESIAN_POINT ( 'NONE',  ( 9.564922557960805705, 16.46253265017160317, 89.58224293864769550 ) ) ;
#130282 = CARTESIAN_POINT ( 'NONE',  ( 19.03943276465977164, -0.05219959533909143690, 108.7489096053143527 ) ) ;
#130283 = CARTESIAN_POINT ( 'NONE',  ( -10.59477242850411649, -90.60836494048552936, 0.000000000000000000 ) ) ;
#130284 = CARTESIAN_POINT ( 'NONE',  ( -16.51473224551069308, -9.474510206698971260, 41.66557627198103120 ) ) ;
#130285 = CARTESIAN_POINT ( 'NONE',  ( 5.823673210054125526, 21.52544592524343514, 54.79057627198104541 ) ) ;
#130286 = CARTESIAN_POINT ( 'NONE',  ( 12.14591786802327356, -12.06949235617739191, 100.6260903946857184 ) ) ;
#130288 = CARTESIAN_POINT ( 'NONE',  ( 9.474510206698971260, -16.51473224551069308, 87.91557627198102409 ) ) ;
#130287 = CARTESIAN_POINT ( 'NONE',  ( 8.224510206698953496, -14.34966873604960469, 97.91557627198103830 ) ) ;
#130289 = CARTESIAN_POINT ( 'NONE',  ( -15.72974639402176322, -15.80617190586768395, 104.3760903946856899 ) ) ;
#130290 = CARTESIAN_POINT ( 'NONE',  ( 13.89961937509977652, -13.97604488694527269, 38.12390960531436690 ) ) ;
#130291 = CARTESIAN_POINT ( 'NONE',  ( 16.55341960407611168, 4.379528057220329451, 93.95724293864770971 ) ) ;
#130292 = CARTESIAN_POINT ( 'NONE',  ( -21.53943276465977519, -0.05219959533937600094, 53.75109039468568994 ) ) ;
#130293 = CARTESIAN_POINT ( 'NONE',  ( 0.05219959533907565091, 21.53943276465977519, 84.99890960531436690 ) ) ;
#130294 = CARTESIAN_POINT ( 'NONE',  ( 19.03943276465977164, 0.05219959533936151252, 46.25109039468566863 ) ) ;
#130295 = CARTESIAN_POINT ( 'NONE',  ( -27.70075874562641616, -28.85686966938180475, -5.145719711754212611 ) ) ;
#130296 = CARTESIAN_POINT ( 'NONE',  ( -16.51473224551069308, -9.474510206698971260, 91.66557627198103830 ) ) ;
#130297 = CARTESIAN_POINT ( 'NONE',  ( -0.05219959533910754901, -16.53943276465976808, 57.49890960531435979 ) ) ;
#130298 = CARTESIAN_POINT ( 'NONE',  ( 5.153800228976615827, -19.02544592524334988, 45.20942372801901143 ) ) ;
#130299 = CARTESIAN_POINT ( 'NONE',  ( 13.89961937509977652, -13.97604488694527269, 53.12390960531434558 ) ) ;
#130300 = CARTESIAN_POINT ( 'NONE',  ( 16.55341960407611168, 4.379528057220329451, 43.95724293864769550 ) ) ;
#130301 = CARTESIAN_POINT ( 'NONE',  ( -16.51473224551082808, 9.474510206698731452, 78.33442372801900433 ) ) ;
#130302 = CARTESIAN_POINT ( 'NONE',  ( -18.56453257813363678, 5.500000000000055955, 85.99000423690684158 ) ) ;
#130303 = CARTESIAN_POINT ( 'NONE',  ( -21.55341960407610458, -5.719274019375992779, 41.45724293864769550 ) ) ;
#130304 = CARTESIAN_POINT ( 'NONE',  ( 14.29746914071049879, -8.314922557960816363, 103.3322429386476955 ) ) ;
#130305 = CARTESIAN_POINT ( 'NONE',  ( -3.573655867282028392E-15, -12.39993551617566503, 175.0000000000000000 ) ) ;
#130307 = CARTESIAN_POINT ( 'NONE',  ( 21.53943276465977519, -0.05219959533907433946, 43.74890960531435979 ) ) ;
#130306 = CARTESIAN_POINT ( 'NONE',  ( 0.05219959533909260263, 19.03943276465977164, 54.99890960531435979 ) ) ;
#130308 = CARTESIAN_POINT ( 'NONE',  ( 16.51473224551069308, 9.474510206698969483, 29.16557627198103475 ) ) ;
#130310 = CARTESIAN_POINT ( 'NONE',  ( -0.05219959533909027116, -19.03943276465977164, 62.49890960531435979 ) ) ;
#130309 = CARTESIAN_POINT ( 'NONE',  ( 14.29746914071037800, 8.314922557961029526, 76.66775706135234714 ) ) ;
#130311 = CARTESIAN_POINT ( 'NONE',  ( -19.02544592524334988, -5.153800228976617603, 38.95942372801900433 ) ) ;
#130312 = CARTESIAN_POINT ( 'NONE',  ( -21.53943276465977519, -0.05219959533937600094, 73.75109039468567573 ) ) ;
#130313 = CARTESIAN_POINT ( 'NONE',  ( -21.52544592524343514, 5.823673210054127303, 46.04057627198103830 ) ) ;
#130314 = CARTESIAN_POINT ( 'NONE',  ( -16.51473224551069308, -9.474510206698971260, 21.66557627198102765 ) ) ;
#130315 = CARTESIAN_POINT ( 'NONE',  ( -16.51473224551082808, 9.474510206698731452, 108.3344237280190043 ) ) ;
#130316 = DIRECTION ( 'NONE',  ( -1.734723475976805517E-15, 0.000000000000000000, -1.000000000000000000 ) ) ;
#130318 = CARTESIAN_POINT ( 'NONE',  ( -5.823673210054116645, -21.52544592524344225, 42.29057627198103120 ) ) ;
#130317 = CARTESIAN_POINT ( 'NONE',  ( 1.300000000000000044, -0.7216878364870319418, 1.249999999999999778 ) ) ;
#130319 = CARTESIAN_POINT ( 'NONE',  ( 16.18388926212234935, -7.379444403734663815, 67.06046848633847901 ) ) ;
#130320 = CARTESIAN_POINT ( 'NONE',  ( 21.52544592524334988, 5.823673210054432836, 86.45942372801901854 ) ) ;
#130321 = CARTESIAN_POINT ( 'NONE',  ( -8.314922557960811034, -14.29746914071050412, 52.08224293864768839 ) ) ;
#130322 = CARTESIAN_POINT ( 'NONE',  ( 4.483927247898545687, 16.52544592524342804, 59.79057627198103120 ) ) ;
#130323 = CARTESIAN_POINT ( 'NONE',  ( 18.62759615963271287, -10.81492255796078972, 83.33224293864769550 ) ) ;
#130324 = CARTESIAN_POINT ( 'NONE',  ( -5.823673210054116645, -21.52544592524344225, 72.29057627198102409 ) ) ;
#130325 = CARTESIAN_POINT ( 'NONE',  ( 18.96320343559638388, -23.46320343559646560, 1.110912703473986074 ) ) ;
#130326 = CARTESIAN_POINT ( 'NONE',  ( -10.72451020669898014, 18.67979575497178502, 35.41557627198102409 ) ) ;
#130327 = CARTESIAN_POINT ( 'NONE',  ( 4.483927247898790824, -16.52544592524335698, 60.20942372801902565 ) ) ;
#130328 = CARTESIAN_POINT ( 'NONE',  ( 8.314922557960818139, 14.29746914071049879, 79.58224293864769550 ) ) ;
#130329 = CARTESIAN_POINT ( 'NONE',  ( 5.049401038298161559, -19.05341960407611168, 57.70724293864769550 ) ) ;
#130330 = CARTESIAN_POINT ( 'NONE',  ( -16.51473224551069308, -9.474510206698971260, 26.66557627198103120 ) ) ;
#130331 = DIRECTION ( 'NONE',  ( -1.000000000000000000, 0.000000000000000000, 0.000000000000000000 ) ) ;
#130332 = ORIENTED_EDGE ( 'NONE', *, *, #29329, .F. ) ;
#130333 = CARTESIAN_POINT ( 'NONE',  ( -16.53943276465976808, -0.05219959533934237506, 88.75109039468567573 ) ) ;
#130334 = CARTESIAN_POINT ( 'NONE',  ( 18.62759615963255655, 10.81492255796105972, 21.66775706135235069 ) ) ;
#130335 = CARTESIAN_POINT ( 'NONE',  ( 19.03943276465977164, -0.05219959533909143690, 83.74890960531436690 ) ) ;
#130336 = CARTESIAN_POINT ( 'NONE',  ( 15.80617190586769283, -15.72974639402175789, 50.62609039468568994 ) ) ;
#130337 = CARTESIAN_POINT ( 'NONE',  ( 16.46253265017160672, -9.564922557960803928, 113.3322429386476955 ) ) ;
#130338 = CARTESIAN_POINT ( 'NONE',  ( -14.22875182907677072, -42.06737590810060112, -22.02417070750285788 ) ) ;
#130339 = ORIENTED_EDGE ( 'NONE', *, *, #83608, .F. ) ;
#130340 = CARTESIAN_POINT ( 'NONE',  ( 21.53943276465977519, 0.05219959533937863772, 46.25109039468567573 ) ) ;
#130342 = CARTESIAN_POINT ( 'NONE',  ( 5.049401038298161559, -19.05341960407611168, 102.7072429386476955 ) ) ;
#130341 = CARTESIAN_POINT ( 'NONE',  ( -16.46253265017160317, 9.564922557960807481, 40.83224293864769550 ) ) ;
#130343 = CARTESIAN_POINT ( 'NONE',  ( 19.02544592524334988, 5.153800228976608722, 51.45942372801900433 ) ) ;
#130344 = CARTESIAN_POINT ( 'NONE',  ( -21.55341960407619339, 5.719274019375674811, 28.54275706135234358 ) ) ;
#130345 = CARTESIAN_POINT ( 'NONE',  ( -19.02544592524334988, -5.153800228976617603, 43.95942372801899012 ) ) ;
#130346 = CARTESIAN_POINT ( 'NONE',  ( 9.564922557960805705, 16.46253265017160317, 29.58224293864769550 ) ) ;
#130347 = CARTESIAN_POINT ( 'NONE',  ( 12.14591786802327356, -12.06949235617739191, 95.62609039468568994 ) ) ;
#130348 = CARTESIAN_POINT ( 'NONE',  ( -13.97604488694547697, 13.89961937509957934, 63.12609039468566152 ) ) ;
#130349 = CARTESIAN_POINT ( 'NONE',  ( -4.483927247898782831, 16.52544592524335698, 107.7094237280190328 ) ) ;
#130350 = LINE ( 'NONE', #161713, #124883 ) ;
#130351 = CARTESIAN_POINT ( 'NONE',  ( -5.049401038298153566, 19.05341960407611168, 85.20724293864766707 ) ) ;
#130352 = CARTESIAN_POINT ( 'NONE',  ( 18.62759615963255655, 10.81492255796105972, 96.66775706135234714 ) ) ;
#130353 = CARTESIAN_POINT ( 'NONE',  ( -18.62759615963255300, -10.81492255796106328, 109.1677570613523613 ) ) ;
#130354 = FACE_OUTER_BOUND ( 'NONE', #82412, .T. ) ;
#130355 = CARTESIAN_POINT ( 'NONE',  ( 16.46253265017160672, -9.564922557960803928, 103.3322429386476955 ) ) ;
#130356 = CARTESIAN_POINT ( 'NONE',  ( -21.52544592524334988, -5.823673210054445271, 73.95942372801901854 ) ) ;
#130357 = CARTESIAN_POINT ( 'NONE',  ( -13.97604488694547697, 13.89961937509957934, 113.1260903946856757 ) ) ;
#130358 = EDGE_CURVE ( 'NONE', #70507, #182160, #161307, .T. ) ;
#130359 = CARTESIAN_POINT ( 'NONE',  ( -16.46253265017160317, 9.564922557960807481, 85.83224293864769550 ) ) ;
#130360 = CARTESIAN_POINT ( 'NONE',  ( 0.05219959533907565091, 21.53943276465977519, 24.99890960531435624 ) ) ;
#130361 = AXIS2_PLACEMENT_3D ( 'NONE', #198724, #60191, #74390 ) ;
#130362 = CARTESIAN_POINT ( 'NONE',  ( 5.049401038298161559, -19.05341960407611168, 87.70724293864769550 ) ) ;
#130363 = CARTESIAN_POINT ( 'NONE',  ( -16.61371651742602396, -7.165104196376147705, 91.14584930007005426 ) ) ;
#130364 = CARTESIAN_POINT ( 'NONE',  ( -19.02544592524342804, 5.153800228976336051, 76.04057627198102409 ) ) ;
#130365 = CARTESIAN_POINT ( 'NONE',  ( -5.049401038298153566, 19.05341960407611168, 70.20724293864769550 ) ) ;
#130366 = CARTESIAN_POINT ( 'NONE',  ( -4.379528057220086978, -16.55341960407618274, 99.79275706135234714 ) ) ;
#130367 = CYLINDRICAL_SURFACE ( 'NONE', #110416, 28.79475375365586487 ) ;
#130368 = CARTESIAN_POINT ( 'NONE',  ( -13.89961937509957401, -13.97604488694547875, 64.37609039468567573 ) ) ;
#130369 = CARTESIAN_POINT ( 'NONE',  ( 0.05219959533909260263, 19.03943276465977164, 89.99890960531436690 ) ) ;
#130370 = CARTESIAN_POINT ( 'NONE',  ( 16.53943276465976808, -0.05219959533910856209, 83.74890960531435269 ) ) ;
#130371 = CARTESIAN_POINT ( 'NONE',  ( 15.72974639402199770, -15.80617190586745480, 28.12390960531435979 ) ) ;
#130372 = CARTESIAN_POINT ( 'NONE',  ( 19.05341960407611168, 5.049401038298154454, 113.9572429386477097 ) ) ;
#130373 = CARTESIAN_POINT ( 'NONE',  ( 0.05219959533910956823, 16.53943276465976808, 89.99890960531438111 ) ) ;
#130374 = DIRECTION ( 'NONE',  ( 1.000000000000000000, 0.000000000000000000, 0.000000000000000000 ) ) ;
#130375 = CARTESIAN_POINT ( 'NONE',  ( 0.05219959533936267826, -19.03943276465977164, 40.00109039468566152 ) ) ;
#130376 = CARTESIAN_POINT ( 'NONE',  ( -8.314922557960811034, -14.29746914071050412, 22.08224293864769194 ) ) ;
#130377 = CARTESIAN_POINT ( 'NONE',  ( 19.02544592524343514, -5.153800228976328945, 103.5405762719809957 ) ) ;
#130378 = CARTESIAN_POINT ( 'NONE',  ( -5.823673210054431948, 21.52544592524334988, 62.70942372801902565 ) ) ;
#130379 = CARTESIAN_POINT ( 'NONE',  ( 18.62759615963271287, -10.81492255796078972, 53.33224293864769550 ) ) ;
#130380 = CARTESIAN_POINT ( 'NONE',  ( 15.72974639402176855, 15.80617190586768217, 31.87609039468567929 ) ) ;
#130381 = CARTESIAN_POINT ( 'NONE',  ( 5.719274019375991003, -21.55341960407610458, 87.70724293864769550 ) ) ;
#130382 = CARTESIAN_POINT ( 'NONE',  ( -18.67979575497193778, 10.72451020669871902, 43.33442372801901143 ) ) ;
#130383 = CARTESIAN_POINT ( 'NONE',  ( -4.483927247898539470, -16.52544592524342804, 112.2905762719810241 ) ) ;
#130384 = EDGE_CURVE ( 'NONE', #172465, #87119, #190306, .T. ) ;
#130385 = CARTESIAN_POINT ( 'NONE',  ( -13.97604488694547697, 13.89961937509957934, 73.12609039468568994 ) ) ;
#130386 = CARTESIAN_POINT ( 'NONE',  ( 19.03943276465977164, -0.05219959533909143690, 48.74890960531435979 ) ) ;
#130388 = CARTESIAN_POINT ( 'NONE',  ( -13.97604488694527625, -13.89961937509977652, 91.87390960531432427 ) ) ;
#130387 = CARTESIAN_POINT ( 'NONE',  ( -14.29746914071049879, 8.314922557960819915, 85.83224293864768129 ) ) ;
#130389 = CARTESIAN_POINT ( 'NONE',  ( -13.89961937509977652, 13.97604488694528158, 90.62390960531432427 ) ) ;
#130390 = CARTESIAN_POINT ( 'NONE',  ( 0.05219959533909260263, 19.03943276465977164, 24.99890960531435269 ) ) ;
#130391 = CARTESIAN_POINT ( 'NONE',  ( -16.53943276465976808, 0.05219959533911058130, 36.24890960531435979 ) ) ;
#130392 = CARTESIAN_POINT ( 'NONE',  ( -16.53943276465976808, -0.05219959533934237506, 93.75109039468567573 ) ) ;
#130393 = CARTESIAN_POINT ( 'NONE',  ( 19.05341960407611168, 5.049401038298154454, 58.95724293864768129 ) ) ;
#130394 = CARTESIAN_POINT ( 'NONE',  ( -19.05341960407611168, -5.049401038298163336, 21.45724293864768839 ) ) ;
#130395 = CARTESIAN_POINT ( 'NONE',  ( -16.46253265017146816, -9.564922557961047289, 29.16775706135232937 ) ) ;
#130397 = CARTESIAN_POINT ( 'NONE',  ( 16.53943276465976808, 0.05219959533934440121, 111.2510903946856899 ) ) ;
#130396 = CARTESIAN_POINT ( 'NONE',  ( -13.89961937509977652, 13.97604488694528158, 110.6239096053143243 ) ) ;
#130398 = CARTESIAN_POINT ( 'NONE',  ( -21.53943276465977519, -0.05219959533937600094, 43.75109039468568284 ) ) ;
#130399 = CARTESIAN_POINT ( 'NONE',  ( 0.05219959533909260263, 19.03943276465977164, 99.99890960531436690 ) ) ;
#130400 = CARTESIAN_POINT ( 'NONE',  ( 0.05219959533934541429, -16.53943276465976808, 50.00109039468568994 ) ) ;
#130401 = CARTESIAN_POINT ( 'NONE',  ( 14.29746914071037800, 8.314922557961029526, 106.6677570613523756 ) ) ;
#130402 = CARTESIAN_POINT ( 'NONE',  ( 13.89961937509977652, -13.97604488694527269, 48.12390960531435979 ) ) ;
#130403 = CARTESIAN_POINT ( 'NONE',  ( -14.34966873604972548, 8.224510206698743886, 88.33442372801901854 ) ) ;
#130404 = CARTESIAN_POINT ( 'NONE',  ( -8.314922557961024197, 14.29746914071037800, 32.91775706135234714 ) ) ;
#130405 = CARTESIAN_POINT ( 'NONE',  ( -16.51473224551069308, -9.474510206698971260, 51.66557627198102409 ) ) ;
#130406 = CARTESIAN_POINT ( 'NONE',  ( -8.224510206698948167, 14.34966873604960824, 110.4155762719810383 ) ) ;
#130407 = CARTESIAN_POINT ( 'NONE',  ( -21.53943276465977519, 0.05219959533907696930, 111.2489096053143669 ) ) ;
#130408 = CARTESIAN_POINT ( 'NONE',  ( -13.97604488694527625, -13.89961937509977652, 51.87390960531436690 ) ) ;
#130409 = CARTESIAN_POINT ( 'NONE',  ( -16.51473224551069308, -9.474510206698971260, 106.6655762719810383 ) ) ;
#130410 = CARTESIAN_POINT ( 'NONE',  ( 13.97604488694527802, 13.89961937509977652, 29.37390960531435979 ) ) ;
#130411 = CARTESIAN_POINT ( 'NONE',  ( -19.02544592524342804, 5.153800228976336051, 111.0405762719810099 ) ) ;
#130412 = CARTESIAN_POINT ( 'NONE',  ( -17.40861289039006010, -6.110651285853200498, 36.37232470827432707 ) ) ;
#130413 = CARTESIAN_POINT ( 'NONE',  ( 9.474510206698971260, -16.51473224551069308, 97.91557627198102409 ) ) ;
#130415 = CARTESIAN_POINT ( 'NONE',  ( 4.379528057220339221, -16.55341960407611168, 102.7072429386476955 ) ) ;
#130414 = CARTESIAN_POINT ( 'NONE',  ( -10.72451020669870658, -18.67979575497194134, 44.58442372801901854 ) ) ;
#130416 = CARTESIAN_POINT ( 'NONE',  ( 19.02544592524343514, -5.153800228976328945, 103.5405762719809957 ) ) ;
#130417 = LINE ( 'NONE', #52593, #28846 ) ;
#130418 = AXIS2_PLACEMENT_3D ( 'NONE', #64155, #78309, #139982 ) ;
#130419 = CARTESIAN_POINT ( 'NONE',  ( 8.314922557961029526, -14.29746914071037800, 60.41775706135235424 ) ) ;
#130420 = CARTESIAN_POINT ( 'NONE',  ( -5.823673210054431948, 21.52544592524334988, 87.70942372801901854 ) ) ;
#130421 = CARTESIAN_POINT ( 'NONE',  ( -16.55341960407617563, 4.379528057220093196, 38.54275706135234714 ) ) ;
#130422 = CARTESIAN_POINT ( 'NONE',  ( -16.51473224551069308, -9.474510206698971260, 81.66557627198103830 ) ) ;
#130423 = CARTESIAN_POINT ( 'NONE',  ( -16.55341960407617563, 4.379528057220093196, 33.54275706135234714 ) ) ;
#130424 = CARTESIAN_POINT ( 'NONE',  ( 0.05219959533934541429, -16.53943276465976808, 20.00109039468568639 ) ) ;
#130425 = CARTESIAN_POINT ( 'NONE',  ( 12.06949235617739724, 12.14591786802326823, 76.87609039468567573 ) ) ;
#130426 = CARTESIAN_POINT ( 'NONE',  ( -5.153800228976607833, 19.02544592524334988, 92.70942372801901854 ) ) ;
#130427 = CARTESIAN_POINT ( 'NONE',  ( -9.564922557960796823, -16.46253265017161027, 82.08224293864768129 ) ) ;
#130428 = CARTESIAN_POINT ( 'NONE',  ( -15.72974639402197994, 15.80617190586746368, 95.62390960531436690 ) ) ;
#130430 = CARTESIAN_POINT ( 'NONE',  ( 13.97604488694548053, -13.89961937509957401, 90.62609039468567573 ) ) ;
#130429 = CARTESIAN_POINT ( 'NONE',  ( 16.55341960407611168, 4.379528057220329451, 88.95724293864769550 ) ) ;
#130431 = CARTESIAN_POINT ( 'NONE',  ( 4.483927247898790824, -16.52544592524335698, 70.20942372801904696 ) ) ;
#130432 = CARTESIAN_POINT ( 'NONE',  ( 24.24385185424126377, 7.025880200331397596, 170.5073520790474788 ) ) ;
#130433 = CARTESIAN_POINT ( 'NONE',  ( -16.51473224551082808, 9.474510206698731452, 73.33442372801900433 ) ) ;
#130434 = CARTESIAN_POINT ( 'NONE',  ( -14.29746914071049879, 8.314922557960819915, 30.83224293864770260 ) ) ;
#130435 = CARTESIAN_POINT ( 'NONE',  ( 8.224510206698953496, -14.34966873604960469, 97.91557627198103830 ) ) ;
#130437 = CARTESIAN_POINT ( 'NONE',  ( -5.049401038297874678, -19.05341960407618274, 44.79275706135232582 ) ) ;
#130436 = CARTESIAN_POINT ( 'NONE',  ( -13.89961937509957401, -13.97604488694547875, 34.37609039468566863 ) ) ;
#130438 = CARTESIAN_POINT ( 'NONE',  ( -10.72451020669898014, 18.67979575497178502, 115.4155762719810241 ) ) ;
#130439 = CARTESIAN_POINT ( 'NONE',  ( 13.97604488694527802, 13.89961937509977652, 109.3739096053143669 ) ) ;
#130440 = CARTESIAN_POINT ( 'NONE',  ( -19.02544592524342804, 5.153800228976336051, 96.04057627198103830 ) ) ;
#130441 = CARTESIAN_POINT ( 'NONE',  ( 0.05219959533937995610, -21.53943276465977519, 95.00109039468568994 ) ) ;
#130442 = CARTESIAN_POINT ( 'NONE',  ( -19.02544592524342804, 5.153800228976336051, 71.04057627198099567 ) ) ;
#130443 = ORIENTED_EDGE ( 'NONE', *, *, #63444, .F. ) ;
#130444 = CARTESIAN_POINT ( 'NONE',  ( -15.80617190586745835, -15.72974639402198527, 41.87390960531435979 ) ) ;
#130445 = CARTESIAN_POINT ( 'NONE',  ( 16.55341960407611168, 4.379528057220329451, 93.95724293864770971 ) ) ;
#130446 = CARTESIAN_POINT ( 'NONE',  ( 16.51473224551069308, 9.474510206698969483, 59.16557627198102409 ) ) ;
#130447 = CARTESIAN_POINT ( 'NONE',  ( -16.52544592524342804, 4.483927247898546575, 116.0405762719810383 ) ) ;
#130448 = AXIS2_PLACEMENT_3D ( 'NONE', #25, #137559, #75884 ) ;
#130449 = CARTESIAN_POINT ( 'NONE',  ( -15.80617190586768217, 15.72974639402176855, 23.12609039468567573 ) ) ;
#130450 = CARTESIAN_POINT ( 'NONE',  ( -18.62759615963255300, -10.81492255796106328, 64.16775706135234714 ) ) ;
#130451 = CARTESIAN_POINT ( 'NONE',  ( -16.51473224551069308, -9.474510206698971260, 46.66557627198102409 ) ) ;
#130452 = CARTESIAN_POINT ( 'NONE',  ( 12.14591786802327356, -12.06949235617739191, 80.62609039468567573 ) ) ;
#130453 = B_SPLINE_CURVE_WITH_KNOTS ( 'NONE', 3,
 ( #66823, #128486, #175013, #51657, #191179, #36477, #98134, #99150, #160839, #22328, #83978, #115336, #64842, #177027, #38497, #100153, #150676, #166840, #12174, #39483, #54653, #73839, #193180, #11168, #57671, #70833, #103166, #84972, #72843, #134513, #41502, #165843 ),
 .UNSPECIFIED., .F., .F.,
 ( 4, 2, 2, 2, 2, 2, 2, 2, 2, 2, 2, 2, 2, 2, 2, 4 ),
 ( 1.684111863762029156E-17, 0.0003712461730036760443, 0.0007424923460073351751, 0.001113738519010994523, 0.001484984692014653654, 0.002227477038021980372, 0.002598723211025658585, 0.002969969384029335930, 0.003341215557033014143, 0.003712461730036691488, 0.004083707903040368833, 0.004454954076044045745, 0.004826200249047724392, 0.005197446422051402171, 0.005568692595055079082, 0.005939938768058757729 ),
 .UNSPECIFIED. ) ;
#130454 = CARTESIAN_POINT ( 'NONE',  ( -21.52544592524343514, 5.823673210054127303, 111.0405762719810525 ) ) ;
#130455 = ORIENTED_EDGE ( 'NONE', *, *, #1987, .T. ) ;
#130456 = CARTESIAN_POINT ( 'NONE',  ( -18.62759615963270932, 10.81492255796079327, 105.8322429386476955 ) ) ;
#130458 = CARTESIAN_POINT ( 'NONE',  ( 13.89961937509977652, -13.97604488694527269, 63.12390960531435979 ) ) ;
#130457 = CARTESIAN_POINT ( 'NONE',  ( 19.05341960407617918, -5.049401038297876454, 56.04275706135234714 ) ) ;
#130459 = CARTESIAN_POINT ( 'NONE',  ( 19.05341960407617918, -5.049401038297876454, 31.04275706135232227 ) ) ;
#130460 = CARTESIAN_POINT ( 'NONE',  ( 0.05219959533937995610, -21.53943276465977519, 75.00109039468568994 ) ) ;
#130461 = CARTESIAN_POINT ( 'NONE',  ( 5.719274019375991003, -21.55341960407610458, 67.70724293864769550 ) ) ;
#130462 = CARTESIAN_POINT ( 'NONE',  ( -4.379528057220328563, 16.55341960407611168, 50.20724293864769550 ) ) ;
#130464 = CARTESIAN_POINT ( 'NONE',  ( -19.02544592524334988, -5.153800228976617603, 33.95942372801897591 ) ) ;
#130463 = CARTESIAN_POINT ( 'NONE',  ( -18.62759615963255300, -10.81492255796106328, 84.16775706135234714 ) ) ;
#130465 = CARTESIAN_POINT ( 'NONE',  ( 14.29746914071049879, -8.314922557960816363, 68.33224293864769550 ) ) ;
#130466 = CARTESIAN_POINT ( 'NONE',  ( -0.05219959533910754901, -16.53943276465976808, 107.4989096053143669 ) ) ;
#130467 = CARTESIAN_POINT ( 'NONE',  ( -19.03943276465977164, -0.05219959533935918106, 63.75109039468566863 ) ) ;
#130468 = CARTESIAN_POINT ( 'NONE',  ( -16.53943276465976808, -0.05219959533934237506, 113.7510903946856757 ) ) ;
#130470 = EDGE_CURVE ( 'NONE', #100463, #105726, #35301, .T. ) ;
#130469 = CARTESIAN_POINT ( 'NONE',  ( 18.62759615963255655, 10.81492255796105972, 66.66775706135234714 ) ) ;
#130471 = CARTESIAN_POINT ( 'NONE',  ( 5.153800228976335163, 19.02544592524342804, 74.79057627198103830 ) ) ;
#130472 = CARTESIAN_POINT ( 'NONE',  ( 9.564922557961047289, -16.46253265017146816, 45.41775706135232582 ) ) ;
#130473 = CARTESIAN_POINT ( 'NONE',  ( -5.823673210054116645, -21.52544592524344225, 52.29057627198102409 ) ) ;
#130474 = CARTESIAN_POINT ( 'NONE',  ( -18.62759615963255300, -10.81492255796106328, 44.16775706135234714 ) ) ;
#130475 = CARTESIAN_POINT ( 'NONE',  ( -5.823673210054116645, -21.52544592524344225, 107.2905762719810525 ) ) ;
#130476 = CARTESIAN_POINT ( 'NONE',  ( -9.564922557961040184, 16.46253265017147172, 102.9177570613523329 ) ) ;
#130477 = CARTESIAN_POINT ( 'NONE',  ( -16.55341960407617563, 4.379528057220093196, 68.54275706135234714 ) ) ;
#130479 = CARTESIAN_POINT ( 'NONE',  ( -21.53943276465977519, 0.05219959533907696930, 101.2489096053143669 ) ) ;
#130478 = CARTESIAN_POINT ( 'NONE',  ( -14.62203461105063873, -16.12203461105573865, -58.56003730381080175 ) ) ;
#130480 = CARTESIAN_POINT ( 'NONE',  ( 4.483927247898545687, 16.52544592524342804, 94.79057627198105251 ) ) ;
#130481 = CARTESIAN_POINT ( 'NONE',  ( -17.49999999999999645, -3.209263204892548238, 30.23803174393719573 ) ) ;
#130482 = CARTESIAN_POINT ( 'NONE',  ( 16.55341960407618274, -4.379528057220086978, 21.04275706135234714 ) ) ;
#130483 = CARTESIAN_POINT ( 'NONE',  ( -18.62759615963270932, 10.81492255796079327, 50.83224293864770971 ) ) ;
#130484 = CARTESIAN_POINT ( 'NONE',  ( 14.34966873604972726, -8.224510206698740333, 90.83442372801901854 ) ) ;
#130485 = CARTESIAN_POINT ( 'NONE',  ( 36.91803858635991986, 1.187467863258684586, -8.000000000000005329 ) ) ;
#130486 = ADVANCED_FACE ( 'NONE', ( #29479 ), #120473, .F. ) ;
#130487 = CARTESIAN_POINT ( 'NONE',  ( -16.53943276465976808, -0.05219959533934237506, 68.75109039468568994 ) ) ;
#130488 = CARTESIAN_POINT ( 'NONE',  ( -5.719274019375665041, -21.55341960407619695, 34.79275706135235424 ) ) ;
#130489 = CARTESIAN_POINT ( 'NONE',  ( 18.62759615963271287, -10.81492255796078972, 58.33224293864768839 ) ) ;
#130490 = CARTESIAN_POINT ( 'NONE',  ( 8.224510206698742110, 14.34966873604972548, 82.08442372801901854 ) ) ;
#130491 = CARTESIAN_POINT ( 'NONE',  ( 5.049401038298161559, -19.05341960407611168, 92.70724293864769550 ) ) ;
#130492 = CARTESIAN_POINT ( 'NONE',  ( -10.72451020669870658, -18.67979575497194134, 69.58442372801900433 ) ) ;
#130493 = CARTESIAN_POINT ( 'NONE',  ( 10.72451020669898902, -18.67979575497178502, 42.91557627198103120 ) ) ;
#130494 = CARTESIAN_POINT ( 'NONE',  ( -18.62759615963270932, 10.81492255796079327, 30.83224293864770260 ) ) ;
#130495 = EDGE_LOOP ( 'NONE', ( #102032, #174043 ) ) ;
#130496 = CARTESIAN_POINT ( 'NONE',  ( -13.97604488694547697, 13.89961937509957934, 58.12609039468566863 ) ) ;
#130497 = CARTESIAN_POINT ( 'NONE',  ( 0.05219959533934541429, -16.53943276465976808, 65.00109039468568994 ) ) ;
#130498 = CARTESIAN_POINT ( 'NONE',  ( 10.72451020669898902, -18.67979575497178502, 32.91557627198102409 ) ) ;
#130499 = VERTEX_POINT ( 'NONE', #152800 ) ;
#130500 = CARTESIAN_POINT ( 'NONE',  ( -5.049401038298153566, 19.05341960407611168, 85.20724293864766707 ) ) ;
#130501 = CARTESIAN_POINT ( 'NONE',  ( 8.314922557960818139, 14.29746914071049879, 24.58224293864768839 ) ) ;
#130502 = CARTESIAN_POINT ( 'NONE',  ( -18.22780087662123805, 5.499999999999981348, 86.01763182126894947 ) ) ;
#130503 = CARTESIAN_POINT ( 'NONE',  ( 4.483927247898545687, 16.52544592524342804, 109.7905762719810383 ) ) ;
#130504 = CARTESIAN_POINT ( 'NONE',  ( -21.52544592524343514, 5.823673210054127303, 46.04057627198103830 ) ) ;
#130505 = CARTESIAN_POINT ( 'NONE',  ( 5.153800228976335163, 19.02544592524342804, 49.79057627198100988 ) ) ;
#130506 = CARTESIAN_POINT ( 'NONE',  ( 4.379528057220092307, 16.55341960407617563, 87.29275706135236135 ) ) ;
#130507 = CARTESIAN_POINT ( 'NONE',  ( -10.81492255796105439, 18.62759615963255655, 27.91775706135234358 ) ) ;
#130508 = CARTESIAN_POINT ( 'NONE',  ( 13.97604488694548053, -13.89961937509957401, 85.62609039468568994 ) ) ;
#130509 = CARTESIAN_POINT ( 'NONE',  ( 16.55341960407611168, 4.379528057220329451, 93.95724293864770971 ) ) ;
#130510 = CARTESIAN_POINT ( 'NONE',  ( -13.89961937509977652, 13.97604488694528158, 50.62390960531435979 ) ) ;
#130511 = CARTESIAN_POINT ( 'NONE',  ( -9.474510206698964154, 16.51473224551069663, 30.41557627198102054 ) ) ;
#130512 = CARTESIAN_POINT ( 'NONE',  ( 21.52544592524334988, 5.823673210054432836, 106.4594237280190328 ) ) ;
#130513 = CARTESIAN_POINT ( 'NONE',  ( -16.51473224551069308, -9.474510206698971260, 71.66557627198102409 ) ) ;
#130514 = CARTESIAN_POINT ( 'NONE',  ( -8.314922557961024197, 14.29746914071037800, 62.91775706135236135 ) ) ;
#130515 = CARTESIAN_POINT ( 'NONE',  ( 18.62759615963255655, 10.81492255796105972, 96.66775706135234714 ) ) ;
#130516 = CARTESIAN_POINT ( 'NONE',  ( -5.823673210054116645, -21.52544592524344225, 52.29057627198102409 ) ) ;
#130517 = CARTESIAN_POINT ( 'NONE',  ( -14.29746914071037622, -8.314922557961029526, 69.16775706135234714 ) ) ;
#130518 = CARTESIAN_POINT ( 'NONE',  ( 16.46253265017146816, 9.564922557961045513, 51.66775706135233293 ) ) ;
#130519 = CARTESIAN_POINT ( 'NONE',  ( 19.05341960407617918, -5.049401038297876454, 61.04275706135232582 ) ) ;
#130520 = ORIENTED_EDGE ( 'NONE', *, *, #93254, .F. ) ;
#130521 = CARTESIAN_POINT ( 'NONE',  ( -5.823673210054431948, 21.52544592524334988, 62.70942372801902565 ) ) ;
#130522 = CARTESIAN_POINT ( 'NONE',  ( -16.46253265017160317, 9.564922557960807481, 60.83224293864769550 ) ) ;
#130523 = CARTESIAN_POINT ( 'NONE',  ( -13.97604488694527625, -13.89961937509977652, 31.87390960531435979 ) ) ;
#130524 = CARTESIAN_POINT ( 'NONE',  ( -16.51473224551082808, 9.474510206698731452, 63.33442372801900433 ) ) ;
#130525 = CARTESIAN_POINT ( 'NONE',  ( -5.049401038298153566, 19.05341960407611168, 115.2072429386477097 ) ) ;
#130526 = CARTESIAN_POINT ( 'NONE',  ( -19.03943276465977164, 0.05219959533909376836, 101.2489096053143669 ) ) ;
#130527 = CARTESIAN_POINT ( 'NONE',  ( -14.34966873604960291, -8.224510206698953496, 51.66557627198102409 ) ) ;
#130528 = CARTESIAN_POINT ( 'NONE',  ( -21.53943276465977519, 0.05219959533907696930, 51.24890960531436690 ) ) ;
#130529 = CARTESIAN_POINT ( 'NONE',  ( 18.22780087662122384, -5.500000000000022204, 91.01540105326107266 ) ) ;
#130530 = CARTESIAN_POINT ( 'NONE',  ( 18.62759615963255655, 10.81492255796105972, 111.6677570613523613 ) ) ;
#130531 = CARTESIAN_POINT ( 'NONE',  ( -16.21995358207303184, -7.366697692864244473, 80.06448998487843483 ) ) ;
#130532 = CARTESIAN_POINT ( 'NONE',  ( 19.05341960407611168, 5.049401038298154454, 53.95724293864770260 ) ) ;
#130533 = CARTESIAN_POINT ( 'NONE',  ( -33.70061762759714696, -5.431516297171048890, 95.88384366041692886 ) ) ;
#130534 = CARTESIAN_POINT ( 'NONE',  ( 8.398485719538898664, -36.04929410000102052, -7.999999999999994671 ) ) ;
#130535 = CARTESIAN_POINT ( 'NONE',  ( 0.05219959533934541429, -16.53943276465976808, 75.00109039468568994 ) ) ;
#130536 = CARTESIAN_POINT ( 'NONE',  ( 15.80617190586746368, 15.72974639402197994, 99.37390960531436690 ) ) ;
#130537 = AXIS2_PLACEMENT_3D ( 'NONE', #16059, #156558, #865 ) ;
#130538 = CARTESIAN_POINT ( 'NONE',  ( 4.483927247898545687, 16.52544592524342804, 54.79057627198104541 ) ) ;
#130540 = DIRECTION ( 'NONE',  ( 0.000000000000000000, 0.000000000000000000, 1.000000000000000000 ) ) ;
#130539 = CARTESIAN_POINT ( 'NONE',  ( 16.46253265017160672, -9.564922557960803928, 43.33224293864769550 ) ) ;
#130541 = CARTESIAN_POINT ( 'NONE',  ( -10.72451020669870658, -18.67979575497194134, 34.58442372801900433 ) ) ;
#130542 = CARTESIAN_POINT ( 'NONE',  ( -5.153800228976607833, 19.02544592524334988, 42.70942372801901143 ) ) ;
#130543 = CARTESIAN_POINT ( 'NONE',  ( 9.474510206698971260, -16.51473224551069308, 42.91557627198103120 ) ) ;
#130544 = CARTESIAN_POINT ( 'NONE',  ( -5.719274019375665041, -21.55341960407619695, 89.79275706135236135 ) ) ;
#130545 = CARTESIAN_POINT ( 'NONE',  ( -0.05219959533909027116, -19.03943276465977164, 22.49890960531436690 ) ) ;
#130546 = ORIENTED_EDGE ( 'NONE', *, *, #189415, .F. ) ;
#130547 = CARTESIAN_POINT ( 'NONE',  ( -14.29746914071049879, 8.314922557960819915, 40.83224293864769550 ) ) ;
#130548 = CARTESIAN_POINT ( 'NONE',  ( 18.22780087662126647, 5.499999999999818812, 41.48236817873107185 ) ) ;
#130549 = CARTESIAN_POINT ( 'NONE',  ( 21.55341960407610458, 5.719274019375980345, 43.95724293864769550 ) ) ;
#130550 = LINE ( 'NONE', #52715, #52864 ) ;
#130551 = CARTESIAN_POINT ( 'NONE',  ( 9.564922557960805705, 16.46253265017160317, 104.5822429386476955 ) ) ;
#130552 = CARTESIAN_POINT ( 'NONE',  ( -16.53943276465976808, 0.05219959533911058130, 86.24890960531436690 ) ) ;
#130553 = CARTESIAN_POINT ( 'NONE',  ( -4.379528057220086978, -16.55341960407618274, 19.79275706135235069 ) ) ;
#130554 = CARTESIAN_POINT ( 'NONE',  ( -8.224510206698735004, -14.34966873604973081, 109.5844237280190328 ) ) ;
#130555 = ORIENTED_EDGE ( 'NONE', *, *, #2746, .T. ) ;
#130557 = CARTESIAN_POINT ( 'NONE',  ( -5.823673210054116645, -21.52544592524344225, 102.2905762719810383 ) ) ;
#130556 = CARTESIAN_POINT ( 'NONE',  ( 16.46253265017160672, -9.564922557960803928, 93.33224293864769550 ) ) ;
#130559 = CARTESIAN_POINT ( 'NONE',  ( 0.05219959533909260263, 19.03943276465977164, 99.99890960531436690 ) ) ;
#130558 = CARTESIAN_POINT ( 'NONE',  ( 16.52544592524342804, -4.483927247898539470, 28.54057627198103120 ) ) ;
#130560 = CARTESIAN_POINT ( 'NONE',  ( 9.474510206698729675, 16.51473224551082808, 77.08442372801900433 ) ) ;
#130561 = CARTESIAN_POINT ( 'NONE',  ( 15.72974639402176855, 15.80617190586768217, 111.8760903946856615 ) ) ;
#130562 = CARTESIAN_POINT ( 'NONE',  ( -15.72974639402197994, 15.80617190586746368, 85.62390960531436690 ) ) ;
#130563 = CARTESIAN_POINT ( 'NONE',  ( -15.72974639402197994, 15.80617190586746368, 50.62390960531435979 ) ) ;
#130564 = AXIS2_PLACEMENT_3D ( 'NONE', #38554, #100211, #40554 ) ;
#130565 = CARTESIAN_POINT ( 'NONE',  ( -9.564922557960796823, -16.46253265017161027, 67.08224293864769550 ) ) ;
#130566 = CARTESIAN_POINT ( 'NONE',  ( -14.34966873604960291, -8.224510206698953496, 31.66557627198102054 ) ) ;
#130567 = CARTESIAN_POINT ( 'NONE',  ( 16.46253265017160672, -9.564922557960803928, 78.33224293864769550 ) ) ;
#130568 = ORIENTED_EDGE ( 'NONE', *, *, #63230, .F. ) ;
#130569 = SPHERICAL_SURFACE ( 'NONE', #182921, 0.5000000000000000000 ) ;
#130570 = CARTESIAN_POINT ( 'NONE',  ( 19.05341960407617918, -5.049401038297876454, 26.04275706135233293 ) ) ;
#130571 = CARTESIAN_POINT ( 'NONE',  ( 16.55341960407611168, 4.379528057220329451, 88.95724293864769550 ) ) ;
#130572 =( GEOMETRIC_REPRESENTATION_CONTEXT ( 3 ) GLOBAL_UNCERTAINTY_ASSIGNED_CONTEXT ( ( #161139 ) ) GLOBAL_UNIT_ASSIGNED_CONTEXT ( ( #150771, #134608, #72939 ) ) REPRESENTATION_CONTEXT ( 'NONE', 'WORKASPACE' ) );
#130573 =( BOUNDED_SURFACE ( )  B_SPLINE_SURFACE ( 3, 2, ( 
 ( #71969, #85122, #147827, #7283, #116476, #129618, #191313, #178165, #39630, #24485, #130631, #68967, #52790, #86136, #54801, #21464, #131645, #176160, #117474, #102309, #175153, #84121, #114458, #192325, #8300, #145800, #69977, #100299, #36620, #37630, #190323, #148822, #98277, #132646, #38642, #99293, #159978, #161977, #9313, #179172, #160979, #23473, #193327, #25495, #163999, #101290, #162980, #70978, #194334, #115481, #22473, #53806, #55802, #40640, #146806, #177169, #87138, #10312, #51800, #113459, #83126, #144802, #6285, #67964, #165987, #166980, #119483, #58783, #15272, #42642, #41648, #56814, #137614, #152779, #184129, #28483, #92088, #59777, #90117, #133643, #73980, #122437, #26486, #72988, #198300, #104304, #164992, #75939, #105292, #88128, #199298, #195334, #181165, #45612, #151801, #27487, #106275, #135649, #149812, #118488, #153777, #136619, #60765, #11318, #44622, #134657, #43629, #13292, #12315, #74957, #121446, #183138, #89130, #180179, #196343, #30442, #150818, #167960, #107264, #29459, #168935, #14270, #91091, #103312, #57811, #197320, #120452, #182145, #46604, #154773, #112248, #156772, #3079, #142581, #169944, #173939, #31435, #17262, #50588, #65738, #62750, #35407, #126417, #34419, #80904, #63762, #97059, #94085, #187131, #158741, #171936, #16270, #78915, #140592, #157767, #2082, #125435, #95084, #48603, #170939, #110255, #49586, #76932, #172940, #123421, #186127, #108265, #33425, #111249, #18266, #188114, #64755, #4060, #79919, #32431, #127406, #138601, #96078, #141592, #19258, #189115, #155764, #93089, #83, #77922, #61753, #47606, #185114, #139589, #1075, #124430, #109260, #81193, #17564, #157068, #95382, #65049, #171246, #138906, #16572, #189406, #140894, #48899, #1379, #142874, #172235, #385, #18564, #32735, #62058, #127706, #79225, #66039, #20530, #33720, #96370, #156066, #126705, #78219, #139890, #188409, #49886, #173237, #2383, #64062, #63058, #34713, #3374, #170249, #80212, #124738, #50883, #112541, #123723, #94387, #186435, #125732, #141883, #187431, #111552, #110554, #185420, #47911, #158058, #109565, #19548, #4354, #174235, #35704, #97351, #159037, #46912, #108572, #31743, #93391, #155077, #36687, #23540, #114527, #115548, #68031, #7347, #164063, #191380, #190393, #5353, #86202, #101356, #132710, #177236, #40704, #8367, #38708, #82178, #22538, #71043, #175222, #21533, #146875, #52856, #113528, #24552, #53874, #98347, #147892, #143873, #129682, #194398, #100365, #176228, #54868, #84185, #160046, #67037, #102374, #85186, #9378, #83194, #128696, #55866, #145865, #117540, #161044, #162044, #70042, #131711, #37697, #51868, #144868, #179238, #69032, #192391, #6351, #99361, #193392, #130697, #116542, #178230, #39694, #163045, #104368, #152842, #107324, #120516, #183202, #42707, #151862, #165055, #26548, #13353, #75017, #59839, #166052, #27552, #88192, #121508, #90179, #56878, #167041, #11381, #14336, #137675, #10378, #119548, #149876, #89192, #43692, #181231, #105354, #135713, #72035, #73051, #25562, #184191, #133708, #168023, #74042, #134723, #195400, #197384, #44684, #76001, #196406, #58849, #28543, #60826, #199361, #136682, #198364, #106337, #29519, #182208, #57876, #118552, #91153, #122500, #45673, #150885, #87206, #148887, #180243, #41712, #103377, #12380, #171997, #172999, #94147, #77982, #32494, #126476, #141650, #125495, #154834, #78978, #157825, #124494, #110315, #4117, #19315, #123484, #33485, #1137, #2144, #16333, #155826, #50643, #139649, #76993, #92152, #34477, #188174, #80963, #63822, #127465, #95143, #187192, #168997, #109322, #142639, #61814, #108326, #156832, #62811, #145, #111310, #140653, #185176, #96136, #30501, #186189, #65796, #48663, #47670, #3140, #171002, #46667, #153838, #189171, #18325, #15335, #170006, #138664, #31497, #17323, #93150, #79982, #64815, #49647, #38465, #144629, #112305, #190151, #162800, #114285, #22297, #174982, #116296 ),
 ( #100121, #130447, #6112, #146624, #175988, #66791, #20287, #160809, #177986, #52623, #23299, #143625, #173995, #24309, #194160, #113291, #83948, #85958, #81933, #131462, #70801, #35464, #53627, #158798, #161804, #9135, #82951, #7108, #147646, #51626, #132469, #37457, #145628, #36446, #39453, #68790, #97115, #192146, #67794, #5110, #101114, #191149, #128455, #98101, #115302, #69795, #129450, #84943, #159799, #21294, #8117, #193149, #54621, #99117, #176995, #195155, #151631, #120282, #86961, #197149, #41470, #182967, #167789, #40460, #149640, #56637, #72812, #73808, #11137, #135480, #165812, #102133, #180002, #55624, #14095, #163817, #198131, #104130, #103134, #25319, #27309, #13125, #44450, #118310, #88957, #58615, #90919, #29288, #181974, #43456, #105125, #59599, #180990, #164815, #119306, #74788, #28311, #12144, #26311, #150647, #106104, #134481, #166811, #152605, #75762, #10135, #89951, #87951, #136450, #196166, #42467, #137440, #57640, #148646, #178992, #121273, #117297, #71796, #133465, #157590, #125262, #93916, #199119, #139419, #187944, #91908, #138432, #63588, #108084, #30264, #141417, #170769, #153601, #2905, #60586, #46426, #111076, #32258, #31262, #171766, #901, #15098, #122262, #19082, #1909, #64583, #76757, #45437, #126248, #62575, #49413, #77753, #17089, #155594, #186960, #92913, #183951, #34246, #172765, #200113, #140418, #154599, #78742, #184941, #124253, #80730, #169769, #107090, #168761, #95906, #18093, #61581, #48431, #123250, #110087, #33255, #16095, #185949, #47433, #109089, #94913, #156598, #79748, #173766, #87481, #116817, #96887, #149168, #3887, #192668, #57159, #178508, #177514, #117827, #147161, #35233, #142409, #103660, #148166, #10658, #158570, #188940, #72321, #85472, #133997, #23822, #163335, #101644, #71323, #38984, #65566, #20059, #195688, #8649, #55146, #7627, #118838, #39974, #127226, #24831, #100640, #50418, #180521, #70323, #41994, #26830, #86481, #102657, #162321, #132986, #81703, #143386, #194677, #56146, #179520, #131990, #193675, #69311, #40989, #9657, #130977, #164342, #54151, #165338, #112077, #115824, #25837, #27834, #105634, #106623, #43972, #168297, #198653, #135006, #12654, #88471, #46945, #196684, #30786, #136964, #135988, #58153, #60119, #184468, #77270, #89475, #121787, #29793, #123756, #419, #14620, #91429, #153116, #92433, #13626, #197659, #152143, #45947, #61105, #44965, #74321, #183481, #138939, #167323, #76277, #73334, #11668, #150168, #104649, #122778, #59125, #28819, #75293, #151166, #119821, #154120, #137955, #90459, #199639, #182491, #107602, #169280, #108605, #185455, #15613, #62093, #181506, #170282, #42984, #166336, #120791, #128731, #158091, #49921, #125764, #66073, #95416, #186470, #139925, #80245, #97385, #172267, #142907, #63093, #31776, #143907, #113562, #32769, #3406, #82216, #1414, #50918, #190427, #93424, #173271, #78252, #19583, #51903, #2416, #126739, #5389, #34745, #174270, #112576, #111586, #96404, #65081, #124772, #35738, #155111, #47947, #109598, #67072, #81226, #4388, #159071, #171281, #16605, #94421, #33757, #156101, #20565, #17599, #79258, #127739, #189441, #140930, #18597, #64096, #48932, #141915, #187464, #188442, #110586, #157101, #177273, #55904, #38744, #100402, #193430, #115585, #69069, #85225, #147927, #195440, #71079, #21568, #84222, #144903, #23577, #9413, #162083, #24589, #101392, #179277, #146916, #130736, #25598, #133745, #194433, #54906, #132745, #116579, #192428, #129719, #8405, #6386, #70080, #145901, #131748, #37735, #53910, #178268, #117577, #98384, #163085, #72072, #86237, #39731, #40742, #102412, #164099, #191416, #83228, #87242, #148925, #10414, #56915, #68065, #175256, #36722, #160081, #176264, #52892, #114567, #99397, #161080, #22575, #7385, #59879, #165092, #106377, #15373, #89230, #13390, #30539, #121545, #60862, #199398, #198401, #183240, #151900, #26586, #137714, #180280, #88229, #196443 ),
 ( #76039, #122537, #105393, #138701, #135750, #28581, #77029, #75054, #57913, #120553, #182246, #184228, #43731, #167079, #136720, #58887, #12417, #90217, #91189, #183, #14373, #149913, #27592, #11420, #44721, #152878, #168059, #29556, #45709, #107360, #169033, #74079, #92191, #118590, #153875, #41750, #103414, #73090, #197421, #134761, #119585, #181268, #42745, #150924, #104407, #166089, #79014, #95183, #46704, #185213, #123520, #78017, #96174, #32530, #140688, #187228, #62847, #61851, #4156, #141687, #2180, #48699, #155861, #126513, #142677, #20326, #97155, #173038, #50687, #108366, #81003, #188211, #3178, #64851, #65835, #110351, #171039, #125531, #19354, #34516, #18365, #47707, #172033, #112344, #17359, #49683, #158838, #174034, #16369, #111348, #94182, #156869, #109357, #33521, #143669, #63860, #170044, #31534, #127505, #189209, #35505, #80018, #81975, #157864, #93187, #154872, #139686, #1172, #124531, #186226, #69834, #114325, #36486, #147687, #177035, #159841, #9174, #66832, #52663, #117337, #38505, #37496, #178024, #7147, #98142, #5150, #163859, #8158, #70841, #21334, #51666, #132509, #145666, #194198, #83987, #23337, #161843, #131501, #99158, #128496, #82992, #55663, #68831, #115345, #67833, #179032, #100161, #190191, #84981, #160847, #113330, #40499, #130490, #102171, #86999, #146663, #162839, #22336, #193188, #144668, #6153, #54661, #116335, #39492, #192186, #53667, #129489, #101152, #24347, #191187, #85998, #176028, #25358, #175023, #133503, #42505, #87990, #165851, #166847, #104169, #28349, #58652, #195195, #72851, #148686, #107126, #56675, #90954, #197188, #196207, #118348, #120318, #44487, #137476, #149678, #182012, #89987, #183987, #60623, #10174, #180042, #26350, #45472, #151668, #74826, #14131, #41511, #168797, #103174, #88993, #122297, #199156, #134521, #30301, #198167, #106143, #152641, #135517, #71834, #27347, #43495, #164854, #105161, #11176, #150684, #12182, #29324, #73846, #13162, #136487, #59637, #121311, #183003, #167825, #57679, #75798, #119347, #181031, #61616, #140452, #64618, #17124, #141453, #18126, #95938, #32294, #185984, #142442, #50449, #111109, #171799, #49446, #110121, #109124, #46460, #1942, #123284, #78776, #62608, #93950, #154634, #170802, #125298, #76794, #15132, #153637, #108120, #126280, #124287, #155628, #63622, #92948, #91944, #34279, #33287, #186994, #48464, #47467, #156631, #172798, #112108, #127260, #2938, #80764, #138465, #157624, #19114, #200146, #79781, #188973, #187977, #94947, #3920, #65600, #173799, #169803, #184975, #31296, #16129, #77784, #139453, #934, #35265, #147438, #117087, #36246, #6902, #85751, #143422, #54424, #193953, #96920, #176786, #81736, #23092, #132262, #5910, #130237, #8926, #38259, #177782, #116094, #115094, #99913, #68581, #4909, #39252, #37251, #128256, #158602, #55416, #161598, #100908, #189954, #66592, #162592, #175777, #24097, #114076, #53417, #191933, #84737, #67587, #20092, #113088, #70594, #98908, #145420, #97899, #51428, #146415, #174780, #7906, #129245, #159590, #21087, #160601, #82744, #144424, #69590, #192945, #52418, #131257, #190941, #22091, #83741, #104916, #12915, #119105, #57432, #118101, #74579, #43248, #9929, #120079, #164607, #105900, #90720, #163606, #72598, #179791, #195959, #196944, #134272, #58412, #88748, #25107, #102922, #178782, #137233, #86751, #121065, #27102, #26101, #148434, #150441, #136247, #167586, #41260, #11937, #181767, #13890, #152403, #166603, #28103, #89742, #182759, #103923, #87744, #42263, #197923, #151428, #135272, #149429, #73600, #29081, #180786, #59391, #75557, #198917, #133254, #44243, #10925, #60386, #165603, #40250, #101924, #71588, #194945, #56421, #126042, #141207, #172552, #16879, #80522, #48218, #78530, #122058, #62365, #110867, #14894, #61377, #186748, #31057, #153396, #64374, #93707, #76555, #187738, #183750, #169560, #34038, #155389, #154393, #94701, #156378, #92705 ),
 ( #45236, #95695, #693, #49209, #3679, #140204, #79537, #139218, #109872, #123048, #184734, #171556, #33046, #17883, #124034, #185733, #46219, #2697, #157383, #138231, #63374, #107872, #18876, #142196, #106890, #15888, #77546, #47222, #1698, #108881, #125051, #32050, #168563, #170560, #30061, #91702, #199913, #7661, #113836, #112851, #35023, #175532, #161360, #54186, #4662, #98667, #6663, #100673, #177549, #191691, #68341, #129991, #69345, #190705, #174542, #129006, #22851, #38020, #21851, #51190, #37006, #115859, #20843, #53173, #162355, #39018, #19855, #114850, #97658, #160361, #36009, #52178, #147195, #159347, #173554, #188725, #131012, #84498, #23856, #83502, #85506, #176544, #145179, #65357, #5669, #127018, #158366, #66354, #99676, #82501, #96678, #192703, #146176, #81495, #50210, #111864, #144183, #143182, #128015, #67345, #189717, #10694, #101679, #8685, #167357, #11703, #151200, #163369, #55181, #12688, #149203, #74354, #87515, #26867, #194711, #136020, #120828, #193712, #102690, #148199, #25871, #88510, #164378, #150205, #118872, #116850, #133021, #70356, #28855, #178541, #197694, #57197, #56180, #40007, #180556, #104685, #59160, #9692, #42030, #73370, #44010, #182528, #135042, #196718, #58187, #105671, #134031, #117863, #72357, #166373, #181539, #165373, #179554, #103694, #90495, #195724, #119855, #132023, #24866, #86515, #43018, #41024, #27869, #89510, #71357, #36517, #63891, #60154, #75328, #158868, #174066, #5181, #49714, #113361, #81030, #111379, #152177, #95213, #143699, #47736, #94213, #19381, #125562, #186258, #97182, #126540, #109389, #20357, #13661, #2210, #66862, #188239, #187259, #127536, #156899, #171069, #136998, #175053, #157892, #82005, #32559, #198687, #128525, #18395, #190219, #33551, #173067, #34544, #142706, #48728, #124561, #155892, #51698, #80046, #64879, #17390, #79046, #96203, #140720, #4185, #110381, #172064, #141715, #3205, #65864, #189238, #50716, #112374, #35534, #24382, #37528, #99191, #86033, #147720, #132542, #38539, #177068, #160879, #194230, #162874, #129518, #39525, #130524, #131538, #84021, #23371, #180074, #7181, #6183, #21365, #102206, #117369, #148718, #193222, #56707, #9207, #54696, #98172, #100195, #87033, #191218, #22370, #70874, #68865, #52692, #40535, #69869, #114356, #163895, #159874, #145699, #10206, #116369, #192221, #55696, #161877, #176061, #83023, #118380, #101185, #25391, #53703, #144697, #71866, #85016, #133534, #146697, #178057, #179066, #195226, #115380, #67863, #8194, #91975, #43526, #151700, #104200, #45503, #74856, #41543, #121341, #135547, #103206, #30334, #120348, #168829, #123315, #136518, #199189, #58681, #167856, #181062, #42537, #29356, #90986, #75830, #182043, #105191, #165881, #137508, #106173, #72883, #183034, #27378, #153669, #15166, #26382, #197219, #89024, #166878, #59669, #28379, #44517, #13193, #88021, #150715, #164888, #200178, #149709, #184021, #90017, #12214, #11208, #198199, #60656, #76825, #73877, #152673, #14162, #138496, #61647, #122329, #107158, #134551, #196240, #57709, #119379, #48498, #142473, #157656, #141486, #170835, #94979, #173830, #140488, #126311, #20122, #35295, #139485, #188007, #19145, #155660, #154666, #143453, #967, #31330, #187027, #156664, #47500, #189003, #18159, #185008, #64649, #78809, #46493, #96951, #63656, #112138, #66622, #79815, #3951, #1976, #111140, #124320, #186018, #172830, #34309, #80795, #125330, #110152, #109156, #65630, #49477, #16162, #95972, #32327, #158631, #81766, #169836, #171830, #93980, #33318, #2969, #127290, #50478, #4938, #92981, #17156, #108154, #77816, #62643, #70628, #176817, #175809, #97930, #38289, #24132, #117120, #67616, #161629, #69622, #163639, #40284, #54455, #131288, #192976, #132295, #53449, #37282, #191963, #85784, #100941, #84768, #114106, #99943, #178814, #83771, #116125, #25141, #101958, #82774, #177814, #160630, #23123, #98939, #115124, #9961 ),
 ( #21118, #129277, #39284, #22121, #159623, #193987, #146446, #144455, #55449, #189984, #145451, #86783, #7939, #6933, #162625, #130268, #5940, #128286, #148468, #147470, #51458, #190972, #174810, #113120, #68612, #36275, #8960, #52449, #179824, #11968, #12950, #88780, #89777, #28137, #182794, #165635, #180817, #167620, #13924, #197957, #181801, #59426, #120111, #42296, #102955, #73633, #41294, #135304, #57465, #27133, #10957, #103956, #196976, #194977, #133287, #56456, #164639, #74615, #119137, #150473, #26134, #118135, #43280, #121100, #104949, #58443, #166635, #151462, #136281, #44277, #75591, #90755, #105935, #29116, #71621, #137270, #152438, #149462, #87777, #72631, #134306, #195992, #146109, #86449, #115792, #6596, #160294, #100607, #117796, #192636, #163301, #83435, #52113, #164311, #133965, #53105, #23789, #102626, #21784, #71292, #10626, #113770, #193643, #98600, #39942, #149136, #22785, #147130, #25804, #55115, #194643, #132955, #131958, #116784, #85439, #145112, #56113, #175466, #68274, #129925, #87450, #178475, #101612, #179489, #191625, #72287, #114783, #54119, #36938, #40953, #37952, #176476, #24800, #9625, #99610, #38951, #161290, #69280, #162290, #84432, #8618, #7593, #177481, #70290, #130946, #148134, #120757, #13591, #135955, #89440, #105599, #168262, #15579, #91393, #41962, #197625, #58119, #12621, #28783, #180490, #118803, #57128, #11635, #29758, #166303, #74285, #26798, #103628, #198617, #137920, #75258, #59091, #182458, #151129, #60084, #76242, #154085, #30751, #106585, #184433, #195657, #14585, #153082, #165304, #183445, #92399, #121752, #136929, #43938, #199604, #167286, #150134, #88439, #90422, #61070, #152107, #122742, #73302, #134973, #107566, #77237, #196649, #44929, #45913, #119788, #169244, #181472, #42950, #104614, #27799, #146694, #52689, #118378, #6180, #40532, #8191, #145696, #67860, #69866, #194227, #87030, #37525, #131535, #39522, #133532, #10203, #24379, #101182, #162871, #102203, #23368, #7178, #161874, #55693, #70871, #54693, #84018, #193219, #148715, #53700, #86030, #195224, #71863, #114353, #147717, #130521, #116366, #68862, #85013, #180072, #192217, #129515, #21362, #163892, #117366, #56705, #178054, #98169, #9205, #132539, #159870, #38536, #83020, #191215, #99188, #179063, #115377, #176057, #25388, #144694, #160876, #22367, #177065, #100192, #153667, #74854, #73875, #14160, #43524, #134549, #41541, #200176, #44515, #88019, #106171, #184019, #121339, #58679, #166876, #135544, #167854, #122327, #61645, #76823, #152671, #30332, #103204, #60654, #199186, #164885, #29354, #138494, #90983, #59667, #197217, #75828, #105189, #196238, #149707, #90015, #107156, #182041, #137506, #72881, #26380, #15163, #123313, #42535, #13190, #91973, #11206, #45501, #57707, #119377, #183032, #181059, #168826, #136516, #104198, #198197, #165879, #27376, #89022, #150713, #12212, #120346, #28377, #151699, #3949, #46490, #154664, #62641, #20120, #64647, #111138, #50476, #77814, #81764, #139483, #125328, #158629, #173828, #170833, #143451, #34307, #142471, #189001, #171829, #4936, #1973, #94977, #66620, #79811, #124317, #187025, #48496, #65628, #110150, #33316, #2967, #156662, #78807, #18157, #157653, #185006, #80793, #31327, #93978, #16160, #141484, #19143, #126309, #95969, #172828, #112136, #188005, #140486, #35292, #108152, #127288, #49475, #96949, #169834, #63654, #965, #92979, #186016, #47497, #155658, #109154, #32325, #17154, #161627, #113117, #51456, #189982, #144453, #162622, #98937, #145449, #159621, #7936, #54452, #193983, #21116, #25137, #82772, #68609, #101953, #117116, #114104, #86779, #177811, #85781, #132291, #115122, #148464, #6931, #38287, #9957, #23121, #5938, #130266, #191961, #8957, #53447, #176815, #146443, #99941, #22119, #84766, #100938, #128284, #24128, #174808, #37280, #97928, #69619, #147467, #131285, #39281, #116122, #55445, #192973, #83769, #178810, #36273 ),
 ( #70625, #67614, #129275, #190969, #52447, #40280, #160628, #163635, #175807, #118131, #74611, #13920, #151458, #88776, #196972, #165631, #136277, #152434, #30093, #106920, #182790, #60416, #71617, #90751, #29112, #194973, #59422, #168593, #197953, #89773, #27129, #105931, #135299, #26130, #179819, #120107, #137266, #11964, #44273, #102951, #133283, #183780, #153428, #72627, #43276, #122089, #41290, #75587, #91732, #56452, #12946, #149458, #167616, #166631, #164635, #28133, #45266, #121096, #198949, #87773, #10953, #134302, #104945, #195988, #57460, #119133, #180813, #42292, #103952, #58439, #150469, #73629, #181797, #114622, #109905, #92738, #16911, #78564, #98445, #140237, #1730, #33077, #155421, #108913, #125083, #190487, #37791, #113619, #61409, #124067, #184766, #63408, #51959, #186781, #67129, #143965, #21627, #48251, #170593, #68121, #176323, #36778, #94733, #175313, #156412, #31090, #123080, #171589, #99455, #17914, #185769, #82273, #77578, #32083, #5445, #199945, #138262, #76586, #154426, #160139, #47256, #93740, #46252, #107906, #128787, #83284, #144958, #6439, #129773, #191469, #52947, #14926, #169592, #15920, #139250, #726, #62398, #180336, #118644, #84278, #148981, #57969, #87297, #179335, #54962, #195497, #24645, #115640, #69124, #9472, #26641, #101450, #72131, #192483, #161135, #73149, #42802, #162137, #132801, #11478, #130791, #41804, #119640, #22631, #102467, #38800, #56971, #55960, #181323, #117636, #134819, #164155, #103471, #165150, #40798, #25652, #194488, #53966, #88284, #145959, #177329, #100457, #196499, #10470, #133805, #149972, #23633, #7440, #85281, #163142, #146973, #8461, #70134, #131806, #193485, #116634, #178323, #39786, #86293, #147983, #71135, #58943, #12474, #152930, #170097, #44777, #15428, #135806, #104464, #16424, #186282, #105451, #76092, #154926, #74135, #123576, #62906, #166147, #45765, #182306, #238, #199451, #1228, #60919, #78071, #107417, #46763, #185271, #184282, #169090, #137767, #197477, #108422, #27650, #120612, #43787, #139739, #30596, #92249, #31591, #167135, #124587, #28635, #106430, #89289, #93241, #90272, #150980, #153934, #61905, #151955, #91240, #13444, #121600, #14427, #75108, #122594, #136775, #168111, #29608, #198461, #77087, #138756, #59933, #183295, #141739, #157915, #20382, #67887, #143725, #94238, #156923, #17414, #96226, #82029, #173092, #97206, #174089, #51721, #188263, #3229, #98196, #6207, #66886, #127562, #5205, #65888, #63915, #155919, #4210, #144721, #34570, #18420, #49738, #110406, #64903, #81054, #32585, #171094, #109415, #125585, #128547, #80069, #126564, #79071, #140745, #50739, #190244, #189264, #111406, #19405, #142730, #112398, #113384, #129540, #83046, #158892, #36540, #47761, #175074, #159899, #2233, #35558, #187282, #21388, #48753, #172088, #33575, #95237, #72909, #132566, #68889, #87058, #86056, #88046, #147745, #103231, #194255, #133561, #71891, #70899, #55722, #24407, #99214, #10231, #52714, #160902, #130549, #26407, #117394, #179093, #56736, #84045, #149734, #145724, #131563, #164913, #180100, #177091, #11235, #40562, #148743, #195251, #178082, #191240, #8219, #101209, #114378, #9232, #192246, #193247, #54720, #118406, #116392, #39550, #102231, #162898, #85041, #163920, #25416, #176082, #41568, #37551, #100219, #22395, #7205, #53727, #115403, #38563, #161900, #23395, #146722, #69895, #185034, #93006, #153694, #14187, #92000, #152698, #150739, #42562, #91012, #31355, #121366, #105216, #136542, #197243, #151724, #167882, #119404, #57734, #196265, #12239, #168853, #166903, #13217, #165906, #181087, #137532, #76849, #75856, #74880, #59695, #28403, #199214, #15190, #154692, #169861, #45528, #123341, #134578, #138520, #14549, #104225, #122356, #16187, #60681, #184045, #90042, #30358, #198223, #89049, #27404, #183059, #61672, #44543, #107182, #73901, #135571, #46521, #58704, #120374, #106198, #182067, #43550, #29381, #108180 ),
 ( #64672, #97957, #95001, #188031, #174837, #172853, #155684, #79839, #141509, #158656, #2994, #126334, #95995, #18182, #171854, #49501, #50502, #159649, #173855, #124346, #187051, #47524, #111164, #112166, #34334, #127317, #3975, #81792, #157680, #33342, #128311, #36302, #96975, #19170, #35321, #80819, #94003, #186041, #142497, #77842, #65655, #48521, #189028, #140511, #156688, #20147, #62666, #992, #139509, #17179, #143479, #110175, #4963, #109180, #170859, #66649, #190011, #51485, #113147, #32350, #78833, #2000, #63679, #125354, #56485, #132325, #9991, #21145, #40312, #178845, #144482, #8991, #118163, #147500, #39313, #115154, #55480, #84797, #175835, #129303, #69651, #86814, #161657, #194017, #52475, #82800, #133318, #102984, #22149, #193007, #71651, #190999, #101989, #179853, #5966, #162657, #98967, #117150, #116154, #41324, #177845, #195007, #24163, #163670, #25172, #100972, #85814, #54484, #114134, #148500, #67644, #37308, #160657, #83799, #70659, #145479, #6960, #68640, #130296, #191990, #53477, #176847, #38318, #99973, #23153, #146476, #7968, #131317, #183811, #26165, #134336, #42325, #199977, #44307, #90784, #30125, #57496, #61442, #119165, #104979, #138296, #153461, #150503, #123114, #13954, #122123, #168625, #151491, #184799, #181832, #74646, #46285, #59457, #103986, #166666, #28167, #45300, #89809, #12982, #182825, #136312, #58474, #197987, #137300, #164669, #60448, #10988, #73663, #196020, #121131, #198981, #105966, #75620, #152468, #91766, #167651, #120141, #14958, #87806, #106952, #29147, #76618, #149492, #180848, #72661, #165665, #27163, #88811, #135335, #12000, #197008, #43311, #141271, #92772, #31124, #169628, #124104, #142260, #78599, #125118, #139284, #154462, #110930, #50273, #187803, #186816, #33111, #1765, #172616, #188790, #66418, #143245, #18941, #96740, #107941, #127082, #65421, #15954, #95761, #4728, #34104, #126107, #63442, #3744, #171623, #62432, #77613, #156449, #173617, #48286, #80586, #761, #185804, #19917, #189782, #108947, #79602, #158429, #47291, #111931, #109941, #94767, #81559, #128079, #35087, #49272, #170628, #157446, #32117, #93774, #64437, #155455, #17949, #140272, #2761, #16945, #68405, #84562, #36074, #174608, #112914, #67411, #85573, #21915, #130057, #82567, #97723, #54250, #193776, #131078, #191757, #176610, #145246, #115922, #132087, #9754, #86577, #162417, #40069, #51254, #70420, #8750, #159413, #39080, #148261, #177612, #69412, #6727, #147260, #114917, #5732, #20908, #99740, #116913, #53240, #23919, #144248, #129066, #163435, #133082, #52242, #22916, #101746, #190767, #55245, #71418, #113899, #192767, #175597, #178606, #146240, #37073, #7726, #24932, #100736, #98733, #160426, #83567, #38084, #161424, #102752, #13723, #56246, #164440, #72420, #29891, #74415, #120891, #60216, #87577, #91529, #149264, #135103, #168396, #183579, #180619, #153216, #44074, #152238, #198751, #181601, #14721, #11766, #104745, #76381, #89574, #134097, #196779, #58247, #75389, #119915, #43078, #12750, #166436, #88573, #27931, #167420, #194772, #90556, #41089, #103757, #25934, #151260, #28916, #136081, #105733, #182590, #197755, #137061, #59222, #121886, #45064, #106722, #150271, #117927, #179617, #10756, #195788, #57260, #165436, #118934, #42092, #26931, #73432, #187566, #64199, #142017, #78355, #31877, #188547, #96502, #157204, #17704, #95518, #156204, #154224, #46046, #94522, #34847, #124875, #108707, #140029, #522, #155216, #171385, #122877, #61205, #199739, #15714, #172368, #170386, #16705, #169380, #184565, #141032, #80345, #79361, #1518, #63195, #93531, #2519, #18698, #158192, #173377, #49033, #126841, #138058, #3506, #65182, #107701, #125866, #19682, #110688, #33858, #186574, #50025, #48047, #92535, #30888, #109703, #111690, #32872, #77374, #139042, #62194, #123858, #185556, #47050, #52993, #131849, #189543, #100502, #39830, #163185, #22677, #159170, #177373 ) ),
 .UNSPECIFIED., .T., .F., .F. ) 
 B_SPLINE_SURFACE_WITH_KNOTS ( ( 4, 3, 4 ),
 ( 3, 2, 2, 2, 2, 2, 2, 2, 2, 2, 2, 2, 2, 2, 2, 2, 2, 2, 2, 2, 2, 2, 2, 2, 2, 2, 2, 2, 2, 2, 2, 2, 2, 2, 2, 2, 2, 2, 2, 2, 2, 2, 2, 2, 2, 2, 2, 2, 2, 2, 2, 2, 2, 2, 2, 2, 2, 2, 2, 2, 2, 2, 2, 2, 2, 2, 2, 2, 2, 2, 2, 2, 2, 2, 2, 2, 2, 2, 2, 2, 2, 2, 2, 2, 2, 2, 2, 2, 2, 2, 2, 2, 2, 2, 2, 2, 2, 2, 2, 2, 2, 2, 2, 2, 2, 2, 2, 2, 2, 2, 2, 2, 2, 2, 2, 2, 2, 2, 2, 2, 2, 2, 2, 2, 2, 2, 2, 2, 2, 2, 2, 2, 2, 2, 2, 2, 2, 2, 2, 2, 2, 2, 2, 2, 2, 2, 2, 2, 2, 2, 2, 2, 2, 2, 2, 2, 2, 2, 2, 2, 2, 2, 2, 2, 2, 2, 2, 2, 2, 2, 2, 2, 2, 2, 2, 2, 2, 2, 2, 2, 2, 2, 2, 2, 2, 2, 2, 2, 2, 2, 2, 2, 2, 2, 2, 2, 2, 2, 2, 2, 2, 2, 2, 2, 2, 2, 2, 2, 2, 2, 2, 2, 2, 2, 2, 2, 2, 2, 2, 2, 2, 2, 2, 2, 2, 2, 2, 2, 3 ),
 ( 0.000000000000000000, 0.5000000000000000000, 1.000000000000000000 ),
 ( 0.000000000000000000, 0.004385964912280701511, 0.008771929824561403022, 0.01315789473684210453, 0.01754385964912280604, 0.02192982456140350755, 0.02631578947368420907, 0.03070175438596491058, 0.03508771929824561209, 0.03947368421052631360, 0.04385964912280701511, 0.04824561403508771662, 0.05263157894736841813, 0.05701754385964911964, 0.06140350877192982115, 0.06578947368421052266, 0.07017543859649122417, 0.07456140350877192569, 0.07894736842105262720, 0.08333333333333332871, 0.08771929824561403022, 0.09210526315789473173, 0.09649122807017543324, 0.1008771929824561348, 0.1052631578947368363, 0.1096491228070175378, 0.1140350877192982393, 0.1184210526315789408, 0.1228070175438596423, 0.1271929824561403577, 0.1315789473684210453, 0.1359649122807017607, 0.1403508771929824483, 0.1447368421052631637, 0.1491228070175438514, 0.1535087719298245668, 0.1578947368421052544, 0.1622807017543859698, 0.1666666666666666574, 0.1710526315789473728, 0.1754385964912280604, 0.1798245614035087758, 0.1842105263157894635, 0.1885964912280701788, 0.1929824561403508665, 0.1973684210526315819, 0.2017543859649122695, 0.2061403508771929849, 0.2105263157894736725, 0.2149122807017543879, 0.2192982456140350755, 0.2236842105263157909, 0.2280701754385964786, 0.2324561403508771940, 0.2368421052631578816, 0.2412280701754385970, 0.2456140350877192846, 0.2500000000000000000, 0.2543859649122807154, 0.2587719298245614308, 0.2631578947368420907, 0.2675438596491228060, 0.2719298245614035214, 0.2763157894736842368, 0.2807017543859648967, 0.2850877192982456121, 0.2894736842105263275, 0.2938596491228070429, 0.2982456140350877027, 0.3026315789473684181, 0.3070175438596491335, 0.3114035087719298489, 0.3157894736842105088, 0.3201754385964912242, 0.3245614035087719396, 0.3289473684210526550, 0.3333333333333333148, 0.3377192982456140302, 0.3421052631578947456, 0.3464912280701754610, 0.3508771929824561209, 0.3552631578947368363, 0.3596491228070175517, 0.3640350877192982670, 0.3684210526315789269, 0.3728070175438596423, 0.3771929824561403577, 0.3815789473684210731, 0.3859649122807017330, 0.3903508771929824483, 0.3947368421052631637, 0.3991228070175438791, 0.4035087719298245390, 0.4078947368421052544, 0.4122807017543859698, 0.4166666666666666852, 0.4210526315789473450, 0.4254385964912280604, 0.4298245614035087758, 0.4342105263157894912, 0.4385964912280701511, 0.4429824561403508665, 0.4473684210526315819, 0.4517543859649122973, 0.4561403508771929571, 0.4605263157894736725, 0.4649122807017543879, 0.4692982456140351033, 0.4736842105263157632, 0.4780701754385964786, 0.4824561403508771940, 0.4868421052631579093, 0.4912280701754385692, 0.4956140350877192846, 0.5000000000000000000, 0.5043859649122807154, 0.5087719298245614308, 0.5131578947368421462, 0.5175438596491228616, 0.5219298245614034659, 0.5263157894736841813, 0.5307017543859648967, 0.5350877192982456121, 0.5394736842105263275, 0.5438596491228070429, 0.5482456140350877583, 0.5526315789473684736, 0.5570175438596490780, 0.5614035087719297934, 0.5657894736842105088, 0.5701754385964912242, 0.5745614035087719396, 0.5789473684210526550, 0.5833333333333333703, 0.5877192982456140857, 0.5921052631578946901, 0.5964912280701754055, 0.6008771929824561209, 0.6052631578947368363, 0.6096491228070175517, 0.6140350877192982670, 0.6184210526315789824, 0.6228070175438596978, 0.6271929824561403022, 0.6315789473684210176, 0.6359649122807017330, 0.6403508771929824483, 0.6447368421052631637, 0.6491228070175438791, 0.6535087719298245945, 0.6578947368421053099, 0.6622807017543859143, 0.6666666666666666297, 0.6710526315789473450, 0.6754385964912280604, 0.6798245614035087758, 0.6842105263157894912, 0.6885964912280702066, 0.6929824561403509220, 0.6973684210526315264, 0.7017543859649122417, 0.7061403508771929571, 0.7105263157894736725, 0.7149122807017543879, 0.7192982456140351033, 0.7236842105263158187, 0.7280701754385965341, 0.7324561403508771384, 0.7368421052631578538, 0.7412280701754385692, 0.7456140350877192846, 0.7500000000000000000, 0.7543859649122807154, 0.7587719298245614308, 0.7631578947368421462, 0.7675438596491228616, 0.7719298245614034659, 0.7763157894736841813, 0.7807017543859648967, 0.7850877192982456121, 0.7894736842105263275, 0.7938596491228070429, 0.7982456140350877583, 0.8026315789473684736, 0.8070175438596490780, 0.8114035087719297934, 0.8157894736842105088, 0.8201754385964912242, 0.8245614035087719396, 0.8289473684210526550, 0.8333333333333333703, 0.8377192982456140857, 0.8421052631578946901, 0.8464912280701754055, 0.8508771929824561209, 0.8552631578947368363, 0.8596491228070175517, 0.8640350877192982670, 0.8684210526315789824, 0.8728070175438596978, 0.8771929824561403022, 0.8815789473684210176, 0.8859649122807017330, 0.8903508771929824483, 0.8947368421052631637, 0.8991228070175438791, 0.9035087719298245945, 0.9078947368421053099, 0.9122807017543859143, 0.9166666666666666297, 0.9210526315789473450, 0.9254385964912280604, 0.9298245614035087758, 0.9342105263157894912, 0.9385964912280702066, 0.9429824561403509220, 0.9473684210526315264, 0.9517543859649122417, 0.9561403508771929571, 0.9605263157894736725, 0.9649122807017543879, 0.9692982456140351033, 0.9736842105263158187, 0.9780701754385965341, 0.9824561403508771384, 0.9868421052631578538, 0.9912280701754385692, 0.9956140350877192846, 1.000000000000000000 ),
 .UNSPECIFIED. ) 
 GEOMETRIC_REPRESENTATION_ITEM ( )  RATIONAL_B_SPLINE_SURFACE ( (
 ( 1.000000000000000000, 0.9659258262890683122, 1.000000000000000000, 0.9659258262890683122, 1.000000000000000000, 0.9659258262890683122, 1.000000000000000000, 0.9659258262890683122, 1.000000000000000000, 0.9659258262890683122, 1.000000000000000000, 0.9659258262890683122, 1.000000000000000000, 0.9659258262890683122, 1.000000000000000000, 0.9659258262890683122, 1.000000000000000000, 0.9659258262890683122, 1.000000000000000000, 0.9659258262890683122, 1.000000000000000000, 0.9659258262890683122, 1.000000000000000000, 0.9659258262890683122, 1.000000000000000000, 0.9659258262890683122, 1.000000000000000000, 0.9659258262890683122, 1.000000000000000000, 0.9659258262890683122, 1.000000000000000000, 0.9659258262890683122, 1.000000000000000000, 0.9659258262890683122, 1.000000000000000000, 0.9659258262890683122, 1.000000000000000000, 0.9659258262890683122, 1.000000000000000000, 0.9659258262890683122, 1.000000000000000000, 0.9659258262890683122, 1.000000000000000000, 0.9659258262890683122, 1.000000000000000000, 0.9659258262890683122, 1.000000000000000000, 0.9659258262890683122, 1.000000000000000000, 0.9659258262890683122, 1.000000000000000000, 0.9659258262890683122, 1.000000000000000000, 0.9659258262890683122, 1.000000000000000000, 0.9659258262890683122, 1.000000000000000000, 0.9659258262890683122, 1.000000000000000000, 0.9659258262890683122, 1.000000000000000000, 0.9659258262890683122, 1.000000000000000000, 0.9659258262890683122, 1.000000000000000000, 0.9659258262890683122, 1.000000000000000000, 0.9659258262890683122, 1.000000000000000000, 0.9659258262890683122, 1.000000000000000000, 0.9659258262890683122, 1.000000000000000000, 0.9659258262890683122, 1.000000000000000000, 0.9659258262890683122, 1.000000000000000000, 0.9659258262890683122, 1.000000000000000000, 0.9659258262890683122, 1.000000000000000000, 0.9659258262890683122, 1.000000000000000000, 0.9659258262890683122, 1.000000000000000000, 0.9659258262890683122, 1.000000000000000000, 0.9659258262890683122, 1.000000000000000000, 0.9659258262890683122, 1.000000000000000000, 0.9659258262890683122, 1.000000000000000000, 0.9659258262890683122, 1.000000000000000000, 0.9659258262890683122, 1.000000000000000000, 0.9659258262890683122, 1.000000000000000000, 0.9659258262890683122, 1.000000000000000000, 0.9659258262890683122, 1.000000000000000000, 0.9659258262890683122, 1.000000000000000000, 0.9659258262890683122, 1.000000000000000000, 0.9659258262890683122, 1.000000000000000000, 0.9659258262890683122, 1.000000000000000000, 0.9659258262890683122, 1.000000000000000000, 0.9659258262890683122, 1.000000000000000000, 0.9659258262890683122, 1.000000000000000000, 0.9659258262890683122, 1.000000000000000000, 0.9659258262890683122, 1.000000000000000000, 0.9659258262890683122, 1.000000000000000000, 0.9659258262890683122, 1.000000000000000000, 0.9659258262890683122, 1.000000000000000000, 0.9659258262890683122, 1.000000000000000000, 0.9659258262890683122, 1.000000000000000000, 0.9659258262890683122, 1.000000000000000000, 0.9659258262890683122, 1.000000000000000000, 0.9659258262890683122, 1.000000000000000000, 0.9659258262890683122, 1.000000000000000000, 0.9659258262890683122, 1.000000000000000000, 0.9659258262890683122, 1.000000000000000000, 0.9659258262890683122, 1.000000000000000000, 0.9659258262890683122, 1.000000000000000000, 0.9659258262890683122, 1.000000000000000000, 0.9659258262890683122, 1.000000000000000000, 0.9659258262890683122, 1.000000000000000000, 0.9659258262890683122, 1.000000000000000000, 0.9659258262890683122, 1.000000000000000000, 0.9659258262890683122, 1.000000000000000000, 0.9659258262890683122, 1.000000000000000000, 0.9659258262890683122, 1.000000000000000000, 0.9659258262890683122, 1.000000000000000000, 0.9659258262890683122, 1.000000000000000000, 0.9659258262890683122, 1.000000000000000000, 0.9659258262890683122, 1.000000000000000000, 0.9659258262890683122, 1.000000000000000000, 0.9659258262890683122, 1.000000000000000000, 0.9659258262890683122, 1.000000000000000000, 0.9659258262890683122, 1.000000000000000000, 0.9659258262890683122, 1.000000000000000000, 0.9659258262890683122, 1.000000000000000000, 0.9659258262890683122, 1.000000000000000000, 0.9659258262890683122, 1.000000000000000000, 0.9659258262890683122, 1.000000000000000000, 0.9659258262890683122, 1.000000000000000000, 0.9659258262890683122, 1.000000000000000000, 0.9659258262890683122, 1.000000000000000000, 0.9659258262890683122, 1.000000000000000000, 0.9659258262890683122, 1.000000000000000000, 0.9659258262890683122, 1.000000000000000000, 0.9659258262890683122, 1.000000000000000000, 0.9659258262890683122, 1.000000000000000000, 0.9659258262890683122, 1.000000000000000000, 0.9659258262890683122, 1.000000000000000000, 0.9659258262890683122, 1.000000000000000000, 0.9659258262890683122, 1.000000000000000000, 0.9659258262890683122, 1.000000000000000000, 0.9659258262890683122, 1.000000000000000000, 0.9659258262890683122, 1.000000000000000000, 0.9659258262890683122, 1.000000000000000000, 0.9659258262890683122, 1.000000000000000000, 0.9659258262890683122, 1.000000000000000000, 0.9659258262890683122, 1.000000000000000000, 0.9659258262890683122, 1.000000000000000000, 0.9659258262890683122, 1.000000000000000000, 0.9659258262890683122, 1.000000000000000000, 0.9659258262890683122, 1.000000000000000000, 0.9659258262890683122, 1.000000000000000000, 0.9659258262890683122, 1.000000000000000000, 0.9659258262890683122, 1.000000000000000000, 0.9659258262890683122, 1.000000000000000000, 0.9659258262890683122, 1.000000000000000000, 0.9659258262890683122, 1.000000000000000000, 0.9659258262890683122, 1.000000000000000000, 0.9659258262890683122, 1.000000000000000000, 0.9659258262890683122, 1.000000000000000000, 0.9659258262890683122, 1.000000000000000000, 0.9659258262890683122, 1.000000000000000000, 0.9659258262890683122, 1.000000000000000000, 0.9659258262890683122, 1.000000000000000000, 0.9659258262890683122, 1.000000000000000000, 0.9659258262890683122, 1.000000000000000000, 0.9659258262890683122, 1.000000000000000000, 0.9659258262890683122, 1.000000000000000000, 0.9659258262890683122, 1.000000000000000000, 0.9659258262890683122, 1.000000000000000000, 0.9659258262890683122, 1.000000000000000000, 0.9659258262890683122, 1.000000000000000000, 0.9659258262890683122, 1.000000000000000000, 0.9659258262890683122, 1.000000000000000000, 0.9659258262890683122, 1.000000000000000000, 0.9659258262890683122, 1.000000000000000000, 0.9659258262890683122, 1.000000000000000000, 0.9659258262890683122, 1.000000000000000000, 0.9659258262890683122, 1.000000000000000000, 0.9659258262890683122, 1.000000000000000000, 0.9659258262890683122, 1.000000000000000000, 0.9659258262890683122, 1.000000000000000000, 0.9659258262890683122, 1.000000000000000000, 0.9659258262890683122, 1.000000000000000000, 0.9659258262890683122, 1.000000000000000000, 0.9659258262890683122, 1.000000000000000000, 0.9659258262890683122, 1.000000000000000000, 0.9659258262890683122, 1.000000000000000000, 0.9659258262890683122, 1.000000000000000000, 0.9659258262890683122, 1.000000000000000000, 0.9659258262890683122, 1.000000000000000000, 0.9659258262890683122, 1.000000000000000000, 0.9659258262890683122, 1.000000000000000000, 0.9659258262890683122, 1.000000000000000000, 0.9659258262890683122, 1.000000000000000000, 0.9659258262890683122, 1.000000000000000000, 0.9659258262890683122, 1.000000000000000000, 0.9659258262890683122, 1.000000000000000000, 0.9659258262890683122, 1.000000000000000000, 0.9659258262890683122, 1.000000000000000000, 0.9659258262890683122, 1.000000000000000000, 0.9659258262890683122, 1.000000000000000000, 0.9659258262890683122, 1.000000000000000000, 0.9659258262890683122, 1.000000000000000000, 0.9659258262890683122, 1.000000000000000000, 0.9659258262890683122, 1.000000000000000000, 0.9659258262890683122, 1.000000000000000000, 0.9659258262890683122, 1.000000000000000000, 0.9659258262890683122, 1.000000000000000000, 0.9659258262890683122, 1.000000000000000000, 0.9659258262890683122, 1.000000000000000000, 0.9659258262890683122, 1.000000000000000000, 0.9659258262890683122, 1.000000000000000000, 0.9659258262890683122, 1.000000000000000000, 0.9659258262890683122, 1.000000000000000000, 0.9659258262890683122, 1.000000000000000000, 0.9659258262890683122, 1.000000000000000000, 0.9659258262890683122, 1.000000000000000000, 0.9659258262890683122, 1.000000000000000000, 0.9659258262890683122, 1.000000000000000000, 0.9659258262890683122, 1.000000000000000000, 0.9659258262890683122, 1.000000000000000000, 0.9659258262890683122, 1.000000000000000000, 0.9659258262890683122, 1.000000000000000000, 0.9659258262890683122, 1.000000000000000000, 0.9659258262890683122, 1.000000000000000000, 0.9659258262890683122, 1.000000000000000000, 0.9659258262890683122, 1.000000000000000000, 0.9659258262890683122, 1.000000000000000000, 0.9659258262890683122, 1.000000000000000000, 0.9659258262890683122, 1.000000000000000000, 0.9659258262890683122, 1.000000000000000000, 0.9659258262890683122, 1.000000000000000000, 0.9659258262890683122, 1.000000000000000000, 0.9659258262890683122, 1.000000000000000000, 0.9659258262890683122, 1.000000000000000000, 0.9659258262890683122, 1.000000000000000000, 0.9659258262890683122, 1.000000000000000000, 0.9659258262890683122, 1.000000000000000000, 0.9659258262890683122, 1.000000000000000000, 0.9659258262890683122, 1.000000000000000000, 0.9659258262890683122, 1.000000000000000000, 0.9659258262890683122, 1.000000000000000000, 0.9659258262890683122, 1.000000000000000000, 0.9659258262890683122, 1.000000000000000000, 0.9659258262890683122, 1.000000000000000000, 0.9659258262890683122, 1.000000000000000000, 0.9659258262890683122, 1.000000000000000000, 0.9659258262890683122, 1.000000000000000000, 0.9659258262890683122, 1.000000000000000000, 0.9659258262890683122, 1.000000000000000000, 0.9659258262890683122, 1.000000000000000000, 0.9659258262890683122, 1.000000000000000000, 0.9659258262890683122, 1.000000000000000000, 0.9659258262890683122, 1.000000000000000000, 0.9659258262890683122, 1.000000000000000000, 0.9659258262890683122, 1.000000000000000000, 0.9659258262890683122, 1.000000000000000000, 0.9659258262890683122, 1.000000000000000000, 0.9659258262890683122, 1.000000000000000000, 0.9659258262890683122, 1.000000000000000000, 0.9659258262890683122, 1.000000000000000000),
 ( 0.3333333333333333703, 0.3219752754296894559, 0.3333333333333333703, 0.3219752754296894559, 0.3333333333333333703, 0.3219752754296894559, 0.3333333333333333703, 0.3219752754296894559, 0.3333333333333333703, 0.3219752754296894559, 0.3333333333333333703, 0.3219752754296894559, 0.3333333333333333703, 0.3219752754296894559, 0.3333333333333333703, 0.3219752754296894559, 0.3333333333333333703, 0.3219752754296894559, 0.3333333333333333703, 0.3219752754296894559, 0.3333333333333333703, 0.3219752754296894559, 0.3333333333333333703, 0.3219752754296894559, 0.3333333333333333703, 0.3219752754296894559, 0.3333333333333333703, 0.3219752754296894559, 0.3333333333333333703, 0.3219752754296894559, 0.3333333333333333703, 0.3219752754296894559, 0.3333333333333333703, 0.3219752754296894559, 0.3333333333333333703, 0.3219752754296894559, 0.3333333333333333703, 0.3219752754296894559, 0.3333333333333333703, 0.3219752754296894559, 0.3333333333333333703, 0.3219752754296894559, 0.3333333333333333703, 0.3219752754296894559, 0.3333333333333333703, 0.3219752754296894559, 0.3333333333333333703, 0.3219752754296894559, 0.3333333333333333703, 0.3219752754296894559, 0.3333333333333333703, 0.3219752754296894559, 0.3333333333333333703, 0.3219752754296894559, 0.3333333333333333703, 0.3219752754296894559, 0.3333333333333333703, 0.3219752754296894559, 0.3333333333333333703, 0.3219752754296894559, 0.3333333333333333703, 0.3219752754296894559, 0.3333333333333333703, 0.3219752754296894559, 0.3333333333333333703, 0.3219752754296894559, 0.3333333333333333703, 0.3219752754296894559, 0.3333333333333333703, 0.3219752754296894559, 0.3333333333333333703, 0.3219752754296894559, 0.3333333333333333703, 0.3219752754296894559, 0.3333333333333333703, 0.3219752754296894559, 0.3333333333333333703, 0.3219752754296894559, 0.3333333333333333703, 0.3219752754296894559, 0.3333333333333333703, 0.3219752754296894559, 0.3333333333333333703, 0.3219752754296894559, 0.3333333333333333703, 0.3219752754296894559, 0.3333333333333333703, 0.3219752754296894559, 0.3333333333333333703, 0.3219752754296894559, 0.3333333333333333703, 0.3219752754296894559, 0.3333333333333333703, 0.3219752754296894559, 0.3333333333333333703, 0.3219752754296894559, 0.3333333333333333703, 0.3219752754296894559, 0.3333333333333333703, 0.3219752754296894559, 0.3333333333333333703, 0.3219752754296894559, 0.3333333333333333703, 0.3219752754296894559, 0.3333333333333333703, 0.3219752754296894559, 0.3333333333333333703, 0.3219752754296894559, 0.3333333333333333703, 0.3219752754296894559, 0.3333333333333333703, 0.3219752754296894559, 0.3333333333333333703, 0.3219752754296894559, 0.3333333333333333703, 0.3219752754296894559, 0.3333333333333333703, 0.3219752754296894559, 0.3333333333333333703, 0.3219752754296894559, 0.3333333333333333703, 0.3219752754296894559, 0.3333333333333333703, 0.3219752754296894559, 0.3333333333333333703, 0.3219752754296894559, 0.3333333333333333703, 0.3219752754296894559, 0.3333333333333333703, 0.3219752754296894559, 0.3333333333333333703, 0.3219752754296894559, 0.3333333333333333703, 0.3219752754296894559, 0.3333333333333333703, 0.3219752754296894559, 0.3333333333333333703, 0.3219752754296894559, 0.3333333333333333703, 0.3219752754296894559, 0.3333333333333333703, 0.3219752754296894559, 0.3333333333333333703, 0.3219752754296894559, 0.3333333333333333703, 0.3219752754296894559, 0.3333333333333333703, 0.3219752754296894559, 0.3333333333333333703, 0.3219752754296894559, 0.3333333333333333703, 0.3219752754296894559, 0.3333333333333333703, 0.3219752754296894559, 0.3333333333333333703, 0.3219752754296894559, 0.3333333333333333703, 0.3219752754296894559, 0.3333333333333333703, 0.3219752754296894559, 0.3333333333333333703, 0.3219752754296894559, 0.3333333333333333703, 0.3219752754296894559, 0.3333333333333333703, 0.3219752754296894559, 0.3333333333333333703, 0.3219752754296894559, 0.3333333333333333703, 0.3219752754296894559, 0.3333333333333333703, 0.3219752754296894559, 0.3333333333333333703, 0.3219752754296894559, 0.3333333333333333703, 0.3219752754296894559, 0.3333333333333333703, 0.3219752754296894559, 0.3333333333333333703, 0.3219752754296894559, 0.3333333333333333703, 0.3219752754296894559, 0.3333333333333333703, 0.3219752754296894559, 0.3333333333333333703, 0.3219752754296894559, 0.3333333333333333703, 0.3219752754296894559, 0.3333333333333333703, 0.3219752754296894559, 0.3333333333333333703, 0.3219752754296894559, 0.3333333333333333703, 0.3219752754296894559, 0.3333333333333333703, 0.3219752754296894559, 0.3333333333333333703, 0.3219752754296894559, 0.3333333333333333703, 0.3219752754296894559, 0.3333333333333333703, 0.3219752754296894559, 0.3333333333333333703, 0.3219752754296894559, 0.3333333333333333703, 0.3219752754296894559, 0.3333333333333333703, 0.3219752754296894559, 0.3333333333333333703, 0.3219752754296894559, 0.3333333333333333703, 0.3219752754296894559, 0.3333333333333333703, 0.3219752754296894559, 0.3333333333333333703, 0.3219752754296894559, 0.3333333333333333703, 0.3219752754296894559, 0.3333333333333333703, 0.3219752754296894559, 0.3333333333333333703, 0.3219752754296894559, 0.3333333333333333703, 0.3219752754296894559, 0.3333333333333333703, 0.3219752754296894559, 0.3333333333333333703, 0.3219752754296894559, 0.3333333333333333703, 0.3219752754296894559, 0.3333333333333333703, 0.3219752754296894559, 0.3333333333333333703, 0.3219752754296894559, 0.3333333333333333703, 0.3219752754296894559, 0.3333333333333333703, 0.3219752754296894559, 0.3333333333333333703, 0.3219752754296894559, 0.3333333333333333703, 0.3219752754296894559, 0.3333333333333333703, 0.3219752754296894559, 0.3333333333333333703, 0.3219752754296894559, 0.3333333333333333703, 0.3219752754296894559, 0.3333333333333333703, 0.3219752754296894559, 0.3333333333333333703, 0.3219752754296894559, 0.3333333333333333703, 0.3219752754296894559, 0.3333333333333333703, 0.3219752754296894559, 0.3333333333333333703, 0.3219752754296894559, 0.3333333333333333703, 0.3219752754296894559, 0.3333333333333333703, 0.3219752754296894559, 0.3333333333333333703, 0.3219752754296894559, 0.3333333333333333703, 0.3219752754296894559, 0.3333333333333333703, 0.3219752754296894559, 0.3333333333333333703, 0.3219752754296894559, 0.3333333333333333703, 0.3219752754296894559, 0.3333333333333333703, 0.3219752754296894559, 0.3333333333333333703, 0.3219752754296894559, 0.3333333333333333703, 0.3219752754296894559, 0.3333333333333333703, 0.3219752754296894559, 0.3333333333333333703, 0.3219752754296894559, 0.3333333333333333703, 0.3219752754296894559, 0.3333333333333333703, 0.3219752754296894559, 0.3333333333333333703, 0.3219752754296894559, 0.3333333333333333703, 0.3219752754296894559, 0.3333333333333333703, 0.3219752754296894559, 0.3333333333333333703, 0.3219752754296894559, 0.3333333333333333703, 0.3219752754296894559, 0.3333333333333333703, 0.3219752754296894559, 0.3333333333333333703, 0.3219752754296894559, 0.3333333333333333703, 0.3219752754296894559, 0.3333333333333333703, 0.3219752754296894559, 0.3333333333333333703, 0.3219752754296894559, 0.3333333333333333703, 0.3219752754296894559, 0.3333333333333333703, 0.3219752754296894559, 0.3333333333333333703, 0.3219752754296894559, 0.3333333333333333703, 0.3219752754296894559, 0.3333333333333333703, 0.3219752754296894559, 0.3333333333333333703, 0.3219752754296894559, 0.3333333333333333703, 0.3219752754296894559, 0.3333333333333333703, 0.3219752754296894559, 0.3333333333333333703, 0.3219752754296894559, 0.3333333333333333703, 0.3219752754296894559, 0.3333333333333333703, 0.3219752754296894559, 0.3333333333333333703, 0.3219752754296894559, 0.3333333333333333703, 0.3219752754296894559, 0.3333333333333333703, 0.3219752754296894559, 0.3333333333333333703, 0.3219752754296894559, 0.3333333333333333703, 0.3219752754296894559, 0.3333333333333333703, 0.3219752754296894559, 0.3333333333333333703, 0.3219752754296894559, 0.3333333333333333703, 0.3219752754296894559, 0.3333333333333333703, 0.3219752754296894559, 0.3333333333333333703, 0.3219752754296894559, 0.3333333333333333703, 0.3219752754296894559, 0.3333333333333333703, 0.3219752754296894559, 0.3333333333333333703, 0.3219752754296894559, 0.3333333333333333703, 0.3219752754296894559, 0.3333333333333333703, 0.3219752754296894559, 0.3333333333333333703, 0.3219752754296894559, 0.3333333333333333703, 0.3219752754296894559, 0.3333333333333333703, 0.3219752754296894559, 0.3333333333333333703, 0.3219752754296894559, 0.3333333333333333703, 0.3219752754296894559, 0.3333333333333333703, 0.3219752754296894559, 0.3333333333333333703, 0.3219752754296894559, 0.3333333333333333703, 0.3219752754296894559, 0.3333333333333333703, 0.3219752754296894559, 0.3333333333333333703, 0.3219752754296894559, 0.3333333333333333703, 0.3219752754296894559, 0.3333333333333333703, 0.3219752754296894559, 0.3333333333333333703, 0.3219752754296894559, 0.3333333333333333703, 0.3219752754296894559, 0.3333333333333333703, 0.3219752754296894559, 0.3333333333333333703, 0.3219752754296894559, 0.3333333333333333703, 0.3219752754296894559, 0.3333333333333333703, 0.3219752754296894559, 0.3333333333333333703, 0.3219752754296894559, 0.3333333333333333703, 0.3219752754296894559, 0.3333333333333333703, 0.3219752754296894559, 0.3333333333333333703, 0.3219752754296894559, 0.3333333333333333703, 0.3219752754296894559, 0.3333333333333333703, 0.3219752754296894559, 0.3333333333333333703, 0.3219752754296894559, 0.3333333333333333703, 0.3219752754296894559, 0.3333333333333333703, 0.3219752754296894559, 0.3333333333333333703, 0.3219752754296894559, 0.3333333333333333703, 0.3219752754296894559, 0.3333333333333333703, 0.3219752754296894559, 0.3333333333333333703, 0.3219752754296894559, 0.3333333333333333703, 0.3219752754296894559, 0.3333333333333333703, 0.3219752754296894559, 0.3333333333333333703, 0.3219752754296894559, 0.3333333333333333703, 0.3219752754296894559, 0.3333333333333333703, 0.3219752754296894559, 0.3333333333333333703, 0.3219752754296894559, 0.3333333333333333703, 0.3219752754296894559, 0.3333333333333333703, 0.3219752754296894559, 0.3333333333333333703, 0.3219752754296894559, 0.3333333333333333703, 0.3219752754296894559, 0.3333333333333333703, 0.3219752754296894559, 0.3333333333333333703, 0.3219752754296894559, 0.3333333333333333703, 0.3219752754296894559, 0.3333333333333333703, 0.3219752754296894559, 0.3333333333333333703, 0.3219752754296894559, 0.3333333333333333703, 0.3219752754296894559, 0.3333333333333333703, 0.3219752754296894559, 0.3333333333333333703, 0.3219752754296894559, 0.3333333333333333703),
 ( 0.3333333333333333703, 0.3219752754296894559, 0.3333333333333333703, 0.3219752754296894559, 0.3333333333333333703, 0.3219752754296894559, 0.3333333333333333703, 0.3219752754296894559, 0.3333333333333333703, 0.3219752754296894559, 0.3333333333333333703, 0.3219752754296894559, 0.3333333333333333703, 0.3219752754296894559, 0.3333333333333333703, 0.3219752754296894559, 0.3333333333333333703, 0.3219752754296894559, 0.3333333333333333703, 0.3219752754296894559, 0.3333333333333333703, 0.3219752754296894559, 0.3333333333333333703, 0.3219752754296894559, 0.3333333333333333703, 0.3219752754296894559, 0.3333333333333333703, 0.3219752754296894559, 0.3333333333333333703, 0.3219752754296894559, 0.3333333333333333703, 0.3219752754296894559, 0.3333333333333333703, 0.3219752754296894559, 0.3333333333333333703, 0.3219752754296894559, 0.3333333333333333703, 0.3219752754296894559, 0.3333333333333333703, 0.3219752754296894559, 0.3333333333333333703, 0.3219752754296894559, 0.3333333333333333703, 0.3219752754296894559, 0.3333333333333333703, 0.3219752754296894559, 0.3333333333333333703, 0.3219752754296894559, 0.3333333333333333703, 0.3219752754296894559, 0.3333333333333333703, 0.3219752754296894559, 0.3333333333333333703, 0.3219752754296894559, 0.3333333333333333703, 0.3219752754296894559, 0.3333333333333333703, 0.3219752754296894559, 0.3333333333333333703, 0.3219752754296894559, 0.3333333333333333703, 0.3219752754296894559, 0.3333333333333333703, 0.3219752754296894559, 0.3333333333333333703, 0.3219752754296894559, 0.3333333333333333703, 0.3219752754296894559, 0.3333333333333333703, 0.3219752754296894559, 0.3333333333333333703, 0.3219752754296894559, 0.3333333333333333703, 0.3219752754296894559, 0.3333333333333333703, 0.3219752754296894559, 0.3333333333333333703, 0.3219752754296894559, 0.3333333333333333703, 0.3219752754296894559, 0.3333333333333333703, 0.3219752754296894559, 0.3333333333333333703, 0.3219752754296894559, 0.3333333333333333703, 0.3219752754296894559, 0.3333333333333333703, 0.3219752754296894559, 0.3333333333333333703, 0.3219752754296894559, 0.3333333333333333703, 0.3219752754296894559, 0.3333333333333333703, 0.3219752754296894559, 0.3333333333333333703, 0.3219752754296894559, 0.3333333333333333703, 0.3219752754296894559, 0.3333333333333333703, 0.3219752754296894559, 0.3333333333333333703, 0.3219752754296894559, 0.3333333333333333703, 0.3219752754296894559, 0.3333333333333333703, 0.3219752754296894559, 0.3333333333333333703, 0.3219752754296894559, 0.3333333333333333703, 0.3219752754296894559, 0.3333333333333333703, 0.3219752754296894559, 0.3333333333333333703, 0.3219752754296894559, 0.3333333333333333703, 0.3219752754296894559, 0.3333333333333333703, 0.3219752754296894559, 0.3333333333333333703, 0.3219752754296894559, 0.3333333333333333703, 0.3219752754296894559, 0.3333333333333333703, 0.3219752754296894559, 0.3333333333333333703, 0.3219752754296894559, 0.3333333333333333703, 0.3219752754296894559, 0.3333333333333333703, 0.3219752754296894559, 0.3333333333333333703, 0.3219752754296894559, 0.3333333333333333703, 0.3219752754296894559, 0.3333333333333333703, 0.3219752754296894559, 0.3333333333333333703, 0.3219752754296894559, 0.3333333333333333703, 0.3219752754296894559, 0.3333333333333333703, 0.3219752754296894559, 0.3333333333333333703, 0.3219752754296894559, 0.3333333333333333703, 0.3219752754296894559, 0.3333333333333333703, 0.3219752754296894559, 0.3333333333333333703, 0.3219752754296894559, 0.3333333333333333703, 0.3219752754296894559, 0.3333333333333333703, 0.3219752754296894559, 0.3333333333333333703, 0.3219752754296894559, 0.3333333333333333703, 0.3219752754296894559, 0.3333333333333333703, 0.3219752754296894559, 0.3333333333333333703, 0.3219752754296894559, 0.3333333333333333703, 0.3219752754296894559, 0.3333333333333333703, 0.3219752754296894559, 0.3333333333333333703, 0.3219752754296894559, 0.3333333333333333703, 0.3219752754296894559, 0.3333333333333333703, 0.3219752754296894559, 0.3333333333333333703, 0.3219752754296894559, 0.3333333333333333703, 0.3219752754296894559, 0.3333333333333333703, 0.3219752754296894559, 0.3333333333333333703, 0.3219752754296894559, 0.3333333333333333703, 0.3219752754296894559, 0.3333333333333333703, 0.3219752754296894559, 0.3333333333333333703, 0.3219752754296894559, 0.3333333333333333703, 0.3219752754296894559, 0.3333333333333333703, 0.3219752754296894559, 0.3333333333333333703, 0.3219752754296894559, 0.3333333333333333703, 0.3219752754296894559, 0.3333333333333333703, 0.3219752754296894559, 0.3333333333333333703, 0.3219752754296894559, 0.3333333333333333703, 0.3219752754296894559, 0.3333333333333333703, 0.3219752754296894559, 0.3333333333333333703, 0.3219752754296894559, 0.3333333333333333703, 0.3219752754296894559, 0.3333333333333333703, 0.3219752754296894559, 0.3333333333333333703, 0.3219752754296894559, 0.3333333333333333703, 0.3219752754296894559, 0.3333333333333333703, 0.3219752754296894559, 0.3333333333333333703, 0.3219752754296894559, 0.3333333333333333703, 0.3219752754296894559, 0.3333333333333333703, 0.3219752754296894559, 0.3333333333333333703, 0.3219752754296894559, 0.3333333333333333703, 0.3219752754296894559, 0.3333333333333333703, 0.3219752754296894559, 0.3333333333333333703, 0.3219752754296894559, 0.3333333333333333703, 0.3219752754296894559, 0.3333333333333333703, 0.3219752754296894559, 0.3333333333333333703, 0.3219752754296894559, 0.3333333333333333703, 0.3219752754296894559, 0.3333333333333333703, 0.3219752754296894559, 0.3333333333333333703, 0.3219752754296894559, 0.3333333333333333703, 0.3219752754296894559, 0.3333333333333333703, 0.3219752754296894559, 0.3333333333333333703, 0.3219752754296894559, 0.3333333333333333703, 0.3219752754296894559, 0.3333333333333333703, 0.3219752754296894559, 0.3333333333333333703, 0.3219752754296894559, 0.3333333333333333703, 0.3219752754296894559, 0.3333333333333333703, 0.3219752754296894559, 0.3333333333333333703, 0.3219752754296894559, 0.3333333333333333703, 0.3219752754296894559, 0.3333333333333333703, 0.3219752754296894559, 0.3333333333333333703, 0.3219752754296894559, 0.3333333333333333703, 0.3219752754296894559, 0.3333333333333333703, 0.3219752754296894559, 0.3333333333333333703, 0.3219752754296894559, 0.3333333333333333703, 0.3219752754296894559, 0.3333333333333333703, 0.3219752754296894559, 0.3333333333333333703, 0.3219752754296894559, 0.3333333333333333703, 0.3219752754296894559, 0.3333333333333333703, 0.3219752754296894559, 0.3333333333333333703, 0.3219752754296894559, 0.3333333333333333703, 0.3219752754296894559, 0.3333333333333333703, 0.3219752754296894559, 0.3333333333333333703, 0.3219752754296894559, 0.3333333333333333703, 0.3219752754296894559, 0.3333333333333333703, 0.3219752754296894559, 0.3333333333333333703, 0.3219752754296894559, 0.3333333333333333703, 0.3219752754296894559, 0.3333333333333333703, 0.3219752754296894559, 0.3333333333333333703, 0.3219752754296894559, 0.3333333333333333703, 0.3219752754296894559, 0.3333333333333333703, 0.3219752754296894559, 0.3333333333333333703, 0.3219752754296894559, 0.3333333333333333703, 0.3219752754296894559, 0.3333333333333333703, 0.3219752754296894559, 0.3333333333333333703, 0.3219752754296894559, 0.3333333333333333703, 0.3219752754296894559, 0.3333333333333333703, 0.3219752754296894559, 0.3333333333333333703, 0.3219752754296894559, 0.3333333333333333703, 0.3219752754296894559, 0.3333333333333333703, 0.3219752754296894559, 0.3333333333333333703, 0.3219752754296894559, 0.3333333333333333703, 0.3219752754296894559, 0.3333333333333333703, 0.3219752754296894559, 0.3333333333333333703, 0.3219752754296894559, 0.3333333333333333703, 0.3219752754296894559, 0.3333333333333333703, 0.3219752754296894559, 0.3333333333333333703, 0.3219752754296894559, 0.3333333333333333703, 0.3219752754296894559, 0.3333333333333333703, 0.3219752754296894559, 0.3333333333333333703, 0.3219752754296894559, 0.3333333333333333703, 0.3219752754296894559, 0.3333333333333333703, 0.3219752754296894559, 0.3333333333333333703, 0.3219752754296894559, 0.3333333333333333703, 0.3219752754296894559, 0.3333333333333333703, 0.3219752754296894559, 0.3333333333333333703, 0.3219752754296894559, 0.3333333333333333703, 0.3219752754296894559, 0.3333333333333333703, 0.3219752754296894559, 0.3333333333333333703, 0.3219752754296894559, 0.3333333333333333703, 0.3219752754296894559, 0.3333333333333333703, 0.3219752754296894559, 0.3333333333333333703, 0.3219752754296894559, 0.3333333333333333703, 0.3219752754296894559, 0.3333333333333333703, 0.3219752754296894559, 0.3333333333333333703, 0.3219752754296894559, 0.3333333333333333703, 0.3219752754296894559, 0.3333333333333333703, 0.3219752754296894559, 0.3333333333333333703, 0.3219752754296894559, 0.3333333333333333703, 0.3219752754296894559, 0.3333333333333333703, 0.3219752754296894559, 0.3333333333333333703, 0.3219752754296894559, 0.3333333333333333703, 0.3219752754296894559, 0.3333333333333333703, 0.3219752754296894559, 0.3333333333333333703, 0.3219752754296894559, 0.3333333333333333703, 0.3219752754296894559, 0.3333333333333333703, 0.3219752754296894559, 0.3333333333333333703, 0.3219752754296894559, 0.3333333333333333703, 0.3219752754296894559, 0.3333333333333333703, 0.3219752754296894559, 0.3333333333333333703, 0.3219752754296894559, 0.3333333333333333703, 0.3219752754296894559, 0.3333333333333333703, 0.3219752754296894559, 0.3333333333333333703, 0.3219752754296894559, 0.3333333333333333703, 0.3219752754296894559, 0.3333333333333333703, 0.3219752754296894559, 0.3333333333333333703, 0.3219752754296894559, 0.3333333333333333703, 0.3219752754296894559, 0.3333333333333333703, 0.3219752754296894559, 0.3333333333333333703, 0.3219752754296894559, 0.3333333333333333703, 0.3219752754296894559, 0.3333333333333333703, 0.3219752754296894559, 0.3333333333333333703, 0.3219752754296894559, 0.3333333333333333703, 0.3219752754296894559, 0.3333333333333333703, 0.3219752754296894559, 0.3333333333333333703, 0.3219752754296894559, 0.3333333333333333703, 0.3219752754296894559, 0.3333333333333333703, 0.3219752754296894559, 0.3333333333333333703, 0.3219752754296894559, 0.3333333333333333703, 0.3219752754296894559, 0.3333333333333333703, 0.3219752754296894559, 0.3333333333333333703, 0.3219752754296894559, 0.3333333333333333703, 0.3219752754296894559, 0.3333333333333333703, 0.3219752754296894559, 0.3333333333333333703, 0.3219752754296894559, 0.3333333333333333703, 0.3219752754296894559, 0.3333333333333333703, 0.3219752754296894559, 0.3333333333333333703, 0.3219752754296894559, 0.3333333333333333703),
 ( 1.000000000000000000, 0.9659258262890683122, 1.000000000000000000, 0.9659258262890683122, 1.000000000000000000, 0.9659258262890683122, 1.000000000000000000, 0.9659258262890683122, 1.000000000000000000, 0.9659258262890683122, 1.000000000000000000, 0.9659258262890683122, 1.000000000000000000, 0.9659258262890683122, 1.000000000000000000, 0.9659258262890683122, 1.000000000000000000, 0.9659258262890683122, 1.000000000000000000, 0.9659258262890683122, 1.000000000000000000, 0.9659258262890683122, 1.000000000000000000, 0.9659258262890683122, 1.000000000000000000, 0.9659258262890683122, 1.000000000000000000, 0.9659258262890683122, 1.000000000000000000, 0.9659258262890683122, 1.000000000000000000, 0.9659258262890683122, 1.000000000000000000, 0.9659258262890683122, 1.000000000000000000, 0.9659258262890683122, 1.000000000000000000, 0.9659258262890683122, 1.000000000000000000, 0.9659258262890683122, 1.000000000000000000, 0.9659258262890683122, 1.000000000000000000, 0.9659258262890683122, 1.000000000000000000, 0.9659258262890683122, 1.000000000000000000, 0.9659258262890683122, 1.000000000000000000, 0.9659258262890683122, 1.000000000000000000, 0.9659258262890683122, 1.000000000000000000, 0.9659258262890683122, 1.000000000000000000, 0.9659258262890683122, 1.000000000000000000, 0.9659258262890683122, 1.000000000000000000, 0.9659258262890683122, 1.000000000000000000, 0.9659258262890683122, 1.000000000000000000, 0.9659258262890683122, 1.000000000000000000, 0.9659258262890683122, 1.000000000000000000, 0.9659258262890683122, 1.000000000000000000, 0.9659258262890683122, 1.000000000000000000, 0.9659258262890683122, 1.000000000000000000, 0.9659258262890683122, 1.000000000000000000, 0.9659258262890683122, 1.000000000000000000, 0.9659258262890683122, 1.000000000000000000, 0.9659258262890683122, 1.000000000000000000, 0.9659258262890683122, 1.000000000000000000, 0.9659258262890683122, 1.000000000000000000, 0.9659258262890683122, 1.000000000000000000, 0.9659258262890683122, 1.000000000000000000, 0.9659258262890683122, 1.000000000000000000, 0.9659258262890683122, 1.000000000000000000, 0.9659258262890683122, 1.000000000000000000, 0.9659258262890683122, 1.000000000000000000, 0.9659258262890683122, 1.000000000000000000, 0.9659258262890683122, 1.000000000000000000, 0.9659258262890683122, 1.000000000000000000, 0.9659258262890683122, 1.000000000000000000, 0.9659258262890683122, 1.000000000000000000, 0.9659258262890683122, 1.000000000000000000, 0.9659258262890683122, 1.000000000000000000, 0.9659258262890683122, 1.000000000000000000, 0.9659258262890683122, 1.000000000000000000, 0.9659258262890683122, 1.000000000000000000, 0.9659258262890683122, 1.000000000000000000, 0.9659258262890683122, 1.000000000000000000, 0.9659258262890683122, 1.000000000000000000, 0.9659258262890683122, 1.000000000000000000, 0.9659258262890683122, 1.000000000000000000, 0.9659258262890683122, 1.000000000000000000, 0.9659258262890683122, 1.000000000000000000, 0.9659258262890683122, 1.000000000000000000, 0.9659258262890683122, 1.000000000000000000, 0.9659258262890683122, 1.000000000000000000, 0.9659258262890683122, 1.000000000000000000, 0.9659258262890683122, 1.000000000000000000, 0.9659258262890683122, 1.000000000000000000, 0.9659258262890683122, 1.000000000000000000, 0.9659258262890683122, 1.000000000000000000, 0.9659258262890683122, 1.000000000000000000, 0.9659258262890683122, 1.000000000000000000, 0.9659258262890683122, 1.000000000000000000, 0.9659258262890683122, 1.000000000000000000, 0.9659258262890683122, 1.000000000000000000, 0.9659258262890683122, 1.000000000000000000, 0.9659258262890683122, 1.000000000000000000, 0.9659258262890683122, 1.000000000000000000, 0.9659258262890683122, 1.000000000000000000, 0.9659258262890683122, 1.000000000000000000, 0.9659258262890683122, 1.000000000000000000, 0.9659258262890683122, 1.000000000000000000, 0.9659258262890683122, 1.000000000000000000, 0.9659258262890683122, 1.000000000000000000, 0.9659258262890683122, 1.000000000000000000, 0.9659258262890683122, 1.000000000000000000, 0.9659258262890683122, 1.000000000000000000, 0.9659258262890683122, 1.000000000000000000, 0.9659258262890683122, 1.000000000000000000, 0.9659258262890683122, 1.000000000000000000, 0.9659258262890683122, 1.000000000000000000, 0.9659258262890683122, 1.000000000000000000, 0.9659258262890683122, 1.000000000000000000, 0.9659258262890683122, 1.000000000000000000, 0.9659258262890683122, 1.000000000000000000, 0.9659258262890683122, 1.000000000000000000, 0.9659258262890683122, 1.000000000000000000, 0.9659258262890683122, 1.000000000000000000, 0.9659258262890683122, 1.000000000000000000, 0.9659258262890683122, 1.000000000000000000, 0.9659258262890683122, 1.000000000000000000, 0.9659258262890683122, 1.000000000000000000, 0.9659258262890683122, 1.000000000000000000, 0.9659258262890683122, 1.000000000000000000, 0.9659258262890683122, 1.000000000000000000, 0.9659258262890683122, 1.000000000000000000, 0.9659258262890683122, 1.000000000000000000, 0.9659258262890683122, 1.000000000000000000, 0.9659258262890683122, 1.000000000000000000, 0.9659258262890683122, 1.000000000000000000, 0.9659258262890683122, 1.000000000000000000, 0.9659258262890683122, 1.000000000000000000, 0.9659258262890683122, 1.000000000000000000, 0.9659258262890683122, 1.000000000000000000, 0.9659258262890683122, 1.000000000000000000, 0.9659258262890683122, 1.000000000000000000, 0.9659258262890683122, 1.000000000000000000, 0.9659258262890683122, 1.000000000000000000, 0.9659258262890683122, 1.000000000000000000, 0.9659258262890683122, 1.000000000000000000, 0.9659258262890683122, 1.000000000000000000, 0.9659258262890683122, 1.000000000000000000, 0.9659258262890683122, 1.000000000000000000, 0.9659258262890683122, 1.000000000000000000, 0.9659258262890683122, 1.000000000000000000, 0.9659258262890683122, 1.000000000000000000, 0.9659258262890683122, 1.000000000000000000, 0.9659258262890683122, 1.000000000000000000, 0.9659258262890683122, 1.000000000000000000, 0.9659258262890683122, 1.000000000000000000, 0.9659258262890683122, 1.000000000000000000, 0.9659258262890683122, 1.000000000000000000, 0.9659258262890683122, 1.000000000000000000, 0.9659258262890683122, 1.000000000000000000, 0.9659258262890683122, 1.000000000000000000, 0.9659258262890683122, 1.000000000000000000, 0.9659258262890683122, 1.000000000000000000, 0.9659258262890683122, 1.000000000000000000, 0.9659258262890683122, 1.000000000000000000, 0.9659258262890683122, 1.000000000000000000, 0.9659258262890683122, 1.000000000000000000, 0.9659258262890683122, 1.000000000000000000, 0.9659258262890683122, 1.000000000000000000, 0.9659258262890683122, 1.000000000000000000, 0.9659258262890683122, 1.000000000000000000, 0.9659258262890683122, 1.000000000000000000, 0.9659258262890683122, 1.000000000000000000, 0.9659258262890683122, 1.000000000000000000, 0.9659258262890683122, 1.000000000000000000, 0.9659258262890683122, 1.000000000000000000, 0.9659258262890683122, 1.000000000000000000, 0.9659258262890683122, 1.000000000000000000, 0.9659258262890683122, 1.000000000000000000, 0.9659258262890683122, 1.000000000000000000, 0.9659258262890683122, 1.000000000000000000, 0.9659258262890683122, 1.000000000000000000, 0.9659258262890683122, 1.000000000000000000, 0.9659258262890683122, 1.000000000000000000, 0.9659258262890683122, 1.000000000000000000, 0.9659258262890683122, 1.000000000000000000, 0.9659258262890683122, 1.000000000000000000, 0.9659258262890683122, 1.000000000000000000, 0.9659258262890683122, 1.000000000000000000, 0.9659258262890683122, 1.000000000000000000, 0.9659258262890683122, 1.000000000000000000, 0.9659258262890683122, 1.000000000000000000, 0.9659258262890683122, 1.000000000000000000, 0.9659258262890683122, 1.000000000000000000, 0.9659258262890683122, 1.000000000000000000, 0.9659258262890683122, 1.000000000000000000, 0.9659258262890683122, 1.000000000000000000, 0.9659258262890683122, 1.000000000000000000, 0.9659258262890683122, 1.000000000000000000, 0.9659258262890683122, 1.000000000000000000, 0.9659258262890683122, 1.000000000000000000, 0.9659258262890683122, 1.000000000000000000, 0.9659258262890683122, 1.000000000000000000, 0.9659258262890683122, 1.000000000000000000, 0.9659258262890683122, 1.000000000000000000, 0.9659258262890683122, 1.000000000000000000, 0.9659258262890683122, 1.000000000000000000, 0.9659258262890683122, 1.000000000000000000, 0.9659258262890683122, 1.000000000000000000, 0.9659258262890683122, 1.000000000000000000, 0.9659258262890683122, 1.000000000000000000, 0.9659258262890683122, 1.000000000000000000, 0.9659258262890683122, 1.000000000000000000, 0.9659258262890683122, 1.000000000000000000, 0.9659258262890683122, 1.000000000000000000, 0.9659258262890683122, 1.000000000000000000, 0.9659258262890683122, 1.000000000000000000, 0.9659258262890683122, 1.000000000000000000, 0.9659258262890683122, 1.000000000000000000, 0.9659258262890683122, 1.000000000000000000, 0.9659258262890683122, 1.000000000000000000, 0.9659258262890683122, 1.000000000000000000, 0.9659258262890683122, 1.000000000000000000, 0.9659258262890683122, 1.000000000000000000, 0.9659258262890683122, 1.000000000000000000, 0.9659258262890683122, 1.000000000000000000, 0.9659258262890683122, 1.000000000000000000, 0.9659258262890683122, 1.000000000000000000, 0.9659258262890683122, 1.000000000000000000, 0.9659258262890683122, 1.000000000000000000, 0.9659258262890683122, 1.000000000000000000, 0.9659258262890683122, 1.000000000000000000, 0.9659258262890683122, 1.000000000000000000, 0.9659258262890683122, 1.000000000000000000, 0.9659258262890683122, 1.000000000000000000, 0.9659258262890683122, 1.000000000000000000, 0.9659258262890683122, 1.000000000000000000, 0.9659258262890683122, 1.000000000000000000, 0.9659258262890683122, 1.000000000000000000, 0.9659258262890683122, 1.000000000000000000, 0.9659258262890683122, 1.000000000000000000, 0.9659258262890683122, 1.000000000000000000, 0.9659258262890683122, 1.000000000000000000, 0.9659258262890683122, 1.000000000000000000, 0.9659258262890683122, 1.000000000000000000, 0.9659258262890683122, 1.000000000000000000, 0.9659258262890683122, 1.000000000000000000, 0.9659258262890683122, 1.000000000000000000, 0.9659258262890683122, 1.000000000000000000, 0.9659258262890683122, 1.000000000000000000, 0.9659258262890683122, 1.000000000000000000),
 ( 0.3333333333333333703, 0.3219752754296894559, 0.3333333333333333703, 0.3219752754296894559, 0.3333333333333333703, 0.3219752754296894559, 0.3333333333333333703, 0.3219752754296894559, 0.3333333333333333703, 0.3219752754296894559, 0.3333333333333333703, 0.3219752754296894559, 0.3333333333333333703, 0.3219752754296894559, 0.3333333333333333703, 0.3219752754296894559, 0.3333333333333333703, 0.3219752754296894559, 0.3333333333333333703, 0.3219752754296894559, 0.3333333333333333703, 0.3219752754296894559, 0.3333333333333333703, 0.3219752754296894559, 0.3333333333333333703, 0.3219752754296894559, 0.3333333333333333703, 0.3219752754296894559, 0.3333333333333333703, 0.3219752754296894559, 0.3333333333333333703, 0.3219752754296894559, 0.3333333333333333703, 0.3219752754296894559, 0.3333333333333333703, 0.3219752754296894559, 0.3333333333333333703, 0.3219752754296894559, 0.3333333333333333703, 0.3219752754296894559, 0.3333333333333333703, 0.3219752754296894559, 0.3333333333333333703, 0.3219752754296894559, 0.3333333333333333703, 0.3219752754296894559, 0.3333333333333333703, 0.3219752754296894559, 0.3333333333333333703, 0.3219752754296894559, 0.3333333333333333703, 0.3219752754296894559, 0.3333333333333333703, 0.3219752754296894559, 0.3333333333333333703, 0.3219752754296894559, 0.3333333333333333703, 0.3219752754296894559, 0.3333333333333333703, 0.3219752754296894559, 0.3333333333333333703, 0.3219752754296894559, 0.3333333333333333703, 0.3219752754296894559, 0.3333333333333333703, 0.3219752754296894559, 0.3333333333333333703, 0.3219752754296894559, 0.3333333333333333703, 0.3219752754296894559, 0.3333333333333333703, 0.3219752754296894559, 0.3333333333333333703, 0.3219752754296894559, 0.3333333333333333703, 0.3219752754296894559, 0.3333333333333333703, 0.3219752754296894559, 0.3333333333333333703, 0.3219752754296894559, 0.3333333333333333703, 0.3219752754296894559, 0.3333333333333333703, 0.3219752754296894559, 0.3333333333333333703, 0.3219752754296894559, 0.3333333333333333703, 0.3219752754296894559, 0.3333333333333333703, 0.3219752754296894559, 0.3333333333333333703, 0.3219752754296894559, 0.3333333333333333703, 0.3219752754296894559, 0.3333333333333333703, 0.3219752754296894559, 0.3333333333333333703, 0.3219752754296894559, 0.3333333333333333703, 0.3219752754296894559, 0.3333333333333333703, 0.3219752754296894559, 0.3333333333333333703, 0.3219752754296894559, 0.3333333333333333703, 0.3219752754296894559, 0.3333333333333333703, 0.3219752754296894559, 0.3333333333333333703, 0.3219752754296894559, 0.3333333333333333703, 0.3219752754296894559, 0.3333333333333333703, 0.3219752754296894559, 0.3333333333333333703, 0.3219752754296894559, 0.3333333333333333703, 0.3219752754296894559, 0.3333333333333333703, 0.3219752754296894559, 0.3333333333333333703, 0.3219752754296894559, 0.3333333333333333703, 0.3219752754296894559, 0.3333333333333333703, 0.3219752754296894559, 0.3333333333333333703, 0.3219752754296894559, 0.3333333333333333703, 0.3219752754296894559, 0.3333333333333333703, 0.3219752754296894559, 0.3333333333333333703, 0.3219752754296894559, 0.3333333333333333703, 0.3219752754296894559, 0.3333333333333333703, 0.3219752754296894559, 0.3333333333333333703, 0.3219752754296894559, 0.3333333333333333703, 0.3219752754296894559, 0.3333333333333333703, 0.3219752754296894559, 0.3333333333333333703, 0.3219752754296894559, 0.3333333333333333703, 0.3219752754296894559, 0.3333333333333333703, 0.3219752754296894559, 0.3333333333333333703, 0.3219752754296894559, 0.3333333333333333703, 0.3219752754296894559, 0.3333333333333333703, 0.3219752754296894559, 0.3333333333333333703, 0.3219752754296894559, 0.3333333333333333703, 0.3219752754296894559, 0.3333333333333333703, 0.3219752754296894559, 0.3333333333333333703, 0.3219752754296894559, 0.3333333333333333703, 0.3219752754296894559, 0.3333333333333333703, 0.3219752754296894559, 0.3333333333333333703, 0.3219752754296894559, 0.3333333333333333703, 0.3219752754296894559, 0.3333333333333333703, 0.3219752754296894559, 0.3333333333333333703, 0.3219752754296894559, 0.3333333333333333703, 0.3219752754296894559, 0.3333333333333333703, 0.3219752754296894559, 0.3333333333333333703, 0.3219752754296894559, 0.3333333333333333703, 0.3219752754296894559, 0.3333333333333333703, 0.3219752754296894559, 0.3333333333333333703, 0.3219752754296894559, 0.3333333333333333703, 0.3219752754296894559, 0.3333333333333333703, 0.3219752754296894559, 0.3333333333333333703, 0.3219752754296894559, 0.3333333333333333703, 0.3219752754296894559, 0.3333333333333333703, 0.3219752754296894559, 0.3333333333333333703, 0.3219752754296894559, 0.3333333333333333703, 0.3219752754296894559, 0.3333333333333333703, 0.3219752754296894559, 0.3333333333333333703, 0.3219752754296894559, 0.3333333333333333703, 0.3219752754296894559, 0.3333333333333333703, 0.3219752754296894559, 0.3333333333333333703, 0.3219752754296894559, 0.3333333333333333703, 0.3219752754296894559, 0.3333333333333333703, 0.3219752754296894559, 0.3333333333333333703, 0.3219752754296894559, 0.3333333333333333703, 0.3219752754296894559, 0.3333333333333333703, 0.3219752754296894559, 0.3333333333333333703, 0.3219752754296894559, 0.3333333333333333703, 0.3219752754296894559, 0.3333333333333333703, 0.3219752754296894559, 0.3333333333333333703, 0.3219752754296894559, 0.3333333333333333703, 0.3219752754296894559, 0.3333333333333333703, 0.3219752754296894559, 0.3333333333333333703, 0.3219752754296894559, 0.3333333333333333703, 0.3219752754296894559, 0.3333333333333333703, 0.3219752754296894559, 0.3333333333333333703, 0.3219752754296894559, 0.3333333333333333703, 0.3219752754296894559, 0.3333333333333333703, 0.3219752754296894559, 0.3333333333333333703, 0.3219752754296894559, 0.3333333333333333703, 0.3219752754296894559, 0.3333333333333333703, 0.3219752754296894559, 0.3333333333333333703, 0.3219752754296894559, 0.3333333333333333703, 0.3219752754296894559, 0.3333333333333333703, 0.3219752754296894559, 0.3333333333333333703, 0.3219752754296894559, 0.3333333333333333703, 0.3219752754296894559, 0.3333333333333333703, 0.3219752754296894559, 0.3333333333333333703, 0.3219752754296894559, 0.3333333333333333703, 0.3219752754296894559, 0.3333333333333333703, 0.3219752754296894559, 0.3333333333333333703, 0.3219752754296894559, 0.3333333333333333703, 0.3219752754296894559, 0.3333333333333333703, 0.3219752754296894559, 0.3333333333333333703, 0.3219752754296894559, 0.3333333333333333703, 0.3219752754296894559, 0.3333333333333333703, 0.3219752754296894559, 0.3333333333333333703, 0.3219752754296894559, 0.3333333333333333703, 0.3219752754296894559, 0.3333333333333333703, 0.3219752754296894559, 0.3333333333333333703, 0.3219752754296894559, 0.3333333333333333703, 0.3219752754296894559, 0.3333333333333333703, 0.3219752754296894559, 0.3333333333333333703, 0.3219752754296894559, 0.3333333333333333703, 0.3219752754296894559, 0.3333333333333333703, 0.3219752754296894559, 0.3333333333333333703, 0.3219752754296894559, 0.3333333333333333703, 0.3219752754296894559, 0.3333333333333333703, 0.3219752754296894559, 0.3333333333333333703, 0.3219752754296894559, 0.3333333333333333703, 0.3219752754296894559, 0.3333333333333333703, 0.3219752754296894559, 0.3333333333333333703, 0.3219752754296894559, 0.3333333333333333703, 0.3219752754296894559, 0.3333333333333333703, 0.3219752754296894559, 0.3333333333333333703, 0.3219752754296894559, 0.3333333333333333703, 0.3219752754296894559, 0.3333333333333333703, 0.3219752754296894559, 0.3333333333333333703, 0.3219752754296894559, 0.3333333333333333703, 0.3219752754296894559, 0.3333333333333333703, 0.3219752754296894559, 0.3333333333333333703, 0.3219752754296894559, 0.3333333333333333703, 0.3219752754296894559, 0.3333333333333333703, 0.3219752754296894559, 0.3333333333333333703, 0.3219752754296894559, 0.3333333333333333703, 0.3219752754296894559, 0.3333333333333333703, 0.3219752754296894559, 0.3333333333333333703, 0.3219752754296894559, 0.3333333333333333703, 0.3219752754296894559, 0.3333333333333333703, 0.3219752754296894559, 0.3333333333333333703, 0.3219752754296894559, 0.3333333333333333703, 0.3219752754296894559, 0.3333333333333333703, 0.3219752754296894559, 0.3333333333333333703, 0.3219752754296894559, 0.3333333333333333703, 0.3219752754296894559, 0.3333333333333333703, 0.3219752754296894559, 0.3333333333333333703, 0.3219752754296894559, 0.3333333333333333703, 0.3219752754296894559, 0.3333333333333333703, 0.3219752754296894559, 0.3333333333333333703, 0.3219752754296894559, 0.3333333333333333703, 0.3219752754296894559, 0.3333333333333333703, 0.3219752754296894559, 0.3333333333333333703, 0.3219752754296894559, 0.3333333333333333703, 0.3219752754296894559, 0.3333333333333333703, 0.3219752754296894559, 0.3333333333333333703, 0.3219752754296894559, 0.3333333333333333703, 0.3219752754296894559, 0.3333333333333333703, 0.3219752754296894559, 0.3333333333333333703, 0.3219752754296894559, 0.3333333333333333703, 0.3219752754296894559, 0.3333333333333333703, 0.3219752754296894559, 0.3333333333333333703, 0.3219752754296894559, 0.3333333333333333703, 0.3219752754296894559, 0.3333333333333333703, 0.3219752754296894559, 0.3333333333333333703, 0.3219752754296894559, 0.3333333333333333703, 0.3219752754296894559, 0.3333333333333333703, 0.3219752754296894559, 0.3333333333333333703, 0.3219752754296894559, 0.3333333333333333703, 0.3219752754296894559, 0.3333333333333333703, 0.3219752754296894559, 0.3333333333333333703, 0.3219752754296894559, 0.3333333333333333703, 0.3219752754296894559, 0.3333333333333333703, 0.3219752754296894559, 0.3333333333333333703, 0.3219752754296894559, 0.3333333333333333703, 0.3219752754296894559, 0.3333333333333333703, 0.3219752754296894559, 0.3333333333333333703, 0.3219752754296894559, 0.3333333333333333703, 0.3219752754296894559, 0.3333333333333333703, 0.3219752754296894559, 0.3333333333333333703, 0.3219752754296894559, 0.3333333333333333703, 0.3219752754296894559, 0.3333333333333333703, 0.3219752754296894559, 0.3333333333333333703, 0.3219752754296894559, 0.3333333333333333703, 0.3219752754296894559, 0.3333333333333333703, 0.3219752754296894559, 0.3333333333333333703, 0.3219752754296894559, 0.3333333333333333703, 0.3219752754296894559, 0.3333333333333333703, 0.3219752754296894559, 0.3333333333333333703, 0.3219752754296894559, 0.3333333333333333703, 0.3219752754296894559, 0.3333333333333333703, 0.3219752754296894559, 0.3333333333333333703, 0.3219752754296894559, 0.3333333333333333703, 0.3219752754296894559, 0.3333333333333333703, 0.3219752754296894559, 0.3333333333333333703),
 ( 0.3333333333333333703, 0.3219752754296894559, 0.3333333333333333703, 0.3219752754296894559, 0.3333333333333333703, 0.3219752754296894559, 0.3333333333333333703, 0.3219752754296894559, 0.3333333333333333703, 0.3219752754296894559, 0.3333333333333333703, 0.3219752754296894559, 0.3333333333333333703, 0.3219752754296894559, 0.3333333333333333703, 0.3219752754296894559, 0.3333333333333333703, 0.3219752754296894559, 0.3333333333333333703, 0.3219752754296894559, 0.3333333333333333703, 0.3219752754296894559, 0.3333333333333333703, 0.3219752754296894559, 0.3333333333333333703, 0.3219752754296894559, 0.3333333333333333703, 0.3219752754296894559, 0.3333333333333333703, 0.3219752754296894559, 0.3333333333333333703, 0.3219752754296894559, 0.3333333333333333703, 0.3219752754296894559, 0.3333333333333333703, 0.3219752754296894559, 0.3333333333333333703, 0.3219752754296894559, 0.3333333333333333703, 0.3219752754296894559, 0.3333333333333333703, 0.3219752754296894559, 0.3333333333333333703, 0.3219752754296894559, 0.3333333333333333703, 0.3219752754296894559, 0.3333333333333333703, 0.3219752754296894559, 0.3333333333333333703, 0.3219752754296894559, 0.3333333333333333703, 0.3219752754296894559, 0.3333333333333333703, 0.3219752754296894559, 0.3333333333333333703, 0.3219752754296894559, 0.3333333333333333703, 0.3219752754296894559, 0.3333333333333333703, 0.3219752754296894559, 0.3333333333333333703, 0.3219752754296894559, 0.3333333333333333703, 0.3219752754296894559, 0.3333333333333333703, 0.3219752754296894559, 0.3333333333333333703, 0.3219752754296894559, 0.3333333333333333703, 0.3219752754296894559, 0.3333333333333333703, 0.3219752754296894559, 0.3333333333333333703, 0.3219752754296894559, 0.3333333333333333703, 0.3219752754296894559, 0.3333333333333333703, 0.3219752754296894559, 0.3333333333333333703, 0.3219752754296894559, 0.3333333333333333703, 0.3219752754296894559, 0.3333333333333333703, 0.3219752754296894559, 0.3333333333333333703, 0.3219752754296894559, 0.3333333333333333703, 0.3219752754296894559, 0.3333333333333333703, 0.3219752754296894559, 0.3333333333333333703, 0.3219752754296894559, 0.3333333333333333703, 0.3219752754296894559, 0.3333333333333333703, 0.3219752754296894559, 0.3333333333333333703, 0.3219752754296894559, 0.3333333333333333703, 0.3219752754296894559, 0.3333333333333333703, 0.3219752754296894559, 0.3333333333333333703, 0.3219752754296894559, 0.3333333333333333703, 0.3219752754296894559, 0.3333333333333333703, 0.3219752754296894559, 0.3333333333333333703, 0.3219752754296894559, 0.3333333333333333703, 0.3219752754296894559, 0.3333333333333333703, 0.3219752754296894559, 0.3333333333333333703, 0.3219752754296894559, 0.3333333333333333703, 0.3219752754296894559, 0.3333333333333333703, 0.3219752754296894559, 0.3333333333333333703, 0.3219752754296894559, 0.3333333333333333703, 0.3219752754296894559, 0.3333333333333333703, 0.3219752754296894559, 0.3333333333333333703, 0.3219752754296894559, 0.3333333333333333703, 0.3219752754296894559, 0.3333333333333333703, 0.3219752754296894559, 0.3333333333333333703, 0.3219752754296894559, 0.3333333333333333703, 0.3219752754296894559, 0.3333333333333333703, 0.3219752754296894559, 0.3333333333333333703, 0.3219752754296894559, 0.3333333333333333703, 0.3219752754296894559, 0.3333333333333333703, 0.3219752754296894559, 0.3333333333333333703, 0.3219752754296894559, 0.3333333333333333703, 0.3219752754296894559, 0.3333333333333333703, 0.3219752754296894559, 0.3333333333333333703, 0.3219752754296894559, 0.3333333333333333703, 0.3219752754296894559, 0.3333333333333333703, 0.3219752754296894559, 0.3333333333333333703, 0.3219752754296894559, 0.3333333333333333703, 0.3219752754296894559, 0.3333333333333333703, 0.3219752754296894559, 0.3333333333333333703, 0.3219752754296894559, 0.3333333333333333703, 0.3219752754296894559, 0.3333333333333333703, 0.3219752754296894559, 0.3333333333333333703, 0.3219752754296894559, 0.3333333333333333703, 0.3219752754296894559, 0.3333333333333333703, 0.3219752754296894559, 0.3333333333333333703, 0.3219752754296894559, 0.3333333333333333703, 0.3219752754296894559, 0.3333333333333333703, 0.3219752754296894559, 0.3333333333333333703, 0.3219752754296894559, 0.3333333333333333703, 0.3219752754296894559, 0.3333333333333333703, 0.3219752754296894559, 0.3333333333333333703, 0.3219752754296894559, 0.3333333333333333703, 0.3219752754296894559, 0.3333333333333333703, 0.3219752754296894559, 0.3333333333333333703, 0.3219752754296894559, 0.3333333333333333703, 0.3219752754296894559, 0.3333333333333333703, 0.3219752754296894559, 0.3333333333333333703, 0.3219752754296894559, 0.3333333333333333703, 0.3219752754296894559, 0.3333333333333333703, 0.3219752754296894559, 0.3333333333333333703, 0.3219752754296894559, 0.3333333333333333703, 0.3219752754296894559, 0.3333333333333333703, 0.3219752754296894559, 0.3333333333333333703, 0.3219752754296894559, 0.3333333333333333703, 0.3219752754296894559, 0.3333333333333333703, 0.3219752754296894559, 0.3333333333333333703, 0.3219752754296894559, 0.3333333333333333703, 0.3219752754296894559, 0.3333333333333333703, 0.3219752754296894559, 0.3333333333333333703, 0.3219752754296894559, 0.3333333333333333703, 0.3219752754296894559, 0.3333333333333333703, 0.3219752754296894559, 0.3333333333333333703, 0.3219752754296894559, 0.3333333333333333703, 0.3219752754296894559, 0.3333333333333333703, 0.3219752754296894559, 0.3333333333333333703, 0.3219752754296894559, 0.3333333333333333703, 0.3219752754296894559, 0.3333333333333333703, 0.3219752754296894559, 0.3333333333333333703, 0.3219752754296894559, 0.3333333333333333703, 0.3219752754296894559, 0.3333333333333333703, 0.3219752754296894559, 0.3333333333333333703, 0.3219752754296894559, 0.3333333333333333703, 0.3219752754296894559, 0.3333333333333333703, 0.3219752754296894559, 0.3333333333333333703, 0.3219752754296894559, 0.3333333333333333703, 0.3219752754296894559, 0.3333333333333333703, 0.3219752754296894559, 0.3333333333333333703, 0.3219752754296894559, 0.3333333333333333703, 0.3219752754296894559, 0.3333333333333333703, 0.3219752754296894559, 0.3333333333333333703, 0.3219752754296894559, 0.3333333333333333703, 0.3219752754296894559, 0.3333333333333333703, 0.3219752754296894559, 0.3333333333333333703, 0.3219752754296894559, 0.3333333333333333703, 0.3219752754296894559, 0.3333333333333333703, 0.3219752754296894559, 0.3333333333333333703, 0.3219752754296894559, 0.3333333333333333703, 0.3219752754296894559, 0.3333333333333333703, 0.3219752754296894559, 0.3333333333333333703, 0.3219752754296894559, 0.3333333333333333703, 0.3219752754296894559, 0.3333333333333333703, 0.3219752754296894559, 0.3333333333333333703, 0.3219752754296894559, 0.3333333333333333703, 0.3219752754296894559, 0.3333333333333333703, 0.3219752754296894559, 0.3333333333333333703, 0.3219752754296894559, 0.3333333333333333703, 0.3219752754296894559, 0.3333333333333333703, 0.3219752754296894559, 0.3333333333333333703, 0.3219752754296894559, 0.3333333333333333703, 0.3219752754296894559, 0.3333333333333333703, 0.3219752754296894559, 0.3333333333333333703, 0.3219752754296894559, 0.3333333333333333703, 0.3219752754296894559, 0.3333333333333333703, 0.3219752754296894559, 0.3333333333333333703, 0.3219752754296894559, 0.3333333333333333703, 0.3219752754296894559, 0.3333333333333333703, 0.3219752754296894559, 0.3333333333333333703, 0.3219752754296894559, 0.3333333333333333703, 0.3219752754296894559, 0.3333333333333333703, 0.3219752754296894559, 0.3333333333333333703, 0.3219752754296894559, 0.3333333333333333703, 0.3219752754296894559, 0.3333333333333333703, 0.3219752754296894559, 0.3333333333333333703, 0.3219752754296894559, 0.3333333333333333703, 0.3219752754296894559, 0.3333333333333333703, 0.3219752754296894559, 0.3333333333333333703, 0.3219752754296894559, 0.3333333333333333703, 0.3219752754296894559, 0.3333333333333333703, 0.3219752754296894559, 0.3333333333333333703, 0.3219752754296894559, 0.3333333333333333703, 0.3219752754296894559, 0.3333333333333333703, 0.3219752754296894559, 0.3333333333333333703, 0.3219752754296894559, 0.3333333333333333703, 0.3219752754296894559, 0.3333333333333333703, 0.3219752754296894559, 0.3333333333333333703, 0.3219752754296894559, 0.3333333333333333703, 0.3219752754296894559, 0.3333333333333333703, 0.3219752754296894559, 0.3333333333333333703, 0.3219752754296894559, 0.3333333333333333703, 0.3219752754296894559, 0.3333333333333333703, 0.3219752754296894559, 0.3333333333333333703, 0.3219752754296894559, 0.3333333333333333703, 0.3219752754296894559, 0.3333333333333333703, 0.3219752754296894559, 0.3333333333333333703, 0.3219752754296894559, 0.3333333333333333703, 0.3219752754296894559, 0.3333333333333333703, 0.3219752754296894559, 0.3333333333333333703, 0.3219752754296894559, 0.3333333333333333703, 0.3219752754296894559, 0.3333333333333333703, 0.3219752754296894559, 0.3333333333333333703, 0.3219752754296894559, 0.3333333333333333703, 0.3219752754296894559, 0.3333333333333333703, 0.3219752754296894559, 0.3333333333333333703, 0.3219752754296894559, 0.3333333333333333703, 0.3219752754296894559, 0.3333333333333333703, 0.3219752754296894559, 0.3333333333333333703, 0.3219752754296894559, 0.3333333333333333703, 0.3219752754296894559, 0.3333333333333333703, 0.3219752754296894559, 0.3333333333333333703, 0.3219752754296894559, 0.3333333333333333703, 0.3219752754296894559, 0.3333333333333333703, 0.3219752754296894559, 0.3333333333333333703, 0.3219752754296894559, 0.3333333333333333703, 0.3219752754296894559, 0.3333333333333333703, 0.3219752754296894559, 0.3333333333333333703, 0.3219752754296894559, 0.3333333333333333703, 0.3219752754296894559, 0.3333333333333333703, 0.3219752754296894559, 0.3333333333333333703, 0.3219752754296894559, 0.3333333333333333703, 0.3219752754296894559, 0.3333333333333333703, 0.3219752754296894559, 0.3333333333333333703, 0.3219752754296894559, 0.3333333333333333703, 0.3219752754296894559, 0.3333333333333333703, 0.3219752754296894559, 0.3333333333333333703, 0.3219752754296894559, 0.3333333333333333703, 0.3219752754296894559, 0.3333333333333333703, 0.3219752754296894559, 0.3333333333333333703, 0.3219752754296894559, 0.3333333333333333703, 0.3219752754296894559, 0.3333333333333333703, 0.3219752754296894559, 0.3333333333333333703, 0.3219752754296894559, 0.3333333333333333703, 0.3219752754296894559, 0.3333333333333333703, 0.3219752754296894559, 0.3333333333333333703, 0.3219752754296894559, 0.3333333333333333703, 0.3219752754296894559, 0.3333333333333333703, 0.3219752754296894559, 0.3333333333333333703),
 ( 1.000000000000000000, 0.9659258262890683122, 1.000000000000000000, 0.9659258262890683122, 1.000000000000000000, 0.9659258262890683122, 1.000000000000000000, 0.9659258262890683122, 1.000000000000000000, 0.9659258262890683122, 1.000000000000000000, 0.9659258262890683122, 1.000000000000000000, 0.9659258262890683122, 1.000000000000000000, 0.9659258262890683122, 1.000000000000000000, 0.9659258262890683122, 1.000000000000000000, 0.9659258262890683122, 1.000000000000000000, 0.9659258262890683122, 1.000000000000000000, 0.9659258262890683122, 1.000000000000000000, 0.9659258262890683122, 1.000000000000000000, 0.9659258262890683122, 1.000000000000000000, 0.9659258262890683122, 1.000000000000000000, 0.9659258262890683122, 1.000000000000000000, 0.9659258262890683122, 1.000000000000000000, 0.9659258262890683122, 1.000000000000000000, 0.9659258262890683122, 1.000000000000000000, 0.9659258262890683122, 1.000000000000000000, 0.9659258262890683122, 1.000000000000000000, 0.9659258262890683122, 1.000000000000000000, 0.9659258262890683122, 1.000000000000000000, 0.9659258262890683122, 1.000000000000000000, 0.9659258262890683122, 1.000000000000000000, 0.9659258262890683122, 1.000000000000000000, 0.9659258262890683122, 1.000000000000000000, 0.9659258262890683122, 1.000000000000000000, 0.9659258262890683122, 1.000000000000000000, 0.9659258262890683122, 1.000000000000000000, 0.9659258262890683122, 1.000000000000000000, 0.9659258262890683122, 1.000000000000000000, 0.9659258262890683122, 1.000000000000000000, 0.9659258262890683122, 1.000000000000000000, 0.9659258262890683122, 1.000000000000000000, 0.9659258262890683122, 1.000000000000000000, 0.9659258262890683122, 1.000000000000000000, 0.9659258262890683122, 1.000000000000000000, 0.9659258262890683122, 1.000000000000000000, 0.9659258262890683122, 1.000000000000000000, 0.9659258262890683122, 1.000000000000000000, 0.9659258262890683122, 1.000000000000000000, 0.9659258262890683122, 1.000000000000000000, 0.9659258262890683122, 1.000000000000000000, 0.9659258262890683122, 1.000000000000000000, 0.9659258262890683122, 1.000000000000000000, 0.9659258262890683122, 1.000000000000000000, 0.9659258262890683122, 1.000000000000000000, 0.9659258262890683122, 1.000000000000000000, 0.9659258262890683122, 1.000000000000000000, 0.9659258262890683122, 1.000000000000000000, 0.9659258262890683122, 1.000000000000000000, 0.9659258262890683122, 1.000000000000000000, 0.9659258262890683122, 1.000000000000000000, 0.9659258262890683122, 1.000000000000000000, 0.9659258262890683122, 1.000000000000000000, 0.9659258262890683122, 1.000000000000000000, 0.9659258262890683122, 1.000000000000000000, 0.9659258262890683122, 1.000000000000000000, 0.9659258262890683122, 1.000000000000000000, 0.9659258262890683122, 1.000000000000000000, 0.9659258262890683122, 1.000000000000000000, 0.9659258262890683122, 1.000000000000000000, 0.9659258262890683122, 1.000000000000000000, 0.9659258262890683122, 1.000000000000000000, 0.9659258262890683122, 1.000000000000000000, 0.9659258262890683122, 1.000000000000000000, 0.9659258262890683122, 1.000000000000000000, 0.9659258262890683122, 1.000000000000000000, 0.9659258262890683122, 1.000000000000000000, 0.9659258262890683122, 1.000000000000000000, 0.9659258262890683122, 1.000000000000000000, 0.9659258262890683122, 1.000000000000000000, 0.9659258262890683122, 1.000000000000000000, 0.9659258262890683122, 1.000000000000000000, 0.9659258262890683122, 1.000000000000000000, 0.9659258262890683122, 1.000000000000000000, 0.9659258262890683122, 1.000000000000000000, 0.9659258262890683122, 1.000000000000000000, 0.9659258262890683122, 1.000000000000000000, 0.9659258262890683122, 1.000000000000000000, 0.9659258262890683122, 1.000000000000000000, 0.9659258262890683122, 1.000000000000000000, 0.9659258262890683122, 1.000000000000000000, 0.9659258262890683122, 1.000000000000000000, 0.9659258262890683122, 1.000000000000000000, 0.9659258262890683122, 1.000000000000000000, 0.9659258262890683122, 1.000000000000000000, 0.9659258262890683122, 1.000000000000000000, 0.9659258262890683122, 1.000000000000000000, 0.9659258262890683122, 1.000000000000000000, 0.9659258262890683122, 1.000000000000000000, 0.9659258262890683122, 1.000000000000000000, 0.9659258262890683122, 1.000000000000000000, 0.9659258262890683122, 1.000000000000000000, 0.9659258262890683122, 1.000000000000000000, 0.9659258262890683122, 1.000000000000000000, 0.9659258262890683122, 1.000000000000000000, 0.9659258262890683122, 1.000000000000000000, 0.9659258262890683122, 1.000000000000000000, 0.9659258262890683122, 1.000000000000000000, 0.9659258262890683122, 1.000000000000000000, 0.9659258262890683122, 1.000000000000000000, 0.9659258262890683122, 1.000000000000000000, 0.9659258262890683122, 1.000000000000000000, 0.9659258262890683122, 1.000000000000000000, 0.9659258262890683122, 1.000000000000000000, 0.9659258262890683122, 1.000000000000000000, 0.9659258262890683122, 1.000000000000000000, 0.9659258262890683122, 1.000000000000000000, 0.9659258262890683122, 1.000000000000000000, 0.9659258262890683122, 1.000000000000000000, 0.9659258262890683122, 1.000000000000000000, 0.9659258262890683122, 1.000000000000000000, 0.9659258262890683122, 1.000000000000000000, 0.9659258262890683122, 1.000000000000000000, 0.9659258262890683122, 1.000000000000000000, 0.9659258262890683122, 1.000000000000000000, 0.9659258262890683122, 1.000000000000000000, 0.9659258262890683122, 1.000000000000000000, 0.9659258262890683122, 1.000000000000000000, 0.9659258262890683122, 1.000000000000000000, 0.9659258262890683122, 1.000000000000000000, 0.9659258262890683122, 1.000000000000000000, 0.9659258262890683122, 1.000000000000000000, 0.9659258262890683122, 1.000000000000000000, 0.9659258262890683122, 1.000000000000000000, 0.9659258262890683122, 1.000000000000000000, 0.9659258262890683122, 1.000000000000000000, 0.9659258262890683122, 1.000000000000000000, 0.9659258262890683122, 1.000000000000000000, 0.9659258262890683122, 1.000000000000000000, 0.9659258262890683122, 1.000000000000000000, 0.9659258262890683122, 1.000000000000000000, 0.9659258262890683122, 1.000000000000000000, 0.9659258262890683122, 1.000000000000000000, 0.9659258262890683122, 1.000000000000000000, 0.9659258262890683122, 1.000000000000000000, 0.9659258262890683122, 1.000000000000000000, 0.9659258262890683122, 1.000000000000000000, 0.9659258262890683122, 1.000000000000000000, 0.9659258262890683122, 1.000000000000000000, 0.9659258262890683122, 1.000000000000000000, 0.9659258262890683122, 1.000000000000000000, 0.9659258262890683122, 1.000000000000000000, 0.9659258262890683122, 1.000000000000000000, 0.9659258262890683122, 1.000000000000000000, 0.9659258262890683122, 1.000000000000000000, 0.9659258262890683122, 1.000000000000000000, 0.9659258262890683122, 1.000000000000000000, 0.9659258262890683122, 1.000000000000000000, 0.9659258262890683122, 1.000000000000000000, 0.9659258262890683122, 1.000000000000000000, 0.9659258262890683122, 1.000000000000000000, 0.9659258262890683122, 1.000000000000000000, 0.9659258262890683122, 1.000000000000000000, 0.9659258262890683122, 1.000000000000000000, 0.9659258262890683122, 1.000000000000000000, 0.9659258262890683122, 1.000000000000000000, 0.9659258262890683122, 1.000000000000000000, 0.9659258262890683122, 1.000000000000000000, 0.9659258262890683122, 1.000000000000000000, 0.9659258262890683122, 1.000000000000000000, 0.9659258262890683122, 1.000000000000000000, 0.9659258262890683122, 1.000000000000000000, 0.9659258262890683122, 1.000000000000000000, 0.9659258262890683122, 1.000000000000000000, 0.9659258262890683122, 1.000000000000000000, 0.9659258262890683122, 1.000000000000000000, 0.9659258262890683122, 1.000000000000000000, 0.9659258262890683122, 1.000000000000000000, 0.9659258262890683122, 1.000000000000000000, 0.9659258262890683122, 1.000000000000000000, 0.9659258262890683122, 1.000000000000000000, 0.9659258262890683122, 1.000000000000000000, 0.9659258262890683122, 1.000000000000000000, 0.9659258262890683122, 1.000000000000000000, 0.9659258262890683122, 1.000000000000000000, 0.9659258262890683122, 1.000000000000000000, 0.9659258262890683122, 1.000000000000000000, 0.9659258262890683122, 1.000000000000000000, 0.9659258262890683122, 1.000000000000000000, 0.9659258262890683122, 1.000000000000000000, 0.9659258262890683122, 1.000000000000000000, 0.9659258262890683122, 1.000000000000000000, 0.9659258262890683122, 1.000000000000000000, 0.9659258262890683122, 1.000000000000000000, 0.9659258262890683122, 1.000000000000000000, 0.9659258262890683122, 1.000000000000000000, 0.9659258262890683122, 1.000000000000000000, 0.9659258262890683122, 1.000000000000000000, 0.9659258262890683122, 1.000000000000000000, 0.9659258262890683122, 1.000000000000000000, 0.9659258262890683122, 1.000000000000000000, 0.9659258262890683122, 1.000000000000000000, 0.9659258262890683122, 1.000000000000000000, 0.9659258262890683122, 1.000000000000000000, 0.9659258262890683122, 1.000000000000000000, 0.9659258262890683122, 1.000000000000000000, 0.9659258262890683122, 1.000000000000000000, 0.9659258262890683122, 1.000000000000000000, 0.9659258262890683122, 1.000000000000000000, 0.9659258262890683122, 1.000000000000000000, 0.9659258262890683122, 1.000000000000000000, 0.9659258262890683122, 1.000000000000000000, 0.9659258262890683122, 1.000000000000000000, 0.9659258262890683122, 1.000000000000000000, 0.9659258262890683122, 1.000000000000000000, 0.9659258262890683122, 1.000000000000000000, 0.9659258262890683122, 1.000000000000000000, 0.9659258262890683122, 1.000000000000000000, 0.9659258262890683122, 1.000000000000000000, 0.9659258262890683122, 1.000000000000000000, 0.9659258262890683122, 1.000000000000000000, 0.9659258262890683122, 1.000000000000000000, 0.9659258262890683122, 1.000000000000000000, 0.9659258262890683122, 1.000000000000000000, 0.9659258262890683122, 1.000000000000000000, 0.9659258262890683122, 1.000000000000000000, 0.9659258262890683122, 1.000000000000000000, 0.9659258262890683122, 1.000000000000000000, 0.9659258262890683122, 1.000000000000000000, 0.9659258262890683122, 1.000000000000000000, 0.9659258262890683122, 1.000000000000000000, 0.9659258262890683122, 1.000000000000000000, 0.9659258262890683122, 1.000000000000000000, 0.9659258262890683122, 1.000000000000000000, 0.9659258262890683122, 1.000000000000000000) ) ) 
 REPRESENTATION_ITEM ( '' )  SURFACE ( )  );
